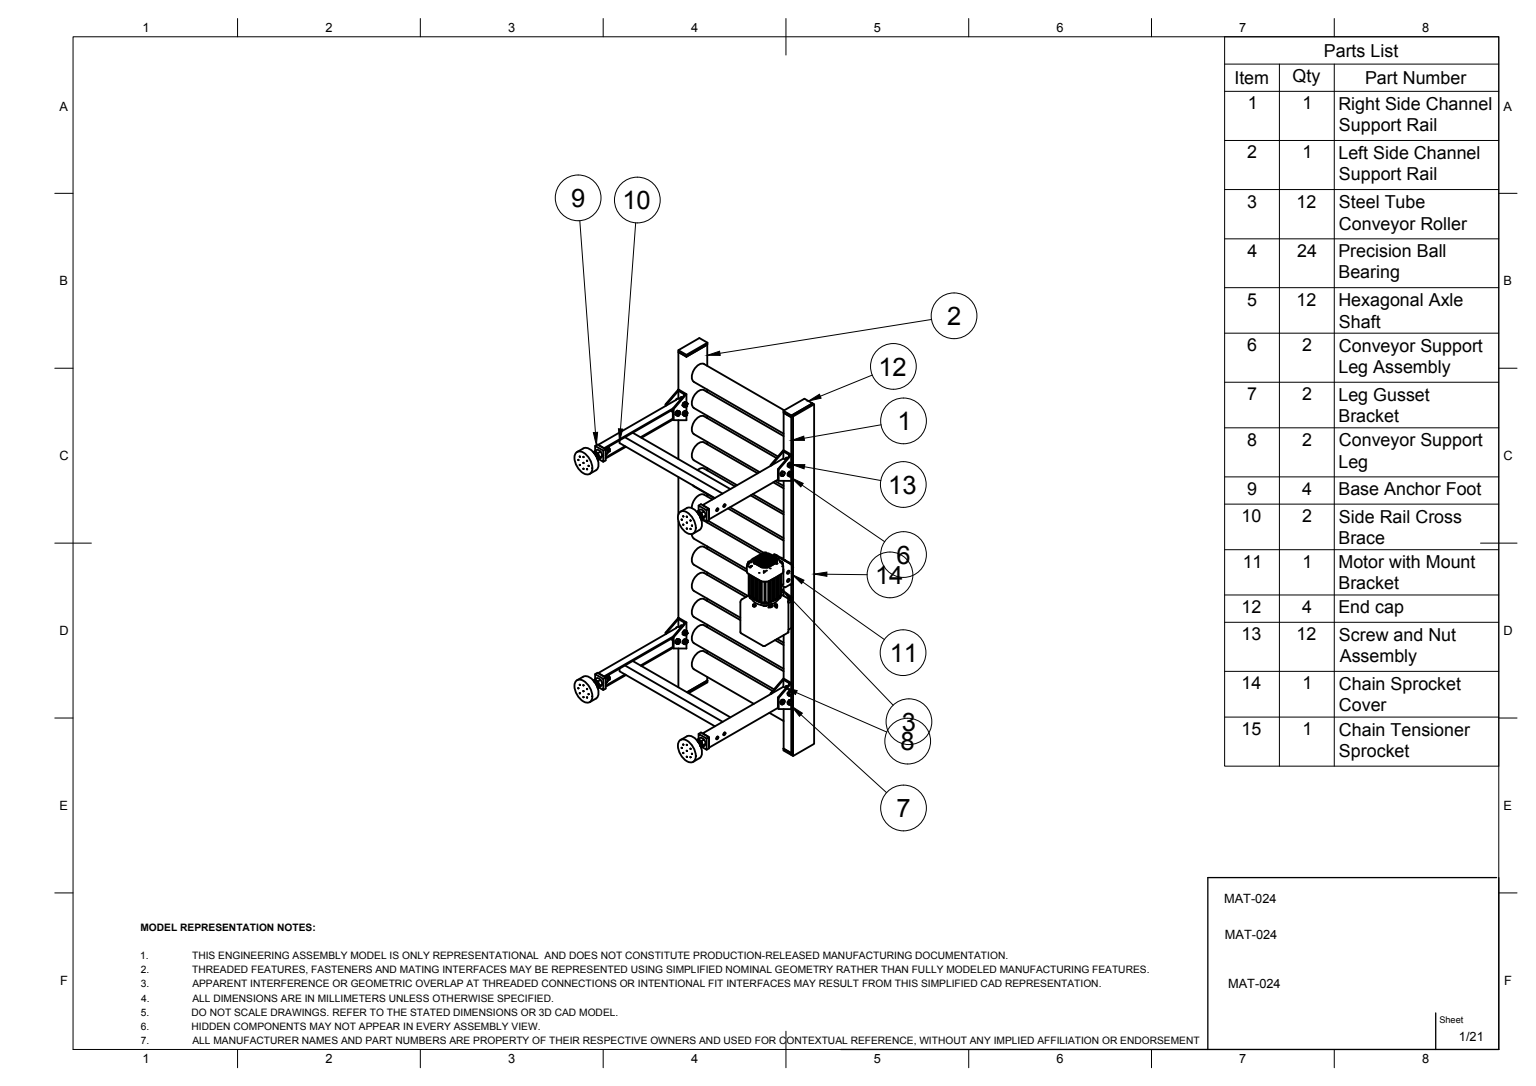
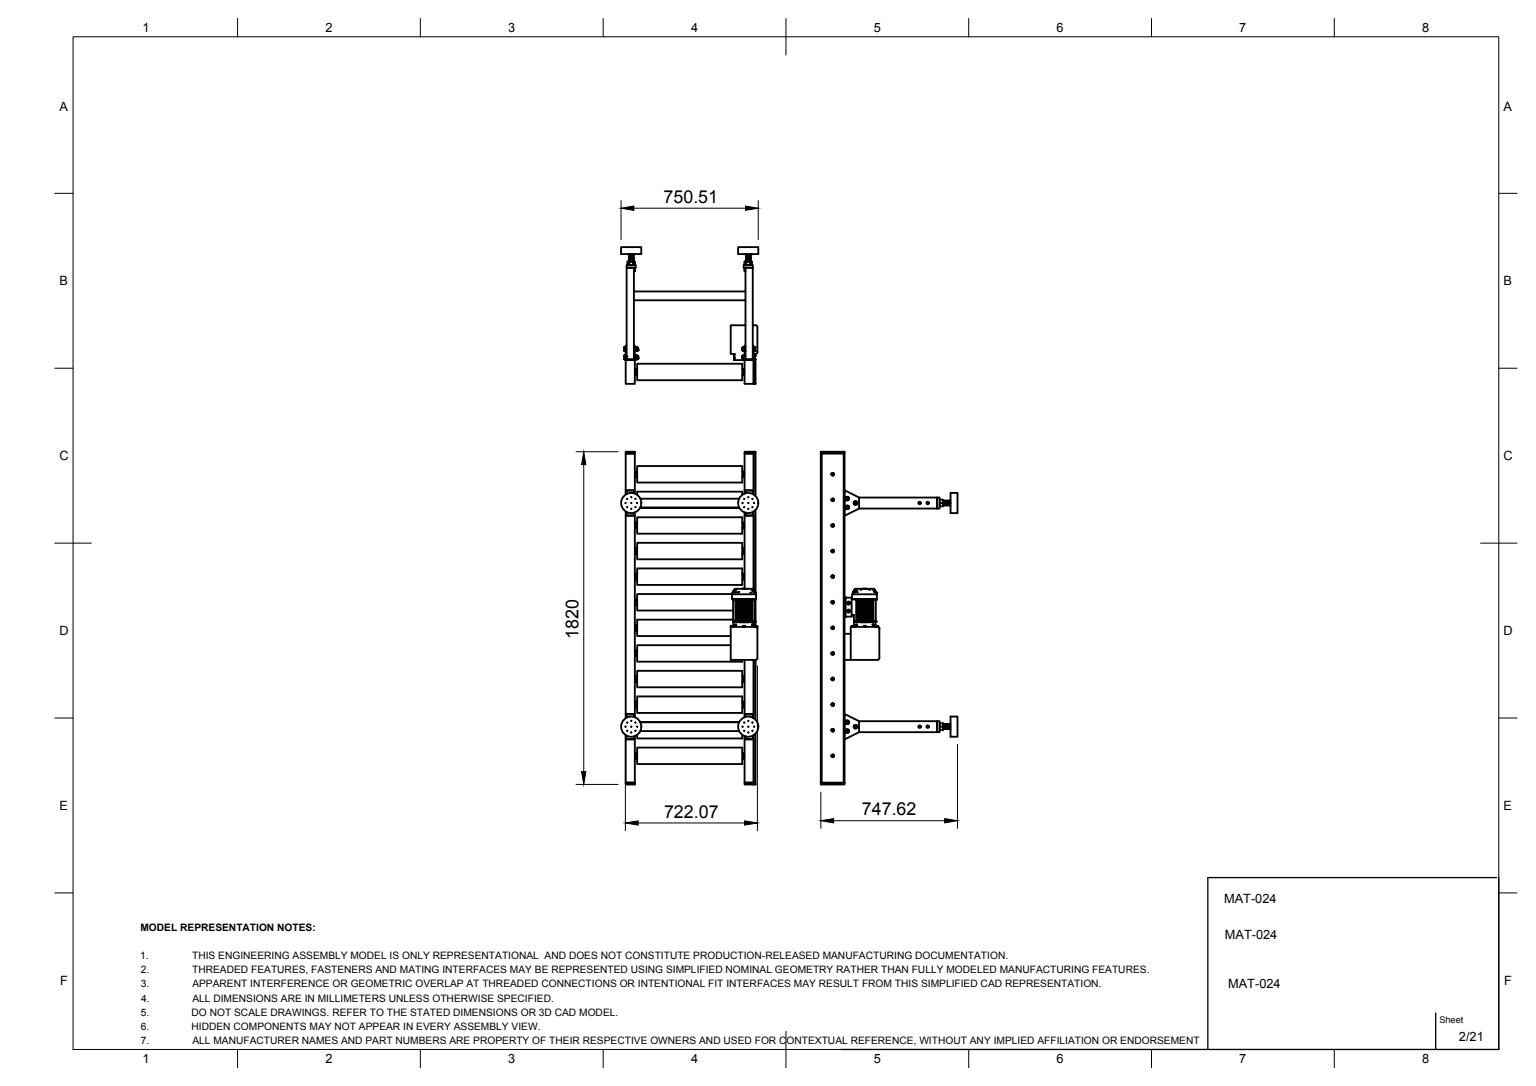
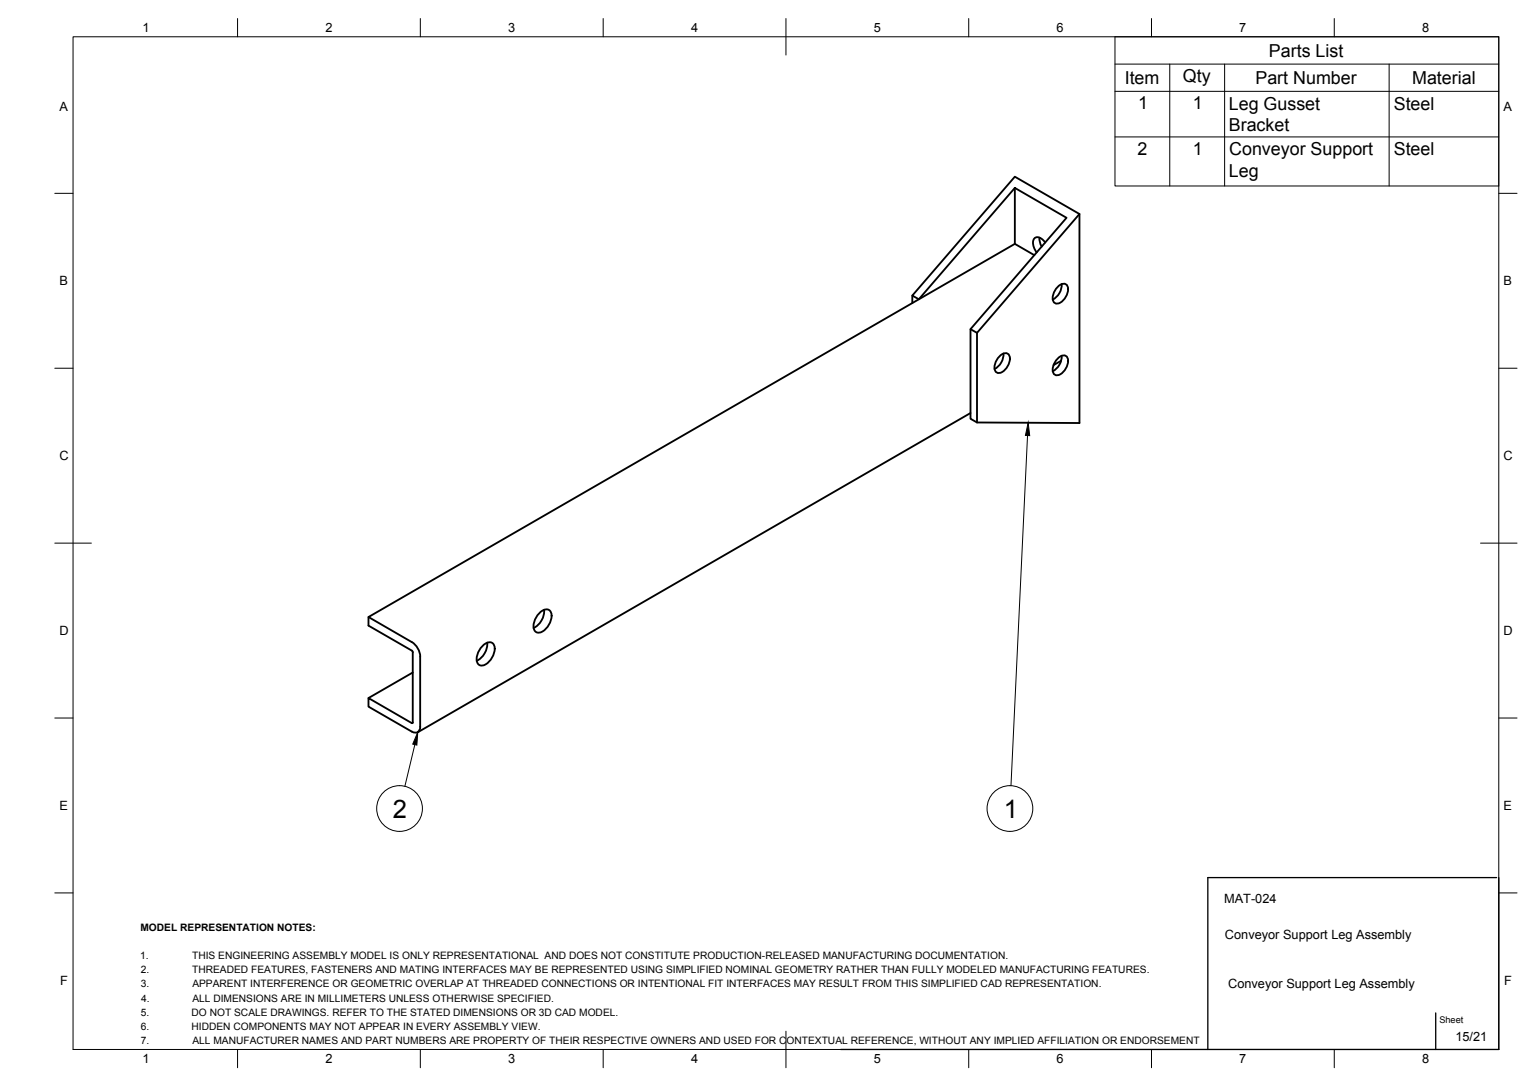
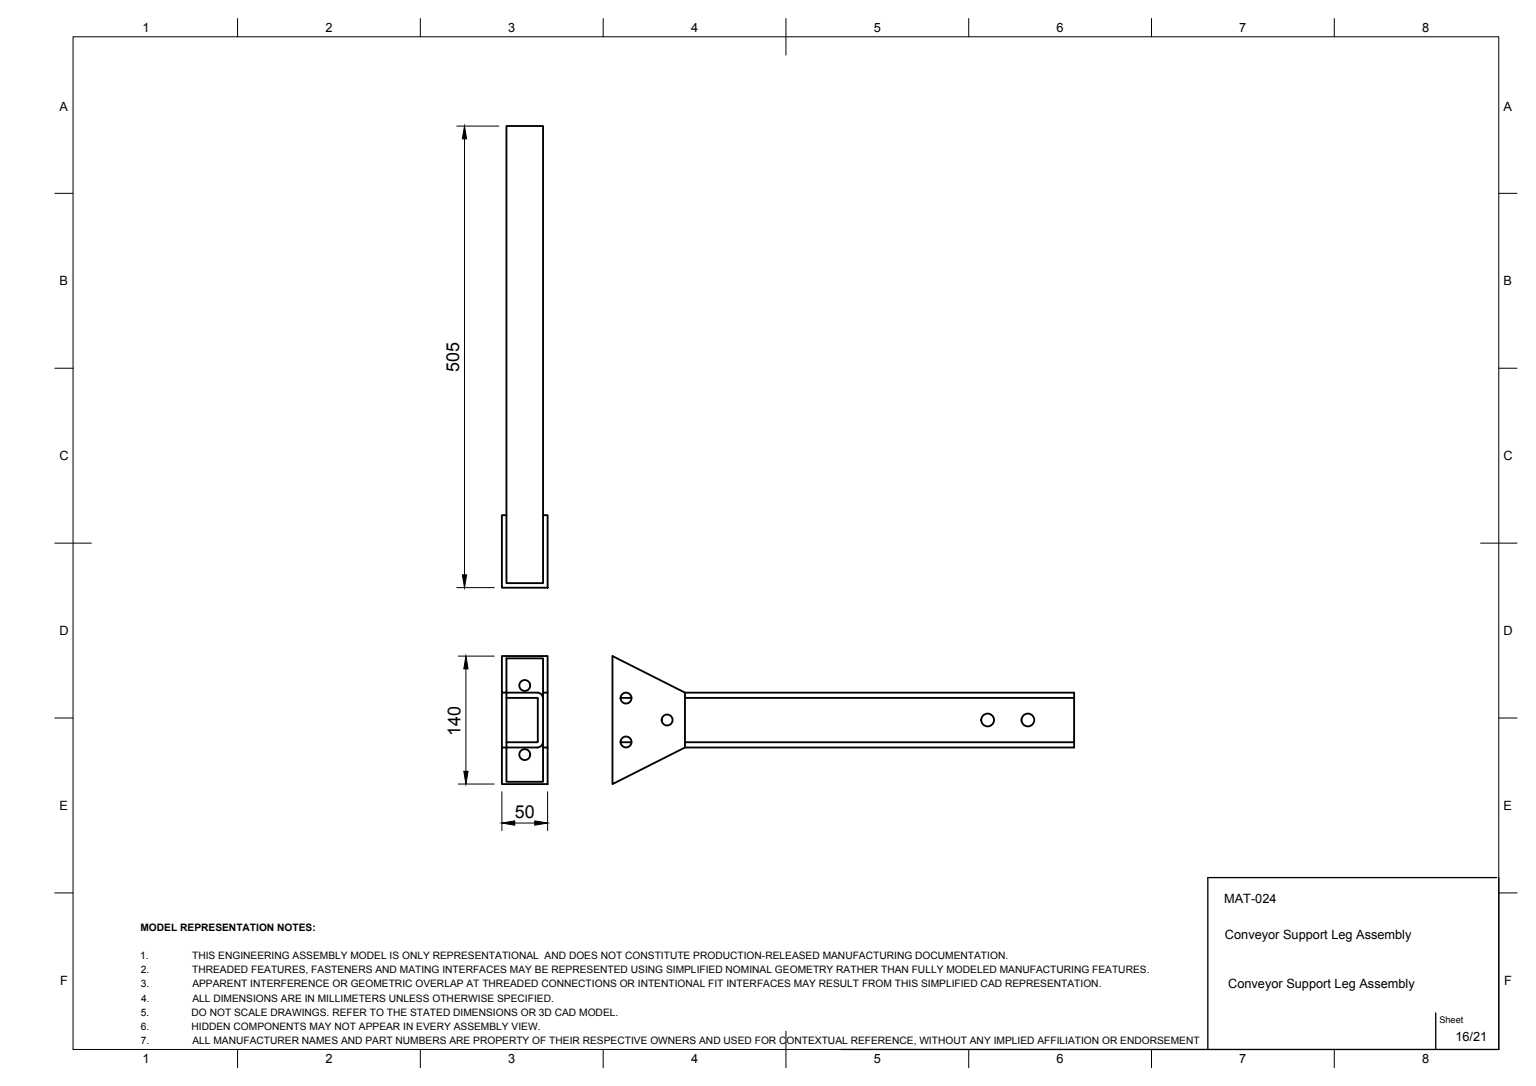
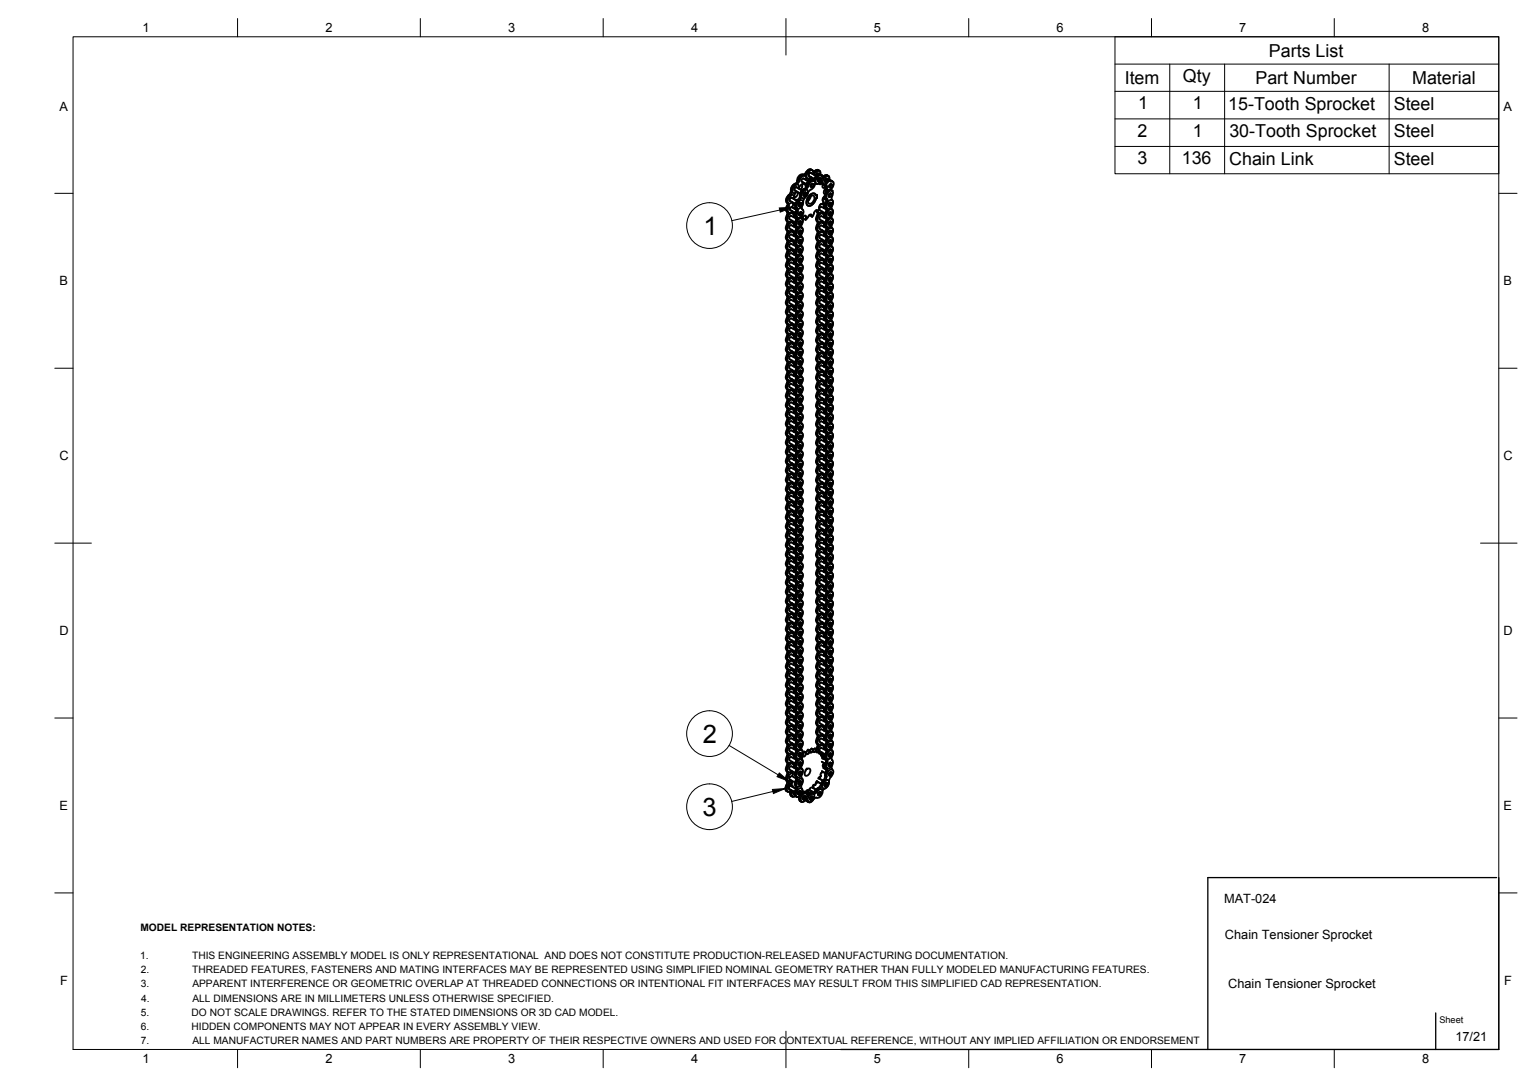
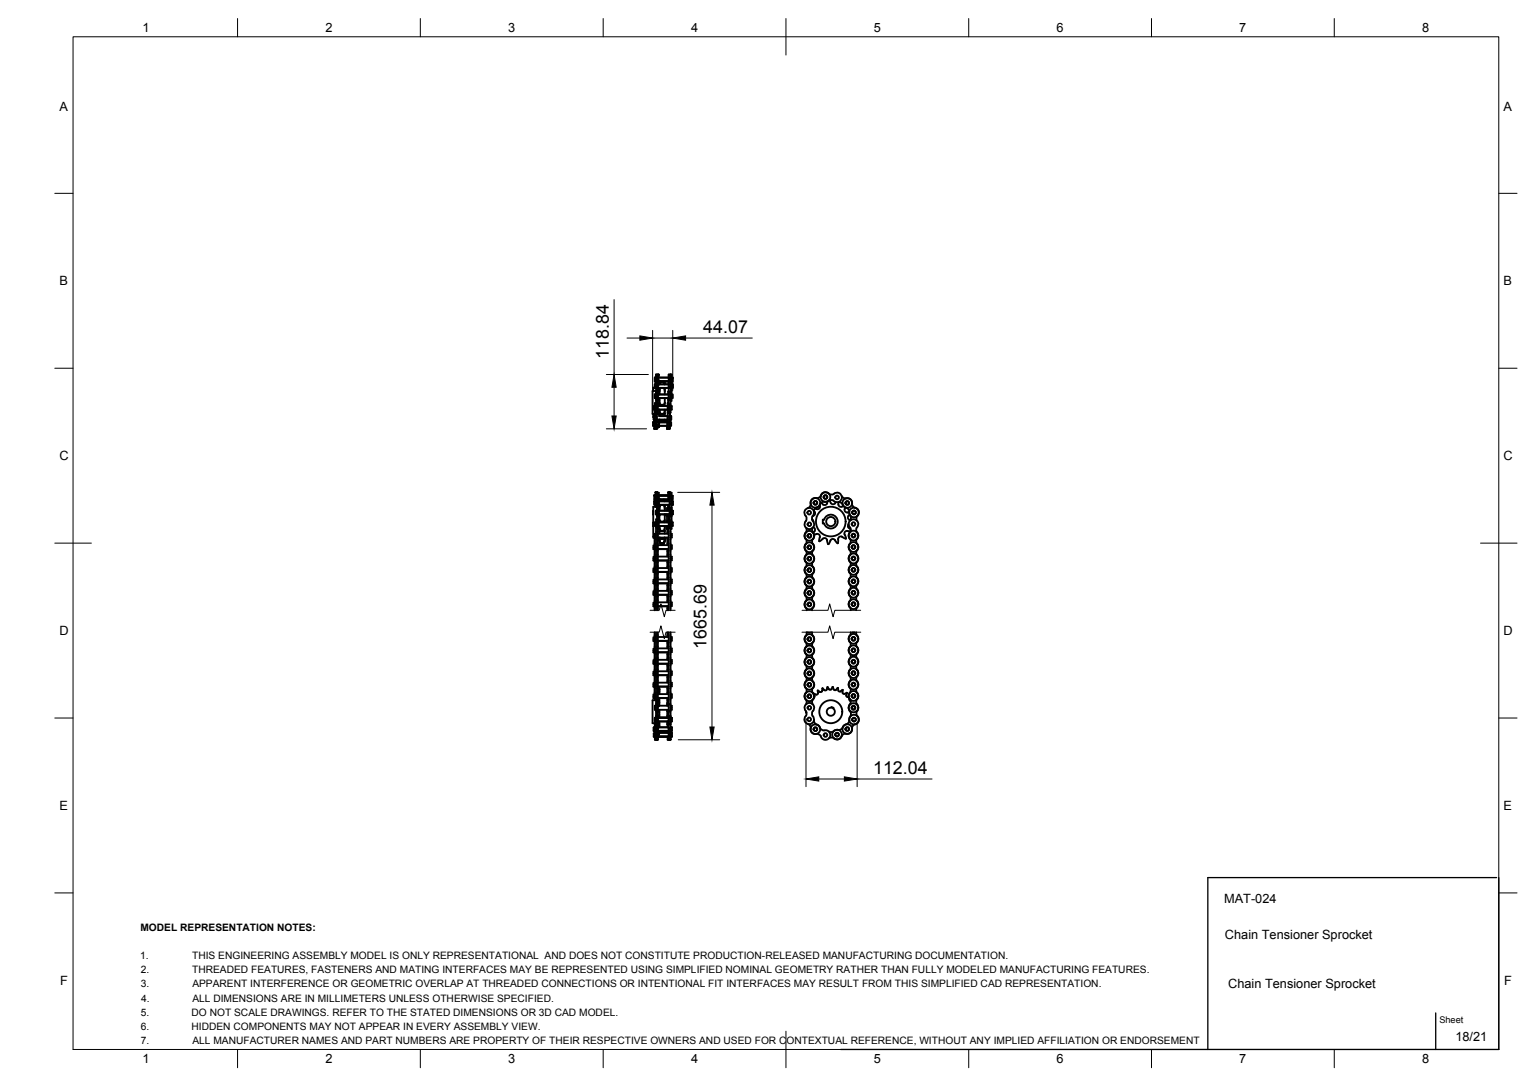
ISO-10303-21;
HEADER;
/* Generated by software containing ST-Developer
 * from STEP Tools, Inc. (www.steptools.com) 
 */

FILE_DESCRIPTION(
/* description */ ('STEP AP214'),
/* implementation_level */ '2;1');

FILE_NAME(
/* name */ 'MAT-024.step',
/* time_stamp */ '2026-11-14T06:34:07-08:00',
/* author */ (''),
/* organization */ (''),
/* preprocessor_version */ 'ST-DEVELOPER v20.2',
/* originating_system */ 'Autodesk Translation Framework v15.17.0.0',
/* authorisation */ '');

FILE_SCHEMA (('AUTOMOTIVE_DESIGN { 1 0 10303 214 3 1 1 }'));
ENDSEC;

DATA;
#10=MECHANICAL_DESIGN_GEOMETRIC_PRESENTATION_REPRESENTATION('',(#7256,#7257,
#7258,#7259,#7260,#7261,#7262,#7263,#7264,#7265,#7266,#7267,#7268,#7269,
#7270,#7271,#7272,#7273,#7274,#7275,#7276,#7277,#7278,#7279,#7280,#7281,
#7282,#7283,#7284,#7285,#7286,#7287,#7288,#7289,#7290,#7291,#7292,#7293,
#7294,#7295,#7296,#7297,#7298,#7299,#7300,#7301,#7302,#7303,#7304,#7305,
#7306,#7307,#7308,#7309,#7310,#7311,#7312,#7313,#7314,#7315,#7316,#7317,
#7318,#7319,#7320,#7321,#7322,#7323),#310623);
#11=ORIENTED_CLOSED_SHELL('',*,#93766,.F.);
#12=BREP_WITH_VOIDS('Body3',#93767,(#11));
#13=ITEM_DEFINED_TRANSFORMATION($,$,#103340,#103974);
#14=ITEM_DEFINED_TRANSFORMATION($,$,#103547,#103975);
#15=ITEM_DEFINED_TRANSFORMATION($,$,#103923,#103976);
#16=ITEM_DEFINED_TRANSFORMATION($,$,#103923,#103977);
#17=ITEM_DEFINED_TRANSFORMATION($,$,#103923,#103978);
#18=ITEM_DEFINED_TRANSFORMATION($,$,#103923,#103979);
#19=ITEM_DEFINED_TRANSFORMATION($,$,#103923,#103980);
#20=ITEM_DEFINED_TRANSFORMATION($,$,#103923,#103981);
#21=ITEM_DEFINED_TRANSFORMATION($,$,#103923,#103982);
#22=ITEM_DEFINED_TRANSFORMATION($,$,#103923,#103983);
#23=ITEM_DEFINED_TRANSFORMATION($,$,#103923,#103984);
#24=ITEM_DEFINED_TRANSFORMATION($,$,#103923,#103985);
#25=ITEM_DEFINED_TRANSFORMATION($,$,#103923,#103986);
#26=ITEM_DEFINED_TRANSFORMATION($,$,#103923,#103987);
#27=ITEM_DEFINED_TRANSFORMATION($,$,#103923,#103988);
#28=ITEM_DEFINED_TRANSFORMATION($,$,#103923,#103989);
#29=ITEM_DEFINED_TRANSFORMATION($,$,#103923,#103990);
#30=ITEM_DEFINED_TRANSFORMATION($,$,#103923,#103991);
#31=ITEM_DEFINED_TRANSFORMATION($,$,#103923,#103992);
#32=ITEM_DEFINED_TRANSFORMATION($,$,#103923,#103993);
#33=ITEM_DEFINED_TRANSFORMATION($,$,#103923,#103994);
#34=ITEM_DEFINED_TRANSFORMATION($,$,#103923,#103995);
#35=ITEM_DEFINED_TRANSFORMATION($,$,#103923,#103996);
#36=ITEM_DEFINED_TRANSFORMATION($,$,#103923,#103997);
#37=ITEM_DEFINED_TRANSFORMATION($,$,#103923,#103998);
#38=ITEM_DEFINED_TRANSFORMATION($,$,#103923,#103999);
#39=ITEM_DEFINED_TRANSFORMATION($,$,#103923,#104000);
#40=ITEM_DEFINED_TRANSFORMATION($,$,#103923,#104001);
#41=ITEM_DEFINED_TRANSFORMATION($,$,#103923,#104002);
#42=ITEM_DEFINED_TRANSFORMATION($,$,#103923,#104003);
#43=ITEM_DEFINED_TRANSFORMATION($,$,#103923,#104004);
#44=ITEM_DEFINED_TRANSFORMATION($,$,#103923,#104005);
#45=ITEM_DEFINED_TRANSFORMATION($,$,#103923,#104006);
#46=ITEM_DEFINED_TRANSFORMATION($,$,#103923,#104007);
#47=ITEM_DEFINED_TRANSFORMATION($,$,#103923,#104008);
#48=ITEM_DEFINED_TRANSFORMATION($,$,#103923,#104009);
#49=ITEM_DEFINED_TRANSFORMATION($,$,#103923,#104010);
#50=ITEM_DEFINED_TRANSFORMATION($,$,#103923,#104011);
#51=ITEM_DEFINED_TRANSFORMATION($,$,#103923,#104012);
#52=ITEM_DEFINED_TRANSFORMATION($,$,#103923,#104013);
#53=ITEM_DEFINED_TRANSFORMATION($,$,#103923,#104014);
#54=ITEM_DEFINED_TRANSFORMATION($,$,#103923,#104015);
#55=ITEM_DEFINED_TRANSFORMATION($,$,#103923,#104016);
#56=ITEM_DEFINED_TRANSFORMATION($,$,#103923,#104017);
#57=ITEM_DEFINED_TRANSFORMATION($,$,#103923,#104018);
#58=ITEM_DEFINED_TRANSFORMATION($,$,#103923,#104019);
#59=ITEM_DEFINED_TRANSFORMATION($,$,#103923,#104020);
#60=ITEM_DEFINED_TRANSFORMATION($,$,#103923,#104021);
#61=ITEM_DEFINED_TRANSFORMATION($,$,#103923,#104022);
#62=ITEM_DEFINED_TRANSFORMATION($,$,#103923,#104023);
#63=ITEM_DEFINED_TRANSFORMATION($,$,#103923,#104024);
#64=ITEM_DEFINED_TRANSFORMATION($,$,#103923,#104025);
#65=ITEM_DEFINED_TRANSFORMATION($,$,#103923,#104026);
#66=ITEM_DEFINED_TRANSFORMATION($,$,#103923,#104027);
#67=ITEM_DEFINED_TRANSFORMATION($,$,#103923,#104028);
#68=ITEM_DEFINED_TRANSFORMATION($,$,#103923,#104029);
#69=ITEM_DEFINED_TRANSFORMATION($,$,#103923,#104030);
#70=ITEM_DEFINED_TRANSFORMATION($,$,#103923,#104031);
#71=ITEM_DEFINED_TRANSFORMATION($,$,#103923,#104032);
#72=ITEM_DEFINED_TRANSFORMATION($,$,#103923,#104033);
#73=ITEM_DEFINED_TRANSFORMATION($,$,#103923,#104034);
#74=ITEM_DEFINED_TRANSFORMATION($,$,#103923,#104035);
#75=ITEM_DEFINED_TRANSFORMATION($,$,#103923,#104036);
#76=ITEM_DEFINED_TRANSFORMATION($,$,#103923,#104037);
#77=ITEM_DEFINED_TRANSFORMATION($,$,#103923,#104038);
#78=ITEM_DEFINED_TRANSFORMATION($,$,#103923,#104039);
#79=ITEM_DEFINED_TRANSFORMATION($,$,#103923,#104040);
#80=ITEM_DEFINED_TRANSFORMATION($,$,#103923,#104041);
#81=ITEM_DEFINED_TRANSFORMATION($,$,#103923,#104042);
#82=ITEM_DEFINED_TRANSFORMATION($,$,#103923,#104043);
#83=ITEM_DEFINED_TRANSFORMATION($,$,#103923,#104044);
#84=ITEM_DEFINED_TRANSFORMATION($,$,#103923,#104045);
#85=ITEM_DEFINED_TRANSFORMATION($,$,#103923,#104046);
#86=ITEM_DEFINED_TRANSFORMATION($,$,#103923,#104047);
#87=ITEM_DEFINED_TRANSFORMATION($,$,#103923,#104048);
#88=ITEM_DEFINED_TRANSFORMATION($,$,#103923,#104049);
#89=ITEM_DEFINED_TRANSFORMATION($,$,#103923,#104050);
#90=ITEM_DEFINED_TRANSFORMATION($,$,#103923,#104051);
#91=ITEM_DEFINED_TRANSFORMATION($,$,#103923,#104052);
#92=ITEM_DEFINED_TRANSFORMATION($,$,#103923,#104053);
#93=ITEM_DEFINED_TRANSFORMATION($,$,#103923,#104054);
#94=ITEM_DEFINED_TRANSFORMATION($,$,#103923,#104055);
#95=ITEM_DEFINED_TRANSFORMATION($,$,#103923,#104056);
#96=ITEM_DEFINED_TRANSFORMATION($,$,#103923,#104057);
#97=ITEM_DEFINED_TRANSFORMATION($,$,#103923,#104058);
#98=ITEM_DEFINED_TRANSFORMATION($,$,#103923,#104059);
#99=ITEM_DEFINED_TRANSFORMATION($,$,#103923,#104060);
#100=ITEM_DEFINED_TRANSFORMATION($,$,#103923,#104061);
#101=ITEM_DEFINED_TRANSFORMATION($,$,#103923,#104062);
#102=ITEM_DEFINED_TRANSFORMATION($,$,#103923,#104063);
#103=ITEM_DEFINED_TRANSFORMATION($,$,#103923,#104064);
#104=ITEM_DEFINED_TRANSFORMATION($,$,#103923,#104065);
#105=ITEM_DEFINED_TRANSFORMATION($,$,#103923,#104066);
#106=ITEM_DEFINED_TRANSFORMATION($,$,#103923,#104067);
#107=ITEM_DEFINED_TRANSFORMATION($,$,#103923,#104068);
#108=ITEM_DEFINED_TRANSFORMATION($,$,#103923,#104069);
#109=ITEM_DEFINED_TRANSFORMATION($,$,#103923,#104070);
#110=ITEM_DEFINED_TRANSFORMATION($,$,#103923,#104071);
#111=ITEM_DEFINED_TRANSFORMATION($,$,#103923,#104072);
#112=ITEM_DEFINED_TRANSFORMATION($,$,#103923,#104073);
#113=ITEM_DEFINED_TRANSFORMATION($,$,#103923,#104074);
#114=ITEM_DEFINED_TRANSFORMATION($,$,#103923,#104075);
#115=ITEM_DEFINED_TRANSFORMATION($,$,#103923,#104076);
#116=ITEM_DEFINED_TRANSFORMATION($,$,#103923,#104077);
#117=ITEM_DEFINED_TRANSFORMATION($,$,#103923,#104078);
#118=ITEM_DEFINED_TRANSFORMATION($,$,#103923,#104079);
#119=ITEM_DEFINED_TRANSFORMATION($,$,#103923,#104080);
#120=ITEM_DEFINED_TRANSFORMATION($,$,#103923,#104081);
#121=ITEM_DEFINED_TRANSFORMATION($,$,#103923,#104082);
#122=ITEM_DEFINED_TRANSFORMATION($,$,#103923,#104083);
#123=ITEM_DEFINED_TRANSFORMATION($,$,#103923,#104084);
#124=ITEM_DEFINED_TRANSFORMATION($,$,#103923,#104085);
#125=ITEM_DEFINED_TRANSFORMATION($,$,#103923,#104086);
#126=ITEM_DEFINED_TRANSFORMATION($,$,#103923,#104087);
#127=ITEM_DEFINED_TRANSFORMATION($,$,#103923,#104088);
#128=ITEM_DEFINED_TRANSFORMATION($,$,#103923,#104089);
#129=ITEM_DEFINED_TRANSFORMATION($,$,#103923,#104090);
#130=ITEM_DEFINED_TRANSFORMATION($,$,#103923,#104091);
#131=ITEM_DEFINED_TRANSFORMATION($,$,#103923,#104092);
#132=ITEM_DEFINED_TRANSFORMATION($,$,#103923,#104093);
#133=ITEM_DEFINED_TRANSFORMATION($,$,#103923,#104094);
#134=ITEM_DEFINED_TRANSFORMATION($,$,#103923,#104095);
#135=ITEM_DEFINED_TRANSFORMATION($,$,#103923,#104096);
#136=ITEM_DEFINED_TRANSFORMATION($,$,#103923,#104097);
#137=ITEM_DEFINED_TRANSFORMATION($,$,#103923,#104098);
#138=ITEM_DEFINED_TRANSFORMATION($,$,#103923,#104099);
#139=ITEM_DEFINED_TRANSFORMATION($,$,#103923,#104100);
#140=ITEM_DEFINED_TRANSFORMATION($,$,#103923,#104101);
#141=ITEM_DEFINED_TRANSFORMATION($,$,#103923,#104102);
#142=ITEM_DEFINED_TRANSFORMATION($,$,#103923,#104103);
#143=ITEM_DEFINED_TRANSFORMATION($,$,#103923,#104104);
#144=ITEM_DEFINED_TRANSFORMATION($,$,#103923,#104105);
#145=ITEM_DEFINED_TRANSFORMATION($,$,#103923,#104106);
#146=ITEM_DEFINED_TRANSFORMATION($,$,#103923,#104107);
#147=ITEM_DEFINED_TRANSFORMATION($,$,#103923,#104108);
#148=ITEM_DEFINED_TRANSFORMATION($,$,#103923,#104109);
#149=ITEM_DEFINED_TRANSFORMATION($,$,#103923,#104110);
#150=ITEM_DEFINED_TRANSFORMATION($,$,#103923,#104111);
#151=ITEM_DEFINED_TRANSFORMATION($,$,#104562,#104634);
#152=ITEM_DEFINED_TRANSFORMATION($,$,#104597,#104635);
#153=ITEM_DEFINED_TRANSFORMATION($,$,#104637,#104781);
#154=ITEM_DEFINED_TRANSFORMATION($,$,#104720,#104782);
#155=ITEM_DEFINED_TRANSFORMATION($,$,#93964,#104783);
#156=ITEM_DEFINED_TRANSFORMATION($,$,#94023,#104784);
#157=ITEM_DEFINED_TRANSFORMATION($,$,#104112,#104785);
#158=ITEM_DEFINED_TRANSFORMATION($,$,#104129,#104786);
#159=ITEM_DEFINED_TRANSFORMATION($,$,#104223,#104787);
#160=ITEM_DEFINED_TRANSFORMATION($,$,#104561,#104788);
#161=ITEM_DEFINED_TRANSFORMATION($,$,#104248,#104789);
#162=ITEM_DEFINED_TRANSFORMATION($,$,#104543,#104790);
#163=ITEM_DEFINED_TRANSFORMATION($,$,#94082,#104791);
#164=ITEM_DEFINED_TRANSFORMATION($,$,#104554,#104792);
#165=ITEM_DEFINED_TRANSFORMATION($,$,#104636,#104793);
#166=ITEM_DEFINED_TRANSFORMATION($,$,#103332,#104794);
#167=ITEM_DEFINED_TRANSFORMATION($,$,#103339,#104795);
#168=ITEM_DEFINED_TRANSFORMATION($,$,#104112,#104796);
#169=ITEM_DEFINED_TRANSFORMATION($,$,#104112,#104797);
#170=ITEM_DEFINED_TRANSFORMATION($,$,#104112,#104798);
#171=ITEM_DEFINED_TRANSFORMATION($,$,#104112,#104799);
#172=ITEM_DEFINED_TRANSFORMATION($,$,#104112,#104800);
#173=ITEM_DEFINED_TRANSFORMATION($,$,#104112,#104801);
#174=ITEM_DEFINED_TRANSFORMATION($,$,#104112,#104802);
#175=ITEM_DEFINED_TRANSFORMATION($,$,#104112,#104803);
#176=ITEM_DEFINED_TRANSFORMATION($,$,#104112,#104804);
#177=ITEM_DEFINED_TRANSFORMATION($,$,#104112,#104805);
#178=ITEM_DEFINED_TRANSFORMATION($,$,#104112,#104806);
#179=ITEM_DEFINED_TRANSFORMATION($,$,#104129,#104807);
#180=ITEM_DEFINED_TRANSFORMATION($,$,#104129,#104808);
#181=ITEM_DEFINED_TRANSFORMATION($,$,#104129,#104809);
#182=ITEM_DEFINED_TRANSFORMATION($,$,#104129,#104810);
#183=ITEM_DEFINED_TRANSFORMATION($,$,#104129,#104811);
#184=ITEM_DEFINED_TRANSFORMATION($,$,#104129,#104812);
#185=ITEM_DEFINED_TRANSFORMATION($,$,#104129,#104813);
#186=ITEM_DEFINED_TRANSFORMATION($,$,#104129,#104814);
#187=ITEM_DEFINED_TRANSFORMATION($,$,#104129,#104815);
#188=ITEM_DEFINED_TRANSFORMATION($,$,#104129,#104816);
#189=ITEM_DEFINED_TRANSFORMATION($,$,#104129,#104817);
#190=ITEM_DEFINED_TRANSFORMATION($,$,#104129,#104818);
#191=ITEM_DEFINED_TRANSFORMATION($,$,#104129,#104819);
#192=ITEM_DEFINED_TRANSFORMATION($,$,#104129,#104820);
#193=ITEM_DEFINED_TRANSFORMATION($,$,#104129,#104821);
#194=ITEM_DEFINED_TRANSFORMATION($,$,#104129,#104822);
#195=ITEM_DEFINED_TRANSFORMATION($,$,#104129,#104823);
#196=ITEM_DEFINED_TRANSFORMATION($,$,#104129,#104824);
#197=ITEM_DEFINED_TRANSFORMATION($,$,#104129,#104825);
#198=ITEM_DEFINED_TRANSFORMATION($,$,#104129,#104826);
#199=ITEM_DEFINED_TRANSFORMATION($,$,#104129,#104827);
#200=ITEM_DEFINED_TRANSFORMATION($,$,#104129,#104828);
#201=ITEM_DEFINED_TRANSFORMATION($,$,#104129,#104829);
#202=ITEM_DEFINED_TRANSFORMATION($,$,#104223,#104830);
#203=ITEM_DEFINED_TRANSFORMATION($,$,#104223,#104831);
#204=ITEM_DEFINED_TRANSFORMATION($,$,#104223,#104832);
#205=ITEM_DEFINED_TRANSFORMATION($,$,#104223,#104833);
#206=ITEM_DEFINED_TRANSFORMATION($,$,#104223,#104834);
#207=ITEM_DEFINED_TRANSFORMATION($,$,#104223,#104835);
#208=ITEM_DEFINED_TRANSFORMATION($,$,#104223,#104836);
#209=ITEM_DEFINED_TRANSFORMATION($,$,#104223,#104837);
#210=ITEM_DEFINED_TRANSFORMATION($,$,#104223,#104838);
#211=ITEM_DEFINED_TRANSFORMATION($,$,#104223,#104839);
#212=ITEM_DEFINED_TRANSFORMATION($,$,#104223,#104840);
#213=ITEM_DEFINED_TRANSFORMATION($,$,#104562,#104841);
#214=ITEM_DEFINED_TRANSFORMATION($,$,#104597,#104842);
#215=ITEM_DEFINED_TRANSFORMATION($,$,#104248,#104843);
#216=ITEM_DEFINED_TRANSFORMATION($,$,#104248,#104844);
#217=ITEM_DEFINED_TRANSFORMATION($,$,#104597,#104845);
#218=ITEM_DEFINED_TRANSFORMATION($,$,#104248,#104846);
#219=ITEM_DEFINED_TRANSFORMATION($,$,#104543,#104847);
#220=ITEM_DEFINED_TRANSFORMATION($,$,#104562,#104848);
#221=ITEM_DEFINED_TRANSFORMATION($,$,#104554,#104849);
#222=ITEM_DEFINED_TRANSFORMATION($,$,#104554,#104850);
#223=ITEM_DEFINED_TRANSFORMATION($,$,#104554,#104851);
#224=ITEM_DEFINED_TRANSFORMATION($,$,#104636,#104852);
#225=ITEM_DEFINED_TRANSFORMATION($,$,#104636,#104853);
#226=ITEM_DEFINED_TRANSFORMATION($,$,#104636,#104854);
#227=ITEM_DEFINED_TRANSFORMATION($,$,#104636,#104855);
#228=ITEM_DEFINED_TRANSFORMATION($,$,#104636,#104856);
#229=ITEM_DEFINED_TRANSFORMATION($,$,#104561,#104857);
#230=ITEM_DEFINED_TRANSFORMATION($,$,#104636,#104858);
#231=ITEM_DEFINED_TRANSFORMATION($,$,#104636,#104859);
#232=ITEM_DEFINED_TRANSFORMATION($,$,#104636,#104860);
#233=ITEM_DEFINED_TRANSFORMATION($,$,#104636,#104861);
#234=ITEM_DEFINED_TRANSFORMATION($,$,#104636,#104862);
#235=ITEM_DEFINED_TRANSFORMATION($,$,#104636,#104863);
#236=(
REPRESENTATION_RELATIONSHIP($,$,#310899,#310898)
REPRESENTATION_RELATIONSHIP_WITH_TRANSFORMATION(#13)
SHAPE_REPRESENTATION_RELATIONSHIP()
);
#237=(
REPRESENTATION_RELATIONSHIP($,$,#310900,#310898)
REPRESENTATION_RELATIONSHIP_WITH_TRANSFORMATION(#14)
SHAPE_REPRESENTATION_RELATIONSHIP()
);
#238=(
REPRESENTATION_RELATIONSHIP($,$,#310901,#310898)
REPRESENTATION_RELATIONSHIP_WITH_TRANSFORMATION(#15)
SHAPE_REPRESENTATION_RELATIONSHIP()
);
#239=(
REPRESENTATION_RELATIONSHIP($,$,#310901,#310898)
REPRESENTATION_RELATIONSHIP_WITH_TRANSFORMATION(#16)
SHAPE_REPRESENTATION_RELATIONSHIP()
);
#240=(
REPRESENTATION_RELATIONSHIP($,$,#310901,#310898)
REPRESENTATION_RELATIONSHIP_WITH_TRANSFORMATION(#17)
SHAPE_REPRESENTATION_RELATIONSHIP()
);
#241=(
REPRESENTATION_RELATIONSHIP($,$,#310901,#310898)
REPRESENTATION_RELATIONSHIP_WITH_TRANSFORMATION(#18)
SHAPE_REPRESENTATION_RELATIONSHIP()
);
#242=(
REPRESENTATION_RELATIONSHIP($,$,#310901,#310898)
REPRESENTATION_RELATIONSHIP_WITH_TRANSFORMATION(#19)
SHAPE_REPRESENTATION_RELATIONSHIP()
);
#243=(
REPRESENTATION_RELATIONSHIP($,$,#310901,#310898)
REPRESENTATION_RELATIONSHIP_WITH_TRANSFORMATION(#20)
SHAPE_REPRESENTATION_RELATIONSHIP()
);
#244=(
REPRESENTATION_RELATIONSHIP($,$,#310901,#310898)
REPRESENTATION_RELATIONSHIP_WITH_TRANSFORMATION(#21)
SHAPE_REPRESENTATION_RELATIONSHIP()
);
#245=(
REPRESENTATION_RELATIONSHIP($,$,#310901,#310898)
REPRESENTATION_RELATIONSHIP_WITH_TRANSFORMATION(#22)
SHAPE_REPRESENTATION_RELATIONSHIP()
);
#246=(
REPRESENTATION_RELATIONSHIP($,$,#310901,#310898)
REPRESENTATION_RELATIONSHIP_WITH_TRANSFORMATION(#23)
SHAPE_REPRESENTATION_RELATIONSHIP()
);
#247=(
REPRESENTATION_RELATIONSHIP($,$,#310901,#310898)
REPRESENTATION_RELATIONSHIP_WITH_TRANSFORMATION(#24)
SHAPE_REPRESENTATION_RELATIONSHIP()
);
#248=(
REPRESENTATION_RELATIONSHIP($,$,#310901,#310898)
REPRESENTATION_RELATIONSHIP_WITH_TRANSFORMATION(#25)
SHAPE_REPRESENTATION_RELATIONSHIP()
);
#249=(
REPRESENTATION_RELATIONSHIP($,$,#310901,#310898)
REPRESENTATION_RELATIONSHIP_WITH_TRANSFORMATION(#26)
SHAPE_REPRESENTATION_RELATIONSHIP()
);
#250=(
REPRESENTATION_RELATIONSHIP($,$,#310901,#310898)
REPRESENTATION_RELATIONSHIP_WITH_TRANSFORMATION(#27)
SHAPE_REPRESENTATION_RELATIONSHIP()
);
#251=(
REPRESENTATION_RELATIONSHIP($,$,#310901,#310898)
REPRESENTATION_RELATIONSHIP_WITH_TRANSFORMATION(#28)
SHAPE_REPRESENTATION_RELATIONSHIP()
);
#252=(
REPRESENTATION_RELATIONSHIP($,$,#310901,#310898)
REPRESENTATION_RELATIONSHIP_WITH_TRANSFORMATION(#29)
SHAPE_REPRESENTATION_RELATIONSHIP()
);
#253=(
REPRESENTATION_RELATIONSHIP($,$,#310901,#310898)
REPRESENTATION_RELATIONSHIP_WITH_TRANSFORMATION(#30)
SHAPE_REPRESENTATION_RELATIONSHIP()
);
#254=(
REPRESENTATION_RELATIONSHIP($,$,#310901,#310898)
REPRESENTATION_RELATIONSHIP_WITH_TRANSFORMATION(#31)
SHAPE_REPRESENTATION_RELATIONSHIP()
);
#255=(
REPRESENTATION_RELATIONSHIP($,$,#310901,#310898)
REPRESENTATION_RELATIONSHIP_WITH_TRANSFORMATION(#32)
SHAPE_REPRESENTATION_RELATIONSHIP()
);
#256=(
REPRESENTATION_RELATIONSHIP($,$,#310901,#310898)
REPRESENTATION_RELATIONSHIP_WITH_TRANSFORMATION(#33)
SHAPE_REPRESENTATION_RELATIONSHIP()
);
#257=(
REPRESENTATION_RELATIONSHIP($,$,#310901,#310898)
REPRESENTATION_RELATIONSHIP_WITH_TRANSFORMATION(#34)
SHAPE_REPRESENTATION_RELATIONSHIP()
);
#258=(
REPRESENTATION_RELATIONSHIP($,$,#310901,#310898)
REPRESENTATION_RELATIONSHIP_WITH_TRANSFORMATION(#35)
SHAPE_REPRESENTATION_RELATIONSHIP()
);
#259=(
REPRESENTATION_RELATIONSHIP($,$,#310901,#310898)
REPRESENTATION_RELATIONSHIP_WITH_TRANSFORMATION(#36)
SHAPE_REPRESENTATION_RELATIONSHIP()
);
#260=(
REPRESENTATION_RELATIONSHIP($,$,#310901,#310898)
REPRESENTATION_RELATIONSHIP_WITH_TRANSFORMATION(#37)
SHAPE_REPRESENTATION_RELATIONSHIP()
);
#261=(
REPRESENTATION_RELATIONSHIP($,$,#310901,#310898)
REPRESENTATION_RELATIONSHIP_WITH_TRANSFORMATION(#38)
SHAPE_REPRESENTATION_RELATIONSHIP()
);
#262=(
REPRESENTATION_RELATIONSHIP($,$,#310901,#310898)
REPRESENTATION_RELATIONSHIP_WITH_TRANSFORMATION(#39)
SHAPE_REPRESENTATION_RELATIONSHIP()
);
#263=(
REPRESENTATION_RELATIONSHIP($,$,#310901,#310898)
REPRESENTATION_RELATIONSHIP_WITH_TRANSFORMATION(#40)
SHAPE_REPRESENTATION_RELATIONSHIP()
);
#264=(
REPRESENTATION_RELATIONSHIP($,$,#310901,#310898)
REPRESENTATION_RELATIONSHIP_WITH_TRANSFORMATION(#41)
SHAPE_REPRESENTATION_RELATIONSHIP()
);
#265=(
REPRESENTATION_RELATIONSHIP($,$,#310901,#310898)
REPRESENTATION_RELATIONSHIP_WITH_TRANSFORMATION(#42)
SHAPE_REPRESENTATION_RELATIONSHIP()
);
#266=(
REPRESENTATION_RELATIONSHIP($,$,#310901,#310898)
REPRESENTATION_RELATIONSHIP_WITH_TRANSFORMATION(#43)
SHAPE_REPRESENTATION_RELATIONSHIP()
);
#267=(
REPRESENTATION_RELATIONSHIP($,$,#310901,#310898)
REPRESENTATION_RELATIONSHIP_WITH_TRANSFORMATION(#44)
SHAPE_REPRESENTATION_RELATIONSHIP()
);
#268=(
REPRESENTATION_RELATIONSHIP($,$,#310901,#310898)
REPRESENTATION_RELATIONSHIP_WITH_TRANSFORMATION(#45)
SHAPE_REPRESENTATION_RELATIONSHIP()
);
#269=(
REPRESENTATION_RELATIONSHIP($,$,#310901,#310898)
REPRESENTATION_RELATIONSHIP_WITH_TRANSFORMATION(#46)
SHAPE_REPRESENTATION_RELATIONSHIP()
);
#270=(
REPRESENTATION_RELATIONSHIP($,$,#310901,#310898)
REPRESENTATION_RELATIONSHIP_WITH_TRANSFORMATION(#47)
SHAPE_REPRESENTATION_RELATIONSHIP()
);
#271=(
REPRESENTATION_RELATIONSHIP($,$,#310901,#310898)
REPRESENTATION_RELATIONSHIP_WITH_TRANSFORMATION(#48)
SHAPE_REPRESENTATION_RELATIONSHIP()
);
#272=(
REPRESENTATION_RELATIONSHIP($,$,#310901,#310898)
REPRESENTATION_RELATIONSHIP_WITH_TRANSFORMATION(#49)
SHAPE_REPRESENTATION_RELATIONSHIP()
);
#273=(
REPRESENTATION_RELATIONSHIP($,$,#310901,#310898)
REPRESENTATION_RELATIONSHIP_WITH_TRANSFORMATION(#50)
SHAPE_REPRESENTATION_RELATIONSHIP()
);
#274=(
REPRESENTATION_RELATIONSHIP($,$,#310901,#310898)
REPRESENTATION_RELATIONSHIP_WITH_TRANSFORMATION(#51)
SHAPE_REPRESENTATION_RELATIONSHIP()
);
#275=(
REPRESENTATION_RELATIONSHIP($,$,#310901,#310898)
REPRESENTATION_RELATIONSHIP_WITH_TRANSFORMATION(#52)
SHAPE_REPRESENTATION_RELATIONSHIP()
);
#276=(
REPRESENTATION_RELATIONSHIP($,$,#310901,#310898)
REPRESENTATION_RELATIONSHIP_WITH_TRANSFORMATION(#53)
SHAPE_REPRESENTATION_RELATIONSHIP()
);
#277=(
REPRESENTATION_RELATIONSHIP($,$,#310901,#310898)
REPRESENTATION_RELATIONSHIP_WITH_TRANSFORMATION(#54)
SHAPE_REPRESENTATION_RELATIONSHIP()
);
#278=(
REPRESENTATION_RELATIONSHIP($,$,#310901,#310898)
REPRESENTATION_RELATIONSHIP_WITH_TRANSFORMATION(#55)
SHAPE_REPRESENTATION_RELATIONSHIP()
);
#279=(
REPRESENTATION_RELATIONSHIP($,$,#310901,#310898)
REPRESENTATION_RELATIONSHIP_WITH_TRANSFORMATION(#56)
SHAPE_REPRESENTATION_RELATIONSHIP()
);
#280=(
REPRESENTATION_RELATIONSHIP($,$,#310901,#310898)
REPRESENTATION_RELATIONSHIP_WITH_TRANSFORMATION(#57)
SHAPE_REPRESENTATION_RELATIONSHIP()
);
#281=(
REPRESENTATION_RELATIONSHIP($,$,#310901,#310898)
REPRESENTATION_RELATIONSHIP_WITH_TRANSFORMATION(#58)
SHAPE_REPRESENTATION_RELATIONSHIP()
);
#282=(
REPRESENTATION_RELATIONSHIP($,$,#310901,#310898)
REPRESENTATION_RELATIONSHIP_WITH_TRANSFORMATION(#59)
SHAPE_REPRESENTATION_RELATIONSHIP()
);
#283=(
REPRESENTATION_RELATIONSHIP($,$,#310901,#310898)
REPRESENTATION_RELATIONSHIP_WITH_TRANSFORMATION(#60)
SHAPE_REPRESENTATION_RELATIONSHIP()
);
#284=(
REPRESENTATION_RELATIONSHIP($,$,#310901,#310898)
REPRESENTATION_RELATIONSHIP_WITH_TRANSFORMATION(#61)
SHAPE_REPRESENTATION_RELATIONSHIP()
);
#285=(
REPRESENTATION_RELATIONSHIP($,$,#310901,#310898)
REPRESENTATION_RELATIONSHIP_WITH_TRANSFORMATION(#62)
SHAPE_REPRESENTATION_RELATIONSHIP()
);
#286=(
REPRESENTATION_RELATIONSHIP($,$,#310901,#310898)
REPRESENTATION_RELATIONSHIP_WITH_TRANSFORMATION(#63)
SHAPE_REPRESENTATION_RELATIONSHIP()
);
#287=(
REPRESENTATION_RELATIONSHIP($,$,#310901,#310898)
REPRESENTATION_RELATIONSHIP_WITH_TRANSFORMATION(#64)
SHAPE_REPRESENTATION_RELATIONSHIP()
);
#288=(
REPRESENTATION_RELATIONSHIP($,$,#310901,#310898)
REPRESENTATION_RELATIONSHIP_WITH_TRANSFORMATION(#65)
SHAPE_REPRESENTATION_RELATIONSHIP()
);
#289=(
REPRESENTATION_RELATIONSHIP($,$,#310901,#310898)
REPRESENTATION_RELATIONSHIP_WITH_TRANSFORMATION(#66)
SHAPE_REPRESENTATION_RELATIONSHIP()
);
#290=(
REPRESENTATION_RELATIONSHIP($,$,#310901,#310898)
REPRESENTATION_RELATIONSHIP_WITH_TRANSFORMATION(#67)
SHAPE_REPRESENTATION_RELATIONSHIP()
);
#291=(
REPRESENTATION_RELATIONSHIP($,$,#310901,#310898)
REPRESENTATION_RELATIONSHIP_WITH_TRANSFORMATION(#68)
SHAPE_REPRESENTATION_RELATIONSHIP()
);
#292=(
REPRESENTATION_RELATIONSHIP($,$,#310901,#310898)
REPRESENTATION_RELATIONSHIP_WITH_TRANSFORMATION(#69)
SHAPE_REPRESENTATION_RELATIONSHIP()
);
#293=(
REPRESENTATION_RELATIONSHIP($,$,#310901,#310898)
REPRESENTATION_RELATIONSHIP_WITH_TRANSFORMATION(#70)
SHAPE_REPRESENTATION_RELATIONSHIP()
);
#294=(
REPRESENTATION_RELATIONSHIP($,$,#310901,#310898)
REPRESENTATION_RELATIONSHIP_WITH_TRANSFORMATION(#71)
SHAPE_REPRESENTATION_RELATIONSHIP()
);
#295=(
REPRESENTATION_RELATIONSHIP($,$,#310901,#310898)
REPRESENTATION_RELATIONSHIP_WITH_TRANSFORMATION(#72)
SHAPE_REPRESENTATION_RELATIONSHIP()
);
#296=(
REPRESENTATION_RELATIONSHIP($,$,#310901,#310898)
REPRESENTATION_RELATIONSHIP_WITH_TRANSFORMATION(#73)
SHAPE_REPRESENTATION_RELATIONSHIP()
);
#297=(
REPRESENTATION_RELATIONSHIP($,$,#310901,#310898)
REPRESENTATION_RELATIONSHIP_WITH_TRANSFORMATION(#74)
SHAPE_REPRESENTATION_RELATIONSHIP()
);
#298=(
REPRESENTATION_RELATIONSHIP($,$,#310901,#310898)
REPRESENTATION_RELATIONSHIP_WITH_TRANSFORMATION(#75)
SHAPE_REPRESENTATION_RELATIONSHIP()
);
#299=(
REPRESENTATION_RELATIONSHIP($,$,#310901,#310898)
REPRESENTATION_RELATIONSHIP_WITH_TRANSFORMATION(#76)
SHAPE_REPRESENTATION_RELATIONSHIP()
);
#300=(
REPRESENTATION_RELATIONSHIP($,$,#310901,#310898)
REPRESENTATION_RELATIONSHIP_WITH_TRANSFORMATION(#77)
SHAPE_REPRESENTATION_RELATIONSHIP()
);
#301=(
REPRESENTATION_RELATIONSHIP($,$,#310901,#310898)
REPRESENTATION_RELATIONSHIP_WITH_TRANSFORMATION(#78)
SHAPE_REPRESENTATION_RELATIONSHIP()
);
#302=(
REPRESENTATION_RELATIONSHIP($,$,#310901,#310898)
REPRESENTATION_RELATIONSHIP_WITH_TRANSFORMATION(#79)
SHAPE_REPRESENTATION_RELATIONSHIP()
);
#303=(
REPRESENTATION_RELATIONSHIP($,$,#310901,#310898)
REPRESENTATION_RELATIONSHIP_WITH_TRANSFORMATION(#80)
SHAPE_REPRESENTATION_RELATIONSHIP()
);
#304=(
REPRESENTATION_RELATIONSHIP($,$,#310901,#310898)
REPRESENTATION_RELATIONSHIP_WITH_TRANSFORMATION(#81)
SHAPE_REPRESENTATION_RELATIONSHIP()
);
#305=(
REPRESENTATION_RELATIONSHIP($,$,#310901,#310898)
REPRESENTATION_RELATIONSHIP_WITH_TRANSFORMATION(#82)
SHAPE_REPRESENTATION_RELATIONSHIP()
);
#306=(
REPRESENTATION_RELATIONSHIP($,$,#310901,#310898)
REPRESENTATION_RELATIONSHIP_WITH_TRANSFORMATION(#83)
SHAPE_REPRESENTATION_RELATIONSHIP()
);
#307=(
REPRESENTATION_RELATIONSHIP($,$,#310901,#310898)
REPRESENTATION_RELATIONSHIP_WITH_TRANSFORMATION(#84)
SHAPE_REPRESENTATION_RELATIONSHIP()
);
#308=(
REPRESENTATION_RELATIONSHIP($,$,#310901,#310898)
REPRESENTATION_RELATIONSHIP_WITH_TRANSFORMATION(#85)
SHAPE_REPRESENTATION_RELATIONSHIP()
);
#309=(
REPRESENTATION_RELATIONSHIP($,$,#310901,#310898)
REPRESENTATION_RELATIONSHIP_WITH_TRANSFORMATION(#86)
SHAPE_REPRESENTATION_RELATIONSHIP()
);
#310=(
REPRESENTATION_RELATIONSHIP($,$,#310901,#310898)
REPRESENTATION_RELATIONSHIP_WITH_TRANSFORMATION(#87)
SHAPE_REPRESENTATION_RELATIONSHIP()
);
#311=(
REPRESENTATION_RELATIONSHIP($,$,#310901,#310898)
REPRESENTATION_RELATIONSHIP_WITH_TRANSFORMATION(#88)
SHAPE_REPRESENTATION_RELATIONSHIP()
);
#312=(
REPRESENTATION_RELATIONSHIP($,$,#310901,#310898)
REPRESENTATION_RELATIONSHIP_WITH_TRANSFORMATION(#89)
SHAPE_REPRESENTATION_RELATIONSHIP()
);
#313=(
REPRESENTATION_RELATIONSHIP($,$,#310901,#310898)
REPRESENTATION_RELATIONSHIP_WITH_TRANSFORMATION(#90)
SHAPE_REPRESENTATION_RELATIONSHIP()
);
#314=(
REPRESENTATION_RELATIONSHIP($,$,#310901,#310898)
REPRESENTATION_RELATIONSHIP_WITH_TRANSFORMATION(#91)
SHAPE_REPRESENTATION_RELATIONSHIP()
);
#315=(
REPRESENTATION_RELATIONSHIP($,$,#310901,#310898)
REPRESENTATION_RELATIONSHIP_WITH_TRANSFORMATION(#92)
SHAPE_REPRESENTATION_RELATIONSHIP()
);
#316=(
REPRESENTATION_RELATIONSHIP($,$,#310901,#310898)
REPRESENTATION_RELATIONSHIP_WITH_TRANSFORMATION(#93)
SHAPE_REPRESENTATION_RELATIONSHIP()
);
#317=(
REPRESENTATION_RELATIONSHIP($,$,#310901,#310898)
REPRESENTATION_RELATIONSHIP_WITH_TRANSFORMATION(#94)
SHAPE_REPRESENTATION_RELATIONSHIP()
);
#318=(
REPRESENTATION_RELATIONSHIP($,$,#310901,#310898)
REPRESENTATION_RELATIONSHIP_WITH_TRANSFORMATION(#95)
SHAPE_REPRESENTATION_RELATIONSHIP()
);
#319=(
REPRESENTATION_RELATIONSHIP($,$,#310901,#310898)
REPRESENTATION_RELATIONSHIP_WITH_TRANSFORMATION(#96)
SHAPE_REPRESENTATION_RELATIONSHIP()
);
#320=(
REPRESENTATION_RELATIONSHIP($,$,#310901,#310898)
REPRESENTATION_RELATIONSHIP_WITH_TRANSFORMATION(#97)
SHAPE_REPRESENTATION_RELATIONSHIP()
);
#321=(
REPRESENTATION_RELATIONSHIP($,$,#310901,#310898)
REPRESENTATION_RELATIONSHIP_WITH_TRANSFORMATION(#98)
SHAPE_REPRESENTATION_RELATIONSHIP()
);
#322=(
REPRESENTATION_RELATIONSHIP($,$,#310901,#310898)
REPRESENTATION_RELATIONSHIP_WITH_TRANSFORMATION(#99)
SHAPE_REPRESENTATION_RELATIONSHIP()
);
#323=(
REPRESENTATION_RELATIONSHIP($,$,#310901,#310898)
REPRESENTATION_RELATIONSHIP_WITH_TRANSFORMATION(#100)
SHAPE_REPRESENTATION_RELATIONSHIP()
);
#324=(
REPRESENTATION_RELATIONSHIP($,$,#310901,#310898)
REPRESENTATION_RELATIONSHIP_WITH_TRANSFORMATION(#101)
SHAPE_REPRESENTATION_RELATIONSHIP()
);
#325=(
REPRESENTATION_RELATIONSHIP($,$,#310901,#310898)
REPRESENTATION_RELATIONSHIP_WITH_TRANSFORMATION(#102)
SHAPE_REPRESENTATION_RELATIONSHIP()
);
#326=(
REPRESENTATION_RELATIONSHIP($,$,#310901,#310898)
REPRESENTATION_RELATIONSHIP_WITH_TRANSFORMATION(#103)
SHAPE_REPRESENTATION_RELATIONSHIP()
);
#327=(
REPRESENTATION_RELATIONSHIP($,$,#310901,#310898)
REPRESENTATION_RELATIONSHIP_WITH_TRANSFORMATION(#104)
SHAPE_REPRESENTATION_RELATIONSHIP()
);
#328=(
REPRESENTATION_RELATIONSHIP($,$,#310901,#310898)
REPRESENTATION_RELATIONSHIP_WITH_TRANSFORMATION(#105)
SHAPE_REPRESENTATION_RELATIONSHIP()
);
#329=(
REPRESENTATION_RELATIONSHIP($,$,#310901,#310898)
REPRESENTATION_RELATIONSHIP_WITH_TRANSFORMATION(#106)
SHAPE_REPRESENTATION_RELATIONSHIP()
);
#330=(
REPRESENTATION_RELATIONSHIP($,$,#310901,#310898)
REPRESENTATION_RELATIONSHIP_WITH_TRANSFORMATION(#107)
SHAPE_REPRESENTATION_RELATIONSHIP()
);
#331=(
REPRESENTATION_RELATIONSHIP($,$,#310901,#310898)
REPRESENTATION_RELATIONSHIP_WITH_TRANSFORMATION(#108)
SHAPE_REPRESENTATION_RELATIONSHIP()
);
#332=(
REPRESENTATION_RELATIONSHIP($,$,#310901,#310898)
REPRESENTATION_RELATIONSHIP_WITH_TRANSFORMATION(#109)
SHAPE_REPRESENTATION_RELATIONSHIP()
);
#333=(
REPRESENTATION_RELATIONSHIP($,$,#310901,#310898)
REPRESENTATION_RELATIONSHIP_WITH_TRANSFORMATION(#110)
SHAPE_REPRESENTATION_RELATIONSHIP()
);
#334=(
REPRESENTATION_RELATIONSHIP($,$,#310901,#310898)
REPRESENTATION_RELATIONSHIP_WITH_TRANSFORMATION(#111)
SHAPE_REPRESENTATION_RELATIONSHIP()
);
#335=(
REPRESENTATION_RELATIONSHIP($,$,#310901,#310898)
REPRESENTATION_RELATIONSHIP_WITH_TRANSFORMATION(#112)
SHAPE_REPRESENTATION_RELATIONSHIP()
);
#336=(
REPRESENTATION_RELATIONSHIP($,$,#310901,#310898)
REPRESENTATION_RELATIONSHIP_WITH_TRANSFORMATION(#113)
SHAPE_REPRESENTATION_RELATIONSHIP()
);
#337=(
REPRESENTATION_RELATIONSHIP($,$,#310901,#310898)
REPRESENTATION_RELATIONSHIP_WITH_TRANSFORMATION(#114)
SHAPE_REPRESENTATION_RELATIONSHIP()
);
#338=(
REPRESENTATION_RELATIONSHIP($,$,#310901,#310898)
REPRESENTATION_RELATIONSHIP_WITH_TRANSFORMATION(#115)
SHAPE_REPRESENTATION_RELATIONSHIP()
);
#339=(
REPRESENTATION_RELATIONSHIP($,$,#310901,#310898)
REPRESENTATION_RELATIONSHIP_WITH_TRANSFORMATION(#116)
SHAPE_REPRESENTATION_RELATIONSHIP()
);
#340=(
REPRESENTATION_RELATIONSHIP($,$,#310901,#310898)
REPRESENTATION_RELATIONSHIP_WITH_TRANSFORMATION(#117)
SHAPE_REPRESENTATION_RELATIONSHIP()
);
#341=(
REPRESENTATION_RELATIONSHIP($,$,#310901,#310898)
REPRESENTATION_RELATIONSHIP_WITH_TRANSFORMATION(#118)
SHAPE_REPRESENTATION_RELATIONSHIP()
);
#342=(
REPRESENTATION_RELATIONSHIP($,$,#310901,#310898)
REPRESENTATION_RELATIONSHIP_WITH_TRANSFORMATION(#119)
SHAPE_REPRESENTATION_RELATIONSHIP()
);
#343=(
REPRESENTATION_RELATIONSHIP($,$,#310901,#310898)
REPRESENTATION_RELATIONSHIP_WITH_TRANSFORMATION(#120)
SHAPE_REPRESENTATION_RELATIONSHIP()
);
#344=(
REPRESENTATION_RELATIONSHIP($,$,#310901,#310898)
REPRESENTATION_RELATIONSHIP_WITH_TRANSFORMATION(#121)
SHAPE_REPRESENTATION_RELATIONSHIP()
);
#345=(
REPRESENTATION_RELATIONSHIP($,$,#310901,#310898)
REPRESENTATION_RELATIONSHIP_WITH_TRANSFORMATION(#122)
SHAPE_REPRESENTATION_RELATIONSHIP()
);
#346=(
REPRESENTATION_RELATIONSHIP($,$,#310901,#310898)
REPRESENTATION_RELATIONSHIP_WITH_TRANSFORMATION(#123)
SHAPE_REPRESENTATION_RELATIONSHIP()
);
#347=(
REPRESENTATION_RELATIONSHIP($,$,#310901,#310898)
REPRESENTATION_RELATIONSHIP_WITH_TRANSFORMATION(#124)
SHAPE_REPRESENTATION_RELATIONSHIP()
);
#348=(
REPRESENTATION_RELATIONSHIP($,$,#310901,#310898)
REPRESENTATION_RELATIONSHIP_WITH_TRANSFORMATION(#125)
SHAPE_REPRESENTATION_RELATIONSHIP()
);
#349=(
REPRESENTATION_RELATIONSHIP($,$,#310901,#310898)
REPRESENTATION_RELATIONSHIP_WITH_TRANSFORMATION(#126)
SHAPE_REPRESENTATION_RELATIONSHIP()
);
#350=(
REPRESENTATION_RELATIONSHIP($,$,#310901,#310898)
REPRESENTATION_RELATIONSHIP_WITH_TRANSFORMATION(#127)
SHAPE_REPRESENTATION_RELATIONSHIP()
);
#351=(
REPRESENTATION_RELATIONSHIP($,$,#310901,#310898)
REPRESENTATION_RELATIONSHIP_WITH_TRANSFORMATION(#128)
SHAPE_REPRESENTATION_RELATIONSHIP()
);
#352=(
REPRESENTATION_RELATIONSHIP($,$,#310901,#310898)
REPRESENTATION_RELATIONSHIP_WITH_TRANSFORMATION(#129)
SHAPE_REPRESENTATION_RELATIONSHIP()
);
#353=(
REPRESENTATION_RELATIONSHIP($,$,#310901,#310898)
REPRESENTATION_RELATIONSHIP_WITH_TRANSFORMATION(#130)
SHAPE_REPRESENTATION_RELATIONSHIP()
);
#354=(
REPRESENTATION_RELATIONSHIP($,$,#310901,#310898)
REPRESENTATION_RELATIONSHIP_WITH_TRANSFORMATION(#131)
SHAPE_REPRESENTATION_RELATIONSHIP()
);
#355=(
REPRESENTATION_RELATIONSHIP($,$,#310901,#310898)
REPRESENTATION_RELATIONSHIP_WITH_TRANSFORMATION(#132)
SHAPE_REPRESENTATION_RELATIONSHIP()
);
#356=(
REPRESENTATION_RELATIONSHIP($,$,#310901,#310898)
REPRESENTATION_RELATIONSHIP_WITH_TRANSFORMATION(#133)
SHAPE_REPRESENTATION_RELATIONSHIP()
);
#357=(
REPRESENTATION_RELATIONSHIP($,$,#310901,#310898)
REPRESENTATION_RELATIONSHIP_WITH_TRANSFORMATION(#134)
SHAPE_REPRESENTATION_RELATIONSHIP()
);
#358=(
REPRESENTATION_RELATIONSHIP($,$,#310901,#310898)
REPRESENTATION_RELATIONSHIP_WITH_TRANSFORMATION(#135)
SHAPE_REPRESENTATION_RELATIONSHIP()
);
#359=(
REPRESENTATION_RELATIONSHIP($,$,#310901,#310898)
REPRESENTATION_RELATIONSHIP_WITH_TRANSFORMATION(#136)
SHAPE_REPRESENTATION_RELATIONSHIP()
);
#360=(
REPRESENTATION_RELATIONSHIP($,$,#310901,#310898)
REPRESENTATION_RELATIONSHIP_WITH_TRANSFORMATION(#137)
SHAPE_REPRESENTATION_RELATIONSHIP()
);
#361=(
REPRESENTATION_RELATIONSHIP($,$,#310901,#310898)
REPRESENTATION_RELATIONSHIP_WITH_TRANSFORMATION(#138)
SHAPE_REPRESENTATION_RELATIONSHIP()
);
#362=(
REPRESENTATION_RELATIONSHIP($,$,#310901,#310898)
REPRESENTATION_RELATIONSHIP_WITH_TRANSFORMATION(#139)
SHAPE_REPRESENTATION_RELATIONSHIP()
);
#363=(
REPRESENTATION_RELATIONSHIP($,$,#310901,#310898)
REPRESENTATION_RELATIONSHIP_WITH_TRANSFORMATION(#140)
SHAPE_REPRESENTATION_RELATIONSHIP()
);
#364=(
REPRESENTATION_RELATIONSHIP($,$,#310901,#310898)
REPRESENTATION_RELATIONSHIP_WITH_TRANSFORMATION(#141)
SHAPE_REPRESENTATION_RELATIONSHIP()
);
#365=(
REPRESENTATION_RELATIONSHIP($,$,#310901,#310898)
REPRESENTATION_RELATIONSHIP_WITH_TRANSFORMATION(#142)
SHAPE_REPRESENTATION_RELATIONSHIP()
);
#366=(
REPRESENTATION_RELATIONSHIP($,$,#310901,#310898)
REPRESENTATION_RELATIONSHIP_WITH_TRANSFORMATION(#143)
SHAPE_REPRESENTATION_RELATIONSHIP()
);
#367=(
REPRESENTATION_RELATIONSHIP($,$,#310901,#310898)
REPRESENTATION_RELATIONSHIP_WITH_TRANSFORMATION(#144)
SHAPE_REPRESENTATION_RELATIONSHIP()
);
#368=(
REPRESENTATION_RELATIONSHIP($,$,#310901,#310898)
REPRESENTATION_RELATIONSHIP_WITH_TRANSFORMATION(#145)
SHAPE_REPRESENTATION_RELATIONSHIP()
);
#369=(
REPRESENTATION_RELATIONSHIP($,$,#310901,#310898)
REPRESENTATION_RELATIONSHIP_WITH_TRANSFORMATION(#146)
SHAPE_REPRESENTATION_RELATIONSHIP()
);
#370=(
REPRESENTATION_RELATIONSHIP($,$,#310901,#310898)
REPRESENTATION_RELATIONSHIP_WITH_TRANSFORMATION(#147)
SHAPE_REPRESENTATION_RELATIONSHIP()
);
#371=(
REPRESENTATION_RELATIONSHIP($,$,#310901,#310898)
REPRESENTATION_RELATIONSHIP_WITH_TRANSFORMATION(#148)
SHAPE_REPRESENTATION_RELATIONSHIP()
);
#372=(
REPRESENTATION_RELATIONSHIP($,$,#310901,#310898)
REPRESENTATION_RELATIONSHIP_WITH_TRANSFORMATION(#149)
SHAPE_REPRESENTATION_RELATIONSHIP()
);
#373=(
REPRESENTATION_RELATIONSHIP($,$,#310901,#310898)
REPRESENTATION_RELATIONSHIP_WITH_TRANSFORMATION(#150)
SHAPE_REPRESENTATION_RELATIONSHIP()
);
#374=(
REPRESENTATION_RELATIONSHIP($,$,#310909,#310908)
REPRESENTATION_RELATIONSHIP_WITH_TRANSFORMATION(#151)
SHAPE_REPRESENTATION_RELATIONSHIP()
);
#375=(
REPRESENTATION_RELATIONSHIP($,$,#310910,#310908)
REPRESENTATION_RELATIONSHIP_WITH_TRANSFORMATION(#152)
SHAPE_REPRESENTATION_RELATIONSHIP()
);
#376=(
REPRESENTATION_RELATIONSHIP($,$,#310912,#310911)
REPRESENTATION_RELATIONSHIP_WITH_TRANSFORMATION(#153)
SHAPE_REPRESENTATION_RELATIONSHIP()
);
#377=(
REPRESENTATION_RELATIONSHIP($,$,#310913,#310911)
REPRESENTATION_RELATIONSHIP_WITH_TRANSFORMATION(#154)
SHAPE_REPRESENTATION_RELATIONSHIP()
);
#378=(
REPRESENTATION_RELATIONSHIP($,$,#310894,#310893)
REPRESENTATION_RELATIONSHIP_WITH_TRANSFORMATION(#155)
SHAPE_REPRESENTATION_RELATIONSHIP()
);
#379=(
REPRESENTATION_RELATIONSHIP($,$,#310895,#310893)
REPRESENTATION_RELATIONSHIP_WITH_TRANSFORMATION(#156)
SHAPE_REPRESENTATION_RELATIONSHIP()
);
#380=(
REPRESENTATION_RELATIONSHIP($,$,#310902,#310893)
REPRESENTATION_RELATIONSHIP_WITH_TRANSFORMATION(#157)
SHAPE_REPRESENTATION_RELATIONSHIP()
);
#381=(
REPRESENTATION_RELATIONSHIP($,$,#310903,#310893)
REPRESENTATION_RELATIONSHIP_WITH_TRANSFORMATION(#158)
SHAPE_REPRESENTATION_RELATIONSHIP()
);
#382=(
REPRESENTATION_RELATIONSHIP($,$,#310904,#310893)
REPRESENTATION_RELATIONSHIP_WITH_TRANSFORMATION(#159)
SHAPE_REPRESENTATION_RELATIONSHIP()
);
#383=(
REPRESENTATION_RELATIONSHIP($,$,#310908,#310893)
REPRESENTATION_RELATIONSHIP_WITH_TRANSFORMATION(#160)
SHAPE_REPRESENTATION_RELATIONSHIP()
);
#384=(
REPRESENTATION_RELATIONSHIP($,$,#310905,#310893)
REPRESENTATION_RELATIONSHIP_WITH_TRANSFORMATION(#161)
SHAPE_REPRESENTATION_RELATIONSHIP()
);
#385=(
REPRESENTATION_RELATIONSHIP($,$,#310906,#310893)
REPRESENTATION_RELATIONSHIP_WITH_TRANSFORMATION(#162)
SHAPE_REPRESENTATION_RELATIONSHIP()
);
#386=(
REPRESENTATION_RELATIONSHIP($,$,#310896,#310893)
REPRESENTATION_RELATIONSHIP_WITH_TRANSFORMATION(#163)
SHAPE_REPRESENTATION_RELATIONSHIP()
);
#387=(
REPRESENTATION_RELATIONSHIP($,$,#310907,#310893)
REPRESENTATION_RELATIONSHIP_WITH_TRANSFORMATION(#164)
SHAPE_REPRESENTATION_RELATIONSHIP()
);
#388=(
REPRESENTATION_RELATIONSHIP($,$,#310911,#310893)
REPRESENTATION_RELATIONSHIP_WITH_TRANSFORMATION(#165)
SHAPE_REPRESENTATION_RELATIONSHIP()
);
#389=(
REPRESENTATION_RELATIONSHIP($,$,#310897,#310893)
REPRESENTATION_RELATIONSHIP_WITH_TRANSFORMATION(#166)
SHAPE_REPRESENTATION_RELATIONSHIP()
);
#390=(
REPRESENTATION_RELATIONSHIP($,$,#310898,#310893)
REPRESENTATION_RELATIONSHIP_WITH_TRANSFORMATION(#167)
SHAPE_REPRESENTATION_RELATIONSHIP()
);
#391=(
REPRESENTATION_RELATIONSHIP($,$,#310902,#310893)
REPRESENTATION_RELATIONSHIP_WITH_TRANSFORMATION(#168)
SHAPE_REPRESENTATION_RELATIONSHIP()
);
#392=(
REPRESENTATION_RELATIONSHIP($,$,#310902,#310893)
REPRESENTATION_RELATIONSHIP_WITH_TRANSFORMATION(#169)
SHAPE_REPRESENTATION_RELATIONSHIP()
);
#393=(
REPRESENTATION_RELATIONSHIP($,$,#310902,#310893)
REPRESENTATION_RELATIONSHIP_WITH_TRANSFORMATION(#170)
SHAPE_REPRESENTATION_RELATIONSHIP()
);
#394=(
REPRESENTATION_RELATIONSHIP($,$,#310902,#310893)
REPRESENTATION_RELATIONSHIP_WITH_TRANSFORMATION(#171)
SHAPE_REPRESENTATION_RELATIONSHIP()
);
#395=(
REPRESENTATION_RELATIONSHIP($,$,#310902,#310893)
REPRESENTATION_RELATIONSHIP_WITH_TRANSFORMATION(#172)
SHAPE_REPRESENTATION_RELATIONSHIP()
);
#396=(
REPRESENTATION_RELATIONSHIP($,$,#310902,#310893)
REPRESENTATION_RELATIONSHIP_WITH_TRANSFORMATION(#173)
SHAPE_REPRESENTATION_RELATIONSHIP()
);
#397=(
REPRESENTATION_RELATIONSHIP($,$,#310902,#310893)
REPRESENTATION_RELATIONSHIP_WITH_TRANSFORMATION(#174)
SHAPE_REPRESENTATION_RELATIONSHIP()
);
#398=(
REPRESENTATION_RELATIONSHIP($,$,#310902,#310893)
REPRESENTATION_RELATIONSHIP_WITH_TRANSFORMATION(#175)
SHAPE_REPRESENTATION_RELATIONSHIP()
);
#399=(
REPRESENTATION_RELATIONSHIP($,$,#310902,#310893)
REPRESENTATION_RELATIONSHIP_WITH_TRANSFORMATION(#176)
SHAPE_REPRESENTATION_RELATIONSHIP()
);
#400=(
REPRESENTATION_RELATIONSHIP($,$,#310902,#310893)
REPRESENTATION_RELATIONSHIP_WITH_TRANSFORMATION(#177)
SHAPE_REPRESENTATION_RELATIONSHIP()
);
#401=(
REPRESENTATION_RELATIONSHIP($,$,#310902,#310893)
REPRESENTATION_RELATIONSHIP_WITH_TRANSFORMATION(#178)
SHAPE_REPRESENTATION_RELATIONSHIP()
);
#402=(
REPRESENTATION_RELATIONSHIP($,$,#310903,#310893)
REPRESENTATION_RELATIONSHIP_WITH_TRANSFORMATION(#179)
SHAPE_REPRESENTATION_RELATIONSHIP()
);
#403=(
REPRESENTATION_RELATIONSHIP($,$,#310903,#310893)
REPRESENTATION_RELATIONSHIP_WITH_TRANSFORMATION(#180)
SHAPE_REPRESENTATION_RELATIONSHIP()
);
#404=(
REPRESENTATION_RELATIONSHIP($,$,#310903,#310893)
REPRESENTATION_RELATIONSHIP_WITH_TRANSFORMATION(#181)
SHAPE_REPRESENTATION_RELATIONSHIP()
);
#405=(
REPRESENTATION_RELATIONSHIP($,$,#310903,#310893)
REPRESENTATION_RELATIONSHIP_WITH_TRANSFORMATION(#182)
SHAPE_REPRESENTATION_RELATIONSHIP()
);
#406=(
REPRESENTATION_RELATIONSHIP($,$,#310903,#310893)
REPRESENTATION_RELATIONSHIP_WITH_TRANSFORMATION(#183)
SHAPE_REPRESENTATION_RELATIONSHIP()
);
#407=(
REPRESENTATION_RELATIONSHIP($,$,#310903,#310893)
REPRESENTATION_RELATIONSHIP_WITH_TRANSFORMATION(#184)
SHAPE_REPRESENTATION_RELATIONSHIP()
);
#408=(
REPRESENTATION_RELATIONSHIP($,$,#310903,#310893)
REPRESENTATION_RELATIONSHIP_WITH_TRANSFORMATION(#185)
SHAPE_REPRESENTATION_RELATIONSHIP()
);
#409=(
REPRESENTATION_RELATIONSHIP($,$,#310903,#310893)
REPRESENTATION_RELATIONSHIP_WITH_TRANSFORMATION(#186)
SHAPE_REPRESENTATION_RELATIONSHIP()
);
#410=(
REPRESENTATION_RELATIONSHIP($,$,#310903,#310893)
REPRESENTATION_RELATIONSHIP_WITH_TRANSFORMATION(#187)
SHAPE_REPRESENTATION_RELATIONSHIP()
);
#411=(
REPRESENTATION_RELATIONSHIP($,$,#310903,#310893)
REPRESENTATION_RELATIONSHIP_WITH_TRANSFORMATION(#188)
SHAPE_REPRESENTATION_RELATIONSHIP()
);
#412=(
REPRESENTATION_RELATIONSHIP($,$,#310903,#310893)
REPRESENTATION_RELATIONSHIP_WITH_TRANSFORMATION(#189)
SHAPE_REPRESENTATION_RELATIONSHIP()
);
#413=(
REPRESENTATION_RELATIONSHIP($,$,#310903,#310893)
REPRESENTATION_RELATIONSHIP_WITH_TRANSFORMATION(#190)
SHAPE_REPRESENTATION_RELATIONSHIP()
);
#414=(
REPRESENTATION_RELATIONSHIP($,$,#310903,#310893)
REPRESENTATION_RELATIONSHIP_WITH_TRANSFORMATION(#191)
SHAPE_REPRESENTATION_RELATIONSHIP()
);
#415=(
REPRESENTATION_RELATIONSHIP($,$,#310903,#310893)
REPRESENTATION_RELATIONSHIP_WITH_TRANSFORMATION(#192)
SHAPE_REPRESENTATION_RELATIONSHIP()
);
#416=(
REPRESENTATION_RELATIONSHIP($,$,#310903,#310893)
REPRESENTATION_RELATIONSHIP_WITH_TRANSFORMATION(#193)
SHAPE_REPRESENTATION_RELATIONSHIP()
);
#417=(
REPRESENTATION_RELATIONSHIP($,$,#310903,#310893)
REPRESENTATION_RELATIONSHIP_WITH_TRANSFORMATION(#194)
SHAPE_REPRESENTATION_RELATIONSHIP()
);
#418=(
REPRESENTATION_RELATIONSHIP($,$,#310903,#310893)
REPRESENTATION_RELATIONSHIP_WITH_TRANSFORMATION(#195)
SHAPE_REPRESENTATION_RELATIONSHIP()
);
#419=(
REPRESENTATION_RELATIONSHIP($,$,#310903,#310893)
REPRESENTATION_RELATIONSHIP_WITH_TRANSFORMATION(#196)
SHAPE_REPRESENTATION_RELATIONSHIP()
);
#420=(
REPRESENTATION_RELATIONSHIP($,$,#310903,#310893)
REPRESENTATION_RELATIONSHIP_WITH_TRANSFORMATION(#197)
SHAPE_REPRESENTATION_RELATIONSHIP()
);
#421=(
REPRESENTATION_RELATIONSHIP($,$,#310903,#310893)
REPRESENTATION_RELATIONSHIP_WITH_TRANSFORMATION(#198)
SHAPE_REPRESENTATION_RELATIONSHIP()
);
#422=(
REPRESENTATION_RELATIONSHIP($,$,#310903,#310893)
REPRESENTATION_RELATIONSHIP_WITH_TRANSFORMATION(#199)
SHAPE_REPRESENTATION_RELATIONSHIP()
);
#423=(
REPRESENTATION_RELATIONSHIP($,$,#310903,#310893)
REPRESENTATION_RELATIONSHIP_WITH_TRANSFORMATION(#200)
SHAPE_REPRESENTATION_RELATIONSHIP()
);
#424=(
REPRESENTATION_RELATIONSHIP($,$,#310903,#310893)
REPRESENTATION_RELATIONSHIP_WITH_TRANSFORMATION(#201)
SHAPE_REPRESENTATION_RELATIONSHIP()
);
#425=(
REPRESENTATION_RELATIONSHIP($,$,#310904,#310893)
REPRESENTATION_RELATIONSHIP_WITH_TRANSFORMATION(#202)
SHAPE_REPRESENTATION_RELATIONSHIP()
);
#426=(
REPRESENTATION_RELATIONSHIP($,$,#310904,#310893)
REPRESENTATION_RELATIONSHIP_WITH_TRANSFORMATION(#203)
SHAPE_REPRESENTATION_RELATIONSHIP()
);
#427=(
REPRESENTATION_RELATIONSHIP($,$,#310904,#310893)
REPRESENTATION_RELATIONSHIP_WITH_TRANSFORMATION(#204)
SHAPE_REPRESENTATION_RELATIONSHIP()
);
#428=(
REPRESENTATION_RELATIONSHIP($,$,#310904,#310893)
REPRESENTATION_RELATIONSHIP_WITH_TRANSFORMATION(#205)
SHAPE_REPRESENTATION_RELATIONSHIP()
);
#429=(
REPRESENTATION_RELATIONSHIP($,$,#310904,#310893)
REPRESENTATION_RELATIONSHIP_WITH_TRANSFORMATION(#206)
SHAPE_REPRESENTATION_RELATIONSHIP()
);
#430=(
REPRESENTATION_RELATIONSHIP($,$,#310904,#310893)
REPRESENTATION_RELATIONSHIP_WITH_TRANSFORMATION(#207)
SHAPE_REPRESENTATION_RELATIONSHIP()
);
#431=(
REPRESENTATION_RELATIONSHIP($,$,#310904,#310893)
REPRESENTATION_RELATIONSHIP_WITH_TRANSFORMATION(#208)
SHAPE_REPRESENTATION_RELATIONSHIP()
);
#432=(
REPRESENTATION_RELATIONSHIP($,$,#310904,#310893)
REPRESENTATION_RELATIONSHIP_WITH_TRANSFORMATION(#209)
SHAPE_REPRESENTATION_RELATIONSHIP()
);
#433=(
REPRESENTATION_RELATIONSHIP($,$,#310904,#310893)
REPRESENTATION_RELATIONSHIP_WITH_TRANSFORMATION(#210)
SHAPE_REPRESENTATION_RELATIONSHIP()
);
#434=(
REPRESENTATION_RELATIONSHIP($,$,#310904,#310893)
REPRESENTATION_RELATIONSHIP_WITH_TRANSFORMATION(#211)
SHAPE_REPRESENTATION_RELATIONSHIP()
);
#435=(
REPRESENTATION_RELATIONSHIP($,$,#310904,#310893)
REPRESENTATION_RELATIONSHIP_WITH_TRANSFORMATION(#212)
SHAPE_REPRESENTATION_RELATIONSHIP()
);
#436=(
REPRESENTATION_RELATIONSHIP($,$,#310909,#310893)
REPRESENTATION_RELATIONSHIP_WITH_TRANSFORMATION(#213)
SHAPE_REPRESENTATION_RELATIONSHIP()
);
#437=(
REPRESENTATION_RELATIONSHIP($,$,#310910,#310893)
REPRESENTATION_RELATIONSHIP_WITH_TRANSFORMATION(#214)
SHAPE_REPRESENTATION_RELATIONSHIP()
);
#438=(
REPRESENTATION_RELATIONSHIP($,$,#310905,#310893)
REPRESENTATION_RELATIONSHIP_WITH_TRANSFORMATION(#215)
SHAPE_REPRESENTATION_RELATIONSHIP()
);
#439=(
REPRESENTATION_RELATIONSHIP($,$,#310905,#310893)
REPRESENTATION_RELATIONSHIP_WITH_TRANSFORMATION(#216)
SHAPE_REPRESENTATION_RELATIONSHIP()
);
#440=(
REPRESENTATION_RELATIONSHIP($,$,#310910,#310893)
REPRESENTATION_RELATIONSHIP_WITH_TRANSFORMATION(#217)
SHAPE_REPRESENTATION_RELATIONSHIP()
);
#441=(
REPRESENTATION_RELATIONSHIP($,$,#310905,#310893)
REPRESENTATION_RELATIONSHIP_WITH_TRANSFORMATION(#218)
SHAPE_REPRESENTATION_RELATIONSHIP()
);
#442=(
REPRESENTATION_RELATIONSHIP($,$,#310906,#310893)
REPRESENTATION_RELATIONSHIP_WITH_TRANSFORMATION(#219)
SHAPE_REPRESENTATION_RELATIONSHIP()
);
#443=(
REPRESENTATION_RELATIONSHIP($,$,#310909,#310893)
REPRESENTATION_RELATIONSHIP_WITH_TRANSFORMATION(#220)
SHAPE_REPRESENTATION_RELATIONSHIP()
);
#444=(
REPRESENTATION_RELATIONSHIP($,$,#310907,#310893)
REPRESENTATION_RELATIONSHIP_WITH_TRANSFORMATION(#221)
SHAPE_REPRESENTATION_RELATIONSHIP()
);
#445=(
REPRESENTATION_RELATIONSHIP($,$,#310907,#310893)
REPRESENTATION_RELATIONSHIP_WITH_TRANSFORMATION(#222)
SHAPE_REPRESENTATION_RELATIONSHIP()
);
#446=(
REPRESENTATION_RELATIONSHIP($,$,#310907,#310893)
REPRESENTATION_RELATIONSHIP_WITH_TRANSFORMATION(#223)
SHAPE_REPRESENTATION_RELATIONSHIP()
);
#447=(
REPRESENTATION_RELATIONSHIP($,$,#310911,#310893)
REPRESENTATION_RELATIONSHIP_WITH_TRANSFORMATION(#224)
SHAPE_REPRESENTATION_RELATIONSHIP()
);
#448=(
REPRESENTATION_RELATIONSHIP($,$,#310911,#310893)
REPRESENTATION_RELATIONSHIP_WITH_TRANSFORMATION(#225)
SHAPE_REPRESENTATION_RELATIONSHIP()
);
#449=(
REPRESENTATION_RELATIONSHIP($,$,#310911,#310893)
REPRESENTATION_RELATIONSHIP_WITH_TRANSFORMATION(#226)
SHAPE_REPRESENTATION_RELATIONSHIP()
);
#450=(
REPRESENTATION_RELATIONSHIP($,$,#310911,#310893)
REPRESENTATION_RELATIONSHIP_WITH_TRANSFORMATION(#227)
SHAPE_REPRESENTATION_RELATIONSHIP()
);
#451=(
REPRESENTATION_RELATIONSHIP($,$,#310911,#310893)
REPRESENTATION_RELATIONSHIP_WITH_TRANSFORMATION(#228)
SHAPE_REPRESENTATION_RELATIONSHIP()
);
#452=(
REPRESENTATION_RELATIONSHIP($,$,#310908,#310893)
REPRESENTATION_RELATIONSHIP_WITH_TRANSFORMATION(#229)
SHAPE_REPRESENTATION_RELATIONSHIP()
);
#453=(
REPRESENTATION_RELATIONSHIP($,$,#310911,#310893)
REPRESENTATION_RELATIONSHIP_WITH_TRANSFORMATION(#230)
SHAPE_REPRESENTATION_RELATIONSHIP()
);
#454=(
REPRESENTATION_RELATIONSHIP($,$,#310911,#310893)
REPRESENTATION_RELATIONSHIP_WITH_TRANSFORMATION(#231)
SHAPE_REPRESENTATION_RELATIONSHIP()
);
#455=(
REPRESENTATION_RELATIONSHIP($,$,#310911,#310893)
REPRESENTATION_RELATIONSHIP_WITH_TRANSFORMATION(#232)
SHAPE_REPRESENTATION_RELATIONSHIP()
);
#456=(
REPRESENTATION_RELATIONSHIP($,$,#310911,#310893)
REPRESENTATION_RELATIONSHIP_WITH_TRANSFORMATION(#233)
SHAPE_REPRESENTATION_RELATIONSHIP()
);
#457=(
REPRESENTATION_RELATIONSHIP($,$,#310911,#310893)
REPRESENTATION_RELATIONSHIP_WITH_TRANSFORMATION(#234)
SHAPE_REPRESENTATION_RELATIONSHIP()
);
#458=(
REPRESENTATION_RELATIONSHIP($,$,#310911,#310893)
REPRESENTATION_RELATIONSHIP_WITH_TRANSFORMATION(#235)
SHAPE_REPRESENTATION_RELATIONSHIP()
);
#459=CONTEXT_DEPENDENT_SHAPE_REPRESENTATION(#236,#310658);
#460=CONTEXT_DEPENDENT_SHAPE_REPRESENTATION(#237,#310659);
#461=CONTEXT_DEPENDENT_SHAPE_REPRESENTATION(#238,#310660);
#462=CONTEXT_DEPENDENT_SHAPE_REPRESENTATION(#239,#310661);
#463=CONTEXT_DEPENDENT_SHAPE_REPRESENTATION(#240,#310662);
#464=CONTEXT_DEPENDENT_SHAPE_REPRESENTATION(#241,#310663);
#465=CONTEXT_DEPENDENT_SHAPE_REPRESENTATION(#242,#310664);
#466=CONTEXT_DEPENDENT_SHAPE_REPRESENTATION(#243,#310665);
#467=CONTEXT_DEPENDENT_SHAPE_REPRESENTATION(#244,#310666);
#468=CONTEXT_DEPENDENT_SHAPE_REPRESENTATION(#245,#310667);
#469=CONTEXT_DEPENDENT_SHAPE_REPRESENTATION(#246,#310668);
#470=CONTEXT_DEPENDENT_SHAPE_REPRESENTATION(#247,#310669);
#471=CONTEXT_DEPENDENT_SHAPE_REPRESENTATION(#248,#310670);
#472=CONTEXT_DEPENDENT_SHAPE_REPRESENTATION(#249,#310671);
#473=CONTEXT_DEPENDENT_SHAPE_REPRESENTATION(#250,#310672);
#474=CONTEXT_DEPENDENT_SHAPE_REPRESENTATION(#251,#310673);
#475=CONTEXT_DEPENDENT_SHAPE_REPRESENTATION(#252,#310674);
#476=CONTEXT_DEPENDENT_SHAPE_REPRESENTATION(#253,#310675);
#477=CONTEXT_DEPENDENT_SHAPE_REPRESENTATION(#254,#310676);
#478=CONTEXT_DEPENDENT_SHAPE_REPRESENTATION(#255,#310677);
#479=CONTEXT_DEPENDENT_SHAPE_REPRESENTATION(#256,#310678);
#480=CONTEXT_DEPENDENT_SHAPE_REPRESENTATION(#257,#310679);
#481=CONTEXT_DEPENDENT_SHAPE_REPRESENTATION(#258,#310680);
#482=CONTEXT_DEPENDENT_SHAPE_REPRESENTATION(#259,#310681);
#483=CONTEXT_DEPENDENT_SHAPE_REPRESENTATION(#260,#310682);
#484=CONTEXT_DEPENDENT_SHAPE_REPRESENTATION(#261,#310683);
#485=CONTEXT_DEPENDENT_SHAPE_REPRESENTATION(#262,#310684);
#486=CONTEXT_DEPENDENT_SHAPE_REPRESENTATION(#263,#310685);
#487=CONTEXT_DEPENDENT_SHAPE_REPRESENTATION(#264,#310686);
#488=CONTEXT_DEPENDENT_SHAPE_REPRESENTATION(#265,#310687);
#489=CONTEXT_DEPENDENT_SHAPE_REPRESENTATION(#266,#310688);
#490=CONTEXT_DEPENDENT_SHAPE_REPRESENTATION(#267,#310689);
#491=CONTEXT_DEPENDENT_SHAPE_REPRESENTATION(#268,#310690);
#492=CONTEXT_DEPENDENT_SHAPE_REPRESENTATION(#269,#310691);
#493=CONTEXT_DEPENDENT_SHAPE_REPRESENTATION(#270,#310692);
#494=CONTEXT_DEPENDENT_SHAPE_REPRESENTATION(#271,#310693);
#495=CONTEXT_DEPENDENT_SHAPE_REPRESENTATION(#272,#310694);
#496=CONTEXT_DEPENDENT_SHAPE_REPRESENTATION(#273,#310695);
#497=CONTEXT_DEPENDENT_SHAPE_REPRESENTATION(#274,#310696);
#498=CONTEXT_DEPENDENT_SHAPE_REPRESENTATION(#275,#310697);
#499=CONTEXT_DEPENDENT_SHAPE_REPRESENTATION(#276,#310698);
#500=CONTEXT_DEPENDENT_SHAPE_REPRESENTATION(#277,#310699);
#501=CONTEXT_DEPENDENT_SHAPE_REPRESENTATION(#278,#310700);
#502=CONTEXT_DEPENDENT_SHAPE_REPRESENTATION(#279,#310701);
#503=CONTEXT_DEPENDENT_SHAPE_REPRESENTATION(#280,#310702);
#504=CONTEXT_DEPENDENT_SHAPE_REPRESENTATION(#281,#310703);
#505=CONTEXT_DEPENDENT_SHAPE_REPRESENTATION(#282,#310704);
#506=CONTEXT_DEPENDENT_SHAPE_REPRESENTATION(#283,#310705);
#507=CONTEXT_DEPENDENT_SHAPE_REPRESENTATION(#284,#310706);
#508=CONTEXT_DEPENDENT_SHAPE_REPRESENTATION(#285,#310707);
#509=CONTEXT_DEPENDENT_SHAPE_REPRESENTATION(#286,#310708);
#510=CONTEXT_DEPENDENT_SHAPE_REPRESENTATION(#287,#310709);
#511=CONTEXT_DEPENDENT_SHAPE_REPRESENTATION(#288,#310710);
#512=CONTEXT_DEPENDENT_SHAPE_REPRESENTATION(#289,#310711);
#513=CONTEXT_DEPENDENT_SHAPE_REPRESENTATION(#290,#310712);
#514=CONTEXT_DEPENDENT_SHAPE_REPRESENTATION(#291,#310713);
#515=CONTEXT_DEPENDENT_SHAPE_REPRESENTATION(#292,#310714);
#516=CONTEXT_DEPENDENT_SHAPE_REPRESENTATION(#293,#310715);
#517=CONTEXT_DEPENDENT_SHAPE_REPRESENTATION(#294,#310716);
#518=CONTEXT_DEPENDENT_SHAPE_REPRESENTATION(#295,#310717);
#519=CONTEXT_DEPENDENT_SHAPE_REPRESENTATION(#296,#310718);
#520=CONTEXT_DEPENDENT_SHAPE_REPRESENTATION(#297,#310719);
#521=CONTEXT_DEPENDENT_SHAPE_REPRESENTATION(#298,#310720);
#522=CONTEXT_DEPENDENT_SHAPE_REPRESENTATION(#299,#310721);
#523=CONTEXT_DEPENDENT_SHAPE_REPRESENTATION(#300,#310722);
#524=CONTEXT_DEPENDENT_SHAPE_REPRESENTATION(#301,#310723);
#525=CONTEXT_DEPENDENT_SHAPE_REPRESENTATION(#302,#310724);
#526=CONTEXT_DEPENDENT_SHAPE_REPRESENTATION(#303,#310725);
#527=CONTEXT_DEPENDENT_SHAPE_REPRESENTATION(#304,#310726);
#528=CONTEXT_DEPENDENT_SHAPE_REPRESENTATION(#305,#310727);
#529=CONTEXT_DEPENDENT_SHAPE_REPRESENTATION(#306,#310728);
#530=CONTEXT_DEPENDENT_SHAPE_REPRESENTATION(#307,#310729);
#531=CONTEXT_DEPENDENT_SHAPE_REPRESENTATION(#308,#310730);
#532=CONTEXT_DEPENDENT_SHAPE_REPRESENTATION(#309,#310731);
#533=CONTEXT_DEPENDENT_SHAPE_REPRESENTATION(#310,#310732);
#534=CONTEXT_DEPENDENT_SHAPE_REPRESENTATION(#311,#310733);
#535=CONTEXT_DEPENDENT_SHAPE_REPRESENTATION(#312,#310734);
#536=CONTEXT_DEPENDENT_SHAPE_REPRESENTATION(#313,#310735);
#537=CONTEXT_DEPENDENT_SHAPE_REPRESENTATION(#314,#310736);
#538=CONTEXT_DEPENDENT_SHAPE_REPRESENTATION(#315,#310737);
#539=CONTEXT_DEPENDENT_SHAPE_REPRESENTATION(#316,#310738);
#540=CONTEXT_DEPENDENT_SHAPE_REPRESENTATION(#317,#310739);
#541=CONTEXT_DEPENDENT_SHAPE_REPRESENTATION(#318,#310740);
#542=CONTEXT_DEPENDENT_SHAPE_REPRESENTATION(#319,#310741);
#543=CONTEXT_DEPENDENT_SHAPE_REPRESENTATION(#320,#310742);
#544=CONTEXT_DEPENDENT_SHAPE_REPRESENTATION(#321,#310743);
#545=CONTEXT_DEPENDENT_SHAPE_REPRESENTATION(#322,#310744);
#546=CONTEXT_DEPENDENT_SHAPE_REPRESENTATION(#323,#310745);
#547=CONTEXT_DEPENDENT_SHAPE_REPRESENTATION(#324,#310746);
#548=CONTEXT_DEPENDENT_SHAPE_REPRESENTATION(#325,#310747);
#549=CONTEXT_DEPENDENT_SHAPE_REPRESENTATION(#326,#310748);
#550=CONTEXT_DEPENDENT_SHAPE_REPRESENTATION(#327,#310749);
#551=CONTEXT_DEPENDENT_SHAPE_REPRESENTATION(#328,#310750);
#552=CONTEXT_DEPENDENT_SHAPE_REPRESENTATION(#329,#310751);
#553=CONTEXT_DEPENDENT_SHAPE_REPRESENTATION(#330,#310752);
#554=CONTEXT_DEPENDENT_SHAPE_REPRESENTATION(#331,#310753);
#555=CONTEXT_DEPENDENT_SHAPE_REPRESENTATION(#332,#310754);
#556=CONTEXT_DEPENDENT_SHAPE_REPRESENTATION(#333,#310755);
#557=CONTEXT_DEPENDENT_SHAPE_REPRESENTATION(#334,#310756);
#558=CONTEXT_DEPENDENT_SHAPE_REPRESENTATION(#335,#310757);
#559=CONTEXT_DEPENDENT_SHAPE_REPRESENTATION(#336,#310758);
#560=CONTEXT_DEPENDENT_SHAPE_REPRESENTATION(#337,#310759);
#561=CONTEXT_DEPENDENT_SHAPE_REPRESENTATION(#338,#310760);
#562=CONTEXT_DEPENDENT_SHAPE_REPRESENTATION(#339,#310761);
#563=CONTEXT_DEPENDENT_SHAPE_REPRESENTATION(#340,#310762);
#564=CONTEXT_DEPENDENT_SHAPE_REPRESENTATION(#341,#310763);
#565=CONTEXT_DEPENDENT_SHAPE_REPRESENTATION(#342,#310764);
#566=CONTEXT_DEPENDENT_SHAPE_REPRESENTATION(#343,#310765);
#567=CONTEXT_DEPENDENT_SHAPE_REPRESENTATION(#344,#310766);
#568=CONTEXT_DEPENDENT_SHAPE_REPRESENTATION(#345,#310767);
#569=CONTEXT_DEPENDENT_SHAPE_REPRESENTATION(#346,#310768);
#570=CONTEXT_DEPENDENT_SHAPE_REPRESENTATION(#347,#310769);
#571=CONTEXT_DEPENDENT_SHAPE_REPRESENTATION(#348,#310770);
#572=CONTEXT_DEPENDENT_SHAPE_REPRESENTATION(#349,#310771);
#573=CONTEXT_DEPENDENT_SHAPE_REPRESENTATION(#350,#310772);
#574=CONTEXT_DEPENDENT_SHAPE_REPRESENTATION(#351,#310773);
#575=CONTEXT_DEPENDENT_SHAPE_REPRESENTATION(#352,#310774);
#576=CONTEXT_DEPENDENT_SHAPE_REPRESENTATION(#353,#310775);
#577=CONTEXT_DEPENDENT_SHAPE_REPRESENTATION(#354,#310776);
#578=CONTEXT_DEPENDENT_SHAPE_REPRESENTATION(#355,#310777);
#579=CONTEXT_DEPENDENT_SHAPE_REPRESENTATION(#356,#310778);
#580=CONTEXT_DEPENDENT_SHAPE_REPRESENTATION(#357,#310779);
#581=CONTEXT_DEPENDENT_SHAPE_REPRESENTATION(#358,#310780);
#582=CONTEXT_DEPENDENT_SHAPE_REPRESENTATION(#359,#310781);
#583=CONTEXT_DEPENDENT_SHAPE_REPRESENTATION(#360,#310782);
#584=CONTEXT_DEPENDENT_SHAPE_REPRESENTATION(#361,#310783);
#585=CONTEXT_DEPENDENT_SHAPE_REPRESENTATION(#362,#310784);
#586=CONTEXT_DEPENDENT_SHAPE_REPRESENTATION(#363,#310785);
#587=CONTEXT_DEPENDENT_SHAPE_REPRESENTATION(#364,#310786);
#588=CONTEXT_DEPENDENT_SHAPE_REPRESENTATION(#365,#310787);
#589=CONTEXT_DEPENDENT_SHAPE_REPRESENTATION(#366,#310788);
#590=CONTEXT_DEPENDENT_SHAPE_REPRESENTATION(#367,#310789);
#591=CONTEXT_DEPENDENT_SHAPE_REPRESENTATION(#368,#310790);
#592=CONTEXT_DEPENDENT_SHAPE_REPRESENTATION(#369,#310791);
#593=CONTEXT_DEPENDENT_SHAPE_REPRESENTATION(#370,#310792);
#594=CONTEXT_DEPENDENT_SHAPE_REPRESENTATION(#371,#310793);
#595=CONTEXT_DEPENDENT_SHAPE_REPRESENTATION(#372,#310794);
#596=CONTEXT_DEPENDENT_SHAPE_REPRESENTATION(#373,#310795);
#597=CONTEXT_DEPENDENT_SHAPE_REPRESENTATION(#374,#310805);
#598=CONTEXT_DEPENDENT_SHAPE_REPRESENTATION(#375,#310806);
#599=CONTEXT_DEPENDENT_SHAPE_REPRESENTATION(#376,#310810);
#600=CONTEXT_DEPENDENT_SHAPE_REPRESENTATION(#377,#310811);
#601=CONTEXT_DEPENDENT_SHAPE_REPRESENTATION(#378,#310812);
#602=CONTEXT_DEPENDENT_SHAPE_REPRESENTATION(#379,#310813);
#603=CONTEXT_DEPENDENT_SHAPE_REPRESENTATION(#380,#310814);
#604=CONTEXT_DEPENDENT_SHAPE_REPRESENTATION(#381,#310815);
#605=CONTEXT_DEPENDENT_SHAPE_REPRESENTATION(#382,#310816);
#606=CONTEXT_DEPENDENT_SHAPE_REPRESENTATION(#383,#310817);
#607=CONTEXT_DEPENDENT_SHAPE_REPRESENTATION(#384,#310818);
#608=CONTEXT_DEPENDENT_SHAPE_REPRESENTATION(#385,#310819);
#609=CONTEXT_DEPENDENT_SHAPE_REPRESENTATION(#386,#310820);
#610=CONTEXT_DEPENDENT_SHAPE_REPRESENTATION(#387,#310821);
#611=CONTEXT_DEPENDENT_SHAPE_REPRESENTATION(#388,#310822);
#612=CONTEXT_DEPENDENT_SHAPE_REPRESENTATION(#389,#310823);
#613=CONTEXT_DEPENDENT_SHAPE_REPRESENTATION(#390,#310824);
#614=CONTEXT_DEPENDENT_SHAPE_REPRESENTATION(#391,#310825);
#615=CONTEXT_DEPENDENT_SHAPE_REPRESENTATION(#392,#310826);
#616=CONTEXT_DEPENDENT_SHAPE_REPRESENTATION(#393,#310827);
#617=CONTEXT_DEPENDENT_SHAPE_REPRESENTATION(#394,#310828);
#618=CONTEXT_DEPENDENT_SHAPE_REPRESENTATION(#395,#310829);
#619=CONTEXT_DEPENDENT_SHAPE_REPRESENTATION(#396,#310830);
#620=CONTEXT_DEPENDENT_SHAPE_REPRESENTATION(#397,#310831);
#621=CONTEXT_DEPENDENT_SHAPE_REPRESENTATION(#398,#310832);
#622=CONTEXT_DEPENDENT_SHAPE_REPRESENTATION(#399,#310833);
#623=CONTEXT_DEPENDENT_SHAPE_REPRESENTATION(#400,#310834);
#624=CONTEXT_DEPENDENT_SHAPE_REPRESENTATION(#401,#310835);
#625=CONTEXT_DEPENDENT_SHAPE_REPRESENTATION(#402,#310836);
#626=CONTEXT_DEPENDENT_SHAPE_REPRESENTATION(#403,#310837);
#627=CONTEXT_DEPENDENT_SHAPE_REPRESENTATION(#404,#310838);
#628=CONTEXT_DEPENDENT_SHAPE_REPRESENTATION(#405,#310839);
#629=CONTEXT_DEPENDENT_SHAPE_REPRESENTATION(#406,#310840);
#630=CONTEXT_DEPENDENT_SHAPE_REPRESENTATION(#407,#310841);
#631=CONTEXT_DEPENDENT_SHAPE_REPRESENTATION(#408,#310842);
#632=CONTEXT_DEPENDENT_SHAPE_REPRESENTATION(#409,#310843);
#633=CONTEXT_DEPENDENT_SHAPE_REPRESENTATION(#410,#310844);
#634=CONTEXT_DEPENDENT_SHAPE_REPRESENTATION(#411,#310845);
#635=CONTEXT_DEPENDENT_SHAPE_REPRESENTATION(#412,#310846);
#636=CONTEXT_DEPENDENT_SHAPE_REPRESENTATION(#413,#310847);
#637=CONTEXT_DEPENDENT_SHAPE_REPRESENTATION(#414,#310848);
#638=CONTEXT_DEPENDENT_SHAPE_REPRESENTATION(#415,#310849);
#639=CONTEXT_DEPENDENT_SHAPE_REPRESENTATION(#416,#310850);
#640=CONTEXT_DEPENDENT_SHAPE_REPRESENTATION(#417,#310851);
#641=CONTEXT_DEPENDENT_SHAPE_REPRESENTATION(#418,#310852);
#642=CONTEXT_DEPENDENT_SHAPE_REPRESENTATION(#419,#310853);
#643=CONTEXT_DEPENDENT_SHAPE_REPRESENTATION(#420,#310854);
#644=CONTEXT_DEPENDENT_SHAPE_REPRESENTATION(#421,#310855);
#645=CONTEXT_DEPENDENT_SHAPE_REPRESENTATION(#422,#310856);
#646=CONTEXT_DEPENDENT_SHAPE_REPRESENTATION(#423,#310857);
#647=CONTEXT_DEPENDENT_SHAPE_REPRESENTATION(#424,#310858);
#648=CONTEXT_DEPENDENT_SHAPE_REPRESENTATION(#425,#310859);
#649=CONTEXT_DEPENDENT_SHAPE_REPRESENTATION(#426,#310860);
#650=CONTEXT_DEPENDENT_SHAPE_REPRESENTATION(#427,#310861);
#651=CONTEXT_DEPENDENT_SHAPE_REPRESENTATION(#428,#310862);
#652=CONTEXT_DEPENDENT_SHAPE_REPRESENTATION(#429,#310863);
#653=CONTEXT_DEPENDENT_SHAPE_REPRESENTATION(#430,#310864);
#654=CONTEXT_DEPENDENT_SHAPE_REPRESENTATION(#431,#310865);
#655=CONTEXT_DEPENDENT_SHAPE_REPRESENTATION(#432,#310866);
#656=CONTEXT_DEPENDENT_SHAPE_REPRESENTATION(#433,#310867);
#657=CONTEXT_DEPENDENT_SHAPE_REPRESENTATION(#434,#310868);
#658=CONTEXT_DEPENDENT_SHAPE_REPRESENTATION(#435,#310869);
#659=CONTEXT_DEPENDENT_SHAPE_REPRESENTATION(#436,#310870);
#660=CONTEXT_DEPENDENT_SHAPE_REPRESENTATION(#437,#310871);
#661=CONTEXT_DEPENDENT_SHAPE_REPRESENTATION(#438,#310872);
#662=CONTEXT_DEPENDENT_SHAPE_REPRESENTATION(#439,#310873);
#663=CONTEXT_DEPENDENT_SHAPE_REPRESENTATION(#440,#310874);
#664=CONTEXT_DEPENDENT_SHAPE_REPRESENTATION(#441,#310875);
#665=CONTEXT_DEPENDENT_SHAPE_REPRESENTATION(#442,#310876);
#666=CONTEXT_DEPENDENT_SHAPE_REPRESENTATION(#443,#310877);
#667=CONTEXT_DEPENDENT_SHAPE_REPRESENTATION(#444,#310878);
#668=CONTEXT_DEPENDENT_SHAPE_REPRESENTATION(#445,#310879);
#669=CONTEXT_DEPENDENT_SHAPE_REPRESENTATION(#446,#310880);
#670=CONTEXT_DEPENDENT_SHAPE_REPRESENTATION(#447,#310881);
#671=CONTEXT_DEPENDENT_SHAPE_REPRESENTATION(#448,#310882);
#672=CONTEXT_DEPENDENT_SHAPE_REPRESENTATION(#449,#310883);
#673=CONTEXT_DEPENDENT_SHAPE_REPRESENTATION(#450,#310884);
#674=CONTEXT_DEPENDENT_SHAPE_REPRESENTATION(#451,#310885);
#675=CONTEXT_DEPENDENT_SHAPE_REPRESENTATION(#452,#310886);
#676=CONTEXT_DEPENDENT_SHAPE_REPRESENTATION(#453,#310887);
#677=CONTEXT_DEPENDENT_SHAPE_REPRESENTATION(#454,#310888);
#678=CONTEXT_DEPENDENT_SHAPE_REPRESENTATION(#455,#310889);
#679=CONTEXT_DEPENDENT_SHAPE_REPRESENTATION(#456,#310890);
#680=CONTEXT_DEPENDENT_SHAPE_REPRESENTATION(#457,#310891);
#681=CONTEXT_DEPENDENT_SHAPE_REPRESENTATION(#458,#310892);
#682=NEXT_ASSEMBLY_USAGE_OCCURRENCE('15-Tooth Sprocket:1',
'15-Tooth Sprocket:1','15-Tooth Sprocket:1',#310920,#310921,
'15-Tooth Sprocket:1');
#683=NEXT_ASSEMBLY_USAGE_OCCURRENCE('30-Tooth Sprocket:1',
'30-Tooth Sprocket:1','30-Tooth Sprocket:1',#310920,#310922,
'30-Tooth Sprocket:1');
#684=NEXT_ASSEMBLY_USAGE_OCCURRENCE('Chain Link:1','Chain Link:1',
'Chain Link:1',#310920,#310923,'Chain Link:1');
#685=NEXT_ASSEMBLY_USAGE_OCCURRENCE('Chain Link:2','Chain Link:2',
'Chain Link:2',#310920,#310923,'Chain Link:2');
#686=NEXT_ASSEMBLY_USAGE_OCCURRENCE('Chain Link:3','Chain Link:3',
'Chain Link:3',#310920,#310923,'Chain Link:3');
#687=NEXT_ASSEMBLY_USAGE_OCCURRENCE('Chain Link:4','Chain Link:4',
'Chain Link:4',#310920,#310923,'Chain Link:4');
#688=NEXT_ASSEMBLY_USAGE_OCCURRENCE('Chain Link:5','Chain Link:5',
'Chain Link:5',#310920,#310923,'Chain Link:5');
#689=NEXT_ASSEMBLY_USAGE_OCCURRENCE('Chain Link:6','Chain Link:6',
'Chain Link:6',#310920,#310923,'Chain Link:6');
#690=NEXT_ASSEMBLY_USAGE_OCCURRENCE('Chain Link:7','Chain Link:7',
'Chain Link:7',#310920,#310923,'Chain Link:7');
#691=NEXT_ASSEMBLY_USAGE_OCCURRENCE('Chain Link:8','Chain Link:8',
'Chain Link:8',#310920,#310923,'Chain Link:8');
#692=NEXT_ASSEMBLY_USAGE_OCCURRENCE('Chain Link:9','Chain Link:9',
'Chain Link:9',#310920,#310923,'Chain Link:9');
#693=NEXT_ASSEMBLY_USAGE_OCCURRENCE('Chain Link:10','Chain Link:10',
'Chain Link:10',#310920,#310923,'Chain Link:10');
#694=NEXT_ASSEMBLY_USAGE_OCCURRENCE('Chain Link:11','Chain Link:11',
'Chain Link:11',#310920,#310923,'Chain Link:11');
#695=NEXT_ASSEMBLY_USAGE_OCCURRENCE('Chain Link:12','Chain Link:12',
'Chain Link:12',#310920,#310923,'Chain Link:12');
#696=NEXT_ASSEMBLY_USAGE_OCCURRENCE('Chain Link:13','Chain Link:13',
'Chain Link:13',#310920,#310923,'Chain Link:13');
#697=NEXT_ASSEMBLY_USAGE_OCCURRENCE('Chain Link:14','Chain Link:14',
'Chain Link:14',#310920,#310923,'Chain Link:14');
#698=NEXT_ASSEMBLY_USAGE_OCCURRENCE('Chain Link:15','Chain Link:15',
'Chain Link:15',#310920,#310923,'Chain Link:15');
#699=NEXT_ASSEMBLY_USAGE_OCCURRENCE('Chain Link:16','Chain Link:16',
'Chain Link:16',#310920,#310923,'Chain Link:16');
#700=NEXT_ASSEMBLY_USAGE_OCCURRENCE('Chain Link:17','Chain Link:17',
'Chain Link:17',#310920,#310923,'Chain Link:17');
#701=NEXT_ASSEMBLY_USAGE_OCCURRENCE('Chain Link:18','Chain Link:18',
'Chain Link:18',#310920,#310923,'Chain Link:18');
#702=NEXT_ASSEMBLY_USAGE_OCCURRENCE('Chain Link:19','Chain Link:19',
'Chain Link:19',#310920,#310923,'Chain Link:19');
#703=NEXT_ASSEMBLY_USAGE_OCCURRENCE('Chain Link:20','Chain Link:20',
'Chain Link:20',#310920,#310923,'Chain Link:20');
#704=NEXT_ASSEMBLY_USAGE_OCCURRENCE('Chain Link:21','Chain Link:21',
'Chain Link:21',#310920,#310923,'Chain Link:21');
#705=NEXT_ASSEMBLY_USAGE_OCCURRENCE('Chain Link:22','Chain Link:22',
'Chain Link:22',#310920,#310923,'Chain Link:22');
#706=NEXT_ASSEMBLY_USAGE_OCCURRENCE('Chain Link:23','Chain Link:23',
'Chain Link:23',#310920,#310923,'Chain Link:23');
#707=NEXT_ASSEMBLY_USAGE_OCCURRENCE('Chain Link:24','Chain Link:24',
'Chain Link:24',#310920,#310923,'Chain Link:24');
#708=NEXT_ASSEMBLY_USAGE_OCCURRENCE('Chain Link:25','Chain Link:25',
'Chain Link:25',#310920,#310923,'Chain Link:25');
#709=NEXT_ASSEMBLY_USAGE_OCCURRENCE('Chain Link:26','Chain Link:26',
'Chain Link:26',#310920,#310923,'Chain Link:26');
#710=NEXT_ASSEMBLY_USAGE_OCCURRENCE('Chain Link:27','Chain Link:27',
'Chain Link:27',#310920,#310923,'Chain Link:27');
#711=NEXT_ASSEMBLY_USAGE_OCCURRENCE('Chain Link:28','Chain Link:28',
'Chain Link:28',#310920,#310923,'Chain Link:28');
#712=NEXT_ASSEMBLY_USAGE_OCCURRENCE('Chain Link:29','Chain Link:29',
'Chain Link:29',#310920,#310923,'Chain Link:29');
#713=NEXT_ASSEMBLY_USAGE_OCCURRENCE('Chain Link:30','Chain Link:30',
'Chain Link:30',#310920,#310923,'Chain Link:30');
#714=NEXT_ASSEMBLY_USAGE_OCCURRENCE('Chain Link:31','Chain Link:31',
'Chain Link:31',#310920,#310923,'Chain Link:31');
#715=NEXT_ASSEMBLY_USAGE_OCCURRENCE('Chain Link:32','Chain Link:32',
'Chain Link:32',#310920,#310923,'Chain Link:32');
#716=NEXT_ASSEMBLY_USAGE_OCCURRENCE('Chain Link:33','Chain Link:33',
'Chain Link:33',#310920,#310923,'Chain Link:33');
#717=NEXT_ASSEMBLY_USAGE_OCCURRENCE('Chain Link:34','Chain Link:34',
'Chain Link:34',#310920,#310923,'Chain Link:34');
#718=NEXT_ASSEMBLY_USAGE_OCCURRENCE('Chain Link:35','Chain Link:35',
'Chain Link:35',#310920,#310923,'Chain Link:35');
#719=NEXT_ASSEMBLY_USAGE_OCCURRENCE('Chain Link:36','Chain Link:36',
'Chain Link:36',#310920,#310923,'Chain Link:36');
#720=NEXT_ASSEMBLY_USAGE_OCCURRENCE('Chain Link:37','Chain Link:37',
'Chain Link:37',#310920,#310923,'Chain Link:37');
#721=NEXT_ASSEMBLY_USAGE_OCCURRENCE('Chain Link:38','Chain Link:38',
'Chain Link:38',#310920,#310923,'Chain Link:38');
#722=NEXT_ASSEMBLY_USAGE_OCCURRENCE('Chain Link:39','Chain Link:39',
'Chain Link:39',#310920,#310923,'Chain Link:39');
#723=NEXT_ASSEMBLY_USAGE_OCCURRENCE('Chain Link:40','Chain Link:40',
'Chain Link:40',#310920,#310923,'Chain Link:40');
#724=NEXT_ASSEMBLY_USAGE_OCCURRENCE('Chain Link:41','Chain Link:41',
'Chain Link:41',#310920,#310923,'Chain Link:41');
#725=NEXT_ASSEMBLY_USAGE_OCCURRENCE('Chain Link:42','Chain Link:42',
'Chain Link:42',#310920,#310923,'Chain Link:42');
#726=NEXT_ASSEMBLY_USAGE_OCCURRENCE('Chain Link:43','Chain Link:43',
'Chain Link:43',#310920,#310923,'Chain Link:43');
#727=NEXT_ASSEMBLY_USAGE_OCCURRENCE('Chain Link:44','Chain Link:44',
'Chain Link:44',#310920,#310923,'Chain Link:44');
#728=NEXT_ASSEMBLY_USAGE_OCCURRENCE('Chain Link:45','Chain Link:45',
'Chain Link:45',#310920,#310923,'Chain Link:45');
#729=NEXT_ASSEMBLY_USAGE_OCCURRENCE('Chain Link:46','Chain Link:46',
'Chain Link:46',#310920,#310923,'Chain Link:46');
#730=NEXT_ASSEMBLY_USAGE_OCCURRENCE('Chain Link:47','Chain Link:47',
'Chain Link:47',#310920,#310923,'Chain Link:47');
#731=NEXT_ASSEMBLY_USAGE_OCCURRENCE('Chain Link:48','Chain Link:48',
'Chain Link:48',#310920,#310923,'Chain Link:48');
#732=NEXT_ASSEMBLY_USAGE_OCCURRENCE('Chain Link:49','Chain Link:49',
'Chain Link:49',#310920,#310923,'Chain Link:49');
#733=NEXT_ASSEMBLY_USAGE_OCCURRENCE('Chain Link:50','Chain Link:50',
'Chain Link:50',#310920,#310923,'Chain Link:50');
#734=NEXT_ASSEMBLY_USAGE_OCCURRENCE('Chain Link:51','Chain Link:51',
'Chain Link:51',#310920,#310923,'Chain Link:51');
#735=NEXT_ASSEMBLY_USAGE_OCCURRENCE('Chain Link:52','Chain Link:52',
'Chain Link:52',#310920,#310923,'Chain Link:52');
#736=NEXT_ASSEMBLY_USAGE_OCCURRENCE('Chain Link:53','Chain Link:53',
'Chain Link:53',#310920,#310923,'Chain Link:53');
#737=NEXT_ASSEMBLY_USAGE_OCCURRENCE('Chain Link:54','Chain Link:54',
'Chain Link:54',#310920,#310923,'Chain Link:54');
#738=NEXT_ASSEMBLY_USAGE_OCCURRENCE('Chain Link:55','Chain Link:55',
'Chain Link:55',#310920,#310923,'Chain Link:55');
#739=NEXT_ASSEMBLY_USAGE_OCCURRENCE('Chain Link:56','Chain Link:56',
'Chain Link:56',#310920,#310923,'Chain Link:56');
#740=NEXT_ASSEMBLY_USAGE_OCCURRENCE('Chain Link:57','Chain Link:57',
'Chain Link:57',#310920,#310923,'Chain Link:57');
#741=NEXT_ASSEMBLY_USAGE_OCCURRENCE('Chain Link:58','Chain Link:58',
'Chain Link:58',#310920,#310923,'Chain Link:58');
#742=NEXT_ASSEMBLY_USAGE_OCCURRENCE('Chain Link:59','Chain Link:59',
'Chain Link:59',#310920,#310923,'Chain Link:59');
#743=NEXT_ASSEMBLY_USAGE_OCCURRENCE('Chain Link:60','Chain Link:60',
'Chain Link:60',#310920,#310923,'Chain Link:60');
#744=NEXT_ASSEMBLY_USAGE_OCCURRENCE('Chain Link:61','Chain Link:61',
'Chain Link:61',#310920,#310923,'Chain Link:61');
#745=NEXT_ASSEMBLY_USAGE_OCCURRENCE('Chain Link:62','Chain Link:62',
'Chain Link:62',#310920,#310923,'Chain Link:62');
#746=NEXT_ASSEMBLY_USAGE_OCCURRENCE('Chain Link:63','Chain Link:63',
'Chain Link:63',#310920,#310923,'Chain Link:63');
#747=NEXT_ASSEMBLY_USAGE_OCCURRENCE('Chain Link:64','Chain Link:64',
'Chain Link:64',#310920,#310923,'Chain Link:64');
#748=NEXT_ASSEMBLY_USAGE_OCCURRENCE('Chain Link:65','Chain Link:65',
'Chain Link:65',#310920,#310923,'Chain Link:65');
#749=NEXT_ASSEMBLY_USAGE_OCCURRENCE('Chain Link:66','Chain Link:66',
'Chain Link:66',#310920,#310923,'Chain Link:66');
#750=NEXT_ASSEMBLY_USAGE_OCCURRENCE('Chain Link:67','Chain Link:67',
'Chain Link:67',#310920,#310923,'Chain Link:67');
#751=NEXT_ASSEMBLY_USAGE_OCCURRENCE('Chain Link:68','Chain Link:68',
'Chain Link:68',#310920,#310923,'Chain Link:68');
#752=NEXT_ASSEMBLY_USAGE_OCCURRENCE('Chain Link:69','Chain Link:69',
'Chain Link:69',#310920,#310923,'Chain Link:69');
#753=NEXT_ASSEMBLY_USAGE_OCCURRENCE('Chain Link:70','Chain Link:70',
'Chain Link:70',#310920,#310923,'Chain Link:70');
#754=NEXT_ASSEMBLY_USAGE_OCCURRENCE('Chain Link:71','Chain Link:71',
'Chain Link:71',#310920,#310923,'Chain Link:71');
#755=NEXT_ASSEMBLY_USAGE_OCCURRENCE('Chain Link:72','Chain Link:72',
'Chain Link:72',#310920,#310923,'Chain Link:72');
#756=NEXT_ASSEMBLY_USAGE_OCCURRENCE('Chain Link:73','Chain Link:73',
'Chain Link:73',#310920,#310923,'Chain Link:73');
#757=NEXT_ASSEMBLY_USAGE_OCCURRENCE('Chain Link:74','Chain Link:74',
'Chain Link:74',#310920,#310923,'Chain Link:74');
#758=NEXT_ASSEMBLY_USAGE_OCCURRENCE('Chain Link:75','Chain Link:75',
'Chain Link:75',#310920,#310923,'Chain Link:75');
#759=NEXT_ASSEMBLY_USAGE_OCCURRENCE('Chain Link:76','Chain Link:76',
'Chain Link:76',#310920,#310923,'Chain Link:76');
#760=NEXT_ASSEMBLY_USAGE_OCCURRENCE('Chain Link:77','Chain Link:77',
'Chain Link:77',#310920,#310923,'Chain Link:77');
#761=NEXT_ASSEMBLY_USAGE_OCCURRENCE('Chain Link:78','Chain Link:78',
'Chain Link:78',#310920,#310923,'Chain Link:78');
#762=NEXT_ASSEMBLY_USAGE_OCCURRENCE('Chain Link:79','Chain Link:79',
'Chain Link:79',#310920,#310923,'Chain Link:79');
#763=NEXT_ASSEMBLY_USAGE_OCCURRENCE('Chain Link:80','Chain Link:80',
'Chain Link:80',#310920,#310923,'Chain Link:80');
#764=NEXT_ASSEMBLY_USAGE_OCCURRENCE('Chain Link:81','Chain Link:81',
'Chain Link:81',#310920,#310923,'Chain Link:81');
#765=NEXT_ASSEMBLY_USAGE_OCCURRENCE('Chain Link:82','Chain Link:82',
'Chain Link:82',#310920,#310923,'Chain Link:82');
#766=NEXT_ASSEMBLY_USAGE_OCCURRENCE('Chain Link:83','Chain Link:83',
'Chain Link:83',#310920,#310923,'Chain Link:83');
#767=NEXT_ASSEMBLY_USAGE_OCCURRENCE('Chain Link:84','Chain Link:84',
'Chain Link:84',#310920,#310923,'Chain Link:84');
#768=NEXT_ASSEMBLY_USAGE_OCCURRENCE('Chain Link:85','Chain Link:85',
'Chain Link:85',#310920,#310923,'Chain Link:85');
#769=NEXT_ASSEMBLY_USAGE_OCCURRENCE('Chain Link:86','Chain Link:86',
'Chain Link:86',#310920,#310923,'Chain Link:86');
#770=NEXT_ASSEMBLY_USAGE_OCCURRENCE('Chain Link:87','Chain Link:87',
'Chain Link:87',#310920,#310923,'Chain Link:87');
#771=NEXT_ASSEMBLY_USAGE_OCCURRENCE('Chain Link:88','Chain Link:88',
'Chain Link:88',#310920,#310923,'Chain Link:88');
#772=NEXT_ASSEMBLY_USAGE_OCCURRENCE('Chain Link:89','Chain Link:89',
'Chain Link:89',#310920,#310923,'Chain Link:89');
#773=NEXT_ASSEMBLY_USAGE_OCCURRENCE('Chain Link:90','Chain Link:90',
'Chain Link:90',#310920,#310923,'Chain Link:90');
#774=NEXT_ASSEMBLY_USAGE_OCCURRENCE('Chain Link:91','Chain Link:91',
'Chain Link:91',#310920,#310923,'Chain Link:91');
#775=NEXT_ASSEMBLY_USAGE_OCCURRENCE('Chain Link:92','Chain Link:92',
'Chain Link:92',#310920,#310923,'Chain Link:92');
#776=NEXT_ASSEMBLY_USAGE_OCCURRENCE('Chain Link:93','Chain Link:93',
'Chain Link:93',#310920,#310923,'Chain Link:93');
#777=NEXT_ASSEMBLY_USAGE_OCCURRENCE('Chain Link:94','Chain Link:94',
'Chain Link:94',#310920,#310923,'Chain Link:94');
#778=NEXT_ASSEMBLY_USAGE_OCCURRENCE('Chain Link:95','Chain Link:95',
'Chain Link:95',#310920,#310923,'Chain Link:95');
#779=NEXT_ASSEMBLY_USAGE_OCCURRENCE('Chain Link:96','Chain Link:96',
'Chain Link:96',#310920,#310923,'Chain Link:96');
#780=NEXT_ASSEMBLY_USAGE_OCCURRENCE('Chain Link:97','Chain Link:97',
'Chain Link:97',#310920,#310923,'Chain Link:97');
#781=NEXT_ASSEMBLY_USAGE_OCCURRENCE('Chain Link:98','Chain Link:98',
'Chain Link:98',#310920,#310923,'Chain Link:98');
#782=NEXT_ASSEMBLY_USAGE_OCCURRENCE('Chain Link:99','Chain Link:99',
'Chain Link:99',#310920,#310923,'Chain Link:99');
#783=NEXT_ASSEMBLY_USAGE_OCCURRENCE('Chain Link:100','Chain Link:100',
'Chain Link:100',#310920,#310923,'Chain Link:100');
#784=NEXT_ASSEMBLY_USAGE_OCCURRENCE('Chain Link:101','Chain Link:101',
'Chain Link:101',#310920,#310923,'Chain Link:101');
#785=NEXT_ASSEMBLY_USAGE_OCCURRENCE('Chain Link:102','Chain Link:102',
'Chain Link:102',#310920,#310923,'Chain Link:102');
#786=NEXT_ASSEMBLY_USAGE_OCCURRENCE('Chain Link:103','Chain Link:103',
'Chain Link:103',#310920,#310923,'Chain Link:103');
#787=NEXT_ASSEMBLY_USAGE_OCCURRENCE('Chain Link:104','Chain Link:104',
'Chain Link:104',#310920,#310923,'Chain Link:104');
#788=NEXT_ASSEMBLY_USAGE_OCCURRENCE('Chain Link:105','Chain Link:105',
'Chain Link:105',#310920,#310923,'Chain Link:105');
#789=NEXT_ASSEMBLY_USAGE_OCCURRENCE('Chain Link:106','Chain Link:106',
'Chain Link:106',#310920,#310923,'Chain Link:106');
#790=NEXT_ASSEMBLY_USAGE_OCCURRENCE('Chain Link:107','Chain Link:107',
'Chain Link:107',#310920,#310923,'Chain Link:107');
#791=NEXT_ASSEMBLY_USAGE_OCCURRENCE('Chain Link:108','Chain Link:108',
'Chain Link:108',#310920,#310923,'Chain Link:108');
#792=NEXT_ASSEMBLY_USAGE_OCCURRENCE('Chain Link:109','Chain Link:109',
'Chain Link:109',#310920,#310923,'Chain Link:109');
#793=NEXT_ASSEMBLY_USAGE_OCCURRENCE('Chain Link:110','Chain Link:110',
'Chain Link:110',#310920,#310923,'Chain Link:110');
#794=NEXT_ASSEMBLY_USAGE_OCCURRENCE('Chain Link:111','Chain Link:111',
'Chain Link:111',#310920,#310923,'Chain Link:111');
#795=NEXT_ASSEMBLY_USAGE_OCCURRENCE('Chain Link:112','Chain Link:112',
'Chain Link:112',#310920,#310923,'Chain Link:112');
#796=NEXT_ASSEMBLY_USAGE_OCCURRENCE('Chain Link:113','Chain Link:113',
'Chain Link:113',#310920,#310923,'Chain Link:113');
#797=NEXT_ASSEMBLY_USAGE_OCCURRENCE('Chain Link:114','Chain Link:114',
'Chain Link:114',#310920,#310923,'Chain Link:114');
#798=NEXT_ASSEMBLY_USAGE_OCCURRENCE('Chain Link:115','Chain Link:115',
'Chain Link:115',#310920,#310923,'Chain Link:115');
#799=NEXT_ASSEMBLY_USAGE_OCCURRENCE('Chain Link:116','Chain Link:116',
'Chain Link:116',#310920,#310923,'Chain Link:116');
#800=NEXT_ASSEMBLY_USAGE_OCCURRENCE('Chain Link:117','Chain Link:117',
'Chain Link:117',#310920,#310923,'Chain Link:117');
#801=NEXT_ASSEMBLY_USAGE_OCCURRENCE('Chain Link:118','Chain Link:118',
'Chain Link:118',#310920,#310923,'Chain Link:118');
#802=NEXT_ASSEMBLY_USAGE_OCCURRENCE('Chain Link:119','Chain Link:119',
'Chain Link:119',#310920,#310923,'Chain Link:119');
#803=NEXT_ASSEMBLY_USAGE_OCCURRENCE('Chain Link:120','Chain Link:120',
'Chain Link:120',#310920,#310923,'Chain Link:120');
#804=NEXT_ASSEMBLY_USAGE_OCCURRENCE('Chain Link:121','Chain Link:121',
'Chain Link:121',#310920,#310923,'Chain Link:121');
#805=NEXT_ASSEMBLY_USAGE_OCCURRENCE('Chain Link:122','Chain Link:122',
'Chain Link:122',#310920,#310923,'Chain Link:122');
#806=NEXT_ASSEMBLY_USAGE_OCCURRENCE('Chain Link:123','Chain Link:123',
'Chain Link:123',#310920,#310923,'Chain Link:123');
#807=NEXT_ASSEMBLY_USAGE_OCCURRENCE('Chain Link:124','Chain Link:124',
'Chain Link:124',#310920,#310923,'Chain Link:124');
#808=NEXT_ASSEMBLY_USAGE_OCCURRENCE('Chain Link:125','Chain Link:125',
'Chain Link:125',#310920,#310923,'Chain Link:125');
#809=NEXT_ASSEMBLY_USAGE_OCCURRENCE('Chain Link:126','Chain Link:126',
'Chain Link:126',#310920,#310923,'Chain Link:126');
#810=NEXT_ASSEMBLY_USAGE_OCCURRENCE('Chain Link:127','Chain Link:127',
'Chain Link:127',#310920,#310923,'Chain Link:127');
#811=NEXT_ASSEMBLY_USAGE_OCCURRENCE('Chain Link:128','Chain Link:128',
'Chain Link:128',#310920,#310923,'Chain Link:128');
#812=NEXT_ASSEMBLY_USAGE_OCCURRENCE('Chain Link:129','Chain Link:129',
'Chain Link:129',#310920,#310923,'Chain Link:129');
#813=NEXT_ASSEMBLY_USAGE_OCCURRENCE('Chain Link:130','Chain Link:130',
'Chain Link:130',#310920,#310923,'Chain Link:130');
#814=NEXT_ASSEMBLY_USAGE_OCCURRENCE('Chain Link:131','Chain Link:131',
'Chain Link:131',#310920,#310923,'Chain Link:131');
#815=NEXT_ASSEMBLY_USAGE_OCCURRENCE('Chain Link:132','Chain Link:132',
'Chain Link:132',#310920,#310923,'Chain Link:132');
#816=NEXT_ASSEMBLY_USAGE_OCCURRENCE('Chain Link:133','Chain Link:133',
'Chain Link:133',#310920,#310923,'Chain Link:133');
#817=NEXT_ASSEMBLY_USAGE_OCCURRENCE('Chain Link:134','Chain Link:134',
'Chain Link:134',#310920,#310923,'Chain Link:134');
#818=NEXT_ASSEMBLY_USAGE_OCCURRENCE('Chain Link:135','Chain Link:135',
'Chain Link:135',#310920,#310923,'Chain Link:135');
#819=NEXT_ASSEMBLY_USAGE_OCCURRENCE('Chain Link:136','Chain Link:136',
'Chain Link:136',#310920,#310923,'Chain Link:136');
#820=NEXT_ASSEMBLY_USAGE_OCCURRENCE('Leg Gusset Bracket:1',
'Leg Gusset Bracket:1','Leg Gusset Bracket:1',#310930,#310931,
'Leg Gusset Bracket:1');
#821=NEXT_ASSEMBLY_USAGE_OCCURRENCE('Conveyor Support Leg:1',
'Conveyor Support Leg:1','Conveyor Support Leg:1',#310930,#310932,
'Conveyor Support Leg:1');
#822=NEXT_ASSEMBLY_USAGE_OCCURRENCE('Class 8.8 Steel Hex Head Screw:1',
'Class 8.8 Steel Hex Head Screw:1','Class 8.8 Steel Hex Head Screw:1',#310933,
#310934,'Class 8.8 Steel Hex Head Screw:1');
#823=NEXT_ASSEMBLY_USAGE_OCCURRENCE('Zinc-Plated Steel Hex Nut:1',
'Zinc-Plated Steel Hex Nut:1','Zinc-Plated Steel Hex Nut:1',#310933,#310935,
'Zinc-Plated Steel Hex Nut:1');
#824=NEXT_ASSEMBLY_USAGE_OCCURRENCE('Right Side Channel Support Rail:1',
'Right Side Channel Support Rail:1','Right Side Channel Support Rail:1',
#310915,#310916,'Right Side Channel Support Rail:1');
#825=NEXT_ASSEMBLY_USAGE_OCCURRENCE('Left Side Channel Support Rail:1',
'Left Side Channel Support Rail:1','Left Side Channel Support Rail:1',#310915,
#310917,'Left Side Channel Support Rail:1');
#826=NEXT_ASSEMBLY_USAGE_OCCURRENCE('Steel Tube Conveyor Roller:1',
'Steel Tube Conveyor Roller:1','Steel Tube Conveyor Roller:1',#310915,#310924,
'Steel Tube Conveyor Roller:1');
#827=NEXT_ASSEMBLY_USAGE_OCCURRENCE('Precision Ball Bearing:1',
'Precision Ball Bearing:1','Precision Ball Bearing:1',#310915,#310925,
'Precision Ball Bearing:1');
#828=NEXT_ASSEMBLY_USAGE_OCCURRENCE('Hexagonal Axle Shaft:1',
'Hexagonal Axle Shaft:1','Hexagonal Axle Shaft:1',#310915,#310926,
'Hexagonal Axle Shaft:1');
#829=NEXT_ASSEMBLY_USAGE_OCCURRENCE('Conveyor Support Leg Assembly:1',
'Conveyor Support Leg Assembly:1','Conveyor Support Leg Assembly:1',#310915,
#310930,'Conveyor Support Leg Assembly:1');
#830=NEXT_ASSEMBLY_USAGE_OCCURRENCE('Base Anchor Foot:1',
'Base Anchor Foot:1','Base Anchor Foot:1',#310915,#310927,
'Base Anchor Foot:1');
#831=NEXT_ASSEMBLY_USAGE_OCCURRENCE('Side Rail Cross Brace:1',
'Side Rail Cross Brace:1','Side Rail Cross Brace:1',#310915,#310928,
'Side Rail Cross Brace:1');
#832=NEXT_ASSEMBLY_USAGE_OCCURRENCE('Motor with Mount Bracket:1',
'Motor with Mount Bracket:1','Motor with Mount Bracket:1',#310915,#310918,
'Motor with Mount Bracket:1');
#833=NEXT_ASSEMBLY_USAGE_OCCURRENCE('End Cap:1','End Cap:1','End Cap:1',
#310915,#310929,'End Cap:1');
#834=NEXT_ASSEMBLY_USAGE_OCCURRENCE('Screw and Nut Assembly:1',
'Screw and Nut Assembly:1','Screw and Nut Assembly:1',#310915,#310933,
'Screw and Nut Assembly:1');
#835=NEXT_ASSEMBLY_USAGE_OCCURRENCE('Chain Sprocket Cover:1',
'Chain Sprocket Cover:1','Chain Sprocket Cover:1',#310915,#310919,
'Chain Sprocket Cover:1');
#836=NEXT_ASSEMBLY_USAGE_OCCURRENCE('Chain Tensioner Sprocket:1',
'Chain Tensioner Sprocket:1','Chain Tensioner Sprocket:1',#310915,#310920,
'Chain Tensioner Sprocket:1');
#837=NEXT_ASSEMBLY_USAGE_OCCURRENCE('Steel Tube Conveyor Roller:2',
'Steel Tube Conveyor Roller:2','Steel Tube Conveyor Roller:2',#310915,#310924,
'Steel Tube Conveyor Roller:2');
#838=NEXT_ASSEMBLY_USAGE_OCCURRENCE('Steel Tube Conveyor Roller:3',
'Steel Tube Conveyor Roller:3','Steel Tube Conveyor Roller:3',#310915,#310924,
'Steel Tube Conveyor Roller:3');
#839=NEXT_ASSEMBLY_USAGE_OCCURRENCE('Steel Tube Conveyor Roller:4',
'Steel Tube Conveyor Roller:4','Steel Tube Conveyor Roller:4',#310915,#310924,
'Steel Tube Conveyor Roller:4');
#840=NEXT_ASSEMBLY_USAGE_OCCURRENCE('Steel Tube Conveyor Roller:5',
'Steel Tube Conveyor Roller:5','Steel Tube Conveyor Roller:5',#310915,#310924,
'Steel Tube Conveyor Roller:5');
#841=NEXT_ASSEMBLY_USAGE_OCCURRENCE('Steel Tube Conveyor Roller:6',
'Steel Tube Conveyor Roller:6','Steel Tube Conveyor Roller:6',#310915,#310924,
'Steel Tube Conveyor Roller:6');
#842=NEXT_ASSEMBLY_USAGE_OCCURRENCE('Steel Tube Conveyor Roller:7',
'Steel Tube Conveyor Roller:7','Steel Tube Conveyor Roller:7',#310915,#310924,
'Steel Tube Conveyor Roller:7');
#843=NEXT_ASSEMBLY_USAGE_OCCURRENCE('Steel Tube Conveyor Roller:8',
'Steel Tube Conveyor Roller:8','Steel Tube Conveyor Roller:8',#310915,#310924,
'Steel Tube Conveyor Roller:8');
#844=NEXT_ASSEMBLY_USAGE_OCCURRENCE('Steel Tube Conveyor Roller:9',
'Steel Tube Conveyor Roller:9','Steel Tube Conveyor Roller:9',#310915,#310924,
'Steel Tube Conveyor Roller:9');
#845=NEXT_ASSEMBLY_USAGE_OCCURRENCE('Steel Tube Conveyor Roller:10',
'Steel Tube Conveyor Roller:10','Steel Tube Conveyor Roller:10',#310915,
#310924,'Steel Tube Conveyor Roller:10');
#846=NEXT_ASSEMBLY_USAGE_OCCURRENCE('Steel Tube Conveyor Roller:11',
'Steel Tube Conveyor Roller:11','Steel Tube Conveyor Roller:11',#310915,
#310924,'Steel Tube Conveyor Roller:11');
#847=NEXT_ASSEMBLY_USAGE_OCCURRENCE('Steel Tube Conveyor Roller:12',
'Steel Tube Conveyor Roller:12','Steel Tube Conveyor Roller:12',#310915,
#310924,'Steel Tube Conveyor Roller:12');
#848=NEXT_ASSEMBLY_USAGE_OCCURRENCE('Precision Ball Bearing:2',
'Precision Ball Bearing:2','Precision Ball Bearing:2',#310915,#310925,
'Precision Ball Bearing:2');
#849=NEXT_ASSEMBLY_USAGE_OCCURRENCE('Precision Ball Bearing:3',
'Precision Ball Bearing:3','Precision Ball Bearing:3',#310915,#310925,
'Precision Ball Bearing:3');
#850=NEXT_ASSEMBLY_USAGE_OCCURRENCE('Precision Ball Bearing:4',
'Precision Ball Bearing:4','Precision Ball Bearing:4',#310915,#310925,
'Precision Ball Bearing:4');
#851=NEXT_ASSEMBLY_USAGE_OCCURRENCE('Precision Ball Bearing:5',
'Precision Ball Bearing:5','Precision Ball Bearing:5',#310915,#310925,
'Precision Ball Bearing:5');
#852=NEXT_ASSEMBLY_USAGE_OCCURRENCE('Precision Ball Bearing:6',
'Precision Ball Bearing:6','Precision Ball Bearing:6',#310915,#310925,
'Precision Ball Bearing:6');
#853=NEXT_ASSEMBLY_USAGE_OCCURRENCE('Precision Ball Bearing:7',
'Precision Ball Bearing:7','Precision Ball Bearing:7',#310915,#310925,
'Precision Ball Bearing:7');
#854=NEXT_ASSEMBLY_USAGE_OCCURRENCE('Precision Ball Bearing:8',
'Precision Ball Bearing:8','Precision Ball Bearing:8',#310915,#310925,
'Precision Ball Bearing:8');
#855=NEXT_ASSEMBLY_USAGE_OCCURRENCE('Precision Ball Bearing:9',
'Precision Ball Bearing:9','Precision Ball Bearing:9',#310915,#310925,
'Precision Ball Bearing:9');
#856=NEXT_ASSEMBLY_USAGE_OCCURRENCE('Precision Ball Bearing:10',
'Precision Ball Bearing:10','Precision Ball Bearing:10',#310915,#310925,
'Precision Ball Bearing:10');
#857=NEXT_ASSEMBLY_USAGE_OCCURRENCE('Precision Ball Bearing:11',
'Precision Ball Bearing:11','Precision Ball Bearing:11',#310915,#310925,
'Precision Ball Bearing:11');
#858=NEXT_ASSEMBLY_USAGE_OCCURRENCE('Precision Ball Bearing:12',
'Precision Ball Bearing:12','Precision Ball Bearing:12',#310915,#310925,
'Precision Ball Bearing:12');
#859=NEXT_ASSEMBLY_USAGE_OCCURRENCE('Precision Ball Bearing:13',
'Precision Ball Bearing:13','Precision Ball Bearing:13',#310915,#310925,
'Precision Ball Bearing:13');
#860=NEXT_ASSEMBLY_USAGE_OCCURRENCE('Precision Ball Bearing:14',
'Precision Ball Bearing:14','Precision Ball Bearing:14',#310915,#310925,
'Precision Ball Bearing:14');
#861=NEXT_ASSEMBLY_USAGE_OCCURRENCE('Precision Ball Bearing:15',
'Precision Ball Bearing:15','Precision Ball Bearing:15',#310915,#310925,
'Precision Ball Bearing:15');
#862=NEXT_ASSEMBLY_USAGE_OCCURRENCE('Precision Ball Bearing:16',
'Precision Ball Bearing:16','Precision Ball Bearing:16',#310915,#310925,
'Precision Ball Bearing:16');
#863=NEXT_ASSEMBLY_USAGE_OCCURRENCE('Precision Ball Bearing:17',
'Precision Ball Bearing:17','Precision Ball Bearing:17',#310915,#310925,
'Precision Ball Bearing:17');
#864=NEXT_ASSEMBLY_USAGE_OCCURRENCE('Precision Ball Bearing:18',
'Precision Ball Bearing:18','Precision Ball Bearing:18',#310915,#310925,
'Precision Ball Bearing:18');
#865=NEXT_ASSEMBLY_USAGE_OCCURRENCE('Precision Ball Bearing:19',
'Precision Ball Bearing:19','Precision Ball Bearing:19',#310915,#310925,
'Precision Ball Bearing:19');
#866=NEXT_ASSEMBLY_USAGE_OCCURRENCE('Precision Ball Bearing:20',
'Precision Ball Bearing:20','Precision Ball Bearing:20',#310915,#310925,
'Precision Ball Bearing:20');
#867=NEXT_ASSEMBLY_USAGE_OCCURRENCE('Precision Ball Bearing:21',
'Precision Ball Bearing:21','Precision Ball Bearing:21',#310915,#310925,
'Precision Ball Bearing:21');
#868=NEXT_ASSEMBLY_USAGE_OCCURRENCE('Precision Ball Bearing:22',
'Precision Ball Bearing:22','Precision Ball Bearing:22',#310915,#310925,
'Precision Ball Bearing:22');
#869=NEXT_ASSEMBLY_USAGE_OCCURRENCE('Precision Ball Bearing:23',
'Precision Ball Bearing:23','Precision Ball Bearing:23',#310915,#310925,
'Precision Ball Bearing:23');
#870=NEXT_ASSEMBLY_USAGE_OCCURRENCE('Precision Ball Bearing:24',
'Precision Ball Bearing:24','Precision Ball Bearing:24',#310915,#310925,
'Precision Ball Bearing:24');
#871=NEXT_ASSEMBLY_USAGE_OCCURRENCE('Hexagonal Axle Shaft:2',
'Hexagonal Axle Shaft:2','Hexagonal Axle Shaft:2',#310915,#310926,
'Hexagonal Axle Shaft:2');
#872=NEXT_ASSEMBLY_USAGE_OCCURRENCE('Hexagonal Axle Shaft:3',
'Hexagonal Axle Shaft:3','Hexagonal Axle Shaft:3',#310915,#310926,
'Hexagonal Axle Shaft:3');
#873=NEXT_ASSEMBLY_USAGE_OCCURRENCE('Hexagonal Axle Shaft:4',
'Hexagonal Axle Shaft:4','Hexagonal Axle Shaft:4',#310915,#310926,
'Hexagonal Axle Shaft:4');
#874=NEXT_ASSEMBLY_USAGE_OCCURRENCE('Hexagonal Axle Shaft:5',
'Hexagonal Axle Shaft:5','Hexagonal Axle Shaft:5',#310915,#310926,
'Hexagonal Axle Shaft:5');
#875=NEXT_ASSEMBLY_USAGE_OCCURRENCE('Hexagonal Axle Shaft:6',
'Hexagonal Axle Shaft:6','Hexagonal Axle Shaft:6',#310915,#310926,
'Hexagonal Axle Shaft:6');
#876=NEXT_ASSEMBLY_USAGE_OCCURRENCE('Hexagonal Axle Shaft:7',
'Hexagonal Axle Shaft:7','Hexagonal Axle Shaft:7',#310915,#310926,
'Hexagonal Axle Shaft:7');
#877=NEXT_ASSEMBLY_USAGE_OCCURRENCE('Hexagonal Axle Shaft:8',
'Hexagonal Axle Shaft:8','Hexagonal Axle Shaft:8',#310915,#310926,
'Hexagonal Axle Shaft:8');
#878=NEXT_ASSEMBLY_USAGE_OCCURRENCE('Hexagonal Axle Shaft:9',
'Hexagonal Axle Shaft:9','Hexagonal Axle Shaft:9',#310915,#310926,
'Hexagonal Axle Shaft:9');
#879=NEXT_ASSEMBLY_USAGE_OCCURRENCE('Hexagonal Axle Shaft:10',
'Hexagonal Axle Shaft:10','Hexagonal Axle Shaft:10',#310915,#310926,
'Hexagonal Axle Shaft:10');
#880=NEXT_ASSEMBLY_USAGE_OCCURRENCE('Hexagonal Axle Shaft:11',
'Hexagonal Axle Shaft:11','Hexagonal Axle Shaft:11',#310915,#310926,
'Hexagonal Axle Shaft:11');
#881=NEXT_ASSEMBLY_USAGE_OCCURRENCE('Hexagonal Axle Shaft:12',
'Hexagonal Axle Shaft:12','Hexagonal Axle Shaft:12',#310915,#310926,
'Hexagonal Axle Shaft:12');
#882=NEXT_ASSEMBLY_USAGE_OCCURRENCE('Leg Gusset Bracket:2',
'Leg Gusset Bracket:2','Leg Gusset Bracket:2',#310915,#310931,
'Leg Gusset Bracket:2');
#883=NEXT_ASSEMBLY_USAGE_OCCURRENCE('Conveyor Support Leg:2',
'Conveyor Support Leg:2','Conveyor Support Leg:2',#310915,#310932,
'Conveyor Support Leg:2');
#884=NEXT_ASSEMBLY_USAGE_OCCURRENCE('Base Anchor Foot:2',
'Base Anchor Foot:2','Base Anchor Foot:2',#310915,#310927,
'Base Anchor Foot:2');
#885=NEXT_ASSEMBLY_USAGE_OCCURRENCE('Base Anchor Foot:3',
'Base Anchor Foot:3','Base Anchor Foot:3',#310915,#310927,
'Base Anchor Foot:3');
#886=NEXT_ASSEMBLY_USAGE_OCCURRENCE('Conveyor Support Leg:3',
'Conveyor Support Leg:3','Conveyor Support Leg:3',#310915,#310932,
'Conveyor Support Leg:3');
#887=NEXT_ASSEMBLY_USAGE_OCCURRENCE('Base Anchor Foot:4',
'Base Anchor Foot:4','Base Anchor Foot:4',#310915,#310927,
'Base Anchor Foot:4');
#888=NEXT_ASSEMBLY_USAGE_OCCURRENCE('Side Rail Cross Brace:2',
'Side Rail Cross Brace:2','Side Rail Cross Brace:2',#310915,#310928,
'Side Rail Cross Brace:2');
#889=NEXT_ASSEMBLY_USAGE_OCCURRENCE('Leg Gusset Bracket:3',
'Leg Gusset Bracket:3','Leg Gusset Bracket:3',#310915,#310931,
'Leg Gusset Bracket:3');
#890=NEXT_ASSEMBLY_USAGE_OCCURRENCE('End Cap:2','End Cap:2','End Cap:2',
#310915,#310929,'End Cap:2');
#891=NEXT_ASSEMBLY_USAGE_OCCURRENCE('End Cap:3','End Cap:3','End Cap:3',
#310915,#310929,'End Cap:3');
#892=NEXT_ASSEMBLY_USAGE_OCCURRENCE('End Cap:4','End Cap:4','End Cap:4',
#310915,#310929,'End Cap:4');
#893=NEXT_ASSEMBLY_USAGE_OCCURRENCE('Screw and Nut Assembly:2',
'Screw and Nut Assembly:2','Screw and Nut Assembly:2',#310915,#310933,
'Screw and Nut Assembly:2');
#894=NEXT_ASSEMBLY_USAGE_OCCURRENCE('Screw and Nut Assembly:3',
'Screw and Nut Assembly:3','Screw and Nut Assembly:3',#310915,#310933,
'Screw and Nut Assembly:3');
#895=NEXT_ASSEMBLY_USAGE_OCCURRENCE('Screw and Nut Assembly:4',
'Screw and Nut Assembly:4','Screw and Nut Assembly:4',#310915,#310933,
'Screw and Nut Assembly:4');
#896=NEXT_ASSEMBLY_USAGE_OCCURRENCE('Screw and Nut Assembly:5',
'Screw and Nut Assembly:5','Screw and Nut Assembly:5',#310915,#310933,
'Screw and Nut Assembly:5');
#897=NEXT_ASSEMBLY_USAGE_OCCURRENCE('Screw and Nut Assembly:6',
'Screw and Nut Assembly:6','Screw and Nut Assembly:6',#310915,#310933,
'Screw and Nut Assembly:6');
#898=NEXT_ASSEMBLY_USAGE_OCCURRENCE('Conveyor Support Leg Assembly:2',
'Conveyor Support Leg Assembly:2','Conveyor Support Leg Assembly:2',#310915,
#310930,'Conveyor Support Leg Assembly:2');
#899=NEXT_ASSEMBLY_USAGE_OCCURRENCE('Screw and Nut Assembly:7',
'Screw and Nut Assembly:7','Screw and Nut Assembly:7',#310915,#310933,
'Screw and Nut Assembly:7');
#900=NEXT_ASSEMBLY_USAGE_OCCURRENCE('Screw and Nut Assembly:8',
'Screw and Nut Assembly:8','Screw and Nut Assembly:8',#310915,#310933,
'Screw and Nut Assembly:8');
#901=NEXT_ASSEMBLY_USAGE_OCCURRENCE('Screw and Nut Assembly:9',
'Screw and Nut Assembly:9','Screw and Nut Assembly:9',#310915,#310933,
'Screw and Nut Assembly:9');
#902=NEXT_ASSEMBLY_USAGE_OCCURRENCE('Screw and Nut Assembly:10',
'Screw and Nut Assembly:10','Screw and Nut Assembly:10',#310915,#310933,
'Screw and Nut Assembly:10');
#903=NEXT_ASSEMBLY_USAGE_OCCURRENCE('Screw and Nut Assembly:11',
'Screw and Nut Assembly:11','Screw and Nut Assembly:11',#310915,#310933,
'Screw and Nut Assembly:11');
#904=NEXT_ASSEMBLY_USAGE_OCCURRENCE('Screw and Nut Assembly:12',
'Screw and Nut Assembly:12','Screw and Nut Assembly:12',#310915,#310933,
'Screw and Nut Assembly:12');
#905=B_SPLINE_SURFACE_WITH_KNOTS('',3,3,((#200297,#200298,#200299,#200300,
#200301,#200302,#200303,#200304,#200305,#200306,#200307,#200308,#200309),
(#200310,#200311,#200312,#200313,#200314,#200315,#200316,#200317,#200318,
#200319,#200320,#200321,#200322),(#200323,#200324,#200325,#200326,#200327,
#200328,#200329,#200330,#200331,#200332,#200333,#200334,#200335),(#200336,
#200337,#200338,#200339,#200340,#200341,#200342,#200343,#200344,#200345,
#200346,#200347,#200348),(#200349,#200350,#200351,#200352,#200353,#200354,
#200355,#200356,#200357,#200358,#200359,#200360,#200361),(#200362,#200363,
#200364,#200365,#200366,#200367,#200368,#200369,#200370,#200371,#200372,
#200373,#200374),(#200375,#200376,#200377,#200378,#200379,#200380,#200381,
#200382,#200383,#200384,#200385,#200386,#200387),(#200388,#200389,#200390,
#200391,#200392,#200393,#200394,#200395,#200396,#200397,#200398,#200399,
#200400),(#200401,#200402,#200403,#200404,#200405,#200406,#200407,#200408,
#200409,#200410,#200411,#200412,#200413),(#200414,#200415,#200416,#200417,
#200418,#200419,#200420,#200421,#200422,#200423,#200424,#200425,#200426),
(#200427,#200428,#200429,#200430,#200431,#200432,#200433,#200434,#200435,
#200436,#200437,#200438,#200439),(#200440,#200441,#200442,#200443,#200444,
#200445,#200446,#200447,#200448,#200449,#200450,#200451,#200452),(#200453,
#200454,#200455,#200456,#200457,#200458,#200459,#200460,#200461,#200462,
#200463,#200464,#200465),(#200466,#200467,#200468,#200469,#200470,#200471,
#200472,#200473,#200474,#200475,#200476,#200477,#200478),(#200479,#200480,
#200481,#200482,#200483,#200484,#200485,#200486,#200487,#200488,#200489,
#200490,#200491),(#200492,#200493,#200494,#200495,#200496,#200497,#200498,
#200499,#200500,#200501,#200502,#200503,#200504),(#200505,#200506,#200507,
#200508,#200509,#200510,#200511,#200512,#200513,#200514,#200515,#200516,
#200517),(#200518,#200519,#200520,#200521,#200522,#200523,#200524,#200525,
#200526,#200527,#200528,#200529,#200530),(#200531,#200532,#200533,#200534,
#200535,#200536,#200537,#200538,#200539,#200540,#200541,#200542,#200543),
(#200544,#200545,#200546,#200547,#200548,#200549,#200550,#200551,#200552,
#200553,#200554,#200555,#200556),(#200557,#200558,#200559,#200560,#200561,
#200562,#200563,#200564,#200565,#200566,#200567,#200568,#200569),(#200570,
#200571,#200572,#200573,#200574,#200575,#200576,#200577,#200578,#200579,
#200580,#200581,#200582),(#200583,#200584,#200585,#200586,#200587,#200588,
#200589,#200590,#200591,#200592,#200593,#200594,#200595),(#200596,#200597,
#200598,#200599,#200600,#200601,#200602,#200603,#200604,#200605,#200606,
#200607,#200608),(#200609,#200610,#200611,#200612,#200613,#200614,#200615,
#200616,#200617,#200618,#200619,#200620,#200621),(#200622,#200623,#200624,
#200625,#200626,#200627,#200628,#200629,#200630,#200631,#200632,#200633,
#200634),(#200635,#200636,#200637,#200638,#200639,#200640,#200641,#200642,
#200643,#200644,#200645,#200646,#200647),(#200648,#200649,#200650,#200651,
#200652,#200653,#200654,#200655,#200656,#200657,#200658,#200659,#200660)),
 .UNSPECIFIED.,.F.,.F.,.F.,(4,3,3,3,3,3,3,3,3,4),(4,3,3,3,4),(-3.98343850650087E-6,
0.125000000000275,0.250000000000551,0.375000000000826,0.500000000001101,
0.625000000001376,0.750000000001651,0.875000000001926,0.937500000002063,
1.0000000000022),(0.0305346534395145,0.148544372614449,0.266554091789383,
0.502573530139252,0.97461240683899),.UNSPECIFIED.);
#906=B_SPLINE_SURFACE_WITH_KNOTS('',3,3,((#200724,#200725,#200726,#200727,
#200728,#200729,#200730,#200731,#200732,#200733,#200734,#200735,#200736),
(#200737,#200738,#200739,#200740,#200741,#200742,#200743,#200744,#200745,
#200746,#200747,#200748,#200749),(#200750,#200751,#200752,#200753,#200754,
#200755,#200756,#200757,#200758,#200759,#200760,#200761,#200762),(#200763,
#200764,#200765,#200766,#200767,#200768,#200769,#200770,#200771,#200772,
#200773,#200774,#200775),(#200776,#200777,#200778,#200779,#200780,#200781,
#200782,#200783,#200784,#200785,#200786,#200787,#200788),(#200789,#200790,
#200791,#200792,#200793,#200794,#200795,#200796,#200797,#200798,#200799,
#200800,#200801),(#200802,#200803,#200804,#200805,#200806,#200807,#200808,
#200809,#200810,#200811,#200812,#200813,#200814),(#200815,#200816,#200817,
#200818,#200819,#200820,#200821,#200822,#200823,#200824,#200825,#200826,
#200827),(#200828,#200829,#200830,#200831,#200832,#200833,#200834,#200835,
#200836,#200837,#200838,#200839,#200840),(#200841,#200842,#200843,#200844,
#200845,#200846,#200847,#200848,#200849,#200850,#200851,#200852,#200853),
(#200854,#200855,#200856,#200857,#200858,#200859,#200860,#200861,#200862,
#200863,#200864,#200865,#200866),(#200867,#200868,#200869,#200870,#200871,
#200872,#200873,#200874,#200875,#200876,#200877,#200878,#200879),(#200880,
#200881,#200882,#200883,#200884,#200885,#200886,#200887,#200888,#200889,
#200890,#200891,#200892),(#200893,#200894,#200895,#200896,#200897,#200898,
#200899,#200900,#200901,#200902,#200903,#200904,#200905),(#200906,#200907,
#200908,#200909,#200910,#200911,#200912,#200913,#200914,#200915,#200916,
#200917,#200918),(#200919,#200920,#200921,#200922,#200923,#200924,#200925,
#200926,#200927,#200928,#200929,#200930,#200931),(#200932,#200933,#200934,
#200935,#200936,#200937,#200938,#200939,#200940,#200941,#200942,#200943,
#200944),(#200945,#200946,#200947,#200948,#200949,#200950,#200951,#200952,
#200953,#200954,#200955,#200956,#200957),(#200958,#200959,#200960,#200961,
#200962,#200963,#200964,#200965,#200966,#200967,#200968,#200969,#200970),
(#200971,#200972,#200973,#200974,#200975,#200976,#200977,#200978,#200979,
#200980,#200981,#200982,#200983),(#200984,#200985,#200986,#200987,#200988,
#200989,#200990,#200991,#200992,#200993,#200994,#200995,#200996),(#200997,
#200998,#200999,#201000,#201001,#201002,#201003,#201004,#201005,#201006,
#201007,#201008,#201009),(#201010,#201011,#201012,#201013,#201014,#201015,
#201016,#201017,#201018,#201019,#201020,#201021,#201022),(#201023,#201024,
#201025,#201026,#201027,#201028,#201029,#201030,#201031,#201032,#201033,
#201034,#201035),(#201036,#201037,#201038,#201039,#201040,#201041,#201042,
#201043,#201044,#201045,#201046,#201047,#201048),(#201049,#201050,#201051,
#201052,#201053,#201054,#201055,#201056,#201057,#201058,#201059,#201060,
#201061),(#201062,#201063,#201064,#201065,#201066,#201067,#201068,#201069,
#201070,#201071,#201072,#201073,#201074),(#201075,#201076,#201077,#201078,
#201079,#201080,#201081,#201082,#201083,#201084,#201085,#201086,#201087),
(#201088,#201089,#201090,#201091,#201092,#201093,#201094,#201095,#201096,
#201097,#201098,#201099,#201100),(#201101,#201102,#201103,#201104,#201105,
#201106,#201107,#201108,#201109,#201110,#201111,#201112,#201113),(#201114,
#201115,#201116,#201117,#201118,#201119,#201120,#201121,#201122,#201123,
#201124,#201125,#201126),(#201127,#201128,#201129,#201130,#201131,#201132,
#201133,#201134,#201135,#201136,#201137,#201138,#201139),(#201140,#201141,
#201142,#201143,#201144,#201145,#201146,#201147,#201148,#201149,#201150,
#201151,#201152),(#201153,#201154,#201155,#201156,#201157,#201158,#201159,
#201160,#201161,#201162,#201163,#201164,#201165),(#201166,#201167,#201168,
#201169,#201170,#201171,#201172,#201173,#201174,#201175,#201176,#201177,
#201178),(#201179,#201180,#201181,#201182,#201183,#201184,#201185,#201186,
#201187,#201188,#201189,#201190,#201191),(#201192,#201193,#201194,#201195,
#201196,#201197,#201198,#201199,#201200,#201201,#201202,#201203,#201204),
(#201205,#201206,#201207,#201208,#201209,#201210,#201211,#201212,#201213,
#201214,#201215,#201216,#201217),(#201218,#201219,#201220,#201221,#201222,
#201223,#201224,#201225,#201226,#201227,#201228,#201229,#201230),(#201231,
#201232,#201233,#201234,#201235,#201236,#201237,#201238,#201239,#201240,
#201241,#201242,#201243),(#201244,#201245,#201246,#201247,#201248,#201249,
#201250,#201251,#201252,#201253,#201254,#201255,#201256),(#201257,#201258,
#201259,#201260,#201261,#201262,#201263,#201264,#201265,#201266,#201267,
#201268,#201269),(#201270,#201271,#201272,#201273,#201274,#201275,#201276,
#201277,#201278,#201279,#201280,#201281,#201282)),.UNSPECIFIED.,.F.,.F.,
 .F.,(4,3,3,3,3,3,3,3,3,3,3,3,3,3,4),(4,3,3,3,4),(0.,0.0628750561902459,
0.125750112380492,0.251500224760983,0.377250337141475,0.503000449521967,
0.628750561902459,0.754500674282951,0.817375730473197,0.880250786663443,
0.943125842853689,0.974563370948812,0.990282134996373,0.998141517020154,
1.00600089904393),(0.0313847250337115,0.149350226349808,0.267315727665905,
0.503246730298099,0.975108735562486),.UNSPECIFIED.);
#907=B_SPLINE_SURFACE_WITH_KNOTS('',3,3,((#201360,#201361,#201362,#201363,
#201364,#201365,#201366,#201367,#201368,#201369,#201370,#201371,#201372),
(#201373,#201374,#201375,#201376,#201377,#201378,#201379,#201380,#201381,
#201382,#201383,#201384,#201385),(#201386,#201387,#201388,#201389,#201390,
#201391,#201392,#201393,#201394,#201395,#201396,#201397,#201398),(#201399,
#201400,#201401,#201402,#201403,#201404,#201405,#201406,#201407,#201408,
#201409,#201410,#201411),(#201412,#201413,#201414,#201415,#201416,#201417,
#201418,#201419,#201420,#201421,#201422,#201423,#201424),(#201425,#201426,
#201427,#201428,#201429,#201430,#201431,#201432,#201433,#201434,#201435,
#201436,#201437),(#201438,#201439,#201440,#201441,#201442,#201443,#201444,
#201445,#201446,#201447,#201448,#201449,#201450),(#201451,#201452,#201453,
#201454,#201455,#201456,#201457,#201458,#201459,#201460,#201461,#201462,
#201463),(#201464,#201465,#201466,#201467,#201468,#201469,#201470,#201471,
#201472,#201473,#201474,#201475,#201476),(#201477,#201478,#201479,#201480,
#201481,#201482,#201483,#201484,#201485,#201486,#201487,#201488,#201489),
(#201490,#201491,#201492,#201493,#201494,#201495,#201496,#201497,#201498,
#201499,#201500,#201501,#201502),(#201503,#201504,#201505,#201506,#201507,
#201508,#201509,#201510,#201511,#201512,#201513,#201514,#201515),(#201516,
#201517,#201518,#201519,#201520,#201521,#201522,#201523,#201524,#201525,
#201526,#201527,#201528),(#201529,#201530,#201531,#201532,#201533,#201534,
#201535,#201536,#201537,#201538,#201539,#201540,#201541),(#201542,#201543,
#201544,#201545,#201546,#201547,#201548,#201549,#201550,#201551,#201552,
#201553,#201554),(#201555,#201556,#201557,#201558,#201559,#201560,#201561,
#201562,#201563,#201564,#201565,#201566,#201567),(#201568,#201569,#201570,
#201571,#201572,#201573,#201574,#201575,#201576,#201577,#201578,#201579,
#201580),(#201581,#201582,#201583,#201584,#201585,#201586,#201587,#201588,
#201589,#201590,#201591,#201592,#201593),(#201594,#201595,#201596,#201597,
#201598,#201599,#201600,#201601,#201602,#201603,#201604,#201605,#201606),
(#201607,#201608,#201609,#201610,#201611,#201612,#201613,#201614,#201615,
#201616,#201617,#201618,#201619),(#201620,#201621,#201622,#201623,#201624,
#201625,#201626,#201627,#201628,#201629,#201630,#201631,#201632),(#201633,
#201634,#201635,#201636,#201637,#201638,#201639,#201640,#201641,#201642,
#201643,#201644,#201645),(#201646,#201647,#201648,#201649,#201650,#201651,
#201652,#201653,#201654,#201655,#201656,#201657,#201658),(#201659,#201660,
#201661,#201662,#201663,#201664,#201665,#201666,#201667,#201668,#201669,
#201670,#201671),(#201672,#201673,#201674,#201675,#201676,#201677,#201678,
#201679,#201680,#201681,#201682,#201683,#201684),(#201685,#201686,#201687,
#201688,#201689,#201690,#201691,#201692,#201693,#201694,#201695,#201696,
#201697),(#201698,#201699,#201700,#201701,#201702,#201703,#201704,#201705,
#201706,#201707,#201708,#201709,#201710),(#201711,#201712,#201713,#201714,
#201715,#201716,#201717,#201718,#201719,#201720,#201721,#201722,#201723)),
 .UNSPECIFIED.,.F.,.F.,.F.,(4,3,3,3,3,3,3,3,3,4),(4,3,3,3,4),(0.,0.125000000000521,
0.250000000001042,0.375000000001564,0.500000000002084,0.625000000002606,
0.750000000003127,0.875000000003648,0.937500000003908,1.00000000000417),
(0.035779394199433,0.153116210014097,0.27045302582876,0.505126657458087,
0.97447392071674),.UNSPECIFIED.);
#908=B_SPLINE_SURFACE_WITH_KNOTS('',3,3,((#201796,#201797,#201798,#201799,
#201800,#201801,#201802,#201803,#201804,#201805),(#201806,#201807,#201808,
#201809,#201810,#201811,#201812,#201813,#201814,#201815),(#201816,#201817,
#201818,#201819,#201820,#201821,#201822,#201823,#201824,#201825),(#201826,
#201827,#201828,#201829,#201830,#201831,#201832,#201833,#201834,#201835),
(#201836,#201837,#201838,#201839,#201840,#201841,#201842,#201843,#201844,
#201845),(#201846,#201847,#201848,#201849,#201850,#201851,#201852,#201853,
#201854,#201855),(#201856,#201857,#201858,#201859,#201860,#201861,#201862,
#201863,#201864,#201865),(#201866,#201867,#201868,#201869,#201870,#201871,
#201872,#201873,#201874,#201875),(#201876,#201877,#201878,#201879,#201880,
#201881,#201882,#201883,#201884,#201885),(#201886,#201887,#201888,#201889,
#201890,#201891,#201892,#201893,#201894,#201895),(#201896,#201897,#201898,
#201899,#201900,#201901,#201902,#201903,#201904,#201905),(#201906,#201907,
#201908,#201909,#201910,#201911,#201912,#201913,#201914,#201915),(#201916,
#201917,#201918,#201919,#201920,#201921,#201922,#201923,#201924,#201925),
(#201926,#201927,#201928,#201929,#201930,#201931,#201932,#201933,#201934,
#201935),(#201936,#201937,#201938,#201939,#201940,#201941,#201942,#201943,
#201944,#201945),(#201946,#201947,#201948,#201949,#201950,#201951,#201952,
#201953,#201954,#201955),(#201956,#201957,#201958,#201959,#201960,#201961,
#201962,#201963,#201964,#201965),(#201966,#201967,#201968,#201969,#201970,
#201971,#201972,#201973,#201974,#201975),(#201976,#201977,#201978,#201979,
#201980,#201981,#201982,#201983,#201984,#201985),(#201986,#201987,#201988,
#201989,#201990,#201991,#201992,#201993,#201994,#201995),(#201996,#201997,
#201998,#201999,#202000,#202001,#202002,#202003,#202004,#202005),(#202006,
#202007,#202008,#202009,#202010,#202011,#202012,#202013,#202014,#202015),
(#202016,#202017,#202018,#202019,#202020,#202021,#202022,#202023,#202024,
#202025),(#202026,#202027,#202028,#202029,#202030,#202031,#202032,#202033,
#202034,#202035),(#202036,#202037,#202038,#202039,#202040,#202041,#202042,
#202043,#202044,#202045),(#202046,#202047,#202048,#202049,#202050,#202051,
#202052,#202053,#202054,#202055),(#202056,#202057,#202058,#202059,#202060,
#202061,#202062,#202063,#202064,#202065),(#202066,#202067,#202068,#202069,
#202070,#202071,#202072,#202073,#202074,#202075),(#202076,#202077,#202078,
#202079,#202080,#202081,#202082,#202083,#202084,#202085),(#202086,#202087,
#202088,#202089,#202090,#202091,#202092,#202093,#202094,#202095),(#202096,
#202097,#202098,#202099,#202100,#202101,#202102,#202103,#202104,#202105),
(#202106,#202107,#202108,#202109,#202110,#202111,#202112,#202113,#202114,
#202115),(#202116,#202117,#202118,#202119,#202120,#202121,#202122,#202123,
#202124,#202125),(#202126,#202127,#202128,#202129,#202130,#202131,#202132,
#202133,#202134,#202135),(#202136,#202137,#202138,#202139,#202140,#202141,
#202142,#202143,#202144,#202145),(#202146,#202147,#202148,#202149,#202150,
#202151,#202152,#202153,#202154,#202155),(#202156,#202157,#202158,#202159,
#202160,#202161,#202162,#202163,#202164,#202165),(#202166,#202167,#202168,
#202169,#202170,#202171,#202172,#202173,#202174,#202175),(#202176,#202177,
#202178,#202179,#202180,#202181,#202182,#202183,#202184,#202185),(#202186,
#202187,#202188,#202189,#202190,#202191,#202192,#202193,#202194,#202195),
(#202196,#202197,#202198,#202199,#202200,#202201,#202202,#202203,#202204,
#202205),(#202206,#202207,#202208,#202209,#202210,#202211,#202212,#202213,
#202214,#202215),(#202216,#202217,#202218,#202219,#202220,#202221,#202222,
#202223,#202224,#202225),(#202226,#202227,#202228,#202229,#202230,#202231,
#202232,#202233,#202234,#202235),(#202236,#202237,#202238,#202239,#202240,
#202241,#202242,#202243,#202244,#202245),(#202246,#202247,#202248,#202249,
#202250,#202251,#202252,#202253,#202254,#202255),(#202256,#202257,#202258,
#202259,#202260,#202261,#202262,#202263,#202264,#202265),(#202266,#202267,
#202268,#202269,#202270,#202271,#202272,#202273,#202274,#202275),(#202276,
#202277,#202278,#202279,#202280,#202281,#202282,#202283,#202284,#202285),
(#202286,#202287,#202288,#202289,#202290,#202291,#202292,#202293,#202294,
#202295),(#202296,#202297,#202298,#202299,#202300,#202301,#202302,#202303,
#202304,#202305),(#202306,#202307,#202308,#202309,#202310,#202311,#202312,
#202313,#202314,#202315)),.UNSPECIFIED.,.F.,.F.,.F.,(4,3,3,3,3,3,3,3,3,
3,3,3,3,3,3,3,3,4),(4,3,3,4),(0.,0.00790626166828645,0.0158125233365729,
0.0316250466731458,0.0632500933462917,0.126500186692583,0.189750280038875,
0.253000373385167,0.37950056007775,0.506000746770334,0.632500933462917,
0.7590011201555,0.885501306848084,0.948751400194375,0.980376446867521,0.996188970204094,
1.00409523187238,1.01200149354067),(0.0341113530318832,0.269267250872974,
0.504423148714065,0.974734944396246),.UNSPECIFIED.);
#909=B_SPLINE_SURFACE_WITH_KNOTS('',3,3,((#202498,#202499,#202500,#202501),
(#202502,#202503,#202504,#202505),(#202506,#202507,#202508,#202509),(#202510,
#202511,#202512,#202513)),.UNSPECIFIED.,.F.,.F.,.F.,(4,4),(4,4),(0.,0.27458600745849),
(0.048728470569204,0.974637180848091),.UNSPECIFIED.);
#910=B_SPLINE_SURFACE_WITH_KNOTS('',3,3,((#202534,#202535,#202536,#202537),
(#202538,#202539,#202540,#202541),(#202542,#202543,#202544,#202545),(#202546,
#202547,#202548,#202549)),.UNSPECIFIED.,.F.,.F.,.F.,(4,4),(4,4),(0.,0.276208371820539),
(0.0491493978854403,0.974752225001403),.UNSPECIFIED.);
#911=B_SPLINE_SURFACE_WITH_KNOTS('',3,3,((#202753,#202754,#202755,#202756),
(#202757,#202758,#202759,#202760),(#202761,#202762,#202763,#202764),(#202765,
#202766,#202767,#202768)),.UNSPECIFIED.,.F.,.F.,.F.,(4,4),(4,4),(0.,0.107439860233905),
(0.0511874640850671,0.974440796609261),.UNSPECIFIED.);
#912=B_SPLINE_SURFACE_WITH_KNOTS('',3,3,((#202889,#202890,#202891,#202892),
(#202893,#202894,#202895,#202896),(#202897,#202898,#202899,#202900),(#202901,
#202902,#202903,#202904)),.UNSPECIFIED.,.F.,.F.,.F.,(4,4),(4,4),(0.,0.0948189441871283),
(0.0504405324641688,0.975107277906268),.UNSPECIFIED.);
#913=B_SPLINE_SURFACE_WITH_KNOTS('',3,3,((#202968,#202969,#202970,#202971,
#202972,#202973,#202974),(#202975,#202976,#202977,#202978,#202979,#202980,
#202981),(#202982,#202983,#202984,#202985,#202986,#202987,#202988),(#202989,
#202990,#202991,#202992,#202993,#202994,#202995),(#202996,#202997,#202998,
#202999,#203000,#203001,#203002),(#203003,#203004,#203005,#203006,#203007,
#203008,#203009),(#203010,#203011,#203012,#203013,#203014,#203015,#203016),
(#203017,#203018,#203019,#203020,#203021,#203022,#203023),(#203024,#203025,
#203026,#203027,#203028,#203029,#203030),(#203031,#203032,#203033,#203034,
#203035,#203036,#203037),(#203038,#203039,#203040,#203041,#203042,#203043,
#203044),(#203045,#203046,#203047,#203048,#203049,#203050,#203051),(#203052,
#203053,#203054,#203055,#203056,#203057,#203058),(#203059,#203060,#203061,
#203062,#203063,#203064,#203065),(#203066,#203067,#203068,#203069,#203070,
#203071,#203072),(#203073,#203074,#203075,#203076,#203077,#203078,#203079),
(#203080,#203081,#203082,#203083,#203084,#203085,#203086),(#203087,#203088,
#203089,#203090,#203091,#203092,#203093),(#203094,#203095,#203096,#203097,
#203098,#203099,#203100),(#203101,#203102,#203103,#203104,#203105,#203106,
#203107),(#203108,#203109,#203110,#203111,#203112,#203113,#203114),(#203115,
#203116,#203117,#203118,#203119,#203120,#203121),(#203122,#203123,#203124,
#203125,#203126,#203127,#203128),(#203129,#203130,#203131,#203132,#203133,
#203134,#203135),(#203136,#203137,#203138,#203139,#203140,#203141,#203142),
(#203143,#203144,#203145,#203146,#203147,#203148,#203149),(#203150,#203151,
#203152,#203153,#203154,#203155,#203156),(#203157,#203158,#203159,#203160,
#203161,#203162,#203163)),.UNSPECIFIED.,.F.,.F.,.F.,(4,3,3,3,3,3,3,3,3,
4),(4,3,4),(0.,0.0078125,0.015625,0.03125,0.0625,0.125,0.25,0.5,0.75,1.),
(0.0332750425089971,0.501824549528,0.970374056547004),.UNSPECIFIED.);
#914=B_SPLINE_SURFACE_WITH_KNOTS('',3,3,((#203245,#203246,#203247,#203248,
#203249,#203250,#203251),(#203252,#203253,#203254,#203255,#203256,#203257,
#203258),(#203259,#203260,#203261,#203262,#203263,#203264,#203265),(#203266,
#203267,#203268,#203269,#203270,#203271,#203272),(#203273,#203274,#203275,
#203276,#203277,#203278,#203279),(#203280,#203281,#203282,#203283,#203284,
#203285,#203286),(#203287,#203288,#203289,#203290,#203291,#203292,#203293),
(#203294,#203295,#203296,#203297,#203298,#203299,#203300),(#203301,#203302,
#203303,#203304,#203305,#203306,#203307),(#203308,#203309,#203310,#203311,
#203312,#203313,#203314),(#203315,#203316,#203317,#203318,#203319,#203320,
#203321),(#203322,#203323,#203324,#203325,#203326,#203327,#203328),(#203329,
#203330,#203331,#203332,#203333,#203334,#203335),(#203336,#203337,#203338,
#203339,#203340,#203341,#203342),(#203343,#203344,#203345,#203346,#203347,
#203348,#203349),(#203350,#203351,#203352,#203353,#203354,#203355,#203356),
(#203357,#203358,#203359,#203360,#203361,#203362,#203363),(#203364,#203365,
#203366,#203367,#203368,#203369,#203370),(#203371,#203372,#203373,#203374,
#203375,#203376,#203377),(#203378,#203379,#203380,#203381,#203382,#203383,
#203384),(#203385,#203386,#203387,#203388,#203389,#203390,#203391),(#203392,
#203393,#203394,#203395,#203396,#203397,#203398),(#203399,#203400,#203401,
#203402,#203403,#203404,#203405),(#203406,#203407,#203408,#203409,#203410,
#203411,#203412),(#203413,#203414,#203415,#203416,#203417,#203418,#203419),
(#203420,#203421,#203422,#203423,#203424,#203425,#203426),(#203427,#203428,
#203429,#203430,#203431,#203432,#203433),(#203434,#203435,#203436,#203437,
#203438,#203439,#203440),(#203441,#203442,#203443,#203444,#203445,#203446,
#203447),(#203448,#203449,#203450,#203451,#203452,#203453,#203454),(#203455,
#203456,#203457,#203458,#203459,#203460,#203461),(#203462,#203463,#203464,
#203465,#203466,#203467,#203468),(#203469,#203470,#203471,#203472,#203473,
#203474,#203475),(#203476,#203477,#203478,#203479,#203480,#203481,#203482),
(#203483,#203484,#203485,#203486,#203487,#203488,#203489),(#203490,#203491,
#203492,#203493,#203494,#203495,#203496),(#203497,#203498,#203499,#203500,
#203501,#203502,#203503),(#203504,#203505,#203506,#203507,#203508,#203509,
#203510),(#203511,#203512,#203513,#203514,#203515,#203516,#203517),(#203518,
#203519,#203520,#203521,#203522,#203523,#203524)),.UNSPECIFIED.,.F.,.F.,
 .F.,(4,3,3,3,3,3,3,3,3,3,3,3,3,4),(4,3,4),(0.,0.0078593752336461,0.0157187504672922,
0.0314375009345845,0.0628750018691691,0.125750003738338,0.251500007476676,
0.503000014953352,0.754500022430028,0.880250026168366,0.943125028037535,
0.974562528972119,0.990281279439412,1.0060000299067),(0.0284242133522742,
0.499005960311874,0.969587707271474),.UNSPECIFIED.);
#915=B_SPLINE_SURFACE_WITH_KNOTS('',3,3,((#203732,#203733,#203734,#203735,
#203736,#203737,#203738),(#203739,#203740,#203741,#203742,#203743,#203744,
#203745),(#203746,#203747,#203748,#203749,#203750,#203751,#203752),(#203753,
#203754,#203755,#203756,#203757,#203758,#203759),(#203760,#203761,#203762,
#203763,#203764,#203765,#203766),(#203767,#203768,#203769,#203770,#203771,
#203772,#203773),(#203774,#203775,#203776,#203777,#203778,#203779,#203780),
(#203781,#203782,#203783,#203784,#203785,#203786,#203787),(#203788,#203789,
#203790,#203791,#203792,#203793,#203794),(#203795,#203796,#203797,#203798,
#203799,#203800,#203801),(#203802,#203803,#203804,#203805,#203806,#203807,
#203808),(#203809,#203810,#203811,#203812,#203813,#203814,#203815),(#203816,
#203817,#203818,#203819,#203820,#203821,#203822),(#203823,#203824,#203825,
#203826,#203827,#203828,#203829),(#203830,#203831,#203832,#203833,#203834,
#203835,#203836),(#203837,#203838,#203839,#203840,#203841,#203842,#203843),
(#203844,#203845,#203846,#203847,#203848,#203849,#203850),(#203851,#203852,
#203853,#203854,#203855,#203856,#203857),(#203858,#203859,#203860,#203861,
#203862,#203863,#203864),(#203865,#203866,#203867,#203868,#203869,#203870,
#203871),(#203872,#203873,#203874,#203875,#203876,#203877,#203878),(#203879,
#203880,#203881,#203882,#203883,#203884,#203885),(#203886,#203887,#203888,
#203889,#203890,#203891,#203892),(#203893,#203894,#203895,#203896,#203897,
#203898,#203899),(#203900,#203901,#203902,#203903,#203904,#203905,#203906),
(#203907,#203908,#203909,#203910,#203911,#203912,#203913),(#203914,#203915,
#203916,#203917,#203918,#203919,#203920),(#203921,#203922,#203923,#203924,
#203925,#203926,#203927),(#203928,#203929,#203930,#203931,#203932,#203933,
#203934),(#203935,#203936,#203937,#203938,#203939,#203940,#203941),(#203942,
#203943,#203944,#203945,#203946,#203947,#203948),(#203949,#203950,#203951,
#203952,#203953,#203954,#203955),(#203956,#203957,#203958,#203959,#203960,
#203961,#203962),(#203963,#203964,#203965,#203966,#203967,#203968,#203969),
(#203970,#203971,#203972,#203973,#203974,#203975,#203976),(#203977,#203978,
#203979,#203980,#203981,#203982,#203983),(#203984,#203985,#203986,#203987,
#203988,#203989,#203990),(#203991,#203992,#203993,#203994,#203995,#203996,
#203997),(#203998,#203999,#204000,#204001,#204002,#204003,#204004),(#204005,
#204006,#204007,#204008,#204009,#204010,#204011),(#204012,#204013,#204014,
#204015,#204016,#204017,#204018),(#204019,#204020,#204021,#204022,#204023,
#204024,#204025),(#204026,#204027,#204028,#204029,#204030,#204031,#204032),
(#204033,#204034,#204035,#204036,#204037,#204038,#204039),(#204040,#204041,
#204042,#204043,#204044,#204045,#204046),(#204047,#204048,#204049,#204050,
#204051,#204052,#204053),(#204054,#204055,#204056,#204057,#204058,#204059,
#204060),(#204061,#204062,#204063,#204064,#204065,#204066,#204067),(#204068,
#204069,#204070,#204071,#204072,#204073,#204074),(#204075,#204076,#204077,
#204078,#204079,#204080,#204081),(#204082,#204083,#204084,#204085,#204086,
#204087,#204088),(#204089,#204090,#204091,#204092,#204093,#204094,#204095),
(#204096,#204097,#204098,#204099,#204100,#204101,#204102),(#204103,#204104,
#204105,#204106,#204107,#204108,#204109),(#204110,#204111,#204112,#204113,
#204114,#204115,#204116),(#204117,#204118,#204119,#204120,#204121,#204122,
#204123),(#204124,#204125,#204126,#204127,#204128,#204129,#204130),(#204131,
#204132,#204133,#204134,#204135,#204136,#204137),(#204138,#204139,#204140,
#204141,#204142,#204143,#204144),(#204145,#204146,#204147,#204148,#204149,
#204150,#204151),(#204152,#204153,#204154,#204155,#204156,#204157,#204158),
(#204159,#204160,#204161,#204162,#204163,#204164,#204165),(#204166,#204167,
#204168,#204169,#204170,#204171,#204172),(#204173,#204174,#204175,#204176,
#204177,#204178,#204179),(#204180,#204181,#204182,#204183,#204184,#204185,
#204186),(#204187,#204188,#204189,#204190,#204191,#204192,#204193),(#204194,
#204195,#204196,#204197,#204198,#204199,#204200),(#204201,#204202,#204203,
#204204,#204205,#204206,#204207),(#204208,#204209,#204210,#204211,#204212,
#204213,#204214),(#204215,#204216,#204217,#204218,#204219,#204220,#204221),
(#204222,#204223,#204224,#204225,#204226,#204227,#204228),(#204229,#204230,
#204231,#204232,#204233,#204234,#204235),(#204236,#204237,#204238,#204239,
#204240,#204241,#204242),(#204243,#204244,#204245,#204246,#204247,#204248,
#204249),(#204250,#204251,#204252,#204253,#204254,#204255,#204256),(#204257,
#204258,#204259,#204260,#204261,#204262,#204263),(#204264,#204265,#204266,
#204267,#204268,#204269,#204270),(#204271,#204272,#204273,#204274,#204275,
#204276,#204277),(#204278,#204279,#204280,#204281,#204282,#204283,#204284),
(#204285,#204286,#204287,#204288,#204289,#204290,#204291),(#204292,#204293,
#204294,#204295,#204296,#204297,#204298),(#204299,#204300,#204301,#204302,
#204303,#204304,#204305),(#204306,#204307,#204308,#204309,#204310,#204311,
#204312),(#204313,#204314,#204315,#204316,#204317,#204318,#204319),(#204320,
#204321,#204322,#204323,#204324,#204325,#204326),(#204327,#204328,#204329,
#204330,#204331,#204332,#204333),(#204334,#204335,#204336,#204337,#204338,
#204339,#204340),(#204341,#204342,#204343,#204344,#204345,#204346,#204347),
(#204348,#204349,#204350,#204351,#204352,#204353,#204354),(#204355,#204356,
#204357,#204358,#204359,#204360,#204361),(#204362,#204363,#204364,#204365,
#204366,#204367,#204368),(#204369,#204370,#204371,#204372,#204373,#204374,
#204375),(#204376,#204377,#204378,#204379,#204380,#204381,#204382),(#204383,
#204384,#204385,#204386,#204387,#204388,#204389),(#204390,#204391,#204392,
#204393,#204394,#204395,#204396),(#204397,#204398,#204399,#204400,#204401,
#204402,#204403),(#204404,#204405,#204406,#204407,#204408,#204409,#204410),
(#204411,#204412,#204413,#204414,#204415,#204416,#204417),(#204418,#204419,
#204420,#204421,#204422,#204423,#204424),(#204425,#204426,#204427,#204428,
#204429,#204430,#204431),(#204432,#204433,#204434,#204435,#204436,#204437,
#204438),(#204439,#204440,#204441,#204442,#204443,#204444,#204445),(#204446,
#204447,#204448,#204449,#204450,#204451,#204452),(#204453,#204454,#204455,
#204456,#204457,#204458,#204459),(#204460,#204461,#204462,#204463,#204464,
#204465,#204466),(#204467,#204468,#204469,#204470,#204471,#204472,#204473),
(#204474,#204475,#204476,#204477,#204478,#204479,#204480),(#204481,#204482,
#204483,#204484,#204485,#204486,#204487),(#204488,#204489,#204490,#204491,
#204492,#204493,#204494),(#204495,#204496,#204497,#204498,#204499,#204500,
#204501),(#204502,#204503,#204504,#204505,#204506,#204507,#204508),(#204509,
#204510,#204511,#204512,#204513,#204514,#204515),(#204516,#204517,#204518,
#204519,#204520,#204521,#204522),(#204523,#204524,#204525,#204526,#204527,
#204528,#204529),(#204530,#204531,#204532,#204533,#204534,#204535,#204536),
(#204537,#204538,#204539,#204540,#204541,#204542,#204543),(#204544,#204545,
#204546,#204547,#204548,#204549,#204550),(#204551,#204552,#204553,#204554,
#204555,#204556,#204557),(#204558,#204559,#204560,#204561,#204562,#204563,
#204564),(#204565,#204566,#204567,#204568,#204569,#204570,#204571),(#204572,
#204573,#204574,#204575,#204576,#204577,#204578),(#204579,#204580,#204581,
#204582,#204583,#204584,#204585),(#204586,#204587,#204588,#204589,#204590,
#204591,#204592),(#204593,#204594,#204595,#204596,#204597,#204598,#204599),
(#204600,#204601,#204602,#204603,#204604,#204605,#204606),(#204607,#204608,
#204609,#204610,#204611,#204612,#204613),(#204614,#204615,#204616,#204617,
#204618,#204619,#204620),(#204621,#204622,#204623,#204624,#204625,#204626,
#204627),(#204628,#204629,#204630,#204631,#204632,#204633,#204634),(#204635,
#204636,#204637,#204638,#204639,#204640,#204641),(#204642,#204643,#204644,
#204645,#204646,#204647,#204648),(#204649,#204650,#204651,#204652,#204653,
#204654,#204655),(#204656,#204657,#204658,#204659,#204660,#204661,#204662),
(#204663,#204664,#204665,#204666,#204667,#204668,#204669),(#204670,#204671,
#204672,#204673,#204674,#204675,#204676),(#204677,#204678,#204679,#204680,
#204681,#204682,#204683),(#204684,#204685,#204686,#204687,#204688,#204689,
#204690),(#204691,#204692,#204693,#204694,#204695,#204696,#204697),(#204698,
#204699,#204700,#204701,#204702,#204703,#204704),(#204705,#204706,#204707,
#204708,#204709,#204710,#204711),(#204712,#204713,#204714,#204715,#204716,
#204717,#204718),(#204719,#204720,#204721,#204722,#204723,#204724,#204725),
(#204726,#204727,#204728,#204729,#204730,#204731,#204732),(#204733,#204734,
#204735,#204736,#204737,#204738,#204739),(#204740,#204741,#204742,#204743,
#204744,#204745,#204746),(#204747,#204748,#204749,#204750,#204751,#204752,
#204753),(#204754,#204755,#204756,#204757,#204758,#204759,#204760),(#204761,
#204762,#204763,#204764,#204765,#204766,#204767),(#204768,#204769,#204770,
#204771,#204772,#204773,#204774),(#204775,#204776,#204777,#204778,#204779,
#204780,#204781),(#204782,#204783,#204784,#204785,#204786,#204787,#204788),
(#204789,#204790,#204791,#204792,#204793,#204794,#204795),(#204796,#204797,
#204798,#204799,#204800,#204801,#204802),(#204803,#204804,#204805,#204806,
#204807,#204808,#204809),(#204810,#204811,#204812,#204813,#204814,#204815,
#204816),(#204817,#204818,#204819,#204820,#204821,#204822,#204823),(#204824,
#204825,#204826,#204827,#204828,#204829,#204830)),.UNSPECIFIED.,.F.,.F.,
 .F.,(4,3,3,3,3,3,3,3,3,3,3,3,3,3,3,3,3,3,3,3,3,3,3,3,3,3,3,3,3,3,3,3,3,
3,3,3,3,3,3,3,3,3,3,3,3,3,3,3,3,3,3,3,4),(4,3,4),(0.,0.125100494684528,
0.156375618355659,0.164194399273443,0.165171746888165,0.166149094502889,
0.168103789732334,0.172013180191225,0.187650742026792,0.250200989369055,
0.281476113040187,0.297113674875754,0.299068370105199,0.301023065334645,
0.304932455793537,0.312751236711319,0.375301484053584,0.406576607724715,
0.422214169560281,0.430032950478064,0.431010298092787,0.431498971900149,
0.43198764570751,0.433942340936955,0.437851731395847,0.500401978738111,
0.562952226080375,0.566861616539267,0.568816311768712,0.569793659383435,
0.570771006998158,0.578589787915941,0.594227349751507,0.625502473422639,
0.688052720764903,0.695871501682686,0.699780892141577,0.7007582397563,0.701246913563662,
0.701735587371023,0.703690282600469,0.719327844436035,0.750602968107167,
0.813153215449431,0.828790777284997,0.832700167743888,0.834654862973334,
0.835632210588057,0.836120884395418,0.83660955820278,0.844428339120562,
0.875703462791694,1.00080395747622),(0.0460660594806178,0.548882757239649,
1.05169945499868),.UNSPECIFIED.);
#916=B_SPLINE_SURFACE_WITH_KNOTS('',3,1,((#204924,#204925),(#204926,#204927),
(#204928,#204929),(#204930,#204931),(#204932,#204933),(#204934,#204935),
(#204936,#204937),(#204938,#204939),(#204940,#204941),(#204942,#204943),
(#204944,#204945),(#204946,#204947),(#204948,#204949),(#204950,#204951),
(#204952,#204953),(#204954,#204955),(#204956,#204957),(#204958,#204959),
(#204960,#204961),(#204962,#204963),(#204964,#204965),(#204966,#204967),
(#204968,#204969),(#204970,#204971),(#204972,#204973),(#204974,#204975),
(#204976,#204977),(#204978,#204979),(#204980,#204981),(#204982,#204983),
(#204984,#204985),(#204986,#204987),(#204988,#204989),(#204990,#204991),
(#204992,#204993),(#204994,#204995),(#204996,#204997),(#204998,#204999),
(#205000,#205001),(#205002,#205003),(#205004,#205005),(#205006,#205007)),
 .UNSPECIFIED.,.F.,.F.,.F.,(4,1,1,1,2,1,1,1,2,1,1,1,2,1,1,1,2,1,1,1,2,1,
1,1,2,1,1,1,2,1,1,1,4),(2,2),(-0.130664626928687,0.0411596607520464,0.0823193215040928,
0.123478982256139,0.164638643008186,0.198458137911997,0.232277632815809,
0.26609712771962,0.299916622623432,0.332619014198497,0.365321405773562,
0.398023797348627,0.430726188923692,0.448044641692768,0.465363094461843,
0.482681547230919,0.499999999999994,0.517318452769073,0.534636905538152,
0.55195535830723,0.569273811076309,0.601976202651373,0.634678594226438,
0.667380985801503,0.700083377376568,0.73390287228038,0.767722367184191,
0.801541862088003,0.835361356991815,0.876521017743861,0.917680678495907,
0.958840339247954,1.12208155081997),(-0.184126650858872,1.18095881489235),
 .UNSPECIFIED.);
#917=B_SPLINE_SURFACE_WITH_KNOTS('',3,3,((#205068,#205069,#205070,#205071,
#205072,#205073,#205074),(#205075,#205076,#205077,#205078,#205079,#205080,
#205081),(#205082,#205083,#205084,#205085,#205086,#205087,#205088),(#205089,
#205090,#205091,#205092,#205093,#205094,#205095),(#205096,#205097,#205098,
#205099,#205100,#205101,#205102),(#205103,#205104,#205105,#205106,#205107,
#205108,#205109),(#205110,#205111,#205112,#205113,#205114,#205115,#205116),
(#205117,#205118,#205119,#205120,#205121,#205122,#205123),(#205124,#205125,
#205126,#205127,#205128,#205129,#205130),(#205131,#205132,#205133,#205134,
#205135,#205136,#205137),(#205138,#205139,#205140,#205141,#205142,#205143,
#205144)),.UNSPECIFIED.,.F.,.F.,.F.,(4,1,1,1,1,1,1,1,4),(4,3,4),(0.,0.124999999999998,
0.249999999999996,0.374999999999993,0.500000000000009,0.625000000000007,
0.75,0.875,1.),(0.,1.,1.01),.UNSPECIFIED.);
#918=B_SPLINE_SURFACE_WITH_KNOTS('',3,3,((#205150,#205151,#205152,#205153,
#205154,#205155,#205156),(#205157,#205158,#205159,#205160,#205161,#205162,
#205163),(#205164,#205165,#205166,#205167,#205168,#205169,#205170),(#205171,
#205172,#205173,#205174,#205175,#205176,#205177),(#205178,#205179,#205180,
#205181,#205182,#205183,#205184),(#205185,#205186,#205187,#205188,#205189,
#205190,#205191),(#205192,#205193,#205194,#205195,#205196,#205197,#205198),
(#205199,#205200,#205201,#205202,#205203,#205204,#205205),(#205206,#205207,
#205208,#205209,#205210,#205211,#205212),(#205213,#205214,#205215,#205216,
#205217,#205218,#205219),(#205220,#205221,#205222,#205223,#205224,#205225,
#205226),(#205227,#205228,#205229,#205230,#205231,#205232,#205233),(#205234,
#205235,#205236,#205237,#205238,#205239,#205240),(#205241,#205242,#205243,
#205244,#205245,#205246,#205247)),.UNSPECIFIED.,.F.,.F.,.F.,(4,3,1,1,1,
1,1,1,1,4),(4,3,4),(-0.01,0.,0.124999999999997,0.249999999999995,0.374999999999992,
0.49999999999999,0.624999999999988,0.749999999999985,0.874999999999983,
1.),(0.,1.,1.01),.UNSPECIFIED.);
#919=B_SPLINE_SURFACE_WITH_KNOTS('',3,3,((#205253,#205254,#205255,#205256,
#205257,#205258,#205259),(#205260,#205261,#205262,#205263,#205264,#205265,
#205266),(#205267,#205268,#205269,#205270,#205271,#205272,#205273),(#205274,
#205275,#205276,#205277,#205278,#205279,#205280),(#205281,#205282,#205283,
#205284,#205285,#205286,#205287),(#205288,#205289,#205290,#205291,#205292,
#205293,#205294),(#205295,#205296,#205297,#205298,#205299,#205300,#205301),
(#205302,#205303,#205304,#205305,#205306,#205307,#205308),(#205309,#205310,
#205311,#205312,#205313,#205314,#205315),(#205316,#205317,#205318,#205319,
#205320,#205321,#205322),(#205323,#205324,#205325,#205326,#205327,#205328,
#205329)),.UNSPECIFIED.,.F.,.F.,.F.,(4,1,1,1,1,1,1,1,4),(4,3,4),(0.,0.124999999999997,
0.249999999999998,0.375,0.5,0.625,0.75,0.875,1.),(0.,1.,1.01),
 .UNSPECIFIED.);
#920=B_SPLINE_SURFACE_WITH_KNOTS('',3,3,((#205335,#205336,#205337,#205338,
#205339,#205340,#205341),(#205342,#205343,#205344,#205345,#205346,#205347,
#205348),(#205349,#205350,#205351,#205352,#205353,#205354,#205355),(#205356,
#205357,#205358,#205359,#205360,#205361,#205362),(#205363,#205364,#205365,
#205366,#205367,#205368,#205369),(#205370,#205371,#205372,#205373,#205374,
#205375,#205376),(#205377,#205378,#205379,#205380,#205381,#205382,#205383),
(#205384,#205385,#205386,#205387,#205388,#205389,#205390),(#205391,#205392,
#205393,#205394,#205395,#205396,#205397),(#205398,#205399,#205400,#205401,
#205402,#205403,#205404),(#205405,#205406,#205407,#205408,#205409,#205410,
#205411),(#205412,#205413,#205414,#205415,#205416,#205417,#205418),(#205419,
#205420,#205421,#205422,#205423,#205424,#205425),(#205426,#205427,#205428,
#205429,#205430,#205431,#205432),(#205433,#205434,#205435,#205436,#205437,
#205438,#205439),(#205440,#205441,#205442,#205443,#205444,#205445,#205446),
(#205447,#205448,#205449,#205450,#205451,#205452,#205453)),
 .UNSPECIFIED.,.F.,.F.,.F.,(4,3,1,1,1,1,1,1,1,3,4),(4,3,4),(-0.01,0.,0.125,
0.25,0.375,0.5,0.625,0.75,0.875,1.,1.01),(0.,1.,1.01),.UNSPECIFIED.);
#921=B_SPLINE_SURFACE_WITH_KNOTS('',3,3,((#205503,#205504,#205505,#205506),
(#205507,#205508,#205509,#205510),(#205511,#205512,#205513,#205514),(#205515,
#205516,#205517,#205518),(#205519,#205520,#205521,#205522),(#205523,#205524,
#205525,#205526),(#205527,#205528,#205529,#205530)),.UNSPECIFIED.,.F.,.F.,
 .F.,(4,1,1,1,4),(4,4),(0.,0.25,0.5,0.75,1.),(0.,1.),.UNSPECIFIED.);
#922=B_SPLINE_SURFACE_WITH_KNOTS('',3,3,((#205531,#205532,#205533,#205534,
#205535,#205536,#205537),(#205538,#205539,#205540,#205541,#205542,#205543,
#205544),(#205545,#205546,#205547,#205548,#205549,#205550,#205551),(#205552,
#205553,#205554,#205555,#205556,#205557,#205558),(#205559,#205560,#205561,
#205562,#205563,#205564,#205565),(#205566,#205567,#205568,#205569,#205570,
#205571,#205572),(#205573,#205574,#205575,#205576,#205577,#205578,#205579)),
 .UNSPECIFIED.,.F.,.F.,.F.,(4,1,1,1,4),(4,3,4),(0.,0.25,0.5,0.75,1.),(0.,
1.,1.01),.UNSPECIFIED.);
#923=B_SPLINE_SURFACE_WITH_KNOTS('',3,3,((#205581,#205582,#205583,#205584,
#205585,#205586,#205587),(#205588,#205589,#205590,#205591,#205592,#205593,
#205594),(#205595,#205596,#205597,#205598,#205599,#205600,#205601),(#205602,
#205603,#205604,#205605,#205606,#205607,#205608),(#205609,#205610,#205611,
#205612,#205613,#205614,#205615),(#205616,#205617,#205618,#205619,#205620,
#205621,#205622),(#205623,#205624,#205625,#205626,#205627,#205628,#205629)),
 .UNSPECIFIED.,.F.,.F.,.F.,(4,1,1,1,4),(4,3,4),(0.,0.25,0.5,0.75,1.),(0.,
1.,1.01),.UNSPECIFIED.);
#924=B_SPLINE_SURFACE_WITH_KNOTS('',3,3,((#205630,#205631,#205632,#205633,
#205634,#205635,#205636),(#205637,#205638,#205639,#205640,#205641,#205642,
#205643),(#205644,#205645,#205646,#205647,#205648,#205649,#205650),(#205651,
#205652,#205653,#205654,#205655,#205656,#205657),(#205658,#205659,#205660,
#205661,#205662,#205663,#205664),(#205665,#205666,#205667,#205668,#205669,
#205670,#205671),(#205672,#205673,#205674,#205675,#205676,#205677,#205678)),
 .UNSPECIFIED.,.F.,.F.,.F.,(4,1,1,1,4),(4,3,4),(0.,0.25,0.5,0.75,1.),(0.,
1.,1.01),.UNSPECIFIED.);
#925=B_SPLINE_SURFACE_WITH_KNOTS('',3,3,((#205680,#205681,#205682,#205683,
#205684,#205685,#205686,#205687,#205688,#205689,#205690,#205691,#205692,
#205693,#205694,#205695),(#205696,#205697,#205698,#205699,#205700,#205701,
#205702,#205703,#205704,#205705,#205706,#205707,#205708,#205709,#205710,
#205711),(#205712,#205713,#205714,#205715,#205716,#205717,#205718,#205719,
#205720,#205721,#205722,#205723,#205724,#205725,#205726,#205727),(#205728,
#205729,#205730,#205731,#205732,#205733,#205734,#205735,#205736,#205737,
#205738,#205739,#205740,#205741,#205742,#205743),(#205744,#205745,#205746,
#205747,#205748,#205749,#205750,#205751,#205752,#205753,#205754,#205755,
#205756,#205757,#205758,#205759),(#205760,#205761,#205762,#205763,#205764,
#205765,#205766,#205767,#205768,#205769,#205770,#205771,#205772,#205773,
#205774,#205775),(#205776,#205777,#205778,#205779,#205780,#205781,#205782,
#205783,#205784,#205785,#205786,#205787,#205788,#205789,#205790,#205791),
(#205792,#205793,#205794,#205795,#205796,#205797,#205798,#205799,#205800,
#205801,#205802,#205803,#205804,#205805,#205806,#205807),(#205808,#205809,
#205810,#205811,#205812,#205813,#205814,#205815,#205816,#205817,#205818,
#205819,#205820,#205821,#205822,#205823),(#205824,#205825,#205826,#205827,
#205828,#205829,#205830,#205831,#205832,#205833,#205834,#205835,#205836,
#205837,#205838,#205839),(#205840,#205841,#205842,#205843,#205844,#205845,
#205846,#205847,#205848,#205849,#205850,#205851,#205852,#205853,#205854,
#205855),(#205856,#205857,#205858,#205859,#205860,#205861,#205862,#205863,
#205864,#205865,#205866,#205867,#205868,#205869,#205870,#205871),(#205872,
#205873,#205874,#205875,#205876,#205877,#205878,#205879,#205880,#205881,
#205882,#205883,#205884,#205885,#205886,#205887),(#205888,#205889,#205890,
#205891,#205892,#205893,#205894,#205895,#205896,#205897,#205898,#205899,
#205900,#205901,#205902,#205903),(#205904,#205905,#205906,#205907,#205908,
#205909,#205910,#205911,#205912,#205913,#205914,#205915,#205916,#205917,
#205918,#205919),(#205920,#205921,#205922,#205923,#205924,#205925,#205926,
#205927,#205928,#205929,#205930,#205931,#205932,#205933,#205934,#205935),
(#205936,#205937,#205938,#205939,#205940,#205941,#205942,#205943,#205944,
#205945,#205946,#205947,#205948,#205949,#205950,#205951),(#205952,#205953,
#205954,#205955,#205956,#205957,#205958,#205959,#205960,#205961,#205962,
#205963,#205964,#205965,#205966,#205967),(#205968,#205969,#205970,#205971,
#205972,#205973,#205974,#205975,#205976,#205977,#205978,#205979,#205980,
#205981,#205982,#205983),(#205984,#205985,#205986,#205987,#205988,#205989,
#205990,#205991,#205992,#205993,#205994,#205995,#205996,#205997,#205998,
#205999),(#206000,#206001,#206002,#206003,#206004,#206005,#206006,#206007,
#206008,#206009,#206010,#206011,#206012,#206013,#206014,#206015),(#206016,
#206017,#206018,#206019,#206020,#206021,#206022,#206023,#206024,#206025,
#206026,#206027,#206028,#206029,#206030,#206031),(#206032,#206033,#206034,
#206035,#206036,#206037,#206038,#206039,#206040,#206041,#206042,#206043,
#206044,#206045,#206046,#206047),(#206048,#206049,#206050,#206051,#206052,
#206053,#206054,#206055,#206056,#206057,#206058,#206059,#206060,#206061,
#206062,#206063),(#206064,#206065,#206066,#206067,#206068,#206069,#206070,
#206071,#206072,#206073,#206074,#206075,#206076,#206077,#206078,#206079),
(#206080,#206081,#206082,#206083,#206084,#206085,#206086,#206087,#206088,
#206089,#206090,#206091,#206092,#206093,#206094,#206095),(#206096,#206097,
#206098,#206099,#206100,#206101,#206102,#206103,#206104,#206105,#206106,
#206107,#206108,#206109,#206110,#206111),(#206112,#206113,#206114,#206115,
#206116,#206117,#206118,#206119,#206120,#206121,#206122,#206123,#206124,
#206125,#206126,#206127),(#206128,#206129,#206130,#206131,#206132,#206133,
#206134,#206135,#206136,#206137,#206138,#206139,#206140,#206141,#206142,
#206143),(#206144,#206145,#206146,#206147,#206148,#206149,#206150,#206151,
#206152,#206153,#206154,#206155,#206156,#206157,#206158,#206159),(#206160,
#206161,#206162,#206163,#206164,#206165,#206166,#206167,#206168,#206169,
#206170,#206171,#206172,#206173,#206174,#206175),(#206176,#206177,#206178,
#206179,#206180,#206181,#206182,#206183,#206184,#206185,#206186,#206187,
#206188,#206189,#206190,#206191),(#206192,#206193,#206194,#206195,#206196,
#206197,#206198,#206199,#206200,#206201,#206202,#206203,#206204,#206205,
#206206,#206207),(#206208,#206209,#206210,#206211,#206212,#206213,#206214,
#206215,#206216,#206217,#206218,#206219,#206220,#206221,#206222,#206223),
(#206224,#206225,#206226,#206227,#206228,#206229,#206230,#206231,#206232,
#206233,#206234,#206235,#206236,#206237,#206238,#206239),(#206240,#206241,
#206242,#206243,#206244,#206245,#206246,#206247,#206248,#206249,#206250,
#206251,#206252,#206253,#206254,#206255),(#206256,#206257,#206258,#206259,
#206260,#206261,#206262,#206263,#206264,#206265,#206266,#206267,#206268,
#206269,#206270,#206271),(#206272,#206273,#206274,#206275,#206276,#206277,
#206278,#206279,#206280,#206281,#206282,#206283,#206284,#206285,#206286,
#206287),(#206288,#206289,#206290,#206291,#206292,#206293,#206294,#206295,
#206296,#206297,#206298,#206299,#206300,#206301,#206302,#206303),(#206304,
#206305,#206306,#206307,#206308,#206309,#206310,#206311,#206312,#206313,
#206314,#206315,#206316,#206317,#206318,#206319),(#206320,#206321,#206322,
#206323,#206324,#206325,#206326,#206327,#206328,#206329,#206330,#206331,
#206332,#206333,#206334,#206335),(#206336,#206337,#206338,#206339,#206340,
#206341,#206342,#206343,#206344,#206345,#206346,#206347,#206348,#206349,
#206350,#206351),(#206352,#206353,#206354,#206355,#206356,#206357,#206358,
#206359,#206360,#206361,#206362,#206363,#206364,#206365,#206366,#206367)),
 .UNSPECIFIED.,.F.,.F.,.F.,(4,3,3,3,3,3,3,1,1,1,3,3,3,3,3,3,4),(4,3,3,3,
3,4),(-364.,-121.,-40.,-13.,-4.,-1.,0.,0.25,0.5,0.75,1.,2.,5.,14.,41.,122.,
365.),(-7.07,-3.03,-1.01,0.,1.,1.01),.UNSPECIFIED.);
#926=B_SPLINE_SURFACE_WITH_KNOTS('',3,3,((#206369,#206370,#206371,#206372,
#206373,#206374,#206375,#206376,#206377,#206378,#206379,#206380,#206381,
#206382,#206383,#206384),(#206385,#206386,#206387,#206388,#206389,#206390,
#206391,#206392,#206393,#206394,#206395,#206396,#206397,#206398,#206399,
#206400),(#206401,#206402,#206403,#206404,#206405,#206406,#206407,#206408,
#206409,#206410,#206411,#206412,#206413,#206414,#206415,#206416),(#206417,
#206418,#206419,#206420,#206421,#206422,#206423,#206424,#206425,#206426,
#206427,#206428,#206429,#206430,#206431,#206432),(#206433,#206434,#206435,
#206436,#206437,#206438,#206439,#206440,#206441,#206442,#206443,#206444,
#206445,#206446,#206447,#206448),(#206449,#206450,#206451,#206452,#206453,
#206454,#206455,#206456,#206457,#206458,#206459,#206460,#206461,#206462,
#206463,#206464),(#206465,#206466,#206467,#206468,#206469,#206470,#206471,
#206472,#206473,#206474,#206475,#206476,#206477,#206478,#206479,#206480),
(#206481,#206482,#206483,#206484,#206485,#206486,#206487,#206488,#206489,
#206490,#206491,#206492,#206493,#206494,#206495,#206496),(#206497,#206498,
#206499,#206500,#206501,#206502,#206503,#206504,#206505,#206506,#206507,
#206508,#206509,#206510,#206511,#206512),(#206513,#206514,#206515,#206516,
#206517,#206518,#206519,#206520,#206521,#206522,#206523,#206524,#206525,
#206526,#206527,#206528),(#206529,#206530,#206531,#206532,#206533,#206534,
#206535,#206536,#206537,#206538,#206539,#206540,#206541,#206542,#206543,
#206544),(#206545,#206546,#206547,#206548,#206549,#206550,#206551,#206552,
#206553,#206554,#206555,#206556,#206557,#206558,#206559,#206560),(#206561,
#206562,#206563,#206564,#206565,#206566,#206567,#206568,#206569,#206570,
#206571,#206572,#206573,#206574,#206575,#206576),(#206577,#206578,#206579,
#206580,#206581,#206582,#206583,#206584,#206585,#206586,#206587,#206588,
#206589,#206590,#206591,#206592),(#206593,#206594,#206595,#206596,#206597,
#206598,#206599,#206600,#206601,#206602,#206603,#206604,#206605,#206606,
#206607,#206608),(#206609,#206610,#206611,#206612,#206613,#206614,#206615,
#206616,#206617,#206618,#206619,#206620,#206621,#206622,#206623,#206624),
(#206625,#206626,#206627,#206628,#206629,#206630,#206631,#206632,#206633,
#206634,#206635,#206636,#206637,#206638,#206639,#206640),(#206641,#206642,
#206643,#206644,#206645,#206646,#206647,#206648,#206649,#206650,#206651,
#206652,#206653,#206654,#206655,#206656),(#206657,#206658,#206659,#206660,
#206661,#206662,#206663,#206664,#206665,#206666,#206667,#206668,#206669,
#206670,#206671,#206672),(#206673,#206674,#206675,#206676,#206677,#206678,
#206679,#206680,#206681,#206682,#206683,#206684,#206685,#206686,#206687,
#206688),(#206689,#206690,#206691,#206692,#206693,#206694,#206695,#206696,
#206697,#206698,#206699,#206700,#206701,#206702,#206703,#206704),(#206705,
#206706,#206707,#206708,#206709,#206710,#206711,#206712,#206713,#206714,
#206715,#206716,#206717,#206718,#206719,#206720),(#206721,#206722,#206723,
#206724,#206725,#206726,#206727,#206728,#206729,#206730,#206731,#206732,
#206733,#206734,#206735,#206736),(#206737,#206738,#206739,#206740,#206741,
#206742,#206743,#206744,#206745,#206746,#206747,#206748,#206749,#206750,
#206751,#206752),(#206753,#206754,#206755,#206756,#206757,#206758,#206759,
#206760,#206761,#206762,#206763,#206764,#206765,#206766,#206767,#206768),
(#206769,#206770,#206771,#206772,#206773,#206774,#206775,#206776,#206777,
#206778,#206779,#206780,#206781,#206782,#206783,#206784),(#206785,#206786,
#206787,#206788,#206789,#206790,#206791,#206792,#206793,#206794,#206795,
#206796,#206797,#206798,#206799,#206800),(#206801,#206802,#206803,#206804,
#206805,#206806,#206807,#206808,#206809,#206810,#206811,#206812,#206813,
#206814,#206815,#206816),(#206817,#206818,#206819,#206820,#206821,#206822,
#206823,#206824,#206825,#206826,#206827,#206828,#206829,#206830,#206831,
#206832),(#206833,#206834,#206835,#206836,#206837,#206838,#206839,#206840,
#206841,#206842,#206843,#206844,#206845,#206846,#206847,#206848),(#206849,
#206850,#206851,#206852,#206853,#206854,#206855,#206856,#206857,#206858,
#206859,#206860,#206861,#206862,#206863,#206864),(#206865,#206866,#206867,
#206868,#206869,#206870,#206871,#206872,#206873,#206874,#206875,#206876,
#206877,#206878,#206879,#206880),(#206881,#206882,#206883,#206884,#206885,
#206886,#206887,#206888,#206889,#206890,#206891,#206892,#206893,#206894,
#206895,#206896),(#206897,#206898,#206899,#206900,#206901,#206902,#206903,
#206904,#206905,#206906,#206907,#206908,#206909,#206910,#206911,#206912),
(#206913,#206914,#206915,#206916,#206917,#206918,#206919,#206920,#206921,
#206922,#206923,#206924,#206925,#206926,#206927,#206928),(#206929,#206930,
#206931,#206932,#206933,#206934,#206935,#206936,#206937,#206938,#206939,
#206940,#206941,#206942,#206943,#206944),(#206945,#206946,#206947,#206948,
#206949,#206950,#206951,#206952,#206953,#206954,#206955,#206956,#206957,
#206958,#206959,#206960)),.UNSPECIFIED.,.F.,.F.,.F.,(4,3,3,3,3,3,1,1,1,
3,3,3,3,3,4),(4,3,3,3,3,4),(-121.,-40.,-13.,-4.,-1.,0.,0.25,0.5,0.75,1.,
2.,5.,14.,41.,122.),(-7.07,-3.03,-1.01,0.,1.,1.01),.UNSPECIFIED.);
#927=B_SPLINE_SURFACE_WITH_KNOTS('',3,3,((#223433,#223434,#223435,#223436,
#223437,#223438,#223439),(#223440,#223441,#223442,#223443,#223444,#223445,
#223446),(#223447,#223448,#223449,#223450,#223451,#223452,#223453),(#223454,
#223455,#223456,#223457,#223458,#223459,#223460),(#223461,#223462,#223463,
#223464,#223465,#223466,#223467),(#223468,#223469,#223470,#223471,#223472,
#223473,#223474),(#223475,#223476,#223477,#223478,#223479,#223480,#223481),
(#223482,#223483,#223484,#223485,#223486,#223487,#223488),(#223489,#223490,
#223491,#223492,#223493,#223494,#223495),(#223496,#223497,#223498,#223499,
#223500,#223501,#223502),(#223503,#223504,#223505,#223506,#223507,#223508,
#223509),(#223510,#223511,#223512,#223513,#223514,#223515,#223516),(#223517,
#223518,#223519,#223520,#223521,#223522,#223523),(#223524,#223525,#223526,
#223527,#223528,#223529,#223530),(#223531,#223532,#223533,#223534,#223535,
#223536,#223537),(#223538,#223539,#223540,#223541,#223542,#223543,#223544),
(#223545,#223546,#223547,#223548,#223549,#223550,#223551),(#223552,#223553,
#223554,#223555,#223556,#223557,#223558),(#223559,#223560,#223561,#223562,
#223563,#223564,#223565),(#223566,#223567,#223568,#223569,#223570,#223571,
#223572),(#223573,#223574,#223575,#223576,#223577,#223578,#223579),(#223580,
#223581,#223582,#223583,#223584,#223585,#223586),(#223587,#223588,#223589,
#223590,#223591,#223592,#223593),(#223594,#223595,#223596,#223597,#223598,
#223599,#223600),(#223601,#223602,#223603,#223604,#223605,#223606,#223607),
(#223608,#223609,#223610,#223611,#223612,#223613,#223614),(#223615,#223616,
#223617,#223618,#223619,#223620,#223621),(#223622,#223623,#223624,#223625,
#223626,#223627,#223628),(#223629,#223630,#223631,#223632,#223633,#223634,
#223635),(#223636,#223637,#223638,#223639,#223640,#223641,#223642),(#223643,
#223644,#223645,#223646,#223647,#223648,#223649),(#223650,#223651,#223652,
#223653,#223654,#223655,#223656),(#223657,#223658,#223659,#223660,#223661,
#223662,#223663),(#223664,#223665,#223666,#223667,#223668,#223669,#223670),
(#223671,#223672,#223673,#223674,#223675,#223676,#223677),(#223678,#223679,
#223680,#223681,#223682,#223683,#223684),(#223685,#223686,#223687,#223688,
#223689,#223690,#223691),(#223692,#223693,#223694,#223695,#223696,#223697,
#223698),(#223699,#223700,#223701,#223702,#223703,#223704,#223705),(#223706,
#223707,#223708,#223709,#223710,#223711,#223712),(#223713,#223714,#223715,
#223716,#223717,#223718,#223719),(#223720,#223721,#223722,#223723,#223724,
#223725,#223726),(#223727,#223728,#223729,#223730,#223731,#223732,#223733),
(#223734,#223735,#223736,#223737,#223738,#223739,#223740),(#223741,#223742,
#223743,#223744,#223745,#223746,#223747),(#223748,#223749,#223750,#223751,
#223752,#223753,#223754),(#223755,#223756,#223757,#223758,#223759,#223760,
#223761),(#223762,#223763,#223764,#223765,#223766,#223767,#223768),(#223769,
#223770,#223771,#223772,#223773,#223774,#223775),(#223776,#223777,#223778,
#223779,#223780,#223781,#223782),(#223783,#223784,#223785,#223786,#223787,
#223788,#223789),(#223790,#223791,#223792,#223793,#223794,#223795,#223796),
(#223797,#223798,#223799,#223800,#223801,#223802,#223803),(#223804,#223805,
#223806,#223807,#223808,#223809,#223810),(#223811,#223812,#223813,#223814,
#223815,#223816,#223817),(#223818,#223819,#223820,#223821,#223822,#223823,
#223824),(#223825,#223826,#223827,#223828,#223829,#223830,#223831),(#223832,
#223833,#223834,#223835,#223836,#223837,#223838),(#223839,#223840,#223841,
#223842,#223843,#223844,#223845),(#223846,#223847,#223848,#223849,#223850,
#223851,#223852),(#223853,#223854,#223855,#223856,#223857,#223858,#223859),
(#223860,#223861,#223862,#223863,#223864,#223865,#223866),(#223867,#223868,
#223869,#223870,#223871,#223872,#223873),(#223874,#223875,#223876,#223877,
#223878,#223879,#223880),(#223881,#223882,#223883,#223884,#223885,#223886,
#223887),(#223888,#223889,#223890,#223891,#223892,#223893,#223894),(#223895,
#223896,#223897,#223898,#223899,#223900,#223901),(#223902,#223903,#223904,
#223905,#223906,#223907,#223908),(#223909,#223910,#223911,#223912,#223913,
#223914,#223915),(#223916,#223917,#223918,#223919,#223920,#223921,#223922),
(#223923,#223924,#223925,#223926,#223927,#223928,#223929),(#223930,#223931,
#223932,#223933,#223934,#223935,#223936),(#223937,#223938,#223939,#223940,
#223941,#223942,#223943),(#223944,#223945,#223946,#223947,#223948,#223949,
#223950),(#223951,#223952,#223953,#223954,#223955,#223956,#223957),(#223958,
#223959,#223960,#223961,#223962,#223963,#223964),(#223965,#223966,#223967,
#223968,#223969,#223970,#223971),(#223972,#223973,#223974,#223975,#223976,
#223977,#223978),(#223979,#223980,#223981,#223982,#223983,#223984,#223985),
(#223986,#223987,#223988,#223989,#223990,#223991,#223992),(#223993,#223994,
#223995,#223996,#223997,#223998,#223999),(#224000,#224001,#224002,#224003,
#224004,#224005,#224006),(#224007,#224008,#224009,#224010,#224011,#224012,
#224013),(#224014,#224015,#224016,#224017,#224018,#224019,#224020),(#224021,
#224022,#224023,#224024,#224025,#224026,#224027),(#224028,#224029,#224030,
#224031,#224032,#224033,#224034),(#224035,#224036,#224037,#224038,#224039,
#224040,#224041),(#224042,#224043,#224044,#224045,#224046,#224047,#224048),
(#224049,#224050,#224051,#224052,#224053,#224054,#224055),(#224056,#224057,
#224058,#224059,#224060,#224061,#224062),(#224063,#224064,#224065,#224066,
#224067,#224068,#224069),(#224070,#224071,#224072,#224073,#224074,#224075,
#224076),(#224077,#224078,#224079,#224080,#224081,#224082,#224083),(#224084,
#224085,#224086,#224087,#224088,#224089,#224090),(#224091,#224092,#224093,
#224094,#224095,#224096,#224097),(#224098,#224099,#224100,#224101,#224102,
#224103,#224104),(#224105,#224106,#224107,#224108,#224109,#224110,#224111),
(#224112,#224113,#224114,#224115,#224116,#224117,#224118),(#224119,#224120,
#224121,#224122,#224123,#224124,#224125),(#224126,#224127,#224128,#224129,
#224130,#224131,#224132),(#224133,#224134,#224135,#224136,#224137,#224138,
#224139),(#224140,#224141,#224142,#224143,#224144,#224145,#224146),(#224147,
#224148,#224149,#224150,#224151,#224152,#224153),(#224154,#224155,#224156,
#224157,#224158,#224159,#224160),(#224161,#224162,#224163,#224164,#224165,
#224166,#224167),(#224168,#224169,#224170,#224171,#224172,#224173,#224174),
(#224175,#224176,#224177,#224178,#224179,#224180,#224181),(#224182,#224183,
#224184,#224185,#224186,#224187,#224188),(#224189,#224190,#224191,#224192,
#224193,#224194,#224195),(#224196,#224197,#224198,#224199,#224200,#224201,
#224202),(#224203,#224204,#224205,#224206,#224207,#224208,#224209),(#224210,
#224211,#224212,#224213,#224214,#224215,#224216),(#224217,#224218,#224219,
#224220,#224221,#224222,#224223),(#224224,#224225,#224226,#224227,#224228,
#224229,#224230),(#224231,#224232,#224233,#224234,#224235,#224236,#224237),
(#224238,#224239,#224240,#224241,#224242,#224243,#224244),(#224245,#224246,
#224247,#224248,#224249,#224250,#224251),(#224252,#224253,#224254,#224255,
#224256,#224257,#224258),(#224259,#224260,#224261,#224262,#224263,#224264,
#224265),(#224266,#224267,#224268,#224269,#224270,#224271,#224272),(#224273,
#224274,#224275,#224276,#224277,#224278,#224279),(#224280,#224281,#224282,
#224283,#224284,#224285,#224286),(#224287,#224288,#224289,#224290,#224291,
#224292,#224293),(#224294,#224295,#224296,#224297,#224298,#224299,#224300),
(#224301,#224302,#224303,#224304,#224305,#224306,#224307),(#224308,#224309,
#224310,#224311,#224312,#224313,#224314),(#224315,#224316,#224317,#224318,
#224319,#224320,#224321),(#224322,#224323,#224324,#224325,#224326,#224327,
#224328),(#224329,#224330,#224331,#224332,#224333,#224334,#224335),(#224336,
#224337,#224338,#224339,#224340,#224341,#224342),(#224343,#224344,#224345,
#224346,#224347,#224348,#224349),(#224350,#224351,#224352,#224353,#224354,
#224355,#224356),(#224357,#224358,#224359,#224360,#224361,#224362,#224363),
(#224364,#224365,#224366,#224367,#224368,#224369,#224370),(#224371,#224372,
#224373,#224374,#224375,#224376,#224377),(#224378,#224379,#224380,#224381,
#224382,#224383,#224384),(#224385,#224386,#224387,#224388,#224389,#224390,
#224391),(#224392,#224393,#224394,#224395,#224396,#224397,#224398),(#224399,
#224400,#224401,#224402,#224403,#224404,#224405),(#224406,#224407,#224408,
#224409,#224410,#224411,#224412),(#224413,#224414,#224415,#224416,#224417,
#224418,#224419),(#224420,#224421,#224422,#224423,#224424,#224425,#224426),
(#224427,#224428,#224429,#224430,#224431,#224432,#224433),(#224434,#224435,
#224436,#224437,#224438,#224439,#224440),(#224441,#224442,#224443,#224444,
#224445,#224446,#224447),(#224448,#224449,#224450,#224451,#224452,#224453,
#224454),(#224455,#224456,#224457,#224458,#224459,#224460,#224461),(#224462,
#224463,#224464,#224465,#224466,#224467,#224468),(#224469,#224470,#224471,
#224472,#224473,#224474,#224475),(#224476,#224477,#224478,#224479,#224480,
#224481,#224482),(#224483,#224484,#224485,#224486,#224487,#224488,#224489),
(#224490,#224491,#224492,#224493,#224494,#224495,#224496),(#224497,#224498,
#224499,#224500,#224501,#224502,#224503),(#224504,#224505,#224506,#224507,
#224508,#224509,#224510),(#224511,#224512,#224513,#224514,#224515,#224516,
#224517),(#224518,#224519,#224520,#224521,#224522,#224523,#224524),(#224525,
#224526,#224527,#224528,#224529,#224530,#224531),(#224532,#224533,#224534,
#224535,#224536,#224537,#224538),(#224539,#224540,#224541,#224542,#224543,
#224544,#224545),(#224546,#224547,#224548,#224549,#224550,#224551,#224552),
(#224553,#224554,#224555,#224556,#224557,#224558,#224559),(#224560,#224561,
#224562,#224563,#224564,#224565,#224566),(#224567,#224568,#224569,#224570,
#224571,#224572,#224573),(#224574,#224575,#224576,#224577,#224578,#224579,
#224580),(#224581,#224582,#224583,#224584,#224585,#224586,#224587),(#224588,
#224589,#224590,#224591,#224592,#224593,#224594),(#224595,#224596,#224597,
#224598,#224599,#224600,#224601),(#224602,#224603,#224604,#224605,#224606,
#224607,#224608),(#224609,#224610,#224611,#224612,#224613,#224614,#224615),
(#224616,#224617,#224618,#224619,#224620,#224621,#224622),(#224623,#224624,
#224625,#224626,#224627,#224628,#224629),(#224630,#224631,#224632,#224633,
#224634,#224635,#224636),(#224637,#224638,#224639,#224640,#224641,#224642,
#224643),(#224644,#224645,#224646,#224647,#224648,#224649,#224650),(#224651,
#224652,#224653,#224654,#224655,#224656,#224657)),.UNSPECIFIED.,.F.,.F.,
 .F.,(4,3,3,3,3,3,3,3,3,3,3,3,3,3,3,3,3,3,3,3,3,3,3,3,3,3,3,3,3,3,3,3,3,
3,3,3,3,3,3,3,3,3,3,3,3,3,3,3,3,3,3,3,3,3,3,3,3,3,4),(4,3,4),(-0.00276391227871182,
0.0600815767561073,0.122927065790926,0.138638438049631,0.1396203988158,
0.140111379198885,0.140602359581969,0.142566281114307,0.146494124178983,
0.154349810308336,0.185772554825745,0.248618043860565,0.264329416119269,
0.272185102248622,0.276112945313298,0.277094906079467,0.278076866845636,
0.280040788377974,0.311463532895383,0.374309021930203,0.405731766447612,
0.421443138706317,0.421934119089401,0.422425099472486,0.423407060238655,
0.425370981770993,0.42929882483567,0.437154510965022,0.468577255482431,
0.499999999999841,0.53142274451725,0.56284548903466,0.570701175164012,0.574629018228689,
0.576592939761027,0.577574900527196,0.57806588091028,0.578556861293365,
0.59426823355207,0.625690978069479,0.688536467104298,0.719959211621708,
0.721923133154046,0.722905093920215,0.723887054686384,0.72781489775106,
0.735670583880413,0.751381956139117,0.814227445173936,0.845650189691346,
0.853505875820698,0.857433718885374,0.859397640417713,0.859888620800797,
0.860379601183882,0.861361561950051,0.877072934208755,0.939918423243574,
1.00276391227839),(-0.034810747309642,0.460156458726841,0.955123664763324),
 .UNSPECIFIED.);
#928=B_SPLINE_SURFACE_WITH_KNOTS('',3,3,((#224988,#224989,#224990,#224991),
(#224992,#224993,#224994,#224995),(#224996,#224997,#224998,#224999),(#225000,
#225001,#225002,#225003),(#225004,#225005,#225006,#225007),(#225008,#225009,
#225010,#225011),(#225012,#225013,#225014,#225015),(#225016,#225017,#225018,
#225019),(#225020,#225021,#225022,#225023),(#225024,#225025,#225026,#225027),
(#225028,#225029,#225030,#225031),(#225032,#225033,#225034,#225035),(#225036,
#225037,#225038,#225039),(#225040,#225041,#225042,#225043),(#225044,#225045,
#225046,#225047),(#225048,#225049,#225050,#225051),(#225052,#225053,#225054,
#225055),(#225056,#225057,#225058,#225059),(#225060,#225061,#225062,#225063),
(#225064,#225065,#225066,#225067),(#225068,#225069,#225070,#225071),(#225072,
#225073,#225074,#225075),(#225076,#225077,#225078,#225079),(#225080,#225081,
#225082,#225083),(#225084,#225085,#225086,#225087),(#225088,#225089,#225090,
#225091),(#225092,#225093,#225094,#225095),(#225096,#225097,#225098,#225099),
(#225100,#225101,#225102,#225103),(#225104,#225105,#225106,#225107),(#225108,
#225109,#225110,#225111),(#225112,#225113,#225114,#225115),(#225116,#225117,
#225118,#225119),(#225120,#225121,#225122,#225123),(#225124,#225125,#225126,
#225127),(#225128,#225129,#225130,#225131),(#225132,#225133,#225134,#225135),
(#225136,#225137,#225138,#225139),(#225140,#225141,#225142,#225143),(#225144,
#225145,#225146,#225147),(#225148,#225149,#225150,#225151),(#225152,#225153,
#225154,#225155),(#225156,#225157,#225158,#225159),(#225160,#225161,#225162,
#225163),(#225164,#225165,#225166,#225167),(#225168,#225169,#225170,#225171),
(#225172,#225173,#225174,#225175),(#225176,#225177,#225178,#225179),(#225180,
#225181,#225182,#225183),(#225184,#225185,#225186,#225187),(#225188,#225189,
#225190,#225191),(#225192,#225193,#225194,#225195),(#225196,#225197,#225198,
#225199),(#225200,#225201,#225202,#225203),(#225204,#225205,#225206,#225207),
(#225208,#225209,#225210,#225211),(#225212,#225213,#225214,#225215),(#225216,
#225217,#225218,#225219),(#225220,#225221,#225222,#225223),(#225224,#225225,
#225226,#225227),(#225228,#225229,#225230,#225231),(#225232,#225233,#225234,
#225235),(#225236,#225237,#225238,#225239),(#225240,#225241,#225242,#225243),
(#225244,#225245,#225246,#225247),(#225248,#225249,#225250,#225251),(#225252,
#225253,#225254,#225255),(#225256,#225257,#225258,#225259),(#225260,#225261,
#225262,#225263),(#225264,#225265,#225266,#225267),(#225268,#225269,#225270,
#225271),(#225272,#225273,#225274,#225275),(#225276,#225277,#225278,#225279),
(#225280,#225281,#225282,#225283),(#225284,#225285,#225286,#225287),(#225288,
#225289,#225290,#225291),(#225292,#225293,#225294,#225295),(#225296,#225297,
#225298,#225299),(#225300,#225301,#225302,#225303),(#225304,#225305,#225306,
#225307),(#225308,#225309,#225310,#225311),(#225312,#225313,#225314,#225315),
(#225316,#225317,#225318,#225319),(#225320,#225321,#225322,#225323),(#225324,
#225325,#225326,#225327),(#225328,#225329,#225330,#225331),(#225332,#225333,
#225334,#225335),(#225336,#225337,#225338,#225339),(#225340,#225341,#225342,
#225343),(#225344,#225345,#225346,#225347),(#225348,#225349,#225350,#225351),
(#225352,#225353,#225354,#225355),(#225356,#225357,#225358,#225359),(#225360,
#225361,#225362,#225363),(#225364,#225365,#225366,#225367),(#225368,#225369,
#225370,#225371),(#225372,#225373,#225374,#225375),(#225376,#225377,#225378,
#225379),(#225380,#225381,#225382,#225383),(#225384,#225385,#225386,#225387),
(#225388,#225389,#225390,#225391),(#225392,#225393,#225394,#225395),(#225396,
#225397,#225398,#225399),(#225400,#225401,#225402,#225403),(#225404,#225405,
#225406,#225407),(#225408,#225409,#225410,#225411),(#225412,#225413,#225414,
#225415),(#225416,#225417,#225418,#225419),(#225420,#225421,#225422,#225423),
(#225424,#225425,#225426,#225427),(#225428,#225429,#225430,#225431),(#225432,
#225433,#225434,#225435),(#225436,#225437,#225438,#225439),(#225440,#225441,
#225442,#225443),(#225444,#225445,#225446,#225447),(#225448,#225449,#225450,
#225451),(#225452,#225453,#225454,#225455),(#225456,#225457,#225458,#225459),
(#225460,#225461,#225462,#225463),(#225464,#225465,#225466,#225467),(#225468,
#225469,#225470,#225471),(#225472,#225473,#225474,#225475),(#225476,#225477,
#225478,#225479),(#225480,#225481,#225482,#225483),(#225484,#225485,#225486,
#225487),(#225488,#225489,#225490,#225491),(#225492,#225493,#225494,#225495),
(#225496,#225497,#225498,#225499),(#225500,#225501,#225502,#225503),(#225504,
#225505,#225506,#225507),(#225508,#225509,#225510,#225511),(#225512,#225513,
#225514,#225515),(#225516,#225517,#225518,#225519),(#225520,#225521,#225522,
#225523),(#225524,#225525,#225526,#225527),(#225528,#225529,#225530,#225531),
(#225532,#225533,#225534,#225535),(#225536,#225537,#225538,#225539),(#225540,
#225541,#225542,#225543),(#225544,#225545,#225546,#225547),(#225548,#225549,
#225550,#225551),(#225552,#225553,#225554,#225555),(#225556,#225557,#225558,
#225559),(#225560,#225561,#225562,#225563),(#225564,#225565,#225566,#225567),
(#225568,#225569,#225570,#225571),(#225572,#225573,#225574,#225575),(#225576,
#225577,#225578,#225579),(#225580,#225581,#225582,#225583),(#225584,#225585,
#225586,#225587),(#225588,#225589,#225590,#225591)),.UNSPECIFIED.,.F.,.F.,
 .F.,(4,3,3,3,3,3,3,3,3,3,3,3,3,3,3,3,3,3,3,3,3,3,3,3,3,3,3,3,3,3,3,3,3,
3,3,3,3,3,3,3,3,3,3,3,3,3,3,3,3,3,4),(4,4),(-0.00109644387045235,0.124177669566463,
0.139836933746078,0.147666565835885,0.151581381880788,0.15353878990324,
0.155496197925692,0.186814726284921,0.249451783003379,0.280770311362608,
0.296429575542222,0.300344391587126,0.302301799609578,0.302791151615191,
0.303280503620803,0.304259207632029,0.312088839721837,0.374725896440295,
0.406044424799524,0.421703688979138,0.42366109700159,0.424639801012816,
0.425618505024042,0.429533321068946,0.437362953158753,0.500000009877211,
0.562637066595668,0.570466698685476,0.574381514730379,0.575360218741605,
0.576338922752831,0.578296330775283,0.593955594954897,0.625274123314126,
0.687911180032584,0.695740812122391,0.696719516133617,0.69720886813923,
0.697698220144843,0.699655628167295,0.703570444212198,0.719229708391813,
0.750548236751042,0.8131852934695,0.844503821828729,0.84646122985118,0.848418637873632,
0.852333453918536,0.860163086008343,0.875822350187958,1.00109646362487),
(0.0477813279241126,1.03891804990681),.UNSPECIFIED.);
#929=B_SPLINE_SURFACE_WITH_KNOTS('',3,3,((#225984,#225985,#225986,#225987,
#225988,#225989,#225990,#225991,#225992,#225993,#225994,#225995,#225996),
(#225997,#225998,#225999,#226000,#226001,#226002,#226003,#226004,#226005,
#226006,#226007,#226008,#226009),(#226010,#226011,#226012,#226013,#226014,
#226015,#226016,#226017,#226018,#226019,#226020,#226021,#226022),(#226023,
#226024,#226025,#226026,#226027,#226028,#226029,#226030,#226031,#226032,
#226033,#226034,#226035),(#226036,#226037,#226038,#226039,#226040,#226041,
#226042,#226043,#226044,#226045,#226046,#226047,#226048),(#226049,#226050,
#226051,#226052,#226053,#226054,#226055,#226056,#226057,#226058,#226059,
#226060,#226061),(#226062,#226063,#226064,#226065,#226066,#226067,#226068,
#226069,#226070,#226071,#226072,#226073,#226074),(#226075,#226076,#226077,
#226078,#226079,#226080,#226081,#226082,#226083,#226084,#226085,#226086,
#226087),(#226088,#226089,#226090,#226091,#226092,#226093,#226094,#226095,
#226096,#226097,#226098,#226099,#226100),(#226101,#226102,#226103,#226104,
#226105,#226106,#226107,#226108,#226109,#226110,#226111,#226112,#226113),
(#226114,#226115,#226116,#226117,#226118,#226119,#226120,#226121,#226122,
#226123,#226124,#226125,#226126),(#226127,#226128,#226129,#226130,#226131,
#226132,#226133,#226134,#226135,#226136,#226137,#226138,#226139),(#226140,
#226141,#226142,#226143,#226144,#226145,#226146,#226147,#226148,#226149,
#226150,#226151,#226152),(#226153,#226154,#226155,#226156,#226157,#226158,
#226159,#226160,#226161,#226162,#226163,#226164,#226165),(#226166,#226167,
#226168,#226169,#226170,#226171,#226172,#226173,#226174,#226175,#226176,
#226177,#226178),(#226179,#226180,#226181,#226182,#226183,#226184,#226185,
#226186,#226187,#226188,#226189,#226190,#226191),(#226192,#226193,#226194,
#226195,#226196,#226197,#226198,#226199,#226200,#226201,#226202,#226203,
#226204),(#226205,#226206,#226207,#226208,#226209,#226210,#226211,#226212,
#226213,#226214,#226215,#226216,#226217),(#226218,#226219,#226220,#226221,
#226222,#226223,#226224,#226225,#226226,#226227,#226228,#226229,#226230),
(#226231,#226232,#226233,#226234,#226235,#226236,#226237,#226238,#226239,
#226240,#226241,#226242,#226243),(#226244,#226245,#226246,#226247,#226248,
#226249,#226250,#226251,#226252,#226253,#226254,#226255,#226256),(#226257,
#226258,#226259,#226260,#226261,#226262,#226263,#226264,#226265,#226266,
#226267,#226268,#226269),(#226270,#226271,#226272,#226273,#226274,#226275,
#226276,#226277,#226278,#226279,#226280,#226281,#226282),(#226283,#226284,
#226285,#226286,#226287,#226288,#226289,#226290,#226291,#226292,#226293,
#226294,#226295),(#226296,#226297,#226298,#226299,#226300,#226301,#226302,
#226303,#226304,#226305,#226306,#226307,#226308),(#226309,#226310,#226311,
#226312,#226313,#226314,#226315,#226316,#226317,#226318,#226319,#226320,
#226321),(#226322,#226323,#226324,#226325,#226326,#226327,#226328,#226329,
#226330,#226331,#226332,#226333,#226334),(#226335,#226336,#226337,#226338,
#226339,#226340,#226341,#226342,#226343,#226344,#226345,#226346,#226347)),
 .UNSPECIFIED.,.F.,.F.,.F.,(4,3,3,3,3,3,3,3,3,4),(4,3,3,3,4),(-2.09329281387815E-12,
0.0624999999980442,0.124999999998182,0.249999999998457,0.374999999998732,
0.499999999999007,0.624999999999282,0.749999999999557,0.874999999999832,
1.00000398343861),(0.0305346534395145,0.148544372614449,0.266554091789383,
0.502573530139252,0.97461240683899),.UNSPECIFIED.);
#930=B_SPLINE_SURFACE_WITH_KNOTS('',3,3,((#226418,#226419,#226420,#226421,
#226422,#226423,#226424,#226425,#226426,#226427,#226428,#226429,#226430),
(#226431,#226432,#226433,#226434,#226435,#226436,#226437,#226438,#226439,
#226440,#226441,#226442,#226443),(#226444,#226445,#226446,#226447,#226448,
#226449,#226450,#226451,#226452,#226453,#226454,#226455,#226456),(#226457,
#226458,#226459,#226460,#226461,#226462,#226463,#226464,#226465,#226466,
#226467,#226468,#226469),(#226470,#226471,#226472,#226473,#226474,#226475,
#226476,#226477,#226478,#226479,#226480,#226481,#226482),(#226483,#226484,
#226485,#226486,#226487,#226488,#226489,#226490,#226491,#226492,#226493,
#226494,#226495),(#226496,#226497,#226498,#226499,#226500,#226501,#226502,
#226503,#226504,#226505,#226506,#226507,#226508),(#226509,#226510,#226511,
#226512,#226513,#226514,#226515,#226516,#226517,#226518,#226519,#226520,
#226521),(#226522,#226523,#226524,#226525,#226526,#226527,#226528,#226529,
#226530,#226531,#226532,#226533,#226534),(#226535,#226536,#226537,#226538,
#226539,#226540,#226541,#226542,#226543,#226544,#226545,#226546,#226547),
(#226548,#226549,#226550,#226551,#226552,#226553,#226554,#226555,#226556,
#226557,#226558,#226559,#226560),(#226561,#226562,#226563,#226564,#226565,
#226566,#226567,#226568,#226569,#226570,#226571,#226572,#226573),(#226574,
#226575,#226576,#226577,#226578,#226579,#226580,#226581,#226582,#226583,
#226584,#226585,#226586),(#226587,#226588,#226589,#226590,#226591,#226592,
#226593,#226594,#226595,#226596,#226597,#226598,#226599),(#226600,#226601,
#226602,#226603,#226604,#226605,#226606,#226607,#226608,#226609,#226610,
#226611,#226612),(#226613,#226614,#226615,#226616,#226617,#226618,#226619,
#226620,#226621,#226622,#226623,#226624,#226625),(#226626,#226627,#226628,
#226629,#226630,#226631,#226632,#226633,#226634,#226635,#226636,#226637,
#226638),(#226639,#226640,#226641,#226642,#226643,#226644,#226645,#226646,
#226647,#226648,#226649,#226650,#226651),(#226652,#226653,#226654,#226655,
#226656,#226657,#226658,#226659,#226660,#226661,#226662,#226663,#226664),
(#226665,#226666,#226667,#226668,#226669,#226670,#226671,#226672,#226673,
#226674,#226675,#226676,#226677),(#226678,#226679,#226680,#226681,#226682,
#226683,#226684,#226685,#226686,#226687,#226688,#226689,#226690),(#226691,
#226692,#226693,#226694,#226695,#226696,#226697,#226698,#226699,#226700,
#226701,#226702,#226703),(#226704,#226705,#226706,#226707,#226708,#226709,
#226710,#226711,#226712,#226713,#226714,#226715,#226716),(#226717,#226718,
#226719,#226720,#226721,#226722,#226723,#226724,#226725,#226726,#226727,
#226728,#226729),(#226730,#226731,#226732,#226733,#226734,#226735,#226736,
#226737,#226738,#226739,#226740,#226741,#226742),(#226743,#226744,#226745,
#226746,#226747,#226748,#226749,#226750,#226751,#226752,#226753,#226754,
#226755),(#226756,#226757,#226758,#226759,#226760,#226761,#226762,#226763,
#226764,#226765,#226766,#226767,#226768),(#226769,#226770,#226771,#226772,
#226773,#226774,#226775,#226776,#226777,#226778,#226779,#226780,#226781),
(#226782,#226783,#226784,#226785,#226786,#226787,#226788,#226789,#226790,
#226791,#226792,#226793,#226794),(#226795,#226796,#226797,#226798,#226799,
#226800,#226801,#226802,#226803,#226804,#226805,#226806,#226807),(#226808,
#226809,#226810,#226811,#226812,#226813,#226814,#226815,#226816,#226817,
#226818,#226819,#226820),(#226821,#226822,#226823,#226824,#226825,#226826,
#226827,#226828,#226829,#226830,#226831,#226832,#226833),(#226834,#226835,
#226836,#226837,#226838,#226839,#226840,#226841,#226842,#226843,#226844,
#226845,#226846),(#226847,#226848,#226849,#226850,#226851,#226852,#226853,
#226854,#226855,#226856,#226857,#226858,#226859),(#226860,#226861,#226862,
#226863,#226864,#226865,#226866,#226867,#226868,#226869,#226870,#226871,
#226872),(#226873,#226874,#226875,#226876,#226877,#226878,#226879,#226880,
#226881,#226882,#226883,#226884,#226885),(#226886,#226887,#226888,#226889,
#226890,#226891,#226892,#226893,#226894,#226895,#226896,#226897,#226898),
(#226899,#226900,#226901,#226902,#226903,#226904,#226905,#226906,#226907,
#226908,#226909,#226910,#226911),(#226912,#226913,#226914,#226915,#226916,
#226917,#226918,#226919,#226920,#226921,#226922,#226923,#226924),(#226925,
#226926,#226927,#226928,#226929,#226930,#226931,#226932,#226933,#226934,
#226935,#226936,#226937),(#226938,#226939,#226940,#226941,#226942,#226943,
#226944,#226945,#226946,#226947,#226948,#226949,#226950),(#226951,#226952,
#226953,#226954,#226955,#226956,#226957,#226958,#226959,#226960,#226961,
#226962,#226963),(#226964,#226965,#226966,#226967,#226968,#226969,#226970,
#226971,#226972,#226973,#226974,#226975,#226976)),.UNSPECIFIED.,.F.,.F.,
 .F.,(4,3,3,3,3,3,3,3,3,3,3,3,3,3,4),(4,3,3,3,4),(-0.00600089904390221,
0.00185848297987854,0.00971786500365927,0.0254366290512207,0.0568741571463437,
0.11974921333659,0.182624269526835,0.245499325717081,0.371249438097573,
0.496999550478065,0.622749662858557,0.748499775239049,0.874249887619541,
0.937124943809787,1.00000000000003),(0.0313847250337115,0.149350226349808,
0.267315727665905,0.503246730298099,0.975108735562486),.UNSPECIFIED.);
#931=B_SPLINE_SURFACE_WITH_KNOTS('',3,3,((#227055,#227056,#227057,#227058,
#227059,#227060,#227061,#227062,#227063,#227064,#227065,#227066,#227067),
(#227068,#227069,#227070,#227071,#227072,#227073,#227074,#227075,#227076,
#227077,#227078,#227079,#227080),(#227081,#227082,#227083,#227084,#227085,
#227086,#227087,#227088,#227089,#227090,#227091,#227092,#227093),(#227094,
#227095,#227096,#227097,#227098,#227099,#227100,#227101,#227102,#227103,
#227104,#227105,#227106),(#227107,#227108,#227109,#227110,#227111,#227112,
#227113,#227114,#227115,#227116,#227117,#227118,#227119),(#227120,#227121,
#227122,#227123,#227124,#227125,#227126,#227127,#227128,#227129,#227130,
#227131,#227132),(#227133,#227134,#227135,#227136,#227137,#227138,#227139,
#227140,#227141,#227142,#227143,#227144,#227145),(#227146,#227147,#227148,
#227149,#227150,#227151,#227152,#227153,#227154,#227155,#227156,#227157,
#227158),(#227159,#227160,#227161,#227162,#227163,#227164,#227165,#227166,
#227167,#227168,#227169,#227170,#227171),(#227172,#227173,#227174,#227175,
#227176,#227177,#227178,#227179,#227180,#227181,#227182,#227183,#227184),
(#227185,#227186,#227187,#227188,#227189,#227190,#227191,#227192,#227193,
#227194,#227195,#227196,#227197),(#227198,#227199,#227200,#227201,#227202,
#227203,#227204,#227205,#227206,#227207,#227208,#227209,#227210),(#227211,
#227212,#227213,#227214,#227215,#227216,#227217,#227218,#227219,#227220,
#227221,#227222,#227223),(#227224,#227225,#227226,#227227,#227228,#227229,
#227230,#227231,#227232,#227233,#227234,#227235,#227236),(#227237,#227238,
#227239,#227240,#227241,#227242,#227243,#227244,#227245,#227246,#227247,
#227248,#227249),(#227250,#227251,#227252,#227253,#227254,#227255,#227256,
#227257,#227258,#227259,#227260,#227261,#227262),(#227263,#227264,#227265,
#227266,#227267,#227268,#227269,#227270,#227271,#227272,#227273,#227274,
#227275),(#227276,#227277,#227278,#227279,#227280,#227281,#227282,#227283,
#227284,#227285,#227286,#227287,#227288),(#227289,#227290,#227291,#227292,
#227293,#227294,#227295,#227296,#227297,#227298,#227299,#227300,#227301),
(#227302,#227303,#227304,#227305,#227306,#227307,#227308,#227309,#227310,
#227311,#227312,#227313,#227314),(#227315,#227316,#227317,#227318,#227319,
#227320,#227321,#227322,#227323,#227324,#227325,#227326,#227327),(#227328,
#227329,#227330,#227331,#227332,#227333,#227334,#227335,#227336,#227337,
#227338,#227339,#227340),(#227341,#227342,#227343,#227344,#227345,#227346,
#227347,#227348,#227349,#227350,#227351,#227352,#227353),(#227354,#227355,
#227356,#227357,#227358,#227359,#227360,#227361,#227362,#227363,#227364,
#227365,#227366),(#227367,#227368,#227369,#227370,#227371,#227372,#227373,
#227374,#227375,#227376,#227377,#227378,#227379),(#227380,#227381,#227382,
#227383,#227384,#227385,#227386,#227387,#227388,#227389,#227390,#227391,
#227392),(#227393,#227394,#227395,#227396,#227397,#227398,#227399,#227400,
#227401,#227402,#227403,#227404,#227405),(#227406,#227407,#227408,#227409,
#227410,#227411,#227412,#227413,#227414,#227415,#227416,#227417,#227418)),
 .UNSPECIFIED.,.F.,.F.,.F.,(4,3,3,3,3,3,3,3,3,4),(4,3,3,3,4),(7.97241441451061E-14,
0.0625000000003403,0.125000000000601,0.250000000001122,0.375000000001643,
0.500000000002164,0.625000000002685,0.750000000003206,0.875000000003727,
1.00000000000425),(0.035779394199433,0.153116210014097,0.27045302582876,
0.505126657458087,0.97447392071674),.UNSPECIFIED.);
#932=B_SPLINE_SURFACE_WITH_KNOTS('',3,3,((#227491,#227492,#227493,#227494,
#227495,#227496,#227497,#227498,#227499,#227500),(#227501,#227502,#227503,
#227504,#227505,#227506,#227507,#227508,#227509,#227510),(#227511,#227512,
#227513,#227514,#227515,#227516,#227517,#227518,#227519,#227520),(#227521,
#227522,#227523,#227524,#227525,#227526,#227527,#227528,#227529,#227530),
(#227531,#227532,#227533,#227534,#227535,#227536,#227537,#227538,#227539,
#227540),(#227541,#227542,#227543,#227544,#227545,#227546,#227547,#227548,
#227549,#227550),(#227551,#227552,#227553,#227554,#227555,#227556,#227557,
#227558,#227559,#227560),(#227561,#227562,#227563,#227564,#227565,#227566,
#227567,#227568,#227569,#227570),(#227571,#227572,#227573,#227574,#227575,
#227576,#227577,#227578,#227579,#227580),(#227581,#227582,#227583,#227584,
#227585,#227586,#227587,#227588,#227589,#227590),(#227591,#227592,#227593,
#227594,#227595,#227596,#227597,#227598,#227599,#227600),(#227601,#227602,
#227603,#227604,#227605,#227606,#227607,#227608,#227609,#227610),(#227611,
#227612,#227613,#227614,#227615,#227616,#227617,#227618,#227619,#227620),
(#227621,#227622,#227623,#227624,#227625,#227626,#227627,#227628,#227629,
#227630),(#227631,#227632,#227633,#227634,#227635,#227636,#227637,#227638,
#227639,#227640),(#227641,#227642,#227643,#227644,#227645,#227646,#227647,
#227648,#227649,#227650),(#227651,#227652,#227653,#227654,#227655,#227656,
#227657,#227658,#227659,#227660),(#227661,#227662,#227663,#227664,#227665,
#227666,#227667,#227668,#227669,#227670),(#227671,#227672,#227673,#227674,
#227675,#227676,#227677,#227678,#227679,#227680),(#227681,#227682,#227683,
#227684,#227685,#227686,#227687,#227688,#227689,#227690),(#227691,#227692,
#227693,#227694,#227695,#227696,#227697,#227698,#227699,#227700),(#227701,
#227702,#227703,#227704,#227705,#227706,#227707,#227708,#227709,#227710),
(#227711,#227712,#227713,#227714,#227715,#227716,#227717,#227718,#227719,
#227720),(#227721,#227722,#227723,#227724,#227725,#227726,#227727,#227728,
#227729,#227730),(#227731,#227732,#227733,#227734,#227735,#227736,#227737,
#227738,#227739,#227740),(#227741,#227742,#227743,#227744,#227745,#227746,
#227747,#227748,#227749,#227750),(#227751,#227752,#227753,#227754,#227755,
#227756,#227757,#227758,#227759,#227760),(#227761,#227762,#227763,#227764,
#227765,#227766,#227767,#227768,#227769,#227770),(#227771,#227772,#227773,
#227774,#227775,#227776,#227777,#227778,#227779,#227780),(#227781,#227782,
#227783,#227784,#227785,#227786,#227787,#227788,#227789,#227790),(#227791,
#227792,#227793,#227794,#227795,#227796,#227797,#227798,#227799,#227800),
(#227801,#227802,#227803,#227804,#227805,#227806,#227807,#227808,#227809,
#227810),(#227811,#227812,#227813,#227814,#227815,#227816,#227817,#227818,
#227819,#227820),(#227821,#227822,#227823,#227824,#227825,#227826,#227827,
#227828,#227829,#227830),(#227831,#227832,#227833,#227834,#227835,#227836,
#227837,#227838,#227839,#227840),(#227841,#227842,#227843,#227844,#227845,
#227846,#227847,#227848,#227849,#227850),(#227851,#227852,#227853,#227854,
#227855,#227856,#227857,#227858,#227859,#227860),(#227861,#227862,#227863,
#227864,#227865,#227866,#227867,#227868,#227869,#227870),(#227871,#227872,
#227873,#227874,#227875,#227876,#227877,#227878,#227879,#227880),(#227881,
#227882,#227883,#227884,#227885,#227886,#227887,#227888,#227889,#227890),
(#227891,#227892,#227893,#227894,#227895,#227896,#227897,#227898,#227899,
#227900),(#227901,#227902,#227903,#227904,#227905,#227906,#227907,#227908,
#227909,#227910),(#227911,#227912,#227913,#227914,#227915,#227916,#227917,
#227918,#227919,#227920),(#227921,#227922,#227923,#227924,#227925,#227926,
#227927,#227928,#227929,#227930),(#227931,#227932,#227933,#227934,#227935,
#227936,#227937,#227938,#227939,#227940),(#227941,#227942,#227943,#227944,
#227945,#227946,#227947,#227948,#227949,#227950),(#227951,#227952,#227953,
#227954,#227955,#227956,#227957,#227958,#227959,#227960),(#227961,#227962,
#227963,#227964,#227965,#227966,#227967,#227968,#227969,#227970),(#227971,
#227972,#227973,#227974,#227975,#227976,#227977,#227978,#227979,#227980),
(#227981,#227982,#227983,#227984,#227985,#227986,#227987,#227988,#227989,
#227990),(#227991,#227992,#227993,#227994,#227995,#227996,#227997,#227998,
#227999,#228000),(#228001,#228002,#228003,#228004,#228005,#228006,#228007,
#228008,#228009,#228010)),.UNSPECIFIED.,.F.,.F.,.F.,(4,3,3,3,3,3,3,3,3,
3,3,3,3,3,3,3,3,4),(4,3,3,4),(-0.00600093757051703,0.00190532409776943,
0.00981158576605589,0.0256241091026288,0.0572491557757747,0.120499249122066,
0.24699943581465,0.373499622507233,0.499999809199817,0.6264999958924,0.753000182584983,
0.816250275931275,0.879500369277567,0.942750462623858,0.974375509297004,
0.990188032633577,0.998094294301864,1.00600055597015),(0.0341113530318832,
0.269267250872974,0.504423148714065,0.974734944396246),.UNSPECIFIED.);
#933=B_SPLINE_SURFACE_WITH_KNOTS('',3,3,((#228207,#228208,#228209,#228210),
(#228211,#228212,#228213,#228214),(#228215,#228216,#228217,#228218),(#228219,
#228220,#228221,#228222)),.UNSPECIFIED.,.F.,.F.,.F.,(4,4),(4,4),(-2.26710392139532E-13,
0.274586007458263),(0.048728470569204,0.974637180848091),.UNSPECIFIED.);
#934=B_SPLINE_SURFACE_WITH_KNOTS('',3,3,((#228243,#228244,#228245,#228246),
(#228247,#228248,#228249,#228250),(#228251,#228252,#228253,#228254),(#228255,
#228256,#228257,#228258)),.UNSPECIFIED.,.F.,.F.,.F.,(4,4),(4,4),(0.723791628179461,
1.),(0.0491493978854403,0.974752225001403),.UNSPECIFIED.);
#935=B_SPLINE_SURFACE_WITH_KNOTS('',3,3,((#228461,#228462,#228463,#228464),
(#228465,#228466,#228467,#228468),(#228469,#228470,#228471,#228472),(#228473,
#228474,#228475,#228476)),.UNSPECIFIED.,.F.,.F.,.F.,(4,4),(4,4),(7.07266882820453E-16,
0.107439860233906),(0.0511874640850671,0.974440796609261),.UNSPECIFIED.);
#936=B_SPLINE_SURFACE_WITH_KNOTS('',3,3,((#228512,#228513,#228514,#228515),
(#228516,#228517,#228518,#228519),(#228520,#228521,#228522,#228523),(#228524,
#228525,#228526,#228527)),.UNSPECIFIED.,.F.,.F.,.F.,(4,4),(4,4),(0.905181055822597,
1.00000000000972),(0.0504405324641688,0.975107277906268),.UNSPECIFIED.);
#937=B_SPLINE_SURFACE_WITH_KNOTS('',3,3,((#228544,#228545,#228546,#228547,
#228548,#228549,#228550),(#228551,#228552,#228553,#228554,#228555,#228556,
#228557),(#228558,#228559,#228560,#228561,#228562,#228563,#228564),(#228565,
#228566,#228567,#228568,#228569,#228570,#228571),(#228572,#228573,#228574,
#228575,#228576,#228577,#228578),(#228579,#228580,#228581,#228582,#228583,
#228584,#228585),(#228586,#228587,#228588,#228589,#228590,#228591,#228592),
(#228593,#228594,#228595,#228596,#228597,#228598,#228599),(#228600,#228601,
#228602,#228603,#228604,#228605,#228606),(#228607,#228608,#228609,#228610,
#228611,#228612,#228613),(#228614,#228615,#228616,#228617,#228618,#228619,
#228620),(#228621,#228622,#228623,#228624,#228625,#228626,#228627),(#228628,
#228629,#228630,#228631,#228632,#228633,#228634),(#228635,#228636,#228637,
#228638,#228639,#228640,#228641),(#228642,#228643,#228644,#228645,#228646,
#228647,#228648),(#228649,#228650,#228651,#228652,#228653,#228654,#228655),
(#228656,#228657,#228658,#228659,#228660,#228661,#228662),(#228663,#228664,
#228665,#228666,#228667,#228668,#228669),(#228670,#228671,#228672,#228673,
#228674,#228675,#228676),(#228677,#228678,#228679,#228680,#228681,#228682,
#228683),(#228684,#228685,#228686,#228687,#228688,#228689,#228690),(#228691,
#228692,#228693,#228694,#228695,#228696,#228697),(#228698,#228699,#228700,
#228701,#228702,#228703,#228704),(#228705,#228706,#228707,#228708,#228709,
#228710,#228711),(#228712,#228713,#228714,#228715,#228716,#228717,#228718),
(#228719,#228720,#228721,#228722,#228723,#228724,#228725),(#228726,#228727,
#228728,#228729,#228730,#228731,#228732),(#228733,#228734,#228735,#228736,
#228737,#228738,#228739)),.UNSPECIFIED.,.F.,.F.,.F.,(4,3,3,3,3,3,3,3,3,
4),(4,3,4),(6.8818812944557E-15,0.250000000000005,0.5,0.75,0.875,0.9375,
0.96875,0.984375,0.9921875,1.),(0.0332750425089971,0.501824549528,0.970374056547004),
 .UNSPECIFIED.);
#938=B_SPLINE_SURFACE_WITH_KNOTS('',3,3,((#228821,#228822,#228823,#228824,
#228825,#228826,#228827),(#228828,#228829,#228830,#228831,#228832,#228833,
#228834),(#228835,#228836,#228837,#228838,#228839,#228840,#228841),(#228842,
#228843,#228844,#228845,#228846,#228847,#228848),(#228849,#228850,#228851,
#228852,#228853,#228854,#228855),(#228856,#228857,#228858,#228859,#228860,
#228861,#228862),(#228863,#228864,#228865,#228866,#228867,#228868,#228869),
(#228870,#228871,#228872,#228873,#228874,#228875,#228876),(#228877,#228878,
#228879,#228880,#228881,#228882,#228883),(#228884,#228885,#228886,#228887,
#228888,#228889,#228890),(#228891,#228892,#228893,#228894,#228895,#228896,
#228897),(#228898,#228899,#228900,#228901,#228902,#228903,#228904),(#228905,
#228906,#228907,#228908,#228909,#228910,#228911),(#228912,#228913,#228914,
#228915,#228916,#228917,#228918),(#228919,#228920,#228921,#228922,#228923,
#228924,#228925),(#228926,#228927,#228928,#228929,#228930,#228931,#228932),
(#228933,#228934,#228935,#228936,#228937,#228938,#228939),(#228940,#228941,
#228942,#228943,#228944,#228945,#228946),(#228947,#228948,#228949,#228950,
#228951,#228952,#228953),(#228954,#228955,#228956,#228957,#228958,#228959,
#228960),(#228961,#228962,#228963,#228964,#228965,#228966,#228967),(#228968,
#228969,#228970,#228971,#228972,#228973,#228974),(#228975,#228976,#228977,
#228978,#228979,#228980,#228981),(#228982,#228983,#228984,#228985,#228986,
#228987,#228988),(#228989,#228990,#228991,#228992,#228993,#228994,#228995),
(#228996,#228997,#228998,#228999,#229000,#229001,#229002),(#229003,#229004,
#229005,#229006,#229007,#229008,#229009),(#229010,#229011,#229012,#229013,
#229014,#229015,#229016),(#229017,#229018,#229019,#229020,#229021,#229022,
#229023),(#229024,#229025,#229026,#229027,#229028,#229029,#229030),(#229031,
#229032,#229033,#229034,#229035,#229036,#229037),(#229038,#229039,#229040,
#229041,#229042,#229043,#229044),(#229045,#229046,#229047,#229048,#229049,
#229050,#229051),(#229052,#229053,#229054,#229055,#229056,#229057,#229058),
(#229059,#229060,#229061,#229062,#229063,#229064,#229065),(#229066,#229067,
#229068,#229069,#229070,#229071,#229072),(#229073,#229074,#229075,#229076,
#229077,#229078,#229079),(#229080,#229081,#229082,#229083,#229084,#229085,
#229086),(#229087,#229088,#229089,#229090,#229091,#229092,#229093),(#229094,
#229095,#229096,#229097,#229098,#229099,#229100)),.UNSPECIFIED.,.F.,.F.,
 .F.,(4,3,3,3,3,3,3,3,3,3,3,3,3,4),(4,3,4),(-0.00600002990670325,0.009718720560589,
0.0254374710278812,0.0568749719624657,0.119749973831635,0.245499977569973,
0.496999985046649,0.748499992523325,0.874249996261663,0.937124998130832,
0.968562499065416,0.984281249532708,0.992140624766354,1.),(0.0284242133522742,
0.499005960311874,0.969587707271474),.UNSPECIFIED.);
#939=B_SPLINE_SURFACE_WITH_KNOTS('',3,3,((#229258,#229259,#229260,#229261,
#229262,#229263,#229264),(#229265,#229266,#229267,#229268,#229269,#229270,
#229271),(#229272,#229273,#229274,#229275,#229276,#229277,#229278),(#229279,
#229280,#229281,#229282,#229283,#229284,#229285),(#229286,#229287,#229288,
#229289,#229290,#229291,#229292),(#229293,#229294,#229295,#229296,#229297,
#229298,#229299),(#229300,#229301,#229302,#229303,#229304,#229305,#229306),
(#229307,#229308,#229309,#229310,#229311,#229312,#229313),(#229314,#229315,
#229316,#229317,#229318,#229319,#229320),(#229321,#229322,#229323,#229324,
#229325,#229326,#229327),(#229328,#229329,#229330,#229331,#229332,#229333,
#229334),(#229335,#229336,#229337,#229338,#229339,#229340,#229341),(#229342,
#229343,#229344,#229345,#229346,#229347,#229348),(#229349,#229350,#229351,
#229352,#229353,#229354,#229355),(#229356,#229357,#229358,#229359,#229360,
#229361,#229362),(#229363,#229364,#229365,#229366,#229367,#229368,#229369),
(#229370,#229371,#229372,#229373,#229374,#229375,#229376),(#229377,#229378,
#229379,#229380,#229381,#229382,#229383),(#229384,#229385,#229386,#229387,
#229388,#229389,#229390),(#229391,#229392,#229393,#229394,#229395,#229396,
#229397),(#229398,#229399,#229400,#229401,#229402,#229403,#229404),(#229405,
#229406,#229407,#229408,#229409,#229410,#229411),(#229412,#229413,#229414,
#229415,#229416,#229417,#229418),(#229419,#229420,#229421,#229422,#229423,
#229424,#229425),(#229426,#229427,#229428,#229429,#229430,#229431,#229432),
(#229433,#229434,#229435,#229436,#229437,#229438,#229439),(#229440,#229441,
#229442,#229443,#229444,#229445,#229446),(#229447,#229448,#229449,#229450,
#229451,#229452,#229453),(#229454,#229455,#229456,#229457,#229458,#229459,
#229460),(#229461,#229462,#229463,#229464,#229465,#229466,#229467),(#229468,
#229469,#229470,#229471,#229472,#229473,#229474),(#229475,#229476,#229477,
#229478,#229479,#229480,#229481),(#229482,#229483,#229484,#229485,#229486,
#229487,#229488),(#229489,#229490,#229491,#229492,#229493,#229494,#229495),
(#229496,#229497,#229498,#229499,#229500,#229501,#229502),(#229503,#229504,
#229505,#229506,#229507,#229508,#229509),(#229510,#229511,#229512,#229513,
#229514,#229515,#229516),(#229517,#229518,#229519,#229520,#229521,#229522,
#229523),(#229524,#229525,#229526,#229527,#229528,#229529,#229530),(#229531,
#229532,#229533,#229534,#229535,#229536,#229537),(#229538,#229539,#229540,
#229541,#229542,#229543,#229544),(#229545,#229546,#229547,#229548,#229549,
#229550,#229551),(#229552,#229553,#229554,#229555,#229556,#229557,#229558),
(#229559,#229560,#229561,#229562,#229563,#229564,#229565),(#229566,#229567,
#229568,#229569,#229570,#229571,#229572),(#229573,#229574,#229575,#229576,
#229577,#229578,#229579),(#229580,#229581,#229582,#229583,#229584,#229585,
#229586),(#229587,#229588,#229589,#229590,#229591,#229592,#229593),(#229594,
#229595,#229596,#229597,#229598,#229599,#229600),(#229601,#229602,#229603,
#229604,#229605,#229606,#229607),(#229608,#229609,#229610,#229611,#229612,
#229613,#229614),(#229615,#229616,#229617,#229618,#229619,#229620,#229621),
(#229622,#229623,#229624,#229625,#229626,#229627,#229628),(#229629,#229630,
#229631,#229632,#229633,#229634,#229635),(#229636,#229637,#229638,#229639,
#229640,#229641,#229642),(#229643,#229644,#229645,#229646,#229647,#229648,
#229649),(#229650,#229651,#229652,#229653,#229654,#229655,#229656),(#229657,
#229658,#229659,#229660,#229661,#229662,#229663),(#229664,#229665,#229666,
#229667,#229668,#229669,#229670),(#229671,#229672,#229673,#229674,#229675,
#229676,#229677),(#229678,#229679,#229680,#229681,#229682,#229683,#229684),
(#229685,#229686,#229687,#229688,#229689,#229690,#229691),(#229692,#229693,
#229694,#229695,#229696,#229697,#229698),(#229699,#229700,#229701,#229702,
#229703,#229704,#229705),(#229706,#229707,#229708,#229709,#229710,#229711,
#229712),(#229713,#229714,#229715,#229716,#229717,#229718,#229719),(#229720,
#229721,#229722,#229723,#229724,#229725,#229726),(#229727,#229728,#229729,
#229730,#229731,#229732,#229733),(#229734,#229735,#229736,#229737,#229738,
#229739,#229740),(#229741,#229742,#229743,#229744,#229745,#229746,#229747),
(#229748,#229749,#229750,#229751,#229752,#229753,#229754),(#229755,#229756,
#229757,#229758,#229759,#229760,#229761),(#229762,#229763,#229764,#229765,
#229766,#229767,#229768),(#229769,#229770,#229771,#229772,#229773,#229774,
#229775),(#229776,#229777,#229778,#229779,#229780,#229781,#229782),(#229783,
#229784,#229785,#229786,#229787,#229788,#229789),(#229790,#229791,#229792,
#229793,#229794,#229795,#229796),(#229797,#229798,#229799,#229800,#229801,
#229802,#229803),(#229804,#229805,#229806,#229807,#229808,#229809,#229810),
(#229811,#229812,#229813,#229814,#229815,#229816,#229817),(#229818,#229819,
#229820,#229821,#229822,#229823,#229824),(#229825,#229826,#229827,#229828,
#229829,#229830,#229831),(#229832,#229833,#229834,#229835,#229836,#229837,
#229838),(#229839,#229840,#229841,#229842,#229843,#229844,#229845),(#229846,
#229847,#229848,#229849,#229850,#229851,#229852),(#229853,#229854,#229855,
#229856,#229857,#229858,#229859),(#229860,#229861,#229862,#229863,#229864,
#229865,#229866),(#229867,#229868,#229869,#229870,#229871,#229872,#229873),
(#229874,#229875,#229876,#229877,#229878,#229879,#229880),(#229881,#229882,
#229883,#229884,#229885,#229886,#229887),(#229888,#229889,#229890,#229891,
#229892,#229893,#229894),(#229895,#229896,#229897,#229898,#229899,#229900,
#229901),(#229902,#229903,#229904,#229905,#229906,#229907,#229908),(#229909,
#229910,#229911,#229912,#229913,#229914,#229915),(#229916,#229917,#229918,
#229919,#229920,#229921,#229922),(#229923,#229924,#229925,#229926,#229927,
#229928,#229929),(#229930,#229931,#229932,#229933,#229934,#229935,#229936),
(#229937,#229938,#229939,#229940,#229941,#229942,#229943),(#229944,#229945,
#229946,#229947,#229948,#229949,#229950),(#229951,#229952,#229953,#229954,
#229955,#229956,#229957),(#229958,#229959,#229960,#229961,#229962,#229963,
#229964),(#229965,#229966,#229967,#229968,#229969,#229970,#229971),(#229972,
#229973,#229974,#229975,#229976,#229977,#229978),(#229979,#229980,#229981,
#229982,#229983,#229984,#229985),(#229986,#229987,#229988,#229989,#229990,
#229991,#229992),(#229993,#229994,#229995,#229996,#229997,#229998,#229999),
(#230000,#230001,#230002,#230003,#230004,#230005,#230006),(#230007,#230008,
#230009,#230010,#230011,#230012,#230013),(#230014,#230015,#230016,#230017,
#230018,#230019,#230020),(#230021,#230022,#230023,#230024,#230025,#230026,
#230027),(#230028,#230029,#230030,#230031,#230032,#230033,#230034),(#230035,
#230036,#230037,#230038,#230039,#230040,#230041),(#230042,#230043,#230044,
#230045,#230046,#230047,#230048),(#230049,#230050,#230051,#230052,#230053,
#230054,#230055),(#230056,#230057,#230058,#230059,#230060,#230061,#230062),
(#230063,#230064,#230065,#230066,#230067,#230068,#230069),(#230070,#230071,
#230072,#230073,#230074,#230075,#230076),(#230077,#230078,#230079,#230080,
#230081,#230082,#230083),(#230084,#230085,#230086,#230087,#230088,#230089,
#230090),(#230091,#230092,#230093,#230094,#230095,#230096,#230097),(#230098,
#230099,#230100,#230101,#230102,#230103,#230104),(#230105,#230106,#230107,
#230108,#230109,#230110,#230111),(#230112,#230113,#230114,#230115,#230116,
#230117,#230118),(#230119,#230120,#230121,#230122,#230123,#230124,#230125),
(#230126,#230127,#230128,#230129,#230130,#230131,#230132),(#230133,#230134,
#230135,#230136,#230137,#230138,#230139),(#230140,#230141,#230142,#230143,
#230144,#230145,#230146),(#230147,#230148,#230149,#230150,#230151,#230152,
#230153),(#230154,#230155,#230156,#230157,#230158,#230159,#230160),(#230161,
#230162,#230163,#230164,#230165,#230166,#230167),(#230168,#230169,#230170,
#230171,#230172,#230173,#230174),(#230175,#230176,#230177,#230178,#230179,
#230180,#230181),(#230182,#230183,#230184,#230185,#230186,#230187,#230188),
(#230189,#230190,#230191,#230192,#230193,#230194,#230195),(#230196,#230197,
#230198,#230199,#230200,#230201,#230202),(#230203,#230204,#230205,#230206,
#230207,#230208,#230209),(#230210,#230211,#230212,#230213,#230214,#230215,
#230216),(#230217,#230218,#230219,#230220,#230221,#230222,#230223),(#230224,
#230225,#230226,#230227,#230228,#230229,#230230),(#230231,#230232,#230233,
#230234,#230235,#230236,#230237),(#230238,#230239,#230240,#230241,#230242,
#230243,#230244),(#230245,#230246,#230247,#230248,#230249,#230250,#230251),
(#230252,#230253,#230254,#230255,#230256,#230257,#230258),(#230259,#230260,
#230261,#230262,#230263,#230264,#230265),(#230266,#230267,#230268,#230269,
#230270,#230271,#230272),(#230273,#230274,#230275,#230276,#230277,#230278,
#230279),(#230280,#230281,#230282,#230283,#230284,#230285,#230286),(#230287,
#230288,#230289,#230290,#230291,#230292,#230293),(#230294,#230295,#230296,
#230297,#230298,#230299,#230300),(#230301,#230302,#230303,#230304,#230305,
#230306,#230307),(#230308,#230309,#230310,#230311,#230312,#230313,#230314),
(#230315,#230316,#230317,#230318,#230319,#230320,#230321),(#230322,#230323,
#230324,#230325,#230326,#230327,#230328),(#230329,#230330,#230331,#230332,
#230333,#230334,#230335),(#230336,#230337,#230338,#230339,#230340,#230341,
#230342),(#230343,#230344,#230345,#230346,#230347,#230348,#230349),(#230350,
#230351,#230352,#230353,#230354,#230355,#230356)),.UNSPECIFIED.,.F.,.F.,
 .F.,(4,3,3,3,3,3,3,3,3,3,3,3,3,3,3,3,3,3,3,3,3,3,3,3,3,3,3,3,3,3,3,3,3,
3,3,3,3,3,3,3,3,3,3,3,3,3,3,3,3,3,3,3,4),(4,3,4),(-7.69660169486442E-5,
0.125023528667579,0.156298652338711,0.164117433256494,0.164606107063856,
0.165094780871217,0.16607212848594,0.168026823715385,0.171936214174277,
0.187573776009843,0.250124023352107,0.281399147023239,0.297036708858805,
0.298991404088251,0.299480077895612,0.299968751702973,0.300946099317697,
0.304855489776588,0.312674270694371,0.375224518036634,0.406499641707767,
0.422137203543333,0.429955984461115,0.430933332075839,0.431910679690562,
0.433865374920007,0.437774765378899,0.500325012721163,0.562875260063426,
0.566784650522318,0.568739345751764,0.569228019559125,0.569716693366486,
0.570694040981209,0.578512821898992,0.594150383734558,0.62542550740569,
0.687975754747954,0.695794535665737,0.699703926124629,0.701658621354074,
0.70361331658352,0.719250878419086,0.750526002090218,0.813076249432482,
0.828713811268048,0.832623201726939,0.834577896956385,0.835555244571108,
0.836532592185831,0.844351373103614,0.875626496774746,1.00072699145927),
(0.0460660594806178,0.548882757239649,1.05169945499868),.UNSPECIFIED.);
#940=B_SPLINE_SURFACE_WITH_KNOTS('',3,1,((#230431,#230432),(#230433,#230434),
(#230435,#230436),(#230437,#230438),(#230439,#230440),(#230441,#230442),
(#230443,#230444),(#230445,#230446),(#230447,#230448),(#230449,#230450),
(#230451,#230452),(#230453,#230454),(#230455,#230456),(#230457,#230458),
(#230459,#230460),(#230461,#230462),(#230463,#230464),(#230465,#230466),
(#230467,#230468),(#230469,#230470),(#230471,#230472),(#230473,#230474),
(#230475,#230476),(#230477,#230478),(#230479,#230480),(#230481,#230482),
(#230483,#230484),(#230485,#230486),(#230487,#230488),(#230489,#230490),
(#230491,#230492),(#230493,#230494),(#230495,#230496),(#230497,#230498),
(#230499,#230500),(#230501,#230502),(#230503,#230504),(#230505,#230506),
(#230507,#230508),(#230509,#230510),(#230511,#230512),(#230513,#230514)),
 .UNSPECIFIED.,.F.,.F.,.F.,(4,1,1,1,2,1,1,1,2,1,1,1,2,1,1,1,2,1,1,1,2,1,
1,1,2,1,1,1,2,1,1,1,4),(2,2),(-0.116364947985043,0.0349237439162043,0.0698474878324086,
0.104771231748613,0.139694975664817,0.174004779710855,0.208314583756892,
0.24262438780293,0.276934191848968,0.313293030205055,0.349651868561143,
0.38601070691723,0.422369545273318,0.441777158954989,0.46118477263666,0.480592386318331,
0.5,0.519407613681673,0.538815227363344,0.558222841045015,0.577630454726686,
0.613989293082773,0.65034813143886,0.686706969794946,0.723065808151033,
0.757375612197071,0.791685416243108,0.825995220289146,0.860305024335184,
0.895228768251388,0.930152512167592,0.965076256083796,1.11636494798509),
(-0.174247524918837,1.18461554289192),.UNSPECIFIED.);
#941=B_SPLINE_SURFACE_WITH_KNOTS('',3,3,((#230515,#230516,#230517,#230518),
(#230519,#230520,#230521,#230522),(#230523,#230524,#230525,#230526),(#230527,
#230528,#230529,#230530),(#230531,#230532,#230533,#230534),(#230535,#230536,
#230537,#230538),(#230539,#230540,#230541,#230542),(#230543,#230544,#230545,
#230546),(#230547,#230548,#230549,#230550),(#230551,#230552,#230553,#230554),
(#230555,#230556,#230557,#230558),(#230559,#230560,#230561,#230562),(#230563,
#230564,#230565,#230566),(#230567,#230568,#230569,#230570),(#230571,#230572,
#230573,#230574),(#230575,#230576,#230577,#230578),(#230579,#230580,#230581,
#230582),(#230583,#230584,#230585,#230586),(#230587,#230588,#230589,#230590),
(#230591,#230592,#230593,#230594),(#230595,#230596,#230597,#230598),(#230599,
#230600,#230601,#230602),(#230603,#230604,#230605,#230606),(#230607,#230608,
#230609,#230610),(#230611,#230612,#230613,#230614),(#230615,#230616,#230617,
#230618),(#230619,#230620,#230621,#230622),(#230623,#230624,#230625,#230626),
(#230627,#230628,#230629,#230630),(#230631,#230632,#230633,#230634),(#230635,
#230636,#230637,#230638),(#230639,#230640,#230641,#230642),(#230643,#230644,
#230645,#230646),(#230647,#230648,#230649,#230650),(#230651,#230652,#230653,
#230654),(#230655,#230656,#230657,#230658),(#230659,#230660,#230661,#230662),
(#230663,#230664,#230665,#230666),(#230667,#230668,#230669,#230670),(#230671,
#230672,#230673,#230674),(#230675,#230676,#230677,#230678),(#230679,#230680,
#230681,#230682)),.UNSPECIFIED.,.F.,.F.,.F.,(4,1,1,1,2,1,1,1,2,1,1,1,2,
1,1,1,2,1,1,1,2,1,1,1,2,1,1,1,2,1,1,1,4),(4,4),(-0.0947053917544244,0.0379780806838576,
0.0759561613677151,0.113934242051573,0.15191232273543,0.189669188200293,
0.227426053665157,0.26518291913002,0.302939784594882,0.333326792628875,
0.363713800662868,0.394100808696861,0.424487816730854,0.44336586254814,
0.462243908365427,0.481121954182713,0.5,0.518878045817286,0.537756091634573,
0.55663413745186,0.575512183269147,0.60589919130314,0.636286199337133,0.666673207371127,
0.697060215405119,0.734817080869983,0.772573946334846,0.810330811799709,
0.848087677264572,0.886065757948429,0.924043838632286,0.962021919316143,
1.09470538922058),(-0.176001360689901,1.1748817259388),.UNSPECIFIED.);
#942=B_SPLINE_SURFACE_WITH_KNOTS('',3,1,((#230683,#230684),(#230685,#230686),
(#230687,#230688),(#230689,#230690),(#230691,#230692),(#230693,#230694),
(#230695,#230696),(#230697,#230698),(#230699,#230700),(#230701,#230702),
(#230703,#230704),(#230705,#230706),(#230707,#230708),(#230709,#230710),
(#230711,#230712),(#230713,#230714),(#230715,#230716),(#230717,#230718),
(#230719,#230720),(#230721,#230722),(#230723,#230724),(#230725,#230726),
(#230727,#230728),(#230729,#230730),(#230731,#230732),(#230733,#230734),
(#230735,#230736),(#230737,#230738),(#230739,#230740),(#230741,#230742),
(#230743,#230744),(#230745,#230746),(#230747,#230748),(#230749,#230750),
(#230751,#230752),(#230753,#230754),(#230755,#230756),(#230757,#230758),
(#230759,#230760),(#230761,#230762),(#230763,#230764),(#230765,#230766)),
 .UNSPECIFIED.,.F.,.F.,.F.,(4,1,1,1,2,1,1,1,2,1,1,1,2,1,1,1,2,1,1,1,2,1,
1,1,2,1,1,1,2,1,1,1,4),(2,2),(-0.130664626928687,0.0411596607520464,0.0823193215040928,
0.123478982256139,0.164638643008186,0.198458137911997,0.232277632815809,
0.26609712771962,0.299916622623432,0.332619014198497,0.365321405773562,
0.398023797348627,0.430726188923692,0.448044641692768,0.465363094461843,
0.482681547230919,0.499999999999994,0.517318452769073,0.534636905538152,
0.55195535830723,0.569273811076309,0.601976202651373,0.634678594226438,
0.667380985801503,0.700083377376568,0.73390287228038,0.767722367184191,
0.801541862088003,0.835361356991815,0.876521017743861,0.917680678495907,
0.958840339247954,1.12208155081997),(-0.184126650858872,1.18095881489235),
 .UNSPECIFIED.);
#943=B_SPLINE_SURFACE_WITH_KNOTS('',3,3,((#230837,#230838,#230839,#230840,
#230841,#230842,#230843),(#230844,#230845,#230846,#230847,#230848,#230849,
#230850),(#230851,#230852,#230853,#230854,#230855,#230856,#230857),(#230858,
#230859,#230860,#230861,#230862,#230863,#230864),(#230865,#230866,#230867,
#230868,#230869,#230870,#230871),(#230872,#230873,#230874,#230875,#230876,
#230877,#230878),(#230879,#230880,#230881,#230882,#230883,#230884,#230885),
(#230886,#230887,#230888,#230889,#230890,#230891,#230892),(#230893,#230894,
#230895,#230896,#230897,#230898,#230899),(#230900,#230901,#230902,#230903,
#230904,#230905,#230906),(#230907,#230908,#230909,#230910,#230911,#230912,
#230913)),.UNSPECIFIED.,.F.,.F.,.F.,(4,1,1,1,1,1,1,1,4),(4,3,4),(0.,0.124999999999998,
0.249999999999996,0.374999999999993,0.500000000000009,0.625000000000007,
0.75,0.875,1.),(0.,1.,1.01),.UNSPECIFIED.);
#944=B_SPLINE_SURFACE_WITH_KNOTS('',3,3,((#230919,#230920,#230921,#230922,
#230923,#230924,#230925),(#230926,#230927,#230928,#230929,#230930,#230931,
#230932),(#230933,#230934,#230935,#230936,#230937,#230938,#230939),(#230940,
#230941,#230942,#230943,#230944,#230945,#230946),(#230947,#230948,#230949,
#230950,#230951,#230952,#230953),(#230954,#230955,#230956,#230957,#230958,
#230959,#230960),(#230961,#230962,#230963,#230964,#230965,#230966,#230967),
(#230968,#230969,#230970,#230971,#230972,#230973,#230974),(#230975,#230976,
#230977,#230978,#230979,#230980,#230981),(#230982,#230983,#230984,#230985,
#230986,#230987,#230988),(#230989,#230990,#230991,#230992,#230993,#230994,
#230995),(#230996,#230997,#230998,#230999,#231000,#231001,#231002),(#231003,
#231004,#231005,#231006,#231007,#231008,#231009),(#231010,#231011,#231012,
#231013,#231014,#231015,#231016)),.UNSPECIFIED.,.F.,.F.,.F.,(4,3,1,1,1,
1,1,1,1,4),(4,3,4),(-0.01,0.,0.124999999999997,0.249999999999995,0.374999999999992,
0.49999999999999,0.624999999999988,0.749999999999985,0.874999999999983,
1.),(0.,1.,1.01),.UNSPECIFIED.);
#945=B_SPLINE_SURFACE_WITH_KNOTS('',3,3,((#231022,#231023,#231024,#231025,
#231026,#231027,#231028),(#231029,#231030,#231031,#231032,#231033,#231034,
#231035),(#231036,#231037,#231038,#231039,#231040,#231041,#231042),(#231043,
#231044,#231045,#231046,#231047,#231048,#231049),(#231050,#231051,#231052,
#231053,#231054,#231055,#231056),(#231057,#231058,#231059,#231060,#231061,
#231062,#231063),(#231064,#231065,#231066,#231067,#231068,#231069,#231070),
(#231071,#231072,#231073,#231074,#231075,#231076,#231077),(#231078,#231079,
#231080,#231081,#231082,#231083,#231084),(#231085,#231086,#231087,#231088,
#231089,#231090,#231091),(#231092,#231093,#231094,#231095,#231096,#231097,
#231098)),.UNSPECIFIED.,.F.,.F.,.F.,(4,1,1,1,1,1,1,1,4),(4,3,4),(0.,0.124999999999997,
0.249999999999998,0.375,0.5,0.625,0.75,0.875,1.),(0.,1.,1.01),
 .UNSPECIFIED.);
#946=B_SPLINE_SURFACE_WITH_KNOTS('',3,3,((#231104,#231105,#231106,#231107,
#231108,#231109,#231110),(#231111,#231112,#231113,#231114,#231115,#231116,
#231117),(#231118,#231119,#231120,#231121,#231122,#231123,#231124),(#231125,
#231126,#231127,#231128,#231129,#231130,#231131),(#231132,#231133,#231134,
#231135,#231136,#231137,#231138),(#231139,#231140,#231141,#231142,#231143,
#231144,#231145),(#231146,#231147,#231148,#231149,#231150,#231151,#231152),
(#231153,#231154,#231155,#231156,#231157,#231158,#231159),(#231160,#231161,
#231162,#231163,#231164,#231165,#231166),(#231167,#231168,#231169,#231170,
#231171,#231172,#231173),(#231174,#231175,#231176,#231177,#231178,#231179,
#231180),(#231181,#231182,#231183,#231184,#231185,#231186,#231187),(#231188,
#231189,#231190,#231191,#231192,#231193,#231194),(#231195,#231196,#231197,
#231198,#231199,#231200,#231201),(#231202,#231203,#231204,#231205,#231206,
#231207,#231208),(#231209,#231210,#231211,#231212,#231213,#231214,#231215),
(#231216,#231217,#231218,#231219,#231220,#231221,#231222)),
 .UNSPECIFIED.,.F.,.F.,.F.,(4,3,1,1,1,1,1,1,1,3,4),(4,3,4),(-0.01,0.,0.125,
0.25,0.375,0.5,0.625,0.75,0.875,1.,1.01),(0.,1.,1.01),.UNSPECIFIED.);
#947=B_SPLINE_SURFACE_WITH_KNOTS('',3,3,((#231279,#231280,#231281,#231282),
(#231283,#231284,#231285,#231286),(#231287,#231288,#231289,#231290),(#231291,
#231292,#231293,#231294),(#231295,#231296,#231297,#231298),(#231299,#231300,
#231301,#231302),(#231303,#231304,#231305,#231306)),.UNSPECIFIED.,.F.,.F.,
 .F.,(4,1,1,1,4),(4,4),(0.,0.25,0.5,0.75,1.),(0.,1.),.UNSPECIFIED.);
#948=B_SPLINE_SURFACE_WITH_KNOTS('',3,3,((#231307,#231308,#231309,#231310,
#231311,#231312,#231313),(#231314,#231315,#231316,#231317,#231318,#231319,
#231320),(#231321,#231322,#231323,#231324,#231325,#231326,#231327),(#231328,
#231329,#231330,#231331,#231332,#231333,#231334),(#231335,#231336,#231337,
#231338,#231339,#231340,#231341),(#231342,#231343,#231344,#231345,#231346,
#231347,#231348),(#231349,#231350,#231351,#231352,#231353,#231354,#231355)),
 .UNSPECIFIED.,.F.,.F.,.F.,(4,1,1,1,4),(4,3,4),(0.,0.25,0.5,0.75,1.),(0.,
1.,1.01),.UNSPECIFIED.);
#949=B_SPLINE_SURFACE_WITH_KNOTS('',3,3,((#231357,#231358,#231359,#231360,
#231361,#231362,#231363),(#231364,#231365,#231366,#231367,#231368,#231369,
#231370),(#231371,#231372,#231373,#231374,#231375,#231376,#231377),(#231378,
#231379,#231380,#231381,#231382,#231383,#231384),(#231385,#231386,#231387,
#231388,#231389,#231390,#231391),(#231392,#231393,#231394,#231395,#231396,
#231397,#231398),(#231399,#231400,#231401,#231402,#231403,#231404,#231405)),
 .UNSPECIFIED.,.F.,.F.,.F.,(4,1,1,1,4),(4,3,4),(0.,0.25,0.5,0.75,1.),(0.,
1.,1.01),.UNSPECIFIED.);
#950=B_SPLINE_SURFACE_WITH_KNOTS('',3,3,((#231408,#231409,#231410,#231411,
#231412,#231413,#231414),(#231415,#231416,#231417,#231418,#231419,#231420,
#231421),(#231422,#231423,#231424,#231425,#231426,#231427,#231428),(#231429,
#231430,#231431,#231432,#231433,#231434,#231435),(#231436,#231437,#231438,
#231439,#231440,#231441,#231442),(#231443,#231444,#231445,#231446,#231447,
#231448,#231449),(#231450,#231451,#231452,#231453,#231454,#231455,#231456)),
 .UNSPECIFIED.,.F.,.F.,.F.,(4,1,1,1,4),(4,3,4),(0.,0.25,0.5,0.75,1.),(0.,
1.,1.01),.UNSPECIFIED.);
#951=B_SPLINE_SURFACE_WITH_KNOTS('',3,3,((#231458,#231459,#231460,#231461,
#231462,#231463,#231464,#231465,#231466,#231467,#231468,#231469,#231470,
#231471,#231472,#231473),(#231474,#231475,#231476,#231477,#231478,#231479,
#231480,#231481,#231482,#231483,#231484,#231485,#231486,#231487,#231488,
#231489),(#231490,#231491,#231492,#231493,#231494,#231495,#231496,#231497,
#231498,#231499,#231500,#231501,#231502,#231503,#231504,#231505),(#231506,
#231507,#231508,#231509,#231510,#231511,#231512,#231513,#231514,#231515,
#231516,#231517,#231518,#231519,#231520,#231521),(#231522,#231523,#231524,
#231525,#231526,#231527,#231528,#231529,#231530,#231531,#231532,#231533,
#231534,#231535,#231536,#231537),(#231538,#231539,#231540,#231541,#231542,
#231543,#231544,#231545,#231546,#231547,#231548,#231549,#231550,#231551,
#231552,#231553),(#231554,#231555,#231556,#231557,#231558,#231559,#231560,
#231561,#231562,#231563,#231564,#231565,#231566,#231567,#231568,#231569),
(#231570,#231571,#231572,#231573,#231574,#231575,#231576,#231577,#231578,
#231579,#231580,#231581,#231582,#231583,#231584,#231585),(#231586,#231587,
#231588,#231589,#231590,#231591,#231592,#231593,#231594,#231595,#231596,
#231597,#231598,#231599,#231600,#231601),(#231602,#231603,#231604,#231605,
#231606,#231607,#231608,#231609,#231610,#231611,#231612,#231613,#231614,
#231615,#231616,#231617),(#231618,#231619,#231620,#231621,#231622,#231623,
#231624,#231625,#231626,#231627,#231628,#231629,#231630,#231631,#231632,
#231633),(#231634,#231635,#231636,#231637,#231638,#231639,#231640,#231641,
#231642,#231643,#231644,#231645,#231646,#231647,#231648,#231649),(#231650,
#231651,#231652,#231653,#231654,#231655,#231656,#231657,#231658,#231659,
#231660,#231661,#231662,#231663,#231664,#231665),(#231666,#231667,#231668,
#231669,#231670,#231671,#231672,#231673,#231674,#231675,#231676,#231677,
#231678,#231679,#231680,#231681),(#231682,#231683,#231684,#231685,#231686,
#231687,#231688,#231689,#231690,#231691,#231692,#231693,#231694,#231695,
#231696,#231697),(#231698,#231699,#231700,#231701,#231702,#231703,#231704,
#231705,#231706,#231707,#231708,#231709,#231710,#231711,#231712,#231713),
(#231714,#231715,#231716,#231717,#231718,#231719,#231720,#231721,#231722,
#231723,#231724,#231725,#231726,#231727,#231728,#231729),(#231730,#231731,
#231732,#231733,#231734,#231735,#231736,#231737,#231738,#231739,#231740,
#231741,#231742,#231743,#231744,#231745),(#231746,#231747,#231748,#231749,
#231750,#231751,#231752,#231753,#231754,#231755,#231756,#231757,#231758,
#231759,#231760,#231761),(#231762,#231763,#231764,#231765,#231766,#231767,
#231768,#231769,#231770,#231771,#231772,#231773,#231774,#231775,#231776,
#231777),(#231778,#231779,#231780,#231781,#231782,#231783,#231784,#231785,
#231786,#231787,#231788,#231789,#231790,#231791,#231792,#231793),(#231794,
#231795,#231796,#231797,#231798,#231799,#231800,#231801,#231802,#231803,
#231804,#231805,#231806,#231807,#231808,#231809),(#231810,#231811,#231812,
#231813,#231814,#231815,#231816,#231817,#231818,#231819,#231820,#231821,
#231822,#231823,#231824,#231825),(#231826,#231827,#231828,#231829,#231830,
#231831,#231832,#231833,#231834,#231835,#231836,#231837,#231838,#231839,
#231840,#231841),(#231842,#231843,#231844,#231845,#231846,#231847,#231848,
#231849,#231850,#231851,#231852,#231853,#231854,#231855,#231856,#231857),
(#231858,#231859,#231860,#231861,#231862,#231863,#231864,#231865,#231866,
#231867,#231868,#231869,#231870,#231871,#231872,#231873),(#231874,#231875,
#231876,#231877,#231878,#231879,#231880,#231881,#231882,#231883,#231884,
#231885,#231886,#231887,#231888,#231889),(#231890,#231891,#231892,#231893,
#231894,#231895,#231896,#231897,#231898,#231899,#231900,#231901,#231902,
#231903,#231904,#231905),(#231906,#231907,#231908,#231909,#231910,#231911,
#231912,#231913,#231914,#231915,#231916,#231917,#231918,#231919,#231920,
#231921),(#231922,#231923,#231924,#231925,#231926,#231927,#231928,#231929,
#231930,#231931,#231932,#231933,#231934,#231935,#231936,#231937),(#231938,
#231939,#231940,#231941,#231942,#231943,#231944,#231945,#231946,#231947,
#231948,#231949,#231950,#231951,#231952,#231953),(#231954,#231955,#231956,
#231957,#231958,#231959,#231960,#231961,#231962,#231963,#231964,#231965,
#231966,#231967,#231968,#231969),(#231970,#231971,#231972,#231973,#231974,
#231975,#231976,#231977,#231978,#231979,#231980,#231981,#231982,#231983,
#231984,#231985),(#231986,#231987,#231988,#231989,#231990,#231991,#231992,
#231993,#231994,#231995,#231996,#231997,#231998,#231999,#232000,#232001),
(#232002,#232003,#232004,#232005,#232006,#232007,#232008,#232009,#232010,
#232011,#232012,#232013,#232014,#232015,#232016,#232017),(#232018,#232019,
#232020,#232021,#232022,#232023,#232024,#232025,#232026,#232027,#232028,
#232029,#232030,#232031,#232032,#232033),(#232034,#232035,#232036,#232037,
#232038,#232039,#232040,#232041,#232042,#232043,#232044,#232045,#232046,
#232047,#232048,#232049),(#232050,#232051,#232052,#232053,#232054,#232055,
#232056,#232057,#232058,#232059,#232060,#232061,#232062,#232063,#232064,
#232065),(#232066,#232067,#232068,#232069,#232070,#232071,#232072,#232073,
#232074,#232075,#232076,#232077,#232078,#232079,#232080,#232081),(#232082,
#232083,#232084,#232085,#232086,#232087,#232088,#232089,#232090,#232091,
#232092,#232093,#232094,#232095,#232096,#232097),(#232098,#232099,#232100,
#232101,#232102,#232103,#232104,#232105,#232106,#232107,#232108,#232109,
#232110,#232111,#232112,#232113),(#232114,#232115,#232116,#232117,#232118,
#232119,#232120,#232121,#232122,#232123,#232124,#232125,#232126,#232127,
#232128,#232129),(#232130,#232131,#232132,#232133,#232134,#232135,#232136,
#232137,#232138,#232139,#232140,#232141,#232142,#232143,#232144,#232145)),
 .UNSPECIFIED.,.F.,.F.,.F.,(4,3,3,3,3,3,3,1,1,1,3,3,3,3,3,3,4),(4,3,3,3,
3,4),(-364.,-121.,-40.,-13.,-4.,-1.,0.,0.25,0.5,0.75,1.,2.,5.,14.,41.,122.,
365.),(-7.07,-3.03,-1.01,0.,1.,1.01),.UNSPECIFIED.);
#952=B_SPLINE_SURFACE_WITH_KNOTS('',3,3,((#232147,#232148,#232149,#232150,
#232151,#232152,#232153,#232154,#232155,#232156,#232157,#232158,#232159,
#232160,#232161,#232162),(#232163,#232164,#232165,#232166,#232167,#232168,
#232169,#232170,#232171,#232172,#232173,#232174,#232175,#232176,#232177,
#232178),(#232179,#232180,#232181,#232182,#232183,#232184,#232185,#232186,
#232187,#232188,#232189,#232190,#232191,#232192,#232193,#232194),(#232195,
#232196,#232197,#232198,#232199,#232200,#232201,#232202,#232203,#232204,
#232205,#232206,#232207,#232208,#232209,#232210),(#232211,#232212,#232213,
#232214,#232215,#232216,#232217,#232218,#232219,#232220,#232221,#232222,
#232223,#232224,#232225,#232226),(#232227,#232228,#232229,#232230,#232231,
#232232,#232233,#232234,#232235,#232236,#232237,#232238,#232239,#232240,
#232241,#232242),(#232243,#232244,#232245,#232246,#232247,#232248,#232249,
#232250,#232251,#232252,#232253,#232254,#232255,#232256,#232257,#232258),
(#232259,#232260,#232261,#232262,#232263,#232264,#232265,#232266,#232267,
#232268,#232269,#232270,#232271,#232272,#232273,#232274),(#232275,#232276,
#232277,#232278,#232279,#232280,#232281,#232282,#232283,#232284,#232285,
#232286,#232287,#232288,#232289,#232290),(#232291,#232292,#232293,#232294,
#232295,#232296,#232297,#232298,#232299,#232300,#232301,#232302,#232303,
#232304,#232305,#232306),(#232307,#232308,#232309,#232310,#232311,#232312,
#232313,#232314,#232315,#232316,#232317,#232318,#232319,#232320,#232321,
#232322),(#232323,#232324,#232325,#232326,#232327,#232328,#232329,#232330,
#232331,#232332,#232333,#232334,#232335,#232336,#232337,#232338),(#232339,
#232340,#232341,#232342,#232343,#232344,#232345,#232346,#232347,#232348,
#232349,#232350,#232351,#232352,#232353,#232354),(#232355,#232356,#232357,
#232358,#232359,#232360,#232361,#232362,#232363,#232364,#232365,#232366,
#232367,#232368,#232369,#232370),(#232371,#232372,#232373,#232374,#232375,
#232376,#232377,#232378,#232379,#232380,#232381,#232382,#232383,#232384,
#232385,#232386),(#232387,#232388,#232389,#232390,#232391,#232392,#232393,
#232394,#232395,#232396,#232397,#232398,#232399,#232400,#232401,#232402),
(#232403,#232404,#232405,#232406,#232407,#232408,#232409,#232410,#232411,
#232412,#232413,#232414,#232415,#232416,#232417,#232418),(#232419,#232420,
#232421,#232422,#232423,#232424,#232425,#232426,#232427,#232428,#232429,
#232430,#232431,#232432,#232433,#232434),(#232435,#232436,#232437,#232438,
#232439,#232440,#232441,#232442,#232443,#232444,#232445,#232446,#232447,
#232448,#232449,#232450),(#232451,#232452,#232453,#232454,#232455,#232456,
#232457,#232458,#232459,#232460,#232461,#232462,#232463,#232464,#232465,
#232466),(#232467,#232468,#232469,#232470,#232471,#232472,#232473,#232474,
#232475,#232476,#232477,#232478,#232479,#232480,#232481,#232482),(#232483,
#232484,#232485,#232486,#232487,#232488,#232489,#232490,#232491,#232492,
#232493,#232494,#232495,#232496,#232497,#232498),(#232499,#232500,#232501,
#232502,#232503,#232504,#232505,#232506,#232507,#232508,#232509,#232510,
#232511,#232512,#232513,#232514),(#232515,#232516,#232517,#232518,#232519,
#232520,#232521,#232522,#232523,#232524,#232525,#232526,#232527,#232528,
#232529,#232530),(#232531,#232532,#232533,#232534,#232535,#232536,#232537,
#232538,#232539,#232540,#232541,#232542,#232543,#232544,#232545,#232546),
(#232547,#232548,#232549,#232550,#232551,#232552,#232553,#232554,#232555,
#232556,#232557,#232558,#232559,#232560,#232561,#232562),(#232563,#232564,
#232565,#232566,#232567,#232568,#232569,#232570,#232571,#232572,#232573,
#232574,#232575,#232576,#232577,#232578),(#232579,#232580,#232581,#232582,
#232583,#232584,#232585,#232586,#232587,#232588,#232589,#232590,#232591,
#232592,#232593,#232594),(#232595,#232596,#232597,#232598,#232599,#232600,
#232601,#232602,#232603,#232604,#232605,#232606,#232607,#232608,#232609,
#232610),(#232611,#232612,#232613,#232614,#232615,#232616,#232617,#232618,
#232619,#232620,#232621,#232622,#232623,#232624,#232625,#232626),(#232627,
#232628,#232629,#232630,#232631,#232632,#232633,#232634,#232635,#232636,
#232637,#232638,#232639,#232640,#232641,#232642),(#232643,#232644,#232645,
#232646,#232647,#232648,#232649,#232650,#232651,#232652,#232653,#232654,
#232655,#232656,#232657,#232658),(#232659,#232660,#232661,#232662,#232663,
#232664,#232665,#232666,#232667,#232668,#232669,#232670,#232671,#232672,
#232673,#232674),(#232675,#232676,#232677,#232678,#232679,#232680,#232681,
#232682,#232683,#232684,#232685,#232686,#232687,#232688,#232689,#232690),
(#232691,#232692,#232693,#232694,#232695,#232696,#232697,#232698,#232699,
#232700,#232701,#232702,#232703,#232704,#232705,#232706),(#232707,#232708,
#232709,#232710,#232711,#232712,#232713,#232714,#232715,#232716,#232717,
#232718,#232719,#232720,#232721,#232722),(#232723,#232724,#232725,#232726,
#232727,#232728,#232729,#232730,#232731,#232732,#232733,#232734,#232735,
#232736,#232737,#232738)),.UNSPECIFIED.,.F.,.F.,.F.,(4,3,3,3,3,3,1,1,1,
3,3,3,3,3,4),(4,3,3,3,3,4),(-121.,-40.,-13.,-4.,-1.,0.,0.25,0.5,0.75,1.,
2.,5.,14.,41.,122.),(-7.07,-3.03,-1.01,0.,1.,1.01),.UNSPECIFIED.);
#953=B_SPLINE_SURFACE_WITH_KNOTS('',1,3,((#244024,#244025,#244026,#244027,
#244028,#244029,#244030,#244031,#244032,#244033,#244034,#244035,#244036,
#244037,#244038,#244039,#244040,#244041,#244042,#244043,#244044,#244045,
#244046,#244047,#244048,#244049,#244050,#244051,#244052,#244053,#244054,
#244055,#244056,#244057,#244058,#244059,#244060,#244061,#244062,#244063,
#244064,#244065,#244066,#244067,#244068,#244069,#244070,#244071,#244072,
#244073,#244074,#244075,#244076,#244077,#244078,#244079,#244080,#244081,
#244082,#244083,#244084,#244085,#244086,#244087,#244088,#244089,#244090,
#244091,#244092,#244093,#244094,#244095,#244096,#244097,#244098,#244099,
#244100,#244101,#244102,#244103,#244104,#244105,#244106,#244107,#244108,
#244109,#244110,#244111,#244112,#244113,#244114,#244115,#244116,#244117,
#244118,#244119,#244120,#244121,#244122,#244123,#244124,#244125,#244126,
#244127,#244128,#244129,#244130,#244131,#244132,#244133,#244134,#244135,
#244136,#244137,#244138,#244139,#244140,#244141,#244142,#244143,#244144,
#244145,#244146,#244147,#244148,#244149,#244150,#244151,#244152,#244153,
#244154,#244155,#244156,#244157,#244158,#244159,#244160,#244161,#244162,
#244163,#244164,#244165,#244166,#244167,#244168,#244169,#244170,#244171,
#244172,#244173,#244174,#244175,#244176,#244177,#244178,#244179,#244180,
#244181,#244182,#244183,#244184,#244185,#244186,#244187,#244188,#244189,
#244190,#244191,#244192,#244193,#244194,#244195,#244196,#244197,#244198),
(#244199,#244200,#244201,#244202,#244203,#244204,#244205,#244206,#244207,
#244208,#244209,#244210,#244211,#244212,#244213,#244214,#244215,#244216,
#244217,#244218,#244219,#244220,#244221,#244222,#244223,#244224,#244225,
#244226,#244227,#244228,#244229,#244230,#244231,#244232,#244233,#244234,
#244235,#244236,#244237,#244238,#244239,#244240,#244241,#244242,#244243,
#244244,#244245,#244246,#244247,#244248,#244249,#244250,#244251,#244252,
#244253,#244254,#244255,#244256,#244257,#244258,#244259,#244260,#244261,
#244262,#244263,#244264,#244265,#244266,#244267,#244268,#244269,#244270,
#244271,#244272,#244273,#244274,#244275,#244276,#244277,#244278,#244279,
#244280,#244281,#244282,#244283,#244284,#244285,#244286,#244287,#244288,
#244289,#244290,#244291,#244292,#244293,#244294,#244295,#244296,#244297,
#244298,#244299,#244300,#244301,#244302,#244303,#244304,#244305,#244306,
#244307,#244308,#244309,#244310,#244311,#244312,#244313,#244314,#244315,
#244316,#244317,#244318,#244319,#244320,#244321,#244322,#244323,#244324,
#244325,#244326,#244327,#244328,#244329,#244330,#244331,#244332,#244333,
#244334,#244335,#244336,#244337,#244338,#244339,#244340,#244341,#244342,
#244343,#244344,#244345,#244346,#244347,#244348,#244349,#244350,#244351,
#244352,#244353,#244354,#244355,#244356,#244357,#244358,#244359,#244360,
#244361,#244362,#244363,#244364,#244365,#244366,#244367,#244368,#244369,
#244370,#244371,#244372,#244373)),.UNSPECIFIED.,.F.,.T.,.F.,(2,2),(4,1,
1,2,1,1,1,1,2,2,1,2,2,2,2,1,1,2,2,2,1,1,1,1,2,2,2,2,2,2,2,2,1,1,1,2,2,2,
2,1,1,1,2,2,2,1,1,1,2,2,2,2,2,2,2,1,2,2,2,2,2,1,1,2,2,2,2,1,2,2,2,1,1,2,
2,2,1,1,1,1,2,2,2,2,2,2,2,1,2,1,1,2,2,2,1,2,2,2,2,2,1,2,2,2,2,4),(0.,4.71475608888856),
(-0.000135430429350568,9.25560474171526E-5,0.000320542524184873,0.000548529000952593,
0.000776515477720314,0.00100450195448803,0.00111849519287189,0.00123248843125575,
0.00134648166963961,0.00146047490802347,0.0016884613847912,0.00191644786155891,
0.00203044109994277,0.00214443433832664,0.00225842757671049,0.00237242081509435,
0.00260040729186208,0.00271440053024594,0.0028283937686298,0.00294238700701366,
0.00305638024539752,0.00317037348378138,0.00328436672216524,0.0033983599605491,
0.00351235319893296,0.00362634643731682,0.00374033967570068,0.0039683261524684,
0.00419631262923612,0.00431030586761998,0.00436730248681191,0.00442429910600384,
0.0045382923443877,0.00465228558277156,0.00488027205953928,0.00499426529792314,
0.005108258536307,0.00522225177469086,0.00533624501307472,0.00556423148984244,
0.0056782247282263,0.00579221796661016,0.00590621120499402,0.00602020444337788,
0.00613419768176174,0.0062481909201456,0.00647617739691333,0.00659017063529719,
0.00670416387368105,0.00681815711206491,0.00693215035044876,0.00716013682721649,
0.00727413006560035,0.00738812330398421,0.00761610978075193,0.00784409625751965,
0.00795808949590351,0.00807208273428737,0.0081290793534793,0.00818607597267123,
0.00830006921105509,0.00852805568782281,0.00864204892620667,0.00875604216459053,
0.00887003540297439,0.00898402864135825,0.00921201511812597,0.00944000159489369,
0.00955399483327755,0.00966798807166141,0.00978198131004527,0.00989597454842913,
0.0101239610251968,0.0102379542635807,0.0103519475019646,0.0104659407403484,
0.0105799339787323,0.0106939272171161,0.0108079204555,0.0109219136938839,
0.0110359069322677,0.0111499001706516,0.0112638934090355,0.0114918798858032,
0.0117198663625709,0.0118338596009548,0.0118908562201467,0.0119478528393386,
0.0120618460777225,0.0121758393161063,0.0124038257928741,0.0125178190312579,
0.0126318122696418,0.0127458055080256,0.0129737919847934,0.0130877852231772,
0.0133157716999449,0.0134297649383288,0.0134867615575207,0.0135437581767127,
0.0137717446534804,0.0139997311302481,0.0142277176070158,0.0142847142262077,
0.0143417108453997,0.0144557040837835),.UNSPECIFIED.);
#954=B_SPLINE_SURFACE_WITH_KNOTS('',1,3,((#245024,#245025,#245026,#245027,
#245028,#245029,#245030,#245031,#245032,#245033,#245034,#245035,#245036,
#245037,#245038,#245039,#245040,#245041,#245042,#245043,#245044,#245045,
#245046,#245047,#245048,#245049,#245050,#245051,#245052,#245053,#245054,
#245055,#245056,#245057,#245058,#245059,#245060,#245061,#245062,#245063,
#245064,#245065,#245066,#245067,#245068,#245069,#245070,#245071,#245072,
#245073,#245074,#245075,#245076,#245077,#245078,#245079,#245080,#245081,
#245082,#245083,#245084,#245085,#245086,#245087,#245088,#245089,#245090,
#245091,#245092,#245093,#245094,#245095,#245096,#245097,#245098,#245099,
#245100,#245101,#245102,#245103,#245104,#245105,#245106,#245107,#245108,
#245109,#245110,#245111,#245112,#245113,#245114,#245115,#245116,#245117,
#245118,#245119,#245120,#245121,#245122,#245123,#245124,#245125,#245126,
#245127,#245128,#245129,#245130,#245131,#245132,#245133,#245134,#245135,
#245136,#245137,#245138,#245139,#245140,#245141,#245142,#245143,#245144,
#245145,#245146,#245147,#245148,#245149,#245150,#245151,#245152,#245153,
#245154,#245155,#245156,#245157,#245158,#245159,#245160,#245161,#245162,
#245163,#245164,#245165,#245166,#245167,#245168,#245169,#245170,#245171,
#245172,#245173,#245174,#245175,#245176,#245177,#245178,#245179,#245180,
#245181,#245182,#245183,#245184,#245185,#245186,#245187,#245188,#245189,
#245190,#245191,#245192,#245193,#245194,#245195,#245196,#245197,#245198),
(#245199,#245200,#245201,#245202,#245203,#245204,#245205,#245206,#245207,
#245208,#245209,#245210,#245211,#245212,#245213,#245214,#245215,#245216,
#245217,#245218,#245219,#245220,#245221,#245222,#245223,#245224,#245225,
#245226,#245227,#245228,#245229,#245230,#245231,#245232,#245233,#245234,
#245235,#245236,#245237,#245238,#245239,#245240,#245241,#245242,#245243,
#245244,#245245,#245246,#245247,#245248,#245249,#245250,#245251,#245252,
#245253,#245254,#245255,#245256,#245257,#245258,#245259,#245260,#245261,
#245262,#245263,#245264,#245265,#245266,#245267,#245268,#245269,#245270,
#245271,#245272,#245273,#245274,#245275,#245276,#245277,#245278,#245279,
#245280,#245281,#245282,#245283,#245284,#245285,#245286,#245287,#245288,
#245289,#245290,#245291,#245292,#245293,#245294,#245295,#245296,#245297,
#245298,#245299,#245300,#245301,#245302,#245303,#245304,#245305,#245306,
#245307,#245308,#245309,#245310,#245311,#245312,#245313,#245314,#245315,
#245316,#245317,#245318,#245319,#245320,#245321,#245322,#245323,#245324,
#245325,#245326,#245327,#245328,#245329,#245330,#245331,#245332,#245333,
#245334,#245335,#245336,#245337,#245338,#245339,#245340,#245341,#245342,
#245343,#245344,#245345,#245346,#245347,#245348,#245349,#245350,#245351,
#245352,#245353,#245354,#245355,#245356,#245357,#245358,#245359,#245360,
#245361,#245362,#245363,#245364,#245365,#245366,#245367,#245368,#245369,
#245370,#245371,#245372,#245373)),.UNSPECIFIED.,.F.,.T.,.F.,(2,2),(4,1,
1,2,1,1,1,1,2,2,1,2,2,2,2,1,1,2,2,2,1,1,1,1,2,2,2,2,2,2,2,2,1,1,1,2,2,2,
2,1,1,1,2,2,2,1,1,1,2,2,2,2,2,2,2,1,2,2,2,2,2,1,1,2,2,2,2,1,2,2,2,1,1,2,
2,2,1,1,1,1,2,2,2,2,2,2,2,1,2,1,1,2,2,2,1,2,2,2,2,2,1,2,2,2,2,4),(0.,5.46382276754873),
(-0.000135430429350568,9.25560474171526E-5,0.000320542524184873,0.000548529000952593,
0.000776515477720314,0.00100450195448803,0.00111849519287189,0.00123248843125575,
0.00134648166963961,0.00146047490802347,0.0016884613847912,0.00191644786155891,
0.00203044109994277,0.00214443433832664,0.00225842757671049,0.00237242081509435,
0.00260040729186208,0.00271440053024594,0.0028283937686298,0.00294238700701366,
0.00305638024539752,0.00317037348378138,0.00328436672216524,0.0033983599605491,
0.00351235319893296,0.00362634643731682,0.00374033967570068,0.0039683261524684,
0.00419631262923612,0.00431030586761998,0.00436730248681191,0.00442429910600384,
0.0045382923443877,0.00465228558277156,0.00488027205953928,0.00499426529792314,
0.005108258536307,0.00522225177469086,0.00533624501307472,0.00556423148984244,
0.0056782247282263,0.00579221796661016,0.00590621120499402,0.00602020444337788,
0.00613419768176174,0.0062481909201456,0.00647617739691333,0.00659017063529719,
0.00670416387368105,0.00681815711206491,0.00693215035044876,0.00716013682721649,
0.00727413006560035,0.00738812330398421,0.00761610978075193,0.00784409625751965,
0.00795808949590351,0.00807208273428737,0.0081290793534793,0.00818607597267123,
0.00830006921105509,0.00852805568782281,0.00864204892620667,0.00875604216459053,
0.00887003540297439,0.00898402864135825,0.00921201511812597,0.00944000159489369,
0.00955399483327755,0.00966798807166141,0.00978198131004527,0.00989597454842913,
0.0101239610251968,0.0102379542635807,0.0103519475019646,0.0104659407403484,
0.0105799339787323,0.0106939272171161,0.0108079204555,0.0109219136938839,
0.0110359069322677,0.0111499001706516,0.0112638934090355,0.0114918798858032,
0.0117198663625709,0.0118338596009548,0.0118908562201467,0.0119478528393386,
0.0120618460777225,0.0121758393161063,0.0124038257928741,0.0125178190312579,
0.0126318122696418,0.0127458055080256,0.0129737919847934,0.0130877852231772,
0.0133157716999449,0.0134297649383288,0.0134867615575207,0.0135437581767127,
0.0137717446534804,0.0139997311302481,0.0142277176070158,0.0142847142262077,
0.0143417108453997,0.0144557040837835),.UNSPECIFIED.);
#955=B_SPLINE_SURFACE_WITH_KNOTS('',1,3,((#249188,#249189,#249190,#249191,
#249192,#249193,#249194,#249195,#249196,#249197,#249198,#249199,#249200,
#249201,#249202,#249203,#249204,#249205,#249206,#249207,#249208,#249209,
#249210,#249211,#249212,#249213,#249214,#249215,#249216,#249217,#249218,
#249219,#249220,#249221,#249222,#249223,#249224,#249225,#249226,#249227,
#249228,#249229,#249230,#249231,#249232,#249233,#249234,#249235,#249236,
#249237,#249238,#249239,#249240,#249241,#249242,#249243,#249244,#249245,
#249246,#249247,#249248,#249249,#249250,#249251,#249252,#249253,#249254,
#249255,#249256,#249257,#249258,#249259,#249260,#249261,#249262,#249263,
#249264,#249265,#249266,#249267,#249268,#249269,#249270,#249271,#249272,
#249273,#249274,#249275,#249276,#249277,#249278,#249279,#249280,#249281,
#249282,#249283,#249284,#249285,#249286,#249287,#249288,#249289,#249290,
#249291,#249292,#249293,#249294,#249295,#249296,#249297,#249298,#249299,
#249300,#249301,#249302,#249303,#249304,#249305,#249306,#249307,#249308,
#249309,#249310,#249311,#249312,#249313,#249314,#249315,#249316,#249317,
#249318,#249319,#249320,#249321,#249322,#249323,#249324,#249325,#249326,
#249327,#249328,#249329,#249330,#249331,#249332,#249333,#249334,#249335,
#249336,#249337,#249338,#249339,#249340,#249341,#249342,#249343,#249344,
#249345,#249346,#249347,#249348,#249349,#249350,#249351,#249352,#249353,
#249354,#249355,#249356,#249357,#249358,#249359,#249360,#249361,#249362,
#249363,#249364,#249365,#249366),(#249367,#249368,#249369,#249370,#249371,
#249372,#249373,#249374,#249375,#249376,#249377,#249378,#249379,#249380,
#249381,#249382,#249383,#249384,#249385,#249386,#249387,#249388,#249389,
#249390,#249391,#249392,#249393,#249394,#249395,#249396,#249397,#249398,
#249399,#249400,#249401,#249402,#249403,#249404,#249405,#249406,#249407,
#249408,#249409,#249410,#249411,#249412,#249413,#249414,#249415,#249416,
#249417,#249418,#249419,#249420,#249421,#249422,#249423,#249424,#249425,
#249426,#249427,#249428,#249429,#249430,#249431,#249432,#249433,#249434,
#249435,#249436,#249437,#249438,#249439,#249440,#249441,#249442,#249443,
#249444,#249445,#249446,#249447,#249448,#249449,#249450,#249451,#249452,
#249453,#249454,#249455,#249456,#249457,#249458,#249459,#249460,#249461,
#249462,#249463,#249464,#249465,#249466,#249467,#249468,#249469,#249470,
#249471,#249472,#249473,#249474,#249475,#249476,#249477,#249478,#249479,
#249480,#249481,#249482,#249483,#249484,#249485,#249486,#249487,#249488,
#249489,#249490,#249491,#249492,#249493,#249494,#249495,#249496,#249497,
#249498,#249499,#249500,#249501,#249502,#249503,#249504,#249505,#249506,
#249507,#249508,#249509,#249510,#249511,#249512,#249513,#249514,#249515,
#249516,#249517,#249518,#249519,#249520,#249521,#249522,#249523,#249524,
#249525,#249526,#249527,#249528,#249529,#249530,#249531,#249532,#249533,
#249534,#249535,#249536,#249537,#249538,#249539,#249540,#249541,#249542,
#249543,#249544,#249545)),.UNSPECIFIED.,.F.,.T.,.F.,(2,2),(4,1,1,2,2,2,
2,1,1,1,2,2,2,1,1,2,2,2,2,2,2,2,2,2,1,1,1,2,2,2,1,2,2,2,1,2,2,2,1,1,1,1,
2,2,2,1,1,1,1,2,2,2,2,2,2,2,1,1,2,2,2,2,1,2,2,2,1,1,2,2,2,2,2,2,2,2,2,2,
1,1,1,2,2,2,1,1,2,2,2,1,2,2,2,2,2,1,2,2,2,2,2,1,1,1,2,2,4),(0.,5.45368304321453),
(-0.000118831294053002,0.000109147352845132,0.000337125999743267,0.000451115323192334,
0.000565104646641402,0.000679093970090469,0.000793083293539536,0.00102106194043767,
0.00113505126388674,0.0012490405873358,0.00136302991078487,0.00142002457250941,
0.00147701923423394,0.00170499788113207,0.00193297652803021,0.00204696585147928,
0.00216095517492835,0.00227494449837741,0.00238893382182648,0.00261691246872462,
0.00284489111562275,0.00290188577734728,0.00295888043907182,0.00307286976252088,
0.00330084840941902,0.00341483773286809,0.00352882705631715,0.00364281637976622,
0.00375680570321528,0.00387079502666435,0.00398478435011342,0.00421276299701156,
0.00444074164390969,0.00466872029080782,0.00489669893770596,0.00512467758460409,
0.00518167224632863,0.00523866690805316,0.00535265623150223,0.0054666455549513,
0.00558063487840036,0.00569462420184943,0.0058086135252985,0.00592260284874756,
0.00603659217219663,0.0061505814956457,0.00626457081909477,0.0064925494659929,
0.00660653878944197,0.00672052811289104,0.0068345174363401,0.00694850675978917,
0.00717648540668731,0.00729047473013637,0.00740446405358544,0.00763244270048357,
0.00786042134738171,0.00797441067083078,0.00808839999427985,0.00820238931772891,
0.00831637864117798,0.00854435728807612,0.00877233593497425,0.00888632525842331,
0.00900031458187238,0.00911430390532145,0.00922829322877052,0.00945627187566865,
0.00957026119911772,0.00968425052256679,0.00974124518429132,0.00979823984601585,
0.00991222916946492,0.0101402078163631,0.0103681864632612,0.0104251811249857,
0.0104821757867103,0.0105961651101593,0.0108241437570575,0.0109381330805065,
0.0110521224039556,0.0111661117274047,0.0112801010508537,0.0113940903743028,
0.0115080796977519,0.01173605834465,0.0118500476680991,0.0119640369915481,
0.0120780263149972,0.0121920156384463,0.0124199942853444,0.0126479729322425,
0.0127049675939671,0.0127619622556916,0.0128759515791407,0.0131039302260388,
0.0133319088729369,0.013445898196386,0.0135028928581105,0.0135598875198351,
0.0136738768432841,0.0137878661667332,0.0140158448136313,0.0141298341370804,
0.0142438234605295,0.0143578127839785,0.0144718021074276),.UNSPECIFIED.);
#956=B_SPLINE_SURFACE_WITH_KNOTS('',1,3,((#250322,#250323,#250324,#250325,
#250326,#250327,#250328,#250329,#250330,#250331,#250332,#250333,#250334,
#250335,#250336,#250337,#250338,#250339,#250340,#250341,#250342,#250343,
#250344,#250345,#250346,#250347,#250348,#250349,#250350,#250351,#250352,
#250353,#250354,#250355,#250356,#250357,#250358,#250359,#250360,#250361,
#250362,#250363,#250364,#250365,#250366,#250367,#250368,#250369,#250370,
#250371,#250372,#250373,#250374,#250375,#250376,#250377,#250378,#250379,
#250380,#250381,#250382,#250383,#250384,#250385,#250386,#250387,#250388,
#250389,#250390,#250391,#250392,#250393,#250394,#250395,#250396,#250397,
#250398,#250399,#250400,#250401,#250402,#250403,#250404,#250405,#250406,
#250407,#250408,#250409,#250410,#250411,#250412,#250413,#250414,#250415,
#250416,#250417,#250418,#250419,#250420,#250421,#250422,#250423,#250424,
#250425,#250426,#250427,#250428,#250429,#250430,#250431,#250432,#250433,
#250434,#250435,#250436,#250437,#250438,#250439,#250440,#250441,#250442,
#250443,#250444,#250445,#250446,#250447,#250448,#250449,#250450,#250451,
#250452,#250453,#250454,#250455,#250456,#250457,#250458,#250459,#250460,
#250461,#250462,#250463,#250464,#250465,#250466,#250467,#250468,#250469,
#250470,#250471,#250472,#250473,#250474,#250475,#250476,#250477,#250478,
#250479,#250480,#250481,#250482,#250483,#250484,#250485,#250486,#250487,
#250488,#250489,#250490,#250491,#250492,#250493,#250494,#250495,#250496,
#250497,#250498,#250499,#250500),(#250501,#250502,#250503,#250504,#250505,
#250506,#250507,#250508,#250509,#250510,#250511,#250512,#250513,#250514,
#250515,#250516,#250517,#250518,#250519,#250520,#250521,#250522,#250523,
#250524,#250525,#250526,#250527,#250528,#250529,#250530,#250531,#250532,
#250533,#250534,#250535,#250536,#250537,#250538,#250539,#250540,#250541,
#250542,#250543,#250544,#250545,#250546,#250547,#250548,#250549,#250550,
#250551,#250552,#250553,#250554,#250555,#250556,#250557,#250558,#250559,
#250560,#250561,#250562,#250563,#250564,#250565,#250566,#250567,#250568,
#250569,#250570,#250571,#250572,#250573,#250574,#250575,#250576,#250577,
#250578,#250579,#250580,#250581,#250582,#250583,#250584,#250585,#250586,
#250587,#250588,#250589,#250590,#250591,#250592,#250593,#250594,#250595,
#250596,#250597,#250598,#250599,#250600,#250601,#250602,#250603,#250604,
#250605,#250606,#250607,#250608,#250609,#250610,#250611,#250612,#250613,
#250614,#250615,#250616,#250617,#250618,#250619,#250620,#250621,#250622,
#250623,#250624,#250625,#250626,#250627,#250628,#250629,#250630,#250631,
#250632,#250633,#250634,#250635,#250636,#250637,#250638,#250639,#250640,
#250641,#250642,#250643,#250644,#250645,#250646,#250647,#250648,#250649,
#250650,#250651,#250652,#250653,#250654,#250655,#250656,#250657,#250658,
#250659,#250660,#250661,#250662,#250663,#250664,#250665,#250666,#250667,
#250668,#250669,#250670,#250671,#250672,#250673,#250674,#250675,#250676,
#250677,#250678,#250679)),.UNSPECIFIED.,.F.,.T.,.F.,(2,2),(4,1,1,2,2,2,
2,1,1,1,2,2,2,1,1,2,2,2,2,2,2,2,2,2,1,1,1,2,2,2,1,2,2,2,1,2,2,2,1,1,1,1,
2,2,2,1,1,1,1,2,2,2,2,2,2,2,1,1,2,2,2,2,1,2,2,2,1,1,2,2,2,2,2,2,2,2,2,2,
1,1,1,2,2,2,1,1,2,2,2,1,2,2,2,2,2,1,2,2,2,2,2,1,1,1,2,2,4),(0.,5.45368304321453),
(-0.000118831294053002,0.000109147352845132,0.000337125999743267,0.000451115323192334,
0.000565104646641402,0.000679093970090469,0.000793083293539536,0.00102106194043767,
0.00113505126388674,0.0012490405873358,0.00136302991078487,0.00142002457250941,
0.00147701923423394,0.00170499788113207,0.00193297652803021,0.00204696585147928,
0.00216095517492835,0.00227494449837741,0.00238893382182648,0.00261691246872462,
0.00284489111562275,0.00290188577734728,0.00295888043907182,0.00307286976252088,
0.00330084840941902,0.00341483773286809,0.00352882705631715,0.00364281637976622,
0.00375680570321528,0.00387079502666435,0.00398478435011342,0.00421276299701156,
0.00444074164390969,0.00466872029080782,0.00489669893770596,0.00512467758460409,
0.00518167224632863,0.00523866690805316,0.00535265623150223,0.0054666455549513,
0.00558063487840036,0.00569462420184943,0.0058086135252985,0.00592260284874756,
0.00603659217219663,0.0061505814956457,0.00626457081909477,0.0064925494659929,
0.00660653878944197,0.00672052811289104,0.0068345174363401,0.00694850675978917,
0.00717648540668731,0.00729047473013637,0.00740446405358544,0.00763244270048357,
0.00786042134738171,0.00797441067083078,0.00808839999427985,0.00820238931772891,
0.00831637864117798,0.00854435728807612,0.00877233593497425,0.00888632525842331,
0.00900031458187238,0.00911430390532145,0.00922829322877052,0.00945627187566865,
0.00957026119911772,0.00968425052256679,0.00974124518429132,0.00979823984601585,
0.00991222916946492,0.0101402078163631,0.0103681864632612,0.0104251811249857,
0.0104821757867103,0.0105961651101593,0.0108241437570575,0.0109381330805065,
0.0110521224039556,0.0111661117274047,0.0112801010508537,0.0113940903743028,
0.0115080796977519,0.01173605834465,0.0118500476680991,0.0119640369915481,
0.0120780263149972,0.0121920156384463,0.0124199942853444,0.0126479729322425,
0.0127049675939671,0.0127619622556916,0.0128759515791407,0.0131039302260388,
0.0133319088729369,0.013445898196386,0.0135028928581105,0.0135598875198351,
0.0136738768432841,0.0137878661667332,0.0140158448136313,0.0141298341370804,
0.0142438234605295,0.0143578127839785,0.0144718021074276),.UNSPECIFIED.);
#957=B_SPLINE_SURFACE_WITH_KNOTS('',1,3,((#250704,#250705,#250706,#250707,
#250708,#250709,#250710,#250711,#250712,#250713,#250714,#250715,#250716,
#250717,#250718,#250719,#250720,#250721,#250722,#250723,#250724,#250725,
#250726,#250727,#250728,#250729,#250730,#250731,#250732,#250733,#250734,
#250735,#250736,#250737,#250738,#250739,#250740,#250741,#250742,#250743,
#250744,#250745,#250746,#250747,#250748,#250749,#250750,#250751,#250752,
#250753,#250754,#250755,#250756,#250757,#250758,#250759,#250760,#250761,
#250762,#250763,#250764,#250765,#250766,#250767,#250768,#250769,#250770,
#250771,#250772,#250773,#250774,#250775,#250776,#250777,#250778,#250779,
#250780,#250781,#250782,#250783,#250784,#250785,#250786,#250787,#250788,
#250789,#250790,#250791,#250792,#250793,#250794,#250795,#250796,#250797,
#250798,#250799,#250800,#250801,#250802,#250803,#250804,#250805,#250806,
#250807,#250808,#250809,#250810,#250811,#250812,#250813,#250814,#250815,
#250816,#250817,#250818,#250819,#250820,#250821,#250822,#250823,#250824,
#250825,#250826,#250827,#250828,#250829,#250830,#250831,#250832,#250833,
#250834,#250835,#250836,#250837,#250838,#250839,#250840,#250841,#250842,
#250843,#250844,#250845,#250846,#250847,#250848,#250849,#250850,#250851,
#250852,#250853,#250854,#250855,#250856,#250857,#250858,#250859,#250860,
#250861,#250862,#250863,#250864,#250865,#250866,#250867,#250868,#250869,
#250870,#250871,#250872,#250873,#250874,#250875,#250876,#250877,#250878,
#250879,#250880,#250881,#250882),(#250883,#250884,#250885,#250886,#250887,
#250888,#250889,#250890,#250891,#250892,#250893,#250894,#250895,#250896,
#250897,#250898,#250899,#250900,#250901,#250902,#250903,#250904,#250905,
#250906,#250907,#250908,#250909,#250910,#250911,#250912,#250913,#250914,
#250915,#250916,#250917,#250918,#250919,#250920,#250921,#250922,#250923,
#250924,#250925,#250926,#250927,#250928,#250929,#250930,#250931,#250932,
#250933,#250934,#250935,#250936,#250937,#250938,#250939,#250940,#250941,
#250942,#250943,#250944,#250945,#250946,#250947,#250948,#250949,#250950,
#250951,#250952,#250953,#250954,#250955,#250956,#250957,#250958,#250959,
#250960,#250961,#250962,#250963,#250964,#250965,#250966,#250967,#250968,
#250969,#250970,#250971,#250972,#250973,#250974,#250975,#250976,#250977,
#250978,#250979,#250980,#250981,#250982,#250983,#250984,#250985,#250986,
#250987,#250988,#250989,#250990,#250991,#250992,#250993,#250994,#250995,
#250996,#250997,#250998,#250999,#251000,#251001,#251002,#251003,#251004,
#251005,#251006,#251007,#251008,#251009,#251010,#251011,#251012,#251013,
#251014,#251015,#251016,#251017,#251018,#251019,#251020,#251021,#251022,
#251023,#251024,#251025,#251026,#251027,#251028,#251029,#251030,#251031,
#251032,#251033,#251034,#251035,#251036,#251037,#251038,#251039,#251040,
#251041,#251042,#251043,#251044,#251045,#251046,#251047,#251048,#251049,
#251050,#251051,#251052,#251053,#251054,#251055,#251056,#251057,#251058,
#251059,#251060,#251061)),.UNSPECIFIED.,.F.,.T.,.F.,(2,2),(4,1,1,2,2,2,
2,1,1,1,2,2,2,1,1,2,2,2,2,2,2,2,2,2,1,1,1,2,2,2,1,2,2,2,1,2,2,2,1,1,1,1,
2,2,2,1,1,1,1,2,2,2,2,2,2,2,1,1,2,2,2,2,1,2,2,2,1,1,2,2,2,2,2,2,2,2,2,2,
1,1,1,2,2,2,1,1,2,2,2,1,2,2,2,2,2,1,2,2,2,2,2,1,1,1,2,2,4),(0.,5.45368304321453),
(-0.000118831294053002,0.000109147352845132,0.000337125999743267,0.000451115323192334,
0.000565104646641402,0.000679093970090469,0.000793083293539536,0.00102106194043767,
0.00113505126388674,0.0012490405873358,0.00136302991078487,0.00142002457250941,
0.00147701923423394,0.00170499788113207,0.00193297652803021,0.00204696585147928,
0.00216095517492835,0.00227494449837741,0.00238893382182648,0.00261691246872462,
0.00284489111562275,0.00290188577734728,0.00295888043907182,0.00307286976252088,
0.00330084840941902,0.00341483773286809,0.00352882705631715,0.00364281637976622,
0.00375680570321528,0.00387079502666435,0.00398478435011342,0.00421276299701156,
0.00444074164390969,0.00466872029080782,0.00489669893770596,0.00512467758460409,
0.00518167224632863,0.00523866690805316,0.00535265623150223,0.0054666455549513,
0.00558063487840036,0.00569462420184943,0.0058086135252985,0.00592260284874756,
0.00603659217219663,0.0061505814956457,0.00626457081909477,0.0064925494659929,
0.00660653878944197,0.00672052811289104,0.0068345174363401,0.00694850675978917,
0.00717648540668731,0.00729047473013637,0.00740446405358544,0.00763244270048357,
0.00786042134738171,0.00797441067083078,0.00808839999427985,0.00820238931772891,
0.00831637864117798,0.00854435728807612,0.00877233593497425,0.00888632525842331,
0.00900031458187238,0.00911430390532145,0.00922829322877052,0.00945627187566865,
0.00957026119911772,0.00968425052256679,0.00974124518429132,0.00979823984601585,
0.00991222916946492,0.0101402078163631,0.0103681864632612,0.0104251811249857,
0.0104821757867103,0.0105961651101593,0.0108241437570575,0.0109381330805065,
0.0110521224039556,0.0111661117274047,0.0112801010508537,0.0113940903743028,
0.0115080796977519,0.01173605834465,0.0118500476680991,0.0119640369915481,
0.0120780263149972,0.0121920156384463,0.0124199942853444,0.0126479729322425,
0.0127049675939671,0.0127619622556916,0.0128759515791407,0.0131039302260388,
0.0133319088729369,0.013445898196386,0.0135028928581105,0.0135598875198351,
0.0136738768432841,0.0137878661667332,0.0140158448136313,0.0141298341370804,
0.0142438234605295,0.0143578127839785,0.0144718021074276),.UNSPECIFIED.);
#958=B_SPLINE_SURFACE_WITH_KNOTS('',1,3,((#251106,#251107,#251108,#251109,
#251110,#251111,#251112,#251113,#251114,#251115,#251116,#251117,#251118,
#251119,#251120,#251121,#251122,#251123,#251124,#251125,#251126,#251127,
#251128,#251129,#251130,#251131,#251132,#251133,#251134,#251135,#251136,
#251137,#251138,#251139,#251140,#251141,#251142,#251143,#251144,#251145,
#251146,#251147,#251148,#251149,#251150,#251151,#251152,#251153,#251154,
#251155,#251156,#251157,#251158,#251159,#251160,#251161,#251162,#251163,
#251164,#251165,#251166,#251167,#251168,#251169,#251170,#251171,#251172,
#251173,#251174,#251175,#251176,#251177,#251178,#251179,#251180,#251181,
#251182,#251183,#251184,#251185,#251186,#251187,#251188,#251189,#251190,
#251191,#251192,#251193,#251194,#251195,#251196,#251197,#251198,#251199,
#251200,#251201,#251202,#251203,#251204,#251205,#251206,#251207,#251208,
#251209,#251210,#251211,#251212,#251213,#251214,#251215,#251216,#251217,
#251218,#251219,#251220,#251221,#251222,#251223,#251224,#251225,#251226,
#251227,#251228,#251229,#251230,#251231,#251232,#251233,#251234,#251235,
#251236,#251237,#251238,#251239,#251240,#251241,#251242,#251243,#251244,
#251245,#251246,#251247,#251248,#251249,#251250,#251251,#251252,#251253,
#251254,#251255,#251256,#251257,#251258,#251259,#251260,#251261,#251262,
#251263,#251264,#251265,#251266,#251267,#251268,#251269,#251270,#251271,
#251272,#251273,#251274,#251275,#251276,#251277,#251278,#251279,#251280,
#251281,#251282,#251283,#251284),(#251285,#251286,#251287,#251288,#251289,
#251290,#251291,#251292,#251293,#251294,#251295,#251296,#251297,#251298,
#251299,#251300,#251301,#251302,#251303,#251304,#251305,#251306,#251307,
#251308,#251309,#251310,#251311,#251312,#251313,#251314,#251315,#251316,
#251317,#251318,#251319,#251320,#251321,#251322,#251323,#251324,#251325,
#251326,#251327,#251328,#251329,#251330,#251331,#251332,#251333,#251334,
#251335,#251336,#251337,#251338,#251339,#251340,#251341,#251342,#251343,
#251344,#251345,#251346,#251347,#251348,#251349,#251350,#251351,#251352,
#251353,#251354,#251355,#251356,#251357,#251358,#251359,#251360,#251361,
#251362,#251363,#251364,#251365,#251366,#251367,#251368,#251369,#251370,
#251371,#251372,#251373,#251374,#251375,#251376,#251377,#251378,#251379,
#251380,#251381,#251382,#251383,#251384,#251385,#251386,#251387,#251388,
#251389,#251390,#251391,#251392,#251393,#251394,#251395,#251396,#251397,
#251398,#251399,#251400,#251401,#251402,#251403,#251404,#251405,#251406,
#251407,#251408,#251409,#251410,#251411,#251412,#251413,#251414,#251415,
#251416,#251417,#251418,#251419,#251420,#251421,#251422,#251423,#251424,
#251425,#251426,#251427,#251428,#251429,#251430,#251431,#251432,#251433,
#251434,#251435,#251436,#251437,#251438,#251439,#251440,#251441,#251442,
#251443,#251444,#251445,#251446,#251447,#251448,#251449,#251450,#251451,
#251452,#251453,#251454,#251455,#251456,#251457,#251458,#251459,#251460,
#251461,#251462,#251463)),.UNSPECIFIED.,.F.,.T.,.F.,(2,2),(4,1,1,2,2,2,
2,1,1,1,2,2,2,1,1,2,2,2,2,2,2,2,2,2,1,1,1,2,2,2,1,2,2,2,1,2,2,2,1,1,1,1,
2,2,2,1,1,1,1,2,2,2,2,2,2,2,1,1,2,2,2,2,1,2,2,2,1,1,2,2,2,2,2,2,2,2,2,2,
1,1,1,2,2,2,1,1,2,2,2,1,2,2,2,2,2,1,2,2,2,2,2,1,1,1,2,2,4),(0.,5.45368304321453),
(-0.000118831294053002,0.000109147352845132,0.000337125999743267,0.000451115323192334,
0.000565104646641402,0.000679093970090469,0.000793083293539536,0.00102106194043767,
0.00113505126388674,0.0012490405873358,0.00136302991078487,0.00142002457250941,
0.00147701923423394,0.00170499788113207,0.00193297652803021,0.00204696585147928,
0.00216095517492835,0.00227494449837741,0.00238893382182648,0.00261691246872462,
0.00284489111562275,0.00290188577734728,0.00295888043907182,0.00307286976252088,
0.00330084840941902,0.00341483773286809,0.00352882705631715,0.00364281637976622,
0.00375680570321528,0.00387079502666435,0.00398478435011342,0.00421276299701156,
0.00444074164390969,0.00466872029080782,0.00489669893770596,0.00512467758460409,
0.00518167224632863,0.00523866690805316,0.00535265623150223,0.0054666455549513,
0.00558063487840036,0.00569462420184943,0.0058086135252985,0.00592260284874756,
0.00603659217219663,0.0061505814956457,0.00626457081909477,0.0064925494659929,
0.00660653878944197,0.00672052811289104,0.0068345174363401,0.00694850675978917,
0.00717648540668731,0.00729047473013637,0.00740446405358544,0.00763244270048357,
0.00786042134738171,0.00797441067083078,0.00808839999427985,0.00820238931772891,
0.00831637864117798,0.00854435728807612,0.00877233593497425,0.00888632525842331,
0.00900031458187238,0.00911430390532145,0.00922829322877052,0.00945627187566865,
0.00957026119911772,0.00968425052256679,0.00974124518429132,0.00979823984601585,
0.00991222916946492,0.0101402078163631,0.0103681864632612,0.0104251811249857,
0.0104821757867103,0.0105961651101593,0.0108241437570575,0.0109381330805065,
0.0110521224039556,0.0111661117274047,0.0112801010508537,0.0113940903743028,
0.0115080796977519,0.01173605834465,0.0118500476680991,0.0119640369915481,
0.0120780263149972,0.0121920156384463,0.0124199942853444,0.0126479729322425,
0.0127049675939671,0.0127619622556916,0.0128759515791407,0.0131039302260388,
0.0133319088729369,0.013445898196386,0.0135028928581105,0.0135598875198351,
0.0136738768432841,0.0137878661667332,0.0140158448136313,0.0141298341370804,
0.0142438234605295,0.0143578127839785,0.0144718021074276),.UNSPECIFIED.);
#959=B_SPLINE_SURFACE_WITH_KNOTS('',1,3,((#251561,#251562,#251563,#251564,
#251565,#251566,#251567,#251568,#251569,#251570,#251571,#251572,#251573,
#251574,#251575,#251576,#251577,#251578,#251579,#251580,#251581,#251582,
#251583,#251584,#251585,#251586,#251587,#251588,#251589,#251590,#251591,
#251592,#251593,#251594,#251595,#251596,#251597,#251598,#251599,#251600,
#251601,#251602,#251603,#251604,#251605,#251606,#251607,#251608,#251609,
#251610,#251611,#251612,#251613,#251614,#251615,#251616,#251617,#251618,
#251619,#251620,#251621,#251622,#251623,#251624,#251625,#251626,#251627,
#251628,#251629,#251630,#251631,#251632,#251633,#251634,#251635,#251636,
#251637,#251638,#251639,#251640,#251641,#251642,#251643,#251644,#251645,
#251646,#251647,#251648,#251649,#251650,#251651,#251652,#251653,#251654,
#251655,#251656,#251657,#251658,#251659,#251660,#251661,#251662,#251663,
#251664,#251665,#251666,#251667,#251668,#251669,#251670,#251671,#251672,
#251673,#251674,#251675,#251676,#251677,#251678,#251679,#251680,#251681,
#251682,#251683,#251684,#251685,#251686,#251687,#251688,#251689,#251690,
#251691,#251692,#251693,#251694,#251695,#251696,#251697,#251698,#251699,
#251700,#251701,#251702,#251703,#251704,#251705,#251706,#251707,#251708,
#251709,#251710,#251711,#251712,#251713,#251714,#251715,#251716,#251717,
#251718,#251719,#251720,#251721,#251722,#251723,#251724,#251725,#251726,
#251727,#251728,#251729,#251730,#251731,#251732,#251733,#251734,#251735,
#251736,#251737,#251738,#251739,#251740,#251741,#251742,#251743,#251744,
#251745,#251746,#251747,#251748,#251749,#251750,#251751,#251752,#251753,
#251754,#251755,#251756,#251757,#251758,#251759,#251760,#251761,#251762,
#251763,#251764,#251765,#251766,#251767,#251768,#251769,#251770,#251771,
#251772,#251773,#251774,#251775,#251776,#251777,#251778,#251779,#251780,
#251781,#251782,#251783,#251784,#251785,#251786),(#251787,#251788,#251789,
#251790,#251791,#251792,#251793,#251794,#251795,#251796,#251797,#251798,
#251799,#251800,#251801,#251802,#251803,#251804,#251805,#251806,#251807,
#251808,#251809,#251810,#251811,#251812,#251813,#251814,#251815,#251816,
#251817,#251818,#251819,#251820,#251821,#251822,#251823,#251824,#251825,
#251826,#251827,#251828,#251829,#251830,#251831,#251832,#251833,#251834,
#251835,#251836,#251837,#251838,#251839,#251840,#251841,#251842,#251843,
#251844,#251845,#251846,#251847,#251848,#251849,#251850,#251851,#251852,
#251853,#251854,#251855,#251856,#251857,#251858,#251859,#251860,#251861,
#251862,#251863,#251864,#251865,#251866,#251867,#251868,#251869,#251870,
#251871,#251872,#251873,#251874,#251875,#251876,#251877,#251878,#251879,
#251880,#251881,#251882,#251883,#251884,#251885,#251886,#251887,#251888,
#251889,#251890,#251891,#251892,#251893,#251894,#251895,#251896,#251897,
#251898,#251899,#251900,#251901,#251902,#251903,#251904,#251905,#251906,
#251907,#251908,#251909,#251910,#251911,#251912,#251913,#251914,#251915,
#251916,#251917,#251918,#251919,#251920,#251921,#251922,#251923,#251924,
#251925,#251926,#251927,#251928,#251929,#251930,#251931,#251932,#251933,
#251934,#251935,#251936,#251937,#251938,#251939,#251940,#251941,#251942,
#251943,#251944,#251945,#251946,#251947,#251948,#251949,#251950,#251951,
#251952,#251953,#251954,#251955,#251956,#251957,#251958,#251959,#251960,
#251961,#251962,#251963,#251964,#251965,#251966,#251967,#251968,#251969,
#251970,#251971,#251972,#251973,#251974,#251975,#251976,#251977,#251978,
#251979,#251980,#251981,#251982,#251983,#251984,#251985,#251986,#251987,
#251988,#251989,#251990,#251991,#251992,#251993,#251994,#251995,#251996,
#251997,#251998,#251999,#252000,#252001,#252002,#252003,#252004,#252005,
#252006,#252007,#252008,#252009,#252010,#252011,#252012)),.UNSPECIFIED.,
 .F.,.T.,.F.,(2,2),(4,2,2,2,2,2,2,2,2,2,2,2,2,2,2,2,2,2,2,2,2,2,2,2,2,2,
2,2,2,2,2,2,2,2,2,2,2,2,2,2,2,2,2,2,2,2,2,2,2,2,2,2,2,2,2,2,2,2,2,2,2,2,
2,2,2,2,2,2,2,2,2,2,2,2,2,2,2,2,2,2,2,2,2,2,2,2,2,2,2,2,2,2,2,2,2,2,2,2,
2,2,2,2,2,2,2,2,2,2,2,2,2,2,4),(-1.02033811129603E-7,1.00000163088848),
(-0.000118831294053002,-4.84197060393493E-6,0.000109147352845132,0.000337125999743267,
0.000451115323192334,0.000565104646641402,0.000679093970090469,0.000793083293539536,
0.00102106194043767,0.00113505126388674,0.0012490405873358,0.00136302991078487,
0.00142002457250941,0.00147701923423394,0.00170499788113207,0.00193297652803021,
0.00204696585147928,0.00216095517492835,0.00227494449837741,0.00238893382182648,
0.00261691246872462,0.00284489111562275,0.00290188577734728,0.00295888043907182,
0.00307286976252088,0.00318685908596995,0.00330084840941902,0.00341483773286809,
0.00352882705631715,0.00364281637976622,0.00375680570321528,0.00387079502666435,
0.00398478435011342,0.00421276299701156,0.00444074164390969,0.00466872029080782,
0.00489669893770596,0.00512467758460409,0.00518167224632863,0.00523866690805316,
0.00535265623150223,0.0054666455549513,0.00558063487840036,0.00569462420184943,
0.0058086135252985,0.00592260284874756,0.00603659217219663,0.0061505814956457,
0.00626457081909477,0.0064925494659929,0.00660653878944197,0.00672052811289104,
0.0068345174363401,0.00694850675978917,0.00706249608323824,0.00717648540668731,
0.00729047473013637,0.00740446405358544,0.00763244270048357,0.00786042134738171,
0.00797441067083078,0.00808839999427985,0.00820238931772891,0.00831637864117798,
0.00854435728807612,0.00865834661152518,0.00877233593497425,0.00888632525842331,
0.00900031458187238,0.00911430390532145,0.00922829322877052,0.00945627187566865,
0.00957026119911772,0.00968425052256679,0.00974124518429132,0.00979823984601585,
0.00991222916946492,0.0101402078163631,0.0103681864632612,0.0104251811249857,
0.0104821757867103,0.0105961651101593,0.0107101544336084,0.0108241437570575,
0.0109381330805065,0.0110521224039556,0.0111661117274047,0.0112801010508537,
0.0113940903743028,0.0115080796977519,0.01173605834465,0.0118500476680991,
0.0119640369915481,0.0120780263149972,0.0121920156384463,0.0124199942853444,
0.0126479729322425,0.0127049675939671,0.0127619622556916,0.0128759515791407,
0.0129899409025897,0.0131039302260388,0.0133319088729369,0.013445898196386,
0.0135028928581105,0.0135598875198351,0.0136738768432841,0.0137878661667332,
0.0140158448136313,0.0141298341370804,0.0142438234605295,0.0143578127839785,
0.0144718021074276),.UNSPECIFIED.);
#960=B_SPLINE_SURFACE_WITH_KNOTS('',1,3,((#254568,#254569,#254570,#254571,
#254572,#254573,#254574,#254575,#254576,#254577,#254578,#254579,#254580,
#254581,#254582,#254583,#254584,#254585,#254586,#254587,#254588,#254589,
#254590,#254591,#254592,#254593,#254594,#254595,#254596,#254597,#254598,
#254599,#254600,#254601,#254602,#254603,#254604,#254605,#254606,#254607,
#254608,#254609,#254610,#254611,#254612,#254613,#254614,#254615,#254616,
#254617,#254618,#254619,#254620,#254621,#254622,#254623,#254624,#254625,
#254626,#254627,#254628,#254629,#254630,#254631,#254632,#254633,#254634,
#254635,#254636,#254637,#254638,#254639,#254640,#254641,#254642,#254643,
#254644,#254645,#254646,#254647,#254648,#254649,#254650,#254651,#254652,
#254653,#254654,#254655,#254656,#254657,#254658,#254659,#254660,#254661,
#254662,#254663,#254664,#254665,#254666,#254667,#254668,#254669,#254670,
#254671,#254672,#254673,#254674,#254675,#254676,#254677,#254678,#254679,
#254680,#254681,#254682,#254683,#254684,#254685,#254686,#254687,#254688,
#254689,#254690,#254691,#254692,#254693,#254694,#254695,#254696,#254697,
#254698,#254699,#254700,#254701,#254702,#254703,#254704,#254705,#254706,
#254707,#254708,#254709,#254710,#254711,#254712,#254713,#254714,#254715,
#254716,#254717,#254718,#254719,#254720,#254721,#254722,#254723,#254724,
#254725,#254726,#254727,#254728,#254729,#254730,#254731,#254732,#254733,
#254734,#254735,#254736,#254737,#254738,#254739,#254740,#254741,#254742,
#254743,#254744,#254745,#254746),(#254747,#254748,#254749,#254750,#254751,
#254752,#254753,#254754,#254755,#254756,#254757,#254758,#254759,#254760,
#254761,#254762,#254763,#254764,#254765,#254766,#254767,#254768,#254769,
#254770,#254771,#254772,#254773,#254774,#254775,#254776,#254777,#254778,
#254779,#254780,#254781,#254782,#254783,#254784,#254785,#254786,#254787,
#254788,#254789,#254790,#254791,#254792,#254793,#254794,#254795,#254796,
#254797,#254798,#254799,#254800,#254801,#254802,#254803,#254804,#254805,
#254806,#254807,#254808,#254809,#254810,#254811,#254812,#254813,#254814,
#254815,#254816,#254817,#254818,#254819,#254820,#254821,#254822,#254823,
#254824,#254825,#254826,#254827,#254828,#254829,#254830,#254831,#254832,
#254833,#254834,#254835,#254836,#254837,#254838,#254839,#254840,#254841,
#254842,#254843,#254844,#254845,#254846,#254847,#254848,#254849,#254850,
#254851,#254852,#254853,#254854,#254855,#254856,#254857,#254858,#254859,
#254860,#254861,#254862,#254863,#254864,#254865,#254866,#254867,#254868,
#254869,#254870,#254871,#254872,#254873,#254874,#254875,#254876,#254877,
#254878,#254879,#254880,#254881,#254882,#254883,#254884,#254885,#254886,
#254887,#254888,#254889,#254890,#254891,#254892,#254893,#254894,#254895,
#254896,#254897,#254898,#254899,#254900,#254901,#254902,#254903,#254904,
#254905,#254906,#254907,#254908,#254909,#254910,#254911,#254912,#254913,
#254914,#254915,#254916,#254917,#254918,#254919,#254920,#254921,#254922,
#254923,#254924,#254925)),.UNSPECIFIED.,.F.,.T.,.F.,(2,2),(4,1,1,2,2,2,
2,1,1,1,2,2,2,1,1,2,2,2,2,2,2,2,2,2,1,1,1,2,2,2,1,2,2,2,1,2,2,2,1,1,1,1,
2,2,2,1,1,1,1,2,2,2,2,2,2,2,1,1,2,2,2,2,1,2,2,2,1,1,2,2,2,2,2,2,2,2,2,2,
1,1,1,2,2,2,1,1,2,2,2,1,2,2,2,2,2,1,2,2,2,2,2,1,1,1,2,2,4),(0.,4.74723717073224),
(-0.000118831294053002,0.000109147352845132,0.000337125999743267,0.000451115323192334,
0.000565104646641402,0.000679093970090469,0.000793083293539536,0.00102106194043767,
0.00113505126388674,0.0012490405873358,0.00136302991078487,0.00142002457250941,
0.00147701923423394,0.00170499788113207,0.00193297652803021,0.00204696585147928,
0.00216095517492835,0.00227494449837741,0.00238893382182648,0.00261691246872462,
0.00284489111562275,0.00290188577734728,0.00295888043907182,0.00307286976252088,
0.00330084840941902,0.00341483773286809,0.00352882705631715,0.00364281637976622,
0.00375680570321528,0.00387079502666435,0.00398478435011342,0.00421276299701156,
0.00444074164390969,0.00466872029080782,0.00489669893770596,0.00512467758460409,
0.00518167224632863,0.00523866690805316,0.00535265623150223,0.0054666455549513,
0.00558063487840036,0.00569462420184943,0.0058086135252985,0.00592260284874756,
0.00603659217219663,0.0061505814956457,0.00626457081909477,0.0064925494659929,
0.00660653878944197,0.00672052811289104,0.0068345174363401,0.00694850675978917,
0.00717648540668731,0.00729047473013637,0.00740446405358544,0.00763244270048357,
0.00786042134738171,0.00797441067083078,0.00808839999427985,0.00820238931772891,
0.00831637864117798,0.00854435728807612,0.00877233593497425,0.00888632525842331,
0.00900031458187238,0.00911430390532145,0.00922829322877052,0.00945627187566865,
0.00957026119911772,0.00968425052256679,0.00974124518429132,0.00979823984601585,
0.00991222916946492,0.0101402078163631,0.0103681864632612,0.0104251811249857,
0.0104821757867103,0.0105961651101593,0.0108241437570575,0.0109381330805065,
0.0110521224039556,0.0111661117274047,0.0112801010508537,0.0113940903743028,
0.0115080796977519,0.01173605834465,0.0118500476680991,0.0119640369915481,
0.0120780263149972,0.0121920156384463,0.0124199942853444,0.0126479729322425,
0.0127049675939671,0.0127619622556916,0.0128759515791407,0.0131039302260388,
0.0133319088729369,0.013445898196386,0.0135028928581105,0.0135598875198351,
0.0136738768432841,0.0137878661667332,0.0140158448136313,0.0141298341370804,
0.0142438234605295,0.0143578127839785,0.0144718021074276),.UNSPECIFIED.);
#961=B_SPLINE_SURFACE_WITH_KNOTS('',1,3,((#254948,#254949,#254950,#254951,
#254952,#254953,#254954,#254955,#254956,#254957,#254958,#254959,#254960,
#254961,#254962,#254963,#254964,#254965,#254966,#254967,#254968,#254969,
#254970,#254971,#254972,#254973,#254974,#254975,#254976,#254977,#254978,
#254979,#254980,#254981,#254982,#254983,#254984,#254985,#254986,#254987,
#254988,#254989,#254990,#254991,#254992,#254993,#254994,#254995,#254996,
#254997,#254998,#254999,#255000,#255001,#255002,#255003,#255004,#255005,
#255006,#255007,#255008,#255009,#255010,#255011,#255012,#255013,#255014,
#255015,#255016,#255017,#255018,#255019,#255020,#255021,#255022,#255023,
#255024,#255025,#255026,#255027,#255028,#255029,#255030,#255031,#255032,
#255033,#255034,#255035,#255036,#255037,#255038,#255039,#255040,#255041,
#255042,#255043,#255044,#255045,#255046,#255047,#255048,#255049,#255050,
#255051,#255052,#255053,#255054,#255055,#255056,#255057,#255058,#255059,
#255060,#255061,#255062,#255063,#255064,#255065,#255066,#255067,#255068,
#255069,#255070,#255071,#255072,#255073,#255074,#255075,#255076,#255077,
#255078,#255079,#255080,#255081,#255082,#255083,#255084,#255085,#255086,
#255087,#255088,#255089,#255090,#255091,#255092,#255093,#255094,#255095,
#255096,#255097,#255098,#255099,#255100,#255101,#255102,#255103,#255104,
#255105,#255106,#255107,#255108,#255109,#255110,#255111,#255112,#255113,
#255114,#255115,#255116,#255117,#255118,#255119,#255120,#255121,#255122,
#255123,#255124,#255125,#255126),(#255127,#255128,#255129,#255130,#255131,
#255132,#255133,#255134,#255135,#255136,#255137,#255138,#255139,#255140,
#255141,#255142,#255143,#255144,#255145,#255146,#255147,#255148,#255149,
#255150,#255151,#255152,#255153,#255154,#255155,#255156,#255157,#255158,
#255159,#255160,#255161,#255162,#255163,#255164,#255165,#255166,#255167,
#255168,#255169,#255170,#255171,#255172,#255173,#255174,#255175,#255176,
#255177,#255178,#255179,#255180,#255181,#255182,#255183,#255184,#255185,
#255186,#255187,#255188,#255189,#255190,#255191,#255192,#255193,#255194,
#255195,#255196,#255197,#255198,#255199,#255200,#255201,#255202,#255203,
#255204,#255205,#255206,#255207,#255208,#255209,#255210,#255211,#255212,
#255213,#255214,#255215,#255216,#255217,#255218,#255219,#255220,#255221,
#255222,#255223,#255224,#255225,#255226,#255227,#255228,#255229,#255230,
#255231,#255232,#255233,#255234,#255235,#255236,#255237,#255238,#255239,
#255240,#255241,#255242,#255243,#255244,#255245,#255246,#255247,#255248,
#255249,#255250,#255251,#255252,#255253,#255254,#255255,#255256,#255257,
#255258,#255259,#255260,#255261,#255262,#255263,#255264,#255265,#255266,
#255267,#255268,#255269,#255270,#255271,#255272,#255273,#255274,#255275,
#255276,#255277,#255278,#255279,#255280,#255281,#255282,#255283,#255284,
#255285,#255286,#255287,#255288,#255289,#255290,#255291,#255292,#255293,
#255294,#255295,#255296,#255297,#255298,#255299,#255300,#255301,#255302,
#255303,#255304,#255305)),.UNSPECIFIED.,.F.,.T.,.F.,(2,2),(4,1,1,2,2,2,
2,1,1,1,2,2,2,1,1,2,2,2,2,2,2,2,2,2,1,1,1,2,2,2,1,2,2,2,1,2,2,2,1,1,1,1,
2,2,2,1,1,1,1,2,2,2,2,2,2,2,1,1,2,2,2,2,1,2,2,2,1,1,2,2,2,2,2,2,2,2,2,2,
1,1,1,2,2,2,1,1,2,2,2,1,2,2,2,2,2,1,2,2,2,2,2,1,1,1,2,2,4),(0.,4.74723717073224),
(-0.000118831294053002,0.000109147352845132,0.000337125999743267,0.000451115323192334,
0.000565104646641402,0.000679093970090469,0.000793083293539536,0.00102106194043767,
0.00113505126388674,0.0012490405873358,0.00136302991078487,0.00142002457250941,
0.00147701923423394,0.00170499788113207,0.00193297652803021,0.00204696585147928,
0.00216095517492835,0.00227494449837741,0.00238893382182648,0.00261691246872462,
0.00284489111562275,0.00290188577734728,0.00295888043907182,0.00307286976252088,
0.00330084840941902,0.00341483773286809,0.00352882705631715,0.00364281637976622,
0.00375680570321528,0.00387079502666435,0.00398478435011342,0.00421276299701156,
0.00444074164390969,0.00466872029080782,0.00489669893770596,0.00512467758460409,
0.00518167224632863,0.00523866690805316,0.00535265623150223,0.0054666455549513,
0.00558063487840036,0.00569462420184943,0.0058086135252985,0.00592260284874756,
0.00603659217219663,0.0061505814956457,0.00626457081909477,0.0064925494659929,
0.00660653878944197,0.00672052811289104,0.0068345174363401,0.00694850675978917,
0.00717648540668731,0.00729047473013637,0.00740446405358544,0.00763244270048357,
0.00786042134738171,0.00797441067083078,0.00808839999427985,0.00820238931772891,
0.00831637864117798,0.00854435728807612,0.00877233593497425,0.00888632525842331,
0.00900031458187238,0.00911430390532145,0.00922829322877052,0.00945627187566865,
0.00957026119911772,0.00968425052256679,0.00974124518429132,0.00979823984601585,
0.00991222916946492,0.0101402078163631,0.0103681864632612,0.0104251811249857,
0.0104821757867103,0.0105961651101593,0.0108241437570575,0.0109381330805065,
0.0110521224039556,0.0111661117274047,0.0112801010508537,0.0113940903743028,
0.0115080796977519,0.01173605834465,0.0118500476680991,0.0119640369915481,
0.0120780263149972,0.0121920156384463,0.0124199942853444,0.0126479729322425,
0.0127049675939671,0.0127619622556916,0.0128759515791407,0.0131039302260388,
0.0133319088729369,0.013445898196386,0.0135028928581105,0.0135598875198351,
0.0136738768432841,0.0137878661667332,0.0140158448136313,0.0141298341370804,
0.0142438234605295,0.0143578127839785,0.0144718021074276),.UNSPECIFIED.);
#962=B_SPLINE_SURFACE_WITH_KNOTS('',1,3,((#255358,#255359,#255360,#255361,
#255362,#255363,#255364,#255365,#255366,#255367,#255368,#255369,#255370,
#255371,#255372,#255373,#255374,#255375,#255376,#255377,#255378,#255379,
#255380,#255381,#255382,#255383,#255384,#255385,#255386,#255387,#255388,
#255389,#255390,#255391,#255392,#255393,#255394,#255395,#255396,#255397,
#255398,#255399,#255400,#255401,#255402,#255403,#255404,#255405,#255406,
#255407,#255408,#255409,#255410,#255411,#255412,#255413,#255414,#255415,
#255416,#255417,#255418,#255419,#255420,#255421,#255422,#255423,#255424,
#255425,#255426,#255427,#255428,#255429,#255430,#255431,#255432,#255433,
#255434,#255435,#255436,#255437,#255438,#255439,#255440,#255441,#255442,
#255443,#255444,#255445,#255446,#255447,#255448,#255449,#255450,#255451,
#255452,#255453,#255454,#255455,#255456,#255457,#255458,#255459,#255460,
#255461,#255462,#255463,#255464,#255465,#255466,#255467,#255468,#255469,
#255470,#255471,#255472,#255473,#255474,#255475,#255476,#255477,#255478,
#255479,#255480,#255481,#255482,#255483,#255484,#255485,#255486,#255487,
#255488,#255489,#255490,#255491,#255492,#255493,#255494,#255495,#255496,
#255497,#255498,#255499,#255500,#255501,#255502,#255503,#255504,#255505,
#255506,#255507,#255508,#255509,#255510,#255511,#255512,#255513,#255514,
#255515,#255516,#255517,#255518,#255519,#255520,#255521,#255522,#255523,
#255524,#255525,#255526,#255527,#255528,#255529,#255530,#255531,#255532,
#255533,#255534,#255535,#255536),(#255537,#255538,#255539,#255540,#255541,
#255542,#255543,#255544,#255545,#255546,#255547,#255548,#255549,#255550,
#255551,#255552,#255553,#255554,#255555,#255556,#255557,#255558,#255559,
#255560,#255561,#255562,#255563,#255564,#255565,#255566,#255567,#255568,
#255569,#255570,#255571,#255572,#255573,#255574,#255575,#255576,#255577,
#255578,#255579,#255580,#255581,#255582,#255583,#255584,#255585,#255586,
#255587,#255588,#255589,#255590,#255591,#255592,#255593,#255594,#255595,
#255596,#255597,#255598,#255599,#255600,#255601,#255602,#255603,#255604,
#255605,#255606,#255607,#255608,#255609,#255610,#255611,#255612,#255613,
#255614,#255615,#255616,#255617,#255618,#255619,#255620,#255621,#255622,
#255623,#255624,#255625,#255626,#255627,#255628,#255629,#255630,#255631,
#255632,#255633,#255634,#255635,#255636,#255637,#255638,#255639,#255640,
#255641,#255642,#255643,#255644,#255645,#255646,#255647,#255648,#255649,
#255650,#255651,#255652,#255653,#255654,#255655,#255656,#255657,#255658,
#255659,#255660,#255661,#255662,#255663,#255664,#255665,#255666,#255667,
#255668,#255669,#255670,#255671,#255672,#255673,#255674,#255675,#255676,
#255677,#255678,#255679,#255680,#255681,#255682,#255683,#255684,#255685,
#255686,#255687,#255688,#255689,#255690,#255691,#255692,#255693,#255694,
#255695,#255696,#255697,#255698,#255699,#255700,#255701,#255702,#255703,
#255704,#255705,#255706,#255707,#255708,#255709,#255710,#255711,#255712,
#255713,#255714,#255715)),.UNSPECIFIED.,.F.,.T.,.F.,(2,2),(4,1,1,2,2,2,
2,1,1,1,2,2,2,1,1,2,2,2,2,2,2,2,2,2,1,1,1,2,2,2,1,2,2,2,1,2,2,2,1,1,1,1,
2,2,2,1,1,1,1,2,2,2,2,2,2,2,1,1,2,2,2,2,1,2,2,2,1,1,2,2,2,2,2,2,2,2,2,2,
1,1,1,2,2,2,1,1,2,2,2,1,2,2,2,2,2,1,2,2,2,2,2,1,1,1,2,2,4),(0.,4.74723717073224),
(-0.000118831294053002,0.000109147352845132,0.000337125999743267,0.000451115323192334,
0.000565104646641402,0.000679093970090469,0.000793083293539536,0.00102106194043767,
0.00113505126388674,0.0012490405873358,0.00136302991078487,0.00142002457250941,
0.00147701923423394,0.00170499788113207,0.00193297652803021,0.00204696585147928,
0.00216095517492835,0.00227494449837741,0.00238893382182648,0.00261691246872462,
0.00284489111562275,0.00290188577734728,0.00295888043907182,0.00307286976252088,
0.00330084840941902,0.00341483773286809,0.00352882705631715,0.00364281637976622,
0.00375680570321528,0.00387079502666435,0.00398478435011342,0.00421276299701156,
0.00444074164390969,0.00466872029080782,0.00489669893770596,0.00512467758460409,
0.00518167224632863,0.00523866690805316,0.00535265623150223,0.0054666455549513,
0.00558063487840036,0.00569462420184943,0.0058086135252985,0.00592260284874756,
0.00603659217219663,0.0061505814956457,0.00626457081909477,0.0064925494659929,
0.00660653878944197,0.00672052811289104,0.0068345174363401,0.00694850675978917,
0.00717648540668731,0.00729047473013637,0.00740446405358544,0.00763244270048357,
0.00786042134738171,0.00797441067083078,0.00808839999427985,0.00820238931772891,
0.00831637864117798,0.00854435728807612,0.00877233593497425,0.00888632525842331,
0.00900031458187238,0.00911430390532145,0.00922829322877052,0.00945627187566865,
0.00957026119911772,0.00968425052256679,0.00974124518429132,0.00979823984601585,
0.00991222916946492,0.0101402078163631,0.0103681864632612,0.0104251811249857,
0.0104821757867103,0.0105961651101593,0.0108241437570575,0.0109381330805065,
0.0110521224039556,0.0111661117274047,0.0112801010508537,0.0113940903743028,
0.0115080796977519,0.01173605834465,0.0118500476680991,0.0119640369915481,
0.0120780263149972,0.0121920156384463,0.0124199942853444,0.0126479729322425,
0.0127049675939671,0.0127619622556916,0.0128759515791407,0.0131039302260388,
0.0133319088729369,0.013445898196386,0.0135028928581105,0.0135598875198351,
0.0136738768432841,0.0137878661667332,0.0140158448136313,0.0141298341370804,
0.0142438234605295,0.0143578127839785,0.0144718021074276),.UNSPECIFIED.);
#963=B_SPLINE_SURFACE_WITH_KNOTS('',1,3,((#255726,#255727,#255728,#255729,
#255730,#255731,#255732,#255733,#255734,#255735,#255736,#255737,#255738,
#255739,#255740,#255741,#255742,#255743,#255744,#255745,#255746,#255747,
#255748,#255749,#255750,#255751,#255752,#255753,#255754,#255755,#255756,
#255757,#255758,#255759,#255760,#255761,#255762,#255763,#255764,#255765,
#255766,#255767,#255768,#255769,#255770,#255771,#255772,#255773,#255774,
#255775,#255776,#255777,#255778,#255779,#255780,#255781,#255782,#255783,
#255784,#255785,#255786,#255787,#255788,#255789,#255790,#255791,#255792,
#255793,#255794,#255795,#255796,#255797,#255798,#255799,#255800,#255801,
#255802,#255803,#255804,#255805,#255806,#255807,#255808,#255809,#255810,
#255811,#255812,#255813,#255814,#255815,#255816,#255817,#255818,#255819,
#255820,#255821,#255822,#255823,#255824,#255825,#255826,#255827,#255828,
#255829,#255830,#255831,#255832,#255833,#255834,#255835,#255836,#255837,
#255838,#255839,#255840,#255841),(#255842,#255843,#255844,#255845,#255846,
#255847,#255848,#255849,#255850,#255851,#255852,#255853,#255854,#255855,
#255856,#255857,#255858,#255859,#255860,#255861,#255862,#255863,#255864,
#255865,#255866,#255867,#255868,#255869,#255870,#255871,#255872,#255873,
#255874,#255875,#255876,#255877,#255878,#255879,#255880,#255881,#255882,
#255883,#255884,#255885,#255886,#255887,#255888,#255889,#255890,#255891,
#255892,#255893,#255894,#255895,#255896,#255897,#255898,#255899,#255900,
#255901,#255902,#255903,#255904,#255905,#255906,#255907,#255908,#255909,
#255910,#255911,#255912,#255913,#255914,#255915,#255916,#255917,#255918,
#255919,#255920,#255921,#255922,#255923,#255924,#255925,#255926,#255927,
#255928,#255929,#255930,#255931,#255932,#255933,#255934,#255935,#255936,
#255937,#255938,#255939,#255940,#255941,#255942,#255943,#255944,#255945,
#255946,#255947,#255948,#255949,#255950,#255951,#255952,#255953,#255954,
#255955,#255956,#255957)),.UNSPECIFIED.,.F.,.F.,.F.,(2,2),(4,2,2,2,2,2,
2,2,2,2,2,2,2,2,2,2,2,2,2,2,2,2,2,2,2,2,2,2,2,2,2,2,2,2,2,2,2,2,2,2,2,2,
2,2,2,2,2,2,2,2,2,2,2,2,2,2,2,4),(0.,1.00000324318157),(0.00717648540668731,
0.00729047473013637,0.00740446405358544,0.00763244270048357,0.00786042134738171,
0.00797441067083078,0.00808839999427985,0.00820238931772891,0.00831637864117798,
0.00854435728807612,0.00865834661152518,0.00877233593497425,0.00888632525842331,
0.00900031458187238,0.00911430390532145,0.00922829322877052,0.00945627187566865,
0.00957026119911772,0.00968425052256679,0.00974124518429132,0.00979823984601585,
0.00991222916946492,0.0101402078163631,0.0103681864632612,0.0104251811249857,
0.0104821757867103,0.0105961651101593,0.0107101544336084,0.0108241437570575,
0.0109381330805065,0.0110521224039556,0.0111661117274047,0.0112801010508537,
0.0113940903743028,0.0115080796977519,0.01173605834465,0.0118500476680991,
0.0119640369915481,0.0120780263149972,0.0121920156384463,0.0124199942853444,
0.0126479729322425,0.0127049675939671,0.0127619622556916,0.0128759515791407,
0.0129899409025897,0.0131039302260388,0.0133319088729369,0.013445898196386,
0.0135028928581105,0.0135598875198351,0.0136738768432841,0.0137878661667332,
0.0140158448136313,0.0141298341370804,0.0142438234605295,0.0143578127839785,
0.0144718021074276),.UNSPECIFIED.);
#964=B_SPLINE_SURFACE_WITH_KNOTS('',1,3,((#258767,#258768,#258769,#258770,
#258771,#258772,#258773,#258774,#258775,#258776,#258777,#258778,#258779,
#258780,#258781,#258782,#258783,#258784,#258785,#258786,#258787,#258788,
#258789,#258790,#258791,#258792,#258793,#258794,#258795,#258796,#258797,
#258798,#258799,#258800,#258801,#258802,#258803,#258804,#258805,#258806,
#258807,#258808,#258809,#258810,#258811,#258812,#258813,#258814,#258815,
#258816,#258817,#258818,#258819,#258820,#258821,#258822,#258823,#258824,
#258825,#258826,#258827,#258828,#258829,#258830,#258831,#258832,#258833,
#258834,#258835,#258836,#258837,#258838,#258839,#258840,#258841,#258842,
#258843,#258844,#258845,#258846,#258847,#258848,#258849,#258850,#258851,
#258852,#258853,#258854,#258855,#258856,#258857,#258858,#258859,#258860,
#258861,#258862,#258863,#258864,#258865,#258866,#258867,#258868,#258869,
#258870,#258871,#258872,#258873,#258874,#258875,#258876,#258877,#258878,
#258879,#258880,#258881,#258882,#258883,#258884,#258885,#258886,#258887,
#258888,#258889,#258890,#258891,#258892,#258893,#258894,#258895,#258896,
#258897,#258898,#258899,#258900,#258901,#258902,#258903,#258904,#258905,
#258906,#258907,#258908,#258909,#258910,#258911,#258912,#258913,#258914,
#258915,#258916,#258917,#258918,#258919,#258920,#258921,#258922,#258923,
#258924,#258925,#258926,#258927,#258928,#258929,#258930,#258931,#258932,
#258933,#258934,#258935,#258936,#258937,#258938,#258939,#258940,#258941),
(#258942,#258943,#258944,#258945,#258946,#258947,#258948,#258949,#258950,
#258951,#258952,#258953,#258954,#258955,#258956,#258957,#258958,#258959,
#258960,#258961,#258962,#258963,#258964,#258965,#258966,#258967,#258968,
#258969,#258970,#258971,#258972,#258973,#258974,#258975,#258976,#258977,
#258978,#258979,#258980,#258981,#258982,#258983,#258984,#258985,#258986,
#258987,#258988,#258989,#258990,#258991,#258992,#258993,#258994,#258995,
#258996,#258997,#258998,#258999,#259000,#259001,#259002,#259003,#259004,
#259005,#259006,#259007,#259008,#259009,#259010,#259011,#259012,#259013,
#259014,#259015,#259016,#259017,#259018,#259019,#259020,#259021,#259022,
#259023,#259024,#259025,#259026,#259027,#259028,#259029,#259030,#259031,
#259032,#259033,#259034,#259035,#259036,#259037,#259038,#259039,#259040,
#259041,#259042,#259043,#259044,#259045,#259046,#259047,#259048,#259049,
#259050,#259051,#259052,#259053,#259054,#259055,#259056,#259057,#259058,
#259059,#259060,#259061,#259062,#259063,#259064,#259065,#259066,#259067,
#259068,#259069,#259070,#259071,#259072,#259073,#259074,#259075,#259076,
#259077,#259078,#259079,#259080,#259081,#259082,#259083,#259084,#259085,
#259086,#259087,#259088,#259089,#259090,#259091,#259092,#259093,#259094,
#259095,#259096,#259097,#259098,#259099,#259100,#259101,#259102,#259103,
#259104,#259105,#259106,#259107,#259108,#259109,#259110,#259111,#259112,
#259113,#259114,#259115,#259116)),.UNSPECIFIED.,.F.,.T.,.F.,(2,2),(4,1,
1,2,1,1,1,1,2,2,1,2,2,2,2,1,1,2,2,2,1,1,1,1,2,2,2,2,2,2,2,2,1,1,1,2,2,2,
2,1,1,1,2,2,2,1,1,1,2,2,2,2,2,2,2,1,2,2,2,2,2,1,1,2,2,2,2,1,2,2,2,1,1,2,
2,2,1,1,1,1,2,2,2,2,2,2,2,1,2,1,1,2,2,2,1,2,2,2,2,2,1,2,2,2,2,4),(0.,4.71475608888856),
(-0.000135430429350568,9.25560474171526E-5,0.000320542524184873,0.000548529000952593,
0.000776515477720314,0.00100450195448803,0.00111849519287189,0.00123248843125575,
0.00134648166963961,0.00146047490802347,0.0016884613847912,0.00191644786155891,
0.00203044109994277,0.00214443433832664,0.00225842757671049,0.00237242081509435,
0.00260040729186208,0.00271440053024594,0.0028283937686298,0.00294238700701366,
0.00305638024539752,0.00317037348378138,0.00328436672216524,0.0033983599605491,
0.00351235319893296,0.00362634643731682,0.00374033967570068,0.0039683261524684,
0.00419631262923612,0.00431030586761998,0.00436730248681191,0.00442429910600384,
0.0045382923443877,0.00465228558277156,0.00488027205953928,0.00499426529792314,
0.005108258536307,0.00522225177469086,0.00533624501307472,0.00556423148984244,
0.0056782247282263,0.00579221796661016,0.00590621120499402,0.00602020444337788,
0.00613419768176174,0.0062481909201456,0.00647617739691333,0.00659017063529719,
0.00670416387368105,0.00681815711206491,0.00693215035044876,0.00716013682721649,
0.00727413006560035,0.00738812330398421,0.00761610978075193,0.00784409625751965,
0.00795808949590351,0.00807208273428737,0.0081290793534793,0.00818607597267123,
0.00830006921105509,0.00852805568782281,0.00864204892620667,0.00875604216459053,
0.00887003540297439,0.00898402864135825,0.00921201511812597,0.00944000159489369,
0.00955399483327755,0.00966798807166141,0.00978198131004527,0.00989597454842913,
0.0101239610251968,0.0102379542635807,0.0103519475019646,0.0104659407403484,
0.0105799339787323,0.0106939272171161,0.0108079204555,0.0109219136938839,
0.0110359069322677,0.0111499001706516,0.0112638934090355,0.0114918798858032,
0.0117198663625709,0.0118338596009548,0.0118908562201467,0.0119478528393386,
0.0120618460777225,0.0121758393161063,0.0124038257928741,0.0125178190312579,
0.0126318122696418,0.0127458055080256,0.0129737919847934,0.0130877852231772,
0.0133157716999449,0.0134297649383288,0.0134867615575207,0.0135437581767127,
0.0137717446534804,0.0139997311302481,0.0142277176070158,0.0142847142262077,
0.0143417108453997,0.0144557040837835),.UNSPECIFIED.);
#965=B_SPLINE_SURFACE_WITH_KNOTS('',1,3,((#259139,#259140,#259141,#259142,
#259143,#259144,#259145,#259146,#259147,#259148,#259149,#259150,#259151,
#259152,#259153,#259154,#259155,#259156,#259157,#259158,#259159,#259160,
#259161,#259162,#259163,#259164,#259165,#259166,#259167,#259168,#259169,
#259170,#259171,#259172,#259173,#259174,#259175,#259176,#259177,#259178,
#259179,#259180,#259181,#259182,#259183,#259184,#259185,#259186,#259187,
#259188,#259189,#259190,#259191,#259192,#259193,#259194,#259195,#259196,
#259197,#259198,#259199,#259200,#259201,#259202,#259203,#259204,#259205,
#259206,#259207,#259208,#259209,#259210,#259211,#259212,#259213,#259214,
#259215,#259216,#259217,#259218,#259219,#259220,#259221,#259222,#259223,
#259224,#259225,#259226,#259227,#259228,#259229,#259230,#259231,#259232,
#259233,#259234,#259235,#259236,#259237,#259238,#259239,#259240,#259241,
#259242,#259243,#259244,#259245,#259246,#259247,#259248,#259249,#259250,
#259251,#259252,#259253,#259254,#259255,#259256,#259257,#259258,#259259,
#259260,#259261,#259262,#259263,#259264,#259265,#259266,#259267,#259268,
#259269,#259270,#259271,#259272,#259273,#259274,#259275,#259276,#259277,
#259278,#259279,#259280,#259281,#259282,#259283,#259284,#259285,#259286,
#259287,#259288,#259289,#259290,#259291,#259292,#259293,#259294,#259295,
#259296,#259297,#259298,#259299,#259300,#259301,#259302,#259303,#259304,
#259305,#259306,#259307,#259308,#259309,#259310,#259311,#259312,#259313),
(#259314,#259315,#259316,#259317,#259318,#259319,#259320,#259321,#259322,
#259323,#259324,#259325,#259326,#259327,#259328,#259329,#259330,#259331,
#259332,#259333,#259334,#259335,#259336,#259337,#259338,#259339,#259340,
#259341,#259342,#259343,#259344,#259345,#259346,#259347,#259348,#259349,
#259350,#259351,#259352,#259353,#259354,#259355,#259356,#259357,#259358,
#259359,#259360,#259361,#259362,#259363,#259364,#259365,#259366,#259367,
#259368,#259369,#259370,#259371,#259372,#259373,#259374,#259375,#259376,
#259377,#259378,#259379,#259380,#259381,#259382,#259383,#259384,#259385,
#259386,#259387,#259388,#259389,#259390,#259391,#259392,#259393,#259394,
#259395,#259396,#259397,#259398,#259399,#259400,#259401,#259402,#259403,
#259404,#259405,#259406,#259407,#259408,#259409,#259410,#259411,#259412,
#259413,#259414,#259415,#259416,#259417,#259418,#259419,#259420,#259421,
#259422,#259423,#259424,#259425,#259426,#259427,#259428,#259429,#259430,
#259431,#259432,#259433,#259434,#259435,#259436,#259437,#259438,#259439,
#259440,#259441,#259442,#259443,#259444,#259445,#259446,#259447,#259448,
#259449,#259450,#259451,#259452,#259453,#259454,#259455,#259456,#259457,
#259458,#259459,#259460,#259461,#259462,#259463,#259464,#259465,#259466,
#259467,#259468,#259469,#259470,#259471,#259472,#259473,#259474,#259475,
#259476,#259477,#259478,#259479,#259480,#259481,#259482,#259483,#259484,
#259485,#259486,#259487,#259488)),.UNSPECIFIED.,.F.,.T.,.F.,(2,2),(4,1,
1,2,1,1,1,1,2,2,1,2,2,2,2,1,1,2,2,2,1,1,1,1,2,2,2,2,2,2,2,2,1,1,1,2,2,2,
2,1,1,1,2,2,2,1,1,1,2,2,2,2,2,2,2,1,2,2,2,2,2,1,1,2,2,2,2,1,2,2,2,1,1,2,
2,2,1,1,1,1,2,2,2,2,2,2,2,1,2,1,1,2,2,2,1,2,2,2,2,2,1,2,2,2,2,4),(0.,4.71475608888856),
(-0.000135430429350568,9.25560474171526E-5,0.000320542524184873,0.000548529000952593,
0.000776515477720314,0.00100450195448803,0.00111849519287189,0.00123248843125575,
0.00134648166963961,0.00146047490802347,0.0016884613847912,0.00191644786155891,
0.00203044109994277,0.00214443433832664,0.00225842757671049,0.00237242081509435,
0.00260040729186208,0.00271440053024594,0.0028283937686298,0.00294238700701366,
0.00305638024539752,0.00317037348378138,0.00328436672216524,0.0033983599605491,
0.00351235319893296,0.00362634643731682,0.00374033967570068,0.0039683261524684,
0.00419631262923612,0.00431030586761998,0.00436730248681191,0.00442429910600384,
0.0045382923443877,0.00465228558277156,0.00488027205953928,0.00499426529792314,
0.005108258536307,0.00522225177469086,0.00533624501307472,0.00556423148984244,
0.0056782247282263,0.00579221796661016,0.00590621120499402,0.00602020444337788,
0.00613419768176174,0.0062481909201456,0.00647617739691333,0.00659017063529719,
0.00670416387368105,0.00681815711206491,0.00693215035044876,0.00716013682721649,
0.00727413006560035,0.00738812330398421,0.00761610978075193,0.00784409625751965,
0.00795808949590351,0.00807208273428737,0.0081290793534793,0.00818607597267123,
0.00830006921105509,0.00852805568782281,0.00864204892620667,0.00875604216459053,
0.00887003540297439,0.00898402864135825,0.00921201511812597,0.00944000159489369,
0.00955399483327755,0.00966798807166141,0.00978198131004527,0.00989597454842913,
0.0101239610251968,0.0102379542635807,0.0103519475019646,0.0104659407403484,
0.0105799339787323,0.0106939272171161,0.0108079204555,0.0109219136938839,
0.0110359069322677,0.0111499001706516,0.0112638934090355,0.0114918798858032,
0.0117198663625709,0.0118338596009548,0.0118908562201467,0.0119478528393386,
0.0120618460777225,0.0121758393161063,0.0124038257928741,0.0125178190312579,
0.0126318122696418,0.0127458055080256,0.0129737919847934,0.0130877852231772,
0.0133157716999449,0.0134297649383288,0.0134867615575207,0.0135437581767127,
0.0137717446534804,0.0139997311302481,0.0142277176070158,0.0142847142262077,
0.0143417108453997,0.0144557040837835),.UNSPECIFIED.);
#966=B_SPLINE_SURFACE_WITH_KNOTS('',1,3,((#259536,#259537,#259538,#259539,
#259540,#259541,#259542,#259543,#259544,#259545,#259546,#259547,#259548,
#259549,#259550,#259551,#259552,#259553,#259554,#259555,#259556,#259557,
#259558,#259559,#259560,#259561,#259562,#259563,#259564,#259565,#259566,
#259567,#259568,#259569,#259570,#259571,#259572,#259573,#259574,#259575,
#259576,#259577,#259578,#259579,#259580,#259581,#259582,#259583,#259584,
#259585,#259586,#259587,#259588,#259589,#259590,#259591,#259592,#259593,
#259594,#259595,#259596,#259597,#259598,#259599,#259600,#259601,#259602,
#259603,#259604,#259605,#259606,#259607,#259608,#259609,#259610,#259611,
#259612,#259613,#259614,#259615,#259616,#259617,#259618,#259619,#259620,
#259621,#259622,#259623,#259624,#259625,#259626,#259627,#259628,#259629,
#259630,#259631,#259632,#259633,#259634,#259635,#259636,#259637,#259638,
#259639,#259640,#259641,#259642,#259643,#259644,#259645,#259646,#259647,
#259648,#259649,#259650,#259651,#259652,#259653,#259654,#259655,#259656,
#259657,#259658,#259659,#259660,#259661,#259662,#259663,#259664,#259665,
#259666,#259667,#259668,#259669,#259670,#259671,#259672,#259673,#259674,
#259675,#259676,#259677,#259678,#259679,#259680,#259681,#259682,#259683,
#259684,#259685,#259686,#259687,#259688,#259689,#259690,#259691,#259692,
#259693,#259694,#259695,#259696,#259697,#259698,#259699,#259700,#259701,
#259702,#259703,#259704,#259705,#259706,#259707,#259708,#259709,#259710),
(#259711,#259712,#259713,#259714,#259715,#259716,#259717,#259718,#259719,
#259720,#259721,#259722,#259723,#259724,#259725,#259726,#259727,#259728,
#259729,#259730,#259731,#259732,#259733,#259734,#259735,#259736,#259737,
#259738,#259739,#259740,#259741,#259742,#259743,#259744,#259745,#259746,
#259747,#259748,#259749,#259750,#259751,#259752,#259753,#259754,#259755,
#259756,#259757,#259758,#259759,#259760,#259761,#259762,#259763,#259764,
#259765,#259766,#259767,#259768,#259769,#259770,#259771,#259772,#259773,
#259774,#259775,#259776,#259777,#259778,#259779,#259780,#259781,#259782,
#259783,#259784,#259785,#259786,#259787,#259788,#259789,#259790,#259791,
#259792,#259793,#259794,#259795,#259796,#259797,#259798,#259799,#259800,
#259801,#259802,#259803,#259804,#259805,#259806,#259807,#259808,#259809,
#259810,#259811,#259812,#259813,#259814,#259815,#259816,#259817,#259818,
#259819,#259820,#259821,#259822,#259823,#259824,#259825,#259826,#259827,
#259828,#259829,#259830,#259831,#259832,#259833,#259834,#259835,#259836,
#259837,#259838,#259839,#259840,#259841,#259842,#259843,#259844,#259845,
#259846,#259847,#259848,#259849,#259850,#259851,#259852,#259853,#259854,
#259855,#259856,#259857,#259858,#259859,#259860,#259861,#259862,#259863,
#259864,#259865,#259866,#259867,#259868,#259869,#259870,#259871,#259872,
#259873,#259874,#259875,#259876,#259877,#259878,#259879,#259880,#259881,
#259882,#259883,#259884,#259885)),.UNSPECIFIED.,.F.,.T.,.F.,(2,2),(4,1,
1,2,1,1,1,1,2,2,1,2,2,2,2,1,1,2,2,2,1,1,1,1,2,2,2,2,2,2,2,2,1,1,1,2,2,2,
2,1,1,1,2,2,2,1,1,1,2,2,2,2,2,2,2,1,2,2,2,2,2,1,1,2,2,2,2,1,2,2,2,1,1,2,
2,2,1,1,1,1,2,2,2,2,2,2,2,1,2,1,1,2,2,2,1,2,2,2,2,2,1,2,2,2,2,4),(0.,4.71475608888856),
(-0.000135430429350568,9.25560474171526E-5,0.000320542524184873,0.000548529000952593,
0.000776515477720314,0.00100450195448803,0.00111849519287189,0.00123248843125575,
0.00134648166963961,0.00146047490802347,0.0016884613847912,0.00191644786155891,
0.00203044109994277,0.00214443433832664,0.00225842757671049,0.00237242081509435,
0.00260040729186208,0.00271440053024594,0.0028283937686298,0.00294238700701366,
0.00305638024539752,0.00317037348378138,0.00328436672216524,0.0033983599605491,
0.00351235319893296,0.00362634643731682,0.00374033967570068,0.0039683261524684,
0.00419631262923612,0.00431030586761998,0.00436730248681191,0.00442429910600384,
0.0045382923443877,0.00465228558277156,0.00488027205953928,0.00499426529792314,
0.005108258536307,0.00522225177469086,0.00533624501307472,0.00556423148984244,
0.0056782247282263,0.00579221796661016,0.00590621120499402,0.00602020444337788,
0.00613419768176174,0.0062481909201456,0.00647617739691333,0.00659017063529719,
0.00670416387368105,0.00681815711206491,0.00693215035044876,0.00716013682721649,
0.00727413006560035,0.00738812330398421,0.00761610978075193,0.00784409625751965,
0.00795808949590351,0.00807208273428737,0.0081290793534793,0.00818607597267123,
0.00830006921105509,0.00852805568782281,0.00864204892620667,0.00875604216459053,
0.00887003540297439,0.00898402864135825,0.00921201511812597,0.00944000159489369,
0.00955399483327755,0.00966798807166141,0.00978198131004527,0.00989597454842913,
0.0101239610251968,0.0102379542635807,0.0103519475019646,0.0104659407403484,
0.0105799339787323,0.0106939272171161,0.0108079204555,0.0109219136938839,
0.0110359069322677,0.0111499001706516,0.0112638934090355,0.0114918798858032,
0.0117198663625709,0.0118338596009548,0.0118908562201467,0.0119478528393386,
0.0120618460777225,0.0121758393161063,0.0124038257928741,0.0125178190312579,
0.0126318122696418,0.0127458055080256,0.0129737919847934,0.0130877852231772,
0.0133157716999449,0.0134297649383288,0.0134867615575207,0.0135437581767127,
0.0137717446534804,0.0139997311302481,0.0142277176070158,0.0142847142262077,
0.0143417108453997,0.0144557040837835),.UNSPECIFIED.);
#967=B_SPLINE_SURFACE_WITH_KNOTS('',1,3,((#259896,#259897,#259898,#259899,
#259900,#259901,#259902,#259903,#259904,#259905,#259906,#259907,#259908,
#259909,#259910,#259911,#259912,#259913,#259914,#259915,#259916,#259917,
#259918,#259919,#259920,#259921,#259922,#259923,#259924,#259925,#259926,
#259927,#259928,#259929,#259930,#259931,#259932,#259933,#259934,#259935,
#259936,#259937,#259938,#259939,#259940,#259941,#259942,#259943,#259944,
#259945,#259946,#259947,#259948,#259949,#259950,#259951,#259952,#259953,
#259954,#259955,#259956,#259957,#259958,#259959,#259960,#259961,#259962,
#259963,#259964,#259965,#259966,#259967,#259968,#259969,#259970,#259971,
#259972,#259973,#259974,#259975,#259976,#259977,#259978,#259979,#259980,
#259981,#259982,#259983,#259984,#259985,#259986,#259987,#259988,#259989,
#259990,#259991,#259992,#259993,#259994,#259995,#259996,#259997,#259998,
#259999,#260000,#260001,#260002,#260003,#260004,#260005,#260006,#260007,
#260008,#260009),(#260010,#260011,#260012,#260013,#260014,#260015,#260016,
#260017,#260018,#260019,#260020,#260021,#260022,#260023,#260024,#260025,
#260026,#260027,#260028,#260029,#260030,#260031,#260032,#260033,#260034,
#260035,#260036,#260037,#260038,#260039,#260040,#260041,#260042,#260043,
#260044,#260045,#260046,#260047,#260048,#260049,#260050,#260051,#260052,
#260053,#260054,#260055,#260056,#260057,#260058,#260059,#260060,#260061,
#260062,#260063,#260064,#260065,#260066,#260067,#260068,#260069,#260070,
#260071,#260072,#260073,#260074,#260075,#260076,#260077,#260078,#260079,
#260080,#260081,#260082,#260083,#260084,#260085,#260086,#260087,#260088,
#260089,#260090,#260091,#260092,#260093,#260094,#260095,#260096,#260097,
#260098,#260099,#260100,#260101,#260102,#260103,#260104,#260105,#260106,
#260107,#260108,#260109,#260110,#260111,#260112,#260113,#260114,#260115,
#260116,#260117,#260118,#260119,#260120,#260121,#260122,#260123)),
 .UNSPECIFIED.,.F.,.F.,.F.,(2,2),(4,2,2,2,2,2,2,2,2,2,2,2,2,2,2,2,2,2,2,
2,2,2,2,2,2,2,2,2,2,2,2,2,2,2,2,2,2,2,2,2,2,2,2,2,2,2,2,2,2,2,2,2,2,2,2,
2,4),(0.,1.00000135803625),(0.00716013682721649,0.00727413006560035,0.00738812330398421,
0.00761610978075193,0.00784409625751965,0.00795808949590351,0.00807208273428737,
0.0081290793534793,0.00818607597267123,0.00830006921105509,0.00852805568782281,
0.00864204892620667,0.00875604216459053,0.00887003540297439,0.00898402864135825,
0.00921201511812597,0.00944000159489369,0.00955399483327755,0.00966798807166141,
0.00978198131004527,0.00989597454842913,0.0101239610251968,0.0102379542635807,
0.0103519475019646,0.0104659407403484,0.0105799339787323,0.0106939272171161,
0.0108079204555,0.0109219136938839,0.0110359069322677,0.0111499001706516,
0.0112638934090355,0.0114918798858032,0.0117198663625709,0.0118338596009548,
0.0118908562201467,0.0119478528393386,0.0120618460777225,0.0121758393161063,
0.0124038257928741,0.0125178190312579,0.0126318122696418,0.0127458055080256,
0.0128597987464095,0.0129737919847934,0.0130877852231772,0.0133157716999449,
0.0134297649383288,0.0134867615575207,0.0135437581767127,0.0136577514150965,
0.0137717446534804,0.0139997311302481,0.0142277176070158,0.0142847142262077,
0.0143417108453997,0.0144557040837835),.UNSPECIFIED.);
#968=B_SPLINE_SURFACE_WITH_KNOTS('',1,3,((#262733,#262734,#262735,#262736,
#262737,#262738,#262739,#262740,#262741,#262742,#262743,#262744,#262745,
#262746,#262747,#262748,#262749,#262750,#262751,#262752,#262753,#262754,
#262755,#262756,#262757,#262758,#262759,#262760,#262761,#262762,#262763,
#262764,#262765,#262766,#262767,#262768,#262769,#262770,#262771,#262772,
#262773,#262774,#262775,#262776,#262777,#262778,#262779,#262780,#262781,
#262782,#262783,#262784,#262785,#262786,#262787,#262788,#262789,#262790,
#262791,#262792,#262793,#262794,#262795,#262796,#262797,#262798,#262799,
#262800,#262801,#262802,#262803,#262804,#262805,#262806,#262807,#262808,
#262809,#262810,#262811,#262812,#262813,#262814,#262815,#262816,#262817,
#262818,#262819,#262820,#262821,#262822,#262823,#262824,#262825,#262826,
#262827,#262828,#262829,#262830,#262831,#262832,#262833,#262834,#262835,
#262836,#262837,#262838,#262839,#262840,#262841,#262842,#262843,#262844,
#262845,#262846,#262847,#262848,#262849,#262850,#262851,#262852,#262853,
#262854,#262855,#262856,#262857,#262858,#262859,#262860,#262861,#262862,
#262863,#262864,#262865,#262866,#262867,#262868,#262869,#262870,#262871,
#262872,#262873,#262874,#262875,#262876,#262877,#262878,#262879,#262880,
#262881,#262882,#262883,#262884,#262885,#262886,#262887,#262888,#262889,
#262890,#262891,#262892,#262893,#262894,#262895,#262896,#262897,#262898,
#262899,#262900,#262901,#262902,#262903,#262904,#262905,#262906,#262907),
(#262908,#262909,#262910,#262911,#262912,#262913,#262914,#262915,#262916,
#262917,#262918,#262919,#262920,#262921,#262922,#262923,#262924,#262925,
#262926,#262927,#262928,#262929,#262930,#262931,#262932,#262933,#262934,
#262935,#262936,#262937,#262938,#262939,#262940,#262941,#262942,#262943,
#262944,#262945,#262946,#262947,#262948,#262949,#262950,#262951,#262952,
#262953,#262954,#262955,#262956,#262957,#262958,#262959,#262960,#262961,
#262962,#262963,#262964,#262965,#262966,#262967,#262968,#262969,#262970,
#262971,#262972,#262973,#262974,#262975,#262976,#262977,#262978,#262979,
#262980,#262981,#262982,#262983,#262984,#262985,#262986,#262987,#262988,
#262989,#262990,#262991,#262992,#262993,#262994,#262995,#262996,#262997,
#262998,#262999,#263000,#263001,#263002,#263003,#263004,#263005,#263006,
#263007,#263008,#263009,#263010,#263011,#263012,#263013,#263014,#263015,
#263016,#263017,#263018,#263019,#263020,#263021,#263022,#263023,#263024,
#263025,#263026,#263027,#263028,#263029,#263030,#263031,#263032,#263033,
#263034,#263035,#263036,#263037,#263038,#263039,#263040,#263041,#263042,
#263043,#263044,#263045,#263046,#263047,#263048,#263049,#263050,#263051,
#263052,#263053,#263054,#263055,#263056,#263057,#263058,#263059,#263060,
#263061,#263062,#263063,#263064,#263065,#263066,#263067,#263068,#263069,
#263070,#263071,#263072,#263073,#263074,#263075,#263076,#263077,#263078,
#263079,#263080,#263081,#263082)),.UNSPECIFIED.,.F.,.T.,.F.,(2,2),(4,1,
1,2,1,1,1,1,2,2,1,2,2,2,2,1,1,2,2,2,1,1,1,1,2,2,2,2,2,2,2,2,1,1,1,2,2,2,
2,1,1,1,2,2,2,1,1,1,2,2,2,2,2,2,2,1,2,2,2,2,2,1,1,2,2,2,2,1,2,2,2,1,1,2,
2,2,1,1,1,1,2,2,2,2,2,2,2,1,2,1,1,2,2,2,1,2,2,2,2,2,1,2,2,2,2,4),(0.,5.46382276754873),
(-0.000135430429350568,9.25560474171526E-5,0.000320542524184873,0.000548529000952593,
0.000776515477720314,0.00100450195448803,0.00111849519287189,0.00123248843125575,
0.00134648166963961,0.00146047490802347,0.0016884613847912,0.00191644786155891,
0.00203044109994277,0.00214443433832664,0.00225842757671049,0.00237242081509435,
0.00260040729186208,0.00271440053024594,0.0028283937686298,0.00294238700701366,
0.00305638024539752,0.00317037348378138,0.00328436672216524,0.0033983599605491,
0.00351235319893296,0.00362634643731682,0.00374033967570068,0.0039683261524684,
0.00419631262923612,0.00431030586761998,0.00436730248681191,0.00442429910600384,
0.0045382923443877,0.00465228558277156,0.00488027205953928,0.00499426529792314,
0.005108258536307,0.00522225177469086,0.00533624501307472,0.00556423148984244,
0.0056782247282263,0.00579221796661016,0.00590621120499402,0.00602020444337788,
0.00613419768176174,0.0062481909201456,0.00647617739691333,0.00659017063529719,
0.00670416387368105,0.00681815711206491,0.00693215035044876,0.00716013682721649,
0.00727413006560035,0.00738812330398421,0.00761610978075193,0.00784409625751965,
0.00795808949590351,0.00807208273428737,0.0081290793534793,0.00818607597267123,
0.00830006921105509,0.00852805568782281,0.00864204892620667,0.00875604216459053,
0.00887003540297439,0.00898402864135825,0.00921201511812597,0.00944000159489369,
0.00955399483327755,0.00966798807166141,0.00978198131004527,0.00989597454842913,
0.0101239610251968,0.0102379542635807,0.0103519475019646,0.0104659407403484,
0.0105799339787323,0.0106939272171161,0.0108079204555,0.0109219136938839,
0.0110359069322677,0.0111499001706516,0.0112638934090355,0.0114918798858032,
0.0117198663625709,0.0118338596009548,0.0118908562201467,0.0119478528393386,
0.0120618460777225,0.0121758393161063,0.0124038257928741,0.0125178190312579,
0.0126318122696418,0.0127458055080256,0.0129737919847934,0.0130877852231772,
0.0133157716999449,0.0134297649383288,0.0134867615575207,0.0135437581767127,
0.0137717446534804,0.0139997311302481,0.0142277176070158,0.0142847142262077,
0.0143417108453997,0.0144557040837835),.UNSPECIFIED.);
#969=B_SPLINE_SURFACE_WITH_KNOTS('',1,3,((#263107,#263108,#263109,#263110,
#263111,#263112,#263113,#263114,#263115,#263116,#263117,#263118,#263119,
#263120,#263121,#263122,#263123,#263124,#263125,#263126,#263127,#263128,
#263129,#263130,#263131,#263132,#263133,#263134,#263135,#263136,#263137,
#263138,#263139,#263140,#263141,#263142,#263143,#263144,#263145,#263146,
#263147,#263148,#263149,#263150,#263151,#263152,#263153,#263154,#263155,
#263156,#263157,#263158,#263159,#263160,#263161,#263162,#263163,#263164,
#263165,#263166,#263167,#263168,#263169,#263170,#263171,#263172,#263173,
#263174,#263175,#263176,#263177,#263178,#263179,#263180,#263181,#263182,
#263183,#263184,#263185,#263186,#263187,#263188,#263189,#263190,#263191,
#263192,#263193,#263194,#263195,#263196,#263197,#263198,#263199,#263200,
#263201,#263202,#263203,#263204,#263205,#263206,#263207,#263208,#263209,
#263210,#263211,#263212,#263213,#263214,#263215,#263216,#263217,#263218,
#263219,#263220,#263221,#263222,#263223,#263224,#263225,#263226,#263227,
#263228,#263229,#263230,#263231,#263232,#263233,#263234,#263235,#263236,
#263237,#263238,#263239,#263240,#263241,#263242,#263243,#263244,#263245,
#263246,#263247,#263248,#263249,#263250,#263251,#263252,#263253,#263254,
#263255,#263256,#263257,#263258,#263259,#263260,#263261,#263262,#263263,
#263264,#263265,#263266,#263267,#263268,#263269,#263270,#263271,#263272,
#263273,#263274,#263275,#263276,#263277,#263278,#263279,#263280,#263281),
(#263282,#263283,#263284,#263285,#263286,#263287,#263288,#263289,#263290,
#263291,#263292,#263293,#263294,#263295,#263296,#263297,#263298,#263299,
#263300,#263301,#263302,#263303,#263304,#263305,#263306,#263307,#263308,
#263309,#263310,#263311,#263312,#263313,#263314,#263315,#263316,#263317,
#263318,#263319,#263320,#263321,#263322,#263323,#263324,#263325,#263326,
#263327,#263328,#263329,#263330,#263331,#263332,#263333,#263334,#263335,
#263336,#263337,#263338,#263339,#263340,#263341,#263342,#263343,#263344,
#263345,#263346,#263347,#263348,#263349,#263350,#263351,#263352,#263353,
#263354,#263355,#263356,#263357,#263358,#263359,#263360,#263361,#263362,
#263363,#263364,#263365,#263366,#263367,#263368,#263369,#263370,#263371,
#263372,#263373,#263374,#263375,#263376,#263377,#263378,#263379,#263380,
#263381,#263382,#263383,#263384,#263385,#263386,#263387,#263388,#263389,
#263390,#263391,#263392,#263393,#263394,#263395,#263396,#263397,#263398,
#263399,#263400,#263401,#263402,#263403,#263404,#263405,#263406,#263407,
#263408,#263409,#263410,#263411,#263412,#263413,#263414,#263415,#263416,
#263417,#263418,#263419,#263420,#263421,#263422,#263423,#263424,#263425,
#263426,#263427,#263428,#263429,#263430,#263431,#263432,#263433,#263434,
#263435,#263436,#263437,#263438,#263439,#263440,#263441,#263442,#263443,
#263444,#263445,#263446,#263447,#263448,#263449,#263450,#263451,#263452,
#263453,#263454,#263455,#263456)),.UNSPECIFIED.,.F.,.T.,.F.,(2,2),(4,1,
1,2,1,1,1,1,2,2,1,2,2,2,2,1,1,2,2,2,1,1,1,1,2,2,2,2,2,2,2,2,1,1,1,2,2,2,
2,1,1,1,2,2,2,1,1,1,2,2,2,2,2,2,2,1,2,2,2,2,2,1,1,2,2,2,2,1,2,2,2,1,1,2,
2,2,1,1,1,1,2,2,2,2,2,2,2,1,2,1,1,2,2,2,1,2,2,2,2,2,1,2,2,2,2,4),(0.,5.46382276754873),
(-0.000135430429350568,9.25560474171526E-5,0.000320542524184873,0.000548529000952593,
0.000776515477720314,0.00100450195448803,0.00111849519287189,0.00123248843125575,
0.00134648166963961,0.00146047490802347,0.0016884613847912,0.00191644786155891,
0.00203044109994277,0.00214443433832664,0.00225842757671049,0.00237242081509435,
0.00260040729186208,0.00271440053024594,0.0028283937686298,0.00294238700701366,
0.00305638024539752,0.00317037348378138,0.00328436672216524,0.0033983599605491,
0.00351235319893296,0.00362634643731682,0.00374033967570068,0.0039683261524684,
0.00419631262923612,0.00431030586761998,0.00436730248681191,0.00442429910600384,
0.0045382923443877,0.00465228558277156,0.00488027205953928,0.00499426529792314,
0.005108258536307,0.00522225177469086,0.00533624501307472,0.00556423148984244,
0.0056782247282263,0.00579221796661016,0.00590621120499402,0.00602020444337788,
0.00613419768176174,0.0062481909201456,0.00647617739691333,0.00659017063529719,
0.00670416387368105,0.00681815711206491,0.00693215035044876,0.00716013682721649,
0.00727413006560035,0.00738812330398421,0.00761610978075193,0.00784409625751965,
0.00795808949590351,0.00807208273428737,0.0081290793534793,0.00818607597267123,
0.00830006921105509,0.00852805568782281,0.00864204892620667,0.00875604216459053,
0.00887003540297439,0.00898402864135825,0.00921201511812597,0.00944000159489369,
0.00955399483327755,0.00966798807166141,0.00978198131004527,0.00989597454842913,
0.0101239610251968,0.0102379542635807,0.0103519475019646,0.0104659407403484,
0.0105799339787323,0.0106939272171161,0.0108079204555,0.0109219136938839,
0.0110359069322677,0.0111499001706516,0.0112638934090355,0.0114918798858032,
0.0117198663625709,0.0118338596009548,0.0118908562201467,0.0119478528393386,
0.0120618460777225,0.0121758393161063,0.0124038257928741,0.0125178190312579,
0.0126318122696418,0.0127458055080256,0.0129737919847934,0.0130877852231772,
0.0133157716999449,0.0134297649383288,0.0134867615575207,0.0135437581767127,
0.0137717446534804,0.0139997311302481,0.0142277176070158,0.0142847142262077,
0.0143417108453997,0.0144557040837835),.UNSPECIFIED.);
#970=B_SPLINE_SURFACE_WITH_KNOTS('',1,3,((#263501,#263502,#263503,#263504,
#263505,#263506,#263507,#263508,#263509,#263510,#263511,#263512,#263513,
#263514,#263515,#263516,#263517,#263518,#263519,#263520,#263521,#263522,
#263523,#263524,#263525,#263526,#263527,#263528,#263529,#263530,#263531,
#263532,#263533,#263534,#263535,#263536,#263537,#263538,#263539,#263540,
#263541,#263542,#263543,#263544,#263545,#263546,#263547,#263548,#263549,
#263550,#263551,#263552,#263553,#263554,#263555,#263556,#263557,#263558,
#263559,#263560,#263561,#263562,#263563,#263564,#263565,#263566,#263567,
#263568,#263569,#263570,#263571,#263572,#263573,#263574,#263575,#263576,
#263577,#263578,#263579,#263580,#263581,#263582,#263583,#263584,#263585,
#263586,#263587,#263588,#263589,#263590,#263591,#263592,#263593,#263594,
#263595,#263596,#263597,#263598,#263599,#263600,#263601,#263602,#263603,
#263604,#263605,#263606,#263607,#263608,#263609,#263610,#263611,#263612,
#263613,#263614,#263615,#263616,#263617,#263618,#263619,#263620,#263621,
#263622,#263623,#263624,#263625,#263626,#263627,#263628,#263629,#263630,
#263631,#263632,#263633,#263634,#263635,#263636,#263637,#263638,#263639,
#263640,#263641,#263642,#263643,#263644,#263645,#263646,#263647,#263648,
#263649,#263650,#263651,#263652,#263653,#263654,#263655,#263656,#263657,
#263658,#263659,#263660,#263661,#263662,#263663,#263664,#263665,#263666,
#263667,#263668,#263669,#263670,#263671,#263672,#263673,#263674,#263675),
(#263676,#263677,#263678,#263679,#263680,#263681,#263682,#263683,#263684,
#263685,#263686,#263687,#263688,#263689,#263690,#263691,#263692,#263693,
#263694,#263695,#263696,#263697,#263698,#263699,#263700,#263701,#263702,
#263703,#263704,#263705,#263706,#263707,#263708,#263709,#263710,#263711,
#263712,#263713,#263714,#263715,#263716,#263717,#263718,#263719,#263720,
#263721,#263722,#263723,#263724,#263725,#263726,#263727,#263728,#263729,
#263730,#263731,#263732,#263733,#263734,#263735,#263736,#263737,#263738,
#263739,#263740,#263741,#263742,#263743,#263744,#263745,#263746,#263747,
#263748,#263749,#263750,#263751,#263752,#263753,#263754,#263755,#263756,
#263757,#263758,#263759,#263760,#263761,#263762,#263763,#263764,#263765,
#263766,#263767,#263768,#263769,#263770,#263771,#263772,#263773,#263774,
#263775,#263776,#263777,#263778,#263779,#263780,#263781,#263782,#263783,
#263784,#263785,#263786,#263787,#263788,#263789,#263790,#263791,#263792,
#263793,#263794,#263795,#263796,#263797,#263798,#263799,#263800,#263801,
#263802,#263803,#263804,#263805,#263806,#263807,#263808,#263809,#263810,
#263811,#263812,#263813,#263814,#263815,#263816,#263817,#263818,#263819,
#263820,#263821,#263822,#263823,#263824,#263825,#263826,#263827,#263828,
#263829,#263830,#263831,#263832,#263833,#263834,#263835,#263836,#263837,
#263838,#263839,#263840,#263841,#263842,#263843,#263844,#263845,#263846,
#263847,#263848,#263849,#263850)),.UNSPECIFIED.,.F.,.T.,.F.,(2,2),(4,1,
1,2,1,1,1,1,2,2,1,2,2,2,2,1,1,2,2,2,1,1,1,1,2,2,2,2,2,2,2,2,1,1,1,2,2,2,
2,1,1,1,2,2,2,1,1,1,2,2,2,2,2,2,2,1,2,2,2,2,2,1,1,2,2,2,2,1,2,2,2,1,1,2,
2,2,1,1,1,1,2,2,2,2,2,2,2,1,2,1,1,2,2,2,1,2,2,2,2,2,1,2,2,2,2,4),(0.,5.46382276754873),
(-0.000135430429350568,9.25560474171526E-5,0.000320542524184873,0.000548529000952593,
0.000776515477720314,0.00100450195448803,0.00111849519287189,0.00123248843125575,
0.00134648166963961,0.00146047490802347,0.0016884613847912,0.00191644786155891,
0.00203044109994277,0.00214443433832664,0.00225842757671049,0.00237242081509435,
0.00260040729186208,0.00271440053024594,0.0028283937686298,0.00294238700701366,
0.00305638024539752,0.00317037348378138,0.00328436672216524,0.0033983599605491,
0.00351235319893296,0.00362634643731682,0.00374033967570068,0.0039683261524684,
0.00419631262923612,0.00431030586761998,0.00436730248681191,0.00442429910600384,
0.0045382923443877,0.00465228558277156,0.00488027205953928,0.00499426529792314,
0.005108258536307,0.00522225177469086,0.00533624501307472,0.00556423148984244,
0.0056782247282263,0.00579221796661016,0.00590621120499402,0.00602020444337788,
0.00613419768176174,0.0062481909201456,0.00647617739691333,0.00659017063529719,
0.00670416387368105,0.00681815711206491,0.00693215035044876,0.00716013682721649,
0.00727413006560035,0.00738812330398421,0.00761610978075193,0.00784409625751965,
0.00795808949590351,0.00807208273428737,0.0081290793534793,0.00818607597267123,
0.00830006921105509,0.00852805568782281,0.00864204892620667,0.00875604216459053,
0.00887003540297439,0.00898402864135825,0.00921201511812597,0.00944000159489369,
0.00955399483327755,0.00966798807166141,0.00978198131004527,0.00989597454842913,
0.0101239610251968,0.0102379542635807,0.0103519475019646,0.0104659407403484,
0.0105799339787323,0.0106939272171161,0.0108079204555,0.0109219136938839,
0.0110359069322677,0.0111499001706516,0.0112638934090355,0.0114918798858032,
0.0117198663625709,0.0118338596009548,0.0118908562201467,0.0119478528393386,
0.0120618460777225,0.0121758393161063,0.0124038257928741,0.0125178190312579,
0.0126318122696418,0.0127458055080256,0.0129737919847934,0.0130877852231772,
0.0133157716999449,0.0134297649383288,0.0134867615575207,0.0135437581767127,
0.0137717446534804,0.0139997311302481,0.0142277176070158,0.0142847142262077,
0.0143417108453997,0.0144557040837835),.UNSPECIFIED.);
#971=B_SPLINE_SURFACE_WITH_KNOTS('',1,3,((#263926,#263927,#263928,#263929,
#263930,#263931,#263932,#263933,#263934,#263935,#263936,#263937,#263938,
#263939,#263940,#263941,#263942,#263943,#263944,#263945,#263946,#263947,
#263948,#263949,#263950,#263951,#263952,#263953,#263954,#263955,#263956,
#263957,#263958,#263959,#263960,#263961,#263962,#263963,#263964,#263965,
#263966,#263967,#263968,#263969,#263970,#263971,#263972,#263973,#263974,
#263975,#263976,#263977,#263978,#263979,#263980,#263981,#263982,#263983,
#263984,#263985,#263986,#263987,#263988,#263989,#263990,#263991,#263992,
#263993,#263994,#263995,#263996,#263997,#263998,#263999,#264000,#264001,
#264002,#264003,#264004,#264005,#264006,#264007,#264008,#264009,#264010,
#264011,#264012,#264013,#264014,#264015,#264016,#264017,#264018,#264019,
#264020,#264021,#264022,#264023,#264024,#264025,#264026,#264027,#264028,
#264029,#264030,#264031,#264032,#264033,#264034,#264035,#264036,#264037,
#264038,#264039,#264040,#264041,#264042,#264043,#264044,#264045,#264046,
#264047,#264048,#264049,#264050,#264051,#264052,#264053,#264054,#264055,
#264056,#264057,#264058,#264059,#264060,#264061,#264062,#264063,#264064,
#264065,#264066,#264067,#264068,#264069,#264070,#264071,#264072,#264073,
#264074,#264075,#264076,#264077,#264078,#264079,#264080,#264081,#264082,
#264083,#264084,#264085,#264086,#264087,#264088,#264089,#264090,#264091,
#264092,#264093,#264094,#264095,#264096,#264097,#264098,#264099,#264100,
#264101,#264102,#264103,#264104,#264105,#264106,#264107,#264108,#264109,
#264110,#264111,#264112,#264113,#264114,#264115,#264116,#264117,#264118,
#264119,#264120,#264121,#264122,#264123,#264124,#264125,#264126,#264127,
#264128,#264129,#264130,#264131,#264132,#264133,#264134,#264135,#264136,
#264137,#264138,#264139,#264140,#264141,#264142,#264143,#264144,#264145,
#264146,#264147,#264148,#264149),(#264150,#264151,#264152,#264153,#264154,
#264155,#264156,#264157,#264158,#264159,#264160,#264161,#264162,#264163,
#264164,#264165,#264166,#264167,#264168,#264169,#264170,#264171,#264172,
#264173,#264174,#264175,#264176,#264177,#264178,#264179,#264180,#264181,
#264182,#264183,#264184,#264185,#264186,#264187,#264188,#264189,#264190,
#264191,#264192,#264193,#264194,#264195,#264196,#264197,#264198,#264199,
#264200,#264201,#264202,#264203,#264204,#264205,#264206,#264207,#264208,
#264209,#264210,#264211,#264212,#264213,#264214,#264215,#264216,#264217,
#264218,#264219,#264220,#264221,#264222,#264223,#264224,#264225,#264226,
#264227,#264228,#264229,#264230,#264231,#264232,#264233,#264234,#264235,
#264236,#264237,#264238,#264239,#264240,#264241,#264242,#264243,#264244,
#264245,#264246,#264247,#264248,#264249,#264250,#264251,#264252,#264253,
#264254,#264255,#264256,#264257,#264258,#264259,#264260,#264261,#264262,
#264263,#264264,#264265,#264266,#264267,#264268,#264269,#264270,#264271,
#264272,#264273,#264274,#264275,#264276,#264277,#264278,#264279,#264280,
#264281,#264282,#264283,#264284,#264285,#264286,#264287,#264288,#264289,
#264290,#264291,#264292,#264293,#264294,#264295,#264296,#264297,#264298,
#264299,#264300,#264301,#264302,#264303,#264304,#264305,#264306,#264307,
#264308,#264309,#264310,#264311,#264312,#264313,#264314,#264315,#264316,
#264317,#264318,#264319,#264320,#264321,#264322,#264323,#264324,#264325,
#264326,#264327,#264328,#264329,#264330,#264331,#264332,#264333,#264334,
#264335,#264336,#264337,#264338,#264339,#264340,#264341,#264342,#264343,
#264344,#264345,#264346,#264347,#264348,#264349,#264350,#264351,#264352,
#264353,#264354,#264355,#264356,#264357,#264358,#264359,#264360,#264361,
#264362,#264363,#264364,#264365,#264366,#264367,#264368,#264369,#264370,
#264371,#264372,#264373)),.UNSPECIFIED.,.F.,.T.,.F.,(2,2),(4,2,2,2,2,2,
2,2,2,2,2,2,2,2,2,2,2,2,2,2,2,2,2,2,2,2,2,2,2,2,2,2,2,2,2,2,2,2,2,2,2,2,
2,2,2,2,2,2,2,2,2,2,2,2,2,2,2,2,2,2,2,2,2,2,2,2,2,2,2,2,2,2,2,2,2,2,2,2,
2,2,2,2,2,2,2,2,2,2,2,2,2,2,2,2,2,2,2,2,2,2,2,2,2,2,2,2,2,2,2,2,2,4),(-1.37747249376985E-7,
1.00000777338949),(-0.000135430429350568,-2.14371909667077E-5,9.25560474171526E-5,
0.000320542524184873,0.000548529000952593,0.000776515477720314,0.00100450195448803,
0.00111849519287189,0.00123248843125575,0.00134648166963961,0.00146047490802347,
0.00157446814640733,0.0016884613847912,0.00191644786155891,0.00203044109994277,
0.00214443433832664,0.00225842757671049,0.00237242081509435,0.00260040729186208,
0.00271440053024594,0.0028283937686298,0.00294238700701366,0.00305638024539752,
0.00317037348378138,0.00328436672216524,0.0033983599605491,0.00351235319893296,
0.00362634643731682,0.00374033967570068,0.0039683261524684,0.00419631262923612,
0.00431030586761998,0.00436730248681191,0.00442429910600384,0.0045382923443877,
0.00465228558277156,0.00488027205953928,0.00499426529792314,0.005108258536307,
0.00522225177469086,0.00533624501307472,0.00545023825145858,0.00556423148984244,
0.0056782247282263,0.00579221796661016,0.00590621120499402,0.00602020444337788,
0.00613419768176174,0.0062481909201456,0.00647617739691333,0.00659017063529719,
0.00670416387368105,0.00681815711206491,0.00693215035044876,0.00704614358883263,
0.00716013682721649,0.00727413006560035,0.00738812330398421,0.00761610978075193,
0.00784409625751965,0.00795808949590351,0.00807208273428737,0.0081290793534793,
0.00818607597267123,0.00830006921105509,0.00852805568782281,0.00864204892620667,
0.00875604216459053,0.00887003540297439,0.00898402864135825,0.00921201511812597,
0.00944000159489369,0.00955399483327755,0.00966798807166141,0.00978198131004527,
0.00989597454842913,0.0101239610251968,0.0102379542635807,0.0103519475019646,
0.0104659407403484,0.0105799339787323,0.0106939272171161,0.0108079204555,
0.0109219136938839,0.0110359069322677,0.0111499001706516,0.0112638934090355,
0.0114918798858032,0.0117198663625709,0.0118338596009548,0.0118908562201467,
0.0119478528393386,0.0120618460777225,0.0121758393161063,0.0124038257928741,
0.0125178190312579,0.0126318122696418,0.0127458055080256,0.0128597987464095,
0.0129737919847934,0.0130877852231772,0.0133157716999449,0.0134297649383288,
0.0134867615575207,0.0135437581767127,0.0136577514150965,0.0137717446534804,
0.0139997311302481,0.0142277176070158,0.0142847142262077,0.0143417108453997,
0.0144557040837835),.UNSPECIFIED.);
#972=B_SPLINE_SURFACE_WITH_KNOTS('',1,3,((#266971,#266972,#266973,#266974,
#266975,#266976,#266977,#266978,#266979,#266980,#266981,#266982,#266983,
#266984,#266985,#266986,#266987,#266988,#266989,#266990,#266991,#266992,
#266993,#266994,#266995,#266996,#266997,#266998,#266999,#267000,#267001,
#267002,#267003,#267004,#267005,#267006,#267007,#267008,#267009,#267010,
#267011,#267012,#267013,#267014,#267015,#267016,#267017,#267018,#267019,
#267020,#267021,#267022,#267023,#267024,#267025,#267026,#267027,#267028,
#267029,#267030,#267031,#267032,#267033,#267034,#267035,#267036,#267037,
#267038,#267039,#267040,#267041,#267042,#267043,#267044,#267045,#267046,
#267047,#267048,#267049,#267050,#267051,#267052,#267053,#267054,#267055,
#267056,#267057,#267058,#267059,#267060,#267061,#267062,#267063,#267064,
#267065,#267066,#267067,#267068,#267069,#267070,#267071,#267072,#267073,
#267074,#267075,#267076,#267077,#267078,#267079,#267080,#267081,#267082,
#267083,#267084,#267085,#267086,#267087,#267088,#267089,#267090,#267091,
#267092,#267093,#267094,#267095,#267096,#267097,#267098,#267099,#267100,
#267101,#267102,#267103,#267104,#267105,#267106,#267107,#267108,#267109,
#267110,#267111,#267112,#267113,#267114,#267115,#267116,#267117,#267118,
#267119,#267120,#267121,#267122,#267123,#267124,#267125,#267126,#267127,
#267128,#267129,#267130,#267131,#267132,#267133,#267134,#267135,#267136,
#267137,#267138,#267139,#267140,#267141,#267142,#267143,#267144,#267145,
#267146,#267147,#267148,#267149,#267150,#267151,#267152,#267153,#267154,
#267155,#267156,#267157,#267158,#267159,#267160,#267161,#267162,#267163,
#267164,#267165,#267166,#267167,#267168,#267169,#267170,#267171,#267172,
#267173,#267174,#267175,#267176,#267177,#267178,#267179,#267180,#267181,
#267182,#267183,#267184,#267185,#267186,#267187,#267188,#267189,#267190,
#267191,#267192,#267193,#267194),(#267195,#267196,#267197,#267198,#267199,
#267200,#267201,#267202,#267203,#267204,#267205,#267206,#267207,#267208,
#267209,#267210,#267211,#267212,#267213,#267214,#267215,#267216,#267217,
#267218,#267219,#267220,#267221,#267222,#267223,#267224,#267225,#267226,
#267227,#267228,#267229,#267230,#267231,#267232,#267233,#267234,#267235,
#267236,#267237,#267238,#267239,#267240,#267241,#267242,#267243,#267244,
#267245,#267246,#267247,#267248,#267249,#267250,#267251,#267252,#267253,
#267254,#267255,#267256,#267257,#267258,#267259,#267260,#267261,#267262,
#267263,#267264,#267265,#267266,#267267,#267268,#267269,#267270,#267271,
#267272,#267273,#267274,#267275,#267276,#267277,#267278,#267279,#267280,
#267281,#267282,#267283,#267284,#267285,#267286,#267287,#267288,#267289,
#267290,#267291,#267292,#267293,#267294,#267295,#267296,#267297,#267298,
#267299,#267300,#267301,#267302,#267303,#267304,#267305,#267306,#267307,
#267308,#267309,#267310,#267311,#267312,#267313,#267314,#267315,#267316,
#267317,#267318,#267319,#267320,#267321,#267322,#267323,#267324,#267325,
#267326,#267327,#267328,#267329,#267330,#267331,#267332,#267333,#267334,
#267335,#267336,#267337,#267338,#267339,#267340,#267341,#267342,#267343,
#267344,#267345,#267346,#267347,#267348,#267349,#267350,#267351,#267352,
#267353,#267354,#267355,#267356,#267357,#267358,#267359,#267360,#267361,
#267362,#267363,#267364,#267365,#267366,#267367,#267368,#267369,#267370,
#267371,#267372,#267373,#267374,#267375,#267376,#267377,#267378,#267379,
#267380,#267381,#267382,#267383,#267384,#267385,#267386,#267387,#267388,
#267389,#267390,#267391,#267392,#267393,#267394,#267395,#267396,#267397,
#267398,#267399,#267400,#267401,#267402,#267403,#267404,#267405,#267406,
#267407,#267408,#267409,#267410,#267411,#267412,#267413,#267414,#267415,
#267416,#267417,#267418)),.UNSPECIFIED.,.F.,.T.,.F.,(2,2),(4,2,2,2,2,2,
2,2,2,2,2,2,2,2,2,2,2,2,2,2,2,2,2,2,2,2,2,2,2,2,2,2,2,2,2,2,2,2,2,2,2,2,
2,2,2,2,2,2,2,2,2,2,2,2,2,2,2,2,2,2,2,2,2,2,2,2,2,2,2,2,2,2,2,2,2,2,2,2,
2,2,2,2,2,2,2,2,2,2,2,2,2,2,2,2,2,2,2,2,2,2,2,2,2,2,2,2,2,2,2,2,2,4),(-3.14488534446183E-8,
1.00000561805477),(-0.000135430429350568,-2.14371909667077E-5,9.25560474171526E-5,
0.000320542524184873,0.000548529000952593,0.000776515477720314,0.00100450195448803,
0.00111849519287189,0.00123248843125575,0.00134648166963961,0.00146047490802347,
0.00157446814640733,0.0016884613847912,0.00191644786155891,0.00203044109994277,
0.00214443433832664,0.00225842757671049,0.00237242081509435,0.00260040729186208,
0.00271440053024594,0.0028283937686298,0.00294238700701366,0.00305638024539752,
0.00317037348378138,0.00328436672216524,0.0033983599605491,0.00351235319893296,
0.00362634643731682,0.00374033967570068,0.0039683261524684,0.00419631262923612,
0.00431030586761998,0.00436730248681191,0.00442429910600384,0.0045382923443877,
0.00465228558277156,0.00488027205953928,0.00499426529792314,0.005108258536307,
0.00522225177469086,0.00533624501307472,0.00545023825145858,0.00556423148984244,
0.0056782247282263,0.00579221796661016,0.00590621120499402,0.00602020444337788,
0.00613419768176174,0.0062481909201456,0.00647617739691333,0.00659017063529719,
0.00670416387368105,0.00681815711206491,0.00693215035044876,0.00704614358883263,
0.00716013682721649,0.00727413006560035,0.00738812330398421,0.00761610978075193,
0.00784409625751965,0.00795808949590351,0.00807208273428737,0.0081290793534793,
0.00818607597267123,0.00830006921105509,0.00852805568782281,0.00864204892620667,
0.00875604216459053,0.00887003540297439,0.00898402864135825,0.00921201511812597,
0.00944000159489369,0.00955399483327755,0.00966798807166141,0.00978198131004527,
0.00989597454842913,0.0101239610251968,0.0102379542635807,0.0103519475019646,
0.0104659407403484,0.0105799339787323,0.0106939272171161,0.0108079204555,
0.0109219136938839,0.0110359069322677,0.0111499001706516,0.0112638934090355,
0.0114918798858032,0.0117198663625709,0.0118338596009548,0.0118908562201467,
0.0119478528393386,0.0120618460777225,0.0121758393161063,0.0124038257928741,
0.0125178190312579,0.0126318122696418,0.0127458055080256,0.0128597987464095,
0.0129737919847934,0.0130877852231772,0.0133157716999449,0.0134297649383288,
0.0134867615575207,0.0135437581767127,0.0136577514150965,0.0137717446534804,
0.0139997311302481,0.0142277176070158,0.0142847142262077,0.0143417108453997,
0.0144557040837835),.UNSPECIFIED.);
#973=B_SPLINE_SURFACE_WITH_KNOTS('',1,3,((#267480,#267481,#267482,#267483,
#267484,#267485,#267486,#267487,#267488,#267489,#267490,#267491,#267492,
#267493,#267494,#267495,#267496,#267497,#267498,#267499,#267500,#267501,
#267502,#267503,#267504,#267505,#267506,#267507,#267508,#267509,#267510,
#267511,#267512,#267513,#267514,#267515,#267516,#267517,#267518,#267519,
#267520,#267521,#267522,#267523,#267524,#267525,#267526,#267527,#267528,
#267529,#267530,#267531,#267532,#267533,#267534,#267535,#267536,#267537,
#267538,#267539,#267540,#267541,#267542,#267543,#267544,#267545,#267546,
#267547,#267548,#267549,#267550,#267551,#267552,#267553,#267554,#267555,
#267556,#267557,#267558,#267559,#267560,#267561,#267562,#267563,#267564,
#267565,#267566,#267567,#267568,#267569,#267570,#267571,#267572,#267573,
#267574,#267575,#267576,#267577,#267578,#267579,#267580,#267581,#267582,
#267583,#267584,#267585,#267586,#267587,#267588,#267589,#267590,#267591,
#267592,#267593,#267594,#267595,#267596,#267597,#267598,#267599,#267600,
#267601,#267602,#267603,#267604,#267605,#267606,#267607,#267608,#267609,
#267610,#267611,#267612,#267613,#267614,#267615,#267616,#267617,#267618,
#267619,#267620,#267621,#267622,#267623,#267624,#267625,#267626,#267627,
#267628,#267629,#267630,#267631,#267632,#267633,#267634,#267635,#267636,
#267637,#267638,#267639,#267640,#267641,#267642,#267643,#267644,#267645,
#267646,#267647,#267648,#267649,#267650,#267651,#267652,#267653,#267654),
(#267655,#267656,#267657,#267658,#267659,#267660,#267661,#267662,#267663,
#267664,#267665,#267666,#267667,#267668,#267669,#267670,#267671,#267672,
#267673,#267674,#267675,#267676,#267677,#267678,#267679,#267680,#267681,
#267682,#267683,#267684,#267685,#267686,#267687,#267688,#267689,#267690,
#267691,#267692,#267693,#267694,#267695,#267696,#267697,#267698,#267699,
#267700,#267701,#267702,#267703,#267704,#267705,#267706,#267707,#267708,
#267709,#267710,#267711,#267712,#267713,#267714,#267715,#267716,#267717,
#267718,#267719,#267720,#267721,#267722,#267723,#267724,#267725,#267726,
#267727,#267728,#267729,#267730,#267731,#267732,#267733,#267734,#267735,
#267736,#267737,#267738,#267739,#267740,#267741,#267742,#267743,#267744,
#267745,#267746,#267747,#267748,#267749,#267750,#267751,#267752,#267753,
#267754,#267755,#267756,#267757,#267758,#267759,#267760,#267761,#267762,
#267763,#267764,#267765,#267766,#267767,#267768,#267769,#267770,#267771,
#267772,#267773,#267774,#267775,#267776,#267777,#267778,#267779,#267780,
#267781,#267782,#267783,#267784,#267785,#267786,#267787,#267788,#267789,
#267790,#267791,#267792,#267793,#267794,#267795,#267796,#267797,#267798,
#267799,#267800,#267801,#267802,#267803,#267804,#267805,#267806,#267807,
#267808,#267809,#267810,#267811,#267812,#267813,#267814,#267815,#267816,
#267817,#267818,#267819,#267820,#267821,#267822,#267823,#267824,#267825,
#267826,#267827,#267828,#267829)),.UNSPECIFIED.,.F.,.T.,.F.,(2,2),(4,1,
1,2,1,1,1,1,2,2,1,2,2,2,2,1,1,2,2,2,1,1,1,1,2,2,2,2,2,2,2,2,1,1,1,2,2,2,
2,1,1,1,2,2,2,1,1,1,2,2,2,2,2,2,2,1,2,2,2,2,2,1,1,2,2,2,2,1,2,2,2,1,1,2,
2,2,1,1,1,1,2,2,2,2,2,2,2,1,2,1,1,2,2,2,1,2,2,2,2,2,1,2,2,2,2,4),(0.,5.46382276754873),
(-0.000135430429350568,9.25560474171526E-5,0.000320542524184873,0.000548529000952593,
0.000776515477720314,0.00100450195448803,0.00111849519287189,0.00123248843125575,
0.00134648166963961,0.00146047490802347,0.0016884613847912,0.00191644786155891,
0.00203044109994277,0.00214443433832664,0.00225842757671049,0.00237242081509435,
0.00260040729186208,0.00271440053024594,0.0028283937686298,0.00294238700701366,
0.00305638024539752,0.00317037348378138,0.00328436672216524,0.0033983599605491,
0.00351235319893296,0.00362634643731682,0.00374033967570068,0.0039683261524684,
0.00419631262923612,0.00431030586761998,0.00436730248681191,0.00442429910600384,
0.0045382923443877,0.00465228558277156,0.00488027205953928,0.00499426529792314,
0.005108258536307,0.00522225177469086,0.00533624501307472,0.00556423148984244,
0.0056782247282263,0.00579221796661016,0.00590621120499402,0.00602020444337788,
0.00613419768176174,0.0062481909201456,0.00647617739691333,0.00659017063529719,
0.00670416387368105,0.00681815711206491,0.00693215035044876,0.00716013682721649,
0.00727413006560035,0.00738812330398421,0.00761610978075193,0.00784409625751965,
0.00795808949590351,0.00807208273428737,0.0081290793534793,0.00818607597267123,
0.00830006921105509,0.00852805568782281,0.00864204892620667,0.00875604216459053,
0.00887003540297439,0.00898402864135825,0.00921201511812597,0.00944000159489369,
0.00955399483327755,0.00966798807166141,0.00978198131004527,0.00989597454842913,
0.0101239610251968,0.0102379542635807,0.0103519475019646,0.0104659407403484,
0.0105799339787323,0.0106939272171161,0.0108079204555,0.0109219136938839,
0.0110359069322677,0.0111499001706516,0.0112638934090355,0.0114918798858032,
0.0117198663625709,0.0118338596009548,0.0118908562201467,0.0119478528393386,
0.0120618460777225,0.0121758393161063,0.0124038257928741,0.0125178190312579,
0.0126318122696418,0.0127458055080256,0.0129737919847934,0.0130877852231772,
0.0133157716999449,0.0134297649383288,0.0134867615575207,0.0135437581767127,
0.0137717446534804,0.0139997311302481,0.0142277176070158,0.0142847142262077,
0.0143417108453997,0.0144557040837835),.UNSPECIFIED.);
#974=B_SPLINE_SURFACE_WITH_KNOTS('',1,3,((#267830,#267831,#267832,#267833,
#267834,#267835,#267836,#267837,#267838,#267839,#267840,#267841,#267842,
#267843,#267844,#267845,#267846,#267847,#267848,#267849,#267850,#267851,
#267852,#267853,#267854,#267855,#267856,#267857,#267858,#267859,#267860,
#267861,#267862,#267863,#267864,#267865,#267866,#267867,#267868,#267869,
#267870,#267871,#267872,#267873,#267874,#267875,#267876,#267877,#267878,
#267879,#267880,#267881,#267882,#267883,#267884,#267885,#267886,#267887,
#267888,#267889,#267890,#267891,#267892,#267893,#267894,#267895,#267896,
#267897,#267898,#267899,#267900,#267901,#267902,#267903,#267904,#267905,
#267906,#267907,#267908,#267909,#267910,#267911,#267912,#267913,#267914,
#267915,#267916,#267917,#267918,#267919,#267920,#267921,#267922,#267923,
#267924,#267925,#267926,#267927,#267928,#267929,#267930,#267931,#267932,
#267933,#267934,#267935,#267936,#267937,#267938,#267939,#267940,#267941,
#267942,#267943,#267944,#267945,#267946,#267947,#267948,#267949,#267950,
#267951,#267952,#267953,#267954,#267955,#267956,#267957,#267958,#267959,
#267960,#267961,#267962,#267963,#267964,#267965,#267966,#267967,#267968,
#267969,#267970,#267971,#267972,#267973,#267974,#267975,#267976,#267977,
#267978,#267979,#267980,#267981,#267982,#267983,#267984,#267985,#267986,
#267987,#267988,#267989,#267990,#267991,#267992,#267993,#267994,#267995,
#267996,#267997,#267998,#267999,#268000,#268001,#268002,#268003,#268004),
(#268005,#268006,#268007,#268008,#268009,#268010,#268011,#268012,#268013,
#268014,#268015,#268016,#268017,#268018,#268019,#268020,#268021,#268022,
#268023,#268024,#268025,#268026,#268027,#268028,#268029,#268030,#268031,
#268032,#268033,#268034,#268035,#268036,#268037,#268038,#268039,#268040,
#268041,#268042,#268043,#268044,#268045,#268046,#268047,#268048,#268049,
#268050,#268051,#268052,#268053,#268054,#268055,#268056,#268057,#268058,
#268059,#268060,#268061,#268062,#268063,#268064,#268065,#268066,#268067,
#268068,#268069,#268070,#268071,#268072,#268073,#268074,#268075,#268076,
#268077,#268078,#268079,#268080,#268081,#268082,#268083,#268084,#268085,
#268086,#268087,#268088,#268089,#268090,#268091,#268092,#268093,#268094,
#268095,#268096,#268097,#268098,#268099,#268100,#268101,#268102,#268103,
#268104,#268105,#268106,#268107,#268108,#268109,#268110,#268111,#268112,
#268113,#268114,#268115,#268116,#268117,#268118,#268119,#268120,#268121,
#268122,#268123,#268124,#268125,#268126,#268127,#268128,#268129,#268130,
#268131,#268132,#268133,#268134,#268135,#268136,#268137,#268138,#268139,
#268140,#268141,#268142,#268143,#268144,#268145,#268146,#268147,#268148,
#268149,#268150,#268151,#268152,#268153,#268154,#268155,#268156,#268157,
#268158,#268159,#268160,#268161,#268162,#268163,#268164,#268165,#268166,
#268167,#268168,#268169,#268170,#268171,#268172,#268173,#268174,#268175,
#268176,#268177,#268178,#268179)),.UNSPECIFIED.,.F.,.T.,.F.,(2,2),(4,1,
1,2,1,1,1,1,2,2,1,2,2,2,2,1,1,2,2,2,1,1,1,1,2,2,2,2,2,2,2,2,1,1,1,2,2,2,
2,1,1,1,2,2,2,1,1,1,2,2,2,2,2,2,2,1,2,2,2,2,2,1,1,2,2,2,2,1,2,2,2,1,1,2,
2,2,1,1,1,1,2,2,2,2,2,2,2,1,2,1,1,2,2,2,1,2,2,2,2,2,1,2,2,2,2,4),(0.,5.46382276754873),
(-0.000135430429350568,9.25560474171526E-5,0.000320542524184873,0.000548529000952593,
0.000776515477720314,0.00100450195448803,0.00111849519287189,0.00123248843125575,
0.00134648166963961,0.00146047490802347,0.0016884613847912,0.00191644786155891,
0.00203044109994277,0.00214443433832664,0.00225842757671049,0.00237242081509435,
0.00260040729186208,0.00271440053024594,0.0028283937686298,0.00294238700701366,
0.00305638024539752,0.00317037348378138,0.00328436672216524,0.0033983599605491,
0.00351235319893296,0.00362634643731682,0.00374033967570068,0.0039683261524684,
0.00419631262923612,0.00431030586761998,0.00436730248681191,0.00442429910600384,
0.0045382923443877,0.00465228558277156,0.00488027205953928,0.00499426529792314,
0.005108258536307,0.00522225177469086,0.00533624501307472,0.00556423148984244,
0.0056782247282263,0.00579221796661016,0.00590621120499402,0.00602020444337788,
0.00613419768176174,0.0062481909201456,0.00647617739691333,0.00659017063529719,
0.00670416387368105,0.00681815711206491,0.00693215035044876,0.00716013682721649,
0.00727413006560035,0.00738812330398421,0.00761610978075193,0.00784409625751965,
0.00795808949590351,0.00807208273428737,0.0081290793534793,0.00818607597267123,
0.00830006921105509,0.00852805568782281,0.00864204892620667,0.00875604216459053,
0.00887003540297439,0.00898402864135825,0.00921201511812597,0.00944000159489369,
0.00955399483327755,0.00966798807166141,0.00978198131004527,0.00989597454842913,
0.0101239610251968,0.0102379542635807,0.0103519475019646,0.0104659407403484,
0.0105799339787323,0.0106939272171161,0.0108079204555,0.0109219136938839,
0.0110359069322677,0.0111499001706516,0.0112638934090355,0.0114918798858032,
0.0117198663625709,0.0118338596009548,0.0118908562201467,0.0119478528393386,
0.0120618460777225,0.0121758393161063,0.0124038257928741,0.0125178190312579,
0.0126318122696418,0.0127458055080256,0.0129737919847934,0.0130877852231772,
0.0133157716999449,0.0134297649383288,0.0134867615575207,0.0135437581767127,
0.0137717446534804,0.0139997311302481,0.0142277176070158,0.0142847142262077,
0.0143417108453997,0.0144557040837835),.UNSPECIFIED.);
#975=B_SPLINE_SURFACE_WITH_KNOTS('',1,3,((#268180,#268181,#268182,#268183,
#268184,#268185,#268186,#268187,#268188,#268189,#268190,#268191,#268192,
#268193,#268194,#268195,#268196,#268197,#268198,#268199,#268200,#268201,
#268202,#268203,#268204,#268205,#268206,#268207,#268208,#268209,#268210,
#268211,#268212,#268213,#268214,#268215,#268216,#268217,#268218,#268219,
#268220,#268221,#268222,#268223,#268224,#268225,#268226,#268227,#268228,
#268229,#268230,#268231,#268232,#268233,#268234,#268235,#268236,#268237,
#268238,#268239,#268240,#268241,#268242,#268243,#268244,#268245,#268246,
#268247,#268248,#268249,#268250,#268251,#268252,#268253,#268254,#268255,
#268256,#268257,#268258,#268259,#268260,#268261,#268262,#268263,#268264,
#268265,#268266,#268267,#268268,#268269,#268270,#268271,#268272,#268273,
#268274,#268275,#268276,#268277,#268278,#268279,#268280,#268281,#268282,
#268283,#268284,#268285,#268286,#268287,#268288,#268289,#268290,#268291),
(#268292,#268293,#268294,#268295,#268296,#268297,#268298,#268299,#268300,
#268301,#268302,#268303,#268304,#268305,#268306,#268307,#268308,#268309,
#268310,#268311,#268312,#268313,#268314,#268315,#268316,#268317,#268318,
#268319,#268320,#268321,#268322,#268323,#268324,#268325,#268326,#268327,
#268328,#268329,#268330,#268331,#268332,#268333,#268334,#268335,#268336,
#268337,#268338,#268339,#268340,#268341,#268342,#268343,#268344,#268345,
#268346,#268347,#268348,#268349,#268350,#268351,#268352,#268353,#268354,
#268355,#268356,#268357,#268358,#268359,#268360,#268361,#268362,#268363,
#268364,#268365,#268366,#268367,#268368,#268369,#268370,#268371,#268372,
#268373,#268374,#268375,#268376,#268377,#268378,#268379,#268380,#268381,
#268382,#268383,#268384,#268385,#268386,#268387,#268388,#268389,#268390,
#268391,#268392,#268393,#268394,#268395,#268396,#268397,#268398,#268399,
#268400,#268401,#268402,#268403)),.UNSPECIFIED.,.F.,.F.,.F.,(2,2),(4,2,
2,2,2,2,2,2,2,2,2,2,2,2,2,2,2,2,2,2,2,2,2,2,2,2,2,2,2,2,2,2,2,2,2,2,2,2,
2,2,2,2,2,2,2,2,2,2,2,2,2,2,2,2,2,4),(0.,1.),(-0.000135430429350568,-2.14371909667077E-5,
9.25560474171526E-5,0.000320542524184873,0.000548529000952593,0.000776515477720314,
0.00100450195448803,0.00111849519287189,0.00123248843125575,0.00134648166963961,
0.00146047490802347,0.00157446814640733,0.0016884613847912,0.00191644786155891,
0.00203044109994277,0.00214443433832664,0.00225842757671049,0.00237242081509435,
0.00260040729186208,0.00271440053024594,0.0028283937686298,0.00294238700701366,
0.00305638024539752,0.00317037348378138,0.00328436672216524,0.0033983599605491,
0.00351235319893296,0.00362634643731682,0.00374033967570068,0.0039683261524684,
0.00419631262923612,0.00431030586761998,0.00436730248681191,0.00442429910600384,
0.0045382923443877,0.00465228558277156,0.00488027205953928,0.00499426529792314,
0.005108258536307,0.00522225177469086,0.00533624501307472,0.00545023825145858,
0.00556423148984244,0.0056782247282263,0.00579221796661016,0.00590621120499402,
0.00602020444337788,0.00613419768176174,0.0062481909201456,0.00647617739691333,
0.00659017063529719,0.00670416387368105,0.00681815711206491,0.00693215035044876,
0.00704614358883263,0.00716013682721649),.UNSPECIFIED.);
#976=B_SPLINE_SURFACE_WITH_KNOTS('',1,3,((#268440,#268441,#268442,#268443,
#268444,#268445,#268446,#268447,#268448,#268449,#268450,#268451,#268452,
#268453,#268454,#268455,#268456,#268457,#268458,#268459,#268460,#268461,
#268462,#268463,#268464,#268465,#268466,#268467,#268468,#268469,#268470,
#268471,#268472,#268473,#268474,#268475,#268476,#268477,#268478,#268479,
#268480,#268481,#268482,#268483,#268484,#268485,#268486,#268487,#268488,
#268489,#268490,#268491,#268492,#268493,#268494,#268495,#268496,#268497,
#268498,#268499,#268500,#268501,#268502,#268503,#268504,#268505,#268506,
#268507,#268508,#268509,#268510,#268511,#268512,#268513,#268514,#268515,
#268516,#268517,#268518,#268519,#268520,#268521,#268522,#268523,#268524,
#268525,#268526,#268527,#268528,#268529,#268530,#268531,#268532,#268533,
#268534,#268535,#268536,#268537,#268538,#268539,#268540,#268541,#268542,
#268543,#268544,#268545,#268546,#268547,#268548,#268549,#268550,#268551,
#268552,#268553,#268554,#268555,#268556,#268557,#268558,#268559,#268560,
#268561,#268562,#268563,#268564,#268565,#268566,#268567,#268568,#268569,
#268570,#268571,#268572,#268573,#268574,#268575,#268576,#268577,#268578,
#268579,#268580,#268581,#268582,#268583,#268584,#268585,#268586,#268587,
#268588,#268589,#268590,#268591,#268592,#268593,#268594,#268595,#268596,
#268597,#268598,#268599,#268600,#268601,#268602,#268603,#268604,#268605,
#268606,#268607,#268608,#268609,#268610,#268611,#268612,#268613,#268614),
(#268615,#268616,#268617,#268618,#268619,#268620,#268621,#268622,#268623,
#268624,#268625,#268626,#268627,#268628,#268629,#268630,#268631,#268632,
#268633,#268634,#268635,#268636,#268637,#268638,#268639,#268640,#268641,
#268642,#268643,#268644,#268645,#268646,#268647,#268648,#268649,#268650,
#268651,#268652,#268653,#268654,#268655,#268656,#268657,#268658,#268659,
#268660,#268661,#268662,#268663,#268664,#268665,#268666,#268667,#268668,
#268669,#268670,#268671,#268672,#268673,#268674,#268675,#268676,#268677,
#268678,#268679,#268680,#268681,#268682,#268683,#268684,#268685,#268686,
#268687,#268688,#268689,#268690,#268691,#268692,#268693,#268694,#268695,
#268696,#268697,#268698,#268699,#268700,#268701,#268702,#268703,#268704,
#268705,#268706,#268707,#268708,#268709,#268710,#268711,#268712,#268713,
#268714,#268715,#268716,#268717,#268718,#268719,#268720,#268721,#268722,
#268723,#268724,#268725,#268726,#268727,#268728,#268729,#268730,#268731,
#268732,#268733,#268734,#268735,#268736,#268737,#268738,#268739,#268740,
#268741,#268742,#268743,#268744,#268745,#268746,#268747,#268748,#268749,
#268750,#268751,#268752,#268753,#268754,#268755,#268756,#268757,#268758,
#268759,#268760,#268761,#268762,#268763,#268764,#268765,#268766,#268767,
#268768,#268769,#268770,#268771,#268772,#268773,#268774,#268775,#268776,
#268777,#268778,#268779,#268780,#268781,#268782,#268783,#268784,#268785,
#268786,#268787,#268788,#268789)),.UNSPECIFIED.,.F.,.T.,.F.,(2,2),(4,1,
1,2,1,1,1,1,2,2,1,2,2,2,2,1,1,2,2,2,1,1,1,1,2,2,2,2,2,2,2,2,1,1,1,2,2,2,
2,1,1,1,2,2,2,1,1,1,2,2,2,2,2,2,2,1,2,2,2,2,2,1,1,2,2,2,2,1,2,2,2,1,1,2,
2,2,1,1,1,1,2,2,2,2,2,2,2,1,2,1,1,2,2,2,1,2,2,2,2,2,1,2,2,2,2,4),(0.,4.71475608888856),
(-0.000135430429350568,9.25560474171526E-5,0.000320542524184873,0.000548529000952593,
0.000776515477720314,0.00100450195448803,0.00111849519287189,0.00123248843125575,
0.00134648166963961,0.00146047490802347,0.0016884613847912,0.00191644786155891,
0.00203044109994277,0.00214443433832664,0.00225842757671049,0.00237242081509435,
0.00260040729186208,0.00271440053024594,0.0028283937686298,0.00294238700701366,
0.00305638024539752,0.00317037348378138,0.00328436672216524,0.0033983599605491,
0.00351235319893296,0.00362634643731682,0.00374033967570068,0.0039683261524684,
0.00419631262923612,0.00431030586761998,0.00436730248681191,0.00442429910600384,
0.0045382923443877,0.00465228558277156,0.00488027205953928,0.00499426529792314,
0.005108258536307,0.00522225177469086,0.00533624501307472,0.00556423148984244,
0.0056782247282263,0.00579221796661016,0.00590621120499402,0.00602020444337788,
0.00613419768176174,0.0062481909201456,0.00647617739691333,0.00659017063529719,
0.00670416387368105,0.00681815711206491,0.00693215035044876,0.00716013682721649,
0.00727413006560035,0.00738812330398421,0.00761610978075193,0.00784409625751965,
0.00795808949590351,0.00807208273428737,0.0081290793534793,0.00818607597267123,
0.00830006921105509,0.00852805568782281,0.00864204892620667,0.00875604216459053,
0.00887003540297439,0.00898402864135825,0.00921201511812597,0.00944000159489369,
0.00955399483327755,0.00966798807166141,0.00978198131004527,0.00989597454842913,
0.0101239610251968,0.0102379542635807,0.0103519475019646,0.0104659407403484,
0.0105799339787323,0.0106939272171161,0.0108079204555,0.0109219136938839,
0.0110359069322677,0.0111499001706516,0.0112638934090355,0.0114918798858032,
0.0117198663625709,0.0118338596009548,0.0118908562201467,0.0119478528393386,
0.0120618460777225,0.0121758393161063,0.0124038257928741,0.0125178190312579,
0.0126318122696418,0.0127458055080256,0.0129737919847934,0.0130877852231772,
0.0133157716999449,0.0134297649383288,0.0134867615575207,0.0135437581767127,
0.0137717446534804,0.0139997311302481,0.0142277176070158,0.0142847142262077,
0.0143417108453997,0.0144557040837835),.UNSPECIFIED.);
#977=B_SPLINE_SURFACE_WITH_KNOTS('',1,3,((#268791,#268792,#268793,#268794,
#268795,#268796,#268797,#268798,#268799,#268800,#268801,#268802,#268803,
#268804,#268805,#268806,#268807,#268808,#268809,#268810,#268811,#268812,
#268813,#268814,#268815,#268816,#268817,#268818,#268819,#268820,#268821,
#268822,#268823,#268824,#268825,#268826,#268827,#268828,#268829,#268830,
#268831,#268832,#268833,#268834,#268835,#268836,#268837,#268838,#268839,
#268840,#268841,#268842,#268843,#268844,#268845,#268846,#268847,#268848,
#268849,#268850,#268851,#268852,#268853,#268854,#268855,#268856,#268857,
#268858,#268859,#268860,#268861,#268862,#268863,#268864,#268865,#268866,
#268867,#268868,#268869,#268870,#268871,#268872,#268873,#268874,#268875,
#268876,#268877,#268878,#268879,#268880,#268881,#268882,#268883,#268884,
#268885,#268886,#268887,#268888,#268889,#268890,#268891,#268892,#268893,
#268894,#268895,#268896,#268897,#268898,#268899,#268900,#268901,#268902,
#268903,#268904,#268905,#268906,#268907,#268908,#268909,#268910,#268911,
#268912,#268913,#268914,#268915,#268916,#268917,#268918,#268919,#268920,
#268921,#268922,#268923,#268924,#268925,#268926,#268927,#268928,#268929,
#268930,#268931,#268932,#268933,#268934,#268935,#268936,#268937,#268938,
#268939,#268940,#268941,#268942,#268943,#268944,#268945,#268946,#268947,
#268948,#268949,#268950,#268951,#268952,#268953,#268954,#268955,#268956,
#268957,#268958,#268959,#268960,#268961,#268962,#268963,#268964,#268965),
(#268966,#268967,#268968,#268969,#268970,#268971,#268972,#268973,#268974,
#268975,#268976,#268977,#268978,#268979,#268980,#268981,#268982,#268983,
#268984,#268985,#268986,#268987,#268988,#268989,#268990,#268991,#268992,
#268993,#268994,#268995,#268996,#268997,#268998,#268999,#269000,#269001,
#269002,#269003,#269004,#269005,#269006,#269007,#269008,#269009,#269010,
#269011,#269012,#269013,#269014,#269015,#269016,#269017,#269018,#269019,
#269020,#269021,#269022,#269023,#269024,#269025,#269026,#269027,#269028,
#269029,#269030,#269031,#269032,#269033,#269034,#269035,#269036,#269037,
#269038,#269039,#269040,#269041,#269042,#269043,#269044,#269045,#269046,
#269047,#269048,#269049,#269050,#269051,#269052,#269053,#269054,#269055,
#269056,#269057,#269058,#269059,#269060,#269061,#269062,#269063,#269064,
#269065,#269066,#269067,#269068,#269069,#269070,#269071,#269072,#269073,
#269074,#269075,#269076,#269077,#269078,#269079,#269080,#269081,#269082,
#269083,#269084,#269085,#269086,#269087,#269088,#269089,#269090,#269091,
#269092,#269093,#269094,#269095,#269096,#269097,#269098,#269099,#269100,
#269101,#269102,#269103,#269104,#269105,#269106,#269107,#269108,#269109,
#269110,#269111,#269112,#269113,#269114,#269115,#269116,#269117,#269118,
#269119,#269120,#269121,#269122,#269123,#269124,#269125,#269126,#269127,
#269128,#269129,#269130,#269131,#269132,#269133,#269134,#269135,#269136,
#269137,#269138,#269139,#269140)),.UNSPECIFIED.,.F.,.T.,.F.,(2,2),(4,1,
1,2,1,1,1,1,2,2,1,2,2,2,2,1,1,2,2,2,1,1,1,1,2,2,2,2,2,2,2,2,1,1,1,2,2,2,
2,1,1,1,2,2,2,1,1,1,2,2,2,2,2,2,2,1,2,2,2,2,2,1,1,2,2,2,2,1,2,2,2,1,1,2,
2,2,1,1,1,1,2,2,2,2,2,2,2,1,2,1,1,2,2,2,1,2,2,2,2,2,1,2,2,2,2,4),(0.,4.71475608888856),
(-0.000135430429350568,9.25560474171526E-5,0.000320542524184873,0.000548529000952593,
0.000776515477720314,0.00100450195448803,0.00111849519287189,0.00123248843125575,
0.00134648166963961,0.00146047490802347,0.0016884613847912,0.00191644786155891,
0.00203044109994277,0.00214443433832664,0.00225842757671049,0.00237242081509435,
0.00260040729186208,0.00271440053024594,0.0028283937686298,0.00294238700701366,
0.00305638024539752,0.00317037348378138,0.00328436672216524,0.0033983599605491,
0.00351235319893296,0.00362634643731682,0.00374033967570068,0.0039683261524684,
0.00419631262923612,0.00431030586761998,0.00436730248681191,0.00442429910600384,
0.0045382923443877,0.00465228558277156,0.00488027205953928,0.00499426529792314,
0.005108258536307,0.00522225177469086,0.00533624501307472,0.00556423148984244,
0.0056782247282263,0.00579221796661016,0.00590621120499402,0.00602020444337788,
0.00613419768176174,0.0062481909201456,0.00647617739691333,0.00659017063529719,
0.00670416387368105,0.00681815711206491,0.00693215035044876,0.00716013682721649,
0.00727413006560035,0.00738812330398421,0.00761610978075193,0.00784409625751965,
0.00795808949590351,0.00807208273428737,0.0081290793534793,0.00818607597267123,
0.00830006921105509,0.00852805568782281,0.00864204892620667,0.00875604216459053,
0.00887003540297439,0.00898402864135825,0.00921201511812597,0.00944000159489369,
0.00955399483327755,0.00966798807166141,0.00978198131004527,0.00989597454842913,
0.0101239610251968,0.0102379542635807,0.0103519475019646,0.0104659407403484,
0.0105799339787323,0.0106939272171161,0.0108079204555,0.0109219136938839,
0.0110359069322677,0.0111499001706516,0.0112638934090355,0.0114918798858032,
0.0117198663625709,0.0118338596009548,0.0118908562201467,0.0119478528393386,
0.0120618460777225,0.0121758393161063,0.0124038257928741,0.0125178190312579,
0.0126318122696418,0.0127458055080256,0.0129737919847934,0.0130877852231772,
0.0133157716999449,0.0134297649383288,0.0134867615575207,0.0135437581767127,
0.0137717446534804,0.0139997311302481,0.0142277176070158,0.0142847142262077,
0.0143417108453997,0.0144557040837835),.UNSPECIFIED.);
#978=B_SPLINE_SURFACE_WITH_KNOTS('',1,3,((#269141,#269142,#269143,#269144,
#269145,#269146,#269147,#269148,#269149,#269150,#269151,#269152,#269153,
#269154,#269155,#269156,#269157,#269158,#269159,#269160,#269161,#269162,
#269163,#269164,#269165,#269166,#269167,#269168,#269169,#269170,#269171,
#269172,#269173,#269174,#269175,#269176,#269177,#269178,#269179,#269180,
#269181,#269182,#269183,#269184,#269185,#269186,#269187,#269188,#269189,
#269190,#269191,#269192,#269193,#269194,#269195,#269196,#269197,#269198,
#269199,#269200,#269201,#269202,#269203,#269204,#269205,#269206,#269207,
#269208,#269209,#269210,#269211,#269212,#269213,#269214,#269215,#269216,
#269217,#269218,#269219,#269220,#269221,#269222,#269223,#269224,#269225,
#269226,#269227,#269228,#269229,#269230,#269231,#269232,#269233,#269234,
#269235,#269236,#269237,#269238,#269239,#269240,#269241,#269242,#269243,
#269244,#269245,#269246,#269247,#269248,#269249,#269250,#269251,#269252),
(#269253,#269254,#269255,#269256,#269257,#269258,#269259,#269260,#269261,
#269262,#269263,#269264,#269265,#269266,#269267,#269268,#269269,#269270,
#269271,#269272,#269273,#269274,#269275,#269276,#269277,#269278,#269279,
#269280,#269281,#269282,#269283,#269284,#269285,#269286,#269287,#269288,
#269289,#269290,#269291,#269292,#269293,#269294,#269295,#269296,#269297,
#269298,#269299,#269300,#269301,#269302,#269303,#269304,#269305,#269306,
#269307,#269308,#269309,#269310,#269311,#269312,#269313,#269314,#269315,
#269316,#269317,#269318,#269319,#269320,#269321,#269322,#269323,#269324,
#269325,#269326,#269327,#269328,#269329,#269330,#269331,#269332,#269333,
#269334,#269335,#269336,#269337,#269338,#269339,#269340,#269341,#269342,
#269343,#269344,#269345,#269346,#269347,#269348,#269349,#269350,#269351,
#269352,#269353,#269354,#269355,#269356,#269357,#269358,#269359,#269360,
#269361,#269362,#269363,#269364)),.UNSPECIFIED.,.F.,.F.,.F.,(2,2),(4,2,
2,2,2,2,2,2,2,2,2,2,2,2,2,2,2,2,2,2,2,2,2,2,2,2,2,2,2,2,2,2,2,2,2,2,2,2,
2,2,2,2,2,2,2,2,2,2,2,2,2,2,2,2,2,4),(0.,1.),(-0.000118831294053002,-4.84197060393493E-6,
0.000109147352845132,0.000337125999743267,0.000451115323192334,0.000565104646641402,
0.000679093970090469,0.000793083293539536,0.00102106194043767,0.00113505126388674,
0.0012490405873358,0.00136302991078487,0.00142002457250941,0.00147701923423394,
0.00170499788113207,0.00193297652803021,0.00204696585147928,0.00216095517492835,
0.00227494449837741,0.00238893382182648,0.00261691246872462,0.00284489111562275,
0.00290188577734728,0.00295888043907182,0.00307286976252088,0.00318685908596995,
0.00330084840941902,0.00341483773286809,0.00352882705631715,0.00364281637976622,
0.00375680570321528,0.00387079502666435,0.00398478435011342,0.00421276299701156,
0.00444074164390969,0.00466872029080782,0.00489669893770596,0.00512467758460409,
0.00518167224632863,0.00523866690805316,0.00535265623150223,0.0054666455549513,
0.00558063487840036,0.00569462420184943,0.0058086135252985,0.00592260284874756,
0.00603659217219663,0.0061505814956457,0.00626457081909477,0.0064925494659929,
0.00660653878944197,0.00672052811289104,0.0068345174363401,0.00694850675978917,
0.00706249608323824,0.00717648540668731),.UNSPECIFIED.);
#979=B_SPLINE_SURFACE_WITH_KNOTS('',1,3,((#269442,#269443,#269444,#269445,
#269446,#269447,#269448,#269449,#269450,#269451,#269452,#269453,#269454,
#269455,#269456,#269457,#269458,#269459,#269460),(#269461,#269462,#269463,
#269464,#269465,#269466,#269467,#269468,#269469,#269470,#269471,#269472,
#269473,#269474,#269475,#269476,#269477,#269478,#269479)),.UNSPECIFIED.,
 .F.,.F.,.F.,(2,2),(4,2,2,2,2,1,1,1,2,2,4),(0.,4.74723717073224),(0.013418536150584,
0.013445898196386,0.0135028928581105,0.0135598875198351,0.0136738768432841,
0.0137878661667332,0.0140158448136313,0.0141298341370804,0.0142438234605295,
0.0143578127839785,0.0144718021074276),.UNSPECIFIED.);
#980=B_SPLINE_SURFACE_WITH_KNOTS('',1,3,((#269481,#269482,#269483,#269484,
#269485,#269486,#269487,#269488,#269489,#269490,#269491,#269492,#269493,
#269494,#269495,#269496,#269497,#269498,#269499,#269500,#269501,#269502,
#269503,#269504,#269505,#269506,#269507,#269508,#269509,#269510,#269511,
#269512,#269513,#269514,#269515,#269516,#269517,#269518,#269519,#269520,
#269521,#269522,#269523,#269524,#269525,#269526,#269527,#269528,#269529,
#269530,#269531,#269532,#269533,#269534,#269535,#269536,#269537,#269538,
#269539,#269540,#269541,#269542,#269543,#269544,#269545,#269546,#269547,
#269548,#269549,#269550,#269551,#269552,#269553,#269554,#269555,#269556,
#269557,#269558,#269559,#269560,#269561,#269562,#269563,#269564,#269565,
#269566,#269567,#269568,#269569,#269570,#269571,#269572,#269573,#269574,
#269575,#269576,#269577,#269578,#269579,#269580,#269581,#269582,#269583,
#269584,#269585,#269586,#269587,#269588,#269589,#269590,#269591,#269592,
#269593,#269594,#269595,#269596,#269597,#269598,#269599,#269600,#269601,
#269602,#269603,#269604,#269605,#269606,#269607,#269608,#269609,#269610,
#269611,#269612,#269613,#269614,#269615,#269616,#269617,#269618,#269619,
#269620,#269621,#269622,#269623,#269624,#269625,#269626,#269627,#269628,
#269629,#269630,#269631,#269632,#269633,#269634,#269635,#269636,#269637,
#269638,#269639,#269640,#269641,#269642,#269643,#269644,#269645,#269646,
#269647,#269648,#269649,#269650,#269651,#269652,#269653,#269654,#269655,
#269656,#269657,#269658,#269659),(#269660,#269661,#269662,#269663,#269664,
#269665,#269666,#269667,#269668,#269669,#269670,#269671,#269672,#269673,
#269674,#269675,#269676,#269677,#269678,#269679,#269680,#269681,#269682,
#269683,#269684,#269685,#269686,#269687,#269688,#269689,#269690,#269691,
#269692,#269693,#269694,#269695,#269696,#269697,#269698,#269699,#269700,
#269701,#269702,#269703,#269704,#269705,#269706,#269707,#269708,#269709,
#269710,#269711,#269712,#269713,#269714,#269715,#269716,#269717,#269718,
#269719,#269720,#269721,#269722,#269723,#269724,#269725,#269726,#269727,
#269728,#269729,#269730,#269731,#269732,#269733,#269734,#269735,#269736,
#269737,#269738,#269739,#269740,#269741,#269742,#269743,#269744,#269745,
#269746,#269747,#269748,#269749,#269750,#269751,#269752,#269753,#269754,
#269755,#269756,#269757,#269758,#269759,#269760,#269761,#269762,#269763,
#269764,#269765,#269766,#269767,#269768,#269769,#269770,#269771,#269772,
#269773,#269774,#269775,#269776,#269777,#269778,#269779,#269780,#269781,
#269782,#269783,#269784,#269785,#269786,#269787,#269788,#269789,#269790,
#269791,#269792,#269793,#269794,#269795,#269796,#269797,#269798,#269799,
#269800,#269801,#269802,#269803,#269804,#269805,#269806,#269807,#269808,
#269809,#269810,#269811,#269812,#269813,#269814,#269815,#269816,#269817,
#269818,#269819,#269820,#269821,#269822,#269823,#269824,#269825,#269826,
#269827,#269828,#269829,#269830,#269831,#269832,#269833,#269834,#269835,
#269836,#269837,#269838)),.UNSPECIFIED.,.F.,.T.,.F.,(2,2),(4,1,1,2,2,2,
2,1,1,1,2,2,2,1,1,2,2,2,2,2,2,2,2,2,1,1,1,2,2,2,1,2,2,2,1,2,2,2,1,1,1,1,
2,2,2,1,1,1,1,2,2,2,2,2,2,2,1,1,2,2,2,2,1,2,2,2,1,1,2,2,2,2,2,2,2,2,2,2,
1,1,1,2,2,2,1,1,2,2,2,1,2,2,2,2,2,1,2,2,2,2,2,1,1,1,2,2,4),(0.,4.74723717073224),
(-0.000118831294053002,0.000109147352845132,0.000337125999743267,0.000451115323192334,
0.000565104646641402,0.000679093970090469,0.000793083293539536,0.00102106194043767,
0.00113505126388674,0.0012490405873358,0.00136302991078487,0.00142002457250941,
0.00147701923423394,0.00170499788113207,0.00193297652803021,0.00204696585147928,
0.00216095517492835,0.00227494449837741,0.00238893382182648,0.00261691246872462,
0.00284489111562275,0.00290188577734728,0.00295888043907182,0.00307286976252088,
0.00330084840941902,0.00341483773286809,0.00352882705631715,0.00364281637976622,
0.00375680570321528,0.00387079502666435,0.00398478435011342,0.00421276299701156,
0.00444074164390969,0.00466872029080782,0.00489669893770596,0.00512467758460409,
0.00518167224632863,0.00523866690805316,0.00535265623150223,0.0054666455549513,
0.00558063487840036,0.00569462420184943,0.0058086135252985,0.00592260284874756,
0.00603659217219663,0.0061505814956457,0.00626457081909477,0.0064925494659929,
0.00660653878944197,0.00672052811289104,0.0068345174363401,0.00694850675978917,
0.00717648540668731,0.00729047473013637,0.00740446405358544,0.00763244270048357,
0.00786042134738171,0.00797441067083078,0.00808839999427985,0.00820238931772891,
0.00831637864117798,0.00854435728807612,0.00877233593497425,0.00888632525842331,
0.00900031458187238,0.00911430390532145,0.00922829322877052,0.00945627187566865,
0.00957026119911772,0.00968425052256679,0.00974124518429132,0.00979823984601585,
0.00991222916946492,0.0101402078163631,0.0103681864632612,0.0104251811249857,
0.0104821757867103,0.0105961651101593,0.0108241437570575,0.0109381330805065,
0.0110521224039556,0.0111661117274047,0.0112801010508537,0.0113940903743028,
0.0115080796977519,0.01173605834465,0.0118500476680991,0.0119640369915481,
0.0120780263149972,0.0121920156384463,0.0124199942853444,0.0126479729322425,
0.0127049675939671,0.0127619622556916,0.0128759515791407,0.0131039302260388,
0.0133319088729369,0.013445898196386,0.0135028928581105,0.0135598875198351,
0.0136738768432841,0.0137878661667332,0.0140158448136313,0.0141298341370804,
0.0142438234605295,0.0143578127839785,0.0144718021074276),.UNSPECIFIED.);
#981=B_SPLINE_SURFACE_WITH_KNOTS('',1,3,((#269839,#269840,#269841,#269842,
#269843,#269844,#269845,#269846,#269847,#269848,#269849,#269850,#269851,
#269852,#269853,#269854,#269855,#269856,#269857,#269858,#269859,#269860,
#269861,#269862,#269863,#269864,#269865,#269866,#269867,#269868,#269869,
#269870,#269871,#269872,#269873,#269874,#269875,#269876,#269877,#269878,
#269879,#269880,#269881,#269882,#269883,#269884,#269885,#269886,#269887,
#269888,#269889,#269890,#269891,#269892,#269893,#269894,#269895,#269896,
#269897,#269898,#269899,#269900,#269901,#269902,#269903,#269904,#269905,
#269906,#269907,#269908,#269909,#269910,#269911,#269912,#269913,#269914,
#269915,#269916,#269917,#269918,#269919,#269920,#269921,#269922,#269923,
#269924,#269925,#269926,#269927,#269928,#269929,#269930,#269931,#269932,
#269933,#269934,#269935,#269936,#269937,#269938,#269939,#269940,#269941,
#269942,#269943,#269944,#269945,#269946,#269947,#269948,#269949,#269950,
#269951,#269952,#269953,#269954,#269955,#269956,#269957,#269958,#269959,
#269960,#269961,#269962,#269963,#269964,#269965,#269966,#269967,#269968,
#269969,#269970,#269971,#269972,#269973,#269974,#269975,#269976,#269977,
#269978,#269979,#269980,#269981,#269982,#269983,#269984,#269985,#269986,
#269987,#269988,#269989,#269990,#269991,#269992,#269993,#269994,#269995,
#269996,#269997,#269998,#269999,#270000,#270001,#270002,#270003,#270004,
#270005,#270006,#270007,#270008,#270009,#270010,#270011,#270012,#270013,
#270014,#270015,#270016,#270017,#270018,#270019,#270020,#270021,#270022,
#270023,#270024,#270025,#270026,#270027,#270028,#270029,#270030,#270031,
#270032,#270033,#270034,#270035,#270036,#270037,#270038,#270039,#270040,
#270041,#270042,#270043,#270044,#270045,#270046,#270047,#270048,#270049,
#270050,#270051,#270052,#270053,#270054,#270055,#270056,#270057,#270058,
#270059,#270060,#270061,#270062,#270063,#270064),(#270065,#270066,#270067,
#270068,#270069,#270070,#270071,#270072,#270073,#270074,#270075,#270076,
#270077,#270078,#270079,#270080,#270081,#270082,#270083,#270084,#270085,
#270086,#270087,#270088,#270089,#270090,#270091,#270092,#270093,#270094,
#270095,#270096,#270097,#270098,#270099,#270100,#270101,#270102,#270103,
#270104,#270105,#270106,#270107,#270108,#270109,#270110,#270111,#270112,
#270113,#270114,#270115,#270116,#270117,#270118,#270119,#270120,#270121,
#270122,#270123,#270124,#270125,#270126,#270127,#270128,#270129,#270130,
#270131,#270132,#270133,#270134,#270135,#270136,#270137,#270138,#270139,
#270140,#270141,#270142,#270143,#270144,#270145,#270146,#270147,#270148,
#270149,#270150,#270151,#270152,#270153,#270154,#270155,#270156,#270157,
#270158,#270159,#270160,#270161,#270162,#270163,#270164,#270165,#270166,
#270167,#270168,#270169,#270170,#270171,#270172,#270173,#270174,#270175,
#270176,#270177,#270178,#270179,#270180,#270181,#270182,#270183,#270184,
#270185,#270186,#270187,#270188,#270189,#270190,#270191,#270192,#270193,
#270194,#270195,#270196,#270197,#270198,#270199,#270200,#270201,#270202,
#270203,#270204,#270205,#270206,#270207,#270208,#270209,#270210,#270211,
#270212,#270213,#270214,#270215,#270216,#270217,#270218,#270219,#270220,
#270221,#270222,#270223,#270224,#270225,#270226,#270227,#270228,#270229,
#270230,#270231,#270232,#270233,#270234,#270235,#270236,#270237,#270238,
#270239,#270240,#270241,#270242,#270243,#270244,#270245,#270246,#270247,
#270248,#270249,#270250,#270251,#270252,#270253,#270254,#270255,#270256,
#270257,#270258,#270259,#270260,#270261,#270262,#270263,#270264,#270265,
#270266,#270267,#270268,#270269,#270270,#270271,#270272,#270273,#270274,
#270275,#270276,#270277,#270278,#270279,#270280,#270281,#270282,#270283,
#270284,#270285,#270286,#270287,#270288,#270289,#270290)),.UNSPECIFIED.,
 .F.,.T.,.F.,(2,2),(4,2,2,2,2,2,2,2,2,2,2,2,2,2,2,2,2,2,2,2,2,2,2,2,2,2,
2,2,2,2,2,2,2,2,2,2,2,2,2,2,2,2,2,2,2,2,2,2,2,2,2,2,2,2,2,2,2,2,2,2,2,2,
2,2,2,2,2,2,2,2,2,2,2,2,2,2,2,2,2,2,2,2,2,2,2,2,2,2,2,2,2,2,2,2,2,2,2,2,
2,2,2,2,2,2,2,2,2,2,2,2,2,2,4),(-1.67052866871372E-8,1.00000923646777),
(-0.000118831294053002,-4.84197060393493E-6,0.000109147352845132,0.000337125999743267,
0.000451115323192334,0.000565104646641402,0.000679093970090469,0.000793083293539536,
0.00102106194043767,0.00113505126388674,0.0012490405873358,0.00136302991078487,
0.00142002457250941,0.00147701923423394,0.00170499788113207,0.00193297652803021,
0.00204696585147928,0.00216095517492835,0.00227494449837741,0.00238893382182648,
0.00261691246872462,0.00284489111562275,0.00290188577734728,0.00295888043907182,
0.00307286976252088,0.00318685908596995,0.00330084840941902,0.00341483773286809,
0.00352882705631715,0.00364281637976622,0.00375680570321528,0.00387079502666435,
0.00398478435011342,0.00421276299701156,0.00444074164390969,0.00466872029080782,
0.00489669893770596,0.00512467758460409,0.00518167224632863,0.00523866690805316,
0.00535265623150223,0.0054666455549513,0.00558063487840036,0.00569462420184943,
0.0058086135252985,0.00592260284874756,0.00603659217219663,0.0061505814956457,
0.00626457081909477,0.0064925494659929,0.00660653878944197,0.00672052811289104,
0.0068345174363401,0.00694850675978917,0.00706249608323824,0.00717648540668731,
0.00729047473013637,0.00740446405358544,0.00763244270048357,0.00786042134738171,
0.00797441067083078,0.00808839999427985,0.00820238931772891,0.00831637864117798,
0.00854435728807612,0.00865834661152518,0.00877233593497425,0.00888632525842331,
0.00900031458187238,0.00911430390532145,0.00922829322877052,0.00945627187566865,
0.00957026119911772,0.00968425052256679,0.00974124518429132,0.00979823984601585,
0.00991222916946492,0.0101402078163631,0.0103681864632612,0.0104251811249857,
0.0104821757867103,0.0105961651101593,0.0107101544336084,0.0108241437570575,
0.0109381330805065,0.0110521224039556,0.0111661117274047,0.0112801010508537,
0.0113940903743028,0.0115080796977519,0.01173605834465,0.0118500476680991,
0.0119640369915481,0.0120780263149972,0.0121920156384463,0.0124199942853444,
0.0126479729322425,0.0127049675939671,0.0127619622556916,0.0128759515791407,
0.0129899409025897,0.0131039302260388,0.0133319088729369,0.013445898196386,
0.0135028928581105,0.0135598875198351,0.0136738768432841,0.0137878661667332,
0.0140158448136313,0.0141298341370804,0.0142438234605295,0.0143578127839785,
0.0144718021074276),.UNSPECIFIED.);
#982=B_SPLINE_SURFACE_WITH_KNOTS('',1,3,((#270358,#270359,#270360,#270361,
#270362,#270363,#270364,#270365,#270366,#270367,#270368,#270369,#270370,
#270371,#270372,#270373,#270374,#270375,#270376,#270377,#270378,#270379,
#270380,#270381,#270382,#270383,#270384,#270385,#270386,#270387,#270388,
#270389,#270390,#270391,#270392,#270393,#270394,#270395,#270396,#270397,
#270398,#270399,#270400,#270401,#270402,#270403,#270404,#270405,#270406,
#270407,#270408,#270409,#270410,#270411,#270412,#270413,#270414,#270415,
#270416,#270417,#270418,#270419,#270420,#270421,#270422,#270423,#270424,
#270425,#270426,#270427,#270428,#270429,#270430,#270431,#270432,#270433,
#270434,#270435,#270436,#270437,#270438,#270439,#270440,#270441,#270442,
#270443,#270444,#270445,#270446,#270447,#270448,#270449,#270450,#270451,
#270452,#270453,#270454,#270455,#270456,#270457,#270458,#270459,#270460,
#270461,#270462,#270463,#270464,#270465,#270466,#270467,#270468,#270469,
#270470,#270471,#270472,#270473,#270474,#270475,#270476,#270477,#270478,
#270479,#270480,#270481,#270482,#270483,#270484,#270485,#270486,#270487,
#270488,#270489,#270490,#270491,#270492,#270493,#270494,#270495,#270496,
#270497,#270498,#270499,#270500,#270501,#270502,#270503,#270504,#270505,
#270506,#270507,#270508,#270509,#270510,#270511,#270512,#270513,#270514,
#270515,#270516,#270517,#270518,#270519,#270520,#270521,#270522,#270523,
#270524,#270525,#270526,#270527,#270528,#270529,#270530,#270531,#270532,
#270533,#270534,#270535,#270536),(#270537,#270538,#270539,#270540,#270541,
#270542,#270543,#270544,#270545,#270546,#270547,#270548,#270549,#270550,
#270551,#270552,#270553,#270554,#270555,#270556,#270557,#270558,#270559,
#270560,#270561,#270562,#270563,#270564,#270565,#270566,#270567,#270568,
#270569,#270570,#270571,#270572,#270573,#270574,#270575,#270576,#270577,
#270578,#270579,#270580,#270581,#270582,#270583,#270584,#270585,#270586,
#270587,#270588,#270589,#270590,#270591,#270592,#270593,#270594,#270595,
#270596,#270597,#270598,#270599,#270600,#270601,#270602,#270603,#270604,
#270605,#270606,#270607,#270608,#270609,#270610,#270611,#270612,#270613,
#270614,#270615,#270616,#270617,#270618,#270619,#270620,#270621,#270622,
#270623,#270624,#270625,#270626,#270627,#270628,#270629,#270630,#270631,
#270632,#270633,#270634,#270635,#270636,#270637,#270638,#270639,#270640,
#270641,#270642,#270643,#270644,#270645,#270646,#270647,#270648,#270649,
#270650,#270651,#270652,#270653,#270654,#270655,#270656,#270657,#270658,
#270659,#270660,#270661,#270662,#270663,#270664,#270665,#270666,#270667,
#270668,#270669,#270670,#270671,#270672,#270673,#270674,#270675,#270676,
#270677,#270678,#270679,#270680,#270681,#270682,#270683,#270684,#270685,
#270686,#270687,#270688,#270689,#270690,#270691,#270692,#270693,#270694,
#270695,#270696,#270697,#270698,#270699,#270700,#270701,#270702,#270703,
#270704,#270705,#270706,#270707,#270708,#270709,#270710,#270711,#270712,
#270713,#270714,#270715)),.UNSPECIFIED.,.F.,.T.,.F.,(2,2),(4,1,1,2,2,2,
2,1,1,1,2,2,2,1,1,2,2,2,2,2,2,2,2,2,1,1,1,2,2,2,1,2,2,2,1,2,2,2,1,1,1,1,
2,2,2,1,1,1,1,2,2,2,2,2,2,2,1,1,2,2,2,2,1,2,2,2,1,1,2,2,2,2,2,2,2,2,2,2,
1,1,1,2,2,2,1,1,2,2,2,1,2,2,2,2,2,1,2,2,2,2,2,1,1,1,2,2,4),(0.,5.45368304321453),
(-0.000118831294053002,0.000109147352845132,0.000337125999743267,0.000451115323192334,
0.000565104646641402,0.000679093970090469,0.000793083293539536,0.00102106194043767,
0.00113505126388674,0.0012490405873358,0.00136302991078487,0.00142002457250941,
0.00147701923423394,0.00170499788113207,0.00193297652803021,0.00204696585147928,
0.00216095517492835,0.00227494449837741,0.00238893382182648,0.00261691246872462,
0.00284489111562275,0.00290188577734728,0.00295888043907182,0.00307286976252088,
0.00330084840941902,0.00341483773286809,0.00352882705631715,0.00364281637976622,
0.00375680570321528,0.00387079502666435,0.00398478435011342,0.00421276299701156,
0.00444074164390969,0.00466872029080782,0.00489669893770596,0.00512467758460409,
0.00518167224632863,0.00523866690805316,0.00535265623150223,0.0054666455549513,
0.00558063487840036,0.00569462420184943,0.0058086135252985,0.00592260284874756,
0.00603659217219663,0.0061505814956457,0.00626457081909477,0.0064925494659929,
0.00660653878944197,0.00672052811289104,0.0068345174363401,0.00694850675978917,
0.00717648540668731,0.00729047473013637,0.00740446405358544,0.00763244270048357,
0.00786042134738171,0.00797441067083078,0.00808839999427985,0.00820238931772891,
0.00831637864117798,0.00854435728807612,0.00877233593497425,0.00888632525842331,
0.00900031458187238,0.00911430390532145,0.00922829322877052,0.00945627187566865,
0.00957026119911772,0.00968425052256679,0.00974124518429132,0.00979823984601585,
0.00991222916946492,0.0101402078163631,0.0103681864632612,0.0104251811249857,
0.0104821757867103,0.0105961651101593,0.0108241437570575,0.0109381330805065,
0.0110521224039556,0.0111661117274047,0.0112801010508537,0.0113940903743028,
0.0115080796977519,0.01173605834465,0.0118500476680991,0.0119640369915481,
0.0120780263149972,0.0121920156384463,0.0124199942853444,0.0126479729322425,
0.0127049675939671,0.0127619622556916,0.0128759515791407,0.0131039302260388,
0.0133319088729369,0.013445898196386,0.0135028928581105,0.0135598875198351,
0.0136738768432841,0.0137878661667332,0.0140158448136313,0.0141298341370804,
0.0142438234605295,0.0143578127839785,0.0144718021074276),.UNSPECIFIED.);
#983=B_SPLINE_SURFACE_WITH_KNOTS('',1,3,((#270716,#270717,#270718,#270719,
#270720,#270721,#270722,#270723,#270724,#270725,#270726,#270727,#270728,
#270729,#270730,#270731,#270732,#270733,#270734,#270735,#270736,#270737,
#270738,#270739,#270740,#270741,#270742,#270743,#270744,#270745,#270746,
#270747,#270748,#270749,#270750,#270751,#270752,#270753,#270754,#270755,
#270756,#270757,#270758,#270759,#270760,#270761,#270762,#270763,#270764,
#270765,#270766,#270767,#270768,#270769,#270770,#270771,#270772,#270773,
#270774,#270775,#270776,#270777,#270778,#270779,#270780,#270781,#270782,
#270783,#270784,#270785,#270786,#270787,#270788,#270789,#270790,#270791,
#270792,#270793,#270794,#270795,#270796,#270797,#270798,#270799,#270800,
#270801,#270802,#270803,#270804,#270805,#270806,#270807,#270808,#270809,
#270810,#270811,#270812,#270813,#270814,#270815,#270816,#270817,#270818,
#270819,#270820,#270821,#270822,#270823,#270824,#270825,#270826,#270827,
#270828,#270829,#270830,#270831,#270832,#270833,#270834,#270835,#270836,
#270837,#270838,#270839,#270840,#270841,#270842,#270843,#270844,#270845,
#270846,#270847,#270848,#270849,#270850,#270851,#270852,#270853,#270854,
#270855,#270856,#270857,#270858,#270859,#270860,#270861,#270862,#270863,
#270864,#270865,#270866,#270867,#270868,#270869,#270870,#270871,#270872,
#270873,#270874,#270875,#270876,#270877,#270878,#270879,#270880,#270881,
#270882,#270883,#270884,#270885,#270886,#270887,#270888,#270889,#270890,
#270891,#270892,#270893,#270894),(#270895,#270896,#270897,#270898,#270899,
#270900,#270901,#270902,#270903,#270904,#270905,#270906,#270907,#270908,
#270909,#270910,#270911,#270912,#270913,#270914,#270915,#270916,#270917,
#270918,#270919,#270920,#270921,#270922,#270923,#270924,#270925,#270926,
#270927,#270928,#270929,#270930,#270931,#270932,#270933,#270934,#270935,
#270936,#270937,#270938,#270939,#270940,#270941,#270942,#270943,#270944,
#270945,#270946,#270947,#270948,#270949,#270950,#270951,#270952,#270953,
#270954,#270955,#270956,#270957,#270958,#270959,#270960,#270961,#270962,
#270963,#270964,#270965,#270966,#270967,#270968,#270969,#270970,#270971,
#270972,#270973,#270974,#270975,#270976,#270977,#270978,#270979,#270980,
#270981,#270982,#270983,#270984,#270985,#270986,#270987,#270988,#270989,
#270990,#270991,#270992,#270993,#270994,#270995,#270996,#270997,#270998,
#270999,#271000,#271001,#271002,#271003,#271004,#271005,#271006,#271007,
#271008,#271009,#271010,#271011,#271012,#271013,#271014,#271015,#271016,
#271017,#271018,#271019,#271020,#271021,#271022,#271023,#271024,#271025,
#271026,#271027,#271028,#271029,#271030,#271031,#271032,#271033,#271034,
#271035,#271036,#271037,#271038,#271039,#271040,#271041,#271042,#271043,
#271044,#271045,#271046,#271047,#271048,#271049,#271050,#271051,#271052,
#271053,#271054,#271055,#271056,#271057,#271058,#271059,#271060,#271061,
#271062,#271063,#271064,#271065,#271066,#271067,#271068,#271069,#271070,
#271071,#271072,#271073)),.UNSPECIFIED.,.F.,.T.,.F.,(2,2),(4,1,1,2,2,2,
2,1,1,1,2,2,2,1,1,2,2,2,2,2,2,2,2,2,1,1,1,2,2,2,1,2,2,2,1,2,2,2,1,1,1,1,
2,2,2,1,1,1,1,2,2,2,2,2,2,2,1,1,2,2,2,2,1,2,2,2,1,1,2,2,2,2,2,2,2,2,2,2,
1,1,1,2,2,2,1,1,2,2,2,1,2,2,2,2,2,1,2,2,2,2,2,1,1,1,2,2,4),(0.,5.45368304321453),
(-0.000118831294053002,0.000109147352845132,0.000337125999743267,0.000451115323192334,
0.000565104646641402,0.000679093970090469,0.000793083293539536,0.00102106194043767,
0.00113505126388674,0.0012490405873358,0.00136302991078487,0.00142002457250941,
0.00147701923423394,0.00170499788113207,0.00193297652803021,0.00204696585147928,
0.00216095517492835,0.00227494449837741,0.00238893382182648,0.00261691246872462,
0.00284489111562275,0.00290188577734728,0.00295888043907182,0.00307286976252088,
0.00330084840941902,0.00341483773286809,0.00352882705631715,0.00364281637976622,
0.00375680570321528,0.00387079502666435,0.00398478435011342,0.00421276299701156,
0.00444074164390969,0.00466872029080782,0.00489669893770596,0.00512467758460409,
0.00518167224632863,0.00523866690805316,0.00535265623150223,0.0054666455549513,
0.00558063487840036,0.00569462420184943,0.0058086135252985,0.00592260284874756,
0.00603659217219663,0.0061505814956457,0.00626457081909477,0.0064925494659929,
0.00660653878944197,0.00672052811289104,0.0068345174363401,0.00694850675978917,
0.00717648540668731,0.00729047473013637,0.00740446405358544,0.00763244270048357,
0.00786042134738171,0.00797441067083078,0.00808839999427985,0.00820238931772891,
0.00831637864117798,0.00854435728807612,0.00877233593497425,0.00888632525842331,
0.00900031458187238,0.00911430390532145,0.00922829322877052,0.00945627187566865,
0.00957026119911772,0.00968425052256679,0.00974124518429132,0.00979823984601585,
0.00991222916946492,0.0101402078163631,0.0103681864632612,0.0104251811249857,
0.0104821757867103,0.0105961651101593,0.0108241437570575,0.0109381330805065,
0.0110521224039556,0.0111661117274047,0.0112801010508537,0.0113940903743028,
0.0115080796977519,0.01173605834465,0.0118500476680991,0.0119640369915481,
0.0120780263149972,0.0121920156384463,0.0124199942853444,0.0126479729322425,
0.0127049675939671,0.0127619622556916,0.0128759515791407,0.0131039302260388,
0.0133319088729369,0.013445898196386,0.0135028928581105,0.0135598875198351,
0.0136738768432841,0.0137878661667332,0.0140158448136313,0.0141298341370804,
0.0142438234605295,0.0143578127839785,0.0144718021074276),.UNSPECIFIED.);
#984=B_SPLINE_SURFACE_WITH_KNOTS('',3,1,((#306944,#306945),(#306946,#306947),
(#306948,#306949),(#306950,#306951),(#306952,#306953),(#306954,#306955),
(#306956,#306957),(#306958,#306959),(#306960,#306961),(#306962,#306963),
(#306964,#306965),(#306966,#306967),(#306968,#306969),(#306970,#306971),
(#306972,#306973),(#306974,#306975),(#306976,#306977),(#306978,#306979),
(#306980,#306981)),.UNSPECIFIED.,.F.,.F.,.F.,(4,1,1,1,1,1,1,1,1,1,1,1,1,
1,1,1,4),(2,2),(0.,0.0580692684342556,0.114001303445375,0.169772099070702,
0.224674954494909,0.280054150165824,0.336957215314267,0.395112576113712,
0.456649482459617,0.519182398591372,0.582165728137028,0.645753825355143,
0.710908012329458,0.778341319290106,0.848949505917864,0.922850140892551,
1.),(0.,0.024),.UNSPECIFIED.);
#985=B_SPLINE_SURFACE_WITH_KNOTS('',3,1,((#307005,#307006),(#307007,#307008),
(#307009,#307010),(#307011,#307012),(#307013,#307014),(#307015,#307016),
(#307017,#307018),(#307019,#307020),(#307021,#307022),(#307023,#307024),
(#307025,#307026),(#307027,#307028),(#307029,#307030),(#307031,#307032),
(#307033,#307034),(#307035,#307036),(#307037,#307038),(#307039,#307040),
(#307041,#307042)),.UNSPECIFIED.,.F.,.F.,.F.,(4,1,1,1,1,1,1,1,1,1,1,1,1,
1,1,1,4),(2,2),(0.,0.0766164418639844,0.150101977842741,0.220268821680907,
0.287483908975341,0.35290178839726,0.417338409308383,0.480866360224848,
0.543808187325834,0.605854592868513,0.665047756996982,0.722013651121557,
0.777789178028364,0.832724479504672,0.887128050755955,0.942855781853261,
1.),(0.,0.024),.UNSPECIFIED.);
#986=B_SPLINE_SURFACE_WITH_KNOTS('',3,1,((#307064,#307065),(#307066,#307067),
(#307068,#307069),(#307070,#307071),(#307072,#307073),(#307074,#307075),
(#307076,#307077),(#307078,#307079),(#307080,#307081),(#307082,#307083),
(#307084,#307085),(#307086,#307087),(#307088,#307089),(#307090,#307091),
(#307092,#307093),(#307094,#307095),(#307096,#307097),(#307098,#307099),
(#307100,#307101)),.UNSPECIFIED.,.F.,.F.,.F.,(4,1,1,1,1,1,1,1,1,1,1,1,1,
1,1,1,4),(2,2),(0.,0.0577170366867072,0.113994474768008,0.16893758423175,
0.224179487123504,0.279968804571931,0.337633163696686,0.397092193126611,
0.459041827583877,0.522525900750905,0.586121573329079,0.650102352916103,
0.71540731027663,0.782762550840158,0.852275272320573,0.924507298607219,
1.),(0.,0.024),.UNSPECIFIED.);
#987=B_SPLINE_SURFACE_WITH_KNOTS('',3,1,((#307123,#307124),(#307125,#307126),
(#307127,#307128),(#307129,#307130),(#307131,#307132),(#307133,#307134),
(#307135,#307136),(#307137,#307138),(#307139,#307140),(#307141,#307142),
(#307143,#307144),(#307145,#307146),(#307147,#307148),(#307149,#307150),
(#307151,#307152),(#307153,#307154),(#307155,#307156),(#307157,#307158),
(#307159,#307160)),.UNSPECIFIED.,.F.,.F.,.F.,(4,1,1,1,1,1,1,1,1,1,1,1,1,
1,1,1,4),(2,2),(0.,0.0768723536038944,0.150603343572851,0.220876273582275,
0.288315870518755,0.35395225660761,0.418604106617997,0.481972048717606,
0.545247561534372,0.606993813632933,0.665860906234417,0.723420981486814,
0.778433488719744,0.833552283298071,0.88813757158342,0.943362448943921,
1.),(0.,0.024),.UNSPECIFIED.);
#988=B_SPLINE_SURFACE_WITH_KNOTS('',3,1,((#307180,#307181),(#307182,#307183),
(#307184,#307185),(#307186,#307187),(#307188,#307189),(#307190,#307191),
(#307192,#307193),(#307194,#307195),(#307196,#307197),(#307198,#307199),
(#307200,#307201)),.UNSPECIFIED.,.F.,.F.,.F.,(4,1,1,1,1,1,1,1,4),(2,2),
(0.,0.113008663357688,0.223447121007772,0.335763095333029,0.457240997711765,
0.584219963833153,0.714811315114105,0.851997802140335,1.),(0.,0.024),
 .UNSPECIFIED.);
#989=B_SPLINE_SURFACE_WITH_KNOTS('',3,1,((#307217,#307218),(#307219,#307220),
(#307221,#307222),(#307223,#307224),(#307225,#307226),(#307227,#307228),
(#307229,#307230),(#307231,#307232),(#307233,#307234),(#307235,#307236),
(#307237,#307238)),.UNSPECIFIED.,.F.,.F.,.F.,(4,1,1,1,1,1,1,1,4),(2,2),
(0.,0.149379665294656,0.288273014687601,0.418942648167458,0.547753389590675,
0.670496533301504,0.782663672045753,0.890203158268387,1.),(0.,0.024),
 .UNSPECIFIED.);
#990=B_SPLINE_SURFACE_WITH_KNOTS('',3,1,((#307252,#307253),(#307254,#307255),
(#307256,#307257),(#307258,#307259),(#307260,#307261),(#307262,#307263),
(#307264,#307265),(#307266,#307267),(#307268,#307269),(#307270,#307271),
(#307272,#307273)),.UNSPECIFIED.,.F.,.F.,.F.,(4,1,1,1,1,1,1,1,4),(2,2),
(0.,0.113035127206385,0.22352787461649,0.337812984577189,0.462304974001557,
0.590889524052717,0.720496476039469,0.855414628911259,1.),(0.,0.024),
 .UNSPECIFIED.);
#991=B_SPLINE_SURFACE_WITH_KNOTS('',3,1,((#307287,#307288),(#307289,#307290),
(#307291,#307292),(#307293,#307294),(#307295,#307296),(#307297,#307298),
(#307299,#307300),(#307301,#307302),(#307303,#307304),(#307305,#307306),
(#307307,#307308)),.UNSPECIFIED.,.F.,.F.,.F.,(4,1,1,1,1,1,1,1,4),(2,2),
(0.,0.153975786043391,0.294620990206987,0.425952943236339,0.551063084753368,
0.669883873511439,0.780296648018842,0.888858324162197,1.),(0.,0.024),
 .UNSPECIFIED.);
#992=B_SPLINE_SURFACE_WITH_KNOTS('',3,1,((#307320,#307321),(#307322,#307323),
(#307324,#307325),(#307326,#307327),(#307328,#307329),(#307330,#307331),
(#307332,#307333),(#307334,#307335),(#307336,#307337),(#307338,#307339),
(#307340,#307341),(#307342,#307343),(#307344,#307345),(#307346,#307347),
(#307348,#307349),(#307350,#307351),(#307352,#307353),(#307354,#307355),
(#307356,#307357)),.UNSPECIFIED.,.F.,.F.,.F.,(4,1,1,1,1,1,1,1,1,1,1,1,1,
1,1,1,4),(2,2),(0.,0.0580692684342556,0.114001303445375,0.169772099070702,
0.224674954494909,0.280054150165824,0.336957215314267,0.395112576113712,
0.456649482459617,0.519182398591372,0.582165728137028,0.645753825355143,
0.710908012329458,0.778341319290106,0.848949505917864,0.922850140892551,
1.),(0.,0.024),.UNSPECIFIED.);
#993=B_SPLINE_SURFACE_WITH_KNOTS('',3,1,((#307381,#307382),(#307383,#307384),
(#307385,#307386),(#307387,#307388),(#307389,#307390),(#307391,#307392),
(#307393,#307394),(#307395,#307396),(#307397,#307398),(#307399,#307400),
(#307401,#307402),(#307403,#307404),(#307405,#307406),(#307407,#307408),
(#307409,#307410),(#307411,#307412),(#307413,#307414),(#307415,#307416),
(#307417,#307418)),.UNSPECIFIED.,.F.,.F.,.F.,(4,1,1,1,1,1,1,1,1,1,1,1,1,
1,1,1,4),(2,2),(0.,0.0766164418639844,0.150101977842741,0.220268821680907,
0.287483908975341,0.35290178839726,0.417338409308383,0.480866360224848,
0.543808187325834,0.605854592868513,0.665047756996982,0.722013651121557,
0.777789178028364,0.832724479504672,0.887128050755955,0.942855781853261,
1.),(0.,0.024),.UNSPECIFIED.);
#994=B_SPLINE_SURFACE_WITH_KNOTS('',3,1,((#307440,#307441),(#307442,#307443),
(#307444,#307445),(#307446,#307447),(#307448,#307449),(#307450,#307451),
(#307452,#307453),(#307454,#307455),(#307456,#307457),(#307458,#307459),
(#307460,#307461),(#307462,#307463),(#307464,#307465),(#307466,#307467),
(#307468,#307469),(#307470,#307471),(#307472,#307473),(#307474,#307475),
(#307476,#307477)),.UNSPECIFIED.,.F.,.F.,.F.,(4,1,1,1,1,1,1,1,1,1,1,1,1,
1,1,1,4),(2,2),(0.,0.0577170366867072,0.113994474768008,0.16893758423175,
0.224179487123505,0.279968804571931,0.337633163696686,0.397092193126611,
0.459041827583877,0.522525900750905,0.586121573329079,0.650102352916103,
0.71540731027663,0.782762550840158,0.852275272320572,0.924507298607219,
1.),(0.,0.024),.UNSPECIFIED.);
#995=B_SPLINE_SURFACE_WITH_KNOTS('',3,1,((#307499,#307500),(#307501,#307502),
(#307503,#307504),(#307505,#307506),(#307507,#307508),(#307509,#307510),
(#307511,#307512),(#307513,#307514),(#307515,#307516),(#307517,#307518),
(#307519,#307520),(#307521,#307522),(#307523,#307524),(#307525,#307526),
(#307527,#307528),(#307529,#307530),(#307531,#307532),(#307533,#307534),
(#307535,#307536)),.UNSPECIFIED.,.F.,.F.,.F.,(4,1,1,1,1,1,1,1,1,1,1,1,1,
1,1,1,4),(2,2),(0.,0.0768723536038944,0.150603343572851,0.220876273582275,
0.288315870518755,0.35395225660761,0.418604106617997,0.481972048717605,
0.545247561534372,0.606993813632933,0.665860906234417,0.723420981486814,
0.778433488719744,0.833552283298071,0.88813757158342,0.943362448943921,
1.),(0.,0.024),.UNSPECIFIED.);
#996=B_SPLINE_SURFACE_WITH_KNOTS('',3,1,((#307556,#307557),(#307558,#307559),
(#307560,#307561),(#307562,#307563),(#307564,#307565),(#307566,#307567),
(#307568,#307569),(#307570,#307571),(#307572,#307573),(#307574,#307575),
(#307576,#307577)),.UNSPECIFIED.,.F.,.F.,.F.,(4,1,1,1,1,1,1,1,4),(2,2),
(0.,0.113008663357688,0.223447121007772,0.335763095333029,0.457240997711765,
0.584219963833153,0.714811315114105,0.851997802140335,1.),(0.,0.024),
 .UNSPECIFIED.);
#997=B_SPLINE_SURFACE_WITH_KNOTS('',3,1,((#307593,#307594),(#307595,#307596),
(#307597,#307598),(#307599,#307600),(#307601,#307602),(#307603,#307604),
(#307605,#307606),(#307607,#307608),(#307609,#307610),(#307611,#307612),
(#307613,#307614)),.UNSPECIFIED.,.F.,.F.,.F.,(4,1,1,1,1,1,1,1,4),(2,2),
(0.,0.149379665294656,0.288273014687601,0.418942648167458,0.547753389590675,
0.670496533301504,0.782663672045753,0.890203158268387,1.),(0.,0.024),
 .UNSPECIFIED.);
#998=B_SPLINE_SURFACE_WITH_KNOTS('',3,1,((#307628,#307629),(#307630,#307631),
(#307632,#307633),(#307634,#307635),(#307636,#307637),(#307638,#307639),
(#307640,#307641),(#307642,#307643),(#307644,#307645),(#307646,#307647),
(#307648,#307649)),.UNSPECIFIED.,.F.,.F.,.F.,(4,1,1,1,1,1,1,1,4),(2,2),
(0.,0.113035127206385,0.22352787461649,0.337812984577189,0.462304974001557,
0.590889524052717,0.720496476039469,0.855414628911259,1.),(0.,0.024),
 .UNSPECIFIED.);
#999=B_SPLINE_SURFACE_WITH_KNOTS('',3,1,((#307663,#307664),(#307665,#307666),
(#307667,#307668),(#307669,#307670),(#307671,#307672),(#307673,#307674),
(#307675,#307676),(#307677,#307678),(#307679,#307680),(#307681,#307682),
(#307683,#307684)),.UNSPECIFIED.,.F.,.F.,.F.,(4,1,1,1,1,1,1,1,4),(2,2),
(0.,0.153975786043391,0.294620990206987,0.42595294323634,0.551063084753368,
0.669883873511439,0.780296648018842,0.888858324162197,1.),(0.,0.024),
 .UNSPECIFIED.);
#1000=B_SPLINE_SURFACE_WITH_KNOTS('',3,1,((#307995,#307996),(#307997,#307998),
(#307999,#308000),(#308001,#308002),(#308003,#308004),(#308005,#308006),
(#308007,#308008),(#308009,#308010),(#308011,#308012),(#308013,#308014),
(#308015,#308016),(#308017,#308018),(#308019,#308020),(#308021,#308022),
(#308023,#308024),(#308025,#308026),(#308027,#308028),(#308029,#308030),
(#308031,#308032)),.UNSPECIFIED.,.F.,.F.,.F.,(4,1,1,1,1,1,1,1,1,1,1,1,1,
1,1,1,4),(2,2),(0.,0.0624074292203441,0.123580758253191,0.183030548059535,
0.241487894622227,0.299476288588136,0.357776621678218,0.416397215359044,
0.475293297309649,0.535174551555035,0.596373380100883,0.65843295832835,
0.722087328991003,0.787866252937039,0.856053064935337,0.926280127267363,
1.),(0.,0.024),.UNSPECIFIED.);
#1001=B_SPLINE_SURFACE_WITH_KNOTS('',3,1,((#308056,#308057),(#308058,#308059),
(#308060,#308061),(#308062,#308063),(#308064,#308065),(#308066,#308067),
(#308068,#308069),(#308070,#308071),(#308072,#308073),(#308074,#308075),
(#308076,#308077)),.UNSPECIFIED.,.F.,.F.,.F.,(4,1,1,1,1,1,1,1,4),(2,2),
(0.,0.140786050719229,0.271192292477146,0.394820533419766,0.51366840541228,
0.630249521887138,0.748635241534156,0.870539222318192,1.),(0.,0.024),
 .UNSPECIFIED.);
#1002=B_SPLINE_SURFACE_WITH_KNOTS('',3,1,((#308091,#308092),(#308093,#308094),
(#308095,#308096),(#308097,#308098),(#308099,#308100),(#308101,#308102),
(#308103,#308104),(#308105,#308106),(#308107,#308108),(#308109,#308110),
(#308111,#308112),(#308113,#308114),(#308115,#308116),(#308117,#308118),
(#308119,#308120),(#308121,#308122),(#308123,#308124),(#308125,#308126),
(#308127,#308128)),.UNSPECIFIED.,.F.,.F.,.F.,(4,1,1,1,1,1,1,1,1,1,1,1,1,
1,1,1,4),(2,2),(0.,0.061579283211466,0.121651367349155,0.179800294989198,
0.237201673292092,0.294780234992934,0.353324880649131,0.412515530286399,
0.474433538402357,0.537108068033057,0.599269077379891,0.66175044463838,
0.725142484567205,0.790290611404277,0.857751363050287,0.927508428952717,
1.),(0.,0.024),.UNSPECIFIED.);
#1003=B_SPLINE_SURFACE_WITH_KNOTS('',3,1,((#308150,#308151),(#308152,#308153),
(#308154,#308155),(#308156,#308157),(#308158,#308159),(#308160,#308161),
(#308162,#308163),(#308164,#308165),(#308166,#308167),(#308168,#308169),
(#308170,#308171),(#308172,#308173),(#308174,#308175),(#308176,#308177),
(#308178,#308179),(#308180,#308181),(#308182,#308183),(#308184,#308185),
(#308186,#308187)),.UNSPECIFIED.,.F.,.F.,.F.,(4,1,1,1,1,1,1,1,1,1,1,1,1,
1,1,1,4),(2,2),(0.,0.0728455592253727,0.142402257701936,0.209648156853246,
0.274427985226561,0.337611609749171,0.399896985087157,0.462371952688158,
0.524655094094133,0.586203391626632,0.645775819776357,0.704006503444922,
0.762043319649332,0.81964939871453,0.877994662833982,0.938199028971844,
1.),(0.,0.024),.UNSPECIFIED.);
#1004=B_SPLINE_SURFACE_WITH_KNOTS('',3,1,((#308209,#308210),(#308211,#308212),
(#308213,#308214),(#308215,#308216),(#308217,#308218),(#308219,#308220),
(#308221,#308222),(#308223,#308224),(#308225,#308226),(#308227,#308228),
(#308229,#308230)),.UNSPECIFIED.,.F.,.F.,.F.,(4,1,1,1,1,1,1,1,4),(2,2),
(0.,0.126037809173243,0.24590192439148,0.362706754432767,0.479405225937116,
0.59860340945283,0.723279815939465,0.85618139156474,1.),(0.,0.024),
 .UNSPECIFIED.);
#1005=B_SPLINE_SURFACE_WITH_KNOTS('',3,1,((#308244,#308245),(#308246,#308247),
(#308248,#308249),(#308250,#308251),(#308252,#308253),(#308254,#308255),
(#308256,#308257),(#308258,#308259),(#308260,#308261),(#308262,#308263),
(#308264,#308265),(#308266,#308267),(#308268,#308269),(#308270,#308271),
(#308272,#308273),(#308274,#308275),(#308276,#308277),(#308278,#308279),
(#308280,#308281)),.UNSPECIFIED.,.F.,.F.,.F.,(4,1,1,1,1,1,1,1,1,1,1,1,1,
1,1,1,4),(2,2),(0.,0.0756779287595513,0.148475385165302,0.218686839383758,
0.285894163869826,0.350394511043543,0.41333034849776,0.475131662182092,
0.535395707628871,0.595069793647295,0.653190706601446,0.71022527848224,
0.767064167323289,0.824126149789293,0.882061797546221,0.940276800846585,
1.),(0.,0.024),.UNSPECIFIED.);
#1006=B_SPLINE_SURFACE_WITH_KNOTS('',3,1,((#308303,#308304),(#308305,#308306),
(#308307,#308308),(#308309,#308310),(#308311,#308312),(#308313,#308314),
(#308315,#308316),(#308317,#308318),(#308319,#308320),(#308321,#308322),
(#308323,#308324),(#308325,#308326),(#308327,#308328),(#308329,#308330),
(#308331,#308332),(#308333,#308334),(#308335,#308336),(#308337,#308338),
(#308339,#308340)),.UNSPECIFIED.,.F.,.F.,.F.,(4,1,1,1,1,1,1,1,1,1,1,1,1,
1,1,1,4),(2,2),(0.,0.061560808552986,0.120975543465591,0.179004419802313,
0.236102291207156,0.293686508428115,0.351514938997191,0.410728891353352,
0.472160594099565,0.534227146274051,0.596384774286223,0.658759168877887,
0.722544817104037,0.787964999387698,0.855593119477614,0.926440609783223,
1.),(0.,0.024),.UNSPECIFIED.);
#1007=B_SPLINE_SURFACE_WITH_KNOTS('',3,1,((#308362,#308363),(#308364,#308365),
(#308366,#308367),(#308368,#308369),(#308370,#308371),(#308372,#308373),
(#308374,#308375),(#308376,#308377),(#308378,#308379),(#308380,#308381),
(#308382,#308383),(#308384,#308385),(#308386,#308387),(#308388,#308389),
(#308390,#308391),(#308392,#308393),(#308394,#308395),(#308396,#308397),
(#308398,#308399)),.UNSPECIFIED.,.F.,.F.,.F.,(4,1,1,1,1,1,1,1,1,1,1,1,1,
1,1,1,4),(2,2),(0.,0.0724843729385586,0.142190024778259,0.209247943639616,
0.274447923967761,0.33802582267117,0.400406532440542,0.463046285981066,
0.525723189050567,0.587758999700955,0.647207274703619,0.705604379270503,
0.76335494041328,0.821014301633402,0.879178712895835,0.938732443992665,
1.),(0.,0.024),.UNSPECIFIED.);
#1008=B_SPLINE_SURFACE_WITH_KNOTS('',3,1,((#308419,#308420),(#308421,#308422),
(#308423,#308424),(#308425,#308426),(#308427,#308428),(#308429,#308430),
(#308431,#308432),(#308433,#308434),(#308435,#308436),(#308437,#308438),
(#308439,#308440),(#308441,#308442),(#308443,#308444),(#308445,#308446),
(#308447,#308448),(#308449,#308450),(#308451,#308452),(#308453,#308454),
(#308455,#308456)),.UNSPECIFIED.,.F.,.F.,.F.,(4,1,1,1,1,1,1,1,1,1,1,1,1,
1,1,1,4),(2,2),(0.,0.0624074292203441,0.123580758253191,0.183030548059535,
0.241487894622227,0.299476288588135,0.357776621678218,0.416397215359044,
0.475293297309649,0.535174551555035,0.596373380100883,0.65843295832835,
0.722087328991003,0.787866252937039,0.856053064935338,0.926280127267363,
1.),(0.,0.024),.UNSPECIFIED.);
#1009=B_SPLINE_SURFACE_WITH_KNOTS('',3,1,((#308480,#308481),(#308482,#308483),
(#308484,#308485),(#308486,#308487),(#308488,#308489),(#308490,#308491),
(#308492,#308493),(#308494,#308495),(#308496,#308497),(#308498,#308499),
(#308500,#308501)),.UNSPECIFIED.,.F.,.F.,.F.,(4,1,1,1,1,1,1,1,4),(2,2),
(0.,0.140786050719229,0.271192292477146,0.394820533419766,0.51366840541228,
0.630249521887138,0.748635241534156,0.870539222318192,1.),(0.,0.024),
 .UNSPECIFIED.);
#1010=B_SPLINE_SURFACE_WITH_KNOTS('',3,1,((#308515,#308516),(#308517,#308518),
(#308519,#308520),(#308521,#308522),(#308523,#308524),(#308525,#308526),
(#308527,#308528),(#308529,#308530),(#308531,#308532),(#308533,#308534),
(#308535,#308536),(#308537,#308538),(#308539,#308540),(#308541,#308542),
(#308543,#308544),(#308545,#308546),(#308547,#308548),(#308549,#308550),
(#308551,#308552)),.UNSPECIFIED.,.F.,.F.,.F.,(4,1,1,1,1,1,1,1,1,1,1,1,1,
1,1,1,4),(2,2),(0.,0.061579283211466,0.121651367349155,0.179800294989198,
0.237201673292092,0.294780234992934,0.353324880649131,0.412515530286399,
0.474433538402357,0.537108068033057,0.599269077379891,0.66175044463838,
0.725142484567205,0.790290611404277,0.857751363050287,0.927508428952717,
1.),(0.,0.024),.UNSPECIFIED.);
#1011=B_SPLINE_SURFACE_WITH_KNOTS('',3,1,((#308574,#308575),(#308576,#308577),
(#308578,#308579),(#308580,#308581),(#308582,#308583),(#308584,#308585),
(#308586,#308587),(#308588,#308589),(#308590,#308591),(#308592,#308593),
(#308594,#308595),(#308596,#308597),(#308598,#308599),(#308600,#308601),
(#308602,#308603),(#308604,#308605),(#308606,#308607),(#308608,#308609),
(#308610,#308611)),.UNSPECIFIED.,.F.,.F.,.F.,(4,1,1,1,1,1,1,1,1,1,1,1,1,
1,1,1,4),(2,2),(0.,0.0728455592253727,0.142402257701936,0.209648156853246,
0.274427985226561,0.337611609749171,0.399896985087157,0.462371952688158,
0.524655094094133,0.586203391626633,0.645775819776357,0.704006503444922,
0.762043319649332,0.81964939871453,0.877994662833982,0.938199028971844,
1.),(0.,0.024),.UNSPECIFIED.);
#1012=B_SPLINE_SURFACE_WITH_KNOTS('',3,1,((#308633,#308634),(#308635,#308636),
(#308637,#308638),(#308639,#308640),(#308641,#308642),(#308643,#308644),
(#308645,#308646),(#308647,#308648),(#308649,#308650),(#308651,#308652),
(#308653,#308654)),.UNSPECIFIED.,.F.,.F.,.F.,(4,1,1,1,1,1,1,1,4),(2,2),
(0.,0.126037809173244,0.24590192439148,0.362706754432767,0.479405225937116,
0.59860340945283,0.723279815939465,0.85618139156474,1.),(0.,0.024),
 .UNSPECIFIED.);
#1013=B_SPLINE_SURFACE_WITH_KNOTS('',3,1,((#308668,#308669),(#308670,#308671),
(#308672,#308673),(#308674,#308675),(#308676,#308677),(#308678,#308679),
(#308680,#308681),(#308682,#308683),(#308684,#308685),(#308686,#308687),
(#308688,#308689),(#308690,#308691),(#308692,#308693),(#308694,#308695),
(#308696,#308697),(#308698,#308699),(#308700,#308701),(#308702,#308703),
(#308704,#308705)),.UNSPECIFIED.,.F.,.F.,.F.,(4,1,1,1,1,1,1,1,1,1,1,1,1,
1,1,1,4),(2,2),(0.,0.0756779287595513,0.148475385165302,0.218686839383758,
0.285894163869826,0.350394511043543,0.41333034849776,0.475131662182092,
0.535395707628871,0.595069793647295,0.653190706601445,0.71022527848224,
0.767064167323289,0.824126149789293,0.882061797546221,0.940276800846584,
1.),(0.,0.024),.UNSPECIFIED.);
#1014=B_SPLINE_SURFACE_WITH_KNOTS('',3,1,((#308727,#308728),(#308729,#308730),
(#308731,#308732),(#308733,#308734),(#308735,#308736),(#308737,#308738),
(#308739,#308740),(#308741,#308742),(#308743,#308744),(#308745,#308746),
(#308747,#308748),(#308749,#308750),(#308751,#308752),(#308753,#308754),
(#308755,#308756),(#308757,#308758),(#308759,#308760),(#308761,#308762),
(#308763,#308764)),.UNSPECIFIED.,.F.,.F.,.F.,(4,1,1,1,1,1,1,1,1,1,1,1,1,
1,1,1,4),(2,2),(0.,0.061560808552986,0.120975543465591,0.179004419802313,
0.236102291207156,0.293686508428115,0.351514938997191,0.410728891353352,
0.472160594099565,0.534227146274051,0.596384774286223,0.658759168877887,
0.722544817104037,0.787964999387698,0.855593119477614,0.926440609783223,
1.),(0.,0.024),.UNSPECIFIED.);
#1015=B_SPLINE_SURFACE_WITH_KNOTS('',3,1,((#308786,#308787),(#308788,#308789),
(#308790,#308791),(#308792,#308793),(#308794,#308795),(#308796,#308797),
(#308798,#308799),(#308800,#308801),(#308802,#308803),(#308804,#308805),
(#308806,#308807),(#308808,#308809),(#308810,#308811),(#308812,#308813),
(#308814,#308815),(#308816,#308817),(#308818,#308819),(#308820,#308821),
(#308822,#308823)),.UNSPECIFIED.,.F.,.F.,.F.,(4,1,1,1,1,1,1,1,1,1,1,1,1,
1,1,1,4),(2,2),(0.,0.0724843729385586,0.142190024778259,0.209247943639616,
0.274447923967761,0.33802582267117,0.400406532440542,0.463046285981066,
0.525723189050567,0.587758999700955,0.647207274703619,0.705604379270503,
0.76335494041328,0.821014301633402,0.879178712895835,0.938732443992665,
1.),(0.,0.024),.UNSPECIFIED.);
#1016=SPHERICAL_SURFACE('',#95826,0.5);
#1017=SPHERICAL_SURFACE('',#96300,0.5);
#1018=SPHERICAL_SURFACE('',#97991,0.5);
#1019=SPHERICAL_SURFACE('',#98013,0.5);
#1020=SPHERICAL_SURFACE('',#98021,0.5);
#1021=SPHERICAL_SURFACE('',#98031,0.5);
#1022=SPHERICAL_SURFACE('',#99893,0.5);
#1023=SPHERICAL_SURFACE('',#99915,0.5);
#1024=SPHERICAL_SURFACE('',#99923,0.5);
#1025=SPHERICAL_SURFACE('',#99933,0.5);
#1026=SPHERICAL_SURFACE('',#101999,20.36);
#1027=SPHERICAL_SURFACE('',#102137,20.36);
#1028=SPHERICAL_SURFACE('',#102743,0.75);
#1029=SPHERICAL_SURFACE('',#102749,0.75);
#1030=SPHERICAL_SURFACE('',#102756,0.75);
#1031=SPHERICAL_SURFACE('',#102764,0.75);
#1032=SPHERICAL_SURFACE('',#102790,0.75);
#1033=SPHERICAL_SURFACE('',#102796,0.75);
#1034=SPHERICAL_SURFACE('',#102803,0.75);
#1035=SPHERICAL_SURFACE('',#102811,0.75);
#1036=SPHERICAL_SURFACE('',#103151,1.);
#1037=SPHERICAL_SURFACE('',#103161,1.);
#1038=SPHERICAL_SURFACE('',#103323,10.);
#1039=SPHERICAL_SURFACE('',#103325,10.);
#1040=SPHERICAL_SURFACE('',#104160,32.6421664440783);
#1041=SPHERICAL_SURFACE('',#104175,5.238);
#1042=SPHERICAL_SURFACE('',#104177,5.238);
#1043=SPHERICAL_SURFACE('',#104179,5.238);
#1044=SPHERICAL_SURFACE('',#104181,5.238);
#1045=SPHERICAL_SURFACE('',#104183,5.238);
#1046=SPHERICAL_SURFACE('',#104185,5.238);
#1047=SPHERICAL_SURFACE('',#104187,5.238);
#1048=SPHERICAL_SURFACE('',#104189,5.238);
#1049=SPHERICAL_SURFACE('',#104191,5.238);
#1050=SPHERICAL_SURFACE('',#104193,5.238);
#1051=SPHERICAL_SURFACE('',#104195,5.238);
#1052=SPHERICAL_SURFACE('',#104197,5.238);
#1053=SPHERICAL_SURFACE('',#104199,5.238);
#1054=SPHERICAL_SURFACE('',#104201,5.238);
#1055=SPHERICAL_SURFACE('',#104203,5.238);
#1056=SPHERICAL_SURFACE('',#104205,5.238);
#1057=SPHERICAL_SURFACE('',#104207,5.238);
#1058=SPHERICAL_SURFACE('',#104209,5.238);
#1059=SPHERICAL_SURFACE('',#104211,5.238);
#1060=SPHERICAL_SURFACE('',#104213,5.238);
#1061=SPHERICAL_SURFACE('',#104215,5.238);
#1062=SPHERICAL_SURFACE('',#104217,5.238);
#1063=SPHERICAL_SURFACE('',#104219,5.238);
#1064=SPHERICAL_SURFACE('',#104221,5.238);
#1065=SPHERICAL_SURFACE('',#104324,64.4688722290585);
#1066=SPHERICAL_SURFACE('',#104326,25.0876428025235);
#1067=SPHERICAL_SURFACE('',#104511,25.2860803025235);
#1068=(
BOUNDED_CURVE()
B_SPLINE_CURVE(3,(#134716,#134717,#134718,#134719,#134720,#134721),
 .UNSPECIFIED.,.F.,.F.)
B_SPLINE_CURVE_WITH_KNOTS((4,2,4),(0.,0.5,1.),.UNSPECIFIED.)
CURVE()
GEOMETRIC_REPRESENTATION_ITEM()
RATIONAL_B_SPLINE_CURVE((0.999999968420324,0.999999972427659,0.999999976025392,
0.999999982652427,0.99999998567993,0.999999988486397))
REPRESENTATION_ITEM('')
);
#1069=(
BOUNDED_CURVE()
B_SPLINE_CURVE(3,(#135210,#135211,#135212,#135213,#135214,#135215,#135216,
#135217,#135218,#135219,#135220,#135221,#135222,#135223),.UNSPECIFIED.,
 .F.,.F.)
B_SPLINE_CURVE_WITH_KNOTS((4,2,2,2,2,2,4),(0.,0.0419812889255314,0.201651074104609,
0.361320859283688,0.520990644462766,0.680660429641844,1.),.UNSPECIFIED.)
CURVE()
GEOMETRIC_REPRESENTATION_ITEM()
RATIONAL_B_SPLINE_CURVE((0.999998374495664,0.999998374493274,0.999998374583376,
0.999998375464702,0.999998377524268,0.999998384150543,0.999998388666334,
0.999998400123408,0.999998406847051,0.999998422090857,0.99999843067397,
0.999998457730094,0.999998478258162,0.999998498329814))
REPRESENTATION_ITEM('')
);
#1070=(
BOUNDED_CURVE()
B_SPLINE_CURVE(3,(#135565,#135566,#135567,#135568,#135569,#135570,#135571,
#135572,#135573,#135574),.UNSPECIFIED.,.F.,.F.)
B_SPLINE_CURVE_WITH_KNOTS((4,2,2,2,4),(4.71238898038469,5.10508806208341,
5.49778714378214,5.89048622548086,6.28318530717959),.UNSPECIFIED.)
CURVE()
GEOMETRIC_REPRESENTATION_ITEM()
RATIONAL_B_SPLINE_CURVE((1.,1.,1.,1.,1.,1.,1.,1.,1.,1.))
REPRESENTATION_ITEM('')
);
#1071=(
BOUNDED_CURVE()
B_SPLINE_CURVE(3,(#136470,#136471,#136472,#136473,#136474,#136475,#136476,
#136477,#136478,#136479),.UNSPECIFIED.,.F.,.F.)
B_SPLINE_CURVE_WITH_KNOTS((4,2,2,2,4),(0.,0.245429606613382,0.496953071075587,
0.748476535537792,1.),.UNSPECIFIED.)
CURVE()
GEOMETRIC_REPRESENTATION_ITEM()
RATIONAL_B_SPLINE_CURVE((0.999999984853823,0.999999984852031,0.99999998484993,
0.999999984845045,0.999999984842238,0.999999984836252,0.999999984832989,
0.999999984826274,0.999999984822825,0.99999998481928))
REPRESENTATION_ITEM('')
);
#1072=(
BOUNDED_CURVE()
B_SPLINE_CURVE(3,(#136618,#136619,#136620,#136621),.UNSPECIFIED.,.F.,.F.)
B_SPLINE_CURVE_WITH_KNOTS((4,4),(0.,0.038317388945353),.UNSPECIFIED.)
CURVE()
GEOMETRIC_REPRESENTATION_ITEM()
RATIONAL_B_SPLINE_CURVE((1.,1.,1.,1.))
REPRESENTATION_ITEM('')
);
#1073=(
BOUNDED_CURVE()
B_SPLINE_CURVE(3,(#136629,#136630,#136631,#136632),.UNSPECIFIED.,.F.,.F.)
B_SPLINE_CURVE_WITH_KNOTS((4,4),(0.,0.0385835973699829),.UNSPECIFIED.)
CURVE()
GEOMETRIC_REPRESENTATION_ITEM()
RATIONAL_B_SPLINE_CURVE((1.,1.,1.,1.))
REPRESENTATION_ITEM('')
);
#1074=(
BOUNDED_CURVE()
B_SPLINE_CURVE(3,(#136756,#136757,#136758,#136759),.UNSPECIFIED.,.F.,.F.)
B_SPLINE_CURVE_WITH_KNOTS((4,4),(0.,0.0372541843113205),.UNSPECIFIED.)
CURVE()
GEOMETRIC_REPRESENTATION_ITEM()
RATIONAL_B_SPLINE_CURVE((1.,1.,1.,1.))
REPRESENTATION_ITEM('')
);
#1075=(
BOUNDED_CURVE()
B_SPLINE_CURVE(3,(#136790,#136791,#136792,#136793),.UNSPECIFIED.,.F.,.F.)
B_SPLINE_CURVE_WITH_KNOTS((4,4),(0.,0.0369876550821707),.UNSPECIFIED.)
CURVE()
GEOMETRIC_REPRESENTATION_ITEM()
RATIONAL_B_SPLINE_CURVE((1.,1.,1.,1.))
REPRESENTATION_ITEM('')
);
#1076=(
BOUNDED_CURVE()
B_SPLINE_CURVE(3,(#136837,#136838,#136839,#136840,#136841,#136842,#136843,
#136844,#136845,#136846,#136847,#136848,#136849,#136850),.UNSPECIFIED.,
 .F.,.F.)
B_SPLINE_CURVE_WITH_KNOTS((4,2,2,2,2,2,4),(0.,0.245468499204218,0.371223749336846,
0.496978999469476,0.622734249602107,0.748489499734738,1.),.UNSPECIFIED.)
CURVE()
GEOMETRIC_REPRESENTATION_ITEM()
RATIONAL_B_SPLINE_CURVE((0.99999993495641,0.999999935048577,0.999999935181178,
0.999999935424418,0.999999935514307,0.999999935708972,0.999999935814682,
0.999999936034834,0.999999936149644,0.999999936388505,0.999999936513549,
0.999999936895779,0.999999937156295,0.999999937422256))
REPRESENTATION_ITEM('')
);
#1077=(
BOUNDED_CURVE()
B_SPLINE_CURVE(3,(#137033,#137034,#137035,#137036),.UNSPECIFIED.,.F.,.F.)
B_SPLINE_CURVE_WITH_KNOTS((4,4),(0.,0.0358270578054484),.UNSPECIFIED.)
CURVE()
GEOMETRIC_REPRESENTATION_ITEM()
RATIONAL_B_SPLINE_CURVE((1.,1.,1.,1.))
REPRESENTATION_ITEM('')
);
#1078=(
BOUNDED_CURVE()
B_SPLINE_CURVE(3,(#137068,#137069,#137070,#137071),.UNSPECIFIED.,.F.,.F.)
B_SPLINE_CURVE_WITH_KNOTS((4,4),(0.,0.0360938777358061),.UNSPECIFIED.)
CURVE()
GEOMETRIC_REPRESENTATION_ITEM()
RATIONAL_B_SPLINE_CURVE((1.,1.,1.,1.))
REPRESENTATION_ITEM('')
);
#1079=(
BOUNDED_CURVE()
B_SPLINE_CURVE(3,(#137082,#137083,#137084,#137085),.UNSPECIFIED.,.F.,.F.)
B_SPLINE_CURVE_WITH_KNOTS((4,4),(0.,1.),.UNSPECIFIED.)
CURVE()
GEOMETRIC_REPRESENTATION_ITEM()
RATIONAL_B_SPLINE_CURVE((0.999999995222607,0.999999995303701,0.999999995402298,
0.999999995544337))
REPRESENTATION_ITEM('')
);
#1080=(
BOUNDED_CURVE()
B_SPLINE_CURVE(3,(#137248,#137249,#137250,#137251),.UNSPECIFIED.,.F.,.F.)
B_SPLINE_CURVE_WITH_KNOTS((4,4),(0.,1.),.UNSPECIFIED.)
CURVE()
GEOMETRIC_REPRESENTATION_ITEM()
RATIONAL_B_SPLINE_CURVE((0.999999920677172,0.999999923035118,0.999999925829014,
0.999999929482952))
REPRESENTATION_ITEM('')
);
#1081=(
BOUNDED_CURVE()
B_SPLINE_CURVE(3,(#137464,#137465,#137466,#137467),.UNSPECIFIED.,.F.,.F.)
B_SPLINE_CURVE_WITH_KNOTS((4,4),(0.,1.),.UNSPECIFIED.)
CURVE()
GEOMETRIC_REPRESENTATION_ITEM()
RATIONAL_B_SPLINE_CURVE((0.999999954619029,0.999999952528045,0.999999951009961,
0.999999949748637))
REPRESENTATION_ITEM('')
);
#1082=(
BOUNDED_CURVE()
B_SPLINE_CURVE(3,(#137900,#137901,#137902,#137903),.UNSPECIFIED.,.F.,.F.)
B_SPLINE_CURVE_WITH_KNOTS((4,4),(-1.38777878078145E-17,0.0332202089949022),
 .UNSPECIFIED.)
CURVE()
GEOMETRIC_REPRESENTATION_ITEM()
RATIONAL_B_SPLINE_CURVE((1.,1.,1.,1.))
REPRESENTATION_ITEM('')
);
#1083=(
BOUNDED_CURVE()
B_SPLINE_CURVE(3,(#137941,#137942,#137943,#137944,#137945,#137946,#137947,
#137948,#137949,#137950,#137951,#137952),.UNSPECIFIED.,.F.,.F.)
B_SPLINE_CURVE_WITH_KNOTS((4,2,2,2,2,4),(0.,0.244321743484906,0.496214495656607,
0.622160871742453,0.748107247828304,1.),.UNSPECIFIED.)
CURVE()
GEOMETRIC_REPRESENTATION_ITEM()
RATIONAL_B_SPLINE_CURVE((0.999999971111316,0.999999971052111,0.999999970982043,
0.999999970817943,0.99999997072254,0.999999970569587,0.999999970516657,
0.999999970406767,0.999999970349674,0.999999970177141,0.999999970058889,
0.999999969937273))
REPRESENTATION_ITEM('')
);
#1084=(
BOUNDED_CURVE()
B_SPLINE_CURVE(3,(#138175,#138176,#138177,#138178,#138179,#138180),
 .UNSPECIFIED.,.F.,.F.)
B_SPLINE_CURVE_WITH_KNOTS((4,2,4),(0.,0.5,1.),.UNSPECIFIED.)
CURVE()
GEOMETRIC_REPRESENTATION_ITEM()
RATIONAL_B_SPLINE_CURVE((0.999999994912409,0.999999994848392,0.999999994777208,
0.999999994613678,0.999999994521381,0.999999994413334))
REPRESENTATION_ITEM('')
);
#1085=(
BOUNDED_CURVE()
B_SPLINE_CURVE(3,(#138365,#138366,#138367,#138368),.UNSPECIFIED.,.F.,.F.)
B_SPLINE_CURVE_WITH_KNOTS((4,4),(0.,1.),.UNSPECIFIED.)
CURVE()
GEOMETRIC_REPRESENTATION_ITEM()
RATIONAL_B_SPLINE_CURVE((0.999999987573952,0.999999987041702,0.999999986704629,
0.99999998643111))
REPRESENTATION_ITEM('')
);
#1086=(
BOUNDED_CURVE()
B_SPLINE_CURVE(3,(#138745,#138746,#138747,#138748),.UNSPECIFIED.,.F.,.F.)
B_SPLINE_CURVE_WITH_KNOTS((4,4),(0.,0.0430361525536219),.UNSPECIFIED.)
CURVE()
GEOMETRIC_REPRESENTATION_ITEM()
RATIONAL_B_SPLINE_CURVE((1.,1.,1.,1.))
REPRESENTATION_ITEM('')
);
#1087=(
BOUNDED_CURVE()
B_SPLINE_CURVE(3,(#138780,#138781,#138782,#138783),.UNSPECIFIED.,.F.,.F.)
B_SPLINE_CURVE_WITH_KNOTS((4,4),(-2.77555756156289E-17,0.0433026927553429),
 .UNSPECIFIED.)
CURVE()
GEOMETRIC_REPRESENTATION_ITEM()
RATIONAL_B_SPLINE_CURVE((1.,1.,1.,1.))
REPRESENTATION_ITEM('')
);
#1088=(
BOUNDED_CURVE()
B_SPLINE_CURVE(3,(#138796,#138797,#138798,#138799),.UNSPECIFIED.,.F.,.F.)
B_SPLINE_CURVE_WITH_KNOTS((4,4),(0.,1.),.UNSPECIFIED.)
CURVE()
GEOMETRIC_REPRESENTATION_ITEM()
RATIONAL_B_SPLINE_CURVE((0.999999999134233,0.999999999123191,0.999999999109547,
0.999999999086375))
REPRESENTATION_ITEM('')
);
#1089=(
BOUNDED_CURVE()
B_SPLINE_CURVE(3,(#138882,#138883,#138884,#138885),.UNSPECIFIED.,.F.,.F.)
B_SPLINE_CURVE_WITH_KNOTS((4,4),(0.,0.044753309356401),.UNSPECIFIED.)
CURVE()
GEOMETRIC_REPRESENTATION_ITEM()
RATIONAL_B_SPLINE_CURVE((1.,1.,1.,1.))
REPRESENTATION_ITEM('')
);
#1090=(
BOUNDED_CURVE()
B_SPLINE_CURVE(3,(#138892,#138893,#138894,#138895),.UNSPECIFIED.,.F.,.F.)
B_SPLINE_CURVE_WITH_KNOTS((4,4),(0.,0.0444870989094409),.UNSPECIFIED.)
CURVE()
GEOMETRIC_REPRESENTATION_ITEM()
RATIONAL_B_SPLINE_CURVE((1.,1.,1.,1.))
REPRESENTATION_ITEM('')
);
#1091=(
BOUNDED_CURVE()
B_SPLINE_CURVE(3,(#138927,#138928,#138929,#138930,#138931,#138932,#138933,
#138934,#138935,#138936),.UNSPECIFIED.,.F.,.F.)
B_SPLINE_CURVE_WITH_KNOTS((4,2,2,2,4),(0.,0.245398115008223,0.49693207667215,
0.748466038336073,1.),.UNSPECIFIED.)
CURVE()
GEOMETRIC_REPRESENTATION_ITEM()
RATIONAL_B_SPLINE_CURVE((0.999999977858779,0.999999977854974,0.999999977850512,
0.999999977840136,0.999999977834171,0.999999977821454,0.999999977814521,
0.999999977800252,0.999999977792922,0.999999977785388))
REPRESENTATION_ITEM('')
);
#1092=(
BOUNDED_CURVE()
B_SPLINE_CURVE(3,(#138951,#138952,#138953,#138954,#138955,#138956,#138957,
#138958,#138959,#138960),.UNSPECIFIED.,.F.,.F.)
B_SPLINE_CURVE_WITH_KNOTS((4,2,2,2,4),(0.,0.251502574391383,0.503005148782772,
0.754507723174155,1.),.UNSPECIFIED.)
CURVE()
GEOMETRIC_REPRESENTATION_ITEM()
RATIONAL_B_SPLINE_CURVE((0.999999995351172,0.999999995351771,0.999999995352353,
0.999999995353486,0.999999995354037,0.999999995355048,0.999999995355522,
0.999999995356347,0.999999995356702,0.999999995357005))
REPRESENTATION_ITEM('')
);
#1093=(
BOUNDED_CURVE()
B_SPLINE_CURVE(3,(#139039,#139040,#139041,#139042),.UNSPECIFIED.,.F.,.F.)
B_SPLINE_CURVE_WITH_KNOTS((4,4),(0.,0.0445045070401677),.UNSPECIFIED.)
CURVE()
GEOMETRIC_REPRESENTATION_ITEM()
RATIONAL_B_SPLINE_CURVE((1.,1.,1.,1.))
REPRESENTATION_ITEM('')
);
#1094=(
BOUNDED_CURVE()
B_SPLINE_CURVE(3,(#139088,#139089,#139090,#139091,#139092,#139093,#139094,
#139095),.UNSPECIFIED.,.F.,.F.)
B_SPLINE_CURVE_WITH_KNOTS((4,2,2,4),(0.,0.233211998637451,0.490844615148963,
1.),.UNSPECIFIED.)
CURVE()
GEOMETRIC_REPRESENTATION_ITEM()
RATIONAL_B_SPLINE_CURVE((0.999999996506968,0.999999996496103,0.99999999647882,
0.999999996429016,0.999999996394958,0.999999996273789,0.999999996166972,
0.999999996039415))
REPRESENTATION_ITEM('')
);
#1095=(
BOUNDED_CURVE()
B_SPLINE_CURVE(3,(#139100,#139101,#139102,#139103),.UNSPECIFIED.,.F.,.F.)
B_SPLINE_CURVE_WITH_KNOTS((4,4),(0.,1.),.UNSPECIFIED.)
CURVE()
GEOMETRIC_REPRESENTATION_ITEM()
RATIONAL_B_SPLINE_CURVE((0.999999998576403,0.999999998611592,0.999999998632289,
0.999999998649038))
REPRESENTATION_ITEM('')
);
#1096=(
BOUNDED_CURVE()
B_SPLINE_CURVE(3,(#139203,#139204,#139205,#139206),.UNSPECIFIED.,.F.,.F.)
B_SPLINE_CURVE_WITH_KNOTS((4,4),(0.,0.0433970829567688),.UNSPECIFIED.)
CURVE()
GEOMETRIC_REPRESENTATION_ITEM()
RATIONAL_B_SPLINE_CURVE((1.,1.,1.,1.))
REPRESENTATION_ITEM('')
);
#1097=(
BOUNDED_CURVE()
B_SPLINE_CURVE(3,(#139237,#139238,#139239,#139240),.UNSPECIFIED.,.F.,.F.)
B_SPLINE_CURVE_WITH_KNOTS((4,4),(-1.38777878078145E-17,0.0431305646498159),
 .UNSPECIFIED.)
CURVE()
GEOMETRIC_REPRESENTATION_ITEM()
RATIONAL_B_SPLINE_CURVE((1.,1.,1.,1.))
REPRESENTATION_ITEM('')
);
#1098=(
BOUNDED_CURVE()
B_SPLINE_CURVE(3,(#139284,#139285,#139286,#139287,#139288,#139289,#139290,
#139291,#139292,#139293,#139294,#139295,#139296,#139297),.UNSPECIFIED.,
 .F.,.F.)
B_SPLINE_CURVE_WITH_KNOTS((4,2,2,2,2,2,4),(0.,0.245486421447413,0.371238684539511,
0.496990947631609,0.622743210723706,0.748495473815804,1.),.UNSPECIFIED.)
CURVE()
GEOMETRIC_REPRESENTATION_ITEM()
RATIONAL_B_SPLINE_CURVE((0.999999936096482,0.999999936209566,0.999999936365119,
0.999999936644208,0.999999936746728,0.999999936967832,0.999999937086967,
0.999999937333646,0.999999937462032,0.999999937728739,0.999999937868259,
0.999999938292486,0.99999993858141,0.99999993887622))
REPRESENTATION_ITEM('')
);
#1099=(
BOUNDED_CURVE()
B_SPLINE_CURVE(3,(#139524,#139525,#139526,#139527),.UNSPECIFIED.,.F.,.F.)
B_SPLINE_CURVE_WITH_KNOTS((4,4),(0.,1.),.UNSPECIFIED.)
CURVE()
GEOMETRIC_REPRESENTATION_ITEM()
RATIONAL_B_SPLINE_CURVE((0.999999988352499,0.999999988581759,0.999999988864347,
0.999999989311818))
REPRESENTATION_ITEM('')
);
#1100=(
BOUNDED_CURVE()
B_SPLINE_CURVE(3,(#139703,#139704,#139705,#139706,#139707,#139708),
 .UNSPECIFIED.,.F.,.F.)
B_SPLINE_CURVE_WITH_KNOTS((4,2,4),(0.,0.500000000000001,1.),
 .UNSPECIFIED.)
CURVE()
GEOMETRIC_REPRESENTATION_ITEM()
RATIONAL_B_SPLINE_CURVE((0.999999994872226,0.999999994962405,0.999999995062978,
0.999999995295095,0.999999995426566,0.999999995581248))
REPRESENTATION_ITEM('')
);
#1101=(
BOUNDED_CURVE()
B_SPLINE_CURVE(3,(#139709,#139710,#139711,#139712,#139713,#139714),
 .UNSPECIFIED.,.F.,.F.)
B_SPLINE_CURVE_WITH_KNOTS((4,2,4),(0.,0.5,1.),.UNSPECIFIED.)
CURVE()
GEOMETRIC_REPRESENTATION_ITEM()
RATIONAL_B_SPLINE_CURVE((0.999999988435972,0.999999988660851,0.999999988852627,
0.999999989192075,0.999999989339638,0.999999989472243))
REPRESENTATION_ITEM('')
);
#1102=(
BOUNDED_CURVE()
B_SPLINE_CURVE(3,(#139852,#139853,#139854,#139855,#139856,#139857,#139858,
#139859,#139860,#139861),.UNSPECIFIED.,.F.,.F.)
B_SPLINE_CURVE_WITH_KNOTS((4,2,2,2,4),(1.18015353016497E-15,0.392699081698726,
0.785398163397449,1.17809724509617,1.5707963267949),.UNSPECIFIED.)
CURVE()
GEOMETRIC_REPRESENTATION_ITEM()
RATIONAL_B_SPLINE_CURVE((1.,1.,1.,1.,1.,1.,1.,1.,1.,1.))
REPRESENTATION_ITEM('')
);
#1103=(
BOUNDED_CURVE()
B_SPLINE_CURVE(3,(#139894,#139895,#139896,#139897,#139898,#139899,#139900,
#139901,#139902,#139903),.UNSPECIFIED.,.F.,.F.)
B_SPLINE_CURVE_WITH_KNOTS((4,2,2,2,4),(4.71238898038469,5.10508806208341,
5.49778714378214,5.89048622548086,6.28318530717959),.UNSPECIFIED.)
CURVE()
GEOMETRIC_REPRESENTATION_ITEM()
RATIONAL_B_SPLINE_CURVE((1.,1.,1.,1.,1.,1.,1.,1.,1.,1.))
REPRESENTATION_ITEM('')
);
#1104=(
BOUNDED_CURVE()
B_SPLINE_CURVE(3,(#139907,#139908,#139909,#139910,#139911,#139912,#139913,
#139914,#139915,#139916),.UNSPECIFIED.,.F.,.F.)
B_SPLINE_CURVE_WITH_KNOTS((4,2,2,2,4),(1.5707963267949,1.96349540849362,
2.35619449019234,2.74889357189107,3.1415926535898),.UNSPECIFIED.)
CURVE()
GEOMETRIC_REPRESENTATION_ITEM()
RATIONAL_B_SPLINE_CURVE((1.,1.,1.,1.,1.,1.,1.,1.,1.,1.))
REPRESENTATION_ITEM('')
);
#1105=(
BOUNDED_CURVE()
B_SPLINE_CURVE(3,(#140064,#140065,#140066,#140067,#140068,#140069,#140070,
#140071,#140072,#140073),.UNSPECIFIED.,.F.,.F.)
B_SPLINE_CURVE_WITH_KNOTS((4,2,2,2,4),(3.1415926535898,3.53429173528852,
3.92699081698724,4.31968989868597,4.71238898038469),.UNSPECIFIED.)
CURVE()
GEOMETRIC_REPRESENTATION_ITEM()
RATIONAL_B_SPLINE_CURVE((1.,1.,1.,1.,1.,1.,1.,1.,1.,1.))
REPRESENTATION_ITEM('')
);
#1106=(
BOUNDED_CURVE()
B_SPLINE_CURVE(3,(#140084,#140085,#140086,#140087,#140088,#140089,#140090,
#140091,#140092,#140093),.UNSPECIFIED.,.F.,.F.)
B_SPLINE_CURVE_WITH_KNOTS((4,2,2,2,4),(4.71238898038469,5.10508806208342,
5.49778714378214,5.89048622548086,6.28318530717959),.UNSPECIFIED.)
CURVE()
GEOMETRIC_REPRESENTATION_ITEM()
RATIONAL_B_SPLINE_CURVE((1.,1.,1.,1.,1.,1.,1.,1.,1.,1.))
REPRESENTATION_ITEM('')
);
#1107=(
BOUNDED_CURVE()
B_SPLINE_CURVE(3,(#140350,#140351,#140352,#140353,#140354,#140355,#140356,
#140357,#140358,#140359),.UNSPECIFIED.,.F.,.F.)
B_SPLINE_CURVE_WITH_KNOTS((4,2,2,2,4),(0.,0.392699081698724,0.785398163397448,
1.17809724509617,1.5707963267949),.UNSPECIFIED.)
CURVE()
GEOMETRIC_REPRESENTATION_ITEM()
RATIONAL_B_SPLINE_CURVE((1.,1.,1.,1.,1.,1.,1.,1.,1.,1.))
REPRESENTATION_ITEM('')
);
#1108=(
BOUNDED_CURVE()
B_SPLINE_CURVE(3,(#140374,#140375,#140376,#140377,#140378,#140379,#140380,
#140381,#140382,#140383),.UNSPECIFIED.,.F.,.F.)
B_SPLINE_CURVE_WITH_KNOTS((4,2,2,2,4),(1.5707963267949,1.96349540849362,
2.35619449019234,2.74889357189107,3.1415926535898),.UNSPECIFIED.)
CURVE()
GEOMETRIC_REPRESENTATION_ITEM()
RATIONAL_B_SPLINE_CURVE((1.,1.,1.,1.,1.,1.,1.,1.,1.,1.))
REPRESENTATION_ITEM('')
);
#1109=(
BOUNDED_CURVE()
B_SPLINE_CURVE(3,(#140585,#140586,#140587,#140588,#140589,#140590,#140591,
#140592,#140593,#140594),.UNSPECIFIED.,.F.,.F.)
B_SPLINE_CURVE_WITH_KNOTS((4,2,2,2,4),(3.1415926535898,3.53429173528852,
3.92699081698724,4.31968989868597,4.71238898038469),.UNSPECIFIED.)
CURVE()
GEOMETRIC_REPRESENTATION_ITEM()
RATIONAL_B_SPLINE_CURVE((1.,1.,1.,1.,1.,1.,1.,1.,1.,1.))
REPRESENTATION_ITEM('')
);
#1110=(
BOUNDED_CURVE()
B_SPLINE_CURVE(3,(#140633,#140634,#140635,#140636,#140637,#140638,#140639,
#140640,#140641,#140642),.UNSPECIFIED.,.F.,.F.)
B_SPLINE_CURVE_WITH_KNOTS((4,2,2,2,4),(3.1415926535898,3.53429173528852,
3.92699081698724,4.31968989868597,4.71238898038469),.UNSPECIFIED.)
CURVE()
GEOMETRIC_REPRESENTATION_ITEM()
RATIONAL_B_SPLINE_CURVE((1.,1.,1.,1.,1.,1.,1.,1.,1.,1.))
REPRESENTATION_ITEM('')
);
#1111=(
BOUNDED_CURVE()
B_SPLINE_CURVE(3,(#140676,#140677,#140678,#140679,#140680,#140681,#140682,
#140683,#140684,#140685),.UNSPECIFIED.,.F.,.F.)
B_SPLINE_CURVE_WITH_KNOTS((4,2,2,2,4),(1.5707963267949,1.96349540849362,
2.35619449019234,2.74889357189106,3.14159265358979),.UNSPECIFIED.)
CURVE()
GEOMETRIC_REPRESENTATION_ITEM()
RATIONAL_B_SPLINE_CURVE((1.,1.,1.,1.,1.,1.,1.,1.,1.,1.))
REPRESENTATION_ITEM('')
);
#1112=(
BOUNDED_CURVE()
B_SPLINE_CURVE(3,(#140968,#140969,#140970,#140971),.UNSPECIFIED.,.F.,.F.)
B_SPLINE_CURVE_WITH_KNOTS((4,4),(0.,0.00407947372412412),.UNSPECIFIED.)
CURVE()
GEOMETRIC_REPRESENTATION_ITEM()
RATIONAL_B_SPLINE_CURVE((1.,1.,1.,1.))
REPRESENTATION_ITEM('')
);
#1113=(
BOUNDED_CURVE()
B_SPLINE_CURVE(3,(#141029,#141030,#141031,#141032,#141033,#141034,#141035,
#141036,#141037,#141038),.UNSPECIFIED.,.F.,.F.)
B_SPLINE_CURVE_WITH_KNOTS((4,2,2,2,4),(-1.77635683940025E-15,0.392699081698723,
0.785398163397447,1.17809724509617,1.5707963267949),.UNSPECIFIED.)
CURVE()
GEOMETRIC_REPRESENTATION_ITEM()
RATIONAL_B_SPLINE_CURVE((1.,1.,1.,1.,1.,1.,1.,1.,1.,1.))
REPRESENTATION_ITEM('')
);
#1114=(
BOUNDED_CURVE()
B_SPLINE_CURVE(3,(#141072,#141073,#141074,#141075,#141076,#141077,#141078,
#141079,#141080,#141081),.UNSPECIFIED.,.F.,.F.)
B_SPLINE_CURVE_WITH_KNOTS((4,2,2,2,4),(4.71238898038469,5.10508806208342,
5.49778714378214,5.89048622548086,6.28318530717959),.UNSPECIFIED.)
CURVE()
GEOMETRIC_REPRESENTATION_ITEM()
RATIONAL_B_SPLINE_CURVE((1.,1.,1.,1.,1.,1.,1.,1.,1.,1.))
REPRESENTATION_ITEM('')
);
#1115=(
BOUNDED_CURVE()
B_SPLINE_CURVE(3,(#141085,#141086,#141087,#141088,#141089,#141090,#141091,
#141092,#141093,#141094),.UNSPECIFIED.,.F.,.F.)
B_SPLINE_CURVE_WITH_KNOTS((4,2,2,2,4),(1.5707963267949,1.96349540849362,
2.35619449019234,2.74889357189107,3.14159265358979),.UNSPECIFIED.)
CURVE()
GEOMETRIC_REPRESENTATION_ITEM()
RATIONAL_B_SPLINE_CURVE((1.,1.,1.,1.,1.,1.,1.,1.,1.,1.))
REPRESENTATION_ITEM('')
);
#1116=(
BOUNDED_CURVE()
B_SPLINE_CURVE(3,(#141118,#141119,#141120,#141121),.UNSPECIFIED.,.F.,.F.)
B_SPLINE_CURVE_WITH_KNOTS((4,4),(-1.00613961606655E-16,0.00454919832189776),
 .UNSPECIFIED.)
CURVE()
GEOMETRIC_REPRESENTATION_ITEM()
RATIONAL_B_SPLINE_CURVE((1.,1.,1.,1.))
REPRESENTATION_ITEM('')
);
#1117=(
BOUNDED_CURVE()
B_SPLINE_CURVE(3,(#141162,#141163,#141164,#141165),.UNSPECIFIED.,.F.,.F.)
B_SPLINE_CURVE_WITH_KNOTS((4,4),(1.7347234759768E-18,0.00426411906192034),
 .UNSPECIFIED.)
CURVE()
GEOMETRIC_REPRESENTATION_ITEM()
RATIONAL_B_SPLINE_CURVE((1.,1.,1.,1.))
REPRESENTATION_ITEM('')
);
#1118=(
BOUNDED_CURVE()
B_SPLINE_CURVE(3,(#141236,#141237,#141238,#141239,#141240,#141241,#141242,
#141243,#141244,#141245),.UNSPECIFIED.,.F.,.F.)
B_SPLINE_CURVE_WITH_KNOTS((4,2,2,2,4),(4.71238898038469,5.10508806208342,
5.49778714378214,5.89048622548086,6.28318530717959),.UNSPECIFIED.)
CURVE()
GEOMETRIC_REPRESENTATION_ITEM()
RATIONAL_B_SPLINE_CURVE((1.,1.,1.,1.,1.,1.,1.,1.,1.,1.))
REPRESENTATION_ITEM('')
);
#1119=(
BOUNDED_CURVE()
B_SPLINE_CURVE(3,(#141275,#141276,#141277,#141278,#141279,#141280,#141281,
#141282,#141283,#141284),.UNSPECIFIED.,.F.,.F.)
B_SPLINE_CURVE_WITH_KNOTS((4,2,2,2,4),(3.1415926535898,3.53429173528852,
3.92699081698724,4.31968989868597,4.71238898038469),.UNSPECIFIED.)
CURVE()
GEOMETRIC_REPRESENTATION_ITEM()
RATIONAL_B_SPLINE_CURVE((1.,1.,1.,1.,1.,1.,1.,1.,1.,1.))
REPRESENTATION_ITEM('')
);
#1120=(
BOUNDED_CURVE()
B_SPLINE_CURVE(3,(#141500,#141501,#141502,#141503,#141504,#141505,#141506,
#141507,#141508,#141509),.UNSPECIFIED.,.F.,.F.)
B_SPLINE_CURVE_WITH_KNOTS((4,2,2,2,4),(-1.77635683940025E-15,0.392699081698723,
0.785398163397447,1.17809724509617,1.5707963267949),.UNSPECIFIED.)
CURVE()
GEOMETRIC_REPRESENTATION_ITEM()
RATIONAL_B_SPLINE_CURVE((1.,1.,1.,1.,1.,1.,1.,1.,1.,1.))
REPRESENTATION_ITEM('')
);
#1121=(
BOUNDED_CURVE()
B_SPLINE_CURVE(3,(#141524,#141525,#141526,#141527,#141528,#141529,#141530,
#141531,#141532,#141533),.UNSPECIFIED.,.F.,.F.)
B_SPLINE_CURVE_WITH_KNOTS((4,2,2,2,4),(1.5707963267949,1.96349540849362,
2.35619449019234,2.74889357189107,3.14159265358979),.UNSPECIFIED.)
CURVE()
GEOMETRIC_REPRESENTATION_ITEM()
RATIONAL_B_SPLINE_CURVE((1.,1.,1.,1.,1.,1.,1.,1.,1.,1.))
REPRESENTATION_ITEM('')
);
#1122=(
BOUNDED_CURVE()
B_SPLINE_CURVE(3,(#141732,#141733,#141734,#141735,#141736,#141737,#141738,
#141739,#141740,#141741),.UNSPECIFIED.,.F.,.F.)
B_SPLINE_CURVE_WITH_KNOTS((4,2,2,2,4),(3.1415926535898,3.53429173528852,
3.92699081698724,4.31968989868597,4.71238898038469),.UNSPECIFIED.)
CURVE()
GEOMETRIC_REPRESENTATION_ITEM()
RATIONAL_B_SPLINE_CURVE((1.,1.,1.,1.,1.,1.,1.,1.,1.,1.))
REPRESENTATION_ITEM('')
);
#1123=(
BOUNDED_CURVE()
B_SPLINE_CURVE(3,(#141935,#141936,#141937,#141938,#141939,#141940,#141941,
#141942,#141943,#141944),.UNSPECIFIED.,.F.,.F.)
B_SPLINE_CURVE_WITH_KNOTS((4,2,2,2,4),(3.1415926535898,3.53429173528852,
3.92699081698724,4.31968989868597,4.71238898038469),.UNSPECIFIED.)
CURVE()
GEOMETRIC_REPRESENTATION_ITEM()
RATIONAL_B_SPLINE_CURVE((1.,1.,1.,1.,1.,1.,1.,1.,1.,1.))
REPRESENTATION_ITEM('')
);
#1124=(
BOUNDED_CURVE()
B_SPLINE_CURVE(3,(#141948,#141949,#141950,#141951,#141952,#141953,#141954,
#141955,#141956,#141957),.UNSPECIFIED.,.F.,.F.)
B_SPLINE_CURVE_WITH_KNOTS((4,2,2,2,4),(4.71238898038469,5.10508806208341,
5.49778714378214,5.89048622548086,6.28318530717959),.UNSPECIFIED.)
CURVE()
GEOMETRIC_REPRESENTATION_ITEM()
RATIONAL_B_SPLINE_CURVE((1.,1.,1.,1.,1.,1.,1.,1.,1.,1.))
REPRESENTATION_ITEM('')
);
#1125=(
BOUNDED_CURVE()
B_SPLINE_CURVE(3,(#142061,#142062,#142063,#142064,#142065,#142066,#142067,
#142068,#142069,#142070),.UNSPECIFIED.,.F.,.F.)
B_SPLINE_CURVE_WITH_KNOTS((4,2,2,2,4),(1.5707963267949,1.96349540849362,
2.35619449019234,2.74889357189107,3.14159265358979),.UNSPECIFIED.)
CURVE()
GEOMETRIC_REPRESENTATION_ITEM()
RATIONAL_B_SPLINE_CURVE((1.,1.,1.,1.,1.,1.,1.,1.,1.,1.))
REPRESENTATION_ITEM('')
);
#1126=(
BOUNDED_CURVE()
B_SPLINE_CURVE(3,(#142094,#142095,#142096,#142097),.UNSPECIFIED.,.F.,.F.)
B_SPLINE_CURVE_WITH_KNOTS((4,4),(-5.03069808033274E-17,0.00385726433182564),
 .UNSPECIFIED.)
CURVE()
GEOMETRIC_REPRESENTATION_ITEM()
RATIONAL_B_SPLINE_CURVE((1.,1.,1.,1.))
REPRESENTATION_ITEM('')
);
#1127=(
BOUNDED_CURVE()
B_SPLINE_CURVE(3,(#142138,#142139,#142140,#142141),.UNSPECIFIED.,.F.,.F.)
B_SPLINE_CURVE_WITH_KNOTS((4,4),(0.,0.00414272899747597),.UNSPECIFIED.)
CURVE()
GEOMETRIC_REPRESENTATION_ITEM()
RATIONAL_B_SPLINE_CURVE((1.,1.,1.,1.))
REPRESENTATION_ITEM('')
);
#1128=(
BOUNDED_CURVE()
B_SPLINE_CURVE(3,(#142159,#142160,#142161,#142162,#142163,#142164,#142165,
#142166,#142167,#142168),.UNSPECIFIED.,.F.,.F.)
B_SPLINE_CURVE_WITH_KNOTS((4,2,2,2,4),(-8.88178419700125E-16,0.392699081698724,
0.785398163397448,1.17809724509617,1.5707963267949),.UNSPECIFIED.)
CURVE()
GEOMETRIC_REPRESENTATION_ITEM()
RATIONAL_B_SPLINE_CURVE((1.,1.,1.,1.,1.,1.,1.,1.,1.,1.))
REPRESENTATION_ITEM('')
);
#1129=(
BOUNDED_CURVE()
B_SPLINE_CURVE(3,(#142266,#142267,#142268,#142269,#142270,#142271,#142272,
#142273,#142274,#142275),.UNSPECIFIED.,.F.,.F.)
B_SPLINE_CURVE_WITH_KNOTS((4,2,2,2,4),(4.71238898038469,5.10508806208341,
5.49778714378214,5.89048622548086,6.28318530717959),.UNSPECIFIED.)
CURVE()
GEOMETRIC_REPRESENTATION_ITEM()
RATIONAL_B_SPLINE_CURVE((1.,1.,1.,1.,1.,1.,1.,1.,1.,1.))
REPRESENTATION_ITEM('')
);
#1130=(
BOUNDED_CURVE()
B_SPLINE_CURVE(3,(#142412,#142413,#142414,#142415,#142416,#142417,#142418,
#142419,#142420,#142421),.UNSPECIFIED.,.F.,.F.)
B_SPLINE_CURVE_WITH_KNOTS((4,2,2,2,4),(1.5707963267949,1.96349540849362,
2.35619449019234,2.74889357189107,3.14159265358979),.UNSPECIFIED.)
CURVE()
GEOMETRIC_REPRESENTATION_ITEM()
RATIONAL_B_SPLINE_CURVE((1.,1.,1.,1.,1.,1.,1.,1.,1.,1.))
REPRESENTATION_ITEM('')
);
#1131=(
BOUNDED_CURVE()
B_SPLINE_CURVE(3,(#142528,#142529,#142530,#142531,#142532,#142533,#142534,
#142535,#142536,#142537),.UNSPECIFIED.,.F.,.F.)
B_SPLINE_CURVE_WITH_KNOTS((4,2,2,2,4),(-8.88178419700125E-16,0.392699081698724,
0.785398163397448,1.17809724509617,1.5707963267949),.UNSPECIFIED.)
CURVE()
GEOMETRIC_REPRESENTATION_ITEM()
RATIONAL_B_SPLINE_CURVE((1.,1.,1.,1.,1.,1.,1.,1.,1.,1.))
REPRESENTATION_ITEM('')
);
#1132=(
BOUNDED_CURVE()
B_SPLINE_CURVE(3,(#144003,#144004,#144005,#144006),.UNSPECIFIED.,.F.,.F.)
B_SPLINE_CURVE_WITH_KNOTS((4,4),(0.,1.),.UNSPECIFIED.)
CURVE()
GEOMETRIC_REPRESENTATION_ITEM()
RATIONAL_B_SPLINE_CURVE((0.999999927380708,0.999999923584106,0.999999920688567,
0.999999918247059))
REPRESENTATION_ITEM('')
);
#1133=(
BOUNDED_CURVE()
B_SPLINE_CURVE(3,(#144057,#144058,#144059,#144060),.UNSPECIFIED.,.F.,.F.)
B_SPLINE_CURVE_WITH_KNOTS((4,4),(0.,1.),.UNSPECIFIED.)
CURVE()
GEOMETRIC_REPRESENTATION_ITEM()
RATIONAL_B_SPLINE_CURVE((0.999999995487232,0.999999995342312,0.999999995242007,
0.999999995159558))
REPRESENTATION_ITEM('')
);
#1134=(
BOUNDED_CURVE()
B_SPLINE_CURVE(3,(#144253,#144254,#144255,#144256),.UNSPECIFIED.,.F.,.F.)
B_SPLINE_CURVE_WITH_KNOTS((4,4),(0.,1.),.UNSPECIFIED.)
CURVE()
GEOMETRIC_REPRESENTATION_ITEM()
RATIONAL_B_SPLINE_CURVE((0.999999999408156,0.999999999401785,0.999999999393965,
0.999999999382027))
REPRESENTATION_ITEM('')
);
#1135=(
BOUNDED_CURVE()
B_SPLINE_CURVE(3,(#144311,#144312,#144313,#144314),.UNSPECIFIED.,.F.,.F.)
B_SPLINE_CURVE_WITH_KNOTS((4,4),(0.,1.),.UNSPECIFIED.)
CURVE()
GEOMETRIC_REPRESENTATION_ITEM()
RATIONAL_B_SPLINE_CURVE((0.99999987960117,0.999999865674974,0.999999841276082,
0.999999808047049))
REPRESENTATION_ITEM('')
);
#1136=(
BOUNDED_CURVE()
B_SPLINE_CURVE(3,(#144668,#144669,#144670,#144671,#144672,#144673),
 .UNSPECIFIED.,.F.,.F.)
B_SPLINE_CURVE_WITH_KNOTS((4,2,4),(0.,0.5,1.),.UNSPECIFIED.)
CURVE()
GEOMETRIC_REPRESENTATION_ITEM()
RATIONAL_B_SPLINE_CURVE((0.999999999903741,0.999999999897905,0.999999999891833,
0.999999999879122,0.999999999872429,0.999999999865662))
REPRESENTATION_ITEM('')
);
#1137=(
BOUNDED_CURVE()
B_SPLINE_CURVE(3,(#144928,#144929,#144930,#144931,#144932,#144933),
 .UNSPECIFIED.,.F.,.F.)
B_SPLINE_CURVE_WITH_KNOTS((4,2,4),(0.,0.499999999999999,0.999999989281006),
 .UNSPECIFIED.)
CURVE()
GEOMETRIC_REPRESENTATION_ITEM()
RATIONAL_B_SPLINE_CURVE((0.999999999934743,0.999999999928937,0.999999999922868,
0.999999999909996,0.99999999990313,0.999999999896125))
REPRESENTATION_ITEM('')
);
#1138=(
BOUNDED_CURVE()
B_SPLINE_CURVE(3,(#145054,#145055,#145056,#145057),.UNSPECIFIED.,.F.,.F.)
B_SPLINE_CURVE_WITH_KNOTS((4,4),(0.,1.),.UNSPECIFIED.)
CURVE()
GEOMETRIC_REPRESENTATION_ITEM()
RATIONAL_B_SPLINE_CURVE((0.999999907463791,0.99999990228317,0.999999898054214,
0.999999894391216))
REPRESENTATION_ITEM('')
);
#1139=(
BOUNDED_CURVE()
B_SPLINE_CURVE(3,(#145708,#145709,#145710,#145711,#145712,#145713),
 .UNSPECIFIED.,.F.,.F.)
B_SPLINE_CURVE_WITH_KNOTS((4,2,4),(0.,0.5,1.),.UNSPECIFIED.)
CURVE()
GEOMETRIC_REPRESENTATION_ITEM()
RATIONAL_B_SPLINE_CURVE((0.999999998284567,0.999999998319219,0.99999999834714,
0.999999998395064,0.999999998415023,0.999999998432575))
REPRESENTATION_ITEM('')
);
#1140=(
BOUNDED_CURVE()
B_SPLINE_CURVE(3,(#145734,#145735,#145736,#145737,#145738,#145739),
 .UNSPECIFIED.,.F.,.F.)
B_SPLINE_CURVE_WITH_KNOTS((4,2,4),(0.,0.499999999999999,1.),
 .UNSPECIFIED.)
CURVE()
GEOMETRIC_REPRESENTATION_ITEM()
RATIONAL_B_SPLINE_CURVE((0.99999999988276,0.999999999875186,0.999999999867293,
0.999999999850728,0.999999999841986,0.999999999833128))
REPRESENTATION_ITEM('')
);
#1141=(
BOUNDED_CURVE()
B_SPLINE_CURVE(3,(#145935,#145936,#145937,#145938),.UNSPECIFIED.,.F.,.F.)
B_SPLINE_CURVE_WITH_KNOTS((4,4),(0.,1.),.UNSPECIFIED.)
CURVE()
GEOMETRIC_REPRESENTATION_ITEM()
RATIONAL_B_SPLINE_CURVE((0.999999985881004,0.999999986166315,0.999999986518015,
0.99999998707511))
REPRESENTATION_ITEM('')
);
#1142=(
BOUNDED_CURVE()
B_SPLINE_CURVE(3,(#146091,#146092,#146093,#146094,#146095,#146096,#146097,
#146098,#146099,#146100,#146101,#146102,#146103,#146104),.UNSPECIFIED.,
 .F.,.F.)
B_SPLINE_CURVE_WITH_KNOTS((4,2,2,2,2,2,4),(0.,0.245502202551198,0.371251835459332,
0.497001468367467,0.622751101275599,0.748500734183734,1.),.UNSPECIFIED.)
CURVE()
GEOMETRIC_REPRESENTATION_ITEM()
RATIONAL_B_SPLINE_CURVE((0.999999945516601,0.999999945630438,0.999999945782265,
0.999999946051757,0.999999946150377,0.999999946362488,0.999999946475958,
0.99999994671043,0.999999946832282,0.999999947085115,0.999999947217219,
0.999999947617593,0.999999947890007,0.999999948167728))
REPRESENTATION_ITEM('')
);
#1143=(
BOUNDED_CURVE()
B_SPLINE_CURVE(3,(#146180,#146181,#146182,#146183),.UNSPECIFIED.,.F.,.F.)
B_SPLINE_CURVE_WITH_KNOTS((4,4),(0.,1.),.UNSPECIFIED.)
CURVE()
GEOMETRIC_REPRESENTATION_ITEM()
RATIONAL_B_SPLINE_CURVE((0.999999999051513,0.999999999075715,0.999999999089916,
0.999999999101407))
REPRESENTATION_ITEM('')
);
#1144=(
BOUNDED_CURVE()
B_SPLINE_CURVE(3,(#146412,#146413,#146414,#146415,#146416,#146417,#146418,
#146419,#146420,#146421),.UNSPECIFIED.,.F.,.F.)
B_SPLINE_CURVE_WITH_KNOTS((4,2,2,2,4),(0.,0.251507516180303,0.50301503236061,
0.754522548540912,1.),.UNSPECIFIED.)
CURVE()
GEOMETRIC_REPRESENTATION_ITEM()
RATIONAL_B_SPLINE_CURVE((0.999999987939898,0.999999987944251,0.999999987948487,
0.999999987956739,0.999999987960767,0.999999987968182,0.999999987971664,
0.999999987977827,0.999999987980498,0.999999987982808))
REPRESENTATION_ITEM('')
);
#1145=(
BOUNDED_CURVE()
B_SPLINE_CURVE(3,(#146520,#146521,#146522,#146523,#146524,#146525,#146526,
#146527,#146528,#146529),.UNSPECIFIED.,.F.,.F.)
B_SPLINE_CURVE_WITH_KNOTS((4,2,2,2,4),(0.,0.24546127409179,0.496974182727859,
0.748487091363931,1.),.UNSPECIFIED.)
CURVE()
GEOMETRIC_REPRESENTATION_ITEM()
RATIONAL_B_SPLINE_CURVE((0.999999992164428,0.999999992163856,0.999999992163196,
0.999999992161673,0.999999992160813,0.999999992158981,0.999999992157986,
0.999999992155948,0.999999992154902,0.999999992153827))
REPRESENTATION_ITEM('')
);
#1146=(
BOUNDED_CURVE()
B_SPLINE_CURVE(3,(#146762,#146763,#146764,#146765),.UNSPECIFIED.,.F.,.F.)
B_SPLINE_CURVE_WITH_KNOTS((4,4),(0.,1.),.UNSPECIFIED.)
CURVE()
GEOMETRIC_REPRESENTATION_ITEM()
RATIONAL_B_SPLINE_CURVE((0.999999998598817,0.999999998581398,0.999999998559873,
0.999999998523147))
REPRESENTATION_ITEM('')
);
#1147=(
BOUNDED_CURVE()
B_SPLINE_CURVE(3,(#147003,#147004,#147005,#147006),.UNSPECIFIED.,.F.,.F.)
B_SPLINE_CURVE_WITH_KNOTS((4,4),(0.,1.),.UNSPECIFIED.)
CURVE()
GEOMETRIC_REPRESENTATION_ITEM()
RATIONAL_B_SPLINE_CURVE((0.99999998938962,0.999999988942626,0.999999988661227,
0.999999988432992))
REPRESENTATION_ITEM('')
);
#1148=(
BOUNDED_CURVE()
B_SPLINE_CURVE(3,(#147124,#147125,#147126,#147127,#147128,#147129),
 .UNSPECIFIED.,.F.,.F.)
B_SPLINE_CURVE_WITH_KNOTS((4,2,4),(0.,0.5,1.),.UNSPECIFIED.)
CURVE()
GEOMETRIC_REPRESENTATION_ITEM()
RATIONAL_B_SPLINE_CURVE((0.999999999894234,0.999999999887496,0.999999999880475,
0.999999999865743,0.999999999857971,0.999999999850097))
REPRESENTATION_ITEM('')
);
#1149=(
BOUNDED_CURVE()
B_SPLINE_CURVE(3,(#148141,#148142,#148143,#148144),.UNSPECIFIED.,.F.,.F.)
B_SPLINE_CURVE_WITH_KNOTS((4,4),(0.,1.),.UNSPECIFIED.)
CURVE()
GEOMETRIC_REPRESENTATION_ITEM()
RATIONAL_B_SPLINE_CURVE((0.999999927469661,0.999999923649506,0.999999920386278,
0.999999917494068))
REPRESENTATION_ITEM('')
);
#1150=(
BOUNDED_CURVE()
B_SPLINE_CURVE(3,(#148246,#148247,#148248,#148249),.UNSPECIFIED.,.F.,.F.)
B_SPLINE_CURVE_WITH_KNOTS((4,4),(0.,1.),.UNSPECIFIED.)
CURVE()
GEOMETRIC_REPRESENTATION_ITEM()
RATIONAL_B_SPLINE_CURVE((0.999999892411738,0.999999896151516,0.999999900365766,
0.999999905288505))
REPRESENTATION_ITEM('')
);
#1151=(
BOUNDED_CURVE()
B_SPLINE_CURVE(3,(#148262,#148263,#148264,#148265),.UNSPECIFIED.,.F.,.F.)
B_SPLINE_CURVE_WITH_KNOTS((4,4),(0.,1.),.UNSPECIFIED.)
CURVE()
GEOMETRIC_REPRESENTATION_ITEM()
RATIONAL_B_SPLINE_CURVE((0.999999978616913,0.999999978977049,0.999999979295994,
0.999999979585313))
REPRESENTATION_ITEM('')
);
#1152=(
BOUNDED_CURVE()
B_SPLINE_CURVE(3,(#148432,#148433,#148434,#148435),.UNSPECIFIED.,.F.,.F.)
B_SPLINE_CURVE_WITH_KNOTS((4,4),(0.,1.),.UNSPECIFIED.)
CURVE()
GEOMETRIC_REPRESENTATION_ITEM()
RATIONAL_B_SPLINE_CURVE((0.999999998794032,0.999999998776629,0.99999999875741,
0.999999998735649))
REPRESENTATION_ITEM('')
);
#1153=(
BOUNDED_CURVE()
B_SPLINE_CURVE(3,(#149798,#149799,#149800,#149801,#149802,#149803),
 .UNSPECIFIED.,.F.,.F.)
B_SPLINE_CURVE_WITH_KNOTS((4,2,4),(0.,0.5,1.),.UNSPECIFIED.)
CURVE()
GEOMETRIC_REPRESENTATION_ITEM()
RATIONAL_B_SPLINE_CURVE((0.999999996854374,0.999999996923258,0.999999996997747,
0.999999997161208,0.999999997250172,0.999999997348475))
REPRESENTATION_ITEM('')
);
#1154=(
BOUNDED_CURVE()
B_SPLINE_CURVE(3,(#150640,#150641,#150642,#150643,#150644,#150645),
 .UNSPECIFIED.,.F.,.F.)
B_SPLINE_CURVE_WITH_KNOTS((4,2,4),(0.,0.5,1.),.UNSPECIFIED.)
CURVE()
GEOMETRIC_REPRESENTATION_ITEM()
RATIONAL_B_SPLINE_CURVE((0.999999996756183,0.999999996827757,0.999999996905132,
0.999999997074846,0.999999997167179,0.999999997269145))
REPRESENTATION_ITEM('')
);
#1155=(
BOUNDED_CURVE()
B_SPLINE_CURVE(3,(#151836,#151837,#151838,#151839,#151840,#151841),
 .UNSPECIFIED.,.F.,.F.)
B_SPLINE_CURVE_WITH_KNOTS((4,2,4),(0.,0.5,1.),.UNSPECIFIED.)
CURVE()
GEOMETRIC_REPRESENTATION_ITEM()
RATIONAL_B_SPLINE_CURVE((0.999999999990438,0.999999999987754,0.999999999984833,
0.999999999978368,0.999999999974827,0.999999999970832))
REPRESENTATION_ITEM('')
);
#1156=(
BOUNDED_CURVE()
B_SPLINE_CURVE(3,(#151873,#151874,#151875,#151876),.UNSPECIFIED.,.F.,.F.)
B_SPLINE_CURVE_WITH_KNOTS((4,4),(0.,1.),.UNSPECIFIED.)
CURVE()
GEOMETRIC_REPRESENTATION_ITEM()
RATIONAL_B_SPLINE_CURVE((0.999999764205276,0.999999729074058,0.999999662874959,
0.999999569832623))
REPRESENTATION_ITEM('')
);
#1157=(
BOUNDED_CURVE()
B_SPLINE_CURVE(3,(#152419,#152420,#152421,#152422,#152423,#152424),
 .UNSPECIFIED.,.F.,.F.)
B_SPLINE_CURVE_WITH_KNOTS((4,2,4),(0.,0.5,1.),.UNSPECIFIED.)
CURVE()
GEOMETRIC_REPRESENTATION_ITEM()
RATIONAL_B_SPLINE_CURVE((0.999999938557239,0.999999946973332,0.999999954433094,
0.999999968051422,0.999999974205021,0.999999979856827))
REPRESENTATION_ITEM('')
);
#1158=(
BOUNDED_CURVE()
B_SPLINE_CURVE(3,(#152846,#152847,#152848,#152849,#152850,#152851,#152852,
#152853),.UNSPECIFIED.,.F.,.F.)
B_SPLINE_CURVE_WITH_KNOTS((4,2,2,4),(0.,0.230529842217703,0.489063635927588,
1.),.UNSPECIFIED.)
CURVE()
GEOMETRIC_REPRESENTATION_ITEM()
RATIONAL_B_SPLINE_CURVE((0.999999995461409,0.999999995444687,0.999999995419802,
0.999999995349838,0.999999995302614,0.999999995136626,0.999999994992415,
0.999999994821643))
REPRESENTATION_ITEM('')
);
#1159=(
BOUNDED_CURVE()
B_SPLINE_CURVE(3,(#165191,#165192,#165193,#165194,#165195,#165196,#165197,
#165198,#165199,#165200),.UNSPECIFIED.,.F.,.F.)
B_SPLINE_CURVE_WITH_KNOTS((4,2,2,2,4),(-8.88178419700125E-16,0.392699081698724,
0.785398163397448,1.17809724509617,1.5707963267949),.UNSPECIFIED.)
CURVE()
GEOMETRIC_REPRESENTATION_ITEM()
RATIONAL_B_SPLINE_CURVE((1.,1.,1.,1.,1.,1.,1.,1.,1.,1.))
REPRESENTATION_ITEM('')
);
#1160=(
BOUNDED_CURVE()
B_SPLINE_CURVE(3,(#165277,#165278,#165279,#165280,#165281,#165282,#165283,
#165284,#165285,#165286),.UNSPECIFIED.,.F.,.F.)
B_SPLINE_CURVE_WITH_KNOTS((4,2,2,2,4),(4.71238898038469,5.10508806208341,
5.49778714378214,5.89048622548086,6.28318530717959),.UNSPECIFIED.)
CURVE()
GEOMETRIC_REPRESENTATION_ITEM()
RATIONAL_B_SPLINE_CURVE((1.,1.,1.,1.,1.,1.,1.,1.,1.,1.))
REPRESENTATION_ITEM('')
);
#1161=(
BOUNDED_CURVE()
B_SPLINE_CURVE(3,(#165729,#165730,#165731,#165732),.UNSPECIFIED.,.F.,.F.)
B_SPLINE_CURVE_WITH_KNOTS((4,4),(-5.03069808033274E-17,0.00385726433182564),
 .UNSPECIFIED.)
CURVE()
GEOMETRIC_REPRESENTATION_ITEM()
RATIONAL_B_SPLINE_CURVE((1.,1.,1.,1.))
REPRESENTATION_ITEM('')
);
#1162=(
BOUNDED_CURVE()
B_SPLINE_CURVE(3,(#165857,#165858,#165859,#165860),.UNSPECIFIED.,.F.,.F.)
B_SPLINE_CURVE_WITH_KNOTS((4,4),(0.,0.00414272899747597),.UNSPECIFIED.)
CURVE()
GEOMETRIC_REPRESENTATION_ITEM()
RATIONAL_B_SPLINE_CURVE((1.,1.,1.,1.))
REPRESENTATION_ITEM('')
);
#1163=(
BOUNDED_CURVE()
B_SPLINE_CURVE(3,(#165944,#165945,#165946,#165947,#165948,#165949,#165950,
#165951,#165952,#165953),.UNSPECIFIED.,.F.,.F.)
B_SPLINE_CURVE_WITH_KNOTS((4,2,2,2,4),(-8.88178419700125E-16,0.392699081698724,
0.785398163397448,1.17809724509617,1.5707963267949),.UNSPECIFIED.)
CURVE()
GEOMETRIC_REPRESENTATION_ITEM()
RATIONAL_B_SPLINE_CURVE((1.,1.,1.,1.,1.,1.,1.,1.,1.,1.))
REPRESENTATION_ITEM('')
);
#1164=(
BOUNDED_CURVE()
B_SPLINE_CURVE(3,(#166125,#166126,#166127,#166128,#166129,#166130,#166131,
#166132,#166133,#166134),.UNSPECIFIED.,.F.,.F.)
B_SPLINE_CURVE_WITH_KNOTS((4,2,2,2,4),(4.71238898038469,5.10508806208341,
5.49778714378214,5.89048622548086,6.28318530717959),.UNSPECIFIED.)
CURVE()
GEOMETRIC_REPRESENTATION_ITEM()
RATIONAL_B_SPLINE_CURVE((1.,1.,1.,1.,1.,1.,1.,1.,1.,1.))
REPRESENTATION_ITEM('')
);
#1165=(
BOUNDED_CURVE()
B_SPLINE_CURVE(3,(#166770,#166771,#166772,#166773,#166774,#166775,#166776,
#166777,#166778,#166779),.UNSPECIFIED.,.F.,.F.)
B_SPLINE_CURVE_WITH_KNOTS((4,2,2,2,4),(3.1415926535898,3.53429173528852,
3.92699081698724,4.31968989868597,4.71238898038469),.UNSPECIFIED.)
CURVE()
GEOMETRIC_REPRESENTATION_ITEM()
RATIONAL_B_SPLINE_CURVE((1.,1.,1.,1.,1.,1.,1.,1.,1.,1.))
REPRESENTATION_ITEM('')
);
#1166=(
BOUNDED_CURVE()
B_SPLINE_CURVE(3,(#166847,#166848,#166849,#166850,#166851,#166852,#166853,
#166854,#166855,#166856),.UNSPECIFIED.,.F.,.F.)
B_SPLINE_CURVE_WITH_KNOTS((4,2,2,2,4),(1.5707963267949,1.96349540849362,
2.35619449019234,2.74889357189107,3.14159265358979),.UNSPECIFIED.)
CURVE()
GEOMETRIC_REPRESENTATION_ITEM()
RATIONAL_B_SPLINE_CURVE((1.,1.,1.,1.,1.,1.,1.,1.,1.,1.))
REPRESENTATION_ITEM('')
);
#1167=(
BOUNDED_CURVE()
B_SPLINE_CURVE(3,(#167521,#167522,#167523,#167524,#167525,#167526,#167527,
#167528,#167529,#167530),.UNSPECIFIED.,.F.,.F.)
B_SPLINE_CURVE_WITH_KNOTS((4,2,2,2,4),(3.1415926535898,3.53429173528852,
3.92699081698724,4.31968989868597,4.71238898038469),.UNSPECIFIED.)
CURVE()
GEOMETRIC_REPRESENTATION_ITEM()
RATIONAL_B_SPLINE_CURVE((1.,1.,1.,1.,1.,1.,1.,1.,1.,1.))
REPRESENTATION_ITEM('')
);
#1168=(
BOUNDED_CURVE()
B_SPLINE_CURVE(3,(#167735,#167736,#167737,#167738),.UNSPECIFIED.,.F.,.F.)
B_SPLINE_CURVE_WITH_KNOTS((4,4),(-1.00613961606655E-16,0.00454919832189776),
 .UNSPECIFIED.)
CURVE()
GEOMETRIC_REPRESENTATION_ITEM()
RATIONAL_B_SPLINE_CURVE((1.,1.,1.,1.))
REPRESENTATION_ITEM('')
);
#1169=(
BOUNDED_CURVE()
B_SPLINE_CURVE(3,(#167862,#167863,#167864,#167865),.UNSPECIFIED.,.F.,.F.)
B_SPLINE_CURVE_WITH_KNOTS((4,4),(1.7347234759768E-18,0.00426411906192034),
 .UNSPECIFIED.)
CURVE()
GEOMETRIC_REPRESENTATION_ITEM()
RATIONAL_B_SPLINE_CURVE((1.,1.,1.,1.))
REPRESENTATION_ITEM('')
);
#1170=(
BOUNDED_CURVE()
B_SPLINE_CURVE(3,(#168044,#168045,#168046,#168047,#168048,#168049,#168050,
#168051,#168052,#168053),.UNSPECIFIED.,.F.,.F.)
B_SPLINE_CURVE_WITH_KNOTS((4,2,2,2,4),(1.5707963267949,1.96349540849362,
2.35619449019234,2.74889357189107,3.14159265358979),.UNSPECIFIED.)
CURVE()
GEOMETRIC_REPRESENTATION_ITEM()
RATIONAL_B_SPLINE_CURVE((1.,1.,1.,1.,1.,1.,1.,1.,1.,1.))
REPRESENTATION_ITEM('')
);
#1171=(
BOUNDED_CURVE()
B_SPLINE_CURVE(3,(#168202,#168203,#168204,#168205),.UNSPECIFIED.,.F.,.F.)
B_SPLINE_CURVE_WITH_KNOTS((4,4),(0.,0.00407947372412412),.UNSPECIFIED.)
CURVE()
GEOMETRIC_REPRESENTATION_ITEM()
RATIONAL_B_SPLINE_CURVE((1.,1.,1.,1.))
REPRESENTATION_ITEM('')
);
#1172=(
BOUNDED_CURVE()
B_SPLINE_CURVE(3,(#169018,#169019,#169020,#169021,#169022,#169023,#169024,
#169025,#169026,#169027),.UNSPECIFIED.,.F.,.F.)
B_SPLINE_CURVE_WITH_KNOTS((4,2,2,2,4),(3.1415926535898,3.53429173528852,
3.92699081698724,4.31968989868597,4.71238898038469),.UNSPECIFIED.)
CURVE()
GEOMETRIC_REPRESENTATION_ITEM()
RATIONAL_B_SPLINE_CURVE((1.,1.,1.,1.,1.,1.,1.,1.,1.,1.))
REPRESENTATION_ITEM('')
);
#1173=(
BOUNDED_CURVE()
B_SPLINE_CURVE(3,(#169095,#169096,#169097,#169098,#169099,#169100,#169101,
#169102,#169103,#169104),.UNSPECIFIED.,.F.,.F.)
B_SPLINE_CURVE_WITH_KNOTS((4,2,2,2,4),(1.5707963267949,1.96349540849362,
2.35619449019234,2.74889357189107,3.1415926535898),.UNSPECIFIED.)
CURVE()
GEOMETRIC_REPRESENTATION_ITEM()
RATIONAL_B_SPLINE_CURVE((1.,1.,1.,1.,1.,1.,1.,1.,1.,1.))
REPRESENTATION_ITEM('')
);
#1174=(
BOUNDED_CURVE()
B_SPLINE_CURVE(3,(#169731,#169732,#169733,#169734,#169735,#169736,#169737,
#169738,#169739,#169740),.UNSPECIFIED.,.F.,.F.)
B_SPLINE_CURVE_WITH_KNOTS((4,2,2,2,4),(3.1415926535898,3.53429173528852,
3.92699081698724,4.31968989868597,4.71238898038469),.UNSPECIFIED.)
CURVE()
GEOMETRIC_REPRESENTATION_ITEM()
RATIONAL_B_SPLINE_CURVE((1.,1.,1.,1.,1.,1.,1.,1.,1.,1.))
REPRESENTATION_ITEM('')
);
#1175=(
BOUNDED_CURVE()
B_SPLINE_CURVE(3,(#170157,#170158,#170159,#170160,#170161,#170162,#170163,
#170164,#170165,#170166),.UNSPECIFIED.,.F.,.F.)
B_SPLINE_CURVE_WITH_KNOTS((4,2,2,2,4),(1.5707963267949,1.96349540849362,
2.35619449019234,2.74889357189107,3.1415926535898),.UNSPECIFIED.)
CURVE()
GEOMETRIC_REPRESENTATION_ITEM()
RATIONAL_B_SPLINE_CURVE((1.,1.,1.,1.,1.,1.,1.,1.,1.,1.))
REPRESENTATION_ITEM('')
);
#1176=(
BOUNDED_CURVE()
B_SPLINE_CURVE(3,(#171513,#171514,#171515,#171516),.UNSPECIFIED.,.F.,.F.)
B_SPLINE_CURVE_WITH_KNOTS((4,4),(0.,0.0433970829567688),.UNSPECIFIED.)
CURVE()
GEOMETRIC_REPRESENTATION_ITEM()
RATIONAL_B_SPLINE_CURVE((1.,1.,1.,1.))
REPRESENTATION_ITEM('')
);
#1177=(
BOUNDED_CURVE()
B_SPLINE_CURVE(3,(#171666,#171667,#171668,#171669),.UNSPECIFIED.,.F.,.F.)
B_SPLINE_CURVE_WITH_KNOTS((4,4),(-1.38777878078145E-17,0.0431305646498159),
 .UNSPECIFIED.)
CURVE()
GEOMETRIC_REPRESENTATION_ITEM()
RATIONAL_B_SPLINE_CURVE((1.,1.,1.,1.))
REPRESENTATION_ITEM('')
);
#1178=(
BOUNDED_CURVE()
B_SPLINE_CURVE(3,(#171908,#171909,#171910,#171911),.UNSPECIFIED.,.F.,.F.)
B_SPLINE_CURVE_WITH_KNOTS((4,4),(0.,0.0445045070401677),.UNSPECIFIED.)
CURVE()
GEOMETRIC_REPRESENTATION_ITEM()
RATIONAL_B_SPLINE_CURVE((1.,1.,1.,1.))
REPRESENTATION_ITEM('')
);
#1179=(
BOUNDED_CURVE()
B_SPLINE_CURVE(3,(#172016,#172017,#172018,#172019),.UNSPECIFIED.,.F.,.F.)
B_SPLINE_CURVE_WITH_KNOTS((4,4),(0.,0.044753309356401),.UNSPECIFIED.)
CURVE()
GEOMETRIC_REPRESENTATION_ITEM()
RATIONAL_B_SPLINE_CURVE((1.,1.,1.,1.))
REPRESENTATION_ITEM('')
);
#1180=(
BOUNDED_CURVE()
B_SPLINE_CURVE(3,(#172070,#172071,#172072,#172073),.UNSPECIFIED.,.F.,.F.)
B_SPLINE_CURVE_WITH_KNOTS((4,4),(0.,0.0444870989094409),.UNSPECIFIED.)
CURVE()
GEOMETRIC_REPRESENTATION_ITEM()
RATIONAL_B_SPLINE_CURVE((1.,1.,1.,1.))
REPRESENTATION_ITEM('')
);
#1181=(
BOUNDED_CURVE()
B_SPLINE_CURVE(3,(#172295,#172296,#172297,#172298),.UNSPECIFIED.,.F.,.F.)
B_SPLINE_CURVE_WITH_KNOTS((4,4),(-2.77555756156289E-17,0.0433026927553429),
 .UNSPECIFIED.)
CURVE()
GEOMETRIC_REPRESENTATION_ITEM()
RATIONAL_B_SPLINE_CURVE((1.,1.,1.,1.))
REPRESENTATION_ITEM('')
);
#1182=(
BOUNDED_CURVE()
B_SPLINE_CURVE(3,(#172425,#172426,#172427,#172428),.UNSPECIFIED.,.F.,.F.)
B_SPLINE_CURVE_WITH_KNOTS((4,4),(0.,0.0430361525536219),.UNSPECIFIED.)
CURVE()
GEOMETRIC_REPRESENTATION_ITEM()
RATIONAL_B_SPLINE_CURVE((1.,1.,1.,1.))
REPRESENTATION_ITEM('')
);
#1183=(
BOUNDED_CURVE()
B_SPLINE_CURVE(3,(#173780,#173781,#173782,#173783),.UNSPECIFIED.,.F.,.F.)
B_SPLINE_CURVE_WITH_KNOTS((4,4),(-1.38777878078145E-17,0.0332202089949022),
 .UNSPECIFIED.)
CURVE()
GEOMETRIC_REPRESENTATION_ITEM()
RATIONAL_B_SPLINE_CURVE((1.,1.,1.,1.))
REPRESENTATION_ITEM('')
);
#1184=(
BOUNDED_CURVE()
B_SPLINE_CURVE(3,(#175236,#175237,#175238,#175239),.UNSPECIFIED.,.F.,.F.)
B_SPLINE_CURVE_WITH_KNOTS((4,4),(0.,0.0360938777358061),.UNSPECIFIED.)
CURVE()
GEOMETRIC_REPRESENTATION_ITEM()
RATIONAL_B_SPLINE_CURVE((1.,1.,1.,1.))
REPRESENTATION_ITEM('')
);
#1185=(
BOUNDED_CURVE()
B_SPLINE_CURVE(3,(#175270,#175271,#175272,#175273),.UNSPECIFIED.,.F.,.F.)
B_SPLINE_CURVE_WITH_KNOTS((4,4),(0.,0.0358270578054484),.UNSPECIFIED.)
CURVE()
GEOMETRIC_REPRESENTATION_ITEM()
RATIONAL_B_SPLINE_CURVE((1.,1.,1.,1.))
REPRESENTATION_ITEM('')
);
#1186=(
BOUNDED_CURVE()
B_SPLINE_CURVE(3,(#175317,#175318,#175319,#175320),.UNSPECIFIED.,.F.,.F.)
B_SPLINE_CURVE_WITH_KNOTS((4,4),(0.,0.0372541843113205),.UNSPECIFIED.)
CURVE()
GEOMETRIC_REPRESENTATION_ITEM()
RATIONAL_B_SPLINE_CURVE((1.,1.,1.,1.))
REPRESENTATION_ITEM('')
);
#1187=(
BOUNDED_CURVE()
B_SPLINE_CURVE(3,(#175490,#175491,#175492,#175493),.UNSPECIFIED.,.F.,.F.)
B_SPLINE_CURVE_WITH_KNOTS((4,4),(0.,0.0369876550821707),.UNSPECIFIED.)
CURVE()
GEOMETRIC_REPRESENTATION_ITEM()
RATIONAL_B_SPLINE_CURVE((1.,1.,1.,1.))
REPRESENTATION_ITEM('')
);
#1188=(
BOUNDED_CURVE()
B_SPLINE_CURVE(3,(#175650,#175651,#175652,#175653),.UNSPECIFIED.,.F.,.F.)
B_SPLINE_CURVE_WITH_KNOTS((4,4),(0.,0.0385835973699829),.UNSPECIFIED.)
CURVE()
GEOMETRIC_REPRESENTATION_ITEM()
RATIONAL_B_SPLINE_CURVE((1.,1.,1.,1.))
REPRESENTATION_ITEM('')
);
#1189=(
BOUNDED_CURVE()
B_SPLINE_CURVE(3,(#175681,#175682,#175683,#175684),.UNSPECIFIED.,.F.,.F.)
B_SPLINE_CURVE_WITH_KNOTS((4,4),(0.,0.038317388945353),.UNSPECIFIED.)
CURVE()
GEOMETRIC_REPRESENTATION_ITEM()
RATIONAL_B_SPLINE_CURVE((1.,1.,1.,1.))
REPRESENTATION_ITEM('')
);
#1190=(
BOUNDED_CURVE()
B_SPLINE_CURVE(3,(#176882,#176883,#176884,#176885,#176886,#176887,#176888,
#176889,#176890,#176891),.UNSPECIFIED.,.F.,.F.)
B_SPLINE_CURVE_WITH_KNOTS((4,2,2,2,4),(4.71238898038469,5.10508806208341,
5.49778714378214,5.89048622548086,6.28318530717959),.UNSPECIFIED.)
CURVE()
GEOMETRIC_REPRESENTATION_ITEM()
RATIONAL_B_SPLINE_CURVE((1.,1.,1.,1.,1.,1.,1.,1.,1.,1.))
REPRESENTATION_ITEM('')
);
#1191=(
BOUNDED_CURVE()
B_SPLINE_CURVE(3,(#177941,#177942,#177943,#177944,#177945,#177946,#177947,
#177948,#177949,#177950),.UNSPECIFIED.,.F.,.F.)
B_SPLINE_CURVE_WITH_KNOTS((4,2,2,2,4),(1.5707963267949,1.96349540849362,
2.35619449019234,2.74889357189107,3.14159265358979),.UNSPECIFIED.)
CURVE()
GEOMETRIC_REPRESENTATION_ITEM()
RATIONAL_B_SPLINE_CURVE((1.,1.,1.,1.,1.,1.,1.,1.,1.,1.))
REPRESENTATION_ITEM('')
);
#1192=(
BOUNDED_CURVE()
B_SPLINE_CURVE(3,(#178325,#178326,#178327,#178328,#178329,#178330,#178331,
#178332,#178333,#178334),.UNSPECIFIED.,.F.,.F.)
B_SPLINE_CURVE_WITH_KNOTS((4,2,2,2,4),(1.5707963267949,1.96349540849362,
2.35619449019234,2.74889357189107,3.14159265358979),.UNSPECIFIED.)
CURVE()
GEOMETRIC_REPRESENTATION_ITEM()
RATIONAL_B_SPLINE_CURVE((1.,1.,1.,1.,1.,1.,1.,1.,1.,1.))
REPRESENTATION_ITEM('')
);
#1193=(
BOUNDED_CURVE()
B_SPLINE_CURVE(3,(#178526,#178527,#178528,#178529,#178530,#178531,#178532,
#178533,#178534,#178535),.UNSPECIFIED.,.F.,.F.)
B_SPLINE_CURVE_WITH_KNOTS((4,2,2,2,4),(3.1415926535898,3.53429173528852,
3.92699081698724,4.31968989868597,4.71238898038469),.UNSPECIFIED.)
CURVE()
GEOMETRIC_REPRESENTATION_ITEM()
RATIONAL_B_SPLINE_CURVE((1.,1.,1.,1.,1.,1.,1.,1.,1.,1.))
REPRESENTATION_ITEM('')
);
#1194=(
BOUNDED_CURVE()
B_SPLINE_CURVE(3,(#178822,#178823,#178824,#178825,#178826,#178827,#178828,
#178829,#178830,#178831),.UNSPECIFIED.,.F.,.F.)
B_SPLINE_CURVE_WITH_KNOTS((4,2,2,2,4),(4.71238898038469,5.10508806208342,
5.49778714378214,5.89048622548086,6.28318530717959),.UNSPECIFIED.)
CURVE()
GEOMETRIC_REPRESENTATION_ITEM()
RATIONAL_B_SPLINE_CURVE((1.,1.,1.,1.,1.,1.,1.,1.,1.,1.))
REPRESENTATION_ITEM('')
);
#1195=(
BOUNDED_CURVE()
B_SPLINE_CURVE(3,(#178949,#178950,#178951,#178952,#178953,#178954,#178955,
#178956,#178957,#178958),.UNSPECIFIED.,.F.,.F.)
B_SPLINE_CURVE_WITH_KNOTS((4,2,2,2,4),(-1.77635683940025E-15,0.392699081698723,
0.785398163397447,1.17809724509617,1.5707963267949),.UNSPECIFIED.)
CURVE()
GEOMETRIC_REPRESENTATION_ITEM()
RATIONAL_B_SPLINE_CURVE((1.,1.,1.,1.,1.,1.,1.,1.,1.,1.))
REPRESENTATION_ITEM('')
);
#1196=(
BOUNDED_CURVE()
B_SPLINE_CURVE(3,(#179176,#179177,#179178,#179179,#179180,#179181,#179182,
#179183,#179184,#179185),.UNSPECIFIED.,.F.,.F.)
B_SPLINE_CURVE_WITH_KNOTS((4,2,2,2,4),(4.71238898038469,5.10508806208342,
5.49778714378214,5.89048622548086,6.28318530717959),.UNSPECIFIED.)
CURVE()
GEOMETRIC_REPRESENTATION_ITEM()
RATIONAL_B_SPLINE_CURVE((1.,1.,1.,1.,1.,1.,1.,1.,1.,1.))
REPRESENTATION_ITEM('')
);
#1197=(
BOUNDED_CURVE()
B_SPLINE_CURVE(3,(#179405,#179406,#179407,#179408,#179409,#179410,#179411,
#179412,#179413,#179414),.UNSPECIFIED.,.F.,.F.)
B_SPLINE_CURVE_WITH_KNOTS((4,2,2,2,4),(-1.77635683940025E-15,0.392699081698723,
0.785398163397447,1.17809724509617,1.5707963267949),.UNSPECIFIED.)
CURVE()
GEOMETRIC_REPRESENTATION_ITEM()
RATIONAL_B_SPLINE_CURVE((1.,1.,1.,1.,1.,1.,1.,1.,1.,1.))
REPRESENTATION_ITEM('')
);
#1198=(
BOUNDED_CURVE()
B_SPLINE_CURVE(3,(#179630,#179631,#179632,#179633,#179634,#179635,#179636,
#179637,#179638,#179639),.UNSPECIFIED.,.F.,.F.)
B_SPLINE_CURVE_WITH_KNOTS((4,2,2,2,4),(1.5707963267949,1.96349540849362,
2.35619449019234,2.74889357189106,3.14159265358979),.UNSPECIFIED.)
CURVE()
GEOMETRIC_REPRESENTATION_ITEM()
RATIONAL_B_SPLINE_CURVE((1.,1.,1.,1.,1.,1.,1.,1.,1.,1.))
REPRESENTATION_ITEM('')
);
#1199=(
BOUNDED_CURVE()
B_SPLINE_CURVE(3,(#180140,#180141,#180142,#180143,#180144,#180145,#180146,
#180147,#180148,#180149),.UNSPECIFIED.,.F.,.F.)
B_SPLINE_CURVE_WITH_KNOTS((4,2,2,2,4),(3.1415926535898,3.53429173528852,
3.92699081698724,4.31968989868597,4.71238898038469),.UNSPECIFIED.)
CURVE()
GEOMETRIC_REPRESENTATION_ITEM()
RATIONAL_B_SPLINE_CURVE((1.,1.,1.,1.,1.,1.,1.,1.,1.,1.))
REPRESENTATION_ITEM('')
);
#1200=(
BOUNDED_CURVE()
B_SPLINE_CURVE(3,(#180362,#180363,#180364,#180365,#180366,#180367,#180368,
#180369,#180370,#180371),.UNSPECIFIED.,.F.,.F.)
B_SPLINE_CURVE_WITH_KNOTS((4,2,2,2,4),(4.71238898038469,5.10508806208341,
5.49778714378214,5.89048622548086,6.28318530717959),.UNSPECIFIED.)
CURVE()
GEOMETRIC_REPRESENTATION_ITEM()
RATIONAL_B_SPLINE_CURVE((1.,1.,1.,1.,1.,1.,1.,1.,1.,1.))
REPRESENTATION_ITEM('')
);
#1201=(
BOUNDED_CURVE()
B_SPLINE_CURVE(3,(#180489,#180490,#180491,#180492,#180493,#180494,#180495,
#180496,#180497,#180498),.UNSPECIFIED.,.F.,.F.)
B_SPLINE_CURVE_WITH_KNOTS((4,2,2,2,4),(0.,0.392699081698724,0.785398163397448,
1.17809724509617,1.5707963267949),.UNSPECIFIED.)
CURVE()
GEOMETRIC_REPRESENTATION_ITEM()
RATIONAL_B_SPLINE_CURVE((1.,1.,1.,1.,1.,1.,1.,1.,1.,1.))
REPRESENTATION_ITEM('')
);
#1202=(
BOUNDED_CURVE()
B_SPLINE_CURVE(3,(#180738,#180739,#180740,#180741,#180742,#180743,#180744,
#180745,#180746,#180747),.UNSPECIFIED.,.F.,.F.)
B_SPLINE_CURVE_WITH_KNOTS((4,2,2,2,4),(4.71238898038469,5.10508806208342,
5.49778714378214,5.89048622548086,6.28318530717959),.UNSPECIFIED.)
CURVE()
GEOMETRIC_REPRESENTATION_ITEM()
RATIONAL_B_SPLINE_CURVE((1.,1.,1.,1.,1.,1.,1.,1.,1.,1.))
REPRESENTATION_ITEM('')
);
#1203=(
BOUNDED_CURVE()
B_SPLINE_CURVE(3,(#180936,#180937,#180938,#180939,#180940,#180941,#180942,
#180943,#180944,#180945),.UNSPECIFIED.,.F.,.F.)
B_SPLINE_CURVE_WITH_KNOTS((4,2,2,2,4),(1.18015353016497E-15,0.392699081698726,
0.785398163397449,1.17809724509617,1.5707963267949),.UNSPECIFIED.)
CURVE()
GEOMETRIC_REPRESENTATION_ITEM()
RATIONAL_B_SPLINE_CURVE((1.,1.,1.,1.,1.,1.,1.,1.,1.,1.))
REPRESENTATION_ITEM('')
);
#1204=(
BOUNDED_CURVE()
B_SPLINE_CURVE(2,(#189315,#189316,#189317),.UNSPECIFIED.,.F.,.F.)
B_SPLINE_CURVE_WITH_KNOTS((3,3),(0.130611113351463,0.388312804292302),
 .UNSPECIFIED.)
CURVE()
GEOMETRIC_REPRESENTATION_ITEM()
RATIONAL_B_SPLINE_CURVE((1.30940107675848,1.51196612828735,1.30940107675849))
REPRESENTATION_ITEM('')
);
#1205=(
BOUNDED_CURVE()
B_SPLINE_CURVE(2,(#189320,#189321,#189322),.UNSPECIFIED.,.F.,.F.)
B_SPLINE_CURVE_WITH_KNOTS((3,3),(-1.16209721084497,-0.594066455576381),
 .UNSPECIFIED.)
CURVE()
GEOMETRIC_REPRESENTATION_ITEM()
RATIONAL_B_SPLINE_CURVE((2.95854811567268,3.41623710198805,2.95854811567267))
REPRESENTATION_ITEM('')
);
#1206=(
BOUNDED_CURVE()
B_SPLINE_CURVE(2,(#189327,#189328,#189329),.UNSPECIFIED.,.F.,.F.)
B_SPLINE_CURVE_WITH_KNOTS((3,3),(0.130611113351462,0.388312804292336),
 .UNSPECIFIED.)
CURVE()
GEOMETRIC_REPRESENTATION_ITEM()
RATIONAL_B_SPLINE_CURVE((1.30940107675853,1.51196612828747,1.30940107675849))
REPRESENTATION_ITEM('')
);
#1207=(
BOUNDED_CURVE()
B_SPLINE_CURVE(2,(#189330,#189331,#189332),.UNSPECIFIED.,.F.,.F.)
B_SPLINE_CURVE_WITH_KNOTS((3,3),(-1.16209721084502,-0.594066455576397),
 .UNSPECIFIED.)
CURVE()
GEOMETRIC_REPRESENTATION_ITEM()
RATIONAL_B_SPLINE_CURVE((2.95854811567274,3.41623710198818,2.95854811567276))
REPRESENTATION_ITEM('')
);
#1208=(
BOUNDED_CURVE()
B_SPLINE_CURVE(2,(#189337,#189338,#189339),.UNSPECIFIED.,.F.,.F.)
B_SPLINE_CURVE_WITH_KNOTS((3,3),(0.130611113351459,0.388312804292314),
 .UNSPECIFIED.)
CURVE()
GEOMETRIC_REPRESENTATION_ITEM()
RATIONAL_B_SPLINE_CURVE((1.30940107675849,1.51196612828739,1.3094010767585))
REPRESENTATION_ITEM('')
);
#1209=(
BOUNDED_CURVE()
B_SPLINE_CURVE(2,(#189340,#189341,#189342),.UNSPECIFIED.,.F.,.F.)
B_SPLINE_CURVE_WITH_KNOTS((3,3),(-1.16209721084514,-0.594066455576369),
 .UNSPECIFIED.)
CURVE()
GEOMETRIC_REPRESENTATION_ITEM()
RATIONAL_B_SPLINE_CURVE((2.95854811567259,3.4162371019884,2.95854811567281))
REPRESENTATION_ITEM('')
);
#1210=(
BOUNDED_CURVE()
B_SPLINE_CURVE(2,(#189347,#189348,#189349),.UNSPECIFIED.,.F.,.F.)
B_SPLINE_CURVE_WITH_KNOTS((3,3),(0.130611113351462,0.388312804292323),
 .UNSPECIFIED.)
CURVE()
GEOMETRIC_REPRESENTATION_ITEM()
RATIONAL_B_SPLINE_CURVE((1.30940107675851,1.51196612828743,1.30940107675851))
REPRESENTATION_ITEM('')
);
#1211=(
BOUNDED_CURVE()
B_SPLINE_CURVE(2,(#189350,#189351,#189352),.UNSPECIFIED.,.F.,.F.)
B_SPLINE_CURVE_WITH_KNOTS((3,3),(-1.16209721084512,-0.594066455576527),
 .UNSPECIFIED.)
CURVE()
GEOMETRIC_REPRESENTATION_ITEM()
RATIONAL_B_SPLINE_CURVE((2.95854811567258,3.41623710198823,2.95854811567305))
REPRESENTATION_ITEM('')
);
#1212=(
BOUNDED_CURVE()
B_SPLINE_CURVE(2,(#189357,#189358,#189359),.UNSPECIFIED.,.F.,.F.)
B_SPLINE_CURVE_WITH_KNOTS((3,3),(0.130611113351459,0.388312804292301),
 .UNSPECIFIED.)
CURVE()
GEOMETRIC_REPRESENTATION_ITEM()
RATIONAL_B_SPLINE_CURVE((1.30940107675849,1.51196612828738,1.30940107675852))
REPRESENTATION_ITEM('')
);
#1213=(
BOUNDED_CURVE()
B_SPLINE_CURVE(2,(#189360,#189361,#189362),.UNSPECIFIED.,.F.,.F.)
B_SPLINE_CURVE_WITH_KNOTS((3,3),(-1.16209721084525,-0.594066455576358),
 .UNSPECIFIED.)
CURVE()
GEOMETRIC_REPRESENTATION_ITEM()
RATIONAL_B_SPLINE_CURVE((2.95854811567222,3.41623710198829,2.95854811567264))
REPRESENTATION_ITEM('')
);
#1214=(
BOUNDED_CURVE()
B_SPLINE_CURVE(2,(#189364,#189365,#189366),.UNSPECIFIED.,.F.,.F.)
B_SPLINE_CURVE_WITH_KNOTS((3,3),(0.130611113351455,0.388312804292296),
 .UNSPECIFIED.)
CURVE()
GEOMETRIC_REPRESENTATION_ITEM()
RATIONAL_B_SPLINE_CURVE((1.30940107675851,1.51196612828741,1.30940107675853))
REPRESENTATION_ITEM('')
);
#1215=(
BOUNDED_CURVE()
B_SPLINE_CURVE(2,(#189367,#189368,#189369),.UNSPECIFIED.,.F.,.F.)
B_SPLINE_CURVE_WITH_KNOTS((3,3),(-1.16209721084501,-0.594066455576361),
 .UNSPECIFIED.)
CURVE()
GEOMETRIC_REPRESENTATION_ITEM()
RATIONAL_B_SPLINE_CURVE((2.95854811567265,3.41623710198812,2.95854811567266))
REPRESENTATION_ITEM('')
);
#1216=(
BOUNDED_CURVE()
B_SPLINE_CURVE(3,(#189448,#189449,#189450,#189451,#189452,#189453),
 .UNSPECIFIED.,.F.,.F.)
B_SPLINE_CURVE_WITH_KNOTS((4,2,4),(0.,0.5,1.),.UNSPECIFIED.)
CURVE()
GEOMETRIC_REPRESENTATION_ITEM()
RATIONAL_B_SPLINE_CURVE((0.999999993165193,0.99999999218853,0.99999999162755,
0.999999991625647,0.999999992188242,0.999999993165193))
REPRESENTATION_ITEM('')
);
#1217=(
BOUNDED_CURVE()
B_SPLINE_CURVE(3,(#195905,#195906,#195907,#195908),.UNSPECIFIED.,.F.,.F.)
B_SPLINE_CURVE_WITH_KNOTS((4,4),(0.,1.),.UNSPECIFIED.)
CURVE()
GEOMETRIC_REPRESENTATION_ITEM()
RATIONAL_B_SPLINE_CURVE((0.999999992674717,0.999999992656022,0.999999992624103,
0.999999992588127))
REPRESENTATION_ITEM('')
);
#1218=(
BOUNDED_CURVE()
B_SPLINE_CURVE(3,(#198545,#198546,#198547,#198548),.UNSPECIFIED.,.F.,.F.)
B_SPLINE_CURVE_WITH_KNOTS((4,4),(0.,1.),.UNSPECIFIED.)
CURVE()
GEOMETRIC_REPRESENTATION_ITEM()
RATIONAL_B_SPLINE_CURVE((0.999999999851496,0.999999999851229,0.999999999850917,
0.999999999850552))
REPRESENTATION_ITEM('')
);
#1219=(
BOUNDED_CURVE()
B_SPLINE_CURVE(3,(#198765,#198766,#198767,#198768,#198769,#198770,#198771,
#198772,#198773,#198774,#198775,#198776,#198777,#198778,#198779,#198780,
#198781,#198782,#198783,#198784),.UNSPECIFIED.,.F.,.F.)
B_SPLINE_CURVE_WITH_KNOTS((4,2,2,2,2,2,2,2,2,4),(0.,0.12500000000001,0.25,
0.37499999999999,0.437500000000004,0.5,0.62499999999999,0.75,0.87499999999999,
1.),.UNSPECIFIED.)
CURVE()
GEOMETRIC_REPRESENTATION_ITEM()
RATIONAL_B_SPLINE_CURVE((0.999999999812713,0.999999999813312,0.999999999814157,
0.999999999815449,0.999999999817637,0.999999999820964,0.999999999822179,
0.999999999824503,0.999999999825349,0.999999999827408,0.999999999828626,
0.999999999831746,0.999999999833571,0.999999999837455,0.999999999839621,
0.999999999844372,0.999999999846902,0.999999999851427,0.999999999853478,
0.999999999855875))
REPRESENTATION_ITEM('')
);
#1220=(
BOUNDED_CURVE()
B_SPLINE_CURVE(3,(#198941,#198942,#198943,#198944),.UNSPECIFIED.,.F.,.F.)
B_SPLINE_CURVE_WITH_KNOTS((4,4),(0.,1.),.UNSPECIFIED.)
CURVE()
GEOMETRIC_REPRESENTATION_ITEM()
RATIONAL_B_SPLINE_CURVE((0.999999998386268,0.999999998378396,0.999999998366988,
0.999999998354755))
REPRESENTATION_ITEM('')
);
#1221=(
BOUNDED_CURVE()
B_SPLINE_CURVE(3,(#199096,#199097,#199098,#199099,#199100,#199101),
 .UNSPECIFIED.,.F.,.F.)
B_SPLINE_CURVE_WITH_KNOTS((4,2,4),(0.,0.494420432466491,1.),
 .UNSPECIFIED.)
CURVE()
GEOMETRIC_REPRESENTATION_ITEM()
RATIONAL_B_SPLINE_CURVE((0.999999966703371,0.999999968198516,0.999999968156611,
0.999999966169366,0.999999964170887,0.999999961536821))
REPRESENTATION_ITEM('')
);
#1222=(
BOUNDED_CURVE()
B_SPLINE_CURVE(2,(#200177,#200178,#200179),.UNSPECIFIED.,.F.,.F.)
B_SPLINE_CURVE_WITH_KNOTS((3,3),(-0.866812823403001,-0.259568682604973),
 .UNSPECIFIED.)
CURVE()
GEOMETRIC_REPRESENTATION_ITEM()
RATIONAL_B_SPLINE_CURVE((1.00000103881537,1.00000117281535,1.00000060925137))
REPRESENTATION_ITEM('')
);
#1223=(
BOUNDED_CURVE()
B_SPLINE_CURVE(2,(#200193,#200194,#200195),.UNSPECIFIED.,.F.,.F.)
B_SPLINE_CURVE_WITH_KNOTS((3,3),(-1.23967788329125,-0.633513201114164),
 .UNSPECIFIED.)
CURVE()
GEOMETRIC_REPRESENTATION_ITEM()
RATIONAL_B_SPLINE_CURVE((1.00000061114393,1.00000117236832,1.00000103863036))
REPRESENTATION_ITEM('')
);
#1224=(
BOUNDED_CURVE()
B_SPLINE_CURVE(2,(#200212,#200213,#200214),.UNSPECIFIED.,.F.,.F.)
B_SPLINE_CURVE_WITH_KNOTS((3,3),(-1.24811202076719,-0.633513201181538),
 .UNSPECIFIED.)
CURVE()
GEOMETRIC_REPRESENTATION_ITEM()
RATIONAL_B_SPLINE_CURVE((1.00000059564287,1.00000117472449,1.00000103906851))
REPRESENTATION_ITEM('')
);
#1225=(
BOUNDED_CURVE()
B_SPLINE_CURVE(2,(#200228,#200229,#200230),.UNSPECIFIED.,.F.,.F.)
B_SPLINE_CURVE_WITH_KNOTS((3,3),(-0.866812823519123,-0.251975230958864),
 .UNSPECIFIED.)
CURVE()
GEOMETRIC_REPRESENTATION_ITEM()
RATIONAL_B_SPLINE_CURVE((1.00000103877905,1.00000117444993,1.00000059502701))
REPRESENTATION_ITEM('')
);
#1226=(
BOUNDED_CURVE()
B_SPLINE_CURVE(2,(#223366,#223367,#223368),.UNSPECIFIED.,.F.,.F.)
B_SPLINE_CURVE_WITH_KNOTS((3,3),(0.633513201322797,1.24075734212083),
 .UNSPECIFIED.)
CURVE()
GEOMETRIC_REPRESENTATION_ITEM()
RATIONAL_B_SPLINE_CURVE((1.00000103881537,1.00000117281535,1.00000060925137))
REPRESENTATION_ITEM('')
);
#1227=(
BOUNDED_CURVE()
B_SPLINE_CURVE(2,(#223382,#223383,#223384),.UNSPECIFIED.,.F.,.F.)
B_SPLINE_CURVE_WITH_KNOTS((3,3),(0.260648141434546,0.866812823611635),
 .UNSPECIFIED.)
CURVE()
GEOMETRIC_REPRESENTATION_ITEM()
RATIONAL_B_SPLINE_CURVE((1.00000061114393,1.00000117236832,1.00000103863036))
REPRESENTATION_ITEM('')
);
#1228=(
BOUNDED_CURVE()
B_SPLINE_CURVE(2,(#223401,#223402,#223403),.UNSPECIFIED.,.F.,.F.)
B_SPLINE_CURVE_WITH_KNOTS((3,3),(0.252214003958614,0.866812823544261),
 .UNSPECIFIED.)
CURVE()
GEOMETRIC_REPRESENTATION_ITEM()
RATIONAL_B_SPLINE_CURVE((1.00000059564287,1.00000117472449,1.00000103906851))
REPRESENTATION_ITEM('')
);
#1229=(
BOUNDED_CURVE()
B_SPLINE_CURVE(2,(#223417,#223418,#223419),.UNSPECIFIED.,.F.,.F.)
B_SPLINE_CURVE_WITH_KNOTS((3,3),(0.633513201206708,1.24835079376697),
 .UNSPECIFIED.)
CURVE()
GEOMETRIC_REPRESENTATION_ITEM()
RATIONAL_B_SPLINE_CURVE((1.00000103877905,1.00000117444993,1.00000059502701))
REPRESENTATION_ITEM('')
);
#1230=(
BOUNDED_CURVE()
B_SPLINE_CURVE(2,(#232817,#232818,#232819),.UNSPECIFIED.,.F.,.F.)
B_SPLINE_CURVE_WITH_KNOTS((3,3),(0.594066455576382,1.16209721084497),
 .UNSPECIFIED.)
CURVE()
GEOMETRIC_REPRESENTATION_ITEM()
RATIONAL_B_SPLINE_CURVE((2.95854811567267,3.41623710198805,2.95854811567268))
REPRESENTATION_ITEM('')
);
#1231=(
BOUNDED_CURVE()
B_SPLINE_CURVE(2,(#232822,#232823,#232824),.UNSPECIFIED.,.F.,.F.)
B_SPLINE_CURVE_WITH_KNOTS((3,3),(-0.388312804292316,-0.130611113351459),
 .UNSPECIFIED.)
CURVE()
GEOMETRIC_REPRESENTATION_ITEM()
RATIONAL_B_SPLINE_CURVE((1.30940107675847,1.51196612828737,1.30940107675848))
REPRESENTATION_ITEM('')
);
#1232=(
BOUNDED_CURVE()
B_SPLINE_CURVE(2,(#232829,#232830,#232831),.UNSPECIFIED.,.F.,.F.)
B_SPLINE_CURVE_WITH_KNOTS((3,3),(0.594066455576367,1.16209721084493),
 .UNSPECIFIED.)
CURVE()
GEOMETRIC_REPRESENTATION_ITEM()
RATIONAL_B_SPLINE_CURVE((2.95854811567267,3.41623710198805,2.95854811567278))
REPRESENTATION_ITEM('')
);
#1233=(
BOUNDED_CURVE()
B_SPLINE_CURVE(2,(#232832,#232833,#232834),.UNSPECIFIED.,.F.,.F.)
B_SPLINE_CURVE_WITH_KNOTS((3,3),(-0.388312804292315,-0.130611113351461),
 .UNSPECIFIED.)
CURVE()
GEOMETRIC_REPRESENTATION_ITEM()
RATIONAL_B_SPLINE_CURVE((1.30940107675852,1.51196612828742,1.30940107675851))
REPRESENTATION_ITEM('')
);
#1234=(
BOUNDED_CURVE()
B_SPLINE_CURVE(2,(#232839,#232840,#232841),.UNSPECIFIED.,.F.,.F.)
B_SPLINE_CURVE_WITH_KNOTS((3,3),(0.594066455576351,1.16209721084505),
 .UNSPECIFIED.)
CURVE()
GEOMETRIC_REPRESENTATION_ITEM()
RATIONAL_B_SPLINE_CURVE((2.95854811567277,3.41623710198832,2.95854811567269))
REPRESENTATION_ITEM('')
);
#1235=(
BOUNDED_CURVE()
B_SPLINE_CURVE(2,(#232842,#232843,#232844),.UNSPECIFIED.,.F.,.F.)
B_SPLINE_CURVE_WITH_KNOTS((3,3),(-0.388312804292322,-0.130611113351455),
 .UNSPECIFIED.)
CURVE()
GEOMETRIC_REPRESENTATION_ITEM()
RATIONAL_B_SPLINE_CURVE((1.30940107675848,1.5119661282874,1.30940107675849))
REPRESENTATION_ITEM('')
);
#1236=(
BOUNDED_CURVE()
B_SPLINE_CURVE(2,(#232849,#232850,#232851),.UNSPECIFIED.,.F.,.F.)
B_SPLINE_CURVE_WITH_KNOTS((3,3),(0.594066455576352,1.16209721084485),
 .UNSPECIFIED.)
CURVE()
GEOMETRIC_REPRESENTATION_ITEM()
RATIONAL_B_SPLINE_CURVE((2.95854811567277,3.41623710198815,2.95854811567302))
REPRESENTATION_ITEM('')
);
#1237=(
BOUNDED_CURVE()
B_SPLINE_CURVE(2,(#232852,#232853,#232854),.UNSPECIFIED.,.F.,.F.)
B_SPLINE_CURVE_WITH_KNOTS((3,3),(-0.388312804292316,-0.130611113351461),
 .UNSPECIFIED.)
CURVE()
GEOMETRIC_REPRESENTATION_ITEM()
RATIONAL_B_SPLINE_CURVE((1.30940107675852,1.51196612828743,1.30940107675851))
REPRESENTATION_ITEM('')
);
#1238=(
BOUNDED_CURVE()
B_SPLINE_CURVE(2,(#232859,#232860,#232861),.UNSPECIFIED.,.F.,.F.)
B_SPLINE_CURVE_WITH_KNOTS((3,3),(0.594066455576162,1.16209721084505),
 .UNSPECIFIED.)
CURVE()
GEOMETRIC_REPRESENTATION_ITEM()
RATIONAL_B_SPLINE_CURVE((2.95854811567234,3.41623710198832,2.95854811567258))
REPRESENTATION_ITEM('')
);
#1239=(
BOUNDED_CURVE()
B_SPLINE_CURVE(2,(#232862,#232863,#232864),.UNSPECIFIED.,.F.,.F.)
B_SPLINE_CURVE_WITH_KNOTS((3,3),(-0.388312804292327,-0.130611113351463),
 .UNSPECIFIED.)
CURVE()
GEOMETRIC_REPRESENTATION_ITEM()
RATIONAL_B_SPLINE_CURVE((1.30940107675851,1.51196612828743,1.30940107675852))
REPRESENTATION_ITEM('')
);
#1240=(
BOUNDED_CURVE()
B_SPLINE_CURVE(2,(#232866,#232867,#232868),.UNSPECIFIED.,.F.,.F.)
B_SPLINE_CURVE_WITH_KNOTS((3,3),(0.594066455576369,1.16209721084496),
 .UNSPECIFIED.)
CURVE()
GEOMETRIC_REPRESENTATION_ITEM()
RATIONAL_B_SPLINE_CURVE((2.95854811567278,3.4162371019882,2.95854811567281))
REPRESENTATION_ITEM('')
);
#1241=(
BOUNDED_CURVE()
B_SPLINE_CURVE(2,(#232869,#232870,#232871),.UNSPECIFIED.,.F.,.F.)
B_SPLINE_CURVE_WITH_KNOTS((3,3),(-0.388312804292311,-0.130611113351464),
 .UNSPECIFIED.)
CURVE()
GEOMETRIC_REPRESENTATION_ITEM()
RATIONAL_B_SPLINE_CURVE((1.30940107675851,1.51196612828742,1.30940107675852))
REPRESENTATION_ITEM('')
);
#1242=(
BOUNDED_CURVE()
B_SPLINE_CURVE(2,(#232916,#232917,#232918),.UNSPECIFIED.,.F.,.F.)
B_SPLINE_CURVE_WITH_KNOTS((3,3),(-1.46410161513778,-1.00000000000002),
 .UNSPECIFIED.)
CURVE()
GEOMETRIC_REPRESENTATION_ITEM()
RATIONAL_B_SPLINE_CURVE((1.39230484541328,1.50000000000003,1.50000000000003))
REPRESENTATION_ITEM('')
);
#1243=(
BOUNDED_CURVE()
B_SPLINE_CURVE(2,(#232919,#232920,#232921),.UNSPECIFIED.,.F.,.F.)
B_SPLINE_CURVE_WITH_KNOTS((3,3),(-1.00000000000002,-0.535898384862265),
 .UNSPECIFIED.)
CURVE()
GEOMETRIC_REPRESENTATION_ITEM()
RATIONAL_B_SPLINE_CURVE((1.50000000000001,1.50000000000001,1.39230484541328))
REPRESENTATION_ITEM('')
);
#1244=(
BOUNDED_CURVE()
B_SPLINE_CURVE(2,(#232924,#232925,#232926),.UNSPECIFIED.,.F.,.F.)
B_SPLINE_CURVE_WITH_KNOTS((3,3),(-1.00000000000002,-0.535898384862256),
 .UNSPECIFIED.)
CURVE()
GEOMETRIC_REPRESENTATION_ITEM()
RATIONAL_B_SPLINE_CURVE((1.50000000000003,1.50000000000003,1.39230484541329))
REPRESENTATION_ITEM('')
);
#1245=(
BOUNDED_CURVE()
B_SPLINE_CURVE(2,(#232927,#232928,#232929),.UNSPECIFIED.,.F.,.F.)
B_SPLINE_CURVE_WITH_KNOTS((3,3),(-1.46410161513777,-1.00000000000001),
 .UNSPECIFIED.)
CURVE()
GEOMETRIC_REPRESENTATION_ITEM()
RATIONAL_B_SPLINE_CURVE((1.39230484541327,1.50000000000001,1.50000000000001))
REPRESENTATION_ITEM('')
);
#1246=(
BOUNDED_CURVE()
B_SPLINE_CURVE(2,(#232932,#232933,#232934),.UNSPECIFIED.,.F.,.F.)
B_SPLINE_CURVE_WITH_KNOTS((3,3),(-1.00000000000001,-0.535898384862254),
 .UNSPECIFIED.)
CURVE()
GEOMETRIC_REPRESENTATION_ITEM()
RATIONAL_B_SPLINE_CURVE((1.50000000000001,1.50000000000001,1.39230484541328))
REPRESENTATION_ITEM('')
);
#1247=(
BOUNDED_CURVE()
B_SPLINE_CURVE(2,(#232935,#232936,#232937),.UNSPECIFIED.,.F.,.F.)
B_SPLINE_CURVE_WITH_KNOTS((3,3),(-1.46410161513775,-1.),.UNSPECIFIED.)
CURVE()
GEOMETRIC_REPRESENTATION_ITEM()
RATIONAL_B_SPLINE_CURVE((1.39230484541327,1.5,1.5))
REPRESENTATION_ITEM('')
);
#1248=(
BOUNDED_CURVE()
B_SPLINE_CURVE(2,(#232940,#232941,#232942),.UNSPECIFIED.,.F.,.F.)
B_SPLINE_CURVE_WITH_KNOTS((3,3),(-1.,-0.535898384862256),.UNSPECIFIED.)
CURVE()
GEOMETRIC_REPRESENTATION_ITEM()
RATIONAL_B_SPLINE_CURVE((1.5,1.5,1.39230484541327))
REPRESENTATION_ITEM('')
);
#1249=(
BOUNDED_CURVE()
B_SPLINE_CURVE(2,(#232943,#232944,#232945),.UNSPECIFIED.,.F.,.F.)
B_SPLINE_CURVE_WITH_KNOTS((3,3),(-1.46410161513776,-1.00000000000001),
 .UNSPECIFIED.)
CURVE()
GEOMETRIC_REPRESENTATION_ITEM()
RATIONAL_B_SPLINE_CURVE((1.39230484541327,1.5,1.5))
REPRESENTATION_ITEM('')
);
#1250=(
BOUNDED_CURVE()
B_SPLINE_CURVE(2,(#232948,#232949,#232950),.UNSPECIFIED.,.F.,.F.)
B_SPLINE_CURVE_WITH_KNOTS((3,3),(-1.00000000000001,-0.535898384862251),
 .UNSPECIFIED.)
CURVE()
GEOMETRIC_REPRESENTATION_ITEM()
RATIONAL_B_SPLINE_CURVE((1.5,1.50000000000001,1.39230484541327))
REPRESENTATION_ITEM('')
);
#1251=(
BOUNDED_CURVE()
B_SPLINE_CURVE(2,(#232951,#232952,#232953),.UNSPECIFIED.,.F.,.F.)
B_SPLINE_CURVE_WITH_KNOTS((3,3),(-1.46410161513775,-1.00000000000001),
 .UNSPECIFIED.)
CURVE()
GEOMETRIC_REPRESENTATION_ITEM()
RATIONAL_B_SPLINE_CURVE((1.39230484541326,1.49999999999999,1.49999999999999))
REPRESENTATION_ITEM('')
);
#1252=(
BOUNDED_CURVE()
B_SPLINE_CURVE(2,(#232956,#232957,#232958),.UNSPECIFIED.,.F.,.F.)
B_SPLINE_CURVE_WITH_KNOTS((3,3),(-1.00000000000001,-0.535898384862264),
 .UNSPECIFIED.)
CURVE()
GEOMETRIC_REPRESENTATION_ITEM()
RATIONAL_B_SPLINE_CURVE((1.49999999999999,1.49999999999999,1.39230484541326))
REPRESENTATION_ITEM('')
);
#1253=(
BOUNDED_CURVE()
B_SPLINE_CURVE(2,(#232959,#232960,#232961),.UNSPECIFIED.,.F.,.F.)
B_SPLINE_CURVE_WITH_KNOTS((3,3),(-1.46410161513776,-1.00000000000002),
 .UNSPECIFIED.)
CURVE()
GEOMETRIC_REPRESENTATION_ITEM()
RATIONAL_B_SPLINE_CURVE((1.39230484541327,1.5,1.50000000000001))
REPRESENTATION_ITEM('')
);
#1254=(
BOUNDED_CURVE()
B_SPLINE_CURVE(2,(#232977,#232978,#232979),.UNSPECIFIED.,.F.,.F.)
B_SPLINE_CURVE_WITH_KNOTS((3,3),(0.82874043787133,1.36602540378442),
 .UNSPECIFIED.)
CURVE()
GEOMETRIC_REPRESENTATION_ITEM()
RATIONAL_B_SPLINE_CURVE((1.73205080756822,1.86602540378445,1.86602540378445))
REPRESENTATION_ITEM('')
);
#1255=(
BOUNDED_CURVE()
B_SPLINE_CURVE(2,(#232980,#232981,#232982),.UNSPECIFIED.,.F.,.F.)
B_SPLINE_CURVE_WITH_KNOTS((3,3),(1.36602540378443,1.90331036969748),
 .UNSPECIFIED.)
CURVE()
GEOMETRIC_REPRESENTATION_ITEM()
RATIONAL_B_SPLINE_CURVE((1.86602540378443,1.86602540378443,1.73205080756823))
REPRESENTATION_ITEM('')
);
#1256=(
BOUNDED_CURVE()
B_SPLINE_CURVE(2,(#232985,#232986,#232987),.UNSPECIFIED.,.F.,.F.)
B_SPLINE_CURVE_WITH_KNOTS((3,3),(0.82874043787135,1.36602540378443),
 .UNSPECIFIED.)
CURVE()
GEOMETRIC_REPRESENTATION_ITEM()
RATIONAL_B_SPLINE_CURVE((1.73205080756821,1.86602540378443,1.86602540378443))
REPRESENTATION_ITEM('')
);
#1257=(
BOUNDED_CURVE()
B_SPLINE_CURVE(2,(#232988,#232989,#232990),.UNSPECIFIED.,.F.,.F.)
B_SPLINE_CURVE_WITH_KNOTS((3,3),(1.36602540378445,1.90331036969754),
 .UNSPECIFIED.)
CURVE()
GEOMETRIC_REPRESENTATION_ITEM()
RATIONAL_B_SPLINE_CURVE((1.86602540378445,1.86602540378445,1.73205080756823))
REPRESENTATION_ITEM('')
);
#1258=(
BOUNDED_CURVE()
B_SPLINE_CURVE(2,(#232993,#232994,#232995),.UNSPECIFIED.,.F.,.F.)
B_SPLINE_CURVE_WITH_KNOTS((3,3),(0.828740437871358,1.36602540378445),
 .UNSPECIFIED.)
CURVE()
GEOMETRIC_REPRESENTATION_ITEM()
RATIONAL_B_SPLINE_CURVE((1.73205080756824,1.86602540378446,1.86602540378445))
REPRESENTATION_ITEM('')
);
#1259=(
BOUNDED_CURVE()
B_SPLINE_CURVE(2,(#232996,#232997,#232998),.UNSPECIFIED.,.F.,.F.)
B_SPLINE_CURVE_WITH_KNOTS((3,3),(1.36602540378445,1.90331036969753),
 .UNSPECIFIED.)
CURVE()
GEOMETRIC_REPRESENTATION_ITEM()
RATIONAL_B_SPLINE_CURVE((1.86602540378444,1.86602540378444,1.73205080756822))
REPRESENTATION_ITEM('')
);
#1260=(
BOUNDED_CURVE()
B_SPLINE_CURVE(2,(#233001,#233002,#233003),.UNSPECIFIED.,.F.,.F.)
B_SPLINE_CURVE_WITH_KNOTS((3,3),(0.828740437871363,1.36602540378445),
 .UNSPECIFIED.)
CURVE()
GEOMETRIC_REPRESENTATION_ITEM()
RATIONAL_B_SPLINE_CURVE((1.73205080756823,1.86602540378444,1.86602540378444))
REPRESENTATION_ITEM('')
);
#1261=(
BOUNDED_CURVE()
B_SPLINE_CURVE(2,(#233004,#233005,#233006),.UNSPECIFIED.,.F.,.F.)
B_SPLINE_CURVE_WITH_KNOTS((3,3),(1.36602540378447,1.90331036969755),
 .UNSPECIFIED.)
CURVE()
GEOMETRIC_REPRESENTATION_ITEM()
RATIONAL_B_SPLINE_CURVE((1.86602540378447,1.86602540378447,1.73205080756825))
REPRESENTATION_ITEM('')
);
#1262=(
BOUNDED_CURVE()
B_SPLINE_CURVE(2,(#233009,#233010,#233011),.UNSPECIFIED.,.F.,.F.)
B_SPLINE_CURVE_WITH_KNOTS((3,3),(0.828740437871365,1.36602540378447),
 .UNSPECIFIED.)
CURVE()
GEOMETRIC_REPRESENTATION_ITEM()
RATIONAL_B_SPLINE_CURVE((1.73205080756825,1.86602540378447,1.86602540378447))
REPRESENTATION_ITEM('')
);
#1263=(
BOUNDED_CURVE()
B_SPLINE_CURVE(2,(#233012,#233013,#233014),.UNSPECIFIED.,.F.,.F.)
B_SPLINE_CURVE_WITH_KNOTS((3,3),(1.36602540378446,1.90331036969757),
 .UNSPECIFIED.)
CURVE()
GEOMETRIC_REPRESENTATION_ITEM()
RATIONAL_B_SPLINE_CURVE((1.8660254037845,1.8660254037845,1.73205080756827))
REPRESENTATION_ITEM('')
);
#1264=(
BOUNDED_CURVE()
B_SPLINE_CURVE(2,(#233017,#233018,#233019),.UNSPECIFIED.,.F.,.F.)
B_SPLINE_CURVE_WITH_KNOTS((3,3),(1.36602540378442,1.90331036969753),
 .UNSPECIFIED.)
CURVE()
GEOMETRIC_REPRESENTATION_ITEM()
RATIONAL_B_SPLINE_CURVE((1.86602540378445,1.86602540378446,1.73205080756824))
REPRESENTATION_ITEM('')
);
#1265=(
BOUNDED_CURVE()
B_SPLINE_CURVE(2,(#233020,#233021,#233022),.UNSPECIFIED.,.F.,.F.)
B_SPLINE_CURVE_WITH_KNOTS((3,3),(0.82874043787136,1.36602540378446),
 .UNSPECIFIED.)
CURVE()
GEOMETRIC_REPRESENTATION_ITEM()
RATIONAL_B_SPLINE_CURVE((1.73205080756826,1.86602540378449,1.8660254037845))
REPRESENTATION_ITEM('')
);
#1266=(
BOUNDED_CURVE()
B_SPLINE_CURVE(2,(#233050,#233051,#233052),.UNSPECIFIED.,.F.,.F.)
B_SPLINE_CURVE_WITH_KNOTS((3,3),(-1.46410161513776,-1.00000000000001),
 .UNSPECIFIED.)
CURVE()
GEOMETRIC_REPRESENTATION_ITEM()
RATIONAL_B_SPLINE_CURVE((1.39230484541327,1.50000000000001,1.50000000000001))
REPRESENTATION_ITEM('')
);
#1267=(
BOUNDED_CURVE()
B_SPLINE_CURVE(2,(#233053,#233054,#233055),.UNSPECIFIED.,.F.,.F.)
B_SPLINE_CURVE_WITH_KNOTS((3,3),(-1.,-0.535898384862256),.UNSPECIFIED.)
CURVE()
GEOMETRIC_REPRESENTATION_ITEM()
RATIONAL_B_SPLINE_CURVE((1.5,1.5,1.39230484541327))
REPRESENTATION_ITEM('')
);
#1268=(
BOUNDED_CURVE()
B_SPLINE_CURVE(2,(#233058,#233059,#233060),.UNSPECIFIED.,.F.,.F.)
B_SPLINE_CURVE_WITH_KNOTS((3,3),(-1.00000000000001,-0.535898384862251),
 .UNSPECIFIED.)
CURVE()
GEOMETRIC_REPRESENTATION_ITEM()
RATIONAL_B_SPLINE_CURVE((1.50000000000001,1.50000000000001,1.39230484541327))
REPRESENTATION_ITEM('')
);
#1269=(
BOUNDED_CURVE()
B_SPLINE_CURVE(2,(#233061,#233062,#233063),.UNSPECIFIED.,.F.,.F.)
B_SPLINE_CURVE_WITH_KNOTS((3,3),(-1.46410161513775,-1.),.UNSPECIFIED.)
CURVE()
GEOMETRIC_REPRESENTATION_ITEM()
RATIONAL_B_SPLINE_CURVE((1.39230484541326,1.5,1.5))
REPRESENTATION_ITEM('')
);
#1270=(
BOUNDED_CURVE()
B_SPLINE_CURVE(2,(#233066,#233067,#233068),.UNSPECIFIED.,.F.,.F.)
B_SPLINE_CURVE_WITH_KNOTS((3,3),(-1.,-0.535898384862256),.UNSPECIFIED.)
CURVE()
GEOMETRIC_REPRESENTATION_ITEM()
RATIONAL_B_SPLINE_CURVE((1.5,1.5,1.39230484541327))
REPRESENTATION_ITEM('')
);
#1271=(
BOUNDED_CURVE()
B_SPLINE_CURVE(2,(#233069,#233070,#233071),.UNSPECIFIED.,.F.,.F.)
B_SPLINE_CURVE_WITH_KNOTS((3,3),(-1.46410161513777,-1.),.UNSPECIFIED.)
CURVE()
GEOMETRIC_REPRESENTATION_ITEM()
RATIONAL_B_SPLINE_CURVE((1.39230484541326,1.5,1.5))
REPRESENTATION_ITEM('')
);
#1272=(
BOUNDED_CURVE()
B_SPLINE_CURVE(2,(#233074,#233075,#233076),.UNSPECIFIED.,.F.,.F.)
B_SPLINE_CURVE_WITH_KNOTS((3,3),(-1.,-0.535898384862258),.UNSPECIFIED.)
CURVE()
GEOMETRIC_REPRESENTATION_ITEM()
RATIONAL_B_SPLINE_CURVE((1.5,1.5,1.39230484541327))
REPRESENTATION_ITEM('')
);
#1273=(
BOUNDED_CURVE()
B_SPLINE_CURVE(2,(#233077,#233078,#233079),.UNSPECIFIED.,.F.,.F.)
B_SPLINE_CURVE_WITH_KNOTS((3,3),(-1.46410161513776,-1.),.UNSPECIFIED.)
CURVE()
GEOMETRIC_REPRESENTATION_ITEM()
RATIONAL_B_SPLINE_CURVE((1.39230484541327,1.50000000000001,1.50000000000001))
REPRESENTATION_ITEM('')
);
#1274=(
BOUNDED_CURVE()
B_SPLINE_CURVE(2,(#233082,#233083,#233084),.UNSPECIFIED.,.F.,.F.)
B_SPLINE_CURVE_WITH_KNOTS((3,3),(-1.,-0.535898384862256),.UNSPECIFIED.)
CURVE()
GEOMETRIC_REPRESENTATION_ITEM()
RATIONAL_B_SPLINE_CURVE((1.50000000000001,1.5,1.39230484541327))
REPRESENTATION_ITEM('')
);
#1275=(
BOUNDED_CURVE()
B_SPLINE_CURVE(2,(#233085,#233086,#233087),.UNSPECIFIED.,.F.,.F.)
B_SPLINE_CURVE_WITH_KNOTS((3,3),(-1.46410161513776,-1.00000000000001),
 .UNSPECIFIED.)
CURVE()
GEOMETRIC_REPRESENTATION_ITEM()
RATIONAL_B_SPLINE_CURVE((1.39230484541328,1.50000000000002,1.50000000000002))
REPRESENTATION_ITEM('')
);
#1276=(
BOUNDED_CURVE()
B_SPLINE_CURVE(2,(#233090,#233091,#233092),.UNSPECIFIED.,.F.,.F.)
B_SPLINE_CURVE_WITH_KNOTS((3,3),(-1.00000000000001,-0.535898384862248),
 .UNSPECIFIED.)
CURVE()
GEOMETRIC_REPRESENTATION_ITEM()
RATIONAL_B_SPLINE_CURVE((1.50000000000002,1.50000000000002,1.39230484541328))
REPRESENTATION_ITEM('')
);
#1277=(
BOUNDED_CURVE()
B_SPLINE_CURVE(2,(#233093,#233094,#233095),.UNSPECIFIED.,.F.,.F.)
B_SPLINE_CURVE_WITH_KNOTS((3,3),(-1.46410161513775,-1.),.UNSPECIFIED.)
CURVE()
GEOMETRIC_REPRESENTATION_ITEM()
RATIONAL_B_SPLINE_CURVE((1.39230484541327,1.5,1.5))
REPRESENTATION_ITEM('')
);
#1278=(
BOUNDED_CURVE()
B_SPLINE_CURVE(2,(#233111,#233112,#233113),.UNSPECIFIED.,.F.,.F.)
B_SPLINE_CURVE_WITH_KNOTS((3,3),(0.828740437871337,1.36602540378444),
 .UNSPECIFIED.)
CURVE()
GEOMETRIC_REPRESENTATION_ITEM()
RATIONAL_B_SPLINE_CURVE((1.73205080756821,1.86602540378444,1.86602540378444))
REPRESENTATION_ITEM('')
);
#1279=(
BOUNDED_CURVE()
B_SPLINE_CURVE(2,(#233114,#233115,#233116),.UNSPECIFIED.,.F.,.F.)
B_SPLINE_CURVE_WITH_KNOTS((3,3),(1.36602540378446,1.90331036969753),
 .UNSPECIFIED.)
CURVE()
GEOMETRIC_REPRESENTATION_ITEM()
RATIONAL_B_SPLINE_CURVE((1.86602540378447,1.86602540378447,1.73205080756826))
REPRESENTATION_ITEM('')
);
#1280=(
BOUNDED_CURVE()
B_SPLINE_CURVE(2,(#233119,#233120,#233121),.UNSPECIFIED.,.F.,.F.)
B_SPLINE_CURVE_WITH_KNOTS((3,3),(0.828740437871367,1.36602540378446),
 .UNSPECIFIED.)
CURVE()
GEOMETRIC_REPRESENTATION_ITEM()
RATIONAL_B_SPLINE_CURVE((1.73205080756825,1.86602540378447,1.86602540378447))
REPRESENTATION_ITEM('')
);
#1281=(
BOUNDED_CURVE()
B_SPLINE_CURVE(2,(#233122,#233123,#233124),.UNSPECIFIED.,.F.,.F.)
B_SPLINE_CURVE_WITH_KNOTS((3,3),(1.36602540378445,1.90331036969753),
 .UNSPECIFIED.)
CURVE()
GEOMETRIC_REPRESENTATION_ITEM()
RATIONAL_B_SPLINE_CURVE((1.86602540378445,1.86602540378445,1.73205080756823))
REPRESENTATION_ITEM('')
);
#1282=(
BOUNDED_CURVE()
B_SPLINE_CURVE(2,(#233127,#233128,#233129),.UNSPECIFIED.,.F.,.F.)
B_SPLINE_CURVE_WITH_KNOTS((3,3),(0.828740437871355,1.36602540378445),
 .UNSPECIFIED.)
CURVE()
GEOMETRIC_REPRESENTATION_ITEM()
RATIONAL_B_SPLINE_CURVE((1.73205080756823,1.86602540378445,1.86602540378445))
REPRESENTATION_ITEM('')
);
#1283=(
BOUNDED_CURVE()
B_SPLINE_CURVE(2,(#233130,#233131,#233132),.UNSPECIFIED.,.F.,.F.)
B_SPLINE_CURVE_WITH_KNOTS((3,3),(1.36602540378444,1.90331036969752),
 .UNSPECIFIED.)
CURVE()
GEOMETRIC_REPRESENTATION_ITEM()
RATIONAL_B_SPLINE_CURVE((1.86602540378444,1.86602540378444,1.73205080756823))
REPRESENTATION_ITEM('')
);
#1284=(
BOUNDED_CURVE()
B_SPLINE_CURVE(2,(#233135,#233136,#233137),.UNSPECIFIED.,.F.,.F.)
B_SPLINE_CURVE_WITH_KNOTS((3,3),(0.828740437871347,1.36602540378444),
 .UNSPECIFIED.)
CURVE()
GEOMETRIC_REPRESENTATION_ITEM()
RATIONAL_B_SPLINE_CURVE((1.73205080756822,1.86602540378444,1.86602540378444))
REPRESENTATION_ITEM('')
);
#1285=(
BOUNDED_CURVE()
B_SPLINE_CURVE(2,(#233138,#233139,#233140),.UNSPECIFIED.,.F.,.F.)
B_SPLINE_CURVE_WITH_KNOTS((3,3),(1.36602540378443,1.90331036969751),
 .UNSPECIFIED.)
CURVE()
GEOMETRIC_REPRESENTATION_ITEM()
RATIONAL_B_SPLINE_CURVE((1.86602540378443,1.86602540378444,1.73205080756823))
REPRESENTATION_ITEM('')
);
#1286=(
BOUNDED_CURVE()
B_SPLINE_CURVE(2,(#233143,#233144,#233145),.UNSPECIFIED.,.F.,.F.)
B_SPLINE_CURVE_WITH_KNOTS((3,3),(0.828740437871352,1.36602540378443),
 .UNSPECIFIED.)
CURVE()
GEOMETRIC_REPRESENTATION_ITEM()
RATIONAL_B_SPLINE_CURVE((1.73205080756822,1.86602540378443,1.86602540378443))
REPRESENTATION_ITEM('')
);
#1287=(
BOUNDED_CURVE()
B_SPLINE_CURVE(2,(#233146,#233147,#233148),.UNSPECIFIED.,.F.,.F.)
B_SPLINE_CURVE_WITH_KNOTS((3,3),(1.36602540378444,1.90331036969754),
 .UNSPECIFIED.)
CURVE()
GEOMETRIC_REPRESENTATION_ITEM()
RATIONAL_B_SPLINE_CURVE((1.86602540378445,1.86602540378445,1.73205080756823))
REPRESENTATION_ITEM('')
);
#1288=(
BOUNDED_CURVE()
B_SPLINE_CURVE(2,(#233151,#233152,#233153),.UNSPECIFIED.,.F.,.F.)
B_SPLINE_CURVE_WITH_KNOTS((3,3),(1.36602540378444,1.90331036969753),
 .UNSPECIFIED.)
CURVE()
GEOMETRIC_REPRESENTATION_ITEM()
RATIONAL_B_SPLINE_CURVE((1.86602540378444,1.86602540378444,1.73205080756822))
REPRESENTATION_ITEM('')
);
#1289=(
BOUNDED_CURVE()
B_SPLINE_CURVE(2,(#233154,#233155,#233156),.UNSPECIFIED.,.F.,.F.)
B_SPLINE_CURVE_WITH_KNOTS((3,3),(0.828740437871356,1.36602540378444),
 .UNSPECIFIED.)
CURVE()
GEOMETRIC_REPRESENTATION_ITEM()
RATIONAL_B_SPLINE_CURVE((1.73205080756823,1.86602540378445,1.86602540378445))
REPRESENTATION_ITEM('')
);
#1290=(
BOUNDED_CURVE()
B_SPLINE_CURVE(2,(#233174,#233175,#233176),.UNSPECIFIED.,.F.,.F.)
B_SPLINE_CURVE_WITH_KNOTS((3,3),(0.130611113351464,0.388312804292288),
 .UNSPECIFIED.)
CURVE()
GEOMETRIC_REPRESENTATION_ITEM()
RATIONAL_B_SPLINE_CURVE((1.30940107675847,1.51196612828731,1.30940107675848))
REPRESENTATION_ITEM('')
);
#1291=(
BOUNDED_CURVE()
B_SPLINE_CURVE(2,(#233179,#233180,#233181),.UNSPECIFIED.,.F.,.F.)
B_SPLINE_CURVE_WITH_KNOTS((3,3),(-1.16209721084502,-0.594066455576398),
 .UNSPECIFIED.)
CURVE()
GEOMETRIC_REPRESENTATION_ITEM()
RATIONAL_B_SPLINE_CURVE((2.95854811567252,3.41623710198795,2.95854811567259))
REPRESENTATION_ITEM('')
);
#1292=(
BOUNDED_CURVE()
B_SPLINE_CURVE(2,(#233186,#233187,#233188),.UNSPECIFIED.,.F.,.F.)
B_SPLINE_CURVE_WITH_KNOTS((3,3),(0.130611113351459,0.388312804292326),
 .UNSPECIFIED.)
CURVE()
GEOMETRIC_REPRESENTATION_ITEM()
RATIONAL_B_SPLINE_CURVE((1.30940107675853,1.51196612828746,1.30940107675851))
REPRESENTATION_ITEM('')
);
#1293=(
BOUNDED_CURVE()
B_SPLINE_CURVE(2,(#233189,#233190,#233191),.UNSPECIFIED.,.F.,.F.)
B_SPLINE_CURVE_WITH_KNOTS((3,3),(-1.16209721084504,-0.594066455576386),
 .UNSPECIFIED.)
CURVE()
GEOMETRIC_REPRESENTATION_ITEM()
RATIONAL_B_SPLINE_CURVE((2.95854811567252,3.416237101988,2.95854811567259))
REPRESENTATION_ITEM('')
);
#1294=(
BOUNDED_CURVE()
B_SPLINE_CURVE(2,(#233196,#233197,#233198),.UNSPECIFIED.,.F.,.F.)
B_SPLINE_CURVE_WITH_KNOTS((3,3),(0.130611113351456,0.388312804292303),
 .UNSPECIFIED.)
CURVE()
GEOMETRIC_REPRESENTATION_ITEM()
RATIONAL_B_SPLINE_CURVE((1.30940107675853,1.51196612828745,1.30940107675855))
REPRESENTATION_ITEM('')
);
#1295=(
BOUNDED_CURVE()
B_SPLINE_CURVE(2,(#233199,#233200,#233201),.UNSPECIFIED.,.F.,.F.)
B_SPLINE_CURVE_WITH_KNOTS((3,3),(-1.16209721084501,-0.594066455576338),
 .UNSPECIFIED.)
CURVE()
GEOMETRIC_REPRESENTATION_ITEM()
RATIONAL_B_SPLINE_CURVE((2.95854811567261,3.41623710198812,2.9585481156726))
REPRESENTATION_ITEM('')
);
#1296=(
BOUNDED_CURVE()
B_SPLINE_CURVE(2,(#233206,#233207,#233208),.UNSPECIFIED.,.F.,.F.)
B_SPLINE_CURVE_WITH_KNOTS((3,3),(0.130611113351459,0.388312804292329),
 .UNSPECIFIED.)
CURVE()
GEOMETRIC_REPRESENTATION_ITEM()
RATIONAL_B_SPLINE_CURVE((1.30940107675851,1.51196612828744,1.3094010767585))
REPRESENTATION_ITEM('')
);
#1297=(
BOUNDED_CURVE()
B_SPLINE_CURVE(2,(#233209,#233210,#233211),.UNSPECIFIED.,.F.,.F.)
B_SPLINE_CURVE_WITH_KNOTS((3,3),(-1.16209721084508,-0.594066455576527),
 .UNSPECIFIED.)
CURVE()
GEOMETRIC_REPRESENTATION_ITEM()
RATIONAL_B_SPLINE_CURVE((2.95854811567269,3.41623710198822,2.95854811567307))
REPRESENTATION_ITEM('')
);
#1298=(
BOUNDED_CURVE()
B_SPLINE_CURVE(2,(#233216,#233217,#233218),.UNSPECIFIED.,.F.,.F.)
B_SPLINE_CURVE_WITH_KNOTS((3,3),(0.130611113351453,0.388312804292305),
 .UNSPECIFIED.)
CURVE()
GEOMETRIC_REPRESENTATION_ITEM()
RATIONAL_B_SPLINE_CURVE((1.30940107675848,1.51196612828739,1.30940107675851))
REPRESENTATION_ITEM('')
);
#1299=(
BOUNDED_CURVE()
B_SPLINE_CURVE(2,(#233219,#233220,#233221),.UNSPECIFIED.,.F.,.F.)
B_SPLINE_CURVE_WITH_KNOTS((3,3),(-1.16209721084514,-0.594066455576349),
 .UNSPECIFIED.)
CURVE()
GEOMETRIC_REPRESENTATION_ITEM()
RATIONAL_B_SPLINE_CURVE((2.9585481156724,3.41623710198821,2.95854811567262))
REPRESENTATION_ITEM('')
);
#1300=(
BOUNDED_CURVE()
B_SPLINE_CURVE(2,(#233223,#233224,#233225),.UNSPECIFIED.,.F.,.F.)
B_SPLINE_CURVE_WITH_KNOTS((3,3),(0.130611113351457,0.388312804292304),
 .UNSPECIFIED.)
CURVE()
GEOMETRIC_REPRESENTATION_ITEM()
RATIONAL_B_SPLINE_CURVE((1.30940107675851,1.51196612828742,1.30940107675852))
REPRESENTATION_ITEM('')
);
#1301=(
BOUNDED_CURVE()
B_SPLINE_CURVE(2,(#233226,#233227,#233228),.UNSPECIFIED.,.F.,.F.)
B_SPLINE_CURVE_WITH_KNOTS((3,3),(-1.16209721084494,-0.594066455576379),
 .UNSPECIFIED.)
CURVE()
GEOMETRIC_REPRESENTATION_ITEM()
RATIONAL_B_SPLINE_CURVE((2.95854811567261,3.41623710198787,2.95854811567254))
REPRESENTATION_ITEM('')
);
#1302=(
BOUNDED_CURVE()
B_SPLINE_CURVE(2,(#234764,#234765,#234766),.UNSPECIFIED.,.F.,.F.)
B_SPLINE_CURVE_WITH_KNOTS((3,3),(-1.46410161513777,-1.00000000000001),
 .UNSPECIFIED.)
CURVE()
GEOMETRIC_REPRESENTATION_ITEM()
RATIONAL_B_SPLINE_CURVE((1.39230484541328,1.50000000000002,1.50000000000002))
REPRESENTATION_ITEM('')
);
#1303=(
BOUNDED_CURVE()
B_SPLINE_CURVE(2,(#234767,#234768,#234769),.UNSPECIFIED.,.F.,.F.)
B_SPLINE_CURVE_WITH_KNOTS((3,3),(-1.00000000000001,-0.535898384862261),
 .UNSPECIFIED.)
CURVE()
GEOMETRIC_REPRESENTATION_ITEM()
RATIONAL_B_SPLINE_CURVE((1.5,1.5,1.39230484541327))
REPRESENTATION_ITEM('')
);
#1304=(
BOUNDED_CURVE()
B_SPLINE_CURVE(2,(#234772,#234773,#234774),.UNSPECIFIED.,.F.,.F.)
B_SPLINE_CURVE_WITH_KNOTS((3,3),(-1.00000000000001,-0.535898384862254),
 .UNSPECIFIED.)
CURVE()
GEOMETRIC_REPRESENTATION_ITEM()
RATIONAL_B_SPLINE_CURVE((1.50000000000002,1.50000000000002,1.39230484541328))
REPRESENTATION_ITEM('')
);
#1305=(
BOUNDED_CURVE()
B_SPLINE_CURVE(2,(#234775,#234776,#234777),.UNSPECIFIED.,.F.,.F.)
B_SPLINE_CURVE_WITH_KNOTS((3,3),(-1.46410161513777,-1.),.UNSPECIFIED.)
CURVE()
GEOMETRIC_REPRESENTATION_ITEM()
RATIONAL_B_SPLINE_CURVE((1.39230484541327,1.50000000000001,1.50000000000001))
REPRESENTATION_ITEM('')
);
#1306=(
BOUNDED_CURVE()
B_SPLINE_CURVE(2,(#234780,#234781,#234782),.UNSPECIFIED.,.F.,.F.)
B_SPLINE_CURVE_WITH_KNOTS((3,3),(-1.,-0.535898384862249),.UNSPECIFIED.)
CURVE()
GEOMETRIC_REPRESENTATION_ITEM()
RATIONAL_B_SPLINE_CURVE((1.50000000000001,1.50000000000001,1.39230484541327))
REPRESENTATION_ITEM('')
);
#1307=(
BOUNDED_CURVE()
B_SPLINE_CURVE(2,(#234783,#234784,#234785),.UNSPECIFIED.,.F.,.F.)
B_SPLINE_CURVE_WITH_KNOTS((3,3),(-1.46410161513774,-0.99999999999999),
 .UNSPECIFIED.)
CURVE()
GEOMETRIC_REPRESENTATION_ITEM()
RATIONAL_B_SPLINE_CURVE((1.39230484541328,1.50000000000001,1.50000000000001))
REPRESENTATION_ITEM('')
);
#1308=(
BOUNDED_CURVE()
B_SPLINE_CURVE(2,(#234788,#234789,#234790),.UNSPECIFIED.,.F.,.F.)
B_SPLINE_CURVE_WITH_KNOTS((3,3),(-0.99999999999999,-0.535898384862251),
 .UNSPECIFIED.)
CURVE()
GEOMETRIC_REPRESENTATION_ITEM()
RATIONAL_B_SPLINE_CURVE((1.50000000000001,1.5,1.39230484541327))
REPRESENTATION_ITEM('')
);
#1309=(
BOUNDED_CURVE()
B_SPLINE_CURVE(2,(#234791,#234792,#234793),.UNSPECIFIED.,.F.,.F.)
B_SPLINE_CURVE_WITH_KNOTS((3,3),(-1.46410161513775,-1.),.UNSPECIFIED.)
CURVE()
GEOMETRIC_REPRESENTATION_ITEM()
RATIONAL_B_SPLINE_CURVE((1.39230484541327,1.5,1.5))
REPRESENTATION_ITEM('')
);
#1310=(
BOUNDED_CURVE()
B_SPLINE_CURVE(2,(#234796,#234797,#234798),.UNSPECIFIED.,.F.,.F.)
B_SPLINE_CURVE_WITH_KNOTS((3,3),(-1.,-0.53589838486225),.UNSPECIFIED.)
CURVE()
GEOMETRIC_REPRESENTATION_ITEM()
RATIONAL_B_SPLINE_CURVE((1.5,1.5,1.39230484541326))
REPRESENTATION_ITEM('')
);
#1311=(
BOUNDED_CURVE()
B_SPLINE_CURVE(2,(#234799,#234800,#234801),.UNSPECIFIED.,.F.,.F.)
B_SPLINE_CURVE_WITH_KNOTS((3,3),(-1.46410161513774,-1.),.UNSPECIFIED.)
CURVE()
GEOMETRIC_REPRESENTATION_ITEM()
RATIONAL_B_SPLINE_CURVE((1.39230484541326,1.49999999999999,1.49999999999999))
REPRESENTATION_ITEM('')
);
#1312=(
BOUNDED_CURVE()
B_SPLINE_CURVE(2,(#234804,#234805,#234806),.UNSPECIFIED.,.F.,.F.)
B_SPLINE_CURVE_WITH_KNOTS((3,3),(-1.,-0.535898384862254),.UNSPECIFIED.)
CURVE()
GEOMETRIC_REPRESENTATION_ITEM()
RATIONAL_B_SPLINE_CURVE((1.49999999999999,1.49999999999999,1.39230484541326))
REPRESENTATION_ITEM('')
);
#1313=(
BOUNDED_CURVE()
B_SPLINE_CURVE(2,(#234807,#234808,#234809),.UNSPECIFIED.,.F.,.F.)
B_SPLINE_CURVE_WITH_KNOTS((3,3),(-1.46410161513775,-1.00000000000001),
 .UNSPECIFIED.)
CURVE()
GEOMETRIC_REPRESENTATION_ITEM()
RATIONAL_B_SPLINE_CURVE((1.39230484541327,1.5,1.5))
REPRESENTATION_ITEM('')
);
#1314=(
BOUNDED_CURVE()
B_SPLINE_CURVE(2,(#234825,#234826,#234827),.UNSPECIFIED.,.F.,.F.)
B_SPLINE_CURVE_WITH_KNOTS((3,3),(0.828740437871318,1.36602540378443),
 .UNSPECIFIED.)
CURVE()
GEOMETRIC_REPRESENTATION_ITEM()
RATIONAL_B_SPLINE_CURVE((1.73205080756821,1.86602540378444,1.86602540378444))
REPRESENTATION_ITEM('')
);
#1315=(
BOUNDED_CURVE()
B_SPLINE_CURVE(2,(#234828,#234829,#234830),.UNSPECIFIED.,.F.,.F.)
B_SPLINE_CURVE_WITH_KNOTS((3,3),(1.36602540378443,1.90331036969749),
 .UNSPECIFIED.)
CURVE()
GEOMETRIC_REPRESENTATION_ITEM()
RATIONAL_B_SPLINE_CURVE((1.86602540378444,1.86602540378444,1.73205080756824))
REPRESENTATION_ITEM('')
);
#1316=(
BOUNDED_CURVE()
B_SPLINE_CURVE(2,(#234833,#234834,#234835),.UNSPECIFIED.,.F.,.F.)
B_SPLINE_CURVE_WITH_KNOTS((3,3),(0.828740437871351,1.36602540378443),
 .UNSPECIFIED.)
CURVE()
GEOMETRIC_REPRESENTATION_ITEM()
RATIONAL_B_SPLINE_CURVE((1.73205080756822,1.86602540378444,1.86602540378444))
REPRESENTATION_ITEM('')
);
#1317=(
BOUNDED_CURVE()
B_SPLINE_CURVE(2,(#234836,#234837,#234838),.UNSPECIFIED.,.F.,.F.)
B_SPLINE_CURVE_WITH_KNOTS((3,3),(1.36602540378444,1.90331036969753),
 .UNSPECIFIED.)
CURVE()
GEOMETRIC_REPRESENTATION_ITEM()
RATIONAL_B_SPLINE_CURVE((1.86602540378444,1.86602540378444,1.73205080756822))
REPRESENTATION_ITEM('')
);
#1318=(
BOUNDED_CURVE()
B_SPLINE_CURVE(2,(#234841,#234842,#234843),.UNSPECIFIED.,.F.,.F.)
B_SPLINE_CURVE_WITH_KNOTS((3,3),(0.82874043787136,1.36602540378444),
 .UNSPECIFIED.)
CURVE()
GEOMETRIC_REPRESENTATION_ITEM()
RATIONAL_B_SPLINE_CURVE((1.73205080756822,1.86602540378444,1.86602540378444))
REPRESENTATION_ITEM('')
);
#1319=(
BOUNDED_CURVE()
B_SPLINE_CURVE(2,(#234844,#234845,#234846),.UNSPECIFIED.,.F.,.F.)
B_SPLINE_CURVE_WITH_KNOTS((3,3),(1.36602540378446,1.90331036969753),
 .UNSPECIFIED.)
CURVE()
GEOMETRIC_REPRESENTATION_ITEM()
RATIONAL_B_SPLINE_CURVE((1.86602540378445,1.86602540378444,1.73205080756823))
REPRESENTATION_ITEM('')
);
#1320=(
BOUNDED_CURVE()
B_SPLINE_CURVE(2,(#234849,#234850,#234851),.UNSPECIFIED.,.F.,.F.)
B_SPLINE_CURVE_WITH_KNOTS((3,3),(0.82874043787137,1.36602540378446),
 .UNSPECIFIED.)
CURVE()
GEOMETRIC_REPRESENTATION_ITEM()
RATIONAL_B_SPLINE_CURVE((1.73205080756824,1.86602540378445,1.86602540378445))
REPRESENTATION_ITEM('')
);
#1321=(
BOUNDED_CURVE()
B_SPLINE_CURVE(2,(#234852,#234853,#234854),.UNSPECIFIED.,.F.,.F.)
B_SPLINE_CURVE_WITH_KNOTS((3,3),(1.36602540378446,1.90331036969755),
 .UNSPECIFIED.)
CURVE()
GEOMETRIC_REPRESENTATION_ITEM()
RATIONAL_B_SPLINE_CURVE((1.86602540378447,1.86602540378446,1.73205080756824))
REPRESENTATION_ITEM('')
);
#1322=(
BOUNDED_CURVE()
B_SPLINE_CURVE(2,(#234857,#234858,#234859),.UNSPECIFIED.,.F.,.F.)
B_SPLINE_CURVE_WITH_KNOTS((3,3),(0.828740437871358,1.36602540378446),
 .UNSPECIFIED.)
CURVE()
GEOMETRIC_REPRESENTATION_ITEM()
RATIONAL_B_SPLINE_CURVE((1.73205080756824,1.86602540378447,1.86602540378447))
REPRESENTATION_ITEM('')
);
#1323=(
BOUNDED_CURVE()
B_SPLINE_CURVE(2,(#234860,#234861,#234862),.UNSPECIFIED.,.F.,.F.)
B_SPLINE_CURVE_WITH_KNOTS((3,3),(1.36602540378446,1.90331036969755),
 .UNSPECIFIED.)
CURVE()
GEOMETRIC_REPRESENTATION_ITEM()
RATIONAL_B_SPLINE_CURVE((1.86602540378446,1.86602540378446,1.73205080756824))
REPRESENTATION_ITEM('')
);
#1324=(
BOUNDED_CURVE()
B_SPLINE_CURVE(2,(#234865,#234866,#234867),.UNSPECIFIED.,.F.,.F.)
B_SPLINE_CURVE_WITH_KNOTS((3,3),(1.36602540378443,1.90331036969752),
 .UNSPECIFIED.)
CURVE()
GEOMETRIC_REPRESENTATION_ITEM()
RATIONAL_B_SPLINE_CURVE((1.86602540378444,1.86602540378445,1.73205080756823))
REPRESENTATION_ITEM('')
);
#1325=(
BOUNDED_CURVE()
B_SPLINE_CURVE(2,(#234868,#234869,#234870),.UNSPECIFIED.,.F.,.F.)
B_SPLINE_CURVE_WITH_KNOTS((3,3),(0.828740437871363,1.36602540378446),
 .UNSPECIFIED.)
CURVE()
GEOMETRIC_REPRESENTATION_ITEM()
RATIONAL_B_SPLINE_CURVE((1.73205080756824,1.86602540378447,1.86602540378446))
REPRESENTATION_ITEM('')
);
#1326=(
BOUNDED_CURVE()
B_SPLINE_CURVE(2,(#234898,#234899,#234900),.UNSPECIFIED.,.F.,.F.)
B_SPLINE_CURVE_WITH_KNOTS((3,3),(-1.46410161513776,-1.00000000000001),
 .UNSPECIFIED.)
CURVE()
GEOMETRIC_REPRESENTATION_ITEM()
RATIONAL_B_SPLINE_CURVE((1.39230484541327,1.5,1.5))
REPRESENTATION_ITEM('')
);
#1327=(
BOUNDED_CURVE()
B_SPLINE_CURVE(2,(#234901,#234902,#234903),.UNSPECIFIED.,.F.,.F.)
B_SPLINE_CURVE_WITH_KNOTS((3,3),(-1.,-0.535898384862256),.UNSPECIFIED.)
CURVE()
GEOMETRIC_REPRESENTATION_ITEM()
RATIONAL_B_SPLINE_CURVE((1.5,1.5,1.39230484541327))
REPRESENTATION_ITEM('')
);
#1328=(
BOUNDED_CURVE()
B_SPLINE_CURVE(2,(#234906,#234907,#234908),.UNSPECIFIED.,.F.,.F.)
B_SPLINE_CURVE_WITH_KNOTS((3,3),(-1.00000000000001,-0.535898384862261),
 .UNSPECIFIED.)
CURVE()
GEOMETRIC_REPRESENTATION_ITEM()
RATIONAL_B_SPLINE_CURVE((1.5,1.5,1.39230484541327))
REPRESENTATION_ITEM('')
);
#1329=(
BOUNDED_CURVE()
B_SPLINE_CURVE(2,(#234909,#234910,#234911),.UNSPECIFIED.,.F.,.F.)
B_SPLINE_CURVE_WITH_KNOTS((3,3),(-1.46410161513776,-1.),.UNSPECIFIED.)
CURVE()
GEOMETRIC_REPRESENTATION_ITEM()
RATIONAL_B_SPLINE_CURVE((1.39230484541328,1.50000000000002,1.50000000000002))
REPRESENTATION_ITEM('')
);
#1330=(
BOUNDED_CURVE()
B_SPLINE_CURVE(2,(#234914,#234915,#234916),.UNSPECIFIED.,.F.,.F.)
B_SPLINE_CURVE_WITH_KNOTS((3,3),(-1.,-0.53589838486225),.UNSPECIFIED.)
CURVE()
GEOMETRIC_REPRESENTATION_ITEM()
RATIONAL_B_SPLINE_CURVE((1.50000000000002,1.50000000000002,1.39230484541328))
REPRESENTATION_ITEM('')
);
#1331=(
BOUNDED_CURVE()
B_SPLINE_CURVE(2,(#234917,#234918,#234919),.UNSPECIFIED.,.F.,.F.)
B_SPLINE_CURVE_WITH_KNOTS((3,3),(-1.46410161513775,-1.00000000000001),
 .UNSPECIFIED.)
CURVE()
GEOMETRIC_REPRESENTATION_ITEM()
RATIONAL_B_SPLINE_CURVE((1.39230484541327,1.5,1.50000000000001))
REPRESENTATION_ITEM('')
);
#1332=(
BOUNDED_CURVE()
B_SPLINE_CURVE(2,(#234922,#234923,#234924),.UNSPECIFIED.,.F.,.F.)
B_SPLINE_CURVE_WITH_KNOTS((3,3),(-1.00000000000001,-0.535898384862254),
 .UNSPECIFIED.)
CURVE()
GEOMETRIC_REPRESENTATION_ITEM()
RATIONAL_B_SPLINE_CURVE((1.50000000000001,1.50000000000001,1.39230484541327))
REPRESENTATION_ITEM('')
);
#1333=(
BOUNDED_CURVE()
B_SPLINE_CURVE(2,(#234925,#234926,#234927),.UNSPECIFIED.,.F.,.F.)
B_SPLINE_CURVE_WITH_KNOTS((3,3),(-1.46410161513775,-1.00000000000001),
 .UNSPECIFIED.)
CURVE()
GEOMETRIC_REPRESENTATION_ITEM()
RATIONAL_B_SPLINE_CURVE((1.39230484541328,1.50000000000001,1.50000000000001))
REPRESENTATION_ITEM('')
);
#1334=(
BOUNDED_CURVE()
B_SPLINE_CURVE(2,(#234930,#234931,#234932),.UNSPECIFIED.,.F.,.F.)
B_SPLINE_CURVE_WITH_KNOTS((3,3),(-1.00000000000001,-0.535898384862257),
 .UNSPECIFIED.)
CURVE()
GEOMETRIC_REPRESENTATION_ITEM()
RATIONAL_B_SPLINE_CURVE((1.5,1.5,1.39230484541327))
REPRESENTATION_ITEM('')
);
#1335=(
BOUNDED_CURVE()
B_SPLINE_CURVE(2,(#234933,#234934,#234935),.UNSPECIFIED.,.F.,.F.)
B_SPLINE_CURVE_WITH_KNOTS((3,3),(-1.46410161513775,-1.00000000000001),
 .UNSPECIFIED.)
CURVE()
GEOMETRIC_REPRESENTATION_ITEM()
RATIONAL_B_SPLINE_CURVE((1.39230484541328,1.50000000000001,1.50000000000001))
REPRESENTATION_ITEM('')
);
#1336=(
BOUNDED_CURVE()
B_SPLINE_CURVE(2,(#234938,#234939,#234940),.UNSPECIFIED.,.F.,.F.)
B_SPLINE_CURVE_WITH_KNOTS((3,3),(-1.00000000000001,-0.535898384862249),
 .UNSPECIFIED.)
CURVE()
GEOMETRIC_REPRESENTATION_ITEM()
RATIONAL_B_SPLINE_CURVE((1.50000000000002,1.50000000000002,1.39230484541328))
REPRESENTATION_ITEM('')
);
#1337=(
BOUNDED_CURVE()
B_SPLINE_CURVE(2,(#234941,#234942,#234943),.UNSPECIFIED.,.F.,.F.)
B_SPLINE_CURVE_WITH_KNOTS((3,3),(-1.46410161513775,-1.),.UNSPECIFIED.)
CURVE()
GEOMETRIC_REPRESENTATION_ITEM()
RATIONAL_B_SPLINE_CURVE((1.39230484541327,1.5,1.5))
REPRESENTATION_ITEM('')
);
#1338=(
BOUNDED_CURVE()
B_SPLINE_CURVE(2,(#234959,#234960,#234961),.UNSPECIFIED.,.F.,.F.)
B_SPLINE_CURVE_WITH_KNOTS((3,3),(0.828740437871322,1.36602540378445),
 .UNSPECIFIED.)
CURVE()
GEOMETRIC_REPRESENTATION_ITEM()
RATIONAL_B_SPLINE_CURVE((1.7320508075682,1.86602540378444,1.86602540378444))
REPRESENTATION_ITEM('')
);
#1339=(
BOUNDED_CURVE()
B_SPLINE_CURVE(2,(#234962,#234963,#234964),.UNSPECIFIED.,.F.,.F.)
B_SPLINE_CURVE_WITH_KNOTS((3,3),(1.36602540378446,1.90331036969753),
 .UNSPECIFIED.)
CURVE()
GEOMETRIC_REPRESENTATION_ITEM()
RATIONAL_B_SPLINE_CURVE((1.86602540378447,1.86602540378447,1.73205080756826))
REPRESENTATION_ITEM('')
);
#1340=(
BOUNDED_CURVE()
B_SPLINE_CURVE(2,(#234967,#234968,#234969),.UNSPECIFIED.,.F.,.F.)
B_SPLINE_CURVE_WITH_KNOTS((3,3),(0.828740437871366,1.36602540378446),
 .UNSPECIFIED.)
CURVE()
GEOMETRIC_REPRESENTATION_ITEM()
RATIONAL_B_SPLINE_CURVE((1.73205080756825,1.86602540378447,1.86602540378447))
REPRESENTATION_ITEM('')
);
#1341=(
BOUNDED_CURVE()
B_SPLINE_CURVE(2,(#234970,#234971,#234972),.UNSPECIFIED.,.F.,.F.)
B_SPLINE_CURVE_WITH_KNOTS((3,3),(1.36602540378446,1.90331036969754),
 .UNSPECIFIED.)
CURVE()
GEOMETRIC_REPRESENTATION_ITEM()
RATIONAL_B_SPLINE_CURVE((1.86602540378445,1.86602540378445,1.73205080756824))
REPRESENTATION_ITEM('')
);
#1342=(
BOUNDED_CURVE()
B_SPLINE_CURVE(2,(#234975,#234976,#234977),.UNSPECIFIED.,.F.,.F.)
B_SPLINE_CURVE_WITH_KNOTS((3,3),(0.828740437871359,1.36602540378446),
 .UNSPECIFIED.)
CURVE()
GEOMETRIC_REPRESENTATION_ITEM()
RATIONAL_B_SPLINE_CURVE((1.73205080756823,1.86602540378446,1.86602540378445))
REPRESENTATION_ITEM('')
);
#1343=(
BOUNDED_CURVE()
B_SPLINE_CURVE(2,(#234978,#234979,#234980),.UNSPECIFIED.,.F.,.F.)
B_SPLINE_CURVE_WITH_KNOTS((3,3),(1.36602540378444,1.90331036969751),
 .UNSPECIFIED.)
CURVE()
GEOMETRIC_REPRESENTATION_ITEM()
RATIONAL_B_SPLINE_CURVE((1.86602540378444,1.86602540378444,1.73205080756823))
REPRESENTATION_ITEM('')
);
#1344=(
BOUNDED_CURVE()
B_SPLINE_CURVE(2,(#234983,#234984,#234985),.UNSPECIFIED.,.F.,.F.)
B_SPLINE_CURVE_WITH_KNOTS((3,3),(0.828740437871355,1.36602540378444),
 .UNSPECIFIED.)
CURVE()
GEOMETRIC_REPRESENTATION_ITEM()
RATIONAL_B_SPLINE_CURVE((1.73205080756823,1.86602540378444,1.86602540378444))
REPRESENTATION_ITEM('')
);
#1345=(
BOUNDED_CURVE()
B_SPLINE_CURVE(2,(#234986,#234987,#234988),.UNSPECIFIED.,.F.,.F.)
B_SPLINE_CURVE_WITH_KNOTS((3,3),(1.36602540378447,1.90331036969758),
 .UNSPECIFIED.)
CURVE()
GEOMETRIC_REPRESENTATION_ITEM()
RATIONAL_B_SPLINE_CURVE((1.8660254037845,1.86602540378449,1.73205080756826))
REPRESENTATION_ITEM('')
);
#1346=(
BOUNDED_CURVE()
B_SPLINE_CURVE(2,(#234991,#234992,#234993),.UNSPECIFIED.,.F.,.F.)
B_SPLINE_CURVE_WITH_KNOTS((3,3),(0.828740437871367,1.36602540378446),
 .UNSPECIFIED.)
CURVE()
GEOMETRIC_REPRESENTATION_ITEM()
RATIONAL_B_SPLINE_CURVE((1.73205080756826,1.86602540378449,1.86602540378449))
REPRESENTATION_ITEM('')
);
#1347=(
BOUNDED_CURVE()
B_SPLINE_CURVE(2,(#234994,#234995,#234996),.UNSPECIFIED.,.F.,.F.)
B_SPLINE_CURVE_WITH_KNOTS((3,3),(1.36602540378445,1.90331036969752),
 .UNSPECIFIED.)
CURVE()
GEOMETRIC_REPRESENTATION_ITEM()
RATIONAL_B_SPLINE_CURVE((1.86602540378444,1.86602540378444,1.73205080756823))
REPRESENTATION_ITEM('')
);
#1348=(
BOUNDED_CURVE()
B_SPLINE_CURVE(2,(#234999,#235000,#235001),.UNSPECIFIED.,.F.,.F.)
B_SPLINE_CURVE_WITH_KNOTS((3,3),(1.36602540378445,1.90331036969753),
 .UNSPECIFIED.)
CURVE()
GEOMETRIC_REPRESENTATION_ITEM()
RATIONAL_B_SPLINE_CURVE((1.86602540378444,1.86602540378444,1.73205080756822))
REPRESENTATION_ITEM('')
);
#1349=(
BOUNDED_CURVE()
B_SPLINE_CURVE(2,(#235002,#235003,#235004),.UNSPECIFIED.,.F.,.F.)
B_SPLINE_CURVE_WITH_KNOTS((3,3),(0.828740437871357,1.36602540378444),
 .UNSPECIFIED.)
CURVE()
GEOMETRIC_REPRESENTATION_ITEM()
RATIONAL_B_SPLINE_CURVE((1.73205080756823,1.86602540378444,1.86602540378444))
REPRESENTATION_ITEM('')
);
#1350=(
BOUNDED_CURVE()
B_SPLINE_CURVE(2,(#235022,#235023,#235024),.UNSPECIFIED.,.F.,.F.)
B_SPLINE_CURVE_WITH_KNOTS((3,3),(0.594066455576395,1.16209721084489),
 .UNSPECIFIED.)
CURVE()
GEOMETRIC_REPRESENTATION_ITEM()
RATIONAL_B_SPLINE_CURVE((2.95854811567256,3.4162371019878,2.95854811567265))
REPRESENTATION_ITEM('')
);
#1351=(
BOUNDED_CURVE()
B_SPLINE_CURVE(2,(#235027,#235028,#235029),.UNSPECIFIED.,.F.,.F.)
B_SPLINE_CURVE_WITH_KNOTS((3,3),(-0.388312804292301,-0.130611113351461),
 .UNSPECIFIED.)
CURVE()
GEOMETRIC_REPRESENTATION_ITEM()
RATIONAL_B_SPLINE_CURVE((1.30940107675846,1.51196612828732,1.30940107675846))
REPRESENTATION_ITEM('')
);
#1352=(
BOUNDED_CURVE()
B_SPLINE_CURVE(2,(#235034,#235035,#235036),.UNSPECIFIED.,.F.,.F.)
B_SPLINE_CURVE_WITH_KNOTS((3,3),(0.594066455576358,1.16209721084491),
 .UNSPECIFIED.)
CURVE()
GEOMETRIC_REPRESENTATION_ITEM()
RATIONAL_B_SPLINE_CURVE((2.95854811567265,3.41623710198804,2.95854811567281))
REPRESENTATION_ITEM('')
);
#1353=(
BOUNDED_CURVE()
B_SPLINE_CURVE(2,(#235037,#235038,#235039),.UNSPECIFIED.,.F.,.F.)
B_SPLINE_CURVE_WITH_KNOTS((3,3),(-0.388312804292316,-0.130611113351459),
 .UNSPECIFIED.)
CURVE()
GEOMETRIC_REPRESENTATION_ITEM()
RATIONAL_B_SPLINE_CURVE((1.30940107675852,1.51196612828743,1.30940107675851))
REPRESENTATION_ITEM('')
);
#1354=(
BOUNDED_CURVE()
B_SPLINE_CURVE(2,(#235044,#235045,#235046),.UNSPECIFIED.,.F.,.F.)
B_SPLINE_CURVE_WITH_KNOTS((3,3),(0.59406645557637,1.16209721084499),
 .UNSPECIFIED.)
CURVE()
GEOMETRIC_REPRESENTATION_ITEM()
RATIONAL_B_SPLINE_CURVE((2.95854811567266,3.41623710198807,2.95854811567265))
REPRESENTATION_ITEM('')
);
#1355=(
BOUNDED_CURVE()
B_SPLINE_CURVE(2,(#235047,#235048,#235049),.UNSPECIFIED.,.F.,.F.)
B_SPLINE_CURVE_WITH_KNOTS((3,3),(-0.38831280429231,-0.130611113351455),
 .UNSPECIFIED.)
CURVE()
GEOMETRIC_REPRESENTATION_ITEM()
RATIONAL_B_SPLINE_CURVE((1.30940107675854,1.51196612828746,1.30940107675852))
REPRESENTATION_ITEM('')
);
#1356=(
BOUNDED_CURVE()
B_SPLINE_CURVE(2,(#235054,#235055,#235056),.UNSPECIFIED.,.F.,.F.)
B_SPLINE_CURVE_WITH_KNOTS((3,3),(0.594066455576365,1.16209721084486),
 .UNSPECIFIED.)
CURVE()
GEOMETRIC_REPRESENTATION_ITEM()
RATIONAL_B_SPLINE_CURVE((2.95854811567265,3.41623710198797,2.95854811567285))
REPRESENTATION_ITEM('')
);
#1357=(
BOUNDED_CURVE()
B_SPLINE_CURVE(2,(#235057,#235058,#235059),.UNSPECIFIED.,.F.,.F.)
B_SPLINE_CURVE_WITH_KNOTS((3,3),(-0.388312804292318,-0.13061111335146),
 .UNSPECIFIED.)
CURVE()
GEOMETRIC_REPRESENTATION_ITEM()
RATIONAL_B_SPLINE_CURVE((1.30940107675852,1.51196612828743,1.30940107675851))
REPRESENTATION_ITEM('')
);
#1358=(
BOUNDED_CURVE()
B_SPLINE_CURVE(2,(#235064,#235065,#235066),.UNSPECIFIED.,.F.,.F.)
B_SPLINE_CURVE_WITH_KNOTS((3,3),(0.594066455576169,1.16209721084492),
 .UNSPECIFIED.)
CURVE()
GEOMETRIC_REPRESENTATION_ITEM()
RATIONAL_B_SPLINE_CURVE((2.95854811567235,3.41623710198821,2.95854811567279))
REPRESENTATION_ITEM('')
);
#1359=(
BOUNDED_CURVE()
B_SPLINE_CURVE(2,(#235067,#235068,#235069),.UNSPECIFIED.,.F.,.F.)
B_SPLINE_CURVE_WITH_KNOTS((3,3),(-0.388312804292328,-0.130611113351469),
 .UNSPECIFIED.)
CURVE()
GEOMETRIC_REPRESENTATION_ITEM()
RATIONAL_B_SPLINE_CURVE((1.3094010767585,1.51196612828743,1.30940107675853))
REPRESENTATION_ITEM('')
);
#1360=(
BOUNDED_CURVE()
B_SPLINE_CURVE(2,(#235071,#235072,#235073),.UNSPECIFIED.,.F.,.F.)
B_SPLINE_CURVE_WITH_KNOTS((3,3),(0.594066455576378,1.16209721084502),
 .UNSPECIFIED.)
CURVE()
GEOMETRIC_REPRESENTATION_ITEM()
RATIONAL_B_SPLINE_CURVE((2.95854811567253,3.41623710198792,2.95854811567244))
REPRESENTATION_ITEM('')
);
#1361=(
BOUNDED_CURVE()
B_SPLINE_CURVE(2,(#235074,#235075,#235076),.UNSPECIFIED.,.F.,.F.)
B_SPLINE_CURVE_WITH_KNOTS((3,3),(-0.388312804292317,-0.13061111335146),
 .UNSPECIFIED.)
CURVE()
GEOMETRIC_REPRESENTATION_ITEM()
RATIONAL_B_SPLINE_CURVE((1.3094010767585,1.51196612828743,1.30940107675851))
REPRESENTATION_ITEM('')
);
#1362=(
BOUNDED_CURVE()
B_SPLINE_CURVE(3,(#235504,#235505,#235506,#235507,#235508,#235509,#235510,
#235511,#235512,#235513),.UNSPECIFIED.,.F.,.F.)
B_SPLINE_CURVE_WITH_KNOTS((4,2,2,2,4),(4.71238898038469,5.10508806208341,
5.49778714378214,5.89048622548086,6.28318530717959),.UNSPECIFIED.)
CURVE()
GEOMETRIC_REPRESENTATION_ITEM()
RATIONAL_B_SPLINE_CURVE((1.,1.,1.,1.,1.,1.,1.,1.,1.,1.))
REPRESENTATION_ITEM('')
);
#1363=(
BOUNDED_CURVE()
B_SPLINE_CURVE(3,(#235591,#235592,#235593,#235594,#235595,#235596,#235597,
#235598,#235599,#235600),.UNSPECIFIED.,.F.,.F.)
B_SPLINE_CURVE_WITH_KNOTS((4,2,2,2,4),(4.71238898038469,5.10508806208341,
5.49778714378214,5.89048622548086,6.28318530717959),.UNSPECIFIED.)
CURVE()
GEOMETRIC_REPRESENTATION_ITEM()
RATIONAL_B_SPLINE_CURVE((1.,1.,1.,1.,1.,1.,1.,1.,1.,1.))
REPRESENTATION_ITEM('')
);
#1364=(
BOUNDED_CURVE()
B_SPLINE_CURVE(2,(#238415,#238416,#238417),.UNSPECIFIED.,.F.,.F.)
B_SPLINE_CURVE_WITH_KNOTS((3,3),(0.809350832147077,0.812919471044032),
 .UNSPECIFIED.)
CURVE()
GEOMETRIC_REPRESENTATION_ITEM()
RATIONAL_B_SPLINE_CURVE((1.,0.934429088195473,0.933042650109519))
REPRESENTATION_ITEM('')
);
#1365=(
BOUNDED_CURVE()
B_SPLINE_CURVE(2,(#238425,#238426,#238427),.UNSPECIFIED.,.F.,.F.)
B_SPLINE_CURVE_WITH_KNOTS((3,3),(0.804347826086956,0.80995470719394),
 .UNSPECIFIED.)
CURVE()
GEOMETRIC_REPRESENTATION_ITEM()
RATIONAL_B_SPLINE_CURVE((1.,0.89633721073752,0.953092503428239))
REPRESENTATION_ITEM('')
);
#1366=(
BOUNDED_CURVE()
B_SPLINE_CURVE(2,(#238433,#238434,#238435,#238436,#238437,#238438,#238439),
 .UNSPECIFIED.,.F.,.F.)
B_SPLINE_CURVE_WITH_KNOTS((3,2,2,3),(0.76560213851751,0.772893587455772,
0.780185036394034,0.78020664750063),.UNSPECIFIED.)
CURVE()
GEOMETRIC_REPRESENTATION_ITEM()
RATIONAL_B_SPLINE_CURVE((1.,0.866025403784439,1.,0.866025403784439,1.,0.99960291304177,
0.999208179933552))
REPRESENTATION_ITEM('')
);
#1367=(
BOUNDED_CURVE()
B_SPLINE_CURVE(2,(#238453,#238454,#238455,#238456,#238457,#238458,#238459),
 .UNSPECIFIED.,.F.,.F.)
B_SPLINE_CURVE_WITH_KNOTS((3,2,2,3),(0.787646415600072,0.794767934270535,
0.802059383208806,0.809350832147077),.UNSPECIFIED.)
CURVE()
GEOMETRIC_REPRESENTATION_ITEM()
RATIONAL_B_SPLINE_CURVE((0.993900866577314,0.86914773779612,1.,0.866025403784439,
1.,0.866025403784439,1.))
REPRESENTATION_ITEM('')
);
#1368=(
BOUNDED_CURVE()
B_SPLINE_CURVE(2,(#238460,#238461,#238462,#238463,#238464,#238465,#238466,
#238467,#238468,#238469,#238470,#238471,#238472),.UNSPECIFIED.,.F.,.F.)
B_SPLINE_CURVE_WITH_KNOTS((3,2,2,2,2,2,3),(0.760869565217391,0.768115942028986,
0.77536231884058,0.782608695652174,0.789855072463768,0.797101449275362,
0.804347826086956),.UNSPECIFIED.)
CURVE()
GEOMETRIC_REPRESENTATION_ITEM()
RATIONAL_B_SPLINE_CURVE((1.,0.866025403784439,1.,0.866025403784439,1.,0.866025403784439,
1.,0.866025403784439,1.,0.866025403784439,1.,0.866025403784439,1.))
REPRESENTATION_ITEM('')
);
#1369=(
BOUNDED_CURVE()
B_SPLINE_CURVE(2,(#238477,#238478,#238479,#238480,#238481,#238482,#238483,
#238484,#238485,#238486,#238487,#238488,#238489),.UNSPECIFIED.,.F.,.F.)
B_SPLINE_CURVE_WITH_KNOTS((3,2,2,2,2,2,3),(0.721853444887938,0.7291448938262,
0.736436342764462,0.743727791702724,0.751019240640986,0.758310689579248,
0.76560213851751),.UNSPECIFIED.)
CURVE()
GEOMETRIC_REPRESENTATION_ITEM()
RATIONAL_B_SPLINE_CURVE((1.,0.866025403784439,1.,0.866025403784439,1.,0.866025403784439,
1.,0.866025403784439,1.,0.866025403784439,1.,0.866025403784439,1.))
REPRESENTATION_ITEM('')
);
#1370=(
BOUNDED_CURVE()
B_SPLINE_CURVE(2,(#238490,#238491,#238492,#238493,#238494,#238495,#238496,
#238497,#238498,#238499,#238500,#238501,#238502),.UNSPECIFIED.,.F.,.F.)
B_SPLINE_CURVE_WITH_KNOTS((3,2,2,2,2,2,3),(0.717391304347826,0.72463768115942,
0.731884057971015,0.739130434782609,0.746376811594203,0.753623188405797,
0.760869565217391),.UNSPECIFIED.)
CURVE()
GEOMETRIC_REPRESENTATION_ITEM()
RATIONAL_B_SPLINE_CURVE((1.,0.866025403784439,1.,0.866025403784439,1.,0.866025403784439,
1.,0.866025403784439,1.,0.866025403784439,1.,0.866025403784439,1.))
REPRESENTATION_ITEM('')
);
#1371=(
BOUNDED_CURVE()
B_SPLINE_CURVE(2,(#238507,#238508,#238509,#238510,#238511,#238512,#238513,
#238514,#238515,#238516,#238517,#238518,#238519),.UNSPECIFIED.,.F.,.F.)
B_SPLINE_CURVE_WITH_KNOTS((3,2,2,2,2,2,3),(0.678104751258366,0.685396200196628,
0.69268764913489,0.699979098073152,0.707270547011414,0.714561995949676,
0.721853444887938),.UNSPECIFIED.)
CURVE()
GEOMETRIC_REPRESENTATION_ITEM()
RATIONAL_B_SPLINE_CURVE((1.,0.866025403784439,1.,0.866025403784439,1.,0.866025403784439,
1.,0.866025403784439,1.,0.866025403784439,1.,0.866025403784439,1.))
REPRESENTATION_ITEM('')
);
#1372=(
BOUNDED_CURVE()
B_SPLINE_CURVE(2,(#238520,#238521,#238522,#238523,#238524,#238525,#238526,
#238527,#238528,#238529,#238530,#238531,#238532),.UNSPECIFIED.,.F.,.F.)
B_SPLINE_CURVE_WITH_KNOTS((3,2,2,2,2,2,3),(0.673913043478261,0.681159420289855,
0.688405797101449,0.695652173913044,0.702898550724638,0.710144927536232,
0.717391304347826),.UNSPECIFIED.)
CURVE()
GEOMETRIC_REPRESENTATION_ITEM()
RATIONAL_B_SPLINE_CURVE((1.,0.866025403784439,1.,0.866025403784439,1.,0.866025403784439,
1.,0.866025403784439,1.,0.866025403784439,1.,0.866025403784439,1.))
REPRESENTATION_ITEM('')
);
#1373=(
BOUNDED_CURVE()
B_SPLINE_CURVE(2,(#238537,#238538,#238539,#238540,#238541,#238542,#238543,
#238544,#238545,#238546,#238547,#238548,#238549),.UNSPECIFIED.,.F.,.F.)
B_SPLINE_CURVE_WITH_KNOTS((3,2,2,2,2,2,3),(0.634356057628794,0.641647506567056,
0.648938955505318,0.65623040444358,0.663521853381842,0.670813302320104,
0.678104751258366),.UNSPECIFIED.)
CURVE()
GEOMETRIC_REPRESENTATION_ITEM()
RATIONAL_B_SPLINE_CURVE((1.,0.866025403784439,1.,0.866025403784439,1.,0.866025403784439,
1.,0.866025403784439,1.,0.866025403784439,1.,0.866025403784439,1.))
REPRESENTATION_ITEM('')
);
#1374=(
BOUNDED_CURVE()
B_SPLINE_CURVE(2,(#238550,#238551,#238552,#238553,#238554,#238555,#238556,
#238557,#238558,#238559,#238560,#238561,#238562),.UNSPECIFIED.,.F.,.F.)
B_SPLINE_CURVE_WITH_KNOTS((3,2,2,2,2,2,3),(0.630434782608696,0.63768115942029,
0.644927536231884,0.652173913043478,0.659420289855073,0.666666666666667,
0.673913043478261),.UNSPECIFIED.)
CURVE()
GEOMETRIC_REPRESENTATION_ITEM()
RATIONAL_B_SPLINE_CURVE((1.,0.866025403784439,1.,0.866025403784439,1.,0.866025403784439,
1.,0.866025403784439,1.,0.866025403784439,1.,0.866025403784439,1.))
REPRESENTATION_ITEM('')
);
#1375=(
BOUNDED_CURVE()
B_SPLINE_CURVE(2,(#238567,#238568,#238569,#238570,#238571,#238572,#238573,
#238574,#238575,#238576,#238577,#238578,#238579),.UNSPECIFIED.,.F.,.F.)
B_SPLINE_CURVE_WITH_KNOTS((3,2,2,2,2,2,3),(0.590607363999222,0.597898812937484,
0.605190261875746,0.612481710814008,0.61977315975227,0.627064608690532,
0.634356057628794),.UNSPECIFIED.)
CURVE()
GEOMETRIC_REPRESENTATION_ITEM()
RATIONAL_B_SPLINE_CURVE((1.,0.866025403784439,1.,0.866025403784439,1.,0.866025403784439,
1.,0.866025403784439,1.,0.866025403784439,1.,0.866025403784439,1.))
REPRESENTATION_ITEM('')
);
#1376=(
BOUNDED_CURVE()
B_SPLINE_CURVE(2,(#238580,#238581,#238582,#238583,#238584,#238585,#238586,
#238587,#238588,#238589,#238590,#238591,#238592),.UNSPECIFIED.,.F.,.F.)
B_SPLINE_CURVE_WITH_KNOTS((3,2,2,2,2,2,3),(0.586956521739131,0.594202898550725,
0.601449275362319,0.608695652173913,0.615942028985507,0.623188405797102,
0.630434782608696),.UNSPECIFIED.)
CURVE()
GEOMETRIC_REPRESENTATION_ITEM()
RATIONAL_B_SPLINE_CURVE((1.,0.866025403784439,1.,0.866025403784439,1.,0.866025403784439,
1.,0.866025403784439,1.,0.866025403784439,1.,0.866025403784439,1.))
REPRESENTATION_ITEM('')
);
#1377=(
BOUNDED_CURVE()
B_SPLINE_CURVE(2,(#238597,#238598,#238599,#238600,#238601,#238602,#238603,
#238604,#238605,#238606,#238607,#238608,#238609),.UNSPECIFIED.,.F.,.F.)
B_SPLINE_CURVE_WITH_KNOTS((3,2,2,2,2,2,3),(0.54685867036965,0.554150119307912,
0.561441568246174,0.568733017184436,0.576024466122698,0.58331591506096,
0.590607363999222),.UNSPECIFIED.)
CURVE()
GEOMETRIC_REPRESENTATION_ITEM()
RATIONAL_B_SPLINE_CURVE((1.,0.866025403784439,1.,0.866025403784439,1.,0.866025403784439,
1.,0.866025403784439,1.,0.866025403784439,1.,0.866025403784439,1.))
REPRESENTATION_ITEM('')
);
#1378=(
BOUNDED_CURVE()
B_SPLINE_CURVE(2,(#238610,#238611,#238612,#238613,#238614,#238615,#238616,
#238617,#238618,#238619,#238620,#238621,#238622),.UNSPECIFIED.,.F.,.F.)
B_SPLINE_CURVE_WITH_KNOTS((3,2,2,2,2,2,3),(0.543478260869565,0.550724637681159,
0.557971014492754,0.565217391304348,0.572463768115942,0.579710144927536,
0.586956521739131),.UNSPECIFIED.)
CURVE()
GEOMETRIC_REPRESENTATION_ITEM()
RATIONAL_B_SPLINE_CURVE((1.,0.866025403784439,1.,0.866025403784439,1.,0.866025403784439,
1.,0.866025403784439,1.,0.866025403784439,1.,0.866025403784439,1.))
REPRESENTATION_ITEM('')
);
#1379=(
BOUNDED_CURVE()
B_SPLINE_CURVE(2,(#238627,#238628,#238629,#238630,#238631,#238632,#238633,
#238634,#238635,#238636,#238637,#238638,#238639),.UNSPECIFIED.,.F.,.F.)
B_SPLINE_CURVE_WITH_KNOTS((3,2,2,2,2,2,3),(0.503109976740078,0.51040142567834,
0.517692874616602,0.524984323554864,0.532275772493126,0.539567221431388,
0.54685867036965),.UNSPECIFIED.)
CURVE()
GEOMETRIC_REPRESENTATION_ITEM()
RATIONAL_B_SPLINE_CURVE((1.,0.866025403784439,1.,0.866025403784439,1.,0.866025403784439,
1.,0.866025403784439,1.,0.866025403784439,1.,0.866025403784439,1.))
REPRESENTATION_ITEM('')
);
#1380=(
BOUNDED_CURVE()
B_SPLINE_CURVE(2,(#238640,#238641,#238642,#238643,#238644,#238645,#238646,
#238647,#238648,#238649,#238650,#238651,#238652),.UNSPECIFIED.,.F.,.F.)
B_SPLINE_CURVE_WITH_KNOTS((3,2,2,2,2,2,3),(0.5,0.507246376811594,0.514492753623189,
0.521739130434783,0.528985507246377,0.536231884057971,0.543478260869565),
 .UNSPECIFIED.)
CURVE()
GEOMETRIC_REPRESENTATION_ITEM()
RATIONAL_B_SPLINE_CURVE((1.,0.866025403784439,1.,0.866025403784439,1.,0.866025403784439,
1.,0.866025403784439,1.,0.866025403784439,1.,0.866025403784439,1.))
REPRESENTATION_ITEM('')
);
#1381=(
BOUNDED_CURVE()
B_SPLINE_CURVE(2,(#238657,#238658,#238659,#238660,#238661,#238662,#238663,
#238664,#238665,#238666,#238667,#238668,#238669),.UNSPECIFIED.,.F.,.F.)
B_SPLINE_CURVE_WITH_KNOTS((3,2,2,2,2,2,3),(0.459361283110506,0.466652732048768,
0.47394418098703,0.481235629925292,0.488527078863554,0.495818527801816,
0.503109976740078),.UNSPECIFIED.)
CURVE()
GEOMETRIC_REPRESENTATION_ITEM()
RATIONAL_B_SPLINE_CURVE((1.,0.866025403784439,1.,0.866025403784439,1.,0.866025403784439,
1.,0.866025403784439,1.,0.866025403784439,1.,0.866025403784439,1.))
REPRESENTATION_ITEM('')
);
#1382=(
BOUNDED_CURVE()
B_SPLINE_CURVE(2,(#238670,#238671,#238672,#238673,#238674,#238675,#238676,
#238677,#238678,#238679,#238680,#238681,#238682),.UNSPECIFIED.,.F.,.F.)
B_SPLINE_CURVE_WITH_KNOTS((3,2,2,2,2,2,3),(0.456521739130435,0.463768115942029,
0.471014492753623,0.478260869565218,0.485507246376812,0.492753623188406,
0.5),.UNSPECIFIED.)
CURVE()
GEOMETRIC_REPRESENTATION_ITEM()
RATIONAL_B_SPLINE_CURVE((1.,0.866025403784439,1.,0.866025403784439,1.,0.866025403784439,
1.,0.866025403784439,1.,0.866025403784439,1.,0.866025403784439,1.))
REPRESENTATION_ITEM('')
);
#1383=(
BOUNDED_CURVE()
B_SPLINE_CURVE(2,(#238687,#238688,#238689,#238690,#238691,#238692,#238693,
#238694,#238695,#238696,#238697,#238698,#238699),.UNSPECIFIED.,.F.,.F.)
B_SPLINE_CURVE_WITH_KNOTS((3,2,2,2,2,2,3),(0.415612589480934,0.422904038419196,
0.430195487357458,0.43748693629572,0.444778385233982,0.452069834172244,
0.459361283110506),.UNSPECIFIED.)
CURVE()
GEOMETRIC_REPRESENTATION_ITEM()
RATIONAL_B_SPLINE_CURVE((1.,0.866025403784439,1.,0.866025403784439,1.,0.866025403784439,
1.,0.866025403784439,1.,0.866025403784439,1.,0.866025403784439,1.))
REPRESENTATION_ITEM('')
);
#1384=(
BOUNDED_CURVE()
B_SPLINE_CURVE(2,(#238700,#238701,#238702,#238703,#238704,#238705,#238706,
#238707,#238708,#238709,#238710,#238711,#238712),.UNSPECIFIED.,.F.,.F.)
B_SPLINE_CURVE_WITH_KNOTS((3,2,2,2,2,2,3),(0.41304347826087,0.420289855072464,
0.427536231884058,0.434782608695652,0.442028985507247,0.449275362318841,
0.456521739130435),.UNSPECIFIED.)
CURVE()
GEOMETRIC_REPRESENTATION_ITEM()
RATIONAL_B_SPLINE_CURVE((1.,0.866025403784439,1.,0.866025403784439,1.,0.866025403784439,
1.,0.866025403784439,1.,0.866025403784439,1.,0.866025403784439,1.))
REPRESENTATION_ITEM('')
);
#1385=(
BOUNDED_CURVE()
B_SPLINE_CURVE(2,(#238717,#238718,#238719,#238720,#238721,#238722,#238723,
#238724,#238725,#238726,#238727,#238728,#238729),.UNSPECIFIED.,.F.,.F.)
B_SPLINE_CURVE_WITH_KNOTS((3,2,2,2,2,2,3),(0.371863895851362,0.379155344789624,
0.386446793727886,0.393738242666148,0.40102969160441,0.408321140542672,
0.415612589480934),.UNSPECIFIED.)
CURVE()
GEOMETRIC_REPRESENTATION_ITEM()
RATIONAL_B_SPLINE_CURVE((1.,0.866025403784439,1.,0.866025403784439,1.,0.866025403784439,
1.,0.866025403784439,1.,0.866025403784439,1.,0.866025403784439,1.))
REPRESENTATION_ITEM('')
);
#1386=(
BOUNDED_CURVE()
B_SPLINE_CURVE(2,(#238730,#238731,#238732,#238733,#238734,#238735,#238736,
#238737,#238738,#238739,#238740,#238741,#238742),.UNSPECIFIED.,.F.,.F.)
B_SPLINE_CURVE_WITH_KNOTS((3,2,2,2,2,2,3),(0.369565217391304,0.376811594202899,
0.384057971014493,0.391304347826087,0.398550724637681,0.405797101449275,
0.41304347826087),.UNSPECIFIED.)
CURVE()
GEOMETRIC_REPRESENTATION_ITEM()
RATIONAL_B_SPLINE_CURVE((1.,0.866025403784439,1.,0.866025403784439,1.,0.866025403784439,
1.,0.866025403784439,1.,0.866025403784439,1.,0.866025403784439,1.))
REPRESENTATION_ITEM('')
);
#1387=(
BOUNDED_CURVE()
B_SPLINE_CURVE(2,(#238747,#238748,#238749,#238750,#238751,#238752,#238753,
#238754,#238755,#238756,#238757,#238758,#238759),.UNSPECIFIED.,.F.,.F.)
B_SPLINE_CURVE_WITH_KNOTS((3,2,2,2,2,2,3),(0.32811520222179,0.335406651160052,
0.342698100098314,0.349989549036576,0.357280997974838,0.3645724469131,0.371863895851362),
 .UNSPECIFIED.)
CURVE()
GEOMETRIC_REPRESENTATION_ITEM()
RATIONAL_B_SPLINE_CURVE((1.,0.866025403784439,1.,0.866025403784439,1.,0.866025403784439,
1.,0.866025403784439,1.,0.866025403784439,1.,0.866025403784439,1.))
REPRESENTATION_ITEM('')
);
#1388=(
BOUNDED_CURVE()
B_SPLINE_CURVE(2,(#238760,#238761,#238762,#238763,#238764,#238765,#238766,
#238767,#238768,#238769,#238770,#238771,#238772),.UNSPECIFIED.,.F.,.F.)
B_SPLINE_CURVE_WITH_KNOTS((3,2,2,2,2,2,3),(0.326086956521739,0.333333333333334,
0.340579710144927,0.347826086956522,0.355072463768116,0.36231884057971,
0.369565217391304),.UNSPECIFIED.)
CURVE()
GEOMETRIC_REPRESENTATION_ITEM()
RATIONAL_B_SPLINE_CURVE((1.,0.866025403784439,1.,0.866025403784439,1.,0.866025403784439,
1.,0.866025403784439,1.,0.866025403784439,1.,0.866025403784439,1.))
REPRESENTATION_ITEM('')
);
#1389=(
BOUNDED_CURVE()
B_SPLINE_CURVE(2,(#238777,#238778,#238779,#238780,#238781,#238782,#238783,
#238784,#238785,#238786,#238787,#238788,#238789),.UNSPECIFIED.,.F.,.F.)
B_SPLINE_CURVE_WITH_KNOTS((3,2,2,2,2,2,3),(0.284366508592218,0.29165795753048,
0.298949406468742,0.306240855407004,0.313532304345266,0.320823753283528,
0.32811520222179),.UNSPECIFIED.)
CURVE()
GEOMETRIC_REPRESENTATION_ITEM()
RATIONAL_B_SPLINE_CURVE((1.,0.866025403784439,1.,0.866025403784439,1.,0.866025403784439,
1.,0.866025403784439,1.,0.866025403784439,1.,0.866025403784439,1.))
REPRESENTATION_ITEM('')
);
#1390=(
BOUNDED_CURVE()
B_SPLINE_CURVE(2,(#238790,#238791,#238792,#238793,#238794,#238795,#238796,
#238797,#238798,#238799,#238800,#238801,#238802),.UNSPECIFIED.,.F.,.F.)
B_SPLINE_CURVE_WITH_KNOTS((3,2,2,2,2,2,3),(0.282608695652174,0.289855072463769,
0.297101449275363,0.304347826086956,0.311594202898551,0.318840579710145,
0.326086956521739),.UNSPECIFIED.)
CURVE()
GEOMETRIC_REPRESENTATION_ITEM()
RATIONAL_B_SPLINE_CURVE((1.,0.866025403784439,1.,0.866025403784439,1.,0.866025403784439,
1.,0.866025403784439,1.,0.866025403784439,1.,0.866025403784439,1.))
REPRESENTATION_ITEM('')
);
#1391=(
BOUNDED_CURVE()
B_SPLINE_CURVE(2,(#238807,#238808,#238809,#238810,#238811,#238812,#238813,
#238814,#238815,#238816,#238817,#238818,#238819),.UNSPECIFIED.,.F.,.F.)
B_SPLINE_CURVE_WITH_KNOTS((3,2,2,2,2,2,3),(0.240617814962646,0.247909263900908,
0.25520071283917,0.262492161777432,0.269783610715694,0.277075059653956,
0.284366508592218),.UNSPECIFIED.)
CURVE()
GEOMETRIC_REPRESENTATION_ITEM()
RATIONAL_B_SPLINE_CURVE((1.,0.866025403784439,1.,0.866025403784439,1.,0.866025403784439,
1.,0.866025403784439,1.,0.866025403784439,1.,0.866025403784439,1.))
REPRESENTATION_ITEM('')
);
#1392=(
BOUNDED_CURVE()
B_SPLINE_CURVE(2,(#238820,#238821,#238822,#238823,#238824,#238825,#238826,
#238827,#238828,#238829,#238830,#238831,#238832),.UNSPECIFIED.,.F.,.F.)
B_SPLINE_CURVE_WITH_KNOTS((3,2,2,2,2,2,3),(0.239130434782609,0.246376811594203,
0.253623188405797,0.260869565217392,0.268115942028985,0.27536231884058,
0.282608695652174),.UNSPECIFIED.)
CURVE()
GEOMETRIC_REPRESENTATION_ITEM()
RATIONAL_B_SPLINE_CURVE((1.,0.866025403784439,1.,0.866025403784439,1.,0.866025403784439,
1.,0.866025403784439,1.,0.866025403784439,1.,0.866025403784439,1.))
REPRESENTATION_ITEM('')
);
#1393=(
BOUNDED_CURVE()
B_SPLINE_CURVE(2,(#238837,#238838,#238839,#238840,#238841,#238842,#238843,
#238844,#238845,#238846,#238847,#238848,#238849),.UNSPECIFIED.,.F.,.F.)
B_SPLINE_CURVE_WITH_KNOTS((3,2,2,2,2,2,3),(0.196869121333074,0.204160570271336,
0.211452019209598,0.21874346814786,0.226034917086122,0.233326366024384,
0.240617814962646),.UNSPECIFIED.)
CURVE()
GEOMETRIC_REPRESENTATION_ITEM()
RATIONAL_B_SPLINE_CURVE((1.,0.866025403784439,1.,0.866025403784439,1.,0.866025403784439,
1.,0.866025403784439,1.,0.866025403784439,1.,0.866025403784439,1.))
REPRESENTATION_ITEM('')
);
#1394=(
BOUNDED_CURVE()
B_SPLINE_CURVE(2,(#238850,#238851,#238852,#238853,#238854,#238855,#238856,
#238857,#238858,#238859,#238860,#238861,#238862),.UNSPECIFIED.,.F.,.F.)
B_SPLINE_CURVE_WITH_KNOTS((3,2,2,2,2,2,3),(0.195652173913044,0.202898550724638,
0.210144927536232,0.217391304347826,0.224637681159421,0.231884057971014,
0.239130434782609),.UNSPECIFIED.)
CURVE()
GEOMETRIC_REPRESENTATION_ITEM()
RATIONAL_B_SPLINE_CURVE((1.,0.866025403784439,1.,0.866025403784439,1.,0.866025403784439,
1.,0.866025403784439,1.,0.866025403784439,1.,0.866025403784439,1.))
REPRESENTATION_ITEM('')
);
#1395=(
BOUNDED_CURVE()
B_SPLINE_CURVE(2,(#238867,#238868,#238869,#238870,#238871,#238872,#238873,
#238874,#238875,#238876,#238877,#238878,#238879),.UNSPECIFIED.,.F.,.F.)
B_SPLINE_CURVE_WITH_KNOTS((3,2,2,2,2,2,3),(0.153120427703502,0.160411876641764,
0.167703325580026,0.174994774518288,0.18228622345655,0.189577672394812,
0.196869121333074),.UNSPECIFIED.)
CURVE()
GEOMETRIC_REPRESENTATION_ITEM()
RATIONAL_B_SPLINE_CURVE((1.,0.866025403784439,1.,0.866025403784439,1.,0.866025403784439,
1.,0.866025403784439,1.,0.866025403784439,1.,0.866025403784439,1.))
REPRESENTATION_ITEM('')
);
#1396=(
BOUNDED_CURVE()
B_SPLINE_CURVE(2,(#238880,#238881,#238882,#238883,#238884,#238885,#238886,
#238887,#238888,#238889,#238890,#238891,#238892),.UNSPECIFIED.,.F.,.F.)
B_SPLINE_CURVE_WITH_KNOTS((3,2,2,2,2,2,3),(0.152173913043478,0.159420289855073,
0.166666666666667,0.173913043478261,0.181159420289855,0.18840579710145,
0.195652173913044),.UNSPECIFIED.)
CURVE()
GEOMETRIC_REPRESENTATION_ITEM()
RATIONAL_B_SPLINE_CURVE((1.,0.866025403784439,1.,0.866025403784439,1.,0.866025403784439,
1.,0.866025403784439,1.,0.866025403784439,1.,0.866025403784439,1.))
REPRESENTATION_ITEM('')
);
#1397=(
BOUNDED_CURVE()
B_SPLINE_CURVE(2,(#238897,#238898,#238899,#238900,#238901,#238902,#238903,
#238904,#238905,#238906,#238907,#238908,#238909),.UNSPECIFIED.,.F.,.F.)
B_SPLINE_CURVE_WITH_KNOTS((3,2,2,2,2,2,3),(0.10937173407393,0.116663183012192,
0.123954631950454,0.131246080888716,0.138537529826978,0.14582897876524,
0.153120427703502),.UNSPECIFIED.)
CURVE()
GEOMETRIC_REPRESENTATION_ITEM()
RATIONAL_B_SPLINE_CURVE((1.,0.866025403784439,1.,0.866025403784439,1.,0.866025403784439,
1.,0.866025403784439,1.,0.866025403784439,1.,0.866025403784439,1.))
REPRESENTATION_ITEM('')
);
#1398=(
BOUNDED_CURVE()
B_SPLINE_CURVE(2,(#238910,#238911,#238912,#238913,#238914,#238915,#238916,
#238917,#238918,#238919,#238920,#238921,#238922),.UNSPECIFIED.,.F.,.F.)
B_SPLINE_CURVE_WITH_KNOTS((3,2,2,2,2,2,3),(0.108695652173913,0.115942028985507,
0.123188405797102,0.130434782608696,0.13768115942029,0.144927536231884,
0.152173913043478),.UNSPECIFIED.)
CURVE()
GEOMETRIC_REPRESENTATION_ITEM()
RATIONAL_B_SPLINE_CURVE((1.,0.866025403784439,1.,0.866025403784439,1.,0.866025403784439,
1.,0.866025403784439,1.,0.866025403784439,1.,0.866025403784439,1.))
REPRESENTATION_ITEM('')
);
#1399=(
BOUNDED_CURVE()
B_SPLINE_CURVE(2,(#238927,#238928,#238929,#238930,#238931,#238932,#238933,
#238934,#238935,#238936,#238937,#238938,#238939),.UNSPECIFIED.,.F.,.F.)
B_SPLINE_CURVE_WITH_KNOTS((3,2,2,2,2,2,3),(0.065623040444358,0.07291448938262,
0.080205938320882,0.087497387259144,0.094788836197406,0.102080285135668,
0.10937173407393),.UNSPECIFIED.)
CURVE()
GEOMETRIC_REPRESENTATION_ITEM()
RATIONAL_B_SPLINE_CURVE((1.,0.866025403784439,1.,0.866025403784439,1.,0.866025403784439,
1.,0.866025403784439,1.,0.866025403784439,1.,0.866025403784439,1.))
REPRESENTATION_ITEM('')
);
#1400=(
BOUNDED_CURVE()
B_SPLINE_CURVE(2,(#238940,#238941,#238942,#238943,#238944,#238945,#238946,
#238947,#238948,#238949,#238950,#238951,#238952),.UNSPECIFIED.,.F.,.F.)
B_SPLINE_CURVE_WITH_KNOTS((3,2,2,2,2,2,3),(0.065217391304348,0.0724637681159422,
0.0797101449275364,0.0869565217391306,0.0942028985507248,0.101449275362319,
0.108695652173913),.UNSPECIFIED.)
CURVE()
GEOMETRIC_REPRESENTATION_ITEM()
RATIONAL_B_SPLINE_CURVE((1.,0.866025403784439,1.,0.866025403784439,1.,0.866025403784439,
1.,0.866025403784439,1.,0.866025403784439,1.,0.866025403784439,1.))
REPRESENTATION_ITEM('')
);
#1401=(
BOUNDED_CURVE()
B_SPLINE_CURVE(2,(#238959,#238960,#238961,#238962,#238963),
 .UNSPECIFIED.,.F.,.F.)
B_SPLINE_CURVE_WITH_KNOTS((3,2,3),(0.0118893770663295,0.014582897876524,
0.021874346814786),.UNSPECIFIED.)
CURVE()
GEOMETRIC_REPRESENTATION_ITEM()
RATIONAL_B_SPLINE_CURVE((0.937582367981151,0.950508689562319,1.,0.866025403784439,
1.))
REPRESENTATION_ITEM('')
);
#1402=(
BOUNDED_CURVE()
B_SPLINE_CURVE(2,(#240349,#240350,#240351),.UNSPECIFIED.,.F.,.F.)
B_SPLINE_CURVE_WITH_KNOTS((3,3),(0.809350832147077,0.812919456587346),
 .UNSPECIFIED.)
CURVE()
GEOMETRIC_REPRESENTATION_ITEM()
RATIONAL_B_SPLINE_CURVE((1.,0.934429353825615,0.933042661343594))
REPRESENTATION_ITEM('')
);
#1403=(
BOUNDED_CURVE()
B_SPLINE_CURVE(2,(#240369,#240370,#240371),.UNSPECIFIED.,.F.,.F.)
B_SPLINE_CURVE_WITH_KNOTS((3,3),(0.804347826086956,0.809954707839571),
 .UNSPECIFIED.)
CURVE()
GEOMETRIC_REPRESENTATION_ITEM()
RATIONAL_B_SPLINE_CURVE((1.,0.896337198800779,0.953092516498953))
REPRESENTATION_ITEM('')
);
#1404=(
BOUNDED_CURVE()
B_SPLINE_CURVE(2,(#240377,#240378,#240379,#240380,#240381,#240382,#240383),
 .UNSPECIFIED.,.F.,.F.)
B_SPLINE_CURVE_WITH_KNOTS((3,2,2,3),(0.76560213851751,0.772893587455772,
0.780185036394034,0.780206648355897),.UNSPECIFIED.)
CURVE()
GEOMETRIC_REPRESENTATION_ITEM()
RATIONAL_B_SPLINE_CURVE((1.,0.866025403784439,1.,0.866025403784439,1.,0.99960289732691,
0.999208148690144))
REPRESENTATION_ITEM('')
);
#1405=(
BOUNDED_CURVE()
B_SPLINE_CURVE(2,(#240397,#240398,#240399,#240400,#240401,#240402,#240403),
 .UNSPECIFIED.,.F.,.F.)
B_SPLINE_CURVE_WITH_KNOTS((3,2,2,3),(0.787646397966073,0.794767934270535,
0.802059383208806,0.809350832147077),.UNSPECIFIED.)
CURVE()
GEOMETRIC_REPRESENTATION_ITEM()
RATIONAL_B_SPLINE_CURVE((0.99390148439558,0.869147413785358,1.,0.866025403784439,
1.,0.866025403784439,1.))
REPRESENTATION_ITEM('')
);
#1406=(
BOUNDED_CURVE()
B_SPLINE_CURVE(2,(#240404,#240405,#240406,#240407,#240408,#240409,#240410,
#240411,#240412,#240413,#240414,#240415,#240416),.UNSPECIFIED.,.F.,.F.)
B_SPLINE_CURVE_WITH_KNOTS((3,2,2,2,2,2,3),(0.760869565217391,0.768115942028986,
0.77536231884058,0.782608695652174,0.789855072463768,0.797101449275362,
0.804347826086956),.UNSPECIFIED.)
CURVE()
GEOMETRIC_REPRESENTATION_ITEM()
RATIONAL_B_SPLINE_CURVE((1.,0.866025403784439,1.,0.866025403784439,1.,0.866025403784439,
1.,0.866025403784439,1.,0.866025403784439,1.,0.866025403784439,1.))
REPRESENTATION_ITEM('')
);
#1407=(
BOUNDED_CURVE()
B_SPLINE_CURVE(2,(#240421,#240422,#240423,#240424,#240425,#240426,#240427,
#240428,#240429,#240430,#240431,#240432,#240433),.UNSPECIFIED.,.F.,.F.)
B_SPLINE_CURVE_WITH_KNOTS((3,2,2,2,2,2,3),(0.721853444887938,0.7291448938262,
0.736436342764462,0.743727791702724,0.751019240640986,0.758310689579248,
0.76560213851751),.UNSPECIFIED.)
CURVE()
GEOMETRIC_REPRESENTATION_ITEM()
RATIONAL_B_SPLINE_CURVE((1.,0.866025403784439,1.,0.866025403784439,1.,0.866025403784439,
1.,0.866025403784439,1.,0.866025403784439,1.,0.866025403784439,1.))
REPRESENTATION_ITEM('')
);
#1408=(
BOUNDED_CURVE()
B_SPLINE_CURVE(2,(#240434,#240435,#240436,#240437,#240438,#240439,#240440,
#240441,#240442,#240443,#240444,#240445,#240446),.UNSPECIFIED.,.F.,.F.)
B_SPLINE_CURVE_WITH_KNOTS((3,2,2,2,2,2,3),(0.717391304347826,0.724637681159421,
0.731884057971015,0.739130434782609,0.746376811594203,0.753623188405797,
0.760869565217391),.UNSPECIFIED.)
CURVE()
GEOMETRIC_REPRESENTATION_ITEM()
RATIONAL_B_SPLINE_CURVE((1.,0.866025403784439,1.,0.866025403784439,1.,0.866025403784439,
1.,0.866025403784439,1.,0.866025403784439,1.,0.866025403784439,1.))
REPRESENTATION_ITEM('')
);
#1409=(
BOUNDED_CURVE()
B_SPLINE_CURVE(2,(#240451,#240452,#240453,#240454,#240455,#240456,#240457,
#240458,#240459,#240460,#240461,#240462,#240463),.UNSPECIFIED.,.F.,.F.)
B_SPLINE_CURVE_WITH_KNOTS((3,2,2,2,2,2,3),(0.678104751258366,0.685396200196628,
0.69268764913489,0.699979098073152,0.707270547011414,0.714561995949676,
0.721853444887938),.UNSPECIFIED.)
CURVE()
GEOMETRIC_REPRESENTATION_ITEM()
RATIONAL_B_SPLINE_CURVE((1.,0.866025403784439,1.,0.866025403784439,1.,0.866025403784439,
1.,0.866025403784439,1.,0.866025403784439,1.,0.866025403784439,1.))
REPRESENTATION_ITEM('')
);
#1410=(
BOUNDED_CURVE()
B_SPLINE_CURVE(2,(#240464,#240465,#240466,#240467,#240468,#240469,#240470,
#240471,#240472,#240473,#240474,#240475,#240476),.UNSPECIFIED.,.F.,.F.)
B_SPLINE_CURVE_WITH_KNOTS((3,2,2,2,2,2,3),(0.673913043478261,0.681159420289855,
0.688405797101449,0.695652173913044,0.702898550724638,0.710144927536232,
0.717391304347826),.UNSPECIFIED.)
CURVE()
GEOMETRIC_REPRESENTATION_ITEM()
RATIONAL_B_SPLINE_CURVE((1.,0.866025403784439,1.,0.866025403784439,1.,0.866025403784439,
1.,0.866025403784439,1.,0.866025403784439,1.,0.866025403784439,1.))
REPRESENTATION_ITEM('')
);
#1411=(
BOUNDED_CURVE()
B_SPLINE_CURVE(2,(#240481,#240482,#240483,#240484,#240485,#240486,#240487,
#240488,#240489,#240490,#240491,#240492,#240493),.UNSPECIFIED.,.F.,.F.)
B_SPLINE_CURVE_WITH_KNOTS((3,2,2,2,2,2,3),(0.634356057628794,0.641647506567056,
0.648938955505318,0.65623040444358,0.663521853381842,0.670813302320104,
0.678104751258366),.UNSPECIFIED.)
CURVE()
GEOMETRIC_REPRESENTATION_ITEM()
RATIONAL_B_SPLINE_CURVE((1.,0.866025403784439,1.,0.866025403784439,1.,0.866025403784439,
1.,0.866025403784439,1.,0.866025403784439,1.,0.866025403784439,1.))
REPRESENTATION_ITEM('')
);
#1412=(
BOUNDED_CURVE()
B_SPLINE_CURVE(2,(#240494,#240495,#240496,#240497,#240498,#240499,#240500,
#240501,#240502,#240503,#240504,#240505,#240506),.UNSPECIFIED.,.F.,.F.)
B_SPLINE_CURVE_WITH_KNOTS((3,2,2,2,2,2,3),(0.630434782608696,0.63768115942029,
0.644927536231884,0.652173913043478,0.659420289855073,0.666666666666667,
0.673913043478261),.UNSPECIFIED.)
CURVE()
GEOMETRIC_REPRESENTATION_ITEM()
RATIONAL_B_SPLINE_CURVE((1.,0.866025403784439,1.,0.866025403784439,1.,0.866025403784439,
1.,0.866025403784439,1.,0.866025403784439,1.,0.866025403784439,1.))
REPRESENTATION_ITEM('')
);
#1413=(
BOUNDED_CURVE()
B_SPLINE_CURVE(2,(#240511,#240512,#240513,#240514,#240515,#240516,#240517,
#240518,#240519,#240520,#240521,#240522,#240523),.UNSPECIFIED.,.F.,.F.)
B_SPLINE_CURVE_WITH_KNOTS((3,2,2,2,2,2,3),(0.590607363999222,0.597898812937484,
0.605190261875746,0.612481710814008,0.61977315975227,0.627064608690532,
0.634356057628794),.UNSPECIFIED.)
CURVE()
GEOMETRIC_REPRESENTATION_ITEM()
RATIONAL_B_SPLINE_CURVE((1.,0.866025403784439,1.,0.866025403784439,1.,0.866025403784439,
1.,0.866025403784439,1.,0.866025403784439,1.,0.866025403784439,1.))
REPRESENTATION_ITEM('')
);
#1414=(
BOUNDED_CURVE()
B_SPLINE_CURVE(2,(#240524,#240525,#240526,#240527,#240528,#240529,#240530,
#240531,#240532,#240533,#240534,#240535,#240536),.UNSPECIFIED.,.F.,.F.)
B_SPLINE_CURVE_WITH_KNOTS((3,2,2,2,2,2,3),(0.586956521739131,0.594202898550725,
0.601449275362319,0.608695652173913,0.615942028985507,0.623188405797101,
0.630434782608696),.UNSPECIFIED.)
CURVE()
GEOMETRIC_REPRESENTATION_ITEM()
RATIONAL_B_SPLINE_CURVE((1.,0.866025403784439,1.,0.866025403784439,1.,0.866025403784439,
1.,0.866025403784439,1.,0.866025403784439,1.,0.866025403784439,1.))
REPRESENTATION_ITEM('')
);
#1415=(
BOUNDED_CURVE()
B_SPLINE_CURVE(2,(#240541,#240542,#240543,#240544,#240545,#240546,#240547,
#240548,#240549,#240550,#240551,#240552,#240553),.UNSPECIFIED.,.F.,.F.)
B_SPLINE_CURVE_WITH_KNOTS((3,2,2,2,2,2,3),(0.54685867036965,0.554150119307912,
0.561441568246174,0.568733017184436,0.576024466122698,0.58331591506096,
0.590607363999222),.UNSPECIFIED.)
CURVE()
GEOMETRIC_REPRESENTATION_ITEM()
RATIONAL_B_SPLINE_CURVE((1.,0.866025403784439,1.,0.866025403784439,1.,0.866025403784439,
1.,0.866025403784439,1.,0.866025403784439,1.,0.866025403784439,1.))
REPRESENTATION_ITEM('')
);
#1416=(
BOUNDED_CURVE()
B_SPLINE_CURVE(2,(#240554,#240555,#240556,#240557,#240558,#240559,#240560,
#240561,#240562,#240563,#240564,#240565,#240566),.UNSPECIFIED.,.F.,.F.)
B_SPLINE_CURVE_WITH_KNOTS((3,2,2,2,2,2,3),(0.543478260869565,0.55072463768116,
0.557971014492754,0.565217391304348,0.572463768115942,0.579710144927536,
0.586956521739131),.UNSPECIFIED.)
CURVE()
GEOMETRIC_REPRESENTATION_ITEM()
RATIONAL_B_SPLINE_CURVE((1.,0.866025403784439,1.,0.866025403784439,1.,0.866025403784439,
1.,0.866025403784439,1.,0.866025403784439,1.,0.866025403784439,1.))
REPRESENTATION_ITEM('')
);
#1417=(
BOUNDED_CURVE()
B_SPLINE_CURVE(2,(#240571,#240572,#240573,#240574,#240575,#240576,#240577,
#240578,#240579,#240580,#240581,#240582,#240583),.UNSPECIFIED.,.F.,.F.)
B_SPLINE_CURVE_WITH_KNOTS((3,2,2,2,2,2,3),(0.503109976740078,0.51040142567834,
0.517692874616602,0.524984323554864,0.532275772493126,0.539567221431388,
0.54685867036965),.UNSPECIFIED.)
CURVE()
GEOMETRIC_REPRESENTATION_ITEM()
RATIONAL_B_SPLINE_CURVE((1.,0.866025403784439,1.,0.866025403784439,1.,0.866025403784439,
1.,0.866025403784439,1.,0.866025403784439,1.,0.866025403784439,1.))
REPRESENTATION_ITEM('')
);
#1418=(
BOUNDED_CURVE()
B_SPLINE_CURVE(2,(#240584,#240585,#240586,#240587,#240588,#240589,#240590,
#240591,#240592,#240593,#240594,#240595,#240596),.UNSPECIFIED.,.F.,.F.)
B_SPLINE_CURVE_WITH_KNOTS((3,2,2,2,2,2,3),(0.5,0.507246376811594,0.514492753623189,
0.521739130434783,0.528985507246377,0.536231884057971,0.543478260869565),
 .UNSPECIFIED.)
CURVE()
GEOMETRIC_REPRESENTATION_ITEM()
RATIONAL_B_SPLINE_CURVE((1.,0.866025403784439,1.,0.866025403784439,1.,0.866025403784439,
1.,0.866025403784439,1.,0.866025403784439,1.,0.866025403784439,1.))
REPRESENTATION_ITEM('')
);
#1419=(
BOUNDED_CURVE()
B_SPLINE_CURVE(2,(#240601,#240602,#240603,#240604,#240605,#240606,#240607,
#240608,#240609,#240610,#240611,#240612,#240613),.UNSPECIFIED.,.F.,.F.)
B_SPLINE_CURVE_WITH_KNOTS((3,2,2,2,2,2,3),(0.459361283110506,0.466652732048768,
0.47394418098703,0.481235629925292,0.488527078863554,0.495818527801816,
0.503109976740078),.UNSPECIFIED.)
CURVE()
GEOMETRIC_REPRESENTATION_ITEM()
RATIONAL_B_SPLINE_CURVE((1.,0.866025403784439,1.,0.866025403784439,1.,0.866025403784439,
1.,0.866025403784439,1.,0.866025403784439,1.,0.866025403784439,1.))
REPRESENTATION_ITEM('')
);
#1420=(
BOUNDED_CURVE()
B_SPLINE_CURVE(2,(#240614,#240615,#240616,#240617,#240618,#240619,#240620,
#240621,#240622,#240623,#240624,#240625,#240626),.UNSPECIFIED.,.F.,.F.)
B_SPLINE_CURVE_WITH_KNOTS((3,2,2,2,2,2,3),(0.456521739130435,0.463768115942029,
0.471014492753623,0.478260869565218,0.485507246376812,0.492753623188406,
0.5),.UNSPECIFIED.)
CURVE()
GEOMETRIC_REPRESENTATION_ITEM()
RATIONAL_B_SPLINE_CURVE((1.,0.866025403784439,1.,0.866025403784439,1.,0.866025403784439,
1.,0.866025403784439,1.,0.866025403784439,1.,0.866025403784439,1.))
REPRESENTATION_ITEM('')
);
#1421=(
BOUNDED_CURVE()
B_SPLINE_CURVE(2,(#240631,#240632,#240633,#240634,#240635,#240636,#240637,
#240638,#240639,#240640,#240641,#240642,#240643),.UNSPECIFIED.,.F.,.F.)
B_SPLINE_CURVE_WITH_KNOTS((3,2,2,2,2,2,3),(0.415612589480934,0.422904038419196,
0.430195487357458,0.43748693629572,0.444778385233982,0.452069834172244,
0.459361283110506),.UNSPECIFIED.)
CURVE()
GEOMETRIC_REPRESENTATION_ITEM()
RATIONAL_B_SPLINE_CURVE((1.,0.866025403784439,1.,0.866025403784439,1.,0.866025403784439,
1.,0.866025403784439,1.,0.866025403784439,1.,0.866025403784439,1.))
REPRESENTATION_ITEM('')
);
#1422=(
BOUNDED_CURVE()
B_SPLINE_CURVE(2,(#240644,#240645,#240646,#240647,#240648,#240649,#240650,
#240651,#240652,#240653,#240654,#240655,#240656),.UNSPECIFIED.,.F.,.F.)
B_SPLINE_CURVE_WITH_KNOTS((3,2,2,2,2,2,3),(0.413043478260869,0.420289855072464,
0.427536231884058,0.434782608695652,0.442028985507246,0.449275362318841,
0.456521739130435),.UNSPECIFIED.)
CURVE()
GEOMETRIC_REPRESENTATION_ITEM()
RATIONAL_B_SPLINE_CURVE((1.,0.866025403784439,1.,0.866025403784439,1.,0.866025403784439,
1.,0.866025403784439,1.,0.866025403784439,1.,0.866025403784439,1.))
REPRESENTATION_ITEM('')
);
#1423=(
BOUNDED_CURVE()
B_SPLINE_CURVE(2,(#240661,#240662,#240663,#240664,#240665,#240666,#240667,
#240668,#240669,#240670,#240671,#240672,#240673),.UNSPECIFIED.,.F.,.F.)
B_SPLINE_CURVE_WITH_KNOTS((3,2,2,2,2,2,3),(0.371863895851362,0.379155344789624,
0.386446793727886,0.393738242666148,0.40102969160441,0.408321140542672,
0.415612589480934),.UNSPECIFIED.)
CURVE()
GEOMETRIC_REPRESENTATION_ITEM()
RATIONAL_B_SPLINE_CURVE((1.,0.866025403784439,1.,0.866025403784439,1.,0.866025403784439,
1.,0.866025403784439,1.,0.866025403784439,1.,0.866025403784439,1.))
REPRESENTATION_ITEM('')
);
#1424=(
BOUNDED_CURVE()
B_SPLINE_CURVE(2,(#240674,#240675,#240676,#240677,#240678,#240679,#240680,
#240681,#240682,#240683,#240684,#240685,#240686),.UNSPECIFIED.,.F.,.F.)
B_SPLINE_CURVE_WITH_KNOTS((3,2,2,2,2,2,3),(0.369565217391304,0.376811594202899,
0.384057971014493,0.391304347826087,0.398550724637682,0.405797101449275,
0.413043478260869),.UNSPECIFIED.)
CURVE()
GEOMETRIC_REPRESENTATION_ITEM()
RATIONAL_B_SPLINE_CURVE((1.,0.866025403784439,1.,0.866025403784439,1.,0.866025403784439,
1.,0.866025403784439,1.,0.866025403784439,1.,0.866025403784439,1.))
REPRESENTATION_ITEM('')
);
#1425=(
BOUNDED_CURVE()
B_SPLINE_CURVE(2,(#240691,#240692,#240693,#240694,#240695,#240696,#240697,
#240698,#240699,#240700,#240701,#240702,#240703),.UNSPECIFIED.,.F.,.F.)
B_SPLINE_CURVE_WITH_KNOTS((3,2,2,2,2,2,3),(0.32811520222179,0.335406651160052,
0.342698100098314,0.349989549036576,0.357280997974838,0.3645724469131,0.371863895851362),
 .UNSPECIFIED.)
CURVE()
GEOMETRIC_REPRESENTATION_ITEM()
RATIONAL_B_SPLINE_CURVE((1.,0.866025403784439,1.,0.866025403784439,1.,0.866025403784439,
1.,0.866025403784439,1.,0.866025403784439,1.,0.866025403784439,1.))
REPRESENTATION_ITEM('')
);
#1426=(
BOUNDED_CURVE()
B_SPLINE_CURVE(2,(#240704,#240705,#240706,#240707,#240708,#240709,#240710,
#240711,#240712,#240713,#240714,#240715,#240716),.UNSPECIFIED.,.F.,.F.)
B_SPLINE_CURVE_WITH_KNOTS((3,2,2,2,2,2,3),(0.326086956521739,0.333333333333334,
0.340579710144927,0.347826086956522,0.355072463768116,0.36231884057971,
0.369565217391304),.UNSPECIFIED.)
CURVE()
GEOMETRIC_REPRESENTATION_ITEM()
RATIONAL_B_SPLINE_CURVE((1.,0.866025403784439,1.,0.866025403784439,1.,0.866025403784439,
1.,0.866025403784439,1.,0.866025403784439,1.,0.866025403784439,1.))
REPRESENTATION_ITEM('')
);
#1427=(
BOUNDED_CURVE()
B_SPLINE_CURVE(2,(#240721,#240722,#240723,#240724,#240725,#240726,#240727,
#240728,#240729,#240730,#240731,#240732,#240733),.UNSPECIFIED.,.F.,.F.)
B_SPLINE_CURVE_WITH_KNOTS((3,2,2,2,2,2,3),(0.284366508592218,0.29165795753048,
0.298949406468742,0.306240855407004,0.313532304345266,0.320823753283528,
0.32811520222179),.UNSPECIFIED.)
CURVE()
GEOMETRIC_REPRESENTATION_ITEM()
RATIONAL_B_SPLINE_CURVE((1.,0.866025403784439,1.,0.866025403784439,1.,0.866025403784439,
1.,0.866025403784439,1.,0.866025403784439,1.,0.866025403784439,1.))
REPRESENTATION_ITEM('')
);
#1428=(
BOUNDED_CURVE()
B_SPLINE_CURVE(2,(#240734,#240735,#240736,#240737,#240738,#240739,#240740,
#240741,#240742,#240743,#240744,#240745,#240746),.UNSPECIFIED.,.F.,.F.)
B_SPLINE_CURVE_WITH_KNOTS((3,2,2,2,2,2,3),(0.282608695652174,0.289855072463769,
0.297101449275363,0.304347826086956,0.311594202898551,0.318840579710145,
0.326086956521739),.UNSPECIFIED.)
CURVE()
GEOMETRIC_REPRESENTATION_ITEM()
RATIONAL_B_SPLINE_CURVE((1.,0.866025403784439,1.,0.866025403784439,1.,0.866025403784439,
1.,0.866025403784439,1.,0.866025403784439,1.,0.866025403784439,1.))
REPRESENTATION_ITEM('')
);
#1429=(
BOUNDED_CURVE()
B_SPLINE_CURVE(2,(#240751,#240752,#240753,#240754,#240755,#240756,#240757,
#240758,#240759,#240760,#240761,#240762,#240763),.UNSPECIFIED.,.F.,.F.)
B_SPLINE_CURVE_WITH_KNOTS((3,2,2,2,2,2,3),(0.240617814962646,0.247909263900908,
0.25520071283917,0.262492161777432,0.269783610715694,0.277075059653956,
0.284366508592218),.UNSPECIFIED.)
CURVE()
GEOMETRIC_REPRESENTATION_ITEM()
RATIONAL_B_SPLINE_CURVE((1.,0.866025403784439,1.,0.866025403784439,1.,0.866025403784439,
1.,0.866025403784439,1.,0.866025403784439,1.,0.866025403784439,1.))
REPRESENTATION_ITEM('')
);
#1430=(
BOUNDED_CURVE()
B_SPLINE_CURVE(2,(#240764,#240765,#240766,#240767,#240768,#240769,#240770,
#240771,#240772,#240773,#240774,#240775,#240776),.UNSPECIFIED.,.F.,.F.)
B_SPLINE_CURVE_WITH_KNOTS((3,2,2,2,2,2,3),(0.239130434782609,0.246376811594203,
0.253623188405797,0.260869565217392,0.268115942028985,0.27536231884058,
0.282608695652174),.UNSPECIFIED.)
CURVE()
GEOMETRIC_REPRESENTATION_ITEM()
RATIONAL_B_SPLINE_CURVE((1.,0.866025403784439,1.,0.866025403784439,1.,0.866025403784439,
1.,0.866025403784439,1.,0.866025403784439,1.,0.866025403784439,1.))
REPRESENTATION_ITEM('')
);
#1431=(
BOUNDED_CURVE()
B_SPLINE_CURVE(2,(#240781,#240782,#240783,#240784,#240785,#240786,#240787,
#240788,#240789,#240790,#240791,#240792,#240793),.UNSPECIFIED.,.F.,.F.)
B_SPLINE_CURVE_WITH_KNOTS((3,2,2,2,2,2,3),(0.196869121333074,0.204160570271336,
0.211452019209598,0.21874346814786,0.226034917086122,0.233326366024384,
0.240617814962646),.UNSPECIFIED.)
CURVE()
GEOMETRIC_REPRESENTATION_ITEM()
RATIONAL_B_SPLINE_CURVE((1.,0.866025403784439,1.,0.866025403784439,1.,0.866025403784439,
1.,0.866025403784439,1.,0.866025403784439,1.,0.866025403784439,1.))
REPRESENTATION_ITEM('')
);
#1432=(
BOUNDED_CURVE()
B_SPLINE_CURVE(2,(#240794,#240795,#240796,#240797,#240798,#240799,#240800,
#240801,#240802,#240803,#240804,#240805,#240806),.UNSPECIFIED.,.F.,.F.)
B_SPLINE_CURVE_WITH_KNOTS((3,2,2,2,2,2,3),(0.195652173913044,0.202898550724638,
0.210144927536232,0.217391304347826,0.224637681159421,0.231884057971015,
0.239130434782609),.UNSPECIFIED.)
CURVE()
GEOMETRIC_REPRESENTATION_ITEM()
RATIONAL_B_SPLINE_CURVE((1.,0.866025403784439,1.,0.866025403784439,1.,0.866025403784439,
1.,0.866025403784439,1.,0.866025403784439,1.,0.866025403784439,1.))
REPRESENTATION_ITEM('')
);
#1433=(
BOUNDED_CURVE()
B_SPLINE_CURVE(2,(#240811,#240812,#240813,#240814,#240815,#240816,#240817,
#240818,#240819,#240820,#240821,#240822,#240823),.UNSPECIFIED.,.F.,.F.)
B_SPLINE_CURVE_WITH_KNOTS((3,2,2,2,2,2,3),(0.153120427703502,0.160411876641764,
0.167703325580026,0.174994774518288,0.18228622345655,0.189577672394812,
0.196869121333074),.UNSPECIFIED.)
CURVE()
GEOMETRIC_REPRESENTATION_ITEM()
RATIONAL_B_SPLINE_CURVE((1.,0.866025403784439,1.,0.866025403784439,1.,0.866025403784439,
1.,0.866025403784439,1.,0.866025403784439,1.,0.866025403784439,1.))
REPRESENTATION_ITEM('')
);
#1434=(
BOUNDED_CURVE()
B_SPLINE_CURVE(2,(#240824,#240825,#240826,#240827,#240828,#240829,#240830,
#240831,#240832,#240833,#240834,#240835,#240836),.UNSPECIFIED.,.F.,.F.)
B_SPLINE_CURVE_WITH_KNOTS((3,2,2,2,2,2,3),(0.152173913043478,0.159420289855073,
0.166666666666667,0.173913043478261,0.181159420289855,0.18840579710145,
0.195652173913044),.UNSPECIFIED.)
CURVE()
GEOMETRIC_REPRESENTATION_ITEM()
RATIONAL_B_SPLINE_CURVE((1.,0.866025403784439,1.,0.866025403784439,1.,0.866025403784439,
1.,0.866025403784439,1.,0.866025403784439,1.,0.866025403784439,1.))
REPRESENTATION_ITEM('')
);
#1435=(
BOUNDED_CURVE()
B_SPLINE_CURVE(2,(#240841,#240842,#240843,#240844,#240845,#240846,#240847,
#240848,#240849,#240850,#240851,#240852,#240853),.UNSPECIFIED.,.F.,.F.)
B_SPLINE_CURVE_WITH_KNOTS((3,2,2,2,2,2,3),(0.10937173407393,0.116663183012192,
0.123954631950454,0.131246080888716,0.138537529826978,0.14582897876524,
0.153120427703502),.UNSPECIFIED.)
CURVE()
GEOMETRIC_REPRESENTATION_ITEM()
RATIONAL_B_SPLINE_CURVE((1.,0.866025403784439,1.,0.866025403784439,1.,0.866025403784439,
1.,0.866025403784439,1.,0.866025403784439,1.,0.866025403784439,1.))
REPRESENTATION_ITEM('')
);
#1436=(
BOUNDED_CURVE()
B_SPLINE_CURVE(2,(#240854,#240855,#240856,#240857,#240858,#240859,#240860,
#240861,#240862,#240863,#240864,#240865,#240866),.UNSPECIFIED.,.F.,.F.)
B_SPLINE_CURVE_WITH_KNOTS((3,2,2,2,2,2,3),(0.108695652173913,0.115942028985507,
0.123188405797102,0.130434782608696,0.13768115942029,0.144927536231884,
0.152173913043478),.UNSPECIFIED.)
CURVE()
GEOMETRIC_REPRESENTATION_ITEM()
RATIONAL_B_SPLINE_CURVE((1.,0.866025403784439,1.,0.866025403784439,1.,0.866025403784439,
1.,0.866025403784439,1.,0.866025403784439,1.,0.866025403784439,1.))
REPRESENTATION_ITEM('')
);
#1437=(
BOUNDED_CURVE()
B_SPLINE_CURVE(2,(#240871,#240872,#240873,#240874,#240875,#240876,#240877,
#240878,#240879,#240880,#240881,#240882,#240883),.UNSPECIFIED.,.F.,.F.)
B_SPLINE_CURVE_WITH_KNOTS((3,2,2,2,2,2,3),(0.065623040444358,0.07291448938262,
0.080205938320882,0.087497387259144,0.094788836197406,0.102080285135668,
0.10937173407393),.UNSPECIFIED.)
CURVE()
GEOMETRIC_REPRESENTATION_ITEM()
RATIONAL_B_SPLINE_CURVE((1.,0.866025403784439,1.,0.866025403784439,1.,0.866025403784439,
1.,0.866025403784439,1.,0.866025403784439,1.,0.866025403784439,1.))
REPRESENTATION_ITEM('')
);
#1438=(
BOUNDED_CURVE()
B_SPLINE_CURVE(2,(#240884,#240885,#240886,#240887,#240888,#240889,#240890,
#240891,#240892,#240893,#240894,#240895,#240896),.UNSPECIFIED.,.F.,.F.)
B_SPLINE_CURVE_WITH_KNOTS((3,2,2,2,2,2,3),(0.065217391304348,0.0724637681159421,
0.0797101449275364,0.0869565217391305,0.0942028985507248,0.101449275362319,
0.108695652173913),.UNSPECIFIED.)
CURVE()
GEOMETRIC_REPRESENTATION_ITEM()
RATIONAL_B_SPLINE_CURVE((1.,0.866025403784439,1.,0.866025403784439,1.,0.866025403784439,
1.,0.866025403784439,1.,0.866025403784439,1.,0.866025403784439,1.))
REPRESENTATION_ITEM('')
);
#1439=(
BOUNDED_CURVE()
B_SPLINE_CURVE(2,(#240903,#240904,#240905,#240906,#240907),
 .UNSPECIFIED.,.F.,.F.)
B_SPLINE_CURVE_WITH_KNOTS((3,2,3),(0.0118893770663288,0.014582897876524,
0.021874346814786),.UNSPECIFIED.)
CURVE()
GEOMETRIC_REPRESENTATION_ITEM()
RATIONAL_B_SPLINE_CURVE((0.937582367981144,0.950508689562306,1.,0.866025403784439,
1.))
REPRESENTATION_ITEM('')
);
#1440=(
BOUNDED_CURVE()
B_SPLINE_CURVE(2,(#242295,#242296,#242297),.UNSPECIFIED.,.F.,.F.)
B_SPLINE_CURVE_WITH_KNOTS((3,3),(0.809350832147077,0.81291946675533),
 .UNSPECIFIED.)
CURVE()
GEOMETRIC_REPRESENTATION_ITEM()
RATIONAL_B_SPLINE_CURVE((1.,0.934429166996968,0.933042653441986))
REPRESENTATION_ITEM('')
);
#1441=(
BOUNDED_CURVE()
B_SPLINE_CURVE(2,(#242305,#242306,#242307),.UNSPECIFIED.,.F.,.F.)
B_SPLINE_CURVE_WITH_KNOTS((3,3),(0.804347826086956,0.809954704477924),
 .UNSPECIFIED.)
CURVE()
GEOMETRIC_REPRESENTATION_ITEM()
RATIONAL_B_SPLINE_CURVE((1.,0.896337260952566,0.953092448442884))
REPRESENTATION_ITEM('')
);
#1442=(
BOUNDED_CURVE()
B_SPLINE_CURVE(2,(#242313,#242314,#242315,#242316,#242317,#242318,#242319),
 .UNSPECIFIED.,.F.,.F.)
B_SPLINE_CURVE_WITH_KNOTS((3,2,2,3),(0.76560213851751,0.772893587455772,
0.780185036394034,0.780206651397652),.UNSPECIFIED.)
CURVE()
GEOMETRIC_REPRESENTATION_ITEM()
RATIONAL_B_SPLINE_CURVE((1.,0.866025403784439,1.,0.866025403784439,1.,0.999602841437075,
0.999208037573154))
REPRESENTATION_ITEM('')
);
#1443=(
BOUNDED_CURVE()
B_SPLINE_CURVE(2,(#242333,#242334,#242335,#242336,#242337,#242338,#242339),
 .UNSPECIFIED.,.F.,.F.)
B_SPLINE_CURVE_WITH_KNOTS((3,2,2,3),(0.787646407455994,0.794767934270535,
0.802059383208806,0.809350832147077),.UNSPECIFIED.)
CURVE()
GEOMETRIC_REPRESENTATION_ITEM()
RATIONAL_B_SPLINE_CURVE((0.993901151909826,0.86914758815514,1.,0.866025403784439,
1.,0.866025403784439,1.))
REPRESENTATION_ITEM('')
);
#1444=(
BOUNDED_CURVE()
B_SPLINE_CURVE(2,(#242340,#242341,#242342,#242343,#242344,#242345,#242346,
#242347,#242348,#242349,#242350,#242351,#242352),.UNSPECIFIED.,.F.,.F.)
B_SPLINE_CURVE_WITH_KNOTS((3,2,2,2,2,2,3),(0.760869565217391,0.768115942028986,
0.77536231884058,0.782608695652174,0.789855072463768,0.797101449275362,
0.804347826086956),.UNSPECIFIED.)
CURVE()
GEOMETRIC_REPRESENTATION_ITEM()
RATIONAL_B_SPLINE_CURVE((1.,0.866025403784439,1.,0.866025403784439,1.,0.866025403784439,
1.,0.866025403784439,1.,0.866025403784439,1.,0.866025403784439,1.))
REPRESENTATION_ITEM('')
);
#1445=(
BOUNDED_CURVE()
B_SPLINE_CURVE(2,(#242357,#242358,#242359,#242360,#242361,#242362,#242363,
#242364,#242365,#242366,#242367,#242368,#242369),.UNSPECIFIED.,.F.,.F.)
B_SPLINE_CURVE_WITH_KNOTS((3,2,2,2,2,2,3),(0.721853444887938,0.7291448938262,
0.736436342764462,0.743727791702724,0.751019240640986,0.758310689579248,
0.76560213851751),.UNSPECIFIED.)
CURVE()
GEOMETRIC_REPRESENTATION_ITEM()
RATIONAL_B_SPLINE_CURVE((1.,0.866025403784439,1.,0.866025403784439,1.,0.866025403784439,
1.,0.866025403784439,1.,0.866025403784439,1.,0.866025403784439,1.))
REPRESENTATION_ITEM('')
);
#1446=(
BOUNDED_CURVE()
B_SPLINE_CURVE(2,(#242370,#242371,#242372,#242373,#242374,#242375,#242376,
#242377,#242378,#242379,#242380,#242381,#242382),.UNSPECIFIED.,.F.,.F.)
B_SPLINE_CURVE_WITH_KNOTS((3,2,2,2,2,2,3),(0.717391304347826,0.72463768115942,
0.731884057971015,0.739130434782609,0.746376811594203,0.753623188405797,
0.760869565217391),.UNSPECIFIED.)
CURVE()
GEOMETRIC_REPRESENTATION_ITEM()
RATIONAL_B_SPLINE_CURVE((1.,0.866025403784439,1.,0.866025403784439,1.,0.866025403784439,
1.,0.866025403784439,1.,0.866025403784439,1.,0.866025403784439,1.))
REPRESENTATION_ITEM('')
);
#1447=(
BOUNDED_CURVE()
B_SPLINE_CURVE(2,(#242387,#242388,#242389,#242390,#242391,#242392,#242393,
#242394,#242395,#242396,#242397,#242398,#242399),.UNSPECIFIED.,.F.,.F.)
B_SPLINE_CURVE_WITH_KNOTS((3,2,2,2,2,2,3),(0.678104751258366,0.685396200196628,
0.69268764913489,0.699979098073152,0.707270547011414,0.714561995949676,
0.721853444887938),.UNSPECIFIED.)
CURVE()
GEOMETRIC_REPRESENTATION_ITEM()
RATIONAL_B_SPLINE_CURVE((1.,0.866025403784439,1.,0.866025403784439,1.,0.866025403784439,
1.,0.866025403784439,1.,0.866025403784439,1.,0.866025403784439,1.))
REPRESENTATION_ITEM('')
);
#1448=(
BOUNDED_CURVE()
B_SPLINE_CURVE(2,(#242400,#242401,#242402,#242403,#242404,#242405,#242406,
#242407,#242408,#242409,#242410,#242411,#242412),.UNSPECIFIED.,.F.,.F.)
B_SPLINE_CURVE_WITH_KNOTS((3,2,2,2,2,2,3),(0.673913043478261,0.681159420289855,
0.688405797101449,0.695652173913044,0.702898550724638,0.710144927536232,
0.717391304347826),.UNSPECIFIED.)
CURVE()
GEOMETRIC_REPRESENTATION_ITEM()
RATIONAL_B_SPLINE_CURVE((1.,0.866025403784439,1.,0.866025403784439,1.,0.866025403784439,
1.,0.866025403784439,1.,0.866025403784439,1.,0.866025403784439,1.))
REPRESENTATION_ITEM('')
);
#1449=(
BOUNDED_CURVE()
B_SPLINE_CURVE(2,(#242417,#242418,#242419,#242420,#242421,#242422,#242423,
#242424,#242425,#242426,#242427,#242428,#242429),.UNSPECIFIED.,.F.,.F.)
B_SPLINE_CURVE_WITH_KNOTS((3,2,2,2,2,2,3),(0.634356057628794,0.641647506567056,
0.648938955505318,0.65623040444358,0.663521853381842,0.670813302320104,
0.678104751258366),.UNSPECIFIED.)
CURVE()
GEOMETRIC_REPRESENTATION_ITEM()
RATIONAL_B_SPLINE_CURVE((1.,0.866025403784439,1.,0.866025403784439,1.,0.866025403784439,
1.,0.866025403784439,1.,0.866025403784439,1.,0.866025403784439,1.))
REPRESENTATION_ITEM('')
);
#1450=(
BOUNDED_CURVE()
B_SPLINE_CURVE(2,(#242430,#242431,#242432,#242433,#242434,#242435,#242436,
#242437,#242438,#242439,#242440,#242441,#242442),.UNSPECIFIED.,.F.,.F.)
B_SPLINE_CURVE_WITH_KNOTS((3,2,2,2,2,2,3),(0.630434782608696,0.63768115942029,
0.644927536231884,0.652173913043478,0.659420289855073,0.666666666666667,
0.673913043478261),.UNSPECIFIED.)
CURVE()
GEOMETRIC_REPRESENTATION_ITEM()
RATIONAL_B_SPLINE_CURVE((1.,0.866025403784439,1.,0.866025403784439,1.,0.866025403784439,
1.,0.866025403784439,1.,0.866025403784439,1.,0.866025403784439,1.))
REPRESENTATION_ITEM('')
);
#1451=(
BOUNDED_CURVE()
B_SPLINE_CURVE(2,(#242447,#242448,#242449,#242450,#242451,#242452,#242453,
#242454,#242455,#242456,#242457,#242458,#242459),.UNSPECIFIED.,.F.,.F.)
B_SPLINE_CURVE_WITH_KNOTS((3,2,2,2,2,2,3),(0.590607363999222,0.597898812937484,
0.605190261875746,0.612481710814008,0.61977315975227,0.627064608690532,
0.634356057628794),.UNSPECIFIED.)
CURVE()
GEOMETRIC_REPRESENTATION_ITEM()
RATIONAL_B_SPLINE_CURVE((1.,0.866025403784439,1.,0.866025403784439,1.,0.866025403784439,
1.,0.866025403784439,1.,0.866025403784439,1.,0.866025403784439,1.))
REPRESENTATION_ITEM('')
);
#1452=(
BOUNDED_CURVE()
B_SPLINE_CURVE(2,(#242460,#242461,#242462,#242463,#242464,#242465,#242466,
#242467,#242468,#242469,#242470,#242471,#242472),.UNSPECIFIED.,.F.,.F.)
B_SPLINE_CURVE_WITH_KNOTS((3,2,2,2,2,2,3),(0.586956521739131,0.594202898550725,
0.601449275362319,0.608695652173913,0.615942028985507,0.623188405797101,
0.630434782608696),.UNSPECIFIED.)
CURVE()
GEOMETRIC_REPRESENTATION_ITEM()
RATIONAL_B_SPLINE_CURVE((1.,0.866025403784439,1.,0.866025403784439,1.,0.866025403784439,
1.,0.866025403784439,1.,0.866025403784439,1.,0.866025403784439,1.))
REPRESENTATION_ITEM('')
);
#1453=(
BOUNDED_CURVE()
B_SPLINE_CURVE(2,(#242477,#242478,#242479,#242480,#242481,#242482,#242483,
#242484,#242485,#242486,#242487,#242488,#242489),.UNSPECIFIED.,.F.,.F.)
B_SPLINE_CURVE_WITH_KNOTS((3,2,2,2,2,2,3),(0.54685867036965,0.554150119307912,
0.561441568246174,0.568733017184436,0.576024466122698,0.58331591506096,
0.590607363999222),.UNSPECIFIED.)
CURVE()
GEOMETRIC_REPRESENTATION_ITEM()
RATIONAL_B_SPLINE_CURVE((1.,0.866025403784439,1.,0.866025403784439,1.,0.866025403784439,
1.,0.866025403784439,1.,0.866025403784439,1.,0.866025403784439,1.))
REPRESENTATION_ITEM('')
);
#1454=(
BOUNDED_CURVE()
B_SPLINE_CURVE(2,(#242490,#242491,#242492,#242493,#242494,#242495,#242496,
#242497,#242498,#242499,#242500,#242501,#242502),.UNSPECIFIED.,.F.,.F.)
B_SPLINE_CURVE_WITH_KNOTS((3,2,2,2,2,2,3),(0.543478260869565,0.55072463768116,
0.557971014492754,0.565217391304348,0.572463768115942,0.579710144927536,
0.586956521739131),.UNSPECIFIED.)
CURVE()
GEOMETRIC_REPRESENTATION_ITEM()
RATIONAL_B_SPLINE_CURVE((1.,0.866025403784439,1.,0.866025403784439,1.,0.866025403784439,
1.,0.866025403784439,1.,0.866025403784439,1.,0.866025403784439,1.))
REPRESENTATION_ITEM('')
);
#1455=(
BOUNDED_CURVE()
B_SPLINE_CURVE(2,(#242507,#242508,#242509,#242510,#242511,#242512,#242513,
#242514,#242515,#242516,#242517,#242518,#242519),.UNSPECIFIED.,.F.,.F.)
B_SPLINE_CURVE_WITH_KNOTS((3,2,2,2,2,2,3),(0.503109976740078,0.51040142567834,
0.517692874616602,0.524984323554864,0.532275772493126,0.539567221431388,
0.54685867036965),.UNSPECIFIED.)
CURVE()
GEOMETRIC_REPRESENTATION_ITEM()
RATIONAL_B_SPLINE_CURVE((1.,0.866025403784439,1.,0.866025403784439,1.,0.866025403784439,
1.,0.866025403784439,1.,0.866025403784439,1.,0.866025403784439,1.))
REPRESENTATION_ITEM('')
);
#1456=(
BOUNDED_CURVE()
B_SPLINE_CURVE(2,(#242520,#242521,#242522,#242523,#242524,#242525,#242526,
#242527,#242528,#242529,#242530,#242531,#242532),.UNSPECIFIED.,.F.,.F.)
B_SPLINE_CURVE_WITH_KNOTS((3,2,2,2,2,2,3),(0.5,0.507246376811594,0.514492753623188,
0.521739130434783,0.528985507246377,0.536231884057971,0.543478260869565),
 .UNSPECIFIED.)
CURVE()
GEOMETRIC_REPRESENTATION_ITEM()
RATIONAL_B_SPLINE_CURVE((1.,0.866025403784439,1.,0.866025403784439,1.,0.866025403784439,
1.,0.866025403784439,1.,0.866025403784439,1.,0.866025403784439,1.))
REPRESENTATION_ITEM('')
);
#1457=(
BOUNDED_CURVE()
B_SPLINE_CURVE(2,(#242537,#242538,#242539,#242540,#242541,#242542,#242543,
#242544,#242545,#242546,#242547,#242548,#242549),.UNSPECIFIED.,.F.,.F.)
B_SPLINE_CURVE_WITH_KNOTS((3,2,2,2,2,2,3),(0.459361283110506,0.466652732048768,
0.47394418098703,0.481235629925292,0.488527078863554,0.495818527801816,
0.503109976740078),.UNSPECIFIED.)
CURVE()
GEOMETRIC_REPRESENTATION_ITEM()
RATIONAL_B_SPLINE_CURVE((1.,0.866025403784439,1.,0.866025403784439,1.,0.866025403784439,
1.,0.866025403784439,1.,0.866025403784439,1.,0.866025403784439,1.))
REPRESENTATION_ITEM('')
);
#1458=(
BOUNDED_CURVE()
B_SPLINE_CURVE(2,(#242550,#242551,#242552,#242553,#242554,#242555,#242556,
#242557,#242558,#242559,#242560,#242561,#242562),.UNSPECIFIED.,.F.,.F.)
B_SPLINE_CURVE_WITH_KNOTS((3,2,2,2,2,2,3),(0.456521739130435,0.463768115942029,
0.471014492753623,0.478260869565218,0.485507246376812,0.492753623188406,
0.5),.UNSPECIFIED.)
CURVE()
GEOMETRIC_REPRESENTATION_ITEM()
RATIONAL_B_SPLINE_CURVE((1.,0.866025403784439,1.,0.866025403784439,1.,0.866025403784439,
1.,0.866025403784439,1.,0.866025403784439,1.,0.866025403784439,1.))
REPRESENTATION_ITEM('')
);
#1459=(
BOUNDED_CURVE()
B_SPLINE_CURVE(2,(#242567,#242568,#242569,#242570,#242571,#242572,#242573,
#242574,#242575,#242576,#242577,#242578,#242579),.UNSPECIFIED.,.F.,.F.)
B_SPLINE_CURVE_WITH_KNOTS((3,2,2,2,2,2,3),(0.415612589480934,0.422904038419196,
0.430195487357458,0.43748693629572,0.444778385233982,0.452069834172244,
0.459361283110506),.UNSPECIFIED.)
CURVE()
GEOMETRIC_REPRESENTATION_ITEM()
RATIONAL_B_SPLINE_CURVE((1.,0.866025403784439,1.,0.866025403784439,1.,0.866025403784439,
1.,0.866025403784439,1.,0.866025403784439,1.,0.866025403784439,1.))
REPRESENTATION_ITEM('')
);
#1460=(
BOUNDED_CURVE()
B_SPLINE_CURVE(2,(#242580,#242581,#242582,#242583,#242584,#242585,#242586,
#242587,#242588,#242589,#242590,#242591,#242592),.UNSPECIFIED.,.F.,.F.)
B_SPLINE_CURVE_WITH_KNOTS((3,2,2,2,2,2,3),(0.41304347826087,0.420289855072464,
0.427536231884058,0.434782608695652,0.442028985507247,0.449275362318841,
0.456521739130435),.UNSPECIFIED.)
CURVE()
GEOMETRIC_REPRESENTATION_ITEM()
RATIONAL_B_SPLINE_CURVE((1.,0.866025403784439,1.,0.866025403784439,1.,0.866025403784439,
1.,0.866025403784439,1.,0.866025403784439,1.,0.866025403784439,1.))
REPRESENTATION_ITEM('')
);
#1461=(
BOUNDED_CURVE()
B_SPLINE_CURVE(2,(#242597,#242598,#242599,#242600,#242601,#242602,#242603,
#242604,#242605,#242606,#242607,#242608,#242609),.UNSPECIFIED.,.F.,.F.)
B_SPLINE_CURVE_WITH_KNOTS((3,2,2,2,2,2,3),(0.371863895851362,0.379155344789624,
0.386446793727886,0.393738242666148,0.40102969160441,0.408321140542672,
0.415612589480934),.UNSPECIFIED.)
CURVE()
GEOMETRIC_REPRESENTATION_ITEM()
RATIONAL_B_SPLINE_CURVE((1.,0.866025403784439,1.,0.866025403784439,1.,0.866025403784439,
1.,0.866025403784439,1.,0.866025403784439,1.,0.866025403784439,1.))
REPRESENTATION_ITEM('')
);
#1462=(
BOUNDED_CURVE()
B_SPLINE_CURVE(2,(#242610,#242611,#242612,#242613,#242614,#242615,#242616,
#242617,#242618,#242619,#242620,#242621,#242622),.UNSPECIFIED.,.F.,.F.)
B_SPLINE_CURVE_WITH_KNOTS((3,2,2,2,2,2,3),(0.369565217391304,0.376811594202899,
0.384057971014493,0.391304347826087,0.398550724637681,0.405797101449275,
0.41304347826087),.UNSPECIFIED.)
CURVE()
GEOMETRIC_REPRESENTATION_ITEM()
RATIONAL_B_SPLINE_CURVE((1.,0.866025403784439,1.,0.866025403784439,1.,0.866025403784439,
1.,0.866025403784439,1.,0.866025403784439,1.,0.866025403784439,1.))
REPRESENTATION_ITEM('')
);
#1463=(
BOUNDED_CURVE()
B_SPLINE_CURVE(2,(#242627,#242628,#242629,#242630,#242631,#242632,#242633,
#242634,#242635,#242636,#242637,#242638,#242639),.UNSPECIFIED.,.F.,.F.)
B_SPLINE_CURVE_WITH_KNOTS((3,2,2,2,2,2,3),(0.32811520222179,0.335406651160052,
0.342698100098314,0.349989549036576,0.357280997974838,0.3645724469131,0.371863895851362),
 .UNSPECIFIED.)
CURVE()
GEOMETRIC_REPRESENTATION_ITEM()
RATIONAL_B_SPLINE_CURVE((1.,0.866025403784439,1.,0.866025403784439,1.,0.866025403784439,
1.,0.866025403784439,1.,0.866025403784439,1.,0.866025403784439,1.))
REPRESENTATION_ITEM('')
);
#1464=(
BOUNDED_CURVE()
B_SPLINE_CURVE(2,(#242640,#242641,#242642,#242643,#242644,#242645,#242646,
#242647,#242648,#242649,#242650,#242651,#242652),.UNSPECIFIED.,.F.,.F.)
B_SPLINE_CURVE_WITH_KNOTS((3,2,2,2,2,2,3),(0.326086956521739,0.333333333333334,
0.340579710144927,0.347826086956522,0.355072463768116,0.36231884057971,
0.369565217391304),.UNSPECIFIED.)
CURVE()
GEOMETRIC_REPRESENTATION_ITEM()
RATIONAL_B_SPLINE_CURVE((1.,0.866025403784439,1.,0.866025403784439,1.,0.866025403784439,
1.,0.866025403784439,1.,0.866025403784439,1.,0.866025403784439,1.))
REPRESENTATION_ITEM('')
);
#1465=(
BOUNDED_CURVE()
B_SPLINE_CURVE(2,(#242657,#242658,#242659,#242660,#242661,#242662,#242663,
#242664,#242665,#242666,#242667,#242668,#242669),.UNSPECIFIED.,.F.,.F.)
B_SPLINE_CURVE_WITH_KNOTS((3,2,2,2,2,2,3),(0.284366508592218,0.29165795753048,
0.298949406468742,0.306240855407004,0.313532304345266,0.320823753283528,
0.32811520222179),.UNSPECIFIED.)
CURVE()
GEOMETRIC_REPRESENTATION_ITEM()
RATIONAL_B_SPLINE_CURVE((1.,0.866025403784439,1.,0.866025403784439,1.,0.866025403784439,
1.,0.866025403784439,1.,0.866025403784439,1.,0.866025403784439,1.))
REPRESENTATION_ITEM('')
);
#1466=(
BOUNDED_CURVE()
B_SPLINE_CURVE(2,(#242670,#242671,#242672,#242673,#242674,#242675,#242676,
#242677,#242678,#242679,#242680,#242681,#242682),.UNSPECIFIED.,.F.,.F.)
B_SPLINE_CURVE_WITH_KNOTS((3,2,2,2,2,2,3),(0.282608695652174,0.289855072463769,
0.297101449275363,0.304347826086956,0.311594202898551,0.318840579710145,
0.326086956521739),.UNSPECIFIED.)
CURVE()
GEOMETRIC_REPRESENTATION_ITEM()
RATIONAL_B_SPLINE_CURVE((1.,0.866025403784439,1.,0.866025403784439,1.,0.866025403784439,
1.,0.866025403784439,1.,0.866025403784439,1.,0.866025403784439,1.))
REPRESENTATION_ITEM('')
);
#1467=(
BOUNDED_CURVE()
B_SPLINE_CURVE(2,(#242687,#242688,#242689,#242690,#242691,#242692,#242693,
#242694,#242695,#242696,#242697,#242698,#242699),.UNSPECIFIED.,.F.,.F.)
B_SPLINE_CURVE_WITH_KNOTS((3,2,2,2,2,2,3),(0.240617814962646,0.247909263900908,
0.25520071283917,0.262492161777432,0.269783610715694,0.277075059653956,
0.284366508592218),.UNSPECIFIED.)
CURVE()
GEOMETRIC_REPRESENTATION_ITEM()
RATIONAL_B_SPLINE_CURVE((1.,0.866025403784439,1.,0.866025403784439,1.,0.866025403784439,
1.,0.866025403784439,1.,0.866025403784439,1.,0.866025403784439,1.))
REPRESENTATION_ITEM('')
);
#1468=(
BOUNDED_CURVE()
B_SPLINE_CURVE(2,(#242700,#242701,#242702,#242703,#242704,#242705,#242706,
#242707,#242708,#242709,#242710,#242711,#242712),.UNSPECIFIED.,.F.,.F.)
B_SPLINE_CURVE_WITH_KNOTS((3,2,2,2,2,2,3),(0.239130434782609,0.246376811594203,
0.253623188405797,0.260869565217392,0.268115942028985,0.27536231884058,
0.282608695652174),.UNSPECIFIED.)
CURVE()
GEOMETRIC_REPRESENTATION_ITEM()
RATIONAL_B_SPLINE_CURVE((1.,0.866025403784439,1.,0.866025403784439,1.,0.866025403784439,
1.,0.866025403784439,1.,0.866025403784439,1.,0.866025403784439,1.))
REPRESENTATION_ITEM('')
);
#1469=(
BOUNDED_CURVE()
B_SPLINE_CURVE(2,(#242717,#242718,#242719,#242720,#242721,#242722,#242723,
#242724,#242725,#242726,#242727,#242728,#242729),.UNSPECIFIED.,.F.,.F.)
B_SPLINE_CURVE_WITH_KNOTS((3,2,2,2,2,2,3),(0.196869121333074,0.204160570271336,
0.211452019209598,0.21874346814786,0.226034917086122,0.233326366024384,
0.240617814962646),.UNSPECIFIED.)
CURVE()
GEOMETRIC_REPRESENTATION_ITEM()
RATIONAL_B_SPLINE_CURVE((1.,0.866025403784439,1.,0.866025403784439,1.,0.866025403784439,
1.,0.866025403784439,1.,0.866025403784439,1.,0.866025403784439,1.))
REPRESENTATION_ITEM('')
);
#1470=(
BOUNDED_CURVE()
B_SPLINE_CURVE(2,(#242730,#242731,#242732,#242733,#242734,#242735,#242736,
#242737,#242738,#242739,#242740,#242741,#242742),.UNSPECIFIED.,.F.,.F.)
B_SPLINE_CURVE_WITH_KNOTS((3,2,2,2,2,2,3),(0.195652173913044,0.202898550724638,
0.210144927536232,0.217391304347826,0.224637681159421,0.231884057971014,
0.239130434782609),.UNSPECIFIED.)
CURVE()
GEOMETRIC_REPRESENTATION_ITEM()
RATIONAL_B_SPLINE_CURVE((1.,0.866025403784439,1.,0.866025403784439,1.,0.866025403784439,
1.,0.866025403784439,1.,0.866025403784439,1.,0.866025403784439,1.))
REPRESENTATION_ITEM('')
);
#1471=(
BOUNDED_CURVE()
B_SPLINE_CURVE(2,(#242747,#242748,#242749,#242750,#242751,#242752,#242753,
#242754,#242755,#242756,#242757,#242758,#242759),.UNSPECIFIED.,.F.,.F.)
B_SPLINE_CURVE_WITH_KNOTS((3,2,2,2,2,2,3),(0.153120427703502,0.160411876641764,
0.167703325580026,0.174994774518288,0.18228622345655,0.189577672394812,
0.196869121333074),.UNSPECIFIED.)
CURVE()
GEOMETRIC_REPRESENTATION_ITEM()
RATIONAL_B_SPLINE_CURVE((1.,0.866025403784439,1.,0.866025403784439,1.,0.866025403784439,
1.,0.866025403784439,1.,0.866025403784439,1.,0.866025403784439,1.))
REPRESENTATION_ITEM('')
);
#1472=(
BOUNDED_CURVE()
B_SPLINE_CURVE(2,(#242760,#242761,#242762,#242763,#242764,#242765,#242766,
#242767,#242768,#242769,#242770,#242771,#242772),.UNSPECIFIED.,.F.,.F.)
B_SPLINE_CURVE_WITH_KNOTS((3,2,2,2,2,2,3),(0.152173913043478,0.159420289855073,
0.166666666666667,0.173913043478261,0.181159420289855,0.18840579710145,
0.195652173913044),.UNSPECIFIED.)
CURVE()
GEOMETRIC_REPRESENTATION_ITEM()
RATIONAL_B_SPLINE_CURVE((1.,0.866025403784439,1.,0.866025403784439,1.,0.866025403784439,
1.,0.866025403784439,1.,0.866025403784439,1.,0.866025403784439,1.))
REPRESENTATION_ITEM('')
);
#1473=(
BOUNDED_CURVE()
B_SPLINE_CURVE(2,(#242777,#242778,#242779,#242780,#242781,#242782,#242783,
#242784,#242785,#242786,#242787,#242788,#242789),.UNSPECIFIED.,.F.,.F.)
B_SPLINE_CURVE_WITH_KNOTS((3,2,2,2,2,2,3),(0.10937173407393,0.116663183012192,
0.123954631950454,0.131246080888716,0.138537529826978,0.14582897876524,
0.153120427703502),.UNSPECIFIED.)
CURVE()
GEOMETRIC_REPRESENTATION_ITEM()
RATIONAL_B_SPLINE_CURVE((1.,0.866025403784439,1.,0.866025403784439,1.,0.866025403784439,
1.,0.866025403784439,1.,0.866025403784439,1.,0.866025403784439,1.))
REPRESENTATION_ITEM('')
);
#1474=(
BOUNDED_CURVE()
B_SPLINE_CURVE(2,(#242790,#242791,#242792,#242793,#242794,#242795,#242796,
#242797,#242798,#242799,#242800,#242801,#242802),.UNSPECIFIED.,.F.,.F.)
B_SPLINE_CURVE_WITH_KNOTS((3,2,2,2,2,2,3),(0.108695652173913,0.115942028985507,
0.123188405797102,0.130434782608696,0.13768115942029,0.144927536231884,
0.152173913043478),.UNSPECIFIED.)
CURVE()
GEOMETRIC_REPRESENTATION_ITEM()
RATIONAL_B_SPLINE_CURVE((1.,0.866025403784439,1.,0.866025403784439,1.,0.866025403784439,
1.,0.866025403784439,1.,0.866025403784439,1.,0.866025403784439,1.))
REPRESENTATION_ITEM('')
);
#1475=(
BOUNDED_CURVE()
B_SPLINE_CURVE(2,(#242807,#242808,#242809,#242810,#242811,#242812,#242813,
#242814,#242815,#242816,#242817,#242818,#242819),.UNSPECIFIED.,.F.,.F.)
B_SPLINE_CURVE_WITH_KNOTS((3,2,2,2,2,2,3),(0.065623040444358,0.07291448938262,
0.080205938320882,0.087497387259144,0.094788836197406,0.102080285135668,
0.10937173407393),.UNSPECIFIED.)
CURVE()
GEOMETRIC_REPRESENTATION_ITEM()
RATIONAL_B_SPLINE_CURVE((1.,0.866025403784439,1.,0.866025403784439,1.,0.866025403784439,
1.,0.866025403784439,1.,0.866025403784439,1.,0.866025403784439,1.))
REPRESENTATION_ITEM('')
);
#1476=(
BOUNDED_CURVE()
B_SPLINE_CURVE(2,(#242820,#242821,#242822,#242823,#242824,#242825,#242826,
#242827,#242828,#242829,#242830,#242831,#242832),.UNSPECIFIED.,.F.,.F.)
B_SPLINE_CURVE_WITH_KNOTS((3,2,2,2,2,2,3),(0.065217391304348,0.0724637681159422,
0.0797101449275364,0.0869565217391306,0.0942028985507248,0.101449275362319,
0.108695652173913),.UNSPECIFIED.)
CURVE()
GEOMETRIC_REPRESENTATION_ITEM()
RATIONAL_B_SPLINE_CURVE((1.,0.866025403784439,1.,0.866025403784439,1.,0.866025403784439,
1.,0.866025403784439,1.,0.866025403784439,1.,0.866025403784439,1.))
REPRESENTATION_ITEM('')
);
#1477=(
BOUNDED_CURVE()
B_SPLINE_CURVE(2,(#242839,#242840,#242841,#242842,#242843),
 .UNSPECIFIED.,.F.,.F.)
B_SPLINE_CURVE_WITH_KNOTS((3,2,3),(0.0118893770663289,0.014582897876524,
0.021874346814786),.UNSPECIFIED.)
CURVE()
GEOMETRIC_REPRESENTATION_ITEM()
RATIONAL_B_SPLINE_CURVE((0.937582367981145,0.950508689562308,1.,0.866025403784439,
1.))
REPRESENTATION_ITEM('')
);
#1478=(
BOUNDED_CURVE()
B_SPLINE_CURVE(2,(#242849,#242850,#242851),.UNSPECIFIED.,.F.,.F.)
B_SPLINE_CURVE_WITH_KNOTS((3,3),(0.809350832147077,0.812919467682267),
 .UNSPECIFIED.)
CURVE()
GEOMETRIC_REPRESENTATION_ITEM()
RATIONAL_B_SPLINE_CURVE((1.,0.934429149965244,0.933042652721709))
REPRESENTATION_ITEM('')
);
#1479=(
BOUNDED_CURVE()
B_SPLINE_CURVE(2,(#242859,#242860,#242861),.UNSPECIFIED.,.F.,.F.)
B_SPLINE_CURVE_WITH_KNOTS((3,3),(0.804347826086957,0.809954707320484),
 .UNSPECIFIED.)
CURVE()
GEOMETRIC_REPRESENTATION_ITEM()
RATIONAL_B_SPLINE_CURVE((1.,0.896337208397912,0.953092505990106))
REPRESENTATION_ITEM('')
);
#1480=(
BOUNDED_CURVE()
B_SPLINE_CURVE(2,(#242867,#242868,#242869,#242870,#242871,#242872,#242873),
 .UNSPECIFIED.,.F.,.F.)
B_SPLINE_CURVE_WITH_KNOTS((3,2,2,3),(0.76560213851751,0.772893587455772,
0.780185036394034,0.780206571546235),.UNSPECIFIED.)
CURVE()
GEOMETRIC_REPRESENTATION_ITEM()
RATIONAL_B_SPLINE_CURVE((1.,0.866025403784439,1.,0.866025403784439,1.,0.99960430864359,
0.999210954620584))
REPRESENTATION_ITEM('')
);
#1481=(
BOUNDED_CURVE()
B_SPLINE_CURVE(2,(#242887,#242888,#242889,#242890,#242891,#242892,#242893),
 .UNSPECIFIED.,.F.,.F.)
B_SPLINE_CURVE_WITH_KNOTS((3,2,2,3),(0.787646418746451,0.794767934270535,
0.802059383208806,0.809350832147077),.UNSPECIFIED.)
CURVE()
GEOMETRIC_REPRESENTATION_ITEM()
RATIONAL_B_SPLINE_CURVE((0.993900756342288,0.869147795608333,1.,0.866025403784439,
1.,0.866025403784439,1.))
REPRESENTATION_ITEM('')
);
#1482=(
BOUNDED_CURVE()
B_SPLINE_CURVE(2,(#242894,#242895,#242896,#242897,#242898,#242899,#242900,
#242901,#242902,#242903,#242904,#242905,#242906),.UNSPECIFIED.,.F.,.F.)
B_SPLINE_CURVE_WITH_KNOTS((3,2,2,2,2,2,3),(0.760869565217391,0.768115942028986,
0.77536231884058,0.782608695652174,0.789855072463768,0.797101449275362,
0.804347826086957),.UNSPECIFIED.)
CURVE()
GEOMETRIC_REPRESENTATION_ITEM()
RATIONAL_B_SPLINE_CURVE((1.,0.866025403784439,1.,0.866025403784439,1.,0.866025403784439,
1.,0.866025403784439,1.,0.866025403784439,1.,0.866025403784439,1.))
REPRESENTATION_ITEM('')
);
#1483=(
BOUNDED_CURVE()
B_SPLINE_CURVE(2,(#242911,#242912,#242913,#242914,#242915,#242916,#242917,
#242918,#242919,#242920,#242921,#242922,#242923),.UNSPECIFIED.,.F.,.F.)
B_SPLINE_CURVE_WITH_KNOTS((3,2,2,2,2,2,3),(0.721853444887938,0.7291448938262,
0.736436342764462,0.743727791702724,0.751019240640986,0.758310689579248,
0.76560213851751),.UNSPECIFIED.)
CURVE()
GEOMETRIC_REPRESENTATION_ITEM()
RATIONAL_B_SPLINE_CURVE((1.,0.866025403784439,1.,0.866025403784439,1.,0.866025403784439,
1.,0.866025403784439,1.,0.866025403784439,1.,0.866025403784439,1.))
REPRESENTATION_ITEM('')
);
#1484=(
BOUNDED_CURVE()
B_SPLINE_CURVE(2,(#242924,#242925,#242926,#242927,#242928,#242929,#242930,
#242931,#242932,#242933,#242934,#242935,#242936),.UNSPECIFIED.,.F.,.F.)
B_SPLINE_CURVE_WITH_KNOTS((3,2,2,2,2,2,3),(0.717391304347826,0.72463768115942,
0.731884057971015,0.739130434782609,0.746376811594203,0.753623188405797,
0.760869565217391),.UNSPECIFIED.)
CURVE()
GEOMETRIC_REPRESENTATION_ITEM()
RATIONAL_B_SPLINE_CURVE((1.,0.866025403784439,1.,0.866025403784439,1.,0.866025403784439,
1.,0.866025403784439,1.,0.866025403784439,1.,0.866025403784439,1.))
REPRESENTATION_ITEM('')
);
#1485=(
BOUNDED_CURVE()
B_SPLINE_CURVE(2,(#242941,#242942,#242943,#242944,#242945,#242946,#242947,
#242948,#242949,#242950,#242951,#242952,#242953),.UNSPECIFIED.,.F.,.F.)
B_SPLINE_CURVE_WITH_KNOTS((3,2,2,2,2,2,3),(0.678104751258366,0.685396200196628,
0.69268764913489,0.699979098073152,0.707270547011414,0.714561995949676,
0.721853444887938),.UNSPECIFIED.)
CURVE()
GEOMETRIC_REPRESENTATION_ITEM()
RATIONAL_B_SPLINE_CURVE((1.,0.866025403784439,1.,0.866025403784439,1.,0.866025403784439,
1.,0.866025403784439,1.,0.866025403784439,1.,0.866025403784439,1.))
REPRESENTATION_ITEM('')
);
#1486=(
BOUNDED_CURVE()
B_SPLINE_CURVE(2,(#242954,#242955,#242956,#242957,#242958,#242959,#242960,
#242961,#242962,#242963,#242964,#242965,#242966),.UNSPECIFIED.,.F.,.F.)
B_SPLINE_CURVE_WITH_KNOTS((3,2,2,2,2,2,3),(0.673913043478261,0.681159420289855,
0.688405797101449,0.695652173913044,0.702898550724638,0.710144927536232,
0.717391304347826),.UNSPECIFIED.)
CURVE()
GEOMETRIC_REPRESENTATION_ITEM()
RATIONAL_B_SPLINE_CURVE((1.,0.866025403784439,1.,0.866025403784439,1.,0.866025403784439,
1.,0.866025403784439,1.,0.866025403784439,1.,0.866025403784439,1.))
REPRESENTATION_ITEM('')
);
#1487=(
BOUNDED_CURVE()
B_SPLINE_CURVE(2,(#242971,#242972,#242973,#242974,#242975,#242976,#242977,
#242978,#242979,#242980,#242981,#242982,#242983),.UNSPECIFIED.,.F.,.F.)
B_SPLINE_CURVE_WITH_KNOTS((3,2,2,2,2,2,3),(0.634356057628794,0.641647506567056,
0.648938955505318,0.65623040444358,0.663521853381842,0.670813302320104,
0.678104751258366),.UNSPECIFIED.)
CURVE()
GEOMETRIC_REPRESENTATION_ITEM()
RATIONAL_B_SPLINE_CURVE((1.,0.866025403784439,1.,0.866025403784439,1.,0.866025403784439,
1.,0.866025403784439,1.,0.866025403784439,1.,0.866025403784439,1.))
REPRESENTATION_ITEM('')
);
#1488=(
BOUNDED_CURVE()
B_SPLINE_CURVE(2,(#242984,#242985,#242986,#242987,#242988,#242989,#242990,
#242991,#242992,#242993,#242994,#242995,#242996),.UNSPECIFIED.,.F.,.F.)
B_SPLINE_CURVE_WITH_KNOTS((3,2,2,2,2,2,3),(0.630434782608696,0.63768115942029,
0.644927536231884,0.652173913043478,0.659420289855073,0.666666666666667,
0.673913043478261),.UNSPECIFIED.)
CURVE()
GEOMETRIC_REPRESENTATION_ITEM()
RATIONAL_B_SPLINE_CURVE((1.,0.866025403784439,1.,0.866025403784439,1.,0.866025403784439,
1.,0.866025403784439,1.,0.866025403784439,1.,0.866025403784439,1.))
REPRESENTATION_ITEM('')
);
#1489=(
BOUNDED_CURVE()
B_SPLINE_CURVE(2,(#243001,#243002,#243003,#243004,#243005,#243006,#243007,
#243008,#243009,#243010,#243011,#243012,#243013),.UNSPECIFIED.,.F.,.F.)
B_SPLINE_CURVE_WITH_KNOTS((3,2,2,2,2,2,3),(0.590607363999222,0.597898812937484,
0.605190261875746,0.612481710814008,0.61977315975227,0.627064608690532,
0.634356057628794),.UNSPECIFIED.)
CURVE()
GEOMETRIC_REPRESENTATION_ITEM()
RATIONAL_B_SPLINE_CURVE((1.,0.866025403784439,1.,0.866025403784439,1.,0.866025403784439,
1.,0.866025403784439,1.,0.866025403784439,1.,0.866025403784439,1.))
REPRESENTATION_ITEM('')
);
#1490=(
BOUNDED_CURVE()
B_SPLINE_CURVE(2,(#243014,#243015,#243016,#243017,#243018,#243019,#243020,
#243021,#243022,#243023,#243024,#243025,#243026),.UNSPECIFIED.,.F.,.F.)
B_SPLINE_CURVE_WITH_KNOTS((3,2,2,2,2,2,3),(0.586956521739131,0.594202898550725,
0.601449275362319,0.608695652173913,0.615942028985507,0.623188405797101,
0.630434782608696),.UNSPECIFIED.)
CURVE()
GEOMETRIC_REPRESENTATION_ITEM()
RATIONAL_B_SPLINE_CURVE((1.,0.866025403784439,1.,0.866025403784439,1.,0.866025403784439,
1.,0.866025403784439,1.,0.866025403784439,1.,0.866025403784439,1.))
REPRESENTATION_ITEM('')
);
#1491=(
BOUNDED_CURVE()
B_SPLINE_CURVE(2,(#243031,#243032,#243033,#243034,#243035,#243036,#243037,
#243038,#243039,#243040,#243041,#243042,#243043),.UNSPECIFIED.,.F.,.F.)
B_SPLINE_CURVE_WITH_KNOTS((3,2,2,2,2,2,3),(0.54685867036965,0.554150119307912,
0.561441568246174,0.568733017184436,0.576024466122698,0.58331591506096,
0.590607363999222),.UNSPECIFIED.)
CURVE()
GEOMETRIC_REPRESENTATION_ITEM()
RATIONAL_B_SPLINE_CURVE((1.,0.866025403784439,1.,0.866025403784439,1.,0.866025403784439,
1.,0.866025403784439,1.,0.866025403784439,1.,0.866025403784439,1.))
REPRESENTATION_ITEM('')
);
#1492=(
BOUNDED_CURVE()
B_SPLINE_CURVE(2,(#243044,#243045,#243046,#243047,#243048,#243049,#243050,
#243051,#243052,#243053,#243054,#243055,#243056),.UNSPECIFIED.,.F.,.F.)
B_SPLINE_CURVE_WITH_KNOTS((3,2,2,2,2,2,3),(0.543478260869565,0.55072463768116,
0.557971014492754,0.565217391304348,0.572463768115942,0.579710144927536,
0.586956521739131),.UNSPECIFIED.)
CURVE()
GEOMETRIC_REPRESENTATION_ITEM()
RATIONAL_B_SPLINE_CURVE((1.,0.866025403784439,1.,0.866025403784439,1.,0.866025403784439,
1.,0.866025403784439,1.,0.866025403784439,1.,0.866025403784439,1.))
REPRESENTATION_ITEM('')
);
#1493=(
BOUNDED_CURVE()
B_SPLINE_CURVE(2,(#243061,#243062,#243063,#243064,#243065,#243066,#243067,
#243068,#243069,#243070,#243071,#243072,#243073),.UNSPECIFIED.,.F.,.F.)
B_SPLINE_CURVE_WITH_KNOTS((3,2,2,2,2,2,3),(0.503109976740078,0.51040142567834,
0.517692874616602,0.524984323554864,0.532275772493126,0.539567221431388,
0.54685867036965),.UNSPECIFIED.)
CURVE()
GEOMETRIC_REPRESENTATION_ITEM()
RATIONAL_B_SPLINE_CURVE((1.,0.866025403784439,1.,0.866025403784439,1.,0.866025403784439,
1.,0.866025403784439,1.,0.866025403784439,1.,0.866025403784439,1.))
REPRESENTATION_ITEM('')
);
#1494=(
BOUNDED_CURVE()
B_SPLINE_CURVE(2,(#243074,#243075,#243076,#243077,#243078,#243079,#243080,
#243081,#243082,#243083,#243084,#243085,#243086),.UNSPECIFIED.,.F.,.F.)
B_SPLINE_CURVE_WITH_KNOTS((3,2,2,2,2,2,3),(0.5,0.507246376811594,0.514492753623189,
0.521739130434783,0.528985507246377,0.536231884057971,0.543478260869565),
 .UNSPECIFIED.)
CURVE()
GEOMETRIC_REPRESENTATION_ITEM()
RATIONAL_B_SPLINE_CURVE((1.,0.866025403784439,1.,0.866025403784439,1.,0.866025403784439,
1.,0.866025403784439,1.,0.866025403784439,1.,0.866025403784439,1.))
REPRESENTATION_ITEM('')
);
#1495=(
BOUNDED_CURVE()
B_SPLINE_CURVE(2,(#243091,#243092,#243093,#243094,#243095,#243096,#243097,
#243098,#243099,#243100,#243101,#243102,#243103),.UNSPECIFIED.,.F.,.F.)
B_SPLINE_CURVE_WITH_KNOTS((3,2,2,2,2,2,3),(0.459361283110506,0.466652732048768,
0.47394418098703,0.481235629925292,0.488527078863554,0.495818527801816,
0.503109976740078),.UNSPECIFIED.)
CURVE()
GEOMETRIC_REPRESENTATION_ITEM()
RATIONAL_B_SPLINE_CURVE((1.,0.866025403784439,1.,0.866025403784439,1.,0.866025403784439,
1.,0.866025403784439,1.,0.866025403784439,1.,0.866025403784439,1.))
REPRESENTATION_ITEM('')
);
#1496=(
BOUNDED_CURVE()
B_SPLINE_CURVE(2,(#243104,#243105,#243106,#243107,#243108,#243109,#243110,
#243111,#243112,#243113,#243114,#243115,#243116),.UNSPECIFIED.,.F.,.F.)
B_SPLINE_CURVE_WITH_KNOTS((3,2,2,2,2,2,3),(0.456521739130435,0.463768115942029,
0.471014492753623,0.478260869565218,0.485507246376812,0.492753623188406,
0.5),.UNSPECIFIED.)
CURVE()
GEOMETRIC_REPRESENTATION_ITEM()
RATIONAL_B_SPLINE_CURVE((1.,0.866025403784439,1.,0.866025403784439,1.,0.866025403784439,
1.,0.866025403784439,1.,0.866025403784439,1.,0.866025403784439,1.))
REPRESENTATION_ITEM('')
);
#1497=(
BOUNDED_CURVE()
B_SPLINE_CURVE(2,(#243121,#243122,#243123,#243124,#243125,#243126,#243127,
#243128,#243129,#243130,#243131,#243132,#243133),.UNSPECIFIED.,.F.,.F.)
B_SPLINE_CURVE_WITH_KNOTS((3,2,2,2,2,2,3),(0.415612589480934,0.422904038419196,
0.430195487357458,0.43748693629572,0.444778385233982,0.452069834172244,
0.459361283110506),.UNSPECIFIED.)
CURVE()
GEOMETRIC_REPRESENTATION_ITEM()
RATIONAL_B_SPLINE_CURVE((1.,0.866025403784439,1.,0.866025403784439,1.,0.866025403784439,
1.,0.866025403784439,1.,0.866025403784439,1.,0.866025403784439,1.))
REPRESENTATION_ITEM('')
);
#1498=(
BOUNDED_CURVE()
B_SPLINE_CURVE(2,(#243134,#243135,#243136,#243137,#243138,#243139,#243140,
#243141,#243142,#243143,#243144,#243145,#243146),.UNSPECIFIED.,.F.,.F.)
B_SPLINE_CURVE_WITH_KNOTS((3,2,2,2,2,2,3),(0.41304347826087,0.420289855072464,
0.427536231884058,0.434782608695652,0.442028985507247,0.449275362318841,
0.456521739130435),.UNSPECIFIED.)
CURVE()
GEOMETRIC_REPRESENTATION_ITEM()
RATIONAL_B_SPLINE_CURVE((1.,0.866025403784439,1.,0.866025403784439,1.,0.866025403784439,
1.,0.866025403784439,1.,0.866025403784439,1.,0.866025403784439,1.))
REPRESENTATION_ITEM('')
);
#1499=(
BOUNDED_CURVE()
B_SPLINE_CURVE(2,(#243151,#243152,#243153,#243154,#243155,#243156,#243157,
#243158,#243159,#243160,#243161,#243162,#243163),.UNSPECIFIED.,.F.,.F.)
B_SPLINE_CURVE_WITH_KNOTS((3,2,2,2,2,2,3),(0.371863895851362,0.379155344789624,
0.386446793727886,0.393738242666148,0.40102969160441,0.408321140542672,
0.415612589480934),.UNSPECIFIED.)
CURVE()
GEOMETRIC_REPRESENTATION_ITEM()
RATIONAL_B_SPLINE_CURVE((1.,0.866025403784439,1.,0.866025403784439,1.,0.866025403784439,
1.,0.866025403784439,1.,0.866025403784439,1.,0.866025403784439,1.))
REPRESENTATION_ITEM('')
);
#1500=(
BOUNDED_CURVE()
B_SPLINE_CURVE(2,(#243164,#243165,#243166,#243167,#243168,#243169,#243170,
#243171,#243172,#243173,#243174,#243175,#243176),.UNSPECIFIED.,.F.,.F.)
B_SPLINE_CURVE_WITH_KNOTS((3,2,2,2,2,2,3),(0.369565217391304,0.376811594202899,
0.384057971014493,0.391304347826087,0.398550724637682,0.405797101449275,
0.41304347826087),.UNSPECIFIED.)
CURVE()
GEOMETRIC_REPRESENTATION_ITEM()
RATIONAL_B_SPLINE_CURVE((1.,0.866025403784439,1.,0.866025403784439,1.,0.866025403784439,
1.,0.866025403784439,1.,0.866025403784439,1.,0.866025403784439,1.))
REPRESENTATION_ITEM('')
);
#1501=(
BOUNDED_CURVE()
B_SPLINE_CURVE(2,(#243181,#243182,#243183,#243184,#243185,#243186,#243187,
#243188,#243189,#243190,#243191,#243192,#243193),.UNSPECIFIED.,.F.,.F.)
B_SPLINE_CURVE_WITH_KNOTS((3,2,2,2,2,2,3),(0.32811520222179,0.335406651160052,
0.342698100098314,0.349989549036576,0.357280997974838,0.3645724469131,0.371863895851362),
 .UNSPECIFIED.)
CURVE()
GEOMETRIC_REPRESENTATION_ITEM()
RATIONAL_B_SPLINE_CURVE((1.,0.866025403784439,1.,0.866025403784439,1.,0.866025403784439,
1.,0.866025403784439,1.,0.866025403784439,1.,0.866025403784439,1.))
REPRESENTATION_ITEM('')
);
#1502=(
BOUNDED_CURVE()
B_SPLINE_CURVE(2,(#243194,#243195,#243196,#243197,#243198,#243199,#243200,
#243201,#243202,#243203,#243204,#243205,#243206),.UNSPECIFIED.,.F.,.F.)
B_SPLINE_CURVE_WITH_KNOTS((3,2,2,2,2,2,3),(0.326086956521739,0.333333333333334,
0.340579710144927,0.347826086956522,0.355072463768116,0.36231884057971,
0.369565217391304),.UNSPECIFIED.)
CURVE()
GEOMETRIC_REPRESENTATION_ITEM()
RATIONAL_B_SPLINE_CURVE((1.,0.866025403784439,1.,0.866025403784439,1.,0.866025403784439,
1.,0.866025403784439,1.,0.866025403784439,1.,0.866025403784439,1.))
REPRESENTATION_ITEM('')
);
#1503=(
BOUNDED_CURVE()
B_SPLINE_CURVE(2,(#243211,#243212,#243213,#243214,#243215,#243216,#243217,
#243218,#243219,#243220,#243221,#243222,#243223),.UNSPECIFIED.,.F.,.F.)
B_SPLINE_CURVE_WITH_KNOTS((3,2,2,2,2,2,3),(0.284366508592218,0.29165795753048,
0.298949406468742,0.306240855407004,0.313532304345266,0.320823753283528,
0.32811520222179),.UNSPECIFIED.)
CURVE()
GEOMETRIC_REPRESENTATION_ITEM()
RATIONAL_B_SPLINE_CURVE((1.,0.866025403784439,1.,0.866025403784439,1.,0.866025403784439,
1.,0.866025403784439,1.,0.866025403784439,1.,0.866025403784439,1.))
REPRESENTATION_ITEM('')
);
#1504=(
BOUNDED_CURVE()
B_SPLINE_CURVE(2,(#243224,#243225,#243226,#243227,#243228,#243229,#243230,
#243231,#243232,#243233,#243234,#243235,#243236),.UNSPECIFIED.,.F.,.F.)
B_SPLINE_CURVE_WITH_KNOTS((3,2,2,2,2,2,3),(0.282608695652174,0.289855072463769,
0.297101449275363,0.304347826086956,0.311594202898551,0.318840579710145,
0.326086956521739),.UNSPECIFIED.)
CURVE()
GEOMETRIC_REPRESENTATION_ITEM()
RATIONAL_B_SPLINE_CURVE((1.,0.866025403784439,1.,0.866025403784439,1.,0.866025403784439,
1.,0.866025403784439,1.,0.866025403784439,1.,0.866025403784439,1.))
REPRESENTATION_ITEM('')
);
#1505=(
BOUNDED_CURVE()
B_SPLINE_CURVE(2,(#243241,#243242,#243243,#243244,#243245,#243246,#243247,
#243248,#243249,#243250,#243251,#243252,#243253),.UNSPECIFIED.,.F.,.F.)
B_SPLINE_CURVE_WITH_KNOTS((3,2,2,2,2,2,3),(0.240617814962646,0.247909263900908,
0.25520071283917,0.262492161777432,0.269783610715694,0.277075059653956,
0.284366508592218),.UNSPECIFIED.)
CURVE()
GEOMETRIC_REPRESENTATION_ITEM()
RATIONAL_B_SPLINE_CURVE((1.,0.866025403784439,1.,0.866025403784439,1.,0.866025403784439,
1.,0.866025403784439,1.,0.866025403784439,1.,0.866025403784439,1.))
REPRESENTATION_ITEM('')
);
#1506=(
BOUNDED_CURVE()
B_SPLINE_CURVE(2,(#243254,#243255,#243256,#243257,#243258,#243259,#243260,
#243261,#243262,#243263,#243264,#243265,#243266),.UNSPECIFIED.,.F.,.F.)
B_SPLINE_CURVE_WITH_KNOTS((3,2,2,2,2,2,3),(0.239130434782609,0.246376811594203,
0.253623188405797,0.260869565217392,0.268115942028985,0.27536231884058,
0.282608695652174),.UNSPECIFIED.)
CURVE()
GEOMETRIC_REPRESENTATION_ITEM()
RATIONAL_B_SPLINE_CURVE((1.,0.866025403784439,1.,0.866025403784439,1.,0.866025403784439,
1.,0.866025403784439,1.,0.866025403784439,1.,0.866025403784439,1.))
REPRESENTATION_ITEM('')
);
#1507=(
BOUNDED_CURVE()
B_SPLINE_CURVE(2,(#243271,#243272,#243273,#243274,#243275,#243276,#243277,
#243278,#243279,#243280,#243281,#243282,#243283),.UNSPECIFIED.,.F.,.F.)
B_SPLINE_CURVE_WITH_KNOTS((3,2,2,2,2,2,3),(0.196869121333074,0.204160570271336,
0.211452019209598,0.21874346814786,0.226034917086122,0.233326366024384,
0.240617814962646),.UNSPECIFIED.)
CURVE()
GEOMETRIC_REPRESENTATION_ITEM()
RATIONAL_B_SPLINE_CURVE((1.,0.866025403784439,1.,0.866025403784439,1.,0.866025403784439,
1.,0.866025403784439,1.,0.866025403784439,1.,0.866025403784439,1.))
REPRESENTATION_ITEM('')
);
#1508=(
BOUNDED_CURVE()
B_SPLINE_CURVE(2,(#243284,#243285,#243286,#243287,#243288,#243289,#243290,
#243291,#243292,#243293,#243294,#243295,#243296),.UNSPECIFIED.,.F.,.F.)
B_SPLINE_CURVE_WITH_KNOTS((3,2,2,2,2,2,3),(0.195652173913044,0.202898550724638,
0.210144927536232,0.217391304347826,0.224637681159421,0.231884057971015,
0.239130434782609),.UNSPECIFIED.)
CURVE()
GEOMETRIC_REPRESENTATION_ITEM()
RATIONAL_B_SPLINE_CURVE((1.,0.866025403784439,1.,0.866025403784439,1.,0.866025403784439,
1.,0.866025403784439,1.,0.866025403784439,1.,0.866025403784439,1.))
REPRESENTATION_ITEM('')
);
#1509=(
BOUNDED_CURVE()
B_SPLINE_CURVE(2,(#243301,#243302,#243303,#243304,#243305,#243306,#243307,
#243308,#243309,#243310,#243311,#243312,#243313),.UNSPECIFIED.,.F.,.F.)
B_SPLINE_CURVE_WITH_KNOTS((3,2,2,2,2,2,3),(0.153120427703502,0.160411876641764,
0.167703325580026,0.174994774518288,0.18228622345655,0.189577672394812,
0.196869121333074),.UNSPECIFIED.)
CURVE()
GEOMETRIC_REPRESENTATION_ITEM()
RATIONAL_B_SPLINE_CURVE((1.,0.866025403784439,1.,0.866025403784439,1.,0.866025403784439,
1.,0.866025403784439,1.,0.866025403784439,1.,0.866025403784439,1.))
REPRESENTATION_ITEM('')
);
#1510=(
BOUNDED_CURVE()
B_SPLINE_CURVE(2,(#243314,#243315,#243316,#243317,#243318,#243319,#243320,
#243321,#243322,#243323,#243324,#243325,#243326),.UNSPECIFIED.,.F.,.F.)
B_SPLINE_CURVE_WITH_KNOTS((3,2,2,2,2,2,3),(0.152173913043478,0.159420289855073,
0.166666666666667,0.173913043478261,0.181159420289855,0.18840579710145,
0.195652173913044),.UNSPECIFIED.)
CURVE()
GEOMETRIC_REPRESENTATION_ITEM()
RATIONAL_B_SPLINE_CURVE((1.,0.866025403784439,1.,0.866025403784439,1.,0.866025403784439,
1.,0.866025403784439,1.,0.866025403784439,1.,0.866025403784439,1.))
REPRESENTATION_ITEM('')
);
#1511=(
BOUNDED_CURVE()
B_SPLINE_CURVE(2,(#243331,#243332,#243333,#243334,#243335,#243336,#243337,
#243338,#243339,#243340,#243341,#243342,#243343),.UNSPECIFIED.,.F.,.F.)
B_SPLINE_CURVE_WITH_KNOTS((3,2,2,2,2,2,3),(0.10937173407393,0.116663183012192,
0.123954631950454,0.131246080888716,0.138537529826978,0.14582897876524,
0.153120427703502),.UNSPECIFIED.)
CURVE()
GEOMETRIC_REPRESENTATION_ITEM()
RATIONAL_B_SPLINE_CURVE((1.,0.866025403784439,1.,0.866025403784439,1.,0.866025403784439,
1.,0.866025403784439,1.,0.866025403784439,1.,0.866025403784439,1.))
REPRESENTATION_ITEM('')
);
#1512=(
BOUNDED_CURVE()
B_SPLINE_CURVE(2,(#243344,#243345,#243346,#243347,#243348,#243349,#243350,
#243351,#243352,#243353,#243354,#243355,#243356),.UNSPECIFIED.,.F.,.F.)
B_SPLINE_CURVE_WITH_KNOTS((3,2,2,2,2,2,3),(0.108695652173913,0.115942028985507,
0.123188405797102,0.130434782608696,0.13768115942029,0.144927536231884,
0.152173913043478),.UNSPECIFIED.)
CURVE()
GEOMETRIC_REPRESENTATION_ITEM()
RATIONAL_B_SPLINE_CURVE((1.,0.866025403784439,1.,0.866025403784439,1.,0.866025403784439,
1.,0.866025403784439,1.,0.866025403784439,1.,0.866025403784439,1.))
REPRESENTATION_ITEM('')
);
#1513=(
BOUNDED_CURVE()
B_SPLINE_CURVE(2,(#243361,#243362,#243363,#243364,#243365,#243366,#243367,
#243368,#243369,#243370,#243371,#243372,#243373),.UNSPECIFIED.,.F.,.F.)
B_SPLINE_CURVE_WITH_KNOTS((3,2,2,2,2,2,3),(0.065623040444358,0.07291448938262,
0.080205938320882,0.087497387259144,0.094788836197406,0.102080285135668,
0.10937173407393),.UNSPECIFIED.)
CURVE()
GEOMETRIC_REPRESENTATION_ITEM()
RATIONAL_B_SPLINE_CURVE((1.,0.866025403784439,1.,0.866025403784439,1.,0.866025403784439,
1.,0.866025403784439,1.,0.866025403784439,1.,0.866025403784439,1.))
REPRESENTATION_ITEM('')
);
#1514=(
BOUNDED_CURVE()
B_SPLINE_CURVE(2,(#243374,#243375,#243376,#243377,#243378,#243379,#243380,
#243381,#243382,#243383,#243384,#243385,#243386),.UNSPECIFIED.,.F.,.F.)
B_SPLINE_CURVE_WITH_KNOTS((3,2,2,2,2,2,3),(0.065217391304348,0.0724637681159422,
0.0797101449275364,0.0869565217391306,0.0942028985507248,0.101449275362319,
0.108695652173913),.UNSPECIFIED.)
CURVE()
GEOMETRIC_REPRESENTATION_ITEM()
RATIONAL_B_SPLINE_CURVE((1.,0.866025403784439,1.,0.866025403784439,1.,0.866025403784439,
1.,0.866025403784439,1.,0.866025403784439,1.,0.866025403784439,1.))
REPRESENTATION_ITEM('')
);
#1515=(
BOUNDED_CURVE()
B_SPLINE_CURVE(2,(#243393,#243394,#243395,#243396,#243397),
 .UNSPECIFIED.,.F.,.F.)
B_SPLINE_CURVE_WITH_KNOTS((3,2,3),(0.0118893770663285,0.014582897876524,
0.021874346814786),.UNSPECIFIED.)
CURVE()
GEOMETRIC_REPRESENTATION_ITEM()
RATIONAL_B_SPLINE_CURVE((0.937582367981142,0.950508689562301,1.,0.866025403784439,
1.))
REPRESENTATION_ITEM('')
);
#1516=(
BOUNDED_CURVE()
B_SPLINE_CURVE(2,(#243949,#243950,#243951),.UNSPECIFIED.,.F.,.F.)
B_SPLINE_CURVE_WITH_KNOTS((3,3),(0.305379135947461,0.795630657118022),
 .UNSPECIFIED.)
CURVE()
GEOMETRIC_REPRESENTATION_ITEM()
RATIONAL_B_SPLINE_CURVE((1.45513171305057,1.68024137247218,1.45513171305058))
REPRESENTATION_ITEM('')
);
#1517=(
BOUNDED_CURVE()
B_SPLINE_CURVE(2,(#243954,#243955,#243956),.UNSPECIFIED.,.F.,.F.)
B_SPLINE_CURVE_WITH_KNOTS((3,3),(-1.92744743716646,-0.984663180908388),
 .UNSPECIFIED.)
CURVE()
GEOMETRIC_REPRESENTATION_ITEM()
RATIONAL_B_SPLINE_CURVE((2.94675698395174,3.40262187584188,2.94675698395181))
REPRESENTATION_ITEM('')
);
#1518=(
BOUNDED_CURVE()
B_SPLINE_CURVE(2,(#243961,#243962,#243963),.UNSPECIFIED.,.F.,.F.)
B_SPLINE_CURVE_WITH_KNOTS((3,3),(0.313853530401117,0.810060947929668),
 .UNSPECIFIED.)
CURVE()
GEOMETRIC_REPRESENTATION_ITEM()
RATIONAL_B_SPLINE_CURVE((1.46945873729773,1.69678479508373,1.46945873729773))
REPRESENTATION_ITEM('')
);
#1519=(
BOUNDED_CURVE()
B_SPLINE_CURVE(2,(#243964,#243965,#243966),.UNSPECIFIED.,.F.,.F.)
B_SPLINE_CURVE_WITH_KNOTS((3,3),(-1.9274474371665,-0.98466318090834),
 .UNSPECIFIED.)
CURVE()
GEOMETRIC_REPRESENTATION_ITEM()
RATIONAL_B_SPLINE_CURVE((2.94675698395173,3.40262187584197,2.94675698395179))
REPRESENTATION_ITEM('')
);
#1520=(
BOUNDED_CURVE()
B_SPLINE_CURVE(2,(#243971,#243972,#243973),.UNSPECIFIED.,.F.,.F.)
B_SPLINE_CURVE_WITH_KNOTS((3,3),(0.337455036462552,0.850307797466422),
 .UNSPECIFIED.)
CURVE()
GEOMETRIC_REPRESENTATION_ITEM()
RATIONAL_B_SPLINE_CURVE((1.5095308677303,1.74305610566815,1.5095308677303))
REPRESENTATION_ITEM('')
);
#1521=(
BOUNDED_CURVE()
B_SPLINE_CURVE(2,(#243974,#243975,#243976),.UNSPECIFIED.,.F.,.F.)
B_SPLINE_CURVE_WITH_KNOTS((3,3),(-1.75023669514897,-0.881692746819963),
 .UNSPECIFIED.)
CURVE()
GEOMETRIC_REPRESENTATION_ITEM()
RATIONAL_B_SPLINE_CURVE((2.72423919983985,3.14568047072895,2.72423919983986))
REPRESENTATION_ITEM('')
);
#1522=(
BOUNDED_CURVE()
B_SPLINE_CURVE(2,(#243981,#243982,#243983),.UNSPECIFIED.,.F.,.F.)
B_SPLINE_CURVE_WITH_KNOTS((3,3),(0.296747814710797,0.78094561467123),
 .UNSPECIFIED.)
CURVE()
GEOMETRIC_REPRESENTATION_ITEM()
RATIONAL_B_SPLINE_CURVE((1.44057579043547,1.66343364079194,1.44057579043547))
REPRESENTATION_ITEM('')
);
#1523=(
BOUNDED_CURVE()
B_SPLINE_CURVE(2,(#243984,#243985,#243986),.UNSPECIFIED.,.F.,.F.)
B_SPLINE_CURVE_WITH_KNOTS((3,3),(-1.65890795248092,-0.828567311293231),
 .UNSPECIFIED.)
CURVE()
GEOMETRIC_REPRESENTATION_ITEM()
RATIONAL_B_SPLINE_CURVE((2.60974794608846,3.01347735838248,2.60974794608845))
REPRESENTATION_ITEM('')
);
#1524=(
BOUNDED_CURVE()
B_SPLINE_CURVE(2,(#243991,#243992,#243993),.UNSPECIFIED.,.F.,.F.)
B_SPLINE_CURVE_WITH_KNOTS((3,3),(0.327461385305039,0.833256095326246),
 .UNSPECIFIED.)
CURVE()
GEOMETRIC_REPRESENTATION_ITEM()
RATIONAL_B_SPLINE_CURVE((1.49253377429497,1.72342955272753,1.49253377429496))
REPRESENTATION_ITEM('')
);
#1525=(
BOUNDED_CURVE()
B_SPLINE_CURVE(2,(#243994,#243995,#243996),.UNSPECIFIED.,.F.,.F.)
B_SPLINE_CURVE_WITH_KNOTS((3,3),(-1.63785199431076,-0.816312569741005),
 .UNSPECIFIED.)
CURVE()
GEOMETRIC_REPRESENTATION_ITEM()
RATIONAL_B_SPLINE_CURVE((2.58337319633923,2.9830224206474,2.58337319633922))
REPRESENTATION_ITEM('')
);
#1526=(
BOUNDED_CURVE()
B_SPLINE_CURVE(2,(#243998,#243999,#244000),.UNSPECIFIED.,.F.,.F.)
B_SPLINE_CURVE_WITH_KNOTS((3,3),(0.336410883504879,0.848525565411443),
 .UNSPECIFIED.)
CURVE()
GEOMETRIC_REPRESENTATION_ITEM()
RATIONAL_B_SPLINE_CURVE((1.50775306979144,1.74100328143105,1.50775306979145))
REPRESENTATION_ITEM('')
);
#1527=(
BOUNDED_CURVE()
B_SPLINE_CURVE(2,(#244001,#244002,#244003),.UNSPECIFIED.,.F.,.F.)
B_SPLINE_CURVE_WITH_KNOTS((3,3),(-1.93645569281037,-0.989894173396402),
 .UNSPECIFIED.)
CURVE()
GEOMETRIC_REPRESENTATION_ITEM()
RATIONAL_B_SPLINE_CURVE((2.9580792886783,3.41569574720537,2.9580792886783))
REPRESENTATION_ITEM('')
);
#1528=(
BOUNDED_CURVE()
B_SPLINE_CURVE(2,(#247964,#247965,#247966),.UNSPECIFIED.,.F.,.F.)
B_SPLINE_CURVE_WITH_KNOTS((3,3),(-1.19817642475198,-1.13405670867392),
 .UNSPECIFIED.)
CURVE()
GEOMETRIC_REPRESENTATION_ITEM()
RATIONAL_B_SPLINE_CURVE((1.00675929761165,1.00683091269735,1.00687550567357))
REPRESENTATION_ITEM('')
);
#1529=(
BOUNDED_CURVE()
B_SPLINE_CURVE(3,(#248095,#248096,#248097,#248098,#248099,#248100),
 .UNSPECIFIED.,.F.,.F.)
B_SPLINE_CURVE_WITH_KNOTS((4,2,4),(0.,0.5,1.),.UNSPECIFIED.)
CURVE()
GEOMETRIC_REPRESENTATION_ITEM()
RATIONAL_B_SPLINE_CURVE((0.99999997576651,0.999999976303432,0.999999976712256,
0.999999977274856,0.999999977413013,0.999999977414642))
REPRESENTATION_ITEM('')
);
#1530=(
BOUNDED_CURVE()
B_SPLINE_CURVE(3,(#248243,#248244,#248245,#248246,#248247,#248248),
 .UNSPECIFIED.,.F.,.F.)
B_SPLINE_CURVE_WITH_KNOTS((4,2,4),(0.,0.5,1.),.UNSPECIFIED.)
CURVE()
GEOMETRIC_REPRESENTATION_ITEM()
RATIONAL_B_SPLINE_CURVE((0.999999975766518,0.999999976303441,0.999999976712265,
0.999999977274864,0.999999977413021,0.99999997741465))
REPRESENTATION_ITEM('')
);
#1531=(
BOUNDED_CURVE()
B_SPLINE_CURVE(2,(#252039,#252040,#252041,#252042,#252043,#252044,#252045,
#252046,#252047,#252048,#252049,#252050,#252051),.UNSPECIFIED.,.F.,.F.)
B_SPLINE_CURVE_WITH_KNOTS((3,2,2,2,2,2,3),(0.021874346814786,0.029165795753048,
0.03645724469131,0.043748693629572,0.051040142567834,0.058331591506096,
0.065623040444358),.UNSPECIFIED.)
CURVE()
GEOMETRIC_REPRESENTATION_ITEM()
RATIONAL_B_SPLINE_CURVE((1.,0.866025403784439,1.,0.866025403784439,1.,0.866025403784439,
1.,0.866025403784439,1.,0.866025403784439,1.,0.866025403784439,1.))
REPRESENTATION_ITEM('')
);
#1532=(
BOUNDED_CURVE()
B_SPLINE_CURVE(2,(#252052,#252053,#252054,#252055,#252056,#252057,#252058,
#252059,#252060,#252061,#252062,#252063,#252064),.UNSPECIFIED.,.F.,.F.)
B_SPLINE_CURVE_WITH_KNOTS((3,2,2,2,2,2,3),(0.0217391304347828,0.028985507246377,
0.0362318840579712,0.0434782608695654,0.0507246376811596,0.0579710144927538,
0.065217391304348),.UNSPECIFIED.)
CURVE()
GEOMETRIC_REPRESENTATION_ITEM()
RATIONAL_B_SPLINE_CURVE((1.,0.866025403784442,1.,0.866025403784439,1.,0.866025403784439,
1.,0.866025403784439,1.,0.866025403784439,1.,0.866025403784439,1.))
REPRESENTATION_ITEM('')
);
#1533=(
BOUNDED_CURVE()
B_SPLINE_CURVE(2,(#256140,#256141,#256142,#256143,#256144,#256145,#256146,
#256147,#256148,#256149,#256150,#256151,#256152),.UNSPECIFIED.,.F.,.F.)
B_SPLINE_CURVE_WITH_KNOTS((3,2,2,2,2,2,3),(0.021874346814786,0.029165795753048,
0.03645724469131,0.043748693629572,0.051040142567834,0.058331591506096,
0.065623040444358),.UNSPECIFIED.)
CURVE()
GEOMETRIC_REPRESENTATION_ITEM()
RATIONAL_B_SPLINE_CURVE((1.,0.866025403784439,1.,0.866025403784439,1.,0.866025403784439,
1.,0.866025403784439,1.,0.866025403784439,1.,0.866025403784439,1.))
REPRESENTATION_ITEM('')
);
#1534=(
BOUNDED_CURVE()
B_SPLINE_CURVE(2,(#256153,#256154,#256155,#256156,#256157,#256158,#256159,
#256160,#256161,#256162,#256163,#256164,#256165),.UNSPECIFIED.,.F.,.F.)
B_SPLINE_CURVE_WITH_KNOTS((3,2,2,2,2,2,3),(0.0217391304347828,0.028985507246377,
0.0362318840579712,0.0434782608695654,0.0507246376811596,0.0579710144927538,
0.065217391304348),.UNSPECIFIED.)
CURVE()
GEOMETRIC_REPRESENTATION_ITEM()
RATIONAL_B_SPLINE_CURVE((1.,0.866025403784442,1.,0.866025403784439,1.,0.866025403784439,
1.,0.866025403784439,1.,0.866025403784439,1.,0.866025403784439,1.))
REPRESENTATION_ITEM('')
);
#1535=(
BOUNDED_CURVE()
B_SPLINE_CURVE(2,(#260278,#260279,#260280,#260281,#260282,#260283,#260284,
#260285,#260286,#260287,#260288,#260289,#260290),.UNSPECIFIED.,.F.,.F.)
B_SPLINE_CURVE_WITH_KNOTS((3,2,2,2,2,2,3),(0.021874346814786,0.029165795753048,
0.03645724469131,0.043748693629572,0.051040142567834,0.058331591506096,
0.065623040444358),.UNSPECIFIED.)
CURVE()
GEOMETRIC_REPRESENTATION_ITEM()
RATIONAL_B_SPLINE_CURVE((1.,0.866025403784439,1.,0.866025403784439,1.,0.866025403784439,
1.,0.866025403784439,1.,0.866025403784439,1.,0.866025403784439,1.))
REPRESENTATION_ITEM('')
);
#1536=(
BOUNDED_CURVE()
B_SPLINE_CURVE(2,(#260291,#260292,#260293,#260294,#260295,#260296,#260297,
#260298,#260299,#260300,#260301,#260302,#260303),.UNSPECIFIED.,.F.,.F.)
B_SPLINE_CURVE_WITH_KNOTS((3,2,2,2,2,2,3),(0.0217391304347828,0.028985507246377,
0.0362318840579711,0.0434782608695653,0.0507246376811596,0.0579710144927538,
0.065217391304348),.UNSPECIFIED.)
CURVE()
GEOMETRIC_REPRESENTATION_ITEM()
RATIONAL_B_SPLINE_CURVE((1.,0.866025403784441,1.,0.866025403784439,1.,0.866025403784439,
1.,0.866025403784439,1.,0.866025403784439,1.,0.866025403784439,1.))
REPRESENTATION_ITEM('')
);
#1537=(
BOUNDED_CURVE()
B_SPLINE_CURVE(2,(#264429,#264430,#264431,#264432,#264433,#264434,#264435,
#264436,#264437,#264438,#264439,#264440,#264441),.UNSPECIFIED.,.F.,.F.)
B_SPLINE_CURVE_WITH_KNOTS((3,2,2,2,2,2,3),(0.021874346814786,0.029165795753048,
0.03645724469131,0.043748693629572,0.051040142567834,0.058331591506096,
0.065623040444358),.UNSPECIFIED.)
CURVE()
GEOMETRIC_REPRESENTATION_ITEM()
RATIONAL_B_SPLINE_CURVE((1.,0.866025403784439,1.,0.866025403784439,1.,0.866025403784439,
1.,0.866025403784439,1.,0.866025403784439,1.,0.866025403784439,1.))
REPRESENTATION_ITEM('')
);
#1538=(
BOUNDED_CURVE()
B_SPLINE_CURVE(2,(#264442,#264443,#264444,#264445,#264446,#264447,#264448,
#264449,#264450,#264451,#264452,#264453,#264454),.UNSPECIFIED.,.F.,.F.)
B_SPLINE_CURVE_WITH_KNOTS((3,2,2,2,2,2,3),(0.0217391304347828,0.028985507246377,
0.0362318840579712,0.0434782608695654,0.0507246376811596,0.0579710144927538,
0.065217391304348),.UNSPECIFIED.)
CURVE()
GEOMETRIC_REPRESENTATION_ITEM()
RATIONAL_B_SPLINE_CURVE((1.,0.866025403784442,1.,0.866025403784439,1.,0.866025403784439,
1.,0.866025403784439,1.,0.866025403784439,1.,0.866025403784439,1.))
REPRESENTATION_ITEM('')
);
#1539=(
BOUNDED_CURVE()
B_SPLINE_CURVE(2,(#275566,#275567,#275568),.UNSPECIFIED.,.F.,.F.)
B_SPLINE_CURVE_WITH_KNOTS((3,3),(0.701923076923077,0.701927534605613),
 .UNSPECIFIED.)
CURVE()
GEOMETRIC_REPRESENTATION_ITEM()
RATIONAL_B_SPLINE_CURVE((1.,0.99988654925346,0.999773624463427))
REPRESENTATION_ITEM('')
);
#1540=(
BOUNDED_CURVE()
B_SPLINE_CURVE(2,(#275574,#275575,#275576,#275577,#275578,#275579,#275580,
#275581,#275582,#275583,#275584,#275585,#275586,#275587,#275588,#275589,
#275590,#275591,#275592),.UNSPECIFIED.,.F.,.F.)
B_SPLINE_CURVE_WITH_KNOTS((3,2,2,2,2,2,2,2,2,3),(0.682692307692308,0.684615384615385,
0.686538461538462,0.688461538461538,0.690384615384615,0.692307692307692,
0.694230769230769,0.696153846153846,0.698076923076923,0.699514511997895),
 .UNSPECIFIED.)
CURVE()
GEOMETRIC_REPRESENTATION_ITEM()
RATIONAL_B_SPLINE_CURVE((1.,0.951056516295154,1.,0.951056516295154,1.,0.951056516295154,
1.,0.951056516295154,1.,0.951056516295154,1.,0.951056516295154,1.,0.951056516295154,
1.,0.951056516295154,1.,0.963412482837523,0.981526687366426))
REPRESENTATION_ITEM('')
);
#1541=(
BOUNDED_CURVE()
B_SPLINE_CURVE(2,(#275594,#275595,#275596,#275597,#275598,#275599,#275600,
#275601,#275602,#275603,#275604,#275605,#275606,#275607,#275608,#275609,
#275610,#275611,#275612,#275613,#275614),.UNSPECIFIED.,.F.,.F.)
B_SPLINE_CURVE_WITH_KNOTS((3,2,2,2,2,2,2,2,2,2,3),(0.682692307692308,0.684615384615385,
0.686538461538462,0.688461538461538,0.690384615384615,0.692307692307692,
0.694230769230769,0.696153846153846,0.698076923076923,0.7,0.701923076923077),
 .UNSPECIFIED.)
CURVE()
GEOMETRIC_REPRESENTATION_ITEM()
RATIONAL_B_SPLINE_CURVE((1.,0.951056516295154,1.,0.951056516295154,1.,0.951056516295154,
1.,0.951056516295154,1.,0.951056516295154,1.,0.951056516295154,1.,0.951056516295154,
1.,0.951056516295154,1.,0.951056516295154,1.,0.951056516295154,1.))
REPRESENTATION_ITEM('')
);
#1542=(
BOUNDED_CURVE()
B_SPLINE_CURVE(2,(#275619,#275620,#275621,#275622,#275623,#275624,#275625,
#275626,#275627,#275628,#275629,#275630,#275631,#275632,#275633,#275634,
#275635,#275636,#275637,#275638,#275639),.UNSPECIFIED.,.F.,.F.)
B_SPLINE_CURVE_WITH_KNOTS((3,2,2,2,2,2,2,2,2,2,3),(0.663461538461538,0.665384615384615,
0.667307692307692,0.669230769230769,0.671153846153846,0.673076923076923,
0.675,0.676923076923077,0.678846153846154,0.680769230769231,0.682692307692308),
 .UNSPECIFIED.)
CURVE()
GEOMETRIC_REPRESENTATION_ITEM()
RATIONAL_B_SPLINE_CURVE((1.,0.951056516295154,1.,0.951056516295154,1.,0.951056516295154,
1.,0.951056516295154,1.,0.951056516295154,1.,0.951056516295154,1.,0.951056516295154,
1.,0.951056516295154,1.,0.951056516295154,1.,0.951056516295154,1.))
REPRESENTATION_ITEM('')
);
#1543=(
BOUNDED_CURVE()
B_SPLINE_CURVE(2,(#275640,#275641,#275642,#275643,#275644,#275645,#275646,
#275647,#275648,#275649,#275650,#275651,#275652,#275653,#275654,#275655,
#275656,#275657,#275658,#275659,#275660),.UNSPECIFIED.,.F.,.F.)
B_SPLINE_CURVE_WITH_KNOTS((3,2,2,2,2,2,2,2,2,2,3),(0.663461538461538,0.665384615384615,
0.667307692307692,0.669230769230769,0.671153846153846,0.673076923076923,
0.675,0.676923076923077,0.678846153846154,0.680769230769231,0.682692307692308),
 .UNSPECIFIED.)
CURVE()
GEOMETRIC_REPRESENTATION_ITEM()
RATIONAL_B_SPLINE_CURVE((1.,0.951056516295154,1.,0.951056516295154,1.,0.951056516295154,
1.,0.951056516295154,1.,0.951056516295154,1.,0.951056516295154,1.,0.951056516295154,
1.,0.951056516295154,1.,0.951056516295154,1.,0.951056516295154,1.))
REPRESENTATION_ITEM('')
);
#1544=(
BOUNDED_CURVE()
B_SPLINE_CURVE(2,(#275665,#275666,#275667,#275668,#275669,#275670,#275671,
#275672,#275673,#275674,#275675,#275676,#275677,#275678,#275679,#275680,
#275681,#275682,#275683,#275684,#275685),.UNSPECIFIED.,.F.,.F.)
B_SPLINE_CURVE_WITH_KNOTS((3,2,2,2,2,2,2,2,2,2,3),(0.644230769230769,0.646153846153846,
0.648076923076923,0.65,0.651923076923077,0.653846153846154,0.655769230769231,
0.657692307692308,0.659615384615385,0.661538461538462,0.663461538461538),
 .UNSPECIFIED.)
CURVE()
GEOMETRIC_REPRESENTATION_ITEM()
RATIONAL_B_SPLINE_CURVE((1.,0.951056516295154,1.,0.951056516295154,1.,0.951056516295154,
1.,0.951056516295154,1.,0.951056516295154,1.,0.951056516295154,1.,0.951056516295154,
1.,0.951056516295154,1.,0.951056516295154,1.,0.951056516295154,1.))
REPRESENTATION_ITEM('')
);
#1545=(
BOUNDED_CURVE()
B_SPLINE_CURVE(2,(#275686,#275687,#275688,#275689,#275690,#275691,#275692,
#275693,#275694,#275695,#275696,#275697,#275698,#275699,#275700,#275701,
#275702,#275703,#275704,#275705,#275706),.UNSPECIFIED.,.F.,.F.)
B_SPLINE_CURVE_WITH_KNOTS((3,2,2,2,2,2,2,2,2,2,3),(0.644230769230769,0.646153846153846,
0.648076923076923,0.65,0.651923076923077,0.653846153846154,0.655769230769231,
0.657692307692308,0.659615384615385,0.661538461538462,0.663461538461538),
 .UNSPECIFIED.)
CURVE()
GEOMETRIC_REPRESENTATION_ITEM()
RATIONAL_B_SPLINE_CURVE((1.,0.951056516295154,1.,0.951056516295154,1.,0.951056516295154,
1.,0.951056516295154,1.,0.951056516295154,1.,0.951056516295154,1.,0.951056516295154,
1.,0.951056516295154,1.,0.951056516295154,1.,0.951056516295154,1.))
REPRESENTATION_ITEM('')
);
#1546=(
BOUNDED_CURVE()
B_SPLINE_CURVE(2,(#275712,#275713,#275714,#275715,#275716,#275717,#275718,
#275719,#275720),.UNSPECIFIED.,.F.,.F.)
B_SPLINE_CURVE_WITH_KNOTS((3,2,2,2,3),(0.618568719050757,0.619230769230769,
0.621153846153846,0.623076923076923,0.625),.UNSPECIFIED.)
CURVE()
GEOMETRIC_REPRESENTATION_ITEM()
RATIONAL_B_SPLINE_CURVE((0.977902315623412,0.983150418057436,1.,0.951056516295154,
1.,0.951056516295154,1.,0.951056516295154,1.))
REPRESENTATION_ITEM('')
);
#1547=(
BOUNDED_CURVE()
B_SPLINE_CURVE(2,(#275723,#275724,#275725,#275726,#275727,#275728,#275729,
#275730,#275731,#275732,#275733),.UNSPECIFIED.,.F.,.F.)
B_SPLINE_CURVE_WITH_KNOTS((3,2,2,2,2,3),(0.616175777003085,0.617307692307692,
0.619230769230769,0.621153846153846,0.623076923076923,0.625),
 .UNSPECIFIED.)
CURVE()
GEOMETRIC_REPRESENTATION_ITEM()
RATIONAL_B_SPLINE_CURVE((0.976296596823935,0.971192063301508,1.,0.951056516295154,
1.,0.951056516295154,1.,0.951056516295154,1.,0.951056516295154,1.))
REPRESENTATION_ITEM('')
);
#1548=(
BOUNDED_CURVE()
B_SPLINE_CURVE(2,(#276333,#276334,#276335),.UNSPECIFIED.,.F.,.F.)
B_SPLINE_CURVE_WITH_KNOTS((3,3),(-7.37746868484566,-5.33580039117808),
 .UNSPECIFIED.)
CURVE()
GEOMETRIC_REPRESENTATION_ITEM()
RATIONAL_B_SPLINE_CURVE((1.82136720504436,1.96225044864938,1.96225044864938))
REPRESENTATION_ITEM('')
);
#1549=(
BOUNDED_CURVE()
B_SPLINE_CURVE(2,(#276339,#276340,#276341),.UNSPECIFIED.,.F.,.F.)
B_SPLINE_CURVE_WITH_KNOTS((3,3),(3.29413209751051,5.33580039117807),
 .UNSPECIFIED.)
CURVE()
GEOMETRIC_REPRESENTATION_ITEM()
RATIONAL_B_SPLINE_CURVE((1.82136720504436,1.96225044864938,1.96225044864938))
REPRESENTATION_ITEM('')
);
#1550=(
BOUNDED_CURVE()
B_SPLINE_CURVE(2,(#276343,#276344,#276345),.UNSPECIFIED.,.F.,.F.)
B_SPLINE_CURVE_WITH_KNOTS((3,3),(5.33580039117807,7.37746868484567),
 .UNSPECIFIED.)
CURVE()
GEOMETRIC_REPRESENTATION_ITEM()
RATIONAL_B_SPLINE_CURVE((1.96225044864938,1.96225044864939,1.82136720504436))
REPRESENTATION_ITEM('')
);
#1551=(
BOUNDED_CURVE()
B_SPLINE_CURVE(2,(#276348,#276349,#276350),.UNSPECIFIED.,.F.,.F.)
B_SPLINE_CURVE_WITH_KNOTS((3,3),(-5.33580039117808,-3.2941320975105),
 .UNSPECIFIED.)
CURVE()
GEOMETRIC_REPRESENTATION_ITEM()
RATIONAL_B_SPLINE_CURVE((1.96225044864938,1.96225044864938,1.82136720504436))
REPRESENTATION_ITEM('')
);
#1552=(
BOUNDED_CURVE()
B_SPLINE_CURVE(2,(#276352,#276353,#276354),.UNSPECIFIED.,.F.,.F.)
B_SPLINE_CURVE_WITH_KNOTS((3,3),(-7.37746868484565,-5.33580039117808),
 .UNSPECIFIED.)
CURVE()
GEOMETRIC_REPRESENTATION_ITEM()
RATIONAL_B_SPLINE_CURVE((1.82136720504435,1.96225044864937,1.96225044864937))
REPRESENTATION_ITEM('')
);
#1553=(
BOUNDED_CURVE()
B_SPLINE_CURVE(2,(#276356,#276357,#276358),.UNSPECIFIED.,.F.,.F.)
B_SPLINE_CURVE_WITH_KNOTS((3,3),(3.29413209751051,5.33580039117807),
 .UNSPECIFIED.)
CURVE()
GEOMETRIC_REPRESENTATION_ITEM()
RATIONAL_B_SPLINE_CURVE((1.82136720504436,1.96225044864937,1.96225044864937))
REPRESENTATION_ITEM('')
);
#1554=(
BOUNDED_CURVE()
B_SPLINE_CURVE(2,(#276360,#276361,#276362),.UNSPECIFIED.,.F.,.F.)
B_SPLINE_CURVE_WITH_KNOTS((3,3),(5.33580039117807,7.37746868484565),
 .UNSPECIFIED.)
CURVE()
GEOMETRIC_REPRESENTATION_ITEM()
RATIONAL_B_SPLINE_CURVE((1.96225044864937,1.96225044864937,1.82136720504436))
REPRESENTATION_ITEM('')
);
#1555=(
BOUNDED_CURVE()
B_SPLINE_CURVE(2,(#276365,#276366,#276367),.UNSPECIFIED.,.F.,.F.)
B_SPLINE_CURVE_WITH_KNOTS((3,3),(-5.33580039117808,-3.29413209751051),
 .UNSPECIFIED.)
CURVE()
GEOMETRIC_REPRESENTATION_ITEM()
RATIONAL_B_SPLINE_CURVE((1.96225044864937,1.96225044864937,1.82136720504436))
REPRESENTATION_ITEM('')
);
#1556=(
BOUNDED_CURVE()
B_SPLINE_CURVE(2,(#276369,#276370,#276371),.UNSPECIFIED.,.F.,.F.)
B_SPLINE_CURVE_WITH_KNOTS((3,3),(-7.37746868484568,-5.33580039117808),
 .UNSPECIFIED.)
CURVE()
GEOMETRIC_REPRESENTATION_ITEM()
RATIONAL_B_SPLINE_CURVE((1.82136720504436,1.96225044864938,1.96225044864938))
REPRESENTATION_ITEM('')
);
#1557=(
BOUNDED_CURVE()
B_SPLINE_CURVE(2,(#276373,#276374,#276375),.UNSPECIFIED.,.F.,.F.)
B_SPLINE_CURVE_WITH_KNOTS((3,3),(3.29413209751049,5.3358003911781),
 .UNSPECIFIED.)
CURVE()
GEOMETRIC_REPRESENTATION_ITEM()
RATIONAL_B_SPLINE_CURVE((1.82136720504436,1.96225044864939,1.96225044864938))
REPRESENTATION_ITEM('')
);
#1558=(
BOUNDED_CURVE()
B_SPLINE_CURVE(2,(#276377,#276378,#276379),.UNSPECIFIED.,.F.,.F.)
B_SPLINE_CURVE_WITH_KNOTS((3,3),(5.3358003911781,7.37746868484565),
 .UNSPECIFIED.)
CURVE()
GEOMETRIC_REPRESENTATION_ITEM()
RATIONAL_B_SPLINE_CURVE((1.96225044864938,1.96225044864938,1.82136720504436))
REPRESENTATION_ITEM('')
);
#1559=(
BOUNDED_CURVE()
B_SPLINE_CURVE(2,(#276382,#276383,#276384),.UNSPECIFIED.,.F.,.F.)
B_SPLINE_CURVE_WITH_KNOTS((3,3),(-5.33580039117808,-3.29413209751051),
 .UNSPECIFIED.)
CURVE()
GEOMETRIC_REPRESENTATION_ITEM()
RATIONAL_B_SPLINE_CURVE((1.96225044864938,1.96225044864938,1.82136720504436))
REPRESENTATION_ITEM('')
);
#1560=(
BOUNDED_CURVE()
B_SPLINE_CURVE(2,(#276386,#276387,#276388),.UNSPECIFIED.,.F.,.F.)
B_SPLINE_CURVE_WITH_KNOTS((3,3),(-7.37746868484567,-5.33580039117808),
 .UNSPECIFIED.)
CURVE()
GEOMETRIC_REPRESENTATION_ITEM()
RATIONAL_B_SPLINE_CURVE((1.82136720504436,1.96225044864938,1.96225044864938))
REPRESENTATION_ITEM('')
);
#1561=(
BOUNDED_CURVE()
B_SPLINE_CURVE(2,(#276390,#276391,#276392),.UNSPECIFIED.,.F.,.F.)
B_SPLINE_CURVE_WITH_KNOTS((3,3),(3.29413209751051,5.33580039117811),
 .UNSPECIFIED.)
CURVE()
GEOMETRIC_REPRESENTATION_ITEM()
RATIONAL_B_SPLINE_CURVE((1.82136720504437,1.96225044864939,1.96225044864939))
REPRESENTATION_ITEM('')
);
#1562=(
BOUNDED_CURVE()
B_SPLINE_CURVE(2,(#276394,#276395,#276396),.UNSPECIFIED.,.F.,.F.)
B_SPLINE_CURVE_WITH_KNOTS((3,3),(5.33580039117811,7.37746868484567),
 .UNSPECIFIED.)
CURVE()
GEOMETRIC_REPRESENTATION_ITEM()
RATIONAL_B_SPLINE_CURVE((1.96225044864939,1.96225044864939,1.82136720504437))
REPRESENTATION_ITEM('')
);
#1563=(
BOUNDED_CURVE()
B_SPLINE_CURVE(2,(#276399,#276400,#276401),.UNSPECIFIED.,.F.,.F.)
B_SPLINE_CURVE_WITH_KNOTS((3,3),(-5.3358003911781,-3.29413209751052),
 .UNSPECIFIED.)
CURVE()
GEOMETRIC_REPRESENTATION_ITEM()
RATIONAL_B_SPLINE_CURVE((1.96225044864939,1.96225044864939,1.82136720504437))
REPRESENTATION_ITEM('')
);
#1564=(
BOUNDED_CURVE()
B_SPLINE_CURVE(2,(#276403,#276404,#276405),.UNSPECIFIED.,.F.,.F.)
B_SPLINE_CURVE_WITH_KNOTS((3,3),(-7.37746868484567,-5.33580039117809),
 .UNSPECIFIED.)
CURVE()
GEOMETRIC_REPRESENTATION_ITEM()
RATIONAL_B_SPLINE_CURVE((1.82136720504437,1.96225044864939,1.96225044864939))
REPRESENTATION_ITEM('')
);
#1565=(
BOUNDED_CURVE()
B_SPLINE_CURVE(2,(#276407,#276408,#276409),.UNSPECIFIED.,.F.,.F.)
B_SPLINE_CURVE_WITH_KNOTS((3,3),(3.29413209751051,5.33580039117809),
 .UNSPECIFIED.)
CURVE()
GEOMETRIC_REPRESENTATION_ITEM()
RATIONAL_B_SPLINE_CURVE((1.82136720504437,1.96225044864939,1.96225044864939))
REPRESENTATION_ITEM('')
);
#1566=(
BOUNDED_CURVE()
B_SPLINE_CURVE(2,(#276411,#276412,#276413),.UNSPECIFIED.,.F.,.F.)
B_SPLINE_CURVE_WITH_KNOTS((3,3),(5.33580039117809,7.37746868484569),
 .UNSPECIFIED.)
CURVE()
GEOMETRIC_REPRESENTATION_ITEM()
RATIONAL_B_SPLINE_CURVE((1.96225044864939,1.96225044864939,1.82136720504436))
REPRESENTATION_ITEM('')
);
#1567=(
BOUNDED_CURVE()
B_SPLINE_CURVE(2,(#276416,#276417,#276418),.UNSPECIFIED.,.F.,.F.)
B_SPLINE_CURVE_WITH_KNOTS((3,3),(-5.33580039117809,-3.29413209751051),
 .UNSPECIFIED.)
CURVE()
GEOMETRIC_REPRESENTATION_ITEM()
RATIONAL_B_SPLINE_CURVE((1.96225044864939,1.96225044864939,1.82136720504436))
REPRESENTATION_ITEM('')
);
#1568=(
BOUNDED_CURVE()
B_SPLINE_CURVE(2,(#276420,#276421,#276422),.UNSPECIFIED.,.F.,.F.)
B_SPLINE_CURVE_WITH_KNOTS((3,3),(-7.37746868484564,-5.33580039117808),
 .UNSPECIFIED.)
CURVE()
GEOMETRIC_REPRESENTATION_ITEM()
RATIONAL_B_SPLINE_CURVE((1.82136720504437,1.96225044864938,1.96225044864938))
REPRESENTATION_ITEM('')
);
#1569=(
BOUNDED_CURVE()
B_SPLINE_CURVE(2,(#276424,#276425,#276426),.UNSPECIFIED.,.F.,.F.)
B_SPLINE_CURVE_WITH_KNOTS((3,3),(3.29413209751051,5.3358003911781),
 .UNSPECIFIED.)
CURVE()
GEOMETRIC_REPRESENTATION_ITEM()
RATIONAL_B_SPLINE_CURVE((1.82136720504436,1.96225044864939,1.96225044864938))
REPRESENTATION_ITEM('')
);
#1570=(
BOUNDED_CURVE()
B_SPLINE_CURVE(2,(#276427,#276428,#276429),.UNSPECIFIED.,.F.,.F.)
B_SPLINE_CURVE_WITH_KNOTS((3,3),(5.3358003911781,7.37746868484565),
 .UNSPECIFIED.)
CURVE()
GEOMETRIC_REPRESENTATION_ITEM()
RATIONAL_B_SPLINE_CURVE((1.96225044864938,1.96225044864938,1.82136720504436))
REPRESENTATION_ITEM('')
);
#1571=(
BOUNDED_CURVE()
B_SPLINE_CURVE(2,(#276430,#276431,#276432),.UNSPECIFIED.,.F.,.F.)
B_SPLINE_CURVE_WITH_KNOTS((3,3),(-5.33580039117809,-3.2941320975105),
 .UNSPECIFIED.)
CURVE()
GEOMETRIC_REPRESENTATION_ITEM()
RATIONAL_B_SPLINE_CURVE((1.96225044864938,1.96225044864938,1.82136720504436))
REPRESENTATION_ITEM('')
);
#1572=(
BOUNDED_CURVE()
B_SPLINE_CURVE(2,(#278526,#278527,#278528,#278529,#278530,#278531,#278532,
#278533,#278534,#278535,#278536,#278537,#278538,#278539,#278540,#278541,
#278542,#278543,#278544,#278545,#278546),.UNSPECIFIED.,.F.,.F.)
B_SPLINE_CURVE_WITH_KNOTS((3,2,2,2,2,2,2,2,2,2,3),(0.625,0.626923076923077,
0.628846153846154,0.630769230769231,0.632692307692308,0.634615384615385,
0.636538461538461,0.638461538461538,0.640384615384615,0.642307692307692,
0.644230769230769),.UNSPECIFIED.)
CURVE()
GEOMETRIC_REPRESENTATION_ITEM()
RATIONAL_B_SPLINE_CURVE((1.,0.951056516295154,1.,0.951056516295154,1.,0.951056516295154,
1.,0.951056516295154,1.,0.951056516295154,1.,0.951056516295154,1.,0.951056516295154,
1.,0.951056516295154,1.,0.951056516295154,1.,0.951056516295154,1.))
REPRESENTATION_ITEM('')
);
#1573=(
BOUNDED_CURVE()
B_SPLINE_CURVE(2,(#280621,#280622,#280623,#280624,#280625,#280626,#280627,
#280628,#280629,#280630,#280631,#280632,#280633,#280634,#280635,#280636,
#280637,#280638,#280639,#280640,#280641),.UNSPECIFIED.,.F.,.F.)
B_SPLINE_CURVE_WITH_KNOTS((3,2,2,2,2,2,2,2,2,2,3),(0.625,0.626923076923077,
0.628846153846154,0.630769230769231,0.632692307692308,0.634615384615385,
0.636538461538461,0.638461538461538,0.640384615384615,0.642307692307692,
0.644230769230769),.UNSPECIFIED.)
CURVE()
GEOMETRIC_REPRESENTATION_ITEM()
RATIONAL_B_SPLINE_CURVE((1.,0.951056516295154,1.,0.951056516295154,1.,0.951056516295154,
1.,0.951056516295154,1.,0.951056516295154,1.,0.951056516295154,1.,0.951056516295154,
1.,0.951056516295154,1.,0.951056516295154,1.,0.951056516295154,1.))
REPRESENTATION_ITEM('')
);
#1574=(
BOUNDED_CURVE()
B_SPLINE_CURVE(2,(#280648,#280649,#280650,#280651,#280652,#280653,#280654,
#280655,#280656),.UNSPECIFIED.,.F.,.F.)
B_SPLINE_CURVE_WITH_KNOTS((3,2,2,2,3),(0.125,0.126923076923077,0.128846153846154,
0.130769230769231,0.132372212319224),.UNSPECIFIED.)
CURVE()
GEOMETRIC_REPRESENTATION_ITEM()
RATIONAL_B_SPLINE_CURVE((1.,0.951056516295154,1.,0.951056516295154,1.,0.951056516295154,
1.,0.959203139286952,0.986418758195375))
REPRESENTATION_ITEM('')
);
#1575=(
BOUNDED_CURVE()
B_SPLINE_CURVE(2,(#280659,#280660,#280661,#280662,#280663,#280664,#280665,
#280666,#280667,#280668,#280669,#280670,#280671),.UNSPECIFIED.,.F.,.F.)
B_SPLINE_CURVE_WITH_KNOTS((3,2,2,2,2,2,3),(0.125,0.126923076923077,0.128846153846154,
0.130769230769231,0.132692307692308,0.134615384615385,0.134791334496805),
 .UNSPECIFIED.)
CURVE()
GEOMETRIC_REPRESENTATION_ITEM()
RATIONAL_B_SPLINE_CURVE((1.,0.951056516295154,1.,0.951056516295154,1.,0.951056516295154,
1.,0.951056516295154,1.,0.951056516295154,1.,0.99552196791982,0.991863361421687))
REPRESENTATION_ITEM('')
);
#1576=(
BOUNDED_CURVE()
B_SPLINE_CURVE(2,(#280676,#280677,#280678,#280679,#280680,#280681,#280682,
#280683,#280684,#280685,#280686,#280687,#280688,#280689,#280690,#280691,
#280692,#280693,#280694,#280695,#280696),.UNSPECIFIED.,.F.,.F.)
B_SPLINE_CURVE_WITH_KNOTS((3,2,2,2,2,2,2,2,2,2,3),(0.105769230769231,0.107692307692308,
0.109615384615385,0.111538461538462,0.113461538461538,0.115384615384615,
0.117307692307692,0.119230769230769,0.121153846153846,0.123076923076923,
0.125),.UNSPECIFIED.)
CURVE()
GEOMETRIC_REPRESENTATION_ITEM()
RATIONAL_B_SPLINE_CURVE((1.,0.951056516295154,1.,0.951056516295154,1.,0.951056516295154,
1.,0.951056516295154,1.,0.951056516295154,1.,0.951056516295154,1.,0.951056516295154,
1.,0.951056516295154,1.,0.951056516295154,1.,0.951056516295154,1.))
REPRESENTATION_ITEM('')
);
#1577=(
BOUNDED_CURVE()
B_SPLINE_CURVE(2,(#280697,#280698,#280699,#280700,#280701,#280702,#280703,
#280704,#280705,#280706,#280707,#280708,#280709,#280710,#280711,#280712,
#280713,#280714,#280715,#280716,#280717),.UNSPECIFIED.,.F.,.F.)
B_SPLINE_CURVE_WITH_KNOTS((3,2,2,2,2,2,2,2,2,2,3),(0.105769230769231,0.107692307692308,
0.109615384615385,0.111538461538462,0.113461538461538,0.115384615384615,
0.117307692307692,0.119230769230769,0.121153846153846,0.123076923076923,
0.125),.UNSPECIFIED.)
CURVE()
GEOMETRIC_REPRESENTATION_ITEM()
RATIONAL_B_SPLINE_CURVE((1.,0.951056516295154,1.,0.951056516295154,1.,0.951056516295154,
1.,0.951056516295154,1.,0.951056516295154,1.,0.951056516295154,1.,0.951056516295154,
1.,0.951056516295154,1.,0.951056516295154,1.,0.951056516295154,1.))
REPRESENTATION_ITEM('')
);
#1578=(
BOUNDED_CURVE()
B_SPLINE_CURVE(2,(#280722,#280723,#280724,#280725,#280726,#280727,#280728,
#280729,#280730,#280731,#280732,#280733,#280734,#280735,#280736,#280737,
#280738,#280739,#280740,#280741,#280742),.UNSPECIFIED.,.F.,.F.)
B_SPLINE_CURVE_WITH_KNOTS((3,2,2,2,2,2,2,2,2,2,3),(0.0865384615384615,0.0884615384615385,
0.0903846153846154,0.0923076923076923,0.0942307692307692,0.0961538461538462,
0.0980769230769231,0.1,0.101923076923077,0.103846153846154,0.105769230769231),
 .UNSPECIFIED.)
CURVE()
GEOMETRIC_REPRESENTATION_ITEM()
RATIONAL_B_SPLINE_CURVE((1.,0.951056516295154,1.,0.951056516295154,1.,0.951056516295154,
1.,0.951056516295154,1.,0.951056516295154,1.,0.951056516295154,1.,0.951056516295154,
1.,0.951056516295154,1.,0.951056516295154,1.,0.951056516295154,1.))
REPRESENTATION_ITEM('')
);
#1579=(
BOUNDED_CURVE()
B_SPLINE_CURVE(2,(#280743,#280744,#280745,#280746,#280747,#280748,#280749,
#280750,#280751,#280752,#280753,#280754,#280755,#280756,#280757,#280758,
#280759,#280760,#280761,#280762,#280763),.UNSPECIFIED.,.F.,.F.)
B_SPLINE_CURVE_WITH_KNOTS((3,2,2,2,2,2,2,2,2,2,3),(0.0865384615384615,0.0884615384615385,
0.0903846153846154,0.0923076923076923,0.0942307692307692,0.0961538461538462,
0.0980769230769231,0.1,0.101923076923077,0.103846153846154,0.105769230769231),
 .UNSPECIFIED.)
CURVE()
GEOMETRIC_REPRESENTATION_ITEM()
RATIONAL_B_SPLINE_CURVE((1.,0.951056516295154,1.,0.951056516295154,1.,0.951056516295154,
1.,0.951056516295154,1.,0.951056516295154,1.,0.951056516295154,1.,0.951056516295154,
1.,0.951056516295154,1.,0.951056516295154,1.,0.951056516295154,1.))
REPRESENTATION_ITEM('')
);
#1580=(
BOUNDED_CURVE()
B_SPLINE_CURVE(2,(#280768,#280769,#280770,#280771,#280772,#280773,#280774,
#280775,#280776,#280777,#280778,#280779,#280780,#280781,#280782,#280783,
#280784,#280785,#280786,#280787,#280788),.UNSPECIFIED.,.F.,.F.)
B_SPLINE_CURVE_WITH_KNOTS((3,2,2,2,2,2,2,2,2,2,3),(0.0673076923076923,0.0692307692307692,
0.0711538461538461,0.0730769230769231,0.075,0.0769230769230769,0.0788461538461538,
0.0807692307692308,0.0826923076923077,0.0846153846153846,0.0865384615384615),
 .UNSPECIFIED.)
CURVE()
GEOMETRIC_REPRESENTATION_ITEM()
RATIONAL_B_SPLINE_CURVE((1.,0.951056516295154,1.,0.951056516295154,1.,0.951056516295154,
1.,0.951056516295154,1.,0.951056516295154,1.,0.951056516295154,1.,0.951056516295154,
1.,0.951056516295154,1.,0.951056516295154,1.,0.951056516295154,1.))
REPRESENTATION_ITEM('')
);
#1581=(
BOUNDED_CURVE()
B_SPLINE_CURVE(2,(#280789,#280790,#280791,#280792,#280793,#280794,#280795,
#280796,#280797,#280798,#280799,#280800,#280801,#280802,#280803,#280804,
#280805,#280806,#280807,#280808,#280809),.UNSPECIFIED.,.F.,.F.)
B_SPLINE_CURVE_WITH_KNOTS((3,2,2,2,2,2,2,2,2,2,3),(0.0673076923076923,0.0692307692307692,
0.0711538461538462,0.0730769230769231,0.075,0.0769230769230769,0.0788461538461538,
0.0807692307692308,0.0826923076923077,0.0846153846153846,0.0865384615384615),
 .UNSPECIFIED.)
CURVE()
GEOMETRIC_REPRESENTATION_ITEM()
RATIONAL_B_SPLINE_CURVE((1.,0.951056516295154,1.,0.951056516295154,1.,0.951056516295154,
1.,0.951056516295154,1.,0.951056516295154,1.,0.951056516295154,1.,0.951056516295154,
1.,0.951056516295154,1.,0.951056516295154,1.,0.951056516295154,1.))
REPRESENTATION_ITEM('')
);
#1582=(
BOUNDED_CURVE()
B_SPLINE_CURVE(2,(#280814,#280815,#280816,#280817,#280818,#280819,#280820,
#280821,#280822,#280823,#280824,#280825,#280826,#280827,#280828,#280829,
#280830,#280831,#280832,#280833,#280834),.UNSPECIFIED.,.F.,.F.)
B_SPLINE_CURVE_WITH_KNOTS((3,2,2,2,2,2,2,2,2,2,3),(0.0480769230769231,0.05,
0.0519230769230769,0.0538461538461538,0.0557692307692308,0.0576923076923077,
0.0596153846153846,0.0615384615384615,0.0634615384615385,0.0653846153846154,
0.0673076923076923),.UNSPECIFIED.)
CURVE()
GEOMETRIC_REPRESENTATION_ITEM()
RATIONAL_B_SPLINE_CURVE((1.,0.951056516295154,1.,0.951056516295154,1.,0.951056516295154,
1.,0.951056516295154,1.,0.951056516295154,1.,0.951056516295154,1.,0.951056516295154,
1.,0.951056516295154,1.,0.951056516295154,1.,0.951056516295154,1.))
REPRESENTATION_ITEM('')
);
#1583=(
BOUNDED_CURVE()
B_SPLINE_CURVE(2,(#280835,#280836,#280837,#280838,#280839,#280840,#280841,
#280842,#280843,#280844,#280845,#280846,#280847,#280848,#280849,#280850,
#280851,#280852,#280853,#280854,#280855),.UNSPECIFIED.,.F.,.F.)
B_SPLINE_CURVE_WITH_KNOTS((3,2,2,2,2,2,2,2,2,2,3),(0.0480769230769231,0.05,
0.0519230769230769,0.0538461538461538,0.0557692307692308,0.0576923076923077,
0.0596153846153846,0.0615384615384615,0.0634615384615385,0.0653846153846154,
0.0673076923076923),.UNSPECIFIED.)
CURVE()
GEOMETRIC_REPRESENTATION_ITEM()
RATIONAL_B_SPLINE_CURVE((1.,0.951056516295154,1.,0.951056516295154,1.,0.951056516295154,
1.,0.951056516295154,1.,0.951056516295154,1.,0.951056516295154,1.,0.951056516295154,
1.,0.951056516295154,1.,0.951056516295154,1.,0.951056516295154,1.))
REPRESENTATION_ITEM('')
);
#1584=(
BOUNDED_CURVE()
B_SPLINE_CURVE(2,(#280862,#280863,#280864,#280865,#280866),
 .UNSPECIFIED.,.F.,.F.)
B_SPLINE_CURVE_WITH_KNOTS((3,2,3),(0.0264333754686713,0.0269230769230769,
0.0288461538461538),.UNSPECIFIED.)
CURVE()
GEOMETRIC_REPRESENTATION_ITEM()
RATIONAL_B_SPLINE_CURVE((0.981420974846885,0.987536798519951,1.,0.951056516295154,
1.))
REPRESENTATION_ITEM('')
);
#1585=(
BOUNDED_CURVE()
B_SPLINE_CURVE(2,(#281378,#281379,#281380),.UNSPECIFIED.,.F.,.F.)
B_SPLINE_CURVE_WITH_KNOTS((3,3),(-3.18750279702086,-0.878323675844115),
 .UNSPECIFIED.)
CURVE()
GEOMETRIC_REPRESENTATION_ITEM()
RATIONAL_B_SPLINE_CURVE((1.1939543172175,1.37865969289105,1.1939543172175))
REPRESENTATION_ITEM('')
);
#1586=(
BOUNDED_CURVE()
B_SPLINE_CURVE(2,(#281382,#281383,#281384),.UNSPECIFIED.,.F.,.F.)
B_SPLINE_CURVE_WITH_KNOTS((3,3),(0.878323675844114,3.18750279702085),
 .UNSPECIFIED.)
CURVE()
GEOMETRIC_REPRESENTATION_ITEM()
RATIONAL_B_SPLINE_CURVE((1.1939543172175,1.37865969289105,1.1939543172175))
REPRESENTATION_ITEM('')
);
#1587=(
BOUNDED_CURVE()
B_SPLINE_CURVE(2,(#281386,#281387,#281388),.UNSPECIFIED.,.F.,.F.)
B_SPLINE_CURVE_WITH_KNOTS((3,3),(0.878323675844118,3.18750279702086),
 .UNSPECIFIED.)
CURVE()
GEOMETRIC_REPRESENTATION_ITEM()
RATIONAL_B_SPLINE_CURVE((1.1939543172175,1.37865969289105,1.1939543172175))
REPRESENTATION_ITEM('')
);
#1588=(
BOUNDED_CURVE()
B_SPLINE_CURVE(2,(#281390,#281391,#281392),.UNSPECIFIED.,.F.,.F.)
B_SPLINE_CURVE_WITH_KNOTS((3,3),(0.878323675844117,2.03291323643249),
 .UNSPECIFIED.)
CURVE()
GEOMETRIC_REPRESENTATION_ITEM()
RATIONAL_B_SPLINE_CURVE((1.1939543172175,1.28630700505428,1.28630700505428))
REPRESENTATION_ITEM('')
);
#1589=(
BOUNDED_CURVE()
B_SPLINE_CURVE(2,(#281397,#281398,#281399),.UNSPECIFIED.,.F.,.F.)
B_SPLINE_CURVE_WITH_KNOTS((3,3),(2.03291323643249,3.18750279702086),
 .UNSPECIFIED.)
CURVE()
GEOMETRIC_REPRESENTATION_ITEM()
RATIONAL_B_SPLINE_CURVE((1.28630700505428,1.28630700505428,1.1939543172175))
REPRESENTATION_ITEM('')
);
#1590=(
BOUNDED_CURVE()
B_SPLINE_CURVE(2,(#281401,#281402,#281403),.UNSPECIFIED.,.F.,.F.)
B_SPLINE_CURVE_WITH_KNOTS((3,3),(-3.18750279702086,-0.878323675844113),
 .UNSPECIFIED.)
CURVE()
GEOMETRIC_REPRESENTATION_ITEM()
RATIONAL_B_SPLINE_CURVE((1.1939543172175,1.37865969289105,1.1939543172175))
REPRESENTATION_ITEM('')
);
#1591=(
BOUNDED_CURVE()
B_SPLINE_CURVE(2,(#281404,#281405,#281406),.UNSPECIFIED.,.F.,.F.)
B_SPLINE_CURVE_WITH_KNOTS((3,3),(-3.18750279702087,-0.878323675844119),
 .UNSPECIFIED.)
CURVE()
GEOMETRIC_REPRESENTATION_ITEM()
RATIONAL_B_SPLINE_CURVE((1.1939543172175,1.37865969289105,1.1939543172175))
REPRESENTATION_ITEM('')
);
#1592=(
BOUNDED_CURVE()
B_SPLINE_CURVE(2,(#283589,#283590,#283591,#283592,#283593,#283594,#283595,
#283596,#283597,#283598,#283599,#283600,#283601,#283602,#283603,#283604,
#283605,#283606,#283607,#283608,#283609),.UNSPECIFIED.,.F.,.F.)
B_SPLINE_CURVE_WITH_KNOTS((3,2,2,2,2,2,2,2,2,2,3),(0.0288461538461538,0.0307692307692308,
0.0326923076923077,0.0346153846153846,0.0365384615384615,0.0384615384615385,
0.0403846153846154,0.0423076923076923,0.0442307692307692,0.0461538461538462,
0.0480769230769231),.UNSPECIFIED.)
CURVE()
GEOMETRIC_REPRESENTATION_ITEM()
RATIONAL_B_SPLINE_CURVE((1.,0.951056516295154,1.,0.951056516295154,1.,0.951056516295154,
1.,0.951056516295154,1.,0.951056516295154,1.,0.951056516295154,1.,0.951056516295154,
1.,0.951056516295154,1.,0.951056516295154,1.,0.951056516295154,1.))
REPRESENTATION_ITEM('')
);
#1593=(
BOUNDED_CURVE()
B_SPLINE_CURVE(2,(#285684,#285685,#285686,#285687,#285688,#285689,#285690,
#285691,#285692,#285693,#285694,#285695,#285696,#285697,#285698,#285699,
#285700,#285701,#285702,#285703,#285704),.UNSPECIFIED.,.F.,.F.)
B_SPLINE_CURVE_WITH_KNOTS((3,2,2,2,2,2,2,2,2,2,3),(0.0288461538461538,0.0307692307692308,
0.0326923076923077,0.0346153846153846,0.0365384615384615,0.0384615384615385,
0.0403846153846154,0.0423076923076923,0.0442307692307692,0.0461538461538462,
0.0480769230769231),.UNSPECIFIED.)
CURVE()
GEOMETRIC_REPRESENTATION_ITEM()
RATIONAL_B_SPLINE_CURVE((1.,0.951056516295154,1.,0.951056516295154,1.,0.951056516295154,
1.,0.951056516295154,1.,0.951056516295154,1.,0.951056516295154,1.,0.951056516295154,
1.,0.951056516295154,1.,0.951056516295154,1.,0.951056516295154,1.))
REPRESENTATION_ITEM('')
);
#1594=(
BOUNDED_CURVE()
B_SPLINE_CURVE(2,(#285711,#285712,#285713,#285714,#285715,#285716,#285717,
#285718,#285719,#285720,#285721,#285722,#285723),.UNSPECIFIED.,.F.,.F.)
B_SPLINE_CURVE_WITH_KNOTS((3,2,2,2,2,2,3),(0.480090915688519,0.480769230769231,
0.482692307692308,0.484615384615385,0.486538461538462,0.488461538461538,
0.490384615384615),.UNSPECIFIED.)
CURVE()
GEOMETRIC_REPRESENTATION_ITEM()
RATIONAL_B_SPLINE_CURVE((0.977651452579507,0.982736466388236,1.,0.951056516295154,
1.,0.951056516295154,1.,0.951056516295154,1.,0.951056516295154,1.,0.951056516295154,
1.))
REPRESENTATION_ITEM('')
);
#1595=(
BOUNDED_CURVE()
B_SPLINE_CURVE(2,(#285726,#285727,#285728,#285729,#285730,#285731,#285732,
#285733,#285734,#285735,#285736),.UNSPECIFIED.,.F.,.F.)
B_SPLINE_CURVE_WITH_KNOTS((3,2,2,2,2,3),(0.482494269360453,0.482692307692308,
0.484615384615385,0.486538461538462,0.488461538461538,0.490384615384615),
 .UNSPECIFIED.)
CURVE()
GEOMETRIC_REPRESENTATION_ITEM()
RATIONAL_B_SPLINE_CURVE((0.990957684919766,0.994959803348612,1.,0.951056516295154,
1.,0.951056516295154,1.,0.951056516295154,1.,0.951056516295154,1.))
REPRESENTATION_ITEM('')
);
#1596=(
BOUNDED_CURVE()
B_SPLINE_CURVE(2,(#285805,#285806,#285807,#285808,#285809,#285810,#285811,
#285812,#285813),.UNSPECIFIED.,.F.,.F.)
B_SPLINE_CURVE_WITH_KNOTS((3,2,2,2,3),(0.48722585646854,0.488461538461539,
0.490384615384615,0.492307692307692,0.493941807988044),.UNSPECIFIED.)
CURVE()
GEOMETRIC_REPRESENTATION_ITEM()
RATIONAL_B_SPLINE_CURVE((0.97751749990519,0.968551137625873,1.,0.951056516295154,
1.,0.951056516295154,1.,0.958410756629963,0.987501613373882))
REPRESENTATION_ITEM('')
);
#1597=(
BOUNDED_CURVE()
B_SPLINE_CURVE(2,(#287903,#287904,#287905,#287906,#287907,#287908,#287909,
#287910,#287911,#287912,#287913),.UNSPECIFIED.,.F.,.F.)
B_SPLINE_CURVE_WITH_KNOTS((3,2,2,2,2,3),(0.490384615384615,0.492307692307692,
0.494230769230769,0.496153846153846,0.498076923076923,0.499312605069927),
 .UNSPECIFIED.)
CURVE()
GEOMETRIC_REPRESENTATION_ITEM()
RATIONAL_B_SPLINE_CURVE((1.,0.951056516295154,1.,0.951056516295154,1.,0.951056516295154,
1.,0.951056516295154,1.,0.968551137625747,0.977517499905262))
REPRESENTATION_ITEM('')
);
#1598=(
BOUNDED_CURVE()
B_SPLINE_CURVE(2,(#290023,#290024,#290025,#290026,#290027,#290028,#290029,
#290030,#290031,#290032,#290033,#290034,#290035),.UNSPECIFIED.,.F.,.F.)
B_SPLINE_CURVE_WITH_KNOTS((3,2,2,2,2,2,3),(0.490384615384615,0.492307692307692,
0.494230769230769,0.496153846153846,0.498076923076923,0.5,0.501715584159741),
 .UNSPECIFIED.)
CURVE()
GEOMETRIC_REPRESENTATION_ITEM()
RATIONAL_B_SPLINE_CURVE((1.,0.951056516295154,1.,0.951056516295154,1.,0.951056516295154,
1.,0.951056516295154,1.,0.951056516295154,1.,0.956337334009382,0.99057792529015))
REPRESENTATION_ITEM('')
);
#1599=(
BOUNDED_CURVE()
B_SPLINE_CURVE(2,(#290044,#290045,#290046,#290047,#290048),
 .UNSPECIFIED.,.F.,.F.)
B_SPLINE_CURVE_WITH_KNOTS((3,2,3),(0.0264333754686713,0.0269230769230769,
0.0288461538461538),.UNSPECIFIED.)
CURVE()
GEOMETRIC_REPRESENTATION_ITEM()
RATIONAL_B_SPLINE_CURVE((0.981420974846885,0.987536798519951,1.,0.951056516295154,
1.))
REPRESENTATION_ITEM('')
);
#1600=(
BOUNDED_CURVE()
B_SPLINE_CURVE(2,(#290054,#290055,#290056,#290057,#290058,#290059,#290060,
#290061,#290062,#290063,#290064,#290065,#290066,#290067,#290068,#290069,
#290070,#290071,#290072,#290073,#290074),.UNSPECIFIED.,.F.,.F.)
B_SPLINE_CURVE_WITH_KNOTS((3,2,2,2,2,2,2,2,2,2,3),(0.0288461538461538,0.0307692307692308,
0.0326923076923077,0.0346153846153846,0.0365384615384615,0.0384615384615385,
0.0403846153846154,0.0423076923076923,0.0442307692307692,0.0461538461538462,
0.0480769230769231),.UNSPECIFIED.)
CURVE()
GEOMETRIC_REPRESENTATION_ITEM()
RATIONAL_B_SPLINE_CURVE((1.,0.951056516295154,1.,0.951056516295154,1.,0.951056516295154,
1.,0.951056516295154,1.,0.951056516295154,1.,0.951056516295154,1.,0.951056516295154,
1.,0.951056516295154,1.,0.951056516295154,1.,0.951056516295154,1.))
REPRESENTATION_ITEM('')
);
#1601=(
BOUNDED_CURVE()
B_SPLINE_CURVE(2,(#290075,#290076,#290077,#290078,#290079,#290080,#290081,
#290082,#290083,#290084,#290085,#290086,#290087,#290088,#290089,#290090,
#290091,#290092,#290093,#290094,#290095),.UNSPECIFIED.,.F.,.F.)
B_SPLINE_CURVE_WITH_KNOTS((3,2,2,2,2,2,2,2,2,2,3),(0.0288461538461538,0.0307692307692308,
0.0326923076923077,0.0346153846153846,0.0365384615384615,0.0384615384615385,
0.0403846153846154,0.0423076923076923,0.0442307692307692,0.0461538461538462,
0.0480769230769231),.UNSPECIFIED.)
CURVE()
GEOMETRIC_REPRESENTATION_ITEM()
RATIONAL_B_SPLINE_CURVE((1.,0.951056516295154,1.,0.951056516295154,1.,0.951056516295154,
1.,0.951056516295154,1.,0.951056516295154,1.,0.951056516295154,1.,0.951056516295154,
1.,0.951056516295154,1.,0.951056516295154,1.,0.951056516295154,1.))
REPRESENTATION_ITEM('')
);
#1602=(
BOUNDED_CURVE()
B_SPLINE_CURVE(2,(#290100,#290101,#290102,#290103,#290104,#290105,#290106,
#290107,#290108,#290109,#290110,#290111,#290112,#290113,#290114,#290115,
#290116,#290117,#290118,#290119,#290120),.UNSPECIFIED.,.F.,.F.)
B_SPLINE_CURVE_WITH_KNOTS((3,2,2,2,2,2,2,2,2,2,3),(0.0480769230769231,0.05,
0.0519230769230769,0.0538461538461538,0.0557692307692308,0.0576923076923077,
0.0596153846153846,0.0615384615384615,0.0634615384615385,0.0653846153846154,
0.0673076923076923),.UNSPECIFIED.)
CURVE()
GEOMETRIC_REPRESENTATION_ITEM()
RATIONAL_B_SPLINE_CURVE((1.,0.951056516295154,1.,0.951056516295154,1.,0.951056516295154,
1.,0.951056516295154,1.,0.951056516295154,1.,0.951056516295154,1.,0.951056516295154,
1.,0.951056516295154,1.,0.951056516295154,1.,0.951056516295154,1.))
REPRESENTATION_ITEM('')
);
#1603=(
BOUNDED_CURVE()
B_SPLINE_CURVE(2,(#290121,#290122,#290123,#290124,#290125,#290126,#290127,
#290128,#290129,#290130,#290131,#290132,#290133,#290134,#290135,#290136,
#290137,#290138,#290139,#290140,#290141),.UNSPECIFIED.,.F.,.F.)
B_SPLINE_CURVE_WITH_KNOTS((3,2,2,2,2,2,2,2,2,2,3),(0.0480769230769231,0.05,
0.0519230769230769,0.0538461538461538,0.0557692307692308,0.0576923076923077,
0.0596153846153846,0.0615384615384615,0.0634615384615385,0.0653846153846154,
0.0673076923076923),.UNSPECIFIED.)
CURVE()
GEOMETRIC_REPRESENTATION_ITEM()
RATIONAL_B_SPLINE_CURVE((1.,0.951056516295154,1.,0.951056516295154,1.,0.951056516295154,
1.,0.951056516295154,1.,0.951056516295154,1.,0.951056516295154,1.,0.951056516295154,
1.,0.951056516295154,1.,0.951056516295154,1.,0.951056516295154,1.))
REPRESENTATION_ITEM('')
);
#1604=(
BOUNDED_CURVE()
B_SPLINE_CURVE(2,(#290146,#290147,#290148,#290149,#290150,#290151,#290152,
#290153,#290154,#290155,#290156,#290157,#290158,#290159,#290160,#290161,
#290162,#290163,#290164,#290165,#290166),.UNSPECIFIED.,.F.,.F.)
B_SPLINE_CURVE_WITH_KNOTS((3,2,2,2,2,2,2,2,2,2,3),(0.0673076923076923,0.0692307692307692,
0.0711538461538462,0.0730769230769231,0.075,0.0769230769230769,0.0788461538461538,
0.0807692307692308,0.0826923076923077,0.0846153846153846,0.0865384615384615),
 .UNSPECIFIED.)
CURVE()
GEOMETRIC_REPRESENTATION_ITEM()
RATIONAL_B_SPLINE_CURVE((1.,0.951056516295154,1.,0.951056516295154,1.,0.951056516295154,
1.,0.951056516295154,1.,0.951056516295154,1.,0.951056516295154,1.,0.951056516295154,
1.,0.951056516295154,1.,0.951056516295154,1.,0.951056516295154,1.))
REPRESENTATION_ITEM('')
);
#1605=(
BOUNDED_CURVE()
B_SPLINE_CURVE(2,(#290167,#290168,#290169,#290170,#290171,#290172,#290173,
#290174,#290175,#290176,#290177,#290178,#290179,#290180,#290181,#290182,
#290183,#290184,#290185,#290186,#290187),.UNSPECIFIED.,.F.,.F.)
B_SPLINE_CURVE_WITH_KNOTS((3,2,2,2,2,2,2,2,2,2,3),(0.0673076923076923,0.0692307692307692,
0.0711538461538462,0.0730769230769231,0.075,0.0769230769230769,0.0788461538461538,
0.0807692307692308,0.0826923076923077,0.0846153846153846,0.0865384615384615),
 .UNSPECIFIED.)
CURVE()
GEOMETRIC_REPRESENTATION_ITEM()
RATIONAL_B_SPLINE_CURVE((1.,0.951056516295154,1.,0.951056516295154,1.,0.951056516295154,
1.,0.951056516295154,1.,0.951056516295154,1.,0.951056516295154,1.,0.951056516295154,
1.,0.951056516295154,1.,0.951056516295154,1.,0.951056516295154,1.))
REPRESENTATION_ITEM('')
);
#1606=(
BOUNDED_CURVE()
B_SPLINE_CURVE(2,(#290192,#290193,#290194,#290195,#290196,#290197,#290198,
#290199,#290200,#290201,#290202,#290203,#290204,#290205,#290206,#290207,
#290208,#290209,#290210,#290211,#290212),.UNSPECIFIED.,.F.,.F.)
B_SPLINE_CURVE_WITH_KNOTS((3,2,2,2,2,2,2,2,2,2,3),(0.0865384615384615,0.0884615384615385,
0.0903846153846154,0.0923076923076923,0.0942307692307692,0.0961538461538462,
0.0980769230769231,0.1,0.101923076923077,0.103846153846154,0.105769230769231),
 .UNSPECIFIED.)
CURVE()
GEOMETRIC_REPRESENTATION_ITEM()
RATIONAL_B_SPLINE_CURVE((1.,0.951056516295154,1.,0.951056516295154,1.,0.951056516295154,
1.,0.951056516295154,1.,0.951056516295154,1.,0.951056516295154,1.,0.951056516295154,
1.,0.951056516295154,1.,0.951056516295154,1.,0.951056516295154,1.))
REPRESENTATION_ITEM('')
);
#1607=(
BOUNDED_CURVE()
B_SPLINE_CURVE(2,(#290213,#290214,#290215,#290216,#290217,#290218,#290219,
#290220,#290221,#290222,#290223,#290224,#290225,#290226,#290227,#290228,
#290229,#290230,#290231,#290232,#290233),.UNSPECIFIED.,.F.,.F.)
B_SPLINE_CURVE_WITH_KNOTS((3,2,2,2,2,2,2,2,2,2,3),(0.0865384615384615,0.0884615384615385,
0.0903846153846154,0.0923076923076923,0.0942307692307692,0.0961538461538462,
0.0980769230769231,0.1,0.101923076923077,0.103846153846154,0.105769230769231),
 .UNSPECIFIED.)
CURVE()
GEOMETRIC_REPRESENTATION_ITEM()
RATIONAL_B_SPLINE_CURVE((1.,0.951056516295154,1.,0.951056516295154,1.,0.951056516295154,
1.,0.951056516295154,1.,0.951056516295154,1.,0.951056516295154,1.,0.951056516295154,
1.,0.951056516295154,1.,0.951056516295154,1.,0.951056516295154,1.))
REPRESENTATION_ITEM('')
);
#1608=(
BOUNDED_CURVE()
B_SPLINE_CURVE(2,(#290238,#290239,#290240,#290241,#290242,#290243,#290244,
#290245,#290246,#290247,#290248,#290249,#290250,#290251,#290252,#290253,
#290254,#290255,#290256,#290257,#290258),.UNSPECIFIED.,.F.,.F.)
B_SPLINE_CURVE_WITH_KNOTS((3,2,2,2,2,2,2,2,2,2,3),(0.105769230769231,0.107692307692308,
0.109615384615385,0.111538461538462,0.113461538461538,0.115384615384615,
0.117307692307692,0.119230769230769,0.121153846153846,0.123076923076923,
0.125),.UNSPECIFIED.)
CURVE()
GEOMETRIC_REPRESENTATION_ITEM()
RATIONAL_B_SPLINE_CURVE((1.,0.951056516295154,1.,0.951056516295154,1.,0.951056516295154,
1.,0.951056516295154,1.,0.951056516295154,1.,0.951056516295154,1.,0.951056516295154,
1.,0.951056516295154,1.,0.951056516295154,1.,0.951056516295154,1.))
REPRESENTATION_ITEM('')
);
#1609=(
BOUNDED_CURVE()
B_SPLINE_CURVE(2,(#290259,#290260,#290261,#290262,#290263,#290264,#290265,
#290266,#290267,#290268,#290269,#290270,#290271,#290272,#290273,#290274,
#290275,#290276,#290277,#290278,#290279),.UNSPECIFIED.,.F.,.F.)
B_SPLINE_CURVE_WITH_KNOTS((3,2,2,2,2,2,2,2,2,2,3),(0.105769230769231,0.107692307692308,
0.109615384615385,0.111538461538462,0.113461538461538,0.115384615384615,
0.117307692307692,0.119230769230769,0.121153846153846,0.123076923076923,
0.125),.UNSPECIFIED.)
CURVE()
GEOMETRIC_REPRESENTATION_ITEM()
RATIONAL_B_SPLINE_CURVE((1.,0.951056516295154,1.,0.951056516295154,1.,0.951056516295154,
1.,0.951056516295154,1.,0.951056516295154,1.,0.951056516295154,1.,0.951056516295154,
1.,0.951056516295154,1.,0.951056516295154,1.,0.951056516295154,1.))
REPRESENTATION_ITEM('')
);
#1610=(
BOUNDED_CURVE()
B_SPLINE_CURVE(2,(#290284,#290285,#290286,#290287,#290288,#290289,#290290,
#290291,#290292,#290293,#290294,#290295,#290296,#290297,#290298,#290299,
#290300,#290301,#290302,#290303,#290304),.UNSPECIFIED.,.F.,.F.)
B_SPLINE_CURVE_WITH_KNOTS((3,2,2,2,2,2,2,2,2,2,3),(0.125,0.126923076923077,
0.128846153846154,0.130769230769231,0.132692307692308,0.134615384615385,
0.136538461538462,0.138461538461538,0.140384615384615,0.142307692307692,
0.144230769230769),.UNSPECIFIED.)
CURVE()
GEOMETRIC_REPRESENTATION_ITEM()
RATIONAL_B_SPLINE_CURVE((1.,0.951056516295154,1.,0.951056516295154,1.,0.951056516295154,
1.,0.951056516295154,1.,0.951056516295154,1.,0.951056516295154,1.,0.951056516295154,
1.,0.951056516295154,1.,0.951056516295154,1.,0.951056516295154,1.))
REPRESENTATION_ITEM('')
);
#1611=(
BOUNDED_CURVE()
B_SPLINE_CURVE(2,(#290305,#290306,#290307,#290308,#290309,#290310,#290311,
#290312,#290313,#290314,#290315,#290316,#290317,#290318,#290319,#290320,
#290321,#290322,#290323,#290324,#290325),.UNSPECIFIED.,.F.,.F.)
B_SPLINE_CURVE_WITH_KNOTS((3,2,2,2,2,2,2,2,2,2,3),(0.125,0.126923076923077,
0.128846153846154,0.130769230769231,0.132692307692308,0.134615384615385,
0.136538461538462,0.138461538461538,0.140384615384615,0.142307692307692,
0.144230769230769),.UNSPECIFIED.)
CURVE()
GEOMETRIC_REPRESENTATION_ITEM()
RATIONAL_B_SPLINE_CURVE((1.,0.951056516295154,1.,0.951056516295154,1.,0.951056516295154,
1.,0.951056516295154,1.,0.951056516295154,1.,0.951056516295154,1.,0.951056516295154,
1.,0.951056516295154,1.,0.951056516295154,1.,0.951056516295154,1.))
REPRESENTATION_ITEM('')
);
#1612=(
BOUNDED_CURVE()
B_SPLINE_CURVE(2,(#290330,#290331,#290332,#290333,#290334,#290335,#290336,
#290337,#290338,#290339,#290340,#290341,#290342,#290343,#290344,#290345,
#290346,#290347,#290348,#290349,#290350),.UNSPECIFIED.,.F.,.F.)
B_SPLINE_CURVE_WITH_KNOTS((3,2,2,2,2,2,2,2,2,2,3),(0.144230769230769,0.146153846153846,
0.148076923076923,0.15,0.151923076923077,0.153846153846154,0.155769230769231,
0.157692307692308,0.159615384615385,0.161538461538462,0.163461538461538),
 .UNSPECIFIED.)
CURVE()
GEOMETRIC_REPRESENTATION_ITEM()
RATIONAL_B_SPLINE_CURVE((1.,0.951056516295154,1.,0.951056516295154,1.,0.951056516295154,
1.,0.951056516295154,1.,0.951056516295154,1.,0.951056516295154,1.,0.951056516295154,
1.,0.951056516295154,1.,0.951056516295154,1.,0.951056516295154,1.))
REPRESENTATION_ITEM('')
);
#1613=(
BOUNDED_CURVE()
B_SPLINE_CURVE(2,(#290351,#290352,#290353,#290354,#290355,#290356,#290357,
#290358,#290359,#290360,#290361,#290362,#290363,#290364,#290365,#290366,
#290367,#290368,#290369,#290370,#290371),.UNSPECIFIED.,.F.,.F.)
B_SPLINE_CURVE_WITH_KNOTS((3,2,2,2,2,2,2,2,2,2,3),(0.144230769230769,0.146153846153846,
0.148076923076923,0.15,0.151923076923077,0.153846153846154,0.155769230769231,
0.157692307692308,0.159615384615385,0.161538461538462,0.163461538461538),
 .UNSPECIFIED.)
CURVE()
GEOMETRIC_REPRESENTATION_ITEM()
RATIONAL_B_SPLINE_CURVE((1.,0.951056516295154,1.,0.951056516295154,1.,0.951056516295154,
1.,0.951056516295154,1.,0.951056516295154,1.,0.951056516295154,1.,0.951056516295154,
1.,0.951056516295154,1.,0.951056516295154,1.,0.951056516295154,1.))
REPRESENTATION_ITEM('')
);
#1614=(
BOUNDED_CURVE()
B_SPLINE_CURVE(2,(#290376,#290377,#290378,#290379,#290380,#290381,#290382,
#290383,#290384,#290385,#290386,#290387,#290388,#290389,#290390,#290391,
#290392,#290393,#290394,#290395,#290396),.UNSPECIFIED.,.F.,.F.)
B_SPLINE_CURVE_WITH_KNOTS((3,2,2,2,2,2,2,2,2,2,3),(0.163461538461538,0.165384615384615,
0.167307692307692,0.169230769230769,0.171153846153846,0.173076923076923,
0.175,0.176923076923077,0.178846153846154,0.180769230769231,0.182692307692308),
 .UNSPECIFIED.)
CURVE()
GEOMETRIC_REPRESENTATION_ITEM()
RATIONAL_B_SPLINE_CURVE((1.,0.951056516295154,1.,0.951056516295154,1.,0.951056516295154,
1.,0.951056516295154,1.,0.951056516295154,1.,0.951056516295154,1.,0.951056516295154,
1.,0.951056516295154,1.,0.951056516295154,1.,0.951056516295154,1.))
REPRESENTATION_ITEM('')
);
#1615=(
BOUNDED_CURVE()
B_SPLINE_CURVE(2,(#290397,#290398,#290399,#290400,#290401,#290402,#290403,
#290404,#290405,#290406,#290407,#290408,#290409,#290410,#290411,#290412,
#290413,#290414,#290415,#290416,#290417),.UNSPECIFIED.,.F.,.F.)
B_SPLINE_CURVE_WITH_KNOTS((3,2,2,2,2,2,2,2,2,2,3),(0.163461538461538,0.165384615384615,
0.167307692307692,0.169230769230769,0.171153846153846,0.173076923076923,
0.175,0.176923076923077,0.178846153846154,0.180769230769231,0.182692307692308),
 .UNSPECIFIED.)
CURVE()
GEOMETRIC_REPRESENTATION_ITEM()
RATIONAL_B_SPLINE_CURVE((1.,0.951056516295154,1.,0.951056516295154,1.,0.951056516295154,
1.,0.951056516295154,1.,0.951056516295154,1.,0.951056516295154,1.,0.951056516295154,
1.,0.951056516295154,1.,0.951056516295154,1.,0.951056516295154,1.))
REPRESENTATION_ITEM('')
);
#1616=(
BOUNDED_CURVE()
B_SPLINE_CURVE(2,(#290422,#290423,#290424,#290425,#290426,#290427,#290428,
#290429,#290430,#290431,#290432,#290433,#290434,#290435,#290436,#290437,
#290438,#290439,#290440,#290441,#290442),.UNSPECIFIED.,.F.,.F.)
B_SPLINE_CURVE_WITH_KNOTS((3,2,2,2,2,2,2,2,2,2,3),(0.182692307692308,0.184615384615385,
0.186538461538462,0.188461538461538,0.190384615384615,0.192307692307692,
0.194230769230769,0.196153846153846,0.198076923076923,0.2,0.201923076923077),
 .UNSPECIFIED.)
CURVE()
GEOMETRIC_REPRESENTATION_ITEM()
RATIONAL_B_SPLINE_CURVE((1.,0.951056516295154,1.,0.951056516295154,1.,0.951056516295154,
1.,0.951056516295154,1.,0.951056516295154,1.,0.951056516295154,1.,0.951056516295154,
1.,0.951056516295154,1.,0.951056516295154,1.,0.951056516295154,1.))
REPRESENTATION_ITEM('')
);
#1617=(
BOUNDED_CURVE()
B_SPLINE_CURVE(2,(#290443,#290444,#290445,#290446,#290447,#290448,#290449,
#290450,#290451,#290452,#290453,#290454,#290455,#290456,#290457,#290458,
#290459,#290460,#290461,#290462,#290463),.UNSPECIFIED.,.F.,.F.)
B_SPLINE_CURVE_WITH_KNOTS((3,2,2,2,2,2,2,2,2,2,3),(0.182692307692308,0.184615384615385,
0.186538461538462,0.188461538461538,0.190384615384615,0.192307692307692,
0.194230769230769,0.196153846153846,0.198076923076923,0.2,0.201923076923077),
 .UNSPECIFIED.)
CURVE()
GEOMETRIC_REPRESENTATION_ITEM()
RATIONAL_B_SPLINE_CURVE((1.,0.951056516295154,1.,0.951056516295154,1.,0.951056516295154,
1.,0.951056516295154,1.,0.951056516295154,1.,0.951056516295154,1.,0.951056516295154,
1.,0.951056516295154,1.,0.951056516295154,1.,0.951056516295154,1.))
REPRESENTATION_ITEM('')
);
#1618=(
BOUNDED_CURVE()
B_SPLINE_CURVE(2,(#290468,#290469,#290470,#290471,#290472,#290473,#290474,
#290475,#290476,#290477,#290478,#290479,#290480,#290481,#290482,#290483,
#290484,#290485,#290486,#290487,#290488),.UNSPECIFIED.,.F.,.F.)
B_SPLINE_CURVE_WITH_KNOTS((3,2,2,2,2,2,2,2,2,2,3),(0.201923076923077,0.203846153846154,
0.205769230769231,0.207692307692308,0.209615384615385,0.211538461538462,
0.213461538461538,0.215384615384615,0.217307692307692,0.219230769230769,
0.221153846153846),.UNSPECIFIED.)
CURVE()
GEOMETRIC_REPRESENTATION_ITEM()
RATIONAL_B_SPLINE_CURVE((1.,0.951056516295154,1.,0.951056516295154,1.,0.951056516295154,
1.,0.951056516295154,1.,0.951056516295154,1.,0.951056516295154,1.,0.951056516295154,
1.,0.951056516295154,1.,0.951056516295154,1.,0.951056516295154,1.))
REPRESENTATION_ITEM('')
);
#1619=(
BOUNDED_CURVE()
B_SPLINE_CURVE(2,(#290489,#290490,#290491,#290492,#290493,#290494,#290495,
#290496,#290497,#290498,#290499,#290500,#290501,#290502,#290503,#290504,
#290505,#290506,#290507,#290508,#290509),.UNSPECIFIED.,.F.,.F.)
B_SPLINE_CURVE_WITH_KNOTS((3,2,2,2,2,2,2,2,2,2,3),(0.201923076923077,0.203846153846154,
0.205769230769231,0.207692307692308,0.209615384615385,0.211538461538462,
0.213461538461538,0.215384615384615,0.217307692307692,0.219230769230769,
0.221153846153846),.UNSPECIFIED.)
CURVE()
GEOMETRIC_REPRESENTATION_ITEM()
RATIONAL_B_SPLINE_CURVE((1.,0.951056516295154,1.,0.951056516295154,1.,0.951056516295154,
1.,0.951056516295154,1.,0.951056516295154,1.,0.951056516295154,1.,0.951056516295154,
1.,0.951056516295154,1.,0.951056516295154,1.,0.951056516295154,1.))
REPRESENTATION_ITEM('')
);
#1620=(
BOUNDED_CURVE()
B_SPLINE_CURVE(2,(#290514,#290515,#290516,#290517,#290518,#290519,#290520,
#290521,#290522,#290523,#290524,#290525,#290526,#290527,#290528,#290529,
#290530,#290531,#290532,#290533,#290534),.UNSPECIFIED.,.F.,.F.)
B_SPLINE_CURVE_WITH_KNOTS((3,2,2,2,2,2,2,2,2,2,3),(0.221153846153846,0.223076923076923,
0.225,0.226923076923077,0.228846153846154,0.230769230769231,0.232692307692308,
0.234615384615385,0.236538461538462,0.238461538461538,0.240384615384615),
 .UNSPECIFIED.)
CURVE()
GEOMETRIC_REPRESENTATION_ITEM()
RATIONAL_B_SPLINE_CURVE((1.,0.951056516295154,1.,0.951056516295154,1.,0.951056516295154,
1.,0.951056516295154,1.,0.951056516295154,1.,0.951056516295154,1.,0.951056516295154,
1.,0.951056516295154,1.,0.951056516295154,1.,0.951056516295154,1.))
REPRESENTATION_ITEM('')
);
#1621=(
BOUNDED_CURVE()
B_SPLINE_CURVE(2,(#290535,#290536,#290537,#290538,#290539,#290540,#290541,
#290542,#290543,#290544,#290545,#290546,#290547,#290548,#290549,#290550,
#290551,#290552,#290553,#290554,#290555),.UNSPECIFIED.,.F.,.F.)
B_SPLINE_CURVE_WITH_KNOTS((3,2,2,2,2,2,2,2,2,2,3),(0.221153846153846,0.223076923076923,
0.225,0.226923076923077,0.228846153846154,0.230769230769231,0.232692307692308,
0.234615384615385,0.236538461538462,0.238461538461538,0.240384615384615),
 .UNSPECIFIED.)
CURVE()
GEOMETRIC_REPRESENTATION_ITEM()
RATIONAL_B_SPLINE_CURVE((1.,0.951056516295154,1.,0.951056516295154,1.,0.951056516295154,
1.,0.951056516295154,1.,0.951056516295154,1.,0.951056516295154,1.,0.951056516295154,
1.,0.951056516295154,1.,0.951056516295154,1.,0.951056516295154,1.))
REPRESENTATION_ITEM('')
);
#1622=(
BOUNDED_CURVE()
B_SPLINE_CURVE(2,(#290560,#290561,#290562,#290563,#290564,#290565,#290566,
#290567,#290568,#290569,#290570,#290571,#290572,#290573,#290574,#290575,
#290576,#290577,#290578,#290579,#290580),.UNSPECIFIED.,.F.,.F.)
B_SPLINE_CURVE_WITH_KNOTS((3,2,2,2,2,2,2,2,2,2,3),(0.240384615384615,0.242307692307692,
0.244230769230769,0.246153846153846,0.248076923076923,0.25,0.251923076923077,
0.253846153846154,0.255769230769231,0.257692307692308,0.259615384615385),
 .UNSPECIFIED.)
CURVE()
GEOMETRIC_REPRESENTATION_ITEM()
RATIONAL_B_SPLINE_CURVE((1.,0.951056516295154,1.,0.951056516295154,1.,0.951056516295154,
1.,0.951056516295154,1.,0.951056516295154,1.,0.951056516295154,1.,0.951056516295154,
1.,0.951056516295154,1.,0.951056516295154,1.,0.951056516295154,1.))
REPRESENTATION_ITEM('')
);
#1623=(
BOUNDED_CURVE()
B_SPLINE_CURVE(2,(#290581,#290582,#290583,#290584,#290585,#290586,#290587,
#290588,#290589,#290590,#290591,#290592,#290593,#290594,#290595,#290596,
#290597,#290598,#290599,#290600,#290601),.UNSPECIFIED.,.F.,.F.)
B_SPLINE_CURVE_WITH_KNOTS((3,2,2,2,2,2,2,2,2,2,3),(0.240384615384615,0.242307692307692,
0.244230769230769,0.246153846153846,0.248076923076923,0.25,0.251923076923077,
0.253846153846154,0.255769230769231,0.257692307692308,0.259615384615385),
 .UNSPECIFIED.)
CURVE()
GEOMETRIC_REPRESENTATION_ITEM()
RATIONAL_B_SPLINE_CURVE((1.,0.951056516295154,1.,0.951056516295154,1.,0.951056516295154,
1.,0.951056516295154,1.,0.951056516295154,1.,0.951056516295154,1.,0.951056516295154,
1.,0.951056516295154,1.,0.951056516295154,1.,0.951056516295154,1.))
REPRESENTATION_ITEM('')
);
#1624=(
BOUNDED_CURVE()
B_SPLINE_CURVE(2,(#290606,#290607,#290608,#290609,#290610,#290611,#290612,
#290613,#290614,#290615,#290616,#290617,#290618,#290619,#290620,#290621,
#290622,#290623,#290624,#290625,#290626),.UNSPECIFIED.,.F.,.F.)
B_SPLINE_CURVE_WITH_KNOTS((3,2,2,2,2,2,2,2,2,2,3),(0.259615384615385,0.261538461538462,
0.263461538461538,0.265384615384615,0.267307692307692,0.269230769230769,
0.271153846153846,0.273076923076923,0.275,0.276923076923077,0.278846153846154),
 .UNSPECIFIED.)
CURVE()
GEOMETRIC_REPRESENTATION_ITEM()
RATIONAL_B_SPLINE_CURVE((1.,0.951056516295154,1.,0.951056516295154,1.,0.951056516295154,
1.,0.951056516295154,1.,0.951056516295154,1.,0.951056516295154,1.,0.951056516295154,
1.,0.951056516295154,1.,0.951056516295154,1.,0.951056516295154,1.))
REPRESENTATION_ITEM('')
);
#1625=(
BOUNDED_CURVE()
B_SPLINE_CURVE(2,(#290627,#290628,#290629,#290630,#290631,#290632,#290633,
#290634,#290635,#290636,#290637,#290638,#290639,#290640,#290641,#290642,
#290643,#290644,#290645,#290646,#290647),.UNSPECIFIED.,.F.,.F.)
B_SPLINE_CURVE_WITH_KNOTS((3,2,2,2,2,2,2,2,2,2,3),(0.259615384615385,0.261538461538462,
0.263461538461538,0.265384615384615,0.267307692307692,0.269230769230769,
0.271153846153846,0.273076923076923,0.275,0.276923076923077,0.278846153846154),
 .UNSPECIFIED.)
CURVE()
GEOMETRIC_REPRESENTATION_ITEM()
RATIONAL_B_SPLINE_CURVE((1.,0.951056516295154,1.,0.951056516295154,1.,0.951056516295154,
1.,0.951056516295154,1.,0.951056516295154,1.,0.951056516295154,1.,0.951056516295154,
1.,0.951056516295154,1.,0.951056516295154,1.,0.951056516295154,1.))
REPRESENTATION_ITEM('')
);
#1626=(
BOUNDED_CURVE()
B_SPLINE_CURVE(2,(#290652,#290653,#290654,#290655,#290656,#290657,#290658,
#290659,#290660,#290661,#290662,#290663,#290664,#290665,#290666,#290667,
#290668,#290669,#290670,#290671,#290672),.UNSPECIFIED.,.F.,.F.)
B_SPLINE_CURVE_WITH_KNOTS((3,2,2,2,2,2,2,2,2,2,3),(0.278846153846154,0.280769230769231,
0.282692307692308,0.284615384615385,0.286538461538462,0.288461538461538,
0.290384615384615,0.292307692307692,0.294230769230769,0.296153846153846,
0.298076923076923),.UNSPECIFIED.)
CURVE()
GEOMETRIC_REPRESENTATION_ITEM()
RATIONAL_B_SPLINE_CURVE((1.,0.951056516295154,1.,0.951056516295154,1.,0.951056516295154,
1.,0.951056516295154,1.,0.951056516295154,1.,0.951056516295154,1.,0.951056516295154,
1.,0.951056516295154,1.,0.951056516295154,1.,0.951056516295154,1.))
REPRESENTATION_ITEM('')
);
#1627=(
BOUNDED_CURVE()
B_SPLINE_CURVE(2,(#290673,#290674,#290675,#290676,#290677,#290678,#290679,
#290680,#290681,#290682,#290683,#290684,#290685,#290686,#290687,#290688,
#290689,#290690,#290691,#290692,#290693),.UNSPECIFIED.,.F.,.F.)
B_SPLINE_CURVE_WITH_KNOTS((3,2,2,2,2,2,2,2,2,2,3),(0.278846153846154,0.280769230769231,
0.282692307692308,0.284615384615385,0.286538461538462,0.288461538461538,
0.290384615384615,0.292307692307692,0.294230769230769,0.296153846153846,
0.298076923076923),.UNSPECIFIED.)
CURVE()
GEOMETRIC_REPRESENTATION_ITEM()
RATIONAL_B_SPLINE_CURVE((1.,0.951056516295154,1.,0.951056516295154,1.,0.951056516295154,
1.,0.951056516295154,1.,0.951056516295154,1.,0.951056516295154,1.,0.951056516295154,
1.,0.951056516295154,1.,0.951056516295154,1.,0.951056516295154,1.))
REPRESENTATION_ITEM('')
);
#1628=(
BOUNDED_CURVE()
B_SPLINE_CURVE(2,(#290698,#290699,#290700,#290701,#290702,#290703,#290704,
#290705,#290706,#290707,#290708,#290709,#290710,#290711,#290712,#290713,
#290714,#290715,#290716,#290717,#290718),.UNSPECIFIED.,.F.,.F.)
B_SPLINE_CURVE_WITH_KNOTS((3,2,2,2,2,2,2,2,2,2,3),(0.298076923076923,0.3,
0.301923076923077,0.303846153846154,0.305769230769231,0.307692307692308,
0.309615384615385,0.311538461538462,0.313461538461538,0.315384615384615,
0.317307692307692),.UNSPECIFIED.)
CURVE()
GEOMETRIC_REPRESENTATION_ITEM()
RATIONAL_B_SPLINE_CURVE((1.,0.951056516295154,1.,0.951056516295154,1.,0.951056516295154,
1.,0.951056516295154,1.,0.951056516295154,1.,0.951056516295154,1.,0.951056516295154,
1.,0.951056516295154,1.,0.951056516295154,1.,0.951056516295154,1.))
REPRESENTATION_ITEM('')
);
#1629=(
BOUNDED_CURVE()
B_SPLINE_CURVE(2,(#290719,#290720,#290721,#290722,#290723,#290724,#290725,
#290726,#290727,#290728,#290729,#290730,#290731,#290732,#290733,#290734,
#290735,#290736,#290737,#290738,#290739),.UNSPECIFIED.,.F.,.F.)
B_SPLINE_CURVE_WITH_KNOTS((3,2,2,2,2,2,2,2,2,2,3),(0.298076923076923,0.3,
0.301923076923077,0.303846153846154,0.305769230769231,0.307692307692308,
0.309615384615385,0.311538461538462,0.313461538461538,0.315384615384615,
0.317307692307692),.UNSPECIFIED.)
CURVE()
GEOMETRIC_REPRESENTATION_ITEM()
RATIONAL_B_SPLINE_CURVE((1.,0.951056516295154,1.,0.951056516295154,1.,0.951056516295154,
1.,0.951056516295154,1.,0.951056516295154,1.,0.951056516295154,1.,0.951056516295154,
1.,0.951056516295154,1.,0.951056516295154,1.,0.951056516295154,1.))
REPRESENTATION_ITEM('')
);
#1630=(
BOUNDED_CURVE()
B_SPLINE_CURVE(2,(#290744,#290745,#290746,#290747,#290748,#290749,#290750,
#290751,#290752,#290753,#290754,#290755,#290756,#290757,#290758,#290759,
#290760,#290761,#290762,#290763,#290764),.UNSPECIFIED.,.F.,.F.)
B_SPLINE_CURVE_WITH_KNOTS((3,2,2,2,2,2,2,2,2,2,3),(0.317307692307692,0.319230769230769,
0.321153846153846,0.323076923076923,0.325,0.326923076923077,0.328846153846154,
0.330769230769231,0.332692307692308,0.334615384615385,0.336538461538462),
 .UNSPECIFIED.)
CURVE()
GEOMETRIC_REPRESENTATION_ITEM()
RATIONAL_B_SPLINE_CURVE((1.,0.951056516295154,1.,0.951056516295154,1.,0.951056516295154,
1.,0.951056516295154,1.,0.951056516295154,1.,0.951056516295154,1.,0.951056516295154,
1.,0.951056516295154,1.,0.951056516295154,1.,0.951056516295154,1.))
REPRESENTATION_ITEM('')
);
#1631=(
BOUNDED_CURVE()
B_SPLINE_CURVE(2,(#290765,#290766,#290767,#290768,#290769,#290770,#290771,
#290772,#290773,#290774,#290775,#290776,#290777,#290778,#290779,#290780,
#290781,#290782,#290783,#290784,#290785),.UNSPECIFIED.,.F.,.F.)
B_SPLINE_CURVE_WITH_KNOTS((3,2,2,2,2,2,2,2,2,2,3),(0.317307692307692,0.319230769230769,
0.321153846153846,0.323076923076923,0.325,0.326923076923077,0.328846153846154,
0.330769230769231,0.332692307692308,0.334615384615385,0.336538461538462),
 .UNSPECIFIED.)
CURVE()
GEOMETRIC_REPRESENTATION_ITEM()
RATIONAL_B_SPLINE_CURVE((1.,0.951056516295154,1.,0.951056516295154,1.,0.951056516295154,
1.,0.951056516295154,1.,0.951056516295154,1.,0.951056516295154,1.,0.951056516295154,
1.,0.951056516295154,1.,0.951056516295154,1.,0.951056516295154,1.))
REPRESENTATION_ITEM('')
);
#1632=(
BOUNDED_CURVE()
B_SPLINE_CURVE(2,(#290790,#290791,#290792,#290793,#290794,#290795,#290796,
#290797,#290798,#290799,#290800,#290801,#290802,#290803,#290804,#290805,
#290806,#290807,#290808,#290809,#290810),.UNSPECIFIED.,.F.,.F.)
B_SPLINE_CURVE_WITH_KNOTS((3,2,2,2,2,2,2,2,2,2,3),(0.336538461538462,0.338461538461538,
0.340384615384615,0.342307692307692,0.344230769230769,0.346153846153846,
0.348076923076923,0.35,0.351923076923077,0.353846153846154,0.355769230769231),
 .UNSPECIFIED.)
CURVE()
GEOMETRIC_REPRESENTATION_ITEM()
RATIONAL_B_SPLINE_CURVE((1.,0.951056516295154,1.,0.951056516295154,1.,0.951056516295154,
1.,0.951056516295154,1.,0.951056516295154,1.,0.951056516295154,1.,0.951056516295154,
1.,0.951056516295154,1.,0.951056516295154,1.,0.951056516295154,1.))
REPRESENTATION_ITEM('')
);
#1633=(
BOUNDED_CURVE()
B_SPLINE_CURVE(2,(#290811,#290812,#290813,#290814,#290815,#290816,#290817,
#290818,#290819,#290820,#290821,#290822,#290823,#290824,#290825,#290826,
#290827,#290828,#290829,#290830,#290831),.UNSPECIFIED.,.F.,.F.)
B_SPLINE_CURVE_WITH_KNOTS((3,2,2,2,2,2,2,2,2,2,3),(0.336538461538462,0.338461538461538,
0.340384615384615,0.342307692307692,0.344230769230769,0.346153846153846,
0.348076923076923,0.35,0.351923076923077,0.353846153846154,0.355769230769231),
 .UNSPECIFIED.)
CURVE()
GEOMETRIC_REPRESENTATION_ITEM()
RATIONAL_B_SPLINE_CURVE((1.,0.951056516295154,1.,0.951056516295154,1.,0.951056516295154,
1.,0.951056516295154,1.,0.951056516295154,1.,0.951056516295154,1.,0.951056516295154,
1.,0.951056516295154,1.,0.951056516295154,1.,0.951056516295154,1.))
REPRESENTATION_ITEM('')
);
#1634=(
BOUNDED_CURVE()
B_SPLINE_CURVE(2,(#290836,#290837,#290838,#290839,#290840,#290841,#290842,
#290843,#290844,#290845,#290846,#290847,#290848,#290849,#290850,#290851,
#290852,#290853,#290854,#290855,#290856),.UNSPECIFIED.,.F.,.F.)
B_SPLINE_CURVE_WITH_KNOTS((3,2,2,2,2,2,2,2,2,2,3),(0.355769230769231,0.357692307692308,
0.359615384615385,0.361538461538462,0.363461538461538,0.365384615384615,
0.367307692307692,0.369230769230769,0.371153846153846,0.373076923076923,
0.375),.UNSPECIFIED.)
CURVE()
GEOMETRIC_REPRESENTATION_ITEM()
RATIONAL_B_SPLINE_CURVE((1.,0.951056516295154,1.,0.951056516295154,1.,0.951056516295154,
1.,0.951056516295154,1.,0.951056516295154,1.,0.951056516295154,1.,0.951056516295154,
1.,0.951056516295154,1.,0.951056516295154,1.,0.951056516295154,1.))
REPRESENTATION_ITEM('')
);
#1635=(
BOUNDED_CURVE()
B_SPLINE_CURVE(2,(#290857,#290858,#290859,#290860,#290861,#290862,#290863,
#290864,#290865,#290866,#290867,#290868,#290869,#290870,#290871,#290872,
#290873,#290874,#290875,#290876,#290877),.UNSPECIFIED.,.F.,.F.)
B_SPLINE_CURVE_WITH_KNOTS((3,2,2,2,2,2,2,2,2,2,3),(0.355769230769231,0.357692307692308,
0.359615384615385,0.361538461538462,0.363461538461538,0.365384615384615,
0.367307692307692,0.369230769230769,0.371153846153846,0.373076923076923,
0.375),.UNSPECIFIED.)
CURVE()
GEOMETRIC_REPRESENTATION_ITEM()
RATIONAL_B_SPLINE_CURVE((1.,0.951056516295154,1.,0.951056516295154,1.,0.951056516295154,
1.,0.951056516295154,1.,0.951056516295154,1.,0.951056516295154,1.,0.951056516295154,
1.,0.951056516295154,1.,0.951056516295154,1.,0.951056516295154,1.))
REPRESENTATION_ITEM('')
);
#1636=(
BOUNDED_CURVE()
B_SPLINE_CURVE(2,(#290882,#290883,#290884,#290885,#290886,#290887,#290888,
#290889,#290890,#290891,#290892,#290893,#290894,#290895,#290896,#290897,
#290898,#290899,#290900,#290901,#290902),.UNSPECIFIED.,.F.,.F.)
B_SPLINE_CURVE_WITH_KNOTS((3,2,2,2,2,2,2,2,2,2,3),(0.375,0.376923076923077,
0.378846153846154,0.380769230769231,0.382692307692308,0.384615384615385,
0.386538461538462,0.388461538461538,0.390384615384615,0.392307692307692,
0.394230769230769),.UNSPECIFIED.)
CURVE()
GEOMETRIC_REPRESENTATION_ITEM()
RATIONAL_B_SPLINE_CURVE((1.,0.951056516295154,1.,0.951056516295154,1.,0.951056516295154,
1.,0.951056516295154,1.,0.951056516295154,1.,0.951056516295154,1.,0.951056516295154,
1.,0.951056516295154,1.,0.951056516295154,1.,0.951056516295154,1.))
REPRESENTATION_ITEM('')
);
#1637=(
BOUNDED_CURVE()
B_SPLINE_CURVE(2,(#290903,#290904,#290905,#290906,#290907,#290908,#290909,
#290910,#290911,#290912,#290913,#290914,#290915,#290916,#290917,#290918,
#290919,#290920,#290921,#290922,#290923),.UNSPECIFIED.,.F.,.F.)
B_SPLINE_CURVE_WITH_KNOTS((3,2,2,2,2,2,2,2,2,2,3),(0.375,0.376923076923077,
0.378846153846154,0.380769230769231,0.382692307692308,0.384615384615385,
0.386538461538462,0.388461538461538,0.390384615384615,0.392307692307692,
0.394230769230769),.UNSPECIFIED.)
CURVE()
GEOMETRIC_REPRESENTATION_ITEM()
RATIONAL_B_SPLINE_CURVE((1.,0.951056516295154,1.,0.951056516295154,1.,0.951056516295154,
1.,0.951056516295154,1.,0.951056516295154,1.,0.951056516295154,1.,0.951056516295154,
1.,0.951056516295154,1.,0.951056516295154,1.,0.951056516295154,1.))
REPRESENTATION_ITEM('')
);
#1638=(
BOUNDED_CURVE()
B_SPLINE_CURVE(2,(#290929,#290930,#290931,#290932,#290933,#290934,#290935,
#290936,#290937,#290938,#290939,#290940,#290941),.UNSPECIFIED.,.F.,.F.)
B_SPLINE_CURVE_WITH_KNOTS((3,2,2,2,2,2,3),(0.595378520967158,0.596153846153846,
0.598076923076923,0.6,0.601923076923077,0.603846153846154,0.605769230769231),
 .UNSPECIFIED.)
CURVE()
GEOMETRIC_REPRESENTATION_ITEM()
RATIONAL_B_SPLINE_CURVE((0.976446068257266,0.980267499866866,1.,0.951056516295154,
1.,0.951056516295154,1.,0.951056516295154,1.,0.951056516295154,1.,0.951056516295154,
1.))
REPRESENTATION_ITEM('')
);
#1639=(
BOUNDED_CURVE()
B_SPLINE_CURVE(2,(#290944,#290945,#290946,#290947,#290948,#290949,#290950,
#290951,#290952,#290953,#290954),.UNSPECIFIED.,.F.,.F.)
B_SPLINE_CURVE_WITH_KNOTS((3,2,2,2,2,3),(0.597778235786775,0.598076923076923,
0.6,0.601923076923077,0.603846153846154,0.605769230769231),
 .UNSPECIFIED.)
CURVE()
GEOMETRIC_REPRESENTATION_ITEM()
RATIONAL_B_SPLINE_CURVE((0.987157827087347,0.992398225810528,1.,0.951056516295154,
1.,0.951056516295154,1.,0.951056516295154,1.,0.951056516295154,1.))
REPRESENTATION_ITEM('')
);
#1640=(
BOUNDED_CURVE()
B_SPLINE_CURVE(2,(#290959,#290960,#290961,#290962,#290963,#290964,#290965,
#290966,#290967,#290968,#290969,#290970,#290971,#290972,#290973,#290974,
#290975,#290976,#290977,#290978,#290979),.UNSPECIFIED.,.F.,.F.)
B_SPLINE_CURVE_WITH_KNOTS((3,2,2,2,2,2,2,2,2,2,3),(0.605769230769231,0.607692307692308,
0.609615384615385,0.611538461538462,0.613461538461539,0.615384615384615,
0.617307692307692,0.619230769230769,0.621153846153846,0.623076923076923,
0.625),.UNSPECIFIED.)
CURVE()
GEOMETRIC_REPRESENTATION_ITEM()
RATIONAL_B_SPLINE_CURVE((1.,0.951056516295154,1.,0.951056516295154,1.,0.951056516295154,
1.,0.951056516295154,1.,0.951056516295154,1.,0.951056516295154,1.,0.951056516295154,
1.,0.951056516295154,1.,0.951056516295154,1.,0.951056516295154,1.))
REPRESENTATION_ITEM('')
);
#1641=(
BOUNDED_CURVE()
B_SPLINE_CURVE(2,(#290980,#290981,#290982,#290983,#290984,#290985,#290986,
#290987,#290988,#290989,#290990,#290991,#290992,#290993,#290994,#290995,
#290996,#290997,#290998,#290999,#291000),.UNSPECIFIED.,.F.,.F.)
B_SPLINE_CURVE_WITH_KNOTS((3,2,2,2,2,2,2,2,2,2,3),(0.605769230769231,0.607692307692308,
0.609615384615385,0.611538461538462,0.613461538461539,0.615384615384615,
0.617307692307692,0.619230769230769,0.621153846153846,0.623076923076923,
0.625),.UNSPECIFIED.)
CURVE()
GEOMETRIC_REPRESENTATION_ITEM()
RATIONAL_B_SPLINE_CURVE((1.,0.951056516295154,1.,0.951056516295154,1.,0.951056516295154,
1.,0.951056516295154,1.,0.951056516295154,1.,0.951056516295154,1.,0.951056516295154,
1.,0.951056516295154,1.,0.951056516295154,1.,0.951056516295154,1.))
REPRESENTATION_ITEM('')
);
#1642=(
BOUNDED_CURVE()
B_SPLINE_CURVE(2,(#291005,#291006,#291007,#291008,#291009,#291010,#291011,
#291012,#291013,#291014,#291015,#291016,#291017,#291018,#291019,#291020,
#291021,#291022,#291023,#291024,#291025),.UNSPECIFIED.,.F.,.F.)
B_SPLINE_CURVE_WITH_KNOTS((3,2,2,2,2,2,2,2,2,2,3),(0.625,0.626923076923077,
0.628846153846154,0.630769230769231,0.632692307692308,0.634615384615385,
0.636538461538461,0.638461538461538,0.640384615384615,0.642307692307692,
0.644230769230769),.UNSPECIFIED.)
CURVE()
GEOMETRIC_REPRESENTATION_ITEM()
RATIONAL_B_SPLINE_CURVE((1.,0.951056516295154,1.,0.951056516295154,1.,0.951056516295154,
1.,0.951056516295154,1.,0.951056516295154,1.,0.951056516295154,1.,0.951056516295154,
1.,0.951056516295154,1.,0.951056516295154,1.,0.951056516295154,1.))
REPRESENTATION_ITEM('')
);
#1643=(
BOUNDED_CURVE()
B_SPLINE_CURVE(2,(#291026,#291027,#291028,#291029,#291030,#291031,#291032,
#291033,#291034,#291035,#291036,#291037,#291038,#291039,#291040,#291041,
#291042,#291043,#291044,#291045,#291046),.UNSPECIFIED.,.F.,.F.)
B_SPLINE_CURVE_WITH_KNOTS((3,2,2,2,2,2,2,2,2,2,3),(0.625,0.626923076923077,
0.628846153846154,0.630769230769231,0.632692307692308,0.634615384615385,
0.636538461538461,0.638461538461538,0.640384615384615,0.642307692307692,
0.644230769230769),.UNSPECIFIED.)
CURVE()
GEOMETRIC_REPRESENTATION_ITEM()
RATIONAL_B_SPLINE_CURVE((1.,0.951056516295154,1.,0.951056516295154,1.,0.951056516295154,
1.,0.951056516295154,1.,0.951056516295154,1.,0.951056516295154,1.,0.951056516295154,
1.,0.951056516295154,1.,0.951056516295154,1.,0.951056516295154,1.))
REPRESENTATION_ITEM('')
);
#1644=(
BOUNDED_CURVE()
B_SPLINE_CURVE(2,(#291051,#291052,#291053,#291054,#291055,#291056,#291057,
#291058,#291059,#291060,#291061,#291062,#291063,#291064,#291065,#291066,
#291067,#291068,#291069,#291070,#291071),.UNSPECIFIED.,.F.,.F.)
B_SPLINE_CURVE_WITH_KNOTS((3,2,2,2,2,2,2,2,2,2,3),(0.644230769230769,0.646153846153846,
0.648076923076923,0.65,0.651923076923077,0.653846153846154,0.655769230769231,
0.657692307692308,0.659615384615385,0.661538461538462,0.663461538461538),
 .UNSPECIFIED.)
CURVE()
GEOMETRIC_REPRESENTATION_ITEM()
RATIONAL_B_SPLINE_CURVE((1.,0.951056516295154,1.,0.951056516295154,1.,0.951056516295154,
1.,0.951056516295154,1.,0.951056516295154,1.,0.951056516295154,1.,0.951056516295154,
1.,0.951056516295154,1.,0.951056516295154,1.,0.951056516295154,1.))
REPRESENTATION_ITEM('')
);
#1645=(
BOUNDED_CURVE()
B_SPLINE_CURVE(2,(#291072,#291073,#291074,#291075,#291076,#291077,#291078,
#291079,#291080,#291081,#291082,#291083,#291084,#291085,#291086,#291087,
#291088,#291089,#291090,#291091,#291092),.UNSPECIFIED.,.F.,.F.)
B_SPLINE_CURVE_WITH_KNOTS((3,2,2,2,2,2,2,2,2,2,3),(0.644230769230769,0.646153846153846,
0.648076923076923,0.65,0.651923076923077,0.653846153846154,0.655769230769231,
0.657692307692308,0.659615384615385,0.661538461538462,0.663461538461538),
 .UNSPECIFIED.)
CURVE()
GEOMETRIC_REPRESENTATION_ITEM()
RATIONAL_B_SPLINE_CURVE((1.,0.951056516295154,1.,0.951056516295154,1.,0.951056516295154,
1.,0.951056516295154,1.,0.951056516295154,1.,0.951056516295154,1.,0.951056516295154,
1.,0.951056516295154,1.,0.951056516295154,1.,0.951056516295154,1.))
REPRESENTATION_ITEM('')
);
#1646=(
BOUNDED_CURVE()
B_SPLINE_CURVE(2,(#291097,#291098,#291099,#291100,#291101,#291102,#291103,
#291104,#291105,#291106,#291107,#291108,#291109,#291110,#291111,#291112,
#291113,#291114,#291115,#291116,#291117),.UNSPECIFIED.,.F.,.F.)
B_SPLINE_CURVE_WITH_KNOTS((3,2,2,2,2,2,2,2,2,2,3),(0.663461538461538,0.665384615384615,
0.667307692307692,0.669230769230769,0.671153846153846,0.673076923076923,
0.675,0.676923076923077,0.678846153846154,0.680769230769231,0.682692307692308),
 .UNSPECIFIED.)
CURVE()
GEOMETRIC_REPRESENTATION_ITEM()
RATIONAL_B_SPLINE_CURVE((1.,0.951056516295154,1.,0.951056516295154,1.,0.951056516295154,
1.,0.951056516295154,1.,0.951056516295154,1.,0.951056516295154,1.,0.951056516295154,
1.,0.951056516295154,1.,0.951056516295154,1.,0.951056516295154,1.))
REPRESENTATION_ITEM('')
);
#1647=(
BOUNDED_CURVE()
B_SPLINE_CURVE(2,(#291118,#291119,#291120,#291121,#291122,#291123,#291124,
#291125,#291126,#291127,#291128,#291129,#291130,#291131,#291132,#291133,
#291134,#291135,#291136,#291137,#291138),.UNSPECIFIED.,.F.,.F.)
B_SPLINE_CURVE_WITH_KNOTS((3,2,2,2,2,2,2,2,2,2,3),(0.663461538461538,0.665384615384615,
0.667307692307692,0.669230769230769,0.671153846153846,0.673076923076923,
0.675,0.676923076923077,0.678846153846154,0.680769230769231,0.682692307692308),
 .UNSPECIFIED.)
CURVE()
GEOMETRIC_REPRESENTATION_ITEM()
RATIONAL_B_SPLINE_CURVE((1.,0.951056516295154,1.,0.951056516295154,1.,0.951056516295154,
1.,0.951056516295154,1.,0.951056516295154,1.,0.951056516295154,1.,0.951056516295154,
1.,0.951056516295154,1.,0.951056516295154,1.,0.951056516295154,1.))
REPRESENTATION_ITEM('')
);
#1648=(
BOUNDED_CURVE()
B_SPLINE_CURVE(2,(#291143,#291144,#291145,#291146,#291147,#291148,#291149,
#291150,#291151,#291152,#291153,#291154,#291155,#291156,#291157,#291158,
#291159,#291160,#291161,#291162,#291163),.UNSPECIFIED.,.F.,.F.)
B_SPLINE_CURVE_WITH_KNOTS((3,2,2,2,2,2,2,2,2,2,3),(0.682692307692308,0.684615384615385,
0.686538461538462,0.688461538461538,0.690384615384615,0.692307692307692,
0.694230769230769,0.696153846153846,0.698076923076923,0.7,0.701923076923077),
 .UNSPECIFIED.)
CURVE()
GEOMETRIC_REPRESENTATION_ITEM()
RATIONAL_B_SPLINE_CURVE((1.,0.951056516295154,1.,0.951056516295154,1.,0.951056516295154,
1.,0.951056516295154,1.,0.951056516295154,1.,0.951056516295154,1.,0.951056516295154,
1.,0.951056516295154,1.,0.951056516295154,1.,0.951056516295154,1.))
REPRESENTATION_ITEM('')
);
#1649=(
BOUNDED_CURVE()
B_SPLINE_CURVE(2,(#291164,#291165,#291166,#291167,#291168,#291169,#291170,
#291171,#291172,#291173,#291174,#291175,#291176,#291177,#291178,#291179,
#291180,#291181,#291182,#291183,#291184),.UNSPECIFIED.,.F.,.F.)
B_SPLINE_CURVE_WITH_KNOTS((3,2,2,2,2,2,2,2,2,2,3),(0.682692307692308,0.684615384615385,
0.686538461538462,0.688461538461538,0.690384615384615,0.692307692307692,
0.694230769230769,0.696153846153846,0.698076923076923,0.7,0.701923076923077),
 .UNSPECIFIED.)
CURVE()
GEOMETRIC_REPRESENTATION_ITEM()
RATIONAL_B_SPLINE_CURVE((1.,0.951056516295154,1.,0.951056516295154,1.,0.951056516295154,
1.,0.951056516295154,1.,0.951056516295154,1.,0.951056516295154,1.,0.951056516295154,
1.,0.951056516295154,1.,0.951056516295154,1.,0.951056516295154,1.))
REPRESENTATION_ITEM('')
);
#1650=(
BOUNDED_CURVE()
B_SPLINE_CURVE(2,(#291189,#291190,#291191,#291192,#291193,#291194,#291195,
#291196,#291197,#291198,#291199,#291200,#291201,#291202,#291203,#291204,
#291205,#291206,#291207,#291208,#291209),.UNSPECIFIED.,.F.,.F.)
B_SPLINE_CURVE_WITH_KNOTS((3,2,2,2,2,2,2,2,2,2,3),(0.701923076923077,0.703846153846154,
0.705769230769231,0.707692307692308,0.709615384615385,0.711538461538462,
0.713461538461538,0.715384615384615,0.717307692307692,0.719230769230769,
0.721153846153846),.UNSPECIFIED.)
CURVE()
GEOMETRIC_REPRESENTATION_ITEM()
RATIONAL_B_SPLINE_CURVE((1.,0.951056516295154,1.,0.951056516295154,1.,0.951056516295154,
1.,0.951056516295154,1.,0.951056516295154,1.,0.951056516295154,1.,0.951056516295154,
1.,0.951056516295154,1.,0.951056516295154,1.,0.951056516295154,1.))
REPRESENTATION_ITEM('')
);
#1651=(
BOUNDED_CURVE()
B_SPLINE_CURVE(2,(#291210,#291211,#291212,#291213,#291214,#291215,#291216,
#291217,#291218,#291219,#291220,#291221,#291222,#291223,#291224,#291225,
#291226,#291227,#291228,#291229,#291230),.UNSPECIFIED.,.F.,.F.)
B_SPLINE_CURVE_WITH_KNOTS((3,2,2,2,2,2,2,2,2,2,3),(0.701923076923077,0.703846153846154,
0.705769230769231,0.707692307692308,0.709615384615385,0.711538461538462,
0.713461538461538,0.715384615384615,0.717307692307692,0.719230769230769,
0.721153846153846),.UNSPECIFIED.)
CURVE()
GEOMETRIC_REPRESENTATION_ITEM()
RATIONAL_B_SPLINE_CURVE((1.,0.951056516295154,1.,0.951056516295154,1.,0.951056516295154,
1.,0.951056516295154,1.,0.951056516295154,1.,0.951056516295154,1.,0.951056516295154,
1.,0.951056516295154,1.,0.951056516295154,1.,0.951056516295154,1.))
REPRESENTATION_ITEM('')
);
#1652=(
BOUNDED_CURVE()
B_SPLINE_CURVE(2,(#291235,#291236,#291237,#291238,#291239,#291240,#291241,
#291242,#291243,#291244,#291245,#291246,#291247,#291248,#291249,#291250,
#291251,#291252,#291253,#291254,#291255),.UNSPECIFIED.,.F.,.F.)
B_SPLINE_CURVE_WITH_KNOTS((3,2,2,2,2,2,2,2,2,2,3),(0.721153846153846,0.723076923076923,
0.725,0.726923076923077,0.728846153846154,0.730769230769231,0.732692307692308,
0.734615384615385,0.736538461538462,0.738461538461539,0.740384615384615),
 .UNSPECIFIED.)
CURVE()
GEOMETRIC_REPRESENTATION_ITEM()
RATIONAL_B_SPLINE_CURVE((1.,0.951056516295154,1.,0.951056516295154,1.,0.951056516295154,
1.,0.951056516295154,1.,0.951056516295154,1.,0.951056516295154,1.,0.951056516295154,
1.,0.951056516295154,1.,0.951056516295154,1.,0.951056516295154,1.))
REPRESENTATION_ITEM('')
);
#1653=(
BOUNDED_CURVE()
B_SPLINE_CURVE(2,(#291256,#291257,#291258,#291259,#291260,#291261,#291262,
#291263,#291264,#291265,#291266,#291267,#291268,#291269,#291270,#291271,
#291272,#291273,#291274,#291275,#291276),.UNSPECIFIED.,.F.,.F.)
B_SPLINE_CURVE_WITH_KNOTS((3,2,2,2,2,2,2,2,2,2,3),(0.721153846153846,0.723076923076923,
0.725,0.726923076923077,0.728846153846154,0.730769230769231,0.732692307692308,
0.734615384615385,0.736538461538462,0.738461538461539,0.740384615384615),
 .UNSPECIFIED.)
CURVE()
GEOMETRIC_REPRESENTATION_ITEM()
RATIONAL_B_SPLINE_CURVE((1.,0.951056516295154,1.,0.951056516295154,1.,0.951056516295154,
1.,0.951056516295154,1.,0.951056516295154,1.,0.951056516295154,1.,0.951056516295154,
1.,0.951056516295154,1.,0.951056516295154,1.,0.951056516295154,1.))
REPRESENTATION_ITEM('')
);
#1654=(
BOUNDED_CURVE()
B_SPLINE_CURVE(2,(#291281,#291282,#291283,#291284,#291285,#291286,#291287,
#291288,#291289,#291290,#291291,#291292,#291293,#291294,#291295,#291296,
#291297,#291298,#291299,#291300,#291301),.UNSPECIFIED.,.F.,.F.)
B_SPLINE_CURVE_WITH_KNOTS((3,2,2,2,2,2,2,2,2,2,3),(0.740384615384615,0.742307692307692,
0.744230769230769,0.746153846153846,0.748076923076923,0.75,0.751923076923077,
0.753846153846154,0.755769230769231,0.757692307692308,0.759615384615385),
 .UNSPECIFIED.)
CURVE()
GEOMETRIC_REPRESENTATION_ITEM()
RATIONAL_B_SPLINE_CURVE((1.,0.951056516295154,1.,0.951056516295154,1.,0.951056516295154,
1.,0.951056516295154,1.,0.951056516295154,1.,0.951056516295154,1.,0.951056516295154,
1.,0.951056516295154,1.,0.951056516295154,1.,0.951056516295154,1.))
REPRESENTATION_ITEM('')
);
#1655=(
BOUNDED_CURVE()
B_SPLINE_CURVE(2,(#291302,#291303,#291304,#291305,#291306,#291307,#291308,
#291309,#291310,#291311,#291312,#291313,#291314,#291315,#291316,#291317,
#291318,#291319,#291320,#291321,#291322),.UNSPECIFIED.,.F.,.F.)
B_SPLINE_CURVE_WITH_KNOTS((3,2,2,2,2,2,2,2,2,2,3),(0.740384615384615,0.742307692307692,
0.744230769230769,0.746153846153846,0.748076923076923,0.75,0.751923076923077,
0.753846153846154,0.755769230769231,0.757692307692308,0.759615384615385),
 .UNSPECIFIED.)
CURVE()
GEOMETRIC_REPRESENTATION_ITEM()
RATIONAL_B_SPLINE_CURVE((1.,0.951056516295154,1.,0.951056516295154,1.,0.951056516295154,
1.,0.951056516295154,1.,0.951056516295154,1.,0.951056516295154,1.,0.951056516295154,
1.,0.951056516295154,1.,0.951056516295154,1.,0.951056516295154,1.))
REPRESENTATION_ITEM('')
);
#1656=(
BOUNDED_CURVE()
B_SPLINE_CURVE(2,(#291327,#291328,#291329,#291330,#291331,#291332,#291333,
#291334,#291335,#291336,#291337,#291338,#291339,#291340,#291341,#291342,
#291343,#291344,#291345,#291346,#291347),.UNSPECIFIED.,.F.,.F.)
B_SPLINE_CURVE_WITH_KNOTS((3,2,2,2,2,2,2,2,2,2,3),(0.759615384615385,0.761538461538461,
0.763461538461538,0.765384615384615,0.767307692307692,0.769230769230769,
0.771153846153846,0.773076923076923,0.775,0.776923076923077,0.778846153846154),
 .UNSPECIFIED.)
CURVE()
GEOMETRIC_REPRESENTATION_ITEM()
RATIONAL_B_SPLINE_CURVE((1.,0.951056516295154,1.,0.951056516295154,1.,0.951056516295154,
1.,0.951056516295154,1.,0.951056516295154,1.,0.951056516295154,1.,0.951056516295154,
1.,0.951056516295154,1.,0.951056516295154,1.,0.951056516295154,1.))
REPRESENTATION_ITEM('')
);
#1657=(
BOUNDED_CURVE()
B_SPLINE_CURVE(2,(#291348,#291349,#291350,#291351,#291352,#291353,#291354,
#291355,#291356,#291357,#291358,#291359,#291360,#291361,#291362,#291363,
#291364,#291365,#291366,#291367,#291368),.UNSPECIFIED.,.F.,.F.)
B_SPLINE_CURVE_WITH_KNOTS((3,2,2,2,2,2,2,2,2,2,3),(0.759615384615385,0.761538461538461,
0.763461538461538,0.765384615384615,0.767307692307692,0.769230769230769,
0.771153846153846,0.773076923076923,0.775,0.776923076923077,0.778846153846154),
 .UNSPECIFIED.)
CURVE()
GEOMETRIC_REPRESENTATION_ITEM()
RATIONAL_B_SPLINE_CURVE((1.,0.951056516295154,1.,0.951056516295154,1.,0.951056516295154,
1.,0.951056516295154,1.,0.951056516295154,1.,0.951056516295154,1.,0.951056516295154,
1.,0.951056516295154,1.,0.951056516295154,1.,0.951056516295154,1.))
REPRESENTATION_ITEM('')
);
#1658=(
BOUNDED_CURVE()
B_SPLINE_CURVE(2,(#291373,#291374,#291375,#291376,#291377,#291378,#291379,
#291380,#291381,#291382,#291383,#291384,#291385,#291386,#291387,#291388,
#291389,#291390,#291391,#291392,#291393),.UNSPECIFIED.,.F.,.F.)
B_SPLINE_CURVE_WITH_KNOTS((3,2,2,2,2,2,2,2,2,2,3),(0.778846153846154,0.780769230769231,
0.782692307692308,0.784615384615385,0.786538461538462,0.788461538461538,
0.790384615384615,0.792307692307692,0.794230769230769,0.796153846153846,
0.798076923076923),.UNSPECIFIED.)
CURVE()
GEOMETRIC_REPRESENTATION_ITEM()
RATIONAL_B_SPLINE_CURVE((1.,0.951056516295154,1.,0.951056516295154,1.,0.951056516295154,
1.,0.951056516295154,1.,0.951056516295154,1.,0.951056516295154,1.,0.951056516295154,
1.,0.951056516295154,1.,0.951056516295154,1.,0.951056516295154,1.))
REPRESENTATION_ITEM('')
);
#1659=(
BOUNDED_CURVE()
B_SPLINE_CURVE(2,(#291394,#291395,#291396,#291397,#291398,#291399,#291400,
#291401,#291402,#291403,#291404,#291405,#291406,#291407,#291408,#291409,
#291410,#291411,#291412,#291413,#291414),.UNSPECIFIED.,.F.,.F.)
B_SPLINE_CURVE_WITH_KNOTS((3,2,2,2,2,2,2,2,2,2,3),(0.778846153846154,0.780769230769231,
0.782692307692308,0.784615384615385,0.786538461538462,0.788461538461538,
0.790384615384615,0.792307692307692,0.794230769230769,0.796153846153846,
0.798076923076923),.UNSPECIFIED.)
CURVE()
GEOMETRIC_REPRESENTATION_ITEM()
RATIONAL_B_SPLINE_CURVE((1.,0.951056516295154,1.,0.951056516295154,1.,0.951056516295154,
1.,0.951056516295154,1.,0.951056516295154,1.,0.951056516295154,1.,0.951056516295154,
1.,0.951056516295154,1.,0.951056516295154,1.,0.951056516295154,1.))
REPRESENTATION_ITEM('')
);
#1660=(
BOUNDED_CURVE()
B_SPLINE_CURVE(2,(#291419,#291420,#291421,#291422,#291423,#291424,#291425,
#291426,#291427,#291428,#291429,#291430,#291431,#291432,#291433,#291434,
#291435,#291436,#291437,#291438,#291439),.UNSPECIFIED.,.F.,.F.)
B_SPLINE_CURVE_WITH_KNOTS((3,2,2,2,2,2,2,2,2,2,3),(0.798076923076923,0.8,
0.801923076923077,0.803846153846154,0.805769230769231,0.807692307692308,
0.809615384615385,0.811538461538462,0.813461538461538,0.815384615384615,
0.817307692307692),.UNSPECIFIED.)
CURVE()
GEOMETRIC_REPRESENTATION_ITEM()
RATIONAL_B_SPLINE_CURVE((1.,0.951056516295154,1.,0.951056516295154,1.,0.951056516295154,
1.,0.951056516295154,1.,0.951056516295154,1.,0.951056516295154,1.,0.951056516295154,
1.,0.951056516295154,1.,0.951056516295154,1.,0.951056516295154,1.))
REPRESENTATION_ITEM('')
);
#1661=(
BOUNDED_CURVE()
B_SPLINE_CURVE(2,(#291440,#291441,#291442,#291443,#291444,#291445,#291446,
#291447,#291448,#291449,#291450,#291451,#291452,#291453,#291454,#291455,
#291456,#291457,#291458,#291459,#291460),.UNSPECIFIED.,.F.,.F.)
B_SPLINE_CURVE_WITH_KNOTS((3,2,2,2,2,2,2,2,2,2,3),(0.798076923076923,0.8,
0.801923076923077,0.803846153846154,0.805769230769231,0.807692307692308,
0.809615384615385,0.811538461538462,0.813461538461538,0.815384615384615,
0.817307692307692),.UNSPECIFIED.)
CURVE()
GEOMETRIC_REPRESENTATION_ITEM()
RATIONAL_B_SPLINE_CURVE((1.,0.951056516295154,1.,0.951056516295154,1.,0.951056516295154,
1.,0.951056516295154,1.,0.951056516295154,1.,0.951056516295154,1.,0.951056516295154,
1.,0.951056516295154,1.,0.951056516295154,1.,0.951056516295154,1.))
REPRESENTATION_ITEM('')
);
#1662=(
BOUNDED_CURVE()
B_SPLINE_CURVE(2,(#291465,#291466,#291467,#291468,#291469,#291470,#291471,
#291472,#291473,#291474,#291475,#291476,#291477,#291478,#291479,#291480,
#291481,#291482,#291483,#291484,#291485),.UNSPECIFIED.,.F.,.F.)
B_SPLINE_CURVE_WITH_KNOTS((3,2,2,2,2,2,2,2,2,2,3),(0.817307692307692,0.819230769230769,
0.821153846153846,0.823076923076923,0.825,0.826923076923077,0.828846153846154,
0.830769230769231,0.832692307692308,0.834615384615385,0.836538461538462),
 .UNSPECIFIED.)
CURVE()
GEOMETRIC_REPRESENTATION_ITEM()
RATIONAL_B_SPLINE_CURVE((1.,0.951056516295154,1.,0.951056516295154,1.,0.951056516295154,
1.,0.951056516295154,1.,0.951056516295154,1.,0.951056516295154,1.,0.951056516295154,
1.,0.951056516295154,1.,0.951056516295154,1.,0.951056516295154,1.))
REPRESENTATION_ITEM('')
);
#1663=(
BOUNDED_CURVE()
B_SPLINE_CURVE(2,(#291486,#291487,#291488,#291489,#291490,#291491,#291492,
#291493,#291494,#291495,#291496,#291497,#291498,#291499,#291500,#291501,
#291502,#291503,#291504,#291505,#291506),.UNSPECIFIED.,.F.,.F.)
B_SPLINE_CURVE_WITH_KNOTS((3,2,2,2,2,2,2,2,2,2,3),(0.817307692307692,0.819230769230769,
0.821153846153846,0.823076923076923,0.825,0.826923076923077,0.828846153846154,
0.830769230769231,0.832692307692308,0.834615384615385,0.836538461538462),
 .UNSPECIFIED.)
CURVE()
GEOMETRIC_REPRESENTATION_ITEM()
RATIONAL_B_SPLINE_CURVE((1.,0.951056516295154,1.,0.951056516295154,1.,0.951056516295154,
1.,0.951056516295154,1.,0.951056516295154,1.,0.951056516295154,1.,0.951056516295154,
1.,0.951056516295154,1.,0.951056516295154,1.,0.951056516295154,1.))
REPRESENTATION_ITEM('')
);
#1664=(
BOUNDED_CURVE()
B_SPLINE_CURVE(2,(#296144,#296145,#296146,#296147,#296148,#296149,#296150,
#296151,#296152,#296153,#296154,#296155,#296156,#296157,#296158),
 .UNSPECIFIED.,.F.,.F.)
B_SPLINE_CURVE_WITH_KNOTS((3,2,2,2,2,2,2,3),(0.836538461538462,0.838461538461538,
0.840384615384615,0.842307692307692,0.844230769230769,0.846153846153846,
0.848076923076923,0.849421797849676),.UNSPECIFIED.)
CURVE()
GEOMETRIC_REPRESENTATION_ITEM()
RATIONAL_B_SPLINE_CURVE((1.,0.951056516295154,1.,0.951056516295154,1.,0.951056516295154,
1.,0.951056516295154,1.,0.951056516295154,1.,0.951056516295154,1.,0.965772114606848,
0.979417737587222))
REPRESENTATION_ITEM('')
);
#1665=(
BOUNDED_CURVE()
B_SPLINE_CURVE(2,(#298251,#298252,#298253,#298254,#298255,#298256,#298257,
#298258,#298259,#298260,#298261,#298262,#298263,#298264,#298265,#298266,
#298267),.UNSPECIFIED.,.F.,.F.)
B_SPLINE_CURVE_WITH_KNOTS((3,2,2,2,2,2,2,2,3),(0.836538461538462,0.838461538461538,
0.840384615384615,0.842307692307692,0.844230769230769,0.846153846153846,
0.848076923076923,0.85,0.851829757961637),.UNSPECIFIED.)
CURVE()
GEOMETRIC_REPRESENTATION_ITEM()
RATIONAL_B_SPLINE_CURVE((1.,0.951056516295154,1.,0.951056516295154,1.,0.951056516295154,
1.,0.951056516295154,1.,0.951056516295154,1.,0.951056516295154,1.,0.951056516295154,
1.,0.953431540930822,0.995480450954353))
REPRESENTATION_ITEM('')
);
#1666=(
BOUNDED_CURVE()
B_SPLINE_CURVE(2,(#298312,#298313,#298314),.UNSPECIFIED.,.F.,.F.)
B_SPLINE_CURVE_WITH_KNOTS((3,3),(3.2941320975105,5.33580039117811),
 .UNSPECIFIED.)
CURVE()
GEOMETRIC_REPRESENTATION_ITEM()
RATIONAL_B_SPLINE_CURVE((1.82136720504436,1.96225044864938,1.96225044864938))
REPRESENTATION_ITEM('')
);
#1667=(
BOUNDED_CURVE()
B_SPLINE_CURVE(2,(#298316,#298317,#298318),.UNSPECIFIED.,.F.,.F.)
B_SPLINE_CURVE_WITH_KNOTS((3,3),(5.33580039117811,7.37746868484565),
 .UNSPECIFIED.)
CURVE()
GEOMETRIC_REPRESENTATION_ITEM()
RATIONAL_B_SPLINE_CURVE((1.96225044864938,1.96225044864938,1.82136720504436))
REPRESENTATION_ITEM('')
);
#1668=(
BOUNDED_CURVE()
B_SPLINE_CURVE(2,(#298322,#298323,#298324),.UNSPECIFIED.,.F.,.F.)
B_SPLINE_CURVE_WITH_KNOTS((3,3),(-5.33580039117806,-3.29413209751052),
 .UNSPECIFIED.)
CURVE()
GEOMETRIC_REPRESENTATION_ITEM()
RATIONAL_B_SPLINE_CURVE((1.96225044864938,1.96225044864937,1.82136720504436))
REPRESENTATION_ITEM('')
);
#1669=(
BOUNDED_CURVE()
B_SPLINE_CURVE(2,(#298325,#298326,#298327),.UNSPECIFIED.,.F.,.F.)
B_SPLINE_CURVE_WITH_KNOTS((3,3),(-7.37746868484564,-5.33580039117806),
 .UNSPECIFIED.)
CURVE()
GEOMETRIC_REPRESENTATION_ITEM()
RATIONAL_B_SPLINE_CURVE((1.82136720504435,1.96225044864937,1.96225044864937))
REPRESENTATION_ITEM('')
);
#1670=(
BOUNDED_CURVE()
B_SPLINE_CURVE(2,(#298329,#298330,#298331),.UNSPECIFIED.,.F.,.F.)
B_SPLINE_CURVE_WITH_KNOTS((3,3),(3.29413209751049,5.33580039117809),
 .UNSPECIFIED.)
CURVE()
GEOMETRIC_REPRESENTATION_ITEM()
RATIONAL_B_SPLINE_CURVE((1.82136720504436,1.96225044864938,1.96225044864938))
REPRESENTATION_ITEM('')
);
#1671=(
BOUNDED_CURVE()
B_SPLINE_CURVE(2,(#298333,#298334,#298335),.UNSPECIFIED.,.F.,.F.)
B_SPLINE_CURVE_WITH_KNOTS((3,3),(5.33580039117807,7.37746868484566),
 .UNSPECIFIED.)
CURVE()
GEOMETRIC_REPRESENTATION_ITEM()
RATIONAL_B_SPLINE_CURVE((1.96225044864938,1.96225044864938,1.82136720504436))
REPRESENTATION_ITEM('')
);
#1672=(
BOUNDED_CURVE()
B_SPLINE_CURVE(2,(#298339,#298340,#298341),.UNSPECIFIED.,.F.,.F.)
B_SPLINE_CURVE_WITH_KNOTS((3,3),(-5.33580039117809,-3.29413209751052),
 .UNSPECIFIED.)
CURVE()
GEOMETRIC_REPRESENTATION_ITEM()
RATIONAL_B_SPLINE_CURVE((1.96225044864938,1.96225044864938,1.82136720504436))
REPRESENTATION_ITEM('')
);
#1673=(
BOUNDED_CURVE()
B_SPLINE_CURVE(2,(#298342,#298343,#298344),.UNSPECIFIED.,.F.,.F.)
B_SPLINE_CURVE_WITH_KNOTS((3,3),(-7.37746868484567,-5.33580039117808),
 .UNSPECIFIED.)
CURVE()
GEOMETRIC_REPRESENTATION_ITEM()
RATIONAL_B_SPLINE_CURVE((1.82136720504436,1.96225044864939,1.96225044864939))
REPRESENTATION_ITEM('')
);
#1674=(
BOUNDED_CURVE()
B_SPLINE_CURVE(2,(#298346,#298347,#298348),.UNSPECIFIED.,.F.,.F.)
B_SPLINE_CURVE_WITH_KNOTS((3,3),(3.2941320975105,5.33580039117809),
 .UNSPECIFIED.)
CURVE()
GEOMETRIC_REPRESENTATION_ITEM()
RATIONAL_B_SPLINE_CURVE((1.82136720504437,1.9622504486494,1.9622504486494))
REPRESENTATION_ITEM('')
);
#1675=(
BOUNDED_CURVE()
B_SPLINE_CURVE(2,(#298350,#298351,#298352),.UNSPECIFIED.,.F.,.F.)
B_SPLINE_CURVE_WITH_KNOTS((3,3),(5.33580039117805,7.37746868484568),
 .UNSPECIFIED.)
CURVE()
GEOMETRIC_REPRESENTATION_ITEM()
RATIONAL_B_SPLINE_CURVE((1.96225044864939,1.9622504486494,1.82136720504437))
REPRESENTATION_ITEM('')
);
#1676=(
BOUNDED_CURVE()
B_SPLINE_CURVE(2,(#298356,#298357,#298358),.UNSPECIFIED.,.F.,.F.)
B_SPLINE_CURVE_WITH_KNOTS((3,3),(-5.33580039117813,-3.29413209751052),
 .UNSPECIFIED.)
CURVE()
GEOMETRIC_REPRESENTATION_ITEM()
RATIONAL_B_SPLINE_CURVE((1.96225044864939,1.96225044864939,1.82136720504437))
REPRESENTATION_ITEM('')
);
#1677=(
BOUNDED_CURVE()
B_SPLINE_CURVE(2,(#298359,#298360,#298361),.UNSPECIFIED.,.F.,.F.)
B_SPLINE_CURVE_WITH_KNOTS((3,3),(-7.37746868484571,-5.33580039117813),
 .UNSPECIFIED.)
CURVE()
GEOMETRIC_REPRESENTATION_ITEM()
RATIONAL_B_SPLINE_CURVE((1.82136720504437,1.96225044864939,1.96225044864939))
REPRESENTATION_ITEM('')
);
#1678=(
BOUNDED_CURVE()
B_SPLINE_CURVE(2,(#298363,#298364,#298365),.UNSPECIFIED.,.F.,.F.)
B_SPLINE_CURVE_WITH_KNOTS((3,3),(3.29413209751053,5.33580039117809),
 .UNSPECIFIED.)
CURVE()
GEOMETRIC_REPRESENTATION_ITEM()
RATIONAL_B_SPLINE_CURVE((1.82136720504437,1.96225044864939,1.96225044864939))
REPRESENTATION_ITEM('')
);
#1679=(
BOUNDED_CURVE()
B_SPLINE_CURVE(2,(#298367,#298368,#298369),.UNSPECIFIED.,.F.,.F.)
B_SPLINE_CURVE_WITH_KNOTS((3,3),(5.33580039117809,7.37746868484569),
 .UNSPECIFIED.)
CURVE()
GEOMETRIC_REPRESENTATION_ITEM()
RATIONAL_B_SPLINE_CURVE((1.96225044864938,1.96225044864938,1.82136720504436))
REPRESENTATION_ITEM('')
);
#1680=(
BOUNDED_CURVE()
B_SPLINE_CURVE(2,(#298373,#298374,#298375),.UNSPECIFIED.,.F.,.F.)
B_SPLINE_CURVE_WITH_KNOTS((3,3),(-5.33580039117811,-3.2941320975105),
 .UNSPECIFIED.)
CURVE()
GEOMETRIC_REPRESENTATION_ITEM()
RATIONAL_B_SPLINE_CURVE((1.96225044864939,1.96225044864939,1.82136720504437))
REPRESENTATION_ITEM('')
);
#1681=(
BOUNDED_CURVE()
B_SPLINE_CURVE(2,(#298376,#298377,#298378),.UNSPECIFIED.,.F.,.F.)
B_SPLINE_CURVE_WITH_KNOTS((3,3),(-7.37746868484567,-5.33580039117811),
 .UNSPECIFIED.)
CURVE()
GEOMETRIC_REPRESENTATION_ITEM()
RATIONAL_B_SPLINE_CURVE((1.82136720504437,1.96225044864939,1.96225044864939))
REPRESENTATION_ITEM('')
);
#1682=(
BOUNDED_CURVE()
B_SPLINE_CURVE(2,(#298380,#298381,#298382),.UNSPECIFIED.,.F.,.F.)
B_SPLINE_CURVE_WITH_KNOTS((3,3),(3.29413209751053,5.33580039117807),
 .UNSPECIFIED.)
CURVE()
GEOMETRIC_REPRESENTATION_ITEM()
RATIONAL_B_SPLINE_CURVE((1.82136720504437,1.96225044864938,1.96225044864938))
REPRESENTATION_ITEM('')
);
#1683=(
BOUNDED_CURVE()
B_SPLINE_CURVE(2,(#298384,#298385,#298386),.UNSPECIFIED.,.F.,.F.)
B_SPLINE_CURVE_WITH_KNOTS((3,3),(5.33580039117811,7.37746868484569),
 .UNSPECIFIED.)
CURVE()
GEOMETRIC_REPRESENTATION_ITEM()
RATIONAL_B_SPLINE_CURVE((1.96225044864938,1.96225044864938,1.82136720504436))
REPRESENTATION_ITEM('')
);
#1684=(
BOUNDED_CURVE()
B_SPLINE_CURVE(2,(#298390,#298391,#298392),.UNSPECIFIED.,.F.,.F.)
B_SPLINE_CURVE_WITH_KNOTS((3,3),(-5.33580039117809,-3.2941320975105),
 .UNSPECIFIED.)
CURVE()
GEOMETRIC_REPRESENTATION_ITEM()
RATIONAL_B_SPLINE_CURVE((1.96225044864938,1.96225044864938,1.82136720504436))
REPRESENTATION_ITEM('')
);
#1685=(
BOUNDED_CURVE()
B_SPLINE_CURVE(2,(#298393,#298394,#298395),.UNSPECIFIED.,.F.,.F.)
B_SPLINE_CURVE_WITH_KNOTS((3,3),(-7.37746868484566,-5.3358003911781),
 .UNSPECIFIED.)
CURVE()
GEOMETRIC_REPRESENTATION_ITEM()
RATIONAL_B_SPLINE_CURVE((1.82136720504436,1.96225044864938,1.96225044864938))
REPRESENTATION_ITEM('')
);
#1686=(
BOUNDED_CURVE()
B_SPLINE_CURVE(2,(#298397,#298398,#298399),.UNSPECIFIED.,.F.,.F.)
B_SPLINE_CURVE_WITH_KNOTS((3,3),(3.29413209751053,5.33580039117807),
 .UNSPECIFIED.)
CURVE()
GEOMETRIC_REPRESENTATION_ITEM()
RATIONAL_B_SPLINE_CURVE((1.82136720504436,1.96225044864937,1.96225044864937))
REPRESENTATION_ITEM('')
);
#1687=(
BOUNDED_CURVE()
B_SPLINE_CURVE(2,(#298400,#298401,#298402),.UNSPECIFIED.,.F.,.F.)
B_SPLINE_CURVE_WITH_KNOTS((3,3),(5.33580039117807,7.37746868484566),
 .UNSPECIFIED.)
CURVE()
GEOMETRIC_REPRESENTATION_ITEM()
RATIONAL_B_SPLINE_CURVE((1.96225044864937,1.96225044864937,1.82136720504435))
REPRESENTATION_ITEM('')
);
#1688=(
BOUNDED_CURVE()
B_SPLINE_CURVE(2,(#298404,#298405,#298406),.UNSPECIFIED.,.F.,.F.)
B_SPLINE_CURVE_WITH_KNOTS((3,3),(-5.33580039117805,-3.29413209751049),
 .UNSPECIFIED.)
CURVE()
GEOMETRIC_REPRESENTATION_ITEM()
RATIONAL_B_SPLINE_CURVE((1.96225044864937,1.96225044864937,1.82136720504435))
REPRESENTATION_ITEM('')
);
#1689=(
BOUNDED_CURVE()
B_SPLINE_CURVE(2,(#298407,#298408,#298409),.UNSPECIFIED.,.F.,.F.)
B_SPLINE_CURVE_WITH_KNOTS((3,3),(-7.37746868484564,-5.33580039117806),
 .UNSPECIFIED.)
CURVE()
GEOMETRIC_REPRESENTATION_ITEM()
RATIONAL_B_SPLINE_CURVE((1.82136720504436,1.96225044864938,1.96225044864938))
REPRESENTATION_ITEM('')
);
#1690=(
BOUNDED_CURVE()
B_SPLINE_CURVE(2,(#300536,#300537,#300538,#300539,#300540),
 .UNSPECIFIED.,.F.,.F.)
B_SPLINE_CURVE_WITH_KNOTS((3,2,3),(0.394230769230769,0.396153846153846,
0.396753325815344),.UNSPECIFIED.)
CURVE()
GEOMETRIC_REPRESENTATION_ITEM()
RATIONAL_B_SPLINE_CURVE((1.,0.951056516295154,1.,0.984742876017165,0.978997940975819))
REPRESENTATION_ITEM('')
);
#1691=(
BOUNDED_CURVE()
B_SPLINE_CURVE(2,(#302615,#302616,#302617,#302618,#302619,#302620,#302621),
 .UNSPECIFIED.,.F.,.F.)
B_SPLINE_CURVE_WITH_KNOTS((3,2,2,3),(0.394230769230769,0.396153846153846,
0.398076923076923,0.399146724305703),.UNSPECIFIED.)
CURVE()
GEOMETRIC_REPRESENTATION_ITEM()
RATIONAL_B_SPLINE_CURVE((1.,0.951056516295154,1.,0.951056516295154,1.,0.972772904515738,
0.975838492444844))
REPRESENTATION_ITEM('')
);
#1692=(
BOUNDED_CURVE()
B_SPLINE_CURVE(2,(#304329,#304330,#304331),.UNSPECIFIED.,.F.,.F.)
B_SPLINE_CURVE_WITH_KNOTS((3,3),(0.868421052631579,0.871442538302458),
 .UNSPECIFIED.)
CURVE()
GEOMETRIC_REPRESENTATION_ITEM()
RATIONAL_B_SPLINE_CURVE((1.,0.971902413407548,0.976065479819744))
REPRESENTATION_ITEM('')
);
#1693=(
BOUNDED_CURVE()
B_SPLINE_CURVE(2,(#304336,#304337,#304338,#304339,#304340,#304341,#304342,
#304343,#304344,#304345,#304346,#304347,#304348,#304349,#304350,#304351,
#304352,#304353,#304354,#304355,#304356),.UNSPECIFIED.,.F.,.F.)
B_SPLINE_CURVE_WITH_KNOTS((3,2,2,2,2,2,2,2,2,2,3),(0.815789473684211,0.821052631578947,
0.826315789473684,0.831578947368421,0.836842105263158,0.842105263157895,
0.847368421052632,0.852631578947368,0.857894736842105,0.863157894736842,
0.868421052631579),.UNSPECIFIED.)
CURVE()
GEOMETRIC_REPRESENTATION_ITEM()
RATIONAL_B_SPLINE_CURVE((1.,0.951056516295154,1.,0.951056516295154,1.,0.951056516295154,
1.,0.951056516295154,1.,0.951056516295154,1.,0.951056516295154,1.,0.951056516295154,
1.,0.951056516295154,1.,0.951056516295154,1.,0.951056516295154,1.))
REPRESENTATION_ITEM('')
);
#1694=(
BOUNDED_CURVE()
B_SPLINE_CURVE(2,(#304357,#304358,#304359,#304360,#304361,#304362,#304363,
#304364,#304365,#304366,#304367,#304368,#304369,#304370,#304371,#304372,
#304373,#304374,#304375,#304376,#304377),.UNSPECIFIED.,.F.,.F.)
B_SPLINE_CURVE_WITH_KNOTS((3,2,2,2,2,2,2,2,2,2,3),(0.815789473684211,0.821052631578947,
0.826315789473684,0.831578947368421,0.836842105263158,0.842105263157895,
0.847368421052632,0.852631578947368,0.857894736842105,0.863157894736842,
0.864892973551299),.UNSPECIFIED.)
CURVE()
GEOMETRIC_REPRESENTATION_ITEM()
RATIONAL_B_SPLINE_CURVE((1.,0.951056516295154,1.,0.951056516295154,1.,0.951056516295154,
1.,0.951056516295154,1.,0.951056516295154,1.,0.951056516295154,1.,0.951056516295154,
1.,0.951056516295154,1.,0.951056516295154,1.,0.983865047680423,0.978368352658793))
REPRESENTATION_ITEM('')
);
#1695=(
BOUNDED_CURVE()
B_SPLINE_CURVE(2,(#304382,#304383,#304384,#304385,#304386,#304387,#304388,
#304389,#304390,#304391,#304392,#304393,#304394,#304395,#304396,#304397,
#304398,#304399,#304400,#304401,#304402),.UNSPECIFIED.,.F.,.F.)
B_SPLINE_CURVE_WITH_KNOTS((3,2,2,2,2,2,2,2,2,2,3),(0.763157894736842,0.768421052631579,
0.773684210526316,0.778947368421053,0.78421052631579,0.789473684210526,
0.794736842105263,0.8,0.805263157894737,0.810526315789474,0.815789473684211),
 .UNSPECIFIED.)
CURVE()
GEOMETRIC_REPRESENTATION_ITEM()
RATIONAL_B_SPLINE_CURVE((1.,0.951056516295154,1.,0.951056516295154,1.,0.951056516295154,
1.,0.951056516295154,1.,0.951056516295154,1.,0.951056516295154,1.,0.951056516295154,
1.,0.951056516295154,1.,0.951056516295154,1.,0.951056516295154,1.))
REPRESENTATION_ITEM('')
);
#1696=(
BOUNDED_CURVE()
B_SPLINE_CURVE(2,(#304403,#304404,#304405,#304406,#304407,#304408,#304409,
#304410,#304411,#304412,#304413,#304414,#304415,#304416,#304417,#304418,
#304419,#304420,#304421,#304422,#304423),.UNSPECIFIED.,.F.,.F.)
B_SPLINE_CURVE_WITH_KNOTS((3,2,2,2,2,2,2,2,2,2,3),(0.763157894736842,0.768421052631579,
0.773684210526316,0.778947368421053,0.78421052631579,0.789473684210526,
0.794736842105263,0.8,0.805263157894737,0.810526315789474,0.815789473684211),
 .UNSPECIFIED.)
CURVE()
GEOMETRIC_REPRESENTATION_ITEM()
RATIONAL_B_SPLINE_CURVE((1.,0.951056516295154,1.,0.951056516295154,1.,0.951056516295154,
1.,0.951056516295154,1.,0.951056516295154,1.,0.951056516295154,1.,0.951056516295154,
1.,0.951056516295154,1.,0.951056516295154,1.,0.951056516295154,1.))
REPRESENTATION_ITEM('')
);
#1697=(
BOUNDED_CURVE()
B_SPLINE_CURVE(2,(#304428,#304429,#304430,#304431,#304432,#304433,#304434,
#304435,#304436,#304437,#304438,#304439,#304440,#304441,#304442,#304443,
#304444,#304445,#304446,#304447,#304448),.UNSPECIFIED.,.F.,.F.)
B_SPLINE_CURVE_WITH_KNOTS((3,2,2,2,2,2,2,2,2,2,3),(0.710526315789474,0.715789473684211,
0.721052631578947,0.726315789473684,0.731578947368421,0.736842105263158,
0.742105263157895,0.747368421052632,0.752631578947368,0.757894736842105,
0.763157894736842),.UNSPECIFIED.)
CURVE()
GEOMETRIC_REPRESENTATION_ITEM()
RATIONAL_B_SPLINE_CURVE((1.,0.951056516295154,1.,0.951056516295154,1.,0.951056516295154,
1.,0.951056516295154,1.,0.951056516295154,1.,0.951056516295154,1.,0.951056516295154,
1.,0.951056516295154,1.,0.951056516295154,1.,0.951056516295154,1.))
REPRESENTATION_ITEM('')
);
#1698=(
BOUNDED_CURVE()
B_SPLINE_CURVE(2,(#304449,#304450,#304451,#304452,#304453,#304454,#304455,
#304456,#304457,#304458,#304459,#304460,#304461,#304462,#304463,#304464,
#304465,#304466,#304467,#304468,#304469),.UNSPECIFIED.,.F.,.F.)
B_SPLINE_CURVE_WITH_KNOTS((3,2,2,2,2,2,2,2,2,2,3),(0.710526315789474,0.715789473684211,
0.721052631578947,0.726315789473684,0.731578947368421,0.736842105263158,
0.742105263157895,0.747368421052632,0.752631578947368,0.757894736842105,
0.763157894736842),.UNSPECIFIED.)
CURVE()
GEOMETRIC_REPRESENTATION_ITEM()
RATIONAL_B_SPLINE_CURVE((1.,0.951056516295154,1.,0.951056516295154,1.,0.951056516295154,
1.,0.951056516295154,1.,0.951056516295154,1.,0.951056516295154,1.,0.951056516295154,
1.,0.951056516295154,1.,0.951056516295154,1.,0.951056516295154,1.))
REPRESENTATION_ITEM('')
);
#1699=(
BOUNDED_CURVE()
B_SPLINE_CURVE(2,(#304474,#304475,#304476,#304477,#304478,#304479,#304480,
#304481,#304482,#304483,#304484,#304485,#304486,#304487,#304488,#304489,
#304490,#304491,#304492,#304493,#304494),.UNSPECIFIED.,.F.,.F.)
B_SPLINE_CURVE_WITH_KNOTS((3,2,2,2,2,2,2,2,2,2,3),(0.657894736842105,0.663157894736842,
0.668421052631579,0.673684210526316,0.678947368421053,0.68421052631579,
0.689473684210526,0.694736842105263,0.7,0.705263157894737,0.710526315789474),
 .UNSPECIFIED.)
CURVE()
GEOMETRIC_REPRESENTATION_ITEM()
RATIONAL_B_SPLINE_CURVE((1.,0.951056516295154,1.,0.951056516295154,1.,0.951056516295154,
1.,0.951056516295154,1.,0.951056516295154,1.,0.951056516295154,1.,0.951056516295154,
1.,0.951056516295154,1.,0.951056516295154,1.,0.951056516295154,1.))
REPRESENTATION_ITEM('')
);
#1700=(
BOUNDED_CURVE()
B_SPLINE_CURVE(2,(#304495,#304496,#304497,#304498,#304499,#304500,#304501,
#304502,#304503,#304504,#304505,#304506,#304507,#304508,#304509,#304510,
#304511,#304512,#304513,#304514,#304515),.UNSPECIFIED.,.F.,.F.)
B_SPLINE_CURVE_WITH_KNOTS((3,2,2,2,2,2,2,2,2,2,3),(0.657894736842105,0.663157894736842,
0.668421052631579,0.673684210526316,0.678947368421053,0.68421052631579,
0.689473684210526,0.694736842105263,0.7,0.705263157894737,0.710526315789474),
 .UNSPECIFIED.)
CURVE()
GEOMETRIC_REPRESENTATION_ITEM()
RATIONAL_B_SPLINE_CURVE((1.,0.951056516295154,1.,0.951056516295154,1.,0.951056516295154,
1.,0.951056516295154,1.,0.951056516295154,1.,0.951056516295154,1.,0.951056516295154,
1.,0.951056516295154,1.,0.951056516295154,1.,0.951056516295154,1.))
REPRESENTATION_ITEM('')
);
#1701=(
BOUNDED_CURVE()
B_SPLINE_CURVE(2,(#304520,#304521,#304522,#304523,#304524,#304525,#304526,
#304527,#304528,#304529,#304530,#304531,#304532,#304533,#304534,#304535,
#304536,#304537,#304538,#304539,#304540),.UNSPECIFIED.,.F.,.F.)
B_SPLINE_CURVE_WITH_KNOTS((3,2,2,2,2,2,2,2,2,2,3),(0.605263157894737,0.610526315789474,
0.615789473684211,0.621052631578947,0.626315789473684,0.631578947368421,
0.636842105263158,0.642105263157895,0.647368421052632,0.652631578947369,
0.657894736842105),.UNSPECIFIED.)
CURVE()
GEOMETRIC_REPRESENTATION_ITEM()
RATIONAL_B_SPLINE_CURVE((1.,0.951056516295154,1.,0.951056516295154,1.,0.951056516295154,
1.,0.951056516295154,1.,0.951056516295154,1.,0.951056516295154,1.,0.951056516295154,
1.,0.951056516295154,1.,0.951056516295154,1.,0.951056516295154,1.))
REPRESENTATION_ITEM('')
);
#1702=(
BOUNDED_CURVE()
B_SPLINE_CURVE(2,(#304541,#304542,#304543,#304544,#304545,#304546,#304547,
#304548,#304549,#304550,#304551,#304552,#304553,#304554,#304555,#304556,
#304557,#304558,#304559,#304560,#304561),.UNSPECIFIED.,.F.,.F.)
B_SPLINE_CURVE_WITH_KNOTS((3,2,2,2,2,2,2,2,2,2,3),(0.605263157894737,0.610526315789474,
0.615789473684211,0.621052631578947,0.626315789473684,0.631578947368421,
0.636842105263158,0.642105263157895,0.647368421052632,0.652631578947369,
0.657894736842105),.UNSPECIFIED.)
CURVE()
GEOMETRIC_REPRESENTATION_ITEM()
RATIONAL_B_SPLINE_CURVE((1.,0.951056516295154,1.,0.951056516295154,1.,0.951056516295154,
1.,0.951056516295154,1.,0.951056516295154,1.,0.951056516295154,1.,0.951056516295154,
1.,0.951056516295154,1.,0.951056516295154,1.,0.951056516295154,1.))
REPRESENTATION_ITEM('')
);
#1703=(
BOUNDED_CURVE()
B_SPLINE_CURVE(2,(#304566,#304567,#304568,#304569,#304570,#304571,#304572,
#304573,#304574,#304575,#304576,#304577,#304578,#304579,#304580,#304581,
#304582,#304583,#304584,#304585,#304586),.UNSPECIFIED.,.F.,.F.)
B_SPLINE_CURVE_WITH_KNOTS((3,2,2,2,2,2,2,2,2,2,3),(0.552631578947369,0.557894736842105,
0.563157894736842,0.568421052631579,0.573684210526316,0.578947368421053,
0.58421052631579,0.589473684210526,0.594736842105263,0.6,0.605263157894737),
 .UNSPECIFIED.)
CURVE()
GEOMETRIC_REPRESENTATION_ITEM()
RATIONAL_B_SPLINE_CURVE((1.,0.951056516295154,1.,0.951056516295154,1.,0.951056516295154,
1.,0.951056516295154,1.,0.951056516295154,1.,0.951056516295154,1.,0.951056516295154,
1.,0.951056516295154,1.,0.951056516295154,1.,0.951056516295154,1.))
REPRESENTATION_ITEM('')
);
#1704=(
BOUNDED_CURVE()
B_SPLINE_CURVE(2,(#304587,#304588,#304589,#304590,#304591,#304592,#304593,
#304594,#304595,#304596,#304597,#304598,#304599,#304600,#304601,#304602,
#304603,#304604,#304605,#304606,#304607),.UNSPECIFIED.,.F.,.F.)
B_SPLINE_CURVE_WITH_KNOTS((3,2,2,2,2,2,2,2,2,2,3),(0.552631578947369,0.557894736842105,
0.563157894736842,0.568421052631579,0.573684210526316,0.578947368421053,
0.58421052631579,0.589473684210526,0.594736842105263,0.6,0.605263157894737),
 .UNSPECIFIED.)
CURVE()
GEOMETRIC_REPRESENTATION_ITEM()
RATIONAL_B_SPLINE_CURVE((1.,0.951056516295154,1.,0.951056516295154,1.,0.951056516295154,
1.,0.951056516295154,1.,0.951056516295154,1.,0.951056516295154,1.,0.951056516295154,
1.,0.951056516295154,1.,0.951056516295154,1.,0.951056516295154,1.))
REPRESENTATION_ITEM('')
);
#1705=(
BOUNDED_CURVE()
B_SPLINE_CURVE(2,(#304612,#304613,#304614,#304615,#304616,#304617,#304618,
#304619,#304620,#304621,#304622,#304623,#304624,#304625,#304626,#304627,
#304628,#304629,#304630,#304631,#304632),.UNSPECIFIED.,.F.,.F.)
B_SPLINE_CURVE_WITH_KNOTS((3,2,2,2,2,2,2,2,2,2,3),(0.5,0.505263157894737,
0.510526315789474,0.515789473684211,0.521052631578947,0.526315789473684,
0.531578947368421,0.536842105263158,0.542105263157895,0.547368421052632,
0.552631578947369),.UNSPECIFIED.)
CURVE()
GEOMETRIC_REPRESENTATION_ITEM()
RATIONAL_B_SPLINE_CURVE((1.,0.951056516295154,1.,0.951056516295154,1.,0.951056516295154,
1.,0.951056516295154,1.,0.951056516295154,1.,0.951056516295154,1.,0.951056516295154,
1.,0.951056516295154,1.,0.951056516295154,1.,0.951056516295154,1.))
REPRESENTATION_ITEM('')
);
#1706=(
BOUNDED_CURVE()
B_SPLINE_CURVE(2,(#304633,#304634,#304635,#304636,#304637,#304638,#304639,
#304640,#304641,#304642,#304643,#304644,#304645,#304646,#304647,#304648,
#304649,#304650,#304651,#304652,#304653),.UNSPECIFIED.,.F.,.F.)
B_SPLINE_CURVE_WITH_KNOTS((3,2,2,2,2,2,2,2,2,2,3),(0.5,0.505263157894737,
0.510526315789474,0.515789473684211,0.521052631578947,0.526315789473684,
0.531578947368421,0.536842105263158,0.542105263157895,0.547368421052632,
0.552631578947369),.UNSPECIFIED.)
CURVE()
GEOMETRIC_REPRESENTATION_ITEM()
RATIONAL_B_SPLINE_CURVE((1.,0.951056516295154,1.,0.951056516295154,1.,0.951056516295154,
1.,0.951056516295154,1.,0.951056516295154,1.,0.951056516295154,1.,0.951056516295154,
1.,0.951056516295154,1.,0.951056516295154,1.,0.951056516295154,1.))
REPRESENTATION_ITEM('')
);
#1707=(
BOUNDED_CURVE()
B_SPLINE_CURVE(2,(#304658,#304659,#304660,#304661,#304662,#304663,#304664,
#304665,#304666,#304667,#304668,#304669,#304670,#304671,#304672,#304673,
#304674,#304675,#304676,#304677,#304678),.UNSPECIFIED.,.F.,.F.)
B_SPLINE_CURVE_WITH_KNOTS((3,2,2,2,2,2,2,2,2,2,3),(0.447368421052632,0.452631578947368,
0.457894736842105,0.463157894736842,0.468421052631579,0.473684210526316,
0.478947368421053,0.48421052631579,0.489473684210526,0.494736842105263,
0.5),.UNSPECIFIED.)
CURVE()
GEOMETRIC_REPRESENTATION_ITEM()
RATIONAL_B_SPLINE_CURVE((1.,0.951056516295154,1.,0.951056516295154,1.,0.951056516295154,
1.,0.951056516295154,1.,0.951056516295154,1.,0.951056516295154,1.,0.951056516295154,
1.,0.951056516295154,1.,0.951056516295154,1.,0.951056516295154,1.))
REPRESENTATION_ITEM('')
);
#1708=(
BOUNDED_CURVE()
B_SPLINE_CURVE(2,(#304679,#304680,#304681,#304682,#304683,#304684,#304685,
#304686,#304687,#304688,#304689,#304690,#304691,#304692,#304693,#304694,
#304695,#304696,#304697,#304698,#304699),.UNSPECIFIED.,.F.,.F.)
B_SPLINE_CURVE_WITH_KNOTS((3,2,2,2,2,2,2,2,2,2,3),(0.447368421052631,0.452631578947369,
0.457894736842105,0.463157894736842,0.468421052631579,0.473684210526316,
0.478947368421053,0.48421052631579,0.489473684210526,0.494736842105263,
0.5),.UNSPECIFIED.)
CURVE()
GEOMETRIC_REPRESENTATION_ITEM()
RATIONAL_B_SPLINE_CURVE((1.,0.951056516295154,1.,0.951056516295154,1.,0.951056516295154,
1.,0.951056516295154,1.,0.951056516295154,1.,0.951056516295154,1.,0.951056516295154,
1.,0.951056516295154,1.,0.951056516295154,1.,0.951056516295154,1.))
REPRESENTATION_ITEM('')
);
#1709=(
BOUNDED_CURVE()
B_SPLINE_CURVE(2,(#304704,#304705,#304706,#304707,#304708,#304709,#304710,
#304711,#304712,#304713,#304714,#304715,#304716,#304717,#304718,#304719,
#304720,#304721,#304722,#304723,#304724),.UNSPECIFIED.,.F.,.F.)
B_SPLINE_CURVE_WITH_KNOTS((3,2,2,2,2,2,2,2,2,2,3),(0.394736842105263,0.4,
0.405263157894737,0.410526315789473,0.415789473684211,0.421052631578948,
0.426315789473684,0.431578947368421,0.436842105263158,0.442105263157895,
0.447368421052632),.UNSPECIFIED.)
CURVE()
GEOMETRIC_REPRESENTATION_ITEM()
RATIONAL_B_SPLINE_CURVE((1.,0.951056516295154,1.,0.951056516295154,1.,0.951056516295154,
1.,0.951056516295154,1.,0.951056516295154,1.,0.951056516295154,1.,0.951056516295154,
1.,0.951056516295154,1.,0.951056516295154,1.,0.951056516295154,1.))
REPRESENTATION_ITEM('')
);
#1710=(
BOUNDED_CURVE()
B_SPLINE_CURVE(2,(#304725,#304726,#304727,#304728,#304729,#304730,#304731,
#304732,#304733,#304734,#304735,#304736,#304737,#304738,#304739,#304740,
#304741,#304742,#304743,#304744,#304745),.UNSPECIFIED.,.F.,.F.)
B_SPLINE_CURVE_WITH_KNOTS((3,2,2,2,2,2,2,2,2,2,3),(0.394736842105263,0.4,
0.405263157894737,0.410526315789473,0.415789473684211,0.421052631578948,
0.426315789473684,0.431578947368421,0.436842105263158,0.442105263157894,
0.447368421052631),.UNSPECIFIED.)
CURVE()
GEOMETRIC_REPRESENTATION_ITEM()
RATIONAL_B_SPLINE_CURVE((1.,0.951056516295154,1.,0.951056516295154,1.,0.951056516295154,
1.,0.951056516295154,1.,0.951056516295154,1.,0.951056516295154,1.,0.951056516295154,
1.,0.951056516295154,1.,0.951056516295154,1.,0.951056516295154,1.))
REPRESENTATION_ITEM('')
);
#1711=(
BOUNDED_CURVE()
B_SPLINE_CURVE(2,(#304750,#304751,#304752,#304753,#304754,#304755,#304756,
#304757,#304758,#304759,#304760,#304761,#304762,#304763,#304764,#304765,
#304766,#304767,#304768,#304769,#304770),.UNSPECIFIED.,.F.,.F.)
B_SPLINE_CURVE_WITH_KNOTS((3,2,2,2,2,2,2,2,2,2,3),(0.342105263157895,0.347368421052631,
0.352631578947369,0.357894736842105,0.363157894736842,0.368421052631579,
0.373684210526316,0.378947368421053,0.38421052631579,0.389473684210526,
0.394736842105263),.UNSPECIFIED.)
CURVE()
GEOMETRIC_REPRESENTATION_ITEM()
RATIONAL_B_SPLINE_CURVE((1.,0.951056516295154,1.,0.951056516295154,1.,0.951056516295154,
1.,0.951056516295154,1.,0.951056516295154,1.,0.951056516295154,1.,0.951056516295154,
1.,0.951056516295154,1.,0.951056516295154,1.,0.951056516295154,1.))
REPRESENTATION_ITEM('')
);
#1712=(
BOUNDED_CURVE()
B_SPLINE_CURVE(2,(#304771,#304772,#304773,#304774,#304775,#304776,#304777,
#304778,#304779,#304780,#304781,#304782,#304783,#304784,#304785,#304786,
#304787,#304788,#304789,#304790,#304791),.UNSPECIFIED.,.F.,.F.)
B_SPLINE_CURVE_WITH_KNOTS((3,2,2,2,2,2,2,2,2,2,3),(0.342105263157895,0.347368421052632,
0.352631578947369,0.357894736842105,0.363157894736842,0.368421052631579,
0.373684210526316,0.378947368421053,0.38421052631579,0.389473684210527,
0.394736842105263),.UNSPECIFIED.)
CURVE()
GEOMETRIC_REPRESENTATION_ITEM()
RATIONAL_B_SPLINE_CURVE((1.,0.951056516295154,1.,0.951056516295154,1.,0.951056516295154,
1.,0.951056516295154,1.,0.951056516295154,1.,0.951056516295154,1.,0.951056516295154,
1.,0.951056516295154,1.,0.951056516295154,1.,0.951056516295154,1.))
REPRESENTATION_ITEM('')
);
#1713=(
BOUNDED_CURVE()
B_SPLINE_CURVE(2,(#304796,#304797,#304798,#304799,#304800,#304801,#304802,
#304803,#304804,#304805,#304806,#304807,#304808,#304809,#304810,#304811,
#304812,#304813,#304814,#304815,#304816),.UNSPECIFIED.,.F.,.F.)
B_SPLINE_CURVE_WITH_KNOTS((3,2,2,2,2,2,2,2,2,2,3),(0.289473684210526,0.294736842105263,
0.3,0.305263157894737,0.310526315789473,0.315789473684211,0.321052631578947,
0.326315789473685,0.331578947368421,0.336842105263158,0.342105263157895),
 .UNSPECIFIED.)
CURVE()
GEOMETRIC_REPRESENTATION_ITEM()
RATIONAL_B_SPLINE_CURVE((1.,0.951056516295154,1.,0.951056516295154,1.,0.951056516295154,
1.,0.951056516295154,1.,0.951056516295154,1.,0.951056516295154,1.,0.951056516295154,
1.,0.951056516295154,1.,0.951056516295154,1.,0.951056516295154,1.))
REPRESENTATION_ITEM('')
);
#1714=(
BOUNDED_CURVE()
B_SPLINE_CURVE(2,(#304817,#304818,#304819,#304820,#304821,#304822,#304823,
#304824,#304825,#304826,#304827,#304828,#304829,#304830,#304831,#304832,
#304833,#304834,#304835,#304836,#304837),.UNSPECIFIED.,.F.,.F.)
B_SPLINE_CURVE_WITH_KNOTS((3,2,2,2,2,2,2,2,2,2,3),(0.289473684210526,0.294736842105263,
0.3,0.305263157894737,0.310526315789473,0.315789473684211,0.321052631578947,
0.326315789473685,0.331578947368421,0.336842105263158,0.342105263157895),
 .UNSPECIFIED.)
CURVE()
GEOMETRIC_REPRESENTATION_ITEM()
RATIONAL_B_SPLINE_CURVE((1.,0.951056516295154,1.,0.951056516295154,1.,0.951056516295154,
1.,0.951056516295154,1.,0.951056516295154,1.,0.951056516295154,1.,0.951056516295154,
1.,0.951056516295154,1.,0.951056516295154,1.,0.951056516295154,1.))
REPRESENTATION_ITEM('')
);
#1715=(
BOUNDED_CURVE()
B_SPLINE_CURVE(2,(#304842,#304843,#304844,#304845,#304846,#304847,#304848,
#304849,#304850,#304851,#304852,#304853,#304854,#304855,#304856,#304857,
#304858,#304859,#304860,#304861,#304862),.UNSPECIFIED.,.F.,.F.)
B_SPLINE_CURVE_WITH_KNOTS((3,2,2,2,2,2,2,2,2,2,3),(0.236842105263158,0.242105263157895,
0.247368421052632,0.252631578947369,0.257894736842106,0.263157894736842,
0.268421052631579,0.273684210526316,0.278947368421052,0.28421052631579,
0.289473684210526),.UNSPECIFIED.)
CURVE()
GEOMETRIC_REPRESENTATION_ITEM()
RATIONAL_B_SPLINE_CURVE((1.,0.951056516295154,1.,0.951056516295154,1.,0.951056516295154,
1.,0.951056516295154,1.,0.951056516295154,1.,0.951056516295154,1.,0.951056516295154,
1.,0.951056516295154,1.,0.951056516295154,1.,0.951056516295154,1.))
REPRESENTATION_ITEM('')
);
#1716=(
BOUNDED_CURVE()
B_SPLINE_CURVE(2,(#304863,#304864,#304865,#304866,#304867,#304868,#304869,
#304870,#304871,#304872,#304873,#304874,#304875,#304876,#304877,#304878,
#304879,#304880,#304881,#304882,#304883),.UNSPECIFIED.,.F.,.F.)
B_SPLINE_CURVE_WITH_KNOTS((3,2,2,2,2,2,2,2,2,2,3),(0.236842105263158,0.242105263157895,
0.247368421052632,0.252631578947369,0.257894736842106,0.263157894736842,
0.268421052631579,0.273684210526316,0.278947368421052,0.28421052631579,
0.289473684210526),.UNSPECIFIED.)
CURVE()
GEOMETRIC_REPRESENTATION_ITEM()
RATIONAL_B_SPLINE_CURVE((1.,0.951056516295154,1.,0.951056516295154,1.,0.951056516295154,
1.,0.951056516295154,1.,0.951056516295154,1.,0.951056516295154,1.,0.951056516295154,
1.,0.951056516295154,1.,0.951056516295154,1.,0.951056516295154,1.))
REPRESENTATION_ITEM('')
);
#1717=(
BOUNDED_CURVE()
B_SPLINE_CURVE(2,(#304888,#304889,#304890,#304891,#304892,#304893,#304894,
#304895,#304896,#304897,#304898,#304899,#304900,#304901,#304902,#304903,
#304904,#304905,#304906,#304907,#304908),.UNSPECIFIED.,.F.,.F.)
B_SPLINE_CURVE_WITH_KNOTS((3,2,2,2,2,2,2,2,2,2,3),(0.18421052631579,0.189473684210526,
0.194736842105263,0.2,0.205263157894737,0.210526315789474,0.215789473684211,
0.221052631578948,0.226315789473684,0.231578947368421,0.236842105263158),
 .UNSPECIFIED.)
CURVE()
GEOMETRIC_REPRESENTATION_ITEM()
RATIONAL_B_SPLINE_CURVE((1.,0.951056516295154,1.,0.951056516295154,1.,0.951056516295154,
1.,0.951056516295154,1.,0.951056516295154,1.,0.951056516295154,1.,0.951056516295154,
1.,0.951056516295154,1.,0.951056516295154,1.,0.951056516295154,1.))
REPRESENTATION_ITEM('')
);
#1718=(
BOUNDED_CURVE()
B_SPLINE_CURVE(2,(#304909,#304910,#304911,#304912,#304913,#304914,#304915,
#304916,#304917,#304918,#304919,#304920,#304921,#304922,#304923,#304924,
#304925,#304926,#304927,#304928,#304929),.UNSPECIFIED.,.F.,.F.)
B_SPLINE_CURVE_WITH_KNOTS((3,2,2,2,2,2,2,2,2,2,3),(0.18421052631579,0.189473684210526,
0.194736842105263,0.2,0.205263157894737,0.210526315789474,0.215789473684211,
0.221052631578948,0.226315789473685,0.231578947368421,0.236842105263158),
 .UNSPECIFIED.)
CURVE()
GEOMETRIC_REPRESENTATION_ITEM()
RATIONAL_B_SPLINE_CURVE((1.,0.951056516295154,1.,0.951056516295154,1.,0.951056516295154,
1.,0.951056516295154,1.,0.951056516295154,1.,0.951056516295154,1.,0.951056516295154,
1.,0.951056516295154,1.,0.951056516295154,1.,0.951056516295154,1.))
REPRESENTATION_ITEM('')
);
#1719=(
BOUNDED_CURVE()
B_SPLINE_CURVE(2,(#304934,#304935,#304936,#304937,#304938,#304939,#304940,
#304941,#304942,#304943,#304944,#304945,#304946,#304947,#304948,#304949,
#304950,#304951,#304952,#304953,#304954),.UNSPECIFIED.,.F.,.F.)
B_SPLINE_CURVE_WITH_KNOTS((3,2,2,2,2,2,2,2,2,2,3),(0.131578947368421,0.136842105263158,
0.142105263157895,0.147368421052632,0.152631578947369,0.157894736842105,
0.163157894736842,0.168421052631579,0.173684210526316,0.178947368421052,
0.18421052631579),.UNSPECIFIED.)
CURVE()
GEOMETRIC_REPRESENTATION_ITEM()
RATIONAL_B_SPLINE_CURVE((1.,0.951056516295154,1.,0.951056516295154,1.,0.951056516295154,
1.,0.951056516295154,1.,0.951056516295154,1.,0.951056516295154,1.,0.951056516295154,
1.,0.951056516295154,1.,0.951056516295154,1.,0.951056516295154,1.))
REPRESENTATION_ITEM('')
);
#1720=(
BOUNDED_CURVE()
B_SPLINE_CURVE(2,(#304955,#304956,#304957,#304958,#304959,#304960,#304961,
#304962,#304963,#304964,#304965,#304966,#304967,#304968,#304969,#304970,
#304971,#304972,#304973,#304974,#304975),.UNSPECIFIED.,.F.,.F.)
B_SPLINE_CURVE_WITH_KNOTS((3,2,2,2,2,2,2,2,2,2,3),(0.131578947368421,0.136842105263158,
0.142105263157895,0.147368421052632,0.152631578947369,0.157894736842105,
0.163157894736842,0.168421052631579,0.173684210526316,0.178947368421053,
0.18421052631579),.UNSPECIFIED.)
CURVE()
GEOMETRIC_REPRESENTATION_ITEM()
RATIONAL_B_SPLINE_CURVE((1.,0.951056516295154,1.,0.951056516295154,1.,0.951056516295154,
1.,0.951056516295154,1.,0.951056516295154,1.,0.951056516295154,1.,0.951056516295154,
1.,0.951056516295154,1.,0.951056516295154,1.,0.951056516295154,1.))
REPRESENTATION_ITEM('')
);
#1721=(
BOUNDED_CURVE()
B_SPLINE_CURVE(2,(#304980,#304981,#304982,#304983,#304984,#304985,#304986,
#304987,#304988,#304989,#304990,#304991,#304992,#304993,#304994,#304995,
#304996,#304997,#304998,#304999,#305000),.UNSPECIFIED.,.F.,.F.)
B_SPLINE_CURVE_WITH_KNOTS((3,2,2,2,2,2,2,2,2,2,3),(0.0789473684210526,0.0842105263157895,
0.0894736842105263,0.0947368421052632,0.1,0.105263157894737,0.110526315789474,
0.11578947368421,0.121052631578947,0.126315789473684,0.131578947368421),
 .UNSPECIFIED.)
CURVE()
GEOMETRIC_REPRESENTATION_ITEM()
RATIONAL_B_SPLINE_CURVE((1.,0.951056516295154,1.,0.951056516295154,1.,0.951056516295154,
1.,0.951056516295154,1.,0.951056516295154,1.,0.951056516295154,1.,0.951056516295154,
1.,0.951056516295154,1.,0.951056516295154,1.,0.951056516295154,1.))
REPRESENTATION_ITEM('')
);
#1722=(
BOUNDED_CURVE()
B_SPLINE_CURVE(2,(#305001,#305002,#305003,#305004,#305005,#305006,#305007,
#305008,#305009,#305010,#305011,#305012,#305013,#305014,#305015,#305016,
#305017,#305018,#305019,#305020,#305021),.UNSPECIFIED.,.F.,.F.)
B_SPLINE_CURVE_WITH_KNOTS((3,2,2,2,2,2,2,2,2,2,3),(0.0789473684210526,0.0842105263157895,
0.0894736842105263,0.0947368421052632,0.1,0.105263157894737,0.110526315789474,
0.11578947368421,0.121052631578947,0.126315789473684,0.131578947368421),
 .UNSPECIFIED.)
CURVE()
GEOMETRIC_REPRESENTATION_ITEM()
RATIONAL_B_SPLINE_CURVE((1.,0.951056516295154,1.,0.951056516295154,1.,0.951056516295154,
1.,0.951056516295154,1.,0.951056516295154,1.,0.951056516295154,1.,0.951056516295154,
1.,0.951056516295154,1.,0.951056516295154,1.,0.951056516295154,1.))
REPRESENTATION_ITEM('')
);
#1723=(
BOUNDED_CURVE()
B_SPLINE_CURVE(2,(#305028,#305029,#305030,#305031,#305032,#305033,#305034,
#305035,#305036,#305037,#305038,#305039,#305040,#305041,#305042,#305043,
#305044,#305045,#305046),.UNSPECIFIED.,.F.,.F.)
B_SPLINE_CURVE_WITH_KNOTS((3,2,2,2,2,2,2,2,2,3),(0.0316055430258635,0.0368421052631579,
0.0421052631578947,0.0473684210526316,0.0526315789473684,0.0578947368421053,
0.0631578947368421,0.068421052631579,0.0736842105263158,0.0789473684210526),
 .UNSPECIFIED.)
CURVE()
GEOMETRIC_REPRESENTATION_ITEM()
RATIONAL_B_SPLINE_CURVE((0.999507859534149,0.951303836279218,1.,0.951056516295154,
1.,0.951056516295154,1.,0.951056516295154,1.,0.951056516295154,1.,0.951056516295154,
1.,0.951056516295154,1.,0.951056516295154,1.,0.951056516295154,1.))
REPRESENTATION_ITEM('')
);
#1724=(
BOUNDED_CURVE()
B_SPLINE_CURVE(2,(#305047,#305048,#305049,#305050,#305051,#305052,#305053,
#305054,#305055,#305056,#305057,#305058,#305059,#305060,#305061,#305062,
#305063,#305064,#305065,#305066,#305067),.UNSPECIFIED.,.F.,.F.)
B_SPLINE_CURVE_WITH_KNOTS((3,2,2,2,2,2,2,2,2,2,3),(0.0263157894736842,0.031578947368421,
0.0368421052631579,0.0421052631578947,0.0473684210526316,0.0526315789473684,
0.0578947368421053,0.0631578947368421,0.068421052631579,0.0736842105263158,
0.0789473684210526),.UNSPECIFIED.)
CURVE()
GEOMETRIC_REPRESENTATION_ITEM()
RATIONAL_B_SPLINE_CURVE((1.,0.951056516295154,1.,0.951056516295154,1.,0.951056516295154,
1.,0.951056516295154,1.,0.951056516295154,1.,0.951056516295154,1.,0.951056516295154,
1.,0.951056516295154,1.,0.951056516295154,1.,0.951056516295154,1.))
REPRESENTATION_ITEM('')
);
#1725=(
BOUNDED_CURVE()
B_SPLINE_CURVE(2,(#305900,#305901,#305902),.UNSPECIFIED.,.F.,.F.)
B_SPLINE_CURVE_WITH_KNOTS((3,3),(0.0250007074989804,0.0263157894736842),
 .UNSPECIFIED.)
CURVE()
GEOMETRIC_REPRESENTATION_ITEM()
RATIONAL_B_SPLINE_CURVE((0.981652774597819,0.987770708292104,1.))
REPRESENTATION_ITEM('')
);
#1726=(
BOUNDED_CURVE()
B_SPLINE_CURVE(2,(#308874,#308875,#308876),.UNSPECIFIED.,.F.,.F.)
B_SPLINE_CURVE_WITH_KNOTS((3,3),(-2.38479811603073,-1.41769287070735),
 .UNSPECIFIED.)
CURVE()
GEOMETRIC_REPRESENTATION_ITEM()
RATIONAL_B_SPLINE_CURVE((1.77486483496503,1.77486483496502,1.6474352731167))
REPRESENTATION_ITEM('')
);
#1727=(
BOUNDED_CURVE()
B_SPLINE_CURVE(2,(#308877,#308878,#308879),.UNSPECIFIED.,.F.,.F.)
B_SPLINE_CURVE_WITH_KNOTS((3,3),(-3.35190336135413,-2.38479811603074),
 .UNSPECIFIED.)
CURVE()
GEOMETRIC_REPRESENTATION_ITEM()
RATIONAL_B_SPLINE_CURVE((1.6474352731167,1.77486483496503,1.77486483496503))
REPRESENTATION_ITEM('')
);
#1728=(
BOUNDED_CURVE()
B_SPLINE_CURVE(2,(#308882,#308883,#308884),.UNSPECIFIED.,.F.,.F.)
B_SPLINE_CURVE_WITH_KNOTS((3,3),(-2.38479811603074,-1.41769287070735),
 .UNSPECIFIED.)
CURVE()
GEOMETRIC_REPRESENTATION_ITEM()
RATIONAL_B_SPLINE_CURVE((1.77486483496503,1.77486483496503,1.6474352731167))
REPRESENTATION_ITEM('')
);
#1729=(
BOUNDED_CURVE()
B_SPLINE_CURVE(2,(#308885,#308886,#308887),.UNSPECIFIED.,.F.,.F.)
B_SPLINE_CURVE_WITH_KNOTS((3,3),(-3.35190336135412,-2.38479811603073),
 .UNSPECIFIED.)
CURVE()
GEOMETRIC_REPRESENTATION_ITEM()
RATIONAL_B_SPLINE_CURVE((1.6474352731167,1.77486483496503,1.77486483496503))
REPRESENTATION_ITEM('')
);
#1730=(
BOUNDED_CURVE()
B_SPLINE_CURVE(2,(#308890,#308891,#308892),.UNSPECIFIED.,.F.,.F.)
B_SPLINE_CURVE_WITH_KNOTS((3,3),(-2.38479811603073,-1.41769287070735),
 .UNSPECIFIED.)
CURVE()
GEOMETRIC_REPRESENTATION_ITEM()
RATIONAL_B_SPLINE_CURVE((1.77486483496503,1.77486483496503,1.6474352731167))
REPRESENTATION_ITEM('')
);
#1731=(
BOUNDED_CURVE()
B_SPLINE_CURVE(2,(#308893,#308894,#308895),.UNSPECIFIED.,.F.,.F.)
B_SPLINE_CURVE_WITH_KNOTS((3,3),(-3.35190336135412,-2.38479811603073),
 .UNSPECIFIED.)
CURVE()
GEOMETRIC_REPRESENTATION_ITEM()
RATIONAL_B_SPLINE_CURVE((1.6474352731167,1.77486483496503,1.77486483496503))
REPRESENTATION_ITEM('')
);
#1732=(
BOUNDED_CURVE()
B_SPLINE_CURVE(2,(#308898,#308899,#308900),.UNSPECIFIED.,.F.,.F.)
B_SPLINE_CURVE_WITH_KNOTS((3,3),(-2.38479811603073,-1.41769287070735),
 .UNSPECIFIED.)
CURVE()
GEOMETRIC_REPRESENTATION_ITEM()
RATIONAL_B_SPLINE_CURVE((1.77486483496503,1.77486483496503,1.6474352731167))
REPRESENTATION_ITEM('')
);
#1733=(
BOUNDED_CURVE()
B_SPLINE_CURVE(2,(#308901,#308902,#308903),.UNSPECIFIED.,.F.,.F.)
B_SPLINE_CURVE_WITH_KNOTS((3,3),(-3.35190336135412,-2.38479811603073),
 .UNSPECIFIED.)
CURVE()
GEOMETRIC_REPRESENTATION_ITEM()
RATIONAL_B_SPLINE_CURVE((1.6474352731167,1.77486483496502,1.77486483496502))
REPRESENTATION_ITEM('')
);
#1734=(
BOUNDED_CURVE()
B_SPLINE_CURVE(2,(#308906,#308907,#308908),.UNSPECIFIED.,.F.,.F.)
B_SPLINE_CURVE_WITH_KNOTS((3,3),(-2.38479811603073,-1.41769287070735),
 .UNSPECIFIED.)
CURVE()
GEOMETRIC_REPRESENTATION_ITEM()
RATIONAL_B_SPLINE_CURVE((1.77486483496503,1.77486483496503,1.6474352731167))
REPRESENTATION_ITEM('')
);
#1735=(
BOUNDED_CURVE()
B_SPLINE_CURVE(2,(#308909,#308910,#308911),.UNSPECIFIED.,.F.,.F.)
B_SPLINE_CURVE_WITH_KNOTS((3,3),(-3.35190336135413,-2.38479811603073),
 .UNSPECIFIED.)
CURVE()
GEOMETRIC_REPRESENTATION_ITEM()
RATIONAL_B_SPLINE_CURVE((1.6474352731167,1.77486483496503,1.77486483496503))
REPRESENTATION_ITEM('')
);
#1736=(
BOUNDED_CURVE()
B_SPLINE_CURVE(2,(#308914,#308915,#308916),.UNSPECIFIED.,.F.,.F.)
B_SPLINE_CURVE_WITH_KNOTS((3,3),(-3.35190336135412,-2.38479811603073),
 .UNSPECIFIED.)
CURVE()
GEOMETRIC_REPRESENTATION_ITEM()
RATIONAL_B_SPLINE_CURVE((1.6474352731167,1.77486483496503,1.77486483496503))
REPRESENTATION_ITEM('')
);
#1737=(
BOUNDED_CURVE()
B_SPLINE_CURVE(2,(#308917,#308918,#308919),.UNSPECIFIED.,.F.,.F.)
B_SPLINE_CURVE_WITH_KNOTS((3,3),(-2.38479811603073,-1.41769287070735),
 .UNSPECIFIED.)
CURVE()
GEOMETRIC_REPRESENTATION_ITEM()
RATIONAL_B_SPLINE_CURVE((1.77486483496502,1.77486483496502,1.6474352731167))
REPRESENTATION_ITEM('')
);
#1738=(
BOUNDED_CURVE()
B_SPLINE_CURVE(2,(#309301,#309302,#309303,#309304,#309305,#309306,#309307,
#309308,#309309,#309310,#309311,#309312,#309313),.UNSPECIFIED.,.F.,.F.)
B_SPLINE_CURVE_WITH_KNOTS((3,2,2,2,2,2,3),(0.670198248522263,0.685091542933869,
0.699984837345475,0.714878131757081,0.729771426168687,0.744664720580293,
0.750623093706636),.UNSPECIFIED.)
CURVE()
GEOMETRIC_REPRESENTATION_ITEM()
RATIONAL_B_SPLINE_CURVE((1.,0.951056516295154,1.,0.951056516295154,1.,0.951056516295154,
1.,0.951056516295154,1.,0.951056516295154,1.,0.980419138307685,0.976505741029048))
REPRESENTATION_ITEM('')
);
#1739=(
BOUNDED_CURVE()
B_SPLINE_CURVE(2,(#309314,#309315,#309316,#309317,#309318,#309319,#309320,
#309321,#309322,#309323,#309324,#309325,#309326,#309327,#309328),
 .UNSPECIFIED.,.F.,.F.)
B_SPLINE_CURVE_WITH_KNOTS((3,2,2,2,2,2,2,3),(0.642857142857143,0.657142857142857,
0.671428571428571,0.685714285714286,0.7,0.714285714285714,0.728571428571428,
0.737776488038992),.UNSPECIFIED.)
CURVE()
GEOMETRIC_REPRESENTATION_ITEM()
RATIONAL_B_SPLINE_CURVE((1.,0.951056516295154,1.,0.951056516295154,1.,0.951056516295154,
1.,0.951056516295154,1.,0.951056516295154,1.,0.951056516295154,1.,0.968463062536303,
0.977568038941547))
REPRESENTATION_ITEM('')
);
#1740=(
BOUNDED_CURVE()
B_SPLINE_CURVE(2,(#309333,#309334,#309335,#309336,#309337,#309338,#309339,
#309340,#309341,#309342,#309343,#309344,#309345,#309346,#309347,#309348,
#309349,#309350,#309351,#309352,#309353),.UNSPECIFIED.,.F.,.F.)
B_SPLINE_CURVE_WITH_KNOTS((3,2,2,2,2,2,2,2,2,2,3),(0.521265304406204,0.53615859881781,
0.551051893229416,0.565945187641022,0.580838482052628,0.595731776464233,
0.610625070875839,0.625518365287445,0.640411659699051,0.655304954110657,
0.670198248522263),.UNSPECIFIED.)
CURVE()
GEOMETRIC_REPRESENTATION_ITEM()
RATIONAL_B_SPLINE_CURVE((1.,0.951056516295154,1.,0.951056516295154,1.,0.951056516295154,
1.,0.951056516295154,1.,0.951056516295154,1.,0.951056516295154,1.,0.951056516295154,
1.,0.951056516295154,1.,0.951056516295154,1.,0.951056516295154,1.))
REPRESENTATION_ITEM('')
);
#1741=(
BOUNDED_CURVE()
B_SPLINE_CURVE(2,(#309354,#309355,#309356,#309357,#309358,#309359,#309360,
#309361,#309362,#309363,#309364,#309365,#309366,#309367,#309368,#309369,
#309370,#309371,#309372,#309373,#309374),.UNSPECIFIED.,.F.,.F.)
B_SPLINE_CURVE_WITH_KNOTS((3,2,2,2,2,2,2,2,2,2,3),(0.5,0.514285714285714,
0.528571428571429,0.542857142857143,0.557142857142857,0.571428571428571,
0.585714285714286,0.6,0.614285714285714,0.628571428571429,0.642857142857143),
 .UNSPECIFIED.)
CURVE()
GEOMETRIC_REPRESENTATION_ITEM()
RATIONAL_B_SPLINE_CURVE((1.,0.951056516295154,1.,0.951056516295154,1.,0.951056516295154,
1.,0.951056516295154,1.,0.951056516295154,1.,0.951056516295154,1.,0.951056516295154,
1.,0.951056516295154,1.,0.951056516295154,1.,0.951056516295154,1.))
REPRESENTATION_ITEM('')
);
#1742=(
BOUNDED_CURVE()
B_SPLINE_CURVE(2,(#309379,#309380,#309381,#309382,#309383,#309384,#309385,
#309386,#309387,#309388,#309389,#309390,#309391,#309392,#309393,#309394,
#309395,#309396,#309397,#309398,#309399),.UNSPECIFIED.,.F.,.F.)
B_SPLINE_CURVE_WITH_KNOTS((3,2,2,2,2,2,2,2,2,2,3),(0.372332360290144,0.38722565470175,
0.402118949113356,0.417012243524962,0.431905537936568,0.446798832348174,
0.46169212675978,0.476585421171386,0.491478715582992,0.506372009994598,
0.521265304406204),.UNSPECIFIED.)
CURVE()
GEOMETRIC_REPRESENTATION_ITEM()
RATIONAL_B_SPLINE_CURVE((1.,0.951056516295154,1.,0.951056516295154,1.,0.951056516295154,
1.,0.951056516295154,1.,0.951056516295154,1.,0.951056516295154,1.,0.951056516295154,
1.,0.951056516295154,1.,0.951056516295154,1.,0.951056516295154,1.))
REPRESENTATION_ITEM('')
);
#1743=(
BOUNDED_CURVE()
B_SPLINE_CURVE(2,(#309400,#309401,#309402,#309403,#309404,#309405,#309406,
#309407,#309408,#309409,#309410,#309411,#309412,#309413,#309414,#309415,
#309416,#309417,#309418,#309419,#309420),.UNSPECIFIED.,.F.,.F.)
B_SPLINE_CURVE_WITH_KNOTS((3,2,2,2,2,2,2,2,2,2,3),(0.357142857142857,0.371428571428571,
0.385714285714286,0.4,0.414285714285715,0.428571428571428,0.442857142857143,
0.457142857142857,0.471428571428571,0.485714285714286,0.5),
 .UNSPECIFIED.)
CURVE()
GEOMETRIC_REPRESENTATION_ITEM()
RATIONAL_B_SPLINE_CURVE((1.,0.951056516295154,1.,0.951056516295154,1.,0.951056516295154,
1.,0.951056516295154,1.,0.951056516295154,1.,0.951056516295154,1.,0.951056516295154,
1.,0.951056516295154,1.,0.951056516295154,1.,0.951056516295154,1.))
REPRESENTATION_ITEM('')
);
#1744=(
BOUNDED_CURVE()
B_SPLINE_CURVE(2,(#309427,#309428,#309429),.UNSPECIFIED.,.F.,.F.)
B_SPLINE_CURVE_WITH_KNOTS((3,3),(0.212227443337166,0.223399416174085),
 .UNSPECIFIED.)
CURVE()
GEOMETRIC_REPRESENTATION_ITEM()
RATIONAL_B_SPLINE_CURVE((0.981652774597814,0.963285808003053,1.))
REPRESENTATION_ITEM('')
);
#1745=(
BOUNDED_CURVE()
B_SPLINE_CURVE(2,(#309746,#309747,#309748,#309749,#309750,#309751,#309752,
#309753,#309754,#309755,#309756,#309757,#309758,#309759,#309760,#309761,
#309762,#309763,#309764,#309765,#309766),.UNSPECIFIED.,.F.,.F.)
B_SPLINE_CURVE_WITH_KNOTS((3,2,2,2,2,2,2,2,2,2,3),(0.223399416174085,0.23829271058569,
0.253186004997297,0.268079299408903,0.282972593820508,0.297865888232115,
0.312759182643721,0.327652477055327,0.342545771466932,0.357439065878539,
0.372332360290144),.UNSPECIFIED.)
CURVE()
GEOMETRIC_REPRESENTATION_ITEM()
RATIONAL_B_SPLINE_CURVE((1.,0.951056516295154,1.,0.951056516295154,1.,0.951056516295154,
1.,0.951056516295154,1.,0.951056516295154,1.,0.951056516295154,1.,0.951056516295154,
1.,0.951056516295154,1.,0.951056516295154,1.,0.951056516295154,1.))
REPRESENTATION_ITEM('')
);
#1746=(
BOUNDED_CURVE()
B_SPLINE_CURVE(2,(#309820,#309821,#309822,#309823,#309824,#309825,#309826,
#309827,#309828,#309829,#309830,#309831,#309832,#309833,#309834,#309835,
#309836,#309837,#309838,#309839,#309840),.UNSPECIFIED.,.F.,.F.)
B_SPLINE_CURVE_WITH_KNOTS((3,2,2,2,2,2,2,2,2,2,3),(0.221361545916683,0.228571428571428,
0.242857142857143,0.257142857142857,0.271428571428572,0.285714285714286,
0.3,0.314285714285715,0.328571428571429,0.342857142857143,0.357142857142857),
 .UNSPECIFIED.)
CURVE()
GEOMETRIC_REPRESENTATION_ITEM()
RATIONAL_B_SPLINE_CURVE((0.975530412919128,0.97529862580415,1.,0.951056516295154,
1.,0.951056516295154,1.,0.951056516295154,1.,0.951056516295154,1.,0.951056516295154,
1.,0.951056516295154,1.,0.951056516295154,1.,0.951056516295154,1.,0.951056516295154,
1.))
REPRESENTATION_ITEM('')
);
#1747=(
BOUNDED_CURVE()
B_SPLINE_CURVE(2,(#310374,#310375,#310376),.UNSPECIFIED.,.F.,.F.)
B_SPLINE_CURVE_WITH_KNOTS((3,3),(1.8359668034886,2.908605540086),
 .UNSPECIFIED.)
CURVE()
GEOMETRIC_REPRESENTATION_ITEM()
RATIONAL_B_SPLINE_CURVE((1.8663905512715,2.00276625701356,2.00276625701356))
REPRESENTATION_ITEM('')
);
#1748=(
BOUNDED_CURVE()
B_SPLINE_CURVE(2,(#310378,#310379,#310380),.UNSPECIFIED.,.F.,.F.)
B_SPLINE_CURVE_WITH_KNOTS((3,3),(2.908605540086,3.98124427668513),
 .UNSPECIFIED.)
CURVE()
GEOMETRIC_REPRESENTATION_ITEM()
RATIONAL_B_SPLINE_CURVE((2.00276625701356,2.00276625701356,1.86639055127106))
REPRESENTATION_ITEM('')
);
#1749=(
BOUNDED_CURVE()
B_SPLINE_CURVE(2,(#310383,#310384,#310385),.UNSPECIFIED.,.F.,.F.)
B_SPLINE_CURVE_WITH_KNOTS((3,3),(1.83596680348874,2.908605540086),
 .UNSPECIFIED.)
CURVE()
GEOMETRIC_REPRESENTATION_ITEM()
RATIONAL_B_SPLINE_CURVE((1.86639055127154,2.00276625701356,2.00276625701356))
REPRESENTATION_ITEM('')
);
#1750=(
BOUNDED_CURVE()
B_SPLINE_CURVE(2,(#310387,#310388,#310389),.UNSPECIFIED.,.F.,.F.)
B_SPLINE_CURVE_WITH_KNOTS((3,3),(2.908605540086,3.98124427668513),
 .UNSPECIFIED.)
CURVE()
GEOMETRIC_REPRESENTATION_ITEM()
RATIONAL_B_SPLINE_CURVE((2.00276625701356,2.00276625701356,1.86639055127106))
REPRESENTATION_ITEM('')
);
#1751=(
BOUNDED_CURVE()
B_SPLINE_CURVE(2,(#310392,#310393,#310394),.UNSPECIFIED.,.F.,.F.)
B_SPLINE_CURVE_WITH_KNOTS((3,3),(1.83596680348874,2.908605540086),
 .UNSPECIFIED.)
CURVE()
GEOMETRIC_REPRESENTATION_ITEM()
RATIONAL_B_SPLINE_CURVE((1.86639055127154,2.00276625701356,2.00276625701356))
REPRESENTATION_ITEM('')
);
#1752=(
BOUNDED_CURVE()
B_SPLINE_CURVE(2,(#310396,#310397,#310398),.UNSPECIFIED.,.F.,.F.)
B_SPLINE_CURVE_WITH_KNOTS((3,3),(2.908605540086,3.9812442766844),
 .UNSPECIFIED.)
CURVE()
GEOMETRIC_REPRESENTATION_ITEM()
RATIONAL_B_SPLINE_CURVE((2.00276625701356,2.00276625701356,1.86639055127125))
REPRESENTATION_ITEM('')
);
#1753=(
BOUNDED_CURVE()
B_SPLINE_CURVE(2,(#310401,#310402,#310403),.UNSPECIFIED.,.F.,.F.)
B_SPLINE_CURVE_WITH_KNOTS((3,3),(1.8359668034886,2.908605540086),
 .UNSPECIFIED.)
CURVE()
GEOMETRIC_REPRESENTATION_ITEM()
RATIONAL_B_SPLINE_CURVE((1.8663905512715,2.00276625701356,2.00276625701356))
REPRESENTATION_ITEM('')
);
#1754=(
BOUNDED_CURVE()
B_SPLINE_CURVE(2,(#310405,#310406,#310407),.UNSPECIFIED.,.F.,.F.)
B_SPLINE_CURVE_WITH_KNOTS((3,3),(2.908605540086,3.98124427668513),
 .UNSPECIFIED.)
CURVE()
GEOMETRIC_REPRESENTATION_ITEM()
RATIONAL_B_SPLINE_CURVE((2.00276625701356,2.00276625701356,1.86639055127106))
REPRESENTATION_ITEM('')
);
#1755=(
BOUNDED_CURVE()
B_SPLINE_CURVE(2,(#310410,#310411,#310412),.UNSPECIFIED.,.F.,.F.)
B_SPLINE_CURVE_WITH_KNOTS((3,3),(1.83596680348875,2.908605540086),
 .UNSPECIFIED.)
CURVE()
GEOMETRIC_REPRESENTATION_ITEM()
RATIONAL_B_SPLINE_CURVE((1.86639055127154,2.00276625701356,2.00276625701356))
REPRESENTATION_ITEM('')
);
#1756=(
BOUNDED_CURVE()
B_SPLINE_CURVE(2,(#310414,#310415,#310416),.UNSPECIFIED.,.F.,.F.)
B_SPLINE_CURVE_WITH_KNOTS((3,3),(2.908605540086,3.98124427668513),
 .UNSPECIFIED.)
CURVE()
GEOMETRIC_REPRESENTATION_ITEM()
RATIONAL_B_SPLINE_CURVE((2.00276625701356,2.00276625701356,1.86639055127106))
REPRESENTATION_ITEM('')
);
#1757=(
BOUNDED_CURVE()
B_SPLINE_CURVE(2,(#310419,#310420,#310421),.UNSPECIFIED.,.F.,.F.)
B_SPLINE_CURVE_WITH_KNOTS((3,3),(1.83596680348874,2.908605540086),
 .UNSPECIFIED.)
CURVE()
GEOMETRIC_REPRESENTATION_ITEM()
RATIONAL_B_SPLINE_CURVE((1.86639055127154,2.00276625701356,2.00276625701356))
REPRESENTATION_ITEM('')
);
#1758=(
BOUNDED_CURVE()
B_SPLINE_CURVE(2,(#310422,#310423,#310424),.UNSPECIFIED.,.F.,.F.)
B_SPLINE_CURVE_WITH_KNOTS((3,3),(2.908605540086,3.9812442766844),
 .UNSPECIFIED.)
CURVE()
GEOMETRIC_REPRESENTATION_ITEM()
RATIONAL_B_SPLINE_CURVE((2.00276625701356,2.00276625701356,1.86639055127125))
REPRESENTATION_ITEM('')
);
#1759=(
BOUNDED_CURVE()
B_SPLINE_CURVE(2,(#310428,#310429,#310430),.UNSPECIFIED.,.F.,.F.)
B_SPLINE_CURVE_WITH_KNOTS((3,3),(-2.908605540086,-1.83596680348895),
 .UNSPECIFIED.)
CURVE()
GEOMETRIC_REPRESENTATION_ITEM()
RATIONAL_B_SPLINE_CURVE((2.00276625701356,2.00276625701356,1.86639055127159))
REPRESENTATION_ITEM('')
);
#1760=(
BOUNDED_CURVE()
B_SPLINE_CURVE(2,(#310432,#310433,#310434),.UNSPECIFIED.,.F.,.F.)
B_SPLINE_CURVE_WITH_KNOTS((3,3),(-3.98124427668322,-2.90860554008599),
 .UNSPECIFIED.)
CURVE()
GEOMETRIC_REPRESENTATION_ITEM()
RATIONAL_B_SPLINE_CURVE((1.86639055127155,2.00276625701356,2.00276625701356))
REPRESENTATION_ITEM('')
);
#1761=(
BOUNDED_CURVE()
B_SPLINE_CURVE(2,(#310437,#310438,#310439),.UNSPECIFIED.,.F.,.F.)
B_SPLINE_CURVE_WITH_KNOTS((3,3),(-2.90860554008599,-1.83596680348895),
 .UNSPECIFIED.)
CURVE()
GEOMETRIC_REPRESENTATION_ITEM()
RATIONAL_B_SPLINE_CURVE((2.00276625701356,2.00276625701356,1.86639055127159))
REPRESENTATION_ITEM('')
);
#1762=(
BOUNDED_CURVE()
B_SPLINE_CURVE(2,(#310441,#310442,#310443),.UNSPECIFIED.,.F.,.F.)
B_SPLINE_CURVE_WITH_KNOTS((3,3),(-3.98124427668324,-2.908605540086),
 .UNSPECIFIED.)
CURVE()
GEOMETRIC_REPRESENTATION_ITEM()
RATIONAL_B_SPLINE_CURVE((1.86639055127154,2.00276625701356,2.00276625701356))
REPRESENTATION_ITEM('')
);
#1763=(
BOUNDED_CURVE()
B_SPLINE_CURVE(2,(#310446,#310447,#310448),.UNSPECIFIED.,.F.,.F.)
B_SPLINE_CURVE_WITH_KNOTS((3,3),(-2.908605540086,-1.83596680348886),
 .UNSPECIFIED.)
CURVE()
GEOMETRIC_REPRESENTATION_ITEM()
RATIONAL_B_SPLINE_CURVE((2.00276625701356,2.00276625701356,1.86639055127157))
REPRESENTATION_ITEM('')
);
#1764=(
BOUNDED_CURVE()
B_SPLINE_CURVE(2,(#310450,#310451,#310452),.UNSPECIFIED.,.F.,.F.)
B_SPLINE_CURVE_WITH_KNOTS((3,3),(-3.98124427668322,-2.908605540086),
 .UNSPECIFIED.)
CURVE()
GEOMETRIC_REPRESENTATION_ITEM()
RATIONAL_B_SPLINE_CURVE((1.86639055127154,2.00276625701356,2.00276625701356))
REPRESENTATION_ITEM('')
);
#1765=(
BOUNDED_CURVE()
B_SPLINE_CURVE(2,(#310455,#310456,#310457),.UNSPECIFIED.,.F.,.F.)
B_SPLINE_CURVE_WITH_KNOTS((3,3),(-2.908605540086,-1.83596680348895),
 .UNSPECIFIED.)
CURVE()
GEOMETRIC_REPRESENTATION_ITEM()
RATIONAL_B_SPLINE_CURVE((2.00276625701356,2.00276625701356,1.86639055127159))
REPRESENTATION_ITEM('')
);
#1766=(
BOUNDED_CURVE()
B_SPLINE_CURVE(2,(#310459,#310460,#310461),.UNSPECIFIED.,.F.,.F.)
B_SPLINE_CURVE_WITH_KNOTS((3,3),(-3.98124427668322,-2.908605540086),
 .UNSPECIFIED.)
CURVE()
GEOMETRIC_REPRESENTATION_ITEM()
RATIONAL_B_SPLINE_CURVE((1.86639055127154,2.00276625701356,2.00276625701356))
REPRESENTATION_ITEM('')
);
#1767=(
BOUNDED_CURVE()
B_SPLINE_CURVE(2,(#310464,#310465,#310466),.UNSPECIFIED.,.F.,.F.)
B_SPLINE_CURVE_WITH_KNOTS((3,3),(-2.908605540086,-1.83596680348895),
 .UNSPECIFIED.)
CURVE()
GEOMETRIC_REPRESENTATION_ITEM()
RATIONAL_B_SPLINE_CURVE((2.00276625701356,2.00276625701356,1.86639055127159))
REPRESENTATION_ITEM('')
);
#1768=(
BOUNDED_CURVE()
B_SPLINE_CURVE(2,(#310468,#310469,#310470),.UNSPECIFIED.,.F.,.F.)
B_SPLINE_CURVE_WITH_KNOTS((3,3),(-3.98124427668324,-2.908605540086),
 .UNSPECIFIED.)
CURVE()
GEOMETRIC_REPRESENTATION_ITEM()
RATIONAL_B_SPLINE_CURVE((1.86639055127154,2.00276625701356,2.00276625701356))
REPRESENTATION_ITEM('')
);
#1769=(
BOUNDED_CURVE()
B_SPLINE_CURVE(2,(#310473,#310474,#310475),.UNSPECIFIED.,.F.,.F.)
B_SPLINE_CURVE_WITH_KNOTS((3,3),(-2.908605540086,-1.83596680348886),
 .UNSPECIFIED.)
CURVE()
GEOMETRIC_REPRESENTATION_ITEM()
RATIONAL_B_SPLINE_CURVE((2.00276625701356,2.00276625701356,1.86639055127157))
REPRESENTATION_ITEM('')
);
#1770=(
BOUNDED_CURVE()
B_SPLINE_CURVE(2,(#310476,#310477,#310478),.UNSPECIFIED.,.F.,.F.)
B_SPLINE_CURVE_WITH_KNOTS((3,3),(-3.98124427668322,-2.908605540086),
 .UNSPECIFIED.)
CURVE()
GEOMETRIC_REPRESENTATION_ITEM()
RATIONAL_B_SPLINE_CURVE((1.86639055127154,2.00276625701356,2.00276625701356))
REPRESENTATION_ITEM('')
);
#1771=ELLIPSE('',#94133,0.937885965405836,0.86675406492929);
#1772=ELLIPSE('',#94142,1.46972525436131,1.19984572304843);
#1773=ELLIPSE('',#94157,1.04665693996376,1.00906146746166);
#1774=ELLIPSE('',#94159,1.37504974877692,1.13183911208508);
#1775=ELLIPSE('',#94174,1.14567646024684,1.02014379851209);
#1776=ELLIPSE('',#94176,1.25196838933939,1.02863480032067);
#1777=ELLIPSE('',#94203,1.29935811091585,1.07153805568279);
#1778=ELLIPSE('',#94205,1.09610411986708,1.01541339803192);
#1779=ELLIPSE('',#94218,1.42337813156552,1.16710237101683);
#1780=ELLIPSE('',#94264,0.908597175301873,0.820141976513812);
#1781=ELLIPSE('',#94283,1.06703722879645,0.943876034909289);
#1782=ELLIPSE('',#94284,1.14336482056826,1.01842172929862);
#1783=ELLIPSE('',#94297,1.3737241452667,1.13065652311915);
#1784=ELLIPSE('',#94298,1.04669178748828,1.00873018684506);
#1785=ELLIPSE('',#94310,1.46903943622045,1.1992965413372);
#1786=ELLIPSE('',#94324,1.47061008469222,1.20045580538409);
#1787=ELLIPSE('',#94336,1.04558723045975,1.0088761098663);
#1788=ELLIPSE('',#94337,1.37669607957637,1.13307292819281);
#1789=ELLIPSE('',#94350,1.14413769841436,1.02008736650461);
#1790=ELLIPSE('',#94351,1.25359260924378,1.03019400968285);
#1791=ELLIPSE('',#94415,0.455015549306865,0.414682781673397);
#1792=ELLIPSE('',#94434,0.470322150347728,0.437408695773927);
#1793=ELLIPSE('',#94470,2.23591051322783,1.82312386243465);
#1794=ELLIPSE('',#94471,1.49234872661747,1.21529881462133);
#1795=ELLIPSE('',#94499,0.796819240888165,0.626540578311605);
#1796=ELLIPSE('',#94501,0.817675517046813,0.657962952441664);
#1797=ELLIPSE('',#94642,1.14142675533965,1.0183769149773);
#1798=ELLIPSE('',#94644,1.25155489583491,1.02861695892357);
#1799=ELLIPSE('',#94658,1.04546867609948,1.00852772291651);
#1800=ELLIPSE('',#94660,1.37581189656266,1.13221924904961);
#1801=ELLIPSE('',#94675,1.47003669918833,1.19998639117251);
#1802=ELLIPSE('',#94690,2.24478172556828,1.82751302619863);
#1803=ELLIPSE('',#94692,6.74379813677969,5.49640701624088);
#1804=ELLIPSE('',#94693,6.74471830677379,5.49677536022385);
#1805=ELLIPSE('',#94694,2.24478717905741,1.82751618959032);
#1806=ELLIPSE('',#94697,2.19060648404767,1.80054773483043);
#1807=ELLIPSE('',#94699,2.19081358780445,1.80064181344396);
#1808=ELLIPSE('',#94703,1.43187143532244,1.37961189378668);
#1809=ELLIPSE('',#94705,2.14457779788183,1.77729531483311);
#1810=ELLIPSE('',#94708,1.45260602254477,1.42951177173056);
#1811=ELLIPSE('',#94712,1.45276135118972,1.42923490730472);
#1812=ELLIPSE('',#94719,1.48146874195372,1.44883544422854);
#1813=ELLIPSE('',#94723,1.48049428484162,1.44867655321776);
#1814=ELLIPSE('',#94726,1.59183749500213,1.48024250564481);
#1815=ELLIPSE('',#94730,1.59230054944377,1.48054973563609);
#1816=ELLIPSE('',#94736,1.34503947636183,1.23514518656413);
#1817=ELLIPSE('',#94748,1.52235692825161,1.4619644584823);
#1818=ELLIPSE('',#94753,1.44688208751335,1.42026986218873);
#1819=ELLIPSE('',#94761,1.43683810397249,1.39553674726878);
#1820=ELLIPSE('',#94764,2.21081023708958,1.81065351492543);
#1821=ELLIPSE('',#94783,1.4677889282425,1.40956355520622);
#1822=ELLIPSE('',#94784,1.59354891790328,1.48067275522773);
#1823=ELLIPSE('',#94787,1.48261995869119,1.44952139994979);
#1824=ELLIPSE('',#94792,1.48262920837846,1.44930064696724);
#1825=ELLIPSE('',#94799,1.45380901900664,1.43054003732522);
#1826=ELLIPSE('',#94801,1.45322066357761,1.43028995785239);
#1827=ELLIPSE('',#94806,2.14181401024915,1.77588874339951);
#1828=ELLIPSE('',#94808,1.43208157244053,1.38029189146704);
#1829=ELLIPSE('',#94812,2.18879207398525,1.79962727559316);
#1830=ELLIPSE('',#94814,2.18901509550273,1.79974914074665);
#1831=ELLIPSE('',#94817,2.2444282619244,1.82733890923556);
#1832=ELLIPSE('',#94819,2.24443876108746,1.82734353773875);
#1833=ELLIPSE('',#94820,6.74573450851259,5.50047048351084);
#1834=ELLIPSE('',#94821,6.74598671172703,5.50057144500526);
#1835=ELLIPSE('',#94826,2.24510297414266,1.8276717674473);
#1836=ELLIPSE('',#94828,6.74390240939121,5.49585078304806);
#1837=ELLIPSE('',#94829,6.74404990886307,5.4959097928901);
#1838=ELLIPSE('',#94830,2.24510748390125,1.82767438434328);
#1839=ELLIPSE('',#94833,2.19238797298482,1.80144123645576);
#1840=ELLIPSE('',#94835,2.19259034569564,1.80153305864657);
#1841=ELLIPSE('',#94839,1.4316254101432,1.37881184106309);
#1842=ELLIPSE('',#94841,2.14692927256853,1.77849116248874);
#1843=ELLIPSE('',#94843,1.45181104759523,1.42845526063355);
#1844=ELLIPSE('',#94848,1.45196348821223,1.42817952802932);
#1845=ELLIPSE('',#94855,1.47984354908539,1.44816756164213);
#1846=ELLIPSE('',#94857,1.47888863188348,1.44801453428131);
#1847=ELLIPSE('',#94861,1.58904382174786,1.4795419860971);
#1848=ELLIPSE('',#94864,1.58949098795625,1.47983751651523);
#1849=ELLIPSE('',#94887,0.749685754907703,0.60185647341446);
#1850=ELLIPSE('',#94890,1.41328440310968,1.18460827309285);
#1851=ELLIPSE('',#94952,2.88179127866164,2.12564226548654);
#1852=ELLIPSE('',#94953,1.43722552537773,1.32204636451836);
#1853=ELLIPSE('',#94954,0.987429753876356,0.693960884248331);
#1854=ELLIPSE('',#94958,1.87599164352097,1.3631837367251);
#1855=ELLIPSE('',#94976,0.977632591669663,0.93380624359465);
#1856=ELLIPSE('',#94979,0.523318313869799,0.469519600058616);
#1857=ELLIPSE('',#95067,17.5713723065032,4.52112060210991);
#1858=ELLIPSE('',#95068,4.50277672631039,3.19320827117429);
#1859=ELLIPSE('',#95108,9.1303217691259,3.27937044288807);
#1860=ELLIPSE('',#95112,5.58690768783904,2.31976556616765);
#1861=ELLIPSE('',#95177,7.49339813124813,6.10504954200232);
#1862=ELLIPSE('',#95180,7.49235439337033,6.10463249190312);
#1863=ELLIPSE('',#95265,1.25100010657953,1.02769269305806);
#1864=ELLIPSE('',#95282,1.14675177068285,1.02017737933149);
#1865=ELLIPSE('',#95308,1.37382679960868,1.13091857689604);
#1866=ELLIPSE('',#95320,1.04756140277279,1.00921649017983);
#1867=ELLIPSE('',#95333,1.46893565132849,1.19930046752296);
#1868=ELLIPSE('',#95338,7.49433291871596,6.10831258037442);
#1869=ELLIPSE('',#95344,7.4940138380099,6.10818593644246);
#1870=ELLIPSE('',#95364,7.49253505210954,6.10416626992353);
#1871=ELLIPSE('',#95367,7.49234362041712,6.10409043317082);
#1872=ELLIPSE('',#95375,1.47091283278985,1.20059247389518);
#1873=ELLIPSE('',#95388,1.04442811078714,1.00835504871987);
#1874=ELLIPSE('',#95400,1.3774591382642,1.13345236867699);
#1875=ELLIPSE('',#95426,1.13994052039406,1.01834002153806);
#1876=ELLIPSE('',#95434,1.25321023290178,1.03018791386508);
#1877=ELLIPSE('',#95475,11.6751690359376,3.71302998352787);
#1878=ELLIPSE('',#95715,0.678690131415711,0.494805844211885);
#1879=ELLIPSE('',#95726,34.5904711318704,5.84597391203818);
#1880=ELLIPSE('',#96078,11.7565014068008,3.72593447424617);
#1881=ELLIPSE('',#96110,7.46086400325983,6.09136338114254);
#1882=ELLIPSE('',#96116,7.53518791407952,6.1247960459708);
#1883=ELLIPSE('',#96150,7.45763201025,6.09058811436398);
#1884=ELLIPSE('',#96203,9.1303217691259,3.27937044288807);
#1885=ELLIPSE('',#96205,6.16525689027633,2.36185455359168);
#1886=ELLIPSE('',#96212,1.33669592490101,1.1019523707532);
#1887=ELLIPSE('',#96213,1.25109689071003,1.02773417463857);
#1888=ELLIPSE('',#96221,5.58690768783904,2.31976556616765);
#1889=ELLIPSE('',#96224,1.44645360831276,1.18341499862822);
#1890=ELLIPSE('',#96225,1.37376569032744,1.13089346959656);
#1891=ELLIPSE('',#96233,1.49685474119579,1.21828695523177);
#1892=ELLIPSE('',#96234,1.46882736484448,1.19925664387663);
#1893=ELLIPSE('',#96242,1.47121822864674,1.20071603818299);
#1894=ELLIPSE('',#96243,1.49679583489779,1.21835526315613);
#1895=ELLIPSE('',#96251,1.37792699674947,1.13364466418821);
#1896=ELLIPSE('',#96252,1.44801280663984,1.18476784522542);
#1897=ELLIPSE('',#96262,1.25404132664573,1.03054296143257);
#1898=ELLIPSE('',#96263,1.3394502339077,1.10450276996805);
#1899=ELLIPSE('',#96432,0.979743096898815,0.937213104467219);
#1900=ELLIPSE('',#96433,0.523318313830269,0.469519600018551);
#1901=ELLIPSE('',#96496,1.43722552532624,1.32204636444341);
#1902=ELLIPSE('',#96498,0.987429753852244,0.693960884240177);
#1903=ELLIPSE('',#96500,1.01009247479397,0.982994833669031);
#1904=ELLIPSE('',#96682,0.749685755431834,0.601856473637416);
#1905=ELLIPSE('',#96752,1.58949098802822,1.479837516555);
#1906=ELLIPSE('',#96760,1.47888863176487,1.4480145341903);
#1907=ELLIPSE('',#96787,1.45196348827863,1.42817952812272);
#1908=ELLIPSE('',#96802,2.14692927256853,1.77849116248874);
#1909=ELLIPSE('',#96814,2.19259034569564,1.80153305864657);
#1910=ELLIPSE('',#96822,7.53325800757047,6.12058869275862);
#1911=ELLIPSE('',#96825,6.74390240934933,5.49585078303102);
#1912=ELLIPSE('',#96829,6.74404990885783,5.49590979288799);
#1913=ELLIPSE('',#96832,2.24510748390125,1.82767438434328);
#1914=ELLIPSE('',#96845,2.24443876108746,1.82734353773875);
#1915=ELLIPSE('',#96848,6.7457345089557,5.50047048368992);
#1916=ELLIPSE('',#96852,6.7459867118041,5.50057144503682);
#1917=ELLIPSE('',#96854,7.46237077505305,6.09538628449527);
#1918=ELLIPSE('',#96863,2.18901509550273,1.79974914074665);
#1919=ELLIPSE('',#96875,1.43208157237843,1.38029189134632);
#1920=ELLIPSE('',#96889,1.45322066372077,1.43028995804929);
#1921=ELLIPSE('',#96916,1.48262920850352,1.44930064705618);
#1922=ELLIPSE('',#96937,1.59354891806686,1.48067275531);
#1923=ELLIPSE('',#96964,4.50277672631039,3.19320827117429);
#1924=ELLIPSE('',#97067,7.540726371712,6.12413561514585);
#1925=ELLIPSE('',#97070,6.743798136932,5.49640701630224);
#1926=ELLIPSE('',#97074,6.74471830680559,5.49677536023675);
#1927=ELLIPSE('',#97084,1.49663539150943,1.21824685106957);
#1928=ELLIPSE('',#97085,2.24478717905741,1.82751618959032);
#1929=ELLIPSE('',#97089,2.19081358780445,1.80064181344396);
#1930=ELLIPSE('',#97090,1.47034339388813,1.20011049466526);
#1931=ELLIPSE('',#97093,1.4468541246316,1.18395401892993);
#1932=ELLIPSE('',#97094,2.14457779788183,1.77729531483311);
#1933=ELLIPSE('',#97098,1.45276135105947,1.42923490713001);
#1934=ELLIPSE('',#97099,1.37628311373034,1.13241299577346);
#1935=ELLIPSE('',#97105,1.33772997969343,1.1031395948871);
#1936=ELLIPSE('',#97106,1.48049428500572,1.4486765533338);
#1937=ELLIPSE('',#97110,1.59230054967801,1.48054973575714);
#1938=ELLIPSE('',#97111,1.25239319344149,1.02897532635693);
#1939=ELLIPSE('',#97183,17.5713723091178,4.52112060324491);
#1940=ELLIPSE('',#97197,0.872532027987849,0.761015579916806);
#1941=ELLIPSE('',#97198,0.872242253742692,0.756153787356879);
#1942=ELLIPSE('',#97289,2.88179127901306,2.12564226561543);
#1943=ELLIPSE('',#97336,1.58904382162818,1.47954198603725);
#1944=ELLIPSE('',#97338,1.25368354036916,1.03023294677774);
#1945=ELLIPSE('',#97342,1.47984354894719,1.44816756153839);
#1946=ELLIPSE('',#97343,1.33964027941621,1.10428915808927);
#1947=ELLIPSE('',#97350,1.45181104761723,1.42845526066408);
#1948=ELLIPSE('',#97352,1.37663299645276,1.13304702413717);
#1949=ELLIPSE('',#97356,1.4316254101432,1.37881184106309);
#1950=ELLIPSE('',#97357,1.44858750676641,1.18492005208182);
#1951=ELLIPSE('',#97361,2.19238797298482,1.80144123645576);
#1952=ELLIPSE('',#97363,1.47050130285363,1.20041179042018);
#1953=ELLIPSE('',#97367,2.24510297414266,1.8276717674473);
#1954=ELLIPSE('',#97368,1.49718443147311,1.21851081499056);
#1955=ELLIPSE('',#97372,2.2444282619244,1.82733890923556);
#1956=ELLIPSE('',#97374,1.496455657919,1.21812538939567);
#1957=ELLIPSE('',#97378,2.18879207398525,1.79962727559316);
#1958=ELLIPSE('',#97379,1.46934753477481,1.19942122868132);
#1959=ELLIPSE('',#97383,2.14181401024915,1.77588874339951);
#1960=ELLIPSE('',#97385,1.44549176500332,1.18299703423917);
#1961=ELLIPSE('',#97389,1.45380901901781,1.43054003733421);
#1962=ELLIPSE('',#97390,1.37419951292197,1.13085206801441);
#1963=ELLIPSE('',#97397,1.48261995859359,1.44952139988389);
#1964=ELLIPSE('',#97399,1.33548546759184,1.10135868188479);
#1965=ELLIPSE('',#97403,1.46778892822304,1.40956355519549);
#1966=ELLIPSE('',#97409,0.470344661252933,0.437456112172233);
#1967=ELLIPSE('',#97411,0.455017224729773,0.414686073541653);
#1968=ELLIPSE('',#97416,2.23591051322783,1.82312386243465);
#1969=ELLIPSE('',#97419,2.21081023703135,1.81065351490182);
#1970=ELLIPSE('',#97421,1.47966360607638,1.20670524509602);
#1971=ELLIPSE('',#97426,1.43683810399907,1.39553674731997);
#1972=ELLIPSE('',#97427,1.42375962264705,1.16725779022872);
#1973=ELLIPSE('',#97431,1.44688208750104,1.42026986217179);
#1974=ELLIPSE('',#97433,1.39004657997782,1.14302890167313);
#1975=ELLIPSE('',#97437,1.52235692801125,1.4619644583464);
#1976=ELLIPSE('',#97438,1.30002012621557,1.07181606140101);
#1977=ELLIPSE('',#97445,1.34503947637202,1.23514518658134);
#1978=ELLIPSE('',#97451,1.59183749527776,1.48024250578175);
#1979=ELLIPSE('',#97453,1.25206291218026,1.02867529869755);
#1980=ELLIPSE('',#97457,1.48146874171335,1.4488354440584);
#1981=ELLIPSE('',#97458,1.33790496197122,1.1029159114908);
#1982=ELLIPSE('',#97465,1.45260602245606,1.42951177160569);
#1983=ELLIPSE('',#97468,1.37498779933069,1.13181366553965);
#1984=ELLIPSE('',#97472,1.4318714352199,1.37961189358987);
#1985=ELLIPSE('',#97473,1.44743072160946,1.18410503354282);
#1986=ELLIPSE('',#97477,2.19060648404767,1.80054773483043);
#1987=ELLIPSE('',#97480,1.46961676159926,1.19980182022532);
#1988=ELLIPSE('',#97484,2.24478172556828,1.82751302619863);
#1989=ELLIPSE('',#97485,1.49702492666268,1.21840253533698);
#1990=ELLIPSE('',#97642,0.872188006859956,0.755196727163197);
#1991=ELLIPSE('',#97644,1.49262340192896,1.21540966767209);
#1992=ELLIPSE('',#97677,0.937885965402937,0.866754064923446);
#1993=ELLIPSE('',#97692,0.908597175301873,0.820141976513812);
#1994=ELLIPSE('',#98012,3.52383305788943,2.05269137889129);
#1995=ELLIPSE('',#98075,61.9730832448324,42.9788571518931);
#1996=ELLIPSE('',#99192,13.1271153497978,2.2815651398259);
#1997=ELLIPSE('',#99195,1.19618791882944,0.501602687323024);
#1998=ELLIPSE('',#99196,1.29981244177848,1.04628846257511);
#1999=ELLIPSE('',#99204,12.6883691454053,2.13068730228645);
#2000=ELLIPSE('',#99207,1.1878650987102,0.0615784629608745);
#2001=ELLIPSE('',#99209,9.77817556377705,5.31069546080688);
#2002=ELLIPSE('',#99212,88.5846814729442,33.7972522652792);
#2003=ELLIPSE('',#99914,3.52785922818763,2.05416344169751);
#2004=ELLIPSE('',#99983,61.9730832448324,42.9788571518931);
#2005=ELLIPSE('',#101082,2.92401254191216,2.73356722767542);
#2006=ELLIPSE('',#101109,5.10101304780922,2.0080086469997);
#2007=ELLIPSE('',#101114,5.6075381031809,3.56592930826501);
#2008=ELLIPSE('',#101127,13.1302942292056,2.28259278464871);
#2009=ELLIPSE('',#101129,4.57456085127438,4.1484359323234);
#2010=ELLIPSE('',#101131,1.29981239432824,1.04628842702785);
#2011=ELLIPSE('',#101132,1.19618830369613,0.501602775052797);
#2012=ELLIPSE('',#101140,12.6871422926546,2.13028400375921);
#2013=ELLIPSE('',#101142,9.77817556377705,5.31069546080688);
#2014=ELLIPSE('',#101144,1.18790481732873,0.0615825826882351);
#2015=ELLIPSE('',#101147,88.5846058090516,33.7973158081396);
#2016=ELLIPSE('',#102738,0.922279678089193,0.749999999999809);
#2017=ELLIPSE('',#102739,1.28870175757961,0.749999999999421);
#2018=ELLIPSE('',#102741,1.2887017575839,0.750000000003065);
#2019=ELLIPSE('',#102777,0.859134505046975,0.499999999989815);
#2020=ELLIPSE('',#102778,0.614853118726872,0.500000000000419);
#2021=ELLIPSE('',#102780,0.859134505053703,0.499999999999708);
#2022=ELLIPSE('',#102785,1.28870175757994,0.749999999999587);
#2023=ELLIPSE('',#102786,0.922279678089253,0.749999999999816);
#2024=ELLIPSE('',#102789,1.28870175760062,0.750000000020496);
#2025=ELLIPSE('',#102824,0.859134505046725,0.499999999989502);
#2026=ELLIPSE('',#102825,0.614853118726913,0.500000000000432);
#2027=ELLIPSE('',#102827,0.859134505054217,0.500000000000012);
#2028=ELLIPSE('',#103055,20.4666308011442,7.0000000000003);
#2029=ELLIPSE('',#103124,2.41725606676382,0.463770738124485);
#2030=ELLIPSE('',#103128,18.7300337971543,16.644499908438);
#2031=ELLIPSE('',#103129,18.4563717977211,16.4307217995611);
#2032=ELLIPSE('',#103137,1.99975887730092,1.99623716560152);
#2033=ELLIPSE('',#103142,2.00289288489225,1.97864499243066);
#2034=ELLIPSE('',#103145,1.70825186416551,1.63934150110833);
#2035=ELLIPSE('',#103294,2.05999726017368,1.96170207629362);
#2036=ELLIPSE('',#103328,14.1421356237285,9.99999999999842);
#2037=ELLIPSE('',#103330,14.14213562373,9.99999999999928);
#2038=(
BOUNDED_SURFACE()
B_SPLINE_SURFACE(3,2,((#131389,#131390,#131391),(#131392,#131393,#131394),
(#131395,#131396,#131397),(#131398,#131399,#131400)),.UNSPECIFIED.,.F.,
 .F.,.F.)
B_SPLINE_SURFACE_WITH_KNOTS((4,4),(3,3),(0.,0.00040046484477139),(0.,1.),
 .UNSPECIFIED.)
GEOMETRIC_REPRESENTATION_ITEM()
RATIONAL_B_SPLINE_SURFACE(((1.,0.707106781186548,1.),(1.,0.718332690797356,
1.),(1.,0.721890377876178,1.),(1.,0.71893387489533,1.)))
REPRESENTATION_ITEM('')
SURFACE()
);
#2039=(
BOUNDED_SURFACE()
B_SPLINE_SURFACE(3,2,((#131632,#131633,#131634),(#131635,#131636,#131637),
(#131638,#131639,#131640),(#131641,#131642,#131643),(#131644,#131645,#131646),
(#131647,#131648,#131649),(#131650,#131651,#131652),(#131653,#131654,#131655)),
 .UNSPECIFIED.,.F.,.F.,.F.)
B_SPLINE_SURFACE_WITH_KNOTS((4,2,2,4),(3,3),(-6.93889390390723E-18,0.000883592517330617,
0.00132538877599593,0.00176718503466124),(0.,1.),.UNSPECIFIED.)
GEOMETRIC_REPRESENTATION_ITEM()
RATIONAL_B_SPLINE_SURFACE(((1.,0.714572220188102,1.),(1.,0.766482020905858,
1.),(1.,0.804713539964754,1.),(1.,0.843200382681728,1.),(1.,0.852495764772597,
1.),(1.,0.865090875406593,1.),(1.,0.86808633519291,1.),(1.,0.868041451421723,
1.)))
REPRESENTATION_ITEM('')
SURFACE()
);
#2040=(
BOUNDED_SURFACE()
B_SPLINE_SURFACE(3,2,((#131704,#131705,#131706),(#131707,#131708,#131709),
(#131710,#131711,#131712),(#131713,#131714,#131715),(#131716,#131717,#131718),
(#131719,#131720,#131721),(#131722,#131723,#131724),(#131725,#131726,#131727),
(#131728,#131729,#131730),(#131731,#131732,#131733)),.UNSPECIFIED.,.F.,
 .F.,.F.)
B_SPLINE_SURFACE_WITH_KNOTS((4,2,2,2,4),(3,3),(-4.62791697325438E-16,0.00043428534736775,
0.000868570694735964,0.00130285604210418,0.00173714138947239),(0.,1.),
 .UNSPECIFIED.)
GEOMETRIC_REPRESENTATION_ITEM()
RATIONAL_B_SPLINE_SURFACE(((1.,0.823084066989561,1.),(1.,0.819254444805576,
1.),(1.,0.813299508531675,1.),(1.,0.797300511206505,1.),(1.,0.787129420739965,
1.),(1.,0.761999300344554,1.),(1.,0.746886433981532,1.),(1.,0.710597168436061,
1.),(1.,0.68930848675479,1.),(1.,0.664389729441784,1.)))
REPRESENTATION_ITEM('')
SURFACE()
);
#2041=(
BOUNDED_SURFACE()
B_SPLINE_SURFACE(3,2,((#131793,#131794,#131795),(#131796,#131797,#131798),
(#131799,#131800,#131801),(#131802,#131803,#131804)),.UNSPECIFIED.,.F.,
 .F.,.F.)
B_SPLINE_SURFACE_WITH_KNOTS((4,4),(3,3),(0.,0.000503800937603746),(0.,1.),
 .UNSPECIFIED.)
GEOMETRIC_REPRESENTATION_ITEM()
RATIONAL_B_SPLINE_SURFACE(((1.,0.816955285488328,1.),(1.,0.819071576866324,
1.),(1.,0.821113754793722,1.),(1.,0.823084066989369,1.)))
REPRESENTATION_ITEM('')
SURFACE()
);
#2042=(
BOUNDED_SURFACE()
B_SPLINE_SURFACE(3,2,((#131810,#131811,#131812),(#131813,#131814,#131815),
(#131816,#131817,#131818),(#131819,#131820,#131821),(#131822,#131823,#131824),
(#131825,#131826,#131827),(#131828,#131829,#131830),(#131831,#131832,#131833),
(#131834,#131835,#131836),(#131837,#131838,#131839)),.UNSPECIFIED.,.F.,
 .F.,.F.)
B_SPLINE_SURFACE_WITH_KNOTS((4,2,2,2,4),(3,3),(-7.15573433840433E-18,0.000392138229924569,
0.000784276459849145,0.00117641468977372,0.00156855291969829),(0.,1.),
 .UNSPECIFIED.)
GEOMETRIC_REPRESENTATION_ITEM()
RATIONAL_B_SPLINE_SURFACE(((1.,0.761454662564716,1.),(1.,0.777350220421001,
1.),(1.,0.789525254479917,1.),(1.,0.80808932428192,1.),(1.,0.814267286660623,
1.),(1.,0.822043050215882,1.),(1.,0.8235601071816,1.),(1.,0.82291335354639,
1.),(1.,0.820747192732019,1.),(1.,0.816955285488498,1.)))
REPRESENTATION_ITEM('')
SURFACE()
);
#2043=(
BOUNDED_SURFACE()
B_SPLINE_SURFACE(3,2,((#131914,#131915,#131916),(#131917,#131918,#131919),
(#131920,#131921,#131922),(#131923,#131924,#131925),(#131926,#131927,#131928),
(#131929,#131930,#131931)),.UNSPECIFIED.,.F.,.F.,.F.)
B_SPLINE_SURFACE_WITH_KNOTS((4,2,4),(3,3),(-9.86081875875566E-17,0.000795696580732677,
0.00159139316146545),(0.,1.),.UNSPECIFIED.)
GEOMETRIC_REPRESENTATION_ITEM()
RATIONAL_B_SPLINE_SURFACE(((1.,0.707106781186548,1.),(1.,0.682426263182222,
1.),(1.,0.657497772192221,1.),(1.,0.621173394621865,1.),(1.,0.609936188780092,
1.),(1.,0.610093408676581,1.)))
REPRESENTATION_ITEM('')
SURFACE()
);
#2044=(
BOUNDED_SURFACE()
B_SPLINE_SURFACE(3,2,((#131953,#131954,#131955),(#131956,#131957,#131958),
(#131959,#131960,#131961),(#131962,#131963,#131964),(#131965,#131966,#131967),
(#131968,#131969,#131970),(#131971,#131972,#131973),(#131974,#131975,#131976),
(#131977,#131978,#131979),(#131980,#131981,#131982)),.UNSPECIFIED.,.F.,
 .F.,.F.)
B_SPLINE_SURFACE_WITH_KNOTS((4,2,2,2,4),(3,3),(0.,0.000399257182160439,
0.000798514364320879,0.00119777154648132,0.00159702872864176),(0.,1.),
 .UNSPECIFIED.)
GEOMETRIC_REPRESENTATION_ITEM()
RATIONAL_B_SPLINE_SURFACE(((1.,0.805613398857371,1.),(1.,0.805643268651268,
1.),(1.,0.802937363700045,1.),(1.,0.792810049002322,1.),(1.,0.785336419192136,
1.),(1.,0.767086380955436,1.),(1.,0.756158224894836,1.),(1.,0.732687821688199,
1.),(1.,0.719866291289219,1.),(1.,0.707106781186559,1.)))
REPRESENTATION_ITEM('')
SURFACE()
);
#2045=(
BOUNDED_SURFACE()
B_SPLINE_SURFACE(3,2,((#132088,#132089,#132090),(#132091,#132092,#132093),
(#132094,#132095,#132096),(#132097,#132098,#132099),(#132100,#132101,#132102),
(#132103,#132104,#132105),(#132106,#132107,#132108),(#132109,#132110,#132111),
(#132112,#132113,#132114),(#132115,#132116,#132117)),.UNSPECIFIED.,.F.,
 .F.,.F.)
B_SPLINE_SURFACE_WITH_KNOTS((4,2,2,2,4),(3,3),(0.,0.000408971318093432,
0.000817942636186865,0.0012269139542803,0.00163588527237373),(0.,1.),
 .UNSPECIFIED.)
GEOMETRIC_REPRESENTATION_ITEM()
RATIONAL_B_SPLINE_SURFACE(((1.,0.707106781186548,1.),(1.,0.688859876352089,
1.),(1.,0.670469148037181,1.),(1.,0.634232875326911,1.),(1.,0.617116919953528,
1.),(1.,0.586509610415134,1.),(1.,0.573603373050602,1.),(1.,0.555466576286827,
1.),(1.,0.550482231415542,1.),(1.,0.55046727607882,1.)))
REPRESENTATION_ITEM('')
SURFACE()
);
#2046=(
BOUNDED_SURFACE()
B_SPLINE_SURFACE(3,2,((#132223,#132224,#132225),(#132226,#132227,#132228),
(#132229,#132230,#132231),(#132232,#132233,#132234),(#132235,#132236,#132237),
(#132238,#132239,#132240)),.UNSPECIFIED.,.F.,.F.,.F.)
B_SPLINE_SURFACE_WITH_KNOTS((4,2,4),(3,3),(0.,0.0008117357936932,0.0016234715873864),
(0.,1.),.UNSPECIFIED.)
GEOMETRIC_REPRESENTATION_ITEM()
RATIONAL_B_SPLINE_SURFACE(((1.,0.707106781186543,1.),(1.,0.739826804639566,
1.),(1.,0.771134330273905,1.),(1.,0.817260896513624,1.),(1.,0.831377708695547,
1.),(1.,0.831289505264087,1.)))
REPRESENTATION_ITEM('')
SURFACE()
);
#2047=(
BOUNDED_SURFACE()
B_SPLINE_SURFACE(3,2,((#132262,#132263,#132264),(#132265,#132266,#132267),
(#132268,#132269,#132270),(#132271,#132272,#132273),(#132274,#132275,#132276),
(#132277,#132278,#132279),(#132280,#132281,#132282),(#132283,#132284,#132285),
(#132286,#132287,#132288),(#132289,#132290,#132291)),.UNSPECIFIED.,.F.,
 .F.,.F.)
B_SPLINE_SURFACE_WITH_KNOTS((4,2,2,2,4),(3,3),(0.,0.000403813407730069,
0.00080762681546014,0.00121144022319021,0.00161525363092028),(0.,1.),
 .UNSPECIFIED.)
GEOMETRIC_REPRESENTATION_ITEM()
RATIONAL_B_SPLINE_SURFACE(((1.,0.574616980402532,1.),(1.,0.574559944255782,
1.),(1.,0.578580805360036,1.),(1.,0.593205211704828,1.),(1.,0.603887596362185,
1.),(1.,0.629170763939607,1.),(1.,0.643946507952345,1.),(1.,0.674809145535283,
1.),(1.,0.691194307570675,1.),(1.,0.707106781186543,1.)))
REPRESENTATION_ITEM('')
SURFACE()
);
#2048=(
BOUNDED_SURFACE()
B_SPLINE_SURFACE(3,2,((#132373,#132374,#132375),(#132376,#132377,#132378),
(#132379,#132380,#132381),(#132382,#132383,#132384),(#132385,#132386,#132387),
(#132388,#132389,#132390),(#132391,#132392,#132393),(#132394,#132395,#132396),
(#132397,#132398,#132399),(#132400,#132401,#132402)),.UNSPECIFIED.,.F.,
 .F.,.F.)
B_SPLINE_SURFACE_WITH_KNOTS((4,2,2,2,4),(3,3),(-3.25260651745651E-18,0.000393055033931551,
0.000786110067863104,0.00117916510179466,0.00157222013572621),(0.,1.),
 .UNSPECIFIED.)
GEOMETRIC_REPRESENTATION_ITEM()
RATIONAL_B_SPLINE_SURFACE(((1.,0.759233451646328,1.),(1.,0.765853834182409,
1.),(1.,0.77182063876785,1.),(1.,0.782085007421256,1.),(1.,0.786377884755709,
1.),(1.,0.792439775573655,1.),(1.,0.794229619467717,1.),(1.,0.793882695203775,
1.),(1.,0.791736824593394,1.),(1.,0.786683372191859,1.)))
REPRESENTATION_ITEM('')
SURFACE()
);
#2049=(
BOUNDED_SURFACE()
B_SPLINE_SURFACE(3,2,((#132459,#132460,#132461),(#132462,#132463,#132464),
(#132465,#132466,#132467),(#132468,#132469,#132470)),.UNSPECIFIED.,.F.,
 .F.,.F.)
B_SPLINE_SURFACE_WITH_KNOTS((4,4),(3,3),(2.16840434497101E-19,0.000504355062152837),
(0.,1.),.UNSPECIFIED.)
GEOMETRIC_REPRESENTATION_ITEM()
RATIONAL_B_SPLINE_SURFACE(((1.,0.759233451646319,1.),(1.,0.762871393877082,
1.),(1.,0.766403968732707,1.),(1.,0.769836971136898,1.)))
REPRESENTATION_ITEM('')
SURFACE()
);
#2050=(
BOUNDED_SURFACE()
B_SPLINE_SURFACE(3,2,((#132476,#132477,#132478),(#132479,#132480,#132481),
(#132482,#132483,#132484),(#132485,#132486,#132487),(#132488,#132489,#132490),
(#132491,#132492,#132493)),.UNSPECIFIED.,.F.,.F.,.F.)
B_SPLINE_SURFACE_WITH_KNOTS((4,2,4),(3,3),(-7.10152422978005E-18,0.000826467086096255,
0.00165293417219252),(0.,1.),.UNSPECIFIED.)
GEOMETRIC_REPRESENTATION_ITEM()
RATIONAL_B_SPLINE_SURFACE(((1.,0.634315526883885,1.),(1.,0.669226935131166,
1.),(1.,0.696507858185965,1.),(1.,0.739984504397939,1.),(1.,0.756420113602562,
1.),(1.,0.769836971137166,1.)))
REPRESENTATION_ITEM('')
SURFACE()
);
#2051=(
BOUNDED_SURFACE()
B_SPLINE_SURFACE(3,2,((#132531,#132532,#132533),(#132534,#132535,#132536),
(#132537,#132538,#132539),(#132540,#132541,#132542),(#132543,#132544,#132545),
(#132546,#132547,#132548),(#132549,#132550,#132551),(#132552,#132553,#132554),
(#132555,#132556,#132557),(#132558,#132559,#132560)),.UNSPECIFIED.,.F.,
 .F.,.F.)
B_SPLINE_SURFACE_WITH_KNOTS((4,2,2,2,4),(3,3),(-9.01822866961737E-5,0.000428050429885702,
0.000856100859773762,0.00128415128966182,0.0018023840062437),(-0.000709751295981599,
1.),.UNSPECIFIED.)
GEOMETRIC_REPRESENTATION_ITEM()
RATIONAL_B_SPLINE_SURFACE(((1.00018329866537,0.870871200656103,1.),(1.00017803427841,
0.874579814490897,1.),(1.00017912606777,0.873810679327735,1.),(1.00019317825117,
0.863911307902413,1.),(1.000204118,0.856204559855697,1.),(1.00023569027009,
0.833962775819186,1.),(1.00025618433367,0.819525279404997,1.),(1.00031175778272,
0.780375333947188,1.),(1.00034836088001,0.754589472410892,1.),(1.00039261225142,
0.723415614990589,1.)))
REPRESENTATION_ITEM('')
SURFACE()
);
#2052=(
BOUNDED_SURFACE()
B_SPLINE_SURFACE(3,2,((#132586,#132587,#132588),(#132589,#132590,#132591),
(#132592,#132593,#132594),(#132595,#132596,#132597)),.UNSPECIFIED.,.F.,
 .F.,.F.)
B_SPLINE_SURFACE_WITH_KNOTS((4,4),(3,3),(0.,0.000504208024932662),(0.,1.),
 .UNSPECIFIED.)
GEOMETRIC_REPRESENTATION_ITEM()
RATIONAL_B_SPLINE_SURFACE(((1.,0.872490094680101,1.),(1.,0.873532316568381,
1.),(1.,0.874514063294085,1.),(1.,0.875436198637085,1.)))
REPRESENTATION_ITEM('')
SURFACE()
);
#2053=(
BOUNDED_SURFACE()
B_SPLINE_SURFACE(3,2,((#132603,#132604,#132605),(#132606,#132607,#132608),
(#132609,#132610,#132611),(#132612,#132613,#132614),(#132615,#132616,#132617),
(#132618,#132619,#132620),(#132621,#132622,#132623),(#132624,#132625,#132626),
(#132627,#132628,#132629),(#132630,#132631,#132632),(#132633,#132634,#132635),
(#132636,#132637,#132638)),.UNSPECIFIED.,.F.,.F.,.F.)
B_SPLINE_SURFACE_WITH_KNOTS((4,2,2,2,2,4),(3,3),(0.,0.000471787629256711,
0.000943575258513421,0.00117946907314178,0.00141536288777013,0.00188715051702685),
(0.,1.),.UNSPECIFIED.)
GEOMETRIC_REPRESENTATION_ITEM()
RATIONAL_B_SPLINE_SURFACE(((1.,0.688859710774758,1.),(1.,0.717278497414175,
1.),(1.,0.742415568607548,1.),(1.,0.786827943379553,1.),(1.,0.806155596178757,
1.),(1.,0.829868996905786,1.),(1.,0.837032764561711,1.),(1.,0.849395444084014,
1.),(1.,0.854694123459555,1.),(1.,0.86824784980175,1.),(1.,0.873676740317145,
1.),(1.,0.875436198637081,1.)))
REPRESENTATION_ITEM('')
SURFACE()
);
#2054=(
BOUNDED_SURFACE()
B_SPLINE_SURFACE(3,2,((#132703,#132704,#132705),(#132706,#132707,#132708),
(#132709,#132710,#132711),(#132712,#132713,#132714)),.UNSPECIFIED.,.F.,
 .F.,.F.)
B_SPLINE_SURFACE_WITH_KNOTS((4,4),(3,3),(0.000909429960036056,0.00157021148057203),
(0.,1.),.UNSPECIFIED.)
GEOMETRIC_REPRESENTATION_ITEM()
RATIONAL_B_SPLINE_SURFACE(((1.,0.72569894652024,1.),(1.,0.728856973451895,
1.),(1.,0.724481780670466,1.),(1.,0.707106781186543,1.)))
REPRESENTATION_ITEM('')
SURFACE()
);
#2055=(
BOUNDED_SURFACE()
B_SPLINE_SURFACE(3,2,((#132727,#132728,#132729),(#132730,#132731,#132732),
(#132733,#132734,#132735),(#132736,#132737,#132738)),.UNSPECIFIED.,.F.,
 .F.,.F.)
B_SPLINE_SURFACE_WITH_KNOTS((4,4),(3,3),(-1.50704101975485E-17,0.000358861832009556),
(0.,1.),.UNSPECIFIED.)
GEOMETRIC_REPRESENTATION_ITEM()
RATIONAL_B_SPLINE_SURFACE(((1.,0.707106781186544,1.),(1.,0.693584131808955,
1.),(1.,0.67719600445086,1.),(1.,0.65799444631037,1.)))
REPRESENTATION_ITEM('')
SURFACE()
);
#2056=(
BOUNDED_SURFACE()
B_SPLINE_SURFACE(3,2,((#133123,#133124,#133125),(#133126,#133127,#133128),
(#133129,#133130,#133131),(#133132,#133133,#133134)),.UNSPECIFIED.,.F.,
 .F.,.F.)
B_SPLINE_SURFACE_WITH_KNOTS((4,4),(3,3),(5.42101086242752E-20,0.000113625826113285),
(0.,1.),.UNSPECIFIED.)
GEOMETRIC_REPRESENTATION_ITEM()
RATIONAL_B_SPLINE_SURFACE(((1.,0.691935594449019,1.),(1.,0.697297182114951,
1.),(1.,0.702351867303478,1.),(1.,0.70710678118654,1.)))
REPRESENTATION_ITEM('')
SURFACE()
);
#2057=(
BOUNDED_SURFACE()
B_SPLINE_SURFACE(3,2,((#133147,#133148,#133149),(#133150,#133151,#133152),
(#133153,#133154,#133155),(#133156,#133157,#133158),(#133159,#133160,#133161),
(#133162,#133163,#133164)),.UNSPECIFIED.,.F.,.F.,.F.)
B_SPLINE_SURFACE_WITH_KNOTS((4,2,4),(3,3),(0.,0.000500133683539797,0.00100026736707959),
(0.,1.),.UNSPECIFIED.)
GEOMETRIC_REPRESENTATION_ITEM()
RATIONAL_B_SPLINE_SURFACE(((1.,0.707106781186538,1.),(1.,0.722794581177,
1.),(1.,0.731463278267736,1.),(1.,0.737752025312339,1.),(1.,0.735567484186947,
1.),(1.,0.732423362569068,1.)))
REPRESENTATION_ITEM('')
SURFACE()
);
#2058=(
BOUNDED_SURFACE()
B_SPLINE_SURFACE(3,2,((#133347,#133348,#133349),(#133350,#133351,#133352),
(#133353,#133354,#133355),(#133356,#133357,#133358),(#133359,#133360,#133361),
(#133362,#133363,#133364)),.UNSPECIFIED.,.F.,.F.,.F.)
B_SPLINE_SURFACE_WITH_KNOTS((4,2,4),(3,3),(0.,0.000635851334990063,0.00127170266998013),
(0.,1.),.UNSPECIFIED.)
GEOMETRIC_REPRESENTATION_ITEM()
RATIONAL_B_SPLINE_SURFACE(((1.,0.549598954535088,1.),(1.,0.549481216714779,
1.),(1.,0.561870616792487,1.),(1.,0.602538835999935,1.),(1.,0.629604434612806,
1.),(1.,0.65799444631184,1.)))
REPRESENTATION_ITEM('')
SURFACE()
);
#2059=(
BOUNDED_SURFACE()
B_SPLINE_SURFACE(3,2,((#133389,#133390,#133391),(#133392,#133393,#133394),
(#133395,#133396,#133397),(#133398,#133399,#133400),(#133401,#133402,#133403),
(#133404,#133405,#133406),(#133407,#133408,#133409),(#133410,#133411,#133412)),
 .UNSPECIFIED.,.F.,.F.,.F.)
B_SPLINE_SURFACE_WITH_KNOTS((4,2,2,4),(3,3),(0.,0.000399389907139719,0.000798779814279438,
0.00159755962855888),(0.,1.),.UNSPECIFIED.)
GEOMETRIC_REPRESENTATION_ITEM()
RATIONAL_B_SPLINE_SURFACE(((1.,0.707106781186543,1.),(1.,0.719972059607527,
1.),(1.,0.732679659198347,1.),(1.,0.756479572209125,1.),(1.,0.767365377234031,
1.),(1.,0.79501980381119,1.),(1.,0.806340389868128,1.),(1.,0.806206028026398,
1.)))
REPRESENTATION_ITEM('')
SURFACE()
);
#2060=(
BOUNDED_SURFACE()
B_SPLINE_SURFACE(3,2,((#133427,#133428,#133429),(#133430,#133431,#133432),
(#133433,#133434,#133435),(#133436,#133437,#133438),(#133439,#133440,#133441),
(#133442,#133443,#133444),(#133445,#133446,#133447),(#133448,#133449,#133450),
(#133451,#133452,#133453),(#133454,#133455,#133456)),.UNSPECIFIED.,.F.,
 .F.,.F.)
B_SPLINE_SURFACE_WITH_KNOTS((4,2,2,2,4),(3,3),(0.,0.000397955182835291,
0.000795910365670582,0.00119386554850587,0.00159182073134117),(0.,1.),
 .UNSPECIFIED.)
GEOMETRIC_REPRESENTATION_ITEM()
RATIONAL_B_SPLINE_SURFACE(((1.,0.60931006565052,1.),(1.,0.60928110676943,
1.),(1.,0.611992414032709,1.),(1.,0.622151576786515,1.),(1.,0.629646305612374,
1.),(1.,0.647895096091951,1.),(1.,0.658798646820943,1.),(1.,0.682038372243284,
1.),(1.,0.694657643733687,1.),(1.,0.707106781186553,1.)))
REPRESENTATION_ITEM('')
SURFACE()
);
#2061=(
BOUNDED_SURFACE()
B_SPLINE_SURFACE(3,2,((#133485,#133486,#133487),(#133488,#133489,#133490),
(#133491,#133492,#133493),(#133494,#133495,#133496),(#133497,#133498,#133499),
(#133500,#133501,#133502),(#133503,#133504,#133505),(#133506,#133507,#133508),
(#133509,#133510,#133511),(#133512,#133513,#133514)),.UNSPECIFIED.,.F.,
 .F.,.F.)
B_SPLINE_SURFACE_WITH_KNOTS((4,2,2,2,4),(3,3),(0.,0.00039329942356206,0.000786598847124121,
0.00117989827068618,0.00157319769424824),(0.,1.),.UNSPECIFIED.)
GEOMETRIC_REPRESENTATION_ITEM()
RATIONAL_B_SPLINE_SURFACE(((1.,0.825370895892916,1.),(1.,0.829081051796027,
1.),(1.,0.831084991111337,1.),(1.,0.831059675364535,1.),(1.,0.829021889329635,
1.),(1.,0.819977402296451,1.),(1.,0.812885056457023,1.),(1.,0.792515337687537,
1.),(1.,0.779105591645567,1.),(1.,0.762081632340355,1.)))
REPRESENTATION_ITEM('')
SURFACE()
);
#2062=(
BOUNDED_SURFACE()
B_SPLINE_SURFACE(3,2,((#133527,#133528,#133529),(#133530,#133531,#133532),
(#133533,#133534,#133535),(#133536,#133537,#133538)),.UNSPECIFIED.,.F.,
 .F.,.F.)
B_SPLINE_SURFACE_WITH_KNOTS((4,4),(3,3),(-2.62810606610486E-16,0.000504136652582459),
(0.,1.),.UNSPECIFIED.)
GEOMETRIC_REPRESENTATION_ITEM()
RATIONAL_B_SPLINE_SURFACE(((1.,0.831517473467334,1.),(1.,0.829540548856785,
1.),(1.,0.827492428459287,1.),(1.,0.825370895892945,1.)))
REPRESENTATION_ITEM('')
SURFACE()
);
#2063=(
BOUNDED_SURFACE()
B_SPLINE_SURFACE(3,2,((#133542,#133543,#133544),(#133545,#133546,#133547),
(#133548,#133549,#133550),(#133551,#133552,#133553),(#133554,#133555,#133556),
(#133557,#133558,#133559),(#133560,#133561,#133562),(#133563,#133564,#133565),
(#133566,#133567,#133568),(#133569,#133570,#133571),(#133572,#133573,#133574),
(#133575,#133576,#133577)),.UNSPECIFIED.,.F.,.F.,.F.)
B_SPLINE_SURFACE_WITH_KNOTS((4,2,2,2,2,4),(3,3),(-0.000176150978763801,
0.000440377446917856,0.000880754893835713,0.00110094361729464,0.00132113234075357,
0.00193766076643857),(0.,1.00051287559994),.UNSPECIFIED.)
GEOMETRIC_REPRESENTATION_ITEM()
RATIONAL_B_SPLINE_SURFACE(((1.,0.629431973271816,1.00038011059806),(1.,
0.671936522340933,1.00033651150585),(1.,0.704322705400091,1.00030329133971),
(1.,0.750691692792477,1.00025572829526),(1.,0.766670204641027,1.00023933831756),
(1.,0.786800026967206,1.00021869012815),(1.,0.792954061695274,1.00021237761965),
(1.,0.80379124513689,1.00020126136573),(1.,0.808563806838397,1.00019636590484),
(1.,0.824745084867243,1.00017976793948),(1.,0.832099980342898,1.00017222364662),
(1.,0.835028609003294,1.00016921960226)))
REPRESENTATION_ITEM('')
SURFACE()
);
#2064=(
BOUNDED_SURFACE()
B_SPLINE_SURFACE(3,2,((#133645,#133646,#133647),(#133648,#133649,#133650),
(#133651,#133652,#133653),(#133654,#133655,#133656),(#133657,#133658,#133659),
(#133660,#133661,#133662),(#133663,#133664,#133665),(#133666,#133667,#133668),
(#133669,#133670,#133671),(#133672,#133673,#133674)),.UNSPECIFIED.,.F.,
 .F.,.F.)
B_SPLINE_SURFACE_WITH_KNOTS((4,2,2,2,4),(3,3),(-0.000135704889425893,0.000453061765036137,
0.000906123530072295,0.00135918529510845,0.00194795194957144),(-0.000781731935573401,
1.00013570488943),.UNSPECIFIED.)
GEOMETRIC_REPRESENTATION_ITEM()
RATIONAL_B_SPLINE_SURFACE(((1.00019390081514,0.8759631402042,1.00003363851682),
(1.00018914318116,0.879006562062377,1.00003281314767),(1.00019402369835,
0.875884532760928,1.00003365983498),(1.00021859753591,0.860164837917186,
1.00003792298079),(1.00023473046334,0.84984472834809,1.00004072177124),
(1.00027794935235,0.822197937521576,1.0000482195186),(1.00030475494617,
0.805050605368179,1.00005286983644),(1.00037753551171,0.758493437481938,
1.00006549603544),(1.00042634862193,0.727268066383258,1.0000739642857),
(1.00048406431786,0.690347779692363,1.00008397698424)))
REPRESENTATION_ITEM('')
SURFACE()
);
#2065=(
BOUNDED_SURFACE()
B_SPLINE_SURFACE(3,2,((#133726,#133727,#133728),(#133729,#133730,#133731),
(#133732,#133733,#133734),(#133735,#133736,#133737)),.UNSPECIFIED.,.F.,
 .F.,.F.)
B_SPLINE_SURFACE_WITH_KNOTS((4,4),(3,3),(0.,0.000503779257761556),(0.,1.),
 .UNSPECIFIED.)
GEOMETRIC_REPRESENTATION_ITEM()
RATIONAL_B_SPLINE_SURFACE(((1.,0.877279917170998,1.),(1.,0.877311423474687,
1.),(1.,0.877285649811871,1.),(1.,0.877202574460126,1.)))
REPRESENTATION_ITEM('')
SURFACE()
);
#2066=(
BOUNDED_SURFACE()
B_SPLINE_SURFACE(3,2,((#133741,#133742,#133743),(#133744,#133745,#133746),
(#133747,#133748,#133749),(#133750,#133751,#133752),(#133753,#133754,#133755),
(#133756,#133757,#133758),(#133759,#133760,#133761),(#133762,#133763,#133764),
(#133765,#133766,#133767),(#133768,#133769,#133770)),.UNSPECIFIED.,.F.,
 .F.,.F.)
B_SPLINE_SURFACE_WITH_KNOTS((4,2,2,2,4),(3,3),(-0.000155617325212005,0.000907880296577857,
0.00113485037072232,0.00136182044486679,0.00197137791837065),(0.,1.00015561732522),
 .UNSPECIFIED.)
GEOMETRIC_REPRESENTATION_ITEM()
RATIONAL_B_SPLINE_SURFACE(((1.,0.68550557359324,1.00009788156287),(1.,0.752540961090915,
1.00007701782747),(1.,0.80291249495684,1.00006134046074),(1.,0.8425596182679,
1.00004900090217),(1.,0.848571644906788,1.00004712975116),(1.,0.858970162163407,
1.00004389337228),(1.,0.8633849038709,1.00004251935169),(1.,0.876162786879574,
1.00003854243174),(1.,0.879321122197454,1.00003755944835),(1.,0.875948401811248,
1.0000386091558)))
REPRESENTATION_ITEM('')
SURFACE()
);
#2067=(
BOUNDED_SURFACE()
B_SPLINE_SURFACE(3,2,((#133838,#133839,#133840),(#133841,#133842,#133843),
(#133844,#133845,#133846),(#133847,#133848,#133849),(#133850,#133851,#133852),
(#133853,#133854,#133855),(#133856,#133857,#133858),(#133859,#133860,#133861),
(#133862,#133863,#133864),(#133865,#133866,#133867)),.UNSPECIFIED.,.F.,
 .F.,.F.)
B_SPLINE_SURFACE_WITH_KNOTS((4,2,2,2,4),(3,3),(-8.34022521184474E-16,0.000443043867974425,
0.000886087735949684,0.00132913160392494,0.00177217547190021),(0.,1.),
 .UNSPECIFIED.)
GEOMETRIC_REPRESENTATION_ITEM()
RATIONAL_B_SPLINE_SURFACE(((1.,0.834143101464621,1.),(1.,0.83044410875076,
1.),(1.,0.824302497883951,1.),(1.,0.80744078994961,1.),(1.,0.79657978834944,
1.),(1.,0.769588124839812,1.),(1.,0.753384767045469,1.),(1.,0.714346006222175,
1.),(1.,0.691706791956038,1.),(1.,0.665108204576645,1.)))
REPRESENTATION_ITEM('')
SURFACE()
);
#2068=(
BOUNDED_SURFACE()
B_SPLINE_SURFACE(3,2,((#133880,#133881,#133882),(#133883,#133884,#133885),
(#133886,#133887,#133888),(#133889,#133890,#133891)),.UNSPECIFIED.,.F.,
 .F.,.F.)
B_SPLINE_SURFACE_WITH_KNOTS((4,4),(3,3),(0.,0.000504125640440226),(0.,1.),
 .UNSPECIFIED.)
GEOMETRIC_REPRESENTATION_ITEM()
RATIONAL_B_SPLINE_SURFACE(((1.,0.828190603154496,1.),(1.,0.830246482056442,
1.),(1.,0.832229943187683,1.),(1.,0.834143101464675,1.)))
REPRESENTATION_ITEM('')
SURFACE()
);
#2069=(
BOUNDED_SURFACE()
B_SPLINE_SURFACE(3,2,((#133895,#133896,#133897),(#133898,#133899,#133900),
(#133901,#133902,#133903),(#133904,#133905,#133906),(#133907,#133908,#133909),
(#133910,#133911,#133912),(#133913,#133914,#133915),(#133916,#133917,#133918)),
 .UNSPECIFIED.,.F.,.F.,.F.)
B_SPLINE_SURFACE_WITH_KNOTS((4,2,2,4),(3,3),(0.,0.000394166264145648,0.000788332528291295,
0.00157666505658259),(0.,1.),.UNSPECIFIED.)
GEOMETRIC_REPRESENTATION_ITEM()
RATIONAL_B_SPLINE_SURFACE(((1.,0.760827176127386,1.),(1.,0.778398802886113,
1.),(1.,0.792083552136379,1.),(1.,0.813520155171949,1.),(1.,0.820889309284053,
1.),(1.,0.835705990917082,1.),(1.,0.835268319089816,1.),(1.,0.828190603154679,
1.)))
REPRESENTATION_ITEM('')
SURFACE()
);
#2070=(
BOUNDED_SURFACE()
B_SPLINE_SURFACE(3,2,((#133945,#133946,#133947),(#133948,#133949,#133950),
(#133951,#133952,#133953),(#133954,#133955,#133956),(#133957,#133958,#133959),
(#133960,#133961,#133962)),.UNSPECIFIED.,.F.,.F.,.F.)
B_SPLINE_SURFACE_WITH_KNOTS((4,2,4),(3,3),(0.,0.000795474163050539,0.00159094832610108),
(0.,1.),.UNSPECIFIED.)
GEOMETRIC_REPRESENTATION_ITEM()
RATIONAL_B_SPLINE_SURFACE(((1.,0.707106781186543,1.),(1.,0.682590952101739,
1.),(1.,0.657853637690047,1.),(1.,0.62184399984072,1.),(1.,0.610720170210845,
1.),(1.,0.610875747200839,1.)))
REPRESENTATION_ITEM('')
SURFACE()
);
#2071=(
BOUNDED_SURFACE()
B_SPLINE_SURFACE(3,2,((#133975,#133976,#133977),(#133978,#133979,#133980),
(#133981,#133982,#133983),(#133984,#133985,#133986),(#133987,#133988,#133989),
(#133990,#133991,#133992),(#133993,#133994,#133995),(#133996,#133997,#133998),
(#133999,#134000,#134001),(#134002,#134003,#134004)),.UNSPECIFIED.,.F.,
 .F.,.F.)
B_SPLINE_SURFACE_WITH_KNOTS((4,2,2,2,4),(3,3),(0.,0.000399133477242608,
0.000798266954485216,0.00119740043172782,0.00159653390897044),(0.,1.),
 .UNSPECIFIED.)
GEOMETRIC_REPRESENTATION_ITEM()
RATIONAL_B_SPLINE_SURFACE(((1.,0.805020333414601,1.),(1.,0.805049923545582,
1.),(1.,0.802360394037482,1.),(1.,0.792292516045722,1.),(1.,0.784862653088995,
1.),(1.,0.766719225973379,1.),(1.,0.755854623801483,1.),(1.,0.732526059701691,
1.),(1.,0.719783513455905,1.),(1.,0.707106781186554,1.)))
REPRESENTATION_ITEM('')
SURFACE()
);
#2072=(
BOUNDED_SURFACE()
B_SPLINE_SURFACE(3,2,((#134060,#134061,#134062),(#134063,#134064,#134065),
(#134066,#134067,#134068),(#134069,#134070,#134071),(#134072,#134073,#134074),
(#134075,#134076,#134077),(#134078,#134079,#134080),(#134081,#134082,#134083)),
 .UNSPECIFIED.,.F.,.F.,.F.)
B_SPLINE_SURFACE_WITH_KNOTS((4,2,2,4),(3,3),(-3.14418630020796E-18,0.000761037462531171,
0.00114155619379676,0.00152207492506235),(0.,1.),.UNSPECIFIED.)
GEOMETRIC_REPRESENTATION_ITEM()
RATIONAL_B_SPLINE_SURFACE(((1.,0.691935594449023,1.),(1.,0.657938057153071,
1.),(1.,0.623321566128117,1.),(1.,0.582569634693765,1.),(1.,0.571407182182735,
1.),(1.,0.5555307216223,1.),(1.,0.551373498869702,1.),(1.,0.551334230064852,
1.)))
REPRESENTATION_ITEM('')
SURFACE()
);
#2073=(
BOUNDED_SURFACE()
B_SPLINE_SURFACE(3,2,((#134122,#134123,#134124),(#134125,#134126,#134127),
(#134128,#134129,#134130),(#134131,#134132,#134133),(#134134,#134135,#134136),
(#134137,#134138,#134139)),.UNSPECIFIED.,.F.,.F.,.F.)
B_SPLINE_SURFACE_WITH_KNOTS((4,2,4),(3,3),(4.71238898038469,5.49778714378214,
6.28318530717959),(0.,1.),.UNSPECIFIED.)
GEOMETRIC_REPRESENTATION_ITEM()
RATIONAL_B_SPLINE_SURFACE(((1.,0.707106781186548,1.),(1.,0.699025295935929,
1.),(1.,0.690860049127223,1.),(1.,0.679082711198032,1.),(1.,0.675526278180878,
1.),(1.,0.675590207615665,1.)))
REPRESENTATION_ITEM('')
SURFACE()
);
#2074=(
BOUNDED_SURFACE()
B_SPLINE_SURFACE(3,2,((#134152,#134153,#134154),(#134155,#134156,#134157),
(#134158,#134159,#134160),(#134161,#134162,#134163),(#134164,#134165,#134166),
(#134167,#134168,#134169)),.UNSPECIFIED.,.F.,.F.,.F.)
B_SPLINE_SURFACE_WITH_KNOTS((4,2,4),(3,3),(1.41124413247309E-15,0.78539816339745,
1.5707963267949),(0.,1.),.UNSPECIFIED.)
GEOMETRIC_REPRESENTATION_ITEM()
RATIONAL_B_SPLINE_SURFACE(((1.,0.73727733681012,1.),(1.,0.737326538316275,
1.),(1.,0.734106258287724,1.),(1.,0.723033691556635,1.),(1.,0.715202981902879,
1.),(1.,0.707106781186548,1.)))
REPRESENTATION_ITEM('')
SURFACE()
);
#2075=(
BOUNDED_SURFACE()
B_SPLINE_SURFACE(3,2,((#134195,#134196,#134197),(#134198,#134199,#134200),
(#134201,#134202,#134203),(#134204,#134205,#134206),(#134207,#134208,#134209),
(#134210,#134211,#134212)),.UNSPECIFIED.,.F.,.F.,.F.)
B_SPLINE_SURFACE_WITH_KNOTS((4,2,4),(3,3),(3.1415926535898,3.72828696246945,
4.31498127134909),(0.,1.),.UNSPECIFIED.)
GEOMETRIC_REPRESENTATION_ITEM()
RATIONAL_B_SPLINE_SURFACE(((1.,0.737277336810115,1.),(1.,0.73729299178243,
1.),(1.,0.735539930277599,1.),(1.,0.729097328045697,1.),(1.,0.724411344440144,
1.),(1.,0.71893387489533,1.)))
REPRESENTATION_ITEM('')
SURFACE()
);
#2076=(
BOUNDED_SURFACE()
B_SPLINE_SURFACE(3,2,((#134225,#134226,#134227),(#134228,#134229,#134230),
(#134231,#134232,#134233),(#134234,#134235,#134236),(#134237,#134238,#134239),
(#134240,#134241,#134242)),.UNSPECIFIED.,.F.,.F.,.F.)
B_SPLINE_SURFACE_WITH_KNOTS((4,2,4),(3,3),(0.,0.00169934430350512,0.00339868860701024),
(0.,1.),.UNSPECIFIED.)
GEOMETRIC_REPRESENTATION_ITEM()
RATIONAL_B_SPLINE_SURFACE(((1.,0.707106781186547,1.),(1.,0.74482559038907,
1.),(1.,0.778551967557851,1.),(1.,0.840511428018892,1.),(1.,0.868726285027217,
1.),(1.,0.894799245647903,1.)))
REPRESENTATION_ITEM('')
SURFACE()
);
#2077=(
BOUNDED_SURFACE()
B_SPLINE_SURFACE(3,2,((#134277,#134278,#134279),(#134280,#134281,#134282),
(#134283,#134284,#134285),(#134286,#134287,#134288),(#134289,#134290,#134291),
(#134292,#134293,#134294)),.UNSPECIFIED.,.F.,.F.,.F.)
B_SPLINE_SURFACE_WITH_KNOTS((4,2,4),(3,3),(4.71238898038469,5.49778714378214,
6.28318530717959),(0.,1.),.UNSPECIFIED.)
GEOMETRIC_REPRESENTATION_ITEM()
RATIONAL_B_SPLINE_SURFACE(((1.,0.707106781186548,1.),(1.,0.699025295935929,
1.),(1.,0.690860049127223,1.),(1.,0.679082711198032,1.),(1.,0.675526278180878,
1.),(1.,0.675590207615665,1.)))
REPRESENTATION_ITEM('')
SURFACE()
);
#2078=(
BOUNDED_SURFACE()
B_SPLINE_SURFACE(3,2,((#134307,#134308,#134309),(#134310,#134311,#134312),
(#134313,#134314,#134315),(#134316,#134317,#134318),(#134319,#134320,#134321),
(#134322,#134323,#134324)),.UNSPECIFIED.,.F.,.F.,.F.)
B_SPLINE_SURFACE_WITH_KNOTS((4,2,4),(3,3),(3.1415926535898,3.92699081698724,
4.71238898038469),(0.,1.),.UNSPECIFIED.)
GEOMETRIC_REPRESENTATION_ITEM()
RATIONAL_B_SPLINE_SURFACE(((1.,0.73727733681012,1.),(1.,0.737326538316634,
1.),(1.,0.734106258287243,1.),(1.,0.723033691557116,1.),(1.,0.715202981902516,
1.),(1.,0.707106781186548,1.)))
REPRESENTATION_ITEM('')
SURFACE()
);
#2079=(
BOUNDED_SURFACE()
B_SPLINE_SURFACE(3,2,((#134339,#134340,#134341),(#134342,#134343,#134344),
(#134345,#134346,#134347),(#134348,#134349,#134350),(#134351,#134352,#134353),
(#134354,#134355,#134356)),.UNSPECIFIED.,.F.,.F.,.F.)
B_SPLINE_SURFACE_WITH_KNOTS((4,2,4),(3,3),(-3.25260651745651E-18,0.00101351621082632,
0.00202703242165263),(0.,1.),.UNSPECIFIED.)
GEOMETRIC_REPRESENTATION_ITEM()
RATIONAL_B_SPLINE_SURFACE(((1.,0.893214344719542,1.),(1.,0.912305000874927,
1.),(1.,0.927255525935639,1.),(1.,0.94789383214718,1.),(1.,0.953590869545161,
1.),(1.,0.953555223991885,1.)))
REPRESENTATION_ITEM('')
SURFACE()
);
#2080=(
BOUNDED_SURFACE()
B_SPLINE_SURFACE(3,2,((#134395,#134396,#134397),(#134398,#134399,#134400),
(#134401,#134402,#134403),(#134404,#134405,#134406),(#134407,#134408,#134409),
(#134410,#134411,#134412)),.UNSPECIFIED.,.F.,.F.,.F.)
B_SPLINE_SURFACE_WITH_KNOTS((4,2,4),(3,3),(4.71238898038469,5.49778714378214,
6.28318530717959),(0.,1.),.UNSPECIFIED.)
GEOMETRIC_REPRESENTATION_ITEM()
RATIONAL_B_SPLINE_SURFACE(((1.,0.707106781186543,1.),(1.,0.715202981902221,
1.),(1.,0.723033691557525,1.),(1.,0.734106258286841,1.),(1.,0.737326538316939,
1.),(1.,0.737277336810125,1.)))
REPRESENTATION_ITEM('')
SURFACE()
);
#2081=(
BOUNDED_SURFACE()
B_SPLINE_SURFACE(3,2,((#134425,#134426,#134427),(#134428,#134429,#134430),
(#134431,#134432,#134433),(#134434,#134435,#134436),(#134437,#134438,#134439),
(#134440,#134441,#134442)),.UNSPECIFIED.,.F.,.F.,.F.)
B_SPLINE_SURFACE_WITH_KNOTS((4,2,4),(3,3),(3.1415926535898,3.92699081698724,
4.71238898038469),(0.,1.),.UNSPECIFIED.)
GEOMETRIC_REPRESENTATION_ITEM()
RATIONAL_B_SPLINE_SURFACE(((1.,0.675590207615659,1.),(1.,0.675526278181242,
1.),(1.,0.679082711197541,1.),(1.,0.690860049127717,1.),(1.,0.699025295935567,
1.),(1.,0.707106781186543,1.)))
REPRESENTATION_ITEM('')
SURFACE()
);
#2082=(
BOUNDED_SURFACE()
B_SPLINE_SURFACE(3,2,((#134455,#134456,#134457),(#134458,#134459,#134460),
(#134461,#134462,#134463),(#134464,#134465,#134466),(#134467,#134468,#134469),
(#134470,#134471,#134472)),.UNSPECIFIED.,.F.,.F.,.F.)
B_SPLINE_SURFACE_WITH_KNOTS((4,2,4),(3,3),(0.,0.00162565899344706,0.00325131798689413),
(0.,1.),.UNSPECIFIED.)
GEOMETRIC_REPRESENTATION_ITEM()
RATIONAL_B_SPLINE_SURFACE(((1.,0.893214344719539,1.),(1.,0.868075018581634,
1.),(1.,0.841018189595232,1.),(1.,0.782003386508022,1.),(1.,0.750058517040659,
1.),(1.,0.714668958264373,1.)))
REPRESENTATION_ITEM('')
SURFACE()
);
#2083=(
BOUNDED_SURFACE()
B_SPLINE_SURFACE(3,2,((#134511,#134512,#134513),(#134514,#134515,#134516),
(#134517,#134518,#134519),(#134520,#134521,#134522),(#134523,#134524,#134525),
(#134526,#134527,#134528)),.UNSPECIFIED.,.F.,.F.,.F.)
B_SPLINE_SURFACE_WITH_KNOTS((4,2,4),(3,3),(1.5707963267949,2.35619449019234,
3.1415926535898),(0.,1.),.UNSPECIFIED.)
GEOMETRIC_REPRESENTATION_ITEM()
RATIONAL_B_SPLINE_SURFACE(((1.,0.707106781186543,1.),(1.,0.71520298190223,
1.),(1.,0.723033691557516,1.),(1.,0.734106258286857,1.),(1.,0.737326538316932,
1.),(1.,0.737277336810125,1.)))
REPRESENTATION_ITEM('')
SURFACE()
);
#2084=(
BOUNDED_SURFACE()
B_SPLINE_SURFACE(3,2,((#134541,#134542,#134543),(#134544,#134545,#134546),
(#134547,#134548,#134549),(#134550,#134551,#134552),(#134553,#134554,#134555),
(#134556,#134557,#134558)),.UNSPECIFIED.,.F.,.F.,.F.)
B_SPLINE_SURFACE_WITH_KNOTS((4,2,4),(3,3),(3.1415926535898,3.92699081698724,
4.71238898038469),(0.,1.),.UNSPECIFIED.)
GEOMETRIC_REPRESENTATION_ITEM()
RATIONAL_B_SPLINE_SURFACE(((1.,0.675590207615659,1.),(1.,0.675526278181249,
1.),(1.,0.679082711197525,1.),(1.,0.69086004912773,1.),(1.,0.699025295935556,
1.),(1.,0.707106781186543,1.)))
REPRESENTATION_ITEM('')
SURFACE()
);
#2085=(
BOUNDED_SURFACE()
B_SPLINE_SURFACE(3,2,((#134603,#134604,#134605),(#134606,#134607,#134608),
(#134609,#134610,#134611),(#134612,#134613,#134614),(#134615,#134616,#134617),
(#134618,#134619,#134620)),.UNSPECIFIED.,.F.,.F.,.F.)
B_SPLINE_SURFACE_WITH_KNOTS((4,2,4),(3,3),(4.71238898038469,5.49778714378214,
6.28318530717959),(0.,1.),.UNSPECIFIED.)
GEOMETRIC_REPRESENTATION_ITEM()
RATIONAL_B_SPLINE_SURFACE(((1.,0.707106781186543,1.),(1.,0.699025295935225,
1.),(1.,0.690860049128176,1.),(1.,0.679082711197064,1.),(1.,0.6755262781816,
1.),(1.,0.675590207615662,1.)))
REPRESENTATION_ITEM('')
SURFACE()
);
#2086=(
BOUNDED_SURFACE()
B_SPLINE_SURFACE(3,2,((#134633,#134634,#134635),(#134636,#134637,#134638),
(#134639,#134640,#134641),(#134642,#134643,#134644),(#134645,#134646,#134647),
(#134648,#134649,#134650)),.UNSPECIFIED.,.F.,.F.,.F.)
B_SPLINE_SURFACE_WITH_KNOTS((4,2,4),(3,3),(0.,0.785398163397448,1.5707963267949),
(0.,1.),.UNSPECIFIED.)
GEOMETRIC_REPRESENTATION_ITEM()
RATIONAL_B_SPLINE_SURFACE(((1.,0.737277336810127,1.),(1.,0.737326538316762,
1.),(1.,0.734106258287074,1.),(1.,0.723033691557295,1.),(1.,0.715202981902387,
1.),(1.,0.707106781186548,1.)))
REPRESENTATION_ITEM('')
SURFACE()
);
#2087=(
BOUNDED_SURFACE()
B_SPLINE_SURFACE(3,2,((#134676,#134677,#134678),(#134679,#134680,#134681),
(#134682,#134683,#134684),(#134685,#134686,#134687)),.UNSPECIFIED.,.F.,
 .F.,.F.)
B_SPLINE_SURFACE_WITH_KNOTS((4,4),(3,3),(3.1415926535898,3.72189740710945),
(0.,1.),.UNSPECIFIED.)
GEOMETRIC_REPRESENTATION_ITEM()
RATIONAL_B_SPLINE_SURFACE(((1.,0.737277336810124,1.),(1.,0.737285953283754,
1.),(1.,0.735586930398308,1.),(1.,0.732423362569238,1.)))
REPRESENTATION_ITEM('')
SURFACE()
);
#2088=(
BOUNDED_SURFACE()
B_SPLINE_SURFACE(3,2,((#134695,#134696,#134697),(#134698,#134699,#134700),
(#134701,#134702,#134703),(#134704,#134705,#134706),(#134707,#134708,#134709),
(#134710,#134711,#134712)),.UNSPECIFIED.,.F.,.F.,.F.)
B_SPLINE_SURFACE_WITH_KNOTS((4,2,4),(3,3),(0.,0.00168309713341273,0.00336619426682545),
(0.,1.),.UNSPECIFIED.)
GEOMETRIC_REPRESENTATION_ITEM()
RATIONAL_B_SPLINE_SURFACE(((1.,0.707106781186545,1.),(1.,0.744273762477552,
1.),(1.,0.7776417896067,1.),(1.,0.83910580954319,1.),(1.,0.867185102973278,
1.),(1.,0.89321434471954,1.)))
REPRESENTATION_ITEM('')
SURFACE()
);
#2089=(
BOUNDED_SURFACE()
B_SPLINE_SURFACE(3,2,((#134756,#134757,#134758),(#134759,#134760,#134761),
(#134762,#134763,#134764),(#134765,#134766,#134767),(#134768,#134769,#134770),
(#134771,#134772,#134773)),.UNSPECIFIED.,.F.,.F.,.F.)
B_SPLINE_SURFACE_WITH_KNOTS((4,2,4),(3,3),(4.71238898038469,5.49778714378214,
6.28318530717959),(0.,1.),.UNSPECIFIED.)
GEOMETRIC_REPRESENTATION_ITEM()
RATIONAL_B_SPLINE_SURFACE(((1.,0.707106781186543,1.),(1.,0.699025295935037,
1.),(1.,0.690860049128415,1.),(1.,0.679082711196836,1.),(1.,0.675526278181767,
1.),(1.,0.675590207615662,1.)))
REPRESENTATION_ITEM('')
SURFACE()
);
#2090=(
BOUNDED_SURFACE()
B_SPLINE_SURFACE(3,2,((#134786,#134787,#134788),(#134789,#134790,#134791),
(#134792,#134793,#134794),(#134795,#134796,#134797),(#134798,#134799,#134800),
(#134801,#134802,#134803)),.UNSPECIFIED.,.F.,.F.,.F.)
B_SPLINE_SURFACE_WITH_KNOTS((4,2,4),(3,3),(3.1415926535898,3.92699081698724,
4.71238898038469),(0.,1.),.UNSPECIFIED.)
GEOMETRIC_REPRESENTATION_ITEM()
RATIONAL_B_SPLINE_SURFACE(((1.,0.737277336810123,1.),(1.,0.737326538316937,
1.),(1.,0.73410625828684,1.),(1.,0.723033691557529,1.),(1.,0.715202981902217,
1.),(1.,0.707106781186543,1.)))
REPRESENTATION_ITEM('')
SURFACE()
);
#2091=(
BOUNDED_SURFACE()
B_SPLINE_SURFACE(3,2,((#134816,#134817,#134818),(#134819,#134820,#134821),
(#134822,#134823,#134824),(#134825,#134826,#134827),(#134828,#134829,#134830),
(#134831,#134832,#134833)),.UNSPECIFIED.,.F.,.F.,.F.)
B_SPLINE_SURFACE_WITH_KNOTS((4,2,4),(3,3),(9.63948754967748E-5,0.00173129457116097,
0.00336619426682516),(0.,1.),.UNSPECIFIED.)
GEOMETRIC_REPRESENTATION_ITEM()
RATIONAL_B_SPLINE_SURFACE(((1.,0.88872394157032,1.),(1.,0.863203710383462,
1.),(1.,0.835728844788038,1.),(1.,0.775725241916869,1.),(1.,0.743211702946043,
1.),(1.,0.707106781186548,1.)))
REPRESENTATION_ITEM('')
SURFACE()
);
#2092=(
BOUNDED_SURFACE()
B_SPLINE_SURFACE(3,2,((#134855,#134856,#134857),(#134858,#134859,#134860),
(#134861,#134862,#134863),(#134864,#134865,#134866)),.UNSPECIFIED.,.F.,
 .F.,.F.)
B_SPLINE_SURFACE_WITH_KNOTS((4,4),(3,3),(2.22847122787664,3.14161440295379),
(-2.1749363990258E-5,1.),.UNSPECIFIED.)
GEOMETRIC_REPRESENTATION_ITEM()
RATIONAL_B_SPLINE_SURFACE(((1.00001193202905,0.725692460307629,1.),(1.00001161526324,
0.732974645844473,1.),(1.00001142611057,0.737323110435419,1.),(1.00001142835037,
0.737271619087495,0.999999999999999)))
REPRESENTATION_ITEM('')
SURFACE()
);
#2093=(
BOUNDED_SURFACE()
B_SPLINE_SURFACE(3,2,((#134887,#134888,#134889),(#134890,#134891,#134892),
(#134893,#134894,#134895),(#134896,#134897,#134898),(#134899,#134900,#134901),
(#134902,#134903,#134904)),.UNSPECIFIED.,.F.,.F.,.F.)
B_SPLINE_SURFACE_WITH_KNOTS((4,2,4),(3,3),(4.71238898038469,5.49778714378214,
6.28318530717959),(0.,1.),.UNSPECIFIED.)
GEOMETRIC_REPRESENTATION_ITEM()
RATIONAL_B_SPLINE_SURFACE(((1.,0.707106781186538,1.),(1.,0.715202981902668,
1.),(1.,0.723033691556936,1.),(1.,0.734106258287417,1.),(1.,0.737326538316498,
1.),(1.,0.737277336810125,1.)))
REPRESENTATION_ITEM('')
SURFACE()
);
#2094=(
BOUNDED_SURFACE()
B_SPLINE_SURFACE(3,2,((#134917,#134918,#134919),(#134920,#134921,#134922),
(#134923,#134924,#134925),(#134926,#134927,#134928),(#134929,#134930,#134931),
(#134932,#134933,#134934)),.UNSPECIFIED.,.F.,.F.,.F.)
B_SPLINE_SURFACE_WITH_KNOTS((4,2,4),(3,3),(0.,0.785398163397448,1.5707963267949),
(0.,1.),.UNSPECIFIED.)
GEOMETRIC_REPRESENTATION_ITEM()
RATIONAL_B_SPLINE_SURFACE(((1.,0.675590207615664,1.),(1.,0.675526278181461,
1.),(1.,0.679082711197251,1.),(1.,0.690860049128011,1.),(1.,0.699025295935341,
1.),(1.,0.707106781186543,1.)))
REPRESENTATION_ITEM('')
SURFACE()
);
#2095=(
BOUNDED_SURFACE()
B_SPLINE_SURFACE(3,2,((#134977,#134978,#134979),(#134980,#134981,#134982),
(#134983,#134984,#134985),(#134986,#134987,#134988),(#134989,#134990,#134991),
(#134992,#134993,#134994)),.UNSPECIFIED.,.F.,.F.,.F.)
B_SPLINE_SURFACE_WITH_KNOTS((4,2,4),(3,3),(1.5707963267949,2.35619449019234,
3.1415926535898),(0.,1.),.UNSPECIFIED.)
GEOMETRIC_REPRESENTATION_ITEM()
RATIONAL_B_SPLINE_SURFACE(((1.,0.707106781186543,1.),(1.,0.715202981902222,
1.),(1.,0.723033691557528,1.),(1.,0.73410625828684,1.),(1.,0.737326538316928,
1.),(1.,0.737277336810125,1.)))
REPRESENTATION_ITEM('')
SURFACE()
);
#2096=(
BOUNDED_SURFACE()
B_SPLINE_SURFACE(3,2,((#135007,#135008,#135009),(#135010,#135011,#135012),
(#135013,#135014,#135015),(#135016,#135017,#135018),(#135019,#135020,#135021),
(#135022,#135023,#135024)),.UNSPECIFIED.,.F.,.F.,.F.)
B_SPLINE_SURFACE_WITH_KNOTS((4,2,4),(3,3),(0.,0.785398163397448,1.5707963267949),
(0.,1.),.UNSPECIFIED.)
GEOMETRIC_REPRESENTATION_ITEM()
RATIONAL_B_SPLINE_SURFACE(((1.,0.675590207615664,1.),(1.,0.675526278181762,
1.),(1.,0.679082711196844,1.),(1.,0.690860049128418,1.),(1.,0.699025295935035,
1.),(1.,0.707106781186543,1.)))
REPRESENTATION_ITEM('')
SURFACE()
);
#2097=(
BOUNDED_SURFACE()
B_SPLINE_SURFACE(3,2,((#135086,#135087,#135088),(#135089,#135090,#135091),
(#135092,#135093,#135094),(#135095,#135096,#135097)),.UNSPECIFIED.,.F.,
 .F.,.F.)
B_SPLINE_SURFACE_WITH_KNOTS((4,4),(3,3),(0.,0.000650162698700256),(0.,1.),
 .UNSPECIFIED.)
GEOMETRIC_REPRESENTATION_ITEM()
RATIONAL_B_SPLINE_SURFACE(((1.,0.690549802660026,1.),(1.,0.689437188232559,
1.),(1.,0.688863085247593,1.),(1.,0.688859710772113,1.)))
REPRESENTATION_ITEM('')
SURFACE()
);
#2098=(
BOUNDED_SURFACE()
B_SPLINE_SURFACE(3,2,((#135103,#135104,#135105),(#135106,#135107,#135108),
(#135109,#135110,#135111),(#135112,#135113,#135114)),.UNSPECIFIED.,.F.,
 .F.,.F.)
B_SPLINE_SURFACE_WITH_KNOTS((4,4),(3,3),(-6.93889390390723E-18,0.0331958858056162),
(0.,1.),.UNSPECIFIED.)
GEOMETRIC_REPRESENTATION_ITEM()
RATIONAL_B_SPLINE_SURFACE(((1.,0.685275128444715,1.),(1.,0.687584548418076,
1.),(1.,0.689209215689052,1.),(1.,0.690549802660031,1.)))
REPRESENTATION_ITEM('')
SURFACE()
);
#2099=(
BOUNDED_SURFACE()
B_SPLINE_SURFACE(3,2,((#135126,#135127,#135128),(#135129,#135130,#135131),
(#135132,#135133,#135134),(#135135,#135136,#135137),(#135138,#135139,#135140),
(#135141,#135142,#135143),(#135144,#135145,#135146),(#135147,#135148,#135149),
(#135150,#135151,#135152),(#135153,#135154,#135155),(#135156,#135157,#135158),
(#135159,#135160,#135161),(#135162,#135163,#135164),(#135165,#135166,#135167)),
 .UNSPECIFIED.,.F.,.F.,.F.)
B_SPLINE_SURFACE_WITH_KNOTS((4,2,2,2,2,2,4),(3,3),(-9.99593665452618E-5,
0.000249898416362892,0.000374847624544338,0.000499796832725785,0.000624746040907231,
0.000749695249088677,0.00109955303199673),(-0.00121399112232759,1.00003012118409),
 .UNSPECIFIED.)
GEOMETRIC_REPRESENTATION_ITEM()
RATIONAL_B_SPLINE_SURFACE(((1.00075881319157,0.687462263241503,1.0000188051834),
(1.0007674207464,0.683917008974209,1.00001901849894),(1.00077151552536,
0.682230463507457,1.00001911997723),(1.00077025819397,0.682748329448053,
1.00001908881759),(1.00076928167011,0.683150537212566,1.00001906461702),
(1.00076613988363,0.684444566951248,1.00001898675613),(1.00076399876361,
0.685326445139633,1.00001893369412),(1.00075856649934,0.687563870106642,
1.00001879906978),(1.000755378547,0.688876914504211,1.00001872006479),(1.0007481508392,
0.69185384145156,1.00001854094512),(1.00074408123656,0.693530017369103,
1.00001844009075),(1.00072783192001,0.700222737891797,1.0000180373943),
(1.00071354413798,0.706107547365276,1.00001768330931),(1.00070077601211,
0.711366445349713,1.00001736688499)))
REPRESENTATION_ITEM('')
SURFACE()
);
#2100=(
BOUNDED_SURFACE()
B_SPLINE_SURFACE(3,2,((#135420,#135421,#135422),(#135423,#135424,#135425),
(#135426,#135427,#135428),(#135429,#135430,#135431),(#135432,#135433,#135434),
(#135435,#135436,#135437)),.UNSPECIFIED.,.F.,.F.,.F.)
B_SPLINE_SURFACE_WITH_KNOTS((4,2,4),(3,3),(0.0202634924775631,0.0220347355863407,
0.0238059786951184),(0.,1.),.UNSPECIFIED.)
GEOMETRIC_REPRESENTATION_ITEM()
RATIONAL_B_SPLINE_SURFACE(((1.,0.707106781186538,1.),(1.,0.681614664404396,
1.),(1.,0.655059254259685,1.),(1.,0.598852069172831,1.),(1.,0.569209502658738,
1.),(1.,0.537299608347133,1.)))
REPRESENTATION_ITEM('')
SURFACE()
);
#2101=(
BOUNDED_SURFACE()
B_SPLINE_SURFACE(3,2,((#135836,#135837,#135838),(#135839,#135840,#135841),
(#135842,#135843,#135844),(#135845,#135846,#135847),(#135848,#135849,#135850),
(#135851,#135852,#135853),(#135854,#135855,#135856),(#135857,#135858,#135859),
(#135860,#135861,#135862),(#135863,#135864,#135865)),.UNSPECIFIED.,.F.,
 .F.,.F.)
B_SPLINE_SURFACE_WITH_KNOTS((4,2,2,2,4),(3,3),(-4.08272591082004E-15,0.000408890006701704,
0.000817780013407491,0.00122667002011328,0.00163556002681907),(0.,1.),
 .UNSPECIFIED.)
GEOMETRIC_REPRESENTATION_ITEM()
RATIONAL_B_SPLINE_SURFACE(((1.,0.707106781186878,1.),(1.,0.688891921544893,
1.),(1.,0.670532818962991,1.),(1.,0.634368444020432,1.),(1.,0.617287210907485,
1.),(1.,0.586753298958185,1.),(1.,0.573879231151052,1.),(1.,0.555793216592158,
1.),(1.,0.550823008344725,1.),(1.,0.550808342809435,1.)))
REPRESENTATION_ITEM('')
SURFACE()
);
#2102=(
BOUNDED_SURFACE()
B_SPLINE_SURFACE(3,2,((#135947,#135948,#135949),(#135950,#135951,#135952),
(#135953,#135954,#135955),(#135956,#135957,#135958),(#135959,#135960,#135961),
(#135962,#135963,#135964),(#135965,#135966,#135967),(#135968,#135969,#135970),
(#135971,#135972,#135973),(#135974,#135975,#135976)),.UNSPECIFIED.,.F.,
 .F.,.F.)
B_SPLINE_SURFACE_WITH_KNOTS((4,2,2,2,4),(3,3),(-5.38853734303535E-5,0.000399221470224828,
0.000798442940449655,0.00119766441067448,0.00165077125432966),(-5.38853734303535E-5,
1.),.UNSPECIFIED.)
GEOMETRIC_REPRESENTATION_ITEM()
RATIONAL_B_SPLINE_SURFACE(((1.00002098681007,0.805264316328848,1.),(1.00002089216129,
0.806142558161274,1.),(1.00002118366649,0.803437694284019,1.),(1.00002234668521,
0.79264609497424,1.),(1.00002315070481,0.785185632613891,1.),(1.00002511413113,
0.766967086537006,1.),(1.0000262898705,0.756057452790845,1.),(1.00002898535259,
0.731046193594127,1.),(1.00003056885291,0.716352964024592,1.),(1.00003212218393,
0.701939674122364,1.)))
REPRESENTATION_ITEM('')
SURFACE()
);
#2103=(
BOUNDED_SURFACE()
B_SPLINE_SURFACE(3,2,((#136069,#136070,#136071),(#136072,#136073,#136074),
(#136075,#136076,#136077),(#136078,#136079,#136080),(#136081,#136082,#136083),
(#136084,#136085,#136086)),.UNSPECIFIED.,.F.,.F.,.F.)
B_SPLINE_SURFACE_WITH_KNOTS((4,2,4),(3,3),(-1.94017978766281E-16,0.000795637462001992,
0.00159127492400417),(0.,1.),.UNSPECIFIED.)
GEOMETRIC_REPRESENTATION_ITEM()
RATIONAL_B_SPLINE_SURFACE(((1.,0.707106781186555,1.),(1.,0.682471170316176,
1.),(1.,0.657591859959034,1.),(1.,0.621346223380964,1.),(1.,0.610136165392898,
1.),(1.,0.610293066582478,1.)))
REPRESENTATION_ITEM('')
SURFACE()
);
#2104=(
BOUNDED_SURFACE()
B_SPLINE_SURFACE(3,2,((#136124,#136125,#136126),(#136127,#136128,#136129),
(#136130,#136131,#136132),(#136133,#136134,#136135),(#136136,#136137,#136138),
(#136139,#136140,#136141),(#136142,#136143,#136144),(#136145,#136146,#136147)),
 .UNSPECIFIED.,.F.,.F.,.F.)
B_SPLINE_SURFACE_WITH_KNOTS((4,2,2,4),(3,3),(0.,0.000393730579424048,0.000787461158848096,
0.00157492231769619),(0.,1.),.UNSPECIFIED.)
GEOMETRIC_REPRESENTATION_ITEM()
RATIONAL_B_SPLINE_SURFACE(((1.,0.761354724782829,1.),(1.,0.778699482201342,
1.),(1.,0.792177303062869,1.),(1.,0.813203501689393,1.),(1.,0.820397856397578,
1.),(1.,0.834724000629532,1.),(1.,0.834081767050111,1.),(1.,0.826892724830075,
1.)))
REPRESENTATION_ITEM('')
SURFACE()
);
#2105=(
BOUNDED_SURFACE()
B_SPLINE_SURFACE(3,2,((#136167,#136168,#136169),(#136170,#136171,#136172),
(#136173,#136174,#136175),(#136176,#136177,#136178)),.UNSPECIFIED.,.F.,
 .F.,.F.)
B_SPLINE_SURFACE_WITH_KNOTS((4,4),(3,3),(-2.30501381870419E-16,0.000504122926429285),
(0.,1.),.UNSPECIFIED.)
GEOMETRIC_REPRESENTATION_ITEM()
RATIONAL_B_SPLINE_SURFACE(((1.,0.832929291663028,1.),(1.,0.830988393206304,
1.),(1.,0.828976922242354,1.),(1.,0.82689272482991,1.)))
REPRESENTATION_ITEM('')
SURFACE()
);
#2106=(
BOUNDED_SURFACE()
B_SPLINE_SURFACE(3,2,((#136184,#136185,#136186),(#136187,#136188,#136189),
(#136190,#136191,#136192),(#136193,#136194,#136195),(#136196,#136197,#136198),
(#136199,#136200,#136201),(#136202,#136203,#136204),(#136205,#136206,#136207),
(#136208,#136209,#136210),(#136211,#136212,#136213)),.UNSPECIFIED.,.F.,
 .F.,.F.)
B_SPLINE_SURFACE_WITH_KNOTS((4,2,2,2,4),(3,3),(-1.86157513015761E-16,0.000442340065143073,
0.000884680130286332,0.00132702019542959,0.00176936026057285),(0.,1.),
 .UNSPECIFIED.)
GEOMETRIC_REPRESENTATION_ITEM()
RATIONAL_B_SPLINE_SURFACE(((1.,0.83292929166297,1.),(1.,0.829173169481911,
1.),(1.,0.823008202027213,1.),(1.,0.806154887727085,1.),(1.,0.795326013033949,
1.),(1.,0.768452086196073,1.),(1.,0.752322946736307,1.),(1.,0.713492386952618,
1.),(1.,0.69094524448308,1.),(1.,0.664473794614023,1.)))
REPRESENTATION_ITEM('')
SURFACE()
);
#2107=(
BOUNDED_SURFACE()
B_SPLINE_SURFACE(3,2,((#136301,#136302,#136303),(#136304,#136305,#136306),
(#136307,#136308,#136309),(#136310,#136311,#136312),(#136313,#136314,#136315),
(#136316,#136317,#136318),(#136319,#136320,#136321),(#136322,#136323,#136324),
(#136325,#136326,#136327),(#136328,#136329,#136330)),.UNSPECIFIED.,.F.,
 .F.,.F.)
B_SPLINE_SURFACE_WITH_KNOTS((4,2,2,2,4),(3,3),(-0.000154485852495398,0.000906588491342359,
0.00113323561417795,0.00135988273701354,0.00196766283517968),(-0.000154485852495398,
1.),.UNSPECIFIED.)
GEOMETRIC_REPRESENTATION_ITEM()
RATIONAL_B_SPLINE_SURFACE(((1.00009689723556,0.686387996056344,1.),(1.00007625016334,
0.753213119168533,1.),(1.00006074765387,0.803387647186572,1.),(1.00004855990641,
0.842833807662968,1.),(1.00004671134296,0.848816761518043,1.),(1.00004351687879,
0.859155779998294,1.),(1.0000421620718,0.863540670176529,1.),(1.00003825071871,
0.876199929974803,1.),(1.00003729591827,0.879290182030031,1.),(1.00003834620117,
0.875890896968986,1.)))
REPRESENTATION_ITEM('')
SURFACE()
);
#2108=(
BOUNDED_SURFACE()
B_SPLINE_SURFACE(3,2,((#136411,#136412,#136413),(#136414,#136415,#136416),
(#136417,#136418,#136419),(#136420,#136421,#136422)),.UNSPECIFIED.,.F.,
 .F.,.F.)
B_SPLINE_SURFACE_WITH_KNOTS((4,4),(3,3),(-2.91650384398601E-17,0.000810744804887501),
(0.,1.),.UNSPECIFIED.)
GEOMETRIC_REPRESENTATION_ITEM()
RATIONAL_B_SPLINE_SURFACE(((1.,0.804104907750019,1.),(1.,0.778265384411316,
1.),(1.,0.743775615594857,1.),(1.,0.707106781186549,1.)))
REPRESENTATION_ITEM('')
SURFACE()
);
#2109=(
BOUNDED_SURFACE()
B_SPLINE_SURFACE(3,2,((#136439,#136440,#136441),(#136442,#136443,#136444),
(#136445,#136446,#136447),(#136448,#136449,#136450),(#136451,#136452,#136453),
(#136454,#136455,#136456),(#136457,#136458,#136459),(#136460,#136461,#136462),
(#136463,#136464,#136465),(#136466,#136467,#136468)),.UNSPECIFIED.,.F.,
 .F.,.F.)
B_SPLINE_SURFACE_WITH_KNOTS((4,2,2,2,4),(3,3),(0.00807567872552143,0.00870243807057167,
0.0093291974156219,0.00995595676067213,0.0105827161057224),(0.,1.),
 .UNSPECIFIED.)
GEOMETRIC_REPRESENTATION_ITEM()
RATIONAL_B_SPLINE_SURFACE(((1.,0.707106781186547,1.),(1.,0.707175173315664,
1.),(1.,0.707241719347897,1.),(1.,0.707371272007346,1.),(1.,0.70743422794471,
1.),(1.,0.707549712034256,1.),(1.,0.707603875852248,1.),(1.,0.707699291327501,
1.),(1.,0.707740674853624,1.),(1.,0.707775806502368,1.)))
REPRESENTATION_ITEM('')
SURFACE()
);
#2110=(
BOUNDED_SURFACE()
B_SPLINE_SURFACE(3,2,((#136516,#136517,#136518),(#136519,#136520,#136521),
(#136522,#136523,#136524),(#136525,#136526,#136527),(#136528,#136529,#136530),
(#136531,#136532,#136533),(#136534,#136535,#136536),(#136537,#136538,#136539),
(#136540,#136541,#136542),(#136543,#136544,#136545),(#136546,#136547,#136548),
(#136549,#136550,#136551)),.UNSPECIFIED.,.F.,.F.,.F.)
B_SPLINE_SURFACE_WITH_KNOTS((4,2,2,2,2,4),(3,3),(0.00807567643991074,0.0087258483708248,
0.00905093433628183,0.00937602030173886,0.0100261922326529,0.010676364163567),
(0.,1.),.UNSPECIFIED.)
GEOMETRIC_REPRESENTATION_ITEM()
RATIONAL_B_SPLINE_SURFACE(((1.,0.707106781186547,1.),(1.,0.707170635637275,
1.),(1.,0.707232744268554,1.),(1.,0.70732338528182,1.),(1.,0.707353375007997,
1.),(1.,0.707410998957093,1.),(1.,0.707438747129451,1.),(1.,0.707518900645085,
1.),(1.,0.707568814651682,1.),(1.,0.707655521042551,1.),(1.,0.707692858707996,
1.),(1.,0.707723858215708,1.)))
REPRESENTATION_ITEM('')
SURFACE()
);
#2111=(
BOUNDED_SURFACE()
B_SPLINE_SURFACE(3,2,((#136601,#136602,#136603),(#136604,#136605,#136606),
(#136607,#136608,#136609),(#136610,#136611,#136612)),.UNSPECIFIED.,.F.,
 .F.,.F.)
B_SPLINE_SURFACE_WITH_KNOTS((4,4),(3,3),(0.,0.000650122897330092),(0.,1.),
 .UNSPECIFIED.)
GEOMETRIC_REPRESENTATION_ITEM()
RATIONAL_B_SPLINE_SURFACE(((1.,0.713892198341303,1.),(1.,0.714340614318511,
1.),(1.,0.714570777789516,1.),(1.,0.714572220188112,1.)))
REPRESENTATION_ITEM('')
SURFACE()
);
#2112=(
BOUNDED_SURFACE()
B_SPLINE_SURFACE(3,2,((#136660,#136661,#136662),(#136663,#136664,#136665),
(#136666,#136667,#136668),(#136669,#136670,#136671)),.UNSPECIFIED.,.F.,
 .F.,.F.)
B_SPLINE_SURFACE_WITH_KNOTS((4,4),(3,3),(0.,0.000650368158908551),(0.,1.),
 .UNSPECIFIED.)
GEOMETRIC_REPRESENTATION_ITEM()
RATIONAL_B_SPLINE_SURFACE(((1.,0.66438972944168,1.),(1.,0.664393217905862,
1.),(1.,0.665747114157887,1.),(1.,0.66841287307604,1.)))
REPRESENTATION_ITEM('')
SURFACE()
);
#2113=(
BOUNDED_SURFACE()
B_SPLINE_SURFACE(3,2,((#136794,#136795,#136796),(#136797,#136798,#136799),
(#136800,#136801,#136802),(#136803,#136804,#136805),(#136806,#136807,#136808),
(#136809,#136810,#136811),(#136812,#136813,#136814),(#136815,#136816,#136817),
(#136818,#136819,#136820),(#136821,#136822,#136823),(#136824,#136825,#136826),
(#136827,#136828,#136829),(#136830,#136831,#136832),(#136833,#136834,#136835)),
 .UNSPECIFIED.,.F.,.F.,.F.)
B_SPLINE_SURFACE_WITH_KNOTS((4,2,2,2,2,2,4),(3,3),(0.00807831625971351,
0.00883535021604665,0.00921386719421322,0.00959238417237979,0.00997090115054636,
0.0103494181287129,0.0111064520850461),(0.,1.),.UNSPECIFIED.)
GEOMETRIC_REPRESENTATION_ITEM()
RATIONAL_B_SPLINE_SURFACE(((1.,0.707106781186548,1.),(1.,0.705861961062141,
1.),(1.,0.704642623504988,1.),(1.,0.702853606538468,1.),(1.,0.702268342990035,
1.),(1.,0.701150362247141,1.),(1.,0.700612993986993,1.),(1.,0.699582583564998,
1.),(1.,0.699087807793684,1.),(1.,0.698176683118393,1.),(1.,0.697755963868462,
1.),(1.,0.696598958196255,1.),(1.,0.695966377684547,1.),(1.,0.695533955710884,
1.)))
REPRESENTATION_ITEM('')
SURFACE()
);
#2114=(
BOUNDED_SURFACE()
B_SPLINE_SURFACE(3,2,((#136852,#136853,#136854),(#136855,#136856,#136857),
(#136858,#136859,#136860),(#136861,#136862,#136863)),.UNSPECIFIED.,.F.,
 .F.,.F.)
B_SPLINE_SURFACE_WITH_KNOTS((4,4),(3,3),(0.0316780996002149,0.0322721596780966),
(0.0854777406552673,1.),.UNSPECIFIED.)
GEOMETRIC_REPRESENTATION_ITEM()
RATIONAL_B_SPLINE_SURFACE(((0.96702384016161,0.807106741558701,1.),(0.966583587972177,
0.804531496904019,1.),(0.966125339262662,0.801850982035457,1.),(0.96564868941755,
0.799062830164232,1.)))
REPRESENTATION_ITEM('')
SURFACE()
);
#2115=(
BOUNDED_SURFACE()
B_SPLINE_SURFACE(3,2,((#136881,#136882,#136883),(#136884,#136885,#136886),
(#136887,#136888,#136889),(#136890,#136891,#136892),(#136893,#136894,#136895),
(#136896,#136897,#136898),(#136899,#136900,#136901),(#136902,#136903,#136904),
(#136905,#136906,#136907),(#136908,#136909,#136910),(#136911,#136912,#136913),
(#136914,#136915,#136916)),.UNSPECIFIED.,.F.,.F.,.F.)
B_SPLINE_SURFACE_WITH_KNOTS((4,2,2,2,2,4),(3,3),(0.00807807165860127,0.00885401549830484,
0.00962995933800841,0.0100179312578602,0.010405903177712,0.0111818470174155),
(0.,1.),.UNSPECIFIED.)
GEOMETRIC_REPRESENTATION_ITEM()
RATIONAL_B_SPLINE_SURFACE(((1.,0.707106781186548,1.),(1.,0.708323960348238,
1.),(1.,0.709510365636766,1.),(1.,0.711820403892163,1.),(1.,0.712901935204825,
1.),(1.,0.714375984986412,1.),(1.,0.714843782196838,1.),(1.,0.715700614088123,
1.),(1.,0.716094239791898,1.),(1.,0.71717000694229,1.),(1.,0.717742537382462,
1.),(1.,0.718120418666571,1.)))
REPRESENTATION_ITEM('')
SURFACE()
);
#2116=(
BOUNDED_SURFACE()
B_SPLINE_SURFACE(3,2,((#136965,#136966,#136967),(#136968,#136969,#136970),
(#136971,#136972,#136973),(#136974,#136975,#136976)),.UNSPECIFIED.,.F.,
 .F.,.F.)
B_SPLINE_SURFACE_WITH_KNOTS((4,4),(3,3),(-6.50599722386063E-5,0.000715659694624667),
(0.,1.00019764385803),.UNSPECIFIED.)
GEOMETRIC_REPRESENTATION_ITEM()
RATIONAL_B_SPLINE_SURFACE(((1.,0.755595413549798,1.00009661013077),(1.,
0.759778183122694,1.00009495673334),(1.,0.761738166948689,1.00009418197581),
(1.,0.761362101277913,1.00009433062995)))
REPRESENTATION_ITEM('')
SURFACE()
);
#2117=(
BOUNDED_SURFACE()
B_SPLINE_SURFACE(3,2,((#137090,#137091,#137092),(#137093,#137094,#137095),
(#137096,#137097,#137098),(#137099,#137100,#137101)),.UNSPECIFIED.,.F.,
 .F.,.F.)
B_SPLINE_SURFACE_WITH_KNOTS((4,4),(3,3),(-6.51392861930307E-5,0.000716532148123338),
(0.,1.00012789259532),.UNSPECIFIED.)
GEOMETRIC_REPRESENTATION_ITEM()
RATIONAL_B_SPLINE_SURFACE(((1.,0.610140967503591,1.00009972016695),(1.,
0.609358872291236,1.00009992021532),(1.,0.613297600455477,1.00009891274699),
(1.,0.621522254435954,1.0000968090023)))
REPRESENTATION_ITEM('')
SURFACE()
);
#2118=(
BOUNDED_SURFACE()
B_SPLINE_SURFACE(3,2,((#137171,#137172,#137173),(#137174,#137175,#137176),
(#137177,#137178,#137179),(#137180,#137181,#137182)),.UNSPECIFIED.,.F.,
 .F.,.F.)
B_SPLINE_SURFACE_WITH_KNOTS((4,4),(3,3),(-6.51938878740145E-5,0.000717132766614092),
(0.,1.00014042207762),.UNSPECIFIED.)
GEOMETRIC_REPRESENTATION_ITEM()
RATIONAL_B_SPLINE_SURFACE(((1.,0.795313299193259,1.00005748506358),(1.,
0.802685972468766,1.00005541449138),(1.,0.806177096184803,1.00005443402969),
(1.,0.805504544806421,1.00005462291181)))
REPRESENTATION_ITEM('')
SURFACE()
);
#2119=(
BOUNDED_SURFACE()
B_SPLINE_SURFACE(3,2,((#137256,#137257,#137258),(#137259,#137260,#137261),
(#137262,#137263,#137264),(#137265,#137266,#137267)),.UNSPECIFIED.,.F.,
 .F.,.F.)
B_SPLINE_SURFACE_WITH_KNOTS((4,4),(3,3),(-3.51472717058904E-5,0.00068864672702981),
(0.,1.00003514727171),.UNSPECIFIED.)
GEOMETRIC_REPRESENTATION_ITEM()
RATIONAL_B_SPLINE_SURFACE(((1.,0.550503741378763,1.00003159713427),(1.,
0.549804011257131,1.00003164632147),(1.,0.556145239310861,1.00003120056774),
(1.,0.568324276981185,1.00003034444785)))
REPRESENTATION_ITEM('')
SURFACE()
);
#2120=(
BOUNDED_SURFACE()
B_SPLINE_SURFACE(3,2,((#137355,#137356,#137357),(#137358,#137359,#137360),
(#137361,#137362,#137363),(#137364,#137365,#137366)),.UNSPECIFIED.,.F.,
 .F.,.F.)
B_SPLINE_SURFACE_WITH_KNOTS((4,4),(3,3),(0.,0.000921798889909707),(0.,1.),
 .UNSPECIFIED.)
GEOMETRIC_REPRESENTATION_ITEM()
RATIONAL_B_SPLINE_SURFACE(((1.,0.831289505264087,1.),(1.,0.831333394817592,
1.),(1.,0.824011622363235,1.),(1.,0.810617639934149,1.)))
REPRESENTATION_ITEM('')
SURFACE()
);
#2121=(
BOUNDED_SURFACE()
B_SPLINE_SURFACE(3,2,((#137438,#137439,#137440),(#137441,#137442,#137443),
(#137444,#137445,#137446),(#137447,#137448,#137449)),.UNSPECIFIED.,.F.,
 .F.,.F.)
B_SPLINE_SURFACE_WITH_KNOTS((4,4),(3,3),(-6.52563961816919E-5,0.000717820357998483),
(0.,1.00007660676733),.UNSPECIFIED.)
GEOMETRIC_REPRESENTATION_ITEM()
RATIONAL_B_SPLINE_SURFACE(((1.,0.590666869146129,1.00006271537583),(1.,
0.579347829852759,1.00006444960585),(1.,0.573596789585218,1.00006533074306),
(0.999999999999999,0.574723554882887,1.00006515810736)))
REPRESENTATION_ITEM('')
SURFACE()
);
#2122=(
BOUNDED_SURFACE()
B_SPLINE_SURFACE(3,2,((#137468,#137469,#137470),(#137471,#137472,#137473),
(#137474,#137475,#137476),(#137477,#137478,#137479)),.UNSPECIFIED.,.F.,
 .F.,.F.)
B_SPLINE_SURFACE_WITH_KNOTS((4,4),(3,3),(-6.51209638471727E-5,0.000716330602318899),
(0.,1.00017301493665),.UNSPECIFIED.)
GEOMETRIC_REPRESENTATION_ITEM()
RATIONAL_B_SPLINE_SURFACE(((1.,0.786579319308494,1.0000738499311),(1.,0.787125222591245,
1.00007366103225),(1.,0.784342967102359,1.00007462377577),(1.,0.778244201129582,
1.00007673413099)))
REPRESENTATION_ITEM('')
SURFACE()
);
#2123=(
BOUNDED_SURFACE()
B_SPLINE_SURFACE(3,2,((#137596,#137597,#137598),(#137599,#137600,#137601),
(#137602,#137603,#137604),(#137605,#137606,#137607),(#137608,#137609,#137610),
(#137611,#137612,#137613),(#137614,#137615,#137616),(#137617,#137618,#137619),
(#137620,#137621,#137622),(#137623,#137624,#137625),(#137626,#137627,#137628),
(#137629,#137630,#137631),(#137632,#137633,#137634),(#137635,#137636,#137637)),
 .UNSPECIFIED.,.F.,.F.,.F.)
B_SPLINE_SURFACE_WITH_KNOTS((4,2,2,2,2,2,4),(3,3),(0.00807568025026493,
0.00898700204274496,0.00944266293898498,0.009898323835225,0.010353984731465,
0.010809645627705,0.0117209674201851),(0.,1.),.UNSPECIFIED.)
GEOMETRIC_REPRESENTATION_ITEM()
RATIONAL_B_SPLINE_SURFACE(((1.,0.707106781186546,1.),(1.,0.707214557916128,
1.),(1.,0.707322930753557,1.),(1.,0.707478596210236,1.),(1.,0.707528365558662,
1.),(1.,0.70762361150633,1.),(1.,0.70766951928712,1.),(1.,0.70775397022188,
1.),(1.,0.707792549798564,1.),(1.,0.707862266510969,1.),(1.,0.707893578069266,
1.),(1.,0.707972242595767,1.),(1.,0.70800597758526,1.),(1.,0.708018339291814,
1.)))
REPRESENTATION_ITEM('')
SURFACE()
);
#2124=(
BOUNDED_SURFACE()
B_SPLINE_SURFACE(3,2,((#137654,#137655,#137656),(#137657,#137658,#137659),
(#137660,#137661,#137662),(#137663,#137664,#137665)),.UNSPECIFIED.,.F.,
 .F.,.F.)
B_SPLINE_SURFACE_WITH_KNOTS((4,4),(3,3),(0.0370067204754696,0.0375452288399126),
(0.,0.906596046514924),.UNSPECIFIED.)
GEOMETRIC_REPRESENTATION_ITEM()
RATIONAL_B_SPLINE_SURFACE(((1.,0.74984328911729,0.953268748425464),(1.,
0.745960134338133,0.952543344408728),(1.,0.741971405566699,0.951798218335465),
(1.,0.737872605222811,0.951032530022135)))
REPRESENTATION_ITEM('')
SURFACE()
);
#2125=(
BOUNDED_SURFACE()
B_SPLINE_SURFACE(3,2,((#137680,#137681,#137682),(#137683,#137684,#137685),
(#137686,#137687,#137688),(#137689,#137690,#137691),(#137692,#137693,#137694),
(#137695,#137696,#137697),(#137698,#137699,#137700),(#137701,#137702,#137703),
(#137704,#137705,#137706),(#137707,#137708,#137709),(#137710,#137711,#137712),
(#137713,#137714,#137715)),.UNSPECIFIED.,.F.,.F.,.F.)
B_SPLINE_SURFACE_WITH_KNOTS((4,2,2,2,2,4),(3,3),(0.00807589507756136,0.00894079878156724,
0.00980570248557312,0.010238154337576,0.010670606189579,0.0115355098935849),
(0.,1.),.UNSPECIFIED.)
GEOMETRIC_REPRESENTATION_ITEM()
RATIONAL_B_SPLINE_SURFACE(((1.,0.707106781186548,1.),(1.,0.706684802682679,
1.),(1.,0.706265611788784,1.),(1.,0.705449765784865,1.),(1.,0.705070572349072,
1.),(1.,0.704559600788765,1.),(1.,0.704402907652403,1.),(1.,0.7041166887103,
1.),(1.,0.703986299022118,1.),(1.,0.703645597188673,1.),(1.,0.703488957328521,
1.),(1.,0.703406029216022,1.)))
REPRESENTATION_ITEM('')
SURFACE()
);
#2126=(
BOUNDED_SURFACE()
B_SPLINE_SURFACE(3,2,((#137779,#137780,#137781),(#137782,#137783,#137784),
(#137785,#137786,#137787),(#137788,#137789,#137790)),.UNSPECIFIED.,.F.,
 .F.,.F.)
B_SPLINE_SURFACE_WITH_KNOTS((4,4),(3,3),(-6.50851503337948E-5,0.000715936653671955),
(0.,1.00015557324313),.UNSPECIFIED.)
GEOMETRIC_REPRESENTATION_ITEM()
RATIONAL_B_SPLINE_SURFACE(((0.999999999999999,0.64270572393334,1.00011117085856),
(1.,0.636685742162938,1.00011304395473),(1.,0.633761479841935,1.00011395382868),
(1.,0.634327701648552,1.00011377765075)))
REPRESENTATION_ITEM('')
SURFACE()
);
#2127=(
BOUNDED_SURFACE()
B_SPLINE_SURFACE(3,2,((#137844,#137845,#137846),(#137847,#137848,#137849),
(#137850,#137851,#137852),(#137853,#137854,#137855)),.UNSPECIFIED.,.F.,
 .F.,.F.)
B_SPLINE_SURFACE_WITH_KNOTS((4,4),(3,3),(0.,0.000650274811908555),(0.,1.),
 .UNSPECIFIED.)
GEOMETRIC_REPRESENTATION_ITEM()
RATIONAL_B_SPLINE_SURFACE(((1.,0.73939111071482,1.),(1.,0.73938749716724,
1.),(1.,0.738423154307972,1.),(1.,0.736495153922513,1.)))
REPRESENTATION_ITEM('')
SURFACE()
);
#2128=(
BOUNDED_SURFACE()
B_SPLINE_SURFACE(3,2,((#137904,#137905,#137906),(#137907,#137908,#137909),
(#137910,#137911,#137912),(#137913,#137914,#137915),(#137916,#137917,#137918),
(#137919,#137920,#137921),(#137922,#137923,#137924),(#137925,#137926,#137927),
(#137928,#137929,#137930),(#137931,#137932,#137933),(#137934,#137935,#137936),
(#137937,#137938,#137939)),.UNSPECIFIED.,.F.,.F.,.F.)
B_SPLINE_SURFACE_WITH_KNOTS((4,2,2,2,2,4),(3,3),(0.00807907499033046,0.00872002967587247,
0.00904050701864348,0.00936098436141448,0.0100019390469565,0.0106428937324985),
(0.,1.),.UNSPECIFIED.)
GEOMETRIC_REPRESENTATION_ITEM()
RATIONAL_B_SPLINE_SURFACE(((1.,0.707106781186548,1.),(1.,0.708291653108703,
1.),(1.,0.709443749235048,1.),(1.,0.71112469687116,1.),(1.,0.711680940824733,
1.),(1.,0.712751570007901,1.),(1.,0.713267249229028,1.),(1.,0.714757432797168,
1.),(1.,0.715686917775259,1.),(1.,0.717310091250008,1.),(1.,0.718010566750711,
1.),(1.,0.718598488256614,1.)))
REPRESENTATION_ITEM('')
SURFACE()
);
#2129=(
BOUNDED_SURFACE()
B_SPLINE_SURFACE(3,2,((#137954,#137955,#137956),(#137957,#137958,#137959),
(#137960,#137961,#137962),(#137963,#137964,#137965)),.UNSPECIFIED.,.F.,
 .F.,.F.)
B_SPLINE_SURFACE_WITH_KNOTS((4,4),(3,3),(0.0283524505452003,0.0289409470909155),
(0.,0.920633110097118),.UNSPECIFIED.)
GEOMETRIC_REPRESENTATION_ITEM()
RATIONAL_B_SPLINE_SURFACE(((1.,0.864312975626627,0.978461885750618),(1.,
0.86308788835206,0.978267423016934),(1.,0.861770510916135,0.978058310717099),
(1.,0.860360064997711,0.977834425305256)))
REPRESENTATION_ITEM('')
SURFACE()
);
#2130=(
BOUNDED_SURFACE()
B_SPLINE_SURFACE(3,2,((#137981,#137982,#137983),(#137984,#137985,#137986),
(#137987,#137988,#137989),(#137990,#137991,#137992),(#137993,#137994,#137995),
(#137996,#137997,#137998),(#137999,#138000,#138001),(#138002,#138003,#138004),
(#138005,#138006,#138007),(#138008,#138009,#138010)),.UNSPECIFIED.,.F.,
 .F.,.F.)
B_SPLINE_SURFACE_WITH_KNOTS((4,2,2,2,4),(3,3),(0.00807856278467327,0.00871080510931882,
0.00934304743396438,0.00997528975860994,0.0106075320832555),(0.,1.),
 .UNSPECIFIED.)
GEOMETRIC_REPRESENTATION_ITEM()
RATIONAL_B_SPLINE_SURFACE(((1.,0.707106781186548,1.),(1.,0.706030220592194,
1.),(1.,0.704978540375902,1.),(1.,0.702923837367757,1.),(1.,0.701922380471311,
1.),(1.,0.700080728636545,1.),(1.,0.699214393311896,1.),(1.,0.697689255248067,
1.),(1.,0.697026914527849,1.),(1.,0.696465765714756,1.)))
REPRESENTATION_ITEM('')
SURFACE()
);
#2131=(
BOUNDED_SURFACE()
B_SPLINE_SURFACE(3,2,((#138152,#138153,#138154),(#138155,#138156,#138157),
(#138158,#138159,#138160),(#138161,#138162,#138163)),.UNSPECIFIED.,.F.,
 .F.,.F.)
B_SPLINE_SURFACE_WITH_KNOTS((4,4),(3,3),(0.00489732211254449,0.00554953903232782),
(0.,1.),.UNSPECIFIED.)
GEOMETRIC_REPRESENTATION_ITEM()
RATIONAL_B_SPLINE_SURFACE(((1.,0.565840417962196,1.),(1.,0.555341099754398,
1.),(1.,0.549566935115175,1.),(1.,0.549598954535096,1.)))
REPRESENTATION_ITEM('')
SURFACE()
);
#2132=(
BOUNDED_SURFACE()
B_SPLINE_SURFACE(3,2,((#138187,#138188,#138189),(#138190,#138191,#138192),
(#138193,#138194,#138195),(#138196,#138197,#138198)),.UNSPECIFIED.,.F.,
 .F.,.F.)
B_SPLINE_SURFACE_WITH_KNOTS((4,4),(3,3),(-6.51926395977061E-5,0.000717119035574751),
(0.,1.00013881592609),.UNSPECIFIED.)
GEOMETRIC_REPRESENTATION_ITEM()
RATIONAL_B_SPLINE_SURFACE(((1.,0.806095432842625,1.00005383408413),(1.,
0.806773570717767,1.00005364581145),(1.,0.803329499666744,1.00005460199528),
(0.999999999999999,0.795829536739348,1.00005668422387)))
REPRESENTATION_ITEM('')
SURFACE()
);
#2133=(
BOUNDED_SURFACE()
B_SPLINE_SURFACE(3,2,((#138272,#138273,#138274),(#138275,#138276,#138277),
(#138278,#138279,#138280),(#138281,#138282,#138283)),.UNSPECIFIED.,.F.,
 .F.,.F.)
B_SPLINE_SURFACE_WITH_KNOTS((4,4),(3,3),(-6.51439314691727E-5,0.000716583246160882),
(0.,1.00012692018127),.UNSPECIFIED.)
GEOMETRIC_REPRESENTATION_ITEM()
RATIONAL_B_SPLINE_SURFACE(((1.,0.620818202688319,1.0000962516449),(1.,0.612618963298309,
1.0000983329428),(1.,0.608569430840875,1.00009936087759),(1.,0.609356995261979,
1.00009916096195)))
REPRESENTATION_ITEM('')
SURFACE()
);
#2134=(
BOUNDED_SURFACE()
B_SPLINE_SURFACE(3,2,((#138369,#138370,#138371),(#138372,#138373,#138374),
(#138375,#138376,#138377),(#138378,#138379,#138380)),.UNSPECIFIED.,.F.,
 .F.,.F.)
B_SPLINE_SURFACE_WITH_KNOTS((4,4),(3,3),(0.,0.00065060314950297),(0.,1.),
 .UNSPECIFIED.)
GEOMETRIC_REPRESENTATION_ITEM()
RATIONAL_B_SPLINE_SURFACE(((1.,0.762081632339421,1.),(1.,0.762075781187422,
1.),(1.,0.760455646763466,1.),(1.,0.757216058458816,1.)))
REPRESENTATION_ITEM('')
SURFACE()
);
#2135=(
BOUNDED_SURFACE()
B_SPLINE_SURFACE(3,2,((#138521,#138522,#138523),(#138524,#138525,#138526),
(#138527,#138528,#138529),(#138530,#138531,#138532),(#138533,#138534,#138535),
(#138536,#138537,#138538),(#138539,#138540,#138541),(#138542,#138543,#138544),
(#138545,#138546,#138547),(#138548,#138549,#138550),(#138551,#138552,#138553),
(#138554,#138555,#138556),(#138557,#138558,#138559),(#138560,#138561,#138562)),
 .UNSPECIFIED.,.F.,.F.,.F.)
B_SPLINE_SURFACE_WITH_KNOTS((4,2,2,2,2,2,4),(3,3),(0.00807895877935271,
0.00883634587130868,0.00921503941728666,0.00959373296326465,0.00997242650924264,
0.0103511200552206,0.0111085071471766),(0.,1.),.UNSPECIFIED.)
GEOMETRIC_REPRESENTATION_ITEM()
RATIONAL_B_SPLINE_SURFACE(((1.,0.707106781186548,1.),(1.,0.708496200821205,
1.),(1.,0.70985049824013,1.),(1.,0.711828637936002,1.),(1.,0.712474210732742,
1.),(1.,0.71370482119381,1.),(1.,0.714294998379545,1.),(1.,0.715424510819791,
1.),(1.,0.715965704866287,1.),(1.,0.716960611510995,1.),(1.,0.71741913219781,
1.),(1.,0.71867831515119,1.),(1.,0.719364099598229,1.),(1.,0.719832136235989,
1.)))
REPRESENTATION_ITEM('')
SURFACE()
);
#2136=(
BOUNDED_SURFACE()
B_SPLINE_SURFACE(3,2,((#138579,#138580,#138581),(#138582,#138583,#138584),
(#138585,#138586,#138587),(#138588,#138589,#138590)),.UNSPECIFIED.,.F.,
 .F.,.F.)
B_SPLINE_SURFACE_WITH_KNOTS((4,4),(3,3),(0.0154746506919765,0.0160816000283851),
(0.0845570889131019,1.),.UNSPECIFIED.)
GEOMETRIC_REPRESENTATION_ITEM()
RATIONAL_B_SPLINE_SURFACE(((0.967520924037566,0.807945871955148,1.),(0.96800421232544,
0.810803635237245,1.),(0.968468725982054,0.813550381031034,1.),(0.968914883389343,
0.81618858329783,1.)))
REPRESENTATION_ITEM('')
SURFACE()
);
#2137=(
BOUNDED_SURFACE()
B_SPLINE_SURFACE(3,2,((#138610,#138611,#138612),(#138613,#138614,#138615),
(#138616,#138617,#138618),(#138619,#138620,#138621),(#138622,#138623,#138624),
(#138625,#138626,#138627),(#138628,#138629,#138630),(#138631,#138632,#138633),
(#138634,#138635,#138636),(#138637,#138638,#138639),(#138640,#138641,#138642),
(#138643,#138644,#138645),(#138646,#138647,#138648),(#138649,#138650,#138651)),
 .UNSPECIFIED.,.F.,.F.,.F.)
B_SPLINE_SURFACE_WITH_KNOTS((4,2,2,2,2,2,4),(3,3),(0.00807922902311453,
0.00881773053780572,0.00918698129515131,0.0095562320524969,0.0099254828098425,
0.0102947335671881,0.0110332350818793),(0.,1.),.UNSPECIFIED.)
GEOMETRIC_REPRESENTATION_ITEM()
RATIONAL_B_SPLINE_SURFACE(((1.,0.707106781186548,1.),(1.,0.705699386801107,
1.),(1.,0.704319784944778,1.),(1.,0.702293838625036,1.),(1.,0.701628229397446,
1.),(1.,0.700355977320158,1.),(1.,0.699743668156969,1.),(1.,0.698567591087498,
1.),(1.,0.698000119405105,1.),(1.,0.696949115865192,1.),(1.,0.696462203809247,
1.),(1.,0.695116916536575,1.),(1.,0.694367821279467,1.),(1.,0.693837065201558,
1.)))
REPRESENTATION_ITEM('')
SURFACE()
);
#2138=(
BOUNDED_SURFACE()
B_SPLINE_SURFACE(3,2,((#138691,#138692,#138693),(#138694,#138695,#138696),
(#138697,#138698,#138699),(#138700,#138701,#138702)),.UNSPECIFIED.,.F.,
 .F.,.F.)
B_SPLINE_SURFACE_WITH_KNOTS((4,4),(3,3),(0.,0.0006503810773206),(0.,1.),
 .UNSPECIFIED.)
GEOMETRIC_REPRESENTATION_ITEM()
RATIONAL_B_SPLINE_SURFACE(((1.,0.667763418073535,1.),(1.,0.665075430476096,
1.),(1.,0.663677894706716,1.),(1.,0.663670476501713,1.)))
REPRESENTATION_ITEM('')
SURFACE()
);
#2139=(
BOUNDED_SURFACE()
B_SPLINE_SURFACE(3,2,((#138804,#138805,#138806),(#138807,#138808,#138809),
(#138810,#138811,#138812),(#138813,#138814,#138815)),.UNSPECIFIED.,.F.,
 .F.,.F.)
B_SPLINE_SURFACE_WITH_KNOTS((4,4),(3,3),(0.,0.000650124307745721),(0.,1.),
 .UNSPECIFIED.)
GEOMETRIC_REPRESENTATION_ITEM()
RATIONAL_B_SPLINE_SURFACE(((1.,0.715240287646145,1.),(1.,0.715239393380683,
1.),(1.,0.714992351911572,1.),(1.,0.71449972514277,1.)))
REPRESENTATION_ITEM('')
SURFACE()
);
#2140=(
BOUNDED_SURFACE()
B_SPLINE_SURFACE(3,2,((#138896,#138897,#138898),(#138899,#138900,#138901),
(#138902,#138903,#138904),(#138905,#138906,#138907),(#138908,#138909,#138910),
(#138911,#138912,#138913),(#138914,#138915,#138916),(#138917,#138918,#138919),
(#138920,#138921,#138922),(#138923,#138924,#138925)),.UNSPECIFIED.,.F.,
 .F.,.F.)
B_SPLINE_SURFACE_WITH_KNOTS((4,2,2,2,4),(3,3),(0.00807569195610403,0.00870260410927289,
0.00932951626244174,0.0099564284156106,0.0105833405687795),(0.,1.),
 .UNSPECIFIED.)
GEOMETRIC_REPRESENTATION_ITEM()
RATIONAL_B_SPLINE_SURFACE(((1.,0.707106781186548,1.),(1.,0.707206112905989,
1.),(1.,0.707302756119535,1.),(1.,0.707490889447615,1.),(1.,0.707582303244654,
1.),(1.,0.707749976398179,1.),(1.,0.707828611057685,1.),(1.,0.70796711497316,
1.),(1.,0.708027180199908,1.),(1.,0.708078164615097,1.)))
REPRESENTATION_ITEM('')
SURFACE()
);
#2141=(
BOUNDED_SURFACE()
B_SPLINE_SURFACE(3,2,((#138938,#138939,#138940),(#138941,#138942,#138943),
(#138944,#138945,#138946),(#138947,#138948,#138949)),.UNSPECIFIED.,.F.,
 .F.,.F.)
B_SPLINE_SURFACE_WITH_KNOTS((4,4),(3,3),(0.0237206528291238,0.0242322821884044),
(0.0789621674491627,1.),.UNSPECIFIED.)
GEOMETRIC_REPRESENTATION_ITEM()
RATIONAL_B_SPLINE_SURFACE(((0.978911250155251,0.866462949751686,1.),(0.978926955451664,
0.866562397986968,1.),(0.9789317875721,0.866592995680722,1.),(0.978925751378407,
0.866554773618892,1.)))
REPRESENTATION_ITEM('')
SURFACE()
);
#2142=(
BOUNDED_SURFACE()
B_SPLINE_SURFACE(3,2,((#138962,#138963,#138964),(#138965,#138966,#138967),
(#138968,#138969,#138970),(#138971,#138972,#138973),(#138974,#138975,#138976),
(#138977,#138978,#138979),(#138980,#138981,#138982),(#138983,#138984,#138985),
(#138986,#138987,#138988),(#138989,#138990,#138991)),.UNSPECIFIED.,.F.,
 .F.,.F.)
B_SPLINE_SURFACE_WITH_KNOTS((4,2,2,2,4),(3,3),(0.00807567041695258,0.00870229794915108,
0.00932892548134959,0.00995555301354809,0.0105821805457466),(0.,1.),
 .UNSPECIFIED.)
GEOMETRIC_REPRESENTATION_ITEM()
RATIONAL_B_SPLINE_SURFACE(((1.,0.707106781186548,1.),(1.,0.707144476742774,
1.),(1.,0.707181156772813,1.),(1.,0.707252569458078,1.),(1.,0.707287275051322,
1.),(1.,0.707350941456054,1.),(1.,0.707380803865577,1.),(1.,0.707433415861318,
1.),(1.,0.707456236659423,1.),(1.,0.707475611987371,1.)))
REPRESENTATION_ITEM('')
SURFACE()
);
#2143=(
BOUNDED_SURFACE()
B_SPLINE_SURFACE(3,2,((#139022,#139023,#139024),(#139025,#139026,#139027),
(#139028,#139029,#139030),(#139031,#139032,#139033)),.UNSPECIFIED.,.F.,
 .F.,.F.)
B_SPLINE_SURFACE_WITH_KNOTS((4,4),(3,3),(0.,0.000650121463573334),(0.,1.),
 .UNSPECIFIED.)
GEOMETRIC_REPRESENTATION_ITEM()
RATIONAL_B_SPLINE_SURFACE(((1.,0.713284154090124,1.),(1.,0.713692564168438,
1.),(1.,0.713902215282654,1.),(1.,0.713903527556066,1.)))
REPRESENTATION_ITEM('')
SURFACE()
);
#2144=(
BOUNDED_SURFACE()
B_SPLINE_SURFACE(3,2,((#139104,#139105,#139106),(#139107,#139108,#139109),
(#139110,#139111,#139112),(#139113,#139114,#139115)),.UNSPECIFIED.,.F.,
 .F.,.F.)
B_SPLINE_SURFACE_WITH_KNOTS((4,4),(3,3),(0.,0.000650359837711272),(0.,1.),
 .UNSPECIFIED.)
GEOMETRIC_REPRESENTATION_ITEM()
RATIONAL_B_SPLINE_SURFACE(((1.,0.665108204576639,1.),(1.,0.66511166059484,
1.),(1.,0.666441892349684,1.),(1.,0.669061697655964,1.)))
REPRESENTATION_ITEM('')
SURFACE()
);
#2145=(
BOUNDED_SURFACE()
B_SPLINE_SURFACE(3,2,((#139241,#139242,#139243),(#139244,#139245,#139246),
(#139247,#139248,#139249),(#139250,#139251,#139252),(#139253,#139254,#139255),
(#139256,#139257,#139258),(#139259,#139260,#139261),(#139262,#139263,#139264),
(#139265,#139266,#139267),(#139268,#139269,#139270),(#139271,#139272,#139273),
(#139274,#139275,#139276),(#139277,#139278,#139279),(#139280,#139281,#139282)),
 .UNSPECIFIED.,.F.,.F.,.F.)
B_SPLINE_SURFACE_WITH_KNOTS((4,2,2,2,2,2,4),(3,3),(0.00807931853788568,
0.00881187542632408,0.00917815387054328,0.00954443231476248,0.00991071075898168,
0.0102769892032009,0.0110095460916393),(0.,1.),.UNSPECIFIED.)
GEOMETRIC_REPRESENTATION_ITEM()
RATIONAL_B_SPLINE_SURFACE(((1.,0.707106781186552,1.),(1.,0.705694108475444,
1.),(1.,0.704309639709031,1.),(1.,0.702276829363826,1.),(1.,0.701608277715413,
1.),(1.,0.700330266875156,1.),(1.,0.699715065357364,1.),(1.,0.698533028725346,
1.),(1.,0.697962156582885,1.),(1.,0.696902668323859,1.),(1.,0.696411414935025,
1.),(1.,0.695052392645847,1.),(1.,0.69429223033984,1.),(1.,0.69374733452232,
1.)))
REPRESENTATION_ITEM('')
SURFACE()
);
#2146=(
BOUNDED_SURFACE()
B_SPLINE_SURFACE(3,2,((#139299,#139300,#139301),(#139302,#139303,#139304),
(#139305,#139306,#139307),(#139308,#139309,#139310)),.UNSPECIFIED.,.F.,
 .F.,.F.)
B_SPLINE_SURFACE_WITH_KNOTS((4,4),(3,3),(0.0318721040045715,0.0324798405467945),
(0.0842204782052437,1.),.UNSPECIFIED.)
GEOMETRIC_REPRESENTATION_ITEM()
RATIONAL_B_SPLINE_SURFACE(((0.96952117077485,0.819053335514945,1.),(0.96908988447244,
0.816492875686171,1.),(0.968640411425079,0.813824444819121,1.),(0.968172353055208,
0.811045676639188,1.)))
REPRESENTATION_ITEM('')
SURFACE()
);
#2147=(
BOUNDED_SURFACE()
B_SPLINE_SURFACE(3,2,((#139330,#139331,#139332),(#139333,#139334,#139335),
(#139336,#139337,#139338),(#139339,#139340,#139341),(#139342,#139343,#139344),
(#139345,#139346,#139347),(#139348,#139349,#139350),(#139351,#139352,#139353),
(#139354,#139355,#139356),(#139357,#139358,#139359),(#139360,#139361,#139362),
(#139363,#139364,#139365),(#139366,#139367,#139368),(#139369,#139370,#139371)),
 .UNSPECIFIED.,.F.,.F.,.F.)
B_SPLINE_SURFACE_WITH_KNOTS((4,2,2,2,2,2,4),(3,3),(0.00807909221698663,
0.00882982802565525,0.00920519592998956,0.00958056383432386,0.00995593173865817,
0.0103312996429925,0.0110820354516611),(0.,1.),.UNSPECIFIED.)
GEOMETRIC_REPRESENTATION_ITEM()
RATIONAL_B_SPLINE_SURFACE(((1.,0.707106781186556,1.),(1.,0.708510771074171,
1.),(1.,0.709878889431803,1.),(1.,0.711876867675041,1.),(1.,0.712529775389558,
1.),(1.,0.713774284861137,1.),(1.,0.714371256763372,1.),(1.,0.715514222535529,
1.),(1.,0.716062813357328,1.),(1.,0.717072969030255,1.),(1.,0.717538977439758,
1.),(1.,0.718820706504871,1.),(1.,0.719523481892828,1.),(1.,0.720009098745653,
1.)))
REPRESENTATION_ITEM('')
SURFACE()
);
#2148=(
BOUNDED_SURFACE()
B_SPLINE_SURFACE(3,2,((#139411,#139412,#139413),(#139414,#139415,#139416),
(#139417,#139418,#139419),(#139420,#139421,#139422)),.UNSPECIFIED.,.F.,
 .F.,.F.)
B_SPLINE_SURFACE_WITH_KNOTS((4,4),(3,3),(-6.50587846610038E-5,0.000715646631271042),
(0.,1.00019802018696),.UNSPECIFIED.)
GEOMETRIC_REPRESENTATION_ITEM()
RATIONAL_B_SPLINE_SURFACE(((1.,0.755032712249889,1.00009701693624),(1.,
0.75916874975514,1.0000953788984),(1.,0.761106752395798,1.00009461137111),
(1.,0.760734912009425,1.00009475863492)))
REPRESENTATION_ITEM('')
SURFACE()
);
#2149=(
BOUNDED_SURFACE()
B_SPLINE_SURFACE(3,2,((#139534,#139535,#139536),(#139537,#139538,#139539),
(#139540,#139541,#139542),(#139543,#139544,#139545)),.UNSPECIFIED.,.F.,
 .F.,.F.)
B_SPLINE_SURFACE_WITH_KNOTS((4,4),(3,3),(-6.5137241604418E-5,0.000716509657648589),
(0.,1.00012888352926),.UNSPECIFIED.)
GEOMETRIC_REPRESENTATION_ITEM()
RATIONAL_B_SPLINE_SURFACE(((1.,0.610922104164594,1.00010029146475),(1.,
0.610147227047923,1.00010049120254),(1.,0.614050298485334,1.0000994851193),
(1.,0.622205101827845,1.00009738307963)))
REPRESENTATION_ITEM('')
SURFACE()
);
#2150=(
BOUNDED_SURFACE()
B_SPLINE_SURFACE(3,2,((#139622,#139623,#139624),(#139625,#139626,#139627),
(#139628,#139629,#139630),(#139631,#139632,#139633)),.UNSPECIFIED.,.F.,
 .F.,.F.)
B_SPLINE_SURFACE_WITH_KNOTS((4,4),(3,3),(-6.51913040321435E-5,0.00071710434435357),
(0.,1.00014170095501),.UNSPECIFIED.)
GEOMETRIC_REPRESENTATION_ITEM()
RATIONAL_B_SPLINE_SURFACE(((1.,0.794778369766658,1.00005816020198),(1.,
0.80210956676765,1.00005608252675),(1.,0.805580179391815,1.0000550989485),
(1.,0.804911641151859,1.00005528841352)))
REPRESENTATION_ITEM('')
SURFACE()
);
#2151=(
BOUNDED_SURFACE()
B_SPLINE_SURFACE(3,2,((#139715,#139716,#139717),(#139718,#139719,#139720),
(#139721,#139722,#139723),(#139724,#139725,#139726)),.UNSPECIFIED.,.F.,
 .F.,.F.)
B_SPLINE_SURFACE_WITH_KNOTS((4,4),(3,3),(-3.67368196064713E-5,0.0006901971826107),
(0.,1.00003673681961),.UNSPECIFIED.)
GEOMETRIC_REPRESENTATION_ITEM()
RATIONAL_B_SPLINE_SURFACE(((1.,0.551374288254534,1.00003296216369),(1.,
0.550645752158029,1.00003301569188),(1.,0.556973926885096,1.00003255073786),
(0.999999999999999,0.569158328192581,1.00003165550555)))
REPRESENTATION_ITEM('')
SURFACE()
);
#2152=(
BOUNDED_SURFACE()
B_SPLINE_SURFACE(3,2,((#139820,#139821,#139822),(#139823,#139824,#139825),
(#139826,#139827,#139828),(#139829,#139830,#139831),(#139832,#139833,#139834),
(#139835,#139836,#139837),(#139838,#139839,#139840),(#139841,#139842,#139843),
(#139844,#139845,#139846),(#139847,#139848,#139849)),.UNSPECIFIED.,.F.,
 .F.,.F.)
B_SPLINE_SURFACE_WITH_KNOTS((4,2,2,2,4),(3,3),(1.18015353016497E-15,0.392699081698726,
0.785398163397449,1.17809724509617,1.5707963267949),(0.,1.),
 .UNSPECIFIED.)
GEOMETRIC_REPRESENTATION_ITEM()
RATIONAL_B_SPLINE_SURFACE(((1.,0.67559020761567,1.),(1.,0.675585785528194,
1.),(1.,0.676431027860885,1.),(1.,0.679650528045421,1.),(1.,0.682027045382314,
1.),(1.,0.687915714942951,1.),(1.,0.691424416305301,1.),(1.,0.699004971484679,
1.),(1.,0.703073130220216,1.),(1.,0.707106781186548,1.)))
REPRESENTATION_ITEM('')
SURFACE()
);
#2153=(
BOUNDED_SURFACE()
B_SPLINE_SURFACE(3,2,((#139862,#139863,#139864),(#139865,#139866,#139867),
(#139868,#139869,#139870),(#139871,#139872,#139873),(#139874,#139875,#139876),
(#139877,#139878,#139879),(#139880,#139881,#139882),(#139883,#139884,#139885),
(#139886,#139887,#139888),(#139889,#139890,#139891)),.UNSPECIFIED.,.F.,
 .F.,.F.)
B_SPLINE_SURFACE_WITH_KNOTS((4,2,2,2,4),(3,3),(4.71238898038469,5.10508806208341,
5.49778714378214,5.89048622548086,6.28318530717959),(0.,1.),
 .UNSPECIFIED.)
GEOMETRIC_REPRESENTATION_ITEM()
RATIONAL_B_SPLINE_SURFACE(((1.,0.707106781186548,1.),(1.,0.71114164850559,
1.),(1.,0.71513624913423,1.),(1.,0.722468048845566,1.),(1.,0.725801833007554,
1.),(1.,0.731338116836806,1.),(1.,0.733539335051299,1.),(1.,0.736509240245015,
1.),(1.,0.737280525008035,1.),(1.,0.73727733681012,1.)))
REPRESENTATION_ITEM('')
SURFACE()
);
#2154=(
BOUNDED_SURFACE()
B_SPLINE_SURFACE(3,2,((#140139,#140140,#140141),(#140142,#140143,#140144),
(#140145,#140146,#140147),(#140148,#140149,#140150),(#140151,#140152,#140153),
(#140154,#140155,#140156),(#140157,#140158,#140159),(#140160,#140161,#140162),
(#140163,#140164,#140165),(#140166,#140167,#140168)),.UNSPECIFIED.,.F.,
 .F.,.F.)
B_SPLINE_SURFACE_WITH_KNOTS((4,2,2,2,4),(3,3),(4.71238898038469,5.10508806208342,
5.49778714378214,5.89048622548086,6.28318530717959),(0.,1.),
 .UNSPECIFIED.)
GEOMETRIC_REPRESENTATION_ITEM()
RATIONAL_B_SPLINE_SURFACE(((1.,0.707106781186548,1.),(1.,0.711141648505921,
1.),(1.,0.715136249133786,1.),(1.,0.722468048846019,1.),(1.,0.725801833007554,
1.),(1.,0.731338116836806,1.),(1.,0.733539335051135,1.),(1.,0.736509240245178,
1.),(1.,0.737280525007913,1.),(1.,0.73727733681012,1.)))
REPRESENTATION_ITEM('')
SURFACE()
);
#2155=(
BOUNDED_SURFACE()
B_SPLINE_SURFACE(3,2,((#140170,#140171,#140172),(#140173,#140174,#140175),
(#140176,#140177,#140178),(#140179,#140180,#140181),(#140182,#140183,#140184),
(#140185,#140186,#140187)),.UNSPECIFIED.,.F.,.F.,.F.)
B_SPLINE_SURFACE_WITH_KNOTS((4,2,4),(3,3),(0.,0.00070803381389838,0.00141606762779676),
(0.,1.),.UNSPECIFIED.)
GEOMETRIC_REPRESENTATION_ITEM()
RATIONAL_B_SPLINE_SURFACE(((1.,0.800108937437262,1.),(1.,0.794442999342884,
1.),(1.,0.785169683107043,1.),(1.,0.763289065038484,1.),(1.,0.750458153314313,
1.),(1.,0.737277336810115,1.)))
REPRESENTATION_ITEM('')
SURFACE()
);
#2156=(
BOUNDED_SURFACE()
B_SPLINE_SURFACE(3,2,((#140318,#140319,#140320),(#140321,#140322,#140323),
(#140324,#140325,#140326),(#140327,#140328,#140329),(#140330,#140331,#140332),
(#140333,#140334,#140335),(#140336,#140337,#140338),(#140339,#140340,#140341),
(#140342,#140343,#140344),(#140345,#140346,#140347)),.UNSPECIFIED.,.F.,
 .F.,.F.)
B_SPLINE_SURFACE_WITH_KNOTS((4,2,2,2,4),(3,3),(0.,0.392699081698724,0.785398163397448,
1.17809724509617,1.5707963267949),(0.,1.),.UNSPECIFIED.)
GEOMETRIC_REPRESENTATION_ITEM()
RATIONAL_B_SPLINE_SURFACE(((1.,0.67559020761567,1.),(1.,0.675585785528568,
1.),(1.,0.676431027860386,1.),(1.,0.679650528045925,1.),(1.,0.682027045382314,
1.),(1.,0.687915714942951,1.),(1.,0.69142441630529,1.),(1.,0.69900497148469,
1.),(1.,0.703073130220208,1.),(1.,0.707106781186548,1.)))
REPRESENTATION_ITEM('')
SURFACE()
);
#2157=(
BOUNDED_SURFACE()
B_SPLINE_SURFACE(3,2,((#140602,#140603,#140604),(#140605,#140606,#140607),
(#140608,#140609,#140610),(#140611,#140612,#140613),(#140614,#140615,#140616),
(#140617,#140618,#140619),(#140620,#140621,#140622),(#140623,#140624,#140625),
(#140626,#140627,#140628),(#140629,#140630,#140631)),.UNSPECIFIED.,.F.,
 .F.,.F.)
B_SPLINE_SURFACE_WITH_KNOTS((4,2,2,2,4),(3,3),(3.1415926535898,3.53429173528852,
3.92699081698724,4.31968989868597,4.71238898038469),(0.,1.),
 .UNSPECIFIED.)
GEOMETRIC_REPRESENTATION_ITEM()
RATIONAL_B_SPLINE_SURFACE(((1.,0.737277336810125,1.),(1.,0.737280525008216,
1.),(1.,0.736509240244793,1.),(1.,0.733539335051535,1.),(1.,0.731338116837053,
1.),(1.,0.725801833007317,1.),(1.,0.722468048845379,1.),(1.,0.715136249134436,
1.),(1.,0.711141648505436,1.),(1.,0.707106781186548,1.)))
REPRESENTATION_ITEM('')
SURFACE()
);
#2158=(
BOUNDED_SURFACE()
B_SPLINE_SURFACE(3,2,((#140644,#140645,#140646),(#140647,#140648,#140649),
(#140650,#140651,#140652),(#140653,#140654,#140655),(#140656,#140657,#140658),
(#140659,#140660,#140661),(#140662,#140663,#140664),(#140665,#140666,#140667),
(#140668,#140669,#140670),(#140671,#140672,#140673)),.UNSPECIFIED.,.F.,
 .F.,.F.)
B_SPLINE_SURFACE_WITH_KNOTS((4,2,2,2,4),(3,3),(1.5707963267949,1.96349540849362,
2.35619449019234,2.74889357189106,3.14159265358979),(0.,1.),
 .UNSPECIFIED.)
GEOMETRIC_REPRESENTATION_ITEM()
RATIONAL_B_SPLINE_SURFACE(((1.,0.707106781186548,1.),(1.,0.703073130219847,
1.),(1.,0.699004971485165,1.),(1.,0.691424416304824,1.),(1.,0.687915714942826,
1.),(1.,0.682027045382428,1.),(1.,0.679650528045614,1.),(1.,0.676431027860685,
1.),(1.,0.675585785528338,1.),(1.,0.675590207615664,1.)))
REPRESENTATION_ITEM('')
SURFACE()
);
#2159=(
BOUNDED_SURFACE()
B_SPLINE_SURFACE(3,2,((#140835,#140836,#140837),(#140838,#140839,#140840),
(#140841,#140842,#140843),(#140844,#140845,#140846),(#140847,#140848,#140849),
(#140850,#140851,#140852),(#140853,#140854,#140855),(#140856,#140857,#140858),
(#140859,#140860,#140861),(#140862,#140863,#140864),(#140865,#140866,#140867),
(#140868,#140869,#140870)),.UNSPECIFIED.,.F.,.F.,.F.)
B_SPLINE_SURFACE_WITH_KNOTS((4,2,2,2,2,4),(3,3),(0.00373720614906648,0.00431441150266452,
0.00489161685626256,0.00518021953306157,0.00546882220986059,0.00604602756345863),
(0.,1.),.UNSPECIFIED.)
GEOMETRIC_REPRESENTATION_ITEM()
RATIONAL_B_SPLINE_SURFACE(((1.,0.702399276808564,1.),(1.,0.697901374758016,
1.),(1.,0.693446103155503,1.),(1.,0.685742881148842,1.),(1.,0.682394877642487,
1.),(1.,0.6786862147386,1.),(1.,0.677675780152448,1.),(1.,0.676083839724519,
1.),(1.,0.675500346164623,1.),(1.,0.674441428307327,1.),(1.,0.674627601820987,
1.),(1.,0.675590207615657,1.)))
REPRESENTATION_ITEM('')
SURFACE()
);
#2160=(
BOUNDED_SURFACE()
B_SPLINE_SURFACE(3,2,((#140872,#140873,#140874),(#140875,#140876,#140877),
(#140878,#140879,#140880),(#140881,#140882,#140883),(#140884,#140885,#140886),
(#140887,#140888,#140889),(#140890,#140891,#140892),(#140893,#140894,#140895),
(#140896,#140897,#140898),(#140899,#140900,#140901)),.UNSPECIFIED.,.F.,
 .F.,.F.)
B_SPLINE_SURFACE_WITH_KNOTS((4,2,2,2,4),(3,3),(1.5707963267949,1.96349540849362,
2.35619449019234,2.74889357189107,3.1415926535898),(0.,1.),
 .UNSPECIFIED.)
GEOMETRIC_REPRESENTATION_ITEM()
RATIONAL_B_SPLINE_SURFACE(((1.,0.707106781186548,1.),(1.,0.711141648505595,
1.),(1.,0.715136249134216,1.),(1.,0.722468048845599,1.),(1.,0.725801833007891,
1.),(1.,0.731338116836469,1.),(1.,0.733539335051304,1.),(1.,0.73650924024502,
1.),(1.,0.737280525008041,1.),(1.,0.737277336810125,1.)))
REPRESENTATION_ITEM('')
SURFACE()
);
#2161=(
BOUNDED_SURFACE()
B_SPLINE_SURFACE(3,2,((#140998,#140999,#141000),(#141001,#141002,#141003),
(#141004,#141005,#141006),(#141007,#141008,#141009),(#141010,#141011,#141012),
(#141013,#141014,#141015),(#141016,#141017,#141018),(#141019,#141020,#141021),
(#141022,#141023,#141024),(#141025,#141026,#141027)),.UNSPECIFIED.,.F.,
 .F.,.F.)
B_SPLINE_SURFACE_WITH_KNOTS((4,2,2,2,4),(3,3),(-1.77635683940025E-15,0.392699081698723,
0.785398163397447,1.17809724509617,1.5707963267949),(0.,1.),
 .UNSPECIFIED.)
GEOMETRIC_REPRESENTATION_ITEM()
RATIONAL_B_SPLINE_SURFACE(((1.,0.675590207615668,1.),(1.,0.675585785528724,
1.),(1.,0.676431027860173,1.),(1.,0.679650528046127,1.),(1.,0.682027045382925,
1.),(1.,0.687915714942339,1.),(1.,0.69142441630503,1.),(1.,0.699004971484955,
1.),(1.,0.703073130220009,1.),(1.,0.70710678118655,1.)))
REPRESENTATION_ITEM('')
SURFACE()
);
#2162=(
BOUNDED_SURFACE()
B_SPLINE_SURFACE(3,2,((#141040,#141041,#141042),(#141043,#141044,#141045),
(#141046,#141047,#141048),(#141049,#141050,#141051),(#141052,#141053,#141054),
(#141055,#141056,#141057),(#141058,#141059,#141060),(#141061,#141062,#141063),
(#141064,#141065,#141066),(#141067,#141068,#141069)),.UNSPECIFIED.,.F.,
 .F.,.F.)
B_SPLINE_SURFACE_WITH_KNOTS((4,2,2,2,4),(3,3),(4.71238898038469,5.10508806208342,
5.49778714378214,5.89048622548086,6.28318530717959),(0.,1.),
 .UNSPECIFIED.)
GEOMETRIC_REPRESENTATION_ITEM()
RATIONAL_B_SPLINE_SURFACE(((1.,0.707106781186545,1.),(1.,0.711141648505882,
1.),(1.,0.715136249133832,1.),(1.,0.722468048845978,1.),(1.,0.725801833007229,
1.),(1.,0.731338116837136,1.),(1.,0.733539335051522,1.),(1.,0.736509240244802,
1.),(1.,0.737280525008203,1.),(1.,0.737277336810123,1.)))
REPRESENTATION_ITEM('')
SURFACE()
);
#2163=(
BOUNDED_SURFACE()
B_SPLINE_SURFACE(3,2,((#141204,#141205,#141206),(#141207,#141208,#141209),
(#141210,#141211,#141212),(#141213,#141214,#141215),(#141216,#141217,#141218),
(#141219,#141220,#141221),(#141222,#141223,#141224),(#141225,#141226,#141227),
(#141228,#141229,#141230),(#141231,#141232,#141233)),.UNSPECIFIED.,.F.,
 .F.,.F.)
B_SPLINE_SURFACE_WITH_KNOTS((4,2,2,2,4),(3,3),(4.71238898038469,5.10508806208342,
5.49778714378214,5.89048622548086,6.28318530717959),(0.,1.),
 .UNSPECIFIED.)
GEOMETRIC_REPRESENTATION_ITEM()
RATIONAL_B_SPLINE_SURFACE(((1.,0.707106781186545,1.),(1.,0.711141648505767,
1.),(1.,0.715136249133983,1.),(1.,0.722468048845823,1.),(1.,0.725801833007033,
1.),(1.,0.731338116837333,1.),(1.,0.73353933505153,1.),(1.,0.736509240244789,
1.),(1.,0.737280525008216,1.),(1.,0.737277336810123,1.)))
REPRESENTATION_ITEM('')
SURFACE()
);
#2164=(
BOUNDED_SURFACE()
B_SPLINE_SURFACE(3,2,((#141417,#141418,#141419),(#141420,#141421,#141422),
(#141423,#141424,#141425),(#141426,#141427,#141428)),.UNSPECIFIED.,.F.,
 .F.,.F.)
B_SPLINE_SURFACE_WITH_KNOTS((4,4),(3,3),(-5.74627151417317E-18,0.000655078443521525),
(0.,1.),.UNSPECIFIED.)
GEOMETRIC_REPRESENTATION_ITEM()
RATIONAL_B_SPLINE_SURFACE(((1.,0.773398994756356,1.),(1.,0.76231666392952,
1.),(1.,0.750153503473797,1.),(1.,0.737277336810164,1.)))
REPRESENTATION_ITEM('')
SURFACE()
);
#2165=(
BOUNDED_SURFACE()
B_SPLINE_SURFACE(3,2,((#141430,#141431,#141432),(#141433,#141434,#141435),
(#141436,#141437,#141438),(#141439,#141440,#141441)),.UNSPECIFIED.,.F.,
 .F.,.F.)
B_SPLINE_SURFACE_WITH_KNOTS((4,4),(3,3),(-8.23993651088983E-18,0.000144871551798125),
(0.,0.546238879221174),.UNSPECIFIED.)
GEOMETRIC_REPRESENTATION_ITEM()
RATIONAL_B_SPLINE_SURFACE(((1.,0.941669523342704,0.947063795072844),(1.,
0.94316141436526,0.948417719357794),(1.,0.944606420735039,0.949729094777561),
(1.,0.946004055482066,0.950997479396062)))
REPRESENTATION_ITEM('')
SURFACE()
);
#2166=(
BOUNDED_SURFACE()
B_SPLINE_SURFACE(3,2,((#141468,#141469,#141470),(#141471,#141472,#141473),
(#141474,#141475,#141476),(#141477,#141478,#141479),(#141480,#141481,#141482),
(#141483,#141484,#141485),(#141486,#141487,#141488),(#141489,#141490,#141491),
(#141492,#141493,#141494),(#141495,#141496,#141497)),.UNSPECIFIED.,.F.,
 .F.,.F.)
B_SPLINE_SURFACE_WITH_KNOTS((4,2,2,2,4),(3,3),(-1.77635683940025E-15,0.392699081698723,
0.785398163397447,1.17809724509617,1.5707963267949),(0.,1.),
 .UNSPECIFIED.)
GEOMETRIC_REPRESENTATION_ITEM()
RATIONAL_B_SPLINE_SURFACE(((1.,0.675590207615662,1.),(1.,0.675585785528387,
1.),(1.,0.676431027860615,1.),(1.,0.679650528045674,1.),(1.,0.682027045382935,
1.),(1.,0.687915714942327,1.),(1.,0.691424416304369,1.),(1.,0.699004971485606,
1.),(1.,0.703073130219524,1.),(1.,0.707106781186548,1.)))
REPRESENTATION_ITEM('')
SURFACE()
);
#2167=(
BOUNDED_SURFACE()
B_SPLINE_SURFACE(3,2,((#141760,#141761,#141762),(#141763,#141764,#141765),
(#141766,#141767,#141768),(#141769,#141770,#141771),(#141772,#141773,#141774),
(#141775,#141776,#141777)),.UNSPECIFIED.,.F.,.F.,.F.)
B_SPLINE_SURFACE_WITH_KNOTS((4,2,4),(3,3),(0.00432986646256736,0.00505584518302534,
0.00578182390348332),(0.,1.),.UNSPECIFIED.)
GEOMETRIC_REPRESENTATION_ITEM()
RATIONAL_B_SPLINE_SURFACE(((1.,0.737277336810087,1.),(1.,0.750110373322841,
1.),(1.,0.762782449795825,1.),(1.,0.783852338027907,1.),(1.,0.792419881107176,
1.),(1.,0.79736306112227,1.)))
REPRESENTATION_ITEM('')
SURFACE()
);
#2168=(
BOUNDED_SURFACE()
B_SPLINE_SURFACE(3,2,((#141903,#141904,#141905),(#141906,#141907,#141908),
(#141909,#141910,#141911),(#141912,#141913,#141914),(#141915,#141916,#141917),
(#141918,#141919,#141920),(#141921,#141922,#141923),(#141924,#141925,#141926),
(#141927,#141928,#141929),(#141930,#141931,#141932)),.UNSPECIFIED.,.F.,
 .F.,.F.)
B_SPLINE_SURFACE_WITH_KNOTS((4,2,2,2,4),(3,3),(3.1415926535898,3.53429173528852,
3.92699081698724,4.31968989868597,4.71238898038469),(0.,1.),
 .UNSPECIFIED.)
GEOMETRIC_REPRESENTATION_ITEM()
RATIONAL_B_SPLINE_SURFACE(((1.,0.73727733681012,1.),(1.,0.737280525007918,
1.),(1.,0.736509240245177,1.),(1.,0.733539335051133,1.),(1.,0.731338116836513,
1.),(1.,0.725801833007847,1.),(1.,0.722468048844965,1.),(1.,0.715136249134831,
1.),(1.,0.711141648505139,1.),(1.,0.707106781186548,1.)))
REPRESENTATION_ITEM('')
SURFACE()
);
#2169=(
BOUNDED_SURFACE()
B_SPLINE_SURFACE(3,2,((#142170,#142171,#142172),(#142173,#142174,#142175),
(#142176,#142177,#142178),(#142179,#142180,#142181),(#142182,#142183,#142184),
(#142185,#142186,#142187),(#142188,#142189,#142190),(#142191,#142192,#142193),
(#142194,#142195,#142196),(#142197,#142198,#142199)),.UNSPECIFIED.,.F.,
 .F.,.F.)
B_SPLINE_SURFACE_WITH_KNOTS((4,2,2,2,4),(3,3),(1.5707963267949,1.96349540849362,
2.35619449019234,2.74889357189107,3.14159265358979),(0.,1.),
 .UNSPECIFIED.)
GEOMETRIC_REPRESENTATION_ITEM()
RATIONAL_B_SPLINE_SURFACE(((1.,0.707106781186548,1.),(1.,0.703073130219484,
1.),(1.,0.699004971485652,1.),(1.,0.691424416304328,1.),(1.,0.687915714942076,
1.),(1.,0.682027045383186,1.),(1.,0.679650528045925,1.),(1.,0.676431027860385,
1.),(1.,0.675585785528569,1.),(1.,0.67559020761567,1.)))
REPRESENTATION_ITEM('')
SURFACE()
);
#2170=(
BOUNDED_SURFACE()
B_SPLINE_SURFACE(3,2,((#142207,#142208,#142209),(#142210,#142211,#142212),
(#142213,#142214,#142215),(#142216,#142217,#142218),(#142219,#142220,#142221),
(#142222,#142223,#142224),(#142225,#142226,#142227),(#142228,#142229,#142230),
(#142231,#142232,#142233),(#142234,#142235,#142236)),.UNSPECIFIED.,.F.,
 .F.,.F.)
B_SPLINE_SURFACE_WITH_KNOTS((4,2,2,2,4),(3,3),(3.1415926535898,3.53429173528852,
3.92699081698724,4.31968989868597,4.71238898038469),(0.,1.),
 .UNSPECIFIED.)
GEOMETRIC_REPRESENTATION_ITEM()
RATIONAL_B_SPLINE_SURFACE(((1.,0.73727733681012,1.),(1.,0.737280525007918,
1.),(1.,0.736509240245186,1.),(1.,0.733539335051142,1.),(1.,0.731338116837293,
1.),(1.,0.725801833007076,1.),(1.,0.722468048845319,1.),(1.,0.715136249134486,
1.),(1.,0.711141648505406,1.),(1.,0.707106781186552,1.)))
REPRESENTATION_ITEM('')
SURFACE()
);
#2171=(
BOUNDED_SURFACE()
B_SPLINE_SURFACE(3,2,((#142380,#142381,#142382),(#142383,#142384,#142385),
(#142386,#142387,#142388),(#142389,#142390,#142391),(#142392,#142393,#142394),
(#142395,#142396,#142397),(#142398,#142399,#142400),(#142401,#142402,#142403),
(#142404,#142405,#142406),(#142407,#142408,#142409)),.UNSPECIFIED.,.F.,
 .F.,.F.)
B_SPLINE_SURFACE_WITH_KNOTS((4,2,2,2,4),(3,3),(1.5707963267949,1.96349540849362,
2.35619449019234,2.74889357189107,3.14159265358979),(0.,1.),
 .UNSPECIFIED.)
GEOMETRIC_REPRESENTATION_ITEM()
RATIONAL_B_SPLINE_SURFACE(((1.,0.707106781186543,1.),(1.,0.703073130219691,
1.),(1.,0.699004971485369,1.),(1.,0.691424416304591,1.),(1.,0.687915714942475,
1.),(1.,0.682027045382777,1.),(1.,0.679650528045923,1.),(1.,0.676431027860383,
1.),(1.,0.675585785528567,1.),(1.,0.675590207615659,1.)))
REPRESENTATION_ITEM('')
SURFACE()
);
#2172=(
BOUNDED_SURFACE()
B_SPLINE_SURFACE(2,2,((#142574,#142575,#142576),(#142577,#142578,#142579),
(#142580,#142581,#142582)),.UNSPECIFIED.,.F.,.F.,.F.)
B_SPLINE_SURFACE_WITH_KNOTS((3,3),(3,3),(-1.5707963267949,-1.75915766232281E-16),
(2.36370134837197,3.14159265358979),.UNSPECIFIED.)
GEOMETRIC_REPRESENTATION_ITEM()
RATIONAL_B_SPLINE_SURFACE(((1.,0.925309396359852,1.),(0.707106781186554,
0.654292548861688,0.707106781186554),(1.,0.925309396359852,1.)))
REPRESENTATION_ITEM('')
SURFACE()
);
#2173=(
BOUNDED_SURFACE()
B_SPLINE_SURFACE(2,2,((#142590,#142591,#142592),(#142593,#142594,#142595),
(#142596,#142597,#142598)),.UNSPECIFIED.,.F.,.F.,.F.)
B_SPLINE_SURFACE_WITH_KNOTS((3,3),(3,3),(-1.5707963267949,0.),(1.5707963267949,
2.40432329481773),.UNSPECIFIED.)
GEOMETRIC_REPRESENTATION_ITEM()
RATIONAL_B_SPLINE_SURFACE(((1.,0.914403878918655,1.),(0.707106781186554,
0.64658118352667,0.707106781186554),(1.,0.914403878918655,1.)))
REPRESENTATION_ITEM('')
SURFACE()
);
#2174=(
BOUNDED_SURFACE()
B_SPLINE_SURFACE(3,2,((#142680,#142681,#142682),(#142683,#142684,#142685),
(#142686,#142687,#142688),(#142689,#142690,#142691),(#142692,#142693,#142694),
(#142695,#142696,#142697),(#142698,#142699,#142700),(#142701,#142702,#142703),
(#142704,#142705,#142706),(#142707,#142708,#142709)),.UNSPECIFIED.,.F.,
 .F.,.F.)
B_SPLINE_SURFACE_WITH_KNOTS((4,2,2,2,4),(3,3),(0.00328497804042337,0.00367780251889487,
0.00407062699736637,0.00446345147583787,0.00485627595430937),(0.,1.),
 .UNSPECIFIED.)
GEOMETRIC_REPRESENTATION_ITEM()
RATIONAL_B_SPLINE_SURFACE(((1.,0.801783725737274,1.),(1.,0.801875346909261,
1.),(1.,0.796940392589261,1.),(1.,0.780100098278086,1.),(1.,0.768150144755555,
1.),(1.,0.743627445145758,1.),(1.,0.730956034974261,1.),(1.,0.712691010436091,
1.),(1.,0.706946596929733,1.),(1.,0.707106781186548,1.)))
REPRESENTATION_ITEM('')
SURFACE()
);
#2175=(
BOUNDED_SURFACE()
B_SPLINE_SURFACE(3,2,((#142721,#142722,#142723),(#142724,#142725,#142726),
(#142727,#142728,#142729),(#142730,#142731,#142732),(#142733,#142734,#142735),
(#142736,#142737,#142738)),.UNSPECIFIED.,.F.,.F.,.F.)
B_SPLINE_SURFACE_WITH_KNOTS((4,2,4),(3,3),(-1.97866896478604E-18,0.00038804539867497,
0.000776090797349943),(0.,1.),.UNSPECIFIED.)
GEOMETRIC_REPRESENTATION_ITEM()
RATIONAL_B_SPLINE_SURFACE(((1.,0.889512696472455,1.),(1.,0.863343118435834,
1.),(1.,0.832896241151233,1.),(1.,0.770252595987774,1.),(1.,0.738321744191135,
1.),(1.,0.707106781186616,1.)))
REPRESENTATION_ITEM('')
SURFACE()
);
#2176=(
BOUNDED_SURFACE()
B_SPLINE_SURFACE(3,2,((#142752,#142753,#142754),(#142755,#142756,#142757),
(#142758,#142759,#142760),(#142761,#142762,#142763)),.UNSPECIFIED.,.F.,
 .F.,.F.)
B_SPLINE_SURFACE_WITH_KNOTS((4,4),(3,3),(-3.41523684332934E-18,0.000418670815451504),
(0.,1.),.UNSPECIFIED.)
GEOMETRIC_REPRESENTATION_ITEM()
RATIONAL_B_SPLINE_SURFACE(((1.,0.80178372573727,1.),(1.,0.801581038760284,
1.),(1.,0.797360979426379,1.),(1.,0.782160982635977,1.)))
REPRESENTATION_ITEM('')
SURFACE()
);
#2177=(
BOUNDED_SURFACE()
B_SPLINE_SURFACE(3,2,((#142770,#142771,#142772),(#142773,#142774,#142775),
(#142776,#142777,#142778),(#142779,#142780,#142781),(#142782,#142783,#142784),
(#142785,#142786,#142787)),.UNSPECIFIED.,.F.,.F.,.F.)
B_SPLINE_SURFACE_WITH_KNOTS((4,2,4),(3,3),(0.,0.00138008432392828,0.00276016864785656),
(0.,1.),.UNSPECIFIED.)
GEOMETRIC_REPRESENTATION_ITEM()
RATIONAL_B_SPLINE_SURFACE(((1.,0.889512696472458,1.),(1.,0.875621469665309,
1.),(1.,0.859481975708513,1.),(1.,0.823331923932046,1.),(1.,0.803217377248123,
1.),(1.,0.782160982635976,1.)))
REPRESENTATION_ITEM('')
SURFACE()
);
#2178=(
BOUNDED_SURFACE()
B_SPLINE_SURFACE(3,2,((#142799,#142800,#142801),(#142802,#142803,#142804),
(#142805,#142806,#142807),(#142808,#142809,#142810),(#142811,#142812,#142813),
(#142814,#142815,#142816),(#142817,#142818,#142819),(#142820,#142821,#142822),
(#142823,#142824,#142825),(#142826,#142827,#142828),(#142829,#142830,#142831),
(#142832,#142833,#142834)),.UNSPECIFIED.,.F.,.F.,.F.)
B_SPLINE_SURFACE_WITH_KNOTS((4,2,2,2,2,4),(3,3),(0.,0.000250417359226946,
0.000375626038840418,0.000500834718453891,0.000751252077680836,0.00100166943690778),
(-0.00140468204160171,1.),.UNSPECIFIED.)
GEOMETRIC_REPRESENTATION_ITEM()
RATIONAL_B_SPLINE_SURFACE(((1.0008239995229,0.706695359341974,1.),(1.00080388922191,
0.713853670046833,1.),(1.00078381509905,0.720999103057124,1.),(1.00075782359272,
0.7302508431544,1.),(1.00074967829203,0.73315018280726,1.),(1.00073524706918,
0.738287011792902,1.),(1.00072896513201,0.740523082654128,1.),(1.00071294399062,
0.746225847024512,1.),(1.00070666903946,0.748459431199004,1.),(1.00070405563711,
0.749389678142165,1.),(1.00070770913775,0.748089205673413,1.),(1.00071606406546,
0.745115248770045,1.)))
REPRESENTATION_ITEM('')
SURFACE()
);
#2179=(
BOUNDED_SURFACE()
B_SPLINE_SURFACE(3,2,((#142836,#142837,#142838),(#142839,#142840,#142841),
(#142842,#142843,#142844),(#142845,#142846,#142847),(#142848,#142849,#142850),
(#142851,#142852,#142853),(#142854,#142855,#142856),(#142857,#142858,#142859),
(#142860,#142861,#142862),(#142863,#142864,#142865),(#142866,#142867,#142868),
(#142869,#142870,#142871)),.UNSPECIFIED.,.F.,.F.,.F.)
B_SPLINE_SURFACE_WITH_KNOTS((4,2,2,2,2,4),(3,3),(-2.00577401909819E-18,
0.000253295312002929,0.000379942968004394,0.00050659062400586,0.000759885936008791,
0.00101318124801172),(0.,1.),.UNSPECIFIED.)
GEOMETRIC_REPRESENTATION_ITEM()
RATIONAL_B_SPLINE_SURFACE(((1.,0.619253049823351,1.),(1.,0.611711019709536,
1.),(1.,0.608322651255403,1.),(1.,0.610256821027379,1.),(1.,0.612081873728276,
1.),(1.,0.61778814027945,1.),(1.,0.621690668847742,1.),(1.,0.636005795097188,
1.),(1.,0.648854597242623,1.),(1.,0.676998182563378,1.),(1.,0.692438011698887,
1.),(1.,0.707106781186548,1.)))
REPRESENTATION_ITEM('')
SURFACE()
);
#2180=(
BOUNDED_SURFACE()
B_SPLINE_SURFACE(3,2,((#142878,#142879,#142880),(#142881,#142882,#142883),
(#142884,#142885,#142886),(#142887,#142888,#142889)),.UNSPECIFIED.,.F.,
 .F.,.F.)
B_SPLINE_SURFACE_WITH_KNOTS((4,4),(3,3),(0.00165976994196512,0.00175987143987977),
(0.,1.),.UNSPECIFIED.)
GEOMETRIC_REPRESENTATION_ITEM()
RATIONAL_B_SPLINE_SURFACE(((1.,0.707106781186549,1.),(1.,0.714158119082749,
1.),(1.,0.721010468727715,1.),(1.,0.727682857483054,1.)))
REPRESENTATION_ITEM('')
SURFACE()
);
#2181=(
BOUNDED_SURFACE()
B_SPLINE_SURFACE(3,2,((#142891,#142892,#142893),(#142894,#142895,#142896),
(#142897,#142898,#142899),(#142900,#142901,#142902),(#142903,#142904,#142905),
(#142906,#142907,#142908),(#142909,#142910,#142911),(#142912,#142913,#142914),
(#142915,#142916,#142917),(#142918,#142919,#142920)),.UNSPECIFIED.,.F.,
 .F.,.F.)
B_SPLINE_SURFACE_WITH_KNOTS((4,2,2,2,4),(3,3),(0.00166905748884283,0.00189688228523533,
0.00212470708162783,0.00235253187802032,0.00258035667441282),(0.,1.),
 .UNSPECIFIED.)
GEOMETRIC_REPRESENTATION_ITEM()
RATIONAL_B_SPLINE_SURFACE(((1.,0.727682857482998,1.),(1.,0.742747587336582,
1.),(1.,0.756565090576503,1.),(1.,0.779563382898484,1.),(1.,0.788904601358709,
1.),(1.,0.801793098601248,1.),(1.,0.805447378128131,1.),(1.,0.806422615061365,
1.),(1.,0.803776299349016,1.),(1.,0.798143461625347,1.)))
REPRESENTATION_ITEM('')
SURFACE()
);
#2182=(
BOUNDED_SURFACE()
B_SPLINE_SURFACE(3,2,((#142922,#142923,#142924),(#142925,#142926,#142927),
(#142928,#142929,#142930),(#142931,#142932,#142933),(#142934,#142935,#142936),
(#142937,#142938,#142939)),.UNSPECIFIED.,.F.,.F.,.F.)
B_SPLINE_SURFACE_WITH_KNOTS((4,2,4),(3,3),(0.19058679356565,0.194723599184011,
0.198860404802373),(0.,1.),.UNSPECIFIED.)
GEOMETRIC_REPRESENTATION_ITEM()
RATIONAL_B_SPLINE_SURFACE(((1.,0.954062806827576,1.),(1.,0.95589180838713,
1.),(1.,0.957713181483215,1.),(1.,0.961295526062221,1.),(1.,0.963047831711069,
1.),(1.,0.964700553047209,1.)))
REPRESENTATION_ITEM('')
SURFACE()
);
#2183=(
BOUNDED_SURFACE()
B_SPLINE_SURFACE(2,2,((#142973,#142974,#142975),(#142976,#142977,#142978),
(#142979,#142980,#142981)),.UNSPECIFIED.,.F.,.F.,.F.)
B_SPLINE_SURFACE_WITH_KNOTS((3,3),(3,3),(-3.74064361396611E-16,1.57079632679501),
(0.,1.5707963267949),.UNSPECIFIED.)
GEOMETRIC_REPRESENTATION_ITEM()
RATIONAL_B_SPLINE_SURFACE(((1.,0.707106781186548,1.),(0.707106781186506,
0.49999999999997,0.707106781186506),(1.,0.707106781186548,1.)))
REPRESENTATION_ITEM('')
SURFACE()
);
#2184=(
BOUNDED_SURFACE()
B_SPLINE_SURFACE(2,2,((#142993,#142994,#142995),(#142996,#142997,#142998),
(#142999,#143000,#143001)),.UNSPECIFIED.,.F.,.F.,.F.)
B_SPLINE_SURFACE_WITH_KNOTS((3,3),(3,3),(0.,1.57079632679501),(1.5707963267949,
3.14159265358979),.UNSPECIFIED.)
GEOMETRIC_REPRESENTATION_ITEM()
RATIONAL_B_SPLINE_SURFACE(((1.,0.707106781186548,1.),(0.707106781186506,
0.49999999999997,0.707106781186506),(1.,0.707106781186548,1.)))
REPRESENTATION_ITEM('')
SURFACE()
);
#2185=(
BOUNDED_SURFACE()
B_SPLINE_SURFACE(2,2,((#143024,#143025,#143026),(#143027,#143028,#143029),
(#143030,#143031,#143032)),.UNSPECIFIED.,.F.,.F.,.F.)
B_SPLINE_SURFACE_WITH_KNOTS((3,3),(3,3),(-3.74064361396611E-16,1.57079632679492),
(0.,1.5707963267949),.UNSPECIFIED.)
GEOMETRIC_REPRESENTATION_ITEM()
RATIONAL_B_SPLINE_SURFACE(((1.,0.707106781186548,1.),(0.707106781186552,
0.500000000000003,0.707106781186552),(1.,0.707106781186548,1.)))
REPRESENTATION_ITEM('')
SURFACE()
);
#2186=(
BOUNDED_SURFACE()
B_SPLINE_SURFACE(2,2,((#143044,#143045,#143046),(#143047,#143048,#143049),
(#143050,#143051,#143052)),.UNSPECIFIED.,.F.,.F.,.F.)
B_SPLINE_SURFACE_WITH_KNOTS((3,3),(3,3),(0.,1.57079632679492),(1.5707963267949,
3.14159265358979),.UNSPECIFIED.)
GEOMETRIC_REPRESENTATION_ITEM()
RATIONAL_B_SPLINE_SURFACE(((1.,0.707106781186548,1.),(0.707106781186552,
0.500000000000003,0.707106781186552),(1.,0.707106781186548,1.)))
REPRESENTATION_ITEM('')
SURFACE()
);
#2187=(
BOUNDED_SURFACE()
B_SPLINE_SURFACE(2,2,((#143072,#143073,#143074),(#143075,#143076,#143077),
(#143078,#143079,#143080)),.UNSPECIFIED.,.F.,.F.,.F.)
B_SPLINE_SURFACE_WITH_KNOTS((3,3),(3,3),(-3.74064361396611E-16,1.57079632679492),
(0.,1.5707963267949),.UNSPECIFIED.)
GEOMETRIC_REPRESENTATION_ITEM()
RATIONAL_B_SPLINE_SURFACE(((1.,0.707106781186548,1.),(0.707106781186552,
0.500000000000003,0.707106781186552),(1.,0.707106781186548,1.)))
REPRESENTATION_ITEM('')
SURFACE()
);
#2188=(
BOUNDED_SURFACE()
B_SPLINE_SURFACE(3,2,((#143089,#143090,#143091),(#143092,#143093,#143094),
(#143095,#143096,#143097),(#143098,#143099,#143100),(#143101,#143102,#143103),
(#143104,#143105,#143106),(#143107,#143108,#143109),(#143110,#143111,#143112),
(#143113,#143114,#143115),(#143116,#143117,#143118)),.UNSPECIFIED.,.F.,
 .F.,.F.)
B_SPLINE_SURFACE_WITH_KNOTS((4,2,2,2,4),(3,3),(0.00116892975483561,0.00173273620432837,
0.00229654265382113,0.00286034910331391,0.00342415555280667),(-8.73672651670295E-5,
1.),.UNSPECIFIED.)
GEOMETRIC_REPRESENTATION_ITEM()
RATIONAL_B_SPLINE_SURFACE(((1.00005118303036,0.707081191907034,1.),(1.00004250803408,
0.75672791175003,1.),(1.00003576403205,0.795323614743255,1.),(1.0000266067815,
0.847730260009664,1.),(1.00002422236724,0.86137618483401,1.),(1.00002421067414,
0.861443104051655,1.),(1.0000265855687,0.847851660205381,1.),(1.00003574715403,
0.795420207077597,1.),(1.00004250128307,0.756766547571557,1.),(1.00005118303036,
0.707081191907034,1.)))
REPRESENTATION_ITEM('')
SURFACE()
);
#2189=(
BOUNDED_SURFACE()
B_SPLINE_SURFACE(3,2,((#143124,#143125,#143126),(#143127,#143128,#143129),
(#143130,#143131,#143132),(#143133,#143134,#143135),(#143136,#143137,#143138),
(#143139,#143140,#143141),(#143142,#143143,#143144),(#143145,#143146,#143147),
(#143148,#143149,#143150),(#143151,#143152,#143153)),.UNSPECIFIED.,.F.,
 .F.,.F.)
B_SPLINE_SURFACE_WITH_KNOTS((4,2,2,2,4),(3,3),(4.71238898038469,5.10508806208341,
5.49778714378214,5.89048622548086,6.28318530717959),(0.,1.),
 .UNSPECIFIED.)
GEOMETRIC_REPRESENTATION_ITEM()
RATIONAL_B_SPLINE_SURFACE(((1.,0.707106781186548,1.),(1.,0.71355026185156,
1.),(1.,0.719894264862189,1.),(1.,0.73149075639733,1.),(1.,0.73673812929671,
1.),(1.,0.745429366938189,1.),(1.,0.748871927696634,1.),(1.,0.753512297096161,
1.),(1.,0.754714219730837,1.),(1.,0.754709580222772,1.)))
REPRESENTATION_ITEM('')
SURFACE()
);
#2190=(
BOUNDED_SURFACE()
B_SPLINE_SURFACE(3,2,((#143170,#143171,#143172),(#143173,#143174,#143175),
(#143176,#143177,#143178),(#143179,#143180,#143181),(#143182,#143183,#143184),
(#143185,#143186,#143187),(#143188,#143189,#143190),(#143191,#143192,#143193),
(#143194,#143195,#143196),(#143197,#143198,#143199)),.UNSPECIFIED.,.F.,
 .F.,.F.)
B_SPLINE_SURFACE_WITH_KNOTS((4,2,2,2,4),(3,3),(8.78519494496445E-16,0.392699081698725,
0.785398163397449,1.17809724509617,1.5707963267949),(0.,1.),
 .UNSPECIFIED.)
GEOMETRIC_REPRESENTATION_ITEM()
RATIONAL_B_SPLINE_SURFACE(((1.,0.754709580222768,1.),(1.,0.754714219644573,
1.),(1.,0.753512297211018,1.),(1.,0.748871927581762,1.),(1.,0.745429367161016,
1.),(1.,0.736738129073881,1.),(1.,0.73149075671205,1.),(1.,0.719894264547496,
1.),(1.,0.713550262087909,1.),(1.,0.707106781186548,1.)))
REPRESENTATION_ITEM('')
SURFACE()
);
#2191=(
BOUNDED_SURFACE()
B_SPLINE_SURFACE(3,2,((#143854,#143855,#143856),(#143857,#143858,#143859),
(#143860,#143861,#143862),(#143863,#143864,#143865),(#143866,#143867,#143868),
(#143869,#143870,#143871),(#143872,#143873,#143874),(#143875,#143876,#143877),
(#143878,#143879,#143880),(#143881,#143882,#143883)),.UNSPECIFIED.,.F.,
 .F.,.F.)
B_SPLINE_SURFACE_WITH_KNOTS((4,2,2,2,4),(3,3),(0.00116892975483565,0.00173273620432837,
0.00229654265382108,0.0028603491033138,0.00342415555280651),(-8.73672651410431E-5,
1.),.UNSPECIFIED.)
GEOMETRIC_REPRESENTATION_ITEM()
RATIONAL_B_SPLINE_SURFACE(((1.00005118303034,0.707081191907037,1.),(1.00004250803407,
0.756727911750281,1.),(1.00003576403204,0.795323614742893,1.),(1.00002660678149,
0.847730260009987,1.),(1.00002422236723,0.861376184832614,1.),(1.00002421067413,
0.861443104052995,1.),(1.00002658556869,0.847851660205354,1.),(1.00003574715402,
0.795420207077597,1.),(1.00004250128306,0.756766547571537,1.),(1.00005118303034,
0.707081191907037,1.)))
REPRESENTATION_ITEM('')
SURFACE()
);
#2192=(
BOUNDED_SURFACE()
B_SPLINE_SURFACE(3,2,((#143900,#143901,#143902),(#143903,#143904,#143905),
(#143906,#143907,#143908),(#143909,#143910,#143911),(#143912,#143913,#143914),
(#143915,#143916,#143917),(#143918,#143919,#143920),(#143921,#143922,#143923),
(#143924,#143925,#143926),(#143927,#143928,#143929)),.UNSPECIFIED.,.F.,
 .F.,.F.)
B_SPLINE_SURFACE_WITH_KNOTS((4,2,2,2,4),(3,3),(0.00108313181642967,0.00175636478508591,
0.00242959775374216,0.0031028307223984,0.00377606369105465),(-0.000209460012303618,
1.),.UNSPECIFIED.)
GEOMETRIC_REPRESENTATION_ITEM()
RATIONAL_B_SPLINE_SURFACE(((1.00012272453493,0.707045431769336,1.),(1.00009434426229,
0.774791710231057,1.),(1.00007166829574,0.828921293970649,1.),(1.0000403086156,
0.903779687679754,1.),(1.00003179560244,0.924101020320101,1.),(1.00003154660919,
0.92469538973271,1.),(1.00003985538718,0.90486158494707,1.),(1.00007114262335,
0.830176121522528,1.),(1.00009383870822,0.775998513536341,1.),(1.00012272453493,
0.707045431769336,1.)))
REPRESENTATION_ITEM('')
SURFACE()
);
#2193=(
BOUNDED_SURFACE()
B_SPLINE_SURFACE(3,2,((#143938,#143939,#143940),(#143941,#143942,#143943),
(#143944,#143945,#143946),(#143947,#143948,#143949),(#143950,#143951,#143952),
(#143953,#143954,#143955),(#143956,#143957,#143958),(#143959,#143960,#143961),
(#143962,#143963,#143964),(#143965,#143966,#143967)),.UNSPECIFIED.,.F.,
 .F.,.F.)
B_SPLINE_SURFACE_WITH_KNOTS((4,2,2,2,4),(3,3),(0.00131180726843869,0.00173116479138241,
0.00215052231432612,0.00256987983726984,0.00298923736021356),(-7.19536616060548E-6,
1.),.UNSPECIFIED.)
GEOMETRIC_REPRESENTATION_ITEM()
RATIONAL_B_SPLINE_SURFACE(((1.00000421497824,0.707104673712593,1.),(1.00000380693473,
0.735459277067922,1.),(1.00000349584298,0.757076784024011,1.),(1.00000307861086,
0.78606989643,1.),(1.00000297270686,0.793429076618424,1.),(1.00000297242631,
0.793448571747567,1.),(1.00000307812254,0.786103829136133,1.),(1.0000034951559,
0.757124528684544,1.),(1.00000380600669,0.735523766261729,1.),(1.00000421497824,
0.707104673712593,1.)))
REPRESENTATION_ITEM('')
SURFACE()
);
#2194=(
BOUNDED_SURFACE()
B_SPLINE_SURFACE(3,2,((#143988,#143989,#143990),(#143991,#143992,#143993),
(#143994,#143995,#143996),(#143997,#143998,#143999)),.UNSPECIFIED.,.F.,
 .F.,.F.)
B_SPLINE_SURFACE_WITH_KNOTS((4,4),(3,3),(-3.51851606259766E-5,0.000688755160509476),
(0.,1.00003518516063),.UNSPECIFIED.)
GEOMETRIC_REPRESENTATION_ITEM()
RATIONAL_B_SPLINE_SURFACE(((1.,0.568606220888424,1.00003035731882),(1.,
0.556584756681385,1.00003120327312),(1.,0.550157943671747,1.00003165553002),
(1.,0.550842070368378,1.0000316073878)))
REPRESENTATION_ITEM('')
SURFACE()
);
#2195=(
BOUNDED_SURFACE()
B_SPLINE_SURFACE(3,2,((#144019,#144020,#144021),(#144022,#144023,#144024),
(#144025,#144026,#144027),(#144028,#144029,#144030)),.UNSPECIFIED.,.F.,
 .F.,.F.)
B_SPLINE_SURFACE_WITH_KNOTS((4,4),(3,3),(-6.51893458122614E-5,0.000717082803934822),
(0.,1.00014047630858),.UNSPECIFIED.)
GEOMETRIC_REPRESENTATION_ITEM()
RATIONAL_B_SPLINE_SURFACE(((1.,0.80532666321776,1.00005469398346),(1.,0.805999592802023,
1.00005450492213),(1.,0.80258142750598,1.00005546526462),(1.,0.795135566176566,
1.00005755719884)))
REPRESENTATION_ITEM('')
SURFACE()
);
#2196=(
BOUNDED_SURFACE()
B_SPLINE_SURFACE(3,2,((#144042,#144043,#144044),(#144045,#144046,#144047),
(#144048,#144049,#144050),(#144051,#144052,#144053)),.UNSPECIFIED.,.F.,
 .F.,.F.)
B_SPLINE_SURFACE_WITH_KNOTS((4,4),(3,3),(-6.51412822692208E-5,0.000716554104961429),
(0.,1.00012817146333),.UNSPECIFIED.)
GEOMETRIC_REPRESENTATION_ITEM()
RATIONAL_B_SPLINE_SURFACE(((1.,0.62167678976432,1.00009698047894),(1.,0.613563994562104,
1.0000990601366),(1.,0.609559936451189,1.00010008654858),(1.,0.610338513229397,
1.00009988696593)))
REPRESENTATION_ITEM('')
SURFACE()
);
#2197=(
BOUNDED_SURFACE()
B_SPLINE_SURFACE(3,2,((#144072,#144073,#144074),(#144075,#144076,#144077),
(#144078,#144079,#144080),(#144081,#144082,#144083)),.UNSPECIFIED.,.F.,
 .F.,.F.)
B_SPLINE_SURFACE_WITH_KNOTS((4,4),(3,3),(0.,0.000650589467290063),(0.,1.),
 .UNSPECIFIED.)
GEOMETRIC_REPRESENTATION_ITEM()
RATIONAL_B_SPLINE_SURFACE(((1.,0.761354724782838,1.),(1.,0.761348936155314,
1.),(1.,0.759749503531854,1.),(1.,0.756551244268667,1.)))
REPRESENTATION_ITEM('')
SURFACE()
);
#2198=(
BOUNDED_SURFACE()
B_SPLINE_SURFACE(3,2,((#144085,#144086,#144087),(#144088,#144089,#144090),
(#144091,#144092,#144093),(#144094,#144095,#144096),(#144097,#144098,#144099),
(#144100,#144101,#144102),(#144103,#144104,#144105),(#144106,#144107,#144108),
(#144109,#144110,#144111),(#144112,#144113,#144114),(#144115,#144116,#144117),
(#144118,#144119,#144120),(#144121,#144122,#144123),(#144124,#144125,#144126)),
 .UNSPECIFIED.,.F.,.F.,.F.)
B_SPLINE_SURFACE_WITH_KNOTS((4,2,2,2,2,2,4),(3,3),(0.00807902625150492,
0.00883280378349999,0.00920969254949752,0.00958658131549505,0.00996347008149258,
0.0103403588474901,0.0110941363794852),(0.,1.),.UNSPECIFIED.)
GEOMETRIC_REPRESENTATION_ITEM()
RATIONAL_B_SPLINE_SURFACE(((1.,0.707106781186548,1.),(1.,0.708503208405905,
1.),(1.,0.709864127404626,1.),(1.,0.711851747119499,1.),(1.,0.712500882329163,
1.),(1.,0.713738228851022,1.),(1.,0.714331705876986,1.),(1.,0.715467776552351,
1.),(1.,0.716012641761659,1.),(1.,0.71701515809269,1.),(1.,0.717477434704573,
1.),(1.,0.718748007011303,1.),(1.,0.719442582755427,1.),(1.,0.719919801430648,
1.)))
REPRESENTATION_ITEM('')
SURFACE()
);
#2199=(
BOUNDED_SURFACE()
B_SPLINE_SURFACE(3,2,((#144143,#144144,#144145),(#144146,#144147,#144148),
(#144149,#144150,#144151),(#144152,#144153,#144154)),.UNSPECIFIED.,.F.,
 .F.,.F.)
B_SPLINE_SURFACE_WITH_KNOTS((4,4),(3,3),(0.0156098999423859,0.0162171358932854),
(0.0843742085712764,1.),.UNSPECIFIED.)
GEOMETRIC_REPRESENTATION_ITEM()
RATIONAL_B_SPLINE_SURFACE(((0.967873953213285,0.809621640719886,1.),(0.968348523789084,
0.812433937177747,1.),(0.968804462122364,0.815135819310926,1.),(0.969242174215226,
0.817729693080374,1.)))
REPRESENTATION_ITEM('')
SURFACE()
);
#2200=(
BOUNDED_SURFACE()
B_SPLINE_SURFACE(3,2,((#144174,#144175,#144176),(#144177,#144178,#144179),
(#144180,#144181,#144182),(#144183,#144184,#144185),(#144186,#144187,#144188),
(#144189,#144190,#144191),(#144192,#144193,#144194),(#144195,#144196,#144197),
(#144198,#144199,#144200),(#144201,#144202,#144203),(#144204,#144205,#144206),
(#144207,#144208,#144209),(#144210,#144211,#144212),(#144213,#144214,#144215)),
 .UNSPECIFIED.,.F.,.F.,.F.)
B_SPLINE_SURFACE_WITH_KNOTS((4,2,2,2,2,2,4),(3,3),(0.00807927244133089,
0.00881458117408921,0.00918223554046837,0.00954988990684753,0.0099175442732267,
0.0102851986396059,0.0110205073723642),(0.,1.),.UNSPECIFIED.)
GEOMETRIC_REPRESENTATION_ITEM()
RATIONAL_B_SPLINE_SURFACE(((1.,0.707106781186548,1.),(1.,0.705697402766896,
1.),(1.,0.704316028414221,1.),(1.,0.702287640598182,1.),(1.,0.70162085852966,
1.),(1.,0.700346303389684,1.),(1.,0.699732822392533,1.),(1.,0.69855427952325,
1.),(1.,0.697985323371657,1.),(1.,0.696930428409623,1.),(1.,0.69644149384419,
1.),(1.,0.695089684342733,1.),(1.,0.694335092820993,1.),(1.,0.693797102764879,
1.)))
REPRESENTATION_ITEM('')
SURFACE()
);
#2201=(
BOUNDED_SURFACE()
B_SPLINE_SURFACE(3,2,((#144217,#144218,#144219),(#144220,#144221,#144222),
(#144223,#144224,#144225),(#144226,#144227,#144228)),.UNSPECIFIED.,.F.,
 .F.,.F.)
B_SPLINE_SURFACE_WITH_KNOTS((4,4),(3,3),(-1.0842021724855E-19,0.000650371461981817),
(0.,1.),.UNSPECIFIED.)
GEOMETRIC_REPRESENTATION_ITEM()
RATIONAL_B_SPLINE_SURFACE(((1.,0.668488966322264,1.),(1.,0.665851831765851,
1.),(1.,0.664481097979681,1.),(1.,0.664473794614064,1.)))
REPRESENTATION_ITEM('')
SURFACE()
);
#2202=(
BOUNDED_SURFACE()
B_SPLINE_SURFACE(3,2,((#144257,#144258,#144259),(#144260,#144261,#144262),
(#144263,#144264,#144265),(#144266,#144267,#144268)),.UNSPECIFIED.,.F.,
 .F.,.F.)
B_SPLINE_SURFACE_WITH_KNOTS((4,4),(3,3),(0.,0.000650122732446382),(0.,1.),
 .UNSPECIFIED.)
GEOMETRIC_REPRESENTATION_ITEM()
RATIONAL_B_SPLINE_SURFACE(((1.,0.714558059459819,1.),(1.,0.714557241617472,
1.),(1.,0.714330794970796,1.),(1.,0.71387929067142,1.)))
REPRESENTATION_ITEM('')
SURFACE()
);
#2203=(
BOUNDED_SURFACE()
B_SPLINE_SURFACE(3,2,((#144273,#144274,#144275),(#144276,#144277,#144278),
(#144279,#144280,#144281),(#144282,#144283,#144284),(#144285,#144286,#144287),
(#144288,#144289,#144290)),.UNSPECIFIED.,.F.,.F.,.F.)
B_SPLINE_SURFACE_WITH_KNOTS((4,2,4),(3,3),(0.,0.000414679582686121,0.000829359165372242),
(0.,1.),.UNSPECIFIED.)
GEOMETRIC_REPRESENTATION_ITEM()
RATIONAL_B_SPLINE_SURFACE(((1.,0.807089511457031,1.),(1.,0.806982451123016,
1.),(1.,0.808254776113455,1.),(1.,0.809251473726326,1.),(1.,0.80886183729917,
1.),(1.,0.804104907750028,1.)))
REPRESENTATION_ITEM('')
SURFACE()
);
#2204=(
BOUNDED_SURFACE()
B_SPLINE_SURFACE(3,2,((#144297,#144298,#144299),(#144300,#144301,#144302),
(#144303,#144304,#144305),(#144306,#144307,#144308)),.UNSPECIFIED.,.F.,
 .F.,.F.)
B_SPLINE_SURFACE_WITH_KNOTS((4,4),(3,3),(2.16840434497101E-19,0.000794016598505311),
(0.,1.),.UNSPECIFIED.)
GEOMETRIC_REPRESENTATION_ITEM()
RATIONAL_B_SPLINE_SURFACE(((1.,0.917068097704896,1.),(1.,0.931812274712855,
1.),(1.,0.942532558511199,1.),(1.,0.948460216910911,1.)))
REPRESENTATION_ITEM('')
SURFACE()
);
#2205=(
BOUNDED_SURFACE()
B_SPLINE_SURFACE(3,2,((#144328,#144329,#144330),(#144331,#144332,#144333),
(#144334,#144335,#144336),(#144337,#144338,#144339)),.UNSPECIFIED.,.F.,
 .F.,.F.)
B_SPLINE_SURFACE_WITH_KNOTS((4,4),(3,3),(0.,0.038317388945353),(0.,1.),
 .UNSPECIFIED.)
GEOMETRIC_REPRESENTATION_ITEM()
RATIONAL_B_SPLINE_SURFACE(((1.,0.716457303923414,1.),(1.,0.715285870443621,
1.),(1.,0.714517981140503,1.),(1.,0.713892198341303,1.)))
REPRESENTATION_ITEM('')
SURFACE()
);
#2206=(
BOUNDED_SURFACE()
B_SPLINE_SURFACE(3,2,((#144341,#144342,#144343),(#144344,#144345,#144346),
(#144347,#144348,#144349),(#144350,#144351,#144352)),.UNSPECIFIED.,.F.,
 .F.,.F.)
B_SPLINE_SURFACE_WITH_KNOTS((4,4),(3,3),(0.,0.0385835973699829),(0.,1.),
 .UNSPECIFIED.)
GEOMETRIC_REPRESENTATION_ITEM()
RATIONAL_B_SPLINE_SURFACE(((1.,0.713879290671428,1.),(1.,0.71450712730611,
1.),(1.,0.715277846561214,1.),(1.,0.716457303923418,1.)))
REPRESENTATION_ITEM('')
SURFACE()
);
#2207=(
BOUNDED_SURFACE()
B_SPLINE_SURFACE(3,2,((#144354,#144355,#144356),(#144357,#144358,#144359),
(#144360,#144361,#144362),(#144363,#144364,#144365)),.UNSPECIFIED.,.F.,
 .F.,.F.)
B_SPLINE_SURFACE_WITH_KNOTS((4,4),(3,3),(0.,0.00195778753723149),(0.,1.),
 .UNSPECIFIED.)
GEOMETRIC_REPRESENTATION_ITEM()
RATIONAL_B_SPLINE_SURFACE(((1.,0.707106781186543,1.),(1.,0.710074099671655,
1.),(1.,0.713236629341983,1.),(1.,0.716457303923398,1.)))
REPRESENTATION_ITEM('')
SURFACE()
);
#2208=(
BOUNDED_SURFACE()
B_SPLINE_SURFACE(3,2,((#144373,#144374,#144375),(#144376,#144377,#144378),
(#144379,#144380,#144381),(#144382,#144383,#144384)),.UNSPECIFIED.,.F.,
 .F.,.F.)
B_SPLINE_SURFACE_WITH_KNOTS((4,4),(3,3),(-4.11996825544492E-18,0.00195778789380024),
(0.,1.),.UNSPECIFIED.)
GEOMETRIC_REPRESENTATION_ITEM()
RATIONAL_B_SPLINE_SURFACE(((1.,0.716457303923414,1.),(1.,0.713268765085681,
1.),(1.,0.710104564531573,1.),(1.,0.707106781186529,1.)))
REPRESENTATION_ITEM('')
SURFACE()
);
#2209=(
BOUNDED_SURFACE()
B_SPLINE_SURFACE(3,2,((#144386,#144387,#144388),(#144389,#144390,#144391),
(#144392,#144393,#144394),(#144395,#144396,#144397),(#144398,#144399,#144400),
(#144401,#144402,#144403)),.UNSPECIFIED.,.F.,.F.,.F.)
B_SPLINE_SURFACE_WITH_KNOTS((4,2,4),(3,3),(0.024832888249526,0.028058706716499,
0.0312845251834718),(0.,1.),.UNSPECIFIED.)
GEOMETRIC_REPRESENTATION_ITEM()
RATIONAL_B_SPLINE_SURFACE(((1.,0.973275621725783,1.),(1.,0.974072863725218,
1.),(1.,0.974738796346974,1.),(1.,0.975743605366306,1.),(1.,0.976080910223402,
1.),(1.,0.976217656750926,1.)))
REPRESENTATION_ITEM('')
SURFACE()
);
#2210=(
BOUNDED_SURFACE()
B_SPLINE_SURFACE(3,2,((#144437,#144438,#144439),(#144440,#144441,#144442),
(#144443,#144444,#144445),(#144446,#144447,#144448)),.UNSPECIFIED.,.F.,
 .F.,.F.)
B_SPLINE_SURFACE_WITH_KNOTS((4,4),(3,3),(0.,0.0369876550821707),(0.,1.),
 .UNSPECIFIED.)
GEOMETRIC_REPRESENTATION_ITEM()
RATIONAL_B_SPLINE_SURFACE(((1.,0.668412873076039,1.),(1.,0.66485630627401,
1.),(1.,0.660493096380151,1.),(1.,0.653853118868808,1.)))
REPRESENTATION_ITEM('')
SURFACE()
);
#2211=(
BOUNDED_SURFACE()
B_SPLINE_SURFACE(3,2,((#144450,#144451,#144452),(#144453,#144454,#144455),
(#144456,#144457,#144458),(#144459,#144460,#144461),(#144462,#144463,#144464),
(#144465,#144466,#144467)),.UNSPECIFIED.,.F.,.F.,.F.)
B_SPLINE_SURFACE_WITH_KNOTS((4,2,4),(3,3),(0.,0.00108572934543333,0.00217145869086666),
(0.,1.),.UNSPECIFIED.)
GEOMETRIC_REPRESENTATION_ITEM()
RATIONAL_B_SPLINE_SURFACE(((1.,0.707106781186548,1.),(1.,0.698862672165929,
1.),(1.,0.690309395332211,1.),(1.,0.672521089753096,1.),(1.,0.663221545283971,
1.),(1.,0.653853118868808,1.)))
REPRESENTATION_ITEM('')
SURFACE()
);
#2212=(
BOUNDED_SURFACE()
B_SPLINE_SURFACE(3,2,((#144473,#144474,#144475),(#144476,#144477,#144478),
(#144479,#144480,#144481),(#144482,#144483,#144484),(#144485,#144486,#144487),
(#144488,#144489,#144490)),.UNSPECIFIED.,.F.,.F.,.F.)
B_SPLINE_SURFACE_WITH_KNOTS((4,2,4),(3,3),(-3.59995409638982E-5,0.00108574887884081,
0.00220749732422829),(0.,1.00003599956655),.UNSPECIFIED.)
GEOMETRIC_REPRESENTATION_ITEM()
RATIONAL_B_SPLINE_SURFACE(((1.,0.652908618523184,1.00002499027857),(1.,
0.662597041194131,1.00002429272054),(1.,0.672048287583566,1.00002361223899),
(1.,0.690435350993111,1.00002228838636),(1.,0.699430385989609,1.00002164075164),
(1.,0.70791464495416,1.00002102989235)))
REPRESENTATION_ITEM('')
SURFACE()
);
#2213=(
BOUNDED_SURFACE()
B_SPLINE_SURFACE(3,2,((#144517,#144518,#144519),(#144520,#144521,#144522),
(#144523,#144524,#144525),(#144526,#144527,#144528)),.UNSPECIFIED.,.F.,
 .F.,.F.)
B_SPLINE_SURFACE_WITH_KNOTS((4,4),(3,3),(0.,0.0372541843113205),(0.,1.),
 .UNSPECIFIED.)
GEOMETRIC_REPRESENTATION_ITEM()
RATIONAL_B_SPLINE_SURFACE(((1.,0.653853118868809,1.),(1.,0.660540277946251,
1.),(1.,0.664920252154014,1.),(1.,0.668488966322263,1.)))
REPRESENTATION_ITEM('')
SURFACE()
);
#2214=(
BOUNDED_SURFACE()
B_SPLINE_SURFACE(3,2,((#144534,#144535,#144536),(#144537,#144538,#144539),
(#144540,#144541,#144542),(#144543,#144544,#144545)),.UNSPECIFIED.,.F.,
 .F.,.F.)
B_SPLINE_SURFACE_WITH_KNOTS((4,4),(3,3),(0.,0.0358270578054484),(0.,1.),
 .UNSPECIFIED.)
GEOMETRIC_REPRESENTATION_ITEM()
RATIONAL_B_SPLINE_SURFACE(((1.,0.773031559588625,1.),(1.,0.765796148320668,
1.),(1.,0.760773695826815,1.),(1.,0.756642830410354,1.)))
REPRESENTATION_ITEM('')
SURFACE()
);
#2215=(
BOUNDED_SURFACE()
B_SPLINE_SURFACE(3,2,((#144547,#144548,#144549),(#144550,#144551,#144552),
(#144553,#144554,#144555),(#144556,#144557,#144558)),.UNSPECIFIED.,.F.,
 .F.,.F.)
B_SPLINE_SURFACE_WITH_KNOTS((4,4),(3,3),(0.,0.0360938777358061),(0.,1.),
 .UNSPECIFIED.)
GEOMETRIC_REPRESENTATION_ITEM()
RATIONAL_B_SPLINE_SURFACE(((1.,0.756551244268665,1.),(1.,0.760698019999951,
1.),(1.,0.765742819248909,1.),(1.,0.77303155958863,1.)))
REPRESENTATION_ITEM('')
SURFACE()
);
#2216=(
BOUNDED_SURFACE()
B_SPLINE_SURFACE(3,2,((#144560,#144561,#144562),(#144563,#144564,#144565),
(#144566,#144567,#144568),(#144569,#144570,#144571),(#144572,#144573,#144574),
(#144575,#144576,#144577)),.UNSPECIFIED.,.F.,.F.,.F.)
B_SPLINE_SURFACE_WITH_KNOTS((4,2,4),(3,3),(-2.53870287234617E-5,0.00117590500970525,
0.00237716614312564),(0.,1.00002538702872),.UNSPECIFIED.)
GEOMETRIC_REPRESENTATION_ITEM()
RATIONAL_B_SPLINE_SURFACE(((1.,0.706372183938724,1.0000149086756),(1.,0.717843868865426,
1.00001432621161),(1.,0.729214574731599,1.00001374887474),(1.,0.751742343795836,
1.0000126050485),(1.,0.762975777222459,1.0000120346815),(1.,0.773705940022985,
1.0000114898676)))
REPRESENTATION_ITEM('')
SURFACE()
);
#2217=(
BOUNDED_SURFACE()
B_SPLINE_SURFACE(3,2,((#144609,#144610,#144611),(#144612,#144613,#144614),
(#144615,#144616,#144617),(#144618,#144619,#144620),(#144621,#144622,#144623),
(#144624,#144625,#144626)),.UNSPECIFIED.,.F.,.F.,.F.)
B_SPLINE_SURFACE_WITH_KNOTS((4,2,4),(3,3),(0.,0.00117596609447381,0.00235193218894761),
(0.,1.),.UNSPECIFIED.)
GEOMETRIC_REPRESENTATION_ITEM()
RATIONAL_B_SPLINE_SURFACE(((1.,0.773031559588625,1.),(1.,0.762507689934388,
1.),(1.,0.751714784265694,1.),(1.,0.729663967046365,1.),(1.,0.718328240933523,
1.),(1.,0.707106781186548,1.)))
REPRESENTATION_ITEM('')
SURFACE()
);
#2218=(
BOUNDED_SURFACE()
B_SPLINE_SURFACE(3,2,((#144633,#144634,#144635),(#144636,#144637,#144638),
(#144639,#144640,#144641),(#144642,#144643,#144644),(#144645,#144646,#144647),
(#144648,#144649,#144650)),.UNSPECIFIED.,.F.,.F.,.F.)
B_SPLINE_SURFACE_WITH_KNOTS((4,2,4),(3,3),(0.0131958327712131,0.0172517018793722,
0.0213075709875312),(0.,1.),.UNSPECIFIED.)
GEOMETRIC_REPRESENTATION_ITEM()
RATIONAL_B_SPLINE_SURFACE(((1.,0.962986864031359,1.),(1.,0.964634124968522,
1.),(1.,0.966223563289428,1.),(1.,0.969200421482677,1.),(1.,0.970562510847277,
1.),(1.,0.97174760310377,1.)))
REPRESENTATION_ITEM('')
SURFACE()
);
#2219=(
BOUNDED_SURFACE()
B_SPLINE_SURFACE(3,2,((#144674,#144675,#144676),(#144677,#144678,#144679),
(#144680,#144681,#144682),(#144683,#144684,#144685)),.UNSPECIFIED.,.F.,
 .F.,.F.)
B_SPLINE_SURFACE_WITH_KNOTS((4,4),(3,3),(0.,0.0319950621716305),(0.,1.),
 .UNSPECIFIED.)
GEOMETRIC_REPRESENTATION_ITEM()
RATIONAL_B_SPLINE_SURFACE(((1.,0.619604282534389,1.),(1.,0.612421729644488,
1.),(1.,0.603704627405285,1.),(1.,0.591243989422539,1.)))
REPRESENTATION_ITEM('')
SURFACE()
);
#2220=(
BOUNDED_SURFACE()
B_SPLINE_SURFACE(3,2,((#144687,#144688,#144689),(#144690,#144691,#144692),
(#144693,#144694,#144695),(#144696,#144697,#144698),(#144699,#144700,#144701),
(#144702,#144703,#144704)),.UNSPECIFIED.,.F.,.F.,.F.)
B_SPLINE_SURFACE_WITH_KNOTS((4,2,4),(3,3),(0.,0.00145467289932797,0.00290934579865593),
(0.,1.),.UNSPECIFIED.)
GEOMETRIC_REPRESENTATION_ITEM()
RATIONAL_B_SPLINE_SURFACE(((1.,0.707106781186548,1.),(1.,0.689351003959322,
1.),(1.,0.670875374619751,1.),(1.,0.63219865253591,1.),(1.,0.61183462187758,
1.),(1.,0.591243989422533,1.)))
REPRESENTATION_ITEM('')
SURFACE()
);
#2221=(
BOUNDED_SURFACE()
B_SPLINE_SURFACE(3,2,((#144710,#144711,#144712),(#144713,#144714,#144715),
(#144716,#144717,#144718),(#144719,#144720,#144721),(#144722,#144723,#144724),
(#144725,#144726,#144727)),.UNSPECIFIED.,.F.,.F.,.F.)
B_SPLINE_SURFACE_WITH_KNOTS((4,2,4),(3,3),(-0.000112903673830276,0.00145505538520654,
0.00302301461672063),(0.,1.00011290384629),.UNSPECIFIED.)
GEOMETRIC_REPRESENTATION_ITEM()
RATIONAL_B_SPLINE_SURFACE(((0.999999999999999,0.586393787062724,1.00009339546458),
(1.,0.608684432923124,1.00008836206527),(1.,0.630255928913141,1.00008349105554),
(1.,0.671993040490121,1.00007406649468),(1.,0.692297992883085,1.00006948148023),
(1.,0.711173028308929,1.00006521935203)))
REPRESENTATION_ITEM('')
SURFACE()
);
#2222=(
BOUNDED_SURFACE()
B_SPLINE_SURFACE(3,2,((#144757,#144758,#144759),(#144760,#144761,#144762),
(#144763,#144764,#144765),(#144766,#144767,#144768)),.UNSPECIFIED.,.F.,
 .F.,.F.)
B_SPLINE_SURFACE_WITH_KNOTS((4,4),(3,3),(0.,0.0322629186945109),(0.,1.),
 .UNSPECIFIED.)
GEOMETRIC_REPRESENTATION_ITEM()
RATIONAL_B_SPLINE_SURFACE(((1.,0.591243989422541,1.),(1.,0.603807915079894,
1.),(1.,0.612569262394175,1.),(1.,0.619783312569531,1.)))
REPRESENTATION_ITEM('')
SURFACE()
);
#2223=(
BOUNDED_SURFACE()
B_SPLINE_SURFACE(3,2,((#144785,#144786,#144787),(#144788,#144789,#144790),
(#144791,#144792,#144793),(#144794,#144795,#144796)),.UNSPECIFIED.,.F.,
 .F.,.F.)
B_SPLINE_SURFACE_WITH_KNOTS((4,4),(3,3),(0.,0.0298008594779328),(0.,1.),
 .UNSPECIFIED.)
GEOMETRIC_REPRESENTATION_ITEM()
RATIONAL_B_SPLINE_SURFACE(((1.,0.819627815321769,1.),(1.,0.81028158060527,
1.),(1.,0.803135207628788,1.),(1.,0.797103929716951,1.)))
REPRESENTATION_ITEM('')
SURFACE()
);
#2224=(
BOUNDED_SURFACE()
B_SPLINE_SURFACE(3,2,((#144798,#144799,#144800),(#144801,#144802,#144803),
(#144804,#144805,#144806),(#144807,#144808,#144809)),.UNSPECIFIED.,.F.,
 .F.,.F.)
B_SPLINE_SURFACE_WITH_KNOTS((4,4),(3,3),(0.,0.0300693678107436),(0.,1.),
 .UNSPECIFIED.)
GEOMETRIC_REPRESENTATION_ITEM()
RATIONAL_B_SPLINE_SURFACE(((1.,0.79694160937888,1.),(1.,0.803005840650144,
1.),(1.,0.810197796192684,1.),(1.,0.819627815321757,1.)))
REPRESENTATION_ITEM('')
SURFACE()
);
#2225=(
BOUNDED_SURFACE()
B_SPLINE_SURFACE(3,2,((#144811,#144812,#144813),(#144814,#144815,#144816),
(#144817,#144818,#144819),(#144820,#144821,#144822),(#144823,#144824,#144825),
(#144826,#144827,#144828)),.UNSPECIFIED.,.F.,.F.,.F.)
B_SPLINE_SURFACE_WITH_KNOTS((4,2,4),(3,3),(-8.43401684374147E-5,0.00160216910094088,
0.00328860201455053),(0.,1.00008434016844),.UNSPECIFIED.)
GEOMETRIC_REPRESENTATION_ITEM()
RATIONAL_B_SPLINE_SURFACE(((1.,0.703841529342767,1.0000499561106),(1.,0.725491849855086,
1.00004630412724),(1.,0.746131243723142,1.00004282266733),(1.,0.785697186856154,
1.00003614867071),(1.,0.804770925859817,1.00003293130599),(1.,0.822243584210538,
1.0000299840121)))
REPRESENTATION_ITEM('')
SURFACE()
);
#2226=(
BOUNDED_SURFACE()
B_SPLINE_SURFACE(3,2,((#144863,#144864,#144865),(#144866,#144867,#144868),
(#144869,#144870,#144871),(#144872,#144873,#144874),(#144875,#144876,#144877),
(#144878,#144879,#144880)),.UNSPECIFIED.,.F.,.F.,.F.)
B_SPLINE_SURFACE_WITH_KNOTS((4,2,4),(3,3),(0.,0.00160286774303482,0.00320573548606963),
(0.,1.),.UNSPECIFIED.)
GEOMETRIC_REPRESENTATION_ITEM()
RATIONAL_B_SPLINE_SURFACE(((1.,0.819627815321769,1.),(1.,0.802865620897526,
1.),(1.,0.785107826354221,1.),(1.,0.747495184421159,1.),(1.,0.727508688529169,
1.),(1.,0.707106781186548,1.)))
REPRESENTATION_ITEM('')
SURFACE()
);
#2227=(
BOUNDED_SURFACE()
B_SPLINE_SURFACE(3,2,((#144893,#144894,#144895),(#144896,#144897,#144898),
(#144899,#144900,#144901),(#144902,#144903,#144904),(#144905,#144906,#144907),
(#144908,#144909,#144910)),.UNSPECIFIED.,.F.,.F.,.F.)
B_SPLINE_SURFACE_WITH_KNOTS((4,2,4),(3,3),(0.28787290846928,0.292960043496213,
0.298047178523145),(0.,1.),.UNSPECIFIED.)
GEOMETRIC_REPRESENTATION_ITEM()
RATIONAL_B_SPLINE_SURFACE(((1.,0.948000837587232,1.),(1.,0.950253148926149,
1.),(1.,0.952526342948766,1.),(1.,0.957029990073055,1.),(1.,0.959243464400477,
1.),(1.,0.961372004230729,1.)))
REPRESENTATION_ITEM('')
SURFACE()
);
#2228=(
BOUNDED_SURFACE()
B_SPLINE_SURFACE(3,2,((#144934,#144935,#144936),(#144937,#144938,#144939),
(#144940,#144941,#144942),(#144943,#144944,#144945)),.UNSPECIFIED.,.F.,
 .F.,.F.)
B_SPLINE_SURFACE_WITH_KNOTS((4,4),(3,3),(1.38777878078145E-17,0.0238258198664154),
(0.,1.),.UNSPECIFIED.)
GEOMETRIC_REPRESENTATION_ITEM()
RATIONAL_B_SPLINE_SURFACE(((1.,0.566606711022863,1.),(1.,0.557709627588123,
1.),(1.,0.547241836069268,1.),(1.,0.533775524284033,1.)))
REPRESENTATION_ITEM('')
SURFACE()
);
#2229=(
BOUNDED_SURFACE()
B_SPLINE_SURFACE(3,2,((#144947,#144948,#144949),(#144950,#144951,#144952),
(#144953,#144954,#144955),(#144956,#144957,#144958),(#144959,#144960,#144961),
(#144962,#144963,#144964)),.UNSPECIFIED.,.F.,.F.,.F.)
B_SPLINE_SURFACE_WITH_KNOTS((4,2,4),(3,3),(0.,0.00196532227871992,0.00393064455743984),
(0.,1.),.UNSPECIFIED.)
GEOMETRIC_REPRESENTATION_ITEM()
RATIONAL_B_SPLINE_SURFACE(((1.,0.70710678118655,1.),(1.,0.681045297773967,
1.),(1.,0.653805231917789,1.),(1.,0.596033371554667,1.),(1.,0.565216504169612,
1.),(1.,0.533775524284038,1.)))
REPRESENTATION_ITEM('')
SURFACE()
);
#2230=(
BOUNDED_SURFACE()
B_SPLINE_SURFACE(3,2,((#144970,#144971,#144972),(#144973,#144974,#144975),
(#144976,#144977,#144978),(#144979,#144980,#144981),(#144982,#144983,#144984),
(#144985,#144986,#144987)),.UNSPECIFIED.,.F.,.F.,.F.)
B_SPLINE_SURFACE_WITH_KNOTS((4,2,4),(3,3),(-0.000393284609852448,0.00196642364705715,
0.00432613202352569),(0.,1.00045991623863),.UNSPECIFIED.)
GEOMETRIC_REPRESENTATION_ITEM()
RATIONAL_B_SPLINE_SURFACE(((1.,0.514485821122662,1.0004465917099),(1.,0.552975432690279,
1.00041118771514),(1.,0.589408021414007,1.0003776758368),(1.,0.658978456167228,
1.00031368269146),(1.,0.692168964479326,1.00028315298398),(1.,0.722275405990915,
1.0002554601013)))
REPRESENTATION_ITEM('')
SURFACE()
);
#2231=(
BOUNDED_SURFACE()
B_SPLINE_SURFACE(3,2,((#145020,#145021,#145022),(#145023,#145024,#145025),
(#145026,#145027,#145028),(#145029,#145030,#145031)),.UNSPECIFIED.,.F.,
 .F.,.F.)
B_SPLINE_SURFACE_WITH_KNOTS((4,4),(3,3),(0.,0.0240963563036403),(0.,1.),
 .UNSPECIFIED.)
GEOMETRIC_REPRESENTATION_ITEM()
RATIONAL_B_SPLINE_SURFACE(((1.,0.533775524284036,1.),(1.,0.547394060950047,
1.),(1.,0.557948204678947,1.),(1.,0.566908467907053,1.)))
REPRESENTATION_ITEM('')
SURFACE()
);
#2232=(
BOUNDED_SURFACE()
B_SPLINE_SURFACE(3,2,((#145058,#145059,#145060),(#145061,#145062,#145063),
(#145064,#145065,#145066),(#145067,#145068,#145069)),.UNSPECIFIED.,.F.,
 .F.,.F.)
B_SPLINE_SURFACE_WITH_KNOTS((4,4),(3,3),(0.,8.95703543583319E-5),(0.,1.),
 .UNSPECIFIED.)
GEOMETRIC_REPRESENTATION_ITEM()
RATIONAL_B_SPLINE_SURFACE(((1.,0.821022196159299,1.),(1.,0.818079073177133,
1.),(1.,0.814610488520586,1.),(1.,0.810617639934139,1.)))
REPRESENTATION_ITEM('')
SURFACE()
);
#2233=(
BOUNDED_SURFACE()
B_SPLINE_SURFACE(3,2,((#145071,#145072,#145073),(#145074,#145075,#145076),
(#145077,#145078,#145079),(#145080,#145081,#145082),(#145083,#145084,#145085),
(#145086,#145087,#145088),(#145089,#145090,#145091),(#145092,#145093,#145094)),
 .UNSPECIFIED.,.F.,.F.,.F.)
B_SPLINE_SURFACE_WITH_KNOTS((4,2,2,4),(3,3),(0.,0.000301902853038141,0.000452854279557211,
0.000603805706076282),(0.,1.),.UNSPECIFIED.)
GEOMETRIC_REPRESENTATION_ITEM()
RATIONAL_B_SPLINE_SURFACE(((1.,0.702399276808562,1.),(1.,0.672208297052869,
1.),(1.,0.639172707788597,1.),(1.,0.593013313775285,1.),(1.,0.577958663413849,
1.),(1.,0.550545486207946,1.),(1.,0.538469268822416,1.),(1.,0.528679393385783,
1.)))
REPRESENTATION_ITEM('')
SURFACE()
);
#2234=(
BOUNDED_SURFACE()
B_SPLINE_SURFACE(3,2,((#145096,#145097,#145098),(#145099,#145100,#145101),
(#145102,#145103,#145104),(#145105,#145106,#145107)),.UNSPECIFIED.,.F.,
 .F.,.F.)
B_SPLINE_SURFACE_WITH_KNOTS((4,4),(3,3),(0.,0.024690830875569),(0.,1.),
 .UNSPECIFIED.)
GEOMETRIC_REPRESENTATION_ITEM()
RATIONAL_B_SPLINE_SURFACE(((1.,0.821022196159299,1.),(1.,0.827229968384993,
1.),(1.,0.834396885388283,1.),(1.,0.84317661051583,1.)))
REPRESENTATION_ITEM('')
SURFACE()
);
#2235=(
BOUNDED_SURFACE()
B_SPLINE_SURFACE(3,2,((#145109,#145110,#145111),(#145112,#145113,#145114),
(#145115,#145116,#145117),(#145118,#145119,#145120),(#145121,#145122,#145123),
(#145124,#145125,#145126)),.UNSPECIFIED.,.F.,.F.,.F.)
B_SPLINE_SURFACE_WITH_KNOTS((4,2,4),(3,3),(-0.000125633631190664,0.00192660600180124,
0.00397876574878657),(0.,1.00012563363119),.UNSPECIFIED.)
GEOMETRIC_REPRESENTATION_ITEM()
RATIONAL_B_SPLINE_SURFACE(((1.,0.702058786892261,1.00007486287297),(1.,
0.729454174087526,1.00006797930903),(1.,0.755057429332917,1.00006154604917),
(1.,0.803448625603955,1.00004938692576),(1.,0.826420664059153,1.00004361480455),
(1.,0.846952528006408,1.0000384558193)))
REPRESENTATION_ITEM('')
SURFACE()
);
#2236=(
BOUNDED_SURFACE()
B_SPLINE_SURFACE(3,2,((#145167,#145168,#145169),(#145170,#145171,#145172),
(#145173,#145174,#145175),(#145176,#145177,#145178),(#145179,#145180,#145181),
(#145182,#145183,#145184)),.UNSPECIFIED.,.F.,.F.,.F.)
B_SPLINE_SURFACE_WITH_KNOTS((4,2,4),(3,3),(-0.000277756685671561,0.00176358033920161,
0.00380491746723071),(0.,1.00027775678883),.UNSPECIFIED.)
GEOMETRIC_REPRESENTATION_ITEM()
RATIONAL_B_SPLINE_SURFACE(((1.,0.541612572103269,1.00025464044002),(1.,
0.573730160641759,1.00023679868351),(1.,0.60443290548972,1.00021974289187),
(1.,0.66339296977674,1.00018698977562),(1.,0.691792553884413,1.00017121342105),
(1.,0.717755310902421,1.00015679075701)))
REPRESENTATION_ITEM('')
SURFACE()
);
#2237=(
BOUNDED_SURFACE()
B_SPLINE_SURFACE(3,2,((#145186,#145187,#145188),(#145189,#145190,#145191),
(#145192,#145193,#145194),(#145195,#145196,#145197)),.UNSPECIFIED.,.F.,
 .F.,.F.)
B_SPLINE_SURFACE_WITH_KNOTS((4,4),(3,3),(0.,0.0278605201857756),(0.,1.),
 .UNSPECIFIED.)
GEOMETRIC_REPRESENTATION_ITEM()
RATIONAL_B_SPLINE_SURFACE(((1.,0.55476848021506,1.),(1.,0.56887897086178,
1.),(1.,0.579290070452688,1.),(1.,0.587985430396658,1.)))
REPRESENTATION_ITEM('')
SURFACE()
);
#2238=(
BOUNDED_SURFACE()
B_SPLINE_SURFACE(3,2,((#145198,#145199,#145200),(#145201,#145202,#145203),
(#145204,#145205,#145206),(#145207,#145208,#145209)),.UNSPECIFIED.,.F.,
 .F.,.F.)
B_SPLINE_SURFACE_WITH_KNOTS((4,4),(3,3),(-1.38777878078145E-17,0.0333345287175385),
(0.,1.),.UNSPECIFIED.)
GEOMETRIC_REPRESENTATION_ITEM()
RATIONAL_B_SPLINE_SURFACE(((1.,0.779737900546642,1.),(1.,0.785266544814036,
1.),(1.,0.791920621206337,1.),(1.,0.801085834760578,1.)))
REPRESENTATION_ITEM('')
SURFACE()
);
#2239=(
BOUNDED_SURFACE()
B_SPLINE_SURFACE(3,2,((#145211,#145212,#145213),(#145214,#145215,#145216),
(#145217,#145218,#145219),(#145220,#145221,#145222)),.UNSPECIFIED.,.F.,
 .F.,.F.)
B_SPLINE_SURFACE_WITH_KNOTS((4,4),(3,3),(0.,9.64176041888312E-5),(0.,1.),
 .UNSPECIFIED.)
GEOMETRIC_REPRESENTATION_ITEM()
RATIONAL_B_SPLINE_SURFACE(((1.,0.801085834760579,1.),(1.,0.800109483270879,
1.),(1.,0.799128688610329,1.),(1.,0.798143461627153,1.)))
REPRESENTATION_ITEM('')
SURFACE()
);
#2240=(
BOUNDED_SURFACE()
B_SPLINE_SURFACE(3,2,((#145223,#145224,#145225),(#145226,#145227,#145228),
(#145229,#145230,#145231),(#145232,#145233,#145234)),.UNSPECIFIED.,.F.,
 .F.,.F.)
B_SPLINE_SURFACE_WITH_KNOTS((4,4),(3,3),(0.,0.0333425790106738),(0.,1.),
 .UNSPECIFIED.)
GEOMETRIC_REPRESENTATION_ITEM()
RATIONAL_B_SPLINE_SURFACE(((1.,0.619253049823353,1.),(1.,0.62903050118076,
1.),(1.,0.635777469330956,1.),(1.,0.641321251913794,1.)))
REPRESENTATION_ITEM('')
SURFACE()
);
#2241=(
BOUNDED_SURFACE()
B_SPLINE_SURFACE(3,2,((#145235,#145236,#145237),(#145238,#145239,#145240),
(#145241,#145242,#145243),(#145244,#145245,#145246)),.UNSPECIFIED.,.F.,
 .F.,.F.)
B_SPLINE_SURFACE_WITH_KNOTS((4,4),(3,3),(-1.38777878078145E-17,0.0332202089949022),
(0.,1.),.UNSPECIFIED.)
GEOMETRIC_REPRESENTATION_ITEM()
RATIONAL_B_SPLINE_SURFACE(((1.,0.736495153922513,1.),(1.,0.738798609451216,
1.),(1.,0.741580133014481,1.),(1.,0.745472778587061,1.)))
REPRESENTATION_ITEM('')
SURFACE()
);
#2242=(
BOUNDED_SURFACE()
B_SPLINE_SURFACE(3,2,((#145285,#145286,#145287),(#145288,#145289,#145290),
(#145291,#145292,#145293),(#145294,#145295,#145296)),.UNSPECIFIED.,.F.,
 .F.,.F.)
B_SPLINE_SURFACE_WITH_KNOTS((4,4),(3,3),(-3.41800396632663E-5,0.000687703280430334),
(0.,1.00003418003966),.UNSPECIFIED.)
GEOMETRIC_REPRESENTATION_ITEM()
RATIONAL_B_SPLINE_SURFACE(((1.,0.549976566282829,1.00003076363763),(1.,
0.549294416403988,1.00003081026945),(1.,0.555643671106273,1.00003037623389),
(1.,0.567819410633178,1.00002954389937)))
REPRESENTATION_ITEM('')
SURFACE()
);
#2243=(
BOUNDED_SURFACE()
B_SPLINE_SURFACE(3,2,((#145300,#145301,#145302),(#145303,#145304,#145305),
(#145306,#145307,#145308),(#145309,#145310,#145311),(#145312,#145313,#145314),
(#145315,#145316,#145317)),.UNSPECIFIED.,.F.,.F.,.F.)
B_SPLINE_SURFACE_WITH_KNOTS((4,2,4),(3,3),(1.38777878078145E-17,0.0146992078328598,
0.0293984156657196),(0.,1.),.UNSPECIFIED.)
GEOMETRIC_REPRESENTATION_ITEM()
RATIONAL_B_SPLINE_SURFACE(((1.,0.566144048133053,1.),(1.,0.560653267979146,
1.),(1.,0.554543800692172,1.),(1.,0.540492753126539,1.),(1.,0.532555598048173,
1.),(1.,0.523250899838466,1.)))
REPRESENTATION_ITEM('')
SURFACE()
);
#2244=(
BOUNDED_SURFACE()
B_SPLINE_SURFACE(3,2,((#145326,#145327,#145328),(#145329,#145330,#145331),
(#145332,#145333,#145334),(#145335,#145336,#145337),(#145338,#145339,#145340),
(#145341,#145342,#145343)),.UNSPECIFIED.,.F.,.F.,.F.)
B_SPLINE_SURFACE_WITH_KNOTS((4,2,4),(3,3),(0.,0.00207126900955203,0.00414253801910405),
(0.,1.),.UNSPECIFIED.)
GEOMETRIC_REPRESENTATION_ITEM()
RATIONAL_B_SPLINE_SURFACE(((1.,0.707106781186548,1.),(1.,0.679626330234824,
1.),(1.,0.650848145227602,1.),(1.,0.589569252159033,1.),(1.,0.556778618705704,
1.),(1.,0.523250899838466,1.)))
REPRESENTATION_ITEM('')
SURFACE()
);
#2245=(
BOUNDED_SURFACE()
B_SPLINE_SURFACE(3,2,((#145356,#145357,#145358),(#145359,#145360,#145361),
(#145362,#145363,#145364),(#145365,#145366,#145367),(#145368,#145369,#145370),
(#145371,#145372,#145373)),.UNSPECIFIED.,.F.,.F.,.F.)
B_SPLINE_SURFACE_WITH_KNOTS((4,2,4),(3,3),(-0.000414433024293954,0.00207216577676188,
0.00455876470887616),(0.,1.00057450279771),.UNSPECIFIED.)
GEOMETRIC_REPRESENTATION_ITEM()
RATIONAL_B_SPLINE_SURFACE(((1.,0.502594029997045,1.00057152224273),(1.,
0.543754583372273,1.00052422853659),(1.,0.582517660127345,1.0004796895445),
(1.,0.656326486548337,1.00039488278995),(1.,0.691338987574868,1.00035465323036),
(1.,0.723071803322265,1.00031819204751)))
REPRESENTATION_ITEM('')
SURFACE()
);
#2246=(
BOUNDED_SURFACE()
B_SPLINE_SURFACE(3,2,((#145406,#145407,#145408),(#145409,#145410,#145411),
(#145412,#145413,#145414),(#145415,#145416,#145417),(#145418,#145419,#145420),
(#145421,#145422,#145423)),.UNSPECIFIED.,.F.,.F.,.F.)
B_SPLINE_SURFACE_WITH_KNOTS((4,2,4),(3,3),(0.,0.0145632072393804,0.0291264144787609),
(0.,1.),.UNSPECIFIED.)
GEOMETRIC_REPRESENTATION_ITEM()
RATIONAL_B_SPLINE_SURFACE(((1.,0.523250899838464,1.),(1.,0.532471350763147,
1.),(1.,0.540347653844846,1.),(1.,0.554302832144208,1.),(1.,0.560377433574518,
1.),(1.,0.565840417962188,1.)))
REPRESENTATION_ITEM('')
SURFACE()
);
#2247=(
BOUNDED_SURFACE()
B_SPLINE_SURFACE(3,2,((#145430,#145431,#145432),(#145433,#145434,#145435),
(#145436,#145437,#145438),(#145439,#145440,#145441),(#145442,#145443,#145444),
(#145445,#145446,#145447)),.UNSPECIFIED.,.F.,.F.,.F.)
B_SPLINE_SURFACE_WITH_KNOTS((4,2,4),(3,3),(0.320579494062015,0.325851056440119,
0.331122618818223),(0.,1.),.UNSPECIFIED.)
GEOMETRIC_REPRESENTATION_ITEM()
RATIONAL_B_SPLINE_SURFACE(((1.,0.944716550693843,1.),(1.,0.947183014496352,
1.),(1.,0.949681733718157,1.),(1.,0.954674150124444,1.),(1.,0.957142659869515,
1.),(1.,0.959530911310534,1.)))
REPRESENTATION_ITEM('')
SURFACE()
);
#2248=(
BOUNDED_SURFACE()
B_SPLINE_SURFACE(3,2,((#145499,#145500,#145501),(#145502,#145503,#145504),
(#145505,#145506,#145507),(#145508,#145509,#145510),(#145511,#145512,#145513),
(#145514,#145515,#145516)),.UNSPECIFIED.,.F.,.F.,.F.)
B_SPLINE_SURFACE_WITH_KNOTS((4,2,4),(3,3),(0.,0.0176980703187956,0.0353961406375911),
(0.,1.),.UNSPECIFIED.)
GEOMETRIC_REPRESENTATION_ITEM()
RATIONAL_B_SPLINE_SURFACE(((1.,0.797648081014877,1.),(1.,0.801243745289675,
1.),(1.,0.805251011590647,1.),(1.,0.814487862093865,1.),(1.,0.819714636457853,
1.),(1.,0.825853968826193,1.)))
REPRESENTATION_ITEM('')
SURFACE()
);
#2249=(
BOUNDED_SURFACE()
B_SPLINE_SURFACE(3,2,((#145518,#145519,#145520),(#145521,#145522,#145523),
(#145524,#145525,#145526),(#145527,#145528,#145529),(#145530,#145531,#145532),
(#145533,#145534,#145535)),.UNSPECIFIED.,.F.,.F.,.F.)
B_SPLINE_SURFACE_WITH_KNOTS((4,2,4),(3,3),(-9.9063038639367E-5,0.00167878022781669,
0.00345653198876773),(0.,1.00009906303864),.UNSPECIFIED.)
GEOMETRIC_REPRESENTATION_ITEM()
RATIONAL_B_SPLINE_SURFACE(((0.999999999999999,0.70321690031505,1.00005880047134),
(1.,0.726378747565388,1.0000542115054),(1.,0.748363388483742,1.00004985577474),
(1.,0.790366013422709,1.00004153395942),(1.,0.810543585884598,1.00003753625614),
(1.,0.828922930782749,1.00003389482864)))
REPRESENTATION_ITEM('')
SURFACE()
);
#2250=(
BOUNDED_SURFACE()
B_SPLINE_SURFACE(3,2,((#145541,#145542,#145543),(#145544,#145545,#145546),
(#145547,#145548,#145549),(#145550,#145551,#145552),(#145553,#145554,#145555),
(#145556,#145557,#145558)),.UNSPECIFIED.,.F.,.F.,.F.)
B_SPLINE_SURFACE_WITH_KNOTS((4,2,4),(3,3),(-3.90312782094781E-18,0.00167965794371986,
0.00335931588743972),(0.,1.),.UNSPECIFIED.)
GEOMETRIC_REPRESENTATION_ITEM()
RATIONAL_B_SPLINE_SURFACE(((1.,0.825853968826192,1.),(1.,0.808295365083271,
1.),(1.,0.789625920673805,1.),(1.,0.749928217285841,1.),(1.,0.728769006116152,
1.),(1.,0.707106781186548,1.)))
REPRESENTATION_ITEM('')
SURFACE()
);
#2251=(
BOUNDED_SURFACE()
B_SPLINE_SURFACE(3,2,((#145567,#145568,#145569),(#145570,#145571,#145572),
(#145573,#145574,#145575),(#145576,#145577,#145578),(#145579,#145580,#145581),
(#145582,#145583,#145584)),.UNSPECIFIED.,.F.,.F.,.F.)
B_SPLINE_SURFACE_WITH_KNOTS((4,2,4),(3,3),(0.,0.0178323395635859,0.0356646791271718),
(0.,1.),.UNSPECIFIED.)
GEOMETRIC_REPRESENTATION_ITEM()
RATIONAL_B_SPLINE_SURFACE(((1.,0.825853968826192,1.),(1.,0.819668171116131,
1.),(1.,0.814408476706928,1.),(1.,0.80512037347301,1.),(1.,0.801094867709694,
1.),(1.,0.79748483152198,1.)))
REPRESENTATION_ITEM('')
SURFACE()
);
#2252=(
BOUNDED_SURFACE()
B_SPLINE_SURFACE(3,2,((#145593,#145594,#145595),(#145596,#145597,#145598),
(#145599,#145600,#145601),(#145602,#145603,#145604)),.UNSPECIFIED.,.F.,
 .F.,.F.)
B_SPLINE_SURFACE_WITH_KNOTS((4,4),(3,3),(-6.51957114117417E-5,0.000717152825529202),
(0.,1.0001395156952),.UNSPECIFIED.)
GEOMETRIC_REPRESENTATION_ITEM()
RATIONAL_B_SPLINE_SURFACE(((1.,0.795687417707187,1.00005700962391),(1.,
0.80308940810469,1.00005494423624),(1.,0.806595093358397,1.00005396604001),
(1.,0.80591968995395,1.00005415449876)))
REPRESENTATION_ITEM('')
SURFACE()
);
#2253=(
BOUNDED_SURFACE()
B_SPLINE_SURFACE(3,2,((#145638,#145639,#145640),(#145641,#145642,#145643),
(#145644,#145645,#145646),(#145647,#145648,#145649),(#145650,#145651,#145652),
(#145653,#145654,#145655)),.UNSPECIFIED.,.F.,.F.,.F.)
B_SPLINE_SURFACE_WITH_KNOTS((4,2,4),(3,3),(0.,0.0188568492058762,0.0377136984117525),
(0.,1.),.UNSPECIFIED.)
GEOMETRIC_REPRESENTATION_ITEM()
RATIONAL_B_SPLINE_SURFACE(((1.,0.583115115460263,1.),(1.,0.591477165975886,
1.),(1.,0.59822556054293,1.),(1.,0.609817503669346,1.),(1.,0.614651018359553,
1.),(1.,0.618903611686376,1.)))
REPRESENTATION_ITEM('')
SURFACE()
);
#2254=(
BOUNDED_SURFACE()
B_SPLINE_SURFACE(3,2,((#145673,#145674,#145675),(#145676,#145677,#145678),
(#145679,#145680,#145681),(#145682,#145683,#145684)),.UNSPECIFIED.,.F.,
 .F.,.F.)
B_SPLINE_SURFACE_WITH_KNOTS((4,4),(3,3),(-6.51408174375087E-5,0.000716548991812596),
(0.,1.00012715075799),.UNSPECIFIED.)
GEOMETRIC_REPRESENTATION_ITEM()
RATIONAL_B_SPLINE_SURFACE(((1.,0.609559938200355,1.00009928949961),(1.,
0.608772413245087,1.0000994897684),(1.,0.612737943163139,1.00009848132813),
(1.,0.621014916147782,1.00009637648136)))
REPRESENTATION_ITEM('')
SURFACE()
);
#2255=(
BOUNDED_SURFACE()
B_SPLINE_SURFACE(3,2,((#145688,#145689,#145690),(#145691,#145692,#145693),
(#145694,#145695,#145696),(#145697,#145698,#145699),(#145700,#145701,#145702),
(#145703,#145704,#145705)),.UNSPECIFIED.,.F.,.F.,.F.)
B_SPLINE_SURFACE_WITH_KNOTS((4,2,4),(3,3),(0.,0.018990790064314,0.0379815801286281),
(0.,1.),.UNSPECIFIED.)
GEOMETRIC_REPRESENTATION_ITEM()
RATIONAL_B_SPLINE_SURFACE(((1.,0.619084183929308,1.),(1.,0.61481875400451,
1.),(1.,0.609968099232784,1.),(1.,0.598321687913226,1.),(1.,0.591536257853193,
1.),(1.,0.583115115460264,1.)))
REPRESENTATION_ITEM('')
SURFACE()
);
#2256=(
BOUNDED_SURFACE()
B_SPLINE_SURFACE(3,2,((#145714,#145715,#145716),(#145717,#145718,#145719),
(#145720,#145721,#145722),(#145723,#145724,#145725),(#145726,#145727,#145728),
(#145729,#145730,#145731)),.UNSPECIFIED.,.F.,.F.,.F.)
B_SPLINE_SURFACE_WITH_KNOTS((4,2,4),(3,3),(0.,0.00151694200897944,0.00303388401795888),
(0.,1.),.UNSPECIFIED.)
GEOMETRIC_REPRESENTATION_ITEM()
RATIONAL_B_SPLINE_SURFACE(((1.,0.70710678118655,1.),(1.,0.688185240537986,
1.),(1.,0.6684652198449,1.),(1.,0.627083641349078,1.),(1.,0.605243055947471,
1.),(1.,0.583115115460264,1.)))
REPRESENTATION_ITEM('')
SURFACE()
);
#2257=(
BOUNDED_SURFACE()
B_SPLINE_SURFACE(3,2,((#145744,#145745,#145746),(#145747,#145748,#145749),
(#145750,#145751,#145752),(#145753,#145754,#145755),(#145756,#145757,#145758),
(#145759,#145760,#145761)),.UNSPECIFIED.,.F.,.F.,.F.)
B_SPLINE_SURFACE_WITH_KNOTS((4,2,4),(3,3),(-0.000134068678628998,0.00151741931723474,
0.00316890735964793),(0.,1.00013406872517),.UNSPECIFIED.)
GEOMETRIC_REPRESENTATION_ITEM()
RATIONAL_B_SPLINE_SURFACE(((1.,0.577176787432037,1.00011337473816),(1.,
0.601399673404762,1.00010687967528),(1.,0.624769559778014,1.00010061333353),
(1.,0.669881131114838,1.00008851723181),(1.,0.691769778729462,1.00008264806565),
(1.,0.712034386796128,1.00007721436531)))
REPRESENTATION_ITEM('')
SURFACE()
);
#2258=(
BOUNDED_SURFACE()
B_SPLINE_SURFACE(3,2,((#145790,#145791,#145792),(#145793,#145794,#145795),
(#145796,#145797,#145798),(#145799,#145800,#145801),(#145802,#145803,#145804),
(#145805,#145806,#145807),(#145808,#145809,#145810),(#145811,#145812,#145813)),
 .UNSPECIFIED.,.F.,.F.,.F.)
B_SPLINE_SURFACE_WITH_KNOTS((4,2,2,4),(3,3),(0.017818580704263,0.0199004486313254,
0.0219823165583878,0.0261460524125126),(0.,1.),.UNSPECIFIED.)
GEOMETRIC_REPRESENTATION_ITEM()
RATIONAL_B_SPLINE_SURFACE(((1.,0.961171308030857,1.),(1.,0.962092810628593,
1.),(1.,0.963001088261132,1.),(1.,0.964780402726978,1.),(1.,0.965653853257041,
1.),(1.,0.968176214233281,1.),(1.,0.969729042204957,1.),(1.,0.971089731516655,
1.)))
REPRESENTATION_ITEM('')
SURFACE()
);
#2259=(
BOUNDED_SURFACE()
B_SPLINE_SURFACE(3,2,((#145859,#145860,#145861),(#145862,#145863,#145864),
(#145865,#145866,#145867),(#145868,#145869,#145870)),.UNSPECIFIED.,.F.,
 .F.,.F.)
B_SPLINE_SURFACE_WITH_KNOTS((4,4),(3,3),(-8.32667268468867E-17,0.0417901757617077),
(0.,1.),.UNSPECIFIED.)
GEOMETRIC_REPRESENTATION_ITEM()
RATIONAL_B_SPLINE_SURFACE(((1.,0.757216058458815,1.),(1.,0.76211005468913,
1.),(1.,0.768141195659961,1.),(1.,0.777664586555055,1.)))
REPRESENTATION_ITEM('')
SURFACE()
);
#2260=(
BOUNDED_SURFACE()
B_SPLINE_SURFACE(3,2,((#145872,#145873,#145874),(#145875,#145876,#145877),
(#145878,#145879,#145880),(#145881,#145882,#145883),(#145884,#145885,#145886),
(#145887,#145888,#145889)),.UNSPECIFIED.,.F.,.F.,.F.)
B_SPLINE_SURFACE_WITH_KNOTS((4,2,4),(3,3),(-2.92956119863222E-5,0.00120613678608598,
0.00244151698435041),(0.,1.00002929561199),.UNSPECIFIED.)
GEOMETRIC_REPRESENTATION_ITEM()
RATIONAL_B_SPLINE_SURFACE(((1.,0.706220266280328,1.00001721291418),(1.,
0.718564407685336,1.00001648965582),(1.,0.730784372547602,1.00001577367312),
(1.,0.754961474849659,1.00001435710711),(1.,0.767001288465581,1.00001365167969),
(1.,0.778473732954666,1.00001297949513)))
REPRESENTATION_ITEM('')
SURFACE()
);
#2261=(
BOUNDED_SURFACE()
B_SPLINE_SURFACE(3,2,((#145895,#145896,#145897),(#145898,#145899,#145900),
(#145901,#145902,#145903),(#145904,#145905,#145906),(#145907,#145908,#145909),
(#145910,#145911,#145912)),.UNSPECIFIED.,.F.,.F.,.F.)
B_SPLINE_SURFACE_WITH_KNOTS((4,2,4),(3,3),(0.,0.00120620763625507,0.00241241527251014),
(0.,1.),.UNSPECIFIED.)
GEOMETRIC_REPRESENTATION_ITEM()
RATIONAL_B_SPLINE_SURFACE(((1.,0.777664586555049,1.),(1.,0.766436783957212,
1.),(1.,0.754901973237173,1.),(1.,0.73129895059372,1.),(1.,0.719146552484787,
1.),(1.,0.707106781186548,1.)))
REPRESENTATION_ITEM('')
SURFACE()
);
#2262=(
BOUNDED_SURFACE()
B_SPLINE_SURFACE(3,2,((#145921,#145922,#145923),(#145924,#145925,#145926),
(#145927,#145928,#145929),(#145930,#145931,#145932)),.UNSPECIFIED.,.F.,
 .F.,.F.)
B_SPLINE_SURFACE_WITH_KNOTS((4,4),(3,3),(0.,0.0420570108120997),(0.,1.),
 .UNSPECIFIED.)
GEOMETRIC_REPRESENTATION_ITEM()
RATIONAL_B_SPLINE_SURFACE(((1.,0.777664586555049,1.),(1.,0.768081385918698,
1.),(1.,0.762031405880593,1.),(1.,0.757123446310248,1.)))
REPRESENTATION_ITEM('')
SURFACE()
);
#2263=(
BOUNDED_SURFACE()
B_SPLINE_SURFACE(3,2,((#145939,#145940,#145941),(#145942,#145943,#145944),
(#145945,#145946,#145947),(#145948,#145949,#145950)),.UNSPECIFIED.,.F.,
 .F.,.F.)
B_SPLINE_SURFACE_WITH_KNOTS((4,4),(3,3),(-6.50609804213592E-5,0.000715670784634903),
(0.,1.00019732104438),.UNSPECIFIED.)
GEOMETRIC_REPRESENTATION_ITEM()
RATIONAL_B_SPLINE_SURFACE(((1.,0.756066809424476,1.00009626630384),(1.,
0.760288887453374,1.00009460009415),(1.,0.762267398805321,1.0000938192903),
(1.,0.761887769744426,1.00009396910791)))
REPRESENTATION_ITEM('')
SURFACE()
);
#2264=(
BOUNDED_SURFACE()
B_SPLINE_SURFACE(3,2,((#145955,#145956,#145957),(#145958,#145959,#145960),
(#145961,#145962,#145963),(#145964,#145965,#145966),(#145967,#145968,#145969),
(#145970,#145971,#145972),(#145973,#145974,#145975),(#145976,#145977,#145978),
(#145979,#145980,#145981),(#145982,#145983,#145984),(#145985,#145986,#145987),
(#145988,#145989,#145990),(#145991,#145992,#145993),(#145994,#145995,#145996)),
 .UNSPECIFIED.,.F.,.F.,.F.)
B_SPLINE_SURFACE_WITH_KNOTS((4,2,2,2,2,2,4),(3,3),(0.00808011141552929,
0.00881517523662049,0.00918270714716608,0.00955023905771168,0.00991777096825728,
0.0102853028788029,0.0110203666998941),(0.,1.),.UNSPECIFIED.)
GEOMETRIC_REPRESENTATION_ITEM()
RATIONAL_B_SPLINE_SURFACE(((1.,0.707106781186548,1.),(1.,0.708672362536739,
1.),(1.,0.710198222857537,1.),(1.,0.712427305746575,1.),(1.,0.71315813872198,
1.),(1.,0.714551782754775,1.),(1.,0.715220876802376,1.),(1.,0.71650348303418,
1.),(1.,0.717121230234592,1.),(1.,0.718264550261012,1.),(1.,0.718793336138408,
1.),(1.,0.720253112545596,1.),(1.,0.721064801594907,1.),(1.,0.721643051700349,
1.)))
REPRESENTATION_ITEM('')
SURFACE()
);
#2265=(
BOUNDED_SURFACE()
B_SPLINE_SURFACE(3,2,((#146035,#146036,#146037),(#146038,#146039,#146040),
(#146041,#146042,#146043),(#146044,#146045,#146046)),.UNSPECIFIED.,.F.,
 .F.,.F.)
B_SPLINE_SURFACE_WITH_KNOTS((4,4),(3,3),(0.,0.0430361525536219),(0.,1.),
 .UNSPECIFIED.)
GEOMETRIC_REPRESENTATION_ITEM()
RATIONAL_B_SPLINE_SURFACE(((1.,0.649397749909071,1.),(1.,0.658290092659334,
1.),(1.,0.663526138769308,1.),(1.,0.667763418073535,1.)))
REPRESENTATION_ITEM('')
SURFACE()
);
#2266=(
BOUNDED_SURFACE()
B_SPLINE_SURFACE(3,2,((#146048,#146049,#146050),(#146051,#146052,#146053),
(#146054,#146055,#146056),(#146057,#146058,#146059),(#146060,#146061,#146062),
(#146063,#146064,#146065),(#146066,#146067,#146068),(#146069,#146070,#146071),
(#146072,#146073,#146074),(#146075,#146076,#146077),(#146078,#146079,#146080),
(#146081,#146082,#146083),(#146084,#146085,#146086),(#146087,#146088,#146089)),
 .UNSPECIFIED.,.F.,.F.,.F.)
B_SPLINE_SURFACE_WITH_KNOTS((4,2,2,2,2,2,4),(3,3),(0.0080803797182093,0.00879690254712659,
0.00915516396158524,0.00951342537604388,0.00987168679050253,0.0102299482049612,
0.0109464710338785),(0.,1.),.UNSPECIFIED.)
GEOMETRIC_REPRESENTATION_ITEM()
RATIONAL_B_SPLINE_SURFACE(((1.,0.707106781186548,1.),(1.,0.705537440672151,
1.),(1.,0.703998083945123,1.),(1.,0.701735656940981,1.),(1.,0.700989163179782,
1.),(1.,0.699560461823081,1.),(1.,0.698871897343629,1.),(1.,0.697546947950716,
1.),(1.,0.696905752213842,1.),(1.,0.695707159507179,1.),(1.,0.695149875554341,
1.),(1.,0.693602432259692,1.),(1.,0.692727265033204,1.),(1.,0.692079067931822,
1.)))
REPRESENTATION_ITEM('')
SURFACE()
);
#2267=(
BOUNDED_SURFACE()
B_SPLINE_SURFACE(3,2,((#146151,#146152,#146153),(#146154,#146155,#146156),
(#146157,#146158,#146159),(#146160,#146161,#146162)),.UNSPECIFIED.,.F.,
 .F.,.F.)
B_SPLINE_SURFACE_WITH_KNOTS((4,4),(3,3),(0.,0.000650375609766158),(0.,1.),
 .UNSPECIFIED.)
GEOMETRIC_REPRESENTATION_ITEM()
RATIONAL_B_SPLINE_SURFACE(((1.,0.663756004792833,1.),(1.,0.663759519746911,
1.),(1.,0.665134391960157,1.),(1.,0.66784082710355,1.)))
REPRESENTATION_ITEM('')
SURFACE()
);
#2268=(
BOUNDED_SURFACE()
B_SPLINE_SURFACE(3,2,((#146166,#146167,#146168),(#146169,#146170,#146171),
(#146172,#146173,#146174),(#146175,#146176,#146177)),.UNSPECIFIED.,.F.,
 .F.,.F.)
B_SPLINE_SURFACE_WITH_KNOTS((4,4),(3,3),(-2.77555756156289E-17,0.0433026927553429),
(0.,1.),.UNSPECIFIED.)
GEOMETRIC_REPRESENTATION_ITEM()
RATIONAL_B_SPLINE_SURFACE(((1.,0.667840827103545,1.),(1.,0.66359300941018,
1.),(1.,0.658343952018749,1.),(1.,0.649397749909072,1.)))
REPRESENTATION_ITEM('')
SURFACE()
);
#2269=(
BOUNDED_SURFACE()
B_SPLINE_SURFACE(3,2,((#146184,#146185,#146186),(#146187,#146188,#146189),
(#146190,#146191,#146192),(#146193,#146194,#146195),(#146196,#146197,#146198),
(#146199,#146200,#146201)),.UNSPECIFIED.,.F.,.F.,.F.)
B_SPLINE_SURFACE_WITH_KNOTS((4,2,4),(3,3),(0.,0.00110388220976991,0.00220776441953981),
(0.,1.),.UNSPECIFIED.)
GEOMETRIC_REPRESENTATION_ITEM()
RATIONAL_B_SPLINE_SURFACE(((1.,0.707106781186548,1.),(1.,0.69822152219183,
1.),(1.,0.68897986867167,1.),(1.,0.66970545013756,1.),(1.,0.659601845960695,
1.),(1.,0.649397749909072,1.)))
REPRESENTATION_ITEM('')
SURFACE()
);
#2270=(
BOUNDED_SURFACE()
B_SPLINE_SURFACE(3,2,((#146215,#146216,#146217),(#146218,#146219,#146220),
(#146221,#146222,#146223),(#146224,#146225,#146226),(#146227,#146228,#146229),
(#146230,#146231,#146232)),.UNSPECIFIED.,.F.,.F.,.F.)
B_SPLINE_SURFACE_WITH_KNOTS((4,2,4),(3,3),(-4.18082381682501E-5,0.00110390261829224,
0.00224961359036052),(0.,1.00004180835378),.UNSPECIFIED.)
GEOMETRIC_REPRESENTATION_ITEM()
RATIONAL_B_SPLINE_SURFACE(((1.,0.648223184306046,1.00002941441912),(1.,
0.658829102191687,1.00002852758719),(1.,0.669145628051642,1.00002766495326),
(1.,0.68916060951258,1.00002599136641),(1.,0.698923845802076,1.00002517499674),
(1.,0.708101577151724,1.00002440758506)))
REPRESENTATION_ITEM('')
SURFACE()
);
#2271=(
BOUNDED_SURFACE()
B_SPLINE_SURFACE(3,2,((#146258,#146259,#146260),(#146261,#146262,#146263),
(#146264,#146265,#146266),(#146267,#146268,#146269),(#146270,#146271,#146272),
(#146273,#146274,#146275)),.UNSPECIFIED.,.F.,.F.,.F.)
B_SPLINE_SURFACE_WITH_KNOTS((4,2,4),(3,3),(0.012499301108314,0.0157975372010094,
0.0190957732937049),(0.,1.),.UNSPECIFIED.)
GEOMETRIC_REPRESENTATION_ITEM()
RATIONAL_B_SPLINE_SURFACE(((1.,0.976191060180328,1.),(1.,0.976018964367352,
1.),(1.,0.975629721882182,1.),(1.,0.974451430140223,1.),(1.,0.97367913510036,
1.),(1.,0.972768244198254,1.)))
REPRESENTATION_ITEM('')
SURFACE()
);
#2272=(
BOUNDED_SURFACE()
B_SPLINE_SURFACE(3,2,((#146300,#146301,#146302),(#146303,#146304,#146305),
(#146306,#146307,#146308),(#146309,#146310,#146311)),.UNSPECIFIED.,.F.,
 .F.,.F.)
B_SPLINE_SURFACE_WITH_KNOTS((4,4),(3,3),(0.,0.0444870989094409),(0.,1.),
 .UNSPECIFIED.)
GEOMETRIC_REPRESENTATION_ITEM()
RATIONAL_B_SPLINE_SURFACE(((1.,0.71449972514277,1.),(1.,0.715296138993144,
1.),(1.,0.71628014758797,1.),(1.,0.717952606100523,1.)))
REPRESENTATION_ITEM('')
SURFACE()
);
#2273=(
BOUNDED_SURFACE()
B_SPLINE_SURFACE(3,2,((#146313,#146314,#146315),(#146316,#146317,#146318),
(#146319,#146320,#146321),(#146322,#146323,#146324)),.UNSPECIFIED.,.F.,
 .F.,.F.)
B_SPLINE_SURFACE_WITH_KNOTS((4,4),(3,3),(0.,0.00196035438616165),(0.,1.),
 .UNSPECIFIED.)
GEOMETRIC_REPRESENTATION_ITEM()
RATIONAL_B_SPLINE_SURFACE(((1.,0.707106781186548,1.),(1.,0.710533388681839,
1.),(1.,0.714200483631581,1.),(1.,0.717952606100467,1.)))
REPRESENTATION_ITEM('')
SURFACE()
);
#2274=(
BOUNDED_SURFACE()
B_SPLINE_SURFACE(3,2,((#146330,#146331,#146332),(#146333,#146334,#146335),
(#146336,#146337,#146338),(#146339,#146340,#146341)),.UNSPECIFIED.,.F.,
 .F.,.F.)
B_SPLINE_SURFACE_WITH_KNOTS((4,4),(3,3),(-3.90312782094781E-18,0.0019603544817943),
(0.,1.),.UNSPECIFIED.)
GEOMETRIC_REPRESENTATION_ITEM()
RATIONAL_B_SPLINE_SURFACE(((1.,0.717952606100523,1.),(1.,0.714237876912109,
1.),(1.,0.710568615888393,1.),(1.,0.707106781186514,1.)))
REPRESENTATION_ITEM('')
SURFACE()
);
#2275=(
BOUNDED_SURFACE()
B_SPLINE_SURFACE(3,2,((#146345,#146346,#146347),(#146348,#146349,#146350),
(#146351,#146352,#146353),(#146354,#146355,#146356)),.UNSPECIFIED.,.F.,
 .F.,.F.)
B_SPLINE_SURFACE_WITH_KNOTS((4,4),(3,3),(0.,0.044753309356401),(0.,1.),
 .UNSPECIFIED.)
GEOMETRIC_REPRESENTATION_ITEM()
RATIONAL_B_SPLINE_SURFACE(((1.,0.717952606100523,1.),(1.,0.716270361073643,
1.),(1.,0.715283994577086,1.),(1.,0.714485667734334,1.)))
REPRESENTATION_ITEM('')
SURFACE()
);
#2276=(
BOUNDED_SURFACE()
B_SPLINE_SURFACE(3,2,((#146363,#146364,#146365),(#146366,#146367,#146368),
(#146369,#146370,#146371),(#146372,#146373,#146374)),.UNSPECIFIED.,.F.,
 .F.,.F.)
B_SPLINE_SURFACE_WITH_KNOTS((4,4),(3,3),(0.,0.000650124428678587),(0.,1.),
 .UNSPECIFIED.)
GEOMETRIC_REPRESENTATION_ITEM()
RATIONAL_B_SPLINE_SURFACE(((1.,0.714485667734326,1.),(1.,0.714973119513317,
1.),(1.,0.715223297464931,1.),(1.,0.715224866856049,1.)))
REPRESENTATION_ITEM('')
SURFACE()
);
#2277=(
BOUNDED_SURFACE()
B_SPLINE_SURFACE(3,2,((#146379,#146380,#146381),(#146382,#146383,#146384),
(#146385,#146386,#146387),(#146388,#146389,#146390),(#146391,#146392,#146393),
(#146394,#146395,#146396),(#146397,#146398,#146399),(#146400,#146401,#146402),
(#146403,#146404,#146405),(#146406,#146407,#146408)),.UNSPECIFIED.,.F.,
 .F.,.F.)
B_SPLINE_SURFACE_WITH_KNOTS((4,2,2,2,4),(3,3),(0.00807569768389314,0.00867847980331418,
0.00928126192273523,0.00988404404215627,0.0104868261615773),(0.,1.),
 .UNSPECIFIED.)
GEOMETRIC_REPRESENTATION_ITEM()
RATIONAL_B_SPLINE_SURFACE(((1.,0.707106781186548,1.),(1.,0.707212493429049,
1.),(1.,0.707315385014487,1.),(1.,0.707515784384109,1.),(1.,0.707613608127955,
1.),(1.,0.707793680404111,1.),(1.,0.707878261047732,1.),(1.,0.708029744860286,
1.),(1.,0.7080959680978,1.),(1.,0.708153025875396,1.)))
REPRESENTATION_ITEM('')
SURFACE()
);
#2278=(
BOUNDED_SURFACE()
B_SPLINE_SURFACE(3,2,((#146476,#146477,#146478),(#146479,#146480,#146481),
(#146482,#146483,#146484),(#146485,#146486,#146487)),.UNSPECIFIED.,.F.,
 .F.,.F.)
B_SPLINE_SURFACE_WITH_KNOTS((4,4),(3,3),(0.,0.0445045070401677),(0.,1.),
 .UNSPECIFIED.)
GEOMETRIC_REPRESENTATION_ITEM()
RATIONAL_B_SPLINE_SURFACE(((1.,0.71617462512364,1.),(1.,0.714773807595299,
1.),(1.,0.713950503107743,1.),(1.,0.713284154090124,1.)))
REPRESENTATION_ITEM('')
SURFACE()
);
#2279=(
BOUNDED_SURFACE()
B_SPLINE_SURFACE(3,2,((#146489,#146490,#146491),(#146492,#146493,#146494),
(#146495,#146496,#146497),(#146498,#146499,#146500),(#146501,#146502,#146503),
(#146504,#146505,#146506),(#146507,#146508,#146509),(#146510,#146511,#146512),
(#146513,#146514,#146515),(#146516,#146517,#146518)),.UNSPECIFIED.,.F.,
 .F.,.F.)
B_SPLINE_SURFACE_WITH_KNOTS((4,2,2,2,4),(3,3),(0.0080756712423913,0.00867825313759154,
0.00928083503279179,0.00988341692799203,0.0104859988231923),(0.,1.),
 .UNSPECIFIED.)
GEOMETRIC_REPRESENTATION_ITEM()
RATIONAL_B_SPLINE_SURFACE(((1.,0.707106781186548,1.),(1.,0.707146901961909,
1.),(1.,0.707185957443845,1.),(1.,0.707262034097608,1.),(1.,0.707299176477847,
1.),(1.,0.7073675568103,1.),(1.,0.707399679105567,1.),(1.,0.707457223307409,
1.),(1.,0.707482383732919,1.),(1.,0.707504065565917,1.)))
REPRESENTATION_ITEM('')
SURFACE()
);
#2280=(
BOUNDED_SURFACE()
B_SPLINE_SURFACE(3,2,((#146545,#146546,#146547),(#146548,#146549,#146550),
(#146551,#146552,#146553),(#146554,#146555,#146556)),.UNSPECIFIED.,.F.,
 .F.,.F.)
B_SPLINE_SURFACE_WITH_KNOTS((4,4),(3,3),(0.,0.000650121327073412),(0.,1.),
 .UNSPECIFIED.)
GEOMETRIC_REPRESENTATION_ITEM()
RATIONAL_B_SPLINE_SURFACE(((1.,0.713890629234418,1.),(1.,0.713889885788569,
1.),(1.,0.71368362023966,1.),(1.,0.713272398106985,1.)))
REPRESENTATION_ITEM('')
SURFACE()
);
#2281=(
BOUNDED_SURFACE()
B_SPLINE_SURFACE(3,2,((#146560,#146561,#146562),(#146563,#146564,#146565),
(#146566,#146567,#146568),(#146569,#146570,#146571)),.UNSPECIFIED.,.F.,
 .F.,.F.)
B_SPLINE_SURFACE_WITH_KNOTS((4,4),(3,3),(0.,0.0447707136167657),(0.,1.),
 .UNSPECIFIED.)
GEOMETRIC_REPRESENTATION_ITEM()
RATIONAL_B_SPLINE_SURFACE(((1.,0.713272398106993,1.),(1.,0.713940344609358,
1.),(1.,0.714765614654658,1.),(1.,0.71617462512364,1.)))
REPRESENTATION_ITEM('')
SURFACE()
);
#2282=(
BOUNDED_SURFACE()
B_SPLINE_SURFACE(3,2,((#146578,#146579,#146580),(#146581,#146582,#146583),
(#146584,#146585,#146586),(#146587,#146588,#146589)),.UNSPECIFIED.,.F.,
 .F.,.F.)
B_SPLINE_SURFACE_WITH_KNOTS((4,4),(3,3),(0.,0.00195732360009946),(0.,1.),
 .UNSPECIFIED.)
GEOMETRIC_REPRESENTATION_ITEM()
RATIONAL_B_SPLINE_SURFACE(((1.,0.707106781186548,1.),(1.,0.709967301734631,
1.),(1.,0.713032729764421,1.),(1.,0.716174625123614,1.)))
REPRESENTATION_ITEM('')
SURFACE()
);
#2283=(
BOUNDED_SURFACE()
B_SPLINE_SURFACE(3,2,((#146597,#146598,#146599),(#146600,#146601,#146602),
(#146603,#146604,#146605),(#146606,#146607,#146608)),.UNSPECIFIED.,.F.,
 .F.,.F.)
B_SPLINE_SURFACE_WITH_KNOTS((4,4),(3,3),(0.,0.00195732365556561),(0.,1.),
 .UNSPECIFIED.)
GEOMETRIC_REPRESENTATION_ITEM()
RATIONAL_B_SPLINE_SURFACE(((1.,0.71617462512364,1.),(1.,0.713064019807532,
1.),(1.,0.709996713322441,1.),(1.,0.707106781186534,1.)))
REPRESENTATION_ITEM('')
SURFACE()
);
#2284=(
BOUNDED_SURFACE()
B_SPLINE_SURFACE(3,2,((#146610,#146611,#146612),(#146613,#146614,#146615),
(#146616,#146617,#146618),(#146619,#146620,#146621),(#146622,#146623,#146624),
(#146625,#146626,#146627),(#146628,#146629,#146630),(#146631,#146632,#146633)),
 .UNSPECIFIED.,.F.,.F.,.F.)
B_SPLINE_SURFACE_WITH_KNOTS((4,2,2,4),(3,3),(0.023727979672696,0.0269788291349169,
0.0286042538660274,0.0302296785971378),(0.,1.),.UNSPECIFIED.)
GEOMETRIC_REPRESENTATION_ITEM()
RATIONAL_B_SPLINE_SURFACE(((1.,0.972985060853882,1.),(1.,0.973867966894579,
1.),(1.,0.974606628833735,1.),(1.,0.975438732489742,1.),(1.,0.975670772749385,
1.),(1.,0.976026965697327,1.),(1.,0.976152018462137,1.),(1.,0.976223679017856,
1.)))
REPRESENTATION_ITEM('')
SURFACE()
);
#2285=(
BOUNDED_SURFACE()
B_SPLINE_SURFACE(3,2,((#146667,#146668,#146669),(#146670,#146671,#146672),
(#146673,#146674,#146675),(#146676,#146677,#146678)),.UNSPECIFIED.,.F.,
 .F.,.F.)
B_SPLINE_SURFACE_WITH_KNOTS((4,4),(3,3),(-1.38777878078145E-17,0.0431305646498159),
(0.,1.),.UNSPECIFIED.)
GEOMETRIC_REPRESENTATION_ITEM()
RATIONAL_B_SPLINE_SURFACE(((1.,0.669061697655964,1.),(1.,0.66495869705799,
1.),(1.,0.659888610517475,1.),(1.,0.65126854630498,1.)))
REPRESENTATION_ITEM('')
SURFACE()
);
#2286=(
BOUNDED_SURFACE()
B_SPLINE_SURFACE(3,2,((#146680,#146681,#146682),(#146683,#146684,#146685),
(#146686,#146687,#146688),(#146689,#146690,#146691),(#146692,#146693,#146694),
(#146695,#146696,#146697)),.UNSPECIFIED.,.F.,.F.,.F.)
B_SPLINE_SURFACE_WITH_KNOTS((4,2,4),(3,3),(0.,0.00109598668217933,0.00219197336435865),
(0.,1.),.UNSPECIFIED.)
GEOMETRIC_REPRESENTATION_ITEM()
RATIONAL_B_SPLINE_SURFACE(((1.,0.707106781186548,1.),(1.,0.698507203291837,
1.),(1.,0.689563761715544,1.),(1.,0.670914228806854,1.),(1.,0.661139818833385,
1.),(1.,0.65126854630498,1.)))
REPRESENTATION_ITEM('')
SURFACE()
);
#2287=(
BOUNDED_SURFACE()
B_SPLINE_SURFACE(3,2,((#146703,#146704,#146705),(#146706,#146707,#146708),
(#146709,#146710,#146711),(#146712,#146713,#146714),(#146715,#146716,#146717),
(#146718,#146719,#146720)),.UNSPECIFIED.,.F.,.F.,.F.)
B_SPLINE_SURFACE_WITH_KNOTS((4,2,4),(3,3),(-4.05963276307181E-5,0.00109600456666539,
0.0022326050184341),(0.,1.00004059633081),.UNSPECIFIED.)
GEOMETRIC_REPRESENTATION_ITEM()
RATIONAL_B_SPLINE_SURFACE(((1.,0.650157040100188,1.00002840468107),(1.,
0.660408047293388,1.00002757237451),(1.,0.670380682621654,1.0000267626697),
(1.,0.689731025456819,1.00002519156386),(1.,0.699171182287062,1.0000244250924),
(1.,0.708048211870778,1.00002370434275)))
REPRESENTATION_ITEM('')
SURFACE()
);
#2288=(
BOUNDED_SURFACE()
B_SPLINE_SURFACE(3,2,((#146748,#146749,#146750),(#146751,#146752,#146753),
(#146754,#146755,#146756),(#146757,#146758,#146759)),.UNSPECIFIED.,.F.,
 .F.,.F.)
B_SPLINE_SURFACE_WITH_KNOTS((4,4),(3,3),(0.,0.0433970829567688),(0.,1.),
 .UNSPECIFIED.)
GEOMETRIC_REPRESENTATION_ITEM()
RATIONAL_B_SPLINE_SURFACE(((1.,0.651268546304981,1.),(1.,0.659940697395559,
1.),(1.,0.665023311775857,1.),(1.,0.669136477740405,1.)))
REPRESENTATION_ITEM('')
SURFACE()
);
#2289=(
BOUNDED_SURFACE()
B_SPLINE_SURFACE(3,2,((#146766,#146767,#146768),(#146769,#146770,#146771),
(#146772,#146773,#146774),(#146775,#146776,#146777)),.UNSPECIFIED.,.F.,
 .F.,.F.)
B_SPLINE_SURFACE_WITH_KNOTS((4,4),(3,3),(0.,0.000650363027228679),(0.,1.),
 .UNSPECIFIED.)
GEOMETRIC_REPRESENTATION_ITEM()
RATIONAL_B_SPLINE_SURFACE(((1.,0.66913647774042,1.),(1.,0.666544790513632,
1.),(1.,0.665198010610878,1.),(1.,0.665190809887722,1.)))
REPRESENTATION_ITEM('')
SURFACE()
);
#2290=(
BOUNDED_SURFACE()
B_SPLINE_SURFACE(3,2,((#146782,#146783,#146784),(#146785,#146786,#146787),
(#146788,#146789,#146790),(#146791,#146792,#146793),(#146794,#146795,#146796),
(#146797,#146798,#146799),(#146800,#146801,#146802),(#146803,#146804,#146805),
(#146806,#146807,#146808),(#146809,#146810,#146811),(#146812,#146813,#146814),
(#146815,#146816,#146817),(#146818,#146819,#146820),(#146821,#146822,#146823)),
 .UNSPECIFIED.,.F.,.F.,.F.)
B_SPLINE_SURFACE_WITH_KNOTS((4,2,2,2,2,2,4),(3,3),(0.00808046157075938,
0.00879095475051749,0.00914620134039654,0.0095014479302756,0.00985669452015465,
0.0102119411100337,0.0109224342897918),(0.,1.),.UNSPECIFIED.)
GEOMETRIC_REPRESENTATION_ITEM()
RATIONAL_B_SPLINE_SURFACE(((1.,0.707106781186552,1.),(1.,0.705538120216095,
1.),(1.,0.703999772329756,1.),(1.,0.701739154413458,1.),(1.,0.700992634705956,
1.),(1.,0.699563445722461,1.),(1.,0.698874516085242,1.),(1.,0.697548436732303,
1.),(1.,0.696906638208049,1.),(1.,0.695703451829647,1.),(1.,0.695143596113536,
1.),(1.,0.693587190992306,1.),(1.,0.692704331853457,1.),(1.,0.69204248906153,
1.)))
REPRESENTATION_ITEM('')
SURFACE()
);
#2291=(
BOUNDED_SURFACE()
B_SPLINE_SURFACE(3,2,((#146895,#146896,#146897),(#146898,#146899,#146900),
(#146901,#146902,#146903),(#146904,#146905,#146906)),.UNSPECIFIED.,.F.,
 .F.,.F.)
B_SPLINE_SURFACE_WITH_KNOTS((4,4),(3,3),(0.,0.0419168978153696),(0.,1.),
 .UNSPECIFIED.)
GEOMETRIC_REPRESENTATION_ITEM()
RATIONAL_B_SPLINE_SURFACE(((1.,0.776159951988518,1.),(1.,0.766788671732685,
1.),(1.,0.760870494736068,1.),(1.,0.756069167758398,1.)))
REPRESENTATION_ITEM('')
SURFACE()
);
#2292=(
BOUNDED_SURFACE()
B_SPLINE_SURFACE(3,2,((#146908,#146909,#146910),(#146911,#146912,#146913),
(#146914,#146915,#146916),(#146917,#146918,#146919),(#146920,#146921,#146922),
(#146923,#146924,#146925),(#146926,#146927,#146928),(#146929,#146930,#146931),
(#146932,#146933,#146934),(#146935,#146936,#146937),(#146938,#146939,#146940),
(#146941,#146942,#146943),(#146944,#146945,#146946),(#146947,#146948,#146949)),
 .UNSPECIFIED.,.F.,.F.,.F.)
B_SPLINE_SURFACE_WITH_KNOTS((4,2,2,2,2,2,4),(3,3),(0.00808024661615471,
0.00880850598034447,0.00917263566243935,0.00953676534453423,0.00990089502662911,
0.010265024708724,0.0109932840729137),(0.,1.),.UNSPECIFIED.)
GEOMETRIC_REPRESENTATION_ITEM()
RATIONAL_B_SPLINE_SURFACE(((1.,0.707106781186552,1.),(1.,0.7086803042033,
1.),(1.,0.710213526000588,1.),(1.,0.712453026336305,1.),(1.,0.713188114139461,
1.),(1.,0.714590095265908,1.),(1.,0.715263343050717,1.),(1.,0.716554408796435,
1.),(1.,0.71717678241798,1.),(1.,0.718331565221162,1.),(1.,0.718866152975084,
1.),(1.,0.720344053893136,1.),(1.,0.721169771392395,1.),(1.,0.721765931188049,
1.)))
REPRESENTATION_ITEM('')
SURFACE()
);
#2293=(
BOUNDED_SURFACE()
B_SPLINE_SURFACE(3,2,((#146974,#146975,#146976),(#146977,#146978,#146979),
(#146980,#146981,#146982),(#146983,#146984,#146985)),.UNSPECIFIED.,.F.,
 .F.,.F.)
B_SPLINE_SURFACE_WITH_KNOTS((4,4),(3,3),(0.,0.000650577858517379),(0.,1.),
 .UNSPECIFIED.)
GEOMETRIC_REPRESENTATION_ITEM()
RATIONAL_B_SPLINE_SURFACE(((1.,0.760728353039955,1.),(1.,0.760722617942438,
1.),(1.,0.759141109939139,1.),(1.,0.755978609126096,1.)))
REPRESENTATION_ITEM('')
SURFACE()
);
#2294=(
BOUNDED_SURFACE()
B_SPLINE_SURFACE(3,2,((#146989,#146990,#146991),(#146992,#146993,#146994),
(#146995,#146996,#146997),(#146998,#146999,#147000)),.UNSPECIFIED.,.F.,
 .F.,.F.)
B_SPLINE_SURFACE_WITH_KNOTS((4,4),(3,3),(0.,0.0421837023697854),(0.,1.),
 .UNSPECIFIED.)
GEOMETRIC_REPRESENTATION_ITEM()
RATIONAL_B_SPLINE_SURFACE(((1.,0.755978609126094,1.),(1.,0.760793534959097,
1.),(1.,0.766730014383061,1.),(1.,0.776159951988524,1.)))
REPRESENTATION_ITEM('')
SURFACE()
);
#2295=(
BOUNDED_SURFACE()
B_SPLINE_SURFACE(3,2,((#147007,#147008,#147009),(#147010,#147011,#147012),
(#147013,#147014,#147015),(#147016,#147017,#147018),(#147019,#147020,#147021),
(#147022,#147023,#147024)),.UNSPECIFIED.,.F.,.F.,.F.)
B_SPLINE_SURFACE_WITH_KNOTS((4,2,4),(3,3),(-2.81603468776107E-5,0.00119589979970271,
0.00241995509742885),(0.,1.00002816034688),.UNSPECIFIED.)
GEOMETRIC_REPRESENTATION_ITEM()
RATIONAL_B_SPLINE_SURFACE(((1.,0.706267412093565,1.00001654322313),(1.,
0.718312133068377,1.00001586485609),(1.,0.730249727038935,1.00001519252251),
(1.,0.753894775002322,1.00001386081701),(1.,0.765682964669419,1.00001319689799),
(1.,0.776930652130126,1.00001256342043)))
REPRESENTATION_ITEM('')
SURFACE()
);
#2296=(
BOUNDED_SURFACE()
B_SPLINE_SURFACE(3,2,((#147056,#147057,#147058),(#147059,#147060,#147061),
(#147062,#147063,#147064),(#147065,#147066,#147067),(#147068,#147069,#147070),
(#147071,#147072,#147073)),.UNSPECIFIED.,.F.,.F.,.F.)
B_SPLINE_SURFACE_WITH_KNOTS((4,2,4),(3,3),(0.,0.00119596402151854,0.00239192804303707),
(0.,1.),.UNSPECIFIED.)
GEOMETRIC_REPRESENTATION_ITEM()
RATIONAL_B_SPLINE_SURFACE(((1.,0.776159951988518,1.),(1.,0.765146332033717,
1.),(1.,0.753844155392208,1.),(1.,0.730744284614809,1.),(1.,0.718864587348138,
1.),(1.,0.707106781186548,1.)))
REPRESENTATION_ITEM('')
SURFACE()
);
#2297=(
BOUNDED_SURFACE()
B_SPLINE_SURFACE(3,2,((#147080,#147081,#147082),(#147083,#147084,#147085),
(#147086,#147087,#147088),(#147089,#147090,#147091),(#147092,#147093,#147094),
(#147095,#147096,#147097),(#147098,#147099,#147100),(#147101,#147102,#147103)),
 .UNSPECIFIED.,.F.,.F.,.F.)
B_SPLINE_SURFACE_WITH_KNOTS((4,2,2,4),(3,3),(0.0758061741912965,0.0799264930317429,
0.081986652451966,0.0840468118721892),(0.,1.),.UNSPECIFIED.)
GEOMETRIC_REPRESENTATION_ITEM()
RATIONAL_B_SPLINE_SURFACE(((1.,0.961573839605902,1.),(1.,0.963379794804551,
1.),(1.,0.965135301445735,1.),(1.,0.967619049505042,1.),(1.,0.968423938543271,
1.),(1.,0.96994350882013,1.),(1.,0.970660771468208,1.),(1.,0.971327129982678,
1.)))
REPRESENTATION_ITEM('')
SURFACE()
);
#2298=(
BOUNDED_SURFACE()
B_SPLINE_SURFACE(3,2,((#147130,#147131,#147132),(#147133,#147134,#147135),
(#147136,#147137,#147138),(#147139,#147140,#147141),(#147142,#147143,#147144),
(#147145,#147146,#147147)),.UNSPECIFIED.,.F.,.F.,.F.)
B_SPLINE_SURFACE_WITH_KNOTS((4,2,4),(3,3),(-1.38777878078145E-17,0.0189537577590876,
0.0379075155181751),(0.,1.),.UNSPECIFIED.)
GEOMETRIC_REPRESENTATION_ITEM()
RATIONAL_B_SPLINE_SURFACE(((1.,0.620304161933054,1.),(1.,0.616101722702546,
1.),(1.,0.61132314280393,1.),(1.,0.599852065362239,1.),(1.,0.593169697629851,
1.),(1.,0.584878694958868,1.)))
REPRESENTATION_ITEM('')
SURFACE()
);
#2299=(
BOUNDED_SURFACE()
B_SPLINE_SURFACE(3,2,((#147149,#147150,#147151),(#147152,#147153,#147154),
(#147155,#147156,#147157),(#147158,#147159,#147160),(#147161,#147162,#147163),
(#147164,#147165,#147166)),.UNSPECIFIED.,.F.,.F.,.F.)
B_SPLINE_SURFACE_WITH_KNOTS((4,2,4),(3,3),(-1.06251812903579E-17,0.00150294083257491,
0.00300588166514984),(0.,1.),.UNSPECIFIED.)
GEOMETRIC_REPRESENTATION_ITEM()
RATIONAL_B_SPLINE_SURFACE(((1.,0.707106781186548,1.),(1.,0.688447591630839,
1.),(1.,0.669002122235948,1.),(1.,0.628207099426844,1.),(1.,0.606682052630604,
1.),(1.,0.584878694958868,1.)))
REPRESENTATION_ITEM('')
SURFACE()
);
#2300=(
BOUNDED_SURFACE()
B_SPLINE_SURFACE(3,2,((#147172,#147173,#147174),(#147175,#147176,#147177),
(#147178,#147179,#147180),(#147181,#147182,#147183),(#147184,#147185,#147186),
(#147187,#147188,#147189)),.UNSPECIFIED.,.F.,.F.,.F.)
B_SPLINE_SURFACE_WITH_KNOTS((4,2,4),(3,3),(-0.000128927283350436,0.00150339017752321,
0.00313570783234569),(0.,1.00012892747725),.UNSPECIFIED.)
GEOMETRIC_REPRESENTATION_ITEM()
RATIONAL_B_SPLINE_SURFACE(((1.,0.579199953812914,1.00010850537676),(1.,
0.603005180155982,1.0001023670812),(1.,0.625981897604081,1.00009644242077),
(1.,0.670345420760658,1.00008500306653),(1.,0.691877771030212,1.00007945084333),
(1.,0.711824716728862,1.00007430742455)))
REPRESENTATION_ITEM('')
SURFACE()
);
#2301=(
BOUNDED_SURFACE()
B_SPLINE_SURFACE(3,2,((#147220,#147221,#147222),(#147223,#147224,#147225),
(#147226,#147227,#147228),(#147229,#147230,#147231),(#147232,#147233,#147234),
(#147235,#147236,#147237)),.UNSPECIFIED.,.F.,.F.,.F.)
B_SPLINE_SURFACE_WITH_KNOTS((4,2,4),(3,3),(0.,0.0190876722191456,0.0381753444382913),
(0.,1.),.UNSPECIFIED.)
GEOMETRIC_REPRESENTATION_ITEM()
RATIONAL_B_SPLINE_SURFACE(((1.,0.584878694958869,1.),(1.,0.593227971935905,
1.),(1.,0.599946751815832,1.),(1.,0.611471310523657,1.),(1.,0.616266665820404,
1.),(1.,0.620481653466,1.)))
REPRESENTATION_ITEM('')
SURFACE()
);
#2302=(
BOUNDED_SURFACE()
B_SPLINE_SURFACE(3,2,((#147246,#147247,#147248),(#147249,#147250,#147251),
(#147252,#147253,#147254),(#147255,#147256,#147257)),.UNSPECIFIED.,.F.,
 .F.,.F.)
B_SPLINE_SURFACE_WITH_KNOTS((4,4),(3,3),(-6.51391992791641E-5,0.000716531192070805),
(0.,1.00012915786925),.UNSPECIFIED.)
GEOMETRIC_REPRESENTATION_ITEM()
RATIONAL_B_SPLINE_SURFACE(((1.,0.622358323103107,1.00009755078866),(1.,
0.614314362823104,1.0000996286702),(1.,0.610346508423654,1.00010065362944),
(1.,0.611117930705946,1.00010045435892)))
REPRESENTATION_ITEM('')
SURFACE()
);
#2303=(
BOUNDED_SURFACE()
B_SPLINE_SURFACE(3,2,((#147285,#147286,#147287),(#147288,#147289,#147290),
(#147291,#147292,#147293),(#147294,#147295,#147296),(#147297,#147298,#147299),
(#147300,#147301,#147302)),.UNSPECIFIED.,.F.,.F.,.F.)
B_SPLINE_SURFACE_WITH_KNOTS((4,2,4),(3,3),(0.,0.0178083890192188,0.0356167780384377),
(0.,1.),.UNSPECIFIED.)
GEOMETRIC_REPRESENTATION_ITEM()
RATIONAL_B_SPLINE_SURFACE(((1.,0.824689321081978,1.),(1.,0.818552442915159,
1.),(1.,0.813336414682689,1.),(1.,0.80412734431217,1.),(1.,0.800137214821899,
1.),(1.,0.796559406694623,1.)))
REPRESENTATION_ITEM('')
SURFACE()
);
#2304=(
BOUNDED_SURFACE()
B_SPLINE_SURFACE(3,2,((#147355,#147356,#147357),(#147358,#147359,#147360),
(#147361,#147362,#147363),(#147364,#147365,#147366)),.UNSPECIFIED.,.F.,
 .F.,.F.)
B_SPLINE_SURFACE_WITH_KNOTS((4,4),(3,3),(-6.5186839171593E-5,0.000717055230887516),
(0.,1.00014173624585),.UNSPECIFIED.)
GEOMETRIC_REPRESENTATION_ITEM()
RATIONAL_B_SPLINE_SURFACE(((1.,0.804734778555417,1.00005535231887),(1.,
0.805403669437747,1.0000551627067),(1.,0.802005595787365,1.00005612596711),
(1.,0.794601667527971,1.0000582247771)))
REPRESENTATION_ITEM('')
SURFACE()
);
#2305=(
BOUNDED_SURFACE()
B_SPLINE_SURFACE(3,2,((#147370,#147371,#147372),(#147373,#147374,#147375),
(#147376,#147377,#147378),(#147379,#147380,#147381),(#147382,#147383,#147384),
(#147385,#147386,#147387)),.UNSPECIFIED.,.F.,.F.,.F.)
B_SPLINE_SURFACE_WITH_KNOTS((4,2,4),(3,3),(0.,0.0179426259581151,0.0358852519162302),
(0.,1.),.UNSPECIFIED.)
GEOMETRIC_REPRESENTATION_ITEM()
RATIONAL_B_SPLINE_SURFACE(((1.,0.796398016704685,1.),(1.,0.799989941027341,
1.),(1.,0.80399801610487,1.),(1.,0.81325769888663,1.),(1.,0.81850629826423,
1.),(1.,0.824689321081979,1.)))
REPRESENTATION_ITEM('')
SURFACE()
);
#2306=(
BOUNDED_SURFACE()
B_SPLINE_SURFACE(3,2,((#147396,#147397,#147398),(#147399,#147400,#147401),
(#147402,#147403,#147404),(#147405,#147406,#147407),(#147408,#147409,#147410),
(#147411,#147412,#147413)),.UNSPECIFIED.,.F.,.F.,.F.)
B_SPLINE_SURFACE_WITH_KNOTS((4,2,4),(3,3),(-9.67458881849461E-5,0.0016638050806964,
0.00342426416910809),(0.,1.00009674588818),.UNSPECIFIED.)
GEOMETRIC_REPRESENTATION_ITEM()
RATIONAL_B_SPLINE_SURFACE(((1.,0.703317663028854,1.0000574055924),(1.,0.726192599003532,
1.0000529794804),(1.,0.747928069556768,1.00004877384559),(1.,0.789487375132482,
1.00004073246173),(1.,0.809468493425914,1.00003686627966),(1.,0.827689223724241,
1.00003334071819)))
REPRESENTATION_ITEM('')
SURFACE()
);
#2307=(
BOUNDED_SURFACE()
B_SPLINE_SURFACE(3,2,((#147448,#147449,#147450),(#147451,#147452,#147453),
(#147454,#147455,#147456),(#147457,#147458,#147459),(#147460,#147461,#147462),
(#147463,#147464,#147465)),.UNSPECIFIED.,.F.,.F.,.F.)
B_SPLINE_SURFACE_WITH_KNOTS((4,2,4),(3,3),(0.,0.00166463949867057,0.00332927899734113),
(0.,1.),.UNSPECIFIED.)
GEOMETRIC_REPRESENTATION_ITEM()
RATIONAL_B_SPLINE_SURFACE(((1.,0.824689321081979,1.),(1.,0.807273117786527,
1.),(1.,0.78876985537206,1.),(1.,0.749461319834452,1.),(1.,0.728524445804063,
1.),(1.,0.707106781186548,1.)))
REPRESENTATION_ITEM('')
SURFACE()
);
#2308=(
BOUNDED_SURFACE()
B_SPLINE_SURFACE(3,2,((#147473,#147474,#147475),(#147476,#147477,#147478),
(#147479,#147480,#147481),(#147482,#147483,#147484),(#147485,#147486,#147487),
(#147488,#147489,#147490)),.UNSPECIFIED.,.F.,.F.,.F.)
B_SPLINE_SURFACE_WITH_KNOTS((4,2,4),(3,3),(0.312244141975826,0.317485429411984,
0.322726716848141),(0.,1.),.UNSPECIFIED.)
GEOMETRIC_REPRESENTATION_ITEM()
RATIONAL_B_SPLINE_SURFACE(((1.,0.945205509755643,1.),(1.,0.94765942841632,
1.),(1.,0.950143082313928,1.),(1.,0.955101624050304,1.),(1.,0.957550590969702,
1.),(1.,0.959916006973269,1.)))
REPRESENTATION_ITEM('')
SURFACE()
);
#2309=(
BOUNDED_SURFACE()
B_SPLINE_SURFACE(3,2,((#147517,#147518,#147519),(#147520,#147521,#147522),
(#147523,#147524,#147525),(#147526,#147527,#147528),(#147529,#147530,#147531),
(#147532,#147533,#147534)),.UNSPECIFIED.,.F.,.F.,.F.)
B_SPLINE_SURFACE_WITH_KNOTS((4,2,4),(3,3),(0.,0.0147014688781887,0.0294029377563774),
(0.,1.),.UNSPECIFIED.)
GEOMETRIC_REPRESENTATION_ITEM()
RATIONAL_B_SPLINE_SURFACE(((1.,0.567371969128416,1.),(1.,0.561922702387361,
1.),(1.,0.555858739311734,1.),(1.,0.541909480588213,1.),(1.,0.534028604774054,
1.),(1.,0.524787419125872,1.)))
REPRESENTATION_ITEM('')
SURFACE()
);
#2310=(
BOUNDED_SURFACE()
B_SPLINE_SURFACE(3,2,((#147536,#147537,#147538),(#147539,#147540,#147541),
(#147542,#147543,#147544),(#147545,#147546,#147547)),.UNSPECIFIED.,.F.,
 .F.,.F.)
B_SPLINE_SURFACE_WITH_KNOTS((4,4),(3,3),(-3.67928601655754E-5,0.000690322634236133),
(0.,1.00003679286017),.UNSPECIFIED.)
GEOMETRIC_REPRESENTATION_ITEM()
RATIONAL_B_SPLINE_SURFACE(((1.,0.569438382608578,1.00003168318676),(1.,
0.557411392496524,1.00003256820149),(1.,0.550996682930264,1.00003304023252),
(1.,0.551710399363625,1.00003298771318)))
REPRESENTATION_ITEM('')
SURFACE()
);
#2311=(
BOUNDED_SURFACE()
B_SPLINE_SURFACE(3,2,((#147575,#147576,#147577),(#147578,#147579,#147580),
(#147581,#147582,#147583),(#147584,#147585,#147586),(#147587,#147588,#147589),
(#147590,#147591,#147592)),.UNSPECIFIED.,.F.,.F.,.F.)
B_SPLINE_SURFACE_WITH_KNOTS((4,2,4),(3,3),(0.,0.002055311285568,0.00411062257113599),
(0.,1.),.UNSPECIFIED.)
GEOMETRIC_REPRESENTATION_ITEM()
RATIONAL_B_SPLINE_SURFACE(((1.,0.707106781186549,1.),(1.,0.67983601545864,
1.),(1.,0.651283059470391,1.),(1.,0.590515772030266,1.),(1.,0.55801180255865,
1.),(1.,0.524787419125864,1.)))
REPRESENTATION_ITEM('')
SURFACE()
);
#2312=(
BOUNDED_SURFACE()
B_SPLINE_SURFACE(3,2,((#147598,#147599,#147600),(#147601,#147602,#147603),
(#147604,#147605,#147606),(#147607,#147608,#147609),(#147610,#147611,#147612),
(#147613,#147614,#147615)),.UNSPECIFIED.,.F.,.F.,.F.)
B_SPLINE_SURFACE_WITH_KNOTS((4,2,4),(3,3),(-0.000411246537817809,0.00205623335330194,
0.00452371337726426),(0.,1.00055466892243),.UNSPECIFIED.)
GEOMETRIC_REPRESENTATION_ITEM()
RATIONAL_B_SPLINE_SURFACE(((1.,0.50433079517456,1.00054986460745),(1.,0.545103499610019,
1.00050463390338),(1.,0.583527669535412,1.00046200851752),(1.,0.656716898757763,
1.00038081693571),(1.,0.691464019865608,1.00034227063927),(1.,0.722954371107003,
1.00030733720088)))
REPRESENTATION_ITEM('')
SURFACE()
);
#2313=(
BOUNDED_SURFACE()
B_SPLINE_SURFACE(3,2,((#147649,#147650,#147651),(#147652,#147653,#147654),
(#147655,#147656,#147657),(#147658,#147659,#147660),(#147661,#147662,#147663),
(#147664,#147665,#147666)),.UNSPECIFIED.,.F.,.F.,.F.)
B_SPLINE_SURFACE_WITH_KNOTS((4,2,4),(3,3),(-6.93889390390723E-18,0.0148367096635454,
0.0296734193270908),(0.,1.),.UNSPECIFIED.)
GEOMETRIC_REPRESENTATION_ITEM()
RATIONAL_B_SPLINE_SURFACE(((1.,0.524787419125867,1.),(1.,0.534113414550019,
1.),(1.,0.542054608658765,1.),(1.,0.556098130983184,1.),(1.,0.562195863398439,
1.),(1.,0.56767185832395,1.)))
REPRESENTATION_ITEM('')
SURFACE()
);
#2314=(
BOUNDED_SURFACE()
B_SPLINE_SURFACE(3,2,((#147673,#147674,#147675),(#147676,#147677,#147678),
(#147679,#147680,#147681),(#147682,#147683,#147684)),.UNSPECIFIED.,.F.,
 .F.,.F.)
B_SPLINE_SURFACE_WITH_KNOTS((4,4),(3,3),(0.,0.000433489251034108),(0.,1.),
 .UNSPECIFIED.)
GEOMETRIC_REPRESENTATION_ITEM()
RATIONAL_B_SPLINE_SURFACE(((1.,0.843391445812886,1.),(1.,0.83955525384858,
1.),(1.,0.835558949072738,1.),(1.,0.831408647420015,1.)))
REPRESENTATION_ITEM('')
SURFACE()
);
#2315=(
BOUNDED_SURFACE()
B_SPLINE_SURFACE(3,2,((#147715,#147716,#147717),(#147718,#147719,#147720),
(#147721,#147722,#147723),(#147724,#147725,#147726),(#147727,#147728,#147729),
(#147730,#147731,#147732),(#147733,#147734,#147735),(#147736,#147737,#147738),
(#147739,#147740,#147741),(#147742,#147743,#147744)),.UNSPECIFIED.,.F.,
 .F.,.F.)
B_SPLINE_SURFACE_WITH_KNOTS((4,2,2,2,4),(3,3),(1.5707963267949,1.96349540849362,
2.35619449019234,2.74889357189107,3.1415926535898),(0.,1.),
 .UNSPECIFIED.)
GEOMETRIC_REPRESENTATION_ITEM()
RATIONAL_B_SPLINE_SURFACE(((1.,0.707106781186548,1.),(1.,0.700666378834291,
1.),(1.,0.694134907060803,1.),(1.,0.681903435451243,1.),(1.,0.676209154064001,
1.),(1.,0.666616044204474,1.),(1.,0.662724068472647,1.),(1.,0.657443209221265,
1.),(1.,0.656051196071914,1.),(1.,0.656059028990508,1.)))
REPRESENTATION_ITEM('')
SURFACE()
);
#2316=(
BOUNDED_SURFACE()
B_SPLINE_SURFACE(3,2,((#147783,#147784,#147785),(#147786,#147787,#147788),
(#147789,#147790,#147791),(#147792,#147793,#147794),(#147795,#147796,#147797),
(#147798,#147799,#147800),(#147801,#147802,#147803),(#147804,#147805,#147806),
(#147807,#147808,#147809),(#147810,#147811,#147812)),.UNSPECIFIED.,.F.,
 .F.,.F.)
B_SPLINE_SURFACE_WITH_KNOTS((4,2,2,2,4),(3,3),(0.,0.000174105410412539,
0.000348210820825077,0.000522316231237617,0.000696421641650155),(0.,1.),
 .UNSPECIFIED.)
GEOMETRIC_REPRESENTATION_ITEM()
RATIONAL_B_SPLINE_SURFACE(((1.,0.4747595709467,1.),(1.,0.487194273605061,
1.),(1.,0.503322485825965,1.),(1.,0.54047069549172,1.),(1.,0.560568699342516,
1.),(1.,0.602438533850501,1.),(1.,0.623450047599376,1.),(1.,0.665484286819028,
1.),(1.,0.686628698725959,1.),(1.,0.707106781186548,1.)))
REPRESENTATION_ITEM('')
SURFACE()
);
#2317=(
BOUNDED_SURFACE()
B_SPLINE_SURFACE(3,2,((#147814,#147815,#147816),(#147817,#147818,#147819),
(#147820,#147821,#147822),(#147823,#147824,#147825),(#147826,#147827,#147828),
(#147829,#147830,#147831),(#147832,#147833,#147834),(#147835,#147836,#147837)),
 .UNSPECIFIED.,.F.,.F.,.F.)
B_SPLINE_SURFACE_WITH_KNOTS((4,2,2,4),(3,3),(0.,0.00267885639561352,0.00401828459342028,
0.00535771279122705),(0.,1.),.UNSPECIFIED.)
GEOMETRIC_REPRESENTATION_ITEM()
RATIONAL_B_SPLINE_SURFACE(((1.,0.707106781186871,1.),(1.,0.673473842386368,
1.),(1.,0.638019211186003,1.),(1.,0.580269195298477,1.),(1.,0.560144321783745,
1.),(1.,0.518526712842715,1.),(1.,0.497044145980004,1.),(1.,0.474759570947005,
1.)))
REPRESENTATION_ITEM('')
SURFACE()
);
#2318=(
BOUNDED_SURFACE()
B_SPLINE_SURFACE(3,2,((#147854,#147855,#147856),(#147857,#147858,#147859),
(#147860,#147861,#147862),(#147863,#147864,#147865),(#147866,#147867,#147868),
(#147869,#147870,#147871),(#147872,#147873,#147874),(#147875,#147876,#147877),
(#147878,#147879,#147880),(#147881,#147882,#147883)),.UNSPECIFIED.,.F.,
 .F.,.F.)
B_SPLINE_SURFACE_WITH_KNOTS((4,2,2,2,4),(3,3),(-0.000563963881013773,0.00140990970253443,
0.00281981940506887,0.0042297291076033,0.0062036026911515),(0.,1.00067621131492),
 .UNSPECIFIED.)
GEOMETRIC_REPRESENTATION_ITEM()
RATIONAL_B_SPLINE_SURFACE(((1.,0.431302648803683,1.00076911916729),(1.,
0.465713233921,1.00072258151327),(1.,0.498089262024449,1.0006787954402),
(1.,0.550868342653017,1.00060741581717),(1.,0.572053437981938,1.00057876461484),
(1.,0.613155696744348,1.00052317698995),(1.,0.632943112728916,1.00049641604078),
(1.,0.678527474844668,1.00043476671789),(1.,0.703702763966988,1.00040071908717),
(1.,0.727897090333189,1.00036799813268)))
REPRESENTATION_ITEM('')
SURFACE()
);
#2319=(
BOUNDED_SURFACE()
B_SPLINE_SURFACE(3,2,((#147929,#147930,#147931),(#147932,#147933,#147934),
(#147935,#147936,#147937),(#147938,#147939,#147940),(#147941,#147942,#147943),
(#147944,#147945,#147946)),.UNSPECIFIED.,.F.,.F.,.F.)
B_SPLINE_SURFACE_WITH_KNOTS((4,2,4),(3,3),(0.00191966951912585,0.00217079434687949,
0.00242191917463315),(0.,1.),.UNSPECIFIED.)
GEOMETRIC_REPRESENTATION_ITEM()
RATIONAL_B_SPLINE_SURFACE(((1.,0.460674285272032,1.),(1.,0.480581991146479,
1.),(1.,0.508992468088204,1.),(1.,0.568988175192947,1.),(1.,0.601196374063936,
1.),(1.,0.631879234223659,1.)))
REPRESENTATION_ITEM('')
SURFACE()
);
#2320=(
BOUNDED_SURFACE()
B_SPLINE_SURFACE(3,2,((#147955,#147956,#147957),(#147958,#147959,#147960),
(#147961,#147962,#147963),(#147964,#147965,#147966)),.UNSPECIFIED.,.F.,
 .F.,.F.)
B_SPLINE_SURFACE_WITH_KNOTS((4,4),(3,3),(-6.9931040125315E-18,0.000203650363220118),
(0.,1.),.UNSPECIFIED.)
GEOMETRIC_REPRESENTATION_ITEM()
RATIONAL_B_SPLINE_SURFACE(((1.,0.707106781186548,1.),(1.,0.683088481213104,
1.),(1.,0.658130799535722,1.),(1.,0.631879234223615,1.)))
REPRESENTATION_ITEM('')
SURFACE()
);
#2321=(
BOUNDED_SURFACE()
B_SPLINE_SURFACE(3,2,((#147988,#147989,#147990),(#147991,#147992,#147993),
(#147994,#147995,#147996),(#147997,#147998,#147999),(#148000,#148001,#148002),
(#148003,#148004,#148005),(#148006,#148007,#148008),(#148009,#148010,#148011),
(#148012,#148013,#148014),(#148015,#148016,#148017)),.UNSPECIFIED.,.F.,
 .F.,.F.)
B_SPLINE_SURFACE_WITH_KNOTS((4,2,2,2,4),(3,3),(0.00116892975483546,0.00173273620432841,
0.00229654265382136,0.0028603491033143,0.00342415555280725),(0.,1.00008736726511),
 .UNSPECIFIED.)
GEOMETRIC_REPRESENTATION_ITEM()
RATIONAL_B_SPLINE_SURFACE(((1.,0.707081191907056,1.00005118303032),(1.,
0.756727911750155,1.00004250803406),(1.,0.795323614743188,1.00003576403202),
(1.,0.847730260009882,1.00002660678148),(1.,0.86137618483429,1.00002422236722),
(1.,0.861443104051581,1.00002421067412),(1.,0.847851660205464,1.00002658556868),
(1.,0.795420207077645,1.00003574715401),(1.,0.756766547571617,1.00004250128304),
(1.,0.707081191907056,1.00005118303032)))
REPRESENTATION_ITEM('')
SURFACE()
);
#2322=(
BOUNDED_SURFACE()
B_SPLINE_SURFACE(3,2,((#148038,#148039,#148040),(#148041,#148042,#148043),
(#148044,#148045,#148046),(#148047,#148048,#148049),(#148050,#148051,#148052),
(#148053,#148054,#148055),(#148056,#148057,#148058),(#148059,#148060,#148061),
(#148062,#148063,#148064),(#148065,#148066,#148067)),.UNSPECIFIED.,.F.,
 .F.,.F.)
B_SPLINE_SURFACE_WITH_KNOTS((4,2,2,2,4),(3,3),(3.1415926535898,3.53429173528852,
3.92699081698724,4.31968989868597,4.71238898038469),(0.,1.),
 .UNSPECIFIED.)
GEOMETRIC_REPRESENTATION_ITEM()
RATIONAL_B_SPLINE_SURFACE(((1.,0.754709580222767,1.),(1.,0.754714219730801,
1.),(1.,0.753512297096199,1.),(1.,0.748871927696587,1.),(1.,0.745429366938708,
1.),(1.,0.736738129296182,1.),(1.,0.731490756397336,1.),(1.,0.719894264862173,
1.),(1.,0.71355026185156,1.),(1.,0.707106781186543,1.)))
REPRESENTATION_ITEM('')
SURFACE()
);
#2323=(
BOUNDED_SURFACE()
B_SPLINE_SURFACE(3,2,((#148080,#148081,#148082),(#148083,#148084,#148085),
(#148086,#148087,#148088),(#148089,#148090,#148091)),.UNSPECIFIED.,.F.,
 .F.,.F.)
B_SPLINE_SURFACE_WITH_KNOTS((4,4),(3,3),(-2.71050543121376E-20,0.00022779825406313),
(0.,1.),.UNSPECIFIED.)
GEOMETRIC_REPRESENTATION_ITEM()
RATIONAL_B_SPLINE_SURFACE(((1.,0.800108937437274,1.),(1.,0.815261773270244,
1.),(1.,0.827452668690902,1.),(1.,0.835963592436001,1.)))
REPRESENTATION_ITEM('')
SURFACE()
);
#2324=(
BOUNDED_SURFACE()
B_SPLINE_SURFACE(3,2,((#148093,#148094,#148095),(#148096,#148097,#148098),
(#148099,#148100,#148101),(#148102,#148103,#148104),(#148105,#148106,#148107),
(#148108,#148109,#148110)),.UNSPECIFIED.,.F.,.F.,.F.)
B_SPLINE_SURFACE_WITH_KNOTS((4,2,4),(3,3),(0.,0.000488238270881924,0.000976476541763847),
(0.,1.),.UNSPECIFIED.)
GEOMETRIC_REPRESENTATION_ITEM()
RATIONAL_B_SPLINE_SURFACE(((1.,0.807089511457258,1.),(1.,0.816558112905035,
1.),(1.,0.821286794224823,1.),(1.,0.825205555407875,1.),(1.,0.824318362071196,
1.),(1.,0.822092089912778,1.)))
REPRESENTATION_ITEM('')
SURFACE()
);
#2325=(
BOUNDED_SURFACE()
B_SPLINE_SURFACE(3,2,((#148112,#148113,#148114),(#148115,#148116,#148117),
(#148118,#148119,#148120),(#148121,#148122,#148123)),.UNSPECIFIED.,.F.,
 .F.,.F.)
B_SPLINE_SURFACE_WITH_KNOTS((4,4),(3,3),(0.,0.000103369667661675),(0.,1.),
 .UNSPECIFIED.)
GEOMETRIC_REPRESENTATION_ITEM()
RATIONAL_B_SPLINE_SURFACE(((1.,0.835735574810027,1.),(1.,0.831946521393585,
1.),(1.,0.827395718030991,1.),(1.,0.822092089912784,1.)))
REPRESENTATION_ITEM('')
SURFACE()
);
#2326=(
BOUNDED_SURFACE()
B_SPLINE_SURFACE(3,2,((#148127,#148128,#148129),(#148130,#148131,#148132),
(#148133,#148134,#148135),(#148136,#148137,#148138)),.UNSPECIFIED.,.F.,
 .F.,.F.)
B_SPLINE_SURFACE_WITH_KNOTS((4,4),(3,3),(0.,0.0206148669995797),(0.,1.),
 .UNSPECIFIED.)
GEOMETRIC_REPRESENTATION_ITEM()
RATIONAL_B_SPLINE_SURFACE(((1.,0.835735574810025,1.),(1.,0.841493793210698,
1.),(1.,0.847990686938055,1.),(1.,0.855596390789697,1.)))
REPRESENTATION_ITEM('')
SURFACE()
);
#2327=(
BOUNDED_SURFACE()
B_SPLINE_SURFACE(3,2,((#148145,#148146,#148147),(#148148,#148149,#148150),
(#148151,#148152,#148153),(#148154,#148155,#148156),(#148157,#148158,#148159),
(#148160,#148161,#148162)),.UNSPECIFIED.,.F.,.F.,.F.)
B_SPLINE_SURFACE_WITH_KNOTS((4,2,4),(3,3),(-0.000138519827310576,0.00213206083322637,
0.00440235036966729),(0.,1.00013851982731),.UNSPECIFIED.)
GEOMETRIC_REPRESENTATION_ITEM()
RATIONAL_B_SPLINE_SURFACE(((1.,0.701536032441349,1.00008268635449),(1.,
0.731888497336716,1.0000742775181),(1.,0.759999697565549,1.0000664896009),
(1.,0.812818114669199,1.00005185680486),(1.,0.837690840276735,1.00004496607355),
(1.,0.859613164458893,1.00003889272043)))
REPRESENTATION_ITEM('')
SURFACE()
);
#2328=(
BOUNDED_SURFACE()
B_SPLINE_SURFACE(3,2,((#148200,#148201,#148202),(#148203,#148204,#148205),
(#148206,#148207,#148208),(#148209,#148210,#148211),(#148212,#148213,#148214),
(#148215,#148216,#148217),(#148218,#148219,#148220),(#148221,#148222,#148223)),
 .UNSPECIFIED.,.F.,.F.,.F.)
B_SPLINE_SURFACE_WITH_KNOTS((4,2,2,4),(3,3),(0.,0.00213290337237644,0.00319935505856466,
0.00426580674475288),(0.,1.),.UNSPECIFIED.)
GEOMETRIC_REPRESENTATION_ITEM()
RATIONAL_B_SPLINE_SURFACE(((1.,0.855596390789701,1.),(1.,0.834565892891844,
1.),(1.,0.811730594666637,1.),(1.,0.77446817058652,1.),(1.,0.761499431653623,
1.),(1.,0.734903385695778,1.),(1.,0.721225679237929,1.),(1.,0.707106781186545,
1.)))
REPRESENTATION_ITEM('')
SURFACE()
);
#2329=(
BOUNDED_SURFACE()
B_SPLINE_SURFACE(3,2,((#148234,#148235,#148236),(#148237,#148238,#148239),
(#148240,#148241,#148242),(#148243,#148244,#148245)),.UNSPECIFIED.,.F.,
 .F.,.F.)
B_SPLINE_SURFACE_WITH_KNOTS((4,4),(3,3),(-2.08166817117217E-17,0.0203430832871546),
(0.,1.),.UNSPECIFIED.)
GEOMETRIC_REPRESENTATION_ITEM()
RATIONAL_B_SPLINE_SURFACE(((1.,0.855596390789699,1.),(1.,0.848090845809161,
1.),(1.,0.841665513049531,1.),(1.,0.835963592435998,1.)))
REPRESENTATION_ITEM('')
SURFACE()
);
#2330=(
BOUNDED_SURFACE()
B_SPLINE_SURFACE(3,2,((#148266,#148267,#148268),(#148269,#148270,#148271),
(#148272,#148273,#148274),(#148275,#148276,#148277),(#148278,#148279,#148280),
(#148281,#148282,#148283),(#148284,#148285,#148286),(#148287,#148288,#148289)),
 .UNSPECIFIED.,.F.,.F.,.F.)
B_SPLINE_SURFACE_WITH_KNOTS((4,2,2,4),(3,3),(-1.5368565794982E-17,0.000158339556725866,
0.000316679113451747,0.000633358226903509),(0.,1.),.UNSPECIFIED.)
GEOMETRIC_REPRESENTATION_ITEM()
RATIONAL_B_SPLINE_SURFACE(((1.,0.507397370006824,1.),(1.,0.519070630879541,
1.),(1.,0.533426892711081,1.),(1.,0.565658432465259,1.),(1.,0.583100719918817,
1.),(1.,0.636529920575075,1.),(1.,0.673198940992506,1.),(1.,0.707106781186548,
1.)))
REPRESENTATION_ITEM('')
SURFACE()
);
#2331=(
BOUNDED_SURFACE()
B_SPLINE_SURFACE(3,2,((#148293,#148294,#148295),(#148296,#148297,#148298),
(#148299,#148300,#148301),(#148302,#148303,#148304)),.UNSPECIFIED.,.F.,
 .F.,.F.)
B_SPLINE_SURFACE_WITH_KNOTS((4,4),(3,3),(0.,0.0125680158145827),(0.,1.),
 .UNSPECIFIED.)
GEOMETRIC_REPRESENTATION_ITEM()
RATIONAL_B_SPLINE_SURFACE(((1.,0.507397370006812,1.),(1.,0.500416139715127,
1.),(1.,0.49272006913241,1.),(1.,0.484030052331115,1.)))
REPRESENTATION_ITEM('')
SURFACE()
);
#2332=(
BOUNDED_SURFACE()
B_SPLINE_SURFACE(3,2,((#148306,#148307,#148308),(#148309,#148310,#148311),
(#148312,#148313,#148314),(#148315,#148316,#148317),(#148318,#148319,#148320),
(#148321,#148322,#148323),(#148324,#148325,#148326),(#148327,#148328,#148329)),
 .UNSPECIFIED.,.F.,.F.,.F.)
B_SPLINE_SURFACE_WITH_KNOTS((4,2,2,4),(3,3),(-5.42101086242752E-20,0.00250485829616721,
0.00375728744425081,0.00500971659233441),(0.,1.),.UNSPECIFIED.)
GEOMETRIC_REPRESENTATION_ITEM()
RATIONAL_B_SPLINE_SURFACE(((1.,0.70710678118722,1.),(1.,0.674452105060394,
1.),(1.,0.640073400404409,1.),(1.,0.584341050151977,1.),(1.,0.564951135845581,
1.),(1.,0.525261922605914,1.),(1.,0.504912110655119,1.),(1.,0.484030052331115,
1.)))
REPRESENTATION_ITEM('')
SURFACE()
);
#2333=(
BOUNDED_SURFACE()
B_SPLINE_SURFACE(3,2,((#148346,#148347,#148348),(#148349,#148350,#148351),
(#148352,#148353,#148354),(#148355,#148356,#148357),(#148358,#148359,#148360),
(#148361,#148362,#148363),(#148364,#148365,#148366),(#148367,#148368,#148369),
(#148370,#148371,#148372),(#148373,#148374,#148375)),.UNSPECIFIED.,.F.,
 .F.,.F.)
B_SPLINE_SURFACE_WITH_KNOTS((4,2,2,2,4),(3,3),(-0.000453575048684217,0.00125260629929845,
0.00250521259859689,0.00375781889789535,0.00546400047376828),(0.,1.00045357527164),
 .UNSPECIFIED.)
GEOMETRIC_REPRESENTATION_ITEM()
RATIONAL_B_SPLINE_SURFACE(((1.,0.460833248862991,1.00048910541122),(1.,
0.4899429330804,1.00046269854536),(1.,0.517846279275575,1.0004373860097),
(1.,0.564400235579759,1.00039515456295),(1.,0.583541342515348,1.00037779069739),
(1.,0.620882778440762,1.00034391639351),(1.,0.63899642320703,1.00032748459082),
(1.,0.680146964965137,1.0002901548545),(1.,0.702746029066762,1.00026965410123),
(1.,0.724519821938228,1.00024990199319)))
REPRESENTATION_ITEM('')
SURFACE()
);
#2334=(
BOUNDED_SURFACE()
B_SPLINE_SURFACE(3,2,((#148418,#148419,#148420),(#148421,#148422,#148423),
(#148424,#148425,#148426),(#148427,#148428,#148429)),.UNSPECIFIED.,.F.,
 .F.,.F.)
B_SPLINE_SURFACE_WITH_KNOTS((4,4),(3,3),(0.,0.01284355850178),(0.,1.),
 .UNSPECIFIED.)
GEOMETRIC_REPRESENTATION_ITEM()
RATIONAL_B_SPLINE_SURFACE(((1.,0.484030052331127,1.),(1.,0.492910462848522,
1.),(1.,0.500753390328389,1.),(1.,0.507855360856573,1.)))
REPRESENTATION_ITEM('')
SURFACE()
);
#2335=(
BOUNDED_SURFACE()
B_SPLINE_SURFACE(3,2,((#148436,#148437,#148438),(#148439,#148440,#148441),
(#148442,#148443,#148444),(#148445,#148446,#148447),(#148448,#148449,#148450),
(#148451,#148452,#148453),(#148454,#148455,#148456),(#148457,#148458,#148459),
(#148460,#148461,#148462),(#148463,#148464,#148465)),.UNSPECIFIED.,.F.,
 .F.,.F.)
B_SPLINE_SURFACE_WITH_KNOTS((4,2,2,2,4),(3,3),(0.,0.000158019212117338,
0.000316038424234677,0.000474057636352015,0.000632076848469353),(0.,1.),
 .UNSPECIFIED.)
GEOMETRIC_REPRESENTATION_ITEM()
RATIONAL_B_SPLINE_SURFACE(((1.,0.707106781186548,1.),(1.,0.690072170678528,
1.),(1.,0.67275310971826,1.),(1.,0.637401910188738,1.),(1.,0.619074074320766,
1.),(1.,0.5836606862513,1.),(1.,0.566468213012793,1.),(1.,0.53406367243224,
1.),(1.,0.519473083497879,1.),(1.,0.507855360856575,1.)))
REPRESENTATION_ITEM('')
SURFACE()
);
#2336=(
BOUNDED_SURFACE()
B_SPLINE_SURFACE(3,2,((#148482,#148483,#148484),(#148485,#148486,#148487),
(#148488,#148489,#148490),(#148491,#148492,#148493),(#148494,#148495,#148496),
(#148497,#148498,#148499),(#148500,#148501,#148502),(#148503,#148504,#148505),
(#148506,#148507,#148508),(#148509,#148510,#148511)),.UNSPECIFIED.,.F.,
 .F.,.F.)
B_SPLINE_SURFACE_WITH_KNOTS((4,2,2,2,4),(3,3),(1.5707963267949,1.96349540849362,
2.35619449019234,2.74889357189107,3.1415926535898),(0.,1.),
 .UNSPECIFIED.)
GEOMETRIC_REPRESENTATION_ITEM()
RATIONAL_B_SPLINE_SURFACE(((1.,0.707106781186548,1.),(1.,0.700666378834307,
1.),(1.,0.694134907060781,1.),(1.,0.681903435451265,1.),(1.,0.676209154064001,
1.),(1.,0.666616044204474,1.),(1.,0.662724068472647,1.),(1.,0.657443209221265,
1.),(1.,0.656051196071904,1.),(1.,0.656059028990508,1.)))
REPRESENTATION_ITEM('')
SURFACE()
);
#2337=(
BOUNDED_SURFACE()
B_SPLINE_SURFACE(3,2,((#148566,#148567,#148568),(#148569,#148570,#148571),
(#148572,#148573,#148574),(#148575,#148576,#148577),(#148578,#148579,#148580),
(#148581,#148582,#148583),(#148584,#148585,#148586),(#148587,#148588,#148589),
(#148590,#148591,#148592),(#148593,#148594,#148595)),.UNSPECIFIED.,.F.,
 .F.,.F.)
B_SPLINE_SURFACE_WITH_KNOTS((4,2,2,2,4),(3,3),(3.1415926535898,3.53429173528852,
3.92699081698724,4.31968989868597,4.71238898038469),(0.,1.),
 .UNSPECIFIED.)
GEOMETRIC_REPRESENTATION_ITEM()
RATIONAL_B_SPLINE_SURFACE(((1.,0.754709580222772,1.),(1.,0.754714219730806,
1.),(1.,0.753512297096203,1.),(1.,0.748871927696591,1.),(1.,0.745429366938691,
1.),(1.,0.736738129296209,1.),(1.,0.73149075639733,1.),(1.,0.719894264862189,
1.),(1.,0.713550261851557,1.),(1.,0.707106781186548,1.)))
REPRESENTATION_ITEM('')
SURFACE()
);
#2338=(
BOUNDED_SURFACE()
B_SPLINE_SURFACE(3,2,((#148612,#148613,#148614),(#148615,#148616,#148617),
(#148618,#148619,#148620),(#148621,#148622,#148623),(#148624,#148625,#148626),
(#148627,#148628,#148629)),.UNSPECIFIED.,.F.,.F.,.F.)
B_SPLINE_SURFACE_WITH_KNOTS((4,2,4),(3,3),(-3.07642366442762E-17,0.000324428028333684,
0.000648856056667399),(0.,1.),.UNSPECIFIED.)
GEOMETRIC_REPRESENTATION_ITEM()
RATIONAL_B_SPLINE_SURFACE(((1.,0.872575378690131,1.),(1.,0.857798601408145,
1.),(1.,0.834121076196936,1.),(1.,0.776835192876573,1.),(1.,0.743446077163894,
1.),(1.,0.707106781186548,1.)))
REPRESENTATION_ITEM('')
SURFACE()
);
#2339=(
BOUNDED_SURFACE()
B_SPLINE_SURFACE(3,2,((#148638,#148639,#148640),(#148641,#148642,#148643),
(#148644,#148645,#148646),(#148647,#148648,#148649)),.UNSPECIFIED.,.F.,
 .F.,.F.)
B_SPLINE_SURFACE_WITH_KNOTS((4,4),(3,3),(-3.46944695195361E-18,0.00904291806877092),
(0.,1.),.UNSPECIFIED.)
GEOMETRIC_REPRESENTATION_ITEM()
RATIONAL_B_SPLINE_SURFACE(((1.,0.872575378690133,1.),(1.,0.875691129720726,
1.),(1.,0.878972255663315,1.),(1.,0.882443751548002,1.)))
REPRESENTATION_ITEM('')
SURFACE()
);
#2340=(
BOUNDED_SURFACE()
B_SPLINE_SURFACE(3,2,((#148656,#148657,#148658),(#148659,#148660,#148661),
(#148662,#148663,#148664),(#148665,#148666,#148667),(#148668,#148669,#148670),
(#148671,#148672,#148673),(#148674,#148675,#148676),(#148677,#148678,#148679)),
 .UNSPECIFIED.,.F.,.F.,.F.)
B_SPLINE_SURFACE_WITH_KNOTS((4,2,2,4),(3,3),(-0.000144062567305207,0.0026640399986995,
0.00399605999804924,0.00547189964699229),(0.,1.00014406256731),
 .UNSPECIFIED.)
GEOMETRIC_REPRESENTATION_ITEM()
RATIONAL_B_SPLINE_SURFACE(((1.,0.701472497284949,1.0000860132769),(1.,0.73797281472355,
1.00007549661803),(1.,0.771217551452112,1.00006591797378),(1.,0.816811286567555,
1.00005278127272),(1.,0.831011743157808,1.00004868976425),(1.,0.859267298198093,
1.00004054862865),(1.,0.873224671977378,1.00003652715845),(1.,0.886265321053273,
1.00003276981968)))
REPRESENTATION_ITEM('')
SURFACE()
);
#2341=(
BOUNDED_SURFACE()
B_SPLINE_SURFACE(3,2,((#148726,#148727,#148728),(#148729,#148730,#148731),
(#148732,#148733,#148734),(#148735,#148736,#148737),(#148738,#148739,#148740),
(#148741,#148742,#148743),(#148744,#148745,#148746),(#148747,#148748,#148749)),
 .UNSPECIFIED.,.F.,.F.,.F.)
B_SPLINE_SURFACE_WITH_KNOTS((4,2,2,4),(3,3),(0.,0.00133214690895888,0.00266429381791776,
0.00532858763583552),(0.,1.),.UNSPECIFIED.)
GEOMETRIC_REPRESENTATION_ITEM()
RATIONAL_B_SPLINE_SURFACE(((1.,0.882443751548025,1.),(1.,0.870504695835311,
1.),(1.,0.857867656996629,1.),(1.,0.831237498116469,1.),(1.,0.81724531074011,
1.),(1.,0.773060112442974,1.),(1.,0.741342239036411,1.),(1.,0.707106781185704,
1.)))
REPRESENTATION_ITEM('')
SURFACE()
);
#2342=(
BOUNDED_SURFACE()
B_SPLINE_SURFACE(3,2,((#148760,#148761,#148762),(#148763,#148764,#148765),
(#148766,#148767,#148768),(#148769,#148770,#148771)),.UNSPECIFIED.,.F.,
 .F.,.F.)
B_SPLINE_SURFACE_WITH_KNOTS((4,4),(3,3),(0.,0.00876509433037234),(0.,1.),
 .UNSPECIFIED.)
GEOMETRIC_REPRESENTATION_ITEM()
RATIONAL_B_SPLINE_SURFACE(((1.,0.882443751548025,1.),(1.,0.879078911067312,
1.),(1.,0.875892933141997,1.),(1.,0.872863017557589,1.)))
REPRESENTATION_ITEM('')
SURFACE()
);
#2343=(
BOUNDED_SURFACE()
B_SPLINE_SURFACE(3,2,((#148777,#148778,#148779),(#148780,#148781,#148782),
(#148783,#148784,#148785),(#148786,#148787,#148788),(#148789,#148790,#148791),
(#148792,#148793,#148794)),.UNSPECIFIED.,.F.,.F.,.F.)
B_SPLINE_SURFACE_WITH_KNOTS((4,2,4),(3,3),(0.,0.000324772070278169,0.000649544140556338),
(0.,1.),.UNSPECIFIED.)
GEOMETRIC_REPRESENTATION_ITEM()
RATIONAL_B_SPLINE_SURFACE(((1.,0.707106781186543,1.),(1.,0.743104095569232,
1.),(1.,0.776957430466177,1.),(1.,0.834022397797079,1.),(1.,0.857828418485942,
1.),(1.,0.872863017557589,1.)))
REPRESENTATION_ITEM('')
SURFACE()
);
#2344=(
BOUNDED_SURFACE()
B_SPLINE_SURFACE(3,2,((#148823,#148824,#148825),(#148826,#148827,#148828),
(#148829,#148830,#148831),(#148832,#148833,#148834),(#148835,#148836,#148837),
(#148838,#148839,#148840)),.UNSPECIFIED.,.F.,.F.,.F.)
B_SPLINE_SURFACE_WITH_KNOTS((4,2,4),(3,3),(0.,0.000315675390911493,0.000631350781822986),
(0.,1.),.UNSPECIFIED.)
GEOMETRIC_REPRESENTATION_ITEM()
RATIONAL_B_SPLINE_SURFACE(((1.,0.860139545375527,1.),(1.,0.846673137247607,
1.),(1.,0.824923291377528,1.),(1.,0.771907958235216,1.),(1.,0.740773829846737,
1.),(1.,0.70710678118655,1.)))
REPRESENTATION_ITEM('')
SURFACE()
);
#2345=(
BOUNDED_SURFACE()
B_SPLINE_SURFACE(3,2,((#148842,#148843,#148844),(#148845,#148846,#148847),
(#148848,#148849,#148850),(#148851,#148852,#148853)),.UNSPECIFIED.,.F.,
 .F.,.F.)
B_SPLINE_SURFACE_WITH_KNOTS((4,4),(3,3),(0.,0.0135233968444947),(0.,1.),
 .UNSPECIFIED.)
GEOMETRIC_REPRESENTATION_ITEM()
RATIONAL_B_SPLINE_SURFACE(((1.,0.860139545375529,1.),(1.,0.864525021855929,
1.),(1.,0.869269442591942,1.),(1.,0.874466916621369,1.)))
REPRESENTATION_ITEM('')
SURFACE()
);
#2346=(
BOUNDED_SURFACE()
B_SPLINE_SURFACE(3,2,((#148860,#148861,#148862),(#148863,#148864,#148865),
(#148866,#148867,#148868),(#148869,#148870,#148871),(#148872,#148873,#148874),
(#148875,#148876,#148877),(#148878,#148879,#148880),(#148881,#148882,#148883)),
 .UNSPECIFIED.,.F.,.F.,.F.)
B_SPLINE_SURFACE_WITH_KNOTS((4,2,2,4),(3,3),(-0.000144843990829094,0.00249252731595781,
0.00373879097393672,0.00512986098279815),(0.,1.00014484399083),
 .UNSPECIFIED.)
GEOMETRIC_REPRESENTATION_ITEM()
RATIONAL_B_SPLINE_SURFACE(((1.,0.70137438171017,1.00008650825263),(1.,0.736070522946198,
1.00007645719751),(1.,0.767818414112902,1.00006726021499),(1.,0.811420652293743,
1.00005462917062),(1.,0.824998507459968,1.00005069582916),(1.,0.852223941818717,
1.00004280894803),(1.,0.865751049224885,1.00003889030759),(1.,0.878438086880466,
1.00003521502526)))
REPRESENTATION_ITEM('')
SURFACE()
);
#2347=(
BOUNDED_SURFACE()
B_SPLINE_SURFACE(3,2,((#148933,#148934,#148935),(#148936,#148937,#148938),
(#148939,#148940,#148941),(#148942,#148943,#148944),(#148945,#148946,#148947),
(#148948,#148949,#148950),(#148951,#148952,#148953),(#148954,#148955,#148956),
(#148957,#148958,#148959),(#148960,#148961,#148962)),.UNSPECIFIED.,.F.,
 .F.,.F.)
B_SPLINE_SURFACE_WITH_KNOTS((4,2,2,2,4),(3,3),(-0.000328574018954638,0.00116432048255243,
0.00232864096510486,0.0034929614476573,0.00498585604475646),(0.,1.00032857411453),
 .UNSPECIFIED.)
GEOMETRIC_REPRESENTATION_ITEM()
RATIONAL_B_SPLINE_SURFACE(((1.,0.483022826201985,1.00033973063422),(1.,
0.508075627896709,1.00032326722996),(1.,0.53225061289853,1.00030738068138),
(1.,0.573877072079261,1.00028002592744),(1.,0.591639012002754,1.00026835370008),
(1.,0.626354777911338,1.00024554029599),(1.,0.643300055532478,1.00023440473681),
(1.,0.680527266030163,1.00020994094136),(1.,0.700545105936671,1.00019678625332),
(1.,0.719876715686407,1.0001840825202)))
REPRESENTATION_ITEM('')
SURFACE()
);
#2348=(
BOUNDED_SURFACE()
B_SPLINE_SURFACE(3,2,((#149004,#149005,#149006),(#149007,#149008,#149009),
(#149010,#149011,#149012),(#149013,#149014,#149015)),.UNSPECIFIED.,.F.,
 .F.,.F.)
B_SPLINE_SURFACE_WITH_KNOTS((4,4),(3,3),(-1.7347234759768E-18,0.0170848224870981),
(0.,1.),.UNSPECIFIED.)
GEOMETRIC_REPRESENTATION_ITEM()
RATIONAL_B_SPLINE_SURFACE(((1.,0.499602392377301,1.),(1.,0.510855798801923,
1.),(1.,0.520331406035946,1.),(1.,0.528679393385783,1.)))
REPRESENTATION_ITEM('')
SURFACE()
);
#2349=(
BOUNDED_SURFACE()
B_SPLINE_SURFACE(3,2,((#149027,#149028,#149029),(#149030,#149031,#149032),
(#149033,#149034,#149035),(#149036,#149037,#149038),(#149039,#149040,#149041),
(#149042,#149043,#149044),(#149045,#149046,#149047),(#149048,#149049,#149050)),
 .UNSPECIFIED.,.F.,.F.,.F.)
B_SPLINE_SURFACE_WITH_KNOTS((4,2,2,4),(3,3),(0.,0.001434338214324,0.002868676428648,
0.005737352857296),(0.,1.),.UNSPECIFIED.)
GEOMETRIC_REPRESENTATION_ITEM()
RATIONAL_B_SPLINE_SURFACE(((1.,0.45339384727684,1.),(1.,0.47771228976057,
1.),(1.,0.501151853233145,1.),(1.,0.546461020466456,1.),(1.,0.568350660511087,
1.),(1.,0.632070189677047,1.),(1.,0.670684004768455,1.),(1.,0.707106781186548,
1.)))
REPRESENTATION_ITEM('')
SURFACE()
);
#2350=(
BOUNDED_SURFACE()
B_SPLINE_SURFACE(3,2,((#149061,#149062,#149063),(#149064,#149065,#149066),
(#149067,#149068,#149069),(#149070,#149071,#149072)),.UNSPECIFIED.,.F.,
 .F.,.F.)
B_SPLINE_SURFACE_WITH_KNOTS((4,4),(3,3),(0.,0.00407947372412412),(0.,1.),
 .UNSPECIFIED.)
GEOMETRIC_REPRESENTATION_ITEM()
RATIONAL_B_SPLINE_SURFACE(((1.,0.453393847276564,1.),(1.,0.456475766016567,
1.),(1.,0.459447353892611,1.),(1.,0.462319489161104,1.)))
REPRESENTATION_ITEM('')
SURFACE()
);
#2351=(
BOUNDED_SURFACE()
B_SPLINE_SURFACE(3,2,((#149078,#149079,#149080),(#149081,#149082,#149083),
(#149084,#149085,#149086),(#149087,#149088,#149089),(#149090,#149091,#149092),
(#149093,#149094,#149095),(#149096,#149097,#149098),(#149099,#149100,#149101)),
 .UNSPECIFIED.,.F.,.F.,.F.)
B_SPLINE_SURFACE_WITH_KNOTS((4,2,2,4),(3,3),(0.,0.000337961269725901,0.000506941904588851,
0.000675922539451801),(0.,1.),.UNSPECIFIED.)
GEOMETRIC_REPRESENTATION_ITEM()
RATIONAL_B_SPLINE_SURFACE(((1.,0.707106781186548,1.),(1.,0.66833529952704,
1.),(1.,0.625126311995779,1.),(1.,0.560329805282816,1.),(1.,0.53845874286336,
1.),(1.,0.497198802480914,1.),(1.,0.478168468596388,1.),(1.,0.462319489161107,
1.)))
REPRESENTATION_ITEM('')
SURFACE()
);
#2352=(
BOUNDED_SURFACE()
B_SPLINE_SURFACE(3,2,((#149126,#149127,#149128),(#149129,#149130,#149131),
(#149132,#149133,#149134),(#149135,#149136,#149137),(#149138,#149139,#149140),
(#149141,#149142,#149143),(#149144,#149145,#149146),(#149147,#149148,#149149),
(#149150,#149151,#149152),(#149153,#149154,#149155)),.UNSPECIFIED.,.F.,
 .F.,.F.)
B_SPLINE_SURFACE_WITH_KNOTS((4,2,2,2,4),(3,3),(1.5707963267949,1.96349540849362,
2.35619449019234,2.74889357189107,3.14159265358979),(0.,1.),
 .UNSPECIFIED.)
GEOMETRIC_REPRESENTATION_ITEM()
RATIONAL_B_SPLINE_SURFACE(((1.,0.70710678118655,1.),(1.,0.7006663788345,
1.),(1.,0.694134907060529,1.),(1.,0.681903435451519,1.),(1.,0.676209154063276,
1.),(1.,0.666616044205195,1.),(1.,0.662724068472661,1.),(1.,0.657443209221257,
1.),(1.,0.656051196071916,1.),(1.,0.656059028990507,1.)))
REPRESENTATION_ITEM('')
SURFACE()
);
#2353=(
BOUNDED_SURFACE()
B_SPLINE_SURFACE(3,2,((#149194,#149195,#149196),(#149197,#149198,#149199),
(#149200,#149201,#149202),(#149203,#149204,#149205),(#149206,#149207,#149208),
(#149209,#149210,#149211),(#149212,#149213,#149214),(#149215,#149216,#149217),
(#149218,#149219,#149220),(#149221,#149222,#149223)),.UNSPECIFIED.,.F.,
 .F.,.F.)
B_SPLINE_SURFACE_WITH_KNOTS((4,2,2,2,4),(3,3),(0.,0.000175112702239915,
0.000350225404479831,0.000525338106719747,0.000700450808959663),(0.,1.),
 .UNSPECIFIED.)
GEOMETRIC_REPRESENTATION_ITEM()
RATIONAL_B_SPLINE_SURFACE(((1.,0.441891116431771,1.),(1.,0.459945578495206,
1.),(1.,0.481391225572596,1.),(1.,0.52725624746098,1.),(1.,0.550835433567685,
1.),(1.,0.597437830540943,1.),(1.,0.62070290968502,1.),(1.,0.665021344579013,
1.),(1.,0.68636937449165,1.),(1.,0.707106781186548,1.)))
REPRESENTATION_ITEM('')
SURFACE()
);
#2354=(
BOUNDED_SURFACE()
B_SPLINE_SURFACE(3,2,((#149225,#149226,#149227),(#149228,#149229,#149230),
(#149231,#149232,#149233),(#149234,#149235,#149236)),.UNSPECIFIED.,.F.,
 .F.,.F.)
B_SPLINE_SURFACE_WITH_KNOTS((4,4),(3,3),(1.7347234759768E-18,0.00426411906192034),
(0.,1.),.UNSPECIFIED.)
GEOMETRIC_REPRESENTATION_ITEM()
RATIONAL_B_SPLINE_SURFACE(((1.,0.441891116431774,1.),(1.,0.438589787881315,
1.),(1.,0.435168043398159,1.),(1.,0.431612184895232,1.)))
REPRESENTATION_ITEM('')
SURFACE()
);
#2355=(
BOUNDED_SURFACE()
B_SPLINE_SURFACE(3,2,((#149243,#149244,#149245),(#149246,#149247,#149248),
(#149249,#149250,#149251),(#149252,#149253,#149254),(#149255,#149256,#149257),
(#149258,#149259,#149260),(#149261,#149262,#149263),(#149264,#149265,#149266),
(#149267,#149268,#149269),(#149270,#149271,#149272)),.UNSPECIFIED.,.F.,
 .F.,.F.)
B_SPLINE_SURFACE_WITH_KNOTS((4,2,2,2,4),(3,3),(-0.000627077628646835,0.00156769407161709,
0.00313538814323418,0.00470308221485126,0.00689785374126868),(0.,1.00120059479706),
 .UNSPECIFIED.)
GEOMETRIC_REPRESENTATION_ITEM()
RATIONAL_B_SPLINE_SURFACE(((1.,0.729847250011682,1.00064868797209),(1.,
0.70323368126333,1.00071259219644),(1.,0.675527972127855,1.00077911885691),
(1.,0.62520314302849,1.00089995831287),(1.,0.603398245983805,1.00095231600475),
(1.,0.55753734457264,1.001062436724),(1.,0.533442814445538,1.00112029225901),
(1.,0.47370313538274,1.00126373855474),(1.,0.436994504158806,1.00135188293805),
(1.,0.398153145892338,1.00144514840334)))
REPRESENTATION_ITEM('')
SURFACE()
);
#2356=(
BOUNDED_SURFACE()
B_SPLINE_SURFACE(3,2,((#149328,#149329,#149330),(#149331,#149332,#149333),
(#149334,#149335,#149336),(#149337,#149338,#149339),(#149340,#149341,#149342),
(#149343,#149344,#149345),(#149346,#149347,#149348),(#149349,#149350,#149351),
(#149352,#149353,#149354),(#149355,#149356,#149357),(#149358,#149359,#149360),
(#149361,#149362,#149363)),.UNSPECIFIED.,.F.,.F.,.F.)
B_SPLINE_SURFACE_WITH_KNOTS((4,2,2,2,2,4),(3,3),(-0.000627228261712472,
0.0015680710888481,0.00235210663327216,0.0031361421776962,0.00470421326654431,
0.00689951279093165),(0.,1.00121732095691),.UNSPECIFIED.)
GEOMETRIC_REPRESENTATION_ITEM()
RATIONAL_B_SPLINE_SURFACE(((1.,0.398113494737596,1.00146537811308),(1.,
0.437012270486998,1.00137067352324),(1.,0.473696248960092,1.00128136117168),
(1.,0.520905142750056,1.00116642442016),(1.,0.533089323815758,1.00113676030225),
(1.,0.557031366991619,1.00107847000043),(1.,0.568823900888959,1.00104975940313),
(1.,0.603302051221277,1.00096581745322),(1.,0.625142666027295,1.00091264337699),
(1.,0.675522559468756,1.00078998637681),(1.,0.703234839482815,1.00072251689836),
(1.,0.729837417574121,1.00065774914672)))
REPRESENTATION_ITEM('')
SURFACE()
);
#2357=(
BOUNDED_SURFACE()
B_SPLINE_SURFACE(3,2,((#149415,#149416,#149417),(#149418,#149419,#149420),
(#149421,#149422,#149423),(#149424,#149425,#149426)),.UNSPECIFIED.,.F.,
 .F.,.F.)
B_SPLINE_SURFACE_WITH_KNOTS((4,4),(3,3),(-1.00613961606655E-16,0.00454919832189776),
(0.,1.),.UNSPECIFIED.)
GEOMETRIC_REPRESENTATION_ITEM()
RATIONAL_B_SPLINE_SURFACE(((1.,0.43161218489519,1.),(1.,0.4354057728044,
1.),(1.,0.439046733702441,1.),(1.,0.442551630563568,1.)))
REPRESENTATION_ITEM('')
SURFACE()
);
#2358=(
BOUNDED_SURFACE()
B_SPLINE_SURFACE(3,2,((#149433,#149434,#149435),(#149436,#149437,#149438),
(#149439,#149440,#149441),(#149442,#149443,#149444),(#149445,#149446,#149447),
(#149448,#149449,#149450),(#149451,#149452,#149453),(#149454,#149455,#149456)),
 .UNSPECIFIED.,.F.,.F.,.F.)
B_SPLINE_SURFACE_WITH_KNOTS((4,2,2,4),(3,3),(0.,0.000350059279280428,0.000525088918920643,
0.000700118558560857),(0.,1.),.UNSPECIFIED.)
GEOMETRIC_REPRESENTATION_ITEM()
RATIONAL_B_SPLINE_SURFACE(((1.,0.707106781186548,1.),(1.,0.666269021153261,
1.),(1.,0.620643690025591,1.),(1.,0.551020195303415,1.),(1.,0.527243635346707,
1.),(1.,0.48184496425994,1.),(1.,0.460546552679624,1.),(1.,0.442551630563558,
1.)))
REPRESENTATION_ITEM('')
SURFACE()
);
#2359=(
BOUNDED_SURFACE()
B_SPLINE_SURFACE(3,2,((#149477,#149478,#149479),(#149480,#149481,#149482),
(#149483,#149484,#149485),(#149486,#149487,#149488),(#149489,#149490,#149491),
(#149492,#149493,#149494),(#149495,#149496,#149497),(#149498,#149499,#149500),
(#149501,#149502,#149503),(#149504,#149505,#149506)),.UNSPECIFIED.,.F.,
 .F.,.F.)
B_SPLINE_SURFACE_WITH_KNOTS((4,2,2,2,4),(3,3),(0.00131180726843867,0.00173116479138242,
0.00215052231432617,0.00256987983726992,0.00298923736021366),(0.,1.00000719536586),
 .UNSPECIFIED.)
GEOMETRIC_REPRESENTATION_ITEM()
RATIONAL_B_SPLINE_SURFACE(((1.,0.70710467371268,1.00000421497806),(1.,0.735459277069437,
1.00000380693457),(1.,0.75707678402216,1.00000349584283),(1.,0.786069896432003,
1.00000307861073),(1.,0.793429076618853,1.00000297270674),(1.,0.793448571747271,
1.00000297242619),(1.,0.786103829137559,1.00000307812241),(1.,0.757124528683257,
1.00000349515575),(1.,0.735523766262829,1.00000380600653),(1.,0.70710467371268,
1.00000421497806)))
REPRESENTATION_ITEM('')
SURFACE()
);
#2360=(
BOUNDED_SURFACE()
B_SPLINE_SURFACE(3,2,((#149527,#149528,#149529),(#149530,#149531,#149532),
(#149533,#149534,#149535),(#149536,#149537,#149538),(#149539,#149540,#149541),
(#149542,#149543,#149544),(#149545,#149546,#149547),(#149548,#149549,#149550),
(#149551,#149552,#149553),(#149554,#149555,#149556)),.UNSPECIFIED.,.F.,
 .F.,.F.)
B_SPLINE_SURFACE_WITH_KNOTS((4,2,2,2,4),(3,3),(3.1415926535898,3.53429173528852,
3.92699081698724,4.31968989868597,4.71238898038469),(0.,1.),
 .UNSPECIFIED.)
GEOMETRIC_REPRESENTATION_ITEM()
RATIONAL_B_SPLINE_SURFACE(((1.,0.754709580222776,1.),(1.,0.75471421973084,
1.),(1.,0.753512297096162,1.),(1.,0.748871927696637,1.),(1.,0.745429366938649,
1.),(1.,0.736738129296255,1.),(1.,0.73149075639724,1.),(1.,0.719894264862275,
1.),(1.,0.713550261851491,1.),(1.,0.707106781186548,1.)))
REPRESENTATION_ITEM('')
SURFACE()
);
#2361=(
BOUNDED_SURFACE()
B_SPLINE_SURFACE(3,2,((#149596,#149597,#149598),(#149599,#149600,#149601),
(#149602,#149603,#149604),(#149605,#149606,#149607),(#149608,#149609,#149610),
(#149611,#149612,#149613)),.UNSPECIFIED.,.F.,.F.,.F.)
B_SPLINE_SURFACE_WITH_KNOTS((4,2,4),(3,3),(-3.80119597236557E-5,0.000488761174293955,
0.00101555203427385),(-3.80296856860089E-5,1.),.UNSPECIFIED.)
GEOMETRIC_REPRESENTATION_ITEM()
RATIONAL_B_SPLINE_SURFACE(((1.00001434166179,0.81144122631948,1.),(1.00001374938095,
0.819228311950262,1.),(1.00001345333693,0.823120587367281,1.),(1.00001327853937,
0.825418760007561,1.),(1.00001340351003,0.823775692776788,1.),(1.00001365395156,
0.820482981788876,1.)))
REPRESENTATION_ITEM('')
SURFACE()
);
#2362=(
BOUNDED_SURFACE()
B_SPLINE_SURFACE(3,2,((#149641,#149642,#149643),(#149644,#149645,#149646),
(#149647,#149648,#149649),(#149650,#149651,#149652)),.UNSPECIFIED.,.F.,
 .F.,.F.)
B_SPLINE_SURFACE_WITH_KNOTS((4,4),(3,3),(0.,0.000106239733749475),(0.,1.),
 .UNSPECIFIED.)
GEOMETRIC_REPRESENTATION_ITEM()
RATIONAL_B_SPLINE_SURFACE(((1.,0.835215680136664,1.),(1.,0.831333836917881,
1.),(1.,0.826651097750167,1.),(1.,0.821176675475199,1.)))
REPRESENTATION_ITEM('')
SURFACE()
);
#2363=(
BOUNDED_SURFACE()
B_SPLINE_SURFACE(3,2,((#149656,#149657,#149658),(#149659,#149660,#149661),
(#149662,#149663,#149664),(#149665,#149666,#149667),(#149668,#149669,#149670),
(#149671,#149672,#149673)),.UNSPECIFIED.,.F.,.F.,.F.)
B_SPLINE_SURFACE_WITH_KNOTS((4,2,4),(3,3),(0.,0.0130414224518927,0.0260828449037854),
(0.,1.),.UNSPECIFIED.)
GEOMETRIC_REPRESENTATION_ITEM()
RATIONAL_B_SPLINE_SURFACE(((1.,0.835215680136663,1.),(1.,0.838844513950773,
1.),(1.,0.842771271110783,1.),(1.,0.851396246528345,1.),(1.,0.856094111052002,
1.),(1.,0.861290731803024,1.)))
REPRESENTATION_ITEM('')
SURFACE()
);
#2364=(
BOUNDED_SURFACE()
B_SPLINE_SURFACE(3,2,((#149682,#149683,#149684),(#149685,#149686,#149687),
(#149688,#149689,#149690),(#149691,#149692,#149693),(#149694,#149695,#149696),
(#149697,#149698,#149699)),.UNSPECIFIED.,.F.,.F.,.F.)
B_SPLINE_SURFACE_WITH_KNOTS((4,2,4),(3,3),(-0.00015233523741089,0.0022325368353913,
0.00461734601372613),(0.,1.00015233523741),.UNSPECIFIED.)
GEOMETRIC_REPRESENTATION_ITEM()
RATIONAL_B_SPLINE_SURFACE(((1.,0.700994279879693,1.00009109821472),(1.,
0.732815663384495,1.0000814031787),(1.,0.762177009942305,1.0000724576433),
(1.,0.817213761356616,1.00005568957012),(1.,0.843031394120544,1.00004782369969),
(1.,0.865639026170535,1.00004093582169)))
REPRESENTATION_ITEM('')
SURFACE()
);
#2365=(
BOUNDED_SURFACE()
B_SPLINE_SURFACE(3,2,((#149743,#149744,#149745),(#149746,#149747,#149748),
(#149749,#149750,#149751),(#149752,#149753,#149754),(#149755,#149756,#149757),
(#149758,#149759,#149760),(#149761,#149762,#149763),(#149764,#149765,#149766)),
 .UNSPECIFIED.,.F.,.F.,.F.)
B_SPLINE_SURFACE_WITH_KNOTS((4,2,2,4),(3,3),(0.,0.00223318354977648,0.00334977532466471,
0.00446636709955295),(0.,1.),.UNSPECIFIED.)
GEOMETRIC_REPRESENTATION_ITEM()
RATIONAL_B_SPLINE_SURFACE(((1.,0.861290731803006,1.),(1.,0.839613661895165,
1.),(1.,0.815980432119487,1.),(1.,0.777267373295742,1.),(1.,0.763786842194511,
1.),(1.,0.736109943319361,1.),(1.,0.721853181403518,1.),(1.,0.707106781186545,
1.)))
REPRESENTATION_ITEM('')
SURFACE()
);
#2366=(
BOUNDED_SURFACE()
B_SPLINE_SURFACE(3,2,((#149779,#149780,#149781),(#149782,#149783,#149784),
(#149785,#149786,#149787),(#149788,#149789,#149790),(#149791,#149792,#149793),
(#149794,#149795,#149796)),.UNSPECIFIED.,.F.,.F.,.F.)
B_SPLINE_SURFACE_WITH_KNOTS((4,2,4),(3,3),(0.,0.0129055642122842,0.0258111284245685),
(0.,1.),.UNSPECIFIED.)
GEOMETRIC_REPRESENTATION_ITEM()
RATIONAL_B_SPLINE_SURFACE(((1.,0.861290731803006,1.),(1.,0.856148221578915,
1.),(1.,0.851494227257712,1.),(1.,0.842943112520738,1.),(1.,0.839046328378941,
1.),(1.,0.835442841040481,1.)))
REPRESENTATION_ITEM('')
SURFACE()
);
#2367=(
BOUNDED_SURFACE()
B_SPLINE_SURFACE(3,2,((#149804,#149805,#149806),(#149807,#149808,#149809),
(#149810,#149811,#149812),(#149813,#149814,#149815)),.UNSPECIFIED.,.F.,
 .F.,.F.)
B_SPLINE_SURFACE_WITH_KNOTS((4,4),(3,3),(0.,0.000212668013534773),(0.,1.),
 .UNSPECIFIED.)
GEOMETRIC_REPRESENTATION_ITEM()
RATIONAL_B_SPLINE_SURFACE(((1.,0.802684671197877,1.),(1.,0.816456497832501,
1.),(1.,0.82752079624252,1.),(1.,0.835442841040483,1.)))
REPRESENTATION_ITEM('')
SURFACE()
);
#2368=(
BOUNDED_SURFACE()
B_SPLINE_SURFACE(3,2,((#149817,#149818,#149819),(#149820,#149821,#149822),
(#149823,#149824,#149825),(#149826,#149827,#149828)),.UNSPECIFIED.,.F.,
 .F.,.F.)
B_SPLINE_SURFACE_WITH_KNOTS((4,4),(3,3),(-1.1328828500301E-15,0.000723745383907254),
(0.,1.),.UNSPECIFIED.)
GEOMETRIC_REPRESENTATION_ITEM()
RATIONAL_B_SPLINE_SURFACE(((1.,0.802684671198269,1.),(1.,0.797620722711664,
1.),(1.,0.787749610789602,1.),(1.,0.773398994756355,1.)))
REPRESENTATION_ITEM('')
SURFACE()
);
#2369=(
BOUNDED_SURFACE()
B_SPLINE_SURFACE(3,2,((#149848,#149849,#149850),(#149851,#149852,#149853),
(#149854,#149855,#149856),(#149857,#149858,#149859),(#149860,#149861,#149862),
(#149863,#149864,#149865),(#149866,#149867,#149868),(#149869,#149870,#149871)),
 .UNSPECIFIED.,.F.,.F.,.F.)
B_SPLINE_SURFACE_WITH_KNOTS((4,2,2,4),(3,3),(-6.50521303491303E-18,0.000158176853950714,
0.000316353707901435,0.000632707415802875),(0.,1.),.UNSPECIFIED.)
GEOMETRIC_REPRESENTATION_ITEM()
RATIONAL_B_SPLINE_SURFACE(((1.,0.50825434412561,1.),(1.,0.519857702736613,
1.),(1.,0.534132547044037,1.),(1.,0.566198696596924,1.),(1.,0.583560620774966,
1.),(1.,0.636763258069658,1.),(1.,0.673308410857549,1.),(1.,0.707106781186552,
1.)))
REPRESENTATION_ITEM('')
SURFACE()
);
#2370=(
BOUNDED_SURFACE()
B_SPLINE_SURFACE(3,2,((#149875,#149876,#149877),(#149878,#149879,#149880),
(#149881,#149882,#149883),(#149884,#149885,#149886)),.UNSPECIFIED.,.F.,
 .F.,.F.)
B_SPLINE_SURFACE_WITH_KNOTS((4,4),(3,3),(-6.93889390390723E-18,0.0177935197894076),
(0.,1.),.UNSPECIFIED.)
GEOMETRIC_REPRESENTATION_ITEM()
RATIONAL_B_SPLINE_SURFACE(((1.,0.508254344125608,1.),(1.,0.498412666571477,
1.),(1.,0.487173250319529,1.),(1.,0.473671517629131,1.)))
REPRESENTATION_ITEM('')
SURFACE()
);
#2371=(
BOUNDED_SURFACE()
B_SPLINE_SURFACE(3,2,((#149888,#149889,#149890),(#149891,#149892,#149893),
(#149894,#149895,#149896),(#149897,#149898,#149899),(#149900,#149901,#149902),
(#149903,#149904,#149905),(#149906,#149907,#149908),(#149909,#149910,#149911)),
 .UNSPECIFIED.,.F.,.F.,.F.)
B_SPLINE_SURFACE_WITH_KNOTS((4,2,2,4),(3,3),(0.,0.00262348010799063,0.00393522016198593,
0.00524696021598125),(0.,1.),.UNSPECIFIED.)
GEOMETRIC_REPRESENTATION_ITEM()
RATIONAL_B_SPLINE_SURFACE(((1.,0.70710678118732,1.),(1.,0.673159051373371,
1.),(1.,0.637356734328886,1.),(1.,0.579048422068377,1.),(1.,0.558729842945168,
1.),(1.,0.517089292555981,1.),(1.,0.495689661102028,1.),(1.,0.473671517629131,
1.)))
REPRESENTATION_ITEM('')
SURFACE()
);
#2372=(
BOUNDED_SURFACE()
B_SPLINE_SURFACE(3,2,((#149928,#149929,#149930),(#149931,#149932,#149933),
(#149934,#149935,#149936),(#149937,#149938,#149939),(#149940,#149941,#149942),
(#149943,#149944,#149945),(#149946,#149947,#149948),(#149949,#149950,#149951),
(#149952,#149953,#149954),(#149955,#149956,#149957)),.UNSPECIFIED.,.F.,
 .F.,.F.)
B_SPLINE_SURFACE_WITH_KNOTS((4,2,2,2,4),(3,3),(-4.33680868994201E-18,0.00131184996336558,
0.00262369992673117,0.00393554989009676,0.00524739985346235),(0.,1.),
 .UNSPECIFIED.)
GEOMETRIC_REPRESENTATION_ITEM()
RATIONAL_B_SPLINE_SURFACE(((1.,0.473671517629133,1.),(1.,0.495707594803631,
1.),(1.,0.517034522428114,1.),(1.,0.558412152901823,1.),(1.,0.578466470542957,
1.),(1.,0.617536962037478,1.),(1.,0.636393525150058,1.),(1.,0.672664546785766,
1.),(1.,0.690145348310819,1.),(1.,0.707106781186548,1.)))
REPRESENTATION_ITEM('')
SURFACE()
);
#2373=(
BOUNDED_SURFACE()
B_SPLINE_SURFACE(3,2,((#149970,#149971,#149972),(#149973,#149974,#149975),
(#149976,#149977,#149978),(#149979,#149980,#149981)),.UNSPECIFIED.,.F.,
 .F.,.F.)
B_SPLINE_SURFACE_WITH_KNOTS((4,4),(3,3),(0.,0.0180689587739334),(0.,1.),
 .UNSPECIFIED.)
GEOMETRIC_REPRESENTATION_ITEM()
RATIONAL_B_SPLINE_SURFACE(((1.,0.473671517629134,1.),(1.,0.487381853083234,
1.),(1.,0.49876090260372,1.),(1.,0.508709923441297,1.)))
REPRESENTATION_ITEM('')
SURFACE()
);
#2374=(
BOUNDED_SURFACE()
B_SPLINE_SURFACE(3,2,((#149988,#149989,#149990),(#149991,#149992,#149993),
(#149994,#149995,#149996),(#149997,#149998,#149999),(#150000,#150001,#150002),
(#150003,#150004,#150005),(#150006,#150007,#150008),(#150009,#150010,#150011),
(#150012,#150013,#150014),(#150015,#150016,#150017)),.UNSPECIFIED.,.F.,
 .F.,.F.)
B_SPLINE_SURFACE_WITH_KNOTS((4,2,2,2,4),(3,3),(0.,0.000157845161260656,
0.000315690322521312,0.000473535483781968,0.000631380645042625),(0.,1.),
 .UNSPECIFIED.)
GEOMETRIC_REPRESENTATION_ITEM()
RATIONAL_B_SPLINE_SURFACE(((1.,0.707106781186548,1.),(1.,0.690126575842363,
1.),(1.,0.672866331348439,1.),(1.,0.637644189799934,1.),(1.,0.619386686649187,
1.),(1.,0.584119465416144,1.),(1.,0.567005655158962,1.),(1.,0.534765171917349,
1.),(1.,0.520258799319389,1.),(1.,0.508709923441296,1.)))
REPRESENTATION_ITEM('')
SURFACE()
);
#2375=(
BOUNDED_SURFACE()
B_SPLINE_SURFACE(3,2,((#150034,#150035,#150036),(#150037,#150038,#150039),
(#150040,#150041,#150042),(#150043,#150044,#150045),(#150046,#150047,#150048),
(#150049,#150050,#150051),(#150052,#150053,#150054),(#150055,#150056,#150057),
(#150058,#150059,#150060),(#150061,#150062,#150063)),.UNSPECIFIED.,.F.,
 .F.,.F.)
B_SPLINE_SURFACE_WITH_KNOTS((4,2,2,2,4),(3,3),(1.5707963267949,1.96349540849362,
2.35619449019234,2.74889357189107,3.14159265358979),(0.,1.),
 .UNSPECIFIED.)
GEOMETRIC_REPRESENTATION_ITEM()
RATIONAL_B_SPLINE_SURFACE(((1.,0.707106781186548,1.),(1.,0.700666378834645,
1.),(1.,0.694134907060333,1.),(1.,0.681903435451719,1.),(1.,0.676209154063922,
1.),(1.,0.666616044204548,1.),(1.,0.662724068472644,1.),(1.,0.657443209221262,
1.),(1.,0.656051196071901,1.),(1.,0.656059028990513,1.)))
REPRESENTATION_ITEM('')
SURFACE()
);
#2376=(
BOUNDED_SURFACE()
B_SPLINE_SURFACE(3,2,((#150118,#150119,#150120),(#150121,#150122,#150123),
(#150124,#150125,#150126),(#150127,#150128,#150129),(#150130,#150131,#150132),
(#150133,#150134,#150135),(#150136,#150137,#150138),(#150139,#150140,#150141),
(#150142,#150143,#150144),(#150145,#150146,#150147)),.UNSPECIFIED.,.F.,
 .F.,.F.)
B_SPLINE_SURFACE_WITH_KNOTS((4,2,2,2,4),(3,3),(3.1415926535898,3.53429173528852,
3.92699081698724,4.31968989868597,4.71238898038469),(0.,1.),
 .UNSPECIFIED.)
GEOMETRIC_REPRESENTATION_ITEM()
RATIONAL_B_SPLINE_SURFACE(((1.,0.754709580222772,1.),(1.,0.754714219730848,
1.),(1.,0.753512297096158,1.),(1.,0.748871927696634,1.),(1.,0.745429366938649,
1.),(1.,0.736738129296255,1.),(1.,0.731490756397077,1.),(1.,0.719894264862441,
1.),(1.,0.713550261851367,1.),(1.,0.707106781186548,1.)))
REPRESENTATION_ITEM('')
SURFACE()
);
#2377=(
BOUNDED_SURFACE()
B_SPLINE_SURFACE(3,2,((#150164,#150165,#150166),(#150167,#150168,#150169),
(#150170,#150171,#150172),(#150173,#150174,#150175),(#150176,#150177,#150178),
(#150179,#150180,#150181)),.UNSPECIFIED.,.F.,.F.,.F.)
B_SPLINE_SURFACE_WITH_KNOTS((4,2,4),(3,3),(0.,0.000324038763230374,0.000648077526460748),
(0.,1.),.UNSPECIFIED.)
GEOMETRIC_REPRESENTATION_ITEM()
RATIONAL_B_SPLINE_SURFACE(((1.,0.87207744658335,1.),(1.,0.857354948275163,
1.),(1.,0.833755771861677,1.),(1.,0.776640613237984,1.),(1.,0.743340108181467,
1.),(1.,0.707106781186543,1.)))
REPRESENTATION_ITEM('')
SURFACE()
);
#2378=(
BOUNDED_SURFACE()
B_SPLINE_SURFACE(3,2,((#150190,#150191,#150192),(#150193,#150194,#150195),
(#150196,#150197,#150198),(#150199,#150200,#150201)),.UNSPECIFIED.,.F.,
 .F.,.F.)
B_SPLINE_SURFACE_WITH_KNOTS((4,4),(3,3),(0.,0.0141656229616797),(0.,1.),
 .UNSPECIFIED.)
GEOMETRIC_REPRESENTATION_ITEM()
RATIONAL_B_SPLINE_SURFACE(((1.,0.872077446583348,1.),(1.,0.876947206822174,
1.),(1.,0.882221222508023,1.),(1.,0.887998771276578,1.)))
REPRESENTATION_ITEM('')
SURFACE()
);
#2379=(
BOUNDED_SURFACE()
B_SPLINE_SURFACE(3,2,((#150208,#150209,#150210),(#150211,#150212,#150213),
(#150214,#150215,#150216),(#150217,#150218,#150219),(#150220,#150221,#150222),
(#150223,#150224,#150225),(#150226,#150227,#150228),(#150229,#150230,#150231)),
 .UNSPECIFIED.,.F.,.F.,.F.)
B_SPLINE_SURFACE_WITH_KNOTS((4,2,2,4),(3,3),(-0.000151407848110819,0.00278824321172774,
0.00418236481759161,0.0057276222743267),(0.,1.00015140784811),
 .UNSPECIFIED.)
GEOMETRIC_REPRESENTATION_ITEM()
RATIONAL_B_SPLINE_SURFACE(((1.,0.701236390783137,1.00009047031033),(1.,
0.739120426865072,1.00007899842957),(1.,0.773512306563008,1.00006858402857),
(1.,0.820586923934616,1.00005432909554),(1.,0.835217331499987,1.00004989877849),
(1.,0.864264001665827,1.00004110299084),(1.,0.878586452051055,1.00003676592805),
(1.,0.891923360613614,1.0000327273028)))
REPRESENTATION_ITEM('')
SURFACE()
);
#2380=(
BOUNDED_SURFACE()
B_SPLINE_SURFACE(3,2,((#150278,#150279,#150280),(#150281,#150282,#150283),
(#150284,#150285,#150286),(#150287,#150288,#150289),(#150290,#150291,#150292),
(#150293,#150294,#150295),(#150296,#150297,#150298),(#150299,#150300,#150301)),
 .UNSPECIFIED.,.F.,.F.,.F.)
B_SPLINE_SURFACE_WITH_KNOTS((4,2,2,4),(3,3),(-8.78076470147105E-5,0.00139422219513554,
0.00278844439027108,0.0056649682329014),(0.,1.00008807945236),
 .UNSPECIFIED.)
GEOMETRIC_REPRESENTATION_ITEM()
RATIONAL_B_SPLINE_SURFACE(((1.,0.890287745294558,1.00001932679062),(1.,
0.87740523386917,1.00002159615973),(1.,0.863663500716923,1.00002401688839),
(1.,0.835397058527914,1.00002899627389),(1.,0.820967815861932,1.00003153811347),
(1.,0.774347259046824,1.0000397507397),(1.,0.740581186868133,1.00004569893399),
(0.999999999999999,0.703701983503653,1.00005219553406)))
REPRESENTATION_ITEM('')
SURFACE()
);
#2381=(
BOUNDED_SURFACE()
B_SPLINE_SURFACE(3,2,((#150350,#150351,#150352),(#150353,#150354,#150355),
(#150356,#150357,#150358),(#150359,#150360,#150361)),.UNSPECIFIED.,.F.,
 .F.,.F.)
B_SPLINE_SURFACE_WITH_KNOTS((4,4),(3,3),(0.,0.0138879247081574),(0.,1.),
 .UNSPECIFIED.)
GEOMETRIC_REPRESENTATION_ITEM()
RATIONAL_B_SPLINE_SURFACE(((1.,0.887998771276556,1.),(1.,0.882334484690674,
1.),(1.,0.877154223922122,1.),(1.,0.872364293278347,1.)))
REPRESENTATION_ITEM('')
SURFACE()
);
#2382=(
BOUNDED_SURFACE()
B_SPLINE_SURFACE(3,2,((#150367,#150368,#150369),(#150370,#150371,#150372),
(#150373,#150374,#150375),(#150376,#150377,#150378),(#150379,#150380,#150381),
(#150382,#150383,#150384)),.UNSPECIFIED.,.F.,.F.,.F.)
B_SPLINE_SURFACE_WITH_KNOTS((4,2,4),(3,3),(0.,0.000324353517959648,0.000648707035919297),
(0.,1.),.UNSPECIFIED.)
GEOMETRIC_REPRESENTATION_ITEM()
RATIONAL_B_SPLINE_SURFACE(((1.,0.707106781186548,1.),(1.,0.742998991655634,
1.),(1.,0.776756965569408,1.),(1.,0.833658724502819,1.),(1.,0.857385369677227,
1.),(1.,0.872364293278349,1.)))
REPRESENTATION_ITEM('')
SURFACE()
);
#2383=(
BOUNDED_SURFACE()
B_SPLINE_SURFACE(3,2,((#150411,#150412,#150413),(#150414,#150415,#150416),
(#150417,#150418,#150419),(#150420,#150421,#150422)),.UNSPECIFIED.,.F.,
 .F.,.F.)
B_SPLINE_SURFACE_WITH_KNOTS((4,4),(3,3),(0.00167806205423436,0.0019221164224989),
(0.,1.),.UNSPECIFIED.)
GEOMETRIC_REPRESENTATION_ITEM()
RATIONAL_B_SPLINE_SURFACE(((1.,0.83648401963888,1.),(1.,0.827500667105214,
1.),(1.,0.81402442184051,1.),(1.,0.797363061122239,1.)))
REPRESENTATION_ITEM('')
SURFACE()
);
#2384=(
BOUNDED_SURFACE()
B_SPLINE_SURFACE(3,2,((#150424,#150425,#150426),(#150427,#150428,#150429),
(#150430,#150431,#150432),(#150433,#150434,#150435),(#150436,#150437,#150438),
(#150439,#150440,#150441),(#150442,#150443,#150444),(#150445,#150446,#150447),
(#150448,#150449,#150450),(#150451,#150452,#150453)),.UNSPECIFIED.,.F.,
 .F.,.F.)
B_SPLINE_SURFACE_WITH_KNOTS((4,2,2,2,4),(3,3),(0.,0.000158289020679031,
0.000316578041358062,0.000474867062037094,0.000633156082716125),(0.,1.),
 .UNSPECIFIED.)
GEOMETRIC_REPRESENTATION_ITEM()
RATIONAL_B_SPLINE_SURFACE(((1.,0.707106781186548,1.),(1.,0.689988873362392,
1.),(1.,0.672579653000586,1.),(1.,0.63703033863955,1.),(1.,0.61859446393025,
1.),(1.,0.582956103977724,1.),(1.,0.565642356156971,1.),(1.,0.532984405418804,
1.),(1.,0.518263379167526,1.),(1.,0.506538946041792,1.)))
REPRESENTATION_ITEM('')
SURFACE()
);
#2385=(
BOUNDED_SURFACE()
B_SPLINE_SURFACE(3,2,((#150456,#150457,#150458),(#150459,#150460,#150461),
(#150462,#150463,#150464),(#150465,#150466,#150467),(#150468,#150469,#150470),
(#150471,#150472,#150473)),.UNSPECIFIED.,.F.,.F.,.F.)
B_SPLINE_SURFACE_WITH_KNOTS((4,2,4),(3,3),(0.,0.000518347860385374,0.00103669572077075),
(0.,1.),.UNSPECIFIED.)
GEOMETRIC_REPRESENTATION_ITEM()
RATIONAL_B_SPLINE_SURFACE(((1.,0.819851970694872,1.),(1.,0.821199393891468,
1.),(1.,0.820620061026224,1.),(1.,0.813565992888811,1.),(1.,0.807280082867884,
1.),(1.,0.797551754323293,1.)))
REPRESENTATION_ITEM('')
SURFACE()
);
#2386=(
BOUNDED_SURFACE()
B_SPLINE_SURFACE(3,2,((#150504,#150505,#150506),(#150507,#150508,#150509),
(#150510,#150511,#150512),(#150513,#150514,#150515),(#150516,#150517,#150518),
(#150519,#150520,#150521)),.UNSPECIFIED.,.F.,.F.,.F.)
B_SPLINE_SURFACE_WITH_KNOTS((4,2,4),(3,3),(0.,0.0127570403976527,0.0255140807953054),
(0.,1.),.UNSPECIFIED.)
GEOMETRIC_REPRESENTATION_ITEM()
RATIONAL_B_SPLINE_SURFACE(((1.,0.83648401963888,1.),(1.,0.840071262854844,
1.),(1.,0.843946769546665,1.),(1.,0.852439323016447,1.),(1.,0.857056062862677,
1.),(1.,0.862148985649771,1.)))
REPRESENTATION_ITEM('')
SURFACE()
);
#2387=(
BOUNDED_SURFACE()
B_SPLINE_SURFACE(3,2,((#150523,#150524,#150525),(#150526,#150527,#150528),
(#150529,#150530,#150531),(#150532,#150533,#150534),(#150535,#150536,#150537),
(#150538,#150539,#150540)),.UNSPECIFIED.,.F.,.F.,.F.)
B_SPLINE_SURFACE_WITH_KNOTS((4,2,4),(3,3),(-0.000152927716596379,0.00224843555189379,
0.00464973688355988),(0.,1.0001529277166),.UNSPECIFIED.)
GEOMETRIC_REPRESENTATION_ITEM()
RATIONAL_B_SPLINE_SURFACE(((1.,0.700973962712928,1.00009145873817),(1.,
0.732997839700047,1.0000816640614),(1.,0.76252859926943,1.00007263191814),
(1.,0.817862932084816,1.00005570761181),(1.,0.843804501741489,1.00004777324178),
(1.,0.866501623387319,1.00004083120381)))
REPRESENTATION_ITEM('')
SURFACE()
);
#2388=(
BOUNDED_SURFACE()
B_SPLINE_SURFACE(3,2,((#150584,#150585,#150586),(#150587,#150588,#150589),
(#150590,#150591,#150592),(#150593,#150594,#150595),(#150596,#150597,#150598),
(#150599,#150600,#150601),(#150602,#150603,#150604),(#150605,#150606,#150607)),
 .UNSPECIFIED.,.F.,.F.,.F.)
B_SPLINE_SURFACE_WITH_KNOTS((4,2,2,4),(3,3),(2.16840434497101E-19,0.00224905873968498,
0.00337358810952747,0.00449811747936996),(0.,1.),.UNSPECIFIED.)
GEOMETRIC_REPRESENTATION_ITEM()
RATIONAL_B_SPLINE_SURFACE(((1.,0.862148985649768,1.),(1.,0.840377424690098,
1.),(1.,0.816625499326475,1.),(1.,0.777693385283957,1.),(1.,0.764135973582955,
1.),(1.,0.736295007876384,1.),(1.,0.721949804627483,1.),(1.,0.707106781186548,
1.)))
REPRESENTATION_ITEM('')
SURFACE()
);
#2389=(
BOUNDED_SURFACE()
B_SPLINE_SURFACE(3,2,((#150620,#150621,#150622),(#150623,#150624,#150625),
(#150626,#150627,#150628),(#150629,#150630,#150631),(#150632,#150633,#150634),
(#150635,#150636,#150637)),.UNSPECIFIED.,.F.,.F.,.F.)
B_SPLINE_SURFACE_WITH_KNOTS((4,2,4),(3,3),(0.,0.0128929585057523,0.0257859170115046),
(0.,1.),.UNSPECIFIED.)
GEOMETRIC_REPRESENTATION_ITEM()
RATIONAL_B_SPLINE_SURFACE(((1.,0.862148985649771,1.),(1.,0.857001824466315,
1.),(1.,0.852340953158334,1.),(1.,0.843773924789864,1.),(1.,0.839868090827823,
1.),(1.,0.83625514626814,1.)))
REPRESENTATION_ITEM('')
SURFACE()
);
#2390=(
BOUNDED_SURFACE()
B_SPLINE_SURFACE(3,2,((#150646,#150647,#150648),(#150649,#150650,#150651),
(#150652,#150653,#150654),(#150655,#150656,#150657)),.UNSPECIFIED.,.F.,
 .F.,.F.)
B_SPLINE_SURFACE_WITH_KNOTS((4,4),(3,3),(-1.68213967061126E-16,0.000120540380538488),
(0.,1.),.UNSPECIFIED.)
GEOMETRIC_REPRESENTATION_ITEM()
RATIONAL_B_SPLINE_SURFACE(((1.,0.819851970694933,1.),(1.,0.826338730586804,
1.),(1.,0.831810971765196,1.),(1.,0.836255146268139,1.)))
REPRESENTATION_ITEM('')
SURFACE()
);
#2391=(
BOUNDED_SURFACE()
B_SPLINE_SURFACE(3,2,((#150659,#150660,#150661),(#150662,#150663,#150664),
(#150665,#150666,#150667),(#150668,#150669,#150670),(#150671,#150672,#150673),
(#150674,#150675,#150676),(#150677,#150678,#150679),(#150680,#150681,#150682),
(#150683,#150684,#150685),(#150686,#150687,#150688)),.UNSPECIFIED.,.F.,
 .F.,.F.)
B_SPLINE_SURFACE_WITH_KNOTS((4,2,2,2,4),(3,3),(4.71238898038469,5.10508806208341,
5.49778714378214,5.89048622548086,6.28318530717959),(0.,1.),
 .UNSPECIFIED.)
GEOMETRIC_REPRESENTATION_ITEM()
RATIONAL_B_SPLINE_SURFACE(((1.,0.707106781186552,1.),(1.,0.713550261851678,
1.),(1.,0.71989426486204,1.),(1.,0.731490756397489,1.),(1.,0.736738129296849,
1.),(1.,0.745429366938066,1.),(1.,0.748871927696599,1.),(1.,0.753512297096214,
1.),(1.,0.754714219730812,1.),(1.,0.754709580222777,1.)))
REPRESENTATION_ITEM('')
SURFACE()
);
#2392=(
BOUNDED_SURFACE()
B_SPLINE_SURFACE(3,2,((#150724,#150725,#150726),(#150727,#150728,#150729),
(#150730,#150731,#150732),(#150733,#150734,#150735),(#150736,#150737,#150738),
(#150739,#150740,#150741),(#150742,#150743,#150744),(#150745,#150746,#150747),
(#150748,#150749,#150750),(#150751,#150752,#150753)),.UNSPECIFIED.,.F.,
 .F.,.F.)
B_SPLINE_SURFACE_WITH_KNOTS((4,2,2,2,4),(3,3),(0.00108313181642978,0.00175636478508586,
0.00242959775374195,0.00310283072239804,0.00377606369105412),(0.,1.00020946001193),
 .UNSPECIFIED.)
GEOMETRIC_REPRESENTATION_ITEM()
RATIONAL_B_SPLINE_SURFACE(((1.,0.707045431769442,1.00012272453471),(1.,
0.774791710231453,1.00009434426212),(1.,0.828921293970199,1.00007166829561),
(1.,0.90377968768014,1.00004030861553),(1.,0.924101020320238,1.00003179560238),
(1.,0.924695389732398,1.00003154660913),(1.,0.904861584946617,1.0000398553871),
(1.,0.830176121522932,1.00007114262322),(1.,0.775998513536094,1.00009383870805),
(1.,0.707045431769442,1.00012272453471)))
REPRESENTATION_ITEM('')
SURFACE()
);
#2393=(
BOUNDED_SURFACE()
B_SPLINE_SURFACE(3,2,((#150784,#150785,#150786),(#150787,#150788,#150789),
(#150790,#150791,#150792),(#150793,#150794,#150795),(#150796,#150797,#150798),
(#150799,#150800,#150801),(#150802,#150803,#150804),(#150805,#150806,#150807),
(#150808,#150809,#150810),(#150811,#150812,#150813)),.UNSPECIFIED.,.F.,
 .F.,.F.)
B_SPLINE_SURFACE_WITH_KNOTS((4,2,2,2,4),(3,3),(-8.88178419700125E-16,0.392699081698724,
0.785398163397448,1.17809724509617,1.5707963267949),(0.,1.),
 .UNSPECIFIED.)
GEOMETRIC_REPRESENTATION_ITEM()
RATIONAL_B_SPLINE_SURFACE(((1.,0.656059028990513,1.),(1.,0.656051196071901,
1.),(1.,0.657443209221259,1.),(1.,0.662724068472642,1.),(1.,0.666616044204551,
1.),(1.,0.676209154063925,1.),(1.,0.681903435451265,1.),(1.,0.694134907060781,
1.),(1.,0.70066637883431,1.),(1.,0.707106781186548,1.)))
REPRESENTATION_ITEM('')
SURFACE()
);
#2394=(
BOUNDED_SURFACE()
B_SPLINE_SURFACE(3,2,((#150830,#150831,#150832),(#150833,#150834,#150835),
(#150836,#150837,#150838),(#150839,#150840,#150841),(#150842,#150843,#150844),
(#150845,#150846,#150847),(#150848,#150849,#150850),(#150851,#150852,#150853),
(#150854,#150855,#150856),(#150857,#150858,#150859)),.UNSPECIFIED.,.F.,
 .F.,.F.)
B_SPLINE_SURFACE_WITH_KNOTS((4,2,2,2,4),(3,3),(-6.16097884514888E-17,0.000175529658750937,
0.000351059317501936,0.000526588976252934,0.000702118635003933),(0.,1.),
 .UNSPECIFIED.)
GEOMETRIC_REPRESENTATION_ITEM()
RATIONAL_B_SPLINE_SURFACE(((1.,0.440584280700845,1.),(1.,0.458788905458512,
1.),(1.,0.480391768923104,1.),(1.,0.526541516020855,1.),(1.,0.550240391579637,
1.),(1.,0.597052366816548,1.),(1.,0.620407250394368,1.),(1.,0.664886737818671,
1.),(1.,0.686305427599538,1.),(1.,0.707106781186548,1.)))
REPRESENTATION_ITEM('')
SURFACE()
);
#2395=(
BOUNDED_SURFACE()
B_SPLINE_SURFACE(3,2,((#150872,#150873,#150874),(#150875,#150876,#150877),
(#150878,#150879,#150880),(#150881,#150882,#150883)),.UNSPECIFIED.,.F.,
 .F.,.F.)
B_SPLINE_SURFACE_WITH_KNOTS((4,4),(3,3),(0.,0.00414272899747597),(0.,1.),
 .UNSPECIFIED.)
GEOMETRIC_REPRESENTATION_ITEM()
RATIONAL_B_SPLINE_SURFACE(((1.,0.440584280700845,1.),(1.,0.437364321804866,
1.),(1.,0.434030421143282,1.),(1.,0.43057004911423,1.)))
REPRESENTATION_ITEM('')
SURFACE()
);
#2396=(
BOUNDED_SURFACE()
B_SPLINE_SURFACE(3,2,((#150890,#150891,#150892),(#150893,#150894,#150895),
(#150896,#150897,#150898),(#150899,#150900,#150901),(#150902,#150903,#150904),
(#150905,#150906,#150907),(#150908,#150909,#150910),(#150911,#150912,#150913),
(#150914,#150915,#150916),(#150917,#150918,#150919)),.UNSPECIFIED.,.F.,
 .F.,.F.)
B_SPLINE_SURFACE_WITH_KNOTS((4,2,2,2,4),(3,3),(-0.000629686196911106,0.00157421549227777,
0.00314843098455553,0.0047226464768333,0.00692654799509362),(0.,1.00122484286925),
 .UNSPECIFIED.)
GEOMETRIC_REPRESENTATION_ITEM()
RATIONAL_B_SPLINE_SURFACE(((1.,0.729910044545915,1.00066163551199),(1.,
0.703216914697168,1.00072702529149),(1.,0.675425262315014,1.00079510610598),
(1.,0.62493198685998,1.00091879876276),(1.,0.603050731781505,1.00097240096126),
(1.,0.557017477276785,1.00108516796832),(1.,0.532829811862376,1.00114442014733),
(1.,0.472843951657849,1.00129136665359),(1.,0.435970647158995,1.00138169466175),
(1.,0.396939037364919,1.00147730983961)))
REPRESENTATION_ITEM('')
SURFACE()
);
#2397=(
BOUNDED_SURFACE()
B_SPLINE_SURFACE(3,2,((#150975,#150976,#150977),(#150978,#150979,#150980),
(#150981,#150982,#150983),(#150984,#150985,#150986),(#150987,#150988,#150989),
(#150990,#150991,#150992),(#150993,#150994,#150995),(#150996,#150997,#150998),
(#150999,#151000,#151001),(#151002,#151003,#151004),(#151005,#151006,#151007),
(#151008,#151009,#151010)),.UNSPECIFIED.,.F.,.F.,.F.)
B_SPLINE_SURFACE_WITH_KNOTS((4,2,2,2,2,4),(3,3),(-0.000629845251684256,
0.00157461356268982,0.00236192034403473,0.00314922712537965,0.00472384068806947,
0.00692829967583523),(0.,1.00123997501886),.UNSPECIFIED.)
GEOMETRIC_REPRESENTATION_ITEM()
RATIONAL_B_SPLINE_SURFACE(((1.,0.396902198869997,1.00149565241467),(1.,
0.435987544303699,1.00139872271078),(1.,0.47283780294273,1.00130733591048),
(1.,0.520247360808013,1.00118976257566),(1.,0.532482074736246,1.0011594210964),
(1.,0.556521348730162,1.00109980489795),(1.,0.568360302311468,1.00107044488457),
(1.,0.602961724073934,1.00098463508736),(1.,0.624876074265694,1.00093028859378),
(1.,0.67542036326162,1.00080494128238),(1.,0.703218088558977,1.00073600431248),
(1.,0.72990104380667,1.0006698319166)))
REPRESENTATION_ITEM('')
SURFACE()
);
#2398=(
BOUNDED_SURFACE()
B_SPLINE_SURFACE(3,2,((#151062,#151063,#151064),(#151065,#151066,#151067),
(#151068,#151069,#151070),(#151071,#151072,#151073)),.UNSPECIFIED.,.F.,
 .F.,.F.)
B_SPLINE_SURFACE_WITH_KNOTS((4,4),(3,3),(-5.03069808033274E-17,0.00385726433182564),
(0.,1.),.UNSPECIFIED.)
GEOMETRIC_REPRESENTATION_ITEM()
RATIONAL_B_SPLINE_SURFACE(((1.,0.430570049114201,1.),(1.,0.433791974258431,
1.),(1.,0.436904245661489,1.),(1.,0.439917019807019,1.)))
REPRESENTATION_ITEM('')
SURFACE()
);
#2399=(
BOUNDED_SURFACE()
B_SPLINE_SURFACE(3,2,((#151080,#151081,#151082),(#151083,#151084,#151085),
(#151086,#151087,#151088),(#151089,#151090,#151091),(#151092,#151093,#151094),
(#151095,#151096,#151097),(#151098,#151099,#151100),(#151101,#151102,#151103)),
 .UNSPECIFIED.,.F.,.F.,.F.)
B_SPLINE_SURFACE_WITH_KNOTS((4,2,2,4),(3,3),(0.,0.000351812098911224,0.000527718148366836,
0.000703624197822447),(0.,1.),.UNSPECIFIED.)
GEOMETRIC_REPRESENTATION_ITEM()
RATIONAL_B_SPLINE_SURFACE(((1.,0.707106781186548,1.),(1.,0.666004685610564,
1.),(1.,0.620075381085077,1.),(1.,0.549819108711631,1.),(1.,0.525790037137517,
1.),(1.,0.479829608303299,1.),(1.,0.458216765529125,1.),(1.,0.439917019807004,
1.)))
REPRESENTATION_ITEM('')
SURFACE()
);
#2400=(
BOUNDED_SURFACE()
B_SPLINE_SURFACE(3,2,((#151131,#151132,#151133),(#151134,#151135,#151136),
(#151137,#151138,#151139),(#151140,#151141,#151142),(#151143,#151144,#151145),
(#151146,#151147,#151148)),.UNSPECIFIED.,.F.,.F.,.F.)
B_SPLINE_SURFACE_WITH_KNOTS((4,2,4),(3,3),(-6.47810798060089E-18,0.000325048915579083,
0.000650097831158172),(0.,1.),.UNSPECIFIED.)
GEOMETRIC_REPRESENTATION_ITEM()
RATIONAL_B_SPLINE_SURFACE(((1.,0.873361457045401,1.),(1.,0.85849847792363,
1.),(1.,0.834696857457215,1.),(1.,0.77714142509596,1.),(1.,0.743612803250452,
1.),(1.,0.707106781186552,1.)))
REPRESENTATION_ITEM('')
SURFACE()
);
#2401=(
BOUNDED_SURFACE()
B_SPLINE_SURFACE(3,2,((#151150,#151151,#151152),(#151153,#151154,#151155),
(#151156,#151157,#151158),(#151159,#151160,#151161)),.UNSPECIFIED.,.F.,
 .F.,.F.)
B_SPLINE_SURFACE_WITH_KNOTS((4,4),(3,3),(-6.93889390390723E-18,0.0135258923233721),
(0.,1.),.UNSPECIFIED.)
GEOMETRIC_REPRESENTATION_ITEM()
RATIONAL_B_SPLINE_SURFACE(((1.,0.873361457045398,1.),(1.,0.878048383336236,
1.),(1.,0.883106305929072,1.),(1.,0.888620714475961,1.)))
REPRESENTATION_ITEM('')
SURFACE()
);
#2402=(
BOUNDED_SURFACE()
B_SPLINE_SURFACE(3,2,((#151168,#151169,#151170),(#151171,#151172,#151173),
(#151174,#151175,#151176),(#151177,#151178,#151179),(#151180,#151181,#151182),
(#151183,#151184,#151185),(#151186,#151187,#151188),(#151189,#151190,#151191)),
 .UNSPECIFIED.,.F.,.F.,.F.)
B_SPLINE_SURFACE_WITH_KNOTS((4,2,2,4),(3,3),(-0.000151078666148884,0.00280275939636971,
0.00420413909455456,0.00575632475223853),(0.,1.00015107866615),
 .UNSPECIFIED.)
GEOMETRIC_REPRESENTATION_ITEM()
RATIONAL_B_SPLINE_SURFACE(((1.,0.701255881851812,1.00009026772578),(1.,
0.739278029586967,1.00007877905505),(1.,0.773783756716406,1.00006835289659),
(1.,0.82101132809148,1.00005408273962),(1.,0.835689666549691,1.00004964757202),
(1.,0.864812919803629,1.00004084776751),(1.,0.879165644906446,1.00003651098639),
(1.,0.892526157585967,1.00003247400952)))
REPRESENTATION_ITEM('')
SURFACE()
);
#2403=(
BOUNDED_SURFACE()
B_SPLINE_SURFACE(3,2,((#151241,#151242,#151243),(#151244,#151245,#151246),
(#151247,#151248,#151249),(#151250,#151251,#151252),(#151253,#151254,#151255),
(#151256,#151257,#151258),(#151259,#151260,#151261),(#151262,#151263,#151264)),
 .UNSPECIFIED.,.F.,.F.,.F.)
B_SPLINE_SURFACE_WITH_KNOTS((4,2,2,4),(3,3),(-9.4832710962814E-5,0.00140148291572316,
0.00280296583144632,0.00570103232705891),(0.,1.00009510066417),
 .UNSPECIFIED.)
GEOMETRIC_REPRESENTATION_ITEM()
RATIONAL_B_SPLINE_SURFACE(((1.,0.891085304843231,1.0000207157197),(1.,0.878122527114681,
1.00002318125724),(1.,0.864284413164116,1.00002581328489),(1.,0.835864397104656,
1.0000312188097),(1.,0.821386039943232,1.00003397261246),(1.,0.774524182759367,
1.00004288579995),(1.,0.740570301233833,1.00004934387332),(1.,0.703433195559746,
1.00005640740015)))
REPRESENTATION_ITEM('')
SURFACE()
);
#2404=(
BOUNDED_SURFACE()
B_SPLINE_SURFACE(3,2,((#151313,#151314,#151315),(#151316,#151317,#151318),
(#151319,#151320,#151321),(#151322,#151323,#151324)),.UNSPECIFIED.,.F.,
 .F.,.F.)
B_SPLINE_SURFACE_WITH_KNOTS((4,4),(3,3),(-6.93889390390723E-18,0.0138038180377133),
(0.,1.),.UNSPECIFIED.)
GEOMETRIC_REPRESENTATION_ITEM()
RATIONAL_B_SPLINE_SURFACE(((1.,0.888620714475959,1.),(1.,0.882992994712188,
1.),(1.,0.877840677983261,1.),(1.,0.873073026815702,1.)))
REPRESENTATION_ITEM('')
SURFACE()
);
#2405=(
BOUNDED_SURFACE()
B_SPLINE_SURFACE(3,2,((#151331,#151332,#151333),(#151334,#151335,#151336),
(#151337,#151338,#151339),(#151340,#151341,#151342),(#151343,#151344,#151345),
(#151346,#151347,#151348)),.UNSPECIFIED.,.F.,.F.,.F.)
B_SPLINE_SURFACE_WITH_KNOTS((4,2,4),(3,3),(0.,0.000324950456877623,0.000649900913755246),
(0.,1.),.UNSPECIFIED.)
GEOMETRIC_REPRESENTATION_ITEM()
RATIONAL_B_SPLINE_SURFACE(((1.,0.707106781186552,1.),(1.,0.743148709395921,
1.),(1.,0.777042261126144,1.),(1.,0.834175818048995,1.),(1.,0.858015095896893,
1.),(1.,0.873073026815704,1.)))
REPRESENTATION_ITEM('')
SURFACE()
);
#2406=(
BOUNDED_SURFACE()
B_SPLINE_SURFACE(3,2,((#151361,#151362,#151363),(#151364,#151365,#151366),
(#151367,#151368,#151369),(#151370,#151371,#151372),(#151373,#151374,#151375),
(#151376,#151377,#151378),(#151379,#151380,#151381),(#151382,#151383,#151384),
(#151385,#151386,#151387),(#151388,#151389,#151390)),.UNSPECIFIED.,.F.,
 .F.,.F.)
B_SPLINE_SURFACE_WITH_KNOTS((4,2,2,2,4),(3,3),(4.71238898038469,5.10508806208341,
5.49778714378214,5.89048622548086,6.28318530717959),(0.,1.),
 .UNSPECIFIED.)
GEOMETRIC_REPRESENTATION_ITEM()
RATIONAL_B_SPLINE_SURFACE(((1.,0.707106781186552,1.),(1.,0.713550261851565,
1.),(1.,0.719894264862192,1.),(1.,0.731490756397333,1.),(1.,0.736738129296254,
1.),(1.,0.745429366938654,1.),(1.,0.748871927696603,1.),(1.,0.753512297096217,
1.),(1.,0.754714219730812,1.),(1.,0.754709580222777,1.)))
REPRESENTATION_ITEM('')
SURFACE()
);
#2407=(
BOUNDED_SURFACE()
B_SPLINE_SURFACE(3,2,((#151448,#151449,#151450),(#151451,#151452,#151453),
(#151454,#151455,#151456),(#151457,#151458,#151459),(#151460,#151461,#151462),
(#151463,#151464,#151465),(#151466,#151467,#151468),(#151469,#151470,#151471),
(#151472,#151473,#151474),(#151475,#151476,#151477)),.UNSPECIFIED.,.F.,
 .F.,.F.)
B_SPLINE_SURFACE_WITH_KNOTS((4,2,2,2,4),(3,3),(-8.88178419700125E-16,0.392699081698724,
0.785398163397448,1.17809724509617,1.5707963267949),(0.,1.),
 .UNSPECIFIED.)
GEOMETRIC_REPRESENTATION_ITEM()
RATIONAL_B_SPLINE_SURFACE(((1.,0.656059028990507,1.),(1.,0.65605119607191,
1.),(1.,0.657443209221259,1.),(1.,0.662724068472642,1.),(1.,0.666616044204551,
1.),(1.,0.676209154063925,1.),(1.,0.681903435451068,1.),(1.,0.694134907060979,
1.),(1.,0.70066637883416,1.),(1.,0.707106781186548,1.)))
REPRESENTATION_ITEM('')
SURFACE()
);
#2408=(
BOUNDED_SURFACE()
B_SPLINE_SURFACE(3,2,((#151494,#151495,#151496),(#151497,#151498,#151499),
(#151500,#151501,#151502),(#151503,#151504,#151505),(#151506,#151507,#151508),
(#151509,#151510,#151511),(#151512,#151513,#151514),(#151515,#151516,#151517)),
 .UNSPECIFIED.,.F.,.F.,.F.)
B_SPLINE_SURFACE_WITH_KNOTS((4,2,2,4),(3,3),(-2.83789918648081E-17,0.000158415844625727,
0.000316831689251482,0.000633663378502992),(0.,1.),.UNSPECIFIED.)
GEOMETRIC_REPRESENTATION_ITEM()
RATIONAL_B_SPLINE_SURFACE(((1.,0.506999357883079,1.),(1.,0.518705031372287,
1.),(1.,0.533099046918872,1.),(1.,0.565407295868411,1.),(1.,0.582886848388227,
1.),(1.,0.636421215472814,1.),(1.,0.67314781771756,1.),(1.,0.707106781186543,
1.)))
REPRESENTATION_ITEM('')
SURFACE()
);
#2409=(
BOUNDED_SURFACE()
B_SPLINE_SURFACE(3,2,((#151528,#151529,#151530),(#151531,#151532,#151533),
(#151534,#151535,#151536),(#151537,#151538,#151539)),.UNSPECIFIED.,.F.,
 .F.,.F.)
B_SPLINE_SURFACE_WITH_KNOTS((4,4),(3,3),(6.93889390390723E-18,0.0177264565684137),
(0.,1.),.UNSPECIFIED.)
GEOMETRIC_REPRESENTATION_ITEM()
RATIONAL_B_SPLINE_SURFACE(((1.,0.506999357883079,1.),(1.,0.497142617029225,
1.),(1.,0.485892200859361,1.),(1.,0.472392340793768,1.)))
REPRESENTATION_ITEM('')
SURFACE()
);
#2410=(
BOUNDED_SURFACE()
B_SPLINE_SURFACE(3,2,((#151546,#151547,#151548),(#151549,#151550,#151551),
(#151552,#151553,#151554),(#151555,#151556,#151557),(#151558,#151559,#151560),
(#151561,#151562,#151563),(#151564,#151565,#151566),(#151567,#151568,#151569)),
 .UNSPECIFIED.,.F.,.F.,.F.)
B_SPLINE_SURFACE_WITH_KNOTS((4,2,2,4),(3,3),(0.,0.00263855694108943,0.00395783541163415,
0.00527711388217887),(0.,1.),.UNSPECIFIED.)
GEOMETRIC_REPRESENTATION_ITEM()
RATIONAL_B_SPLINE_SURFACE(((1.,0.707106781186999,1.),(1.,0.673000035720727,
1.),(1.,0.63702309328796,1.),(1.,0.578397249219397,1.),(1.,0.557964247865131,
1.),(1.,0.516081850109694,1.),(1.,0.494551837223282,1.),(1.,0.472392340793768,
1.)))
REPRESENTATION_ITEM('')
SURFACE()
);
#2411=(
BOUNDED_SURFACE()
B_SPLINE_SURFACE(3,2,((#151586,#151587,#151588),(#151589,#151590,#151591),
(#151592,#151593,#151594),(#151595,#151596,#151597),(#151598,#151599,#151600),
(#151601,#151602,#151603),(#151604,#151605,#151606),(#151607,#151608,#151609)),
 .UNSPECIFIED.,.F.,.F.,.F.)
B_SPLINE_SURFACE_WITH_KNOTS((4,2,2,4),(3,3),(-0.00052775387520704,0.0013193848583342,
0.00263876971666841,0.00580529337667048),(0.,1.00056372827132),
 .UNSPECIFIED.)
GEOMETRIC_REPRESENTATION_ITEM()
RATIONAL_B_SPLINE_SURFACE(((1.,0.445116797210528,1.00062560669739),(1.,
0.477005124809063,1.0005896539938),(1.,0.507425993631993,1.00055535578622),
(1.,0.557401754212246,1.00049901028798),(1.,0.577581621789236,1.00047625836425),
(1.,0.644406491906409,1.00040091622722),(1.,0.687357348800982,1.0003524910026),
(1.,0.727074127757439,1.00030771206032)))
REPRESENTATION_ITEM('')
SURFACE()
);
#2412=(
BOUNDED_SURFACE()
B_SPLINE_SURFACE(3,2,((#151654,#151655,#151656),(#151657,#151658,#151659),
(#151660,#151661,#151662),(#151663,#151664,#151665)),.UNSPECIFIED.,.F.,
 .F.,.F.)
B_SPLINE_SURFACE_WITH_KNOTS((4,4),(3,3),(0.,0.0174508326761739),(0.,1.),
 .UNSPECIFIED.)
GEOMETRIC_REPRESENTATION_ITEM()
RATIONAL_B_SPLINE_SURFACE(((1.,0.472392340793765,1.),(1.,0.485682667654673,
1.),(1.,0.49679147679375,1.),(1.,0.506538946041787,1.)))
REPRESENTATION_ITEM('')
SURFACE()
);
#2413=(
BOUNDED_SURFACE()
B_SPLINE_SURFACE(3,2,((#151677,#151678,#151679),(#151680,#151681,#151682),
(#151683,#151684,#151685),(#151686,#151687,#151688),(#151689,#151690,#151691),
(#151692,#151693,#151694)),.UNSPECIFIED.,.F.,.F.,.F.)
B_SPLINE_SURFACE_WITH_KNOTS((4,2,4),(3,3),(0.269041526988586,0.27511900362718,
0.281196480265774),(0.,1.),.UNSPECIFIED.)
GEOMETRIC_REPRESENTATION_ITEM()
RATIONAL_B_SPLINE_SURFACE(((1.,0.936757701036177,1.),(1.,0.939378149853558,
1.),(1.,0.942051042550488,1.),(1.,0.947449038066665,1.),(1.,0.950158897999453,
1.),(1.,0.952840299126697,1.)))
REPRESENTATION_ITEM('')
SURFACE()
);
#2414=(
BOUNDED_SURFACE()
B_SPLINE_SURFACE(3,2,((#151695,#151696,#151697),(#151698,#151699,#151700),
(#151701,#151702,#151703),(#151704,#151705,#151706),(#151707,#151708,#151709),
(#151710,#151711,#151712)),.UNSPECIFIED.,.F.,.F.,.F.)
B_SPLINE_SURFACE_WITH_KNOTS((4,2,4),(3,3),(0.0740543944727613,0.0811932403219739,
0.0883320861711864),(0.,1.),.UNSPECIFIED.)
GEOMETRIC_REPRESENTATION_ITEM()
RATIONAL_B_SPLINE_SURFACE(((1.,0.918849788108586,1.),(1.,0.921623427170992,
1.),(1.,0.924482745526459,1.),(1.,0.930368049939493,1.),(1.,0.933390296558584,
1.),(1.,0.936467000373499,1.)))
REPRESENTATION_ITEM('')
SURFACE()
);
#2415=(
BOUNDED_SURFACE()
B_SPLINE_SURFACE(3,2,((#151730,#151731,#151732),(#151733,#151734,#151735),
(#151736,#151737,#151738),(#151739,#151740,#151741),(#151742,#151743,#151744),
(#151745,#151746,#151747)),.UNSPECIFIED.,.F.,.F.,.F.)
B_SPLINE_SURFACE_WITH_KNOTS((4,2,4),(3,3),(4.71238898038469,5.49778714378214,
6.28318530717959),(0.,1.),.UNSPECIFIED.)
GEOMETRIC_REPRESENTATION_ITEM()
RATIONAL_B_SPLINE_SURFACE(((1.,0.707106781186552,1.),(1.,0.720039765645528,
1.),(1.,0.732392511163776,1.),(1.,0.749774985071127,1.),(1.,0.754782222113857,
1.),(1.,0.754709580222772,1.)))
REPRESENTATION_ITEM('')
SURFACE()
);
#2416=(
BOUNDED_SURFACE()
B_SPLINE_SURFACE(3,2,((#151752,#151753,#151754),(#151755,#151756,#151757),
(#151758,#151759,#151760),(#151761,#151762,#151763),(#151764,#151765,#151766),
(#151767,#151768,#151769)),.UNSPECIFIED.,.F.,.F.,.F.)
B_SPLINE_SURFACE_WITH_KNOTS((4,2,4),(3,3),(0.,0.785398163397448,1.5707963267949),
(0.,1.),.UNSPECIFIED.)
GEOMETRIC_REPRESENTATION_ITEM()
RATIONAL_B_SPLINE_SURFACE(((1.,0.656059028990507,1.),(1.,0.655948674699742,
1.),(1.,0.661819490286637,1.),(1.,0.681005707981833,1.),(1.,0.694211427469263,
1.),(1.,0.707106781186548,1.)))
REPRESENTATION_ITEM('')
SURFACE()
);
#2417=(
BOUNDED_SURFACE()
B_SPLINE_SURFACE(3,2,((#151772,#151773,#151774),(#151775,#151776,#151777),
(#151778,#151779,#151780),(#151781,#151782,#151783),(#151784,#151785,#151786),
(#151787,#151788,#151789)),.UNSPECIFIED.,.F.,.F.,.F.)
B_SPLINE_SURFACE_WITH_KNOTS((4,2,4),(3,3),(1.5707963267949,2.35619449019234,
3.1415926535898),(0.,1.),.UNSPECIFIED.)
GEOMETRIC_REPRESENTATION_ITEM()
RATIONAL_B_SPLINE_SURFACE(((1.,0.707106781186548,1.),(1.,0.72003976564552,
1.),(1.,0.732392511163791,1.),(1.,0.749774985071113,1.),(1.,0.75478222211386,
1.),(1.,0.754709580222772,1.)))
REPRESENTATION_ITEM('')
SURFACE()
);
#2418=(
BOUNDED_SURFACE()
B_SPLINE_SURFACE(3,2,((#151794,#151795,#151796),(#151797,#151798,#151799),
(#151800,#151801,#151802),(#151803,#151804,#151805),(#151806,#151807,#151808),
(#151809,#151810,#151811)),.UNSPECIFIED.,.F.,.F.,.F.)
B_SPLINE_SURFACE_WITH_KNOTS((4,2,4),(3,3),(0.,0.785398163397448,1.5707963267949),
(0.,1.),.UNSPECIFIED.)
GEOMETRIC_REPRESENTATION_ITEM()
RATIONAL_B_SPLINE_SURFACE(((1.,0.656059028990507,1.),(1.,0.655948674699894,
1.),(1.,0.661819490286433,1.),(1.,0.681005707982038,1.),(1.,0.694211427469109,
1.),(1.,0.707106781186548,1.)))
REPRESENTATION_ITEM('')
SURFACE()
);
#2419=(
BOUNDED_SURFACE()
B_SPLINE_SURFACE(3,2,((#151816,#151817,#151818),(#151819,#151820,#151821),
(#151822,#151823,#151824),(#151825,#151826,#151827),(#151828,#151829,#151830),
(#151831,#151832,#151833)),.UNSPECIFIED.,.F.,.F.,.F.)
B_SPLINE_SURFACE_WITH_KNOTS((4,2,4),(3,3),(-4.77048955893622E-18,0.00191432655883667,
0.00382865311767335),(0.,1.),.UNSPECIFIED.)
GEOMETRIC_REPRESENTATION_ITEM()
RATIONAL_B_SPLINE_SURFACE(((1.,0.903978945212085,1.),(1.,0.877037193452108,
1.),(1.,0.847703426978615,1.),(1.,0.782785838918396,1.),(1.,0.74722569047758,
1.),(1.,0.707106781186548,1.)))
REPRESENTATION_ITEM('')
SURFACE()
);
#2420=(
BOUNDED_SURFACE()
B_SPLINE_SURFACE(3,2,((#151842,#151843,#151844),(#151845,#151846,#151847),
(#151848,#151849,#151850),(#151851,#151852,#151853),(#151854,#151855,#151856),
(#151857,#151858,#151859)),.UNSPECIFIED.,.F.,.F.,.F.)
B_SPLINE_SURFACE_WITH_KNOTS((4,2,4),(3,3),(0.,0.000512893057734432,0.00102578611546886),
(0.,1.),.UNSPECIFIED.)
GEOMETRIC_REPRESENTATION_ITEM()
RATIONAL_B_SPLINE_SURFACE(((1.,0.813073674901549,1.),(1.,0.812982901655522,
1.),(1.,0.811992001632673,1.),(1.,0.803971289951385,1.),(1.,0.796694115012665,
1.),(1.,0.78334887142417,1.)))
REPRESENTATION_ITEM('')
SURFACE()
);
#2421=(
BOUNDED_SURFACE()
B_SPLINE_SURFACE(3,2,((#151861,#151862,#151863),(#151864,#151865,#151866),
(#151867,#151868,#151869),(#151870,#151871,#151872)),.UNSPECIFIED.,.F.,
 .F.,.F.)
B_SPLINE_SURFACE_WITH_KNOTS((4,4),(3,3),(0.,0.00123332093723591),(0.,1.),
 .UNSPECIFIED.)
GEOMETRIC_REPRESENTATION_ITEM()
RATIONAL_B_SPLINE_SURFACE(((1.,0.903978945212084,1.),(1.,0.925250261712233,
1.),(1.,0.940236171156205,1.),(1.,0.947923524237147,1.)))
REPRESENTATION_ITEM('')
SURFACE()
);
#2422=(
BOUNDED_SURFACE()
B_SPLINE_SURFACE(3,2,((#151877,#151878,#151879),(#151880,#151881,#151882),
(#151883,#151884,#151885),(#151886,#151887,#151888)),.UNSPECIFIED.,.F.,
 .F.,.F.)
B_SPLINE_SURFACE_WITH_KNOTS((4,4),(3,3),(-2.22874639202747E-5,0.000633198052120762),
(-2.22874639202404E-5,1.),.UNSPECIFIED.)
GEOMETRIC_REPRESENTATION_ITEM()
RATIONAL_B_SPLINE_SURFACE(((1.00000954900466,0.785776329440857,1.),(1.00001060519385,
0.762081637234299,1.),(1.0000118597036,0.733937794771298,1.),(1.00001319156803,
0.70405856681235,1.)))
REPRESENTATION_ITEM('')
SURFACE()
);
#2423=(
BOUNDED_SURFACE()
B_SPLINE_SURFACE(3,2,((#151893,#151894,#151895),(#151896,#151897,#151898),
(#151899,#151900,#151901),(#151902,#151903,#151904),(#151905,#151906,#151907),
(#151908,#151909,#151910),(#151911,#151912,#151913),(#151914,#151915,#151916),
(#151917,#151918,#151919),(#151920,#151921,#151922)),.UNSPECIFIED.,.F.,
 .F.,.F.)
B_SPLINE_SURFACE_WITH_KNOTS((4,2,2,2,4),(3,3),(0.,0.000408689684844658,
0.000817379369689317,0.00122606905453398,0.00163475873937863),(0.,1.),
 .UNSPECIFIED.)
GEOMETRIC_REPRESENTATION_ITEM()
RATIONAL_B_SPLINE_SURFACE(((1.,0.707106781186864,1.),(1.,0.688970136944317,
1.),(1.,0.670689426918774,1.),(1.,0.634705388858963,1.),(1.,0.617712576312848,
1.),(1.,0.58736619029857,1.),(1.,0.574575334017929,1.),(1.,0.556620432342278,
1.),(1.,0.551687087704826,1.),(1.,0.55167311003777,1.)))
REPRESENTATION_ITEM('')
SURFACE()
);
#2424=(
BOUNDED_SURFACE()
B_SPLINE_SURFACE(3,2,((#151925,#151926,#151927),(#151928,#151929,#151930),
(#151931,#151932,#151933),(#151934,#151935,#151936),(#151937,#151938,#151939),
(#151940,#151941,#151942),(#151943,#151944,#151945),(#151946,#151947,#151948),
(#151949,#151950,#151951),(#151952,#151953,#151954)),.UNSPECIFIED.,.F.,
 .F.,.F.)
B_SPLINE_SURFACE_WITH_KNOTS((4,2,2,2,4),(3,3),(-5.33083174934941E-5,0.000399098307138592,
0.000798196614277184,0.00119729492141578,0.00164970154604786),(-5.33083174934941E-5,
1.),.UNSPECIFIED.)
GEOMETRIC_REPRESENTATION_ITEM()
RATIONAL_B_SPLINE_SURFACE(((1.00002082472519,0.804676585507141,1.),(1.00002073272724,
0.805539470966454,1.),(1.00002101939354,0.802850713304667,1.),(1.00002216245292,
0.792129502840601,1.),(1.0000229532041,0.784712731694325,1.),(1.00002488425564,
0.766600628144248,1.),(1.00002604063762,0.755754459706965,1.),(1.00002868939129,
0.730910741180952,1.),(1.00003024414844,0.716328052911061,1.),(1.00003176891541,
0.702026654549035,1.)))
REPRESENTATION_ITEM('')
SURFACE()
);
#2425=(
BOUNDED_SURFACE()
B_SPLINE_SURFACE(3,2,((#151960,#151961,#151962),(#151963,#151964,#151965),
(#151966,#151967,#151968),(#151969,#151970,#151971)),.UNSPECIFIED.,.F.,
 .F.,.F.)
B_SPLINE_SURFACE_WITH_KNOTS((4,4),(3,3),(0.00330239163309442,0.00410592895993832),
(0.,1.),.UNSPECIFIED.)
GEOMETRIC_REPRESENTATION_ITEM()
RATIONAL_B_SPLINE_SURFACE(((1.,0.707106781186551,1.),(1.,0.682330721002586,
1.),(1.,0.657517255942454,1.),(1.,0.639433225268795,1.)))
REPRESENTATION_ITEM('')
SURFACE()
);
#2426=(
BOUNDED_SURFACE()
B_SPLINE_SURFACE(3,2,((#151977,#151978,#151979),(#151980,#151981,#151982),
(#151983,#151984,#151985),(#151986,#151987,#151988)),.UNSPECIFIED.,.F.,
 .F.,.F.)
B_SPLINE_SURFACE_WITH_KNOTS((4,4),(3,3),(-3.25260651745652E-19,0.0007884708222344),
(0.,1.),.UNSPECIFIED.)
GEOMETRIC_REPRESENTATION_ITEM()
RATIONAL_B_SPLINE_SURFACE(((1.,0.639433225268789,1.),(1.,0.625985289878347,
1.),(1.,0.614551947533885,1.),(1.,0.61107365918432,1.)))
REPRESENTATION_ITEM('')
SURFACE()
);
#2427=(
BOUNDED_SURFACE()
B_SPLINE_SURFACE(3,2,((#151991,#151992,#151993),(#151994,#151995,#151996),
(#151997,#151998,#151999),(#152000,#152001,#152002),(#152003,#152004,#152005),
(#152006,#152007,#152008)),.UNSPECIFIED.,.F.,.F.,.F.)
B_SPLINE_SURFACE_WITH_KNOTS((4,2,4),(3,3),(0.,0.000792989481313416,0.00158597896262684),
(0.,1.),.UNSPECIFIED.)
GEOMETRIC_REPRESENTATION_ITEM()
RATIONAL_B_SPLINE_SURFACE(((1.,0.760728353039959,1.),(1.,0.798498231399495,
1.),(1.,0.82089578223655,1.),(1.,0.844341385725833,1.),(1.,0.844813563409958,
1.),(1.,0.837989542743388,1.)))
REPRESENTATION_ITEM('')
SURFACE()
);
#2428=(
BOUNDED_SURFACE()
B_SPLINE_SURFACE(3,2,((#152010,#152011,#152012),(#152013,#152014,#152015),
(#152016,#152017,#152018),(#152019,#152020,#152021)),.UNSPECIFIED.,.F.,
 .F.,.F.)
B_SPLINE_SURFACE_WITH_KNOTS((4,4),(3,3),(0.,0.000504443591143906),(0.,1.),
 .UNSPECIFIED.)
GEOMETRIC_REPRESENTATION_ITEM()
RATIONAL_B_SPLINE_SURFACE(((1.,0.843854525156016,1.),(1.,0.841969285469978,
1.),(1.,0.840014967913779,1.),(1.,0.837989542743208,1.)))
REPRESENTATION_ITEM('')
SURFACE()
);
#2429=(
BOUNDED_SURFACE()
B_SPLINE_SURFACE(3,2,((#152024,#152025,#152026),(#152027,#152028,#152029),
(#152030,#152031,#152032),(#152033,#152034,#152035),(#152036,#152037,#152038),
(#152039,#152040,#152041),(#152042,#152043,#152044),(#152045,#152046,#152047),
(#152048,#152049,#152050),(#152051,#152052,#152053)),.UNSPECIFIED.,.F.,
 .F.,.F.)
B_SPLINE_SURFACE_WITH_KNOTS((4,2,2,2,4),(3,3),(-0.000180960259681038,0.00045240064920256,
0.00090480129840513,0.0013572019476077,0.0019905628564913),(-0.000555000723925246,
1.),.UNSPECIFIED.)
GEOMETRIC_REPRESENTATION_ITEM()
RATIONAL_B_SPLINE_SURFACE(((1.00017007065858,0.846783390316832,1.),(1.00017222379657,
0.844843628895718,1.),(1.00018057705553,0.837318180189595,1.),(1.00020429784683,
0.815948125808373,1.),(1.00021713987135,0.804378749442043,1.),(1.00024916216878,
0.775529870463418,1.),(1.00026828613008,0.758301098979412,1.),(1.00032368050176,
0.708396324719543,1.),(1.00036234037351,0.673567656857712,1.),(1.00041151994587,
0.629261793605653,1.)))
REPRESENTATION_ITEM('')
SURFACE()
);
#2430=(
BOUNDED_SURFACE()
B_SPLINE_SURFACE(3,2,((#152056,#152057,#152058),(#152059,#152060,#152061),
(#152062,#152063,#152064),(#152065,#152066,#152067),(#152068,#152069,#152070),
(#152071,#152072,#152073),(#152074,#152075,#152076),(#152077,#152078,#152079),
(#152080,#152081,#152082),(#152083,#152084,#152085),(#152086,#152087,#152088),
(#152089,#152090,#152091)),.UNSPECIFIED.,.F.,.F.,.F.)
B_SPLINE_SURFACE_WITH_KNOTS((4,2,2,2,2,4),(3,3),(0.,0.000464847896993965,
0.00092969579398793,0.00116211974248491,0.00139454369098189,0.00185939158797586),
(0.,1.),.UNSPECIFIED.)
GEOMETRIC_REPRESENTATION_ITEM()
RATIONAL_B_SPLINE_SURFACE(((1.,0.713890629234418,1.),(1.,0.74043984709427,
1.),(1.,0.764405928904485,1.),(1.,0.806784773788238,1.),(1.,0.825414433535011,
1.),(1.,0.847876574774264,1.),(1.,0.854606009430438,1.),(1.,0.866028143804753,
1.),(1.,0.87079122929337,1.),(1.,0.882487982894785,1.),(1.,0.886433234017275,
1.),(1.,0.886392435203049,1.)))
REPRESENTATION_ITEM('')
SURFACE()
);
#2431=(
BOUNDED_SURFACE()
B_SPLINE_SURFACE(3,2,((#152093,#152094,#152095),(#152096,#152097,#152098),
(#152099,#152100,#152101),(#152102,#152103,#152104)),.UNSPECIFIED.,.F.,
 .F.,.F.)
B_SPLINE_SURFACE_WITH_KNOTS((4,4),(3,3),(0.,0.000504070263719173),(0.,1.),
 .UNSPECIFIED.)
GEOMETRIC_REPRESENTATION_ITEM()
RATIONAL_B_SPLINE_SURFACE(((1.,0.886316114436169,1.),(1.,0.886398092028818,
1.),(1.,0.886423525277845,1.),(1.,0.886392435202391,1.)))
REPRESENTATION_ITEM('')
SURFACE()
);
#2432=(
BOUNDED_SURFACE()
B_SPLINE_SURFACE(3,2,((#152107,#152108,#152109),(#152110,#152111,#152112),
(#152113,#152114,#152115),(#152116,#152117,#152118),(#152119,#152120,#152121),
(#152122,#152123,#152124),(#152125,#152126,#152127),(#152128,#152129,#152130)),
 .UNSPECIFIED.,.F.,.F.,.F.)
B_SPLINE_SURFACE_WITH_KNOTS((4,2,2,4),(3,3),(-0.00017279642425018,0.000466811173310166,
0.000933622346620337,0.00204004111749139),(-0.000172796424253642,1.),
 .UNSPECIFIED.)
GEOMETRIC_REPRESENTATION_ITEM()
RATIONAL_B_SPLINE_SURFACE(((1.00003993733279,0.884438196676905,1.),(1.00003842620951,
0.888810750363417,1.),(1.00003959918162,0.885416663590792,1.),(1.00004581699226,
0.867424941052306,1.),(1.00004978263944,0.855950030055177,1.),(1.00006709382113,
0.805858768736276,1.),(1.0000858454205,0.751599545903121,1.),(1.0001089190889,
0.684834077514369,1.)))
REPRESENTATION_ITEM('')
SURFACE()
);
#2433=(
BOUNDED_SURFACE()
B_SPLINE_SURFACE(3,2,((#152133,#152134,#152135),(#152136,#152137,#152138),
(#152139,#152140,#152141),(#152142,#152143,#152144),(#152145,#152146,#152147),
(#152148,#152149,#152150),(#152151,#152152,#152153),(#152154,#152155,#152156)),
 .UNSPECIFIED.,.F.,.F.,.F.)
B_SPLINE_SURFACE_WITH_KNOTS((4,2,2,4),(3,3),(-0.00017992504535195,0.000899625226760169,
0.00134943784014025,0.00197917549887237),(-0.000964860374386562,1.),
 .UNSPECIFIED.)
GEOMETRIC_REPRESENTATION_ITEM()
RATIONAL_B_SPLINE_SURFACE(((1.00071732884499,0.628273238267874,1.),(1.00057400293934,
0.702546112070203,1.),(1.00047742991241,0.75259119087058,1.),(1.00038270957014,
0.801676190515576,1.),(1.00036092726382,0.812963992823138,1.),(1.00031924704205,
0.83456308781941,1.),(1.00030545716438,0.841709136113667,1.),(1.00029954974065,
0.844770420362849,1.)))
REPRESENTATION_ITEM('')
SURFACE()
);
#2434=(
BOUNDED_SURFACE()
B_SPLINE_SURFACE(3,2,((#152158,#152159,#152160),(#152161,#152162,#152163),
(#152164,#152165,#152166),(#152167,#152168,#152169)),.UNSPECIFIED.,.F.,
 .F.,.F.)
B_SPLINE_SURFACE_WITH_KNOTS((4,4),(3,3),(-2.16840434497101E-19,0.000504456607560921),
(0.,1.),.UNSPECIFIED.)
GEOMETRIC_REPRESENTATION_ITEM()
RATIONAL_B_SPLINE_SURFACE(((1.,0.835211735760659,1.),(1.,0.83730162444359,
1.),(1.,0.839319452171524,1.),(1.,0.841267344812682,1.)))
REPRESENTATION_ITEM('')
SURFACE()
);
#2435=(
BOUNDED_SURFACE()
B_SPLINE_SURFACE(3,2,((#152172,#152173,#152174),(#152175,#152176,#152177),
(#152178,#152179,#152180),(#152181,#152182,#152183),(#152184,#152185,#152186),
(#152187,#152188,#152189),(#152190,#152191,#152192),(#152193,#152194,#152195),
(#152196,#152197,#152198),(#152199,#152200,#152201)),.UNSPECIFIED.,.F.,
 .F.,.F.)
B_SPLINE_SURFACE_WITH_KNOTS((4,2,2,2,4),(3,3),(0.,0.00039540981677153,0.00079081963354306,
0.00118622945031459,0.00158163926708612),(0.,1.),.UNSPECIFIED.)
GEOMETRIC_REPRESENTATION_ITEM()
RATIONAL_B_SPLINE_SURFACE(((1.,0.835211735760644,1.),(1.,0.838806334780784,
1.),(1.,0.840513202341181,1.),(1.,0.839504260685003,1.),(1.,0.836771095032971,
1.),(1.,0.825966649242057,1.),(1.,0.817815337411177,1.),(1.,0.795024845130666,
1.),(1.,0.780342956064905,1.),(1.,0.761980581628842,1.)))
REPRESENTATION_ITEM('')
SURFACE()
);
#2436=(
BOUNDED_SURFACE()
B_SPLINE_SURFACE(3,2,((#152204,#152205,#152206),(#152207,#152208,#152209),
(#152210,#152211,#152212),(#152213,#152214,#152215)),.UNSPECIFIED.,.F.,
 .F.,.F.)
B_SPLINE_SURFACE_WITH_KNOTS((4,4),(3,3),(0.,0.000372129922795447),(0.,1.),
 .UNSPECIFIED.)
GEOMETRIC_REPRESENTATION_ITEM()
RATIONAL_B_SPLINE_SURFACE(((1.,0.609511474287707,1.),(1.,0.609908567799612,
1.),(1.,0.612427474748796,1.),(1.,0.616304832905386,1.)))
REPRESENTATION_ITEM('')
SURFACE()
);
#2437=(
BOUNDED_SURFACE()
B_SPLINE_SURFACE(3,2,((#152217,#152218,#152219),(#152220,#152221,#152222),
(#152223,#152224,#152225),(#152226,#152227,#152228),(#152229,#152230,#152231),
(#152232,#152233,#152234)),.UNSPECIFIED.,.F.,.F.,.F.)
B_SPLINE_SURFACE_WITH_KNOTS((4,2,4),(3,3),(0.0033044647217104,0.00391466500066162,
0.00452486527961284),(0.,1.),.UNSPECIFIED.)
GEOMETRIC_REPRESENTATION_ITEM()
RATIONAL_B_SPLINE_SURFACE(((1.,0.707106781186548,1.),(1.,0.688071275370979,
1.),(1.,0.668909963668733,1.),(1.,0.636714772442526,1.),(1.,0.623520947306417,
1.),(1.,0.61630483290538,1.)))
REPRESENTATION_ITEM('')
SURFACE()
);
#2438=(
BOUNDED_SURFACE()
B_SPLINE_SURFACE(3,2,((#152246,#152247,#152248),(#152249,#152250,#152251),
(#152252,#152253,#152254),(#152255,#152256,#152257),(#152258,#152259,#152260),
(#152261,#152262,#152263),(#152264,#152265,#152266),(#152267,#152268,#152269)),
 .UNSPECIFIED.,.F.,.F.,.F.)
B_SPLINE_SURFACE_WITH_KNOTS((4,2,2,4),(3,3),(-1.29128478743024E-16,0.000399353616616221,
0.00079870723323257,0.00159741446646527),(0.,1.),.UNSPECIFIED.)
GEOMETRIC_REPRESENTATION_ITEM()
RATIONAL_B_SPLINE_SURFACE(((1.,0.70710678118656,1.),(1.,0.719948338626786,
1.),(1.,0.732633692835949,1.),(1.,0.756391361283625,1.),(1.,0.767258343653063,
1.),(1.,0.794863148134095,1.),(1.,0.806163077037293,1.),(1.,0.806028661642745,
1.)))
REPRESENTATION_ITEM('')
SURFACE()
);
#2439=(
BOUNDED_SURFACE()
B_SPLINE_SURFACE(3,2,((#152272,#152273,#152274),(#152275,#152276,#152277),
(#152278,#152279,#152280),(#152281,#152282,#152283),(#152284,#152285,#152286),
(#152287,#152288,#152289),(#152290,#152291,#152292),(#152293,#152294,#152295),
(#152296,#152297,#152298),(#152299,#152300,#152301)),.UNSPECIFIED.,.F.,
 .F.,.F.)
B_SPLINE_SURFACE_WITH_KNOTS((4,2,2,2,4),(3,3),(0.,0.000409091700616903,
0.000818183401233805,0.00122727510185071,0.00163636680246761),(0.,1.),
 .UNSPECIFIED.)
GEOMETRIC_REPRESENTATION_ITEM()
RATIONAL_B_SPLINE_SURFACE(((1.,0.549942215762897,1.),(1.,0.54985788278214,
1.),(1.,0.554957454495403,1.),(1.,0.573078296428378,1.),(1.,0.58619337630722,
1.),(1.,0.61662144853447,1.),(1.,0.634085743304818,1.),(1.,0.670152902628418,
1.),(1.,0.688944445542904,1.),(1.,0.707106781186548,1.)))
REPRESENTATION_ITEM('')
SURFACE()
);
#2440=(
BOUNDED_SURFACE()
B_SPLINE_SURFACE(3,2,((#152306,#152307,#152308),(#152309,#152310,#152311),
(#152312,#152313,#152314),(#152315,#152316,#152317)),.UNSPECIFIED.,.F.,
 .F.,.F.)
B_SPLINE_SURFACE_WITH_KNOTS((4,4),(3,3),(0.,0.000344272120907045),(0.,1.),
 .UNSPECIFIED.)
GEOMETRIC_REPRESENTATION_ITEM()
RATIONAL_B_SPLINE_SURFACE(((1.,0.707106781186548,1.),(1.,0.722743638846974,
1.),(1.,0.737730816488031,1.),(1.,0.752153393551655,1.)))
REPRESENTATION_ITEM('')
SURFACE()
);
#2441=(
BOUNDED_SURFACE()
B_SPLINE_SURFACE(3,2,((#152319,#152320,#152321),(#152322,#152323,#152324),
(#152325,#152326,#152327),(#152328,#152329,#152330),(#152331,#152332,#152333),
(#152334,#152335,#152336)),.UNSPECIFIED.,.F.,.F.,.F.)
B_SPLINE_SURFACE_WITH_KNOTS((4,2,4),(3,3),(-1.54498809579185E-17,0.000643111039450966,
0.00128622207890195),(0.,1.),.UNSPECIFIED.)
GEOMETRIC_REPRESENTATION_ITEM()
RATIONAL_B_SPLINE_SURFACE(((1.,0.752153393551656,1.),(1.,0.774602351077688,
1.),(1.,0.786049290204429,1.),(1.,0.797170335299084,1.),(1.,0.797315472489739,
1.),(1.,0.797551754323297,1.)))
REPRESENTATION_ITEM('')
SURFACE()
);
#2442=(
BOUNDED_SURFACE()
B_SPLINE_SURFACE(3,2,((#152337,#152338,#152339),(#152340,#152341,#152342),
(#152343,#152344,#152345),(#152346,#152347,#152348)),.UNSPECIFIED.,.F.,
 .F.,.F.)
B_SPLINE_SURFACE_WITH_KNOTS((4,4),(3,3),(0.,0.00096907076046529),(0.,1.),
 .UNSPECIFIED.)
GEOMETRIC_REPRESENTATION_ITEM()
RATIONAL_B_SPLINE_SURFACE(((1.,0.903978945212084,1.),(1.,0.920702565586523,
1.),(1.,0.933513016958348,1.),(1.,0.941989694367876,1.)))
REPRESENTATION_ITEM('')
SURFACE()
);
#2443=(
BOUNDED_SURFACE()
B_SPLINE_SURFACE(3,2,((#152357,#152358,#152359),(#152360,#152361,#152362),
(#152363,#152364,#152365),(#152366,#152367,#152368),(#152369,#152370,#152371),
(#152372,#152373,#152374)),.UNSPECIFIED.,.F.,.F.,.F.)
B_SPLINE_SURFACE_WITH_KNOTS((4,2,4),(3,3),(4.71238898038469,5.49778714378214,
6.28318530717959),(0.,1.),.UNSPECIFIED.)
GEOMETRIC_REPRESENTATION_ITEM()
RATIONAL_B_SPLINE_SURFACE(((1.,0.707106781186552,1.),(1.,0.694211427469738,
1.),(1.,0.681005707981193,1.),(1.,0.661819490287278,1.),(1.,0.65594867469926,
1.),(1.,0.656059028990507,1.)))
REPRESENTATION_ITEM('')
SURFACE()
);
#2444=(
BOUNDED_SURFACE()
B_SPLINE_SURFACE(3,2,((#152379,#152380,#152381),(#152382,#152383,#152384),
(#152385,#152386,#152387),(#152388,#152389,#152390),(#152391,#152392,#152393),
(#152394,#152395,#152396)),.UNSPECIFIED.,.F.,.F.,.F.)
B_SPLINE_SURFACE_WITH_KNOTS((4,2,4),(3,3),(0.,0.785398163397448,1.5707963267949),
(0.,1.),.UNSPECIFIED.)
GEOMETRIC_REPRESENTATION_ITEM()
RATIONAL_B_SPLINE_SURFACE(((1.,0.754709580222772,1.),(1.,0.754782222114301,
1.),(1.,0.749774985070531,1.),(1.,0.732392511164381,1.),(1.,0.720039765645079,
1.),(1.,0.707106781186548,1.)))
REPRESENTATION_ITEM('')
SURFACE()
);
#2445=(
BOUNDED_SURFACE()
B_SPLINE_SURFACE(3,2,((#152399,#152400,#152401),(#152402,#152403,#152404),
(#152405,#152406,#152407),(#152408,#152409,#152410),(#152411,#152412,#152413),
(#152414,#152415,#152416)),.UNSPECIFIED.,.F.,.F.,.F.)
B_SPLINE_SURFACE_WITH_KNOTS((4,2,4),(3,3),(0.,0.00191432655883665,0.0038286531176733),
(0.,1.),.UNSPECIFIED.)
GEOMETRIC_REPRESENTATION_ITEM()
RATIONAL_B_SPLINE_SURFACE(((1.,0.707106781186548,1.),(1.,0.747225690478532,
1.),(1.,0.78278583891712,1.),(1.,0.847703426979888,1.),(1.,0.877037193451153,
1.),(1.,0.903978945212084,1.)))
REPRESENTATION_ITEM('')
SURFACE()
);
#2446=(
BOUNDED_SURFACE()
B_SPLINE_SURFACE(3,2,((#152427,#152428,#152429),(#152430,#152431,#152432),
(#152433,#152434,#152435),(#152436,#152437,#152438),(#152439,#152440,#152441),
(#152442,#152443,#152444)),.UNSPECIFIED.,.F.,.F.,.F.)
B_SPLINE_SURFACE_WITH_KNOTS((4,2,4),(3,3),(4.71238898038469,5.49778714378214,
6.28318530717959),(0.,1.),.UNSPECIFIED.)
GEOMETRIC_REPRESENTATION_ITEM()
RATIONAL_B_SPLINE_SURFACE(((1.,0.707106781186548,1.),(1.,0.694211427468419,
1.),(1.,0.68100570798296,1.),(1.,0.661819490285511,1.),(1.,0.655948674700594,
1.),(1.,0.656059028990501,1.)))
REPRESENTATION_ITEM('')
SURFACE()
);
#2447=(
BOUNDED_SURFACE()
B_SPLINE_SURFACE(3,2,((#152449,#152450,#152451),(#152452,#152453,#152454),
(#152455,#152456,#152457),(#152458,#152459,#152460),(#152461,#152462,#152463),
(#152464,#152465,#152466)),.UNSPECIFIED.,.F.,.F.,.F.)
B_SPLINE_SURFACE_WITH_KNOTS((4,2,4),(3,3),(3.1415926535898,3.92699081698724,
4.71238898038469),(0.,1.),.UNSPECIFIED.)
GEOMETRIC_REPRESENTATION_ITEM()
RATIONAL_B_SPLINE_SURFACE(((1.,0.754709580222777,1.),(1.,0.754782222115066,
1.),(1.,0.749774985069503,1.),(1.,0.732392511165393,1.),(1.,0.720039765644325,
1.),(1.,0.707106781186548,1.)))
REPRESENTATION_ITEM('')
SURFACE()
);
#2448=(
BOUNDED_SURFACE()
B_SPLINE_SURFACE(3,2,((#152474,#152475,#152476),(#152477,#152478,#152479),
(#152480,#152481,#152482),(#152483,#152484,#152485),(#152486,#152487,#152488),
(#152489,#152490,#152491)),.UNSPECIFIED.,.F.,.F.,.F.)
B_SPLINE_SURFACE_WITH_KNOTS((4,2,4),(3,3),(4.71238898038469,5.49778714378214,
6.28318530717959),(0.,1.),.UNSPECIFIED.)
GEOMETRIC_REPRESENTATION_ITEM()
RATIONAL_B_SPLINE_SURFACE(((1.,0.707106781186548,1.),(1.,0.720039765645103,
1.),(1.,0.732392511164345,1.),(1.,0.749774985070558,1.),(1.,0.754782222114279,
1.),(1.,0.754709580222763,1.)))
REPRESENTATION_ITEM('')
SURFACE()
);
#2449=(
BOUNDED_SURFACE()
B_SPLINE_SURFACE(3,2,((#152496,#152497,#152498),(#152499,#152500,#152501),
(#152502,#152503,#152504),(#152505,#152506,#152507),(#152508,#152509,#152510),
(#152511,#152512,#152513)),.UNSPECIFIED.,.F.,.F.,.F.)
B_SPLINE_SURFACE_WITH_KNOTS((4,2,4),(3,3),(8.78519494496442E-16,0.785398163397449,
1.5707963267949),(0.,1.),.UNSPECIFIED.)
GEOMETRIC_REPRESENTATION_ITEM()
RATIONAL_B_SPLINE_SURFACE(((1.,0.656059028990513,1.),(1.,0.655948674700453,
1.),(1.,0.661819490285707,1.),(1.,0.681005707982772,1.),(1.,0.694211427468564,
1.),(1.,0.707106781186548,1.)))
REPRESENTATION_ITEM('')
SURFACE()
);
#2450=(
BOUNDED_SURFACE()
B_SPLINE_SURFACE(3,2,((#152516,#152517,#152518),(#152519,#152520,#152521),
(#152522,#152523,#152524),(#152525,#152526,#152527),(#152528,#152529,#152530),
(#152531,#152532,#152533)),.UNSPECIFIED.,.F.,.F.,.F.)
B_SPLINE_SURFACE_WITH_KNOTS((4,2,4),(3,3),(1.5707963267949,2.35619449019234,
3.1415926535898),(0.,1.),.UNSPECIFIED.)
GEOMETRIC_REPRESENTATION_ITEM()
RATIONAL_B_SPLINE_SURFACE(((1.,0.707106781186548,1.),(1.,0.720039765645106,
1.),(1.,0.732392511164342,1.),(1.,0.749774985070554,1.),(1.,0.754782222114274,
1.),(1.,0.754709580222767,1.)))
REPRESENTATION_ITEM('')
SURFACE()
);
#2451=(
BOUNDED_SURFACE()
B_SPLINE_SURFACE(3,2,((#152538,#152539,#152540),(#152541,#152542,#152543),
(#152544,#152545,#152546),(#152547,#152548,#152549),(#152550,#152551,#152552),
(#152553,#152554,#152555)),.UNSPECIFIED.,.F.,.F.,.F.)
B_SPLINE_SURFACE_WITH_KNOTS((4,2,4),(3,3),(8.78519494496442E-16,0.785398163397449,
1.5707963267949),(0.,1.),.UNSPECIFIED.)
GEOMETRIC_REPRESENTATION_ITEM()
RATIONAL_B_SPLINE_SURFACE(((1.,0.656059028990513,1.),(1.,0.65594867470042,
1.),(1.,0.661819490285751,1.),(1.,0.681005707982728,1.),(1.,0.694211427468597,
1.),(1.,0.707106781186548,1.)))
REPRESENTATION_ITEM('')
SURFACE()
);
#2452=(
BOUNDED_SURFACE()
B_SPLINE_SURFACE(3,2,((#152560,#152561,#152562),(#152563,#152564,#152565),
(#152566,#152567,#152568),(#152569,#152570,#152571),(#152572,#152573,#152574),
(#152575,#152576,#152577),(#152578,#152579,#152580),(#152581,#152582,#152583)),
 .UNSPECIFIED.,.F.,.F.,.F.)
B_SPLINE_SURFACE_WITH_KNOTS((4,2,2,4),(3,3),(0.,0.00103600378053286,0.00207200756106572,
0.00414401512213144),(0.,1.),.UNSPECIFIED.)
GEOMETRIC_REPRESENTATION_ITEM()
RATIONAL_B_SPLINE_SURFACE(((1.,0.917068097704898,1.),(1.,0.902969174287913,
1.),(1.,0.888154932928049,1.),(1.,0.856959094818643,1.),(1.,0.840579087750432,
1.),(1.,0.788725570722382,1.),(1.,0.750598222445163,1.),(1.,0.707106781186548,
1.)))
REPRESENTATION_ITEM('')
SURFACE()
);
#2453=(
BOUNDED_SURFACE()
B_SPLINE_SURFACE(2,2,((#152592,#152593,#152594),(#152595,#152596,#152597),
(#152598,#152599,#152600)),.UNSPECIFIED.,.F.,.F.,.F.)
B_SPLINE_SURFACE_WITH_KNOTS((3,3),(3,3),(0.,1.5707963267949),(0.,1.5707963267949),
 .UNSPECIFIED.)
GEOMETRIC_REPRESENTATION_ITEM()
RATIONAL_B_SPLINE_SURFACE(((1.,0.707106781186547,1.),(0.707106781186621,
0.500000000000052,0.707106781186621),(1.,0.707106781186547,1.)))
REPRESENTATION_ITEM('')
SURFACE()
);
#2454=(
BOUNDED_SURFACE()
B_SPLINE_SURFACE(3,2,((#152601,#152602,#152603),(#152604,#152605,#152606),
(#152607,#152608,#152609),(#152610,#152611,#152612),(#152613,#152614,#152615),
(#152616,#152617,#152618)),.UNSPECIFIED.,.F.,.F.,.F.)
B_SPLINE_SURFACE_WITH_KNOTS((4,2,4),(3,3),(0.283188163394013,0.288276169473932,
0.293364175553851),(0.,1.),.UNSPECIFIED.)
GEOMETRIC_REPRESENTATION_ITEM()
RATIONAL_B_SPLINE_SURFACE(((1.,0.948000855586274,1.),(1.,0.950253931198463,
1.),(1.,0.952523267214703,1.),(1.,0.957028867337525,1.),(1.,0.959243070764605,
1.),(1.,0.961372018922465,1.)))
REPRESENTATION_ITEM('')
SURFACE()
);
#2455=(
BOUNDED_SURFACE()
B_SPLINE_SURFACE(3,2,((#152640,#152641,#152642),(#152643,#152644,#152645),
(#152646,#152647,#152648),(#152649,#152650,#152651),(#152652,#152653,#152654),
(#152655,#152656,#152657)),.UNSPECIFIED.,.F.,.F.,.F.)
B_SPLINE_SURFACE_WITH_KNOTS((4,2,4),(3,3),(0.0131888298509929,0.0172446796820237,
0.0213005295130545),(0.,1.),.UNSPECIFIED.)
GEOMETRIC_REPRESENTATION_ITEM()
RATIONAL_B_SPLINE_SURFACE(((1.,0.962986864789684,1.),(1.,0.964634105108703,
1.),(1.,0.96622351418111,1.),(1.,0.969200309542686,1.),(1.,0.970562566403692,
1.),(1.,0.971747603318281,1.)))
REPRESENTATION_ITEM('')
SURFACE()
);
#2456=(
BOUNDED_SURFACE()
B_SPLINE_SURFACE(3,2,((#152674,#152675,#152676),(#152677,#152678,#152679),
(#152680,#152681,#152682),(#152683,#152684,#152685),(#152686,#152687,#152688),
(#152689,#152690,#152691),(#152692,#152693,#152694),(#152695,#152696,#152697)),
 .UNSPECIFIED.,.F.,.F.,.F.)
B_SPLINE_SURFACE_WITH_KNOTS((4,2,2,4),(3,3),(0.0122567706991037,0.0155118977534076,
0.0171394612805594,0.0187670248077113),(0.,1.),.UNSPECIFIED.)
GEOMETRIC_REPRESENTATION_ITEM()
RATIONAL_B_SPLINE_SURFACE(((1.,0.976217638119343,1.),(1.,0.976078404720299,
1.),(1.,0.975752989031438,1.),(1.,0.975002468017128,1.),(1.,0.974707022042782,
1.),(1.,0.97404359369431,1.),(1.,0.973675473821347,1.),(1.,0.973275528580344,
1.)))
REPRESENTATION_ITEM('')
SURFACE()
);
#2457=(
BOUNDED_SURFACE()
B_SPLINE_SURFACE(3,2,((#152745,#152746,#152747),(#152748,#152749,#152750),
(#152751,#152752,#152753),(#152754,#152755,#152756),(#152757,#152758,#152759),
(#152760,#152761,#152762)),.UNSPECIFIED.,.F.,.F.,.F.)
B_SPLINE_SURFACE_WITH_KNOTS((4,2,4),(3,3),(0.320593732793275,0.325865292398914,
0.331136852004555),(0.,1.),.UNSPECIFIED.)
GEOMETRIC_REPRESENTATION_ITEM()
RATIONAL_B_SPLINE_SURFACE(((1.,0.944716550630948,1.),(1.,0.947183012056064,
1.),(1.,0.949681743560583,1.),(1.,0.954674153969892,1.),(1.,0.957142661330136,
1.),(1.,0.959530911256235,1.)))
REPRESENTATION_ITEM('')
SURFACE()
);
#2458=(
BOUNDED_SURFACE()
B_SPLINE_SURFACE(3,2,((#152798,#152799,#152800),(#152801,#152802,#152803),
(#152804,#152805,#152806),(#152807,#152808,#152809),(#152810,#152811,#152812),
(#152813,#152814,#152815)),.UNSPECIFIED.,.F.,.F.,.F.)
B_SPLINE_SURFACE_WITH_KNOTS((4,2,4),(3,3),(0.0161036610523817,0.0202680863362144,
0.0244325116200472),(0.,1.),.UNSPECIFIED.)
GEOMETRIC_REPRESENTATION_ITEM()
RATIONAL_B_SPLINE_SURFACE(((1.,0.961171400688072,1.),(1.,0.963011198169074,
1.),(1.,0.964799382389448,1.),(1.,0.968173271553358,1.),(1.,0.969728922082773,
1.),(1.,0.971089741366958,1.)))
REPRESENTATION_ITEM('')
SURFACE()
);
#2459=(
BOUNDED_SURFACE()
B_SPLINE_SURFACE(3,2,((#152833,#152834,#152835),(#152836,#152837,#152838),
(#152839,#152840,#152841),(#152842,#152843,#152844)),.UNSPECIFIED.,.F.,
 .F.,.F.)
B_SPLINE_SURFACE_WITH_KNOTS((4,4),(3,3),(0.0324061838408421,0.0330259723062236),
(0.0834883624373275,1.),.UNSPECIFIED.)
GEOMETRIC_REPRESENTATION_ITEM()
RATIONAL_B_SPLINE_SURFACE(((0.97106385378676,0.826705510992856,1.),(0.97062009002177,
0.824047872538613,1.),(0.970157734863912,0.821278892860728,1.),(0.969676371182953,
0.8183960738252,1.)))
REPRESENTATION_ITEM('')
SURFACE()
);
#2460=(
BOUNDED_SURFACE()
B_SPLINE_SURFACE(3,2,((#152854,#152855,#152856),(#152857,#152858,#152859),
(#152860,#152861,#152862),(#152863,#152864,#152865),(#152866,#152867,#152868),
(#152869,#152870,#152871),(#152872,#152873,#152874),(#152875,#152876,#152877)),
 .UNSPECIFIED.,.F.,.F.,.F.)
B_SPLINE_SURFACE_WITH_KNOTS((4,2,2,4),(3,3),(0.0238269657788709,0.0270983492768517,
0.0287340410258421,0.0303697327748325),(0.,1.),.UNSPECIFIED.)
GEOMETRIC_REPRESENTATION_ITEM()
RATIONAL_B_SPLINE_SURFACE(((1.,0.972768240458926,1.),(1.,0.973679370262107,
1.),(1.,0.974448100441956,1.),(1.,0.975326902749563,1.),(1.,0.975574944117527,
1.),(1.,0.975963474394985,1.),(1.,0.976104268047958,1.),(1.,0.976191081059459,
1.)))
REPRESENTATION_ITEM('')
SURFACE()
);
#2461=(
BOUNDED_SURFACE()
B_SPLINE_SURFACE(3,2,((#152904,#152905,#152906),(#152907,#152908,#152909),
(#152910,#152911,#152912),(#152913,#152914,#152915)),.UNSPECIFIED.,.F.,
 .F.,.F.)
B_SPLINE_SURFACE_WITH_KNOTS((4,4),(3,3),(0.0242632023351278,0.0247749981337221),
(0.078087948024069,1.),.UNSPECIFIED.)
GEOMETRIC_REPRESENTATION_ITEM()
RATIONAL_B_SPLINE_SURFACE(((0.980707816377885,0.876471439509661,1.),(0.980713728265565,
0.876509293543672,1.),(0.98070899383337,0.876478978800394,1.),(0.980693615408901,
0.876380510183544,1.)))
REPRESENTATION_ITEM('')
SURFACE()
);
#2462=(
BOUNDED_SURFACE()
B_SPLINE_SURFACE(3,2,((#152923,#152924,#152925),(#152926,#152927,#152928),
(#152929,#152930,#152931),(#152932,#152933,#152934),(#152935,#152936,#152937),
(#152938,#152939,#152940)),.UNSPECIFIED.,.F.,.F.,.F.)
B_SPLINE_SURFACE_WITH_KNOTS((4,2,4),(3,3),(0.0123698333451925,0.0156488944469233,
0.018927955548654),(0.,1.),.UNSPECIFIED.)
GEOMETRIC_REPRESENTATION_ITEM()
RATIONAL_B_SPLINE_SURFACE(((1.,0.976223664541016,1.),(1.,0.976080968954893,
1.),(1.,0.975725566325668,1.),(1.,0.974611093487067,1.),(1.,0.973867270455976,
1.),(1.,0.972985060473524,1.)))
REPRESENTATION_ITEM('')
SURFACE()
);
#2463=(
BOUNDED_SURFACE()
B_SPLINE_SURFACE(3,2,((#152961,#152962,#152963),(#152964,#152965,#152966),
(#152967,#152968,#152969),(#152970,#152971,#152972)),.UNSPECIFIED.,.F.,
 .F.,.F.)
B_SPLINE_SURFACE_WITH_KNOTS((4,4),(3,3),(0.0160154644119955,0.0166352988433916),
(0.0831643362494566,1.),.UNSPECIFIED.)
GEOMETRIC_REPRESENTATION_ITEM()
RATIONAL_B_SPLINE_SURFACE(((0.970304695662226,0.821466113499056,1.),(0.970770685596721,
0.824267734695772,1.),(0.971217880665933,0.826956357544095,1.),(0.971646673892332,
0.829534344970778,1.)))
REPRESENTATION_ITEM('')
SURFACE()
);
#2464=(
BOUNDED_SURFACE()
B_SPLINE_SURFACE(3,2,((#152982,#152983,#152984),(#152985,#152986,#152987),
(#152988,#152989,#152990),(#152991,#152992,#152993),(#152994,#152995,#152996),
(#152997,#152998,#152999),(#153000,#153001,#153002),(#153003,#153004,#153005)),
 .UNSPECIFIED.,.F.,.F.,.F.)
B_SPLINE_SURFACE_WITH_KNOTS((4,2,2,4),(3,3),(0.0125275809691397,0.0146002660392865,
0.0166729511094333,0.0208183212497269),(0.,1.),.UNSPECIFIED.)
GEOMETRIC_REPRESENTATION_ITEM()
RATIONAL_B_SPLINE_SURFACE(((1.,0.971326932216839,1.),(1.,0.970663335907126,
1.),(1.,0.969949535519179,1.),(1.,0.968438208203061,1.),(1.,0.967638304877362,
1.),(1.,0.965155032314022,1.),(1.,0.963392662012641,1.),(1.,0.961573369372794,
1.)))
REPRESENTATION_ITEM('')
SURFACE()
);
#2465=(
BOUNDED_SURFACE()
B_SPLINE_SURFACE(3,2,((#153041,#153042,#153043),(#153044,#153045,#153046),
(#153047,#153048,#153049),(#153050,#153051,#153052),(#153053,#153054,#153055),
(#153056,#153057,#153058)),.UNSPECIFIED.,.F.,.F.,.F.)
B_SPLINE_SURFACE_WITH_KNOTS((4,2,4),(3,3),(0.312823500866356,0.318064669632816,
0.323305838399276),(0.,1.),.UNSPECIFIED.)
GEOMETRIC_REPRESENTATION_ITEM()
RATIONAL_B_SPLINE_SURFACE(((1.,0.945205507217168,1.),(1.,0.947659322083022,
1.),(1.,0.950143491189858,1.),(1.,0.955101782056076,1.),(1.,0.957550650194803,
1.),(1.,0.959916004770377,1.)))
REPRESENTATION_ITEM('')
SURFACE()
);
#2466=(
BOUNDED_SURFACE()
B_SPLINE_SURFACE(3,2,((#153082,#153083,#153084),(#153085,#153086,#153087),
(#153088,#153089,#153090),(#153091,#153092,#153093)),.UNSPECIFIED.,.F.,
 .F.,.F.)
B_SPLINE_SURFACE_WITH_KNOTS((4,4),(3,3),(0.419404298305653,0.433181348372439),
(0.,1.),.UNSPECIFIED.)
GEOMETRIC_REPRESENTATION_ITEM()
RATIONAL_B_SPLINE_SURFACE(((1.,0.914650799019394,1.),(1.,0.919810342661608,
1.),(1.,0.925303402418372,1.),(1.,0.931052782541994,1.)))
REPRESENTATION_ITEM('')
SURFACE()
);
#2467=(
BOUNDED_SURFACE()
B_SPLINE_SURFACE(3,2,((#153113,#153114,#153115),(#153116,#153117,#153118),
(#153119,#153120,#153121),(#153122,#153123,#153124)),.UNSPECIFIED.,.F.,
 .F.,.F.)
B_SPLINE_SURFACE_WITH_KNOTS((4,4),(3,3),(0.419208811459411,0.43319545022518),
(0.,1.),.UNSPECIFIED.)
GEOMETRIC_REPRESENTATION_ITEM()
RATIONAL_B_SPLINE_SURFACE(((1.,0.914416798650558,1.),(1.,0.91964499776707,
1.),(1.,0.925217323809603,1.),(1.,0.931054338234342,1.)))
REPRESENTATION_ITEM('')
SURFACE()
);
#2468=(
BOUNDED_SURFACE()
B_SPLINE_SURFACE(3,2,((#153131,#153132,#153133),(#153134,#153135,#153136),
(#153137,#153138,#153139),(#153140,#153141,#153142)),.UNSPECIFIED.,.F.,
 .F.,.F.)
B_SPLINE_SURFACE_WITH_KNOTS((4,4),(3,3),(0.,0.000244695081784474),(0.27005445281224,
1.),.UNSPECIFIED.)
GEOMETRIC_REPRESENTATION_ITEM()
RATIONAL_B_SPLINE_SURFACE(((0.938257063314061,0.885684283219602,1.),(0.937405524229094,
0.884107676953533,1.),(0.936533776434415,0.882493654696909,1.),(0.935642351405452,
0.88084320046503,1.)))
REPRESENTATION_ITEM('')
SURFACE()
);
#2469=(
BOUNDED_SURFACE()
B_SPLINE_SURFACE(2,2,((#153148,#153149,#153150),(#153151,#153152,#153153),
(#153154,#153155,#153156)),.UNSPECIFIED.,.F.,.F.,.F.)
B_SPLINE_SURFACE_WITH_KNOTS((3,3),(3,3),(-1.5707963267949,2.46935726117696E-16),
(0.,1.5707963267949),.UNSPECIFIED.)
GEOMETRIC_REPRESENTATION_ITEM()
RATIONAL_B_SPLINE_SURFACE(((1.,0.707106781186548,1.),(0.707106781186554,
0.500000000000005,0.707106781186554),(1.,0.707106781186548,1.)))
REPRESENTATION_ITEM('')
SURFACE()
);
#2470=(
BOUNDED_SURFACE()
B_SPLINE_SURFACE(3,2,((#153162,#153163,#153164),(#153165,#153166,#153167),
(#153168,#153169,#153170),(#153171,#153172,#153173)),.UNSPECIFIED.,.F.,
 .F.,.F.)
B_SPLINE_SURFACE_WITH_KNOTS((4,4),(3,3),(0.38512996553569,0.397461118597566),
(0.,1.),.UNSPECIFIED.)
GEOMETRIC_REPRESENTATION_ITEM()
RATIONAL_B_SPLINE_SURFACE(((1.,0.93107684669709,1.),(1.,0.936225605355842,
1.),(1.,0.941660652469138,1.),(1.,0.947109873173451,1.)))
REPRESENTATION_ITEM('')
SURFACE()
);
#2471=(
BOUNDED_SURFACE()
B_SPLINE_SURFACE(3,2,((#153183,#153184,#153185),(#153186,#153187,#153188),
(#153189,#153190,#153191),(#153192,#153193,#153194)),.UNSPECIFIED.,.F.,
 .F.,.F.)
B_SPLINE_SURFACE_WITH_KNOTS((4,4),(3,3),(0.385104144430477,0.397435259869197),
(0.,1.),.UNSPECIFIED.)
GEOMETRIC_REPRESENTATION_ITEM()
RATIONAL_B_SPLINE_SURFACE(((1.,0.931076847239609,1.),(1.,0.936225547402437,
1.),(1.,0.941660619426866,1.),(1.,0.947109873449768,1.)))
REPRESENTATION_ITEM('')
SURFACE()
);
#2472=(
BOUNDED_SURFACE()
B_SPLINE_SURFACE(3,2,((#153213,#153214,#153215),(#153216,#153217,#153218),
(#153219,#153220,#153221),(#153222,#153223,#153224)),.UNSPECIFIED.,.F.,
 .F.,.F.)
B_SPLINE_SURFACE_WITH_KNOTS((4,4),(3,3),(0.404488952792596,0.419203847024178),
(0.,1.),.UNSPECIFIED.)
GEOMETRIC_REPRESENTATION_ITEM()
RATIONAL_B_SPLINE_SURFACE(((1.,0.909299925506085,1.),(1.,0.914893743921987,
1.),(1.,0.920902622704526,1.),(1.,0.927264329586823,1.)))
REPRESENTATION_ITEM('')
SURFACE()
);
#2473=(
BOUNDED_SURFACE()
B_SPLINE_SURFACE(3,2,((#153234,#153235,#153236),(#153237,#153238,#153239),
(#153240,#153241,#153242),(#153243,#153244,#153245)),.UNSPECIFIED.,.F.,
 .F.,.F.)
B_SPLINE_SURFACE_WITH_KNOTS((4,4),(3,3),(0.404502936988592,0.419217840791179),
(0.,1.),.UNSPECIFIED.)
GEOMETRIC_REPRESENTATION_ITEM()
RATIONAL_B_SPLINE_SURFACE(((1.,0.909299925389086,1.),(1.,0.914893755639716,
1.),(1.,0.920902631303307,1.),(1.,0.927264329485076,1.)))
REPRESENTATION_ITEM('')
SURFACE()
);
#2474=(
BOUNDED_SURFACE()
B_SPLINE_SURFACE(3,2,((#153266,#153267,#153268),(#153269,#153270,#153271),
(#153272,#153273,#153274),(#153275,#153276,#153277),(#153278,#153279,#153280),
(#153281,#153282,#153283)),.UNSPECIFIED.,.F.,.F.,.F.)
B_SPLINE_SURFACE_WITH_KNOTS((4,2,4),(3,3),(0.369267573830044,0.375649620241937,
0.382031666653828),(0.,1.),.UNSPECIFIED.)
GEOMETRIC_REPRESENTATION_ITEM()
RATIONAL_B_SPLINE_SURFACE(((1.,0.927093956641406,1.),(1.,0.929854789980195,
1.),(1.,0.932694024545401,1.),(1.,0.938495042437814,1.),(1.,0.941445780893249,
1.),(1.,0.944420998665188,1.)))
REPRESENTATION_ITEM('')
SURFACE()
);
#2475=(
BOUNDED_SURFACE()
B_SPLINE_SURFACE(3,2,((#153311,#153312,#153313),(#153314,#153315,#153316),
(#153317,#153318,#153319),(#153320,#153321,#153322),(#153323,#153324,#153325),
(#153326,#153327,#153328)),.UNSPECIFIED.,.F.,.F.,.F.)
B_SPLINE_SURFACE_WITH_KNOTS((4,2,4),(3,3),(0.369297600957186,0.375679664308256,
0.382061727659326),(0.,1.),.UNSPECIFIED.)
GEOMETRIC_REPRESENTATION_ITEM()
RATIONAL_B_SPLINE_SURFACE(((1.,0.927093956100417,1.),(1.,0.929854781017749,
1.),(1.,0.932694090912752,1.),(1.,0.938495064212398,1.),(1.,0.941445786720263,
1.),(1.,0.944420998446809,1.)))
REPRESENTATION_ITEM('')
SURFACE()
);
#2476=(
BOUNDED_SURFACE()
B_SPLINE_SURFACE(3,2,((#153335,#153336,#153337),(#153338,#153339,#153340),
(#153341,#153342,#153343),(#153344,#153345,#153346),(#153347,#153348,#153349),
(#153350,#153351,#153352)),.UNSPECIFIED.,.F.,.F.,.F.)
B_SPLINE_SURFACE_WITH_KNOTS((4,2,4),(3,3),(0.370125164623157,0.376536577097884,
0.382947989572612),(0.,1.),.UNSPECIFIED.)
GEOMETRIC_REPRESENTATION_ITEM()
RATIONAL_B_SPLINE_SURFACE(((1.,0.926591820711723,1.),(1.,0.929356779319319,
1.),(1.,0.932200966596534,1.),(1.,0.938014929520768,1.),(1.,0.94097390228205,
1.),(1.,0.943959859033813,1.)))
REPRESENTATION_ITEM('')
SURFACE()
);
#2477=(
BOUNDED_SURFACE()
B_SPLINE_SURFACE(3,2,((#153380,#153381,#153382),(#153383,#153384,#153385),
(#153386,#153387,#153388),(#153389,#153390,#153391),(#153392,#153393,#153394),
(#153395,#153396,#153397)),.UNSPECIFIED.,.F.,.F.,.F.)
B_SPLINE_SURFACE_WITH_KNOTS((4,2,4),(3,3),(0.370163239489449,0.376574672522443,
0.382986105555437),(0.,1.),.UNSPECIFIED.)
GEOMETRIC_REPRESENTATION_ITEM()
RATIONAL_B_SPLINE_SURFACE(((1.,0.926591820049981,1.),(1.,0.929356768176447,
1.),(1.,0.932201048041363,1.),(1.,0.938014956099503,1.),(1.,0.940973909290998,
1.),(1.,0.943959858771035,1.)))
REPRESENTATION_ITEM('')
SURFACE()
);
#2478=(
BOUNDED_SURFACE()
B_SPLINE_SURFACE(3,2,((#153423,#153424,#153425),(#153426,#153427,#153428),
(#153429,#153430,#153431),(#153432,#153433,#153434)),.UNSPECIFIED.,.F.,
 .F.,.F.)
B_SPLINE_SURFACE_WITH_KNOTS((4,4),(3,3),(0.405561464018681,0.420324995017399),
(0.,1.),.UNSPECIFIED.)
GEOMETRIC_REPRESENTATION_ITEM()
RATIONAL_B_SPLINE_SURFACE(((1.,0.908824629255916,1.),(1.,0.914415103092982,
1.),(1.,0.920421753472993,1.),(1.,0.926785562004255,1.)))
REPRESENTATION_ITEM('')
SURFACE()
);
#2479=(
BOUNDED_SURFACE()
B_SPLINE_SURFACE(3,2,((#153444,#153445,#153446),(#153447,#153448,#153449),
(#153450,#153451,#153452),(#153453,#153454,#153455)),.UNSPECIFIED.,.F.,
 .F.,.F.)
B_SPLINE_SURFACE_WITH_KNOTS((4,4),(3,3),(0.410308427502393,0.42507565892922),
(0.,1.),.UNSPECIFIED.)
GEOMETRIC_REPRESENTATION_ITEM()
RATIONAL_B_SPLINE_SURFACE(((1.,0.908824587192128,1.),(1.,0.914419456338754,
1.),(1.,0.920423871098494,1.),(1.,0.926785532009406,1.)))
REPRESENTATION_ITEM('')
SURFACE()
);
#2480=(
BOUNDED_SURFACE()
B_SPLINE_SURFACE(3,2,((#153537,#153538,#153539),(#153540,#153541,#153542),
(#153543,#153544,#153545),(#153546,#153547,#153548)),.UNSPECIFIED.,.F.,
 .F.,.F.)
B_SPLINE_SURFACE_WITH_KNOTS((4,4),(3,3),(0.410308427502393,0.42507565892922),
(0.,1.),.UNSPECIFIED.)
GEOMETRIC_REPRESENTATION_ITEM()
RATIONAL_B_SPLINE_SURFACE(((1.,0.908824587192128,1.),(1.,0.914419456338754,
1.),(1.,0.920423871098494,1.),(1.,0.926785532009406,1.)))
REPRESENTATION_ITEM('')
SURFACE()
);
#2481=(
BOUNDED_SURFACE()
B_SPLINE_SURFACE(3,2,((#153800,#153801,#153802),(#153803,#153804,#153805),
(#153806,#153807,#153808),(#153809,#153810,#153811)),.UNSPECIFIED.,.F.,
 .F.,.F.)
B_SPLINE_SURFACE_WITH_KNOTS((4,4),(3,3),(0.405561464018681,0.420324995017399),
(0.,1.),.UNSPECIFIED.)
GEOMETRIC_REPRESENTATION_ITEM()
RATIONAL_B_SPLINE_SURFACE(((1.,0.908824629255916,1.),(1.,0.914415103092982,
1.),(1.,0.920421753472993,1.),(1.,0.926785562004255,1.)))
REPRESENTATION_ITEM('')
SURFACE()
);
#2482=(
BOUNDED_SURFACE()
B_SPLINE_SURFACE(3,2,((#154434,#154435,#154436),(#154437,#154438,#154439),
(#154440,#154441,#154442),(#154443,#154444,#154445),(#154446,#154447,#154448),
(#154449,#154450,#154451)),.UNSPECIFIED.,.F.,.F.,.F.)
B_SPLINE_SURFACE_WITH_KNOTS((4,2,4),(3,3),(0.370163239489449,0.376574672522443,
0.382986105555437),(0.,1.),.UNSPECIFIED.)
GEOMETRIC_REPRESENTATION_ITEM()
RATIONAL_B_SPLINE_SURFACE(((1.,0.926591820049981,1.),(1.,0.929356768176447,
1.),(1.,0.932201048041363,1.),(1.,0.938014956099503,1.),(1.,0.940973909290998,
1.),(1.,0.943959858771035,1.)))
REPRESENTATION_ITEM('')
SURFACE()
);
#2483=(
BOUNDED_SURFACE()
B_SPLINE_SURFACE(3,2,((#154619,#154620,#154621),(#154622,#154623,#154624),
(#154625,#154626,#154627),(#154628,#154629,#154630),(#154631,#154632,#154633),
(#154634,#154635,#154636)),.UNSPECIFIED.,.F.,.F.,.F.)
B_SPLINE_SURFACE_WITH_KNOTS((4,2,4),(3,3),(0.370125164623157,0.376536577097884,
0.382947989572612),(0.,1.),.UNSPECIFIED.)
GEOMETRIC_REPRESENTATION_ITEM()
RATIONAL_B_SPLINE_SURFACE(((1.,0.926591820711723,1.),(1.,0.929356779319319,
1.),(1.,0.932200966596534,1.),(1.,0.938014929520768,1.),(1.,0.94097390228205,
1.),(1.,0.943959859033813,1.)))
REPRESENTATION_ITEM('')
SURFACE()
);
#2484=(
BOUNDED_SURFACE()
B_SPLINE_SURFACE(3,2,((#154835,#154836,#154837),(#154838,#154839,#154840),
(#154841,#154842,#154843),(#154844,#154845,#154846),(#154847,#154848,#154849),
(#154850,#154851,#154852)),.UNSPECIFIED.,.F.,.F.,.F.)
B_SPLINE_SURFACE_WITH_KNOTS((4,2,4),(3,3),(0.369297600957186,0.375679664308256,
0.382061727659326),(0.,1.),.UNSPECIFIED.)
GEOMETRIC_REPRESENTATION_ITEM()
RATIONAL_B_SPLINE_SURFACE(((1.,0.927093956100417,1.),(1.,0.929854781017749,
1.),(1.,0.932694090912752,1.),(1.,0.938495064212398,1.),(1.,0.941445786720263,
1.),(1.,0.944420998446809,1.)))
REPRESENTATION_ITEM('')
SURFACE()
);
#2485=(
BOUNDED_SURFACE()
B_SPLINE_SURFACE(3,2,((#154999,#155000,#155001),(#155002,#155003,#155004),
(#155005,#155006,#155007),(#155008,#155009,#155010),(#155011,#155012,#155013),
(#155014,#155015,#155016)),.UNSPECIFIED.,.F.,.F.,.F.)
B_SPLINE_SURFACE_WITH_KNOTS((4,2,4),(3,3),(0.369267573830044,0.375649620241937,
0.382031666653828),(0.,1.),.UNSPECIFIED.)
GEOMETRIC_REPRESENTATION_ITEM()
RATIONAL_B_SPLINE_SURFACE(((1.,0.927093956641406,1.),(1.,0.929854789980195,
1.),(1.,0.932694024545401,1.),(1.,0.938495042437814,1.),(1.,0.941445780893249,
1.),(1.,0.944420998665188,1.)))
REPRESENTATION_ITEM('')
SURFACE()
);
#2486=(
BOUNDED_SURFACE()
B_SPLINE_SURFACE(3,2,((#155557,#155558,#155559),(#155560,#155561,#155562),
(#155563,#155564,#155565),(#155566,#155567,#155568)),.UNSPECIFIED.,.F.,
 .F.,.F.)
B_SPLINE_SURFACE_WITH_KNOTS((4,4),(3,3),(0.404502936988592,0.419217840791179),
(0.,1.),.UNSPECIFIED.)
GEOMETRIC_REPRESENTATION_ITEM()
RATIONAL_B_SPLINE_SURFACE(((1.,0.909299925389086,1.),(1.,0.914893755639716,
1.),(1.,0.920902631303307,1.),(1.,0.927264329485076,1.)))
REPRESENTATION_ITEM('')
SURFACE()
);
#2487=(
BOUNDED_SURFACE()
B_SPLINE_SURFACE(3,2,((#155817,#155818,#155819),(#155820,#155821,#155822),
(#155823,#155824,#155825),(#155826,#155827,#155828)),.UNSPECIFIED.,.F.,
 .F.,.F.)
B_SPLINE_SURFACE_WITH_KNOTS((4,4),(3,3),(0.404488952792596,0.419203847024178),
(0.,1.00010378411472),.UNSPECIFIED.)
GEOMETRIC_REPRESENTATION_ITEM()
RATIONAL_B_SPLINE_SURFACE(((1.,0.909290512279149,1.00001882840776),(1.,
0.914884911244543,1.00001766718827),(1.,0.920894413653247,1.0000164198065),
(1.,0.927256780779661,1.00001509918122)))
REPRESENTATION_ITEM('')
SURFACE()
);
#2488=(
BOUNDED_SURFACE()
B_SPLINE_SURFACE(3,2,((#156265,#156266,#156267),(#156268,#156269,#156270),
(#156271,#156272,#156273),(#156274,#156275,#156276)),.UNSPECIFIED.,.F.,
 .F.,.F.)
B_SPLINE_SURFACE_WITH_KNOTS((4,4),(3,3),(0.385104144430477,0.397435259869197),
(0.,1.),.UNSPECIFIED.)
GEOMETRIC_REPRESENTATION_ITEM()
RATIONAL_B_SPLINE_SURFACE(((1.,0.931076847239609,1.),(1.,0.936225547402437,
1.),(1.,0.941660619426866,1.),(1.,0.947109873449768,1.)))
REPRESENTATION_ITEM('')
SURFACE()
);
#2489=(
BOUNDED_SURFACE()
B_SPLINE_SURFACE(3,2,((#156429,#156430,#156431),(#156432,#156433,#156434),
(#156435,#156436,#156437),(#156438,#156439,#156440)),.UNSPECIFIED.,.F.,
 .F.,.F.)
B_SPLINE_SURFACE_WITH_KNOTS((4,4),(3,3),(0.38512996553569,0.397461118597566),
(0.,1.),.UNSPECIFIED.)
GEOMETRIC_REPRESENTATION_ITEM()
RATIONAL_B_SPLINE_SURFACE(((1.,0.93107684669709,1.),(1.,0.936225605355842,
1.),(1.,0.941660652469138,1.),(1.,0.947109873173451,1.)))
REPRESENTATION_ITEM('')
SURFACE()
);
#2490=(
BOUNDED_SURFACE()
B_SPLINE_SURFACE(2,2,((#156689,#156690,#156691),(#156692,#156693,#156694),
(#156695,#156696,#156697)),.UNSPECIFIED.,.F.,.F.,.F.)
B_SPLINE_SURFACE_WITH_KNOTS((3,3),(3,3),(-1.5707963267949,2.46935726117696E-16),
(-1.5707963267949,0.),.UNSPECIFIED.)
GEOMETRIC_REPRESENTATION_ITEM()
RATIONAL_B_SPLINE_SURFACE(((1.,0.707106781186548,1.),(0.707106781186554,
0.500000000000005,0.707106781186554),(1.,0.707106781186548,1.)))
REPRESENTATION_ITEM('')
SURFACE()
);
#2491=(
BOUNDED_SURFACE()
B_SPLINE_SURFACE(3,2,((#156786,#156787,#156788),(#156789,#156790,#156791),
(#156792,#156793,#156794),(#156795,#156796,#156797)),.UNSPECIFIED.,.F.,
 .F.,.F.)
B_SPLINE_SURFACE_WITH_KNOTS((4,4),(3,3),(0.,0.000244695081784474),(0.,0.729945547187775),
 .UNSPECIFIED.)
GEOMETRIC_REPRESENTATION_ITEM()
RATIONAL_B_SPLINE_SURFACE(((1.,0.8856842832196,0.938257063314063),(1.,0.884107676953531,
0.937405524229096),(1.,0.882493654696906,0.936533776434417),(1.,0.880843200465028,
0.935642351405454)))
REPRESENTATION_ITEM('')
SURFACE()
);
#2492=(
BOUNDED_SURFACE()
B_SPLINE_SURFACE(3,2,((#156852,#156853,#156854),(#156855,#156856,#156857),
(#156858,#156859,#156860),(#156861,#156862,#156863)),.UNSPECIFIED.,.F.,
 .F.,.F.)
B_SPLINE_SURFACE_WITH_KNOTS((4,4),(3,3),(0.419208811459411,0.43319545022518),
(0.,1.),.UNSPECIFIED.)
GEOMETRIC_REPRESENTATION_ITEM()
RATIONAL_B_SPLINE_SURFACE(((1.,0.914416798650558,1.),(1.,0.91964499776707,
1.),(1.,0.925217323809603,1.),(1.,0.931054338234342,1.)))
REPRESENTATION_ITEM('')
SURFACE()
);
#2493=(
BOUNDED_SURFACE()
B_SPLINE_SURFACE(3,2,((#157146,#157147,#157148),(#157149,#157150,#157151),
(#157152,#157153,#157154),(#157155,#157156,#157157)),.UNSPECIFIED.,.F.,
 .F.,.F.)
B_SPLINE_SURFACE_WITH_KNOTS((4,4),(3,3),(0.419404298305653,0.433181348372439),
(0.,1.),.UNSPECIFIED.)
GEOMETRIC_REPRESENTATION_ITEM()
RATIONAL_B_SPLINE_SURFACE(((1.,0.914650799019394,1.),(1.,0.919810342661608,
1.),(1.,0.925303402418372,1.),(1.,0.931052782541994,1.)))
REPRESENTATION_ITEM('')
SURFACE()
);
#2494=(
BOUNDED_SURFACE()
B_SPLINE_SURFACE(3,2,((#157401,#157402,#157403),(#157404,#157405,#157406),
(#157407,#157408,#157409),(#157410,#157411,#157412),(#157413,#157414,#157415),
(#157416,#157417,#157418)),.UNSPECIFIED.,.F.,.F.,.F.)
B_SPLINE_SURFACE_WITH_KNOTS((4,2,4),(3,3),(0.312823500866356,0.318064669632816,
0.323305838399276),(-5.72660618870878E-8,1.),.UNSPECIFIED.)
GEOMETRIC_REPRESENTATION_ITEM()
RATIONAL_B_SPLINE_SURFACE(((1.00000000627573,0.945205504079303,1.),(1.00000000599469,
0.947659319085678,1.),(1.00000000571017,0.950143488334772,1.),(1.00000000514229,
0.955101779484932,1.),(1.00000000486181,0.957550647763896,1.),(1.00000000459091,
0.959916002474924,1.)))
REPRESENTATION_ITEM('')
SURFACE()
);
#2495=(
BOUNDED_SURFACE()
B_SPLINE_SURFACE(3,2,((#157744,#157745,#157746),(#157747,#157748,#157749),
(#157750,#157751,#157752),(#157753,#157754,#157755),(#157756,#157757,#157758),
(#157759,#157760,#157761),(#157762,#157763,#157764),(#157765,#157766,#157767)),
 .UNSPECIFIED.,.F.,.F.,.F.)
B_SPLINE_SURFACE_WITH_KNOTS((4,2,2,4),(3,3),(0.0125275809691397,0.0146002660392865,
0.0166729511094333,0.0208183212497269),(0.,1.),.UNSPECIFIED.)
GEOMETRIC_REPRESENTATION_ITEM()
RATIONAL_B_SPLINE_SURFACE(((1.,0.971326932216839,1.),(1.,0.970663335907126,
1.),(1.,0.969949535519179,1.),(1.,0.968438208203061,1.),(1.,0.967638304877362,
1.),(1.,0.965155032314022,1.),(1.,0.963392662012641,1.),(1.,0.961573369372794,
1.)))
REPRESENTATION_ITEM('')
SURFACE()
);
#2496=(
BOUNDED_SURFACE()
B_SPLINE_SURFACE(3,2,((#157998,#157999,#158000),(#158001,#158002,#158003),
(#158004,#158005,#158006),(#158007,#158008,#158009)),.UNSPECIFIED.,.F.,
 .F.,.F.)
B_SPLINE_SURFACE_WITH_KNOTS((4,4),(3,3),(0.0160154644119955,0.0166352988433916),
(0.,0.916835663750545),.UNSPECIFIED.)
GEOMETRIC_REPRESENTATION_ITEM()
RATIONAL_B_SPLINE_SURFACE(((1.,0.821466113499055,0.970304695662227),(1.,
0.824267734695769,0.970770685596721),(1.,0.826956357544096,0.971217880665933),
(1.,0.829534344970778,0.971646673892332)))
REPRESENTATION_ITEM('')
SURFACE()
);
#2497=(
BOUNDED_SURFACE()
B_SPLINE_SURFACE(3,2,((#158282,#158283,#158284),(#158285,#158286,#158287),
(#158288,#158289,#158290),(#158291,#158292,#158293),(#158294,#158295,#158296),
(#158297,#158298,#158299)),.UNSPECIFIED.,.F.,.F.,.F.)
B_SPLINE_SURFACE_WITH_KNOTS((4,2,4),(3,3),(0.0123698333451925,0.0156488944469233,
0.018927955548654),(0.,1.00002228978397),.UNSPECIFIED.)
GEOMETRIC_REPRESENTATION_ITEM()
RATIONAL_B_SPLINE_SURFACE(((1.,0.976223134571635,1.00000105996239),(1.,
0.976080435804858,1.00000106632384),(1.,0.975725025253786,1.00000108216789),
(1.,0.974610527573826,1.00000113185171),(1.,0.97386668796308,1.00000116501176),
(1.,0.972984458316358,1.00000120434118)))
REPRESENTATION_ITEM('')
SURFACE()
);
#2498=(
BOUNDED_SURFACE()
B_SPLINE_SURFACE(3,2,((#158421,#158422,#158423),(#158424,#158425,#158426),
(#158427,#158428,#158429),(#158430,#158431,#158432)),.UNSPECIFIED.,.F.,
 .F.,.F.)
B_SPLINE_SURFACE_WITH_KNOTS((4,4),(3,3),(0.0242632023351278,0.0247749981337221),
(0.,0.921912051975923),.UNSPECIFIED.)
GEOMETRIC_REPRESENTATION_ITEM()
RATIONAL_B_SPLINE_SURFACE(((1.,0.876471439509662,0.980707816377883),(1.,
0.876509293543674,0.980713728265564),(1.,0.876478978800395,0.980708993833368),
(1.,0.876380510183545,0.980693615408899)))
REPRESENTATION_ITEM('')
SURFACE()
);
#2499=(
BOUNDED_SURFACE()
B_SPLINE_SURFACE(3,2,((#158594,#158595,#158596),(#158597,#158598,#158599),
(#158600,#158601,#158602),(#158603,#158604,#158605),(#158606,#158607,#158608),
(#158609,#158610,#158611),(#158612,#158613,#158614),(#158615,#158616,#158617)),
 .UNSPECIFIED.,.F.,.F.,.F.)
B_SPLINE_SURFACE_WITH_KNOTS((4,2,2,4),(3,3),(0.0238269657788709,0.0270983492768517,
0.0287340410258421,0.0303697327748325),(0.,1.),.UNSPECIFIED.)
GEOMETRIC_REPRESENTATION_ITEM()
RATIONAL_B_SPLINE_SURFACE(((1.,0.972768240458926,1.),(1.,0.973679370262107,
1.),(1.,0.974448100441956,1.),(1.,0.975326902749563,1.),(1.,0.975574944117527,
1.),(1.,0.975963474394985,1.),(1.,0.976104268047958,1.),(1.,0.976191081059459,
1.)))
REPRESENTATION_ITEM('')
SURFACE()
);
#2500=(
BOUNDED_SURFACE()
B_SPLINE_SURFACE(3,2,((#158773,#158774,#158775),(#158776,#158777,#158778),
(#158779,#158780,#158781),(#158782,#158783,#158784)),.UNSPECIFIED.,.F.,
 .F.,.F.)
B_SPLINE_SURFACE_WITH_KNOTS((4,4),(3,3),(0.0324061838408421,0.0330259723062236),
(0.,0.916511637562676),.UNSPECIFIED.)
GEOMETRIC_REPRESENTATION_ITEM()
RATIONAL_B_SPLINE_SURFACE(((1.,0.826705510992856,0.971063853786761),(1.,
0.824047872538611,0.970620090021771),(1.,0.821278892860727,0.970157734863913),
(1.,0.818396073825199,0.969676371182954)))
REPRESENTATION_ITEM('')
SURFACE()
);
#2501=(
BOUNDED_SURFACE()
B_SPLINE_SURFACE(3,2,((#158996,#158997,#158998),(#158999,#159000,#159001),
(#159002,#159003,#159004),(#159005,#159006,#159007),(#159008,#159009,#159010),
(#159011,#159012,#159013)),.UNSPECIFIED.,.F.,.F.,.F.)
B_SPLINE_SURFACE_WITH_KNOTS((4,2,4),(3,3),(0.0161036610523817,0.0202680863362144,
0.0244325116200472),(0.,1.),.UNSPECIFIED.)
GEOMETRIC_REPRESENTATION_ITEM()
RATIONAL_B_SPLINE_SURFACE(((1.,0.961171400688072,1.),(1.,0.963011198169074,
1.),(1.,0.964799382389448,1.),(1.,0.968173271553358,1.),(1.,0.969728922082773,
1.),(1.,0.971089741366958,1.)))
REPRESENTATION_ITEM('')
SURFACE()
);
#2502=(
BOUNDED_SURFACE()
B_SPLINE_SURFACE(3,2,((#159339,#159340,#159341),(#159342,#159343,#159344),
(#159345,#159346,#159347),(#159348,#159349,#159350),(#159351,#159352,#159353),
(#159354,#159355,#159356)),.UNSPECIFIED.,.F.,.F.,.F.)
B_SPLINE_SURFACE_WITH_KNOTS((4,2,4),(3,3),(0.320593732793275,0.325865292398914,
0.331136852004555),(0.,1.),.UNSPECIFIED.)
GEOMETRIC_REPRESENTATION_ITEM()
RATIONAL_B_SPLINE_SURFACE(((1.,0.944716550630948,1.),(1.,0.947183012056064,
1.),(1.,0.949681743560583,1.),(1.,0.954674153969892,1.),(1.,0.957142661330136,
1.),(1.,0.959530911256235,1.)))
REPRESENTATION_ITEM('')
SURFACE()
);
#2503=(
BOUNDED_SURFACE()
B_SPLINE_SURFACE(3,2,((#159807,#159808,#159809),(#159810,#159811,#159812),
(#159813,#159814,#159815),(#159816,#159817,#159818),(#159819,#159820,#159821),
(#159822,#159823,#159824),(#159825,#159826,#159827),(#159828,#159829,#159830)),
 .UNSPECIFIED.,.F.,.F.,.F.)
B_SPLINE_SURFACE_WITH_KNOTS((4,2,2,4),(3,3),(0.0122567706991037,0.0155118977534076,
0.0171394612805594,0.0187670248077113),(0.,1.00001496733849),
 .UNSPECIFIED.)
GEOMETRIC_REPRESENTATION_ITEM()
RATIONAL_B_SPLINE_SURFACE(((1.,0.976217282160683,1.00000071192798),(1.,
0.976078046677685,1.00000071609595),(1.,0.975752626118217,1.0000007258373),
(1.,0.975002093870605,1.00000074830424),(1.,0.97470664347422,1.00000075714846),
(1.,0.974043205195991,1.00000077700827),(1.,0.973675079813253,1.00000078802798),
(1.,0.973275128586134,1.00000080000039)))
REPRESENTATION_ITEM('')
SURFACE()
);
#2504=(
BOUNDED_SURFACE()
B_SPLINE_SURFACE(3,2,((#159910,#159911,#159912),(#159913,#159914,#159915),
(#159916,#159917,#159918),(#159919,#159920,#159921),(#159922,#159923,#159924),
(#159925,#159926,#159927)),.UNSPECIFIED.,.F.,.F.,.F.)
B_SPLINE_SURFACE_WITH_KNOTS((4,2,4),(3,3),(0.0131888298509929,0.0172446796820237,
0.0213005295130545),(0.,1.),.UNSPECIFIED.)
GEOMETRIC_REPRESENTATION_ITEM()
RATIONAL_B_SPLINE_SURFACE(((1.,0.962986864789684,1.),(1.,0.964634105108703,
1.),(1.,0.96622351418111,1.),(1.,0.969200309542686,1.),(1.,0.970562566403692,
1.),(1.,0.971747603318281,1.)))
REPRESENTATION_ITEM('')
SURFACE()
);
#2505=(
BOUNDED_SURFACE()
B_SPLINE_SURFACE(3,2,((#160107,#160108,#160109),(#160110,#160111,#160112),
(#160113,#160114,#160115),(#160116,#160117,#160118),(#160119,#160120,#160121),
(#160122,#160123,#160124)),.UNSPECIFIED.,.F.,.F.,.F.)
B_SPLINE_SURFACE_WITH_KNOTS((4,2,4),(3,3),(0.283188163394013,0.288276169473932,
0.293364175553851),(0.,1.),.UNSPECIFIED.)
GEOMETRIC_REPRESENTATION_ITEM()
RATIONAL_B_SPLINE_SURFACE(((1.,0.948000855586274,1.),(1.,0.950253931198463,
1.),(1.,0.952523267214703,1.),(1.,0.957028867337525,1.),(1.,0.959243070764605,
1.),(1.,0.961372018922465,1.)))
REPRESENTATION_ITEM('')
SURFACE()
);
#2506=(
BOUNDED_SURFACE()
B_SPLINE_SURFACE(2,2,((#160355,#160356,#160357),(#160358,#160359,#160360),
(#160361,#160362,#160363)),.UNSPECIFIED.,.F.,.F.,.F.)
B_SPLINE_SURFACE_WITH_KNOTS((3,3),(3,3),(0.,1.5707963267949),(-1.5707963267949,
0.),.UNSPECIFIED.)
GEOMETRIC_REPRESENTATION_ITEM()
RATIONAL_B_SPLINE_SURFACE(((1.,0.707106781186547,1.),(0.707106781186621,
0.500000000000052,0.707106781186621),(1.,0.707106781186547,1.)))
REPRESENTATION_ITEM('')
SURFACE()
);
#2507=(
BOUNDED_SURFACE()
B_SPLINE_SURFACE(3,2,((#160372,#160373,#160374),(#160375,#160376,#160377),
(#160378,#160379,#160380),(#160381,#160382,#160383),(#160384,#160385,#160386),
(#160387,#160388,#160389),(#160390,#160391,#160392),(#160393,#160394,#160395)),
 .UNSPECIFIED.,.F.,.F.,.F.)
B_SPLINE_SURFACE_WITH_KNOTS((4,2,2,4),(3,3),(0.,0.00103600378053286,0.00207200756106572,
0.00414401512213144),(0.,1.),.UNSPECIFIED.)
GEOMETRIC_REPRESENTATION_ITEM()
RATIONAL_B_SPLINE_SURFACE(((1.,0.917068097704898,1.),(1.,0.902969174287913,
1.),(1.,0.888154932928049,1.),(1.,0.856959094818643,1.),(1.,0.840579087750432,
1.),(1.,0.788725570722382,1.),(1.,0.750598222445163,1.),(1.,0.707106781186548,
1.)))
REPRESENTATION_ITEM('')
SURFACE()
);
#2508=(
BOUNDED_SURFACE()
B_SPLINE_SURFACE(3,2,((#160489,#160490,#160491),(#160492,#160493,#160494),
(#160495,#160496,#160497),(#160498,#160499,#160500),(#160501,#160502,#160503),
(#160504,#160505,#160506)),.UNSPECIFIED.,.F.,.F.,.F.)
B_SPLINE_SURFACE_WITH_KNOTS((4,2,4),(3,3),(8.78519494496442E-16,0.785398163397449,
1.5707963267949),(0.,1.),.UNSPECIFIED.)
GEOMETRIC_REPRESENTATION_ITEM()
RATIONAL_B_SPLINE_SURFACE(((1.,0.656059028990513,1.),(1.,0.65594867470042,
1.),(1.,0.661819490285751,1.),(1.,0.681005707982728,1.),(1.,0.694211427468597,
1.),(1.,0.707106781186548,1.)))
REPRESENTATION_ITEM('')
SURFACE()
);
#2509=(
BOUNDED_SURFACE()
B_SPLINE_SURFACE(3,2,((#160578,#160579,#160580),(#160581,#160582,#160583),
(#160584,#160585,#160586),(#160587,#160588,#160589),(#160590,#160591,#160592),
(#160593,#160594,#160595)),.UNSPECIFIED.,.F.,.F.,.F.)
B_SPLINE_SURFACE_WITH_KNOTS((4,2,4),(3,3),(1.5707963267949,2.35619449019234,
3.1415926535898),(0.,1.),.UNSPECIFIED.)
GEOMETRIC_REPRESENTATION_ITEM()
RATIONAL_B_SPLINE_SURFACE(((1.,0.707106781186548,1.),(1.,0.720039765645106,
1.),(1.,0.732392511164342,1.),(1.,0.749774985070554,1.),(1.,0.754782222114274,
1.),(1.,0.754709580222767,1.)))
REPRESENTATION_ITEM('')
SURFACE()
);
#2510=(
BOUNDED_SURFACE()
B_SPLINE_SURFACE(3,2,((#160799,#160800,#160801),(#160802,#160803,#160804),
(#160805,#160806,#160807),(#160808,#160809,#160810),(#160811,#160812,#160813),
(#160814,#160815,#160816)),.UNSPECIFIED.,.F.,.F.,.F.)
B_SPLINE_SURFACE_WITH_KNOTS((4,2,4),(3,3),(8.78519494496442E-16,0.785398163397449,
1.5707963267949),(0.,1.),.UNSPECIFIED.)
GEOMETRIC_REPRESENTATION_ITEM()
RATIONAL_B_SPLINE_SURFACE(((1.,0.656059028990513,1.),(1.,0.655948674700453,
1.),(1.,0.661819490285707,1.),(1.,0.681005707982772,1.),(1.,0.694211427468564,
1.),(1.,0.707106781186548,1.)))
REPRESENTATION_ITEM('')
SURFACE()
);
#2511=(
BOUNDED_SURFACE()
B_SPLINE_SURFACE(3,2,((#160888,#160889,#160890),(#160891,#160892,#160893),
(#160894,#160895,#160896),(#160897,#160898,#160899),(#160900,#160901,#160902),
(#160903,#160904,#160905)),.UNSPECIFIED.,.F.,.F.,.F.)
B_SPLINE_SURFACE_WITH_KNOTS((4,2,4),(3,3),(4.71238898038469,5.49778714378214,
6.28318530717959),(0.,1.),.UNSPECIFIED.)
GEOMETRIC_REPRESENTATION_ITEM()
RATIONAL_B_SPLINE_SURFACE(((1.,0.707106781186548,1.),(1.,0.720039765645103,
1.),(1.,0.732392511164345,1.),(1.,0.749774985070558,1.),(1.,0.754782222114279,
1.),(1.,0.754709580222763,1.)))
REPRESENTATION_ITEM('')
SURFACE()
);
#2512=(
BOUNDED_SURFACE()
B_SPLINE_SURFACE(3,2,((#161058,#161059,#161060),(#161061,#161062,#161063),
(#161064,#161065,#161066),(#161067,#161068,#161069),(#161070,#161071,#161072),
(#161073,#161074,#161075)),.UNSPECIFIED.,.F.,.F.,.F.)
B_SPLINE_SURFACE_WITH_KNOTS((4,2,4),(3,3),(3.1415926535898,3.92699081698724,
4.71238898038469),(0.,1.),.UNSPECIFIED.)
GEOMETRIC_REPRESENTATION_ITEM()
RATIONAL_B_SPLINE_SURFACE(((1.,0.754709580222777,1.),(1.,0.754782222115066,
1.),(1.,0.749774985069503,1.),(1.,0.732392511165393,1.),(1.,0.720039765644325,
1.),(1.,0.707106781186548,1.)))
REPRESENTATION_ITEM('')
SURFACE()
);
#2513=(
BOUNDED_SURFACE()
B_SPLINE_SURFACE(3,2,((#161141,#161142,#161143),(#161144,#161145,#161146),
(#161147,#161148,#161149),(#161150,#161151,#161152),(#161153,#161154,#161155),
(#161156,#161157,#161158)),.UNSPECIFIED.,.F.,.F.,.F.)
B_SPLINE_SURFACE_WITH_KNOTS((4,2,4),(3,3),(4.71232237546293,5.49778714378214,
6.28325191210135),(-6.66049217571579E-5,1.),.UNSPECIFIED.)
GEOMETRIC_REPRESENTATION_ITEM()
RATIONAL_B_SPLINE_SURFACE(((1.00003901842147,0.707090554001954,1.),(1.0000407364626,
0.694193300415841,1.),(1.0000424959016,0.680985274981482,1.),(1.00004505208164,
0.661796152210739,1.),(1.00004583420842,0.655924763411915,1.),(1.00004581937076,
0.656036149035425,1.)))
REPRESENTATION_ITEM('')
SURFACE()
);
#2514=(
BOUNDED_SURFACE()
B_SPLINE_SURFACE(3,2,((#161302,#161303,#161304),(#161305,#161306,#161307),
(#161308,#161309,#161310),(#161311,#161312,#161313),(#161314,#161315,#161316),
(#161317,#161318,#161319)),.UNSPECIFIED.,.F.,.F.,.F.)
B_SPLINE_SURFACE_WITH_KNOTS((4,2,4),(3,3),(0.,0.00191432655883665,0.0038286531176733),
(0.,1.),.UNSPECIFIED.)
GEOMETRIC_REPRESENTATION_ITEM()
RATIONAL_B_SPLINE_SURFACE(((1.,0.707106781186548,1.),(1.,0.747225690478532,
1.),(1.,0.78278583891712,1.),(1.,0.847703426979888,1.),(1.,0.877037193451153,
1.),(1.,0.903978945212084,1.)))
REPRESENTATION_ITEM('')
SURFACE()
);
#2515=(
BOUNDED_SURFACE()
B_SPLINE_SURFACE(3,2,((#161410,#161411,#161412),(#161413,#161414,#161415),
(#161416,#161417,#161418),(#161419,#161420,#161421),(#161422,#161423,#161424),
(#161425,#161426,#161427)),.UNSPECIFIED.,.F.,.F.,.F.)
B_SPLINE_SURFACE_WITH_KNOTS((4,2,4),(3,3),(0.,0.785398163397448,1.5707963267949),
(0.,1.),.UNSPECIFIED.)
GEOMETRIC_REPRESENTATION_ITEM()
RATIONAL_B_SPLINE_SURFACE(((1.,0.754709580222772,1.),(1.,0.754782222114301,
1.),(1.,0.749774985070531,1.),(1.,0.732392511164381,1.),(1.,0.720039765645079,
1.),(1.,0.707106781186548,1.)))
REPRESENTATION_ITEM('')
SURFACE()
);
#2516=(
BOUNDED_SURFACE()
B_SPLINE_SURFACE(3,2,((#161493,#161494,#161495),(#161496,#161497,#161498),
(#161499,#161500,#161501),(#161502,#161503,#161504),(#161505,#161506,#161507),
(#161508,#161509,#161510)),.UNSPECIFIED.,.F.,.F.,.F.)
B_SPLINE_SURFACE_WITH_KNOTS((4,2,4),(3,3),(4.71232237546302,5.49778714378214,
6.28325191210126),(-6.6604921673139E-5,1.),.UNSPECIFIED.)
GEOMETRIC_REPRESENTATION_ITEM()
RATIONAL_B_SPLINE_SURFACE(((1.00003901842142,0.707090554001977,0.999999999999999),
(1.00004073646254,0.694193300417183,1.),(1.00004249590154,0.68098527497974,
1.),(1.00004505208158,0.661796152212536,1.),(1.00004583420837,0.65592476341061,
1.),(1.0000458193707,0.65603614903546,1.)))
REPRESENTATION_ITEM('')
SURFACE()
);
#2517=(
BOUNDED_SURFACE()
B_SPLINE_SURFACE(3,2,((#161723,#161724,#161725),(#161726,#161727,#161728),
(#161729,#161730,#161731),(#161732,#161733,#161734)),.UNSPECIFIED.,.F.,
 .F.,.F.)
B_SPLINE_SURFACE_WITH_KNOTS((4,4),(3,3),(0.,0.00096907076046529),(0.,1.),
 .UNSPECIFIED.)
GEOMETRIC_REPRESENTATION_ITEM()
RATIONAL_B_SPLINE_SURFACE(((1.,0.903978945212084,1.),(1.,0.920702565586523,
1.),(1.,0.933513016958348,1.),(1.,0.941989694367876,1.)))
REPRESENTATION_ITEM('')
SURFACE()
);
#2518=(
BOUNDED_SURFACE()
B_SPLINE_SURFACE(3,2,((#161807,#161808,#161809),(#161810,#161811,#161812),
(#161813,#161814,#161815),(#161816,#161817,#161818),(#161819,#161820,#161821),
(#161822,#161823,#161824)),.UNSPECIFIED.,.F.,.F.,.F.)
B_SPLINE_SURFACE_WITH_KNOTS((4,2,4),(3,3),(-0.000128622207890212,0.000643111039450966,
0.00141484428679216),(-0.00251732068448168,1.),.UNSPECIFIED.)
GEOMETRIC_REPRESENTATION_ITEM()
RATIONAL_B_SPLINE_SURFACE(((1.00132581435537,0.736661609395596,1.),(1.00116195192182,
0.769208601633366,1.),(1.0010854898064,0.784395803624051,1.),(1.00101813210278,
0.797774652021856,1.),(1.00102381299662,0.796646290850486,1.),(1.00102082699956,
0.797239381168936,1.)))
REPRESENTATION_ITEM('')
SURFACE()
);
#2519=(
BOUNDED_SURFACE()
B_SPLINE_SURFACE(3,2,((#161873,#161874,#161875),(#161876,#161877,#161878),
(#161879,#161880,#161881),(#161882,#161883,#161884)),.UNSPECIFIED.,.F.,
 .F.,.F.)
B_SPLINE_SURFACE_WITH_KNOTS((4,4),(3,3),(0.,0.000344272120907045),(0.,1.),
 .UNSPECIFIED.)
GEOMETRIC_REPRESENTATION_ITEM()
RATIONAL_B_SPLINE_SURFACE(((1.,0.707106781186548,1.),(1.,0.722743638846974,
1.),(1.,0.737730816488031,1.),(1.,0.752153393551655,1.)))
REPRESENTATION_ITEM('')
SURFACE()
);
#2520=(
BOUNDED_SURFACE()
B_SPLINE_SURFACE(3,2,((#161893,#161894,#161895),(#161896,#161897,#161898),
(#161899,#161900,#161901),(#161902,#161903,#161904),(#161905,#161906,#161907),
(#161908,#161909,#161910),(#161911,#161912,#161913),(#161914,#161915,#161916),
(#161917,#161918,#161919),(#161920,#161921,#161922)),.UNSPECIFIED.,.F.,
 .F.,.F.)
B_SPLINE_SURFACE_WITH_KNOTS((4,2,2,2,4),(3,3),(0.,0.000409091700616903,
0.000818183401233805,0.00122727510185071,0.00163636680246761),(0.,1.),
 .UNSPECIFIED.)
GEOMETRIC_REPRESENTATION_ITEM()
RATIONAL_B_SPLINE_SURFACE(((1.,0.549942215762897,1.),(1.,0.54985788278214,
1.),(1.,0.554957454495403,1.),(1.,0.573078296428378,1.),(1.,0.58619337630722,
1.),(1.,0.61662144853447,1.),(1.,0.634085743304818,1.),(1.,0.670152902628418,
1.),(1.,0.688944445542904,1.),(1.,0.707106781186548,1.)))
REPRESENTATION_ITEM('')
SURFACE()
);
#2521=(
BOUNDED_SURFACE()
B_SPLINE_SURFACE(3,2,((#162039,#162040,#162041),(#162042,#162043,#162044),
(#162045,#162046,#162047),(#162048,#162049,#162050),(#162051,#162052,#162053),
(#162054,#162055,#162056),(#162057,#162058,#162059),(#162060,#162061,#162062)),
 .UNSPECIFIED.,.F.,.F.,.F.)
B_SPLINE_SURFACE_WITH_KNOTS((4,2,2,4),(3,3),(-0.000109471601813517,0.000399353616616221,
0.00079870723323257,0.00170688606827854),(-0.000609991948385842,1.),
 .UNSPECIFIED.)
GEOMETRIC_REPRESENTATION_ITEM()
RATIONAL_B_SPLINE_SURFACE(((1.00037046105782,0.696339387097673,1.),(1.00035043066668,
0.712757957212574,1.),(1.00033035655321,0.729212365766033,1.),(1.00029737990511,
0.756242761975451,1.),(1.00028411427462,0.767116373116637,1.),(1.00024733719763,
0.797261916093909,1.),(1.00023300379127,0.809010764906677,1.),(1.00023765398644,
0.805199079207076,1.)))
REPRESENTATION_ITEM('')
SURFACE()
);
#2522=(
BOUNDED_SURFACE()
B_SPLINE_SURFACE(3,2,((#162155,#162156,#162157),(#162158,#162159,#162160),
(#162161,#162162,#162163),(#162164,#162165,#162166),(#162167,#162168,#162169),
(#162170,#162171,#162172)),.UNSPECIFIED.,.F.,.F.,.F.)
B_SPLINE_SURFACE_WITH_KNOTS((4,2,4),(3,3),(0.0033044647217104,0.00391466500066162,
0.00452486527961284),(0.,1.),.UNSPECIFIED.)
GEOMETRIC_REPRESENTATION_ITEM()
RATIONAL_B_SPLINE_SURFACE(((1.,0.707106781186548,1.),(1.,0.688071275370979,
1.),(1.,0.668909963668733,1.),(1.,0.636714772442526,1.),(1.,0.623520947306417,
1.),(1.,0.61630483290538,1.)))
REPRESENTATION_ITEM('')
SURFACE()
);
#2523=(
BOUNDED_SURFACE()
B_SPLINE_SURFACE(3,2,((#162206,#162207,#162208),(#162209,#162210,#162211),
(#162212,#162213,#162214),(#162215,#162216,#162217)),.UNSPECIFIED.,.F.,
 .F.,.F.)
B_SPLINE_SURFACE_WITH_KNOTS((4,4),(3,3),(-3.72129922795447E-5,0.000409342915074972),
(0.,1.00007018282617),.UNSPECIFIED.)
GEOMETRIC_REPRESENTATION_ITEM()
RATIONAL_B_SPLINE_SURFACE(((1.,0.609429354571442,1.00005482270343),(1.,
0.60938746827453,1.00005482858282),(1.,0.612511139640593,1.00005439012666),
(1.,0.617481186158951,1.00005369250283)))
REPRESENTATION_ITEM('')
SURFACE()
);
#2524=(
BOUNDED_SURFACE()
B_SPLINE_SURFACE(3,2,((#162238,#162239,#162240),(#162241,#162242,#162243),
(#162244,#162245,#162246),(#162247,#162248,#162249),(#162250,#162251,#162252),
(#162253,#162254,#162255),(#162256,#162257,#162258),(#162259,#162260,#162261),
(#162262,#162263,#162264),(#162265,#162266,#162267)),.UNSPECIFIED.,.F.,
 .F.,.F.)
B_SPLINE_SURFACE_WITH_KNOTS((4,2,2,2,4),(3,3),(0.,0.00039540981677153,0.00079081963354306,
0.00118622945031459,0.00158163926708612),(0.,1.),.UNSPECIFIED.)
GEOMETRIC_REPRESENTATION_ITEM()
RATIONAL_B_SPLINE_SURFACE(((1.,0.835211735760644,1.),(1.,0.838806334780784,
1.),(1.,0.840513202341181,1.),(1.,0.839504260685003,1.),(1.,0.836771095032971,
1.),(1.,0.825966649242057,1.),(1.,0.817815337411177,1.),(1.,0.795024845130666,
1.),(1.,0.780342956064905,1.),(1.,0.761980581628842,1.)))
REPRESENTATION_ITEM('')
SURFACE()
);
#2525=(
BOUNDED_SURFACE()
B_SPLINE_SURFACE(3,2,((#162380,#162381,#162382),(#162383,#162384,#162385),
(#162386,#162387,#162388),(#162389,#162390,#162391)),.UNSPECIFIED.,.F.,
 .F.,.F.)
B_SPLINE_SURFACE_WITH_KNOTS((4,4),(3,3),(-2.16840434497101E-19,0.000504456607560921),
(0.,1.),.UNSPECIFIED.)
GEOMETRIC_REPRESENTATION_ITEM()
RATIONAL_B_SPLINE_SURFACE(((1.,0.835211735760659,1.),(1.,0.83730162444359,
1.),(1.,0.839319452171524,1.),(1.,0.841267344812682,1.)))
REPRESENTATION_ITEM('')
SURFACE()
);
#2526=(
BOUNDED_SURFACE()
B_SPLINE_SURFACE(3,2,((#162395,#162396,#162397),(#162398,#162399,#162400),
(#162401,#162402,#162403),(#162404,#162405,#162406),(#162407,#162408,#162409),
(#162410,#162411,#162412),(#162413,#162414,#162415),(#162416,#162417,#162418)),
 .UNSPECIFIED.,.F.,.F.,.F.)
B_SPLINE_SURFACE_WITH_KNOTS((4,2,2,4),(3,3),(-0.000179925045351958,0.000899625226760169,
0.00134943784014025,0.00197917549887236),(0.,1.00242125618315),
 .UNSPECIFIED.)
GEOMETRIC_REPRESENTATION_ITEM()
RATIONAL_B_SPLINE_SURFACE(((1.,0.627732378823926,1.00180271055912),(1.,
0.702113319059347,1.00144251993621),(1.,0.752231213046251,1.00119982341481),
(1.,0.801387630970335,1.00096178285313),(1.,0.812691856939329,1.00090704199908),
(1.,0.834322378444833,1.0008022959312),(1.,0.841478824181795,1.00076764075422),
(1.,0.8445445625749,1.00075279487814)))
REPRESENTATION_ITEM('')
SURFACE()
);
#2527=(
BOUNDED_SURFACE()
B_SPLINE_SURFACE(3,2,((#162525,#162526,#162527),(#162528,#162529,#162530),
(#162531,#162532,#162533),(#162534,#162535,#162536),(#162537,#162538,#162539),
(#162540,#162541,#162542),(#162543,#162544,#162545),(#162546,#162547,#162548)),
 .UNSPECIFIED.,.F.,.F.,.F.)
B_SPLINE_SURFACE_WITH_KNOTS((4,2,2,4),(3,3),(-5.14996031930615E-18,0.000466811173310166,
0.000933622346620337,0.00186724469324068),(-0.00180391133637782,1.),
 .UNSPECIFIED.)
GEOMETRIC_REPRESENTATION_ITEM()
RATIONAL_B_SPLINE_SURFACE(((1.00041089117644,0.886111038786231,1.),(1.00041028049095,
0.886280305833524,1.),(1.0004242246253,0.882415333629096,1.),(1.0004790873429,
0.867208733256615,1.),(1.00052055430255,0.855715108594697,1.),(1.00068168753861,
0.811052925699315,1.),(1.00083807861781,0.767705152435299,1.),(1.00102927155329,
0.714711157767394,1.)))
REPRESENTATION_ITEM('')
SURFACE()
);
#2528=(
BOUNDED_SURFACE()
B_SPLINE_SURFACE(3,2,((#162647,#162648,#162649),(#162650,#162651,#162652),
(#162653,#162654,#162655),(#162656,#162657,#162658)),.UNSPECIFIED.,.F.,
 .F.,.F.)
B_SPLINE_SURFACE_WITH_KNOTS((4,4),(3,3),(0.,0.000504070263719173),(0.,1.),
 .UNSPECIFIED.)
GEOMETRIC_REPRESENTATION_ITEM()
RATIONAL_B_SPLINE_SURFACE(((1.,0.886316114436169,1.),(1.,0.886398092028818,
1.),(1.,0.886423525277845,1.),(1.,0.886392435202391,1.)))
REPRESENTATION_ITEM('')
SURFACE()
);
#2529=(
BOUNDED_SURFACE()
B_SPLINE_SURFACE(3,2,((#162662,#162663,#162664),(#162665,#162666,#162667),
(#162668,#162669,#162670),(#162671,#162672,#162673),(#162674,#162675,#162676),
(#162677,#162678,#162679),(#162680,#162681,#162682),(#162683,#162684,#162685),
(#162686,#162687,#162688),(#162689,#162690,#162691),(#162692,#162693,#162694),
(#162695,#162696,#162697)),.UNSPECIFIED.,.F.,.F.,.F.)
B_SPLINE_SURFACE_WITH_KNOTS((4,2,2,2,2,4),(3,3),(0.,0.000464847896993965,
0.00092969579398793,0.00116211974248491,0.00139454369098189,0.00185939158797586),
(0.,1.),.UNSPECIFIED.)
GEOMETRIC_REPRESENTATION_ITEM()
RATIONAL_B_SPLINE_SURFACE(((1.,0.713890629234418,1.),(1.,0.74043984709427,
1.),(1.,0.764405928904485,1.),(1.,0.806784773788238,1.),(1.,0.825414433535011,
1.),(1.,0.847876574774264,1.),(1.,0.854606009430438,1.),(1.,0.866028143804753,
1.),(1.,0.87079122929337,1.),(1.,0.882487982894785,1.),(1.,0.886433234017274,
1.),(1.,0.886392435203049,1.)))
REPRESENTATION_ITEM('')
SURFACE()
);
#2530=(
BOUNDED_SURFACE()
B_SPLINE_SURFACE(3,2,((#162835,#162836,#162837),(#162838,#162839,#162840),
(#162841,#162842,#162843),(#162844,#162845,#162846),(#162847,#162848,#162849),
(#162850,#162851,#162852),(#162853,#162854,#162855),(#162856,#162857,#162858),
(#162859,#162860,#162861),(#162862,#162863,#162864)),.UNSPECIFIED.,.F.,
 .F.,.F.)
B_SPLINE_SURFACE_WITH_KNOTS((4,2,2,2,4),(3,3),(-1.01915004213637E-17,0.00045240064920256,
0.00090480129840513,0.0013572019476077,0.00180960259681027),(0.,1.),
 .UNSPECIFIED.)
GEOMETRIC_REPRESENTATION_ITEM()
RATIONAL_B_SPLINE_SURFACE(((1.,0.843854525155974,1.),(1.,0.840228746359808,
1.),(1.,0.833848718540882,1.),(1.,0.81605021807051,1.),(1.,0.804487259154749,
1.),(1.,0.775654382443571,1.),(1.,0.758435167636249,1.),(1.,0.716870923938366,
1.),(1.,0.693173303079418,1.),(1.,0.665190809887608,1.)))
REPRESENTATION_ITEM('')
SURFACE()
);
#2531=(
BOUNDED_SURFACE()
B_SPLINE_SURFACE(3,2,((#162989,#162990,#162991),(#162992,#162993,#162994),
(#162995,#162996,#162997),(#162998,#162999,#163000)),.UNSPECIFIED.,.F.,
 .F.,.F.)
B_SPLINE_SURFACE_WITH_KNOTS((4,4),(3,3),(0.,0.000504443591143906),(0.,1.),
 .UNSPECIFIED.)
GEOMETRIC_REPRESENTATION_ITEM()
RATIONAL_B_SPLINE_SURFACE(((1.,0.843854525156016,1.),(1.,0.841969285469978,
1.),(1.,0.840014967913779,1.),(1.,0.837989542743208,1.)))
REPRESENTATION_ITEM('')
SURFACE()
);
#2532=(
BOUNDED_SURFACE()
B_SPLINE_SURFACE(3,2,((#163004,#163005,#163006),(#163007,#163008,#163009),
(#163010,#163011,#163012),(#163013,#163014,#163015),(#163016,#163017,#163018),
(#163019,#163020,#163021)),.UNSPECIFIED.,.F.,.F.,.F.)
B_SPLINE_SURFACE_WITH_KNOTS((4,2,4),(3,3),(-0.000158597896262736,0.000792989481313416,
0.00174457685888895),(-0.00240453499929849,1.),.UNSPECIFIED.)
GEOMETRIC_REPRESENTATION_ITEM()
RATIONAL_B_SPLINE_SURFACE(((1.00127175946673,0.735549811688094,1.),(1.00101661270767,
0.788605134055686,1.),(1.00087469807204,0.81811492195007,1.),(1.00073907087598,
0.846317297066205,1.),(1.00074935587393,0.844178630349327,1.),(1.00080479888491,
0.832649787767144,1.)))
REPRESENTATION_ITEM('')
SURFACE()
);
#2533=(
BOUNDED_SURFACE()
B_SPLINE_SURFACE(3,2,((#163108,#163109,#163110),(#163111,#163112,#163113),
(#163114,#163115,#163116),(#163117,#163118,#163119)),.UNSPECIFIED.,.F.,
 .F.,.F.)
B_SPLINE_SURFACE_WITH_KNOTS((4,4),(3,3),(-3.25260651745652E-19,0.0007884708222344),
(0.,1.),.UNSPECIFIED.)
GEOMETRIC_REPRESENTATION_ITEM()
RATIONAL_B_SPLINE_SURFACE(((1.,0.639433225268789,1.),(1.,0.625985289878347,
1.),(1.,0.614551947533885,1.),(1.,0.61107365918432,1.)))
REPRESENTATION_ITEM('')
SURFACE()
);
#2534=(
BOUNDED_SURFACE()
B_SPLINE_SURFACE(3,2,((#163168,#163169,#163170),(#163171,#163172,#163173),
(#163174,#163175,#163176),(#163177,#163178,#163179)),.UNSPECIFIED.,.F.,
 .F.,.F.)
B_SPLINE_SURFACE_WITH_KNOTS((4,4),(3,3),(0.00330239163309442,0.00410592895993832),
(0.,1.),.UNSPECIFIED.)
GEOMETRIC_REPRESENTATION_ITEM()
RATIONAL_B_SPLINE_SURFACE(((1.,0.707106781186551,1.),(1.,0.682330721002586,
1.),(1.,0.657517255942454,1.),(1.,0.639433225268795,1.)))
REPRESENTATION_ITEM('')
SURFACE()
);
#2535=(
BOUNDED_SURFACE()
B_SPLINE_SURFACE(3,2,((#163214,#163215,#163216),(#163217,#163218,#163219),
(#163220,#163221,#163222),(#163223,#163224,#163225),(#163226,#163227,#163228),
(#163229,#163230,#163231),(#163232,#163233,#163234),(#163235,#163236,#163237),
(#163238,#163239,#163240),(#163241,#163242,#163243)),.UNSPECIFIED.,.F.,
 .F.,.F.)
B_SPLINE_SURFACE_WITH_KNOTS((4,2,2,2,4),(3,3),(-0.000159639322855436,0.000399098307138592,
0.000798196614277184,0.00119729492141578,0.0017560325514098),(0.,1.00227173482475),
 .UNSPECIFIED.)
GEOMETRIC_REPRESENTATION_ITEM()
RATIONAL_B_SPLINE_SURFACE(((1.,0.803036549228823,1.00089489746064),(1.,
0.806208297931994,1.00088048671667),(1.,0.80375514797508,1.00089163252905),
(1.,0.791668382001202,1.00094654838341),(1.,0.784235158170282,1.00098032101028),
(1.,0.766082876391421,1.00106279535161),(1.,0.755212647809181,1.00111218390526),
(1.,0.727204596596005,1.00123943763589),(1.,0.708752138742072,1.00132327581811),
(1.,0.691327715635498,1.00140244315565)))
REPRESENTATION_ITEM('')
SURFACE()
);
#2536=(
BOUNDED_SURFACE()
B_SPLINE_SURFACE(3,2,((#163315,#163316,#163317),(#163318,#163319,#163320),
(#163321,#163322,#163323),(#163324,#163325,#163326),(#163327,#163328,#163329),
(#163330,#163331,#163332),(#163333,#163334,#163335),(#163336,#163337,#163338),
(#163339,#163340,#163341),(#163342,#163343,#163344)),.UNSPECIFIED.,.F.,
 .F.,.F.)
B_SPLINE_SURFACE_WITH_KNOTS((4,2,2,2,4),(3,3),(0.,0.000408689684844658,
0.000817379369689317,0.00122606905453398,0.00163475873937863),(0.,1.),
 .UNSPECIFIED.)
GEOMETRIC_REPRESENTATION_ITEM()
RATIONAL_B_SPLINE_SURFACE(((1.,0.707106781186864,1.),(1.,0.688970136944317,
1.),(1.,0.670689426918774,1.),(1.,0.634705388858963,1.),(1.,0.617712576312848,
1.),(1.,0.58736619029857,1.),(1.,0.574575334017929,1.),(1.,0.556620432342278,
1.),(1.,0.551687087704826,1.),(1.,0.55167311003777,1.)))
REPRESENTATION_ITEM('')
SURFACE()
);
#2537=(
BOUNDED_SURFACE()
B_SPLINE_SURFACE(3,2,((#163467,#163468,#163469),(#163470,#163471,#163472),
(#163473,#163474,#163475),(#163476,#163477,#163478)),.UNSPECIFIED.,.F.,
 .F.,.F.)
B_SPLINE_SURFACE_WITH_KNOTS((4,4),(3,3),(-6.10910588200899E-5,0.000672001647020572),
(-0.000116090865111071,1.),.UNSPECIFIED.)
GEOMETRIC_REPRESENTATION_ITEM()
RATIONAL_B_SPLINE_SURFACE(((1.00004877735551,0.789917339908843,1.),(1.00005479149462,
0.764014616617302,1.),(1.00006214451632,0.73234536470319,1.),(1.00006995490833,
0.698706232130948,1.)))
REPRESENTATION_ITEM('')
SURFACE()
);
#2538=(
BOUNDED_SURFACE()
B_SPLINE_SURFACE(3,2,((#163526,#163527,#163528),(#163529,#163530,#163531),
(#163532,#163533,#163534),(#163535,#163536,#163537)),.UNSPECIFIED.,.F.,
 .F.,.F.)
B_SPLINE_SURFACE_WITH_KNOTS((4,4),(3,3),(0.,0.00123332093723591),(0.,1.),
 .UNSPECIFIED.)
GEOMETRIC_REPRESENTATION_ITEM()
RATIONAL_B_SPLINE_SURFACE(((1.,0.903978945212084,1.),(1.,0.925250261712233,
1.),(1.,0.940236171156205,1.),(1.,0.947923524237147,1.)))
REPRESENTATION_ITEM('')
SURFACE()
);
#2539=(
BOUNDED_SURFACE()
B_SPLINE_SURFACE(3,2,((#163612,#163613,#163614),(#163615,#163616,#163617),
(#163618,#163619,#163620),(#163621,#163622,#163623),(#163624,#163625,#163626),
(#163627,#163628,#163629)),.UNSPECIFIED.,.F.,.F.,.F.)
B_SPLINE_SURFACE_WITH_KNOTS((4,2,4),(3,3),(-2.91766628346879E-5,0.000512893057734432,
0.00105496277830351),(-0.00146324405675922,1.00002917666283),
 .UNSPECIFIED.)
GEOMETRIC_REPRESENTATION_ITEM()
RATIONAL_B_SPLINE_SURFACE(((1.00054781718412,0.812801839713216,1.00001090767416),
(1.0005478023828,0.812806897568977,1.00001090737945),(1.00055033964304,
0.811939873927939,1.00001095789923),(1.00057518372836,0.80345024052436,
1.00001145257373),(1.00059830034578,0.795550911371957,1.00001191285233),
(1.00064180365305,0.780685114305911,1.00001277905353)))
REPRESENTATION_ITEM('')
SURFACE()
);
#2540=(
BOUNDED_SURFACE()
B_SPLINE_SURFACE(3,2,((#163651,#163652,#163653),(#163654,#163655,#163656),
(#163657,#163658,#163659),(#163660,#163661,#163662),(#163663,#163664,#163665),
(#163666,#163667,#163668)),.UNSPECIFIED.,.F.,.F.,.F.)
B_SPLINE_SURFACE_WITH_KNOTS((4,2,4),(3,3),(-4.77048955893622E-18,0.00191432655883667,
0.00382865311767335),(0.,1.),.UNSPECIFIED.)
GEOMETRIC_REPRESENTATION_ITEM()
RATIONAL_B_SPLINE_SURFACE(((1.,0.903978945212085,1.),(1.,0.877037193452108,
1.),(1.,0.847703426978615,1.),(1.,0.782785838918396,1.),(1.,0.74722569047758,
1.),(1.,0.707106781186548,1.)))
REPRESENTATION_ITEM('')
SURFACE()
);
#2541=(
BOUNDED_SURFACE()
B_SPLINE_SURFACE(3,2,((#163760,#163761,#163762),(#163763,#163764,#163765),
(#163766,#163767,#163768),(#163769,#163770,#163771),(#163772,#163773,#163774),
(#163775,#163776,#163777)),.UNSPECIFIED.,.F.,.F.,.F.)
B_SPLINE_SURFACE_WITH_KNOTS((4,2,4),(3,3),(0.,0.785398163397448,1.5707963267949),
(0.,1.),.UNSPECIFIED.)
GEOMETRIC_REPRESENTATION_ITEM()
RATIONAL_B_SPLINE_SURFACE(((1.,0.656059028990507,1.),(1.,0.655948674699894,
1.),(1.,0.661819490286433,1.),(1.,0.681005707982038,1.),(1.,0.694211427469109,
1.),(1.,0.707106781186548,1.)))
REPRESENTATION_ITEM('')
SURFACE()
);
#2542=(
BOUNDED_SURFACE()
B_SPLINE_SURFACE(3,2,((#163849,#163850,#163851),(#163852,#163853,#163854),
(#163855,#163856,#163857),(#163858,#163859,#163860),(#163861,#163862,#163863),
(#163864,#163865,#163866)),.UNSPECIFIED.,.F.,.F.,.F.)
B_SPLINE_SURFACE_WITH_KNOTS((4,2,4),(3,3),(1.5707963267949,2.35619449019234,
3.1415926535898),(0.,1.),.UNSPECIFIED.)
GEOMETRIC_REPRESENTATION_ITEM()
RATIONAL_B_SPLINE_SURFACE(((1.,0.707106781186548,1.),(1.,0.72003976564552,
1.),(1.,0.732392511163791,1.),(1.,0.749774985071113,1.),(1.,0.75478222211386,
1.),(1.,0.754709580222772,1.)))
REPRESENTATION_ITEM('')
SURFACE()
);
#2543=(
BOUNDED_SURFACE()
B_SPLINE_SURFACE(3,2,((#164070,#164071,#164072),(#164073,#164074,#164075),
(#164076,#164077,#164078),(#164079,#164080,#164081),(#164082,#164083,#164084),
(#164085,#164086,#164087)),.UNSPECIFIED.,.F.,.F.,.F.)
B_SPLINE_SURFACE_WITH_KNOTS((4,2,4),(3,3),(0.,0.785398163397448,1.5707963267949),
(0.,1.),.UNSPECIFIED.)
GEOMETRIC_REPRESENTATION_ITEM()
RATIONAL_B_SPLINE_SURFACE(((1.,0.656059028990507,1.),(1.,0.655948674699742,
1.),(1.,0.661819490286637,1.),(1.,0.681005707981833,1.),(1.,0.694211427469263,
1.),(1.,0.707106781186548,1.)))
REPRESENTATION_ITEM('')
SURFACE()
);
#2544=(
BOUNDED_SURFACE()
B_SPLINE_SURFACE(3,2,((#164159,#164160,#164161),(#164162,#164163,#164164),
(#164165,#164166,#164167),(#164168,#164169,#164170),(#164171,#164172,#164173),
(#164174,#164175,#164176)),.UNSPECIFIED.,.F.,.F.,.F.)
B_SPLINE_SURFACE_WITH_KNOTS((4,2,4),(3,3),(4.71238898038469,5.49778714378214,
6.28318530717959),(0.,1.),.UNSPECIFIED.)
GEOMETRIC_REPRESENTATION_ITEM()
RATIONAL_B_SPLINE_SURFACE(((1.,0.707106781186552,1.),(1.,0.720039765645528,
1.),(1.,0.732392511163776,1.),(1.,0.749774985071127,1.),(1.,0.754782222113857,
1.),(1.,0.754709580222772,1.)))
REPRESENTATION_ITEM('')
SURFACE()
);
#2545=(
BOUNDED_SURFACE()
B_SPLINE_SURFACE(3,2,((#164411,#164412,#164413),(#164414,#164415,#164416),
(#164417,#164418,#164419),(#164420,#164421,#164422),(#164423,#164424,#164425),
(#164426,#164427,#164428)),.UNSPECIFIED.,.F.,.F.,.F.)
B_SPLINE_SURFACE_WITH_KNOTS((4,2,4),(3,3),(0.0740543944727613,0.0811932403219739,
0.0883320861711864),(0.,1.),.UNSPECIFIED.)
GEOMETRIC_REPRESENTATION_ITEM()
RATIONAL_B_SPLINE_SURFACE(((1.,0.918849788108586,1.),(1.,0.921623427170992,
1.),(1.,0.924482745526459,1.),(1.,0.930368049939493,1.),(1.,0.933390296558584,
1.),(1.,0.936467000373499,1.)))
REPRESENTATION_ITEM('')
SURFACE()
);
#2546=(
BOUNDED_SURFACE()
B_SPLINE_SURFACE(3,2,((#164641,#164642,#164643),(#164644,#164645,#164646),
(#164647,#164648,#164649),(#164650,#164651,#164652),(#164653,#164654,#164655),
(#164656,#164657,#164658)),.UNSPECIFIED.,.F.,.F.,.F.)
B_SPLINE_SURFACE_WITH_KNOTS((4,2,4),(3,3),(0.269041526988586,0.27511900362718,
0.281196480265774),(0.,1.),.UNSPECIFIED.)
GEOMETRIC_REPRESENTATION_ITEM()
RATIONAL_B_SPLINE_SURFACE(((1.,0.936757701036177,1.),(1.,0.939378149853558,
1.),(1.,0.942051042550488,1.),(1.,0.947449038066665,1.),(1.,0.950158897999453,
1.),(1.,0.952840299126697,1.)))
REPRESENTATION_ITEM('')
SURFACE()
);
#2547=(
BOUNDED_SURFACE()
B_SPLINE_SURFACE(3,2,((#164959,#164960,#164961),(#164962,#164963,#164964),
(#164965,#164966,#164967),(#164968,#164969,#164970)),.UNSPECIFIED.,.F.,
 .F.,.F.)
B_SPLINE_SURFACE_WITH_KNOTS((4,4),(3,3),(0.,0.0174508326761739),(0.,1.),
 .UNSPECIFIED.)
GEOMETRIC_REPRESENTATION_ITEM()
RATIONAL_B_SPLINE_SURFACE(((1.,0.472392340793765,1.),(1.,0.485682667654673,
1.),(1.,0.49679147679375,1.),(1.,0.506538946041787,1.)))
REPRESENTATION_ITEM('')
SURFACE()
);
#2548=(
BOUNDED_SURFACE()
B_SPLINE_SURFACE(3,2,((#164996,#164997,#164998),(#164999,#165000,#165001),
(#165002,#165003,#165004),(#165005,#165006,#165007),(#165008,#165009,#165010),
(#165011,#165012,#165013),(#165014,#165015,#165016),(#165017,#165018,#165019)),
 .UNSPECIFIED.,.F.,.F.,.F.)
B_SPLINE_SURFACE_WITH_KNOTS((4,2,2,4),(3,3),(0.,0.0013193848583342,0.00263876971666841,
0.00527753943333681),(0.,1.),.UNSPECIFIED.)
GEOMETRIC_REPRESENTATION_ITEM()
RATIONAL_B_SPLINE_SURFACE(((1.,0.472392340793765,1.),(1.,0.494569863951139,
1.),(1.,0.516028114800238,1.),(1.,0.557651118782376,1.),(1.,0.577819616806839,
1.),(1.,0.636749517047671,1.),(1.,0.673107462854922,1.),(1.,0.707106781186548,
1.)))
REPRESENTATION_ITEM('')
SURFACE()
);
#2549=(
BOUNDED_SURFACE()
B_SPLINE_SURFACE(3,2,((#165054,#165055,#165056),(#165057,#165058,#165059),
(#165060,#165061,#165062),(#165063,#165064,#165065),(#165066,#165067,#165068),
(#165069,#165070,#165071),(#165072,#165073,#165074),(#165075,#165076,#165077)),
 .UNSPECIFIED.,.F.,.F.,.F.)
B_SPLINE_SURFACE_WITH_KNOTS((4,2,2,4),(3,3),(-0.000342067638939368,0.00263855694108943,
0.00395783541163415,0.00561918145328965),(-0.00153661657981784,1.),
 .UNSPECIFIED.)
GEOMETRIC_REPRESENTATION_ITEM()
RATIONAL_B_SPLINE_SURFACE(((1.00086096519304,0.71985035032541,1.),(1.00097794016698,
0.681787838351873,1.),(1.00110163105103,0.641540034937012,1.),(1.00129767452272,
0.577749407442451,1.),(1.00136056639245,0.557285008399528,1.),(1.00150619096957,
0.509900195875283,1.),(1.00159023347395,0.482553587266646,1.),(1.00167739996307,
0.454190464588956,1.)))
REPRESENTATION_ITEM('')
SURFACE()
);
#2550=(
BOUNDED_SURFACE()
B_SPLINE_SURFACE(3,2,((#165096,#165097,#165098),(#165099,#165100,#165101),
(#165102,#165103,#165104),(#165105,#165106,#165107)),.UNSPECIFIED.,.F.,
 .F.,.F.)
B_SPLINE_SURFACE_WITH_KNOTS((4,4),(3,3),(6.93889390390723E-18,0.0177264565684137),
(0.,1.),.UNSPECIFIED.)
GEOMETRIC_REPRESENTATION_ITEM()
RATIONAL_B_SPLINE_SURFACE(((1.,0.506999357883079,1.),(1.,0.497142617029225,
1.),(1.,0.485892200859361,1.),(1.,0.472392340793768,1.)))
REPRESENTATION_ITEM('')
SURFACE()
);
#2551=(
BOUNDED_SURFACE()
B_SPLINE_SURFACE(3,2,((#165114,#165115,#165116),(#165117,#165118,#165119),
(#165120,#165121,#165122),(#165123,#165124,#165125),(#165126,#165127,#165128),
(#165129,#165130,#165131),(#165132,#165133,#165134),(#165135,#165136,#165137)),
 .UNSPECIFIED.,.F.,.F.,.F.)
B_SPLINE_SURFACE_WITH_KNOTS((4,2,2,4),(3,3),(-2.83789918648081E-17,0.000158415844625727,
0.000316831689251482,0.000633663378502992),(0.,1.),.UNSPECIFIED.)
GEOMETRIC_REPRESENTATION_ITEM()
RATIONAL_B_SPLINE_SURFACE(((1.,0.506999357883079,1.),(1.,0.518705031372287,
1.),(1.,0.533099046918872,1.),(1.,0.565407295868411,1.),(1.,0.582886848388227,
1.),(1.,0.636421215472814,1.),(1.,0.67314781771756,1.),(1.,0.707106781186543,
1.)))
REPRESENTATION_ITEM('')
SURFACE()
);
#2552=(
BOUNDED_SURFACE()
B_SPLINE_SURFACE(3,2,((#165157,#165158,#165159),(#165160,#165161,#165162),
(#165163,#165164,#165165),(#165166,#165167,#165168),(#165169,#165170,#165171),
(#165172,#165173,#165174),(#165175,#165176,#165177),(#165178,#165179,#165180),
(#165181,#165182,#165183),(#165184,#165185,#165186)),.UNSPECIFIED.,.F.,
 .F.,.F.)
B_SPLINE_SURFACE_WITH_KNOTS((4,2,2,2,4),(3,3),(-8.88178419700125E-16,0.392699081698724,
0.785398163397448,1.17809724509617,1.5707963267949),(0.,1.),
 .UNSPECIFIED.)
GEOMETRIC_REPRESENTATION_ITEM()
RATIONAL_B_SPLINE_SURFACE(((1.,0.656059028990507,1.),(1.,0.65605119607191,
1.),(1.,0.657443209221259,1.),(1.,0.662724068472642,1.),(1.,0.666616044204551,
1.),(1.,0.676209154063925,1.),(1.,0.681903435451068,1.),(1.,0.694134907060979,
1.),(1.,0.70066637883416,1.),(1.,0.707106781186548,1.)))
REPRESENTATION_ITEM('')
SURFACE()
);
#2553=(
BOUNDED_SURFACE()
B_SPLINE_SURFACE(3,2,((#165246,#165247,#165248),(#165249,#165250,#165251),
(#165252,#165253,#165254),(#165255,#165256,#165257),(#165258,#165259,#165260),
(#165261,#165262,#165263),(#165264,#165265,#165266),(#165267,#165268,#165269),
(#165270,#165271,#165272),(#165273,#165274,#165275)),.UNSPECIFIED.,.F.,
 .F.,.F.)
B_SPLINE_SURFACE_WITH_KNOTS((4,2,2,2,4),(3,3),(4.71238898038469,5.10508806208341,
5.49778714378214,5.89048622548086,6.28318530717959),(0.,1.),
 .UNSPECIFIED.)
GEOMETRIC_REPRESENTATION_ITEM()
RATIONAL_B_SPLINE_SURFACE(((1.,0.707106781186552,1.),(1.,0.713550261851565,
1.),(1.,0.719894264862192,1.),(1.,0.731490756397333,1.),(1.,0.736738129296254,
1.),(1.,0.745429366938654,1.),(1.,0.748871927696603,1.),(1.,0.753512297096217,
1.),(1.,0.754714219730812,1.),(1.,0.754709580222777,1.)))
REPRESENTATION_ITEM('')
SURFACE()
);
#2554=(
BOUNDED_SURFACE()
B_SPLINE_SURFACE(3,2,((#165292,#165293,#165294),(#165295,#165296,#165297),
(#165298,#165299,#165300),(#165301,#165302,#165303),(#165304,#165305,#165306),
(#165307,#165308,#165309)),.UNSPECIFIED.,.F.,.F.,.F.)
B_SPLINE_SURFACE_WITH_KNOTS((4,2,4),(3,3),(-6.49900913755202E-5,0.000324950456877623,
0.000714891005130771),(-0.0004124377275279,1.),.UNSPECIFIED.)
GEOMETRIC_REPRESENTATION_ITEM()
RATIONAL_B_SPLINE_SURFACE(((1.0002597372525,0.685119431172141,1.),(1.00022332133393,
0.7292666031402,1.),(1.00018870296933,0.771234592847265,1.),(1.00013212596193,
0.839823137995945,1.),(1.00010945519713,0.867307001975368,1.),(1.00009818284526,
0.880972521781153,1.)))
REPRESENTATION_ITEM('')
SURFACE()
);
#2555=(
BOUNDED_SURFACE()
B_SPLINE_SURFACE(3,2,((#165334,#165335,#165336),(#165337,#165338,#165339),
(#165340,#165341,#165342),(#165343,#165344,#165345)),.UNSPECIFIED.,.F.,
 .F.,.F.)
B_SPLINE_SURFACE_WITH_KNOTS((4,4),(3,3),(-6.93889390390723E-18,0.0138038180377133),
(0.,1.),.UNSPECIFIED.)
GEOMETRIC_REPRESENTATION_ITEM()
RATIONAL_B_SPLINE_SURFACE(((1.,0.888620714475959,1.),(1.,0.882992994712188,
1.),(1.,0.877840677983261,1.),(1.,0.873073026815702,1.)))
REPRESENTATION_ITEM('')
SURFACE()
);
#2556=(
BOUNDED_SURFACE()
B_SPLINE_SURFACE(3,2,((#165352,#165353,#165354),(#165355,#165356,#165357),
(#165358,#165359,#165360),(#165361,#165362,#165363),(#165364,#165365,#165366),
(#165367,#165368,#165369),(#165370,#165371,#165372),(#165373,#165374,#165375)),
 .UNSPECIFIED.,.F.,.F.,.F.)
B_SPLINE_SURFACE_WITH_KNOTS((4,2,2,4),(3,3),(0.,0.00140148291572316,0.00280296583144632,
0.00560593166289265),(0.,1.),.UNSPECIFIED.)
GEOMETRIC_REPRESENTATION_ITEM()
RATIONAL_B_SPLINE_SURFACE(((1.,0.888620714475959,1.),(1.,0.876376872535401,
1.),(1.,0.863367339892611,1.),(1.,0.835880005025182,1.),(1.,0.821403024634208,
1.),(1.,0.775582050820272,1.),(1.,0.742820617730576,1.),(1.,0.707106781185993,
1.)))
REPRESENTATION_ITEM('')
SURFACE()
);
#2557=(
BOUNDED_SURFACE()
B_SPLINE_SURFACE(3,2,((#165401,#165402,#165403),(#165404,#165405,#165406),
(#165407,#165408,#165409),(#165410,#165411,#165412),(#165413,#165414,#165415),
(#165416,#165417,#165418),(#165419,#165420,#165421),(#165422,#165423,#165424)),
 .UNSPECIFIED.,.F.,.F.,.F.)
B_SPLINE_SURFACE_WITH_KNOTS((4,2,2,4),(3,3),(0.,0.00280275939636971,0.00420413909455456,
0.00560551879273941),(0.,1.),.UNSPECIFIED.)
GEOMETRIC_REPRESENTATION_ITEM()
RATIONAL_B_SPLINE_SURFACE(((1.,0.707106781186548,1.),(1.,0.742840106247676,
1.),(1.,0.77545596336237,1.),(1.,0.821038365376531,1.),(1.,0.835714486585925,
1.),(1.,0.863346562356171,1.),(1.,0.876386389875133,1.),(1.,0.888620714475965,
1.)))
REPRESENTATION_ITEM('')
SURFACE()
);
#2558=(
BOUNDED_SURFACE()
B_SPLINE_SURFACE(3,2,((#165443,#165444,#165445),(#165446,#165447,#165448),
(#165449,#165450,#165451),(#165452,#165453,#165454)),.UNSPECIFIED.,.F.,
 .F.,.F.)
B_SPLINE_SURFACE_WITH_KNOTS((4,4),(3,3),(-6.93889390390723E-18,0.0135258923233721),
(0.,1.),.UNSPECIFIED.)
GEOMETRIC_REPRESENTATION_ITEM()
RATIONAL_B_SPLINE_SURFACE(((1.,0.873361457045398,1.),(1.,0.878048383336236,
1.),(1.,0.883106305929072,1.),(1.,0.888620714475961,1.)))
REPRESENTATION_ITEM('')
SURFACE()
);
#2559=(
BOUNDED_SURFACE()
B_SPLINE_SURFACE(3,2,((#165461,#165462,#165463),(#165464,#165465,#165466),
(#165467,#165468,#165469),(#165470,#165471,#165472),(#165473,#165474,#165475),
(#165476,#165477,#165478)),.UNSPECIFIED.,.F.,.F.,.F.)
B_SPLINE_SURFACE_WITH_KNOTS((4,2,4),(3,3),(-6.47810798060089E-18,0.000325048915579083,
0.000650097831158172),(0.,1.),.UNSPECIFIED.)
GEOMETRIC_REPRESENTATION_ITEM()
RATIONAL_B_SPLINE_SURFACE(((1.,0.873361457045401,1.),(1.,0.85849847792363,
1.),(1.,0.834696857457215,1.),(1.,0.77714142509596,1.),(1.,0.743612803250452,
1.),(1.,0.707106781186552,1.)))
REPRESENTATION_ITEM('')
SURFACE()
);
#2560=(
BOUNDED_SURFACE()
B_SPLINE_SURFACE(3,2,((#165671,#165672,#165673),(#165674,#165675,#165676),
(#165677,#165678,#165679),(#165680,#165681,#165682),(#165683,#165684,#165685),
(#165686,#165687,#165688),(#165689,#165690,#165691),(#165692,#165693,#165694)),
 .UNSPECIFIED.,.F.,.F.,.F.)
B_SPLINE_SURFACE_WITH_KNOTS((4,2,2,4),(3,3),(0.,0.000351812098911224,0.000527718148366836,
0.000703624197822447),(0.,1.),.UNSPECIFIED.)
GEOMETRIC_REPRESENTATION_ITEM()
RATIONAL_B_SPLINE_SURFACE(((1.,0.707106781186548,1.),(1.,0.666004685610564,
1.),(1.,0.620075381085077,1.),(1.,0.549819108711631,1.),(1.,0.525790037137517,
1.),(1.,0.479829608303299,1.),(1.,0.458216765529125,1.),(1.,0.439917019807004,
1.)))
REPRESENTATION_ITEM('')
SURFACE()
);
#2561=(
BOUNDED_SURFACE()
B_SPLINE_SURFACE(3,2,((#165716,#165717,#165718),(#165719,#165720,#165721),
(#165722,#165723,#165724),(#165725,#165726,#165727)),.UNSPECIFIED.,.F.,
 .F.,.F.)
B_SPLINE_SURFACE_WITH_KNOTS((4,4),(3,3),(-5.03069808033274E-17,0.00385726433182564),
(0.,1.),.UNSPECIFIED.)
GEOMETRIC_REPRESENTATION_ITEM()
RATIONAL_B_SPLINE_SURFACE(((1.,0.430570049114201,1.),(1.,0.433791974258431,
1.),(1.,0.436904245661489,1.),(1.,0.439917019807019,1.)))
REPRESENTATION_ITEM('')
SURFACE()
);
#2562=(
BOUNDED_SURFACE()
B_SPLINE_SURFACE(3,2,((#165734,#165735,#165736),(#165737,#165738,#165739),
(#165740,#165741,#165742),(#165743,#165744,#165745),(#165746,#165747,#165748),
(#165749,#165750,#165751),(#165752,#165753,#165754),(#165755,#165756,#165757),
(#165758,#165759,#165760),(#165761,#165762,#165763),(#165764,#165765,#165766),
(#165767,#165768,#165769)),.UNSPECIFIED.,.F.,.F.,.F.)
B_SPLINE_SURFACE_WITH_KNOTS((4,2,2,2,2,4),(3,3),(0.,0.00157461356268982,
0.00236192034403473,0.00314922712537965,0.00472384068806947,0.0062984542507593),
(0.,1.),.UNSPECIFIED.)
GEOMETRIC_REPRESENTATION_ITEM()
RATIONAL_B_SPLINE_SURFACE(((1.,0.430570049114667,1.),(1.,0.457560960025303,
1.),(1.,0.483459257940472,1.),(1.,0.520841505371429,1.),(1.,0.533061067348069,
1.),(1.,0.557070570158285,1.),(1.,0.5688948619132,1.),(1.,0.603453431912179,
1.),(1.,0.625340642509566,1.),(1.,0.667408719974356,1.),(1.,0.687583394050722,
1.),(1.,0.707106781186543,1.)))
REPRESENTATION_ITEM('')
SURFACE()
);
#2563=(
BOUNDED_SURFACE()
B_SPLINE_SURFACE(3,2,((#165795,#165796,#165797),(#165798,#165799,#165800),
(#165801,#165802,#165803),(#165804,#165805,#165806),(#165807,#165808,#165809),
(#165810,#165811,#165812),(#165813,#165814,#165815),(#165816,#165817,#165818),
(#165819,#165820,#165821),(#165822,#165823,#165824)),.UNSPECIFIED.,.F.,
 .F.,.F.)
B_SPLINE_SURFACE_WITH_KNOTS((4,2,2,2,4),(3,3),(0.,0.00157421549227777,0.00314843098455553,
0.0047226464768333,0.00629686196911106),(0.,1.),.UNSPECIFIED.)
GEOMETRIC_REPRESENTATION_ITEM()
RATIONAL_B_SPLINE_SURFACE(((1.,0.707106781187362,1.),(1.,0.68758289696825,
1.),(1.,0.667417078226011,1.),(1.,0.625390824237668,1.),(1.,0.60353633747147,
1.),(1.,0.557559397493831,1.),(1.,0.533401321926016,1.),(1.,0.483474255638482,
1.),(1.,0.457551920277023,1.),(1.,0.430570049114227,1.)))
REPRESENTATION_ITEM('')
SURFACE()
);
#2564=(
BOUNDED_SURFACE()
B_SPLINE_SURFACE(3,2,((#165843,#165844,#165845),(#165846,#165847,#165848),
(#165849,#165850,#165851),(#165852,#165853,#165854)),.UNSPECIFIED.,.F.,
 .F.,.F.)
B_SPLINE_SURFACE_WITH_KNOTS((4,4),(3,3),(0.,0.00414272899747597),(0.,1.),
 .UNSPECIFIED.)
GEOMETRIC_REPRESENTATION_ITEM()
RATIONAL_B_SPLINE_SURFACE(((1.,0.440584280700845,1.),(1.,0.437364321804866,
1.),(1.,0.434030421143282,1.),(1.,0.43057004911423,1.)))
REPRESENTATION_ITEM('')
SURFACE()
);
#2565=(
BOUNDED_SURFACE()
B_SPLINE_SURFACE(3,2,((#165861,#165862,#165863),(#165864,#165865,#165866),
(#165867,#165868,#165869),(#165870,#165871,#165872),(#165873,#165874,#165875),
(#165876,#165877,#165878),(#165879,#165880,#165881),(#165882,#165883,#165884),
(#165885,#165886,#165887),(#165888,#165889,#165890)),.UNSPECIFIED.,.F.,
 .F.,.F.)
B_SPLINE_SURFACE_WITH_KNOTS((4,2,2,2,4),(3,3),(-6.16097884514888E-17,0.000175529658750937,
0.000351059317501936,0.000526588976252934,0.000702118635003933),(0.,1.),
 .UNSPECIFIED.)
GEOMETRIC_REPRESENTATION_ITEM()
RATIONAL_B_SPLINE_SURFACE(((1.,0.440584280700845,1.),(1.,0.458788905458512,
1.),(1.,0.480391768923104,1.),(1.,0.526541516020855,1.),(1.,0.550240391579637,
1.),(1.,0.597052366816548,1.),(1.,0.620407250394368,1.),(1.,0.664886737818671,
1.),(1.,0.686305427599538,1.),(1.,0.707106781186548,1.)))
REPRESENTATION_ITEM('')
SURFACE()
);
#2566=(
BOUNDED_SURFACE()
B_SPLINE_SURFACE(3,2,((#165910,#165911,#165912),(#165913,#165914,#165915),
(#165916,#165917,#165918),(#165919,#165920,#165921),(#165922,#165923,#165924),
(#165925,#165926,#165927),(#165928,#165929,#165930),(#165931,#165932,#165933),
(#165934,#165935,#165936),(#165937,#165938,#165939)),.UNSPECIFIED.,.F.,
 .F.,.F.)
B_SPLINE_SURFACE_WITH_KNOTS((4,2,2,2,4),(3,3),(-8.88178419700125E-16,0.392699081698724,
0.785398163397448,1.17809724509617,1.5707963267949),(0.,1.),
 .UNSPECIFIED.)
GEOMETRIC_REPRESENTATION_ITEM()
RATIONAL_B_SPLINE_SURFACE(((1.,0.656059028990513,1.),(1.,0.656051196071901,
1.),(1.,0.657443209221259,1.),(1.,0.662724068472642,1.),(1.,0.666616044204551,
1.),(1.,0.676209154063925,1.),(1.,0.681903435451265,1.),(1.,0.694134907060781,
1.),(1.,0.70066637883431,1.),(1.,0.707106781186548,1.)))
REPRESENTATION_ITEM('')
SURFACE()
);
#2567=(
BOUNDED_SURFACE()
B_SPLINE_SURFACE(3,2,((#165987,#165988,#165989),(#165990,#165991,#165992),
(#165993,#165994,#165995),(#165996,#165997,#165998),(#165999,#166000,#166001),
(#166002,#166003,#166004),(#166005,#166006,#166007),(#166008,#166009,#166010),
(#166011,#166012,#166013),(#166014,#166015,#166016)),.UNSPECIFIED.,.F.,
 .F.,.F.)
B_SPLINE_SURFACE_WITH_KNOTS((4,2,2,2,4),(3,3),(0.00108313181642978,0.00175636478508586,
0.00242959775374195,0.00310283072239804,0.00377606369105412),(-0.000209460012389645,
1.),.UNSPECIFIED.)
GEOMETRIC_REPRESENTATION_ITEM()
RATIONAL_B_SPLINE_SURFACE(((1.00012272453498,0.707045431769307,1.),(1.00009434426233,
0.774791710231349,1.),(1.00007166829577,0.82892129397012,1.),(1.00004030861562,
0.903779687680096,1.),(1.00003179560245,0.924101020320203,1.),(1.0000315466092,
0.924695389732363,1.),(1.00003985538719,0.904861584947119,1.),(1.00007114262338,
0.830176121522307,1.),(1.00009383870826,0.775998513536397,1.),(1.00012272453498,
0.707045431769307,1.)))
REPRESENTATION_ITEM('')
SURFACE()
);
#2568=(
BOUNDED_SURFACE()
B_SPLINE_SURFACE(3,2,((#166095,#166096,#166097),(#166098,#166099,#166100),
(#166101,#166102,#166103),(#166104,#166105,#166106),(#166107,#166108,#166109),
(#166110,#166111,#166112),(#166113,#166114,#166115),(#166116,#166117,#166118),
(#166119,#166120,#166121),(#166122,#166123,#166124)),.UNSPECIFIED.,.F.,
 .F.,.F.)
B_SPLINE_SURFACE_WITH_KNOTS((4,2,2,2,4),(3,3),(4.71238898038469,5.10508806208341,
5.49778714378214,5.89048622548086,6.28318530717959),(0.,1.),
 .UNSPECIFIED.)
GEOMETRIC_REPRESENTATION_ITEM()
RATIONAL_B_SPLINE_SURFACE(((1.,0.707106781186552,1.),(1.,0.713550261851678,
1.),(1.,0.71989426486204,1.),(1.,0.731490756397489,1.),(1.,0.736738129296849,
1.),(1.,0.745429366938066,1.),(1.,0.748871927696599,1.),(1.,0.753512297096214,
1.),(1.,0.754714219730812,1.),(1.,0.754709580222777,1.)))
REPRESENTATION_ITEM('')
SURFACE()
);
#2569=(
BOUNDED_SURFACE()
B_SPLINE_SURFACE(3,2,((#166135,#166136,#166137),(#166138,#166139,#166140),
(#166141,#166142,#166143),(#166144,#166145,#166146)),.UNSPECIFIED.,.F.,
 .F.,.F.)
B_SPLINE_SURFACE_WITH_KNOTS((4,4),(3,3),(-1.68213967061126E-16,0.000120540380538488),
(0.,1.),.UNSPECIFIED.)
GEOMETRIC_REPRESENTATION_ITEM()
RATIONAL_B_SPLINE_SURFACE(((1.,0.819851970694933,1.),(1.,0.826338730586804,
1.),(1.,0.831810971765196,1.),(1.,0.836255146268139,1.)))
REPRESENTATION_ITEM('')
SURFACE()
);
#2570=(
BOUNDED_SURFACE()
B_SPLINE_SURFACE(3,2,((#166155,#166156,#166157),(#166158,#166159,#166160),
(#166161,#166162,#166163),(#166164,#166165,#166166),(#166167,#166168,#166169),
(#166170,#166171,#166172)),.UNSPECIFIED.,.F.,.F.,.F.)
B_SPLINE_SURFACE_WITH_KNOTS((4,2,4),(3,3),(0.,0.0128929585057523,0.0257859170115046),
(0.,1.),.UNSPECIFIED.)
GEOMETRIC_REPRESENTATION_ITEM()
RATIONAL_B_SPLINE_SURFACE(((1.,0.862148985649771,1.),(1.,0.857001824466315,
1.),(1.,0.852340953158334,1.),(1.,0.843773924789864,1.),(1.,0.839868090827823,
1.),(1.,0.83625514626814,1.)))
REPRESENTATION_ITEM('')
SURFACE()
);
#2571=(
BOUNDED_SURFACE()
B_SPLINE_SURFACE(3,2,((#166182,#166183,#166184),(#166185,#166186,#166187),
(#166188,#166189,#166190),(#166191,#166192,#166193),(#166194,#166195,#166196),
(#166197,#166198,#166199),(#166200,#166201,#166202),(#166203,#166204,#166205)),
 .UNSPECIFIED.,.F.,.F.,.F.)
B_SPLINE_SURFACE_WITH_KNOTS((4,2,2,4),(3,3),(-0.000114297678441313,0.00224905873968498,
0.00337358810952747,0.00461247683191633),(-0.000114359352546393,1.),
 .UNSPECIFIED.)
GEOMETRIC_REPRESENTATION_ITEM()
RATIONAL_B_SPLINE_SURFACE(((1.0000307769399,0.865437591192138,1.),(1.00003596191931,
0.842767913115381,1.),(1.0000416442543,0.817923705527529,1.),(1.00005085149573,
0.777667962443431,1.),(1.00005395268399,0.764109000325605,1.),(1.00006064498396,
0.734849041160352,1.),(1.00006427096229,0.718995600871095,1.),(1.00006803721689,
0.702528847114332,1.)))
REPRESENTATION_ITEM('')
SURFACE()
);
#2572=(
BOUNDED_SURFACE()
B_SPLINE_SURFACE(3,2,((#166228,#166229,#166230),(#166231,#166232,#166233),
(#166234,#166235,#166236),(#166237,#166238,#166239),(#166240,#166241,#166242),
(#166243,#166244,#166245)),.UNSPECIFIED.,.F.,.F.,.F.)
B_SPLINE_SURFACE_WITH_KNOTS((4,2,4),(3,3),(0.,0.00224843555189379,0.00449687110378757),
(0.,1.),.UNSPECIFIED.)
GEOMETRIC_REPRESENTATION_ITEM()
RATIONAL_B_SPLINE_SURFACE(((1.,0.707106781186548,1.),(1.,0.736791791485942,
1.),(1.,0.764326610725229,1.),(1.,0.81612979408374,1.),(1.,0.840519041516535,
1.),(1.,0.862148985649773,1.)))
REPRESENTATION_ITEM('')
SURFACE()
);
#2573=(
BOUNDED_SURFACE()
B_SPLINE_SURFACE(3,2,((#166273,#166274,#166275),(#166276,#166277,#166278),
(#166279,#166280,#166281),(#166282,#166283,#166284),(#166285,#166286,#166287),
(#166288,#166289,#166290)),.UNSPECIFIED.,.F.,.F.,.F.)
B_SPLINE_SURFACE_WITH_KNOTS((4,2,4),(3,3),(0.,0.0127570403976527,0.0255140807953054),
(0.,1.),.UNSPECIFIED.)
GEOMETRIC_REPRESENTATION_ITEM()
RATIONAL_B_SPLINE_SURFACE(((1.,0.83648401963888,1.),(1.,0.840071262854844,
1.),(1.,0.843946769546665,1.),(1.,0.852439323016447,1.),(1.,0.857056062862677,
1.),(1.,0.862148985649771,1.)))
REPRESENTATION_ITEM('')
SURFACE()
);
#2574=(
BOUNDED_SURFACE()
B_SPLINE_SURFACE(3,2,((#166346,#166347,#166348),(#166349,#166350,#166351),
(#166352,#166353,#166354),(#166355,#166356,#166357),(#166358,#166359,#166360),
(#166361,#166362,#166363)),.UNSPECIFIED.,.F.,.F.,.F.)
B_SPLINE_SURFACE_WITH_KNOTS((4,2,4),(3,3),(0.,0.000518347860385374,0.00103669572077075),
(0.,1.),.UNSPECIFIED.)
GEOMETRIC_REPRESENTATION_ITEM()
RATIONAL_B_SPLINE_SURFACE(((1.,0.819851970694872,1.),(1.,0.821199393891468,
1.),(1.,0.820620061026224,1.),(1.,0.813565992888811,1.),(1.,0.807280082867884,
1.),(1.,0.797551754323293,1.)))
REPRESENTATION_ITEM('')
SURFACE()
);
#2575=(
BOUNDED_SURFACE()
B_SPLINE_SURFACE(3,2,((#166377,#166378,#166379),(#166380,#166381,#166382),
(#166383,#166384,#166385),(#166386,#166387,#166388),(#166389,#166390,#166391),
(#166392,#166393,#166394),(#166395,#166396,#166397),(#166398,#166399,#166400),
(#166401,#166402,#166403),(#166404,#166405,#166406)),.UNSPECIFIED.,.F.,
 .F.,.F.)
B_SPLINE_SURFACE_WITH_KNOTS((4,2,2,2,4),(3,3),(0.,0.000158289020679031,
0.000316578041358062,0.000474867062037094,0.000633156082716125),(-0.000663546784200084,
1.),.UNSPECIFIED.)
GEOMETRIC_REPRESENTATION_ITEM()
RATIONAL_B_SPLINE_SURFACE(((1.00038895462537,0.70691243283309,1.),(1.00041168676458,
0.689783166476245,1.),(1.00043480575931,0.672362394282253,1.),(1.00048201433009,
0.636789491287992,1.),(1.00050649669526,0.618341383513315,1.),(1.00055382351628,
0.582679375841648,1.),(1.00057681572595,0.565354139539206,1.),(1.00062018464055,
0.532674518722848,1.),(1.00063973378298,0.517943724381941,1.),(1.00065530352718,
0.50621151154631,1.)))
REPRESENTATION_ITEM('')
SURFACE()
);
#2576=(
BOUNDED_SURFACE()
B_SPLINE_SURFACE(3,2,((#166442,#166443,#166444),(#166445,#166446,#166447),
(#166448,#166449,#166450),(#166451,#166452,#166453)),.UNSPECIFIED.,.F.,
 .F.,.F.)
B_SPLINE_SURFACE_WITH_KNOTS((4,4),(3,3),(0.00167806205423436,0.0019221164224989),
(0.,1.),.UNSPECIFIED.)
GEOMETRIC_REPRESENTATION_ITEM()
RATIONAL_B_SPLINE_SURFACE(((1.,0.83648401963888,1.),(1.,0.827500667105214,
1.),(1.,0.81402442184051,1.),(1.,0.797363061122239,1.)))
REPRESENTATION_ITEM('')
SURFACE()
);
#2577=(
BOUNDED_SURFACE()
B_SPLINE_SURFACE(3,2,((#166471,#166472,#166473),(#166474,#166475,#166476),
(#166477,#166478,#166479),(#166480,#166481,#166482),(#166483,#166484,#166485),
(#166486,#166487,#166488)),.UNSPECIFIED.,.F.,.F.,.F.)
B_SPLINE_SURFACE_WITH_KNOTS((4,2,4),(3,3),(-6.48707035919281E-5,0.000324353517959648,
0.000713577739511227),(-0.000405636278254878,1.),.UNSPECIFIED.)
GEOMETRIC_REPRESENTATION_ITEM()
RATIONAL_B_SPLINE_SURFACE(((1.00025537797947,0.685213092166142,1.),(1.00021971394,
0.729173705886148,1.),(1.00018580256851,0.770973926060662,1.),(1.0001303846956,
0.839283734482019,1.),(1.0001081970018,0.866632981809814,1.),(1.00009717328087,
0.88022116601206,1.)))
REPRESENTATION_ITEM('')
SURFACE()
);
#2578=(
BOUNDED_SURFACE()
B_SPLINE_SURFACE(3,2,((#166571,#166572,#166573),(#166574,#166575,#166576),
(#166577,#166578,#166579),(#166580,#166581,#166582)),.UNSPECIFIED.,.F.,
 .F.,.F.)
B_SPLINE_SURFACE_WITH_KNOTS((4,4),(3,3),(0.,0.0138879247081574),(0.,1.),
 .UNSPECIFIED.)
GEOMETRIC_REPRESENTATION_ITEM()
RATIONAL_B_SPLINE_SURFACE(((1.,0.887998771276556,1.),(1.,0.882334484690674,
1.),(1.,0.877154223922122,1.),(1.,0.872364293278347,1.)))
REPRESENTATION_ITEM('')
SURFACE()
);
#2579=(
BOUNDED_SURFACE()
B_SPLINE_SURFACE(3,2,((#166589,#166590,#166591),(#166592,#166593,#166594),
(#166595,#166596,#166597),(#166598,#166599,#166600),(#166601,#166602,#166603),
(#166604,#166605,#166606),(#166607,#166608,#166609),(#166610,#166611,#166612)),
 .UNSPECIFIED.,.F.,.F.,.F.)
B_SPLINE_SURFACE_WITH_KNOTS((4,2,2,4),(3,3),(0.,0.00139422219513554,0.00278844439027108,
0.00557688878054216),(-0.000307172053122608,1.),.UNSPECIFIED.)
GEOMETRIC_REPRESENTATION_ITEM()
RATIONAL_B_SPLINE_SURFACE(((1.00006882843044,0.887964367629177,1.),(1.00007633423115,
0.875746783638711,1.),(1.00008430612713,0.862770512034486,1.),(1.00010114500028,
0.835360998417529,1.),(1.00011001146245,0.820928594689669,1.),(1.00013806798131,
0.775259533038872,1.),(1.00015813805149,0.742590431185938,1.),(1.00017999249442,
0.707016812574673,1.)))
REPRESENTATION_ITEM('')
SURFACE()
);
#2580=(
BOUNDED_SURFACE()
B_SPLINE_SURFACE(3,2,((#166638,#166639,#166640),(#166641,#166642,#166643),
(#166644,#166645,#166646),(#166647,#166648,#166649),(#166650,#166651,#166652),
(#166653,#166654,#166655),(#166656,#166657,#166658),(#166659,#166660,#166661)),
 .UNSPECIFIED.,.F.,.F.,.F.)
B_SPLINE_SURFACE_WITH_KNOTS((4,2,2,4),(3,3),(0.,0.00278824321172774,0.00418236481759161,
0.00557648642345548),(0.,1.),.UNSPECIFIED.)
GEOMETRIC_REPRESENTATION_ITEM()
RATIONAL_B_SPLINE_SURFACE(((1.,0.707106781186548,1.),(1.,0.742695591047798,
1.),(1.,0.775190977638611,1.),(1.,0.820614084370083,1.),(1.,0.835242277112269,
1.),(1.,0.862791265741296,1.),(1.,0.875794541967241,1.),(1.,0.887998771276056,
1.)))
REPRESENTATION_ITEM('')
SURFACE()
);
#2581=(
BOUNDED_SURFACE()
B_SPLINE_SURFACE(3,2,((#166680,#166681,#166682),(#166683,#166684,#166685),
(#166686,#166687,#166688),(#166689,#166690,#166691)),.UNSPECIFIED.,.F.,
 .F.,.F.)
B_SPLINE_SURFACE_WITH_KNOTS((4,4),(3,3),(0.,0.0141656229616797),(0.,1.),
 .UNSPECIFIED.)
GEOMETRIC_REPRESENTATION_ITEM()
RATIONAL_B_SPLINE_SURFACE(((1.,0.872077446583348,1.),(1.,0.876947206822174,
1.),(1.,0.882221222508023,1.),(1.,0.887998771276578,1.)))
REPRESENTATION_ITEM('')
SURFACE()
);
#2582=(
BOUNDED_SURFACE()
B_SPLINE_SURFACE(3,2,((#166698,#166699,#166700),(#166701,#166702,#166703),
(#166704,#166705,#166706),(#166707,#166708,#166709),(#166710,#166711,#166712),
(#166713,#166714,#166715)),.UNSPECIFIED.,.F.,.F.,.F.)
B_SPLINE_SURFACE_WITH_KNOTS((4,2,4),(3,3),(-6.48077526460634E-5,0.000324038763230374,
0.000712885279106823),(-0.000106163867131493,1.),.UNSPECIFIED.)
GEOMETRIC_REPRESENTATION_ITEM()
RATIONAL_B_SPLINE_SURFACE(((1.00002552144573,0.879801638625688,1.),(1.00002832831616,
0.866582120070106,1.),(1.00003408916573,0.839450244950509,1.),(1.00004864326935,
0.770904778322745,1.),(1.00005737063385,0.729801506857169,1.),(1.00006688410924,
0.684995888682771,1.)))
REPRESENTATION_ITEM('')
SURFACE()
);
#2583=(
BOUNDED_SURFACE()
B_SPLINE_SURFACE(3,2,((#166738,#166739,#166740),(#166741,#166742,#166743),
(#166744,#166745,#166746),(#166747,#166748,#166749),(#166750,#166751,#166752),
(#166753,#166754,#166755),(#166756,#166757,#166758),(#166759,#166760,#166761),
(#166762,#166763,#166764),(#166765,#166766,#166767)),.UNSPECIFIED.,.F.,
 .F.,.F.)
B_SPLINE_SURFACE_WITH_KNOTS((4,2,2,2,4),(3,3),(3.1415926535898,3.53429173528852,
3.92699081698724,4.31968989868597,4.71238898038469),(0.,1.),
 .UNSPECIFIED.)
GEOMETRIC_REPRESENTATION_ITEM()
RATIONAL_B_SPLINE_SURFACE(((1.,0.754709580222772,1.),(1.,0.754714219730848,
1.),(1.,0.753512297096158,1.),(1.,0.748871927696634,1.),(1.,0.745429366938649,
1.),(1.,0.736738129296255,1.),(1.,0.731490756397077,1.),(1.,0.719894264862441,
1.),(1.,0.713550261851367,1.),(1.,0.707106781186548,1.)))
REPRESENTATION_ITEM('')
SURFACE()
);
#2584=(
BOUNDED_SURFACE()
B_SPLINE_SURFACE(3,2,((#166816,#166817,#166818),(#166819,#166820,#166821),
(#166822,#166823,#166824),(#166825,#166826,#166827),(#166828,#166829,#166830),
(#166831,#166832,#166833),(#166834,#166835,#166836),(#166837,#166838,#166839),
(#166840,#166841,#166842),(#166843,#166844,#166845)),.UNSPECIFIED.,.F.,
 .F.,.F.)
B_SPLINE_SURFACE_WITH_KNOTS((4,2,2,2,4),(3,3),(1.5706633618744,1.96349540849362,
2.35619449019234,2.74889357189107,3.14172561851029),(0.,1.0001329649205),
 .UNSPECIFIED.)
GEOMETRIC_REPRESENTATION_ITEM()
RATIONAL_B_SPLINE_SURFACE(((1.,0.707074379515176,1.00007789766368),(1.,
0.700631001612551,1.00007961115014),(1.,0.694096308749504,1.00008134891997),
(1.,0.681861139767303,1.00008460261652),(1.,0.676166101239835,1.00008611709721),
(1.,0.666571715833371,1.00008866853059),(1.,0.662679222605223,1.0000897036607),
(1.,0.657396767036559,1.00009110842327),(1.,0.656004520314218,1.00009147866321),
(0.999999999999999,0.65601330534573,1.00009147632701)))
REPRESENTATION_ITEM('')
SURFACE()
);
#2585=(
BOUNDED_SURFACE()
B_SPLINE_SURFACE(3,2,((#166862,#166863,#166864),(#166865,#166866,#166867),
(#166868,#166869,#166870),(#166871,#166872,#166873),(#166874,#166875,#166876),
(#166877,#166878,#166879),(#166880,#166881,#166882),(#166883,#166884,#166885),
(#166886,#166887,#166888),(#166889,#166890,#166891)),.UNSPECIFIED.,.F.,
 .F.,.F.)
B_SPLINE_SURFACE_WITH_KNOTS((4,2,2,2,4),(3,3),(0.,0.000157845161260656,
0.000315690322521312,0.000473535483781968,0.000631380645042625),(-0.000656128803624682,
1.),.UNSPECIFIED.)
GEOMETRIC_REPRESENTATION_ITEM()
RATIONAL_B_SPLINE_SURFACE(((1.00038460353849,0.706914605509298,1.),(1.00040690056226,
0.689923258963295,1.),(1.00042956531064,0.672651689525801,1.),(1.00047581616045,
0.637406437715701,1.),(1.00049979042774,0.619136955291255,1.),(1.00054610047252,
0.583846594218537,1.),(1.00056857293538,0.566721555097505,1.),(1.00061090851415,
0.534459917946195,1.),(1.00062995710208,0.519944027299337,1.),(1.00064512214601,
0.508387573871131,1.)))
REPRESENTATION_ITEM('')
SURFACE()
);
#2586=(
BOUNDED_SURFACE()
B_SPLINE_SURFACE(3,2,((#166913,#166914,#166915),(#166916,#166917,#166918),
(#166919,#166920,#166921),(#166922,#166923,#166924)),.UNSPECIFIED.,.F.,
 .F.,.F.)
B_SPLINE_SURFACE_WITH_KNOTS((4,4),(3,3),(0.,0.0180689587739334),(0.,1.),
 .UNSPECIFIED.)
GEOMETRIC_REPRESENTATION_ITEM()
RATIONAL_B_SPLINE_SURFACE(((1.,0.473671517629134,1.),(1.,0.487381853083234,
1.),(1.,0.49876090260372,1.),(1.,0.508709923441297,1.)))
REPRESENTATION_ITEM('')
SURFACE()
);
#2587=(
BOUNDED_SURFACE()
B_SPLINE_SURFACE(3,2,((#166931,#166932,#166933),(#166934,#166935,#166936),
(#166937,#166938,#166939),(#166940,#166941,#166942),(#166943,#166944,#166945),
(#166946,#166947,#166948),(#166949,#166950,#166951),(#166952,#166953,#166954),
(#166955,#166956,#166957),(#166958,#166959,#166960)),.UNSPECIFIED.,.F.,
 .F.,.F.)
B_SPLINE_SURFACE_WITH_KNOTS((4,2,2,2,4),(3,3),(-4.33680868994201E-18,0.00131184996336558,
0.00262369992673117,0.00393554989009676,0.00524739985346235),(0.,1.),
 .UNSPECIFIED.)
GEOMETRIC_REPRESENTATION_ITEM()
RATIONAL_B_SPLINE_SURFACE(((1.,0.473671517629133,1.),(1.,0.495707594803631,
1.),(1.,0.517034522428114,1.),(1.,0.558412152901823,1.),(1.,0.578466470542957,
1.),(1.,0.617536962037478,1.),(1.,0.636393525150058,1.),(1.,0.672664546785766,
1.),(1.,0.690145348310819,1.),(1.,0.707106781186548,1.)))
REPRESENTATION_ITEM('')
SURFACE()
);
#2588=(
BOUNDED_SURFACE()
B_SPLINE_SURFACE(3,2,((#166983,#166984,#166985),(#166986,#166987,#166988),
(#166989,#166990,#166991),(#166992,#166993,#166994),(#166995,#166996,#166997),
(#166998,#166999,#167000),(#167001,#167002,#167003),(#167004,#167005,#167006)),
 .UNSPECIFIED.,.F.,.F.,.F.)
B_SPLINE_SURFACE_WITH_KNOTS((4,2,2,4),(3,3),(0.,0.00262348010799063,0.00393522016198593,
0.00524696021598125),(0.,1.),.UNSPECIFIED.)
GEOMETRIC_REPRESENTATION_ITEM()
RATIONAL_B_SPLINE_SURFACE(((1.,0.70710678118732,1.),(1.,0.673159051373371,
1.),(1.,0.637356734328886,1.),(1.,0.579048422068377,1.),(1.,0.558729842945168,
1.),(1.,0.517089292555981,1.),(1.,0.495689661102028,1.),(1.,0.473671517629131,
1.)))
REPRESENTATION_ITEM('')
SURFACE()
);
#2589=(
BOUNDED_SURFACE()
B_SPLINE_SURFACE(3,2,((#167025,#167026,#167027),(#167028,#167029,#167030),
(#167031,#167032,#167033),(#167034,#167035,#167036)),.UNSPECIFIED.,.F.,
 .F.,.F.)
B_SPLINE_SURFACE_WITH_KNOTS((4,4),(3,3),(-6.93889390390723E-18,0.0177935197894076),
(0.,1.),.UNSPECIFIED.)
GEOMETRIC_REPRESENTATION_ITEM()
RATIONAL_B_SPLINE_SURFACE(((1.,0.508254344125608,1.),(1.,0.498412666571477,
1.),(1.,0.487173250319529,1.),(1.,0.473671517629131,1.)))
REPRESENTATION_ITEM('')
SURFACE()
);
#2590=(
BOUNDED_SURFACE()
B_SPLINE_SURFACE(3,2,((#167072,#167073,#167074),(#167075,#167076,#167077),
(#167078,#167079,#167080),(#167081,#167082,#167083),(#167084,#167085,#167086),
(#167087,#167088,#167089),(#167090,#167091,#167092),(#167093,#167094,#167095)),
 .UNSPECIFIED.,.F.,.F.,.F.)
B_SPLINE_SURFACE_WITH_KNOTS((4,2,2,4),(3,3),(-6.50521303491303E-18,0.000158176853950714,
0.000316353707901435,0.000632707415802875),(0.,1.),.UNSPECIFIED.)
GEOMETRIC_REPRESENTATION_ITEM()
RATIONAL_B_SPLINE_SURFACE(((1.,0.50825434412561,1.),(1.,0.519857702736613,
1.),(1.,0.534132547044037,1.),(1.,0.566198696596924,1.),(1.,0.583560620774966,
1.),(1.,0.636763258069658,1.),(1.,0.673308410857549,1.),(1.,0.707106781186552,
1.)))
REPRESENTATION_ITEM('')
SURFACE()
);
#2591=(
BOUNDED_SURFACE()
B_SPLINE_SURFACE(3,2,((#167226,#167227,#167228),(#167229,#167230,#167231),
(#167232,#167233,#167234),(#167235,#167236,#167237)),.UNSPECIFIED.,.F.,
 .F.,.F.)
B_SPLINE_SURFACE_WITH_KNOTS((4,4),(3,3),(-1.1328828500301E-15,0.000723745383907254),
(0.,1.),.UNSPECIFIED.)
GEOMETRIC_REPRESENTATION_ITEM()
RATIONAL_B_SPLINE_SURFACE(((1.,0.802684671198269,1.),(1.,0.797620722711664,
1.),(1.,0.787749610789602,1.),(1.,0.773398994756355,1.)))
REPRESENTATION_ITEM('')
SURFACE()
);
#2592=(
BOUNDED_SURFACE()
B_SPLINE_SURFACE(3,2,((#167258,#167259,#167260),(#167261,#167262,#167263),
(#167264,#167265,#167266),(#167267,#167268,#167269)),.UNSPECIFIED.,.F.,
 .F.,.F.)
B_SPLINE_SURFACE_WITH_KNOTS((4,4),(3,3),(-2.12668013510612E-5,0.00023393481488825),
(-2.58890273307494E-5,1.),.UNSPECIFIED.)
GEOMETRIC_REPRESENTATION_ITEM()
RATIONAL_B_SPLINE_SURFACE(((1.00001043498075,0.798467114731324,1.),(1.00000954588804,
0.815638341296739,1.),(1.00000885543353,0.828973228358054,1.),(1.00000840251418,
0.837720550997796,0.999999999999999)))
REPRESENTATION_ITEM('')
SURFACE()
);
#2593=(
BOUNDED_SURFACE()
B_SPLINE_SURFACE(3,2,((#167274,#167275,#167276),(#167277,#167278,#167279),
(#167280,#167281,#167282),(#167283,#167284,#167285),(#167286,#167287,#167288),
(#167289,#167290,#167291)),.UNSPECIFIED.,.F.,.F.,.F.)
B_SPLINE_SURFACE_WITH_KNOTS((4,2,4),(3,3),(0.,0.0129055642122842,0.0258111284245685),
(0.,1.),.UNSPECIFIED.)
GEOMETRIC_REPRESENTATION_ITEM()
RATIONAL_B_SPLINE_SURFACE(((1.,0.861290731803006,1.),(1.,0.856148221578915,
1.),(1.,0.851494227257712,1.),(1.,0.842943112520738,1.),(1.,0.839046328378941,
1.),(1.,0.835442841040481,1.)))
REPRESENTATION_ITEM('')
SURFACE()
);
#2594=(
BOUNDED_SURFACE()
B_SPLINE_SURFACE(3,2,((#167301,#167302,#167303),(#167304,#167305,#167306),
(#167307,#167308,#167309),(#167310,#167311,#167312),(#167313,#167314,#167315),
(#167316,#167317,#167318),(#167319,#167320,#167321),(#167322,#167323,#167324)),
 .UNSPECIFIED.,.F.,.F.,.F.)
B_SPLINE_SURFACE_WITH_KNOTS((4,2,2,4),(3,3),(-0.000118679703551729,0.00223318354977648,
0.00334977532466471,0.00458504680310467),(-0.000118679703551729,1.),
 .UNSPECIFIED.)
GEOMETRIC_REPRESENTATION_ITEM()
RATIONAL_B_SPLINE_SURFACE(((1.00003211137202,0.864714137900249,1.),(1.00003747888505,
0.842100696538067,1.),(1.00004335836542,0.817330326405749,1.),(1.00005287395854,
0.777240939453633,1.),(1.00005607406915,0.763758808486968,1.),(1.00006299338349,
0.734607596724851,1.),(1.00006674915501,0.718784455078024,1.),(1.00007064938466,
0.702352708408401,0.999999999999999)))
REPRESENTATION_ITEM('')
SURFACE()
);
#2595=(
BOUNDED_SURFACE()
B_SPLINE_SURFACE(3,2,((#167347,#167348,#167349),(#167350,#167351,#167352),
(#167353,#167354,#167355),(#167356,#167357,#167358),(#167359,#167360,#167361),
(#167362,#167363,#167364)),.UNSPECIFIED.,.F.,.F.,.F.)
B_SPLINE_SURFACE_WITH_KNOTS((4,2,4),(3,3),(4.33680868994202E-19,0.0022325368353913,
0.00446507367078261),(0.,1.),.UNSPECIFIED.)
GEOMETRIC_REPRESENTATION_ITEM()
RATIONAL_B_SPLINE_SURFACE(((1.,0.707106781186548,1.),(1.,0.736599220372578,
1.),(1.,0.763970742639471,1.),(1.,0.815484818127782,1.),(1.,0.839751912193024,
1.),(1.,0.861290731802537,1.)))
REPRESENTATION_ITEM('')
SURFACE()
);
#2596=(
BOUNDED_SURFACE()
B_SPLINE_SURFACE(3,2,((#167392,#167393,#167394),(#167395,#167396,#167397),
(#167398,#167399,#167400),(#167401,#167402,#167403),(#167404,#167405,#167406),
(#167407,#167408,#167409)),.UNSPECIFIED.,.F.,.F.,.F.)
B_SPLINE_SURFACE_WITH_KNOTS((4,2,4),(3,3),(0.,0.0130414224518927,0.0260828449037854),
(0.,1.),.UNSPECIFIED.)
GEOMETRIC_REPRESENTATION_ITEM()
RATIONAL_B_SPLINE_SURFACE(((1.,0.835215680136663,1.),(1.,0.838844513950773,
1.),(1.,0.842771271110783,1.),(1.,0.851396246528345,1.),(1.,0.856094111052002,
1.),(1.,0.861290731803024,1.)))
REPRESENTATION_ITEM('')
SURFACE()
);
#2597=(
BOUNDED_SURFACE()
B_SPLINE_SURFACE(3,2,((#167419,#167420,#167421),(#167422,#167423,#167424),
(#167425,#167426,#167427),(#167428,#167429,#167430)),.UNSPECIFIED.,.F.,
 .F.,.F.)
B_SPLINE_SURFACE_WITH_KNOTS((4,4),(3,3),(0.,0.000106239733749475),(0.,1.),
 .UNSPECIFIED.)
GEOMETRIC_REPRESENTATION_ITEM()
RATIONAL_B_SPLINE_SURFACE(((1.,0.835215680136664,1.),(1.,0.831333836917881,
1.),(1.,0.826651097750167,1.),(1.,0.821176675475199,1.)))
REPRESENTATION_ITEM('')
SURFACE()
);
#2598=(
BOUNDED_SURFACE()
B_SPLINE_SURFACE(3,2,((#167437,#167438,#167439),(#167440,#167441,#167442),
(#167443,#167444,#167445),(#167446,#167447,#167448),(#167449,#167450,#167451),
(#167452,#167453,#167454)),.UNSPECIFIED.,.F.,.F.,.F.)
B_SPLINE_SURFACE_WITH_KNOTS((4,2,4),(3,3),(0.,0.000488761174293955,0.00097752234858791),
(0.,1.),.UNSPECIFIED.)
GEOMETRIC_REPRESENTATION_ITEM()
RATIONAL_B_SPLINE_SURFACE(((1.,0.813073674901529,1.),(1.,0.819782614828204,
1.),(1.,0.82321022732318,1.),(1.,0.825342446816795,1.),(1.,0.824005064313242,
1.),(1.,0.821176675475194,1.)))
REPRESENTATION_ITEM('')
SURFACE()
);
#2599=(
BOUNDED_SURFACE()
B_SPLINE_SURFACE(3,2,((#167489,#167490,#167491),(#167492,#167493,#167494),
(#167495,#167496,#167497),(#167498,#167499,#167500),(#167501,#167502,#167503),
(#167504,#167505,#167506),(#167507,#167508,#167509),(#167510,#167511,#167512),
(#167513,#167514,#167515),(#167516,#167517,#167518)),.UNSPECIFIED.,.F.,
 .F.,.F.)
B_SPLINE_SURFACE_WITH_KNOTS((4,2,2,2,4),(3,3),(3.1415926535898,3.53429173528852,
3.92699081698724,4.31968989868597,4.71238898038469),(0.,1.),
 .UNSPECIFIED.)
GEOMETRIC_REPRESENTATION_ITEM()
RATIONAL_B_SPLINE_SURFACE(((1.,0.754709580222776,1.),(1.,0.75471421973084,
1.),(1.,0.753512297096162,1.),(1.,0.748871927696637,1.),(1.,0.745429366938649,
1.),(1.,0.736738129296255,1.),(1.,0.73149075639724,1.),(1.,0.719894264862275,
1.),(1.,0.713550261851491,1.),(1.,0.707106781186548,1.)))
REPRESENTATION_ITEM('')
SURFACE()
);
#2600=(
BOUNDED_SURFACE()
B_SPLINE_SURFACE(3,2,((#167546,#167547,#167548),(#167549,#167550,#167551),
(#167552,#167553,#167554),(#167555,#167556,#167557),(#167558,#167559,#167560),
(#167561,#167562,#167563),(#167564,#167565,#167566),(#167567,#167568,#167569),
(#167570,#167571,#167572),(#167573,#167574,#167575)),.UNSPECIFIED.,.F.,
 .F.,.F.)
B_SPLINE_SURFACE_WITH_KNOTS((4,2,2,2,4),(3,3),(0.00131180726843867,0.00173116479138242,
0.00215052231432617,0.00256987983726992,0.00298923736021366),(-7.19536585550859E-6,
1.),.UNSPECIFIED.)
GEOMETRIC_REPRESENTATION_ITEM()
RATIONAL_B_SPLINE_SURFACE(((1.00000421497806,0.707104673712682,1.),(1.00000380693457,
0.735459277069438,1.),(1.00000349584283,0.757076784022164,1.),(1.00000307861073,
0.786069896432006,1.),(1.00000297270674,0.793429076618855,1.),(1.00000297242619,
0.793448571747273,1.),(1.00000307812241,0.786103829137561,1.),(1.00000349515575,
0.757124528683259,1.),(1.00000380600652,0.735523766262835,1.),(1.00000421497806,
0.707104673712682,1.)))
REPRESENTATION_ITEM('')
SURFACE()
);
#2601=(
BOUNDED_SURFACE()
B_SPLINE_SURFACE(3,2,((#167676,#167677,#167678),(#167679,#167680,#167681),
(#167682,#167683,#167684),(#167685,#167686,#167687),(#167688,#167689,#167690),
(#167691,#167692,#167693),(#167694,#167695,#167696),(#167697,#167698,#167699)),
 .UNSPECIFIED.,.F.,.F.,.F.)
B_SPLINE_SURFACE_WITH_KNOTS((4,2,2,4),(3,3),(0.,0.000350059279280428,0.000525088918920643,
0.000700118558560857),(0.,1.),.UNSPECIFIED.)
GEOMETRIC_REPRESENTATION_ITEM()
RATIONAL_B_SPLINE_SURFACE(((1.,0.707106781186548,1.),(1.,0.666269021153261,
1.),(1.,0.620643690025591,1.),(1.,0.551020195303415,1.),(1.,0.527243635346707,
1.),(1.,0.48184496425994,1.),(1.,0.460546552679624,1.),(1.,0.442551630563558,
1.)))
REPRESENTATION_ITEM('')
SURFACE()
);
#2602=(
BOUNDED_SURFACE()
B_SPLINE_SURFACE(3,2,((#167721,#167722,#167723),(#167724,#167725,#167726),
(#167727,#167728,#167729),(#167730,#167731,#167732)),.UNSPECIFIED.,.F.,
 .F.,.F.)
B_SPLINE_SURFACE_WITH_KNOTS((4,4),(3,3),(-1.00613961606655E-16,0.00454919832189776),
(0.,1.),.UNSPECIFIED.)
GEOMETRIC_REPRESENTATION_ITEM()
RATIONAL_B_SPLINE_SURFACE(((1.,0.43161218489519,1.),(1.,0.4354057728044,
1.),(1.,0.439046733702441,1.),(1.,0.442551630563568,1.)))
REPRESENTATION_ITEM('')
SURFACE()
);
#2603=(
BOUNDED_SURFACE()
B_SPLINE_SURFACE(3,2,((#167739,#167740,#167741),(#167742,#167743,#167744),
(#167745,#167746,#167747),(#167748,#167749,#167750),(#167751,#167752,#167753),
(#167754,#167755,#167756),(#167757,#167758,#167759),(#167760,#167761,#167762),
(#167763,#167764,#167765),(#167766,#167767,#167768),(#167769,#167770,#167771),
(#167772,#167773,#167774)),.UNSPECIFIED.,.F.,.F.,.F.)
B_SPLINE_SURFACE_WITH_KNOTS((4,2,2,2,2,4),(3,3),(0.,0.0015680710888481,
0.00235210663327216,0.0031361421776962,0.00470421326654431,0.00627228435539241),
(0.,1.),.UNSPECIFIED.)
GEOMETRIC_REPRESENTATION_ITEM()
RATIONAL_B_SPLINE_SURFACE(((1.,0.431612184896198,1.),(1.,0.458478767119797,
1.),(1.,0.484262778995081,1.),(1.,0.521487645866883,1.),(1.,0.533657012907055,
1.),(1.,0.557569946367873,1.),(1.,0.569348142420323,1.),(1.,0.603784372807714,
1.),(1.,0.625598432901225,1.),(1.,0.667530632490446,1.),(1.,0.687642674416921,
1.),(1.,0.707106781186545,1.)))
REPRESENTATION_ITEM('')
SURFACE()
);
#2604=(
BOUNDED_SURFACE()
B_SPLINE_SURFACE(3,2,((#167800,#167801,#167802),(#167803,#167804,#167805),
(#167806,#167807,#167808),(#167809,#167810,#167811),(#167812,#167813,#167814),
(#167815,#167816,#167817),(#167818,#167819,#167820),(#167821,#167822,#167823),
(#167824,#167825,#167826),(#167827,#167828,#167829)),.UNSPECIFIED.,.F.,
 .F.,.F.)
B_SPLINE_SURFACE_WITH_KNOTS((4,2,2,2,4),(3,3),(0.,0.00156769407161709,0.00313538814323418,
0.00470308221485126,0.00627077628646835),(0.,1.),.UNSPECIFIED.)
GEOMETRIC_REPRESENTATION_ITEM()
RATIONAL_B_SPLINE_SURFACE(((1.,0.707106781185944,1.),(1.,0.687642132810167,
1.),(1.,0.6675396507768,1.),(1.,0.625652582590125,1.),(1.,0.603873832998886,
1.),(1.,0.558067925921433,1.),(1.,0.534002288872959,1.),(1.,0.484278918307038,
1.),(1.,0.458469143464434,1.),(1.,0.431612184895232,1.)))
REPRESENTATION_ITEM('')
SURFACE()
);
#2605=(
BOUNDED_SURFACE()
B_SPLINE_SURFACE(3,2,((#167848,#167849,#167850),(#167851,#167852,#167853),
(#167854,#167855,#167856),(#167857,#167858,#167859)),.UNSPECIFIED.,.F.,
 .F.,.F.)
B_SPLINE_SURFACE_WITH_KNOTS((4,4),(3,3),(1.7347234759768E-18,0.00426411906192034),
(0.,1.),.UNSPECIFIED.)
GEOMETRIC_REPRESENTATION_ITEM()
RATIONAL_B_SPLINE_SURFACE(((1.,0.441891116431774,1.),(1.,0.438589787881315,
1.),(1.,0.435168043398159,1.),(1.,0.431612184895232,1.)))
REPRESENTATION_ITEM('')
SURFACE()
);
#2606=(
BOUNDED_SURFACE()
B_SPLINE_SURFACE(3,2,((#167866,#167867,#167868),(#167869,#167870,#167871),
(#167872,#167873,#167874),(#167875,#167876,#167877),(#167878,#167879,#167880),
(#167881,#167882,#167883),(#167884,#167885,#167886),(#167887,#167888,#167889),
(#167890,#167891,#167892),(#167893,#167894,#167895)),.UNSPECIFIED.,.F.,
 .F.,.F.)
B_SPLINE_SURFACE_WITH_KNOTS((4,2,2,2,4),(3,3),(0.,0.000175112702239915,
0.000350225404479831,0.000525338106719747,0.000700450808959663),(0.,1.),
 .UNSPECIFIED.)
GEOMETRIC_REPRESENTATION_ITEM()
RATIONAL_B_SPLINE_SURFACE(((1.,0.441891116431771,1.),(1.,0.459945578495206,
1.),(1.,0.481391225572596,1.),(1.,0.52725624746098,1.),(1.,0.550835433567685,
1.),(1.,0.597437830540943,1.),(1.,0.62070290968502,1.),(1.,0.665021344579013,
1.),(1.,0.68636937449165,1.),(1.,0.707106781186548,1.)))
REPRESENTATION_ITEM('')
SURFACE()
);
#2607=(
BOUNDED_SURFACE()
B_SPLINE_SURFACE(3,2,((#168014,#168015,#168016),(#168017,#168018,#168019),
(#168020,#168021,#168022),(#168023,#168024,#168025),(#168026,#168027,#168028),
(#168029,#168030,#168031),(#168032,#168033,#168034),(#168035,#168036,#168037),
(#168038,#168039,#168040),(#168041,#168042,#168043)),.UNSPECIFIED.,.F.,
 .F.,.F.)
B_SPLINE_SURFACE_WITH_KNOTS((4,2,2,2,4),(3,3),(1.57066336187496,1.96349540849362,
2.35619449019234,2.74889357189107,3.14172561850969),(0.,1.00013296491993),
 .UNSPECIFIED.)
GEOMETRIC_REPRESENTATION_ITEM()
RATIONAL_B_SPLINE_SURFACE(((1.,0.707074379515315,1.00007789766335),(1.,
0.700631001612556,1.0000796111498),(1.,0.694096308749865,1.00008134891963),
(1.,0.681861139767284,1.00008460261615),(1.,0.676166101239372,1.00008611709684),
(1.,0.666571715834207,1.00008866853021),(1.,0.662679222605431,1.00008970366031),
(1.,0.657396767036752,1.00009110842288),(1.,0.656004520314433,1.00009147866283),
(1.,0.656013305345919,1.00009147632662)))
REPRESENTATION_ITEM('')
SURFACE()
);
#2608=(
BOUNDED_SURFACE()
B_SPLINE_SURFACE(3,2,((#168068,#168069,#168070),(#168071,#168072,#168073),
(#168074,#168075,#168076),(#168077,#168078,#168079),(#168080,#168081,#168082),
(#168083,#168084,#168085),(#168086,#168087,#168088),(#168089,#168090,#168091)),
 .UNSPECIFIED.,.F.,.F.,.F.)
B_SPLINE_SURFACE_WITH_KNOTS((4,2,2,4),(3,3),(0.,0.000337961269725901,0.000506941904588851,
0.000675922539451801),(0.,1.),.UNSPECIFIED.)
GEOMETRIC_REPRESENTATION_ITEM()
RATIONAL_B_SPLINE_SURFACE(((1.,0.707106781186548,1.),(1.,0.66833529952704,
1.),(1.,0.625126311995779,1.),(1.,0.560329805282816,1.),(1.,0.53845874286336,
1.),(1.,0.497198802480914,1.),(1.,0.478168468596388,1.),(1.,0.462319489161107,
1.)))
REPRESENTATION_ITEM('')
SURFACE()
);
#2609=(
BOUNDED_SURFACE()
B_SPLINE_SURFACE(3,2,((#168189,#168190,#168191),(#168192,#168193,#168194),
(#168195,#168196,#168197),(#168198,#168199,#168200)),.UNSPECIFIED.,.F.,
 .F.,.F.)
B_SPLINE_SURFACE_WITH_KNOTS((4,4),(3,3),(0.,0.00407947372412412),(0.,1.),
 .UNSPECIFIED.)
GEOMETRIC_REPRESENTATION_ITEM()
RATIONAL_B_SPLINE_SURFACE(((1.,0.453393847276564,1.),(1.,0.456475766016567,
1.),(1.,0.459447353892611,1.),(1.,0.462319489161104,1.)))
REPRESENTATION_ITEM('')
SURFACE()
);
#2610=(
BOUNDED_SURFACE()
B_SPLINE_SURFACE(3,2,((#168207,#168208,#168209),(#168210,#168211,#168212),
(#168213,#168214,#168215),(#168216,#168217,#168218),(#168219,#168220,#168221),
(#168222,#168223,#168224),(#168225,#168226,#168227),(#168228,#168229,#168230)),
 .UNSPECIFIED.,.F.,.F.,.F.)
B_SPLINE_SURFACE_WITH_KNOTS((4,2,2,4),(3,3),(0.,0.001434338214324,0.002868676428648,
0.005737352857296),(0.,1.),.UNSPECIFIED.)
GEOMETRIC_REPRESENTATION_ITEM()
RATIONAL_B_SPLINE_SURFACE(((1.,0.45339384727684,1.),(1.,0.47771228976057,
1.),(1.,0.501151853233145,1.),(1.,0.546461020466456,1.),(1.,0.568350660511087,
1.),(1.,0.632070189677047,1.),(1.,0.670684004768455,1.),(1.,0.707106781186548,
1.)))
REPRESENTATION_ITEM('')
SURFACE()
);
#2611=(
BOUNDED_SURFACE()
B_SPLINE_SURFACE(3,2,((#168399,#168400,#168401),(#168402,#168403,#168404),
(#168405,#168406,#168407),(#168408,#168409,#168410)),.UNSPECIFIED.,.F.,
 .F.,.F.)
B_SPLINE_SURFACE_WITH_KNOTS((4,4),(3,3),(-1.7347234759768E-18,0.0170848224870981),
(0.,1.),.UNSPECIFIED.)
GEOMETRIC_REPRESENTATION_ITEM()
RATIONAL_B_SPLINE_SURFACE(((1.,0.499602392377301,1.),(1.,0.510855798801923,
1.),(1.,0.520331406035946,1.),(1.,0.528679393385783,1.)))
REPRESENTATION_ITEM('')
SURFACE()
);
#2612=(
BOUNDED_SURFACE()
B_SPLINE_SURFACE(3,2,((#168436,#168437,#168438),(#168439,#168440,#168441),
(#168442,#168443,#168444),(#168445,#168446,#168447),(#168448,#168449,#168450),
(#168451,#168452,#168453),(#168454,#168455,#168456),(#168457,#168458,#168459),
(#168460,#168461,#168462),(#168463,#168464,#168465)),.UNSPECIFIED.,.F.,
 .F.,.F.)
B_SPLINE_SURFACE_WITH_KNOTS((4,2,2,2,4),(3,3),(-1.8702487475375E-18,0.00116432048255243,
0.00232864096510486,0.0034929614476573,0.00465728193020974),(0.,1.),
 .UNSPECIFIED.)
GEOMETRIC_REPRESENTATION_ITEM()
RATIONAL_B_SPLINE_SURFACE(((1.,0.499602392377304,1.),(1.,0.518836986211321,
1.),(1.,0.537549820773013,1.),(1.,0.574017039053458,1.),(1.,0.591773144780234,
1.),(1.,0.62647750773349,1.),(1.,0.643417219403868,1.),(1.,0.676030436791849,
1.),(1.,0.691791372953169,1.),(1.,0.707106781186548,1.)))
REPRESENTATION_ITEM('')
SURFACE()
);
#2613=(
BOUNDED_SURFACE()
B_SPLINE_SURFACE(3,2,((#168516,#168517,#168518),(#168519,#168520,#168521),
(#168522,#168523,#168524),(#168525,#168526,#168527),(#168528,#168529,#168530),
(#168531,#168532,#168533),(#168534,#168535,#168536),(#168537,#168538,#168539)),
 .UNSPECIFIED.,.F.,.F.,.F.)
B_SPLINE_SURFACE_WITH_KNOTS((4,2,2,4),(3,3),(-4.33680868994202E-19,0.00249252731595781,
0.00373879097393672,0.00498505463191562),(0.,1.),.UNSPECIFIED.)
GEOMETRIC_REPRESENTATION_ITEM()
RATIONAL_B_SPLINE_SURFACE(((1.,0.70710678118655,1.),(1.,0.739588972045703,
1.),(1.,0.769477992255324,1.),(1.,0.811447962923272,1.),(1.,0.825023851703587,
1.),(1.,0.850750710603259,1.),(1.,0.862945608551043,1.),(1.,0.874466916621005,
1.)))
REPRESENTATION_ITEM('')
SURFACE()
);
#2614=(
BOUNDED_SURFACE()
B_SPLINE_SURFACE(3,2,((#168555,#168556,#168557),(#168558,#168559,#168560),
(#168561,#168562,#168563),(#168564,#168565,#168566)),.UNSPECIFIED.,.F.,
 .F.,.F.)
B_SPLINE_SURFACE_WITH_KNOTS((4,4),(3,3),(0.,0.0135233968444947),(0.,1.),
 .UNSPECIFIED.)
GEOMETRIC_REPRESENTATION_ITEM()
RATIONAL_B_SPLINE_SURFACE(((1.,0.860139545375529,1.),(1.,0.864525021855929,
1.),(1.,0.869269442591942,1.),(1.,0.874466916621369,1.)))
REPRESENTATION_ITEM('')
SURFACE()
);
#2615=(
BOUNDED_SURFACE()
B_SPLINE_SURFACE(3,2,((#168573,#168574,#168575),(#168576,#168577,#168578),
(#168579,#168580,#168581),(#168582,#168583,#168584),(#168585,#168586,#168587),
(#168588,#168589,#168590)),.UNSPECIFIED.,.F.,.F.,.F.)
B_SPLINE_SURFACE_WITH_KNOTS((4,2,4),(3,3),(0.,0.000315675390911493,0.000631350781822986),
(0.,1.),.UNSPECIFIED.)
GEOMETRIC_REPRESENTATION_ITEM()
RATIONAL_B_SPLINE_SURFACE(((1.,0.860139545375527,1.),(1.,0.846673137247607,
1.),(1.,0.824923291377528,1.),(1.,0.771907958235216,1.),(1.,0.740773829846737,
1.),(1.,0.70710678118655,1.)))
REPRESENTATION_ITEM('')
SURFACE()
);
#2616=(
BOUNDED_SURFACE()
B_SPLINE_SURFACE(3,2,((#168713,#168714,#168715),(#168716,#168717,#168718),
(#168719,#168720,#168721),(#168722,#168723,#168724),(#168725,#168726,#168727),
(#168728,#168729,#168730)),.UNSPECIFIED.,.F.,.F.,.F.)
B_SPLINE_SURFACE_WITH_KNOTS((4,2,4),(3,3),(-6.4954414055628E-5,0.000324772070278169,
0.000714498554611972),(-0.000410438713922671,1.),.UNSPECIFIED.)
GEOMETRIC_REPRESENTATION_ITEM()
RATIONAL_B_SPLINE_SURFACE(((1.00025845542913,0.685147355296338,1.),(1.0002222617227,
0.729238842293541,1.),(1.00018785201525,0.771157046260518,1.),(1.00013161693134,
0.839663113063761,1.),(1.00010908866185,0.867107246289421,1.),(1.00009788969732,
0.880749921969343,1.)))
REPRESENTATION_ITEM('')
SURFACE()
);
#2617=(
BOUNDED_SURFACE()
B_SPLINE_SURFACE(3,2,((#168813,#168814,#168815),(#168816,#168817,#168818),
(#168819,#168820,#168821),(#168822,#168823,#168824)),.UNSPECIFIED.,.F.,
 .F.,.F.)
B_SPLINE_SURFACE_WITH_KNOTS((4,4),(3,3),(0.,0.00876509433037234),(0.,1.),
 .UNSPECIFIED.)
GEOMETRIC_REPRESENTATION_ITEM()
RATIONAL_B_SPLINE_SURFACE(((1.,0.882443751548025,1.),(1.,0.879078911067312,
1.),(1.,0.875892933141997,1.),(1.,0.872863017557589,1.)))
REPRESENTATION_ITEM('')
SURFACE()
);
#2618=(
BOUNDED_SURFACE()
B_SPLINE_SURFACE(3,2,((#168831,#168832,#168833),(#168834,#168835,#168836),
(#168837,#168838,#168839),(#168840,#168841,#168842),(#168843,#168844,#168845),
(#168846,#168847,#168848),(#168849,#168850,#168851),(#168852,#168853,#168854)),
 .UNSPECIFIED.,.F.,.F.,.F.)
B_SPLINE_SURFACE_WITH_KNOTS((4,2,2,4),(3,3),(-4.21496351932344E-5,0.00133214690895888,
0.00266429381791776,0.00537073727101886),(-0.000298701407012629,1.),
 .UNSPECIFIED.)
GEOMETRIC_REPRESENTATION_ITEM()
RATIONAL_B_SPLINE_SURFACE(((1.00006957344384,0.883540147100468,1.),(1.0000769064979,
0.871265256709866,1.),(1.00008468386698,0.858246621887947,1.),(1.00010084930836,
0.831187088519705,1.),(1.00010921077731,0.81719072165729,1.),(1.00013589350388,
0.772526173817441,1.),(1.00015516908062,0.740260546179961,1.),(1.00017599959926,
0.705392081983662,0.999999999999999)))
REPRESENTATION_ITEM('')
SURFACE()
);
#2619=(
BOUNDED_SURFACE()
B_SPLINE_SURFACE(3,2,((#168886,#168887,#168888),(#168889,#168890,#168891),
(#168892,#168893,#168894),(#168895,#168896,#168897),(#168898,#168899,#168900),
(#168901,#168902,#168903),(#168904,#168905,#168906),(#168907,#168908,#168909)),
 .UNSPECIFIED.,.F.,.F.,.F.)
B_SPLINE_SURFACE_WITH_KNOTS((4,2,2,4),(3,3),(0.,0.0026640399986995,0.00399605999804924,
0.00532807999739899),(0.,1.),.UNSPECIFIED.)
GEOMETRIC_REPRESENTATION_ITEM()
RATIONAL_B_SPLINE_SURFACE(((1.,0.707106781186548,1.),(1.,0.741415034329509,
1.),(1.,0.772836788298617,1.),(1.,0.816837673402558,1.),(1.,0.831036084533252,
1.),(1.,0.857840517676878,1.),(1.,0.87051456122688,1.),(1.,0.882443751548482,
1.)))
REPRESENTATION_ITEM('')
SURFACE()
);
#2620=(
BOUNDED_SURFACE()
B_SPLINE_SURFACE(3,2,((#168928,#168929,#168930),(#168931,#168932,#168933),
(#168934,#168935,#168936),(#168937,#168938,#168939)),.UNSPECIFIED.,.F.,
 .F.,.F.)
B_SPLINE_SURFACE_WITH_KNOTS((4,4),(3,3),(-3.46944695195361E-18,0.00904291806877092),
(0.,1.),.UNSPECIFIED.)
GEOMETRIC_REPRESENTATION_ITEM()
RATIONAL_B_SPLINE_SURFACE(((1.,0.872575378690133,1.),(1.,0.875691129720726,
1.),(1.,0.878972255663315,1.),(1.,0.882443751548002,1.)))
REPRESENTATION_ITEM('')
SURFACE()
);
#2621=(
BOUNDED_SURFACE()
B_SPLINE_SURFACE(3,2,((#168946,#168947,#168948),(#168949,#168950,#168951),
(#168952,#168953,#168954),(#168955,#168956,#168957),(#168958,#168959,#168960),
(#168961,#168962,#168963)),.UNSPECIFIED.,.F.,.F.,.F.)
B_SPLINE_SURFACE_WITH_KNOTS((4,2,4),(3,3),(-6.48856056667737E-5,0.000324428028333684,
0.000713741662334142),(-0.000106621799618699,1.),.UNSPECIFIED.)
GEOMETRIC_REPRESENTATION_ITEM()
RATIONAL_B_SPLINE_SURFACE(((1.00002551905035,0.880329114491097,1.),(1.00002834928183,
0.867056821704917,1.),(1.0000341546752,0.839832589011995,1.),(1.0000488152557,
0.771082199518792,1.),(1.00005760311273,0.729871785430903,1.),(1.00006718666931,
0.68492996016543,1.)))
REPRESENTATION_ITEM('')
SURFACE()
);
#2622=(
BOUNDED_SURFACE()
B_SPLINE_SURFACE(3,2,((#168986,#168987,#168988),(#168989,#168990,#168991),
(#168992,#168993,#168994),(#168995,#168996,#168997),(#168998,#168999,#169000),
(#169001,#169002,#169003),(#169004,#169005,#169006),(#169007,#169008,#169009),
(#169010,#169011,#169012),(#169013,#169014,#169015)),.UNSPECIFIED.,.F.,
 .F.,.F.)
B_SPLINE_SURFACE_WITH_KNOTS((4,2,2,2,4),(3,3),(3.1415926535898,3.53429173528852,
3.92699081698724,4.31968989868597,4.71238898038469),(0.,1.),
 .UNSPECIFIED.)
GEOMETRIC_REPRESENTATION_ITEM()
RATIONAL_B_SPLINE_SURFACE(((1.,0.754709580222772,1.),(1.,0.754714219730806,
1.),(1.,0.753512297096203,1.),(1.,0.748871927696591,1.),(1.,0.745429366938691,
1.),(1.,0.736738129296209,1.),(1.,0.73149075639733,1.),(1.,0.719894264862189,
1.),(1.,0.713550261851557,1.),(1.,0.707106781186548,1.)))
REPRESENTATION_ITEM('')
SURFACE()
);
#2623=(
BOUNDED_SURFACE()
B_SPLINE_SURFACE(3,2,((#169064,#169065,#169066),(#169067,#169068,#169069),
(#169070,#169071,#169072),(#169073,#169074,#169075),(#169076,#169077,#169078),
(#169079,#169080,#169081),(#169082,#169083,#169084),(#169085,#169086,#169087),
(#169088,#169089,#169090),(#169091,#169092,#169093)),.UNSPECIFIED.,.F.,
 .F.,.F.)
B_SPLINE_SURFACE_WITH_KNOTS((4,2,2,2,4),(3,3),(1.57066336187449,1.96349540849362,
2.35619449019234,2.74889357189107,3.1417256185102),(0.,1.00013296492041),
 .UNSPECIFIED.)
GEOMETRIC_REPRESENTATION_ITEM()
RATIONAL_B_SPLINE_SURFACE(((1.,0.707074379515197,1.00007789766363),(1.,
0.700631001612236,1.00007961115009),(1.,0.694096308749978,1.00008134891992),
(1.,0.681861139766877,1.00008460261646),(1.,0.676166101239942,1.00008611709715),
(1.,0.666571715833326,1.00008866853053),(1.,0.662679222605256,1.00008970366064),
(1.,0.657396767036593,1.00009110842321),(1.,0.656004520314252,1.00009147866316),
(1.,0.656013305345755,1.00009147632695)))
REPRESENTATION_ITEM('')
SURFACE()
);
#2624=(
BOUNDED_SURFACE()
B_SPLINE_SURFACE(3,2,((#169110,#169111,#169112),(#169113,#169114,#169115),
(#169116,#169117,#169118),(#169119,#169120,#169121),(#169122,#169123,#169124),
(#169125,#169126,#169127),(#169128,#169129,#169130),(#169131,#169132,#169133),
(#169134,#169135,#169136),(#169137,#169138,#169139)),.UNSPECIFIED.,.F.,
 .F.,.F.)
B_SPLINE_SURFACE_WITH_KNOTS((4,2,2,2,4),(3,3),(0.,0.000158019212117338,
0.000316038424234677,0.000474057636352015,0.000632076848469353),(-0.000659009817274179,
1.),.UNSPECIFIED.)
GEOMETRIC_REPRESENTATION_ITEM()
RATIONAL_B_SPLINE_SURFACE(((1.00038629341672,0.706913761679937,1.),(1.00040876016389,
0.689867925196359,1.),(1.00043160206942,0.672537450804892,1.),(1.00047822635013,
0.637162954487827,1.),(1.000502398717,0.618823040396089,1.),(1.00054910501744,
0.583386314556222,1.),(1.0005717799679,0.566182511309068,1.),(1.00061451793483,
0.533756615818148,1.),(1.00063376129073,0.519156411542439,1.),(1.0006490837683,
0.507531032707861,1.)))
REPRESENTATION_ITEM('')
SURFACE()
);
#2625=(
BOUNDED_SURFACE()
B_SPLINE_SURFACE(3,2,((#169161,#169162,#169163),(#169164,#169165,#169166),
(#169167,#169168,#169169),(#169170,#169171,#169172)),.UNSPECIFIED.,.F.,
 .F.,.F.)
B_SPLINE_SURFACE_WITH_KNOTS((4,4),(3,3),(0.,0.01284355850178),(0.,1.),
 .UNSPECIFIED.)
GEOMETRIC_REPRESENTATION_ITEM()
RATIONAL_B_SPLINE_SURFACE(((1.,0.484030052331127,1.),(1.,0.492910462848522,
1.),(1.,0.500753390328389,1.),(1.,0.507855360856573,1.)))
REPRESENTATION_ITEM('')
SURFACE()
);
#2626=(
BOUNDED_SURFACE()
B_SPLINE_SURFACE(3,2,((#169179,#169180,#169181),(#169182,#169183,#169184),
(#169185,#169186,#169187),(#169188,#169189,#169190),(#169191,#169192,#169193),
(#169194,#169195,#169196),(#169197,#169198,#169199),(#169200,#169201,#169202),
(#169203,#169204,#169205),(#169206,#169207,#169208)),.UNSPECIFIED.,.F.,
 .F.,.F.)
B_SPLINE_SURFACE_WITH_KNOTS((4,2,2,2,4),(3,3),(-4.33680868994201E-18,0.00125260629929845,
0.00250521259859689,0.00375781889789535,0.0050104251971938),(0.,1.),
 .UNSPECIFIED.)
GEOMETRIC_REPRESENTATION_ITEM()
RATIONAL_B_SPLINE_SURFACE(((1.,0.484030052331112,1.),(1.,0.504928485114276,
1.),(1.,0.525198247435633,1.),(1.,0.564597723285694,1.),(1.,0.583730152224629,
1.),(1.,0.62105465867689,1.),(1.,0.639160091266653,1.),(1.,0.67398655458045,
1.),(1.,0.690790819130117,1.),(1.,0.707106781186548,1.)))
REPRESENTATION_ITEM('')
SURFACE()
);
#2627=(
BOUNDED_SURFACE()
B_SPLINE_SURFACE(3,2,((#169231,#169232,#169233),(#169234,#169235,#169236),
(#169237,#169238,#169239),(#169240,#169241,#169242),(#169243,#169244,#169245),
(#169246,#169247,#169248),(#169249,#169250,#169251),(#169252,#169253,#169254)),
 .UNSPECIFIED.,.F.,.F.,.F.)
B_SPLINE_SURFACE_WITH_KNOTS((4,2,2,4),(3,3),(-5.42101086242752E-20,0.00250485829616721,
0.00375728744425081,0.00500971659233441),(0.,1.),.UNSPECIFIED.)
GEOMETRIC_REPRESENTATION_ITEM()
RATIONAL_B_SPLINE_SURFACE(((1.,0.70710678118722,1.),(1.,0.674452105060394,
1.),(1.,0.640073400404409,1.),(1.,0.584341050151977,1.),(1.,0.564951135845581,
1.),(1.,0.525261922605914,1.),(1.,0.504912110655119,1.),(1.,0.484030052331115,
1.)))
REPRESENTATION_ITEM('')
SURFACE()
);
#2628=(
BOUNDED_SURFACE()
B_SPLINE_SURFACE(3,2,((#169270,#169271,#169272),(#169273,#169274,#169275),
(#169276,#169277,#169278),(#169279,#169280,#169281)),.UNSPECIFIED.,.F.,
 .F.,.F.)
B_SPLINE_SURFACE_WITH_KNOTS((4,4),(3,3),(0.,0.0125680158145827),(0.,1.),
 .UNSPECIFIED.)
GEOMETRIC_REPRESENTATION_ITEM()
RATIONAL_B_SPLINE_SURFACE(((1.,0.507397370006812,1.),(1.,0.500416139715127,
1.),(1.,0.49272006913241,1.),(1.,0.484030052331115,1.)))
REPRESENTATION_ITEM('')
SURFACE()
);
#2629=(
BOUNDED_SURFACE()
B_SPLINE_SURFACE(3,2,((#169311,#169312,#169313),(#169314,#169315,#169316),
(#169317,#169318,#169319),(#169320,#169321,#169322),(#169323,#169324,#169325),
(#169326,#169327,#169328),(#169329,#169330,#169331),(#169332,#169333,#169334)),
 .UNSPECIFIED.,.F.,.F.,.F.)
B_SPLINE_SURFACE_WITH_KNOTS((4,2,2,4),(3,3),(-1.5368565794982E-17,0.000158339556725866,
0.000316679113451747,0.000633358226903509),(0.,1.),.UNSPECIFIED.)
GEOMETRIC_REPRESENTATION_ITEM()
RATIONAL_B_SPLINE_SURFACE(((1.,0.507397370006824,1.),(1.,0.519070630879541,
1.),(1.,0.533426892711081,1.),(1.,0.565658432465259,1.),(1.,0.583100719918817,
1.),(1.,0.636529920575075,1.),(1.,0.673198940992506,1.),(1.,0.707106781186548,
1.)))
REPRESENTATION_ITEM('')
SURFACE()
);
#2630=(
BOUNDED_SURFACE()
B_SPLINE_SURFACE(3,2,((#169453,#169454,#169455),(#169456,#169457,#169458),
(#169459,#169460,#169461),(#169462,#169463,#169464)),.UNSPECIFIED.,.F.,
 .F.,.F.)
B_SPLINE_SURFACE_WITH_KNOTS((4,4),(3,3),(-2.08166817117217E-17,0.0203430832871546),
(0.,1.),.UNSPECIFIED.)
GEOMETRIC_REPRESENTATION_ITEM()
RATIONAL_B_SPLINE_SURFACE(((1.,0.855596390789699,1.),(1.,0.848090845809161,
1.),(1.,0.841665513049531,1.),(1.,0.835963592435998,1.)))
REPRESENTATION_ITEM('')
SURFACE()
);
#2631=(
BOUNDED_SURFACE()
B_SPLINE_SURFACE(3,2,((#169473,#169474,#169475),(#169476,#169477,#169478),
(#169479,#169480,#169481),(#169482,#169483,#169484),(#169485,#169486,#169487),
(#169488,#169489,#169490),(#169491,#169492,#169493),(#169494,#169495,#169496)),
 .UNSPECIFIED.,.F.,.F.,.F.)
B_SPLINE_SURFACE_WITH_KNOTS((4,2,2,4),(3,3),(-0.000280270643381287,0.00213290337237644,
0.00319935505856466,0.00454607738813407),(-0.00139944814386632,1.),
 .UNSPECIFIED.)
GEOMETRIC_REPRESENTATION_ITEM()
RATIONAL_B_SPLINE_SURFACE(((1.0003817605577,0.863603178378214,1.),(1.00044695755931,
0.840309352917159,1.),(1.00051853483077,0.814735961086389,1.),(1.00063212358804,
0.774152550486465,1.),(1.00066847254068,0.76116566247594,1.),(1.00075281158742,
0.731032696452739,1.),(1.00080157579018,0.713610042037807,1.),(1.00085238418929,
0.695457029605283,1.)))
REPRESENTATION_ITEM('')
SURFACE()
);
#2632=(
BOUNDED_SURFACE()
B_SPLINE_SURFACE(3,2,((#169516,#169517,#169518),(#169519,#169520,#169521),
(#169522,#169523,#169524),(#169525,#169526,#169527),(#169528,#169529,#169530),
(#169531,#169532,#169533)),.UNSPECIFIED.,.F.,.F.,.F.)
B_SPLINE_SURFACE_WITH_KNOTS((4,2,4),(3,3),(0.,0.00213206083322637,0.00426412166645274),
(0.,1.),.UNSPECIFIED.)
GEOMETRIC_REPRESENTATION_ITEM()
RATIONAL_B_SPLINE_SURFACE(((1.,0.707106781186545,1.),(1.,0.735348751818402,
1.),(1.,0.761643947187706,1.),(1.,0.811236415877723,1.),(1.,0.834679252508647,
1.),(1.,0.855596390789698,1.)))
REPRESENTATION_ITEM('')
SURFACE()
);
#2633=(
BOUNDED_SURFACE()
B_SPLINE_SURFACE(3,2,((#169558,#169559,#169560),(#169561,#169562,#169563),
(#169564,#169565,#169566),(#169567,#169568,#169569)),.UNSPECIFIED.,.F.,
 .F.,.F.)
B_SPLINE_SURFACE_WITH_KNOTS((4,4),(3,3),(0.,0.0206148669995797),(0.,1.),
 .UNSPECIFIED.)
GEOMETRIC_REPRESENTATION_ITEM()
RATIONAL_B_SPLINE_SURFACE(((1.,0.835735574810025,1.),(1.,0.841493793210698,
1.),(1.,0.847990686938055,1.),(1.,0.855596390789697,1.)))
REPRESENTATION_ITEM('')
SURFACE()
);
#2634=(
BOUNDED_SURFACE()
B_SPLINE_SURFACE(3,2,((#169576,#169577,#169578),(#169579,#169580,#169581),
(#169582,#169583,#169584),(#169585,#169586,#169587)),.UNSPECIFIED.,.F.,
 .F.,.F.)
B_SPLINE_SURFACE_WITH_KNOTS((4,4),(3,3),(0.,0.000103369667661675),(0.,1.),
 .UNSPECIFIED.)
GEOMETRIC_REPRESENTATION_ITEM()
RATIONAL_B_SPLINE_SURFACE(((1.,0.835735574810027,1.),(1.,0.831946521393585,
1.),(1.,0.827395718030991,1.),(1.,0.822092089912784,1.)))
REPRESENTATION_ITEM('')
SURFACE()
);
#2635=(
BOUNDED_SURFACE()
B_SPLINE_SURFACE(3,2,((#169594,#169595,#169596),(#169597,#169598,#169599),
(#169600,#169601,#169602),(#169603,#169604,#169605),(#169606,#169607,#169608),
(#169609,#169610,#169611)),.UNSPECIFIED.,.F.,.F.,.F.)
B_SPLINE_SURFACE_WITH_KNOTS((4,2,4),(3,3),(0.,0.000488238270881924,0.000976476541763847),
(0.,1.),.UNSPECIFIED.)
GEOMETRIC_REPRESENTATION_ITEM()
RATIONAL_B_SPLINE_SURFACE(((1.,0.807089511457258,1.),(1.,0.816558112905035,
1.),(1.,0.821286794224823,1.),(1.,0.825205555407875,1.),(1.,0.824318362071196,
1.),(1.,0.822092089912778,1.)))
REPRESENTATION_ITEM('')
SURFACE()
);
#2636=(
BOUNDED_SURFACE()
B_SPLINE_SURFACE(3,2,((#169662,#169663,#169664),(#169665,#169666,#169667),
(#169668,#169669,#169670),(#169671,#169672,#169673)),.UNSPECIFIED.,.F.,
 .F.,.F.)
B_SPLINE_SURFACE_WITH_KNOTS((4,4),(3,3),(-2.2779825405953E-5,0.000250578079469443),
(-9.62977912475538E-5,1.),.UNSPECIFIED.)
GEOMETRIC_REPRESENTATION_ITEM()
RATIONAL_B_SPLINE_SURFACE(((1.00003939441504,0.795455251195445,1.),(1.00003575677157,
0.814342722165374,1.),(1.00003292074913,0.829067994671566,1.),(1.00003112533526,
0.838390191208877,1.)))
REPRESENTATION_ITEM('')
SURFACE()
);
#2637=(
BOUNDED_SURFACE()
B_SPLINE_SURFACE(3,2,((#169699,#169700,#169701),(#169702,#169703,#169704),
(#169705,#169706,#169707),(#169708,#169709,#169710),(#169711,#169712,#169713),
(#169714,#169715,#169716),(#169717,#169718,#169719),(#169720,#169721,#169722),
(#169723,#169724,#169725),(#169726,#169727,#169728)),.UNSPECIFIED.,.F.,
 .F.,.F.)
B_SPLINE_SURFACE_WITH_KNOTS((4,2,2,2,4),(3,3),(3.1415926535898,3.53429173528852,
3.92699081698724,4.31968989868597,4.71238898038469),(0.,1.),
 .UNSPECIFIED.)
GEOMETRIC_REPRESENTATION_ITEM()
RATIONAL_B_SPLINE_SURFACE(((1.,0.754709580222767,1.),(1.,0.754714219730801,
1.),(1.,0.753512297096199,1.),(1.,0.748871927696587,1.),(1.,0.745429366938708,
1.),(1.,0.736738129296182,1.),(1.,0.731490756397336,1.),(1.,0.719894264862173,
1.),(1.,0.71355026185156,1.),(1.,0.707106781186543,1.)))
REPRESENTATION_ITEM('')
SURFACE()
);
#2638=(
BOUNDED_SURFACE()
B_SPLINE_SURFACE(3,2,((#169756,#169757,#169758),(#169759,#169760,#169761),
(#169762,#169763,#169764),(#169765,#169766,#169767),(#169768,#169769,#169770),
(#169771,#169772,#169773),(#169774,#169775,#169776),(#169777,#169778,#169779),
(#169780,#169781,#169782),(#169783,#169784,#169785)),.UNSPECIFIED.,.F.,
 .F.,.F.)
B_SPLINE_SURFACE_WITH_KNOTS((4,2,2,2,4),(3,3),(0.00116892975483546,0.00173273620432841,
0.00229654265382136,0.0028603491033143,0.00342415555280725),(-8.73672651017134E-5,
1.),.UNSPECIFIED.)
GEOMETRIC_REPRESENTATION_ITEM()
RATIONAL_B_SPLINE_SURFACE(((1.00005118303032,0.707081191907057,1.),(1.00004250803405,
0.756727911750157,1.),(1.00003576403202,0.795323614743189,1.),(1.00002660678148,
0.847730260009883,1.),(1.00002422236722,0.86137618483429,1.),(1.00002421067412,
0.861443104051582,1.),(1.00002658556867,0.847851660205465,1.),(1.00003574715401,
0.795420207077646,1.),(1.00004250128304,0.756766547571618,1.),(1.00005118303032,
0.707081191907057,1.)))
REPRESENTATION_ITEM('')
SURFACE()
);
#2639=(
BOUNDED_SURFACE()
B_SPLINE_SURFACE(3,2,((#169873,#169874,#169875),(#169876,#169877,#169878),
(#169879,#169880,#169881),(#169882,#169883,#169884)),.UNSPECIFIED.,.F.,
 .F.,.F.)
B_SPLINE_SURFACE_WITH_KNOTS((4,4),(3,3),(-6.9931040125315E-18,0.000203650363220118),
(0.,1.),.UNSPECIFIED.)
GEOMETRIC_REPRESENTATION_ITEM()
RATIONAL_B_SPLINE_SURFACE(((1.,0.707106781186548,1.),(1.,0.683088481213104,
1.),(1.,0.658130799535722,1.),(1.,0.631879234223615,1.)))
REPRESENTATION_ITEM('')
SURFACE()
);
#2640=(
BOUNDED_SURFACE()
B_SPLINE_SURFACE(3,2,((#169891,#169892,#169893),(#169894,#169895,#169896),
(#169897,#169898,#169899),(#169900,#169901,#169902),(#169903,#169904,#169905),
(#169906,#169907,#169908)),.UNSPECIFIED.,.F.,.F.,.F.)
B_SPLINE_SURFACE_WITH_KNOTS((4,2,4),(3,3),(0.00191966951912585,0.00217079434687949,
0.00242191917463315),(0.,1.),.UNSPECIFIED.)
GEOMETRIC_REPRESENTATION_ITEM()
RATIONAL_B_SPLINE_SURFACE(((1.,0.460674285272032,1.),(1.,0.480581991146479,
1.),(1.,0.508992468088204,1.),(1.,0.568988175192947,1.),(1.,0.601196374063936,
1.),(1.,0.631879234223659,1.)))
REPRESENTATION_ITEM('')
SURFACE()
);
#2641=(
BOUNDED_SURFACE()
B_SPLINE_SURFACE(3,2,((#169936,#169937,#169938),(#169939,#169940,#169941),
(#169942,#169943,#169944),(#169945,#169946,#169947),(#169948,#169949,#169950),
(#169951,#169952,#169953),(#169954,#169955,#169956),(#169957,#169958,#169959),
(#169960,#169961,#169962),(#169963,#169964,#169965)),.UNSPECIFIED.,.F.,
 .F.,.F.)
B_SPLINE_SURFACE_WITH_KNOTS((4,2,2,2,4),(3,3),(0.,0.00140990970253443,0.00281981940506887,
0.0042297291076033,0.00563963881013773),(0.,1.),.UNSPECIFIED.)
GEOMETRIC_REPRESENTATION_ITEM()
RATIONAL_B_SPLINE_SURFACE(((1.,0.460674285271834,1.),(1.,0.484432802265468,
1.),(1.,0.507218999550826,1.),(1.,0.55117184532966,1.),(1.,0.572342624738,
1.),(1.,0.613417108469756,1.),(1.,0.633191153021656,1.),(1.,0.671152451591827,
1.),(1.,0.689411349760462,1.),(1.,0.707106781186548,1.)))
REPRESENTATION_ITEM('')
SURFACE()
);
#2642=(
BOUNDED_SURFACE()
B_SPLINE_SURFACE(3,2,((#169988,#169989,#169990),(#169991,#169992,#169993),
(#169994,#169995,#169996),(#169997,#169998,#169999),(#170000,#170001,#170002),
(#170003,#170004,#170005),(#170006,#170007,#170008),(#170009,#170010,#170011)),
 .UNSPECIFIED.,.F.,.F.,.F.)
B_SPLINE_SURFACE_WITH_KNOTS((4,2,2,4),(3,3),(0.,0.00267885639561352,0.00401828459342028,
0.00535771279122705),(0.,1.),.UNSPECIFIED.)
GEOMETRIC_REPRESENTATION_ITEM()
RATIONAL_B_SPLINE_SURFACE(((1.,0.707106781186871,1.),(1.,0.673473842386368,
1.),(1.,0.638019211186003,1.),(1.,0.580269195298477,1.),(1.,0.560144321783745,
1.),(1.,0.518526712842715,1.),(1.,0.497044145980004,1.),(1.,0.474759570947005,
1.)))
REPRESENTATION_ITEM('')
SURFACE()
);
#2643=(
BOUNDED_SURFACE()
B_SPLINE_SURFACE(3,2,((#170027,#170028,#170029),(#170030,#170031,#170032),
(#170033,#170034,#170035),(#170036,#170037,#170038),(#170039,#170040,#170041),
(#170042,#170043,#170044),(#170045,#170046,#170047),(#170048,#170049,#170050),
(#170051,#170052,#170053),(#170054,#170055,#170056)),.UNSPECIFIED.,.F.,
 .F.,.F.)
B_SPLINE_SURFACE_WITH_KNOTS((4,2,2,2,4),(3,3),(0.,0.000174105410412539,
0.000348210820825077,0.000522316231237617,0.000696421641650155),(-0.000483059379797502,
1.),.UNSPECIFIED.)
GEOMETRIC_REPRESENTATION_ITEM()
RATIONAL_B_SPLINE_SURFACE(((1.0005076897577,0.474505848630797,1.),(1.000495670555,
0.486946557988912,1.),(1.0004800812597,0.503082561094009,1.),(1.00044417434065,
0.540248715550885,1.),(1.00042474790251,0.560356427930957,1.),(1.00038427712958,
0.602246488055232,1.),(1.00036396770606,0.623268151612906,1.),(1.00032333802193,
0.665322695866086,1.),(1.00030290014099,0.686477321779519,1.),(1.00028310632439,
0.706965296369921,1.)))
REPRESENTATION_ITEM('')
SURFACE()
);
#2644=(
BOUNDED_SURFACE()
B_SPLINE_SURFACE(3,2,((#170127,#170128,#170129),(#170130,#170131,#170132),
(#170133,#170134,#170135),(#170136,#170137,#170138),(#170139,#170140,#170141),
(#170142,#170143,#170144),(#170145,#170146,#170147),(#170148,#170149,#170150),
(#170151,#170152,#170153),(#170154,#170155,#170156)),.UNSPECIFIED.,.F.,
 .F.,.F.)
B_SPLINE_SURFACE_WITH_KNOTS((4,2,2,2,4),(3,3),(1.57066336187483,1.96349540849362,
2.35619449019234,2.74889357189107,3.14172561850986),(0.,1.00013296492006),
 .UNSPECIFIED.)
GEOMETRIC_REPRESENTATION_ITEM()
RATIONAL_B_SPLINE_SURFACE(((1.,0.707074379515281,1.00007789766343),(1.,
0.700631001612311,1.00007961114988),(1.,0.6940963087501,1.00008134891971),
(1.,0.681861139766965,1.00008460261624),(1.,0.676166101240053,1.00008611709693),
(1.,0.666571715833441,1.0000886685303),(1.,0.662679222605372,1.00008970366041),
(1.,0.657396767036713,1.00009110842297),(1.,0.656004520314383,1.00009147866292),
(1.,0.656013305345874,1.00009147632672)))
REPRESENTATION_ITEM('')
SURFACE()
);
#2645=(
BOUNDED_SURFACE()
B_SPLINE_SURFACE(3,2,((#170183,#170184,#170185),(#170186,#170187,#170188),
(#170189,#170190,#170191),(#170192,#170193,#170194)),.UNSPECIFIED.,.F.,
 .F.,.F.)
B_SPLINE_SURFACE_WITH_KNOTS((4,4),(3,3),(0.,0.000433489251034108),(0.,1.),
 .UNSPECIFIED.)
GEOMETRIC_REPRESENTATION_ITEM()
RATIONAL_B_SPLINE_SURFACE(((1.,0.843391445812886,1.),(1.,0.83955525384858,
1.),(1.,0.835558949072738,1.),(1.,0.831408647420015,1.)))
REPRESENTATION_ITEM('')
SURFACE()
);
#2646=(
BOUNDED_SURFACE()
B_SPLINE_SURFACE(3,2,((#170199,#170200,#170201),(#170202,#170203,#170204),
(#170205,#170206,#170207),(#170208,#170209,#170210),(#170211,#170212,#170213),
(#170214,#170215,#170216)),.UNSPECIFIED.,.F.,.F.,.F.)
B_SPLINE_SURFACE_WITH_KNOTS((4,2,4),(3,3),(-6.93889390390723E-18,0.0148367096635454,
0.0296734193270908),(0.,1.),.UNSPECIFIED.)
GEOMETRIC_REPRESENTATION_ITEM()
RATIONAL_B_SPLINE_SURFACE(((1.,0.524787419125867,1.),(1.,0.534113414550019,
1.),(1.,0.542054608658765,1.),(1.,0.556098130983184,1.),(1.,0.562195863398439,
1.),(1.,0.56767185832395,1.)))
REPRESENTATION_ITEM('')
SURFACE()
);
#2647=(
BOUNDED_SURFACE()
B_SPLINE_SURFACE(3,2,((#170228,#170229,#170230),(#170231,#170232,#170233),
(#170234,#170235,#170236),(#170237,#170238,#170239),(#170240,#170241,#170242),
(#170243,#170244,#170245)),.UNSPECIFIED.,.F.,.F.,.F.)
B_SPLINE_SURFACE_WITH_KNOTS((4,2,4),(3,3),(-0.000210164559996447,0.00205623335330194,
0.00432263126660034),(-0.000445187292128403,1.),.UNSPECIFIED.)
GEOMETRIC_REPRESENTATION_ITEM()
RATIONAL_B_SPLINE_SURFACE(((1.0004324500486,0.514305488672343,1.),(1.00039941933963,
0.551403031161431,1.),(1.00036812081892,0.58655511350849,1.),(1.00030827208983,
0.653772585966662,1.),(1.00027973535443,0.68582284425181,1.),(1.00025355847735,
0.71522269184906,1.)))
REPRESENTATION_ITEM('')
SURFACE()
);
#2648=(
BOUNDED_SURFACE()
B_SPLINE_SURFACE(3,2,((#170277,#170278,#170279),(#170280,#170281,#170282),
(#170283,#170284,#170285),(#170286,#170287,#170288),(#170289,#170290,#170291),
(#170292,#170293,#170294)),.UNSPECIFIED.,.F.,.F.,.F.)
B_SPLINE_SURFACE_WITH_KNOTS((4,2,4),(3,3),(0.,0.002055311285568,0.00411062257113599),
(0.,1.),.UNSPECIFIED.)
GEOMETRIC_REPRESENTATION_ITEM()
RATIONAL_B_SPLINE_SURFACE(((1.,0.707106781186549,1.),(1.,0.67983601545864,
1.),(1.,0.651283059470391,1.),(1.,0.590515772030266,1.),(1.,0.55801180255865,
1.),(1.,0.524787419125864,1.)))
REPRESENTATION_ITEM('')
SURFACE()
);
#2649=(
BOUNDED_SURFACE()
B_SPLINE_SURFACE(3,2,((#170376,#170377,#170378),(#170379,#170380,#170381),
(#170382,#170383,#170384),(#170385,#170386,#170387)),.UNSPECIFIED.,.F.,
 .F.,.F.)
B_SPLINE_SURFACE_WITH_KNOTS((4,4),(3,3),(-3.67928601881599E-5,0.000690322634258718),
(-3.67928601881599E-5,1.),.UNSPECIFIED.)
GEOMETRIC_REPRESENTATION_ITEM()
RATIONAL_B_SPLINE_SURFACE(((1.00003168318678,0.569438382609689,1.),(1.00003256820151,
0.557411392496539,1.),(1.00003304023254,0.550996682929833,1.),(1.0000329877132,
0.551710399363681,1.)))
REPRESENTATION_ITEM('')
SURFACE()
);
#2650=(
BOUNDED_SURFACE()
B_SPLINE_SURFACE(3,2,((#170389,#170390,#170391),(#170392,#170393,#170394),
(#170395,#170396,#170397),(#170398,#170399,#170400),(#170401,#170402,#170403),
(#170404,#170405,#170406)),.UNSPECIFIED.,.F.,.F.,.F.)
B_SPLINE_SURFACE_WITH_KNOTS((4,2,4),(3,3),(-3.37037386498138E-5,0.0147014688781887,
0.0294366414950272),(0.,1.00003370373865),.UNSPECIFIED.)
GEOMETRIC_REPRESENTATION_ITEM()
RATIONAL_B_SPLINE_SURFACE(((1.,0.567394857543477,1.00002916082132),(1.,
0.561935737478507,1.00002952880683),(1.,0.555859760262213,1.00002993837313),
(1.,0.541878051053617,1.00003088084487),(1.,0.533976759333239,1.00003141345102),
(1.,0.524707821662759,1.00003203824672)))
REPRESENTATION_ITEM('')
SURFACE()
);
#2651=(
BOUNDED_SURFACE()
B_SPLINE_SURFACE(3,2,((#170433,#170434,#170435),(#170436,#170437,#170438),
(#170439,#170440,#170441),(#170442,#170443,#170444),(#170445,#170446,#170447),
(#170448,#170449,#170450)),.UNSPECIFIED.,.F.,.F.,.F.)
B_SPLINE_SURFACE_WITH_KNOTS((4,2,4),(3,3),(0.312244141975826,0.317485429411984,
0.322726716848141),(0.,1.),.UNSPECIFIED.)
GEOMETRIC_REPRESENTATION_ITEM()
RATIONAL_B_SPLINE_SURFACE(((1.,0.945205509755643,1.),(1.,0.94765942841632,
1.),(1.,0.950143082313928,1.),(1.,0.955101624050304,1.),(1.,0.957550590969702,
1.),(1.,0.959916006973269,1.)))
REPRESENTATION_ITEM('')
SURFACE()
);
#2652=(
BOUNDED_SURFACE()
B_SPLINE_SURFACE(3,2,((#170550,#170551,#170552),(#170553,#170554,#170555),
(#170556,#170557,#170558),(#170559,#170560,#170561),(#170562,#170563,#170564),
(#170565,#170566,#170567)),.UNSPECIFIED.,.F.,.F.,.F.)
B_SPLINE_SURFACE_WITH_KNOTS((4,2,4),(3,3),(0.,0.00166463949867057,0.00332927899734113),
(0.,1.),.UNSPECIFIED.)
GEOMETRIC_REPRESENTATION_ITEM()
RATIONAL_B_SPLINE_SURFACE(((1.,0.824689321081979,1.),(1.,0.807273117786527,
1.),(1.,0.78876985537206,1.),(1.,0.749461319834452,1.),(1.,0.728524445804063,
1.),(1.,0.707106781186548,1.)))
REPRESENTATION_ITEM('')
SURFACE()
);
#2653=(
BOUNDED_SURFACE()
B_SPLINE_SURFACE(3,2,((#170584,#170585,#170586),(#170587,#170588,#170589),
(#170590,#170591,#170592),(#170593,#170594,#170595),(#170596,#170597,#170598),
(#170599,#170600,#170601)),.UNSPECIFIED.,.F.,.F.,.F.)
B_SPLINE_SURFACE_WITH_KNOTS((4,2,4),(3,3),(0.,0.0016638050806964,0.0033276101613928),
(0.,1.),.UNSPECIFIED.)
GEOMETRIC_REPRESENTATION_ITEM()
RATIONAL_B_SPLINE_SURFACE(((1.,0.707106781186548,1.),(1.,0.728604788113201,
1.),(1.,0.749094258011124,1.),(1.,0.788367019884298,1.),(1.,0.807290696029469,
1.),(1.,0.824689321081979,1.)))
REPRESENTATION_ITEM('')
SURFACE()
);
#2654=(
BOUNDED_SURFACE()
B_SPLINE_SURFACE(3,2,((#170620,#170621,#170622),(#170623,#170624,#170625),
(#170626,#170627,#170628),(#170629,#170630,#170631),(#170632,#170633,#170634),
(#170635,#170636,#170637)),.UNSPECIFIED.,.F.,.F.,.F.)
B_SPLINE_SURFACE_WITH_KNOTS((4,2,4),(3,3),(0.,0.0179426259581151,0.0358852519162302),
(0.,1.),.UNSPECIFIED.)
GEOMETRIC_REPRESENTATION_ITEM()
RATIONAL_B_SPLINE_SURFACE(((1.,0.796398016704685,1.),(1.,0.799989941027341,
1.),(1.,0.80399801610487,1.),(1.,0.81325769888663,1.),(1.,0.81850629826423,
1.),(1.,0.824689321081979,1.)))
REPRESENTATION_ITEM('')
SURFACE()
);
#2655=(
BOUNDED_SURFACE()
B_SPLINE_SURFACE(3,2,((#170647,#170648,#170649),(#170650,#170651,#170652),
(#170653,#170654,#170655),(#170656,#170657,#170658)),.UNSPECIFIED.,.F.,
 .F.,.F.)
B_SPLINE_SURFACE_WITH_KNOTS((4,4),(3,3),(-6.51868391715497E-5,0.000717055230887523),
(-0.00014173624593116,1.),.UNSPECIFIED.)
GEOMETRIC_REPRESENTATION_ITEM()
RATIONAL_B_SPLINE_SURFACE(((1.0000553523189,0.804734778555401,1.),(1.00005516270673,
0.805403669437731,1.),(1.00005612596714,0.802005595787349,1.),(1.00005822477713,
0.794601667527954,1.)))
REPRESENTATION_ITEM('')
SURFACE()
);
#2656=(
BOUNDED_SURFACE()
B_SPLINE_SURFACE(3,2,((#170677,#170678,#170679),(#170680,#170681,#170682),
(#170683,#170684,#170685),(#170686,#170687,#170688),(#170689,#170690,#170691),
(#170692,#170693,#170694)),.UNSPECIFIED.,.F.,.F.,.F.)
B_SPLINE_SURFACE_WITH_KNOTS((4,2,4),(3,3),(0.,0.0178083890192188,0.0356167780384377),
(0.,1.),.UNSPECIFIED.)
GEOMETRIC_REPRESENTATION_ITEM()
RATIONAL_B_SPLINE_SURFACE(((1.,0.824689321081978,1.),(1.,0.818552442915159,
1.),(1.,0.813336414682689,1.),(1.,0.80412734431217,1.),(1.,0.800137214821899,
1.),(1.,0.796559406694623,1.)))
REPRESENTATION_ITEM('')
SURFACE()
);
#2657=(
BOUNDED_SURFACE()
B_SPLINE_SURFACE(3,2,((#170763,#170764,#170765),(#170766,#170767,#170768),
(#170769,#170770,#170771),(#170772,#170773,#170774)),.UNSPECIFIED.,.F.,
 .F.,.F.)
B_SPLINE_SURFACE_WITH_KNOTS((4,4),(3,3),(-6.51391992791641E-5,0.00071653119207077),
(-0.000129157869248124,1.),.UNSPECIFIED.)
GEOMETRIC_REPRESENTATION_ITEM()
RATIONAL_B_SPLINE_SURFACE(((1.00009755078865,0.622358323103109,1.),(1.00009962867019,
0.614314362823106,1.),(1.00010065362943,0.610346508423656,1.),(1.00010045435892,
0.611117930705948,1.)))
REPRESENTATION_ITEM('')
SURFACE()
);
#2658=(
BOUNDED_SURFACE()
B_SPLINE_SURFACE(3,2,((#170778,#170779,#170780),(#170781,#170782,#170783),
(#170784,#170785,#170786),(#170787,#170788,#170789),(#170790,#170791,#170792),
(#170793,#170794,#170795)),.UNSPECIFIED.,.F.,.F.,.F.)
B_SPLINE_SURFACE_WITH_KNOTS((4,2,4),(3,3),(0.,0.0190876722191456,0.0381753444382913),
(0.,1.),.UNSPECIFIED.)
GEOMETRIC_REPRESENTATION_ITEM()
RATIONAL_B_SPLINE_SURFACE(((1.,0.584878694958869,1.),(1.,0.593227971935905,
1.),(1.,0.599946751815832,1.),(1.,0.611471310523657,1.),(1.,0.616266665820404,
1.),(1.,0.620481653466,1.)))
REPRESENTATION_ITEM('')
SURFACE()
);
#2659=(
BOUNDED_SURFACE()
B_SPLINE_SURFACE(3,2,((#170805,#170806,#170807),(#170808,#170809,#170810),
(#170811,#170812,#170813),(#170814,#170815,#170816),(#170817,#170818,#170819),
(#170820,#170821,#170822)),.UNSPECIFIED.,.F.,.F.,.F.)
B_SPLINE_SURFACE_WITH_KNOTS((4,2,4),(3,3),(-3.90312782094781E-18,0.00150339017752321,
0.00300678035504644),(0.,1.),.UNSPECIFIED.)
GEOMETRIC_REPRESENTATION_ITEM()
RATIONAL_B_SPLINE_SURFACE(((1.,0.58487869495887,1.),(1.,0.60668052563981,
1.),(1.,0.627781895260115,1.),(1.,0.668636131517873,1.),(1.,0.688512443471572,
1.),(1.,0.707106781186547,1.)))
REPRESENTATION_ITEM('')
SURFACE()
);
#2660=(
BOUNDED_SURFACE()
B_SPLINE_SURFACE(3,2,((#170845,#170846,#170847),(#170848,#170849,#170850),
(#170851,#170852,#170853),(#170854,#170855,#170856),(#170857,#170858,#170859),
(#170860,#170861,#170862)),.UNSPECIFIED.,.F.,.F.,.F.)
B_SPLINE_SURFACE_WITH_KNOTS((4,2,4),(3,3),(-1.06251812903579E-17,0.00150294083257491,
0.00300588166514984),(0.,1.),.UNSPECIFIED.)
GEOMETRIC_REPRESENTATION_ITEM()
RATIONAL_B_SPLINE_SURFACE(((1.,0.707106781186548,1.),(1.,0.688447591630839,
1.),(1.,0.669002122235948,1.),(1.,0.628207099426844,1.),(1.,0.606682052630604,
1.),(1.,0.584878694958868,1.)))
REPRESENTATION_ITEM('')
SURFACE()
);
#2661=(
BOUNDED_SURFACE()
B_SPLINE_SURFACE(3,2,((#170982,#170983,#170984),(#170985,#170986,#170987),
(#170988,#170989,#170990),(#170991,#170992,#170993),(#170994,#170995,#170996),
(#170997,#170998,#170999)),.UNSPECIFIED.,.F.,.F.,.F.)
B_SPLINE_SURFACE_WITH_KNOTS((4,2,4),(3,3),(-1.83478794364492E-5,0.0189537577590876,
0.0379258633976115),(0.,1.00001834787944),.UNSPECIFIED.)
GEOMETRIC_REPRESENTATION_ITEM()
RATIONAL_B_SPLINE_SURFACE(((0.999999999999999,0.620309398234657,1.00001393303477),
(1.,0.616103929910579,1.00001408735762),(1.,0.611321563705418,1.00001426285018),
(1.,0.599839171198574,1.00001468420528),(1.,0.593149294515289,1.00001492969539),
(0.999999999999999,0.584846995484289,1.00001523435455)))
REPRESENTATION_ITEM('')
SURFACE()
);
#2662=(
BOUNDED_SURFACE()
B_SPLINE_SURFACE(3,2,((#171026,#171027,#171028),(#171029,#171030,#171031),
(#171032,#171033,#171034),(#171035,#171036,#171037),(#171038,#171039,#171040),
(#171041,#171042,#171043),(#171044,#171045,#171046),(#171047,#171048,#171049)),
 .UNSPECIFIED.,.F.,.F.,.F.)
B_SPLINE_SURFACE_WITH_KNOTS((4,2,2,4),(3,3),(0.0758061741912965,0.0799264930317429,
0.081986652451966,0.0840468118721892),(0.,1.00000233834524),
 .UNSPECIFIED.)
GEOMETRIC_REPRESENTATION_ITEM()
RATIONAL_B_SPLINE_SURFACE(((1.,0.961573749752273,1.00000017970768),(1.,
0.963379709173868,1.00000017126177),(1.,0.965135219920033,1.00000016305179),
(1.,0.9676189737872,1.00000015143604),(1.,0.968423864707538,1.00000014767181),
(1.,0.969943438537677,1.00000014056524),(1.,0.970660702862963,1.00000013721081),
(1.,0.971327062935609,1.00000013409445)))
REPRESENTATION_ITEM('')
SURFACE()
);
#2663=(
BOUNDED_SURFACE()
B_SPLINE_SURFACE(3,2,((#171155,#171156,#171157),(#171158,#171159,#171160),
(#171161,#171162,#171163),(#171164,#171165,#171166),(#171167,#171168,#171169),
(#171170,#171171,#171172)),.UNSPECIFIED.,.F.,.F.,.F.)
B_SPLINE_SURFACE_WITH_KNOTS((4,2,4),(3,3),(-0.00011033835690659,0.00119596402151854,
0.00250226639994571),(-0.000284389303992256,1.),.UNSPECIFIED.)
GEOMETRIC_REPRESENTATION_ITEM()
RATIONAL_B_SPLINE_SURFACE(((1.00012562153941,0.779138072972314,1.),(1.00013243243221,
0.767163479163878,1.),(1.00013944174136,0.754840038985303,1.),(1.00015379669844,
0.729601823486879,1.),(1.00016119800703,0.716589188185346,1.),(1.00016848829712,
0.703771740441114,1.)))
REPRESENTATION_ITEM('')
SURFACE()
);
#2664=(
BOUNDED_SURFACE()
B_SPLINE_SURFACE(3,2,((#171194,#171195,#171196),(#171197,#171198,#171199),
(#171200,#171201,#171202),(#171203,#171204,#171205),(#171206,#171207,#171208),
(#171209,#171210,#171211)),.UNSPECIFIED.,.F.,.F.,.F.)
B_SPLINE_SURFACE_WITH_KNOTS((4,2,4),(3,3),(0.,0.00119589979970271,0.00239179959940542),
(0.,1.),.UNSPECIFIED.)
GEOMETRIC_REPRESENTATION_ITEM()
RATIONAL_B_SPLINE_SURFACE(((1.,0.707106781186548,1.),(1.,0.718869254063191,
1.),(1.,0.730529301274249,1.),(1.,0.753629773858896,1.),(1.,0.765147260447909,
1.),(1.,0.776159951988232,1.)))
REPRESENTATION_ITEM('')
SURFACE()
);
#2665=(
BOUNDED_SURFACE()
B_SPLINE_SURFACE(3,2,((#171227,#171228,#171229),(#171230,#171231,#171232),
(#171233,#171234,#171235),(#171236,#171237,#171238)),.UNSPECIFIED.,.F.,
 .F.,.F.)
B_SPLINE_SURFACE_WITH_KNOTS((4,4),(3,3),(0.,0.0421837023697854),(0.,1.),
 .UNSPECIFIED.)
GEOMETRIC_REPRESENTATION_ITEM()
RATIONAL_B_SPLINE_SURFACE(((1.,0.755978609126094,1.),(1.,0.760793534959097,
1.),(1.,0.766730014383061,1.),(1.,0.776159951988524,1.)))
REPRESENTATION_ITEM('')
SURFACE()
);
#2666=(
BOUNDED_SURFACE()
B_SPLINE_SURFACE(3,2,((#171245,#171246,#171247),(#171248,#171249,#171250),
(#171251,#171252,#171253),(#171254,#171255,#171256)),.UNSPECIFIED.,.F.,
 .F.,.F.)
B_SPLINE_SURFACE_WITH_KNOTS((4,4),(3,3),(0.,0.000650577858517379),(0.,1.),
 .UNSPECIFIED.)
GEOMETRIC_REPRESENTATION_ITEM()
RATIONAL_B_SPLINE_SURFACE(((1.,0.760728353039955,1.),(1.,0.760722617942438,
1.),(1.,0.759141109939139,1.),(1.,0.755978609126096,1.)))
REPRESENTATION_ITEM('')
SURFACE()
);
#2667=(
BOUNDED_SURFACE()
B_SPLINE_SURFACE(3,2,((#171263,#171264,#171265),(#171266,#171267,#171268),
(#171269,#171270,#171271),(#171272,#171273,#171274),(#171275,#171276,#171277),
(#171278,#171279,#171280),(#171281,#171282,#171283),(#171284,#171285,#171286),
(#171287,#171288,#171289),(#171290,#171291,#171292),(#171293,#171294,#171295),
(#171296,#171297,#171298),(#171299,#171300,#171301),(#171302,#171303,#171304)),
 .UNSPECIFIED.,.F.,.F.,.F.)
B_SPLINE_SURFACE_WITH_KNOTS((4,2,2,2,2,2,4),(3,3),(0.00808024661615471,
0.00880850598034447,0.00917263566243935,0.00953676534453423,0.00990089502662911,
0.010265024708724,0.0109932840729137),(0.,1.),.UNSPECIFIED.)
GEOMETRIC_REPRESENTATION_ITEM()
RATIONAL_B_SPLINE_SURFACE(((1.,0.707106781186552,1.),(1.,0.7086803042033,
1.),(1.,0.710213526000588,1.),(1.,0.712453026336305,1.),(1.,0.713188114139461,
1.),(1.,0.714590095265908,1.),(1.,0.715263343050717,1.),(1.,0.716554408796435,
1.),(1.,0.71717678241798,1.),(1.,0.718331565221162,1.),(1.,0.718866152975084,
1.),(1.,0.720344053893136,1.),(1.,0.721169771392395,1.),(1.,0.721765931188049,
1.)))
REPRESENTATION_ITEM('')
SURFACE()
);
#2668=(
BOUNDED_SURFACE()
B_SPLINE_SURFACE(3,2,((#171347,#171348,#171349),(#171350,#171351,#171352),
(#171353,#171354,#171355),(#171356,#171357,#171358)),.UNSPECIFIED.,.F.,
 .F.,.F.)
B_SPLINE_SURFACE_WITH_KNOTS((4,4),(3,3),(0.,0.0419168978153696),(0.,1.),
 .UNSPECIFIED.)
GEOMETRIC_REPRESENTATION_ITEM()
RATIONAL_B_SPLINE_SURFACE(((1.,0.776159951988518,1.),(1.,0.766788671732685,
1.),(1.,0.760870494736068,1.),(1.,0.756069167758398,1.)))
REPRESENTATION_ITEM('')
SURFACE()
);
#2669=(
BOUNDED_SURFACE()
B_SPLINE_SURFACE(3,2,((#171401,#171402,#171403),(#171404,#171405,#171406),
(#171407,#171408,#171409),(#171410,#171411,#171412),(#171413,#171414,#171415),
(#171416,#171417,#171418),(#171419,#171420,#171421),(#171422,#171423,#171424),
(#171425,#171426,#171427),(#171428,#171429,#171430),(#171431,#171432,#171433),
(#171434,#171435,#171436),(#171437,#171438,#171439),(#171440,#171441,#171442)),
 .UNSPECIFIED.,.F.,.F.,.F.)
B_SPLINE_SURFACE_WITH_KNOTS((4,2,2,2,2,2,4),(3,3),(0.00808046157075938,
0.00879095475051749,0.00914620134039654,0.0095014479302756,0.00985669452015465,
0.0102119411100337,0.0109224342897918),(0.,1.),.UNSPECIFIED.)
GEOMETRIC_REPRESENTATION_ITEM()
RATIONAL_B_SPLINE_SURFACE(((1.,0.707106781186552,1.),(1.,0.705538120216095,
1.),(1.,0.703999772329756,1.),(1.,0.701739154413458,1.),(1.,0.700992634705956,
1.),(1.,0.699563445722461,1.),(1.,0.698874516085242,1.),(1.,0.697548436732303,
1.),(1.,0.696906638208049,1.),(1.,0.695703451829647,1.),(1.,0.695143596113536,
1.),(1.,0.693587190992306,1.),(1.,0.692704331853457,1.),(1.,0.69204248906153,
1.)))
REPRESENTATION_ITEM('')
SURFACE()
);
#2670=(
BOUNDED_SURFACE()
B_SPLINE_SURFACE(3,2,((#171485,#171486,#171487),(#171488,#171489,#171490),
(#171491,#171492,#171493),(#171494,#171495,#171496)),.UNSPECIFIED.,.F.,
 .F.,.F.)
B_SPLINE_SURFACE_WITH_KNOTS((4,4),(3,3),(0.,0.000650363027228679),(0.,1.),
 .UNSPECIFIED.)
GEOMETRIC_REPRESENTATION_ITEM()
RATIONAL_B_SPLINE_SURFACE(((1.,0.66913647774042,1.),(1.,0.666544790513632,
1.),(1.,0.665198010610878,1.),(1.,0.665190809887722,1.)))
REPRESENTATION_ITEM('')
SURFACE()
);
#2671=(
BOUNDED_SURFACE()
B_SPLINE_SURFACE(3,2,((#171500,#171501,#171502),(#171503,#171504,#171505),
(#171506,#171507,#171508),(#171509,#171510,#171511)),.UNSPECIFIED.,.F.,
 .F.,.F.)
B_SPLINE_SURFACE_WITH_KNOTS((4,4),(3,3),(0.,0.0433970829567688),(0.,1.),
 .UNSPECIFIED.)
GEOMETRIC_REPRESENTATION_ITEM()
RATIONAL_B_SPLINE_SURFACE(((1.,0.651268546304981,1.),(1.,0.659940697395559,
1.),(1.,0.665023311775857,1.),(1.,0.669136477740405,1.)))
REPRESENTATION_ITEM('')
SURFACE()
);
#2672=(
BOUNDED_SURFACE()
B_SPLINE_SURFACE(3,2,((#171518,#171519,#171520),(#171521,#171522,#171523),
(#171524,#171525,#171526),(#171527,#171528,#171529),(#171530,#171531,#171532),
(#171533,#171534,#171535)),.UNSPECIFIED.,.F.,.F.,.F.)
B_SPLINE_SURFACE_WITH_KNOTS((4,2,4),(3,3),(-0.00017231904915643,0.00109600456666539,
0.00236432773995983),(-0.000172319052339097,1.),.UNSPECIFIED.)
GEOMETRIC_REPRESENTATION_ITEM()
RATIONAL_B_SPLINE_SURFACE(((1.00012181741146,0.646535279167556,1.),(1.00011784985333,
0.658047523674751,1.),(1.0001140008242,0.669215845107308,1.),(1.00010655811155,
0.690811578565519,1.),(1.00010293762449,0.701316763613497,1.),(1.00009957515527,
0.711073285509502,1.)))
REPRESENTATION_ITEM('')
SURFACE()
);
#2673=(
BOUNDED_SURFACE()
B_SPLINE_SURFACE(3,2,((#171555,#171556,#171557),(#171558,#171559,#171560),
(#171561,#171562,#171563),(#171564,#171565,#171566),(#171567,#171568,#171569),
(#171570,#171571,#171572)),.UNSPECIFIED.,.F.,.F.,.F.)
B_SPLINE_SURFACE_WITH_KNOTS((4,2,4),(3,3),(0.,0.00109598668217933,0.00219197336435865),
(0.,1.),.UNSPECIFIED.)
GEOMETRIC_REPRESENTATION_ITEM()
RATIONAL_B_SPLINE_SURFACE(((1.,0.707106781186548,1.),(1.,0.698507203291837,
1.),(1.,0.689563761715544,1.),(1.,0.670914228806854,1.),(1.,0.661139818833385,
1.),(1.,0.65126854630498,1.)))
REPRESENTATION_ITEM('')
SURFACE()
);
#2674=(
BOUNDED_SURFACE()
B_SPLINE_SURFACE(3,2,((#171653,#171654,#171655),(#171656,#171657,#171658),
(#171659,#171660,#171661),(#171662,#171663,#171664)),.UNSPECIFIED.,.F.,
 .F.,.F.)
B_SPLINE_SURFACE_WITH_KNOTS((4,4),(3,3),(-1.38777878078145E-17,0.0431305646498159),
(0.,1.),.UNSPECIFIED.)
GEOMETRIC_REPRESENTATION_ITEM()
RATIONAL_B_SPLINE_SURFACE(((1.,0.669061697655964,1.),(1.,0.66495869705799,
1.),(1.,0.659888610517475,1.),(1.,0.65126854630498,1.)))
REPRESENTATION_ITEM('')
SURFACE()
);
#2675=(
BOUNDED_SURFACE()
B_SPLINE_SURFACE(3,2,((#171688,#171689,#171690),(#171691,#171692,#171693),
(#171694,#171695,#171696),(#171697,#171698,#171699),(#171700,#171701,#171702),
(#171703,#171704,#171705),(#171706,#171707,#171708),(#171709,#171710,#171711)),
 .UNSPECIFIED.,.F.,.F.,.F.)
B_SPLINE_SURFACE_WITH_KNOTS((4,2,2,4),(3,3),(0.023727979672696,0.0269788291349169,
0.0286042538660274,0.0302296785971378),(0.,1.),.UNSPECIFIED.)
GEOMETRIC_REPRESENTATION_ITEM()
RATIONAL_B_SPLINE_SURFACE(((1.,0.972985060853882,1.),(1.,0.973867966894579,
1.),(1.,0.974606628833735,1.),(1.,0.975438732489742,1.),(1.,0.975670772749385,
1.),(1.,0.976026965697327,1.),(1.,0.976152018462137,1.),(1.,0.976223679017856,
1.)))
REPRESENTATION_ITEM('')
SURFACE()
);
#2676=(
BOUNDED_SURFACE()
B_SPLINE_SURFACE(3,2,((#171754,#171755,#171756),(#171757,#171758,#171759),
(#171760,#171761,#171762),(#171763,#171764,#171765)),.UNSPECIFIED.,.F.,
 .F.,.F.)
B_SPLINE_SURFACE_WITH_KNOTS((4,4),(3,3),(0.,0.00195732365556561),(0.,1.),
 .UNSPECIFIED.)
GEOMETRIC_REPRESENTATION_ITEM()
RATIONAL_B_SPLINE_SURFACE(((1.,0.71617462512364,1.),(1.,0.713064019807532,
1.),(1.,0.709996713322441,1.),(1.,0.707106781186534,1.)))
REPRESENTATION_ITEM('')
SURFACE()
);
#2677=(
BOUNDED_SURFACE()
B_SPLINE_SURFACE(3,2,((#171775,#171776,#171777),(#171778,#171779,#171780),
(#171781,#171782,#171783),(#171784,#171785,#171786)),.UNSPECIFIED.,.F.,
 .F.,.F.)
B_SPLINE_SURFACE_WITH_KNOTS((4,4),(3,3),(0.,0.00195732360009946),(0.,1.),
 .UNSPECIFIED.)
GEOMETRIC_REPRESENTATION_ITEM()
RATIONAL_B_SPLINE_SURFACE(((1.,0.707106781186548,1.),(1.,0.709967301734631,
1.),(1.,0.713032729764421,1.),(1.,0.716174625123614,1.)))
REPRESENTATION_ITEM('')
SURFACE()
);
#2678=(
BOUNDED_SURFACE()
B_SPLINE_SURFACE(3,2,((#171790,#171791,#171792),(#171793,#171794,#171795),
(#171796,#171797,#171798),(#171799,#171800,#171801)),.UNSPECIFIED.,.F.,
 .F.,.F.)
B_SPLINE_SURFACE_WITH_KNOTS((4,4),(3,3),(0.,0.0447707136167657),(0.,1.),
 .UNSPECIFIED.)
GEOMETRIC_REPRESENTATION_ITEM()
RATIONAL_B_SPLINE_SURFACE(((1.,0.713272398106993,1.),(1.,0.713940344609358,
1.),(1.,0.714765614654658,1.),(1.,0.71617462512364,1.)))
REPRESENTATION_ITEM('')
SURFACE()
);
#2679=(
BOUNDED_SURFACE()
B_SPLINE_SURFACE(3,2,((#171808,#171809,#171810),(#171811,#171812,#171813),
(#171814,#171815,#171816),(#171817,#171818,#171819)),.UNSPECIFIED.,.F.,
 .F.,.F.)
B_SPLINE_SURFACE_WITH_KNOTS((4,4),(3,3),(0.,0.000650121327073412),(0.,1.),
 .UNSPECIFIED.)
GEOMETRIC_REPRESENTATION_ITEM()
RATIONAL_B_SPLINE_SURFACE(((1.,0.713890629234418,1.),(1.,0.713889885788569,
1.),(1.,0.71368362023966,1.),(1.,0.713272398106985,1.)))
REPRESENTATION_ITEM('')
SURFACE()
);
#2680=(
BOUNDED_SURFACE()
B_SPLINE_SURFACE(3,2,((#171826,#171827,#171828),(#171829,#171830,#171831),
(#171832,#171833,#171834),(#171835,#171836,#171837),(#171838,#171839,#171840),
(#171841,#171842,#171843),(#171844,#171845,#171846),(#171847,#171848,#171849),
(#171850,#171851,#171852),(#171853,#171854,#171855)),.UNSPECIFIED.,.F.,
 .F.,.F.)
B_SPLINE_SURFACE_WITH_KNOTS((4,2,2,2,4),(3,3),(0.0080756712423913,0.00867825313759154,
0.00928083503279179,0.00988341692799203,0.0104859988231923),(0.,1.),
 .UNSPECIFIED.)
GEOMETRIC_REPRESENTATION_ITEM()
RATIONAL_B_SPLINE_SURFACE(((1.,0.707106781186548,1.),(1.,0.707146901961909,
1.),(1.,0.707185957443845,1.),(1.,0.707262034097608,1.),(1.,0.707299176477847,
1.),(1.,0.7073675568103,1.),(1.,0.707399679105567,1.),(1.,0.707457223307409,
1.),(1.,0.707482383732919,1.),(1.,0.707504065565917,1.)))
REPRESENTATION_ITEM('')
SURFACE()
);
#2681=(
BOUNDED_SURFACE()
B_SPLINE_SURFACE(3,2,((#171883,#171884,#171885),(#171886,#171887,#171888),
(#171889,#171890,#171891),(#171892,#171893,#171894)),.UNSPECIFIED.,.F.,
 .F.,.F.)
B_SPLINE_SURFACE_WITH_KNOTS((4,4),(3,3),(0.,0.0445045070401677),(0.,1.),
 .UNSPECIFIED.)
GEOMETRIC_REPRESENTATION_ITEM()
RATIONAL_B_SPLINE_SURFACE(((1.,0.71617462512364,1.),(1.,0.714773807595299,
1.),(1.,0.713950503107743,1.),(1.,0.713284154090124,1.)))
REPRESENTATION_ITEM('')
SURFACE()
);
#2682=(
BOUNDED_SURFACE()
B_SPLINE_SURFACE(3,2,((#171928,#171929,#171930),(#171931,#171932,#171933),
(#171934,#171935,#171936),(#171937,#171938,#171939),(#171940,#171941,#171942),
(#171943,#171944,#171945),(#171946,#171947,#171948),(#171949,#171950,#171951),
(#171952,#171953,#171954),(#171955,#171956,#171957)),.UNSPECIFIED.,.F.,
 .F.,.F.)
B_SPLINE_SURFACE_WITH_KNOTS((4,2,2,2,4),(3,3),(0.00807569768389314,0.00867847980331418,
0.00928126192273523,0.00988404404215627,0.0104868261615773),(0.,1.),
 .UNSPECIFIED.)
GEOMETRIC_REPRESENTATION_ITEM()
RATIONAL_B_SPLINE_SURFACE(((1.,0.707106781186548,1.),(1.,0.707212493429049,
1.),(1.,0.707315385014487,1.),(1.,0.707515784384109,1.),(1.,0.707613608127955,
1.),(1.,0.707793680404111,1.),(1.,0.707878261047732,1.),(1.,0.708029744860286,
1.),(1.,0.7080959680978,1.),(1.,0.708153025875396,1.)))
REPRESENTATION_ITEM('')
SURFACE()
);
#2683=(
BOUNDED_SURFACE()
B_SPLINE_SURFACE(3,2,((#171988,#171989,#171990),(#171991,#171992,#171993),
(#171994,#171995,#171996),(#171997,#171998,#171999)),.UNSPECIFIED.,.F.,
 .F.,.F.)
B_SPLINE_SURFACE_WITH_KNOTS((4,4),(3,3),(0.,0.000650124428678587),(0.,1.),
 .UNSPECIFIED.)
GEOMETRIC_REPRESENTATION_ITEM()
RATIONAL_B_SPLINE_SURFACE(((1.,0.714485667734326,1.),(1.,0.714973119513317,
1.),(1.,0.715223297464931,1.),(1.,0.715224866856049,1.)))
REPRESENTATION_ITEM('')
SURFACE()
);
#2684=(
BOUNDED_SURFACE()
B_SPLINE_SURFACE(3,2,((#172003,#172004,#172005),(#172006,#172007,#172008),
(#172009,#172010,#172011),(#172012,#172013,#172014)),.UNSPECIFIED.,.F.,
 .F.,.F.)
B_SPLINE_SURFACE_WITH_KNOTS((4,4),(3,3),(0.,0.044753309356401),(0.,1.),
 .UNSPECIFIED.)
GEOMETRIC_REPRESENTATION_ITEM()
RATIONAL_B_SPLINE_SURFACE(((1.,0.717952606100523,1.),(1.,0.716270361073643,
1.),(1.,0.715283994577086,1.),(1.,0.714485667734334,1.)))
REPRESENTATION_ITEM('')
SURFACE()
);
#2685=(
BOUNDED_SURFACE()
B_SPLINE_SURFACE(3,2,((#172021,#172022,#172023),(#172024,#172025,#172026),
(#172027,#172028,#172029),(#172030,#172031,#172032)),.UNSPECIFIED.,.F.,
 .F.,.F.)
B_SPLINE_SURFACE_WITH_KNOTS((4,4),(3,3),(-3.90312782094781E-18,0.0019603544817943),
(0.,1.),.UNSPECIFIED.)
GEOMETRIC_REPRESENTATION_ITEM()
RATIONAL_B_SPLINE_SURFACE(((1.,0.717952606100523,1.),(1.,0.714237876912109,
1.),(1.,0.710568615888393,1.),(1.,0.707106781186514,1.)))
REPRESENTATION_ITEM('')
SURFACE()
);
#2686=(
BOUNDED_SURFACE()
B_SPLINE_SURFACE(3,2,((#172040,#172041,#172042),(#172043,#172044,#172045),
(#172046,#172047,#172048),(#172049,#172050,#172051)),.UNSPECIFIED.,.F.,
 .F.,.F.)
B_SPLINE_SURFACE_WITH_KNOTS((4,4),(3,3),(0.,0.00196035438616165),(0.,1.),
 .UNSPECIFIED.)
GEOMETRIC_REPRESENTATION_ITEM()
RATIONAL_B_SPLINE_SURFACE(((1.,0.707106781186548,1.),(1.,0.710533388681839,
1.),(1.,0.714200483631581,1.),(1.,0.717952606100467,1.)))
REPRESENTATION_ITEM('')
SURFACE()
);
#2687=(
BOUNDED_SURFACE()
B_SPLINE_SURFACE(3,2,((#172057,#172058,#172059),(#172060,#172061,#172062),
(#172063,#172064,#172065),(#172066,#172067,#172068)),.UNSPECIFIED.,.F.,
 .F.,.F.)
B_SPLINE_SURFACE_WITH_KNOTS((4,4),(3,3),(0.,0.0444870989094409),(0.,1.),
 .UNSPECIFIED.)
GEOMETRIC_REPRESENTATION_ITEM()
RATIONAL_B_SPLINE_SURFACE(((1.,0.71449972514277,1.),(1.,0.715296138993144,
1.),(1.,0.71628014758797,1.),(1.,0.717952606100523,1.)))
REPRESENTATION_ITEM('')
SURFACE()
);
#2688=(
BOUNDED_SURFACE()
B_SPLINE_SURFACE(3,2,((#172101,#172102,#172103),(#172104,#172105,#172106),
(#172107,#172108,#172109),(#172110,#172111,#172112),(#172113,#172114,#172115),
(#172116,#172117,#172118)),.UNSPECIFIED.,.F.,.F.,.F.)
B_SPLINE_SURFACE_WITH_KNOTS((4,2,4),(3,3),(0.012499301108314,0.0157975372010094,
0.0190957732937049),(0.,1.),.UNSPECIFIED.)
GEOMETRIC_REPRESENTATION_ITEM()
RATIONAL_B_SPLINE_SURFACE(((1.,0.976191060180328,1.),(1.,0.976018964367352,
1.),(1.,0.975629721882182,1.),(1.,0.974451430140223,1.),(1.,0.97367913510036,
1.),(1.,0.972768244198254,1.)))
REPRESENTATION_ITEM('')
SURFACE()
);
#2689=(
BOUNDED_SURFACE()
B_SPLINE_SURFACE(3,2,((#172209,#172210,#172211),(#172212,#172213,#172214),
(#172215,#172216,#172217),(#172218,#172219,#172220),(#172221,#172222,#172223),
(#172224,#172225,#172226)),.UNSPECIFIED.,.F.,.F.,.F.)
B_SPLINE_SURFACE_WITH_KNOTS((4,2,4),(3,3),(-0.00018317133585458,0.00110390261829224,
0.00239097668804685),(-0.000183171451462374,1.),.UNSPECIFIED.)
GEOMETRIC_REPRESENTATION_ITEM()
RATIONAL_B_SPLINE_SURFACE(((1.00013033238588,0.644233899891368,1.),(1.00012593769652,
0.656230008786567,1.),(1.00012167569773,0.667863914494213,1.),(1.00011343748823,
0.690351615044338,1.),(1.00010943132374,0.701287174225601,1.),(1.00010571535824,
0.711430582116219,1.)))
REPRESENTATION_ITEM('')
SURFACE()
);
#2690=(
BOUNDED_SURFACE()
B_SPLINE_SURFACE(3,2,((#172248,#172249,#172250),(#172251,#172252,#172253),
(#172254,#172255,#172256),(#172257,#172258,#172259),(#172260,#172261,#172262),
(#172263,#172264,#172265)),.UNSPECIFIED.,.F.,.F.,.F.)
B_SPLINE_SURFACE_WITH_KNOTS((4,2,4),(3,3),(0.,0.00110388220976991,0.00220776441953981),
(0.,1.),.UNSPECIFIED.)
GEOMETRIC_REPRESENTATION_ITEM()
RATIONAL_B_SPLINE_SURFACE(((1.,0.707106781186548,1.),(1.,0.69822152219183,
1.),(1.,0.68897986867167,1.),(1.,0.66970545013756,1.),(1.,0.659601845960695,
1.),(1.,0.649397749909072,1.)))
REPRESENTATION_ITEM('')
SURFACE()
);
#2691=(
BOUNDED_SURFACE()
B_SPLINE_SURFACE(3,2,((#172281,#172282,#172283),(#172284,#172285,#172286),
(#172287,#172288,#172289),(#172290,#172291,#172292)),.UNSPECIFIED.,.F.,
 .F.,.F.)
B_SPLINE_SURFACE_WITH_KNOTS((4,4),(3,3),(-2.77555756156289E-17,0.0433026927553429),
(0.,1.),.UNSPECIFIED.)
GEOMETRIC_REPRESENTATION_ITEM()
RATIONAL_B_SPLINE_SURFACE(((1.,0.667840827103545,1.),(1.,0.66359300941018,
1.),(1.,0.658343952018749,1.),(1.,0.649397749909072,1.)))
REPRESENTATION_ITEM('')
SURFACE()
);
#2692=(
BOUNDED_SURFACE()
B_SPLINE_SURFACE(3,2,((#172299,#172300,#172301),(#172302,#172303,#172304),
(#172305,#172306,#172307),(#172308,#172309,#172310)),.UNSPECIFIED.,.F.,
 .F.,.F.)
B_SPLINE_SURFACE_WITH_KNOTS((4,4),(3,3),(0.,0.000650375609766158),(0.,1.),
 .UNSPECIFIED.)
GEOMETRIC_REPRESENTATION_ITEM()
RATIONAL_B_SPLINE_SURFACE(((1.,0.663756004792833,1.),(1.,0.663759519746911,
1.),(1.,0.665134391960157,1.),(1.,0.66784082710355,1.)))
REPRESENTATION_ITEM('')
SURFACE()
);
#2693=(
BOUNDED_SURFACE()
B_SPLINE_SURFACE(3,2,((#172317,#172318,#172319),(#172320,#172321,#172322),
(#172323,#172324,#172325),(#172326,#172327,#172328),(#172329,#172330,#172331),
(#172332,#172333,#172334),(#172335,#172336,#172337),(#172338,#172339,#172340),
(#172341,#172342,#172343),(#172344,#172345,#172346),(#172347,#172348,#172349),
(#172350,#172351,#172352),(#172353,#172354,#172355),(#172356,#172357,#172358)),
 .UNSPECIFIED.,.F.,.F.,.F.)
B_SPLINE_SURFACE_WITH_KNOTS((4,2,2,2,2,2,4),(3,3),(0.0080803797182093,0.00879690254712659,
0.00915516396158524,0.00951342537604388,0.00987168679050253,0.0102299482049612,
0.0109464710338785),(0.,1.),.UNSPECIFIED.)
GEOMETRIC_REPRESENTATION_ITEM()
RATIONAL_B_SPLINE_SURFACE(((1.,0.707106781186548,1.),(1.,0.705537440672151,
1.),(1.,0.703998083945123,1.),(1.,0.701735656940981,1.),(1.,0.700989163179782,
1.),(1.,0.699560461823081,1.),(1.,0.698871897343629,1.),(1.,0.697546947950716,
1.),(1.,0.696905752213842,1.),(1.,0.695707159507179,1.),(1.,0.695149875554341,
1.),(1.,0.693602432259692,1.),(1.,0.692727265033204,1.),(1.,0.692079067931822,
1.)))
REPRESENTATION_ITEM('')
SURFACE()
);
#2694=(
BOUNDED_SURFACE()
B_SPLINE_SURFACE(3,2,((#172395,#172396,#172397),(#172398,#172399,#172400),
(#172401,#172402,#172403),(#172404,#172405,#172406)),.UNSPECIFIED.,.F.,
 .F.,.F.)
B_SPLINE_SURFACE_WITH_KNOTS((4,4),(3,3),(0.,0.0430361525536219),(0.,1.),
 .UNSPECIFIED.)
GEOMETRIC_REPRESENTATION_ITEM()
RATIONAL_B_SPLINE_SURFACE(((1.,0.649397749909071,1.),(1.,0.658290092659334,
1.),(1.,0.663526138769308,1.),(1.,0.667763418073535,1.)))
REPRESENTATION_ITEM('')
SURFACE()
);
#2695=(
BOUNDED_SURFACE()
B_SPLINE_SURFACE(3,2,((#172448,#172449,#172450),(#172451,#172452,#172453),
(#172454,#172455,#172456),(#172457,#172458,#172459),(#172460,#172461,#172462),
(#172463,#172464,#172465),(#172466,#172467,#172468),(#172469,#172470,#172471),
(#172472,#172473,#172474),(#172475,#172476,#172477),(#172478,#172479,#172480),
(#172481,#172482,#172483),(#172484,#172485,#172486),(#172487,#172488,#172489)),
 .UNSPECIFIED.,.F.,.F.,.F.)
B_SPLINE_SURFACE_WITH_KNOTS((4,2,2,2,2,2,4),(3,3),(0.00808011141552929,
0.00881517523662049,0.00918270714716608,0.00955023905771168,0.00991777096825728,
0.0102853028788029,0.0110203666998941),(0.,1.),.UNSPECIFIED.)
GEOMETRIC_REPRESENTATION_ITEM()
RATIONAL_B_SPLINE_SURFACE(((1.,0.707106781186548,1.),(1.,0.708672362536739,
1.),(1.,0.710198222857537,1.),(1.,0.712427305746575,1.),(1.,0.71315813872198,
1.),(1.,0.714551782754775,1.),(1.,0.715220876802376,1.),(1.,0.71650348303418,
1.),(1.,0.717121230234592,1.),(1.,0.718264550261012,1.),(1.,0.718793336138408,
1.),(1.,0.720253112545596,1.),(1.,0.721064801594907,1.),(1.,0.721643051700349,
1.)))
REPRESENTATION_ITEM('')
SURFACE()
);
#2696=(
BOUNDED_SURFACE()
B_SPLINE_SURFACE(3,2,((#172532,#172533,#172534),(#172535,#172536,#172537),
(#172538,#172539,#172540),(#172541,#172542,#172543)),.UNSPECIFIED.,.F.,
 .F.,.F.)
B_SPLINE_SURFACE_WITH_KNOTS((4,4),(3,3),(-6.5060980421357E-5,0.000715670784634951),
(-0.000197321044369628,1.),.UNSPECIFIED.)
GEOMETRIC_REPRESENTATION_ITEM()
RATIONAL_B_SPLINE_SURFACE(((1.00009626630384,0.756066809424477,1.),(1.00009460009415,
0.760288887453376,1.),(1.0000938192903,0.762267398805323,1.),(1.0000939691079,
0.761887769744427,1.)))
REPRESENTATION_ITEM('')
SURFACE()
);
#2697=(
BOUNDED_SURFACE()
B_SPLINE_SURFACE(3,2,((#172547,#172548,#172549),(#172550,#172551,#172552),
(#172553,#172554,#172555),(#172556,#172557,#172558)),.UNSPECIFIED.,.F.,
 .F.,.F.)
B_SPLINE_SURFACE_WITH_KNOTS((4,4),(3,3),(0.,0.0420570108120997),(0.,1.),
 .UNSPECIFIED.)
GEOMETRIC_REPRESENTATION_ITEM()
RATIONAL_B_SPLINE_SURFACE(((1.,0.777664586555049,1.),(1.,0.768081385918698,
1.),(1.,0.762031405880593,1.),(1.,0.757123446310248,1.)))
REPRESENTATION_ITEM('')
SURFACE()
);
#2698=(
BOUNDED_SURFACE()
B_SPLINE_SURFACE(3,2,((#172565,#172566,#172567),(#172568,#172569,#172570),
(#172571,#172572,#172573),(#172574,#172575,#172576),(#172577,#172578,#172579),
(#172580,#172581,#172582)),.UNSPECIFIED.,.F.,.F.,.F.)
B_SPLINE_SURFACE_WITH_KNOTS((4,2,4),(3,3),(0.,0.00120620763625507,0.00241241527251014),
(0.,1.),.UNSPECIFIED.)
GEOMETRIC_REPRESENTATION_ITEM()
RATIONAL_B_SPLINE_SURFACE(((1.,0.777664586555049,1.),(1.,0.766436783957212,
1.),(1.,0.754901973237173,1.),(1.,0.73129895059372,1.),(1.,0.719146552484787,
1.),(1.,0.707106781186548,1.)))
REPRESENTATION_ITEM('')
SURFACE()
);
#2699=(
BOUNDED_SURFACE()
B_SPLINE_SURFACE(3,2,((#172602,#172603,#172604),(#172605,#172606,#172607),
(#172608,#172609,#172610),(#172611,#172612,#172613),(#172614,#172615,#172616),
(#172617,#172618,#172619)),.UNSPECIFIED.,.F.,.F.,.F.)
B_SPLINE_SURFACE_WITH_KNOTS((4,2,4),(3,3),(0.,0.00120613678608598,0.00241227357217196),
(0.,1.),.UNSPECIFIED.)
GEOMETRIC_REPRESENTATION_ITEM()
RATIONAL_B_SPLINE_SURFACE(((1.,0.707106781186548,1.),(1.,0.719152101713129,
1.),(1.,0.731078910702522,1.),(1.,0.754682512407923,1.),(1.,0.766438100601174,
1.),(1.,0.777664586554854,1.)))
REPRESENTATION_ITEM('')
SURFACE()
);
#2700=(
BOUNDED_SURFACE()
B_SPLINE_SURFACE(3,2,((#172700,#172701,#172702),(#172703,#172704,#172705),
(#172706,#172707,#172708),(#172709,#172710,#172711)),.UNSPECIFIED.,.F.,
 .F.,.F.)
B_SPLINE_SURFACE_WITH_KNOTS((4,4),(3,3),(-8.32667268468867E-17,0.0417901757617077),
(0.,1.),.UNSPECIFIED.)
GEOMETRIC_REPRESENTATION_ITEM()
RATIONAL_B_SPLINE_SURFACE(((1.,0.757216058458815,1.),(1.,0.76211005468913,
1.),(1.,0.768141195659961,1.),(1.,0.777664586555055,1.)))
REPRESENTATION_ITEM('')
SURFACE()
);
#2701=(
BOUNDED_SURFACE()
B_SPLINE_SURFACE(3,2,((#172735,#172736,#172737),(#172738,#172739,#172740),
(#172741,#172742,#172743),(#172744,#172745,#172746),(#172747,#172748,#172749),
(#172750,#172751,#172752),(#172753,#172754,#172755),(#172756,#172757,#172758)),
 .UNSPECIFIED.,.F.,.F.,.F.)
B_SPLINE_SURFACE_WITH_KNOTS((4,2,2,4),(3,3),(0.017818580704263,0.0199004486313254,
0.0219823165583878,0.0261460524125126),(0.,1.),.UNSPECIFIED.)
GEOMETRIC_REPRESENTATION_ITEM()
RATIONAL_B_SPLINE_SURFACE(((1.,0.961171308030857,1.),(1.,0.962092810628593,
1.),(1.,0.963001088261132,1.),(1.,0.964780402726978,1.),(1.,0.965653853257041,
1.),(1.,0.968176214233281,1.),(1.,0.969729042204957,1.),(1.,0.971089731516655,
1.)))
REPRESENTATION_ITEM('')
SURFACE()
);
#2702=(
BOUNDED_SURFACE()
B_SPLINE_SURFACE(3,2,((#172864,#172865,#172866),(#172867,#172868,#172869),
(#172870,#172871,#172872),(#172873,#172874,#172875),(#172876,#172877,#172878),
(#172879,#172880,#172881)),.UNSPECIFIED.,.F.,.F.,.F.)
B_SPLINE_SURFACE_WITH_KNOTS((4,2,4),(3,3),(-1.5178830414797E-17,0.00151741931723474,
0.0030348386344695),(0.,1.),.UNSPECIFIED.)
GEOMETRIC_REPRESENTATION_ITEM()
RATIONAL_B_SPLINE_SURFACE(((1.,0.583115115460263,1.),(1.,0.605241592753533,
1.),(1.,0.62665070495839,1.),(1.,0.668094537904905,1.),(1.,0.688253312209368,
1.),(1.,0.70710678118655,1.)))
REPRESENTATION_ITEM('')
SURFACE()
);
#2703=(
BOUNDED_SURFACE()
B_SPLINE_SURFACE(3,2,((#172906,#172907,#172908),(#172909,#172910,#172911),
(#172912,#172913,#172914),(#172915,#172916,#172917),(#172918,#172919,#172920),
(#172921,#172922,#172923)),.UNSPECIFIED.,.F.,.F.,.F.)
B_SPLINE_SURFACE_WITH_KNOTS((4,2,4),(3,3),(0.,0.00151694200897944,0.00303388401795888),
(0.,1.),.UNSPECIFIED.)
GEOMETRIC_REPRESENTATION_ITEM()
RATIONAL_B_SPLINE_SURFACE(((1.,0.70710678118655,1.),(1.,0.688185240537986,
1.),(1.,0.6684652198449,1.),(1.,0.627083641349078,1.),(1.,0.605243055947471,
1.),(1.,0.583115115460264,1.)))
REPRESENTATION_ITEM('')
SURFACE()
);
#2704=(
BOUNDED_SURFACE()
B_SPLINE_SURFACE(3,2,((#172939,#172940,#172941),(#172942,#172943,#172944),
(#172945,#172946,#172947),(#172948,#172949,#172950),(#172951,#172952,#172953),
(#172954,#172955,#172956)),.UNSPECIFIED.,.F.,.F.,.F.)
B_SPLINE_SURFACE_WITH_KNOTS((4,2,4),(3,3),(-1.94201995013153E-5,0.018990790064314,
0.0380010003281294),(0.,1.0000194201995),.UNSPECIFIED.)
GEOMETRIC_REPRESENTATION_ITEM()
RATIONAL_B_SPLINE_SURFACE(((1.,0.619089870519235,1.00001479470141),(1.,
0.61482119355377,1.00001496049853),(1.,0.60996647972793,1.00001514905755),
(1.,0.5983079322478,1.00001560188019),(1.,0.59151444641303,1.00001586574189),
(0.999999999999999,0.58308117916846,1.00001619329335)))
REPRESENTATION_ITEM('')
SURFACE()
);
#2705=(
BOUNDED_SURFACE()
B_SPLINE_SURFACE(3,2,((#172966,#172967,#172968),(#172969,#172970,#172971),
(#172972,#172973,#172974),(#172975,#172976,#172977)),.UNSPECIFIED.,.F.,
 .F.,.F.)
B_SPLINE_SURFACE_WITH_KNOTS((4,4),(3,3),(-6.51408174375083E-5,0.000716548991812596),
(-0.000127150757950157,1.),.UNSPECIFIED.)
GEOMETRIC_REPRESENTATION_ITEM()
RATIONAL_B_SPLINE_SURFACE(((1.00009928949958,0.60955993820037,1.),(1.00009948976837,
0.608772413245102,1.),(1.0000984813281,0.612737943163154,1.),(1.00009637648133,
0.621014916147796,1.)))
REPRESENTATION_ITEM('')
SURFACE()
);
#2706=(
BOUNDED_SURFACE()
B_SPLINE_SURFACE(3,2,((#172992,#172993,#172994),(#172995,#172996,#172997),
(#172998,#172999,#173000),(#173001,#173002,#173003),(#173004,#173005,#173006),
(#173007,#173008,#173009)),.UNSPECIFIED.,.F.,.F.,.F.)
B_SPLINE_SURFACE_WITH_KNOTS((4,2,4),(3,3),(0.,0.0188568492058762,0.0377136984117525),
(0.,1.),.UNSPECIFIED.)
GEOMETRIC_REPRESENTATION_ITEM()
RATIONAL_B_SPLINE_SURFACE(((1.,0.583115115460263,1.),(1.,0.591477165975886,
1.),(1.,0.59822556054293,1.),(1.,0.609817503669346,1.),(1.,0.614651018359553,
1.),(1.,0.618903611686376,1.)))
REPRESENTATION_ITEM('')
SURFACE()
);
#2707=(
BOUNDED_SURFACE()
B_SPLINE_SURFACE(3,2,((#173094,#173095,#173096),(#173097,#173098,#173099),
(#173100,#173101,#173102),(#173103,#173104,#173105)),.UNSPECIFIED.,.F.,
 .F.,.F.)
B_SPLINE_SURFACE_WITH_KNOTS((4,4),(3,3),(-6.51957114117336E-5,0.000717152825529202),
(-0.000139515695195982,1.),.UNSPECIFIED.)
GEOMETRIC_REPRESENTATION_ITEM()
RATIONAL_B_SPLINE_SURFACE(((1.00005700962391,0.795687417707188,1.),(1.00005494423624,
0.80308940810469,1.),(1.00005396604001,0.806595093358397,1.),(1.00005415449876,
0.805919689953951,1.)))
REPRESENTATION_ITEM('')
SURFACE()
);
#2708=(
BOUNDED_SURFACE()
B_SPLINE_SURFACE(3,2,((#173109,#173110,#173111),(#173112,#173113,#173114),
(#173115,#173116,#173117),(#173118,#173119,#173120),(#173121,#173122,#173123),
(#173124,#173125,#173126)),.UNSPECIFIED.,.F.,.F.,.F.)
B_SPLINE_SURFACE_WITH_KNOTS((4,2,4),(3,3),(0.,0.0178323395635859,0.0356646791271718),
(0.,1.),.UNSPECIFIED.)
GEOMETRIC_REPRESENTATION_ITEM()
RATIONAL_B_SPLINE_SURFACE(((1.,0.825853968826192,1.),(1.,0.819668171116131,
1.),(1.,0.814408476706928,1.),(1.,0.80512037347301,1.),(1.,0.801094867709694,
1.),(1.,0.79748483152198,1.)))
REPRESENTATION_ITEM('')
SURFACE()
);
#2709=(
BOUNDED_SURFACE()
B_SPLINE_SURFACE(3,2,((#173136,#173137,#173138),(#173139,#173140,#173141),
(#173142,#173143,#173144),(#173145,#173146,#173147),(#173148,#173149,#173150),
(#173151,#173152,#173153)),.UNSPECIFIED.,.F.,.F.,.F.)
B_SPLINE_SURFACE_WITH_KNOTS((4,2,4),(3,3),(-3.90312782094781E-18,0.00167965794371986,
0.00335931588743972),(0.,1.),.UNSPECIFIED.)
GEOMETRIC_REPRESENTATION_ITEM()
RATIONAL_B_SPLINE_SURFACE(((1.,0.825853968826192,1.),(1.,0.808295365083271,
1.),(1.,0.789625920673805,1.),(1.,0.749928217285841,1.),(1.,0.728769006116152,
1.),(1.,0.707106781186548,1.)))
REPRESENTATION_ITEM('')
SURFACE()
);
#2710=(
BOUNDED_SURFACE()
B_SPLINE_SURFACE(3,2,((#173168,#173169,#173170),(#173171,#173172,#173173),
(#173174,#173175,#173176),(#173177,#173178,#173179),(#173180,#173181,#173182),
(#173183,#173184,#173185)),.UNSPECIFIED.,.F.,.F.,.F.)
B_SPLINE_SURFACE_WITH_KNOTS((4,2,4),(3,3),(0.,0.00167878022781669,0.00335756045563338),
(0.,1.),.UNSPECIFIED.)
GEOMETRIC_REPRESENTATION_ITEM()
RATIONAL_B_SPLINE_SURFACE(((1.,0.707106781186548,1.),(1.,0.728852565122502,
1.),(1.,0.749558440272865,1.),(1.,0.789217732831704,1.),(1.,0.808313359696353,
1.),(1.,0.825853968826191,1.)))
REPRESENTATION_ITEM('')
SURFACE()
);
#2711=(
BOUNDED_SURFACE()
B_SPLINE_SURFACE(3,2,((#173302,#173303,#173304),(#173305,#173306,#173307),
(#173308,#173309,#173310),(#173311,#173312,#173313),(#173314,#173315,#173316),
(#173317,#173318,#173319)),.UNSPECIFIED.,.F.,.F.,.F.)
B_SPLINE_SURFACE_WITH_KNOTS((4,2,4),(3,3),(0.,0.0176980703187956,0.0353961406375911),
(0.,1.),.UNSPECIFIED.)
GEOMETRIC_REPRESENTATION_ITEM()
RATIONAL_B_SPLINE_SURFACE(((1.,0.797648081014877,1.),(1.,0.801243745289675,
1.),(1.,0.805251011590647,1.),(1.,0.814487862093865,1.),(1.,0.819714636457853,
1.),(1.,0.825853968826193,1.)))
REPRESENTATION_ITEM('')
SURFACE()
);
#2712=(
BOUNDED_SURFACE()
B_SPLINE_SURFACE(3,2,((#173361,#173362,#173363),(#173364,#173365,#173366),
(#173367,#173368,#173369),(#173370,#173371,#173372),(#173373,#173374,#173375),
(#173376,#173377,#173378)),.UNSPECIFIED.,.F.,.F.,.F.)
B_SPLINE_SURFACE_WITH_KNOTS((4,2,4),(3,3),(0.320579494062015,0.325851056440119,
0.331122618818223),(0.,1.),.UNSPECIFIED.)
GEOMETRIC_REPRESENTATION_ITEM()
RATIONAL_B_SPLINE_SURFACE(((1.,0.944716550693843,1.),(1.,0.947183014496352,
1.),(1.,0.949681733718157,1.),(1.,0.954674150124444,1.),(1.,0.957142659869515,
1.),(1.,0.959530911310534,1.)))
REPRESENTATION_ITEM('')
SURFACE()
);
#2713=(
BOUNDED_SURFACE()
B_SPLINE_SURFACE(3,2,((#173512,#173513,#173514),(#173515,#173516,#173517),
(#173518,#173519,#173520),(#173521,#173522,#173523),(#173524,#173525,#173526),
(#173527,#173528,#173529)),.UNSPECIFIED.,.F.,.F.,.F.)
B_SPLINE_SURFACE_WITH_KNOTS((4,2,4),(3,3),(0.,0.0145632072393804,0.0291264144787609),
(0.,1.),.UNSPECIFIED.)
GEOMETRIC_REPRESENTATION_ITEM()
RATIONAL_B_SPLINE_SURFACE(((1.,0.523250899838464,1.),(1.,0.532471350763147,
1.),(1.,0.540347653844846,1.),(1.,0.554302832144208,1.),(1.,0.560377433574518,
1.),(1.,0.565840417962188,1.)))
REPRESENTATION_ITEM('')
SURFACE()
);
#2714=(
BOUNDED_SURFACE()
B_SPLINE_SURFACE(3,2,((#173582,#173583,#173584),(#173585,#173586,#173587),
(#173588,#173589,#173590),(#173591,#173592,#173593),(#173594,#173595,#173596),
(#173597,#173598,#173599)),.UNSPECIFIED.,.F.,.F.,.F.)
B_SPLINE_SURFACE_WITH_KNOTS((4,2,4),(3,3),(-0.000106024816734168,0.00207216577676188,
0.00425035650131637),(-0.000106024947792593,1.),.UNSPECIFIED.)
GEOMETRIC_REPRESENTATION_ITEM()
RATIONAL_B_SPLINE_SURFACE(((1.00010220266629,0.518025387314371,1.),(1.00009466956028,
0.553550545186674,1.),(1.00008751550017,0.587288171340496,1.),(1.00007381194872,
0.651912355251542,1.),(1.00006726786479,0.682773412363203,1.),(1.00006122918042,
0.711251070175717,1.)))
REPRESENTATION_ITEM('')
SURFACE()
);
#2715=(
BOUNDED_SURFACE()
B_SPLINE_SURFACE(3,2,((#173631,#173632,#173633),(#173634,#173635,#173636),
(#173637,#173638,#173639),(#173640,#173641,#173642),(#173643,#173644,#173645),
(#173646,#173647,#173648)),.UNSPECIFIED.,.F.,.F.,.F.)
B_SPLINE_SURFACE_WITH_KNOTS((4,2,4),(3,3),(0.,0.00207126900955203,0.00414253801910405),
(0.,1.),.UNSPECIFIED.)
GEOMETRIC_REPRESENTATION_ITEM()
RATIONAL_B_SPLINE_SURFACE(((1.,0.707106781186548,1.),(1.,0.679626330234824,
1.),(1.,0.650848145227602,1.),(1.,0.589569252159033,1.),(1.,0.556778618705704,
1.),(1.,0.523250899838466,1.)))
REPRESENTATION_ITEM('')
SURFACE()
);
#2716=(
BOUNDED_SURFACE()
B_SPLINE_SURFACE(3,2,((#173673,#173674,#173675),(#173676,#173677,#173678),
(#173679,#173680,#173681),(#173682,#173683,#173684),(#173685,#173686,#173687),
(#173688,#173689,#173690)),.UNSPECIFIED.,.F.,.F.,.F.)
B_SPLINE_SURFACE_WITH_KNOTS((4,2,4),(3,3),(-3.45632130015141E-5,0.0146992078328598,
0.029432978878721),(0.,1.000034563213),.UNSPECIFIED.)
GEOMETRIC_REPRESENTATION_ITEM()
RATIONAL_B_SPLINE_SURFACE(((1.,0.566167776253824,1.00002998927111),(1.,
0.560666809856082,1.00003036953326),(1.,0.554544924441235,1.00003079271732),
(1.,0.540460350933127,1.00003176633355),(1.,0.532502109028823,1.00003231645837),
(1.,0.523168760654905,1.00003296163938)))
REPRESENTATION_ITEM('')
SURFACE()
);
#2717=(
BOUNDED_SURFACE()
B_SPLINE_SURFACE(3,2,((#173700,#173701,#173702),(#173703,#173704,#173705),
(#173706,#173707,#173708),(#173709,#173710,#173711)),.UNSPECIFIED.,.F.,
 .F.,.F.)
B_SPLINE_SURFACE_WITH_KNOTS((4,4),(3,3),(-3.41800396463488E-5,0.000687703280413445),
(-3.41800396463774E-5,1.),.UNSPECIFIED.)
GEOMETRIC_REPRESENTATION_ITEM()
RATIONAL_B_SPLINE_SURFACE(((1.00003076363761,0.549976566282789,1.),(1.00003081026943,
0.549294416404309,1.),(1.00003037623388,0.555643671106268,1.),(1.00002954389936,
0.56781941063233,1.)))
REPRESENTATION_ITEM('')
SURFACE()
);
#2718=(
BOUNDED_SURFACE()
B_SPLINE_SURFACE(3,2,((#173748,#173749,#173750),(#173751,#173752,#173753),
(#173754,#173755,#173756),(#173757,#173758,#173759)),.UNSPECIFIED.,.F.,
 .F.,.F.)
B_SPLINE_SURFACE_WITH_KNOTS((4,4),(3,3),(-1.38777878078145E-17,0.0332202089949022),
(0.,1.),.UNSPECIFIED.)
GEOMETRIC_REPRESENTATION_ITEM()
RATIONAL_B_SPLINE_SURFACE(((1.,0.736495153922513,1.),(1.,0.738798609451216,
1.),(1.,0.741580133014481,1.),(1.,0.745472778587061,1.)))
REPRESENTATION_ITEM('')
SURFACE()
);
#2719=(
BOUNDED_SURFACE()
B_SPLINE_SURFACE(3,2,((#173784,#173785,#173786),(#173787,#173788,#173789),
(#173790,#173791,#173792),(#173793,#173794,#173795)),.UNSPECIFIED.,.F.,
 .F.,.F.)
B_SPLINE_SURFACE_WITH_KNOTS((4,4),(3,3),(0.,0.0333425790106738),(0.,1.),
 .UNSPECIFIED.)
GEOMETRIC_REPRESENTATION_ITEM()
RATIONAL_B_SPLINE_SURFACE(((1.,0.619253049823353,1.),(1.,0.62903050118076,
1.),(1.,0.635777469330956,1.),(1.,0.641321251913794,1.)))
REPRESENTATION_ITEM('')
SURFACE()
);
#2720=(
BOUNDED_SURFACE()
B_SPLINE_SURFACE(3,2,((#173820,#173821,#173822),(#173823,#173824,#173825),
(#173826,#173827,#173828),(#173829,#173830,#173831)),.UNSPECIFIED.,.F.,
 .F.,.F.)
B_SPLINE_SURFACE_WITH_KNOTS((4,4),(3,3),(0.,9.64176041888312E-5),(0.,1.),
 .UNSPECIFIED.)
GEOMETRIC_REPRESENTATION_ITEM()
RATIONAL_B_SPLINE_SURFACE(((1.,0.801085834760579,1.),(1.,0.800109483270879,
1.),(1.,0.799128688610329,1.),(1.,0.798143461627153,1.)))
REPRESENTATION_ITEM('')
SURFACE()
);
#2721=(
BOUNDED_SURFACE()
B_SPLINE_SURFACE(3,2,((#173843,#173844,#173845),(#173846,#173847,#173848),
(#173849,#173850,#173851),(#173852,#173853,#173854)),.UNSPECIFIED.,.F.,
 .F.,.F.)
B_SPLINE_SURFACE_WITH_KNOTS((4,4),(3,3),(-1.38777878078145E-17,0.0333345287175385),
(0.,1.),.UNSPECIFIED.)
GEOMETRIC_REPRESENTATION_ITEM()
RATIONAL_B_SPLINE_SURFACE(((1.,0.779737900546642,1.),(1.,0.785266544814036,
1.),(1.,0.791920621206337,1.),(1.,0.801085834760578,1.)))
REPRESENTATION_ITEM('')
SURFACE()
);
#2722=(
BOUNDED_SURFACE()
B_SPLINE_SURFACE(3,2,((#173881,#173882,#173883),(#173884,#173885,#173886),
(#173887,#173888,#173889),(#173890,#173891,#173892)),.UNSPECIFIED.,.F.,
 .F.,.F.)
B_SPLINE_SURFACE_WITH_KNOTS((4,4),(3,3),(0.,0.0278605201857756),(0.,1.),
 .UNSPECIFIED.)
GEOMETRIC_REPRESENTATION_ITEM()
RATIONAL_B_SPLINE_SURFACE(((1.,0.55476848021506,1.),(1.,0.56887897086178,
1.),(1.,0.579290070452688,1.),(1.,0.587985430396658,1.)))
REPRESENTATION_ITEM('')
SURFACE()
);
#2723=(
BOUNDED_SURFACE()
B_SPLINE_SURFACE(3,2,((#173922,#173923,#173924),(#173925,#173926,#173927),
(#173928,#173929,#173930),(#173931,#173932,#173933),(#173934,#173935,#173936),
(#173937,#173938,#173939)),.UNSPECIFIED.,.F.,.F.,.F.)
B_SPLINE_SURFACE_WITH_KNOTS((4,2,4),(3,3),(-1.95156391047391E-18,0.00176358033920161,
0.00352716067840323),(0.,1.),.UNSPECIFIED.)
GEOMETRIC_REPRESENTATION_ITEM()
RATIONAL_B_SPLINE_SURFACE(((1.,0.554768480215054,1.),(1.,0.582178779071266,
1.),(1.,0.608552864303934,1.),(1.,0.659476319336264,1.),(1.,0.684131843499319,
1.),(1.,0.707106781186548,1.)))
REPRESENTATION_ITEM('')
SURFACE()
);
#2724=(
BOUNDED_SURFACE()
B_SPLINE_SURFACE(3,2,((#174089,#174090,#174091),(#174092,#174093,#174094),
(#174095,#174096,#174097),(#174098,#174099,#174100),(#174101,#174102,#174103),
(#174104,#174105,#174106)),.UNSPECIFIED.,.F.,.F.,.F.)
B_SPLINE_SURFACE_WITH_KNOTS((4,2,4),(3,3),(0.,0.00192660600180124,0.00385321200360248),
(0.,1.),.UNSPECIFIED.)
GEOMETRIC_REPRESENTATION_ITEM()
RATIONAL_B_SPLINE_SURFACE(((1.,0.707106781186548,1.),(1.,0.732617243564259,
1.),(1.,0.7565692429617,1.),(1.,0.801993213239136,1.),(1.,0.823627327095932,
1.),(1.,0.843176610515832,1.)))
REPRESENTATION_ITEM('')
SURFACE()
);
#2725=(
BOUNDED_SURFACE()
B_SPLINE_SURFACE(3,2,((#174125,#174126,#174127),(#174128,#174129,#174130),
(#174131,#174132,#174133),(#174134,#174135,#174136)),.UNSPECIFIED.,.F.,
 .F.,.F.)
B_SPLINE_SURFACE_WITH_KNOTS((4,4),(3,3),(0.,0.024690830875569),(0.,1.),
 .UNSPECIFIED.)
GEOMETRIC_REPRESENTATION_ITEM()
RATIONAL_B_SPLINE_SURFACE(((1.,0.821022196159299,1.),(1.,0.827229968384993,
1.),(1.,0.834396885388283,1.),(1.,0.84317661051583,1.)))
REPRESENTATION_ITEM('')
SURFACE()
);
#2726=(
BOUNDED_SURFACE()
B_SPLINE_SURFACE(3,2,((#174163,#174164,#174165),(#174166,#174167,#174168),
(#174169,#174170,#174171),(#174172,#174173,#174174),(#174175,#174176,#174177),
(#174178,#174179,#174180),(#174181,#174182,#174183),(#174184,#174185,#174186)),
 .UNSPECIFIED.,.F.,.F.,.F.)
B_SPLINE_SURFACE_WITH_KNOTS((4,2,2,4),(3,3),(0.,0.000301902853038141,0.000452854279557211,
0.000603805706076282),(0.,1.),.UNSPECIFIED.)
GEOMETRIC_REPRESENTATION_ITEM()
RATIONAL_B_SPLINE_SURFACE(((1.,0.702399276808562,1.),(1.,0.672208297052869,
1.),(1.,0.639172707788597,1.),(1.,0.593013313775285,1.),(1.,0.577958663413849,
1.),(1.,0.550545486207946,1.),(1.,0.538469268822416,1.),(1.,0.528679393385783,
1.)))
REPRESENTATION_ITEM('')
SURFACE()
);
#2727=(
BOUNDED_SURFACE()
B_SPLINE_SURFACE(3,2,((#174264,#174265,#174266),(#174267,#174268,#174269),
(#174270,#174271,#174272),(#174273,#174274,#174275)),.UNSPECIFIED.,.F.,
 .F.,.F.)
B_SPLINE_SURFACE_WITH_KNOTS((4,4),(3,3),(0.,8.95703543583319E-5),(0.,1.),
 .UNSPECIFIED.)
GEOMETRIC_REPRESENTATION_ITEM()
RATIONAL_B_SPLINE_SURFACE(((1.,0.821022196159299,1.),(1.,0.818079073177133,
1.),(1.,0.814610488520586,1.),(1.,0.810617639934139,1.)))
REPRESENTATION_ITEM('')
SURFACE()
);
#2728=(
BOUNDED_SURFACE()
B_SPLINE_SURFACE(3,2,((#174299,#174300,#174301),(#174302,#174303,#174304),
(#174305,#174306,#174307),(#174308,#174309,#174310)),.UNSPECIFIED.,.F.,
 .F.,.F.)
B_SPLINE_SURFACE_WITH_KNOTS((4,4),(3,3),(0.,0.0240963563036403),(0.,1.),
 .UNSPECIFIED.)
GEOMETRIC_REPRESENTATION_ITEM()
RATIONAL_B_SPLINE_SURFACE(((1.,0.533775524284036,1.),(1.,0.547394060950047,
1.),(1.,0.557948204678947,1.),(1.,0.566908467907053,1.)))
REPRESENTATION_ITEM('')
SURFACE()
);
#2729=(
BOUNDED_SURFACE()
B_SPLINE_SURFACE(3,2,((#174339,#174340,#174341),(#174342,#174343,#174344),
(#174345,#174346,#174347),(#174348,#174349,#174350),(#174351,#174352,#174353),
(#174354,#174355,#174356)),.UNSPECIFIED.,.F.,.F.,.F.)
B_SPLINE_SURFACE_WITH_KNOTS((4,2,4),(3,3),(0.,0.00196642364705715,0.0039328472941143),
(0.,1.),.UNSPECIFIED.)
GEOMETRIC_REPRESENTATION_ITEM()
RATIONAL_B_SPLINE_SURFACE(((1.,0.533775524284043,1.),(1.,0.565273803175765,
1.),(1.,0.595391641981992,1.),(1.,0.653340354191305,1.),(1.,0.681207781927973,
1.),(1.,0.707106781186552,1.)))
REPRESENTATION_ITEM('')
SURFACE()
);
#2730=(
BOUNDED_SURFACE()
B_SPLINE_SURFACE(3,2,((#174388,#174389,#174390),(#174391,#174392,#174393),
(#174394,#174395,#174396),(#174397,#174398,#174399),(#174400,#174401,#174402),
(#174403,#174404,#174405)),.UNSPECIFIED.,.F.,.F.,.F.)
B_SPLINE_SURFACE_WITH_KNOTS((4,2,4),(3,3),(0.,0.00196532227871992,0.00393064455743984),
(0.,1.),.UNSPECIFIED.)
GEOMETRIC_REPRESENTATION_ITEM()
RATIONAL_B_SPLINE_SURFACE(((1.,0.70710678118655,1.),(1.,0.681045297773967,
1.),(1.,0.653805231917789,1.),(1.,0.596033371554667,1.),(1.,0.565216504169612,
1.),(1.,0.533775524284038,1.)))
REPRESENTATION_ITEM('')
SURFACE()
);
#2731=(
BOUNDED_SURFACE()
B_SPLINE_SURFACE(3,2,((#174467,#174468,#174469),(#174470,#174471,#174472),
(#174473,#174474,#174475),(#174476,#174477,#174478)),.UNSPECIFIED.,.F.,
 .F.,.F.)
B_SPLINE_SURFACE_WITH_KNOTS((4,4),(3,3),(1.38777878078145E-17,0.0238258198664154),
(0.,1.),.UNSPECIFIED.)
GEOMETRIC_REPRESENTATION_ITEM()
RATIONAL_B_SPLINE_SURFACE(((1.,0.566606711022863,1.),(1.,0.557709627588123,
1.),(1.,0.547241836069268,1.),(1.,0.533775524284033,1.)))
REPRESENTATION_ITEM('')
SURFACE()
);
#2732=(
BOUNDED_SURFACE()
B_SPLINE_SURFACE(3,2,((#174505,#174506,#174507),(#174508,#174509,#174510),
(#174511,#174512,#174513),(#174514,#174515,#174516),(#174517,#174518,#174519),
(#174520,#174521,#174522)),.UNSPECIFIED.,.F.,.F.,.F.)
B_SPLINE_SURFACE_WITH_KNOTS((4,2,4),(3,3),(0.28787290846928,0.292960043496213,
0.298047178523145),(0.,1.),.UNSPECIFIED.)
GEOMETRIC_REPRESENTATION_ITEM()
RATIONAL_B_SPLINE_SURFACE(((1.,0.948000837587232,1.),(1.,0.950253148926149,
1.),(1.,0.952526342948766,1.),(1.,0.957029990073055,1.),(1.,0.959243464400477,
1.),(1.,0.961372004230729,1.)))
REPRESENTATION_ITEM('')
SURFACE()
);
#2733=(
BOUNDED_SURFACE()
B_SPLINE_SURFACE(3,2,((#174589,#174590,#174591),(#174592,#174593,#174594),
(#174595,#174596,#174597),(#174598,#174599,#174600),(#174601,#174602,#174603),
(#174604,#174605,#174606)),.UNSPECIFIED.,.F.,.F.,.F.)
B_SPLINE_SURFACE_WITH_KNOTS((4,2,4),(3,3),(0.,0.00160286774303482,0.00320573548606963),
(0.,1.),.UNSPECIFIED.)
GEOMETRIC_REPRESENTATION_ITEM()
RATIONAL_B_SPLINE_SURFACE(((1.,0.819627815321769,1.),(1.,0.802865620897526,
1.),(1.,0.785107826354221,1.),(1.,0.747495184421159,1.),(1.,0.727508688529169,
1.),(1.,0.707106781186548,1.)))
REPRESENTATION_ITEM('')
SURFACE()
);
#2734=(
BOUNDED_SURFACE()
B_SPLINE_SURFACE(3,2,((#174631,#174632,#174633),(#174634,#174635,#174636),
(#174637,#174638,#174639),(#174640,#174641,#174642),(#174643,#174644,#174645),
(#174646,#174647,#174648)),.UNSPECIFIED.,.F.,.F.,.F.)
B_SPLINE_SURFACE_WITH_KNOTS((4,2,4),(3,3),(0.,0.00160216910094088,0.00320433820188177),
(0.,1.),.UNSPECIFIED.)
GEOMETRIC_REPRESENTATION_ITEM()
RATIONAL_B_SPLINE_SURFACE(((1.,0.707106781186548,1.),(1.,0.727576984679287,
1.),(1.,0.747141913282259,1.),(1.,0.784726895243881,1.),(1.,0.80287971578069,
1.),(1.,0.819627815322113,1.)))
REPRESENTATION_ITEM('')
SURFACE()
);
#2735=(
BOUNDED_SURFACE()
B_SPLINE_SURFACE(3,2,((#174664,#174665,#174666),(#174667,#174668,#174669),
(#174670,#174671,#174672),(#174673,#174674,#174675)),.UNSPECIFIED.,.F.,
 .F.,.F.)
B_SPLINE_SURFACE_WITH_KNOTS((4,4),(3,3),(0.,0.0300693678107436),(0.,1.),
 .UNSPECIFIED.)
GEOMETRIC_REPRESENTATION_ITEM()
RATIONAL_B_SPLINE_SURFACE(((1.,0.79694160937888,1.),(1.,0.803005840650144,
1.),(1.,0.810197796192684,1.),(1.,0.819627815321757,1.)))
REPRESENTATION_ITEM('')
SURFACE()
);
#2736=(
BOUNDED_SURFACE()
B_SPLINE_SURFACE(3,2,((#174702,#174703,#174704),(#174705,#174706,#174707),
(#174708,#174709,#174710),(#174711,#174712,#174713)),.UNSPECIFIED.,.F.,
 .F.,.F.)
B_SPLINE_SURFACE_WITH_KNOTS((4,4),(3,3),(0.,0.0298008594779328),(0.,1.),
 .UNSPECIFIED.)
GEOMETRIC_REPRESENTATION_ITEM()
RATIONAL_B_SPLINE_SURFACE(((1.,0.819627815321769,1.),(1.,0.81028158060527,
1.),(1.,0.803135207628788,1.),(1.,0.797103929716951,1.)))
REPRESENTATION_ITEM('')
SURFACE()
);
#2737=(
BOUNDED_SURFACE()
B_SPLINE_SURFACE(3,2,((#174764,#174765,#174766),(#174767,#174768,#174769),
(#174770,#174771,#174772),(#174773,#174774,#174775)),.UNSPECIFIED.,.F.,
 .F.,.F.)
B_SPLINE_SURFACE_WITH_KNOTS((4,4),(3,3),(0.,0.0322629186945109),(0.,1.),
 .UNSPECIFIED.)
GEOMETRIC_REPRESENTATION_ITEM()
RATIONAL_B_SPLINE_SURFACE(((1.,0.591243989422541,1.),(1.,0.603807915079894,
1.),(1.,0.612569262394175,1.),(1.,0.619783312569531,1.)))
REPRESENTATION_ITEM('')
SURFACE()
);
#2738=(
BOUNDED_SURFACE()
B_SPLINE_SURFACE(3,2,((#174804,#174805,#174806),(#174807,#174808,#174809),
(#174810,#174811,#174812),(#174813,#174814,#174815),(#174816,#174817,#174818),
(#174819,#174820,#174821)),.UNSPECIFIED.,.F.,.F.,.F.)
B_SPLINE_SURFACE_WITH_KNOTS((4,2,4),(3,3),(-4.11996825544492E-18,0.00145505538520654,
0.00291011077041309),(0.,1.),.UNSPECIFIED.)
GEOMETRIC_REPRESENTATION_ITEM()
RATIONAL_B_SPLINE_SURFACE(((1.,0.591243989422539,1.),(1.,0.611831201619161,
1.),(1.,0.631800177390031,1.),(1.,0.67052755959961,1.),(1.,0.68940594547505,
1.),(1.,0.707106781186548,1.)))
REPRESENTATION_ITEM('')
SURFACE()
);
#2739=(
BOUNDED_SURFACE()
B_SPLINE_SURFACE(3,2,((#174844,#174845,#174846),(#174847,#174848,#174849),
(#174850,#174851,#174852),(#174853,#174854,#174855),(#174856,#174857,#174858),
(#174859,#174860,#174861)),.UNSPECIFIED.,.F.,.F.,.F.)
B_SPLINE_SURFACE_WITH_KNOTS((4,2,4),(3,3),(0.,0.00145467289932797,0.00290934579865593),
(0.,1.),.UNSPECIFIED.)
GEOMETRIC_REPRESENTATION_ITEM()
RATIONAL_B_SPLINE_SURFACE(((1.,0.707106781186548,1.),(1.,0.689351003959322,
1.),(1.,0.670875374619751,1.),(1.,0.63219865253591,1.),(1.,0.61183462187758,
1.),(1.,0.591243989422533,1.)))
REPRESENTATION_ITEM('')
SURFACE()
);
#2740=(
BOUNDED_SURFACE()
B_SPLINE_SURFACE(3,2,((#174975,#174976,#174977),(#174978,#174979,#174980),
(#174981,#174982,#174983),(#174984,#174985,#174986)),.UNSPECIFIED.,.F.,
 .F.,.F.)
B_SPLINE_SURFACE_WITH_KNOTS((4,4),(3,3),(0.,0.0319950621716305),(0.,1.),
 .UNSPECIFIED.)
GEOMETRIC_REPRESENTATION_ITEM()
RATIONAL_B_SPLINE_SURFACE(((1.,0.619604282534389,1.),(1.,0.612421729644488,
1.),(1.,0.603704627405285,1.),(1.,0.591243989422539,1.)))
REPRESENTATION_ITEM('')
SURFACE()
);
#2741=(
BOUNDED_SURFACE()
B_SPLINE_SURFACE(3,2,((#175013,#175014,#175015),(#175016,#175017,#175018),
(#175019,#175020,#175021),(#175022,#175023,#175024),(#175025,#175026,#175027),
(#175028,#175029,#175030)),.UNSPECIFIED.,.F.,.F.,.F.)
B_SPLINE_SURFACE_WITH_KNOTS((4,2,4),(3,3),(0.0131958327712131,0.0172517018793722,
0.0213075709875312),(0.,1.),.UNSPECIFIED.)
GEOMETRIC_REPRESENTATION_ITEM()
RATIONAL_B_SPLINE_SURFACE(((1.,0.962986864031359,1.),(1.,0.964634124968522,
1.),(1.,0.966223563289428,1.),(1.,0.969200421482677,1.),(1.,0.970562510847277,
1.),(1.,0.97174760310377,1.)))
REPRESENTATION_ITEM('')
SURFACE()
);
#2742=(
BOUNDED_SURFACE()
B_SPLINE_SURFACE(3,2,((#175133,#175134,#175135),(#175136,#175137,#175138),
(#175139,#175140,#175141),(#175142,#175143,#175144),(#175145,#175146,#175147),
(#175148,#175149,#175150)),.UNSPECIFIED.,.F.,.F.,.F.)
B_SPLINE_SURFACE_WITH_KNOTS((4,2,4),(3,3),(0.,0.00117596609447381,0.00235193218894761),
(0.,1.),.UNSPECIFIED.)
GEOMETRIC_REPRESENTATION_ITEM()
RATIONAL_B_SPLINE_SURFACE(((1.,0.773031559588625,1.),(1.,0.762507689934388,
1.),(1.,0.751714784265694,1.),(1.,0.729663967046365,1.),(1.,0.718328240933523,
1.),(1.,0.707106781186548,1.)))
REPRESENTATION_ITEM('')
SURFACE()
);
#2743=(
BOUNDED_SURFACE()
B_SPLINE_SURFACE(3,2,((#175172,#175173,#175174),(#175175,#175176,#175177),
(#175178,#175179,#175180),(#175181,#175182,#175183),(#175184,#175185,#175186),
(#175187,#175188,#175189)),.UNSPECIFIED.,.F.,.F.,.F.)
B_SPLINE_SURFACE_WITH_KNOTS((4,2,4),(3,3),(0.,0.00117590500970525,0.00235181001941051),
(0.,1.),.UNSPECIFIED.)
GEOMETRIC_REPRESENTATION_ITEM()
RATIONAL_B_SPLINE_SURFACE(((1.,0.707106781186548,1.),(1.,0.718331568550412,
1.),(1.,0.729459486848599,1.),(1.,0.751510898082342,1.),(1.,0.762507564122321,
1.),(1.,0.773031559588357,1.)))
REPRESENTATION_ITEM('')
SURFACE()
);
#2744=(
BOUNDED_SURFACE()
B_SPLINE_SURFACE(3,2,((#175205,#175206,#175207),(#175208,#175209,#175210),
(#175211,#175212,#175213),(#175214,#175215,#175216)),.UNSPECIFIED.,.F.,
 .F.,.F.)
B_SPLINE_SURFACE_WITH_KNOTS((4,4),(3,3),(0.,0.0360938777358061),(0.,1.),
 .UNSPECIFIED.)
GEOMETRIC_REPRESENTATION_ITEM()
RATIONAL_B_SPLINE_SURFACE(((1.,0.756551244268665,1.),(1.,0.760698019999951,
1.),(1.,0.765742819248909,1.),(1.,0.77303155958863,1.)))
REPRESENTATION_ITEM('')
SURFACE()
);
#2745=(
BOUNDED_SURFACE()
B_SPLINE_SURFACE(3,2,((#175240,#175241,#175242),(#175243,#175244,#175245),
(#175246,#175247,#175248),(#175249,#175250,#175251)),.UNSPECIFIED.,.F.,
 .F.,.F.)
B_SPLINE_SURFACE_WITH_KNOTS((4,4),(3,3),(0.,0.0358270578054484),(0.,1.),
 .UNSPECIFIED.)
GEOMETRIC_REPRESENTATION_ITEM()
RATIONAL_B_SPLINE_SURFACE(((1.,0.773031559588625,1.),(1.,0.765796148320668,
1.),(1.,0.760773695826815,1.),(1.,0.756642830410354,1.)))
REPRESENTATION_ITEM('')
SURFACE()
);
#2746=(
BOUNDED_SURFACE()
B_SPLINE_SURFACE(3,2,((#175301,#175302,#175303),(#175304,#175305,#175306),
(#175307,#175308,#175309),(#175310,#175311,#175312)),.UNSPECIFIED.,.F.,
 .F.,.F.)
B_SPLINE_SURFACE_WITH_KNOTS((4,4),(3,3),(0.,0.0372541843113205),(0.,1.),
 .UNSPECIFIED.)
GEOMETRIC_REPRESENTATION_ITEM()
RATIONAL_B_SPLINE_SURFACE(((1.,0.653853118868809,1.),(1.,0.660540277946251,
1.),(1.,0.664920252154014,1.),(1.,0.668488966322263,1.)))
REPRESENTATION_ITEM('')
SURFACE()
);
#2747=(
BOUNDED_SURFACE()
B_SPLINE_SURFACE(3,2,((#175336,#175337,#175338),(#175339,#175340,#175341),
(#175342,#175343,#175344),(#175345,#175346,#175347),(#175348,#175349,#175350),
(#175351,#175352,#175353)),.UNSPECIFIED.,.F.,.F.,.F.)
B_SPLINE_SURFACE_WITH_KNOTS((4,2,4),(3,3),(-0.000172720172426045,0.00108574887884081,
0.00234421795569043),(-0.000172720198008812,1.),.UNSPECIFIED.)
GEOMETRIC_REPRESENTATION_ITEM()
RATIONAL_B_SPLINE_SURFACE(((1.00012114331385,0.649307622257087,1.),(1.00011736582696,
0.660242900607159,1.),(1.00011369038462,0.670882774756897,1.),(1.0001065636278,
0.691513705317947,1.),(1.00010308656314,0.70157930476702,1.),(1.00009984815327,
0.710954033119057,1.)))
REPRESENTATION_ITEM('')
SURFACE()
);
#2748=(
BOUNDED_SURFACE()
B_SPLINE_SURFACE(3,2,((#175373,#175374,#175375),(#175376,#175377,#175378),
(#175379,#175380,#175381),(#175382,#175383,#175384),(#175385,#175386,#175387),
(#175388,#175389,#175390)),.UNSPECIFIED.,.F.,.F.,.F.)
B_SPLINE_SURFACE_WITH_KNOTS((4,2,4),(3,3),(0.,0.00108572934543333,0.00217145869086666),
(0.,1.),.UNSPECIFIED.)
GEOMETRIC_REPRESENTATION_ITEM()
RATIONAL_B_SPLINE_SURFACE(((1.,0.707106781186548,1.),(1.,0.698862672165929,
1.),(1.,0.690309395332211,1.),(1.,0.672521089753096,1.),(1.,0.663221545283971,
1.),(1.,0.653853118868808,1.)))
REPRESENTATION_ITEM('')
SURFACE()
);
#2749=(
BOUNDED_SURFACE()
B_SPLINE_SURFACE(3,2,((#175477,#175478,#175479),(#175480,#175481,#175482),
(#175483,#175484,#175485),(#175486,#175487,#175488)),.UNSPECIFIED.,.F.,
 .F.,.F.)
B_SPLINE_SURFACE_WITH_KNOTS((4,4),(3,3),(0.,0.0369876550821707),(0.,1.),
 .UNSPECIFIED.)
GEOMETRIC_REPRESENTATION_ITEM()
RATIONAL_B_SPLINE_SURFACE(((1.,0.668412873076039,1.),(1.,0.66485630627401,
1.),(1.,0.660493096380151,1.),(1.,0.653853118868808,1.)))
REPRESENTATION_ITEM('')
SURFACE()
);
#2750=(
BOUNDED_SURFACE()
B_SPLINE_SURFACE(3,2,((#175554,#175555,#175556),(#175557,#175558,#175559),
(#175560,#175561,#175562),(#175563,#175564,#175565),(#175566,#175567,#175568),
(#175569,#175570,#175571)),.UNSPECIFIED.,.F.,.F.,.F.)
B_SPLINE_SURFACE_WITH_KNOTS((4,2,4),(3,3),(0.024832888249526,0.028058706716499,
0.0312845251834718),(0.,1.),.UNSPECIFIED.)
GEOMETRIC_REPRESENTATION_ITEM()
RATIONAL_B_SPLINE_SURFACE(((1.,0.973275621725783,1.),(1.,0.974072863725218,
1.),(1.,0.974738796346974,1.),(1.,0.975743605366306,1.),(1.,0.976080910223402,
1.),(1.,0.976217656750926,1.)))
REPRESENTATION_ITEM('')
SURFACE()
);
#2751=(
BOUNDED_SURFACE()
B_SPLINE_SURFACE(3,2,((#175587,#175588,#175589),(#175590,#175591,#175592),
(#175593,#175594,#175595),(#175596,#175597,#175598)),.UNSPECIFIED.,.F.,
 .F.,.F.)
B_SPLINE_SURFACE_WITH_KNOTS((4,4),(3,3),(-4.11996825544492E-18,0.00195778789380024),
(0.,1.),.UNSPECIFIED.)
GEOMETRIC_REPRESENTATION_ITEM()
RATIONAL_B_SPLINE_SURFACE(((1.,0.716457303923414,1.),(1.,0.713268765085681,
1.),(1.,0.710104564531573,1.),(1.,0.707106781186529,1.)))
REPRESENTATION_ITEM('')
SURFACE()
);
#2752=(
BOUNDED_SURFACE()
B_SPLINE_SURFACE(3,2,((#175608,#175609,#175610),(#175611,#175612,#175613),
(#175614,#175615,#175616),(#175617,#175618,#175619)),.UNSPECIFIED.,.F.,
 .F.,.F.)
B_SPLINE_SURFACE_WITH_KNOTS((4,4),(3,3),(0.,0.00195778753723149),(0.,1.),
 .UNSPECIFIED.)
GEOMETRIC_REPRESENTATION_ITEM()
RATIONAL_B_SPLINE_SURFACE(((1.,0.707106781186543,1.),(1.,0.710074099671655,
1.),(1.,0.713236629341983,1.),(1.,0.716457303923398,1.)))
REPRESENTATION_ITEM('')
SURFACE()
);
#2753=(
BOUNDED_SURFACE()
B_SPLINE_SURFACE(3,2,((#175623,#175624,#175625),(#175626,#175627,#175628),
(#175629,#175630,#175631),(#175632,#175633,#175634)),.UNSPECIFIED.,.F.,
 .F.,.F.)
B_SPLINE_SURFACE_WITH_KNOTS((4,4),(3,3),(0.,0.0385835973699829),(0.,1.),
 .UNSPECIFIED.)
GEOMETRIC_REPRESENTATION_ITEM()
RATIONAL_B_SPLINE_SURFACE(((1.,0.713879290671428,1.),(1.,0.71450712730611,
1.),(1.,0.715277846561214,1.),(1.,0.716457303923418,1.)))
REPRESENTATION_ITEM('')
SURFACE()
);
#2754=(
BOUNDED_SURFACE()
B_SPLINE_SURFACE(3,2,((#175654,#175655,#175656),(#175657,#175658,#175659),
(#175660,#175661,#175662),(#175663,#175664,#175665)),.UNSPECIFIED.,.F.,
 .F.,.F.)
B_SPLINE_SURFACE_WITH_KNOTS((4,4),(3,3),(0.,0.038317388945353),(0.,1.),
 .UNSPECIFIED.)
GEOMETRIC_REPRESENTATION_ITEM()
RATIONAL_B_SPLINE_SURFACE(((1.,0.716457303923414,1.),(1.,0.715285870443621,
1.),(1.,0.714517981140503,1.),(1.,0.713892198341303,1.)))
REPRESENTATION_ITEM('')
SURFACE()
);
#2755=(
BOUNDED_SURFACE()
B_SPLINE_SURFACE(3,2,((#175747,#175748,#175749),(#175750,#175751,#175752),
(#175753,#175754,#175755),(#175756,#175757,#175758)),.UNSPECIFIED.,.F.,
 .F.,.F.)
B_SPLINE_SURFACE_WITH_KNOTS((4,4),(3,3),(-1.62187915626604E-5,0.000794016598505311),
(0.,1.00001621879156),.UNSPECIFIED.)
GEOMETRIC_REPRESENTATION_ITEM()
RATIONAL_B_SPLINE_SURFACE(((1.,0.916158202477454,1.00000271962528),(1.,
0.931371211352859,1.00000222615204),(1.,0.942410544587803,1.00000186806275),
(1.,0.948459380997912,1.00000167185311)))
REPRESENTATION_ITEM('')
SURFACE()
);
#2756=(
BOUNDED_SURFACE()
B_SPLINE_SURFACE(3,2,((#175770,#175771,#175772),(#175773,#175774,#175775),
(#175776,#175777,#175778),(#175779,#175780,#175781),(#175782,#175783,#175784),
(#175785,#175786,#175787)),.UNSPECIFIED.,.F.,.F.,.F.)
B_SPLINE_SURFACE_WITH_KNOTS((4,2,4),(3,3),(-2.35539541778838E-5,0.000414679582686121,
0.000852913119550131),(-0.00068744155822166,1.00002355395418),
 .UNSPECIFIED.)
GEOMETRIC_REPRESENTATION_ITEM()
RATIONAL_B_SPLINE_SURFACE(((1.00026536769246,0.806984358134055,1.00000908631671),
(1.00026576129372,0.806698071587169,1.00000909979381),(1.00026384744406,
0.80809011338651,1.00000903426268),(1.00026239826983,0.809144172726734,
1.00000898464226),(1.00026303812725,0.808678771345985,1.00000900655128),
(1.00027069226676,0.803111519968988,1.00000926863268)))
REPRESENTATION_ITEM('')
SURFACE()
);
#2757=(
BOUNDED_SURFACE()
B_SPLINE_SURFACE(3,2,((#175807,#175808,#175809),(#175810,#175811,#175812),
(#175813,#175814,#175815),(#175816,#175817,#175818)),.UNSPECIFIED.,.F.,
 .F.,.F.)
B_SPLINE_SURFACE_WITH_KNOTS((4,4),(3,3),(0.,0.000650122732446382),(0.,1.),
 .UNSPECIFIED.)
GEOMETRIC_REPRESENTATION_ITEM()
RATIONAL_B_SPLINE_SURFACE(((1.,0.714558059459819,1.),(1.,0.714557241617472,
1.),(1.,0.714330794970796,1.),(1.,0.71387929067142,1.)))
REPRESENTATION_ITEM('')
SURFACE()
);
#2758=(
BOUNDED_SURFACE()
B_SPLINE_SURFACE(3,2,((#175826,#175827,#175828),(#175829,#175830,#175831),
(#175832,#175833,#175834),(#175835,#175836,#175837)),.UNSPECIFIED.,.F.,
 .F.,.F.)
B_SPLINE_SURFACE_WITH_KNOTS((4,4),(3,3),(-1.0842021724855E-19,0.000650371461981817),
(0.,1.),.UNSPECIFIED.)
GEOMETRIC_REPRESENTATION_ITEM()
RATIONAL_B_SPLINE_SURFACE(((1.,0.668488966322264,1.),(1.,0.665851831765851,
1.),(1.,0.664481097979681,1.),(1.,0.664473794614064,1.)))
REPRESENTATION_ITEM('')
SURFACE()
);
#2759=(
BOUNDED_SURFACE()
B_SPLINE_SURFACE(3,2,((#175843,#175844,#175845),(#175846,#175847,#175848),
(#175849,#175850,#175851),(#175852,#175853,#175854),(#175855,#175856,#175857),
(#175858,#175859,#175860),(#175861,#175862,#175863),(#175864,#175865,#175866),
(#175867,#175868,#175869),(#175870,#175871,#175872),(#175873,#175874,#175875),
(#175876,#175877,#175878),(#175879,#175880,#175881),(#175882,#175883,#175884)),
 .UNSPECIFIED.,.F.,.F.,.F.)
B_SPLINE_SURFACE_WITH_KNOTS((4,2,2,2,2,2,4),(3,3),(0.00807927244133089,
0.00881458117408921,0.00918223554046837,0.00954988990684753,0.0099175442732267,
0.0102851986396059,0.0110205073723642),(0.,1.),.UNSPECIFIED.)
GEOMETRIC_REPRESENTATION_ITEM()
RATIONAL_B_SPLINE_SURFACE(((1.,0.707106781186548,1.),(1.,0.705697402766896,
1.),(1.,0.704316028414221,1.),(1.,0.702287640598182,1.),(1.,0.70162085852966,
1.),(1.,0.700346303389684,1.),(1.,0.699732822392533,1.),(1.,0.69855427952325,
1.),(1.,0.697985323371657,1.),(1.,0.696930428409623,1.),(1.,0.69644149384419,
1.),(1.,0.695089684342733,1.),(1.,0.694335092820993,1.),(1.,0.693797102764879,
1.)))
REPRESENTATION_ITEM('')
SURFACE()
);
#2760=(
BOUNDED_SURFACE()
B_SPLINE_SURFACE(3,2,((#176024,#176025,#176026),(#176027,#176028,#176029),
(#176030,#176031,#176032),(#176033,#176034,#176035)),.UNSPECIFIED.,.F.,
 .F.,.F.)
B_SPLINE_SURFACE_WITH_KNOTS((4,4),(3,3),(0.0156098999423859,0.0162171358932854),
(0.,0.915625791428726),.UNSPECIFIED.)
GEOMETRIC_REPRESENTATION_ITEM()
RATIONAL_B_SPLINE_SURFACE(((1.,0.809621640719886,0.967873953213285),(1.,
0.812433937177746,0.968348523789085),(1.,0.815135819310926,0.968804462122364),
(1.,0.817729693080373,0.969242174215226)))
REPRESENTATION_ITEM('')
SURFACE()
);
#2761=(
BOUNDED_SURFACE()
B_SPLINE_SURFACE(3,2,((#176070,#176071,#176072),(#176073,#176074,#176075),
(#176076,#176077,#176078),(#176079,#176080,#176081),(#176082,#176083,#176084),
(#176085,#176086,#176087),(#176088,#176089,#176090),(#176091,#176092,#176093),
(#176094,#176095,#176096),(#176097,#176098,#176099),(#176100,#176101,#176102),
(#176103,#176104,#176105),(#176106,#176107,#176108),(#176109,#176110,#176111)),
 .UNSPECIFIED.,.F.,.F.,.F.)
B_SPLINE_SURFACE_WITH_KNOTS((4,2,2,2,2,2,4),(3,3),(0.00807902625150492,
0.00883280378349999,0.00920969254949752,0.00958658131549505,0.00996347008149258,
0.0103403588474901,0.0110941363794852),(0.,1.),.UNSPECIFIED.)
GEOMETRIC_REPRESENTATION_ITEM()
RATIONAL_B_SPLINE_SURFACE(((1.,0.707106781186548,1.),(1.,0.708503208405905,
1.),(1.,0.709864127404626,1.),(1.,0.711851747119499,1.),(1.,0.712500882329163,
1.),(1.,0.713738228851022,1.),(1.,0.714331705876986,1.),(1.,0.715467776552351,
1.),(1.,0.716012641761659,1.),(1.,0.71701515809269,1.),(1.,0.717477434704573,
1.),(1.,0.718748007011303,1.),(1.,0.719442582755427,1.),(1.,0.719919801430648,
1.)))
REPRESENTATION_ITEM('')
SURFACE()
);
#2762=(
BOUNDED_SURFACE()
B_SPLINE_SURFACE(3,2,((#176211,#176212,#176213),(#176214,#176215,#176216),
(#176217,#176218,#176219),(#176220,#176221,#176222)),.UNSPECIFIED.,.F.,
 .F.,.F.)
B_SPLINE_SURFACE_WITH_KNOTS((4,4),(3,3),(0.,0.000650589467290063),(0.,1.),
 .UNSPECIFIED.)
GEOMETRIC_REPRESENTATION_ITEM()
RATIONAL_B_SPLINE_SURFACE(((1.,0.761354724782838,1.),(1.,0.761348936155314,
1.),(1.,0.759749503531854,1.),(1.,0.756551244268667,1.)))
REPRESENTATION_ITEM('')
SURFACE()
);
#2763=(
BOUNDED_SURFACE()
B_SPLINE_SURFACE(3,2,((#176230,#176231,#176232),(#176233,#176234,#176235),
(#176236,#176237,#176238),(#176239,#176240,#176241)),.UNSPECIFIED.,.F.,
 .F.,.F.)
B_SPLINE_SURFACE_WITH_KNOTS((4,4),(3,3),(-6.51412822692206E-5,0.000716554104961429),
(-0.000128171463349183,1.),.UNSPECIFIED.)
GEOMETRIC_REPRESENTATION_ITEM()
RATIONAL_B_SPLINE_SURFACE(((1.00009698047895,0.621676789764313,1.),(1.00009906013662,
0.613563994562098,1.),(1.00010008654859,0.609559936451183,1.),(1.00009988696594,
0.610338513229391,1.)))
REPRESENTATION_ITEM('')
SURFACE()
);
#2764=(
BOUNDED_SURFACE()
B_SPLINE_SURFACE(3,2,((#176291,#176292,#176293),(#176294,#176295,#176296),
(#176297,#176298,#176299),(#176300,#176301,#176302)),.UNSPECIFIED.,.F.,
 .F.,.F.)
B_SPLINE_SURFACE_WITH_KNOTS((4,4),(3,3),(-6.51893458122614E-5,0.000717082803934875),
(-0.000140476308568739,1.),.UNSPECIFIED.)
GEOMETRIC_REPRESENTATION_ITEM()
RATIONAL_B_SPLINE_SURFACE(((1.00005469398346,0.805326663217762,1.),(1.00005450492213,
0.805999592802024,1.),(1.00005546526461,0.802581427505982,1.),(1.00005755719884,
0.795135566176566,1.)))
REPRESENTATION_ITEM('')
SURFACE()
);
#2765=(
BOUNDED_SURFACE()
B_SPLINE_SURFACE(3,2,((#176310,#176311,#176312),(#176313,#176314,#176315),
(#176316,#176317,#176318),(#176319,#176320,#176321)),.UNSPECIFIED.,.F.,
 .F.,.F.)
B_SPLINE_SURFACE_WITH_KNOTS((4,4),(3,3),(-3.51851606592903E-5,0.00068875516054279),
(-3.51851606592598E-5,1.),.UNSPECIFIED.)
GEOMETRIC_REPRESENTATION_ITEM()
RATIONAL_B_SPLINE_SURFACE(((1.00003035731885,0.568606220890069,1.),(1.00003120327315,
0.556584756681408,1.),(1.00003165553005,0.550157943671109,1.),(1.00003160738783,
0.550842070368458,1.)))
REPRESENTATION_ITEM('')
SURFACE()
);
#2766=(
BOUNDED_SURFACE()
B_SPLINE_SURFACE(3,2,((#176408,#176409,#176410),(#176411,#176412,#176413),
(#176414,#176415,#176416),(#176417,#176418,#176419),(#176420,#176421,#176422),
(#176423,#176424,#176425),(#176426,#176427,#176428),(#176429,#176430,#176431),
(#176432,#176433,#176434),(#176435,#176436,#176437)),.UNSPECIFIED.,.F.,
 .F.,.F.)
B_SPLINE_SURFACE_WITH_KNOTS((4,2,2,2,4),(3,3),(0.00131180726843869,0.00173116479138241,
0.00215052231432612,0.00256987983726984,0.00298923736021356),(0.,1.00000719536613),
 .UNSPECIFIED.)
GEOMETRIC_REPRESENTATION_ITEM()
RATIONAL_B_SPLINE_SURFACE(((1.,0.707104673712603,1.00000421497822),(1.,
0.735459277067931,1.00000380693471),(1.,0.757076784024019,1.00000349584296),
(1.,0.786069896430007,1.00000307861084),(1.,0.793429076618431,1.00000297270685),
(1.,0.793448571747574,1.0000029724263),(1.,0.78610382913614,1.00000307812252),
(1.,0.757124528684552,1.00000349515588),(1.,0.735523766261738,1.00000380600667),
(1.,0.707104673712603,1.00000421497822)))
REPRESENTATION_ITEM('')
SURFACE()
);
#2767=(
BOUNDED_SURFACE()
B_SPLINE_SURFACE(3,2,((#176476,#176477,#176478),(#176479,#176480,#176481),
(#176482,#176483,#176484),(#176485,#176486,#176487),(#176488,#176489,#176490),
(#176491,#176492,#176493),(#176494,#176495,#176496),(#176497,#176498,#176499),
(#176500,#176501,#176502),(#176503,#176504,#176505)),.UNSPECIFIED.,.F.,
 .F.,.F.)
B_SPLINE_SURFACE_WITH_KNOTS((4,2,2,2,4),(3,3),(0.00108313181642967,0.00175636478508591,
0.00242959775374216,0.0031028307223984,0.00377606369105465),(0.,1.00020946001139),
 .UNSPECIFIED.)
GEOMETRIC_REPRESENTATION_ITEM()
RATIONAL_B_SPLINE_SURFACE(((1.,0.707045431769604,1.00012272453439),(1.,
0.774791710231264,1.00009434426188),(1.,0.828921293970805,1.00007166829543),
(1.,0.903779687679842,1.00004030861543),(1.,0.92410102032017,1.0000317956023),
(1.,0.924695389732779,1.00003154660905),(1.,0.904861584947158,1.000039855387),
(1.,0.830176121522683,1.00007114262304),(1.,0.775998513536546,1.00009383870781),
(1.,0.707045431769604,1.00012272453439)))
REPRESENTATION_ITEM('')
SURFACE()
);
#2768=(
BOUNDED_SURFACE()
B_SPLINE_SURFACE(3,2,((#176567,#176568,#176569),(#176570,#176571,#176572),
(#176573,#176574,#176575),(#176576,#176577,#176578),(#176579,#176580,#176581),
(#176582,#176583,#176584),(#176585,#176586,#176587),(#176588,#176589,#176590),
(#176591,#176592,#176593),(#176594,#176595,#176596)),.UNSPECIFIED.,.F.,
 .F.,.F.)
B_SPLINE_SURFACE_WITH_KNOTS((4,2,2,2,4),(3,3),(0.00116892975483565,0.00173273620432837,
0.00229654265382108,0.0028603491033138,0.00342415555280651),(0.,1.00008736726516),
 .UNSPECIFIED.)
GEOMETRIC_REPRESENTATION_ITEM()
RATIONAL_B_SPLINE_SURFACE(((1.,0.707081191907032,1.00005118303035),(1.,
0.756727911750276,1.00004250803408),(1.,0.79532361474289,1.00003576403205),
(1.,0.847730260009984,1.0000266067815),(1.,0.861376184832611,1.00002422236723),
(1.,0.861443104052992,1.00002421067414),(1.,0.847851660205351,1.00002658556869),
(1.,0.795420207077594,1.00003574715403),(1.,0.756766547571532,1.00004250128307),
(1.,0.707081191907032,1.00005118303035)))
REPRESENTATION_ITEM('')
SURFACE()
);
#2769=(
BOUNDED_SURFACE()
B_SPLINE_SURFACE(3,2,((#176718,#176719,#176720),(#176721,#176722,#176723),
(#176724,#176725,#176726),(#176727,#176728,#176729),(#176730,#176731,#176732),
(#176733,#176734,#176735),(#176736,#176737,#176738),(#176739,#176740,#176741),
(#176742,#176743,#176744),(#176745,#176746,#176747)),.UNSPECIFIED.,.F.,
 .F.,.F.)
B_SPLINE_SURFACE_WITH_KNOTS((4,2,2,2,4),(3,3),(8.78519494496445E-16,0.392699081698725,
0.785398163397449,1.17809724509617,1.5707963267949),(0.,1.),
 .UNSPECIFIED.)
GEOMETRIC_REPRESENTATION_ITEM()
RATIONAL_B_SPLINE_SURFACE(((1.,0.754709580222768,1.),(1.,0.754714219644573,
1.),(1.,0.753512297211018,1.),(1.,0.748871927581762,1.),(1.,0.745429367161016,
1.),(1.,0.736738129073881,1.),(1.,0.73149075671205,1.),(1.,0.719894264547496,
1.),(1.,0.713550262087909,1.),(1.,0.707106781186548,1.)))
REPRESENTATION_ITEM('')
SURFACE()
);
#2770=(
BOUNDED_SURFACE()
B_SPLINE_SURFACE(3,2,((#176850,#176851,#176852),(#176853,#176854,#176855),
(#176856,#176857,#176858),(#176859,#176860,#176861),(#176862,#176863,#176864),
(#176865,#176866,#176867),(#176868,#176869,#176870),(#176871,#176872,#176873),
(#176874,#176875,#176876),(#176877,#176878,#176879)),.UNSPECIFIED.,.F.,
 .F.,.F.)
B_SPLINE_SURFACE_WITH_KNOTS((4,2,2,2,4),(3,3),(4.71238898038469,5.10508806208341,
5.49778714378214,5.89048622548086,6.28318530717959),(0.,1.),
 .UNSPECIFIED.)
GEOMETRIC_REPRESENTATION_ITEM()
RATIONAL_B_SPLINE_SURFACE(((1.,0.707106781186548,1.),(1.,0.71355026185156,
1.),(1.,0.719894264862189,1.),(1.,0.73149075639733,1.),(1.,0.73673812929671,
1.),(1.,0.745429366938189,1.),(1.,0.748871927696634,1.),(1.,0.753512297096161,
1.),(1.,0.754714219730837,1.),(1.,0.754709580222772,1.)))
REPRESENTATION_ITEM('')
SURFACE()
);
#2771=(
BOUNDED_SURFACE()
B_SPLINE_SURFACE(3,2,((#176896,#176897,#176898),(#176899,#176900,#176901),
(#176902,#176903,#176904),(#176905,#176906,#176907),(#176908,#176909,#176910),
(#176911,#176912,#176913),(#176914,#176915,#176916),(#176917,#176918,#176919),
(#176920,#176921,#176922),(#176923,#176924,#176925)),.UNSPECIFIED.,.F.,
 .F.,.F.)
B_SPLINE_SURFACE_WITH_KNOTS((4,2,2,2,4),(3,3),(0.00116892975483561,0.00173273620432837,
0.00229654265382113,0.00286034910331391,0.00342415555280667),(0.,1.00008736726517),
 .UNSPECIFIED.)
GEOMETRIC_REPRESENTATION_ITEM()
RATIONAL_B_SPLINE_SURFACE(((1.,0.707081191907034,1.00005118303036),(1.,
0.75672791175003,1.00004250803408),(1.,0.795323614743255,1.00003576403205),
(1.,0.847730260009664,1.0000266067815),(1.,0.861376184834009,1.00002422236724),
(1.,0.861443104051655,1.00002421067414),(1.,0.847851660205381,1.0000265855687),
(1.,0.795420207077597,1.00003574715403),(1.,0.756766547571556,1.00004250128307),
(1.,0.707081191907034,1.00005118303036)))
REPRESENTATION_ITEM('')
SURFACE()
);
#2772=(
BOUNDED_SURFACE()
B_SPLINE_SURFACE(2,2,((#176985,#176986,#176987),(#176988,#176989,#176990),
(#176991,#176992,#176993)),.UNSPECIFIED.,.F.,.F.,.F.)
B_SPLINE_SURFACE_WITH_KNOTS((3,3),(3,3),(-3.74064361396611E-16,1.57079632679492),
(-1.5707963267949,0.),.UNSPECIFIED.)
GEOMETRIC_REPRESENTATION_ITEM()
RATIONAL_B_SPLINE_SURFACE(((1.,0.707106781186548,1.),(0.707106781186552,
0.500000000000003,0.707106781186552),(1.,0.707106781186548,1.)))
REPRESENTATION_ITEM('')
SURFACE()
);
#2773=(
BOUNDED_SURFACE()
B_SPLINE_SURFACE(2,2,((#177001,#177002,#177003),(#177004,#177005,#177006),
(#177007,#177008,#177009)),.UNSPECIFIED.,.F.,.F.,.F.)
B_SPLINE_SURFACE_WITH_KNOTS((3,3),(3,3),(0.,1.57079632679492),(-3.14159265358979,
-1.5707963267949),.UNSPECIFIED.)
GEOMETRIC_REPRESENTATION_ITEM()
RATIONAL_B_SPLINE_SURFACE(((1.,0.707106781186548,1.),(0.707106781186552,
0.500000000000003,0.707106781186552),(1.,0.707106781186548,1.)))
REPRESENTATION_ITEM('')
SURFACE()
);
#2774=(
BOUNDED_SURFACE()
B_SPLINE_SURFACE(2,2,((#177029,#177030,#177031),(#177032,#177033,#177034),
(#177035,#177036,#177037)),.UNSPECIFIED.,.F.,.F.,.F.)
B_SPLINE_SURFACE_WITH_KNOTS((3,3),(3,3),(-3.74064361396611E-16,1.57079632679492),
(-1.5707963267949,0.),.UNSPECIFIED.)
GEOMETRIC_REPRESENTATION_ITEM()
RATIONAL_B_SPLINE_SURFACE(((1.,0.707106781186548,1.),(0.707106781186552,
0.500000000000003,0.707106781186552),(1.,0.707106781186548,1.)))
REPRESENTATION_ITEM('')
SURFACE()
);
#2775=(
BOUNDED_SURFACE()
B_SPLINE_SURFACE(2,2,((#177045,#177046,#177047),(#177048,#177049,#177050),
(#177051,#177052,#177053)),.UNSPECIFIED.,.F.,.F.,.F.)
B_SPLINE_SURFACE_WITH_KNOTS((3,3),(3,3),(0.,1.57079632679501),(-3.14159265358979,
-1.5707963267949),.UNSPECIFIED.)
GEOMETRIC_REPRESENTATION_ITEM()
RATIONAL_B_SPLINE_SURFACE(((1.,0.707106781186548,1.),(0.707106781186506,
0.49999999999997,0.707106781186506),(1.,0.707106781186548,1.)))
REPRESENTATION_ITEM('')
SURFACE()
);
#2776=(
BOUNDED_SURFACE()
B_SPLINE_SURFACE(2,2,((#177073,#177074,#177075),(#177076,#177077,#177078),
(#177079,#177080,#177081)),.UNSPECIFIED.,.F.,.F.,.F.)
B_SPLINE_SURFACE_WITH_KNOTS((3,3),(3,3),(-3.74064361396611E-16,1.57079632679501),
(-1.5707963267949,0.),.UNSPECIFIED.)
GEOMETRIC_REPRESENTATION_ITEM()
RATIONAL_B_SPLINE_SURFACE(((1.,0.707106781186548,1.),(0.707106781186506,
0.49999999999997,0.707106781186506),(1.,0.707106781186548,1.)))
REPRESENTATION_ITEM('')
SURFACE()
);
#2777=(
BOUNDED_SURFACE()
B_SPLINE_SURFACE(3,2,((#177091,#177092,#177093),(#177094,#177095,#177096),
(#177097,#177098,#177099),(#177100,#177101,#177102),(#177103,#177104,#177105),
(#177106,#177107,#177108)),.UNSPECIFIED.,.F.,.F.,.F.)
B_SPLINE_SURFACE_WITH_KNOTS((4,2,4),(3,3),(0.19058679356565,0.194723599184011,
0.198860404802373),(0.,1.),.UNSPECIFIED.)
GEOMETRIC_REPRESENTATION_ITEM()
RATIONAL_B_SPLINE_SURFACE(((1.,0.954062806827576,1.),(1.,0.95589180838713,
1.),(1.,0.957713181483215,1.),(1.,0.961295526062221,1.),(1.,0.963047831711069,
1.),(1.,0.964700553047209,1.)))
REPRESENTATION_ITEM('')
SURFACE()
);
#2778=(
BOUNDED_SURFACE()
B_SPLINE_SURFACE(3,2,((#177180,#177181,#177182),(#177183,#177184,#177185),
(#177186,#177187,#177188),(#177189,#177190,#177191),(#177192,#177193,#177194),
(#177195,#177196,#177197),(#177198,#177199,#177200),(#177201,#177202,#177203),
(#177204,#177205,#177206),(#177207,#177208,#177209)),.UNSPECIFIED.,.F.,
 .F.,.F.)
B_SPLINE_SURFACE_WITH_KNOTS((4,2,2,2,4),(3,3),(0.00166905748884283,0.00189688228523533,
0.00212470708162783,0.00235253187802032,0.00258035667441282),(0.,1.),
 .UNSPECIFIED.)
GEOMETRIC_REPRESENTATION_ITEM()
RATIONAL_B_SPLINE_SURFACE(((1.,0.727682857482998,1.),(1.,0.742747587336582,
1.),(1.,0.756565090576503,1.),(1.,0.779563382898484,1.),(1.,0.788904601358709,
1.),(1.,0.801793098601248,1.),(1.,0.805447378128131,1.),(1.,0.806422615061365,
1.),(1.,0.803776299349016,1.),(1.,0.798143461625347,1.)))
REPRESENTATION_ITEM('')
SURFACE()
);
#2779=(
BOUNDED_SURFACE()
B_SPLINE_SURFACE(3,2,((#177347,#177348,#177349),(#177350,#177351,#177352),
(#177353,#177354,#177355),(#177356,#177357,#177358)),.UNSPECIFIED.,.F.,
 .F.,.F.)
B_SPLINE_SURFACE_WITH_KNOTS((4,4),(3,3),(0.00165976994196512,0.00175987143987977),
(0.,1.),.UNSPECIFIED.)
GEOMETRIC_REPRESENTATION_ITEM()
RATIONAL_B_SPLINE_SURFACE(((1.,0.707106781186549,1.),(1.,0.714158119082749,
1.),(1.,0.721010468727715,1.),(1.,0.727682857483054,1.)))
REPRESENTATION_ITEM('')
SURFACE()
);
#2780=(
BOUNDED_SURFACE()
B_SPLINE_SURFACE(3,2,((#177385,#177386,#177387),(#177388,#177389,#177390),
(#177391,#177392,#177393),(#177394,#177395,#177396),(#177397,#177398,#177399),
(#177400,#177401,#177402),(#177403,#177404,#177405),(#177406,#177407,#177408),
(#177409,#177410,#177411),(#177412,#177413,#177414),(#177415,#177416,#177417),
(#177418,#177419,#177420)),.UNSPECIFIED.,.F.,.F.,.F.)
B_SPLINE_SURFACE_WITH_KNOTS((4,2,2,2,2,4),(3,3),(-2.00577401909819E-18,
0.000253295312002929,0.000379942968004394,0.00050659062400586,0.000759885936008791,
0.00107305843962858),(-0.000819314453937797,1.),.UNSPECIFIED.)
GEOMETRIC_REPRESENTATION_ITEM()
RATIONAL_B_SPLINE_SURFACE(((1.00062441413186,0.618941098343779,1.),(1.000636782846,
0.611392888935679,1.),(1.00064233967356,0.608001744342297,1.),(1.00063916769033,
0.609937498807523,1.),(1.00063617465599,0.611764046800477,1.),(1.0006268165417,
0.617474988578315,1.),(1.00062041650623,0.621380714544669,1.),(1.00059694010773,
0.635707569383962,1.),(1.00057586843891,0.64856689873871,1.),(1.00052425844524,
0.680062738598407,1.),(1.00049229616275,0.699568242459855,1.),(1.00046353459627,
0.717120457208093,1.)))
REPRESENTATION_ITEM('')
SURFACE()
);
#2781=(
BOUNDED_SURFACE()
B_SPLINE_SURFACE(3,2,((#177478,#177479,#177480),(#177481,#177482,#177483),
(#177484,#177485,#177486),(#177487,#177488,#177489),(#177490,#177491,#177492),
(#177493,#177494,#177495),(#177496,#177497,#177498),(#177499,#177500,#177501),
(#177502,#177503,#177504),(#177505,#177506,#177507),(#177508,#177509,#177510),
(#177511,#177512,#177513)),.UNSPECIFIED.,.F.,.F.,.F.)
B_SPLINE_SURFACE_WITH_KNOTS((4,2,2,2,2,4),(3,3),(0.,0.000250417359226946,
0.000375626038840418,0.000500834718453891,0.000751252077680836,0.00100166943690778),
(0.,1.00140468204324),.UNSPECIFIED.)
GEOMETRIC_REPRESENTATION_ITEM()
RATIONAL_B_SPLINE_SURFACE(((1.,0.706695359341495,1.00082399952386),(1.,
0.713853670046366,1.00080388922285),(1.,0.720999103056668,1.00078381509997),
(1.,0.73025084315396,1.0007578235936),(1.,0.733150182806824,1.00074967829291),
(1.,0.738287011792474,1.00073524707003),(1.,0.740523082653704,1.00072896513286),
(1.,0.746225847024098,1.00071294399145),(1.,0.748459431198593,1.00070666904028),
(1.,0.749389678141756,1.00070405563793),(1.,0.748089205673001,1.00070770913858),
(1.,0.745115248769628,1.0007160640663)))
REPRESENTATION_ITEM('')
SURFACE()
);
#2782=(
BOUNDED_SURFACE()
B_SPLINE_SURFACE(3,2,((#177610,#177611,#177612),(#177613,#177614,#177615),
(#177616,#177617,#177618),(#177619,#177620,#177621),(#177622,#177623,#177624),
(#177625,#177626,#177627)),.UNSPECIFIED.,.F.,.F.,.F.)
B_SPLINE_SURFACE_WITH_KNOTS((4,2,4),(3,3),(0.,0.00138008432392828,0.00276016864785656),
(0.,1.),.UNSPECIFIED.)
GEOMETRIC_REPRESENTATION_ITEM()
RATIONAL_B_SPLINE_SURFACE(((1.,0.889512696472458,1.),(1.,0.875621469665309,
1.),(1.,0.859481975708513,1.),(1.,0.823331923932046,1.),(1.,0.803217377248123,
1.),(1.,0.782160982635976,1.)))
REPRESENTATION_ITEM('')
SURFACE()
);
#2783=(
BOUNDED_SURFACE()
B_SPLINE_SURFACE(3,2,((#177678,#177679,#177680),(#177681,#177682,#177683),
(#177684,#177685,#177686),(#177687,#177688,#177689)),.UNSPECIFIED.,.F.,
 .F.,.F.)
B_SPLINE_SURFACE_WITH_KNOTS((4,4),(3,3),(-3.41523684332934E-18,0.000418670815451504),
(0.,1.),.UNSPECIFIED.)
GEOMETRIC_REPRESENTATION_ITEM()
RATIONAL_B_SPLINE_SURFACE(((1.,0.80178372573727,1.),(1.,0.801581038760284,
1.),(1.,0.797360979426379,1.),(1.,0.782160982635977,1.)))
REPRESENTATION_ITEM('')
SURFACE()
);
#2784=(
BOUNDED_SURFACE()
B_SPLINE_SURFACE(3,2,((#177736,#177737,#177738),(#177739,#177740,#177741),
(#177742,#177743,#177744),(#177745,#177746,#177747),(#177748,#177749,#177750),
(#177751,#177752,#177753)),.UNSPECIFIED.,.F.,.F.,.F.)
B_SPLINE_SURFACE_WITH_KNOTS((4,2,4),(3,3),(-1.97866896478604E-18,0.00038804539867497,
0.000776090797349943),(0.,1.),.UNSPECIFIED.)
GEOMETRIC_REPRESENTATION_ITEM()
RATIONAL_B_SPLINE_SURFACE(((1.,0.889512696472455,1.),(1.,0.863343118435834,
1.),(1.,0.832896241151233,1.),(1.,0.770252595987774,1.),(1.,0.738321744191135,
1.),(1.,0.707106781186616,1.)))
REPRESENTATION_ITEM('')
SURFACE()
);
#2785=(
BOUNDED_SURFACE()
B_SPLINE_SURFACE(3,2,((#177788,#177789,#177790),(#177791,#177792,#177793),
(#177794,#177795,#177796),(#177797,#177798,#177799),(#177800,#177801,#177802),
(#177803,#177804,#177805),(#177806,#177807,#177808),(#177809,#177810,#177811),
(#177812,#177813,#177814),(#177815,#177816,#177817)),.UNSPECIFIED.,.F.,
 .F.,.F.)
B_SPLINE_SURFACE_WITH_KNOTS((4,2,2,2,4),(3,3),(0.00312784824903477,0.00367780251889487,
0.00407062699736637,0.00446345147583787,0.00501340574569797),(0.,1.00073967576989),
 .UNSPECIFIED.)
GEOMETRIC_REPRESENTATION_ITEM()
RATIONAL_B_SPLINE_SURFACE(((1.,0.799013820880279,1.00029732921356),(1.,
0.805121639253135,1.00028829360304),(1.,0.800160744451582,1.00029563251041),
(1.,0.77993744364898,1.00032554988159),(1.,0.767978651035377,1.00034324113985),
(1.,0.743437812578867,1.00037954566701),(1.,0.730757029672295,1.00039830500273),
(1.,0.708822787991186,1.00043075345694),(1.,0.70267339919749,1.00043985056472),
(1.,0.710079976844615,1.00042889363267)))
REPRESENTATION_ITEM('')
SURFACE()
);
#2786=(
BOUNDED_SURFACE()
B_SPLINE_SURFACE(2,2,((#177886,#177887,#177888),(#177889,#177890,#177891),
(#177892,#177893,#177894)),.UNSPECIFIED.,.F.,.F.,.F.)
B_SPLINE_SURFACE_WITH_KNOTS((3,3),(3,3),(-1.5707963267949,0.),(-2.40432329481773,
-1.5707963267949),.UNSPECIFIED.)
GEOMETRIC_REPRESENTATION_ITEM()
RATIONAL_B_SPLINE_SURFACE(((1.,0.914403878918655,1.),(0.707106781186554,
0.64658118352667,0.707106781186554),(1.,0.914403878918655,1.)))
REPRESENTATION_ITEM('')
SURFACE()
);
#2787=(
BOUNDED_SURFACE()
B_SPLINE_SURFACE(2,2,((#177902,#177903,#177904),(#177905,#177906,#177907),
(#177908,#177909,#177910)),.UNSPECIFIED.,.F.,.F.,.F.)
B_SPLINE_SURFACE_WITH_KNOTS((3,3),(3,3),(-1.5707963267949,-1.75915766232281E-16),
(-3.14159265358979,-2.36370134837197),.UNSPECIFIED.)
GEOMETRIC_REPRESENTATION_ITEM()
RATIONAL_B_SPLINE_SURFACE(((1.,0.925309396359852,1.),(0.707106781186554,
0.654292548861688,0.707106781186554),(1.,0.925309396359852,1.)))
REPRESENTATION_ITEM('')
SURFACE()
);
#2788=(
BOUNDED_SURFACE()
B_SPLINE_SURFACE(3,2,((#177954,#177955,#177956),(#177957,#177958,#177959),
(#177960,#177961,#177962),(#177963,#177964,#177965),(#177966,#177967,#177968),
(#177969,#177970,#177971),(#177972,#177973,#177974),(#177975,#177976,#177977),
(#177978,#177979,#177980),(#177981,#177982,#177983)),.UNSPECIFIED.,.F.,
 .F.,.F.)
B_SPLINE_SURFACE_WITH_KNOTS((4,2,2,2,4),(3,3),(1.57071221042854,1.96349540849362,
2.35619449019234,2.74889357189107,3.14167676995614),(0.,1.00008411636635),
 .UNSPECIFIED.)
GEOMETRIC_REPRESENTATION_ITEM()
RATIONAL_B_SPLINE_SURFACE(((1.,0.707084736317511,1.00004927793526),(1.,
0.703049896773505,1.00004995672734),(1.,0.698980464825185,1.000050641339),
(1.,0.691398460047746,1.00005191688038),(1.,0.68788946354642,1.00005250720845),
(1.,0.682000298653236,1.00005349795876),(1.,0.679623581412379,1.00005389780039),
(1.,0.676403465575794,1.00005443952928),(1.,0.675558134885499,1.00005458174157),
(1.,0.675562922401557,1.00005458093616)))
REPRESENTATION_ITEM('')
SURFACE()
);
#2789=(
BOUNDED_SURFACE()
B_SPLINE_SURFACE(3,2,((#178188,#178189,#178190),(#178191,#178192,#178193),
(#178194,#178195,#178196),(#178197,#178198,#178199),(#178200,#178201,#178202),
(#178203,#178204,#178205),(#178206,#178207,#178208),(#178209,#178210,#178211),
(#178212,#178213,#178214),(#178215,#178216,#178217)),.UNSPECIFIED.,.F.,
 .F.,.F.)
B_SPLINE_SURFACE_WITH_KNOTS((4,2,2,2,4),(3,3),(3.1415926535898,3.53429173528852,
3.92699081698724,4.31968989868597,4.71238898038469),(0.,1.),
 .UNSPECIFIED.)
GEOMETRIC_REPRESENTATION_ITEM()
RATIONAL_B_SPLINE_SURFACE(((1.,0.73727733681012,1.),(1.,0.737280525007918,
1.),(1.,0.736509240245186,1.),(1.,0.733539335051142,1.),(1.,0.731338116837293,
1.),(1.,0.725801833007076,1.),(1.,0.722468048845319,1.),(1.,0.715136249134486,
1.),(1.,0.711141648505406,1.),(1.,0.707106781186552,1.)))
REPRESENTATION_ITEM('')
SURFACE()
);
#2790=(
BOUNDED_SURFACE()
B_SPLINE_SURFACE(3,2,((#178292,#178293,#178294),(#178295,#178296,#178297),
(#178298,#178299,#178300),(#178301,#178302,#178303),(#178304,#178305,#178306),
(#178307,#178308,#178309),(#178310,#178311,#178312),(#178313,#178314,#178315),
(#178316,#178317,#178318),(#178319,#178320,#178321)),.UNSPECIFIED.,.F.,
 .F.,.F.)
B_SPLINE_SURFACE_WITH_KNOTS((4,2,2,2,4),(3,3),(1.57071221043463,1.96349540849362,
2.35619449019234,2.74889357189107,3.14167676995005),(0.,1.00008411636026),
 .UNSPECIFIED.)
GEOMETRIC_REPRESENTATION_ITEM()
RATIONAL_B_SPLINE_SURFACE(((0.999999999999999,0.707084736319112,1.00004927793169),
(1.,0.70304989677498,1.00004995672372),(1.,0.698980464827243,1.00005064133533),
(1.,0.691398460049362,1.00005191687662),(1.,0.687889463547922,1.00005250720465),
(1.,0.682000298655582,1.00005349795488),(1.,0.679623581414333,1.00005389779649),
(1.,0.676403465577792,1.00005443952534),(1.,0.675558134887503,1.00005458173762),
(1.,0.675562922403545,1.0000545809322)))
REPRESENTATION_ITEM('')
SURFACE()
);
#2791=(
BOUNDED_SURFACE()
B_SPLINE_SURFACE(3,2,((#178536,#178537,#178538),(#178539,#178540,#178541),
(#178542,#178543,#178544),(#178545,#178546,#178547),(#178548,#178549,#178550),
(#178551,#178552,#178553),(#178554,#178555,#178556),(#178557,#178558,#178559),
(#178560,#178561,#178562),(#178563,#178564,#178565)),.UNSPECIFIED.,.F.,
 .F.,.F.)
B_SPLINE_SURFACE_WITH_KNOTS((4,2,2,2,4),(3,3),(3.1415926535898,3.53429173528852,
3.92699081698724,4.31968989868597,4.71238898038469),(0.,1.),
 .UNSPECIFIED.)
GEOMETRIC_REPRESENTATION_ITEM()
RATIONAL_B_SPLINE_SURFACE(((1.,0.73727733681012,1.),(1.,0.737280525007918,
1.),(1.,0.736509240245177,1.),(1.,0.733539335051133,1.),(1.,0.731338116836513,
1.),(1.,0.725801833007847,1.),(1.,0.722468048844965,1.),(1.,0.715136249134831,
1.),(1.,0.711141648505139,1.),(1.,0.707106781186548,1.)))
REPRESENTATION_ITEM('')
SURFACE()
);
#2792=(
BOUNDED_SURFACE()
B_SPLINE_SURFACE(3,2,((#178674,#178675,#178676),(#178677,#178678,#178679),
(#178680,#178681,#178682),(#178683,#178684,#178685),(#178686,#178687,#178688),
(#178689,#178690,#178691)),.UNSPECIFIED.,.F.,.F.,.F.)
B_SPLINE_SURFACE_WITH_KNOTS((4,2,4),(3,3),(0.00432986646256736,0.00505584518302534,
0.00578182390348332),(0.,1.),.UNSPECIFIED.)
GEOMETRIC_REPRESENTATION_ITEM()
RATIONAL_B_SPLINE_SURFACE(((1.,0.737277336810087,1.),(1.,0.750110373322841,
1.),(1.,0.762782449795825,1.),(1.,0.783852338027907,1.),(1.,0.792419881107176,
1.),(1.,0.79736306112227,1.)))
REPRESENTATION_ITEM('')
SURFACE()
);
#2793=(
BOUNDED_SURFACE()
B_SPLINE_SURFACE(3,2,((#178959,#178960,#178961),(#178962,#178963,#178964),
(#178965,#178966,#178967),(#178968,#178969,#178970),(#178971,#178972,#178973),
(#178974,#178975,#178976),(#178977,#178978,#178979),(#178980,#178981,#178982),
(#178983,#178984,#178985),(#178986,#178987,#178988)),.UNSPECIFIED.,.F.,
 .F.,.F.)
B_SPLINE_SURFACE_WITH_KNOTS((4,2,2,2,4),(3,3),(-1.77635683940025E-15,0.392699081698723,
0.785398163397447,1.17809724509617,1.5707963267949),(0.,1.),
 .UNSPECIFIED.)
GEOMETRIC_REPRESENTATION_ITEM()
RATIONAL_B_SPLINE_SURFACE(((1.,0.675590207615662,1.),(1.,0.675585785528387,
1.),(1.,0.676431027860615,1.),(1.,0.679650528045674,1.),(1.,0.682027045382935,
1.),(1.,0.687915714942327,1.),(1.,0.691424416304369,1.),(1.,0.699004971485606,
1.),(1.,0.703073130219524,1.),(1.,0.707106781186548,1.)))
REPRESENTATION_ITEM('')
SURFACE()
);
#2794=(
BOUNDED_SURFACE()
B_SPLINE_SURFACE(3,2,((#179098,#179099,#179100),(#179101,#179102,#179103),
(#179104,#179105,#179106),(#179107,#179108,#179109)),.UNSPECIFIED.,.F.,
 .F.,.F.)
B_SPLINE_SURFACE_WITH_KNOTS((4,4),(3,3),(-8.23993651088983E-18,0.000144871551798125),
(0.453761120778822,1.),.UNSPECIFIED.)
GEOMETRIC_REPRESENTATION_ITEM()
RATIONAL_B_SPLINE_SURFACE(((0.947063795072845,0.941669523342704,1.),(0.948417719357794,
0.943161414365259,1.),(0.949729094777561,0.944606420735039,1.),(0.950997479396062,
0.946004055482066,1.)))
REPRESENTATION_ITEM('')
SURFACE()
);
#2795=(
BOUNDED_SURFACE()
B_SPLINE_SURFACE(3,2,((#179111,#179112,#179113),(#179114,#179115,#179116),
(#179117,#179118,#179119),(#179120,#179121,#179122)),.UNSPECIFIED.,.F.,
 .F.,.F.)
B_SPLINE_SURFACE_WITH_KNOTS((4,4),(3,3),(-5.74627151417317E-18,0.000655078443521525),
(0.,1.),.UNSPECIFIED.)
GEOMETRIC_REPRESENTATION_ITEM()
RATIONAL_B_SPLINE_SURFACE(((1.,0.773398994756356,1.),(1.,0.76231666392952,
1.),(1.,0.750153503473797,1.),(1.,0.737277336810164,1.)))
REPRESENTATION_ITEM('')
SURFACE()
);
#2796=(
BOUNDED_SURFACE()
B_SPLINE_SURFACE(3,2,((#179189,#179190,#179191),(#179192,#179193,#179194),
(#179195,#179196,#179197),(#179198,#179199,#179200),(#179201,#179202,#179203),
(#179204,#179205,#179206),(#179207,#179208,#179209),(#179210,#179211,#179212),
(#179213,#179214,#179215),(#179216,#179217,#179218)),.UNSPECIFIED.,.F.,
 .F.,.F.)
B_SPLINE_SURFACE_WITH_KNOTS((4,2,2,2,4),(3,3),(4.71238898038469,5.10508806208342,
5.49778714378214,5.89048622548086,6.28318530717959),(0.,1.),
 .UNSPECIFIED.)
GEOMETRIC_REPRESENTATION_ITEM()
RATIONAL_B_SPLINE_SURFACE(((1.,0.707106781186545,1.),(1.,0.711141648505767,
1.),(1.,0.715136249133983,1.),(1.,0.722468048845823,1.),(1.,0.725801833007033,
1.),(1.,0.731338116837333,1.),(1.,0.73353933505153,1.),(1.,0.736509240244789,
1.),(1.,0.737280525008216,1.),(1.,0.737277336810123,1.)))
REPRESENTATION_ITEM('')
SURFACE()
);
#2797=(
BOUNDED_SURFACE()
B_SPLINE_SURFACE(3,2,((#179415,#179416,#179417),(#179418,#179419,#179420),
(#179421,#179422,#179423),(#179424,#179425,#179426),(#179427,#179428,#179429),
(#179430,#179431,#179432),(#179433,#179434,#179435),(#179436,#179437,#179438),
(#179439,#179440,#179441),(#179442,#179443,#179444)),.UNSPECIFIED.,.F.,
 .F.,.F.)
B_SPLINE_SURFACE_WITH_KNOTS((4,2,2,2,4),(3,3),(4.71238898038469,5.10508806208342,
5.49778714378214,5.89048622548086,6.28318530717959),(0.,1.),
 .UNSPECIFIED.)
GEOMETRIC_REPRESENTATION_ITEM()
RATIONAL_B_SPLINE_SURFACE(((1.,0.707106781186545,1.),(1.,0.711141648505882,
1.),(1.,0.715136249133832,1.),(1.,0.722468048845978,1.),(1.,0.725801833007229,
1.),(1.,0.731338116837136,1.),(1.,0.733539335051522,1.),(1.,0.736509240244802,
1.),(1.,0.737280525008203,1.),(1.,0.737277336810123,1.)))
REPRESENTATION_ITEM('')
SURFACE()
);
#2798=(
BOUNDED_SURFACE()
B_SPLINE_SURFACE(3,2,((#179517,#179518,#179519),(#179520,#179521,#179522),
(#179523,#179524,#179525),(#179526,#179527,#179528),(#179529,#179530,#179531),
(#179532,#179533,#179534),(#179535,#179536,#179537),(#179538,#179539,#179540),
(#179541,#179542,#179543),(#179544,#179545,#179546)),.UNSPECIFIED.,.F.,
 .F.,.F.)
B_SPLINE_SURFACE_WITH_KNOTS((4,2,2,2,4),(3,3),(-1.77635683940025E-15,0.392699081698723,
0.785398163397447,1.17809724509617,1.5707963267949),(0.,1.),
 .UNSPECIFIED.)
GEOMETRIC_REPRESENTATION_ITEM()
RATIONAL_B_SPLINE_SURFACE(((1.,0.675590207615668,1.),(1.,0.675585785528724,
1.),(1.,0.676431027860173,1.),(1.,0.679650528046127,1.),(1.,0.682027045382925,
1.),(1.,0.687915714942339,1.),(1.,0.69142441630503,1.),(1.,0.699004971484955,
1.),(1.,0.703073130220009,1.),(1.,0.70710678118655,1.)))
REPRESENTATION_ITEM('')
SURFACE()
);
#2799=(
BOUNDED_SURFACE()
B_SPLINE_SURFACE(3,2,((#179770,#179771,#179772),(#179773,#179774,#179775),
(#179776,#179777,#179778),(#179779,#179780,#179781),(#179782,#179783,#179784),
(#179785,#179786,#179787),(#179788,#179789,#179790),(#179791,#179792,#179793),
(#179794,#179795,#179796),(#179797,#179798,#179799)),.UNSPECIFIED.,.F.,
 .F.,.F.)
B_SPLINE_SURFACE_WITH_KNOTS((4,2,2,2,4),(3,3),(1.5707963267949,1.96349540849362,
2.35619449019234,2.74889357189107,3.1415926535898),(0.,1.),
 .UNSPECIFIED.)
GEOMETRIC_REPRESENTATION_ITEM()
RATIONAL_B_SPLINE_SURFACE(((1.,0.707106781186548,1.),(1.,0.711141648505595,
1.),(1.,0.715136249134216,1.),(1.,0.722468048845599,1.),(1.,0.725801833007891,
1.),(1.,0.731338116836469,1.),(1.,0.733539335051304,1.),(1.,0.73650924024502,
1.),(1.,0.737280525008041,1.),(1.,0.737277336810125,1.)))
REPRESENTATION_ITEM('')
SURFACE()
);
#2800=(
BOUNDED_SURFACE()
B_SPLINE_SURFACE(3,2,((#179872,#179873,#179874),(#179875,#179876,#179877),
(#179878,#179879,#179880),(#179881,#179882,#179883),(#179884,#179885,#179886),
(#179887,#179888,#179889),(#179890,#179891,#179892),(#179893,#179894,#179895),
(#179896,#179897,#179898),(#179899,#179900,#179901),(#179902,#179903,#179904),
(#179905,#179906,#179907)),.UNSPECIFIED.,.F.,.F.,.F.)
B_SPLINE_SURFACE_WITH_KNOTS((4,2,2,2,2,4),(3,3),(0.00373720614906648,0.00431441150266452,
0.00489161685626256,0.00518021953306157,0.00546882220986059,0.00604602756345863),
(0.,1.),.UNSPECIFIED.)
GEOMETRIC_REPRESENTATION_ITEM()
RATIONAL_B_SPLINE_SURFACE(((1.,0.702399276808564,1.),(1.,0.697901374758016,
1.),(1.,0.693446103155503,1.),(1.,0.685742881148842,1.),(1.,0.682394877642487,
1.),(1.,0.6786862147386,1.),(1.,0.677675780152448,1.),(1.,0.676083839724519,
1.),(1.,0.675500346164623,1.),(1.,0.674441428307327,1.),(1.,0.674627601820987,
1.),(1.,0.675590207615657,1.)))
REPRESENTATION_ITEM('')
SURFACE()
);
#2801=(
BOUNDED_SURFACE()
B_SPLINE_SURFACE(3,2,((#180151,#180152,#180153),(#180154,#180155,#180156),
(#180157,#180158,#180159),(#180160,#180161,#180162),(#180163,#180164,#180165),
(#180166,#180167,#180168),(#180169,#180170,#180171),(#180172,#180173,#180174),
(#180175,#180176,#180177),(#180178,#180179,#180180)),.UNSPECIFIED.,.F.,
 .F.,.F.)
B_SPLINE_SURFACE_WITH_KNOTS((4,2,2,2,4),(3,3),(1.5707122104307,1.96349540849362,
2.35619449019234,2.74889357189106,3.14167676995398),(0.,1.0000841163642),
 .UNSPECIFIED.)
GEOMETRIC_REPRESENTATION_ITEM()
RATIONAL_B_SPLINE_SURFACE(((1.,0.70708473631808,1.000049277934),(1.,0.703049896774256,
1.00004995672606),(1.,0.698980464825608,1.0000506413377),(1.,0.691398460048643,
1.00005191687905),(1.,0.687889463547443,1.00005250720711),(1.,0.682000298653572,
1.00005349795739),(1.,0.67962358141276,1.00005389779901),(1.,0.676403465576801,
1.00005443952789),(1.,0.675558134885977,1.00005458174018),(1.,0.675562922402261,
1.00005458093476)))
REPRESENTATION_ITEM('')
SURFACE()
);
#2802=(
BOUNDED_SURFACE()
B_SPLINE_SURFACE(3,2,((#180256,#180257,#180258),(#180259,#180260,#180261),
(#180262,#180263,#180264),(#180265,#180266,#180267),(#180268,#180269,#180270),
(#180271,#180272,#180273),(#180274,#180275,#180276),(#180277,#180278,#180279),
(#180280,#180281,#180282),(#180283,#180284,#180285)),.UNSPECIFIED.,.F.,
 .F.,.F.)
B_SPLINE_SURFACE_WITH_KNOTS((4,2,2,2,4),(3,3),(3.1415926535898,3.53429173528852,
3.92699081698724,4.31968989868597,4.71238898038469),(0.,1.),
 .UNSPECIFIED.)
GEOMETRIC_REPRESENTATION_ITEM()
RATIONAL_B_SPLINE_SURFACE(((1.,0.737277336810125,1.),(1.,0.737280525008216,
1.),(1.,0.736509240244793,1.),(1.,0.733539335051535,1.),(1.,0.731338116837053,
1.),(1.,0.725801833007317,1.),(1.,0.722468048845379,1.),(1.,0.715136249134436,
1.),(1.,0.711141648505436,1.),(1.,0.707106781186548,1.)))
REPRESENTATION_ITEM('')
SURFACE()
);
#2803=(
BOUNDED_SURFACE()
B_SPLINE_SURFACE(3,2,((#180499,#180500,#180501),(#180502,#180503,#180504),
(#180505,#180506,#180507),(#180508,#180509,#180510),(#180511,#180512,#180513),
(#180514,#180515,#180516),(#180517,#180518,#180519),(#180520,#180521,#180522),
(#180523,#180524,#180525),(#180526,#180527,#180528)),.UNSPECIFIED.,.F.,
 .F.,.F.)
B_SPLINE_SURFACE_WITH_KNOTS((4,2,2,2,4),(3,3),(0.,0.392699081698724,0.785398163397448,
1.17809724509617,1.5707963267949),(0.,1.),.UNSPECIFIED.)
GEOMETRIC_REPRESENTATION_ITEM()
RATIONAL_B_SPLINE_SURFACE(((1.,0.67559020761567,1.),(1.,0.675585785528568,
1.),(1.,0.676431027860386,1.),(1.,0.679650528045925,1.),(1.,0.682027045382314,
1.),(1.,0.687915714942951,1.),(1.,0.69142441630529,1.),(1.,0.69900497148469,
1.),(1.,0.703073130220208,1.),(1.,0.707106781186548,1.)))
REPRESENTATION_ITEM('')
SURFACE()
);
#2804=(
BOUNDED_SURFACE()
B_SPLINE_SURFACE(3,2,((#180669,#180670,#180671),(#180672,#180673,#180674),
(#180675,#180676,#180677),(#180678,#180679,#180680),(#180681,#180682,#180683),
(#180684,#180685,#180686)),.UNSPECIFIED.,.F.,.F.,.F.)
B_SPLINE_SURFACE_WITH_KNOTS((4,2,4),(3,3),(-0.000141606762778327,0.00070803381389838,
0.00155767439057644),(0.,1.00109719399777),.UNSPECIFIED.)
GEOMETRIC_REPRESENTATION_ITEM()
RATIONAL_B_SPLINE_SURFACE(((1.,0.802844010548984,1.0004326367365),(1.,0.797864106908113,
1.00044356457727),(1.,0.787124435107925,1.00046713158414),(1.,0.7608388846863,
1.00052481228045),(1.,0.744970654526623,1.00055963333422),(1.,0.729042216494434,
1.00059458650742)))
REPRESENTATION_ITEM('')
SURFACE()
);
#2805=(
BOUNDED_SURFACE()
B_SPLINE_SURFACE(3,2,((#180705,#180706,#180707),(#180708,#180709,#180710),
(#180711,#180712,#180713),(#180714,#180715,#180716),(#180717,#180718,#180719),
(#180720,#180721,#180722),(#180723,#180724,#180725),(#180726,#180727,#180728),
(#180729,#180730,#180731),(#180732,#180733,#180734)),.UNSPECIFIED.,.F.,
 .F.,.F.)
B_SPLINE_SURFACE_WITH_KNOTS((4,2,2,2,4),(3,3),(4.71238898038469,5.10508806208342,
5.49778714378214,5.89048622548086,6.28318530717959),(0.,1.),
 .UNSPECIFIED.)
GEOMETRIC_REPRESENTATION_ITEM()
RATIONAL_B_SPLINE_SURFACE(((1.,0.707106781186548,1.),(1.,0.711141648505921,
1.),(1.,0.715136249133786,1.),(1.,0.722468048846019,1.),(1.,0.725801833007554,
1.),(1.,0.731338116836806,1.),(1.,0.733539335051135,1.),(1.,0.736509240245178,
1.),(1.,0.737280525007913,1.),(1.,0.73727733681012,1.)))
REPRESENTATION_ITEM('')
SURFACE()
);
#2806=(
BOUNDED_SURFACE()
B_SPLINE_SURFACE(3,2,((#180946,#180947,#180948),(#180949,#180950,#180951),
(#180952,#180953,#180954),(#180955,#180956,#180957),(#180958,#180959,#180960),
(#180961,#180962,#180963),(#180964,#180965,#180966),(#180967,#180968,#180969),
(#180970,#180971,#180972),(#180973,#180974,#180975)),.UNSPECIFIED.,.F.,
 .F.,.F.)
B_SPLINE_SURFACE_WITH_KNOTS((4,2,2,2,4),(3,3),(4.71238898038469,5.10508806208341,
5.49778714378214,5.89048622548086,6.28318530717959),(0.,1.),
 .UNSPECIFIED.)
GEOMETRIC_REPRESENTATION_ITEM()
RATIONAL_B_SPLINE_SURFACE(((1.,0.707106781186548,1.),(1.,0.71114164850559,
1.),(1.,0.71513624913423,1.),(1.,0.722468048845566,1.),(1.,0.725801833007554,
1.),(1.,0.731338116836806,1.),(1.,0.733539335051299,1.),(1.,0.736509240245015,
1.),(1.,0.737280525008035,1.),(1.,0.73727733681012,1.)))
REPRESENTATION_ITEM('')
SURFACE()
);
#2807=(
BOUNDED_SURFACE()
B_SPLINE_SURFACE(3,2,((#181048,#181049,#181050),(#181051,#181052,#181053),
(#181054,#181055,#181056),(#181057,#181058,#181059),(#181060,#181061,#181062),
(#181063,#181064,#181065),(#181066,#181067,#181068),(#181069,#181070,#181071),
(#181072,#181073,#181074),(#181075,#181076,#181077)),.UNSPECIFIED.,.F.,
 .F.,.F.)
B_SPLINE_SURFACE_WITH_KNOTS((4,2,2,2,4),(3,3),(1.18015353016497E-15,0.392699081698726,
0.785398163397449,1.17809724509617,1.5707963267949),(0.,1.),
 .UNSPECIFIED.)
GEOMETRIC_REPRESENTATION_ITEM()
RATIONAL_B_SPLINE_SURFACE(((1.,0.67559020761567,1.),(1.,0.675585785528194,
1.),(1.,0.676431027860885,1.),(1.,0.679650528045421,1.),(1.,0.682027045382314,
1.),(1.,0.687915714942951,1.),(1.,0.691424416305301,1.),(1.,0.699004971484679,
1.),(1.,0.703073130220216,1.),(1.,0.707106781186548,1.)))
REPRESENTATION_ITEM('')
SURFACE()
);
#2808=(
BOUNDED_SURFACE()
B_SPLINE_SURFACE(3,2,((#181164,#181165,#181166),(#181167,#181168,#181169),
(#181170,#181171,#181172),(#181173,#181174,#181175)),.UNSPECIFIED.,.F.,
 .F.,.F.)
B_SPLINE_SURFACE_WITH_KNOTS((4,4),(3,3),(-3.67368196280255E-5,0.000690197182632251),
(-3.67368196280259E-5,1.),.UNSPECIFIED.)
GEOMETRIC_REPRESENTATION_ITEM()
RATIONAL_B_SPLINE_SURFACE(((1.00003296216371,0.551374288254589,1.),(1.0000330156919,
0.550645752157623,1.),(1.00003255073788,0.5569739268851,1.),(1.00003165550557,
0.569158328193655,1.)))
REPRESENTATION_ITEM('')
SURFACE()
);
#2809=(
BOUNDED_SURFACE()
B_SPLINE_SURFACE(3,2,((#181187,#181188,#181189),(#181190,#181191,#181192),
(#181193,#181194,#181195),(#181196,#181197,#181198)),.UNSPECIFIED.,.F.,
 .F.,.F.)
B_SPLINE_SURFACE_WITH_KNOTS((4,4),(3,3),(-6.51913040321377E-5,0.000717104344353579),
(-0.000141700954976534,1.),.UNSPECIFIED.)
GEOMETRIC_REPRESENTATION_ITEM()
RATIONAL_B_SPLINE_SURFACE(((1.00005816020197,0.794778369766663,1.),(1.00005608252674,
0.802109566767656,1.),(1.00005509894849,0.805580179391821,1.),(1.00005528841351,
0.804911641151865,1.)))
REPRESENTATION_ITEM('')
SURFACE()
);
#2810=(
BOUNDED_SURFACE()
B_SPLINE_SURFACE(3,2,((#181286,#181287,#181288),(#181289,#181290,#181291),
(#181292,#181293,#181294),(#181295,#181296,#181297)),.UNSPECIFIED.,.F.,
 .F.,.F.)
B_SPLINE_SURFACE_WITH_KNOTS((4,4),(3,3),(-6.5137241604418E-5,0.000716509657648598),
(-0.000128883529287276,1.),.UNSPECIFIED.)
GEOMETRIC_REPRESENTATION_ITEM()
RATIONAL_B_SPLINE_SURFACE(((1.00010029146477,0.610922104164585,1.),(1.00010049120256,
0.610147227047914,1.),(1.00009948511932,0.614050298485325,1.),(1.00009738307965,
0.622205101827837,1.)))
REPRESENTATION_ITEM('')
SURFACE()
);
#2811=(
BOUNDED_SURFACE()
B_SPLINE_SURFACE(3,2,((#181345,#181346,#181347),(#181348,#181349,#181350),
(#181351,#181352,#181353),(#181354,#181355,#181356)),.UNSPECIFIED.,.F.,
 .F.,.F.)
B_SPLINE_SURFACE_WITH_KNOTS((4,4),(3,3),(-6.50587846610001E-5,0.000715646631271033),
(-0.000198020186981615,1.),.UNSPECIFIED.)
GEOMETRIC_REPRESENTATION_ITEM()
RATIONAL_B_SPLINE_SURFACE(((1.00009701693625,0.755032712249884,1.),(1.00009537889841,
0.759168749755136,1.),(1.00009461137112,0.761106752395794,1.),(1.00009475863492,
0.760734912009421,1.)))
REPRESENTATION_ITEM('')
SURFACE()
);
#2812=(
BOUNDED_SURFACE()
B_SPLINE_SURFACE(3,2,((#181360,#181361,#181362),(#181363,#181364,#181365),
(#181366,#181367,#181368),(#181369,#181370,#181371),(#181372,#181373,#181374),
(#181375,#181376,#181377),(#181378,#181379,#181380),(#181381,#181382,#181383),
(#181384,#181385,#181386),(#181387,#181388,#181389),(#181390,#181391,#181392),
(#181393,#181394,#181395),(#181396,#181397,#181398),(#181399,#181400,#181401)),
 .UNSPECIFIED.,.F.,.F.,.F.)
B_SPLINE_SURFACE_WITH_KNOTS((4,2,2,2,2,2,4),(3,3),(0.00807909221698663,
0.00882982802565525,0.00920519592998956,0.00958056383432386,0.00995593173865817,
0.0103312996429925,0.0110820354516611),(0.,1.),.UNSPECIFIED.)
GEOMETRIC_REPRESENTATION_ITEM()
RATIONAL_B_SPLINE_SURFACE(((1.,0.707106781186556,1.),(1.,0.708510771074171,
1.),(1.,0.709878889431803,1.),(1.,0.711876867675041,1.),(1.,0.712529775389558,
1.),(1.,0.713774284861137,1.),(1.,0.714371256763372,1.),(1.,0.715514222535529,
1.),(1.,0.716062813357328,1.),(1.,0.717072969030255,1.),(1.,0.717538977439758,
1.),(1.,0.718820706504871,1.),(1.,0.719523481892828,1.),(1.,0.720009098745653,
1.)))
REPRESENTATION_ITEM('')
SURFACE()
);
#2813=(
BOUNDED_SURFACE()
B_SPLINE_SURFACE(3,2,((#181447,#181448,#181449),(#181450,#181451,#181452),
(#181453,#181454,#181455),(#181456,#181457,#181458)),.UNSPECIFIED.,.F.,
 .F.,.F.)
B_SPLINE_SURFACE_WITH_KNOTS((4,4),(3,3),(0.0318721040045715,0.0324798405467945),
(0.,0.915779521794752),.UNSPECIFIED.)
GEOMETRIC_REPRESENTATION_ITEM()
RATIONAL_B_SPLINE_SURFACE(((1.,0.819053335514945,0.969521170774848),(1.,
0.81649287568617,0.969089884472439),(1.,0.813824444819125,0.968640411425078),
(1.,0.811045676639188,0.968172353055207)))
REPRESENTATION_ITEM('')
SURFACE()
);
#2814=(
BOUNDED_SURFACE()
B_SPLINE_SURFACE(3,2,((#181591,#181592,#181593),(#181594,#181595,#181596),
(#181597,#181598,#181599),(#181600,#181601,#181602),(#181603,#181604,#181605),
(#181606,#181607,#181608),(#181609,#181610,#181611),(#181612,#181613,#181614),
(#181615,#181616,#181617),(#181618,#181619,#181620),(#181621,#181622,#181623),
(#181624,#181625,#181626),(#181627,#181628,#181629),(#181630,#181631,#181632)),
 .UNSPECIFIED.,.F.,.F.,.F.)
B_SPLINE_SURFACE_WITH_KNOTS((4,2,2,2,2,2,4),(3,3),(0.00807931853788568,
0.00881187542632408,0.00917815387054328,0.00954443231476248,0.00991071075898168,
0.0102769892032009,0.0110095460916393),(0.,1.),.UNSPECIFIED.)
GEOMETRIC_REPRESENTATION_ITEM()
RATIONAL_B_SPLINE_SURFACE(((1.,0.707106781186552,1.),(1.,0.705694108475444,
1.),(1.,0.704309639709031,1.),(1.,0.702276829363826,1.),(1.,0.701608277715413,
1.),(1.,0.700330266875156,1.),(1.,0.699715065357364,1.),(1.,0.698533028725346,
1.),(1.,0.697962156582885,1.),(1.,0.696902668323859,1.),(1.,0.696411414935025,
1.),(1.,0.695052392645847,1.),(1.,0.69429223033984,1.),(1.,0.69374733452232,
1.)))
REPRESENTATION_ITEM('')
SURFACE()
);
#2815=(
BOUNDED_SURFACE()
B_SPLINE_SURFACE(3,2,((#181733,#181734,#181735),(#181736,#181737,#181738),
(#181739,#181740,#181741),(#181742,#181743,#181744)),.UNSPECIFIED.,.F.,
 .F.,.F.)
B_SPLINE_SURFACE_WITH_KNOTS((4,4),(3,3),(0.,0.000650359837711272),(0.,1.),
 .UNSPECIFIED.)
GEOMETRIC_REPRESENTATION_ITEM()
RATIONAL_B_SPLINE_SURFACE(((1.,0.665108204576639,1.),(1.,0.66511166059484,
1.),(1.,0.666441892349684,1.),(1.,0.669061697655964,1.)))
REPRESENTATION_ITEM('')
SURFACE()
);
#2816=(
BOUNDED_SURFACE()
B_SPLINE_SURFACE(3,2,((#181783,#181784,#181785),(#181786,#181787,#181788),
(#181789,#181790,#181791),(#181792,#181793,#181794)),.UNSPECIFIED.,.F.,
 .F.,.F.)
B_SPLINE_SURFACE_WITH_KNOTS((4,4),(3,3),(0.,0.000650121463573334),(0.,1.),
 .UNSPECIFIED.)
GEOMETRIC_REPRESENTATION_ITEM()
RATIONAL_B_SPLINE_SURFACE(((1.,0.713284154090124,1.),(1.,0.713692564168438,
1.),(1.,0.713902215282654,1.),(1.,0.713903527556066,1.)))
REPRESENTATION_ITEM('')
SURFACE()
);
#2817=(
BOUNDED_SURFACE()
B_SPLINE_SURFACE(3,2,((#181798,#181799,#181800),(#181801,#181802,#181803),
(#181804,#181805,#181806),(#181807,#181808,#181809),(#181810,#181811,#181812),
(#181813,#181814,#181815),(#181816,#181817,#181818),(#181819,#181820,#181821),
(#181822,#181823,#181824),(#181825,#181826,#181827)),.UNSPECIFIED.,.F.,
 .F.,.F.)
B_SPLINE_SURFACE_WITH_KNOTS((4,2,2,2,4),(3,3),(0.00807567041695258,0.00870229794915108,
0.00932892548134959,0.00995555301354809,0.0105821805457466),(0.,1.),
 .UNSPECIFIED.)
GEOMETRIC_REPRESENTATION_ITEM()
RATIONAL_B_SPLINE_SURFACE(((1.,0.707106781186548,1.),(1.,0.707144476742774,
1.),(1.,0.707181156772813,1.),(1.,0.707252569458078,1.),(1.,0.707287275051322,
1.),(1.,0.707350941456054,1.),(1.,0.707380803865577,1.),(1.,0.707433415861318,
1.),(1.,0.707456236659423,1.),(1.,0.707475611987371,1.)))
REPRESENTATION_ITEM('')
SURFACE()
);
#2818=(
BOUNDED_SURFACE()
B_SPLINE_SURFACE(3,2,((#181942,#181943,#181944),(#181945,#181946,#181947),
(#181948,#181949,#181950),(#181951,#181952,#181953)),.UNSPECIFIED.,.F.,
 .F.,.F.)
B_SPLINE_SURFACE_WITH_KNOTS((4,4),(3,3),(0.0237206528291238,0.0242322821884044),
(0.,0.921037832550836),.UNSPECIFIED.)
GEOMETRIC_REPRESENTATION_ITEM()
RATIONAL_B_SPLINE_SURFACE(((1.,0.866462949751686,0.97891125015525),(1.,
0.866562397986968,0.978926955451664),(1.,0.866592995680722,0.9789317875721),
(1.,0.866554773618892,0.978925751378407)))
REPRESENTATION_ITEM('')
SURFACE()
);
#2819=(
BOUNDED_SURFACE()
B_SPLINE_SURFACE(3,2,((#182017,#182018,#182019),(#182020,#182021,#182022),
(#182023,#182024,#182025),(#182026,#182027,#182028),(#182029,#182030,#182031),
(#182032,#182033,#182034),(#182035,#182036,#182037),(#182038,#182039,#182040),
(#182041,#182042,#182043),(#182044,#182045,#182046)),.UNSPECIFIED.,.F.,
 .F.,.F.)
B_SPLINE_SURFACE_WITH_KNOTS((4,2,2,2,4),(3,3),(0.00807569195610403,0.00870260410927289,
0.00932951626244174,0.0099564284156106,0.0105833405687795),(0.,1.),
 .UNSPECIFIED.)
GEOMETRIC_REPRESENTATION_ITEM()
RATIONAL_B_SPLINE_SURFACE(((1.,0.707106781186548,1.),(1.,0.707206112905989,
1.),(1.,0.707302756119535,1.),(1.,0.707490889447615,1.),(1.,0.707582303244654,
1.),(1.,0.707749976398179,1.),(1.,0.707828611057685,1.),(1.,0.70796711497316,
1.),(1.,0.708027180199908,1.),(1.,0.708078164615097,1.)))
REPRESENTATION_ITEM('')
SURFACE()
);
#2820=(
BOUNDED_SURFACE()
B_SPLINE_SURFACE(3,2,((#182150,#182151,#182152),(#182153,#182154,#182155),
(#182156,#182157,#182158),(#182159,#182160,#182161)),.UNSPECIFIED.,.F.,
 .F.,.F.)
B_SPLINE_SURFACE_WITH_KNOTS((4,4),(3,3),(0.,0.000650124307745721),(0.,1.),
 .UNSPECIFIED.)
GEOMETRIC_REPRESENTATION_ITEM()
RATIONAL_B_SPLINE_SURFACE(((1.,0.715240287646145,1.),(1.,0.715239393380683,
1.),(1.,0.714992351911572,1.),(1.,0.71449972514277,1.)))
REPRESENTATION_ITEM('')
SURFACE()
);
#2821=(
BOUNDED_SURFACE()
B_SPLINE_SURFACE(3,2,((#182209,#182210,#182211),(#182212,#182213,#182214),
(#182215,#182216,#182217),(#182218,#182219,#182220)),.UNSPECIFIED.,.F.,
 .F.,.F.)
B_SPLINE_SURFACE_WITH_KNOTS((4,4),(3,3),(0.,0.0006503810773206),(0.,1.),
 .UNSPECIFIED.)
GEOMETRIC_REPRESENTATION_ITEM()
RATIONAL_B_SPLINE_SURFACE(((1.,0.667763418073535,1.),(1.,0.665075430476096,
1.),(1.,0.663677894706716,1.),(1.,0.663670476501713,1.)))
REPRESENTATION_ITEM('')
SURFACE()
);
#2822=(
BOUNDED_SURFACE()
B_SPLINE_SURFACE(3,2,((#182224,#182225,#182226),(#182227,#182228,#182229),
(#182230,#182231,#182232),(#182233,#182234,#182235),(#182236,#182237,#182238),
(#182239,#182240,#182241),(#182242,#182243,#182244),(#182245,#182246,#182247),
(#182248,#182249,#182250),(#182251,#182252,#182253),(#182254,#182255,#182256),
(#182257,#182258,#182259),(#182260,#182261,#182262),(#182263,#182264,#182265)),
 .UNSPECIFIED.,.F.,.F.,.F.)
B_SPLINE_SURFACE_WITH_KNOTS((4,2,2,2,2,2,4),(3,3),(0.00807922902311453,
0.00881773053780572,0.00918698129515131,0.0095562320524969,0.0099254828098425,
0.0102947335671881,0.0110332350818793),(0.,1.),.UNSPECIFIED.)
GEOMETRIC_REPRESENTATION_ITEM()
RATIONAL_B_SPLINE_SURFACE(((1.,0.707106781186548,1.),(1.,0.705699386801107,
1.),(1.,0.704319784944778,1.),(1.,0.702293838625036,1.),(1.,0.701628229397446,
1.),(1.,0.700355977320158,1.),(1.,0.699743668156969,1.),(1.,0.698567591087498,
1.),(1.,0.698000119405105,1.),(1.,0.696949115865192,1.),(1.,0.696462203809247,
1.),(1.,0.695116916536575,1.),(1.,0.694367821279467,1.),(1.,0.693837065201558,
1.)))
REPRESENTATION_ITEM('')
SURFACE()
);
#2823=(
BOUNDED_SURFACE()
B_SPLINE_SURFACE(3,2,((#182373,#182374,#182375),(#182376,#182377,#182378),
(#182379,#182380,#182381),(#182382,#182383,#182384)),.UNSPECIFIED.,.F.,
 .F.,.F.)
B_SPLINE_SURFACE_WITH_KNOTS((4,4),(3,3),(0.0154746506919765,0.0160816000283851),
(0.,0.915442911086902),.UNSPECIFIED.)
GEOMETRIC_REPRESENTATION_ITEM()
RATIONAL_B_SPLINE_SURFACE(((1.,0.807945871955147,0.967520924037568),(1.,
0.810803635237244,0.968004212325442),(1.,0.813550381031034,0.968468725982056),
(1.,0.816188583297829,0.968914883389344)))
REPRESENTATION_ITEM('')
SURFACE()
);
#2824=(
BOUNDED_SURFACE()
B_SPLINE_SURFACE(3,2,((#182419,#182420,#182421),(#182422,#182423,#182424),
(#182425,#182426,#182427),(#182428,#182429,#182430),(#182431,#182432,#182433),
(#182434,#182435,#182436),(#182437,#182438,#182439),(#182440,#182441,#182442),
(#182443,#182444,#182445),(#182446,#182447,#182448),(#182449,#182450,#182451),
(#182452,#182453,#182454),(#182455,#182456,#182457),(#182458,#182459,#182460)),
 .UNSPECIFIED.,.F.,.F.,.F.)
B_SPLINE_SURFACE_WITH_KNOTS((4,2,2,2,2,2,4),(3,3),(0.00807895877935271,
0.00883634587130868,0.00921503941728666,0.00959373296326465,0.00997242650924264,
0.0103511200552206,0.0111085071471766),(0.,1.),.UNSPECIFIED.)
GEOMETRIC_REPRESENTATION_ITEM()
RATIONAL_B_SPLINE_SURFACE(((1.,0.707106781186548,1.),(1.,0.708496200821205,
1.),(1.,0.70985049824013,1.),(1.,0.711828637936002,1.),(1.,0.712474210732742,
1.),(1.,0.71370482119381,1.),(1.,0.714294998379545,1.),(1.,0.715424510819791,
1.),(1.,0.715965704866287,1.),(1.,0.716960611510995,1.),(1.,0.71741913219781,
1.),(1.,0.71867831515119,1.),(1.,0.719364099598229,1.),(1.,0.719832136235989,
1.)))
REPRESENTATION_ITEM('')
SURFACE()
);
#2825=(
BOUNDED_SURFACE()
B_SPLINE_SURFACE(3,2,((#182582,#182583,#182584),(#182585,#182586,#182587),
(#182588,#182589,#182590),(#182591,#182592,#182593)),.UNSPECIFIED.,.F.,
 .F.,.F.)
B_SPLINE_SURFACE_WITH_KNOTS((4,4),(3,3),(0.,0.00065060314950297),(0.,1.),
 .UNSPECIFIED.)
GEOMETRIC_REPRESENTATION_ITEM()
RATIONAL_B_SPLINE_SURFACE(((1.,0.762081632339421,1.),(1.,0.762075781187422,
1.),(1.,0.760455646763466,1.),(1.,0.757216058458816,1.)))
REPRESENTATION_ITEM('')
SURFACE()
);
#2826=(
BOUNDED_SURFACE()
B_SPLINE_SURFACE(3,2,((#182605,#182606,#182607),(#182608,#182609,#182610),
(#182611,#182612,#182613),(#182614,#182615,#182616)),.UNSPECIFIED.,.F.,
 .F.,.F.)
B_SPLINE_SURFACE_WITH_KNOTS((4,4),(3,3),(-6.51439314691719E-5,0.0007165832461609),
(-0.00012692018125823,1.),.UNSPECIFIED.)
GEOMETRIC_REPRESENTATION_ITEM()
RATIONAL_B_SPLINE_SURFACE(((1.00009625164489,0.620818202688323,1.),(1.00009833294279,
0.612618963298313,1.),(1.00009936087757,0.608569430840879,1.),(1.00009916096194,
0.609356995261984,1.)))
REPRESENTATION_ITEM('')
SURFACE()
);
#2827=(
BOUNDED_SURFACE()
B_SPLINE_SURFACE(3,2,((#182759,#182760,#182761),(#182762,#182763,#182764),
(#182765,#182766,#182767),(#182768,#182769,#182770)),.UNSPECIFIED.,.F.,
 .F.,.F.)
B_SPLINE_SURFACE_WITH_KNOTS((4,4),(3,3),(-6.51926395977004E-5,0.000717119035574768),
(-0.000138815926047248,1.),.UNSPECIFIED.)
GEOMETRIC_REPRESENTATION_ITEM()
RATIONAL_B_SPLINE_SURFACE(((1.00005383408411,0.806095432842632,1.),(1.00005364581143,
0.806773570717775,1.),(1.00005460199526,0.803329499666753,1.),(1.00005668422386,
0.795829536739356,1.)))
REPRESENTATION_ITEM('')
SURFACE()
);
#2828=(
BOUNDED_SURFACE()
B_SPLINE_SURFACE(3,2,((#182776,#182777,#182778),(#182779,#182780,#182781),
(#182782,#182783,#182784),(#182785,#182786,#182787)),.UNSPECIFIED.,.F.,
 .F.,.F.)
B_SPLINE_SURFACE_WITH_KNOTS((4,4),(3,3),(0.00485453262895891,0.0055923285159134),
(0.,1.00004278948359),.UNSPECIFIED.)
GEOMETRIC_REPRESENTATION_ITEM()
RATIONAL_B_SPLINE_SURFACE(((1.,0.567949101515402,1.00003697446966),(1.,
0.55537551727941,1.00003805050401),(1.,0.548757935635794,1.00003861682981),
(1.,0.549661265383694,1.00003853952379)))
REPRESENTATION_ITEM('')
SURFACE()
);
#2829=(
BOUNDED_SURFACE()
B_SPLINE_SURFACE(3,2,((#183025,#183026,#183027),(#183028,#183029,#183030),
(#183031,#183032,#183033),(#183034,#183035,#183036),(#183037,#183038,#183039),
(#183040,#183041,#183042),(#183043,#183044,#183045),(#183046,#183047,#183048),
(#183049,#183050,#183051),(#183052,#183053,#183054)),.UNSPECIFIED.,.F.,
 .F.,.F.)
B_SPLINE_SURFACE_WITH_KNOTS((4,2,2,2,4),(3,3),(0.00807856278467327,0.00871080510931882,
0.00934304743396438,0.00997528975860994,0.0106075320832555),(0.,1.),
 .UNSPECIFIED.)
GEOMETRIC_REPRESENTATION_ITEM()
RATIONAL_B_SPLINE_SURFACE(((1.,0.707106781186548,1.),(1.,0.706030220592194,
1.),(1.,0.704978540375902,1.),(1.,0.702923837367757,1.),(1.,0.701922380471311,
1.),(1.,0.700080728636545,1.),(1.,0.699214393311896,1.),(1.,0.697689255248067,
1.),(1.,0.697026914527849,1.),(1.,0.696465765714756,1.)))
REPRESENTATION_ITEM('')
SURFACE()
);
#2830=(
BOUNDED_SURFACE()
B_SPLINE_SURFACE(3,2,((#183211,#183212,#183213),(#183214,#183215,#183216),
(#183217,#183218,#183219),(#183220,#183221,#183222)),.UNSPECIFIED.,.F.,
 .F.,.F.)
B_SPLINE_SURFACE_WITH_KNOTS((4,4),(3,3),(0.0283524505452003,0.0289409470909155),
(0.0793668899028847,1.),.UNSPECIFIED.)
GEOMETRIC_REPRESENTATION_ITEM()
RATIONAL_B_SPLINE_SURFACE(((0.978461885750617,0.864312975626627,1.),(0.978267423016933,
0.863087888352061,1.),(0.978058310717098,0.861770510916135,1.),(0.977834425305255,
0.860360064997711,1.)))
REPRESENTATION_ITEM('')
SURFACE()
);
#2831=(
BOUNDED_SURFACE()
B_SPLINE_SURFACE(3,2,((#183319,#183320,#183321),(#183322,#183323,#183324),
(#183325,#183326,#183327),(#183328,#183329,#183330),(#183331,#183332,#183333),
(#183334,#183335,#183336),(#183337,#183338,#183339),(#183340,#183341,#183342),
(#183343,#183344,#183345),(#183346,#183347,#183348),(#183349,#183350,#183351),
(#183352,#183353,#183354)),.UNSPECIFIED.,.F.,.F.,.F.)
B_SPLINE_SURFACE_WITH_KNOTS((4,2,2,2,2,4),(3,3),(0.00807907499033046,0.00872002967587247,
0.00904050701864348,0.00936098436141448,0.0100019390469565,0.0106428937324985),
(0.,1.),.UNSPECIFIED.)
GEOMETRIC_REPRESENTATION_ITEM()
RATIONAL_B_SPLINE_SURFACE(((1.,0.707106781186548,1.),(1.,0.708291653108703,
1.),(1.,0.709443749235048,1.),(1.,0.71112469687116,1.),(1.,0.711680940824733,
1.),(1.,0.712751570007901,1.),(1.,0.713267249229028,1.),(1.,0.714757432797168,
1.),(1.,0.715686917775259,1.),(1.,0.717310091250008,1.),(1.,0.718010566750711,
1.),(1.,0.718598488256614,1.)))
REPRESENTATION_ITEM('')
SURFACE()
);
#2832=(
BOUNDED_SURFACE()
B_SPLINE_SURFACE(3,2,((#183462,#183463,#183464),(#183465,#183466,#183467),
(#183468,#183469,#183470),(#183471,#183472,#183473)),.UNSPECIFIED.,.F.,
 .F.,.F.)
B_SPLINE_SURFACE_WITH_KNOTS((4,4),(3,3),(0.,0.000650274811908555),(0.,1.),
 .UNSPECIFIED.)
GEOMETRIC_REPRESENTATION_ITEM()
RATIONAL_B_SPLINE_SURFACE(((1.,0.73939111071482,1.),(1.,0.73938749716724,
1.),(1.,0.738423154307972,1.),(1.,0.736495153922513,1.)))
REPRESENTATION_ITEM('')
SURFACE()
);
#2833=(
BOUNDED_SURFACE()
B_SPLINE_SURFACE(3,2,((#183547,#183548,#183549),(#183550,#183551,#183552),
(#183553,#183554,#183555),(#183556,#183557,#183558)),.UNSPECIFIED.,.F.,
 .F.,.F.)
B_SPLINE_SURFACE_WITH_KNOTS((4,4),(3,3),(-6.5085150333794E-5,0.000715936653671951),
(-0.00015557324309298,1.),.UNSPECIFIED.)
GEOMETRIC_REPRESENTATION_ITEM()
RATIONAL_B_SPLINE_SURFACE(((1.00011117085853,0.642705723933352,1.),(1.00011304395471,
0.636685742162949,1.),(1.00011395382865,0.633761479841946,1.),(1.00011377765073,
0.634327701648564,1.)))
REPRESENTATION_ITEM('')
SURFACE()
);
#2834=(
BOUNDED_SURFACE()
B_SPLINE_SURFACE(3,2,((#183562,#183563,#183564),(#183565,#183566,#183567),
(#183568,#183569,#183570),(#183571,#183572,#183573),(#183574,#183575,#183576),
(#183577,#183578,#183579),(#183580,#183581,#183582),(#183583,#183584,#183585),
(#183586,#183587,#183588),(#183589,#183590,#183591),(#183592,#183593,#183594),
(#183595,#183596,#183597)),.UNSPECIFIED.,.F.,.F.,.F.)
B_SPLINE_SURFACE_WITH_KNOTS((4,2,2,2,2,4),(3,3),(0.00807589507756136,0.00894079878156724,
0.00980570248557312,0.010238154337576,0.010670606189579,0.0115355098935849),
(0.,1.),.UNSPECIFIED.)
GEOMETRIC_REPRESENTATION_ITEM()
RATIONAL_B_SPLINE_SURFACE(((1.,0.707106781186548,1.),(1.,0.706684802682679,
1.),(1.,0.706265611788784,1.),(1.,0.705449765784865,1.),(1.,0.705070572349072,
1.),(1.,0.704559600788765,1.),(1.,0.704402907652403,1.),(1.,0.7041166887103,
1.),(1.,0.703986299022118,1.),(1.,0.703645597188673,1.),(1.,0.703488957328521,
1.),(1.,0.703406029216022,1.)))
REPRESENTATION_ITEM('')
SURFACE()
);
#2835=(
BOUNDED_SURFACE()
B_SPLINE_SURFACE(3,2,((#183769,#183770,#183771),(#183772,#183773,#183774),
(#183775,#183776,#183777),(#183778,#183779,#183780)),.UNSPECIFIED.,.F.,
 .F.,.F.)
B_SPLINE_SURFACE_WITH_KNOTS((4,4),(3,3),(0.0370067204754696,0.0375452288399126),
(0.093403953485077,1.),.UNSPECIFIED.)
GEOMETRIC_REPRESENTATION_ITEM()
RATIONAL_B_SPLINE_SURFACE(((0.953268748425463,0.74984328911729,1.),(0.952543344408727,
0.745960134338133,1.),(0.951798218335464,0.741971405566697,1.),(0.951032530022134,
0.737872605222811,1.)))
REPRESENTATION_ITEM('')
SURFACE()
);
#2836=(
BOUNDED_SURFACE()
B_SPLINE_SURFACE(3,2,((#183865,#183866,#183867),(#183868,#183869,#183870),
(#183871,#183872,#183873),(#183874,#183875,#183876),(#183877,#183878,#183879),
(#183880,#183881,#183882),(#183883,#183884,#183885),(#183886,#183887,#183888),
(#183889,#183890,#183891),(#183892,#183893,#183894),(#183895,#183896,#183897),
(#183898,#183899,#183900),(#183901,#183902,#183903),(#183904,#183905,#183906)),
 .UNSPECIFIED.,.F.,.F.,.F.)
B_SPLINE_SURFACE_WITH_KNOTS((4,2,2,2,2,2,4),(3,3),(0.00807568025026493,
0.00898700204274496,0.00944266293898498,0.009898323835225,0.010353984731465,
0.010809645627705,0.0117209674201851),(0.,1.),.UNSPECIFIED.)
GEOMETRIC_REPRESENTATION_ITEM()
RATIONAL_B_SPLINE_SURFACE(((1.,0.707106781186546,1.),(1.,0.707214557916128,
1.),(1.,0.707322930753557,1.),(1.,0.707478596210236,1.),(1.,0.707528365558662,
1.),(1.,0.70762361150633,1.),(1.,0.70766951928712,1.),(1.,0.70775397022188,
1.),(1.,0.707792549798564,1.),(1.,0.707862266510969,1.),(1.,0.707893578069266,
1.),(1.,0.707972242595767,1.),(1.,0.70800597758526,1.),(1.,0.708018339291814,
1.)))
REPRESENTATION_ITEM('')
SURFACE()
);
#2837=(
BOUNDED_SURFACE()
B_SPLINE_SURFACE(3,2,((#184041,#184042,#184043),(#184044,#184045,#184046),
(#184047,#184048,#184049),(#184050,#184051,#184052)),.UNSPECIFIED.,.F.,
 .F.,.F.)
B_SPLINE_SURFACE_WITH_KNOTS((4,4),(3,3),(-6.51209638471711E-5,0.0007163306023189),
(-0.000173014936682415,1.),.UNSPECIFIED.)
GEOMETRIC_REPRESENTATION_ITEM()
RATIONAL_B_SPLINE_SURFACE(((1.00007384993111,0.786579319308486,1.),(1.00007366103227,
0.787125222591237,1.),(1.00007462377578,0.784342967102351,1.),(1.000076734131,
0.778244201129574,1.)))
REPRESENTATION_ITEM('')
SURFACE()
);
#2838=(
BOUNDED_SURFACE()
B_SPLINE_SURFACE(3,2,((#184058,#184059,#184060),(#184061,#184062,#184063),
(#184064,#184065,#184066),(#184067,#184068,#184069)),.UNSPECIFIED.,.F.,
 .F.,.F.)
B_SPLINE_SURFACE_WITH_KNOTS((4,4),(3,3),(-6.52563961816873E-5,0.000717820357998492),
(-7.66067673815307E-5,1.),.UNSPECIFIED.)
GEOMETRIC_REPRESENTATION_ITEM()
RATIONAL_B_SPLINE_SURFACE(((1.00006271537587,0.590666869146107,1.),(1.00006444960589,
0.579347829852736,1.),(1.0000653307431,0.573596789585195,1.),(1.00006515810741,
0.574723554882865,1.)))
REPRESENTATION_ITEM('')
SURFACE()
);
#2839=(
BOUNDED_SURFACE()
B_SPLINE_SURFACE(3,2,((#184193,#184194,#184195),(#184196,#184197,#184198),
(#184199,#184200,#184201),(#184202,#184203,#184204)),.UNSPECIFIED.,.F.,
 .F.,.F.)
B_SPLINE_SURFACE_WITH_KNOTS((4,4),(3,3),(0.,0.000921798889909707),(0.,1.),
 .UNSPECIFIED.)
GEOMETRIC_REPRESENTATION_ITEM()
RATIONAL_B_SPLINE_SURFACE(((1.,0.831289505264087,1.),(1.,0.831333394817592,
1.),(1.,0.824011622363235,1.),(1.,0.810617639934149,1.)))
REPRESENTATION_ITEM('')
SURFACE()
);
#2840=(
BOUNDED_SURFACE()
B_SPLINE_SURFACE(3,2,((#184372,#184373,#184374),(#184375,#184376,#184377),
(#184378,#184379,#184380),(#184381,#184382,#184383)),.UNSPECIFIED.,.F.,
 .F.,.F.)
B_SPLINE_SURFACE_WITH_KNOTS((4,4),(3,3),(-3.51472716647773E-5,0.000688646726988702),
(-3.51472716647773E-5,1.),.UNSPECIFIED.)
GEOMETRIC_REPRESENTATION_ITEM()
RATIONAL_B_SPLINE_SURFACE(((1.00003159713423,0.550503741378662,1.),(1.00003164632144,
0.54980401125791,1.),(1.00003120056771,0.556145239310851,1.),(1.00003034444782,
0.568324276979128,1.)))
REPRESENTATION_ITEM('')
SURFACE()
);
#2841=(
BOUNDED_SURFACE()
B_SPLINE_SURFACE(3,2,((#184396,#184397,#184398),(#184399,#184400,#184401),
(#184402,#184403,#184404),(#184405,#184406,#184407)),.UNSPECIFIED.,.F.,
 .F.,.F.)
B_SPLINE_SURFACE_WITH_KNOTS((4,4),(3,3),(-6.51938878740144E-5,0.000717132766614092),
(-0.000140422077604399,1.),.UNSPECIFIED.)
GEOMETRIC_REPRESENTATION_ITEM()
RATIONAL_B_SPLINE_SURFACE(((1.00005748506357,0.795313299193262,1.),(1.00005541449137,
0.802685972468769,1.),(1.00005443402968,0.806177096184806,1.),(1.00005462291181,
0.805504544806424,1.)))
REPRESENTATION_ITEM('')
SURFACE()
);
#2842=(
BOUNDED_SURFACE()
B_SPLINE_SURFACE(3,2,((#184496,#184497,#184498),(#184499,#184500,#184501),
(#184502,#184503,#184504),(#184505,#184506,#184507)),.UNSPECIFIED.,.F.,
 .F.,.F.)
B_SPLINE_SURFACE_WITH_KNOTS((4,4),(3,3),(-6.51392861930307E-5,0.000716532148123338),
(-0.000127892595311363,1.),.UNSPECIFIED.)
GEOMETRIC_REPRESENTATION_ITEM()
RATIONAL_B_SPLINE_SURFACE(((1.00009972016694,0.610140967503593,1.),(1.00009992021532,
0.609358872291238,1.),(1.00009891274698,0.613297600455479,1.),(1.0000968090023,
0.621522254435956,1.)))
REPRESENTATION_ITEM('')
SURFACE()
);
#2843=(
BOUNDED_SURFACE()
B_SPLINE_SURFACE(3,2,((#184567,#184568,#184569),(#184570,#184571,#184572),
(#184573,#184574,#184575),(#184576,#184577,#184578)),.UNSPECIFIED.,.F.,
 .F.,.F.)
B_SPLINE_SURFACE_WITH_KNOTS((4,4),(3,3),(-6.5059972238603E-5,0.000715659694624669),
(-0.000197643858000933,1.),.UNSPECIFIED.)
GEOMETRIC_REPRESENTATION_ITEM()
RATIONAL_B_SPLINE_SURFACE(((1.00009661013076,0.755595413549805,1.),(1.00009495673333,
0.759778183122702,1.),(1.0000941819758,0.761738166948696,1.),(1.00009433062994,
0.761362101277921,1.)))
REPRESENTATION_ITEM('')
SURFACE()
);
#2844=(
BOUNDED_SURFACE()
B_SPLINE_SURFACE(3,2,((#184582,#184583,#184584),(#184585,#184586,#184587),
(#184588,#184589,#184590),(#184591,#184592,#184593),(#184594,#184595,#184596),
(#184597,#184598,#184599),(#184600,#184601,#184602),(#184603,#184604,#184605),
(#184606,#184607,#184608),(#184609,#184610,#184611),(#184612,#184613,#184614),
(#184615,#184616,#184617)),.UNSPECIFIED.,.F.,.F.,.F.)
B_SPLINE_SURFACE_WITH_KNOTS((4,2,2,2,2,4),(3,3),(0.00807807165860127,0.00885401549830484,
0.00962995933800841,0.0100179312578602,0.010405903177712,0.0111818470174155),
(0.,1.),.UNSPECIFIED.)
GEOMETRIC_REPRESENTATION_ITEM()
RATIONAL_B_SPLINE_SURFACE(((1.,0.707106781186548,1.),(1.,0.708323960348238,
1.),(1.,0.709510365636766,1.),(1.,0.711820403892163,1.),(1.,0.712901935204825,
1.),(1.,0.714375984986412,1.),(1.,0.714843782196838,1.),(1.,0.715700614088123,
1.),(1.,0.716094239791898,1.),(1.,0.71717000694229,1.),(1.,0.717742537382462,
1.),(1.,0.718120418666571,1.)))
REPRESENTATION_ITEM('')
SURFACE()
);
#2845=(
BOUNDED_SURFACE()
B_SPLINE_SURFACE(3,2,((#184765,#184766,#184767),(#184768,#184769,#184770),
(#184771,#184772,#184773),(#184774,#184775,#184776)),.UNSPECIFIED.,.F.,
 .F.,.F.)
B_SPLINE_SURFACE_WITH_KNOTS((4,4),(3,3),(0.0316780996002149,0.032272159678108),
(0.,0.914522259344732),.UNSPECIFIED.)
GEOMETRIC_REPRESENTATION_ITEM()
RATIONAL_B_SPLINE_SURFACE(((1.,0.807106741558702,0.96702384016161),(1.,
0.804531496903973,0.966583587972169),(1.,0.801850982035351,0.966125339262643),
(1.,0.799062830164071,0.965648689417522)))
REPRESENTATION_ITEM('')
SURFACE()
);
#2846=(
BOUNDED_SURFACE()
B_SPLINE_SURFACE(3,2,((#184867,#184868,#184869),(#184870,#184871,#184872),
(#184873,#184874,#184875),(#184876,#184877,#184878),(#184879,#184880,#184881),
(#184882,#184883,#184884),(#184885,#184886,#184887),(#184888,#184889,#184890),
(#184891,#184892,#184893),(#184894,#184895,#184896),(#184897,#184898,#184899),
(#184900,#184901,#184902),(#184903,#184904,#184905),(#184906,#184907,#184908)),
 .UNSPECIFIED.,.F.,.F.,.F.)
B_SPLINE_SURFACE_WITH_KNOTS((4,2,2,2,2,2,4),(3,3),(0.00807831625971351,
0.00883535021604665,0.00921386719421322,0.00959238417237979,0.00997090115054636,
0.0103494181287129,0.0111064520850461),(0.,1.),.UNSPECIFIED.)
GEOMETRIC_REPRESENTATION_ITEM()
RATIONAL_B_SPLINE_SURFACE(((1.,0.707106781186548,1.),(1.,0.705861961062141,
1.),(1.,0.704642623504988,1.),(1.,0.702853606538468,1.),(1.,0.702268342990035,
1.),(1.,0.701150362247141,1.),(1.,0.700612993986993,1.),(1.,0.699582583564998,
1.),(1.,0.699087807793684,1.),(1.,0.698176683118393,1.),(1.,0.697755963868462,
1.),(1.,0.696598958196255,1.),(1.,0.695966377684547,1.),(1.,0.695533955710884,
1.)))
REPRESENTATION_ITEM('')
SURFACE()
);
#2847=(
BOUNDED_SURFACE()
B_SPLINE_SURFACE(3,2,((#185016,#185017,#185018),(#185019,#185020,#185021),
(#185022,#185023,#185024),(#185025,#185026,#185027)),.UNSPECIFIED.,.F.,
 .F.,.F.)
B_SPLINE_SURFACE_WITH_KNOTS((4,4),(3,3),(0.,0.000650368158908551),(0.,1.),
 .UNSPECIFIED.)
GEOMETRIC_REPRESENTATION_ITEM()
RATIONAL_B_SPLINE_SURFACE(((1.,0.66438972944168,1.),(1.,0.664393217905862,
1.),(1.,0.665747114157887,1.),(1.,0.66841287307604,1.)))
REPRESENTATION_ITEM('')
SURFACE()
);
#2848=(
BOUNDED_SURFACE()
B_SPLINE_SURFACE(3,2,((#185110,#185111,#185112),(#185113,#185114,#185115),
(#185116,#185117,#185118),(#185119,#185120,#185121)),.UNSPECIFIED.,.F.,
 .F.,.F.)
B_SPLINE_SURFACE_WITH_KNOTS((4,4),(3,3),(0.,0.000650122897330092),(0.,1.),
 .UNSPECIFIED.)
GEOMETRIC_REPRESENTATION_ITEM()
RATIONAL_B_SPLINE_SURFACE(((1.,0.713892198341303,1.),(1.,0.714340614318511,
1.),(1.,0.714570777789516,1.),(1.,0.714572220188112,1.)))
REPRESENTATION_ITEM('')
SURFACE()
);
#2849=(
BOUNDED_SURFACE()
B_SPLINE_SURFACE(3,2,((#185125,#185126,#185127),(#185128,#185129,#185130),
(#185131,#185132,#185133),(#185134,#185135,#185136),(#185137,#185138,#185139),
(#185140,#185141,#185142),(#185143,#185144,#185145),(#185146,#185147,#185148),
(#185149,#185150,#185151),(#185152,#185153,#185154),(#185155,#185156,#185157),
(#185158,#185159,#185160)),.UNSPECIFIED.,.F.,.F.,.F.)
B_SPLINE_SURFACE_WITH_KNOTS((4,2,2,2,2,4),(3,3),(0.00807567643991074,0.0087258483708248,
0.00905093433628183,0.00937602030173886,0.0100261922326529,0.010676364163567),
(0.,1.),.UNSPECIFIED.)
GEOMETRIC_REPRESENTATION_ITEM()
RATIONAL_B_SPLINE_SURFACE(((1.,0.707106781186547,1.),(1.,0.707170635637275,
1.),(1.,0.707232744268554,1.),(1.,0.70732338528182,1.),(1.,0.707353375007997,
1.),(1.,0.707410998957093,1.),(1.,0.707438747129451,1.),(1.,0.707518900645085,
1.),(1.,0.707568814651682,1.),(1.,0.707655521042551,1.),(1.,0.707692858707996,
1.),(1.,0.707723858215708,1.)))
REPRESENTATION_ITEM('')
SURFACE()
);
#2850=(
BOUNDED_SURFACE()
B_SPLINE_SURFACE(3,2,((#185275,#185276,#185277),(#185278,#185279,#185280),
(#185281,#185282,#185283),(#185284,#185285,#185286),(#185287,#185288,#185289),
(#185290,#185291,#185292),(#185293,#185294,#185295),(#185296,#185297,#185298),
(#185299,#185300,#185301),(#185302,#185303,#185304)),.UNSPECIFIED.,.F.,
 .F.,.F.)
B_SPLINE_SURFACE_WITH_KNOTS((4,2,2,2,4),(3,3),(0.00807567872552143,0.00870243807057167,
0.0093291974156219,0.00995595676067213,0.0105827161057224),(0.,1.),
 .UNSPECIFIED.)
GEOMETRIC_REPRESENTATION_ITEM()
RATIONAL_B_SPLINE_SURFACE(((1.,0.707106781186547,1.),(1.,0.707175173315664,
1.),(1.,0.707241719347897,1.),(1.,0.707371272007346,1.),(1.,0.70743422794471,
1.),(1.,0.707549712034256,1.),(1.,0.707603875852248,1.),(1.,0.707699291327501,
1.),(1.,0.707740674853624,1.),(1.,0.707775806502368,1.)))
REPRESENTATION_ITEM('')
SURFACE()
);
#2851=(
BOUNDED_SURFACE()
B_SPLINE_SURFACE(3,2,((#185425,#185426,#185427),(#185428,#185429,#185430),
(#185431,#185432,#185433),(#185434,#185435,#185436)),.UNSPECIFIED.,.F.,
 .F.,.F.)
B_SPLINE_SURFACE_WITH_KNOTS((4,4),(3,3),(-2.91650384398601E-17,0.000810744804887501),
(0.,1.),.UNSPECIFIED.)
GEOMETRIC_REPRESENTATION_ITEM()
RATIONAL_B_SPLINE_SURFACE(((1.,0.804104907750019,1.),(1.,0.778265384411316,
1.),(1.,0.743775615594857,1.),(1.,0.707106781186549,1.)))
REPRESENTATION_ITEM('')
SURFACE()
);
#2852=(
BOUNDED_SURFACE()
B_SPLINE_SURFACE(3,2,((#185472,#185473,#185474),(#185475,#185476,#185477),
(#185478,#185479,#185480),(#185481,#185482,#185483),(#185484,#185485,#185486),
(#185487,#185488,#185489),(#185490,#185491,#185492),(#185493,#185494,#185495),
(#185496,#185497,#185498),(#185499,#185500,#185501)),.UNSPECIFIED.,.F.,
 .F.,.F.)
B_SPLINE_SURFACE_WITH_KNOTS((4,2,2,2,4),(3,3),(-0.00010658318899339,0.000906588491342359,
0.00113323561417795,0.00135988273701354,0.00191976017167813),(-0.00126250237001865,
1.),.UNSPECIFIED.)
GEOMETRIC_REPRESENTATION_ITEM()
RATIONAL_B_SPLINE_SURFACE(((1.0007701286604,0.694999122897755,1.),(1.0006124677188,
0.757438982554043,1.),(1.0004932878644,0.804638836285473,1.),(1.00039728502394,
0.842659691824301,1.),(1.00038216130089,0.848649273867104,1.),(1.00035602630873,
0.858999746381121,1.),(1.00034494217433,0.863389494339642,1.),(1.00031477912816,
0.875335232776448,1.),(1.00030645813634,0.878630668891778,1.),(1.00031199678186,
0.876437150031478,1.)))
REPRESENTATION_ITEM('')
SURFACE()
);
#2853=(
BOUNDED_SURFACE()
B_SPLINE_SURFACE(3,2,((#185532,#185533,#185534),(#185535,#185536,#185537),
(#185538,#185539,#185540),(#185541,#185542,#185543),(#185544,#185545,#185546),
(#185547,#185548,#185549),(#185550,#185551,#185552),(#185553,#185554,#185555),
(#185556,#185557,#185558),(#185559,#185560,#185561)),.UNSPECIFIED.,.F.,
 .F.,.F.)
B_SPLINE_SURFACE_WITH_KNOTS((4,2,2,2,4),(3,3),(-1.86157513015761E-16,0.000442340065143073,
0.000884680130286332,0.00132702019542959,0.00176936026057285),(0.,1.),
 .UNSPECIFIED.)
GEOMETRIC_REPRESENTATION_ITEM()
RATIONAL_B_SPLINE_SURFACE(((1.,0.83292929166297,1.),(1.,0.829173169481905,
1.),(1.,0.823008202027213,1.),(1.,0.806154887727085,1.),(1.,0.795326013033949,
1.),(1.,0.768452086196073,1.),(1.,0.752322946736307,1.),(1.,0.713492386952618,
1.),(1.,0.690945244483084,1.),(1.,0.664473794614023,1.)))
REPRESENTATION_ITEM('')
SURFACE()
);
#2854=(
BOUNDED_SURFACE()
B_SPLINE_SURFACE(3,2,((#185616,#185617,#185618),(#185619,#185620,#185621),
(#185622,#185623,#185624),(#185625,#185626,#185627)),.UNSPECIFIED.,.F.,
 .F.,.F.)
B_SPLINE_SURFACE_WITH_KNOTS((4,4),(3,3),(-2.30501381870419E-16,0.000504122926429285),
(0.,1.),.UNSPECIFIED.)
GEOMETRIC_REPRESENTATION_ITEM()
RATIONAL_B_SPLINE_SURFACE(((1.,0.832929291663028,1.),(1.,0.830988393206304,
1.),(1.,0.828976922242354,1.),(1.,0.82689272482991,1.)))
REPRESENTATION_ITEM('')
SURFACE()
);
#2855=(
BOUNDED_SURFACE()
B_SPLINE_SURFACE(3,2,((#185631,#185632,#185633),(#185634,#185635,#185636),
(#185637,#185638,#185639),(#185640,#185641,#185642),(#185643,#185644,#185645),
(#185646,#185647,#185648),(#185649,#185650,#185651),(#185652,#185653,#185654)),
 .UNSPECIFIED.,.F.,.F.,.F.)
B_SPLINE_SURFACE_WITH_KNOTS((4,2,2,4),(3,3),(-0.000157492231769603,0.000393730579424047,
0.000787461158848095,0.00173241454946589),(-0.00194680660466252,1.),
 .UNSPECIFIED.)
GEOMETRIC_REPRESENTATION_ITEM()
RATIONAL_B_SPLINE_SURFACE(((1.00101966603795,0.738118302171479,1.),(1.00090725032211,
0.766990126307879,1.),(1.00082716197042,0.787559285950097,1.),(1.00072872925164,
0.812839845032754,1.),(1.0007006626831,0.820048205758201,1.),(1.00063732175048,
0.836316111484255,1.),(1.00064987188718,0.833092849177034,1.),(1.00069510349992,
0.82147597551466,1.)))
REPRESENTATION_ITEM('')
SURFACE()
);
#2856=(
BOUNDED_SURFACE()
B_SPLINE_SURFACE(3,2,((#185690,#185691,#185692),(#185693,#185694,#185695),
(#185696,#185697,#185698),(#185699,#185700,#185701),(#185702,#185703,#185704),
(#185705,#185706,#185707)),.UNSPECIFIED.,.F.,.F.,.F.)
B_SPLINE_SURFACE_WITH_KNOTS((4,2,4),(3,3),(-0.000159127492400632,0.000795637462001992,
0.00175040241640461),(-0.00149890992630704,1.),.UNSPECIFIED.)
GEOMETRIC_REPRESENTATION_ITEM()
RATIONAL_B_SPLINE_SURFACE(((1.00083523485068,0.721385909846626,1.),(1.00092263143497,
0.692232528860078,1.),(1.00101713444213,0.66070861755133,1.),(1.00114771935088,
0.617148658924304,1.),(1.00118312565315,0.605337975155434,1.),(1.0011655374311,
0.611204979483453,1.)))
REPRESENTATION_ITEM('')
SURFACE()
);
#2857=(
BOUNDED_SURFACE()
B_SPLINE_SURFACE(3,2,((#185736,#185737,#185738),(#185739,#185740,#185741),
(#185742,#185743,#185744),(#185745,#185746,#185747),(#185748,#185749,#185750),
(#185751,#185752,#185753),(#185754,#185755,#185756),(#185757,#185758,#185759),
(#185760,#185761,#185762),(#185763,#185764,#185765)),.UNSPECIFIED.,.F.,
 .F.,.F.)
B_SPLINE_SURFACE_WITH_KNOTS((4,2,2,2,4),(3,3),(-0.000159688588089931,0.000399221470224828,
0.000798442940449655,0.00119766441067448,0.00175657446898924),(0.,1.0022804026225),
 .UNSPECIFIED.)
GEOMETRIC_REPRESENTATION_ITEM()
RATIONAL_B_SPLINE_SURFACE(((1.,0.803619719160217,1.00089565221487),(1.,
0.806811279572102,1.0008810961294),(1.,0.804342659083832,1.00089235502667),
(1.,0.792184442804338,1.00094780628325),(1.,0.784707370490891,1.00098190775387),
(1.,0.766448262692597,1.00106518398849),(1.,0.75551433976755,1.00111505148151),
(1.,0.727335726940382,1.00124356864669),(1.,0.708767918151572,1.00132825280641),
(1.,0.691224111502863,1.00140826669179)))
REPRESENTATION_ITEM('')
SURFACE()
);
#2858=(
BOUNDED_SURFACE()
B_SPLINE_SURFACE(3,2,((#185822,#185823,#185824),(#185825,#185826,#185827),
(#185828,#185829,#185830),(#185831,#185832,#185833),(#185834,#185835,#185836),
(#185837,#185838,#185839),(#185840,#185841,#185842),(#185843,#185844,#185845),
(#185846,#185847,#185848),(#185849,#185850,#185851)),.UNSPECIFIED.,.F.,
 .F.,.F.)
B_SPLINE_SURFACE_WITH_KNOTS((4,2,2,2,4),(3,3),(-4.08272591082004E-15,0.000408890006701704,
0.000817780013407491,0.00122667002011328,0.00163556002681907),(0.,1.),
 .UNSPECIFIED.)
GEOMETRIC_REPRESENTATION_ITEM()
RATIONAL_B_SPLINE_SURFACE(((1.,0.707106781186878,1.),(1.,0.688891921544893,
1.),(1.,0.670532818962991,1.),(1.,0.634368444020432,1.),(1.,0.617287210907485,
1.),(1.,0.586753298958185,1.),(1.,0.573879231151052,1.),(1.,0.555793216592158,
1.),(1.,0.550823008344725,1.),(1.,0.550808342809435,1.)))
REPRESENTATION_ITEM('')
SURFACE()
);
#2859=(
BOUNDED_SURFACE()
B_SPLINE_SURFACE(3,2,((#186037,#186038,#186039),(#186040,#186041,#186042),
(#186043,#186044,#186045),(#186046,#186047,#186048),(#186049,#186050,#186051),
(#186052,#186053,#186054)),.UNSPECIFIED.,.F.,.F.,.F.)
B_SPLINE_SURFACE_WITH_KNOTS((4,2,4),(3,3),(0.0202634924775631,0.0220347355863407,
0.0238059786951184),(0.,1.),.UNSPECIFIED.)
GEOMETRIC_REPRESENTATION_ITEM()
RATIONAL_B_SPLINE_SURFACE(((1.,0.707106781186538,1.),(1.,0.681614664404396,
1.),(1.,0.655059254259685,1.),(1.,0.598852069172831,1.),(1.,0.569209502658738,
1.),(1.,0.537299608347133,1.)))
REPRESENTATION_ITEM('')
SURFACE()
);
#2860=(
BOUNDED_SURFACE()
B_SPLINE_SURFACE(3,2,((#186115,#186116,#186117),(#186118,#186119,#186120),
(#186121,#186122,#186123),(#186124,#186125,#186126),(#186127,#186128,#186129),
(#186130,#186131,#186132),(#186133,#186134,#186135),(#186136,#186137,#186138),
(#186139,#186140,#186141),(#186142,#186143,#186144),(#186145,#186146,#186147),
(#186148,#186149,#186150),(#186151,#186152,#186153),(#186154,#186155,#186156)),
 .UNSPECIFIED.,.F.,.F.,.F.)
B_SPLINE_SURFACE_WITH_KNOTS((4,2,2,2,2,2,4),(3,3),(-9.99593665452691E-5,
0.000249898416362892,0.000374847624544338,0.000499796832725785,0.000624746040907231,
0.000749695249088677,0.00109955303199673),(0.,1.00121399112233),
 .UNSPECIFIED.)
GEOMETRIC_REPRESENTATION_ITEM()
RATIONAL_B_SPLINE_SURFACE(((1.,0.68747168837863,1.00075881319157),(1.,0.683926541024849,
1.0007674207464),(1.,0.682240046418907,1.00077151552536),(1.,0.682757896742324,
1.00077025819397),(1.,0.68316009237754,1.00076928167011),(1.,0.684454083092429,
1.00076613988363),(1.,0.685335934686193,1.00076399876362),(1.,0.687573292179631,
1.00075856649935),(1.,0.688886296979987,1.000755378547),(1.,0.691863134152753,
1.0007481508392),(1.,0.693539259522199,1.00074408123657),(1.,0.700231778213878,
1.00072783192001),(1.,0.706116410220352,1.00071354413798),(1.,0.711375149613269,
1.00070077601211)))
REPRESENTATION_ITEM('')
SURFACE()
);
#2861=(
BOUNDED_SURFACE()
B_SPLINE_SURFACE(3,2,((#186234,#186235,#186236),(#186237,#186238,#186239),
(#186240,#186241,#186242),(#186243,#186244,#186245)),.UNSPECIFIED.,.F.,
 .F.,.F.)
B_SPLINE_SURFACE_WITH_KNOTS((4,4),(3,3),(-6.93889390390723E-18,0.0331958858056162),
(0.,1.),.UNSPECIFIED.)
GEOMETRIC_REPRESENTATION_ITEM()
RATIONAL_B_SPLINE_SURFACE(((1.,0.685275128444715,1.),(1.,0.687584548418076,
1.),(1.,0.689209215689052,1.),(1.,0.690549802660031,1.)))
REPRESENTATION_ITEM('')
SURFACE()
);
#2862=(
BOUNDED_SURFACE()
B_SPLINE_SURFACE(3,2,((#186258,#186259,#186260),(#186261,#186262,#186263),
(#186264,#186265,#186266),(#186267,#186268,#186269)),.UNSPECIFIED.,.F.,
 .F.,.F.)
B_SPLINE_SURFACE_WITH_KNOTS((4,4),(3,3),(0.,0.000650162698700256),(0.,1.),
 .UNSPECIFIED.)
GEOMETRIC_REPRESENTATION_ITEM()
RATIONAL_B_SPLINE_SURFACE(((1.,0.690549802660026,1.),(1.,0.689437188232559,
1.),(1.,0.688863085247593,1.),(1.,0.688859710772113,1.)))
REPRESENTATION_ITEM('')
SURFACE()
);
#2863=(
BOUNDED_SURFACE()
B_SPLINE_SURFACE(3,2,((#186361,#186362,#186363),(#186364,#186365,#186366),
(#186367,#186368,#186369),(#186370,#186371,#186372),(#186373,#186374,#186375),
(#186376,#186377,#186378)),.UNSPECIFIED.,.F.,.F.,.F.)
B_SPLINE_SURFACE_WITH_KNOTS((4,2,4),(3,3),(0.,0.785398163397448,1.5707963267949),
(0.,1.),.UNSPECIFIED.)
GEOMETRIC_REPRESENTATION_ITEM()
RATIONAL_B_SPLINE_SURFACE(((1.,0.675590207615664,1.),(1.,0.675526278181762,
1.),(1.,0.679082711196844,1.),(1.,0.690860049128418,1.),(1.,0.699025295935035,
1.),(1.,0.707106781186543,1.)))
REPRESENTATION_ITEM('')
SURFACE()
);
#2864=(
BOUNDED_SURFACE()
B_SPLINE_SURFACE(3,2,((#186392,#186393,#186394),(#186395,#186396,#186397),
(#186398,#186399,#186400),(#186401,#186402,#186403),(#186404,#186405,#186406),
(#186407,#186408,#186409)),.UNSPECIFIED.,.F.,.F.,.F.)
B_SPLINE_SURFACE_WITH_KNOTS((4,2,4),(3,3),(1.5707963267949,2.35619449019234,
3.1415926535898),(0.,1.),.UNSPECIFIED.)
GEOMETRIC_REPRESENTATION_ITEM()
RATIONAL_B_SPLINE_SURFACE(((1.,0.707106781186543,1.),(1.,0.715202981902222,
1.),(1.,0.723033691557528,1.),(1.,0.73410625828684,1.),(1.,0.737326538316928,
1.),(1.,0.737277336810125,1.)))
REPRESENTATION_ITEM('')
SURFACE()
);
#2865=(
BOUNDED_SURFACE()
B_SPLINE_SURFACE(3,2,((#186427,#186428,#186429),(#186430,#186431,#186432),
(#186433,#186434,#186435),(#186436,#186437,#186438),(#186439,#186440,#186441),
(#186442,#186443,#186444)),.UNSPECIFIED.,.F.,.F.,.F.)
B_SPLINE_SURFACE_WITH_KNOTS((4,2,4),(3,3),(0.,0.785398163397448,1.5707963267949),
(0.,1.),.UNSPECIFIED.)
GEOMETRIC_REPRESENTATION_ITEM()
RATIONAL_B_SPLINE_SURFACE(((1.,0.675590207615664,1.),(1.,0.675526278181461,
1.),(1.,0.679082711197251,1.),(1.,0.690860049128011,1.),(1.,0.699025295935341,
1.),(1.,0.707106781186543,1.)))
REPRESENTATION_ITEM('')
SURFACE()
);
#2866=(
BOUNDED_SURFACE()
B_SPLINE_SURFACE(3,2,((#186458,#186459,#186460),(#186461,#186462,#186463),
(#186464,#186465,#186466),(#186467,#186468,#186469),(#186470,#186471,#186472),
(#186473,#186474,#186475)),.UNSPECIFIED.,.F.,.F.,.F.)
B_SPLINE_SURFACE_WITH_KNOTS((4,2,4),(3,3),(4.71238898038469,5.49778714378214,
6.28318530717959),(0.,1.),.UNSPECIFIED.)
GEOMETRIC_REPRESENTATION_ITEM()
RATIONAL_B_SPLINE_SURFACE(((1.,0.707106781186538,1.),(1.,0.715202981902668,
1.),(1.,0.723033691556936,1.),(1.,0.734106258287417,1.),(1.,0.737326538316498,
1.),(1.,0.737277336810125,1.)))
REPRESENTATION_ITEM('')
SURFACE()
);
#2867=(
BOUNDED_SURFACE()
B_SPLINE_SURFACE(3,2,((#186491,#186492,#186493),(#186494,#186495,#186496),
(#186497,#186498,#186499),(#186500,#186501,#186502)),.UNSPECIFIED.,.F.,
 .F.,.F.)
B_SPLINE_SURFACE_WITH_KNOTS((4,4),(3,3),(2.22847122787663,3.14161440295379),
(0.,1.000021749364),.UNSPECIFIED.)
GEOMETRIC_REPRESENTATION_ITEM()
RATIONAL_B_SPLINE_SURFACE(((1.,0.725692460307628,1.00001193202905),(1.,
0.732974645844472,1.00001161526325),(1.,0.737323110435418,1.00001142611057),
(1.,0.737271619087494,1.00001142835038)))
REPRESENTATION_ITEM('')
SURFACE()
);
#2868=(
BOUNDED_SURFACE()
B_SPLINE_SURFACE(3,2,((#186510,#186511,#186512),(#186513,#186514,#186515),
(#186516,#186517,#186518),(#186519,#186520,#186521),(#186522,#186523,#186524),
(#186525,#186526,#186527)),.UNSPECIFIED.,.F.,.F.,.F.)
B_SPLINE_SURFACE_WITH_KNOTS((4,2,4),(3,3),(9.63948754967748E-5,0.00173129457116097,
0.00336619426682516),(0.,1.),.UNSPECIFIED.)
GEOMETRIC_REPRESENTATION_ITEM()
RATIONAL_B_SPLINE_SURFACE(((1.,0.88872394157032,1.),(1.,0.863203710383462,
1.),(1.,0.835728844788038,1.),(1.,0.775725241916869,1.),(1.,0.743211702946043,
1.),(1.,0.707106781186548,1.)))
REPRESENTATION_ITEM('')
SURFACE()
);
#2869=(
BOUNDED_SURFACE()
B_SPLINE_SURFACE(3,2,((#186551,#186552,#186553),(#186554,#186555,#186556),
(#186557,#186558,#186559),(#186560,#186561,#186562),(#186563,#186564,#186565),
(#186566,#186567,#186568)),.UNSPECIFIED.,.F.,.F.,.F.)
B_SPLINE_SURFACE_WITH_KNOTS((4,2,4),(3,3),(3.1415926535898,3.92699081698724,
4.71238898038469),(0.,1.),.UNSPECIFIED.)
GEOMETRIC_REPRESENTATION_ITEM()
RATIONAL_B_SPLINE_SURFACE(((1.,0.737277336810123,1.),(1.,0.737326538316937,
1.),(1.,0.73410625828684,1.),(1.,0.723033691557529,1.),(1.,0.715202981902217,
1.),(1.,0.707106781186543,1.)))
REPRESENTATION_ITEM('')
SURFACE()
);
#2870=(
BOUNDED_SURFACE()
B_SPLINE_SURFACE(3,2,((#186582,#186583,#186584),(#186585,#186586,#186587),
(#186588,#186589,#186590),(#186591,#186592,#186593),(#186594,#186595,#186596),
(#186597,#186598,#186599)),.UNSPECIFIED.,.F.,.F.,.F.)
B_SPLINE_SURFACE_WITH_KNOTS((4,2,4),(3,3),(4.71234651107924,5.49778714378214,
6.28322777648504),(-4.24693054514115E-5,1.),.UNSPECIFIED.)
GEOMETRIC_REPRESENTATION_ITEM()
RATIONAL_B_SPLINE_SURFACE(((1.00002487888834,0.707095653254892,1.),(1.00002556538397,
0.699013396841122,1.),(1.00002625900611,0.690847238604463,1.),(1.00002725945341,
0.679068763627425,1.),(1.00002756155034,0.675512113380383,1.),(1.00002755608648,
0.675576440559981,1.)))
REPRESENTATION_ITEM('')
SURFACE()
);
#2871=(
BOUNDED_SURFACE()
B_SPLINE_SURFACE(3,2,((#186615,#186616,#186617),(#186618,#186619,#186620),
(#186621,#186622,#186623),(#186624,#186625,#186626),(#186627,#186628,#186629),
(#186630,#186631,#186632)),.UNSPECIFIED.,.F.,.F.,.F.)
B_SPLINE_SURFACE_WITH_KNOTS((4,2,4),(3,3),(0.,0.00168309713341273,0.00336619426682545),
(0.,1.),.UNSPECIFIED.)
GEOMETRIC_REPRESENTATION_ITEM()
RATIONAL_B_SPLINE_SURFACE(((1.,0.707106781186545,1.),(1.,0.744273762477552,
1.),(1.,0.7776417896067,1.),(1.,0.83910580954319,1.),(1.,0.867185102973278,
1.),(1.,0.89321434471954,1.)))
REPRESENTATION_ITEM('')
SURFACE()
);
#2872=(
BOUNDED_SURFACE()
B_SPLINE_SURFACE(3,2,((#186656,#186657,#186658),(#186659,#186660,#186661),
(#186662,#186663,#186664),(#186665,#186666,#186667)),.UNSPECIFIED.,.F.,
 .F.,.F.)
B_SPLINE_SURFACE_WITH_KNOTS((4,4),(3,3),(3.1415926535898,3.72189740710945),
(0.,1.),.UNSPECIFIED.)
GEOMETRIC_REPRESENTATION_ITEM()
RATIONAL_B_SPLINE_SURFACE(((1.,0.737277336810124,1.),(1.,0.737285953283754,
1.),(1.,0.735586930398308,1.),(1.,0.732423362569238,1.)))
REPRESENTATION_ITEM('')
SURFACE()
);
#2873=(
BOUNDED_SURFACE()
B_SPLINE_SURFACE(3,2,((#186679,#186680,#186681),(#186682,#186683,#186684),
(#186685,#186686,#186687),(#186688,#186689,#186690),(#186691,#186692,#186693),
(#186694,#186695,#186696)),.UNSPECIFIED.,.F.,.F.,.F.)
B_SPLINE_SURFACE_WITH_KNOTS((4,2,4),(3,3),(0.,0.785398163397448,1.5707963267949),
(0.,1.),.UNSPECIFIED.)
GEOMETRIC_REPRESENTATION_ITEM()
RATIONAL_B_SPLINE_SURFACE(((1.,0.737277336810127,1.),(1.,0.737326538316762,
1.),(1.,0.734106258287074,1.),(1.,0.723033691557295,1.),(1.,0.715202981902387,
1.),(1.,0.707106781186548,1.)))
REPRESENTATION_ITEM('')
SURFACE()
);
#2874=(
BOUNDED_SURFACE()
B_SPLINE_SURFACE(3,2,((#186710,#186711,#186712),(#186713,#186714,#186715),
(#186716,#186717,#186718),(#186719,#186720,#186721),(#186722,#186723,#186724),
(#186725,#186726,#186727)),.UNSPECIFIED.,.F.,.F.,.F.)
B_SPLINE_SURFACE_WITH_KNOTS((4,2,4),(3,3),(4.7123465110751,5.49778714378214,
6.28322777648918),(-4.24693095901446E-5,1.),.UNSPECIFIED.)
GEOMETRIC_REPRESENTATION_ITEM()
RATIONAL_B_SPLINE_SURFACE(((1.00002487889076,0.707095653253807,0.999999999999999),
(1.00002556538646,0.69901339684015,1.),(1.00002625900867,0.690847238602975,
1.),(1.00002725945607,0.679068763626294,1.),(1.00002756155303,0.675512113378835,
1.),(1.00002755608917,0.675576440558639,0.999999999999999)))
REPRESENTATION_ITEM('')
SURFACE()
);
#2875=(
BOUNDED_SURFACE()
B_SPLINE_SURFACE(3,2,((#186751,#186752,#186753),(#186754,#186755,#186756),
(#186757,#186758,#186759),(#186760,#186761,#186762),(#186763,#186764,#186765),
(#186766,#186767,#186768)),.UNSPECIFIED.,.F.,.F.,.F.)
B_SPLINE_SURFACE_WITH_KNOTS((4,2,4),(3,3),(3.1415926535898,3.92699081698724,
4.71238898038469),(0.,1.),.UNSPECIFIED.)
GEOMETRIC_REPRESENTATION_ITEM()
RATIONAL_B_SPLINE_SURFACE(((1.,0.675590207615659,1.),(1.,0.675526278181249,
1.),(1.,0.679082711197525,1.),(1.,0.69086004912773,1.),(1.,0.699025295935556,
1.),(1.,0.707106781186543,1.)))
REPRESENTATION_ITEM('')
SURFACE()
);
#2876=(
BOUNDED_SURFACE()
B_SPLINE_SURFACE(3,2,((#186782,#186783,#186784),(#186785,#186786,#186787),
(#186788,#186789,#186790),(#186791,#186792,#186793),(#186794,#186795,#186796),
(#186797,#186798,#186799)),.UNSPECIFIED.,.F.,.F.,.F.)
B_SPLINE_SURFACE_WITH_KNOTS((4,2,4),(3,3),(1.5707963267949,2.35619449019234,
3.1415926535898),(0.,1.),.UNSPECIFIED.)
GEOMETRIC_REPRESENTATION_ITEM()
RATIONAL_B_SPLINE_SURFACE(((1.,0.707106781186543,1.),(1.,0.71520298190223,
1.),(1.,0.723033691557516,1.),(1.,0.734106258286857,1.),(1.,0.737326538316932,
1.),(1.,0.737277336810125,1.)))
REPRESENTATION_ITEM('')
SURFACE()
);
#2877=(
BOUNDED_SURFACE()
B_SPLINE_SURFACE(3,2,((#186815,#186816,#186817),(#186818,#186819,#186820),
(#186821,#186822,#186823),(#186824,#186825,#186826),(#186827,#186828,#186829),
(#186830,#186831,#186832)),.UNSPECIFIED.,.F.,.F.,.F.)
B_SPLINE_SURFACE_WITH_KNOTS((4,2,4),(3,3),(0.,0.00162565899344706,0.00325131798689413),
(0.,1.),.UNSPECIFIED.)
GEOMETRIC_REPRESENTATION_ITEM()
RATIONAL_B_SPLINE_SURFACE(((1.,0.893214344719539,1.),(1.,0.868075018581634,
1.),(1.,0.841018189595232,1.),(1.,0.782003386508022,1.),(1.,0.750058517040659,
1.),(1.,0.714668958264373,1.)))
REPRESENTATION_ITEM('')
SURFACE()
);
#2878=(
BOUNDED_SURFACE()
B_SPLINE_SURFACE(3,2,((#186855,#186856,#186857),(#186858,#186859,#186860),
(#186861,#186862,#186863),(#186864,#186865,#186866),(#186867,#186868,#186869),
(#186870,#186871,#186872)),.UNSPECIFIED.,.F.,.F.,.F.)
B_SPLINE_SURFACE_WITH_KNOTS((4,2,4),(3,3),(3.1415926535898,3.92699081698724,
4.71238898038469),(0.,1.),.UNSPECIFIED.)
GEOMETRIC_REPRESENTATION_ITEM()
RATIONAL_B_SPLINE_SURFACE(((1.,0.675590207615659,1.),(1.,0.675526278181242,
1.),(1.,0.679082711197541,1.),(1.,0.690860049127717,1.),(1.,0.699025295935567,
1.),(1.,0.707106781186543,1.)))
REPRESENTATION_ITEM('')
SURFACE()
);
#2879=(
BOUNDED_SURFACE()
B_SPLINE_SURFACE(3,2,((#186886,#186887,#186888),(#186889,#186890,#186891),
(#186892,#186893,#186894),(#186895,#186896,#186897),(#186898,#186899,#186900),
(#186901,#186902,#186903)),.UNSPECIFIED.,.F.,.F.,.F.)
B_SPLINE_SURFACE_WITH_KNOTS((4,2,4),(3,3),(4.71238898038469,5.49778714378214,
6.28318530717959),(0.,1.),.UNSPECIFIED.)
GEOMETRIC_REPRESENTATION_ITEM()
RATIONAL_B_SPLINE_SURFACE(((1.,0.707106781186543,1.),(1.,0.715202981902221,
1.),(1.,0.723033691557525,1.),(1.,0.734106258286841,1.),(1.,0.737326538316939,
1.),(1.,0.737277336810125,1.)))
REPRESENTATION_ITEM('')
SURFACE()
);
#2880=(
BOUNDED_SURFACE()
B_SPLINE_SURFACE(3,2,((#186917,#186918,#186919),(#186920,#186921,#186922),
(#186923,#186924,#186925),(#186926,#186927,#186928),(#186929,#186930,#186931),
(#186932,#186933,#186934)),.UNSPECIFIED.,.F.,.F.,.F.)
B_SPLINE_SURFACE_WITH_KNOTS((4,2,4),(3,3),(-3.25260651745651E-18,0.00101351621082632,
0.00202703242165263),(0.,1.),.UNSPECIFIED.)
GEOMETRIC_REPRESENTATION_ITEM()
RATIONAL_B_SPLINE_SURFACE(((1.,0.893214344719542,1.),(1.,0.912305000874927,
1.),(1.,0.927255525935639,1.),(1.,0.94789383214718,1.),(1.,0.953590869545161,
1.),(1.,0.953555223991885,1.)))
REPRESENTATION_ITEM('')
SURFACE()
);
#2881=(
BOUNDED_SURFACE()
B_SPLINE_SURFACE(3,2,((#187005,#187006,#187007),(#187008,#187009,#187010),
(#187011,#187012,#187013),(#187014,#187015,#187016),(#187017,#187018,#187019),
(#187020,#187021,#187022)),.UNSPECIFIED.,.F.,.F.,.F.)
B_SPLINE_SURFACE_WITH_KNOTS((4,2,4),(3,3),(3.1415926535898,3.92699081698724,
4.71238898038469),(0.,1.),.UNSPECIFIED.)
GEOMETRIC_REPRESENTATION_ITEM()
RATIONAL_B_SPLINE_SURFACE(((1.,0.73727733681012,1.),(1.,0.737326538316634,
1.),(1.,0.734106258287243,1.),(1.,0.723033691557116,1.),(1.,0.715202981902516,
1.),(1.,0.707106781186548,1.)))
REPRESENTATION_ITEM('')
SURFACE()
);
#2882=(
BOUNDED_SURFACE()
B_SPLINE_SURFACE(3,2,((#187036,#187037,#187038),(#187039,#187040,#187041),
(#187042,#187043,#187044),(#187045,#187046,#187047),(#187048,#187049,#187050),
(#187051,#187052,#187053)),.UNSPECIFIED.,.F.,.F.,.F.)
B_SPLINE_SURFACE_WITH_KNOTS((4,2,4),(3,3),(4.71234651106924,5.49778714378214,
6.28322777649504),(-4.24693154496904E-5,1.),.UNSPECIFIED.)
GEOMETRIC_REPRESENTATION_ITEM()
RATIONAL_B_SPLINE_SURFACE(((1.0000248788942,0.707095653252277,1.),(1.00002556538999,
0.699013396839213,1.),(1.00002625901229,0.690847238600254,1.),(1.00002725945983,
0.679068763625337,1.),(1.00002756155683,0.675512113376159,1.),(1.00002755609297,
0.675576440556743,1.)))
REPRESENTATION_ITEM('')
SURFACE()
);
#2883=(
BOUNDED_SURFACE()
B_SPLINE_SURFACE(3,2,((#187069,#187070,#187071),(#187072,#187073,#187074),
(#187075,#187076,#187077),(#187078,#187079,#187080),(#187081,#187082,#187083),
(#187084,#187085,#187086)),.UNSPECIFIED.,.F.,.F.,.F.)
B_SPLINE_SURFACE_WITH_KNOTS((4,2,4),(3,3),(0.,0.00169934430350512,0.00339868860701024),
(0.,1.),.UNSPECIFIED.)
GEOMETRIC_REPRESENTATION_ITEM()
RATIONAL_B_SPLINE_SURFACE(((1.,0.707106781186547,1.),(1.,0.74482559038907,
1.),(1.,0.778551967557851,1.),(1.,0.840511428018892,1.),(1.,0.868726285027217,
1.),(1.,0.894799245647903,1.)))
REPRESENTATION_ITEM('')
SURFACE()
);
#2884=(
BOUNDED_SURFACE()
B_SPLINE_SURFACE(3,2,((#187110,#187111,#187112),(#187113,#187114,#187115),
(#187116,#187117,#187118),(#187119,#187120,#187121),(#187122,#187123,#187124),
(#187125,#187126,#187127)),.UNSPECIFIED.,.F.,.F.,.F.)
B_SPLINE_SURFACE_WITH_KNOTS((4,2,4),(3,3),(3.1415926535898,3.72828696246945,
4.31498127134909),(0.,1.),.UNSPECIFIED.)
GEOMETRIC_REPRESENTATION_ITEM()
RATIONAL_B_SPLINE_SURFACE(((1.,0.737277336810115,1.),(1.,0.73729299178243,
1.),(1.,0.735539930277599,1.),(1.,0.729097328045697,1.),(1.,0.724411344440144,
1.),(1.,0.71893387489533,1.)))
REPRESENTATION_ITEM('')
SURFACE()
);
#2885=(
BOUNDED_SURFACE()
B_SPLINE_SURFACE(3,2,((#187175,#187176,#187177),(#187178,#187179,#187180),
(#187181,#187182,#187183),(#187184,#187185,#187186),(#187187,#187188,#187189),
(#187190,#187191,#187192)),.UNSPECIFIED.,.F.,.F.,.F.)
B_SPLINE_SURFACE_WITH_KNOTS((4,2,4),(3,3),(1.41124413247309E-15,0.78539816339745,
1.5707963267949),(0.,1.),.UNSPECIFIED.)
GEOMETRIC_REPRESENTATION_ITEM()
RATIONAL_B_SPLINE_SURFACE(((1.,0.73727733681012,1.),(1.,0.737326538316275,
1.),(1.,0.734106258287724,1.),(1.,0.723033691556635,1.),(1.,0.715202981902879,
1.),(1.,0.707106781186548,1.)))
REPRESENTATION_ITEM('')
SURFACE()
);
#2886=(
BOUNDED_SURFACE()
B_SPLINE_SURFACE(3,2,((#187206,#187207,#187208),(#187209,#187210,#187211),
(#187212,#187213,#187214),(#187215,#187216,#187217),(#187218,#187219,#187220),
(#187221,#187222,#187223)),.UNSPECIFIED.,.F.,.F.,.F.)
B_SPLINE_SURFACE_WITH_KNOTS((4,2,4),(3,3),(4.71234651107879,5.49778714378214,
6.28322777648549),(-4.24693058989126E-5,1.),.UNSPECIFIED.)
GEOMETRIC_REPRESENTATION_ITEM()
RATIONAL_B_SPLINE_SURFACE(((1.0000248788886,0.70709565325478,1.),(1.00002556538424,
0.699013396841888,1.),(1.00002625900639,0.690847238603135,1.),(1.0000272594537,
0.679068763628474,1.),(1.00002756155063,0.675512113379344,1.),(1.00002755608677,
0.675576440559839,1.)))
REPRESENTATION_ITEM('')
SURFACE()
);
#2887=(
BOUNDED_SURFACE()
B_SPLINE_SURFACE(3,2,((#187237,#187238,#187239),(#187240,#187241,#187242),
(#187243,#187244,#187245),(#187246,#187247,#187248),(#187249,#187250,#187251),
(#187252,#187253,#187254),(#187255,#187256,#187257),(#187258,#187259,#187260)),
 .UNSPECIFIED.,.F.,.F.,.F.)
B_SPLINE_SURFACE_WITH_KNOTS((4,2,2,4),(3,3),(-3.14418630020796E-18,0.000761037462531171,
0.00114155619379676,0.00152207492506235),(0.,1.),.UNSPECIFIED.)
GEOMETRIC_REPRESENTATION_ITEM()
RATIONAL_B_SPLINE_SURFACE(((1.,0.691935594449023,1.),(1.,0.657938057153071,
1.),(1.,0.623321566128117,1.),(1.,0.582569634693765,1.),(1.,0.571407182182735,
1.),(1.,0.5555307216223,1.),(1.,0.551373498869702,1.),(1.,0.551334230064852,
1.)))
REPRESENTATION_ITEM('')
SURFACE()
);
#2888=(
BOUNDED_SURFACE()
B_SPLINE_SURFACE(3,2,((#187340,#187341,#187342),(#187343,#187344,#187345),
(#187346,#187347,#187348),(#187349,#187350,#187351),(#187352,#187353,#187354),
(#187355,#187356,#187357),(#187358,#187359,#187360),(#187361,#187362,#187363),
(#187364,#187365,#187366),(#187367,#187368,#187369)),.UNSPECIFIED.,.F.,
 .F.,.F.)
B_SPLINE_SURFACE_WITH_KNOTS((4,2,2,2,4),(3,3),(-0.000159653390897044,0.000399133477242608,
0.000798266954485216,0.00119740043172782,0.00175618729986758),(-0.00202899497456342,
1.),.UNSPECIFIED.)
GEOMETRIC_REPRESENTATION_ITEM()
RATIONAL_B_SPLINE_SURFACE(((1.00079837996119,0.803257284714785,1.),(1.00078548688006,
0.806434493454874,1.),(1.00079545917955,0.803977045403331,1.),(1.00084458507115,
0.791871078604599,1.),(1.00087479655517,0.784426140493272,1.),(1.00094857178652,
0.766245900455217,1.),(1.00099274968817,0.755359254060113,1.),(1.00110658067738,
0.727308176893173,1.),(1.00118157563583,0.70882736264828,1.),(1.0012523988413,
0.691374582737139,1.)))
REPRESENTATION_ITEM('')
SURFACE()
);
#2889=(
BOUNDED_SURFACE()
B_SPLINE_SURFACE(3,2,((#187419,#187420,#187421),(#187422,#187423,#187424),
(#187425,#187426,#187427),(#187428,#187429,#187430),(#187431,#187432,#187433),
(#187434,#187435,#187436)),.UNSPECIFIED.,.F.,.F.,.F.)
B_SPLINE_SURFACE_WITH_KNOTS((4,2,4),(3,3),(-0.000140547083940185,0.000795474163050539,
0.00173149541004126),(-0.000140547083940185,1.00127446610899),
 .UNSPECIFIED.)
GEOMETRIC_REPRESENTATION_ITEM()
RATIONAL_B_SPLINE_SURFACE(((1.00007870553575,0.719646060326318,1.00071450264019),
(1.00008671779993,0.691105884499127,1.00078723937792),(1.00009529453502,
0.660555028733005,1.00086510048138),(1.00010720671514,0.618123113407254,
1.0009732413392),(1.0001104843585,0.606447946977011,1.00100299635976),(1.00010906895813,
0.611489689798581,1.00099014710727)))
REPRESENTATION_ITEM('')
SURFACE()
);
#2890=(
BOUNDED_SURFACE()
B_SPLINE_SURFACE(3,2,((#187466,#187467,#187468),(#187469,#187470,#187471),
(#187472,#187473,#187474),(#187475,#187476,#187477),(#187478,#187479,#187480),
(#187481,#187482,#187483),(#187484,#187485,#187486),(#187487,#187488,#187489)),
 .UNSPECIFIED.,.F.,.F.,.F.)
B_SPLINE_SURFACE_WITH_KNOTS((4,2,2,4),(3,3),(-0.000157666505658259,0.000394166264145648,
0.000788332528291295,0.00173433156224098),(-0.00241203109543842,1.00210445955167),
 .UNSPECIFIED.)
GEOMETRIC_REPRESENTATION_ITEM()
RATIONAL_B_SPLINE_SURFACE(((1.00126783966346,0.736629804805208,1.00110583094575),
(1.00112683188768,0.765921557145529,1.00098284160685),(1.00102615333431,
0.786835660891743,1.0008950280898),(1.00090176020874,0.812676027545364,
1.00078653032651),(1.00086612520509,0.820078539185068,1.00075544888071),
(1.00078492300801,0.836946790835935,1.00068462296716),(1.00079943453383,
0.833932290266678,1.00069728016253),(1.00085506469522,0.822376155144815,
1.00074580171913)))
REPRESENTATION_ITEM('')
SURFACE()
);
#2891=(
BOUNDED_SURFACE()
B_SPLINE_SURFACE(3,2,((#187520,#187521,#187522),(#187523,#187524,#187525),
(#187526,#187527,#187528),(#187529,#187530,#187531)),.UNSPECIFIED.,.F.,
 .F.,.F.)
B_SPLINE_SURFACE_WITH_KNOTS((4,4),(3,3),(0.,0.000504125640440226),(0.,1.),
 .UNSPECIFIED.)
GEOMETRIC_REPRESENTATION_ITEM()
RATIONAL_B_SPLINE_SURFACE(((1.,0.828190603154496,1.),(1.,0.830246482056442,
1.),(1.,0.832229943187683,1.),(1.,0.834143101464675,1.)))
REPRESENTATION_ITEM('')
SURFACE()
);
#2892=(
BOUNDED_SURFACE()
B_SPLINE_SURFACE(3,2,((#187535,#187536,#187537),(#187538,#187539,#187540),
(#187541,#187542,#187543),(#187544,#187545,#187546),(#187547,#187548,#187549),
(#187550,#187551,#187552),(#187553,#187554,#187555),(#187556,#187557,#187558),
(#187559,#187560,#187561),(#187562,#187563,#187564)),.UNSPECIFIED.,.F.,
 .F.,.F.)
B_SPLINE_SURFACE_WITH_KNOTS((4,2,2,2,4),(3,3),(-8.34022521184474E-16,0.000443043867974425,
0.000886087735949684,0.00132913160392494,0.00177217547190021),(0.,1.),
 .UNSPECIFIED.)
GEOMETRIC_REPRESENTATION_ITEM()
RATIONAL_B_SPLINE_SURFACE(((1.,0.834143101464621,1.),(1.,0.830444108750761,
1.),(1.,0.824302497883951,1.),(1.,0.80744078994961,1.),(1.,0.79657978834944,
1.),(1.,0.769588124839812,1.),(1.,0.753384767045469,1.),(1.,0.714346006222175,
1.),(1.,0.691706791956038,1.),(1.,0.665108204576645,1.)))
REPRESENTATION_ITEM('')
SURFACE()
);
#2893=(
BOUNDED_SURFACE()
B_SPLINE_SURFACE(3,2,((#187627,#187628,#187629),(#187630,#187631,#187632),
(#187633,#187634,#187635),(#187636,#187637,#187638),(#187639,#187640,#187641),
(#187642,#187643,#187644),(#187645,#187646,#187647),(#187648,#187649,#187650),
(#187651,#187652,#187653),(#187654,#187655,#187656)),.UNSPECIFIED.,.F.,
 .F.,.F.)
B_SPLINE_SURFACE_WITH_KNOTS((4,2,2,2,4),(3,3),(-0.000173686186586184,0.000907880296577857,
0.00113485037072232,0.00136182044486679,0.00198944677974189),(0.,1.00144242662926),
 .UNSPECIFIED.)
GEOMETRIC_REPRESENTATION_ITEM()
RATIONAL_B_SPLINE_SURFACE(((1.,0.681665301346584,1.00091834889271),(1.,
0.750503632449571,1.00071976040892),(1.,0.8021030753377,1.00057090358796),
(1.,0.842357054042358,1.00045477676633),(1.,0.848376815809341,1.00043741063698),
(1.,0.858788711892737,1.00040737384464),(1.,0.863209133647019,1.00039462157653),
(1.,0.876279812131844,1.00035691458712),(1.,0.879347925892028,1.00034806352914),
(1.,0.875471233314833,1.00035924721835)))
REPRESENTATION_ITEM('')
SURFACE()
);
#2894=(
BOUNDED_SURFACE()
B_SPLINE_SURFACE(3,2,((#187676,#187677,#187678),(#187679,#187680,#187681),
(#187682,#187683,#187684),(#187685,#187686,#187687)),.UNSPECIFIED.,.F.,
 .F.,.F.)
B_SPLINE_SURFACE_WITH_KNOTS((4,4),(3,3),(0.,0.000503779257761556),(0.,1.),
 .UNSPECIFIED.)
GEOMETRIC_REPRESENTATION_ITEM()
RATIONAL_B_SPLINE_SURFACE(((1.,0.877279917170998,1.),(1.,0.877311423474942,
1.),(1.,0.87728564981134,1.),(1.,0.877202574460556,1.)))
REPRESENTATION_ITEM('')
SURFACE()
);
#2895=(
BOUNDED_SURFACE()
B_SPLINE_SURFACE(3,2,((#187691,#187692,#187693),(#187694,#187695,#187696),
(#187697,#187698,#187699),(#187700,#187701,#187702),(#187703,#187704,#187705),
(#187706,#187707,#187708),(#187709,#187710,#187711),(#187712,#187713,#187714),
(#187715,#187716,#187717),(#187718,#187719,#187720)),.UNSPECIFIED.,.F.,
 .F.,.F.)
B_SPLINE_SURFACE_WITH_KNOTS((4,2,2,2,4),(3,3),(-0.000115990203183372,0.000453061765036137,
0.000906123530072295,0.00135918529510845,0.00192823726332794),(0.,1.00079444254916),
 .UNSPECIFIED.)
GEOMETRIC_REPRESENTATION_ITEM()
RATIONAL_B_SPLINE_SURFACE(((1.,0.876263374194623,1.00019660328086),(1.,
0.878805941473907,1.0001925634336),(1.,0.875602380876755,1.00019765352329),
(1.,0.86018205071516,1.0002221546561),(1.,0.849863211484357,1.00023855010598),
(1.,0.822219823797783,1.00028247227274),(1.,0.805074602369326,1.00030971405958),
(1.,0.759404065674411,1.00038227929477),(1.,0.729387016381409,1.00042997293708),
(1.,0.694075111441602,1.00048607949663)))
REPRESENTATION_ITEM('')
SURFACE()
);
#2896=(
BOUNDED_SURFACE()
B_SPLINE_SURFACE(3,2,((#187753,#187754,#187755),(#187756,#187757,#187758),
(#187759,#187760,#187761),(#187762,#187763,#187764),(#187765,#187766,#187767),
(#187768,#187769,#187770),(#187771,#187772,#187773),(#187774,#187775,#187776),
(#187777,#187778,#187779),(#187780,#187781,#187782),(#187783,#187784,#187785),
(#187786,#187787,#187788)),.UNSPECIFIED.,.F.,.F.,.F.)
B_SPLINE_SURFACE_WITH_KNOTS((4,2,2,2,2,4),(3,3),(0.,0.000440377446917856,
0.000880754893835713,0.00110094361729464,0.00132113234075357,0.00176150978767142),
(0.,1.),.UNSPECIFIED.)
GEOMETRIC_REPRESENTATION_ITEM()
RATIONAL_B_SPLINE_SURFACE(((1.,0.663670476503535,1.),(1.,0.690166095882704,
1.),(1.,0.712198476344476,1.),(1.,0.750819491395322,1.),(1.,0.766789812455876,
1.),(1.,0.786909315979615,1.),(1.,0.793060196071366,1.),(1.,0.803891824235189,
1.),(1.,0.808661939460988,1.),(1.,0.821430084171777,1.),(1.,0.827612685850937,
1.),(1.,0.831517473467322,1.)))
REPRESENTATION_ITEM('')
SURFACE()
);
#2897=(
BOUNDED_SURFACE()
B_SPLINE_SURFACE(3,2,((#187834,#187835,#187836),(#187837,#187838,#187839),
(#187840,#187841,#187842),(#187843,#187844,#187845)),.UNSPECIFIED.,.F.,
 .F.,.F.)
B_SPLINE_SURFACE_WITH_KNOTS((4,4),(3,3),(-2.62810606610486E-16,0.000504136652582459),
(0.,1.),.UNSPECIFIED.)
GEOMETRIC_REPRESENTATION_ITEM()
RATIONAL_B_SPLINE_SURFACE(((1.,0.831517473467334,1.),(1.,0.829540548856785,
1.),(1.,0.827492428459287,1.),(1.,0.825370895892945,1.)))
REPRESENTATION_ITEM('')
SURFACE()
);
#2898=(
BOUNDED_SURFACE()
B_SPLINE_SURFACE(3,2,((#187849,#187850,#187851),(#187852,#187853,#187854),
(#187855,#187856,#187857),(#187858,#187859,#187860),(#187861,#187862,#187863),
(#187864,#187865,#187866),(#187867,#187868,#187869),(#187870,#187871,#187872),
(#187873,#187874,#187875),(#187876,#187877,#187878)),.UNSPECIFIED.,.F.,
 .F.,.F.)
B_SPLINE_SURFACE_WITH_KNOTS((4,2,2,2,4),(3,3),(0.,0.00039329942356206,0.000786598847124121,
0.00117989827068618,0.00157319769424824),(0.,1.),.UNSPECIFIED.)
GEOMETRIC_REPRESENTATION_ITEM()
RATIONAL_B_SPLINE_SURFACE(((1.,0.825370895892916,1.),(1.,0.829081051796028,
1.),(1.,0.831084991111337,1.),(1.,0.831059675364535,1.),(1.,0.829021889329635,
1.),(1.,0.819977402296451,1.),(1.,0.812885056457023,1.),(1.,0.792515337687537,
1.),(1.,0.779105591645567,1.),(1.,0.762081632340355,1.)))
REPRESENTATION_ITEM('')
SURFACE()
);
#2899=(
BOUNDED_SURFACE()
B_SPLINE_SURFACE(3,2,((#187935,#187936,#187937),(#187938,#187939,#187940),
(#187941,#187942,#187943),(#187944,#187945,#187946),(#187947,#187948,#187949),
(#187950,#187951,#187952),(#187953,#187954,#187955),(#187956,#187957,#187958),
(#187959,#187960,#187961),(#187962,#187963,#187964)),.UNSPECIFIED.,.F.,
 .F.,.F.)
B_SPLINE_SURFACE_WITH_KNOTS((4,2,2,2,4),(3,3),(0.,0.000397955182835291,
0.000795910365670582,0.00119386554850587,0.00159182073134117),(0.,1.),
 .UNSPECIFIED.)
GEOMETRIC_REPRESENTATION_ITEM()
RATIONAL_B_SPLINE_SURFACE(((1.,0.60931006565052,1.),(1.,0.60928110676943,
1.),(1.,0.611992414032709,1.),(1.,0.622151576786515,1.),(1.,0.629646305612374,
1.),(1.,0.647895096091951,1.),(1.,0.658798646820943,1.),(1.,0.682038372243284,
1.),(1.,0.694657643733687,1.),(1.,0.707106781186553,1.)))
REPRESENTATION_ITEM('')
SURFACE()
);
#2900=(
BOUNDED_SURFACE()
B_SPLINE_SURFACE(3,2,((#188014,#188015,#188016),(#188017,#188018,#188019),
(#188020,#188021,#188022),(#188023,#188024,#188025),(#188026,#188027,#188028),
(#188029,#188030,#188031),(#188032,#188033,#188034),(#188035,#188036,#188037)),
 .UNSPECIFIED.,.F.,.F.,.F.)
B_SPLINE_SURFACE_WITH_KNOTS((4,2,2,4),(3,3),(0.,0.000399389907139719,0.000798779814279438,
0.00159755962855888),(0.,1.),.UNSPECIFIED.)
GEOMETRIC_REPRESENTATION_ITEM()
RATIONAL_B_SPLINE_SURFACE(((1.,0.707106781186543,1.),(1.,0.719972059607527,
1.),(1.,0.732679659198347,1.),(1.,0.756479572209125,1.),(1.,0.767365377234031,
1.),(1.,0.79501980381119,1.),(1.,0.806340389868128,1.),(1.,0.806206028026398,
1.)))
REPRESENTATION_ITEM('')
SURFACE()
);
#2901=(
BOUNDED_SURFACE()
B_SPLINE_SURFACE(3,2,((#188109,#188110,#188111),(#188112,#188113,#188114),
(#188115,#188116,#188117),(#188118,#188119,#188120),(#188121,#188122,#188123),
(#188124,#188125,#188126)),.UNSPECIFIED.,.F.,.F.,.F.)
B_SPLINE_SURFACE_WITH_KNOTS((4,2,4),(3,3),(0.,0.000635851334990063,0.00127170266998013),
(0.,1.),.UNSPECIFIED.)
GEOMETRIC_REPRESENTATION_ITEM()
RATIONAL_B_SPLINE_SURFACE(((1.,0.549598954535088,1.),(1.,0.549481216714779,
1.),(1.,0.561870616792487,1.),(1.,0.602538835999935,1.),(1.,0.629604434612806,
1.),(1.,0.65799444631184,1.)))
REPRESENTATION_ITEM('')
SURFACE()
);
#2902=(
BOUNDED_SURFACE()
B_SPLINE_SURFACE(3,2,((#188207,#188208,#188209),(#188210,#188211,#188212),
(#188213,#188214,#188215),(#188216,#188217,#188218),(#188219,#188220,#188221),
(#188222,#188223,#188224)),.UNSPECIFIED.,.F.,.F.,.F.)
B_SPLINE_SURFACE_WITH_KNOTS((4,2,4),(3,3),(0.,0.000500133683539797,0.00100026736707959),
(-0.00102329236961724,1.),.UNSPECIFIED.)
GEOMETRIC_REPRESENTATION_ITEM()
RATIONAL_B_SPLINE_SURFACE(((1.0006000441848,0.706807065790613,1.),(1.00056790491851,
0.722510918987102,1.),(1.00055014554087,0.731188486689425,1.),(1.0005372619169,
0.737483668960894,1.),(1.00054173734042,0.735296892411237,1.),(1.00054817863633,
0.732149553437697,1.)))
REPRESENTATION_ITEM('')
SURFACE()
);
#2903=(
BOUNDED_SURFACE()
B_SPLINE_SURFACE(3,2,((#188242,#188243,#188244),(#188245,#188246,#188247),
(#188248,#188249,#188250),(#188251,#188252,#188253)),.UNSPECIFIED.,.F.,
 .F.,.F.)
B_SPLINE_SURFACE_WITH_KNOTS((4,4),(3,3),(5.42101086242752E-20,0.000113625826113285),
(0.,1.),.UNSPECIFIED.)
GEOMETRIC_REPRESENTATION_ITEM()
RATIONAL_B_SPLINE_SURFACE(((1.,0.691935594449019,1.),(1.,0.697297182114951,
1.),(1.,0.702351867303478,1.),(1.,0.70710678118654,1.)))
REPRESENTATION_ITEM('')
SURFACE()
);
#2904=(
BOUNDED_SURFACE()
B_SPLINE_SURFACE(3,2,((#188263,#188264,#188265),(#188266,#188267,#188268),
(#188269,#188270,#188271),(#188272,#188273,#188274)),.UNSPECIFIED.,.F.,
 .F.,.F.)
B_SPLINE_SURFACE_WITH_KNOTS((4,4),(3,3),(-1.50704101975485E-17,0.000358861832009556),
(0.,1.),.UNSPECIFIED.)
GEOMETRIC_REPRESENTATION_ITEM()
RATIONAL_B_SPLINE_SURFACE(((1.,0.707106781186544,1.),(1.,0.693584131808955,
1.),(1.,0.67719600445086,1.),(1.,0.65799444631037,1.)))
REPRESENTATION_ITEM('')
SURFACE()
);
#2905=(
BOUNDED_SURFACE()
B_SPLINE_SURFACE(3,2,((#188288,#188289,#188290),(#188291,#188292,#188293),
(#188294,#188295,#188296),(#188297,#188298,#188299)),.UNSPECIFIED.,.F.,
 .F.,.F.)
B_SPLINE_SURFACE_WITH_KNOTS((4,4),(3,3),(0.000909429960036056,0.00157021148057203),
(0.,1.),.UNSPECIFIED.)
GEOMETRIC_REPRESENTATION_ITEM()
RATIONAL_B_SPLINE_SURFACE(((1.,0.72569894652024,1.),(1.,0.728856973451895,
1.),(1.,0.724481780670466,1.),(1.,0.707106781186543,1.)))
REPRESENTATION_ITEM('')
SURFACE()
);
#2906=(
BOUNDED_SURFACE()
B_SPLINE_SURFACE(3,2,((#188335,#188336,#188337),(#188338,#188339,#188340),
(#188341,#188342,#188343),(#188344,#188345,#188346),(#188347,#188348,#188349),
(#188350,#188351,#188352),(#188353,#188354,#188355),(#188356,#188357,#188358),
(#188359,#188360,#188361),(#188362,#188363,#188364),(#188365,#188366,#188367),
(#188368,#188369,#188370)),.UNSPECIFIED.,.F.,.F.,.F.)
B_SPLINE_SURFACE_WITH_KNOTS((4,2,2,2,2,4),(3,3),(0.,0.000471787629256711,
0.000943575258513421,0.00117946907314178,0.00141536288777013,0.00188715051702685),
(0.,1.),.UNSPECIFIED.)
GEOMETRIC_REPRESENTATION_ITEM()
RATIONAL_B_SPLINE_SURFACE(((1.,0.688859710774758,1.),(1.,0.717278497414175,
1.),(1.,0.742415568607548,1.),(1.,0.786827943379553,1.),(1.,0.806155596178757,
1.),(1.,0.829868996905786,1.),(1.,0.837032764561711,1.),(1.,0.849395444084014,
1.),(1.,0.854694123459555,1.),(1.,0.86824784980175,1.),(1.,0.873676740317143,
1.),(1.,0.875436198637081,1.)))
REPRESENTATION_ITEM('')
SURFACE()
);
#2907=(
BOUNDED_SURFACE()
B_SPLINE_SURFACE(3,2,((#188416,#188417,#188418),(#188419,#188420,#188421),
(#188422,#188423,#188424),(#188425,#188426,#188427)),.UNSPECIFIED.,.F.,
 .F.,.F.)
B_SPLINE_SURFACE_WITH_KNOTS((4,4),(3,3),(0.,0.000504208024932662),(0.,1.),
 .UNSPECIFIED.)
GEOMETRIC_REPRESENTATION_ITEM()
RATIONAL_B_SPLINE_SURFACE(((1.,0.872490094680101,1.),(1.,0.873532316568381,
1.),(1.,0.874514063294085,1.),(1.,0.875436198637085,1.)))
REPRESENTATION_ITEM('')
SURFACE()
);
#2908=(
BOUNDED_SURFACE()
B_SPLINE_SURFACE(3,2,((#188431,#188432,#188433),(#188434,#188435,#188436),
(#188437,#188438,#188439),(#188440,#188441,#188442),(#188443,#188444,#188445),
(#188446,#188447,#188448),(#188449,#188450,#188451),(#188452,#188453,#188454),
(#188455,#188456,#188457),(#188458,#188459,#188460)),.UNSPECIFIED.,.F.,
 .F.,.F.)
B_SPLINE_SURFACE_WITH_KNOTS((4,2,2,2,4),(3,3),(-9.01822866958479E-5,0.000428050429885702,
0.000856100859773762,0.00128415128966182,0.00180238400624337),(0.,1.00070975129598),
 .UNSPECIFIED.)
GEOMETRIC_REPRESENTATION_ITEM()
RATIONAL_B_SPLINE_SURFACE(((1.,0.87087120065611,1.00018329866537),(1.,0.874579814490895,
1.00017803427842),(1.,0.873810679327731,1.00017912606777),(1.,0.863911307902413,
1.00019317825117),(1.,0.856204559855697,1.000204118),(1.,0.833962775819185,
1.00023569027009),(1.,0.819525279404997,1.00025618433367),(1.,0.780375333947201,
1.00031175778272),(1.,0.754589472410923,1.00034836088001),(1.,0.723415614990647,
1.00039261225142)))
REPRESENTATION_ITEM('')
SURFACE()
);
#2909=(
BOUNDED_SURFACE()
B_SPLINE_SURFACE(3,2,((#188483,#188484,#188485),(#188486,#188487,#188488),
(#188489,#188490,#188491),(#188492,#188493,#188494),(#188495,#188496,#188497),
(#188498,#188499,#188500)),.UNSPECIFIED.,.F.,.F.,.F.)
B_SPLINE_SURFACE_WITH_KNOTS((4,2,4),(3,3),(-0.000165293417219257,0.000826467086096255,
0.0018182275894121),(-0.00110131312783401,1.00167262876028),
 .UNSPECIFIED.)
GEOMETRIC_REPRESENTATION_ITEM()
RATIONAL_B_SPLINE_SURFACE(((1.00085459808061,0.61135981365314,1.00129866887682),
(1.00075392303127,0.657143171733025,1.00114568052331),(1.00067880279221,
0.691305129694834,1.00103152590643),(1.00056376087147,0.743622019388052,
1.00085670529147),(1.00052307748563,0.762123346519561,1.00079488178847),
(1.00049052902468,0.77692520509168,1.00074542032329)))
REPRESENTATION_ITEM('')
SURFACE()
);
#2910=(
BOUNDED_SURFACE()
B_SPLINE_SURFACE(3,2,((#188515,#188516,#188517),(#188518,#188519,#188520),
(#188521,#188522,#188523),(#188524,#188525,#188526)),.UNSPECIFIED.,.F.,
 .F.,.F.)
B_SPLINE_SURFACE_WITH_KNOTS((4,4),(3,3),(2.16840434497101E-19,0.000504355062152837),
(0.,1.),.UNSPECIFIED.)
GEOMETRIC_REPRESENTATION_ITEM()
RATIONAL_B_SPLINE_SURFACE(((1.,0.759233451646319,1.),(1.,0.762871393877082,
1.),(1.,0.766403968732707,1.),(1.,0.769836971136898,1.)))
REPRESENTATION_ITEM('')
SURFACE()
);
#2911=(
BOUNDED_SURFACE()
B_SPLINE_SURFACE(3,2,((#188530,#188531,#188532),(#188533,#188534,#188535),
(#188536,#188537,#188538),(#188539,#188540,#188541),(#188542,#188543,#188544),
(#188545,#188546,#188547),(#188548,#188549,#188550),(#188551,#188552,#188553),
(#188554,#188555,#188556),(#188557,#188558,#188559)),.UNSPECIFIED.,.F.,
 .F.,.F.)
B_SPLINE_SURFACE_WITH_KNOTS((4,2,2,2,4),(3,3),(-3.25260651745651E-18,0.000393055033931551,
0.000786110067863104,0.00117916510179466,0.00157222013572621),(0.,1.),
 .UNSPECIFIED.)
GEOMETRIC_REPRESENTATION_ITEM()
RATIONAL_B_SPLINE_SURFACE(((1.,0.759233451646328,1.),(1.,0.765853834182409,
1.),(1.,0.77182063876785,1.),(1.,0.782085007421256,1.),(1.,0.786377884755709,
1.),(1.,0.792439775573655,1.),(1.,0.794229619467717,1.),(1.,0.793882695203775,
1.),(1.,0.791736824593394,1.),(1.,0.786683372191859,1.)))
REPRESENTATION_ITEM('')
SURFACE()
);
#2912=(
BOUNDED_SURFACE()
B_SPLINE_SURFACE(3,2,((#188613,#188614,#188615),(#188616,#188617,#188618),
(#188619,#188620,#188621),(#188622,#188623,#188624),(#188625,#188626,#188627),
(#188628,#188629,#188630),(#188631,#188632,#188633),(#188634,#188635,#188636),
(#188637,#188638,#188639),(#188640,#188641,#188642)),.UNSPECIFIED.,.F.,
 .F.,.F.)
B_SPLINE_SURFACE_WITH_KNOTS((4,2,2,2,4),(3,3),(0.,0.000403813407730069,
0.00080762681546014,0.00121144022319021,0.00161525363092028),(0.,1.),
 .UNSPECIFIED.)
GEOMETRIC_REPRESENTATION_ITEM()
RATIONAL_B_SPLINE_SURFACE(((1.,0.574616980402532,1.),(1.,0.574559944255782,
1.),(1.,0.578580805360036,1.),(1.,0.593205211704828,1.),(1.,0.603887596362185,
1.),(1.,0.629170763939607,1.),(1.,0.643946507952345,1.),(1.,0.674809145535283,
1.),(1.,0.691194307570675,1.),(1.,0.707106781186543,1.)))
REPRESENTATION_ITEM('')
SURFACE()
);
#2913=(
BOUNDED_SURFACE()
B_SPLINE_SURFACE(3,2,((#188695,#188696,#188697),(#188698,#188699,#188700),
(#188701,#188702,#188703),(#188704,#188705,#188706),(#188707,#188708,#188709),
(#188710,#188711,#188712)),.UNSPECIFIED.,.F.,.F.,.F.)
B_SPLINE_SURFACE_WITH_KNOTS((4,2,4),(3,3),(-0.00016234715873864,0.0008117357936932,
0.00178581874612504),(-0.00233857113343664,1.00211339902085),
 .UNSPECIFIED.)
GEOMETRIC_REPRESENTATION_ITEM()
RATIONAL_B_SPLINE_SURFACE(((1.00146568173025,0.685964966691454,1.00132425925821),
(1.00127996764077,0.725755822420716,1.00115646457449),(1.00109456509479,
0.765479927253636,1.00098895137367),(1.00083507105024,0.821078778791707,
1.00075449570444),(1.00076572018014,0.83593780469964,1.000691836445),(1.00079936494528,
0.828729121720177,1.00072223485333)))
REPRESENTATION_ITEM('')
SURFACE()
);
#2914=(
BOUNDED_SURFACE()
B_SPLINE_SURFACE(3,2,((#188743,#188744,#188745),(#188746,#188747,#188748),
(#188749,#188750,#188751),(#188752,#188753,#188754),(#188755,#188756,#188757),
(#188758,#188759,#188760),(#188761,#188762,#188763),(#188764,#188765,#188766),
(#188767,#188768,#188769),(#188770,#188771,#188772)),.UNSPECIFIED.,.F.,
 .F.,.F.)
B_SPLINE_SURFACE_WITH_KNOTS((4,2,2,2,4),(3,3),(0.,0.000408971318093432,
0.000817942636186865,0.0012269139542803,0.00163588527237373),(0.,1.),
 .UNSPECIFIED.)
GEOMETRIC_REPRESENTATION_ITEM()
RATIONAL_B_SPLINE_SURFACE(((1.,0.707106781186548,1.),(1.,0.688859876352089,
1.),(1.,0.670469148037181,1.),(1.,0.634232875326911,1.),(1.,0.617116919953528,
1.),(1.,0.586509610415134,1.),(1.,0.573603373050602,1.),(1.,0.555466576286827,
1.),(1.,0.550482231415542,1.),(1.,0.55046727607882,1.)))
REPRESENTATION_ITEM('')
SURFACE()
);
#2915=(
BOUNDED_SURFACE()
B_SPLINE_SURFACE(3,2,((#188826,#188827,#188828),(#188829,#188830,#188831),
(#188832,#188833,#188834),(#188835,#188836,#188837),(#188838,#188839,#188840),
(#188841,#188842,#188843),(#188844,#188845,#188846),(#188847,#188848,#188849),
(#188850,#188851,#188852),(#188853,#188854,#188855)),.UNSPECIFIED.,.F.,
 .F.,.F.)
B_SPLINE_SURFACE_WITH_KNOTS((4,2,2,2,4),(3,3),(-0.000159702872864176,0.000399257182160439,
0.000798514364320879,0.00119777154648132,0.00175673160150589),(-0.00203488447750748,
1.),.UNSPECIFIED.)
GEOMETRIC_REPRESENTATION_ITEM()
RATIONAL_B_SPLINE_SURFACE(((1.00079831838497,0.803841841197695,1.),(1.00078530711036,
0.807038896055489,1.),(1.00079537143545,0.804565948522982,1.),(1.00084493107595,
0.792388441387141,1.),(1.00087540891547,0.784899603603664,1.),(1.00094983349238,
0.766612428647442,1.),(1.00099439906428,0.755662035051707,1.),(1.00110925525072,
0.727440239732745,1.),(1.00118493769597,0.708843988672124,1.),(1.00125645292226,
0.691271682458585,1.)))
REPRESENTATION_ITEM('')
SURFACE()
);
#2916=(
BOUNDED_SURFACE()
B_SPLINE_SURFACE(3,2,((#188905,#188906,#188907),(#188908,#188909,#188910),
(#188911,#188912,#188913),(#188914,#188915,#188916),(#188917,#188918,#188919),
(#188920,#188921,#188922)),.UNSPECIFIED.,.F.,.F.,.F.)
B_SPLINE_SURFACE_WITH_KNOTS((4,2,4),(3,3),(-9.2024572792766E-5,0.000795696580732677,
0.00168341773425804),(0.,1.00126533647542),.UNSPECIFIED.)
GEOMETRIC_REPRESENTATION_ITEM()
RATIONAL_B_SPLINE_SURFACE(((1.,0.715289297039673,1.0007205096748),(1.,0.687888441120641,
1.0007898522797),(1.,0.659167558273284,1.00086253544105),(1.,0.618590884857398,
1.0009652217309),(1.,0.606932851144685,1.00099472440148),(1.,0.610119385799617,
1.00098666032442)))
REPRESENTATION_ITEM('')
SURFACE()
);
#2917=(
BOUNDED_SURFACE()
B_SPLINE_SURFACE(3,2,((#188952,#188953,#188954),(#188955,#188956,#188957),
(#188958,#188959,#188960),(#188961,#188962,#188963),(#188964,#188965,#188966),
(#188967,#188968,#188969),(#188970,#188971,#188972),(#188973,#188974,#188975),
(#188976,#188977,#188978),(#188979,#188980,#188981)),.UNSPECIFIED.,.F.,
 .F.,.F.)
B_SPLINE_SURFACE_WITH_KNOTS((4,2,2,2,4),(3,3),(-7.15573433840433E-18,0.000392138229924569,
0.000784276459849145,0.00117641468977372,0.00156855291969829),(0.,1.),
 .UNSPECIFIED.)
GEOMETRIC_REPRESENTATION_ITEM()
RATIONAL_B_SPLINE_SURFACE(((1.,0.761454662564716,1.),(1.,0.777350220421001,
1.),(1.,0.789525254479917,1.),(1.,0.80808932428192,1.),(1.,0.814267286660623,
1.),(1.,0.822043050215882,1.),(1.,0.823560107182087,1.),(1.,0.822913353545903,
1.),(1.,0.820747192732385,1.),(1.,0.816955285488498,1.)))
REPRESENTATION_ITEM('')
SURFACE()
);
#2918=(
BOUNDED_SURFACE()
B_SPLINE_SURFACE(3,2,((#189021,#189022,#189023),(#189024,#189025,#189026),
(#189027,#189028,#189029),(#189030,#189031,#189032)),.UNSPECIFIED.,.F.,
 .F.,.F.)
B_SPLINE_SURFACE_WITH_KNOTS((4,4),(3,3),(0.,0.000503800937603746),(0.,1.),
 .UNSPECIFIED.)
GEOMETRIC_REPRESENTATION_ITEM()
RATIONAL_B_SPLINE_SURFACE(((1.,0.816955285488328,1.),(1.,0.819071576866324,
1.),(1.,0.821113754793722,1.),(1.,0.823084066989369,1.)))
REPRESENTATION_ITEM('')
SURFACE()
);
#2919=(
BOUNDED_SURFACE()
B_SPLINE_SURFACE(3,2,((#189036,#189037,#189038),(#189039,#189040,#189041),
(#189042,#189043,#189044),(#189045,#189046,#189047),(#189048,#189049,#189050),
(#189051,#189052,#189053),(#189054,#189055,#189056),(#189057,#189058,#189059),
(#189060,#189061,#189062),(#189063,#189064,#189065)),.UNSPECIFIED.,.F.,
 .F.,.F.)
B_SPLINE_SURFACE_WITH_KNOTS((4,2,2,2,4),(3,3),(-4.62791697325438E-16,0.00043428534736775,
0.000868570694735964,0.00130285604210418,0.00173714138947239),(0.,1.),
 .UNSPECIFIED.)
GEOMETRIC_REPRESENTATION_ITEM()
RATIONAL_B_SPLINE_SURFACE(((1.,0.823084066989561,1.),(1.,0.819254444805576,
1.),(1.,0.813299508531675,1.),(1.,0.797300511206505,1.),(1.,0.787129420739965,
1.),(1.,0.761999300344554,1.),(1.,0.746886433981532,1.),(1.,0.710597168436061,
1.),(1.,0.68930848675479,1.),(1.,0.664389729441784,1.)))
REPRESENTATION_ITEM('')
SURFACE()
);
#2920=(
BOUNDED_SURFACE()
B_SPLINE_SURFACE(3,2,((#189124,#189125,#189126),(#189127,#189128,#189129),
(#189130,#189131,#189132),(#189133,#189134,#189135),(#189136,#189137,#189138),
(#189139,#189140,#189141),(#189142,#189143,#189144),(#189145,#189146,#189147)),
 .UNSPECIFIED.,.F.,.F.,.F.)
B_SPLINE_SURFACE_WITH_KNOTS((4,2,2,4),(3,3),(-2.3396834471962E-5,0.000883592517330617,
0.00132538877599593,0.00179058186913343),(0.,1.00056892075226),
 .UNSPECIFIED.)
GEOMETRIC_REPRESENTATION_ITEM()
RATIONAL_B_SPLINE_SURFACE(((1.,0.710255087975394,1.00032968378662),(1.,
0.764314513729547,1.00026817272829),(1.,0.803922650049074,1.00022310494687),
(1.,0.84311117612549,1.0001785146154),(1.,0.852411846552129,1.00016793192657),
(1.,0.865347821163161,1.00015321283775),(1.,0.86831947063463,1.00014983157165),
(1.,0.867933686036368,1.00015027053338)))
REPRESENTATION_ITEM('')
SURFACE()
);
#2921=(
BOUNDED_SURFACE()
B_SPLINE_SURFACE(3,2,((#189196,#189197,#189198),(#189199,#189200,#189201),
(#189202,#189203,#189204),(#189205,#189206,#189207)),.UNSPECIFIED.,.F.,
 .F.,.F.)
B_SPLINE_SURFACE_WITH_KNOTS((4,4),(3,3),(0.,0.00040046484477139),(0.,1.),
 .UNSPECIFIED.)
GEOMETRIC_REPRESENTATION_ITEM()
RATIONAL_B_SPLINE_SURFACE(((1.,0.707106781186548,1.),(1.,0.718332690797356,
1.),(1.,0.721890377876178,1.),(1.,0.71893387489533,1.)))
REPRESENTATION_ITEM('')
SURFACE()
);
#2922=(
BOUNDED_SURFACE()
B_SPLINE_SURFACE(3,2,((#189227,#189228,#189229),(#189230,#189231,#189232),
(#189233,#189234,#189235),(#189236,#189237,#189238)),.UNSPECIFIED.,.F.,
 .F.,.F.)
B_SPLINE_SURFACE_WITH_KNOTS((4,4),(3,3),(0.,0.000502699148463484),(0.,1.),
 .UNSPECIFIED.)
GEOMETRIC_REPRESENTATION_ITEM()
RATIONAL_B_SPLINE_SURFACE(((1.,0.868041451421792,1.),(1.,0.868099423952364,
1.),(1.,0.868099396145349,1.),(1.,0.868041451421496,1.)))
REPRESENTATION_ITEM('')
SURFACE()
);
#2923=(
BOUNDED_SURFACE()
B_SPLINE_SURFACE(3,2,((#189240,#189241,#189242),(#189243,#189244,#189245),
(#189246,#189247,#189248),(#189249,#189250,#189251)),.UNSPECIFIED.,.F.,
 .F.,.F.)
B_SPLINE_SURFACE_WITH_KNOTS((4,4),(3,3),(0.0235251249547107,0.0240364247854912),
(0.,0.920133931130292),.UNSPECIFIED.)
GEOMETRIC_REPRESENTATION_ITEM()
RATIONAL_B_SPLINE_SURFACE(((1.,0.856496456488226,0.977077872221683),(1.,
0.856565845946365,0.977088955948168),(1.,0.856565846106366,0.977088955973725),
(1.,0.85649645648538,0.977077872221228)))
REPRESENTATION_ITEM('')
SURFACE()
);
#2924=(
BOUNDED_SURFACE()
B_SPLINE_SURFACE(3,2,((#189255,#189256,#189257),(#189258,#189259,#189260),
(#189261,#189262,#189263),(#189264,#189265,#189266)),.UNSPECIFIED.,.F.,
 .F.,.F.)
B_SPLINE_SURFACE_WITH_KNOTS((4,4),(3,3),(0.0238558353156833,0.0243674807756399),
(0.,0.921037717824849),.UNSPECIFIED.)
GEOMETRIC_REPRESENTATION_ITEM()
RATIONAL_B_SPLINE_SURFACE(((1.,0.866519190723957,0.978920101345955),(1.,
0.866587888331177,0.978930950385647),(1.,0.866587880203078,0.978930949102021),
(1.,0.866519190868502,0.978920101368782)))
REPRESENTATION_ITEM('')
SURFACE()
);
#2925=(
BOUNDED_SURFACE()
B_SPLINE_SURFACE(3,2,((#189268,#189269,#189270),(#189271,#189272,#189273),
(#189274,#189275,#189276),(#189277,#189278,#189279)),.UNSPECIFIED.,.F.,
 .F.,.F.)
B_SPLINE_SURFACE_WITH_KNOTS((4,4),(3,3),(-8.67361737988404E-19,0.00050299424914367),
(0.,1.),.UNSPECIFIED.)
GEOMETRIC_REPRESENTATION_ITEM()
RATIONAL_B_SPLINE_SURFACE(((1.,0.877250029438358,1.),(1.,0.877307222991301,
1.),(1.,0.877307195652826,1.),(1.,0.877250029437921,1.)))
REPRESENTATION_ITEM('')
SURFACE()
);
#2926=(
BOUNDED_SURFACE()
B_SPLINE_SURFACE(3,2,((#189418,#189419,#189420),(#189421,#189422,#189423),
(#189424,#189425,#189426),(#189427,#189428,#189429),(#189430,#189431,#189432),
(#189433,#189434,#189435)),.UNSPECIFIED.,.F.,.F.,.F.)
B_SPLINE_SURFACE_WITH_KNOTS((4,2,4),(3,3),(0.,0.000611885440421095,0.00122377088084219),
(0.,1.),.UNSPECIFIED.)
GEOMETRIC_REPRESENTATION_ITEM()
RATIONAL_B_SPLINE_SURFACE(((1.,0.713250449154079,1.),(1.,0.672263173507019,
1.),(1.,0.648659882421647,1.),(1.,0.648739723662275,1.),(1.,0.672275262307808,
1.),(1.,0.713250449154082,1.)))
REPRESENTATION_ITEM('')
SURFACE()
);
#2927=(
BOUNDED_SURFACE()
B_SPLINE_SURFACE(3,2,((#189462,#189463,#189464),(#189465,#189466,#189467),
(#189468,#189469,#189470),(#189471,#189472,#189473),(#189474,#189475,#189476),
(#189477,#189478,#189479),(#189480,#189481,#189482),(#189483,#189484,#189485),
(#189486,#189487,#189488),(#189489,#189490,#189491)),.UNSPECIFIED.,.F.,
 .F.,.F.)
B_SPLINE_SURFACE_WITH_KNOTS((4,2,2,2,4),(3,3),(-1.10588621593521E-17,0.00061030576480229,
0.00122061152960459,0.00183091729440689,0.0024412230592092),(0.,1.),
 .UNSPECIFIED.)
GEOMETRIC_REPRESENTATION_ITEM()
RATIONAL_B_SPLINE_SURFACE(((1.,0.727552664059041,1.),(1.,0.745088511631937,
1.),(1.,0.761651043043578,1.),(1.,0.793171709476032,1.),(1.,0.808261553244041,
1.),(1.,0.836218122215552,1.),(1.,0.8491155211034,1.),(1.,0.872797166619207,
1.),(1.,0.883451618896772,1.),(1.,0.892325300547709,1.)))
REPRESENTATION_ITEM('')
SURFACE()
);
#2928=(
BOUNDED_SURFACE()
B_SPLINE_SURFACE(3,2,((#189539,#189540,#189541),(#189542,#189543,#189544),
(#189545,#189546,#189547),(#189548,#189549,#189550)),.UNSPECIFIED.,.F.,
 .F.,.F.)
B_SPLINE_SURFACE_WITH_KNOTS((4,4),(3,3),(0.,0.010514647628205),(0.,1.),
 .UNSPECIFIED.)
GEOMETRIC_REPRESENTATION_ITEM()
RATIONAL_B_SPLINE_SURFACE(((1.,0.727552664059029,1.),(1.,0.728396913847474,
1.),(1.,0.728235528042243,1.),(1.,0.727880838895167,1.)))
REPRESENTATION_ITEM('')
SURFACE()
);
#2929=(
BOUNDED_SURFACE()
B_SPLINE_SURFACE(3,2,((#189581,#189582,#189583),(#189584,#189585,#189586),
(#189587,#189588,#189589),(#189590,#189591,#189592),(#189593,#189594,#189595),
(#189596,#189597,#189598),(#189599,#189600,#189601),(#189602,#189603,#189604),
(#189605,#189606,#189607),(#189608,#189609,#189610)),.UNSPECIFIED.,.F.,
 .F.,.F.)
B_SPLINE_SURFACE_WITH_KNOTS((4,2,2,2,4),(3,3),(-0.000237785429372242,0.000594463573430658,
0.00118892714686131,0.00178339072029198,0.00261563972309489),(0.,1.00128235392051),
 .UNSPECIFIED.)
GEOMETRIC_REPRESENTATION_ITEM()
RATIONAL_B_SPLINE_SURFACE(((1.,0.922004222179873,1.00020003638294),(1.,
0.933851150468113,1.00016965247307),(1.,0.92880531270258,1.00018259357275),
(1.,0.902012680283328,1.0002513088472),(1.,0.885879697912423,1.00029268523358),
(1.,0.848390934561697,1.0003888329589),(1.,0.826950983044361,1.00044382017067),
(1.,0.770649871834025,1.00058821607204),(1.,0.734476704092988,1.00068098967898),
(1.,0.693640011354707,1.00078572386505)))
REPRESENTATION_ITEM('')
SURFACE()
);
#2930=(
BOUNDED_SURFACE()
B_SPLINE_SURFACE(3,2,((#189682,#189683,#189684),(#189685,#189686,#189687),
(#189688,#189689,#189690),(#189691,#189692,#189693),(#189694,#189695,#189696),
(#189697,#189698,#189699)),.UNSPECIFIED.,.F.,.F.,.F.)
B_SPLINE_SURFACE_WITH_KNOTS((4,2,4),(3,3),(-1.38777878078145E-17,0.0041604828508626,
0.00832096570172521),(0.,1.),.UNSPECIFIED.)
GEOMETRIC_REPRESENTATION_ITEM()
RATIONAL_B_SPLINE_SURFACE(((1.,0.928260885086434,1.),(1.,0.928493402693592,
1.),(1.,0.928615016565842,1.),(1.,0.928561249118847,1.),(1.,0.928391240061757,
1.),(1.,0.928132015153712,1.)))
REPRESENTATION_ITEM('')
SURFACE()
);
#2931=(
BOUNDED_SURFACE()
B_SPLINE_SURFACE(3,2,((#189722,#189723,#189724),(#189725,#189726,#189727),
(#189728,#189729,#189730),(#189731,#189732,#189733),(#189734,#189735,#189736),
(#189737,#189738,#189739),(#189740,#189741,#189742),(#189743,#189744,#189745),
(#189746,#189747,#189748),(#189749,#189750,#189751)),.UNSPECIFIED.,.F.,
 .F.,.F.)
B_SPLINE_SURFACE_WITH_KNOTS((4,2,2,2,4),(3,3),(-0.00023493367097703,0.000587334177442414,
0.00117466835488487,0.00176200253232733,0.00258427038074678),(0.,1.00065879078994),
 .UNSPECIFIED.)
GEOMETRIC_REPRESENTATION_ITEM()
RATIONAL_B_SPLINE_SURFACE(((1.,0.701334864614367,1.00039351568094),(1.,
0.741616670565157,1.00034044111541),(1.,0.777121913763768,1.00029366006098),
(1.,0.832030184715688,1.00022131393459),(1.,0.853267713621314,1.00019333175771),
(1.,0.889718813400979,1.00014530446007),(1.,0.905272975779917,1.00012481058223),
(1.,0.930301816583754,1.00009183304262),(1.,0.933805909408884,1.00008721611446),
(1.,0.920947462794136,1.00010415816686)))
REPRESENTATION_ITEM('')
SURFACE()
);
#2932=(
BOUNDED_SURFACE()
B_SPLINE_SURFACE(3,2,((#189820,#189821,#189822),(#189823,#189824,#189825),
(#189826,#189827,#189828),(#189829,#189830,#189831)),.UNSPECIFIED.,.F.,
 .F.,.F.)
B_SPLINE_SURFACE_WITH_KNOTS((4,4),(3,3),(0.,0.0107001581246114),(0.,1.),
 .UNSPECIFIED.)
GEOMETRIC_REPRESENTATION_ITEM()
RATIONAL_B_SPLINE_SURFACE(((1.,0.73489735095993,1.),(1.,0.734875794442845,
1.),(1.,0.734252034560147,1.),(1.,0.73129868040477,1.)))
REPRESENTATION_ITEM('')
SURFACE()
);
#2933=(
BOUNDED_SURFACE()
B_SPLINE_SURFACE(3,2,((#189843,#189844,#189845),(#189846,#189847,#189848),
(#189849,#189850,#189851),(#189852,#189853,#189854)),.UNSPECIFIED.,.F.,
 .F.,.F.)
B_SPLINE_SURFACE_WITH_KNOTS((4,4),(3,3),(0.,0.000517122404042923),(0.,1.),
 .UNSPECIFIED.)
GEOMETRIC_REPRESENTATION_ITEM()
RATIONAL_B_SPLINE_SURFACE(((1.,0.707106781186546,1.),(1.,0.731070766440982,
1.),(1.,0.753745435486364,1.),(1.,0.77196935846749,1.)))
REPRESENTATION_ITEM('')
SURFACE()
);
#2934=(
BOUNDED_SURFACE()
B_SPLINE_SURFACE(3,2,((#189866,#189867,#189868),(#189869,#189870,#189871),
(#189872,#189873,#189874),(#189875,#189876,#189877),(#189878,#189879,#189880),
(#189881,#189882,#189883)),.UNSPECIFIED.,.F.,.F.,.F.)
B_SPLINE_SURFACE_WITH_KNOTS((4,2,4),(3,3),(-2.92626166353837E-16,0.00117037761632422,
0.00247736720267303),(0.,1.00013661197002),.UNSPECIFIED.)
GEOMETRIC_REPRESENTATION_ITEM()
RATIONAL_B_SPLINE_SURFACE(((1.,0.888632222864986,1.00003042834286),(1.,
0.871230572502141,1.00003518289034),(1.,0.84777527697816,1.0000415914386),
(1.,0.791539704054847,1.0000569563434),(1.,0.757531651118529,1.00006624815762),
(1.,0.719456177971868,1.00007665128841)))
REPRESENTATION_ITEM('')
SURFACE()
);
#2935=(
BOUNDED_SURFACE()
B_SPLINE_SURFACE(3,2,((#189921,#189922,#189923),(#189924,#189925,#189926),
(#189927,#189928,#189929),(#189930,#189931,#189932),(#189933,#189934,#189935),
(#189936,#189937,#189938),(#189939,#189940,#189941),(#189942,#189943,#189944),
(#189945,#189946,#189947),(#189948,#189949,#189950),(#189951,#189952,#189953),
(#189954,#189955,#189956)),.UNSPECIFIED.,.F.,.F.,.F.)
B_SPLINE_SURFACE_WITH_KNOTS((4,2,2,2,2,4),(3,3),(-0.000229639107487331,
0.000574097768718188,0.00114819553743641,0.00143524442179553,0.00172229330615464,
0.00252603018236012),(0.,1.0004970139285),.UNSPECIFIED.)
GEOMETRIC_REPRESENTATION_ITEM()
RATIONAL_B_SPLINE_SURFACE(((1.,0.700923021341121,1.00029729084818),(1.,
0.7401895073962,1.00025825886719),(1.,0.774929246625952,1.00022372659865),
(1.,0.828726764317455,1.00017025036743),(1.,0.848866331641938,1.00015023107648),
(1.,0.875086581874444,1.00012416741733),(1.,0.883052096108772,1.00011624947429),
(1.,0.896973719729107,1.00010241099259),(1.,0.903053458090336,1.0000963675633),
(1.,0.921003114707731,1.0000785251046),(1.,0.923996083572407,1.00007555001017),
(1.,0.912082123762018,1.00008739281811)))
REPRESENTATION_ITEM('')
SURFACE()
);
#2936=(
BOUNDED_SURFACE()
B_SPLINE_SURFACE(3,2,((#190030,#190031,#190032),(#190033,#190034,#190035),
(#190036,#190037,#190038),(#190039,#190040,#190041)),.UNSPECIFIED.,.F.,
 .F.,.F.)
B_SPLINE_SURFACE_WITH_KNOTS((4,4),(3,3),(-0.00012025625334337,0.00992992973959445),
(0.,1.00012025625329),.UNSPECIFIED.)
GEOMETRIC_REPRESENTATION_ITEM()
RATIONAL_B_SPLINE_SURFACE(((1.,0.733625250090197,1.00006406645879),(1.,
0.732900523743408,1.00006424076454),(1.,0.731718785769699,1.0000645249873),
(1.,0.729605009136797,1.00006503337702)))
REPRESENTATION_ITEM('')
SURFACE()
);
#2937=(
BOUNDED_SURFACE()
B_SPLINE_SURFACE(3,2,((#190062,#190063,#190064),(#190065,#190066,#190067),
(#190068,#190069,#190070),(#190071,#190072,#190073),(#190074,#190075,#190076),
(#190077,#190078,#190079)),.UNSPECIFIED.,.F.,.F.,.F.)
B_SPLINE_SURFACE_WITH_KNOTS((4,2,4),(3,3),(-1.04083408558608E-17,0.00416021787251448,
0.00832043574502897),(0.,1.),.UNSPECIFIED.)
GEOMETRIC_REPRESENTATION_ITEM()
RATIONAL_B_SPLINE_SURFACE(((1.,0.91815876419713,1.),(1.,0.918478576988139,
1.),(1.,0.918702883828552,1.),(1.,0.918900670636956,1.),(1.,0.918880394705029,
1.),(1.,0.918792784744087,1.)))
REPRESENTATION_ITEM('')
SURFACE()
);
#2938=(
BOUNDED_SURFACE()
B_SPLINE_SURFACE(3,2,((#190115,#190116,#190117),(#190118,#190119,#190120),
(#190121,#190122,#190123),(#190124,#190125,#190126),(#190127,#190128,#190129),
(#190130,#190131,#190132)),.UNSPECIFIED.,.F.,.F.,.F.)
B_SPLINE_SURFACE_WITH_KNOTS((4,2,4),(3,3),(0.,0.00128099832444667,0.00256199664889334),
(0.,1.),.UNSPECIFIED.)
GEOMETRIC_REPRESENTATION_ITEM()
RATIONAL_B_SPLINE_SURFACE(((1.,0.901968956514557,1.),(1.,0.883369478136272,
1.),(1.,0.857628018061933,1.),(1.,0.799434735382796,1.),(1.,0.766284883168506,
1.),(1.,0.729712990977659,1.)))
REPRESENTATION_ITEM('')
SURFACE()
);
#2939=(
BOUNDED_SURFACE()
B_SPLINE_SURFACE(3,2,((#190148,#190149,#190150),(#190151,#190152,#190153),
(#190154,#190155,#190156),(#190157,#190158,#190159),(#190160,#190161,#190162),
(#190163,#190164,#190165),(#190166,#190167,#190168),(#190169,#190170,#190171),
(#190172,#190173,#190174),(#190175,#190176,#190177)),.UNSPECIFIED.,.F.,
 .F.,.F.)
B_SPLINE_SURFACE_WITH_KNOTS((4,2,2,2,4),(3,3),(-0.000230073755017583,0.000575184387543924,
0.00115036877508786,0.00172555316263179,0.0025308113051933),(0.,1.00091870395598),
 .UNSPECIFIED.)
GEOMETRIC_REPRESENTATION_ITEM()
RATIONAL_B_SPLINE_SURFACE(((1.,0.912190934045583,1.00016134107253),(1.,
0.923169507875512,1.00014116895411),(1.,0.919328473509897,1.00014822650104),
(1.,0.895550804689188,1.00019191577786),(1.,0.880755800234217,1.00021910023611),
(1.,0.845438547487969,1.00028399243573),(1.,0.825154962787659,1.00032126165474),
(1.,0.771085355509094,1.00042060957895),(1.,0.736236157458662,1.00048464177118),
(1.,0.696833914618885,1.00055703976392)))
REPRESENTATION_ITEM('')
SURFACE()
);
#2940=(
BOUNDED_SURFACE()
B_SPLINE_SURFACE(3,2,((#190247,#190248,#190249),(#190250,#190251,#190252),
(#190253,#190254,#190255),(#190256,#190257,#190258)),.UNSPECIFIED.,.F.,
 .F.,.F.)
B_SPLINE_SURFACE_WITH_KNOTS((4,4),(3,3),(-8.33055367281454E-5,0.00981269153950731),
(0.,1.00008330553673),.UNSPECIFIED.)
GEOMETRIC_REPRESENTATION_ITEM()
RATIONAL_B_SPLINE_SURFACE(((1.,0.729482986426254,1.00004507113002),(1.,
0.730583093938839,1.00004488783993),(1.,0.730289958374372,1.00004493667956),
(1.,0.729733000633497,1.00004502947488)))
REPRESENTATION_ITEM('')
SURFACE()
);
#2941=(
BOUNDED_SURFACE()
B_SPLINE_SURFACE(3,2,((#190285,#190286,#190287),(#190288,#190289,#190290),
(#190291,#190292,#190293),(#190294,#190295,#190296)),.UNSPECIFIED.,.F.,
 .F.,.F.)
B_SPLINE_SURFACE_WITH_KNOTS((4,4),(3,3),(-6.39679281766448E-18,3.42512019832298E-5),
(0.,1.),.UNSPECIFIED.)
GEOMETRIC_REPRESENTATION_ITEM()
RATIONAL_B_SPLINE_SURFACE(((1.,0.707106781186548,1.),(1.,0.70842711846827,
1.),(1.,0.709730890158149,1.),(1.,0.711017327239758,1.)))
REPRESENTATION_ITEM('')
SURFACE()
);
#2942=(
BOUNDED_SURFACE()
B_SPLINE_SURFACE(3,2,((#190308,#190309,#190310),(#190311,#190312,#190313),
(#190314,#190315,#190316),(#190317,#190318,#190319),(#190320,#190321,#190322),
(#190323,#190324,#190325),(#190326,#190327,#190328),(#190329,#190330,#190331)),
 .UNSPECIFIED.,.F.,.F.,.F.)
B_SPLINE_SURFACE_WITH_KNOTS((4,2,2,4),(3,3),(-4.40186082029115E-17,0.00128517876997136,
0.00192776815495707,0.00257035753994277),(0.,1.),.UNSPECIFIED.)
GEOMETRIC_REPRESENTATION_ITEM()
RATIONAL_B_SPLINE_SURFACE(((1.,0.729533004763577,1.),(1.,0.766429181343272,
1.),(1.,0.799163813689396,1.),(1.,0.843673470277402,1.),(1.,0.857403797497954,
1.),(1.,0.882315838156852,1.),(1.,0.8936522353954,1.),(1.,0.903015666115932,
1.)))
REPRESENTATION_ITEM('')
SURFACE()
);
#2943=(
BOUNDED_SURFACE()
B_SPLINE_SURFACE(3,2,((#190367,#190368,#190369),(#190370,#190371,#190372),
(#190373,#190374,#190375),(#190376,#190377,#190378)),.UNSPECIFIED.,.F.,
 .F.,.F.)
B_SPLINE_SURFACE_WITH_KNOTS((4,4),(3,3),(-6.61363325216158E-18,2.21589532008063E-5),
(0.,1.),.UNSPECIFIED.)
GEOMETRIC_REPRESENTATION_ITEM()
RATIONAL_B_SPLINE_SURFACE(((1.,0.707106781186552,1.),(1.,0.707961610595566,
1.),(1.,0.708809519028292,1.),(1.,0.709650295730098,1.)))
REPRESENTATION_ITEM('')
SURFACE()
);
#2944=(
BOUNDED_SURFACE()
B_SPLINE_SURFACE(3,2,((#190438,#190439,#190440),(#190441,#190442,#190443),
(#190444,#190445,#190446),(#190447,#190448,#190449)),.UNSPECIFIED.,.F.,
 .F.,.F.)
B_SPLINE_SURFACE_WITH_KNOTS((4,4),(3,3),(0.00880203782093236,0.00917783640854858),
(0.,1.),.UNSPECIFIED.)
GEOMETRIC_REPRESENTATION_ITEM()
RATIONAL_B_SPLINE_SURFACE(((1.,0.928452770819608,1.),(1.,0.928460035446427,
1.),(1.,0.928468213633899,1.),(1.,0.928477160954731,1.)))
REPRESENTATION_ITEM('')
SURFACE()
);
#2945=(
BOUNDED_SURFACE()
B_SPLINE_SURFACE(3,2,((#190455,#190456,#190457),(#190458,#190459,#190460),
(#190461,#190462,#190463),(#190464,#190465,#190466)),.UNSPECIFIED.,.F.,
 .F.,.F.)
B_SPLINE_SURFACE_WITH_KNOTS((4,4),(3,3),(0.,0.000210836370419711),(0.,1.),
 .UNSPECIFIED.)
GEOMETRIC_REPRESENTATION_ITEM()
RATIONAL_B_SPLINE_SURFACE(((1.,0.928492930368189,1.),(1.,0.928487440815482,
1.),(1.,0.928482179049582,1.),(1.,0.928477160954739,1.)))
REPRESENTATION_ITEM('')
SURFACE()
);
#2946=(
BOUNDED_SURFACE()
B_SPLINE_SURFACE(3,2,((#190475,#190476,#190477),(#190478,#190479,#190480),
(#190481,#190482,#190483),(#190484,#190485,#190486),(#190487,#190488,#190489),
(#190490,#190491,#190492),(#190493,#190494,#190495),(#190496,#190497,#190498),
(#190499,#190500,#190501),(#190502,#190503,#190504),(#190505,#190506,#190507),
(#190508,#190509,#190510)),.UNSPECIFIED.,.F.,.F.,.F.)
B_SPLINE_SURFACE_WITH_KNOTS((4,2,2,2,2,4),(3,3),(0.,0.000515857252641128,
0.00103171450528226,0.00154757175792339,0.00180550038424395,0.00206342901056451),
(0.,1.),.UNSPECIFIED.)
GEOMETRIC_REPRESENTATION_ITEM()
RATIONAL_B_SPLINE_SURFACE(((1.,0.833636261310757,1.),(1.,0.852503152936051,
1.),(1.,0.870009925957043,1.),(1.,0.902231799969848,1.),(1.,0.917257297026174,
1.),(1.,0.941890812780404,1.),(1.,0.951540383616161,1.),(1.,0.957012273115604,
1.),(1.,0.957266013039511,1.),(1.,0.954585364787499,1.),(1.,0.951691174223743,
1.),(1.,0.94762543845782,1.)))
REPRESENTATION_ITEM('')
SURFACE()
);
#2947=(
BOUNDED_SURFACE()
B_SPLINE_SURFACE(3,2,((#190538,#190539,#190540),(#190541,#190542,#190543),
(#190544,#190545,#190546),(#190547,#190548,#190549),(#190550,#190551,#190552),
(#190553,#190554,#190555),(#190556,#190557,#190558),(#190559,#190560,#190561),
(#190562,#190563,#190564),(#190565,#190566,#190567),(#190568,#190569,#190570),
(#190571,#190572,#190573)),.UNSPECIFIED.,.F.,.F.,.F.)
B_SPLINE_SURFACE_WITH_KNOTS((4,2,2,2,2,4),(3,3),(-0.000236631349860531,
0.000591578374651329,0.000887367561976994,0.00118315674930266,0.00177473512395399,
0.00260294484846585),(-0.000316350823376031,1.),.UNSPECIFIED.)
GEOMETRIC_REPRESENTATION_ITEM()
RATIONAL_B_SPLINE_SURFACE(((1.00005654889587,0.910623125196701,1.),(1.00004251824259,
0.932798906393937,1.),(1.00003076168259,0.951380429072687,1.),(1.00002821571298,
0.95540439459059,1.),(1.00002884406971,0.954411261834663,1.),(1.0000324794467,
0.94866546204241,1.),(1.00003543438326,0.943995114528206,1.),(1.00004647347567,
0.926547566441873,1.),(1.00005663693604,0.910483975614549,1.),(1.00008366922795,
0.867758795350838,1.),(1.00010211678816,0.838601987700274,1.),(1.00012218890575,
0.806877528490201,1.)))
REPRESENTATION_ITEM('')
SURFACE()
);
#2948=(
BOUNDED_SURFACE()
B_SPLINE_SURFACE(3,2,((#190623,#190624,#190625),(#190626,#190627,#190628),
(#190629,#190630,#190631),(#190632,#190633,#190634)),.UNSPECIFIED.,.F.,
 .F.,.F.)
B_SPLINE_SURFACE_WITH_KNOTS((4,4),(3,3),(-5.20417042793042E-18,0.000729297262992661),
(0.,1.),.UNSPECIFIED.)
GEOMETRIC_REPRESENTATION_ITEM()
RATIONAL_B_SPLINE_SURFACE(((1.,0.833636261310766,1.),(1.,0.833189131672253,
1.),(1.,0.83273693675361,1.),(1.,0.832279622729512,1.)))
REPRESENTATION_ITEM('')
SURFACE()
);
#2949=(
BOUNDED_SURFACE()
B_SPLINE_SURFACE(3,2,((#190640,#190641,#190642),(#190643,#190644,#190645),
(#190646,#190647,#190648),(#190649,#190650,#190651)),.UNSPECIFIED.,.F.,
 .F.,.F.)
B_SPLINE_SURFACE_WITH_KNOTS((4,4),(3,3),(-1.04083408558608E-17,0.000723082784825488),
(0.,1.),.UNSPECIFIED.)
GEOMETRIC_REPRESENTATION_ITEM()
RATIONAL_B_SPLINE_SURFACE(((1.,0.832455503270619,1.),(1.,0.832789231498785,
1.),(1.,0.833122604759493,1.),(1.,0.833454935865631,1.)))
REPRESENTATION_ITEM('')
SURFACE()
);
#2950=(
BOUNDED_SURFACE()
B_SPLINE_SURFACE(3,2,((#190657,#190658,#190659),(#190660,#190661,#190662),
(#190663,#190664,#190665),(#190666,#190667,#190668)),.UNSPECIFIED.,.F.,
 .F.,.F.)
B_SPLINE_SURFACE_WITH_KNOTS((4,4),(3,3),(-5.74122752815573E-5,0.0016458175534959),
(0.,1.0000582174393),.UNSPECIFIED.)
GEOMETRIC_REPRESENTATION_ITEM()
RATIONAL_B_SPLINE_SURFACE(((1.,0.831178243785979,1.00001965674069),(1.,
0.842029459925232,1.00001839328066),(1.,0.851208165407911,1.0000173245592),
(1.,0.858742600214373,1.0000164472882)))
REPRESENTATION_ITEM('')
SURFACE()
);
#2951=(
BOUNDED_SURFACE()
B_SPLINE_SURFACE(3,2,((#190695,#190696,#190697),(#190698,#190699,#190700),
(#190701,#190702,#190703),(#190704,#190705,#190706)),.UNSPECIFIED.,.F.,
 .F.,.F.)
B_SPLINE_SURFACE_WITH_KNOTS((4,4),(3,3),(-5.23390230695915E-5,0.00157016878280004),
(0.,1.00005233902307),.UNSPECIFIED.)
GEOMETRIC_REPRESENTATION_ITEM()
RATIONAL_B_SPLINE_SURFACE(((1.,0.857807746985037,1.00001488440722),(1.,
0.850509611749564,1.00001564836176),(1.,0.841739216144316,1.00001656642963),
(1.,0.831471023017743,1.00001764128403)))
REPRESENTATION_ITEM('')
SURFACE()
);
#2952=(
BOUNDED_SURFACE()
B_SPLINE_SURFACE(3,2,((#190733,#190734,#190735),(#190736,#190737,#190738),
(#190739,#190740,#190741),(#190742,#190743,#190744),(#190745,#190746,#190747),
(#190748,#190749,#190750),(#190751,#190752,#190753),(#190754,#190755,#190756)),
 .UNSPECIFIED.,.F.,.F.,.F.)
B_SPLINE_SURFACE_WITH_KNOTS((4,2,2,4),(3,3),(-2.40757934422131E-15,0.000787383129295151,
0.00157476625859271,0.00314953251718783),(0.,1.),.UNSPECIFIED.)
GEOMETRIC_REPRESENTATION_ITEM()
RATIONAL_B_SPLINE_SURFACE(((1.,0.989234343678173,1.),(1.,0.988443605143724,
1.),(1.,0.984599769902277,1.),(1.,0.971863446961927,1.),(1.,0.962926004132788,
1.),(1.,0.929467293227288,1.),(1.,0.898004938874792,1.),(1.,0.857972509692102,
1.)))
REPRESENTATION_ITEM('')
SURFACE()
);
#2953=(
BOUNDED_SURFACE()
B_SPLINE_SURFACE(3,2,((#190776,#190777,#190778),(#190779,#190780,#190781),
(#190782,#190783,#190784),(#190785,#190786,#190787),(#190788,#190789,#190790),
(#190791,#190792,#190793),(#190794,#190795,#190796),(#190797,#190798,#190799)),
 .UNSPECIFIED.,.F.,.F.,.F.)
B_SPLINE_SURFACE_WITH_KNOTS((4,2,2,4),(3,3),(2.16840434497101E-19,0.00157702467408662,
0.00236553701112993,0.00315404934817324),(0.,1.),.UNSPECIFIED.)
GEOMETRIC_REPRESENTATION_ITEM()
RATIONAL_B_SPLINE_SURFACE(((1.,0.857104357126295,1.),(1.,0.897186993221649,
1.),(1.,0.928714693488658,1.),(1.,0.962508133039243,1.),(1.,0.971517540750285,
1.),(1.,0.984393580256014,1.),(1.,0.988371316630897,1.),(1.,0.989172917436462,
1.)))
REPRESENTATION_ITEM('')
SURFACE()
);
#2954=(
BOUNDED_SURFACE()
B_SPLINE_SURFACE(3,2,((#190819,#190820,#190821),(#190822,#190823,#190824),
(#190825,#190826,#190827),(#190828,#190829,#190830),(#190831,#190832,#190833),
(#190834,#190835,#190836),(#190837,#190838,#190839),(#190840,#190841,#190842),
(#190843,#190844,#190845),(#190846,#190847,#190848),(#190849,#190850,#190851),
(#190852,#190853,#190854),(#190855,#190856,#190857),(#190858,#190859,#190860),
(#190861,#190862,#190863),(#190864,#190865,#190866),(#190867,#190868,#190869),
(#190870,#190871,#190872)),.UNSPECIFIED.,.F.,.F.,.F.)
B_SPLINE_SURFACE_WITH_KNOTS((4,2,2,2,2,2,2,2,4),(3,3),(-0.000508741685376785,
0.00254370842688261,0.00381556264032431,0.00445148974704516,0.00476945330040559,
0.0049284350770858,0.00500792596542591,0.00504767140959596,0.0055961585391427),
(0.,1.00567142871774),.UNSPECIFIED.)
GEOMETRIC_REPRESENTATION_ITEM()
RATIONAL_B_SPLINE_SURFACE(((1.,0.988073899798154,1.00013527605435),(1.,
0.990274117753828,1.00011031929575),(1.,0.992465877278408,1.00008545847993),
(1.,0.995553721434854,1.00005043350388),(1.,0.996459905831034,1.00004015478347),
(1.,0.997814118238599,1.00002479414519),(1.,0.998264976714179,1.00001968012178),
(1.,0.99893609089222,1.00001206776933),(1.,0.999159203039956,1.00000953704005),
(1.,0.999488994833662,1.00000579625875),(1.,0.999598301582193,1.00000455640789),
(1.,0.999757142399174,1.00000275469914),(1.,0.999809501617783,1.00000216079599),
(1.,0.999882023724343,1.00000133818808),(1.,0.999905504951442,1.00000107184386),
(1.,1.00019880923877,0.999997744935148),(1.,0.999814228249837,1.00000210718248),
(1.,0.965387876575238,1.00039260038155)))
REPRESENTATION_ITEM('')
SURFACE()
);
#2955=(
BOUNDED_SURFACE()
B_SPLINE_SURFACE(3,2,((#190912,#190913,#190914),(#190915,#190916,#190917),
(#190918,#190919,#190920),(#190921,#190922,#190923),(#190924,#190925,#190926),
(#190927,#190928,#190929),(#190930,#190931,#190932),(#190933,#190934,#190935),
(#190936,#190937,#190938),(#190939,#190940,#190941),(#190942,#190943,#190944),
(#190945,#190946,#190947),(#190948,#190949,#190950),(#190951,#190952,#190953),
(#190954,#190955,#190956),(#190957,#190958,#190959),(#190960,#190961,#190962),
(#190963,#190964,#190965)),.UNSPECIFIED.,.F.,.F.,.F.)
B_SPLINE_SURFACE_WITH_KNOTS((4,2,2,2,2,2,2,2,4),(3,3),(-7.45388993583784E-20,
4.05793239028379E-5,8.11586478056759E-5,0.000162317295611352,0.000324634591222704,
0.000649269182445408,0.00129853836489082,0.00259707672978163,0.00519415345956326),
(0.,1.),.UNSPECIFIED.)
GEOMETRIC_REPRESENTATION_ITEM()
RATIONAL_B_SPLINE_SURFACE(((1.,0.999961923064171,1.),(1.,0.999961833753432,
1.),(1.,0.999944633098586,1.),(1.,0.999904212270329,1.),(1.,0.99988023258917,
1.),(1.,0.999806855851567,1.),(1.,0.999754783512162,1.),(1.,0.999595776401296,
1.),(1.,0.999485889992571,1.),(1.,0.999156267866573,1.),(1.,0.998933623645324,
1.),(1.,0.998262897761582,1.),(1.,0.997812273447783,1.),(1.,0.996459235447427,
1.),(1.,0.995553264664008,1.),(1.,0.992828768547989,1.),(1.,0.991003554465269,
1.),(1.,0.989172917436461,1.)))
REPRESENTATION_ITEM('')
SURFACE()
);
#2956=(
BOUNDED_SURFACE()
B_SPLINE_SURFACE(3,2,((#191015,#191016,#191017),(#191018,#191019,#191020),
(#191021,#191022,#191023),(#191024,#191025,#191026),(#191027,#191028,#191029),
(#191030,#191031,#191032),(#191033,#191034,#191035),(#191036,#191037,#191038),
(#191039,#191040,#191041),(#191042,#191043,#191044),(#191045,#191046,#191047),
(#191048,#191049,#191050),(#191051,#191052,#191053),(#191054,#191055,#191056),
(#191057,#191058,#191059),(#191060,#191061,#191062),(#191063,#191064,#191065),
(#191066,#191067,#191068)),.UNSPECIFIED.,.F.,.F.,.F.)
B_SPLINE_SURFACE_WITH_KNOTS((4,2,2,2,2,2,2,2,4),(3,3),(-0.000525941938450675,
0.00262970969225337,0.00394456453838006,0.00460199196144341,0.00493070567297508,
0.00509506252874091,0.00517724095662383,0.00521833017056529,0.00578536132295742),
(0.,1.00671701195453),.UNSPECIFIED.)
GEOMETRIC_REPRESENTATION_ITEM()
RATIONAL_B_SPLINE_SURFACE(((1.,0.987652440486347,1.00016587740972),(1.,
0.989930475499347,1.00013527423289),(1.,0.992199484515042,1.00010479231153),
(1.,0.995396092253403,1.00006184900674),(1.,0.996334181463897,1.00004924669386),
(1.,0.997736167759121,1.00003041237645),(1.,0.998202686027925,1.00002414515887),
(1.,0.998897407157577,1.00001481225861),(1.,0.999128412532823,1.00001170892687),
(1.,0.999469951933241,1.0000071206784),(1.,0.999583268571811,1.00000559837997),
(1.,0.999747958495426,1.0000033859316),(1.,0.999802181877435,1.00000265749339),
(1.,0.999877976982937,1.00000163926013),(1.,0.999902135273186,1.00000131471708),
(1.,1.000210891347,0.999997166880602),(1.,0.999880980100307,1.00000159891618),
(1.,0.96165859498486,1.00051507935168)))
REPRESENTATION_ITEM('')
SURFACE()
);
#2957=(
BOUNDED_SURFACE()
B_SPLINE_SURFACE(3,2,((#191117,#191118,#191119),(#191120,#191121,#191122),
(#191123,#191124,#191125),(#191126,#191127,#191128),(#191129,#191130,#191131),
(#191132,#191133,#191134),(#191135,#191136,#191137),(#191138,#191139,#191140)),
 .UNSPECIFIED.,.F.,.F.,.F.)
B_SPLINE_SURFACE_WITH_KNOTS((4,2,2,4),(3,3),(0.,0.000786373253240854,0.0015727465064817,
0.00314549301296342),(0.,1.),.UNSPECIFIED.)
GEOMETRIC_REPRESENTATION_ITEM()
RATIONAL_B_SPLINE_SURFACE(((1.,0.988865480076014,1.),(1.,0.988061700311495,
1.),(1.,0.984209057857027,1.),(1.,0.971450599512814,1.),(1.,0.962500813802613,
1.),(1.,0.929017994266129,1.),(1.,0.897560549282588,1.),(1.,0.857509777230937,
1.)))
REPRESENTATION_ITEM('')
SURFACE()
);
#2958=(
BOUNDED_SURFACE()
B_SPLINE_SURFACE(3,2,((#191160,#191161,#191162),(#191163,#191164,#191165),
(#191166,#191167,#191168),(#191169,#191170,#191171),(#191172,#191173,#191174),
(#191175,#191176,#191177),(#191178,#191179,#191180),(#191181,#191182,#191183),
(#191184,#191185,#191186),(#191187,#191188,#191189),(#191190,#191191,#191192),
(#191193,#191194,#191195),(#191196,#191197,#191198),(#191199,#191200,#191201),
(#191202,#191203,#191204),(#191205,#191206,#191207),(#191208,#191209,#191210),
(#191211,#191212,#191213)),.UNSPECIFIED.,.F.,.F.,.F.)
B_SPLINE_SURFACE_WITH_KNOTS((4,2,2,2,2,2,2,2,4),(3,3),(-1.32137139771671E-19,
4.17669388829254E-5,8.35338777658508E-5,0.000167067755531702,0.000334135511063404,
0.000668271022126808,0.00133654204425361,0.00267308408850723,0.00534616817701446),
(0.,1.),.UNSPECIFIED.)
GEOMETRIC_REPRESENTATION_ITEM()
RATIONAL_B_SPLINE_SURFACE(((1.,0.999961923064171,1.),(1.,0.999961782802257,
1.),(1.,0.999943671528414,1.),(1.,0.999901604878771,1.),(1.,0.999876750335241,
1.),(1.,0.999800908054986,1.),(1.,0.99974715657318,1.),(1.,0.999583072363253,
1.),(1.,0.999469900307565,1.),(1.,0.999130340955253,1.),(1.,0.998901033022514,
1.),(1.,0.998210264756137,1.),(1.,0.997746391825068,1.),(1.,0.996353373847482,
1.),(1.,0.9954206326127,1.),(1.,0.992615540215937,1.),(1.,0.990736373728666,
1.),(1.,0.988851372352096,1.)))
REPRESENTATION_ITEM('')
SURFACE()
);
#2959=(
BOUNDED_SURFACE()
B_SPLINE_SURFACE(3,2,((#191260,#191261,#191262),(#191263,#191264,#191265),
(#191266,#191267,#191268),(#191269,#191270,#191271)),.UNSPECIFIED.,.F.,
 .F.,.F.)
B_SPLINE_SURFACE_WITH_KNOTS((4,4),(3,3),(-1.85521401386541E-5,0.00125436719122141),
(0.,1.00001918161636),.UNSPECIFIED.)
GEOMETRIC_REPRESENTATION_ITEM()
RATIONAL_B_SPLINE_SURFACE(((1.,0.837815237008462,1.0000062219318),(1.,0.84540513832919,
1.00000593075865),(1.,0.852052930826092,1.00000567572784),(1.,0.857765949207726,
1.00000545655799)))
REPRESENTATION_ITEM('')
SURFACE()
);
#2960=(
BOUNDED_SURFACE()
B_SPLINE_SURFACE(3,2,((#191295,#191296,#191297),(#191298,#191299,#191300),
(#191301,#191302,#191303),(#191304,#191305,#191306),(#191307,#191308,#191309),
(#191310,#191311,#191312),(#191313,#191314,#191315),(#191316,#191317,#191318)),
 .UNSPECIFIED.,.F.,.F.,.F.)
B_SPLINE_SURFACE_WITH_KNOTS((4,2,2,4),(3,3),(8.13151629364128E-20,0.00157235613934946,
0.00235853420902418,0.00314471227869891),(0.,1.),.UNSPECIFIED.)
GEOMETRIC_REPRESENTATION_ITEM()
RATIONAL_B_SPLINE_SURFACE(((1.,0.857407773863101,1.),(1.,0.897293426532578,
1.),(1.,0.928679392158714,1.),(1.,0.962320286971746,1.),(1.,0.971291611639875,
1.),(1.,0.984107082217988,1.),(1.,0.988059746314391,1.),(1.,0.988851372352099,
1.)))
REPRESENTATION_ITEM('')
SURFACE()
);
#2961=(
BOUNDED_SURFACE()
B_SPLINE_SURFACE(3,2,((#191348,#191349,#191350),(#191351,#191352,#191353),
(#191354,#191355,#191356),(#191357,#191358,#191359)),.UNSPECIFIED.,.F.,
 .F.,.F.)
B_SPLINE_SURFACE_WITH_KNOTS((4,4),(3,3),(0.,0.000753104234298227),(0.,1.),
 .UNSPECIFIED.)
GEOMETRIC_REPRESENTATION_ITEM()
RATIONAL_B_SPLINE_SURFACE(((1.,0.839275484760762,1.),(1.,0.838901603374917,
1.),(1.,0.838526082980222,1.),(1.,0.83814959787298,1.)))
REPRESENTATION_ITEM('')
SURFACE()
);
#2962=(
BOUNDED_SURFACE()
B_SPLINE_SURFACE(3,2,((#191365,#191366,#191367),(#191368,#191369,#191370),
(#191371,#191372,#191373),(#191374,#191375,#191376)),.UNSPECIFIED.,.F.,
 .F.,.F.)
B_SPLINE_SURFACE_WITH_KNOTS((4,4),(3,3),(0.,0.00121469382512386),(0.,1.),
 .UNSPECIFIED.)
GEOMETRIC_REPRESENTATION_ITEM()
RATIONAL_B_SPLINE_SURFACE(((1.,0.857407773863101,1.),(1.,0.851918824817362,
1.),(1.,0.845578741226857,1.),(1.,0.83838293312654,1.)))
REPRESENTATION_ITEM('')
SURFACE()
);
#2963=(
BOUNDED_SURFACE()
B_SPLINE_SURFACE(3,2,((#191397,#191398,#191399),(#191400,#191401,#191402),
(#191403,#191404,#191405),(#191406,#191407,#191408),(#191409,#191410,#191411),
(#191412,#191413,#191414),(#191415,#191416,#191417),(#191418,#191419,#191420),
(#191421,#191422,#191423),(#191424,#191425,#191426),(#191427,#191428,#191429),
(#191430,#191431,#191432),(#191433,#191434,#191435),(#191436,#191437,#191438)),
 .UNSPECIFIED.,.F.,.F.,.F.)
B_SPLINE_SURFACE_WITH_KNOTS((4,2,2,2,2,2,4),(3,3),(-0.000226840284413293,
0.000567100711032879,0.000850651066549369,0.00113420142206586,0.00141775177758235,
0.00170130213309884,0.00249524312854497),(-0.000282176477353801,1.00009539139101),
 .UNSPECIFIED.)
GEOMETRIC_REPRESENTATION_ITEM()
RATIONAL_B_SPLINE_SURFACE(((1.00010528003724,0.813432211160089,1.0000355838799),
(1.00008775714205,0.844484705969625,1.00002966126993),(1.00007212354181,
0.872189162633845,1.00002437722779),(1.00005392748604,0.90443457190974,
1.00001822709449),(1.0000494556467,0.912359162369374,1.00001671564561),
(1.00004150285258,0.926452386996823,1.00001402765957),(1.00003795528609,
0.932739064433654,1.00001282860813),(1.00003236888526,0.942638780270556,
1.00001094044565),(1.00003027209024,0.946354531320264,1.00001023174432),
(1.00002812425189,0.950160736773148,1.00000950579073),(1.00002807138552,
0.950254421792609,1.00000948792228),(1.00003175744819,0.943722313910005,
1.00001073378441),(1.00004241856759,0.924829639419119,1.00001433716452),
(1.00005485908397,0.902783678063587,1.00001854196775)))
REPRESENTATION_ITEM('')
SURFACE()
);
#2964=(
BOUNDED_SURFACE()
B_SPLINE_SURFACE(3,2,((#191537,#191538,#191539),(#191540,#191541,#191542),
(#191543,#191544,#191545),(#191546,#191547,#191548)),.UNSPECIFIED.,.F.,
 .F.,.F.)
B_SPLINE_SURFACE_WITH_KNOTS((4,4),(3,3),(0.,0.000758627814399393),(0.,1.),
 .UNSPECIFIED.)
GEOMETRIC_REPRESENTATION_ITEM()
RATIONAL_B_SPLINE_SURFACE(((1.,0.838382933127103,1.),(1.,0.838759998356351,
1.),(1.,0.839135655634363,1.),(1.,0.839509576764081,1.)))
REPRESENTATION_ITEM('')
SURFACE()
);
#2965=(
BOUNDED_SURFACE()
B_SPLINE_SURFACE(3,2,((#191554,#191555,#191556),(#191557,#191558,#191559),
(#191560,#191561,#191562),(#191563,#191564,#191565),(#191566,#191567,#191568),
(#191569,#191570,#191571),(#191572,#191573,#191574),(#191575,#191576,#191577),
(#191578,#191579,#191580),(#191581,#191582,#191583),(#191584,#191585,#191586),
(#191587,#191588,#191589)),.UNSPECIFIED.,.F.,.F.,.F.)
B_SPLINE_SURFACE_WITH_KNOTS((4,2,2,2,2,4),(3,3),(-0.000216256680534375,
0.000582607613633213,0.000867916290121638,0.00115322496661006,0.00172384231958692,
0.00252270661375451),(-0.000244207734780689,1.),.UNSPECIFIED.)
GEOMETRIC_REPRESENTATION_ITEM()
RATIONAL_B_SPLINE_SURFACE(((1.00004816059777,0.901394200701356,1.),(1.00003731388615,
0.923602161531115,1.),(1.00002813164864,0.942402216152368,1.),(1.00002468431679,
0.94946041162475,1.),(1.00002465107978,0.949528462309686,1.),(1.00002636666531,
0.946015908672132,1.),(1.00002810233345,0.942462237161793,1.),(1.00003527537775,
0.927775879444964,1.),(1.0000424644099,0.913056787614755,1.),(1.0000622011378,
0.872647076777095,1.),(1.00007580610643,0.844791757926684,1.),(1.00009107581698,
0.813527984557883,1.)))
REPRESENTATION_ITEM('')
SURFACE()
);
#2966=(
BOUNDED_SURFACE()
B_SPLINE_SURFACE(2,2,((#191642,#191643,#191644),(#191645,#191646,#191647),
(#191648,#191649,#191650)),.UNSPECIFIED.,.F.,.F.,.F.)
B_SPLINE_SURFACE_WITH_KNOTS((3,3),(3,3),(1.74317346290508E-16,1.57079632679495),
(-0.736541846753928,0.787072384273275),.UNSPECIFIED.)
GEOMETRIC_REPRESENTATION_ITEM()
RATIONAL_B_SPLINE_SURFACE(((1.,0.723589867251388,1.),(0.707106781186616,
0.51165530193138,0.707106781186616),(1.,0.723589867251388,1.)))
REPRESENTATION_ITEM('')
SURFACE()
);
#2967=(
BOUNDED_SURFACE()
B_SPLINE_SURFACE(2,2,((#191663,#191664,#191665),(#191666,#191667,#191668),
(#191669,#191670,#191671)),.UNSPECIFIED.,.F.,.F.,.F.)
B_SPLINE_SURFACE_WITH_KNOTS((3,3),(3,3),(-1.74317346290519E-16,1.57079632679496),
(-2.35452026931659,-0.830906038289448),.UNSPECIFIED.)
GEOMETRIC_REPRESENTATION_ITEM()
RATIONAL_B_SPLINE_SURFACE(((1.,0.72358986725141,1.),(0.707106781186587,
0.511655301931375,0.707106781186587),(1.,0.72358986725141,1.)))
REPRESENTATION_ITEM('')
SURFACE()
);
#2968=(
BOUNDED_SURFACE()
B_SPLINE_SURFACE(2,2,((#191686,#191687,#191688),(#191689,#191690,#191691),
(#191692,#191693,#191694)),.UNSPECIFIED.,.F.,.F.,.F.)
B_SPLINE_SURFACE_WITH_KNOTS((3,3),(3,3),(1.81714697791953E-16,1.57079632679495),
(-0.74383310368946,0.26549733202973),.UNSPECIFIED.)
GEOMETRIC_REPRESENTATION_ITEM()
RATIONAL_B_SPLINE_SURFACE(((1.,0.875336395469216,1.),(0.707106781186606,
0.618956301055724,0.707106781186606),(1.,0.875336395469216,1.)))
REPRESENTATION_ITEM('')
SURFACE()
);
#2969=(
BOUNDED_SURFACE()
B_SPLINE_SURFACE(2,2,((#191706,#191707,#191708),(#191709,#191710,#191711),
(#191712,#191713,#191714)),.UNSPECIFIED.,.F.,.F.,.F.)
B_SPLINE_SURFACE_WITH_KNOTS((3,3),(3,3),(-6.30291942997115E-17,1.57079632679495),
(-1.82889777036346,-0.819567334644225),.UNSPECIFIED.)
GEOMETRIC_REPRESENTATION_ITEM()
RATIONAL_B_SPLINE_SURFACE(((1.,0.875336395469206,1.),(0.707106781186601,
0.618956301055712,0.707106781186601),(1.,0.875336395469206,1.)))
REPRESENTATION_ITEM('')
SURFACE()
);
#2970=(
BOUNDED_SURFACE()
B_SPLINE_SURFACE(2,2,((#191729,#191730,#191731),(#191732,#191733,#191734),
(#191735,#191736,#191737)),.UNSPECIFIED.,.F.,.F.,.F.)
B_SPLINE_SURFACE_WITH_KNOTS((3,3),(3,3),(-1.57079632679491,1.68131336473773E-16),
(-1.83117576062825,-0.821845324909055),.UNSPECIFIED.)
GEOMETRIC_REPRESENTATION_ITEM()
RATIONAL_B_SPLINE_SURFACE(((1.,0.875336395469216,1.),(0.70710678118653,
0.618956301055656,0.70710678118653),(1.,0.875336395469216,1.)))
REPRESENTATION_ITEM('')
SURFACE()
);
#2971=(
BOUNDED_SURFACE()
B_SPLINE_SURFACE(2,2,((#191749,#191750,#191751),(#191752,#191753,#191754),
(#191755,#191756,#191757)),.UNSPECIFIED.,.F.,.F.,.F.)
B_SPLINE_SURFACE_WITH_KNOTS((3,3),(3,3),(-1.5707963267949,2.47147205475768E-16),
(-0.746111093954295,0.263219341764958),.UNSPECIFIED.)
GEOMETRIC_REPRESENTATION_ITEM()
RATIONAL_B_SPLINE_SURFACE(((1.,0.875336395469201,1.),(0.707106781186519,
0.618956301055637,0.707106781186519),(1.,0.875336395469201,1.)))
REPRESENTATION_ITEM('')
SURFACE()
);
#2972=(
BOUNDED_SURFACE()
B_SPLINE_SURFACE(2,2,((#191772,#191773,#191774),(#191775,#191776,#191777),
(#191778,#191779,#191780)),.UNSPECIFIED.,.F.,.F.,.F.)
B_SPLINE_SURFACE_WITH_KNOTS((3,3),(3,3),(-1.57079632679491,1.67905497988288E-16),
(-2.34670754812599,-0.823093317098874),.UNSPECIFIED.)
GEOMETRIC_REPRESENTATION_ITEM()
RATIONAL_B_SPLINE_SURFACE(((1.,0.723589867251417,1.),(0.70710678118653,
0.511655301931338,0.70710678118653),(1.,0.723589867251417,1.)))
REPRESENTATION_ITEM('')
SURFACE()
);
#2973=(
BOUNDED_SURFACE()
B_SPLINE_SURFACE(2,2,((#191792,#191793,#191794),(#191795,#191796,#191797),
(#191798,#191799,#191800)),.UNSPECIFIED.,.F.,.F.,.F.)
B_SPLINE_SURFACE_WITH_KNOTS((3,3),(3,3),(-1.57079632679491,2.478375474118E-16),
(-0.728729125563299,0.794885105463935),.UNSPECIFIED.)
GEOMETRIC_REPRESENTATION_ITEM()
RATIONAL_B_SPLINE_SURFACE(((1.,0.723589867251377,1.),(0.70710678118653,
0.511655301931309,0.70710678118653),(1.,0.723589867251377,1.)))
REPRESENTATION_ITEM('')
SURFACE()
);
#2974=(
BOUNDED_SURFACE()
B_SPLINE_SURFACE(3,2,((#193720,#193721,#193722),(#193723,#193724,#193725),
(#193726,#193727,#193728),(#193729,#193730,#193731),(#193732,#193733,#193734),
(#193735,#193736,#193737),(#193738,#193739,#193740),(#193741,#193742,#193743),
(#193744,#193745,#193746),(#193747,#193748,#193749),(#193750,#193751,#193752),
(#193753,#193754,#193755),(#193756,#193757,#193758),(#193759,#193760,#193761),
(#193762,#193763,#193764),(#193765,#193766,#193767),(#193768,#193769,#193770),
(#193771,#193772,#193773),(#193774,#193775,#193776),(#193777,#193778,#193779),
(#193780,#193781,#193782),(#193783,#193784,#193785),(#193786,#193787,#193788),
(#193789,#193790,#193791),(#193792,#193793,#193794),(#193795,#193796,#193797),
(#193798,#193799,#193800),(#193801,#193802,#193803),(#193804,#193805,#193806),
(#193807,#193808,#193809),(#193810,#193811,#193812),(#193813,#193814,#193815),
(#193816,#193817,#193818),(#193819,#193820,#193821),(#193822,#193823,#193824),
(#193825,#193826,#193827),(#193828,#193829,#193830),(#193831,#193832,#193833),
(#193834,#193835,#193836),(#193837,#193838,#193839),(#193840,#193841,#193842),
(#193843,#193844,#193845),(#193846,#193847,#193848),(#193849,#193850,#193851),
(#193852,#193853,#193854),(#193855,#193856,#193857),(#193858,#193859,#193860),
(#193861,#193862,#193863)),.UNSPECIFIED.,.F.,.F.,.F.)
B_SPLINE_SURFACE_WITH_KNOTS((4,2,2,2,2,2,2,2,2,2,2,2,2,2,2,2,2,2,2,2,2,
2,2,4),(3,3),(0.,0.0059149619404375,0.00739370242554688,0.00743991306570655,
0.00748612370586621,0.00757854498618555,0.00776338754682422,0.00813307266810157,
0.00887244291065625,0.011829923880875,0.0133086643659844,0.0140480346085391,
0.0140942452486987,0.0141404558888584,0.0142328771691777,0.0144177197298164,
0.0147874048510938,0.0177448858213125,0.0192236263064219,0.0199629965489765,
0.0201478391096152,0.0203326816702539,0.0207023667915313,0.02365984776175),
(-0.000128696703876237,1.),.UNSPECIFIED.)
GEOMETRIC_REPRESENTATION_ITEM()
RATIONAL_B_SPLINE_SURFACE(((1.00003576453942,0.861051066802645,1.),(1.00003300380643,
0.871776799904612,1.),(1.00003114473836,0.878999471558354,1.),(1.00002957069443,
0.885114794930814,1.),(1.0000292946172,0.886187383506178,1.),(1.00002904679648,
0.887150192641286,1.),(1.00002905930675,0.887101588964017,1.),(1.00002907039925,
0.88705849344574,1.),(1.00002907595876,0.887036894169038,1.),(1.0000290926768,
0.886971942860521,1.),(1.00002910387483,0.886928437357747,1.),(1.00002913762479,
0.886797315265569,1.),(1.00002916033256,0.886709093220405,1.),(1.00002922906338,
0.886442066884952,1.),(1.00002927569335,0.886260904621482,1.),(1.00002941790449,
0.885708399652157,1.),(1.00002951579679,0.885328077943985,1.),(1.00003001983054,
0.883369854726223,1.),(1.0000304754155,0.881599860064861,1.),(1.00003124833757,
0.878596977882908,1.),(1.00003152026012,0.877540530673196,1.),(1.00003195407994,
0.875855095812049,1.),(1.00003210266429,0.875277830252333,1.),(1.00003226456337,
0.874648835593434,1.),(1.00003223907406,0.874747864199818,1.),(1.00003222073887,
0.87481909833159,1.),(1.00003221161445,0.874854547615397,1.),(1.00003218436966,
0.874960396475737,1.),(1.00003216637769,0.875030297104221,1.),(1.00003211290697,
0.875238036387284,1.),(1.0000320779332,0.87537391310078,1.),(1.00003197496994,
0.875773936029893,1.),(1.00003190893599,0.876030484733642,1.),(1.00003133689918,
0.878252906904018,1.),(1.00003098535817,0.879618680051682,1.),(1.00003066804144,
0.880851488372246,1.),(1.00003059686398,0.881128020145932,1.),(1.00003054204845,
0.88134098415604,1.),(1.00003053232869,0.881378746411579,1.),(1.00003053090852,
0.881384263936795,1.),(1.00003053116352,0.881383273219239,1.),(1.00003053276312,
0.881377058605224,1.),(1.00003053808665,0.881356376158469,1.),(1.00003051977626,
0.881427513909725,1.),(1.00003050821747,0.881472421022649,1.),(1.00003041011411,
0.88185356269165,1.),(1.0000303659271,0.882025233799165,1.),(1.00003036612293,
0.882024472999063,1.)))
REPRESENTATION_ITEM('')
SURFACE()
);
#2975=(
BOUNDED_SURFACE()
B_SPLINE_SURFACE(3,2,((#194043,#194044,#194045),(#194046,#194047,#194048),
(#194049,#194050,#194051),(#194052,#194053,#194054)),.UNSPECIFIED.,.F.,
 .F.,.F.)
B_SPLINE_SURFACE_WITH_KNOTS((4,4),(3,3),(1.0842021724855E-19,0.000322395538615675),
(0.,1.),.UNSPECIFIED.)
GEOMETRIC_REPRESENTATION_ITEM()
RATIONAL_B_SPLINE_SURFACE(((1.,0.861068946771251,1.),(1.,0.868023491094222,
1.),(1.,0.874094710294855,1.),(1.,0.879223463974629,1.)))
REPRESENTATION_ITEM('')
SURFACE()
);
#2976=(
BOUNDED_SURFACE()
B_SPLINE_SURFACE(3,2,((#194066,#194067,#194068),(#194069,#194070,#194071),
(#194072,#194073,#194074),(#194075,#194076,#194077)),.UNSPECIFIED.,.F.,
 .F.,.F.)
B_SPLINE_SURFACE_WITH_KNOTS((4,4),(3,3),(-1.56125112837912E-17,0.00371972595076131),
(0.,1.),.UNSPECIFIED.)
GEOMETRIC_REPRESENTATION_ITEM()
RATIONAL_B_SPLINE_SURFACE(((1.,0.879223463974645,1.),(1.,0.879197541860131,
1.),(1.,0.879166735457461,1.),(1.,0.879131676488835,1.)))
REPRESENTATION_ITEM('')
SURFACE()
);
#2977=(
BOUNDED_SURFACE()
B_SPLINE_SURFACE(3,2,((#194083,#194084,#194085),(#194086,#194087,#194088),
(#194089,#194090,#194091),(#194092,#194093,#194094),(#194095,#194096,#194097),
(#194098,#194099,#194100),(#194101,#194102,#194103),(#194104,#194105,#194106),
(#194107,#194108,#194109),(#194110,#194111,#194112),(#194113,#194114,#194115),
(#194116,#194117,#194118),(#194119,#194120,#194121),(#194122,#194123,#194124),
(#194125,#194126,#194127),(#194128,#194129,#194130),(#194131,#194132,#194133),
(#194134,#194135,#194136),(#194137,#194138,#194139),(#194140,#194141,#194142),
(#194143,#194144,#194145),(#194146,#194147,#194148),(#194149,#194150,#194151),
(#194152,#194153,#194154),(#194155,#194156,#194157),(#194158,#194159,#194160)),
 .UNSPECIFIED.,.F.,.F.,.F.)
B_SPLINE_SURFACE_WITH_KNOTS((4,2,2,2,2,2,2,2,2,2,2,2,4),(3,3),(0.,0.000191440896835587,
0.00028716134525338,0.000382881793671173,0.00057432269050676,0.000670043138924553,
0.000765763587342347,0.000957204484177933,0.00114864538101352,0.00124436582943131,
0.00129222605364021,0.00134008627784911,0.00153152717468469),(0.,1.),
 .UNSPECIFIED.)
GEOMETRIC_REPRESENTATION_ITEM()
RATIONAL_B_SPLINE_SURFACE(((1.,0.879131676489345,1.),(1.,0.880626887596785,
1.),(1.,0.882841814432506,1.),(1.,0.886761296901068,1.),(1.,0.888121788557817,
1.),(1.,0.890288150019219,1.),(1.,0.891026608347966,1.),(1.,0.892657535905197,
1.),(1.,0.894092695678742,1.),(1.,0.897075330661339,1.),(1.,0.898026040345514,
1.),(1.,0.899562222232299,1.),(1.,0.900146620417538,1.),(1.,0.901818107518504,
1.),(1.,0.902658365336305,1.),(1.,0.905247057738554,1.),(1.,0.906646088930788,
1.),(1.,0.907839183414567,1.),(1.,0.908162443627513,1.),(1.,0.90858816846029,
1.),(1.,0.908692441152182,1.),(1.,0.909187146997205,1.),(1.,0.909555346803908,
1.),(1.,0.911583034137221,1.),(1.,0.912990115533129,1.),(1.,0.913476533865317,
1.)))
REPRESENTATION_ITEM('')
SURFACE()
);
#2978=(
BOUNDED_SURFACE()
B_SPLINE_SURFACE(3,2,((#194227,#194228,#194229),(#194230,#194231,#194232),
(#194233,#194234,#194235),(#194236,#194237,#194238),(#194239,#194240,#194241),
(#194242,#194243,#194244),(#194245,#194246,#194247),(#194248,#194249,#194250),
(#194251,#194252,#194253),(#194254,#194255,#194256),(#194257,#194258,#194259),
(#194260,#194261,#194262)),.UNSPECIFIED.,.F.,.F.,.F.)
B_SPLINE_SURFACE_WITH_KNOTS((4,2,2,2,2,4),(3,3),(-0.000409539429897566,
0.00646885457540742,0.0129377091508148,0.0161721364385186,0.0194065637262222,
0.0262849577315271),(0.,1.0004095394299),.UNSPECIFIED.)
GEOMETRIC_REPRESENTATION_ITEM()
RATIONAL_B_SPLINE_SURFACE(((1.,0.913179721902361,1.00007111265439),(1.,
0.914649363023394,1.00006990890242),(1.,0.916017546687799,1.0000687882521),
(1.,0.918006651041594,1.00006715901878),(1.,0.918577734918004,1.00006669125605),
(1.,0.918977605127172,1.00006636373081),(1.,0.919016659308045,1.00006633174236),
(1.,0.918937808682391,1.00006639632724),(1.,0.918820432299286,1.00006649246775),
(1.,0.918221056281877,1.00006698340398),(1.,0.917500522000491,1.00006757357837),
(0.999999999999999,0.916883429763216,1.00006807902558)))
REPRESENTATION_ITEM('')
SURFACE()
);
#2979=(
BOUNDED_SURFACE()
B_SPLINE_SURFACE(3,2,((#194367,#194368,#194369),(#194370,#194371,#194372),
(#194373,#194374,#194375),(#194376,#194377,#194378),(#194379,#194380,#194381),
(#194382,#194383,#194384),(#194385,#194386,#194387),(#194388,#194389,#194390),
(#194391,#194392,#194393),(#194394,#194395,#194396),(#194397,#194398,#194399),
(#194400,#194401,#194402),(#194403,#194404,#194405),(#194406,#194407,#194408),
(#194409,#194410,#194411),(#194412,#194413,#194414),(#194415,#194416,#194417),
(#194418,#194419,#194420),(#194421,#194422,#194423),(#194424,#194425,#194426),
(#194427,#194428,#194429),(#194430,#194431,#194432),(#194433,#194434,#194435),
(#194436,#194437,#194438),(#194439,#194440,#194441),(#194442,#194443,#194444),
(#194445,#194446,#194447),(#194448,#194449,#194450),(#194451,#194452,#194453),
(#194454,#194455,#194456),(#194457,#194458,#194459),(#194460,#194461,#194462),
(#194463,#194464,#194465),(#194466,#194467,#194468)),.UNSPECIFIED.,.F.,
 .F.,.F.)
B_SPLINE_SURFACE_WITH_KNOTS((4,2,2,2,2,2,2,2,2,2,2,2,2,2,2,2,4),(3,3),(0.,
0.000127304511784401,0.000254609023568802,0.000318261279461002,0.000381913535353202,
0.000509218047137603,0.000636522558922004,0.000763827070706405,0.000891131582490806,
0.00101843609427521,0.00114574060605961,0.00127304511784401,0.00140034962962841,
0.00152765414141281,0.00165495865319721,0.00178226316498161,0.00203687218855042),
(0.,1.),.UNSPECIFIED.)
GEOMETRIC_REPRESENTATION_ITEM()
RATIONAL_B_SPLINE_SURFACE(((1.,0.91702864701937,1.),(1.,0.916747691343526,
1.),(1.,0.916396650974015,1.),(1.,0.915391285047532,1.),(1.,0.91466902297872,
1.),(1.,0.913617961828943,1.),(1.,0.913301894872966,1.),(1.,0.91288722963512,
1.),(1.,0.912808085796895,1.),(1.,0.912445288290209,1.),(1.,0.912155502184342,
1.),(1.,0.911390085208123,1.),(1.,0.910897099188983,1.),(1.,0.909571313750726,
1.),(1.,0.908903094531974,1.),(1.,0.907795271007775,1.),(1.,0.907436030525757,
1.),(1.,0.9066073942613,1.),(1.,0.906098571567135,1.),(1.,0.904785338999927,
1.),(1.,0.903901015235201,1.),(1.,0.9022896096654,1.),(1.,0.90153583977931,
1.),(1.,0.900209640235172,1.),(1.,0.899552878447653,1.),(1.,0.897909996734079,
1.),(1.,0.896964437998137,1.),(1.,0.894976204823856,1.),(1.,0.894010134201253,
1.),(1.,0.892205555807536,1.),(1.,0.89146980148389,1.),(1.,0.88870491520376,
1.),(1.,0.885769567646591,1.),(1.,0.884000563436218,1.)))
REPRESENTATION_ITEM('')
SURFACE()
);
#2980=(
BOUNDED_SURFACE()
B_SPLINE_SURFACE(3,2,((#194555,#194556,#194557),(#194558,#194559,#194560),
(#194561,#194562,#194563),(#194564,#194565,#194566)),.UNSPECIFIED.,.F.,
 .F.,.F.)
B_SPLINE_SURFACE_WITH_KNOTS((4,4),(3,3),(0.,0.00767500517967513),(0.,1.),
 .UNSPECIFIED.)
GEOMETRIC_REPRESENTATION_ITEM()
RATIONAL_B_SPLINE_SURFACE(((1.,0.884000563436129,1.),(1.,0.883607612825216,
1.),(1.,0.883267077927119,1.),(1.,0.882986276630499,1.)))
REPRESENTATION_ITEM('')
SURFACE()
);
#2981=(
BOUNDED_SURFACE()
B_SPLINE_SURFACE(3,2,((#194572,#194573,#194574),(#194575,#194576,#194577),
(#194578,#194579,#194580),(#194581,#194582,#194583)),.UNSPECIFIED.,.F.,
 .F.,.F.)
B_SPLINE_SURFACE_WITH_KNOTS((4,4),(3,3),(-1.19804340059648E-17,0.000463834979289297),
(0.,1.),.UNSPECIFIED.)
GEOMETRIC_REPRESENTATION_ITEM()
RATIONAL_B_SPLINE_SURFACE(((1.,0.882986276630509,1.),(1.,0.873185362893501,
1.),(1.,0.861832566029531,1.),(1.,0.849056746210421,1.)))
REPRESENTATION_ITEM('')
SURFACE()
);
#2982=(
BOUNDED_SURFACE()
B_SPLINE_SURFACE(3,2,((#194595,#194596,#194597),(#194598,#194599,#194600),
(#194601,#194602,#194603),(#194604,#194605,#194606),(#194607,#194608,#194609),
(#194610,#194611,#194612),(#194613,#194614,#194615),(#194616,#194617,#194618),
(#194619,#194620,#194621),(#194622,#194623,#194624),(#194625,#194626,#194627),
(#194628,#194629,#194630),(#194631,#194632,#194633),(#194634,#194635,#194636),
(#194637,#194638,#194639),(#194640,#194641,#194642),(#194643,#194644,#194645),
(#194646,#194647,#194648),(#194649,#194650,#194651),(#194652,#194653,#194654),
(#194655,#194656,#194657),(#194658,#194659,#194660),(#194661,#194662,#194663),
(#194664,#194665,#194666),(#194667,#194668,#194669),(#194670,#194671,#194672),
(#194673,#194674,#194675),(#194676,#194677,#194678),(#194679,#194680,#194681),
(#194682,#194683,#194684),(#194685,#194686,#194687),(#194688,#194689,#194690),
(#194691,#194692,#194693),(#194694,#194695,#194696),(#194697,#194698,#194699),
(#194700,#194701,#194702),(#194703,#194704,#194705),(#194706,#194707,#194708),
(#194709,#194710,#194711),(#194712,#194713,#194714),(#194715,#194716,#194717),
(#194718,#194719,#194720),(#194721,#194722,#194723),(#194724,#194725,#194726),
(#194727,#194728,#194729),(#194730,#194731,#194732),(#194733,#194734,#194735),
(#194736,#194737,#194738),(#194739,#194740,#194741),(#194742,#194743,#194744),
(#194745,#194746,#194747),(#194748,#194749,#194750),(#194751,#194752,#194753),
(#194754,#194755,#194756),(#194757,#194758,#194759),(#194760,#194761,#194762),
(#194763,#194764,#194765),(#194766,#194767,#194768),(#194769,#194770,#194771),
(#194772,#194773,#194774),(#194775,#194776,#194777),(#194778,#194779,#194780),
(#194781,#194782,#194783),(#194784,#194785,#194786),(#194787,#194788,#194789),
(#194790,#194791,#194792),(#194793,#194794,#194795),(#194796,#194797,#194798),
(#194799,#194800,#194801),(#194802,#194803,#194804),(#194805,#194806,#194807),
(#194808,#194809,#194810),(#194811,#194812,#194813),(#194814,#194815,#194816),
(#194817,#194818,#194819),(#194820,#194821,#194822),(#194823,#194824,#194825),
(#194826,#194827,#194828),(#194829,#194830,#194831),(#194832,#194833,#194834),
(#194835,#194836,#194837),(#194838,#194839,#194840),(#194841,#194842,#194843),
(#194844,#194845,#194846),(#194847,#194848,#194849),(#194850,#194851,#194852),
(#194853,#194854,#194855),(#194856,#194857,#194858),(#194859,#194860,#194861),
(#194862,#194863,#194864),(#194865,#194866,#194867),(#194868,#194869,#194870),
(#194871,#194872,#194873),(#194874,#194875,#194876),(#194877,#194878,#194879),
(#194880,#194881,#194882),(#194883,#194884,#194885),(#194886,#194887,#194888),
(#194889,#194890,#194891),(#194892,#194893,#194894),(#194895,#194896,#194897),
(#194898,#194899,#194900),(#194901,#194902,#194903),(#194904,#194905,#194906)),
 .UNSPECIFIED.,.F.,.F.,.F.)
B_SPLINE_SURFACE_WITH_KNOTS((4,2,2,2,2,2,2,2,2,2,2,2,2,2,2,2,2,2,2,2,2,
2,2,2,2,2,2,2,2,2,2,2,2,2,2,2,2,2,2,2,2,2,2,2,2,2,2,2,2,2,2,4),(3,3),(-1.90819582357449E-17,
0.00250327328955147,0.00500654657910296,0.0062581832238787,0.00688400154626657,
0.00696222883656506,0.00704045612686354,0.00719691070746051,0.00750981986865445,
0.0100130931582059,0.0112647298029817,0.0115776389641756,0.0117340935447726,
0.0117732071899218,0.0118123208350711,0.0118905481253695,0.0125163664477574,
0.0137680030925332,0.0150196397373089,0.0175229130268604,0.0175620266720097,
0.0176011403171589,0.0176793676074573,0.0178358221880543,0.0181487313492483,
0.0187745496716362,0.0200261863164119,0.0225294596059634,0.0226076868962618,
0.0226468005414111,0.0226859141865603,0.0228423687671573,0.0231552779283512,
0.0237810962507391,0.0250327328955148,0.0275360061850663,0.0281618245074543,
0.0283182790880512,0.0283965063783497,0.0284356200234989,0.0284747336686481,
0.0287876428298421,0.0300392794746179,0.0325425527641693,0.0331683710865572,
0.0332465983768557,0.0333248256671542,0.0334812802477511,0.0337941894089451,
0.0350458260537208,0.0375490993432723,0.0401656877060997),(0.,1.00015179601854),
 .UNSPECIFIED.)
GEOMETRIC_REPRESENTATION_ITEM()
RATIONAL_B_SPLINE_SURFACE(((1.,0.849033833625475,1.00004583212598),(1.,
0.857897119742638,1.00004314130289),(1.,0.865043679059864,1.00004097166439),
(1.,0.876686517055576,1.00003743699149),(1.,0.881205024794411,1.00003606520852),
(1.,0.886414625564822,1.00003448361521),(1.,0.887881243937061,1.00003403836155),
(1.,0.889692656429651,1.00003348843114),(1.,0.890232954947349,1.00003332440081),
(1.,0.890771831880103,1.00003316080207),(1.,0.890856320713948,1.00003313515193),
(1.,0.890681329796628,1.00003318827778),(1.,0.890593656796271,1.0000332148946),
(1.,0.890330116618983,1.0000332949033),(1.,0.890153728390971,1.00003334845336),
(1.,0.889622566425299,1.00003350970991),(1.,0.889265797639508,1.00003361802207),
(1.,0.886032789860672,1.00003459953749),(1.,0.883009418597165,1.00003551740893),
(1.,0.878217284280675,1.00003697226275),(1.,0.876593412053755,1.00003746525742),
(1.,0.874525462184782,1.00003809307054),(1.,0.874110131143723,1.00003821916173),
(1.,0.873484749154558,1.00003840902273),(1.,0.873275890241246,1.00003847243063),
(1.,0.873014337068072,1.00003855183609),(1.,0.872962002442414,1.00003856772447),
(1.,0.872857285608954,1.00003859951566),(1.,0.872731930863508,1.00003863757236),
(1.,0.872890560350215,1.00003858941372),(1.,0.872995125812693,1.00003855766847),
(1.,0.873925639885731,1.00003827517181),(1.,0.874677728758358,1.00003804684362),
(1.,0.876724634752812,1.00003742541926),(1.,0.877812640553407,1.00003709510936),
(1.,0.879464189151955,1.00003659371236),(1.,0.880031794826061,1.00003642139179),
(1.,0.880962615838148,1.00003613880195),(1.,0.880576605528814,1.0000362559916),
(1.,0.879126719140342,1.00003669616556),(1.,0.879157178625721,1.00003668691831),
(1.,0.879182665775382,1.00003667918061),(1.,0.879195407511513,1.00003667531232),
(1.,0.879233627689003,1.00003666370898),(1.,0.879259101093747,1.00003665597546),
(1.,0.879335505234512,1.00003663277977),(1.,0.879386419815118,1.00003661732251),
(1.,0.879539134556379,1.00003657095953),(1.,0.879640904470776,1.00003654006299),
(1.,0.879946424969611,1.0000364473094),(1.,0.88014929469008,1.00003638571977),
(1.,0.880757599478193,1.00003620104328),(1.,0.881161368633861,1.00003607846218),
(1.,0.882351219988641,1.00003571723278),(1.,0.883116027430274,1.00003548504333),
(1.,0.883884077234136,1.00003525186953),(1.,0.883907336025334,1.00003524480835),
(1.,0.883942203551939,1.00003523422284),(1.,0.883958490107036,1.00003522927837),
(1.,0.883961132532197,1.00003522847615),(1.,0.883962211382421,1.00003522814862),
(1.,0.883966395700204,1.0000352268783),(1.,0.883965871907594,1.00003522703732),
(1.,0.883952745623932,1.00003523102235),(1.,0.883928595048457,1.00003523835428),
(1.,0.883810165971008,1.0000352743084),(1.,0.883670016928064,1.00003531685653),
(1.,0.88306386319684,1.00003550087998),(1.,0.882412138697386,1.00003569873835),
(1.,0.879709919903232,1.00003651911046),(1.,0.876914343405723,1.00003736782522),
(1.,0.871931382756172,1.00003888061239),(1.,0.870860364968084,1.00003920576487),
(1.,0.869420643269702,1.00003964285291),(1.,0.869127634755716,1.00003973180796),
(1.,0.868680339242782,1.00003986760332),(1.,0.86852994348834,1.00003991326227),
(1.,0.868302379480849,1.00003998234889),(1.,0.868226196408592,1.00004000547747),
(1.,0.868073169270762,1.00004005193529),(1.,0.86818422111107,1.00004001822083),
(1.,0.868924411953888,1.00003979350479),(1.,0.869577997769037,1.00003959508134),
(1.,0.872822984740276,1.00003860992913),(1.,0.87533860305511,1.00003784620744),
(1.,0.882672172604018,1.00003561979413),(1.,0.88727751836787,1.00003422164782),
(1.,0.892665553038707,1.0000325858834),(1.,0.893724673510805,1.00003226434286),
(1.,0.894892968317747,1.00003190965786),(1.,0.89502245580098,1.00003187034649),
(1.,0.895280775266388,1.00003179192276),(1.,0.89516331129965,1.00003182758388),
(1.,0.894880513654593,1.000031913439),(1.,0.894687925962448,1.00003197190709),
(1.,0.894097865318725,1.0000321510448),(1.,0.893688100021225,1.00003227544628),
(1.,0.891555270434203,1.00003292295636),(1.,0.889581836674106,1.00003352207513),
(1.,0.882741932058345,1.00003559861571),(1.,0.877005189271263,1.00003734024514),
(1.,0.862041840928008,1.00004188299854),(1.,0.852645436799408,1.00004473567201),
(0.999999999999999,0.840867469721541,1.00004831136903)))
REPRESENTATION_ITEM('')
SURFACE()
);
#2983=(
BOUNDED_SURFACE()
B_SPLINE_SURFACE(3,2,((#195298,#195299,#195300),(#195301,#195302,#195303),
(#195304,#195305,#195306),(#195307,#195308,#195309)),.UNSPECIFIED.,.F.,
 .F.,.F.)
B_SPLINE_SURFACE_WITH_KNOTS((4,4),(3,3),(-8.29532866279615E-6,0.00052578299168427),
(-8.29532866279615E-6,1.),.UNSPECIFIED.)
GEOMETRIC_REPRESENTATION_ITEM()
RATIONAL_B_SPLINE_SURFACE(((1.00000262679448,0.841670258828196,1.),(1.00000236409525,
0.857504425499066,1.),(1.00000212772213,0.871751788438872,1.),(1.00000191989843,
0.884278338845134,1.)))
REPRESENTATION_ITEM('')
SURFACE()
);
#2984=(
BOUNDED_SURFACE()
B_SPLINE_SURFACE(3,2,((#195321,#195322,#195323),(#195324,#195325,#195326),
(#195327,#195328,#195329),(#195330,#195331,#195332)),.UNSPECIFIED.,.F.,
 .F.,.F.)
B_SPLINE_SURFACE_WITH_KNOTS((4,4),(3,3),(1.7347234759768E-18,0.00761738954978064),
(0.,1.),.UNSPECIFIED.)
GEOMETRIC_REPRESENTATION_ITEM()
RATIONAL_B_SPLINE_SURFACE(((1.,0.883694369886725,1.),(1.,0.884057799195121,
1.),(1.,0.884477978068247,1.),(1.,0.884949126929568,1.)))
REPRESENTATION_ITEM('')
SURFACE()
);
#2985=(
BOUNDED_SURFACE()
B_SPLINE_SURFACE(3,2,((#195338,#195339,#195340),(#195341,#195342,#195343),
(#195344,#195345,#195346),(#195347,#195348,#195349),(#195350,#195351,#195352),
(#195353,#195354,#195355),(#195356,#195357,#195358),(#195359,#195360,#195361),
(#195362,#195363,#195364),(#195365,#195366,#195367),(#195368,#195369,#195370),
(#195371,#195372,#195373),(#195374,#195375,#195376),(#195377,#195378,#195379),
(#195380,#195381,#195382),(#195383,#195384,#195385),(#195386,#195387,#195388),
(#195389,#195390,#195391),(#195392,#195393,#195394),(#195395,#195396,#195397),
(#195398,#195399,#195400),(#195401,#195402,#195403),(#195404,#195405,#195406),
(#195407,#195408,#195409),(#195410,#195411,#195412),(#195413,#195414,#195415),
(#195416,#195417,#195418),(#195419,#195420,#195421),(#195422,#195423,#195424),
(#195425,#195426,#195427),(#195428,#195429,#195430),(#195431,#195432,#195433)),
 .UNSPECIFIED.,.F.,.F.,.F.)
B_SPLINE_SURFACE_WITH_KNOTS((4,2,2,2,2,2,2,2,2,2,2,2,2,2,2,4),(3,3),(0.,
0.0002498236013634,0.0003747354020451,0.0004996472027268,0.0006245590034085,
0.0007494708040902,0.0008743826047719,0.0009992944054536,0.001249118006817,
0.0013740298074987,0.0014989416081804,0.0016238534088621,0.00168630930920295,
0.0017487652095438,0.0018736770102255,0.0019985888109072),(0.,1.),
 .UNSPECIFIED.)
GEOMETRIC_REPRESENTATION_ITEM()
RATIONAL_B_SPLINE_SURFACE(((1.,0.884949126929531,1.),(1.,0.887143782528108,
1.),(1.,0.890918336240603,1.),(1.,0.894210449378273,1.),(1.,0.895128089226685,
1.),(1.,0.897367518060138,1.),(1.,0.898575478737319,1.),(1.,0.901068236159139,
1.),(1.,0.902188804939834,1.),(1.,0.904118344604245,1.),(1.,0.904836730307214,
1.),(1.,0.906457435203586,1.),(1.,0.907401903391372,1.),(1.,0.909436312125094,
1.),(1.,0.910504885825633,1.),(1.,0.912732113906766,1.),(1.,0.913182649173379,
1.),(1.,0.915295706676324,1.),(1.,0.916179642793504,1.),(1.,0.917783643221206,
1.),(1.,0.918289173478595,1.),(1.,0.919115574923275,1.),(1.,0.919419128152901,
1.),(1.,0.919791548547683,1.),(1.,0.91988587489381,1.),(1.,0.920431178830713,
1.),(1.,0.920846680282669,1.),(1.,0.922176939320294,1.),(1.,0.923013849094452,
1.),(1.,0.924153386273243,1.),(1.,0.924540045823644,1.),(1.,0.924853416885498,
1.)))
REPRESENTATION_ITEM('')
SURFACE()
);
#2986=(
BOUNDED_SURFACE()
B_SPLINE_SURFACE(3,2,((#195515,#195516,#195517),(#195518,#195519,#195520),
(#195521,#195522,#195523),(#195524,#195525,#195526),(#195527,#195528,#195529),
(#195530,#195531,#195532),(#195533,#195534,#195535),(#195536,#195537,#195538),
(#195539,#195540,#195541),(#195542,#195543,#195544),(#195545,#195546,#195547),
(#195548,#195549,#195550)),.UNSPECIFIED.,.F.,.F.,.F.)
B_SPLINE_SURFACE_WITH_KNOTS((4,2,2,2,2,4),(3,3),(-0.000625729109945204,
0.00715193125010649,0.014303862500213,0.0178798281252662,0.0214557937503195,
0.0292334541103712),(0.,1.00062572910995),.UNSPECIFIED.)
GEOMETRIC_REPRESENTATION_ITEM()
RATIONAL_B_SPLINE_SURFACE(((1.,0.924499160265099,1.00009448614649),(1.,
0.925778544860493,1.00009288505013),(1.,0.926988832520574,1.00009137042569),
(1.,0.928403005961066,1.00008960064671),(1.,0.928672278179807,1.00008926366378),
(1.,0.928396618697272,1.0000896086401),(1.,0.928197998538414,1.00008985720493),
(1.,0.927602144330102,1.00009060289158),(1.,0.927204819604613,1.00009110012687),
(1.,0.925564164183759,1.00009315333859),(1.,0.923967382217261,1.0000951516445),
(1.,0.922538732838579,1.00009693953951)))
REPRESENTATION_ITEM('')
SURFACE()
);
#2987=(
BOUNDED_SURFACE()
B_SPLINE_SURFACE(3,2,((#195664,#195665,#195666),(#195667,#195668,#195669),
(#195670,#195671,#195672),(#195673,#195674,#195675),(#195676,#195677,#195678),
(#195679,#195680,#195681),(#195682,#195683,#195684),(#195685,#195686,#195687),
(#195688,#195689,#195690),(#195691,#195692,#195693),(#195694,#195695,#195696),
(#195697,#195698,#195699),(#195700,#195701,#195702),(#195703,#195704,#195705),
(#195706,#195707,#195708),(#195709,#195710,#195711),(#195712,#195713,#195714),
(#195715,#195716,#195717),(#195718,#195719,#195720),(#195721,#195722,#195723),
(#195724,#195725,#195726),(#195727,#195728,#195729),(#195730,#195731,#195732),
(#195733,#195734,#195735),(#195736,#195737,#195738),(#195739,#195740,#195741),
(#195742,#195743,#195744),(#195745,#195746,#195747),(#195748,#195749,#195750),
(#195751,#195752,#195753),(#195754,#195755,#195756),(#195757,#195758,#195759),
(#195760,#195761,#195762),(#195763,#195764,#195765)),.UNSPECIFIED.,.F.,
 .F.,.F.)
B_SPLINE_SURFACE_WITH_KNOTS((4,2,2,2,2,2,2,2,2,2,2,2,2,2,2,2,4),(3,3),(0.,
0.000209917658866865,0.000262397073583582,0.000314876488300298,0.000419835317733731,
0.000524794147167163,0.000629752976600596,0.000839670635467461,0.000892150050184177,
0.000944629464900893,0.00104958829433433,0.00115454712376776,0.00125950595320119,
0.00136446478263462,0.00146942361206806,0.00157438244150149,0.00167934127093492),
(0.,1.),.UNSPECIFIED.)
GEOMETRIC_REPRESENTATION_ITEM()
RATIONAL_B_SPLINE_SURFACE(((1.,0.922934699314368,1.),(1.,0.922418139396395,
1.),(1.,0.921306581502972,1.),(1.,0.918237743219156,1.),(1.,0.917652150959428,
1.),(1.,0.91703035541482,1.),(1.,0.917005626549279,1.),(1.,0.916857059572335,
1.),(1.,0.916688851599089,1.),(1.,0.916103666089295,1.),(1.,0.915719829580818,
1.),(1.,0.914172806704204,1.),(1.,0.912988290535927,1.),(1.,0.910591006023012,
1.),(1.,0.910578234409646,1.),(1.,0.908859123022388,1.),(1.,0.908450616432512,
1.),(1.,0.90741169941527,1.),(1.,0.906720027731936,1.),(1.,0.904857077146999,
1.),(1.,0.903782469918774,1.),(1.,0.902111434863952,1.),(1.,0.901503491191089,
1.),(1.,0.899540977424082,1.),(1.,0.898323167261007,1.),(1.,0.895415117868645,
1.),(1.,0.894063264652639,1.),(1.,0.891702659041491,1.),(1.,0.890819635354087,
1.),(1.,0.888591057203743,1.),(1.,0.88687758303178,1.),(1.,0.883673322831122,
1.),(1.,0.882221756932481,1.),(1.,0.881068987522013,1.)))
REPRESENTATION_ITEM('')
SURFACE()
);
#2988=(
BOUNDED_SURFACE()
B_SPLINE_SURFACE(3,2,((#195852,#195853,#195854),(#195855,#195856,#195857),
(#195858,#195859,#195860),(#195861,#195862,#195863)),.UNSPECIFIED.,.F.,
 .F.,.F.)
B_SPLINE_SURFACE_WITH_KNOTS((4,4),(3,3),(-6.93889390390723E-18,0.00418923766731893),
(0.,1.),.UNSPECIFIED.)
GEOMETRIC_REPRESENTATION_ITEM()
RATIONAL_B_SPLINE_SURFACE(((1.,0.881068987521719,1.),(1.,0.880840248614593,
1.),(1.,0.880630793895676,1.),(1.,0.880439575617234,1.)))
REPRESENTATION_ITEM('')
SURFACE()
);
#2989=(
BOUNDED_SURFACE()
B_SPLINE_SURFACE(3,2,((#195869,#195870,#195871),(#195872,#195873,#195874),
(#195875,#195876,#195877),(#195878,#195879,#195880)),.UNSPECIFIED.,.F.,
 .F.,.F.)
B_SPLINE_SURFACE_WITH_KNOTS((4,4),(3,3),(-7.25197858200355E-6,0.00049505136265659),
(-7.25197858200355E-6,1.),.UNSPECIFIED.)
GEOMETRIC_REPRESENTATION_ITEM()
RATIONAL_B_SPLINE_SURFACE(((1.00000172705636,0.880925161180393,1.),(1.00000188960186,
0.86971818519116,1.),(1.00000207656143,0.856827939964767,1.),(1.00000228609307,
0.842381424617121,0.999999999999999)))
REPRESENTATION_ITEM('')
SURFACE()
);
#2990=(
BOUNDED_SURFACE()
B_SPLINE_SURFACE(3,2,((#195892,#195893,#195894),(#195895,#195896,#195897),
(#195898,#195899,#195900),(#195901,#195902,#195903)),.UNSPECIFIED.,.F.,
 .F.,.F.)
B_SPLINE_SURFACE_WITH_KNOTS((4,4),(3,3),(0.0429271655601134,0.046749382327419),
(0.,1.),.UNSPECIFIED.)
GEOMETRIC_REPRESENTATION_ITEM()
RATIONAL_B_SPLINE_SURFACE(((1.,0.922487559402275,1.),(1.,0.922290239059189,
1.),(1.,0.921950699598134,1.),(1.,0.921567721510049,1.)))
REPRESENTATION_ITEM('')
SURFACE()
);
#2991=(
BOUNDED_SURFACE()
B_SPLINE_SURFACE(3,2,((#195912,#195913,#195914),(#195915,#195916,#195917),
(#195918,#195919,#195920),(#195921,#195922,#195923)),.UNSPECIFIED.,.F.,
 .F.,.F.)
B_SPLINE_SURFACE_WITH_KNOTS((4,4),(3,3),(0.0243367909416761,0.0248833749525317),
(0.,1.),.UNSPECIFIED.)
GEOMETRIC_REPRESENTATION_ITEM()
RATIONAL_B_SPLINE_SURFACE(((1.,0.920889968635124,1.),(1.,0.921315643311136,
1.),(1.,0.921538438398832,1.),(1.,0.921567721510049,1.)))
REPRESENTATION_ITEM('')
SURFACE()
);
#2992=(
BOUNDED_SURFACE()
B_SPLINE_SURFACE(3,2,((#195929,#195930,#195931),(#195932,#195933,#195934),
(#195935,#195936,#195937),(#195938,#195939,#195940),(#195941,#195942,#195943),
(#195944,#195945,#195946),(#195947,#195948,#195949),(#195950,#195951,#195952),
(#195953,#195954,#195955),(#195956,#195957,#195958),(#195959,#195960,#195961),
(#195962,#195963,#195964),(#195965,#195966,#195967),(#195968,#195969,#195970),
(#195971,#195972,#195973),(#195974,#195975,#195976),(#195977,#195978,#195979),
(#195980,#195981,#195982),(#195983,#195984,#195985),(#195986,#195987,#195988),
(#195989,#195990,#195991),(#195992,#195993,#195994),(#195995,#195996,#195997),
(#195998,#195999,#196000),(#196001,#196002,#196003),(#196004,#196005,#196006)),
 .UNSPECIFIED.,.F.,.F.,.F.)
B_SPLINE_SURFACE_WITH_KNOTS((4,2,2,2,2,2,2,2,2,2,2,2,4),(3,3),(0.0236362382318929,
0.0238608230039569,0.023973115389989,0.0240854077760209,0.0243099925480849,
0.0245345773201489,0.0249837468642769,0.0252083316363409,0.0254329164084048,
0.0258820859525328,0.0263312554966607,0.0267804250407887,0.0272295945849166),
(0.,1.),.UNSPECIFIED.)
GEOMETRIC_REPRESENTATION_ITEM()
RATIONAL_B_SPLINE_SURFACE(((1.,0.920889968635126,1.),(1.,0.921094720125926,
1.),(1.,0.92133483228952,1.),(1.,0.921629553215121,1.),(1.,0.921717663867405,
1.),(1.,0.921866856601366,1.),(1.,0.92191190374927,1.),(1.,0.922251469700973,
1.),(1.,0.922692650412903,1.),(1.,0.923603719687576,1.),(1.,0.924055408647065,
1.),(1.,0.925181588378585,1.),(1.,0.925771557037175,1.),(1.,0.927073550275403,
1.),(1.,0.927638435549014,1.),(1.,0.92876341969282,1.),(1.,0.929280825357496,
1.),(1.,0.930786786259919,1.),(1.,0.931716896300058,1.),(1.,0.933882873767671,
1.),(1.,0.935142096438581,1.),(1.,0.937701084319509,1.),(1.,0.938925602458109,
1.),(1.,0.941308524649693,1.),(1.,0.942521337023694,1.),(1.,0.944221776843192,
1.)))
REPRESENTATION_ITEM('')
SURFACE()
);
#2993=(
BOUNDED_SURFACE()
B_SPLINE_SURFACE(3,2,((#196062,#196063,#196064),(#196065,#196066,#196067),
(#196068,#196069,#196070),(#196071,#196072,#196073),(#196074,#196075,#196076),
(#196077,#196078,#196079),(#196080,#196081,#196082),(#196083,#196084,#196085)),
 .UNSPECIFIED.,.F.,.F.,.F.)
B_SPLINE_SURFACE_WITH_KNOTS((4,2,2,4),(3,3),(0.,0.00023361260625816,0.00046722521251632,
0.000934450425032639),(0.,1.),.UNSPECIFIED.)
GEOMETRIC_REPRESENTATION_ITEM()
RATIONAL_B_SPLINE_SURFACE(((1.,0.957684062981954,1.),(1.,0.956682131117891,
1.),(1.,0.955470098743404,1.),(1.,0.953098741844667,1.),(1.,0.951960835596806,
1.),(1.,0.948724989903624,1.),(1.,0.946647027979619,1.),(1.,0.944221776843184,
1.)))
REPRESENTATION_ITEM('')
SURFACE()
);
#2994=(
BOUNDED_SURFACE()
B_SPLINE_SURFACE(3,2,((#196135,#196136,#196137),(#196138,#196139,#196140),
(#196141,#196142,#196143),(#196144,#196145,#196146)),.UNSPECIFIED.,.F.,
 .F.,.F.)
B_SPLINE_SURFACE_WITH_KNOTS((4,4),(3,3),(0.0114568846502287,0.0192019541084939),
(0.,1.),.UNSPECIFIED.)
GEOMETRIC_REPRESENTATION_ITEM()
RATIONAL_B_SPLINE_SURFACE(((1.,0.957684062981984,1.),(1.,0.957879658663776,
1.),(1.,0.958058054935734,1.),(1.,0.958218732174581,1.)))
REPRESENTATION_ITEM('')
SURFACE()
);
#2995=(
BOUNDED_SURFACE()
B_SPLINE_SURFACE(3,2,((#196162,#196163,#196164),(#196165,#196166,#196167),
(#196168,#196169,#196170),(#196171,#196172,#196173)),.UNSPECIFIED.,.F.,
 .F.,.F.)
B_SPLINE_SURFACE_WITH_KNOTS((4,4),(3,3),(0.00545299542660057,0.00564442024814154),
(0.,1.),.UNSPECIFIED.)
GEOMETRIC_REPRESENTATION_ITEM()
RATIONAL_B_SPLINE_SURFACE(((1.,0.992160193962408,1.),(1.,0.99307558921891,
1.),(1.,0.993813024865429,1.),(1.,0.994220746859028,1.)))
REPRESENTATION_ITEM('')
SURFACE()
);
#2996=(
BOUNDED_SURFACE()
B_SPLINE_SURFACE(3,2,((#196188,#196189,#196190),(#196191,#196192,#196193),
(#196194,#196195,#196196),(#196197,#196198,#196199),(#196200,#196201,#196202),
(#196203,#196204,#196205)),.UNSPECIFIED.,.F.,.F.,.F.)
B_SPLINE_SURFACE_WITH_KNOTS((4,2,4),(3,3),(-1.09829680072782E-16,0.000498949606022071,
0.000997899212044251),(0.,1.),.UNSPECIFIED.)
GEOMETRIC_REPRESENTATION_ITEM()
RATIONAL_B_SPLINE_SURFACE(((1.,0.994220746859027,1.),(1.,0.996098915568006,
1.),(1.,0.997550054459957,1.),(1.,0.99950507842482,1.),(1.,1.00000638742927,
1.),(1.,1.,1.)))
REPRESENTATION_ITEM('')
SURFACE()
);
#2997=(
BOUNDED_SURFACE()
B_SPLINE_SURFACE(3,2,((#196264,#196265,#196266),(#196267,#196268,#196269),
(#196270,#196271,#196272),(#196273,#196274,#196275),(#196276,#196277,#196278),
(#196279,#196280,#196281),(#196282,#196283,#196284),(#196285,#196286,#196287),
(#196288,#196289,#196290),(#196291,#196292,#196293),(#196294,#196295,#196296),
(#196297,#196298,#196299),(#196300,#196301,#196302),(#196303,#196304,#196305),
(#196306,#196307,#196308),(#196309,#196310,#196311),(#196312,#196313,#196314),
(#196315,#196316,#196317),(#196318,#196319,#196320),(#196321,#196322,#196323),
(#196324,#196325,#196326),(#196327,#196328,#196329),(#196330,#196331,#196332),
(#196333,#196334,#196335),(#196336,#196337,#196338),(#196339,#196340,#196341),
(#196342,#196343,#196344),(#196345,#196346,#196347),(#196348,#196349,#196350),
(#196351,#196352,#196353),(#196354,#196355,#196356),(#196357,#196358,#196359),
(#196360,#196361,#196362),(#196363,#196364,#196365),(#196366,#196367,#196368),
(#196369,#196370,#196371),(#196372,#196373,#196374),(#196375,#196376,#196377),
(#196378,#196379,#196380),(#196381,#196382,#196383),(#196384,#196385,#196386),
(#196387,#196388,#196389),(#196390,#196391,#196392),(#196393,#196394,#196395),
(#196396,#196397,#196398),(#196399,#196400,#196401),(#196402,#196403,#196404),
(#196405,#196406,#196407),(#196408,#196409,#196410),(#196411,#196412,#196413),
(#196414,#196415,#196416),(#196417,#196418,#196419),(#196420,#196421,#196422),
(#196423,#196424,#196425),(#196426,#196427,#196428),(#196429,#196430,#196431),
(#196432,#196433,#196434),(#196435,#196436,#196437),(#196438,#196439,#196440),
(#196441,#196442,#196443),(#196444,#196445,#196446),(#196447,#196448,#196449),
(#196450,#196451,#196452),(#196453,#196454,#196455),(#196456,#196457,#196458),
(#196459,#196460,#196461),(#196462,#196463,#196464),(#196465,#196466,#196467),
(#196468,#196469,#196470),(#196471,#196472,#196473),(#196474,#196475,#196476),
(#196477,#196478,#196479),(#196480,#196481,#196482),(#196483,#196484,#196485),
(#196486,#196487,#196488),(#196489,#196490,#196491),(#196492,#196493,#196494),
(#196495,#196496,#196497),(#196498,#196499,#196500),(#196501,#196502,#196503),
(#196504,#196505,#196506),(#196507,#196508,#196509),(#196510,#196511,#196512),
(#196513,#196514,#196515),(#196516,#196517,#196518),(#196519,#196520,#196521),
(#196522,#196523,#196524),(#196525,#196526,#196527),(#196528,#196529,#196530),
(#196531,#196532,#196533),(#196534,#196535,#196536),(#196537,#196538,#196539),
(#196540,#196541,#196542),(#196543,#196544,#196545),(#196546,#196547,#196548),
(#196549,#196550,#196551),(#196552,#196553,#196554),(#196555,#196556,#196557),
(#196558,#196559,#196560),(#196561,#196562,#196563),(#196564,#196565,#196566),
(#196567,#196568,#196569),(#196570,#196571,#196572),(#196573,#196574,#196575),
(#196576,#196577,#196578),(#196579,#196580,#196581),(#196582,#196583,#196584),
(#196585,#196586,#196587),(#196588,#196589,#196590),(#196591,#196592,#196593),
(#196594,#196595,#196596),(#196597,#196598,#196599),(#196600,#196601,#196602),
(#196603,#196604,#196605),(#196606,#196607,#196608),(#196609,#196610,#196611),
(#196612,#196613,#196614),(#196615,#196616,#196617),(#196618,#196619,#196620),
(#196621,#196622,#196623),(#196624,#196625,#196626),(#196627,#196628,#196629),
(#196630,#196631,#196632),(#196633,#196634,#196635),(#196636,#196637,#196638),
(#196639,#196640,#196641),(#196642,#196643,#196644),(#196645,#196646,#196647),
(#196648,#196649,#196650),(#196651,#196652,#196653),(#196654,#196655,#196656),
(#196657,#196658,#196659),(#196660,#196661,#196662),(#196663,#196664,#196665)),
 .UNSPECIFIED.,.F.,.F.,.F.)
B_SPLINE_SURFACE_WITH_KNOTS((4,2,2,2,2,2,2,2,2,2,2,2,2,2,2,2,2,2,2,2,2,
2,2,2,2,2,2,2,2,2,2,2,2,2,2,2,2,2,2,2,2,2,2,2,2,2,2,2,2,2,2,2,2,2,2,2,2,
2,2,2,2,2,2,2,2,2,4),(3,3),(0.0401209448553485,0.0422079288610133,0.0442949128666782,
0.046381896872343,0.0484688808780079,0.0526428488893376,0.0527732853896916,
0.0528385036398687,0.0529037218900457,0.0531645948907538,0.05368634089217,
0.0547298328950024,0.0568168169006673,0.0578603089034997,0.0589038009063321,
0.0599472929091645,0.0602081659098726,0.0603386024102267,0.0603712115353152,
0.0604038206604037,0.0604690389105808,0.060990784911997,0.0651647529233267,
0.0693387209346564,0.0698604669360726,0.0701213399367807,0.0701865581869577,
0.0702191673120462,0.0702517764371347,0.0703822129374888,0.0714257049403212,
0.0724691969431537,0.0735126889459861,0.0755996729516509,0.0766431649544833,
0.0771649109558996,0.0774257839566077,0.0775562204569617,0.0776214387071387,
0.0776540478322272,0.0776866569573158,0.0818606249686455,0.0860345929799752,
0.0870780849828076,0.0873389579835157,0.0874041762336927,0.0874367853587812,
0.0874530899213255,0.0874693944838697,0.0875998309842238,0.08812157698564,
0.0902085609913048,0.0943825290026346,0.0946434020033427,0.0947086202535197,
0.0947412293786082,0.0947738385036967,0.0949042750040508,0.095426021005467,
0.0964695130082994,0.0985564970139642,0.100643481019629,0.101686973022461,
0.102730465025294,0.104817449030959,0.105860941033791,0.106904433036624),
(-0.000150331225571141,1.),.UNSPECIFIED.)
GEOMETRIC_REPRESENTATION_ITEM()
RATIONAL_B_SPLINE_SURFACE(((1.00000971526928,0.967687121417261,1.),(1.00000979368702,
0.967426304860057,1.),(1.00000993438659,0.966958339653348,1.),(1.00001029017888,
0.965774978398451,1.),(1.00001050549399,0.965058842720181,1.),(1.00001098728375,
0.963456415296758,1.),(1.00001125422659,0.962568566336671,1.),(1.0000118294071,
0.960655522326197,1.),(1.00001213342102,0.959644375358026,1.),(1.00001308594142,
0.956476303020351,1.),(1.00001377412596,0.954187408806267,1.),(1.00001454155145,
0.951634960071011,1.),(1.00001456486356,0.951557424250059,1.),(1.00001459991773,
0.951440834491396,1.),(1.00001457230817,0.951532663561032,1.),(1.00001453962294,
0.951641374304724,1.),(1.00001452333201,0.951695557756684,1.),(1.00001444213708,
0.951965611176811,1.),(1.00001437801212,0.952178890092796,1.),(1.00001418818244,
0.952810261506986,1.),(1.00001406502106,0.953219894923565,1.),(1.0000137061962,
0.954413342436734,1.),(1.00001348115785,0.955161817519688,1.),(1.00001285359615,
0.957249080809413,1.),(1.00001250436141,0.958410631712903,1.),(1.00001210988278,
0.95972266329395,1.),(1.00001200110933,0.960084442603283,1.),(1.00001183261586,
0.960644850011032,1.),(1.00001177287885,0.960843534658787,1.),(1.00001170804724,
0.96105916386307,1.),(1.00001170266968,0.961077049592171,1.),(1.00001173086546,
0.960983270719707,1.),(1.00001173825265,0.960958701013246,1.),(1.00001175198371,
0.960913031660308,1.),(1.00001175700248,0.960896339292811,1.),(1.00001176383135,
0.960873626543695,1.),(1.00001176522489,0.960868991626948,1.),(1.00001176806761,
0.960859536780326,1.),(1.00001177105464,0.960849601956462,1.),(1.00001176869476,
0.960857450901041,1.),(1.00001176715196,0.96086258223084,1.),(1.00001175353863,
0.960907860010547,1.),(1.00001174336965,0.96094168192141,1.),(1.0000116681701,
0.961191794790978,1.),(1.00001171285899,0.961043160058672,1.),(1.00001196988856,
0.96018828251794,1.),(1.00001218283227,0.959480034084875,1.),(1.00001253635177,
0.958304232125271,1.),(1.00001257727477,0.958168122675296,1.),(1.00001264122898,
0.957955411672161,1.),(1.00001266294138,0.957883196469429,1.),(1.00001269058339,
0.957791259469782,1.),(1.00001269613687,0.957772788660441,1.),(1.00001270450487,
0.957744956766385,1.),(1.0000127126013,0.957718028118306,1.),(1.00001270395433,
0.957746787852822,1.),(1.00001269965221,0.9577610966519,1.),(1.00001267824887,
0.957832283944761,1.),(1.00001266146939,0.957888092294895,1.),(1.00001251358919,
0.958379940224678,1.),(1.00001240455658,0.958742581485571,1.),(1.00001223534349,
0.959305382336318,1.),(1.00001217514497,0.959505601958515,1.),(1.00001210726764,
0.959731361219486,1.),(1.00001209931732,0.959757803879631,1.),(1.00001215129706,
0.959584919863517,1.),(1.0000122874652,0.959132026118958,1.),(1.00001262675854,
0.95800354019393,1.),(1.00001276231487,0.957552681348205,1.),(1.00001299609705,
0.956775124398884,1.),(1.00001307914247,0.95649891625436,1.),(1.00001321097066,
0.956060457128587,1.),(1.0000132561197,0.955910291938057,1.),(1.00001332558918,
0.955679237196541,1.),(1.00001334903664,0.955601251202993,1.),(1.00001338463613,
0.955482847702871,1.),(1.000013396574,0.955443142455131,1.),(1.00001341458686,
0.955383231893246,1.),(1.00001342060882,0.955363202924128,1.),(1.00001343268791,
0.955323027998288,1.),(1.00001342097891,0.955361972010516,1.),(1.0000128917049,
0.957122331530358,1.),(1.00001245359404,0.958579483414712,1.),(1.00001173531401,
0.960968474900111,1.),(1.00001145207891,0.96191051170025,1.),(1.00001123165748,
0.962643630951223,1.),(1.00001119459058,0.962766915069294,1.),(1.00001115856949,
0.962886720799798,1.),(1.00001115188289,0.962908960376103,1.),(1.00001114420108,
0.962934509975404,1.),(1.00001114269855,0.962939507370241,1.),(1.00001114049609,
0.962946832741217,1.),(1.00001113977049,0.962949246077756,1.),(1.000011138695,
0.962952823156129,1.),(1.00001113833865,0.962954008361232,1.),(1.00001113763027,
0.962956364421279,1.),(1.00001113829343,0.962954158761119,1.),(1.00001114110855,
0.962944795699858,1.),(1.00001114414817,0.962934685949314,1.),(1.00001116199795,
0.962875317780209,1.),(1.00001118475773,0.962799619030819,1.),(1.00001133896015,
0.96228674347642,1.),(1.00001159320074,0.961441142056957,1.),(1.00001265659516,
0.957904303941762,1.),(1.00001376678907,0.954211811223626,1.),(1.00001513580773,
0.949658470243662,1.),(1.0000152171122,0.949388052460497,1.),(1.00001531968671,
0.949046890784209,1.),(1.00001534024882,0.948978501441861,1.),(1.00001537116238,
0.948875683285007,1.),(1.00001538147863,0.948841371541406,1.),(1.00001540213453,
0.948772670228394,1.),(1.00001538091888,0.948843233269349,1.),(1.00001534454108,
0.948964225425651,1.),(1.00001531549173,0.94906084323558,1.),(1.00001517050652,
0.949543062447052,1.),(1.0000150553548,0.949926055790804,1.),(1.00001471230728,
0.951067028082035,1.),(1.00001448692643,0.951816642300841,1.),(1.00001381880759,
0.954038798202261,1.),(1.00001338374559,0.955485809633019,1.),(1.00001253497379,
0.958308815288275,1.),(1.00001212137949,0.959684425368754,1.),(1.00001152065592,
0.961682425350425,1.),(1.00001132312401,0.962339414286871,1.),(1.00001094046962,
0.963612118576129,1.),(1.00001075510022,0.964228655148104,1.),(1.00001021993682,
0.966008602726101,1.),(1.00000989010539,0.967105618448797,1.),(1.0000094600318,
0.968536038448202,1.),(1.00000932763788,0.968976379179426,1.),(1.00000909187148,
0.969760535622473,1.),(1.00000898814038,0.970105544128433,1.),(1.0000089057079,
0.97037971365699,1.)))
REPRESENTATION_ITEM('')
SURFACE()
);
#2998=(
BOUNDED_SURFACE()
B_SPLINE_SURFACE(3,2,((#197269,#197270,#197271),(#197272,#197273,#197274),
(#197275,#197276,#197277),(#197278,#197279,#197280),(#197281,#197282,#197283),
(#197284,#197285,#197286)),.UNSPECIFIED.,.F.,.F.,.F.)
B_SPLINE_SURFACE_WITH_KNOTS((4,2,4),(3,3),(-2.65828754408143E-15,0.000518614521426172,
0.001037229042855),(0.,1.),.UNSPECIFIED.)
GEOMETRIC_REPRESENTATION_ITEM()
RATIONAL_B_SPLINE_SURFACE(((1.,0.994246489501235,1.),(1.,0.99609478928193,
1.),(1.,0.997541267372286,1.),(1.,0.999499888835022,1.),(1.,1.00000732330262,
1.),(1.,1.,1.)))
REPRESENTATION_ITEM('')
SURFACE()
);
#2999=(
BOUNDED_SURFACE()
B_SPLINE_SURFACE(3,2,((#197303,#197304,#197305),(#197306,#197307,#197308),
(#197309,#197310,#197311),(#197312,#197313,#197314)),.UNSPECIFIED.,.F.,
 .F.,.F.)
B_SPLINE_SURFACE_WITH_KNOTS((4,4),(3,3),(0.0119444722538381,0.0121107952282446),
(0.,1.00002036952005),.UNSPECIFIED.)
GEOMETRIC_REPRESENTATION_ITEM()
RATIONAL_B_SPLINE_SURFACE(((1.,0.99280936423786,1.0000002929396),(1.,0.993510643385736,
1.00000026437016),(1.,0.994041174404923,1.00000024275684),(1.,0.99432165622759,
1.00000023133027)))
REPRESENTATION_ITEM('')
SURFACE()
);
#3000=(
BOUNDED_SURFACE()
B_SPLINE_SURFACE(3,2,((#197329,#197330,#197331),(#197332,#197333,#197334),
(#197335,#197336,#197337),(#197338,#197339,#197340)),.UNSPECIFIED.,.F.,
 .F.,.F.)
B_SPLINE_SURFACE_WITH_KNOTS((4,4),(3,3),(0.0657640091385094,0.0735516090029935),
(0.,1.),.UNSPECIFIED.)
GEOMETRIC_REPRESENTATION_ITEM()
RATIONAL_B_SPLINE_SURFACE(((1.,0.958250447061442,1.),(1.,0.958411329127679,
1.),(1.,0.958554518262528,1.),(1.,0.958680046125676,1.)))
REPRESENTATION_ITEM('')
SURFACE()
);
#3001=(
BOUNDED_SURFACE()
B_SPLINE_SURFACE(3,2,((#197346,#197347,#197348),(#197349,#197350,#197351),
(#197352,#197353,#197354),(#197355,#197356,#197357),(#197358,#197359,#197360),
(#197361,#197362,#197363)),.UNSPECIFIED.,.F.,.F.,.F.)
B_SPLINE_SURFACE_WITH_KNOTS((4,2,4),(3,3),(-3.33934269125535E-17,0.000375063365810863,
0.00075012673162176),(0.,1.),.UNSPECIFIED.)
GEOMETRIC_REPRESENTATION_ITEM()
RATIONAL_B_SPLINE_SURFACE(((1.,0.949971414633671,1.),(1.,0.951436745841567,
1.),(1.,0.952767928482916,1.),(1.,0.955568668815872,1.),(1.,0.957047312721609,
1.),(1.,0.958250447045288,1.)))
REPRESENTATION_ITEM('')
SURFACE()
);
#3002=(
BOUNDED_SURFACE()
B_SPLINE_SURFACE(3,2,((#197380,#197381,#197382),(#197383,#197384,#197385),
(#197386,#197387,#197388),(#197389,#197390,#197391),(#197392,#197393,#197394),
(#197395,#197396,#197397),(#197398,#197399,#197400),(#197401,#197402,#197403),
(#197404,#197405,#197406),(#197407,#197408,#197409),(#197410,#197411,#197412),
(#197413,#197414,#197415),(#197416,#197417,#197418),(#197419,#197420,#197421),
(#197422,#197423,#197424),(#197425,#197426,#197427),(#197428,#197429,#197430),
(#197431,#197432,#197433),(#197434,#197435,#197436),(#197437,#197438,#197439),
(#197440,#197441,#197442),(#197443,#197444,#197445),(#197446,#197447,#197448),
(#197449,#197450,#197451),(#197452,#197453,#197454),(#197455,#197456,#197457)),
 .UNSPECIFIED.,.F.,.F.,.F.)
B_SPLINE_SURFACE_WITH_KNOTS((4,2,2,2,2,2,2,2,2,2,2,2,4),(3,3),(0.0241420258550515,
0.0246199912180732,0.0250868407533039,0.0255536902885345,0.0260205398237651,
0.0262539645913804,0.0264873893589957,0.0269542388942264,0.0271876636618417,
0.0274210884294571,0.0275378008132647,0.0276545131970724,0.0278990537924757),
(0.,1.00001111582779),.UNSPECIFIED.)
GEOMETRIC_REPRESENTATION_ITEM()
RATIONAL_B_SPLINE_SURFACE(((1.,0.950055426454912,1.00000111035056),(1.,
0.948849226790929,1.00000113716637),(1.,0.947384468413781,1.00000116973038),
(1.,0.945196499226927,1.00000121837255),(1.,0.944259740621461,1.00000123919825),
(1.,0.942078306513855,1.00000128769514),(1.,0.940957878707281,1.00000131260411),
(1.,0.938972382400276,1.00000135674498),(1.,0.938140754494424,1.00000137523344),
(1.,0.936869151046711,1.00000140350329),(1.,0.936440925028753,1.00000141302346),
(1.,0.93553683485142,1.00000143312289),(1.,0.935022314137583,1.00000144456153),
(1.,0.933816624278113,1.00000147136601),(1.,0.933295910820293,1.00000148294234),
(1.,0.932361200720811,1.00000150372249),(1.,0.932002008792242,1.00000151170792),
(1.,0.931284282765525,1.00000152766416),(1.,0.930932917594263,1.00000153547559),
(1.,0.930603729964699,1.00000154279397),(1.,0.930541982836373,1.00000154416671),
(1.,0.930392431492657,1.00000154749149),(1.,0.93030830454879,1.00000154936177),
(1.,0.930032458299446,1.00000155549429),(1.,0.929822127885655,1.00000156017028),
(1.,0.929675939651775,1.00000156342029)))
REPRESENTATION_ITEM('')
SURFACE()
);
#3003=(
BOUNDED_SURFACE()
B_SPLINE_SURFACE(3,2,((#197620,#197621,#197622),(#197623,#197624,#197625),
(#197626,#197627,#197628),(#197629,#197630,#197631)),.UNSPECIFIED.,.F.,
 .F.,.F.)
B_SPLINE_SURFACE_WITH_KNOTS((4,4),(3,3),(0.0249863231317726,0.0253614725245169),
(0.,1.),.UNSPECIFIED.)
GEOMETRIC_REPRESENTATION_ITEM()
RATIONAL_B_SPLINE_SURFACE(((1.,0.930070526504304,1.),(1.,0.930041043693298,
1.),(1.,0.929915461335265,1.),(1.,0.929697045866142,1.)))
REPRESENTATION_ITEM('')
SURFACE()
);
#3004=(
BOUNDED_SURFACE()
B_SPLINE_SURFACE(3,2,((#197637,#197638,#197639),(#197640,#197641,#197642),
(#197643,#197644,#197645),(#197646,#197647,#197648)),.UNSPECIFIED.,.F.,
 .F.,.F.)
B_SPLINE_SURFACE_WITH_KNOTS((4,4),(3,3),(0.0387340315057144,0.0427072915207099),
(0.,1.),.UNSPECIFIED.)
GEOMETRIC_REPRESENTATION_ITEM()
RATIONAL_B_SPLINE_SURFACE(((1.,0.930070526504304,1.),(1.,0.930612186341166,
1.),(1.,0.931191283587817,1.),(1.,0.931676951123116,1.)))
REPRESENTATION_ITEM('')
SURFACE()
);
#3005=(
BOUNDED_SURFACE()
B_SPLINE_SURFACE(3,2,((#197654,#197655,#197656),(#197657,#197658,#197659),
(#197660,#197661,#197662),(#197663,#197664,#197665)),.UNSPECIFIED.,.F.,
 .F.,.F.)
B_SPLINE_SURFACE_WITH_KNOTS((4,4),(3,3),(-0.000102945165535128,0.00102945165511774),
(0.,1.00671370076984),.UNSPECIFIED.)
GEOMETRIC_REPRESENTATION_ITEM()
RATIONAL_B_SPLINE_SURFACE(((0.999999999999999,0.997903207556182,1.00002815447409),
(1.,0.999219022833365,1.00001048649401),(1.,1.00001169204399,0.99999984300623),
(1.,1.,1.)))
REPRESENTATION_ITEM('')
SURFACE()
);
#3006=(
BOUNDED_SURFACE()
B_SPLINE_SURFACE(3,2,((#197735,#197736,#197737),(#197738,#197739,#197740),
(#197741,#197742,#197743),(#197744,#197745,#197746)),.UNSPECIFIED.,.F.,
 .F.,.F.)
B_SPLINE_SURFACE_WITH_KNOTS((4,4),(3,3),(0.0105620870905992,0.0106719618085628),
(0.,1.),.UNSPECIFIED.)
GEOMETRIC_REPRESENTATION_ITEM()
RATIONAL_B_SPLINE_SURFACE(((1.,0.997703261465162,1.),(1.,0.997980295466877,
1.),(1.,0.998184609657421,1.),(1.,0.998260562486345,1.)))
REPRESENTATION_ITEM('')
SURFACE()
);
#3007=(
BOUNDED_SURFACE()
B_SPLINE_SURFACE(3,2,((#197752,#197753,#197754),(#197755,#197756,#197757),
(#197758,#197759,#197760),(#197761,#197762,#197763)),.UNSPECIFIED.,.F.,
 .F.,.F.)
B_SPLINE_SURFACE_WITH_KNOTS((4,4),(3,3),(0.0270627267990643,0.0348275700538469),
(0.,1.),.UNSPECIFIED.)
GEOMETRIC_REPRESENTATION_ITEM()
RATIONAL_B_SPLINE_SURFACE(((1.,0.959662285900567,1.),(1.,0.959827071897822,
1.),(1.,0.959976275192286,1.),(1.,0.960109658705298,1.)))
REPRESENTATION_ITEM('')
SURFACE()
);
#3008=(
BOUNDED_SURFACE()
B_SPLINE_SURFACE(3,2,((#197769,#197770,#197771),(#197772,#197773,#197774),
(#197775,#197776,#197777),(#197778,#197779,#197780),(#197781,#197782,#197783),
(#197784,#197785,#197786),(#197787,#197788,#197789),(#197790,#197791,#197792),
(#197793,#197794,#197795),(#197796,#197797,#197798)),.UNSPECIFIED.,.F.,
 .F.,.F.)
B_SPLINE_SURFACE_WITH_KNOTS((4,2,2,2,4),(3,3),(-8.76035355368288E-17,0.000261575538067988,
0.000523151076136064,0.00078472661420414,0.00104630215227222),(0.,1.),
 .UNSPECIFIED.)
GEOMETRIC_REPRESENTATION_ITEM()
RATIONAL_B_SPLINE_SURFACE(((1.,0.941539462223513,1.),(1.,0.942944078103832,
1.),(1.,0.944666632267536,1.),(1.,0.947704870094427,1.),(1.,0.949116332566031,
1.),(1.,0.951938364158755,1.),(1.,0.953364849053626,1.),(1.,0.956562808919945,
1.),(1.,0.958303880696362,1.),(1.,0.959662285866081,1.)))
REPRESENTATION_ITEM('')
SURFACE()
);
#3009=(
BOUNDED_SURFACE()
B_SPLINE_SURFACE(3,2,((#197825,#197826,#197827),(#197828,#197829,#197830),
(#197831,#197832,#197833),(#197834,#197835,#197836),(#197837,#197838,#197839),
(#197840,#197841,#197842),(#197843,#197844,#197845),(#197846,#197847,#197848),
(#197849,#197850,#197851),(#197852,#197853,#197854),(#197855,#197856,#197857),
(#197858,#197859,#197860),(#197861,#197862,#197863),(#197864,#197865,#197866),
(#197867,#197868,#197869),(#197870,#197871,#197872),(#197873,#197874,#197875),
(#197876,#197877,#197878),(#197879,#197880,#197881),(#197882,#197883,#197884),
(#197885,#197886,#197887),(#197888,#197889,#197890),(#197891,#197892,#197893),
(#197894,#197895,#197896),(#197897,#197898,#197899),(#197900,#197901,#197902)),
 .UNSPECIFIED.,.F.,.F.,.F.)
B_SPLINE_SURFACE_WITH_KNOTS((4,2,2,2,2,2,2,2,2,2,2,2,4),(3,3),(0.0234563246751814,
0.0238865203213557,0.0243167159675301,0.0247469116137044,0.0251771072598787,
0.0253922050829658,0.0256073029060529,0.0260374985522272,0.0262525963753144,
0.0264676941984016,0.0265752431099451,0.0266827920214887,0.0268978898445759),
(0.,1.),.UNSPECIFIED.)
GEOMETRIC_REPRESENTATION_ITEM()
RATIONAL_B_SPLINE_SURFACE(((1.,0.941539462223482,1.),(1.,0.94001314415555,
1.),(1.,0.938778552928411,1.),(1.,0.936146669124993,1.),(1.,0.934687355972348,
1.),(1.,0.931881901141109,1.),(1.,0.930584405145522,1.),(1.,0.928334675540862,
1.),(1.,0.927304800261896,1.),(1.,0.925560477902519,1.),(1.,0.924898629931803,
1.),(1.,0.923648361190968,1.),(1.,0.923163635402122,1.),(1.,0.921866592945891,
1.),(1.,0.921255551609143,1.),(1.,0.919961545322548,1.),(1.,0.91942646515046,
1.),(1.,0.918406367469313,1.),(1.,0.917958926413567,1.),(1.,0.917720801012666,
1.),(1.,0.917685854938757,1.),(1.,0.917559269654572,1.),(1.,0.917489604007006,
1.),(1.,0.917284127651096,1.),(1.,0.917152514069398,1.),(1.,0.917108339181246,
1.)))
REPRESENTATION_ITEM('')
SURFACE()
);
#3010=(
BOUNDED_SURFACE()
B_SPLINE_SURFACE(3,2,((#197958,#197959,#197960),(#197961,#197962,#197963),
(#197964,#197965,#197966),(#197967,#197968,#197969)),.UNSPECIFIED.,.F.,
 .F.,.F.)
B_SPLINE_SURFACE_WITH_KNOTS((4,4),(3,3),(0.0245397910410617,0.0252336582652646),
(0.,1.),.UNSPECIFIED.)
GEOMETRIC_REPRESENTATION_ITEM()
RATIONAL_B_SPLINE_SURFACE(((1.,0.91828031569264,1.),(1.,0.918191277007662,
1.),(1.,0.917795655860169,1.),(1.,0.917108339181228,1.)))
REPRESENTATION_ITEM('')
SURFACE()
);
#3011=(
BOUNDED_SURFACE()
B_SPLINE_SURFACE(3,2,((#197984,#197985,#197986),(#197987,#197988,#197989),
(#197990,#197991,#197992),(#197993,#197994,#197995)),.UNSPECIFIED.,.F.,
 .F.,.F.)
B_SPLINE_SURFACE_WITH_KNOTS((4,4),(3,3),(0.0408577781618264,0.0446742483522374),
(0.,1.),.UNSPECIFIED.)
GEOMETRIC_REPRESENTATION_ITEM()
RATIONAL_B_SPLINE_SURFACE(((1.,0.918280315692642,1.),(1.,0.919146142525415,
1.),(1.,0.920060572994544,1.),(1.,0.920885718130539,1.)))
REPRESENTATION_ITEM('')
SURFACE()
);
#3012=(
BOUNDED_SURFACE()
B_SPLINE_SURFACE(3,2,((#198010,#198011,#198012),(#198013,#198014,#198015),
(#198016,#198017,#198018),(#198019,#198020,#198021),(#198022,#198023,#198024),
(#198025,#198026,#198027),(#198028,#198029,#198030),(#198031,#198032,#198033),
(#198034,#198035,#198036),(#198037,#198038,#198039),(#198040,#198041,#198042),
(#198043,#198044,#198045),(#198046,#198047,#198048),(#198049,#198050,#198051),
(#198052,#198053,#198054),(#198055,#198056,#198057),(#198058,#198059,#198060),
(#198061,#198062,#198063),(#198064,#198065,#198066),(#198067,#198068,#198069),
(#198070,#198071,#198072),(#198073,#198074,#198075),(#198076,#198077,#198078),
(#198079,#198080,#198081),(#198082,#198083,#198084),(#198085,#198086,#198087),
(#198088,#198089,#198090),(#198091,#198092,#198093),(#198094,#198095,#198096),
(#198097,#198098,#198099),(#198100,#198101,#198102),(#198103,#198104,#198105),
(#198106,#198107,#198108),(#198109,#198110,#198111),(#198112,#198113,#198114),
(#198115,#198116,#198117),(#198118,#198119,#198120),(#198121,#198122,#198123),
(#198124,#198125,#198126),(#198127,#198128,#198129),(#198130,#198131,#198132),
(#198133,#198134,#198135),(#198136,#198137,#198138),(#198139,#198140,#198141),
(#198142,#198143,#198144),(#198145,#198146,#198147),(#198148,#198149,#198150),
(#198151,#198152,#198153),(#198154,#198155,#198156),(#198157,#198158,#198159),
(#198160,#198161,#198162),(#198163,#198164,#198165),(#198166,#198167,#198168),
(#198169,#198170,#198171),(#198172,#198173,#198174),(#198175,#198176,#198177),
(#198178,#198179,#198180),(#198181,#198182,#198183),(#198184,#198185,#198186),
(#198187,#198188,#198189),(#198190,#198191,#198192),(#198193,#198194,#198195)),
 .UNSPECIFIED.,.F.,.F.,.F.)
B_SPLINE_SURFACE_WITH_KNOTS((4,2,2,2,2,2,2,2,2,2,2,2,2,2,2,2,2,2,2,2,2,
2,2,2,2,2,2,2,2,2,4),(3,3),(8.67361737988404E-19,0.00422017278643856,0.00435205318601475,
0.00438502328590881,0.00441799338580286,0.00448393358559096,0.00474769438474337,
0.00527521598304819,0.00633025917965783,0.00844034557287711,0.0126605183593157,
0.0137155615559253,0.0137815017557134,0.0138474419555015,0.0139793223550777,
0.0142430831542301,0.0147706047525349,0.0168806911457542,0.0211008639321928,
0.0221559071288024,0.0224196679279548,0.0224856081277429,0.0225185782276369,
0.022551548327531,0.0226834287271072,0.0232109503254121,0.0253210367186313,
0.0274311231118506,0.0284861663084603,0.0295412095050698,0.0337613822915084),
(-3.60075492201877E-5,1.),.UNSPECIFIED.)
GEOMETRIC_REPRESENTATION_ITEM()
RATIONAL_B_SPLINE_SURFACE(((1.00000292637104,0.959364479127511,1.),(1.00000292757611,
0.959347745547871,1.),(1.0000029869754,0.958522928388227,1.),(1.00000309965914,
0.956958204480126,1.),(1.00000310312445,0.956910085312184,1.),(1.00000310752022,
0.956849045791879,1.),(1.0000031057735,0.956873300638878,1.),(1.0000031039675,
0.956898378742207,1.),(1.00000310306648,0.956910890223367,1.),(1.0000031003694,
0.956948341850289,1.),(1.0000030985793,0.956973199179412,1.),(1.00000308966864,
0.957096932329961,1.),(1.00000308266768,0.957194147589323,1.),(1.00000306205115,
0.957480428238286,1.),(1.00000304882204,0.957664127258792,1.),(1.00000301070718,
0.958193389415057,1.),(1.00000298738066,0.958517300910559,1.),(1.00000292394881,
0.95939811406461,1.),(1.00000289040681,0.959863877542923,1.),(1.0000028158029,
0.960899825671287,1.),(1.00000280023093,0.961116057785621,1.),(1.00000283026338,
0.960699027834766,1.),(1.0000028387997,0.960580492677261,1.),(1.0000028506814,
0.96041550366659,1.),(1.00000285139065,0.960405655023073,1.),(1.00000285282986,
0.960385670240394,1.),(1.00000285177099,0.96040037370118,1.),(1.00000285025679,
0.960421399773948,1.),(1.000002849315,0.960434477515303,1.),(1.00000284669049,
0.960470921313707,1.),(1.00000284520862,0.960491498623802,1.),(1.00000284155124,
0.960542284905421,1.),(1.00000284016333,0.960561557334819,1.),(1.00000283831761,
0.960587186968871,1.),(1.00000285326178,0.960379672542332,1.),(1.00000294182501,
0.959149885586877,1.),(1.00000306027874,0.957505039829061,1.),(1.00000326284385,
0.954692225357289,1.),(1.00000330607674,0.954091894504147,1.),(1.00000336322261,
0.953298368221104,1.),(1.00000337481016,0.953137463832346,1.),(1.00000338949359,
0.952933570057739,1.),(1.00000339244022,0.952892653107387,1.),(1.00000339687514,
0.952831070026665,1.),(1.00000339835593,0.952810507723471,1.),(1.00000340132251,
0.952769313832698,1.),(1.00000340517493,0.952715819204016,1.),(1.00000339803007,
0.9528150326048,1.),(1.0000033923405,0.952894037921842,1.),(1.0000033640243,
0.953287236017829,1.),(1.0000033417926,0.953595944837787,1.),(1.00000323275155,
0.95511008637556,1.),(1.00000315226282,0.956227751003349,1.),(1.00000300554034,
0.95826513604973,1.),(1.00000293927507,0.959185294029097,1.),(1.0000028519299,
0.960398167032383,1.),(1.00000282483424,0.960774416805573,1.),(1.00000277506302,
0.961465538790771,1.),(1.00000275232028,0.961781343928606,1.),(1.00000265174015,
0.96317799730065,1.),(1.00000261355939,0.963708174443108,1.),(1.00000263292298,
0.963439292028068,1.)))
REPRESENTATION_ITEM('')
SURFACE()
);
#3013=(
BOUNDED_SURFACE()
B_SPLINE_SURFACE(3,2,((#198480,#198481,#198482),(#198483,#198484,#198485),
(#198486,#198487,#198488),(#198489,#198490,#198491),(#198492,#198493,#198494),
(#198495,#198496,#198497)),.UNSPECIFIED.,.F.,.F.,.F.)
B_SPLINE_SURFACE_WITH_KNOTS((4,2,4),(3,3),(-0.000109518730889342,0.000547593654446629,
0.00109518730889329),(-0.00197443491225529,1.),.UNSPECIFIED.)
GEOMETRIC_REPRESENTATION_ITEM()
RATIONAL_B_SPLINE_SURFACE(((1.00002435441833,0.993832559842802,1.),(1.00001601188437,
0.995945198226732,1.),(1.0000094741473,0.997600795233666,1.),(1.00000179564523,
0.999545276164647,1.),(0.999999971260214,1.00000727797757,1.),(1.,1.,1.)))
REPRESENTATION_ITEM('')
SURFACE()
);
#3014=(
BOUNDED_SURFACE()
B_SPLINE_SURFACE(3,2,((#198531,#198532,#198533),(#198534,#198535,#198536),
(#198537,#198538,#198539),(#198540,#198541,#198542)),.UNSPECIFIED.,.F.,
 .F.,.F.)
B_SPLINE_SURFACE_WITH_KNOTS((4,4),(3,3),(0.0169795328233838,0.0259332885708231),
(0.,1.),.UNSPECIFIED.)
GEOMETRIC_REPRESENTATION_ITEM()
RATIONAL_B_SPLINE_SURFACE(((1.,0.957225253293536,1.),(1.,0.957330219064779,
1.),(1.,0.957420194105006,1.),(1.,0.95749691742527,1.)))
REPRESENTATION_ITEM('')
SURFACE()
);
#3015=(
BOUNDED_SURFACE()
B_SPLINE_SURFACE(3,2,((#198553,#198554,#198555),(#198556,#198557,#198558),
(#198559,#198560,#198561),(#198562,#198563,#198564)),.UNSPECIFIED.,.F.,
 .F.,.F.)
B_SPLINE_SURFACE_WITH_KNOTS((4,4),(3,3),(0.00708837036243835,0.00717746991701786),
(0.,1.),.UNSPECIFIED.)
GEOMETRIC_REPRESENTATION_ITEM()
RATIONAL_B_SPLINE_SURFACE(((1.,0.994244619571122,1.),(1.,0.994515217115564,
1.),(1.,0.994723691418642,1.),(1.,0.99486030168986,1.)))
REPRESENTATION_ITEM('')
SURFACE()
);
#3016=(
BOUNDED_SURFACE()
B_SPLINE_SURFACE(3,2,((#198574,#198575,#198576),(#198577,#198578,#198579),
(#198580,#198581,#198582),(#198583,#198584,#198585),(#198586,#198587,#198588),
(#198589,#198590,#198591),(#198592,#198593,#198594),(#198595,#198596,#198597),
(#198598,#198599,#198600),(#198601,#198602,#198603)),.UNSPECIFIED.,.F.,
 .F.,.F.)
B_SPLINE_SURFACE_WITH_KNOTS((4,2,2,2,4),(3,3),(2.16840434497101E-19,0.000213802025234883,
0.000427604050469766,0.000641406075704648,0.00085520810093953),(0.,1.),
 .UNSPECIFIED.)
GEOMETRIC_REPRESENTATION_ITEM()
RATIONAL_B_SPLINE_SURFACE(((1.,0.946111573410138,1.),(1.,0.947006419495448,
1.),(1.,0.94806750540417,1.),(1.,0.949985245580726,1.),(1.,0.950885821685186,
1.),(1.,0.952671230936143,1.),(1.,0.95357069077605,1.),(1.,0.955449705779053,
1.),(1.,0.956409634187462,1.),(1.,0.957225253284162,1.)))
REPRESENTATION_ITEM('')
SURFACE()
);
#3017=(
BOUNDED_SURFACE()
B_SPLINE_SURFACE(3,2,((#198702,#198703,#198704),(#198705,#198706,#198707),
(#198708,#198709,#198710),(#198711,#198712,#198713),(#198714,#198715,#198716),
(#198717,#198718,#198719),(#198720,#198721,#198722),(#198723,#198724,#198725),
(#198726,#198727,#198728),(#198729,#198730,#198731),(#198732,#198733,#198734),
(#198735,#198736,#198737),(#198738,#198739,#198740),(#198741,#198742,#198743),
(#198744,#198745,#198746),(#198747,#198748,#198749),(#198750,#198751,#198752),
(#198753,#198754,#198755),(#198756,#198757,#198758),(#198759,#198760,#198761)),
 .UNSPECIFIED.,.F.,.F.,.F.)
B_SPLINE_SURFACE_WITH_KNOTS((4,2,2,2,2,2,2,2,2,4),(3,3),(0.0241892472826494,
0.0245055239061063,0.0248218005295631,0.0251380771530199,0.0252962154647483,
0.0254543537764767,0.0257706303999336,0.0260869070233904,0.0264031836468472,
0.0267194602703041),(0.,1.),.UNSPECIFIED.)
GEOMETRIC_REPRESENTATION_ITEM()
RATIONAL_B_SPLINE_SURFACE(((1.,0.929973550212778,1.),(1.,0.930197351202751,
1.),(1.,0.930513290387209,1.),(1.,0.930996534931652,1.),(1.,0.931814475301649,
1.),(1.,0.93305861889435,1.),(1.,0.933512667464957,1.),(1.,0.934381592790984,
1.),(1.,0.934697923125669,1.),(1.,0.935467938930732,1.),(1.,0.935923141258381,
1.),(1.,0.937089763990058,1.),(1.,0.937772194692309,1.),(1.,0.939224429356622,
1.),(1.,0.94003447069213,1.),(1.,0.941810586362858,1.),(1.,0.942756891232808,
1.),(1.,0.944448481966905,1.),(1.,0.945215424202475,1.),(1.,0.946111573410157,
1.)))
REPRESENTATION_ITEM('')
SURFACE()
);
#3018=(
BOUNDED_SURFACE()
B_SPLINE_SURFACE(3,2,((#198912,#198913,#198914),(#198915,#198916,#198917),
(#198918,#198919,#198920),(#198921,#198922,#198923)),.UNSPECIFIED.,.F.,
 .F.,.F.)
B_SPLINE_SURFACE_WITH_KNOTS((4,4),(3,3),(0.0252170418335343,0.0258229913570786),
(0.,1.),.UNSPECIFIED.)
GEOMETRIC_REPRESENTATION_ITEM()
RATIONAL_B_SPLINE_SURFACE(((1.,0.930836001346604,1.),(1.,0.9307923293152,
1.),(1.,0.930500666506043,1.),(1.,0.929973550212784,1.)))
REPRESENTATION_ITEM('')
SURFACE()
);
#3019=(
BOUNDED_SURFACE()
B_SPLINE_SURFACE(3,2,((#198929,#198930,#198931),(#198932,#198933,#198934),
(#198935,#198936,#198937),(#198938,#198939,#198940)),.UNSPECIFIED.,.F.,
 .F.,.F.)
B_SPLINE_SURFACE_WITH_KNOTS((4,4),(3,3),(0.0413352581734093,0.045313001148136),
(0.,1.),.UNSPECIFIED.)
GEOMETRIC_REPRESENTATION_ITEM()
RATIONAL_B_SPLINE_SURFACE(((1.,0.932166688794147,1.),(1.,0.93183558573748,
1.),(1.,0.931353352247314,1.),(1.,0.930836001346602,1.)))
REPRESENTATION_ITEM('')
SURFACE()
);
#3020=(
BOUNDED_SURFACE()
B_SPLINE_SURFACE(3,2,((#198949,#198950,#198951),(#198952,#198953,#198954),
(#198955,#198956,#198957),(#198958,#198959,#198960),(#198961,#198962,#198963),
(#198964,#198965,#198966)),.UNSPECIFIED.,.F.,.F.,.F.)
B_SPLINE_SURFACE_WITH_KNOTS((4,2,4),(3,3),(0.0163865690223841,0.0292596031542503,
0.0419823306135875),(0.,1.00027232565654),.UNSPECIFIED.)
GEOMETRIC_REPRESENTATION_ITEM()
RATIONAL_B_SPLINE_SURFACE(((1.,0.997741854080557,1.00000122990214),(1.,
0.997128059065537,1.0000015642064),(1.,0.996318687779106,1.00000200503153),
(1.,0.994008737908883,1.00000326314876),(1.,0.992515369868671,1.00000407651363),
(1.,0.990483423032272,1.00000518321614)))
REPRESENTATION_ITEM('')
SURFACE()
);
#3021=(
BOUNDED_SURFACE()
B_SPLINE_SURFACE(3,2,((#198996,#198997,#198998),(#198999,#199000,#199001),
(#199002,#199003,#199004),(#199005,#199006,#199007)),.UNSPECIFIED.,.F.,
 .F.,.F.)
B_SPLINE_SURFACE_WITH_KNOTS((4,4),(3,3),(0.0181935747412957,0.0490322053436587),
(0.,1.00237065770204),.UNSPECIFIED.)
GEOMETRIC_REPRESENTATION_ITEM()
RATIONAL_B_SPLINE_SURFACE(((1.,0.989924970143594,1.00004776889425),(1.,
0.991156791509079,1.00004192844064),(1.,0.991768207325747,1.00003902952541),
(1.,0.992256661054546,1.00003671361222)))
REPRESENTATION_ITEM('')
SURFACE()
);
#3022=(
BOUNDED_SURFACE()
B_SPLINE_SURFACE(3,2,((#199037,#199038,#199039),(#199040,#199041,#199042),
(#199043,#199044,#199045),(#199046,#199047,#199048)),.UNSPECIFIED.,.F.,
 .F.,.F.)
B_SPLINE_SURFACE_WITH_KNOTS((4,4),(3,3),(0.0486839608469686,0.0783506339606883),
(0.,1.00251465406579),.UNSPECIFIED.)
GEOMETRIC_REPRESENTATION_ITEM()
RATIONAL_B_SPLINE_SURFACE(((1.,0.993081781376145,1.00003479385318),(1.,
0.992621487987293,1.00003710881046),(1.,0.992054572782517,1.00003996000171),
(1.,0.990843694193378,1.00004604988325)))
REPRESENTATION_ITEM('')
SURFACE()
);
#3023=(
BOUNDED_SURFACE()
B_SPLINE_SURFACE(3,2,((#199078,#199079,#199080),(#199081,#199082,#199083),
(#199084,#199085,#199086),(#199087,#199088,#199089),(#199090,#199091,#199092),
(#199093,#199094,#199095)),.UNSPECIFIED.,.F.,.F.,.F.)
B_SPLINE_SURFACE_WITH_KNOTS((4,2,4),(3,3),(0.0166253761100808,0.0283648343214889,
0.0401042925328971),(0.,1.),.UNSPECIFIED.)
GEOMETRIC_REPRESENTATION_ITEM()
RATIONAL_B_SPLINE_SURFACE(((1.,0.99500220761949,1.),(1.,0.995241643636696,
1.),(1.,0.995238480184742,1.),(1.,0.994937803535913,1.),(1.,0.99463876407346,
1.),(1.,0.994244619571122,1.)))
REPRESENTATION_ITEM('')
SURFACE()
);
#3024=(
BOUNDED_SURFACE()
B_SPLINE_SURFACE(3,2,((#207098,#207099,#207100),(#207101,#207102,#207103),
(#207104,#207105,#207106),(#207107,#207108,#207109),(#207110,#207111,#207112),
(#207113,#207114,#207115)),.UNSPECIFIED.,.F.,.F.,.F.)
B_SPLINE_SURFACE_WITH_KNOTS((4,2,4),(3,3),(0.,0.000611885440421095,0.00122377088084219),
(0.,1.),.UNSPECIFIED.)
GEOMETRIC_REPRESENTATION_ITEM()
RATIONAL_B_SPLINE_SURFACE(((1.,0.713250449154079,1.),(1.,0.672263173507019,
1.),(1.,0.648659882421647,1.),(1.,0.648739723662275,1.),(1.,0.672275262307808,
1.),(1.,0.713250449154082,1.)))
REPRESENTATION_ITEM('')
SURFACE()
);
#3025=(
BOUNDED_SURFACE()
B_SPLINE_SURFACE(3,2,((#207212,#207213,#207214),(#207215,#207216,#207217),
(#207218,#207219,#207220),(#207221,#207222,#207223),(#207224,#207225,#207226),
(#207227,#207228,#207229),(#207230,#207231,#207232),(#207233,#207234,#207235),
(#207236,#207237,#207238),(#207239,#207240,#207241)),.UNSPECIFIED.,.F.,
 .F.,.F.)
B_SPLINE_SURFACE_WITH_KNOTS((4,2,2,2,4),(3,3),(-1.10588621593521E-17,0.00061030576480229,
0.00122061152960459,0.00183091729440689,0.0024412230592092),(0.,1.),
 .UNSPECIFIED.)
GEOMETRIC_REPRESENTATION_ITEM()
RATIONAL_B_SPLINE_SURFACE(((1.,0.727552664059041,1.),(1.,0.745088511631937,
1.),(1.,0.761651043043578,1.),(1.,0.793171709476032,1.),(1.,0.808261553243384,
1.),(1.,0.836218122216209,1.),(1.,0.849115521102991,1.),(1.,0.872797166619617,
1.),(1.,0.883451618896464,1.),(1.,0.892325300547709,1.)))
REPRESENTATION_ITEM('')
SURFACE()
);
#3026=(
BOUNDED_SURFACE()
B_SPLINE_SURFACE(3,2,((#207358,#207359,#207360),(#207361,#207362,#207363),
(#207364,#207365,#207366),(#207367,#207368,#207369)),.UNSPECIFIED.,.F.,
 .F.,.F.)
B_SPLINE_SURFACE_WITH_KNOTS((4,4),(3,3),(0.,0.010514647628205),(0.,1.),
 .UNSPECIFIED.)
GEOMETRIC_REPRESENTATION_ITEM()
RATIONAL_B_SPLINE_SURFACE(((1.,0.727552664059029,1.),(1.,0.728396913847474,
1.),(1.,0.728235528042243,1.),(1.,0.727880838895167,1.)))
REPRESENTATION_ITEM('')
SURFACE()
);
#3027=(
BOUNDED_SURFACE()
B_SPLINE_SURFACE(3,2,((#207427,#207428,#207429),(#207430,#207431,#207432),
(#207433,#207434,#207435),(#207436,#207437,#207438),(#207439,#207440,#207441),
(#207442,#207443,#207444),(#207445,#207446,#207447),(#207448,#207449,#207450),
(#207451,#207452,#207453),(#207454,#207455,#207456)),.UNSPECIFIED.,.F.,
 .F.,.F.)
B_SPLINE_SURFACE_WITH_KNOTS((4,2,2,2,4),(3,3),(-8.17201003445707E-5,0.000594463573430658,
0.00118892714686131,0.00178339072029198,0.00245957439406716),(0.,1.00071180428484),
 .UNSPECIFIED.)
GEOMETRIC_REPRESENTATION_ITEM()
RATIONAL_B_SPLINE_SURFACE(((1.,0.926970074644159,1.00010396602758),(1.,
0.931625564084532,1.00009733843292),(1.,0.925916756569445,1.00010546554022),
(1.,0.902068515312624,1.00013941610084),(1.,0.885944725818379,1.00016237006574),
(1.,0.848477324278585,1.00021570897966),(1.,0.827049589649371,1.0002462136863),
(1.,0.776935720203443,1.00031755622031),(1.,0.74806977061884,1.00035865003351),
(1.,0.716291963603933,1.0004038891919)))
REPRESENTATION_ITEM('')
SURFACE()
);
#3028=(
BOUNDED_SURFACE()
B_SPLINE_SURFACE(3,2,((#207529,#207530,#207531),(#207532,#207533,#207534),
(#207535,#207536,#207537),(#207538,#207539,#207540),(#207541,#207542,#207543),
(#207544,#207545,#207546)),.UNSPECIFIED.,.F.,.F.,.F.)
B_SPLINE_SURFACE_WITH_KNOTS((4,2,4),(3,3),(-1.38777878078145E-17,0.0041604828508626,
0.00832096570172521),(0.,1.),.UNSPECIFIED.)
GEOMETRIC_REPRESENTATION_ITEM()
RATIONAL_B_SPLINE_SURFACE(((1.,0.928260885086434,1.),(1.,0.928493402693592,
1.),(1.,0.928615016565842,1.),(1.,0.928561249118847,1.),(1.,0.928391240061757,
1.),(1.,0.928132015153712,1.)))
REPRESENTATION_ITEM('')
SURFACE()
);
#3029=(
BOUNDED_SURFACE()
B_SPLINE_SURFACE(3,2,((#207588,#207589,#207590),(#207591,#207592,#207593),
(#207594,#207595,#207596),(#207597,#207598,#207599),(#207600,#207601,#207602),
(#207603,#207604,#207605),(#207606,#207607,#207608),(#207609,#207610,#207611),
(#207612,#207613,#207614),(#207615,#207616,#207617)),.UNSPECIFIED.,.F.,
 .F.,.F.)
B_SPLINE_SURFACE_WITH_KNOTS((4,2,2,2,4),(3,3),(-0.00023493367097703,0.000587334177442414,
0.00117466835488487,0.00176200253232733,0.00258427038074678),(-0.000330771740685424,
1.),.UNSPECIFIED.)
GEOMETRIC_REPRESENTATION_ITEM()
RATIONAL_B_SPLINE_SURFACE(((1.0001975152061,0.701432767973641,1.),(1.00017087577531,
0.741701369416836,1.),(1.00014739521264,0.777194973892298,1.),(1.00011108291111,
0.832085245739731,1.),(1.00009703796778,0.853315812919012,1.),(1.00007293188498,
0.889754963915332,1.),(1.00006264550326,0.905304027592269,1.),(1.00004609326443,
0.930324663863228,1.),(1.00004377591455,0.933827608038183,1.),(1.00005227954766,
0.920973376459142,1.)))
REPRESENTATION_ITEM('')
SURFACE()
);
#3030=(
BOUNDED_SURFACE()
B_SPLINE_SURFACE(3,2,((#207749,#207750,#207751),(#207752,#207753,#207754),
(#207755,#207756,#207757),(#207758,#207759,#207760)),.UNSPECIFIED.,.F.,
 .F.,.F.)
B_SPLINE_SURFACE_WITH_KNOTS((4,4),(3,3),(0.,0.0107001581246114),(0.,1.),
 .UNSPECIFIED.)
GEOMETRIC_REPRESENTATION_ITEM()
RATIONAL_B_SPLINE_SURFACE(((1.,0.73489735095993,1.),(1.,0.734875794442845,
1.),(1.,0.734252034560147,1.),(1.,0.73129868040477,1.)))
REPRESENTATION_ITEM('')
SURFACE()
);
#3031=(
BOUNDED_SURFACE()
B_SPLINE_SURFACE(3,2,((#207783,#207784,#207785),(#207786,#207787,#207788),
(#207789,#207790,#207791),(#207792,#207793,#207794)),.UNSPECIFIED.,.F.,
 .F.,.F.)
B_SPLINE_SURFACE_WITH_KNOTS((4,4),(3,3),(0.,0.000517122404042923),(0.,1.),
 .UNSPECIFIED.)
GEOMETRIC_REPRESENTATION_ITEM()
RATIONAL_B_SPLINE_SURFACE(((1.,0.707106781186546,1.),(1.,0.731070766440982,
1.),(1.,0.753745435486364,1.),(1.,0.77196935846749,1.)))
REPRESENTATION_ITEM('')
SURFACE()
);
#3032=(
BOUNDED_SURFACE()
B_SPLINE_SURFACE(3,2,((#207836,#207837,#207838),(#207839,#207840,#207841),
(#207842,#207843,#207844),(#207845,#207846,#207847),(#207848,#207849,#207850),
(#207851,#207852,#207853)),.UNSPECIFIED.,.F.,.F.,.F.)
B_SPLINE_SURFACE_WITH_KNOTS((4,2,4),(3,3),(-2.92626166353837E-16,0.00117037761632422,
0.00234075523264872),(0.,1.),.UNSPECIFIED.)
GEOMETRIC_REPRESENTATION_ITEM()
RATIONAL_B_SPLINE_SURFACE(((1.,0.888647434958264,1.),(1.,0.871248161544161,
1.),(1.,0.84779606985727,1.),(1.,0.794668809935237,1.),(1.,0.764625718490638,
1.),(1.,0.731298680404815,1.)))
REPRESENTATION_ITEM('')
SURFACE()
);
#3033=(
BOUNDED_SURFACE()
B_SPLINE_SURFACE(3,2,((#207964,#207965,#207966),(#207967,#207968,#207969),
(#207970,#207971,#207972),(#207973,#207974,#207975),(#207976,#207977,#207978),
(#207979,#207980,#207981),(#207982,#207983,#207984),(#207985,#207986,#207987),
(#207988,#207989,#207990),(#207991,#207992,#207993),(#207994,#207995,#207996),
(#207997,#207998,#207999)),.UNSPECIFIED.,.F.,.F.,.F.)
B_SPLINE_SURFACE_WITH_KNOTS((4,2,2,2,2,4),(3,3),(-0.000229639107487331,
0.000574097768718188,0.00114819553743641,0.00143524442179553,0.00172229330615464,
0.00252603018236012),(-0.000695063111154208,1.00310110558421),
 .UNSPECIFIED.)
GEOMETRIC_REPRESENTATION_ITEM()
RATIONAL_B_SPLINE_SURFACE(((1.00041583704952,0.699935521594427,1.00185976660778),
(1.00036124087235,0.739331658718599,1.00161559368639),(1.00031293869035,
0.774186102461259,1.00139956968065),(1.00023813854648,0.82816125013087,
1.00106503765666),(1.0002101364639,0.848367314777069,1.00093980269216),
(1.00017367979131,0.874674139669543,1.00077675588718),(1.00016260452917,
0.882665954637282,1.0007272234977),(1.00014324788421,0.896633545018679,
1.00064065390999),(1.00013479460749,0.902733357609951,1.00060284794298),
(1.00010983737982,0.920742280843341,1.0004912306191),(1.00010567595172,
0.92374513197171,1.00047261927834),(1.00012224113811,0.911791834348499,
1.00054670450126)))
REPRESENTATION_ITEM('')
SURFACE()
);
#3034=(
BOUNDED_SURFACE()
B_SPLINE_SURFACE(3,2,((#208067,#208068,#208069),(#208070,#208071,#208072),
(#208073,#208074,#208075),(#208076,#208077,#208078)),.UNSPECIFIED.,.F.,
 .F.,.F.)
B_SPLINE_SURFACE_WITH_KNOTS((4,4),(3,3),(0.,0.00980967348625105),(0.,1.),
 .UNSPECIFIED.)
GEOMETRIC_REPRESENTATION_ITEM()
RATIONAL_B_SPLINE_SURFACE(((1.,0.733631070205817,1.),(1.,0.732913032274794,
1.),(1.,0.731754232439324,1.),(1.,0.729712990977684,1.)))
REPRESENTATION_ITEM('')
SURFACE()
);
#3035=(
BOUNDED_SURFACE()
B_SPLINE_SURFACE(3,2,((#208090,#208091,#208092),(#208093,#208094,#208095),
(#208096,#208097,#208098),(#208099,#208100,#208101),(#208102,#208103,#208104),
(#208105,#208106,#208107)),.UNSPECIFIED.,.F.,.F.,.F.)
B_SPLINE_SURFACE_WITH_KNOTS((4,2,4),(3,3),(-1.04083408558608E-17,0.00416021787251448,
0.00832043574502897),(0.,1.),.UNSPECIFIED.)
GEOMETRIC_REPRESENTATION_ITEM()
RATIONAL_B_SPLINE_SURFACE(((1.,0.91815876419713,1.),(1.,0.918478576988139,
1.),(1.,0.918702883828552,1.),(1.,0.918900670636956,1.),(1.,0.918880394705029,
1.),(1.,0.918792784744087,1.)))
REPRESENTATION_ITEM('')
SURFACE()
);
#3036=(
BOUNDED_SURFACE()
B_SPLINE_SURFACE(3,2,((#208140,#208141,#208142),(#208143,#208144,#208145),
(#208146,#208147,#208148),(#208149,#208150,#208151),(#208152,#208153,#208154),
(#208155,#208156,#208157)),.UNSPECIFIED.,.F.,.F.,.F.)
B_SPLINE_SURFACE_WITH_KNOTS((4,2,4),(3,3),(0.,0.00128099832444667,0.00256199664889334),
(0.,1.),.UNSPECIFIED.)
GEOMETRIC_REPRESENTATION_ITEM()
RATIONAL_B_SPLINE_SURFACE(((1.,0.901968956514557,1.),(1.,0.883369478142107,
1.),(1.,0.857628018054164,1.),(1.,0.799434735390564,1.),(1.,0.766284883162671,
1.),(1.,0.729712990977659,1.)))
REPRESENTATION_ITEM('')
SURFACE()
);
#3037=(
BOUNDED_SURFACE()
B_SPLINE_SURFACE(3,2,((#208301,#208302,#208303),(#208304,#208305,#208306),
(#208307,#208308,#208309),(#208310,#208311,#208312),(#208313,#208314,#208315),
(#208316,#208317,#208318),(#208319,#208320,#208321),(#208322,#208323,#208324),
(#208325,#208326,#208327),(#208328,#208329,#208330)),.UNSPECIFIED.,.F.,
 .F.,.F.)
B_SPLINE_SURFACE_WITH_KNOTS((4,2,2,2,4),(3,3),(-9.48676900924816E-18,0.000575184387543924,
0.00115036877508786,0.00172555316263179,0.00230073755017573),(0.,1.00079242647114),
 .UNSPECIFIED.)
GEOMETRIC_REPRESENTATION_ITEM()
RATIONAL_B_SPLINE_SURFACE(((1.,0.918093911035446,1.00012980910609),(1.,
0.92016598823334,1.00012652516844),(1.,0.91537620632456,1.00013411626839),
(1.,0.895563982165149,1.00016551573015),(1.,0.880770844269308,1.00018896067827),
(1.,0.8454580472065,1.00024492626859),(1.,0.825177021514163,1.00027706871183),
(1.,0.780124700037101,1.00034847001608),(1.,0.75591069420419,1.00038684565447),
(1.,0.729555383368477,1.00042861494639)))
REPRESENTATION_ITEM('')
SURFACE()
);
#3038=(
BOUNDED_SURFACE()
B_SPLINE_SURFACE(3,2,((#208401,#208402,#208403),(#208404,#208405,#208406),
(#208407,#208408,#208409),(#208410,#208411,#208412)),.UNSPECIFIED.,.F.,
 .F.,.F.)
B_SPLINE_SURFACE_WITH_KNOTS((4,4),(3,3),(0.,0.00972938600277916),(0.,1.),
 .UNSPECIFIED.)
GEOMETRIC_REPRESENTATION_ITEM()
RATIONAL_B_SPLINE_SURFACE(((1.,0.729533004763605,1.),(1.,0.730591519138966,
1.),(1.,0.730312610923774,1.),(1.,0.729769521153222,1.)))
REPRESENTATION_ITEM('')
SURFACE()
);
#3039=(
BOUNDED_SURFACE()
B_SPLINE_SURFACE(3,2,((#208435,#208436,#208437),(#208438,#208439,#208440),
(#208441,#208442,#208443),(#208444,#208445,#208446)),.UNSPECIFIED.,.F.,
 .F.,.F.)
B_SPLINE_SURFACE_WITH_KNOTS((4,4),(3,3),(-6.39679281766448E-18,3.42512019832298E-5),
(0.,1.),.UNSPECIFIED.)
GEOMETRIC_REPRESENTATION_ITEM()
RATIONAL_B_SPLINE_SURFACE(((1.,0.707106781186548,1.),(1.,0.70842711846827,
1.),(1.,0.709730890158149,1.),(1.,0.711017327239758,1.)))
REPRESENTATION_ITEM('')
SURFACE()
);
#3040=(
BOUNDED_SURFACE()
B_SPLINE_SURFACE(3,2,((#208458,#208459,#208460),(#208461,#208462,#208463),
(#208464,#208465,#208466),(#208467,#208468,#208469),(#208470,#208471,#208472),
(#208473,#208474,#208475),(#208476,#208477,#208478),(#208479,#208480,#208481)),
 .UNSPECIFIED.,.F.,.F.,.F.)
B_SPLINE_SURFACE_WITH_KNOTS((4,2,2,4),(3,3),(-4.40186082029115E-17,0.00128517876997136,
0.00192776815495707,0.00257035753994277),(0.,1.),.UNSPECIFIED.)
GEOMETRIC_REPRESENTATION_ITEM()
RATIONAL_B_SPLINE_SURFACE(((1.,0.729533004763577,1.),(1.,0.766429181343272,
1.),(1.,0.799163813689396,1.),(1.,0.843673470277402,1.),(1.,0.857403797499188,
1.),(1.,0.882315838155618,1.),(1.,0.893652235396326,1.),(1.,0.903015666115932,
1.)))
REPRESENTATION_ITEM('')
SURFACE()
);
#3041=(
BOUNDED_SURFACE()
B_SPLINE_SURFACE(3,2,((#208605,#208606,#208607),(#208608,#208609,#208610),
(#208611,#208612,#208613),(#208614,#208615,#208616)),.UNSPECIFIED.,.F.,
 .F.,.F.)
B_SPLINE_SURFACE_WITH_KNOTS((4,4),(3,3),(-6.61363325216158E-18,2.21589532008063E-5),
(0.,1.),.UNSPECIFIED.)
GEOMETRIC_REPRESENTATION_ITEM()
RATIONAL_B_SPLINE_SURFACE(((1.,0.707106781186552,1.),(1.,0.707961610595566,
1.),(1.,0.708809519028292,1.),(1.,0.709650295730098,1.)))
REPRESENTATION_ITEM('')
SURFACE()
);
#3042=(
BOUNDED_SURFACE()
B_SPLINE_SURFACE(3,2,((#208682,#208683,#208684),(#208685,#208686,#208687),
(#208688,#208689,#208690),(#208691,#208692,#208693)),.UNSPECIFIED.,.F.,
 .F.,.F.)
B_SPLINE_SURFACE_WITH_KNOTS((4,4),(3,3),(0.00880203782093267,0.00917783640854858),
(0.,1.),.UNSPECIFIED.)
GEOMETRIC_REPRESENTATION_ITEM()
RATIONAL_B_SPLINE_SURFACE(((1.,0.928452770819611,1.),(1.,0.928460035446405,
1.),(1.,0.928468213633922,1.),(1.,0.928477160954726,1.)))
REPRESENTATION_ITEM('')
SURFACE()
);
#3043=(
BOUNDED_SURFACE()
B_SPLINE_SURFACE(3,2,((#208699,#208700,#208701),(#208702,#208703,#208704),
(#208705,#208706,#208707),(#208708,#208709,#208710)),.UNSPECIFIED.,.F.,
 .F.,.F.)
B_SPLINE_SURFACE_WITH_KNOTS((4,4),(3,3),(0.,0.000210836370419711),(0.,1.),
 .UNSPECIFIED.)
GEOMETRIC_REPRESENTATION_ITEM()
RATIONAL_B_SPLINE_SURFACE(((1.,0.928492930368189,1.),(1.,0.928487440815482,
1.),(1.,0.928482179049582,1.),(1.,0.928477160954739,1.)))
REPRESENTATION_ITEM('')
SURFACE()
);
#3044=(
BOUNDED_SURFACE()
B_SPLINE_SURFACE(3,2,((#208719,#208720,#208721),(#208722,#208723,#208724),
(#208725,#208726,#208727),(#208728,#208729,#208730),(#208731,#208732,#208733),
(#208734,#208735,#208736),(#208737,#208738,#208739),(#208740,#208741,#208742),
(#208743,#208744,#208745),(#208746,#208747,#208748),(#208749,#208750,#208751),
(#208752,#208753,#208754)),.UNSPECIFIED.,.F.,.F.,.F.)
B_SPLINE_SURFACE_WITH_KNOTS((4,2,2,2,2,4),(3,3),(-0.000206342901056451,
0.000515857252641128,0.00103171450528226,0.00154757175792339,0.00180550038424395,
0.00226977191162085),(-0.00146001009681673,1.00056090637502),
 .UNSPECIFIED.)
GEOMETRIC_REPRESENTATION_ITEM()
RATIONAL_B_SPLINE_SURFACE(((1.00055460374899,0.809961833654899,1.00021287626228),
(1.00047293149373,0.837947301944298,1.00018152760215),(1.00039897300112,
0.863289605070118,1.00015313975317),(1.00028590192954,0.90203405847295,
1.00010973913222),(1.00024196311713,0.917089945412939,1.00009287388352),
(1.00016992773463,0.941773283793271,1.00006522419127),(1.00014170965431,
0.951442371408365,1.00005439310786),(1.00012570829839,0.956925328102896,
1.00004825122936),(1.00012496629093,0.957179581229155,1.00004796642102),
(1.00013594085639,0.953419083216919,1.00005217884201),(1.00015771831893,
0.945956910345841,1.00006053779169),(1.00018769789889,0.935684234741691,
1.0000720450001)))
REPRESENTATION_ITEM('')
SURFACE()
);
#3045=(
BOUNDED_SURFACE()
B_SPLINE_SURFACE(3,2,((#208813,#208814,#208815),(#208816,#208817,#208818),
(#208819,#208820,#208821),(#208822,#208823,#208824),(#208825,#208826,#208827),
(#208828,#208829,#208830),(#208831,#208832,#208833),(#208834,#208835,#208836),
(#208837,#208838,#208839),(#208840,#208841,#208842),(#208843,#208844,#208845),
(#208846,#208847,#208848)),.UNSPECIFIED.,.F.,.F.,.F.)
B_SPLINE_SURFACE_WITH_KNOTS((4,2,2,2,2,4),(3,3),(-0.000236631349860531,
0.000591578374651329,0.000887367561976994,0.00118315674930266,0.00177473512395399,
0.00260294484846584),(-0.00119575409929547,1.),.UNSPECIFIED.)
GEOMETRIC_REPRESENTATION_ITEM()
RATIONAL_B_SPLINE_SURFACE(((1.00021393343793,0.910544551738771,1.),(1.00016085325225,
0.932739828219605,1.),(1.00011637632197,0.951337686385449,1.),(1.00010674451532,
0.955365189471307,1.),(1.00010912168845,0.954371183627145,1.),(1.00012287489593,
0.948620332558914,1.),(1.0001340538894,0.943945879224083,1.),(1.00017581652603,
0.926482992559179,1.),(1.00021426650785,0.910405279824543,1.),(1.00031653395365,
0.86764253878067,1.),(1.00038632399849,0.838460098645234,1.),(1.0004622600014,
0.80670774966673,1.)))
REPRESENTATION_ITEM('')
SURFACE()
);
#3046=(
BOUNDED_SURFACE()
B_SPLINE_SURFACE(3,2,((#208999,#209000,#209001),(#209002,#209003,#209004),
(#209005,#209006,#209007),(#209008,#209009,#209010)),.UNSPECIFIED.,.F.,
 .F.,.F.)
B_SPLINE_SURFACE_WITH_KNOTS((4,4),(3,3),(-5.20417042793042E-18,0.000729297262992661),
(0.,1.),.UNSPECIFIED.)
GEOMETRIC_REPRESENTATION_ITEM()
RATIONAL_B_SPLINE_SURFACE(((1.,0.833636261310766,1.),(1.,0.833189131672253,
1.),(1.,0.83273693675361,1.),(1.,0.832279622729512,1.)))
REPRESENTATION_ITEM('')
SURFACE()
);
#3047=(
BOUNDED_SURFACE()
B_SPLINE_SURFACE(3,2,((#209016,#209017,#209018),(#209019,#209020,#209021),
(#209022,#209023,#209024),(#209025,#209026,#209027)),.UNSPECIFIED.,.F.,
 .F.,.F.)
B_SPLINE_SURFACE_WITH_KNOTS((4,4),(3,3),(-1.04083408558608E-17,0.000723082784825488),
(0.,1.),.UNSPECIFIED.)
GEOMETRIC_REPRESENTATION_ITEM()
RATIONAL_B_SPLINE_SURFACE(((1.,0.832455503270619,1.),(1.,0.832789231498785,
1.),(1.,0.833122604759493,1.),(1.,0.833454935865631,1.)))
REPRESENTATION_ITEM('')
SURFACE()
);
#3048=(
BOUNDED_SURFACE()
B_SPLINE_SURFACE(3,2,((#209033,#209034,#209035),(#209036,#209037,#209038),
(#209039,#209040,#209041),(#209042,#209043,#209044)),.UNSPECIFIED.,.F.,
 .F.,.F.)
B_SPLINE_SURFACE_WITH_KNOTS((4,4),(3,3),(0.,0.00158760011419447),(0.,1.),
 .UNSPECIFIED.)
GEOMETRIC_REPRESENTATION_ITEM()
RATIONAL_B_SPLINE_SURFACE(((1.,0.832279622729481,1.),(1.,0.842288514399813,
1.),(1.,0.850845187132399,1.),(1.,0.857972509692097,1.)))
REPRESENTATION_ITEM('')
SURFACE()
);
#3049=(
BOUNDED_SURFACE()
B_SPLINE_SURFACE(3,2,((#209107,#209108,#209109),(#209110,#209111,#209112),
(#209113,#209114,#209115),(#209116,#209117,#209118)),.UNSPECIFIED.,.F.,
 .F.,.F.)
B_SPLINE_SURFACE_WITH_KNOTS((4,4),(3,3),(-3.10081821330854E-17,0.00151853748946949),
(0.,1.),.UNSPECIFIED.)
GEOMETRIC_REPRESENTATION_ITEM()
RATIONAL_B_SPLINE_SURFACE(((1.,0.857104357126303,1.),(1.,0.850185325699861,
1.),(1.,0.84197601930101,1.),(1.,0.83245550327062,1.)))
REPRESENTATION_ITEM('')
SURFACE()
);
#3050=(
BOUNDED_SURFACE()
B_SPLINE_SURFACE(3,2,((#209184,#209185,#209186),(#209187,#209188,#209189),
(#209190,#209191,#209192),(#209193,#209194,#209195),(#209196,#209197,#209198),
(#209199,#209200,#209201),(#209202,#209203,#209204),(#209205,#209206,#209207)),
 .UNSPECIFIED.,.F.,.F.,.F.)
B_SPLINE_SURFACE_WITH_KNOTS((4,2,2,4),(3,3),(-0.000314953251722383,0.000787383129295151,
0.00157476625859271,0.00346448576890691),(0.,1.00393321929414),
 .UNSPECIFIED.)
GEOMETRIC_REPRESENTATION_ITEM()
RATIONAL_B_SPLINE_SURFACE(((1.,0.988639393495295,1.00008936751339),(1.,
0.99107983362604,1.00007016994098),(1.,0.987096480958425,1.00010150474011),
(1.,0.971752779728647,1.00022220502355),(1.,0.962780183976932,1.00029278739701),
(1.,0.924711164443769,1.00059225500129),(1.,0.884601626384202,1.00090777421924),
(1.,0.832272209417737,1.00131942036416)))
REPRESENTATION_ITEM('')
SURFACE()
);
#3051=(
BOUNDED_SURFACE()
B_SPLINE_SURFACE(3,2,((#209353,#209354,#209355),(#209356,#209357,#209358),
(#209359,#209360,#209361),(#209362,#209363,#209364),(#209365,#209366,#209367),
(#209368,#209369,#209370),(#209371,#209372,#209373),(#209374,#209375,#209376)),
 .UNSPECIFIED.,.F.,.F.,.F.)
B_SPLINE_SURFACE_WITH_KNOTS((4,2,2,4),(3,3),(-0.000315404934817324,0.00157702467408662,
0.00236553701112993,0.00346945428299001),(0.,1.00901231170094),
 .UNSPECIFIED.)
GEOMETRIC_REPRESENTATION_ITEM()
RATIONAL_B_SPLINE_SURFACE(((1.,0.830517951234993,1.00305485010237),(1.,
0.88317248166518,1.00210577202096),(1.,0.923525848545179,1.00137841777995),
(1.,0.962170244647943,1.00068186709361),(1.,0.971260847949517,1.0005180123926),
(1.,0.986851346814187,1.00023699952192),(1.,0.99108019029668,1.00016077621072),
(1.,0.988461418308015,1.00020797858959)))
REPRESENTATION_ITEM('')
SURFACE()
);
#3052=(
BOUNDED_SURFACE()
B_SPLINE_SURFACE(3,2,((#209509,#209510,#209511),(#209512,#209513,#209514),
(#209515,#209516,#209517),(#209518,#209519,#209520),(#209521,#209522,#209523),
(#209524,#209525,#209526),(#209527,#209528,#209529),(#209530,#209531,#209532),
(#209533,#209534,#209535),(#209536,#209537,#209538),(#209539,#209540,#209541),
(#209542,#209543,#209544),(#209545,#209546,#209547),(#209548,#209549,#209550),
(#209551,#209552,#209553),(#209554,#209555,#209556),(#209557,#209558,#209559),
(#209560,#209561,#209562)),.UNSPECIFIED.,.F.,.F.,.F.)
B_SPLINE_SURFACE_WITH_KNOTS((4,2,2,2,2,2,2,2,4),(3,3),(-0.000508741685376785,
0.00254370842688261,0.00381556264032431,0.00445148974704516,0.00476945330040559,
0.0049284350770858,0.00500792596542591,0.00504767140959596,0.0055961585391427),
(-0.00567142872297958,1.),.UNSPECIFIED.)
GEOMETRIC_REPRESENTATION_ITEM()
RATIONAL_B_SPLINE_SURFACE(((1.00013527605448,0.988073899798091,1.),(1.00011031929585,
0.990274117753778,1.),(1.00008545848001,0.992465877278369,1.),(1.00005043350393,
0.995553721434831,1.),(1.0000401547835,0.996459905831016,1.),(1.00002479414521,
0.997814118238588,1.),(1.0000196801218,0.99826497671417,1.),(1.00001206776935,
0.998936090892214,1.),(1.00000953704006,0.999159203039952,1.),(1.00000579625876,
0.999488994833659,1.),(1.00000455640789,0.999598301582191,1.),(1.00000275469915,
0.999757142399172,1.),(1.00000216079599,0.999809501617783,1.),(1.00000133818808,
0.999882023724343,1.),(1.00000107184386,0.999905504951442,1.),(0.999997744935146,
1.00019880923877,1.),(1.00000210718248,0.999814228249836,1.),(1.00039260038191,
0.965387876575058,1.)))
REPRESENTATION_ITEM('')
SURFACE()
);
#3053=(
BOUNDED_SURFACE()
B_SPLINE_SURFACE(3,2,((#209681,#209682,#209683),(#209684,#209685,#209686),
(#209687,#209688,#209689),(#209690,#209691,#209692),(#209693,#209694,#209695),
(#209696,#209697,#209698),(#209699,#209700,#209701),(#209702,#209703,#209704),
(#209705,#209706,#209707),(#209708,#209709,#209710),(#209711,#209712,#209713),
(#209714,#209715,#209716),(#209717,#209718,#209719),(#209720,#209721,#209722),
(#209723,#209724,#209725),(#209726,#209727,#209728),(#209729,#209730,#209731),
(#209732,#209733,#209734)),.UNSPECIFIED.,.F.,.F.,.F.)
B_SPLINE_SURFACE_WITH_KNOTS((4,2,2,2,2,2,2,2,4),(3,3),(-7.45388993583784E-20,
4.05793239028379E-5,8.11586478056759E-5,0.000162317295611352,0.000324634591222704,
0.000649269182445408,0.00129853836489082,0.00259707672978163,0.00519415345956326),
(0.,1.),.UNSPECIFIED.)
GEOMETRIC_REPRESENTATION_ITEM()
RATIONAL_B_SPLINE_SURFACE(((1.,0.999961923064171,1.),(1.,0.999961833753432,
1.),(1.,0.999944633098586,1.),(1.,0.999904212270329,1.),(1.,0.99988023258917,
1.),(1.,0.999806855851567,1.),(1.,0.999754783512162,1.),(1.,0.999595776401296,
1.),(1.,0.999485889992571,1.),(1.,0.999156267866573,1.),(1.,0.998933623645324,
1.),(1.,0.998262897761582,1.),(1.,0.997812273447783,1.),(1.,0.996459235447427,
1.),(1.,0.995553264664008,1.),(1.,0.992828768547989,1.),(1.,0.991003554465269,
1.),(1.,0.989172917436461,1.)))
REPRESENTATION_ITEM('')
SURFACE()
);
#3054=(
BOUNDED_SURFACE()
B_SPLINE_SURFACE(3,2,((#209860,#209861,#209862),(#209863,#209864,#209865),
(#209866,#209867,#209868),(#209869,#209870,#209871),(#209872,#209873,#209874),
(#209875,#209876,#209877),(#209878,#209879,#209880),(#209881,#209882,#209883),
(#209884,#209885,#209886),(#209887,#209888,#209889),(#209890,#209891,#209892),
(#209893,#209894,#209895),(#209896,#209897,#209898),(#209899,#209900,#209901),
(#209902,#209903,#209904),(#209905,#209906,#209907),(#209908,#209909,#209910),
(#209911,#209912,#209913)),.UNSPECIFIED.,.F.,.F.,.F.)
B_SPLINE_SURFACE_WITH_KNOTS((4,2,2,2,2,2,2,2,4),(3,3),(-0.000525941938450675,
0.00262970969225337,0.00394456453838006,0.00460199196144341,0.00493070567297508,
0.00509506252874091,0.00517724095662383,0.00521833017056529,0.00578536132295742),
(-0.00671701195452941,1.),.UNSPECIFIED.)
GEOMETRIC_REPRESENTATION_ITEM()
RATIONAL_B_SPLINE_SURFACE(((1.00016587740973,0.987652440486347,1.),(1.00013527423289,
0.989930475499347,1.),(1.00010479231153,0.992199484515042,1.),(1.00006184900674,
0.995396092253403,1.),(1.00004924669386,0.996334181463897,1.),(1.00003041237645,
0.997736167759121,1.),(1.00002414515887,0.998202686027925,1.),(1.00001481225861,
0.998897407157577,1.),(1.00001170892687,0.999128412532823,1.),(1.0000071206784,
0.999469951933241,1.),(1.00000559837997,0.999583268571811,1.),(1.0000033859316,
0.999747958495426,1.),(1.00000265749339,0.999802181877435,1.),(1.00000163926013,
0.999877976982937,1.),(1.00000131471708,0.999902135273186,1.),(0.999997166880602,
1.000210891347,1.),(1.00000159891618,0.999880980100307,1.),(1.00051507935168,
0.96165859498486,1.)))
REPRESENTATION_ITEM('')
SURFACE()
);
#3055=(
BOUNDED_SURFACE()
B_SPLINE_SURFACE(3,2,((#210041,#210042,#210043),(#210044,#210045,#210046),
(#210047,#210048,#210049),(#210050,#210051,#210052),(#210053,#210054,#210055),
(#210056,#210057,#210058),(#210059,#210060,#210061),(#210062,#210063,#210064)),
 .UNSPECIFIED.,.F.,.F.,.F.)
B_SPLINE_SURFACE_WITH_KNOTS((4,2,2,4),(3,3),(-0.000314549301296344,0.000786373253240854,
0.0015727465064817,0.00346004231425976),(0.,1.00377255784672),
 .UNSPECIFIED.)
GEOMETRIC_REPRESENTATION_ITEM()
RATIONAL_B_SPLINE_SURFACE(((1.,0.988289122120854,1.00008835992847),(1.,
0.990704624856171,1.00007013468087),(1.,0.986710803687609,1.00010026852365),
(1.,0.971342895247987,1.00021622117079),(1.,0.962359345953478,1.00028400308956),
(1.,0.924268992488747,1.00057139921325),(1.,0.884176841333546,1.00087389913212),
(1.,0.831820369843143,1.00126893476681)))
REPRESENTATION_ITEM('')
SURFACE()
);
#3056=(
BOUNDED_SURFACE()
B_SPLINE_SURFACE(3,2,((#210203,#210204,#210205),(#210206,#210207,#210208),
(#210209,#210210,#210211),(#210212,#210213,#210214),(#210215,#210216,#210217),
(#210218,#210219,#210220),(#210221,#210222,#210223),(#210224,#210225,#210226),
(#210227,#210228,#210229),(#210230,#210231,#210232),(#210233,#210234,#210235),
(#210236,#210237,#210238),(#210239,#210240,#210241),(#210242,#210243,#210244),
(#210245,#210246,#210247),(#210248,#210249,#210250),(#210251,#210252,#210253),
(#210254,#210255,#210256)),.UNSPECIFIED.,.F.,.F.,.F.)
B_SPLINE_SURFACE_WITH_KNOTS((4,2,2,2,2,2,2,2,4),(3,3),(-1.32137139771671E-19,
4.17669388829254E-5,8.35338777658508E-5,0.000167067755531702,0.000334135511063404,
0.000668271022126808,0.00133654204425361,0.00267308408850723,0.00534616817701446),
(0.,1.),.UNSPECIFIED.)
GEOMETRIC_REPRESENTATION_ITEM()
RATIONAL_B_SPLINE_SURFACE(((1.,0.999961923064171,1.),(1.,0.999961782802257,
1.),(1.,0.999943671528414,1.),(1.,0.999901604878771,1.),(1.,0.999876750335241,
1.),(1.,0.999800908054986,1.),(1.,0.99974715657318,1.),(1.,0.999583072363253,
1.),(1.,0.999469900307565,1.),(1.,0.999130340955253,1.),(1.,0.998901033022514,
1.),(1.,0.998210264756137,1.),(1.,0.997746391825068,1.),(1.,0.996353373847482,
1.),(1.,0.9954206326127,1.),(1.,0.992615540215937,1.),(1.,0.990736373728666,
1.),(1.,0.988851372352096,1.)))
REPRESENTATION_ITEM('')
SURFACE()
);
#3057=(
BOUNDED_SURFACE()
B_SPLINE_SURFACE(3,2,((#210379,#210380,#210381),(#210382,#210383,#210384),
(#210385,#210386,#210387),(#210388,#210389,#210390)),.UNSPECIFIED.,.F.,
 .F.,.F.)
B_SPLINE_SURFACE_WITH_KNOTS((4,4),(3,3),(-1.02728155843001E-17,0.0012351855748658),
(0.,1.),.UNSPECIFIED.)
GEOMETRIC_REPRESENTATION_ITEM()
RATIONAL_B_SPLINE_SURFACE(((1.,0.838149597872977,1.),(1.,0.845487721431554,
1.),(1.,0.851938880735554,1.),(1.,0.857509777230923,1.)))
REPRESENTATION_ITEM('')
SURFACE()
);
#3058=(
BOUNDED_SURFACE()
B_SPLINE_SURFACE(3,2,((#210447,#210448,#210449),(#210450,#210451,#210452),
(#210453,#210454,#210455),(#210456,#210457,#210458),(#210459,#210460,#210461),
(#210462,#210463,#210464),(#210465,#210466,#210467),(#210468,#210469,#210470)),
 .UNSPECIFIED.,.F.,.F.,.F.)
B_SPLINE_SURFACE_WITH_KNOTS((4,2,2,4),(3,3),(-0.000314471227869891,0.00157235613934946,
0.00235853420902418,0.00345918350656882),(-0.0010818761735745,1.00850572874588),
 .UNSPECIFIED.)
GEOMETRIC_REPRESENTATION_ITEM()
RATIONAL_B_SPLINE_SURFACE(((1.00036290706551,0.830850702039335,1.00287434018484),
(1.0002504422033,0.883270052049706,1.00198358245771),(1.00016420299662,
0.923465745801804,1.00130054032154),(1.0000816177724,0.961958335301367,
1.00064643889664),(1.00006218504651,0.971015838596884,1.00049252548399),
(1.00002887364119,0.986542129924704,1.00022868848542),(1.00001986509788,
0.990740970126149,1.00015733793731),(1.00002547576192,0.988125865671606,
1.00020177619341)))
REPRESENTATION_ITEM('')
SURFACE()
);
#3059=(
BOUNDED_SURFACE()
B_SPLINE_SURFACE(3,2,((#210542,#210543,#210544),(#210545,#210546,#210547),
(#210548,#210549,#210550),(#210551,#210552,#210553)),.UNSPECIFIED.,.F.,
 .F.,.F.)
B_SPLINE_SURFACE_WITH_KNOTS((4,4),(3,3),(0.,0.000753104234298227),(0.,1.),
 .UNSPECIFIED.)
GEOMETRIC_REPRESENTATION_ITEM()
RATIONAL_B_SPLINE_SURFACE(((1.,0.839275484760762,1.),(1.,0.838901603374917,
1.),(1.,0.838526082980222,1.),(1.,0.83814959787298,1.)))
REPRESENTATION_ITEM('')
SURFACE()
);
#3060=(
BOUNDED_SURFACE()
B_SPLINE_SURFACE(3,2,((#210559,#210560,#210561),(#210562,#210563,#210564),
(#210565,#210566,#210567),(#210568,#210569,#210570)),.UNSPECIFIED.,.F.,
 .F.,.F.)
B_SPLINE_SURFACE_WITH_KNOTS((4,4),(3,3),(0.,0.00121469382512386),(0.,1.),
 .UNSPECIFIED.)
GEOMETRIC_REPRESENTATION_ITEM()
RATIONAL_B_SPLINE_SURFACE(((1.,0.857407773863101,1.),(1.,0.851918824817362,
1.),(1.,0.845578741226857,1.),(1.,0.83838293312654,1.)))
REPRESENTATION_ITEM('')
SURFACE()
);
#3061=(
BOUNDED_SURFACE()
B_SPLINE_SURFACE(3,2,((#210627,#210628,#210629),(#210630,#210631,#210632),
(#210633,#210634,#210635),(#210636,#210637,#210638),(#210639,#210640,#210641),
(#210642,#210643,#210644),(#210645,#210646,#210647),(#210648,#210649,#210650),
(#210651,#210652,#210653),(#210654,#210655,#210656),(#210657,#210658,#210659),
(#210660,#210661,#210662),(#210663,#210664,#210665),(#210666,#210667,#210668)),
 .UNSPECIFIED.,.F.,.F.,.F.)
B_SPLINE_SURFACE_WITH_KNOTS((4,2,2,2,2,2,4),(3,3),(-0.000226840284413363,
0.000567100711032879,0.000850651066549369,0.00113420142206586,0.00141775177758235,
0.00170130213309884,0.00249524312854497),(-0.00170901498463875,1.00351063153609),
 .UNSPECIFIED.)
GEOMETRIC_REPRESENTATION_ITEM()
RATIONAL_B_SPLINE_SURFACE(((1.00063854299496,0.812526948435515,1.00131404403671),
(1.00053226337854,0.843730115906702,1.00109533347645),(1.00043744268712,
0.871568999916444,1.00090020399402),(1.0003270802267,0.903970870106644,
1.00067309143599),(1.00029995768986,0.911933912200606,1.00061727654478),
(1.00025172251529,0.926095519859969,1.00051801440582),(1.00023020586516,
0.932412701462029,1.00047373574954),(1.00019632330569,0.942360452621125,
1.00040400955167),(1.00018360585421,0.946094233207541,1.00037783857897),
(1.00017057881538,0.949918907100824,1.00035103051306),(1.000170258171,0.950013046697734,
1.00035037066582),(1.00019261482622,0.943449243773019,1.00039637795071),
(1.00025727649706,0.924464898400181,1.00052944382668),(1.0003327305413,
0.902311965806151,1.00068471909813)))
REPRESENTATION_ITEM('')
SURFACE()
);
#3062=(
BOUNDED_SURFACE()
B_SPLINE_SURFACE(3,2,((#210720,#210721,#210722),(#210723,#210724,#210725),
(#210726,#210727,#210728),(#210729,#210730,#210731)),.UNSPECIFIED.,.F.,
 .F.,.F.)
B_SPLINE_SURFACE_WITH_KNOTS((4,4),(3,3),(0.,0.000758627814399393),(0.,1.),
 .UNSPECIFIED.)
GEOMETRIC_REPRESENTATION_ITEM()
RATIONAL_B_SPLINE_SURFACE(((1.,0.838382933127103,1.),(1.,0.838759998356351,
1.),(1.,0.839135655634363,1.),(1.,0.839509576764081,1.)))
REPRESENTATION_ITEM('')
SURFACE()
);
#3063=(
BOUNDED_SURFACE()
B_SPLINE_SURFACE(3,2,((#210737,#210738,#210739),(#210740,#210741,#210742),
(#210743,#210744,#210745),(#210746,#210747,#210748),(#210749,#210750,#210751),
(#210752,#210753,#210754),(#210755,#210756,#210757),(#210758,#210759,#210760),
(#210761,#210762,#210763),(#210764,#210765,#210766),(#210767,#210768,#210769),
(#210770,#210771,#210772)),.UNSPECIFIED.,.F.,.F.,.F.)
B_SPLINE_SURFACE_WITH_KNOTS((4,2,2,2,2,4),(3,3),(-0.000216256680534387,
0.000582607613633213,0.000867916290121638,0.00115322496661006,0.00172384231958692,
0.00252270661375453),(-0.00157135189843493,1.00088857311935),
 .UNSPECIFIED.)
GEOMETRIC_REPRESENTATION_ITEM()
RATIONAL_B_SPLINE_SURFACE(((1.00031029998659,0.901175496173816,1.00017534981439),
(1.00024041434093,0.923432713562446,1.00013585759549),(1.00018125294539,
0.942274466099237,1.00010242562586),(1.00015904169639,0.949348316427786,
1.00008987409973),(1.00015882754949,0.949416518046249,1.00008975308581),
(1.0001698811118,0.945896173676258,1.00009599942865),(1.00018106406685,
0.942334620236191,1.00010231889103),(1.00022728017823,0.927615688644421,
1.00012843551011),(1.00027359929972,0.912863950337352,1.00015461033998),
(1.00040076355192,0.872364612049113,1.00022647056873),(1.00048842071942,
0.844447510986039,1.00027600543408),(1.00058680386245,0.813114395566315,
1.00033160152371)))
REPRESENTATION_ITEM('')
SURFACE()
);
#3064=(
BOUNDED_SURFACE()
B_SPLINE_SURFACE(2,2,((#210835,#210836,#210837),(#210838,#210839,#210840),
(#210841,#210842,#210843)),.UNSPECIFIED.,.F.,.F.,.F.)
B_SPLINE_SURFACE_WITH_KNOTS((3,3),(3,3),(1.74317346290508E-16,1.57079632679495),
(-0.787072384273275,0.736541846753928),.UNSPECIFIED.)
GEOMETRIC_REPRESENTATION_ITEM()
RATIONAL_B_SPLINE_SURFACE(((1.,0.723589867251388,1.),(0.707106781186616,
0.51165530193138,0.707106781186616),(1.,0.723589867251388,1.)))
REPRESENTATION_ITEM('')
SURFACE()
);
#3065=(
BOUNDED_SURFACE()
B_SPLINE_SURFACE(2,2,((#210856,#210857,#210858),(#210859,#210860,#210861),
(#210862,#210863,#210864)),.UNSPECIFIED.,.F.,.F.,.F.)
B_SPLINE_SURFACE_WITH_KNOTS((3,3),(3,3),(-1.74317346290519E-16,1.57079632679496),
(0.830906038289448,2.35452026931659),.UNSPECIFIED.)
GEOMETRIC_REPRESENTATION_ITEM()
RATIONAL_B_SPLINE_SURFACE(((1.,0.72358986725141,1.),(0.707106781186587,
0.511655301931375,0.707106781186587),(1.,0.72358986725141,1.)))
REPRESENTATION_ITEM('')
SURFACE()
);
#3066=(
BOUNDED_SURFACE()
B_SPLINE_SURFACE(2,2,((#210879,#210880,#210881),(#210882,#210883,#210884),
(#210885,#210886,#210887)),.UNSPECIFIED.,.F.,.F.,.F.)
B_SPLINE_SURFACE_WITH_KNOTS((3,3),(3,3),(1.81714697791953E-16,1.57079632679495),
(-0.26549733202973,0.74383310368946),.UNSPECIFIED.)
GEOMETRIC_REPRESENTATION_ITEM()
RATIONAL_B_SPLINE_SURFACE(((1.,0.875336395469216,1.),(0.707106781186606,
0.618956301055724,0.707106781186606),(1.,0.875336395469216,1.)))
REPRESENTATION_ITEM('')
SURFACE()
);
#3067=(
BOUNDED_SURFACE()
B_SPLINE_SURFACE(2,2,((#210899,#210900,#210901),(#210902,#210903,#210904),
(#210905,#210906,#210907)),.UNSPECIFIED.,.F.,.F.,.F.)
B_SPLINE_SURFACE_WITH_KNOTS((3,3),(3,3),(-6.30291942997115E-17,1.57079632679495),
(0.819567334644225,1.82889777036346),.UNSPECIFIED.)
GEOMETRIC_REPRESENTATION_ITEM()
RATIONAL_B_SPLINE_SURFACE(((1.,0.875336395469206,1.),(0.707106781186601,
0.618956301055712,0.707106781186601),(1.,0.875336395469206,1.)))
REPRESENTATION_ITEM('')
SURFACE()
);
#3068=(
BOUNDED_SURFACE()
B_SPLINE_SURFACE(2,2,((#210922,#210923,#210924),(#210925,#210926,#210927),
(#210928,#210929,#210930)),.UNSPECIFIED.,.F.,.F.,.F.)
B_SPLINE_SURFACE_WITH_KNOTS((3,3),(3,3),(-1.57079632679491,1.68131336473773E-16),
(0.821845324909055,1.83117576062825),.UNSPECIFIED.)
GEOMETRIC_REPRESENTATION_ITEM()
RATIONAL_B_SPLINE_SURFACE(((1.,0.875336395469216,1.),(0.70710678118653,
0.618956301055656,0.70710678118653),(1.,0.875336395469216,1.)))
REPRESENTATION_ITEM('')
SURFACE()
);
#3069=(
BOUNDED_SURFACE()
B_SPLINE_SURFACE(2,2,((#210942,#210943,#210944),(#210945,#210946,#210947),
(#210948,#210949,#210950)),.UNSPECIFIED.,.F.,.F.,.F.)
B_SPLINE_SURFACE_WITH_KNOTS((3,3),(3,3),(-1.5707963267949,2.47147205475768E-16),
(-0.263219341764958,0.746111093954295),.UNSPECIFIED.)
GEOMETRIC_REPRESENTATION_ITEM()
RATIONAL_B_SPLINE_SURFACE(((1.,0.875336395469201,1.),(0.707106781186519,
0.618956301055637,0.707106781186519),(1.,0.875336395469201,1.)))
REPRESENTATION_ITEM('')
SURFACE()
);
#3070=(
BOUNDED_SURFACE()
B_SPLINE_SURFACE(2,2,((#210965,#210966,#210967),(#210968,#210969,#210970),
(#210971,#210972,#210973)),.UNSPECIFIED.,.F.,.F.,.F.)
B_SPLINE_SURFACE_WITH_KNOTS((3,3),(3,3),(-1.57079632679491,1.67905497988288E-16),
(0.823093317098874,2.34670754812599),.UNSPECIFIED.)
GEOMETRIC_REPRESENTATION_ITEM()
RATIONAL_B_SPLINE_SURFACE(((1.,0.723589867251417,1.),(0.70710678118653,
0.511655301931338,0.70710678118653),(1.,0.723589867251417,1.)))
REPRESENTATION_ITEM('')
SURFACE()
);
#3071=(
BOUNDED_SURFACE()
B_SPLINE_SURFACE(2,2,((#210985,#210986,#210987),(#210988,#210989,#210990),
(#210991,#210992,#210993)),.UNSPECIFIED.,.F.,.F.,.F.)
B_SPLINE_SURFACE_WITH_KNOTS((3,3),(3,3),(-1.57079632679491,2.478375474118E-16),
(-0.794885105463935,0.728729125563299),.UNSPECIFIED.)
GEOMETRIC_REPRESENTATION_ITEM()
RATIONAL_B_SPLINE_SURFACE(((1.,0.723589867251377,1.),(0.70710678118653,
0.511655301931309,0.70710678118653),(1.,0.723589867251377,1.)))
REPRESENTATION_ITEM('')
SURFACE()
);
#3072=(
BOUNDED_SURFACE()
B_SPLINE_SURFACE(3,2,((#212943,#212944,#212945),(#212946,#212947,#212948),
(#212949,#212950,#212951),(#212952,#212953,#212954),(#212955,#212956,#212957),
(#212958,#212959,#212960),(#212961,#212962,#212963),(#212964,#212965,#212966),
(#212967,#212968,#212969),(#212970,#212971,#212972),(#212973,#212974,#212975),
(#212976,#212977,#212978),(#212979,#212980,#212981),(#212982,#212983,#212984),
(#212985,#212986,#212987),(#212988,#212989,#212990),(#212991,#212992,#212993),
(#212994,#212995,#212996),(#212997,#212998,#212999),(#213000,#213001,#213002),
(#213003,#213004,#213005),(#213006,#213007,#213008),(#213009,#213010,#213011),
(#213012,#213013,#213014),(#213015,#213016,#213017),(#213018,#213019,#213020),
(#213021,#213022,#213023),(#213024,#213025,#213026),(#213027,#213028,#213029),
(#213030,#213031,#213032),(#213033,#213034,#213035),(#213036,#213037,#213038),
(#213039,#213040,#213041),(#213042,#213043,#213044),(#213045,#213046,#213047),
(#213048,#213049,#213050),(#213051,#213052,#213053),(#213054,#213055,#213056),
(#213057,#213058,#213059),(#213060,#213061,#213062),(#213063,#213064,#213065),
(#213066,#213067,#213068),(#213069,#213070,#213071),(#213072,#213073,#213074),
(#213075,#213076,#213077),(#213078,#213079,#213080),(#213081,#213082,#213083),
(#213084,#213085,#213086)),.UNSPECIFIED.,.F.,.F.,.F.)
B_SPLINE_SURFACE_WITH_KNOTS((4,2,2,2,2,2,2,2,2,2,2,2,2,2,2,2,2,2,2,2,2,
2,2,4),(3,3),(0.,0.0059149619408077,0.00739370242600962,0.00743991306617218,
0.00748612370633474,0.00757854498665986,0.0077633875473101,0.00813307266861059,
0.00887244291121155,0.0118299238816154,0.0133086643668173,0.0140480346094183,
0.0140942452495808,0.0141404558897434,0.0142328771700685,0.0144177197307188,
0.0147874048520192,0.0177448858224231,0.019223626307625,0.019962996550226,
0.0201478391108762,0.0203326816715265,0.0207023667928269,0.0236598477632308),
(0.,1.),.UNSPECIFIED.)
GEOMETRIC_REPRESENTATION_ITEM()
RATIONAL_B_SPLINE_SURFACE(((1.,0.861068946771262,1.),(1.,0.871793299675347,
1.),(1.,0.879015041937488,1.),(1.,0.885129578373153,1.),(1.,0.886202028929654,
1.),(1.,0.887164714171582,1.),(1.,0.887116116747139,1.),(1.,0.887073026774255,
1.),(1.,0.887051430276885,1.),(1.,0.886986487326662,1.),(1.,0.886942987422201,
1.),(1.,0.886811882202044,1.),(1.,0.886723671509742,1.),(1.,0.886456679535479,
1.),(1.,0.886275540586052,1.),(1.,0.88572310670639,1.),(1.,0.885342833942064,
1.),(1.,0.883384862710688,1.),(1.,0.881615095800445,1.),(1.,0.878612600044596,
1.),(1.,0.877556288775192,1.),(1.,0.875871070793252,1.),(1.,0.875293879519929,
1.),(1.,0.874664965796897,1.),(1.,0.874763981664806,1.),(1.,0.874835206629783,
1.),(1.,0.874870651351952,1.),(1.,0.87497648659221,1.),(1.,0.875046378225363,
1.),(1.,0.875254090776843,1.),(1.,0.875389950005275,1.),(1.,0.875789921459867,
1.),(1.,0.876046437149636,1.),(1.,0.878268573346079,1.),(1.,0.879634170738163,
1.),(1.,0.880866820420691,1.),(1.,0.881143316614213,1.),(1.,0.881356253213235,
1.),(1.,0.881394010610288,1.),(1.,0.88139952742701,1.),(1.,0.881398536837081,
1.),(1.,0.881392323021745,1.),(1.,0.881371643237072,1.),(1.,0.881442771835474,
1.),(1.,0.881487673169753,1.),(1.,0.881868765786043,1.),(1.,0.882040414813943,
1.),(1.,0.88203965410677,1.)))
REPRESENTATION_ITEM('')
SURFACE()
);
#3073=(
BOUNDED_SURFACE()
B_SPLINE_SURFACE(3,2,((#213396,#213397,#213398),(#213399,#213400,#213401),
(#213402,#213403,#213404),(#213405,#213406,#213407)),.UNSPECIFIED.,.F.,
 .F.,.F.)
B_SPLINE_SURFACE_WITH_KNOTS((4,4),(3,3),(-8.16115679863473E-6,0.000330556732041574),
(-8.16118966828803E-6,1.),.UNSPECIFIED.)
GEOMETRIC_REPRESENTATION_ITEM()
RATIONAL_B_SPLINE_SURFACE(((1.0000022763522,0.860537967104879,1.),(1.00000215632319,
0.867891613986121,1.),(1.00000205218217,0.874271873585881,1.),(1.00000196504864,
0.8796101599594,1.)))
REPRESENTATION_ITEM('')
SURFACE()
);
#3074=(
BOUNDED_SURFACE()
B_SPLINE_SURFACE(3,2,((#213416,#213417,#213418),(#213419,#213420,#213421),
(#213422,#213423,#213424),(#213425,#213426,#213427)),.UNSPECIFIED.,.F.,
 .F.,.F.)
B_SPLINE_SURFACE_WITH_KNOTS((4,4),(3,3),(-1.56125112837912E-17,0.00371972595076131),
(0.,1.),.UNSPECIFIED.)
GEOMETRIC_REPRESENTATION_ITEM()
RATIONAL_B_SPLINE_SURFACE(((1.,0.879223463974645,1.),(1.,0.879197541860131,
1.),(1.,0.879166735457461,1.),(1.,0.879131676488835,1.)))
REPRESENTATION_ITEM('')
SURFACE()
);
#3075=(
BOUNDED_SURFACE()
B_SPLINE_SURFACE(3,2,((#213433,#213434,#213435),(#213436,#213437,#213438),
(#213439,#213440,#213441),(#213442,#213443,#213444),(#213445,#213446,#213447),
(#213448,#213449,#213450),(#213451,#213452,#213453),(#213454,#213455,#213456),
(#213457,#213458,#213459),(#213460,#213461,#213462),(#213463,#213464,#213465),
(#213466,#213467,#213468),(#213469,#213470,#213471),(#213472,#213473,#213474),
(#213475,#213476,#213477),(#213478,#213479,#213480),(#213481,#213482,#213483),
(#213484,#213485,#213486),(#213487,#213488,#213489),(#213490,#213491,#213492),
(#213493,#213494,#213495),(#213496,#213497,#213498),(#213499,#213500,#213501),
(#213502,#213503,#213504),(#213505,#213506,#213507),(#213508,#213509,#213510)),
 .UNSPECIFIED.,.F.,.F.,.F.)
B_SPLINE_SURFACE_WITH_KNOTS((4,2,2,2,2,2,2,2,2,2,2,2,4),(3,3),(-2.020502013395E-5,
0.000191440896835587,0.00028716134525338,0.000382881793671173,0.00057432269050676,
0.000670043138924553,0.000765763587342347,0.000957204484177933,0.00114864538101352,
0.00124436582943131,0.00129222605364021,0.00134008627784911,0.00155173219481786),
(-0.000614322987741022,1.),.UNSPECIFIED.)
GEOMETRIC_REPRESENTATION_ITEM()
RATIONAL_B_SPLINE_SURFACE(((1.00014914760104,0.878608155632912,1.),(1.00014732673166,
0.880090168686671,1.),(1.00014437340606,0.882493892513453,1.),(1.00013921574776,
0.886691731762652,1.),(1.00013754315828,0.888053059200701,1.),(1.00013487983185,
0.890220751507748,1.),(1.00013397197062,0.890959663488422,1.),(1.00013196690704,
0.892591592961943,1.),(1.00013020252052,0.894027634387128,1.),(1.00012653566681,
0.897012101670959,1.),(1.0001253668636,0.897963395397947,1.),(1.00012347828042,
0.899500520996579,1.),(1.00012275982084,0.900085278191057,1.),(1.00012070489333,
0.901757792124973,1.),(1.00011967187973,0.902598566132467,1.),(1.00011648933932,
0.905188848827967,1.),(1.00011476936931,0.906588739477223,1.),(1.00011330257804,
0.90778256690637,1.),(1.00011290516169,0.908106025705496,1.),(1.00011238177525,
0.908532012070824,1.),(1.00011225358233,0.908636348819827,1.),(1.00011164539059,
0.909131358574023,1.),(1.00011119272546,0.909499784574332,1.),(1.00010848940599,
0.911700027382186,1.),(1.0001066078168,0.913231460541444,1.),(1.00010622151568,
0.913545872609453,1.)))
REPRESENTATION_ITEM('')
SURFACE()
);
#3076=(
BOUNDED_SURFACE()
B_SPLINE_SURFACE(3,2,((#213626,#213627,#213628),(#213629,#213630,#213631),
(#213632,#213633,#213634),(#213635,#213636,#213637),(#213638,#213639,#213640),
(#213641,#213642,#213643),(#213644,#213645,#213646),(#213647,#213648,#213649),
(#213650,#213651,#213652),(#213653,#213654,#213655),(#213656,#213657,#213658),
(#213659,#213660,#213661)),.UNSPECIFIED.,.F.,.F.,.F.)
B_SPLINE_SURFACE_WITH_KNOTS((4,2,2,2,2,4),(3,3),(0.,0.00646885457540742,
0.0129377091508148,0.0161721364385186,0.0194065637262222,0.0258754183016297),
(0.,1.),.UNSPECIFIED.)
GEOMETRIC_REPRESENTATION_ITEM()
RATIONAL_B_SPLINE_SURFACE(((1.,0.913476533865333,1.),(1.,0.914845943871889,
1.),(1.,0.916112934302359,1.),(1.,0.918040216804478,1.),(1.,0.918611066895268,
1.),(1.,0.919010773408858,1.),(1.,0.919049811602052,1.),(1.,0.918970993255618,
1.),(1.,0.918853664923092,1.),(1.,0.918278797297209,1.),(1.,0.917618952389758,
1.),(1.,0.917028647019402,1.)))
REPRESENTATION_ITEM('')
SURFACE()
);
#3077=(
BOUNDED_SURFACE()
B_SPLINE_SURFACE(3,2,((#213793,#213794,#213795),(#213796,#213797,#213798),
(#213799,#213800,#213801),(#213802,#213803,#213804),(#213805,#213806,#213807),
(#213808,#213809,#213810),(#213811,#213812,#213813),(#213814,#213815,#213816),
(#213817,#213818,#213819),(#213820,#213821,#213822),(#213823,#213824,#213825),
(#213826,#213827,#213828),(#213829,#213830,#213831),(#213832,#213833,#213834),
(#213835,#213836,#213837),(#213838,#213839,#213840),(#213841,#213842,#213843),
(#213844,#213845,#213846),(#213847,#213848,#213849),(#213850,#213851,#213852),
(#213853,#213854,#213855),(#213856,#213857,#213858),(#213859,#213860,#213861),
(#213862,#213863,#213864),(#213865,#213866,#213867),(#213868,#213869,#213870),
(#213871,#213872,#213873),(#213874,#213875,#213876),(#213877,#213878,#213879),
(#213880,#213881,#213882),(#213883,#213884,#213885),(#213886,#213887,#213888),
(#213889,#213890,#213891),(#213892,#213893,#213894)),.UNSPECIFIED.,.F.,
 .F.,.F.)
B_SPLINE_SURFACE_WITH_KNOTS((4,2,2,2,2,2,2,2,2,2,2,2,2,2,2,2,4),(3,3),(0.,
0.000127304511784401,0.000254609023568802,0.000318261279461002,0.000381913535353202,
0.000509218047137603,0.000636522558922004,0.000763827070706405,0.000891131582490806,
0.00101843609427521,0.00114574060605961,0.00127304511784401,0.00140034962962841,
0.00152765414141281,0.00165495865319721,0.00178226316498161,0.00203687218855042),
(-0.000961805720933131,1.),.UNSPECIFIED.)
GEOMETRIC_REPRESENTATION_ITEM()
RATIONAL_B_SPLINE_SURFACE(((1.0001597581526,0.916948844697399,1.),(1.00016029912196,
0.916667618796779,1.),(1.00016097503671,0.916316240794633,1.),(1.00016291083017,
0.91530990790145,1.),(1.00016430151804,0.914586951156848,1.),(1.0001663252959,
0.913534879090444,1.),(1.00016693387069,0.913218508139461,1.),(1.00016773229267,
0.912803444074217,1.),(1.00016788468109,0.912724224114995,1.),(1.00016858323375,
0.912361077667592,1.),(1.00016914120577,0.91207101284379,1.),(1.00017061498675,
0.911304859685145,1.),(1.00017156421239,0.910811399509231,1.),(1.00017411696132,
0.909484338922955,1.),(1.00017540359175,0.908815477007135,1.),(1.00017753666339,
0.907706587971933,1.),(1.00017822836713,0.907347001970364,1.),(1.00017982387443,
0.906517568718808,1.),(1.00018080359298,0.906008256636064,1.),(1.00018333217183,
0.90469376099426,1.),(1.00018503490327,0.903808586681878,1.),(1.00018813760279,
0.902195631252981,1.),(1.00018958895774,0.901441136386703,1.),(1.00019214250402,
0.900113661296256,1.),(1.00019340707361,0.899456267831493,1.),(1.00019657037923,
0.897811805984888,1.),(1.00019839101625,0.896865337805144,1.),(1.00020221928284,
0.894875192336821,1.),(1.00020407941471,0.893908192541967,1.),(1.00020755406108,
0.892101878494427,1.),(1.00020897072777,0.891365416518063,1.),(1.00021429441008,
0.888597870954491,1.),(1.00021994630903,0.885659700163249,1.),(1.00022335245868,
0.883888994514506,1.)))
REPRESENTATION_ITEM('')
SURFACE()
);
#3078=(
BOUNDED_SURFACE()
B_SPLINE_SURFACE(3,2,((#214040,#214041,#214042),(#214043,#214044,#214045),
(#214046,#214047,#214048),(#214049,#214050,#214051)),.UNSPECIFIED.,.F.,
 .F.,.F.)
B_SPLINE_SURFACE_WITH_KNOTS((4,4),(3,3),(0.,0.00767500517967513),(0.,1.),
 .UNSPECIFIED.)
GEOMETRIC_REPRESENTATION_ITEM()
RATIONAL_B_SPLINE_SURFACE(((1.,0.884000563436129,1.),(1.,0.883607612825216,
1.),(1.,0.883267077927119,1.),(1.,0.882986276630499,1.)))
REPRESENTATION_ITEM('')
SURFACE()
);
#3079=(
BOUNDED_SURFACE()
B_SPLINE_SURFACE(3,2,((#214057,#214058,#214059),(#214060,#214061,#214062),
(#214063,#214064,#214065),(#214066,#214067,#214068)),.UNSPECIFIED.,.F.,
 .F.,.F.)
B_SPLINE_SURFACE_WITH_KNOTS((4,4),(3,3),(-4.63829152513897E-5,0.000510218477218229),
(-8.53868048819074E-5,1.),.UNSPECIFIED.)
GEOMETRIC_REPRESENTATION_ITEM()
RATIONAL_B_SPLINE_SURFACE(((1.00001949037752,0.885870085279226,1.),(1.0000214351582,
0.874482021962947,1.),(1.00002376476953,0.860840503630916,1.),(1.00002644118215,
0.845168218973911,1.)))
REPRESENTATION_ITEM('')
SURFACE()
);
#3080=(
BOUNDED_SURFACE()
B_SPLINE_SURFACE(3,2,((#214089,#214090,#214091),(#214092,#214093,#214094),
(#214095,#214096,#214097),(#214098,#214099,#214100),(#214101,#214102,#214103),
(#214104,#214105,#214106),(#214107,#214108,#214109),(#214110,#214111,#214112),
(#214113,#214114,#214115),(#214116,#214117,#214118),(#214119,#214120,#214121),
(#214122,#214123,#214124),(#214125,#214126,#214127),(#214128,#214129,#214130),
(#214131,#214132,#214133),(#214134,#214135,#214136),(#214137,#214138,#214139),
(#214140,#214141,#214142),(#214143,#214144,#214145),(#214146,#214147,#214148),
(#214149,#214150,#214151),(#214152,#214153,#214154),(#214155,#214156,#214157),
(#214158,#214159,#214160),(#214161,#214162,#214163),(#214164,#214165,#214166),
(#214167,#214168,#214169),(#214170,#214171,#214172),(#214173,#214174,#214175),
(#214176,#214177,#214178),(#214179,#214180,#214181),(#214182,#214183,#214184),
(#214185,#214186,#214187),(#214188,#214189,#214190),(#214191,#214192,#214193),
(#214194,#214195,#214196),(#214197,#214198,#214199),(#214200,#214201,#214202),
(#214203,#214204,#214205),(#214206,#214207,#214208),(#214209,#214210,#214211),
(#214212,#214213,#214214),(#214215,#214216,#214217),(#214218,#214219,#214220),
(#214221,#214222,#214223),(#214224,#214225,#214226),(#214227,#214228,#214229),
(#214230,#214231,#214232),(#214233,#214234,#214235),(#214236,#214237,#214238),
(#214239,#214240,#214241),(#214242,#214243,#214244),(#214245,#214246,#214247),
(#214248,#214249,#214250),(#214251,#214252,#214253),(#214254,#214255,#214256),
(#214257,#214258,#214259),(#214260,#214261,#214262),(#214263,#214264,#214265),
(#214266,#214267,#214268),(#214269,#214270,#214271),(#214272,#214273,#214274),
(#214275,#214276,#214277),(#214278,#214279,#214280),(#214281,#214282,#214283),
(#214284,#214285,#214286),(#214287,#214288,#214289),(#214290,#214291,#214292),
(#214293,#214294,#214295),(#214296,#214297,#214298),(#214299,#214300,#214301),
(#214302,#214303,#214304),(#214305,#214306,#214307),(#214308,#214309,#214310),
(#214311,#214312,#214313),(#214314,#214315,#214316),(#214317,#214318,#214319),
(#214320,#214321,#214322),(#214323,#214324,#214325),(#214326,#214327,#214328),
(#214329,#214330,#214331),(#214332,#214333,#214334),(#214335,#214336,#214337),
(#214338,#214339,#214340),(#214341,#214342,#214343),(#214344,#214345,#214346),
(#214347,#214348,#214349),(#214350,#214351,#214352),(#214353,#214354,#214355),
(#214356,#214357,#214358),(#214359,#214360,#214361),(#214362,#214363,#214364),
(#214365,#214366,#214367),(#214368,#214369,#214370),(#214371,#214372,#214373),
(#214374,#214375,#214376),(#214377,#214378,#214379),(#214380,#214381,#214382),
(#214383,#214384,#214385),(#214386,#214387,#214388),(#214389,#214390,#214391),
(#214392,#214393,#214394),(#214395,#214396,#214397),(#214398,#214399,#214400)),
 .UNSPECIFIED.,.F.,.F.,.F.)
B_SPLINE_SURFACE_WITH_KNOTS((4,2,2,2,2,2,2,2,2,2,2,2,2,2,2,2,2,2,2,2,2,
2,2,2,2,2,2,2,2,2,2,2,2,2,2,2,2,2,2,2,2,2,2,2,2,2,2,2,2,2,2,4),(3,3),(-1.90819582357449E-17,
0.00250327328955147,0.00500654657910296,0.0062581832238787,0.00688400154626657,
0.00696222883656506,0.00704045612686354,0.00719691070746051,0.00750981986865445,
0.0100130931582059,0.0112647298029817,0.0115776389641756,0.0117340935447726,
0.0117732071899218,0.0118123208350711,0.0118905481253695,0.0125163664477574,
0.0137680030925332,0.0150196397373089,0.0175229130268604,0.0175620266720097,
0.0176011403171589,0.0176793676074573,0.0178358221880543,0.0181487313492483,
0.0187745496716362,0.0200261863164119,0.0225294596059634,0.0226076868962618,
0.0226468005414111,0.0226859141865603,0.0228423687671573,0.0231552779283512,
0.0237810962507391,0.0250327328955148,0.0275360061850663,0.0281618245074543,
0.0283182790880512,0.0283965063783497,0.0284356200234989,0.0284747336686481,
0.0287876428298421,0.0300392794746179,0.0325425527641693,0.0331683710865572,
0.0332465983768557,0.0333248256671542,0.0334812802477511,0.0337941894089451,
0.0350458260537208,0.0375490993432723,0.0400523726328238),(-0.0381612915992707,
1.),.UNSPECIFIED.)
GEOMETRIC_REPRESENTATION_ITEM()
RATIONAL_B_SPLINE_SURFACE(((1.01196001158971,0.843296556687619,1.),(1.01125783435868,
0.85249668070863,1.),(1.01069166159088,0.859914835913468,1.),(1.00976927957171,
0.872000145143153,1.),(1.00941130926471,0.876690373015487,1.),(1.00899858840752,
0.882097958030137,1.),(1.00888239831572,0.883620313366265,1.),(1.00873889255595,
0.885500566284285,1.),(1.00869608841852,0.886061398159222,1.),(1.00865339690349,
0.886620754423689,1.),(1.00864670343397,0.88670845414809,1.),(1.00866056676143,
0.886526812923762,1.),(1.00866751249057,0.886435808022655,1.),(1.00868839096718,
0.886162252336477,1.),(1.00870236499396,0.885979160698443,1.),(1.00874444530519,
0.885427812598559,1.),(1.00877270964358,0.885057485269314,1.),(1.00902883862555,
0.881701611146218,1.),(1.00926835954748,0.878563340507299,1.),(1.00964800740727,
0.873589087227618,1.),(1.00977665564098,0.871903501804282,1.),(1.00994048509359,
0.869756962133522,1.),(1.00997338891691,0.869325846965062,1.),(1.01002293363291,
0.868676698129656,1.),(1.01003948008887,0.86845990179927,1.),(1.01006020114881,
0.868188408630767,1.),(1.01006434726144,0.868134085094295,1.),(1.01007264325631,
0.868025388630908,1.),(1.01008257425108,0.867895269937968,1.),(1.0100700071273,
0.868059927936344,1.),(1.01006172312451,0.868168467276088,1.),(1.00998800489105,
0.86913434435171,1.),(1.00992842205968,0.869915015404356,1.),(1.00976625976859,
0.87203971145494,1.),(1.00968006454818,0.873169065530701,1.),(1.0095492237058,
0.87488337913093,1.),(1.00950425621008,0.875472555935985,1.),(1.00943051365994,
0.876438751615483,1.),(1.00946109460324,0.876038071475825,1.),(1.00957595913498,
0.874533084001203,1.),(1.00957354603934,0.874564701060542,1.),(1.00957152686768,
0.874591156816875,1.),(1.00957051742751,0.874604382786464,1.),(1.00956748950558,
0.874644055473136,1.),(1.00956547142283,0.874670496962195,1.),(1.00955941844798,
0.874749804745048,1.),(1.00955538483576,0.874802654269464,1.),(1.0095432862966,
0.874961172740026,1.),(1.00953522376587,0.875066810290442,1.),(1.00951101947695,
0.875383941706837,1.),(1.00949494750357,0.875594521232732,1.),(1.00944675569682,
0.876225943869802,1.),(1.00941476784221,0.876645057758139,1.),(1.00932050409865,
0.877880127898698,1.),(1.00925991366249,0.878674000873372,1.),(1.00919906635626,
0.879471239432123,1.),(1.00919722372212,0.879495382144067,1.),(1.00919446140767,
0.879531574766626,1.),(1.00919317113587,0.879548480271513,1.),(1.00919296179469,
0.879551223118678,1.),(1.0091928763248,0.879552342969231,1.),(1.00919254483007,
0.879556686306683,1.),(1.00919258632655,0.879556142608002,1.),(1.00919362623178,
0.879542517476642,1.),(1.00919553951585,0.879517449089296,1.),(1.00920492183756,
0.879394519265546,1.),(1.00921602488281,0.879249044036668,1.),(1.00926404627612,
0.878619854204664,1.),(1.00931567792812,0.877943361745405,1.),(1.00952975614758,
0.875138448566535,1.),(1.00975123045612,0.872236629743661,1.),(1.01014599617449,
0.867064298019097,1.),(1.01023084555145,0.865952577563629,1.),(1.01034490480467,
0.864458141075202,1.),(1.01036811785504,0.86415399714571,1.),(1.01040355400373,
0.863689702736319,1.),(1.0104154688255,0.863533591382718,1.),(1.01043349715749,
0.863297379094865,1.),(1.01043953261861,0.863218300781946,1.),(1.0104516559068,
0.863059458042581,1.),(1.01044285803288,0.863174730266686,1.),(1.01038421780063,
0.863943051120049,1.),(1.01033243868938,0.864621475631935,1.),(1.01007536067835,
0.867989784201389,1.),(1.00987606553213,0.870601005387309,1.),(1.00929507722922,
0.878213277909576,1.),(1.00893022734244,0.882993643975501,1.),(1.00850337039391,
0.888586444043777,1.),(1.00841946355952,0.889685815040908,1.),(1.00832690759306,
0.890898509404476,1.),(1.00831664918989,0.891032917894642,1.),(1.00829618431438,
0.891301054462431,1.),(1.008305490177,0.891179126427196,1.),(1.00832789429041,
0.890885581417706,1.),(1.00834315168937,0.89068567467553,1.),(1.00838989813797,
0.890073189528329,1.),(1.00842236102569,0.889647851622424,1.),(1.00859133045236,
0.887433966562537,1.),(1.00874767204339,0.88538553496503,1.),(1.0092895506672,
0.878285688483144,1.),(1.00974403336268,0.872330928090653,1.),(1.01090323982987,
0.857142678183397,1.),(1.01160967330184,0.847886787693706,1.),(1.01248680792497,
0.836394322601919,1.)))
REPRESENTATION_ITEM('')
SURFACE()
);
#3081=(
BOUNDED_SURFACE()
B_SPLINE_SURFACE(3,2,((#214913,#214914,#214915),(#214916,#214917,#214918),
(#214919,#214920,#214921),(#214922,#214923,#214924)),.UNSPECIFIED.,.F.,
 .F.,.F.)
B_SPLINE_SURFACE_WITH_KNOTS((4,4),(3,3),(-5.17487663021493E-5,0.000569235683520745),
(-0.000120686675199996,1.00000829533119),.UNSPECIFIED.)
GEOMETRIC_REPRESENTATION_ITEM()
RATIONAL_B_SPLINE_SURFACE(((1.0000391614481,0.837754362995105,1.00000269143776),
(1.00003464486359,0.856466544625889,1.00000238102774),(1.00003064258142,
0.873047974894796,1.00000210596402),(1.00002720545249,0.887287978772295,
1.00000186974144)))
REPRESENTATION_ITEM('')
SURFACE()
);
#3082=(
BOUNDED_SURFACE()
B_SPLINE_SURFACE(3,2,((#214948,#214949,#214950),(#214951,#214952,#214953),
(#214954,#214955,#214956),(#214957,#214958,#214959)),.UNSPECIFIED.,.F.,
 .F.,.F.)
B_SPLINE_SURFACE_WITH_KNOTS((4,4),(3,3),(1.7347234759768E-18,0.00761738954978064),
(0.,1.),.UNSPECIFIED.)
GEOMETRIC_REPRESENTATION_ITEM()
RATIONAL_B_SPLINE_SURFACE(((1.,0.883694369886725,1.),(1.,0.884057799195121,
1.),(1.,0.884477978068247,1.),(1.,0.884949126929568,1.)))
REPRESENTATION_ITEM('')
SURFACE()
);
#3083=(
BOUNDED_SURFACE()
B_SPLINE_SURFACE(3,2,((#214965,#214966,#214967),(#214968,#214969,#214970),
(#214971,#214972,#214973),(#214974,#214975,#214976),(#214977,#214978,#214979),
(#214980,#214981,#214982),(#214983,#214984,#214985),(#214986,#214987,#214988),
(#214989,#214990,#214991),(#214992,#214993,#214994),(#214995,#214996,#214997),
(#214998,#214999,#215000),(#215001,#215002,#215003),(#215004,#215005,#215006),
(#215007,#215008,#215009),(#215010,#215011,#215012),(#215013,#215014,#215015),
(#215016,#215017,#215018),(#215019,#215020,#215021),(#215022,#215023,#215024),
(#215025,#215026,#215027),(#215028,#215029,#215030),(#215031,#215032,#215033),
(#215034,#215035,#215036),(#215037,#215038,#215039),(#215040,#215041,#215042),
(#215043,#215044,#215045),(#215046,#215047,#215048),(#215049,#215050,#215051),
(#215052,#215053,#215054),(#215055,#215056,#215057),(#215058,#215059,#215060)),
 .UNSPECIFIED.,.F.,.F.,.F.)
B_SPLINE_SURFACE_WITH_KNOTS((4,2,2,2,2,2,2,2,2,2,2,2,2,2,2,4),(3,3),(-4.4986094344704E-5,
0.0002498236013634,0.0003747354020451,0.0004996472027268,0.0006245590034085,
0.0007494708040902,0.0008743826047719,0.0009992944054536,0.001249118006817,
0.0013740298074987,0.0014989416081804,0.0016238534088621,0.00168630930920295,
0.0017487652095438,0.0018736770102255,0.00204357490525167),(-0.000928863206409833,
1.),.UNSPECIFIED.)
GEOMETRIC_REPRESENTATION_ITEM()
RATIONAL_B_SPLINE_SURFACE(((1.00021581603045,0.883827872090034,1.),(1.00021247367029,
0.885627039143543,1.),(1.00020356699106,0.890421436842798,1.),(1.00019671059006,
0.894112185357078,1.),(1.00019500428282,0.895030677567382,1.),(1.00019084017243,
0.897272186523882,1.),(1.00018859402754,0.89848126923129,1.),(1.0001839588648,
0.900976342083762,1.),(1.00018187522096,0.902097951719568,1.),(1.0001782873346,
0.904029283662378,1.),(1.00017695153087,0.904748336647395,1.),(1.00017393790794,
0.906370546956913,1.),(1.00017218171469,0.907315892426449,1.),(1.00016839882933,
0.90935219084759,1.),(1.00016641186784,0.910421757106923,1.),(1.00016227044416,
0.912651053978273,1.),(1.00016143269546,0.913102007730518,1.),(1.00015750356649,
0.915217027974831,1.),(1.00015585992972,0.916101785147747,1.),(1.00015287736794,
0.917707275472429,1.),(1.0001519373587,0.918213275298274,1.),(1.00015040070489,
0.91904044435685,1.),(1.00014983626223,0.919344279545902,1.),(1.00014914376439,
0.919717045868286,1.),(1.00014896836908,0.919811459830685,1.),(1.00014795440259,
0.920357270280351,1.),(1.00014718179759,0.920773157676318,1.),(1.00014470824478,
0.922104652342618,1.),(1.00014315205124,0.922942339491473,1.),(1.00014065158056,
0.924288323840175,1.),(1.00013984045591,0.924724946070919,1.),(1.00013914538674,
0.925099096520833,1.)))
REPRESENTATION_ITEM('')
SURFACE()
);
#3084=(
BOUNDED_SURFACE()
B_SPLINE_SURFACE(3,2,((#215354,#215355,#215356),(#215357,#215358,#215359),
(#215360,#215361,#215362),(#215363,#215364,#215365),(#215366,#215367,#215368),
(#215369,#215370,#215371),(#215372,#215373,#215374),(#215375,#215376,#215377),
(#215378,#215379,#215380),(#215381,#215382,#215383),(#215384,#215385,#215386),
(#215387,#215388,#215389)),.UNSPECIFIED.,.F.,.F.,.F.)
B_SPLINE_SURFACE_WITH_KNOTS((4,2,2,2,2,4),(3,3),(0.,0.00715193125010649,
0.014303862500213,0.0178798281252662,0.0214557937503195,0.028607725000426),
(0.,1.),.UNSPECIFIED.)
GEOMETRIC_REPRESENTATION_ITEM()
RATIONAL_B_SPLINE_SURFACE(((1.,0.924853416885499,1.),(1.,0.926016513677579,
1.),(1.,0.927093722943951,1.),(1.,0.928447778269084,1.),(1.,0.928716882101724,
1.),(1.,0.928441394999488,1.),(1.,0.928242899045327,1.),(1.,0.927647417447185,
1.),(1.,0.927250341183873,1.),(1.,0.92570107615163,1.),(1.,0.924268637781389,
1.),(1.,0.922934699314373,1.)))
REPRESENTATION_ITEM('')
SURFACE()
);
#3085=(
BOUNDED_SURFACE()
B_SPLINE_SURFACE(3,2,((#215533,#215534,#215535),(#215536,#215537,#215538),
(#215539,#215540,#215541),(#215542,#215543,#215544),(#215545,#215546,#215547),
(#215548,#215549,#215550),(#215551,#215552,#215553),(#215554,#215555,#215556),
(#215557,#215558,#215559),(#215560,#215561,#215562),(#215563,#215564,#215565),
(#215566,#215567,#215568),(#215569,#215570,#215571),(#215572,#215573,#215574),
(#215575,#215576,#215577),(#215578,#215579,#215580),(#215581,#215582,#215583),
(#215584,#215585,#215586),(#215587,#215588,#215589),(#215590,#215591,#215592),
(#215593,#215594,#215595),(#215596,#215597,#215598),(#215599,#215600,#215601),
(#215602,#215603,#215604),(#215605,#215606,#215607),(#215608,#215609,#215610),
(#215611,#215612,#215613),(#215614,#215615,#215616),(#215617,#215618,#215619),
(#215620,#215621,#215622),(#215623,#215624,#215625),(#215626,#215627,#215628),
(#215629,#215630,#215631),(#215632,#215633,#215634)),.UNSPECIFIED.,.F.,
 .F.,.F.)
B_SPLINE_SURFACE_WITH_KNOTS((4,2,2,2,2,2,2,2,2,2,2,2,2,2,2,2,4),(3,3),(-0.00016793412709353,
0.000209917658866865,0.000262397073583582,0.000314876488300298,0.000419835317733731,
0.000524794147167163,0.000629752976600596,0.000839670635467461,0.000892150050184177,
0.000944629464900893,0.00104958829433433,0.00115454712376776,0.00125950595320119,
0.00136446478263462,0.00146942361206806,0.00157438244150149,0.00184727539802677),
(-0.00143652655570475,1.),.UNSPECIFIED.)
GEOMETRIC_REPRESENTATION_ITEM()
RATIONAL_B_SPLINE_SURFACE(((1.00022034803097,0.923305270586211,1.),(1.00022057389735,
0.923226655130542,1.),(1.00022076421095,0.923160414238506,1.),(1.00023524475682,
0.918120289566036,1.),(1.00023692961135,0.917533856087476,1.),(1.00023871862926,
0.916911167317056,1.),(1.00023878977867,0.916886402927843,1.),(1.00023921723265,
0.916737622530491,1.),(1.00023970119732,0.916569172922025,1.),(1.00024138488156,
0.915983146777706,1.),(1.00024248924841,0.915598758877892,1.),(1.0002469403122,
0.914049513661833,1.),(1.00025034837882,0.912863295904625,1.),(1.00025724579866,
0.910462567628845,1.),(1.0002572825449,0.910449777668718,1.),(1.00026222873836,
0.9087281967323,1.),(1.00026340408549,0.908319103311859,1.),(1.00026639323709,
0.907278693862733,1.),(1.00026838330125,0.906586028574658,1.),(1.00027374334603,
0.904720401811733,1.),(1.00027683518481,0.903644250881688,1.),(1.00028164305399,
0.901970815340634,1.),(1.00028339221757,0.901361998340541,1.),(1.00028903872358,
0.899396665370392,1.),(1.00029254258302,0.898177105790678,1.),(1.00030090956553,
0.895264878908138,1.),(1.00030479909101,0.893911083719088,1.),(1.00031159097903,
0.891547087035292,1.),(1.00031413159742,0.890662794860912,1.),(1.00032054361863,
0.888431015298873,1.),(1.00032547359281,0.88671507967576,1.),(1.00034206821476,
0.880939125905835,1.),(1.00035112478508,0.877786879858916,1.),(1.00034975691482,
0.87826298322615,1.)))
REPRESENTATION_ITEM('')
SURFACE()
);
#3086=(
BOUNDED_SURFACE()
B_SPLINE_SURFACE(3,2,((#215761,#215762,#215763),(#215764,#215765,#215766),
(#215767,#215768,#215769),(#215770,#215771,#215772)),.UNSPECIFIED.,.F.,
 .F.,.F.)
B_SPLINE_SURFACE_WITH_KNOTS((4,4),(3,3),(-6.93889390390723E-18,0.00418923766731893),
(0.,1.),.UNSPECIFIED.)
GEOMETRIC_REPRESENTATION_ITEM()
RATIONAL_B_SPLINE_SURFACE(((1.,0.881068987521719,1.),(1.,0.880840248614593,
1.),(1.,0.880630793895676,1.),(1.,0.880439575617234,1.)))
REPRESENTATION_ITEM('')
SURFACE()
);
#3087=(
BOUNDED_SURFACE()
B_SPLINE_SURFACE(3,2,((#215778,#215779,#215780),(#215781,#215782,#215783),
(#215784,#215785,#215786),(#215787,#215788,#215789)),.UNSPECIFIED.,.F.,
 .F.,.F.)
B_SPLINE_SURFACE_WITH_KNOTS((4,4),(3,3),(-4.87796775942825E-5,0.000536579322482048),
(-9.19097232831942E-5,1.00000725198376),.UNSPECIFIED.)
GEOMETRIC_REPRESENTATION_ITEM()
RATIONAL_B_SPLINE_SURFACE(((1.00002138549554,0.883659476497807,1.0000016872441),
(1.00002372657649,0.870923620884117,1.00000187194756),(1.00002649051571,
0.85588734854124,1.00000209001312),(1.00002964036462,0.838751665603248,
1.00000233852567)))
REPRESENTATION_ITEM('')
SURFACE()
);
#3088=(
BOUNDED_SURFACE()
B_SPLINE_SURFACE(3,2,((#215810,#215811,#215812),(#215813,#215814,#215815),
(#215816,#215817,#215818),(#215819,#215820,#215821),(#215822,#215823,#215824),
(#215825,#215826,#215827),(#215828,#215829,#215830),(#215831,#215832,#215833),
(#215834,#215835,#215836),(#215837,#215838,#215839),(#215840,#215841,#215842),
(#215843,#215844,#215845),(#215846,#215847,#215848),(#215849,#215850,#215851),
(#215852,#215853,#215854),(#215855,#215856,#215857),(#215858,#215859,#215860),
(#215861,#215862,#215863),(#215864,#215865,#215866),(#215867,#215868,#215869),
(#215870,#215871,#215872),(#215873,#215874,#215875),(#215876,#215877,#215878),
(#215879,#215880,#215881),(#215882,#215883,#215884),(#215885,#215886,#215887),
(#215888,#215889,#215890),(#215891,#215892,#215893),(#215894,#215895,#215896),
(#215897,#215898,#215899),(#215900,#215901,#215902),(#215903,#215904,#215905),
(#215906,#215907,#215908),(#215909,#215910,#215911),(#215912,#215913,#215914),
(#215915,#215916,#215917),(#215918,#215919,#215920),(#215921,#215922,#215923),
(#215924,#215925,#215926),(#215927,#215928,#215929),(#215930,#215931,#215932),
(#215933,#215934,#215935),(#215936,#215937,#215938),(#215939,#215940,#215941),
(#215942,#215943,#215944),(#215945,#215946,#215947),(#215948,#215949,#215950),
(#215951,#215952,#215953),(#215954,#215955,#215956),(#215957,#215958,#215959),
(#215960,#215961,#215962),(#215963,#215964,#215965),(#215966,#215967,#215968),
(#215969,#215970,#215971),(#215972,#215973,#215974),(#215975,#215976,#215977),
(#215978,#215979,#215980),(#215981,#215982,#215983),(#215984,#215985,#215986),
(#215987,#215988,#215989),(#215990,#215991,#215992),(#215993,#215994,#215995),
(#215996,#215997,#215998),(#215999,#216000,#216001),(#216002,#216003,#216004),
(#216005,#216006,#216007),(#216008,#216009,#216010),(#216011,#216012,#216013),
(#216014,#216015,#216016),(#216017,#216018,#216019),(#216020,#216021,#216022),
(#216023,#216024,#216025),(#216026,#216027,#216028),(#216029,#216030,#216031),
(#216032,#216033,#216034),(#216035,#216036,#216037),(#216038,#216039,#216040),
(#216041,#216042,#216043),(#216044,#216045,#216046),(#216047,#216048,#216049),
(#216050,#216051,#216052),(#216053,#216054,#216055),(#216056,#216057,#216058),
(#216059,#216060,#216061),(#216062,#216063,#216064),(#216065,#216066,#216067),
(#216068,#216069,#216070),(#216071,#216072,#216073),(#216074,#216075,#216076),
(#216077,#216078,#216079),(#216080,#216081,#216082),(#216083,#216084,#216085),
(#216086,#216087,#216088),(#216089,#216090,#216091),(#216092,#216093,#216094),
(#216095,#216096,#216097),(#216098,#216099,#216100),(#216101,#216102,#216103),
(#216104,#216105,#216106),(#216107,#216108,#216109),(#216110,#216111,#216112),
(#216113,#216114,#216115),(#216116,#216117,#216118),(#216119,#216120,#216121)),
 .UNSPECIFIED.,.F.,.F.,.F.)
B_SPLINE_SURFACE_WITH_KNOTS((4,2,2,2,2,2,2,2,2,2,2,2,2,2,2,2,2,2,2,2,2,
2,2,2,2,2,2,2,2,2,2,2,2,2,2,2,2,2,2,2,2,2,2,2,2,2,2,2,2,2,2,4),(3,3),(-3.46944695195361E-18,
0.00252618215747139,0.00505236431494278,0.00631545539367848,0.00639439858609946,
0.00647334177852044,0.0066312281633624,0.00694700093304633,0.00757854647241417,
0.0101047286298856,0.0107362741692534,0.0110520469389373,0.0111309901313583,
0.0111704617275688,0.0112099333237793,0.0113678197086213,0.012630910787357,
0.0151570929448283,0.016420184023564,0.0170517295629319,0.0173675023326158,
0.0174464455250368,0.0174859171212473,0.0175253887174578,0.0176832751022998,
0.0189463661810354,0.0202094572597711,0.0227356394172426,0.0228145826096635,
0.022854054205874,0.0228935258020845,0.0230514121869265,0.0233671849566104,
0.0239987304959783,0.025261821574714,0.0277880037321854,0.029051094810921,
0.029208981195763,0.029287924388184,0.029366867580605,0.0296826403502888,
0.0303141858896567,0.0328403680471281,0.0341034591258638,0.0341824023182848,
0.0342218739144953,0.0342613455107057,0.0344192318955477,0.0347350046652317,
0.0353665502045995,0.0378927323620709,0.0404189145195423),(-0.00400343516766361,
1.),.UNSPECIFIED.)
GEOMETRIC_REPRESENTATION_ITEM()
RATIONAL_B_SPLINE_SURFACE(((1.00126205257496,0.842378791948742,1.),(1.00116206025281,
0.854867107353403,1.),(1.00108355000387,0.864672467707073,1.),(1.00095888244726,
0.880242540830635,1.),(1.00091226223324,0.886065067244628,1.),(1.00086179031195,
0.892368643945316,1.),(1.00084832168461,0.894050777759472,1.),(1.00083725616009,
0.89543278147101,1.),(1.00083939692912,0.89516541495365,1.),(1.0008423307566,
0.894799001192412,1.),(1.00084380125902,0.894615346111281,1.),(1.00084822302296,
0.894063099883762,1.),(1.00085118454391,0.893693227408759,1.),(1.00086010596924,
0.892579006126042,1.),(1.00086610276788,0.891830049494227,1.),(1.00088420600063,
0.889569087096759,1.),(1.00089642239576,0.888043347997252,1.),(1.00095780436928,
0.880377184946395,1.),(1.00100879881346,0.874008348928721,1.),(1.00107119105981,
0.866216010132179,1.),(1.00108365614793,0.864659211083758,1.),(1.00110223373256,
0.862339005579313,1.),(1.00110840636504,0.86156808857656,1.),(1.0011160880171,
0.860608705979043,1.),(1.00111762264437,0.860417042169444,1.),(1.0011199218686,
0.860129885748125,1.),(1.00112136395188,0.859949780012029,1.),(1.00111940556711,
0.860194368058238,1.),(1.0011184314474,0.860316028541052,1.),(1.00111358603219,
0.86092118573824,1.),(1.00110979027839,0.861395247842052,1.),(1.00107633361689,
0.86557374207204,1.),(1.00105157373995,0.868666071022459,1.),(1.00098953843601,
0.876413830301835,1.),(1.00096444592774,0.879547702492012,1.),(1.00094661068597,
0.8817751947611,1.),(1.00094402396992,0.882098256823662,1.),(1.00094525304224,
0.881944754610406,1.),(1.00094651635627,0.881786975855158,1.),(1.00094973604407,
0.881384860213925,1.),(1.00095103043371,0.881223200342202,1.),(1.00095293246182,
0.880985650833325,1.),(1.00095332707769,0.880936366175553,1.),(1.00095394048422,
0.88085975615034,1.),(1.00095414853362,0.880833772290365,1.),(1.00095457182273,
0.880780906552175,1.),(1.00095468954101,0.880766204393413,1.),(1.00095544962206,
0.880671275785742,1.),(1.0009560445374,0.880596975178003,1.),(1.00096127208582,
0.879944092315028,1.),(1.0009650012442,0.879478347496011,1.),(1.00096997719539,
0.878856887301876,1.),(1.00097130929268,0.878690518017464,1.),(1.00097096264402,
0.878733811919358,1.),(1.00096516997834,0.879457273826079,1.),(1.0009556328047,
0.880648397604047,1.),(1.00095534056217,0.880684896575533,1.),(1.0009548975107,
0.880740230488282,1.),(1.00095474904569,0.880758772690539,1.),(1.00095445058259,
0.880796048566581,1.),(1.00095424553061,0.880821658070792,1.),(1.00095323023239,
0.880948461449914,1.),(1.00095247254334,0.881043091314579,1.),(1.00095036084046,
0.881306827679129,1.),(1.00094916809947,0.881455792373385,1.),(1.00094622018284,
0.881823965768153,1.),(1.00094509490487,0.881964504820641,1.),(1.00094416392081,
0.882080777973223,1.),(1.00094679343264,0.881752371027292,1.),(1.00096430182822,
0.879565699475922,1.),(1.00098858666124,0.876532700064088,1.),(1.00104815881752,
0.869092570052193,1.),(1.00107185053063,0.866133647012636,1.),(1.00110348918137,
0.862182209133539,1.),(1.00110707459538,0.861734416942979,1.),(1.00111256022933,
0.861049301070322,1.),(1.00111440669401,0.860818691031526,1.),(1.00111813589513,
0.860352940874234,1.),(1.00112173560586,0.859903363126305,1.),(1.00111433813456,
0.860827253609506,1.),(1.00110838255543,0.861571062223461,1.),(1.00109042205054,
0.863814198947867,1.),(1.00107832275572,0.865325313066906,1.),(1.00101749555892,
0.872922188531655,1.),(1.00096720718229,0.879202841836596,1.),(1.00089304098,
0.888465662287133,1.),(1.00086839099238,0.891544266859536,1.),(1.00084316866518,
0.894694352491815,1.),(1.00084168868037,0.894879191853632,1.),(1.00083947448171,
0.895155729198434,1.),(1.00083873737851,0.895247788038785,1.),(1.00083726514029,
0.895431659908763,1.),(1.0008378809652,0.895354747846773,1.),(1.00083952894906,
0.89514892662193,1.),(1.00084089654681,0.894978123586918,1.),(1.00084514785539,
0.894447165996617,1.),(1.0008481799721,0.894068476623283,1.),(1.00085788119072,
0.892856864818009,1.),(1.000865153556,0.891948599169143,1.),(1.0009057894337,
0.886873472934737,1.),(1.00095157280583,0.881155461999917,1.),(1.00107806329298,
0.865357718081277,1.),(1.00116014641827,0.855106131398954,1.),(1.00126205257496,
0.842378791948798,1.)))
REPRESENTATION_ITEM('')
SURFACE()
);
#3089=(
BOUNDED_SURFACE()
B_SPLINE_SURFACE(3,2,((#216727,#216728,#216729),(#216730,#216731,#216732),
(#216733,#216734,#216735),(#216736,#216737,#216738)),.UNSPECIFIED.,.F.,
 .F.,.F.)
B_SPLINE_SURFACE_WITH_KNOTS((4,4),(3,3),(0.0429271655601134,0.046749382327419),
(0.,1.),.UNSPECIFIED.)
GEOMETRIC_REPRESENTATION_ITEM()
RATIONAL_B_SPLINE_SURFACE(((1.,0.922487559402275,1.),(1.,0.922290239059189,
1.),(1.,0.921950699598134,1.),(1.,0.921567721510049,1.)))
REPRESENTATION_ITEM('')
SURFACE()
);
#3090=(
BOUNDED_SURFACE()
B_SPLINE_SURFACE(3,2,((#216765,#216766,#216767),(#216768,#216769,#216770),
(#216771,#216772,#216773),(#216774,#216775,#216776)),.UNSPECIFIED.,.F.,
 .F.,.F.)
B_SPLINE_SURFACE_WITH_KNOTS((4,4),(3,3),(0.0243367909416761,0.0248833749525317),
(0.,1.),.UNSPECIFIED.)
GEOMETRIC_REPRESENTATION_ITEM()
RATIONAL_B_SPLINE_SURFACE(((1.,0.920889968635124,1.),(1.,0.921315643311137,
1.),(1.,0.921538438398832,1.),(1.,0.921567721510049,1.)))
REPRESENTATION_ITEM('')
SURFACE()
);
#3091=(
BOUNDED_SURFACE()
B_SPLINE_SURFACE(3,2,((#216782,#216783,#216784),(#216785,#216786,#216787),
(#216788,#216789,#216790),(#216791,#216792,#216793),(#216794,#216795,#216796),
(#216797,#216798,#216799),(#216800,#216801,#216802),(#216803,#216804,#216805),
(#216806,#216807,#216808),(#216809,#216810,#216811),(#216812,#216813,#216814),
(#216815,#216816,#216817),(#216818,#216819,#216820),(#216821,#216822,#216823),
(#216824,#216825,#216826),(#216827,#216828,#216829),(#216830,#216831,#216832),
(#216833,#216834,#216835),(#216836,#216837,#216838),(#216839,#216840,#216841),
(#216842,#216843,#216844),(#216845,#216846,#216847),(#216848,#216849,#216850),
(#216851,#216852,#216853),(#216854,#216855,#216856),(#216857,#216858,#216859)),
 .UNSPECIFIED.,.F.,.F.,.F.)
B_SPLINE_SURFACE_WITH_KNOTS((4,2,2,2,2,2,2,2,2,2,2,2,4),(3,3),(0.0235924208938234,
0.0238608230039568,0.0239731153899888,0.0240854077760208,0.0243099925480848,
0.0245345773201488,0.0249837468642768,0.0252083316363408,0.0254329164084048,
0.0258820859525327,0.0263312554966607,0.0267804250407887,0.0272734119229856),
(-0.000493556320524505,1.),.UNSPECIFIED.)
GEOMETRIC_REPRESENTATION_ITEM()
RATIONAL_B_SPLINE_SURFACE(((1.00007824284398,0.920735647859346,1.),(1.00007802101355,
0.920960374425325,1.),(1.00007772756555,0.921257653567913,1.),(1.00007739864045,
0.921590872985578,1.),(1.00007731162238,0.92167902712557,1.),(1.00007716427966,
0.921828293494607,1.),(1.00007711979111,0.92187336287521,1.),(1.00007678443583,
0.922213096423567,1.),(1.00007634872583,0.922654494882402,1.),(1.00007544895396,
0.92356601382016,1.),(1.00007500286602,0.924017925712546,1.),(1.0000738906511,
0.925144661281554,1.),(1.00007330799815,0.92573492111959,1.),(1.00007202214984,
0.927037556965429,1.),(1.00007146426924,0.927602721040608,1.),(1.00007035323508,
0.928728260429265,1.),(1.00006984224533,0.929245921461416,1.),(1.00006835495859,
0.930752625641717,1.),(1.00006743638207,0.931683194740616,1.),(1.00006529726307,
0.933850241244143,1.),(1.00006405365497,0.935110085410391,1.),(1.00006152639895,
0.937670336295846,1.),(1.00006031706504,0.938895458806362,1.),(1.00005784890346,
0.941395843745346,1.),(1.0000565320274,0.942729912423448,1.),(1.00005458091539,
0.944706497397475,1.)))
REPRESENTATION_ITEM('')
SURFACE()
);
#3092=(
BOUNDED_SURFACE()
B_SPLINE_SURFACE(3,2,((#217189,#217190,#217191),(#217192,#217193,#217194),
(#217195,#217196,#217197),(#217198,#217199,#217200),(#217201,#217202,#217203),
(#217204,#217205,#217206),(#217207,#217208,#217209),(#217210,#217211,#217212)),
 .UNSPECIFIED.,.F.,.F.,.F.)
B_SPLINE_SURFACE_WITH_KNOTS((4,2,2,4),(3,3),(-6.62670003357417E-5,0.000233612606258176,
0.000467225212516351,0.00100071742536861),(0.,1.00006626700034),
 .UNSPECIFIED.)
GEOMETRIC_REPRESENTATION_ITEM()
RATIONAL_B_SPLINE_SURFACE(((1.,0.958477827751749,1.0000055030996),(1.,0.957369041680115,
1.00000565005146),(1.,0.955803501995477,1.0000058575387),(1.,0.953095633837129,
1.0000062164233),(1.,0.951957652185137,1.00000636724456),(1.,0.9484156097212,
1.00000683668562),(1.,0.946055609381867,1.0000071494659),(1.,0.943163908413987,
1.0000075327146)))
REPRESENTATION_ITEM('')
SURFACE()
);
#3093=(
BOUNDED_SURFACE()
B_SPLINE_SURFACE(3,2,((#217248,#217249,#217250),(#217251,#217252,#217253),
(#217254,#217255,#217256),(#217257,#217258,#217259)),.UNSPECIFIED.,.F.,
 .F.,.F.)
B_SPLINE_SURFACE_WITH_KNOTS((4,4),(3,3),(0.0114568846502287,0.0192019541084939),
(0.,1.),.UNSPECIFIED.)
GEOMETRIC_REPRESENTATION_ITEM()
RATIONAL_B_SPLINE_SURFACE(((1.,0.957684062981984,1.),(1.,0.957879658663776,
1.),(1.,0.958058054935734,1.),(1.,0.958218732174581,1.)))
REPRESENTATION_ITEM('')
SURFACE()
);
#3094=(
BOUNDED_SURFACE()
B_SPLINE_SURFACE(3,2,((#217281,#217282,#217283),(#217284,#217285,#217286),
(#217287,#217288,#217289),(#217290,#217291,#217292)),.UNSPECIFIED.,.F.,
 .F.,.F.)
B_SPLINE_SURFACE_WITH_KNOTS((4,4),(3,3),(0.00543385294581827,0.00566356273029558),
(0.,1.0000263042412),.UNSPECIFIED.)
GEOMETRIC_REPRESENTATION_ITEM()
RATIONAL_B_SPLINE_SURFACE(((1.,0.991880174791391,1.00000042717168),(1.,
0.993019568317563,1.00000036722992),(1.,0.993924546422819,1.00000031962039),
(0.999999999999999,0.994332871227875,1.00000029813904)))
REPRESENTATION_ITEM('')
SURFACE()
);
#3095=(
BOUNDED_SURFACE()
B_SPLINE_SURFACE(3,2,((#217307,#217308,#217309),(#217310,#217311,#217312),
(#217313,#217314,#217315),(#217316,#217317,#217318),(#217319,#217320,#217321),
(#217322,#217323,#217324)),.UNSPECIFIED.,.F.,.F.,.F.)
B_SPLINE_SURFACE_WITH_KNOTS((4,2,4),(3,3),(-1.09829680072782E-16,0.000498949606022071,
0.000997899212044251),(0.,1.),.UNSPECIFIED.)
GEOMETRIC_REPRESENTATION_ITEM()
RATIONAL_B_SPLINE_SURFACE(((1.,0.994220746859027,1.),(1.,0.996098915568006,
1.),(1.,0.997550054459957,1.),(1.,0.99950507842482,1.),(1.,1.00000638742927,
1.),(1.,1.,1.)))
REPRESENTATION_ITEM('')
SURFACE()
);
#3096=(
BOUNDED_SURFACE()
B_SPLINE_SURFACE(3,2,((#217350,#217351,#217352),(#217353,#217354,#217355),
(#217356,#217357,#217358),(#217359,#217360,#217361),(#217362,#217363,#217364),
(#217365,#217366,#217367),(#217368,#217369,#217370),(#217371,#217372,#217373),
(#217374,#217375,#217376),(#217377,#217378,#217379),(#217380,#217381,#217382),
(#217383,#217384,#217385),(#217386,#217387,#217388),(#217389,#217390,#217391),
(#217392,#217393,#217394),(#217395,#217396,#217397),(#217398,#217399,#217400),
(#217401,#217402,#217403),(#217404,#217405,#217406),(#217407,#217408,#217409),
(#217410,#217411,#217412),(#217413,#217414,#217415),(#217416,#217417,#217418),
(#217419,#217420,#217421),(#217422,#217423,#217424),(#217425,#217426,#217427),
(#217428,#217429,#217430),(#217431,#217432,#217433),(#217434,#217435,#217436),
(#217437,#217438,#217439),(#217440,#217441,#217442),(#217443,#217444,#217445),
(#217446,#217447,#217448),(#217449,#217450,#217451),(#217452,#217453,#217454),
(#217455,#217456,#217457),(#217458,#217459,#217460),(#217461,#217462,#217463),
(#217464,#217465,#217466),(#217467,#217468,#217469),(#217470,#217471,#217472),
(#217473,#217474,#217475),(#217476,#217477,#217478),(#217479,#217480,#217481),
(#217482,#217483,#217484),(#217485,#217486,#217487),(#217488,#217489,#217490),
(#217491,#217492,#217493),(#217494,#217495,#217496),(#217497,#217498,#217499),
(#217500,#217501,#217502),(#217503,#217504,#217505),(#217506,#217507,#217508),
(#217509,#217510,#217511),(#217512,#217513,#217514),(#217515,#217516,#217517),
(#217518,#217519,#217520),(#217521,#217522,#217523),(#217524,#217525,#217526),
(#217527,#217528,#217529),(#217530,#217531,#217532),(#217533,#217534,#217535),
(#217536,#217537,#217538),(#217539,#217540,#217541),(#217542,#217543,#217544),
(#217545,#217546,#217547),(#217548,#217549,#217550),(#217551,#217552,#217553),
(#217554,#217555,#217556),(#217557,#217558,#217559),(#217560,#217561,#217562),
(#217563,#217564,#217565),(#217566,#217567,#217568),(#217569,#217570,#217571),
(#217572,#217573,#217574),(#217575,#217576,#217577),(#217578,#217579,#217580),
(#217581,#217582,#217583),(#217584,#217585,#217586),(#217587,#217588,#217589),
(#217590,#217591,#217592),(#217593,#217594,#217595),(#217596,#217597,#217598),
(#217599,#217600,#217601),(#217602,#217603,#217604),(#217605,#217606,#217607),
(#217608,#217609,#217610),(#217611,#217612,#217613),(#217614,#217615,#217616),
(#217617,#217618,#217619),(#217620,#217621,#217622),(#217623,#217624,#217625),
(#217626,#217627,#217628),(#217629,#217630,#217631),(#217632,#217633,#217634),
(#217635,#217636,#217637),(#217638,#217639,#217640),(#217641,#217642,#217643),
(#217644,#217645,#217646),(#217647,#217648,#217649),(#217650,#217651,#217652),
(#217653,#217654,#217655),(#217656,#217657,#217658),(#217659,#217660,#217661),
(#217662,#217663,#217664),(#217665,#217666,#217667),(#217668,#217669,#217670),
(#217671,#217672,#217673),(#217674,#217675,#217676),(#217677,#217678,#217679),
(#217680,#217681,#217682),(#217683,#217684,#217685),(#217686,#217687,#217688),
(#217689,#217690,#217691),(#217692,#217693,#217694),(#217695,#217696,#217697),
(#217698,#217699,#217700),(#217701,#217702,#217703),(#217704,#217705,#217706),
(#217707,#217708,#217709),(#217710,#217711,#217712),(#217713,#217714,#217715),
(#217716,#217717,#217718),(#217719,#217720,#217721),(#217722,#217723,#217724),
(#217725,#217726,#217727),(#217728,#217729,#217730),(#217731,#217732,#217733),
(#217734,#217735,#217736),(#217737,#217738,#217739),(#217740,#217741,#217742),
(#217743,#217744,#217745),(#217746,#217747,#217748),(#217749,#217750,#217751)),
 .UNSPECIFIED.,.F.,.F.,.F.)
B_SPLINE_SURFACE_WITH_KNOTS((4,2,2,2,2,2,2,2,2,2,2,2,2,2,2,2,2,2,2,2,2,
2,2,2,2,2,2,2,2,2,2,2,2,2,2,2,2,2,2,2,2,2,2,2,2,2,2,2,2,2,2,2,2,2,2,2,2,
2,2,2,2,2,2,2,2,2,4),(3,3),(0.0401209448553485,0.0422079288610133,0.0442949128666782,
0.046381896872343,0.0484688808780079,0.0526428488893376,0.0527732853896916,
0.0528385036398687,0.0529037218900457,0.0531645948907538,0.05368634089217,
0.0547298328950024,0.0568168169006673,0.0578603089034997,0.0589038009063321,
0.0599472929091645,0.0602081659098726,0.0603386024102267,0.0603712115353152,
0.0604038206604037,0.0604690389105808,0.060990784911997,0.0651647529233267,
0.0693387209346564,0.0698604669360726,0.0701213399367807,0.0701865581869577,
0.0702191673120462,0.0702517764371347,0.0703822129374888,0.0714257049403212,
0.0724691969431537,0.0735126889459861,0.0755996729516509,0.0766431649544833,
0.0771649109558996,0.0774257839566077,0.0775562204569617,0.0776214387071387,
0.0776540478322272,0.0776866569573158,0.0818606249686455,0.0860345929799752,
0.0870780849828076,0.0873389579835157,0.0874041762336927,0.0874367853587812,
0.0874530899213255,0.0874693944838697,0.0875998309842238,0.08812157698564,
0.0902085609913048,0.0943825290026346,0.0946434020033427,0.0947086202535197,
0.0947412293786082,0.0947738385036967,0.0949042750040508,0.095426021005467,
0.0964695130082994,0.0985564970139642,0.100643481019629,0.101686973022461,
0.102730465025294,0.104817449030959,0.105860941033791,0.106904433036624),
(0.,1.00211619801959),.UNSPECIFIED.)
GEOMETRIC_REPRESENTATION_ITEM()
RATIONAL_B_SPLINE_SURFACE(((1.,0.967623608150263,1.00013702971263),(1.,
0.967362278939665,1.00013813576134),(1.,0.966893393913631,1.00014012026847),
(1.,0.965707706678196,1.00014513856643),(1.,0.964990163383989,1.00014817549383),
(1.,0.9633845862752,1.00015497093202),(1.,0.962494992184358,1.00015873604653),
(1.,0.960578187950096,1.00016684872118),(1.,0.959565053500142,1.00017113670741),
(1.,0.956390754090381,1.00018457159966),(1.,0.954097360891505,1.00019427814795),
(1.,0.951539895136251,1.00020510235588),(1.,0.951462206912974,1.00020543116321),
(1.,0.951345387989037,1.00020592558716),(1.,0.951437397555211,1.00020553616624),
(1.,0.951546321977574,1.00020507515495),(1.,0.951600611930997,1.00020484537836),
(1.,0.951871196160378,1.00020370015874),(1.,0.95208489429128,1.00020279570362),
(1.,0.952717506711006,1.00020011823732),(1.,0.9531279452915,1.0001983810987),
(1.,0.954323738610181,1.00019332002779),(1.,0.955073684874735,1.00019014595819),
(1.,0.957165050829292,1.00018129446921),(1.,0.95832888484391,1.00017636866273),
(1.,0.959643495316587,1.00017080471058),(1.,0.96000598572915,1.00016927050759),
(1.,0.960567494657221,1.00016689397943),(1.,0.960766569834018,1.00016605141444),
(1.,0.960982622872878,1.00016513699241),(1.,0.961000543757655,1.00016506114413),
(1.,0.96090658055613,1.00016545883361),(1.,0.960881962556224,1.00016556302674),
(1.,0.960836203436817,1.00016575669745),(1.,0.960819478259316,1.00016582748503),
(1.,0.960796720866671,1.00016592380333),(1.,0.960792076839665,1.00016594345869),
(1.,0.960782603408868,1.000165983554),(1.,0.960772649057408,1.00016602568476),
(1.,0.960780513429616,1.00016599239962),(1.,0.960785654845429,1.00016597063911),
(1.,0.960831021621874,1.00016577862895),(1.,0.960864910012085,1.00016563519986),
(1.,0.961115514496332,1.00016457454243),(1.,0.960966587611861,1.00016520485999),
(1.,0.960110029748364,1.0001688301521),(1.,0.959400389202501,1.00017183363193),
(1.,0.958222276120302,1.00017681987307),(1.,0.958085899137497,1.00017739707448),
(1.,0.957872770035717,1.00017829912124),(1.,0.957800412888855,1.00017860536534),
(1.,0.95770829518048,1.00017899524397),(1.,0.957689788065446,1.00017907357341),
(1.,0.957661901465818,1.00017919160054),(1.,0.95763491988757,1.00017930579727),
(1.,0.957663736151373,1.00017918383543),(1.,0.957678073075429,1.00017912315589),
(1.,0.95774940029199,1.00017882127086),(1.,0.957805318337416,1.00017858460354),
(1.,0.958298133029376,1.00017649881659),(1.,0.958661487087527,1.00017496095832),
(1.,0.959225394163478,1.00017257428024),(1.,0.95942600733162,1.00017172520586),
(1.,0.959652210338516,1.00017076782515),(1.,0.959678704973595,1.00017065568936),
(1.,0.959505481141619,1.00017138884122),(1.,0.959051697202111,1.00017330943457),
(1.,0.957920993157528,1.00017809502189),(1.,0.957469248115843,1.00018000698582),
(1.,0.956690162824021,1.00018330438332),(1.,0.956413411772314,1.00018447570338),
(1.,0.955974090823865,1.00018633508362),(1.,0.955823630472945,1.00018697189141),
(1.,0.955592121576858,1.00018795172875),(1.,0.955513982296279,1.00018828244513),
(1.,0.955395346065634,1.00018878456064),(1.,0.955355562774398,1.00018895293929),
(1.,0.955295534454033,1.00018920700291),(1.,0.955275466116547,1.00018929194006),
(1.,0.955235212224026,1.00018946231048),(1.,0.955274232783486,1.00018929716002),
(1.,0.957038052415492,1.00018183197679),(1.,0.95849806843578,1.00017565261077),
(1.,0.960891755654296,1.00016552157847),(1.,0.961835644094202,1.00016152666877),
(1.,0.962570204344262,1.00015841771888),(1.,0.962693730785603,1.00015789490606),
(1.,0.962813772003151,1.00015738684409),(1.,0.962836055292866,1.00015729253238),
(1.,0.96286165511172,1.00015718418381),(1.,0.962866662329318,1.00015716299128),
(1.,0.962874002098797,1.00015713192647),(1.,0.962876420178934,1.00015712169219),
(1.,0.962880004288309,1.00015710652282),(1.,0.962881191823016,1.00015710149671),
(1.,0.962883552514071,1.00015709150533),(1.,0.962881342518526,1.0001571008589),
(1.,0.9628719610535,1.00015714056498),(1.,0.9628618314315,1.00015718343755),
(1.,0.96280234657013,1.00015743520104),(1.,0.962726499029366,1.00015775621787),
(1.,0.962212615381494,1.00015993117699),(1.,0.961365351871455,1.00016351713171),
(1.,0.957821561850805,1.00017851585456),(1.,0.954121811281669,1.00019417466422),
(1.,0.949559520376701,1.00021348408617),(1.,0.949288571068739,1.00021463085095),
(1.,0.948946738814693,1.00021607762043),(1.,0.948878215048348,1.00021636764015),
(1.,0.94877519479492,1.00021680366266),(1.,0.948740815609189,1.00021694916899),
(1.,0.948671979258847,1.00021724051168),(1.,0.94874268099657,1.00021694127393),
(1.,0.948863910971176,1.00021642818066),(1.,0.948960718690678,1.00021601845206),
(1.,0.949443885738123,1.00021397349776),(1.,0.949827631882834,1.0002123493321),
(1.,0.950970846836433,1.00020751079365),(1.,0.951721934475459,1.00020433189331),
(1.,0.95394845818276,1.00019490836319),(1.,0.955398313814889,1.00018877199995),
(1.,0.958226868294617,1.00017680043717),(1.,0.95960518223231,1.00017096686672),
(1.,0.961607109424986,1.000162493918),(1.,0.962265389719952,1.00015970781509),
(1.,0.963540595600696,1.00015431063877),(1.,0.96415834401959,1.00015169608281),
(1.,0.965941790209826,1.00014414783222),(1.,0.967040962196452,1.00013949570105),
(1.,0.96847419378806,1.00013342969734),(1.,0.968915400040616,1.00013156233775),
(1.,0.969701097798822,1.00012823695367),(1.,0.970046784443818,1.00012677387088),
(1.,0.970321492872041,1.00012561119602)))
REPRESENTATION_ITEM('')
SURFACE()
);
#3097=(
BOUNDED_SURFACE()
B_SPLINE_SURFACE(3,2,((#218553,#218554,#218555),(#218556,#218557,#218558),
(#218559,#218560,#218561),(#218562,#218563,#218564),(#218565,#218566,#218567),
(#218568,#218569,#218570)),.UNSPECIFIED.,.F.,.F.,.F.)
B_SPLINE_SURFACE_WITH_KNOTS((4,2,4),(3,3),(-2.65828754408143E-15,0.000518614521426172,
0.001037229042855),(0.,1.),.UNSPECIFIED.)
GEOMETRIC_REPRESENTATION_ITEM()
RATIONAL_B_SPLINE_SURFACE(((1.,0.994246489501235,1.),(1.,0.99609478928193,
1.),(1.,0.997541267372286,1.),(1.,0.999499888835022,1.),(1.,1.00000732330262,
1.),(1.,1.,1.)))
REPRESENTATION_ITEM('')
SURFACE()
);
#3098=(
BOUNDED_SURFACE()
B_SPLINE_SURFACE(3,2,((#218579,#218580,#218581),(#218582,#218583,#218584),
(#218585,#218586,#218587),(#218588,#218589,#218590)),.UNSPECIFIED.,.F.,
 .F.,.F.)
B_SPLINE_SURFACE_WITH_KNOTS((4,4),(3,3),(0.0119444722538381,0.0121107952282447),
(-2.03695309557864E-5,1.),.UNSPECIFIED.)
GEOMETRIC_REPRESENTATION_ITEM()
RATIONAL_B_SPLINE_SURFACE(((1.00000029293976,0.992809364237771,1.),(1.0000002643703,
0.993510643385671,1.),(1.00000024275696,0.994041174404857,1.),(1.0000002313304,
0.994321656227528,1.)))
REPRESENTATION_ITEM('')
SURFACE()
);
#3099=(
BOUNDED_SURFACE()
B_SPLINE_SURFACE(3,2,((#218605,#218606,#218607),(#218608,#218609,#218610),
(#218611,#218612,#218613),(#218614,#218615,#218616)),.UNSPECIFIED.,.F.,
 .F.,.F.)
B_SPLINE_SURFACE_WITH_KNOTS((4,4),(3,3),(0.0657640091385094,0.0735516090029935),
(0.,1.),.UNSPECIFIED.)
GEOMETRIC_REPRESENTATION_ITEM()
RATIONAL_B_SPLINE_SURFACE(((1.,0.958250447061442,1.),(1.,0.958411329127679,
1.),(1.,0.958554518262528,1.),(1.,0.958680046125676,1.)))
REPRESENTATION_ITEM('')
SURFACE()
);
#3100=(
BOUNDED_SURFACE()
B_SPLINE_SURFACE(3,2,((#218622,#218623,#218624),(#218625,#218626,#218627),
(#218628,#218629,#218630),(#218631,#218632,#218633),(#218634,#218635,#218636),
(#218637,#218638,#218639)),.UNSPECIFIED.,.F.,.F.,.F.)
B_SPLINE_SURFACE_WITH_KNOTS((4,2,4),(3,3),(-7.50126731622146E-5,0.000375063365810873,
0.000825139404783385),(0.,1.00007657360774),.UNSPECIFIED.)
GEOMETRIC_REPRESENTATION_ITEM()
RATIONAL_B_SPLINE_SURFACE(((1.,0.949070591842026,1.00000779969705),(1.,
0.950903281061525,1.00000751902579),(1.,0.952484216272804,1.00000727690997),
(1.,0.955845362028548,1.00000676215986),(1.,0.957638657720463,1.00000648752161),
(1.,0.95893329183817,1.000006289252)))
REPRESENTATION_ITEM('')
SURFACE()
);
#3101=(
BOUNDED_SURFACE()
B_SPLINE_SURFACE(3,2,((#218663,#218664,#218665),(#218666,#218667,#218668),
(#218669,#218670,#218671),(#218672,#218673,#218674),(#218675,#218676,#218677),
(#218678,#218679,#218680),(#218681,#218682,#218683),(#218684,#218685,#218686),
(#218687,#218688,#218689),(#218690,#218691,#218692),(#218693,#218694,#218695),
(#218696,#218697,#218698),(#218699,#218700,#218701),(#218702,#218703,#218704),
(#218705,#218706,#218707),(#218708,#218709,#218710),(#218711,#218712,#218713),
(#218714,#218715,#218716),(#218717,#218718,#218719),(#218720,#218721,#218722),
(#218723,#218724,#218725),(#218726,#218727,#218728),(#218729,#218730,#218731),
(#218732,#218733,#218734),(#218735,#218736,#218737),(#218738,#218739,#218740)),
 .UNSPECIFIED.,.F.,.F.,.F.)
B_SPLINE_SURFACE_WITH_KNOTS((4,2,2,2,2,2,2,2,2,2,2,2,4),(3,3),(0.0241531416828426,
0.0246199912180733,0.0250868407533039,0.0255536902885345,0.0260205398237651,
0.0262539645913804,0.0264873893589958,0.0269542388942264,0.0271876636618417,
0.0274210884294571,0.0275378008132647,0.0276545131970724,0.0278879379646877),
(-0.000276129488825748,1.),.UNSPECIFIED.)
GEOMETRIC_REPRESENTATION_ITEM()
RATIONAL_B_SPLINE_SURFACE(((1.00002763636452,0.949957600265961,1.),(1.00002829348857,
0.948767716395043,1.),(1.00002907932003,0.947344776267276,1.),(1.00003027374605,
0.945181975713108,1.),(1.0000307912165,0.944244968855354,1.),(1.00003199625233,
0.942062956644543,1.),(1.00003261518263,0.940942231912179,1.),(1.00003371198137,
0.938956209428044,1.),(1.00003417137706,0.938124361131481,1.),(1.00003487381759,
0.936852420695295,1.),(1.00003511037192,0.936424081193685,1.),(1.00003560979616,
0.935519751421037,1.),(1.00003589402015,0.935005094353774,1.),(1.00003656004965,
0.933799084975963,1.),(1.00003684769454,0.933278233520713,1.),(1.00003736403339,
0.93234327571486,1.),(1.00003756245292,0.931983988594581,1.),(1.00003795892861,
0.931266072365573,1.),(1.0000381530246,0.930914614077073,1.),(1.0000383348696,
0.930585339209706,1.),(1.00003836897905,0.930523575717338,1.),(1.000038451592,
0.930373984741388,1.),(1.00003849806418,0.930289835502992,1.),(1.00003864575439,
0.930022406245385,1.),(1.00003875609486,0.929822607823737,1.),(1.00003883615842,
0.929677633147427,1.)))
REPRESENTATION_ITEM('')
SURFACE()
);
#3102=(
BOUNDED_SURFACE()
B_SPLINE_SURFACE(3,2,((#219004,#219005,#219006),(#219007,#219008,#219009),
(#219010,#219011,#219012),(#219013,#219014,#219015)),.UNSPECIFIED.,.F.,
 .F.,.F.)
B_SPLINE_SURFACE_WITH_KNOTS((4,4),(3,3),(0.0249863231317726,0.0253614725245169),
(0.,1.),.UNSPECIFIED.)
GEOMETRIC_REPRESENTATION_ITEM()
RATIONAL_B_SPLINE_SURFACE(((1.,0.930070526504304,1.),(1.,0.930041043693297,
1.),(1.,0.929915461335265,1.),(1.,0.929697045866144,1.)))
REPRESENTATION_ITEM('')
SURFACE()
);
#3103=(
BOUNDED_SURFACE()
B_SPLINE_SURFACE(3,2,((#219021,#219022,#219023),(#219024,#219025,#219026),
(#219027,#219028,#219029),(#219030,#219031,#219032)),.UNSPECIFIED.,.F.,
 .F.,.F.)
B_SPLINE_SURFACE_WITH_KNOTS((4,4),(3,3),(0.0387340315057144,0.0427072915207103),
(0.,1.),.UNSPECIFIED.)
GEOMETRIC_REPRESENTATION_ITEM()
RATIONAL_B_SPLINE_SURFACE(((1.,0.930070526504304,1.),(1.,0.930612186341169,
1.),(1.,0.931191283587816,1.),(1.,0.931676951123116,1.)))
REPRESENTATION_ITEM('')
SURFACE()
);
#3104=(
BOUNDED_SURFACE()
B_SPLINE_SURFACE(3,2,((#219068,#219069,#219070),(#219071,#219072,#219073),
(#219074,#219075,#219076),(#219077,#219078,#219079),(#219080,#219081,#219082),
(#219083,#219084,#219085),(#219086,#219087,#219088),(#219089,#219090,#219091),
(#219092,#219093,#219094),(#219095,#219096,#219097),(#219098,#219099,#219100),
(#219101,#219102,#219103),(#219104,#219105,#219106),(#219107,#219108,#219109),
(#219110,#219111,#219112),(#219113,#219114,#219115),(#219116,#219117,#219118),
(#219119,#219120,#219121),(#219122,#219123,#219124),(#219125,#219126,#219127),
(#219128,#219129,#219130),(#219131,#219132,#219133),(#219134,#219135,#219136),
(#219137,#219138,#219139),(#219140,#219141,#219142),(#219143,#219144,#219145),
(#219146,#219147,#219148),(#219149,#219150,#219151),(#219152,#219153,#219154),
(#219155,#219156,#219157),(#219158,#219159,#219160),(#219161,#219162,#219163),
(#219164,#219165,#219166),(#219167,#219168,#219169),(#219170,#219171,#219172),
(#219173,#219174,#219175),(#219176,#219177,#219178),(#219179,#219180,#219181),
(#219182,#219183,#219184),(#219185,#219186,#219187),(#219188,#219189,#219190),
(#219191,#219192,#219193),(#219194,#219195,#219196),(#219197,#219198,#219199),
(#219200,#219201,#219202),(#219203,#219204,#219205),(#219206,#219207,#219208),
(#219209,#219210,#219211),(#219212,#219213,#219214),(#219215,#219216,#219217),
(#219218,#219219,#219220),(#219221,#219222,#219223),(#219224,#219225,#219226),
(#219227,#219228,#219229),(#219230,#219231,#219232),(#219233,#219234,#219235),
(#219236,#219237,#219238),(#219239,#219240,#219241),(#219242,#219243,#219244),
(#219245,#219246,#219247),(#219248,#219249,#219250),(#219251,#219252,#219253),
(#219254,#219255,#219256),(#219257,#219258,#219259),(#219260,#219261,#219262),
(#219263,#219264,#219265),(#219266,#219267,#219268),(#219269,#219270,#219271),
(#219272,#219273,#219274),(#219275,#219276,#219277),(#219278,#219279,#219280),
(#219281,#219282,#219283),(#219284,#219285,#219286),(#219287,#219288,#219289),
(#219290,#219291,#219292),(#219293,#219294,#219295),(#219296,#219297,#219298),
(#219299,#219300,#219301),(#219302,#219303,#219304),(#219305,#219306,#219307),
(#219308,#219309,#219310),(#219311,#219312,#219313),(#219314,#219315,#219316),
(#219317,#219318,#219319),(#219320,#219321,#219322),(#219323,#219324,#219325),
(#219326,#219327,#219328),(#219329,#219330,#219331),(#219332,#219333,#219334),
(#219335,#219336,#219337),(#219338,#219339,#219340),(#219341,#219342,#219343),
(#219344,#219345,#219346),(#219347,#219348,#219349),(#219350,#219351,#219352),
(#219353,#219354,#219355),(#219356,#219357,#219358),(#219359,#219360,#219361),
(#219362,#219363,#219364),(#219365,#219366,#219367),(#219368,#219369,#219370),
(#219371,#219372,#219373),(#219374,#219375,#219376),(#219377,#219378,#219379),
(#219380,#219381,#219382),(#219383,#219384,#219385),(#219386,#219387,#219388),
(#219389,#219390,#219391),(#219392,#219393,#219394),(#219395,#219396,#219397),
(#219398,#219399,#219400),(#219401,#219402,#219403),(#219404,#219405,#219406),
(#219407,#219408,#219409),(#219410,#219411,#219412),(#219413,#219414,#219415),
(#219416,#219417,#219418),(#219419,#219420,#219421),(#219422,#219423,#219424),
(#219425,#219426,#219427),(#219428,#219429,#219430),(#219431,#219432,#219433),
(#219434,#219435,#219436),(#219437,#219438,#219439),(#219440,#219441,#219442),
(#219443,#219444,#219445)),.UNSPECIFIED.,.F.,.F.,.F.)
B_SPLINE_SURFACE_WITH_KNOTS((4,2,2,2,2,2,2,2,2,2,2,2,2,2,2,2,2,2,2,2,2,
2,2,2,2,2,2,2,2,2,2,2,2,2,2,2,2,2,2,2,2,2,2,2,2,2,2,2,2,2,2,2,2,2,2,2,2,
2,2,2,2,2,4),(3,3),(-0.0208001925820885,-0.0186971148351636,-0.0165940370882388,
-0.0123878815943892,-0.0113363427209268,-0.0108105732841956,-0.0107448521046042,
-0.0106791309250128,-0.01054768856583,-0.0102848038474644,-0.00818172610053958,
-0.00397557060668997,-0.00292403173322756,-0.00279258937404477,-0.00272686819445337,
-0.00266114701486196,-0.00239826229649636,-0.00187249285976516,0.000230584887159648,
0.00443674038100926,0.00653981812793407,0.00759135700139648,0.00811712643812768,
0.00824856879731048,0.00831428997690188,0.00834715056669758,0.00838001115649328,
0.00864289587485888,0.0107459736217837,0.0117975124952461,0.0128490513687085,
0.0139005902421709,0.0149521291156333,0.0170552068625581,0.0181067457360205,
0.0181724669156119,0.0182053275054076,0.0182381880952033,0.0183696304543861,
0.0186325151727517,0.0191582846094829,0.0212613623564077,0.0254675178502573,
0.0275705955971822,0.0286221344706445,0.0291479039073758,0.0291807644971715,
0.0292136250869671,0.0292464856767628,0.0292793462665586,0.0294107886257414,
0.029673673344107,0.0338798288379566,0.0359829065848814,0.0365086760216126,
0.0367715607399782,0.036903003099161,0.0369687242787524,0.0370344454583438,
0.0380859843318062,0.0422921398256558,0.0443952175725807,0.0464982953195054),
(-0.000276885655367279,1.),.UNSPECIFIED.)
GEOMETRIC_REPRESENTATION_ITEM()
RATIONAL_B_SPLINE_SURFACE(((1.0000178221674,0.967816737606249,1.),(1.00001842741335,
0.966723784718768,1.),(1.00001902799113,0.965639261620645,1.),(1.00002019116422,
0.963538804148879,1.),(1.00002075669582,0.962517567422574,1.),(1.00002238403677,
0.959578915815827,1.),(1.00002337031455,0.957797895819759,1.),(1.00002455994145,
0.955649668060796,1.),(1.00002479580039,0.955223754076267,1.),(1.00002514701149,
0.954589537228534,1.),(1.00002526365088,0.954378909864324,1.),(1.00002539442655,
0.954142755210289,1.),(1.00002535993735,0.954205035799784,1.),(1.00002530498449,
0.954304269644752,1.),(1.00002527759341,0.95435373244978,1.),(1.00002519567715,
0.954501656806086,1.),(1.00002514140894,0.954599654306862,1.),(1.00002497963994,
0.954891776693891,1.),(1.00002487317471,0.955084031573329,1.),(1.00002392760603,
0.956791539099975,1.),(1.00002317337716,0.958153525278607,1.),(1.00002124289493,
0.961639589270802,1.),(1.00002040044771,0.963160880111278,1.),(1.00002005485079,
0.963784958886781,1.),(1.00002002036804,0.96384722781288,1.),(1.00002002020255,
0.96384752666274,1.),(1.00002002072063,0.963846591104061,1.),(1.00002002230128,
0.963843736761046,1.),(1.00002003224056,0.963825788430608,1.),(1.00002004614413,
0.963800681366758,1.),(1.0000200530961,0.963788127505428,1.),(1.00002008785585,
0.963725358348255,1.),(1.00002011566327,0.963675143731717,1.),(1.00002019904931,
0.963524565254967,1.),(1.00002025459039,0.963424269201259,1.),(1.00002053167059,
0.962923917881688,1.),(1.00002075111335,0.962527648246921,1.),(1.00002139578426,
0.961363501776867,1.),(1.00002180611404,0.960622528444111,1.),(1.00002240703783,
0.959537380513288,1.),(1.00002260586054,0.959178346540822,1.),(1.00002290466648,
0.958638762910466,1.),(1.00002300423325,0.958458965270393,1.),(1.00002315445808,
0.958187689342807,1.),(1.00002320468023,0.958096998204385,1.),(1.00002326775072,
0.957983105536474,1.),(1.00002328037942,0.957960300638801,1.),(1.00002329935517,
0.957926034231589,1.),(1.00002330568552,0.957914602889172,1.),(1.00002331518898,
0.957897441554315,1.),(1.00002331835812,0.957891718722412,1.),(1.00002332469909,
0.957880268198829,1.),(1.0000233342893,0.957862950189563,1.),(1.00002326570032,
0.957986808148111,1.),(1.00002320624477,0.958094172961626,1.),(1.00002268469492,
0.959035987448788,1.),(1.00002231597137,0.959701828289977,1.),(1.00002192048742,
0.960415993042883,1.),(1.00002181534814,0.960605853508497,1.),(1.00002165963563,
0.960887039090721,1.),(1.00002161074628,0.960975323464167,1.),(1.00002156885829,
0.961050964778899,1.),(1.00002157262121,0.961044169689148,1.),(1.00002163274295,
0.960935601880239,1.),(1.00002169236395,0.960827938305037,1.),(1.00002195462671,
0.960354344324168,1.),(1.00002223986213,0.959839266325176,1.),(1.00002282165689,
0.95878866158457,1.),(1.00002304014723,0.958394111825039,1.),(1.00002329817088,
0.957928172825059,1.),(1.00002331344442,0.957900591864297,1.),(1.00002333649845,
0.957858960912326,1.),(1.00002332375725,0.957881968962704,1.),(1.00002331736747,
0.957893507631862,1.),(1.00002331417392,0.957899274538583,1.),(1.00002329821279,
0.957928097152465,1.),(1.000023285465,0.957951117104651,1.),(1.0000232472804,
0.9580200708351,1.),(1.00002322190232,0.958065898550066,1.),(1.00002314596772,
0.958203021226092,1.),(1.00002309561029,0.958293956657091,1.),(1.00002284471333,
0.958747026277197,1.),(1.00002264663059,0.959104724004719,1.),(1.00002204771429,
0.960186246811101,1.),(1.00002164152455,0.960919744067784,1.),(1.00002099795675,
0.962081898526066,1.),(1.00002077788797,0.962479298636387,1.),(1.00002044118626,
0.963087314445631,1.),(1.00002032779168,0.963292082332173,1.),(1.00002015724606,
0.963600053539546,1.),(1.0000201003211,0.963702848610252,1.),(1.00002003985951,
0.963812030128801,1.),(1.00002003630303,0.963818452413985,1.),(1.0000200291903,
0.963831296571643,1.),(1.00002002404297,0.963840591621128,1.),(1.00002002011293,
0.963847688499234,1.),(1.00002002151763,0.963845151877356,1.),(1.0000200210696,
0.963845960940693,1.),(1.00002002088064,0.963846302169928,1.),(1.00002002011118,
0.963847691658443,1.),(1.00002002005674,0.963847789958493,1.),(1.0000200215801,
0.963845039083613,1.),(1.00002002484447,0.96383914428714,1.),(1.00002011873487,
0.963669597025071,1.),(1.00002080897953,0.962423153516154,1.),(1.00002261635824,
0.95915938980657,1.),(1.00002334790121,0.957838369809624,1.),(1.00002438902999,
0.955958299899251,1.),(1.00002460376163,0.955570537600982,1.),(1.00002493505981,
0.954972279475213,1.),(1.00002504702576,0.954770091421123,1.),(1.00002521723854,
0.954462721246432,1.),(1.00002527435347,0.954359583139847,1.),(1.00002536058752,
0.954203861714998,1.),(1.0000253934109,0.954144589270825,1.),(1.00002536300565,
0.954199495063233,1.),(1.00002534779637,0.954226959973017,1.),(1.0000250891242,
0.954694070074855,1.),(1.00002484395155,0.955136802747112,1.),(1.00002360770641,
0.95736921369098,1.),(1.00002258796812,0.959210656666961,1.),(1.00002090417295,
0.962251253288119,1.),(1.000020317103,0.963311383954806,1.),(1.00001908992458,
0.965527422225216,1.),(1.0000184437515,0.966694281295037,1.),(1.00001779951518,
0.967857642975733,1.)))
REPRESENTATION_ITEM('')
SURFACE()
);
#3105=(
BOUNDED_SURFACE()
B_SPLINE_SURFACE(3,2,((#220102,#220103,#220104),(#220105,#220106,#220107),
(#220108,#220109,#220110),(#220111,#220112,#220113)),.UNSPECIFIED.,.F.,
 .F.,.F.)
B_SPLINE_SURFACE_WITH_KNOTS((4,4),(3,3),(-0.000102945165535282,0.00102945165511775),
(0.,1.00456220410723),.UNSPECIFIED.)
GEOMETRIC_REPRESENTATION_ITEM()
RATIONAL_B_SPLINE_SURFACE(((1.,0.99790768871298,1.00001909110229),(1.,0.999220691897535,
1.00000711072525),(1.,1.00001166705636,0.999999893545015),(1.,1.,1.)))
REPRESENTATION_ITEM('')
SURFACE()
);
#3106=(
BOUNDED_SURFACE()
B_SPLINE_SURFACE(3,2,((#220117,#220118,#220119),(#220120,#220121,#220122),
(#220123,#220124,#220125),(#220126,#220127,#220128)),.UNSPECIFIED.,.F.,
 .F.,.F.)
B_SPLINE_SURFACE_WITH_KNOTS((4,4),(3,3),(0.0105620870905992,0.0106719618085628),
(0.,1.),.UNSPECIFIED.)
GEOMETRIC_REPRESENTATION_ITEM()
RATIONAL_B_SPLINE_SURFACE(((1.,0.997703261465161,1.),(1.,0.997980295466883,
1.),(1.,0.998184609657418,1.),(1.,0.998260562486346,1.)))
REPRESENTATION_ITEM('')
SURFACE()
);
#3107=(
BOUNDED_SURFACE()
B_SPLINE_SURFACE(3,2,((#220134,#220135,#220136),(#220137,#220138,#220139),
(#220140,#220141,#220142),(#220143,#220144,#220145)),.UNSPECIFIED.,.F.,
 .F.,.F.)
B_SPLINE_SURFACE_WITH_KNOTS((4,4),(3,3),(0.0270627267990834,0.0348275700538468),
(0.,1.),.UNSPECIFIED.)
GEOMETRIC_REPRESENTATION_ITEM()
RATIONAL_B_SPLINE_SURFACE(((1.,0.959662285900572,1.),(1.,0.959827071897818,
1.),(1.,0.959976275192295,1.),(1.,0.960109658705296,1.)))
REPRESENTATION_ITEM('')
SURFACE()
);
#3108=(
BOUNDED_SURFACE()
B_SPLINE_SURFACE(3,2,((#220151,#220152,#220153),(#220154,#220155,#220156),
(#220157,#220158,#220159),(#220160,#220161,#220162),(#220163,#220164,#220165),
(#220166,#220167,#220168),(#220169,#220170,#220171),(#220172,#220173,#220174),
(#220175,#220176,#220177),(#220178,#220179,#220180)),.UNSPECIFIED.,.F.,
 .F.,.F.)
B_SPLINE_SURFACE_WITH_KNOTS((4,2,2,2,4),(3,3),(-8.76035355368288E-17,0.000261575538067988,
0.000523151076136064,0.00078472661420414,0.00104630215227222),(0.,1.),
 .UNSPECIFIED.)
GEOMETRIC_REPRESENTATION_ITEM()
RATIONAL_B_SPLINE_SURFACE(((1.,0.941539462223513,1.),(1.,0.942944078103613,
1.),(1.,0.944666632267826,1.),(1.,0.947704870094144,1.),(1.,0.949116332566215,
1.),(1.,0.951938364158571,1.),(1.,0.953364849054759,1.),(1.,0.956562808918851,
1.),(1.,0.958303880697236,1.),(1.,0.959662285866025,1.)))
REPRESENTATION_ITEM('')
SURFACE()
);
#3109=(
BOUNDED_SURFACE()
B_SPLINE_SURFACE(3,2,((#220318,#220319,#220320),(#220321,#220322,#220323),
(#220324,#220325,#220326),(#220327,#220328,#220329),(#220330,#220331,#220332),
(#220333,#220334,#220335),(#220336,#220337,#220338),(#220339,#220340,#220341),
(#220342,#220343,#220344),(#220345,#220346,#220347),(#220348,#220349,#220350),
(#220351,#220352,#220353),(#220354,#220355,#220356),(#220357,#220358,#220359),
(#220360,#220361,#220362),(#220363,#220364,#220365),(#220366,#220367,#220368),
(#220369,#220370,#220371),(#220372,#220373,#220374),(#220375,#220376,#220377),
(#220378,#220379,#220380),(#220381,#220382,#220383),(#220384,#220385,#220386),
(#220387,#220388,#220389),(#220390,#220391,#220392),(#220393,#220394,#220395)),
 .UNSPECIFIED.,.F.,.F.,.F.)
B_SPLINE_SURFACE_WITH_KNOTS((4,2,2,2,2,2,2,2,2,2,2,2,4),(3,3),(0.0232773420264243,
0.0238865203213561,0.0243167159675304,0.0247469116137046,0.0251771072598788,
0.025392205082966,0.0256073029060531,0.0260374985522273,0.0262525963753145,
0.0264676941984016,0.0265752431099451,0.0266827920214887,0.0270768724933326),
(-0.000622430556160899,1.),.UNSPECIFIED.)
GEOMETRIC_REPRESENTATION_ITEM()
RATIONAL_B_SPLINE_SURFACE(((1.00007022535184,0.94358780176874,1.),(1.00007345968059,
0.940989657513307,1.),(1.00007557765372,0.939288284476128,1.),(1.00007953800459,
0.936106924857717,1.),(1.00008135577751,0.93464670339122,1.),(1.00008485035292,
0.931839502350726,1.),(1.00008646656058,0.930541198756514,1.),(1.00008926890465,
0.928290068854851,1.),(1.00009055175433,0.927259552546139,1.),(1.00009272454497,
0.925514144470467,1.),(1.00009354896659,0.924851884544549,1.),(1.00009510634629,
0.923600837597642,1.),(1.00009571013816,0.923115810099967,1.),(1.00009732578087,
0.92181796032787,1.),(1.00009808691593,0.921206538657284,1.),(1.00009969877668,
0.919911726943257,1.),(1.00010036529178,0.919376313722562,1.),(1.00010163596213,
0.918355581096937,1.),(1.00010219331079,0.917907861542757,1.),(1.00010248992835,
0.917669587924958,1.),(1.00010253345844,0.917634620099449,1.),(1.00010269113762,
0.917507956025272,1.),(1.00010277791566,0.917438247014893,1.),(1.00010317584749,
0.917118587394104,1.),(1.00010346600792,0.916885500804008,1.),(1.00010310505887,
0.917175452062668,1.)))
REPRESENTATION_ITEM('')
SURFACE()
);
#3110=(
BOUNDED_SURFACE()
B_SPLINE_SURFACE(3,2,((#220594,#220595,#220596),(#220597,#220598,#220599),
(#220600,#220601,#220602),(#220603,#220604,#220605)),.UNSPECIFIED.,.F.,
 .F.,.F.)
B_SPLINE_SURFACE_WITH_KNOTS((4,4),(3,3),(0.0245397910410617,0.0252336582652646),
(0.,1.),.UNSPECIFIED.)
GEOMETRIC_REPRESENTATION_ITEM()
RATIONAL_B_SPLINE_SURFACE(((1.,0.91828031569264,1.),(1.,0.918191277007669,
1.),(1.,0.917795655860158,1.),(1.,0.917108339181228,1.)))
REPRESENTATION_ITEM('')
SURFACE()
);
#3111=(
BOUNDED_SURFACE()
B_SPLINE_SURFACE(3,2,((#220620,#220621,#220622),(#220623,#220624,#220625),
(#220626,#220627,#220628),(#220629,#220630,#220631)),.UNSPECIFIED.,.F.,
 .F.,.F.)
B_SPLINE_SURFACE_WITH_KNOTS((4,4),(3,3),(0.0408577781618264,0.0446742483522374),
(0.,1.),.UNSPECIFIED.)
GEOMETRIC_REPRESENTATION_ITEM()
RATIONAL_B_SPLINE_SURFACE(((1.,0.918280315692642,1.),(1.,0.919146142525415,
1.),(1.,0.920060572994544,1.),(1.,0.920885718130539,1.)))
REPRESENTATION_ITEM('')
SURFACE()
);
#3112=(
BOUNDED_SURFACE()
B_SPLINE_SURFACE(3,2,((#220649,#220650,#220651),(#220652,#220653,#220654),
(#220655,#220656,#220657),(#220658,#220659,#220660),(#220661,#220662,#220663),
(#220664,#220665,#220666),(#220667,#220668,#220669),(#220670,#220671,#220672),
(#220673,#220674,#220675),(#220676,#220677,#220678),(#220679,#220680,#220681),
(#220682,#220683,#220684),(#220685,#220686,#220687),(#220688,#220689,#220690),
(#220691,#220692,#220693),(#220694,#220695,#220696),(#220697,#220698,#220699),
(#220700,#220701,#220702),(#220703,#220704,#220705),(#220706,#220707,#220708),
(#220709,#220710,#220711),(#220712,#220713,#220714),(#220715,#220716,#220717),
(#220718,#220719,#220720),(#220721,#220722,#220723),(#220724,#220725,#220726),
(#220727,#220728,#220729),(#220730,#220731,#220732),(#220733,#220734,#220735),
(#220736,#220737,#220738),(#220739,#220740,#220741),(#220742,#220743,#220744),
(#220745,#220746,#220747),(#220748,#220749,#220750),(#220751,#220752,#220753),
(#220754,#220755,#220756),(#220757,#220758,#220759),(#220760,#220761,#220762),
(#220763,#220764,#220765),(#220766,#220767,#220768),(#220769,#220770,#220771),
(#220772,#220773,#220774),(#220775,#220776,#220777),(#220778,#220779,#220780),
(#220781,#220782,#220783),(#220784,#220785,#220786),(#220787,#220788,#220789),
(#220790,#220791,#220792),(#220793,#220794,#220795),(#220796,#220797,#220798),
(#220799,#220800,#220801),(#220802,#220803,#220804),(#220805,#220806,#220807),
(#220808,#220809,#220810),(#220811,#220812,#220813),(#220814,#220815,#220816),
(#220817,#220818,#220819),(#220820,#220821,#220822),(#220823,#220824,#220825),
(#220826,#220827,#220828),(#220829,#220830,#220831),(#220832,#220833,#220834)),
 .UNSPECIFIED.,.F.,.F.,.F.)
B_SPLINE_SURFACE_WITH_KNOTS((4,2,2,2,2,2,2,2,2,2,2,2,2,2,2,2,2,2,2,2,2,
2,2,2,2,2,2,2,2,2,4),(3,3),(8.67361737988404E-19,0.00422017278643856,0.00435205318601475,
0.00438502328590881,0.00441799338580286,0.00448393358559096,0.00474769438474337,
0.00527521598304819,0.00633025917965783,0.00844034557287711,0.0126605183593157,
0.0137155615559253,0.0137815017557134,0.0138474419555015,0.0139793223550777,
0.0142430831542301,0.0147706047525349,0.0168806911457542,0.0211008639321928,
0.0221559071288024,0.0224196679279548,0.0224856081277429,0.0225185782276369,
0.022551548327531,0.0226834287271072,0.0232109503254121,0.0253210367186313,
0.0274311231118506,0.0284861663084603,0.0295412095050698,0.0337613822915084),
(0.,1.00028876552603),.UNSPECIFIED.)
GEOMETRIC_REPRESENTATION_ITEM()
RATIONAL_B_SPLINE_SURFACE(((1.,0.959354208545287,1.0000234742067),(1.,0.959337470736254,
1.0000234838733),(1.,0.958512445104999,1.00002396035123),(1.,0.95694732571469,
1.00002486425627),(1.,0.956899194384682,1.00002489205361),(1.,0.956838139436707,
1.00002492731474),(1.,0.956862400414095,1.00002491330327),(1.,0.956887484855878,
1.00002489881623),(1.,0.956899999499305,1.00002489158863),(1.,0.956937460592084,
1.00002486995369),(1.,0.956962324203891,1.00002485559418),(1.,0.957086088627733,
1.00002478411638),(1.,0.957183328458195,1.00002472795736),(1.,0.957469681464417,
1.00002456257961),(1.,0.957653426914545,1.0000244564609),(1.,0.958182822841225,
1.00002415071832),(1.,0.958506816204993,1.00002396360209),(1.,0.959387851983579,
1.00002345477657),(1.,0.959853733183088,1.00002318571571),(1.,0.960889943146176,
1.00002258727228),(1.,0.961106229913013,1.00002246235996),(1.,0.960689094558209,
1.00002270326858),(1.,0.960570529441095,1.00002277174361),(1.,0.960405498729637,
1.00002286705397),(1.,0.960395647596876,1.00002287274331),(1.,0.960375657763087,
1.00002288428806),(1.,0.960390364940156,1.00002287579421),(1.,0.960411396327207,
1.00002286364793),(1.,0.960424477373958,1.00002285609322),(1.,0.960460930383527,
1.00002283504047),(1.,0.960481512894489,1.00002282315343),(1.,0.960532312012284,
1.00002279381537),(1.,0.960551589312845,1.00002278268213),(1.,0.960577225424367,
1.00002276787648),(1.,0.960369658550149,1.00002288775279),(1.,0.959139560764285,
1.00002359817246),(1.,0.957494299277627,1.00002454836206),(1.,0.954680773867681,
1.00002617326035),(1.,0.954080291282266,1.00002652005769),(1.,0.953286564436122,
1.00002697845959),(1.,0.95312561937944,1.00002707141035),(1.,0.952921674070366,
1.0000271891951),(1.,0.952880746778416,1.00002721283189),(1.,0.952819148132629,
1.00002724840702),(1.,0.952798580632323,1.00002726028539),(1.,0.952757376329878,
1.00002728408215),(1.,0.952703868180498,1.00002731498477),(1.,0.952803106657217,
1.00002725767147),(1.,0.952882131942925,1.00002721203191),(1.,0.953275429419064,
1.0000269848904),(1.,0.953584216264606,1.00002680655641),(1.,0.955098740501949,
1.00002593187164),(1.,0.956216687617054,1.00002528622246),(1.,0.958254587609343,
1.00002410927194),(1.,0.959174978159034,1.00002357771781),(1.,0.960388157713114,
1.00002287706895),(1.,0.960764502584019,1.0000226597181),(1.,0.961455799248518,
1.00002226047281),(1.,0.961771684206244,1.00002207803944),(1.,0.963168690580858,
1.00002127122488),(1.,0.963699001724993,1.00002096495372),(1.,0.963430051350225,
1.00002112028092)))
REPRESENTATION_ITEM('')
SURFACE()
);
#3113=(
BOUNDED_SURFACE()
B_SPLINE_SURFACE(3,2,((#221269,#221270,#221271),(#221272,#221273,#221274),
(#221275,#221276,#221277),(#221278,#221279,#221280),(#221281,#221282,#221283),
(#221284,#221285,#221286)),.UNSPECIFIED.,.F.,.F.,.F.)
B_SPLINE_SURFACE_WITH_KNOTS((4,2,4),(3,3),(-3.10081821330854E-17,0.000547593654446629,
0.00109518730889329),(0.,1.),.UNSPECIFIED.)
GEOMETRIC_REPRESENTATION_ITEM()
RATIONAL_B_SPLINE_SURFACE(((1.,0.994860301689857,1.),(1.,0.996487472179808,
1.),(1.,0.997781945631374,1.),(1.,0.999546172218064,1.),(1.,1.00000726363599,
1.),(1.,1.,1.)))
REPRESENTATION_ITEM('')
SURFACE()
);
#3114=(
BOUNDED_SURFACE()
B_SPLINE_SURFACE(3,2,((#221317,#221318,#221319),(#221320,#221321,#221322),
(#221323,#221324,#221325),(#221326,#221327,#221328)),.UNSPECIFIED.,.F.,
 .F.,.F.)
B_SPLINE_SURFACE_WITH_KNOTS((4,4),(3,3),(0.0169795328233838,0.0259332885708231),
(0.,1.),.UNSPECIFIED.)
GEOMETRIC_REPRESENTATION_ITEM()
RATIONAL_B_SPLINE_SURFACE(((1.,0.957225253293536,1.),(1.,0.957330219064779,
1.),(1.,0.957420194105006,1.),(1.,0.95749691742527,1.)))
REPRESENTATION_ITEM('')
SURFACE()
);
#3115=(
BOUNDED_SURFACE()
B_SPLINE_SURFACE(3,2,((#221345,#221346,#221347),(#221348,#221349,#221350),
(#221351,#221352,#221353),(#221354,#221355,#221356)),.UNSPECIFIED.,.F.,
 .F.,.F.)
B_SPLINE_SURFACE_WITH_KNOTS((4,4),(3,3),(0.00708837036243835,0.00717746991701786),
(0.,1.),.UNSPECIFIED.)
GEOMETRIC_REPRESENTATION_ITEM()
RATIONAL_B_SPLINE_SURFACE(((1.,0.994244619571122,1.),(1.,0.99451521711556,
1.),(1.,0.994723691418652,1.),(1.,0.994860301689858,1.)))
REPRESENTATION_ITEM('')
SURFACE()
);
#3116=(
BOUNDED_SURFACE()
B_SPLINE_SURFACE(3,2,((#221366,#221367,#221368),(#221369,#221370,#221371),
(#221372,#221373,#221374),(#221375,#221376,#221377),(#221378,#221379,#221380),
(#221381,#221382,#221383),(#221384,#221385,#221386),(#221387,#221388,#221389),
(#221390,#221391,#221392),(#221393,#221394,#221395)),.UNSPECIFIED.,.F.,
 .F.,.F.)
B_SPLINE_SURFACE_WITH_KNOTS((4,2,2,2,4),(3,3),(-3.64042682515704E-5,0.000213802025234883,
0.000427604050469766,0.000641406075704648,0.000891612369191551),(-3.64042682525183E-5,
1.),.UNSPECIFIED.)
GEOMETRIC_REPRESENTATION_ITEM()
RATIONAL_B_SPLINE_SURFACE(((1.00000395581295,0.945668280974287,1.),(1.00000388505117,
0.946640169426575,1.),(1.00000379315429,0.947902341199865,1.),(1.00000364163364,
0.949983424830958,1.),(1.00000357606162,0.950884033719279,1.),(1.00000344606386,
0.95266950796714,1.),(1.00000338057312,0.953569000549728,1.),(1.00000323211214,
0.955608060593106,1.),(1.0000031500215,0.956735547071876,1.),(1.00000308511796,
0.957626974709355,1.)))
REPRESENTATION_ITEM('')
SURFACE()
);
#3117=(
BOUNDED_SURFACE()
B_SPLINE_SURFACE(3,2,((#221439,#221440,#221441),(#221442,#221443,#221444),
(#221445,#221446,#221447),(#221448,#221449,#221450),(#221451,#221452,#221453),
(#221454,#221455,#221456),(#221457,#221458,#221459),(#221460,#221461,#221462),
(#221463,#221464,#221465),(#221466,#221467,#221468),(#221469,#221470,#221471),
(#221472,#221473,#221474),(#221475,#221476,#221477),(#221478,#221479,#221480),
(#221481,#221482,#221483),(#221484,#221485,#221486),(#221487,#221488,#221489),
(#221490,#221491,#221492),(#221493,#221494,#221495),(#221496,#221497,#221498)),
 .UNSPECIFIED.,.F.,.F.,.F.)
B_SPLINE_SURFACE_WITH_KNOTS((4,2,2,2,2,2,2,2,2,4),(3,3),(0.0241832201811484,
0.0245055239061063,0.0248218005295632,0.02513807715302,0.0252962154647484,
0.0254543537764769,0.0257706303999337,0.0260869070233905,0.0264031836468474,
0.0267254873718053),(-6.02710150104311E-6,1.),.UNSPECIFIED.)
GEOMETRIC_REPRESENTATION_ITEM()
RATIONAL_B_SPLINE_SURFACE(((1.00000084427113,0.929960435071147,1.),(1.00000084156585,
0.930184862090941,1.),(1.00000083766746,0.930508267100976,1.),(1.00000083178679,
0.930996119039314,1.),(1.00000082192711,0.931814064338866,1.),(1.00000080692986,
0.933058215433481,1.),(1.00000080145663,0.933512266741312,1.),(1.00000079098237,
0.934381197300965,1.),(1.00000078716924,0.934697529544281,1.),(1.00000077788725,
0.935467549988599,1.),(1.00000077240012,0.935922755061344,1.),(1.00000075833733,
0.937089384822285,1.),(1.00000075011112,0.937771819638465,1.),(1.00000073260548,
0.939224063056665,1.),(1.00000072284102,0.940034109274095,1.),(1.00000070143123,
0.941810235649062,1.),(1.00000069002421,0.942756546224953,1.),(1.00000066943902,
0.944464265082494,1.),(1.00000066003637,0.945244295905894,1.),(1.00000064896667,
0.946162623330347,1.)))
REPRESENTATION_ITEM('')
SURFACE()
);
#3118=(
BOUNDED_SURFACE()
B_SPLINE_SURFACE(3,2,((#221813,#221814,#221815),(#221816,#221817,#221818),
(#221819,#221820,#221821),(#221822,#221823,#221824)),.UNSPECIFIED.,.F.,
 .F.,.F.)
B_SPLINE_SURFACE_WITH_KNOTS((4,4),(3,3),(0.0252170418335343,0.0258229913570787),
(0.,1.),.UNSPECIFIED.)
GEOMETRIC_REPRESENTATION_ITEM()
RATIONAL_B_SPLINE_SURFACE(((1.,0.930836001346604,1.),(1.,0.930792329315189,
1.),(1.,0.93050066650605,1.),(1.,0.929973550212784,1.)))
REPRESENTATION_ITEM('')
SURFACE()
);
#3119=(
BOUNDED_SURFACE()
B_SPLINE_SURFACE(3,2,((#221842,#221843,#221844),(#221845,#221846,#221847),
(#221848,#221849,#221850),(#221851,#221852,#221853)),.UNSPECIFIED.,.F.,
 .F.,.F.)
B_SPLINE_SURFACE_WITH_KNOTS((4,4),(3,3),(0.0413352581734094,0.0453130011481359),
(0.,1.),.UNSPECIFIED.)
GEOMETRIC_REPRESENTATION_ITEM()
RATIONAL_B_SPLINE_SURFACE(((1.,0.932166688794147,1.),(1.,0.931835585737477,
1.),(1.,0.931353352247319,1.),(1.,0.930836001346601,1.)))
REPRESENTATION_ITEM('')
SURFACE()
);
#3120=(
BOUNDED_SURFACE()
B_SPLINE_SURFACE(3,2,((#221886,#221887,#221888),(#221889,#221890,#221891),
(#221892,#221893,#221894),(#221895,#221896,#221897),(#221898,#221899,#221900),
(#221901,#221902,#221903)),.UNSPECIFIED.,.F.,.F.,.F.)
B_SPLINE_SURFACE_WITH_KNOTS((4,2,4),(3,3),(0.0166588946789198,0.0292596031542503,
0.0418603116295807),(0.,1.),.UNSPECIFIED.)
GEOMETRIC_REPRESENTATION_ITEM()
RATIONAL_B_SPLINE_SURFACE(((1.,0.997703261465172,1.),(1.,0.997094448547928,
1.),(1.,0.996295120040444,1.),(1.,0.994021377933446,1.),(1.,0.992546012713842,
1.),(1.,0.990544312570191,1.)))
REPRESENTATION_ITEM('')
SURFACE()
);
#3121=(
BOUNDED_SURFACE()
B_SPLINE_SURFACE(3,2,((#221942,#221943,#221944),(#221945,#221946,#221947),
(#221948,#221949,#221950),(#221951,#221952,#221953)),.UNSPECIFIED.,.F.,
 .F.,.F.)
B_SPLINE_SURFACE_WITH_KNOTS((4,4),(3,3),(0.0204076478587134,0.0466615476412126),
(0.,1.),.UNSPECIFIED.)
GEOMETRIC_REPRESENTATION_ITEM()
RATIONAL_B_SPLINE_SURFACE(((1.,0.990204100637796,1.),(1.,0.991176825451801,
1.),(1.,0.991726788386978,1.),(1.,0.99216019396246,1.)))
REPRESENTATION_ITEM('')
SURFACE()
);
#3122=(
BOUNDED_SURFACE()
B_SPLINE_SURFACE(3,2,((#222037,#222038,#222039),(#222040,#222041,#222042),
(#222043,#222044,#222045),(#222046,#222047,#222048)),.UNSPECIFIED.,.F.,
 .F.,.F.)
B_SPLINE_SURFACE_WITH_KNOTS((4,4),(3,3),(0.0511685324324545,0.0760142482873155),
(0.,1.),.UNSPECIFIED.)
GEOMETRIC_REPRESENTATION_ITEM()
RATIONAL_B_SPLINE_SURFACE(((1.,0.992981223849425,1.),(1.,0.992578629089082,
1.),(1.,0.992069952154663,1.),(1.,0.99114034013539,1.)))
REPRESENTATION_ITEM('')
SURFACE()
);
#3123=(
BOUNDED_SURFACE()
B_SPLINE_SURFACE(3,2,((#222119,#222120,#222121),(#222122,#222123,#222124),
(#222125,#222126,#222127),(#222128,#222129,#222130),(#222131,#222132,#222133),
(#222134,#222135,#222136)),.UNSPECIFIED.,.F.,.F.,.F.)
B_SPLINE_SURFACE_WITH_KNOTS((4,2,4),(3,3),(0.0166253761100813,0.0283648343214891,
0.0402199721685829),(-0.000115679635685861,1.),.UNSPECIFIED.)
GEOMETRIC_REPRESENTATION_ITEM()
RATIONAL_B_SPLINE_SURFACE(((1.00000115641936,0.995001629476687,1.),(1.00000110101721,
0.995241093190461,1.),(1.00000110174919,0.995237929375604,1.),(1.00000117166435,
0.994935736348517,1.),(1.00000124188212,0.994632235347241,1.),(1.00000133441707,
0.994232273186486,1.)))
REPRESENTATION_ITEM('')
SURFACE()
);
#3124=(
BOUNDED_SURFACE()
B_SPLINE_SURFACE(3,2,((#235472,#235473,#235474),(#235475,#235476,#235477),
(#235478,#235479,#235480),(#235481,#235482,#235483),(#235484,#235485,#235486),
(#235487,#235488,#235489),(#235490,#235491,#235492),(#235493,#235494,#235495),
(#235496,#235497,#235498),(#235499,#235500,#235501)),.UNSPECIFIED.,.F.,
 .F.,.F.)
B_SPLINE_SURFACE_WITH_KNOTS((4,2,2,2,4),(3,3),(4.71238898038469,5.10508806208341,
5.49778714378214,5.89048622548086,6.28318530717959),(0.,1.),
 .UNSPECIFIED.)
GEOMETRIC_REPRESENTATION_ITEM()
RATIONAL_B_SPLINE_SURFACE(((1.,0.707106781186554,1.),(1.,0.7340577581143,
1.),(1.,0.759389607022087,1.),(1.,0.804397146462884,1.),(1.,0.824065680681991,
1.),(1.,0.856126418973412,1.),(1.,0.868523258375879,1.),(1.,0.885147394261533,
1.),(1.,0.889385678509254,1.),(1.,0.889376480585547,1.)))
REPRESENTATION_ITEM('')
SURFACE()
);
#3125=(
BOUNDED_SURFACE()
B_SPLINE_SURFACE(3,2,((#235559,#235560,#235561),(#235562,#235563,#235564),
(#235565,#235566,#235567),(#235568,#235569,#235570),(#235571,#235572,#235573),
(#235574,#235575,#235576),(#235577,#235578,#235579),(#235580,#235581,#235582),
(#235583,#235584,#235585),(#235586,#235587,#235588)),.UNSPECIFIED.,.F.,
 .F.,.F.)
B_SPLINE_SURFACE_WITH_KNOTS((4,2,2,2,4),(3,3),(4.71238898038469,5.10508806208341,
5.49778714378214,5.89048622548086,6.28318530717959),(0.,1.),
 .UNSPECIFIED.)
GEOMETRIC_REPRESENTATION_ITEM()
RATIONAL_B_SPLINE_SURFACE(((1.,0.707106781186555,1.),(1.,0.7340577581143,
1.),(1.,0.759389607022087,1.),(1.,0.804397146462884,1.),(1.,0.82406568068196,
1.),(1.,0.856126418973443,1.),(1.,0.868523258375851,1.),(1.,0.885147394261561,
1.),(1.,0.889385678509233,1.),(1.,0.889376480585547,1.)))
REPRESENTATION_ITEM('')
SURFACE()
);
#3126=(
BOUNDED_SURFACE()
B_SPLINE_SURFACE(1,2,((#244439,#244440,#244441,#244442,#244443,#244444,
#244445,#244446,#244447,#244448,#244449,#244450,#244451,#244452,#244453,
#244454,#244455,#244456,#244457,#244458,#244459,#244460,#244461,#244462,
#244463,#244464,#244465,#244466,#244467,#244468,#244469,#244470,#244471,
#244472,#244473,#244474,#244475,#244476,#244477,#244478,#244479,#244480,
#244481,#244482,#244483,#244484,#244485,#244486,#244487,#244488,#244489,
#244490,#244491,#244492,#244493,#244494,#244495,#244496,#244497,#244498,
#244499,#244500,#244501,#244502,#244503,#244504,#244505,#244506,#244507,
#244508,#244509,#244510,#244511,#244512,#244513,#244514,#244515,#244516,
#244517,#244518,#244519,#244520,#244521,#244522,#244523,#244524,#244525,
#244526,#244527,#244528,#244529,#244530,#244531,#244532,#244533,#244534,
#244535,#244536,#244537,#244538,#244539,#244540,#244541,#244542,#244543,
#244544,#244545,#244546,#244547,#244548,#244549,#244550,#244551,#244552,
#244553,#244554,#244555,#244556,#244557,#244558,#244559,#244560,#244561,
#244562,#244563,#244564,#244565,#244566,#244567,#244568,#244569,#244570,
#244571,#244572,#244573,#244574,#244575,#244576,#244577,#244578,#244579,
#244580,#244581,#244582,#244583,#244584,#244585,#244586,#244587,#244588,
#244589,#244590,#244591,#244592,#244593,#244594,#244595,#244596,#244597,
#244598,#244599,#244600,#244601,#244602,#244603,#244604,#244605,#244606,
#244607,#244608,#244609,#244610,#244611,#244612,#244613,#244614,#244615,
#244616,#244617,#244618,#244619,#244620,#244621,#244622,#244623,#244624,
#244625,#244626,#244627,#244628,#244629,#244630,#244631,#244632,#244633,
#244634,#244635,#244636,#244637,#244638,#244639,#244640,#244641,#244642,
#244643,#244644,#244645,#244646,#244647,#244648,#244649,#244650,#244651,
#244652,#244653,#244654,#244655,#244656,#244657,#244658,#244659,#244660,
#244661,#244662,#244663,#244664,#244665,#244666,#244667,#244668,#244669,
#244670,#244671,#244672,#244673,#244674,#244675,#244676,#244677,#244678,
#244679,#244680,#244681,#244682,#244683,#244684,#244685,#244686,#244687,
#244688,#244689,#244690,#244691,#244692,#244693,#244694,#244695,#244696,
#244697,#244698,#244699,#244700,#244701,#244702,#244703,#244704,#244705,
#244706,#244707,#244708,#244709,#244710,#244711,#244712,#244713,#244714,
#244715),(#244716,#244717,#244718,#244719,#244720,#244721,#244722,#244723,
#244724,#244725,#244726,#244727,#244728,#244729,#244730,#244731,#244732,
#244733,#244734,#244735,#244736,#244737,#244738,#244739,#244740,#244741,
#244742,#244743,#244744,#244745,#244746,#244747,#244748,#244749,#244750,
#244751,#244752,#244753,#244754,#244755,#244756,#244757,#244758,#244759,
#244760,#244761,#244762,#244763,#244764,#244765,#244766,#244767,#244768,
#244769,#244770,#244771,#244772,#244773,#244774,#244775,#244776,#244777,
#244778,#244779,#244780,#244781,#244782,#244783,#244784,#244785,#244786,
#244787,#244788,#244789,#244790,#244791,#244792,#244793,#244794,#244795,
#244796,#244797,#244798,#244799,#244800,#244801,#244802,#244803,#244804,
#244805,#244806,#244807,#244808,#244809,#244810,#244811,#244812,#244813,
#244814,#244815,#244816,#244817,#244818,#244819,#244820,#244821,#244822,
#244823,#244824,#244825,#244826,#244827,#244828,#244829,#244830,#244831,
#244832,#244833,#244834,#244835,#244836,#244837,#244838,#244839,#244840,
#244841,#244842,#244843,#244844,#244845,#244846,#244847,#244848,#244849,
#244850,#244851,#244852,#244853,#244854,#244855,#244856,#244857,#244858,
#244859,#244860,#244861,#244862,#244863,#244864,#244865,#244866,#244867,
#244868,#244869,#244870,#244871,#244872,#244873,#244874,#244875,#244876,
#244877,#244878,#244879,#244880,#244881,#244882,#244883,#244884,#244885,
#244886,#244887,#244888,#244889,#244890,#244891,#244892,#244893,#244894,
#244895,#244896,#244897,#244898,#244899,#244900,#244901,#244902,#244903,
#244904,#244905,#244906,#244907,#244908,#244909,#244910,#244911,#244912,
#244913,#244914,#244915,#244916,#244917,#244918,#244919,#244920,#244921,
#244922,#244923,#244924,#244925,#244926,#244927,#244928,#244929,#244930,
#244931,#244932,#244933,#244934,#244935,#244936,#244937,#244938,#244939,
#244940,#244941,#244942,#244943,#244944,#244945,#244946,#244947,#244948,
#244949,#244950,#244951,#244952,#244953,#244954,#244955,#244956,#244957,
#244958,#244959,#244960,#244961,#244962,#244963,#244964,#244965,#244966,
#244967,#244968,#244969,#244970,#244971,#244972,#244973,#244974,#244975,
#244976,#244977,#244978,#244979,#244980,#244981,#244982,#244983,#244984,
#244985,#244986,#244987,#244988,#244989,#244990,#244991,#244992)),
 .UNSPECIFIED.,.F.,.F.,.F.)
B_SPLINE_SURFACE_WITH_KNOTS((2,2),(3,2,2,2,2,2,2,2,2,2,2,2,2,2,2,2,2,2,
2,2,2,2,2,2,2,2,2,2,2,2,2,2,2,2,2,2,2,2,2,2,2,2,2,2,2,2,2,2,2,2,2,2,2,2,
2,2,2,2,2,2,2,2,2,2,2,2,2,2,2,2,2,2,2,2,2,2,2,2,2,2,2,2,2,2,2,2,2,2,2,2,
2,2,2,2,2,2,2,2,2,2,2,2,2,2,2,2,2,2,2,2,2,2,2,2,2,2,2,2,2,2,2,2,2,2,2,2,
2,2,2,2,2,2,2,2,2,2,2,2,3),(0.,1.),(0.,0.0072463768115942,0.0144927536231884,
0.0217391304347826,0.0289855072463768,0.036231884057971,0.0434782608695652,
0.0507246376811594,0.0579710144927536,0.0652173913043478,0.072463768115942,
0.0797101449275362,0.0869565217391304,0.0942028985507246,0.101449275362319,
0.108695652173913,0.115942028985507,0.123188405797101,0.130434782608696,
0.13768115942029,0.144927536231884,0.152173913043478,0.159420289855073,
0.166666666666667,0.173913043478261,0.181159420289855,0.18840579710145,
0.195652173913044,0.202898550724637,0.210144927536232,0.217391304347826,
0.224637681159421,0.231884057971014,0.239130434782609,0.246376811594203,
0.253623188405797,0.260869565217392,0.268115942028985,0.275362318840579,
0.282608695652174,0.289855072463768,0.297101449275363,0.304347826086956,
0.31159420289855,0.318840579710145,0.326086956521739,0.333333333333334,
0.340579710144927,0.347826086956521,0.355072463768116,0.36231884057971,
0.369565217391304,0.376811594202899,0.384057971014493,0.391304347826087,
0.398550724637681,0.405797101449275,0.41304347826087,0.420289855072463,
0.427536231884058,0.434782608695652,0.442028985507247,0.449275362318841,
0.456521739130435,0.463768115942029,0.471014492753623,0.478260869565218,
0.485507246376812,0.492753623188406,0.5,0.507246376811594,0.514492753623188,
0.521739130434783,0.528985507246377,0.536231884057971,0.543478260869565,
0.550724637681159,0.557971014492754,0.565217391304348,0.572463768115942,
0.579710144927536,0.586956521739131,0.594202898550725,0.601449275362319,
0.608695652173913,0.615942028985507,0.623188405797101,0.630434782608696,
0.63768115942029,0.644927536231884,0.652173913043478,0.659420289855073,
0.666666666666667,0.673913043478261,0.681159420289855,0.688405797101449,
0.695652173913044,0.702898550724638,0.710144927536232,0.717391304347826,
0.72463768115942,0.731884057971015,0.739130434782609,0.746376811594203,
0.753623188405797,0.760869565217391,0.768115942028986,0.77536231884058,
0.782608695652174,0.789855072463768,0.797101449275362,0.804347826086956,
0.811594202898551,0.818840579710145,0.826086956521739,0.833333333333333,
0.840579710144928,0.847826086956522,0.855072463768116,0.86231884057971,
0.869565217391304,0.876811594202899,0.884057971014493,0.891304347826087,
0.898550724637681,0.905797101449275,0.91304347826087,0.920289855072464,
0.927536231884058,0.934782608695652,0.942028985507246,0.94927536231884,
0.956521739130435,0.963768115942029,0.971014492753623,0.978260869565217,
0.985507246376812,0.992753623188406,0.993818585798284),.UNSPECIFIED.)
GEOMETRIC_REPRESENTATION_ITEM()
RATIONAL_B_SPLINE_SURFACE(((1.,0.866025403784439,1.,0.866025403784439,1.,
0.866025403784439,1.,0.866025403784439,1.,0.866025403784439,1.,0.866025403784439,
1.,0.866025403784439,1.,0.866025403784439,1.,0.866025403784439,1.,0.866025403784439,
1.,0.866025403784439,1.,0.866025403784439,1.,0.866025403784439,1.,0.866025403784439,
1.,0.866025403784439,1.,0.866025403784439,1.,0.866025403784439,1.,0.866025403784439,
1.,0.866025403784439,1.,0.866025403784439,1.,0.866025403784439,1.,0.866025403784439,
1.,0.866025403784439,1.,0.866025403784439,1.,0.866025403784439,1.,0.866025403784439,
1.,0.866025403784439,1.,0.866025403784439,1.,0.866025403784439,1.,0.866025403784439,
1.,0.866025403784439,1.,0.866025403784439,1.,0.866025403784439,1.,0.866025403784439,
1.,0.866025403784439,1.,0.866025403784439,1.,0.866025403784439,1.,0.866025403784439,
1.,0.866025403784439,1.,0.866025403784439,1.,0.866025403784439,1.,0.866025403784439,
1.,0.866025403784439,1.,0.866025403784439,1.,0.866025403784439,1.,0.866025403784439,
1.,0.866025403784439,1.,0.866025403784439,1.,0.866025403784439,1.,0.866025403784439,
1.,0.866025403784439,1.,0.866025403784439,1.,0.866025403784439,1.,0.866025403784439,
1.,0.866025403784439,1.,0.866025403784439,1.,0.866025403784439,1.,0.866025403784439,
1.,0.866025403784439,1.,0.866025403784439,1.,0.866025403784439,1.,0.866025403784439,
1.,0.866025403784439,1.,0.866025403784439,1.,0.866025403784439,1.,0.866025403784439,
1.,0.866025403784439,1.,0.866025403784439,1.,0.866025403784439,1.,0.866025403784439,
1.,0.866025403784439,1.,0.866025403784439,1.,0.866025403784439,1.,0.866025403784439,
1.,0.866025403784439,1.,0.866025403784439,1.,0.866025403784439,1.,0.866025403784439,
1.,0.866025403784439,1.,0.866025403784439,1.,0.866025403784439,1.,0.866025403784439,
1.,0.866025403784439,1.,0.866025403784439,1.,0.866025403784439,1.,0.866025403784439,
1.,0.866025403784439,1.,0.866025403784439,1.,0.866025403784439,1.,0.866025403784439,
1.,0.866025403784439,1.,0.866025403784439,1.,0.866025403784439,1.,0.866025403784439,
1.,0.866025403784439,1.,0.866025403784439,1.,0.866025403784439,1.,0.866025403784439,
1.,0.866025403784439,1.,0.866025403784439,1.,0.866025403784439,1.,0.866025403784439,
1.,0.866025403784439,1.,0.866025403784439,1.,0.866025403784439,1.,0.866025403784439,
1.,0.866025403784439,1.,0.866025403784439,1.,0.866025403784439,1.,0.866025403784439,
1.,0.866025403784439,1.,0.866025403784439,1.,0.866025403784439,1.,0.866025403784439,
1.,0.866025403784439,1.,0.866025403784439,1.,0.866025403784439,1.,0.866025403784439,
1.,0.866025403784439,1.,0.866025403784439,1.,0.866025403784439,1.,0.866025403784439,
1.,0.866025403784439,1.,0.866025403784439,1.,0.866025403784439,1.,0.866025403784439,
1.,0.866025403784439,1.,0.866025403784439,1.,0.866025403784439,1.,0.866025403784439,
1.,0.866025403784439,1.,0.866025403784439,1.,0.866025403784439,1.,0.866025403784439,
1.,0.866025403784439,1.,0.866025403784439,1.,0.866025403784439,1.,0.98031044488126,
0.966408234404338),(1.,0.866025403784439,1.,0.866025403784439,1.,0.866025403784439,
1.,0.866025403784439,1.,0.866025403784439,1.,0.866025403784439,1.,0.866025403784439,
1.,0.866025403784439,1.,0.866025403784439,1.,0.866025403784439,1.,0.866025403784439,
1.,0.866025403784439,1.,0.866025403784439,1.,0.866025403784439,1.,0.866025403784439,
1.,0.866025403784439,1.,0.866025403784439,1.,0.866025403784439,1.,0.866025403784439,
1.,0.866025403784439,1.,0.866025403784439,1.,0.866025403784439,1.,0.866025403784439,
1.,0.866025403784439,1.,0.866025403784439,1.,0.866025403784439,1.,0.866025403784439,
1.,0.866025403784439,1.,0.866025403784439,1.,0.866025403784439,1.,0.866025403784439,
1.,0.866025403784439,1.,0.866025403784439,1.,0.866025403784439,1.,0.866025403784439,
1.,0.866025403784439,1.,0.866025403784439,1.,0.866025403784439,1.,0.866025403784439,
1.,0.866025403784439,1.,0.866025403784439,1.,0.866025403784439,1.,0.866025403784439,
1.,0.866025403784439,1.,0.866025403784439,1.,0.866025403784439,1.,0.866025403784439,
1.,0.866025403784439,1.,0.866025403784439,1.,0.866025403784439,1.,0.866025403784439,
1.,0.866025403784439,1.,0.866025403784439,1.,0.866025403784439,1.,0.866025403784439,
1.,0.866025403784439,1.,0.866025403784439,1.,0.866025403784439,1.,0.866025403784439,
1.,0.866025403784439,1.,0.866025403784439,1.,0.866025403784439,1.,0.866025403784439,
1.,0.866025403784439,1.,0.866025403784439,1.,0.866025403784439,1.,0.866025403784439,
1.,0.866025403784439,1.,0.866025403784439,1.,0.866025403784439,1.,0.866025403784439,
1.,0.866025403784439,1.,0.866025403784439,1.,0.866025403784439,1.,0.866025403784439,
1.,0.866025403784439,1.,0.866025403784439,1.,0.866025403784439,1.,0.866025403784439,
1.,0.866025403784439,1.,0.866025403784439,1.,0.866025403784439,1.,0.866025403784439,
1.,0.866025403784439,1.,0.866025403784439,1.,0.866025403784439,1.,0.866025403784439,
1.,0.866025403784439,1.,0.866025403784439,1.,0.866025403784439,1.,0.866025403784439,
1.,0.866025403784439,1.,0.866025403784439,1.,0.866025403784439,1.,0.866025403784439,
1.,0.866025403784439,1.,0.866025403784439,1.,0.866025403784439,1.,0.866025403784439,
1.,0.866025403784439,1.,0.866025403784439,1.,0.866025403784439,1.,0.866025403784439,
1.,0.866025403784439,1.,0.866025403784439,1.,0.866025403784439,1.,0.866025403784439,
1.,0.866025403784439,1.,0.866025403784439,1.,0.866025403784439,1.,0.866025403784439,
1.,0.866025403784439,1.,0.866025403784439,1.,0.866025403784439,1.,0.866025403784439,
1.,0.866025403784439,1.,0.866025403784439,1.,0.866025403784439,1.,0.866025403784439,
1.,0.866025403784439,1.,0.866025403784439,1.,0.866025403784439,1.,0.866025403784439,
1.,0.866025403784439,1.,0.866025403784439,1.,0.866025403784439,1.,0.866025403784439,
1.,0.866025403784439,1.,0.866025403784439,1.,0.866025403784439,1.,0.866025403784439,
1.,0.866025403784439,1.,0.866025403784439,1.,0.866025403784439,1.,0.866025403784439,
1.,0.866025403784439,1.,0.866025403784439,1.,0.98031044488126,0.966408234404338)))
REPRESENTATION_ITEM('')
SURFACE()
);
#3127=(
BOUNDED_SURFACE()
B_SPLINE_SURFACE(1,2,((#245436,#245437,#245438,#245439,#245440,#245441,
#245442,#245443,#245444,#245445,#245446,#245447,#245448,#245449,#245450,
#245451,#245452,#245453,#245454,#245455,#245456,#245457,#245458,#245459,
#245460,#245461,#245462,#245463,#245464,#245465,#245466,#245467,#245468,
#245469,#245470,#245471,#245472,#245473,#245474,#245475,#245476,#245477,
#245478,#245479,#245480,#245481,#245482,#245483,#245484,#245485,#245486,
#245487,#245488,#245489,#245490,#245491,#245492,#245493,#245494,#245495,
#245496,#245497,#245498,#245499,#245500,#245501,#245502,#245503,#245504,
#245505,#245506,#245507,#245508,#245509,#245510,#245511,#245512,#245513,
#245514,#245515,#245516,#245517,#245518,#245519,#245520,#245521,#245522,
#245523,#245524,#245525,#245526,#245527,#245528,#245529,#245530,#245531,
#245532,#245533,#245534,#245535,#245536,#245537,#245538,#245539,#245540,
#245541,#245542,#245543,#245544,#245545,#245546,#245547,#245548,#245549,
#245550,#245551,#245552,#245553,#245554,#245555,#245556,#245557,#245558,
#245559,#245560,#245561,#245562,#245563,#245564,#245565,#245566,#245567,
#245568,#245569,#245570,#245571,#245572,#245573,#245574,#245575,#245576,
#245577,#245578,#245579,#245580,#245581,#245582,#245583,#245584,#245585,
#245586,#245587,#245588,#245589,#245590,#245591,#245592,#245593,#245594,
#245595,#245596,#245597,#245598,#245599,#245600,#245601,#245602,#245603,
#245604,#245605,#245606,#245607,#245608,#245609,#245610,#245611,#245612,
#245613,#245614,#245615,#245616,#245617,#245618,#245619,#245620,#245621,
#245622,#245623,#245624,#245625,#245626,#245627,#245628,#245629,#245630,
#245631,#245632,#245633,#245634,#245635,#245636,#245637,#245638,#245639,
#245640,#245641,#245642,#245643,#245644,#245645,#245646,#245647,#245648,
#245649,#245650,#245651,#245652,#245653,#245654,#245655,#245656,#245657,
#245658,#245659,#245660,#245661,#245662,#245663,#245664,#245665,#245666,
#245667,#245668,#245669,#245670,#245671,#245672,#245673,#245674,#245675,
#245676,#245677,#245678,#245679,#245680,#245681,#245682,#245683,#245684,
#245685,#245686,#245687,#245688,#245689,#245690,#245691,#245692,#245693,
#245694,#245695,#245696,#245697,#245698,#245699,#245700,#245701,#245702,
#245703,#245704,#245705,#245706,#245707,#245708,#245709,#245710,#245711,
#245712),(#245713,#245714,#245715,#245716,#245717,#245718,#245719,#245720,
#245721,#245722,#245723,#245724,#245725,#245726,#245727,#245728,#245729,
#245730,#245731,#245732,#245733,#245734,#245735,#245736,#245737,#245738,
#245739,#245740,#245741,#245742,#245743,#245744,#245745,#245746,#245747,
#245748,#245749,#245750,#245751,#245752,#245753,#245754,#245755,#245756,
#245757,#245758,#245759,#245760,#245761,#245762,#245763,#245764,#245765,
#245766,#245767,#245768,#245769,#245770,#245771,#245772,#245773,#245774,
#245775,#245776,#245777,#245778,#245779,#245780,#245781,#245782,#245783,
#245784,#245785,#245786,#245787,#245788,#245789,#245790,#245791,#245792,
#245793,#245794,#245795,#245796,#245797,#245798,#245799,#245800,#245801,
#245802,#245803,#245804,#245805,#245806,#245807,#245808,#245809,#245810,
#245811,#245812,#245813,#245814,#245815,#245816,#245817,#245818,#245819,
#245820,#245821,#245822,#245823,#245824,#245825,#245826,#245827,#245828,
#245829,#245830,#245831,#245832,#245833,#245834,#245835,#245836,#245837,
#245838,#245839,#245840,#245841,#245842,#245843,#245844,#245845,#245846,
#245847,#245848,#245849,#245850,#245851,#245852,#245853,#245854,#245855,
#245856,#245857,#245858,#245859,#245860,#245861,#245862,#245863,#245864,
#245865,#245866,#245867,#245868,#245869,#245870,#245871,#245872,#245873,
#245874,#245875,#245876,#245877,#245878,#245879,#245880,#245881,#245882,
#245883,#245884,#245885,#245886,#245887,#245888,#245889,#245890,#245891,
#245892,#245893,#245894,#245895,#245896,#245897,#245898,#245899,#245900,
#245901,#245902,#245903,#245904,#245905,#245906,#245907,#245908,#245909,
#245910,#245911,#245912,#245913,#245914,#245915,#245916,#245917,#245918,
#245919,#245920,#245921,#245922,#245923,#245924,#245925,#245926,#245927,
#245928,#245929,#245930,#245931,#245932,#245933,#245934,#245935,#245936,
#245937,#245938,#245939,#245940,#245941,#245942,#245943,#245944,#245945,
#245946,#245947,#245948,#245949,#245950,#245951,#245952,#245953,#245954,
#245955,#245956,#245957,#245958,#245959,#245960,#245961,#245962,#245963,
#245964,#245965,#245966,#245967,#245968,#245969,#245970,#245971,#245972,
#245973,#245974,#245975,#245976,#245977,#245978,#245979,#245980,#245981,
#245982,#245983,#245984,#245985,#245986,#245987,#245988,#245989)),
 .UNSPECIFIED.,.F.,.F.,.F.)
B_SPLINE_SURFACE_WITH_KNOTS((2,2),(3,2,2,2,2,2,2,2,2,2,2,2,2,2,2,2,2,2,
2,2,2,2,2,2,2,2,2,2,2,2,2,2,2,2,2,2,2,2,2,2,2,2,2,2,2,2,2,2,2,2,2,2,2,2,
2,2,2,2,2,2,2,2,2,2,2,2,2,2,2,2,2,2,2,2,2,2,2,2,2,2,2,2,2,2,2,2,2,2,2,2,
2,2,2,2,2,2,2,2,2,2,2,2,2,2,2,2,2,2,2,2,2,2,2,2,2,2,2,2,2,2,2,2,2,2,2,2,
2,2,2,2,2,2,2,2,2,2,2,2,3),(0.,1.),(0.,0.0072463768115942,0.0144927536231884,
0.0217391304347826,0.0289855072463768,0.036231884057971,0.0434782608695652,
0.0507246376811594,0.0579710144927536,0.0652173913043478,0.072463768115942,
0.0797101449275362,0.0869565217391304,0.0942028985507246,0.101449275362319,
0.108695652173913,0.115942028985507,0.123188405797101,0.130434782608696,
0.13768115942029,0.144927536231884,0.152173913043478,0.159420289855073,
0.166666666666667,0.173913043478261,0.181159420289855,0.18840579710145,
0.195652173913044,0.202898550724637,0.210144927536232,0.217391304347826,
0.224637681159421,0.231884057971014,0.239130434782609,0.246376811594203,
0.253623188405797,0.260869565217392,0.268115942028985,0.275362318840579,
0.282608695652174,0.289855072463768,0.297101449275363,0.304347826086956,
0.31159420289855,0.318840579710145,0.326086956521739,0.333333333333334,
0.340579710144927,0.347826086956521,0.355072463768116,0.36231884057971,
0.369565217391304,0.376811594202899,0.384057971014493,0.391304347826087,
0.398550724637681,0.405797101449275,0.41304347826087,0.420289855072463,
0.427536231884058,0.434782608695652,0.442028985507247,0.449275362318841,
0.456521739130435,0.463768115942029,0.471014492753623,0.478260869565218,
0.485507246376812,0.492753623188406,0.5,0.507246376811594,0.514492753623188,
0.521739130434783,0.528985507246377,0.536231884057971,0.543478260869565,
0.550724637681159,0.557971014492754,0.565217391304348,0.572463768115942,
0.579710144927536,0.586956521739131,0.594202898550725,0.601449275362319,
0.608695652173913,0.615942028985507,0.623188405797101,0.630434782608696,
0.63768115942029,0.644927536231884,0.652173913043478,0.659420289855073,
0.666666666666667,0.673913043478261,0.681159420289855,0.688405797101449,
0.695652173913044,0.702898550724638,0.710144927536232,0.717391304347826,
0.72463768115942,0.731884057971015,0.739130434782609,0.746376811594203,
0.753623188405797,0.760869565217391,0.768115942028986,0.77536231884058,
0.782608695652174,0.789855072463768,0.797101449275362,0.804347826086956,
0.811594202898551,0.818840579710145,0.826086956521739,0.833333333333333,
0.840579710144928,0.847826086956522,0.855072463768116,0.86231884057971,
0.869565217391304,0.876811594202899,0.884057971014493,0.891304347826087,
0.898550724637681,0.905797101449275,0.91304347826087,0.920289855072464,
0.927536231884058,0.934782608695652,0.942028985507246,0.94927536231884,
0.956521739130435,0.963768115942029,0.971014492753623,0.978260869565217,
0.985507246376812,0.992753623188406,0.993818585798284),.UNSPECIFIED.)
GEOMETRIC_REPRESENTATION_ITEM()
RATIONAL_B_SPLINE_SURFACE(((1.,0.866025403784439,1.,0.866025403784439,1.,
0.866025403784439,1.,0.866025403784439,1.,0.866025403784439,1.,0.866025403784439,
1.,0.866025403784439,1.,0.866025403784439,1.,0.866025403784439,1.,0.866025403784439,
1.,0.866025403784439,1.,0.866025403784439,1.,0.866025403784439,1.,0.866025403784439,
1.,0.866025403784439,1.,0.866025403784439,1.,0.866025403784439,1.,0.866025403784439,
1.,0.866025403784439,1.,0.866025403784439,1.,0.866025403784439,1.,0.866025403784439,
1.,0.866025403784439,1.,0.866025403784439,1.,0.866025403784439,1.,0.866025403784439,
1.,0.866025403784439,1.,0.866025403784439,1.,0.866025403784439,1.,0.866025403784439,
1.,0.866025403784439,1.,0.866025403784439,1.,0.866025403784439,1.,0.866025403784439,
1.,0.866025403784439,1.,0.866025403784439,1.,0.866025403784439,1.,0.866025403784439,
1.,0.866025403784439,1.,0.866025403784439,1.,0.866025403784439,1.,0.866025403784439,
1.,0.866025403784439,1.,0.866025403784439,1.,0.866025403784439,1.,0.866025403784439,
1.,0.866025403784439,1.,0.866025403784439,1.,0.866025403784439,1.,0.866025403784439,
1.,0.866025403784439,1.,0.866025403784439,1.,0.866025403784439,1.,0.866025403784439,
1.,0.866025403784439,1.,0.866025403784439,1.,0.866025403784439,1.,0.866025403784439,
1.,0.866025403784439,1.,0.866025403784439,1.,0.866025403784439,1.,0.866025403784439,
1.,0.866025403784439,1.,0.866025403784439,1.,0.866025403784439,1.,0.866025403784439,
1.,0.866025403784439,1.,0.866025403784439,1.,0.866025403784439,1.,0.866025403784439,
1.,0.866025403784439,1.,0.866025403784439,1.,0.866025403784439,1.,0.866025403784439,
1.,0.866025403784439,1.,0.866025403784439,1.,0.866025403784439,1.,0.866025403784439,
1.,0.866025403784439,1.,0.866025403784439,1.,0.866025403784439,1.,0.866025403784439,
1.,0.866025403784439,1.,0.866025403784439,1.,0.866025403784439,1.,0.866025403784439,
1.,0.866025403784439,1.,0.866025403784439,1.,0.866025403784439,1.,0.866025403784439,
1.,0.866025403784439,1.,0.866025403784439,1.,0.866025403784439,1.,0.866025403784439,
1.,0.866025403784439,1.,0.866025403784439,1.,0.866025403784439,1.,0.866025403784439,
1.,0.866025403784439,1.,0.866025403784439,1.,0.866025403784439,1.,0.866025403784439,
1.,0.866025403784439,1.,0.866025403784439,1.,0.866025403784439,1.,0.866025403784439,
1.,0.866025403784439,1.,0.866025403784439,1.,0.866025403784439,1.,0.866025403784439,
1.,0.866025403784439,1.,0.866025403784439,1.,0.866025403784439,1.,0.866025403784439,
1.,0.866025403784439,1.,0.866025403784439,1.,0.866025403784439,1.,0.866025403784439,
1.,0.866025403784439,1.,0.866025403784439,1.,0.866025403784439,1.,0.866025403784439,
1.,0.866025403784439,1.,0.866025403784439,1.,0.866025403784439,1.,0.866025403784439,
1.,0.866025403784439,1.,0.866025403784439,1.,0.866025403784439,1.,0.866025403784439,
1.,0.866025403784439,1.,0.866025403784439,1.,0.866025403784439,1.,0.866025403784439,
1.,0.866025403784439,1.,0.866025403784439,1.,0.866025403784439,1.,0.98031044488126,
0.966408234404338),(1.,0.866025403784439,1.,0.866025403784439,1.,0.866025403784439,
1.,0.866025403784439,1.,0.866025403784439,1.,0.866025403784439,1.,0.866025403784439,
1.,0.866025403784439,1.,0.866025403784439,1.,0.866025403784439,1.,0.866025403784439,
1.,0.866025403784439,1.,0.866025403784439,1.,0.866025403784439,1.,0.866025403784439,
1.,0.866025403784439,1.,0.866025403784439,1.,0.866025403784439,1.,0.866025403784439,
1.,0.866025403784439,1.,0.866025403784439,1.,0.866025403784439,1.,0.866025403784439,
1.,0.866025403784439,1.,0.866025403784439,1.,0.866025403784439,1.,0.866025403784439,
1.,0.866025403784439,1.,0.866025403784439,1.,0.866025403784439,1.,0.866025403784439,
1.,0.866025403784439,1.,0.866025403784439,1.,0.866025403784439,1.,0.866025403784439,
1.,0.866025403784439,1.,0.866025403784439,1.,0.866025403784439,1.,0.866025403784439,
1.,0.866025403784439,1.,0.866025403784439,1.,0.866025403784439,1.,0.866025403784439,
1.,0.866025403784439,1.,0.866025403784439,1.,0.866025403784439,1.,0.866025403784439,
1.,0.866025403784439,1.,0.866025403784439,1.,0.866025403784439,1.,0.866025403784439,
1.,0.866025403784439,1.,0.866025403784439,1.,0.866025403784439,1.,0.866025403784439,
1.,0.866025403784439,1.,0.866025403784439,1.,0.866025403784439,1.,0.866025403784439,
1.,0.866025403784439,1.,0.866025403784439,1.,0.866025403784439,1.,0.866025403784439,
1.,0.866025403784439,1.,0.866025403784439,1.,0.866025403784439,1.,0.866025403784439,
1.,0.866025403784439,1.,0.866025403784439,1.,0.866025403784439,1.,0.866025403784439,
1.,0.866025403784439,1.,0.866025403784439,1.,0.866025403784439,1.,0.866025403784439,
1.,0.866025403784439,1.,0.866025403784439,1.,0.866025403784439,1.,0.866025403784439,
1.,0.866025403784439,1.,0.866025403784439,1.,0.866025403784439,1.,0.866025403784439,
1.,0.866025403784439,1.,0.866025403784439,1.,0.866025403784439,1.,0.866025403784439,
1.,0.866025403784439,1.,0.866025403784439,1.,0.866025403784439,1.,0.866025403784439,
1.,0.866025403784439,1.,0.866025403784439,1.,0.866025403784439,1.,0.866025403784439,
1.,0.866025403784439,1.,0.866025403784439,1.,0.866025403784439,1.,0.866025403784439,
1.,0.866025403784439,1.,0.866025403784439,1.,0.866025403784439,1.,0.866025403784439,
1.,0.866025403784439,1.,0.866025403784439,1.,0.866025403784439,1.,0.866025403784439,
1.,0.866025403784439,1.,0.866025403784439,1.,0.866025403784439,1.,0.866025403784439,
1.,0.866025403784439,1.,0.866025403784439,1.,0.866025403784439,1.,0.866025403784439,
1.,0.866025403784439,1.,0.866025403784439,1.,0.866025403784439,1.,0.866025403784439,
1.,0.866025403784439,1.,0.866025403784439,1.,0.866025403784439,1.,0.866025403784439,
1.,0.866025403784439,1.,0.866025403784439,1.,0.866025403784439,1.,0.866025403784439,
1.,0.866025403784439,1.,0.866025403784439,1.,0.866025403784439,1.,0.866025403784439,
1.,0.866025403784439,1.,0.866025403784439,1.,0.866025403784439,1.,0.866025403784439,
1.,0.866025403784439,1.,0.866025403784439,1.,0.98031044488126,0.966408234404338)))
REPRESENTATION_ITEM('')
SURFACE()
);
#3128=(
BOUNDED_SURFACE()
B_SPLINE_SURFACE(3,2,((#246021,#246022,#246023),(#246024,#246025,#246026),
(#246027,#246028,#246029),(#246030,#246031,#246032)),.UNSPECIFIED.,.F.,
 .F.,.F.)
B_SPLINE_SURFACE_WITH_KNOTS((4,4),(3,3),(0.,0.000928457009668218),(0.,0.749952265697638),
 .UNSPECIFIED.)
GEOMETRIC_REPRESENTATION_ITEM()
RATIONAL_B_SPLINE_SURFACE(((1.,0.97561107945597,0.98780321135177),(1.,0.97592437041105,
0.98795988673876),(1.,0.97623752029395,0.988116491576193),(1.,0.97655053044864,
0.988273026536181)))
REPRESENTATION_ITEM('')
SURFACE()
);
#3129=(
BOUNDED_SURFACE()
B_SPLINE_SURFACE(3,2,((#246039,#246040,#246041),(#246042,#246043,#246044),
(#246045,#246046,#246047),(#246048,#246049,#246050),(#246051,#246052,#246053),
(#246054,#246055,#246056),(#246057,#246058,#246059),(#246060,#246061,#246062),
(#246063,#246064,#246065),(#246066,#246067,#246068),(#246069,#246070,#246071),
(#246072,#246073,#246074),(#246075,#246076,#246077),(#246078,#246079,#246080)),
 .UNSPECIFIED.,.F.,.F.,.F.)
B_SPLINE_SURFACE_WITH_KNOTS((4,2,2,2,2,2,4),(3,3),(0.012210545256649,0.012913253531591,
0.0134151880136936,0.0136661552547448,0.0139171224957961,0.0141680897368473,
0.0144191053734446),(-0.00118607011455501,1.00106010974999),
 .UNSPECIFIED.)
GEOMETRIC_REPRESENTATION_ITEM()
RATIONAL_B_SPLINE_SURFACE(((1.00042223753196,0.821812523909012,1.00037734852569),
(1.00036561497319,0.845707677874531,1.00032674563643),(1.00031052998004,
0.868953967361828,1.00027751685078),(1.00022051976633,0.906938967721429,
1.00019707582205),(1.00018420004347,0.922266169259384,1.00016461732929),
(1.0001333136267,0.943740627317328,1.00011914076008),(1.00011734829418,
0.950478120060816,1.00010487273738),(1.00008857958998,0.962618733823534,
1.00007916249778),(1.00007587856666,0.967978663051886,1.00006781174835),
(1.00005828162361,0.975404707950268,1.00005208557525),(1.00005406471308,
0.977184276526349,1.00004831697381),(1.00005807698422,0.975491067339927,
1.00005190269153),(1.00006613372506,0.972091060928923,1.00005910290242),
(1.00007724141785,0.96740352939868,1.00006902971182)))
REPRESENTATION_ITEM('')
SURFACE()
);
#3130=(
BOUNDED_SURFACE()
B_SPLINE_SURFACE(3,2,((#246236,#246237,#246238),(#246239,#246240,#246241),
(#246242,#246243,#246244),(#246245,#246246,#246247)),.UNSPECIFIED.,.F.,
 .F.,.F.)
B_SPLINE_SURFACE_WITH_KNOTS((4,4),(3,3),(2.58410722075169,2.75084833243122),
(0.,1.),.UNSPECIFIED.)
GEOMETRIC_REPRESENTATION_ITEM()
RATIONAL_B_SPLINE_SURFACE(((1.,0.832178067339829,1.),(1.,0.836186490185363,
1.),(1.,0.83962897728861,1.),(1.,0.84247914424116,1.)))
REPRESENTATION_ITEM('')
SURFACE()
);
#3131=(
BOUNDED_SURFACE()
B_SPLINE_SURFACE(3,2,((#246253,#246254,#246255),(#246256,#246257,#246258),
(#246259,#246260,#246261),(#246262,#246263,#246264)),.UNSPECIFIED.,.F.,
 .F.,.F.)
B_SPLINE_SURFACE_WITH_KNOTS((4,4),(3,3),(0.,0.00132498435822727),(0.,1.),
 .UNSPECIFIED.)
GEOMETRIC_REPRESENTATION_ITEM()
RATIONAL_B_SPLINE_SURFACE(((1.,0.832178067339829,1.),(1.,0.82686356673151,
1.),(1.,0.821151298721319,1.),(1.,0.815289268529491,1.)))
REPRESENTATION_ITEM('')
SURFACE()
);
#3132=(
BOUNDED_SURFACE()
B_SPLINE_SURFACE(3,2,((#246297,#246298,#246299),(#246300,#246301,#246302),
(#246303,#246304,#246305),(#246306,#246307,#246308),(#246309,#246310,#246311),
(#246312,#246313,#246314),(#246315,#246316,#246317),(#246318,#246319,#246320),
(#246321,#246322,#246323),(#246324,#246325,#246326)),.UNSPECIFIED.,.F.,
 .F.,.F.)
B_SPLINE_SURFACE_WITH_KNOTS((4,2,2,2,4),(3,3),(-3.38271077815477E-17,0.0053077668156845,
0.00663470851960563,0.00796165022352677,0.010615533631369),(0.,1.),
 .UNSPECIFIED.)
GEOMETRIC_REPRESENTATION_ITEM()
RATIONAL_B_SPLINE_SURFACE(((1.,0.815289268529492,1.),(1.,0.819667585266128,
1.),(1.,0.820338423873395,1.),(1.,0.816466016787285,1.),(1.,0.815452764187778,
1.),(1.,0.812995487572161,1.),(1.,0.81154866816968,1.),(1.,0.806583085327115,
1.),(1.,0.802440012727956,1.),(1.,0.797521159322293,1.)))
REPRESENTATION_ITEM('')
SURFACE()
);
#3133=(
BOUNDED_SURFACE()
B_SPLINE_SURFACE(3,2,((#246443,#246444,#246445),(#246446,#246447,#246448),
(#246449,#246450,#246451),(#246452,#246453,#246454),(#246455,#246456,#246457),
(#246458,#246459,#246460)),.UNSPECIFIED.,.F.,.F.,.F.)
B_SPLINE_SURFACE_WITH_KNOTS((4,2,4),(3,3),(0.00808931143172237,0.0087165405671442,
0.00934376970256604),(0.,1.),.UNSPECIFIED.)
GEOMETRIC_REPRESENTATION_ITEM()
RATIONAL_B_SPLINE_SURFACE(((1.,0.797521159322292,1.),(1.,0.820509064499797,
1.),(1.,0.842744492243191,1.),(1.,0.885608693575932,1.),(1.,0.906523136189702,
1.),(1.,0.925255145240244,1.)))
REPRESENTATION_ITEM('')
SURFACE()
);
#3134=(
BOUNDED_SURFACE()
B_SPLINE_SURFACE(3,2,((#246523,#246524,#246525),(#246526,#246527,#246528),
(#246529,#246530,#246531),(#246532,#246533,#246534),(#246535,#246536,#246537),
(#246538,#246539,#246540),(#246541,#246542,#246543),(#246544,#246545,#246546),
(#246547,#246548,#246549),(#246550,#246551,#246552),(#246553,#246554,#246555),
(#246556,#246557,#246558),(#246559,#246560,#246561),(#246562,#246563,#246564),
(#246565,#246566,#246567),(#246568,#246569,#246570),(#246571,#246572,#246573),
(#246574,#246575,#246576),(#246577,#246578,#246579),(#246580,#246581,#246582)),
 .UNSPECIFIED.,.F.,.F.,.F.)
B_SPLINE_SURFACE_WITH_KNOTS((4,2,2,2,2,2,2,2,2,4),(3,3),(0.00111929193439265,
0.00178147539823544,0.00211256713015685,0.00227811299611754,0.00236088592909789,
0.00240227239558807,0.00242296562883316,0.00243331224545569,0.00243848555376697,
0.00244365886207824),(0.,1.),.UNSPECIFIED.)
GEOMETRIC_REPRESENTATION_ITEM()
RATIONAL_B_SPLINE_SURFACE(((1.,0.849234981733232,1.),(1.,0.870241987650574,
1.),(1.,0.895121832531114,1.),(1.,0.933989529870412,1.),(1.,0.947468186626281,
1.),(1.,0.967283733305218,1.),(1.,0.973827959689554,1.),(1.,0.983885895426172,
1.),(1.,0.987109304535727,1.),(1.,0.991867531035233,1.),(1.,0.993380275833142,
1.),(1.,0.996085964157165,1.),(1.,0.99695187264233,1.),(1.,0.99815729362421,
1.),(1.,0.998544146160859,1.),(1.,0.999082128717776,1.),(1.,0.999255712640949,
1.),(1.,0.999568658539456,1.),(1.,0.999758809035204,1.),(1.,0.99967095488344,
1.)))
REPRESENTATION_ITEM('')
SURFACE()
);
#3135=(
BOUNDED_SURFACE()
B_SPLINE_SURFACE(3,2,((#246601,#246602,#246603),(#246604,#246605,#246606),
(#246607,#246608,#246609),(#246610,#246611,#246612),(#246613,#246614,#246615),
(#246616,#246617,#246618)),.UNSPECIFIED.,.F.,.F.,.F.)
B_SPLINE_SURFACE_WITH_KNOTS((4,2,4),(3,3),(-1.368745591061E-5,0.000558644410170963,
0.00113103749536398),(0.,1.0001876508054),.UNSPECIFIED.)
GEOMETRIC_REPRESENTATION_ITEM()
RATIONAL_B_SPLINE_SURFACE(((1.,0.776510200206641,1.00008387608186),(1.,
0.780671305424827,1.00008231441237),(1.,0.789444453094105,1.00007902183592),
(1.,0.815105956743532,1.00006939103226),(1.,0.831679493744461,1.00006317095713),
(1.,0.850563496104669,1.00005608376062)))
REPRESENTATION_ITEM('')
SURFACE()
);
#3136=(
BOUNDED_SURFACE()
B_SPLINE_SURFACE(3,2,((#246676,#246677,#246678),(#246679,#246680,#246681),
(#246682,#246683,#246684),(#246685,#246686,#246687)),.UNSPECIFIED.,.F.,
 .F.,.F.)
B_SPLINE_SURFACE_WITH_KNOTS((4,4),(3,3),(0.00612686414750675,0.00733563944177598),
(0.,1.),.UNSPECIFIED.)
GEOMETRIC_REPRESENTATION_ITEM()
RATIONAL_B_SPLINE_SURFACE(((1.,0.776858520243962,1.),(1.,0.757903633195438,
1.),(1.,0.733510495431111,1.),(1.,0.707106781186548,1.)))
REPRESENTATION_ITEM('')
SURFACE()
);
#3137=(
BOUNDED_SURFACE()
B_SPLINE_SURFACE(3,2,((#246689,#246690,#246691),(#246692,#246693,#246694),
(#246695,#246696,#246697),(#246698,#246699,#246700)),.UNSPECIFIED.,.F.,
 .F.,.F.)
B_SPLINE_SURFACE_WITH_KNOTS((4,4),(3,3),(0.00603197572710737,0.00723932307207816),
(0.,1.),.UNSPECIFIED.)
GEOMETRIC_REPRESENTATION_ITEM()
RATIONAL_B_SPLINE_SURFACE(((1.,0.707106781186549,1.),(1.,0.733656875693368,
1.),(1.,0.758260023147512,1.),(1.,0.776858520243961,1.)))
REPRESENTATION_ITEM('')
SURFACE()
);
#3138=(
BOUNDED_SURFACE()
B_SPLINE_SURFACE(3,2,((#246704,#246705,#246706),(#246707,#246708,#246709),
(#246710,#246711,#246712),(#246713,#246714,#246715),(#246716,#246717,#246718),
(#246719,#246720,#246721)),.UNSPECIFIED.,.F.,.F.,.F.)
B_SPLINE_SURFACE_WITH_KNOTS((4,2,4),(3,3),(-0.000111927549594358,0.000559637745952908,
0.00123115031984094),(0.,1.00031845895621),.UNSPECIFIED.)
GEOMETRIC_REPRESENTATION_ITEM()
RATIONAL_B_SPLINE_SURFACE(((1.,0.860513397693372,1.00008884151555),(1.,
0.837277590186421,1.00010364081756),(1.,0.817467037853214,1.0001162585132),
(1.,0.787333305184159,1.0001354512273),(1.,0.777597790956806,1.0001416519507),
(1.,0.774832571355172,1.0001434131686)))
REPRESENTATION_ITEM('')
SURFACE()
);
#3139=(
BOUNDED_SURFACE()
B_SPLINE_SURFACE(3,2,((#246776,#246777,#246778),(#246779,#246780,#246781),
(#246782,#246783,#246784),(#246785,#246786,#246787),(#246788,#246789,#246790),
(#246791,#246792,#246793),(#246794,#246795,#246796),(#246797,#246798,#246799),
(#246800,#246801,#246802),(#246803,#246804,#246805),(#246806,#246807,#246808),
(#246809,#246810,#246811),(#246812,#246813,#246814),(#246815,#246816,#246817),
(#246818,#246819,#246820),(#246821,#246822,#246823),(#246824,#246825,#246826),
(#246827,#246828,#246829),(#246830,#246831,#246832),(#246833,#246834,#246835)),
 .UNSPECIFIED.,.F.,.F.,.F.)
B_SPLINE_SURFACE_WITH_KNOTS((4,2,2,2,2,2,2,2,2,4),(3,3),(0.00111929193439371,
0.00178158198025093,0.00211272700317955,0.00227829951464385,0.00236108577037601,
0.00240247889824208,0.00242317546217512,0.00243352374414164,0.0024386978851249,
0.00244387202610816),(0.,1.),.UNSPECIFIED.)
GEOMETRIC_REPRESENTATION_ITEM()
RATIONAL_B_SPLINE_SURFACE(((1.,0.849234981733213,1.),(1.,0.870241987653356,
1.),(1.,0.89512183252925,1.),(1.,0.933989529872486,1.),(1.,0.947468186625073,
1.),(1.,0.967283733305516,1.),(1.,0.973827959687474,1.),(1.,0.983885895428084,
1.),(1.,0.98710930453863,1.),(1.,0.99186753103398,1.),(1.,0.993380275830688,
1.),(1.,0.996085964157665,1.),(1.,0.99695187264221,1.),(1.,0.998157293624355,
1.),(1.,0.998544146162347,1.),(1.,0.999082128717726,1.),(1.,0.999255712642408,
1.),(1.,0.999568658539312,1.),(1.,0.999758809037123,1.),(1.,0.999670954879881,
1.)))
REPRESENTATION_ITEM('')
SURFACE()
);
#3140=(
BOUNDED_SURFACE()
B_SPLINE_SURFACE(3,2,((#246852,#246853,#246854),(#246855,#246856,#246857),
(#246858,#246859,#246860),(#246861,#246862,#246863)),.UNSPECIFIED.,.F.,
 .F.,.F.)
B_SPLINE_SURFACE_WITH_KNOTS((4,4),(3,3),(0.0408455795445267,0.042773718086462),
(0.,1.),.UNSPECIFIED.)
GEOMETRIC_REPRESENTATION_ITEM()
RATIONAL_B_SPLINE_SURFACE(((1.,0.967701496827011,1.),(1.,0.968545704393032,
1.),(1.,0.969390043334334,1.),(1.,0.970233777086396,1.)))
REPRESENTATION_ITEM('')
SURFACE()
);
#3141=(
BOUNDED_SURFACE()
B_SPLINE_SURFACE(3,2,((#246884,#246885,#246886),(#246887,#246888,#246889),
(#246890,#246891,#246892),(#246893,#246894,#246895),(#246896,#246897,#246898),
(#246899,#246900,#246901),(#246902,#246903,#246904),(#246905,#246906,#246907),
(#246908,#246909,#246910),(#246911,#246912,#246913),(#246914,#246915,#246916),
(#246917,#246918,#246919),(#246920,#246921,#246922),(#246923,#246924,#246925)),
 .UNSPECIFIED.,.F.,.F.,.F.)
B_SPLINE_SURFACE_WITH_KNOTS((4,2,2,2,2,2,4),(3,3),(0.00641476504360471,
0.00720885616391255,0.00758281066823651,0.00795676517256048,0.00833071967688444,
0.0087046741812084,0.00945258318985632),(0.,1.00004618211165),
 .UNSPECIFIED.)
GEOMETRIC_REPRESENTATION_ITEM()
RATIONAL_B_SPLINE_SURFACE(((1.,0.706895776308564,1.00002707234397),(1.,
0.708010377644408,1.00002696939468),(1.,0.709414341304934,1.00002683971867),
(1.,0.712474126198451,1.00002655710402),(1.,0.713589100039244,1.00002645412032),
(1.,0.716224859765459,1.00002621067042),(1.,0.717766798011333,1.00002606825049),
(1.,0.721310542436779,1.00002574093529),(1.,0.723318075519062,1.00002555551106),
(1.,0.727854283400673,1.00002513652774),(1.,0.730408561181452,1.00002490060386),
(1.,0.738132660070436,1.00002418717346),(1.,0.743606172212938,1.00002368161677),
(1.,0.745071384918521,1.00002354628353)))
REPRESENTATION_ITEM('')
SURFACE()
);
#3142=(
BOUNDED_SURFACE()
B_SPLINE_SURFACE(3,2,((#247118,#247119,#247120),(#247121,#247122,#247123),
(#247124,#247125,#247126),(#247127,#247128,#247129),(#247130,#247131,#247132),
(#247133,#247134,#247135),(#247136,#247137,#247138),(#247139,#247140,#247141),
(#247142,#247143,#247144),(#247145,#247146,#247147)),.UNSPECIFIED.,.F.,
 .F.,.F.)
B_SPLINE_SURFACE_WITH_KNOTS((4,2,2,2,4),(3,3),(0.,0.392699081698725,0.785398163397449,
1.17809724509617,1.5707963267949),(0.,1.),.UNSPECIFIED.)
GEOMETRIC_REPRESENTATION_ITEM()
RATIONAL_B_SPLINE_SURFACE(((1.,0.819152044288993,1.),(1.,0.819160091424011,
1.),(1.,0.816447805244711,1.),(1.,0.805887184900773,1.),(1.,0.798030050106979,
1.),(1.,0.777942514786192,1.),(1.,0.765710795400617,1.),(1.,0.738207714616384,
1.),(1.,0.722944887324406,1.),(1.,0.707106781186549,1.)))
REPRESENTATION_ITEM('')
SURFACE()
);
#3143=(
BOUNDED_SURFACE()
B_SPLINE_SURFACE(3,2,((#247249,#247250,#247251),(#247252,#247253,#247254),
(#247255,#247256,#247257),(#247258,#247259,#247260),(#247261,#247262,#247263),
(#247264,#247265,#247266),(#247267,#247268,#247269),(#247270,#247271,#247272),
(#247273,#247274,#247275),(#247276,#247277,#247278),(#247279,#247280,#247281),
(#247282,#247283,#247284),(#247285,#247286,#247287),(#247288,#247289,#247290)),
 .UNSPECIFIED.,.F.,.F.,.F.)
B_SPLINE_SURFACE_WITH_KNOTS((4,2,2,2,2,2,4),(3,3),(0.00646808747938269,
0.00724932038878676,0.00763316097925953,0.0080170015697323,0.00840084216020507,
0.00878468275067784,0.00955236393162338),(-1.35517284585259E-5,1.),
 .UNSPECIFIED.)
GEOMETRIC_REPRESENTATION_ITEM()
RATIONAL_B_SPLINE_SURFACE(((1.00000793151294,0.707361574991507,1.),(1.00000806626139,
0.7023899417983,1.),(1.00000820227477,0.697371638210326,1.),(1.00000839312539,
0.690330078134294,1.),(1.00000845317796,0.688114398442112,1.),(1.00000856755574,
0.683894354745816,1.),(1.00000862230378,0.681874389455888,1.),(1.00000872143439,
0.678216899825171,1.),(1.00000876629923,0.676561581859308,1.),(1.00000884629199,
0.673610195926044,1.),(1.00000888117563,0.672323140891743,1.),(1.00000896617579,
0.669187003750694,1.),(1.00000899882615,0.667982347216541,1.),(1.0000090031805,
0.667821690638002,1.)))
REPRESENTATION_ITEM('')
SURFACE()
);
#3144=(
BOUNDED_SURFACE()
B_SPLINE_SURFACE(3,2,((#247491,#247492,#247493),(#247494,#247495,#247496),
(#247497,#247498,#247499),(#247500,#247501,#247502),(#247503,#247504,#247505),
(#247506,#247507,#247508),(#247509,#247510,#247511),(#247512,#247513,#247514),
(#247515,#247516,#247517),(#247518,#247519,#247520)),.UNSPECIFIED.,.F.,
 .F.,.F.)
B_SPLINE_SURFACE_WITH_KNOTS((4,2,2,2,4),(3,3),(1.5707963267949,1.96585160298382,
2.36090687917273,2.75596215536165,3.15101743155057),(0.,1.),
 .UNSPECIFIED.)
GEOMETRIC_REPRESENTATION_ITEM()
RATIONAL_B_SPLINE_SURFACE(((1.,0.707106781186549,1.),(1.,0.723040087310248,
1.),(1.,0.738390656304015,1.),(1.,0.766022585770263,1.),(1.,0.778295218542395,
1.),(1.,0.7983986260281,1.),(1.,0.806230755417563,1.),(1.,0.816669539143349,
1.),(1.,0.819285194795031,1.),(1.,0.819147408352828,1.)))
REPRESENTATION_ITEM('')
SURFACE()
);
#3145=(
BOUNDED_SURFACE()
B_SPLINE_SURFACE(3,2,((#247631,#247632,#247633),(#247634,#247635,#247636),
(#247637,#247638,#247639),(#247640,#247641,#247642)),.UNSPECIFIED.,.F.,
 .F.,.F.)
B_SPLINE_SURFACE_WITH_KNOTS((4,4),(3,3),(0.,0.000561888377921629),(0.,1.),
 .UNSPECIFIED.)
GEOMETRIC_REPRESENTATION_ITEM()
RATIONAL_B_SPLINE_SURFACE(((1.,0.721830660407024,1.),(1.,0.726161642227015,
1.),(1.,0.730217605430419,1.),(1.,0.734028581001202,1.)))
REPRESENTATION_ITEM('')
SURFACE()
);
#3146=(
BOUNDED_SURFACE()
B_SPLINE_SURFACE(3,2,((#247648,#247649,#247650),(#247651,#247652,#247653),
(#247654,#247655,#247656),(#247657,#247658,#247659)),.UNSPECIFIED.,.F.,
 .F.,.F.)
B_SPLINE_SURFACE_WITH_KNOTS((4,4),(3,3),(-8.67361737988403E-18,0.0027255914917872),
(0.,1.),.UNSPECIFIED.)
GEOMETRIC_REPRESENTATION_ITEM()
RATIONAL_B_SPLINE_SURFACE(((1.,0.721830660407024,1.),(1.,0.722050915678773,
1.),(1.,0.722280885253549,1.),(1.,0.722521956262064,1.)))
REPRESENTATION_ITEM('')
SURFACE()
);
#3147=(
BOUNDED_SURFACE()
B_SPLINE_SURFACE(3,2,((#247675,#247676,#247677),(#247678,#247679,#247680),
(#247681,#247682,#247683),(#247684,#247685,#247686),(#247687,#247688,#247689),
(#247690,#247691,#247692),(#247693,#247694,#247695),(#247696,#247697,#247698),
(#247699,#247700,#247701),(#247702,#247703,#247704),(#247705,#247706,#247707),
(#247708,#247709,#247710)),.UNSPECIFIED.,.F.,.F.,.F.)
B_SPLINE_SURFACE_WITH_KNOTS((4,2,2,2,2,4),(3,3),(-2.71050543121376E-20,
0.000196917635222578,0.000295376452833867,0.000393835270445156,0.000590752905667733,
0.000787670540890311),(0.,1.),.UNSPECIFIED.)
GEOMETRIC_REPRESENTATION_ITEM()
RATIONAL_B_SPLINE_SURFACE(((1.,0.768827303401079,1.),(1.,0.768839794086584,
1.),(1.,0.767245932333086,1.),(1.,0.76267317155594,1.),(1.,0.760806266526503,
1.),(1.,0.756383065794974,1.),(1.,0.753812076955945,1.),(1.,0.745366037508728,
1.),(1.,0.738532036970522,1.),(1.,0.723650553821477,1.),(1.,0.715418707911078,
1.),(1.,0.707106781186548,1.)))
REPRESENTATION_ITEM('')
SURFACE()
);
#3148=(
BOUNDED_SURFACE()
B_SPLINE_SURFACE(3,2,((#247840,#247841,#247842),(#247843,#247844,#247845),
(#247846,#247847,#247848),(#247849,#247850,#247851)),.UNSPECIFIED.,.F.,
 .F.,.F.)
B_SPLINE_SURFACE_WITH_KNOTS((4,4),(3,3),(0.,0.00308554567306433),(0.,1.),
 .UNSPECIFIED.)
GEOMETRIC_REPRESENTATION_ITEM()
RATIONAL_B_SPLINE_SURFACE(((1.,0.722521956262063,1.),(1.,0.722249049952648,
1.),(1.,0.721990362413173,1.),(1.,0.721743903804635,1.)))
REPRESENTATION_ITEM('')
SURFACE()
);
#3149=(
BOUNDED_SURFACE()
B_SPLINE_SURFACE(3,2,((#247867,#247868,#247869),(#247870,#247871,#247872),
(#247873,#247874,#247875),(#247876,#247877,#247878),(#247879,#247880,#247881),
(#247882,#247883,#247884),(#247885,#247886,#247887),(#247888,#247889,#247890),
(#247891,#247892,#247893),(#247894,#247895,#247896),(#247897,#247898,#247899),
(#247900,#247901,#247902)),.UNSPECIFIED.,.F.,.F.,.F.)
B_SPLINE_SURFACE_WITH_KNOTS((4,2,2,2,2,4),(3,3),(0.,0.000196919474660801,
0.000295379211991202,0.000393838949321602,0.000590758423982404,0.000787677898643205),
(0.,1.),.UNSPECIFIED.)
GEOMETRIC_REPRESENTATION_ITEM()
RATIONAL_B_SPLINE_SURFACE(((1.,0.707106781186546,1.),(1.,0.715396063584809,
1.),(1.,0.723543617208936,1.),(1.,0.734788510950855,1.),(1.,0.738325118179662,
1.),(1.,0.744992206539526,1.),(1.,0.748144662339383,1.),(1.,0.756608512730963,
1.),(1.,0.761139004306969,1.),(1.,0.767215293085605,1.),(1.,0.768836106148694,
1.),(1.,0.768827303401081,1.)))
REPRESENTATION_ITEM('')
SURFACE()
);
#3150=(
BOUNDED_SURFACE()
B_SPLINE_SURFACE(3,2,((#248044,#248045,#248046),(#248047,#248048,#248049),
(#248050,#248051,#248052),(#248053,#248054,#248055)),.UNSPECIFIED.,.F.,
 .F.,.F.)
B_SPLINE_SURFACE_WITH_KNOTS((4,4),(3,3),(0.,0.00168726762248989),(0.,1.),
 .UNSPECIFIED.)
GEOMETRIC_REPRESENTATION_ITEM()
RATIONAL_B_SPLINE_SURFACE(((1.,0.788010753606719,1.),(1.,0.787995580138724,
1.),(1.,0.785892129585524,1.),(1.,0.781757935428468,1.)))
REPRESENTATION_ITEM('')
SURFACE()
);
#3151=(
BOUNDED_SURFACE()
B_SPLINE_SURFACE(3,2,((#248107,#248108,#248109),(#248110,#248111,#248112),
(#248113,#248114,#248115),(#248116,#248117,#248118),(#248119,#248120,#248121),
(#248122,#248123,#248124)),.UNSPECIFIED.,.F.,.F.,.F.)
B_SPLINE_SURFACE_WITH_KNOTS((4,2,4),(3,3),(0.,0.000492064922826377,0.000984129845652755),
(0.,1.),.UNSPECIFIED.)
GEOMETRIC_REPRESENTATION_ITEM()
RATIONAL_B_SPLINE_SURFACE(((1.,0.788010753606719,1.),(1.,0.787995463701203,
1.),(1.,0.786698704019208,1.),(1.,0.781418067371145,1.),(1.,0.777580790644453,
1.),(1.,0.772541161150265,1.)))
REPRESENTATION_ITEM('')
SURFACE()
);
#3152=(
BOUNDED_SURFACE()
B_SPLINE_SURFACE(3,2,((#248148,#248149,#248150),(#248151,#248152,#248153),
(#248154,#248155,#248156),(#248157,#248158,#248159),(#248160,#248161,#248162),
(#248163,#248164,#248165)),.UNSPECIFIED.,.F.,.F.,.F.)
B_SPLINE_SURFACE_WITH_KNOTS((4,2,4),(3,3),(1.0842021724855E-19,0.000492127602558551,
0.000984255205117102),(0.,1.),.UNSPECIFIED.)
GEOMETRIC_REPRESENTATION_ITEM()
RATIONAL_B_SPLINE_SURFACE(((1.,0.772541161150265,1.),(1.,0.7775811913717,
1.),(1.,0.781415995839735,1.),(1.,0.786696090924191,1.),(1.,0.787997416142609,
1.),(1.,0.788010753606718,1.)))
REPRESENTATION_ITEM('')
SURFACE()
);
#3153=(
BOUNDED_SURFACE()
B_SPLINE_SURFACE(3,2,((#248192,#248193,#248194),(#248195,#248196,#248197),
(#248198,#248199,#248200),(#248201,#248202,#248203)),.UNSPECIFIED.,.F.,
 .F.,.F.)
B_SPLINE_SURFACE_WITH_KNOTS((4,4),(3,3),(-3.46944695195361E-18,0.00168726762248988),
(0.,1.),.UNSPECIFIED.)
GEOMETRIC_REPRESENTATION_ITEM()
RATIONAL_B_SPLINE_SURFACE(((1.,0.781757935428468,1.),(1.,0.785892129585526,
1.),(1.,0.787995580138721,1.),(1.,0.78801075360672,1.)))
REPRESENTATION_ITEM('')
SURFACE()
);
#3154=(
BOUNDED_SURFACE()
B_SPLINE_SURFACE(3,2,((#248257,#248258,#248259),(#248260,#248261,#248262),
(#248263,#248264,#248265),(#248266,#248267,#248268),(#248269,#248270,#248271),
(#248272,#248273,#248274)),.UNSPECIFIED.,.F.,.F.,.F.)
B_SPLINE_SURFACE_WITH_KNOTS((4,2,4),(3,3),(0.,0.000492064922826383,0.000984129845652766),
(0.,1.),.UNSPECIFIED.)
GEOMETRIC_REPRESENTATION_ITEM()
RATIONAL_B_SPLINE_SURFACE(((1.,0.78801075360672,1.),(1.,0.787995463701083,
1.),(1.,0.786698704019365,1.),(1.,0.781418067370988,1.),(1.,0.777580790644572,
1.),(1.,0.772541161150265,1.)))
REPRESENTATION_ITEM('')
SURFACE()
);
#3155=(
BOUNDED_SURFACE()
B_SPLINE_SURFACE(3,2,((#248298,#248299,#248300),(#248301,#248302,#248303),
(#248304,#248305,#248306),(#248307,#248308,#248309),(#248310,#248311,#248312),
(#248313,#248314,#248315)),.UNSPECIFIED.,.F.,.F.,.F.)
B_SPLINE_SURFACE_WITH_KNOTS((4,2,4),(3,3),(0.,0.000492127602558548,0.000984255205117095),
(0.,1.),.UNSPECIFIED.)
GEOMETRIC_REPRESENTATION_ITEM()
RATIONAL_B_SPLINE_SURFACE(((1.,0.772541161150265,1.),(1.,0.777581191371582,
1.),(1.,0.781415995839892,1.),(1.,0.786696090924034,1.),(1.,0.787997416142728,
1.),(1.,0.78801075360672,1.)))
REPRESENTATION_ITEM('')
SURFACE()
);
#3156=(
BOUNDED_SURFACE()
B_SPLINE_SURFACE(3,2,((#248342,#248343,#248344),(#248345,#248346,#248347),
(#248348,#248349,#248350),(#248351,#248352,#248353)),.UNSPECIFIED.,.F.,
 .F.,.F.)
B_SPLINE_SURFACE_WITH_KNOTS((4,4),(3,3),(0.,0.00168726762248988),(0.,1.),
 .UNSPECIFIED.)
GEOMETRIC_REPRESENTATION_ITEM()
RATIONAL_B_SPLINE_SURFACE(((1.,0.78175793542847,1.),(1.,0.785892129585525,
1.),(1.,0.787995580138723,1.),(1.,0.788010753606719,1.)))
REPRESENTATION_ITEM('')
SURFACE()
);
#3157=(
BOUNDED_SURFACE()
B_SPLINE_SURFACE(3,2,((#248371,#248372,#248373),(#248374,#248375,#248376),
(#248377,#248378,#248379),(#248380,#248381,#248382)),.UNSPECIFIED.,.F.,
 .F.,.F.)
B_SPLINE_SURFACE_WITH_KNOTS((4,4),(3,3),(-0.000914415610118037,0.0178445500057952),
(0.,1.00091441561012),.UNSPECIFIED.)
GEOMETRIC_REPRESENTATION_ITEM()
RATIONAL_B_SPLINE_SURFACE(((1.,0.771817621836307,1.00041730705709),(1.,
0.77533655889149,1.00041087151514),(1.,0.779001978127809,1.00040416808201),
(1.,0.782001690466344,1.00039868211443)))
REPRESENTATION_ITEM('')
SURFACE()
);
#3158=(
BOUNDED_SURFACE()
B_SPLINE_SURFACE(3,2,((#248413,#248414,#248415),(#248416,#248417,#248418),
(#248419,#248420,#248421),(#248422,#248423,#248424)),.UNSPECIFIED.,.F.,
 .F.,.F.)
B_SPLINE_SURFACE_WITH_KNOTS((4,4),(3,3),(-0.000914415609804201,0.0178445500054813),
(0.,1.0009144156098),.UNSPECIFIED.)
GEOMETRIC_REPRESENTATION_ITEM()
RATIONAL_B_SPLINE_SURFACE(((1.,0.771817621836556,1.00041730705695),(1.,
0.77533655889162,1.000410871515),(1.,0.779001978127809,1.00040416808187),
(0.999999999999999,0.782001690466259,1.0003986821143)))
REPRESENTATION_ITEM('')
SURFACE()
);
#3159=(
BOUNDED_SURFACE()
B_SPLINE_SURFACE(3,2,((#248455,#248456,#248457),(#248458,#248459,#248460),
(#248461,#248462,#248463),(#248464,#248465,#248466)),.UNSPECIFIED.,.F.,
 .F.,.F.)
B_SPLINE_SURFACE_WITH_KNOTS((4,4),(3,3),(-0.000914415609905059,0.0178445500055823),
(0.,1.00091441560991),.UNSPECIFIED.)
GEOMETRIC_REPRESENTATION_ITEM()
RATIONAL_B_SPLINE_SURFACE(((0.999999999999999,0.782001690466286,1.00039868211434),
(1.,0.779001978127807,1.00040416808192),(1.,0.775336558891579,1.00041087151505),
(1.,0.771817621836475,1.000417307057)))
REPRESENTATION_ITEM('')
SURFACE()
);
#3160=(
BOUNDED_SURFACE()
B_SPLINE_SURFACE(3,2,((#248606,#248607,#248608),(#248609,#248610,#248611),
(#248612,#248613,#248614),(#248615,#248616,#248617)),.UNSPECIFIED.,.F.,
 .F.,.F.)
B_SPLINE_SURFACE_WITH_KNOTS((4,4),(3,3),(0.,0.00168726762248989),(0.,1.),
 .UNSPECIFIED.)
GEOMETRIC_REPRESENTATION_ITEM()
RATIONAL_B_SPLINE_SURFACE(((1.,0.788010753606719,1.),(1.,0.787995580138724,
1.),(1.,0.785892129585524,1.),(1.,0.781757935428468,1.)))
REPRESENTATION_ITEM('')
SURFACE()
);
#3161=(
BOUNDED_SURFACE()
B_SPLINE_SURFACE(3,2,((#248701,#248702,#248703),(#248704,#248705,#248706),
(#248707,#248708,#248709),(#248710,#248711,#248712),(#248713,#248714,#248715),
(#248716,#248717,#248718)),.UNSPECIFIED.,.F.,.F.,.F.)
B_SPLINE_SURFACE_WITH_KNOTS((4,2,4),(3,3),(0.,0.000492064922826377,0.000984129845652755),
(0.,1.),.UNSPECIFIED.)
GEOMETRIC_REPRESENTATION_ITEM()
RATIONAL_B_SPLINE_SURFACE(((1.,0.788010753606719,1.),(1.,0.787995463701203,
1.),(1.,0.786698704019208,1.),(1.,0.781418067371145,1.),(1.,0.777580790644453,
1.),(1.,0.772541161150265,1.)))
REPRESENTATION_ITEM('')
SURFACE()
);
#3162=(
BOUNDED_SURFACE()
B_SPLINE_SURFACE(3,2,((#248742,#248743,#248744),(#248745,#248746,#248747),
(#248748,#248749,#248750),(#248751,#248752,#248753),(#248754,#248755,#248756),
(#248757,#248758,#248759)),.UNSPECIFIED.,.F.,.F.,.F.)
B_SPLINE_SURFACE_WITH_KNOTS((4,2,4),(3,3),(1.0842021724855E-19,0.000492127602558551,
0.000984255205117102),(0.,1.),.UNSPECIFIED.)
GEOMETRIC_REPRESENTATION_ITEM()
RATIONAL_B_SPLINE_SURFACE(((1.,0.772541161150265,1.),(1.,0.7775811913717,
1.),(1.,0.781415995839735,1.),(1.,0.786696090924191,1.),(1.,0.787997416142609,
1.),(1.,0.788010753606718,1.)))
REPRESENTATION_ITEM('')
SURFACE()
);
#3163=(
BOUNDED_SURFACE()
B_SPLINE_SURFACE(3,2,((#248786,#248787,#248788),(#248789,#248790,#248791),
(#248792,#248793,#248794),(#248795,#248796,#248797)),.UNSPECIFIED.,.F.,
 .F.,.F.)
B_SPLINE_SURFACE_WITH_KNOTS((4,4),(3,3),(-3.46944695195361E-18,0.00168726762248988),
(0.,1.),.UNSPECIFIED.)
GEOMETRIC_REPRESENTATION_ITEM()
RATIONAL_B_SPLINE_SURFACE(((1.,0.781757935428468,1.),(1.,0.785892129585526,
1.),(1.,0.787995580138721,1.),(1.,0.78801075360672,1.)))
REPRESENTATION_ITEM('')
SURFACE()
);
#3164=(
BOUNDED_SURFACE()
B_SPLINE_SURFACE(3,2,((#248818,#248819,#248820),(#248821,#248822,#248823),
(#248824,#248825,#248826),(#248827,#248828,#248829)),.UNSPECIFIED.,.F.,
 .F.,.F.)
B_SPLINE_SURFACE_WITH_KNOTS((4,4),(3,3),(0.,0.00168726762248987),(0.,1.),
 .UNSPECIFIED.)
GEOMETRIC_REPRESENTATION_ITEM()
RATIONAL_B_SPLINE_SURFACE(((1.,0.78801075360672,1.),(1.,0.787995580138721,
1.),(1.,0.785892129585525,1.),(1.,0.78175793542847,1.)))
REPRESENTATION_ITEM('')
SURFACE()
);
#3165=(
BOUNDED_SURFACE()
B_SPLINE_SURFACE(3,2,((#248913,#248914,#248915),(#248916,#248917,#248918),
(#248919,#248920,#248921),(#248922,#248923,#248924),(#248925,#248926,#248927),
(#248928,#248929,#248930)),.UNSPECIFIED.,.F.,.F.,.F.)
B_SPLINE_SURFACE_WITH_KNOTS((4,2,4),(3,3),(0.,0.000492064922826383,0.000984129845652766),
(0.,1.),.UNSPECIFIED.)
GEOMETRIC_REPRESENTATION_ITEM()
RATIONAL_B_SPLINE_SURFACE(((1.,0.78801075360672,1.),(1.,0.787995463701083,
1.),(1.,0.786698704019365,1.),(1.,0.781418067370988,1.),(1.,0.777580790644572,
1.),(1.,0.772541161150265,1.)))
REPRESENTATION_ITEM('')
SURFACE()
);
#3166=(
BOUNDED_SURFACE()
B_SPLINE_SURFACE(3,2,((#248954,#248955,#248956),(#248957,#248958,#248959),
(#248960,#248961,#248962),(#248963,#248964,#248965),(#248966,#248967,#248968),
(#248969,#248970,#248971)),.UNSPECIFIED.,.F.,.F.,.F.)
B_SPLINE_SURFACE_WITH_KNOTS((4,2,4),(3,3),(0.,0.000492127602558548,0.000984255205117095),
(0.,1.),.UNSPECIFIED.)
GEOMETRIC_REPRESENTATION_ITEM()
RATIONAL_B_SPLINE_SURFACE(((1.,0.772541161150265,1.),(1.,0.777581191371582,
1.),(1.,0.781415995839892,1.),(1.,0.786696090924034,1.),(1.,0.787997416142728,
1.),(1.,0.78801075360672,1.)))
REPRESENTATION_ITEM('')
SURFACE()
);
#3167=(
BOUNDED_SURFACE()
B_SPLINE_SURFACE(3,2,((#248998,#248999,#249000),(#249001,#249002,#249003),
(#249004,#249005,#249006),(#249007,#249008,#249009)),.UNSPECIFIED.,.F.,
 .F.,.F.)
B_SPLINE_SURFACE_WITH_KNOTS((4,4),(3,3),(0.,0.00168726762248988),(0.,1.),
 .UNSPECIFIED.)
GEOMETRIC_REPRESENTATION_ITEM()
RATIONAL_B_SPLINE_SURFACE(((1.,0.78175793542847,1.),(1.,0.785892129585525,
1.),(1.,0.787995580138723,1.),(1.,0.788010753606719,1.)))
REPRESENTATION_ITEM('')
SURFACE()
);
#3168=(
BOUNDED_SURFACE()
B_SPLINE_SURFACE(3,2,((#249041,#249042,#249043),(#249044,#249045,#249046),
(#249047,#249048,#249049),(#249050,#249051,#249052)),.UNSPECIFIED.,.F.,
 .F.,.F.)
B_SPLINE_SURFACE_WITH_KNOTS((4,4),(3,3),(-1.38777878078145E-17,0.0169301343956772),
(0.,1.),.UNSPECIFIED.)
GEOMETRIC_REPRESENTATION_ITEM()
RATIONAL_B_SPLINE_SURFACE(((1.,0.772541161150265,1.),(1.,0.775725268487667,
1.),(1.,0.778996361886149,1.),(1.,0.78175793542847,1.)))
REPRESENTATION_ITEM('')
SURFACE()
);
#3169=(
BOUNDED_SURFACE()
B_SPLINE_SURFACE(3,2,((#249071,#249072,#249073),(#249074,#249075,#249076),
(#249077,#249078,#249079),(#249080,#249081,#249082)),.UNSPECIFIED.,.F.,
 .F.,.F.)
B_SPLINE_SURFACE_WITH_KNOTS((4,4),(3,3),(-6.93889390390723E-18,0.0169301343956773),
(0.,1.),.UNSPECIFIED.)
GEOMETRIC_REPRESENTATION_ITEM()
RATIONAL_B_SPLINE_SURFACE(((1.,0.781757935428468,1.),(1.,0.778996361886152,
1.),(1.,0.775725268487663,1.),(1.,0.772541161150265,1.)))
REPRESENTATION_ITEM('')
SURFACE()
);
#3170=(
BOUNDED_SURFACE()
B_SPLINE_SURFACE(3,2,((#249102,#249103,#249104),(#249105,#249106,#249107),
(#249108,#249109,#249110),(#249111,#249112,#249113)),.UNSPECIFIED.,.F.,
 .F.,.F.)
B_SPLINE_SURFACE_WITH_KNOTS((4,4),(3,3),(-6.93889390390723E-18,0.0169301343956771),
(0.,1.),.UNSPECIFIED.)
GEOMETRIC_REPRESENTATION_ITEM()
RATIONAL_B_SPLINE_SURFACE(((1.,0.772541161150265,1.),(1.,0.775725268487663,
1.),(1.,0.778996361886151,1.),(1.,0.781757935428468,1.)))
REPRESENTATION_ITEM('')
SURFACE()
);
#3171=(
BOUNDED_SURFACE()
B_SPLINE_SURFACE(3,2,((#249132,#249133,#249134),(#249135,#249136,#249137),
(#249138,#249139,#249140),(#249141,#249142,#249143)),.UNSPECIFIED.,.F.,
 .F.,.F.)
B_SPLINE_SURFACE_WITH_KNOTS((4,4),(3,3),(0.,0.0169301343956772),(0.,1.),
 .UNSPECIFIED.)
GEOMETRIC_REPRESENTATION_ITEM()
RATIONAL_B_SPLINE_SURFACE(((1.,0.781757935428468,1.),(1.,0.778996361886149,
1.),(1.,0.775725268487665,1.),(1.,0.772541161150265,1.)))
REPRESENTATION_ITEM('')
SURFACE()
);
#3172=(
BOUNDED_SURFACE()
B_SPLINE_SURFACE(3,2,((#249172,#249173,#249174),(#249175,#249176,#249177),
(#249178,#249179,#249180),(#249181,#249182,#249183)),.UNSPECIFIED.,.F.,
 .F.,.F.)
B_SPLINE_SURFACE_WITH_KNOTS((4,4),(3,3),(0.00337631140392896,0.0169301343956773),
(0.,1.),.UNSPECIFIED.)
GEOMETRIC_REPRESENTATION_ITEM()
RATIONAL_B_SPLINE_SURFACE(((1.,0.780050659744625,1.),(1.,0.777690973944284,
1.),(1.,0.775093372307372,1.),(1.,0.772541161150265,1.)))
REPRESENTATION_ITEM('')
SURFACE()
);
#3173=(
BOUNDED_SURFACE()
B_SPLINE_SURFACE(1,2,((#249602,#249603,#249604,#249605,#249606,#249607,
#249608,#249609,#249610,#249611,#249612,#249613,#249614,#249615,#249616,
#249617,#249618,#249619,#249620,#249621,#249622,#249623,#249624,#249625,
#249626,#249627,#249628,#249629,#249630,#249631,#249632,#249633,#249634,
#249635,#249636,#249637,#249638,#249639,#249640,#249641,#249642,#249643,
#249644,#249645,#249646,#249647,#249648,#249649,#249650,#249651,#249652,
#249653,#249654,#249655,#249656,#249657,#249658,#249659,#249660,#249661,
#249662,#249663,#249664,#249665,#249666,#249667,#249668,#249669,#249670,
#249671,#249672,#249673,#249674,#249675,#249676,#249677,#249678,#249679,
#249680,#249681,#249682,#249683,#249684,#249685,#249686,#249687,#249688,
#249689,#249690,#249691,#249692,#249693,#249694,#249695,#249696,#249697,
#249698,#249699,#249700,#249701,#249702,#249703,#249704,#249705,#249706,
#249707,#249708,#249709,#249710,#249711,#249712,#249713,#249714,#249715,
#249716,#249717,#249718,#249719,#249720,#249721,#249722,#249723,#249724,
#249725,#249726,#249727,#249728,#249729,#249730,#249731,#249732,#249733,
#249734,#249735,#249736,#249737,#249738,#249739,#249740,#249741,#249742,
#249743,#249744,#249745,#249746,#249747,#249748,#249749,#249750,#249751,
#249752,#249753,#249754,#249755,#249756,#249757,#249758,#249759,#249760,
#249761,#249762,#249763,#249764,#249765,#249766,#249767,#249768,#249769,
#249770,#249771,#249772,#249773,#249774,#249775,#249776,#249777,#249778,
#249779,#249780,#249781,#249782,#249783,#249784,#249785,#249786,#249787,
#249788,#249789,#249790,#249791,#249792,#249793,#249794,#249795,#249796,
#249797,#249798,#249799,#249800,#249801,#249802,#249803,#249804,#249805,
#249806,#249807,#249808,#249809,#249810,#249811,#249812,#249813,#249814,
#249815,#249816,#249817,#249818,#249819,#249820,#249821,#249822,#249823,
#249824,#249825,#249826,#249827,#249828,#249829,#249830,#249831,#249832,
#249833,#249834,#249835,#249836,#249837,#249838,#249839,#249840,#249841,
#249842,#249843,#249844,#249845,#249846,#249847,#249848,#249849,#249850,
#249851,#249852,#249853,#249854,#249855,#249856,#249857,#249858,#249859,
#249860,#249861,#249862,#249863,#249864,#249865,#249866,#249867,#249868,
#249869,#249870,#249871,#249872,#249873,#249874,#249875,#249876,#249877,
#249878),(#249879,#249880,#249881,#249882,#249883,#249884,#249885,#249886,
#249887,#249888,#249889,#249890,#249891,#249892,#249893,#249894,#249895,
#249896,#249897,#249898,#249899,#249900,#249901,#249902,#249903,#249904,
#249905,#249906,#249907,#249908,#249909,#249910,#249911,#249912,#249913,
#249914,#249915,#249916,#249917,#249918,#249919,#249920,#249921,#249922,
#249923,#249924,#249925,#249926,#249927,#249928,#249929,#249930,#249931,
#249932,#249933,#249934,#249935,#249936,#249937,#249938,#249939,#249940,
#249941,#249942,#249943,#249944,#249945,#249946,#249947,#249948,#249949,
#249950,#249951,#249952,#249953,#249954,#249955,#249956,#249957,#249958,
#249959,#249960,#249961,#249962,#249963,#249964,#249965,#249966,#249967,
#249968,#249969,#249970,#249971,#249972,#249973,#249974,#249975,#249976,
#249977,#249978,#249979,#249980,#249981,#249982,#249983,#249984,#249985,
#249986,#249987,#249988,#249989,#249990,#249991,#249992,#249993,#249994,
#249995,#249996,#249997,#249998,#249999,#250000,#250001,#250002,#250003,
#250004,#250005,#250006,#250007,#250008,#250009,#250010,#250011,#250012,
#250013,#250014,#250015,#250016,#250017,#250018,#250019,#250020,#250021,
#250022,#250023,#250024,#250025,#250026,#250027,#250028,#250029,#250030,
#250031,#250032,#250033,#250034,#250035,#250036,#250037,#250038,#250039,
#250040,#250041,#250042,#250043,#250044,#250045,#250046,#250047,#250048,
#250049,#250050,#250051,#250052,#250053,#250054,#250055,#250056,#250057,
#250058,#250059,#250060,#250061,#250062,#250063,#250064,#250065,#250066,
#250067,#250068,#250069,#250070,#250071,#250072,#250073,#250074,#250075,
#250076,#250077,#250078,#250079,#250080,#250081,#250082,#250083,#250084,
#250085,#250086,#250087,#250088,#250089,#250090,#250091,#250092,#250093,
#250094,#250095,#250096,#250097,#250098,#250099,#250100,#250101,#250102,
#250103,#250104,#250105,#250106,#250107,#250108,#250109,#250110,#250111,
#250112,#250113,#250114,#250115,#250116,#250117,#250118,#250119,#250120,
#250121,#250122,#250123,#250124,#250125,#250126,#250127,#250128,#250129,
#250130,#250131,#250132,#250133,#250134,#250135,#250136,#250137,#250138,
#250139,#250140,#250141,#250142,#250143,#250144,#250145,#250146,#250147,
#250148,#250149,#250150,#250151,#250152,#250153,#250154,#250155)),
 .UNSPECIFIED.,.F.,.F.,.F.)
B_SPLINE_SURFACE_WITH_KNOTS((2,2),(3,2,2,2,2,2,2,2,2,2,2,2,2,2,2,2,2,2,
2,2,2,2,2,2,2,2,2,2,2,2,2,2,2,2,2,2,2,2,2,2,2,2,2,2,2,2,2,2,2,2,2,2,2,2,
2,2,2,2,2,2,2,2,2,2,2,2,2,2,2,2,2,2,2,2,2,2,2,2,2,2,2,2,2,2,2,2,2,2,2,2,
2,2,2,2,2,2,2,2,2,2,2,2,2,2,2,2,2,2,2,2,2,2,2,2,2,2,2,2,2,2,2,2,2,2,2,2,
2,2,2,2,2,2,2,2,2,2,2,2,3),(0.,1.),(0.,0.0072463768115942,0.0144927536231884,
0.0217391304347826,0.0289855072463768,0.036231884057971,0.0434782608695652,
0.0507246376811594,0.0579710144927536,0.0652173913043478,0.072463768115942,
0.0797101449275362,0.0869565217391304,0.0942028985507246,0.101449275362319,
0.108695652173913,0.115942028985507,0.123188405797101,0.130434782608696,
0.13768115942029,0.144927536231884,0.152173913043478,0.159420289855073,
0.166666666666667,0.173913043478261,0.181159420289855,0.18840579710145,
0.195652173913044,0.202898550724637,0.210144927536232,0.217391304347826,
0.224637681159421,0.231884057971014,0.239130434782609,0.246376811594203,
0.253623188405797,0.260869565217392,0.268115942028985,0.275362318840579,
0.282608695652174,0.289855072463768,0.297101449275363,0.304347826086956,
0.31159420289855,0.318840579710145,0.326086956521739,0.333333333333334,
0.340579710144927,0.347826086956521,0.355072463768116,0.36231884057971,
0.369565217391304,0.376811594202899,0.384057971014493,0.391304347826087,
0.398550724637681,0.405797101449275,0.41304347826087,0.420289855072463,
0.427536231884058,0.434782608695652,0.442028985507247,0.449275362318841,
0.456521739130435,0.463768115942029,0.471014492753623,0.478260869565218,
0.485507246376812,0.492753623188406,0.5,0.507246376811594,0.514492753623188,
0.521739130434783,0.528985507246377,0.536231884057971,0.543478260869565,
0.550724637681159,0.557971014492754,0.565217391304348,0.572463768115942,
0.579710144927536,0.586956521739131,0.594202898550725,0.601449275362319,
0.608695652173913,0.615942028985507,0.623188405797101,0.630434782608696,
0.63768115942029,0.644927536231884,0.652173913043478,0.659420289855073,
0.666666666666667,0.673913043478261,0.681159420289855,0.688405797101449,
0.695652173913044,0.702898550724638,0.710144927536232,0.717391304347826,
0.72463768115942,0.731884057971015,0.739130434782609,0.746376811594203,
0.753623188405797,0.760869565217391,0.768115942028986,0.77536231884058,
0.782608695652174,0.789855072463768,0.797101449275362,0.804347826086956,
0.811594202898551,0.818840579710145,0.826086956521739,0.833333333333333,
0.840579710144928,0.847826086956522,0.855072463768116,0.86231884057971,
0.869565217391304,0.876811594202899,0.884057971014493,0.891304347826087,
0.898550724637681,0.905797101449275,0.91304347826087,0.920289855072464,
0.927536231884058,0.934782608695652,0.942028985507246,0.94927536231884,
0.956521739130435,0.963768115942029,0.971014492753623,0.978260869565217,
0.985507246376812,0.992753623188406,0.993818585798284),.UNSPECIFIED.)
GEOMETRIC_REPRESENTATION_ITEM()
RATIONAL_B_SPLINE_SURFACE(((1.,0.866025403784439,1.,0.866025403784439,1.,
0.866025403784439,1.,0.866025403784439,1.,0.866025403784439,1.,0.866025403784439,
1.,0.866025403784439,1.,0.866025403784439,1.,0.866025403784439,1.,0.866025403784439,
1.,0.866025403784439,1.,0.866025403784439,1.,0.866025403784439,1.,0.866025403784439,
1.,0.866025403784439,1.,0.866025403784439,1.,0.866025403784439,1.,0.866025403784439,
1.,0.866025403784439,1.,0.866025403784439,1.,0.866025403784439,1.,0.866025403784439,
1.,0.866025403784439,1.,0.866025403784439,1.,0.866025403784439,1.,0.866025403784439,
1.,0.866025403784439,1.,0.866025403784439,1.,0.866025403784439,1.,0.866025403784439,
1.,0.866025403784439,1.,0.866025403784439,1.,0.866025403784439,1.,0.866025403784439,
1.,0.866025403784439,1.,0.866025403784439,1.,0.866025403784439,1.,0.866025403784439,
1.,0.866025403784439,1.,0.866025403784439,1.,0.866025403784439,1.,0.866025403784439,
1.,0.866025403784439,1.,0.866025403784439,1.,0.866025403784439,1.,0.866025403784439,
1.,0.866025403784439,1.,0.866025403784439,1.,0.866025403784439,1.,0.866025403784439,
1.,0.866025403784439,1.,0.866025403784439,1.,0.866025403784439,1.,0.866025403784439,
1.,0.866025403784439,1.,0.866025403784439,1.,0.866025403784439,1.,0.866025403784439,
1.,0.866025403784439,1.,0.866025403784439,1.,0.866025403784439,1.,0.866025403784439,
1.,0.866025403784439,1.,0.866025403784439,1.,0.866025403784439,1.,0.866025403784439,
1.,0.866025403784439,1.,0.866025403784439,1.,0.866025403784439,1.,0.866025403784439,
1.,0.866025403784439,1.,0.866025403784439,1.,0.866025403784439,1.,0.866025403784439,
1.,0.866025403784439,1.,0.866025403784439,1.,0.866025403784439,1.,0.866025403784439,
1.,0.866025403784439,1.,0.866025403784439,1.,0.866025403784439,1.,0.866025403784439,
1.,0.866025403784439,1.,0.866025403784439,1.,0.866025403784439,1.,0.866025403784439,
1.,0.866025403784439,1.,0.866025403784439,1.,0.866025403784439,1.,0.866025403784439,
1.,0.866025403784439,1.,0.866025403784439,1.,0.866025403784439,1.,0.866025403784439,
1.,0.866025403784439,1.,0.866025403784439,1.,0.866025403784439,1.,0.866025403784439,
1.,0.866025403784439,1.,0.866025403784439,1.,0.866025403784439,1.,0.866025403784439,
1.,0.866025403784439,1.,0.866025403784439,1.,0.866025403784439,1.,0.866025403784439,
1.,0.866025403784439,1.,0.866025403784439,1.,0.866025403784439,1.,0.866025403784439,
1.,0.866025403784439,1.,0.866025403784439,1.,0.866025403784439,1.,0.866025403784439,
1.,0.866025403784439,1.,0.866025403784439,1.,0.866025403784439,1.,0.866025403784439,
1.,0.866025403784439,1.,0.866025403784439,1.,0.866025403784439,1.,0.866025403784439,
1.,0.866025403784439,1.,0.866025403784439,1.,0.866025403784439,1.,0.866025403784439,
1.,0.866025403784439,1.,0.866025403784439,1.,0.866025403784439,1.,0.866025403784439,
1.,0.866025403784439,1.,0.866025403784439,1.,0.866025403784439,1.,0.866025403784439,
1.,0.866025403784439,1.,0.866025403784439,1.,0.866025403784439,1.,0.98031044488126,
0.966408234404338),(1.,0.866025403784439,1.,0.866025403784439,1.,0.866025403784439,
1.,0.866025403784439,1.,0.866025403784439,1.,0.866025403784439,1.,0.866025403784439,
1.,0.866025403784439,1.,0.866025403784439,1.,0.866025403784439,1.,0.866025403784439,
1.,0.866025403784439,1.,0.866025403784439,1.,0.866025403784439,1.,0.866025403784439,
1.,0.866025403784439,1.,0.866025403784439,1.,0.866025403784439,1.,0.866025403784439,
1.,0.866025403784439,1.,0.866025403784439,1.,0.866025403784439,1.,0.866025403784439,
1.,0.866025403784439,1.,0.866025403784439,1.,0.866025403784439,1.,0.866025403784439,
1.,0.866025403784439,1.,0.866025403784439,1.,0.866025403784439,1.,0.866025403784439,
1.,0.866025403784439,1.,0.866025403784439,1.,0.866025403784439,1.,0.866025403784439,
1.,0.866025403784439,1.,0.866025403784439,1.,0.866025403784439,1.,0.866025403784439,
1.,0.866025403784439,1.,0.866025403784439,1.,0.866025403784439,1.,0.866025403784439,
1.,0.866025403784439,1.,0.866025403784439,1.,0.866025403784439,1.,0.866025403784439,
1.,0.866025403784439,1.,0.866025403784439,1.,0.866025403784439,1.,0.866025403784439,
1.,0.866025403784439,1.,0.866025403784439,1.,0.866025403784439,1.,0.866025403784439,
1.,0.866025403784439,1.,0.866025403784439,1.,0.866025403784439,1.,0.866025403784439,
1.,0.866025403784439,1.,0.866025403784439,1.,0.866025403784439,1.,0.866025403784439,
1.,0.866025403784439,1.,0.866025403784439,1.,0.866025403784439,1.,0.866025403784439,
1.,0.866025403784439,1.,0.866025403784439,1.,0.866025403784439,1.,0.866025403784439,
1.,0.866025403784439,1.,0.866025403784439,1.,0.866025403784439,1.,0.866025403784439,
1.,0.866025403784439,1.,0.866025403784439,1.,0.866025403784439,1.,0.866025403784439,
1.,0.866025403784439,1.,0.866025403784439,1.,0.866025403784439,1.,0.866025403784439,
1.,0.866025403784439,1.,0.866025403784439,1.,0.866025403784439,1.,0.866025403784439,
1.,0.866025403784439,1.,0.866025403784439,1.,0.866025403784439,1.,0.866025403784439,
1.,0.866025403784439,1.,0.866025403784439,1.,0.866025403784439,1.,0.866025403784439,
1.,0.866025403784439,1.,0.866025403784439,1.,0.866025403784439,1.,0.866025403784439,
1.,0.866025403784439,1.,0.866025403784439,1.,0.866025403784439,1.,0.866025403784439,
1.,0.866025403784439,1.,0.866025403784439,1.,0.866025403784439,1.,0.866025403784439,
1.,0.866025403784439,1.,0.866025403784439,1.,0.866025403784439,1.,0.866025403784439,
1.,0.866025403784439,1.,0.866025403784439,1.,0.866025403784439,1.,0.866025403784439,
1.,0.866025403784439,1.,0.866025403784439,1.,0.866025403784439,1.,0.866025403784439,
1.,0.866025403784439,1.,0.866025403784439,1.,0.866025403784439,1.,0.866025403784439,
1.,0.866025403784439,1.,0.866025403784439,1.,0.866025403784439,1.,0.866025403784439,
1.,0.866025403784439,1.,0.866025403784439,1.,0.866025403784439,1.,0.866025403784439,
1.,0.866025403784439,1.,0.866025403784439,1.,0.866025403784439,1.,0.866025403784439,
1.,0.866025403784439,1.,0.866025403784439,1.,0.98031044488126,0.966408234404338)))
REPRESENTATION_ITEM('')
SURFACE()
);
#3174=(
BOUNDED_SURFACE()
B_SPLINE_SURFACE(1,2,((#252065,#252066,#252067,#252068,#252069,#252070,
#252071,#252072,#252073,#252074,#252075,#252076,#252077,#252078,#252079,
#252080,#252081,#252082,#252083,#252084,#252085,#252086,#252087,#252088,
#252089,#252090,#252091,#252092,#252093,#252094,#252095,#252096,#252097,
#252098,#252099,#252100,#252101,#252102,#252103,#252104,#252105,#252106,
#252107,#252108,#252109,#252110,#252111,#252112,#252113,#252114,#252115,
#252116,#252117,#252118,#252119,#252120,#252121,#252122,#252123,#252124,
#252125,#252126,#252127,#252128,#252129,#252130,#252131,#252132,#252133,
#252134,#252135,#252136,#252137,#252138,#252139,#252140,#252141,#252142,
#252143,#252144,#252145,#252146,#252147,#252148,#252149,#252150,#252151,
#252152,#252153,#252154,#252155,#252156,#252157,#252158,#252159,#252160,
#252161,#252162,#252163,#252164,#252165,#252166,#252167,#252168,#252169,
#252170,#252171,#252172,#252173,#252174,#252175,#252176,#252177,#252178,
#252179,#252180,#252181,#252182,#252183,#252184,#252185,#252186,#252187,
#252188,#252189,#252190,#252191,#252192,#252193,#252194,#252195,#252196,
#252197,#252198,#252199,#252200,#252201,#252202,#252203,#252204,#252205,
#252206,#252207,#252208,#252209,#252210,#252211,#252212,#252213,#252214,
#252215,#252216,#252217,#252218,#252219,#252220,#252221,#252222,#252223,
#252224,#252225,#252226,#252227,#252228,#252229,#252230,#252231,#252232,
#252233,#252234,#252235,#252236,#252237,#252238,#252239,#252240,#252241,
#252242,#252243,#252244,#252245,#252246,#252247,#252248,#252249,#252250,
#252251,#252252,#252253,#252254,#252255,#252256,#252257,#252258,#252259,
#252260,#252261,#252262,#252263,#252264,#252265,#252266,#252267,#252268,
#252269,#252270,#252271,#252272,#252273,#252274,#252275,#252276,#252277,
#252278,#252279,#252280,#252281,#252282,#252283,#252284,#252285,#252286,
#252287,#252288,#252289,#252290,#252291,#252292,#252293,#252294,#252295,
#252296,#252297,#252298,#252299,#252300,#252301,#252302,#252303,#252304,
#252305,#252306,#252307,#252308,#252309,#252310,#252311,#252312,#252313,
#252314,#252315,#252316,#252317,#252318,#252319,#252320,#252321,#252322,
#252323,#252324,#252325,#252326,#252327,#252328,#252329,#252330,#252331,
#252332,#252333,#252334,#252335,#252336,#252337,#252338,#252339,#252340,
#252341),(#252342,#252343,#252344,#252345,#252346,#252347,#252348,#252349,
#252350,#252351,#252352,#252353,#252354,#252355,#252356,#252357,#252358,
#252359,#252360,#252361,#252362,#252363,#252364,#252365,#252366,#252367,
#252368,#252369,#252370,#252371,#252372,#252373,#252374,#252375,#252376,
#252377,#252378,#252379,#252380,#252381,#252382,#252383,#252384,#252385,
#252386,#252387,#252388,#252389,#252390,#252391,#252392,#252393,#252394,
#252395,#252396,#252397,#252398,#252399,#252400,#252401,#252402,#252403,
#252404,#252405,#252406,#252407,#252408,#252409,#252410,#252411,#252412,
#252413,#252414,#252415,#252416,#252417,#252418,#252419,#252420,#252421,
#252422,#252423,#252424,#252425,#252426,#252427,#252428,#252429,#252430,
#252431,#252432,#252433,#252434,#252435,#252436,#252437,#252438,#252439,
#252440,#252441,#252442,#252443,#252444,#252445,#252446,#252447,#252448,
#252449,#252450,#252451,#252452,#252453,#252454,#252455,#252456,#252457,
#252458,#252459,#252460,#252461,#252462,#252463,#252464,#252465,#252466,
#252467,#252468,#252469,#252470,#252471,#252472,#252473,#252474,#252475,
#252476,#252477,#252478,#252479,#252480,#252481,#252482,#252483,#252484,
#252485,#252486,#252487,#252488,#252489,#252490,#252491,#252492,#252493,
#252494,#252495,#252496,#252497,#252498,#252499,#252500,#252501,#252502,
#252503,#252504,#252505,#252506,#252507,#252508,#252509,#252510,#252511,
#252512,#252513,#252514,#252515,#252516,#252517,#252518,#252519,#252520,
#252521,#252522,#252523,#252524,#252525,#252526,#252527,#252528,#252529,
#252530,#252531,#252532,#252533,#252534,#252535,#252536,#252537,#252538,
#252539,#252540,#252541,#252542,#252543,#252544,#252545,#252546,#252547,
#252548,#252549,#252550,#252551,#252552,#252553,#252554,#252555,#252556,
#252557,#252558,#252559,#252560,#252561,#252562,#252563,#252564,#252565,
#252566,#252567,#252568,#252569,#252570,#252571,#252572,#252573,#252574,
#252575,#252576,#252577,#252578,#252579,#252580,#252581,#252582,#252583,
#252584,#252585,#252586,#252587,#252588,#252589,#252590,#252591,#252592,
#252593,#252594,#252595,#252596,#252597,#252598,#252599,#252600,#252601,
#252602,#252603,#252604,#252605,#252606,#252607,#252608,#252609,#252610,
#252611,#252612,#252613,#252614,#252615,#252616,#252617,#252618)),
 .UNSPECIFIED.,.F.,.F.,.F.)
B_SPLINE_SURFACE_WITH_KNOTS((2,2),(3,2,2,2,2,2,2,2,2,2,2,2,2,2,2,2,2,2,
2,2,2,2,2,2,2,2,2,2,2,2,2,2,2,2,2,2,2,2,2,2,2,2,2,2,2,2,2,2,2,2,2,2,2,2,
2,2,2,2,2,2,2,2,2,2,2,2,2,2,2,2,2,2,2,2,2,2,2,2,2,2,2,2,2,2,2,2,2,2,2,2,
2,2,2,2,2,2,2,2,2,2,2,2,2,2,2,2,2,2,2,2,2,2,2,2,2,2,2,2,2,2,2,2,2,2,2,2,
2,2,2,2,2,2,2,2,2,2,2,2,3),(0.,1.),(0.,0.0072463768115942,0.0144927536231884,
0.0217391304347826,0.0289855072463768,0.036231884057971,0.0434782608695652,
0.0507246376811594,0.0579710144927536,0.0652173913043478,0.072463768115942,
0.0797101449275362,0.0869565217391304,0.0942028985507246,0.101449275362319,
0.108695652173913,0.115942028985507,0.123188405797101,0.130434782608696,
0.13768115942029,0.144927536231884,0.152173913043478,0.159420289855073,
0.166666666666667,0.173913043478261,0.181159420289855,0.18840579710145,
0.195652173913044,0.202898550724637,0.210144927536232,0.217391304347826,
0.224637681159421,0.231884057971014,0.239130434782609,0.246376811594203,
0.253623188405797,0.260869565217392,0.268115942028985,0.275362318840579,
0.282608695652174,0.289855072463768,0.297101449275363,0.304347826086956,
0.31159420289855,0.318840579710145,0.326086956521739,0.333333333333334,
0.340579710144927,0.347826086956521,0.355072463768116,0.36231884057971,
0.369565217391304,0.376811594202899,0.384057971014493,0.391304347826087,
0.398550724637681,0.405797101449275,0.41304347826087,0.420289855072463,
0.427536231884058,0.434782608695652,0.442028985507247,0.449275362318841,
0.456521739130435,0.463768115942029,0.471014492753623,0.478260869565218,
0.485507246376812,0.492753623188406,0.5,0.507246376811594,0.514492753623188,
0.521739130434783,0.528985507246377,0.536231884057971,0.543478260869565,
0.550724637681159,0.557971014492754,0.565217391304348,0.572463768115942,
0.579710144927536,0.586956521739131,0.594202898550725,0.601449275362319,
0.608695652173913,0.615942028985507,0.623188405797101,0.630434782608696,
0.63768115942029,0.644927536231884,0.652173913043478,0.659420289855073,
0.666666666666667,0.673913043478261,0.681159420289855,0.688405797101449,
0.695652173913044,0.702898550724638,0.710144927536232,0.717391304347826,
0.72463768115942,0.731884057971015,0.739130434782609,0.746376811594203,
0.753623188405797,0.760869565217391,0.768115942028986,0.77536231884058,
0.782608695652174,0.789855072463768,0.797101449275362,0.804347826086956,
0.811594202898551,0.818840579710145,0.826086956521739,0.833333333333333,
0.840579710144928,0.847826086956522,0.855072463768116,0.86231884057971,
0.869565217391304,0.876811594202899,0.884057971014493,0.891304347826087,
0.898550724637681,0.905797101449275,0.91304347826087,0.920289855072464,
0.927536231884058,0.934782608695652,0.942028985507246,0.94927536231884,
0.956521739130435,0.963768115942029,0.971014492753623,0.978260869565217,
0.985507246376812,0.992753623188406,0.993818495192186),.UNSPECIFIED.)
GEOMETRIC_REPRESENTATION_ITEM()
RATIONAL_B_SPLINE_SURFACE(((1.,0.866025403784439,1.,0.866025403784439,1.,
0.866025403784439,1.,0.866025403784439,1.,0.866025403784439,1.,0.866025403784439,
1.,0.866025403784439,1.,0.866025403784439,1.,0.866025403784439,1.,0.866025403784439,
1.,0.866025403784439,1.,0.866025403784439,1.,0.866025403784439,1.,0.866025403784439,
1.,0.866025403784439,1.,0.866025403784439,1.,0.866025403784439,1.,0.866025403784439,
1.,0.866025403784439,1.,0.866025403784439,1.,0.866025403784439,1.,0.866025403784439,
1.,0.866025403784439,1.,0.866025403784439,1.,0.866025403784439,1.,0.866025403784439,
1.,0.866025403784439,1.,0.866025403784439,1.,0.866025403784439,1.,0.866025403784439,
1.,0.866025403784439,1.,0.866025403784439,1.,0.866025403784439,1.,0.866025403784439,
1.,0.866025403784439,1.,0.866025403784439,1.,0.866025403784439,1.,0.866025403784439,
1.,0.866025403784439,1.,0.866025403784439,1.,0.866025403784439,1.,0.866025403784439,
1.,0.866025403784439,1.,0.866025403784439,1.,0.866025403784439,1.,0.866025403784439,
1.,0.866025403784439,1.,0.866025403784439,1.,0.866025403784439,1.,0.866025403784439,
1.,0.866025403784439,1.,0.866025403784439,1.,0.866025403784439,1.,0.866025403784439,
1.,0.866025403784439,1.,0.866025403784439,1.,0.866025403784439,1.,0.866025403784439,
1.,0.866025403784439,1.,0.866025403784439,1.,0.866025403784439,1.,0.866025403784439,
1.,0.866025403784439,1.,0.866025403784439,1.,0.866025403784439,1.,0.866025403784439,
1.,0.866025403784439,1.,0.866025403784439,1.,0.866025403784439,1.,0.866025403784439,
1.,0.866025403784439,1.,0.866025403784439,1.,0.866025403784439,1.,0.866025403784439,
1.,0.866025403784439,1.,0.866025403784439,1.,0.866025403784439,1.,0.866025403784439,
1.,0.866025403784439,1.,0.866025403784439,1.,0.866025403784439,1.,0.866025403784439,
1.,0.866025403784439,1.,0.866025403784439,1.,0.866025403784439,1.,0.866025403784439,
1.,0.866025403784439,1.,0.866025403784439,1.,0.866025403784439,1.,0.866025403784439,
1.,0.866025403784439,1.,0.866025403784439,1.,0.866025403784439,1.,0.866025403784439,
1.,0.866025403784439,1.,0.866025403784439,1.,0.866025403784439,1.,0.866025403784439,
1.,0.866025403784439,1.,0.866025403784439,1.,0.866025403784439,1.,0.866025403784439,
1.,0.866025403784439,1.,0.866025403784439,1.,0.866025403784439,1.,0.866025403784439,
1.,0.866025403784439,1.,0.866025403784439,1.,0.866025403784439,1.,0.866025403784439,
1.,0.866025403784439,1.,0.866025403784439,1.,0.866025403784439,1.,0.866025403784439,
1.,0.866025403784439,1.,0.866025403784439,1.,0.866025403784439,1.,0.866025403784439,
1.,0.866025403784439,1.,0.866025403784439,1.,0.866025403784439,1.,0.866025403784439,
1.,0.866025403784439,1.,0.866025403784439,1.,0.866025403784439,1.,0.866025403784439,
1.,0.866025403784439,1.,0.866025403784439,1.,0.866025403784439,1.,0.866025403784439,
1.,0.866025403784439,1.,0.866025403784439,1.,0.866025403784439,1.,0.866025403784439,
1.,0.866025403784439,1.,0.866025403784439,1.,0.866025403784439,1.,0.980312120051573,
0.966410600022306),(1.,0.866025403784439,1.,0.866025403784439,1.,0.866025403784439,
1.,0.866025403784439,1.,0.866025403784439,1.,0.866025403784439,1.,0.866025403784439,
1.,0.866025403784439,1.,0.866025403784439,1.,0.866025403784439,1.,0.866025403784439,
1.,0.866025403784439,1.,0.866025403784439,1.,0.866025403784439,1.,0.866025403784439,
1.,0.866025403784439,1.,0.866025403784439,1.,0.866025403784439,1.,0.866025403784439,
1.,0.866025403784439,1.,0.866025403784439,1.,0.866025403784439,1.,0.866025403784439,
1.,0.866025403784439,1.,0.866025403784439,1.,0.866025403784439,1.,0.866025403784439,
1.,0.866025403784439,1.,0.866025403784439,1.,0.866025403784439,1.,0.866025403784439,
1.,0.866025403784439,1.,0.866025403784439,1.,0.866025403784439,1.,0.866025403784439,
1.,0.866025403784439,1.,0.866025403784439,1.,0.866025403784439,1.,0.866025403784439,
1.,0.866025403784439,1.,0.866025403784439,1.,0.866025403784439,1.,0.866025403784439,
1.,0.866025403784439,1.,0.866025403784439,1.,0.866025403784439,1.,0.866025403784439,
1.,0.866025403784439,1.,0.866025403784439,1.,0.866025403784439,1.,0.866025403784439,
1.,0.866025403784439,1.,0.866025403784439,1.,0.866025403784439,1.,0.866025403784439,
1.,0.866025403784439,1.,0.866025403784439,1.,0.866025403784439,1.,0.866025403784439,
1.,0.866025403784439,1.,0.866025403784439,1.,0.866025403784439,1.,0.866025403784439,
1.,0.866025403784439,1.,0.866025403784439,1.,0.866025403784439,1.,0.866025403784439,
1.,0.866025403784439,1.,0.866025403784439,1.,0.866025403784439,1.,0.866025403784439,
1.,0.866025403784439,1.,0.866025403784439,1.,0.866025403784439,1.,0.866025403784439,
1.,0.866025403784439,1.,0.866025403784439,1.,0.866025403784439,1.,0.866025403784439,
1.,0.866025403784439,1.,0.866025403784439,1.,0.866025403784439,1.,0.866025403784439,
1.,0.866025403784439,1.,0.866025403784439,1.,0.866025403784439,1.,0.866025403784439,
1.,0.866025403784439,1.,0.866025403784439,1.,0.866025403784439,1.,0.866025403784439,
1.,0.866025403784439,1.,0.866025403784439,1.,0.866025403784439,1.,0.866025403784439,
1.,0.866025403784439,1.,0.866025403784439,1.,0.866025403784439,1.,0.866025403784439,
1.,0.866025403784439,1.,0.866025403784439,1.,0.866025403784439,1.,0.866025403784439,
1.,0.866025403784439,1.,0.866025403784439,1.,0.866025403784439,1.,0.866025403784439,
1.,0.866025403784439,1.,0.866025403784439,1.,0.866025403784439,1.,0.866025403784439,
1.,0.866025403784439,1.,0.866025403784439,1.,0.866025403784439,1.,0.866025403784439,
1.,0.866025403784439,1.,0.866025403784439,1.,0.866025403784439,1.,0.866025403784439,
1.,0.866025403784439,1.,0.866025403784439,1.,0.866025403784439,1.,0.866025403784439,
1.,0.866025403784439,1.,0.866025403784439,1.,0.866025403784439,1.,0.866025403784439,
1.,0.866025403784439,1.,0.866025403784439,1.,0.866025403784439,1.,0.866025403784439,
1.,0.866025403784439,1.,0.866025403784439,1.,0.866025403784439,1.,0.866025403784439,
1.,0.866025403784439,1.,0.866025403784439,1.,0.980312120051573,0.966410600022306)))
REPRESENTATION_ITEM('')
SURFACE()
);
#3175=(
BOUNDED_SURFACE()
B_SPLINE_SURFACE(1,2,((#252619,#252620,#252621,#252622,#252623,#252624,
#252625,#252626,#252627,#252628,#252629,#252630,#252631,#252632,#252633,
#252634,#252635,#252636,#252637,#252638,#252639,#252640,#252641,#252642,
#252643,#252644,#252645,#252646,#252647,#252648,#252649,#252650,#252651,
#252652,#252653,#252654,#252655,#252656,#252657,#252658,#252659,#252660,
#252661,#252662,#252663,#252664,#252665,#252666,#252667,#252668,#252669,
#252670,#252671,#252672,#252673,#252674,#252675,#252676,#252677,#252678,
#252679,#252680,#252681,#252682,#252683,#252684,#252685,#252686,#252687,
#252688,#252689,#252690,#252691,#252692,#252693,#252694,#252695,#252696,
#252697,#252698,#252699,#252700,#252701,#252702,#252703,#252704,#252705,
#252706,#252707,#252708,#252709,#252710,#252711,#252712,#252713,#252714,
#252715,#252716,#252717,#252718,#252719,#252720,#252721,#252722,#252723,
#252724,#252725,#252726,#252727,#252728,#252729,#252730,#252731,#252732,
#252733,#252734,#252735,#252736,#252737,#252738,#252739,#252740,#252741,
#252742,#252743,#252744,#252745,#252746,#252747,#252748,#252749,#252750,
#252751,#252752,#252753,#252754,#252755,#252756,#252757,#252758,#252759,
#252760,#252761,#252762,#252763,#252764,#252765,#252766,#252767,#252768,
#252769,#252770,#252771,#252772,#252773,#252774,#252775,#252776,#252777,
#252778,#252779,#252780,#252781,#252782,#252783,#252784,#252785,#252786,
#252787,#252788,#252789,#252790,#252791,#252792,#252793,#252794,#252795,
#252796,#252797,#252798,#252799,#252800,#252801,#252802,#252803,#252804,
#252805,#252806,#252807,#252808,#252809,#252810,#252811,#252812,#252813,
#252814,#252815,#252816,#252817,#252818,#252819,#252820,#252821,#252822,
#252823,#252824,#252825,#252826,#252827,#252828,#252829,#252830,#252831,
#252832,#252833,#252834,#252835,#252836,#252837,#252838,#252839,#252840,
#252841,#252842,#252843,#252844,#252845,#252846,#252847,#252848,#252849,
#252850,#252851,#252852,#252853,#252854,#252855,#252856,#252857,#252858,
#252859,#252860,#252861,#252862,#252863,#252864,#252865,#252866,#252867,
#252868,#252869,#252870,#252871,#252872,#252873,#252874,#252875,#252876,
#252877,#252878,#252879,#252880,#252881,#252882,#252883,#252884,#252885,
#252886,#252887,#252888,#252889,#252890,#252891,#252892,#252893,#252894,
#252895),(#252896,#252897,#252898,#252899,#252900,#252901,#252902,#252903,
#252904,#252905,#252906,#252907,#252908,#252909,#252910,#252911,#252912,
#252913,#252914,#252915,#252916,#252917,#252918,#252919,#252920,#252921,
#252922,#252923,#252924,#252925,#252926,#252927,#252928,#252929,#252930,
#252931,#252932,#252933,#252934,#252935,#252936,#252937,#252938,#252939,
#252940,#252941,#252942,#252943,#252944,#252945,#252946,#252947,#252948,
#252949,#252950,#252951,#252952,#252953,#252954,#252955,#252956,#252957,
#252958,#252959,#252960,#252961,#252962,#252963,#252964,#252965,#252966,
#252967,#252968,#252969,#252970,#252971,#252972,#252973,#252974,#252975,
#252976,#252977,#252978,#252979,#252980,#252981,#252982,#252983,#252984,
#252985,#252986,#252987,#252988,#252989,#252990,#252991,#252992,#252993,
#252994,#252995,#252996,#252997,#252998,#252999,#253000,#253001,#253002,
#253003,#253004,#253005,#253006,#253007,#253008,#253009,#253010,#253011,
#253012,#253013,#253014,#253015,#253016,#253017,#253018,#253019,#253020,
#253021,#253022,#253023,#253024,#253025,#253026,#253027,#253028,#253029,
#253030,#253031,#253032,#253033,#253034,#253035,#253036,#253037,#253038,
#253039,#253040,#253041,#253042,#253043,#253044,#253045,#253046,#253047,
#253048,#253049,#253050,#253051,#253052,#253053,#253054,#253055,#253056,
#253057,#253058,#253059,#253060,#253061,#253062,#253063,#253064,#253065,
#253066,#253067,#253068,#253069,#253070,#253071,#253072,#253073,#253074,
#253075,#253076,#253077,#253078,#253079,#253080,#253081,#253082,#253083,
#253084,#253085,#253086,#253087,#253088,#253089,#253090,#253091,#253092,
#253093,#253094,#253095,#253096,#253097,#253098,#253099,#253100,#253101,
#253102,#253103,#253104,#253105,#253106,#253107,#253108,#253109,#253110,
#253111,#253112,#253113,#253114,#253115,#253116,#253117,#253118,#253119,
#253120,#253121,#253122,#253123,#253124,#253125,#253126,#253127,#253128,
#253129,#253130,#253131,#253132,#253133,#253134,#253135,#253136,#253137,
#253138,#253139,#253140,#253141,#253142,#253143,#253144,#253145,#253146,
#253147,#253148,#253149,#253150,#253151,#253152,#253153,#253154,#253155,
#253156,#253157,#253158,#253159,#253160,#253161,#253162,#253163,#253164,
#253165,#253166,#253167,#253168,#253169,#253170,#253171,#253172)),
 .UNSPECIFIED.,.F.,.F.,.F.)
B_SPLINE_SURFACE_WITH_KNOTS((2,2),(3,2,2,2,2,2,2,2,2,2,2,2,2,2,2,2,2,2,
2,2,2,2,2,2,2,2,2,2,2,2,2,2,2,2,2,2,2,2,2,2,2,2,2,2,2,2,2,2,2,2,2,2,2,2,
2,2,2,2,2,2,2,2,2,2,2,2,2,2,2,2,2,2,2,2,2,2,2,2,2,2,2,2,2,2,2,2,2,2,2,2,
2,2,2,2,2,2,2,2,2,2,2,2,2,2,2,2,2,2,2,2,2,2,2,2,2,2,2,2,2,2,2,2,2,2,2,2,
2,2,2,2,2,2,2,2,2,2,2,2,3),(0.,1.00000048160228),(0.,0.0072463768115942,
0.0144927536231884,0.0217391304347826,0.0289855072463768,0.036231884057971,
0.0434782608695652,0.0507246376811594,0.0579710144927536,0.0652173913043478,
0.072463768115942,0.0797101449275362,0.0869565217391304,0.0942028985507246,
0.101449275362319,0.108695652173913,0.115942028985507,0.123188405797101,
0.130434782608696,0.13768115942029,0.144927536231884,0.152173913043478,
0.159420289855073,0.166666666666667,0.173913043478261,0.181159420289855,
0.18840579710145,0.195652173913044,0.202898550724637,0.210144927536232,
0.217391304347826,0.224637681159421,0.231884057971014,0.239130434782609,
0.246376811594203,0.253623188405797,0.260869565217392,0.268115942028985,
0.275362318840579,0.282608695652174,0.289855072463768,0.297101449275363,
0.304347826086956,0.31159420289855,0.318840579710145,0.326086956521739,
0.333333333333334,0.340579710144927,0.347826086956521,0.355072463768116,
0.36231884057971,0.369565217391304,0.376811594202899,0.384057971014493,
0.391304347826087,0.398550724637681,0.405797101449275,0.41304347826087,
0.420289855072463,0.427536231884058,0.434782608695652,0.442028985507247,
0.449275362318841,0.456521739130435,0.463768115942029,0.471014492753623,
0.478260869565218,0.485507246376812,0.492753623188406,0.5,0.507246376811594,
0.514492753623188,0.521739130434783,0.528985507246377,0.536231884057971,
0.543478260869565,0.550724637681159,0.557971014492754,0.565217391304348,
0.572463768115942,0.579710144927536,0.586956521739131,0.594202898550725,
0.601449275362319,0.608695652173913,0.615942028985507,0.623188405797101,
0.630434782608696,0.63768115942029,0.644927536231884,0.652173913043478,
0.659420289855073,0.666666666666667,0.673913043478261,0.681159420289855,
0.688405797101449,0.695652173913044,0.702898550724638,0.710144927536232,
0.717391304347826,0.72463768115942,0.731884057971015,0.739130434782609,
0.746376811594203,0.753623188405797,0.760869565217391,0.768115942028986,
0.77536231884058,0.782608695652174,0.789855072463768,0.797101449275362,
0.804347826086956,0.811594202898551,0.818840579710145,0.826086956521739,
0.833333333333333,0.840579710144928,0.847826086956522,0.855072463768116,
0.86231884057971,0.869565217391304,0.876811594202899,0.884057971014493,
0.891304347826087,0.898550724637681,0.905797101449275,0.91304347826087,
0.920289855072464,0.927536231884058,0.934782608695652,0.942028985507246,
0.94927536231884,0.956521739130435,0.963768115942029,0.971014492753623,
0.978260869565217,0.985507246376812,0.992753623188406,0.993818495192186),
 .UNSPECIFIED.)
GEOMETRIC_REPRESENTATION_ITEM()
RATIONAL_B_SPLINE_SURFACE(((1.,0.866025403784439,1.,0.866025403784439,1.,
0.866025403784439,1.,0.866025403784439,1.,0.866025403784439,1.,0.866025403784439,
1.,0.866025403784439,1.,0.866025403784439,1.,0.866025403784439,1.,0.866025403784439,
1.,0.866025403784439,1.,0.866025403784439,1.,0.866025403784439,1.,0.866025403784439,
1.,0.866025403784439,1.,0.866025403784439,1.,0.866025403784439,1.,0.866025403784439,
1.,0.866025403784439,1.,0.866025403784439,1.,0.866025403784439,1.,0.866025403784439,
1.,0.866025403784439,1.,0.866025403784439,1.,0.866025403784439,1.,0.866025403784439,
1.,0.866025403784439,1.,0.866025403784439,1.,0.866025403784439,1.,0.866025403784439,
1.,0.866025403784439,1.,0.866025403784439,1.,0.866025403784439,1.,0.866025403784439,
1.,0.866025403784439,1.,0.866025403784439,1.,0.866025403784439,1.,0.866025403784439,
1.,0.866025403784439,1.,0.866025403784439,1.,0.866025403784439,1.,0.866025403784439,
1.,0.866025403784439,1.,0.866025403784439,1.,0.866025403784439,1.,0.866025403784439,
1.,0.866025403784439,1.,0.866025403784439,1.,0.866025403784439,1.,0.866025403784439,
1.,0.866025403784439,1.,0.866025403784439,1.,0.866025403784439,1.,0.866025403784439,
1.,0.866025403784439,1.,0.866025403784439,1.,0.866025403784439,1.,0.866025403784439,
1.,0.866025403784439,1.,0.866025403784439,1.,0.866025403784439,1.,0.866025403784439,
1.,0.866025403784439,1.,0.866025403784439,1.,0.866025403784439,1.,0.866025403784439,
1.,0.866025403784439,1.,0.866025403784439,1.,0.866025403784439,1.,0.866025403784439,
1.,0.866025403784439,1.,0.866025403784439,1.,0.866025403784439,1.,0.866025403784439,
1.,0.866025403784439,1.,0.866025403784439,1.,0.866025403784439,1.,0.866025403784439,
1.,0.866025403784439,1.,0.866025403784439,1.,0.866025403784439,1.,0.866025403784439,
1.,0.866025403784439,1.,0.866025403784439,1.,0.866025403784439,1.,0.866025403784439,
1.,0.866025403784439,1.,0.866025403784439,1.,0.866025403784439,1.,0.866025403784439,
1.,0.866025403784439,1.,0.866025403784439,1.,0.866025403784439,1.,0.866025403784439,
1.,0.866025403784439,1.,0.866025403784439,1.,0.866025403784439,1.,0.866025403784439,
1.,0.866025403784439,1.,0.866025403784439,1.,0.866025403784439,1.,0.866025403784439,
1.,0.866025403784439,1.,0.866025403784439,1.,0.866025403784439,1.,0.866025403784439,
1.,0.866025403784439,1.,0.866025403784439,1.,0.866025403784439,1.,0.866025403784439,
1.,0.866025403784439,1.,0.866025403784439,1.,0.866025403784439,1.,0.866025403784439,
1.,0.866025403784439,1.,0.866025403784439,1.,0.866025403784439,1.,0.866025403784439,
1.,0.866025403784439,1.,0.866025403784439,1.,0.866025403784439,1.,0.866025403784439,
1.,0.866025403784439,1.,0.866025403784439,1.,0.866025403784439,1.,0.866025403784439,
1.,0.866025403784439,1.,0.866025403784439,1.,0.866025403784439,1.,0.866025403784439,
1.,0.866025403784439,1.,0.866025403784439,1.,0.866025403784439,1.,0.866025403784439,
1.,0.866025403784439,1.,0.866025403784439,1.,0.866025403784439,1.,0.980312120051573,
0.966410600022306),(1.,0.866025403784439,1.,0.866025403784439,1.,0.866025403784439,
1.,0.866025403784439,1.,0.866025403784439,1.,0.866025403784439,1.,0.866025403784439,
1.,0.866025403784439,1.,0.866025403784439,1.,0.866025403784439,1.,0.866025403784439,
1.,0.866025403784439,1.,0.866025403784439,1.,0.866025403784439,1.,0.866025403784439,
1.,0.866025403784439,1.,0.866025403784439,1.,0.866025403784439,1.,0.866025403784439,
1.,0.866025403784439,1.,0.866025403784439,1.,0.866025403784439,1.,0.866025403784439,
1.,0.866025403784439,1.,0.866025403784439,1.,0.866025403784439,1.,0.866025403784439,
1.,0.866025403784439,1.,0.866025403784439,1.,0.866025403784439,1.,0.866025403784439,
1.,0.866025403784439,1.,0.866025403784439,1.,0.866025403784439,1.,0.866025403784439,
1.,0.866025403784439,1.,0.866025403784439,1.,0.866025403784439,1.,0.866025403784439,
1.,0.866025403784439,1.,0.866025403784439,1.,0.866025403784439,1.,0.866025403784439,
1.,0.866025403784439,1.,0.866025403784439,1.,0.866025403784439,1.,0.866025403784439,
1.,0.866025403784439,1.,0.866025403784439,1.,0.866025403784439,1.,0.866025403784439,
1.,0.866025403784439,1.,0.866025403784439,1.,0.866025403784439,1.,0.866025403784439,
1.,0.866025403784439,1.,0.866025403784439,1.,0.866025403784439,1.,0.866025403784439,
1.,0.866025403784439,1.,0.866025403784439,1.,0.866025403784439,1.,0.866025403784439,
1.,0.866025403784439,1.,0.866025403784439,1.,0.866025403784439,1.,0.866025403784439,
1.,0.866025403784439,1.,0.866025403784439,1.,0.866025403784439,1.,0.866025403784439,
1.,0.866025403784439,1.,0.866025403784439,1.,0.866025403784439,1.,0.866025403784439,
1.,0.866025403784439,1.,0.866025403784439,1.,0.866025403784439,1.,0.866025403784439,
1.,0.866025403784439,1.,0.866025403784439,1.,0.866025403784439,1.,0.866025403784439,
1.,0.866025403784439,1.,0.866025403784439,1.,0.866025403784439,1.,0.866025403784439,
1.,0.866025403784439,1.,0.866025403784439,1.,0.866025403784439,1.,0.866025403784439,
1.,0.866025403784439,1.,0.866025403784439,1.,0.866025403784439,1.,0.866025403784439,
1.,0.866025403784439,1.,0.866025403784439,1.,0.866025403784439,1.,0.866025403784439,
1.,0.866025403784439,1.,0.866025403784439,1.,0.866025403784439,1.,0.866025403784439,
1.,0.866025403784439,1.,0.866025403784439,1.,0.866025403784439,1.,0.866025403784439,
1.,0.866025403784439,1.,0.866025403784439,1.,0.866025403784439,1.,0.866025403784439,
1.,0.866025403784439,1.,0.866025403784439,1.,0.866025403784439,1.,0.866025403784439,
1.,0.866025403784439,1.,0.866025403784439,1.,0.866025403784439,1.,0.866025403784439,
1.,0.866025403784439,1.,0.866025403784439,1.,0.866025403784439,1.,0.866025403784439,
1.,0.866025403784439,1.,0.866025403784439,1.,0.866025403784439,1.,0.866025403784439,
1.,0.866025403784439,1.,0.866025403784439,1.,0.866025403784439,1.,0.866025403784439,
1.,0.866025403784439,1.,0.866025403784439,1.,0.866025403784439,1.,0.866025403784439,
1.,0.866025403784439,1.,0.866025403784439,1.,0.980312120051573,0.966410600022306)))
REPRESENTATION_ITEM('')
SURFACE()
);
#3176=(
BOUNDED_SURFACE()
B_SPLINE_SURFACE(1,2,((#253229,#253230,#253231,#253232,#253233,#253234,
#253235,#253236,#253237,#253238,#253239,#253240,#253241,#253242,#253243,
#253244,#253245,#253246,#253247,#253248,#253249,#253250,#253251,#253252,
#253253,#253254,#253255,#253256,#253257,#253258,#253259,#253260,#253261,
#253262,#253263,#253264,#253265,#253266,#253267,#253268,#253269,#253270,
#253271,#253272,#253273,#253274,#253275,#253276,#253277,#253278,#253279,
#253280,#253281,#253282,#253283,#253284,#253285,#253286,#253287,#253288,
#253289,#253290,#253291,#253292,#253293,#253294,#253295,#253296,#253297,
#253298,#253299,#253300,#253301,#253302,#253303,#253304,#253305,#253306,
#253307,#253308,#253309,#253310,#253311,#253312,#253313,#253314,#253315,
#253316,#253317,#253318,#253319,#253320,#253321,#253322,#253323,#253324,
#253325,#253326,#253327,#253328,#253329,#253330,#253331,#253332,#253333,
#253334,#253335,#253336,#253337,#253338,#253339,#253340,#253341,#253342,
#253343,#253344,#253345,#253346,#253347,#253348,#253349,#253350,#253351,
#253352,#253353,#253354,#253355,#253356,#253357,#253358,#253359,#253360,
#253361,#253362,#253363,#253364,#253365,#253366,#253367,#253368,#253369,
#253370,#253371,#253372,#253373,#253374,#253375,#253376,#253377,#253378,
#253379,#253380,#253381,#253382,#253383,#253384,#253385,#253386,#253387,
#253388,#253389,#253390,#253391,#253392,#253393,#253394,#253395,#253396,
#253397,#253398,#253399,#253400,#253401,#253402,#253403,#253404,#253405,
#253406,#253407,#253408,#253409,#253410,#253411,#253412,#253413,#253414,
#253415,#253416,#253417,#253418,#253419,#253420,#253421,#253422,#253423,
#253424,#253425,#253426,#253427,#253428,#253429,#253430,#253431,#253432,
#253433,#253434,#253435,#253436,#253437,#253438,#253439,#253440,#253441,
#253442,#253443,#253444,#253445,#253446,#253447,#253448,#253449,#253450,
#253451,#253452,#253453,#253454,#253455,#253456,#253457,#253458,#253459,
#253460,#253461,#253462,#253463,#253464,#253465,#253466,#253467,#253468,
#253469,#253470,#253471,#253472,#253473,#253474,#253475,#253476,#253477,
#253478,#253479,#253480,#253481,#253482,#253483,#253484,#253485,#253486,
#253487,#253488,#253489,#253490,#253491,#253492,#253493,#253494,#253495,
#253496,#253497,#253498,#253499,#253500,#253501,#253502,#253503,#253504,
#253505),(#253506,#253507,#253508,#253509,#253510,#253511,#253512,#253513,
#253514,#253515,#253516,#253517,#253518,#253519,#253520,#253521,#253522,
#253523,#253524,#253525,#253526,#253527,#253528,#253529,#253530,#253531,
#253532,#253533,#253534,#253535,#253536,#253537,#253538,#253539,#253540,
#253541,#253542,#253543,#253544,#253545,#253546,#253547,#253548,#253549,
#253550,#253551,#253552,#253553,#253554,#253555,#253556,#253557,#253558,
#253559,#253560,#253561,#253562,#253563,#253564,#253565,#253566,#253567,
#253568,#253569,#253570,#253571,#253572,#253573,#253574,#253575,#253576,
#253577,#253578,#253579,#253580,#253581,#253582,#253583,#253584,#253585,
#253586,#253587,#253588,#253589,#253590,#253591,#253592,#253593,#253594,
#253595,#253596,#253597,#253598,#253599,#253600,#253601,#253602,#253603,
#253604,#253605,#253606,#253607,#253608,#253609,#253610,#253611,#253612,
#253613,#253614,#253615,#253616,#253617,#253618,#253619,#253620,#253621,
#253622,#253623,#253624,#253625,#253626,#253627,#253628,#253629,#253630,
#253631,#253632,#253633,#253634,#253635,#253636,#253637,#253638,#253639,
#253640,#253641,#253642,#253643,#253644,#253645,#253646,#253647,#253648,
#253649,#253650,#253651,#253652,#253653,#253654,#253655,#253656,#253657,
#253658,#253659,#253660,#253661,#253662,#253663,#253664,#253665,#253666,
#253667,#253668,#253669,#253670,#253671,#253672,#253673,#253674,#253675,
#253676,#253677,#253678,#253679,#253680,#253681,#253682,#253683,#253684,
#253685,#253686,#253687,#253688,#253689,#253690,#253691,#253692,#253693,
#253694,#253695,#253696,#253697,#253698,#253699,#253700,#253701,#253702,
#253703,#253704,#253705,#253706,#253707,#253708,#253709,#253710,#253711,
#253712,#253713,#253714,#253715,#253716,#253717,#253718,#253719,#253720,
#253721,#253722,#253723,#253724,#253725,#253726,#253727,#253728,#253729,
#253730,#253731,#253732,#253733,#253734,#253735,#253736,#253737,#253738,
#253739,#253740,#253741,#253742,#253743,#253744,#253745,#253746,#253747,
#253748,#253749,#253750,#253751,#253752,#253753,#253754,#253755,#253756,
#253757,#253758,#253759,#253760,#253761,#253762,#253763,#253764,#253765,
#253766,#253767,#253768,#253769,#253770,#253771,#253772,#253773,#253774,
#253775,#253776,#253777,#253778,#253779,#253780,#253781,#253782)),
 .UNSPECIFIED.,.F.,.F.,.F.)
B_SPLINE_SURFACE_WITH_KNOTS((2,2),(3,2,2,2,2,2,2,2,2,2,2,2,2,2,2,2,2,2,
2,2,2,2,2,2,2,2,2,2,2,2,2,2,2,2,2,2,2,2,2,2,2,2,2,2,2,2,2,2,2,2,2,2,2,2,
2,2,2,2,2,2,2,2,2,2,2,2,2,2,2,2,2,2,2,2,2,2,2,2,2,2,2,2,2,2,2,2,2,2,2,2,
2,2,2,2,2,2,2,2,2,2,2,2,2,2,2,2,2,2,2,2,2,2,2,2,2,2,2,2,2,2,2,2,2,2,2,2,
2,2,2,2,2,2,2,2,2,2,2,2,3),(0.,1.),(0.,0.0072463768115942,0.0144927536231884,
0.0217391304347826,0.0289855072463768,0.036231884057971,0.0434782608695652,
0.0507246376811594,0.0579710144927536,0.0652173913043478,0.072463768115942,
0.0797101449275362,0.0869565217391304,0.0942028985507246,0.101449275362319,
0.108695652173913,0.115942028985507,0.123188405797101,0.130434782608696,
0.13768115942029,0.144927536231884,0.152173913043478,0.159420289855073,
0.166666666666667,0.173913043478261,0.181159420289855,0.18840579710145,
0.195652173913044,0.202898550724637,0.210144927536232,0.217391304347826,
0.224637681159421,0.231884057971014,0.239130434782609,0.246376811594203,
0.253623188405797,0.260869565217392,0.268115942028985,0.275362318840579,
0.282608695652174,0.289855072463768,0.297101449275363,0.304347826086956,
0.31159420289855,0.318840579710145,0.326086956521739,0.333333333333334,
0.340579710144927,0.347826086956521,0.355072463768116,0.36231884057971,
0.369565217391304,0.376811594202899,0.384057971014493,0.391304347826087,
0.398550724637681,0.405797101449275,0.41304347826087,0.420289855072463,
0.427536231884058,0.434782608695652,0.442028985507247,0.449275362318841,
0.456521739130435,0.463768115942029,0.471014492753623,0.478260869565218,
0.485507246376812,0.492753623188406,0.5,0.507246376811594,0.514492753623188,
0.521739130434783,0.528985507246377,0.536231884057971,0.543478260869565,
0.550724637681159,0.557971014492754,0.565217391304348,0.572463768115942,
0.579710144927536,0.586956521739131,0.594202898550725,0.601449275362319,
0.608695652173913,0.615942028985507,0.623188405797101,0.630434782608696,
0.63768115942029,0.644927536231884,0.652173913043478,0.659420289855073,
0.666666666666667,0.673913043478261,0.681159420289855,0.688405797101449,
0.695652173913044,0.702898550724638,0.710144927536232,0.717391304347826,
0.72463768115942,0.731884057971015,0.739130434782609,0.746376811594203,
0.753623188405797,0.760869565217391,0.768115942028986,0.77536231884058,
0.782608695652174,0.789855072463768,0.797101449275362,0.804347826086956,
0.811594202898551,0.818840579710145,0.826086956521739,0.833333333333333,
0.840579710144928,0.847826086956522,0.855072463768116,0.86231884057971,
0.869565217391304,0.876811594202899,0.884057971014493,0.891304347826087,
0.898550724637681,0.905797101449275,0.91304347826087,0.920289855072464,
0.927536231884058,0.934782608695652,0.942028985507246,0.94927536231884,
0.956521739130435,0.963768115942029,0.971014492753623,0.978260869565217,
0.985507246376812,0.992753623188406,0.993818585798284),.UNSPECIFIED.)
GEOMETRIC_REPRESENTATION_ITEM()
RATIONAL_B_SPLINE_SURFACE(((1.,0.866025403784439,1.,0.866025403784439,1.,
0.866025403784439,1.,0.866025403784439,1.,0.866025403784439,1.,0.866025403784439,
1.,0.866025403784439,1.,0.866025403784439,1.,0.866025403784439,1.,0.866025403784439,
1.,0.866025403784439,1.,0.866025403784439,1.,0.866025403784439,1.,0.866025403784439,
1.,0.866025403784439,1.,0.866025403784439,1.,0.866025403784439,1.,0.866025403784439,
1.,0.866025403784439,1.,0.866025403784439,1.,0.866025403784439,1.,0.866025403784439,
1.,0.866025403784439,1.,0.866025403784439,1.,0.866025403784439,1.,0.866025403784439,
1.,0.866025403784439,1.,0.866025403784439,1.,0.866025403784439,1.,0.866025403784439,
1.,0.866025403784439,1.,0.866025403784439,1.,0.866025403784439,1.,0.866025403784439,
1.,0.866025403784439,1.,0.866025403784439,1.,0.866025403784439,1.,0.866025403784439,
1.,0.866025403784439,1.,0.866025403784439,1.,0.866025403784439,1.,0.866025403784439,
1.,0.866025403784439,1.,0.866025403784439,1.,0.866025403784439,1.,0.866025403784439,
1.,0.866025403784439,1.,0.866025403784439,1.,0.866025403784439,1.,0.866025403784439,
1.,0.866025403784439,1.,0.866025403784439,1.,0.866025403784439,1.,0.866025403784439,
1.,0.866025403784439,1.,0.866025403784439,1.,0.866025403784439,1.,0.866025403784439,
1.,0.866025403784439,1.,0.866025403784439,1.,0.866025403784439,1.,0.866025403784439,
1.,0.866025403784439,1.,0.866025403784439,1.,0.866025403784439,1.,0.866025403784439,
1.,0.866025403784439,1.,0.866025403784439,1.,0.866025403784439,1.,0.866025403784439,
1.,0.866025403784439,1.,0.866025403784439,1.,0.866025403784439,1.,0.866025403784439,
1.,0.866025403784439,1.,0.866025403784439,1.,0.866025403784439,1.,0.866025403784439,
1.,0.866025403784439,1.,0.866025403784439,1.,0.866025403784439,1.,0.866025403784439,
1.,0.866025403784439,1.,0.866025403784439,1.,0.866025403784439,1.,0.866025403784439,
1.,0.866025403784439,1.,0.866025403784439,1.,0.866025403784439,1.,0.866025403784439,
1.,0.866025403784439,1.,0.866025403784439,1.,0.866025403784439,1.,0.866025403784439,
1.,0.866025403784439,1.,0.866025403784439,1.,0.866025403784439,1.,0.866025403784439,
1.,0.866025403784439,1.,0.866025403784439,1.,0.866025403784439,1.,0.866025403784439,
1.,0.866025403784439,1.,0.866025403784439,1.,0.866025403784439,1.,0.866025403784439,
1.,0.866025403784439,1.,0.866025403784439,1.,0.866025403784439,1.,0.866025403784439,
1.,0.866025403784439,1.,0.866025403784439,1.,0.866025403784439,1.,0.866025403784439,
1.,0.866025403784439,1.,0.866025403784439,1.,0.866025403784439,1.,0.866025403784439,
1.,0.866025403784439,1.,0.866025403784439,1.,0.866025403784439,1.,0.866025403784439,
1.,0.866025403784439,1.,0.866025403784439,1.,0.866025403784439,1.,0.866025403784439,
1.,0.866025403784439,1.,0.866025403784439,1.,0.866025403784439,1.,0.866025403784439,
1.,0.866025403784439,1.,0.866025403784439,1.,0.866025403784439,1.,0.866025403784439,
1.,0.866025403784439,1.,0.866025403784439,1.,0.866025403784439,1.,0.98031044488126,
0.966408234404338),(1.,0.866025403784439,1.,0.866025403784439,1.,0.866025403784439,
1.,0.866025403784439,1.,0.866025403784439,1.,0.866025403784439,1.,0.866025403784439,
1.,0.866025403784439,1.,0.866025403784439,1.,0.866025403784439,1.,0.866025403784439,
1.,0.866025403784439,1.,0.866025403784439,1.,0.866025403784439,1.,0.866025403784439,
1.,0.866025403784439,1.,0.866025403784439,1.,0.866025403784439,1.,0.866025403784439,
1.,0.866025403784439,1.,0.866025403784439,1.,0.866025403784439,1.,0.866025403784439,
1.,0.866025403784439,1.,0.866025403784439,1.,0.866025403784439,1.,0.866025403784439,
1.,0.866025403784439,1.,0.866025403784439,1.,0.866025403784439,1.,0.866025403784439,
1.,0.866025403784439,1.,0.866025403784439,1.,0.866025403784439,1.,0.866025403784439,
1.,0.866025403784439,1.,0.866025403784439,1.,0.866025403784439,1.,0.866025403784439,
1.,0.866025403784439,1.,0.866025403784439,1.,0.866025403784439,1.,0.866025403784439,
1.,0.866025403784439,1.,0.866025403784439,1.,0.866025403784439,1.,0.866025403784439,
1.,0.866025403784439,1.,0.866025403784439,1.,0.866025403784439,1.,0.866025403784439,
1.,0.866025403784439,1.,0.866025403784439,1.,0.866025403784439,1.,0.866025403784439,
1.,0.866025403784439,1.,0.866025403784439,1.,0.866025403784439,1.,0.866025403784439,
1.,0.866025403784439,1.,0.866025403784439,1.,0.866025403784439,1.,0.866025403784439,
1.,0.866025403784439,1.,0.866025403784439,1.,0.866025403784439,1.,0.866025403784439,
1.,0.866025403784439,1.,0.866025403784439,1.,0.866025403784439,1.,0.866025403784439,
1.,0.866025403784439,1.,0.866025403784439,1.,0.866025403784439,1.,0.866025403784439,
1.,0.866025403784439,1.,0.866025403784439,1.,0.866025403784439,1.,0.866025403784439,
1.,0.866025403784439,1.,0.866025403784439,1.,0.866025403784439,1.,0.866025403784439,
1.,0.866025403784439,1.,0.866025403784439,1.,0.866025403784439,1.,0.866025403784439,
1.,0.866025403784439,1.,0.866025403784439,1.,0.866025403784439,1.,0.866025403784439,
1.,0.866025403784439,1.,0.866025403784439,1.,0.866025403784439,1.,0.866025403784439,
1.,0.866025403784439,1.,0.866025403784439,1.,0.866025403784439,1.,0.866025403784439,
1.,0.866025403784439,1.,0.866025403784439,1.,0.866025403784439,1.,0.866025403784439,
1.,0.866025403784439,1.,0.866025403784439,1.,0.866025403784439,1.,0.866025403784439,
1.,0.866025403784439,1.,0.866025403784439,1.,0.866025403784439,1.,0.866025403784439,
1.,0.866025403784439,1.,0.866025403784439,1.,0.866025403784439,1.,0.866025403784439,
1.,0.866025403784439,1.,0.866025403784439,1.,0.866025403784439,1.,0.866025403784439,
1.,0.866025403784439,1.,0.866025403784439,1.,0.866025403784439,1.,0.866025403784439,
1.,0.866025403784439,1.,0.866025403784439,1.,0.866025403784439,1.,0.866025403784439,
1.,0.866025403784439,1.,0.866025403784439,1.,0.866025403784439,1.,0.866025403784439,
1.,0.866025403784439,1.,0.866025403784439,1.,0.866025403784439,1.,0.866025403784439,
1.,0.866025403784439,1.,0.866025403784439,1.,0.98031044488126,0.966408234404338)))
REPRESENTATION_ITEM('')
SURFACE()
);
#3177=(
BOUNDED_SURFACE()
B_SPLINE_SURFACE(1,2,((#253816,#253817,#253818,#253819,#253820,#253821,
#253822,#253823,#253824,#253825,#253826,#253827,#253828,#253829,#253830,
#253831,#253832,#253833,#253834,#253835,#253836,#253837,#253838,#253839,
#253840,#253841,#253842,#253843,#253844,#253845,#253846,#253847,#253848,
#253849,#253850,#253851,#253852,#253853,#253854,#253855,#253856,#253857,
#253858,#253859,#253860,#253861,#253862,#253863,#253864,#253865,#253866,
#253867,#253868,#253869,#253870,#253871,#253872,#253873,#253874,#253875,
#253876,#253877,#253878,#253879,#253880,#253881,#253882,#253883,#253884,
#253885,#253886,#253887,#253888,#253889,#253890,#253891,#253892,#253893,
#253894,#253895,#253896,#253897,#253898,#253899,#253900,#253901,#253902,
#253903,#253904,#253905,#253906,#253907,#253908,#253909,#253910,#253911,
#253912,#253913,#253914,#253915,#253916,#253917,#253918,#253919,#253920,
#253921,#253922,#253923,#253924,#253925,#253926,#253927,#253928,#253929,
#253930,#253931,#253932,#253933,#253934,#253935,#253936,#253937,#253938,
#253939,#253940,#253941,#253942,#253943,#253944,#253945,#253946,#253947,
#253948,#253949,#253950,#253951,#253952,#253953,#253954,#253955,#253956,
#253957,#253958,#253959,#253960,#253961,#253962,#253963,#253964,#253965,
#253966,#253967,#253968,#253969,#253970,#253971,#253972,#253973,#253974,
#253975,#253976,#253977,#253978,#253979,#253980,#253981,#253982,#253983,
#253984,#253985,#253986,#253987,#253988,#253989,#253990,#253991,#253992,
#253993,#253994,#253995,#253996,#253997,#253998,#253999,#254000,#254001,
#254002,#254003,#254004,#254005,#254006,#254007,#254008,#254009,#254010,
#254011,#254012,#254013,#254014,#254015,#254016,#254017,#254018,#254019,
#254020,#254021,#254022,#254023,#254024,#254025,#254026,#254027,#254028,
#254029,#254030,#254031,#254032,#254033,#254034,#254035,#254036,#254037,
#254038,#254039,#254040,#254041,#254042,#254043,#254044,#254045,#254046,
#254047,#254048,#254049,#254050,#254051,#254052,#254053,#254054,#254055,
#254056,#254057,#254058,#254059,#254060,#254061,#254062,#254063,#254064,
#254065,#254066,#254067,#254068,#254069,#254070,#254071,#254072,#254073,
#254074,#254075,#254076,#254077,#254078,#254079,#254080,#254081,#254082,
#254083,#254084,#254085,#254086,#254087,#254088,#254089,#254090,#254091,
#254092),(#254093,#254094,#254095,#254096,#254097,#254098,#254099,#254100,
#254101,#254102,#254103,#254104,#254105,#254106,#254107,#254108,#254109,
#254110,#254111,#254112,#254113,#254114,#254115,#254116,#254117,#254118,
#254119,#254120,#254121,#254122,#254123,#254124,#254125,#254126,#254127,
#254128,#254129,#254130,#254131,#254132,#254133,#254134,#254135,#254136,
#254137,#254138,#254139,#254140,#254141,#254142,#254143,#254144,#254145,
#254146,#254147,#254148,#254149,#254150,#254151,#254152,#254153,#254154,
#254155,#254156,#254157,#254158,#254159,#254160,#254161,#254162,#254163,
#254164,#254165,#254166,#254167,#254168,#254169,#254170,#254171,#254172,
#254173,#254174,#254175,#254176,#254177,#254178,#254179,#254180,#254181,
#254182,#254183,#254184,#254185,#254186,#254187,#254188,#254189,#254190,
#254191,#254192,#254193,#254194,#254195,#254196,#254197,#254198,#254199,
#254200,#254201,#254202,#254203,#254204,#254205,#254206,#254207,#254208,
#254209,#254210,#254211,#254212,#254213,#254214,#254215,#254216,#254217,
#254218,#254219,#254220,#254221,#254222,#254223,#254224,#254225,#254226,
#254227,#254228,#254229,#254230,#254231,#254232,#254233,#254234,#254235,
#254236,#254237,#254238,#254239,#254240,#254241,#254242,#254243,#254244,
#254245,#254246,#254247,#254248,#254249,#254250,#254251,#254252,#254253,
#254254,#254255,#254256,#254257,#254258,#254259,#254260,#254261,#254262,
#254263,#254264,#254265,#254266,#254267,#254268,#254269,#254270,#254271,
#254272,#254273,#254274,#254275,#254276,#254277,#254278,#254279,#254280,
#254281,#254282,#254283,#254284,#254285,#254286,#254287,#254288,#254289,
#254290,#254291,#254292,#254293,#254294,#254295,#254296,#254297,#254298,
#254299,#254300,#254301,#254302,#254303,#254304,#254305,#254306,#254307,
#254308,#254309,#254310,#254311,#254312,#254313,#254314,#254315,#254316,
#254317,#254318,#254319,#254320,#254321,#254322,#254323,#254324,#254325,
#254326,#254327,#254328,#254329,#254330,#254331,#254332,#254333,#254334,
#254335,#254336,#254337,#254338,#254339,#254340,#254341,#254342,#254343,
#254344,#254345,#254346,#254347,#254348,#254349,#254350,#254351,#254352,
#254353,#254354,#254355,#254356,#254357,#254358,#254359,#254360,#254361,
#254362,#254363,#254364,#254365,#254366,#254367,#254368,#254369)),
 .UNSPECIFIED.,.F.,.F.,.F.)
B_SPLINE_SURFACE_WITH_KNOTS((2,2),(3,2,2,2,2,2,2,2,2,2,2,2,2,2,2,2,2,2,
2,2,2,2,2,2,2,2,2,2,2,2,2,2,2,2,2,2,2,2,2,2,2,2,2,2,2,2,2,2,2,2,2,2,2,2,
2,2,2,2,2,2,2,2,2,2,2,2,2,2,2,2,2,2,2,2,2,2,2,2,2,2,2,2,2,2,2,2,2,2,2,2,
2,2,2,2,2,2,2,2,2,2,2,2,2,2,2,2,2,2,2,2,2,2,2,2,2,2,2,2,2,2,2,2,2,2,2,2,
2,2,2,2,2,2,2,2,2,2,2,2,3),(0.,1.),(0.,0.0072463768115942,0.0144927536231884,
0.0217391304347826,0.0289855072463768,0.036231884057971,0.0434782608695652,
0.0507246376811594,0.0579710144927536,0.0652173913043478,0.072463768115942,
0.0797101449275362,0.0869565217391304,0.0942028985507246,0.101449275362319,
0.108695652173913,0.115942028985507,0.123188405797101,0.130434782608696,
0.13768115942029,0.144927536231884,0.152173913043478,0.159420289855073,
0.166666666666667,0.173913043478261,0.181159420289855,0.18840579710145,
0.195652173913044,0.202898550724637,0.210144927536232,0.217391304347826,
0.224637681159421,0.231884057971014,0.239130434782609,0.246376811594203,
0.253623188405797,0.260869565217392,0.268115942028985,0.275362318840579,
0.282608695652174,0.289855072463768,0.297101449275363,0.304347826086956,
0.31159420289855,0.318840579710145,0.326086956521739,0.333333333333334,
0.340579710144927,0.347826086956521,0.355072463768116,0.36231884057971,
0.369565217391304,0.376811594202899,0.384057971014493,0.391304347826087,
0.398550724637681,0.405797101449275,0.41304347826087,0.420289855072463,
0.427536231884058,0.434782608695652,0.442028985507247,0.449275362318841,
0.456521739130435,0.463768115942029,0.471014492753623,0.478260869565218,
0.485507246376812,0.492753623188406,0.5,0.507246376811594,0.514492753623188,
0.521739130434783,0.528985507246377,0.536231884057971,0.543478260869565,
0.550724637681159,0.557971014492754,0.565217391304348,0.572463768115942,
0.579710144927536,0.586956521739131,0.594202898550725,0.601449275362319,
0.608695652173913,0.615942028985507,0.623188405797101,0.630434782608696,
0.63768115942029,0.644927536231884,0.652173913043478,0.659420289855073,
0.666666666666667,0.673913043478261,0.681159420289855,0.688405797101449,
0.695652173913044,0.702898550724638,0.710144927536232,0.717391304347826,
0.72463768115942,0.731884057971015,0.739130434782609,0.746376811594203,
0.753623188405797,0.760869565217391,0.768115942028986,0.77536231884058,
0.782608695652174,0.789855072463768,0.797101449275362,0.804347826086956,
0.811594202898551,0.818840579710145,0.826086956521739,0.833333333333333,
0.840579710144928,0.847826086956522,0.855072463768116,0.86231884057971,
0.869565217391304,0.876811594202899,0.884057971014493,0.891304347826087,
0.898550724637681,0.905797101449275,0.91304347826087,0.920289855072464,
0.927536231884058,0.934782608695652,0.942028985507246,0.94927536231884,
0.956521739130435,0.963768115942029,0.971014492753623,0.978260869565217,
0.985507246376812,0.992753623188406,0.993818585798284),.UNSPECIFIED.)
GEOMETRIC_REPRESENTATION_ITEM()
RATIONAL_B_SPLINE_SURFACE(((1.,0.866025403784439,1.,0.866025403784439,1.,
0.866025403784439,1.,0.866025403784439,1.,0.866025403784439,1.,0.866025403784439,
1.,0.866025403784439,1.,0.866025403784439,1.,0.866025403784439,1.,0.866025403784439,
1.,0.866025403784439,1.,0.866025403784439,1.,0.866025403784439,1.,0.866025403784439,
1.,0.866025403784439,1.,0.866025403784439,1.,0.866025403784439,1.,0.866025403784439,
1.,0.866025403784439,1.,0.866025403784439,1.,0.866025403784439,1.,0.866025403784439,
1.,0.866025403784439,1.,0.866025403784439,1.,0.866025403784439,1.,0.866025403784439,
1.,0.866025403784439,1.,0.866025403784439,1.,0.866025403784439,1.,0.866025403784439,
1.,0.866025403784439,1.,0.866025403784439,1.,0.866025403784439,1.,0.866025403784439,
1.,0.866025403784439,1.,0.866025403784439,1.,0.866025403784439,1.,0.866025403784439,
1.,0.866025403784439,1.,0.866025403784439,1.,0.866025403784439,1.,0.866025403784439,
1.,0.866025403784439,1.,0.866025403784439,1.,0.866025403784439,1.,0.866025403784439,
1.,0.866025403784439,1.,0.866025403784439,1.,0.866025403784439,1.,0.866025403784439,
1.,0.866025403784439,1.,0.866025403784439,1.,0.866025403784439,1.,0.866025403784439,
1.,0.866025403784439,1.,0.866025403784439,1.,0.866025403784439,1.,0.866025403784439,
1.,0.866025403784439,1.,0.866025403784439,1.,0.866025403784439,1.,0.866025403784439,
1.,0.866025403784439,1.,0.866025403784439,1.,0.866025403784439,1.,0.866025403784439,
1.,0.866025403784439,1.,0.866025403784439,1.,0.866025403784439,1.,0.866025403784439,
1.,0.866025403784439,1.,0.866025403784439,1.,0.866025403784439,1.,0.866025403784439,
1.,0.866025403784439,1.,0.866025403784439,1.,0.866025403784439,1.,0.866025403784439,
1.,0.866025403784439,1.,0.866025403784439,1.,0.866025403784439,1.,0.866025403784439,
1.,0.866025403784439,1.,0.866025403784439,1.,0.866025403784439,1.,0.866025403784439,
1.,0.866025403784439,1.,0.866025403784439,1.,0.866025403784439,1.,0.866025403784439,
1.,0.866025403784439,1.,0.866025403784439,1.,0.866025403784439,1.,0.866025403784439,
1.,0.866025403784439,1.,0.866025403784439,1.,0.866025403784439,1.,0.866025403784439,
1.,0.866025403784439,1.,0.866025403784439,1.,0.866025403784439,1.,0.866025403784439,
1.,0.866025403784439,1.,0.866025403784439,1.,0.866025403784439,1.,0.866025403784439,
1.,0.866025403784439,1.,0.866025403784439,1.,0.866025403784439,1.,0.866025403784439,
1.,0.866025403784439,1.,0.866025403784439,1.,0.866025403784439,1.,0.866025403784439,
1.,0.866025403784439,1.,0.866025403784439,1.,0.866025403784439,1.,0.866025403784439,
1.,0.866025403784439,1.,0.866025403784439,1.,0.866025403784439,1.,0.866025403784439,
1.,0.866025403784439,1.,0.866025403784439,1.,0.866025403784439,1.,0.866025403784439,
1.,0.866025403784439,1.,0.866025403784439,1.,0.866025403784439,1.,0.866025403784439,
1.,0.866025403784439,1.,0.866025403784439,1.,0.866025403784439,1.,0.866025403784439,
1.,0.866025403784439,1.,0.866025403784439,1.,0.866025403784439,1.,0.98031044488126,
0.966408234404338),(1.,0.866025403784439,1.,0.866025403784439,1.,0.866025403784439,
1.,0.866025403784439,1.,0.866025403784439,1.,0.866025403784439,1.,0.866025403784439,
1.,0.866025403784439,1.,0.866025403784439,1.,0.866025403784439,1.,0.866025403784439,
1.,0.866025403784439,1.,0.866025403784439,1.,0.866025403784439,1.,0.866025403784439,
1.,0.866025403784439,1.,0.866025403784439,1.,0.866025403784439,1.,0.866025403784439,
1.,0.866025403784439,1.,0.866025403784439,1.,0.866025403784439,1.,0.866025403784439,
1.,0.866025403784439,1.,0.866025403784439,1.,0.866025403784439,1.,0.866025403784439,
1.,0.866025403784439,1.,0.866025403784439,1.,0.866025403784439,1.,0.866025403784439,
1.,0.866025403784439,1.,0.866025403784439,1.,0.866025403784439,1.,0.866025403784439,
1.,0.866025403784439,1.,0.866025403784439,1.,0.866025403784439,1.,0.866025403784439,
1.,0.866025403784439,1.,0.866025403784439,1.,0.866025403784439,1.,0.866025403784439,
1.,0.866025403784439,1.,0.866025403784439,1.,0.866025403784439,1.,0.866025403784439,
1.,0.866025403784439,1.,0.866025403784439,1.,0.866025403784439,1.,0.866025403784439,
1.,0.866025403784439,1.,0.866025403784439,1.,0.866025403784439,1.,0.866025403784439,
1.,0.866025403784439,1.,0.866025403784439,1.,0.866025403784439,1.,0.866025403784439,
1.,0.866025403784439,1.,0.866025403784439,1.,0.866025403784439,1.,0.866025403784439,
1.,0.866025403784439,1.,0.866025403784439,1.,0.866025403784439,1.,0.866025403784439,
1.,0.866025403784439,1.,0.866025403784439,1.,0.866025403784439,1.,0.866025403784439,
1.,0.866025403784439,1.,0.866025403784439,1.,0.866025403784439,1.,0.866025403784439,
1.,0.866025403784439,1.,0.866025403784439,1.,0.866025403784439,1.,0.866025403784439,
1.,0.866025403784439,1.,0.866025403784439,1.,0.866025403784439,1.,0.866025403784439,
1.,0.866025403784439,1.,0.866025403784439,1.,0.866025403784439,1.,0.866025403784439,
1.,0.866025403784439,1.,0.866025403784439,1.,0.866025403784439,1.,0.866025403784439,
1.,0.866025403784439,1.,0.866025403784439,1.,0.866025403784439,1.,0.866025403784439,
1.,0.866025403784439,1.,0.866025403784439,1.,0.866025403784439,1.,0.866025403784439,
1.,0.866025403784439,1.,0.866025403784439,1.,0.866025403784439,1.,0.866025403784439,
1.,0.866025403784439,1.,0.866025403784439,1.,0.866025403784439,1.,0.866025403784439,
1.,0.866025403784439,1.,0.866025403784439,1.,0.866025403784439,1.,0.866025403784439,
1.,0.866025403784439,1.,0.866025403784439,1.,0.866025403784439,1.,0.866025403784439,
1.,0.866025403784439,1.,0.866025403784439,1.,0.866025403784439,1.,0.866025403784439,
1.,0.866025403784439,1.,0.866025403784439,1.,0.866025403784439,1.,0.866025403784439,
1.,0.866025403784439,1.,0.866025403784439,1.,0.866025403784439,1.,0.866025403784439,
1.,0.866025403784439,1.,0.866025403784439,1.,0.866025403784439,1.,0.866025403784439,
1.,0.866025403784439,1.,0.866025403784439,1.,0.866025403784439,1.,0.866025403784439,
1.,0.866025403784439,1.,0.866025403784439,1.,0.98031044488126,0.966408234404338)))
REPRESENTATION_ITEM('')
SURFACE()
);
#3178=(
BOUNDED_SURFACE()
B_SPLINE_SURFACE(1,2,((#256166,#256167,#256168,#256169,#256170,#256171,
#256172,#256173,#256174,#256175,#256176,#256177,#256178,#256179,#256180,
#256181,#256182,#256183,#256184,#256185,#256186,#256187,#256188,#256189,
#256190,#256191,#256192,#256193,#256194,#256195,#256196,#256197,#256198,
#256199,#256200,#256201,#256202,#256203,#256204,#256205,#256206,#256207,
#256208,#256209,#256210,#256211,#256212,#256213,#256214,#256215,#256216,
#256217,#256218,#256219,#256220,#256221,#256222,#256223,#256224,#256225,
#256226,#256227,#256228,#256229,#256230,#256231,#256232,#256233,#256234,
#256235,#256236,#256237,#256238,#256239,#256240,#256241,#256242,#256243,
#256244,#256245,#256246,#256247,#256248,#256249,#256250,#256251,#256252,
#256253,#256254,#256255,#256256,#256257,#256258,#256259,#256260,#256261,
#256262,#256263,#256264,#256265,#256266,#256267,#256268,#256269,#256270,
#256271,#256272,#256273,#256274,#256275,#256276,#256277,#256278,#256279,
#256280,#256281,#256282,#256283,#256284,#256285,#256286,#256287,#256288,
#256289,#256290,#256291,#256292,#256293,#256294,#256295,#256296,#256297,
#256298,#256299,#256300,#256301,#256302,#256303,#256304,#256305,#256306,
#256307,#256308,#256309,#256310,#256311,#256312,#256313,#256314,#256315,
#256316,#256317,#256318,#256319,#256320,#256321,#256322,#256323,#256324,
#256325,#256326,#256327,#256328,#256329,#256330,#256331,#256332,#256333,
#256334,#256335,#256336,#256337,#256338,#256339,#256340,#256341,#256342,
#256343,#256344,#256345,#256346,#256347,#256348,#256349,#256350,#256351,
#256352,#256353,#256354,#256355,#256356,#256357,#256358,#256359,#256360,
#256361,#256362,#256363,#256364,#256365,#256366,#256367,#256368,#256369,
#256370,#256371,#256372,#256373,#256374,#256375,#256376,#256377,#256378,
#256379,#256380,#256381,#256382,#256383,#256384,#256385,#256386,#256387,
#256388,#256389,#256390,#256391,#256392,#256393,#256394,#256395,#256396,
#256397,#256398,#256399,#256400,#256401,#256402,#256403,#256404,#256405,
#256406,#256407,#256408,#256409,#256410,#256411,#256412,#256413,#256414,
#256415,#256416,#256417,#256418,#256419,#256420,#256421,#256422,#256423,
#256424,#256425,#256426,#256427,#256428,#256429,#256430,#256431,#256432,
#256433,#256434,#256435,#256436,#256437,#256438,#256439,#256440,#256441,
#256442),(#256443,#256444,#256445,#256446,#256447,#256448,#256449,#256450,
#256451,#256452,#256453,#256454,#256455,#256456,#256457,#256458,#256459,
#256460,#256461,#256462,#256463,#256464,#256465,#256466,#256467,#256468,
#256469,#256470,#256471,#256472,#256473,#256474,#256475,#256476,#256477,
#256478,#256479,#256480,#256481,#256482,#256483,#256484,#256485,#256486,
#256487,#256488,#256489,#256490,#256491,#256492,#256493,#256494,#256495,
#256496,#256497,#256498,#256499,#256500,#256501,#256502,#256503,#256504,
#256505,#256506,#256507,#256508,#256509,#256510,#256511,#256512,#256513,
#256514,#256515,#256516,#256517,#256518,#256519,#256520,#256521,#256522,
#256523,#256524,#256525,#256526,#256527,#256528,#256529,#256530,#256531,
#256532,#256533,#256534,#256535,#256536,#256537,#256538,#256539,#256540,
#256541,#256542,#256543,#256544,#256545,#256546,#256547,#256548,#256549,
#256550,#256551,#256552,#256553,#256554,#256555,#256556,#256557,#256558,
#256559,#256560,#256561,#256562,#256563,#256564,#256565,#256566,#256567,
#256568,#256569,#256570,#256571,#256572,#256573,#256574,#256575,#256576,
#256577,#256578,#256579,#256580,#256581,#256582,#256583,#256584,#256585,
#256586,#256587,#256588,#256589,#256590,#256591,#256592,#256593,#256594,
#256595,#256596,#256597,#256598,#256599,#256600,#256601,#256602,#256603,
#256604,#256605,#256606,#256607,#256608,#256609,#256610,#256611,#256612,
#256613,#256614,#256615,#256616,#256617,#256618,#256619,#256620,#256621,
#256622,#256623,#256624,#256625,#256626,#256627,#256628,#256629,#256630,
#256631,#256632,#256633,#256634,#256635,#256636,#256637,#256638,#256639,
#256640,#256641,#256642,#256643,#256644,#256645,#256646,#256647,#256648,
#256649,#256650,#256651,#256652,#256653,#256654,#256655,#256656,#256657,
#256658,#256659,#256660,#256661,#256662,#256663,#256664,#256665,#256666,
#256667,#256668,#256669,#256670,#256671,#256672,#256673,#256674,#256675,
#256676,#256677,#256678,#256679,#256680,#256681,#256682,#256683,#256684,
#256685,#256686,#256687,#256688,#256689,#256690,#256691,#256692,#256693,
#256694,#256695,#256696,#256697,#256698,#256699,#256700,#256701,#256702,
#256703,#256704,#256705,#256706,#256707,#256708,#256709,#256710,#256711,
#256712,#256713,#256714,#256715,#256716,#256717,#256718,#256719)),
 .UNSPECIFIED.,.F.,.F.,.F.)
B_SPLINE_SURFACE_WITH_KNOTS((2,2),(3,2,2,2,2,2,2,2,2,2,2,2,2,2,2,2,2,2,
2,2,2,2,2,2,2,2,2,2,2,2,2,2,2,2,2,2,2,2,2,2,2,2,2,2,2,2,2,2,2,2,2,2,2,2,
2,2,2,2,2,2,2,2,2,2,2,2,2,2,2,2,2,2,2,2,2,2,2,2,2,2,2,2,2,2,2,2,2,2,2,2,
2,2,2,2,2,2,2,2,2,2,2,2,2,2,2,2,2,2,2,2,2,2,2,2,2,2,2,2,2,2,2,2,2,2,2,2,
2,2,2,2,2,2,2,2,2,2,2,2,3),(0.,1.),(0.,0.0072463768115942,0.0144927536231884,
0.0217391304347826,0.0289855072463768,0.036231884057971,0.0434782608695652,
0.0507246376811594,0.0579710144927536,0.0652173913043478,0.072463768115942,
0.0797101449275362,0.0869565217391304,0.0942028985507246,0.101449275362319,
0.108695652173913,0.115942028985507,0.123188405797101,0.130434782608696,
0.13768115942029,0.144927536231884,0.152173913043478,0.159420289855073,
0.166666666666667,0.173913043478261,0.181159420289855,0.18840579710145,
0.195652173913044,0.202898550724637,0.210144927536232,0.217391304347826,
0.224637681159421,0.231884057971014,0.239130434782609,0.246376811594203,
0.253623188405797,0.260869565217392,0.268115942028985,0.275362318840579,
0.282608695652174,0.289855072463768,0.297101449275363,0.304347826086956,
0.31159420289855,0.318840579710145,0.326086956521739,0.333333333333334,
0.340579710144927,0.347826086956521,0.355072463768116,0.36231884057971,
0.369565217391304,0.376811594202899,0.384057971014493,0.391304347826087,
0.398550724637681,0.405797101449275,0.41304347826087,0.420289855072463,
0.427536231884058,0.434782608695652,0.442028985507247,0.449275362318841,
0.456521739130435,0.463768115942029,0.471014492753623,0.478260869565218,
0.485507246376812,0.492753623188406,0.5,0.507246376811594,0.514492753623188,
0.521739130434783,0.528985507246377,0.536231884057971,0.543478260869565,
0.550724637681159,0.557971014492754,0.565217391304348,0.572463768115942,
0.579710144927536,0.586956521739131,0.594202898550725,0.601449275362319,
0.608695652173913,0.615942028985507,0.623188405797101,0.630434782608696,
0.63768115942029,0.644927536231884,0.652173913043478,0.659420289855073,
0.666666666666667,0.673913043478261,0.681159420289855,0.688405797101449,
0.695652173913044,0.702898550724638,0.710144927536232,0.717391304347826,
0.72463768115942,0.731884057971015,0.739130434782609,0.746376811594203,
0.753623188405797,0.760869565217391,0.768115942028986,0.77536231884058,
0.782608695652174,0.789855072463768,0.797101449275362,0.804347826086956,
0.811594202898551,0.818840579710145,0.826086956521739,0.833333333333333,
0.840579710144928,0.847826086956522,0.855072463768116,0.86231884057971,
0.869565217391304,0.876811594202899,0.884057971014493,0.891304347826087,
0.898550724637681,0.905797101449275,0.91304347826087,0.920289855072464,
0.927536231884058,0.934782608695652,0.942028985507246,0.94927536231884,
0.956521739130435,0.963768115942029,0.971014492753623,0.978260869565217,
0.985507246376812,0.992753623188406,0.993818495192186),.UNSPECIFIED.)
GEOMETRIC_REPRESENTATION_ITEM()
RATIONAL_B_SPLINE_SURFACE(((1.,0.866025403784439,1.,0.866025403784439,1.,
0.866025403784439,1.,0.866025403784439,1.,0.866025403784439,1.,0.866025403784439,
1.,0.866025403784439,1.,0.866025403784439,1.,0.866025403784439,1.,0.866025403784439,
1.,0.866025403784439,1.,0.866025403784439,1.,0.866025403784439,1.,0.866025403784439,
1.,0.866025403784439,1.,0.866025403784439,1.,0.866025403784439,1.,0.866025403784439,
1.,0.866025403784439,1.,0.866025403784439,1.,0.866025403784439,1.,0.866025403784439,
1.,0.866025403784439,1.,0.866025403784439,1.,0.866025403784439,1.,0.866025403784439,
1.,0.866025403784439,1.,0.866025403784439,1.,0.866025403784439,1.,0.866025403784439,
1.,0.866025403784439,1.,0.866025403784439,1.,0.866025403784439,1.,0.866025403784439,
1.,0.866025403784439,1.,0.866025403784439,1.,0.866025403784439,1.,0.866025403784439,
1.,0.866025403784439,1.,0.866025403784439,1.,0.866025403784439,1.,0.866025403784439,
1.,0.866025403784439,1.,0.866025403784439,1.,0.866025403784439,1.,0.866025403784439,
1.,0.866025403784439,1.,0.866025403784439,1.,0.866025403784439,1.,0.866025403784439,
1.,0.866025403784439,1.,0.866025403784439,1.,0.866025403784439,1.,0.866025403784439,
1.,0.866025403784439,1.,0.866025403784439,1.,0.866025403784439,1.,0.866025403784439,
1.,0.866025403784439,1.,0.866025403784439,1.,0.866025403784439,1.,0.866025403784439,
1.,0.866025403784439,1.,0.866025403784439,1.,0.866025403784439,1.,0.866025403784439,
1.,0.866025403784439,1.,0.866025403784439,1.,0.866025403784439,1.,0.866025403784439,
1.,0.866025403784439,1.,0.866025403784439,1.,0.866025403784439,1.,0.866025403784439,
1.,0.866025403784439,1.,0.866025403784439,1.,0.866025403784439,1.,0.866025403784439,
1.,0.866025403784439,1.,0.866025403784439,1.,0.866025403784439,1.,0.866025403784439,
1.,0.866025403784439,1.,0.866025403784439,1.,0.866025403784439,1.,0.866025403784439,
1.,0.866025403784439,1.,0.866025403784439,1.,0.866025403784439,1.,0.866025403784439,
1.,0.866025403784439,1.,0.866025403784439,1.,0.866025403784439,1.,0.866025403784439,
1.,0.866025403784439,1.,0.866025403784439,1.,0.866025403784439,1.,0.866025403784439,
1.,0.866025403784439,1.,0.866025403784439,1.,0.866025403784439,1.,0.866025403784439,
1.,0.866025403784439,1.,0.866025403784439,1.,0.866025403784439,1.,0.866025403784439,
1.,0.866025403784439,1.,0.866025403784439,1.,0.866025403784439,1.,0.866025403784439,
1.,0.866025403784439,1.,0.866025403784439,1.,0.866025403784439,1.,0.866025403784439,
1.,0.866025403784439,1.,0.866025403784439,1.,0.866025403784439,1.,0.866025403784439,
1.,0.866025403784439,1.,0.866025403784439,1.,0.866025403784439,1.,0.866025403784439,
1.,0.866025403784439,1.,0.866025403784439,1.,0.866025403784439,1.,0.866025403784439,
1.,0.866025403784439,1.,0.866025403784439,1.,0.866025403784439,1.,0.866025403784439,
1.,0.866025403784439,1.,0.866025403784439,1.,0.866025403784439,1.,0.866025403784439,
1.,0.866025403784439,1.,0.866025403784439,1.,0.866025403784439,1.,0.980312120051573,
0.966410600022306),(1.,0.866025403784439,1.,0.866025403784439,1.,0.866025403784439,
1.,0.866025403784439,1.,0.866025403784439,1.,0.866025403784439,1.,0.866025403784439,
1.,0.866025403784439,1.,0.866025403784439,1.,0.866025403784439,1.,0.866025403784439,
1.,0.866025403784439,1.,0.866025403784439,1.,0.866025403784439,1.,0.866025403784439,
1.,0.866025403784439,1.,0.866025403784439,1.,0.866025403784439,1.,0.866025403784439,
1.,0.866025403784439,1.,0.866025403784439,1.,0.866025403784439,1.,0.866025403784439,
1.,0.866025403784439,1.,0.866025403784439,1.,0.866025403784439,1.,0.866025403784439,
1.,0.866025403784439,1.,0.866025403784439,1.,0.866025403784439,1.,0.866025403784439,
1.,0.866025403784439,1.,0.866025403784439,1.,0.866025403784439,1.,0.866025403784439,
1.,0.866025403784439,1.,0.866025403784439,1.,0.866025403784439,1.,0.866025403784439,
1.,0.866025403784439,1.,0.866025403784439,1.,0.866025403784439,1.,0.866025403784439,
1.,0.866025403784439,1.,0.866025403784439,1.,0.866025403784439,1.,0.866025403784439,
1.,0.866025403784439,1.,0.866025403784439,1.,0.866025403784439,1.,0.866025403784439,
1.,0.866025403784439,1.,0.866025403784439,1.,0.866025403784439,1.,0.866025403784439,
1.,0.866025403784439,1.,0.866025403784439,1.,0.866025403784439,1.,0.866025403784439,
1.,0.866025403784439,1.,0.866025403784439,1.,0.866025403784439,1.,0.866025403784439,
1.,0.866025403784439,1.,0.866025403784439,1.,0.866025403784439,1.,0.866025403784439,
1.,0.866025403784439,1.,0.866025403784439,1.,0.866025403784439,1.,0.866025403784439,
1.,0.866025403784439,1.,0.866025403784439,1.,0.866025403784439,1.,0.866025403784439,
1.,0.866025403784439,1.,0.866025403784439,1.,0.866025403784439,1.,0.866025403784439,
1.,0.866025403784439,1.,0.866025403784439,1.,0.866025403784439,1.,0.866025403784439,
1.,0.866025403784439,1.,0.866025403784439,1.,0.866025403784439,1.,0.866025403784439,
1.,0.866025403784439,1.,0.866025403784439,1.,0.866025403784439,1.,0.866025403784439,
1.,0.866025403784439,1.,0.866025403784439,1.,0.866025403784439,1.,0.866025403784439,
1.,0.866025403784439,1.,0.866025403784439,1.,0.866025403784439,1.,0.866025403784439,
1.,0.866025403784439,1.,0.866025403784439,1.,0.866025403784439,1.,0.866025403784439,
1.,0.866025403784439,1.,0.866025403784439,1.,0.866025403784439,1.,0.866025403784439,
1.,0.866025403784439,1.,0.866025403784439,1.,0.866025403784439,1.,0.866025403784439,
1.,0.866025403784439,1.,0.866025403784439,1.,0.866025403784439,1.,0.866025403784439,
1.,0.866025403784439,1.,0.866025403784439,1.,0.866025403784439,1.,0.866025403784439,
1.,0.866025403784439,1.,0.866025403784439,1.,0.866025403784439,1.,0.866025403784439,
1.,0.866025403784439,1.,0.866025403784439,1.,0.866025403784439,1.,0.866025403784439,
1.,0.866025403784439,1.,0.866025403784439,1.,0.866025403784439,1.,0.866025403784439,
1.,0.866025403784439,1.,0.866025403784439,1.,0.866025403784439,1.,0.866025403784439,
1.,0.866025403784439,1.,0.866025403784439,1.,0.980312120051573,0.966410600022306)))
REPRESENTATION_ITEM('')
SURFACE()
);
#3179=(
BOUNDED_SURFACE()
B_SPLINE_SURFACE(1,2,((#256742,#256743,#256744,#256745,#256746,#256747,
#256748,#256749,#256750,#256751,#256752,#256753,#256754,#256755,#256756,
#256757,#256758,#256759,#256760,#256761,#256762,#256763,#256764,#256765,
#256766,#256767,#256768,#256769,#256770,#256771,#256772,#256773,#256774,
#256775,#256776,#256777,#256778,#256779,#256780,#256781,#256782,#256783,
#256784,#256785,#256786,#256787,#256788,#256789,#256790,#256791,#256792,
#256793,#256794,#256795,#256796,#256797,#256798,#256799,#256800,#256801,
#256802,#256803,#256804,#256805,#256806,#256807,#256808,#256809,#256810,
#256811,#256812,#256813,#256814,#256815,#256816,#256817,#256818,#256819,
#256820,#256821,#256822,#256823,#256824,#256825,#256826,#256827,#256828,
#256829,#256830,#256831,#256832,#256833,#256834,#256835,#256836,#256837,
#256838,#256839,#256840,#256841,#256842,#256843,#256844,#256845,#256846,
#256847,#256848,#256849,#256850,#256851,#256852,#256853,#256854,#256855,
#256856,#256857,#256858,#256859,#256860,#256861,#256862,#256863,#256864,
#256865,#256866,#256867,#256868,#256869,#256870,#256871,#256872,#256873,
#256874,#256875,#256876,#256877,#256878,#256879,#256880,#256881,#256882,
#256883,#256884,#256885,#256886,#256887,#256888,#256889,#256890,#256891,
#256892,#256893,#256894,#256895,#256896,#256897,#256898,#256899,#256900,
#256901,#256902,#256903,#256904,#256905,#256906,#256907,#256908,#256909,
#256910,#256911,#256912,#256913,#256914,#256915,#256916,#256917,#256918,
#256919,#256920,#256921,#256922,#256923,#256924,#256925,#256926,#256927,
#256928,#256929,#256930,#256931,#256932,#256933,#256934,#256935,#256936,
#256937,#256938,#256939,#256940,#256941,#256942,#256943,#256944,#256945,
#256946,#256947,#256948,#256949,#256950,#256951,#256952,#256953,#256954,
#256955,#256956,#256957,#256958,#256959,#256960,#256961,#256962,#256963,
#256964,#256965,#256966,#256967,#256968,#256969,#256970,#256971,#256972,
#256973,#256974,#256975,#256976,#256977,#256978,#256979,#256980,#256981,
#256982,#256983,#256984,#256985,#256986,#256987,#256988,#256989,#256990,
#256991,#256992,#256993,#256994,#256995,#256996,#256997,#256998,#256999,
#257000,#257001,#257002,#257003,#257004,#257005,#257006,#257007,#257008,
#257009,#257010,#257011,#257012,#257013,#257014,#257015,#257016,#257017,
#257018),(#257019,#257020,#257021,#257022,#257023,#257024,#257025,#257026,
#257027,#257028,#257029,#257030,#257031,#257032,#257033,#257034,#257035,
#257036,#257037,#257038,#257039,#257040,#257041,#257042,#257043,#257044,
#257045,#257046,#257047,#257048,#257049,#257050,#257051,#257052,#257053,
#257054,#257055,#257056,#257057,#257058,#257059,#257060,#257061,#257062,
#257063,#257064,#257065,#257066,#257067,#257068,#257069,#257070,#257071,
#257072,#257073,#257074,#257075,#257076,#257077,#257078,#257079,#257080,
#257081,#257082,#257083,#257084,#257085,#257086,#257087,#257088,#257089,
#257090,#257091,#257092,#257093,#257094,#257095,#257096,#257097,#257098,
#257099,#257100,#257101,#257102,#257103,#257104,#257105,#257106,#257107,
#257108,#257109,#257110,#257111,#257112,#257113,#257114,#257115,#257116,
#257117,#257118,#257119,#257120,#257121,#257122,#257123,#257124,#257125,
#257126,#257127,#257128,#257129,#257130,#257131,#257132,#257133,#257134,
#257135,#257136,#257137,#257138,#257139,#257140,#257141,#257142,#257143,
#257144,#257145,#257146,#257147,#257148,#257149,#257150,#257151,#257152,
#257153,#257154,#257155,#257156,#257157,#257158,#257159,#257160,#257161,
#257162,#257163,#257164,#257165,#257166,#257167,#257168,#257169,#257170,
#257171,#257172,#257173,#257174,#257175,#257176,#257177,#257178,#257179,
#257180,#257181,#257182,#257183,#257184,#257185,#257186,#257187,#257188,
#257189,#257190,#257191,#257192,#257193,#257194,#257195,#257196,#257197,
#257198,#257199,#257200,#257201,#257202,#257203,#257204,#257205,#257206,
#257207,#257208,#257209,#257210,#257211,#257212,#257213,#257214,#257215,
#257216,#257217,#257218,#257219,#257220,#257221,#257222,#257223,#257224,
#257225,#257226,#257227,#257228,#257229,#257230,#257231,#257232,#257233,
#257234,#257235,#257236,#257237,#257238,#257239,#257240,#257241,#257242,
#257243,#257244,#257245,#257246,#257247,#257248,#257249,#257250,#257251,
#257252,#257253,#257254,#257255,#257256,#257257,#257258,#257259,#257260,
#257261,#257262,#257263,#257264,#257265,#257266,#257267,#257268,#257269,
#257270,#257271,#257272,#257273,#257274,#257275,#257276,#257277,#257278,
#257279,#257280,#257281,#257282,#257283,#257284,#257285,#257286,#257287,
#257288,#257289,#257290,#257291,#257292,#257293,#257294,#257295)),
 .UNSPECIFIED.,.F.,.F.,.F.)
B_SPLINE_SURFACE_WITH_KNOTS((2,2),(3,2,2,2,2,2,2,2,2,2,2,2,2,2,2,2,2,2,
2,2,2,2,2,2,2,2,2,2,2,2,2,2,2,2,2,2,2,2,2,2,2,2,2,2,2,2,2,2,2,2,2,2,2,2,
2,2,2,2,2,2,2,2,2,2,2,2,2,2,2,2,2,2,2,2,2,2,2,2,2,2,2,2,2,2,2,2,2,2,2,2,
2,2,2,2,2,2,2,2,2,2,2,2,2,2,2,2,2,2,2,2,2,2,2,2,2,2,2,2,2,2,2,2,2,2,2,2,
2,2,2,2,2,2,2,2,2,2,2,2,3),(0.,1.00000038849803),(0.,0.0072463768115942,
0.0144927536231884,0.0217391304347826,0.0289855072463768,0.036231884057971,
0.0434782608695652,0.0507246376811594,0.0579710144927536,0.0652173913043478,
0.072463768115942,0.0797101449275362,0.0869565217391304,0.0942028985507246,
0.101449275362319,0.108695652173913,0.115942028985507,0.123188405797101,
0.130434782608696,0.13768115942029,0.144927536231884,0.152173913043478,
0.159420289855073,0.166666666666667,0.173913043478261,0.181159420289855,
0.18840579710145,0.195652173913044,0.202898550724637,0.210144927536232,
0.217391304347826,0.224637681159421,0.231884057971014,0.239130434782609,
0.246376811594203,0.253623188405797,0.260869565217392,0.268115942028985,
0.275362318840579,0.282608695652174,0.289855072463768,0.297101449275363,
0.304347826086956,0.31159420289855,0.318840579710145,0.326086956521739,
0.333333333333334,0.340579710144927,0.347826086956521,0.355072463768116,
0.36231884057971,0.369565217391304,0.376811594202899,0.384057971014493,
0.391304347826087,0.398550724637681,0.405797101449275,0.41304347826087,
0.420289855072463,0.427536231884058,0.434782608695652,0.442028985507247,
0.449275362318841,0.456521739130435,0.463768115942029,0.471014492753623,
0.478260869565218,0.485507246376812,0.492753623188406,0.5,0.507246376811594,
0.514492753623188,0.521739130434783,0.528985507246377,0.536231884057971,
0.543478260869565,0.550724637681159,0.557971014492754,0.565217391304348,
0.572463768115942,0.579710144927536,0.586956521739131,0.594202898550725,
0.601449275362319,0.608695652173913,0.615942028985507,0.623188405797101,
0.630434782608696,0.63768115942029,0.644927536231884,0.652173913043478,
0.659420289855073,0.666666666666667,0.673913043478261,0.681159420289855,
0.688405797101449,0.695652173913044,0.702898550724638,0.710144927536232,
0.717391304347826,0.72463768115942,0.731884057971015,0.739130434782609,
0.746376811594203,0.753623188405797,0.760869565217391,0.768115942028986,
0.77536231884058,0.782608695652174,0.789855072463768,0.797101449275362,
0.804347826086956,0.811594202898551,0.818840579710145,0.826086956521739,
0.833333333333333,0.840579710144928,0.847826086956522,0.855072463768116,
0.86231884057971,0.869565217391304,0.876811594202899,0.884057971014493,
0.891304347826087,0.898550724637681,0.905797101449275,0.91304347826087,
0.920289855072464,0.927536231884058,0.934782608695652,0.942028985507246,
0.94927536231884,0.956521739130435,0.963768115942029,0.971014492753623,
0.978260869565217,0.985507246376812,0.992753623188406,0.993818495192186),
 .UNSPECIFIED.)
GEOMETRIC_REPRESENTATION_ITEM()
RATIONAL_B_SPLINE_SURFACE(((1.,0.866025403784439,1.,0.866025403784439,1.,
0.866025403784439,1.,0.866025403784439,1.,0.866025403784439,1.,0.866025403784439,
1.,0.866025403784439,1.,0.866025403784439,1.,0.866025403784439,1.,0.866025403784439,
1.,0.866025403784439,1.,0.866025403784439,1.,0.866025403784439,1.,0.866025403784439,
1.,0.866025403784439,1.,0.866025403784439,1.,0.866025403784439,1.,0.866025403784439,
1.,0.866025403784439,1.,0.866025403784439,1.,0.866025403784439,1.,0.866025403784439,
1.,0.866025403784439,1.,0.866025403784439,1.,0.866025403784439,1.,0.866025403784439,
1.,0.866025403784439,1.,0.866025403784439,1.,0.866025403784439,1.,0.866025403784439,
1.,0.866025403784439,1.,0.866025403784439,1.,0.866025403784439,1.,0.866025403784439,
1.,0.866025403784439,1.,0.866025403784439,1.,0.866025403784439,1.,0.866025403784439,
1.,0.866025403784439,1.,0.866025403784439,1.,0.866025403784439,1.,0.866025403784439,
1.,0.866025403784439,1.,0.866025403784439,1.,0.866025403784439,1.,0.866025403784439,
1.,0.866025403784439,1.,0.866025403784439,1.,0.866025403784439,1.,0.866025403784439,
1.,0.866025403784439,1.,0.866025403784439,1.,0.866025403784439,1.,0.866025403784439,
1.,0.866025403784439,1.,0.866025403784439,1.,0.866025403784439,1.,0.866025403784439,
1.,0.866025403784439,1.,0.866025403784439,1.,0.866025403784439,1.,0.866025403784439,
1.,0.866025403784439,1.,0.866025403784439,1.,0.866025403784439,1.,0.866025403784439,
1.,0.866025403784439,1.,0.866025403784439,1.,0.866025403784439,1.,0.866025403784439,
1.,0.866025403784439,1.,0.866025403784439,1.,0.866025403784439,1.,0.866025403784439,
1.,0.866025403784439,1.,0.866025403784439,1.,0.866025403784439,1.,0.866025403784439,
1.,0.866025403784439,1.,0.866025403784439,1.,0.866025403784439,1.,0.866025403784439,
1.,0.866025403784439,1.,0.866025403784439,1.,0.866025403784439,1.,0.866025403784439,
1.,0.866025403784439,1.,0.866025403784439,1.,0.866025403784439,1.,0.866025403784439,
1.,0.866025403784439,1.,0.866025403784439,1.,0.866025403784439,1.,0.866025403784439,
1.,0.866025403784439,1.,0.866025403784439,1.,0.866025403784439,1.,0.866025403784439,
1.,0.866025403784439,1.,0.866025403784439,1.,0.866025403784439,1.,0.866025403784439,
1.,0.866025403784439,1.,0.866025403784439,1.,0.866025403784439,1.,0.866025403784439,
1.,0.866025403784439,1.,0.866025403784439,1.,0.866025403784439,1.,0.866025403784439,
1.,0.866025403784439,1.,0.866025403784439,1.,0.866025403784439,1.,0.866025403784439,
1.,0.866025403784439,1.,0.866025403784439,1.,0.866025403784439,1.,0.866025403784439,
1.,0.866025403784439,1.,0.866025403784439,1.,0.866025403784439,1.,0.866025403784439,
1.,0.866025403784439,1.,0.866025403784439,1.,0.866025403784439,1.,0.866025403784439,
1.,0.866025403784439,1.,0.866025403784439,1.,0.866025403784439,1.,0.866025403784439,
1.,0.866025403784439,1.,0.866025403784439,1.,0.866025403784439,1.,0.866025403784439,
1.,0.866025403784439,1.,0.866025403784439,1.,0.866025403784439,1.,0.980312120051573,
0.966410600022306),(1.,0.866025403784439,1.,0.866025403784439,1.,0.866025403784439,
1.,0.866025403784439,1.,0.866025403784439,1.,0.866025403784439,1.,0.866025403784439,
1.,0.866025403784439,1.,0.866025403784439,1.,0.866025403784439,1.,0.866025403784439,
1.,0.866025403784439,1.,0.866025403784439,1.,0.866025403784439,1.,0.866025403784439,
1.,0.866025403784439,1.,0.866025403784439,1.,0.866025403784439,1.,0.866025403784439,
1.,0.866025403784439,1.,0.866025403784439,1.,0.866025403784439,1.,0.866025403784439,
1.,0.866025403784439,1.,0.866025403784439,1.,0.866025403784439,1.,0.866025403784439,
1.,0.866025403784439,1.,0.866025403784439,1.,0.866025403784439,1.,0.866025403784439,
1.,0.866025403784439,1.,0.866025403784439,1.,0.866025403784439,1.,0.866025403784439,
1.,0.866025403784439,1.,0.866025403784439,1.,0.866025403784439,1.,0.866025403784439,
1.,0.866025403784439,1.,0.866025403784439,1.,0.866025403784439,1.,0.866025403784439,
1.,0.866025403784439,1.,0.866025403784439,1.,0.866025403784439,1.,0.866025403784439,
1.,0.866025403784439,1.,0.866025403784439,1.,0.866025403784439,1.,0.866025403784439,
1.,0.866025403784439,1.,0.866025403784439,1.,0.866025403784439,1.,0.866025403784439,
1.,0.866025403784439,1.,0.866025403784439,1.,0.866025403784439,1.,0.866025403784439,
1.,0.866025403784439,1.,0.866025403784439,1.,0.866025403784439,1.,0.866025403784439,
1.,0.866025403784439,1.,0.866025403784439,1.,0.866025403784439,1.,0.866025403784439,
1.,0.866025403784439,1.,0.866025403784439,1.,0.866025403784439,1.,0.866025403784439,
1.,0.866025403784439,1.,0.866025403784439,1.,0.866025403784439,1.,0.866025403784439,
1.,0.866025403784439,1.,0.866025403784439,1.,0.866025403784439,1.,0.866025403784439,
1.,0.866025403784439,1.,0.866025403784439,1.,0.866025403784439,1.,0.866025403784439,
1.,0.866025403784439,1.,0.866025403784439,1.,0.866025403784439,1.,0.866025403784439,
1.,0.866025403784439,1.,0.866025403784439,1.,0.866025403784439,1.,0.866025403784439,
1.,0.866025403784439,1.,0.866025403784439,1.,0.866025403784439,1.,0.866025403784439,
1.,0.866025403784439,1.,0.866025403784439,1.,0.866025403784439,1.,0.866025403784439,
1.,0.866025403784439,1.,0.866025403784439,1.,0.866025403784439,1.,0.866025403784439,
1.,0.866025403784439,1.,0.866025403784439,1.,0.866025403784439,1.,0.866025403784439,
1.,0.866025403784439,1.,0.866025403784439,1.,0.866025403784439,1.,0.866025403784439,
1.,0.866025403784439,1.,0.866025403784439,1.,0.866025403784439,1.,0.866025403784439,
1.,0.866025403784439,1.,0.866025403784439,1.,0.866025403784439,1.,0.866025403784439,
1.,0.866025403784439,1.,0.866025403784439,1.,0.866025403784439,1.,0.866025403784439,
1.,0.866025403784439,1.,0.866025403784439,1.,0.866025403784439,1.,0.866025403784439,
1.,0.866025403784439,1.,0.866025403784439,1.,0.866025403784439,1.,0.866025403784439,
1.,0.866025403784439,1.,0.866025403784439,1.,0.866025403784439,1.,0.866025403784439,
1.,0.866025403784439,1.,0.866025403784439,1.,0.980312120051573,0.966410600022306)))
REPRESENTATION_ITEM('')
SURFACE()
);
#3180=(
BOUNDED_SURFACE()
B_SPLINE_SURFACE(1,2,((#257346,#257347,#257348,#257349,#257350,#257351,
#257352,#257353,#257354,#257355,#257356,#257357,#257358,#257359,#257360,
#257361,#257362,#257363,#257364,#257365,#257366,#257367,#257368,#257369,
#257370,#257371,#257372,#257373,#257374,#257375,#257376,#257377,#257378,
#257379,#257380,#257381,#257382,#257383,#257384,#257385,#257386,#257387,
#257388,#257389,#257390,#257391,#257392,#257393,#257394,#257395,#257396,
#257397,#257398,#257399,#257400,#257401,#257402,#257403,#257404,#257405,
#257406,#257407,#257408,#257409,#257410,#257411,#257412,#257413,#257414,
#257415,#257416,#257417,#257418,#257419,#257420,#257421,#257422,#257423,
#257424,#257425,#257426,#257427,#257428,#257429,#257430,#257431,#257432,
#257433,#257434,#257435,#257436,#257437,#257438,#257439,#257440,#257441,
#257442,#257443,#257444,#257445,#257446,#257447,#257448,#257449,#257450,
#257451,#257452,#257453,#257454,#257455,#257456,#257457,#257458,#257459,
#257460,#257461,#257462,#257463,#257464,#257465,#257466,#257467,#257468,
#257469,#257470,#257471,#257472,#257473,#257474,#257475,#257476,#257477,
#257478,#257479,#257480,#257481,#257482,#257483,#257484,#257485,#257486,
#257487,#257488,#257489,#257490,#257491,#257492,#257493,#257494,#257495,
#257496,#257497,#257498,#257499,#257500,#257501,#257502,#257503,#257504,
#257505,#257506,#257507,#257508,#257509,#257510,#257511,#257512,#257513,
#257514,#257515,#257516,#257517,#257518,#257519,#257520,#257521,#257522,
#257523,#257524,#257525,#257526,#257527,#257528,#257529,#257530,#257531,
#257532,#257533,#257534,#257535,#257536,#257537,#257538,#257539,#257540,
#257541,#257542,#257543,#257544,#257545,#257546,#257547,#257548,#257549,
#257550,#257551,#257552,#257553,#257554,#257555,#257556,#257557,#257558,
#257559,#257560,#257561,#257562,#257563,#257564,#257565,#257566,#257567,
#257568,#257569,#257570,#257571,#257572,#257573,#257574,#257575,#257576,
#257577,#257578,#257579,#257580,#257581,#257582,#257583,#257584,#257585,
#257586,#257587,#257588,#257589,#257590,#257591,#257592,#257593,#257594,
#257595,#257596,#257597,#257598,#257599,#257600,#257601,#257602,#257603,
#257604,#257605,#257606,#257607,#257608,#257609,#257610,#257611,#257612,
#257613,#257614,#257615,#257616,#257617,#257618,#257619,#257620,#257621,
#257622),(#257623,#257624,#257625,#257626,#257627,#257628,#257629,#257630,
#257631,#257632,#257633,#257634,#257635,#257636,#257637,#257638,#257639,
#257640,#257641,#257642,#257643,#257644,#257645,#257646,#257647,#257648,
#257649,#257650,#257651,#257652,#257653,#257654,#257655,#257656,#257657,
#257658,#257659,#257660,#257661,#257662,#257663,#257664,#257665,#257666,
#257667,#257668,#257669,#257670,#257671,#257672,#257673,#257674,#257675,
#257676,#257677,#257678,#257679,#257680,#257681,#257682,#257683,#257684,
#257685,#257686,#257687,#257688,#257689,#257690,#257691,#257692,#257693,
#257694,#257695,#257696,#257697,#257698,#257699,#257700,#257701,#257702,
#257703,#257704,#257705,#257706,#257707,#257708,#257709,#257710,#257711,
#257712,#257713,#257714,#257715,#257716,#257717,#257718,#257719,#257720,
#257721,#257722,#257723,#257724,#257725,#257726,#257727,#257728,#257729,
#257730,#257731,#257732,#257733,#257734,#257735,#257736,#257737,#257738,
#257739,#257740,#257741,#257742,#257743,#257744,#257745,#257746,#257747,
#257748,#257749,#257750,#257751,#257752,#257753,#257754,#257755,#257756,
#257757,#257758,#257759,#257760,#257761,#257762,#257763,#257764,#257765,
#257766,#257767,#257768,#257769,#257770,#257771,#257772,#257773,#257774,
#257775,#257776,#257777,#257778,#257779,#257780,#257781,#257782,#257783,
#257784,#257785,#257786,#257787,#257788,#257789,#257790,#257791,#257792,
#257793,#257794,#257795,#257796,#257797,#257798,#257799,#257800,#257801,
#257802,#257803,#257804,#257805,#257806,#257807,#257808,#257809,#257810,
#257811,#257812,#257813,#257814,#257815,#257816,#257817,#257818,#257819,
#257820,#257821,#257822,#257823,#257824,#257825,#257826,#257827,#257828,
#257829,#257830,#257831,#257832,#257833,#257834,#257835,#257836,#257837,
#257838,#257839,#257840,#257841,#257842,#257843,#257844,#257845,#257846,
#257847,#257848,#257849,#257850,#257851,#257852,#257853,#257854,#257855,
#257856,#257857,#257858,#257859,#257860,#257861,#257862,#257863,#257864,
#257865,#257866,#257867,#257868,#257869,#257870,#257871,#257872,#257873,
#257874,#257875,#257876,#257877,#257878,#257879,#257880,#257881,#257882,
#257883,#257884,#257885,#257886,#257887,#257888,#257889,#257890,#257891,
#257892,#257893,#257894,#257895,#257896,#257897,#257898,#257899)),
 .UNSPECIFIED.,.F.,.F.,.F.)
B_SPLINE_SURFACE_WITH_KNOTS((2,2),(3,2,2,2,2,2,2,2,2,2,2,2,2,2,2,2,2,2,
2,2,2,2,2,2,2,2,2,2,2,2,2,2,2,2,2,2,2,2,2,2,2,2,2,2,2,2,2,2,2,2,2,2,2,2,
2,2,2,2,2,2,2,2,2,2,2,2,2,2,2,2,2,2,2,2,2,2,2,2,2,2,2,2,2,2,2,2,2,2,2,2,
2,2,2,2,2,2,2,2,2,2,2,2,2,2,2,2,2,2,2,2,2,2,2,2,2,2,2,2,2,2,2,2,2,2,2,2,
2,2,2,2,2,2,2,2,2,2,2,2,3),(0.,1.),(0.,0.0072463768115942,0.0144927536231884,
0.0217391304347826,0.0289855072463768,0.036231884057971,0.0434782608695652,
0.0507246376811594,0.0579710144927536,0.0652173913043478,0.072463768115942,
0.0797101449275362,0.0869565217391304,0.0942028985507246,0.101449275362319,
0.108695652173913,0.115942028985507,0.123188405797101,0.130434782608696,
0.13768115942029,0.144927536231884,0.152173913043478,0.159420289855073,
0.166666666666667,0.173913043478261,0.181159420289855,0.18840579710145,
0.195652173913044,0.202898550724637,0.210144927536232,0.217391304347826,
0.224637681159421,0.231884057971014,0.239130434782609,0.246376811594203,
0.253623188405797,0.260869565217392,0.268115942028985,0.275362318840579,
0.282608695652174,0.289855072463768,0.297101449275363,0.304347826086956,
0.31159420289855,0.318840579710145,0.326086956521739,0.333333333333334,
0.340579710144927,0.347826086956521,0.355072463768116,0.36231884057971,
0.369565217391304,0.376811594202899,0.384057971014493,0.391304347826087,
0.398550724637681,0.405797101449275,0.41304347826087,0.420289855072463,
0.427536231884058,0.434782608695652,0.442028985507247,0.449275362318841,
0.456521739130435,0.463768115942029,0.471014492753623,0.478260869565218,
0.485507246376812,0.492753623188406,0.5,0.507246376811594,0.514492753623188,
0.521739130434783,0.528985507246377,0.536231884057971,0.543478260869565,
0.550724637681159,0.557971014492754,0.565217391304348,0.572463768115942,
0.579710144927536,0.586956521739131,0.594202898550725,0.601449275362319,
0.608695652173913,0.615942028985507,0.623188405797101,0.630434782608696,
0.63768115942029,0.644927536231884,0.652173913043478,0.659420289855073,
0.666666666666667,0.673913043478261,0.681159420289855,0.688405797101449,
0.695652173913044,0.702898550724638,0.710144927536232,0.717391304347826,
0.72463768115942,0.731884057971015,0.739130434782609,0.746376811594203,
0.753623188405797,0.760869565217391,0.768115942028986,0.77536231884058,
0.782608695652174,0.789855072463768,0.797101449275362,0.804347826086956,
0.811594202898551,0.818840579710145,0.826086956521739,0.833333333333333,
0.840579710144928,0.847826086956522,0.855072463768116,0.86231884057971,
0.869565217391304,0.876811594202899,0.884057971014493,0.891304347826087,
0.898550724637681,0.905797101449275,0.91304347826087,0.920289855072464,
0.927536231884058,0.934782608695652,0.942028985507246,0.94927536231884,
0.956521739130435,0.963768115942029,0.971014492753623,0.978260869565217,
0.985507246376812,0.992753623188406,0.993818585798284),.UNSPECIFIED.)
GEOMETRIC_REPRESENTATION_ITEM()
RATIONAL_B_SPLINE_SURFACE(((1.,0.866025403784439,1.,0.866025403784439,1.,
0.866025403784439,1.,0.866025403784439,1.,0.866025403784439,1.,0.866025403784439,
1.,0.866025403784439,1.,0.866025403784439,1.,0.866025403784439,1.,0.866025403784439,
1.,0.866025403784439,1.,0.866025403784439,1.,0.866025403784439,1.,0.866025403784439,
1.,0.866025403784439,1.,0.866025403784439,1.,0.866025403784439,1.,0.866025403784439,
1.,0.866025403784439,1.,0.866025403784439,1.,0.866025403784439,1.,0.866025403784439,
1.,0.866025403784439,1.,0.866025403784439,1.,0.866025403784439,1.,0.866025403784439,
1.,0.866025403784439,1.,0.866025403784439,1.,0.866025403784439,1.,0.866025403784439,
1.,0.866025403784439,1.,0.866025403784439,1.,0.866025403784439,1.,0.866025403784439,
1.,0.866025403784439,1.,0.866025403784439,1.,0.866025403784439,1.,0.866025403784439,
1.,0.866025403784439,1.,0.866025403784439,1.,0.866025403784439,1.,0.866025403784439,
1.,0.866025403784439,1.,0.866025403784439,1.,0.866025403784439,1.,0.866025403784439,
1.,0.866025403784439,1.,0.866025403784439,1.,0.866025403784439,1.,0.866025403784439,
1.,0.866025403784439,1.,0.866025403784439,1.,0.866025403784439,1.,0.866025403784439,
1.,0.866025403784439,1.,0.866025403784439,1.,0.866025403784439,1.,0.866025403784439,
1.,0.866025403784439,1.,0.866025403784439,1.,0.866025403784439,1.,0.866025403784439,
1.,0.866025403784439,1.,0.866025403784439,1.,0.866025403784439,1.,0.866025403784439,
1.,0.866025403784439,1.,0.866025403784439,1.,0.866025403784439,1.,0.866025403784439,
1.,0.866025403784439,1.,0.866025403784439,1.,0.866025403784439,1.,0.866025403784439,
1.,0.866025403784439,1.,0.866025403784439,1.,0.866025403784439,1.,0.866025403784439,
1.,0.866025403784439,1.,0.866025403784439,1.,0.866025403784439,1.,0.866025403784439,
1.,0.866025403784439,1.,0.866025403784439,1.,0.866025403784439,1.,0.866025403784439,
1.,0.866025403784439,1.,0.866025403784439,1.,0.866025403784439,1.,0.866025403784439,
1.,0.866025403784439,1.,0.866025403784439,1.,0.866025403784439,1.,0.866025403784439,
1.,0.866025403784439,1.,0.866025403784439,1.,0.866025403784439,1.,0.866025403784439,
1.,0.866025403784439,1.,0.866025403784439,1.,0.866025403784439,1.,0.866025403784439,
1.,0.866025403784439,1.,0.866025403784439,1.,0.866025403784439,1.,0.866025403784439,
1.,0.866025403784439,1.,0.866025403784439,1.,0.866025403784439,1.,0.866025403784439,
1.,0.866025403784439,1.,0.866025403784439,1.,0.866025403784439,1.,0.866025403784439,
1.,0.866025403784439,1.,0.866025403784439,1.,0.866025403784439,1.,0.866025403784439,
1.,0.866025403784439,1.,0.866025403784439,1.,0.866025403784439,1.,0.866025403784439,
1.,0.866025403784439,1.,0.866025403784439,1.,0.866025403784439,1.,0.866025403784439,
1.,0.866025403784439,1.,0.866025403784439,1.,0.866025403784439,1.,0.866025403784439,
1.,0.866025403784439,1.,0.866025403784439,1.,0.866025403784439,1.,0.866025403784439,
1.,0.866025403784439,1.,0.866025403784439,1.,0.866025403784439,1.,0.98031044488126,
0.966408234404338),(1.,0.866025403784439,1.,0.866025403784439,1.,0.866025403784439,
1.,0.866025403784439,1.,0.866025403784439,1.,0.866025403784439,1.,0.866025403784439,
1.,0.866025403784439,1.,0.866025403784439,1.,0.866025403784439,1.,0.866025403784439,
1.,0.866025403784439,1.,0.866025403784439,1.,0.866025403784439,1.,0.866025403784439,
1.,0.866025403784439,1.,0.866025403784439,1.,0.866025403784439,1.,0.866025403784439,
1.,0.866025403784439,1.,0.866025403784439,1.,0.866025403784439,1.,0.866025403784439,
1.,0.866025403784439,1.,0.866025403784439,1.,0.866025403784439,1.,0.866025403784439,
1.,0.866025403784439,1.,0.866025403784439,1.,0.866025403784439,1.,0.866025403784439,
1.,0.866025403784439,1.,0.866025403784439,1.,0.866025403784439,1.,0.866025403784439,
1.,0.866025403784439,1.,0.866025403784439,1.,0.866025403784439,1.,0.866025403784439,
1.,0.866025403784439,1.,0.866025403784439,1.,0.866025403784439,1.,0.866025403784439,
1.,0.866025403784439,1.,0.866025403784439,1.,0.866025403784439,1.,0.866025403784439,
1.,0.866025403784439,1.,0.866025403784439,1.,0.866025403784439,1.,0.866025403784439,
1.,0.866025403784439,1.,0.866025403784439,1.,0.866025403784439,1.,0.866025403784439,
1.,0.866025403784439,1.,0.866025403784439,1.,0.866025403784439,1.,0.866025403784439,
1.,0.866025403784439,1.,0.866025403784439,1.,0.866025403784439,1.,0.866025403784439,
1.,0.866025403784439,1.,0.866025403784439,1.,0.866025403784439,1.,0.866025403784439,
1.,0.866025403784439,1.,0.866025403784439,1.,0.866025403784439,1.,0.866025403784439,
1.,0.866025403784439,1.,0.866025403784439,1.,0.866025403784439,1.,0.866025403784439,
1.,0.866025403784439,1.,0.866025403784439,1.,0.866025403784439,1.,0.866025403784439,
1.,0.866025403784439,1.,0.866025403784439,1.,0.866025403784439,1.,0.866025403784439,
1.,0.866025403784439,1.,0.866025403784439,1.,0.866025403784439,1.,0.866025403784439,
1.,0.866025403784439,1.,0.866025403784439,1.,0.866025403784439,1.,0.866025403784439,
1.,0.866025403784439,1.,0.866025403784439,1.,0.866025403784439,1.,0.866025403784439,
1.,0.866025403784439,1.,0.866025403784439,1.,0.866025403784439,1.,0.866025403784439,
1.,0.866025403784439,1.,0.866025403784439,1.,0.866025403784439,1.,0.866025403784439,
1.,0.866025403784439,1.,0.866025403784439,1.,0.866025403784439,1.,0.866025403784439,
1.,0.866025403784439,1.,0.866025403784439,1.,0.866025403784439,1.,0.866025403784439,
1.,0.866025403784439,1.,0.866025403784439,1.,0.866025403784439,1.,0.866025403784439,
1.,0.866025403784439,1.,0.866025403784439,1.,0.866025403784439,1.,0.866025403784439,
1.,0.866025403784439,1.,0.866025403784439,1.,0.866025403784439,1.,0.866025403784439,
1.,0.866025403784439,1.,0.866025403784439,1.,0.866025403784439,1.,0.866025403784439,
1.,0.866025403784439,1.,0.866025403784439,1.,0.866025403784439,1.,0.866025403784439,
1.,0.866025403784439,1.,0.866025403784439,1.,0.866025403784439,1.,0.866025403784439,
1.,0.866025403784439,1.,0.866025403784439,1.,0.98031044488126,0.966408234404338)))
REPRESENTATION_ITEM('')
SURFACE()
);
#3181=(
BOUNDED_SURFACE()
B_SPLINE_SURFACE(1,2,((#257947,#257948,#257949,#257950,#257951,#257952,
#257953,#257954,#257955,#257956,#257957,#257958,#257959,#257960,#257961,
#257962,#257963,#257964,#257965,#257966,#257967,#257968,#257969,#257970,
#257971,#257972,#257973,#257974,#257975,#257976,#257977,#257978,#257979,
#257980,#257981,#257982,#257983,#257984,#257985,#257986,#257987,#257988,
#257989,#257990,#257991,#257992,#257993,#257994,#257995,#257996,#257997,
#257998,#257999,#258000,#258001,#258002,#258003,#258004,#258005,#258006,
#258007,#258008,#258009,#258010,#258011,#258012,#258013,#258014,#258015,
#258016,#258017,#258018,#258019,#258020,#258021,#258022,#258023,#258024,
#258025,#258026,#258027,#258028,#258029,#258030,#258031,#258032,#258033,
#258034,#258035,#258036,#258037,#258038,#258039,#258040,#258041,#258042,
#258043,#258044,#258045,#258046,#258047,#258048,#258049,#258050,#258051,
#258052,#258053,#258054,#258055,#258056,#258057,#258058,#258059,#258060,
#258061,#258062,#258063,#258064,#258065,#258066,#258067,#258068,#258069,
#258070,#258071,#258072,#258073,#258074,#258075,#258076,#258077,#258078,
#258079,#258080,#258081,#258082,#258083,#258084,#258085,#258086,#258087,
#258088,#258089,#258090,#258091,#258092,#258093,#258094,#258095,#258096,
#258097,#258098,#258099,#258100,#258101,#258102,#258103,#258104,#258105,
#258106,#258107,#258108,#258109,#258110,#258111,#258112,#258113,#258114,
#258115,#258116,#258117,#258118,#258119,#258120,#258121,#258122,#258123,
#258124,#258125,#258126,#258127,#258128,#258129,#258130,#258131,#258132,
#258133,#258134,#258135,#258136,#258137,#258138,#258139,#258140,#258141,
#258142,#258143,#258144,#258145,#258146,#258147,#258148,#258149,#258150,
#258151,#258152,#258153,#258154,#258155,#258156,#258157,#258158,#258159,
#258160,#258161,#258162,#258163,#258164,#258165,#258166,#258167,#258168,
#258169,#258170,#258171,#258172,#258173,#258174,#258175,#258176,#258177,
#258178,#258179,#258180,#258181,#258182,#258183,#258184,#258185,#258186,
#258187,#258188,#258189,#258190,#258191,#258192,#258193,#258194,#258195,
#258196,#258197,#258198,#258199,#258200,#258201,#258202,#258203,#258204,
#258205,#258206,#258207,#258208,#258209,#258210,#258211,#258212,#258213,
#258214,#258215,#258216,#258217,#258218,#258219,#258220,#258221,#258222,
#258223),(#258224,#258225,#258226,#258227,#258228,#258229,#258230,#258231,
#258232,#258233,#258234,#258235,#258236,#258237,#258238,#258239,#258240,
#258241,#258242,#258243,#258244,#258245,#258246,#258247,#258248,#258249,
#258250,#258251,#258252,#258253,#258254,#258255,#258256,#258257,#258258,
#258259,#258260,#258261,#258262,#258263,#258264,#258265,#258266,#258267,
#258268,#258269,#258270,#258271,#258272,#258273,#258274,#258275,#258276,
#258277,#258278,#258279,#258280,#258281,#258282,#258283,#258284,#258285,
#258286,#258287,#258288,#258289,#258290,#258291,#258292,#258293,#258294,
#258295,#258296,#258297,#258298,#258299,#258300,#258301,#258302,#258303,
#258304,#258305,#258306,#258307,#258308,#258309,#258310,#258311,#258312,
#258313,#258314,#258315,#258316,#258317,#258318,#258319,#258320,#258321,
#258322,#258323,#258324,#258325,#258326,#258327,#258328,#258329,#258330,
#258331,#258332,#258333,#258334,#258335,#258336,#258337,#258338,#258339,
#258340,#258341,#258342,#258343,#258344,#258345,#258346,#258347,#258348,
#258349,#258350,#258351,#258352,#258353,#258354,#258355,#258356,#258357,
#258358,#258359,#258360,#258361,#258362,#258363,#258364,#258365,#258366,
#258367,#258368,#258369,#258370,#258371,#258372,#258373,#258374,#258375,
#258376,#258377,#258378,#258379,#258380,#258381,#258382,#258383,#258384,
#258385,#258386,#258387,#258388,#258389,#258390,#258391,#258392,#258393,
#258394,#258395,#258396,#258397,#258398,#258399,#258400,#258401,#258402,
#258403,#258404,#258405,#258406,#258407,#258408,#258409,#258410,#258411,
#258412,#258413,#258414,#258415,#258416,#258417,#258418,#258419,#258420,
#258421,#258422,#258423,#258424,#258425,#258426,#258427,#258428,#258429,
#258430,#258431,#258432,#258433,#258434,#258435,#258436,#258437,#258438,
#258439,#258440,#258441,#258442,#258443,#258444,#258445,#258446,#258447,
#258448,#258449,#258450,#258451,#258452,#258453,#258454,#258455,#258456,
#258457,#258458,#258459,#258460,#258461,#258462,#258463,#258464,#258465,
#258466,#258467,#258468,#258469,#258470,#258471,#258472,#258473,#258474,
#258475,#258476,#258477,#258478,#258479,#258480,#258481,#258482,#258483,
#258484,#258485,#258486,#258487,#258488,#258489,#258490,#258491,#258492,
#258493,#258494,#258495,#258496,#258497,#258498,#258499,#258500)),
 .UNSPECIFIED.,.F.,.F.,.F.)
B_SPLINE_SURFACE_WITH_KNOTS((2,2),(3,2,2,2,2,2,2,2,2,2,2,2,2,2,2,2,2,2,
2,2,2,2,2,2,2,2,2,2,2,2,2,2,2,2,2,2,2,2,2,2,2,2,2,2,2,2,2,2,2,2,2,2,2,2,
2,2,2,2,2,2,2,2,2,2,2,2,2,2,2,2,2,2,2,2,2,2,2,2,2,2,2,2,2,2,2,2,2,2,2,2,
2,2,2,2,2,2,2,2,2,2,2,2,2,2,2,2,2,2,2,2,2,2,2,2,2,2,2,2,2,2,2,2,2,2,2,2,
2,2,2,2,2,2,2,2,2,2,2,2,3),(0.,1.),(0.,0.0072463768115942,0.0144927536231884,
0.0217391304347826,0.0289855072463768,0.036231884057971,0.0434782608695652,
0.0507246376811594,0.0579710144927536,0.0652173913043478,0.072463768115942,
0.0797101449275362,0.0869565217391304,0.0942028985507246,0.101449275362319,
0.108695652173913,0.115942028985507,0.123188405797101,0.130434782608696,
0.13768115942029,0.144927536231884,0.152173913043478,0.159420289855073,
0.166666666666667,0.173913043478261,0.181159420289855,0.18840579710145,
0.195652173913044,0.202898550724637,0.210144927536232,0.217391304347826,
0.224637681159421,0.231884057971014,0.239130434782609,0.246376811594203,
0.253623188405797,0.260869565217392,0.268115942028985,0.275362318840579,
0.282608695652174,0.289855072463768,0.297101449275363,0.304347826086956,
0.31159420289855,0.318840579710145,0.326086956521739,0.333333333333334,
0.340579710144927,0.347826086956521,0.355072463768116,0.36231884057971,
0.369565217391304,0.376811594202899,0.384057971014493,0.391304347826087,
0.398550724637681,0.405797101449275,0.41304347826087,0.420289855072463,
0.427536231884058,0.434782608695652,0.442028985507247,0.449275362318841,
0.456521739130435,0.463768115942029,0.471014492753623,0.478260869565218,
0.485507246376812,0.492753623188406,0.5,0.507246376811594,0.514492753623188,
0.521739130434783,0.528985507246377,0.536231884057971,0.543478260869565,
0.550724637681159,0.557971014492754,0.565217391304348,0.572463768115942,
0.579710144927536,0.586956521739131,0.594202898550725,0.601449275362319,
0.608695652173913,0.615942028985507,0.623188405797101,0.630434782608696,
0.63768115942029,0.644927536231884,0.652173913043478,0.659420289855073,
0.666666666666667,0.673913043478261,0.681159420289855,0.688405797101449,
0.695652173913044,0.702898550724638,0.710144927536232,0.717391304347826,
0.72463768115942,0.731884057971015,0.739130434782609,0.746376811594203,
0.753623188405797,0.760869565217391,0.768115942028986,0.77536231884058,
0.782608695652174,0.789855072463768,0.797101449275362,0.804347826086956,
0.811594202898551,0.818840579710145,0.826086956521739,0.833333333333333,
0.840579710144928,0.847826086956522,0.855072463768116,0.86231884057971,
0.869565217391304,0.876811594202899,0.884057971014493,0.891304347826087,
0.898550724637681,0.905797101449275,0.91304347826087,0.920289855072464,
0.927536231884058,0.934782608695652,0.942028985507246,0.94927536231884,
0.956521739130435,0.963768115942029,0.971014492753623,0.978260869565217,
0.985507246376812,0.992753623188406,0.993818585798284),.UNSPECIFIED.)
GEOMETRIC_REPRESENTATION_ITEM()
RATIONAL_B_SPLINE_SURFACE(((1.,0.866025403784439,1.,0.866025403784439,1.,
0.866025403784439,1.,0.866025403784439,1.,0.866025403784439,1.,0.866025403784439,
1.,0.866025403784439,1.,0.866025403784439,1.,0.866025403784439,1.,0.866025403784439,
1.,0.866025403784439,1.,0.866025403784439,1.,0.866025403784439,1.,0.866025403784439,
1.,0.866025403784439,1.,0.866025403784439,1.,0.866025403784439,1.,0.866025403784439,
1.,0.866025403784439,1.,0.866025403784439,1.,0.866025403784439,1.,0.866025403784439,
1.,0.866025403784439,1.,0.866025403784439,1.,0.866025403784439,1.,0.866025403784439,
1.,0.866025403784439,1.,0.866025403784439,1.,0.866025403784439,1.,0.866025403784439,
1.,0.866025403784439,1.,0.866025403784439,1.,0.866025403784439,1.,0.866025403784439,
1.,0.866025403784439,1.,0.866025403784439,1.,0.866025403784439,1.,0.866025403784439,
1.,0.866025403784439,1.,0.866025403784439,1.,0.866025403784439,1.,0.866025403784439,
1.,0.866025403784439,1.,0.866025403784439,1.,0.866025403784439,1.,0.866025403784439,
1.,0.866025403784439,1.,0.866025403784439,1.,0.866025403784439,1.,0.866025403784439,
1.,0.866025403784439,1.,0.866025403784439,1.,0.866025403784439,1.,0.866025403784439,
1.,0.866025403784439,1.,0.866025403784439,1.,0.866025403784439,1.,0.866025403784439,
1.,0.866025403784439,1.,0.866025403784439,1.,0.866025403784439,1.,0.866025403784439,
1.,0.866025403784439,1.,0.866025403784439,1.,0.866025403784439,1.,0.866025403784439,
1.,0.866025403784439,1.,0.866025403784439,1.,0.866025403784439,1.,0.866025403784439,
1.,0.866025403784439,1.,0.866025403784439,1.,0.866025403784439,1.,0.866025403784439,
1.,0.866025403784439,1.,0.866025403784439,1.,0.866025403784439,1.,0.866025403784439,
1.,0.866025403784439,1.,0.866025403784439,1.,0.866025403784439,1.,0.866025403784439,
1.,0.866025403784439,1.,0.866025403784439,1.,0.866025403784439,1.,0.866025403784439,
1.,0.866025403784439,1.,0.866025403784439,1.,0.866025403784439,1.,0.866025403784439,
1.,0.866025403784439,1.,0.866025403784439,1.,0.866025403784439,1.,0.866025403784439,
1.,0.866025403784439,1.,0.866025403784439,1.,0.866025403784439,1.,0.866025403784439,
1.,0.866025403784439,1.,0.866025403784439,1.,0.866025403784439,1.,0.866025403784439,
1.,0.866025403784439,1.,0.866025403784439,1.,0.866025403784439,1.,0.866025403784439,
1.,0.866025403784439,1.,0.866025403784439,1.,0.866025403784439,1.,0.866025403784439,
1.,0.866025403784439,1.,0.866025403784439,1.,0.866025403784439,1.,0.866025403784439,
1.,0.866025403784439,1.,0.866025403784439,1.,0.866025403784439,1.,0.866025403784439,
1.,0.866025403784439,1.,0.866025403784439,1.,0.866025403784439,1.,0.866025403784439,
1.,0.866025403784439,1.,0.866025403784439,1.,0.866025403784439,1.,0.866025403784439,
1.,0.866025403784439,1.,0.866025403784439,1.,0.866025403784439,1.,0.866025403784439,
1.,0.866025403784439,1.,0.866025403784439,1.,0.866025403784439,1.,0.866025403784439,
1.,0.866025403784439,1.,0.866025403784439,1.,0.866025403784439,1.,0.98031044488126,
0.966408234404338),(1.,0.866025403784439,1.,0.866025403784439,1.,0.866025403784439,
1.,0.866025403784439,1.,0.866025403784439,1.,0.866025403784439,1.,0.866025403784439,
1.,0.866025403784439,1.,0.866025403784439,1.,0.866025403784439,1.,0.866025403784439,
1.,0.866025403784439,1.,0.866025403784439,1.,0.866025403784439,1.,0.866025403784439,
1.,0.866025403784439,1.,0.866025403784439,1.,0.866025403784439,1.,0.866025403784439,
1.,0.866025403784439,1.,0.866025403784439,1.,0.866025403784439,1.,0.866025403784439,
1.,0.866025403784439,1.,0.866025403784439,1.,0.866025403784439,1.,0.866025403784439,
1.,0.866025403784439,1.,0.866025403784439,1.,0.866025403784439,1.,0.866025403784439,
1.,0.866025403784439,1.,0.866025403784439,1.,0.866025403784439,1.,0.866025403784439,
1.,0.866025403784439,1.,0.866025403784439,1.,0.866025403784439,1.,0.866025403784439,
1.,0.866025403784439,1.,0.866025403784439,1.,0.866025403784439,1.,0.866025403784439,
1.,0.866025403784439,1.,0.866025403784439,1.,0.866025403784439,1.,0.866025403784439,
1.,0.866025403784439,1.,0.866025403784439,1.,0.866025403784439,1.,0.866025403784439,
1.,0.866025403784439,1.,0.866025403784439,1.,0.866025403784439,1.,0.866025403784439,
1.,0.866025403784439,1.,0.866025403784439,1.,0.866025403784439,1.,0.866025403784439,
1.,0.866025403784439,1.,0.866025403784439,1.,0.866025403784439,1.,0.866025403784439,
1.,0.866025403784439,1.,0.866025403784439,1.,0.866025403784439,1.,0.866025403784439,
1.,0.866025403784439,1.,0.866025403784439,1.,0.866025403784439,1.,0.866025403784439,
1.,0.866025403784439,1.,0.866025403784439,1.,0.866025403784439,1.,0.866025403784439,
1.,0.866025403784439,1.,0.866025403784439,1.,0.866025403784439,1.,0.866025403784439,
1.,0.866025403784439,1.,0.866025403784439,1.,0.866025403784439,1.,0.866025403784439,
1.,0.866025403784439,1.,0.866025403784439,1.,0.866025403784439,1.,0.866025403784439,
1.,0.866025403784439,1.,0.866025403784439,1.,0.866025403784439,1.,0.866025403784439,
1.,0.866025403784439,1.,0.866025403784439,1.,0.866025403784439,1.,0.866025403784439,
1.,0.866025403784439,1.,0.866025403784439,1.,0.866025403784439,1.,0.866025403784439,
1.,0.866025403784439,1.,0.866025403784439,1.,0.866025403784439,1.,0.866025403784439,
1.,0.866025403784439,1.,0.866025403784439,1.,0.866025403784439,1.,0.866025403784439,
1.,0.866025403784439,1.,0.866025403784439,1.,0.866025403784439,1.,0.866025403784439,
1.,0.866025403784439,1.,0.866025403784439,1.,0.866025403784439,1.,0.866025403784439,
1.,0.866025403784439,1.,0.866025403784439,1.,0.866025403784439,1.,0.866025403784439,
1.,0.866025403784439,1.,0.866025403784439,1.,0.866025403784439,1.,0.866025403784439,
1.,0.866025403784439,1.,0.866025403784439,1.,0.866025403784439,1.,0.866025403784439,
1.,0.866025403784439,1.,0.866025403784439,1.,0.866025403784439,1.,0.866025403784439,
1.,0.866025403784439,1.,0.866025403784439,1.,0.866025403784439,1.,0.866025403784439,
1.,0.866025403784439,1.,0.866025403784439,1.,0.98031044488126,0.966408234404338)))
REPRESENTATION_ITEM('')
SURFACE()
);
#3182=(
BOUNDED_SURFACE()
B_SPLINE_SURFACE(1,2,((#260304,#260305,#260306,#260307,#260308,#260309,
#260310,#260311,#260312,#260313,#260314,#260315,#260316,#260317,#260318,
#260319,#260320,#260321,#260322,#260323,#260324,#260325,#260326,#260327,
#260328,#260329,#260330,#260331,#260332,#260333,#260334,#260335,#260336,
#260337,#260338,#260339,#260340,#260341,#260342,#260343,#260344,#260345,
#260346,#260347,#260348,#260349,#260350,#260351,#260352,#260353,#260354,
#260355,#260356,#260357,#260358,#260359,#260360,#260361,#260362,#260363,
#260364,#260365,#260366,#260367,#260368,#260369,#260370,#260371,#260372,
#260373,#260374,#260375,#260376,#260377,#260378,#260379,#260380,#260381,
#260382,#260383,#260384,#260385,#260386,#260387,#260388,#260389,#260390,
#260391,#260392,#260393,#260394,#260395,#260396,#260397,#260398,#260399,
#260400,#260401,#260402,#260403,#260404,#260405,#260406,#260407,#260408,
#260409,#260410,#260411,#260412,#260413,#260414,#260415,#260416,#260417,
#260418,#260419,#260420,#260421,#260422,#260423,#260424,#260425,#260426,
#260427,#260428,#260429,#260430,#260431,#260432,#260433,#260434,#260435,
#260436,#260437,#260438,#260439,#260440,#260441,#260442,#260443,#260444,
#260445,#260446,#260447,#260448,#260449,#260450,#260451,#260452,#260453,
#260454,#260455,#260456,#260457,#260458,#260459,#260460,#260461,#260462,
#260463,#260464,#260465,#260466,#260467,#260468,#260469,#260470,#260471,
#260472,#260473,#260474,#260475,#260476,#260477,#260478,#260479,#260480,
#260481,#260482,#260483,#260484,#260485,#260486,#260487,#260488,#260489,
#260490,#260491,#260492,#260493,#260494,#260495,#260496,#260497,#260498,
#260499,#260500,#260501,#260502,#260503,#260504,#260505,#260506,#260507,
#260508,#260509,#260510,#260511,#260512,#260513,#260514,#260515,#260516,
#260517,#260518,#260519,#260520,#260521,#260522,#260523,#260524,#260525,
#260526,#260527,#260528,#260529,#260530,#260531,#260532,#260533,#260534,
#260535,#260536,#260537,#260538,#260539,#260540,#260541,#260542,#260543,
#260544,#260545,#260546,#260547,#260548,#260549,#260550,#260551,#260552,
#260553,#260554,#260555,#260556,#260557,#260558,#260559,#260560,#260561,
#260562,#260563,#260564,#260565,#260566,#260567,#260568,#260569,#260570,
#260571,#260572,#260573,#260574,#260575,#260576,#260577,#260578,#260579,
#260580),(#260581,#260582,#260583,#260584,#260585,#260586,#260587,#260588,
#260589,#260590,#260591,#260592,#260593,#260594,#260595,#260596,#260597,
#260598,#260599,#260600,#260601,#260602,#260603,#260604,#260605,#260606,
#260607,#260608,#260609,#260610,#260611,#260612,#260613,#260614,#260615,
#260616,#260617,#260618,#260619,#260620,#260621,#260622,#260623,#260624,
#260625,#260626,#260627,#260628,#260629,#260630,#260631,#260632,#260633,
#260634,#260635,#260636,#260637,#260638,#260639,#260640,#260641,#260642,
#260643,#260644,#260645,#260646,#260647,#260648,#260649,#260650,#260651,
#260652,#260653,#260654,#260655,#260656,#260657,#260658,#260659,#260660,
#260661,#260662,#260663,#260664,#260665,#260666,#260667,#260668,#260669,
#260670,#260671,#260672,#260673,#260674,#260675,#260676,#260677,#260678,
#260679,#260680,#260681,#260682,#260683,#260684,#260685,#260686,#260687,
#260688,#260689,#260690,#260691,#260692,#260693,#260694,#260695,#260696,
#260697,#260698,#260699,#260700,#260701,#260702,#260703,#260704,#260705,
#260706,#260707,#260708,#260709,#260710,#260711,#260712,#260713,#260714,
#260715,#260716,#260717,#260718,#260719,#260720,#260721,#260722,#260723,
#260724,#260725,#260726,#260727,#260728,#260729,#260730,#260731,#260732,
#260733,#260734,#260735,#260736,#260737,#260738,#260739,#260740,#260741,
#260742,#260743,#260744,#260745,#260746,#260747,#260748,#260749,#260750,
#260751,#260752,#260753,#260754,#260755,#260756,#260757,#260758,#260759,
#260760,#260761,#260762,#260763,#260764,#260765,#260766,#260767,#260768,
#260769,#260770,#260771,#260772,#260773,#260774,#260775,#260776,#260777,
#260778,#260779,#260780,#260781,#260782,#260783,#260784,#260785,#260786,
#260787,#260788,#260789,#260790,#260791,#260792,#260793,#260794,#260795,
#260796,#260797,#260798,#260799,#260800,#260801,#260802,#260803,#260804,
#260805,#260806,#260807,#260808,#260809,#260810,#260811,#260812,#260813,
#260814,#260815,#260816,#260817,#260818,#260819,#260820,#260821,#260822,
#260823,#260824,#260825,#260826,#260827,#260828,#260829,#260830,#260831,
#260832,#260833,#260834,#260835,#260836,#260837,#260838,#260839,#260840,
#260841,#260842,#260843,#260844,#260845,#260846,#260847,#260848,#260849,
#260850,#260851,#260852,#260853,#260854,#260855,#260856,#260857)),
 .UNSPECIFIED.,.F.,.F.,.F.)
B_SPLINE_SURFACE_WITH_KNOTS((2,2),(3,2,2,2,2,2,2,2,2,2,2,2,2,2,2,2,2,2,
2,2,2,2,2,2,2,2,2,2,2,2,2,2,2,2,2,2,2,2,2,2,2,2,2,2,2,2,2,2,2,2,2,2,2,2,
2,2,2,2,2,2,2,2,2,2,2,2,2,2,2,2,2,2,2,2,2,2,2,2,2,2,2,2,2,2,2,2,2,2,2,2,
2,2,2,2,2,2,2,2,2,2,2,2,2,2,2,2,2,2,2,2,2,2,2,2,2,2,2,2,2,2,2,2,2,2,2,2,
2,2,2,2,2,2,2,2,2,2,2,2,3),(0.,1.),(0.,0.0072463768115942,0.0144927536231884,
0.0217391304347826,0.0289855072463768,0.036231884057971,0.0434782608695652,
0.0507246376811594,0.0579710144927536,0.0652173913043478,0.072463768115942,
0.0797101449275362,0.0869565217391304,0.0942028985507246,0.101449275362319,
0.108695652173913,0.115942028985507,0.123188405797101,0.130434782608696,
0.13768115942029,0.144927536231884,0.152173913043478,0.159420289855073,
0.166666666666667,0.173913043478261,0.181159420289855,0.18840579710145,
0.195652173913044,0.202898550724637,0.210144927536232,0.217391304347826,
0.224637681159421,0.231884057971014,0.239130434782609,0.246376811594203,
0.253623188405797,0.260869565217392,0.268115942028985,0.275362318840579,
0.282608695652174,0.289855072463768,0.297101449275363,0.304347826086956,
0.31159420289855,0.318840579710145,0.326086956521739,0.333333333333334,
0.340579710144927,0.347826086956521,0.355072463768116,0.36231884057971,
0.369565217391304,0.376811594202899,0.384057971014493,0.391304347826087,
0.398550724637681,0.405797101449275,0.41304347826087,0.420289855072463,
0.427536231884058,0.434782608695652,0.442028985507247,0.449275362318841,
0.456521739130435,0.463768115942029,0.471014492753623,0.478260869565218,
0.485507246376812,0.492753623188406,0.5,0.507246376811594,0.514492753623188,
0.521739130434783,0.528985507246377,0.536231884057971,0.543478260869565,
0.550724637681159,0.557971014492754,0.565217391304348,0.572463768115942,
0.579710144927536,0.586956521739131,0.594202898550725,0.601449275362319,
0.608695652173913,0.615942028985507,0.623188405797101,0.630434782608696,
0.63768115942029,0.644927536231884,0.652173913043478,0.659420289855073,
0.666666666666667,0.673913043478261,0.681159420289855,0.688405797101449,
0.695652173913044,0.702898550724638,0.710144927536232,0.717391304347826,
0.72463768115942,0.731884057971015,0.739130434782609,0.746376811594203,
0.753623188405797,0.760869565217391,0.768115942028986,0.77536231884058,
0.782608695652174,0.789855072463768,0.797101449275362,0.804347826086956,
0.811594202898551,0.818840579710145,0.826086956521739,0.833333333333333,
0.840579710144928,0.847826086956522,0.855072463768116,0.86231884057971,
0.869565217391304,0.876811594202899,0.884057971014493,0.891304347826087,
0.898550724637681,0.905797101449275,0.91304347826087,0.920289855072464,
0.927536231884058,0.934782608695652,0.942028985507246,0.94927536231884,
0.956521739130435,0.963768115942029,0.971014492753623,0.978260869565217,
0.985507246376812,0.992753623188406,0.993818495192186),.UNSPECIFIED.)
GEOMETRIC_REPRESENTATION_ITEM()
RATIONAL_B_SPLINE_SURFACE(((1.,0.866025403784439,1.,0.866025403784439,1.,
0.866025403784439,1.,0.866025403784439,1.,0.866025403784439,1.,0.866025403784439,
1.,0.866025403784439,1.,0.866025403784439,1.,0.866025403784439,1.,0.866025403784439,
1.,0.866025403784439,1.,0.866025403784439,1.,0.866025403784439,1.,0.866025403784439,
1.,0.866025403784439,1.,0.866025403784439,1.,0.866025403784439,1.,0.866025403784439,
1.,0.866025403784439,1.,0.866025403784439,1.,0.866025403784439,1.,0.866025403784439,
1.,0.866025403784439,1.,0.866025403784439,1.,0.866025403784439,1.,0.866025403784439,
1.,0.866025403784439,1.,0.866025403784439,1.,0.866025403784439,1.,0.866025403784439,
1.,0.866025403784439,1.,0.866025403784439,1.,0.866025403784439,1.,0.866025403784439,
1.,0.866025403784439,1.,0.866025403784439,1.,0.866025403784439,1.,0.866025403784439,
1.,0.866025403784439,1.,0.866025403784439,1.,0.866025403784439,1.,0.866025403784439,
1.,0.866025403784439,1.,0.866025403784439,1.,0.866025403784439,1.,0.866025403784439,
1.,0.866025403784439,1.,0.866025403784439,1.,0.866025403784439,1.,0.866025403784439,
1.,0.866025403784439,1.,0.866025403784439,1.,0.866025403784439,1.,0.866025403784439,
1.,0.866025403784439,1.,0.866025403784439,1.,0.866025403784439,1.,0.866025403784439,
1.,0.866025403784439,1.,0.866025403784439,1.,0.866025403784439,1.,0.866025403784439,
1.,0.866025403784439,1.,0.866025403784439,1.,0.866025403784439,1.,0.866025403784439,
1.,0.866025403784439,1.,0.866025403784439,1.,0.866025403784439,1.,0.866025403784439,
1.,0.866025403784439,1.,0.866025403784439,1.,0.866025403784439,1.,0.866025403784439,
1.,0.866025403784439,1.,0.866025403784439,1.,0.866025403784439,1.,0.866025403784439,
1.,0.866025403784439,1.,0.866025403784439,1.,0.866025403784439,1.,0.866025403784439,
1.,0.866025403784439,1.,0.866025403784439,1.,0.866025403784439,1.,0.866025403784439,
1.,0.866025403784439,1.,0.866025403784439,1.,0.866025403784439,1.,0.866025403784439,
1.,0.866025403784439,1.,0.866025403784439,1.,0.866025403784439,1.,0.866025403784439,
1.,0.866025403784439,1.,0.866025403784439,1.,0.866025403784439,1.,0.866025403784439,
1.,0.866025403784439,1.,0.866025403784439,1.,0.866025403784439,1.,0.866025403784439,
1.,0.866025403784439,1.,0.866025403784439,1.,0.866025403784439,1.,0.866025403784439,
1.,0.866025403784439,1.,0.866025403784439,1.,0.866025403784439,1.,0.866025403784439,
1.,0.866025403784439,1.,0.866025403784439,1.,0.866025403784439,1.,0.866025403784439,
1.,0.866025403784439,1.,0.866025403784439,1.,0.866025403784439,1.,0.866025403784439,
1.,0.866025403784439,1.,0.866025403784439,1.,0.866025403784439,1.,0.866025403784439,
1.,0.866025403784439,1.,0.866025403784439,1.,0.866025403784439,1.,0.866025403784439,
1.,0.866025403784439,1.,0.866025403784439,1.,0.866025403784439,1.,0.866025403784439,
1.,0.866025403784439,1.,0.866025403784439,1.,0.866025403784439,1.,0.866025403784439,
1.,0.866025403784439,1.,0.866025403784439,1.,0.866025403784439,1.,0.980312120051573,
0.966410600022306),(1.,0.866025403784439,1.,0.866025403784439,1.,0.866025403784439,
1.,0.866025403784439,1.,0.866025403784439,1.,0.866025403784439,1.,0.866025403784439,
1.,0.866025403784439,1.,0.866025403784439,1.,0.866025403784439,1.,0.866025403784439,
1.,0.866025403784439,1.,0.866025403784439,1.,0.866025403784439,1.,0.866025403784439,
1.,0.866025403784439,1.,0.866025403784439,1.,0.866025403784439,1.,0.866025403784439,
1.,0.866025403784439,1.,0.866025403784439,1.,0.866025403784439,1.,0.866025403784439,
1.,0.866025403784439,1.,0.866025403784439,1.,0.866025403784439,1.,0.866025403784439,
1.,0.866025403784439,1.,0.866025403784439,1.,0.866025403784439,1.,0.866025403784439,
1.,0.866025403784439,1.,0.866025403784439,1.,0.866025403784439,1.,0.866025403784439,
1.,0.866025403784439,1.,0.866025403784439,1.,0.866025403784439,1.,0.866025403784439,
1.,0.866025403784439,1.,0.866025403784439,1.,0.866025403784439,1.,0.866025403784439,
1.,0.866025403784439,1.,0.866025403784439,1.,0.866025403784439,1.,0.866025403784439,
1.,0.866025403784439,1.,0.866025403784439,1.,0.866025403784439,1.,0.866025403784439,
1.,0.866025403784439,1.,0.866025403784439,1.,0.866025403784439,1.,0.866025403784439,
1.,0.866025403784439,1.,0.866025403784439,1.,0.866025403784439,1.,0.866025403784439,
1.,0.866025403784439,1.,0.866025403784439,1.,0.866025403784439,1.,0.866025403784439,
1.,0.866025403784439,1.,0.866025403784439,1.,0.866025403784439,1.,0.866025403784439,
1.,0.866025403784439,1.,0.866025403784439,1.,0.866025403784439,1.,0.866025403784439,
1.,0.866025403784439,1.,0.866025403784439,1.,0.866025403784439,1.,0.866025403784439,
1.,0.866025403784439,1.,0.866025403784439,1.,0.866025403784439,1.,0.866025403784439,
1.,0.866025403784439,1.,0.866025403784439,1.,0.866025403784439,1.,0.866025403784439,
1.,0.866025403784439,1.,0.866025403784439,1.,0.866025403784439,1.,0.866025403784439,
1.,0.866025403784439,1.,0.866025403784439,1.,0.866025403784439,1.,0.866025403784439,
1.,0.866025403784439,1.,0.866025403784439,1.,0.866025403784439,1.,0.866025403784439,
1.,0.866025403784439,1.,0.866025403784439,1.,0.866025403784439,1.,0.866025403784439,
1.,0.866025403784439,1.,0.866025403784439,1.,0.866025403784439,1.,0.866025403784439,
1.,0.866025403784439,1.,0.866025403784439,1.,0.866025403784439,1.,0.866025403784439,
1.,0.866025403784439,1.,0.866025403784439,1.,0.866025403784439,1.,0.866025403784439,
1.,0.866025403784439,1.,0.866025403784439,1.,0.866025403784439,1.,0.866025403784439,
1.,0.866025403784439,1.,0.866025403784439,1.,0.866025403784439,1.,0.866025403784439,
1.,0.866025403784439,1.,0.866025403784439,1.,0.866025403784439,1.,0.866025403784439,
1.,0.866025403784439,1.,0.866025403784439,1.,0.866025403784439,1.,0.866025403784439,
1.,0.866025403784439,1.,0.866025403784439,1.,0.866025403784439,1.,0.866025403784439,
1.,0.866025403784439,1.,0.866025403784439,1.,0.866025403784439,1.,0.866025403784439,
1.,0.866025403784439,1.,0.866025403784439,1.,0.980312120051573,0.966410600022306)))
REPRESENTATION_ITEM('')
SURFACE()
);
#3183=(
BOUNDED_SURFACE()
B_SPLINE_SURFACE(1,2,((#260880,#260881,#260882,#260883,#260884,#260885,
#260886,#260887,#260888,#260889,#260890,#260891,#260892,#260893,#260894,
#260895,#260896,#260897,#260898,#260899,#260900,#260901,#260902,#260903,
#260904,#260905,#260906,#260907,#260908,#260909,#260910,#260911,#260912,
#260913,#260914,#260915,#260916,#260917,#260918,#260919,#260920,#260921,
#260922,#260923,#260924,#260925,#260926,#260927,#260928,#260929,#260930,
#260931,#260932,#260933,#260934,#260935,#260936,#260937,#260938,#260939,
#260940,#260941,#260942,#260943,#260944,#260945,#260946,#260947,#260948,
#260949,#260950,#260951,#260952,#260953,#260954,#260955,#260956,#260957,
#260958,#260959,#260960,#260961,#260962,#260963,#260964,#260965,#260966,
#260967,#260968,#260969,#260970,#260971,#260972,#260973,#260974,#260975,
#260976,#260977,#260978,#260979,#260980,#260981,#260982,#260983,#260984,
#260985,#260986,#260987,#260988,#260989,#260990,#260991,#260992,#260993,
#260994,#260995,#260996,#260997,#260998,#260999,#261000,#261001,#261002,
#261003,#261004,#261005,#261006,#261007,#261008,#261009,#261010,#261011,
#261012,#261013,#261014,#261015,#261016,#261017,#261018,#261019,#261020,
#261021,#261022,#261023,#261024,#261025,#261026,#261027,#261028,#261029,
#261030,#261031,#261032,#261033,#261034,#261035,#261036,#261037,#261038,
#261039,#261040,#261041,#261042,#261043,#261044,#261045,#261046,#261047,
#261048,#261049,#261050,#261051,#261052,#261053,#261054,#261055,#261056,
#261057,#261058,#261059,#261060,#261061,#261062,#261063,#261064,#261065,
#261066,#261067,#261068,#261069,#261070,#261071,#261072,#261073,#261074,
#261075,#261076,#261077,#261078,#261079,#261080,#261081,#261082,#261083,
#261084,#261085,#261086,#261087,#261088,#261089,#261090,#261091,#261092,
#261093,#261094,#261095,#261096,#261097,#261098,#261099,#261100,#261101,
#261102,#261103,#261104,#261105,#261106,#261107,#261108,#261109,#261110,
#261111,#261112,#261113,#261114,#261115,#261116,#261117,#261118,#261119,
#261120,#261121,#261122,#261123,#261124,#261125,#261126,#261127,#261128,
#261129,#261130,#261131,#261132,#261133,#261134,#261135,#261136,#261137,
#261138,#261139,#261140,#261141,#261142,#261143,#261144,#261145,#261146,
#261147,#261148,#261149,#261150,#261151,#261152,#261153,#261154,#261155,
#261156),(#261157,#261158,#261159,#261160,#261161,#261162,#261163,#261164,
#261165,#261166,#261167,#261168,#261169,#261170,#261171,#261172,#261173,
#261174,#261175,#261176,#261177,#261178,#261179,#261180,#261181,#261182,
#261183,#261184,#261185,#261186,#261187,#261188,#261189,#261190,#261191,
#261192,#261193,#261194,#261195,#261196,#261197,#261198,#261199,#261200,
#261201,#261202,#261203,#261204,#261205,#261206,#261207,#261208,#261209,
#261210,#261211,#261212,#261213,#261214,#261215,#261216,#261217,#261218,
#261219,#261220,#261221,#261222,#261223,#261224,#261225,#261226,#261227,
#261228,#261229,#261230,#261231,#261232,#261233,#261234,#261235,#261236,
#261237,#261238,#261239,#261240,#261241,#261242,#261243,#261244,#261245,
#261246,#261247,#261248,#261249,#261250,#261251,#261252,#261253,#261254,
#261255,#261256,#261257,#261258,#261259,#261260,#261261,#261262,#261263,
#261264,#261265,#261266,#261267,#261268,#261269,#261270,#261271,#261272,
#261273,#261274,#261275,#261276,#261277,#261278,#261279,#261280,#261281,
#261282,#261283,#261284,#261285,#261286,#261287,#261288,#261289,#261290,
#261291,#261292,#261293,#261294,#261295,#261296,#261297,#261298,#261299,
#261300,#261301,#261302,#261303,#261304,#261305,#261306,#261307,#261308,
#261309,#261310,#261311,#261312,#261313,#261314,#261315,#261316,#261317,
#261318,#261319,#261320,#261321,#261322,#261323,#261324,#261325,#261326,
#261327,#261328,#261329,#261330,#261331,#261332,#261333,#261334,#261335,
#261336,#261337,#261338,#261339,#261340,#261341,#261342,#261343,#261344,
#261345,#261346,#261347,#261348,#261349,#261350,#261351,#261352,#261353,
#261354,#261355,#261356,#261357,#261358,#261359,#261360,#261361,#261362,
#261363,#261364,#261365,#261366,#261367,#261368,#261369,#261370,#261371,
#261372,#261373,#261374,#261375,#261376,#261377,#261378,#261379,#261380,
#261381,#261382,#261383,#261384,#261385,#261386,#261387,#261388,#261389,
#261390,#261391,#261392,#261393,#261394,#261395,#261396,#261397,#261398,
#261399,#261400,#261401,#261402,#261403,#261404,#261405,#261406,#261407,
#261408,#261409,#261410,#261411,#261412,#261413,#261414,#261415,#261416,
#261417,#261418,#261419,#261420,#261421,#261422,#261423,#261424,#261425,
#261426,#261427,#261428,#261429,#261430,#261431,#261432,#261433)),
 .UNSPECIFIED.,.F.,.F.,.F.)
B_SPLINE_SURFACE_WITH_KNOTS((2,2),(3,2,2,2,2,2,2,2,2,2,2,2,2,2,2,2,2,2,
2,2,2,2,2,2,2,2,2,2,2,2,2,2,2,2,2,2,2,2,2,2,2,2,2,2,2,2,2,2,2,2,2,2,2,2,
2,2,2,2,2,2,2,2,2,2,2,2,2,2,2,2,2,2,2,2,2,2,2,2,2,2,2,2,2,2,2,2,2,2,2,2,
2,2,2,2,2,2,2,2,2,2,2,2,2,2,2,2,2,2,2,2,2,2,2,2,2,2,2,2,2,2,2,2,2,2,2,2,
2,2,2,2,2,2,2,2,2,2,2,2,3),(0.,1.00000038195933),(0.,0.0072463768115942,
0.0144927536231884,0.0217391304347826,0.0289855072463768,0.036231884057971,
0.0434782608695652,0.0507246376811594,0.0579710144927536,0.0652173913043478,
0.072463768115942,0.0797101449275362,0.0869565217391304,0.0942028985507246,
0.101449275362319,0.108695652173913,0.115942028985507,0.123188405797101,
0.130434782608696,0.13768115942029,0.144927536231884,0.152173913043478,
0.159420289855073,0.166666666666667,0.173913043478261,0.181159420289855,
0.18840579710145,0.195652173913044,0.202898550724637,0.210144927536232,
0.217391304347826,0.224637681159421,0.231884057971014,0.239130434782609,
0.246376811594203,0.253623188405797,0.260869565217392,0.268115942028985,
0.275362318840579,0.282608695652174,0.289855072463768,0.297101449275363,
0.304347826086956,0.31159420289855,0.318840579710145,0.326086956521739,
0.333333333333334,0.340579710144927,0.347826086956521,0.355072463768116,
0.36231884057971,0.369565217391304,0.376811594202899,0.384057971014493,
0.391304347826087,0.398550724637681,0.405797101449275,0.41304347826087,
0.420289855072463,0.427536231884058,0.434782608695652,0.442028985507247,
0.449275362318841,0.456521739130435,0.463768115942029,0.471014492753623,
0.478260869565218,0.485507246376812,0.492753623188406,0.5,0.507246376811594,
0.514492753623188,0.521739130434783,0.528985507246377,0.536231884057971,
0.543478260869565,0.550724637681159,0.557971014492754,0.565217391304348,
0.572463768115942,0.579710144927536,0.586956521739131,0.594202898550725,
0.601449275362319,0.608695652173913,0.615942028985507,0.623188405797101,
0.630434782608696,0.63768115942029,0.644927536231884,0.652173913043478,
0.659420289855073,0.666666666666667,0.673913043478261,0.681159420289855,
0.688405797101449,0.695652173913044,0.702898550724638,0.710144927536232,
0.717391304347826,0.72463768115942,0.731884057971015,0.739130434782609,
0.746376811594203,0.753623188405797,0.760869565217391,0.768115942028986,
0.77536231884058,0.782608695652174,0.789855072463768,0.797101449275362,
0.804347826086956,0.811594202898551,0.818840579710145,0.826086956521739,
0.833333333333333,0.840579710144928,0.847826086956522,0.855072463768116,
0.86231884057971,0.869565217391304,0.876811594202899,0.884057971014493,
0.891304347826087,0.898550724637681,0.905797101449275,0.91304347826087,
0.920289855072464,0.927536231884058,0.934782608695652,0.942028985507246,
0.94927536231884,0.956521739130435,0.963768115942029,0.971014492753623,
0.978260869565217,0.985507246376812,0.992753623188406,0.993818495192186),
 .UNSPECIFIED.)
GEOMETRIC_REPRESENTATION_ITEM()
RATIONAL_B_SPLINE_SURFACE(((1.,0.866025403784439,1.,0.866025403784439,1.,
0.866025403784439,1.,0.866025403784439,1.,0.866025403784439,1.,0.866025403784439,
1.,0.866025403784439,1.,0.866025403784439,1.,0.866025403784439,1.,0.866025403784439,
1.,0.866025403784439,1.,0.866025403784439,1.,0.866025403784439,1.,0.866025403784439,
1.,0.866025403784439,1.,0.866025403784439,1.,0.866025403784439,1.,0.866025403784439,
1.,0.866025403784439,1.,0.866025403784439,1.,0.866025403784439,1.,0.866025403784439,
1.,0.866025403784439,1.,0.866025403784439,1.,0.866025403784439,1.,0.866025403784439,
1.,0.866025403784439,1.,0.866025403784439,1.,0.866025403784439,1.,0.866025403784439,
1.,0.866025403784439,1.,0.866025403784439,1.,0.866025403784439,1.,0.866025403784439,
1.,0.866025403784439,1.,0.866025403784439,1.,0.866025403784439,1.,0.866025403784439,
1.,0.866025403784439,1.,0.866025403784439,1.,0.866025403784439,1.,0.866025403784439,
1.,0.866025403784439,1.,0.866025403784439,1.,0.866025403784439,1.,0.866025403784439,
1.,0.866025403784439,1.,0.866025403784439,1.,0.866025403784439,1.,0.866025403784439,
1.,0.866025403784439,1.,0.866025403784439,1.,0.866025403784439,1.,0.866025403784439,
1.,0.866025403784439,1.,0.866025403784439,1.,0.866025403784439,1.,0.866025403784439,
1.,0.866025403784439,1.,0.866025403784439,1.,0.866025403784439,1.,0.866025403784439,
1.,0.866025403784439,1.,0.866025403784439,1.,0.866025403784439,1.,0.866025403784439,
1.,0.866025403784439,1.,0.866025403784439,1.,0.866025403784439,1.,0.866025403784439,
1.,0.866025403784439,1.,0.866025403784439,1.,0.866025403784439,1.,0.866025403784439,
1.,0.866025403784439,1.,0.866025403784439,1.,0.866025403784439,1.,0.866025403784439,
1.,0.866025403784439,1.,0.866025403784439,1.,0.866025403784439,1.,0.866025403784439,
1.,0.866025403784439,1.,0.866025403784439,1.,0.866025403784439,1.,0.866025403784439,
1.,0.866025403784439,1.,0.866025403784439,1.,0.866025403784439,1.,0.866025403784439,
1.,0.866025403784439,1.,0.866025403784439,1.,0.866025403784439,1.,0.866025403784439,
1.,0.866025403784439,1.,0.866025403784439,1.,0.866025403784439,1.,0.866025403784439,
1.,0.866025403784439,1.,0.866025403784439,1.,0.866025403784439,1.,0.866025403784439,
1.,0.866025403784439,1.,0.866025403784439,1.,0.866025403784439,1.,0.866025403784439,
1.,0.866025403784439,1.,0.866025403784439,1.,0.866025403784439,1.,0.866025403784439,
1.,0.866025403784439,1.,0.866025403784439,1.,0.866025403784439,1.,0.866025403784439,
1.,0.866025403784439,1.,0.866025403784439,1.,0.866025403784439,1.,0.866025403784439,
1.,0.866025403784439,1.,0.866025403784439,1.,0.866025403784439,1.,0.866025403784439,
1.,0.866025403784439,1.,0.866025403784439,1.,0.866025403784439,1.,0.866025403784439,
1.,0.866025403784439,1.,0.866025403784439,1.,0.866025403784439,1.,0.866025403784439,
1.,0.866025403784439,1.,0.866025403784439,1.,0.866025403784439,1.,0.866025403784439,
1.,0.866025403784439,1.,0.866025403784439,1.,0.866025403784439,1.,0.980312120051573,
0.966410600022306),(1.,0.866025403784439,1.,0.866025403784439,1.,0.866025403784439,
1.,0.866025403784439,1.,0.866025403784439,1.,0.866025403784439,1.,0.866025403784439,
1.,0.866025403784439,1.,0.866025403784439,1.,0.866025403784439,1.,0.866025403784439,
1.,0.866025403784439,1.,0.866025403784439,1.,0.866025403784439,1.,0.866025403784439,
1.,0.866025403784439,1.,0.866025403784439,1.,0.866025403784439,1.,0.866025403784439,
1.,0.866025403784439,1.,0.866025403784439,1.,0.866025403784439,1.,0.866025403784439,
1.,0.866025403784439,1.,0.866025403784439,1.,0.866025403784439,1.,0.866025403784439,
1.,0.866025403784439,1.,0.866025403784439,1.,0.866025403784439,1.,0.866025403784439,
1.,0.866025403784439,1.,0.866025403784439,1.,0.866025403784439,1.,0.866025403784439,
1.,0.866025403784439,1.,0.866025403784439,1.,0.866025403784439,1.,0.866025403784439,
1.,0.866025403784439,1.,0.866025403784439,1.,0.866025403784439,1.,0.866025403784439,
1.,0.866025403784439,1.,0.866025403784439,1.,0.866025403784439,1.,0.866025403784439,
1.,0.866025403784439,1.,0.866025403784439,1.,0.866025403784439,1.,0.866025403784439,
1.,0.866025403784439,1.,0.866025403784439,1.,0.866025403784439,1.,0.866025403784439,
1.,0.866025403784439,1.,0.866025403784439,1.,0.866025403784439,1.,0.866025403784439,
1.,0.866025403784439,1.,0.866025403784439,1.,0.866025403784439,1.,0.866025403784439,
1.,0.866025403784439,1.,0.866025403784439,1.,0.866025403784439,1.,0.866025403784439,
1.,0.866025403784439,1.,0.866025403784439,1.,0.866025403784439,1.,0.866025403784439,
1.,0.866025403784439,1.,0.866025403784439,1.,0.866025403784439,1.,0.866025403784439,
1.,0.866025403784439,1.,0.866025403784439,1.,0.866025403784439,1.,0.866025403784439,
1.,0.866025403784439,1.,0.866025403784439,1.,0.866025403784439,1.,0.866025403784439,
1.,0.866025403784439,1.,0.866025403784439,1.,0.866025403784439,1.,0.866025403784439,
1.,0.866025403784439,1.,0.866025403784439,1.,0.866025403784439,1.,0.866025403784439,
1.,0.866025403784439,1.,0.866025403784439,1.,0.866025403784439,1.,0.866025403784439,
1.,0.866025403784439,1.,0.866025403784439,1.,0.866025403784439,1.,0.866025403784439,
1.,0.866025403784439,1.,0.866025403784439,1.,0.866025403784439,1.,0.866025403784439,
1.,0.866025403784439,1.,0.866025403784439,1.,0.866025403784439,1.,0.866025403784439,
1.,0.866025403784439,1.,0.866025403784439,1.,0.866025403784439,1.,0.866025403784439,
1.,0.866025403784439,1.,0.866025403784439,1.,0.866025403784439,1.,0.866025403784439,
1.,0.866025403784439,1.,0.866025403784439,1.,0.866025403784439,1.,0.866025403784439,
1.,0.866025403784439,1.,0.866025403784439,1.,0.866025403784439,1.,0.866025403784439,
1.,0.866025403784439,1.,0.866025403784439,1.,0.866025403784439,1.,0.866025403784439,
1.,0.866025403784439,1.,0.866025403784439,1.,0.866025403784439,1.,0.866025403784439,
1.,0.866025403784439,1.,0.866025403784439,1.,0.866025403784439,1.,0.866025403784439,
1.,0.866025403784439,1.,0.866025403784439,1.,0.980312120051573,0.966410600022306)))
REPRESENTATION_ITEM('')
SURFACE()
);
#3184=(
BOUNDED_SURFACE()
B_SPLINE_SURFACE(1,2,((#261448,#261449,#261450,#261451,#261452,#261453,
#261454,#261455,#261456,#261457,#261458,#261459,#261460,#261461,#261462,
#261463,#261464,#261465,#261466,#261467,#261468,#261469,#261470,#261471,
#261472,#261473,#261474,#261475,#261476,#261477,#261478,#261479,#261480,
#261481,#261482,#261483,#261484,#261485,#261486,#261487,#261488,#261489,
#261490,#261491,#261492,#261493,#261494,#261495,#261496,#261497,#261498,
#261499,#261500,#261501,#261502,#261503,#261504,#261505,#261506,#261507,
#261508,#261509,#261510,#261511,#261512,#261513,#261514,#261515,#261516,
#261517,#261518,#261519,#261520,#261521,#261522,#261523,#261524,#261525,
#261526,#261527,#261528,#261529,#261530,#261531,#261532,#261533,#261534,
#261535,#261536,#261537,#261538,#261539,#261540,#261541,#261542,#261543,
#261544,#261545,#261546,#261547,#261548,#261549,#261550,#261551,#261552,
#261553,#261554,#261555,#261556,#261557,#261558,#261559,#261560,#261561,
#261562,#261563,#261564,#261565,#261566,#261567,#261568,#261569,#261570,
#261571,#261572,#261573,#261574,#261575,#261576,#261577,#261578,#261579,
#261580,#261581,#261582,#261583,#261584,#261585,#261586,#261587,#261588,
#261589,#261590,#261591,#261592,#261593,#261594,#261595,#261596,#261597,
#261598,#261599,#261600,#261601,#261602,#261603,#261604,#261605,#261606,
#261607,#261608,#261609,#261610,#261611,#261612,#261613,#261614,#261615,
#261616,#261617,#261618,#261619,#261620,#261621,#261622,#261623,#261624,
#261625,#261626,#261627,#261628,#261629,#261630,#261631,#261632,#261633,
#261634,#261635,#261636,#261637,#261638,#261639,#261640,#261641,#261642,
#261643,#261644,#261645,#261646,#261647,#261648,#261649,#261650,#261651,
#261652,#261653,#261654,#261655,#261656,#261657,#261658,#261659,#261660,
#261661,#261662,#261663,#261664,#261665,#261666,#261667,#261668,#261669,
#261670,#261671,#261672,#261673,#261674,#261675,#261676,#261677,#261678,
#261679,#261680,#261681,#261682,#261683,#261684,#261685,#261686,#261687,
#261688,#261689,#261690,#261691,#261692,#261693,#261694,#261695,#261696,
#261697,#261698,#261699,#261700,#261701,#261702,#261703,#261704,#261705,
#261706,#261707,#261708,#261709,#261710,#261711,#261712,#261713,#261714,
#261715,#261716,#261717,#261718,#261719,#261720,#261721,#261722,#261723,
#261724),(#261725,#261726,#261727,#261728,#261729,#261730,#261731,#261732,
#261733,#261734,#261735,#261736,#261737,#261738,#261739,#261740,#261741,
#261742,#261743,#261744,#261745,#261746,#261747,#261748,#261749,#261750,
#261751,#261752,#261753,#261754,#261755,#261756,#261757,#261758,#261759,
#261760,#261761,#261762,#261763,#261764,#261765,#261766,#261767,#261768,
#261769,#261770,#261771,#261772,#261773,#261774,#261775,#261776,#261777,
#261778,#261779,#261780,#261781,#261782,#261783,#261784,#261785,#261786,
#261787,#261788,#261789,#261790,#261791,#261792,#261793,#261794,#261795,
#261796,#261797,#261798,#261799,#261800,#261801,#261802,#261803,#261804,
#261805,#261806,#261807,#261808,#261809,#261810,#261811,#261812,#261813,
#261814,#261815,#261816,#261817,#261818,#261819,#261820,#261821,#261822,
#261823,#261824,#261825,#261826,#261827,#261828,#261829,#261830,#261831,
#261832,#261833,#261834,#261835,#261836,#261837,#261838,#261839,#261840,
#261841,#261842,#261843,#261844,#261845,#261846,#261847,#261848,#261849,
#261850,#261851,#261852,#261853,#261854,#261855,#261856,#261857,#261858,
#261859,#261860,#261861,#261862,#261863,#261864,#261865,#261866,#261867,
#261868,#261869,#261870,#261871,#261872,#261873,#261874,#261875,#261876,
#261877,#261878,#261879,#261880,#261881,#261882,#261883,#261884,#261885,
#261886,#261887,#261888,#261889,#261890,#261891,#261892,#261893,#261894,
#261895,#261896,#261897,#261898,#261899,#261900,#261901,#261902,#261903,
#261904,#261905,#261906,#261907,#261908,#261909,#261910,#261911,#261912,
#261913,#261914,#261915,#261916,#261917,#261918,#261919,#261920,#261921,
#261922,#261923,#261924,#261925,#261926,#261927,#261928,#261929,#261930,
#261931,#261932,#261933,#261934,#261935,#261936,#261937,#261938,#261939,
#261940,#261941,#261942,#261943,#261944,#261945,#261946,#261947,#261948,
#261949,#261950,#261951,#261952,#261953,#261954,#261955,#261956,#261957,
#261958,#261959,#261960,#261961,#261962,#261963,#261964,#261965,#261966,
#261967,#261968,#261969,#261970,#261971,#261972,#261973,#261974,#261975,
#261976,#261977,#261978,#261979,#261980,#261981,#261982,#261983,#261984,
#261985,#261986,#261987,#261988,#261989,#261990,#261991,#261992,#261993,
#261994,#261995,#261996,#261997,#261998,#261999,#262000,#262001)),
 .UNSPECIFIED.,.F.,.F.,.F.)
B_SPLINE_SURFACE_WITH_KNOTS((2,2),(3,2,2,2,2,2,2,2,2,2,2,2,2,2,2,2,2,2,
2,2,2,2,2,2,2,2,2,2,2,2,2,2,2,2,2,2,2,2,2,2,2,2,2,2,2,2,2,2,2,2,2,2,2,2,
2,2,2,2,2,2,2,2,2,2,2,2,2,2,2,2,2,2,2,2,2,2,2,2,2,2,2,2,2,2,2,2,2,2,2,2,
2,2,2,2,2,2,2,2,2,2,2,2,2,2,2,2,2,2,2,2,2,2,2,2,2,2,2,2,2,2,2,2,2,2,2,2,
2,2,2,2,2,2,2,2,2,2,2,2,3),(0.,1.),(0.,0.0072463768115942,0.0144927536231884,
0.0217391304347826,0.0289855072463768,0.036231884057971,0.0434782608695652,
0.0507246376811594,0.0579710144927536,0.0652173913043478,0.072463768115942,
0.0797101449275362,0.0869565217391304,0.0942028985507246,0.101449275362319,
0.108695652173913,0.115942028985507,0.123188405797101,0.130434782608696,
0.13768115942029,0.144927536231884,0.152173913043478,0.159420289855073,
0.166666666666667,0.173913043478261,0.181159420289855,0.18840579710145,
0.195652173913044,0.202898550724637,0.210144927536232,0.217391304347826,
0.224637681159421,0.231884057971014,0.239130434782609,0.246376811594203,
0.253623188405797,0.260869565217392,0.268115942028985,0.275362318840579,
0.282608695652174,0.289855072463768,0.297101449275363,0.304347826086956,
0.31159420289855,0.318840579710145,0.326086956521739,0.333333333333334,
0.340579710144927,0.347826086956521,0.355072463768116,0.36231884057971,
0.369565217391304,0.376811594202899,0.384057971014493,0.391304347826087,
0.398550724637681,0.405797101449275,0.41304347826087,0.420289855072463,
0.427536231884058,0.434782608695652,0.442028985507247,0.449275362318841,
0.456521739130435,0.463768115942029,0.471014492753623,0.478260869565218,
0.485507246376812,0.492753623188406,0.5,0.507246376811594,0.514492753623188,
0.521739130434783,0.528985507246377,0.536231884057971,0.543478260869565,
0.550724637681159,0.557971014492754,0.565217391304348,0.572463768115942,
0.579710144927536,0.586956521739131,0.594202898550725,0.601449275362319,
0.608695652173913,0.615942028985507,0.623188405797101,0.630434782608696,
0.63768115942029,0.644927536231884,0.652173913043478,0.659420289855073,
0.666666666666667,0.673913043478261,0.681159420289855,0.688405797101449,
0.695652173913044,0.702898550724638,0.710144927536232,0.717391304347826,
0.72463768115942,0.731884057971015,0.739130434782609,0.746376811594203,
0.753623188405797,0.760869565217391,0.768115942028986,0.77536231884058,
0.782608695652174,0.789855072463768,0.797101449275362,0.804347826086956,
0.811594202898551,0.818840579710145,0.826086956521739,0.833333333333333,
0.840579710144928,0.847826086956522,0.855072463768116,0.86231884057971,
0.869565217391304,0.876811594202899,0.884057971014493,0.891304347826087,
0.898550724637681,0.905797101449275,0.91304347826087,0.920289855072464,
0.927536231884058,0.934782608695652,0.942028985507246,0.94927536231884,
0.956521739130435,0.963768115942029,0.971014492753623,0.978260869565217,
0.985507246376812,0.992753623188406,0.993818585798284),.UNSPECIFIED.)
GEOMETRIC_REPRESENTATION_ITEM()
RATIONAL_B_SPLINE_SURFACE(((1.,0.866025403784439,1.,0.866025403784439,1.,
0.866025403784439,1.,0.866025403784439,1.,0.866025403784439,1.,0.866025403784439,
1.,0.866025403784439,1.,0.866025403784439,1.,0.866025403784439,1.,0.866025403784439,
1.,0.866025403784439,1.,0.866025403784439,1.,0.866025403784439,1.,0.866025403784439,
1.,0.866025403784439,1.,0.866025403784439,1.,0.866025403784439,1.,0.866025403784439,
1.,0.866025403784439,1.,0.866025403784439,1.,0.866025403784439,1.,0.866025403784439,
1.,0.866025403784439,1.,0.866025403784439,1.,0.866025403784439,1.,0.866025403784439,
1.,0.866025403784439,1.,0.866025403784439,1.,0.866025403784439,1.,0.866025403784439,
1.,0.866025403784439,1.,0.866025403784439,1.,0.866025403784439,1.,0.866025403784439,
1.,0.866025403784439,1.,0.866025403784439,1.,0.866025403784439,1.,0.866025403784439,
1.,0.866025403784439,1.,0.866025403784439,1.,0.866025403784439,1.,0.866025403784439,
1.,0.866025403784439,1.,0.866025403784439,1.,0.866025403784439,1.,0.866025403784439,
1.,0.866025403784439,1.,0.866025403784439,1.,0.866025403784439,1.,0.866025403784439,
1.,0.866025403784439,1.,0.866025403784439,1.,0.866025403784439,1.,0.866025403784439,
1.,0.866025403784439,1.,0.866025403784439,1.,0.866025403784439,1.,0.866025403784439,
1.,0.866025403784439,1.,0.866025403784439,1.,0.866025403784439,1.,0.866025403784439,
1.,0.866025403784439,1.,0.866025403784439,1.,0.866025403784439,1.,0.866025403784439,
1.,0.866025403784439,1.,0.866025403784439,1.,0.866025403784439,1.,0.866025403784439,
1.,0.866025403784439,1.,0.866025403784439,1.,0.866025403784439,1.,0.866025403784439,
1.,0.866025403784439,1.,0.866025403784439,1.,0.866025403784439,1.,0.866025403784439,
1.,0.866025403784439,1.,0.866025403784439,1.,0.866025403784439,1.,0.866025403784439,
1.,0.866025403784439,1.,0.866025403784439,1.,0.866025403784439,1.,0.866025403784439,
1.,0.866025403784439,1.,0.866025403784439,1.,0.866025403784439,1.,0.866025403784439,
1.,0.866025403784439,1.,0.866025403784439,1.,0.866025403784439,1.,0.866025403784439,
1.,0.866025403784439,1.,0.866025403784439,1.,0.866025403784439,1.,0.866025403784439,
1.,0.866025403784439,1.,0.866025403784439,1.,0.866025403784439,1.,0.866025403784439,
1.,0.866025403784439,1.,0.866025403784439,1.,0.866025403784439,1.,0.866025403784439,
1.,0.866025403784439,1.,0.866025403784439,1.,0.866025403784439,1.,0.866025403784439,
1.,0.866025403784439,1.,0.866025403784439,1.,0.866025403784439,1.,0.866025403784439,
1.,0.866025403784439,1.,0.866025403784439,1.,0.866025403784439,1.,0.866025403784439,
1.,0.866025403784439,1.,0.866025403784439,1.,0.866025403784439,1.,0.866025403784439,
1.,0.866025403784439,1.,0.866025403784439,1.,0.866025403784439,1.,0.866025403784439,
1.,0.866025403784439,1.,0.866025403784439,1.,0.866025403784439,1.,0.866025403784439,
1.,0.866025403784439,1.,0.866025403784439,1.,0.866025403784439,1.,0.866025403784439,
1.,0.866025403784439,1.,0.866025403784439,1.,0.866025403784439,1.,0.98031044488126,
0.966408234404338),(1.,0.866025403784439,1.,0.866025403784439,1.,0.866025403784439,
1.,0.866025403784439,1.,0.866025403784439,1.,0.866025403784439,1.,0.866025403784439,
1.,0.866025403784439,1.,0.866025403784439,1.,0.866025403784439,1.,0.866025403784439,
1.,0.866025403784439,1.,0.866025403784439,1.,0.866025403784439,1.,0.866025403784439,
1.,0.866025403784439,1.,0.866025403784439,1.,0.866025403784439,1.,0.866025403784439,
1.,0.866025403784439,1.,0.866025403784439,1.,0.866025403784439,1.,0.866025403784439,
1.,0.866025403784439,1.,0.866025403784439,1.,0.866025403784439,1.,0.866025403784439,
1.,0.866025403784439,1.,0.866025403784439,1.,0.866025403784439,1.,0.866025403784439,
1.,0.866025403784439,1.,0.866025403784439,1.,0.866025403784439,1.,0.866025403784439,
1.,0.866025403784439,1.,0.866025403784439,1.,0.866025403784439,1.,0.866025403784439,
1.,0.866025403784439,1.,0.866025403784439,1.,0.866025403784439,1.,0.866025403784439,
1.,0.866025403784439,1.,0.866025403784439,1.,0.866025403784439,1.,0.866025403784439,
1.,0.866025403784439,1.,0.866025403784439,1.,0.866025403784439,1.,0.866025403784439,
1.,0.866025403784439,1.,0.866025403784439,1.,0.866025403784439,1.,0.866025403784439,
1.,0.866025403784439,1.,0.866025403784439,1.,0.866025403784439,1.,0.866025403784439,
1.,0.866025403784439,1.,0.866025403784439,1.,0.866025403784439,1.,0.866025403784439,
1.,0.866025403784439,1.,0.866025403784439,1.,0.866025403784439,1.,0.866025403784439,
1.,0.866025403784439,1.,0.866025403784439,1.,0.866025403784439,1.,0.866025403784439,
1.,0.866025403784439,1.,0.866025403784439,1.,0.866025403784439,1.,0.866025403784439,
1.,0.866025403784439,1.,0.866025403784439,1.,0.866025403784439,1.,0.866025403784439,
1.,0.866025403784439,1.,0.866025403784439,1.,0.866025403784439,1.,0.866025403784439,
1.,0.866025403784439,1.,0.866025403784439,1.,0.866025403784439,1.,0.866025403784439,
1.,0.866025403784439,1.,0.866025403784439,1.,0.866025403784439,1.,0.866025403784439,
1.,0.866025403784439,1.,0.866025403784439,1.,0.866025403784439,1.,0.866025403784439,
1.,0.866025403784439,1.,0.866025403784439,1.,0.866025403784439,1.,0.866025403784439,
1.,0.866025403784439,1.,0.866025403784439,1.,0.866025403784439,1.,0.866025403784439,
1.,0.866025403784439,1.,0.866025403784439,1.,0.866025403784439,1.,0.866025403784439,
1.,0.866025403784439,1.,0.866025403784439,1.,0.866025403784439,1.,0.866025403784439,
1.,0.866025403784439,1.,0.866025403784439,1.,0.866025403784439,1.,0.866025403784439,
1.,0.866025403784439,1.,0.866025403784439,1.,0.866025403784439,1.,0.866025403784439,
1.,0.866025403784439,1.,0.866025403784439,1.,0.866025403784439,1.,0.866025403784439,
1.,0.866025403784439,1.,0.866025403784439,1.,0.866025403784439,1.,0.866025403784439,
1.,0.866025403784439,1.,0.866025403784439,1.,0.866025403784439,1.,0.866025403784439,
1.,0.866025403784439,1.,0.866025403784439,1.,0.866025403784439,1.,0.866025403784439,
1.,0.866025403784439,1.,0.866025403784439,1.,0.98031044488126,0.966408234404338)))
REPRESENTATION_ITEM('')
SURFACE()
);
#3185=(
BOUNDED_SURFACE()
B_SPLINE_SURFACE(1,2,((#262037,#262038,#262039,#262040,#262041,#262042,
#262043,#262044,#262045,#262046,#262047,#262048,#262049,#262050,#262051,
#262052,#262053,#262054,#262055,#262056,#262057,#262058,#262059,#262060,
#262061,#262062,#262063,#262064,#262065,#262066,#262067,#262068,#262069,
#262070,#262071,#262072,#262073,#262074,#262075,#262076,#262077,#262078,
#262079,#262080,#262081,#262082,#262083,#262084,#262085,#262086,#262087,
#262088,#262089,#262090,#262091,#262092,#262093,#262094,#262095,#262096,
#262097,#262098,#262099,#262100,#262101,#262102,#262103,#262104,#262105,
#262106,#262107,#262108,#262109,#262110,#262111,#262112,#262113,#262114,
#262115,#262116,#262117,#262118,#262119,#262120,#262121,#262122,#262123,
#262124,#262125,#262126,#262127,#262128,#262129,#262130,#262131,#262132,
#262133,#262134,#262135,#262136,#262137,#262138,#262139,#262140,#262141,
#262142,#262143,#262144,#262145,#262146,#262147,#262148,#262149,#262150,
#262151,#262152,#262153,#262154,#262155,#262156,#262157,#262158,#262159,
#262160,#262161,#262162,#262163,#262164,#262165,#262166,#262167,#262168,
#262169,#262170,#262171,#262172,#262173,#262174,#262175,#262176,#262177,
#262178,#262179,#262180,#262181,#262182,#262183,#262184,#262185,#262186,
#262187,#262188,#262189,#262190,#262191,#262192,#262193,#262194,#262195,
#262196,#262197,#262198,#262199,#262200,#262201,#262202,#262203,#262204,
#262205,#262206,#262207,#262208,#262209,#262210,#262211,#262212,#262213,
#262214,#262215,#262216,#262217,#262218,#262219,#262220,#262221,#262222,
#262223,#262224,#262225,#262226,#262227,#262228,#262229,#262230,#262231,
#262232,#262233,#262234,#262235,#262236,#262237,#262238,#262239,#262240,
#262241,#262242,#262243,#262244,#262245,#262246,#262247,#262248,#262249,
#262250,#262251,#262252,#262253,#262254,#262255,#262256,#262257,#262258,
#262259,#262260,#262261,#262262,#262263,#262264,#262265,#262266,#262267,
#262268,#262269,#262270,#262271,#262272,#262273,#262274,#262275,#262276,
#262277,#262278,#262279,#262280,#262281,#262282,#262283,#262284,#262285,
#262286,#262287,#262288,#262289,#262290,#262291,#262292,#262293,#262294,
#262295,#262296,#262297,#262298,#262299,#262300,#262301,#262302,#262303,
#262304,#262305,#262306,#262307,#262308,#262309,#262310,#262311,#262312,
#262313),(#262314,#262315,#262316,#262317,#262318,#262319,#262320,#262321,
#262322,#262323,#262324,#262325,#262326,#262327,#262328,#262329,#262330,
#262331,#262332,#262333,#262334,#262335,#262336,#262337,#262338,#262339,
#262340,#262341,#262342,#262343,#262344,#262345,#262346,#262347,#262348,
#262349,#262350,#262351,#262352,#262353,#262354,#262355,#262356,#262357,
#262358,#262359,#262360,#262361,#262362,#262363,#262364,#262365,#262366,
#262367,#262368,#262369,#262370,#262371,#262372,#262373,#262374,#262375,
#262376,#262377,#262378,#262379,#262380,#262381,#262382,#262383,#262384,
#262385,#262386,#262387,#262388,#262389,#262390,#262391,#262392,#262393,
#262394,#262395,#262396,#262397,#262398,#262399,#262400,#262401,#262402,
#262403,#262404,#262405,#262406,#262407,#262408,#262409,#262410,#262411,
#262412,#262413,#262414,#262415,#262416,#262417,#262418,#262419,#262420,
#262421,#262422,#262423,#262424,#262425,#262426,#262427,#262428,#262429,
#262430,#262431,#262432,#262433,#262434,#262435,#262436,#262437,#262438,
#262439,#262440,#262441,#262442,#262443,#262444,#262445,#262446,#262447,
#262448,#262449,#262450,#262451,#262452,#262453,#262454,#262455,#262456,
#262457,#262458,#262459,#262460,#262461,#262462,#262463,#262464,#262465,
#262466,#262467,#262468,#262469,#262470,#262471,#262472,#262473,#262474,
#262475,#262476,#262477,#262478,#262479,#262480,#262481,#262482,#262483,
#262484,#262485,#262486,#262487,#262488,#262489,#262490,#262491,#262492,
#262493,#262494,#262495,#262496,#262497,#262498,#262499,#262500,#262501,
#262502,#262503,#262504,#262505,#262506,#262507,#262508,#262509,#262510,
#262511,#262512,#262513,#262514,#262515,#262516,#262517,#262518,#262519,
#262520,#262521,#262522,#262523,#262524,#262525,#262526,#262527,#262528,
#262529,#262530,#262531,#262532,#262533,#262534,#262535,#262536,#262537,
#262538,#262539,#262540,#262541,#262542,#262543,#262544,#262545,#262546,
#262547,#262548,#262549,#262550,#262551,#262552,#262553,#262554,#262555,
#262556,#262557,#262558,#262559,#262560,#262561,#262562,#262563,#262564,
#262565,#262566,#262567,#262568,#262569,#262570,#262571,#262572,#262573,
#262574,#262575,#262576,#262577,#262578,#262579,#262580,#262581,#262582,
#262583,#262584,#262585,#262586,#262587,#262588,#262589,#262590)),
 .UNSPECIFIED.,.F.,.F.,.F.)
B_SPLINE_SURFACE_WITH_KNOTS((2,2),(3,2,2,2,2,2,2,2,2,2,2,2,2,2,2,2,2,2,
2,2,2,2,2,2,2,2,2,2,2,2,2,2,2,2,2,2,2,2,2,2,2,2,2,2,2,2,2,2,2,2,2,2,2,2,
2,2,2,2,2,2,2,2,2,2,2,2,2,2,2,2,2,2,2,2,2,2,2,2,2,2,2,2,2,2,2,2,2,2,2,2,
2,2,2,2,2,2,2,2,2,2,2,2,2,2,2,2,2,2,2,2,2,2,2,2,2,2,2,2,2,2,2,2,2,2,2,2,
2,2,2,2,2,2,2,2,2,2,2,2,3),(0.,1.),(0.,0.0072463768115942,0.0144927536231884,
0.0217391304347826,0.0289855072463768,0.036231884057971,0.0434782608695652,
0.0507246376811594,0.0579710144927536,0.0652173913043478,0.072463768115942,
0.0797101449275362,0.0869565217391304,0.0942028985507246,0.101449275362319,
0.108695652173913,0.115942028985507,0.123188405797101,0.130434782608696,
0.13768115942029,0.144927536231884,0.152173913043478,0.159420289855073,
0.166666666666667,0.173913043478261,0.181159420289855,0.18840579710145,
0.195652173913044,0.202898550724637,0.210144927536232,0.217391304347826,
0.224637681159421,0.231884057971014,0.239130434782609,0.246376811594203,
0.253623188405797,0.260869565217392,0.268115942028985,0.275362318840579,
0.282608695652174,0.289855072463768,0.297101449275363,0.304347826086956,
0.31159420289855,0.318840579710145,0.326086956521739,0.333333333333334,
0.340579710144927,0.347826086956521,0.355072463768116,0.36231884057971,
0.369565217391304,0.376811594202899,0.384057971014493,0.391304347826087,
0.398550724637681,0.405797101449275,0.41304347826087,0.420289855072463,
0.427536231884058,0.434782608695652,0.442028985507247,0.449275362318841,
0.456521739130435,0.463768115942029,0.471014492753623,0.478260869565218,
0.485507246376812,0.492753623188406,0.5,0.507246376811594,0.514492753623188,
0.521739130434783,0.528985507246377,0.536231884057971,0.543478260869565,
0.550724637681159,0.557971014492754,0.565217391304348,0.572463768115942,
0.579710144927536,0.586956521739131,0.594202898550725,0.601449275362319,
0.608695652173913,0.615942028985507,0.623188405797101,0.630434782608696,
0.63768115942029,0.644927536231884,0.652173913043478,0.659420289855073,
0.666666666666667,0.673913043478261,0.681159420289855,0.688405797101449,
0.695652173913044,0.702898550724638,0.710144927536232,0.717391304347826,
0.72463768115942,0.731884057971015,0.739130434782609,0.746376811594203,
0.753623188405797,0.760869565217391,0.768115942028986,0.77536231884058,
0.782608695652174,0.789855072463768,0.797101449275362,0.804347826086956,
0.811594202898551,0.818840579710145,0.826086956521739,0.833333333333333,
0.840579710144928,0.847826086956522,0.855072463768116,0.86231884057971,
0.869565217391304,0.876811594202899,0.884057971014493,0.891304347826087,
0.898550724637681,0.905797101449275,0.91304347826087,0.920289855072464,
0.927536231884058,0.934782608695652,0.942028985507246,0.94927536231884,
0.956521739130435,0.963768115942029,0.971014492753623,0.978260869565217,
0.985507246376812,0.992753623188406,0.993818585798284),.UNSPECIFIED.)
GEOMETRIC_REPRESENTATION_ITEM()
RATIONAL_B_SPLINE_SURFACE(((1.,0.866025403784439,1.,0.866025403784439,1.,
0.866025403784439,1.,0.866025403784439,1.,0.866025403784439,1.,0.866025403784439,
1.,0.866025403784439,1.,0.866025403784439,1.,0.866025403784439,1.,0.866025403784439,
1.,0.866025403784439,1.,0.866025403784439,1.,0.866025403784439,1.,0.866025403784439,
1.,0.866025403784439,1.,0.866025403784439,1.,0.866025403784439,1.,0.866025403784439,
1.,0.866025403784439,1.,0.866025403784439,1.,0.866025403784439,1.,0.866025403784439,
1.,0.866025403784439,1.,0.866025403784439,1.,0.866025403784439,1.,0.866025403784439,
1.,0.866025403784439,1.,0.866025403784439,1.,0.866025403784439,1.,0.866025403784439,
1.,0.866025403784439,1.,0.866025403784439,1.,0.866025403784439,1.,0.866025403784439,
1.,0.866025403784439,1.,0.866025403784439,1.,0.866025403784439,1.,0.866025403784439,
1.,0.866025403784439,1.,0.866025403784439,1.,0.866025403784439,1.,0.866025403784439,
1.,0.866025403784439,1.,0.866025403784439,1.,0.866025403784439,1.,0.866025403784439,
1.,0.866025403784439,1.,0.866025403784439,1.,0.866025403784439,1.,0.866025403784439,
1.,0.866025403784439,1.,0.866025403784439,1.,0.866025403784439,1.,0.866025403784439,
1.,0.866025403784439,1.,0.866025403784439,1.,0.866025403784439,1.,0.866025403784439,
1.,0.866025403784439,1.,0.866025403784439,1.,0.866025403784439,1.,0.866025403784439,
1.,0.866025403784439,1.,0.866025403784439,1.,0.866025403784439,1.,0.866025403784439,
1.,0.866025403784439,1.,0.866025403784439,1.,0.866025403784439,1.,0.866025403784439,
1.,0.866025403784439,1.,0.866025403784439,1.,0.866025403784439,1.,0.866025403784439,
1.,0.866025403784439,1.,0.866025403784439,1.,0.866025403784439,1.,0.866025403784439,
1.,0.866025403784439,1.,0.866025403784439,1.,0.866025403784439,1.,0.866025403784439,
1.,0.866025403784439,1.,0.866025403784439,1.,0.866025403784439,1.,0.866025403784439,
1.,0.866025403784439,1.,0.866025403784439,1.,0.866025403784439,1.,0.866025403784439,
1.,0.866025403784439,1.,0.866025403784439,1.,0.866025403784439,1.,0.866025403784439,
1.,0.866025403784439,1.,0.866025403784439,1.,0.866025403784439,1.,0.866025403784439,
1.,0.866025403784439,1.,0.866025403784439,1.,0.866025403784439,1.,0.866025403784439,
1.,0.866025403784439,1.,0.866025403784439,1.,0.866025403784439,1.,0.866025403784439,
1.,0.866025403784439,1.,0.866025403784439,1.,0.866025403784439,1.,0.866025403784439,
1.,0.866025403784439,1.,0.866025403784439,1.,0.866025403784439,1.,0.866025403784439,
1.,0.866025403784439,1.,0.866025403784439,1.,0.866025403784439,1.,0.866025403784439,
1.,0.866025403784439,1.,0.866025403784439,1.,0.866025403784439,1.,0.866025403784439,
1.,0.866025403784439,1.,0.866025403784439,1.,0.866025403784439,1.,0.866025403784439,
1.,0.866025403784439,1.,0.866025403784439,1.,0.866025403784439,1.,0.866025403784439,
1.,0.866025403784439,1.,0.866025403784439,1.,0.866025403784439,1.,0.866025403784439,
1.,0.866025403784439,1.,0.866025403784439,1.,0.866025403784439,1.,0.98031044488126,
0.966408234404338),(1.,0.866025403784439,1.,0.866025403784439,1.,0.866025403784439,
1.,0.866025403784439,1.,0.866025403784439,1.,0.866025403784439,1.,0.866025403784439,
1.,0.866025403784439,1.,0.866025403784439,1.,0.866025403784439,1.,0.866025403784439,
1.,0.866025403784439,1.,0.866025403784439,1.,0.866025403784439,1.,0.866025403784439,
1.,0.866025403784439,1.,0.866025403784439,1.,0.866025403784439,1.,0.866025403784439,
1.,0.866025403784439,1.,0.866025403784439,1.,0.866025403784439,1.,0.866025403784439,
1.,0.866025403784439,1.,0.866025403784439,1.,0.866025403784439,1.,0.866025403784439,
1.,0.866025403784439,1.,0.866025403784439,1.,0.866025403784439,1.,0.866025403784439,
1.,0.866025403784439,1.,0.866025403784439,1.,0.866025403784439,1.,0.866025403784439,
1.,0.866025403784439,1.,0.866025403784439,1.,0.866025403784439,1.,0.866025403784439,
1.,0.866025403784439,1.,0.866025403784439,1.,0.866025403784439,1.,0.866025403784439,
1.,0.866025403784439,1.,0.866025403784439,1.,0.866025403784439,1.,0.866025403784439,
1.,0.866025403784439,1.,0.866025403784439,1.,0.866025403784439,1.,0.866025403784439,
1.,0.866025403784439,1.,0.866025403784439,1.,0.866025403784439,1.,0.866025403784439,
1.,0.866025403784439,1.,0.866025403784439,1.,0.866025403784439,1.,0.866025403784439,
1.,0.866025403784439,1.,0.866025403784439,1.,0.866025403784439,1.,0.866025403784439,
1.,0.866025403784439,1.,0.866025403784439,1.,0.866025403784439,1.,0.866025403784439,
1.,0.866025403784439,1.,0.866025403784439,1.,0.866025403784439,1.,0.866025403784439,
1.,0.866025403784439,1.,0.866025403784439,1.,0.866025403784439,1.,0.866025403784439,
1.,0.866025403784439,1.,0.866025403784439,1.,0.866025403784439,1.,0.866025403784439,
1.,0.866025403784439,1.,0.866025403784439,1.,0.866025403784439,1.,0.866025403784439,
1.,0.866025403784439,1.,0.866025403784439,1.,0.866025403784439,1.,0.866025403784439,
1.,0.866025403784439,1.,0.866025403784439,1.,0.866025403784439,1.,0.866025403784439,
1.,0.866025403784439,1.,0.866025403784439,1.,0.866025403784439,1.,0.866025403784439,
1.,0.866025403784439,1.,0.866025403784439,1.,0.866025403784439,1.,0.866025403784439,
1.,0.866025403784439,1.,0.866025403784439,1.,0.866025403784439,1.,0.866025403784439,
1.,0.866025403784439,1.,0.866025403784439,1.,0.866025403784439,1.,0.866025403784439,
1.,0.866025403784439,1.,0.866025403784439,1.,0.866025403784439,1.,0.866025403784439,
1.,0.866025403784439,1.,0.866025403784439,1.,0.866025403784439,1.,0.866025403784439,
1.,0.866025403784439,1.,0.866025403784439,1.,0.866025403784439,1.,0.866025403784439,
1.,0.866025403784439,1.,0.866025403784439,1.,0.866025403784439,1.,0.866025403784439,
1.,0.866025403784439,1.,0.866025403784439,1.,0.866025403784439,1.,0.866025403784439,
1.,0.866025403784439,1.,0.866025403784439,1.,0.866025403784439,1.,0.866025403784439,
1.,0.866025403784439,1.,0.866025403784439,1.,0.866025403784439,1.,0.866025403784439,
1.,0.866025403784439,1.,0.866025403784439,1.,0.98031044488126,0.966408234404338)))
REPRESENTATION_ITEM('')
SURFACE()
);
#3186=(
BOUNDED_SURFACE()
B_SPLINE_SURFACE(1,2,((#264455,#264456,#264457,#264458,#264459,#264460,
#264461,#264462,#264463,#264464,#264465,#264466,#264467,#264468,#264469,
#264470,#264471,#264472,#264473,#264474,#264475,#264476,#264477,#264478,
#264479,#264480,#264481,#264482,#264483,#264484,#264485,#264486,#264487,
#264488,#264489,#264490,#264491,#264492,#264493,#264494,#264495,#264496,
#264497,#264498,#264499,#264500,#264501,#264502,#264503,#264504,#264505,
#264506,#264507,#264508,#264509,#264510,#264511,#264512,#264513,#264514,
#264515,#264516,#264517,#264518,#264519,#264520,#264521,#264522,#264523,
#264524,#264525,#264526,#264527,#264528,#264529,#264530,#264531,#264532,
#264533,#264534,#264535,#264536,#264537,#264538,#264539,#264540,#264541,
#264542,#264543,#264544,#264545,#264546,#264547,#264548,#264549,#264550,
#264551,#264552,#264553,#264554,#264555,#264556,#264557,#264558,#264559,
#264560,#264561,#264562,#264563,#264564,#264565,#264566,#264567,#264568,
#264569,#264570,#264571,#264572,#264573,#264574,#264575,#264576,#264577,
#264578,#264579,#264580,#264581,#264582,#264583,#264584,#264585,#264586,
#264587,#264588,#264589,#264590,#264591,#264592,#264593,#264594,#264595,
#264596,#264597,#264598,#264599,#264600,#264601,#264602,#264603,#264604,
#264605,#264606,#264607,#264608,#264609,#264610,#264611,#264612,#264613,
#264614,#264615,#264616,#264617,#264618,#264619,#264620,#264621,#264622,
#264623,#264624,#264625,#264626,#264627,#264628,#264629,#264630,#264631,
#264632,#264633,#264634,#264635,#264636,#264637,#264638,#264639,#264640,
#264641,#264642,#264643,#264644,#264645,#264646,#264647,#264648,#264649,
#264650,#264651,#264652,#264653,#264654,#264655,#264656,#264657,#264658,
#264659,#264660,#264661,#264662,#264663,#264664,#264665,#264666,#264667,
#264668,#264669,#264670,#264671,#264672,#264673,#264674,#264675,#264676,
#264677,#264678,#264679,#264680,#264681,#264682,#264683,#264684,#264685,
#264686,#264687,#264688,#264689,#264690,#264691,#264692,#264693,#264694,
#264695,#264696,#264697,#264698,#264699,#264700,#264701,#264702,#264703,
#264704,#264705,#264706,#264707,#264708,#264709,#264710,#264711,#264712,
#264713,#264714,#264715,#264716,#264717,#264718,#264719,#264720,#264721,
#264722,#264723,#264724,#264725,#264726,#264727,#264728,#264729,#264730,
#264731),(#264732,#264733,#264734,#264735,#264736,#264737,#264738,#264739,
#264740,#264741,#264742,#264743,#264744,#264745,#264746,#264747,#264748,
#264749,#264750,#264751,#264752,#264753,#264754,#264755,#264756,#264757,
#264758,#264759,#264760,#264761,#264762,#264763,#264764,#264765,#264766,
#264767,#264768,#264769,#264770,#264771,#264772,#264773,#264774,#264775,
#264776,#264777,#264778,#264779,#264780,#264781,#264782,#264783,#264784,
#264785,#264786,#264787,#264788,#264789,#264790,#264791,#264792,#264793,
#264794,#264795,#264796,#264797,#264798,#264799,#264800,#264801,#264802,
#264803,#264804,#264805,#264806,#264807,#264808,#264809,#264810,#264811,
#264812,#264813,#264814,#264815,#264816,#264817,#264818,#264819,#264820,
#264821,#264822,#264823,#264824,#264825,#264826,#264827,#264828,#264829,
#264830,#264831,#264832,#264833,#264834,#264835,#264836,#264837,#264838,
#264839,#264840,#264841,#264842,#264843,#264844,#264845,#264846,#264847,
#264848,#264849,#264850,#264851,#264852,#264853,#264854,#264855,#264856,
#264857,#264858,#264859,#264860,#264861,#264862,#264863,#264864,#264865,
#264866,#264867,#264868,#264869,#264870,#264871,#264872,#264873,#264874,
#264875,#264876,#264877,#264878,#264879,#264880,#264881,#264882,#264883,
#264884,#264885,#264886,#264887,#264888,#264889,#264890,#264891,#264892,
#264893,#264894,#264895,#264896,#264897,#264898,#264899,#264900,#264901,
#264902,#264903,#264904,#264905,#264906,#264907,#264908,#264909,#264910,
#264911,#264912,#264913,#264914,#264915,#264916,#264917,#264918,#264919,
#264920,#264921,#264922,#264923,#264924,#264925,#264926,#264927,#264928,
#264929,#264930,#264931,#264932,#264933,#264934,#264935,#264936,#264937,
#264938,#264939,#264940,#264941,#264942,#264943,#264944,#264945,#264946,
#264947,#264948,#264949,#264950,#264951,#264952,#264953,#264954,#264955,
#264956,#264957,#264958,#264959,#264960,#264961,#264962,#264963,#264964,
#264965,#264966,#264967,#264968,#264969,#264970,#264971,#264972,#264973,
#264974,#264975,#264976,#264977,#264978,#264979,#264980,#264981,#264982,
#264983,#264984,#264985,#264986,#264987,#264988,#264989,#264990,#264991,
#264992,#264993,#264994,#264995,#264996,#264997,#264998,#264999,#265000,
#265001,#265002,#265003,#265004,#265005,#265006,#265007,#265008)),
 .UNSPECIFIED.,.F.,.F.,.F.)
B_SPLINE_SURFACE_WITH_KNOTS((2,2),(3,2,2,2,2,2,2,2,2,2,2,2,2,2,2,2,2,2,
2,2,2,2,2,2,2,2,2,2,2,2,2,2,2,2,2,2,2,2,2,2,2,2,2,2,2,2,2,2,2,2,2,2,2,2,
2,2,2,2,2,2,2,2,2,2,2,2,2,2,2,2,2,2,2,2,2,2,2,2,2,2,2,2,2,2,2,2,2,2,2,2,
2,2,2,2,2,2,2,2,2,2,2,2,2,2,2,2,2,2,2,2,2,2,2,2,2,2,2,2,2,2,2,2,2,2,2,2,
2,2,2,2,2,2,2,2,2,2,2,2,3),(0.,1.),(0.,0.0072463768115942,0.0144927536231884,
0.0217391304347826,0.0289855072463768,0.036231884057971,0.0434782608695652,
0.0507246376811594,0.0579710144927536,0.0652173913043478,0.072463768115942,
0.0797101449275362,0.0869565217391304,0.0942028985507246,0.101449275362319,
0.108695652173913,0.115942028985507,0.123188405797101,0.130434782608696,
0.13768115942029,0.144927536231884,0.152173913043478,0.159420289855073,
0.166666666666667,0.173913043478261,0.181159420289855,0.18840579710145,
0.195652173913044,0.202898550724637,0.210144927536232,0.217391304347826,
0.224637681159421,0.231884057971014,0.239130434782609,0.246376811594203,
0.253623188405797,0.260869565217392,0.268115942028985,0.275362318840579,
0.282608695652174,0.289855072463768,0.297101449275363,0.304347826086956,
0.31159420289855,0.318840579710145,0.326086956521739,0.333333333333334,
0.340579710144927,0.347826086956521,0.355072463768116,0.36231884057971,
0.369565217391304,0.376811594202899,0.384057971014493,0.391304347826087,
0.398550724637681,0.405797101449275,0.41304347826087,0.420289855072463,
0.427536231884058,0.434782608695652,0.442028985507247,0.449275362318841,
0.456521739130435,0.463768115942029,0.471014492753623,0.478260869565218,
0.485507246376812,0.492753623188406,0.5,0.507246376811594,0.514492753623188,
0.521739130434783,0.528985507246377,0.536231884057971,0.543478260869565,
0.550724637681159,0.557971014492754,0.565217391304348,0.572463768115942,
0.579710144927536,0.586956521739131,0.594202898550725,0.601449275362319,
0.608695652173913,0.615942028985507,0.623188405797101,0.630434782608696,
0.63768115942029,0.644927536231884,0.652173913043478,0.659420289855073,
0.666666666666667,0.673913043478261,0.681159420289855,0.688405797101449,
0.695652173913044,0.702898550724638,0.710144927536232,0.717391304347826,
0.72463768115942,0.731884057971015,0.739130434782609,0.746376811594203,
0.753623188405797,0.760869565217391,0.768115942028986,0.77536231884058,
0.782608695652174,0.789855072463768,0.797101449275362,0.804347826086956,
0.811594202898551,0.818840579710145,0.826086956521739,0.833333333333333,
0.840579710144928,0.847826086956522,0.855072463768116,0.86231884057971,
0.869565217391304,0.876811594202899,0.884057971014493,0.891304347826087,
0.898550724637681,0.905797101449275,0.91304347826087,0.920289855072464,
0.927536231884058,0.934782608695652,0.942028985507246,0.94927536231884,
0.956521739130435,0.963768115942029,0.971014492753623,0.978260869565217,
0.985507246376812,0.992753623188406,0.993818495192186),.UNSPECIFIED.)
GEOMETRIC_REPRESENTATION_ITEM()
RATIONAL_B_SPLINE_SURFACE(((1.,0.866025403784439,1.,0.866025403784439,1.,
0.866025403784439,1.,0.866025403784439,1.,0.866025403784439,1.,0.866025403784439,
1.,0.866025403784439,1.,0.866025403784439,1.,0.866025403784439,1.,0.866025403784439,
1.,0.866025403784439,1.,0.866025403784439,1.,0.866025403784439,1.,0.866025403784439,
1.,0.866025403784439,1.,0.866025403784439,1.,0.866025403784439,1.,0.866025403784439,
1.,0.866025403784439,1.,0.866025403784439,1.,0.866025403784439,1.,0.866025403784439,
1.,0.866025403784439,1.,0.866025403784439,1.,0.866025403784439,1.,0.866025403784439,
1.,0.866025403784439,1.,0.866025403784439,1.,0.866025403784439,1.,0.866025403784439,
1.,0.866025403784439,1.,0.866025403784439,1.,0.866025403784439,1.,0.866025403784439,
1.,0.866025403784439,1.,0.866025403784439,1.,0.866025403784439,1.,0.866025403784439,
1.,0.866025403784439,1.,0.866025403784439,1.,0.866025403784439,1.,0.866025403784439,
1.,0.866025403784439,1.,0.866025403784439,1.,0.866025403784439,1.,0.866025403784439,
1.,0.866025403784439,1.,0.866025403784439,1.,0.866025403784439,1.,0.866025403784439,
1.,0.866025403784439,1.,0.866025403784439,1.,0.866025403784439,1.,0.866025403784439,
1.,0.866025403784439,1.,0.866025403784439,1.,0.866025403784439,1.,0.866025403784439,
1.,0.866025403784439,1.,0.866025403784439,1.,0.866025403784439,1.,0.866025403784439,
1.,0.866025403784439,1.,0.866025403784439,1.,0.866025403784439,1.,0.866025403784439,
1.,0.866025403784439,1.,0.866025403784439,1.,0.866025403784439,1.,0.866025403784439,
1.,0.866025403784439,1.,0.866025403784439,1.,0.866025403784439,1.,0.866025403784439,
1.,0.866025403784439,1.,0.866025403784439,1.,0.866025403784439,1.,0.866025403784439,
1.,0.866025403784439,1.,0.866025403784439,1.,0.866025403784439,1.,0.866025403784439,
1.,0.866025403784439,1.,0.866025403784439,1.,0.866025403784439,1.,0.866025403784439,
1.,0.866025403784439,1.,0.866025403784439,1.,0.866025403784439,1.,0.866025403784439,
1.,0.866025403784439,1.,0.866025403784439,1.,0.866025403784439,1.,0.866025403784439,
1.,0.866025403784439,1.,0.866025403784439,1.,0.866025403784439,1.,0.866025403784439,
1.,0.866025403784439,1.,0.866025403784439,1.,0.866025403784439,1.,0.866025403784439,
1.,0.866025403784439,1.,0.866025403784439,1.,0.866025403784439,1.,0.866025403784439,
1.,0.866025403784439,1.,0.866025403784439,1.,0.866025403784439,1.,0.866025403784439,
1.,0.866025403784439,1.,0.866025403784439,1.,0.866025403784439,1.,0.866025403784439,
1.,0.866025403784439,1.,0.866025403784439,1.,0.866025403784439,1.,0.866025403784439,
1.,0.866025403784439,1.,0.866025403784439,1.,0.866025403784439,1.,0.866025403784439,
1.,0.866025403784439,1.,0.866025403784439,1.,0.866025403784439,1.,0.866025403784439,
1.,0.866025403784439,1.,0.866025403784439,1.,0.866025403784439,1.,0.866025403784439,
1.,0.866025403784439,1.,0.866025403784439,1.,0.866025403784439,1.,0.866025403784439,
1.,0.866025403784439,1.,0.866025403784439,1.,0.866025403784439,1.,0.980312120051573,
0.966410600022306),(1.,0.866025403784439,1.,0.866025403784439,1.,0.866025403784439,
1.,0.866025403784439,1.,0.866025403784439,1.,0.866025403784439,1.,0.866025403784439,
1.,0.866025403784439,1.,0.866025403784439,1.,0.866025403784439,1.,0.866025403784439,
1.,0.866025403784439,1.,0.866025403784439,1.,0.866025403784439,1.,0.866025403784439,
1.,0.866025403784439,1.,0.866025403784439,1.,0.866025403784439,1.,0.866025403784439,
1.,0.866025403784439,1.,0.866025403784439,1.,0.866025403784439,1.,0.866025403784439,
1.,0.866025403784439,1.,0.866025403784439,1.,0.866025403784439,1.,0.866025403784439,
1.,0.866025403784439,1.,0.866025403784439,1.,0.866025403784439,1.,0.866025403784439,
1.,0.866025403784439,1.,0.866025403784439,1.,0.866025403784439,1.,0.866025403784439,
1.,0.866025403784439,1.,0.866025403784439,1.,0.866025403784439,1.,0.866025403784439,
1.,0.866025403784439,1.,0.866025403784439,1.,0.866025403784439,1.,0.866025403784439,
1.,0.866025403784439,1.,0.866025403784439,1.,0.866025403784439,1.,0.866025403784439,
1.,0.866025403784439,1.,0.866025403784439,1.,0.866025403784439,1.,0.866025403784439,
1.,0.866025403784439,1.,0.866025403784439,1.,0.866025403784439,1.,0.866025403784439,
1.,0.866025403784439,1.,0.866025403784439,1.,0.866025403784439,1.,0.866025403784439,
1.,0.866025403784439,1.,0.866025403784439,1.,0.866025403784439,1.,0.866025403784439,
1.,0.866025403784439,1.,0.866025403784439,1.,0.866025403784439,1.,0.866025403784439,
1.,0.866025403784439,1.,0.866025403784439,1.,0.866025403784439,1.,0.866025403784439,
1.,0.866025403784439,1.,0.866025403784439,1.,0.866025403784439,1.,0.866025403784439,
1.,0.866025403784439,1.,0.866025403784439,1.,0.866025403784439,1.,0.866025403784439,
1.,0.866025403784439,1.,0.866025403784439,1.,0.866025403784439,1.,0.866025403784439,
1.,0.866025403784439,1.,0.866025403784439,1.,0.866025403784439,1.,0.866025403784439,
1.,0.866025403784439,1.,0.866025403784439,1.,0.866025403784439,1.,0.866025403784439,
1.,0.866025403784439,1.,0.866025403784439,1.,0.866025403784439,1.,0.866025403784439,
1.,0.866025403784439,1.,0.866025403784439,1.,0.866025403784439,1.,0.866025403784439,
1.,0.866025403784439,1.,0.866025403784439,1.,0.866025403784439,1.,0.866025403784439,
1.,0.866025403784439,1.,0.866025403784439,1.,0.866025403784439,1.,0.866025403784439,
1.,0.866025403784439,1.,0.866025403784439,1.,0.866025403784439,1.,0.866025403784439,
1.,0.866025403784439,1.,0.866025403784439,1.,0.866025403784439,1.,0.866025403784439,
1.,0.866025403784439,1.,0.866025403784439,1.,0.866025403784439,1.,0.866025403784439,
1.,0.866025403784439,1.,0.866025403784439,1.,0.866025403784439,1.,0.866025403784439,
1.,0.866025403784439,1.,0.866025403784439,1.,0.866025403784439,1.,0.866025403784439,
1.,0.866025403784439,1.,0.866025403784439,1.,0.866025403784439,1.,0.866025403784439,
1.,0.866025403784439,1.,0.866025403784439,1.,0.866025403784439,1.,0.866025403784439,
1.,0.866025403784439,1.,0.866025403784439,1.,0.980312120051573,0.966410600022306)))
REPRESENTATION_ITEM('')
SURFACE()
);
#3187=(
BOUNDED_SURFACE()
B_SPLINE_SURFACE(1,2,((#265009,#265010,#265011,#265012,#265013,#265014,
#265015,#265016,#265017,#265018,#265019,#265020,#265021,#265022,#265023,
#265024,#265025,#265026,#265027,#265028,#265029,#265030,#265031,#265032,
#265033,#265034,#265035,#265036,#265037,#265038,#265039,#265040,#265041,
#265042,#265043,#265044,#265045,#265046,#265047,#265048,#265049,#265050,
#265051,#265052,#265053,#265054,#265055,#265056,#265057,#265058,#265059,
#265060,#265061,#265062,#265063,#265064,#265065,#265066,#265067,#265068,
#265069,#265070,#265071,#265072,#265073,#265074,#265075,#265076,#265077,
#265078,#265079,#265080,#265081,#265082,#265083,#265084,#265085,#265086,
#265087,#265088,#265089,#265090,#265091,#265092,#265093,#265094,#265095,
#265096,#265097,#265098,#265099,#265100,#265101,#265102,#265103,#265104,
#265105,#265106,#265107,#265108,#265109,#265110,#265111,#265112,#265113,
#265114,#265115,#265116,#265117,#265118,#265119,#265120,#265121,#265122,
#265123,#265124,#265125,#265126,#265127,#265128,#265129,#265130,#265131,
#265132,#265133,#265134,#265135,#265136,#265137,#265138,#265139,#265140,
#265141,#265142,#265143,#265144,#265145,#265146,#265147,#265148,#265149,
#265150,#265151,#265152,#265153,#265154,#265155,#265156,#265157,#265158,
#265159,#265160,#265161,#265162,#265163,#265164,#265165,#265166,#265167,
#265168,#265169,#265170,#265171,#265172,#265173,#265174,#265175,#265176,
#265177,#265178,#265179,#265180,#265181,#265182,#265183,#265184,#265185,
#265186,#265187,#265188,#265189,#265190,#265191,#265192,#265193,#265194,
#265195,#265196,#265197,#265198,#265199,#265200,#265201,#265202,#265203,
#265204,#265205,#265206,#265207,#265208,#265209,#265210,#265211,#265212,
#265213,#265214,#265215,#265216,#265217,#265218,#265219,#265220,#265221,
#265222,#265223,#265224,#265225,#265226,#265227,#265228,#265229,#265230,
#265231,#265232,#265233,#265234,#265235,#265236,#265237,#265238,#265239,
#265240,#265241,#265242,#265243,#265244,#265245,#265246,#265247,#265248,
#265249,#265250,#265251,#265252,#265253,#265254,#265255,#265256,#265257,
#265258,#265259,#265260,#265261,#265262,#265263,#265264,#265265,#265266,
#265267,#265268,#265269,#265270,#265271,#265272,#265273,#265274,#265275,
#265276,#265277,#265278,#265279,#265280,#265281,#265282,#265283,#265284,
#265285),(#265286,#265287,#265288,#265289,#265290,#265291,#265292,#265293,
#265294,#265295,#265296,#265297,#265298,#265299,#265300,#265301,#265302,
#265303,#265304,#265305,#265306,#265307,#265308,#265309,#265310,#265311,
#265312,#265313,#265314,#265315,#265316,#265317,#265318,#265319,#265320,
#265321,#265322,#265323,#265324,#265325,#265326,#265327,#265328,#265329,
#265330,#265331,#265332,#265333,#265334,#265335,#265336,#265337,#265338,
#265339,#265340,#265341,#265342,#265343,#265344,#265345,#265346,#265347,
#265348,#265349,#265350,#265351,#265352,#265353,#265354,#265355,#265356,
#265357,#265358,#265359,#265360,#265361,#265362,#265363,#265364,#265365,
#265366,#265367,#265368,#265369,#265370,#265371,#265372,#265373,#265374,
#265375,#265376,#265377,#265378,#265379,#265380,#265381,#265382,#265383,
#265384,#265385,#265386,#265387,#265388,#265389,#265390,#265391,#265392,
#265393,#265394,#265395,#265396,#265397,#265398,#265399,#265400,#265401,
#265402,#265403,#265404,#265405,#265406,#265407,#265408,#265409,#265410,
#265411,#265412,#265413,#265414,#265415,#265416,#265417,#265418,#265419,
#265420,#265421,#265422,#265423,#265424,#265425,#265426,#265427,#265428,
#265429,#265430,#265431,#265432,#265433,#265434,#265435,#265436,#265437,
#265438,#265439,#265440,#265441,#265442,#265443,#265444,#265445,#265446,
#265447,#265448,#265449,#265450,#265451,#265452,#265453,#265454,#265455,
#265456,#265457,#265458,#265459,#265460,#265461,#265462,#265463,#265464,
#265465,#265466,#265467,#265468,#265469,#265470,#265471,#265472,#265473,
#265474,#265475,#265476,#265477,#265478,#265479,#265480,#265481,#265482,
#265483,#265484,#265485,#265486,#265487,#265488,#265489,#265490,#265491,
#265492,#265493,#265494,#265495,#265496,#265497,#265498,#265499,#265500,
#265501,#265502,#265503,#265504,#265505,#265506,#265507,#265508,#265509,
#265510,#265511,#265512,#265513,#265514,#265515,#265516,#265517,#265518,
#265519,#265520,#265521,#265522,#265523,#265524,#265525,#265526,#265527,
#265528,#265529,#265530,#265531,#265532,#265533,#265534,#265535,#265536,
#265537,#265538,#265539,#265540,#265541,#265542,#265543,#265544,#265545,
#265546,#265547,#265548,#265549,#265550,#265551,#265552,#265553,#265554,
#265555,#265556,#265557,#265558,#265559,#265560,#265561,#265562)),
 .UNSPECIFIED.,.F.,.F.,.F.)
B_SPLINE_SURFACE_WITH_KNOTS((2,2),(3,2,2,2,2,2,2,2,2,2,2,2,2,2,2,2,2,2,
2,2,2,2,2,2,2,2,2,2,2,2,2,2,2,2,2,2,2,2,2,2,2,2,2,2,2,2,2,2,2,2,2,2,2,2,
2,2,2,2,2,2,2,2,2,2,2,2,2,2,2,2,2,2,2,2,2,2,2,2,2,2,2,2,2,2,2,2,2,2,2,2,
2,2,2,2,2,2,2,2,2,2,2,2,2,2,2,2,2,2,2,2,2,2,2,2,2,2,2,2,2,2,2,2,2,2,2,2,
2,2,2,2,2,2,2,2,2,2,2,2,3),(0.,1.00000035866471),(0.,0.0072463768115942,
0.0144927536231884,0.0217391304347826,0.0289855072463768,0.036231884057971,
0.0434782608695652,0.0507246376811594,0.0579710144927536,0.0652173913043478,
0.072463768115942,0.0797101449275362,0.0869565217391304,0.0942028985507246,
0.101449275362319,0.108695652173913,0.115942028985507,0.123188405797101,
0.130434782608696,0.13768115942029,0.144927536231884,0.152173913043478,
0.159420289855073,0.166666666666667,0.173913043478261,0.181159420289855,
0.18840579710145,0.195652173913044,0.202898550724637,0.210144927536232,
0.217391304347826,0.224637681159421,0.231884057971014,0.239130434782609,
0.246376811594203,0.253623188405797,0.260869565217392,0.268115942028985,
0.275362318840579,0.282608695652174,0.289855072463768,0.297101449275363,
0.304347826086956,0.31159420289855,0.318840579710145,0.326086956521739,
0.333333333333334,0.340579710144927,0.347826086956521,0.355072463768116,
0.36231884057971,0.369565217391304,0.376811594202899,0.384057971014493,
0.391304347826087,0.398550724637681,0.405797101449275,0.41304347826087,
0.420289855072463,0.427536231884058,0.434782608695652,0.442028985507247,
0.449275362318841,0.456521739130435,0.463768115942029,0.471014492753623,
0.478260869565218,0.485507246376812,0.492753623188406,0.5,0.507246376811594,
0.514492753623188,0.521739130434783,0.528985507246377,0.536231884057971,
0.543478260869565,0.550724637681159,0.557971014492754,0.565217391304348,
0.572463768115942,0.579710144927536,0.586956521739131,0.594202898550725,
0.601449275362319,0.608695652173913,0.615942028985507,0.623188405797101,
0.630434782608696,0.63768115942029,0.644927536231884,0.652173913043478,
0.659420289855073,0.666666666666667,0.673913043478261,0.681159420289855,
0.688405797101449,0.695652173913044,0.702898550724638,0.710144927536232,
0.717391304347826,0.72463768115942,0.731884057971015,0.739130434782609,
0.746376811594203,0.753623188405797,0.760869565217391,0.768115942028986,
0.77536231884058,0.782608695652174,0.789855072463768,0.797101449275362,
0.804347826086956,0.811594202898551,0.818840579710145,0.826086956521739,
0.833333333333333,0.840579710144928,0.847826086956522,0.855072463768116,
0.86231884057971,0.869565217391304,0.876811594202899,0.884057971014493,
0.891304347826087,0.898550724637681,0.905797101449275,0.91304347826087,
0.920289855072464,0.927536231884058,0.934782608695652,0.942028985507246,
0.94927536231884,0.956521739130435,0.963768115942029,0.971014492753623,
0.978260869565217,0.985507246376812,0.992753623188406,0.993818495192186),
 .UNSPECIFIED.)
GEOMETRIC_REPRESENTATION_ITEM()
RATIONAL_B_SPLINE_SURFACE(((1.,0.866025403784439,1.,0.866025403784439,1.,
0.866025403784439,1.,0.866025403784439,1.,0.866025403784439,1.,0.866025403784439,
1.,0.866025403784439,1.,0.866025403784439,1.,0.866025403784439,1.,0.866025403784439,
1.,0.866025403784439,1.,0.866025403784439,1.,0.866025403784439,1.,0.866025403784439,
1.,0.866025403784439,1.,0.866025403784439,1.,0.866025403784439,1.,0.866025403784439,
1.,0.866025403784439,1.,0.866025403784439,1.,0.866025403784439,1.,0.866025403784439,
1.,0.866025403784439,1.,0.866025403784439,1.,0.866025403784439,1.,0.866025403784439,
1.,0.866025403784439,1.,0.866025403784439,1.,0.866025403784439,1.,0.866025403784439,
1.,0.866025403784439,1.,0.866025403784439,1.,0.866025403784439,1.,0.866025403784439,
1.,0.866025403784439,1.,0.866025403784439,1.,0.866025403784439,1.,0.866025403784439,
1.,0.866025403784439,1.,0.866025403784439,1.,0.866025403784439,1.,0.866025403784439,
1.,0.866025403784439,1.,0.866025403784439,1.,0.866025403784439,1.,0.866025403784439,
1.,0.866025403784439,1.,0.866025403784439,1.,0.866025403784439,1.,0.866025403784439,
1.,0.866025403784439,1.,0.866025403784439,1.,0.866025403784439,1.,0.866025403784439,
1.,0.866025403784439,1.,0.866025403784439,1.,0.866025403784439,1.,0.866025403784439,
1.,0.866025403784439,1.,0.866025403784439,1.,0.866025403784439,1.,0.866025403784439,
1.,0.866025403784439,1.,0.866025403784439,1.,0.866025403784439,1.,0.866025403784439,
1.,0.866025403784439,1.,0.866025403784439,1.,0.866025403784439,1.,0.866025403784439,
1.,0.866025403784439,1.,0.866025403784439,1.,0.866025403784439,1.,0.866025403784439,
1.,0.866025403784439,1.,0.866025403784439,1.,0.866025403784439,1.,0.866025403784439,
1.,0.866025403784439,1.,0.866025403784439,1.,0.866025403784439,1.,0.866025403784439,
1.,0.866025403784439,1.,0.866025403784439,1.,0.866025403784439,1.,0.866025403784439,
1.,0.866025403784439,1.,0.866025403784439,1.,0.866025403784439,1.,0.866025403784439,
1.,0.866025403784439,1.,0.866025403784439,1.,0.866025403784439,1.,0.866025403784439,
1.,0.866025403784439,1.,0.866025403784439,1.,0.866025403784439,1.,0.866025403784439,
1.,0.866025403784439,1.,0.866025403784439,1.,0.866025403784439,1.,0.866025403784439,
1.,0.866025403784439,1.,0.866025403784439,1.,0.866025403784439,1.,0.866025403784439,
1.,0.866025403784439,1.,0.866025403784439,1.,0.866025403784439,1.,0.866025403784439,
1.,0.866025403784439,1.,0.866025403784439,1.,0.866025403784439,1.,0.866025403784439,
1.,0.866025403784439,1.,0.866025403784439,1.,0.866025403784439,1.,0.866025403784439,
1.,0.866025403784439,1.,0.866025403784439,1.,0.866025403784439,1.,0.866025403784439,
1.,0.866025403784439,1.,0.866025403784439,1.,0.866025403784439,1.,0.866025403784439,
1.,0.866025403784439,1.,0.866025403784439,1.,0.866025403784439,1.,0.866025403784439,
1.,0.866025403784439,1.,0.866025403784439,1.,0.866025403784439,1.,0.866025403784439,
1.,0.866025403784439,1.,0.866025403784439,1.,0.866025403784439,1.,0.980312120051573,
0.966410600022306),(1.,0.866025403784439,1.,0.866025403784439,1.,0.866025403784439,
1.,0.866025403784439,1.,0.866025403784439,1.,0.866025403784439,1.,0.866025403784439,
1.,0.866025403784439,1.,0.866025403784439,1.,0.866025403784439,1.,0.866025403784439,
1.,0.866025403784439,1.,0.866025403784439,1.,0.866025403784439,1.,0.866025403784439,
1.,0.866025403784439,1.,0.866025403784439,1.,0.866025403784439,1.,0.866025403784439,
1.,0.866025403784439,1.,0.866025403784439,1.,0.866025403784439,1.,0.866025403784439,
1.,0.866025403784439,1.,0.866025403784439,1.,0.866025403784439,1.,0.866025403784439,
1.,0.866025403784439,1.,0.866025403784439,1.,0.866025403784439,1.,0.866025403784439,
1.,0.866025403784439,1.,0.866025403784439,1.,0.866025403784439,1.,0.866025403784439,
1.,0.866025403784439,1.,0.866025403784439,1.,0.866025403784439,1.,0.866025403784439,
1.,0.866025403784439,1.,0.866025403784439,1.,0.866025403784439,1.,0.866025403784439,
1.,0.866025403784439,1.,0.866025403784439,1.,0.866025403784439,1.,0.866025403784439,
1.,0.866025403784439,1.,0.866025403784439,1.,0.866025403784439,1.,0.866025403784439,
1.,0.866025403784439,1.,0.866025403784439,1.,0.866025403784439,1.,0.866025403784439,
1.,0.866025403784439,1.,0.866025403784439,1.,0.866025403784439,1.,0.866025403784439,
1.,0.866025403784439,1.,0.866025403784439,1.,0.866025403784439,1.,0.866025403784439,
1.,0.866025403784439,1.,0.866025403784439,1.,0.866025403784439,1.,0.866025403784439,
1.,0.866025403784439,1.,0.866025403784439,1.,0.866025403784439,1.,0.866025403784439,
1.,0.866025403784439,1.,0.866025403784439,1.,0.866025403784439,1.,0.866025403784439,
1.,0.866025403784439,1.,0.866025403784439,1.,0.866025403784439,1.,0.866025403784439,
1.,0.866025403784439,1.,0.866025403784439,1.,0.866025403784439,1.,0.866025403784439,
1.,0.866025403784439,1.,0.866025403784439,1.,0.866025403784439,1.,0.866025403784439,
1.,0.866025403784439,1.,0.866025403784439,1.,0.866025403784439,1.,0.866025403784439,
1.,0.866025403784439,1.,0.866025403784439,1.,0.866025403784439,1.,0.866025403784439,
1.,0.866025403784439,1.,0.866025403784439,1.,0.866025403784439,1.,0.866025403784439,
1.,0.866025403784439,1.,0.866025403784439,1.,0.866025403784439,1.,0.866025403784439,
1.,0.866025403784439,1.,0.866025403784439,1.,0.866025403784439,1.,0.866025403784439,
1.,0.866025403784439,1.,0.866025403784439,1.,0.866025403784439,1.,0.866025403784439,
1.,0.866025403784439,1.,0.866025403784439,1.,0.866025403784439,1.,0.866025403784439,
1.,0.866025403784439,1.,0.866025403784439,1.,0.866025403784439,1.,0.866025403784439,
1.,0.866025403784439,1.,0.866025403784439,1.,0.866025403784439,1.,0.866025403784439,
1.,0.866025403784439,1.,0.866025403784439,1.,0.866025403784439,1.,0.866025403784439,
1.,0.866025403784439,1.,0.866025403784439,1.,0.866025403784439,1.,0.866025403784439,
1.,0.866025403784439,1.,0.866025403784439,1.,0.866025403784439,1.,0.866025403784439,
1.,0.866025403784439,1.,0.866025403784439,1.,0.980312120051573,0.966410600022306)))
REPRESENTATION_ITEM('')
SURFACE()
);
#3188=(
BOUNDED_SURFACE()
B_SPLINE_SURFACE(1,2,((#265569,#265570,#265571,#265572,#265573,#265574,
#265575,#265576,#265577,#265578,#265579,#265580,#265581,#265582,#265583,
#265584,#265585,#265586,#265587,#265588,#265589,#265590,#265591,#265592,
#265593,#265594,#265595,#265596,#265597,#265598,#265599,#265600,#265601,
#265602,#265603,#265604,#265605,#265606,#265607,#265608,#265609,#265610,
#265611,#265612,#265613,#265614,#265615,#265616,#265617,#265618,#265619,
#265620,#265621,#265622,#265623,#265624,#265625,#265626,#265627,#265628,
#265629,#265630,#265631,#265632,#265633,#265634,#265635,#265636,#265637,
#265638,#265639,#265640,#265641,#265642,#265643,#265644,#265645,#265646,
#265647,#265648,#265649,#265650,#265651,#265652,#265653,#265654,#265655,
#265656,#265657,#265658,#265659,#265660,#265661,#265662,#265663,#265664,
#265665,#265666,#265667,#265668,#265669,#265670,#265671,#265672,#265673,
#265674,#265675,#265676,#265677,#265678,#265679,#265680,#265681,#265682,
#265683,#265684,#265685,#265686,#265687,#265688,#265689,#265690,#265691,
#265692,#265693,#265694,#265695,#265696,#265697,#265698,#265699,#265700,
#265701,#265702,#265703,#265704,#265705,#265706,#265707,#265708,#265709,
#265710,#265711,#265712,#265713,#265714,#265715,#265716,#265717,#265718,
#265719,#265720,#265721,#265722,#265723,#265724,#265725,#265726,#265727,
#265728,#265729,#265730,#265731,#265732,#265733,#265734,#265735,#265736,
#265737,#265738,#265739,#265740,#265741,#265742,#265743,#265744,#265745,
#265746,#265747,#265748,#265749,#265750,#265751,#265752,#265753,#265754,
#265755,#265756,#265757,#265758,#265759,#265760,#265761,#265762,#265763,
#265764,#265765,#265766,#265767,#265768,#265769,#265770,#265771,#265772,
#265773,#265774,#265775,#265776,#265777,#265778,#265779,#265780,#265781,
#265782,#265783,#265784,#265785,#265786,#265787,#265788,#265789,#265790,
#265791,#265792,#265793,#265794,#265795,#265796,#265797,#265798,#265799,
#265800,#265801,#265802,#265803,#265804,#265805,#265806,#265807,#265808,
#265809,#265810,#265811,#265812,#265813,#265814,#265815,#265816,#265817,
#265818,#265819,#265820,#265821,#265822,#265823,#265824,#265825,#265826,
#265827,#265828,#265829,#265830,#265831,#265832,#265833,#265834,#265835,
#265836,#265837,#265838,#265839,#265840,#265841,#265842,#265843,#265844,
#265845),(#265846,#265847,#265848,#265849,#265850,#265851,#265852,#265853,
#265854,#265855,#265856,#265857,#265858,#265859,#265860,#265861,#265862,
#265863,#265864,#265865,#265866,#265867,#265868,#265869,#265870,#265871,
#265872,#265873,#265874,#265875,#265876,#265877,#265878,#265879,#265880,
#265881,#265882,#265883,#265884,#265885,#265886,#265887,#265888,#265889,
#265890,#265891,#265892,#265893,#265894,#265895,#265896,#265897,#265898,
#265899,#265900,#265901,#265902,#265903,#265904,#265905,#265906,#265907,
#265908,#265909,#265910,#265911,#265912,#265913,#265914,#265915,#265916,
#265917,#265918,#265919,#265920,#265921,#265922,#265923,#265924,#265925,
#265926,#265927,#265928,#265929,#265930,#265931,#265932,#265933,#265934,
#265935,#265936,#265937,#265938,#265939,#265940,#265941,#265942,#265943,
#265944,#265945,#265946,#265947,#265948,#265949,#265950,#265951,#265952,
#265953,#265954,#265955,#265956,#265957,#265958,#265959,#265960,#265961,
#265962,#265963,#265964,#265965,#265966,#265967,#265968,#265969,#265970,
#265971,#265972,#265973,#265974,#265975,#265976,#265977,#265978,#265979,
#265980,#265981,#265982,#265983,#265984,#265985,#265986,#265987,#265988,
#265989,#265990,#265991,#265992,#265993,#265994,#265995,#265996,#265997,
#265998,#265999,#266000,#266001,#266002,#266003,#266004,#266005,#266006,
#266007,#266008,#266009,#266010,#266011,#266012,#266013,#266014,#266015,
#266016,#266017,#266018,#266019,#266020,#266021,#266022,#266023,#266024,
#266025,#266026,#266027,#266028,#266029,#266030,#266031,#266032,#266033,
#266034,#266035,#266036,#266037,#266038,#266039,#266040,#266041,#266042,
#266043,#266044,#266045,#266046,#266047,#266048,#266049,#266050,#266051,
#266052,#266053,#266054,#266055,#266056,#266057,#266058,#266059,#266060,
#266061,#266062,#266063,#266064,#266065,#266066,#266067,#266068,#266069,
#266070,#266071,#266072,#266073,#266074,#266075,#266076,#266077,#266078,
#266079,#266080,#266081,#266082,#266083,#266084,#266085,#266086,#266087,
#266088,#266089,#266090,#266091,#266092,#266093,#266094,#266095,#266096,
#266097,#266098,#266099,#266100,#266101,#266102,#266103,#266104,#266105,
#266106,#266107,#266108,#266109,#266110,#266111,#266112,#266113,#266114,
#266115,#266116,#266117,#266118,#266119,#266120,#266121,#266122)),
 .UNSPECIFIED.,.F.,.F.,.F.)
B_SPLINE_SURFACE_WITH_KNOTS((2,2),(3,2,2,2,2,2,2,2,2,2,2,2,2,2,2,2,2,2,
2,2,2,2,2,2,2,2,2,2,2,2,2,2,2,2,2,2,2,2,2,2,2,2,2,2,2,2,2,2,2,2,2,2,2,2,
2,2,2,2,2,2,2,2,2,2,2,2,2,2,2,2,2,2,2,2,2,2,2,2,2,2,2,2,2,2,2,2,2,2,2,2,
2,2,2,2,2,2,2,2,2,2,2,2,2,2,2,2,2,2,2,2,2,2,2,2,2,2,2,2,2,2,2,2,2,2,2,2,
2,2,2,2,2,2,2,2,2,2,2,2,3),(0.,1.),(0.,0.0072463768115942,0.0144927536231884,
0.0217391304347826,0.0289855072463768,0.036231884057971,0.0434782608695652,
0.0507246376811594,0.0579710144927536,0.0652173913043478,0.072463768115942,
0.0797101449275362,0.0869565217391304,0.0942028985507246,0.101449275362319,
0.108695652173913,0.115942028985507,0.123188405797101,0.130434782608696,
0.13768115942029,0.144927536231884,0.152173913043478,0.159420289855073,
0.166666666666667,0.173913043478261,0.181159420289855,0.18840579710145,
0.195652173913044,0.202898550724637,0.210144927536232,0.217391304347826,
0.224637681159421,0.231884057971014,0.239130434782609,0.246376811594203,
0.253623188405797,0.260869565217392,0.268115942028985,0.275362318840579,
0.282608695652174,0.289855072463768,0.297101449275363,0.304347826086956,
0.31159420289855,0.318840579710145,0.326086956521739,0.333333333333334,
0.340579710144927,0.347826086956521,0.355072463768116,0.36231884057971,
0.369565217391304,0.376811594202899,0.384057971014493,0.391304347826087,
0.398550724637681,0.405797101449275,0.41304347826087,0.420289855072463,
0.427536231884058,0.434782608695652,0.442028985507247,0.449275362318841,
0.456521739130435,0.463768115942029,0.471014492753623,0.478260869565218,
0.485507246376812,0.492753623188406,0.5,0.507246376811594,0.514492753623188,
0.521739130434783,0.528985507246377,0.536231884057971,0.543478260869565,
0.550724637681159,0.557971014492754,0.565217391304348,0.572463768115942,
0.579710144927536,0.586956521739131,0.594202898550725,0.601449275362319,
0.608695652173913,0.615942028985507,0.623188405797101,0.630434782608696,
0.63768115942029,0.644927536231884,0.652173913043478,0.659420289855073,
0.666666666666667,0.673913043478261,0.681159420289855,0.688405797101449,
0.695652173913044,0.702898550724638,0.710144927536232,0.717391304347826,
0.72463768115942,0.731884057971015,0.739130434782609,0.746376811594203,
0.753623188405797,0.760869565217391,0.768115942028986,0.77536231884058,
0.782608695652174,0.789855072463768,0.797101449275362,0.804347826086956,
0.811594202898551,0.818840579710145,0.826086956521739,0.833333333333333,
0.840579710144928,0.847826086956522,0.855072463768116,0.86231884057971,
0.869565217391304,0.876811594202899,0.884057971014493,0.891304347826087,
0.898550724637681,0.905797101449275,0.91304347826087,0.920289855072464,
0.927536231884058,0.934782608695652,0.942028985507246,0.94927536231884,
0.956521739130435,0.963768115942029,0.971014492753623,0.978260869565217,
0.985507246376812,0.992753623188406,0.993818585798284),.UNSPECIFIED.)
GEOMETRIC_REPRESENTATION_ITEM()
RATIONAL_B_SPLINE_SURFACE(((1.,0.866025403784439,1.,0.866025403784439,1.,
0.866025403784439,1.,0.866025403784439,1.,0.866025403784439,1.,0.866025403784439,
1.,0.866025403784439,1.,0.866025403784439,1.,0.866025403784439,1.,0.866025403784439,
1.,0.866025403784439,1.,0.866025403784439,1.,0.866025403784439,1.,0.866025403784439,
1.,0.866025403784439,1.,0.866025403784439,1.,0.866025403784439,1.,0.866025403784439,
1.,0.866025403784439,1.,0.866025403784439,1.,0.866025403784439,1.,0.866025403784439,
1.,0.866025403784439,1.,0.866025403784439,1.,0.866025403784439,1.,0.866025403784439,
1.,0.866025403784439,1.,0.866025403784439,1.,0.866025403784439,1.,0.866025403784439,
1.,0.866025403784439,1.,0.866025403784439,1.,0.866025403784439,1.,0.866025403784439,
1.,0.866025403784439,1.,0.866025403784439,1.,0.866025403784439,1.,0.866025403784439,
1.,0.866025403784439,1.,0.866025403784439,1.,0.866025403784439,1.,0.866025403784439,
1.,0.866025403784439,1.,0.866025403784439,1.,0.866025403784439,1.,0.866025403784439,
1.,0.866025403784439,1.,0.866025403784439,1.,0.866025403784439,1.,0.866025403784439,
1.,0.866025403784439,1.,0.866025403784439,1.,0.866025403784439,1.,0.866025403784439,
1.,0.866025403784439,1.,0.866025403784439,1.,0.866025403784439,1.,0.866025403784439,
1.,0.866025403784439,1.,0.866025403784439,1.,0.866025403784439,1.,0.866025403784439,
1.,0.866025403784439,1.,0.866025403784439,1.,0.866025403784439,1.,0.866025403784439,
1.,0.866025403784439,1.,0.866025403784439,1.,0.866025403784439,1.,0.866025403784439,
1.,0.866025403784439,1.,0.866025403784439,1.,0.866025403784439,1.,0.866025403784439,
1.,0.866025403784439,1.,0.866025403784439,1.,0.866025403784439,1.,0.866025403784439,
1.,0.866025403784439,1.,0.866025403784439,1.,0.866025403784439,1.,0.866025403784439,
1.,0.866025403784439,1.,0.866025403784439,1.,0.866025403784439,1.,0.866025403784439,
1.,0.866025403784439,1.,0.866025403784439,1.,0.866025403784439,1.,0.866025403784439,
1.,0.866025403784439,1.,0.866025403784439,1.,0.866025403784439,1.,0.866025403784439,
1.,0.866025403784439,1.,0.866025403784439,1.,0.866025403784439,1.,0.866025403784439,
1.,0.866025403784439,1.,0.866025403784439,1.,0.866025403784439,1.,0.866025403784439,
1.,0.866025403784439,1.,0.866025403784439,1.,0.866025403784439,1.,0.866025403784439,
1.,0.866025403784439,1.,0.866025403784439,1.,0.866025403784439,1.,0.866025403784439,
1.,0.866025403784439,1.,0.866025403784439,1.,0.866025403784439,1.,0.866025403784439,
1.,0.866025403784439,1.,0.866025403784439,1.,0.866025403784439,1.,0.866025403784439,
1.,0.866025403784439,1.,0.866025403784439,1.,0.866025403784439,1.,0.866025403784439,
1.,0.866025403784439,1.,0.866025403784439,1.,0.866025403784439,1.,0.866025403784439,
1.,0.866025403784439,1.,0.866025403784439,1.,0.866025403784439,1.,0.866025403784439,
1.,0.866025403784439,1.,0.866025403784439,1.,0.866025403784439,1.,0.866025403784439,
1.,0.866025403784439,1.,0.866025403784439,1.,0.866025403784439,1.,0.98031044488126,
0.966408234404338),(1.,0.866025403784439,1.,0.866025403784439,1.,0.866025403784439,
1.,0.866025403784439,1.,0.866025403784439,1.,0.866025403784439,1.,0.866025403784439,
1.,0.866025403784439,1.,0.866025403784439,1.,0.866025403784439,1.,0.866025403784439,
1.,0.866025403784439,1.,0.866025403784439,1.,0.866025403784439,1.,0.866025403784439,
1.,0.866025403784439,1.,0.866025403784439,1.,0.866025403784439,1.,0.866025403784439,
1.,0.866025403784439,1.,0.866025403784439,1.,0.866025403784439,1.,0.866025403784439,
1.,0.866025403784439,1.,0.866025403784439,1.,0.866025403784439,1.,0.866025403784439,
1.,0.866025403784439,1.,0.866025403784439,1.,0.866025403784439,1.,0.866025403784439,
1.,0.866025403784439,1.,0.866025403784439,1.,0.866025403784439,1.,0.866025403784439,
1.,0.866025403784439,1.,0.866025403784439,1.,0.866025403784439,1.,0.866025403784439,
1.,0.866025403784439,1.,0.866025403784439,1.,0.866025403784439,1.,0.866025403784439,
1.,0.866025403784439,1.,0.866025403784439,1.,0.866025403784439,1.,0.866025403784439,
1.,0.866025403784439,1.,0.866025403784439,1.,0.866025403784439,1.,0.866025403784439,
1.,0.866025403784439,1.,0.866025403784439,1.,0.866025403784439,1.,0.866025403784439,
1.,0.866025403784439,1.,0.866025403784439,1.,0.866025403784439,1.,0.866025403784439,
1.,0.866025403784439,1.,0.866025403784439,1.,0.866025403784439,1.,0.866025403784439,
1.,0.866025403784439,1.,0.866025403784439,1.,0.866025403784439,1.,0.866025403784439,
1.,0.866025403784439,1.,0.866025403784439,1.,0.866025403784439,1.,0.866025403784439,
1.,0.866025403784439,1.,0.866025403784439,1.,0.866025403784439,1.,0.866025403784439,
1.,0.866025403784439,1.,0.866025403784439,1.,0.866025403784439,1.,0.866025403784439,
1.,0.866025403784439,1.,0.866025403784439,1.,0.866025403784439,1.,0.866025403784439,
1.,0.866025403784439,1.,0.866025403784439,1.,0.866025403784439,1.,0.866025403784439,
1.,0.866025403784439,1.,0.866025403784439,1.,0.866025403784439,1.,0.866025403784439,
1.,0.866025403784439,1.,0.866025403784439,1.,0.866025403784439,1.,0.866025403784439,
1.,0.866025403784439,1.,0.866025403784439,1.,0.866025403784439,1.,0.866025403784439,
1.,0.866025403784439,1.,0.866025403784439,1.,0.866025403784439,1.,0.866025403784439,
1.,0.866025403784439,1.,0.866025403784439,1.,0.866025403784439,1.,0.866025403784439,
1.,0.866025403784439,1.,0.866025403784439,1.,0.866025403784439,1.,0.866025403784439,
1.,0.866025403784439,1.,0.866025403784439,1.,0.866025403784439,1.,0.866025403784439,
1.,0.866025403784439,1.,0.866025403784439,1.,0.866025403784439,1.,0.866025403784439,
1.,0.866025403784439,1.,0.866025403784439,1.,0.866025403784439,1.,0.866025403784439,
1.,0.866025403784439,1.,0.866025403784439,1.,0.866025403784439,1.,0.866025403784439,
1.,0.866025403784439,1.,0.866025403784439,1.,0.866025403784439,1.,0.866025403784439,
1.,0.866025403784439,1.,0.866025403784439,1.,0.866025403784439,1.,0.866025403784439,
1.,0.866025403784439,1.,0.866025403784439,1.,0.98031044488126,0.966408234404338)))
REPRESENTATION_ITEM('')
SURFACE()
);
#3189=(
BOUNDED_SURFACE()
B_SPLINE_SURFACE(1,2,((#266133,#266134,#266135,#266136,#266137,#266138,
#266139,#266140,#266141,#266142,#266143,#266144,#266145,#266146,#266147,
#266148,#266149,#266150,#266151,#266152,#266153,#266154,#266155,#266156,
#266157,#266158,#266159,#266160,#266161,#266162,#266163,#266164,#266165,
#266166,#266167,#266168,#266169,#266170,#266171,#266172,#266173,#266174,
#266175,#266176,#266177,#266178,#266179,#266180,#266181,#266182,#266183,
#266184,#266185,#266186,#266187,#266188,#266189,#266190,#266191,#266192,
#266193,#266194,#266195,#266196,#266197,#266198,#266199,#266200,#266201,
#266202,#266203,#266204,#266205,#266206,#266207,#266208,#266209,#266210,
#266211,#266212,#266213,#266214,#266215,#266216,#266217,#266218,#266219,
#266220,#266221,#266222,#266223,#266224,#266225,#266226,#266227,#266228,
#266229,#266230,#266231,#266232,#266233,#266234,#266235,#266236,#266237,
#266238,#266239,#266240,#266241,#266242,#266243,#266244,#266245,#266246,
#266247,#266248,#266249,#266250,#266251,#266252,#266253,#266254,#266255,
#266256,#266257,#266258,#266259,#266260,#266261,#266262,#266263,#266264,
#266265,#266266,#266267,#266268,#266269,#266270,#266271,#266272,#266273,
#266274,#266275,#266276,#266277,#266278,#266279,#266280,#266281,#266282,
#266283,#266284,#266285,#266286,#266287,#266288,#266289,#266290,#266291,
#266292,#266293,#266294,#266295,#266296,#266297,#266298,#266299,#266300,
#266301,#266302,#266303,#266304,#266305,#266306,#266307,#266308,#266309,
#266310,#266311,#266312,#266313,#266314,#266315,#266316,#266317,#266318,
#266319,#266320,#266321,#266322,#266323,#266324,#266325,#266326,#266327,
#266328,#266329,#266330,#266331,#266332,#266333,#266334,#266335,#266336,
#266337,#266338,#266339,#266340,#266341,#266342,#266343,#266344,#266345,
#266346,#266347,#266348,#266349,#266350,#266351,#266352,#266353,#266354,
#266355,#266356,#266357,#266358,#266359,#266360,#266361,#266362,#266363,
#266364,#266365,#266366,#266367,#266368,#266369,#266370,#266371,#266372,
#266373,#266374,#266375,#266376,#266377,#266378,#266379,#266380,#266381,
#266382,#266383,#266384,#266385,#266386,#266387,#266388,#266389,#266390,
#266391,#266392,#266393,#266394,#266395,#266396,#266397,#266398,#266399,
#266400,#266401,#266402,#266403,#266404,#266405,#266406,#266407,#266408,
#266409),(#266410,#266411,#266412,#266413,#266414,#266415,#266416,#266417,
#266418,#266419,#266420,#266421,#266422,#266423,#266424,#266425,#266426,
#266427,#266428,#266429,#266430,#266431,#266432,#266433,#266434,#266435,
#266436,#266437,#266438,#266439,#266440,#266441,#266442,#266443,#266444,
#266445,#266446,#266447,#266448,#266449,#266450,#266451,#266452,#266453,
#266454,#266455,#266456,#266457,#266458,#266459,#266460,#266461,#266462,
#266463,#266464,#266465,#266466,#266467,#266468,#266469,#266470,#266471,
#266472,#266473,#266474,#266475,#266476,#266477,#266478,#266479,#266480,
#266481,#266482,#266483,#266484,#266485,#266486,#266487,#266488,#266489,
#266490,#266491,#266492,#266493,#266494,#266495,#266496,#266497,#266498,
#266499,#266500,#266501,#266502,#266503,#266504,#266505,#266506,#266507,
#266508,#266509,#266510,#266511,#266512,#266513,#266514,#266515,#266516,
#266517,#266518,#266519,#266520,#266521,#266522,#266523,#266524,#266525,
#266526,#266527,#266528,#266529,#266530,#266531,#266532,#266533,#266534,
#266535,#266536,#266537,#266538,#266539,#266540,#266541,#266542,#266543,
#266544,#266545,#266546,#266547,#266548,#266549,#266550,#266551,#266552,
#266553,#266554,#266555,#266556,#266557,#266558,#266559,#266560,#266561,
#266562,#266563,#266564,#266565,#266566,#266567,#266568,#266569,#266570,
#266571,#266572,#266573,#266574,#266575,#266576,#266577,#266578,#266579,
#266580,#266581,#266582,#266583,#266584,#266585,#266586,#266587,#266588,
#266589,#266590,#266591,#266592,#266593,#266594,#266595,#266596,#266597,
#266598,#266599,#266600,#266601,#266602,#266603,#266604,#266605,#266606,
#266607,#266608,#266609,#266610,#266611,#266612,#266613,#266614,#266615,
#266616,#266617,#266618,#266619,#266620,#266621,#266622,#266623,#266624,
#266625,#266626,#266627,#266628,#266629,#266630,#266631,#266632,#266633,
#266634,#266635,#266636,#266637,#266638,#266639,#266640,#266641,#266642,
#266643,#266644,#266645,#266646,#266647,#266648,#266649,#266650,#266651,
#266652,#266653,#266654,#266655,#266656,#266657,#266658,#266659,#266660,
#266661,#266662,#266663,#266664,#266665,#266666,#266667,#266668,#266669,
#266670,#266671,#266672,#266673,#266674,#266675,#266676,#266677,#266678,
#266679,#266680,#266681,#266682,#266683,#266684,#266685,#266686)),
 .UNSPECIFIED.,.F.,.F.,.F.)
B_SPLINE_SURFACE_WITH_KNOTS((2,2),(3,2,2,2,2,2,2,2,2,2,2,2,2,2,2,2,2,2,
2,2,2,2,2,2,2,2,2,2,2,2,2,2,2,2,2,2,2,2,2,2,2,2,2,2,2,2,2,2,2,2,2,2,2,2,
2,2,2,2,2,2,2,2,2,2,2,2,2,2,2,2,2,2,2,2,2,2,2,2,2,2,2,2,2,2,2,2,2,2,2,2,
2,2,2,2,2,2,2,2,2,2,2,2,2,2,2,2,2,2,2,2,2,2,2,2,2,2,2,2,2,2,2,2,2,2,2,2,
2,2,2,2,2,2,2,2,2,2,2,2,3),(0.,1.),(0.,0.0072463768115942,0.0144927536231884,
0.0217391304347826,0.0289855072463768,0.036231884057971,0.0434782608695652,
0.0507246376811594,0.0579710144927536,0.0652173913043478,0.072463768115942,
0.0797101449275362,0.0869565217391304,0.0942028985507246,0.101449275362319,
0.108695652173913,0.115942028985507,0.123188405797101,0.130434782608696,
0.13768115942029,0.144927536231884,0.152173913043478,0.159420289855073,
0.166666666666667,0.173913043478261,0.181159420289855,0.18840579710145,
0.195652173913044,0.202898550724637,0.210144927536232,0.217391304347826,
0.224637681159421,0.231884057971014,0.239130434782609,0.246376811594203,
0.253623188405797,0.260869565217392,0.268115942028985,0.275362318840579,
0.282608695652174,0.289855072463768,0.297101449275363,0.304347826086956,
0.31159420289855,0.318840579710145,0.326086956521739,0.333333333333334,
0.340579710144927,0.347826086956521,0.355072463768116,0.36231884057971,
0.369565217391304,0.376811594202899,0.384057971014493,0.391304347826087,
0.398550724637681,0.405797101449275,0.41304347826087,0.420289855072463,
0.427536231884058,0.434782608695652,0.442028985507247,0.449275362318841,
0.456521739130435,0.463768115942029,0.471014492753623,0.478260869565218,
0.485507246376812,0.492753623188406,0.5,0.507246376811594,0.514492753623188,
0.521739130434783,0.528985507246377,0.536231884057971,0.543478260869565,
0.550724637681159,0.557971014492754,0.565217391304348,0.572463768115942,
0.579710144927536,0.586956521739131,0.594202898550725,0.601449275362319,
0.608695652173913,0.615942028985507,0.623188405797101,0.630434782608696,
0.63768115942029,0.644927536231884,0.652173913043478,0.659420289855073,
0.666666666666667,0.673913043478261,0.681159420289855,0.688405797101449,
0.695652173913044,0.702898550724638,0.710144927536232,0.717391304347826,
0.72463768115942,0.731884057971015,0.739130434782609,0.746376811594203,
0.753623188405797,0.760869565217391,0.768115942028986,0.77536231884058,
0.782608695652174,0.789855072463768,0.797101449275362,0.804347826086956,
0.811594202898551,0.818840579710145,0.826086956521739,0.833333333333333,
0.840579710144928,0.847826086956522,0.855072463768116,0.86231884057971,
0.869565217391304,0.876811594202899,0.884057971014493,0.891304347826087,
0.898550724637681,0.905797101449275,0.91304347826087,0.920289855072464,
0.927536231884058,0.934782608695652,0.942028985507246,0.94927536231884,
0.956521739130435,0.963768115942029,0.971014492753623,0.978260869565217,
0.985507246376812,0.992753623188406,0.993818585798284),.UNSPECIFIED.)
GEOMETRIC_REPRESENTATION_ITEM()
RATIONAL_B_SPLINE_SURFACE(((1.,0.866025403784439,1.,0.866025403784439,1.,
0.866025403784439,1.,0.866025403784439,1.,0.866025403784439,1.,0.866025403784439,
1.,0.866025403784439,1.,0.866025403784439,1.,0.866025403784439,1.,0.866025403784439,
1.,0.866025403784439,1.,0.866025403784439,1.,0.866025403784439,1.,0.866025403784439,
1.,0.866025403784439,1.,0.866025403784439,1.,0.866025403784439,1.,0.866025403784439,
1.,0.866025403784439,1.,0.866025403784439,1.,0.866025403784439,1.,0.866025403784439,
1.,0.866025403784439,1.,0.866025403784439,1.,0.866025403784439,1.,0.866025403784439,
1.,0.866025403784439,1.,0.866025403784439,1.,0.866025403784439,1.,0.866025403784439,
1.,0.866025403784439,1.,0.866025403784439,1.,0.866025403784439,1.,0.866025403784439,
1.,0.866025403784439,1.,0.866025403784439,1.,0.866025403784439,1.,0.866025403784439,
1.,0.866025403784439,1.,0.866025403784439,1.,0.866025403784439,1.,0.866025403784439,
1.,0.866025403784439,1.,0.866025403784439,1.,0.866025403784439,1.,0.866025403784439,
1.,0.866025403784439,1.,0.866025403784439,1.,0.866025403784439,1.,0.866025403784439,
1.,0.866025403784439,1.,0.866025403784439,1.,0.866025403784439,1.,0.866025403784439,
1.,0.866025403784439,1.,0.866025403784439,1.,0.866025403784439,1.,0.866025403784439,
1.,0.866025403784439,1.,0.866025403784439,1.,0.866025403784439,1.,0.866025403784439,
1.,0.866025403784439,1.,0.866025403784439,1.,0.866025403784439,1.,0.866025403784439,
1.,0.866025403784439,1.,0.866025403784439,1.,0.866025403784439,1.,0.866025403784439,
1.,0.866025403784439,1.,0.866025403784439,1.,0.866025403784439,1.,0.866025403784439,
1.,0.866025403784439,1.,0.866025403784439,1.,0.866025403784439,1.,0.866025403784439,
1.,0.866025403784439,1.,0.866025403784439,1.,0.866025403784439,1.,0.866025403784439,
1.,0.866025403784439,1.,0.866025403784439,1.,0.866025403784439,1.,0.866025403784439,
1.,0.866025403784439,1.,0.866025403784439,1.,0.866025403784439,1.,0.866025403784439,
1.,0.866025403784439,1.,0.866025403784439,1.,0.866025403784439,1.,0.866025403784439,
1.,0.866025403784439,1.,0.866025403784439,1.,0.866025403784439,1.,0.866025403784439,
1.,0.866025403784439,1.,0.866025403784439,1.,0.866025403784439,1.,0.866025403784439,
1.,0.866025403784439,1.,0.866025403784439,1.,0.866025403784439,1.,0.866025403784439,
1.,0.866025403784439,1.,0.866025403784439,1.,0.866025403784439,1.,0.866025403784439,
1.,0.866025403784439,1.,0.866025403784439,1.,0.866025403784439,1.,0.866025403784439,
1.,0.866025403784439,1.,0.866025403784439,1.,0.866025403784439,1.,0.866025403784439,
1.,0.866025403784439,1.,0.866025403784439,1.,0.866025403784439,1.,0.866025403784439,
1.,0.866025403784439,1.,0.866025403784439,1.,0.866025403784439,1.,0.866025403784439,
1.,0.866025403784439,1.,0.866025403784439,1.,0.866025403784439,1.,0.866025403784439,
1.,0.866025403784439,1.,0.866025403784439,1.,0.866025403784439,1.,0.866025403784439,
1.,0.866025403784439,1.,0.866025403784439,1.,0.866025403784439,1.,0.98031044488126,
0.966408234404338),(1.,0.866025403784439,1.,0.866025403784439,1.,0.866025403784439,
1.,0.866025403784439,1.,0.866025403784439,1.,0.866025403784439,1.,0.866025403784439,
1.,0.866025403784439,1.,0.866025403784439,1.,0.866025403784439,1.,0.866025403784439,
1.,0.866025403784439,1.,0.866025403784439,1.,0.866025403784439,1.,0.866025403784439,
1.,0.866025403784439,1.,0.866025403784439,1.,0.866025403784439,1.,0.866025403784439,
1.,0.866025403784439,1.,0.866025403784439,1.,0.866025403784439,1.,0.866025403784439,
1.,0.866025403784439,1.,0.866025403784439,1.,0.866025403784439,1.,0.866025403784439,
1.,0.866025403784439,1.,0.866025403784439,1.,0.866025403784439,1.,0.866025403784439,
1.,0.866025403784439,1.,0.866025403784439,1.,0.866025403784439,1.,0.866025403784439,
1.,0.866025403784439,1.,0.866025403784439,1.,0.866025403784439,1.,0.866025403784439,
1.,0.866025403784439,1.,0.866025403784439,1.,0.866025403784439,1.,0.866025403784439,
1.,0.866025403784439,1.,0.866025403784439,1.,0.866025403784439,1.,0.866025403784439,
1.,0.866025403784439,1.,0.866025403784439,1.,0.866025403784439,1.,0.866025403784439,
1.,0.866025403784439,1.,0.866025403784439,1.,0.866025403784439,1.,0.866025403784439,
1.,0.866025403784439,1.,0.866025403784439,1.,0.866025403784439,1.,0.866025403784439,
1.,0.866025403784439,1.,0.866025403784439,1.,0.866025403784439,1.,0.866025403784439,
1.,0.866025403784439,1.,0.866025403784439,1.,0.866025403784439,1.,0.866025403784439,
1.,0.866025403784439,1.,0.866025403784439,1.,0.866025403784439,1.,0.866025403784439,
1.,0.866025403784439,1.,0.866025403784439,1.,0.866025403784439,1.,0.866025403784439,
1.,0.866025403784439,1.,0.866025403784439,1.,0.866025403784439,1.,0.866025403784439,
1.,0.866025403784439,1.,0.866025403784439,1.,0.866025403784439,1.,0.866025403784439,
1.,0.866025403784439,1.,0.866025403784439,1.,0.866025403784439,1.,0.866025403784439,
1.,0.866025403784439,1.,0.866025403784439,1.,0.866025403784439,1.,0.866025403784439,
1.,0.866025403784439,1.,0.866025403784439,1.,0.866025403784439,1.,0.866025403784439,
1.,0.866025403784439,1.,0.866025403784439,1.,0.866025403784439,1.,0.866025403784439,
1.,0.866025403784439,1.,0.866025403784439,1.,0.866025403784439,1.,0.866025403784439,
1.,0.866025403784439,1.,0.866025403784439,1.,0.866025403784439,1.,0.866025403784439,
1.,0.866025403784439,1.,0.866025403784439,1.,0.866025403784439,1.,0.866025403784439,
1.,0.866025403784439,1.,0.866025403784439,1.,0.866025403784439,1.,0.866025403784439,
1.,0.866025403784439,1.,0.866025403784439,1.,0.866025403784439,1.,0.866025403784439,
1.,0.866025403784439,1.,0.866025403784439,1.,0.866025403784439,1.,0.866025403784439,
1.,0.866025403784439,1.,0.866025403784439,1.,0.866025403784439,1.,0.866025403784439,
1.,0.866025403784439,1.,0.866025403784439,1.,0.866025403784439,1.,0.866025403784439,
1.,0.866025403784439,1.,0.866025403784439,1.,0.866025403784439,1.,0.866025403784439,
1.,0.866025403784439,1.,0.866025403784439,1.,0.98031044488126,0.966408234404338)))
REPRESENTATION_ITEM('')
SURFACE()
);
#3190=(
BOUNDED_SURFACE()
B_SPLINE_SURFACE(3,2,((#271081,#271082,#271083),(#271084,#271085,#271086),
(#271087,#271088,#271089),(#271090,#271091,#271092),(#271093,#271094,#271095),
(#271096,#271097,#271098),(#271099,#271100,#271101),(#271102,#271103,#271104),
(#271105,#271106,#271107),(#271108,#271109,#271110),(#271111,#271112,#271113),
(#271114,#271115,#271116),(#271117,#271118,#271119),(#271120,#271121,#271122),
(#271123,#271124,#271125),(#271126,#271127,#271128)),.UNSPECIFIED.,.F.,
 .F.,.F.)
B_SPLINE_SURFACE_WITH_KNOTS((4,2,2,2,2,2,2,4),(3,3),(0.021246894993388,
0.0219851502508119,0.0226493629442376,0.0233135756376633,0.023977788331089,
0.0246420010245147,0.0253062137179403,0.02670868166879),(-7.40425639982891E-5,
1.),.UNSPECIFIED.)
GEOMETRIC_REPRESENTATION_ITEM()
RATIONAL_B_SPLINE_SURFACE(((1.00002710501715,0.816963272991268,1.),(1.00002702241829,
0.817521052555119,1.),(1.00002733502832,0.815410036827724,1.),(1.00002846649364,
0.807769395738777,1.),(1.00002922674044,0.802635545928914,1.),(1.00003092826825,
0.791145345435121,1.),(1.00003186568695,0.784815076400909,1.),(1.00003372138338,
0.772283794894346,1.),(1.00003464066055,0.76607603331725,1.),(1.00003637793641,
0.754344430769809,1.),(1.00003719750955,0.748809957783788,1.),(1.00003871890084,
0.738536196261916,1.),(1.00003942162688,0.733790776873006,1.),(1.00004143922335,
0.720166205006836,1.),(1.00004256778357,0.712545181611092,1.),(1.00004353016739,
0.706046326330694,1.)))
REPRESENTATION_ITEM('')
SURFACE()
);
#3191=(
BOUNDED_SURFACE()
B_SPLINE_SURFACE(3,2,((#271130,#271131,#271132),(#271133,#271134,#271135),
(#271136,#271137,#271138),(#271139,#271140,#271141),(#271142,#271143,#271144),
(#271145,#271146,#271147),(#271148,#271149,#271150),(#271151,#271152,#271153),
(#271154,#271155,#271156),(#271157,#271158,#271159),(#271160,#271161,#271162),
(#271163,#271164,#271165),(#271166,#271167,#271168),(#271169,#271170,#271171),
(#271172,#271173,#271174),(#271175,#271176,#271177)),.UNSPECIFIED.,.F.,
 .F.,.F.)
B_SPLINE_SURFACE_WITH_KNOTS((4,2,2,2,2,2,2,4),(3,3),(0.0159102555591329,
0.0173176440494504,0.0179848596341063,0.0186520752187623,0.0193192908034183,
0.0199865063880743,0.0206537219727303,0.0213938948783918),(-7.2957321005512E-5,
1.),.UNSPECIFIED.)
GEOMETRIC_REPRESENTATION_ITEM()
RATIONAL_B_SPLINE_SURFACE(((1.00004288879452,0.706069288657398,1.),(1.00004194432714,
0.71254202756886,1.),(1.00004082887242,0.720186597774606,1.),(1.00003884013724,
0.733816039950407,1.),(1.00003814748,0.7385630429368,1.),(1.00003664903336,
0.748832379971001,1.),(1.00003584236797,0.754360717483753,1.),(1.00003413328098,
0.766073640691051,1.),(1.00003322932712,0.772268727405263,1.),(1.0000314042151,
0.78477680737215,1.),(1.00003048201287,0.791096956071881,1.),(1.00002880594349,
0.802583598909048,1.),(1.00002805569383,0.807725301287472,1.),(1.00002693784998,
0.815386244970287,1.),(1.00002662695858,0.817516883782438,1.),(1.00002670733337,
0.816966049480649,1.)))
REPRESENTATION_ITEM('')
SURFACE()
);
#3192=(
BOUNDED_SURFACE()
B_SPLINE_SURFACE(1,2,((#276452,#276453,#276454,#276455,#276456,#276457,
#276458,#276459,#276460,#276461,#276462,#276463,#276464,#276465,#276466,
#276467,#276468,#276469,#276470,#276471,#276472,#276473,#276474,#276475,
#276476,#276477,#276478,#276479,#276480,#276481,#276482,#276483,#276484,
#276485,#276486,#276487,#276488,#276489,#276490,#276491,#276492,#276493,
#276494,#276495,#276496,#276497,#276498,#276499,#276500,#276501,#276502,
#276503,#276504,#276505,#276506,#276507,#276508,#276509,#276510,#276511,
#276512,#276513,#276514,#276515,#276516,#276517,#276518,#276519,#276520,
#276521,#276522,#276523,#276524,#276525,#276526,#276527,#276528,#276529,
#276530,#276531,#276532,#276533,#276534,#276535,#276536,#276537,#276538,
#276539,#276540,#276541,#276542,#276543,#276544,#276545,#276546,#276547,
#276548,#276549,#276550,#276551,#276552,#276553,#276554,#276555,#276556,
#276557,#276558,#276559,#276560,#276561,#276562,#276563,#276564,#276565,
#276566,#276567,#276568,#276569,#276570,#276571,#276572,#276573,#276574,
#276575,#276576,#276577,#276578,#276579,#276580,#276581,#276582,#276583,
#276584,#276585,#276586,#276587,#276588,#276589,#276590,#276591,#276592,
#276593,#276594,#276595,#276596,#276597,#276598,#276599,#276600,#276601,
#276602,#276603,#276604,#276605,#276606,#276607,#276608,#276609,#276610,
#276611,#276612,#276613,#276614,#276615,#276616,#276617,#276618,#276619,
#276620,#276621,#276622,#276623,#276624,#276625,#276626,#276627,#276628,
#276629,#276630,#276631,#276632,#276633,#276634,#276635,#276636,#276637,
#276638,#276639,#276640,#276641,#276642,#276643,#276644,#276645,#276646,
#276647,#276648,#276649,#276650,#276651,#276652,#276653,#276654,#276655,
#276656,#276657,#276658,#276659,#276660,#276661,#276662,#276663,#276664,
#276665,#276666,#276667,#276668,#276669,#276670,#276671,#276672,#276673,
#276674,#276675,#276676,#276677,#276678,#276679,#276680,#276681,#276682,
#276683,#276684,#276685,#276686,#276687,#276688,#276689,#276690,#276691,
#276692,#276693,#276694,#276695,#276696,#276697,#276698,#276699,#276700,
#276701,#276702,#276703,#276704,#276705,#276706,#276707,#276708,#276709,
#276710,#276711,#276712,#276713,#276714,#276715,#276716,#276717,#276718,
#276719,#276720,#276721,#276722,#276723,#276724,#276725,#276726,#276727,
#276728,#276729,#276730,#276731,#276732,#276733,#276734,#276735,#276736,
#276737,#276738,#276739,#276740,#276741,#276742,#276743,#276744,#276745,
#276746,#276747,#276748,#276749,#276750,#276751,#276752,#276753,#276754,
#276755,#276756,#276757,#276758,#276759,#276760,#276761,#276762,#276763,
#276764,#276765,#276766,#276767,#276768,#276769,#276770,#276771,#276772,
#276773,#276774,#276775,#276776,#276777,#276778,#276779,#276780,#276781,
#276782,#276783,#276784,#276785,#276786,#276787,#276788,#276789,#276790,
#276791,#276792,#276793,#276794,#276795,#276796,#276797,#276798,#276799,
#276800,#276801,#276802,#276803,#276804,#276805,#276806,#276807,#276808,
#276809,#276810,#276811,#276812,#276813,#276814,#276815,#276816,#276817,
#276818,#276819,#276820,#276821,#276822,#276823,#276824,#276825,#276826,
#276827,#276828,#276829,#276830,#276831,#276832,#276833,#276834,#276835,
#276836,#276837,#276838,#276839,#276840,#276841,#276842,#276843,#276844,
#276845,#276846,#276847,#276848,#276849,#276850,#276851,#276852,#276853,
#276854,#276855,#276856,#276857,#276858,#276859,#276860,#276861,#276862,
#276863,#276864,#276865,#276866,#276867,#276868,#276869,#276870,#276871,
#276872,#276873,#276874,#276875,#276876,#276877,#276878,#276879,#276880,
#276881,#276882,#276883,#276884,#276885,#276886,#276887,#276888,#276889,
#276890,#276891,#276892,#276893,#276894,#276895,#276896,#276897,#276898,
#276899,#276900,#276901,#276902,#276903,#276904,#276905,#276906,#276907,
#276908,#276909,#276910,#276911,#276912,#276913,#276914,#276915,#276916,
#276917,#276918,#276919,#276920,#276921,#276922,#276923,#276924,#276925,
#276926,#276927,#276928,#276929,#276930,#276931,#276932,#276933,#276934,
#276935,#276936,#276937,#276938,#276939,#276940,#276941,#276942,#276943,
#276944,#276945,#276946,#276947,#276948,#276949,#276950,#276951,#276952,
#276953,#276954,#276955,#276956,#276957,#276958,#276959,#276960,#276961,
#276962,#276963,#276964,#276965,#276966,#276967,#276968,#276969,#276970,
#276971,#276972,#276973,#276974,#276975,#276976,#276977,#276978,#276979,
#276980,#276981,#276982,#276983,#276984,#276985,#276986,#276987,#276988,
#276989,#276990,#276991,#276992,#276993,#276994,#276995,#276996,#276997,
#276998,#276999,#277000,#277001,#277002,#277003,#277004,#277005,#277006,
#277007,#277008,#277009,#277010,#277011,#277012,#277013,#277014,#277015,
#277016,#277017,#277018,#277019,#277020,#277021,#277022,#277023,#277024,
#277025,#277026,#277027,#277028,#277029,#277030,#277031,#277032,#277033,
#277034,#277035,#277036,#277037,#277038,#277039,#277040,#277041,#277042,
#277043,#277044,#277045,#277046,#277047,#277048,#277049,#277050,#277051,
#277052,#277053,#277054,#277055,#277056,#277057,#277058,#277059,#277060,
#277061,#277062,#277063,#277064,#277065,#277066,#277067,#277068,#277069,
#277070,#277071,#277072,#277073,#277074,#277075,#277076,#277077,#277078,
#277079,#277080,#277081,#277082,#277083,#277084,#277085,#277086,#277087,
#277088,#277089,#277090,#277091,#277092,#277093,#277094,#277095,#277096,
#277097,#277098,#277099,#277100,#277101,#277102,#277103,#277104,#277105,
#277106,#277107,#277108,#277109,#277110,#277111,#277112,#277113,#277114,
#277115,#277116,#277117,#277118,#277119,#277120,#277121,#277122,#277123,
#277124,#277125,#277126,#277127,#277128,#277129,#277130,#277131,#277132,
#277133,#277134,#277135,#277136,#277137,#277138,#277139,#277140,#277141,
#277142,#277143,#277144,#277145,#277146,#277147,#277148,#277149,#277150,
#277151,#277152,#277153,#277154,#277155,#277156,#277157,#277158,#277159,
#277160,#277161,#277162,#277163,#277164,#277165,#277166,#277167,#277168,
#277169,#277170,#277171,#277172,#277173,#277174,#277175,#277176,#277177,
#277178,#277179,#277180,#277181,#277182,#277183,#277184,#277185,#277186,
#277187,#277188,#277189,#277190,#277191,#277192,#277193,#277194,#277195,
#277196,#277197,#277198,#277199,#277200,#277201,#277202,#277203,#277204,
#277205,#277206,#277207,#277208,#277209,#277210,#277211,#277212,#277213,
#277214,#277215,#277216,#277217,#277218,#277219,#277220,#277221,#277222,
#277223,#277224,#277225,#277226,#277227,#277228,#277229,#277230,#277231,
#277232,#277233,#277234,#277235,#277236,#277237,#277238,#277239,#277240,
#277241,#277242,#277243,#277244,#277245,#277246,#277247,#277248,#277249,
#277250,#277251,#277252,#277253,#277254,#277255,#277256,#277257,#277258,
#277259,#277260,#277261,#277262,#277263,#277264,#277265,#277266,#277267,
#277268,#277269,#277270,#277271,#277272,#277273,#277274,#277275,#277276,
#277277,#277278,#277279,#277280,#277281,#277282,#277283,#277284,#277285,
#277286,#277287,#277288,#277289,#277290,#277291,#277292,#277293,#277294,
#277295,#277296,#277297,#277298,#277299,#277300,#277301,#277302,#277303,
#277304,#277305,#277306,#277307,#277308,#277309,#277310,#277311,#277312,
#277313,#277314,#277315,#277316,#277317,#277318,#277319,#277320,#277321,
#277322,#277323,#277324,#277325,#277326,#277327,#277328,#277329,#277330,
#277331,#277332,#277333,#277334,#277335,#277336,#277337,#277338,#277339,
#277340,#277341,#277342,#277343,#277344,#277345,#277346,#277347,#277348,
#277349,#277350,#277351,#277352,#277353,#277354,#277355,#277356,#277357,
#277358,#277359,#277360,#277361,#277362,#277363,#277364,#277365,#277366,
#277367,#277368,#277369,#277370,#277371,#277372,#277373,#277374,#277375,
#277376,#277377,#277378,#277379,#277380,#277381,#277382,#277383,#277384,
#277385,#277386,#277387,#277388,#277389,#277390,#277391,#277392,#277393,
#277394,#277395,#277396,#277397,#277398,#277399,#277400,#277401,#277402,
#277403,#277404,#277405,#277406,#277407,#277408,#277409,#277410,#277411,
#277412,#277413,#277414,#277415,#277416,#277417,#277418,#277419,#277420,
#277421,#277422,#277423,#277424,#277425,#277426,#277427,#277428,#277429,
#277430,#277431,#277432,#277433,#277434,#277435,#277436,#277437,#277438,
#277439,#277440,#277441,#277442,#277443,#277444,#277445,#277446,#277447,
#277448,#277449,#277450,#277451,#277452,#277453,#277454,#277455,#277456,
#277457,#277458,#277459,#277460,#277461,#277462,#277463,#277464,#277465,
#277466,#277467,#277468,#277469,#277470,#277471,#277472,#277473,#277474,
#277475,#277476,#277477,#277478,#277479,#277480,#277481,#277482,#277483,
#277484,#277485,#277486,#277487,#277488),(#277489,#277490,#277491,#277492,
#277493,#277494,#277495,#277496,#277497,#277498,#277499,#277500,#277501,
#277502,#277503,#277504,#277505,#277506,#277507,#277508,#277509,#277510,
#277511,#277512,#277513,#277514,#277515,#277516,#277517,#277518,#277519,
#277520,#277521,#277522,#277523,#277524,#277525,#277526,#277527,#277528,
#277529,#277530,#277531,#277532,#277533,#277534,#277535,#277536,#277537,
#277538,#277539,#277540,#277541,#277542,#277543,#277544,#277545,#277546,
#277547,#277548,#277549,#277550,#277551,#277552,#277553,#277554,#277555,
#277556,#277557,#277558,#277559,#277560,#277561,#277562,#277563,#277564,
#277565,#277566,#277567,#277568,#277569,#277570,#277571,#277572,#277573,
#277574,#277575,#277576,#277577,#277578,#277579,#277580,#277581,#277582,
#277583,#277584,#277585,#277586,#277587,#277588,#277589,#277590,#277591,
#277592,#277593,#277594,#277595,#277596,#277597,#277598,#277599,#277600,
#277601,#277602,#277603,#277604,#277605,#277606,#277607,#277608,#277609,
#277610,#277611,#277612,#277613,#277614,#277615,#277616,#277617,#277618,
#277619,#277620,#277621,#277622,#277623,#277624,#277625,#277626,#277627,
#277628,#277629,#277630,#277631,#277632,#277633,#277634,#277635,#277636,
#277637,#277638,#277639,#277640,#277641,#277642,#277643,#277644,#277645,
#277646,#277647,#277648,#277649,#277650,#277651,#277652,#277653,#277654,
#277655,#277656,#277657,#277658,#277659,#277660,#277661,#277662,#277663,
#277664,#277665,#277666,#277667,#277668,#277669,#277670,#277671,#277672,
#277673,#277674,#277675,#277676,#277677,#277678,#277679,#277680,#277681,
#277682,#277683,#277684,#277685,#277686,#277687,#277688,#277689,#277690,
#277691,#277692,#277693,#277694,#277695,#277696,#277697,#277698,#277699,
#277700,#277701,#277702,#277703,#277704,#277705,#277706,#277707,#277708,
#277709,#277710,#277711,#277712,#277713,#277714,#277715,#277716,#277717,
#277718,#277719,#277720,#277721,#277722,#277723,#277724,#277725,#277726,
#277727,#277728,#277729,#277730,#277731,#277732,#277733,#277734,#277735,
#277736,#277737,#277738,#277739,#277740,#277741,#277742,#277743,#277744,
#277745,#277746,#277747,#277748,#277749,#277750,#277751,#277752,#277753,
#277754,#277755,#277756,#277757,#277758,#277759,#277760,#277761,#277762,
#277763,#277764,#277765,#277766,#277767,#277768,#277769,#277770,#277771,
#277772,#277773,#277774,#277775,#277776,#277777,#277778,#277779,#277780,
#277781,#277782,#277783,#277784,#277785,#277786,#277787,#277788,#277789,
#277790,#277791,#277792,#277793,#277794,#277795,#277796,#277797,#277798,
#277799,#277800,#277801,#277802,#277803,#277804,#277805,#277806,#277807,
#277808,#277809,#277810,#277811,#277812,#277813,#277814,#277815,#277816,
#277817,#277818,#277819,#277820,#277821,#277822,#277823,#277824,#277825,
#277826,#277827,#277828,#277829,#277830,#277831,#277832,#277833,#277834,
#277835,#277836,#277837,#277838,#277839,#277840,#277841,#277842,#277843,
#277844,#277845,#277846,#277847,#277848,#277849,#277850,#277851,#277852,
#277853,#277854,#277855,#277856,#277857,#277858,#277859,#277860,#277861,
#277862,#277863,#277864,#277865,#277866,#277867,#277868,#277869,#277870,
#277871,#277872,#277873,#277874,#277875,#277876,#277877,#277878,#277879,
#277880,#277881,#277882,#277883,#277884,#277885,#277886,#277887,#277888,
#277889,#277890,#277891,#277892,#277893,#277894,#277895,#277896,#277897,
#277898,#277899,#277900,#277901,#277902,#277903,#277904,#277905,#277906,
#277907,#277908,#277909,#277910,#277911,#277912,#277913,#277914,#277915,
#277916,#277917,#277918,#277919,#277920,#277921,#277922,#277923,#277924,
#277925,#277926,#277927,#277928,#277929,#277930,#277931,#277932,#277933,
#277934,#277935,#277936,#277937,#277938,#277939,#277940,#277941,#277942,
#277943,#277944,#277945,#277946,#277947,#277948,#277949,#277950,#277951,
#277952,#277953,#277954,#277955,#277956,#277957,#277958,#277959,#277960,
#277961,#277962,#277963,#277964,#277965,#277966,#277967,#277968,#277969,
#277970,#277971,#277972,#277973,#277974,#277975,#277976,#277977,#277978,
#277979,#277980,#277981,#277982,#277983,#277984,#277985,#277986,#277987,
#277988,#277989,#277990,#277991,#277992,#277993,#277994,#277995,#277996,
#277997,#277998,#277999,#278000,#278001,#278002,#278003,#278004,#278005,
#278006,#278007,#278008,#278009,#278010,#278011,#278012,#278013,#278014,
#278015,#278016,#278017,#278018,#278019,#278020,#278021,#278022,#278023,
#278024,#278025,#278026,#278027,#278028,#278029,#278030,#278031,#278032,
#278033,#278034,#278035,#278036,#278037,#278038,#278039,#278040,#278041,
#278042,#278043,#278044,#278045,#278046,#278047,#278048,#278049,#278050,
#278051,#278052,#278053,#278054,#278055,#278056,#278057,#278058,#278059,
#278060,#278061,#278062,#278063,#278064,#278065,#278066,#278067,#278068,
#278069,#278070,#278071,#278072,#278073,#278074,#278075,#278076,#278077,
#278078,#278079,#278080,#278081,#278082,#278083,#278084,#278085,#278086,
#278087,#278088,#278089,#278090,#278091,#278092,#278093,#278094,#278095,
#278096,#278097,#278098,#278099,#278100,#278101,#278102,#278103,#278104,
#278105,#278106,#278107,#278108,#278109,#278110,#278111,#278112,#278113,
#278114,#278115,#278116,#278117,#278118,#278119,#278120,#278121,#278122,
#278123,#278124,#278125,#278126,#278127,#278128,#278129,#278130,#278131,
#278132,#278133,#278134,#278135,#278136,#278137,#278138,#278139,#278140,
#278141,#278142,#278143,#278144,#278145,#278146,#278147,#278148,#278149,
#278150,#278151,#278152,#278153,#278154,#278155,#278156,#278157,#278158,
#278159,#278160,#278161,#278162,#278163,#278164,#278165,#278166,#278167,
#278168,#278169,#278170,#278171,#278172,#278173,#278174,#278175,#278176,
#278177,#278178,#278179,#278180,#278181,#278182,#278183,#278184,#278185,
#278186,#278187,#278188,#278189,#278190,#278191,#278192,#278193,#278194,
#278195,#278196,#278197,#278198,#278199,#278200,#278201,#278202,#278203,
#278204,#278205,#278206,#278207,#278208,#278209,#278210,#278211,#278212,
#278213,#278214,#278215,#278216,#278217,#278218,#278219,#278220,#278221,
#278222,#278223,#278224,#278225,#278226,#278227,#278228,#278229,#278230,
#278231,#278232,#278233,#278234,#278235,#278236,#278237,#278238,#278239,
#278240,#278241,#278242,#278243,#278244,#278245,#278246,#278247,#278248,
#278249,#278250,#278251,#278252,#278253,#278254,#278255,#278256,#278257,
#278258,#278259,#278260,#278261,#278262,#278263,#278264,#278265,#278266,
#278267,#278268,#278269,#278270,#278271,#278272,#278273,#278274,#278275,
#278276,#278277,#278278,#278279,#278280,#278281,#278282,#278283,#278284,
#278285,#278286,#278287,#278288,#278289,#278290,#278291,#278292,#278293,
#278294,#278295,#278296,#278297,#278298,#278299,#278300,#278301,#278302,
#278303,#278304,#278305,#278306,#278307,#278308,#278309,#278310,#278311,
#278312,#278313,#278314,#278315,#278316,#278317,#278318,#278319,#278320,
#278321,#278322,#278323,#278324,#278325,#278326,#278327,#278328,#278329,
#278330,#278331,#278332,#278333,#278334,#278335,#278336,#278337,#278338,
#278339,#278340,#278341,#278342,#278343,#278344,#278345,#278346,#278347,
#278348,#278349,#278350,#278351,#278352,#278353,#278354,#278355,#278356,
#278357,#278358,#278359,#278360,#278361,#278362,#278363,#278364,#278365,
#278366,#278367,#278368,#278369,#278370,#278371,#278372,#278373,#278374,
#278375,#278376,#278377,#278378,#278379,#278380,#278381,#278382,#278383,
#278384,#278385,#278386,#278387,#278388,#278389,#278390,#278391,#278392,
#278393,#278394,#278395,#278396,#278397,#278398,#278399,#278400,#278401,
#278402,#278403,#278404,#278405,#278406,#278407,#278408,#278409,#278410,
#278411,#278412,#278413,#278414,#278415,#278416,#278417,#278418,#278419,
#278420,#278421,#278422,#278423,#278424,#278425,#278426,#278427,#278428,
#278429,#278430,#278431,#278432,#278433,#278434,#278435,#278436,#278437,
#278438,#278439,#278440,#278441,#278442,#278443,#278444,#278445,#278446,
#278447,#278448,#278449,#278450,#278451,#278452,#278453,#278454,#278455,
#278456,#278457,#278458,#278459,#278460,#278461,#278462,#278463,#278464,
#278465,#278466,#278467,#278468,#278469,#278470,#278471,#278472,#278473,
#278474,#278475,#278476,#278477,#278478,#278479,#278480,#278481,#278482,
#278483,#278484,#278485,#278486,#278487,#278488,#278489,#278490,#278491,
#278492,#278493,#278494,#278495,#278496,#278497,#278498,#278499,#278500,
#278501,#278502,#278503,#278504,#278505,#278506,#278507,#278508,#278509,
#278510,#278511,#278512,#278513,#278514,#278515,#278516,#278517,#278518,
#278519,#278520,#278521,#278522,#278523,#278524,#278525)),.UNSPECIFIED.,
 .F.,.F.,.F.)
B_SPLINE_SURFACE_WITH_KNOTS((2,2),(3,2,2,2,2,2,2,2,2,2,2,2,2,2,2,2,2,2,
2,2,2,2,2,2,2,2,2,2,2,2,2,2,2,2,2,2,2,2,2,2,2,2,2,2,2,2,2,2,2,2,2,2,2,2,
2,2,2,2,2,2,2,2,2,2,2,2,2,2,2,2,2,2,2,2,2,2,2,2,2,2,2,2,2,2,2,2,2,2,2,2,
2,2,2,2,2,2,2,2,2,2,2,2,2,2,2,2,2,2,2,2,2,2,2,2,2,2,2,2,2,2,2,2,2,2,2,2,
2,2,2,2,2,2,2,2,2,2,2,2,2,2,2,2,2,2,2,2,2,2,2,2,2,2,2,2,2,2,2,2,2,2,2,2,
2,2,2,2,2,2,2,2,2,2,2,2,2,2,2,2,2,2,2,2,2,2,2,2,2,2,2,2,2,2,2,2,2,2,2,2,
2,2,2,2,2,2,2,2,2,2,2,2,2,2,2,2,2,2,2,2,2,2,2,2,2,2,2,2,2,2,2,2,2,2,2,2,
2,2,2,2,2,2,2,2,2,2,2,2,2,2,2,2,2,2,2,2,2,2,2,2,2,2,2,2,2,2,2,2,2,2,2,2,
2,2,2,2,2,2,2,2,2,2,2,2,2,2,2,2,2,2,2,2,2,2,2,2,2,2,2,2,2,2,2,2,2,2,2,2,
2,2,2,2,2,2,2,2,2,2,2,2,2,2,2,2,2,2,2,2,2,2,2,2,2,2,2,2,2,2,2,2,2,2,2,2,
2,2,2,2,2,2,2,2,2,2,2,2,2,2,2,2,2,2,2,2,2,2,2,2,2,2,2,2,2,2,2,2,2,2,2,2,
2,2,2,2,2,2,2,2,2,2,2,2,2,2,2,2,2,2,2,2,2,2,2,2,2,2,2,2,2,2,2,2,2,2,2,2,
2,2,2,2,2,2,2,2,2,2,2,2,2,2,2,2,2,2,2,2,2,2,2,2,2,2,2,2,2,2,2,2,2,2,2,2,
2,2,2,2,2,2,2,2,2,2,2,2,2,2,2,2,2,2,2,2,2,2,2,2,2,2,2,2,2,2,2,2,2,2,2,2,
2,2,2,2,2,2,2,2,2,2,2,2,2,2,2,2,2,2,2,2,2,2,2,2,2,2,2,2,2,2,2,2,3),(-2.04414063882605E-6,
1.),(0.,0.00192307692307692,0.00384615384615385,0.00576923076923077,0.00769230769230769,
0.00961538461538462,0.0115384615384615,0.0134615384615385,0.0153846153846154,
0.0173076923076923,0.0192307692307692,0.0211538461538462,0.0230769230769231,
0.025,0.0269230769230769,0.0288461538461538,0.0307692307692308,0.0326923076923077,
0.0346153846153846,0.0365384615384615,0.0384615384615385,0.0403846153846154,
0.0423076923076923,0.0442307692307692,0.0461538461538462,0.0480769230769231,
0.05,0.0519230769230769,0.0538461538461538,0.0557692307692308,0.0576923076923077,
0.0596153846153846,0.0615384615384615,0.0634615384615385,0.0653846153846154,
0.0673076923076923,0.0692307692307692,0.0711538461538462,0.0730769230769231,
0.075,0.0769230769230769,0.0788461538461538,0.0807692307692308,0.0826923076923077,
0.0846153846153846,0.0865384615384615,0.0884615384615385,0.0903846153846154,
0.0923076923076923,0.0942307692307692,0.0961538461538462,0.0980769230769231,
0.1,0.101923076923077,0.103846153846154,0.105769230769231,0.107692307692308,
0.109615384615385,0.111538461538462,0.113461538461538,0.115384615384615,
0.117307692307692,0.119230769230769,0.121153846153846,0.123076923076923,
0.125,0.126923076923077,0.128846153846154,0.130769230769231,0.132692307692308,
0.134615384615385,0.136538461538462,0.138461538461538,0.140384615384615,
0.142307692307692,0.144230769230769,0.146153846153846,0.148076923076923,
0.15,0.151923076923077,0.153846153846154,0.155769230769231,0.157692307692308,
0.159615384615385,0.161538461538462,0.163461538461538,0.165384615384615,
0.167307692307692,0.169230769230769,0.171153846153846,0.173076923076923,
0.175,0.176923076923077,0.178846153846154,0.180769230769231,0.182692307692308,
0.184615384615385,0.186538461538462,0.188461538461538,0.190384615384615,
0.192307692307692,0.194230769230769,0.196153846153846,0.198076923076923,
0.2,0.201923076923077,0.203846153846154,0.205769230769231,0.207692307692308,
0.209615384615385,0.211538461538462,0.213461538461538,0.215384615384615,
0.217307692307692,0.219230769230769,0.221153846153846,0.223076923076923,
0.225,0.226923076923077,0.228846153846154,0.230769230769231,0.232692307692308,
0.234615384615385,0.236538461538462,0.238461538461538,0.240384615384615,
0.242307692307692,0.244230769230769,0.246153846153846,0.248076923076923,
0.25,0.251923076923077,0.253846153846154,0.255769230769231,0.257692307692308,
0.259615384615385,0.261538461538462,0.263461538461538,0.265384615384615,
0.267307692307692,0.269230769230769,0.271153846153846,0.273076923076923,
0.275,0.276923076923077,0.278846153846154,0.280769230769231,0.282692307692308,
0.284615384615385,0.286538461538462,0.288461538461538,0.290384615384615,
0.292307692307692,0.294230769230769,0.296153846153846,0.298076923076923,
0.3,0.301923076923077,0.303846153846154,0.305769230769231,0.307692307692308,
0.309615384615385,0.311538461538462,0.313461538461538,0.315384615384615,
0.317307692307692,0.319230769230769,0.321153846153846,0.323076923076923,
0.325,0.326923076923077,0.328846153846154,0.330769230769231,0.332692307692308,
0.334615384615385,0.336538461538462,0.338461538461538,0.340384615384615,
0.342307692307692,0.344230769230769,0.346153846153846,0.348076923076923,
0.35,0.351923076923077,0.353846153846154,0.355769230769231,0.357692307692308,
0.359615384615385,0.361538461538462,0.363461538461538,0.365384615384615,
0.367307692307692,0.369230769230769,0.371153846153846,0.373076923076923,
0.375,0.376923076923077,0.378846153846154,0.380769230769231,0.382692307692308,
0.384615384615385,0.386538461538462,0.388461538461538,0.390384615384615,
0.392307692307692,0.394230769230769,0.396153846153846,0.398076923076923,
0.4,0.401923076923077,0.403846153846154,0.405769230769231,0.407692307692308,
0.409615384615385,0.411538461538462,0.413461538461538,0.415384615384615,
0.417307692307692,0.419230769230769,0.421153846153846,0.423076923076923,
0.425,0.426923076923077,0.428846153846154,0.430769230769231,0.432692307692308,
0.434615384615385,0.436538461538462,0.438461538461538,0.440384615384615,
0.442307692307692,0.444230769230769,0.446153846153846,0.448076923076923,
0.45,0.451923076923077,0.453846153846154,0.455769230769231,0.457692307692308,
0.459615384615385,0.461538461538462,0.463461538461538,0.465384615384615,
0.467307692307692,0.469230769230769,0.471153846153846,0.473076923076923,
0.475,0.476923076923077,0.478846153846154,0.480769230769231,0.482692307692308,
0.484615384615385,0.486538461538462,0.488461538461538,0.490384615384615,
0.492307692307692,0.494230769230769,0.496153846153846,0.498076923076923,
0.5,0.501923076923077,0.503846153846154,0.505769230769231,0.507692307692308,
0.509615384615385,0.511538461538461,0.513461538461538,0.515384615384615,
0.517307692307692,0.519230769230769,0.521153846153846,0.523076923076923,
0.525,0.526923076923077,0.528846153846154,0.530769230769231,0.532692307692308,
0.534615384615385,0.536538461538462,0.538461538461538,0.540384615384615,
0.542307692307692,0.544230769230769,0.546153846153846,0.548076923076923,
0.55,0.551923076923077,0.553846153846154,0.555769230769231,0.557692307692308,
0.559615384615385,0.561538461538462,0.563461538461538,0.565384615384615,
0.567307692307692,0.569230769230769,0.571153846153846,0.573076923076923,
0.575,0.576923076923077,0.578846153846154,0.580769230769231,0.582692307692308,
0.584615384615385,0.586538461538462,0.588461538461538,0.590384615384615,
0.592307692307692,0.594230769230769,0.596153846153846,0.598076923076923,
0.6,0.601923076923077,0.603846153846154,0.605769230769231,0.607692307692308,
0.609615384615385,0.611538461538462,0.613461538461539,0.615384615384615,
0.617307692307692,0.619230769230769,0.621153846153846,0.623076923076923,
0.625,0.626923076923077,0.628846153846154,0.630769230769231,0.632692307692308,
0.634615384615385,0.636538461538461,0.638461538461538,0.640384615384615,
0.642307692307692,0.644230769230769,0.646153846153846,0.648076923076923,
0.65,0.651923076923077,0.653846153846154,0.655769230769231,0.657692307692308,
0.659615384615385,0.661538461538462,0.663461538461538,0.665384615384615,
0.667307692307692,0.669230769230769,0.671153846153846,0.673076923076923,
0.675,0.676923076923077,0.678846153846154,0.680769230769231,0.682692307692308,
0.684615384615385,0.686538461538462,0.688461538461538,0.690384615384615,
0.692307692307692,0.694230769230769,0.696153846153846,0.698076923076923,
0.7,0.701923076923077,0.703846153846154,0.705769230769231,0.707692307692308,
0.709615384615385,0.711538461538462,0.713461538461538,0.715384615384615,
0.717307692307692,0.719230769230769,0.721153846153846,0.723076923076923,
0.725,0.726923076923077,0.728846153846154,0.730769230769231,0.732692307692308,
0.734615384615385,0.736538461538462,0.738461538461539,0.740384615384615,
0.742307692307692,0.744230769230769,0.746153846153846,0.748076923076923,
0.75,0.751923076923077,0.753846153846154,0.755769230769231,0.757692307692308,
0.759615384615385,0.761538461538461,0.763461538461538,0.765384615384615,
0.767307692307692,0.769230769230769,0.771153846153846,0.773076923076923,
0.775,0.776923076923077,0.778846153846154,0.780769230769231,0.782692307692308,
0.784615384615385,0.786538461538462,0.788461538461538,0.790384615384615,
0.792307692307692,0.794230769230769,0.796153846153846,0.798076923076923,
0.8,0.801923076923077,0.803846153846154,0.805769230769231,0.807692307692308,
0.809615384615385,0.811538461538462,0.813461538461538,0.815384615384615,
0.817307692307692,0.819230769230769,0.821153846153846,0.823076923076923,
0.825,0.826923076923077,0.828846153846154,0.830769230769231,0.832692307692308,
0.834615384615385,0.836538461538462,0.838461538461538,0.840384615384615,
0.842307692307692,0.844230769230769,0.846153846153846,0.848076923076923,
0.85,0.851923076923077,0.853846153846154,0.855769230769231,0.857692307692308,
0.859615384615385,0.861538461538462,0.863461538461539,0.865384615384615,
0.867307692307692,0.869230769230769,0.871153846153846,0.873076923076923,
0.875,0.876923076923077,0.878846153846154,0.880769230769231,0.882692307692308,
0.884615384615385,0.886538461538461,0.888461538461538,0.890384615384615,
0.892307692307692,0.894230769230769,0.896153846153846,0.898076923076923,
0.9,0.901923076923077,0.903846153846154,0.905769230769231,0.907692307692308,
0.909615384615385,0.911538461538462,0.913461538461538,0.915384615384615,
0.917307692307692,0.919230769230769,0.921153846153846,0.923076923076923,
0.925,0.926923076923077,0.928846153846154,0.930769230769231,0.932692307692308,
0.934615384615385,0.936538461538462,0.938461538461538,0.940384615384615,
0.942307692307692,0.944230769230769,0.946153846153846,0.948076923076923,
0.95,0.951923076923077,0.953846153846154,0.955769230769231,0.957692307692308,
0.959615384615385,0.961538461538462,0.963461538461538,0.965384615384615,
0.967307692307692,0.969230769230769,0.971153846153846,0.973076923076923,
0.975,0.976923076923077,0.978846153846154,0.980769230769231,0.982692307692308,
0.984615384615385,0.986538461538462,0.988461538461539,0.990384615384615,
0.992307692307692,0.994230769230769,0.996153846153846),.UNSPECIFIED.)
GEOMETRIC_REPRESENTATION_ITEM()
RATIONAL_B_SPLINE_SURFACE(((1.,0.951056516295153,1.,0.951056516295153,1.,
0.951056516295153,1.,0.951056516295153,1.,0.951056516295153,1.,0.951056516295153,
1.,0.951056516295153,1.,0.951056516295153,1.,0.951056516295153,1.,0.951056516295153,
1.,0.951056516295153,1.,0.951056516295153,1.,0.951056516295153,1.,0.951056516295153,
1.,0.951056516295153,1.,0.951056516295153,1.,0.951056516295153,1.,0.951056516295153,
1.,0.951056516295153,1.,0.951056516295153,1.,0.951056516295153,1.,0.951056516295153,
1.,0.951056516295153,1.,0.951056516295153,1.,0.951056516295153,1.,0.951056516295153,
1.,0.951056516295153,1.,0.951056516295153,1.,0.951056516295153,1.,0.951056516295153,
1.,0.951056516295153,1.,0.951056516295153,1.,0.951056516295153,1.,0.951056516295153,
1.,0.951056516295153,1.,0.951056516295153,1.,0.951056516295153,1.,0.951056516295153,
1.,0.951056516295153,1.,0.951056516295153,1.,0.951056516295153,1.,0.951056516295153,
1.,0.951056516295153,1.,0.951056516295153,1.,0.951056516295153,1.,0.951056516295153,
1.,0.951056516295153,1.,0.951056516295153,1.,0.951056516295153,1.,0.951056516295153,
1.,0.951056516295153,1.,0.951056516295153,1.,0.951056516295153,1.,0.951056516295153,
1.,0.951056516295153,1.,0.951056516295153,1.,0.951056516295153,1.,0.951056516295153,
1.,0.951056516295153,1.,0.951056516295153,1.,0.951056516295153,1.,0.951056516295153,
1.,0.951056516295153,1.,0.951056516295153,1.,0.951056516295153,1.,0.951056516295153,
1.,0.951056516295153,1.,0.951056516295153,1.,0.951056516295153,1.,0.951056516295153,
1.,0.951056516295153,1.,0.951056516295153,1.,0.951056516295153,1.,0.951056516295153,
1.,0.951056516295153,1.,0.951056516295153,1.,0.951056516295153,1.,0.951056516295153,
1.,0.951056516295153,1.,0.951056516295153,1.,0.951056516295153,1.,0.951056516295153,
1.,0.951056516295153,1.,0.951056516295153,1.,0.951056516295153,1.,0.951056516295153,
1.,0.951056516295153,1.,0.951056516295153,1.,0.951056516295153,1.,0.951056516295153,
1.,0.951056516295153,1.,0.951056516295153,1.,0.951056516295153,1.,0.951056516295153,
1.,0.951056516295153,1.,0.951056516295153,1.,0.951056516295153,1.,0.951056516295153,
1.,0.951056516295153,1.,0.951056516295153,1.,0.951056516295153,1.,0.951056516295153,
1.,0.951056516295153,1.,0.951056516295153,1.,0.951056516295153,1.,0.951056516295153,
1.,0.951056516295153,1.,0.951056516295153,1.,0.951056516295153,1.,0.951056516295153,
1.,0.951056516295153,1.,0.951056516295153,1.,0.951056516295153,1.,0.951056516295153,
1.,0.951056516295153,1.,0.951056516295153,1.,0.951056516295153,1.,0.951056516295153,
1.,0.951056516295153,1.,0.951056516295153,1.,0.951056516295153,1.,0.951056516295153,
1.,0.951056516295153,1.,0.951056516295153,1.,0.951056516295153,1.,0.951056516295153,
1.,0.951056516295153,1.,0.951056516295153,1.,0.951056516295153,1.,0.951056516295153,
1.,0.951056516295153,1.,0.951056516295153,1.,0.951056516295153,1.,0.951056516295153,
1.,0.951056516295153,1.,0.951056516295153,1.,0.951056516295153,1.,0.951056516295153,
1.,0.951056516295153,1.,0.951056516295153,1.,0.951056516295153,1.,0.951056516295153,
1.,0.951056516295153,1.,0.951056516295153,1.,0.951056516295153,1.,0.951056516295153,
1.,0.951056516295153,1.,0.951056516295153,1.,0.951056516295153,1.,0.951056516295153,
1.,0.951056516295153,1.,0.951056516295153,1.,0.951056516295153,1.,0.951056516295153,
1.,0.951056516295153,1.,0.951056516295153,1.,0.951056516295153,1.,0.951056516295153,
1.,0.951056516295153,1.,0.951056516295153,1.,0.951056516295153,1.,0.951056516295153,
1.,0.951056516295153,1.,0.951056516295153,1.,0.951056516295153,1.,0.951056516295153,
1.,0.951056516295153,1.,0.951056516295153,1.,0.951056516295153,1.,0.951056516295153,
1.,0.951056516295153,1.,0.951056516295153,1.,0.951056516295153,1.,0.951056516295153,
1.,0.951056516295153,1.,0.951056516295153,1.,0.951056516295153,1.,0.951056516295153,
1.,0.951056516295153,1.,0.951056516295153,1.,0.951056516295153,1.,0.951056516295153,
1.,0.951056516295153,1.,0.951056516295153,1.,0.951056516295153,1.,0.951056516295153,
1.,0.951056516295153,1.,0.951056516295153,1.,0.951056516295153,1.,0.951056516295153,
1.,0.951056516295153,1.,0.951056516295153,1.,0.951056516295153,1.,0.951056516295153,
1.,0.951056516295153,1.,0.951056516295153,1.,0.951056516295153,1.,0.951056516295153,
1.,0.951056516295153,1.,0.951056516295153,1.,0.951056516295153,1.,0.951056516295153,
1.,0.951056516295153,1.,0.951056516295153,1.,0.951056516295153,1.,0.951056516295153,
1.,0.951056516295153,1.,0.951056516295153,1.,0.951056516295153,1.,0.951056516295153,
1.,0.951056516295153,1.,0.951056516295153,1.,0.951056516295153,1.,0.951056516295153,
1.,0.951056516295153,1.,0.951056516295153,1.,0.951056516295153,1.,0.951056516295153,
1.,0.951056516295153,1.,0.951056516295153,1.,0.951056516295153,1.,0.951056516295153,
1.,0.951056516295153,1.,0.951056516295153,1.,0.951056516295153,1.,0.951056516295153,
1.,0.951056516295153,1.,0.951056516295153,1.,0.951056516295153,1.,0.951056516295153,
1.,0.951056516295153,1.,0.951056516295153,1.,0.951056516295153,1.,0.951056516295153,
1.,0.951056516295153,1.,0.951056516295153,1.,0.951056516295153,1.,0.951056516295153,
1.,0.951056516295153,1.,0.951056516295153,1.,0.951056516295153,1.,0.951056516295153,
1.,0.951056516295153,1.,0.951056516295153,1.,0.951056516295153,1.,0.951056516295153,
1.,0.951056516295153,1.,0.951056516295153,1.,0.951056516295153,1.,0.951056516295153,
1.,0.951056516295153,1.,0.951056516295153,1.,0.951056516295153,1.,0.951056516295153,
1.,0.951056516295153,1.,0.951056516295153,1.,0.951056516295153,1.,0.951056516295153,
1.,0.951056516295153,1.,0.951056516295153,1.,0.951056516295153,1.,0.951056516295153,
1.,0.951056516295153,1.,0.951056516295153,1.,0.951056516295153,1.,0.951056516295153,
1.,0.951056516295153,1.,0.951056516295153,1.,0.951056516295153,1.,0.951056516295153,
1.,0.951056516295153,1.,0.951056516295153,1.,0.951056516295153,1.,0.951056516295153,
1.,0.951056516295153,1.,0.951056516295153,1.,0.951056516295153,1.,0.951056516295153,
1.,0.951056516295153,1.,0.951056516295153,1.,0.951056516295153,1.,0.951056516295153,
1.,0.951056516295153,1.,0.951056516295153,1.,0.951056516295153,1.,0.951056516295153,
1.,0.951056516295153,1.,0.951056516295153,1.,0.951056516295153,1.,0.951056516295153,
1.,0.951056516295153,1.,0.951056516295153,1.,0.951056516295153,1.,0.951056516295153,
1.,0.951056516295153,1.,0.951056516295153,1.,0.951056516295153,1.,0.951056516295153,
1.,0.951056516295153,1.,0.951056516295153,1.,0.951056516295153,1.,0.951056516295153,
1.,0.951056516295153,1.,0.951056516295153,1.,0.951056516295153,1.,0.951056516295153,
1.,0.951056516295153,1.,0.951056516295153,1.,0.951056516295153,1.,0.951056516295153,
1.,0.951056516295153,1.,0.951056516295153,1.,0.951056516295153,1.,0.951056516295153,
1.,0.951056516295153,1.,0.951056516295153,1.,0.951056516295153,1.,0.951056516295153,
1.,0.951056516295153,1.,0.951056516295153,1.,0.951056516295153,1.,0.951056516295153,
1.,0.951056516295153,1.,0.951056516295153,1.,0.951056516295153,1.,0.951056516295153,
1.,0.951056516295153,1.,0.951056516295153,1.,0.951056516295153,1.,0.951056516295153,
1.,0.951056516295153,1.,0.951056516295153,1.,0.951056516295153,1.,0.951056516295153,
1.,0.951056516295153,1.,0.951056516295153,1.,0.951056516295153,1.,0.951056516295153,
1.,0.951056516295153,1.,0.951056516295153,1.,0.951056516295153,1.,0.951056516295153,
1.,0.951056516295153,1.,0.951056516295153,1.,0.951056516295153,1.,0.951056516295153,
1.,0.951056516295153,1.,0.951056516295153,1.,0.951056516295153,1.,0.951056516295153,
1.,0.951056516295153,1.,0.951056516295153,1.,0.951056516295153,1.,0.951056516295153,
1.,0.951056516295153,1.,0.951056516295153,1.,0.951056516295153,1.,0.951056516295153,
1.,0.951056516295153,1.,0.951056516295153,1.,0.951056516295153,1.,0.951056516295153,
1.,0.951056516295153,1.,0.951056516295153,1.,0.951056516295153,1.,0.951056516295153,
1.,0.951056516295153,1.,0.951056516295153,1.,0.951056516295153,1.,0.951056516295153,
1.,0.951056516295153,1.,0.951056516295153,1.,0.951056516295153,1.,0.951056516295153,
1.,0.951056516295153,1.,0.951056516295153,1.,0.951056516295153,1.,0.951056516295153,
1.,0.951056516295153,1.,0.951056516295153,1.,0.951056516295153,1.,0.951056516295153,
1.,0.951056516295153,1.,0.951056516295153,1.,0.951056516295153,1.,0.951056516295153,
1.,0.951056516295153,1.,0.951056516295153,1.,0.951056516295153,1.,0.951056516295153,
1.,0.951056516295153,1.,0.951056516295153,1.,0.951056516295153,1.,0.951056516295153,
1.,0.951056516295153,1.,0.951056516295153,1.,0.951056516295153,1.,0.951056516295153,
1.,0.951056516295153,1.,0.951056516295153,1.,0.951056516295153,1.,0.951056516295153,
1.,0.951056516295153,1.,0.951056516295153,1.,0.951056516295153,1.,0.951056516295153,
1.,0.951056516295153,1.,0.951056516295153,1.,0.951056516295153,1.,0.951056516295153,
1.,0.951056516295153,1.,0.951056516295153,1.,0.951056516295153,1.,0.951056516295153,
1.,0.951056516295153,1.,0.951056516295153,1.,0.951056516295153,1.,0.951056516295153,
1.,0.951056516295153,1.,0.951056516295153,1.,0.951056516295153,1.,0.951056516295153,
1.,0.951056516295153,1.,0.951056516295153,1.,0.951056516295153,1.,0.951056516295153,
1.,0.951056516295153,1.,0.951056516295153,1.,0.951056516295153,1.,0.951056516295153,
1.,0.951056516295153,1.,0.951056516295153,1.,0.951056516295153,1.,0.951056516295153,
1.,0.951056516295153,1.,0.951056516295153,1.,0.951056516295153,1.,0.951056516295153,
1.,0.951056516295153,1.,0.951056516295153,1.,0.951056516295153,1.,0.951056516295153,
1.,0.951056516295153,1.,0.951056516295153,1.,0.951056516295153,1.,0.951056516295153,
1.,0.951056516295153,1.,0.951056516295153,1.,0.951056516295153,1.,0.951056516295153,
1.,0.951056516295153,1.,0.951056516295153,1.,0.951056516295153,1.,0.951056516295153,
1.,0.951056516295153,1.,0.951056516295153,1.,0.951056516295153,1.,0.951056516295153,
1.,0.951056516295153,1.,0.951056516295153,1.,0.951056516295153,1.,0.951056516295153,
1.,0.951056516295153,1.,0.951056516295153,1.,0.951056516295153,1.,0.951056516295153,
1.,0.951056516295153,1.,0.951056516295153,1.,0.951056516295153,1.,0.951056516295153,
1.,0.951056516295153,1.,0.951056516295153,1.,0.951056516295153,1.,0.951056516295153,
1.,0.951056516295153,1.,0.951056516295153,1.,0.951056516295153,1.,0.951056516295153,
1.,0.951056516295153,1.,0.951056516295153,1.,0.951056516295153,1.,0.951056516295153,
1.,0.951056516295153,1.,0.951056516295153,1.,0.951056516295153,1.,0.951056516295153,
1.,0.951056516295153,1.,0.951056516295153,1.,0.951056516295153,1.,0.951056516295153,
1.,0.951056516295153,1.,0.951056516295153,1.,0.951056516295153,1.,0.951056516295153,
1.,0.951056516295153,1.,0.951056516295153,1.,0.951056516295153,1.,0.951056516295153,
1.,0.951056516295153,1.,0.951056516295153,1.,0.951056516295153,1.,0.951056516295153,
1.,0.951056516295153,1.,0.951056516295153,1.,0.951056516295153,1.,0.951056516295153,
1.,0.951056516295153,1.,0.951056516295153,1.,0.951056516295153,1.,0.951056516295153,
1.,0.951056516295153,1.,0.951056516295153,1.,0.951056516295153,1.,0.951056516295153,
1.,0.951056516295153,1.,0.951056516295153,1.,0.951056516295153,1.,0.951056516295153,
1.),(1.,0.951056516295154,1.,0.951056516295154,1.,0.951056516295154,1.,
0.951056516295154,1.,0.951056516295154,1.,0.951056516295154,1.,0.951056516295154,
1.,0.951056516295154,1.,0.951056516295154,1.,0.951056516295154,1.,0.951056516295154,
1.,0.951056516295154,1.,0.951056516295154,1.,0.951056516295154,1.,0.951056516295154,
1.,0.951056516295154,1.,0.951056516295154,1.,0.951056516295154,1.,0.951056516295154,
1.,0.951056516295154,1.,0.951056516295154,1.,0.951056516295154,1.,0.951056516295154,
1.,0.951056516295154,1.,0.951056516295154,1.,0.951056516295154,1.,0.951056516295154,
1.,0.951056516295154,1.,0.951056516295154,1.,0.951056516295154,1.,0.951056516295154,
1.,0.951056516295154,1.,0.951056516295154,1.,0.951056516295154,1.,0.951056516295154,
1.,0.951056516295154,1.,0.951056516295154,1.,0.951056516295154,1.,0.951056516295154,
1.,0.951056516295154,1.,0.951056516295154,1.,0.951056516295154,1.,0.951056516295154,
1.,0.951056516295154,1.,0.951056516295154,1.,0.951056516295154,1.,0.951056516295154,
1.,0.951056516295154,1.,0.951056516295154,1.,0.951056516295154,1.,0.951056516295154,
1.,0.951056516295154,1.,0.951056516295154,1.,0.951056516295154,1.,0.951056516295154,
1.,0.951056516295154,1.,0.951056516295154,1.,0.951056516295154,1.,0.951056516295154,
1.,0.951056516295154,1.,0.951056516295154,1.,0.951056516295154,1.,0.951056516295154,
1.,0.951056516295154,1.,0.951056516295154,1.,0.951056516295154,1.,0.951056516295154,
1.,0.951056516295154,1.,0.951056516295154,1.,0.951056516295154,1.,0.951056516295154,
1.,0.951056516295154,1.,0.951056516295154,1.,0.951056516295154,1.,0.951056516295154,
1.,0.951056516295154,1.,0.951056516295154,1.,0.951056516295154,1.,0.951056516295154,
1.,0.951056516295154,1.,0.951056516295154,1.,0.951056516295154,1.,0.951056516295154,
1.,0.951056516295154,1.,0.951056516295154,1.,0.951056516295154,1.,0.951056516295154,
1.,0.951056516295154,1.,0.951056516295154,1.,0.951056516295154,1.,0.951056516295154,
1.,0.951056516295154,1.,0.951056516295154,1.,0.951056516295154,1.,0.951056516295154,
1.,0.951056516295154,1.,0.951056516295154,1.,0.951056516295154,1.,0.951056516295154,
1.,0.951056516295154,1.,0.951056516295154,1.,0.951056516295154,1.,0.951056516295154,
1.,0.951056516295154,1.,0.951056516295154,1.,0.951056516295154,1.,0.951056516295154,
1.,0.951056516295154,1.,0.951056516295154,1.,0.951056516295154,1.,0.951056516295154,
1.,0.951056516295154,1.,0.951056516295154,1.,0.951056516295154,1.,0.951056516295154,
1.,0.951056516295154,1.,0.951056516295154,1.,0.951056516295154,1.,0.951056516295154,
1.,0.951056516295154,1.,0.951056516295154,1.,0.951056516295154,1.,0.951056516295154,
1.,0.951056516295154,1.,0.951056516295154,1.,0.951056516295154,1.,0.951056516295154,
1.,0.951056516295154,1.,0.951056516295154,1.,0.951056516295154,1.,0.951056516295154,
1.,0.951056516295154,1.,0.951056516295154,1.,0.951056516295154,1.,0.951056516295154,
1.,0.951056516295154,1.,0.951056516295154,1.,0.951056516295154,1.,0.951056516295154,
1.,0.951056516295154,1.,0.951056516295154,1.,0.951056516295154,1.,0.951056516295154,
1.,0.951056516295154,1.,0.951056516295154,1.,0.951056516295154,1.,0.951056516295154,
1.,0.951056516295154,1.,0.951056516295154,1.,0.951056516295154,1.,0.951056516295154,
1.,0.951056516295154,1.,0.951056516295154,1.,0.951056516295154,1.,0.951056516295154,
1.,0.951056516295154,1.,0.951056516295154,1.,0.951056516295154,1.,0.951056516295154,
1.,0.951056516295154,1.,0.951056516295154,1.,0.951056516295154,1.,0.951056516295154,
1.,0.951056516295154,1.,0.951056516295154,1.,0.951056516295154,1.,0.951056516295154,
1.,0.951056516295154,1.,0.951056516295154,1.,0.951056516295154,1.,0.951056516295154,
1.,0.951056516295154,1.,0.951056516295154,1.,0.951056516295154,1.,0.951056516295154,
1.,0.951056516295154,1.,0.951056516295154,1.,0.951056516295154,1.,0.951056516295154,
1.,0.951056516295154,1.,0.951056516295154,1.,0.951056516295154,1.,0.951056516295154,
1.,0.951056516295154,1.,0.951056516295154,1.,0.951056516295154,1.,0.951056516295154,
1.,0.951056516295154,1.,0.951056516295154,1.,0.951056516295154,1.,0.951056516295154,
1.,0.951056516295154,1.,0.951056516295154,1.,0.951056516295154,1.,0.951056516295154,
1.,0.951056516295154,1.,0.951056516295154,1.,0.951056516295154,1.,0.951056516295154,
1.,0.951056516295154,1.,0.951056516295154,1.,0.951056516295154,1.,0.951056516295154,
1.,0.951056516295154,1.,0.951056516295154,1.,0.951056516295154,1.,0.951056516295154,
1.,0.951056516295154,1.,0.951056516295154,1.,0.951056516295154,1.,0.951056516295154,
1.,0.951056516295154,1.,0.951056516295154,1.,0.951056516295154,1.,0.951056516295154,
1.,0.951056516295154,1.,0.951056516295154,1.,0.951056516295154,1.,0.951056516295154,
1.,0.951056516295154,1.,0.951056516295154,1.,0.951056516295154,1.,0.951056516295154,
1.,0.951056516295154,1.,0.951056516295154,1.,0.951056516295154,1.,0.951056516295154,
1.,0.951056516295154,1.,0.951056516295154,1.,0.951056516295154,1.,0.951056516295154,
1.,0.951056516295154,1.,0.951056516295154,1.,0.951056516295154,1.,0.951056516295154,
1.,0.951056516295154,1.,0.951056516295154,1.,0.951056516295154,1.,0.951056516295154,
1.,0.951056516295154,1.,0.951056516295154,1.,0.951056516295154,1.,0.951056516295154,
1.,0.951056516295154,1.,0.951056516295154,1.,0.951056516295154,1.,0.951056516295154,
1.,0.951056516295154,1.,0.951056516295154,1.,0.951056516295154,1.,0.951056516295154,
1.,0.951056516295154,1.,0.951056516295154,1.,0.951056516295154,1.,0.951056516295154,
1.,0.951056516295154,1.,0.951056516295154,1.,0.951056516295154,1.,0.951056516295154,
1.,0.951056516295154,1.,0.951056516295154,1.,0.951056516295154,1.,0.951056516295154,
1.,0.951056516295154,1.,0.951056516295154,1.,0.951056516295154,1.,0.951056516295154,
1.,0.951056516295154,1.,0.951056516295154,1.,0.951056516295154,1.,0.951056516295154,
1.,0.951056516295154,1.,0.951056516295154,1.,0.951056516295154,1.,0.951056516295154,
1.,0.951056516295154,1.,0.951056516295154,1.,0.951056516295154,1.,0.951056516295154,
1.,0.951056516295154,1.,0.951056516295154,1.,0.951056516295154,1.,0.951056516295154,
1.,0.951056516295154,1.,0.951056516295154,1.,0.951056516295154,1.,0.951056516295154,
1.,0.951056516295154,1.,0.951056516295154,1.,0.951056516295154,1.,0.951056516295154,
1.,0.951056516295154,1.,0.951056516295154,1.,0.951056516295154,1.,0.951056516295154,
1.,0.951056516295154,1.,0.951056516295154,1.,0.951056516295154,1.,0.951056516295154,
1.,0.951056516295154,1.,0.951056516295154,1.,0.951056516295154,1.,0.951056516295154,
1.,0.951056516295154,1.,0.951056516295154,1.,0.951056516295154,1.,0.951056516295154,
1.,0.951056516295154,1.,0.951056516295154,1.,0.951056516295154,1.,0.951056516295154,
1.,0.951056516295154,1.,0.951056516295154,1.,0.951056516295154,1.,0.951056516295154,
1.,0.951056516295154,1.,0.951056516295154,1.,0.951056516295154,1.,0.951056516295154,
1.,0.951056516295154,1.,0.951056516295154,1.,0.951056516295154,1.,0.951056516295154,
1.,0.951056516295154,1.,0.951056516295154,1.,0.951056516295154,1.,0.951056516295154,
1.,0.951056516295154,1.,0.951056516295154,1.,0.951056516295154,1.,0.951056516295154,
1.,0.951056516295154,1.,0.951056516295154,1.,0.951056516295154,1.,0.951056516295154,
1.,0.951056516295154,1.,0.951056516295154,1.,0.951056516295154,1.,0.951056516295154,
1.,0.951056516295154,1.,0.951056516295154,1.,0.951056516295154,1.,0.951056516295154,
1.,0.951056516295154,1.,0.951056516295154,1.,0.951056516295154,1.,0.951056516295154,
1.,0.951056516295154,1.,0.951056516295154,1.,0.951056516295154,1.,0.951056516295154,
1.,0.951056516295154,1.,0.951056516295154,1.,0.951056516295154,1.,0.951056516295154,
1.,0.951056516295154,1.,0.951056516295154,1.,0.951056516295154,1.,0.951056516295154,
1.,0.951056516295154,1.,0.951056516295154,1.,0.951056516295154,1.,0.951056516295154,
1.,0.951056516295154,1.,0.951056516295154,1.,0.951056516295154,1.,0.951056516295154,
1.,0.951056516295154,1.,0.951056516295154,1.,0.951056516295154,1.,0.951056516295154,
1.,0.951056516295154,1.,0.951056516295154,1.,0.951056516295154,1.,0.951056516295154,
1.,0.951056516295154,1.,0.951056516295154,1.,0.951056516295154,1.,0.951056516295154,
1.,0.951056516295154,1.,0.951056516295154,1.,0.951056516295154,1.,0.951056516295154,
1.,0.951056516295154,1.,0.951056516295154,1.,0.951056516295154,1.,0.951056516295154,
1.,0.951056516295154,1.,0.951056516295154,1.,0.951056516295154,1.,0.951056516295154,
1.,0.951056516295154,1.,0.951056516295154,1.,0.951056516295154,1.,0.951056516295154,
1.,0.951056516295154,1.,0.951056516295154,1.,0.951056516295154,1.,0.951056516295154,
1.,0.951056516295154,1.,0.951056516295154,1.,0.951056516295154,1.,0.951056516295154,
1.,0.951056516295154,1.,0.951056516295154,1.,0.951056516295154,1.,0.951056516295154,
1.,0.951056516295154,1.,0.951056516295154,1.,0.951056516295154,1.,0.951056516295154,
1.,0.951056516295154,1.,0.951056516295154,1.,0.951056516295154,1.,0.951056516295154,
1.,0.951056516295154,1.,0.951056516295154,1.,0.951056516295154,1.,0.951056516295154,
1.,0.951056516295154,1.,0.951056516295154,1.,0.951056516295154,1.,0.951056516295154,
1.,0.951056516295154,1.,0.951056516295154,1.,0.951056516295154,1.,0.951056516295154,
1.,0.951056516295154,1.,0.951056516295154,1.,0.951056516295154,1.,0.951056516295154,
1.,0.951056516295154,1.,0.951056516295154,1.,0.951056516295154,1.,0.951056516295154,
1.,0.951056516295154,1.,0.951056516295154,1.,0.951056516295154,1.,0.951056516295154,
1.,0.951056516295154,1.,0.951056516295154,1.,0.951056516295154,1.,0.951056516295154,
1.,0.951056516295154,1.,0.951056516295154,1.,0.951056516295154,1.,0.951056516295154,
1.,0.951056516295154,1.,0.951056516295154,1.,0.951056516295154,1.,0.951056516295154,
1.,0.951056516295154,1.,0.951056516295154,1.,0.951056516295154,1.,0.951056516295154,
1.,0.951056516295154,1.,0.951056516295154,1.,0.951056516295154,1.,0.951056516295154,
1.,0.951056516295154,1.,0.951056516295154,1.,0.951056516295154,1.,0.951056516295154,
1.,0.951056516295154,1.,0.951056516295154,1.,0.951056516295154,1.,0.951056516295154,
1.,0.951056516295154,1.,0.951056516295154,1.,0.951056516295154,1.,0.951056516295154,
1.,0.951056516295154,1.,0.951056516295154,1.,0.951056516295154,1.,0.951056516295154,
1.,0.951056516295154,1.,0.951056516295154,1.,0.951056516295154,1.,0.951056516295154,
1.,0.951056516295154,1.,0.951056516295154,1.,0.951056516295154,1.,0.951056516295154,
1.,0.951056516295154,1.,0.951056516295154,1.,0.951056516295154,1.,0.951056516295154,
1.,0.951056516295154,1.,0.951056516295154,1.,0.951056516295154,1.,0.951056516295154,
1.,0.951056516295154,1.,0.951056516295154,1.,0.951056516295154,1.,0.951056516295154,
1.,0.951056516295154,1.,0.951056516295154,1.,0.951056516295154,1.,0.951056516295154,
1.,0.951056516295154,1.,0.951056516295154,1.,0.951056516295154,1.,0.951056516295154,
1.,0.951056516295154,1.,0.951056516295154,1.,0.951056516295154,1.,0.951056516295154,
1.,0.951056516295154,1.,0.951056516295154,1.,0.951056516295154,1.,0.951056516295154,
1.,0.951056516295154,1.,0.951056516295154,1.,0.951056516295154,1.,0.951056516295154,
1.,0.951056516295154,1.,0.951056516295154,1.,0.951056516295154,1.)))
REPRESENTATION_ITEM('')
SURFACE()
);
#3193=(
BOUNDED_SURFACE()
B_SPLINE_SURFACE(1,2,((#278547,#278548,#278549,#278550,#278551,#278552,
#278553,#278554,#278555,#278556,#278557,#278558,#278559,#278560,#278561,
#278562,#278563,#278564,#278565,#278566,#278567,#278568,#278569,#278570,
#278571,#278572,#278573,#278574,#278575,#278576,#278577,#278578,#278579,
#278580,#278581,#278582,#278583,#278584,#278585,#278586,#278587,#278588,
#278589,#278590,#278591,#278592,#278593,#278594,#278595,#278596,#278597,
#278598,#278599,#278600,#278601,#278602,#278603,#278604,#278605,#278606,
#278607,#278608,#278609,#278610,#278611,#278612,#278613,#278614,#278615,
#278616,#278617,#278618,#278619,#278620,#278621,#278622,#278623,#278624,
#278625,#278626,#278627,#278628,#278629,#278630,#278631,#278632,#278633,
#278634,#278635,#278636,#278637,#278638,#278639,#278640,#278641,#278642,
#278643,#278644,#278645,#278646,#278647,#278648,#278649,#278650,#278651,
#278652,#278653,#278654,#278655,#278656,#278657,#278658,#278659,#278660,
#278661,#278662,#278663,#278664,#278665,#278666,#278667,#278668,#278669,
#278670,#278671,#278672,#278673,#278674,#278675,#278676,#278677,#278678,
#278679,#278680,#278681,#278682,#278683,#278684,#278685,#278686,#278687,
#278688,#278689,#278690,#278691,#278692,#278693,#278694,#278695,#278696,
#278697,#278698,#278699,#278700,#278701,#278702,#278703,#278704,#278705,
#278706,#278707,#278708,#278709,#278710,#278711,#278712,#278713,#278714,
#278715,#278716,#278717,#278718,#278719,#278720,#278721,#278722,#278723,
#278724,#278725,#278726,#278727,#278728,#278729,#278730,#278731,#278732,
#278733,#278734,#278735,#278736,#278737,#278738,#278739,#278740,#278741,
#278742,#278743,#278744,#278745,#278746,#278747,#278748,#278749,#278750,
#278751,#278752,#278753,#278754,#278755,#278756,#278757,#278758,#278759,
#278760,#278761,#278762,#278763,#278764,#278765,#278766,#278767,#278768,
#278769,#278770,#278771,#278772,#278773,#278774,#278775,#278776,#278777,
#278778,#278779,#278780,#278781,#278782,#278783,#278784,#278785,#278786,
#278787,#278788,#278789,#278790,#278791,#278792,#278793,#278794,#278795,
#278796,#278797,#278798,#278799,#278800,#278801,#278802,#278803,#278804,
#278805,#278806,#278807,#278808,#278809,#278810,#278811,#278812,#278813,
#278814,#278815,#278816,#278817,#278818,#278819,#278820,#278821,#278822,
#278823,#278824,#278825,#278826,#278827,#278828,#278829,#278830,#278831,
#278832,#278833,#278834,#278835,#278836,#278837,#278838,#278839,#278840,
#278841,#278842,#278843,#278844,#278845,#278846,#278847,#278848,#278849,
#278850,#278851,#278852,#278853,#278854,#278855,#278856,#278857,#278858,
#278859,#278860,#278861,#278862,#278863,#278864,#278865,#278866,#278867,
#278868,#278869,#278870,#278871,#278872,#278873,#278874,#278875,#278876,
#278877,#278878,#278879,#278880,#278881,#278882,#278883,#278884,#278885,
#278886,#278887,#278888,#278889,#278890,#278891,#278892,#278893,#278894,
#278895,#278896,#278897,#278898,#278899,#278900,#278901,#278902,#278903,
#278904,#278905,#278906,#278907,#278908,#278909,#278910,#278911,#278912,
#278913,#278914,#278915,#278916,#278917,#278918,#278919,#278920,#278921,
#278922,#278923,#278924,#278925,#278926,#278927,#278928,#278929,#278930,
#278931,#278932,#278933,#278934,#278935,#278936,#278937,#278938,#278939,
#278940,#278941,#278942,#278943,#278944,#278945,#278946,#278947,#278948,
#278949,#278950,#278951,#278952,#278953,#278954,#278955,#278956,#278957,
#278958,#278959,#278960,#278961,#278962,#278963,#278964,#278965,#278966,
#278967,#278968,#278969,#278970,#278971,#278972,#278973,#278974,#278975,
#278976,#278977,#278978,#278979,#278980,#278981,#278982,#278983,#278984,
#278985,#278986,#278987,#278988,#278989,#278990,#278991,#278992,#278993,
#278994,#278995,#278996,#278997,#278998,#278999,#279000,#279001,#279002,
#279003,#279004,#279005,#279006,#279007,#279008,#279009,#279010,#279011,
#279012,#279013,#279014,#279015,#279016,#279017,#279018,#279019,#279020,
#279021,#279022,#279023,#279024,#279025,#279026,#279027,#279028,#279029,
#279030,#279031,#279032,#279033,#279034,#279035,#279036,#279037,#279038,
#279039,#279040,#279041,#279042,#279043,#279044,#279045,#279046,#279047,
#279048,#279049,#279050,#279051,#279052,#279053,#279054,#279055,#279056,
#279057,#279058,#279059,#279060,#279061,#279062,#279063,#279064,#279065,
#279066,#279067,#279068,#279069,#279070,#279071,#279072,#279073,#279074,
#279075,#279076,#279077,#279078,#279079,#279080,#279081,#279082,#279083,
#279084,#279085,#279086,#279087,#279088,#279089,#279090,#279091,#279092,
#279093,#279094,#279095,#279096,#279097,#279098,#279099,#279100,#279101,
#279102,#279103,#279104,#279105,#279106,#279107,#279108,#279109,#279110,
#279111,#279112,#279113,#279114,#279115,#279116,#279117,#279118,#279119,
#279120,#279121,#279122,#279123,#279124,#279125,#279126,#279127,#279128,
#279129,#279130,#279131,#279132,#279133,#279134,#279135,#279136,#279137,
#279138,#279139,#279140,#279141,#279142,#279143,#279144,#279145,#279146,
#279147,#279148,#279149,#279150,#279151,#279152,#279153,#279154,#279155,
#279156,#279157,#279158,#279159,#279160,#279161,#279162,#279163,#279164,
#279165,#279166,#279167,#279168,#279169,#279170,#279171,#279172,#279173,
#279174,#279175,#279176,#279177,#279178,#279179,#279180,#279181,#279182,
#279183,#279184,#279185,#279186,#279187,#279188,#279189,#279190,#279191,
#279192,#279193,#279194,#279195,#279196,#279197,#279198,#279199,#279200,
#279201,#279202,#279203,#279204,#279205,#279206,#279207,#279208,#279209,
#279210,#279211,#279212,#279213,#279214,#279215,#279216,#279217,#279218,
#279219,#279220,#279221,#279222,#279223,#279224,#279225,#279226,#279227,
#279228,#279229,#279230,#279231,#279232,#279233,#279234,#279235,#279236,
#279237,#279238,#279239,#279240,#279241,#279242,#279243,#279244,#279245,
#279246,#279247,#279248,#279249,#279250,#279251,#279252,#279253,#279254,
#279255,#279256,#279257,#279258,#279259,#279260,#279261,#279262,#279263,
#279264,#279265,#279266,#279267,#279268,#279269,#279270,#279271,#279272,
#279273,#279274,#279275,#279276,#279277,#279278,#279279,#279280,#279281,
#279282,#279283,#279284,#279285,#279286,#279287,#279288,#279289,#279290,
#279291,#279292,#279293,#279294,#279295,#279296,#279297,#279298,#279299,
#279300,#279301,#279302,#279303,#279304,#279305,#279306,#279307,#279308,
#279309,#279310,#279311,#279312,#279313,#279314,#279315,#279316,#279317,
#279318,#279319,#279320,#279321,#279322,#279323,#279324,#279325,#279326,
#279327,#279328,#279329,#279330,#279331,#279332,#279333,#279334,#279335,
#279336,#279337,#279338,#279339,#279340,#279341,#279342,#279343,#279344,
#279345,#279346,#279347,#279348,#279349,#279350,#279351,#279352,#279353,
#279354,#279355,#279356,#279357,#279358,#279359,#279360,#279361,#279362,
#279363,#279364,#279365,#279366,#279367,#279368,#279369,#279370,#279371,
#279372,#279373,#279374,#279375,#279376,#279377,#279378,#279379,#279380,
#279381,#279382,#279383,#279384,#279385,#279386,#279387,#279388,#279389,
#279390,#279391,#279392,#279393,#279394,#279395,#279396,#279397,#279398,
#279399,#279400,#279401,#279402,#279403,#279404,#279405,#279406,#279407,
#279408,#279409,#279410,#279411,#279412,#279413,#279414,#279415,#279416,
#279417,#279418,#279419,#279420,#279421,#279422,#279423,#279424,#279425,
#279426,#279427,#279428,#279429,#279430,#279431,#279432,#279433,#279434,
#279435,#279436,#279437,#279438,#279439,#279440,#279441,#279442,#279443,
#279444,#279445,#279446,#279447,#279448,#279449,#279450,#279451,#279452,
#279453,#279454,#279455,#279456,#279457,#279458,#279459,#279460,#279461,
#279462,#279463,#279464,#279465,#279466,#279467,#279468,#279469,#279470,
#279471,#279472,#279473,#279474,#279475,#279476,#279477,#279478,#279479,
#279480,#279481,#279482,#279483,#279484,#279485,#279486,#279487,#279488,
#279489,#279490,#279491,#279492,#279493,#279494,#279495,#279496,#279497,
#279498,#279499,#279500,#279501,#279502,#279503,#279504,#279505,#279506,
#279507,#279508,#279509,#279510,#279511,#279512,#279513,#279514,#279515,
#279516,#279517,#279518,#279519,#279520,#279521,#279522,#279523,#279524,
#279525,#279526,#279527,#279528,#279529,#279530,#279531,#279532,#279533,
#279534,#279535,#279536,#279537,#279538,#279539,#279540,#279541,#279542,
#279543,#279544,#279545,#279546,#279547,#279548,#279549,#279550,#279551,
#279552,#279553,#279554,#279555,#279556,#279557,#279558,#279559,#279560,
#279561,#279562,#279563,#279564,#279565,#279566,#279567,#279568,#279569,
#279570,#279571,#279572,#279573,#279574,#279575,#279576,#279577,#279578,
#279579,#279580,#279581,#279582,#279583),(#279584,#279585,#279586,#279587,
#279588,#279589,#279590,#279591,#279592,#279593,#279594,#279595,#279596,
#279597,#279598,#279599,#279600,#279601,#279602,#279603,#279604,#279605,
#279606,#279607,#279608,#279609,#279610,#279611,#279612,#279613,#279614,
#279615,#279616,#279617,#279618,#279619,#279620,#279621,#279622,#279623,
#279624,#279625,#279626,#279627,#279628,#279629,#279630,#279631,#279632,
#279633,#279634,#279635,#279636,#279637,#279638,#279639,#279640,#279641,
#279642,#279643,#279644,#279645,#279646,#279647,#279648,#279649,#279650,
#279651,#279652,#279653,#279654,#279655,#279656,#279657,#279658,#279659,
#279660,#279661,#279662,#279663,#279664,#279665,#279666,#279667,#279668,
#279669,#279670,#279671,#279672,#279673,#279674,#279675,#279676,#279677,
#279678,#279679,#279680,#279681,#279682,#279683,#279684,#279685,#279686,
#279687,#279688,#279689,#279690,#279691,#279692,#279693,#279694,#279695,
#279696,#279697,#279698,#279699,#279700,#279701,#279702,#279703,#279704,
#279705,#279706,#279707,#279708,#279709,#279710,#279711,#279712,#279713,
#279714,#279715,#279716,#279717,#279718,#279719,#279720,#279721,#279722,
#279723,#279724,#279725,#279726,#279727,#279728,#279729,#279730,#279731,
#279732,#279733,#279734,#279735,#279736,#279737,#279738,#279739,#279740,
#279741,#279742,#279743,#279744,#279745,#279746,#279747,#279748,#279749,
#279750,#279751,#279752,#279753,#279754,#279755,#279756,#279757,#279758,
#279759,#279760,#279761,#279762,#279763,#279764,#279765,#279766,#279767,
#279768,#279769,#279770,#279771,#279772,#279773,#279774,#279775,#279776,
#279777,#279778,#279779,#279780,#279781,#279782,#279783,#279784,#279785,
#279786,#279787,#279788,#279789,#279790,#279791,#279792,#279793,#279794,
#279795,#279796,#279797,#279798,#279799,#279800,#279801,#279802,#279803,
#279804,#279805,#279806,#279807,#279808,#279809,#279810,#279811,#279812,
#279813,#279814,#279815,#279816,#279817,#279818,#279819,#279820,#279821,
#279822,#279823,#279824,#279825,#279826,#279827,#279828,#279829,#279830,
#279831,#279832,#279833,#279834,#279835,#279836,#279837,#279838,#279839,
#279840,#279841,#279842,#279843,#279844,#279845,#279846,#279847,#279848,
#279849,#279850,#279851,#279852,#279853,#279854,#279855,#279856,#279857,
#279858,#279859,#279860,#279861,#279862,#279863,#279864,#279865,#279866,
#279867,#279868,#279869,#279870,#279871,#279872,#279873,#279874,#279875,
#279876,#279877,#279878,#279879,#279880,#279881,#279882,#279883,#279884,
#279885,#279886,#279887,#279888,#279889,#279890,#279891,#279892,#279893,
#279894,#279895,#279896,#279897,#279898,#279899,#279900,#279901,#279902,
#279903,#279904,#279905,#279906,#279907,#279908,#279909,#279910,#279911,
#279912,#279913,#279914,#279915,#279916,#279917,#279918,#279919,#279920,
#279921,#279922,#279923,#279924,#279925,#279926,#279927,#279928,#279929,
#279930,#279931,#279932,#279933,#279934,#279935,#279936,#279937,#279938,
#279939,#279940,#279941,#279942,#279943,#279944,#279945,#279946,#279947,
#279948,#279949,#279950,#279951,#279952,#279953,#279954,#279955,#279956,
#279957,#279958,#279959,#279960,#279961,#279962,#279963,#279964,#279965,
#279966,#279967,#279968,#279969,#279970,#279971,#279972,#279973,#279974,
#279975,#279976,#279977,#279978,#279979,#279980,#279981,#279982,#279983,
#279984,#279985,#279986,#279987,#279988,#279989,#279990,#279991,#279992,
#279993,#279994,#279995,#279996,#279997,#279998,#279999,#280000,#280001,
#280002,#280003,#280004,#280005,#280006,#280007,#280008,#280009,#280010,
#280011,#280012,#280013,#280014,#280015,#280016,#280017,#280018,#280019,
#280020,#280021,#280022,#280023,#280024,#280025,#280026,#280027,#280028,
#280029,#280030,#280031,#280032,#280033,#280034,#280035,#280036,#280037,
#280038,#280039,#280040,#280041,#280042,#280043,#280044,#280045,#280046,
#280047,#280048,#280049,#280050,#280051,#280052,#280053,#280054,#280055,
#280056,#280057,#280058,#280059,#280060,#280061,#280062,#280063,#280064,
#280065,#280066,#280067,#280068,#280069,#280070,#280071,#280072,#280073,
#280074,#280075,#280076,#280077,#280078,#280079,#280080,#280081,#280082,
#280083,#280084,#280085,#280086,#280087,#280088,#280089,#280090,#280091,
#280092,#280093,#280094,#280095,#280096,#280097,#280098,#280099,#280100,
#280101,#280102,#280103,#280104,#280105,#280106,#280107,#280108,#280109,
#280110,#280111,#280112,#280113,#280114,#280115,#280116,#280117,#280118,
#280119,#280120,#280121,#280122,#280123,#280124,#280125,#280126,#280127,
#280128,#280129,#280130,#280131,#280132,#280133,#280134,#280135,#280136,
#280137,#280138,#280139,#280140,#280141,#280142,#280143,#280144,#280145,
#280146,#280147,#280148,#280149,#280150,#280151,#280152,#280153,#280154,
#280155,#280156,#280157,#280158,#280159,#280160,#280161,#280162,#280163,
#280164,#280165,#280166,#280167,#280168,#280169,#280170,#280171,#280172,
#280173,#280174,#280175,#280176,#280177,#280178,#280179,#280180,#280181,
#280182,#280183,#280184,#280185,#280186,#280187,#280188,#280189,#280190,
#280191,#280192,#280193,#280194,#280195,#280196,#280197,#280198,#280199,
#280200,#280201,#280202,#280203,#280204,#280205,#280206,#280207,#280208,
#280209,#280210,#280211,#280212,#280213,#280214,#280215,#280216,#280217,
#280218,#280219,#280220,#280221,#280222,#280223,#280224,#280225,#280226,
#280227,#280228,#280229,#280230,#280231,#280232,#280233,#280234,#280235,
#280236,#280237,#280238,#280239,#280240,#280241,#280242,#280243,#280244,
#280245,#280246,#280247,#280248,#280249,#280250,#280251,#280252,#280253,
#280254,#280255,#280256,#280257,#280258,#280259,#280260,#280261,#280262,
#280263,#280264,#280265,#280266,#280267,#280268,#280269,#280270,#280271,
#280272,#280273,#280274,#280275,#280276,#280277,#280278,#280279,#280280,
#280281,#280282,#280283,#280284,#280285,#280286,#280287,#280288,#280289,
#280290,#280291,#280292,#280293,#280294,#280295,#280296,#280297,#280298,
#280299,#280300,#280301,#280302,#280303,#280304,#280305,#280306,#280307,
#280308,#280309,#280310,#280311,#280312,#280313,#280314,#280315,#280316,
#280317,#280318,#280319,#280320,#280321,#280322,#280323,#280324,#280325,
#280326,#280327,#280328,#280329,#280330,#280331,#280332,#280333,#280334,
#280335,#280336,#280337,#280338,#280339,#280340,#280341,#280342,#280343,
#280344,#280345,#280346,#280347,#280348,#280349,#280350,#280351,#280352,
#280353,#280354,#280355,#280356,#280357,#280358,#280359,#280360,#280361,
#280362,#280363,#280364,#280365,#280366,#280367,#280368,#280369,#280370,
#280371,#280372,#280373,#280374,#280375,#280376,#280377,#280378,#280379,
#280380,#280381,#280382,#280383,#280384,#280385,#280386,#280387,#280388,
#280389,#280390,#280391,#280392,#280393,#280394,#280395,#280396,#280397,
#280398,#280399,#280400,#280401,#280402,#280403,#280404,#280405,#280406,
#280407,#280408,#280409,#280410,#280411,#280412,#280413,#280414,#280415,
#280416,#280417,#280418,#280419,#280420,#280421,#280422,#280423,#280424,
#280425,#280426,#280427,#280428,#280429,#280430,#280431,#280432,#280433,
#280434,#280435,#280436,#280437,#280438,#280439,#280440,#280441,#280442,
#280443,#280444,#280445,#280446,#280447,#280448,#280449,#280450,#280451,
#280452,#280453,#280454,#280455,#280456,#280457,#280458,#280459,#280460,
#280461,#280462,#280463,#280464,#280465,#280466,#280467,#280468,#280469,
#280470,#280471,#280472,#280473,#280474,#280475,#280476,#280477,#280478,
#280479,#280480,#280481,#280482,#280483,#280484,#280485,#280486,#280487,
#280488,#280489,#280490,#280491,#280492,#280493,#280494,#280495,#280496,
#280497,#280498,#280499,#280500,#280501,#280502,#280503,#280504,#280505,
#280506,#280507,#280508,#280509,#280510,#280511,#280512,#280513,#280514,
#280515,#280516,#280517,#280518,#280519,#280520,#280521,#280522,#280523,
#280524,#280525,#280526,#280527,#280528,#280529,#280530,#280531,#280532,
#280533,#280534,#280535,#280536,#280537,#280538,#280539,#280540,#280541,
#280542,#280543,#280544,#280545,#280546,#280547,#280548,#280549,#280550,
#280551,#280552,#280553,#280554,#280555,#280556,#280557,#280558,#280559,
#280560,#280561,#280562,#280563,#280564,#280565,#280566,#280567,#280568,
#280569,#280570,#280571,#280572,#280573,#280574,#280575,#280576,#280577,
#280578,#280579,#280580,#280581,#280582,#280583,#280584,#280585,#280586,
#280587,#280588,#280589,#280590,#280591,#280592,#280593,#280594,#280595,
#280596,#280597,#280598,#280599,#280600,#280601,#280602,#280603,#280604,
#280605,#280606,#280607,#280608,#280609,#280610,#280611,#280612,#280613,
#280614,#280615,#280616,#280617,#280618,#280619,#280620)),.UNSPECIFIED.,
 .F.,.F.,.F.)
B_SPLINE_SURFACE_WITH_KNOTS((2,2),(3,2,2,2,2,2,2,2,2,2,2,2,2,2,2,2,2,2,
2,2,2,2,2,2,2,2,2,2,2,2,2,2,2,2,2,2,2,2,2,2,2,2,2,2,2,2,2,2,2,2,2,2,2,2,
2,2,2,2,2,2,2,2,2,2,2,2,2,2,2,2,2,2,2,2,2,2,2,2,2,2,2,2,2,2,2,2,2,2,2,2,
2,2,2,2,2,2,2,2,2,2,2,2,2,2,2,2,2,2,2,2,2,2,2,2,2,2,2,2,2,2,2,2,2,2,2,2,
2,2,2,2,2,2,2,2,2,2,2,2,2,2,2,2,2,2,2,2,2,2,2,2,2,2,2,2,2,2,2,2,2,2,2,2,
2,2,2,2,2,2,2,2,2,2,2,2,2,2,2,2,2,2,2,2,2,2,2,2,2,2,2,2,2,2,2,2,2,2,2,2,
2,2,2,2,2,2,2,2,2,2,2,2,2,2,2,2,2,2,2,2,2,2,2,2,2,2,2,2,2,2,2,2,2,2,2,2,
2,2,2,2,2,2,2,2,2,2,2,2,2,2,2,2,2,2,2,2,2,2,2,2,2,2,2,2,2,2,2,2,2,2,2,2,
2,2,2,2,2,2,2,2,2,2,2,2,2,2,2,2,2,2,2,2,2,2,2,2,2,2,2,2,2,2,2,2,2,2,2,2,
2,2,2,2,2,2,2,2,2,2,2,2,2,2,2,2,2,2,2,2,2,2,2,2,2,2,2,2,2,2,2,2,2,2,2,2,
2,2,2,2,2,2,2,2,2,2,2,2,2,2,2,2,2,2,2,2,2,2,2,2,2,2,2,2,2,2,2,2,2,2,2,2,
2,2,2,2,2,2,2,2,2,2,2,2,2,2,2,2,2,2,2,2,2,2,2,2,2,2,2,2,2,2,2,2,2,2,2,2,
2,2,2,2,2,2,2,2,2,2,2,2,2,2,2,2,2,2,2,2,2,2,2,2,2,2,2,2,2,2,2,2,2,2,2,2,
2,2,2,2,2,2,2,2,2,2,2,2,2,2,2,2,2,2,2,2,2,2,2,2,2,2,2,2,2,2,2,2,2,2,2,2,
2,2,2,2,2,2,2,2,2,2,2,2,2,2,2,2,2,2,2,2,2,2,2,2,2,2,2,2,2,2,2,2,3),(0.,
1.00000707949272),(0.,0.00192307692307692,0.00384615384615385,0.00576923076923077,
0.00769230769230769,0.00961538461538462,0.0115384615384615,0.0134615384615385,
0.0153846153846154,0.0173076923076923,0.0192307692307692,0.0211538461538462,
0.0230769230769231,0.025,0.0269230769230769,0.0288461538461538,0.0307692307692308,
0.0326923076923077,0.0346153846153846,0.0365384615384615,0.0384615384615385,
0.0403846153846154,0.0423076923076923,0.0442307692307692,0.0461538461538462,
0.0480769230769231,0.05,0.0519230769230769,0.0538461538461538,0.0557692307692308,
0.0576923076923077,0.0596153846153846,0.0615384615384615,0.0634615384615385,
0.0653846153846154,0.0673076923076923,0.0692307692307692,0.0711538461538462,
0.0730769230769231,0.075,0.0769230769230769,0.0788461538461538,0.0807692307692308,
0.0826923076923077,0.0846153846153846,0.0865384615384615,0.0884615384615385,
0.0903846153846154,0.0923076923076923,0.0942307692307692,0.0961538461538462,
0.0980769230769231,0.1,0.101923076923077,0.103846153846154,0.105769230769231,
0.107692307692308,0.109615384615385,0.111538461538462,0.113461538461538,
0.115384615384615,0.117307692307692,0.119230769230769,0.121153846153846,
0.123076923076923,0.125,0.126923076923077,0.128846153846154,0.130769230769231,
0.132692307692308,0.134615384615385,0.136538461538462,0.138461538461538,
0.140384615384615,0.142307692307692,0.144230769230769,0.146153846153846,
0.148076923076923,0.15,0.151923076923077,0.153846153846154,0.155769230769231,
0.157692307692308,0.159615384615385,0.161538461538462,0.163461538461538,
0.165384615384615,0.167307692307692,0.169230769230769,0.171153846153846,
0.173076923076923,0.175,0.176923076923077,0.178846153846154,0.180769230769231,
0.182692307692308,0.184615384615385,0.186538461538462,0.188461538461538,
0.190384615384615,0.192307692307692,0.194230769230769,0.196153846153846,
0.198076923076923,0.2,0.201923076923077,0.203846153846154,0.205769230769231,
0.207692307692308,0.209615384615385,0.211538461538462,0.213461538461538,
0.215384615384615,0.217307692307692,0.219230769230769,0.221153846153846,
0.223076923076923,0.225,0.226923076923077,0.228846153846154,0.230769230769231,
0.232692307692308,0.234615384615385,0.236538461538462,0.238461538461538,
0.240384615384615,0.242307692307692,0.244230769230769,0.246153846153846,
0.248076923076923,0.25,0.251923076923077,0.253846153846154,0.255769230769231,
0.257692307692308,0.259615384615385,0.261538461538462,0.263461538461538,
0.265384615384615,0.267307692307692,0.269230769230769,0.271153846153846,
0.273076923076923,0.275,0.276923076923077,0.278846153846154,0.280769230769231,
0.282692307692308,0.284615384615385,0.286538461538462,0.288461538461538,
0.290384615384615,0.292307692307692,0.294230769230769,0.296153846153846,
0.298076923076923,0.3,0.301923076923077,0.303846153846154,0.305769230769231,
0.307692307692308,0.309615384615385,0.311538461538462,0.313461538461538,
0.315384615384615,0.317307692307692,0.319230769230769,0.321153846153846,
0.323076923076923,0.325,0.326923076923077,0.328846153846154,0.330769230769231,
0.332692307692308,0.334615384615385,0.336538461538462,0.338461538461538,
0.340384615384615,0.342307692307692,0.344230769230769,0.346153846153846,
0.348076923076923,0.35,0.351923076923077,0.353846153846154,0.355769230769231,
0.357692307692308,0.359615384615385,0.361538461538462,0.363461538461538,
0.365384615384615,0.367307692307692,0.369230769230769,0.371153846153846,
0.373076923076923,0.375,0.376923076923077,0.378846153846154,0.380769230769231,
0.382692307692308,0.384615384615385,0.386538461538462,0.388461538461538,
0.390384615384615,0.392307692307692,0.394230769230769,0.396153846153846,
0.398076923076923,0.4,0.401923076923077,0.403846153846154,0.405769230769231,
0.407692307692308,0.409615384615385,0.411538461538462,0.413461538461538,
0.415384615384615,0.417307692307692,0.419230769230769,0.421153846153846,
0.423076923076923,0.425,0.426923076923077,0.428846153846154,0.430769230769231,
0.432692307692308,0.434615384615385,0.436538461538462,0.438461538461538,
0.440384615384615,0.442307692307692,0.444230769230769,0.446153846153846,
0.448076923076923,0.45,0.451923076923077,0.453846153846154,0.455769230769231,
0.457692307692308,0.459615384615385,0.461538461538462,0.463461538461538,
0.465384615384615,0.467307692307692,0.469230769230769,0.471153846153846,
0.473076923076923,0.475,0.476923076923077,0.478846153846154,0.480769230769231,
0.482692307692308,0.484615384615385,0.486538461538462,0.488461538461538,
0.490384615384615,0.492307692307692,0.494230769230769,0.496153846153846,
0.498076923076923,0.5,0.501923076923077,0.503846153846154,0.505769230769231,
0.507692307692308,0.509615384615385,0.511538461538461,0.513461538461538,
0.515384615384615,0.517307692307692,0.519230769230769,0.521153846153846,
0.523076923076923,0.525,0.526923076923077,0.528846153846154,0.530769230769231,
0.532692307692308,0.534615384615385,0.536538461538462,0.538461538461538,
0.540384615384615,0.542307692307692,0.544230769230769,0.546153846153846,
0.548076923076923,0.55,0.551923076923077,0.553846153846154,0.555769230769231,
0.557692307692308,0.559615384615385,0.561538461538462,0.563461538461538,
0.565384615384615,0.567307692307692,0.569230769230769,0.571153846153846,
0.573076923076923,0.575,0.576923076923077,0.578846153846154,0.580769230769231,
0.582692307692308,0.584615384615385,0.586538461538462,0.588461538461538,
0.590384615384615,0.592307692307692,0.594230769230769,0.596153846153846,
0.598076923076923,0.6,0.601923076923077,0.603846153846154,0.605769230769231,
0.607692307692308,0.609615384615385,0.611538461538462,0.613461538461539,
0.615384615384615,0.617307692307692,0.619230769230769,0.621153846153846,
0.623076923076923,0.625,0.626923076923077,0.628846153846154,0.630769230769231,
0.632692307692308,0.634615384615385,0.636538461538461,0.638461538461538,
0.640384615384615,0.642307692307692,0.644230769230769,0.646153846153846,
0.648076923076923,0.65,0.651923076923077,0.653846153846154,0.655769230769231,
0.657692307692308,0.659615384615385,0.661538461538462,0.663461538461538,
0.665384615384615,0.667307692307692,0.669230769230769,0.671153846153846,
0.673076923076923,0.675,0.676923076923077,0.678846153846154,0.680769230769231,
0.682692307692308,0.684615384615385,0.686538461538462,0.688461538461538,
0.690384615384615,0.692307692307692,0.694230769230769,0.696153846153846,
0.698076923076923,0.7,0.701923076923077,0.703846153846154,0.705769230769231,
0.707692307692308,0.709615384615385,0.711538461538462,0.713461538461538,
0.715384615384615,0.717307692307692,0.719230769230769,0.721153846153846,
0.723076923076923,0.725,0.726923076923077,0.728846153846154,0.730769230769231,
0.732692307692308,0.734615384615385,0.736538461538462,0.738461538461539,
0.740384615384615,0.742307692307692,0.744230769230769,0.746153846153846,
0.748076923076923,0.75,0.751923076923077,0.753846153846154,0.755769230769231,
0.757692307692308,0.759615384615385,0.761538461538461,0.763461538461538,
0.765384615384615,0.767307692307692,0.769230769230769,0.771153846153846,
0.773076923076923,0.775,0.776923076923077,0.778846153846154,0.780769230769231,
0.782692307692308,0.784615384615385,0.786538461538462,0.788461538461538,
0.790384615384615,0.792307692307692,0.794230769230769,0.796153846153846,
0.798076923076923,0.8,0.801923076923077,0.803846153846154,0.805769230769231,
0.807692307692308,0.809615384615385,0.811538461538462,0.813461538461538,
0.815384615384615,0.817307692307692,0.819230769230769,0.821153846153846,
0.823076923076923,0.825,0.826923076923077,0.828846153846154,0.830769230769231,
0.832692307692308,0.834615384615385,0.836538461538462,0.838461538461538,
0.840384615384615,0.842307692307692,0.844230769230769,0.846153846153846,
0.848076923076923,0.85,0.851923076923077,0.853846153846154,0.855769230769231,
0.857692307692308,0.859615384615385,0.861538461538462,0.863461538461539,
0.865384615384615,0.867307692307692,0.869230769230769,0.871153846153846,
0.873076923076923,0.875,0.876923076923077,0.878846153846154,0.880769230769231,
0.882692307692308,0.884615384615385,0.886538461538461,0.888461538461538,
0.890384615384615,0.892307692307692,0.894230769230769,0.896153846153846,
0.898076923076923,0.9,0.901923076923077,0.903846153846154,0.905769230769231,
0.907692307692308,0.909615384615385,0.911538461538462,0.913461538461538,
0.915384615384615,0.917307692307692,0.919230769230769,0.921153846153846,
0.923076923076923,0.925,0.926923076923077,0.928846153846154,0.930769230769231,
0.932692307692308,0.934615384615385,0.936538461538462,0.938461538461538,
0.940384615384615,0.942307692307692,0.944230769230769,0.946153846153846,
0.948076923076923,0.95,0.951923076923077,0.953846153846154,0.955769230769231,
0.957692307692308,0.959615384615385,0.961538461538462,0.963461538461538,
0.965384615384615,0.967307692307692,0.969230769230769,0.971153846153846,
0.973076923076923,0.975,0.976923076923077,0.978846153846154,0.980769230769231,
0.982692307692308,0.984615384615385,0.986538461538462,0.988461538461539,
0.990384615384615,0.992307692307692,0.994230769230769,0.996153846153846),
 .UNSPECIFIED.)
GEOMETRIC_REPRESENTATION_ITEM()
RATIONAL_B_SPLINE_SURFACE(((1.,0.951056516295154,1.,0.951056516295154,1.,
0.951056516295154,1.,0.951056516295154,1.,0.951056516295154,1.,0.951056516295154,
1.,0.951056516295154,1.,0.951056516295154,1.,0.951056516295154,1.,0.951056516295154,
1.,0.951056516295154,1.,0.951056516295154,1.,0.951056516295154,1.,0.951056516295154,
1.,0.951056516295154,1.,0.951056516295154,1.,0.951056516295154,1.,0.951056516295154,
1.,0.951056516295154,1.,0.951056516295154,1.,0.951056516295154,1.,0.951056516295154,
1.,0.951056516295154,1.,0.951056516295154,1.,0.951056516295154,1.,0.951056516295154,
1.,0.951056516295154,1.,0.951056516295154,1.,0.951056516295154,1.,0.951056516295154,
1.,0.951056516295154,1.,0.951056516295154,1.,0.951056516295154,1.,0.951056516295154,
1.,0.951056516295154,1.,0.951056516295154,1.,0.951056516295154,1.,0.951056516295154,
1.,0.951056516295154,1.,0.951056516295154,1.,0.951056516295154,1.,0.951056516295154,
1.,0.951056516295154,1.,0.951056516295154,1.,0.951056516295154,1.,0.951056516295154,
1.,0.951056516295154,1.,0.951056516295154,1.,0.951056516295154,1.,0.951056516295154,
1.,0.951056516295154,1.,0.951056516295154,1.,0.951056516295154,1.,0.951056516295154,
1.,0.951056516295154,1.,0.951056516295154,1.,0.951056516295154,1.,0.951056516295154,
1.,0.951056516295154,1.,0.951056516295154,1.,0.951056516295154,1.,0.951056516295154,
1.,0.951056516295154,1.,0.951056516295154,1.,0.951056516295154,1.,0.951056516295154,
1.,0.951056516295154,1.,0.951056516295154,1.,0.951056516295154,1.,0.951056516295154,
1.,0.951056516295154,1.,0.951056516295154,1.,0.951056516295154,1.,0.951056516295154,
1.,0.951056516295154,1.,0.951056516295154,1.,0.951056516295154,1.,0.951056516295154,
1.,0.951056516295154,1.,0.951056516295154,1.,0.951056516295154,1.,0.951056516295154,
1.,0.951056516295154,1.,0.951056516295154,1.,0.951056516295154,1.,0.951056516295154,
1.,0.951056516295154,1.,0.951056516295154,1.,0.951056516295154,1.,0.951056516295154,
1.,0.951056516295154,1.,0.951056516295154,1.,0.951056516295154,1.,0.951056516295154,
1.,0.951056516295154,1.,0.951056516295154,1.,0.951056516295154,1.,0.951056516295154,
1.,0.951056516295154,1.,0.951056516295154,1.,0.951056516295154,1.,0.951056516295154,
1.,0.951056516295154,1.,0.951056516295154,1.,0.951056516295154,1.,0.951056516295154,
1.,0.951056516295154,1.,0.951056516295154,1.,0.951056516295154,1.,0.951056516295154,
1.,0.951056516295154,1.,0.951056516295154,1.,0.951056516295154,1.,0.951056516295154,
1.,0.951056516295154,1.,0.951056516295154,1.,0.951056516295154,1.,0.951056516295154,
1.,0.951056516295154,1.,0.951056516295154,1.,0.951056516295154,1.,0.951056516295154,
1.,0.951056516295154,1.,0.951056516295154,1.,0.951056516295154,1.,0.951056516295154,
1.,0.951056516295154,1.,0.951056516295154,1.,0.951056516295154,1.,0.951056516295154,
1.,0.951056516295154,1.,0.951056516295154,1.,0.951056516295154,1.,0.951056516295154,
1.,0.951056516295154,1.,0.951056516295154,1.,0.951056516295154,1.,0.951056516295154,
1.,0.951056516295154,1.,0.951056516295154,1.,0.951056516295154,1.,0.951056516295154,
1.,0.951056516295154,1.,0.951056516295154,1.,0.951056516295154,1.,0.951056516295154,
1.,0.951056516295154,1.,0.951056516295154,1.,0.951056516295154,1.,0.951056516295154,
1.,0.951056516295154,1.,0.951056516295154,1.,0.951056516295154,1.,0.951056516295154,
1.,0.951056516295154,1.,0.951056516295154,1.,0.951056516295154,1.,0.951056516295154,
1.,0.951056516295154,1.,0.951056516295154,1.,0.951056516295154,1.,0.951056516295154,
1.,0.951056516295154,1.,0.951056516295154,1.,0.951056516295154,1.,0.951056516295154,
1.,0.951056516295154,1.,0.951056516295154,1.,0.951056516295154,1.,0.951056516295154,
1.,0.951056516295154,1.,0.951056516295154,1.,0.951056516295154,1.,0.951056516295154,
1.,0.951056516295154,1.,0.951056516295154,1.,0.951056516295154,1.,0.951056516295154,
1.,0.951056516295154,1.,0.951056516295154,1.,0.951056516295154,1.,0.951056516295154,
1.,0.951056516295154,1.,0.951056516295154,1.,0.951056516295154,1.,0.951056516295154,
1.,0.951056516295154,1.,0.951056516295154,1.,0.951056516295154,1.,0.951056516295154,
1.,0.951056516295154,1.,0.951056516295154,1.,0.951056516295154,1.,0.951056516295154,
1.,0.951056516295154,1.,0.951056516295154,1.,0.951056516295154,1.,0.951056516295154,
1.,0.951056516295154,1.,0.951056516295154,1.,0.951056516295154,1.,0.951056516295154,
1.,0.951056516295154,1.,0.951056516295154,1.,0.951056516295154,1.,0.951056516295154,
1.,0.951056516295154,1.,0.951056516295154,1.,0.951056516295154,1.,0.951056516295154,
1.,0.951056516295154,1.,0.951056516295154,1.,0.951056516295154,1.,0.951056516295154,
1.,0.951056516295154,1.,0.951056516295154,1.,0.951056516295154,1.,0.951056516295154,
1.,0.951056516295154,1.,0.951056516295154,1.,0.951056516295154,1.,0.951056516295154,
1.,0.951056516295154,1.,0.951056516295154,1.,0.951056516295154,1.,0.951056516295154,
1.,0.951056516295154,1.,0.951056516295154,1.,0.951056516295154,1.,0.951056516295154,
1.,0.951056516295154,1.,0.951056516295154,1.,0.951056516295154,1.,0.951056516295154,
1.,0.951056516295154,1.,0.951056516295154,1.,0.951056516295154,1.,0.951056516295154,
1.,0.951056516295154,1.,0.951056516295154,1.,0.951056516295154,1.,0.951056516295154,
1.,0.951056516295154,1.,0.951056516295154,1.,0.951056516295154,1.,0.951056516295154,
1.,0.951056516295154,1.,0.951056516295154,1.,0.951056516295154,1.,0.951056516295154,
1.,0.951056516295154,1.,0.951056516295154,1.,0.951056516295154,1.,0.951056516295154,
1.,0.951056516295154,1.,0.951056516295154,1.,0.951056516295154,1.,0.951056516295154,
1.,0.951056516295154,1.,0.951056516295154,1.,0.951056516295154,1.,0.951056516295154,
1.,0.951056516295154,1.,0.951056516295154,1.,0.951056516295154,1.,0.951056516295154,
1.,0.951056516295154,1.,0.951056516295154,1.,0.951056516295154,1.,0.951056516295154,
1.,0.951056516295154,1.,0.951056516295154,1.,0.951056516295154,1.,0.951056516295154,
1.,0.951056516295154,1.,0.951056516295154,1.,0.951056516295154,1.,0.951056516295154,
1.,0.951056516295154,1.,0.951056516295154,1.,0.951056516295154,1.,0.951056516295154,
1.,0.951056516295154,1.,0.951056516295154,1.,0.951056516295154,1.,0.951056516295154,
1.,0.951056516295154,1.,0.951056516295154,1.,0.951056516295154,1.,0.951056516295154,
1.,0.951056516295154,1.,0.951056516295154,1.,0.951056516295154,1.,0.951056516295154,
1.,0.951056516295154,1.,0.951056516295154,1.,0.951056516295154,1.,0.951056516295154,
1.,0.951056516295154,1.,0.951056516295154,1.,0.951056516295154,1.,0.951056516295154,
1.,0.951056516295154,1.,0.951056516295154,1.,0.951056516295154,1.,0.951056516295154,
1.,0.951056516295154,1.,0.951056516295154,1.,0.951056516295154,1.,0.951056516295154,
1.,0.951056516295154,1.,0.951056516295154,1.,0.951056516295154,1.,0.951056516295154,
1.,0.951056516295154,1.,0.951056516295154,1.,0.951056516295154,1.,0.951056516295154,
1.,0.951056516295154,1.,0.951056516295154,1.,0.951056516295154,1.,0.951056516295154,
1.,0.951056516295154,1.,0.951056516295154,1.,0.951056516295154,1.,0.951056516295154,
1.,0.951056516295154,1.,0.951056516295154,1.,0.951056516295154,1.,0.951056516295154,
1.,0.951056516295154,1.,0.951056516295154,1.,0.951056516295154,1.,0.951056516295154,
1.,0.951056516295154,1.,0.951056516295154,1.,0.951056516295154,1.,0.951056516295154,
1.,0.951056516295154,1.,0.951056516295154,1.,0.951056516295154,1.,0.951056516295154,
1.,0.951056516295154,1.,0.951056516295154,1.,0.951056516295154,1.,0.951056516295154,
1.,0.951056516295154,1.,0.951056516295154,1.,0.951056516295154,1.,0.951056516295154,
1.,0.951056516295154,1.,0.951056516295154,1.,0.951056516295154,1.,0.951056516295154,
1.,0.951056516295154,1.,0.951056516295154,1.,0.951056516295154,1.,0.951056516295154,
1.,0.951056516295154,1.,0.951056516295154,1.,0.951056516295154,1.,0.951056516295154,
1.,0.951056516295154,1.,0.951056516295154,1.,0.951056516295154,1.,0.951056516295154,
1.,0.951056516295154,1.,0.951056516295154,1.,0.951056516295154,1.,0.951056516295154,
1.,0.951056516295154,1.,0.951056516295154,1.,0.951056516295154,1.,0.951056516295154,
1.,0.951056516295154,1.,0.951056516295154,1.,0.951056516295154,1.,0.951056516295154,
1.,0.951056516295154,1.,0.951056516295154,1.,0.951056516295154,1.,0.951056516295154,
1.,0.951056516295154,1.,0.951056516295154,1.,0.951056516295154,1.,0.951056516295154,
1.,0.951056516295154,1.,0.951056516295154,1.,0.951056516295154,1.,0.951056516295154,
1.,0.951056516295154,1.,0.951056516295154,1.,0.951056516295154,1.,0.951056516295154,
1.,0.951056516295154,1.,0.951056516295154,1.,0.951056516295154,1.,0.951056516295154,
1.,0.951056516295154,1.,0.951056516295154,1.,0.951056516295154,1.,0.951056516295154,
1.,0.951056516295154,1.,0.951056516295154,1.,0.951056516295154,1.,0.951056516295154,
1.,0.951056516295154,1.,0.951056516295154,1.,0.951056516295154,1.,0.951056516295154,
1.,0.951056516295154,1.,0.951056516295154,1.,0.951056516295154,1.,0.951056516295154,
1.,0.951056516295154,1.,0.951056516295154,1.,0.951056516295154,1.,0.951056516295154,
1.,0.951056516295154,1.,0.951056516295154,1.,0.951056516295154,1.,0.951056516295154,
1.,0.951056516295154,1.,0.951056516295154,1.,0.951056516295154,1.,0.951056516295154,
1.,0.951056516295154,1.,0.951056516295154,1.,0.951056516295154,1.,0.951056516295154,
1.,0.951056516295154,1.,0.951056516295154,1.,0.951056516295154,1.,0.951056516295154,
1.,0.951056516295154,1.,0.951056516295154,1.,0.951056516295154,1.,0.951056516295154,
1.,0.951056516295154,1.,0.951056516295154,1.,0.951056516295154,1.,0.951056516295154,
1.,0.951056516295154,1.,0.951056516295154,1.,0.951056516295154,1.,0.951056516295154,
1.,0.951056516295154,1.,0.951056516295154,1.,0.951056516295154,1.,0.951056516295154,
1.,0.951056516295154,1.,0.951056516295154,1.,0.951056516295154,1.,0.951056516295154,
1.,0.951056516295154,1.,0.951056516295154,1.,0.951056516295154,1.,0.951056516295154,
1.,0.951056516295154,1.,0.951056516295154,1.,0.951056516295154,1.,0.951056516295154,
1.,0.951056516295154,1.,0.951056516295154,1.,0.951056516295154,1.,0.951056516295154,
1.,0.951056516295154,1.,0.951056516295154,1.,0.951056516295154,1.,0.951056516295154,
1.,0.951056516295154,1.,0.951056516295154,1.,0.951056516295154,1.,0.951056516295154,
1.,0.951056516295154,1.,0.951056516295154,1.,0.951056516295154,1.,0.951056516295154,
1.,0.951056516295154,1.,0.951056516295154,1.,0.951056516295154,1.,0.951056516295154,
1.,0.951056516295154,1.,0.951056516295154,1.,0.951056516295154,1.,0.951056516295154,
1.,0.951056516295154,1.,0.951056516295154,1.,0.951056516295154,1.,0.951056516295154,
1.,0.951056516295154,1.,0.951056516295154,1.,0.951056516295154,1.,0.951056516295154,
1.,0.951056516295154,1.,0.951056516295154,1.,0.951056516295154,1.,0.951056516295154,
1.,0.951056516295154,1.,0.951056516295154,1.,0.951056516295154,1.,0.951056516295154,
1.,0.951056516295154,1.,0.951056516295154,1.,0.951056516295154,1.,0.951056516295154,
1.,0.951056516295154,1.,0.951056516295154,1.,0.951056516295154,1.,0.951056516295154,
1.,0.951056516295154,1.,0.951056516295154,1.,0.951056516295154,1.,0.951056516295154,
1.,0.951056516295154,1.,0.951056516295154,1.,0.951056516295154,1.,0.951056516295154,
1.),(1.,0.951056516295154,1.,0.951056516295154,1.,0.951056516295154,1.,
0.951056516295154,1.,0.951056516295154,1.,0.951056516295154,1.,0.951056516295154,
1.,0.951056516295154,1.,0.951056516295154,1.,0.951056516295154,1.,0.951056516295154,
1.,0.951056516295154,1.,0.951056516295154,1.,0.951056516295154,1.,0.951056516295154,
1.,0.951056516295154,1.,0.951056516295154,1.,0.951056516295154,1.,0.951056516295154,
1.,0.951056516295154,1.,0.951056516295154,1.,0.951056516295154,1.,0.951056516295154,
1.,0.951056516295154,1.,0.951056516295154,1.,0.951056516295154,1.,0.951056516295154,
1.,0.951056516295154,1.,0.951056516295154,1.,0.951056516295154,1.,0.951056516295154,
1.,0.951056516295154,1.,0.951056516295154,1.,0.951056516295154,1.,0.951056516295154,
1.,0.951056516295154,1.,0.951056516295154,1.,0.951056516295154,1.,0.951056516295154,
1.,0.951056516295154,1.,0.951056516295154,1.,0.951056516295154,1.,0.951056516295154,
1.,0.951056516295154,1.,0.951056516295154,1.,0.951056516295154,1.,0.951056516295154,
1.,0.951056516295154,1.,0.951056516295154,1.,0.951056516295154,1.,0.951056516295154,
1.,0.951056516295154,1.,0.951056516295154,1.,0.951056516295154,1.,0.951056516295154,
1.,0.951056516295154,1.,0.951056516295154,1.,0.951056516295154,1.,0.951056516295154,
1.,0.951056516295154,1.,0.951056516295154,1.,0.951056516295154,1.,0.951056516295154,
1.,0.951056516295154,1.,0.951056516295154,1.,0.951056516295154,1.,0.951056516295154,
1.,0.951056516295154,1.,0.951056516295154,1.,0.951056516295154,1.,0.951056516295154,
1.,0.951056516295154,1.,0.951056516295154,1.,0.951056516295154,1.,0.951056516295154,
1.,0.951056516295154,1.,0.951056516295154,1.,0.951056516295154,1.,0.951056516295154,
1.,0.951056516295154,1.,0.951056516295154,1.,0.951056516295154,1.,0.951056516295154,
1.,0.951056516295154,1.,0.951056516295154,1.,0.951056516295154,1.,0.951056516295154,
1.,0.951056516295154,1.,0.951056516295154,1.,0.951056516295154,1.,0.951056516295154,
1.,0.951056516295154,1.,0.951056516295154,1.,0.951056516295154,1.,0.951056516295154,
1.,0.951056516295154,1.,0.951056516295154,1.,0.951056516295154,1.,0.951056516295154,
1.,0.951056516295154,1.,0.951056516295154,1.,0.951056516295154,1.,0.951056516295154,
1.,0.951056516295154,1.,0.951056516295154,1.,0.951056516295154,1.,0.951056516295154,
1.,0.951056516295154,1.,0.951056516295154,1.,0.951056516295154,1.,0.951056516295154,
1.,0.951056516295154,1.,0.951056516295154,1.,0.951056516295154,1.,0.951056516295154,
1.,0.951056516295154,1.,0.951056516295154,1.,0.951056516295154,1.,0.951056516295154,
1.,0.951056516295154,1.,0.951056516295154,1.,0.951056516295154,1.,0.951056516295154,
1.,0.951056516295154,1.,0.951056516295154,1.,0.951056516295154,1.,0.951056516295154,
1.,0.951056516295154,1.,0.951056516295154,1.,0.951056516295154,1.,0.951056516295154,
1.,0.951056516295154,1.,0.951056516295154,1.,0.951056516295154,1.,0.951056516295154,
1.,0.951056516295154,1.,0.951056516295154,1.,0.951056516295154,1.,0.951056516295154,
1.,0.951056516295154,1.,0.951056516295154,1.,0.951056516295154,1.,0.951056516295154,
1.,0.951056516295154,1.,0.951056516295154,1.,0.951056516295154,1.,0.951056516295154,
1.,0.951056516295154,1.,0.951056516295154,1.,0.951056516295154,1.,0.951056516295154,
1.,0.951056516295154,1.,0.951056516295154,1.,0.951056516295154,1.,0.951056516295154,
1.,0.951056516295154,1.,0.951056516295154,1.,0.951056516295154,1.,0.951056516295154,
1.,0.951056516295154,1.,0.951056516295154,1.,0.951056516295154,1.,0.951056516295154,
1.,0.951056516295154,1.,0.951056516295154,1.,0.951056516295154,1.,0.951056516295154,
1.,0.951056516295154,1.,0.951056516295154,1.,0.951056516295154,1.,0.951056516295154,
1.,0.951056516295154,1.,0.951056516295154,1.,0.951056516295154,1.,0.951056516295154,
1.,0.951056516295154,1.,0.951056516295154,1.,0.951056516295154,1.,0.951056516295154,
1.,0.951056516295154,1.,0.951056516295154,1.,0.951056516295154,1.,0.951056516295154,
1.,0.951056516295154,1.,0.951056516295154,1.,0.951056516295154,1.,0.951056516295154,
1.,0.951056516295154,1.,0.951056516295154,1.,0.951056516295154,1.,0.951056516295154,
1.,0.951056516295154,1.,0.951056516295154,1.,0.951056516295154,1.,0.951056516295154,
1.,0.951056516295154,1.,0.951056516295154,1.,0.951056516295154,1.,0.951056516295154,
1.,0.951056516295154,1.,0.951056516295154,1.,0.951056516295154,1.,0.951056516295154,
1.,0.951056516295154,1.,0.951056516295154,1.,0.951056516295154,1.,0.951056516295154,
1.,0.951056516295154,1.,0.951056516295154,1.,0.951056516295154,1.,0.951056516295154,
1.,0.951056516295154,1.,0.951056516295154,1.,0.951056516295154,1.,0.951056516295154,
1.,0.951056516295154,1.,0.951056516295154,1.,0.951056516295154,1.,0.951056516295154,
1.,0.951056516295154,1.,0.951056516295154,1.,0.951056516295154,1.,0.951056516295154,
1.,0.951056516295154,1.,0.951056516295154,1.,0.951056516295154,1.,0.951056516295154,
1.,0.951056516295154,1.,0.951056516295154,1.,0.951056516295154,1.,0.951056516295154,
1.,0.951056516295154,1.,0.951056516295154,1.,0.951056516295154,1.,0.951056516295154,
1.,0.951056516295154,1.,0.951056516295154,1.,0.951056516295154,1.,0.951056516295154,
1.,0.951056516295154,1.,0.951056516295154,1.,0.951056516295154,1.,0.951056516295154,
1.,0.951056516295154,1.,0.951056516295154,1.,0.951056516295154,1.,0.951056516295154,
1.,0.951056516295154,1.,0.951056516295154,1.,0.951056516295154,1.,0.951056516295154,
1.,0.951056516295154,1.,0.951056516295154,1.,0.951056516295154,1.,0.951056516295154,
1.,0.951056516295154,1.,0.951056516295154,1.,0.951056516295154,1.,0.951056516295154,
1.,0.951056516295154,1.,0.951056516295154,1.,0.951056516295154,1.,0.951056516295154,
1.,0.951056516295154,1.,0.951056516295154,1.,0.951056516295154,1.,0.951056516295154,
1.,0.951056516295154,1.,0.951056516295154,1.,0.951056516295154,1.,0.951056516295154,
1.,0.951056516295154,1.,0.951056516295154,1.,0.951056516295154,1.,0.951056516295154,
1.,0.951056516295154,1.,0.951056516295154,1.,0.951056516295154,1.,0.951056516295154,
1.,0.951056516295154,1.,0.951056516295154,1.,0.951056516295154,1.,0.951056516295154,
1.,0.951056516295154,1.,0.951056516295154,1.,0.951056516295154,1.,0.951056516295154,
1.,0.951056516295154,1.,0.951056516295154,1.,0.951056516295154,1.,0.951056516295154,
1.,0.951056516295154,1.,0.951056516295154,1.,0.951056516295154,1.,0.951056516295154,
1.,0.951056516295154,1.,0.951056516295154,1.,0.951056516295154,1.,0.951056516295154,
1.,0.951056516295154,1.,0.951056516295154,1.,0.951056516295154,1.,0.951056516295154,
1.,0.951056516295154,1.,0.951056516295154,1.,0.951056516295154,1.,0.951056516295154,
1.,0.951056516295154,1.,0.951056516295154,1.,0.951056516295154,1.,0.951056516295154,
1.,0.951056516295154,1.,0.951056516295154,1.,0.951056516295154,1.,0.951056516295154,
1.,0.951056516295154,1.,0.951056516295154,1.,0.951056516295154,1.,0.951056516295154,
1.,0.951056516295154,1.,0.951056516295154,1.,0.951056516295154,1.,0.951056516295154,
1.,0.951056516295154,1.,0.951056516295154,1.,0.951056516295154,1.,0.951056516295154,
1.,0.951056516295154,1.,0.951056516295154,1.,0.951056516295154,1.,0.951056516295154,
1.,0.951056516295154,1.,0.951056516295154,1.,0.951056516295154,1.,0.951056516295154,
1.,0.951056516295154,1.,0.951056516295154,1.,0.951056516295154,1.,0.951056516295154,
1.,0.951056516295154,1.,0.951056516295154,1.,0.951056516295154,1.,0.951056516295154,
1.,0.951056516295154,1.,0.951056516295154,1.,0.951056516295154,1.,0.951056516295154,
1.,0.951056516295154,1.,0.951056516295154,1.,0.951056516295154,1.,0.951056516295154,
1.,0.951056516295154,1.,0.951056516295154,1.,0.951056516295154,1.,0.951056516295154,
1.,0.951056516295154,1.,0.951056516295154,1.,0.951056516295154,1.,0.951056516295154,
1.,0.951056516295154,1.,0.951056516295154,1.,0.951056516295154,1.,0.951056516295154,
1.,0.951056516295154,1.,0.951056516295154,1.,0.951056516295154,1.,0.951056516295154,
1.,0.951056516295154,1.,0.951056516295154,1.,0.951056516295154,1.,0.951056516295154,
1.,0.951056516295154,1.,0.951056516295154,1.,0.951056516295154,1.,0.951056516295154,
1.,0.951056516295154,1.,0.951056516295154,1.,0.951056516295154,1.,0.951056516295154,
1.,0.951056516295154,1.,0.951056516295154,1.,0.951056516295154,1.,0.951056516295154,
1.,0.951056516295154,1.,0.951056516295154,1.,0.951056516295154,1.,0.951056516295154,
1.,0.951056516295154,1.,0.951056516295154,1.,0.951056516295154,1.,0.951056516295154,
1.,0.951056516295154,1.,0.951056516295154,1.,0.951056516295154,1.,0.951056516295154,
1.,0.951056516295154,1.,0.951056516295154,1.,0.951056516295154,1.,0.951056516295154,
1.,0.951056516295154,1.,0.951056516295154,1.,0.951056516295154,1.,0.951056516295154,
1.,0.951056516295154,1.,0.951056516295154,1.,0.951056516295154,1.,0.951056516295154,
1.,0.951056516295154,1.,0.951056516295154,1.,0.951056516295154,1.,0.951056516295154,
1.,0.951056516295154,1.,0.951056516295154,1.,0.951056516295154,1.,0.951056516295154,
1.,0.951056516295154,1.,0.951056516295154,1.,0.951056516295154,1.,0.951056516295154,
1.,0.951056516295154,1.,0.951056516295154,1.,0.951056516295154,1.,0.951056516295154,
1.,0.951056516295154,1.,0.951056516295154,1.,0.951056516295154,1.,0.951056516295154,
1.,0.951056516295154,1.,0.951056516295154,1.,0.951056516295154,1.,0.951056516295154,
1.,0.951056516295154,1.,0.951056516295154,1.,0.951056516295154,1.,0.951056516295154,
1.,0.951056516295154,1.,0.951056516295154,1.,0.951056516295154,1.,0.951056516295154,
1.,0.951056516295154,1.,0.951056516295154,1.,0.951056516295154,1.,0.951056516295154,
1.,0.951056516295154,1.,0.951056516295154,1.,0.951056516295154,1.,0.951056516295154,
1.,0.951056516295154,1.,0.951056516295154,1.,0.951056516295154,1.,0.951056516295154,
1.,0.951056516295154,1.,0.951056516295154,1.,0.951056516295154,1.,0.951056516295154,
1.,0.951056516295154,1.,0.951056516295154,1.,0.951056516295154,1.,0.951056516295154,
1.,0.951056516295154,1.,0.951056516295154,1.,0.951056516295154,1.,0.951056516295154,
1.,0.951056516295154,1.,0.951056516295154,1.,0.951056516295154,1.,0.951056516295154,
1.,0.951056516295154,1.,0.951056516295154,1.,0.951056516295154,1.,0.951056516295154,
1.,0.951056516295154,1.,0.951056516295154,1.,0.951056516295154,1.,0.951056516295154,
1.,0.951056516295154,1.,0.951056516295154,1.,0.951056516295154,1.,0.951056516295154,
1.,0.951056516295154,1.,0.951056516295154,1.,0.951056516295154,1.,0.951056516295154,
1.,0.951056516295154,1.,0.951056516295154,1.,0.951056516295154,1.,0.951056516295154,
1.,0.951056516295154,1.,0.951056516295154,1.,0.951056516295154,1.,0.951056516295154,
1.,0.951056516295154,1.,0.951056516295154,1.,0.951056516295154,1.,0.951056516295154,
1.,0.951056516295154,1.,0.951056516295154,1.,0.951056516295154,1.,0.951056516295154,
1.,0.951056516295154,1.,0.951056516295154,1.,0.951056516295154,1.,0.951056516295154,
1.,0.951056516295154,1.,0.951056516295154,1.,0.951056516295154,1.,0.951056516295154,
1.,0.951056516295154,1.,0.951056516295154,1.,0.951056516295154,1.,0.951056516295154,
1.,0.951056516295154,1.,0.951056516295154,1.,0.951056516295154,1.,0.951056516295154,
1.,0.951056516295154,1.,0.951056516295154,1.,0.951056516295154,1.)))
REPRESENTATION_ITEM('')
SURFACE()
);
#3194=(
BOUNDED_SURFACE()
B_SPLINE_SURFACE(1,2,((#281515,#281516,#281517,#281518,#281519,#281520,
#281521,#281522,#281523,#281524,#281525,#281526,#281527,#281528,#281529,
#281530,#281531,#281532,#281533,#281534,#281535,#281536,#281537,#281538,
#281539,#281540,#281541,#281542,#281543,#281544,#281545,#281546,#281547,
#281548,#281549,#281550,#281551,#281552,#281553,#281554,#281555,#281556,
#281557,#281558,#281559,#281560,#281561,#281562,#281563,#281564,#281565,
#281566,#281567,#281568,#281569,#281570,#281571,#281572,#281573,#281574,
#281575,#281576,#281577,#281578,#281579,#281580,#281581,#281582,#281583,
#281584,#281585,#281586,#281587,#281588,#281589,#281590,#281591,#281592,
#281593,#281594,#281595,#281596,#281597,#281598,#281599,#281600,#281601,
#281602,#281603,#281604,#281605,#281606,#281607,#281608,#281609,#281610,
#281611,#281612,#281613,#281614,#281615,#281616,#281617,#281618,#281619,
#281620,#281621,#281622,#281623,#281624,#281625,#281626,#281627,#281628,
#281629,#281630,#281631,#281632,#281633,#281634,#281635,#281636,#281637,
#281638,#281639,#281640,#281641,#281642,#281643,#281644,#281645,#281646,
#281647,#281648,#281649,#281650,#281651,#281652,#281653,#281654,#281655,
#281656,#281657,#281658,#281659,#281660,#281661,#281662,#281663,#281664,
#281665,#281666,#281667,#281668,#281669,#281670,#281671,#281672,#281673,
#281674,#281675,#281676,#281677,#281678,#281679,#281680,#281681,#281682,
#281683,#281684,#281685,#281686,#281687,#281688,#281689,#281690,#281691,
#281692,#281693,#281694,#281695,#281696,#281697,#281698,#281699,#281700,
#281701,#281702,#281703,#281704,#281705,#281706,#281707,#281708,#281709,
#281710,#281711,#281712,#281713,#281714,#281715,#281716,#281717,#281718,
#281719,#281720,#281721,#281722,#281723,#281724,#281725,#281726,#281727,
#281728,#281729,#281730,#281731,#281732,#281733,#281734,#281735,#281736,
#281737,#281738,#281739,#281740,#281741,#281742,#281743,#281744,#281745,
#281746,#281747,#281748,#281749,#281750,#281751,#281752,#281753,#281754,
#281755,#281756,#281757,#281758,#281759,#281760,#281761,#281762,#281763,
#281764,#281765,#281766,#281767,#281768,#281769,#281770,#281771,#281772,
#281773,#281774,#281775,#281776,#281777,#281778,#281779,#281780,#281781,
#281782,#281783,#281784,#281785,#281786,#281787,#281788,#281789,#281790,
#281791,#281792,#281793,#281794,#281795,#281796,#281797,#281798,#281799,
#281800,#281801,#281802,#281803,#281804,#281805,#281806,#281807,#281808,
#281809,#281810,#281811,#281812,#281813,#281814,#281815,#281816,#281817,
#281818,#281819,#281820,#281821,#281822,#281823,#281824,#281825,#281826,
#281827,#281828,#281829,#281830,#281831,#281832,#281833,#281834,#281835,
#281836,#281837,#281838,#281839,#281840,#281841,#281842,#281843,#281844,
#281845,#281846,#281847,#281848,#281849,#281850,#281851,#281852,#281853,
#281854,#281855,#281856,#281857,#281858,#281859,#281860,#281861,#281862,
#281863,#281864,#281865,#281866,#281867,#281868,#281869,#281870,#281871,
#281872,#281873,#281874,#281875,#281876,#281877,#281878,#281879,#281880,
#281881,#281882,#281883,#281884,#281885,#281886,#281887,#281888,#281889,
#281890,#281891,#281892,#281893,#281894,#281895,#281896,#281897,#281898,
#281899,#281900,#281901,#281902,#281903,#281904,#281905,#281906,#281907,
#281908,#281909,#281910,#281911,#281912,#281913,#281914,#281915,#281916,
#281917,#281918,#281919,#281920,#281921,#281922,#281923,#281924,#281925,
#281926,#281927,#281928,#281929,#281930,#281931,#281932,#281933,#281934,
#281935,#281936,#281937,#281938,#281939,#281940,#281941,#281942,#281943,
#281944,#281945,#281946,#281947,#281948,#281949,#281950,#281951,#281952,
#281953,#281954,#281955,#281956,#281957,#281958,#281959,#281960,#281961,
#281962,#281963,#281964,#281965,#281966,#281967,#281968,#281969,#281970,
#281971,#281972,#281973,#281974,#281975,#281976,#281977,#281978,#281979,
#281980,#281981,#281982,#281983,#281984,#281985,#281986,#281987,#281988,
#281989,#281990,#281991,#281992,#281993,#281994,#281995,#281996,#281997,
#281998,#281999,#282000,#282001,#282002,#282003,#282004,#282005,#282006,
#282007,#282008,#282009,#282010,#282011,#282012,#282013,#282014,#282015,
#282016,#282017,#282018,#282019,#282020,#282021,#282022,#282023,#282024,
#282025,#282026,#282027,#282028,#282029,#282030,#282031,#282032,#282033,
#282034,#282035,#282036,#282037,#282038,#282039,#282040,#282041,#282042,
#282043,#282044,#282045,#282046,#282047,#282048,#282049,#282050,#282051,
#282052,#282053,#282054,#282055,#282056,#282057,#282058,#282059,#282060,
#282061,#282062,#282063,#282064,#282065,#282066,#282067,#282068,#282069,
#282070,#282071,#282072,#282073,#282074,#282075,#282076,#282077,#282078,
#282079,#282080,#282081,#282082,#282083,#282084,#282085,#282086,#282087,
#282088,#282089,#282090,#282091,#282092,#282093,#282094,#282095,#282096,
#282097,#282098,#282099,#282100,#282101,#282102,#282103,#282104,#282105,
#282106,#282107,#282108,#282109,#282110,#282111,#282112,#282113,#282114,
#282115,#282116,#282117,#282118,#282119,#282120,#282121,#282122,#282123,
#282124,#282125,#282126,#282127,#282128,#282129,#282130,#282131,#282132,
#282133,#282134,#282135,#282136,#282137,#282138,#282139,#282140,#282141,
#282142,#282143,#282144,#282145,#282146,#282147,#282148,#282149,#282150,
#282151,#282152,#282153,#282154,#282155,#282156,#282157,#282158,#282159,
#282160,#282161,#282162,#282163,#282164,#282165,#282166,#282167,#282168,
#282169,#282170,#282171,#282172,#282173,#282174,#282175,#282176,#282177,
#282178,#282179,#282180,#282181,#282182,#282183,#282184,#282185,#282186,
#282187,#282188,#282189,#282190,#282191,#282192,#282193,#282194,#282195,
#282196,#282197,#282198,#282199,#282200,#282201,#282202,#282203,#282204,
#282205,#282206,#282207,#282208,#282209,#282210,#282211,#282212,#282213,
#282214,#282215,#282216,#282217,#282218,#282219,#282220,#282221,#282222,
#282223,#282224,#282225,#282226,#282227,#282228,#282229,#282230,#282231,
#282232,#282233,#282234,#282235,#282236,#282237,#282238,#282239,#282240,
#282241,#282242,#282243,#282244,#282245,#282246,#282247,#282248,#282249,
#282250,#282251,#282252,#282253,#282254,#282255,#282256,#282257,#282258,
#282259,#282260,#282261,#282262,#282263,#282264,#282265,#282266,#282267,
#282268,#282269,#282270,#282271,#282272,#282273,#282274,#282275,#282276,
#282277,#282278,#282279,#282280,#282281,#282282,#282283,#282284,#282285,
#282286,#282287,#282288,#282289,#282290,#282291,#282292,#282293,#282294,
#282295,#282296,#282297,#282298,#282299,#282300,#282301,#282302,#282303,
#282304,#282305,#282306,#282307,#282308,#282309,#282310,#282311,#282312,
#282313,#282314,#282315,#282316,#282317,#282318,#282319,#282320,#282321,
#282322,#282323,#282324,#282325,#282326,#282327,#282328,#282329,#282330,
#282331,#282332,#282333,#282334,#282335,#282336,#282337,#282338,#282339,
#282340,#282341,#282342,#282343,#282344,#282345,#282346,#282347,#282348,
#282349,#282350,#282351,#282352,#282353,#282354,#282355,#282356,#282357,
#282358,#282359,#282360,#282361,#282362,#282363,#282364,#282365,#282366,
#282367,#282368,#282369,#282370,#282371,#282372,#282373,#282374,#282375,
#282376,#282377,#282378,#282379,#282380,#282381,#282382,#282383,#282384,
#282385,#282386,#282387,#282388,#282389,#282390,#282391,#282392,#282393,
#282394,#282395,#282396,#282397,#282398,#282399,#282400,#282401,#282402,
#282403,#282404,#282405,#282406,#282407,#282408,#282409,#282410,#282411,
#282412,#282413,#282414,#282415,#282416,#282417,#282418,#282419,#282420,
#282421,#282422,#282423,#282424,#282425,#282426,#282427,#282428,#282429,
#282430,#282431,#282432,#282433,#282434,#282435,#282436,#282437,#282438,
#282439,#282440,#282441,#282442,#282443,#282444,#282445,#282446,#282447,
#282448,#282449,#282450,#282451,#282452,#282453,#282454,#282455,#282456,
#282457,#282458,#282459,#282460,#282461,#282462,#282463,#282464,#282465,
#282466,#282467,#282468,#282469,#282470,#282471,#282472,#282473,#282474,
#282475,#282476,#282477,#282478,#282479,#282480,#282481,#282482,#282483,
#282484,#282485,#282486,#282487,#282488,#282489,#282490,#282491,#282492,
#282493,#282494,#282495,#282496,#282497,#282498,#282499,#282500,#282501,
#282502,#282503,#282504,#282505,#282506,#282507,#282508,#282509,#282510,
#282511,#282512,#282513,#282514,#282515,#282516,#282517,#282518,#282519,
#282520,#282521,#282522,#282523,#282524,#282525,#282526,#282527,#282528,
#282529,#282530,#282531,#282532,#282533,#282534,#282535,#282536,#282537,
#282538,#282539,#282540,#282541,#282542,#282543,#282544,#282545,#282546,
#282547,#282548,#282549,#282550,#282551),(#282552,#282553,#282554,#282555,
#282556,#282557,#282558,#282559,#282560,#282561,#282562,#282563,#282564,
#282565,#282566,#282567,#282568,#282569,#282570,#282571,#282572,#282573,
#282574,#282575,#282576,#282577,#282578,#282579,#282580,#282581,#282582,
#282583,#282584,#282585,#282586,#282587,#282588,#282589,#282590,#282591,
#282592,#282593,#282594,#282595,#282596,#282597,#282598,#282599,#282600,
#282601,#282602,#282603,#282604,#282605,#282606,#282607,#282608,#282609,
#282610,#282611,#282612,#282613,#282614,#282615,#282616,#282617,#282618,
#282619,#282620,#282621,#282622,#282623,#282624,#282625,#282626,#282627,
#282628,#282629,#282630,#282631,#282632,#282633,#282634,#282635,#282636,
#282637,#282638,#282639,#282640,#282641,#282642,#282643,#282644,#282645,
#282646,#282647,#282648,#282649,#282650,#282651,#282652,#282653,#282654,
#282655,#282656,#282657,#282658,#282659,#282660,#282661,#282662,#282663,
#282664,#282665,#282666,#282667,#282668,#282669,#282670,#282671,#282672,
#282673,#282674,#282675,#282676,#282677,#282678,#282679,#282680,#282681,
#282682,#282683,#282684,#282685,#282686,#282687,#282688,#282689,#282690,
#282691,#282692,#282693,#282694,#282695,#282696,#282697,#282698,#282699,
#282700,#282701,#282702,#282703,#282704,#282705,#282706,#282707,#282708,
#282709,#282710,#282711,#282712,#282713,#282714,#282715,#282716,#282717,
#282718,#282719,#282720,#282721,#282722,#282723,#282724,#282725,#282726,
#282727,#282728,#282729,#282730,#282731,#282732,#282733,#282734,#282735,
#282736,#282737,#282738,#282739,#282740,#282741,#282742,#282743,#282744,
#282745,#282746,#282747,#282748,#282749,#282750,#282751,#282752,#282753,
#282754,#282755,#282756,#282757,#282758,#282759,#282760,#282761,#282762,
#282763,#282764,#282765,#282766,#282767,#282768,#282769,#282770,#282771,
#282772,#282773,#282774,#282775,#282776,#282777,#282778,#282779,#282780,
#282781,#282782,#282783,#282784,#282785,#282786,#282787,#282788,#282789,
#282790,#282791,#282792,#282793,#282794,#282795,#282796,#282797,#282798,
#282799,#282800,#282801,#282802,#282803,#282804,#282805,#282806,#282807,
#282808,#282809,#282810,#282811,#282812,#282813,#282814,#282815,#282816,
#282817,#282818,#282819,#282820,#282821,#282822,#282823,#282824,#282825,
#282826,#282827,#282828,#282829,#282830,#282831,#282832,#282833,#282834,
#282835,#282836,#282837,#282838,#282839,#282840,#282841,#282842,#282843,
#282844,#282845,#282846,#282847,#282848,#282849,#282850,#282851,#282852,
#282853,#282854,#282855,#282856,#282857,#282858,#282859,#282860,#282861,
#282862,#282863,#282864,#282865,#282866,#282867,#282868,#282869,#282870,
#282871,#282872,#282873,#282874,#282875,#282876,#282877,#282878,#282879,
#282880,#282881,#282882,#282883,#282884,#282885,#282886,#282887,#282888,
#282889,#282890,#282891,#282892,#282893,#282894,#282895,#282896,#282897,
#282898,#282899,#282900,#282901,#282902,#282903,#282904,#282905,#282906,
#282907,#282908,#282909,#282910,#282911,#282912,#282913,#282914,#282915,
#282916,#282917,#282918,#282919,#282920,#282921,#282922,#282923,#282924,
#282925,#282926,#282927,#282928,#282929,#282930,#282931,#282932,#282933,
#282934,#282935,#282936,#282937,#282938,#282939,#282940,#282941,#282942,
#282943,#282944,#282945,#282946,#282947,#282948,#282949,#282950,#282951,
#282952,#282953,#282954,#282955,#282956,#282957,#282958,#282959,#282960,
#282961,#282962,#282963,#282964,#282965,#282966,#282967,#282968,#282969,
#282970,#282971,#282972,#282973,#282974,#282975,#282976,#282977,#282978,
#282979,#282980,#282981,#282982,#282983,#282984,#282985,#282986,#282987,
#282988,#282989,#282990,#282991,#282992,#282993,#282994,#282995,#282996,
#282997,#282998,#282999,#283000,#283001,#283002,#283003,#283004,#283005,
#283006,#283007,#283008,#283009,#283010,#283011,#283012,#283013,#283014,
#283015,#283016,#283017,#283018,#283019,#283020,#283021,#283022,#283023,
#283024,#283025,#283026,#283027,#283028,#283029,#283030,#283031,#283032,
#283033,#283034,#283035,#283036,#283037,#283038,#283039,#283040,#283041,
#283042,#283043,#283044,#283045,#283046,#283047,#283048,#283049,#283050,
#283051,#283052,#283053,#283054,#283055,#283056,#283057,#283058,#283059,
#283060,#283061,#283062,#283063,#283064,#283065,#283066,#283067,#283068,
#283069,#283070,#283071,#283072,#283073,#283074,#283075,#283076,#283077,
#283078,#283079,#283080,#283081,#283082,#283083,#283084,#283085,#283086,
#283087,#283088,#283089,#283090,#283091,#283092,#283093,#283094,#283095,
#283096,#283097,#283098,#283099,#283100,#283101,#283102,#283103,#283104,
#283105,#283106,#283107,#283108,#283109,#283110,#283111,#283112,#283113,
#283114,#283115,#283116,#283117,#283118,#283119,#283120,#283121,#283122,
#283123,#283124,#283125,#283126,#283127,#283128,#283129,#283130,#283131,
#283132,#283133,#283134,#283135,#283136,#283137,#283138,#283139,#283140,
#283141,#283142,#283143,#283144,#283145,#283146,#283147,#283148,#283149,
#283150,#283151,#283152,#283153,#283154,#283155,#283156,#283157,#283158,
#283159,#283160,#283161,#283162,#283163,#283164,#283165,#283166,#283167,
#283168,#283169,#283170,#283171,#283172,#283173,#283174,#283175,#283176,
#283177,#283178,#283179,#283180,#283181,#283182,#283183,#283184,#283185,
#283186,#283187,#283188,#283189,#283190,#283191,#283192,#283193,#283194,
#283195,#283196,#283197,#283198,#283199,#283200,#283201,#283202,#283203,
#283204,#283205,#283206,#283207,#283208,#283209,#283210,#283211,#283212,
#283213,#283214,#283215,#283216,#283217,#283218,#283219,#283220,#283221,
#283222,#283223,#283224,#283225,#283226,#283227,#283228,#283229,#283230,
#283231,#283232,#283233,#283234,#283235,#283236,#283237,#283238,#283239,
#283240,#283241,#283242,#283243,#283244,#283245,#283246,#283247,#283248,
#283249,#283250,#283251,#283252,#283253,#283254,#283255,#283256,#283257,
#283258,#283259,#283260,#283261,#283262,#283263,#283264,#283265,#283266,
#283267,#283268,#283269,#283270,#283271,#283272,#283273,#283274,#283275,
#283276,#283277,#283278,#283279,#283280,#283281,#283282,#283283,#283284,
#283285,#283286,#283287,#283288,#283289,#283290,#283291,#283292,#283293,
#283294,#283295,#283296,#283297,#283298,#283299,#283300,#283301,#283302,
#283303,#283304,#283305,#283306,#283307,#283308,#283309,#283310,#283311,
#283312,#283313,#283314,#283315,#283316,#283317,#283318,#283319,#283320,
#283321,#283322,#283323,#283324,#283325,#283326,#283327,#283328,#283329,
#283330,#283331,#283332,#283333,#283334,#283335,#283336,#283337,#283338,
#283339,#283340,#283341,#283342,#283343,#283344,#283345,#283346,#283347,
#283348,#283349,#283350,#283351,#283352,#283353,#283354,#283355,#283356,
#283357,#283358,#283359,#283360,#283361,#283362,#283363,#283364,#283365,
#283366,#283367,#283368,#283369,#283370,#283371,#283372,#283373,#283374,
#283375,#283376,#283377,#283378,#283379,#283380,#283381,#283382,#283383,
#283384,#283385,#283386,#283387,#283388,#283389,#283390,#283391,#283392,
#283393,#283394,#283395,#283396,#283397,#283398,#283399,#283400,#283401,
#283402,#283403,#283404,#283405,#283406,#283407,#283408,#283409,#283410,
#283411,#283412,#283413,#283414,#283415,#283416,#283417,#283418,#283419,
#283420,#283421,#283422,#283423,#283424,#283425,#283426,#283427,#283428,
#283429,#283430,#283431,#283432,#283433,#283434,#283435,#283436,#283437,
#283438,#283439,#283440,#283441,#283442,#283443,#283444,#283445,#283446,
#283447,#283448,#283449,#283450,#283451,#283452,#283453,#283454,#283455,
#283456,#283457,#283458,#283459,#283460,#283461,#283462,#283463,#283464,
#283465,#283466,#283467,#283468,#283469,#283470,#283471,#283472,#283473,
#283474,#283475,#283476,#283477,#283478,#283479,#283480,#283481,#283482,
#283483,#283484,#283485,#283486,#283487,#283488,#283489,#283490,#283491,
#283492,#283493,#283494,#283495,#283496,#283497,#283498,#283499,#283500,
#283501,#283502,#283503,#283504,#283505,#283506,#283507,#283508,#283509,
#283510,#283511,#283512,#283513,#283514,#283515,#283516,#283517,#283518,
#283519,#283520,#283521,#283522,#283523,#283524,#283525,#283526,#283527,
#283528,#283529,#283530,#283531,#283532,#283533,#283534,#283535,#283536,
#283537,#283538,#283539,#283540,#283541,#283542,#283543,#283544,#283545,
#283546,#283547,#283548,#283549,#283550,#283551,#283552,#283553,#283554,
#283555,#283556,#283557,#283558,#283559,#283560,#283561,#283562,#283563,
#283564,#283565,#283566,#283567,#283568,#283569,#283570,#283571,#283572,
#283573,#283574,#283575,#283576,#283577,#283578,#283579,#283580,#283581,
#283582,#283583,#283584,#283585,#283586,#283587,#283588)),.UNSPECIFIED.,
 .F.,.F.,.F.)
B_SPLINE_SURFACE_WITH_KNOTS((2,2),(3,2,2,2,2,2,2,2,2,2,2,2,2,2,2,2,2,2,
2,2,2,2,2,2,2,2,2,2,2,2,2,2,2,2,2,2,2,2,2,2,2,2,2,2,2,2,2,2,2,2,2,2,2,2,
2,2,2,2,2,2,2,2,2,2,2,2,2,2,2,2,2,2,2,2,2,2,2,2,2,2,2,2,2,2,2,2,2,2,2,2,
2,2,2,2,2,2,2,2,2,2,2,2,2,2,2,2,2,2,2,2,2,2,2,2,2,2,2,2,2,2,2,2,2,2,2,2,
2,2,2,2,2,2,2,2,2,2,2,2,2,2,2,2,2,2,2,2,2,2,2,2,2,2,2,2,2,2,2,2,2,2,2,2,
2,2,2,2,2,2,2,2,2,2,2,2,2,2,2,2,2,2,2,2,2,2,2,2,2,2,2,2,2,2,2,2,2,2,2,2,
2,2,2,2,2,2,2,2,2,2,2,2,2,2,2,2,2,2,2,2,2,2,2,2,2,2,2,2,2,2,2,2,2,2,2,2,
2,2,2,2,2,2,2,2,2,2,2,2,2,2,2,2,2,2,2,2,2,2,2,2,2,2,2,2,2,2,2,2,2,2,2,2,
2,2,2,2,2,2,2,2,2,2,2,2,2,2,2,2,2,2,2,2,2,2,2,2,2,2,2,2,2,2,2,2,2,2,2,2,
2,2,2,2,2,2,2,2,2,2,2,2,2,2,2,2,2,2,2,2,2,2,2,2,2,2,2,2,2,2,2,2,2,2,2,2,
2,2,2,2,2,2,2,2,2,2,2,2,2,2,2,2,2,2,2,2,2,2,2,2,2,2,2,2,2,2,2,2,2,2,2,2,
2,2,2,2,2,2,2,2,2,2,2,2,2,2,2,2,2,2,2,2,2,2,2,2,2,2,2,2,2,2,2,2,2,2,2,2,
2,2,2,2,2,2,2,2,2,2,2,2,2,2,2,2,2,2,2,2,2,2,2,2,2,2,2,2,2,2,2,2,2,2,2,2,
2,2,2,2,2,2,2,2,2,2,2,2,2,2,2,2,2,2,2,2,2,2,2,2,2,2,2,2,2,2,2,2,2,2,2,2,
2,2,2,2,2,2,2,2,2,2,2,2,2,2,2,2,2,2,2,2,2,2,2,2,2,2,2,2,2,2,2,2,3),(-2.99434144680572E-6,
1.),(0.,0.00192307692307692,0.00384615384615385,0.00576923076923077,0.00769230769230769,
0.00961538461538462,0.0115384615384615,0.0134615384615385,0.0153846153846154,
0.0173076923076923,0.0192307692307692,0.0211538461538462,0.0230769230769231,
0.025,0.0269230769230769,0.0288461538461538,0.0307692307692308,0.0326923076923077,
0.0346153846153846,0.0365384615384615,0.0384615384615385,0.0403846153846154,
0.0423076923076923,0.0442307692307692,0.0461538461538462,0.0480769230769231,
0.05,0.0519230769230769,0.0538461538461538,0.0557692307692308,0.0576923076923077,
0.0596153846153846,0.0615384615384615,0.0634615384615385,0.0653846153846154,
0.0673076923076923,0.0692307692307692,0.0711538461538462,0.0730769230769231,
0.075,0.0769230769230769,0.0788461538461538,0.0807692307692308,0.0826923076923077,
0.0846153846153846,0.0865384615384615,0.0884615384615385,0.0903846153846154,
0.0923076923076923,0.0942307692307692,0.0961538461538462,0.0980769230769231,
0.1,0.101923076923077,0.103846153846154,0.105769230769231,0.107692307692308,
0.109615384615385,0.111538461538462,0.113461538461538,0.115384615384615,
0.117307692307692,0.119230769230769,0.121153846153846,0.123076923076923,
0.125,0.126923076923077,0.128846153846154,0.130769230769231,0.132692307692308,
0.134615384615385,0.136538461538462,0.138461538461538,0.140384615384615,
0.142307692307692,0.144230769230769,0.146153846153846,0.148076923076923,
0.15,0.151923076923077,0.153846153846154,0.155769230769231,0.157692307692308,
0.159615384615385,0.161538461538462,0.163461538461538,0.165384615384615,
0.167307692307692,0.169230769230769,0.171153846153846,0.173076923076923,
0.175,0.176923076923077,0.178846153846154,0.180769230769231,0.182692307692308,
0.184615384615385,0.186538461538462,0.188461538461538,0.190384615384615,
0.192307692307692,0.194230769230769,0.196153846153846,0.198076923076923,
0.2,0.201923076923077,0.203846153846154,0.205769230769231,0.207692307692308,
0.209615384615385,0.211538461538462,0.213461538461538,0.215384615384615,
0.217307692307692,0.219230769230769,0.221153846153846,0.223076923076923,
0.225,0.226923076923077,0.228846153846154,0.230769230769231,0.232692307692308,
0.234615384615385,0.236538461538462,0.238461538461538,0.240384615384615,
0.242307692307692,0.244230769230769,0.246153846153846,0.248076923076923,
0.25,0.251923076923077,0.253846153846154,0.255769230769231,0.257692307692308,
0.259615384615385,0.261538461538462,0.263461538461538,0.265384615384615,
0.267307692307692,0.269230769230769,0.271153846153846,0.273076923076923,
0.275,0.276923076923077,0.278846153846154,0.280769230769231,0.282692307692308,
0.284615384615385,0.286538461538462,0.288461538461538,0.290384615384615,
0.292307692307692,0.294230769230769,0.296153846153846,0.298076923076923,
0.3,0.301923076923077,0.303846153846154,0.305769230769231,0.307692307692308,
0.309615384615385,0.311538461538462,0.313461538461538,0.315384615384615,
0.317307692307692,0.319230769230769,0.321153846153846,0.323076923076923,
0.325,0.326923076923077,0.328846153846154,0.330769230769231,0.332692307692308,
0.334615384615385,0.336538461538462,0.338461538461538,0.340384615384615,
0.342307692307692,0.344230769230769,0.346153846153846,0.348076923076923,
0.35,0.351923076923077,0.353846153846154,0.355769230769231,0.357692307692308,
0.359615384615385,0.361538461538462,0.363461538461538,0.365384615384615,
0.367307692307692,0.369230769230769,0.371153846153846,0.373076923076923,
0.375,0.376923076923077,0.378846153846154,0.380769230769231,0.382692307692308,
0.384615384615385,0.386538461538462,0.388461538461538,0.390384615384615,
0.392307692307692,0.394230769230769,0.396153846153846,0.398076923076923,
0.4,0.401923076923077,0.403846153846154,0.405769230769231,0.407692307692308,
0.409615384615385,0.411538461538462,0.413461538461538,0.415384615384615,
0.417307692307692,0.419230769230769,0.421153846153846,0.423076923076923,
0.425,0.426923076923077,0.428846153846154,0.430769230769231,0.432692307692308,
0.434615384615385,0.436538461538462,0.438461538461538,0.440384615384615,
0.442307692307692,0.444230769230769,0.446153846153846,0.448076923076923,
0.45,0.451923076923077,0.453846153846154,0.455769230769231,0.457692307692308,
0.459615384615385,0.461538461538462,0.463461538461538,0.465384615384615,
0.467307692307692,0.469230769230769,0.471153846153846,0.473076923076923,
0.475,0.476923076923077,0.478846153846154,0.480769230769231,0.482692307692308,
0.484615384615385,0.486538461538462,0.488461538461538,0.490384615384615,
0.492307692307692,0.494230769230769,0.496153846153846,0.498076923076923,
0.5,0.501923076923077,0.503846153846154,0.505769230769231,0.507692307692308,
0.509615384615385,0.511538461538461,0.513461538461538,0.515384615384615,
0.517307692307692,0.519230769230769,0.521153846153846,0.523076923076923,
0.525,0.526923076923077,0.528846153846154,0.530769230769231,0.532692307692308,
0.534615384615385,0.536538461538462,0.538461538461538,0.540384615384615,
0.542307692307692,0.544230769230769,0.546153846153846,0.548076923076923,
0.55,0.551923076923077,0.553846153846154,0.555769230769231,0.557692307692308,
0.559615384615385,0.561538461538462,0.563461538461538,0.565384615384615,
0.567307692307692,0.569230769230769,0.571153846153846,0.573076923076923,
0.575,0.576923076923077,0.578846153846154,0.580769230769231,0.582692307692308,
0.584615384615385,0.586538461538462,0.588461538461538,0.590384615384615,
0.592307692307692,0.594230769230769,0.596153846153846,0.598076923076923,
0.6,0.601923076923077,0.603846153846154,0.605769230769231,0.607692307692308,
0.609615384615385,0.611538461538462,0.613461538461539,0.615384615384615,
0.617307692307692,0.619230769230769,0.621153846153846,0.623076923076923,
0.625,0.626923076923077,0.628846153846154,0.630769230769231,0.632692307692308,
0.634615384615385,0.636538461538461,0.638461538461538,0.640384615384615,
0.642307692307692,0.644230769230769,0.646153846153846,0.648076923076923,
0.65,0.651923076923077,0.653846153846154,0.655769230769231,0.657692307692308,
0.659615384615385,0.661538461538462,0.663461538461538,0.665384615384615,
0.667307692307692,0.669230769230769,0.671153846153846,0.673076923076923,
0.675,0.676923076923077,0.678846153846154,0.680769230769231,0.682692307692308,
0.684615384615385,0.686538461538462,0.688461538461538,0.690384615384615,
0.692307692307692,0.694230769230769,0.696153846153846,0.698076923076923,
0.7,0.701923076923077,0.703846153846154,0.705769230769231,0.707692307692308,
0.709615384615385,0.711538461538462,0.713461538461538,0.715384615384615,
0.717307692307692,0.719230769230769,0.721153846153846,0.723076923076923,
0.725,0.726923076923077,0.728846153846154,0.730769230769231,0.732692307692308,
0.734615384615385,0.736538461538462,0.738461538461539,0.740384615384615,
0.742307692307692,0.744230769230769,0.746153846153846,0.748076923076923,
0.75,0.751923076923077,0.753846153846154,0.755769230769231,0.757692307692308,
0.759615384615385,0.761538461538461,0.763461538461538,0.765384615384615,
0.767307692307692,0.769230769230769,0.771153846153846,0.773076923076923,
0.775,0.776923076923077,0.778846153846154,0.780769230769231,0.782692307692308,
0.784615384615385,0.786538461538462,0.788461538461538,0.790384615384615,
0.792307692307692,0.794230769230769,0.796153846153846,0.798076923076923,
0.8,0.801923076923077,0.803846153846154,0.805769230769231,0.807692307692308,
0.809615384615385,0.811538461538462,0.813461538461538,0.815384615384615,
0.817307692307692,0.819230769230769,0.821153846153846,0.823076923076923,
0.825,0.826923076923077,0.828846153846154,0.830769230769231,0.832692307692308,
0.834615384615385,0.836538461538462,0.838461538461538,0.840384615384615,
0.842307692307692,0.844230769230769,0.846153846153846,0.848076923076923,
0.85,0.851923076923077,0.853846153846154,0.855769230769231,0.857692307692308,
0.859615384615385,0.861538461538462,0.863461538461539,0.865384615384615,
0.867307692307692,0.869230769230769,0.871153846153846,0.873076923076923,
0.875,0.876923076923077,0.878846153846154,0.880769230769231,0.882692307692308,
0.884615384615385,0.886538461538461,0.888461538461538,0.890384615384615,
0.892307692307692,0.894230769230769,0.896153846153846,0.898076923076923,
0.9,0.901923076923077,0.903846153846154,0.905769230769231,0.907692307692308,
0.909615384615385,0.911538461538462,0.913461538461538,0.915384615384615,
0.917307692307692,0.919230769230769,0.921153846153846,0.923076923076923,
0.925,0.926923076923077,0.928846153846154,0.930769230769231,0.932692307692308,
0.934615384615385,0.936538461538462,0.938461538461538,0.940384615384615,
0.942307692307692,0.944230769230769,0.946153846153846,0.948076923076923,
0.95,0.951923076923077,0.953846153846154,0.955769230769231,0.957692307692308,
0.959615384615385,0.961538461538462,0.963461538461538,0.965384615384615,
0.967307692307692,0.969230769230769,0.971153846153846,0.973076923076923,
0.975,0.976923076923077,0.978846153846154,0.980769230769231,0.982692307692308,
0.984615384615385,0.986538461538462,0.988461538461539,0.990384615384615,
0.992307692307692,0.994230769230769,0.996153846153846),.UNSPECIFIED.)
GEOMETRIC_REPRESENTATION_ITEM()
RATIONAL_B_SPLINE_SURFACE(((1.,0.951056516295154,1.,0.951056516295154,1.,
0.951056516295154,1.,0.951056516295154,1.,0.951056516295154,1.,0.951056516295154,
1.,0.951056516295154,1.,0.951056516295154,1.,0.951056516295154,1.,0.951056516295154,
1.,0.951056516295154,1.,0.951056516295154,1.,0.951056516295154,1.,0.951056516295154,
1.,0.951056516295154,1.,0.951056516295154,1.,0.951056516295154,1.,0.951056516295154,
1.,0.951056516295154,1.,0.951056516295154,1.,0.951056516295154,1.,0.951056516295154,
1.,0.951056516295154,1.,0.951056516295154,1.,0.951056516295154,1.,0.951056516295154,
1.,0.951056516295154,1.,0.951056516295154,1.,0.951056516295154,1.,0.951056516295154,
1.,0.951056516295154,1.,0.951056516295154,1.,0.951056516295154,1.,0.951056516295154,
1.,0.951056516295154,1.,0.951056516295154,1.,0.951056516295154,1.,0.951056516295154,
1.,0.951056516295154,1.,0.951056516295154,1.,0.951056516295154,1.,0.951056516295154,
1.,0.951056516295154,1.,0.951056516295154,1.,0.951056516295154,1.,0.951056516295154,
1.,0.951056516295154,1.,0.951056516295154,1.,0.951056516295154,1.,0.951056516295154,
1.,0.951056516295154,1.,0.951056516295154,1.,0.951056516295154,1.,0.951056516295154,
1.,0.951056516295154,1.,0.951056516295154,1.,0.951056516295154,1.,0.951056516295154,
1.,0.951056516295154,1.,0.951056516295154,1.,0.951056516295154,1.,0.951056516295154,
1.,0.951056516295154,1.,0.951056516295154,1.,0.951056516295154,1.,0.951056516295154,
1.,0.951056516295154,1.,0.951056516295154,1.,0.951056516295154,1.,0.951056516295154,
1.,0.951056516295154,1.,0.951056516295154,1.,0.951056516295154,1.,0.951056516295154,
1.,0.951056516295154,1.,0.951056516295154,1.,0.951056516295154,1.,0.951056516295154,
1.,0.951056516295154,1.,0.951056516295154,1.,0.951056516295154,1.,0.951056516295154,
1.,0.951056516295154,1.,0.951056516295154,1.,0.951056516295154,1.,0.951056516295154,
1.,0.951056516295154,1.,0.951056516295154,1.,0.951056516295154,1.,0.951056516295154,
1.,0.951056516295154,1.,0.951056516295154,1.,0.951056516295154,1.,0.951056516295154,
1.,0.951056516295154,1.,0.951056516295154,1.,0.951056516295154,1.,0.951056516295154,
1.,0.951056516295154,1.,0.951056516295154,1.,0.951056516295154,1.,0.951056516295154,
1.,0.951056516295154,1.,0.951056516295154,1.,0.951056516295154,1.,0.951056516295154,
1.,0.951056516295154,1.,0.951056516295154,1.,0.951056516295154,1.,0.951056516295154,
1.,0.951056516295154,1.,0.951056516295154,1.,0.951056516295154,1.,0.951056516295154,
1.,0.951056516295154,1.,0.951056516295154,1.,0.951056516295154,1.,0.951056516295154,
1.,0.951056516295154,1.,0.951056516295154,1.,0.951056516295154,1.,0.951056516295154,
1.,0.951056516295154,1.,0.951056516295154,1.,0.951056516295154,1.,0.951056516295154,
1.,0.951056516295154,1.,0.951056516295154,1.,0.951056516295154,1.,0.951056516295154,
1.,0.951056516295154,1.,0.951056516295154,1.,0.951056516295154,1.,0.951056516295154,
1.,0.951056516295154,1.,0.951056516295154,1.,0.951056516295154,1.,0.951056516295154,
1.,0.951056516295154,1.,0.951056516295154,1.,0.951056516295154,1.,0.951056516295154,
1.,0.951056516295154,1.,0.951056516295154,1.,0.951056516295154,1.,0.951056516295154,
1.,0.951056516295154,1.,0.951056516295154,1.,0.951056516295154,1.,0.951056516295154,
1.,0.951056516295154,1.,0.951056516295154,1.,0.951056516295154,1.,0.951056516295154,
1.,0.951056516295154,1.,0.951056516295154,1.,0.951056516295154,1.,0.951056516295154,
1.,0.951056516295154,1.,0.951056516295154,1.,0.951056516295154,1.,0.951056516295154,
1.,0.951056516295154,1.,0.951056516295154,1.,0.951056516295154,1.,0.951056516295154,
1.,0.951056516295154,1.,0.951056516295154,1.,0.951056516295154,1.,0.951056516295154,
1.,0.951056516295154,1.,0.951056516295154,1.,0.951056516295154,1.,0.951056516295154,
1.,0.951056516295154,1.,0.951056516295154,1.,0.951056516295154,1.,0.951056516295154,
1.,0.951056516295154,1.,0.951056516295154,1.,0.951056516295154,1.,0.951056516295154,
1.,0.951056516295154,1.,0.951056516295154,1.,0.951056516295154,1.,0.951056516295154,
1.,0.951056516295154,1.,0.951056516295154,1.,0.951056516295154,1.,0.951056516295154,
1.,0.951056516295154,1.,0.951056516295154,1.,0.951056516295154,1.,0.951056516295154,
1.,0.951056516295154,1.,0.951056516295154,1.,0.951056516295154,1.,0.951056516295154,
1.,0.951056516295154,1.,0.951056516295154,1.,0.951056516295154,1.,0.951056516295154,
1.,0.951056516295154,1.,0.951056516295154,1.,0.951056516295154,1.,0.951056516295154,
1.,0.951056516295154,1.,0.951056516295154,1.,0.951056516295154,1.,0.951056516295154,
1.,0.951056516295154,1.,0.951056516295154,1.,0.951056516295154,1.,0.951056516295154,
1.,0.951056516295154,1.,0.951056516295154,1.,0.951056516295154,1.,0.951056516295154,
1.,0.951056516295154,1.,0.951056516295154,1.,0.951056516295154,1.,0.951056516295154,
1.,0.951056516295154,1.,0.951056516295154,1.,0.951056516295154,1.,0.951056516295154,
1.,0.951056516295154,1.,0.951056516295154,1.,0.951056516295154,1.,0.951056516295154,
1.,0.951056516295154,1.,0.951056516295154,1.,0.951056516295154,1.,0.951056516295154,
1.,0.951056516295154,1.,0.951056516295154,1.,0.951056516295154,1.,0.951056516295154,
1.,0.951056516295154,1.,0.951056516295154,1.,0.951056516295154,1.,0.951056516295154,
1.,0.951056516295154,1.,0.951056516295154,1.,0.951056516295154,1.,0.951056516295154,
1.,0.951056516295154,1.,0.951056516295154,1.,0.951056516295154,1.,0.951056516295154,
1.,0.951056516295154,1.,0.951056516295154,1.,0.951056516295154,1.,0.951056516295154,
1.,0.951056516295154,1.,0.951056516295154,1.,0.951056516295154,1.,0.951056516295154,
1.,0.951056516295154,1.,0.951056516295154,1.,0.951056516295154,1.,0.951056516295154,
1.,0.951056516295154,1.,0.951056516295154,1.,0.951056516295154,1.,0.951056516295154,
1.,0.951056516295154,1.,0.951056516295154,1.,0.951056516295154,1.,0.951056516295154,
1.,0.951056516295154,1.,0.951056516295154,1.,0.951056516295154,1.,0.951056516295154,
1.,0.951056516295154,1.,0.951056516295154,1.,0.951056516295154,1.,0.951056516295154,
1.,0.951056516295154,1.,0.951056516295154,1.,0.951056516295154,1.,0.951056516295154,
1.,0.951056516295154,1.,0.951056516295154,1.,0.951056516295154,1.,0.951056516295154,
1.,0.951056516295154,1.,0.951056516295154,1.,0.951056516295154,1.,0.951056516295154,
1.,0.951056516295154,1.,0.951056516295154,1.,0.951056516295154,1.,0.951056516295154,
1.,0.951056516295154,1.,0.951056516295154,1.,0.951056516295154,1.,0.951056516295154,
1.,0.951056516295154,1.,0.951056516295154,1.,0.951056516295154,1.,0.951056516295154,
1.,0.951056516295154,1.,0.951056516295154,1.,0.951056516295154,1.,0.951056516295154,
1.,0.951056516295154,1.,0.951056516295154,1.,0.951056516295154,1.,0.951056516295154,
1.,0.951056516295154,1.,0.951056516295154,1.,0.951056516295154,1.,0.951056516295154,
1.,0.951056516295154,1.,0.951056516295154,1.,0.951056516295154,1.,0.951056516295154,
1.,0.951056516295154,1.,0.951056516295154,1.,0.951056516295154,1.,0.951056516295154,
1.,0.951056516295154,1.,0.951056516295154,1.,0.951056516295154,1.,0.951056516295154,
1.,0.951056516295154,1.,0.951056516295154,1.,0.951056516295154,1.,0.951056516295154,
1.,0.951056516295154,1.,0.951056516295154,1.,0.951056516295154,1.,0.951056516295154,
1.,0.951056516295154,1.,0.951056516295154,1.,0.951056516295154,1.,0.951056516295154,
1.,0.951056516295154,1.,0.951056516295154,1.,0.951056516295154,1.,0.951056516295154,
1.,0.951056516295154,1.,0.951056516295154,1.,0.951056516295154,1.,0.951056516295154,
1.,0.951056516295154,1.,0.951056516295154,1.,0.951056516295154,1.,0.951056516295154,
1.,0.951056516295154,1.,0.951056516295154,1.,0.951056516295154,1.,0.951056516295154,
1.,0.951056516295154,1.,0.951056516295154,1.,0.951056516295154,1.,0.951056516295154,
1.,0.951056516295154,1.,0.951056516295154,1.,0.951056516295154,1.,0.951056516295154,
1.,0.951056516295154,1.,0.951056516295154,1.,0.951056516295154,1.,0.951056516295154,
1.,0.951056516295154,1.,0.951056516295154,1.,0.951056516295154,1.,0.951056516295154,
1.,0.951056516295154,1.,0.951056516295154,1.,0.951056516295154,1.,0.951056516295154,
1.,0.951056516295154,1.,0.951056516295154,1.,0.951056516295154,1.,0.951056516295154,
1.,0.951056516295154,1.,0.951056516295154,1.,0.951056516295154,1.,0.951056516295154,
1.,0.951056516295154,1.,0.951056516295154,1.,0.951056516295154,1.,0.951056516295154,
1.,0.951056516295154,1.,0.951056516295154,1.,0.951056516295154,1.,0.951056516295154,
1.,0.951056516295154,1.,0.951056516295154,1.,0.951056516295154,1.,0.951056516295154,
1.,0.951056516295154,1.,0.951056516295154,1.,0.951056516295154,1.,0.951056516295154,
1.,0.951056516295154,1.,0.951056516295154,1.,0.951056516295154,1.,0.951056516295154,
1.,0.951056516295154,1.,0.951056516295154,1.,0.951056516295154,1.,0.951056516295154,
1.,0.951056516295154,1.,0.951056516295154,1.,0.951056516295154,1.,0.951056516295154,
1.,0.951056516295154,1.,0.951056516295154,1.,0.951056516295154,1.,0.951056516295154,
1.,0.951056516295154,1.,0.951056516295154,1.,0.951056516295154,1.,0.951056516295154,
1.,0.951056516295154,1.,0.951056516295154,1.,0.951056516295154,1.,0.951056516295154,
1.,0.951056516295154,1.,0.951056516295154,1.,0.951056516295154,1.,0.951056516295154,
1.,0.951056516295154,1.,0.951056516295154,1.,0.951056516295154,1.,0.951056516295154,
1.,0.951056516295154,1.,0.951056516295154,1.,0.951056516295154,1.,0.951056516295154,
1.,0.951056516295154,1.,0.951056516295154,1.,0.951056516295154,1.,0.951056516295154,
1.,0.951056516295154,1.,0.951056516295154,1.,0.951056516295154,1.,0.951056516295154,
1.,0.951056516295154,1.,0.951056516295154,1.,0.951056516295154,1.,0.951056516295154,
1.,0.951056516295154,1.,0.951056516295154,1.,0.951056516295154,1.,0.951056516295154,
1.,0.951056516295154,1.,0.951056516295154,1.,0.951056516295154,1.,0.951056516295154,
1.,0.951056516295154,1.,0.951056516295154,1.,0.951056516295154,1.,0.951056516295154,
1.,0.951056516295154,1.,0.951056516295154,1.,0.951056516295154,1.,0.951056516295154,
1.,0.951056516295154,1.,0.951056516295154,1.,0.951056516295154,1.,0.951056516295154,
1.,0.951056516295154,1.,0.951056516295154,1.,0.951056516295154,1.,0.951056516295154,
1.,0.951056516295154,1.,0.951056516295154,1.,0.951056516295154,1.,0.951056516295154,
1.,0.951056516295154,1.,0.951056516295154,1.,0.951056516295154,1.,0.951056516295154,
1.,0.951056516295154,1.,0.951056516295154,1.,0.951056516295154,1.,0.951056516295154,
1.,0.951056516295154,1.,0.951056516295154,1.,0.951056516295154,1.,0.951056516295154,
1.,0.951056516295154,1.,0.951056516295154,1.,0.951056516295154,1.,0.951056516295154,
1.,0.951056516295154,1.,0.951056516295154,1.,0.951056516295154,1.,0.951056516295154,
1.,0.951056516295154,1.,0.951056516295154,1.,0.951056516295154,1.,0.951056516295154,
1.,0.951056516295154,1.,0.951056516295154,1.,0.951056516295154,1.,0.951056516295154,
1.,0.951056516295154,1.,0.951056516295154,1.,0.951056516295154,1.,0.951056516295154,
1.,0.951056516295154,1.,0.951056516295154,1.,0.951056516295154,1.,0.951056516295154,
1.,0.951056516295154,1.,0.951056516295154,1.,0.951056516295154,1.,0.951056516295154,
1.,0.951056516295154,1.,0.951056516295154,1.,0.951056516295154,1.,0.951056516295154,
1.),(1.,0.951056516295154,1.,0.951056516295154,1.,0.951056516295154,1.,
0.951056516295154,1.,0.951056516295154,1.,0.951056516295154,1.,0.951056516295154,
1.,0.951056516295154,1.,0.951056516295154,1.,0.951056516295154,1.,0.951056516295154,
1.,0.951056516295154,1.,0.951056516295154,1.,0.951056516295154,1.,0.951056516295154,
1.,0.951056516295154,1.,0.951056516295154,1.,0.951056516295154,1.,0.951056516295154,
1.,0.951056516295154,1.,0.951056516295154,1.,0.951056516295154,1.,0.951056516295154,
1.,0.951056516295154,1.,0.951056516295154,1.,0.951056516295154,1.,0.951056516295154,
1.,0.951056516295154,1.,0.951056516295154,1.,0.951056516295154,1.,0.951056516295154,
1.,0.951056516295154,1.,0.951056516295154,1.,0.951056516295154,1.,0.951056516295154,
1.,0.951056516295154,1.,0.951056516295154,1.,0.951056516295154,1.,0.951056516295154,
1.,0.951056516295154,1.,0.951056516295154,1.,0.951056516295154,1.,0.951056516295154,
1.,0.951056516295154,1.,0.951056516295154,1.,0.951056516295154,1.,0.951056516295154,
1.,0.951056516295154,1.,0.951056516295154,1.,0.951056516295154,1.,0.951056516295154,
1.,0.951056516295154,1.,0.951056516295154,1.,0.951056516295154,1.,0.951056516295154,
1.,0.951056516295154,1.,0.951056516295154,1.,0.951056516295154,1.,0.951056516295154,
1.,0.951056516295154,1.,0.951056516295154,1.,0.951056516295154,1.,0.951056516295154,
1.,0.951056516295154,1.,0.951056516295154,1.,0.951056516295154,1.,0.951056516295154,
1.,0.951056516295154,1.,0.951056516295154,1.,0.951056516295154,1.,0.951056516295154,
1.,0.951056516295154,1.,0.951056516295154,1.,0.951056516295154,1.,0.951056516295154,
1.,0.951056516295154,1.,0.951056516295154,1.,0.951056516295154,1.,0.951056516295154,
1.,0.951056516295154,1.,0.951056516295154,1.,0.951056516295154,1.,0.951056516295154,
1.,0.951056516295154,1.,0.951056516295154,1.,0.951056516295154,1.,0.951056516295154,
1.,0.951056516295154,1.,0.951056516295154,1.,0.951056516295154,1.,0.951056516295154,
1.,0.951056516295154,1.,0.951056516295154,1.,0.951056516295154,1.,0.951056516295154,
1.,0.951056516295154,1.,0.951056516295154,1.,0.951056516295154,1.,0.951056516295154,
1.,0.951056516295154,1.,0.951056516295154,1.,0.951056516295154,1.,0.951056516295154,
1.,0.951056516295154,1.,0.951056516295154,1.,0.951056516295154,1.,0.951056516295154,
1.,0.951056516295154,1.,0.951056516295154,1.,0.951056516295154,1.,0.951056516295154,
1.,0.951056516295154,1.,0.951056516295154,1.,0.951056516295154,1.,0.951056516295154,
1.,0.951056516295154,1.,0.951056516295154,1.,0.951056516295154,1.,0.951056516295154,
1.,0.951056516295154,1.,0.951056516295154,1.,0.951056516295154,1.,0.951056516295154,
1.,0.951056516295154,1.,0.951056516295154,1.,0.951056516295154,1.,0.951056516295154,
1.,0.951056516295154,1.,0.951056516295154,1.,0.951056516295154,1.,0.951056516295154,
1.,0.951056516295154,1.,0.951056516295154,1.,0.951056516295154,1.,0.951056516295154,
1.,0.951056516295154,1.,0.951056516295154,1.,0.951056516295154,1.,0.951056516295154,
1.,0.951056516295154,1.,0.951056516295154,1.,0.951056516295154,1.,0.951056516295154,
1.,0.951056516295154,1.,0.951056516295154,1.,0.951056516295154,1.,0.951056516295154,
1.,0.951056516295154,1.,0.951056516295154,1.,0.951056516295154,1.,0.951056516295154,
1.,0.951056516295154,1.,0.951056516295154,1.,0.951056516295154,1.,0.951056516295154,
1.,0.951056516295154,1.,0.951056516295154,1.,0.951056516295154,1.,0.951056516295154,
1.,0.951056516295154,1.,0.951056516295154,1.,0.951056516295154,1.,0.951056516295154,
1.,0.951056516295154,1.,0.951056516295154,1.,0.951056516295154,1.,0.951056516295154,
1.,0.951056516295154,1.,0.951056516295154,1.,0.951056516295154,1.,0.951056516295154,
1.,0.951056516295154,1.,0.951056516295154,1.,0.951056516295154,1.,0.951056516295154,
1.,0.951056516295154,1.,0.951056516295154,1.,0.951056516295154,1.,0.951056516295154,
1.,0.951056516295154,1.,0.951056516295154,1.,0.951056516295154,1.,0.951056516295154,
1.,0.951056516295154,1.,0.951056516295154,1.,0.951056516295154,1.,0.951056516295154,
1.,0.951056516295154,1.,0.951056516295154,1.,0.951056516295154,1.,0.951056516295154,
1.,0.951056516295154,1.,0.951056516295154,1.,0.951056516295154,1.,0.951056516295154,
1.,0.951056516295154,1.,0.951056516295154,1.,0.951056516295154,1.,0.951056516295154,
1.,0.951056516295154,1.,0.951056516295154,1.,0.951056516295154,1.,0.951056516295154,
1.,0.951056516295154,1.,0.951056516295154,1.,0.951056516295154,1.,0.951056516295154,
1.,0.951056516295154,1.,0.951056516295154,1.,0.951056516295154,1.,0.951056516295154,
1.,0.951056516295154,1.,0.951056516295154,1.,0.951056516295154,1.,0.951056516295154,
1.,0.951056516295154,1.,0.951056516295154,1.,0.951056516295154,1.,0.951056516295154,
1.,0.951056516295154,1.,0.951056516295154,1.,0.951056516295154,1.,0.951056516295154,
1.,0.951056516295154,1.,0.951056516295154,1.,0.951056516295154,1.,0.951056516295154,
1.,0.951056516295154,1.,0.951056516295154,1.,0.951056516295154,1.,0.951056516295154,
1.,0.951056516295154,1.,0.951056516295154,1.,0.951056516295154,1.,0.951056516295154,
1.,0.951056516295154,1.,0.951056516295154,1.,0.951056516295154,1.,0.951056516295154,
1.,0.951056516295154,1.,0.951056516295154,1.,0.951056516295154,1.,0.951056516295154,
1.,0.951056516295154,1.,0.951056516295154,1.,0.951056516295154,1.,0.951056516295154,
1.,0.951056516295154,1.,0.951056516295154,1.,0.951056516295154,1.,0.951056516295154,
1.,0.951056516295154,1.,0.951056516295154,1.,0.951056516295154,1.,0.951056516295154,
1.,0.951056516295154,1.,0.951056516295154,1.,0.951056516295154,1.,0.951056516295154,
1.,0.951056516295154,1.,0.951056516295154,1.,0.951056516295154,1.,0.951056516295154,
1.,0.951056516295154,1.,0.951056516295154,1.,0.951056516295154,1.,0.951056516295154,
1.,0.951056516295154,1.,0.951056516295154,1.,0.951056516295154,1.,0.951056516295154,
1.,0.951056516295154,1.,0.951056516295154,1.,0.951056516295154,1.,0.951056516295154,
1.,0.951056516295154,1.,0.951056516295154,1.,0.951056516295154,1.,0.951056516295154,
1.,0.951056516295154,1.,0.951056516295154,1.,0.951056516295154,1.,0.951056516295154,
1.,0.951056516295154,1.,0.951056516295154,1.,0.951056516295154,1.,0.951056516295154,
1.,0.951056516295154,1.,0.951056516295154,1.,0.951056516295154,1.,0.951056516295154,
1.,0.951056516295154,1.,0.951056516295154,1.,0.951056516295154,1.,0.951056516295154,
1.,0.951056516295154,1.,0.951056516295154,1.,0.951056516295154,1.,0.951056516295154,
1.,0.951056516295154,1.,0.951056516295154,1.,0.951056516295154,1.,0.951056516295154,
1.,0.951056516295154,1.,0.951056516295154,1.,0.951056516295154,1.,0.951056516295154,
1.,0.951056516295154,1.,0.951056516295154,1.,0.951056516295154,1.,0.951056516295154,
1.,0.951056516295154,1.,0.951056516295154,1.,0.951056516295154,1.,0.951056516295154,
1.,0.951056516295154,1.,0.951056516295154,1.,0.951056516295154,1.,0.951056516295154,
1.,0.951056516295154,1.,0.951056516295154,1.,0.951056516295154,1.,0.951056516295154,
1.,0.951056516295154,1.,0.951056516295154,1.,0.951056516295154,1.,0.951056516295154,
1.,0.951056516295154,1.,0.951056516295154,1.,0.951056516295154,1.,0.951056516295154,
1.,0.951056516295154,1.,0.951056516295154,1.,0.951056516295154,1.,0.951056516295154,
1.,0.951056516295154,1.,0.951056516295154,1.,0.951056516295154,1.,0.951056516295154,
1.,0.951056516295154,1.,0.951056516295154,1.,0.951056516295154,1.,0.951056516295154,
1.,0.951056516295154,1.,0.951056516295154,1.,0.951056516295154,1.,0.951056516295154,
1.,0.951056516295154,1.,0.951056516295154,1.,0.951056516295154,1.,0.951056516295154,
1.,0.951056516295154,1.,0.951056516295154,1.,0.951056516295154,1.,0.951056516295154,
1.,0.951056516295154,1.,0.951056516295154,1.,0.951056516295154,1.,0.951056516295154,
1.,0.951056516295154,1.,0.951056516295154,1.,0.951056516295154,1.,0.951056516295154,
1.,0.951056516295154,1.,0.951056516295154,1.,0.951056516295154,1.,0.951056516295154,
1.,0.951056516295154,1.,0.951056516295154,1.,0.951056516295154,1.,0.951056516295154,
1.,0.951056516295154,1.,0.951056516295154,1.,0.951056516295154,1.,0.951056516295154,
1.,0.951056516295154,1.,0.951056516295154,1.,0.951056516295154,1.,0.951056516295154,
1.,0.951056516295154,1.,0.951056516295154,1.,0.951056516295154,1.,0.951056516295154,
1.,0.951056516295154,1.,0.951056516295154,1.,0.951056516295154,1.,0.951056516295154,
1.,0.951056516295154,1.,0.951056516295154,1.,0.951056516295154,1.,0.951056516295154,
1.,0.951056516295154,1.,0.951056516295154,1.,0.951056516295154,1.,0.951056516295154,
1.,0.951056516295154,1.,0.951056516295154,1.,0.951056516295154,1.,0.951056516295154,
1.,0.951056516295154,1.,0.951056516295154,1.,0.951056516295154,1.,0.951056516295154,
1.,0.951056516295154,1.,0.951056516295154,1.,0.951056516295154,1.,0.951056516295154,
1.,0.951056516295154,1.,0.951056516295154,1.,0.951056516295154,1.,0.951056516295154,
1.,0.951056516295154,1.,0.951056516295154,1.,0.951056516295154,1.,0.951056516295154,
1.,0.951056516295154,1.,0.951056516295154,1.,0.951056516295154,1.,0.951056516295154,
1.,0.951056516295154,1.,0.951056516295154,1.,0.951056516295154,1.,0.951056516295154,
1.,0.951056516295154,1.,0.951056516295154,1.,0.951056516295154,1.,0.951056516295154,
1.,0.951056516295154,1.,0.951056516295154,1.,0.951056516295154,1.,0.951056516295154,
1.,0.951056516295154,1.,0.951056516295154,1.,0.951056516295154,1.,0.951056516295154,
1.,0.951056516295154,1.,0.951056516295154,1.,0.951056516295154,1.,0.951056516295154,
1.,0.951056516295154,1.,0.951056516295154,1.,0.951056516295154,1.,0.951056516295154,
1.,0.951056516295154,1.,0.951056516295154,1.,0.951056516295154,1.,0.951056516295154,
1.,0.951056516295154,1.,0.951056516295154,1.,0.951056516295154,1.,0.951056516295154,
1.,0.951056516295154,1.,0.951056516295154,1.,0.951056516295154,1.,0.951056516295154,
1.,0.951056516295154,1.,0.951056516295154,1.,0.951056516295154,1.,0.951056516295154,
1.,0.951056516295154,1.,0.951056516295154,1.,0.951056516295154,1.,0.951056516295154,
1.,0.951056516295154,1.,0.951056516295154,1.,0.951056516295154,1.,0.951056516295154,
1.,0.951056516295154,1.,0.951056516295154,1.,0.951056516295154,1.,0.951056516295154,
1.,0.951056516295154,1.,0.951056516295154,1.,0.951056516295154,1.,0.951056516295154,
1.,0.951056516295154,1.,0.951056516295154,1.,0.951056516295154,1.,0.951056516295154,
1.,0.951056516295154,1.,0.951056516295154,1.,0.951056516295154,1.,0.951056516295154,
1.,0.951056516295154,1.,0.951056516295154,1.,0.951056516295154,1.,0.951056516295154,
1.,0.951056516295154,1.,0.951056516295154,1.,0.951056516295154,1.,0.951056516295154,
1.,0.951056516295154,1.,0.951056516295154,1.,0.951056516295154,1.,0.951056516295154,
1.,0.951056516295154,1.,0.951056516295154,1.,0.951056516295154,1.,0.951056516295154,
1.,0.951056516295154,1.,0.951056516295154,1.,0.951056516295154,1.,0.951056516295154,
1.,0.951056516295154,1.,0.951056516295154,1.,0.951056516295154,1.,0.951056516295154,
1.,0.951056516295154,1.,0.951056516295154,1.,0.951056516295154,1.,0.951056516295154,
1.,0.951056516295154,1.,0.951056516295154,1.,0.951056516295154,1.,0.951056516295154,
1.,0.951056516295154,1.,0.951056516295154,1.,0.951056516295154,1.)))
REPRESENTATION_ITEM('')
SURFACE()
);
#3195=(
BOUNDED_SURFACE()
B_SPLINE_SURFACE(1,2,((#283610,#283611,#283612,#283613,#283614,#283615,
#283616,#283617,#283618,#283619,#283620,#283621,#283622,#283623,#283624,
#283625,#283626,#283627,#283628,#283629,#283630,#283631,#283632,#283633,
#283634,#283635,#283636,#283637,#283638,#283639,#283640,#283641,#283642,
#283643,#283644,#283645,#283646,#283647,#283648,#283649,#283650,#283651,
#283652,#283653,#283654,#283655,#283656,#283657,#283658,#283659,#283660,
#283661,#283662,#283663,#283664,#283665,#283666,#283667,#283668,#283669,
#283670,#283671,#283672,#283673,#283674,#283675,#283676,#283677,#283678,
#283679,#283680,#283681,#283682,#283683,#283684,#283685,#283686,#283687,
#283688,#283689,#283690,#283691,#283692,#283693,#283694,#283695,#283696,
#283697,#283698,#283699,#283700,#283701,#283702,#283703,#283704,#283705,
#283706,#283707,#283708,#283709,#283710,#283711,#283712,#283713,#283714,
#283715,#283716,#283717,#283718,#283719,#283720,#283721,#283722,#283723,
#283724,#283725,#283726,#283727,#283728,#283729,#283730,#283731,#283732,
#283733,#283734,#283735,#283736,#283737,#283738,#283739,#283740,#283741,
#283742,#283743,#283744,#283745,#283746,#283747,#283748,#283749,#283750,
#283751,#283752,#283753,#283754,#283755,#283756,#283757,#283758,#283759,
#283760,#283761,#283762,#283763,#283764,#283765,#283766,#283767,#283768,
#283769,#283770,#283771,#283772,#283773,#283774,#283775,#283776,#283777,
#283778,#283779,#283780,#283781,#283782,#283783,#283784,#283785,#283786,
#283787,#283788,#283789,#283790,#283791,#283792,#283793,#283794,#283795,
#283796,#283797,#283798,#283799,#283800,#283801,#283802,#283803,#283804,
#283805,#283806,#283807,#283808,#283809,#283810,#283811,#283812,#283813,
#283814,#283815,#283816,#283817,#283818,#283819,#283820,#283821,#283822,
#283823,#283824,#283825,#283826,#283827,#283828,#283829,#283830,#283831,
#283832,#283833,#283834,#283835,#283836,#283837,#283838,#283839,#283840,
#283841,#283842,#283843,#283844,#283845,#283846,#283847,#283848,#283849,
#283850,#283851,#283852,#283853,#283854,#283855,#283856,#283857,#283858,
#283859,#283860,#283861,#283862,#283863,#283864,#283865,#283866,#283867,
#283868,#283869,#283870,#283871,#283872,#283873,#283874,#283875,#283876,
#283877,#283878,#283879,#283880,#283881,#283882,#283883,#283884,#283885,
#283886,#283887,#283888,#283889,#283890,#283891,#283892,#283893,#283894,
#283895,#283896,#283897,#283898,#283899,#283900,#283901,#283902,#283903,
#283904,#283905,#283906,#283907,#283908,#283909,#283910,#283911,#283912,
#283913,#283914,#283915,#283916,#283917,#283918,#283919,#283920,#283921,
#283922,#283923,#283924,#283925,#283926,#283927,#283928,#283929,#283930,
#283931,#283932,#283933,#283934,#283935,#283936,#283937,#283938,#283939,
#283940,#283941,#283942,#283943,#283944,#283945,#283946,#283947,#283948,
#283949,#283950,#283951,#283952,#283953,#283954,#283955,#283956,#283957,
#283958,#283959,#283960,#283961,#283962,#283963,#283964,#283965,#283966,
#283967,#283968,#283969,#283970,#283971,#283972,#283973,#283974,#283975,
#283976,#283977,#283978,#283979,#283980,#283981,#283982,#283983,#283984,
#283985,#283986,#283987,#283988,#283989,#283990,#283991,#283992,#283993,
#283994,#283995,#283996,#283997,#283998,#283999,#284000,#284001,#284002,
#284003,#284004,#284005,#284006,#284007,#284008,#284009,#284010,#284011,
#284012,#284013,#284014,#284015,#284016,#284017,#284018,#284019,#284020,
#284021,#284022,#284023,#284024,#284025,#284026,#284027,#284028,#284029,
#284030,#284031,#284032,#284033,#284034,#284035,#284036,#284037,#284038,
#284039,#284040,#284041,#284042,#284043,#284044,#284045,#284046,#284047,
#284048,#284049,#284050,#284051,#284052,#284053,#284054,#284055,#284056,
#284057,#284058,#284059,#284060,#284061,#284062,#284063,#284064,#284065,
#284066,#284067,#284068,#284069,#284070,#284071,#284072,#284073,#284074,
#284075,#284076,#284077,#284078,#284079,#284080,#284081,#284082,#284083,
#284084,#284085,#284086,#284087,#284088,#284089,#284090,#284091,#284092,
#284093,#284094,#284095,#284096,#284097,#284098,#284099,#284100,#284101,
#284102,#284103,#284104,#284105,#284106,#284107,#284108,#284109,#284110,
#284111,#284112,#284113,#284114,#284115,#284116,#284117,#284118,#284119,
#284120,#284121,#284122,#284123,#284124,#284125,#284126,#284127,#284128,
#284129,#284130,#284131,#284132,#284133,#284134,#284135,#284136,#284137,
#284138,#284139,#284140,#284141,#284142,#284143,#284144,#284145,#284146,
#284147,#284148,#284149,#284150,#284151,#284152,#284153,#284154,#284155,
#284156,#284157,#284158,#284159,#284160,#284161,#284162,#284163,#284164,
#284165,#284166,#284167,#284168,#284169,#284170,#284171,#284172,#284173,
#284174,#284175,#284176,#284177,#284178,#284179,#284180,#284181,#284182,
#284183,#284184,#284185,#284186,#284187,#284188,#284189,#284190,#284191,
#284192,#284193,#284194,#284195,#284196,#284197,#284198,#284199,#284200,
#284201,#284202,#284203,#284204,#284205,#284206,#284207,#284208,#284209,
#284210,#284211,#284212,#284213,#284214,#284215,#284216,#284217,#284218,
#284219,#284220,#284221,#284222,#284223,#284224,#284225,#284226,#284227,
#284228,#284229,#284230,#284231,#284232,#284233,#284234,#284235,#284236,
#284237,#284238,#284239,#284240,#284241,#284242,#284243,#284244,#284245,
#284246,#284247,#284248,#284249,#284250,#284251,#284252,#284253,#284254,
#284255,#284256,#284257,#284258,#284259,#284260,#284261,#284262,#284263,
#284264,#284265,#284266,#284267,#284268,#284269,#284270,#284271,#284272,
#284273,#284274,#284275,#284276,#284277,#284278,#284279,#284280,#284281,
#284282,#284283,#284284,#284285,#284286,#284287,#284288,#284289,#284290,
#284291,#284292,#284293,#284294,#284295,#284296,#284297,#284298,#284299,
#284300,#284301,#284302,#284303,#284304,#284305,#284306,#284307,#284308,
#284309,#284310,#284311,#284312,#284313,#284314,#284315,#284316,#284317,
#284318,#284319,#284320,#284321,#284322,#284323,#284324,#284325,#284326,
#284327,#284328,#284329,#284330,#284331,#284332,#284333,#284334,#284335,
#284336,#284337,#284338,#284339,#284340,#284341,#284342,#284343,#284344,
#284345,#284346,#284347,#284348,#284349,#284350,#284351,#284352,#284353,
#284354,#284355,#284356,#284357,#284358,#284359,#284360,#284361,#284362,
#284363,#284364,#284365,#284366,#284367,#284368,#284369,#284370,#284371,
#284372,#284373,#284374,#284375,#284376,#284377,#284378,#284379,#284380,
#284381,#284382,#284383,#284384,#284385,#284386,#284387,#284388,#284389,
#284390,#284391,#284392,#284393,#284394,#284395,#284396,#284397,#284398,
#284399,#284400,#284401,#284402,#284403,#284404,#284405,#284406,#284407,
#284408,#284409,#284410,#284411,#284412,#284413,#284414,#284415,#284416,
#284417,#284418,#284419,#284420,#284421,#284422,#284423,#284424,#284425,
#284426,#284427,#284428,#284429,#284430,#284431,#284432,#284433,#284434,
#284435,#284436,#284437,#284438,#284439,#284440,#284441,#284442,#284443,
#284444,#284445,#284446,#284447,#284448,#284449,#284450,#284451,#284452,
#284453,#284454,#284455,#284456,#284457,#284458,#284459,#284460,#284461,
#284462,#284463,#284464,#284465,#284466,#284467,#284468,#284469,#284470,
#284471,#284472,#284473,#284474,#284475,#284476,#284477,#284478,#284479,
#284480,#284481,#284482,#284483,#284484,#284485,#284486,#284487,#284488,
#284489,#284490,#284491,#284492,#284493,#284494,#284495,#284496,#284497,
#284498,#284499,#284500,#284501,#284502,#284503,#284504,#284505,#284506,
#284507,#284508,#284509,#284510,#284511,#284512,#284513,#284514,#284515,
#284516,#284517,#284518,#284519,#284520,#284521,#284522,#284523,#284524,
#284525,#284526,#284527,#284528,#284529,#284530,#284531,#284532,#284533,
#284534,#284535,#284536,#284537,#284538,#284539,#284540,#284541,#284542,
#284543,#284544,#284545,#284546,#284547,#284548,#284549,#284550,#284551,
#284552,#284553,#284554,#284555,#284556,#284557,#284558,#284559,#284560,
#284561,#284562,#284563,#284564,#284565,#284566,#284567,#284568,#284569,
#284570,#284571,#284572,#284573,#284574,#284575,#284576,#284577,#284578,
#284579,#284580,#284581,#284582,#284583,#284584,#284585,#284586,#284587,
#284588,#284589,#284590,#284591,#284592,#284593,#284594,#284595,#284596,
#284597,#284598,#284599,#284600,#284601,#284602,#284603,#284604,#284605,
#284606,#284607,#284608,#284609,#284610,#284611,#284612,#284613,#284614,
#284615,#284616,#284617,#284618,#284619,#284620,#284621,#284622,#284623,
#284624,#284625,#284626,#284627,#284628,#284629,#284630,#284631,#284632,
#284633,#284634,#284635,#284636,#284637,#284638,#284639,#284640,#284641,
#284642,#284643,#284644,#284645,#284646),(#284647,#284648,#284649,#284650,
#284651,#284652,#284653,#284654,#284655,#284656,#284657,#284658,#284659,
#284660,#284661,#284662,#284663,#284664,#284665,#284666,#284667,#284668,
#284669,#284670,#284671,#284672,#284673,#284674,#284675,#284676,#284677,
#284678,#284679,#284680,#284681,#284682,#284683,#284684,#284685,#284686,
#284687,#284688,#284689,#284690,#284691,#284692,#284693,#284694,#284695,
#284696,#284697,#284698,#284699,#284700,#284701,#284702,#284703,#284704,
#284705,#284706,#284707,#284708,#284709,#284710,#284711,#284712,#284713,
#284714,#284715,#284716,#284717,#284718,#284719,#284720,#284721,#284722,
#284723,#284724,#284725,#284726,#284727,#284728,#284729,#284730,#284731,
#284732,#284733,#284734,#284735,#284736,#284737,#284738,#284739,#284740,
#284741,#284742,#284743,#284744,#284745,#284746,#284747,#284748,#284749,
#284750,#284751,#284752,#284753,#284754,#284755,#284756,#284757,#284758,
#284759,#284760,#284761,#284762,#284763,#284764,#284765,#284766,#284767,
#284768,#284769,#284770,#284771,#284772,#284773,#284774,#284775,#284776,
#284777,#284778,#284779,#284780,#284781,#284782,#284783,#284784,#284785,
#284786,#284787,#284788,#284789,#284790,#284791,#284792,#284793,#284794,
#284795,#284796,#284797,#284798,#284799,#284800,#284801,#284802,#284803,
#284804,#284805,#284806,#284807,#284808,#284809,#284810,#284811,#284812,
#284813,#284814,#284815,#284816,#284817,#284818,#284819,#284820,#284821,
#284822,#284823,#284824,#284825,#284826,#284827,#284828,#284829,#284830,
#284831,#284832,#284833,#284834,#284835,#284836,#284837,#284838,#284839,
#284840,#284841,#284842,#284843,#284844,#284845,#284846,#284847,#284848,
#284849,#284850,#284851,#284852,#284853,#284854,#284855,#284856,#284857,
#284858,#284859,#284860,#284861,#284862,#284863,#284864,#284865,#284866,
#284867,#284868,#284869,#284870,#284871,#284872,#284873,#284874,#284875,
#284876,#284877,#284878,#284879,#284880,#284881,#284882,#284883,#284884,
#284885,#284886,#284887,#284888,#284889,#284890,#284891,#284892,#284893,
#284894,#284895,#284896,#284897,#284898,#284899,#284900,#284901,#284902,
#284903,#284904,#284905,#284906,#284907,#284908,#284909,#284910,#284911,
#284912,#284913,#284914,#284915,#284916,#284917,#284918,#284919,#284920,
#284921,#284922,#284923,#284924,#284925,#284926,#284927,#284928,#284929,
#284930,#284931,#284932,#284933,#284934,#284935,#284936,#284937,#284938,
#284939,#284940,#284941,#284942,#284943,#284944,#284945,#284946,#284947,
#284948,#284949,#284950,#284951,#284952,#284953,#284954,#284955,#284956,
#284957,#284958,#284959,#284960,#284961,#284962,#284963,#284964,#284965,
#284966,#284967,#284968,#284969,#284970,#284971,#284972,#284973,#284974,
#284975,#284976,#284977,#284978,#284979,#284980,#284981,#284982,#284983,
#284984,#284985,#284986,#284987,#284988,#284989,#284990,#284991,#284992,
#284993,#284994,#284995,#284996,#284997,#284998,#284999,#285000,#285001,
#285002,#285003,#285004,#285005,#285006,#285007,#285008,#285009,#285010,
#285011,#285012,#285013,#285014,#285015,#285016,#285017,#285018,#285019,
#285020,#285021,#285022,#285023,#285024,#285025,#285026,#285027,#285028,
#285029,#285030,#285031,#285032,#285033,#285034,#285035,#285036,#285037,
#285038,#285039,#285040,#285041,#285042,#285043,#285044,#285045,#285046,
#285047,#285048,#285049,#285050,#285051,#285052,#285053,#285054,#285055,
#285056,#285057,#285058,#285059,#285060,#285061,#285062,#285063,#285064,
#285065,#285066,#285067,#285068,#285069,#285070,#285071,#285072,#285073,
#285074,#285075,#285076,#285077,#285078,#285079,#285080,#285081,#285082,
#285083,#285084,#285085,#285086,#285087,#285088,#285089,#285090,#285091,
#285092,#285093,#285094,#285095,#285096,#285097,#285098,#285099,#285100,
#285101,#285102,#285103,#285104,#285105,#285106,#285107,#285108,#285109,
#285110,#285111,#285112,#285113,#285114,#285115,#285116,#285117,#285118,
#285119,#285120,#285121,#285122,#285123,#285124,#285125,#285126,#285127,
#285128,#285129,#285130,#285131,#285132,#285133,#285134,#285135,#285136,
#285137,#285138,#285139,#285140,#285141,#285142,#285143,#285144,#285145,
#285146,#285147,#285148,#285149,#285150,#285151,#285152,#285153,#285154,
#285155,#285156,#285157,#285158,#285159,#285160,#285161,#285162,#285163,
#285164,#285165,#285166,#285167,#285168,#285169,#285170,#285171,#285172,
#285173,#285174,#285175,#285176,#285177,#285178,#285179,#285180,#285181,
#285182,#285183,#285184,#285185,#285186,#285187,#285188,#285189,#285190,
#285191,#285192,#285193,#285194,#285195,#285196,#285197,#285198,#285199,
#285200,#285201,#285202,#285203,#285204,#285205,#285206,#285207,#285208,
#285209,#285210,#285211,#285212,#285213,#285214,#285215,#285216,#285217,
#285218,#285219,#285220,#285221,#285222,#285223,#285224,#285225,#285226,
#285227,#285228,#285229,#285230,#285231,#285232,#285233,#285234,#285235,
#285236,#285237,#285238,#285239,#285240,#285241,#285242,#285243,#285244,
#285245,#285246,#285247,#285248,#285249,#285250,#285251,#285252,#285253,
#285254,#285255,#285256,#285257,#285258,#285259,#285260,#285261,#285262,
#285263,#285264,#285265,#285266,#285267,#285268,#285269,#285270,#285271,
#285272,#285273,#285274,#285275,#285276,#285277,#285278,#285279,#285280,
#285281,#285282,#285283,#285284,#285285,#285286,#285287,#285288,#285289,
#285290,#285291,#285292,#285293,#285294,#285295,#285296,#285297,#285298,
#285299,#285300,#285301,#285302,#285303,#285304,#285305,#285306,#285307,
#285308,#285309,#285310,#285311,#285312,#285313,#285314,#285315,#285316,
#285317,#285318,#285319,#285320,#285321,#285322,#285323,#285324,#285325,
#285326,#285327,#285328,#285329,#285330,#285331,#285332,#285333,#285334,
#285335,#285336,#285337,#285338,#285339,#285340,#285341,#285342,#285343,
#285344,#285345,#285346,#285347,#285348,#285349,#285350,#285351,#285352,
#285353,#285354,#285355,#285356,#285357,#285358,#285359,#285360,#285361,
#285362,#285363,#285364,#285365,#285366,#285367,#285368,#285369,#285370,
#285371,#285372,#285373,#285374,#285375,#285376,#285377,#285378,#285379,
#285380,#285381,#285382,#285383,#285384,#285385,#285386,#285387,#285388,
#285389,#285390,#285391,#285392,#285393,#285394,#285395,#285396,#285397,
#285398,#285399,#285400,#285401,#285402,#285403,#285404,#285405,#285406,
#285407,#285408,#285409,#285410,#285411,#285412,#285413,#285414,#285415,
#285416,#285417,#285418,#285419,#285420,#285421,#285422,#285423,#285424,
#285425,#285426,#285427,#285428,#285429,#285430,#285431,#285432,#285433,
#285434,#285435,#285436,#285437,#285438,#285439,#285440,#285441,#285442,
#285443,#285444,#285445,#285446,#285447,#285448,#285449,#285450,#285451,
#285452,#285453,#285454,#285455,#285456,#285457,#285458,#285459,#285460,
#285461,#285462,#285463,#285464,#285465,#285466,#285467,#285468,#285469,
#285470,#285471,#285472,#285473,#285474,#285475,#285476,#285477,#285478,
#285479,#285480,#285481,#285482,#285483,#285484,#285485,#285486,#285487,
#285488,#285489,#285490,#285491,#285492,#285493,#285494,#285495,#285496,
#285497,#285498,#285499,#285500,#285501,#285502,#285503,#285504,#285505,
#285506,#285507,#285508,#285509,#285510,#285511,#285512,#285513,#285514,
#285515,#285516,#285517,#285518,#285519,#285520,#285521,#285522,#285523,
#285524,#285525,#285526,#285527,#285528,#285529,#285530,#285531,#285532,
#285533,#285534,#285535,#285536,#285537,#285538,#285539,#285540,#285541,
#285542,#285543,#285544,#285545,#285546,#285547,#285548,#285549,#285550,
#285551,#285552,#285553,#285554,#285555,#285556,#285557,#285558,#285559,
#285560,#285561,#285562,#285563,#285564,#285565,#285566,#285567,#285568,
#285569,#285570,#285571,#285572,#285573,#285574,#285575,#285576,#285577,
#285578,#285579,#285580,#285581,#285582,#285583,#285584,#285585,#285586,
#285587,#285588,#285589,#285590,#285591,#285592,#285593,#285594,#285595,
#285596,#285597,#285598,#285599,#285600,#285601,#285602,#285603,#285604,
#285605,#285606,#285607,#285608,#285609,#285610,#285611,#285612,#285613,
#285614,#285615,#285616,#285617,#285618,#285619,#285620,#285621,#285622,
#285623,#285624,#285625,#285626,#285627,#285628,#285629,#285630,#285631,
#285632,#285633,#285634,#285635,#285636,#285637,#285638,#285639,#285640,
#285641,#285642,#285643,#285644,#285645,#285646,#285647,#285648,#285649,
#285650,#285651,#285652,#285653,#285654,#285655,#285656,#285657,#285658,
#285659,#285660,#285661,#285662,#285663,#285664,#285665,#285666,#285667,
#285668,#285669,#285670,#285671,#285672,#285673,#285674,#285675,#285676,
#285677,#285678,#285679,#285680,#285681,#285682,#285683)),.UNSPECIFIED.,
 .F.,.F.,.F.)
B_SPLINE_SURFACE_WITH_KNOTS((2,2),(3,2,2,2,2,2,2,2,2,2,2,2,2,2,2,2,2,2,
2,2,2,2,2,2,2,2,2,2,2,2,2,2,2,2,2,2,2,2,2,2,2,2,2,2,2,2,2,2,2,2,2,2,2,2,
2,2,2,2,2,2,2,2,2,2,2,2,2,2,2,2,2,2,2,2,2,2,2,2,2,2,2,2,2,2,2,2,2,2,2,2,
2,2,2,2,2,2,2,2,2,2,2,2,2,2,2,2,2,2,2,2,2,2,2,2,2,2,2,2,2,2,2,2,2,2,2,2,
2,2,2,2,2,2,2,2,2,2,2,2,2,2,2,2,2,2,2,2,2,2,2,2,2,2,2,2,2,2,2,2,2,2,2,2,
2,2,2,2,2,2,2,2,2,2,2,2,2,2,2,2,2,2,2,2,2,2,2,2,2,2,2,2,2,2,2,2,2,2,2,2,
2,2,2,2,2,2,2,2,2,2,2,2,2,2,2,2,2,2,2,2,2,2,2,2,2,2,2,2,2,2,2,2,2,2,2,2,
2,2,2,2,2,2,2,2,2,2,2,2,2,2,2,2,2,2,2,2,2,2,2,2,2,2,2,2,2,2,2,2,2,2,2,2,
2,2,2,2,2,2,2,2,2,2,2,2,2,2,2,2,2,2,2,2,2,2,2,2,2,2,2,2,2,2,2,2,2,2,2,2,
2,2,2,2,2,2,2,2,2,2,2,2,2,2,2,2,2,2,2,2,2,2,2,2,2,2,2,2,2,2,2,2,2,2,2,2,
2,2,2,2,2,2,2,2,2,2,2,2,2,2,2,2,2,2,2,2,2,2,2,2,2,2,2,2,2,2,2,2,2,2,2,2,
2,2,2,2,2,2,2,2,2,2,2,2,2,2,2,2,2,2,2,2,2,2,2,2,2,2,2,2,2,2,2,2,2,2,2,2,
2,2,2,2,2,2,2,2,2,2,2,2,2,2,2,2,2,2,2,2,2,2,2,2,2,2,2,2,2,2,2,2,2,2,2,2,
2,2,2,2,2,2,2,2,2,2,2,2,2,2,2,2,2,2,2,2,2,2,2,2,2,2,2,2,2,2,2,2,2,2,2,2,
2,2,2,2,2,2,2,2,2,2,2,2,2,2,2,2,2,2,2,2,2,2,2,2,2,2,2,2,2,2,2,2,3),(0.,
1.00000449367228),(0.,0.00192307692307692,0.00384615384615385,0.00576923076923077,
0.00769230769230769,0.00961538461538462,0.0115384615384615,0.0134615384615385,
0.0153846153846154,0.0173076923076923,0.0192307692307692,0.0211538461538462,
0.0230769230769231,0.025,0.0269230769230769,0.0288461538461538,0.0307692307692308,
0.0326923076923077,0.0346153846153846,0.0365384615384615,0.0384615384615385,
0.0403846153846154,0.0423076923076923,0.0442307692307692,0.0461538461538462,
0.0480769230769231,0.05,0.0519230769230769,0.0538461538461538,0.0557692307692308,
0.0576923076923077,0.0596153846153846,0.0615384615384615,0.0634615384615385,
0.0653846153846154,0.0673076923076923,0.0692307692307692,0.0711538461538462,
0.0730769230769231,0.075,0.0769230769230769,0.0788461538461538,0.0807692307692308,
0.0826923076923077,0.0846153846153846,0.0865384615384615,0.0884615384615385,
0.0903846153846154,0.0923076923076923,0.0942307692307692,0.0961538461538462,
0.0980769230769231,0.1,0.101923076923077,0.103846153846154,0.105769230769231,
0.107692307692308,0.109615384615385,0.111538461538462,0.113461538461538,
0.115384615384615,0.117307692307692,0.119230769230769,0.121153846153846,
0.123076923076923,0.125,0.126923076923077,0.128846153846154,0.130769230769231,
0.132692307692308,0.134615384615385,0.136538461538462,0.138461538461538,
0.140384615384615,0.142307692307692,0.144230769230769,0.146153846153846,
0.148076923076923,0.15,0.151923076923077,0.153846153846154,0.155769230769231,
0.157692307692308,0.159615384615385,0.161538461538462,0.163461538461538,
0.165384615384615,0.167307692307692,0.169230769230769,0.171153846153846,
0.173076923076923,0.175,0.176923076923077,0.178846153846154,0.180769230769231,
0.182692307692308,0.184615384615385,0.186538461538462,0.188461538461538,
0.190384615384615,0.192307692307692,0.194230769230769,0.196153846153846,
0.198076923076923,0.2,0.201923076923077,0.203846153846154,0.205769230769231,
0.207692307692308,0.209615384615385,0.211538461538462,0.213461538461538,
0.215384615384615,0.217307692307692,0.219230769230769,0.221153846153846,
0.223076923076923,0.225,0.226923076923077,0.228846153846154,0.230769230769231,
0.232692307692308,0.234615384615385,0.236538461538462,0.238461538461538,
0.240384615384615,0.242307692307692,0.244230769230769,0.246153846153846,
0.248076923076923,0.25,0.251923076923077,0.253846153846154,0.255769230769231,
0.257692307692308,0.259615384615385,0.261538461538462,0.263461538461538,
0.265384615384615,0.267307692307692,0.269230769230769,0.271153846153846,
0.273076923076923,0.275,0.276923076923077,0.278846153846154,0.280769230769231,
0.282692307692308,0.284615384615385,0.286538461538462,0.288461538461538,
0.290384615384615,0.292307692307692,0.294230769230769,0.296153846153846,
0.298076923076923,0.3,0.301923076923077,0.303846153846154,0.305769230769231,
0.307692307692308,0.309615384615385,0.311538461538462,0.313461538461538,
0.315384615384615,0.317307692307692,0.319230769230769,0.321153846153846,
0.323076923076923,0.325,0.326923076923077,0.328846153846154,0.330769230769231,
0.332692307692308,0.334615384615385,0.336538461538462,0.338461538461538,
0.340384615384615,0.342307692307692,0.344230769230769,0.346153846153846,
0.348076923076923,0.35,0.351923076923077,0.353846153846154,0.355769230769231,
0.357692307692308,0.359615384615385,0.361538461538462,0.363461538461538,
0.365384615384615,0.367307692307692,0.369230769230769,0.371153846153846,
0.373076923076923,0.375,0.376923076923077,0.378846153846154,0.380769230769231,
0.382692307692308,0.384615384615385,0.386538461538462,0.388461538461538,
0.390384615384615,0.392307692307692,0.394230769230769,0.396153846153846,
0.398076923076923,0.4,0.401923076923077,0.403846153846154,0.405769230769231,
0.407692307692308,0.409615384615385,0.411538461538462,0.413461538461538,
0.415384615384615,0.417307692307692,0.419230769230769,0.421153846153846,
0.423076923076923,0.425,0.426923076923077,0.428846153846154,0.430769230769231,
0.432692307692308,0.434615384615385,0.436538461538462,0.438461538461538,
0.440384615384615,0.442307692307692,0.444230769230769,0.446153846153846,
0.448076923076923,0.45,0.451923076923077,0.453846153846154,0.455769230769231,
0.457692307692308,0.459615384615385,0.461538461538462,0.463461538461538,
0.465384615384615,0.467307692307692,0.469230769230769,0.471153846153846,
0.473076923076923,0.475,0.476923076923077,0.478846153846154,0.480769230769231,
0.482692307692308,0.484615384615385,0.486538461538462,0.488461538461538,
0.490384615384615,0.492307692307692,0.494230769230769,0.496153846153846,
0.498076923076923,0.5,0.501923076923077,0.503846153846154,0.505769230769231,
0.507692307692308,0.509615384615385,0.511538461538461,0.513461538461538,
0.515384615384615,0.517307692307692,0.519230769230769,0.521153846153846,
0.523076923076923,0.525,0.526923076923077,0.528846153846154,0.530769230769231,
0.532692307692308,0.534615384615385,0.536538461538462,0.538461538461538,
0.540384615384615,0.542307692307692,0.544230769230769,0.546153846153846,
0.548076923076923,0.55,0.551923076923077,0.553846153846154,0.555769230769231,
0.557692307692308,0.559615384615385,0.561538461538462,0.563461538461538,
0.565384615384615,0.567307692307692,0.569230769230769,0.571153846153846,
0.573076923076923,0.575,0.576923076923077,0.578846153846154,0.580769230769231,
0.582692307692308,0.584615384615385,0.586538461538462,0.588461538461538,
0.590384615384615,0.592307692307692,0.594230769230769,0.596153846153846,
0.598076923076923,0.6,0.601923076923077,0.603846153846154,0.605769230769231,
0.607692307692308,0.609615384615385,0.611538461538462,0.613461538461539,
0.615384615384615,0.617307692307692,0.619230769230769,0.621153846153846,
0.623076923076923,0.625,0.626923076923077,0.628846153846154,0.630769230769231,
0.632692307692308,0.634615384615385,0.636538461538461,0.638461538461538,
0.640384615384615,0.642307692307692,0.644230769230769,0.646153846153846,
0.648076923076923,0.65,0.651923076923077,0.653846153846154,0.655769230769231,
0.657692307692308,0.659615384615385,0.661538461538462,0.663461538461538,
0.665384615384615,0.667307692307692,0.669230769230769,0.671153846153846,
0.673076923076923,0.675,0.676923076923077,0.678846153846154,0.680769230769231,
0.682692307692308,0.684615384615385,0.686538461538462,0.688461538461538,
0.690384615384615,0.692307692307692,0.694230769230769,0.696153846153846,
0.698076923076923,0.7,0.701923076923077,0.703846153846154,0.705769230769231,
0.707692307692308,0.709615384615385,0.711538461538462,0.713461538461538,
0.715384615384615,0.717307692307692,0.719230769230769,0.721153846153846,
0.723076923076923,0.725,0.726923076923077,0.728846153846154,0.730769230769231,
0.732692307692308,0.734615384615385,0.736538461538462,0.738461538461539,
0.740384615384615,0.742307692307692,0.744230769230769,0.746153846153846,
0.748076923076923,0.75,0.751923076923077,0.753846153846154,0.755769230769231,
0.757692307692308,0.759615384615385,0.761538461538461,0.763461538461538,
0.765384615384615,0.767307692307692,0.769230769230769,0.771153846153846,
0.773076923076923,0.775,0.776923076923077,0.778846153846154,0.780769230769231,
0.782692307692308,0.784615384615385,0.786538461538462,0.788461538461538,
0.790384615384615,0.792307692307692,0.794230769230769,0.796153846153846,
0.798076923076923,0.8,0.801923076923077,0.803846153846154,0.805769230769231,
0.807692307692308,0.809615384615385,0.811538461538462,0.813461538461538,
0.815384615384615,0.817307692307692,0.819230769230769,0.821153846153846,
0.823076923076923,0.825,0.826923076923077,0.828846153846154,0.830769230769231,
0.832692307692308,0.834615384615385,0.836538461538462,0.838461538461538,
0.840384615384615,0.842307692307692,0.844230769230769,0.846153846153846,
0.848076923076923,0.85,0.851923076923077,0.853846153846154,0.855769230769231,
0.857692307692308,0.859615384615385,0.861538461538462,0.863461538461539,
0.865384615384615,0.867307692307692,0.869230769230769,0.871153846153846,
0.873076923076923,0.875,0.876923076923077,0.878846153846154,0.880769230769231,
0.882692307692308,0.884615384615385,0.886538461538461,0.888461538461538,
0.890384615384615,0.892307692307692,0.894230769230769,0.896153846153846,
0.898076923076923,0.9,0.901923076923077,0.903846153846154,0.905769230769231,
0.907692307692308,0.909615384615385,0.911538461538462,0.913461538461538,
0.915384615384615,0.917307692307692,0.919230769230769,0.921153846153846,
0.923076923076923,0.925,0.926923076923077,0.928846153846154,0.930769230769231,
0.932692307692308,0.934615384615385,0.936538461538462,0.938461538461538,
0.940384615384615,0.942307692307692,0.944230769230769,0.946153846153846,
0.948076923076923,0.95,0.951923076923077,0.953846153846154,0.955769230769231,
0.957692307692308,0.959615384615385,0.961538461538462,0.963461538461538,
0.965384615384615,0.967307692307692,0.969230769230769,0.971153846153846,
0.973076923076923,0.975,0.976923076923077,0.978846153846154,0.980769230769231,
0.982692307692308,0.984615384615385,0.986538461538462,0.988461538461539,
0.990384615384615,0.992307692307692,0.994230769230769,0.996153846153846),
 .UNSPECIFIED.)
GEOMETRIC_REPRESENTATION_ITEM()
RATIONAL_B_SPLINE_SURFACE(((1.,0.951056516295154,1.,0.951056516295154,1.,
0.951056516295154,1.,0.951056516295154,1.,0.951056516295154,1.,0.951056516295154,
1.,0.951056516295154,1.,0.951056516295154,1.,0.951056516295154,1.,0.951056516295154,
1.,0.951056516295154,1.,0.951056516295154,1.,0.951056516295154,1.,0.951056516295154,
1.,0.951056516295154,1.,0.951056516295154,1.,0.951056516295154,1.,0.951056516295154,
1.,0.951056516295154,1.,0.951056516295154,1.,0.951056516295154,1.,0.951056516295154,
1.,0.951056516295154,1.,0.951056516295154,1.,0.951056516295154,1.,0.951056516295154,
1.,0.951056516295154,1.,0.951056516295154,1.,0.951056516295154,1.,0.951056516295154,
1.,0.951056516295154,1.,0.951056516295154,1.,0.951056516295154,1.,0.951056516295154,
1.,0.951056516295154,1.,0.951056516295154,1.,0.951056516295154,1.,0.951056516295154,
1.,0.951056516295154,1.,0.951056516295154,1.,0.951056516295154,1.,0.951056516295154,
1.,0.951056516295154,1.,0.951056516295154,1.,0.951056516295154,1.,0.951056516295154,
1.,0.951056516295154,1.,0.951056516295154,1.,0.951056516295154,1.,0.951056516295154,
1.,0.951056516295154,1.,0.951056516295154,1.,0.951056516295154,1.,0.951056516295154,
1.,0.951056516295154,1.,0.951056516295154,1.,0.951056516295154,1.,0.951056516295154,
1.,0.951056516295154,1.,0.951056516295154,1.,0.951056516295154,1.,0.951056516295154,
1.,0.951056516295154,1.,0.951056516295154,1.,0.951056516295154,1.,0.951056516295154,
1.,0.951056516295154,1.,0.951056516295154,1.,0.951056516295154,1.,0.951056516295154,
1.,0.951056516295154,1.,0.951056516295154,1.,0.951056516295154,1.,0.951056516295154,
1.,0.951056516295154,1.,0.951056516295154,1.,0.951056516295154,1.,0.951056516295154,
1.,0.951056516295154,1.,0.951056516295154,1.,0.951056516295154,1.,0.951056516295154,
1.,0.951056516295154,1.,0.951056516295154,1.,0.951056516295154,1.,0.951056516295154,
1.,0.951056516295154,1.,0.951056516295154,1.,0.951056516295154,1.,0.951056516295154,
1.,0.951056516295154,1.,0.951056516295154,1.,0.951056516295154,1.,0.951056516295154,
1.,0.951056516295154,1.,0.951056516295154,1.,0.951056516295154,1.,0.951056516295154,
1.,0.951056516295154,1.,0.951056516295154,1.,0.951056516295154,1.,0.951056516295154,
1.,0.951056516295154,1.,0.951056516295154,1.,0.951056516295154,1.,0.951056516295154,
1.,0.951056516295154,1.,0.951056516295154,1.,0.951056516295154,1.,0.951056516295154,
1.,0.951056516295154,1.,0.951056516295154,1.,0.951056516295154,1.,0.951056516295154,
1.,0.951056516295154,1.,0.951056516295154,1.,0.951056516295154,1.,0.951056516295154,
1.,0.951056516295154,1.,0.951056516295154,1.,0.951056516295154,1.,0.951056516295154,
1.,0.951056516295154,1.,0.951056516295154,1.,0.951056516295154,1.,0.951056516295154,
1.,0.951056516295154,1.,0.951056516295154,1.,0.951056516295154,1.,0.951056516295154,
1.,0.951056516295154,1.,0.951056516295154,1.,0.951056516295154,1.,0.951056516295154,
1.,0.951056516295154,1.,0.951056516295154,1.,0.951056516295154,1.,0.951056516295154,
1.,0.951056516295154,1.,0.951056516295154,1.,0.951056516295154,1.,0.951056516295154,
1.,0.951056516295154,1.,0.951056516295154,1.,0.951056516295154,1.,0.951056516295154,
1.,0.951056516295154,1.,0.951056516295154,1.,0.951056516295154,1.,0.951056516295154,
1.,0.951056516295154,1.,0.951056516295154,1.,0.951056516295154,1.,0.951056516295154,
1.,0.951056516295154,1.,0.951056516295154,1.,0.951056516295154,1.,0.951056516295154,
1.,0.951056516295154,1.,0.951056516295154,1.,0.951056516295154,1.,0.951056516295154,
1.,0.951056516295154,1.,0.951056516295154,1.,0.951056516295154,1.,0.951056516295154,
1.,0.951056516295154,1.,0.951056516295154,1.,0.951056516295154,1.,0.951056516295154,
1.,0.951056516295154,1.,0.951056516295154,1.,0.951056516295154,1.,0.951056516295154,
1.,0.951056516295154,1.,0.951056516295154,1.,0.951056516295154,1.,0.951056516295154,
1.,0.951056516295154,1.,0.951056516295154,1.,0.951056516295154,1.,0.951056516295154,
1.,0.951056516295154,1.,0.951056516295154,1.,0.951056516295154,1.,0.951056516295154,
1.,0.951056516295154,1.,0.951056516295154,1.,0.951056516295154,1.,0.951056516295154,
1.,0.951056516295154,1.,0.951056516295154,1.,0.951056516295154,1.,0.951056516295154,
1.,0.951056516295154,1.,0.951056516295154,1.,0.951056516295154,1.,0.951056516295154,
1.,0.951056516295154,1.,0.951056516295154,1.,0.951056516295154,1.,0.951056516295154,
1.,0.951056516295154,1.,0.951056516295154,1.,0.951056516295154,1.,0.951056516295154,
1.,0.951056516295154,1.,0.951056516295154,1.,0.951056516295154,1.,0.951056516295154,
1.,0.951056516295154,1.,0.951056516295154,1.,0.951056516295154,1.,0.951056516295154,
1.,0.951056516295154,1.,0.951056516295154,1.,0.951056516295154,1.,0.951056516295154,
1.,0.951056516295154,1.,0.951056516295154,1.,0.951056516295154,1.,0.951056516295154,
1.,0.951056516295154,1.,0.951056516295154,1.,0.951056516295154,1.,0.951056516295154,
1.,0.951056516295154,1.,0.951056516295154,1.,0.951056516295154,1.,0.951056516295154,
1.,0.951056516295154,1.,0.951056516295154,1.,0.951056516295154,1.,0.951056516295154,
1.,0.951056516295154,1.,0.951056516295154,1.,0.951056516295154,1.,0.951056516295154,
1.,0.951056516295154,1.,0.951056516295154,1.,0.951056516295154,1.,0.951056516295154,
1.,0.951056516295154,1.,0.951056516295154,1.,0.951056516295154,1.,0.951056516295154,
1.,0.951056516295154,1.,0.951056516295154,1.,0.951056516295154,1.,0.951056516295154,
1.,0.951056516295154,1.,0.951056516295154,1.,0.951056516295154,1.,0.951056516295154,
1.,0.951056516295154,1.,0.951056516295154,1.,0.951056516295154,1.,0.951056516295154,
1.,0.951056516295154,1.,0.951056516295154,1.,0.951056516295154,1.,0.951056516295154,
1.,0.951056516295154,1.,0.951056516295154,1.,0.951056516295154,1.,0.951056516295154,
1.,0.951056516295154,1.,0.951056516295154,1.,0.951056516295154,1.,0.951056516295154,
1.,0.951056516295154,1.,0.951056516295154,1.,0.951056516295154,1.,0.951056516295154,
1.,0.951056516295154,1.,0.951056516295154,1.,0.951056516295154,1.,0.951056516295154,
1.,0.951056516295154,1.,0.951056516295154,1.,0.951056516295154,1.,0.951056516295154,
1.,0.951056516295154,1.,0.951056516295154,1.,0.951056516295154,1.,0.951056516295154,
1.,0.951056516295154,1.,0.951056516295154,1.,0.951056516295154,1.,0.951056516295154,
1.,0.951056516295154,1.,0.951056516295154,1.,0.951056516295154,1.,0.951056516295154,
1.,0.951056516295154,1.,0.951056516295154,1.,0.951056516295154,1.,0.951056516295154,
1.,0.951056516295154,1.,0.951056516295154,1.,0.951056516295154,1.,0.951056516295154,
1.,0.951056516295154,1.,0.951056516295154,1.,0.951056516295154,1.,0.951056516295154,
1.,0.951056516295154,1.,0.951056516295154,1.,0.951056516295154,1.,0.951056516295154,
1.,0.951056516295154,1.,0.951056516295154,1.,0.951056516295154,1.,0.951056516295154,
1.,0.951056516295154,1.,0.951056516295154,1.,0.951056516295154,1.,0.951056516295154,
1.,0.951056516295154,1.,0.951056516295154,1.,0.951056516295154,1.,0.951056516295154,
1.,0.951056516295154,1.,0.951056516295154,1.,0.951056516295154,1.,0.951056516295154,
1.,0.951056516295154,1.,0.951056516295154,1.,0.951056516295154,1.,0.951056516295154,
1.,0.951056516295154,1.,0.951056516295154,1.,0.951056516295154,1.,0.951056516295154,
1.,0.951056516295154,1.,0.951056516295154,1.,0.951056516295154,1.,0.951056516295154,
1.,0.951056516295154,1.,0.951056516295154,1.,0.951056516295154,1.,0.951056516295154,
1.,0.951056516295154,1.,0.951056516295154,1.,0.951056516295154,1.,0.951056516295154,
1.,0.951056516295154,1.,0.951056516295154,1.,0.951056516295154,1.,0.951056516295154,
1.,0.951056516295154,1.,0.951056516295154,1.,0.951056516295154,1.,0.951056516295154,
1.,0.951056516295154,1.,0.951056516295154,1.,0.951056516295154,1.,0.951056516295154,
1.,0.951056516295154,1.,0.951056516295154,1.,0.951056516295154,1.,0.951056516295154,
1.,0.951056516295154,1.,0.951056516295154,1.,0.951056516295154,1.,0.951056516295154,
1.,0.951056516295154,1.,0.951056516295154,1.,0.951056516295154,1.,0.951056516295154,
1.,0.951056516295154,1.,0.951056516295154,1.,0.951056516295154,1.,0.951056516295154,
1.,0.951056516295154,1.,0.951056516295154,1.,0.951056516295154,1.,0.951056516295154,
1.,0.951056516295154,1.,0.951056516295154,1.,0.951056516295154,1.,0.951056516295154,
1.,0.951056516295154,1.,0.951056516295154,1.,0.951056516295154,1.,0.951056516295154,
1.,0.951056516295154,1.,0.951056516295154,1.,0.951056516295154,1.,0.951056516295154,
1.,0.951056516295154,1.,0.951056516295154,1.,0.951056516295154,1.,0.951056516295154,
1.,0.951056516295154,1.,0.951056516295154,1.,0.951056516295154,1.,0.951056516295154,
1.,0.951056516295154,1.,0.951056516295154,1.,0.951056516295154,1.,0.951056516295154,
1.,0.951056516295154,1.,0.951056516295154,1.,0.951056516295154,1.,0.951056516295154,
1.,0.951056516295154,1.,0.951056516295154,1.,0.951056516295154,1.,0.951056516295154,
1.,0.951056516295154,1.,0.951056516295154,1.,0.951056516295154,1.,0.951056516295154,
1.,0.951056516295154,1.,0.951056516295154,1.,0.951056516295154,1.,0.951056516295154,
1.,0.951056516295154,1.,0.951056516295154,1.,0.951056516295154,1.,0.951056516295154,
1.,0.951056516295154,1.,0.951056516295154,1.,0.951056516295154,1.,0.951056516295154,
1.,0.951056516295154,1.,0.951056516295154,1.,0.951056516295154,1.,0.951056516295154,
1.,0.951056516295154,1.,0.951056516295154,1.,0.951056516295154,1.,0.951056516295154,
1.,0.951056516295154,1.,0.951056516295154,1.,0.951056516295154,1.,0.951056516295154,
1.,0.951056516295154,1.,0.951056516295154,1.,0.951056516295154,1.,0.951056516295154,
1.,0.951056516295154,1.,0.951056516295154,1.,0.951056516295154,1.,0.951056516295154,
1.,0.951056516295154,1.,0.951056516295154,1.,0.951056516295154,1.,0.951056516295154,
1.,0.951056516295154,1.,0.951056516295154,1.,0.951056516295154,1.,0.951056516295154,
1.,0.951056516295154,1.,0.951056516295154,1.,0.951056516295154,1.,0.951056516295154,
1.,0.951056516295154,1.,0.951056516295154,1.,0.951056516295154,1.,0.951056516295154,
1.,0.951056516295154,1.,0.951056516295154,1.,0.951056516295154,1.,0.951056516295154,
1.,0.951056516295154,1.,0.951056516295154,1.,0.951056516295154,1.,0.951056516295154,
1.,0.951056516295154,1.,0.951056516295154,1.,0.951056516295154,1.,0.951056516295154,
1.,0.951056516295154,1.,0.951056516295154,1.,0.951056516295154,1.,0.951056516295154,
1.,0.951056516295154,1.,0.951056516295154,1.,0.951056516295154,1.,0.951056516295154,
1.,0.951056516295154,1.,0.951056516295154,1.,0.951056516295154,1.,0.951056516295154,
1.,0.951056516295154,1.,0.951056516295154,1.,0.951056516295154,1.,0.951056516295154,
1.,0.951056516295154,1.,0.951056516295154,1.,0.951056516295154,1.,0.951056516295154,
1.,0.951056516295154,1.,0.951056516295154,1.,0.951056516295154,1.,0.951056516295154,
1.,0.951056516295154,1.,0.951056516295154,1.,0.951056516295154,1.,0.951056516295154,
1.,0.951056516295154,1.,0.951056516295154,1.,0.951056516295154,1.,0.951056516295154,
1.,0.951056516295154,1.,0.951056516295154,1.,0.951056516295154,1.,0.951056516295154,
1.,0.951056516295154,1.,0.951056516295154,1.,0.951056516295154,1.,0.951056516295154,
1.,0.951056516295154,1.,0.951056516295154,1.,0.951056516295154,1.,0.951056516295154,
1.),(1.,0.951056516295154,1.,0.951056516295154,1.,0.951056516295154,1.,
0.951056516295154,1.,0.951056516295154,1.,0.951056516295154,1.,0.951056516295154,
1.,0.951056516295154,1.,0.951056516295154,1.,0.951056516295154,1.,0.951056516295154,
1.,0.951056516295154,1.,0.951056516295154,1.,0.951056516295154,1.,0.951056516295154,
1.,0.951056516295154,1.,0.951056516295154,1.,0.951056516295154,1.,0.951056516295154,
1.,0.951056516295154,1.,0.951056516295154,1.,0.951056516295154,1.,0.951056516295154,
1.,0.951056516295154,1.,0.951056516295154,1.,0.951056516295154,1.,0.951056516295154,
1.,0.951056516295154,1.,0.951056516295154,1.,0.951056516295154,1.,0.951056516295154,
1.,0.951056516295154,1.,0.951056516295154,1.,0.951056516295154,1.,0.951056516295154,
1.,0.951056516295154,1.,0.951056516295154,1.,0.951056516295154,1.,0.951056516295154,
1.,0.951056516295154,1.,0.951056516295154,1.,0.951056516295154,1.,0.951056516295154,
1.,0.951056516295154,1.,0.951056516295154,1.,0.951056516295154,1.,0.951056516295154,
1.,0.951056516295154,1.,0.951056516295154,1.,0.951056516295154,1.,0.951056516295154,
1.,0.951056516295154,1.,0.951056516295154,1.,0.951056516295154,1.,0.951056516295154,
1.,0.951056516295154,1.,0.951056516295154,1.,0.951056516295154,1.,0.951056516295154,
1.,0.951056516295154,1.,0.951056516295154,1.,0.951056516295154,1.,0.951056516295154,
1.,0.951056516295154,1.,0.951056516295154,1.,0.951056516295154,1.,0.951056516295154,
1.,0.951056516295154,1.,0.951056516295154,1.,0.951056516295154,1.,0.951056516295154,
1.,0.951056516295154,1.,0.951056516295154,1.,0.951056516295154,1.,0.951056516295154,
1.,0.951056516295154,1.,0.951056516295154,1.,0.951056516295154,1.,0.951056516295154,
1.,0.951056516295154,1.,0.951056516295154,1.,0.951056516295154,1.,0.951056516295154,
1.,0.951056516295154,1.,0.951056516295154,1.,0.951056516295154,1.,0.951056516295154,
1.,0.951056516295154,1.,0.951056516295154,1.,0.951056516295154,1.,0.951056516295154,
1.,0.951056516295154,1.,0.951056516295154,1.,0.951056516295154,1.,0.951056516295154,
1.,0.951056516295154,1.,0.951056516295154,1.,0.951056516295154,1.,0.951056516295154,
1.,0.951056516295154,1.,0.951056516295154,1.,0.951056516295154,1.,0.951056516295154,
1.,0.951056516295154,1.,0.951056516295154,1.,0.951056516295154,1.,0.951056516295154,
1.,0.951056516295154,1.,0.951056516295154,1.,0.951056516295154,1.,0.951056516295154,
1.,0.951056516295154,1.,0.951056516295154,1.,0.951056516295154,1.,0.951056516295154,
1.,0.951056516295154,1.,0.951056516295154,1.,0.951056516295154,1.,0.951056516295154,
1.,0.951056516295154,1.,0.951056516295154,1.,0.951056516295154,1.,0.951056516295154,
1.,0.951056516295154,1.,0.951056516295154,1.,0.951056516295154,1.,0.951056516295154,
1.,0.951056516295154,1.,0.951056516295154,1.,0.951056516295154,1.,0.951056516295154,
1.,0.951056516295154,1.,0.951056516295154,1.,0.951056516295154,1.,0.951056516295154,
1.,0.951056516295154,1.,0.951056516295154,1.,0.951056516295154,1.,0.951056516295154,
1.,0.951056516295154,1.,0.951056516295154,1.,0.951056516295154,1.,0.951056516295154,
1.,0.951056516295154,1.,0.951056516295154,1.,0.951056516295154,1.,0.951056516295154,
1.,0.951056516295154,1.,0.951056516295154,1.,0.951056516295154,1.,0.951056516295154,
1.,0.951056516295154,1.,0.951056516295154,1.,0.951056516295154,1.,0.951056516295154,
1.,0.951056516295154,1.,0.951056516295154,1.,0.951056516295154,1.,0.951056516295154,
1.,0.951056516295154,1.,0.951056516295154,1.,0.951056516295154,1.,0.951056516295154,
1.,0.951056516295154,1.,0.951056516295154,1.,0.951056516295154,1.,0.951056516295154,
1.,0.951056516295154,1.,0.951056516295154,1.,0.951056516295154,1.,0.951056516295154,
1.,0.951056516295154,1.,0.951056516295154,1.,0.951056516295154,1.,0.951056516295154,
1.,0.951056516295154,1.,0.951056516295154,1.,0.951056516295154,1.,0.951056516295154,
1.,0.951056516295154,1.,0.951056516295154,1.,0.951056516295154,1.,0.951056516295154,
1.,0.951056516295154,1.,0.951056516295154,1.,0.951056516295154,1.,0.951056516295154,
1.,0.951056516295154,1.,0.951056516295154,1.,0.951056516295154,1.,0.951056516295154,
1.,0.951056516295154,1.,0.951056516295154,1.,0.951056516295154,1.,0.951056516295154,
1.,0.951056516295154,1.,0.951056516295154,1.,0.951056516295154,1.,0.951056516295154,
1.,0.951056516295154,1.,0.951056516295154,1.,0.951056516295154,1.,0.951056516295154,
1.,0.951056516295154,1.,0.951056516295154,1.,0.951056516295154,1.,0.951056516295154,
1.,0.951056516295154,1.,0.951056516295154,1.,0.951056516295154,1.,0.951056516295154,
1.,0.951056516295154,1.,0.951056516295154,1.,0.951056516295154,1.,0.951056516295154,
1.,0.951056516295154,1.,0.951056516295154,1.,0.951056516295154,1.,0.951056516295154,
1.,0.951056516295154,1.,0.951056516295154,1.,0.951056516295154,1.,0.951056516295154,
1.,0.951056516295154,1.,0.951056516295154,1.,0.951056516295154,1.,0.951056516295154,
1.,0.951056516295154,1.,0.951056516295154,1.,0.951056516295154,1.,0.951056516295154,
1.,0.951056516295154,1.,0.951056516295154,1.,0.951056516295154,1.,0.951056516295154,
1.,0.951056516295154,1.,0.951056516295154,1.,0.951056516295154,1.,0.951056516295154,
1.,0.951056516295154,1.,0.951056516295154,1.,0.951056516295154,1.,0.951056516295154,
1.,0.951056516295154,1.,0.951056516295154,1.,0.951056516295154,1.,0.951056516295154,
1.,0.951056516295154,1.,0.951056516295154,1.,0.951056516295154,1.,0.951056516295154,
1.,0.951056516295154,1.,0.951056516295154,1.,0.951056516295154,1.,0.951056516295154,
1.,0.951056516295154,1.,0.951056516295154,1.,0.951056516295154,1.,0.951056516295154,
1.,0.951056516295154,1.,0.951056516295154,1.,0.951056516295154,1.,0.951056516295154,
1.,0.951056516295154,1.,0.951056516295154,1.,0.951056516295154,1.,0.951056516295154,
1.,0.951056516295154,1.,0.951056516295154,1.,0.951056516295154,1.,0.951056516295154,
1.,0.951056516295154,1.,0.951056516295154,1.,0.951056516295154,1.,0.951056516295154,
1.,0.951056516295154,1.,0.951056516295154,1.,0.951056516295154,1.,0.951056516295154,
1.,0.951056516295154,1.,0.951056516295154,1.,0.951056516295154,1.,0.951056516295154,
1.,0.951056516295154,1.,0.951056516295154,1.,0.951056516295154,1.,0.951056516295154,
1.,0.951056516295154,1.,0.951056516295154,1.,0.951056516295154,1.,0.951056516295154,
1.,0.951056516295154,1.,0.951056516295154,1.,0.951056516295154,1.,0.951056516295154,
1.,0.951056516295154,1.,0.951056516295154,1.,0.951056516295154,1.,0.951056516295154,
1.,0.951056516295154,1.,0.951056516295154,1.,0.951056516295154,1.,0.951056516295154,
1.,0.951056516295154,1.,0.951056516295154,1.,0.951056516295154,1.,0.951056516295154,
1.,0.951056516295154,1.,0.951056516295154,1.,0.951056516295154,1.,0.951056516295154,
1.,0.951056516295154,1.,0.951056516295154,1.,0.951056516295154,1.,0.951056516295154,
1.,0.951056516295154,1.,0.951056516295154,1.,0.951056516295154,1.,0.951056516295154,
1.,0.951056516295154,1.,0.951056516295154,1.,0.951056516295154,1.,0.951056516295154,
1.,0.951056516295154,1.,0.951056516295154,1.,0.951056516295154,1.,0.951056516295154,
1.,0.951056516295154,1.,0.951056516295154,1.,0.951056516295154,1.,0.951056516295154,
1.,0.951056516295154,1.,0.951056516295154,1.,0.951056516295154,1.,0.951056516295154,
1.,0.951056516295154,1.,0.951056516295154,1.,0.951056516295154,1.,0.951056516295154,
1.,0.951056516295154,1.,0.951056516295154,1.,0.951056516295154,1.,0.951056516295154,
1.,0.951056516295154,1.,0.951056516295154,1.,0.951056516295154,1.,0.951056516295154,
1.,0.951056516295154,1.,0.951056516295154,1.,0.951056516295154,1.,0.951056516295154,
1.,0.951056516295154,1.,0.951056516295154,1.,0.951056516295154,1.,0.951056516295154,
1.,0.951056516295154,1.,0.951056516295154,1.,0.951056516295154,1.,0.951056516295154,
1.,0.951056516295154,1.,0.951056516295154,1.,0.951056516295154,1.,0.951056516295154,
1.,0.951056516295154,1.,0.951056516295154,1.,0.951056516295154,1.,0.951056516295154,
1.,0.951056516295154,1.,0.951056516295154,1.,0.951056516295154,1.,0.951056516295154,
1.,0.951056516295154,1.,0.951056516295154,1.,0.951056516295154,1.,0.951056516295154,
1.,0.951056516295154,1.,0.951056516295154,1.,0.951056516295154,1.,0.951056516295154,
1.,0.951056516295154,1.,0.951056516295154,1.,0.951056516295154,1.,0.951056516295154,
1.,0.951056516295154,1.,0.951056516295154,1.,0.951056516295154,1.,0.951056516295154,
1.,0.951056516295154,1.,0.951056516295154,1.,0.951056516295154,1.,0.951056516295154,
1.,0.951056516295154,1.,0.951056516295154,1.,0.951056516295154,1.,0.951056516295154,
1.,0.951056516295154,1.,0.951056516295154,1.,0.951056516295154,1.,0.951056516295154,
1.,0.951056516295154,1.,0.951056516295154,1.,0.951056516295154,1.,0.951056516295154,
1.,0.951056516295154,1.,0.951056516295154,1.,0.951056516295154,1.,0.951056516295154,
1.,0.951056516295154,1.,0.951056516295154,1.,0.951056516295154,1.,0.951056516295154,
1.,0.951056516295154,1.,0.951056516295154,1.,0.951056516295154,1.,0.951056516295154,
1.,0.951056516295154,1.,0.951056516295154,1.,0.951056516295154,1.,0.951056516295154,
1.,0.951056516295154,1.,0.951056516295154,1.,0.951056516295154,1.,0.951056516295154,
1.,0.951056516295154,1.,0.951056516295154,1.,0.951056516295154,1.,0.951056516295154,
1.,0.951056516295154,1.,0.951056516295154,1.,0.951056516295154,1.,0.951056516295154,
1.,0.951056516295154,1.,0.951056516295154,1.,0.951056516295154,1.,0.951056516295154,
1.,0.951056516295154,1.,0.951056516295154,1.,0.951056516295154,1.,0.951056516295154,
1.,0.951056516295154,1.,0.951056516295154,1.,0.951056516295154,1.,0.951056516295154,
1.,0.951056516295154,1.,0.951056516295154,1.,0.951056516295154,1.,0.951056516295154,
1.,0.951056516295154,1.,0.951056516295154,1.,0.951056516295154,1.,0.951056516295154,
1.,0.951056516295154,1.,0.951056516295154,1.,0.951056516295154,1.,0.951056516295154,
1.,0.951056516295154,1.,0.951056516295154,1.,0.951056516295154,1.,0.951056516295154,
1.,0.951056516295154,1.,0.951056516295154,1.,0.951056516295154,1.,0.951056516295154,
1.,0.951056516295154,1.,0.951056516295154,1.,0.951056516295154,1.,0.951056516295154,
1.,0.951056516295154,1.,0.951056516295154,1.,0.951056516295154,1.,0.951056516295154,
1.,0.951056516295154,1.,0.951056516295154,1.,0.951056516295154,1.,0.951056516295154,
1.,0.951056516295154,1.,0.951056516295154,1.,0.951056516295154,1.,0.951056516295154,
1.,0.951056516295154,1.,0.951056516295154,1.,0.951056516295154,1.,0.951056516295154,
1.,0.951056516295154,1.,0.951056516295154,1.,0.951056516295154,1.,0.951056516295154,
1.,0.951056516295154,1.,0.951056516295154,1.,0.951056516295154,1.,0.951056516295154,
1.,0.951056516295154,1.,0.951056516295154,1.,0.951056516295154,1.,0.951056516295154,
1.,0.951056516295154,1.,0.951056516295154,1.,0.951056516295154,1.,0.951056516295154,
1.,0.951056516295154,1.,0.951056516295154,1.,0.951056516295154,1.,0.951056516295154,
1.,0.951056516295154,1.,0.951056516295154,1.,0.951056516295154,1.,0.951056516295154,
1.,0.951056516295154,1.,0.951056516295154,1.,0.951056516295154,1.,0.951056516295154,
1.,0.951056516295154,1.,0.951056516295154,1.,0.951056516295154,1.,0.951056516295154,
1.,0.951056516295154,1.,0.951056516295154,1.,0.951056516295154,1.)))
REPRESENTATION_ITEM('')
SURFACE()
);
#3196=(
BOUNDED_SURFACE()
B_SPLINE_SURFACE(1,2,((#285828,#285829,#285830,#285831,#285832,#285833,
#285834,#285835,#285836,#285837,#285838,#285839,#285840,#285841,#285842,
#285843,#285844,#285845,#285846,#285847,#285848,#285849,#285850,#285851,
#285852,#285853,#285854,#285855,#285856,#285857,#285858,#285859,#285860,
#285861,#285862,#285863,#285864,#285865,#285866,#285867,#285868,#285869,
#285870,#285871,#285872,#285873,#285874,#285875,#285876,#285877,#285878,
#285879,#285880,#285881,#285882,#285883,#285884,#285885,#285886,#285887,
#285888,#285889,#285890,#285891,#285892,#285893,#285894,#285895,#285896,
#285897,#285898,#285899,#285900,#285901,#285902,#285903,#285904,#285905,
#285906,#285907,#285908,#285909,#285910,#285911,#285912,#285913,#285914,
#285915,#285916,#285917,#285918,#285919,#285920,#285921,#285922,#285923,
#285924,#285925,#285926,#285927,#285928,#285929,#285930,#285931,#285932,
#285933,#285934,#285935,#285936,#285937,#285938,#285939,#285940,#285941,
#285942,#285943,#285944,#285945,#285946,#285947,#285948,#285949,#285950,
#285951,#285952,#285953,#285954,#285955,#285956,#285957,#285958,#285959,
#285960,#285961,#285962,#285963,#285964,#285965,#285966,#285967,#285968,
#285969,#285970,#285971,#285972,#285973,#285974,#285975,#285976,#285977,
#285978,#285979,#285980,#285981,#285982,#285983,#285984,#285985,#285986,
#285987,#285988,#285989,#285990,#285991,#285992,#285993,#285994,#285995,
#285996,#285997,#285998,#285999,#286000,#286001,#286002,#286003,#286004,
#286005,#286006,#286007,#286008,#286009,#286010,#286011,#286012,#286013,
#286014,#286015,#286016,#286017,#286018,#286019,#286020,#286021,#286022,
#286023,#286024,#286025,#286026,#286027,#286028,#286029,#286030,#286031,
#286032,#286033,#286034,#286035,#286036,#286037,#286038,#286039,#286040,
#286041,#286042,#286043,#286044,#286045,#286046,#286047,#286048,#286049,
#286050,#286051,#286052,#286053,#286054,#286055,#286056,#286057,#286058,
#286059,#286060,#286061,#286062,#286063,#286064,#286065,#286066,#286067,
#286068,#286069,#286070,#286071,#286072,#286073,#286074,#286075,#286076,
#286077,#286078,#286079,#286080,#286081,#286082,#286083,#286084,#286085,
#286086,#286087,#286088,#286089,#286090,#286091,#286092,#286093,#286094,
#286095,#286096,#286097,#286098,#286099,#286100,#286101,#286102,#286103,
#286104,#286105,#286106,#286107,#286108,#286109,#286110,#286111,#286112,
#286113,#286114,#286115,#286116,#286117,#286118,#286119,#286120,#286121,
#286122,#286123,#286124,#286125,#286126,#286127,#286128,#286129,#286130,
#286131,#286132,#286133,#286134,#286135,#286136,#286137,#286138,#286139,
#286140,#286141,#286142,#286143,#286144,#286145,#286146,#286147,#286148,
#286149,#286150,#286151,#286152,#286153,#286154,#286155,#286156,#286157,
#286158,#286159,#286160,#286161,#286162,#286163,#286164,#286165,#286166,
#286167,#286168,#286169,#286170,#286171,#286172,#286173,#286174,#286175,
#286176,#286177,#286178,#286179,#286180,#286181,#286182,#286183,#286184,
#286185,#286186,#286187,#286188,#286189,#286190,#286191,#286192,#286193,
#286194,#286195,#286196,#286197,#286198,#286199,#286200,#286201,#286202,
#286203,#286204,#286205,#286206,#286207,#286208,#286209,#286210,#286211,
#286212,#286213,#286214,#286215,#286216,#286217,#286218,#286219,#286220,
#286221,#286222,#286223,#286224,#286225,#286226,#286227,#286228,#286229,
#286230,#286231,#286232,#286233,#286234,#286235,#286236,#286237,#286238,
#286239,#286240,#286241,#286242,#286243,#286244,#286245,#286246,#286247,
#286248,#286249,#286250,#286251,#286252,#286253,#286254,#286255,#286256,
#286257,#286258,#286259,#286260,#286261,#286262,#286263,#286264,#286265,
#286266,#286267,#286268,#286269,#286270,#286271,#286272,#286273,#286274,
#286275,#286276,#286277,#286278,#286279,#286280,#286281,#286282,#286283,
#286284,#286285,#286286,#286287,#286288,#286289,#286290,#286291,#286292,
#286293,#286294,#286295,#286296,#286297,#286298,#286299,#286300,#286301,
#286302,#286303,#286304,#286305,#286306,#286307,#286308,#286309,#286310,
#286311,#286312,#286313,#286314,#286315,#286316,#286317,#286318,#286319,
#286320,#286321,#286322,#286323,#286324,#286325,#286326,#286327,#286328,
#286329,#286330,#286331,#286332,#286333,#286334,#286335,#286336,#286337,
#286338,#286339,#286340,#286341,#286342,#286343,#286344,#286345,#286346,
#286347,#286348,#286349,#286350,#286351,#286352,#286353,#286354,#286355,
#286356,#286357,#286358,#286359,#286360,#286361,#286362,#286363,#286364,
#286365,#286366,#286367,#286368,#286369,#286370,#286371,#286372,#286373,
#286374,#286375,#286376,#286377,#286378,#286379,#286380,#286381,#286382,
#286383,#286384,#286385,#286386,#286387,#286388,#286389,#286390,#286391,
#286392,#286393,#286394,#286395,#286396,#286397,#286398,#286399,#286400,
#286401,#286402,#286403,#286404,#286405,#286406,#286407,#286408,#286409,
#286410,#286411,#286412,#286413,#286414,#286415,#286416,#286417,#286418,
#286419,#286420,#286421,#286422,#286423,#286424,#286425,#286426,#286427,
#286428,#286429,#286430,#286431,#286432,#286433,#286434,#286435,#286436,
#286437,#286438,#286439,#286440,#286441,#286442,#286443,#286444,#286445,
#286446,#286447,#286448,#286449,#286450,#286451,#286452,#286453,#286454,
#286455,#286456,#286457,#286458,#286459,#286460,#286461,#286462,#286463,
#286464,#286465,#286466,#286467,#286468,#286469,#286470,#286471,#286472,
#286473,#286474,#286475,#286476,#286477,#286478,#286479,#286480,#286481,
#286482,#286483,#286484,#286485,#286486,#286487,#286488,#286489,#286490,
#286491,#286492,#286493,#286494,#286495,#286496,#286497,#286498,#286499,
#286500,#286501,#286502,#286503,#286504,#286505,#286506,#286507,#286508,
#286509,#286510,#286511,#286512,#286513,#286514,#286515,#286516,#286517,
#286518,#286519,#286520,#286521,#286522,#286523,#286524,#286525,#286526,
#286527,#286528,#286529,#286530,#286531,#286532,#286533,#286534,#286535,
#286536,#286537,#286538,#286539,#286540,#286541,#286542,#286543,#286544,
#286545,#286546,#286547,#286548,#286549,#286550,#286551,#286552,#286553,
#286554,#286555,#286556,#286557,#286558,#286559,#286560,#286561,#286562,
#286563,#286564,#286565,#286566,#286567,#286568,#286569,#286570,#286571,
#286572,#286573,#286574,#286575,#286576,#286577,#286578,#286579,#286580,
#286581,#286582,#286583,#286584,#286585,#286586,#286587,#286588,#286589,
#286590,#286591,#286592,#286593,#286594,#286595,#286596,#286597,#286598,
#286599,#286600,#286601,#286602,#286603,#286604,#286605,#286606,#286607,
#286608,#286609,#286610,#286611,#286612,#286613,#286614,#286615,#286616,
#286617,#286618,#286619,#286620,#286621,#286622,#286623,#286624,#286625,
#286626,#286627,#286628,#286629,#286630,#286631,#286632,#286633,#286634,
#286635,#286636,#286637,#286638,#286639,#286640,#286641,#286642,#286643,
#286644,#286645,#286646,#286647,#286648,#286649,#286650,#286651,#286652,
#286653,#286654,#286655,#286656,#286657,#286658,#286659,#286660,#286661,
#286662,#286663,#286664,#286665,#286666,#286667,#286668,#286669,#286670,
#286671,#286672,#286673,#286674,#286675,#286676,#286677,#286678,#286679,
#286680,#286681,#286682,#286683,#286684,#286685,#286686,#286687,#286688,
#286689,#286690,#286691,#286692,#286693,#286694,#286695,#286696,#286697,
#286698,#286699,#286700,#286701,#286702,#286703,#286704,#286705,#286706,
#286707,#286708,#286709,#286710,#286711,#286712,#286713,#286714,#286715,
#286716,#286717,#286718,#286719,#286720,#286721,#286722,#286723,#286724,
#286725,#286726,#286727,#286728,#286729,#286730,#286731,#286732,#286733,
#286734,#286735,#286736,#286737,#286738,#286739,#286740,#286741,#286742,
#286743,#286744,#286745,#286746,#286747,#286748,#286749,#286750,#286751,
#286752,#286753,#286754,#286755,#286756,#286757,#286758,#286759,#286760,
#286761,#286762,#286763,#286764,#286765,#286766,#286767,#286768,#286769,
#286770,#286771,#286772,#286773,#286774,#286775,#286776,#286777,#286778,
#286779,#286780,#286781,#286782,#286783,#286784,#286785,#286786,#286787,
#286788,#286789,#286790,#286791,#286792,#286793,#286794,#286795,#286796,
#286797,#286798,#286799,#286800,#286801,#286802,#286803,#286804,#286805,
#286806,#286807,#286808,#286809,#286810,#286811,#286812,#286813,#286814,
#286815,#286816,#286817,#286818,#286819,#286820,#286821,#286822,#286823,
#286824,#286825,#286826,#286827,#286828,#286829,#286830,#286831,#286832,
#286833,#286834,#286835,#286836,#286837,#286838,#286839,#286840,#286841,
#286842,#286843,#286844,#286845,#286846,#286847,#286848,#286849,#286850,
#286851,#286852,#286853,#286854,#286855,#286856,#286857,#286858,#286859,
#286860,#286861,#286862,#286863,#286864),(#286865,#286866,#286867,#286868,
#286869,#286870,#286871,#286872,#286873,#286874,#286875,#286876,#286877,
#286878,#286879,#286880,#286881,#286882,#286883,#286884,#286885,#286886,
#286887,#286888,#286889,#286890,#286891,#286892,#286893,#286894,#286895,
#286896,#286897,#286898,#286899,#286900,#286901,#286902,#286903,#286904,
#286905,#286906,#286907,#286908,#286909,#286910,#286911,#286912,#286913,
#286914,#286915,#286916,#286917,#286918,#286919,#286920,#286921,#286922,
#286923,#286924,#286925,#286926,#286927,#286928,#286929,#286930,#286931,
#286932,#286933,#286934,#286935,#286936,#286937,#286938,#286939,#286940,
#286941,#286942,#286943,#286944,#286945,#286946,#286947,#286948,#286949,
#286950,#286951,#286952,#286953,#286954,#286955,#286956,#286957,#286958,
#286959,#286960,#286961,#286962,#286963,#286964,#286965,#286966,#286967,
#286968,#286969,#286970,#286971,#286972,#286973,#286974,#286975,#286976,
#286977,#286978,#286979,#286980,#286981,#286982,#286983,#286984,#286985,
#286986,#286987,#286988,#286989,#286990,#286991,#286992,#286993,#286994,
#286995,#286996,#286997,#286998,#286999,#287000,#287001,#287002,#287003,
#287004,#287005,#287006,#287007,#287008,#287009,#287010,#287011,#287012,
#287013,#287014,#287015,#287016,#287017,#287018,#287019,#287020,#287021,
#287022,#287023,#287024,#287025,#287026,#287027,#287028,#287029,#287030,
#287031,#287032,#287033,#287034,#287035,#287036,#287037,#287038,#287039,
#287040,#287041,#287042,#287043,#287044,#287045,#287046,#287047,#287048,
#287049,#287050,#287051,#287052,#287053,#287054,#287055,#287056,#287057,
#287058,#287059,#287060,#287061,#287062,#287063,#287064,#287065,#287066,
#287067,#287068,#287069,#287070,#287071,#287072,#287073,#287074,#287075,
#287076,#287077,#287078,#287079,#287080,#287081,#287082,#287083,#287084,
#287085,#287086,#287087,#287088,#287089,#287090,#287091,#287092,#287093,
#287094,#287095,#287096,#287097,#287098,#287099,#287100,#287101,#287102,
#287103,#287104,#287105,#287106,#287107,#287108,#287109,#287110,#287111,
#287112,#287113,#287114,#287115,#287116,#287117,#287118,#287119,#287120,
#287121,#287122,#287123,#287124,#287125,#287126,#287127,#287128,#287129,
#287130,#287131,#287132,#287133,#287134,#287135,#287136,#287137,#287138,
#287139,#287140,#287141,#287142,#287143,#287144,#287145,#287146,#287147,
#287148,#287149,#287150,#287151,#287152,#287153,#287154,#287155,#287156,
#287157,#287158,#287159,#287160,#287161,#287162,#287163,#287164,#287165,
#287166,#287167,#287168,#287169,#287170,#287171,#287172,#287173,#287174,
#287175,#287176,#287177,#287178,#287179,#287180,#287181,#287182,#287183,
#287184,#287185,#287186,#287187,#287188,#287189,#287190,#287191,#287192,
#287193,#287194,#287195,#287196,#287197,#287198,#287199,#287200,#287201,
#287202,#287203,#287204,#287205,#287206,#287207,#287208,#287209,#287210,
#287211,#287212,#287213,#287214,#287215,#287216,#287217,#287218,#287219,
#287220,#287221,#287222,#287223,#287224,#287225,#287226,#287227,#287228,
#287229,#287230,#287231,#287232,#287233,#287234,#287235,#287236,#287237,
#287238,#287239,#287240,#287241,#287242,#287243,#287244,#287245,#287246,
#287247,#287248,#287249,#287250,#287251,#287252,#287253,#287254,#287255,
#287256,#287257,#287258,#287259,#287260,#287261,#287262,#287263,#287264,
#287265,#287266,#287267,#287268,#287269,#287270,#287271,#287272,#287273,
#287274,#287275,#287276,#287277,#287278,#287279,#287280,#287281,#287282,
#287283,#287284,#287285,#287286,#287287,#287288,#287289,#287290,#287291,
#287292,#287293,#287294,#287295,#287296,#287297,#287298,#287299,#287300,
#287301,#287302,#287303,#287304,#287305,#287306,#287307,#287308,#287309,
#287310,#287311,#287312,#287313,#287314,#287315,#287316,#287317,#287318,
#287319,#287320,#287321,#287322,#287323,#287324,#287325,#287326,#287327,
#287328,#287329,#287330,#287331,#287332,#287333,#287334,#287335,#287336,
#287337,#287338,#287339,#287340,#287341,#287342,#287343,#287344,#287345,
#287346,#287347,#287348,#287349,#287350,#287351,#287352,#287353,#287354,
#287355,#287356,#287357,#287358,#287359,#287360,#287361,#287362,#287363,
#287364,#287365,#287366,#287367,#287368,#287369,#287370,#287371,#287372,
#287373,#287374,#287375,#287376,#287377,#287378,#287379,#287380,#287381,
#287382,#287383,#287384,#287385,#287386,#287387,#287388,#287389,#287390,
#287391,#287392,#287393,#287394,#287395,#287396,#287397,#287398,#287399,
#287400,#287401,#287402,#287403,#287404,#287405,#287406,#287407,#287408,
#287409,#287410,#287411,#287412,#287413,#287414,#287415,#287416,#287417,
#287418,#287419,#287420,#287421,#287422,#287423,#287424,#287425,#287426,
#287427,#287428,#287429,#287430,#287431,#287432,#287433,#287434,#287435,
#287436,#287437,#287438,#287439,#287440,#287441,#287442,#287443,#287444,
#287445,#287446,#287447,#287448,#287449,#287450,#287451,#287452,#287453,
#287454,#287455,#287456,#287457,#287458,#287459,#287460,#287461,#287462,
#287463,#287464,#287465,#287466,#287467,#287468,#287469,#287470,#287471,
#287472,#287473,#287474,#287475,#287476,#287477,#287478,#287479,#287480,
#287481,#287482,#287483,#287484,#287485,#287486,#287487,#287488,#287489,
#287490,#287491,#287492,#287493,#287494,#287495,#287496,#287497,#287498,
#287499,#287500,#287501,#287502,#287503,#287504,#287505,#287506,#287507,
#287508,#287509,#287510,#287511,#287512,#287513,#287514,#287515,#287516,
#287517,#287518,#287519,#287520,#287521,#287522,#287523,#287524,#287525,
#287526,#287527,#287528,#287529,#287530,#287531,#287532,#287533,#287534,
#287535,#287536,#287537,#287538,#287539,#287540,#287541,#287542,#287543,
#287544,#287545,#287546,#287547,#287548,#287549,#287550,#287551,#287552,
#287553,#287554,#287555,#287556,#287557,#287558,#287559,#287560,#287561,
#287562,#287563,#287564,#287565,#287566,#287567,#287568,#287569,#287570,
#287571,#287572,#287573,#287574,#287575,#287576,#287577,#287578,#287579,
#287580,#287581,#287582,#287583,#287584,#287585,#287586,#287587,#287588,
#287589,#287590,#287591,#287592,#287593,#287594,#287595,#287596,#287597,
#287598,#287599,#287600,#287601,#287602,#287603,#287604,#287605,#287606,
#287607,#287608,#287609,#287610,#287611,#287612,#287613,#287614,#287615,
#287616,#287617,#287618,#287619,#287620,#287621,#287622,#287623,#287624,
#287625,#287626,#287627,#287628,#287629,#287630,#287631,#287632,#287633,
#287634,#287635,#287636,#287637,#287638,#287639,#287640,#287641,#287642,
#287643,#287644,#287645,#287646,#287647,#287648,#287649,#287650,#287651,
#287652,#287653,#287654,#287655,#287656,#287657,#287658,#287659,#287660,
#287661,#287662,#287663,#287664,#287665,#287666,#287667,#287668,#287669,
#287670,#287671,#287672,#287673,#287674,#287675,#287676,#287677,#287678,
#287679,#287680,#287681,#287682,#287683,#287684,#287685,#287686,#287687,
#287688,#287689,#287690,#287691,#287692,#287693,#287694,#287695,#287696,
#287697,#287698,#287699,#287700,#287701,#287702,#287703,#287704,#287705,
#287706,#287707,#287708,#287709,#287710,#287711,#287712,#287713,#287714,
#287715,#287716,#287717,#287718,#287719,#287720,#287721,#287722,#287723,
#287724,#287725,#287726,#287727,#287728,#287729,#287730,#287731,#287732,
#287733,#287734,#287735,#287736,#287737,#287738,#287739,#287740,#287741,
#287742,#287743,#287744,#287745,#287746,#287747,#287748,#287749,#287750,
#287751,#287752,#287753,#287754,#287755,#287756,#287757,#287758,#287759,
#287760,#287761,#287762,#287763,#287764,#287765,#287766,#287767,#287768,
#287769,#287770,#287771,#287772,#287773,#287774,#287775,#287776,#287777,
#287778,#287779,#287780,#287781,#287782,#287783,#287784,#287785,#287786,
#287787,#287788,#287789,#287790,#287791,#287792,#287793,#287794,#287795,
#287796,#287797,#287798,#287799,#287800,#287801,#287802,#287803,#287804,
#287805,#287806,#287807,#287808,#287809,#287810,#287811,#287812,#287813,
#287814,#287815,#287816,#287817,#287818,#287819,#287820,#287821,#287822,
#287823,#287824,#287825,#287826,#287827,#287828,#287829,#287830,#287831,
#287832,#287833,#287834,#287835,#287836,#287837,#287838,#287839,#287840,
#287841,#287842,#287843,#287844,#287845,#287846,#287847,#287848,#287849,
#287850,#287851,#287852,#287853,#287854,#287855,#287856,#287857,#287858,
#287859,#287860,#287861,#287862,#287863,#287864,#287865,#287866,#287867,
#287868,#287869,#287870,#287871,#287872,#287873,#287874,#287875,#287876,
#287877,#287878,#287879,#287880,#287881,#287882,#287883,#287884,#287885,
#287886,#287887,#287888,#287889,#287890,#287891,#287892,#287893,#287894,
#287895,#287896,#287897,#287898,#287899,#287900,#287901)),.UNSPECIFIED.,
 .F.,.F.,.F.)
B_SPLINE_SURFACE_WITH_KNOTS((2,2),(3,2,2,2,2,2,2,2,2,2,2,2,2,2,2,2,2,2,
2,2,2,2,2,2,2,2,2,2,2,2,2,2,2,2,2,2,2,2,2,2,2,2,2,2,2,2,2,2,2,2,2,2,2,2,
2,2,2,2,2,2,2,2,2,2,2,2,2,2,2,2,2,2,2,2,2,2,2,2,2,2,2,2,2,2,2,2,2,2,2,2,
2,2,2,2,2,2,2,2,2,2,2,2,2,2,2,2,2,2,2,2,2,2,2,2,2,2,2,2,2,2,2,2,2,2,2,2,
2,2,2,2,2,2,2,2,2,2,2,2,2,2,2,2,2,2,2,2,2,2,2,2,2,2,2,2,2,2,2,2,2,2,2,2,
2,2,2,2,2,2,2,2,2,2,2,2,2,2,2,2,2,2,2,2,2,2,2,2,2,2,2,2,2,2,2,2,2,2,2,2,
2,2,2,2,2,2,2,2,2,2,2,2,2,2,2,2,2,2,2,2,2,2,2,2,2,2,2,2,2,2,2,2,2,2,2,2,
2,2,2,2,2,2,2,2,2,2,2,2,2,2,2,2,2,2,2,2,2,2,2,2,2,2,2,2,2,2,2,2,2,2,2,2,
2,2,2,2,2,2,2,2,2,2,2,2,2,2,2,2,2,2,2,2,2,2,2,2,2,2,2,2,2,2,2,2,2,2,2,2,
2,2,2,2,2,2,2,2,2,2,2,2,2,2,2,2,2,2,2,2,2,2,2,2,2,2,2,2,2,2,2,2,2,2,2,2,
2,2,2,2,2,2,2,2,2,2,2,2,2,2,2,2,2,2,2,2,2,2,2,2,2,2,2,2,2,2,2,2,2,2,2,2,
2,2,2,2,2,2,2,2,2,2,2,2,2,2,2,2,2,2,2,2,2,2,2,2,2,2,2,2,2,2,2,2,2,2,2,2,
2,2,2,2,2,2,2,2,2,2,2,2,2,2,2,2,2,2,2,2,2,2,2,2,2,2,2,2,2,2,2,2,2,2,2,2,
2,2,2,2,2,2,2,2,2,2,2,2,2,2,2,2,2,2,2,2,2,2,2,2,2,2,2,2,2,2,2,2,2,2,2,2,
2,2,2,2,2,2,2,2,2,2,2,2,2,2,2,2,2,2,2,2,2,2,2,2,2,2,2,2,2,2,2,2,3),(0.,
1.),(0.,0.00192307692307692,0.00384615384615385,0.00576923076923077,0.00769230769230769,
0.00961538461538462,0.0115384615384615,0.0134615384615385,0.0153846153846154,
0.0173076923076923,0.0192307692307692,0.0211538461538462,0.0230769230769231,
0.025,0.0269230769230769,0.0288461538461538,0.0307692307692308,0.0326923076923077,
0.0346153846153846,0.0365384615384615,0.0384615384615385,0.0403846153846154,
0.0423076923076923,0.0442307692307692,0.0461538461538462,0.0480769230769231,
0.05,0.0519230769230769,0.0538461538461538,0.0557692307692308,0.0576923076923077,
0.0596153846153846,0.0615384615384615,0.0634615384615385,0.0653846153846154,
0.0673076923076923,0.0692307692307692,0.0711538461538462,0.0730769230769231,
0.075,0.0769230769230769,0.0788461538461538,0.0807692307692308,0.0826923076923077,
0.0846153846153846,0.0865384615384615,0.0884615384615385,0.0903846153846154,
0.0923076923076923,0.0942307692307692,0.0961538461538462,0.0980769230769231,
0.1,0.101923076923077,0.103846153846154,0.105769230769231,0.107692307692308,
0.109615384615385,0.111538461538462,0.113461538461538,0.115384615384615,
0.117307692307692,0.119230769230769,0.121153846153846,0.123076923076923,
0.125,0.126923076923077,0.128846153846154,0.130769230769231,0.132692307692308,
0.134615384615385,0.136538461538462,0.138461538461538,0.140384615384615,
0.142307692307692,0.144230769230769,0.146153846153846,0.148076923076923,
0.15,0.151923076923077,0.153846153846154,0.155769230769231,0.157692307692308,
0.159615384615385,0.161538461538462,0.163461538461538,0.165384615384615,
0.167307692307692,0.169230769230769,0.171153846153846,0.173076923076923,
0.175,0.176923076923077,0.178846153846154,0.180769230769231,0.182692307692308,
0.184615384615385,0.186538461538462,0.188461538461538,0.190384615384615,
0.192307692307692,0.194230769230769,0.196153846153846,0.198076923076923,
0.2,0.201923076923077,0.203846153846154,0.205769230769231,0.207692307692308,
0.209615384615385,0.211538461538462,0.213461538461538,0.215384615384615,
0.217307692307692,0.219230769230769,0.221153846153846,0.223076923076923,
0.225,0.226923076923077,0.228846153846154,0.230769230769231,0.232692307692308,
0.234615384615385,0.236538461538462,0.238461538461538,0.240384615384615,
0.242307692307692,0.244230769230769,0.246153846153846,0.248076923076923,
0.25,0.251923076923077,0.253846153846154,0.255769230769231,0.257692307692308,
0.259615384615385,0.261538461538462,0.263461538461538,0.265384615384615,
0.267307692307692,0.269230769230769,0.271153846153846,0.273076923076923,
0.275,0.276923076923077,0.278846153846154,0.280769230769231,0.282692307692308,
0.284615384615385,0.286538461538462,0.288461538461538,0.290384615384615,
0.292307692307692,0.294230769230769,0.296153846153846,0.298076923076923,
0.3,0.301923076923077,0.303846153846154,0.305769230769231,0.307692307692308,
0.309615384615385,0.311538461538462,0.313461538461538,0.315384615384615,
0.317307692307692,0.319230769230769,0.321153846153846,0.323076923076923,
0.325,0.326923076923077,0.328846153846154,0.330769230769231,0.332692307692308,
0.334615384615385,0.336538461538462,0.338461538461538,0.340384615384615,
0.342307692307692,0.344230769230769,0.346153846153846,0.348076923076923,
0.35,0.351923076923077,0.353846153846154,0.355769230769231,0.357692307692308,
0.359615384615385,0.361538461538462,0.363461538461538,0.365384615384615,
0.367307692307692,0.369230769230769,0.371153846153846,0.373076923076923,
0.375,0.376923076923077,0.378846153846154,0.380769230769231,0.382692307692308,
0.384615384615385,0.386538461538462,0.388461538461538,0.390384615384615,
0.392307692307692,0.394230769230769,0.396153846153846,0.398076923076923,
0.4,0.401923076923077,0.403846153846154,0.405769230769231,0.407692307692308,
0.409615384615385,0.411538461538462,0.413461538461538,0.415384615384615,
0.417307692307692,0.419230769230769,0.421153846153846,0.423076923076923,
0.425,0.426923076923077,0.428846153846154,0.430769230769231,0.432692307692308,
0.434615384615385,0.436538461538462,0.438461538461538,0.440384615384615,
0.442307692307692,0.444230769230769,0.446153846153846,0.448076923076923,
0.45,0.451923076923077,0.453846153846154,0.455769230769231,0.457692307692308,
0.459615384615385,0.461538461538462,0.463461538461538,0.465384615384615,
0.467307692307692,0.469230769230769,0.471153846153846,0.473076923076923,
0.475,0.476923076923077,0.478846153846154,0.480769230769231,0.482692307692308,
0.484615384615385,0.486538461538462,0.488461538461538,0.490384615384615,
0.492307692307692,0.494230769230769,0.496153846153846,0.498076923076923,
0.5,0.501923076923077,0.503846153846154,0.505769230769231,0.507692307692308,
0.509615384615385,0.511538461538461,0.513461538461538,0.515384615384615,
0.517307692307692,0.519230769230769,0.521153846153846,0.523076923076923,
0.525,0.526923076923077,0.528846153846154,0.530769230769231,0.532692307692308,
0.534615384615385,0.536538461538462,0.538461538461538,0.540384615384615,
0.542307692307692,0.544230769230769,0.546153846153846,0.548076923076923,
0.55,0.551923076923077,0.553846153846154,0.555769230769231,0.557692307692308,
0.559615384615385,0.561538461538462,0.563461538461538,0.565384615384615,
0.567307692307692,0.569230769230769,0.571153846153846,0.573076923076923,
0.575,0.576923076923077,0.578846153846154,0.580769230769231,0.582692307692308,
0.584615384615385,0.586538461538462,0.588461538461538,0.590384615384615,
0.592307692307692,0.594230769230769,0.596153846153846,0.598076923076923,
0.6,0.601923076923077,0.603846153846154,0.605769230769231,0.607692307692308,
0.609615384615385,0.611538461538462,0.613461538461539,0.615384615384615,
0.617307692307692,0.619230769230769,0.621153846153846,0.623076923076923,
0.625,0.626923076923077,0.628846153846154,0.630769230769231,0.632692307692308,
0.634615384615385,0.636538461538461,0.638461538461538,0.640384615384615,
0.642307692307692,0.644230769230769,0.646153846153846,0.648076923076923,
0.65,0.651923076923077,0.653846153846154,0.655769230769231,0.657692307692308,
0.659615384615385,0.661538461538462,0.663461538461538,0.665384615384615,
0.667307692307692,0.669230769230769,0.671153846153846,0.673076923076923,
0.675,0.676923076923077,0.678846153846154,0.680769230769231,0.682692307692308,
0.684615384615385,0.686538461538462,0.688461538461538,0.690384615384615,
0.692307692307692,0.694230769230769,0.696153846153846,0.698076923076923,
0.7,0.701923076923077,0.703846153846154,0.705769230769231,0.707692307692308,
0.709615384615385,0.711538461538462,0.713461538461538,0.715384615384615,
0.717307692307692,0.719230769230769,0.721153846153846,0.723076923076923,
0.725,0.726923076923077,0.728846153846154,0.730769230769231,0.732692307692308,
0.734615384615385,0.736538461538462,0.738461538461539,0.740384615384615,
0.742307692307692,0.744230769230769,0.746153846153846,0.748076923076923,
0.75,0.751923076923077,0.753846153846154,0.755769230769231,0.757692307692308,
0.759615384615385,0.761538461538461,0.763461538461538,0.765384615384615,
0.767307692307692,0.769230769230769,0.771153846153846,0.773076923076923,
0.775,0.776923076923077,0.778846153846154,0.780769230769231,0.782692307692308,
0.784615384615385,0.786538461538462,0.788461538461538,0.790384615384615,
0.792307692307692,0.794230769230769,0.796153846153846,0.798076923076923,
0.8,0.801923076923077,0.803846153846154,0.805769230769231,0.807692307692308,
0.809615384615385,0.811538461538462,0.813461538461538,0.815384615384615,
0.817307692307692,0.819230769230769,0.821153846153846,0.823076923076923,
0.825,0.826923076923077,0.828846153846154,0.830769230769231,0.832692307692308,
0.834615384615385,0.836538461538462,0.838461538461538,0.840384615384615,
0.842307692307692,0.844230769230769,0.846153846153846,0.848076923076923,
0.85,0.851923076923077,0.853846153846154,0.855769230769231,0.857692307692308,
0.859615384615385,0.861538461538462,0.863461538461539,0.865384615384615,
0.867307692307692,0.869230769230769,0.871153846153846,0.873076923076923,
0.875,0.876923076923077,0.878846153846154,0.880769230769231,0.882692307692308,
0.884615384615385,0.886538461538461,0.888461538461538,0.890384615384615,
0.892307692307692,0.894230769230769,0.896153846153846,0.898076923076923,
0.9,0.901923076923077,0.903846153846154,0.905769230769231,0.907692307692308,
0.909615384615385,0.911538461538462,0.913461538461538,0.915384615384615,
0.917307692307692,0.919230769230769,0.921153846153846,0.923076923076923,
0.925,0.926923076923077,0.928846153846154,0.930769230769231,0.932692307692308,
0.934615384615385,0.936538461538462,0.938461538461538,0.940384615384615,
0.942307692307692,0.944230769230769,0.946153846153846,0.948076923076923,
0.95,0.951923076923077,0.953846153846154,0.955769230769231,0.957692307692308,
0.959615384615385,0.961538461538462,0.963461538461538,0.965384615384615,
0.967307692307692,0.969230769230769,0.971153846153846,0.973076923076923,
0.975,0.976923076923077,0.978846153846154,0.980769230769231,0.982692307692308,
0.984615384615385,0.986538461538462,0.988461538461539,0.990384615384615,
0.992307692307692,0.994230769230769,0.996153846153846),.UNSPECIFIED.)
GEOMETRIC_REPRESENTATION_ITEM()
RATIONAL_B_SPLINE_SURFACE(((1.,0.951056516295154,1.,0.951056516295154,1.,
0.951056516295154,1.,0.951056516295154,1.,0.951056516295154,1.,0.951056516295154,
1.,0.951056516295154,1.,0.951056516295154,1.,0.951056516295154,1.,0.951056516295154,
1.,0.951056516295154,1.,0.951056516295154,1.,0.951056516295154,1.,0.951056516295154,
1.,0.951056516295154,1.,0.951056516295154,1.,0.951056516295154,1.,0.951056516295154,
1.,0.951056516295154,1.,0.951056516295154,1.,0.951056516295154,1.,0.951056516295154,
1.,0.951056516295154,1.,0.951056516295154,1.,0.951056516295154,1.,0.951056516295154,
1.,0.951056516295154,1.,0.951056516295154,1.,0.951056516295154,1.,0.951056516295154,
1.,0.951056516295154,1.,0.951056516295154,1.,0.951056516295154,1.,0.951056516295154,
1.,0.951056516295154,1.,0.951056516295154,1.,0.951056516295154,1.,0.951056516295154,
1.,0.951056516295154,1.,0.951056516295154,1.,0.951056516295154,1.,0.951056516295154,
1.,0.951056516295154,1.,0.951056516295154,1.,0.951056516295154,1.,0.951056516295154,
1.,0.951056516295154,1.,0.951056516295154,1.,0.951056516295154,1.,0.951056516295154,
1.,0.951056516295154,1.,0.951056516295154,1.,0.951056516295154,1.,0.951056516295154,
1.,0.951056516295154,1.,0.951056516295154,1.,0.951056516295154,1.,0.951056516295154,
1.,0.951056516295154,1.,0.951056516295154,1.,0.951056516295154,1.,0.951056516295154,
1.,0.951056516295154,1.,0.951056516295154,1.,0.951056516295154,1.,0.951056516295154,
1.,0.951056516295154,1.,0.951056516295154,1.,0.951056516295154,1.,0.951056516295154,
1.,0.951056516295154,1.,0.951056516295154,1.,0.951056516295154,1.,0.951056516295154,
1.,0.951056516295154,1.,0.951056516295154,1.,0.951056516295154,1.,0.951056516295154,
1.,0.951056516295154,1.,0.951056516295154,1.,0.951056516295154,1.,0.951056516295154,
1.,0.951056516295154,1.,0.951056516295154,1.,0.951056516295154,1.,0.951056516295154,
1.,0.951056516295154,1.,0.951056516295154,1.,0.951056516295154,1.,0.951056516295154,
1.,0.951056516295154,1.,0.951056516295154,1.,0.951056516295154,1.,0.951056516295154,
1.,0.951056516295154,1.,0.951056516295154,1.,0.951056516295154,1.,0.951056516295154,
1.,0.951056516295154,1.,0.951056516295154,1.,0.951056516295154,1.,0.951056516295154,
1.,0.951056516295154,1.,0.951056516295154,1.,0.951056516295154,1.,0.951056516295154,
1.,0.951056516295154,1.,0.951056516295154,1.,0.951056516295154,1.,0.951056516295154,
1.,0.951056516295154,1.,0.951056516295154,1.,0.951056516295154,1.,0.951056516295154,
1.,0.951056516295154,1.,0.951056516295154,1.,0.951056516295154,1.,0.951056516295154,
1.,0.951056516295154,1.,0.951056516295154,1.,0.951056516295154,1.,0.951056516295154,
1.,0.951056516295154,1.,0.951056516295154,1.,0.951056516295154,1.,0.951056516295154,
1.,0.951056516295154,1.,0.951056516295154,1.,0.951056516295154,1.,0.951056516295154,
1.,0.951056516295154,1.,0.951056516295154,1.,0.951056516295154,1.,0.951056516295154,
1.,0.951056516295154,1.,0.951056516295154,1.,0.951056516295154,1.,0.951056516295154,
1.,0.951056516295154,1.,0.951056516295154,1.,0.951056516295154,1.,0.951056516295154,
1.,0.951056516295154,1.,0.951056516295154,1.,0.951056516295154,1.,0.951056516295154,
1.,0.951056516295154,1.,0.951056516295154,1.,0.951056516295154,1.,0.951056516295154,
1.,0.951056516295154,1.,0.951056516295154,1.,0.951056516295154,1.,0.951056516295154,
1.,0.951056516295154,1.,0.951056516295154,1.,0.951056516295154,1.,0.951056516295154,
1.,0.951056516295154,1.,0.951056516295154,1.,0.951056516295154,1.,0.951056516295154,
1.,0.951056516295154,1.,0.951056516295154,1.,0.951056516295154,1.,0.951056516295154,
1.,0.951056516295154,1.,0.951056516295154,1.,0.951056516295154,1.,0.951056516295154,
1.,0.951056516295154,1.,0.951056516295154,1.,0.951056516295154,1.,0.951056516295154,
1.,0.951056516295154,1.,0.951056516295154,1.,0.951056516295154,1.,0.951056516295154,
1.,0.951056516295154,1.,0.951056516295154,1.,0.951056516295154,1.,0.951056516295154,
1.,0.951056516295154,1.,0.951056516295154,1.,0.951056516295154,1.,0.951056516295154,
1.,0.951056516295154,1.,0.951056516295154,1.,0.951056516295154,1.,0.951056516295154,
1.,0.951056516295154,1.,0.951056516295154,1.,0.951056516295154,1.,0.951056516295154,
1.,0.951056516295154,1.,0.951056516295154,1.,0.951056516295154,1.,0.951056516295154,
1.,0.951056516295154,1.,0.951056516295154,1.,0.951056516295154,1.,0.951056516295154,
1.,0.951056516295154,1.,0.951056516295154,1.,0.951056516295154,1.,0.951056516295154,
1.,0.951056516295154,1.,0.951056516295154,1.,0.951056516295154,1.,0.951056516295154,
1.,0.951056516295154,1.,0.951056516295154,1.,0.951056516295154,1.,0.951056516295154,
1.,0.951056516295154,1.,0.951056516295154,1.,0.951056516295154,1.,0.951056516295154,
1.,0.951056516295154,1.,0.951056516295154,1.,0.951056516295154,1.,0.951056516295154,
1.,0.951056516295154,1.,0.951056516295154,1.,0.951056516295154,1.,0.951056516295154,
1.,0.951056516295154,1.,0.951056516295154,1.,0.951056516295154,1.,0.951056516295154,
1.,0.951056516295154,1.,0.951056516295154,1.,0.951056516295154,1.,0.951056516295154,
1.,0.951056516295154,1.,0.951056516295154,1.,0.951056516295154,1.,0.951056516295154,
1.,0.951056516295154,1.,0.951056516295154,1.,0.951056516295154,1.,0.951056516295154,
1.,0.951056516295154,1.,0.951056516295154,1.,0.951056516295154,1.,0.951056516295154,
1.,0.951056516295154,1.,0.951056516295154,1.,0.951056516295154,1.,0.951056516295154,
1.,0.951056516295154,1.,0.951056516295154,1.,0.951056516295154,1.,0.951056516295154,
1.,0.951056516295154,1.,0.951056516295154,1.,0.951056516295154,1.,0.951056516295154,
1.,0.951056516295154,1.,0.951056516295154,1.,0.951056516295154,1.,0.951056516295154,
1.,0.951056516295154,1.,0.951056516295154,1.,0.951056516295154,1.,0.951056516295154,
1.,0.951056516295154,1.,0.951056516295154,1.,0.951056516295154,1.,0.951056516295154,
1.,0.951056516295154,1.,0.951056516295154,1.,0.951056516295154,1.,0.951056516295154,
1.,0.951056516295154,1.,0.951056516295154,1.,0.951056516295154,1.,0.951056516295154,
1.,0.951056516295154,1.,0.951056516295154,1.,0.951056516295154,1.,0.951056516295154,
1.,0.951056516295154,1.,0.951056516295154,1.,0.951056516295154,1.,0.951056516295154,
1.,0.951056516295154,1.,0.951056516295154,1.,0.951056516295154,1.,0.951056516295154,
1.,0.951056516295154,1.,0.951056516295154,1.,0.951056516295154,1.,0.951056516295154,
1.,0.951056516295154,1.,0.951056516295154,1.,0.951056516295154,1.,0.951056516295154,
1.,0.951056516295154,1.,0.951056516295154,1.,0.951056516295154,1.,0.951056516295154,
1.,0.951056516295154,1.,0.951056516295154,1.,0.951056516295154,1.,0.951056516295154,
1.,0.951056516295154,1.,0.951056516295154,1.,0.951056516295154,1.,0.951056516295154,
1.,0.951056516295154,1.,0.951056516295154,1.,0.951056516295154,1.,0.951056516295154,
1.,0.951056516295154,1.,0.951056516295154,1.,0.951056516295154,1.,0.951056516295154,
1.,0.951056516295154,1.,0.951056516295154,1.,0.951056516295154,1.,0.951056516295154,
1.,0.951056516295154,1.,0.951056516295154,1.,0.951056516295154,1.,0.951056516295154,
1.,0.951056516295154,1.,0.951056516295154,1.,0.951056516295154,1.,0.951056516295154,
1.,0.951056516295154,1.,0.951056516295154,1.,0.951056516295154,1.,0.951056516295154,
1.,0.951056516295154,1.,0.951056516295154,1.,0.951056516295154,1.,0.951056516295154,
1.,0.951056516295154,1.,0.951056516295154,1.,0.951056516295154,1.,0.951056516295154,
1.,0.951056516295154,1.,0.951056516295154,1.,0.951056516295154,1.,0.951056516295154,
1.,0.951056516295154,1.,0.951056516295154,1.,0.951056516295154,1.,0.951056516295154,
1.,0.951056516295154,1.,0.951056516295154,1.,0.951056516295154,1.,0.951056516295154,
1.,0.951056516295154,1.,0.951056516295154,1.,0.951056516295154,1.,0.951056516295154,
1.,0.951056516295154,1.,0.951056516295154,1.,0.951056516295154,1.,0.951056516295154,
1.,0.951056516295154,1.,0.951056516295154,1.,0.951056516295154,1.,0.951056516295154,
1.,0.951056516295154,1.,0.951056516295154,1.,0.951056516295154,1.,0.951056516295154,
1.,0.951056516295154,1.,0.951056516295154,1.,0.951056516295154,1.,0.951056516295154,
1.,0.951056516295154,1.,0.951056516295154,1.,0.951056516295154,1.,0.951056516295154,
1.,0.951056516295154,1.,0.951056516295154,1.,0.951056516295154,1.,0.951056516295154,
1.,0.951056516295154,1.,0.951056516295154,1.,0.951056516295154,1.,0.951056516295154,
1.,0.951056516295154,1.,0.951056516295154,1.,0.951056516295154,1.,0.951056516295154,
1.,0.951056516295154,1.,0.951056516295154,1.,0.951056516295154,1.,0.951056516295154,
1.,0.951056516295154,1.,0.951056516295154,1.,0.951056516295154,1.,0.951056516295154,
1.,0.951056516295154,1.,0.951056516295154,1.,0.951056516295154,1.,0.951056516295154,
1.,0.951056516295154,1.,0.951056516295154,1.,0.951056516295154,1.,0.951056516295154,
1.,0.951056516295154,1.,0.951056516295154,1.,0.951056516295154,1.,0.951056516295154,
1.,0.951056516295154,1.,0.951056516295154,1.,0.951056516295154,1.,0.951056516295154,
1.,0.951056516295154,1.,0.951056516295154,1.,0.951056516295154,1.,0.951056516295154,
1.,0.951056516295154,1.,0.951056516295154,1.,0.951056516295154,1.,0.951056516295154,
1.,0.951056516295154,1.,0.951056516295154,1.,0.951056516295154,1.,0.951056516295154,
1.,0.951056516295154,1.,0.951056516295154,1.,0.951056516295154,1.,0.951056516295154,
1.,0.951056516295154,1.,0.951056516295154,1.,0.951056516295154,1.,0.951056516295154,
1.,0.951056516295154,1.,0.951056516295154,1.,0.951056516295154,1.,0.951056516295154,
1.,0.951056516295154,1.,0.951056516295154,1.,0.951056516295154,1.,0.951056516295154,
1.,0.951056516295154,1.,0.951056516295154,1.,0.951056516295154,1.,0.951056516295154,
1.,0.951056516295154,1.,0.951056516295154,1.,0.951056516295154,1.,0.951056516295154,
1.,0.951056516295154,1.,0.951056516295154,1.,0.951056516295154,1.,0.951056516295154,
1.,0.951056516295154,1.,0.951056516295154,1.,0.951056516295154,1.,0.951056516295154,
1.,0.951056516295154,1.,0.951056516295154,1.,0.951056516295154,1.,0.951056516295154,
1.,0.951056516295154,1.,0.951056516295154,1.,0.951056516295154,1.,0.951056516295154,
1.,0.951056516295154,1.,0.951056516295154,1.,0.951056516295154,1.,0.951056516295154,
1.,0.951056516295154,1.,0.951056516295154,1.,0.951056516295154,1.,0.951056516295154,
1.,0.951056516295154,1.,0.951056516295154,1.,0.951056516295154,1.,0.951056516295154,
1.,0.951056516295154,1.,0.951056516295154,1.,0.951056516295154,1.,0.951056516295154,
1.,0.951056516295154,1.,0.951056516295154,1.,0.951056516295154,1.,0.951056516295154,
1.,0.951056516295154,1.,0.951056516295154,1.,0.951056516295154,1.,0.951056516295154,
1.,0.951056516295154,1.,0.951056516295154,1.,0.951056516295154,1.,0.951056516295154,
1.,0.951056516295154,1.,0.951056516295154,1.,0.951056516295154,1.,0.951056516295154,
1.,0.951056516295154,1.,0.951056516295154,1.,0.951056516295154,1.,0.951056516295154,
1.,0.951056516295154,1.,0.951056516295154,1.,0.951056516295154,1.,0.951056516295154,
1.,0.951056516295154,1.,0.951056516295154,1.,0.951056516295154,1.,0.951056516295154,
1.,0.951056516295154,1.,0.951056516295154,1.,0.951056516295154,1.,0.951056516295154,
1.,0.951056516295154,1.,0.951056516295154,1.,0.951056516295154,1.,0.951056516295154,
1.),(1.,0.951056516295154,1.,0.951056516295154,1.,0.951056516295154,1.,
0.951056516295154,1.,0.951056516295154,1.,0.951056516295154,1.,0.951056516295154,
1.,0.951056516295154,1.,0.951056516295154,1.,0.951056516295154,1.,0.951056516295154,
1.,0.951056516295154,1.,0.951056516295154,1.,0.951056516295154,1.,0.951056516295154,
1.,0.951056516295154,1.,0.951056516295154,1.,0.951056516295154,1.,0.951056516295154,
1.,0.951056516295154,1.,0.951056516295154,1.,0.951056516295154,1.,0.951056516295154,
1.,0.951056516295154,1.,0.951056516295154,1.,0.951056516295154,1.,0.951056516295154,
1.,0.951056516295154,1.,0.951056516295154,1.,0.951056516295154,1.,0.951056516295154,
1.,0.951056516295154,1.,0.951056516295154,1.,0.951056516295154,1.,0.951056516295154,
1.,0.951056516295154,1.,0.951056516295154,1.,0.951056516295154,1.,0.951056516295154,
1.,0.951056516295154,1.,0.951056516295154,1.,0.951056516295154,1.,0.951056516295154,
1.,0.951056516295154,1.,0.951056516295154,1.,0.951056516295154,1.,0.951056516295154,
1.,0.951056516295154,1.,0.951056516295154,1.,0.951056516295154,1.,0.951056516295154,
1.,0.951056516295154,1.,0.951056516295154,1.,0.951056516295154,1.,0.951056516295154,
1.,0.951056516295154,1.,0.951056516295154,1.,0.951056516295154,1.,0.951056516295154,
1.,0.951056516295154,1.,0.951056516295154,1.,0.951056516295154,1.,0.951056516295154,
1.,0.951056516295154,1.,0.951056516295154,1.,0.951056516295154,1.,0.951056516295154,
1.,0.951056516295154,1.,0.951056516295154,1.,0.951056516295154,1.,0.951056516295154,
1.,0.951056516295154,1.,0.951056516295154,1.,0.951056516295154,1.,0.951056516295154,
1.,0.951056516295154,1.,0.951056516295154,1.,0.951056516295154,1.,0.951056516295154,
1.,0.951056516295154,1.,0.951056516295154,1.,0.951056516295154,1.,0.951056516295154,
1.,0.951056516295154,1.,0.951056516295154,1.,0.951056516295154,1.,0.951056516295154,
1.,0.951056516295154,1.,0.951056516295154,1.,0.951056516295154,1.,0.951056516295154,
1.,0.951056516295154,1.,0.951056516295154,1.,0.951056516295154,1.,0.951056516295154,
1.,0.951056516295154,1.,0.951056516295154,1.,0.951056516295154,1.,0.951056516295154,
1.,0.951056516295154,1.,0.951056516295154,1.,0.951056516295154,1.,0.951056516295154,
1.,0.951056516295154,1.,0.951056516295154,1.,0.951056516295154,1.,0.951056516295154,
1.,0.951056516295154,1.,0.951056516295154,1.,0.951056516295154,1.,0.951056516295154,
1.,0.951056516295154,1.,0.951056516295154,1.,0.951056516295154,1.,0.951056516295154,
1.,0.951056516295154,1.,0.951056516295154,1.,0.951056516295154,1.,0.951056516295154,
1.,0.951056516295154,1.,0.951056516295154,1.,0.951056516295154,1.,0.951056516295154,
1.,0.951056516295154,1.,0.951056516295154,1.,0.951056516295154,1.,0.951056516295154,
1.,0.951056516295154,1.,0.951056516295154,1.,0.951056516295154,1.,0.951056516295154,
1.,0.951056516295154,1.,0.951056516295154,1.,0.951056516295154,1.,0.951056516295154,
1.,0.951056516295154,1.,0.951056516295154,1.,0.951056516295154,1.,0.951056516295154,
1.,0.951056516295154,1.,0.951056516295154,1.,0.951056516295154,1.,0.951056516295154,
1.,0.951056516295154,1.,0.951056516295154,1.,0.951056516295154,1.,0.951056516295154,
1.,0.951056516295154,1.,0.951056516295154,1.,0.951056516295154,1.,0.951056516295154,
1.,0.951056516295154,1.,0.951056516295154,1.,0.951056516295154,1.,0.951056516295154,
1.,0.951056516295154,1.,0.951056516295154,1.,0.951056516295154,1.,0.951056516295154,
1.,0.951056516295154,1.,0.951056516295154,1.,0.951056516295154,1.,0.951056516295154,
1.,0.951056516295154,1.,0.951056516295154,1.,0.951056516295154,1.,0.951056516295154,
1.,0.951056516295154,1.,0.951056516295154,1.,0.951056516295154,1.,0.951056516295154,
1.,0.951056516295154,1.,0.951056516295154,1.,0.951056516295154,1.,0.951056516295154,
1.,0.951056516295154,1.,0.951056516295154,1.,0.951056516295154,1.,0.951056516295154,
1.,0.951056516295154,1.,0.951056516295154,1.,0.951056516295154,1.,0.951056516295154,
1.,0.951056516295154,1.,0.951056516295154,1.,0.951056516295154,1.,0.951056516295154,
1.,0.951056516295154,1.,0.951056516295154,1.,0.951056516295154,1.,0.951056516295154,
1.,0.951056516295154,1.,0.951056516295154,1.,0.951056516295154,1.,0.951056516295154,
1.,0.951056516295154,1.,0.951056516295154,1.,0.951056516295154,1.,0.951056516295154,
1.,0.951056516295154,1.,0.951056516295154,1.,0.951056516295154,1.,0.951056516295154,
1.,0.951056516295154,1.,0.951056516295154,1.,0.951056516295154,1.,0.951056516295154,
1.,0.951056516295154,1.,0.951056516295154,1.,0.951056516295154,1.,0.951056516295154,
1.,0.951056516295154,1.,0.951056516295154,1.,0.951056516295154,1.,0.951056516295154,
1.,0.951056516295154,1.,0.951056516295154,1.,0.951056516295154,1.,0.951056516295154,
1.,0.951056516295154,1.,0.951056516295154,1.,0.951056516295154,1.,0.951056516295154,
1.,0.951056516295154,1.,0.951056516295154,1.,0.951056516295154,1.,0.951056516295154,
1.,0.951056516295154,1.,0.951056516295154,1.,0.951056516295154,1.,0.951056516295154,
1.,0.951056516295154,1.,0.951056516295154,1.,0.951056516295154,1.,0.951056516295154,
1.,0.951056516295154,1.,0.951056516295154,1.,0.951056516295154,1.,0.951056516295154,
1.,0.951056516295154,1.,0.951056516295154,1.,0.951056516295154,1.,0.951056516295154,
1.,0.951056516295154,1.,0.951056516295154,1.,0.951056516295154,1.,0.951056516295154,
1.,0.951056516295154,1.,0.951056516295154,1.,0.951056516295154,1.,0.951056516295154,
1.,0.951056516295154,1.,0.951056516295154,1.,0.951056516295154,1.,0.951056516295154,
1.,0.951056516295154,1.,0.951056516295154,1.,0.951056516295154,1.,0.951056516295154,
1.,0.951056516295154,1.,0.951056516295154,1.,0.951056516295154,1.,0.951056516295154,
1.,0.951056516295154,1.,0.951056516295154,1.,0.951056516295154,1.,0.951056516295154,
1.,0.951056516295154,1.,0.951056516295154,1.,0.951056516295154,1.,0.951056516295154,
1.,0.951056516295154,1.,0.951056516295154,1.,0.951056516295154,1.,0.951056516295154,
1.,0.951056516295154,1.,0.951056516295154,1.,0.951056516295154,1.,0.951056516295154,
1.,0.951056516295154,1.,0.951056516295154,1.,0.951056516295154,1.,0.951056516295154,
1.,0.951056516295154,1.,0.951056516295154,1.,0.951056516295154,1.,0.951056516295154,
1.,0.951056516295154,1.,0.951056516295154,1.,0.951056516295154,1.,0.951056516295154,
1.,0.951056516295154,1.,0.951056516295154,1.,0.951056516295154,1.,0.951056516295154,
1.,0.951056516295154,1.,0.951056516295154,1.,0.951056516295154,1.,0.951056516295154,
1.,0.951056516295154,1.,0.951056516295154,1.,0.951056516295154,1.,0.951056516295154,
1.,0.951056516295154,1.,0.951056516295154,1.,0.951056516295154,1.,0.951056516295154,
1.,0.951056516295154,1.,0.951056516295154,1.,0.951056516295154,1.,0.951056516295154,
1.,0.951056516295154,1.,0.951056516295154,1.,0.951056516295154,1.,0.951056516295154,
1.,0.951056516295154,1.,0.951056516295154,1.,0.951056516295154,1.,0.951056516295154,
1.,0.951056516295154,1.,0.951056516295154,1.,0.951056516295154,1.,0.951056516295154,
1.,0.951056516295154,1.,0.951056516295154,1.,0.951056516295154,1.,0.951056516295154,
1.,0.951056516295154,1.,0.951056516295154,1.,0.951056516295154,1.,0.951056516295154,
1.,0.951056516295154,1.,0.951056516295154,1.,0.951056516295154,1.,0.951056516295154,
1.,0.951056516295154,1.,0.951056516295154,1.,0.951056516295154,1.,0.951056516295154,
1.,0.951056516295154,1.,0.951056516295154,1.,0.951056516295154,1.,0.951056516295154,
1.,0.951056516295154,1.,0.951056516295154,1.,0.951056516295154,1.,0.951056516295154,
1.,0.951056516295154,1.,0.951056516295154,1.,0.951056516295154,1.,0.951056516295154,
1.,0.951056516295154,1.,0.951056516295154,1.,0.951056516295154,1.,0.951056516295154,
1.,0.951056516295154,1.,0.951056516295154,1.,0.951056516295154,1.,0.951056516295154,
1.,0.951056516295154,1.,0.951056516295154,1.,0.951056516295154,1.,0.951056516295154,
1.,0.951056516295154,1.,0.951056516295154,1.,0.951056516295154,1.,0.951056516295154,
1.,0.951056516295154,1.,0.951056516295154,1.,0.951056516295154,1.,0.951056516295154,
1.,0.951056516295154,1.,0.951056516295154,1.,0.951056516295154,1.,0.951056516295154,
1.,0.951056516295154,1.,0.951056516295154,1.,0.951056516295154,1.,0.951056516295154,
1.,0.951056516295154,1.,0.951056516295154,1.,0.951056516295154,1.,0.951056516295154,
1.,0.951056516295154,1.,0.951056516295154,1.,0.951056516295154,1.,0.951056516295154,
1.,0.951056516295154,1.,0.951056516295154,1.,0.951056516295154,1.,0.951056516295154,
1.,0.951056516295154,1.,0.951056516295154,1.,0.951056516295154,1.,0.951056516295154,
1.,0.951056516295154,1.,0.951056516295154,1.,0.951056516295154,1.,0.951056516295154,
1.,0.951056516295154,1.,0.951056516295154,1.,0.951056516295154,1.,0.951056516295154,
1.,0.951056516295154,1.,0.951056516295154,1.,0.951056516295154,1.,0.951056516295154,
1.,0.951056516295154,1.,0.951056516295154,1.,0.951056516295154,1.,0.951056516295154,
1.,0.951056516295154,1.,0.951056516295154,1.,0.951056516295154,1.,0.951056516295154,
1.,0.951056516295154,1.,0.951056516295154,1.,0.951056516295154,1.,0.951056516295154,
1.,0.951056516295154,1.,0.951056516295154,1.,0.951056516295154,1.,0.951056516295154,
1.,0.951056516295154,1.,0.951056516295154,1.,0.951056516295154,1.,0.951056516295154,
1.,0.951056516295154,1.,0.951056516295154,1.,0.951056516295154,1.,0.951056516295154,
1.,0.951056516295154,1.,0.951056516295154,1.,0.951056516295154,1.,0.951056516295154,
1.,0.951056516295154,1.,0.951056516295154,1.,0.951056516295154,1.,0.951056516295154,
1.,0.951056516295154,1.,0.951056516295154,1.,0.951056516295154,1.,0.951056516295154,
1.,0.951056516295154,1.,0.951056516295154,1.,0.951056516295154,1.,0.951056516295154,
1.,0.951056516295154,1.,0.951056516295154,1.,0.951056516295154,1.,0.951056516295154,
1.,0.951056516295154,1.,0.951056516295154,1.,0.951056516295154,1.,0.951056516295154,
1.,0.951056516295154,1.,0.951056516295154,1.,0.951056516295154,1.,0.951056516295154,
1.,0.951056516295154,1.,0.951056516295154,1.,0.951056516295154,1.,0.951056516295154,
1.,0.951056516295154,1.,0.951056516295154,1.,0.951056516295154,1.,0.951056516295154,
1.,0.951056516295154,1.,0.951056516295154,1.,0.951056516295154,1.,0.951056516295154,
1.,0.951056516295154,1.,0.951056516295154,1.,0.951056516295154,1.,0.951056516295154,
1.,0.951056516295154,1.,0.951056516295154,1.,0.951056516295154,1.,0.951056516295154,
1.,0.951056516295154,1.,0.951056516295154,1.,0.951056516295154,1.,0.951056516295154,
1.,0.951056516295154,1.,0.951056516295154,1.,0.951056516295154,1.,0.951056516295154,
1.,0.951056516295154,1.,0.951056516295154,1.,0.951056516295154,1.,0.951056516295154,
1.,0.951056516295154,1.,0.951056516295154,1.,0.951056516295154,1.,0.951056516295154,
1.,0.951056516295154,1.,0.951056516295154,1.,0.951056516295154,1.,0.951056516295154,
1.,0.951056516295154,1.,0.951056516295154,1.,0.951056516295154,1.,0.951056516295154,
1.,0.951056516295154,1.,0.951056516295154,1.,0.951056516295154,1.,0.951056516295154,
1.,0.951056516295154,1.,0.951056516295154,1.,0.951056516295154,1.,0.951056516295154,
1.,0.951056516295154,1.,0.951056516295154,1.,0.951056516295154,1.,0.951056516295154,
1.,0.951056516295154,1.,0.951056516295154,1.,0.951056516295154,1.)))
REPRESENTATION_ITEM('')
SURFACE()
);
#3197=(
BOUNDED_SURFACE()
B_SPLINE_SURFACE(1,2,((#287932,#287933,#287934,#287935,#287936,#287937,
#287938,#287939,#287940,#287941,#287942,#287943,#287944,#287945,#287946,
#287947,#287948,#287949,#287950,#287951,#287952,#287953,#287954,#287955,
#287956,#287957,#287958,#287959,#287960,#287961,#287962,#287963,#287964,
#287965,#287966,#287967,#287968,#287969,#287970,#287971,#287972,#287973,
#287974,#287975,#287976,#287977,#287978,#287979,#287980,#287981,#287982,
#287983,#287984,#287985,#287986,#287987,#287988,#287989,#287990,#287991,
#287992,#287993,#287994,#287995,#287996,#287997,#287998,#287999,#288000,
#288001,#288002,#288003,#288004,#288005,#288006,#288007,#288008,#288009,
#288010,#288011,#288012,#288013,#288014,#288015,#288016,#288017,#288018,
#288019,#288020,#288021,#288022,#288023,#288024,#288025,#288026,#288027,
#288028,#288029,#288030,#288031,#288032,#288033,#288034,#288035,#288036,
#288037,#288038,#288039,#288040,#288041,#288042,#288043,#288044,#288045,
#288046,#288047,#288048,#288049,#288050,#288051,#288052,#288053,#288054,
#288055,#288056,#288057,#288058,#288059,#288060,#288061,#288062,#288063,
#288064,#288065,#288066,#288067,#288068,#288069,#288070,#288071,#288072,
#288073,#288074,#288075,#288076,#288077,#288078,#288079,#288080,#288081,
#288082,#288083,#288084,#288085,#288086,#288087,#288088,#288089,#288090,
#288091,#288092,#288093,#288094,#288095,#288096,#288097,#288098,#288099,
#288100,#288101,#288102,#288103,#288104,#288105,#288106,#288107,#288108,
#288109,#288110,#288111,#288112,#288113,#288114,#288115,#288116,#288117,
#288118,#288119,#288120,#288121,#288122,#288123,#288124,#288125,#288126,
#288127,#288128,#288129,#288130,#288131,#288132,#288133,#288134,#288135,
#288136,#288137,#288138,#288139,#288140,#288141,#288142,#288143,#288144,
#288145,#288146,#288147,#288148,#288149,#288150,#288151,#288152,#288153,
#288154,#288155,#288156,#288157,#288158,#288159,#288160,#288161,#288162,
#288163,#288164,#288165,#288166,#288167,#288168,#288169,#288170,#288171,
#288172,#288173,#288174,#288175,#288176,#288177,#288178,#288179,#288180,
#288181,#288182,#288183,#288184,#288185,#288186,#288187,#288188,#288189,
#288190,#288191,#288192,#288193,#288194,#288195,#288196,#288197,#288198,
#288199,#288200,#288201,#288202,#288203,#288204,#288205,#288206,#288207,
#288208,#288209,#288210,#288211,#288212,#288213,#288214,#288215,#288216,
#288217,#288218,#288219,#288220,#288221,#288222,#288223,#288224,#288225,
#288226,#288227,#288228,#288229,#288230,#288231,#288232,#288233,#288234,
#288235,#288236,#288237,#288238,#288239,#288240,#288241,#288242,#288243,
#288244,#288245,#288246,#288247,#288248,#288249,#288250,#288251,#288252,
#288253,#288254,#288255,#288256,#288257,#288258,#288259,#288260,#288261,
#288262,#288263,#288264,#288265,#288266,#288267,#288268,#288269,#288270,
#288271,#288272,#288273,#288274,#288275,#288276,#288277,#288278,#288279,
#288280,#288281,#288282,#288283,#288284,#288285,#288286,#288287,#288288,
#288289,#288290,#288291,#288292,#288293,#288294,#288295,#288296,#288297,
#288298,#288299,#288300,#288301,#288302,#288303,#288304,#288305,#288306,
#288307,#288308,#288309,#288310,#288311,#288312,#288313,#288314,#288315,
#288316,#288317,#288318,#288319,#288320,#288321,#288322,#288323,#288324,
#288325,#288326,#288327,#288328,#288329,#288330,#288331,#288332,#288333,
#288334,#288335,#288336,#288337,#288338,#288339,#288340,#288341,#288342,
#288343,#288344,#288345,#288346,#288347,#288348,#288349,#288350,#288351,
#288352,#288353,#288354,#288355,#288356,#288357,#288358,#288359,#288360,
#288361,#288362,#288363,#288364,#288365,#288366,#288367,#288368,#288369,
#288370,#288371,#288372,#288373,#288374,#288375,#288376,#288377,#288378,
#288379,#288380,#288381,#288382,#288383,#288384,#288385,#288386,#288387,
#288388,#288389,#288390,#288391,#288392,#288393,#288394,#288395,#288396,
#288397,#288398,#288399,#288400,#288401,#288402,#288403,#288404,#288405,
#288406,#288407,#288408,#288409,#288410,#288411,#288412,#288413,#288414,
#288415,#288416,#288417,#288418,#288419,#288420,#288421,#288422,#288423,
#288424,#288425,#288426,#288427,#288428,#288429,#288430,#288431,#288432,
#288433,#288434,#288435,#288436,#288437,#288438,#288439,#288440,#288441,
#288442,#288443,#288444,#288445,#288446,#288447,#288448,#288449,#288450,
#288451,#288452,#288453,#288454,#288455,#288456,#288457,#288458,#288459,
#288460,#288461,#288462,#288463,#288464,#288465,#288466,#288467,#288468,
#288469,#288470,#288471,#288472,#288473,#288474,#288475,#288476,#288477,
#288478,#288479,#288480,#288481,#288482,#288483,#288484,#288485,#288486,
#288487,#288488,#288489,#288490,#288491,#288492,#288493,#288494,#288495,
#288496,#288497,#288498,#288499,#288500,#288501,#288502,#288503,#288504,
#288505,#288506,#288507,#288508,#288509,#288510,#288511,#288512,#288513,
#288514,#288515,#288516,#288517,#288518,#288519,#288520,#288521,#288522,
#288523,#288524,#288525,#288526,#288527,#288528,#288529,#288530,#288531,
#288532,#288533,#288534,#288535,#288536,#288537,#288538,#288539,#288540,
#288541,#288542,#288543,#288544,#288545,#288546,#288547,#288548,#288549,
#288550,#288551,#288552,#288553,#288554,#288555,#288556,#288557,#288558,
#288559,#288560,#288561,#288562,#288563,#288564,#288565,#288566,#288567,
#288568,#288569,#288570,#288571,#288572,#288573,#288574,#288575,#288576,
#288577,#288578,#288579,#288580,#288581,#288582,#288583,#288584,#288585,
#288586,#288587,#288588,#288589,#288590,#288591,#288592,#288593,#288594,
#288595,#288596,#288597,#288598,#288599,#288600,#288601,#288602,#288603,
#288604,#288605,#288606,#288607,#288608,#288609,#288610,#288611,#288612,
#288613,#288614,#288615,#288616,#288617,#288618,#288619,#288620,#288621,
#288622,#288623,#288624,#288625,#288626,#288627,#288628,#288629,#288630,
#288631,#288632,#288633,#288634,#288635,#288636,#288637,#288638,#288639,
#288640,#288641,#288642,#288643,#288644,#288645,#288646,#288647,#288648,
#288649,#288650,#288651,#288652,#288653,#288654,#288655,#288656,#288657,
#288658,#288659,#288660,#288661,#288662,#288663,#288664,#288665,#288666,
#288667,#288668,#288669,#288670,#288671,#288672,#288673,#288674,#288675,
#288676,#288677,#288678,#288679,#288680,#288681,#288682,#288683,#288684,
#288685,#288686,#288687,#288688,#288689,#288690,#288691,#288692,#288693,
#288694,#288695,#288696,#288697,#288698,#288699,#288700,#288701,#288702,
#288703,#288704,#288705,#288706,#288707,#288708,#288709,#288710,#288711,
#288712,#288713,#288714,#288715,#288716,#288717,#288718,#288719,#288720,
#288721,#288722,#288723,#288724,#288725,#288726,#288727,#288728,#288729,
#288730,#288731,#288732,#288733,#288734,#288735,#288736,#288737,#288738,
#288739,#288740,#288741,#288742,#288743,#288744,#288745,#288746,#288747,
#288748,#288749,#288750,#288751,#288752,#288753,#288754,#288755,#288756,
#288757,#288758,#288759,#288760,#288761,#288762,#288763,#288764,#288765,
#288766,#288767,#288768,#288769,#288770,#288771,#288772,#288773,#288774,
#288775,#288776,#288777,#288778,#288779,#288780,#288781,#288782,#288783,
#288784,#288785,#288786,#288787,#288788,#288789,#288790,#288791,#288792,
#288793,#288794,#288795,#288796,#288797,#288798,#288799,#288800,#288801,
#288802,#288803,#288804,#288805,#288806,#288807,#288808,#288809,#288810,
#288811,#288812,#288813,#288814,#288815,#288816,#288817,#288818,#288819,
#288820,#288821,#288822,#288823,#288824,#288825,#288826,#288827,#288828,
#288829,#288830,#288831,#288832,#288833,#288834,#288835,#288836,#288837,
#288838,#288839,#288840,#288841,#288842,#288843,#288844,#288845,#288846,
#288847,#288848,#288849,#288850,#288851,#288852,#288853,#288854,#288855,
#288856,#288857,#288858,#288859,#288860,#288861,#288862,#288863,#288864,
#288865,#288866,#288867,#288868,#288869,#288870,#288871,#288872,#288873,
#288874,#288875,#288876,#288877,#288878,#288879,#288880,#288881,#288882,
#288883,#288884,#288885,#288886,#288887,#288888,#288889,#288890,#288891,
#288892,#288893,#288894,#288895,#288896,#288897,#288898,#288899,#288900,
#288901,#288902,#288903,#288904,#288905,#288906,#288907,#288908,#288909,
#288910,#288911,#288912,#288913,#288914,#288915,#288916,#288917,#288918,
#288919,#288920,#288921,#288922,#288923,#288924,#288925,#288926,#288927,
#288928,#288929,#288930,#288931,#288932,#288933,#288934,#288935,#288936,
#288937,#288938,#288939,#288940,#288941,#288942,#288943,#288944,#288945,
#288946,#288947,#288948,#288949,#288950,#288951,#288952,#288953,#288954,
#288955,#288956,#288957,#288958,#288959,#288960,#288961,#288962,#288963,
#288964,#288965,#288966,#288967,#288968),(#288969,#288970,#288971,#288972,
#288973,#288974,#288975,#288976,#288977,#288978,#288979,#288980,#288981,
#288982,#288983,#288984,#288985,#288986,#288987,#288988,#288989,#288990,
#288991,#288992,#288993,#288994,#288995,#288996,#288997,#288998,#288999,
#289000,#289001,#289002,#289003,#289004,#289005,#289006,#289007,#289008,
#289009,#289010,#289011,#289012,#289013,#289014,#289015,#289016,#289017,
#289018,#289019,#289020,#289021,#289022,#289023,#289024,#289025,#289026,
#289027,#289028,#289029,#289030,#289031,#289032,#289033,#289034,#289035,
#289036,#289037,#289038,#289039,#289040,#289041,#289042,#289043,#289044,
#289045,#289046,#289047,#289048,#289049,#289050,#289051,#289052,#289053,
#289054,#289055,#289056,#289057,#289058,#289059,#289060,#289061,#289062,
#289063,#289064,#289065,#289066,#289067,#289068,#289069,#289070,#289071,
#289072,#289073,#289074,#289075,#289076,#289077,#289078,#289079,#289080,
#289081,#289082,#289083,#289084,#289085,#289086,#289087,#289088,#289089,
#289090,#289091,#289092,#289093,#289094,#289095,#289096,#289097,#289098,
#289099,#289100,#289101,#289102,#289103,#289104,#289105,#289106,#289107,
#289108,#289109,#289110,#289111,#289112,#289113,#289114,#289115,#289116,
#289117,#289118,#289119,#289120,#289121,#289122,#289123,#289124,#289125,
#289126,#289127,#289128,#289129,#289130,#289131,#289132,#289133,#289134,
#289135,#289136,#289137,#289138,#289139,#289140,#289141,#289142,#289143,
#289144,#289145,#289146,#289147,#289148,#289149,#289150,#289151,#289152,
#289153,#289154,#289155,#289156,#289157,#289158,#289159,#289160,#289161,
#289162,#289163,#289164,#289165,#289166,#289167,#289168,#289169,#289170,
#289171,#289172,#289173,#289174,#289175,#289176,#289177,#289178,#289179,
#289180,#289181,#289182,#289183,#289184,#289185,#289186,#289187,#289188,
#289189,#289190,#289191,#289192,#289193,#289194,#289195,#289196,#289197,
#289198,#289199,#289200,#289201,#289202,#289203,#289204,#289205,#289206,
#289207,#289208,#289209,#289210,#289211,#289212,#289213,#289214,#289215,
#289216,#289217,#289218,#289219,#289220,#289221,#289222,#289223,#289224,
#289225,#289226,#289227,#289228,#289229,#289230,#289231,#289232,#289233,
#289234,#289235,#289236,#289237,#289238,#289239,#289240,#289241,#289242,
#289243,#289244,#289245,#289246,#289247,#289248,#289249,#289250,#289251,
#289252,#289253,#289254,#289255,#289256,#289257,#289258,#289259,#289260,
#289261,#289262,#289263,#289264,#289265,#289266,#289267,#289268,#289269,
#289270,#289271,#289272,#289273,#289274,#289275,#289276,#289277,#289278,
#289279,#289280,#289281,#289282,#289283,#289284,#289285,#289286,#289287,
#289288,#289289,#289290,#289291,#289292,#289293,#289294,#289295,#289296,
#289297,#289298,#289299,#289300,#289301,#289302,#289303,#289304,#289305,
#289306,#289307,#289308,#289309,#289310,#289311,#289312,#289313,#289314,
#289315,#289316,#289317,#289318,#289319,#289320,#289321,#289322,#289323,
#289324,#289325,#289326,#289327,#289328,#289329,#289330,#289331,#289332,
#289333,#289334,#289335,#289336,#289337,#289338,#289339,#289340,#289341,
#289342,#289343,#289344,#289345,#289346,#289347,#289348,#289349,#289350,
#289351,#289352,#289353,#289354,#289355,#289356,#289357,#289358,#289359,
#289360,#289361,#289362,#289363,#289364,#289365,#289366,#289367,#289368,
#289369,#289370,#289371,#289372,#289373,#289374,#289375,#289376,#289377,
#289378,#289379,#289380,#289381,#289382,#289383,#289384,#289385,#289386,
#289387,#289388,#289389,#289390,#289391,#289392,#289393,#289394,#289395,
#289396,#289397,#289398,#289399,#289400,#289401,#289402,#289403,#289404,
#289405,#289406,#289407,#289408,#289409,#289410,#289411,#289412,#289413,
#289414,#289415,#289416,#289417,#289418,#289419,#289420,#289421,#289422,
#289423,#289424,#289425,#289426,#289427,#289428,#289429,#289430,#289431,
#289432,#289433,#289434,#289435,#289436,#289437,#289438,#289439,#289440,
#289441,#289442,#289443,#289444,#289445,#289446,#289447,#289448,#289449,
#289450,#289451,#289452,#289453,#289454,#289455,#289456,#289457,#289458,
#289459,#289460,#289461,#289462,#289463,#289464,#289465,#289466,#289467,
#289468,#289469,#289470,#289471,#289472,#289473,#289474,#289475,#289476,
#289477,#289478,#289479,#289480,#289481,#289482,#289483,#289484,#289485,
#289486,#289487,#289488,#289489,#289490,#289491,#289492,#289493,#289494,
#289495,#289496,#289497,#289498,#289499,#289500,#289501,#289502,#289503,
#289504,#289505,#289506,#289507,#289508,#289509,#289510,#289511,#289512,
#289513,#289514,#289515,#289516,#289517,#289518,#289519,#289520,#289521,
#289522,#289523,#289524,#289525,#289526,#289527,#289528,#289529,#289530,
#289531,#289532,#289533,#289534,#289535,#289536,#289537,#289538,#289539,
#289540,#289541,#289542,#289543,#289544,#289545,#289546,#289547,#289548,
#289549,#289550,#289551,#289552,#289553,#289554,#289555,#289556,#289557,
#289558,#289559,#289560,#289561,#289562,#289563,#289564,#289565,#289566,
#289567,#289568,#289569,#289570,#289571,#289572,#289573,#289574,#289575,
#289576,#289577,#289578,#289579,#289580,#289581,#289582,#289583,#289584,
#289585,#289586,#289587,#289588,#289589,#289590,#289591,#289592,#289593,
#289594,#289595,#289596,#289597,#289598,#289599,#289600,#289601,#289602,
#289603,#289604,#289605,#289606,#289607,#289608,#289609,#289610,#289611,
#289612,#289613,#289614,#289615,#289616,#289617,#289618,#289619,#289620,
#289621,#289622,#289623,#289624,#289625,#289626,#289627,#289628,#289629,
#289630,#289631,#289632,#289633,#289634,#289635,#289636,#289637,#289638,
#289639,#289640,#289641,#289642,#289643,#289644,#289645,#289646,#289647,
#289648,#289649,#289650,#289651,#289652,#289653,#289654,#289655,#289656,
#289657,#289658,#289659,#289660,#289661,#289662,#289663,#289664,#289665,
#289666,#289667,#289668,#289669,#289670,#289671,#289672,#289673,#289674,
#289675,#289676,#289677,#289678,#289679,#289680,#289681,#289682,#289683,
#289684,#289685,#289686,#289687,#289688,#289689,#289690,#289691,#289692,
#289693,#289694,#289695,#289696,#289697,#289698,#289699,#289700,#289701,
#289702,#289703,#289704,#289705,#289706,#289707,#289708,#289709,#289710,
#289711,#289712,#289713,#289714,#289715,#289716,#289717,#289718,#289719,
#289720,#289721,#289722,#289723,#289724,#289725,#289726,#289727,#289728,
#289729,#289730,#289731,#289732,#289733,#289734,#289735,#289736,#289737,
#289738,#289739,#289740,#289741,#289742,#289743,#289744,#289745,#289746,
#289747,#289748,#289749,#289750,#289751,#289752,#289753,#289754,#289755,
#289756,#289757,#289758,#289759,#289760,#289761,#289762,#289763,#289764,
#289765,#289766,#289767,#289768,#289769,#289770,#289771,#289772,#289773,
#289774,#289775,#289776,#289777,#289778,#289779,#289780,#289781,#289782,
#289783,#289784,#289785,#289786,#289787,#289788,#289789,#289790,#289791,
#289792,#289793,#289794,#289795,#289796,#289797,#289798,#289799,#289800,
#289801,#289802,#289803,#289804,#289805,#289806,#289807,#289808,#289809,
#289810,#289811,#289812,#289813,#289814,#289815,#289816,#289817,#289818,
#289819,#289820,#289821,#289822,#289823,#289824,#289825,#289826,#289827,
#289828,#289829,#289830,#289831,#289832,#289833,#289834,#289835,#289836,
#289837,#289838,#289839,#289840,#289841,#289842,#289843,#289844,#289845,
#289846,#289847,#289848,#289849,#289850,#289851,#289852,#289853,#289854,
#289855,#289856,#289857,#289858,#289859,#289860,#289861,#289862,#289863,
#289864,#289865,#289866,#289867,#289868,#289869,#289870,#289871,#289872,
#289873,#289874,#289875,#289876,#289877,#289878,#289879,#289880,#289881,
#289882,#289883,#289884,#289885,#289886,#289887,#289888,#289889,#289890,
#289891,#289892,#289893,#289894,#289895,#289896,#289897,#289898,#289899,
#289900,#289901,#289902,#289903,#289904,#289905,#289906,#289907,#289908,
#289909,#289910,#289911,#289912,#289913,#289914,#289915,#289916,#289917,
#289918,#289919,#289920,#289921,#289922,#289923,#289924,#289925,#289926,
#289927,#289928,#289929,#289930,#289931,#289932,#289933,#289934,#289935,
#289936,#289937,#289938,#289939,#289940,#289941,#289942,#289943,#289944,
#289945,#289946,#289947,#289948,#289949,#289950,#289951,#289952,#289953,
#289954,#289955,#289956,#289957,#289958,#289959,#289960,#289961,#289962,
#289963,#289964,#289965,#289966,#289967,#289968,#289969,#289970,#289971,
#289972,#289973,#289974,#289975,#289976,#289977,#289978,#289979,#289980,
#289981,#289982,#289983,#289984,#289985,#289986,#289987,#289988,#289989,
#289990,#289991,#289992,#289993,#289994,#289995,#289996,#289997,#289998,
#289999,#290000,#290001,#290002,#290003,#290004,#290005)),.UNSPECIFIED.,
 .F.,.F.,.F.)
B_SPLINE_SURFACE_WITH_KNOTS((2,2),(3,2,2,2,2,2,2,2,2,2,2,2,2,2,2,2,2,2,
2,2,2,2,2,2,2,2,2,2,2,2,2,2,2,2,2,2,2,2,2,2,2,2,2,2,2,2,2,2,2,2,2,2,2,2,
2,2,2,2,2,2,2,2,2,2,2,2,2,2,2,2,2,2,2,2,2,2,2,2,2,2,2,2,2,2,2,2,2,2,2,2,
2,2,2,2,2,2,2,2,2,2,2,2,2,2,2,2,2,2,2,2,2,2,2,2,2,2,2,2,2,2,2,2,2,2,2,2,
2,2,2,2,2,2,2,2,2,2,2,2,2,2,2,2,2,2,2,2,2,2,2,2,2,2,2,2,2,2,2,2,2,2,2,2,
2,2,2,2,2,2,2,2,2,2,2,2,2,2,2,2,2,2,2,2,2,2,2,2,2,2,2,2,2,2,2,2,2,2,2,2,
2,2,2,2,2,2,2,2,2,2,2,2,2,2,2,2,2,2,2,2,2,2,2,2,2,2,2,2,2,2,2,2,2,2,2,2,
2,2,2,2,2,2,2,2,2,2,2,2,2,2,2,2,2,2,2,2,2,2,2,2,2,2,2,2,2,2,2,2,2,2,2,2,
2,2,2,2,2,2,2,2,2,2,2,2,2,2,2,2,2,2,2,2,2,2,2,2,2,2,2,2,2,2,2,2,2,2,2,2,
2,2,2,2,2,2,2,2,2,2,2,2,2,2,2,2,2,2,2,2,2,2,2,2,2,2,2,2,2,2,2,2,2,2,2,2,
2,2,2,2,2,2,2,2,2,2,2,2,2,2,2,2,2,2,2,2,2,2,2,2,2,2,2,2,2,2,2,2,2,2,2,2,
2,2,2,2,2,2,2,2,2,2,2,2,2,2,2,2,2,2,2,2,2,2,2,2,2,2,2,2,2,2,2,2,2,2,2,2,
2,2,2,2,2,2,2,2,2,2,2,2,2,2,2,2,2,2,2,2,2,2,2,2,2,2,2,2,2,2,2,2,2,2,2,2,
2,2,2,2,2,2,2,2,2,2,2,2,2,2,2,2,2,2,2,2,2,2,2,2,2,2,2,2,2,2,2,2,2,2,2,2,
2,2,2,2,2,2,2,2,2,2,2,2,2,2,2,2,2,2,2,2,2,2,2,2,2,2,2,2,2,2,2,2,3),(0.,
1.),(0.,0.00192307692307692,0.00384615384615385,0.00576923076923077,0.00769230769230769,
0.00961538461538462,0.0115384615384615,0.0134615384615385,0.0153846153846154,
0.0173076923076923,0.0192307692307692,0.0211538461538462,0.0230769230769231,
0.025,0.0269230769230769,0.0288461538461538,0.0307692307692308,0.0326923076923077,
0.0346153846153846,0.0365384615384615,0.0384615384615385,0.0403846153846154,
0.0423076923076923,0.0442307692307692,0.0461538461538462,0.0480769230769231,
0.05,0.0519230769230769,0.0538461538461538,0.0557692307692308,0.0576923076923077,
0.0596153846153846,0.0615384615384615,0.0634615384615385,0.0653846153846154,
0.0673076923076923,0.0692307692307692,0.0711538461538462,0.0730769230769231,
0.075,0.0769230769230769,0.0788461538461538,0.0807692307692308,0.0826923076923077,
0.0846153846153846,0.0865384615384615,0.0884615384615385,0.0903846153846154,
0.0923076923076923,0.0942307692307692,0.0961538461538462,0.0980769230769231,
0.1,0.101923076923077,0.103846153846154,0.105769230769231,0.107692307692308,
0.109615384615385,0.111538461538462,0.113461538461538,0.115384615384615,
0.117307692307692,0.119230769230769,0.121153846153846,0.123076923076923,
0.125,0.126923076923077,0.128846153846154,0.130769230769231,0.132692307692308,
0.134615384615385,0.136538461538462,0.138461538461538,0.140384615384615,
0.142307692307692,0.144230769230769,0.146153846153846,0.148076923076923,
0.15,0.151923076923077,0.153846153846154,0.155769230769231,0.157692307692308,
0.159615384615385,0.161538461538462,0.163461538461538,0.165384615384615,
0.167307692307692,0.169230769230769,0.171153846153846,0.173076923076923,
0.175,0.176923076923077,0.178846153846154,0.180769230769231,0.182692307692308,
0.184615384615385,0.186538461538462,0.188461538461538,0.190384615384615,
0.192307692307692,0.194230769230769,0.196153846153846,0.198076923076923,
0.2,0.201923076923077,0.203846153846154,0.205769230769231,0.207692307692308,
0.209615384615385,0.211538461538462,0.213461538461538,0.215384615384615,
0.217307692307692,0.219230769230769,0.221153846153846,0.223076923076923,
0.225,0.226923076923077,0.228846153846154,0.230769230769231,0.232692307692308,
0.234615384615385,0.236538461538462,0.238461538461538,0.240384615384615,
0.242307692307692,0.244230769230769,0.246153846153846,0.248076923076923,
0.25,0.251923076923077,0.253846153846154,0.255769230769231,0.257692307692308,
0.259615384615385,0.261538461538462,0.263461538461538,0.265384615384615,
0.267307692307692,0.269230769230769,0.271153846153846,0.273076923076923,
0.275,0.276923076923077,0.278846153846154,0.280769230769231,0.282692307692308,
0.284615384615385,0.286538461538462,0.288461538461538,0.290384615384615,
0.292307692307692,0.294230769230769,0.296153846153846,0.298076923076923,
0.3,0.301923076923077,0.303846153846154,0.305769230769231,0.307692307692308,
0.309615384615385,0.311538461538462,0.313461538461538,0.315384615384615,
0.317307692307692,0.319230769230769,0.321153846153846,0.323076923076923,
0.325,0.326923076923077,0.328846153846154,0.330769230769231,0.332692307692308,
0.334615384615385,0.336538461538462,0.338461538461538,0.340384615384615,
0.342307692307692,0.344230769230769,0.346153846153846,0.348076923076923,
0.35,0.351923076923077,0.353846153846154,0.355769230769231,0.357692307692308,
0.359615384615385,0.361538461538462,0.363461538461538,0.365384615384615,
0.367307692307692,0.369230769230769,0.371153846153846,0.373076923076923,
0.375,0.376923076923077,0.378846153846154,0.380769230769231,0.382692307692308,
0.384615384615385,0.386538461538462,0.388461538461538,0.390384615384615,
0.392307692307692,0.394230769230769,0.396153846153846,0.398076923076923,
0.4,0.401923076923077,0.403846153846154,0.405769230769231,0.407692307692308,
0.409615384615385,0.411538461538462,0.413461538461538,0.415384615384615,
0.417307692307692,0.419230769230769,0.421153846153846,0.423076923076923,
0.425,0.426923076923077,0.428846153846154,0.430769230769231,0.432692307692308,
0.434615384615385,0.436538461538462,0.438461538461538,0.440384615384615,
0.442307692307692,0.444230769230769,0.446153846153846,0.448076923076923,
0.45,0.451923076923077,0.453846153846154,0.455769230769231,0.457692307692308,
0.459615384615385,0.461538461538462,0.463461538461538,0.465384615384615,
0.467307692307692,0.469230769230769,0.471153846153846,0.473076923076923,
0.475,0.476923076923077,0.478846153846154,0.480769230769231,0.482692307692308,
0.484615384615385,0.486538461538462,0.488461538461538,0.490384615384615,
0.492307692307692,0.494230769230769,0.496153846153846,0.498076923076923,
0.5,0.501923076923077,0.503846153846154,0.505769230769231,0.507692307692308,
0.509615384615385,0.511538461538461,0.513461538461538,0.515384615384615,
0.517307692307692,0.519230769230769,0.521153846153846,0.523076923076923,
0.525,0.526923076923077,0.528846153846154,0.530769230769231,0.532692307692308,
0.534615384615385,0.536538461538462,0.538461538461538,0.540384615384615,
0.542307692307692,0.544230769230769,0.546153846153846,0.548076923076923,
0.55,0.551923076923077,0.553846153846154,0.555769230769231,0.557692307692308,
0.559615384615385,0.561538461538462,0.563461538461538,0.565384615384615,
0.567307692307692,0.569230769230769,0.571153846153846,0.573076923076923,
0.575,0.576923076923077,0.578846153846154,0.580769230769231,0.582692307692308,
0.584615384615385,0.586538461538462,0.588461538461538,0.590384615384615,
0.592307692307692,0.594230769230769,0.596153846153846,0.598076923076923,
0.6,0.601923076923077,0.603846153846154,0.605769230769231,0.607692307692308,
0.609615384615385,0.611538461538462,0.613461538461539,0.615384615384615,
0.617307692307692,0.619230769230769,0.621153846153846,0.623076923076923,
0.625,0.626923076923077,0.628846153846154,0.630769230769231,0.632692307692308,
0.634615384615385,0.636538461538461,0.638461538461538,0.640384615384615,
0.642307692307692,0.644230769230769,0.646153846153846,0.648076923076923,
0.65,0.651923076923077,0.653846153846154,0.655769230769231,0.657692307692308,
0.659615384615385,0.661538461538462,0.663461538461538,0.665384615384615,
0.667307692307692,0.669230769230769,0.671153846153846,0.673076923076923,
0.675,0.676923076923077,0.678846153846154,0.680769230769231,0.682692307692308,
0.684615384615385,0.686538461538462,0.688461538461538,0.690384615384615,
0.692307692307692,0.694230769230769,0.696153846153846,0.698076923076923,
0.7,0.701923076923077,0.703846153846154,0.705769230769231,0.707692307692308,
0.709615384615385,0.711538461538462,0.713461538461538,0.715384615384615,
0.717307692307692,0.719230769230769,0.721153846153846,0.723076923076923,
0.725,0.726923076923077,0.728846153846154,0.730769230769231,0.732692307692308,
0.734615384615385,0.736538461538462,0.738461538461539,0.740384615384615,
0.742307692307692,0.744230769230769,0.746153846153846,0.748076923076923,
0.75,0.751923076923077,0.753846153846154,0.755769230769231,0.757692307692308,
0.759615384615385,0.761538461538461,0.763461538461538,0.765384615384615,
0.767307692307692,0.769230769230769,0.771153846153846,0.773076923076923,
0.775,0.776923076923077,0.778846153846154,0.780769230769231,0.782692307692308,
0.784615384615385,0.786538461538462,0.788461538461538,0.790384615384615,
0.792307692307692,0.794230769230769,0.796153846153846,0.798076923076923,
0.8,0.801923076923077,0.803846153846154,0.805769230769231,0.807692307692308,
0.809615384615385,0.811538461538462,0.813461538461538,0.815384615384615,
0.817307692307692,0.819230769230769,0.821153846153846,0.823076923076923,
0.825,0.826923076923077,0.828846153846154,0.830769230769231,0.832692307692308,
0.834615384615385,0.836538461538462,0.838461538461538,0.840384615384615,
0.842307692307692,0.844230769230769,0.846153846153846,0.848076923076923,
0.85,0.851923076923077,0.853846153846154,0.855769230769231,0.857692307692308,
0.859615384615385,0.861538461538462,0.863461538461539,0.865384615384615,
0.867307692307692,0.869230769230769,0.871153846153846,0.873076923076923,
0.875,0.876923076923077,0.878846153846154,0.880769230769231,0.882692307692308,
0.884615384615385,0.886538461538461,0.888461538461538,0.890384615384615,
0.892307692307692,0.894230769230769,0.896153846153846,0.898076923076923,
0.9,0.901923076923077,0.903846153846154,0.905769230769231,0.907692307692308,
0.909615384615385,0.911538461538462,0.913461538461538,0.915384615384615,
0.917307692307692,0.919230769230769,0.921153846153846,0.923076923076923,
0.925,0.926923076923077,0.928846153846154,0.930769230769231,0.932692307692308,
0.934615384615385,0.936538461538462,0.938461538461538,0.940384615384615,
0.942307692307692,0.944230769230769,0.946153846153846,0.948076923076923,
0.95,0.951923076923077,0.953846153846154,0.955769230769231,0.957692307692308,
0.959615384615385,0.961538461538462,0.963461538461538,0.965384615384615,
0.967307692307692,0.969230769230769,0.971153846153846,0.973076923076923,
0.975,0.976923076923077,0.978846153846154,0.980769230769231,0.982692307692308,
0.984615384615385,0.986538461538462,0.988461538461539,0.990384615384615,
0.992307692307692,0.994230769230769,0.996153846153846),.UNSPECIFIED.)
GEOMETRIC_REPRESENTATION_ITEM()
RATIONAL_B_SPLINE_SURFACE(((1.,0.951056516295154,1.,0.951056516295154,1.,
0.951056516295154,1.,0.951056516295154,1.,0.951056516295154,1.,0.951056516295154,
1.,0.951056516295154,1.,0.951056516295154,1.,0.951056516295154,1.,0.951056516295154,
1.,0.951056516295154,1.,0.951056516295154,1.,0.951056516295154,1.,0.951056516295154,
1.,0.951056516295154,1.,0.951056516295154,1.,0.951056516295154,1.,0.951056516295154,
1.,0.951056516295154,1.,0.951056516295154,1.,0.951056516295154,1.,0.951056516295154,
1.,0.951056516295154,1.,0.951056516295154,1.,0.951056516295154,1.,0.951056516295154,
1.,0.951056516295154,1.,0.951056516295154,1.,0.951056516295154,1.,0.951056516295154,
1.,0.951056516295154,1.,0.951056516295154,1.,0.951056516295154,1.,0.951056516295154,
1.,0.951056516295154,1.,0.951056516295154,1.,0.951056516295154,1.,0.951056516295154,
1.,0.951056516295154,1.,0.951056516295154,1.,0.951056516295154,1.,0.951056516295154,
1.,0.951056516295154,1.,0.951056516295154,1.,0.951056516295154,1.,0.951056516295154,
1.,0.951056516295154,1.,0.951056516295154,1.,0.951056516295154,1.,0.951056516295154,
1.,0.951056516295154,1.,0.951056516295154,1.,0.951056516295154,1.,0.951056516295154,
1.,0.951056516295154,1.,0.951056516295154,1.,0.951056516295154,1.,0.951056516295154,
1.,0.951056516295154,1.,0.951056516295154,1.,0.951056516295154,1.,0.951056516295154,
1.,0.951056516295154,1.,0.951056516295154,1.,0.951056516295154,1.,0.951056516295154,
1.,0.951056516295154,1.,0.951056516295154,1.,0.951056516295154,1.,0.951056516295154,
1.,0.951056516295154,1.,0.951056516295154,1.,0.951056516295154,1.,0.951056516295154,
1.,0.951056516295154,1.,0.951056516295154,1.,0.951056516295154,1.,0.951056516295154,
1.,0.951056516295154,1.,0.951056516295154,1.,0.951056516295154,1.,0.951056516295154,
1.,0.951056516295154,1.,0.951056516295154,1.,0.951056516295154,1.,0.951056516295154,
1.,0.951056516295154,1.,0.951056516295154,1.,0.951056516295154,1.,0.951056516295154,
1.,0.951056516295154,1.,0.951056516295154,1.,0.951056516295154,1.,0.951056516295154,
1.,0.951056516295154,1.,0.951056516295154,1.,0.951056516295154,1.,0.951056516295154,
1.,0.951056516295154,1.,0.951056516295154,1.,0.951056516295154,1.,0.951056516295154,
1.,0.951056516295154,1.,0.951056516295154,1.,0.951056516295154,1.,0.951056516295154,
1.,0.951056516295154,1.,0.951056516295154,1.,0.951056516295154,1.,0.951056516295154,
1.,0.951056516295154,1.,0.951056516295154,1.,0.951056516295154,1.,0.951056516295154,
1.,0.951056516295154,1.,0.951056516295154,1.,0.951056516295154,1.,0.951056516295154,
1.,0.951056516295154,1.,0.951056516295154,1.,0.951056516295154,1.,0.951056516295154,
1.,0.951056516295154,1.,0.951056516295154,1.,0.951056516295154,1.,0.951056516295154,
1.,0.951056516295154,1.,0.951056516295154,1.,0.951056516295154,1.,0.951056516295154,
1.,0.951056516295154,1.,0.951056516295154,1.,0.951056516295154,1.,0.951056516295154,
1.,0.951056516295154,1.,0.951056516295154,1.,0.951056516295154,1.,0.951056516295154,
1.,0.951056516295154,1.,0.951056516295154,1.,0.951056516295154,1.,0.951056516295154,
1.,0.951056516295154,1.,0.951056516295154,1.,0.951056516295154,1.,0.951056516295154,
1.,0.951056516295154,1.,0.951056516295154,1.,0.951056516295154,1.,0.951056516295154,
1.,0.951056516295154,1.,0.951056516295154,1.,0.951056516295154,1.,0.951056516295154,
1.,0.951056516295154,1.,0.951056516295154,1.,0.951056516295154,1.,0.951056516295154,
1.,0.951056516295154,1.,0.951056516295154,1.,0.951056516295154,1.,0.951056516295154,
1.,0.951056516295154,1.,0.951056516295154,1.,0.951056516295154,1.,0.951056516295154,
1.,0.951056516295154,1.,0.951056516295154,1.,0.951056516295154,1.,0.951056516295154,
1.,0.951056516295154,1.,0.951056516295154,1.,0.951056516295154,1.,0.951056516295154,
1.,0.951056516295154,1.,0.951056516295154,1.,0.951056516295154,1.,0.951056516295154,
1.,0.951056516295154,1.,0.951056516295154,1.,0.951056516295154,1.,0.951056516295154,
1.,0.951056516295154,1.,0.951056516295154,1.,0.951056516295154,1.,0.951056516295154,
1.,0.951056516295154,1.,0.951056516295154,1.,0.951056516295154,1.,0.951056516295154,
1.,0.951056516295154,1.,0.951056516295154,1.,0.951056516295154,1.,0.951056516295154,
1.,0.951056516295154,1.,0.951056516295154,1.,0.951056516295154,1.,0.951056516295154,
1.,0.951056516295154,1.,0.951056516295154,1.,0.951056516295154,1.,0.951056516295154,
1.,0.951056516295154,1.,0.951056516295154,1.,0.951056516295154,1.,0.951056516295154,
1.,0.951056516295154,1.,0.951056516295154,1.,0.951056516295154,1.,0.951056516295154,
1.,0.951056516295154,1.,0.951056516295154,1.,0.951056516295154,1.,0.951056516295154,
1.,0.951056516295154,1.,0.951056516295154,1.,0.951056516295154,1.,0.951056516295154,
1.,0.951056516295154,1.,0.951056516295154,1.,0.951056516295154,1.,0.951056516295154,
1.,0.951056516295154,1.,0.951056516295154,1.,0.951056516295154,1.,0.951056516295154,
1.,0.951056516295154,1.,0.951056516295154,1.,0.951056516295154,1.,0.951056516295154,
1.,0.951056516295154,1.,0.951056516295154,1.,0.951056516295154,1.,0.951056516295154,
1.,0.951056516295154,1.,0.951056516295154,1.,0.951056516295154,1.,0.951056516295154,
1.,0.951056516295154,1.,0.951056516295154,1.,0.951056516295154,1.,0.951056516295154,
1.,0.951056516295154,1.,0.951056516295154,1.,0.951056516295154,1.,0.951056516295154,
1.,0.951056516295154,1.,0.951056516295154,1.,0.951056516295154,1.,0.951056516295154,
1.,0.951056516295154,1.,0.951056516295154,1.,0.951056516295154,1.,0.951056516295154,
1.,0.951056516295154,1.,0.951056516295154,1.,0.951056516295154,1.,0.951056516295154,
1.,0.951056516295154,1.,0.951056516295154,1.,0.951056516295154,1.,0.951056516295154,
1.,0.951056516295154,1.,0.951056516295154,1.,0.951056516295154,1.,0.951056516295154,
1.,0.951056516295154,1.,0.951056516295154,1.,0.951056516295154,1.,0.951056516295154,
1.,0.951056516295154,1.,0.951056516295154,1.,0.951056516295154,1.,0.951056516295154,
1.,0.951056516295154,1.,0.951056516295154,1.,0.951056516295154,1.,0.951056516295154,
1.,0.951056516295154,1.,0.951056516295154,1.,0.951056516295154,1.,0.951056516295154,
1.,0.951056516295154,1.,0.951056516295154,1.,0.951056516295154,1.,0.951056516295154,
1.,0.951056516295154,1.,0.951056516295154,1.,0.951056516295154,1.,0.951056516295154,
1.,0.951056516295154,1.,0.951056516295154,1.,0.951056516295154,1.,0.951056516295154,
1.,0.951056516295154,1.,0.951056516295154,1.,0.951056516295154,1.,0.951056516295154,
1.,0.951056516295154,1.,0.951056516295154,1.,0.951056516295154,1.,0.951056516295154,
1.,0.951056516295154,1.,0.951056516295154,1.,0.951056516295154,1.,0.951056516295154,
1.,0.951056516295154,1.,0.951056516295154,1.,0.951056516295154,1.,0.951056516295154,
1.,0.951056516295154,1.,0.951056516295154,1.,0.951056516295154,1.,0.951056516295154,
1.,0.951056516295154,1.,0.951056516295154,1.,0.951056516295154,1.,0.951056516295154,
1.,0.951056516295154,1.,0.951056516295154,1.,0.951056516295154,1.,0.951056516295154,
1.,0.951056516295154,1.,0.951056516295154,1.,0.951056516295154,1.,0.951056516295154,
1.,0.951056516295154,1.,0.951056516295154,1.,0.951056516295154,1.,0.951056516295154,
1.,0.951056516295154,1.,0.951056516295154,1.,0.951056516295154,1.,0.951056516295154,
1.,0.951056516295154,1.,0.951056516295154,1.,0.951056516295154,1.,0.951056516295154,
1.,0.951056516295154,1.,0.951056516295154,1.,0.951056516295154,1.,0.951056516295154,
1.,0.951056516295154,1.,0.951056516295154,1.,0.951056516295154,1.,0.951056516295154,
1.,0.951056516295154,1.,0.951056516295154,1.,0.951056516295154,1.,0.951056516295154,
1.,0.951056516295154,1.,0.951056516295154,1.,0.951056516295154,1.,0.951056516295154,
1.,0.951056516295154,1.,0.951056516295154,1.,0.951056516295154,1.,0.951056516295154,
1.,0.951056516295154,1.,0.951056516295154,1.,0.951056516295154,1.,0.951056516295154,
1.,0.951056516295154,1.,0.951056516295154,1.,0.951056516295154,1.,0.951056516295154,
1.,0.951056516295154,1.,0.951056516295154,1.,0.951056516295154,1.,0.951056516295154,
1.,0.951056516295154,1.,0.951056516295154,1.,0.951056516295154,1.,0.951056516295154,
1.,0.951056516295154,1.,0.951056516295154,1.,0.951056516295154,1.,0.951056516295154,
1.,0.951056516295154,1.,0.951056516295154,1.,0.951056516295154,1.,0.951056516295154,
1.,0.951056516295154,1.,0.951056516295154,1.,0.951056516295154,1.,0.951056516295154,
1.,0.951056516295154,1.,0.951056516295154,1.,0.951056516295154,1.,0.951056516295154,
1.,0.951056516295154,1.,0.951056516295154,1.,0.951056516295154,1.,0.951056516295154,
1.,0.951056516295154,1.,0.951056516295154,1.,0.951056516295154,1.,0.951056516295154,
1.,0.951056516295154,1.,0.951056516295154,1.,0.951056516295154,1.,0.951056516295154,
1.,0.951056516295154,1.,0.951056516295154,1.,0.951056516295154,1.,0.951056516295154,
1.,0.951056516295154,1.,0.951056516295154,1.,0.951056516295154,1.,0.951056516295154,
1.,0.951056516295154,1.,0.951056516295154,1.,0.951056516295154,1.,0.951056516295154,
1.,0.951056516295154,1.,0.951056516295154,1.,0.951056516295154,1.,0.951056516295154,
1.,0.951056516295154,1.,0.951056516295154,1.,0.951056516295154,1.,0.951056516295154,
1.,0.951056516295154,1.,0.951056516295154,1.,0.951056516295154,1.,0.951056516295154,
1.,0.951056516295154,1.,0.951056516295154,1.,0.951056516295154,1.,0.951056516295154,
1.,0.951056516295154,1.,0.951056516295154,1.,0.951056516295154,1.,0.951056516295154,
1.,0.951056516295154,1.,0.951056516295154,1.,0.951056516295154,1.,0.951056516295154,
1.,0.951056516295154,1.,0.951056516295154,1.,0.951056516295154,1.,0.951056516295154,
1.,0.951056516295154,1.,0.951056516295154,1.,0.951056516295154,1.,0.951056516295154,
1.,0.951056516295154,1.,0.951056516295154,1.,0.951056516295154,1.,0.951056516295154,
1.,0.951056516295154,1.,0.951056516295154,1.,0.951056516295154,1.,0.951056516295154,
1.,0.951056516295154,1.,0.951056516295154,1.,0.951056516295154,1.,0.951056516295154,
1.,0.951056516295154,1.,0.951056516295154,1.,0.951056516295154,1.,0.951056516295154,
1.,0.951056516295154,1.,0.951056516295154,1.,0.951056516295154,1.,0.951056516295154,
1.,0.951056516295154,1.,0.951056516295154,1.,0.951056516295154,1.,0.951056516295154,
1.,0.951056516295154,1.,0.951056516295154,1.,0.951056516295154,1.,0.951056516295154,
1.,0.951056516295154,1.,0.951056516295154,1.,0.951056516295154,1.,0.951056516295154,
1.,0.951056516295154,1.,0.951056516295154,1.,0.951056516295154,1.,0.951056516295154,
1.,0.951056516295154,1.,0.951056516295154,1.,0.951056516295154,1.,0.951056516295154,
1.,0.951056516295154,1.,0.951056516295154,1.,0.951056516295154,1.,0.951056516295154,
1.,0.951056516295154,1.,0.951056516295154,1.,0.951056516295154,1.,0.951056516295154,
1.,0.951056516295154,1.,0.951056516295154,1.,0.951056516295154,1.,0.951056516295154,
1.,0.951056516295154,1.,0.951056516295154,1.,0.951056516295154,1.,0.951056516295154,
1.,0.951056516295154,1.,0.951056516295154,1.,0.951056516295154,1.,0.951056516295154,
1.,0.951056516295154,1.,0.951056516295154,1.,0.951056516295154,1.,0.951056516295154,
1.,0.951056516295154,1.,0.951056516295154,1.,0.951056516295154,1.,0.951056516295154,
1.,0.951056516295154,1.,0.951056516295154,1.,0.951056516295154,1.,0.951056516295154,
1.),(1.,0.951056516295154,1.,0.951056516295154,1.,0.951056516295154,1.,
0.951056516295154,1.,0.951056516295154,1.,0.951056516295154,1.,0.951056516295154,
1.,0.951056516295154,1.,0.951056516295154,1.,0.951056516295154,1.,0.951056516295154,
1.,0.951056516295154,1.,0.951056516295154,1.,0.951056516295154,1.,0.951056516295154,
1.,0.951056516295154,1.,0.951056516295154,1.,0.951056516295154,1.,0.951056516295154,
1.,0.951056516295154,1.,0.951056516295154,1.,0.951056516295154,1.,0.951056516295154,
1.,0.951056516295154,1.,0.951056516295154,1.,0.951056516295154,1.,0.951056516295154,
1.,0.951056516295154,1.,0.951056516295154,1.,0.951056516295154,1.,0.951056516295154,
1.,0.951056516295154,1.,0.951056516295154,1.,0.951056516295154,1.,0.951056516295154,
1.,0.951056516295154,1.,0.951056516295154,1.,0.951056516295154,1.,0.951056516295154,
1.,0.951056516295154,1.,0.951056516295154,1.,0.951056516295154,1.,0.951056516295154,
1.,0.951056516295154,1.,0.951056516295154,1.,0.951056516295154,1.,0.951056516295154,
1.,0.951056516295154,1.,0.951056516295154,1.,0.951056516295154,1.,0.951056516295154,
1.,0.951056516295154,1.,0.951056516295154,1.,0.951056516295154,1.,0.951056516295154,
1.,0.951056516295154,1.,0.951056516295154,1.,0.951056516295154,1.,0.951056516295154,
1.,0.951056516295154,1.,0.951056516295154,1.,0.951056516295154,1.,0.951056516295154,
1.,0.951056516295154,1.,0.951056516295154,1.,0.951056516295154,1.,0.951056516295154,
1.,0.951056516295154,1.,0.951056516295154,1.,0.951056516295154,1.,0.951056516295154,
1.,0.951056516295154,1.,0.951056516295154,1.,0.951056516295154,1.,0.951056516295154,
1.,0.951056516295154,1.,0.951056516295154,1.,0.951056516295154,1.,0.951056516295154,
1.,0.951056516295154,1.,0.951056516295154,1.,0.951056516295154,1.,0.951056516295154,
1.,0.951056516295154,1.,0.951056516295154,1.,0.951056516295154,1.,0.951056516295154,
1.,0.951056516295154,1.,0.951056516295154,1.,0.951056516295154,1.,0.951056516295154,
1.,0.951056516295154,1.,0.951056516295154,1.,0.951056516295154,1.,0.951056516295154,
1.,0.951056516295154,1.,0.951056516295154,1.,0.951056516295154,1.,0.951056516295154,
1.,0.951056516295154,1.,0.951056516295154,1.,0.951056516295154,1.,0.951056516295154,
1.,0.951056516295154,1.,0.951056516295154,1.,0.951056516295154,1.,0.951056516295154,
1.,0.951056516295154,1.,0.951056516295154,1.,0.951056516295154,1.,0.951056516295154,
1.,0.951056516295154,1.,0.951056516295154,1.,0.951056516295154,1.,0.951056516295154,
1.,0.951056516295154,1.,0.951056516295154,1.,0.951056516295154,1.,0.951056516295154,
1.,0.951056516295154,1.,0.951056516295154,1.,0.951056516295154,1.,0.951056516295154,
1.,0.951056516295154,1.,0.951056516295154,1.,0.951056516295154,1.,0.951056516295154,
1.,0.951056516295154,1.,0.951056516295154,1.,0.951056516295154,1.,0.951056516295154,
1.,0.951056516295154,1.,0.951056516295154,1.,0.951056516295154,1.,0.951056516295154,
1.,0.951056516295154,1.,0.951056516295154,1.,0.951056516295154,1.,0.951056516295154,
1.,0.951056516295154,1.,0.951056516295154,1.,0.951056516295154,1.,0.951056516295154,
1.,0.951056516295154,1.,0.951056516295154,1.,0.951056516295154,1.,0.951056516295154,
1.,0.951056516295154,1.,0.951056516295154,1.,0.951056516295154,1.,0.951056516295154,
1.,0.951056516295154,1.,0.951056516295154,1.,0.951056516295154,1.,0.951056516295154,
1.,0.951056516295154,1.,0.951056516295154,1.,0.951056516295154,1.,0.951056516295154,
1.,0.951056516295154,1.,0.951056516295154,1.,0.951056516295154,1.,0.951056516295154,
1.,0.951056516295154,1.,0.951056516295154,1.,0.951056516295154,1.,0.951056516295154,
1.,0.951056516295154,1.,0.951056516295154,1.,0.951056516295154,1.,0.951056516295154,
1.,0.951056516295154,1.,0.951056516295154,1.,0.951056516295154,1.,0.951056516295154,
1.,0.951056516295154,1.,0.951056516295154,1.,0.951056516295154,1.,0.951056516295154,
1.,0.951056516295154,1.,0.951056516295154,1.,0.951056516295154,1.,0.951056516295154,
1.,0.951056516295154,1.,0.951056516295154,1.,0.951056516295154,1.,0.951056516295154,
1.,0.951056516295154,1.,0.951056516295154,1.,0.951056516295154,1.,0.951056516295154,
1.,0.951056516295154,1.,0.951056516295154,1.,0.951056516295154,1.,0.951056516295154,
1.,0.951056516295154,1.,0.951056516295154,1.,0.951056516295154,1.,0.951056516295154,
1.,0.951056516295154,1.,0.951056516295154,1.,0.951056516295154,1.,0.951056516295154,
1.,0.951056516295154,1.,0.951056516295154,1.,0.951056516295154,1.,0.951056516295154,
1.,0.951056516295154,1.,0.951056516295154,1.,0.951056516295154,1.,0.951056516295154,
1.,0.951056516295154,1.,0.951056516295154,1.,0.951056516295154,1.,0.951056516295154,
1.,0.951056516295154,1.,0.951056516295154,1.,0.951056516295154,1.,0.951056516295154,
1.,0.951056516295154,1.,0.951056516295154,1.,0.951056516295154,1.,0.951056516295154,
1.,0.951056516295154,1.,0.951056516295154,1.,0.951056516295154,1.,0.951056516295154,
1.,0.951056516295154,1.,0.951056516295154,1.,0.951056516295154,1.,0.951056516295154,
1.,0.951056516295154,1.,0.951056516295154,1.,0.951056516295154,1.,0.951056516295154,
1.,0.951056516295154,1.,0.951056516295154,1.,0.951056516295154,1.,0.951056516295154,
1.,0.951056516295154,1.,0.951056516295154,1.,0.951056516295154,1.,0.951056516295154,
1.,0.951056516295154,1.,0.951056516295154,1.,0.951056516295154,1.,0.951056516295154,
1.,0.951056516295154,1.,0.951056516295154,1.,0.951056516295154,1.,0.951056516295154,
1.,0.951056516295154,1.,0.951056516295154,1.,0.951056516295154,1.,0.951056516295154,
1.,0.951056516295154,1.,0.951056516295154,1.,0.951056516295154,1.,0.951056516295154,
1.,0.951056516295154,1.,0.951056516295154,1.,0.951056516295154,1.,0.951056516295154,
1.,0.951056516295154,1.,0.951056516295154,1.,0.951056516295154,1.,0.951056516295154,
1.,0.951056516295154,1.,0.951056516295154,1.,0.951056516295154,1.,0.951056516295154,
1.,0.951056516295154,1.,0.951056516295154,1.,0.951056516295154,1.,0.951056516295154,
1.,0.951056516295154,1.,0.951056516295154,1.,0.951056516295154,1.,0.951056516295154,
1.,0.951056516295154,1.,0.951056516295154,1.,0.951056516295154,1.,0.951056516295154,
1.,0.951056516295154,1.,0.951056516295154,1.,0.951056516295154,1.,0.951056516295154,
1.,0.951056516295154,1.,0.951056516295154,1.,0.951056516295154,1.,0.951056516295154,
1.,0.951056516295154,1.,0.951056516295154,1.,0.951056516295154,1.,0.951056516295154,
1.,0.951056516295154,1.,0.951056516295154,1.,0.951056516295154,1.,0.951056516295154,
1.,0.951056516295154,1.,0.951056516295154,1.,0.951056516295154,1.,0.951056516295154,
1.,0.951056516295154,1.,0.951056516295154,1.,0.951056516295154,1.,0.951056516295154,
1.,0.951056516295154,1.,0.951056516295154,1.,0.951056516295154,1.,0.951056516295154,
1.,0.951056516295154,1.,0.951056516295154,1.,0.951056516295154,1.,0.951056516295154,
1.,0.951056516295154,1.,0.951056516295154,1.,0.951056516295154,1.,0.951056516295154,
1.,0.951056516295154,1.,0.951056516295154,1.,0.951056516295154,1.,0.951056516295154,
1.,0.951056516295154,1.,0.951056516295154,1.,0.951056516295154,1.,0.951056516295154,
1.,0.951056516295154,1.,0.951056516295154,1.,0.951056516295154,1.,0.951056516295154,
1.,0.951056516295154,1.,0.951056516295154,1.,0.951056516295154,1.,0.951056516295154,
1.,0.951056516295154,1.,0.951056516295154,1.,0.951056516295154,1.,0.951056516295154,
1.,0.951056516295154,1.,0.951056516295154,1.,0.951056516295154,1.,0.951056516295154,
1.,0.951056516295154,1.,0.951056516295154,1.,0.951056516295154,1.,0.951056516295154,
1.,0.951056516295154,1.,0.951056516295154,1.,0.951056516295154,1.,0.951056516295154,
1.,0.951056516295154,1.,0.951056516295154,1.,0.951056516295154,1.,0.951056516295154,
1.,0.951056516295154,1.,0.951056516295154,1.,0.951056516295154,1.,0.951056516295154,
1.,0.951056516295154,1.,0.951056516295154,1.,0.951056516295154,1.,0.951056516295154,
1.,0.951056516295154,1.,0.951056516295154,1.,0.951056516295154,1.,0.951056516295154,
1.,0.951056516295154,1.,0.951056516295154,1.,0.951056516295154,1.,0.951056516295154,
1.,0.951056516295154,1.,0.951056516295154,1.,0.951056516295154,1.,0.951056516295154,
1.,0.951056516295154,1.,0.951056516295154,1.,0.951056516295154,1.,0.951056516295154,
1.,0.951056516295154,1.,0.951056516295154,1.,0.951056516295154,1.,0.951056516295154,
1.,0.951056516295154,1.,0.951056516295154,1.,0.951056516295154,1.,0.951056516295154,
1.,0.951056516295154,1.,0.951056516295154,1.,0.951056516295154,1.,0.951056516295154,
1.,0.951056516295154,1.,0.951056516295154,1.,0.951056516295154,1.,0.951056516295154,
1.,0.951056516295154,1.,0.951056516295154,1.,0.951056516295154,1.,0.951056516295154,
1.,0.951056516295154,1.,0.951056516295154,1.,0.951056516295154,1.,0.951056516295154,
1.,0.951056516295154,1.,0.951056516295154,1.,0.951056516295154,1.,0.951056516295154,
1.,0.951056516295154,1.,0.951056516295154,1.,0.951056516295154,1.,0.951056516295154,
1.,0.951056516295154,1.,0.951056516295154,1.,0.951056516295154,1.,0.951056516295154,
1.,0.951056516295154,1.,0.951056516295154,1.,0.951056516295154,1.,0.951056516295154,
1.,0.951056516295154,1.,0.951056516295154,1.,0.951056516295154,1.,0.951056516295154,
1.,0.951056516295154,1.,0.951056516295154,1.,0.951056516295154,1.,0.951056516295154,
1.,0.951056516295154,1.,0.951056516295154,1.,0.951056516295154,1.,0.951056516295154,
1.,0.951056516295154,1.,0.951056516295154,1.,0.951056516295154,1.,0.951056516295154,
1.,0.951056516295154,1.,0.951056516295154,1.,0.951056516295154,1.,0.951056516295154,
1.,0.951056516295154,1.,0.951056516295154,1.,0.951056516295154,1.,0.951056516295154,
1.,0.951056516295154,1.,0.951056516295154,1.,0.951056516295154,1.,0.951056516295154,
1.,0.951056516295154,1.,0.951056516295154,1.,0.951056516295154,1.,0.951056516295154,
1.,0.951056516295154,1.,0.951056516295154,1.,0.951056516295154,1.,0.951056516295154,
1.,0.951056516295154,1.,0.951056516295154,1.,0.951056516295154,1.,0.951056516295154,
1.,0.951056516295154,1.,0.951056516295154,1.,0.951056516295154,1.,0.951056516295154,
1.,0.951056516295154,1.,0.951056516295154,1.,0.951056516295154,1.,0.951056516295154,
1.,0.951056516295154,1.,0.951056516295154,1.,0.951056516295154,1.,0.951056516295154,
1.,0.951056516295154,1.,0.951056516295154,1.,0.951056516295154,1.,0.951056516295154,
1.,0.951056516295154,1.,0.951056516295154,1.,0.951056516295154,1.,0.951056516295154,
1.,0.951056516295154,1.,0.951056516295154,1.,0.951056516295154,1.,0.951056516295154,
1.,0.951056516295154,1.,0.951056516295154,1.,0.951056516295154,1.,0.951056516295154,
1.,0.951056516295154,1.,0.951056516295154,1.,0.951056516295154,1.,0.951056516295154,
1.,0.951056516295154,1.,0.951056516295154,1.,0.951056516295154,1.,0.951056516295154,
1.,0.951056516295154,1.,0.951056516295154,1.,0.951056516295154,1.,0.951056516295154,
1.,0.951056516295154,1.,0.951056516295154,1.,0.951056516295154,1.,0.951056516295154,
1.,0.951056516295154,1.,0.951056516295154,1.,0.951056516295154,1.,0.951056516295154,
1.,0.951056516295154,1.,0.951056516295154,1.,0.951056516295154,1.,0.951056516295154,
1.,0.951056516295154,1.,0.951056516295154,1.,0.951056516295154,1.,0.951056516295154,
1.,0.951056516295154,1.,0.951056516295154,1.,0.951056516295154,1.)))
REPRESENTATION_ITEM('')
SURFACE()
);
#3198=(
BOUNDED_SURFACE()
B_SPLINE_SURFACE(1,2,((#294054,#294055,#294056,#294057,#294058,#294059,
#294060,#294061,#294062,#294063,#294064,#294065,#294066,#294067,#294068,
#294069,#294070,#294071,#294072,#294073,#294074,#294075,#294076,#294077,
#294078,#294079,#294080,#294081,#294082,#294083,#294084,#294085,#294086,
#294087,#294088,#294089,#294090,#294091,#294092,#294093,#294094,#294095,
#294096,#294097,#294098,#294099,#294100,#294101,#294102,#294103,#294104,
#294105,#294106,#294107,#294108,#294109,#294110,#294111,#294112,#294113,
#294114,#294115,#294116,#294117,#294118,#294119,#294120,#294121,#294122,
#294123,#294124,#294125,#294126,#294127,#294128,#294129,#294130,#294131,
#294132,#294133,#294134,#294135,#294136,#294137,#294138,#294139,#294140,
#294141,#294142,#294143,#294144,#294145,#294146,#294147,#294148,#294149,
#294150,#294151,#294152,#294153,#294154,#294155,#294156,#294157,#294158,
#294159,#294160,#294161,#294162,#294163,#294164,#294165,#294166,#294167,
#294168,#294169,#294170,#294171,#294172,#294173,#294174,#294175,#294176,
#294177,#294178,#294179,#294180,#294181,#294182,#294183,#294184,#294185,
#294186,#294187,#294188,#294189,#294190,#294191,#294192,#294193,#294194,
#294195,#294196,#294197,#294198,#294199,#294200,#294201,#294202,#294203,
#294204,#294205,#294206,#294207,#294208,#294209,#294210,#294211,#294212,
#294213,#294214,#294215,#294216,#294217,#294218,#294219,#294220,#294221,
#294222,#294223,#294224,#294225,#294226,#294227,#294228,#294229,#294230,
#294231,#294232,#294233,#294234,#294235,#294236,#294237,#294238,#294239,
#294240,#294241,#294242,#294243,#294244,#294245,#294246,#294247,#294248,
#294249,#294250,#294251,#294252,#294253,#294254,#294255,#294256,#294257,
#294258,#294259,#294260,#294261,#294262,#294263,#294264,#294265,#294266,
#294267,#294268,#294269,#294270,#294271,#294272,#294273,#294274,#294275,
#294276,#294277,#294278,#294279,#294280,#294281,#294282,#294283,#294284,
#294285,#294286,#294287,#294288,#294289,#294290,#294291,#294292,#294293,
#294294,#294295,#294296,#294297,#294298,#294299,#294300,#294301,#294302,
#294303,#294304,#294305,#294306,#294307,#294308,#294309,#294310,#294311,
#294312,#294313,#294314,#294315,#294316,#294317,#294318,#294319,#294320,
#294321,#294322,#294323,#294324,#294325,#294326,#294327,#294328,#294329,
#294330,#294331,#294332,#294333,#294334,#294335,#294336,#294337,#294338,
#294339,#294340,#294341,#294342,#294343,#294344,#294345,#294346,#294347,
#294348,#294349,#294350,#294351,#294352,#294353,#294354,#294355,#294356,
#294357,#294358,#294359,#294360,#294361,#294362,#294363,#294364,#294365,
#294366,#294367,#294368,#294369,#294370,#294371,#294372,#294373,#294374,
#294375,#294376,#294377,#294378,#294379,#294380,#294381,#294382,#294383,
#294384,#294385,#294386,#294387,#294388,#294389,#294390,#294391,#294392,
#294393,#294394,#294395,#294396,#294397,#294398,#294399,#294400,#294401,
#294402,#294403,#294404,#294405,#294406,#294407,#294408,#294409,#294410,
#294411,#294412,#294413,#294414,#294415,#294416,#294417,#294418,#294419,
#294420,#294421,#294422,#294423,#294424,#294425,#294426,#294427,#294428,
#294429,#294430,#294431,#294432,#294433,#294434,#294435,#294436,#294437,
#294438,#294439,#294440,#294441,#294442,#294443,#294444,#294445,#294446,
#294447,#294448,#294449,#294450,#294451,#294452,#294453,#294454,#294455,
#294456,#294457,#294458,#294459,#294460,#294461,#294462,#294463,#294464,
#294465,#294466,#294467,#294468,#294469,#294470,#294471,#294472,#294473,
#294474,#294475,#294476,#294477,#294478,#294479,#294480,#294481,#294482,
#294483,#294484,#294485,#294486,#294487,#294488,#294489,#294490,#294491,
#294492,#294493,#294494,#294495,#294496,#294497,#294498,#294499,#294500,
#294501,#294502,#294503,#294504,#294505,#294506,#294507,#294508,#294509,
#294510,#294511,#294512,#294513,#294514,#294515,#294516,#294517,#294518,
#294519,#294520,#294521,#294522,#294523,#294524,#294525,#294526,#294527,
#294528,#294529,#294530,#294531,#294532,#294533,#294534,#294535,#294536,
#294537,#294538,#294539,#294540,#294541,#294542,#294543,#294544,#294545,
#294546,#294547,#294548,#294549,#294550,#294551,#294552,#294553,#294554,
#294555,#294556,#294557,#294558,#294559,#294560,#294561,#294562,#294563,
#294564,#294565,#294566,#294567,#294568,#294569,#294570,#294571,#294572,
#294573,#294574,#294575,#294576,#294577,#294578,#294579,#294580,#294581,
#294582,#294583,#294584,#294585,#294586,#294587,#294588,#294589,#294590,
#294591,#294592,#294593,#294594,#294595,#294596,#294597,#294598,#294599,
#294600,#294601,#294602,#294603,#294604,#294605,#294606,#294607,#294608,
#294609,#294610,#294611,#294612,#294613,#294614,#294615,#294616,#294617,
#294618,#294619,#294620,#294621,#294622,#294623,#294624,#294625,#294626,
#294627,#294628,#294629,#294630,#294631,#294632,#294633,#294634,#294635,
#294636,#294637,#294638,#294639,#294640,#294641,#294642,#294643,#294644,
#294645,#294646,#294647,#294648,#294649,#294650,#294651,#294652,#294653,
#294654,#294655,#294656,#294657,#294658,#294659,#294660,#294661,#294662,
#294663,#294664,#294665,#294666,#294667,#294668,#294669,#294670,#294671,
#294672,#294673,#294674,#294675,#294676,#294677,#294678,#294679,#294680,
#294681,#294682,#294683,#294684,#294685,#294686,#294687,#294688,#294689,
#294690,#294691,#294692,#294693,#294694,#294695,#294696,#294697,#294698,
#294699,#294700,#294701,#294702,#294703,#294704,#294705,#294706,#294707,
#294708,#294709,#294710,#294711,#294712,#294713,#294714,#294715,#294716,
#294717,#294718,#294719,#294720,#294721,#294722,#294723,#294724,#294725,
#294726,#294727,#294728,#294729,#294730,#294731,#294732,#294733,#294734,
#294735,#294736,#294737,#294738,#294739,#294740,#294741,#294742,#294743,
#294744,#294745,#294746,#294747,#294748,#294749,#294750,#294751,#294752,
#294753,#294754,#294755,#294756,#294757,#294758,#294759,#294760,#294761,
#294762,#294763,#294764,#294765,#294766,#294767,#294768,#294769,#294770,
#294771,#294772,#294773,#294774,#294775,#294776,#294777,#294778,#294779,
#294780,#294781,#294782,#294783,#294784,#294785,#294786,#294787,#294788,
#294789,#294790,#294791,#294792,#294793,#294794,#294795,#294796,#294797,
#294798,#294799,#294800,#294801,#294802,#294803,#294804,#294805,#294806,
#294807,#294808,#294809,#294810,#294811,#294812,#294813,#294814,#294815,
#294816,#294817,#294818,#294819,#294820,#294821,#294822,#294823,#294824,
#294825,#294826,#294827,#294828,#294829,#294830,#294831,#294832,#294833,
#294834,#294835,#294836,#294837,#294838,#294839,#294840,#294841,#294842,
#294843,#294844,#294845,#294846,#294847,#294848,#294849,#294850,#294851,
#294852,#294853,#294854,#294855,#294856,#294857,#294858,#294859,#294860,
#294861,#294862,#294863,#294864,#294865,#294866,#294867,#294868,#294869,
#294870,#294871,#294872,#294873,#294874,#294875,#294876,#294877,#294878,
#294879,#294880,#294881,#294882,#294883,#294884,#294885,#294886,#294887,
#294888,#294889,#294890,#294891,#294892,#294893,#294894,#294895,#294896,
#294897,#294898,#294899,#294900,#294901,#294902,#294903,#294904,#294905,
#294906,#294907,#294908,#294909,#294910,#294911,#294912,#294913,#294914,
#294915,#294916,#294917,#294918,#294919,#294920,#294921,#294922,#294923,
#294924,#294925,#294926,#294927,#294928,#294929,#294930,#294931,#294932,
#294933,#294934,#294935,#294936,#294937,#294938,#294939,#294940,#294941,
#294942,#294943,#294944,#294945,#294946,#294947,#294948,#294949,#294950,
#294951,#294952,#294953,#294954,#294955,#294956,#294957,#294958,#294959,
#294960,#294961,#294962,#294963,#294964,#294965,#294966,#294967,#294968,
#294969,#294970,#294971,#294972,#294973,#294974,#294975,#294976,#294977,
#294978,#294979,#294980,#294981,#294982,#294983,#294984,#294985,#294986,
#294987,#294988,#294989,#294990,#294991,#294992,#294993,#294994,#294995,
#294996,#294997,#294998,#294999,#295000,#295001,#295002,#295003,#295004,
#295005,#295006,#295007,#295008,#295009,#295010,#295011,#295012,#295013,
#295014,#295015,#295016,#295017,#295018,#295019,#295020,#295021,#295022,
#295023,#295024,#295025,#295026,#295027,#295028,#295029,#295030,#295031,
#295032,#295033,#295034,#295035,#295036,#295037,#295038,#295039,#295040,
#295041,#295042,#295043,#295044,#295045,#295046,#295047,#295048,#295049,
#295050,#295051,#295052,#295053,#295054,#295055,#295056,#295057,#295058,
#295059,#295060,#295061,#295062,#295063,#295064,#295065,#295066,#295067,
#295068,#295069,#295070,#295071,#295072,#295073,#295074,#295075,#295076,
#295077,#295078,#295079,#295080,#295081,#295082,#295083,#295084,#295085,
#295086,#295087,#295088,#295089,#295090),(#295091,#295092,#295093,#295094,
#295095,#295096,#295097,#295098,#295099,#295100,#295101,#295102,#295103,
#295104,#295105,#295106,#295107,#295108,#295109,#295110,#295111,#295112,
#295113,#295114,#295115,#295116,#295117,#295118,#295119,#295120,#295121,
#295122,#295123,#295124,#295125,#295126,#295127,#295128,#295129,#295130,
#295131,#295132,#295133,#295134,#295135,#295136,#295137,#295138,#295139,
#295140,#295141,#295142,#295143,#295144,#295145,#295146,#295147,#295148,
#295149,#295150,#295151,#295152,#295153,#295154,#295155,#295156,#295157,
#295158,#295159,#295160,#295161,#295162,#295163,#295164,#295165,#295166,
#295167,#295168,#295169,#295170,#295171,#295172,#295173,#295174,#295175,
#295176,#295177,#295178,#295179,#295180,#295181,#295182,#295183,#295184,
#295185,#295186,#295187,#295188,#295189,#295190,#295191,#295192,#295193,
#295194,#295195,#295196,#295197,#295198,#295199,#295200,#295201,#295202,
#295203,#295204,#295205,#295206,#295207,#295208,#295209,#295210,#295211,
#295212,#295213,#295214,#295215,#295216,#295217,#295218,#295219,#295220,
#295221,#295222,#295223,#295224,#295225,#295226,#295227,#295228,#295229,
#295230,#295231,#295232,#295233,#295234,#295235,#295236,#295237,#295238,
#295239,#295240,#295241,#295242,#295243,#295244,#295245,#295246,#295247,
#295248,#295249,#295250,#295251,#295252,#295253,#295254,#295255,#295256,
#295257,#295258,#295259,#295260,#295261,#295262,#295263,#295264,#295265,
#295266,#295267,#295268,#295269,#295270,#295271,#295272,#295273,#295274,
#295275,#295276,#295277,#295278,#295279,#295280,#295281,#295282,#295283,
#295284,#295285,#295286,#295287,#295288,#295289,#295290,#295291,#295292,
#295293,#295294,#295295,#295296,#295297,#295298,#295299,#295300,#295301,
#295302,#295303,#295304,#295305,#295306,#295307,#295308,#295309,#295310,
#295311,#295312,#295313,#295314,#295315,#295316,#295317,#295318,#295319,
#295320,#295321,#295322,#295323,#295324,#295325,#295326,#295327,#295328,
#295329,#295330,#295331,#295332,#295333,#295334,#295335,#295336,#295337,
#295338,#295339,#295340,#295341,#295342,#295343,#295344,#295345,#295346,
#295347,#295348,#295349,#295350,#295351,#295352,#295353,#295354,#295355,
#295356,#295357,#295358,#295359,#295360,#295361,#295362,#295363,#295364,
#295365,#295366,#295367,#295368,#295369,#295370,#295371,#295372,#295373,
#295374,#295375,#295376,#295377,#295378,#295379,#295380,#295381,#295382,
#295383,#295384,#295385,#295386,#295387,#295388,#295389,#295390,#295391,
#295392,#295393,#295394,#295395,#295396,#295397,#295398,#295399,#295400,
#295401,#295402,#295403,#295404,#295405,#295406,#295407,#295408,#295409,
#295410,#295411,#295412,#295413,#295414,#295415,#295416,#295417,#295418,
#295419,#295420,#295421,#295422,#295423,#295424,#295425,#295426,#295427,
#295428,#295429,#295430,#295431,#295432,#295433,#295434,#295435,#295436,
#295437,#295438,#295439,#295440,#295441,#295442,#295443,#295444,#295445,
#295446,#295447,#295448,#295449,#295450,#295451,#295452,#295453,#295454,
#295455,#295456,#295457,#295458,#295459,#295460,#295461,#295462,#295463,
#295464,#295465,#295466,#295467,#295468,#295469,#295470,#295471,#295472,
#295473,#295474,#295475,#295476,#295477,#295478,#295479,#295480,#295481,
#295482,#295483,#295484,#295485,#295486,#295487,#295488,#295489,#295490,
#295491,#295492,#295493,#295494,#295495,#295496,#295497,#295498,#295499,
#295500,#295501,#295502,#295503,#295504,#295505,#295506,#295507,#295508,
#295509,#295510,#295511,#295512,#295513,#295514,#295515,#295516,#295517,
#295518,#295519,#295520,#295521,#295522,#295523,#295524,#295525,#295526,
#295527,#295528,#295529,#295530,#295531,#295532,#295533,#295534,#295535,
#295536,#295537,#295538,#295539,#295540,#295541,#295542,#295543,#295544,
#295545,#295546,#295547,#295548,#295549,#295550,#295551,#295552,#295553,
#295554,#295555,#295556,#295557,#295558,#295559,#295560,#295561,#295562,
#295563,#295564,#295565,#295566,#295567,#295568,#295569,#295570,#295571,
#295572,#295573,#295574,#295575,#295576,#295577,#295578,#295579,#295580,
#295581,#295582,#295583,#295584,#295585,#295586,#295587,#295588,#295589,
#295590,#295591,#295592,#295593,#295594,#295595,#295596,#295597,#295598,
#295599,#295600,#295601,#295602,#295603,#295604,#295605,#295606,#295607,
#295608,#295609,#295610,#295611,#295612,#295613,#295614,#295615,#295616,
#295617,#295618,#295619,#295620,#295621,#295622,#295623,#295624,#295625,
#295626,#295627,#295628,#295629,#295630,#295631,#295632,#295633,#295634,
#295635,#295636,#295637,#295638,#295639,#295640,#295641,#295642,#295643,
#295644,#295645,#295646,#295647,#295648,#295649,#295650,#295651,#295652,
#295653,#295654,#295655,#295656,#295657,#295658,#295659,#295660,#295661,
#295662,#295663,#295664,#295665,#295666,#295667,#295668,#295669,#295670,
#295671,#295672,#295673,#295674,#295675,#295676,#295677,#295678,#295679,
#295680,#295681,#295682,#295683,#295684,#295685,#295686,#295687,#295688,
#295689,#295690,#295691,#295692,#295693,#295694,#295695,#295696,#295697,
#295698,#295699,#295700,#295701,#295702,#295703,#295704,#295705,#295706,
#295707,#295708,#295709,#295710,#295711,#295712,#295713,#295714,#295715,
#295716,#295717,#295718,#295719,#295720,#295721,#295722,#295723,#295724,
#295725,#295726,#295727,#295728,#295729,#295730,#295731,#295732,#295733,
#295734,#295735,#295736,#295737,#295738,#295739,#295740,#295741,#295742,
#295743,#295744,#295745,#295746,#295747,#295748,#295749,#295750,#295751,
#295752,#295753,#295754,#295755,#295756,#295757,#295758,#295759,#295760,
#295761,#295762,#295763,#295764,#295765,#295766,#295767,#295768,#295769,
#295770,#295771,#295772,#295773,#295774,#295775,#295776,#295777,#295778,
#295779,#295780,#295781,#295782,#295783,#295784,#295785,#295786,#295787,
#295788,#295789,#295790,#295791,#295792,#295793,#295794,#295795,#295796,
#295797,#295798,#295799,#295800,#295801,#295802,#295803,#295804,#295805,
#295806,#295807,#295808,#295809,#295810,#295811,#295812,#295813,#295814,
#295815,#295816,#295817,#295818,#295819,#295820,#295821,#295822,#295823,
#295824,#295825,#295826,#295827,#295828,#295829,#295830,#295831,#295832,
#295833,#295834,#295835,#295836,#295837,#295838,#295839,#295840,#295841,
#295842,#295843,#295844,#295845,#295846,#295847,#295848,#295849,#295850,
#295851,#295852,#295853,#295854,#295855,#295856,#295857,#295858,#295859,
#295860,#295861,#295862,#295863,#295864,#295865,#295866,#295867,#295868,
#295869,#295870,#295871,#295872,#295873,#295874,#295875,#295876,#295877,
#295878,#295879,#295880,#295881,#295882,#295883,#295884,#295885,#295886,
#295887,#295888,#295889,#295890,#295891,#295892,#295893,#295894,#295895,
#295896,#295897,#295898,#295899,#295900,#295901,#295902,#295903,#295904,
#295905,#295906,#295907,#295908,#295909,#295910,#295911,#295912,#295913,
#295914,#295915,#295916,#295917,#295918,#295919,#295920,#295921,#295922,
#295923,#295924,#295925,#295926,#295927,#295928,#295929,#295930,#295931,
#295932,#295933,#295934,#295935,#295936,#295937,#295938,#295939,#295940,
#295941,#295942,#295943,#295944,#295945,#295946,#295947,#295948,#295949,
#295950,#295951,#295952,#295953,#295954,#295955,#295956,#295957,#295958,
#295959,#295960,#295961,#295962,#295963,#295964,#295965,#295966,#295967,
#295968,#295969,#295970,#295971,#295972,#295973,#295974,#295975,#295976,
#295977,#295978,#295979,#295980,#295981,#295982,#295983,#295984,#295985,
#295986,#295987,#295988,#295989,#295990,#295991,#295992,#295993,#295994,
#295995,#295996,#295997,#295998,#295999,#296000,#296001,#296002,#296003,
#296004,#296005,#296006,#296007,#296008,#296009,#296010,#296011,#296012,
#296013,#296014,#296015,#296016,#296017,#296018,#296019,#296020,#296021,
#296022,#296023,#296024,#296025,#296026,#296027,#296028,#296029,#296030,
#296031,#296032,#296033,#296034,#296035,#296036,#296037,#296038,#296039,
#296040,#296041,#296042,#296043,#296044,#296045,#296046,#296047,#296048,
#296049,#296050,#296051,#296052,#296053,#296054,#296055,#296056,#296057,
#296058,#296059,#296060,#296061,#296062,#296063,#296064,#296065,#296066,
#296067,#296068,#296069,#296070,#296071,#296072,#296073,#296074,#296075,
#296076,#296077,#296078,#296079,#296080,#296081,#296082,#296083,#296084,
#296085,#296086,#296087,#296088,#296089,#296090,#296091,#296092,#296093,
#296094,#296095,#296096,#296097,#296098,#296099,#296100,#296101,#296102,
#296103,#296104,#296105,#296106,#296107,#296108,#296109,#296110,#296111,
#296112,#296113,#296114,#296115,#296116,#296117,#296118,#296119,#296120,
#296121,#296122,#296123,#296124,#296125,#296126,#296127)),.UNSPECIFIED.,
 .F.,.F.,.F.)
B_SPLINE_SURFACE_WITH_KNOTS((2,2),(3,2,2,2,2,2,2,2,2,2,2,2,2,2,2,2,2,2,
2,2,2,2,2,2,2,2,2,2,2,2,2,2,2,2,2,2,2,2,2,2,2,2,2,2,2,2,2,2,2,2,2,2,2,2,
2,2,2,2,2,2,2,2,2,2,2,2,2,2,2,2,2,2,2,2,2,2,2,2,2,2,2,2,2,2,2,2,2,2,2,2,
2,2,2,2,2,2,2,2,2,2,2,2,2,2,2,2,2,2,2,2,2,2,2,2,2,2,2,2,2,2,2,2,2,2,2,2,
2,2,2,2,2,2,2,2,2,2,2,2,2,2,2,2,2,2,2,2,2,2,2,2,2,2,2,2,2,2,2,2,2,2,2,2,
2,2,2,2,2,2,2,2,2,2,2,2,2,2,2,2,2,2,2,2,2,2,2,2,2,2,2,2,2,2,2,2,2,2,2,2,
2,2,2,2,2,2,2,2,2,2,2,2,2,2,2,2,2,2,2,2,2,2,2,2,2,2,2,2,2,2,2,2,2,2,2,2,
2,2,2,2,2,2,2,2,2,2,2,2,2,2,2,2,2,2,2,2,2,2,2,2,2,2,2,2,2,2,2,2,2,2,2,2,
2,2,2,2,2,2,2,2,2,2,2,2,2,2,2,2,2,2,2,2,2,2,2,2,2,2,2,2,2,2,2,2,2,2,2,2,
2,2,2,2,2,2,2,2,2,2,2,2,2,2,2,2,2,2,2,2,2,2,2,2,2,2,2,2,2,2,2,2,2,2,2,2,
2,2,2,2,2,2,2,2,2,2,2,2,2,2,2,2,2,2,2,2,2,2,2,2,2,2,2,2,2,2,2,2,2,2,2,2,
2,2,2,2,2,2,2,2,2,2,2,2,2,2,2,2,2,2,2,2,2,2,2,2,2,2,2,2,2,2,2,2,2,2,2,2,
2,2,2,2,2,2,2,2,2,2,2,2,2,2,2,2,2,2,2,2,2,2,2,2,2,2,2,2,2,2,2,2,2,2,2,2,
2,2,2,2,2,2,2,2,2,2,2,2,2,2,2,2,2,2,2,2,2,2,2,2,2,2,2,2,2,2,2,2,2,2,2,2,
2,2,2,2,2,2,2,2,2,2,2,2,2,2,2,2,2,2,2,2,2,2,2,2,2,2,2,2,2,2,2,2,3),(0.,
1.),(0.,0.00192307692307692,0.00384615384615385,0.00576923076923077,0.00769230769230769,
0.00961538461538462,0.0115384615384615,0.0134615384615385,0.0153846153846154,
0.0173076923076923,0.0192307692307692,0.0211538461538462,0.0230769230769231,
0.025,0.0269230769230769,0.0288461538461538,0.0307692307692308,0.0326923076923077,
0.0346153846153846,0.0365384615384615,0.0384615384615385,0.0403846153846154,
0.0423076923076923,0.0442307692307692,0.0461538461538462,0.0480769230769231,
0.05,0.0519230769230769,0.0538461538461538,0.0557692307692308,0.0576923076923077,
0.0596153846153846,0.0615384615384615,0.0634615384615385,0.0653846153846154,
0.0673076923076923,0.0692307692307692,0.0711538461538462,0.0730769230769231,
0.075,0.0769230769230769,0.0788461538461538,0.0807692307692308,0.0826923076923077,
0.0846153846153846,0.0865384615384615,0.0884615384615385,0.0903846153846154,
0.0923076923076923,0.0942307692307692,0.0961538461538462,0.0980769230769231,
0.1,0.101923076923077,0.103846153846154,0.105769230769231,0.107692307692308,
0.109615384615385,0.111538461538462,0.113461538461538,0.115384615384615,
0.117307692307692,0.119230769230769,0.121153846153846,0.123076923076923,
0.125,0.126923076923077,0.128846153846154,0.130769230769231,0.132692307692308,
0.134615384615385,0.136538461538462,0.138461538461538,0.140384615384615,
0.142307692307692,0.144230769230769,0.146153846153846,0.148076923076923,
0.15,0.151923076923077,0.153846153846154,0.155769230769231,0.157692307692308,
0.159615384615385,0.161538461538462,0.163461538461538,0.165384615384615,
0.167307692307692,0.169230769230769,0.171153846153846,0.173076923076923,
0.175,0.176923076923077,0.178846153846154,0.180769230769231,0.182692307692308,
0.184615384615385,0.186538461538462,0.188461538461538,0.190384615384615,
0.192307692307692,0.194230769230769,0.196153846153846,0.198076923076923,
0.2,0.201923076923077,0.203846153846154,0.205769230769231,0.207692307692308,
0.209615384615385,0.211538461538462,0.213461538461538,0.215384615384615,
0.217307692307692,0.219230769230769,0.221153846153846,0.223076923076923,
0.225,0.226923076923077,0.228846153846154,0.230769230769231,0.232692307692308,
0.234615384615385,0.236538461538462,0.238461538461538,0.240384615384615,
0.242307692307692,0.244230769230769,0.246153846153846,0.248076923076923,
0.25,0.251923076923077,0.253846153846154,0.255769230769231,0.257692307692308,
0.259615384615385,0.261538461538462,0.263461538461538,0.265384615384615,
0.267307692307692,0.269230769230769,0.271153846153846,0.273076923076923,
0.275,0.276923076923077,0.278846153846154,0.280769230769231,0.282692307692308,
0.284615384615385,0.286538461538462,0.288461538461538,0.290384615384615,
0.292307692307692,0.294230769230769,0.296153846153846,0.298076923076923,
0.3,0.301923076923077,0.303846153846154,0.305769230769231,0.307692307692308,
0.309615384615385,0.311538461538462,0.313461538461538,0.315384615384615,
0.317307692307692,0.319230769230769,0.321153846153846,0.323076923076923,
0.325,0.326923076923077,0.328846153846154,0.330769230769231,0.332692307692308,
0.334615384615385,0.336538461538462,0.338461538461538,0.340384615384615,
0.342307692307692,0.344230769230769,0.346153846153846,0.348076923076923,
0.35,0.351923076923077,0.353846153846154,0.355769230769231,0.357692307692308,
0.359615384615385,0.361538461538462,0.363461538461538,0.365384615384615,
0.367307692307692,0.369230769230769,0.371153846153846,0.373076923076923,
0.375,0.376923076923077,0.378846153846154,0.380769230769231,0.382692307692308,
0.384615384615385,0.386538461538462,0.388461538461538,0.390384615384615,
0.392307692307692,0.394230769230769,0.396153846153846,0.398076923076923,
0.4,0.401923076923077,0.403846153846154,0.405769230769231,0.407692307692308,
0.409615384615385,0.411538461538462,0.413461538461538,0.415384615384615,
0.417307692307692,0.419230769230769,0.421153846153846,0.423076923076923,
0.425,0.426923076923077,0.428846153846154,0.430769230769231,0.432692307692308,
0.434615384615385,0.436538461538462,0.438461538461538,0.440384615384615,
0.442307692307692,0.444230769230769,0.446153846153846,0.448076923076923,
0.45,0.451923076923077,0.453846153846154,0.455769230769231,0.457692307692308,
0.459615384615385,0.461538461538462,0.463461538461538,0.465384615384615,
0.467307692307692,0.469230769230769,0.471153846153846,0.473076923076923,
0.475,0.476923076923077,0.478846153846154,0.480769230769231,0.482692307692308,
0.484615384615385,0.486538461538462,0.488461538461538,0.490384615384615,
0.492307692307692,0.494230769230769,0.496153846153846,0.498076923076923,
0.5,0.501923076923077,0.503846153846154,0.505769230769231,0.507692307692308,
0.509615384615385,0.511538461538461,0.513461538461538,0.515384615384615,
0.517307692307692,0.519230769230769,0.521153846153846,0.523076923076923,
0.525,0.526923076923077,0.528846153846154,0.530769230769231,0.532692307692308,
0.534615384615385,0.536538461538462,0.538461538461538,0.540384615384615,
0.542307692307692,0.544230769230769,0.546153846153846,0.548076923076923,
0.55,0.551923076923077,0.553846153846154,0.555769230769231,0.557692307692308,
0.559615384615385,0.561538461538462,0.563461538461538,0.565384615384615,
0.567307692307692,0.569230769230769,0.571153846153846,0.573076923076923,
0.575,0.576923076923077,0.578846153846154,0.580769230769231,0.582692307692308,
0.584615384615385,0.586538461538462,0.588461538461538,0.590384615384615,
0.592307692307692,0.594230769230769,0.596153846153846,0.598076923076923,
0.6,0.601923076923077,0.603846153846154,0.605769230769231,0.607692307692308,
0.609615384615385,0.611538461538462,0.613461538461539,0.615384615384615,
0.617307692307692,0.619230769230769,0.621153846153846,0.623076923076923,
0.625,0.626923076923077,0.628846153846154,0.630769230769231,0.632692307692308,
0.634615384615385,0.636538461538461,0.638461538461538,0.640384615384615,
0.642307692307692,0.644230769230769,0.646153846153846,0.648076923076923,
0.65,0.651923076923077,0.653846153846154,0.655769230769231,0.657692307692308,
0.659615384615385,0.661538461538462,0.663461538461538,0.665384615384615,
0.667307692307692,0.669230769230769,0.671153846153846,0.673076923076923,
0.675,0.676923076923077,0.678846153846154,0.680769230769231,0.682692307692308,
0.684615384615385,0.686538461538462,0.688461538461538,0.690384615384615,
0.692307692307692,0.694230769230769,0.696153846153846,0.698076923076923,
0.7,0.701923076923077,0.703846153846154,0.705769230769231,0.707692307692308,
0.709615384615385,0.711538461538462,0.713461538461538,0.715384615384615,
0.717307692307692,0.719230769230769,0.721153846153846,0.723076923076923,
0.725,0.726923076923077,0.728846153846154,0.730769230769231,0.732692307692308,
0.734615384615385,0.736538461538462,0.738461538461539,0.740384615384615,
0.742307692307692,0.744230769230769,0.746153846153846,0.748076923076923,
0.75,0.751923076923077,0.753846153846154,0.755769230769231,0.757692307692308,
0.759615384615385,0.761538461538461,0.763461538461538,0.765384615384615,
0.767307692307692,0.769230769230769,0.771153846153846,0.773076923076923,
0.775,0.776923076923077,0.778846153846154,0.780769230769231,0.782692307692308,
0.784615384615385,0.786538461538462,0.788461538461538,0.790384615384615,
0.792307692307692,0.794230769230769,0.796153846153846,0.798076923076923,
0.8,0.801923076923077,0.803846153846154,0.805769230769231,0.807692307692308,
0.809615384615385,0.811538461538462,0.813461538461538,0.815384615384615,
0.817307692307692,0.819230769230769,0.821153846153846,0.823076923076923,
0.825,0.826923076923077,0.828846153846154,0.830769230769231,0.832692307692308,
0.834615384615385,0.836538461538462,0.838461538461538,0.840384615384615,
0.842307692307692,0.844230769230769,0.846153846153846,0.848076923076923,
0.85,0.851923076923077,0.853846153846154,0.855769230769231,0.857692307692308,
0.859615384615385,0.861538461538462,0.863461538461539,0.865384615384615,
0.867307692307692,0.869230769230769,0.871153846153846,0.873076923076923,
0.875,0.876923076923077,0.878846153846154,0.880769230769231,0.882692307692308,
0.884615384615385,0.886538461538461,0.888461538461538,0.890384615384615,
0.892307692307692,0.894230769230769,0.896153846153846,0.898076923076923,
0.9,0.901923076923077,0.903846153846154,0.905769230769231,0.907692307692308,
0.909615384615385,0.911538461538462,0.913461538461538,0.915384615384615,
0.917307692307692,0.919230769230769,0.921153846153846,0.923076923076923,
0.925,0.926923076923077,0.928846153846154,0.930769230769231,0.932692307692308,
0.934615384615385,0.936538461538462,0.938461538461538,0.940384615384615,
0.942307692307692,0.944230769230769,0.946153846153846,0.948076923076923,
0.95,0.951923076923077,0.953846153846154,0.955769230769231,0.957692307692308,
0.959615384615385,0.961538461538462,0.963461538461538,0.965384615384615,
0.967307692307692,0.969230769230769,0.971153846153846,0.973076923076923,
0.975,0.976923076923077,0.978846153846154,0.980769230769231,0.982692307692308,
0.984615384615385,0.986538461538462,0.988461538461539,0.990384615384615,
0.992307692307692,0.994230769230769,0.996153846153846),.UNSPECIFIED.)
GEOMETRIC_REPRESENTATION_ITEM()
RATIONAL_B_SPLINE_SURFACE(((1.,0.951056516295154,1.,0.951056516295154,1.,
0.951056516295154,1.,0.951056516295154,1.,0.951056516295154,1.,0.951056516295154,
1.,0.951056516295154,1.,0.951056516295154,1.,0.951056516295154,1.,0.951056516295154,
1.,0.951056516295154,1.,0.951056516295154,1.,0.951056516295154,1.,0.951056516295154,
1.,0.951056516295154,1.,0.951056516295154,1.,0.951056516295154,1.,0.951056516295154,
1.,0.951056516295154,1.,0.951056516295154,1.,0.951056516295154,1.,0.951056516295154,
1.,0.951056516295154,1.,0.951056516295154,1.,0.951056516295154,1.,0.951056516295154,
1.,0.951056516295154,1.,0.951056516295154,1.,0.951056516295154,1.,0.951056516295154,
1.,0.951056516295154,1.,0.951056516295154,1.,0.951056516295154,1.,0.951056516295154,
1.,0.951056516295154,1.,0.951056516295154,1.,0.951056516295154,1.,0.951056516295154,
1.,0.951056516295154,1.,0.951056516295154,1.,0.951056516295154,1.,0.951056516295154,
1.,0.951056516295154,1.,0.951056516295154,1.,0.951056516295154,1.,0.951056516295154,
1.,0.951056516295154,1.,0.951056516295154,1.,0.951056516295154,1.,0.951056516295154,
1.,0.951056516295154,1.,0.951056516295154,1.,0.951056516295154,1.,0.951056516295154,
1.,0.951056516295154,1.,0.951056516295154,1.,0.951056516295154,1.,0.951056516295154,
1.,0.951056516295154,1.,0.951056516295154,1.,0.951056516295154,1.,0.951056516295154,
1.,0.951056516295154,1.,0.951056516295154,1.,0.951056516295154,1.,0.951056516295154,
1.,0.951056516295154,1.,0.951056516295154,1.,0.951056516295154,1.,0.951056516295154,
1.,0.951056516295154,1.,0.951056516295154,1.,0.951056516295154,1.,0.951056516295154,
1.,0.951056516295154,1.,0.951056516295154,1.,0.951056516295154,1.,0.951056516295154,
1.,0.951056516295154,1.,0.951056516295154,1.,0.951056516295154,1.,0.951056516295154,
1.,0.951056516295154,1.,0.951056516295154,1.,0.951056516295154,1.,0.951056516295154,
1.,0.951056516295154,1.,0.951056516295154,1.,0.951056516295154,1.,0.951056516295154,
1.,0.951056516295154,1.,0.951056516295154,1.,0.951056516295154,1.,0.951056516295154,
1.,0.951056516295154,1.,0.951056516295154,1.,0.951056516295154,1.,0.951056516295154,
1.,0.951056516295154,1.,0.951056516295154,1.,0.951056516295154,1.,0.951056516295154,
1.,0.951056516295154,1.,0.951056516295154,1.,0.951056516295154,1.,0.951056516295154,
1.,0.951056516295154,1.,0.951056516295154,1.,0.951056516295154,1.,0.951056516295154,
1.,0.951056516295154,1.,0.951056516295154,1.,0.951056516295154,1.,0.951056516295154,
1.,0.951056516295154,1.,0.951056516295154,1.,0.951056516295154,1.,0.951056516295154,
1.,0.951056516295154,1.,0.951056516295154,1.,0.951056516295154,1.,0.951056516295154,
1.,0.951056516295154,1.,0.951056516295154,1.,0.951056516295154,1.,0.951056516295154,
1.,0.951056516295154,1.,0.951056516295154,1.,0.951056516295154,1.,0.951056516295154,
1.,0.951056516295154,1.,0.951056516295154,1.,0.951056516295154,1.,0.951056516295154,
1.,0.951056516295154,1.,0.951056516295154,1.,0.951056516295154,1.,0.951056516295154,
1.,0.951056516295154,1.,0.951056516295154,1.,0.951056516295154,1.,0.951056516295154,
1.,0.951056516295154,1.,0.951056516295154,1.,0.951056516295154,1.,0.951056516295154,
1.,0.951056516295154,1.,0.951056516295154,1.,0.951056516295154,1.,0.951056516295154,
1.,0.951056516295154,1.,0.951056516295154,1.,0.951056516295154,1.,0.951056516295154,
1.,0.951056516295154,1.,0.951056516295154,1.,0.951056516295154,1.,0.951056516295154,
1.,0.951056516295154,1.,0.951056516295154,1.,0.951056516295154,1.,0.951056516295154,
1.,0.951056516295154,1.,0.951056516295154,1.,0.951056516295154,1.,0.951056516295154,
1.,0.951056516295154,1.,0.951056516295154,1.,0.951056516295154,1.,0.951056516295154,
1.,0.951056516295154,1.,0.951056516295154,1.,0.951056516295154,1.,0.951056516295154,
1.,0.951056516295154,1.,0.951056516295154,1.,0.951056516295154,1.,0.951056516295154,
1.,0.951056516295154,1.,0.951056516295154,1.,0.951056516295154,1.,0.951056516295154,
1.,0.951056516295154,1.,0.951056516295154,1.,0.951056516295154,1.,0.951056516295154,
1.,0.951056516295154,1.,0.951056516295154,1.,0.951056516295154,1.,0.951056516295154,
1.,0.951056516295154,1.,0.951056516295154,1.,0.951056516295154,1.,0.951056516295154,
1.,0.951056516295154,1.,0.951056516295154,1.,0.951056516295154,1.,0.951056516295154,
1.,0.951056516295154,1.,0.951056516295154,1.,0.951056516295154,1.,0.951056516295154,
1.,0.951056516295154,1.,0.951056516295154,1.,0.951056516295154,1.,0.951056516295154,
1.,0.951056516295154,1.,0.951056516295154,1.,0.951056516295154,1.,0.951056516295154,
1.,0.951056516295154,1.,0.951056516295154,1.,0.951056516295154,1.,0.951056516295154,
1.,0.951056516295154,1.,0.951056516295154,1.,0.951056516295154,1.,0.951056516295154,
1.,0.951056516295154,1.,0.951056516295154,1.,0.951056516295154,1.,0.951056516295154,
1.,0.951056516295154,1.,0.951056516295154,1.,0.951056516295154,1.,0.951056516295154,
1.,0.951056516295154,1.,0.951056516295154,1.,0.951056516295154,1.,0.951056516295154,
1.,0.951056516295154,1.,0.951056516295154,1.,0.951056516295154,1.,0.951056516295154,
1.,0.951056516295154,1.,0.951056516295154,1.,0.951056516295154,1.,0.951056516295154,
1.,0.951056516295154,1.,0.951056516295154,1.,0.951056516295154,1.,0.951056516295154,
1.,0.951056516295154,1.,0.951056516295154,1.,0.951056516295154,1.,0.951056516295154,
1.,0.951056516295154,1.,0.951056516295154,1.,0.951056516295154,1.,0.951056516295154,
1.,0.951056516295154,1.,0.951056516295154,1.,0.951056516295154,1.,0.951056516295154,
1.,0.951056516295154,1.,0.951056516295154,1.,0.951056516295154,1.,0.951056516295154,
1.,0.951056516295154,1.,0.951056516295154,1.,0.951056516295154,1.,0.951056516295154,
1.,0.951056516295154,1.,0.951056516295154,1.,0.951056516295154,1.,0.951056516295154,
1.,0.951056516295154,1.,0.951056516295154,1.,0.951056516295154,1.,0.951056516295154,
1.,0.951056516295154,1.,0.951056516295154,1.,0.951056516295154,1.,0.951056516295154,
1.,0.951056516295154,1.,0.951056516295154,1.,0.951056516295154,1.,0.951056516295154,
1.,0.951056516295154,1.,0.951056516295154,1.,0.951056516295154,1.,0.951056516295154,
1.,0.951056516295154,1.,0.951056516295154,1.,0.951056516295154,1.,0.951056516295154,
1.,0.951056516295154,1.,0.951056516295154,1.,0.951056516295154,1.,0.951056516295154,
1.,0.951056516295154,1.,0.951056516295154,1.,0.951056516295154,1.,0.951056516295154,
1.,0.951056516295154,1.,0.951056516295154,1.,0.951056516295154,1.,0.951056516295154,
1.,0.951056516295154,1.,0.951056516295154,1.,0.951056516295154,1.,0.951056516295154,
1.,0.951056516295154,1.,0.951056516295154,1.,0.951056516295154,1.,0.951056516295154,
1.,0.951056516295154,1.,0.951056516295154,1.,0.951056516295154,1.,0.951056516295154,
1.,0.951056516295154,1.,0.951056516295154,1.,0.951056516295154,1.,0.951056516295154,
1.,0.951056516295154,1.,0.951056516295154,1.,0.951056516295154,1.,0.951056516295154,
1.,0.951056516295154,1.,0.951056516295154,1.,0.951056516295154,1.,0.951056516295154,
1.,0.951056516295154,1.,0.951056516295154,1.,0.951056516295154,1.,0.951056516295154,
1.,0.951056516295154,1.,0.951056516295154,1.,0.951056516295154,1.,0.951056516295154,
1.,0.951056516295154,1.,0.951056516295154,1.,0.951056516295154,1.,0.951056516295154,
1.,0.951056516295154,1.,0.951056516295154,1.,0.951056516295154,1.,0.951056516295154,
1.,0.951056516295154,1.,0.951056516295154,1.,0.951056516295154,1.,0.951056516295154,
1.,0.951056516295154,1.,0.951056516295154,1.,0.951056516295154,1.,0.951056516295154,
1.,0.951056516295154,1.,0.951056516295154,1.,0.951056516295154,1.,0.951056516295154,
1.,0.951056516295154,1.,0.951056516295154,1.,0.951056516295154,1.,0.951056516295154,
1.,0.951056516295154,1.,0.951056516295154,1.,0.951056516295154,1.,0.951056516295154,
1.,0.951056516295154,1.,0.951056516295154,1.,0.951056516295154,1.,0.951056516295154,
1.,0.951056516295154,1.,0.951056516295154,1.,0.951056516295154,1.,0.951056516295154,
1.,0.951056516295154,1.,0.951056516295154,1.,0.951056516295154,1.,0.951056516295154,
1.,0.951056516295154,1.,0.951056516295154,1.,0.951056516295154,1.,0.951056516295154,
1.,0.951056516295154,1.,0.951056516295154,1.,0.951056516295154,1.,0.951056516295154,
1.,0.951056516295154,1.,0.951056516295154,1.,0.951056516295154,1.,0.951056516295154,
1.,0.951056516295154,1.,0.951056516295154,1.,0.951056516295154,1.,0.951056516295154,
1.,0.951056516295154,1.,0.951056516295154,1.,0.951056516295154,1.,0.951056516295154,
1.,0.951056516295154,1.,0.951056516295154,1.,0.951056516295154,1.,0.951056516295154,
1.,0.951056516295154,1.,0.951056516295154,1.,0.951056516295154,1.,0.951056516295154,
1.,0.951056516295154,1.,0.951056516295154,1.,0.951056516295154,1.,0.951056516295154,
1.,0.951056516295154,1.,0.951056516295154,1.,0.951056516295154,1.,0.951056516295154,
1.,0.951056516295154,1.,0.951056516295154,1.,0.951056516295154,1.,0.951056516295154,
1.,0.951056516295154,1.,0.951056516295154,1.,0.951056516295154,1.,0.951056516295154,
1.,0.951056516295154,1.,0.951056516295154,1.,0.951056516295154,1.,0.951056516295154,
1.,0.951056516295154,1.,0.951056516295154,1.,0.951056516295154,1.,0.951056516295154,
1.,0.951056516295154,1.,0.951056516295154,1.,0.951056516295154,1.,0.951056516295154,
1.,0.951056516295154,1.,0.951056516295154,1.,0.951056516295154,1.,0.951056516295154,
1.,0.951056516295154,1.,0.951056516295154,1.,0.951056516295154,1.,0.951056516295154,
1.,0.951056516295154,1.,0.951056516295154,1.,0.951056516295154,1.,0.951056516295154,
1.,0.951056516295154,1.,0.951056516295154,1.,0.951056516295154,1.,0.951056516295154,
1.,0.951056516295154,1.,0.951056516295154,1.,0.951056516295154,1.,0.951056516295154,
1.,0.951056516295154,1.,0.951056516295154,1.,0.951056516295154,1.,0.951056516295154,
1.,0.951056516295154,1.,0.951056516295154,1.,0.951056516295154,1.,0.951056516295154,
1.,0.951056516295154,1.,0.951056516295154,1.,0.951056516295154,1.,0.951056516295154,
1.,0.951056516295154,1.,0.951056516295154,1.,0.951056516295154,1.,0.951056516295154,
1.,0.951056516295154,1.,0.951056516295154,1.,0.951056516295154,1.,0.951056516295154,
1.,0.951056516295154,1.,0.951056516295154,1.,0.951056516295154,1.,0.951056516295154,
1.,0.951056516295154,1.,0.951056516295154,1.,0.951056516295154,1.,0.951056516295154,
1.,0.951056516295154,1.,0.951056516295154,1.,0.951056516295154,1.,0.951056516295154,
1.,0.951056516295154,1.,0.951056516295154,1.,0.951056516295154,1.,0.951056516295154,
1.,0.951056516295154,1.,0.951056516295154,1.,0.951056516295154,1.,0.951056516295154,
1.,0.951056516295154,1.,0.951056516295154,1.,0.951056516295154,1.,0.951056516295154,
1.,0.951056516295154,1.,0.951056516295154,1.,0.951056516295154,1.,0.951056516295154,
1.,0.951056516295154,1.,0.951056516295154,1.,0.951056516295154,1.,0.951056516295154,
1.,0.951056516295154,1.,0.951056516295154,1.,0.951056516295154,1.,0.951056516295154,
1.,0.951056516295154,1.,0.951056516295154,1.,0.951056516295154,1.,0.951056516295154,
1.,0.951056516295154,1.,0.951056516295154,1.,0.951056516295154,1.,0.951056516295154,
1.,0.951056516295154,1.,0.951056516295154,1.,0.951056516295154,1.,0.951056516295154,
1.,0.951056516295154,1.,0.951056516295154,1.,0.951056516295154,1.,0.951056516295154,
1.),(1.,0.951056516295154,1.,0.951056516295154,1.,0.951056516295154,1.,
0.951056516295154,1.,0.951056516295154,1.,0.951056516295154,1.,0.951056516295154,
1.,0.951056516295154,1.,0.951056516295154,1.,0.951056516295154,1.,0.951056516295154,
1.,0.951056516295154,1.,0.951056516295154,1.,0.951056516295154,1.,0.951056516295154,
1.,0.951056516295154,1.,0.951056516295154,1.,0.951056516295154,1.,0.951056516295154,
1.,0.951056516295154,1.,0.951056516295154,1.,0.951056516295154,1.,0.951056516295154,
1.,0.951056516295154,1.,0.951056516295154,1.,0.951056516295154,1.,0.951056516295154,
1.,0.951056516295154,1.,0.951056516295154,1.,0.951056516295154,1.,0.951056516295154,
1.,0.951056516295154,1.,0.951056516295154,1.,0.951056516295154,1.,0.951056516295154,
1.,0.951056516295154,1.,0.951056516295154,1.,0.951056516295154,1.,0.951056516295154,
1.,0.951056516295154,1.,0.951056516295154,1.,0.951056516295154,1.,0.951056516295154,
1.,0.951056516295154,1.,0.951056516295154,1.,0.951056516295154,1.,0.951056516295154,
1.,0.951056516295154,1.,0.951056516295154,1.,0.951056516295154,1.,0.951056516295154,
1.,0.951056516295154,1.,0.951056516295154,1.,0.951056516295154,1.,0.951056516295154,
1.,0.951056516295154,1.,0.951056516295154,1.,0.951056516295154,1.,0.951056516295154,
1.,0.951056516295154,1.,0.951056516295154,1.,0.951056516295154,1.,0.951056516295154,
1.,0.951056516295154,1.,0.951056516295154,1.,0.951056516295154,1.,0.951056516295154,
1.,0.951056516295154,1.,0.951056516295154,1.,0.951056516295154,1.,0.951056516295154,
1.,0.951056516295154,1.,0.951056516295154,1.,0.951056516295154,1.,0.951056516295154,
1.,0.951056516295154,1.,0.951056516295154,1.,0.951056516295154,1.,0.951056516295154,
1.,0.951056516295154,1.,0.951056516295154,1.,0.951056516295154,1.,0.951056516295154,
1.,0.951056516295154,1.,0.951056516295154,1.,0.951056516295154,1.,0.951056516295154,
1.,0.951056516295154,1.,0.951056516295154,1.,0.951056516295154,1.,0.951056516295154,
1.,0.951056516295154,1.,0.951056516295154,1.,0.951056516295154,1.,0.951056516295154,
1.,0.951056516295154,1.,0.951056516295154,1.,0.951056516295154,1.,0.951056516295154,
1.,0.951056516295154,1.,0.951056516295154,1.,0.951056516295154,1.,0.951056516295154,
1.,0.951056516295154,1.,0.951056516295154,1.,0.951056516295154,1.,0.951056516295154,
1.,0.951056516295154,1.,0.951056516295154,1.,0.951056516295154,1.,0.951056516295154,
1.,0.951056516295154,1.,0.951056516295154,1.,0.951056516295154,1.,0.951056516295154,
1.,0.951056516295154,1.,0.951056516295154,1.,0.951056516295154,1.,0.951056516295154,
1.,0.951056516295154,1.,0.951056516295154,1.,0.951056516295154,1.,0.951056516295154,
1.,0.951056516295154,1.,0.951056516295154,1.,0.951056516295154,1.,0.951056516295154,
1.,0.951056516295154,1.,0.951056516295154,1.,0.951056516295154,1.,0.951056516295154,
1.,0.951056516295154,1.,0.951056516295154,1.,0.951056516295154,1.,0.951056516295154,
1.,0.951056516295154,1.,0.951056516295154,1.,0.951056516295154,1.,0.951056516295154,
1.,0.951056516295154,1.,0.951056516295154,1.,0.951056516295154,1.,0.951056516295154,
1.,0.951056516295154,1.,0.951056516295154,1.,0.951056516295154,1.,0.951056516295154,
1.,0.951056516295154,1.,0.951056516295154,1.,0.951056516295154,1.,0.951056516295154,
1.,0.951056516295154,1.,0.951056516295154,1.,0.951056516295154,1.,0.951056516295154,
1.,0.951056516295154,1.,0.951056516295154,1.,0.951056516295154,1.,0.951056516295154,
1.,0.951056516295154,1.,0.951056516295154,1.,0.951056516295154,1.,0.951056516295154,
1.,0.951056516295154,1.,0.951056516295154,1.,0.951056516295154,1.,0.951056516295154,
1.,0.951056516295154,1.,0.951056516295154,1.,0.951056516295154,1.,0.951056516295154,
1.,0.951056516295154,1.,0.951056516295154,1.,0.951056516295154,1.,0.951056516295154,
1.,0.951056516295154,1.,0.951056516295154,1.,0.951056516295154,1.,0.951056516295154,
1.,0.951056516295154,1.,0.951056516295154,1.,0.951056516295154,1.,0.951056516295154,
1.,0.951056516295154,1.,0.951056516295154,1.,0.951056516295154,1.,0.951056516295154,
1.,0.951056516295154,1.,0.951056516295154,1.,0.951056516295154,1.,0.951056516295154,
1.,0.951056516295154,1.,0.951056516295154,1.,0.951056516295154,1.,0.951056516295154,
1.,0.951056516295154,1.,0.951056516295154,1.,0.951056516295154,1.,0.951056516295154,
1.,0.951056516295154,1.,0.951056516295154,1.,0.951056516295154,1.,0.951056516295154,
1.,0.951056516295154,1.,0.951056516295154,1.,0.951056516295154,1.,0.951056516295154,
1.,0.951056516295154,1.,0.951056516295154,1.,0.951056516295154,1.,0.951056516295154,
1.,0.951056516295154,1.,0.951056516295154,1.,0.951056516295154,1.,0.951056516295154,
1.,0.951056516295154,1.,0.951056516295154,1.,0.951056516295154,1.,0.951056516295154,
1.,0.951056516295154,1.,0.951056516295154,1.,0.951056516295154,1.,0.951056516295154,
1.,0.951056516295154,1.,0.951056516295154,1.,0.951056516295154,1.,0.951056516295154,
1.,0.951056516295154,1.,0.951056516295154,1.,0.951056516295154,1.,0.951056516295154,
1.,0.951056516295154,1.,0.951056516295154,1.,0.951056516295154,1.,0.951056516295154,
1.,0.951056516295154,1.,0.951056516295154,1.,0.951056516295154,1.,0.951056516295154,
1.,0.951056516295154,1.,0.951056516295154,1.,0.951056516295154,1.,0.951056516295154,
1.,0.951056516295154,1.,0.951056516295154,1.,0.951056516295154,1.,0.951056516295154,
1.,0.951056516295154,1.,0.951056516295154,1.,0.951056516295154,1.,0.951056516295154,
1.,0.951056516295154,1.,0.951056516295154,1.,0.951056516295154,1.,0.951056516295154,
1.,0.951056516295154,1.,0.951056516295154,1.,0.951056516295154,1.,0.951056516295154,
1.,0.951056516295154,1.,0.951056516295154,1.,0.951056516295154,1.,0.951056516295154,
1.,0.951056516295154,1.,0.951056516295154,1.,0.951056516295154,1.,0.951056516295154,
1.,0.951056516295154,1.,0.951056516295154,1.,0.951056516295154,1.,0.951056516295154,
1.,0.951056516295154,1.,0.951056516295154,1.,0.951056516295154,1.,0.951056516295154,
1.,0.951056516295154,1.,0.951056516295154,1.,0.951056516295154,1.,0.951056516295154,
1.,0.951056516295154,1.,0.951056516295154,1.,0.951056516295154,1.,0.951056516295154,
1.,0.951056516295154,1.,0.951056516295154,1.,0.951056516295154,1.,0.951056516295154,
1.,0.951056516295154,1.,0.951056516295154,1.,0.951056516295154,1.,0.951056516295154,
1.,0.951056516295154,1.,0.951056516295154,1.,0.951056516295154,1.,0.951056516295154,
1.,0.951056516295154,1.,0.951056516295154,1.,0.951056516295154,1.,0.951056516295154,
1.,0.951056516295154,1.,0.951056516295154,1.,0.951056516295154,1.,0.951056516295154,
1.,0.951056516295154,1.,0.951056516295154,1.,0.951056516295154,1.,0.951056516295154,
1.,0.951056516295154,1.,0.951056516295154,1.,0.951056516295154,1.,0.951056516295154,
1.,0.951056516295154,1.,0.951056516295154,1.,0.951056516295154,1.,0.951056516295154,
1.,0.951056516295154,1.,0.951056516295154,1.,0.951056516295154,1.,0.951056516295154,
1.,0.951056516295154,1.,0.951056516295154,1.,0.951056516295154,1.,0.951056516295154,
1.,0.951056516295154,1.,0.951056516295154,1.,0.951056516295154,1.,0.951056516295154,
1.,0.951056516295154,1.,0.951056516295154,1.,0.951056516295154,1.,0.951056516295154,
1.,0.951056516295154,1.,0.951056516295154,1.,0.951056516295154,1.,0.951056516295154,
1.,0.951056516295154,1.,0.951056516295154,1.,0.951056516295154,1.,0.951056516295154,
1.,0.951056516295154,1.,0.951056516295154,1.,0.951056516295154,1.,0.951056516295154,
1.,0.951056516295154,1.,0.951056516295154,1.,0.951056516295154,1.,0.951056516295154,
1.,0.951056516295154,1.,0.951056516295154,1.,0.951056516295154,1.,0.951056516295154,
1.,0.951056516295154,1.,0.951056516295154,1.,0.951056516295154,1.,0.951056516295154,
1.,0.951056516295154,1.,0.951056516295154,1.,0.951056516295154,1.,0.951056516295154,
1.,0.951056516295154,1.,0.951056516295154,1.,0.951056516295154,1.,0.951056516295154,
1.,0.951056516295154,1.,0.951056516295154,1.,0.951056516295154,1.,0.951056516295154,
1.,0.951056516295154,1.,0.951056516295154,1.,0.951056516295154,1.,0.951056516295154,
1.,0.951056516295154,1.,0.951056516295154,1.,0.951056516295154,1.,0.951056516295154,
1.,0.951056516295154,1.,0.951056516295154,1.,0.951056516295154,1.,0.951056516295154,
1.,0.951056516295154,1.,0.951056516295154,1.,0.951056516295154,1.,0.951056516295154,
1.,0.951056516295154,1.,0.951056516295154,1.,0.951056516295154,1.,0.951056516295154,
1.,0.951056516295154,1.,0.951056516295154,1.,0.951056516295154,1.,0.951056516295154,
1.,0.951056516295154,1.,0.951056516295154,1.,0.951056516295154,1.,0.951056516295154,
1.,0.951056516295154,1.,0.951056516295154,1.,0.951056516295154,1.,0.951056516295154,
1.,0.951056516295154,1.,0.951056516295154,1.,0.951056516295154,1.,0.951056516295154,
1.,0.951056516295154,1.,0.951056516295154,1.,0.951056516295154,1.,0.951056516295154,
1.,0.951056516295154,1.,0.951056516295154,1.,0.951056516295154,1.,0.951056516295154,
1.,0.951056516295154,1.,0.951056516295154,1.,0.951056516295154,1.,0.951056516295154,
1.,0.951056516295154,1.,0.951056516295154,1.,0.951056516295154,1.,0.951056516295154,
1.,0.951056516295154,1.,0.951056516295154,1.,0.951056516295154,1.,0.951056516295154,
1.,0.951056516295154,1.,0.951056516295154,1.,0.951056516295154,1.,0.951056516295154,
1.,0.951056516295154,1.,0.951056516295154,1.,0.951056516295154,1.,0.951056516295154,
1.,0.951056516295154,1.,0.951056516295154,1.,0.951056516295154,1.,0.951056516295154,
1.,0.951056516295154,1.,0.951056516295154,1.,0.951056516295154,1.,0.951056516295154,
1.,0.951056516295154,1.,0.951056516295154,1.,0.951056516295154,1.,0.951056516295154,
1.,0.951056516295154,1.,0.951056516295154,1.,0.951056516295154,1.,0.951056516295154,
1.,0.951056516295154,1.,0.951056516295154,1.,0.951056516295154,1.,0.951056516295154,
1.,0.951056516295154,1.,0.951056516295154,1.,0.951056516295154,1.,0.951056516295154,
1.,0.951056516295154,1.,0.951056516295154,1.,0.951056516295154,1.,0.951056516295154,
1.,0.951056516295154,1.,0.951056516295154,1.,0.951056516295154,1.,0.951056516295154,
1.,0.951056516295154,1.,0.951056516295154,1.,0.951056516295154,1.,0.951056516295154,
1.,0.951056516295154,1.,0.951056516295154,1.,0.951056516295154,1.,0.951056516295154,
1.,0.951056516295154,1.,0.951056516295154,1.,0.951056516295154,1.,0.951056516295154,
1.,0.951056516295154,1.,0.951056516295154,1.,0.951056516295154,1.,0.951056516295154,
1.,0.951056516295154,1.,0.951056516295154,1.,0.951056516295154,1.,0.951056516295154,
1.,0.951056516295154,1.,0.951056516295154,1.,0.951056516295154,1.,0.951056516295154,
1.,0.951056516295154,1.,0.951056516295154,1.,0.951056516295154,1.,0.951056516295154,
1.,0.951056516295154,1.,0.951056516295154,1.,0.951056516295154,1.,0.951056516295154,
1.,0.951056516295154,1.,0.951056516295154,1.,0.951056516295154,1.,0.951056516295154,
1.,0.951056516295154,1.,0.951056516295154,1.,0.951056516295154,1.,0.951056516295154,
1.,0.951056516295154,1.,0.951056516295154,1.,0.951056516295154,1.,0.951056516295154,
1.,0.951056516295154,1.,0.951056516295154,1.,0.951056516295154,1.,0.951056516295154,
1.,0.951056516295154,1.,0.951056516295154,1.,0.951056516295154,1.,0.951056516295154,
1.,0.951056516295154,1.,0.951056516295154,1.,0.951056516295154,1.)))
REPRESENTATION_ITEM('')
SURFACE()
);
#3199=(
BOUNDED_SURFACE()
B_SPLINE_SURFACE(1,2,((#296159,#296160,#296161,#296162,#296163,#296164,
#296165,#296166,#296167,#296168,#296169,#296170,#296171,#296172,#296173,
#296174,#296175,#296176,#296177,#296178,#296179,#296180,#296181,#296182,
#296183,#296184,#296185,#296186,#296187,#296188,#296189,#296190,#296191,
#296192,#296193,#296194,#296195,#296196,#296197,#296198,#296199,#296200,
#296201,#296202,#296203,#296204,#296205,#296206,#296207,#296208,#296209,
#296210,#296211,#296212,#296213,#296214,#296215,#296216,#296217,#296218,
#296219,#296220,#296221,#296222,#296223,#296224,#296225,#296226,#296227,
#296228,#296229,#296230,#296231,#296232,#296233,#296234,#296235,#296236,
#296237,#296238,#296239,#296240,#296241,#296242,#296243,#296244,#296245,
#296246,#296247,#296248,#296249,#296250,#296251,#296252,#296253,#296254,
#296255,#296256,#296257,#296258,#296259,#296260,#296261,#296262,#296263,
#296264,#296265,#296266,#296267,#296268,#296269,#296270,#296271,#296272,
#296273,#296274,#296275,#296276,#296277,#296278,#296279,#296280,#296281,
#296282,#296283,#296284,#296285,#296286,#296287,#296288,#296289,#296290,
#296291,#296292,#296293,#296294,#296295,#296296,#296297,#296298,#296299,
#296300,#296301,#296302,#296303,#296304,#296305,#296306,#296307,#296308,
#296309,#296310,#296311,#296312,#296313,#296314,#296315,#296316,#296317,
#296318,#296319,#296320,#296321,#296322,#296323,#296324,#296325,#296326,
#296327,#296328,#296329,#296330,#296331,#296332,#296333,#296334,#296335,
#296336,#296337,#296338,#296339,#296340,#296341,#296342,#296343,#296344,
#296345,#296346,#296347,#296348,#296349,#296350,#296351,#296352,#296353,
#296354,#296355,#296356,#296357,#296358,#296359,#296360,#296361,#296362,
#296363,#296364,#296365,#296366,#296367,#296368,#296369,#296370,#296371,
#296372,#296373,#296374,#296375,#296376,#296377,#296378,#296379,#296380,
#296381,#296382,#296383,#296384,#296385,#296386,#296387,#296388,#296389,
#296390,#296391,#296392,#296393,#296394,#296395,#296396,#296397,#296398,
#296399,#296400,#296401,#296402,#296403,#296404,#296405,#296406,#296407,
#296408,#296409,#296410,#296411,#296412,#296413,#296414,#296415,#296416,
#296417,#296418,#296419,#296420,#296421,#296422,#296423,#296424,#296425,
#296426,#296427,#296428,#296429,#296430,#296431,#296432,#296433,#296434,
#296435,#296436,#296437,#296438,#296439,#296440,#296441,#296442,#296443,
#296444,#296445,#296446,#296447,#296448,#296449,#296450,#296451,#296452,
#296453,#296454,#296455,#296456,#296457,#296458,#296459,#296460,#296461,
#296462,#296463,#296464,#296465,#296466,#296467,#296468,#296469,#296470,
#296471,#296472,#296473,#296474,#296475,#296476,#296477,#296478,#296479,
#296480,#296481,#296482,#296483,#296484,#296485,#296486,#296487,#296488,
#296489,#296490,#296491,#296492,#296493,#296494,#296495,#296496,#296497,
#296498,#296499,#296500,#296501,#296502,#296503,#296504,#296505,#296506,
#296507,#296508,#296509,#296510,#296511,#296512,#296513,#296514,#296515,
#296516,#296517,#296518,#296519,#296520,#296521,#296522,#296523,#296524,
#296525,#296526,#296527,#296528,#296529,#296530,#296531,#296532,#296533,
#296534,#296535,#296536,#296537,#296538,#296539,#296540,#296541,#296542,
#296543,#296544,#296545,#296546,#296547,#296548,#296549,#296550,#296551,
#296552,#296553,#296554,#296555,#296556,#296557,#296558,#296559,#296560,
#296561,#296562,#296563,#296564,#296565,#296566,#296567,#296568,#296569,
#296570,#296571,#296572,#296573,#296574,#296575,#296576,#296577,#296578,
#296579,#296580,#296581,#296582,#296583,#296584,#296585,#296586,#296587,
#296588,#296589,#296590,#296591,#296592,#296593,#296594,#296595,#296596,
#296597,#296598,#296599,#296600,#296601,#296602,#296603,#296604,#296605,
#296606,#296607,#296608,#296609,#296610,#296611,#296612,#296613,#296614,
#296615,#296616,#296617,#296618,#296619,#296620,#296621,#296622,#296623,
#296624,#296625,#296626,#296627,#296628,#296629,#296630,#296631,#296632,
#296633,#296634,#296635,#296636,#296637,#296638,#296639,#296640,#296641,
#296642,#296643,#296644,#296645,#296646,#296647,#296648,#296649,#296650,
#296651,#296652,#296653,#296654,#296655,#296656,#296657,#296658,#296659,
#296660,#296661,#296662,#296663,#296664,#296665,#296666,#296667,#296668,
#296669,#296670,#296671,#296672,#296673,#296674,#296675,#296676,#296677,
#296678,#296679,#296680,#296681,#296682,#296683,#296684,#296685,#296686,
#296687,#296688,#296689,#296690,#296691,#296692,#296693,#296694,#296695,
#296696,#296697,#296698,#296699,#296700,#296701,#296702,#296703,#296704,
#296705,#296706,#296707,#296708,#296709,#296710,#296711,#296712,#296713,
#296714,#296715,#296716,#296717,#296718,#296719,#296720,#296721,#296722,
#296723,#296724,#296725,#296726,#296727,#296728,#296729,#296730,#296731,
#296732,#296733,#296734,#296735,#296736,#296737,#296738,#296739,#296740,
#296741,#296742,#296743,#296744,#296745,#296746,#296747,#296748,#296749,
#296750,#296751,#296752,#296753,#296754,#296755,#296756,#296757,#296758,
#296759,#296760,#296761,#296762,#296763,#296764,#296765,#296766,#296767,
#296768,#296769,#296770,#296771,#296772,#296773,#296774,#296775,#296776,
#296777,#296778,#296779,#296780,#296781,#296782,#296783,#296784,#296785,
#296786,#296787,#296788,#296789,#296790,#296791,#296792,#296793,#296794,
#296795,#296796,#296797,#296798,#296799,#296800,#296801,#296802,#296803,
#296804,#296805,#296806,#296807,#296808,#296809,#296810,#296811,#296812,
#296813,#296814,#296815,#296816,#296817,#296818,#296819,#296820,#296821,
#296822,#296823,#296824,#296825,#296826,#296827,#296828,#296829,#296830,
#296831,#296832,#296833,#296834,#296835,#296836,#296837,#296838,#296839,
#296840,#296841,#296842,#296843,#296844,#296845,#296846,#296847,#296848,
#296849,#296850,#296851,#296852,#296853,#296854,#296855,#296856,#296857,
#296858,#296859,#296860,#296861,#296862,#296863,#296864,#296865,#296866,
#296867,#296868,#296869,#296870,#296871,#296872,#296873,#296874,#296875,
#296876,#296877,#296878,#296879,#296880,#296881,#296882,#296883,#296884,
#296885,#296886,#296887,#296888,#296889,#296890,#296891,#296892,#296893,
#296894,#296895,#296896,#296897,#296898,#296899,#296900,#296901,#296902,
#296903,#296904,#296905,#296906,#296907,#296908,#296909,#296910,#296911,
#296912,#296913,#296914,#296915,#296916,#296917,#296918,#296919,#296920,
#296921,#296922,#296923,#296924,#296925,#296926,#296927,#296928,#296929,
#296930,#296931,#296932,#296933,#296934,#296935,#296936,#296937,#296938,
#296939,#296940,#296941,#296942,#296943,#296944,#296945,#296946,#296947,
#296948,#296949,#296950,#296951,#296952,#296953,#296954,#296955,#296956,
#296957,#296958,#296959,#296960,#296961,#296962,#296963,#296964,#296965,
#296966,#296967,#296968,#296969,#296970,#296971,#296972,#296973,#296974,
#296975,#296976,#296977,#296978,#296979,#296980,#296981,#296982,#296983,
#296984,#296985,#296986,#296987,#296988,#296989,#296990,#296991,#296992,
#296993,#296994,#296995,#296996,#296997,#296998,#296999,#297000,#297001,
#297002,#297003,#297004,#297005,#297006,#297007,#297008,#297009,#297010,
#297011,#297012,#297013,#297014,#297015,#297016,#297017,#297018,#297019,
#297020,#297021,#297022,#297023,#297024,#297025,#297026,#297027,#297028,
#297029,#297030,#297031,#297032,#297033,#297034,#297035,#297036,#297037,
#297038,#297039,#297040,#297041,#297042,#297043,#297044,#297045,#297046,
#297047,#297048,#297049,#297050,#297051,#297052,#297053,#297054,#297055,
#297056,#297057,#297058,#297059,#297060,#297061,#297062,#297063,#297064,
#297065,#297066,#297067,#297068,#297069,#297070,#297071,#297072,#297073,
#297074,#297075,#297076,#297077,#297078,#297079,#297080,#297081,#297082,
#297083,#297084,#297085,#297086,#297087,#297088,#297089,#297090,#297091,
#297092,#297093,#297094,#297095,#297096,#297097,#297098,#297099,#297100,
#297101,#297102,#297103,#297104,#297105,#297106,#297107,#297108,#297109,
#297110,#297111,#297112,#297113,#297114,#297115,#297116,#297117,#297118,
#297119,#297120,#297121,#297122,#297123,#297124,#297125,#297126,#297127,
#297128,#297129,#297130,#297131,#297132,#297133,#297134,#297135,#297136,
#297137,#297138,#297139,#297140,#297141,#297142,#297143,#297144,#297145,
#297146,#297147,#297148,#297149,#297150,#297151,#297152,#297153,#297154,
#297155,#297156,#297157,#297158,#297159,#297160,#297161,#297162,#297163,
#297164,#297165,#297166,#297167,#297168,#297169,#297170,#297171,#297172,
#297173,#297174,#297175,#297176,#297177,#297178,#297179,#297180,#297181,
#297182,#297183,#297184,#297185,#297186,#297187,#297188,#297189,#297190,
#297191,#297192,#297193,#297194,#297195),(#297196,#297197,#297198,#297199,
#297200,#297201,#297202,#297203,#297204,#297205,#297206,#297207,#297208,
#297209,#297210,#297211,#297212,#297213,#297214,#297215,#297216,#297217,
#297218,#297219,#297220,#297221,#297222,#297223,#297224,#297225,#297226,
#297227,#297228,#297229,#297230,#297231,#297232,#297233,#297234,#297235,
#297236,#297237,#297238,#297239,#297240,#297241,#297242,#297243,#297244,
#297245,#297246,#297247,#297248,#297249,#297250,#297251,#297252,#297253,
#297254,#297255,#297256,#297257,#297258,#297259,#297260,#297261,#297262,
#297263,#297264,#297265,#297266,#297267,#297268,#297269,#297270,#297271,
#297272,#297273,#297274,#297275,#297276,#297277,#297278,#297279,#297280,
#297281,#297282,#297283,#297284,#297285,#297286,#297287,#297288,#297289,
#297290,#297291,#297292,#297293,#297294,#297295,#297296,#297297,#297298,
#297299,#297300,#297301,#297302,#297303,#297304,#297305,#297306,#297307,
#297308,#297309,#297310,#297311,#297312,#297313,#297314,#297315,#297316,
#297317,#297318,#297319,#297320,#297321,#297322,#297323,#297324,#297325,
#297326,#297327,#297328,#297329,#297330,#297331,#297332,#297333,#297334,
#297335,#297336,#297337,#297338,#297339,#297340,#297341,#297342,#297343,
#297344,#297345,#297346,#297347,#297348,#297349,#297350,#297351,#297352,
#297353,#297354,#297355,#297356,#297357,#297358,#297359,#297360,#297361,
#297362,#297363,#297364,#297365,#297366,#297367,#297368,#297369,#297370,
#297371,#297372,#297373,#297374,#297375,#297376,#297377,#297378,#297379,
#297380,#297381,#297382,#297383,#297384,#297385,#297386,#297387,#297388,
#297389,#297390,#297391,#297392,#297393,#297394,#297395,#297396,#297397,
#297398,#297399,#297400,#297401,#297402,#297403,#297404,#297405,#297406,
#297407,#297408,#297409,#297410,#297411,#297412,#297413,#297414,#297415,
#297416,#297417,#297418,#297419,#297420,#297421,#297422,#297423,#297424,
#297425,#297426,#297427,#297428,#297429,#297430,#297431,#297432,#297433,
#297434,#297435,#297436,#297437,#297438,#297439,#297440,#297441,#297442,
#297443,#297444,#297445,#297446,#297447,#297448,#297449,#297450,#297451,
#297452,#297453,#297454,#297455,#297456,#297457,#297458,#297459,#297460,
#297461,#297462,#297463,#297464,#297465,#297466,#297467,#297468,#297469,
#297470,#297471,#297472,#297473,#297474,#297475,#297476,#297477,#297478,
#297479,#297480,#297481,#297482,#297483,#297484,#297485,#297486,#297487,
#297488,#297489,#297490,#297491,#297492,#297493,#297494,#297495,#297496,
#297497,#297498,#297499,#297500,#297501,#297502,#297503,#297504,#297505,
#297506,#297507,#297508,#297509,#297510,#297511,#297512,#297513,#297514,
#297515,#297516,#297517,#297518,#297519,#297520,#297521,#297522,#297523,
#297524,#297525,#297526,#297527,#297528,#297529,#297530,#297531,#297532,
#297533,#297534,#297535,#297536,#297537,#297538,#297539,#297540,#297541,
#297542,#297543,#297544,#297545,#297546,#297547,#297548,#297549,#297550,
#297551,#297552,#297553,#297554,#297555,#297556,#297557,#297558,#297559,
#297560,#297561,#297562,#297563,#297564,#297565,#297566,#297567,#297568,
#297569,#297570,#297571,#297572,#297573,#297574,#297575,#297576,#297577,
#297578,#297579,#297580,#297581,#297582,#297583,#297584,#297585,#297586,
#297587,#297588,#297589,#297590,#297591,#297592,#297593,#297594,#297595,
#297596,#297597,#297598,#297599,#297600,#297601,#297602,#297603,#297604,
#297605,#297606,#297607,#297608,#297609,#297610,#297611,#297612,#297613,
#297614,#297615,#297616,#297617,#297618,#297619,#297620,#297621,#297622,
#297623,#297624,#297625,#297626,#297627,#297628,#297629,#297630,#297631,
#297632,#297633,#297634,#297635,#297636,#297637,#297638,#297639,#297640,
#297641,#297642,#297643,#297644,#297645,#297646,#297647,#297648,#297649,
#297650,#297651,#297652,#297653,#297654,#297655,#297656,#297657,#297658,
#297659,#297660,#297661,#297662,#297663,#297664,#297665,#297666,#297667,
#297668,#297669,#297670,#297671,#297672,#297673,#297674,#297675,#297676,
#297677,#297678,#297679,#297680,#297681,#297682,#297683,#297684,#297685,
#297686,#297687,#297688,#297689,#297690,#297691,#297692,#297693,#297694,
#297695,#297696,#297697,#297698,#297699,#297700,#297701,#297702,#297703,
#297704,#297705,#297706,#297707,#297708,#297709,#297710,#297711,#297712,
#297713,#297714,#297715,#297716,#297717,#297718,#297719,#297720,#297721,
#297722,#297723,#297724,#297725,#297726,#297727,#297728,#297729,#297730,
#297731,#297732,#297733,#297734,#297735,#297736,#297737,#297738,#297739,
#297740,#297741,#297742,#297743,#297744,#297745,#297746,#297747,#297748,
#297749,#297750,#297751,#297752,#297753,#297754,#297755,#297756,#297757,
#297758,#297759,#297760,#297761,#297762,#297763,#297764,#297765,#297766,
#297767,#297768,#297769,#297770,#297771,#297772,#297773,#297774,#297775,
#297776,#297777,#297778,#297779,#297780,#297781,#297782,#297783,#297784,
#297785,#297786,#297787,#297788,#297789,#297790,#297791,#297792,#297793,
#297794,#297795,#297796,#297797,#297798,#297799,#297800,#297801,#297802,
#297803,#297804,#297805,#297806,#297807,#297808,#297809,#297810,#297811,
#297812,#297813,#297814,#297815,#297816,#297817,#297818,#297819,#297820,
#297821,#297822,#297823,#297824,#297825,#297826,#297827,#297828,#297829,
#297830,#297831,#297832,#297833,#297834,#297835,#297836,#297837,#297838,
#297839,#297840,#297841,#297842,#297843,#297844,#297845,#297846,#297847,
#297848,#297849,#297850,#297851,#297852,#297853,#297854,#297855,#297856,
#297857,#297858,#297859,#297860,#297861,#297862,#297863,#297864,#297865,
#297866,#297867,#297868,#297869,#297870,#297871,#297872,#297873,#297874,
#297875,#297876,#297877,#297878,#297879,#297880,#297881,#297882,#297883,
#297884,#297885,#297886,#297887,#297888,#297889,#297890,#297891,#297892,
#297893,#297894,#297895,#297896,#297897,#297898,#297899,#297900,#297901,
#297902,#297903,#297904,#297905,#297906,#297907,#297908,#297909,#297910,
#297911,#297912,#297913,#297914,#297915,#297916,#297917,#297918,#297919,
#297920,#297921,#297922,#297923,#297924,#297925,#297926,#297927,#297928,
#297929,#297930,#297931,#297932,#297933,#297934,#297935,#297936,#297937,
#297938,#297939,#297940,#297941,#297942,#297943,#297944,#297945,#297946,
#297947,#297948,#297949,#297950,#297951,#297952,#297953,#297954,#297955,
#297956,#297957,#297958,#297959,#297960,#297961,#297962,#297963,#297964,
#297965,#297966,#297967,#297968,#297969,#297970,#297971,#297972,#297973,
#297974,#297975,#297976,#297977,#297978,#297979,#297980,#297981,#297982,
#297983,#297984,#297985,#297986,#297987,#297988,#297989,#297990,#297991,
#297992,#297993,#297994,#297995,#297996,#297997,#297998,#297999,#298000,
#298001,#298002,#298003,#298004,#298005,#298006,#298007,#298008,#298009,
#298010,#298011,#298012,#298013,#298014,#298015,#298016,#298017,#298018,
#298019,#298020,#298021,#298022,#298023,#298024,#298025,#298026,#298027,
#298028,#298029,#298030,#298031,#298032,#298033,#298034,#298035,#298036,
#298037,#298038,#298039,#298040,#298041,#298042,#298043,#298044,#298045,
#298046,#298047,#298048,#298049,#298050,#298051,#298052,#298053,#298054,
#298055,#298056,#298057,#298058,#298059,#298060,#298061,#298062,#298063,
#298064,#298065,#298066,#298067,#298068,#298069,#298070,#298071,#298072,
#298073,#298074,#298075,#298076,#298077,#298078,#298079,#298080,#298081,
#298082,#298083,#298084,#298085,#298086,#298087,#298088,#298089,#298090,
#298091,#298092,#298093,#298094,#298095,#298096,#298097,#298098,#298099,
#298100,#298101,#298102,#298103,#298104,#298105,#298106,#298107,#298108,
#298109,#298110,#298111,#298112,#298113,#298114,#298115,#298116,#298117,
#298118,#298119,#298120,#298121,#298122,#298123,#298124,#298125,#298126,
#298127,#298128,#298129,#298130,#298131,#298132,#298133,#298134,#298135,
#298136,#298137,#298138,#298139,#298140,#298141,#298142,#298143,#298144,
#298145,#298146,#298147,#298148,#298149,#298150,#298151,#298152,#298153,
#298154,#298155,#298156,#298157,#298158,#298159,#298160,#298161,#298162,
#298163,#298164,#298165,#298166,#298167,#298168,#298169,#298170,#298171,
#298172,#298173,#298174,#298175,#298176,#298177,#298178,#298179,#298180,
#298181,#298182,#298183,#298184,#298185,#298186,#298187,#298188,#298189,
#298190,#298191,#298192,#298193,#298194,#298195,#298196,#298197,#298198,
#298199,#298200,#298201,#298202,#298203,#298204,#298205,#298206,#298207,
#298208,#298209,#298210,#298211,#298212,#298213,#298214,#298215,#298216,
#298217,#298218,#298219,#298220,#298221,#298222,#298223,#298224,#298225,
#298226,#298227,#298228,#298229,#298230,#298231,#298232)),.UNSPECIFIED.,
 .F.,.F.,.F.)
B_SPLINE_SURFACE_WITH_KNOTS((2,2),(3,2,2,2,2,2,2,2,2,2,2,2,2,2,2,2,2,2,
2,2,2,2,2,2,2,2,2,2,2,2,2,2,2,2,2,2,2,2,2,2,2,2,2,2,2,2,2,2,2,2,2,2,2,2,
2,2,2,2,2,2,2,2,2,2,2,2,2,2,2,2,2,2,2,2,2,2,2,2,2,2,2,2,2,2,2,2,2,2,2,2,
2,2,2,2,2,2,2,2,2,2,2,2,2,2,2,2,2,2,2,2,2,2,2,2,2,2,2,2,2,2,2,2,2,2,2,2,
2,2,2,2,2,2,2,2,2,2,2,2,2,2,2,2,2,2,2,2,2,2,2,2,2,2,2,2,2,2,2,2,2,2,2,2,
2,2,2,2,2,2,2,2,2,2,2,2,2,2,2,2,2,2,2,2,2,2,2,2,2,2,2,2,2,2,2,2,2,2,2,2,
2,2,2,2,2,2,2,2,2,2,2,2,2,2,2,2,2,2,2,2,2,2,2,2,2,2,2,2,2,2,2,2,2,2,2,2,
2,2,2,2,2,2,2,2,2,2,2,2,2,2,2,2,2,2,2,2,2,2,2,2,2,2,2,2,2,2,2,2,2,2,2,2,
2,2,2,2,2,2,2,2,2,2,2,2,2,2,2,2,2,2,2,2,2,2,2,2,2,2,2,2,2,2,2,2,2,2,2,2,
2,2,2,2,2,2,2,2,2,2,2,2,2,2,2,2,2,2,2,2,2,2,2,2,2,2,2,2,2,2,2,2,2,2,2,2,
2,2,2,2,2,2,2,2,2,2,2,2,2,2,2,2,2,2,2,2,2,2,2,2,2,2,2,2,2,2,2,2,2,2,2,2,
2,2,2,2,2,2,2,2,2,2,2,2,2,2,2,2,2,2,2,2,2,2,2,2,2,2,2,2,2,2,2,2,2,2,2,2,
2,2,2,2,2,2,2,2,2,2,2,2,2,2,2,2,2,2,2,2,2,2,2,2,2,2,2,2,2,2,2,2,2,2,2,2,
2,2,2,2,2,2,2,2,2,2,2,2,2,2,2,2,2,2,2,2,2,2,2,2,2,2,2,2,2,2,2,2,2,2,2,2,
2,2,2,2,2,2,2,2,2,2,2,2,2,2,2,2,2,2,2,2,2,2,2,2,2,2,2,2,2,2,2,2,3),(0.,
1.),(0.,0.00192307692307692,0.00384615384615385,0.00576923076923077,0.00769230769230769,
0.00961538461538462,0.0115384615384615,0.0134615384615385,0.0153846153846154,
0.0173076923076923,0.0192307692307692,0.0211538461538462,0.0230769230769231,
0.025,0.0269230769230769,0.0288461538461538,0.0307692307692308,0.0326923076923077,
0.0346153846153846,0.0365384615384615,0.0384615384615385,0.0403846153846154,
0.0423076923076923,0.0442307692307692,0.0461538461538462,0.0480769230769231,
0.05,0.0519230769230769,0.0538461538461538,0.0557692307692308,0.0576923076923077,
0.0596153846153846,0.0615384615384615,0.0634615384615385,0.0653846153846154,
0.0673076923076923,0.0692307692307692,0.0711538461538462,0.0730769230769231,
0.075,0.0769230769230769,0.0788461538461538,0.0807692307692308,0.0826923076923077,
0.0846153846153846,0.0865384615384615,0.0884615384615385,0.0903846153846154,
0.0923076923076923,0.0942307692307692,0.0961538461538462,0.0980769230769231,
0.1,0.101923076923077,0.103846153846154,0.105769230769231,0.107692307692308,
0.109615384615385,0.111538461538462,0.113461538461538,0.115384615384615,
0.117307692307692,0.119230769230769,0.121153846153846,0.123076923076923,
0.125,0.126923076923077,0.128846153846154,0.130769230769231,0.132692307692308,
0.134615384615385,0.136538461538462,0.138461538461538,0.140384615384615,
0.142307692307692,0.144230769230769,0.146153846153846,0.148076923076923,
0.15,0.151923076923077,0.153846153846154,0.155769230769231,0.157692307692308,
0.159615384615385,0.161538461538462,0.163461538461538,0.165384615384615,
0.167307692307692,0.169230769230769,0.171153846153846,0.173076923076923,
0.175,0.176923076923077,0.178846153846154,0.180769230769231,0.182692307692308,
0.184615384615385,0.186538461538462,0.188461538461538,0.190384615384615,
0.192307692307692,0.194230769230769,0.196153846153846,0.198076923076923,
0.2,0.201923076923077,0.203846153846154,0.205769230769231,0.207692307692308,
0.209615384615385,0.211538461538462,0.213461538461538,0.215384615384615,
0.217307692307692,0.219230769230769,0.221153846153846,0.223076923076923,
0.225,0.226923076923077,0.228846153846154,0.230769230769231,0.232692307692308,
0.234615384615385,0.236538461538462,0.238461538461538,0.240384615384615,
0.242307692307692,0.244230769230769,0.246153846153846,0.248076923076923,
0.25,0.251923076923077,0.253846153846154,0.255769230769231,0.257692307692308,
0.259615384615385,0.261538461538462,0.263461538461538,0.265384615384615,
0.267307692307692,0.269230769230769,0.271153846153846,0.273076923076923,
0.275,0.276923076923077,0.278846153846154,0.280769230769231,0.282692307692308,
0.284615384615385,0.286538461538462,0.288461538461538,0.290384615384615,
0.292307692307692,0.294230769230769,0.296153846153846,0.298076923076923,
0.3,0.301923076923077,0.303846153846154,0.305769230769231,0.307692307692308,
0.309615384615385,0.311538461538462,0.313461538461538,0.315384615384615,
0.317307692307692,0.319230769230769,0.321153846153846,0.323076923076923,
0.325,0.326923076923077,0.328846153846154,0.330769230769231,0.332692307692308,
0.334615384615385,0.336538461538462,0.338461538461538,0.340384615384615,
0.342307692307692,0.344230769230769,0.346153846153846,0.348076923076923,
0.35,0.351923076923077,0.353846153846154,0.355769230769231,0.357692307692308,
0.359615384615385,0.361538461538462,0.363461538461538,0.365384615384615,
0.367307692307692,0.369230769230769,0.371153846153846,0.373076923076923,
0.375,0.376923076923077,0.378846153846154,0.380769230769231,0.382692307692308,
0.384615384615385,0.386538461538462,0.388461538461538,0.390384615384615,
0.392307692307692,0.394230769230769,0.396153846153846,0.398076923076923,
0.4,0.401923076923077,0.403846153846154,0.405769230769231,0.407692307692308,
0.409615384615385,0.411538461538462,0.413461538461538,0.415384615384615,
0.417307692307692,0.419230769230769,0.421153846153846,0.423076923076923,
0.425,0.426923076923077,0.428846153846154,0.430769230769231,0.432692307692308,
0.434615384615385,0.436538461538462,0.438461538461538,0.440384615384615,
0.442307692307692,0.444230769230769,0.446153846153846,0.448076923076923,
0.45,0.451923076923077,0.453846153846154,0.455769230769231,0.457692307692308,
0.459615384615385,0.461538461538462,0.463461538461538,0.465384615384615,
0.467307692307692,0.469230769230769,0.471153846153846,0.473076923076923,
0.475,0.476923076923077,0.478846153846154,0.480769230769231,0.482692307692308,
0.484615384615385,0.486538461538462,0.488461538461538,0.490384615384615,
0.492307692307692,0.494230769230769,0.496153846153846,0.498076923076923,
0.5,0.501923076923077,0.503846153846154,0.505769230769231,0.507692307692308,
0.509615384615385,0.511538461538461,0.513461538461538,0.515384615384615,
0.517307692307692,0.519230769230769,0.521153846153846,0.523076923076923,
0.525,0.526923076923077,0.528846153846154,0.530769230769231,0.532692307692308,
0.534615384615385,0.536538461538462,0.538461538461538,0.540384615384615,
0.542307692307692,0.544230769230769,0.546153846153846,0.548076923076923,
0.55,0.551923076923077,0.553846153846154,0.555769230769231,0.557692307692308,
0.559615384615385,0.561538461538462,0.563461538461538,0.565384615384615,
0.567307692307692,0.569230769230769,0.571153846153846,0.573076923076923,
0.575,0.576923076923077,0.578846153846154,0.580769230769231,0.582692307692308,
0.584615384615385,0.586538461538462,0.588461538461538,0.590384615384615,
0.592307692307692,0.594230769230769,0.596153846153846,0.598076923076923,
0.6,0.601923076923077,0.603846153846154,0.605769230769231,0.607692307692308,
0.609615384615385,0.611538461538462,0.613461538461539,0.615384615384615,
0.617307692307692,0.619230769230769,0.621153846153846,0.623076923076923,
0.625,0.626923076923077,0.628846153846154,0.630769230769231,0.632692307692308,
0.634615384615385,0.636538461538461,0.638461538461538,0.640384615384615,
0.642307692307692,0.644230769230769,0.646153846153846,0.648076923076923,
0.65,0.651923076923077,0.653846153846154,0.655769230769231,0.657692307692308,
0.659615384615385,0.661538461538462,0.663461538461538,0.665384615384615,
0.667307692307692,0.669230769230769,0.671153846153846,0.673076923076923,
0.675,0.676923076923077,0.678846153846154,0.680769230769231,0.682692307692308,
0.684615384615385,0.686538461538462,0.688461538461538,0.690384615384615,
0.692307692307692,0.694230769230769,0.696153846153846,0.698076923076923,
0.7,0.701923076923077,0.703846153846154,0.705769230769231,0.707692307692308,
0.709615384615385,0.711538461538462,0.713461538461538,0.715384615384615,
0.717307692307692,0.719230769230769,0.721153846153846,0.723076923076923,
0.725,0.726923076923077,0.728846153846154,0.730769230769231,0.732692307692308,
0.734615384615385,0.736538461538462,0.738461538461539,0.740384615384615,
0.742307692307692,0.744230769230769,0.746153846153846,0.748076923076923,
0.75,0.751923076923077,0.753846153846154,0.755769230769231,0.757692307692308,
0.759615384615385,0.761538461538461,0.763461538461538,0.765384615384615,
0.767307692307692,0.769230769230769,0.771153846153846,0.773076923076923,
0.775,0.776923076923077,0.778846153846154,0.780769230769231,0.782692307692308,
0.784615384615385,0.786538461538462,0.788461538461538,0.790384615384615,
0.792307692307692,0.794230769230769,0.796153846153846,0.798076923076923,
0.8,0.801923076923077,0.803846153846154,0.805769230769231,0.807692307692308,
0.809615384615385,0.811538461538462,0.813461538461538,0.815384615384615,
0.817307692307692,0.819230769230769,0.821153846153846,0.823076923076923,
0.825,0.826923076923077,0.828846153846154,0.830769230769231,0.832692307692308,
0.834615384615385,0.836538461538462,0.838461538461538,0.840384615384615,
0.842307692307692,0.844230769230769,0.846153846153846,0.848076923076923,
0.85,0.851923076923077,0.853846153846154,0.855769230769231,0.857692307692308,
0.859615384615385,0.861538461538462,0.863461538461539,0.865384615384615,
0.867307692307692,0.869230769230769,0.871153846153846,0.873076923076923,
0.875,0.876923076923077,0.878846153846154,0.880769230769231,0.882692307692308,
0.884615384615385,0.886538461538461,0.888461538461538,0.890384615384615,
0.892307692307692,0.894230769230769,0.896153846153846,0.898076923076923,
0.9,0.901923076923077,0.903846153846154,0.905769230769231,0.907692307692308,
0.909615384615385,0.911538461538462,0.913461538461538,0.915384615384615,
0.917307692307692,0.919230769230769,0.921153846153846,0.923076923076923,
0.925,0.926923076923077,0.928846153846154,0.930769230769231,0.932692307692308,
0.934615384615385,0.936538461538462,0.938461538461538,0.940384615384615,
0.942307692307692,0.944230769230769,0.946153846153846,0.948076923076923,
0.95,0.951923076923077,0.953846153846154,0.955769230769231,0.957692307692308,
0.959615384615385,0.961538461538462,0.963461538461538,0.965384615384615,
0.967307692307692,0.969230769230769,0.971153846153846,0.973076923076923,
0.975,0.976923076923077,0.978846153846154,0.980769230769231,0.982692307692308,
0.984615384615385,0.986538461538462,0.988461538461539,0.990384615384615,
0.992307692307692,0.994230769230769,0.996153846153846),.UNSPECIFIED.)
GEOMETRIC_REPRESENTATION_ITEM()
RATIONAL_B_SPLINE_SURFACE(((1.,0.951056516295154,1.,0.951056516295154,1.,
0.951056516295154,1.,0.951056516295154,1.,0.951056516295154,1.,0.951056516295154,
1.,0.951056516295154,1.,0.951056516295154,1.,0.951056516295154,1.,0.951056516295154,
1.,0.951056516295154,1.,0.951056516295154,1.,0.951056516295154,1.,0.951056516295154,
1.,0.951056516295154,1.,0.951056516295154,1.,0.951056516295154,1.,0.951056516295154,
1.,0.951056516295154,1.,0.951056516295154,1.,0.951056516295154,1.,0.951056516295154,
1.,0.951056516295154,1.,0.951056516295154,1.,0.951056516295154,1.,0.951056516295154,
1.,0.951056516295154,1.,0.951056516295154,1.,0.951056516295154,1.,0.951056516295154,
1.,0.951056516295154,1.,0.951056516295154,1.,0.951056516295154,1.,0.951056516295154,
1.,0.951056516295154,1.,0.951056516295154,1.,0.951056516295154,1.,0.951056516295154,
1.,0.951056516295154,1.,0.951056516295154,1.,0.951056516295154,1.,0.951056516295154,
1.,0.951056516295154,1.,0.951056516295154,1.,0.951056516295154,1.,0.951056516295154,
1.,0.951056516295154,1.,0.951056516295154,1.,0.951056516295154,1.,0.951056516295154,
1.,0.951056516295154,1.,0.951056516295154,1.,0.951056516295154,1.,0.951056516295154,
1.,0.951056516295154,1.,0.951056516295154,1.,0.951056516295154,1.,0.951056516295154,
1.,0.951056516295154,1.,0.951056516295154,1.,0.951056516295154,1.,0.951056516295154,
1.,0.951056516295154,1.,0.951056516295154,1.,0.951056516295154,1.,0.951056516295154,
1.,0.951056516295154,1.,0.951056516295154,1.,0.951056516295154,1.,0.951056516295154,
1.,0.951056516295154,1.,0.951056516295154,1.,0.951056516295154,1.,0.951056516295154,
1.,0.951056516295154,1.,0.951056516295154,1.,0.951056516295154,1.,0.951056516295154,
1.,0.951056516295154,1.,0.951056516295154,1.,0.951056516295154,1.,0.951056516295154,
1.,0.951056516295154,1.,0.951056516295154,1.,0.951056516295154,1.,0.951056516295154,
1.,0.951056516295154,1.,0.951056516295154,1.,0.951056516295154,1.,0.951056516295154,
1.,0.951056516295154,1.,0.951056516295154,1.,0.951056516295154,1.,0.951056516295154,
1.,0.951056516295154,1.,0.951056516295154,1.,0.951056516295154,1.,0.951056516295154,
1.,0.951056516295154,1.,0.951056516295154,1.,0.951056516295154,1.,0.951056516295154,
1.,0.951056516295154,1.,0.951056516295154,1.,0.951056516295154,1.,0.951056516295154,
1.,0.951056516295154,1.,0.951056516295154,1.,0.951056516295154,1.,0.951056516295154,
1.,0.951056516295154,1.,0.951056516295154,1.,0.951056516295154,1.,0.951056516295154,
1.,0.951056516295154,1.,0.951056516295154,1.,0.951056516295154,1.,0.951056516295154,
1.,0.951056516295154,1.,0.951056516295154,1.,0.951056516295154,1.,0.951056516295154,
1.,0.951056516295154,1.,0.951056516295154,1.,0.951056516295154,1.,0.951056516295154,
1.,0.951056516295154,1.,0.951056516295154,1.,0.951056516295154,1.,0.951056516295154,
1.,0.951056516295154,1.,0.951056516295154,1.,0.951056516295154,1.,0.951056516295154,
1.,0.951056516295154,1.,0.951056516295154,1.,0.951056516295154,1.,0.951056516295154,
1.,0.951056516295154,1.,0.951056516295154,1.,0.951056516295154,1.,0.951056516295154,
1.,0.951056516295154,1.,0.951056516295154,1.,0.951056516295154,1.,0.951056516295154,
1.,0.951056516295154,1.,0.951056516295154,1.,0.951056516295154,1.,0.951056516295154,
1.,0.951056516295154,1.,0.951056516295154,1.,0.951056516295154,1.,0.951056516295154,
1.,0.951056516295154,1.,0.951056516295154,1.,0.951056516295154,1.,0.951056516295154,
1.,0.951056516295154,1.,0.951056516295154,1.,0.951056516295154,1.,0.951056516295154,
1.,0.951056516295154,1.,0.951056516295154,1.,0.951056516295154,1.,0.951056516295154,
1.,0.951056516295154,1.,0.951056516295154,1.,0.951056516295154,1.,0.951056516295154,
1.,0.951056516295154,1.,0.951056516295154,1.,0.951056516295154,1.,0.951056516295154,
1.,0.951056516295154,1.,0.951056516295154,1.,0.951056516295154,1.,0.951056516295154,
1.,0.951056516295154,1.,0.951056516295154,1.,0.951056516295154,1.,0.951056516295154,
1.,0.951056516295154,1.,0.951056516295154,1.,0.951056516295154,1.,0.951056516295154,
1.,0.951056516295154,1.,0.951056516295154,1.,0.951056516295154,1.,0.951056516295154,
1.,0.951056516295154,1.,0.951056516295154,1.,0.951056516295154,1.,0.951056516295154,
1.,0.951056516295154,1.,0.951056516295154,1.,0.951056516295154,1.,0.951056516295154,
1.,0.951056516295154,1.,0.951056516295154,1.,0.951056516295154,1.,0.951056516295154,
1.,0.951056516295154,1.,0.951056516295154,1.,0.951056516295154,1.,0.951056516295154,
1.,0.951056516295154,1.,0.951056516295154,1.,0.951056516295154,1.,0.951056516295154,
1.,0.951056516295154,1.,0.951056516295154,1.,0.951056516295154,1.,0.951056516295154,
1.,0.951056516295154,1.,0.951056516295154,1.,0.951056516295154,1.,0.951056516295154,
1.,0.951056516295154,1.,0.951056516295154,1.,0.951056516295154,1.,0.951056516295154,
1.,0.951056516295154,1.,0.951056516295154,1.,0.951056516295154,1.,0.951056516295154,
1.,0.951056516295154,1.,0.951056516295154,1.,0.951056516295154,1.,0.951056516295154,
1.,0.951056516295154,1.,0.951056516295154,1.,0.951056516295154,1.,0.951056516295154,
1.,0.951056516295154,1.,0.951056516295154,1.,0.951056516295154,1.,0.951056516295154,
1.,0.951056516295154,1.,0.951056516295154,1.,0.951056516295154,1.,0.951056516295154,
1.,0.951056516295154,1.,0.951056516295154,1.,0.951056516295154,1.,0.951056516295154,
1.,0.951056516295154,1.,0.951056516295154,1.,0.951056516295154,1.,0.951056516295154,
1.,0.951056516295154,1.,0.951056516295154,1.,0.951056516295154,1.,0.951056516295154,
1.,0.951056516295154,1.,0.951056516295154,1.,0.951056516295154,1.,0.951056516295154,
1.,0.951056516295154,1.,0.951056516295154,1.,0.951056516295154,1.,0.951056516295154,
1.,0.951056516295154,1.,0.951056516295154,1.,0.951056516295154,1.,0.951056516295154,
1.,0.951056516295154,1.,0.951056516295154,1.,0.951056516295154,1.,0.951056516295154,
1.,0.951056516295154,1.,0.951056516295154,1.,0.951056516295154,1.,0.951056516295154,
1.,0.951056516295154,1.,0.951056516295154,1.,0.951056516295154,1.,0.951056516295154,
1.,0.951056516295154,1.,0.951056516295154,1.,0.951056516295154,1.,0.951056516295154,
1.,0.951056516295154,1.,0.951056516295154,1.,0.951056516295154,1.,0.951056516295154,
1.,0.951056516295154,1.,0.951056516295154,1.,0.951056516295154,1.,0.951056516295154,
1.,0.951056516295154,1.,0.951056516295154,1.,0.951056516295154,1.,0.951056516295154,
1.,0.951056516295154,1.,0.951056516295154,1.,0.951056516295154,1.,0.951056516295154,
1.,0.951056516295154,1.,0.951056516295154,1.,0.951056516295154,1.,0.951056516295154,
1.,0.951056516295154,1.,0.951056516295154,1.,0.951056516295154,1.,0.951056516295154,
1.,0.951056516295154,1.,0.951056516295154,1.,0.951056516295154,1.,0.951056516295154,
1.,0.951056516295154,1.,0.951056516295154,1.,0.951056516295154,1.,0.951056516295154,
1.,0.951056516295154,1.,0.951056516295154,1.,0.951056516295154,1.,0.951056516295154,
1.,0.951056516295154,1.,0.951056516295154,1.,0.951056516295154,1.,0.951056516295154,
1.,0.951056516295154,1.,0.951056516295154,1.,0.951056516295154,1.,0.951056516295154,
1.,0.951056516295154,1.,0.951056516295154,1.,0.951056516295154,1.,0.951056516295154,
1.,0.951056516295154,1.,0.951056516295154,1.,0.951056516295154,1.,0.951056516295154,
1.,0.951056516295154,1.,0.951056516295154,1.,0.951056516295154,1.,0.951056516295154,
1.,0.951056516295154,1.,0.951056516295154,1.,0.951056516295154,1.,0.951056516295154,
1.,0.951056516295154,1.,0.951056516295154,1.,0.951056516295154,1.,0.951056516295154,
1.,0.951056516295154,1.,0.951056516295154,1.,0.951056516295154,1.,0.951056516295154,
1.,0.951056516295154,1.,0.951056516295154,1.,0.951056516295154,1.,0.951056516295154,
1.,0.951056516295154,1.,0.951056516295154,1.,0.951056516295154,1.,0.951056516295154,
1.,0.951056516295154,1.,0.951056516295154,1.,0.951056516295154,1.,0.951056516295154,
1.,0.951056516295154,1.,0.951056516295154,1.,0.951056516295154,1.,0.951056516295154,
1.,0.951056516295154,1.,0.951056516295154,1.,0.951056516295154,1.,0.951056516295154,
1.,0.951056516295154,1.,0.951056516295154,1.,0.951056516295154,1.,0.951056516295154,
1.,0.951056516295154,1.,0.951056516295154,1.,0.951056516295154,1.,0.951056516295154,
1.,0.951056516295154,1.,0.951056516295154,1.,0.951056516295154,1.,0.951056516295154,
1.,0.951056516295154,1.,0.951056516295154,1.,0.951056516295154,1.,0.951056516295154,
1.,0.951056516295154,1.,0.951056516295154,1.,0.951056516295154,1.,0.951056516295154,
1.,0.951056516295154,1.,0.951056516295154,1.,0.951056516295154,1.,0.951056516295154,
1.,0.951056516295154,1.,0.951056516295154,1.,0.951056516295154,1.,0.951056516295154,
1.,0.951056516295154,1.,0.951056516295154,1.,0.951056516295154,1.,0.951056516295154,
1.,0.951056516295154,1.,0.951056516295154,1.,0.951056516295154,1.,0.951056516295154,
1.,0.951056516295154,1.,0.951056516295154,1.,0.951056516295154,1.,0.951056516295154,
1.,0.951056516295154,1.,0.951056516295154,1.,0.951056516295154,1.,0.951056516295154,
1.,0.951056516295154,1.,0.951056516295154,1.,0.951056516295154,1.,0.951056516295154,
1.,0.951056516295154,1.,0.951056516295154,1.,0.951056516295154,1.,0.951056516295154,
1.,0.951056516295154,1.,0.951056516295154,1.,0.951056516295154,1.,0.951056516295154,
1.,0.951056516295154,1.,0.951056516295154,1.,0.951056516295154,1.,0.951056516295154,
1.,0.951056516295154,1.,0.951056516295154,1.,0.951056516295154,1.,0.951056516295154,
1.,0.951056516295154,1.,0.951056516295154,1.,0.951056516295154,1.,0.951056516295154,
1.,0.951056516295154,1.,0.951056516295154,1.,0.951056516295154,1.,0.951056516295154,
1.,0.951056516295154,1.,0.951056516295154,1.,0.951056516295154,1.,0.951056516295154,
1.,0.951056516295154,1.,0.951056516295154,1.,0.951056516295154,1.,0.951056516295154,
1.,0.951056516295154,1.,0.951056516295154,1.,0.951056516295154,1.,0.951056516295154,
1.,0.951056516295154,1.,0.951056516295154,1.,0.951056516295154,1.,0.951056516295154,
1.,0.951056516295154,1.,0.951056516295154,1.,0.951056516295154,1.,0.951056516295154,
1.,0.951056516295154,1.,0.951056516295154,1.,0.951056516295154,1.,0.951056516295154,
1.,0.951056516295154,1.,0.951056516295154,1.,0.951056516295154,1.,0.951056516295154,
1.,0.951056516295154,1.,0.951056516295154,1.,0.951056516295154,1.,0.951056516295154,
1.,0.951056516295154,1.,0.951056516295154,1.,0.951056516295154,1.,0.951056516295154,
1.,0.951056516295154,1.,0.951056516295154,1.,0.951056516295154,1.,0.951056516295154,
1.,0.951056516295154,1.,0.951056516295154,1.,0.951056516295154,1.,0.951056516295154,
1.,0.951056516295154,1.,0.951056516295154,1.,0.951056516295154,1.,0.951056516295154,
1.,0.951056516295154,1.,0.951056516295154,1.,0.951056516295154,1.,0.951056516295154,
1.,0.951056516295154,1.,0.951056516295154,1.,0.951056516295154,1.,0.951056516295154,
1.,0.951056516295154,1.,0.951056516295154,1.,0.951056516295154,1.,0.951056516295154,
1.,0.951056516295154,1.,0.951056516295154,1.,0.951056516295154,1.,0.951056516295154,
1.,0.951056516295154,1.,0.951056516295154,1.,0.951056516295154,1.,0.951056516295154,
1.,0.951056516295154,1.,0.951056516295154,1.,0.951056516295154,1.,0.951056516295154,
1.,0.951056516295154,1.,0.951056516295154,1.,0.951056516295154,1.,0.951056516295154,
1.),(1.,0.951056516295154,1.,0.951056516295154,1.,0.951056516295154,1.,
0.951056516295154,1.,0.951056516295154,1.,0.951056516295154,1.,0.951056516295154,
1.,0.951056516295154,1.,0.951056516295154,1.,0.951056516295154,1.,0.951056516295154,
1.,0.951056516295154,1.,0.951056516295154,1.,0.951056516295154,1.,0.951056516295154,
1.,0.951056516295154,1.,0.951056516295154,1.,0.951056516295154,1.,0.951056516295154,
1.,0.951056516295154,1.,0.951056516295154,1.,0.951056516295154,1.,0.951056516295154,
1.,0.951056516295154,1.,0.951056516295154,1.,0.951056516295154,1.,0.951056516295154,
1.,0.951056516295154,1.,0.951056516295154,1.,0.951056516295154,1.,0.951056516295154,
1.,0.951056516295154,1.,0.951056516295154,1.,0.951056516295154,1.,0.951056516295154,
1.,0.951056516295154,1.,0.951056516295154,1.,0.951056516295154,1.,0.951056516295154,
1.,0.951056516295154,1.,0.951056516295154,1.,0.951056516295154,1.,0.951056516295154,
1.,0.951056516295154,1.,0.951056516295154,1.,0.951056516295154,1.,0.951056516295154,
1.,0.951056516295154,1.,0.951056516295154,1.,0.951056516295154,1.,0.951056516295154,
1.,0.951056516295154,1.,0.951056516295154,1.,0.951056516295154,1.,0.951056516295154,
1.,0.951056516295154,1.,0.951056516295154,1.,0.951056516295154,1.,0.951056516295154,
1.,0.951056516295154,1.,0.951056516295154,1.,0.951056516295154,1.,0.951056516295154,
1.,0.951056516295154,1.,0.951056516295154,1.,0.951056516295154,1.,0.951056516295154,
1.,0.951056516295154,1.,0.951056516295154,1.,0.951056516295154,1.,0.951056516295154,
1.,0.951056516295154,1.,0.951056516295154,1.,0.951056516295154,1.,0.951056516295154,
1.,0.951056516295154,1.,0.951056516295154,1.,0.951056516295154,1.,0.951056516295154,
1.,0.951056516295154,1.,0.951056516295154,1.,0.951056516295154,1.,0.951056516295154,
1.,0.951056516295154,1.,0.951056516295154,1.,0.951056516295154,1.,0.951056516295154,
1.,0.951056516295154,1.,0.951056516295154,1.,0.951056516295154,1.,0.951056516295154,
1.,0.951056516295154,1.,0.951056516295154,1.,0.951056516295154,1.,0.951056516295154,
1.,0.951056516295154,1.,0.951056516295154,1.,0.951056516295154,1.,0.951056516295154,
1.,0.951056516295154,1.,0.951056516295154,1.,0.951056516295154,1.,0.951056516295154,
1.,0.951056516295154,1.,0.951056516295154,1.,0.951056516295154,1.,0.951056516295154,
1.,0.951056516295154,1.,0.951056516295154,1.,0.951056516295154,1.,0.951056516295154,
1.,0.951056516295154,1.,0.951056516295154,1.,0.951056516295154,1.,0.951056516295154,
1.,0.951056516295154,1.,0.951056516295154,1.,0.951056516295154,1.,0.951056516295154,
1.,0.951056516295154,1.,0.951056516295154,1.,0.951056516295154,1.,0.951056516295154,
1.,0.951056516295154,1.,0.951056516295154,1.,0.951056516295154,1.,0.951056516295154,
1.,0.951056516295154,1.,0.951056516295154,1.,0.951056516295154,1.,0.951056516295154,
1.,0.951056516295154,1.,0.951056516295154,1.,0.951056516295154,1.,0.951056516295154,
1.,0.951056516295154,1.,0.951056516295154,1.,0.951056516295154,1.,0.951056516295154,
1.,0.951056516295154,1.,0.951056516295154,1.,0.951056516295154,1.,0.951056516295154,
1.,0.951056516295154,1.,0.951056516295154,1.,0.951056516295154,1.,0.951056516295154,
1.,0.951056516295154,1.,0.951056516295154,1.,0.951056516295154,1.,0.951056516295154,
1.,0.951056516295154,1.,0.951056516295154,1.,0.951056516295154,1.,0.951056516295154,
1.,0.951056516295154,1.,0.951056516295154,1.,0.951056516295154,1.,0.951056516295154,
1.,0.951056516295154,1.,0.951056516295154,1.,0.951056516295154,1.,0.951056516295154,
1.,0.951056516295154,1.,0.951056516295154,1.,0.951056516295154,1.,0.951056516295154,
1.,0.951056516295154,1.,0.951056516295154,1.,0.951056516295154,1.,0.951056516295154,
1.,0.951056516295154,1.,0.951056516295154,1.,0.951056516295154,1.,0.951056516295154,
1.,0.951056516295154,1.,0.951056516295154,1.,0.951056516295154,1.,0.951056516295154,
1.,0.951056516295154,1.,0.951056516295154,1.,0.951056516295154,1.,0.951056516295154,
1.,0.951056516295154,1.,0.951056516295154,1.,0.951056516295154,1.,0.951056516295154,
1.,0.951056516295154,1.,0.951056516295154,1.,0.951056516295154,1.,0.951056516295154,
1.,0.951056516295154,1.,0.951056516295154,1.,0.951056516295154,1.,0.951056516295154,
1.,0.951056516295154,1.,0.951056516295154,1.,0.951056516295154,1.,0.951056516295154,
1.,0.951056516295154,1.,0.951056516295154,1.,0.951056516295154,1.,0.951056516295154,
1.,0.951056516295154,1.,0.951056516295154,1.,0.951056516295154,1.,0.951056516295154,
1.,0.951056516295154,1.,0.951056516295154,1.,0.951056516295154,1.,0.951056516295154,
1.,0.951056516295154,1.,0.951056516295154,1.,0.951056516295154,1.,0.951056516295154,
1.,0.951056516295154,1.,0.951056516295154,1.,0.951056516295154,1.,0.951056516295154,
1.,0.951056516295154,1.,0.951056516295154,1.,0.951056516295154,1.,0.951056516295154,
1.,0.951056516295154,1.,0.951056516295154,1.,0.951056516295154,1.,0.951056516295154,
1.,0.951056516295154,1.,0.951056516295154,1.,0.951056516295154,1.,0.951056516295154,
1.,0.951056516295154,1.,0.951056516295154,1.,0.951056516295154,1.,0.951056516295154,
1.,0.951056516295154,1.,0.951056516295154,1.,0.951056516295154,1.,0.951056516295154,
1.,0.951056516295154,1.,0.951056516295154,1.,0.951056516295154,1.,0.951056516295154,
1.,0.951056516295154,1.,0.951056516295154,1.,0.951056516295154,1.,0.951056516295154,
1.,0.951056516295154,1.,0.951056516295154,1.,0.951056516295154,1.,0.951056516295154,
1.,0.951056516295154,1.,0.951056516295154,1.,0.951056516295154,1.,0.951056516295154,
1.,0.951056516295154,1.,0.951056516295154,1.,0.951056516295154,1.,0.951056516295154,
1.,0.951056516295154,1.,0.951056516295154,1.,0.951056516295154,1.,0.951056516295154,
1.,0.951056516295154,1.,0.951056516295154,1.,0.951056516295154,1.,0.951056516295154,
1.,0.951056516295154,1.,0.951056516295154,1.,0.951056516295154,1.,0.951056516295154,
1.,0.951056516295154,1.,0.951056516295154,1.,0.951056516295154,1.,0.951056516295154,
1.,0.951056516295154,1.,0.951056516295154,1.,0.951056516295154,1.,0.951056516295154,
1.,0.951056516295154,1.,0.951056516295154,1.,0.951056516295154,1.,0.951056516295154,
1.,0.951056516295154,1.,0.951056516295154,1.,0.951056516295154,1.,0.951056516295154,
1.,0.951056516295154,1.,0.951056516295154,1.,0.951056516295154,1.,0.951056516295154,
1.,0.951056516295154,1.,0.951056516295154,1.,0.951056516295154,1.,0.951056516295154,
1.,0.951056516295154,1.,0.951056516295154,1.,0.951056516295154,1.,0.951056516295154,
1.,0.951056516295154,1.,0.951056516295154,1.,0.951056516295154,1.,0.951056516295154,
1.,0.951056516295154,1.,0.951056516295154,1.,0.951056516295154,1.,0.951056516295154,
1.,0.951056516295154,1.,0.951056516295154,1.,0.951056516295154,1.,0.951056516295154,
1.,0.951056516295154,1.,0.951056516295154,1.,0.951056516295154,1.,0.951056516295154,
1.,0.951056516295154,1.,0.951056516295154,1.,0.951056516295154,1.,0.951056516295154,
1.,0.951056516295154,1.,0.951056516295154,1.,0.951056516295154,1.,0.951056516295154,
1.,0.951056516295154,1.,0.951056516295154,1.,0.951056516295154,1.,0.951056516295154,
1.,0.951056516295154,1.,0.951056516295154,1.,0.951056516295154,1.,0.951056516295154,
1.,0.951056516295154,1.,0.951056516295154,1.,0.951056516295154,1.,0.951056516295154,
1.,0.951056516295154,1.,0.951056516295154,1.,0.951056516295154,1.,0.951056516295154,
1.,0.951056516295154,1.,0.951056516295154,1.,0.951056516295154,1.,0.951056516295154,
1.,0.951056516295154,1.,0.951056516295154,1.,0.951056516295154,1.,0.951056516295154,
1.,0.951056516295154,1.,0.951056516295154,1.,0.951056516295154,1.,0.951056516295154,
1.,0.951056516295154,1.,0.951056516295154,1.,0.951056516295154,1.,0.951056516295154,
1.,0.951056516295154,1.,0.951056516295154,1.,0.951056516295154,1.,0.951056516295154,
1.,0.951056516295154,1.,0.951056516295154,1.,0.951056516295154,1.,0.951056516295154,
1.,0.951056516295154,1.,0.951056516295154,1.,0.951056516295154,1.,0.951056516295154,
1.,0.951056516295154,1.,0.951056516295154,1.,0.951056516295154,1.,0.951056516295154,
1.,0.951056516295154,1.,0.951056516295154,1.,0.951056516295154,1.,0.951056516295154,
1.,0.951056516295154,1.,0.951056516295154,1.,0.951056516295154,1.,0.951056516295154,
1.,0.951056516295154,1.,0.951056516295154,1.,0.951056516295154,1.,0.951056516295154,
1.,0.951056516295154,1.,0.951056516295154,1.,0.951056516295154,1.,0.951056516295154,
1.,0.951056516295154,1.,0.951056516295154,1.,0.951056516295154,1.,0.951056516295154,
1.,0.951056516295154,1.,0.951056516295154,1.,0.951056516295154,1.,0.951056516295154,
1.,0.951056516295154,1.,0.951056516295154,1.,0.951056516295154,1.,0.951056516295154,
1.,0.951056516295154,1.,0.951056516295154,1.,0.951056516295154,1.,0.951056516295154,
1.,0.951056516295154,1.,0.951056516295154,1.,0.951056516295154,1.,0.951056516295154,
1.,0.951056516295154,1.,0.951056516295154,1.,0.951056516295154,1.,0.951056516295154,
1.,0.951056516295154,1.,0.951056516295154,1.,0.951056516295154,1.,0.951056516295154,
1.,0.951056516295154,1.,0.951056516295154,1.,0.951056516295154,1.,0.951056516295154,
1.,0.951056516295154,1.,0.951056516295154,1.,0.951056516295154,1.,0.951056516295154,
1.,0.951056516295154,1.,0.951056516295154,1.,0.951056516295154,1.,0.951056516295154,
1.,0.951056516295154,1.,0.951056516295154,1.,0.951056516295154,1.,0.951056516295154,
1.,0.951056516295154,1.,0.951056516295154,1.,0.951056516295154,1.,0.951056516295154,
1.,0.951056516295154,1.,0.951056516295154,1.,0.951056516295154,1.,0.951056516295154,
1.,0.951056516295154,1.,0.951056516295154,1.,0.951056516295154,1.,0.951056516295154,
1.,0.951056516295154,1.,0.951056516295154,1.,0.951056516295154,1.,0.951056516295154,
1.,0.951056516295154,1.,0.951056516295154,1.,0.951056516295154,1.,0.951056516295154,
1.,0.951056516295154,1.,0.951056516295154,1.,0.951056516295154,1.,0.951056516295154,
1.,0.951056516295154,1.,0.951056516295154,1.,0.951056516295154,1.,0.951056516295154,
1.,0.951056516295154,1.,0.951056516295154,1.,0.951056516295154,1.,0.951056516295154,
1.,0.951056516295154,1.,0.951056516295154,1.,0.951056516295154,1.,0.951056516295154,
1.,0.951056516295154,1.,0.951056516295154,1.,0.951056516295154,1.,0.951056516295154,
1.,0.951056516295154,1.,0.951056516295154,1.,0.951056516295154,1.,0.951056516295154,
1.,0.951056516295154,1.,0.951056516295154,1.,0.951056516295154,1.,0.951056516295154,
1.,0.951056516295154,1.,0.951056516295154,1.,0.951056516295154,1.,0.951056516295154,
1.,0.951056516295154,1.,0.951056516295154,1.,0.951056516295154,1.,0.951056516295154,
1.,0.951056516295154,1.,0.951056516295154,1.,0.951056516295154,1.,0.951056516295154,
1.,0.951056516295154,1.,0.951056516295154,1.,0.951056516295154,1.,0.951056516295154,
1.,0.951056516295154,1.,0.951056516295154,1.,0.951056516295154,1.,0.951056516295154,
1.,0.951056516295154,1.,0.951056516295154,1.,0.951056516295154,1.,0.951056516295154,
1.,0.951056516295154,1.,0.951056516295154,1.,0.951056516295154,1.,0.951056516295154,
1.,0.951056516295154,1.,0.951056516295154,1.,0.951056516295154,1.,0.951056516295154,
1.,0.951056516295154,1.,0.951056516295154,1.,0.951056516295154,1.,0.951056516295154,
1.,0.951056516295154,1.,0.951056516295154,1.,0.951056516295154,1.)))
REPRESENTATION_ITEM('')
SURFACE()
);
#3200=(
BOUNDED_SURFACE()
B_SPLINE_SURFACE(1,2,((#298462,#298463,#298464,#298465,#298466,#298467,
#298468,#298469,#298470,#298471,#298472,#298473,#298474,#298475,#298476,
#298477,#298478,#298479,#298480,#298481,#298482,#298483,#298484,#298485,
#298486,#298487,#298488,#298489,#298490,#298491,#298492,#298493,#298494,
#298495,#298496,#298497,#298498,#298499,#298500,#298501,#298502,#298503,
#298504,#298505,#298506,#298507,#298508,#298509,#298510,#298511,#298512,
#298513,#298514,#298515,#298516,#298517,#298518,#298519,#298520,#298521,
#298522,#298523,#298524,#298525,#298526,#298527,#298528,#298529,#298530,
#298531,#298532,#298533,#298534,#298535,#298536,#298537,#298538,#298539,
#298540,#298541,#298542,#298543,#298544,#298545,#298546,#298547,#298548,
#298549,#298550,#298551,#298552,#298553,#298554,#298555,#298556,#298557,
#298558,#298559,#298560,#298561,#298562,#298563,#298564,#298565,#298566,
#298567,#298568,#298569,#298570,#298571,#298572,#298573,#298574,#298575,
#298576,#298577,#298578,#298579,#298580,#298581,#298582,#298583,#298584,
#298585,#298586,#298587,#298588,#298589,#298590,#298591,#298592,#298593,
#298594,#298595,#298596,#298597,#298598,#298599,#298600,#298601,#298602,
#298603,#298604,#298605,#298606,#298607,#298608,#298609,#298610,#298611,
#298612,#298613,#298614,#298615,#298616,#298617,#298618,#298619,#298620,
#298621,#298622,#298623,#298624,#298625,#298626,#298627,#298628,#298629,
#298630,#298631,#298632,#298633,#298634,#298635,#298636,#298637,#298638,
#298639,#298640,#298641,#298642,#298643,#298644,#298645,#298646,#298647,
#298648,#298649,#298650,#298651,#298652,#298653,#298654,#298655,#298656,
#298657,#298658,#298659,#298660,#298661,#298662,#298663,#298664,#298665,
#298666,#298667,#298668,#298669,#298670,#298671,#298672,#298673,#298674,
#298675,#298676,#298677,#298678,#298679,#298680,#298681,#298682,#298683,
#298684,#298685,#298686,#298687,#298688,#298689,#298690,#298691,#298692,
#298693,#298694,#298695,#298696,#298697,#298698,#298699,#298700,#298701,
#298702,#298703,#298704,#298705,#298706,#298707,#298708,#298709,#298710,
#298711,#298712,#298713,#298714,#298715,#298716,#298717,#298718,#298719,
#298720,#298721,#298722,#298723,#298724,#298725,#298726,#298727,#298728,
#298729,#298730,#298731,#298732,#298733,#298734,#298735,#298736,#298737,
#298738,#298739,#298740,#298741,#298742,#298743,#298744,#298745,#298746,
#298747,#298748,#298749,#298750,#298751,#298752,#298753,#298754,#298755,
#298756,#298757,#298758,#298759,#298760,#298761,#298762,#298763,#298764,
#298765,#298766,#298767,#298768,#298769,#298770,#298771,#298772,#298773,
#298774,#298775,#298776,#298777,#298778,#298779,#298780,#298781,#298782,
#298783,#298784,#298785,#298786,#298787,#298788,#298789,#298790,#298791,
#298792,#298793,#298794,#298795,#298796,#298797,#298798,#298799,#298800,
#298801,#298802,#298803,#298804,#298805,#298806,#298807,#298808,#298809,
#298810,#298811,#298812,#298813,#298814,#298815,#298816,#298817,#298818,
#298819,#298820,#298821,#298822,#298823,#298824,#298825,#298826,#298827,
#298828,#298829,#298830,#298831,#298832,#298833,#298834,#298835,#298836,
#298837,#298838,#298839,#298840,#298841,#298842,#298843,#298844,#298845,
#298846,#298847,#298848,#298849,#298850,#298851,#298852,#298853,#298854,
#298855,#298856,#298857,#298858,#298859,#298860,#298861,#298862,#298863,
#298864,#298865,#298866,#298867,#298868,#298869,#298870,#298871,#298872,
#298873,#298874,#298875,#298876,#298877,#298878,#298879,#298880,#298881,
#298882,#298883,#298884,#298885,#298886,#298887,#298888,#298889,#298890,
#298891,#298892,#298893,#298894,#298895,#298896,#298897,#298898,#298899,
#298900,#298901,#298902,#298903,#298904,#298905,#298906,#298907,#298908,
#298909,#298910,#298911,#298912,#298913,#298914,#298915,#298916,#298917,
#298918,#298919,#298920,#298921,#298922,#298923,#298924,#298925,#298926,
#298927,#298928,#298929,#298930,#298931,#298932,#298933,#298934,#298935,
#298936,#298937,#298938,#298939,#298940,#298941,#298942,#298943,#298944,
#298945,#298946,#298947,#298948,#298949,#298950,#298951,#298952,#298953,
#298954,#298955,#298956,#298957,#298958,#298959,#298960,#298961,#298962,
#298963,#298964,#298965,#298966,#298967,#298968,#298969,#298970,#298971,
#298972,#298973,#298974,#298975,#298976,#298977,#298978,#298979,#298980,
#298981,#298982,#298983,#298984,#298985,#298986,#298987,#298988,#298989,
#298990,#298991,#298992,#298993,#298994,#298995,#298996,#298997,#298998,
#298999,#299000,#299001,#299002,#299003,#299004,#299005,#299006,#299007,
#299008,#299009,#299010,#299011,#299012,#299013,#299014,#299015,#299016,
#299017,#299018,#299019,#299020,#299021,#299022,#299023,#299024,#299025,
#299026,#299027,#299028,#299029,#299030,#299031,#299032,#299033,#299034,
#299035,#299036,#299037,#299038,#299039,#299040,#299041,#299042,#299043,
#299044,#299045,#299046,#299047,#299048,#299049,#299050,#299051,#299052,
#299053,#299054,#299055,#299056,#299057,#299058,#299059,#299060,#299061,
#299062,#299063,#299064,#299065,#299066,#299067,#299068,#299069,#299070,
#299071,#299072,#299073,#299074,#299075,#299076,#299077,#299078,#299079,
#299080,#299081,#299082,#299083,#299084,#299085,#299086,#299087,#299088,
#299089,#299090,#299091,#299092,#299093,#299094,#299095,#299096,#299097,
#299098,#299099,#299100,#299101,#299102,#299103,#299104,#299105,#299106,
#299107,#299108,#299109,#299110,#299111,#299112,#299113,#299114,#299115,
#299116,#299117,#299118,#299119,#299120,#299121,#299122,#299123,#299124,
#299125,#299126,#299127,#299128,#299129,#299130,#299131,#299132,#299133,
#299134,#299135,#299136,#299137,#299138,#299139,#299140,#299141,#299142,
#299143,#299144,#299145,#299146,#299147,#299148,#299149,#299150,#299151,
#299152,#299153,#299154,#299155,#299156,#299157,#299158,#299159,#299160,
#299161,#299162,#299163,#299164,#299165,#299166,#299167,#299168,#299169,
#299170,#299171,#299172,#299173,#299174,#299175,#299176,#299177,#299178,
#299179,#299180,#299181,#299182,#299183,#299184,#299185,#299186,#299187,
#299188,#299189,#299190,#299191,#299192,#299193,#299194,#299195,#299196,
#299197,#299198,#299199,#299200,#299201,#299202,#299203,#299204,#299205,
#299206,#299207,#299208,#299209,#299210,#299211,#299212,#299213,#299214,
#299215,#299216,#299217,#299218,#299219,#299220,#299221,#299222,#299223,
#299224,#299225,#299226,#299227,#299228,#299229,#299230,#299231,#299232,
#299233,#299234,#299235,#299236,#299237,#299238,#299239,#299240,#299241,
#299242,#299243,#299244,#299245,#299246,#299247,#299248,#299249,#299250,
#299251,#299252,#299253,#299254,#299255,#299256,#299257,#299258,#299259,
#299260,#299261,#299262,#299263,#299264,#299265,#299266,#299267,#299268,
#299269,#299270,#299271,#299272,#299273,#299274,#299275,#299276,#299277,
#299278,#299279,#299280,#299281,#299282,#299283,#299284,#299285,#299286,
#299287,#299288,#299289,#299290,#299291,#299292,#299293,#299294,#299295,
#299296,#299297,#299298,#299299,#299300,#299301,#299302,#299303,#299304,
#299305,#299306,#299307,#299308,#299309,#299310,#299311,#299312,#299313,
#299314,#299315,#299316,#299317,#299318,#299319,#299320,#299321,#299322,
#299323,#299324,#299325,#299326,#299327,#299328,#299329,#299330,#299331,
#299332,#299333,#299334,#299335,#299336,#299337,#299338,#299339,#299340,
#299341,#299342,#299343,#299344,#299345,#299346,#299347,#299348,#299349,
#299350,#299351,#299352,#299353,#299354,#299355,#299356,#299357,#299358,
#299359,#299360,#299361,#299362,#299363,#299364,#299365,#299366,#299367,
#299368,#299369,#299370,#299371,#299372,#299373,#299374,#299375,#299376,
#299377,#299378,#299379,#299380,#299381,#299382,#299383,#299384,#299385,
#299386,#299387,#299388,#299389,#299390,#299391,#299392,#299393,#299394,
#299395,#299396,#299397,#299398,#299399,#299400,#299401,#299402,#299403,
#299404,#299405,#299406,#299407,#299408,#299409,#299410,#299411,#299412,
#299413,#299414,#299415,#299416,#299417,#299418,#299419,#299420,#299421,
#299422,#299423,#299424,#299425,#299426,#299427,#299428,#299429,#299430,
#299431,#299432,#299433,#299434,#299435,#299436,#299437,#299438,#299439,
#299440,#299441,#299442,#299443,#299444,#299445,#299446,#299447,#299448,
#299449,#299450,#299451,#299452,#299453,#299454,#299455,#299456,#299457,
#299458,#299459,#299460,#299461,#299462,#299463,#299464,#299465,#299466,
#299467,#299468,#299469,#299470,#299471,#299472,#299473,#299474,#299475,
#299476,#299477,#299478,#299479,#299480,#299481,#299482,#299483,#299484,
#299485,#299486,#299487,#299488,#299489,#299490,#299491,#299492,#299493,
#299494,#299495,#299496,#299497,#299498),(#299499,#299500,#299501,#299502,
#299503,#299504,#299505,#299506,#299507,#299508,#299509,#299510,#299511,
#299512,#299513,#299514,#299515,#299516,#299517,#299518,#299519,#299520,
#299521,#299522,#299523,#299524,#299525,#299526,#299527,#299528,#299529,
#299530,#299531,#299532,#299533,#299534,#299535,#299536,#299537,#299538,
#299539,#299540,#299541,#299542,#299543,#299544,#299545,#299546,#299547,
#299548,#299549,#299550,#299551,#299552,#299553,#299554,#299555,#299556,
#299557,#299558,#299559,#299560,#299561,#299562,#299563,#299564,#299565,
#299566,#299567,#299568,#299569,#299570,#299571,#299572,#299573,#299574,
#299575,#299576,#299577,#299578,#299579,#299580,#299581,#299582,#299583,
#299584,#299585,#299586,#299587,#299588,#299589,#299590,#299591,#299592,
#299593,#299594,#299595,#299596,#299597,#299598,#299599,#299600,#299601,
#299602,#299603,#299604,#299605,#299606,#299607,#299608,#299609,#299610,
#299611,#299612,#299613,#299614,#299615,#299616,#299617,#299618,#299619,
#299620,#299621,#299622,#299623,#299624,#299625,#299626,#299627,#299628,
#299629,#299630,#299631,#299632,#299633,#299634,#299635,#299636,#299637,
#299638,#299639,#299640,#299641,#299642,#299643,#299644,#299645,#299646,
#299647,#299648,#299649,#299650,#299651,#299652,#299653,#299654,#299655,
#299656,#299657,#299658,#299659,#299660,#299661,#299662,#299663,#299664,
#299665,#299666,#299667,#299668,#299669,#299670,#299671,#299672,#299673,
#299674,#299675,#299676,#299677,#299678,#299679,#299680,#299681,#299682,
#299683,#299684,#299685,#299686,#299687,#299688,#299689,#299690,#299691,
#299692,#299693,#299694,#299695,#299696,#299697,#299698,#299699,#299700,
#299701,#299702,#299703,#299704,#299705,#299706,#299707,#299708,#299709,
#299710,#299711,#299712,#299713,#299714,#299715,#299716,#299717,#299718,
#299719,#299720,#299721,#299722,#299723,#299724,#299725,#299726,#299727,
#299728,#299729,#299730,#299731,#299732,#299733,#299734,#299735,#299736,
#299737,#299738,#299739,#299740,#299741,#299742,#299743,#299744,#299745,
#299746,#299747,#299748,#299749,#299750,#299751,#299752,#299753,#299754,
#299755,#299756,#299757,#299758,#299759,#299760,#299761,#299762,#299763,
#299764,#299765,#299766,#299767,#299768,#299769,#299770,#299771,#299772,
#299773,#299774,#299775,#299776,#299777,#299778,#299779,#299780,#299781,
#299782,#299783,#299784,#299785,#299786,#299787,#299788,#299789,#299790,
#299791,#299792,#299793,#299794,#299795,#299796,#299797,#299798,#299799,
#299800,#299801,#299802,#299803,#299804,#299805,#299806,#299807,#299808,
#299809,#299810,#299811,#299812,#299813,#299814,#299815,#299816,#299817,
#299818,#299819,#299820,#299821,#299822,#299823,#299824,#299825,#299826,
#299827,#299828,#299829,#299830,#299831,#299832,#299833,#299834,#299835,
#299836,#299837,#299838,#299839,#299840,#299841,#299842,#299843,#299844,
#299845,#299846,#299847,#299848,#299849,#299850,#299851,#299852,#299853,
#299854,#299855,#299856,#299857,#299858,#299859,#299860,#299861,#299862,
#299863,#299864,#299865,#299866,#299867,#299868,#299869,#299870,#299871,
#299872,#299873,#299874,#299875,#299876,#299877,#299878,#299879,#299880,
#299881,#299882,#299883,#299884,#299885,#299886,#299887,#299888,#299889,
#299890,#299891,#299892,#299893,#299894,#299895,#299896,#299897,#299898,
#299899,#299900,#299901,#299902,#299903,#299904,#299905,#299906,#299907,
#299908,#299909,#299910,#299911,#299912,#299913,#299914,#299915,#299916,
#299917,#299918,#299919,#299920,#299921,#299922,#299923,#299924,#299925,
#299926,#299927,#299928,#299929,#299930,#299931,#299932,#299933,#299934,
#299935,#299936,#299937,#299938,#299939,#299940,#299941,#299942,#299943,
#299944,#299945,#299946,#299947,#299948,#299949,#299950,#299951,#299952,
#299953,#299954,#299955,#299956,#299957,#299958,#299959,#299960,#299961,
#299962,#299963,#299964,#299965,#299966,#299967,#299968,#299969,#299970,
#299971,#299972,#299973,#299974,#299975,#299976,#299977,#299978,#299979,
#299980,#299981,#299982,#299983,#299984,#299985,#299986,#299987,#299988,
#299989,#299990,#299991,#299992,#299993,#299994,#299995,#299996,#299997,
#299998,#299999,#300000,#300001,#300002,#300003,#300004,#300005,#300006,
#300007,#300008,#300009,#300010,#300011,#300012,#300013,#300014,#300015,
#300016,#300017,#300018,#300019,#300020,#300021,#300022,#300023,#300024,
#300025,#300026,#300027,#300028,#300029,#300030,#300031,#300032,#300033,
#300034,#300035,#300036,#300037,#300038,#300039,#300040,#300041,#300042,
#300043,#300044,#300045,#300046,#300047,#300048,#300049,#300050,#300051,
#300052,#300053,#300054,#300055,#300056,#300057,#300058,#300059,#300060,
#300061,#300062,#300063,#300064,#300065,#300066,#300067,#300068,#300069,
#300070,#300071,#300072,#300073,#300074,#300075,#300076,#300077,#300078,
#300079,#300080,#300081,#300082,#300083,#300084,#300085,#300086,#300087,
#300088,#300089,#300090,#300091,#300092,#300093,#300094,#300095,#300096,
#300097,#300098,#300099,#300100,#300101,#300102,#300103,#300104,#300105,
#300106,#300107,#300108,#300109,#300110,#300111,#300112,#300113,#300114,
#300115,#300116,#300117,#300118,#300119,#300120,#300121,#300122,#300123,
#300124,#300125,#300126,#300127,#300128,#300129,#300130,#300131,#300132,
#300133,#300134,#300135,#300136,#300137,#300138,#300139,#300140,#300141,
#300142,#300143,#300144,#300145,#300146,#300147,#300148,#300149,#300150,
#300151,#300152,#300153,#300154,#300155,#300156,#300157,#300158,#300159,
#300160,#300161,#300162,#300163,#300164,#300165,#300166,#300167,#300168,
#300169,#300170,#300171,#300172,#300173,#300174,#300175,#300176,#300177,
#300178,#300179,#300180,#300181,#300182,#300183,#300184,#300185,#300186,
#300187,#300188,#300189,#300190,#300191,#300192,#300193,#300194,#300195,
#300196,#300197,#300198,#300199,#300200,#300201,#300202,#300203,#300204,
#300205,#300206,#300207,#300208,#300209,#300210,#300211,#300212,#300213,
#300214,#300215,#300216,#300217,#300218,#300219,#300220,#300221,#300222,
#300223,#300224,#300225,#300226,#300227,#300228,#300229,#300230,#300231,
#300232,#300233,#300234,#300235,#300236,#300237,#300238,#300239,#300240,
#300241,#300242,#300243,#300244,#300245,#300246,#300247,#300248,#300249,
#300250,#300251,#300252,#300253,#300254,#300255,#300256,#300257,#300258,
#300259,#300260,#300261,#300262,#300263,#300264,#300265,#300266,#300267,
#300268,#300269,#300270,#300271,#300272,#300273,#300274,#300275,#300276,
#300277,#300278,#300279,#300280,#300281,#300282,#300283,#300284,#300285,
#300286,#300287,#300288,#300289,#300290,#300291,#300292,#300293,#300294,
#300295,#300296,#300297,#300298,#300299,#300300,#300301,#300302,#300303,
#300304,#300305,#300306,#300307,#300308,#300309,#300310,#300311,#300312,
#300313,#300314,#300315,#300316,#300317,#300318,#300319,#300320,#300321,
#300322,#300323,#300324,#300325,#300326,#300327,#300328,#300329,#300330,
#300331,#300332,#300333,#300334,#300335,#300336,#300337,#300338,#300339,
#300340,#300341,#300342,#300343,#300344,#300345,#300346,#300347,#300348,
#300349,#300350,#300351,#300352,#300353,#300354,#300355,#300356,#300357,
#300358,#300359,#300360,#300361,#300362,#300363,#300364,#300365,#300366,
#300367,#300368,#300369,#300370,#300371,#300372,#300373,#300374,#300375,
#300376,#300377,#300378,#300379,#300380,#300381,#300382,#300383,#300384,
#300385,#300386,#300387,#300388,#300389,#300390,#300391,#300392,#300393,
#300394,#300395,#300396,#300397,#300398,#300399,#300400,#300401,#300402,
#300403,#300404,#300405,#300406,#300407,#300408,#300409,#300410,#300411,
#300412,#300413,#300414,#300415,#300416,#300417,#300418,#300419,#300420,
#300421,#300422,#300423,#300424,#300425,#300426,#300427,#300428,#300429,
#300430,#300431,#300432,#300433,#300434,#300435,#300436,#300437,#300438,
#300439,#300440,#300441,#300442,#300443,#300444,#300445,#300446,#300447,
#300448,#300449,#300450,#300451,#300452,#300453,#300454,#300455,#300456,
#300457,#300458,#300459,#300460,#300461,#300462,#300463,#300464,#300465,
#300466,#300467,#300468,#300469,#300470,#300471,#300472,#300473,#300474,
#300475,#300476,#300477,#300478,#300479,#300480,#300481,#300482,#300483,
#300484,#300485,#300486,#300487,#300488,#300489,#300490,#300491,#300492,
#300493,#300494,#300495,#300496,#300497,#300498,#300499,#300500,#300501,
#300502,#300503,#300504,#300505,#300506,#300507,#300508,#300509,#300510,
#300511,#300512,#300513,#300514,#300515,#300516,#300517,#300518,#300519,
#300520,#300521,#300522,#300523,#300524,#300525,#300526,#300527,#300528,
#300529,#300530,#300531,#300532,#300533,#300534,#300535)),.UNSPECIFIED.,
 .F.,.F.,.F.)
B_SPLINE_SURFACE_WITH_KNOTS((2,2),(3,2,2,2,2,2,2,2,2,2,2,2,2,2,2,2,2,2,
2,2,2,2,2,2,2,2,2,2,2,2,2,2,2,2,2,2,2,2,2,2,2,2,2,2,2,2,2,2,2,2,2,2,2,2,
2,2,2,2,2,2,2,2,2,2,2,2,2,2,2,2,2,2,2,2,2,2,2,2,2,2,2,2,2,2,2,2,2,2,2,2,
2,2,2,2,2,2,2,2,2,2,2,2,2,2,2,2,2,2,2,2,2,2,2,2,2,2,2,2,2,2,2,2,2,2,2,2,
2,2,2,2,2,2,2,2,2,2,2,2,2,2,2,2,2,2,2,2,2,2,2,2,2,2,2,2,2,2,2,2,2,2,2,2,
2,2,2,2,2,2,2,2,2,2,2,2,2,2,2,2,2,2,2,2,2,2,2,2,2,2,2,2,2,2,2,2,2,2,2,2,
2,2,2,2,2,2,2,2,2,2,2,2,2,2,2,2,2,2,2,2,2,2,2,2,2,2,2,2,2,2,2,2,2,2,2,2,
2,2,2,2,2,2,2,2,2,2,2,2,2,2,2,2,2,2,2,2,2,2,2,2,2,2,2,2,2,2,2,2,2,2,2,2,
2,2,2,2,2,2,2,2,2,2,2,2,2,2,2,2,2,2,2,2,2,2,2,2,2,2,2,2,2,2,2,2,2,2,2,2,
2,2,2,2,2,2,2,2,2,2,2,2,2,2,2,2,2,2,2,2,2,2,2,2,2,2,2,2,2,2,2,2,2,2,2,2,
2,2,2,2,2,2,2,2,2,2,2,2,2,2,2,2,2,2,2,2,2,2,2,2,2,2,2,2,2,2,2,2,2,2,2,2,
2,2,2,2,2,2,2,2,2,2,2,2,2,2,2,2,2,2,2,2,2,2,2,2,2,2,2,2,2,2,2,2,2,2,2,2,
2,2,2,2,2,2,2,2,2,2,2,2,2,2,2,2,2,2,2,2,2,2,2,2,2,2,2,2,2,2,2,2,2,2,2,2,
2,2,2,2,2,2,2,2,2,2,2,2,2,2,2,2,2,2,2,2,2,2,2,2,2,2,2,2,2,2,2,2,2,2,2,2,
2,2,2,2,2,2,2,2,2,2,2,2,2,2,2,2,2,2,2,2,2,2,2,2,2,2,2,2,2,2,2,2,3),(0.,
1.),(0.,0.00192307692307692,0.00384615384615385,0.00576923076923077,0.00769230769230769,
0.00961538461538462,0.0115384615384615,0.0134615384615385,0.0153846153846154,
0.0173076923076923,0.0192307692307692,0.0211538461538462,0.0230769230769231,
0.025,0.0269230769230769,0.0288461538461538,0.0307692307692308,0.0326923076923077,
0.0346153846153846,0.0365384615384615,0.0384615384615385,0.0403846153846154,
0.0423076923076923,0.0442307692307692,0.0461538461538462,0.0480769230769231,
0.05,0.0519230769230769,0.0538461538461538,0.0557692307692308,0.0576923076923077,
0.0596153846153846,0.0615384615384615,0.0634615384615385,0.0653846153846154,
0.0673076923076923,0.0692307692307692,0.0711538461538462,0.0730769230769231,
0.075,0.0769230769230769,0.0788461538461538,0.0807692307692308,0.0826923076923077,
0.0846153846153846,0.0865384615384615,0.0884615384615385,0.0903846153846154,
0.0923076923076923,0.0942307692307692,0.0961538461538462,0.0980769230769231,
0.1,0.101923076923077,0.103846153846154,0.105769230769231,0.107692307692308,
0.109615384615385,0.111538461538462,0.113461538461538,0.115384615384615,
0.117307692307692,0.119230769230769,0.121153846153846,0.123076923076923,
0.125,0.126923076923077,0.128846153846154,0.130769230769231,0.132692307692308,
0.134615384615385,0.136538461538462,0.138461538461538,0.140384615384615,
0.142307692307692,0.144230769230769,0.146153846153846,0.148076923076923,
0.15,0.151923076923077,0.153846153846154,0.155769230769231,0.157692307692308,
0.159615384615385,0.161538461538462,0.163461538461538,0.165384615384615,
0.167307692307692,0.169230769230769,0.171153846153846,0.173076923076923,
0.175,0.176923076923077,0.178846153846154,0.180769230769231,0.182692307692308,
0.184615384615385,0.186538461538462,0.188461538461538,0.190384615384615,
0.192307692307692,0.194230769230769,0.196153846153846,0.198076923076923,
0.2,0.201923076923077,0.203846153846154,0.205769230769231,0.207692307692308,
0.209615384615385,0.211538461538462,0.213461538461538,0.215384615384615,
0.217307692307692,0.219230769230769,0.221153846153846,0.223076923076923,
0.225,0.226923076923077,0.228846153846154,0.230769230769231,0.232692307692308,
0.234615384615385,0.236538461538462,0.238461538461538,0.240384615384615,
0.242307692307692,0.244230769230769,0.246153846153846,0.248076923076923,
0.25,0.251923076923077,0.253846153846154,0.255769230769231,0.257692307692308,
0.259615384615385,0.261538461538462,0.263461538461538,0.265384615384615,
0.267307692307692,0.269230769230769,0.271153846153846,0.273076923076923,
0.275,0.276923076923077,0.278846153846154,0.280769230769231,0.282692307692308,
0.284615384615385,0.286538461538462,0.288461538461538,0.290384615384615,
0.292307692307692,0.294230769230769,0.296153846153846,0.298076923076923,
0.3,0.301923076923077,0.303846153846154,0.305769230769231,0.307692307692308,
0.309615384615385,0.311538461538462,0.313461538461538,0.315384615384615,
0.317307692307692,0.319230769230769,0.321153846153846,0.323076923076923,
0.325,0.326923076923077,0.328846153846154,0.330769230769231,0.332692307692308,
0.334615384615385,0.336538461538462,0.338461538461538,0.340384615384615,
0.342307692307692,0.344230769230769,0.346153846153846,0.348076923076923,
0.35,0.351923076923077,0.353846153846154,0.355769230769231,0.357692307692308,
0.359615384615385,0.361538461538462,0.363461538461538,0.365384615384615,
0.367307692307692,0.369230769230769,0.371153846153846,0.373076923076923,
0.375,0.376923076923077,0.378846153846154,0.380769230769231,0.382692307692308,
0.384615384615385,0.386538461538462,0.388461538461538,0.390384615384615,
0.392307692307692,0.394230769230769,0.396153846153846,0.398076923076923,
0.4,0.401923076923077,0.403846153846154,0.405769230769231,0.407692307692308,
0.409615384615385,0.411538461538462,0.413461538461538,0.415384615384615,
0.417307692307692,0.419230769230769,0.421153846153846,0.423076923076923,
0.425,0.426923076923077,0.428846153846154,0.430769230769231,0.432692307692308,
0.434615384615385,0.436538461538462,0.438461538461538,0.440384615384615,
0.442307692307692,0.444230769230769,0.446153846153846,0.448076923076923,
0.45,0.451923076923077,0.453846153846154,0.455769230769231,0.457692307692308,
0.459615384615385,0.461538461538462,0.463461538461538,0.465384615384615,
0.467307692307692,0.469230769230769,0.471153846153846,0.473076923076923,
0.475,0.476923076923077,0.478846153846154,0.480769230769231,0.482692307692308,
0.484615384615385,0.486538461538462,0.488461538461538,0.490384615384615,
0.492307692307692,0.494230769230769,0.496153846153846,0.498076923076923,
0.5,0.501923076923077,0.503846153846154,0.505769230769231,0.507692307692308,
0.509615384615385,0.511538461538461,0.513461538461538,0.515384615384615,
0.517307692307692,0.519230769230769,0.521153846153846,0.523076923076923,
0.525,0.526923076923077,0.528846153846154,0.530769230769231,0.532692307692308,
0.534615384615385,0.536538461538462,0.538461538461538,0.540384615384615,
0.542307692307692,0.544230769230769,0.546153846153846,0.548076923076923,
0.55,0.551923076923077,0.553846153846154,0.555769230769231,0.557692307692308,
0.559615384615385,0.561538461538462,0.563461538461538,0.565384615384615,
0.567307692307692,0.569230769230769,0.571153846153846,0.573076923076923,
0.575,0.576923076923077,0.578846153846154,0.580769230769231,0.582692307692308,
0.584615384615385,0.586538461538462,0.588461538461538,0.590384615384615,
0.592307692307692,0.594230769230769,0.596153846153846,0.598076923076923,
0.6,0.601923076923077,0.603846153846154,0.605769230769231,0.607692307692308,
0.609615384615385,0.611538461538462,0.613461538461539,0.615384615384615,
0.617307692307692,0.619230769230769,0.621153846153846,0.623076923076923,
0.625,0.626923076923077,0.628846153846154,0.630769230769231,0.632692307692308,
0.634615384615385,0.636538461538461,0.638461538461538,0.640384615384615,
0.642307692307692,0.644230769230769,0.646153846153846,0.648076923076923,
0.65,0.651923076923077,0.653846153846154,0.655769230769231,0.657692307692308,
0.659615384615385,0.661538461538462,0.663461538461538,0.665384615384615,
0.667307692307692,0.669230769230769,0.671153846153846,0.673076923076923,
0.675,0.676923076923077,0.678846153846154,0.680769230769231,0.682692307692308,
0.684615384615385,0.686538461538462,0.688461538461538,0.690384615384615,
0.692307692307692,0.694230769230769,0.696153846153846,0.698076923076923,
0.7,0.701923076923077,0.703846153846154,0.705769230769231,0.707692307692308,
0.709615384615385,0.711538461538462,0.713461538461538,0.715384615384615,
0.717307692307692,0.719230769230769,0.721153846153846,0.723076923076923,
0.725,0.726923076923077,0.728846153846154,0.730769230769231,0.732692307692308,
0.734615384615385,0.736538461538462,0.738461538461539,0.740384615384615,
0.742307692307692,0.744230769230769,0.746153846153846,0.748076923076923,
0.75,0.751923076923077,0.753846153846154,0.755769230769231,0.757692307692308,
0.759615384615385,0.761538461538461,0.763461538461538,0.765384615384615,
0.767307692307692,0.769230769230769,0.771153846153846,0.773076923076923,
0.775,0.776923076923077,0.778846153846154,0.780769230769231,0.782692307692308,
0.784615384615385,0.786538461538462,0.788461538461538,0.790384615384615,
0.792307692307692,0.794230769230769,0.796153846153846,0.798076923076923,
0.8,0.801923076923077,0.803846153846154,0.805769230769231,0.807692307692308,
0.809615384615385,0.811538461538462,0.813461538461538,0.815384615384615,
0.817307692307692,0.819230769230769,0.821153846153846,0.823076923076923,
0.825,0.826923076923077,0.828846153846154,0.830769230769231,0.832692307692308,
0.834615384615385,0.836538461538462,0.838461538461538,0.840384615384615,
0.842307692307692,0.844230769230769,0.846153846153846,0.848076923076923,
0.85,0.851923076923077,0.853846153846154,0.855769230769231,0.857692307692308,
0.859615384615385,0.861538461538462,0.863461538461539,0.865384615384615,
0.867307692307692,0.869230769230769,0.871153846153846,0.873076923076923,
0.875,0.876923076923077,0.878846153846154,0.880769230769231,0.882692307692308,
0.884615384615385,0.886538461538461,0.888461538461538,0.890384615384615,
0.892307692307692,0.894230769230769,0.896153846153846,0.898076923076923,
0.9,0.901923076923077,0.903846153846154,0.905769230769231,0.907692307692308,
0.909615384615385,0.911538461538462,0.913461538461538,0.915384615384615,
0.917307692307692,0.919230769230769,0.921153846153846,0.923076923076923,
0.925,0.926923076923077,0.928846153846154,0.930769230769231,0.932692307692308,
0.934615384615385,0.936538461538462,0.938461538461538,0.940384615384615,
0.942307692307692,0.944230769230769,0.946153846153846,0.948076923076923,
0.95,0.951923076923077,0.953846153846154,0.955769230769231,0.957692307692308,
0.959615384615385,0.961538461538462,0.963461538461538,0.965384615384615,
0.967307692307692,0.969230769230769,0.971153846153846,0.973076923076923,
0.975,0.976923076923077,0.978846153846154,0.980769230769231,0.982692307692308,
0.984615384615385,0.986538461538462,0.988461538461539,0.990384615384615,
0.992307692307692,0.994230769230769,0.996153846153846),.UNSPECIFIED.)
GEOMETRIC_REPRESENTATION_ITEM()
RATIONAL_B_SPLINE_SURFACE(((1.,0.951056516295154,1.,0.951056516295154,1.,
0.951056516295154,1.,0.951056516295154,1.,0.951056516295154,1.,0.951056516295154,
1.,0.951056516295154,1.,0.951056516295154,1.,0.951056516295154,1.,0.951056516295154,
1.,0.951056516295154,1.,0.951056516295154,1.,0.951056516295154,1.,0.951056516295154,
1.,0.951056516295154,1.,0.951056516295154,1.,0.951056516295154,1.,0.951056516295154,
1.,0.951056516295154,1.,0.951056516295154,1.,0.951056516295154,1.,0.951056516295154,
1.,0.951056516295154,1.,0.951056516295154,1.,0.951056516295154,1.,0.951056516295154,
1.,0.951056516295154,1.,0.951056516295154,1.,0.951056516295154,1.,0.951056516295154,
1.,0.951056516295154,1.,0.951056516295154,1.,0.951056516295154,1.,0.951056516295154,
1.,0.951056516295154,1.,0.951056516295154,1.,0.951056516295154,1.,0.951056516295154,
1.,0.951056516295154,1.,0.951056516295154,1.,0.951056516295154,1.,0.951056516295154,
1.,0.951056516295154,1.,0.951056516295154,1.,0.951056516295154,1.,0.951056516295154,
1.,0.951056516295154,1.,0.951056516295154,1.,0.951056516295154,1.,0.951056516295154,
1.,0.951056516295154,1.,0.951056516295154,1.,0.951056516295154,1.,0.951056516295154,
1.,0.951056516295154,1.,0.951056516295154,1.,0.951056516295154,1.,0.951056516295154,
1.,0.951056516295154,1.,0.951056516295154,1.,0.951056516295154,1.,0.951056516295154,
1.,0.951056516295154,1.,0.951056516295154,1.,0.951056516295154,1.,0.951056516295154,
1.,0.951056516295154,1.,0.951056516295154,1.,0.951056516295154,1.,0.951056516295154,
1.,0.951056516295154,1.,0.951056516295154,1.,0.951056516295154,1.,0.951056516295154,
1.,0.951056516295154,1.,0.951056516295154,1.,0.951056516295154,1.,0.951056516295154,
1.,0.951056516295154,1.,0.951056516295154,1.,0.951056516295154,1.,0.951056516295154,
1.,0.951056516295154,1.,0.951056516295154,1.,0.951056516295154,1.,0.951056516295154,
1.,0.951056516295154,1.,0.951056516295154,1.,0.951056516295154,1.,0.951056516295154,
1.,0.951056516295154,1.,0.951056516295154,1.,0.951056516295154,1.,0.951056516295154,
1.,0.951056516295154,1.,0.951056516295154,1.,0.951056516295154,1.,0.951056516295154,
1.,0.951056516295154,1.,0.951056516295154,1.,0.951056516295154,1.,0.951056516295154,
1.,0.951056516295154,1.,0.951056516295154,1.,0.951056516295154,1.,0.951056516295154,
1.,0.951056516295154,1.,0.951056516295154,1.,0.951056516295154,1.,0.951056516295154,
1.,0.951056516295154,1.,0.951056516295154,1.,0.951056516295154,1.,0.951056516295154,
1.,0.951056516295154,1.,0.951056516295154,1.,0.951056516295154,1.,0.951056516295154,
1.,0.951056516295154,1.,0.951056516295154,1.,0.951056516295154,1.,0.951056516295154,
1.,0.951056516295154,1.,0.951056516295154,1.,0.951056516295154,1.,0.951056516295154,
1.,0.951056516295154,1.,0.951056516295154,1.,0.951056516295154,1.,0.951056516295154,
1.,0.951056516295154,1.,0.951056516295154,1.,0.951056516295154,1.,0.951056516295154,
1.,0.951056516295154,1.,0.951056516295154,1.,0.951056516295154,1.,0.951056516295154,
1.,0.951056516295154,1.,0.951056516295154,1.,0.951056516295154,1.,0.951056516295154,
1.,0.951056516295154,1.,0.951056516295154,1.,0.951056516295154,1.,0.951056516295154,
1.,0.951056516295154,1.,0.951056516295154,1.,0.951056516295154,1.,0.951056516295154,
1.,0.951056516295154,1.,0.951056516295154,1.,0.951056516295154,1.,0.951056516295154,
1.,0.951056516295154,1.,0.951056516295154,1.,0.951056516295154,1.,0.951056516295154,
1.,0.951056516295154,1.,0.951056516295154,1.,0.951056516295154,1.,0.951056516295154,
1.,0.951056516295154,1.,0.951056516295154,1.,0.951056516295154,1.,0.951056516295154,
1.,0.951056516295154,1.,0.951056516295154,1.,0.951056516295154,1.,0.951056516295154,
1.,0.951056516295154,1.,0.951056516295154,1.,0.951056516295154,1.,0.951056516295154,
1.,0.951056516295154,1.,0.951056516295154,1.,0.951056516295154,1.,0.951056516295154,
1.,0.951056516295154,1.,0.951056516295154,1.,0.951056516295154,1.,0.951056516295154,
1.,0.951056516295154,1.,0.951056516295154,1.,0.951056516295154,1.,0.951056516295154,
1.,0.951056516295154,1.,0.951056516295154,1.,0.951056516295154,1.,0.951056516295154,
1.,0.951056516295154,1.,0.951056516295154,1.,0.951056516295154,1.,0.951056516295154,
1.,0.951056516295154,1.,0.951056516295154,1.,0.951056516295154,1.,0.951056516295154,
1.,0.951056516295154,1.,0.951056516295154,1.,0.951056516295154,1.,0.951056516295154,
1.,0.951056516295154,1.,0.951056516295154,1.,0.951056516295154,1.,0.951056516295154,
1.,0.951056516295154,1.,0.951056516295154,1.,0.951056516295154,1.,0.951056516295154,
1.,0.951056516295154,1.,0.951056516295154,1.,0.951056516295154,1.,0.951056516295154,
1.,0.951056516295154,1.,0.951056516295154,1.,0.951056516295154,1.,0.951056516295154,
1.,0.951056516295154,1.,0.951056516295154,1.,0.951056516295154,1.,0.951056516295154,
1.,0.951056516295154,1.,0.951056516295154,1.,0.951056516295154,1.,0.951056516295154,
1.,0.951056516295154,1.,0.951056516295154,1.,0.951056516295154,1.,0.951056516295154,
1.,0.951056516295154,1.,0.951056516295154,1.,0.951056516295154,1.,0.951056516295154,
1.,0.951056516295154,1.,0.951056516295154,1.,0.951056516295154,1.,0.951056516295154,
1.,0.951056516295154,1.,0.951056516295154,1.,0.951056516295154,1.,0.951056516295154,
1.,0.951056516295154,1.,0.951056516295154,1.,0.951056516295154,1.,0.951056516295154,
1.,0.951056516295154,1.,0.951056516295154,1.,0.951056516295154,1.,0.951056516295154,
1.,0.951056516295154,1.,0.951056516295154,1.,0.951056516295154,1.,0.951056516295154,
1.,0.951056516295154,1.,0.951056516295154,1.,0.951056516295154,1.,0.951056516295154,
1.,0.951056516295154,1.,0.951056516295154,1.,0.951056516295154,1.,0.951056516295154,
1.,0.951056516295154,1.,0.951056516295154,1.,0.951056516295154,1.,0.951056516295154,
1.,0.951056516295154,1.,0.951056516295154,1.,0.951056516295154,1.,0.951056516295154,
1.,0.951056516295154,1.,0.951056516295154,1.,0.951056516295154,1.,0.951056516295154,
1.,0.951056516295154,1.,0.951056516295154,1.,0.951056516295154,1.,0.951056516295154,
1.,0.951056516295154,1.,0.951056516295154,1.,0.951056516295154,1.,0.951056516295154,
1.,0.951056516295154,1.,0.951056516295154,1.,0.951056516295154,1.,0.951056516295154,
1.,0.951056516295154,1.,0.951056516295154,1.,0.951056516295154,1.,0.951056516295154,
1.,0.951056516295154,1.,0.951056516295154,1.,0.951056516295154,1.,0.951056516295154,
1.,0.951056516295154,1.,0.951056516295154,1.,0.951056516295154,1.,0.951056516295154,
1.,0.951056516295154,1.,0.951056516295154,1.,0.951056516295154,1.,0.951056516295154,
1.,0.951056516295154,1.,0.951056516295154,1.,0.951056516295154,1.,0.951056516295154,
1.,0.951056516295154,1.,0.951056516295154,1.,0.951056516295154,1.,0.951056516295154,
1.,0.951056516295154,1.,0.951056516295154,1.,0.951056516295154,1.,0.951056516295154,
1.,0.951056516295154,1.,0.951056516295154,1.,0.951056516295154,1.,0.951056516295154,
1.,0.951056516295154,1.,0.951056516295154,1.,0.951056516295154,1.,0.951056516295154,
1.,0.951056516295154,1.,0.951056516295154,1.,0.951056516295154,1.,0.951056516295154,
1.,0.951056516295154,1.,0.951056516295154,1.,0.951056516295154,1.,0.951056516295154,
1.,0.951056516295154,1.,0.951056516295154,1.,0.951056516295154,1.,0.951056516295154,
1.,0.951056516295154,1.,0.951056516295154,1.,0.951056516295154,1.,0.951056516295154,
1.,0.951056516295154,1.,0.951056516295154,1.,0.951056516295154,1.,0.951056516295154,
1.,0.951056516295154,1.,0.951056516295154,1.,0.951056516295154,1.,0.951056516295154,
1.,0.951056516295154,1.,0.951056516295154,1.,0.951056516295154,1.,0.951056516295154,
1.,0.951056516295154,1.,0.951056516295154,1.,0.951056516295154,1.,0.951056516295154,
1.,0.951056516295154,1.,0.951056516295154,1.,0.951056516295154,1.,0.951056516295154,
1.,0.951056516295154,1.,0.951056516295154,1.,0.951056516295154,1.,0.951056516295154,
1.,0.951056516295154,1.,0.951056516295154,1.,0.951056516295154,1.,0.951056516295154,
1.,0.951056516295154,1.,0.951056516295154,1.,0.951056516295154,1.,0.951056516295154,
1.,0.951056516295154,1.,0.951056516295154,1.,0.951056516295154,1.,0.951056516295154,
1.,0.951056516295154,1.,0.951056516295154,1.,0.951056516295154,1.,0.951056516295154,
1.,0.951056516295154,1.,0.951056516295154,1.,0.951056516295154,1.,0.951056516295154,
1.,0.951056516295154,1.,0.951056516295154,1.,0.951056516295154,1.,0.951056516295154,
1.,0.951056516295154,1.,0.951056516295154,1.,0.951056516295154,1.,0.951056516295154,
1.,0.951056516295154,1.,0.951056516295154,1.,0.951056516295154,1.,0.951056516295154,
1.,0.951056516295154,1.,0.951056516295154,1.,0.951056516295154,1.,0.951056516295154,
1.,0.951056516295154,1.,0.951056516295154,1.,0.951056516295154,1.,0.951056516295154,
1.,0.951056516295154,1.,0.951056516295154,1.,0.951056516295154,1.,0.951056516295154,
1.,0.951056516295154,1.,0.951056516295154,1.,0.951056516295154,1.,0.951056516295154,
1.,0.951056516295154,1.,0.951056516295154,1.,0.951056516295154,1.,0.951056516295154,
1.,0.951056516295154,1.,0.951056516295154,1.,0.951056516295154,1.,0.951056516295154,
1.,0.951056516295154,1.,0.951056516295154,1.,0.951056516295154,1.,0.951056516295154,
1.,0.951056516295154,1.,0.951056516295154,1.,0.951056516295154,1.,0.951056516295154,
1.,0.951056516295154,1.,0.951056516295154,1.,0.951056516295154,1.,0.951056516295154,
1.,0.951056516295154,1.,0.951056516295154,1.,0.951056516295154,1.,0.951056516295154,
1.,0.951056516295154,1.,0.951056516295154,1.,0.951056516295154,1.,0.951056516295154,
1.,0.951056516295154,1.,0.951056516295154,1.,0.951056516295154,1.,0.951056516295154,
1.,0.951056516295154,1.,0.951056516295154,1.,0.951056516295154,1.,0.951056516295154,
1.,0.951056516295154,1.,0.951056516295154,1.,0.951056516295154,1.,0.951056516295154,
1.,0.951056516295154,1.,0.951056516295154,1.,0.951056516295154,1.,0.951056516295154,
1.,0.951056516295154,1.,0.951056516295154,1.,0.951056516295154,1.,0.951056516295154,
1.,0.951056516295154,1.,0.951056516295154,1.,0.951056516295154,1.,0.951056516295154,
1.,0.951056516295154,1.,0.951056516295154,1.,0.951056516295154,1.,0.951056516295154,
1.,0.951056516295154,1.,0.951056516295154,1.,0.951056516295154,1.,0.951056516295154,
1.,0.951056516295154,1.,0.951056516295154,1.,0.951056516295154,1.,0.951056516295154,
1.,0.951056516295154,1.,0.951056516295154,1.,0.951056516295154,1.,0.951056516295154,
1.,0.951056516295154,1.,0.951056516295154,1.,0.951056516295154,1.,0.951056516295154,
1.,0.951056516295154,1.,0.951056516295154,1.,0.951056516295154,1.,0.951056516295154,
1.,0.951056516295154,1.,0.951056516295154,1.,0.951056516295154,1.,0.951056516295154,
1.,0.951056516295154,1.,0.951056516295154,1.,0.951056516295154,1.,0.951056516295154,
1.,0.951056516295154,1.,0.951056516295154,1.,0.951056516295154,1.,0.951056516295154,
1.,0.951056516295154,1.,0.951056516295154,1.,0.951056516295154,1.,0.951056516295154,
1.,0.951056516295154,1.,0.951056516295154,1.,0.951056516295154,1.,0.951056516295154,
1.,0.951056516295154,1.,0.951056516295154,1.,0.951056516295154,1.,0.951056516295154,
1.,0.951056516295154,1.,0.951056516295154,1.,0.951056516295154,1.,0.951056516295154,
1.,0.951056516295154,1.,0.951056516295154,1.,0.951056516295154,1.,0.951056516295154,
1.),(1.,0.951056516295154,1.,0.951056516295154,1.,0.951056516295154,1.,
0.951056516295154,1.,0.951056516295154,1.,0.951056516295154,1.,0.951056516295154,
1.,0.951056516295154,1.,0.951056516295154,1.,0.951056516295154,1.,0.951056516295154,
1.,0.951056516295154,1.,0.951056516295154,1.,0.951056516295154,1.,0.951056516295154,
1.,0.951056516295154,1.,0.951056516295154,1.,0.951056516295154,1.,0.951056516295154,
1.,0.951056516295154,1.,0.951056516295154,1.,0.951056516295154,1.,0.951056516295154,
1.,0.951056516295154,1.,0.951056516295154,1.,0.951056516295154,1.,0.951056516295154,
1.,0.951056516295154,1.,0.951056516295154,1.,0.951056516295154,1.,0.951056516295154,
1.,0.951056516295154,1.,0.951056516295154,1.,0.951056516295154,1.,0.951056516295154,
1.,0.951056516295154,1.,0.951056516295154,1.,0.951056516295154,1.,0.951056516295154,
1.,0.951056516295154,1.,0.951056516295154,1.,0.951056516295154,1.,0.951056516295154,
1.,0.951056516295154,1.,0.951056516295154,1.,0.951056516295154,1.,0.951056516295154,
1.,0.951056516295154,1.,0.951056516295154,1.,0.951056516295154,1.,0.951056516295154,
1.,0.951056516295154,1.,0.951056516295154,1.,0.951056516295154,1.,0.951056516295154,
1.,0.951056516295154,1.,0.951056516295154,1.,0.951056516295154,1.,0.951056516295154,
1.,0.951056516295154,1.,0.951056516295154,1.,0.951056516295154,1.,0.951056516295154,
1.,0.951056516295154,1.,0.951056516295154,1.,0.951056516295154,1.,0.951056516295154,
1.,0.951056516295154,1.,0.951056516295154,1.,0.951056516295154,1.,0.951056516295154,
1.,0.951056516295154,1.,0.951056516295154,1.,0.951056516295154,1.,0.951056516295154,
1.,0.951056516295154,1.,0.951056516295154,1.,0.951056516295154,1.,0.951056516295154,
1.,0.951056516295154,1.,0.951056516295154,1.,0.951056516295154,1.,0.951056516295154,
1.,0.951056516295154,1.,0.951056516295154,1.,0.951056516295154,1.,0.951056516295154,
1.,0.951056516295154,1.,0.951056516295154,1.,0.951056516295154,1.,0.951056516295154,
1.,0.951056516295154,1.,0.951056516295154,1.,0.951056516295154,1.,0.951056516295154,
1.,0.951056516295154,1.,0.951056516295154,1.,0.951056516295154,1.,0.951056516295154,
1.,0.951056516295154,1.,0.951056516295154,1.,0.951056516295154,1.,0.951056516295154,
1.,0.951056516295154,1.,0.951056516295154,1.,0.951056516295154,1.,0.951056516295154,
1.,0.951056516295154,1.,0.951056516295154,1.,0.951056516295154,1.,0.951056516295154,
1.,0.951056516295154,1.,0.951056516295154,1.,0.951056516295154,1.,0.951056516295154,
1.,0.951056516295154,1.,0.951056516295154,1.,0.951056516295154,1.,0.951056516295154,
1.,0.951056516295154,1.,0.951056516295154,1.,0.951056516295154,1.,0.951056516295154,
1.,0.951056516295154,1.,0.951056516295154,1.,0.951056516295154,1.,0.951056516295154,
1.,0.951056516295154,1.,0.951056516295154,1.,0.951056516295154,1.,0.951056516295154,
1.,0.951056516295154,1.,0.951056516295154,1.,0.951056516295154,1.,0.951056516295154,
1.,0.951056516295154,1.,0.951056516295154,1.,0.951056516295154,1.,0.951056516295154,
1.,0.951056516295154,1.,0.951056516295154,1.,0.951056516295154,1.,0.951056516295154,
1.,0.951056516295154,1.,0.951056516295154,1.,0.951056516295154,1.,0.951056516295154,
1.,0.951056516295154,1.,0.951056516295154,1.,0.951056516295154,1.,0.951056516295154,
1.,0.951056516295154,1.,0.951056516295154,1.,0.951056516295154,1.,0.951056516295154,
1.,0.951056516295154,1.,0.951056516295154,1.,0.951056516295154,1.,0.951056516295154,
1.,0.951056516295154,1.,0.951056516295154,1.,0.951056516295154,1.,0.951056516295154,
1.,0.951056516295154,1.,0.951056516295154,1.,0.951056516295154,1.,0.951056516295154,
1.,0.951056516295154,1.,0.951056516295154,1.,0.951056516295154,1.,0.951056516295154,
1.,0.951056516295154,1.,0.951056516295154,1.,0.951056516295154,1.,0.951056516295154,
1.,0.951056516295154,1.,0.951056516295154,1.,0.951056516295154,1.,0.951056516295154,
1.,0.951056516295154,1.,0.951056516295154,1.,0.951056516295154,1.,0.951056516295154,
1.,0.951056516295154,1.,0.951056516295154,1.,0.951056516295154,1.,0.951056516295154,
1.,0.951056516295154,1.,0.951056516295154,1.,0.951056516295154,1.,0.951056516295154,
1.,0.951056516295154,1.,0.951056516295154,1.,0.951056516295154,1.,0.951056516295154,
1.,0.951056516295154,1.,0.951056516295154,1.,0.951056516295154,1.,0.951056516295154,
1.,0.951056516295154,1.,0.951056516295154,1.,0.951056516295154,1.,0.951056516295154,
1.,0.951056516295154,1.,0.951056516295154,1.,0.951056516295154,1.,0.951056516295154,
1.,0.951056516295154,1.,0.951056516295154,1.,0.951056516295154,1.,0.951056516295154,
1.,0.951056516295154,1.,0.951056516295154,1.,0.951056516295154,1.,0.951056516295154,
1.,0.951056516295154,1.,0.951056516295154,1.,0.951056516295154,1.,0.951056516295154,
1.,0.951056516295154,1.,0.951056516295154,1.,0.951056516295154,1.,0.951056516295154,
1.,0.951056516295154,1.,0.951056516295154,1.,0.951056516295154,1.,0.951056516295154,
1.,0.951056516295154,1.,0.951056516295154,1.,0.951056516295154,1.,0.951056516295154,
1.,0.951056516295154,1.,0.951056516295154,1.,0.951056516295154,1.,0.951056516295154,
1.,0.951056516295154,1.,0.951056516295154,1.,0.951056516295154,1.,0.951056516295154,
1.,0.951056516295154,1.,0.951056516295154,1.,0.951056516295154,1.,0.951056516295154,
1.,0.951056516295154,1.,0.951056516295154,1.,0.951056516295154,1.,0.951056516295154,
1.,0.951056516295154,1.,0.951056516295154,1.,0.951056516295154,1.,0.951056516295154,
1.,0.951056516295154,1.,0.951056516295154,1.,0.951056516295154,1.,0.951056516295154,
1.,0.951056516295154,1.,0.951056516295154,1.,0.951056516295154,1.,0.951056516295154,
1.,0.951056516295154,1.,0.951056516295154,1.,0.951056516295154,1.,0.951056516295154,
1.,0.951056516295154,1.,0.951056516295154,1.,0.951056516295154,1.,0.951056516295154,
1.,0.951056516295154,1.,0.951056516295154,1.,0.951056516295154,1.,0.951056516295154,
1.,0.951056516295154,1.,0.951056516295154,1.,0.951056516295154,1.,0.951056516295154,
1.,0.951056516295154,1.,0.951056516295154,1.,0.951056516295154,1.,0.951056516295154,
1.,0.951056516295154,1.,0.951056516295154,1.,0.951056516295154,1.,0.951056516295154,
1.,0.951056516295154,1.,0.951056516295154,1.,0.951056516295154,1.,0.951056516295154,
1.,0.951056516295154,1.,0.951056516295154,1.,0.951056516295154,1.,0.951056516295154,
1.,0.951056516295154,1.,0.951056516295154,1.,0.951056516295154,1.,0.951056516295154,
1.,0.951056516295154,1.,0.951056516295154,1.,0.951056516295154,1.,0.951056516295154,
1.,0.951056516295154,1.,0.951056516295154,1.,0.951056516295154,1.,0.951056516295154,
1.,0.951056516295154,1.,0.951056516295154,1.,0.951056516295154,1.,0.951056516295154,
1.,0.951056516295154,1.,0.951056516295154,1.,0.951056516295154,1.,0.951056516295154,
1.,0.951056516295154,1.,0.951056516295154,1.,0.951056516295154,1.,0.951056516295154,
1.,0.951056516295154,1.,0.951056516295154,1.,0.951056516295154,1.,0.951056516295154,
1.,0.951056516295154,1.,0.951056516295154,1.,0.951056516295154,1.,0.951056516295154,
1.,0.951056516295154,1.,0.951056516295154,1.,0.951056516295154,1.,0.951056516295154,
1.,0.951056516295154,1.,0.951056516295154,1.,0.951056516295154,1.,0.951056516295154,
1.,0.951056516295154,1.,0.951056516295154,1.,0.951056516295154,1.,0.951056516295154,
1.,0.951056516295154,1.,0.951056516295154,1.,0.951056516295154,1.,0.951056516295154,
1.,0.951056516295154,1.,0.951056516295154,1.,0.951056516295154,1.,0.951056516295154,
1.,0.951056516295154,1.,0.951056516295154,1.,0.951056516295154,1.,0.951056516295154,
1.,0.951056516295154,1.,0.951056516295154,1.,0.951056516295154,1.,0.951056516295154,
1.,0.951056516295154,1.,0.951056516295154,1.,0.951056516295154,1.,0.951056516295154,
1.,0.951056516295154,1.,0.951056516295154,1.,0.951056516295154,1.,0.951056516295154,
1.,0.951056516295154,1.,0.951056516295154,1.,0.951056516295154,1.,0.951056516295154,
1.,0.951056516295154,1.,0.951056516295154,1.,0.951056516295154,1.,0.951056516295154,
1.,0.951056516295154,1.,0.951056516295154,1.,0.951056516295154,1.,0.951056516295154,
1.,0.951056516295154,1.,0.951056516295154,1.,0.951056516295154,1.,0.951056516295154,
1.,0.951056516295154,1.,0.951056516295154,1.,0.951056516295154,1.,0.951056516295154,
1.,0.951056516295154,1.,0.951056516295154,1.,0.951056516295154,1.,0.951056516295154,
1.,0.951056516295154,1.,0.951056516295154,1.,0.951056516295154,1.,0.951056516295154,
1.,0.951056516295154,1.,0.951056516295154,1.,0.951056516295154,1.,0.951056516295154,
1.,0.951056516295154,1.,0.951056516295154,1.,0.951056516295154,1.,0.951056516295154,
1.,0.951056516295154,1.,0.951056516295154,1.,0.951056516295154,1.,0.951056516295154,
1.,0.951056516295154,1.,0.951056516295154,1.,0.951056516295154,1.,0.951056516295154,
1.,0.951056516295154,1.,0.951056516295154,1.,0.951056516295154,1.,0.951056516295154,
1.,0.951056516295154,1.,0.951056516295154,1.,0.951056516295154,1.,0.951056516295154,
1.,0.951056516295154,1.,0.951056516295154,1.,0.951056516295154,1.,0.951056516295154,
1.,0.951056516295154,1.,0.951056516295154,1.,0.951056516295154,1.,0.951056516295154,
1.,0.951056516295154,1.,0.951056516295154,1.,0.951056516295154,1.,0.951056516295154,
1.,0.951056516295154,1.,0.951056516295154,1.,0.951056516295154,1.,0.951056516295154,
1.,0.951056516295154,1.,0.951056516295154,1.,0.951056516295154,1.,0.951056516295154,
1.,0.951056516295154,1.,0.951056516295154,1.,0.951056516295154,1.,0.951056516295154,
1.,0.951056516295154,1.,0.951056516295154,1.,0.951056516295154,1.,0.951056516295154,
1.,0.951056516295154,1.,0.951056516295154,1.,0.951056516295154,1.,0.951056516295154,
1.,0.951056516295154,1.,0.951056516295154,1.,0.951056516295154,1.,0.951056516295154,
1.,0.951056516295154,1.,0.951056516295154,1.,0.951056516295154,1.,0.951056516295154,
1.,0.951056516295154,1.,0.951056516295154,1.,0.951056516295154,1.,0.951056516295154,
1.,0.951056516295154,1.,0.951056516295154,1.,0.951056516295154,1.,0.951056516295154,
1.,0.951056516295154,1.,0.951056516295154,1.,0.951056516295154,1.,0.951056516295154,
1.,0.951056516295154,1.,0.951056516295154,1.,0.951056516295154,1.,0.951056516295154,
1.,0.951056516295154,1.,0.951056516295154,1.,0.951056516295154,1.,0.951056516295154,
1.,0.951056516295154,1.,0.951056516295154,1.,0.951056516295154,1.,0.951056516295154,
1.,0.951056516295154,1.,0.951056516295154,1.,0.951056516295154,1.,0.951056516295154,
1.,0.951056516295154,1.,0.951056516295154,1.,0.951056516295154,1.,0.951056516295154,
1.,0.951056516295154,1.,0.951056516295154,1.,0.951056516295154,1.,0.951056516295154,
1.,0.951056516295154,1.,0.951056516295154,1.,0.951056516295154,1.,0.951056516295154,
1.,0.951056516295154,1.,0.951056516295154,1.,0.951056516295154,1.,0.951056516295154,
1.,0.951056516295154,1.,0.951056516295154,1.,0.951056516295154,1.,0.951056516295154,
1.,0.951056516295154,1.,0.951056516295154,1.,0.951056516295154,1.,0.951056516295154,
1.,0.951056516295154,1.,0.951056516295154,1.,0.951056516295154,1.,0.951056516295154,
1.,0.951056516295154,1.,0.951056516295154,1.,0.951056516295154,1.,0.951056516295154,
1.,0.951056516295154,1.,0.951056516295154,1.,0.951056516295154,1.,0.951056516295154,
1.,0.951056516295154,1.,0.951056516295154,1.,0.951056516295154,1.)))
REPRESENTATION_ITEM('')
SURFACE()
);
#3201=(
BOUNDED_SURFACE()
B_SPLINE_SURFACE(1,2,((#300541,#300542,#300543,#300544,#300545,#300546,
#300547,#300548,#300549,#300550,#300551,#300552,#300553,#300554,#300555,
#300556,#300557,#300558,#300559,#300560,#300561,#300562,#300563,#300564,
#300565,#300566,#300567,#300568,#300569,#300570,#300571,#300572,#300573,
#300574,#300575,#300576,#300577,#300578,#300579,#300580,#300581,#300582,
#300583,#300584,#300585,#300586,#300587,#300588,#300589,#300590,#300591,
#300592,#300593,#300594,#300595,#300596,#300597,#300598,#300599,#300600,
#300601,#300602,#300603,#300604,#300605,#300606,#300607,#300608,#300609,
#300610,#300611,#300612,#300613,#300614,#300615,#300616,#300617,#300618,
#300619,#300620,#300621,#300622,#300623,#300624,#300625,#300626,#300627,
#300628,#300629,#300630,#300631,#300632,#300633,#300634,#300635,#300636,
#300637,#300638,#300639,#300640,#300641,#300642,#300643,#300644,#300645,
#300646,#300647,#300648,#300649,#300650,#300651,#300652,#300653,#300654,
#300655,#300656,#300657,#300658,#300659,#300660,#300661,#300662,#300663,
#300664,#300665,#300666,#300667,#300668,#300669,#300670,#300671,#300672,
#300673,#300674,#300675,#300676,#300677,#300678,#300679,#300680,#300681,
#300682,#300683,#300684,#300685,#300686,#300687,#300688,#300689,#300690,
#300691,#300692,#300693,#300694,#300695,#300696,#300697,#300698,#300699,
#300700,#300701,#300702,#300703,#300704,#300705,#300706,#300707,#300708,
#300709,#300710,#300711,#300712,#300713,#300714,#300715,#300716,#300717,
#300718,#300719,#300720,#300721,#300722,#300723,#300724,#300725,#300726,
#300727,#300728,#300729,#300730,#300731,#300732,#300733,#300734,#300735,
#300736,#300737,#300738,#300739,#300740,#300741,#300742,#300743,#300744,
#300745,#300746,#300747,#300748,#300749,#300750,#300751,#300752,#300753,
#300754,#300755,#300756,#300757,#300758,#300759,#300760,#300761,#300762,
#300763,#300764,#300765,#300766,#300767,#300768,#300769,#300770,#300771,
#300772,#300773,#300774,#300775,#300776,#300777,#300778,#300779,#300780,
#300781,#300782,#300783,#300784,#300785,#300786,#300787,#300788,#300789,
#300790,#300791,#300792,#300793,#300794,#300795,#300796,#300797,#300798,
#300799,#300800,#300801,#300802,#300803,#300804,#300805,#300806,#300807,
#300808,#300809,#300810,#300811,#300812,#300813,#300814,#300815,#300816,
#300817,#300818,#300819,#300820,#300821,#300822,#300823,#300824,#300825,
#300826,#300827,#300828,#300829,#300830,#300831,#300832,#300833,#300834,
#300835,#300836,#300837,#300838,#300839,#300840,#300841,#300842,#300843,
#300844,#300845,#300846,#300847,#300848,#300849,#300850,#300851,#300852,
#300853,#300854,#300855,#300856,#300857,#300858,#300859,#300860,#300861,
#300862,#300863,#300864,#300865,#300866,#300867,#300868,#300869,#300870,
#300871,#300872,#300873,#300874,#300875,#300876,#300877,#300878,#300879,
#300880,#300881,#300882,#300883,#300884,#300885,#300886,#300887,#300888,
#300889,#300890,#300891,#300892,#300893,#300894,#300895,#300896,#300897,
#300898,#300899,#300900,#300901,#300902,#300903,#300904,#300905,#300906,
#300907,#300908,#300909,#300910,#300911,#300912,#300913,#300914,#300915,
#300916,#300917,#300918,#300919,#300920,#300921,#300922,#300923,#300924,
#300925,#300926,#300927,#300928,#300929,#300930,#300931,#300932,#300933,
#300934,#300935,#300936,#300937,#300938,#300939,#300940,#300941,#300942,
#300943,#300944,#300945,#300946,#300947,#300948,#300949,#300950,#300951,
#300952,#300953,#300954,#300955,#300956,#300957,#300958,#300959,#300960,
#300961,#300962,#300963,#300964,#300965,#300966,#300967,#300968,#300969,
#300970,#300971,#300972,#300973,#300974,#300975,#300976,#300977,#300978,
#300979,#300980,#300981,#300982,#300983,#300984,#300985,#300986,#300987,
#300988,#300989,#300990,#300991,#300992,#300993,#300994,#300995,#300996,
#300997,#300998,#300999,#301000,#301001,#301002,#301003,#301004,#301005,
#301006,#301007,#301008,#301009,#301010,#301011,#301012,#301013,#301014,
#301015,#301016,#301017,#301018,#301019,#301020,#301021,#301022,#301023,
#301024,#301025,#301026,#301027,#301028,#301029,#301030,#301031,#301032,
#301033,#301034,#301035,#301036,#301037,#301038,#301039,#301040,#301041,
#301042,#301043,#301044,#301045,#301046,#301047,#301048,#301049,#301050,
#301051,#301052,#301053,#301054,#301055,#301056,#301057,#301058,#301059,
#301060,#301061,#301062,#301063,#301064,#301065,#301066,#301067,#301068,
#301069,#301070,#301071,#301072,#301073,#301074,#301075,#301076,#301077,
#301078,#301079,#301080,#301081,#301082,#301083,#301084,#301085,#301086,
#301087,#301088,#301089,#301090,#301091,#301092,#301093,#301094,#301095,
#301096,#301097,#301098,#301099,#301100,#301101,#301102,#301103,#301104,
#301105,#301106,#301107,#301108,#301109,#301110,#301111,#301112,#301113,
#301114,#301115,#301116,#301117,#301118,#301119,#301120,#301121,#301122,
#301123,#301124,#301125,#301126,#301127,#301128,#301129,#301130,#301131,
#301132,#301133,#301134,#301135,#301136,#301137,#301138,#301139,#301140,
#301141,#301142,#301143,#301144,#301145,#301146,#301147,#301148,#301149,
#301150,#301151,#301152,#301153,#301154,#301155,#301156,#301157,#301158,
#301159,#301160,#301161,#301162,#301163,#301164,#301165,#301166,#301167,
#301168,#301169,#301170,#301171,#301172,#301173,#301174,#301175,#301176,
#301177,#301178,#301179,#301180,#301181,#301182,#301183,#301184,#301185,
#301186,#301187,#301188,#301189,#301190,#301191,#301192,#301193,#301194,
#301195,#301196,#301197,#301198,#301199,#301200,#301201,#301202,#301203,
#301204,#301205,#301206,#301207,#301208,#301209,#301210,#301211,#301212,
#301213,#301214,#301215,#301216,#301217,#301218,#301219,#301220,#301221,
#301222,#301223,#301224,#301225,#301226,#301227,#301228,#301229,#301230,
#301231,#301232,#301233,#301234,#301235,#301236,#301237,#301238,#301239,
#301240,#301241,#301242,#301243,#301244,#301245,#301246,#301247,#301248,
#301249,#301250,#301251,#301252,#301253,#301254,#301255,#301256,#301257,
#301258,#301259,#301260,#301261,#301262,#301263,#301264,#301265,#301266,
#301267,#301268,#301269,#301270,#301271,#301272,#301273,#301274,#301275,
#301276,#301277,#301278,#301279,#301280,#301281,#301282,#301283,#301284,
#301285,#301286,#301287,#301288,#301289,#301290,#301291,#301292,#301293,
#301294,#301295,#301296,#301297,#301298,#301299,#301300,#301301,#301302,
#301303,#301304,#301305,#301306,#301307,#301308,#301309,#301310,#301311,
#301312,#301313,#301314,#301315,#301316,#301317,#301318,#301319,#301320,
#301321,#301322,#301323,#301324,#301325,#301326,#301327,#301328,#301329,
#301330,#301331,#301332,#301333,#301334,#301335,#301336,#301337,#301338,
#301339,#301340,#301341,#301342,#301343,#301344,#301345,#301346,#301347,
#301348,#301349,#301350,#301351,#301352,#301353,#301354,#301355,#301356,
#301357,#301358,#301359,#301360,#301361,#301362,#301363,#301364,#301365,
#301366,#301367,#301368,#301369,#301370,#301371,#301372,#301373,#301374,
#301375,#301376,#301377,#301378,#301379,#301380,#301381,#301382,#301383,
#301384,#301385,#301386,#301387,#301388,#301389,#301390,#301391,#301392,
#301393,#301394,#301395,#301396,#301397,#301398,#301399,#301400,#301401,
#301402,#301403,#301404,#301405,#301406,#301407,#301408,#301409,#301410,
#301411,#301412,#301413,#301414,#301415,#301416,#301417,#301418,#301419,
#301420,#301421,#301422,#301423,#301424,#301425,#301426,#301427,#301428,
#301429,#301430,#301431,#301432,#301433,#301434,#301435,#301436,#301437,
#301438,#301439,#301440,#301441,#301442,#301443,#301444,#301445,#301446,
#301447,#301448,#301449,#301450,#301451,#301452,#301453,#301454,#301455,
#301456,#301457,#301458,#301459,#301460,#301461,#301462,#301463,#301464,
#301465,#301466,#301467,#301468,#301469,#301470,#301471,#301472,#301473,
#301474,#301475,#301476,#301477,#301478,#301479,#301480,#301481,#301482,
#301483,#301484,#301485,#301486,#301487,#301488,#301489,#301490,#301491,
#301492,#301493,#301494,#301495,#301496,#301497,#301498,#301499,#301500,
#301501,#301502,#301503,#301504,#301505,#301506,#301507,#301508,#301509,
#301510,#301511,#301512,#301513,#301514,#301515,#301516,#301517,#301518,
#301519,#301520,#301521,#301522,#301523,#301524,#301525,#301526,#301527,
#301528,#301529,#301530,#301531,#301532,#301533,#301534,#301535,#301536,
#301537,#301538,#301539,#301540,#301541,#301542,#301543,#301544,#301545,
#301546,#301547,#301548,#301549,#301550,#301551,#301552,#301553,#301554,
#301555,#301556,#301557,#301558,#301559,#301560,#301561,#301562,#301563,
#301564,#301565,#301566,#301567,#301568,#301569,#301570,#301571,#301572,
#301573,#301574,#301575,#301576,#301577),(#301578,#301579,#301580,#301581,
#301582,#301583,#301584,#301585,#301586,#301587,#301588,#301589,#301590,
#301591,#301592,#301593,#301594,#301595,#301596,#301597,#301598,#301599,
#301600,#301601,#301602,#301603,#301604,#301605,#301606,#301607,#301608,
#301609,#301610,#301611,#301612,#301613,#301614,#301615,#301616,#301617,
#301618,#301619,#301620,#301621,#301622,#301623,#301624,#301625,#301626,
#301627,#301628,#301629,#301630,#301631,#301632,#301633,#301634,#301635,
#301636,#301637,#301638,#301639,#301640,#301641,#301642,#301643,#301644,
#301645,#301646,#301647,#301648,#301649,#301650,#301651,#301652,#301653,
#301654,#301655,#301656,#301657,#301658,#301659,#301660,#301661,#301662,
#301663,#301664,#301665,#301666,#301667,#301668,#301669,#301670,#301671,
#301672,#301673,#301674,#301675,#301676,#301677,#301678,#301679,#301680,
#301681,#301682,#301683,#301684,#301685,#301686,#301687,#301688,#301689,
#301690,#301691,#301692,#301693,#301694,#301695,#301696,#301697,#301698,
#301699,#301700,#301701,#301702,#301703,#301704,#301705,#301706,#301707,
#301708,#301709,#301710,#301711,#301712,#301713,#301714,#301715,#301716,
#301717,#301718,#301719,#301720,#301721,#301722,#301723,#301724,#301725,
#301726,#301727,#301728,#301729,#301730,#301731,#301732,#301733,#301734,
#301735,#301736,#301737,#301738,#301739,#301740,#301741,#301742,#301743,
#301744,#301745,#301746,#301747,#301748,#301749,#301750,#301751,#301752,
#301753,#301754,#301755,#301756,#301757,#301758,#301759,#301760,#301761,
#301762,#301763,#301764,#301765,#301766,#301767,#301768,#301769,#301770,
#301771,#301772,#301773,#301774,#301775,#301776,#301777,#301778,#301779,
#301780,#301781,#301782,#301783,#301784,#301785,#301786,#301787,#301788,
#301789,#301790,#301791,#301792,#301793,#301794,#301795,#301796,#301797,
#301798,#301799,#301800,#301801,#301802,#301803,#301804,#301805,#301806,
#301807,#301808,#301809,#301810,#301811,#301812,#301813,#301814,#301815,
#301816,#301817,#301818,#301819,#301820,#301821,#301822,#301823,#301824,
#301825,#301826,#301827,#301828,#301829,#301830,#301831,#301832,#301833,
#301834,#301835,#301836,#301837,#301838,#301839,#301840,#301841,#301842,
#301843,#301844,#301845,#301846,#301847,#301848,#301849,#301850,#301851,
#301852,#301853,#301854,#301855,#301856,#301857,#301858,#301859,#301860,
#301861,#301862,#301863,#301864,#301865,#301866,#301867,#301868,#301869,
#301870,#301871,#301872,#301873,#301874,#301875,#301876,#301877,#301878,
#301879,#301880,#301881,#301882,#301883,#301884,#301885,#301886,#301887,
#301888,#301889,#301890,#301891,#301892,#301893,#301894,#301895,#301896,
#301897,#301898,#301899,#301900,#301901,#301902,#301903,#301904,#301905,
#301906,#301907,#301908,#301909,#301910,#301911,#301912,#301913,#301914,
#301915,#301916,#301917,#301918,#301919,#301920,#301921,#301922,#301923,
#301924,#301925,#301926,#301927,#301928,#301929,#301930,#301931,#301932,
#301933,#301934,#301935,#301936,#301937,#301938,#301939,#301940,#301941,
#301942,#301943,#301944,#301945,#301946,#301947,#301948,#301949,#301950,
#301951,#301952,#301953,#301954,#301955,#301956,#301957,#301958,#301959,
#301960,#301961,#301962,#301963,#301964,#301965,#301966,#301967,#301968,
#301969,#301970,#301971,#301972,#301973,#301974,#301975,#301976,#301977,
#301978,#301979,#301980,#301981,#301982,#301983,#301984,#301985,#301986,
#301987,#301988,#301989,#301990,#301991,#301992,#301993,#301994,#301995,
#301996,#301997,#301998,#301999,#302000,#302001,#302002,#302003,#302004,
#302005,#302006,#302007,#302008,#302009,#302010,#302011,#302012,#302013,
#302014,#302015,#302016,#302017,#302018,#302019,#302020,#302021,#302022,
#302023,#302024,#302025,#302026,#302027,#302028,#302029,#302030,#302031,
#302032,#302033,#302034,#302035,#302036,#302037,#302038,#302039,#302040,
#302041,#302042,#302043,#302044,#302045,#302046,#302047,#302048,#302049,
#302050,#302051,#302052,#302053,#302054,#302055,#302056,#302057,#302058,
#302059,#302060,#302061,#302062,#302063,#302064,#302065,#302066,#302067,
#302068,#302069,#302070,#302071,#302072,#302073,#302074,#302075,#302076,
#302077,#302078,#302079,#302080,#302081,#302082,#302083,#302084,#302085,
#302086,#302087,#302088,#302089,#302090,#302091,#302092,#302093,#302094,
#302095,#302096,#302097,#302098,#302099,#302100,#302101,#302102,#302103,
#302104,#302105,#302106,#302107,#302108,#302109,#302110,#302111,#302112,
#302113,#302114,#302115,#302116,#302117,#302118,#302119,#302120,#302121,
#302122,#302123,#302124,#302125,#302126,#302127,#302128,#302129,#302130,
#302131,#302132,#302133,#302134,#302135,#302136,#302137,#302138,#302139,
#302140,#302141,#302142,#302143,#302144,#302145,#302146,#302147,#302148,
#302149,#302150,#302151,#302152,#302153,#302154,#302155,#302156,#302157,
#302158,#302159,#302160,#302161,#302162,#302163,#302164,#302165,#302166,
#302167,#302168,#302169,#302170,#302171,#302172,#302173,#302174,#302175,
#302176,#302177,#302178,#302179,#302180,#302181,#302182,#302183,#302184,
#302185,#302186,#302187,#302188,#302189,#302190,#302191,#302192,#302193,
#302194,#302195,#302196,#302197,#302198,#302199,#302200,#302201,#302202,
#302203,#302204,#302205,#302206,#302207,#302208,#302209,#302210,#302211,
#302212,#302213,#302214,#302215,#302216,#302217,#302218,#302219,#302220,
#302221,#302222,#302223,#302224,#302225,#302226,#302227,#302228,#302229,
#302230,#302231,#302232,#302233,#302234,#302235,#302236,#302237,#302238,
#302239,#302240,#302241,#302242,#302243,#302244,#302245,#302246,#302247,
#302248,#302249,#302250,#302251,#302252,#302253,#302254,#302255,#302256,
#302257,#302258,#302259,#302260,#302261,#302262,#302263,#302264,#302265,
#302266,#302267,#302268,#302269,#302270,#302271,#302272,#302273,#302274,
#302275,#302276,#302277,#302278,#302279,#302280,#302281,#302282,#302283,
#302284,#302285,#302286,#302287,#302288,#302289,#302290,#302291,#302292,
#302293,#302294,#302295,#302296,#302297,#302298,#302299,#302300,#302301,
#302302,#302303,#302304,#302305,#302306,#302307,#302308,#302309,#302310,
#302311,#302312,#302313,#302314,#302315,#302316,#302317,#302318,#302319,
#302320,#302321,#302322,#302323,#302324,#302325,#302326,#302327,#302328,
#302329,#302330,#302331,#302332,#302333,#302334,#302335,#302336,#302337,
#302338,#302339,#302340,#302341,#302342,#302343,#302344,#302345,#302346,
#302347,#302348,#302349,#302350,#302351,#302352,#302353,#302354,#302355,
#302356,#302357,#302358,#302359,#302360,#302361,#302362,#302363,#302364,
#302365,#302366,#302367,#302368,#302369,#302370,#302371,#302372,#302373,
#302374,#302375,#302376,#302377,#302378,#302379,#302380,#302381,#302382,
#302383,#302384,#302385,#302386,#302387,#302388,#302389,#302390,#302391,
#302392,#302393,#302394,#302395,#302396,#302397,#302398,#302399,#302400,
#302401,#302402,#302403,#302404,#302405,#302406,#302407,#302408,#302409,
#302410,#302411,#302412,#302413,#302414,#302415,#302416,#302417,#302418,
#302419,#302420,#302421,#302422,#302423,#302424,#302425,#302426,#302427,
#302428,#302429,#302430,#302431,#302432,#302433,#302434,#302435,#302436,
#302437,#302438,#302439,#302440,#302441,#302442,#302443,#302444,#302445,
#302446,#302447,#302448,#302449,#302450,#302451,#302452,#302453,#302454,
#302455,#302456,#302457,#302458,#302459,#302460,#302461,#302462,#302463,
#302464,#302465,#302466,#302467,#302468,#302469,#302470,#302471,#302472,
#302473,#302474,#302475,#302476,#302477,#302478,#302479,#302480,#302481,
#302482,#302483,#302484,#302485,#302486,#302487,#302488,#302489,#302490,
#302491,#302492,#302493,#302494,#302495,#302496,#302497,#302498,#302499,
#302500,#302501,#302502,#302503,#302504,#302505,#302506,#302507,#302508,
#302509,#302510,#302511,#302512,#302513,#302514,#302515,#302516,#302517,
#302518,#302519,#302520,#302521,#302522,#302523,#302524,#302525,#302526,
#302527,#302528,#302529,#302530,#302531,#302532,#302533,#302534,#302535,
#302536,#302537,#302538,#302539,#302540,#302541,#302542,#302543,#302544,
#302545,#302546,#302547,#302548,#302549,#302550,#302551,#302552,#302553,
#302554,#302555,#302556,#302557,#302558,#302559,#302560,#302561,#302562,
#302563,#302564,#302565,#302566,#302567,#302568,#302569,#302570,#302571,
#302572,#302573,#302574,#302575,#302576,#302577,#302578,#302579,#302580,
#302581,#302582,#302583,#302584,#302585,#302586,#302587,#302588,#302589,
#302590,#302591,#302592,#302593,#302594,#302595,#302596,#302597,#302598,
#302599,#302600,#302601,#302602,#302603,#302604,#302605,#302606,#302607,
#302608,#302609,#302610,#302611,#302612,#302613,#302614)),.UNSPECIFIED.,
 .F.,.F.,.F.)
B_SPLINE_SURFACE_WITH_KNOTS((2,2),(3,2,2,2,2,2,2,2,2,2,2,2,2,2,2,2,2,2,
2,2,2,2,2,2,2,2,2,2,2,2,2,2,2,2,2,2,2,2,2,2,2,2,2,2,2,2,2,2,2,2,2,2,2,2,
2,2,2,2,2,2,2,2,2,2,2,2,2,2,2,2,2,2,2,2,2,2,2,2,2,2,2,2,2,2,2,2,2,2,2,2,
2,2,2,2,2,2,2,2,2,2,2,2,2,2,2,2,2,2,2,2,2,2,2,2,2,2,2,2,2,2,2,2,2,2,2,2,
2,2,2,2,2,2,2,2,2,2,2,2,2,2,2,2,2,2,2,2,2,2,2,2,2,2,2,2,2,2,2,2,2,2,2,2,
2,2,2,2,2,2,2,2,2,2,2,2,2,2,2,2,2,2,2,2,2,2,2,2,2,2,2,2,2,2,2,2,2,2,2,2,
2,2,2,2,2,2,2,2,2,2,2,2,2,2,2,2,2,2,2,2,2,2,2,2,2,2,2,2,2,2,2,2,2,2,2,2,
2,2,2,2,2,2,2,2,2,2,2,2,2,2,2,2,2,2,2,2,2,2,2,2,2,2,2,2,2,2,2,2,2,2,2,2,
2,2,2,2,2,2,2,2,2,2,2,2,2,2,2,2,2,2,2,2,2,2,2,2,2,2,2,2,2,2,2,2,2,2,2,2,
2,2,2,2,2,2,2,2,2,2,2,2,2,2,2,2,2,2,2,2,2,2,2,2,2,2,2,2,2,2,2,2,2,2,2,2,
2,2,2,2,2,2,2,2,2,2,2,2,2,2,2,2,2,2,2,2,2,2,2,2,2,2,2,2,2,2,2,2,2,2,2,2,
2,2,2,2,2,2,2,2,2,2,2,2,2,2,2,2,2,2,2,2,2,2,2,2,2,2,2,2,2,2,2,2,2,2,2,2,
2,2,2,2,2,2,2,2,2,2,2,2,2,2,2,2,2,2,2,2,2,2,2,2,2,2,2,2,2,2,2,2,2,2,2,2,
2,2,2,2,2,2,2,2,2,2,2,2,2,2,2,2,2,2,2,2,2,2,2,2,2,2,2,2,2,2,2,2,2,2,2,2,
2,2,2,2,2,2,2,2,2,2,2,2,2,2,2,2,2,2,2,2,2,2,2,2,2,2,2,2,2,2,2,2,3),(0.,
1.),(0.,0.00192307692307692,0.00384615384615385,0.00576923076923077,0.00769230769230769,
0.00961538461538462,0.0115384615384615,0.0134615384615385,0.0153846153846154,
0.0173076923076923,0.0192307692307692,0.0211538461538462,0.0230769230769231,
0.025,0.0269230769230769,0.0288461538461538,0.0307692307692308,0.0326923076923077,
0.0346153846153846,0.0365384615384615,0.0384615384615385,0.0403846153846154,
0.0423076923076923,0.0442307692307692,0.0461538461538462,0.0480769230769231,
0.05,0.0519230769230769,0.0538461538461538,0.0557692307692308,0.0576923076923077,
0.0596153846153846,0.0615384615384615,0.0634615384615385,0.0653846153846154,
0.0673076923076923,0.0692307692307692,0.0711538461538462,0.0730769230769231,
0.075,0.0769230769230769,0.0788461538461538,0.0807692307692308,0.0826923076923077,
0.0846153846153846,0.0865384615384615,0.0884615384615385,0.0903846153846154,
0.0923076923076923,0.0942307692307692,0.0961538461538462,0.0980769230769231,
0.1,0.101923076923077,0.103846153846154,0.105769230769231,0.107692307692308,
0.109615384615385,0.111538461538462,0.113461538461538,0.115384615384615,
0.117307692307692,0.119230769230769,0.121153846153846,0.123076923076923,
0.125,0.126923076923077,0.128846153846154,0.130769230769231,0.132692307692308,
0.134615384615385,0.136538461538462,0.138461538461538,0.140384615384615,
0.142307692307692,0.144230769230769,0.146153846153846,0.148076923076923,
0.15,0.151923076923077,0.153846153846154,0.155769230769231,0.157692307692308,
0.159615384615385,0.161538461538462,0.163461538461538,0.165384615384615,
0.167307692307692,0.169230769230769,0.171153846153846,0.173076923076923,
0.175,0.176923076923077,0.178846153846154,0.180769230769231,0.182692307692308,
0.184615384615385,0.186538461538462,0.188461538461538,0.190384615384615,
0.192307692307692,0.194230769230769,0.196153846153846,0.198076923076923,
0.2,0.201923076923077,0.203846153846154,0.205769230769231,0.207692307692308,
0.209615384615385,0.211538461538462,0.213461538461538,0.215384615384615,
0.217307692307692,0.219230769230769,0.221153846153846,0.223076923076923,
0.225,0.226923076923077,0.228846153846154,0.230769230769231,0.232692307692308,
0.234615384615385,0.236538461538462,0.238461538461538,0.240384615384615,
0.242307692307692,0.244230769230769,0.246153846153846,0.248076923076923,
0.25,0.251923076923077,0.253846153846154,0.255769230769231,0.257692307692308,
0.259615384615385,0.261538461538462,0.263461538461538,0.265384615384615,
0.267307692307692,0.269230769230769,0.271153846153846,0.273076923076923,
0.275,0.276923076923077,0.278846153846154,0.280769230769231,0.282692307692308,
0.284615384615385,0.286538461538462,0.288461538461538,0.290384615384615,
0.292307692307692,0.294230769230769,0.296153846153846,0.298076923076923,
0.3,0.301923076923077,0.303846153846154,0.305769230769231,0.307692307692308,
0.309615384615385,0.311538461538462,0.313461538461538,0.315384615384615,
0.317307692307692,0.319230769230769,0.321153846153846,0.323076923076923,
0.325,0.326923076923077,0.328846153846154,0.330769230769231,0.332692307692308,
0.334615384615385,0.336538461538462,0.338461538461538,0.340384615384615,
0.342307692307692,0.344230769230769,0.346153846153846,0.348076923076923,
0.35,0.351923076923077,0.353846153846154,0.355769230769231,0.357692307692308,
0.359615384615385,0.361538461538462,0.363461538461538,0.365384615384615,
0.367307692307692,0.369230769230769,0.371153846153846,0.373076923076923,
0.375,0.376923076923077,0.378846153846154,0.380769230769231,0.382692307692308,
0.384615384615385,0.386538461538462,0.388461538461538,0.390384615384615,
0.392307692307692,0.394230769230769,0.396153846153846,0.398076923076923,
0.4,0.401923076923077,0.403846153846154,0.405769230769231,0.407692307692308,
0.409615384615385,0.411538461538462,0.413461538461538,0.415384615384615,
0.417307692307692,0.419230769230769,0.421153846153846,0.423076923076923,
0.425,0.426923076923077,0.428846153846154,0.430769230769231,0.432692307692308,
0.434615384615385,0.436538461538462,0.438461538461538,0.440384615384615,
0.442307692307692,0.444230769230769,0.446153846153846,0.448076923076923,
0.45,0.451923076923077,0.453846153846154,0.455769230769231,0.457692307692308,
0.459615384615385,0.461538461538462,0.463461538461538,0.465384615384615,
0.467307692307692,0.469230769230769,0.471153846153846,0.473076923076923,
0.475,0.476923076923077,0.478846153846154,0.480769230769231,0.482692307692308,
0.484615384615385,0.486538461538462,0.488461538461538,0.490384615384615,
0.492307692307692,0.494230769230769,0.496153846153846,0.498076923076923,
0.5,0.501923076923077,0.503846153846154,0.505769230769231,0.507692307692308,
0.509615384615385,0.511538461538461,0.513461538461538,0.515384615384615,
0.517307692307692,0.519230769230769,0.521153846153846,0.523076923076923,
0.525,0.526923076923077,0.528846153846154,0.530769230769231,0.532692307692308,
0.534615384615385,0.536538461538462,0.538461538461538,0.540384615384615,
0.542307692307692,0.544230769230769,0.546153846153846,0.548076923076923,
0.55,0.551923076923077,0.553846153846154,0.555769230769231,0.557692307692308,
0.559615384615385,0.561538461538462,0.563461538461538,0.565384615384615,
0.567307692307692,0.569230769230769,0.571153846153846,0.573076923076923,
0.575,0.576923076923077,0.578846153846154,0.580769230769231,0.582692307692308,
0.584615384615385,0.586538461538462,0.588461538461538,0.590384615384615,
0.592307692307692,0.594230769230769,0.596153846153846,0.598076923076923,
0.6,0.601923076923077,0.603846153846154,0.605769230769231,0.607692307692308,
0.609615384615385,0.611538461538462,0.613461538461539,0.615384615384615,
0.617307692307692,0.619230769230769,0.621153846153846,0.623076923076923,
0.625,0.626923076923077,0.628846153846154,0.630769230769231,0.632692307692308,
0.634615384615385,0.636538461538461,0.638461538461538,0.640384615384615,
0.642307692307692,0.644230769230769,0.646153846153846,0.648076923076923,
0.65,0.651923076923077,0.653846153846154,0.655769230769231,0.657692307692308,
0.659615384615385,0.661538461538462,0.663461538461538,0.665384615384615,
0.667307692307692,0.669230769230769,0.671153846153846,0.673076923076923,
0.675,0.676923076923077,0.678846153846154,0.680769230769231,0.682692307692308,
0.684615384615385,0.686538461538462,0.688461538461538,0.690384615384615,
0.692307692307692,0.694230769230769,0.696153846153846,0.698076923076923,
0.7,0.701923076923077,0.703846153846154,0.705769230769231,0.707692307692308,
0.709615384615385,0.711538461538462,0.713461538461538,0.715384615384615,
0.717307692307692,0.719230769230769,0.721153846153846,0.723076923076923,
0.725,0.726923076923077,0.728846153846154,0.730769230769231,0.732692307692308,
0.734615384615385,0.736538461538462,0.738461538461539,0.740384615384615,
0.742307692307692,0.744230769230769,0.746153846153846,0.748076923076923,
0.75,0.751923076923077,0.753846153846154,0.755769230769231,0.757692307692308,
0.759615384615385,0.761538461538461,0.763461538461538,0.765384615384615,
0.767307692307692,0.769230769230769,0.771153846153846,0.773076923076923,
0.775,0.776923076923077,0.778846153846154,0.780769230769231,0.782692307692308,
0.784615384615385,0.786538461538462,0.788461538461538,0.790384615384615,
0.792307692307692,0.794230769230769,0.796153846153846,0.798076923076923,
0.8,0.801923076923077,0.803846153846154,0.805769230769231,0.807692307692308,
0.809615384615385,0.811538461538462,0.813461538461538,0.815384615384615,
0.817307692307692,0.819230769230769,0.821153846153846,0.823076923076923,
0.825,0.826923076923077,0.828846153846154,0.830769230769231,0.832692307692308,
0.834615384615385,0.836538461538462,0.838461538461538,0.840384615384615,
0.842307692307692,0.844230769230769,0.846153846153846,0.848076923076923,
0.85,0.851923076923077,0.853846153846154,0.855769230769231,0.857692307692308,
0.859615384615385,0.861538461538462,0.863461538461539,0.865384615384615,
0.867307692307692,0.869230769230769,0.871153846153846,0.873076923076923,
0.875,0.876923076923077,0.878846153846154,0.880769230769231,0.882692307692308,
0.884615384615385,0.886538461538461,0.888461538461538,0.890384615384615,
0.892307692307692,0.894230769230769,0.896153846153846,0.898076923076923,
0.9,0.901923076923077,0.903846153846154,0.905769230769231,0.907692307692308,
0.909615384615385,0.911538461538462,0.913461538461538,0.915384615384615,
0.917307692307692,0.919230769230769,0.921153846153846,0.923076923076923,
0.925,0.926923076923077,0.928846153846154,0.930769230769231,0.932692307692308,
0.934615384615385,0.936538461538462,0.938461538461538,0.940384615384615,
0.942307692307692,0.944230769230769,0.946153846153846,0.948076923076923,
0.95,0.951923076923077,0.953846153846154,0.955769230769231,0.957692307692308,
0.959615384615385,0.961538461538462,0.963461538461538,0.965384615384615,
0.967307692307692,0.969230769230769,0.971153846153846,0.973076923076923,
0.975,0.976923076923077,0.978846153846154,0.980769230769231,0.982692307692308,
0.984615384615385,0.986538461538462,0.988461538461539,0.990384615384615,
0.992307692307692,0.994230769230769,0.996153846153846),.UNSPECIFIED.)
GEOMETRIC_REPRESENTATION_ITEM()
RATIONAL_B_SPLINE_SURFACE(((1.,0.951056516295154,1.,0.951056516295154,1.,
0.951056516295154,1.,0.951056516295154,1.,0.951056516295154,1.,0.951056516295154,
1.,0.951056516295154,1.,0.951056516295154,1.,0.951056516295154,1.,0.951056516295154,
1.,0.951056516295154,1.,0.951056516295154,1.,0.951056516295154,1.,0.951056516295154,
1.,0.951056516295154,1.,0.951056516295154,1.,0.951056516295154,1.,0.951056516295154,
1.,0.951056516295154,1.,0.951056516295154,1.,0.951056516295154,1.,0.951056516295154,
1.,0.951056516295154,1.,0.951056516295154,1.,0.951056516295154,1.,0.951056516295154,
1.,0.951056516295154,1.,0.951056516295154,1.,0.951056516295154,1.,0.951056516295154,
1.,0.951056516295154,1.,0.951056516295154,1.,0.951056516295154,1.,0.951056516295154,
1.,0.951056516295154,1.,0.951056516295154,1.,0.951056516295154,1.,0.951056516295154,
1.,0.951056516295154,1.,0.951056516295154,1.,0.951056516295154,1.,0.951056516295154,
1.,0.951056516295154,1.,0.951056516295154,1.,0.951056516295154,1.,0.951056516295154,
1.,0.951056516295154,1.,0.951056516295154,1.,0.951056516295154,1.,0.951056516295154,
1.,0.951056516295154,1.,0.951056516295154,1.,0.951056516295154,1.,0.951056516295154,
1.,0.951056516295154,1.,0.951056516295154,1.,0.951056516295154,1.,0.951056516295154,
1.,0.951056516295154,1.,0.951056516295154,1.,0.951056516295154,1.,0.951056516295154,
1.,0.951056516295154,1.,0.951056516295154,1.,0.951056516295154,1.,0.951056516295154,
1.,0.951056516295154,1.,0.951056516295154,1.,0.951056516295154,1.,0.951056516295154,
1.,0.951056516295154,1.,0.951056516295154,1.,0.951056516295154,1.,0.951056516295154,
1.,0.951056516295154,1.,0.951056516295154,1.,0.951056516295154,1.,0.951056516295154,
1.,0.951056516295154,1.,0.951056516295154,1.,0.951056516295154,1.,0.951056516295154,
1.,0.951056516295154,1.,0.951056516295154,1.,0.951056516295154,1.,0.951056516295154,
1.,0.951056516295154,1.,0.951056516295154,1.,0.951056516295154,1.,0.951056516295154,
1.,0.951056516295154,1.,0.951056516295154,1.,0.951056516295154,1.,0.951056516295154,
1.,0.951056516295154,1.,0.951056516295154,1.,0.951056516295154,1.,0.951056516295154,
1.,0.951056516295154,1.,0.951056516295154,1.,0.951056516295154,1.,0.951056516295154,
1.,0.951056516295154,1.,0.951056516295154,1.,0.951056516295154,1.,0.951056516295154,
1.,0.951056516295154,1.,0.951056516295154,1.,0.951056516295154,1.,0.951056516295154,
1.,0.951056516295154,1.,0.951056516295154,1.,0.951056516295154,1.,0.951056516295154,
1.,0.951056516295154,1.,0.951056516295154,1.,0.951056516295154,1.,0.951056516295154,
1.,0.951056516295154,1.,0.951056516295154,1.,0.951056516295154,1.,0.951056516295154,
1.,0.951056516295154,1.,0.951056516295154,1.,0.951056516295154,1.,0.951056516295154,
1.,0.951056516295154,1.,0.951056516295154,1.,0.951056516295154,1.,0.951056516295154,
1.,0.951056516295154,1.,0.951056516295154,1.,0.951056516295154,1.,0.951056516295154,
1.,0.951056516295154,1.,0.951056516295154,1.,0.951056516295154,1.,0.951056516295154,
1.,0.951056516295154,1.,0.951056516295154,1.,0.951056516295154,1.,0.951056516295154,
1.,0.951056516295154,1.,0.951056516295154,1.,0.951056516295154,1.,0.951056516295154,
1.,0.951056516295154,1.,0.951056516295154,1.,0.951056516295154,1.,0.951056516295154,
1.,0.951056516295154,1.,0.951056516295154,1.,0.951056516295154,1.,0.951056516295154,
1.,0.951056516295154,1.,0.951056516295154,1.,0.951056516295154,1.,0.951056516295154,
1.,0.951056516295154,1.,0.951056516295154,1.,0.951056516295154,1.,0.951056516295154,
1.,0.951056516295154,1.,0.951056516295154,1.,0.951056516295154,1.,0.951056516295154,
1.,0.951056516295154,1.,0.951056516295154,1.,0.951056516295154,1.,0.951056516295154,
1.,0.951056516295154,1.,0.951056516295154,1.,0.951056516295154,1.,0.951056516295154,
1.,0.951056516295154,1.,0.951056516295154,1.,0.951056516295154,1.,0.951056516295154,
1.,0.951056516295154,1.,0.951056516295154,1.,0.951056516295154,1.,0.951056516295154,
1.,0.951056516295154,1.,0.951056516295154,1.,0.951056516295154,1.,0.951056516295154,
1.,0.951056516295154,1.,0.951056516295154,1.,0.951056516295154,1.,0.951056516295154,
1.,0.951056516295154,1.,0.951056516295154,1.,0.951056516295154,1.,0.951056516295154,
1.,0.951056516295154,1.,0.951056516295154,1.,0.951056516295154,1.,0.951056516295154,
1.,0.951056516295154,1.,0.951056516295154,1.,0.951056516295154,1.,0.951056516295154,
1.,0.951056516295154,1.,0.951056516295154,1.,0.951056516295154,1.,0.951056516295154,
1.,0.951056516295154,1.,0.951056516295154,1.,0.951056516295154,1.,0.951056516295154,
1.,0.951056516295154,1.,0.951056516295154,1.,0.951056516295154,1.,0.951056516295154,
1.,0.951056516295154,1.,0.951056516295154,1.,0.951056516295154,1.,0.951056516295154,
1.,0.951056516295154,1.,0.951056516295154,1.,0.951056516295154,1.,0.951056516295154,
1.,0.951056516295154,1.,0.951056516295154,1.,0.951056516295154,1.,0.951056516295154,
1.,0.951056516295154,1.,0.951056516295154,1.,0.951056516295154,1.,0.951056516295154,
1.,0.951056516295154,1.,0.951056516295154,1.,0.951056516295154,1.,0.951056516295154,
1.,0.951056516295154,1.,0.951056516295154,1.,0.951056516295154,1.,0.951056516295154,
1.,0.951056516295154,1.,0.951056516295154,1.,0.951056516295154,1.,0.951056516295154,
1.,0.951056516295154,1.,0.951056516295154,1.,0.951056516295154,1.,0.951056516295154,
1.,0.951056516295154,1.,0.951056516295154,1.,0.951056516295154,1.,0.951056516295154,
1.,0.951056516295154,1.,0.951056516295154,1.,0.951056516295154,1.,0.951056516295154,
1.,0.951056516295154,1.,0.951056516295154,1.,0.951056516295154,1.,0.951056516295154,
1.,0.951056516295154,1.,0.951056516295154,1.,0.951056516295154,1.,0.951056516295154,
1.,0.951056516295154,1.,0.951056516295154,1.,0.951056516295154,1.,0.951056516295154,
1.,0.951056516295154,1.,0.951056516295154,1.,0.951056516295154,1.,0.951056516295154,
1.,0.951056516295154,1.,0.951056516295154,1.,0.951056516295154,1.,0.951056516295154,
1.,0.951056516295154,1.,0.951056516295154,1.,0.951056516295154,1.,0.951056516295154,
1.,0.951056516295154,1.,0.951056516295154,1.,0.951056516295154,1.,0.951056516295154,
1.,0.951056516295154,1.,0.951056516295154,1.,0.951056516295154,1.,0.951056516295154,
1.,0.951056516295154,1.,0.951056516295154,1.,0.951056516295154,1.,0.951056516295154,
1.,0.951056516295154,1.,0.951056516295154,1.,0.951056516295154,1.,0.951056516295154,
1.,0.951056516295154,1.,0.951056516295154,1.,0.951056516295154,1.,0.951056516295154,
1.,0.951056516295154,1.,0.951056516295154,1.,0.951056516295154,1.,0.951056516295154,
1.,0.951056516295154,1.,0.951056516295154,1.,0.951056516295154,1.,0.951056516295154,
1.,0.951056516295154,1.,0.951056516295154,1.,0.951056516295154,1.,0.951056516295154,
1.,0.951056516295154,1.,0.951056516295154,1.,0.951056516295154,1.,0.951056516295154,
1.,0.951056516295154,1.,0.951056516295154,1.,0.951056516295154,1.,0.951056516295154,
1.,0.951056516295154,1.,0.951056516295154,1.,0.951056516295154,1.,0.951056516295154,
1.,0.951056516295154,1.,0.951056516295154,1.,0.951056516295154,1.,0.951056516295154,
1.,0.951056516295154,1.,0.951056516295154,1.,0.951056516295154,1.,0.951056516295154,
1.,0.951056516295154,1.,0.951056516295154,1.,0.951056516295154,1.,0.951056516295154,
1.,0.951056516295154,1.,0.951056516295154,1.,0.951056516295154,1.,0.951056516295154,
1.,0.951056516295154,1.,0.951056516295154,1.,0.951056516295154,1.,0.951056516295154,
1.,0.951056516295154,1.,0.951056516295154,1.,0.951056516295154,1.,0.951056516295154,
1.,0.951056516295154,1.,0.951056516295154,1.,0.951056516295154,1.,0.951056516295154,
1.,0.951056516295154,1.,0.951056516295154,1.,0.951056516295154,1.,0.951056516295154,
1.,0.951056516295154,1.,0.951056516295154,1.,0.951056516295154,1.,0.951056516295154,
1.,0.951056516295154,1.,0.951056516295154,1.,0.951056516295154,1.,0.951056516295154,
1.,0.951056516295154,1.,0.951056516295154,1.,0.951056516295154,1.,0.951056516295154,
1.,0.951056516295154,1.,0.951056516295154,1.,0.951056516295154,1.,0.951056516295154,
1.,0.951056516295154,1.,0.951056516295154,1.,0.951056516295154,1.,0.951056516295154,
1.,0.951056516295154,1.,0.951056516295154,1.,0.951056516295154,1.,0.951056516295154,
1.,0.951056516295154,1.,0.951056516295154,1.,0.951056516295154,1.,0.951056516295154,
1.,0.951056516295154,1.,0.951056516295154,1.,0.951056516295154,1.,0.951056516295154,
1.,0.951056516295154,1.,0.951056516295154,1.,0.951056516295154,1.,0.951056516295154,
1.,0.951056516295154,1.,0.951056516295154,1.,0.951056516295154,1.,0.951056516295154,
1.,0.951056516295154,1.,0.951056516295154,1.,0.951056516295154,1.,0.951056516295154,
1.,0.951056516295154,1.,0.951056516295154,1.,0.951056516295154,1.,0.951056516295154,
1.,0.951056516295154,1.,0.951056516295154,1.,0.951056516295154,1.,0.951056516295154,
1.,0.951056516295154,1.,0.951056516295154,1.,0.951056516295154,1.,0.951056516295154,
1.,0.951056516295154,1.,0.951056516295154,1.,0.951056516295154,1.,0.951056516295154,
1.,0.951056516295154,1.,0.951056516295154,1.,0.951056516295154,1.,0.951056516295154,
1.,0.951056516295154,1.,0.951056516295154,1.,0.951056516295154,1.,0.951056516295154,
1.,0.951056516295154,1.,0.951056516295154,1.,0.951056516295154,1.,0.951056516295154,
1.,0.951056516295154,1.,0.951056516295154,1.,0.951056516295154,1.,0.951056516295154,
1.,0.951056516295154,1.,0.951056516295154,1.,0.951056516295154,1.,0.951056516295154,
1.,0.951056516295154,1.,0.951056516295154,1.,0.951056516295154,1.,0.951056516295154,
1.,0.951056516295154,1.,0.951056516295154,1.,0.951056516295154,1.,0.951056516295154,
1.,0.951056516295154,1.,0.951056516295154,1.,0.951056516295154,1.,0.951056516295154,
1.,0.951056516295154,1.,0.951056516295154,1.,0.951056516295154,1.,0.951056516295154,
1.,0.951056516295154,1.,0.951056516295154,1.,0.951056516295154,1.,0.951056516295154,
1.,0.951056516295154,1.,0.951056516295154,1.,0.951056516295154,1.,0.951056516295154,
1.,0.951056516295154,1.,0.951056516295154,1.,0.951056516295154,1.,0.951056516295154,
1.,0.951056516295154,1.,0.951056516295154,1.,0.951056516295154,1.,0.951056516295154,
1.,0.951056516295154,1.,0.951056516295154,1.,0.951056516295154,1.,0.951056516295154,
1.,0.951056516295154,1.,0.951056516295154,1.,0.951056516295154,1.,0.951056516295154,
1.,0.951056516295154,1.,0.951056516295154,1.,0.951056516295154,1.,0.951056516295154,
1.,0.951056516295154,1.,0.951056516295154,1.,0.951056516295154,1.,0.951056516295154,
1.,0.951056516295154,1.,0.951056516295154,1.,0.951056516295154,1.,0.951056516295154,
1.,0.951056516295154,1.,0.951056516295154,1.,0.951056516295154,1.,0.951056516295154,
1.,0.951056516295154,1.,0.951056516295154,1.,0.951056516295154,1.,0.951056516295154,
1.,0.951056516295154,1.,0.951056516295154,1.,0.951056516295154,1.,0.951056516295154,
1.,0.951056516295154,1.,0.951056516295154,1.,0.951056516295154,1.,0.951056516295154,
1.,0.951056516295154,1.,0.951056516295154,1.,0.951056516295154,1.,0.951056516295154,
1.,0.951056516295154,1.,0.951056516295154,1.,0.951056516295154,1.,0.951056516295154,
1.,0.951056516295154,1.,0.951056516295154,1.,0.951056516295154,1.,0.951056516295154,
1.,0.951056516295154,1.,0.951056516295154,1.,0.951056516295154,1.,0.951056516295154,
1.),(1.,0.951056516295154,1.,0.951056516295154,1.,0.951056516295154,1.,
0.951056516295154,1.,0.951056516295154,1.,0.951056516295154,1.,0.951056516295154,
1.,0.951056516295154,1.,0.951056516295154,1.,0.951056516295154,1.,0.951056516295154,
1.,0.951056516295154,1.,0.951056516295154,1.,0.951056516295154,1.,0.951056516295154,
1.,0.951056516295154,1.,0.951056516295154,1.,0.951056516295154,1.,0.951056516295154,
1.,0.951056516295154,1.,0.951056516295154,1.,0.951056516295154,1.,0.951056516295154,
1.,0.951056516295154,1.,0.951056516295154,1.,0.951056516295154,1.,0.951056516295154,
1.,0.951056516295154,1.,0.951056516295154,1.,0.951056516295154,1.,0.951056516295154,
1.,0.951056516295154,1.,0.951056516295154,1.,0.951056516295154,1.,0.951056516295154,
1.,0.951056516295154,1.,0.951056516295154,1.,0.951056516295154,1.,0.951056516295154,
1.,0.951056516295154,1.,0.951056516295154,1.,0.951056516295154,1.,0.951056516295154,
1.,0.951056516295154,1.,0.951056516295154,1.,0.951056516295154,1.,0.951056516295154,
1.,0.951056516295154,1.,0.951056516295154,1.,0.951056516295154,1.,0.951056516295154,
1.,0.951056516295154,1.,0.951056516295154,1.,0.951056516295154,1.,0.951056516295154,
1.,0.951056516295154,1.,0.951056516295154,1.,0.951056516295154,1.,0.951056516295154,
1.,0.951056516295154,1.,0.951056516295154,1.,0.951056516295154,1.,0.951056516295154,
1.,0.951056516295154,1.,0.951056516295154,1.,0.951056516295154,1.,0.951056516295154,
1.,0.951056516295154,1.,0.951056516295154,1.,0.951056516295154,1.,0.951056516295154,
1.,0.951056516295154,1.,0.951056516295154,1.,0.951056516295154,1.,0.951056516295154,
1.,0.951056516295154,1.,0.951056516295154,1.,0.951056516295154,1.,0.951056516295154,
1.,0.951056516295154,1.,0.951056516295154,1.,0.951056516295154,1.,0.951056516295154,
1.,0.951056516295154,1.,0.951056516295154,1.,0.951056516295154,1.,0.951056516295154,
1.,0.951056516295154,1.,0.951056516295154,1.,0.951056516295154,1.,0.951056516295154,
1.,0.951056516295154,1.,0.951056516295154,1.,0.951056516295154,1.,0.951056516295154,
1.,0.951056516295154,1.,0.951056516295154,1.,0.951056516295154,1.,0.951056516295154,
1.,0.951056516295154,1.,0.951056516295154,1.,0.951056516295154,1.,0.951056516295154,
1.,0.951056516295154,1.,0.951056516295154,1.,0.951056516295154,1.,0.951056516295154,
1.,0.951056516295154,1.,0.951056516295154,1.,0.951056516295154,1.,0.951056516295154,
1.,0.951056516295154,1.,0.951056516295154,1.,0.951056516295154,1.,0.951056516295154,
1.,0.951056516295154,1.,0.951056516295154,1.,0.951056516295154,1.,0.951056516295154,
1.,0.951056516295154,1.,0.951056516295154,1.,0.951056516295154,1.,0.951056516295154,
1.,0.951056516295154,1.,0.951056516295154,1.,0.951056516295154,1.,0.951056516295154,
1.,0.951056516295154,1.,0.951056516295154,1.,0.951056516295154,1.,0.951056516295154,
1.,0.951056516295154,1.,0.951056516295154,1.,0.951056516295154,1.,0.951056516295154,
1.,0.951056516295154,1.,0.951056516295154,1.,0.951056516295154,1.,0.951056516295154,
1.,0.951056516295154,1.,0.951056516295154,1.,0.951056516295154,1.,0.951056516295154,
1.,0.951056516295154,1.,0.951056516295154,1.,0.951056516295154,1.,0.951056516295154,
1.,0.951056516295154,1.,0.951056516295154,1.,0.951056516295154,1.,0.951056516295154,
1.,0.951056516295154,1.,0.951056516295154,1.,0.951056516295154,1.,0.951056516295154,
1.,0.951056516295154,1.,0.951056516295154,1.,0.951056516295154,1.,0.951056516295154,
1.,0.951056516295154,1.,0.951056516295154,1.,0.951056516295154,1.,0.951056516295154,
1.,0.951056516295154,1.,0.951056516295154,1.,0.951056516295154,1.,0.951056516295154,
1.,0.951056516295154,1.,0.951056516295154,1.,0.951056516295154,1.,0.951056516295154,
1.,0.951056516295154,1.,0.951056516295154,1.,0.951056516295154,1.,0.951056516295154,
1.,0.951056516295154,1.,0.951056516295154,1.,0.951056516295154,1.,0.951056516295154,
1.,0.951056516295154,1.,0.951056516295154,1.,0.951056516295154,1.,0.951056516295154,
1.,0.951056516295154,1.,0.951056516295154,1.,0.951056516295154,1.,0.951056516295154,
1.,0.951056516295154,1.,0.951056516295154,1.,0.951056516295154,1.,0.951056516295154,
1.,0.951056516295154,1.,0.951056516295154,1.,0.951056516295154,1.,0.951056516295154,
1.,0.951056516295154,1.,0.951056516295154,1.,0.951056516295154,1.,0.951056516295154,
1.,0.951056516295154,1.,0.951056516295154,1.,0.951056516295154,1.,0.951056516295154,
1.,0.951056516295154,1.,0.951056516295154,1.,0.951056516295154,1.,0.951056516295154,
1.,0.951056516295154,1.,0.951056516295154,1.,0.951056516295154,1.,0.951056516295154,
1.,0.951056516295154,1.,0.951056516295154,1.,0.951056516295154,1.,0.951056516295154,
1.,0.951056516295154,1.,0.951056516295154,1.,0.951056516295154,1.,0.951056516295154,
1.,0.951056516295154,1.,0.951056516295154,1.,0.951056516295154,1.,0.951056516295154,
1.,0.951056516295154,1.,0.951056516295154,1.,0.951056516295154,1.,0.951056516295154,
1.,0.951056516295154,1.,0.951056516295154,1.,0.951056516295154,1.,0.951056516295154,
1.,0.951056516295154,1.,0.951056516295154,1.,0.951056516295154,1.,0.951056516295154,
1.,0.951056516295154,1.,0.951056516295154,1.,0.951056516295154,1.,0.951056516295154,
1.,0.951056516295154,1.,0.951056516295154,1.,0.951056516295154,1.,0.951056516295154,
1.,0.951056516295154,1.,0.951056516295154,1.,0.951056516295154,1.,0.951056516295154,
1.,0.951056516295154,1.,0.951056516295154,1.,0.951056516295154,1.,0.951056516295154,
1.,0.951056516295154,1.,0.951056516295154,1.,0.951056516295154,1.,0.951056516295154,
1.,0.951056516295154,1.,0.951056516295154,1.,0.951056516295154,1.,0.951056516295154,
1.,0.951056516295154,1.,0.951056516295154,1.,0.951056516295154,1.,0.951056516295154,
1.,0.951056516295154,1.,0.951056516295154,1.,0.951056516295154,1.,0.951056516295154,
1.,0.951056516295154,1.,0.951056516295154,1.,0.951056516295154,1.,0.951056516295154,
1.,0.951056516295154,1.,0.951056516295154,1.,0.951056516295154,1.,0.951056516295154,
1.,0.951056516295154,1.,0.951056516295154,1.,0.951056516295154,1.,0.951056516295154,
1.,0.951056516295154,1.,0.951056516295154,1.,0.951056516295154,1.,0.951056516295154,
1.,0.951056516295154,1.,0.951056516295154,1.,0.951056516295154,1.,0.951056516295154,
1.,0.951056516295154,1.,0.951056516295154,1.,0.951056516295154,1.,0.951056516295154,
1.,0.951056516295154,1.,0.951056516295154,1.,0.951056516295154,1.,0.951056516295154,
1.,0.951056516295154,1.,0.951056516295154,1.,0.951056516295154,1.,0.951056516295154,
1.,0.951056516295154,1.,0.951056516295154,1.,0.951056516295154,1.,0.951056516295154,
1.,0.951056516295154,1.,0.951056516295154,1.,0.951056516295154,1.,0.951056516295154,
1.,0.951056516295154,1.,0.951056516295154,1.,0.951056516295154,1.,0.951056516295154,
1.,0.951056516295154,1.,0.951056516295154,1.,0.951056516295154,1.,0.951056516295154,
1.,0.951056516295154,1.,0.951056516295154,1.,0.951056516295154,1.,0.951056516295154,
1.,0.951056516295154,1.,0.951056516295154,1.,0.951056516295154,1.,0.951056516295154,
1.,0.951056516295154,1.,0.951056516295154,1.,0.951056516295154,1.,0.951056516295154,
1.,0.951056516295154,1.,0.951056516295154,1.,0.951056516295154,1.,0.951056516295154,
1.,0.951056516295154,1.,0.951056516295154,1.,0.951056516295154,1.,0.951056516295154,
1.,0.951056516295154,1.,0.951056516295154,1.,0.951056516295154,1.,0.951056516295154,
1.,0.951056516295154,1.,0.951056516295154,1.,0.951056516295154,1.,0.951056516295154,
1.,0.951056516295154,1.,0.951056516295154,1.,0.951056516295154,1.,0.951056516295154,
1.,0.951056516295154,1.,0.951056516295154,1.,0.951056516295154,1.,0.951056516295154,
1.,0.951056516295154,1.,0.951056516295154,1.,0.951056516295154,1.,0.951056516295154,
1.,0.951056516295154,1.,0.951056516295154,1.,0.951056516295154,1.,0.951056516295154,
1.,0.951056516295154,1.,0.951056516295154,1.,0.951056516295154,1.,0.951056516295154,
1.,0.951056516295154,1.,0.951056516295154,1.,0.951056516295154,1.,0.951056516295154,
1.,0.951056516295154,1.,0.951056516295154,1.,0.951056516295154,1.,0.951056516295154,
1.,0.951056516295154,1.,0.951056516295154,1.,0.951056516295154,1.,0.951056516295154,
1.,0.951056516295154,1.,0.951056516295154,1.,0.951056516295154,1.,0.951056516295154,
1.,0.951056516295154,1.,0.951056516295154,1.,0.951056516295154,1.,0.951056516295154,
1.,0.951056516295154,1.,0.951056516295154,1.,0.951056516295154,1.,0.951056516295154,
1.,0.951056516295154,1.,0.951056516295154,1.,0.951056516295154,1.,0.951056516295154,
1.,0.951056516295154,1.,0.951056516295154,1.,0.951056516295154,1.,0.951056516295154,
1.,0.951056516295154,1.,0.951056516295154,1.,0.951056516295154,1.,0.951056516295154,
1.,0.951056516295154,1.,0.951056516295154,1.,0.951056516295154,1.,0.951056516295154,
1.,0.951056516295154,1.,0.951056516295154,1.,0.951056516295154,1.,0.951056516295154,
1.,0.951056516295154,1.,0.951056516295154,1.,0.951056516295154,1.,0.951056516295154,
1.,0.951056516295154,1.,0.951056516295154,1.,0.951056516295154,1.,0.951056516295154,
1.,0.951056516295154,1.,0.951056516295154,1.,0.951056516295154,1.,0.951056516295154,
1.,0.951056516295154,1.,0.951056516295154,1.,0.951056516295154,1.,0.951056516295154,
1.,0.951056516295154,1.,0.951056516295154,1.,0.951056516295154,1.,0.951056516295154,
1.,0.951056516295154,1.,0.951056516295154,1.,0.951056516295154,1.,0.951056516295154,
1.,0.951056516295154,1.,0.951056516295154,1.,0.951056516295154,1.,0.951056516295154,
1.,0.951056516295154,1.,0.951056516295154,1.,0.951056516295154,1.,0.951056516295154,
1.,0.951056516295154,1.,0.951056516295154,1.,0.951056516295154,1.,0.951056516295154,
1.,0.951056516295154,1.,0.951056516295154,1.,0.951056516295154,1.,0.951056516295154,
1.,0.951056516295154,1.,0.951056516295154,1.,0.951056516295154,1.,0.951056516295154,
1.,0.951056516295154,1.,0.951056516295154,1.,0.951056516295154,1.,0.951056516295154,
1.,0.951056516295154,1.,0.951056516295154,1.,0.951056516295154,1.,0.951056516295154,
1.,0.951056516295154,1.,0.951056516295154,1.,0.951056516295154,1.,0.951056516295154,
1.,0.951056516295154,1.,0.951056516295154,1.,0.951056516295154,1.,0.951056516295154,
1.,0.951056516295154,1.,0.951056516295154,1.,0.951056516295154,1.,0.951056516295154,
1.,0.951056516295154,1.,0.951056516295154,1.,0.951056516295154,1.,0.951056516295154,
1.,0.951056516295154,1.,0.951056516295154,1.,0.951056516295154,1.,0.951056516295154,
1.,0.951056516295154,1.,0.951056516295154,1.,0.951056516295154,1.,0.951056516295154,
1.,0.951056516295154,1.,0.951056516295154,1.,0.951056516295154,1.,0.951056516295154,
1.,0.951056516295154,1.,0.951056516295154,1.,0.951056516295154,1.,0.951056516295154,
1.,0.951056516295154,1.,0.951056516295154,1.,0.951056516295154,1.,0.951056516295154,
1.,0.951056516295154,1.,0.951056516295154,1.,0.951056516295154,1.,0.951056516295154,
1.,0.951056516295154,1.,0.951056516295154,1.,0.951056516295154,1.,0.951056516295154,
1.,0.951056516295154,1.,0.951056516295154,1.,0.951056516295154,1.,0.951056516295154,
1.,0.951056516295154,1.,0.951056516295154,1.,0.951056516295154,1.,0.951056516295154,
1.,0.951056516295154,1.,0.951056516295154,1.,0.951056516295154,1.,0.951056516295154,
1.,0.951056516295154,1.,0.951056516295154,1.,0.951056516295154,1.)))
REPRESENTATION_ITEM('')
SURFACE()
);
#3202=(
BOUNDED_SURFACE()
B_SPLINE_SURFACE(1,2,((#305134,#305135,#305136,#305137,#305138,#305139,
#305140,#305141,#305142,#305143,#305144,#305145,#305146,#305147,#305148,
#305149,#305150,#305151,#305152,#305153,#305154,#305155,#305156,#305157,
#305158,#305159,#305160,#305161,#305162,#305163,#305164,#305165,#305166,
#305167,#305168,#305169,#305170,#305171,#305172,#305173,#305174,#305175,
#305176,#305177,#305178,#305179,#305180,#305181,#305182,#305183,#305184,
#305185,#305186,#305187,#305188,#305189,#305190,#305191,#305192,#305193,
#305194,#305195,#305196,#305197,#305198,#305199,#305200,#305201,#305202,
#305203,#305204,#305205,#305206,#305207,#305208,#305209,#305210,#305211,
#305212,#305213,#305214,#305215,#305216,#305217,#305218,#305219,#305220,
#305221,#305222,#305223,#305224,#305225,#305226,#305227,#305228,#305229,
#305230,#305231,#305232,#305233,#305234,#305235,#305236,#305237,#305238,
#305239,#305240,#305241,#305242,#305243,#305244,#305245,#305246,#305247,
#305248,#305249,#305250,#305251,#305252,#305253,#305254,#305255,#305256,
#305257,#305258,#305259,#305260,#305261,#305262,#305263,#305264,#305265,
#305266,#305267,#305268,#305269,#305270,#305271,#305272,#305273,#305274,
#305275,#305276,#305277,#305278,#305279,#305280,#305281,#305282,#305283,
#305284,#305285,#305286,#305287,#305288,#305289,#305290,#305291,#305292,
#305293,#305294,#305295,#305296,#305297,#305298,#305299,#305300,#305301,
#305302,#305303,#305304,#305305,#305306,#305307,#305308,#305309,#305310,
#305311,#305312,#305313,#305314,#305315,#305316,#305317,#305318,#305319,
#305320,#305321,#305322,#305323,#305324,#305325,#305326,#305327,#305328,
#305329,#305330,#305331,#305332,#305333,#305334,#305335,#305336,#305337,
#305338,#305339,#305340,#305341,#305342,#305343,#305344,#305345,#305346,
#305347,#305348,#305349,#305350,#305351,#305352,#305353,#305354,#305355,
#305356,#305357,#305358,#305359,#305360,#305361,#305362,#305363,#305364,
#305365,#305366,#305367,#305368,#305369,#305370,#305371,#305372,#305373,
#305374,#305375,#305376,#305377,#305378,#305379,#305380,#305381,#305382,
#305383,#305384,#305385,#305386,#305387,#305388,#305389,#305390,#305391,
#305392,#305393,#305394,#305395,#305396,#305397,#305398,#305399,#305400,
#305401,#305402,#305403,#305404,#305405,#305406,#305407,#305408,#305409,
#305410,#305411,#305412,#305413,#305414,#305415,#305416,#305417,#305418,
#305419,#305420,#305421,#305422,#305423,#305424,#305425,#305426,#305427,
#305428,#305429,#305430,#305431,#305432,#305433,#305434,#305435,#305436,
#305437,#305438,#305439,#305440,#305441,#305442,#305443,#305444,#305445,
#305446,#305447,#305448,#305449,#305450,#305451,#305452,#305453,#305454,
#305455,#305456,#305457,#305458,#305459,#305460,#305461,#305462,#305463,
#305464,#305465,#305466,#305467,#305468,#305469,#305470,#305471,#305472,
#305473,#305474,#305475,#305476,#305477,#305478,#305479,#305480,#305481,
#305482,#305483,#305484,#305485,#305486,#305487,#305488,#305489,#305490,
#305491,#305492,#305493,#305494,#305495,#305496,#305497,#305498),(#305499,
#305500,#305501,#305502,#305503,#305504,#305505,#305506,#305507,#305508,
#305509,#305510,#305511,#305512,#305513,#305514,#305515,#305516,#305517,
#305518,#305519,#305520,#305521,#305522,#305523,#305524,#305525,#305526,
#305527,#305528,#305529,#305530,#305531,#305532,#305533,#305534,#305535,
#305536,#305537,#305538,#305539,#305540,#305541,#305542,#305543,#305544,
#305545,#305546,#305547,#305548,#305549,#305550,#305551,#305552,#305553,
#305554,#305555,#305556,#305557,#305558,#305559,#305560,#305561,#305562,
#305563,#305564,#305565,#305566,#305567,#305568,#305569,#305570,#305571,
#305572,#305573,#305574,#305575,#305576,#305577,#305578,#305579,#305580,
#305581,#305582,#305583,#305584,#305585,#305586,#305587,#305588,#305589,
#305590,#305591,#305592,#305593,#305594,#305595,#305596,#305597,#305598,
#305599,#305600,#305601,#305602,#305603,#305604,#305605,#305606,#305607,
#305608,#305609,#305610,#305611,#305612,#305613,#305614,#305615,#305616,
#305617,#305618,#305619,#305620,#305621,#305622,#305623,#305624,#305625,
#305626,#305627,#305628,#305629,#305630,#305631,#305632,#305633,#305634,
#305635,#305636,#305637,#305638,#305639,#305640,#305641,#305642,#305643,
#305644,#305645,#305646,#305647,#305648,#305649,#305650,#305651,#305652,
#305653,#305654,#305655,#305656,#305657,#305658,#305659,#305660,#305661,
#305662,#305663,#305664,#305665,#305666,#305667,#305668,#305669,#305670,
#305671,#305672,#305673,#305674,#305675,#305676,#305677,#305678,#305679,
#305680,#305681,#305682,#305683,#305684,#305685,#305686,#305687,#305688,
#305689,#305690,#305691,#305692,#305693,#305694,#305695,#305696,#305697,
#305698,#305699,#305700,#305701,#305702,#305703,#305704,#305705,#305706,
#305707,#305708,#305709,#305710,#305711,#305712,#305713,#305714,#305715,
#305716,#305717,#305718,#305719,#305720,#305721,#305722,#305723,#305724,
#305725,#305726,#305727,#305728,#305729,#305730,#305731,#305732,#305733,
#305734,#305735,#305736,#305737,#305738,#305739,#305740,#305741,#305742,
#305743,#305744,#305745,#305746,#305747,#305748,#305749,#305750,#305751,
#305752,#305753,#305754,#305755,#305756,#305757,#305758,#305759,#305760,
#305761,#305762,#305763,#305764,#305765,#305766,#305767,#305768,#305769,
#305770,#305771,#305772,#305773,#305774,#305775,#305776,#305777,#305778,
#305779,#305780,#305781,#305782,#305783,#305784,#305785,#305786,#305787,
#305788,#305789,#305790,#305791,#305792,#305793,#305794,#305795,#305796,
#305797,#305798,#305799,#305800,#305801,#305802,#305803,#305804,#305805,
#305806,#305807,#305808,#305809,#305810,#305811,#305812,#305813,#305814,
#305815,#305816,#305817,#305818,#305819,#305820,#305821,#305822,#305823,
#305824,#305825,#305826,#305827,#305828,#305829,#305830,#305831,#305832,
#305833,#305834,#305835,#305836,#305837,#305838,#305839,#305840,#305841,
#305842,#305843,#305844,#305845,#305846,#305847,#305848,#305849,#305850,
#305851,#305852,#305853,#305854,#305855,#305856,#305857,#305858,#305859,
#305860,#305861,#305862,#305863)),.UNSPECIFIED.,.F.,.F.,.F.)
B_SPLINE_SURFACE_WITH_KNOTS((2,2),(3,2,2,2,2,2,2,2,2,2,2,2,2,2,2,2,2,2,
2,2,2,2,2,2,2,2,2,2,2,2,2,2,2,2,2,2,2,2,2,2,2,2,2,2,2,2,2,2,2,2,2,2,2,2,
2,2,2,2,2,2,2,2,2,2,2,2,2,2,2,2,2,2,2,2,2,2,2,2,2,2,2,2,2,2,2,2,2,2,2,2,
2,2,2,2,2,2,2,2,2,2,2,2,2,2,2,2,2,2,2,2,2,2,2,2,2,2,2,2,2,2,2,2,2,2,2,2,
2,2,2,2,2,2,2,2,2,2,2,2,2,2,2,2,2,2,2,2,2,2,2,2,2,2,2,2,2,2,2,2,2,2,2,2,
2,2,2,2,2,2,2,2,2,2,2,2,2,2,2,2,2,2,2,2,3),(0.,1.00001329281699),(0.,0.00526315789473684,
0.0105263157894737,0.0157894736842105,0.0210526315789474,0.0263157894736842,
0.031578947368421,0.0368421052631579,0.0421052631578947,0.0473684210526316,
0.0526315789473684,0.0578947368421053,0.0631578947368421,0.068421052631579,
0.0736842105263158,0.0789473684210526,0.0842105263157895,0.0894736842105263,
0.0947368421052632,0.1,0.105263157894737,0.110526315789474,0.11578947368421,
0.121052631578947,0.126315789473684,0.131578947368421,0.136842105263158,
0.142105263157895,0.147368421052632,0.152631578947369,0.157894736842105,
0.163157894736842,0.168421052631579,0.173684210526316,0.178947368421052,
0.18421052631579,0.189473684210526,0.194736842105263,0.2,0.205263157894737,
0.210526315789474,0.215789473684211,0.221052631578948,0.226315789473684,
0.231578947368421,0.236842105263158,0.242105263157895,0.247368421052632,
0.252631578947369,0.257894736842106,0.263157894736842,0.268421052631579,
0.273684210526316,0.278947368421052,0.28421052631579,0.289473684210526,
0.294736842105263,0.3,0.305263157894737,0.310526315789473,0.315789473684211,
0.321052631578947,0.326315789473685,0.331578947368421,0.336842105263158,
0.342105263157895,0.347368421052631,0.352631578947369,0.357894736842105,
0.363157894736842,0.368421052631579,0.373684210526316,0.378947368421053,
0.38421052631579,0.389473684210526,0.394736842105263,0.4,0.405263157894737,
0.410526315789473,0.415789473684211,0.421052631578948,0.426315789473684,
0.431578947368421,0.436842105263158,0.442105263157895,0.447368421052632,
0.452631578947369,0.457894736842105,0.463157894736842,0.468421052631579,
0.473684210526316,0.478947368421053,0.48421052631579,0.489473684210526,
0.494736842105263,0.5,0.505263157894737,0.510526315789474,0.515789473684211,
0.521052631578947,0.526315789473684,0.531578947368421,0.536842105263158,
0.542105263157895,0.547368421052632,0.552631578947369,0.557894736842105,
0.563157894736842,0.568421052631579,0.573684210526316,0.578947368421053,
0.58421052631579,0.589473684210526,0.594736842105263,0.6,0.605263157894737,
0.610526315789474,0.615789473684211,0.621052631578947,0.626315789473684,
0.631578947368421,0.636842105263158,0.642105263157895,0.647368421052632,
0.652631578947369,0.657894736842105,0.663157894736842,0.668421052631579,
0.673684210526316,0.678947368421053,0.68421052631579,0.689473684210526,
0.694736842105263,0.7,0.705263157894737,0.710526315789474,0.715789473684211,
0.721052631578947,0.726315789473684,0.731578947368421,0.736842105263158,
0.742105263157895,0.747368421052632,0.752631578947368,0.757894736842105,
0.763157894736842,0.768421052631579,0.773684210526316,0.778947368421053,
0.78421052631579,0.789473684210526,0.794736842105263,0.8,0.805263157894737,
0.810526315789474,0.815789473684211,0.821052631578947,0.826315789473684,
0.831578947368421,0.836842105263158,0.842105263157895,0.847368421052632,
0.852631578947368,0.857894736842105,0.863157894736842,0.868421052631579,
0.873684210526316,0.878947368421053,0.884210526315789,0.889473684210526,
0.894736842105263,0.9,0.905263157894737,0.910526315789474,0.91578947368421,
0.921052631578947,0.926315789473684,0.931578947368421,0.936842105263158,
0.942105263157895,0.947368421052632,0.952631578947368,0.954890265398446),
 .UNSPECIFIED.)
GEOMETRIC_REPRESENTATION_ITEM()
RATIONAL_B_SPLINE_SURFACE(((1.,0.951056516295154,1.,0.951056516295154,1.,
0.951056516295154,1.,0.951056516295154,1.,0.951056516295154,1.,0.951056516295154,
1.,0.951056516295154,1.,0.951056516295154,1.,0.951056516295154,1.,0.951056516295154,
1.,0.951056516295154,1.,0.951056516295154,1.,0.951056516295154,1.,0.951056516295154,
1.,0.951056516295154,1.,0.951056516295154,1.,0.951056516295154,1.,0.951056516295154,
1.,0.951056516295154,1.,0.951056516295154,1.,0.951056516295154,1.,0.951056516295154,
1.,0.951056516295154,1.,0.951056516295154,1.,0.951056516295154,1.,0.951056516295154,
1.,0.951056516295154,1.,0.951056516295154,1.,0.951056516295154,1.,0.951056516295154,
1.,0.951056516295154,1.,0.951056516295154,1.,0.951056516295154,1.,0.951056516295154,
1.,0.951056516295154,1.,0.951056516295154,1.,0.951056516295154,1.,0.951056516295154,
1.,0.951056516295154,1.,0.951056516295154,1.,0.951056516295154,1.,0.951056516295154,
1.,0.951056516295154,1.,0.951056516295154,1.,0.951056516295154,1.,0.951056516295154,
1.,0.951056516295154,1.,0.951056516295154,1.,0.951056516295154,1.,0.951056516295154,
1.,0.951056516295154,1.,0.951056516295154,1.,0.951056516295154,1.,0.951056516295154,
1.,0.951056516295154,1.,0.951056516295154,1.,0.951056516295154,1.,0.951056516295154,
1.,0.951056516295154,1.,0.951056516295154,1.,0.951056516295154,1.,0.951056516295154,
1.,0.951056516295154,1.,0.951056516295154,1.,0.951056516295154,1.,0.951056516295154,
1.,0.951056516295154,1.,0.951056516295154,1.,0.951056516295154,1.,0.951056516295154,
1.,0.951056516295154,1.,0.951056516295154,1.,0.951056516295154,1.,0.951056516295154,
1.,0.951056516295154,1.,0.951056516295154,1.,0.951056516295154,1.,0.951056516295154,
1.,0.951056516295154,1.,0.951056516295154,1.,0.951056516295154,1.,0.951056516295154,
1.,0.951056516295154,1.,0.951056516295154,1.,0.951056516295154,1.,0.951056516295154,
1.,0.951056516295154,1.,0.951056516295154,1.,0.951056516295154,1.,0.951056516295154,
1.,0.951056516295154,1.,0.951056516295154,1.,0.951056516295154,1.,0.951056516295154,
1.,0.951056516295154,1.,0.951056516295154,1.,0.951056516295154,1.,0.951056516295154,
1.,0.951056516295154,1.,0.951056516295154,1.,0.951056516295154,1.,0.951056516295154,
1.,0.951056516295154,1.,0.951056516295154,1.,0.951056516295154,1.,0.951056516295154,
1.,0.951056516295154,1.,0.951056516295154,1.,0.951056516295154,1.,0.951056516295154,
1.,0.951056516295154,1.,0.951056516295154,1.,0.951056516295154,1.,0.951056516295154,
1.,0.951056516295154,1.,0.951056516295154,1.,0.951056516295154,1.,0.951056516295154,
1.,0.951056516295154,1.,0.951056516295154,1.,0.951056516295154,1.,0.951056516295154,
1.,0.951056516295154,1.,0.951056516295154,1.,0.951056516295154,1.,0.951056516295154,
1.,0.951056516295154,1.,0.951056516295154,1.,0.951056516295154,1.,0.951056516295154,
1.,0.951056516295154,1.,0.951056516295154,1.,0.951056516295154,1.,0.951056516295154,
1.,0.951056516295154,1.,0.951056516295154,1.,0.951056516295154,1.,0.951056516295154,
1.,0.951056516295154,1.,0.951056516295154,1.,0.951056516295154,1.,0.951056516295154,
1.,0.951056516295154,1.,0.951056516295154,1.,0.951056516295154,1.,0.951056516295154,
1.,0.951056516295154,1.,0.951056516295154,1.,0.951056516295154,1.,0.951056516295154,
1.,0.951056516295154,1.,0.951056516295154,1.,0.951056516295154,1.,0.951056516295154,
1.,0.951056516295154,1.,0.951056516295154,1.,0.951056516295154,1.,0.951056516295154,
1.,0.951056516295154,1.,0.951056516295154,1.,0.951056516295154,1.,0.951056516295154,
1.,0.951056516295154,1.,0.951056516295154,1.,0.951056516295154,1.,0.951056516295154,
1.,0.951056516295154,1.,0.951056516295154,1.,0.951056516295154,1.,0.951056516295154,
1.,0.951056516295154,1.,0.951056516295154,1.,0.951056516295154,1.,0.951056516295154,
1.,0.951056516295154,1.,0.951056516295154,1.,0.951056516295154,1.,0.951056516295154,
1.,0.951056516295154,1.,0.951056516295154,1.,0.951056516295154,1.,0.978995883132586,
0.976019617655583),(1.,0.951056516295154,1.,0.951056516295154,1.,0.951056516295154,
1.,0.951056516295154,1.,0.951056516295154,1.,0.951056516295154,1.,0.951056516295154,
1.,0.951056516295154,1.,0.951056516295154,1.,0.951056516295154,1.,0.951056516295154,
1.,0.951056516295154,1.,0.951056516295154,1.,0.951056516295154,1.,0.951056516295154,
1.,0.951056516295154,1.,0.951056516295154,1.,0.951056516295154,1.,0.951056516295154,
1.,0.951056516295154,1.,0.951056516295154,1.,0.951056516295154,1.,0.951056516295154,
1.,0.951056516295154,1.,0.951056516295154,1.,0.951056516295154,1.,0.951056516295154,
1.,0.951056516295154,1.,0.951056516295154,1.,0.951056516295154,1.,0.951056516295154,
1.,0.951056516295154,1.,0.951056516295154,1.,0.951056516295154,1.,0.951056516295154,
1.,0.951056516295154,1.,0.951056516295154,1.,0.951056516295154,1.,0.951056516295154,
1.,0.951056516295154,1.,0.951056516295154,1.,0.951056516295154,1.,0.951056516295154,
1.,0.951056516295154,1.,0.951056516295154,1.,0.951056516295154,1.,0.951056516295154,
1.,0.951056516295154,1.,0.951056516295154,1.,0.951056516295154,1.,0.951056516295154,
1.,0.951056516295154,1.,0.951056516295154,1.,0.951056516295154,1.,0.951056516295154,
1.,0.951056516295154,1.,0.951056516295154,1.,0.951056516295154,1.,0.951056516295154,
1.,0.951056516295154,1.,0.951056516295154,1.,0.951056516295154,1.,0.951056516295154,
1.,0.951056516295154,1.,0.951056516295154,1.,0.951056516295154,1.,0.951056516295154,
1.,0.951056516295154,1.,0.951056516295154,1.,0.951056516295154,1.,0.951056516295154,
1.,0.951056516295154,1.,0.951056516295154,1.,0.951056516295154,1.,0.951056516295154,
1.,0.951056516295154,1.,0.951056516295154,1.,0.951056516295154,1.,0.951056516295154,
1.,0.951056516295154,1.,0.951056516295154,1.,0.951056516295154,1.,0.951056516295154,
1.,0.951056516295154,1.,0.951056516295154,1.,0.951056516295154,1.,0.951056516295154,
1.,0.951056516295154,1.,0.951056516295154,1.,0.951056516295154,1.,0.951056516295154,
1.,0.951056516295154,1.,0.951056516295154,1.,0.951056516295154,1.,0.951056516295154,
1.,0.951056516295154,1.,0.951056516295154,1.,0.951056516295154,1.,0.951056516295154,
1.,0.951056516295154,1.,0.951056516295154,1.,0.951056516295154,1.,0.951056516295154,
1.,0.951056516295154,1.,0.951056516295154,1.,0.951056516295154,1.,0.951056516295154,
1.,0.951056516295154,1.,0.951056516295154,1.,0.951056516295154,1.,0.951056516295154,
1.,0.951056516295154,1.,0.951056516295154,1.,0.951056516295154,1.,0.951056516295154,
1.,0.951056516295154,1.,0.951056516295154,1.,0.951056516295154,1.,0.951056516295154,
1.,0.951056516295154,1.,0.951056516295154,1.,0.951056516295154,1.,0.951056516295154,
1.,0.951056516295154,1.,0.951056516295154,1.,0.951056516295154,1.,0.951056516295154,
1.,0.951056516295154,1.,0.951056516295154,1.,0.951056516295154,1.,0.951056516295154,
1.,0.951056516295154,1.,0.951056516295154,1.,0.951056516295154,1.,0.951056516295154,
1.,0.951056516295154,1.,0.951056516295154,1.,0.951056516295154,1.,0.951056516295154,
1.,0.951056516295154,1.,0.951056516295154,1.,0.951056516295154,1.,0.951056516295154,
1.,0.951056516295154,1.,0.951056516295154,1.,0.951056516295154,1.,0.951056516295154,
1.,0.951056516295154,1.,0.951056516295154,1.,0.951056516295154,1.,0.951056516295154,
1.,0.951056516295154,1.,0.951056516295154,1.,0.951056516295154,1.,0.951056516295154,
1.,0.951056516295154,1.,0.951056516295154,1.,0.951056516295154,1.,0.951056516295154,
1.,0.951056516295154,1.,0.951056516295154,1.,0.951056516295154,1.,0.951056516295154,
1.,0.951056516295154,1.,0.951056516295154,1.,0.951056516295154,1.,0.951056516295154,
1.,0.951056516295154,1.,0.951056516295154,1.,0.951056516295154,1.,0.951056516295154,
1.,0.951056516295154,1.,0.951056516295154,1.,0.951056516295154,1.,0.951056516295154,
1.,0.951056516295154,1.,0.951056516295154,1.,0.951056516295154,1.,0.951056516295154,
1.,0.951056516295154,1.,0.951056516295154,1.,0.978995883132586,0.976019617655583)))
REPRESENTATION_ITEM('')
SURFACE()
);
#3203=(
BOUNDED_SURFACE()
B_SPLINE_SURFACE(1,2,((#305903,#305904,#305905,#305906,#305907,#305908,
#305909,#305910,#305911,#305912,#305913,#305914,#305915,#305916,#305917,
#305918,#305919,#305920,#305921,#305922,#305923,#305924,#305925,#305926,
#305927,#305928,#305929,#305930,#305931,#305932,#305933,#305934,#305935,
#305936,#305937,#305938,#305939,#305940,#305941,#305942,#305943,#305944,
#305945,#305946,#305947,#305948,#305949,#305950,#305951,#305952,#305953,
#305954,#305955,#305956,#305957,#305958,#305959,#305960,#305961,#305962,
#305963,#305964,#305965,#305966,#305967,#305968,#305969,#305970,#305971,
#305972,#305973,#305974,#305975,#305976,#305977,#305978,#305979,#305980,
#305981,#305982,#305983,#305984,#305985,#305986,#305987,#305988,#305989,
#305990,#305991,#305992,#305993,#305994,#305995,#305996,#305997,#305998,
#305999,#306000,#306001,#306002,#306003,#306004,#306005,#306006,#306007,
#306008,#306009,#306010,#306011,#306012,#306013,#306014,#306015,#306016,
#306017,#306018,#306019,#306020,#306021,#306022,#306023,#306024,#306025,
#306026,#306027,#306028,#306029,#306030,#306031,#306032,#306033,#306034,
#306035,#306036,#306037,#306038,#306039,#306040,#306041,#306042,#306043,
#306044,#306045,#306046,#306047,#306048,#306049,#306050,#306051,#306052,
#306053,#306054,#306055,#306056,#306057,#306058,#306059,#306060,#306061,
#306062,#306063,#306064,#306065,#306066,#306067,#306068,#306069,#306070,
#306071,#306072,#306073,#306074,#306075,#306076,#306077,#306078,#306079,
#306080,#306081,#306082,#306083,#306084,#306085,#306086,#306087,#306088,
#306089,#306090,#306091,#306092,#306093,#306094,#306095,#306096,#306097,
#306098,#306099,#306100,#306101,#306102,#306103,#306104,#306105,#306106,
#306107,#306108,#306109,#306110,#306111,#306112,#306113,#306114,#306115,
#306116,#306117,#306118,#306119,#306120,#306121,#306122,#306123,#306124,
#306125,#306126,#306127,#306128,#306129,#306130,#306131,#306132,#306133,
#306134,#306135,#306136,#306137,#306138,#306139,#306140,#306141,#306142,
#306143,#306144,#306145,#306146,#306147,#306148,#306149,#306150,#306151,
#306152,#306153,#306154,#306155,#306156,#306157,#306158,#306159,#306160,
#306161,#306162,#306163,#306164,#306165,#306166,#306167,#306168,#306169,
#306170,#306171,#306172,#306173,#306174,#306175,#306176,#306177,#306178,
#306179,#306180,#306181,#306182,#306183,#306184,#306185,#306186,#306187,
#306188,#306189,#306190,#306191,#306192,#306193,#306194,#306195,#306196,
#306197,#306198,#306199,#306200,#306201,#306202,#306203,#306204,#306205,
#306206,#306207,#306208,#306209,#306210,#306211,#306212,#306213,#306214,
#306215,#306216,#306217,#306218,#306219,#306220,#306221,#306222,#306223,
#306224,#306225,#306226,#306227,#306228,#306229,#306230,#306231,#306232,
#306233,#306234,#306235,#306236,#306237,#306238,#306239,#306240,#306241,
#306242,#306243,#306244,#306245,#306246,#306247,#306248,#306249,#306250,
#306251,#306252,#306253,#306254,#306255,#306256,#306257,#306258,#306259,
#306260,#306261,#306262,#306263,#306264,#306265,#306266,#306267),(#306268,
#306269,#306270,#306271,#306272,#306273,#306274,#306275,#306276,#306277,
#306278,#306279,#306280,#306281,#306282,#306283,#306284,#306285,#306286,
#306287,#306288,#306289,#306290,#306291,#306292,#306293,#306294,#306295,
#306296,#306297,#306298,#306299,#306300,#306301,#306302,#306303,#306304,
#306305,#306306,#306307,#306308,#306309,#306310,#306311,#306312,#306313,
#306314,#306315,#306316,#306317,#306318,#306319,#306320,#306321,#306322,
#306323,#306324,#306325,#306326,#306327,#306328,#306329,#306330,#306331,
#306332,#306333,#306334,#306335,#306336,#306337,#306338,#306339,#306340,
#306341,#306342,#306343,#306344,#306345,#306346,#306347,#306348,#306349,
#306350,#306351,#306352,#306353,#306354,#306355,#306356,#306357,#306358,
#306359,#306360,#306361,#306362,#306363,#306364,#306365,#306366,#306367,
#306368,#306369,#306370,#306371,#306372,#306373,#306374,#306375,#306376,
#306377,#306378,#306379,#306380,#306381,#306382,#306383,#306384,#306385,
#306386,#306387,#306388,#306389,#306390,#306391,#306392,#306393,#306394,
#306395,#306396,#306397,#306398,#306399,#306400,#306401,#306402,#306403,
#306404,#306405,#306406,#306407,#306408,#306409,#306410,#306411,#306412,
#306413,#306414,#306415,#306416,#306417,#306418,#306419,#306420,#306421,
#306422,#306423,#306424,#306425,#306426,#306427,#306428,#306429,#306430,
#306431,#306432,#306433,#306434,#306435,#306436,#306437,#306438,#306439,
#306440,#306441,#306442,#306443,#306444,#306445,#306446,#306447,#306448,
#306449,#306450,#306451,#306452,#306453,#306454,#306455,#306456,#306457,
#306458,#306459,#306460,#306461,#306462,#306463,#306464,#306465,#306466,
#306467,#306468,#306469,#306470,#306471,#306472,#306473,#306474,#306475,
#306476,#306477,#306478,#306479,#306480,#306481,#306482,#306483,#306484,
#306485,#306486,#306487,#306488,#306489,#306490,#306491,#306492,#306493,
#306494,#306495,#306496,#306497,#306498,#306499,#306500,#306501,#306502,
#306503,#306504,#306505,#306506,#306507,#306508,#306509,#306510,#306511,
#306512,#306513,#306514,#306515,#306516,#306517,#306518,#306519,#306520,
#306521,#306522,#306523,#306524,#306525,#306526,#306527,#306528,#306529,
#306530,#306531,#306532,#306533,#306534,#306535,#306536,#306537,#306538,
#306539,#306540,#306541,#306542,#306543,#306544,#306545,#306546,#306547,
#306548,#306549,#306550,#306551,#306552,#306553,#306554,#306555,#306556,
#306557,#306558,#306559,#306560,#306561,#306562,#306563,#306564,#306565,
#306566,#306567,#306568,#306569,#306570,#306571,#306572,#306573,#306574,
#306575,#306576,#306577,#306578,#306579,#306580,#306581,#306582,#306583,
#306584,#306585,#306586,#306587,#306588,#306589,#306590,#306591,#306592,
#306593,#306594,#306595,#306596,#306597,#306598,#306599,#306600,#306601,
#306602,#306603,#306604,#306605,#306606,#306607,#306608,#306609,#306610,
#306611,#306612,#306613,#306614,#306615,#306616,#306617,#306618,#306619,
#306620,#306621,#306622,#306623,#306624,#306625,#306626,#306627,#306628,
#306629,#306630,#306631,#306632)),.UNSPECIFIED.,.F.,.F.,.F.)
B_SPLINE_SURFACE_WITH_KNOTS((2,2),(3,2,2,2,2,2,2,2,2,2,2,2,2,2,2,2,2,2,
2,2,2,2,2,2,2,2,2,2,2,2,2,2,2,2,2,2,2,2,2,2,2,2,2,2,2,2,2,2,2,2,2,2,2,2,
2,2,2,2,2,2,2,2,2,2,2,2,2,2,2,2,2,2,2,2,2,2,2,2,2,2,2,2,2,2,2,2,2,2,2,2,
2,2,2,2,2,2,2,2,2,2,2,2,2,2,2,2,2,2,2,2,2,2,2,2,2,2,2,2,2,2,2,2,2,2,2,2,
2,2,2,2,2,2,2,2,2,2,2,2,2,2,2,2,2,2,2,2,2,2,2,2,2,2,2,2,2,2,2,2,2,2,2,2,
2,2,2,2,2,2,2,2,2,2,2,2,2,2,2,2,2,2,2,2,3),(-9.0530534475071E-6,1.),(0.,
0.00526315789473684,0.0105263157894737,0.0157894736842105,0.0210526315789474,
0.0263157894736842,0.031578947368421,0.0368421052631579,0.0421052631578947,
0.0473684210526316,0.0526315789473684,0.0578947368421053,0.0631578947368421,
0.068421052631579,0.0736842105263158,0.0789473684210526,0.0842105263157895,
0.0894736842105263,0.0947368421052632,0.1,0.105263157894737,0.110526315789474,
0.11578947368421,0.121052631578947,0.126315789473684,0.131578947368421,
0.136842105263158,0.142105263157895,0.147368421052632,0.152631578947369,
0.157894736842105,0.163157894736842,0.168421052631579,0.173684210526316,
0.178947368421052,0.18421052631579,0.189473684210526,0.194736842105263,
0.2,0.205263157894737,0.210526315789474,0.215789473684211,0.221052631578948,
0.226315789473684,0.231578947368421,0.236842105263158,0.242105263157895,
0.247368421052632,0.252631578947369,0.257894736842106,0.263157894736842,
0.268421052631579,0.273684210526316,0.278947368421052,0.28421052631579,
0.289473684210526,0.294736842105263,0.3,0.305263157894737,0.310526315789473,
0.315789473684211,0.321052631578947,0.326315789473685,0.331578947368421,
0.336842105263158,0.342105263157895,0.347368421052631,0.352631578947369,
0.357894736842105,0.363157894736842,0.368421052631579,0.373684210526316,
0.378947368421053,0.38421052631579,0.389473684210526,0.394736842105263,
0.4,0.405263157894737,0.410526315789473,0.415789473684211,0.421052631578948,
0.426315789473684,0.431578947368421,0.436842105263158,0.442105263157895,
0.447368421052632,0.452631578947369,0.457894736842105,0.463157894736842,
0.468421052631579,0.473684210526316,0.478947368421053,0.48421052631579,
0.489473684210526,0.494736842105263,0.5,0.505263157894737,0.510526315789474,
0.515789473684211,0.521052631578947,0.526315789473684,0.531578947368421,
0.536842105263158,0.542105263157895,0.547368421052632,0.552631578947369,
0.557894736842105,0.563157894736842,0.568421052631579,0.573684210526316,
0.578947368421053,0.58421052631579,0.589473684210526,0.594736842105263,
0.6,0.605263157894737,0.610526315789474,0.615789473684211,0.621052631578947,
0.626315789473684,0.631578947368421,0.636842105263158,0.642105263157895,
0.647368421052632,0.652631578947369,0.657894736842105,0.663157894736842,
0.668421052631579,0.673684210526316,0.678947368421053,0.68421052631579,
0.689473684210526,0.694736842105263,0.7,0.705263157894737,0.710526315789474,
0.715789473684211,0.721052631578947,0.726315789473684,0.731578947368421,
0.736842105263158,0.742105263157895,0.747368421052632,0.752631578947368,
0.757894736842105,0.763157894736842,0.768421052631579,0.773684210526316,
0.778947368421053,0.78421052631579,0.789473684210526,0.794736842105263,
0.8,0.805263157894737,0.810526315789474,0.815789473684211,0.821052631578947,
0.826315789473684,0.831578947368421,0.836842105263158,0.842105263157895,
0.847368421052632,0.852631578947368,0.857894736842105,0.863157894736842,
0.868421052631579,0.873684210526316,0.878947368421053,0.884210526315789,
0.889473684210526,0.894736842105263,0.9,0.905263157894737,0.910526315789474,
0.91578947368421,0.921052631578947,0.926315789473684,0.931578947368421,
0.936842105263158,0.942105263157895,0.947368421052632,0.952631578947368,
0.954890272715098),.UNSPECIFIED.)
GEOMETRIC_REPRESENTATION_ITEM()
RATIONAL_B_SPLINE_SURFACE(((1.,0.951056516295154,1.,0.951056516295154,1.,
0.951056516295154,1.,0.951056516295154,1.,0.951056516295154,1.,0.951056516295154,
1.,0.951056516295154,1.,0.951056516295154,1.,0.951056516295154,1.,0.951056516295154,
1.,0.951056516295154,1.,0.951056516295154,1.,0.951056516295154,1.,0.951056516295154,
1.,0.951056516295154,1.,0.951056516295154,1.,0.951056516295154,1.,0.951056516295154,
1.,0.951056516295154,1.,0.951056516295154,1.,0.951056516295154,1.,0.951056516295154,
1.,0.951056516295154,1.,0.951056516295154,1.,0.951056516295154,1.,0.951056516295154,
1.,0.951056516295154,1.,0.951056516295154,1.,0.951056516295154,1.,0.951056516295154,
1.,0.951056516295154,1.,0.951056516295154,1.,0.951056516295154,1.,0.951056516295154,
1.,0.951056516295154,1.,0.951056516295154,1.,0.951056516295154,1.,0.951056516295154,
1.,0.951056516295154,1.,0.951056516295154,1.,0.951056516295154,1.,0.951056516295154,
1.,0.951056516295154,1.,0.951056516295154,1.,0.951056516295154,1.,0.951056516295154,
1.,0.951056516295154,1.,0.951056516295154,1.,0.951056516295154,1.,0.951056516295154,
1.,0.951056516295154,1.,0.951056516295154,1.,0.951056516295154,1.,0.951056516295154,
1.,0.951056516295154,1.,0.951056516295154,1.,0.951056516295154,1.,0.951056516295154,
1.,0.951056516295154,1.,0.951056516295154,1.,0.951056516295154,1.,0.951056516295154,
1.,0.951056516295154,1.,0.951056516295154,1.,0.951056516295154,1.,0.951056516295154,
1.,0.951056516295154,1.,0.951056516295154,1.,0.951056516295154,1.,0.951056516295154,
1.,0.951056516295154,1.,0.951056516295154,1.,0.951056516295154,1.,0.951056516295154,
1.,0.951056516295154,1.,0.951056516295154,1.,0.951056516295154,1.,0.951056516295154,
1.,0.951056516295154,1.,0.951056516295154,1.,0.951056516295154,1.,0.951056516295154,
1.,0.951056516295154,1.,0.951056516295154,1.,0.951056516295154,1.,0.951056516295154,
1.,0.951056516295154,1.,0.951056516295154,1.,0.951056516295154,1.,0.951056516295154,
1.,0.951056516295154,1.,0.951056516295154,1.,0.951056516295154,1.,0.951056516295154,
1.,0.951056516295154,1.,0.951056516295154,1.,0.951056516295154,1.,0.951056516295154,
1.,0.951056516295154,1.,0.951056516295154,1.,0.951056516295154,1.,0.951056516295154,
1.,0.951056516295154,1.,0.951056516295154,1.,0.951056516295154,1.,0.951056516295154,
1.,0.951056516295154,1.,0.951056516295154,1.,0.951056516295154,1.,0.951056516295154,
1.,0.951056516295154,1.,0.951056516295154,1.,0.951056516295154,1.,0.951056516295154,
1.,0.951056516295154,1.,0.951056516295154,1.,0.951056516295154,1.,0.951056516295154,
1.,0.951056516295154,1.,0.951056516295154,1.,0.951056516295154,1.,0.951056516295154,
1.,0.951056516295154,1.,0.951056516295154,1.,0.951056516295154,1.,0.951056516295154,
1.,0.951056516295154,1.,0.951056516295154,1.,0.951056516295154,1.,0.951056516295154,
1.,0.951056516295154,1.,0.951056516295154,1.,0.951056516295154,1.,0.951056516295154,
1.,0.951056516295154,1.,0.951056516295154,1.,0.951056516295154,1.,0.951056516295154,
1.,0.951056516295154,1.,0.951056516295154,1.,0.951056516295154,1.,0.951056516295154,
1.,0.951056516295154,1.,0.951056516295154,1.,0.951056516295154,1.,0.951056516295154,
1.,0.951056516295154,1.,0.951056516295154,1.,0.951056516295154,1.,0.951056516295154,
1.,0.951056516295154,1.,0.951056516295154,1.,0.951056516295154,1.,0.951056516295154,
1.,0.951056516295154,1.,0.951056516295154,1.,0.951056516295154,1.,0.951056516295154,
1.,0.951056516295154,1.,0.951056516295154,1.,0.951056516295154,1.,0.951056516295154,
1.,0.951056516295154,1.,0.951056516295154,1.,0.951056516295154,1.,0.951056516295154,
1.,0.951056516295154,1.,0.951056516295154,1.,0.951056516295154,1.,0.951056516295154,
1.,0.951056516295154,1.,0.951056516295154,1.,0.951056516295154,1.,0.951056516295154,
1.,0.951056516295154,1.,0.951056516295154,1.,0.951056516295154,1.,0.951056516295154,
1.,0.951056516295154,1.,0.951056516295154,1.,0.951056516295154,1.,0.978995815093128,
0.976019598373506),(1.,0.951056516295154,1.,0.951056516295154,1.,0.951056516295154,
1.,0.951056516295154,1.,0.951056516295154,1.,0.951056516295154,1.,0.951056516295154,
1.,0.951056516295154,1.,0.951056516295154,1.,0.951056516295154,1.,0.951056516295154,
1.,0.951056516295154,1.,0.951056516295154,1.,0.951056516295154,1.,0.951056516295154,
1.,0.951056516295154,1.,0.951056516295154,1.,0.951056516295154,1.,0.951056516295154,
1.,0.951056516295154,1.,0.951056516295154,1.,0.951056516295154,1.,0.951056516295154,
1.,0.951056516295154,1.,0.951056516295154,1.,0.951056516295154,1.,0.951056516295154,
1.,0.951056516295154,1.,0.951056516295154,1.,0.951056516295154,1.,0.951056516295154,
1.,0.951056516295154,1.,0.951056516295154,1.,0.951056516295154,1.,0.951056516295154,
1.,0.951056516295154,1.,0.951056516295154,1.,0.951056516295154,1.,0.951056516295154,
1.,0.951056516295154,1.,0.951056516295154,1.,0.951056516295154,1.,0.951056516295154,
1.,0.951056516295154,1.,0.951056516295154,1.,0.951056516295154,1.,0.951056516295154,
1.,0.951056516295154,1.,0.951056516295154,1.,0.951056516295154,1.,0.951056516295154,
1.,0.951056516295154,1.,0.951056516295154,1.,0.951056516295154,1.,0.951056516295154,
1.,0.951056516295154,1.,0.951056516295154,1.,0.951056516295154,1.,0.951056516295154,
1.,0.951056516295154,1.,0.951056516295154,1.,0.951056516295154,1.,0.951056516295154,
1.,0.951056516295154,1.,0.951056516295154,1.,0.951056516295154,1.,0.951056516295154,
1.,0.951056516295154,1.,0.951056516295154,1.,0.951056516295154,1.,0.951056516295154,
1.,0.951056516295154,1.,0.951056516295154,1.,0.951056516295154,1.,0.951056516295154,
1.,0.951056516295154,1.,0.951056516295154,1.,0.951056516295154,1.,0.951056516295154,
1.,0.951056516295154,1.,0.951056516295154,1.,0.951056516295154,1.,0.951056516295154,
1.,0.951056516295154,1.,0.951056516295154,1.,0.951056516295154,1.,0.951056516295154,
1.,0.951056516295154,1.,0.951056516295154,1.,0.951056516295154,1.,0.951056516295154,
1.,0.951056516295154,1.,0.951056516295154,1.,0.951056516295154,1.,0.951056516295154,
1.,0.951056516295154,1.,0.951056516295154,1.,0.951056516295154,1.,0.951056516295154,
1.,0.951056516295154,1.,0.951056516295154,1.,0.951056516295154,1.,0.951056516295154,
1.,0.951056516295154,1.,0.951056516295154,1.,0.951056516295154,1.,0.951056516295154,
1.,0.951056516295154,1.,0.951056516295154,1.,0.951056516295154,1.,0.951056516295154,
1.,0.951056516295154,1.,0.951056516295154,1.,0.951056516295154,1.,0.951056516295154,
1.,0.951056516295154,1.,0.951056516295154,1.,0.951056516295154,1.,0.951056516295154,
1.,0.951056516295154,1.,0.951056516295154,1.,0.951056516295154,1.,0.951056516295154,
1.,0.951056516295154,1.,0.951056516295154,1.,0.951056516295154,1.,0.951056516295154,
1.,0.951056516295154,1.,0.951056516295154,1.,0.951056516295154,1.,0.951056516295154,
1.,0.951056516295154,1.,0.951056516295154,1.,0.951056516295154,1.,0.951056516295154,
1.,0.951056516295154,1.,0.951056516295154,1.,0.951056516295154,1.,0.951056516295154,
1.,0.951056516295154,1.,0.951056516295154,1.,0.951056516295154,1.,0.951056516295154,
1.,0.951056516295154,1.,0.951056516295154,1.,0.951056516295154,1.,0.951056516295154,
1.,0.951056516295154,1.,0.951056516295154,1.,0.951056516295154,1.,0.951056516295154,
1.,0.951056516295154,1.,0.951056516295154,1.,0.951056516295154,1.,0.951056516295154,
1.,0.951056516295154,1.,0.951056516295154,1.,0.951056516295154,1.,0.951056516295154,
1.,0.951056516295154,1.,0.951056516295154,1.,0.951056516295154,1.,0.951056516295154,
1.,0.951056516295154,1.,0.951056516295154,1.,0.951056516295154,1.,0.951056516295154,
1.,0.951056516295154,1.,0.951056516295154,1.,0.951056516295154,1.,0.951056516295154,
1.,0.951056516295154,1.,0.951056516295154,1.,0.951056516295154,1.,0.951056516295154,
1.,0.951056516295154,1.,0.951056516295154,1.,0.951056516295154,1.,0.951056516295154,
1.,0.951056516295154,1.,0.951056516295154,1.,0.978995815093128,0.976019598373506)))
REPRESENTATION_ITEM('')
SURFACE()
);
#3204=(
BOUNDED_SURFACE()
B_SPLINE_SURFACE(1,2,((#309430,#309431,#309432,#309433,#309434,#309435,
#309436,#309437,#309438,#309439,#309440,#309441,#309442,#309443,#309444,
#309445,#309446,#309447,#309448,#309449,#309450,#309451,#309452,#309453,
#309454,#309455,#309456,#309457,#309458,#309459,#309460,#309461,#309462,
#309463,#309464,#309465,#309466,#309467,#309468,#309469,#309470,#309471,
#309472,#309473,#309474,#309475,#309476,#309477,#309478,#309479,#309480,
#309481,#309482,#309483,#309484,#309485,#309486,#309487,#309488,#309489,
#309490,#309491,#309492,#309493,#309494,#309495,#309496,#309497,#309498,
#309499,#309500,#309501,#309502,#309503,#309504,#309505,#309506,#309507,
#309508,#309509,#309510,#309511,#309512,#309513,#309514,#309515,#309516,
#309517,#309518,#309519,#309520,#309521,#309522,#309523,#309524,#309525,
#309526,#309527,#309528,#309529,#309530,#309531,#309532,#309533,#309534,
#309535,#309536,#309537,#309538,#309539,#309540,#309541,#309542,#309543,
#309544,#309545,#309546,#309547,#309548,#309549,#309550,#309551,#309552,
#309553,#309554,#309555,#309556,#309557,#309558,#309559,#309560,#309561,
#309562,#309563,#309564,#309565,#309566),(#309567,#309568,#309569,#309570,
#309571,#309572,#309573,#309574,#309575,#309576,#309577,#309578,#309579,
#309580,#309581,#309582,#309583,#309584,#309585,#309586,#309587,#309588,
#309589,#309590,#309591,#309592,#309593,#309594,#309595,#309596,#309597,
#309598,#309599,#309600,#309601,#309602,#309603,#309604,#309605,#309606,
#309607,#309608,#309609,#309610,#309611,#309612,#309613,#309614,#309615,
#309616,#309617,#309618,#309619,#309620,#309621,#309622,#309623,#309624,
#309625,#309626,#309627,#309628,#309629,#309630,#309631,#309632,#309633,
#309634,#309635,#309636,#309637,#309638,#309639,#309640,#309641,#309642,
#309643,#309644,#309645,#309646,#309647,#309648,#309649,#309650,#309651,
#309652,#309653,#309654,#309655,#309656,#309657,#309658,#309659,#309660,
#309661,#309662,#309663,#309664,#309665,#309666,#309667,#309668,#309669,
#309670,#309671,#309672,#309673,#309674,#309675,#309676,#309677,#309678,
#309679,#309680,#309681,#309682,#309683,#309684,#309685,#309686,#309687,
#309688,#309689,#309690,#309691,#309692,#309693,#309694,#309695,#309696,
#309697,#309698,#309699,#309700,#309701,#309702,#309703)),.UNSPECIFIED.,
 .F.,.F.,.F.)
B_SPLINE_SURFACE_WITH_KNOTS((2,2),(3,2,2,2,2,2,2,2,2,2,2,2,2,2,2,2,2,2,
2,2,2,2,2,2,2,2,2,2,2,2,2,2,2,2,2,2,2,2,2,2,2,2,2,2,2,2,2,2,2,2,2,2,2,2,
2,2,2,2,2,2,2,2,2,2,2,2,2,2,3),(0.,1.00001687186328),(0.,0.0142857142857143,
0.0285714285714285,0.0428571428571429,0.0571428571428571,0.0714285714285714,
0.0857142857142857,0.1,0.114285714285714,0.128571428571429,0.142857142857143,
0.157142857142857,0.171428571428572,0.185714285714285,0.2,0.214285714285714,
0.228571428571428,0.242857142857143,0.257142857142857,0.271428571428572,
0.285714285714286,0.3,0.314285714285715,0.328571428571429,0.342857142857143,
0.357142857142857,0.371428571428571,0.385714285714286,0.4,0.414285714285715,
0.428571428571428,0.442857142857143,0.457142857142857,0.471428571428571,
0.485714285714286,0.5,0.514285714285714,0.528571428571429,0.542857142857143,
0.557142857142857,0.571428571428571,0.585714285714286,0.6,0.614285714285714,
0.628571428571429,0.642857142857143,0.657142857142857,0.671428571428571,
0.685714285714286,0.7,0.714285714285714,0.728571428571428,0.742857142857143,
0.757142857142857,0.771428571428571,0.785714285714286,0.8,0.814285714285714,
0.828571428571429,0.842857142857143,0.857142857142857,0.871428571428571,
0.885714285714286,0.9,0.914285714285714,0.928571428571429,0.942857142857143,
0.957142857142857,0.95920445073468),.UNSPECIFIED.)
GEOMETRIC_REPRESENTATION_ITEM()
RATIONAL_B_SPLINE_SURFACE(((1.,0.951056516295154,1.,0.951056516295154,1.,
0.951056516295154,1.,0.951056516295154,1.,0.951056516295154,1.,0.951056516295154,
1.,0.951056516295154,1.,0.951056516295154,1.,0.951056516295154,1.,0.951056516295154,
1.,0.951056516295154,1.,0.951056516295154,1.,0.951056516295154,1.,0.951056516295154,
1.,0.951056516295154,1.,0.951056516295154,1.,0.951056516295154,1.,0.951056516295154,
1.,0.951056516295154,1.,0.951056516295154,1.,0.951056516295154,1.,0.951056516295154,
1.,0.951056516295154,1.,0.951056516295154,1.,0.951056516295154,1.,0.951056516295154,
1.,0.951056516295154,1.,0.951056516295154,1.,0.951056516295154,1.,0.951056516295154,
1.,0.951056516295154,1.,0.951056516295154,1.,0.951056516295154,1.,0.951056516295154,
1.,0.951056516295154,1.,0.951056516295154,1.,0.951056516295154,1.,0.951056516295154,
1.,0.951056516295154,1.,0.951056516295154,1.,0.951056516295154,1.,0.951056516295154,
1.,0.951056516295154,1.,0.951056516295154,1.,0.951056516295154,1.,0.951056516295154,
1.,0.951056516295154,1.,0.951056516295154,1.,0.951056516295154,1.,0.951056516295154,
1.,0.951056516295154,1.,0.951056516295154,1.,0.951056516295154,1.,0.951056516295154,
1.,0.951056516295154,1.,0.951056516295154,1.,0.951056516295154,1.,0.951056516295154,
1.,0.951056516295154,1.,0.951056516295154,1.,0.951056516295154,1.,0.951056516295154,
1.,0.951056516295154,1.,0.951056516295154,1.,0.951056516295154,1.,0.951056516295154,
1.,0.951056516295154,1.,0.99293688993428,0.987912356611537),(1.,0.951056516295154,
1.,0.951056516295154,1.,0.951056516295154,1.,0.951056516295154,1.,0.951056516295154,
1.,0.951056516295154,1.,0.951056516295154,1.,0.951056516295154,1.,0.951056516295154,
1.,0.951056516295154,1.,0.951056516295154,1.,0.951056516295154,1.,0.951056516295154,
1.,0.951056516295154,1.,0.951056516295154,1.,0.951056516295154,1.,0.951056516295154,
1.,0.951056516295154,1.,0.951056516295154,1.,0.951056516295154,1.,0.951056516295154,
1.,0.951056516295154,1.,0.951056516295154,1.,0.951056516295154,1.,0.951056516295154,
1.,0.951056516295154,1.,0.951056516295154,1.,0.951056516295154,1.,0.951056516295154,
1.,0.951056516295154,1.,0.951056516295154,1.,0.951056516295154,1.,0.951056516295154,
1.,0.951056516295154,1.,0.951056516295154,1.,0.951056516295154,1.,0.951056516295154,
1.,0.951056516295154,1.,0.951056516295154,1.,0.951056516295154,1.,0.951056516295154,
1.,0.951056516295154,1.,0.951056516295154,1.,0.951056516295154,1.,0.951056516295154,
1.,0.951056516295154,1.,0.951056516295154,1.,0.951056516295154,1.,0.951056516295154,
1.,0.951056516295154,1.,0.951056516295154,1.,0.951056516295154,1.,0.951056516295154,
1.,0.951056516295154,1.,0.951056516295154,1.,0.951056516295154,1.,0.951056516295154,
1.,0.951056516295154,1.,0.951056516295154,1.,0.951056516295154,1.,0.951056516295154,
1.,0.951056516295154,1.,0.951056516295154,1.,0.951056516295154,1.,0.951056516295154,
1.,0.951056516295154,1.,0.951056516295154,1.,0.99293688993428,0.987912356611537)))
REPRESENTATION_ITEM('')
SURFACE()
);
#3205=(
BOUNDED_SURFACE()
B_SPLINE_SURFACE(1,2,((#309842,#309843,#309844,#309845,#309846,#309847,
#309848,#309849,#309850,#309851,#309852,#309853,#309854,#309855,#309856,
#309857,#309858,#309859,#309860,#309861,#309862,#309863,#309864,#309865,
#309866,#309867,#309868,#309869,#309870,#309871,#309872,#309873,#309874,
#309875,#309876,#309877,#309878,#309879,#309880,#309881,#309882,#309883,
#309884,#309885,#309886,#309887,#309888,#309889,#309890,#309891,#309892,
#309893,#309894,#309895,#309896,#309897,#309898,#309899,#309900,#309901,
#309902,#309903,#309904,#309905,#309906,#309907,#309908,#309909,#309910,
#309911,#309912,#309913,#309914,#309915,#309916,#309917,#309918,#309919,
#309920,#309921,#309922,#309923,#309924,#309925,#309926,#309927,#309928,
#309929,#309930,#309931,#309932,#309933,#309934,#309935,#309936,#309937,
#309938,#309939,#309940,#309941,#309942,#309943,#309944,#309945,#309946,
#309947,#309948,#309949,#309950,#309951,#309952,#309953,#309954,#309955,
#309956,#309957,#309958,#309959,#309960,#309961,#309962,#309963,#309964,
#309965,#309966,#309967,#309968,#309969,#309970,#309971,#309972,#309973,
#309974,#309975,#309976,#309977,#309978),(#309979,#309980,#309981,#309982,
#309983,#309984,#309985,#309986,#309987,#309988,#309989,#309990,#309991,
#309992,#309993,#309994,#309995,#309996,#309997,#309998,#309999,#310000,
#310001,#310002,#310003,#310004,#310005,#310006,#310007,#310008,#310009,
#310010,#310011,#310012,#310013,#310014,#310015,#310016,#310017,#310018,
#310019,#310020,#310021,#310022,#310023,#310024,#310025,#310026,#310027,
#310028,#310029,#310030,#310031,#310032,#310033,#310034,#310035,#310036,
#310037,#310038,#310039,#310040,#310041,#310042,#310043,#310044,#310045,
#310046,#310047,#310048,#310049,#310050,#310051,#310052,#310053,#310054,
#310055,#310056,#310057,#310058,#310059,#310060,#310061,#310062,#310063,
#310064,#310065,#310066,#310067,#310068,#310069,#310070,#310071,#310072,
#310073,#310074,#310075,#310076,#310077,#310078,#310079,#310080,#310081,
#310082,#310083,#310084,#310085,#310086,#310087,#310088,#310089,#310090,
#310091,#310092,#310093,#310094,#310095,#310096,#310097,#310098,#310099,
#310100,#310101,#310102,#310103,#310104,#310105,#310106,#310107,#310108,
#310109,#310110,#310111,#310112,#310113,#310114,#310115)),.UNSPECIFIED.,
 .F.,.F.,.F.)
B_SPLINE_SURFACE_WITH_KNOTS((2,2),(3,2,2,2,2,2,2,2,2,2,2,2,2,2,2,2,2,2,
2,2,2,2,2,2,2,2,2,2,2,2,2,2,2,2,2,2,2,2,2,2,2,2,2,2,2,2,2,2,2,2,2,2,2,2,
2,2,2,2,2,2,2,2,2,2,2,2,2,2,3),(-5.49146708075157E-6,1.),(0.,0.0142857142857143,
0.0285714285714285,0.0428571428571429,0.0571428571428571,0.0714285714285714,
0.0857142857142857,0.1,0.114285714285714,0.128571428571429,0.142857142857143,
0.157142857142857,0.171428571428572,0.185714285714285,0.2,0.214285714285714,
0.228571428571428,0.242857142857143,0.257142857142857,0.271428571428572,
0.285714285714286,0.3,0.314285714285715,0.328571428571429,0.342857142857143,
0.357142857142857,0.371428571428571,0.385714285714286,0.4,0.414285714285715,
0.428571428571428,0.442857142857143,0.457142857142857,0.471428571428571,
0.485714285714286,0.5,0.514285714285714,0.528571428571429,0.542857142857143,
0.557142857142857,0.571428571428571,0.585714285714286,0.6,0.614285714285714,
0.628571428571429,0.642857142857143,0.657142857142857,0.671428571428571,
0.685714285714286,0.7,0.714285714285714,0.728571428571428,0.742857142857143,
0.757142857142857,0.771428571428571,0.785714285714286,0.8,0.814285714285714,
0.828571428571429,0.842857142857143,0.857142857142857,0.871428571428571,
0.885714285714286,0.9,0.914285714285714,0.928571428571429,0.942857142857143,
0.957142857142857,0.959204499671976),.UNSPECIFIED.)
GEOMETRIC_REPRESENTATION_ITEM()
RATIONAL_B_SPLINE_SURFACE(((1.,0.951056516295154,1.,0.951056516295154,1.,
0.951056516295154,1.,0.951056516295154,1.,0.951056516295154,1.,0.951056516295154,
1.,0.951056516295154,1.,0.951056516295154,1.,0.951056516295154,1.,0.951056516295154,
1.,0.951056516295154,1.,0.951056516295154,1.,0.951056516295154,1.,0.951056516295154,
1.,0.951056516295154,1.,0.951056516295154,1.,0.951056516295154,1.,0.951056516295154,
1.,0.951056516295154,1.,0.951056516295154,1.,0.951056516295154,1.,0.951056516295154,
1.,0.951056516295154,1.,0.951056516295154,1.,0.951056516295154,1.,0.951056516295154,
1.,0.951056516295154,1.,0.951056516295154,1.,0.951056516295154,1.,0.951056516295154,
1.,0.951056516295154,1.,0.951056516295154,1.,0.951056516295154,1.,0.951056516295154,
1.,0.951056516295154,1.,0.951056516295154,1.,0.951056516295154,1.,0.951056516295154,
1.,0.951056516295154,1.,0.951056516295154,1.,0.951056516295154,1.,0.951056516295154,
1.,0.951056516295154,1.,0.951056516295154,1.,0.951056516295154,1.,0.951056516295154,
1.,0.951056516295154,1.,0.951056516295154,1.,0.951056516295154,1.,0.951056516295154,
1.,0.951056516295154,1.,0.951056516295154,1.,0.951056516295154,1.,0.951056516295154,
1.,0.951056516295154,1.,0.951056516295154,1.,0.951056516295154,1.,0.951056516295154,
1.,0.951056516295154,1.,0.951056516295154,1.,0.951056516295154,1.,0.951056516295154,
1.,0.951056516295154,1.,0.951056516295154,1.,0.951056516295154,1.,0.951056516295154,
1.,0.951056516295154,1.,0.992936722272959,0.987912118071905),(1.,0.951056516295154,
1.,0.951056516295154,1.,0.951056516295154,1.,0.951056516295154,1.,0.951056516295154,
1.,0.951056516295154,1.,0.951056516295154,1.,0.951056516295154,1.,0.951056516295154,
1.,0.951056516295154,1.,0.951056516295154,1.,0.951056516295154,1.,0.951056516295154,
1.,0.951056516295154,1.,0.951056516295154,1.,0.951056516295154,1.,0.951056516295154,
1.,0.951056516295154,1.,0.951056516295154,1.,0.951056516295154,1.,0.951056516295154,
1.,0.951056516295154,1.,0.951056516295154,1.,0.951056516295154,1.,0.951056516295154,
1.,0.951056516295154,1.,0.951056516295154,1.,0.951056516295154,1.,0.951056516295154,
1.,0.951056516295154,1.,0.951056516295154,1.,0.951056516295154,1.,0.951056516295154,
1.,0.951056516295154,1.,0.951056516295154,1.,0.951056516295154,1.,0.951056516295154,
1.,0.951056516295154,1.,0.951056516295154,1.,0.951056516295154,1.,0.951056516295154,
1.,0.951056516295154,1.,0.951056516295154,1.,0.951056516295154,1.,0.951056516295154,
1.,0.951056516295154,1.,0.951056516295154,1.,0.951056516295154,1.,0.951056516295154,
1.,0.951056516295154,1.,0.951056516295154,1.,0.951056516295154,1.,0.951056516295154,
1.,0.951056516295154,1.,0.951056516295154,1.,0.951056516295154,1.,0.951056516295154,
1.,0.951056516295154,1.,0.951056516295154,1.,0.951056516295154,1.,0.951056516295154,
1.,0.951056516295154,1.,0.951056516295154,1.,0.951056516295154,1.,0.951056516295154,
1.,0.951056516295154,1.,0.951056516295154,1.,0.992936722272959,0.987912118071905)))
REPRESENTATION_ITEM('')
SURFACE()
);
#3206=TOROIDAL_SURFACE('',#94111,2.5,0.5);
#3207=TOROIDAL_SURFACE('',#94120,2.,1.);
#3208=TOROIDAL_SURFACE('',#94128,2.,1.);
#3209=TOROIDAL_SURFACE('',#94138,57.3875000000282,1.);
#3210=TOROIDAL_SURFACE('',#94155,57.3875000000282,1.);
#3211=TOROIDAL_SURFACE('',#94165,58.8875000000282,0.5);
#3212=TOROIDAL_SURFACE('',#94172,57.3875000000282,1.);
#3213=TOROIDAL_SURFACE('',#94181,58.8875000000282,0.5);
#3214=TOROIDAL_SURFACE('',#94186,57.3875000000282,1.);
#3215=TOROIDAL_SURFACE('',#94194,58.8875000000282,0.5);
#3216=TOROIDAL_SURFACE('',#94201,57.3875000000282,1.);
#3217=TOROIDAL_SURFACE('',#94216,57.3875000000282,1.);
#3218=TOROIDAL_SURFACE('',#94233,4.5,0.5);
#3219=TOROIDAL_SURFACE('',#94256,4.5,0.5);
#3220=TOROIDAL_SURFACE('',#94265,2.,1.);
#3221=TOROIDAL_SURFACE('',#94273,2.,1.);
#3222=TOROIDAL_SURFACE('',#94281,57.3875000000282,1.);
#3223=TOROIDAL_SURFACE('',#94289,58.8875000000282,0.5);
#3224=TOROIDAL_SURFACE('',#94295,57.3875000000282,1.);
#3225=TOROIDAL_SURFACE('',#94308,57.3875000000282,1.);
#3226=TOROIDAL_SURFACE('',#94321,57.3875000000282,1.);
#3227=TOROIDAL_SURFACE('',#94334,57.3875000000282,1.);
#3228=TOROIDAL_SURFACE('',#94342,58.8875000000282,0.5);
#3229=TOROIDAL_SURFACE('',#94348,57.3875000000282,1.);
#3230=TOROIDAL_SURFACE('',#94474,1.,0.5);
#3231=TOROIDAL_SURFACE('',#94486,1.,0.5);
#3232=TOROIDAL_SURFACE('',#94492,1.,0.5);
#3233=TOROIDAL_SURFACE('',#94498,45.1752328136335,1.);
#3234=TOROIDAL_SURFACE('',#94506,1.,0.5);
#3235=TOROIDAL_SURFACE('',#94512,1.,0.5);
#3236=TOROIDAL_SURFACE('',#94518,45.1752328136335,1.);
#3237=TOROIDAL_SURFACE('',#94528,1.,0.5);
#3238=TOROIDAL_SURFACE('',#94534,1.,0.5);
#3239=TOROIDAL_SURFACE('',#94546,1.,0.5);
#3240=TOROIDAL_SURFACE('',#94552,1.,0.5);
#3241=TOROIDAL_SURFACE('',#94566,4.5,0.5);
#3242=TOROIDAL_SURFACE('',#94575,5.25,0.25);
#3243=TOROIDAL_SURFACE('',#94581,2.75,0.25);
#3244=TOROIDAL_SURFACE('',#94585,67.25,0.25);
#3245=TOROIDAL_SURFACE('',#94589,2.75,0.25);
#3246=TOROIDAL_SURFACE('',#94595,5.25,0.25);
#3247=TOROIDAL_SURFACE('',#94599,58.25,0.25);
#3248=TOROIDAL_SURFACE('',#94603,5.25,0.25);
#3249=TOROIDAL_SURFACE('',#94609,2.75,0.25);
#3250=TOROIDAL_SURFACE('',#94613,67.25,0.25);
#3251=TOROIDAL_SURFACE('',#94617,2.75,0.25);
#3252=TOROIDAL_SURFACE('',#94623,3.25,0.25);
#3253=TOROIDAL_SURFACE('',#94640,57.5,1.);
#3254=TOROIDAL_SURFACE('',#94649,59.,0.5);
#3255=TOROIDAL_SURFACE('',#94656,57.5,1.);
#3256=TOROIDAL_SURFACE('',#94671,57.5,1.);
#3257=TOROIDAL_SURFACE('',#94683,59.,0.5);
#3258=TOROIDAL_SURFACE('',#94733,59.024570260837,1.);
#3259=TOROIDAL_SURFACE('',#94888,59.024570260837,1.);
#3260=TOROIDAL_SURFACE('',#94956,59.024570260837,1.);
#3261=TOROIDAL_SURFACE('',#94973,59.024570260837,1.);
#3262=TOROIDAL_SURFACE('',#95024,59.,0.5);
#3263=TOROIDAL_SURFACE('',#95044,2.5,0.5);
#3264=TOROIDAL_SURFACE('',#95052,3.5,0.5);
#3265=TOROIDAL_SURFACE('',#95199,2.5,0.5);
#3266=TOROIDAL_SURFACE('',#95204,2.5,0.5);
#3267=TOROIDAL_SURFACE('',#95208,2.5,0.5);
#3268=TOROIDAL_SURFACE('',#95217,2.5,0.5);
#3269=TOROIDAL_SURFACE('',#95224,2.5,0.5);
#3270=TOROIDAL_SURFACE('',#95229,2.5,0.5);
#3271=TOROIDAL_SURFACE('',#95236,2.5,0.5);
#3272=TOROIDAL_SURFACE('',#95240,2.5,0.5);
#3273=TOROIDAL_SURFACE('',#95245,2.5,0.5);
#3274=TOROIDAL_SURFACE('',#95250,2.5,0.5);
#3275=TOROIDAL_SURFACE('',#95252,2.5,0.5);
#3276=TOROIDAL_SURFACE('',#95257,2.5,0.5);
#3277=TOROIDAL_SURFACE('',#95273,2.5,0.5);
#3278=TOROIDAL_SURFACE('',#95287,2.5,0.5);
#3279=TOROIDAL_SURFACE('',#95292,2.5,0.5);
#3280=TOROIDAL_SURFACE('',#95296,2.5,0.5);
#3281=TOROIDAL_SURFACE('',#95301,2.5,0.5);
#3282=TOROIDAL_SURFACE('',#95403,2.5,0.5);
#3283=TOROIDAL_SURFACE('',#95409,2.5,0.5);
#3284=TOROIDAL_SURFACE('',#95413,2.5,0.5);
#3285=TOROIDAL_SURFACE('',#95418,2.5,0.5);
#3286=TOROIDAL_SURFACE('',#95439,2.5,0.5);
#3287=TOROIDAL_SURFACE('',#95452,59.024570260837,1.);
#3288=TOROIDAL_SURFACE('',#95461,2.5,0.5);
#3289=TOROIDAL_SURFACE('',#95466,2.5,0.5);
#3290=TOROIDAL_SURFACE('',#95479,2.5,0.5);
#3291=TOROIDAL_SURFACE('',#95491,2.5,0.5);
#3292=TOROIDAL_SURFACE('',#95511,2.5,0.5);
#3293=TOROIDAL_SURFACE('',#95531,2.5,0.5);
#3294=TOROIDAL_SURFACE('',#95536,2.5,0.5);
#3295=TOROIDAL_SURFACE('',#95540,2.5,0.5);
#3296=TOROIDAL_SURFACE('',#95559,2.5,0.5);
#3297=TOROIDAL_SURFACE('',#95561,59.024570260837,1.);
#3298=TOROIDAL_SURFACE('',#95571,2.5,0.5);
#3299=TOROIDAL_SURFACE('',#95575,2.5,0.5);
#3300=TOROIDAL_SURFACE('',#95582,2.5,0.5);
#3301=TOROIDAL_SURFACE('',#95586,2.5,0.5);
#3302=TOROIDAL_SURFACE('',#95591,59.024570260837,1.);
#3303=TOROIDAL_SURFACE('',#95604,2.5,0.5);
#3304=TOROIDAL_SURFACE('',#95609,2.5,0.5);
#3305=TOROIDAL_SURFACE('',#95622,2.5,0.5);
#3306=TOROIDAL_SURFACE('',#95627,2.5,0.5);
#3307=TOROIDAL_SURFACE('',#95655,2.5,0.5);
#3308=TOROIDAL_SURFACE('',#95675,2.5,0.5);
#3309=TOROIDAL_SURFACE('',#95680,2.5,0.5);
#3310=TOROIDAL_SURFACE('',#95684,2.5,0.5);
#3311=TOROIDAL_SURFACE('',#95703,2.5,0.5);
#3312=TOROIDAL_SURFACE('',#95716,2.5,0.5);
#3313=TOROIDAL_SURFACE('',#95733,2.5,0.5);
#3314=TOROIDAL_SURFACE('',#95738,2.5,0.5);
#3315=TOROIDAL_SURFACE('',#95748,2.5,0.5);
#3316=TOROIDAL_SURFACE('',#95770,2.5,0.5);
#3317=TOROIDAL_SURFACE('',#95772,59.024570260837,1.);
#3318=TOROIDAL_SURFACE('',#95791,2.5,0.5);
#3319=TOROIDAL_SURFACE('',#95796,2.5,0.5);
#3320=TOROIDAL_SURFACE('',#95800,2.5,0.5);
#3321=TOROIDAL_SURFACE('',#95820,2.5,0.5);
#3322=TOROIDAL_SURFACE('',#95829,2.,1.);
#3323=TOROIDAL_SURFACE('',#95831,66.5,1.);
#3324=TOROIDAL_SURFACE('',#95833,2.,1.);
#3325=TOROIDAL_SURFACE('',#95848,59.,0.5);
#3326=TOROIDAL_SURFACE('',#95851,57.5,1.);
#3327=TOROIDAL_SURFACE('',#95854,59.,0.5);
#3328=TOROIDAL_SURFACE('',#95858,57.5,1.);
#3329=TOROIDAL_SURFACE('',#95863,57.5,1.);
#3330=TOROIDAL_SURFACE('',#95868,57.5,1.);
#3331=TOROIDAL_SURFACE('',#95873,57.5,1.);
#3332=TOROIDAL_SURFACE('',#95877,59.,0.5);
#3333=TOROIDAL_SURFACE('',#95880,57.5,1.);
#3334=TOROIDAL_SURFACE('',#95883,59.,0.5);
#3335=TOROIDAL_SURFACE('',#95899,2.,1.);
#3336=TOROIDAL_SURFACE('',#95901,66.5,1.);
#3337=TOROIDAL_SURFACE('',#95903,2.,1.);
#3338=TOROIDAL_SURFACE('',#95916,59.1370702608075,1.);
#3339=TOROIDAL_SURFACE('',#95957,59.1370702608075,1.);
#3340=TOROIDAL_SURFACE('',#95976,59.1370702608075,1.);
#3341=TOROIDAL_SURFACE('',#95979,59.1370702608075,1.);
#3342=TOROIDAL_SURFACE('',#95991,59.1370702608075,1.);
#3343=TOROIDAL_SURFACE('',#95998,59.1370702608075,1.);
#3344=TOROIDAL_SURFACE('',#96019,59.1370702608075,1.);
#3345=TOROIDAL_SURFACE('',#96027,59.1370702608075,1.);
#3346=TOROIDAL_SURFACE('',#96042,59.1370702608075,1.);
#3347=TOROIDAL_SURFACE('',#96046,59.1370702608075,1.);
#3348=TOROIDAL_SURFACE('',#96077,59.1370702608075,1.);
#3349=TOROIDAL_SURFACE('',#96148,59.1370702608075,1.);
#3350=TOROIDAL_SURFACE('',#96174,2.,1.);
#3351=TOROIDAL_SURFACE('',#96178,66.5,1.);
#3352=TOROIDAL_SURFACE('',#96182,2.,1.);
#3353=TOROIDAL_SURFACE('',#96206,59.,0.5);
#3354=TOROIDAL_SURFACE('',#96210,57.5,1.);
#3355=TOROIDAL_SURFACE('',#96216,59.,0.5);
#3356=TOROIDAL_SURFACE('',#96222,57.5,1.);
#3357=TOROIDAL_SURFACE('',#96231,57.5,1.);
#3358=TOROIDAL_SURFACE('',#96240,57.5,1.);
#3359=TOROIDAL_SURFACE('',#96249,57.5,1.);
#3360=TOROIDAL_SURFACE('',#96256,59.,0.5);
#3361=TOROIDAL_SURFACE('',#96260,57.5,1.);
#3362=TOROIDAL_SURFACE('',#96266,59.,0.5);
#3363=TOROIDAL_SURFACE('',#96287,2.,1.);
#3364=TOROIDAL_SURFACE('',#96291,66.5,1.);
#3365=TOROIDAL_SURFACE('',#96295,2.,1.);
#3366=TOROIDAL_SURFACE('',#96309,2.5,0.5);
#3367=TOROIDAL_SURFACE('',#96332,2.5,0.5);
#3368=TOROIDAL_SURFACE('',#96338,2.5,0.5);
#3369=TOROIDAL_SURFACE('',#96344,2.5,0.5);
#3370=TOROIDAL_SURFACE('',#96363,59.024570260837,1.);
#3371=TOROIDAL_SURFACE('',#96365,2.5,0.5);
#3372=TOROIDAL_SURFACE('',#96388,2.5,0.5);
#3373=TOROIDAL_SURFACE('',#96402,2.5,0.5);
#3374=TOROIDAL_SURFACE('',#96408,2.5,0.5);
#3375=TOROIDAL_SURFACE('',#96425,2.5,0.5);
#3376=TOROIDAL_SURFACE('',#96436,2.5,0.5);
#3377=TOROIDAL_SURFACE('',#96456,2.5,0.5);
#3378=TOROIDAL_SURFACE('',#96462,2.5,0.5);
#3379=TOROIDAL_SURFACE('',#96468,2.5,0.5);
#3380=TOROIDAL_SURFACE('',#96489,2.5,0.5);
#3381=TOROIDAL_SURFACE('',#96520,2.5,0.5);
#3382=TOROIDAL_SURFACE('',#96529,2.5,0.5);
#3383=TOROIDAL_SURFACE('',#96546,2.5,0.5);
#3384=TOROIDAL_SURFACE('',#96552,2.5,0.5);
#3385=TOROIDAL_SURFACE('',#96563,59.024570260837,1.);
#3386=TOROIDAL_SURFACE('',#96571,2.5,0.5);
#3387=TOROIDAL_SURFACE('',#96578,2.5,0.5);
#3388=TOROIDAL_SURFACE('',#96590,2.5,0.5);
#3389=TOROIDAL_SURFACE('',#96597,2.5,0.5);
#3390=TOROIDAL_SURFACE('',#96611,59.024570260837,1.);
#3391=TOROIDAL_SURFACE('',#96613,2.5,0.5);
#3392=TOROIDAL_SURFACE('',#96633,2.5,0.5);
#3393=TOROIDAL_SURFACE('',#96639,2.5,0.5);
#3394=TOROIDAL_SURFACE('',#96645,2.5,0.5);
#3395=TOROIDAL_SURFACE('',#96666,2.5,0.5);
#3396=TOROIDAL_SURFACE('',#96690,2.5,0.5);
#3397=TOROIDAL_SURFACE('',#96701,2.5,0.5);
#3398=TOROIDAL_SURFACE('',#96717,2.5,0.5);
#3399=TOROIDAL_SURFACE('',#96723,2.5,0.5);
#3400=TOROIDAL_SURFACE('',#96730,59.024570260837,1.);
#3401=TOROIDAL_SURFACE('',#96746,2.5,0.5);
#3402=TOROIDAL_SURFACE('',#96765,2.5,0.5);
#3403=TOROIDAL_SURFACE('',#96771,2.5,0.5);
#3404=TOROIDAL_SURFACE('',#96777,2.5,0.5);
#3405=TOROIDAL_SURFACE('',#96783,2.5,0.5);
#3406=TOROIDAL_SURFACE('',#96892,2.5,0.5);
#3407=TOROIDAL_SURFACE('',#96898,2.5,0.5);
#3408=TOROIDAL_SURFACE('',#96904,2.5,0.5);
#3409=TOROIDAL_SURFACE('',#96910,2.5,0.5);
#3410=TOROIDAL_SURFACE('',#96924,2.5,0.5);
#3411=TOROIDAL_SURFACE('',#96941,2.5,0.5);
#3412=TOROIDAL_SURFACE('',#96947,2.5,0.5);
#3413=TOROIDAL_SURFACE('',#96950,2.5,0.5);
#3414=TOROIDAL_SURFACE('',#96956,2.5,0.5);
#3415=TOROIDAL_SURFACE('',#96972,2.5,0.5);
#3416=TOROIDAL_SURFACE('',#96979,2.5,0.5);
#3417=TOROIDAL_SURFACE('',#96994,2.5,0.5);
#3418=TOROIDAL_SURFACE('',#97001,2.5,0.5);
#3419=TOROIDAL_SURFACE('',#97011,2.5,0.5);
#3420=TOROIDAL_SURFACE('',#97024,2.5,0.5);
#3421=TOROIDAL_SURFACE('',#97030,2.5,0.5);
#3422=TOROIDAL_SURFACE('',#97036,2.5,0.5);
#3423=TOROIDAL_SURFACE('',#97212,3.5,0.5);
#3424=TOROIDAL_SURFACE('',#97220,2.5,0.5);
#3425=TOROIDAL_SURFACE('',#97242,59.,0.5);
#3426=TOROIDAL_SURFACE('',#97277,59.024570260837,1.);
#3427=TOROIDAL_SURFACE('',#97286,59.024570260837,1.);
#3428=TOROIDAL_SURFACE('',#97323,59.024570260837,1.);
#3429=TOROIDAL_SURFACE('',#97447,59.024570260837,1.);
#3430=TOROIDAL_SURFACE('',#97490,59.,0.5);
#3431=TOROIDAL_SURFACE('',#97499,57.5,1.);
#3432=TOROIDAL_SURFACE('',#97508,57.5,1.);
#3433=TOROIDAL_SURFACE('',#97513,59.,0.5);
#3434=TOROIDAL_SURFACE('',#97518,57.5,1.);
#3435=TOROIDAL_SURFACE('',#97526,3.25,0.25);
#3436=TOROIDAL_SURFACE('',#97532,2.75,0.25);
#3437=TOROIDAL_SURFACE('',#97535,67.25,0.25);
#3438=TOROIDAL_SURFACE('',#97538,2.75,0.25);
#3439=TOROIDAL_SURFACE('',#97543,5.25,0.25);
#3440=TOROIDAL_SURFACE('',#97546,58.25,0.25);
#3441=TOROIDAL_SURFACE('',#97549,5.25,0.25);
#3442=TOROIDAL_SURFACE('',#97554,2.75,0.25);
#3443=TOROIDAL_SURFACE('',#97557,67.25,0.25);
#3444=TOROIDAL_SURFACE('',#97560,2.75,0.25);
#3445=TOROIDAL_SURFACE('',#97565,5.25,0.25);
#3446=TOROIDAL_SURFACE('',#97573,4.5,0.5);
#3447=TOROIDAL_SURFACE('',#97584,1.,0.5);
#3448=TOROIDAL_SURFACE('',#97589,1.,0.5);
#3449=TOROIDAL_SURFACE('',#97596,1.,0.5);
#3450=TOROIDAL_SURFACE('',#97601,1.,0.5);
#3451=TOROIDAL_SURFACE('',#97608,45.1752328136335,1.);
#3452=TOROIDAL_SURFACE('',#97612,1.,0.5);
#3453=TOROIDAL_SURFACE('',#97617,1.,0.5);
#3454=TOROIDAL_SURFACE('',#97621,45.1752328136335,1.);
#3455=TOROIDAL_SURFACE('',#97625,1.,0.5);
#3456=TOROIDAL_SURFACE('',#97630,1.,0.5);
#3457=TOROIDAL_SURFACE('',#97639,1.,0.5);
#3458=TOROIDAL_SURFACE('',#97753,57.3875000000282,1.);
#3459=TOROIDAL_SURFACE('',#97758,58.8875000000282,0.5);
#3460=TOROIDAL_SURFACE('',#97763,57.3875000000282,1.);
#3461=TOROIDAL_SURFACE('',#97772,57.3875000000282,1.);
#3462=TOROIDAL_SURFACE('',#97781,57.3875000000282,1.);
#3463=TOROIDAL_SURFACE('',#97790,57.3875000000282,1.);
#3464=TOROIDAL_SURFACE('',#97795,58.8875000000282,0.5);
#3465=TOROIDAL_SURFACE('',#97800,57.3875000000282,1.);
#3466=TOROIDAL_SURFACE('',#97806,2.,1.);
#3467=TOROIDAL_SURFACE('',#97811,2.,1.);
#3468=TOROIDAL_SURFACE('',#97817,4.5,0.5);
#3469=TOROIDAL_SURFACE('',#97826,4.5,0.5);
#3470=TOROIDAL_SURFACE('',#97836,57.3875000000282,1.);
#3471=TOROIDAL_SURFACE('',#97845,57.3875000000282,1.);
#3472=TOROIDAL_SURFACE('',#97850,58.8875000000282,0.5);
#3473=TOROIDAL_SURFACE('',#97855,57.3875000000282,1.);
#3474=TOROIDAL_SURFACE('',#97859,58.8875000000282,0.5);
#3475=TOROIDAL_SURFACE('',#97865,57.3875000000282,1.);
#3476=TOROIDAL_SURFACE('',#97870,58.8875000000282,0.5);
#3477=TOROIDAL_SURFACE('',#97875,57.3875000000282,1.);
#3478=TOROIDAL_SURFACE('',#97885,57.3875000000282,1.);
#3479=TOROIDAL_SURFACE('',#97894,2.,1.);
#3480=TOROIDAL_SURFACE('',#97899,2.,1.);
#3481=TOROIDAL_SURFACE('',#97905,2.5,0.5);
#3482=TOROIDAL_SURFACE('',#97917,58.25,0.25);
#3483=TOROIDAL_SURFACE('',#97921,58.25,0.25);
#3484=TOROIDAL_SURFACE('',#97925,59.,0.5);
#3485=TOROIDAL_SURFACE('',#97931,45.1752328136335,1.);
#3486=TOROIDAL_SURFACE('',#97935,57.3875000000282,1.);
#3487=TOROIDAL_SURFACE('',#97961,3.,0.25);
#3488=TOROIDAL_SURFACE('',#97983,4.01589928084081,0.5);
#3489=TOROIDAL_SURFACE('',#97995,2.,0.5);
#3490=TOROIDAL_SURFACE('',#98000,74.3,0.5);
#3491=TOROIDAL_SURFACE('',#98005,2.,0.5);
#3492=TOROIDAL_SURFACE('',#98027,2.,0.5);
#3493=TOROIDAL_SURFACE('',#98034,74.3,0.5);
#3494=TOROIDAL_SURFACE('',#98039,2.,0.5);
#3495=TOROIDAL_SURFACE('',#98042,12.0057534629026,0.5);
#3496=TOROIDAL_SURFACE('',#98047,77.6552534828746,0.5);
#3497=TOROIDAL_SURFACE('',#98051,12.0057534629026,0.5);
#3498=TOROIDAL_SURFACE('',#98055,1067.5427534629,0.5);
#3499=TOROIDAL_SURFACE('',#98059,12.0057534629025,0.5);
#3500=TOROIDAL_SURFACE('',#98063,77.6552534828746,0.5);
#3501=TOROIDAL_SURFACE('',#98067,12.0057534629026,0.5);
#3502=TOROIDAL_SURFACE('',#98090,77.6139048513169,0.5);
#3503=TOROIDAL_SURFACE('',#98095,77.6139048513167,0.5);
#3504=TOROIDAL_SURFACE('',#98115,73.05,0.75);
#3505=TOROIDAL_SURFACE('',#98129,76.3639048513167,0.75);
#3506=TOROIDAL_SURFACE('',#98142,76.3639048513169,0.75);
#3507=TOROIDAL_SURFACE('',#98155,73.05,0.75);
#3508=TOROIDAL_SURFACE('',#98171,1.2,0.45);
#3509=TOROIDAL_SURFACE('',#98178,204.945690815561,0.45);
#3510=TOROIDAL_SURFACE('',#98182,1.2,0.45);
#3511=TOROIDAL_SURFACE('',#98186,1.45,0.45);
#3512=TOROIDAL_SURFACE('',#98192,48.45,0.45);
#3513=TOROIDAL_SURFACE('',#98196,1.2,0.45);
#3514=TOROIDAL_SURFACE('',#98200,1.2,0.45);
#3515=TOROIDAL_SURFACE('',#98205,1.2,0.45);
#3516=TOROIDAL_SURFACE('',#98212,204.945690815561,0.45);
#3517=TOROIDAL_SURFACE('',#98216,1.2,0.45);
#3518=TOROIDAL_SURFACE('',#98220,1.2,0.45);
#3519=TOROIDAL_SURFACE('',#98228,1.2,0.45);
#3520=TOROIDAL_SURFACE('',#98231,1.2,0.45);
#3521=TOROIDAL_SURFACE('',#98238,204.945690815561,0.45);
#3522=TOROIDAL_SURFACE('',#98242,1.2,0.45);
#3523=TOROIDAL_SURFACE('',#98246,1.2,0.45);
#3524=TOROIDAL_SURFACE('',#98254,1.2,0.45);
#3525=TOROIDAL_SURFACE('',#98257,1.2,0.45);
#3526=TOROIDAL_SURFACE('',#98266,1.2,0.45);
#3527=TOROIDAL_SURFACE('',#98270,1.2,0.45);
#3528=TOROIDAL_SURFACE('',#98278,1.2,0.45);
#3529=TOROIDAL_SURFACE('',#98281,1.2,0.45);
#3530=TOROIDAL_SURFACE('',#98290,1.2,0.45);
#3531=TOROIDAL_SURFACE('',#98294,1.2,0.45);
#3532=TOROIDAL_SURFACE('',#98298,12.6555395526668,0.45);
#3533=TOROIDAL_SURFACE('',#98304,10.45,0.45);
#3534=TOROIDAL_SURFACE('',#98308,1.2,0.45);
#3535=TOROIDAL_SURFACE('',#98311,1.2,0.45);
#3536=TOROIDAL_SURFACE('',#98320,1.2,0.45);
#3537=TOROIDAL_SURFACE('',#98324,1.2,0.45);
#3538=TOROIDAL_SURFACE('',#98332,1.2,0.45);
#3539=TOROIDAL_SURFACE('',#98335,1.2,0.45);
#3540=TOROIDAL_SURFACE('',#98344,1.2,0.45);
#3541=TOROIDAL_SURFACE('',#98348,1.2,0.45);
#3542=TOROIDAL_SURFACE('',#98356,1.2,0.45);
#3543=TOROIDAL_SURFACE('',#98359,1.2,0.45);
#3544=TOROIDAL_SURFACE('',#98368,1.2,0.45);
#3545=TOROIDAL_SURFACE('',#98372,1.2,0.45);
#3546=TOROIDAL_SURFACE('',#98380,1.2,0.45);
#3547=TOROIDAL_SURFACE('',#98383,1.2,0.45);
#3548=TOROIDAL_SURFACE('',#98392,1.2,0.45);
#3549=TOROIDAL_SURFACE('',#98396,1.2,0.45);
#3550=TOROIDAL_SURFACE('',#98404,1.2,0.45);
#3551=TOROIDAL_SURFACE('',#98407,1.2,0.45);
#3552=TOROIDAL_SURFACE('',#98416,1.2,0.45);
#3553=TOROIDAL_SURFACE('',#98420,1.2,0.45);
#3554=TOROIDAL_SURFACE('',#98426,677.884816028482,0.45);
#3555=TOROIDAL_SURFACE('',#98430,1.2,0.45);
#3556=TOROIDAL_SURFACE('',#98433,1.2,0.45);
#3557=TOROIDAL_SURFACE('',#98442,1.2,0.45);
#3558=TOROIDAL_SURFACE('',#98446,1.2,0.45);
#3559=TOROIDAL_SURFACE('',#98452,48.45,0.45);
#3560=TOROIDAL_SURFACE('',#98456,1.2,0.45);
#3561=TOROIDAL_SURFACE('',#98460,1.45,0.45);
#3562=TOROIDAL_SURFACE('',#98464,677.884816028482,0.45);
#3563=TOROIDAL_SURFACE('',#98467,1.2,0.45);
#3564=TOROIDAL_SURFACE('',#98476,1.2,0.45);
#3565=TOROIDAL_SURFACE('',#98480,1.2,0.45);
#3566=TOROIDAL_SURFACE('',#98486,677.884816028482,0.45);
#3567=TOROIDAL_SURFACE('',#98490,1.2,0.45);
#3568=TOROIDAL_SURFACE('',#98493,1.2,0.45);
#3569=TOROIDAL_SURFACE('',#98502,1.2,0.45);
#3570=TOROIDAL_SURFACE('',#98506,1.2,0.45);
#3571=TOROIDAL_SURFACE('',#98514,1.2,0.45);
#3572=TOROIDAL_SURFACE('',#98517,1.2,0.45);
#3573=TOROIDAL_SURFACE('',#98524,11.6555395526668,0.45);
#3574=TOROIDAL_SURFACE('',#98528,1.2,0.45);
#3575=TOROIDAL_SURFACE('',#98532,10.45,0.45);
#3576=TOROIDAL_SURFACE('',#98540,1.2,0.45);
#3577=TOROIDAL_SURFACE('',#98544,1.2,0.45);
#3578=TOROIDAL_SURFACE('',#98549,1.2,0.45);
#3579=TOROIDAL_SURFACE('',#98558,1.2,0.45);
#3580=TOROIDAL_SURFACE('',#98562,10.45,0.45);
#3581=TOROIDAL_SURFACE('',#98568,11.6555395526668,0.45);
#3582=TOROIDAL_SURFACE('',#98572,1.2,0.45);
#3583=TOROIDAL_SURFACE('',#98576,1.2,0.45);
#3584=TOROIDAL_SURFACE('',#98581,1.2,0.45);
#3585=TOROIDAL_SURFACE('',#98590,1.2,0.45);
#3586=TOROIDAL_SURFACE('',#98594,1.2,0.45);
#3587=TOROIDAL_SURFACE('',#98602,1.2,0.45);
#3588=TOROIDAL_SURFACE('',#98605,1.2,0.45);
#3589=TOROIDAL_SURFACE('',#98614,1.2,0.45);
#3590=TOROIDAL_SURFACE('',#98618,1.2,0.45);
#3591=TOROIDAL_SURFACE('',#98622,677.884816028482,0.45);
#3592=TOROIDAL_SURFACE('',#98628,1.2,0.45);
#3593=TOROIDAL_SURFACE('',#98631,1.2,0.45);
#3594=TOROIDAL_SURFACE('',#98640,1.2,0.45);
#3595=TOROIDAL_SURFACE('',#98644,1.2,0.45);
#3596=TOROIDAL_SURFACE('',#98652,1.2,0.45);
#3597=TOROIDAL_SURFACE('',#98655,1.2,0.45);
#3598=TOROIDAL_SURFACE('',#98664,1.2,0.45);
#3599=TOROIDAL_SURFACE('',#98668,1.2,0.45);
#3600=TOROIDAL_SURFACE('',#98676,1.2,0.45);
#3601=TOROIDAL_SURFACE('',#98679,1.2,0.45);
#3602=TOROIDAL_SURFACE('',#98688,1.2,0.45);
#3603=TOROIDAL_SURFACE('',#98692,1.2,0.45);
#3604=TOROIDAL_SURFACE('',#98698,12.6555395526668,0.45);
#3605=TOROIDAL_SURFACE('',#98702,1.2,0.45);
#3606=TOROIDAL_SURFACE('',#98706,10.45,0.45);
#3607=TOROIDAL_SURFACE('',#98709,1.2,0.45);
#3608=TOROIDAL_SURFACE('',#98718,1.2,0.45);
#3609=TOROIDAL_SURFACE('',#98722,1.2,0.45);
#3610=TOROIDAL_SURFACE('',#98726,677.884816028482,0.45);
#3611=TOROIDAL_SURFACE('',#98732,1.2,0.45);
#3612=TOROIDAL_SURFACE('',#98735,1.2,0.45);
#3613=TOROIDAL_SURFACE('',#98744,1.2,0.45);
#3614=TOROIDAL_SURFACE('',#98748,1.2,0.45);
#3615=TOROIDAL_SURFACE('',#98752,48.45,0.45);
#3616=TOROIDAL_SURFACE('',#98758,1.45,0.45);
#3617=TOROIDAL_SURFACE('',#98762,1.2,0.45);
#3618=TOROIDAL_SURFACE('',#98766,677.884816028482,0.45);
#3619=TOROIDAL_SURFACE('',#98769,1.2,0.45);
#3620=TOROIDAL_SURFACE('',#98778,1.2,0.45);
#3621=TOROIDAL_SURFACE('',#98782,1.2,0.45);
#3622=TOROIDAL_SURFACE('',#98790,1.2,0.45);
#3623=TOROIDAL_SURFACE('',#98793,1.2,0.45);
#3624=TOROIDAL_SURFACE('',#98802,1.2,0.45);
#3625=TOROIDAL_SURFACE('',#98806,1.2,0.45);
#3626=TOROIDAL_SURFACE('',#98812,48.45,0.45);
#3627=TOROIDAL_SURFACE('',#98816,1.2,0.45);
#3628=TOROIDAL_SURFACE('',#98820,1.44999999999996,0.45);
#3629=TOROIDAL_SURFACE('',#98824,677.884816028482,0.45);
#3630=TOROIDAL_SURFACE('',#98827,1.2,0.45);
#3631=TOROIDAL_SURFACE('',#98836,1.2,0.45);
#3632=TOROIDAL_SURFACE('',#98840,1.2,0.45);
#3633=TOROIDAL_SURFACE('',#98846,677.884816028482,0.45);
#3634=TOROIDAL_SURFACE('',#98850,1.2,0.45);
#3635=TOROIDAL_SURFACE('',#98853,1.2,0.45);
#3636=TOROIDAL_SURFACE('',#98862,1.2,0.45);
#3637=TOROIDAL_SURFACE('',#98866,1.2,0.45);
#3638=TOROIDAL_SURFACE('',#98874,1.2,0.45);
#3639=TOROIDAL_SURFACE('',#98877,1.2,0.45);
#3640=TOROIDAL_SURFACE('',#98886,1.2,0.45);
#3641=TOROIDAL_SURFACE('',#98890,1.2,0.45);
#3642=TOROIDAL_SURFACE('',#98896,677.884816028482,0.45);
#3643=TOROIDAL_SURFACE('',#98900,1.2,0.45);
#3644=TOROIDAL_SURFACE('',#98903,1.2,0.45);
#3645=TOROIDAL_SURFACE('',#98912,1.2,0.45);
#3646=TOROIDAL_SURFACE('',#98916,1.2,0.45);
#3647=TOROIDAL_SURFACE('',#98924,1.2,0.45);
#3648=TOROIDAL_SURFACE('',#98927,1.2,0.45);
#3649=TOROIDAL_SURFACE('',#98934,48.45,0.45);
#3650=TOROIDAL_SURFACE('',#98938,1.2,0.45);
#3651=TOROIDAL_SURFACE('',#98942,1.2,0.45);
#3652=TOROIDAL_SURFACE('',#98947,1.2,0.45);
#3653=TOROIDAL_SURFACE('',#98954,48.45,0.45);
#3654=TOROIDAL_SURFACE('',#98958,1.2,0.45);
#3655=TOROIDAL_SURFACE('',#98962,1.2,0.45);
#3656=TOROIDAL_SURFACE('',#98967,6.44999999999992,0.45);
#3657=TOROIDAL_SURFACE('',#98972,53.45,0.45);
#3658=TOROIDAL_SURFACE('',#98976,6.45,0.45);
#3659=TOROIDAL_SURFACE('',#98980,682.884816028482,0.45);
#3660=TOROIDAL_SURFACE('',#98984,6.45,0.45);
#3661=TOROIDAL_SURFACE('',#98988,53.45,0.45);
#3662=TOROIDAL_SURFACE('',#98992,6.45,0.45);
#3663=TOROIDAL_SURFACE('',#98996,4.34999999999995,0.45);
#3664=TOROIDAL_SURFACE('',#99001,51.35,0.45);
#3665=TOROIDAL_SURFACE('',#99005,4.35,0.45);
#3666=TOROIDAL_SURFACE('',#99009,680.784816028482,0.45);
#3667=TOROIDAL_SURFACE('',#99013,4.35,0.45);
#3668=TOROIDAL_SURFACE('',#99017,51.35,0.45);
#3669=TOROIDAL_SURFACE('',#99021,4.35,0.45);
#3670=TOROIDAL_SURFACE('',#99025,1.2,0.45);
#3671=TOROIDAL_SURFACE('',#99031,1.2,0.45);
#3672=TOROIDAL_SURFACE('',#99035,11.5555395526669,0.45);
#3673=TOROIDAL_SURFACE('',#99039,1.2,0.45);
#3674=TOROIDAL_SURFACE('',#99045,1.2,0.45);
#3675=TOROIDAL_SURFACE('',#99048,1.2,0.45);
#3676=TOROIDAL_SURFACE('',#99054,1.2,0.45);
#3677=TOROIDAL_SURFACE('',#99058,11.5555395526669,0.45);
#3678=TOROIDAL_SURFACE('',#99062,1.2,0.45);
#3679=TOROIDAL_SURFACE('',#99068,1.2,0.45);
#3680=TOROIDAL_SURFACE('',#99071,1.2,0.45);
#3681=TOROIDAL_SURFACE('',#99077,1.2,0.45);
#3682=TOROIDAL_SURFACE('',#99081,11.5555395526669,0.45);
#3683=TOROIDAL_SURFACE('',#99085,1.2,0.45);
#3684=TOROIDAL_SURFACE('',#99091,1.2,0.45);
#3685=TOROIDAL_SURFACE('',#99094,1.2,0.45);
#3686=TOROIDAL_SURFACE('',#99100,1.2,0.45);
#3687=TOROIDAL_SURFACE('',#99104,11.5555395526669,0.45);
#3688=TOROIDAL_SURFACE('',#99108,1.2,0.45);
#3689=TOROIDAL_SURFACE('',#99114,1.2,0.45);
#3690=TOROIDAL_SURFACE('',#99117,12.5403589366713,1.5);
#3691=TOROIDAL_SURFACE('',#99122,78.1898589566432,1.5);
#3692=TOROIDAL_SURFACE('',#99126,12.5403589366712,1.5);
#3693=TOROIDAL_SURFACE('',#99130,1068.07735893667,1.5);
#3694=TOROIDAL_SURFACE('',#99134,12.5403589366712,1.5);
#3695=TOROIDAL_SURFACE('',#99138,78.1898589566432,1.5);
#3696=TOROIDAL_SURFACE('',#99142,12.5403589366713,1.5);
#3697=TOROIDAL_SURFACE('',#99205,17.1605488438955,4.99999999963848);
#3698=TOROIDAL_SURFACE('',#99881,4.01589928084003,0.5);
#3699=TOROIDAL_SURFACE('',#99885,4.01589928084081,0.5);
#3700=TOROIDAL_SURFACE('',#99897,2.,0.5);
#3701=TOROIDAL_SURFACE('',#99902,74.3,0.5);
#3702=TOROIDAL_SURFACE('',#99907,2.,0.5);
#3703=TOROIDAL_SURFACE('',#99929,2.,0.5);
#3704=TOROIDAL_SURFACE('',#99936,74.3,0.5);
#3705=TOROIDAL_SURFACE('',#99941,2.,0.5);
#3706=TOROIDAL_SURFACE('',#99944,232.542753462903,0.5);
#3707=TOROIDAL_SURFACE('',#99948,12.0057534629026,0.5);
#3708=TOROIDAL_SURFACE('',#99952,77.6552534828746,0.5);
#3709=TOROIDAL_SURFACE('',#99956,12.0057534629026,0.5);
#3710=TOROIDAL_SURFACE('',#99960,1067.5427534629,0.5);
#3711=TOROIDAL_SURFACE('',#99964,12.0057534629025,0.5);
#3712=TOROIDAL_SURFACE('',#99968,77.6552534828746,0.5);
#3713=TOROIDAL_SURFACE('',#99972,12.0057534629026,0.5);
#3714=TOROIDAL_SURFACE('',#99976,1067.5427534629,0.5);
#3715=TOROIDAL_SURFACE('',#99998,77.6139048513169,0.5);
#3716=TOROIDAL_SURFACE('',#100003,77.6139048513167,0.5);
#3717=TOROIDAL_SURFACE('',#100023,73.05,0.75);
#3718=TOROIDAL_SURFACE('',#100037,76.3639048513167,0.75);
#3719=TOROIDAL_SURFACE('',#100050,76.3639048513169,0.75);
#3720=TOROIDAL_SURFACE('',#100063,73.05,0.75);
#3721=TOROIDAL_SURFACE('',#100079,1.2,0.45);
#3722=TOROIDAL_SURFACE('',#100086,204.945690815561,0.45);
#3723=TOROIDAL_SURFACE('',#100090,1.2,0.45);
#3724=TOROIDAL_SURFACE('',#100094,1.45,0.45);
#3725=TOROIDAL_SURFACE('',#100100,48.45,0.45);
#3726=TOROIDAL_SURFACE('',#100104,1.2,0.45);
#3727=TOROIDAL_SURFACE('',#100108,1.2,0.45);
#3728=TOROIDAL_SURFACE('',#100113,1.2,0.45);
#3729=TOROIDAL_SURFACE('',#100120,204.945690815561,0.45);
#3730=TOROIDAL_SURFACE('',#100124,1.2,0.45);
#3731=TOROIDAL_SURFACE('',#100128,1.2,0.45);
#3732=TOROIDAL_SURFACE('',#100136,1.2,0.45);
#3733=TOROIDAL_SURFACE('',#100139,1.2,0.45);
#3734=TOROIDAL_SURFACE('',#100146,204.945690815561,0.45);
#3735=TOROIDAL_SURFACE('',#100150,1.2,0.45);
#3736=TOROIDAL_SURFACE('',#100154,1.2,0.45);
#3737=TOROIDAL_SURFACE('',#100162,1.2,0.45);
#3738=TOROIDAL_SURFACE('',#100165,1.2,0.45);
#3739=TOROIDAL_SURFACE('',#100174,1.2,0.45);
#3740=TOROIDAL_SURFACE('',#100178,1.2,0.45);
#3741=TOROIDAL_SURFACE('',#100186,1.2,0.45);
#3742=TOROIDAL_SURFACE('',#100189,1.2,0.45);
#3743=TOROIDAL_SURFACE('',#100198,1.2,0.45);
#3744=TOROIDAL_SURFACE('',#100202,1.2,0.45);
#3745=TOROIDAL_SURFACE('',#100206,12.6555395526668,0.45);
#3746=TOROIDAL_SURFACE('',#100212,10.45,0.45);
#3747=TOROIDAL_SURFACE('',#100216,1.2,0.45);
#3748=TOROIDAL_SURFACE('',#100219,1.2,0.45);
#3749=TOROIDAL_SURFACE('',#100228,1.2,0.45);
#3750=TOROIDAL_SURFACE('',#100232,1.2,0.45);
#3751=TOROIDAL_SURFACE('',#100240,1.2,0.45);
#3752=TOROIDAL_SURFACE('',#100243,1.2,0.45);
#3753=TOROIDAL_SURFACE('',#100252,1.2,0.45);
#3754=TOROIDAL_SURFACE('',#100256,1.2,0.45);
#3755=TOROIDAL_SURFACE('',#100264,1.2,0.45);
#3756=TOROIDAL_SURFACE('',#100267,1.2,0.45);
#3757=TOROIDAL_SURFACE('',#100276,1.2,0.45);
#3758=TOROIDAL_SURFACE('',#100280,1.2,0.45);
#3759=TOROIDAL_SURFACE('',#100288,1.2,0.45);
#3760=TOROIDAL_SURFACE('',#100291,1.2,0.45);
#3761=TOROIDAL_SURFACE('',#100300,1.2,0.45);
#3762=TOROIDAL_SURFACE('',#100304,1.2,0.45);
#3763=TOROIDAL_SURFACE('',#100312,1.2,0.45);
#3764=TOROIDAL_SURFACE('',#100315,1.2,0.45);
#3765=TOROIDAL_SURFACE('',#100324,1.2,0.45);
#3766=TOROIDAL_SURFACE('',#100328,1.2,0.45);
#3767=TOROIDAL_SURFACE('',#100334,677.884816028482,0.45);
#3768=TOROIDAL_SURFACE('',#100338,1.2,0.45);
#3769=TOROIDAL_SURFACE('',#100341,1.2,0.45);
#3770=TOROIDAL_SURFACE('',#100350,1.2,0.45);
#3771=TOROIDAL_SURFACE('',#100354,1.2,0.45);
#3772=TOROIDAL_SURFACE('',#100360,48.45,0.45);
#3773=TOROIDAL_SURFACE('',#100364,1.2,0.45);
#3774=TOROIDAL_SURFACE('',#100368,1.45,0.45);
#3775=TOROIDAL_SURFACE('',#100372,677.884816028482,0.45);
#3776=TOROIDAL_SURFACE('',#100375,1.2,0.45);
#3777=TOROIDAL_SURFACE('',#100384,1.2,0.45);
#3778=TOROIDAL_SURFACE('',#100388,1.2,0.45);
#3779=TOROIDAL_SURFACE('',#100394,677.884816028482,0.45);
#3780=TOROIDAL_SURFACE('',#100398,1.2,0.45);
#3781=TOROIDAL_SURFACE('',#100401,1.2,0.45);
#3782=TOROIDAL_SURFACE('',#100410,1.2,0.45);
#3783=TOROIDAL_SURFACE('',#100414,1.2,0.45);
#3784=TOROIDAL_SURFACE('',#100422,1.2,0.45);
#3785=TOROIDAL_SURFACE('',#100425,1.2,0.45);
#3786=TOROIDAL_SURFACE('',#100432,11.6555395526668,0.45);
#3787=TOROIDAL_SURFACE('',#100436,1.2,0.45);
#3788=TOROIDAL_SURFACE('',#100440,10.45,0.45);
#3789=TOROIDAL_SURFACE('',#100448,1.2,0.45);
#3790=TOROIDAL_SURFACE('',#100452,1.2,0.45);
#3791=TOROIDAL_SURFACE('',#100457,1.2,0.45);
#3792=TOROIDAL_SURFACE('',#100466,1.2,0.45);
#3793=TOROIDAL_SURFACE('',#100470,10.45,0.45);
#3794=TOROIDAL_SURFACE('',#100476,11.6555395526668,0.45);
#3795=TOROIDAL_SURFACE('',#100480,1.2,0.45);
#3796=TOROIDAL_SURFACE('',#100484,1.2,0.45);
#3797=TOROIDAL_SURFACE('',#100489,1.2,0.45);
#3798=TOROIDAL_SURFACE('',#100498,1.2,0.45);
#3799=TOROIDAL_SURFACE('',#100502,1.2,0.45);
#3800=TOROIDAL_SURFACE('',#100510,1.2,0.45);
#3801=TOROIDAL_SURFACE('',#100513,1.2,0.45);
#3802=TOROIDAL_SURFACE('',#100522,1.2,0.45);
#3803=TOROIDAL_SURFACE('',#100526,1.2,0.45);
#3804=TOROIDAL_SURFACE('',#100530,677.884816028482,0.45);
#3805=TOROIDAL_SURFACE('',#100536,1.2,0.45);
#3806=TOROIDAL_SURFACE('',#100539,1.2,0.45);
#3807=TOROIDAL_SURFACE('',#100548,1.2,0.45);
#3808=TOROIDAL_SURFACE('',#100552,1.2,0.45);
#3809=TOROIDAL_SURFACE('',#100560,1.2,0.45);
#3810=TOROIDAL_SURFACE('',#100563,1.2,0.45);
#3811=TOROIDAL_SURFACE('',#100572,1.2,0.45);
#3812=TOROIDAL_SURFACE('',#100576,1.2,0.45);
#3813=TOROIDAL_SURFACE('',#100584,1.2,0.45);
#3814=TOROIDAL_SURFACE('',#100587,1.2,0.45);
#3815=TOROIDAL_SURFACE('',#100596,1.2,0.45);
#3816=TOROIDAL_SURFACE('',#100600,1.2,0.45);
#3817=TOROIDAL_SURFACE('',#100606,12.6555395526668,0.45);
#3818=TOROIDAL_SURFACE('',#100610,1.2,0.45);
#3819=TOROIDAL_SURFACE('',#100614,10.45,0.45);
#3820=TOROIDAL_SURFACE('',#100617,1.2,0.45);
#3821=TOROIDAL_SURFACE('',#100626,1.2,0.45);
#3822=TOROIDAL_SURFACE('',#100630,1.2,0.45);
#3823=TOROIDAL_SURFACE('',#100634,677.884816028482,0.45);
#3824=TOROIDAL_SURFACE('',#100640,1.2,0.45);
#3825=TOROIDAL_SURFACE('',#100643,1.2,0.45);
#3826=TOROIDAL_SURFACE('',#100652,1.2,0.45);
#3827=TOROIDAL_SURFACE('',#100656,1.2,0.45);
#3828=TOROIDAL_SURFACE('',#100660,48.45,0.45);
#3829=TOROIDAL_SURFACE('',#100666,1.45,0.45);
#3830=TOROIDAL_SURFACE('',#100670,1.2,0.45);
#3831=TOROIDAL_SURFACE('',#100674,677.884816028482,0.45);
#3832=TOROIDAL_SURFACE('',#100677,1.2,0.45);
#3833=TOROIDAL_SURFACE('',#100686,1.2,0.45);
#3834=TOROIDAL_SURFACE('',#100690,1.2,0.45);
#3835=TOROIDAL_SURFACE('',#100698,1.2,0.45);
#3836=TOROIDAL_SURFACE('',#100701,1.2,0.45);
#3837=TOROIDAL_SURFACE('',#100710,1.2,0.45);
#3838=TOROIDAL_SURFACE('',#100714,1.2,0.45);
#3839=TOROIDAL_SURFACE('',#100720,48.45,0.45);
#3840=TOROIDAL_SURFACE('',#100724,1.2,0.45);
#3841=TOROIDAL_SURFACE('',#100728,1.44999999999996,0.45);
#3842=TOROIDAL_SURFACE('',#100732,677.884816028482,0.45);
#3843=TOROIDAL_SURFACE('',#100735,1.2,0.45);
#3844=TOROIDAL_SURFACE('',#100744,1.2,0.45);
#3845=TOROIDAL_SURFACE('',#100748,1.2,0.45);
#3846=TOROIDAL_SURFACE('',#100754,677.884816028482,0.45);
#3847=TOROIDAL_SURFACE('',#100758,1.2,0.45);
#3848=TOROIDAL_SURFACE('',#100761,1.2,0.45);
#3849=TOROIDAL_SURFACE('',#100770,1.2,0.45);
#3850=TOROIDAL_SURFACE('',#100774,1.2,0.45);
#3851=TOROIDAL_SURFACE('',#100782,1.2,0.45);
#3852=TOROIDAL_SURFACE('',#100785,1.2,0.45);
#3853=TOROIDAL_SURFACE('',#100794,1.2,0.45);
#3854=TOROIDAL_SURFACE('',#100798,1.2,0.45);
#3855=TOROIDAL_SURFACE('',#100804,677.884816028482,0.45);
#3856=TOROIDAL_SURFACE('',#100808,1.2,0.45);
#3857=TOROIDAL_SURFACE('',#100811,1.2,0.45);
#3858=TOROIDAL_SURFACE('',#100820,1.2,0.45);
#3859=TOROIDAL_SURFACE('',#100824,1.2,0.45);
#3860=TOROIDAL_SURFACE('',#100832,1.2,0.45);
#3861=TOROIDAL_SURFACE('',#100835,1.2,0.45);
#3862=TOROIDAL_SURFACE('',#100842,48.45,0.45);
#3863=TOROIDAL_SURFACE('',#100846,1.2,0.45);
#3864=TOROIDAL_SURFACE('',#100850,1.2,0.45);
#3865=TOROIDAL_SURFACE('',#100855,1.2,0.45);
#3866=TOROIDAL_SURFACE('',#100862,48.45,0.45);
#3867=TOROIDAL_SURFACE('',#100866,1.2,0.45);
#3868=TOROIDAL_SURFACE('',#100870,1.2,0.45);
#3869=TOROIDAL_SURFACE('',#100875,7.65553955266686,0.45);
#3870=TOROIDAL_SURFACE('',#100879,5.07535,0.45);
#3871=TOROIDAL_SURFACE('',#100883,682.884816028482,0.45);
#3872=TOROIDAL_SURFACE('',#100887,6.44999999999992,0.45);
#3873=TOROIDAL_SURFACE('',#100891,53.45,0.45);
#3874=TOROIDAL_SURFACE('',#100895,6.45,0.45);
#3875=TOROIDAL_SURFACE('',#100899,682.884816028482,0.45);
#3876=TOROIDAL_SURFACE('',#100903,6.45,0.45);
#3877=TOROIDAL_SURFACE('',#100907,53.45,0.45);
#3878=TOROIDAL_SURFACE('',#100911,6.45,0.45);
#3879=TOROIDAL_SURFACE('',#100915,209.945690815561,0.45);
#3880=TOROIDAL_SURFACE('',#100918,680.784816028482,0.45);
#3881=TOROIDAL_SURFACE('',#100922,4.34999999999995,0.45);
#3882=TOROIDAL_SURFACE('',#100926,51.35,0.45);
#3883=TOROIDAL_SURFACE('',#100930,4.35,0.45);
#3884=TOROIDAL_SURFACE('',#100934,680.784816028482,0.45);
#3885=TOROIDAL_SURFACE('',#100938,4.35,0.45);
#3886=TOROIDAL_SURFACE('',#100942,51.35,0.45);
#3887=TOROIDAL_SURFACE('',#100946,4.35,0.45);
#3888=TOROIDAL_SURFACE('',#100950,207.845690815561,0.45);
#3889=TOROIDAL_SURFACE('',#100953,1.2,0.45);
#3890=TOROIDAL_SURFACE('',#100959,1.2,0.45);
#3891=TOROIDAL_SURFACE('',#100963,11.5555395526669,0.45);
#3892=TOROIDAL_SURFACE('',#100967,1.2,0.45);
#3893=TOROIDAL_SURFACE('',#100973,1.2,0.45);
#3894=TOROIDAL_SURFACE('',#100976,1.2,0.45);
#3895=TOROIDAL_SURFACE('',#100982,1.2,0.45);
#3896=TOROIDAL_SURFACE('',#100986,11.5555395526669,0.45);
#3897=TOROIDAL_SURFACE('',#100990,1.2,0.45);
#3898=TOROIDAL_SURFACE('',#100996,1.2,0.45);
#3899=TOROIDAL_SURFACE('',#100999,1.2,0.45);
#3900=TOROIDAL_SURFACE('',#101005,1.2,0.45);
#3901=TOROIDAL_SURFACE('',#101009,11.5555395526669,0.45);
#3902=TOROIDAL_SURFACE('',#101013,1.2,0.45);
#3903=TOROIDAL_SURFACE('',#101019,1.2,0.45);
#3904=TOROIDAL_SURFACE('',#101022,1.2,0.45);
#3905=TOROIDAL_SURFACE('',#101028,1.2,0.45);
#3906=TOROIDAL_SURFACE('',#101032,11.5555395526669,0.45);
#3907=TOROIDAL_SURFACE('',#101036,1.2,0.45);
#3908=TOROIDAL_SURFACE('',#101042,1.2,0.45);
#3909=TOROIDAL_SURFACE('',#101045,233.077358936672,1.5);
#3910=TOROIDAL_SURFACE('',#101049,12.5403589366713,1.5);
#3911=TOROIDAL_SURFACE('',#101053,78.1898589566432,1.5);
#3912=TOROIDAL_SURFACE('',#101057,12.5403589366712,1.5);
#3913=TOROIDAL_SURFACE('',#101061,1068.07735893667,1.5);
#3914=TOROIDAL_SURFACE('',#101065,12.5403589366712,1.5);
#3915=TOROIDAL_SURFACE('',#101069,78.1898589566432,1.5);
#3916=TOROIDAL_SURFACE('',#101073,12.5403589366713,1.5);
#3917=TOROIDAL_SURFACE('',#101077,1068.07735893667,1.5);
#3918=TOROIDAL_SURFACE('',#101141,17.1621953438396,5.00000000078575);
#3919=TOROIDAL_SURFACE('',#101878,4.01589928084003,0.5);
#3920=TOROIDAL_SURFACE('',#101898,3.,0.25);
#3921=TOROIDAL_SURFACE('',#101990,3.,0.25);
#3922=TOROIDAL_SURFACE('',#102003,8.55,0.25);
#3923=TOROIDAL_SURFACE('',#102007,8.55,0.25);
#3924=TOROIDAL_SURFACE('',#102036,6.5,0.5);
#3925=TOROIDAL_SURFACE('',#102045,6.5,0.5);
#3926=TOROIDAL_SURFACE('',#102049,6.5,0.5);
#3927=TOROIDAL_SURFACE('',#102057,6.5,0.5);
#3928=TOROIDAL_SURFACE('',#102068,5.,1.);
#3929=TOROIDAL_SURFACE('',#102075,5.,1.);
#3930=TOROIDAL_SURFACE('',#102081,3.,1.);
#3931=TOROIDAL_SURFACE('',#102085,3.,1.);
#3932=TOROIDAL_SURFACE('',#102098,3.,1.);
#3933=TOROIDAL_SURFACE('',#102101,3.,1.);
#3934=TOROIDAL_SURFACE('',#102107,5.,1.);
#3935=TOROIDAL_SURFACE('',#102113,5.,1.);
#3936=TOROIDAL_SURFACE('',#102141,8.55,0.25);
#3937=TOROIDAL_SURFACE('',#102145,8.55,0.25);
#3938=TOROIDAL_SURFACE('',#102165,1.,0.5);
#3939=TOROIDAL_SURFACE('',#102171,1.,0.5);
#3940=TOROIDAL_SURFACE('',#102179,1.,0.5);
#3941=TOROIDAL_SURFACE('',#102185,1.,0.5);
#3942=TOROIDAL_SURFACE('',#102193,2.5,0.5);
#3943=TOROIDAL_SURFACE('',#102199,1.,0.5);
#3944=TOROIDAL_SURFACE('',#102205,1.,0.5);
#3945=TOROIDAL_SURFACE('',#102211,2.5,0.5);
#3946=TOROIDAL_SURFACE('',#102220,2.5,0.5);
#3947=TOROIDAL_SURFACE('',#102226,1.,0.5);
#3948=TOROIDAL_SURFACE('',#102234,2.5,0.5);
#3949=TOROIDAL_SURFACE('',#102240,1.,0.5);
#3950=TOROIDAL_SURFACE('',#102244,5.5,0.5);
#3951=TOROIDAL_SURFACE('',#102250,1.,0.5);
#3952=TOROIDAL_SURFACE('',#102256,2.5,0.5);
#3953=TOROIDAL_SURFACE('',#102265,2.5,0.5);
#3954=TOROIDAL_SURFACE('',#102271,1.,0.5);
#3955=TOROIDAL_SURFACE('',#102275,58.,0.5);
#3956=TOROIDAL_SURFACE('',#102279,1.,0.5);
#3957=TOROIDAL_SURFACE('',#102285,2.5,0.5);
#3958=TOROIDAL_SURFACE('',#102294,2.5,0.5);
#3959=TOROIDAL_SURFACE('',#102300,1.,0.5);
#3960=TOROIDAL_SURFACE('',#102304,58.,0.5);
#3961=TOROIDAL_SURFACE('',#102308,1.,0.5);
#3962=TOROIDAL_SURFACE('',#102314,2.5,0.5);
#3963=TOROIDAL_SURFACE('',#102323,2.5,0.5);
#3964=TOROIDAL_SURFACE('',#102329,1.,0.5);
#3965=TOROIDAL_SURFACE('',#102333,58.,0.5);
#3966=TOROIDAL_SURFACE('',#102337,1.,0.5);
#3967=TOROIDAL_SURFACE('',#102343,2.5,0.5);
#3968=TOROIDAL_SURFACE('',#102352,2.5,0.5);
#3969=TOROIDAL_SURFACE('',#102358,1.,0.5);
#3970=TOROIDAL_SURFACE('',#102362,58.,0.5);
#3971=TOROIDAL_SURFACE('',#102366,1.,0.5);
#3972=TOROIDAL_SURFACE('',#102372,2.5,0.5);
#3973=TOROIDAL_SURFACE('',#102381,2.5,0.5);
#3974=TOROIDAL_SURFACE('',#102387,1.,0.5);
#3975=TOROIDAL_SURFACE('',#102391,58.,0.5);
#3976=TOROIDAL_SURFACE('',#102395,1.,0.5);
#3977=TOROIDAL_SURFACE('',#102401,2.5,0.5);
#3978=TOROIDAL_SURFACE('',#102410,2.5,0.5);
#3979=TOROIDAL_SURFACE('',#102416,1.,0.5);
#3980=TOROIDAL_SURFACE('',#102420,58.,0.5);
#3981=TOROIDAL_SURFACE('',#102424,1.,0.5);
#3982=TOROIDAL_SURFACE('',#102430,2.5,0.5);
#3983=TOROIDAL_SURFACE('',#102439,2.5,0.5);
#3984=TOROIDAL_SURFACE('',#102445,1.,0.5);
#3985=TOROIDAL_SURFACE('',#102451,5.5,0.5);
#3986=TOROIDAL_SURFACE('',#102455,1.,0.5);
#3987=TOROIDAL_SURFACE('',#102461,2.5,0.5);
#3988=TOROIDAL_SURFACE('',#102470,2.5,0.5);
#3989=TOROIDAL_SURFACE('',#102476,1.,0.5);
#3990=TOROIDAL_SURFACE('',#102482,1.,0.5);
#3991=TOROIDAL_SURFACE('',#102488,2.5,0.5);
#3992=TOROIDAL_SURFACE('',#102496,1.,0.5);
#3993=TOROIDAL_SURFACE('',#102502,2.5,0.5);
#3994=TOROIDAL_SURFACE('',#102728,3.,0.25);
#3995=TOROIDAL_SURFACE('',#102752,1.75,0.75);
#3996=TOROIDAL_SURFACE('',#102759,493.060657452016,0.75);
#3997=TOROIDAL_SURFACE('',#102761,493.060657452016,0.75);
#3998=TOROIDAL_SURFACE('',#102767,1.75,0.75);
#3999=TOROIDAL_SURFACE('',#102770,1.75,0.75);
#4000=TOROIDAL_SURFACE('',#102773,1.75,0.75);
#4001=TOROIDAL_SURFACE('',#102799,1.75,0.75);
#4002=TOROIDAL_SURFACE('',#102806,493.060657452016,0.75);
#4003=TOROIDAL_SURFACE('',#102808,493.060657452016,0.75);
#4004=TOROIDAL_SURFACE('',#102814,1.75,0.75);
#4005=TOROIDAL_SURFACE('',#102817,1.75,0.75);
#4006=TOROIDAL_SURFACE('',#102820,1.75,0.75);
#4007=TOROIDAL_SURFACE('',#102838,6.25,0.75);
#4008=TOROIDAL_SURFACE('',#102845,6.25,0.75);
#4009=TOROIDAL_SURFACE('',#102863,6.25,0.75);
#4010=TOROIDAL_SURFACE('',#102870,6.25,0.75);
#4011=TOROIDAL_SURFACE('',#103086,6.75,0.25);
#4012=TOROIDAL_SURFACE('',#103090,5.89644660940673,0.25);
#4013=TOROIDAL_SURFACE('',#103095,6.75,0.25);
#4014=TOROIDAL_SURFACE('',#103212,66.,1.5);
#4015=TOROIDAL_SURFACE('',#103214,66.,1.5);
#4016=TOROIDAL_SURFACE('',#103267,56.8875000000281,1.5);
#4017=TOROIDAL_SURFACE('',#103269,54.8875000000282,1.);
#4018=TOROIDAL_SURFACE('',#103272,55.3875000000282,1.5);
#4019=TOROIDAL_SURFACE('',#103274,56.8875000000281,1.5);
#4020=TOROIDAL_SURFACE('',#103276,56.8875000000281,1.5);
#4021=TOROIDAL_SURFACE('',#103278,66.,1.5);
#4022=TOROIDAL_SURFACE('',#103280,66.,1.5);
#4023=TOROIDAL_SURFACE('',#103287,56.8875000000281,1.5);
#4024=TOROIDAL_SURFACE('',#103341,32.976,0.576);
#4025=TOROIDAL_SURFACE('',#103396,40.6764810164406,18.288);
#4026=TOROIDAL_SURFACE('',#103398,40.6764810164406,18.288);
#4027=TOROIDAL_SURFACE('',#103400,40.6764810164406,18.288);
#4028=TOROIDAL_SURFACE('',#103402,40.6764810164406,18.288);
#4029=TOROIDAL_SURFACE('',#103404,40.6764810164406,18.288);
#4030=TOROIDAL_SURFACE('',#103406,40.6764810164406,18.288);
#4031=TOROIDAL_SURFACE('',#103408,40.6764810164406,18.288);
#4032=TOROIDAL_SURFACE('',#103410,40.6764810164406,18.288);
#4033=TOROIDAL_SURFACE('',#103412,40.6764810164406,18.288);
#4034=TOROIDAL_SURFACE('',#103414,40.6764810164406,18.288);
#4035=TOROIDAL_SURFACE('',#103416,40.6764810164406,18.288);
#4036=TOROIDAL_SURFACE('',#103418,40.6764810164406,18.288);
#4037=TOROIDAL_SURFACE('',#103420,40.6764810164406,18.288);
#4038=TOROIDAL_SURFACE('',#103422,40.6764810164406,18.288);
#4039=TOROIDAL_SURFACE('',#103452,40.6764810164406,18.288);
#4040=TOROIDAL_SURFACE('',#103454,40.6764810164406,18.288);
#4041=TOROIDAL_SURFACE('',#103456,40.6764810164406,18.288);
#4042=TOROIDAL_SURFACE('',#103458,40.6764810164406,18.288);
#4043=TOROIDAL_SURFACE('',#103460,40.6764810164406,18.288);
#4044=TOROIDAL_SURFACE('',#103462,40.6764810164406,18.288);
#4045=TOROIDAL_SURFACE('',#103464,40.6764810164406,18.288);
#4046=TOROIDAL_SURFACE('',#103466,40.6764810164406,18.288);
#4047=TOROIDAL_SURFACE('',#103468,40.6764810164406,18.288);
#4048=TOROIDAL_SURFACE('',#103470,40.6764810164406,18.288);
#4049=TOROIDAL_SURFACE('',#103472,40.6764810164406,18.288);
#4050=TOROIDAL_SURFACE('',#103474,40.6764810164406,18.288);
#4051=TOROIDAL_SURFACE('',#103476,40.6764810164406,18.288);
#4052=TOROIDAL_SURFACE('',#103478,40.6764810164406,18.288);
#4053=TOROIDAL_SURFACE('',#103480,40.6764810164406,18.288);
#4054=TOROIDAL_SURFACE('',#103484,40.6764810164406,18.288);
#4055=TOROIDAL_SURFACE('',#103548,25.536,0.336);
#4056=TOROIDAL_SURFACE('',#103592,49.1019873874548,10.668);
#4057=TOROIDAL_SURFACE('',#103597,49.1019873874548,10.668);
#4058=TOROIDAL_SURFACE('',#103651,49.1019873874548,10.668);
#4059=TOROIDAL_SURFACE('',#103653,49.1019873874548,10.668);
#4060=TOROIDAL_SURFACE('',#103655,49.1019873874548,10.668);
#4061=TOROIDAL_SURFACE('',#103657,49.1019873874548,10.668);
#4062=TOROIDAL_SURFACE('',#103659,49.1019873874548,10.668);
#4063=TOROIDAL_SURFACE('',#103661,49.1019873874548,10.668);
#4064=TOROIDAL_SURFACE('',#103663,49.1019873874548,10.668);
#4065=TOROIDAL_SURFACE('',#103665,49.1019873874548,10.668);
#4066=TOROIDAL_SURFACE('',#103667,49.1019873874548,10.668);
#4067=TOROIDAL_SURFACE('',#103669,49.1019873874548,10.668);
#4068=TOROIDAL_SURFACE('',#103671,49.1019873874548,10.668);
#4069=TOROIDAL_SURFACE('',#103673,49.1019873874548,10.668);
#4070=TOROIDAL_SURFACE('',#103675,49.1019873874548,10.668);
#4071=TOROIDAL_SURFACE('',#103677,49.1019873874548,10.668);
#4072=TOROIDAL_SURFACE('',#103679,49.1019873874548,10.668);
#4073=TOROIDAL_SURFACE('',#103681,49.1019873874548,10.668);
#4074=TOROIDAL_SURFACE('',#103683,49.1019873874548,10.668);
#4075=TOROIDAL_SURFACE('',#103685,49.1019873874548,10.668);
#4076=TOROIDAL_SURFACE('',#103687,49.1019873874548,10.668);
#4077=TOROIDAL_SURFACE('',#103689,49.1019873874548,10.668);
#4078=TOROIDAL_SURFACE('',#103691,49.1019873874548,10.668);
#4079=TOROIDAL_SURFACE('',#103693,49.1019873874548,10.668);
#4080=TOROIDAL_SURFACE('',#103695,49.1019873874548,10.668);
#4081=TOROIDAL_SURFACE('',#103697,49.1019873874548,10.668);
#4082=TOROIDAL_SURFACE('',#103699,49.1019873874548,10.668);
#4083=TOROIDAL_SURFACE('',#103701,49.1019873874548,10.668);
#4084=TOROIDAL_SURFACE('',#103703,49.1019873874548,10.668);
#4085=TOROIDAL_SURFACE('',#103705,49.1019873874548,10.668);
#4086=TOROIDAL_SURFACE('',#103763,49.1019873874548,10.668);
#4087=TOROIDAL_SURFACE('',#103765,49.1019873874548,10.668);
#4088=TOROIDAL_SURFACE('',#103767,49.1019873874548,10.668);
#4089=TOROIDAL_SURFACE('',#103769,49.1019873874548,10.668);
#4090=TOROIDAL_SURFACE('',#103771,49.1019873874548,10.668);
#4091=TOROIDAL_SURFACE('',#103773,49.1019873874548,10.668);
#4092=TOROIDAL_SURFACE('',#103775,49.1019873874548,10.668);
#4093=TOROIDAL_SURFACE('',#103777,49.1019873874548,10.668);
#4094=TOROIDAL_SURFACE('',#103779,49.1019873874548,10.668);
#4095=TOROIDAL_SURFACE('',#103781,49.1019873874548,10.668);
#4096=TOROIDAL_SURFACE('',#103783,49.1019873874548,10.668);
#4097=TOROIDAL_SURFACE('',#103785,49.1019873874548,10.668);
#4098=TOROIDAL_SURFACE('',#103787,49.1019873874548,10.668);
#4099=TOROIDAL_SURFACE('',#103789,49.1019873874548,10.668);
#4100=TOROIDAL_SURFACE('',#103791,49.1019873874548,10.668);
#4101=TOROIDAL_SURFACE('',#103793,49.1019873874548,10.668);
#4102=TOROIDAL_SURFACE('',#103795,49.1019873874548,10.668);
#4103=TOROIDAL_SURFACE('',#103797,49.1019873874548,10.668);
#4104=TOROIDAL_SURFACE('',#103799,49.1019873874548,10.668);
#4105=TOROIDAL_SURFACE('',#103801,49.1019873874548,10.668);
#4106=TOROIDAL_SURFACE('',#103803,49.1019873874548,10.668);
#4107=TOROIDAL_SURFACE('',#103805,49.1019873874548,10.668);
#4108=TOROIDAL_SURFACE('',#103807,49.1019873874548,10.668);
#4109=TOROIDAL_SURFACE('',#103809,49.1019873874548,10.668);
#4110=TOROIDAL_SURFACE('',#103811,49.1019873874548,10.668);
#4111=TOROIDAL_SURFACE('',#103813,49.1019873874548,10.668);
#4112=TOROIDAL_SURFACE('',#103815,49.1019873874548,10.668);
#4113=TOROIDAL_SURFACE('',#103817,49.1019873874548,10.668);
#4114=TOROIDAL_SURFACE('',#103819,49.1019873874548,10.668);
#4115=TOROIDAL_SURFACE('',#103823,49.1019873874548,10.668);
#4116=TOROIDAL_SURFACE('',#104130,16.0425342723895,1.);
#4117=TOROIDAL_SURFACE('',#104134,26.5598538869239,5.238);
#4118=TOROIDAL_SURFACE('',#104138,26.5598538869239,5.238);
#4119=TOROIDAL_SURFACE('',#104144,17.0841991774145,1.);
#4120=TOROIDAL_SURFACE('',#104147,22.4,1.);
#4121=TOROIDAL_SURFACE('',#104155,22.4,1.);
#4122=TOROIDAL_SURFACE('',#104164,35.,1.);
#4123=TOROIDAL_SURFACE('',#104170,35.,1.);
#4124=TOROIDAL_SURFACE('',#104514,44.9676630434783,0.396875);
#4125=TOROIDAL_SURFACE('',#104518,17.2301371659243,0.396875);
#4126=TOROIDAL_SURFACE('',#104524,43.9357880434783,0.635000000000001);
#4127=B_SPLINE_CURVE_WITH_KNOTS('',3,(#131356,#131357,#131358,#131359,#131360,
#131361,#131362),.UNSPECIFIED.,.F.,.F.,(4,3,4),(0.,0.00021456400433525,
0.000397824826383788),.UNSPECIFIED.);
#4128=B_SPLINE_CURVE_WITH_KNOTS('',3,(#131365,#131366,#131367,#131368),
 .UNSPECIFIED.,.F.,.F.,(4,4),(0.,1.),.UNSPECIFIED.);
#4129=B_SPLINE_CURVE_WITH_KNOTS('',3,(#131379,#131380,#131381,#131382),
 .UNSPECIFIED.,.F.,.F.,(4,4),(0.,1.),.UNSPECIFIED.);
#4130=B_SPLINE_CURVE_WITH_KNOTS('',3,(#131403,#131404,#131405,#131406,#131407,
#131408,#131409,#131410,#131411,#131412),.UNSPECIFIED.,.F.,.F.,(4,3,3,4),
(0.,0.360016030384402,0.739381400890229,1.),.UNSPECIFIED.);
#4131=B_SPLINE_CURVE_WITH_KNOTS('',3,(#131429,#131430,#131431,#131432,#131433,
#131434,#131435),.UNSPECIFIED.,.F.,.F.,(4,3,4),(1.57079632679491,2.35619449019235,
3.14159265358979),.UNSPECIFIED.);
#4132=B_SPLINE_CURVE_WITH_KNOTS('',3,(#131439,#131440,#131441,#131442,#131443,
#131444,#131445),.UNSPECIFIED.,.F.,.F.,(4,3,4),(-1.77635683940025E-15,0.785398163397447,
1.57079632679489),.UNSPECIFIED.);
#4133=B_SPLINE_CURVE_WITH_KNOTS('',3,(#131451,#131452,#131453,#131454,#131455,
#131456,#131457,#131458,#131459,#131460,#131461,#131462,#131463,#131464,
#131465,#131466,#131467,#131468,#131469),.UNSPECIFIED.,.F.,.F.,(4,3,3,3,
3,3,4),(0.00047266192456923,0.000857724029065683,0.00153872216954601,0.0018499707510604,
0.00201291034255504,0.00292749448068747,0.00355315876054085),
 .UNSPECIFIED.);
#4134=B_SPLINE_CURVE_WITH_KNOTS('',3,(#131472,#131473,#131474,#131475,#131476,
#131477,#131478,#131479,#131480,#131481,#131482,#131483,#131484,#131485,
#131486,#131487,#131488,#131489,#131490,#131491,#131492,#131493,#131494,
#131495,#131496,#131497,#131498,#131499,#131500,#131501,#131502,#131503,
#131504,#131505,#131506,#131507,#131508),.UNSPECIFIED.,.F.,.F.,(4,3,3,3,
3,3,3,3,3,3,3,3,4),(1.96820403583049,2.07447029970642,2.18239924823465,
2.29295513021916,2.40448289443547,2.51591247508908,2.55489944283297,2.66627384567102,
2.77787483330248,2.88775468513439,2.99605880939301,3.10223763839193,3.14159265358979),
 .UNSPECIFIED.);
#4135=B_SPLINE_CURVE_WITH_KNOTS('',3,(#131515,#131516,#131517,#131518,#131519,
#131520,#131521),.UNSPECIFIED.,.F.,.F.,(4,3,4),(4.7123889803847,5.49778714378215,
6.28318530717959),.UNSPECIFIED.);
#4136=B_SPLINE_CURVE_WITH_KNOTS('',3,(#131525,#131526,#131527,#131528,#131529,
#131530,#131531),.UNSPECIFIED.,.F.,.F.,(4,3,4),(-1.77635683940025E-15,0.785398163397447,
1.57079632679489),.UNSPECIFIED.);
#4137=B_SPLINE_CURVE_WITH_KNOTS('',3,(#131560,#131561,#131562,#131563,#131564,
#131565,#131566,#131567,#131568,#131569,#131570,#131571,#131572,#131573,
#131574,#131575,#131576,#131577,#131578),.UNSPECIFIED.,.F.,.F.,(4,3,3,3,
3,3,4),(0.,0.000905681138571635,0.00148255506350336,0.00163490147399828,
0.00222383259525504,0.00274053607505753,0.00296511012700672),
 .UNSPECIFIED.);
#4138=B_SPLINE_CURVE_WITH_KNOTS('',3,(#131584,#131585,#131586,#131587,#131588,
#131589,#131590),.UNSPECIFIED.,.F.,.F.,(4,3,4),(4.7123889803847,5.4977871437821,
6.28318530717959),.UNSPECIFIED.);
#4139=B_SPLINE_CURVE_WITH_KNOTS('',3,(#131594,#131595,#131596,#131597,#131598,
#131599,#131600),.UNSPECIFIED.,.F.,.F.,(4,3,4),(3.1415926535898,3.92699081698724,
4.71238898038469),.UNSPECIFIED.);
#4140=B_SPLINE_CURVE_WITH_KNOTS('',3,(#131608,#131609,#131610,#131611,#131612,
#131613,#131614),.UNSPECIFIED.,.F.,.F.,(4,3,4),(4.7123889803847,5.49778714378215,
6.28318530717959),.UNSPECIFIED.);
#4141=B_SPLINE_CURVE_WITH_KNOTS('',3,(#131618,#131619,#131620,#131621,#131622,
#131623,#131624),.UNSPECIFIED.,.F.,.F.,(4,3,4),(1.23467863058848E-16,0.785398163397455,
1.57079632679491),.UNSPECIFIED.);
#4142=B_SPLINE_CURVE_WITH_KNOTS('',3,(#131660,#131661,#131662,#131663,#131664,
#131665,#131666,#131667),.UNSPECIFIED.,.F.,.F.,(4,2,2,4),(9.50038252796028E-8,
0.5,0.75,1.),.UNSPECIFIED.);
#4143=B_SPLINE_CURVE_WITH_KNOTS('',3,(#131670,#131671,#131672,#131673,#131674,
#131675,#131676,#131677),.UNSPECIFIED.,.F.,.F.,(4,2,2,4),(0.,0.25,0.5,1.),
 .UNSPECIFIED.);
#4144=B_SPLINE_CURVE_WITH_KNOTS('',3,(#131735,#131736,#131737,#131738,#131739,
#131740,#131741,#131742,#131743,#131744,#131745,#131746,#131747,#131748,
#131749,#131750,#131751,#131752,#131753,#131754,#131755,#131756,#131757,
#131758,#131759,#131760,#131761,#131762,#131763,#131764,#131765,#131766,
#131767,#131768,#131769,#131770,#131771,#131772,#131773,#131774,#131775,
#131776,#131777,#131778,#131779,#131780),.UNSPECIFIED.,.F.,.F.,(4,3,3,3,
3,3,3,3,3,3,3,3,3,3,3,4),(0.,0.000143086625661407,0.000288513574061178,
0.000426569889101407,0.000433940522460948,0.000435486060835305,0.000709558652807024,
0.000867881044921896,0.000870195056295089,0.00115300716696448,0.00130182156738284,
0.00130356397838256,0.00142320462553202,0.00154203711262815,0.00165601506682433,
0.00173576208984379),.UNSPECIFIED.);
#4145=B_SPLINE_CURVE_WITH_KNOTS('',3,(#131783,#131784,#131785,#131786,#131787,
#131788,#131789,#131790,#131791,#131792),.UNSPECIFIED.,.F.,.F.,(4,2,2,2,
4),(0.,0.25,0.5,0.75,1.),.UNSPECIFIED.);
#4146=B_SPLINE_CURVE_WITH_KNOTS('',3,(#131841,#131842,#131843,#131844,#131845,
#131846,#131847,#131848,#131849,#131850,#131851,#131852,#131853,#131854,
#131855,#131856,#131857,#131858,#131859,#131860,#131861,#131862,#131863,
#131864,#131865,#131866,#131867,#131868,#131869,#131870,#131871,#131872,
#131873,#131874,#131875,#131876,#131877),.UNSPECIFIED.,.F.,.F.,(4,3,3,3,
3,3,3,3,3,3,3,3,4),(0.,0.000202328389738336,0.000393070531576854,0.000394637415448944,
0.000657523627602419,0.000787104044603762,0.000789274830897888,0.0010065772809709,
0.00118241998772925,0.00118391224634683,0.00131758895200357,0.00145591556828473,
0.00157854966179577),.UNSPECIFIED.);
#4147=B_SPLINE_CURVE_WITH_KNOTS('',3,(#131880,#131881,#131882,#131883,#131884,
#131885,#131886,#131887,#131888,#131889),.UNSPECIFIED.,.F.,.F.,(4,2,2,2,
4),(0.,0.25,0.500000000000001,0.75,1.),.UNSPECIFIED.);
#4148=B_SPLINE_CURVE_WITH_KNOTS('',3,(#131933,#131934,#131935,#131936,#131937,
#131938),.UNSPECIFIED.,.F.,.F.,(4,2,4),(0.,0.499999999999999,1.),
 .UNSPECIFIED.);
#4149=B_SPLINE_CURVE_WITH_KNOTS('',3,(#131941,#131942,#131943,#131944,#131945,
#131946),.UNSPECIFIED.,.F.,.F.,(4,2,4),(0.,0.500000000000001,1.),
 .UNSPECIFIED.);
#4150=B_SPLINE_CURVE_WITH_KNOTS('',3,(#131984,#131985,#131986,#131987,#131988,
#131989,#131990,#131991,#131992,#131993,#131994,#131995,#131996,#131997,
#131998,#131999,#132000,#132001,#132002,#132003,#132004,#132005,#132006,
#132007,#132008,#132009,#132010,#132011,#132012,#132013,#132014,#132015,
#132016,#132017,#132018,#132019,#132020,#132021,#132022,#132023,#132024,
#132025,#132026),.UNSPECIFIED.,.F.,.F.,(4,3,3,3,3,3,3,3,3,3,3,3,3,3,4),
(0.,0.000126914134949751,0.000262536143227196,0.000398158151504642,0.000399655746142223,
0.000648709723489428,0.000797160169367613,0.000799311492284445,0.00106908297786168,
0.00119740971470135,0.00119896723842667,0.00131358784144406,0.00142842585215498,
0.00154010419706602,0.00159862298456889),.UNSPECIFIED.);
#4151=B_SPLINE_CURVE_WITH_KNOTS('',3,(#132029,#132030,#132031,#132032,#132033,
#132034,#132035,#132036,#132037,#132038,#132039,#132040,#132041,#132042,
#132043,#132044,#132045,#132046,#132047,#132048,#132049,#132050,#132051,
#132052,#132053,#132054,#132055,#132056,#132057,#132058,#132059,#132060,
#132061,#132062,#132063,#132064,#132065),.UNSPECIFIED.,.F.,.F.,(4,3,3,3,
3,3,3,3,3,3,3,3,4),(0.,0.0847666443586869,0.169627705088856,0.25,0.337926927638317,
0.426118365859893,0.499999999999999,0.587394748316425,0.674958582364191,
0.749999999999999,0.835586424041094,0.921207988122376,1.),.UNSPECIFIED.);
#4152=B_SPLINE_CURVE_WITH_KNOTS('',3,(#132119,#132120,#132121,#132122,#132123,
#132124,#132125,#132126,#132127,#132128,#132129,#132130,#132131,#132132,
#132133,#132134,#132135,#132136,#132137,#132138,#132139,#132140,#132141,
#132142,#132143,#132144,#132145,#132146,#132147,#132148,#132149,#132150,
#132151,#132152,#132153,#132154,#132155,#132156,#132157,#132158,#132159,
#132160,#132161),.UNSPECIFIED.,.F.,.F.,(4,3,3,3,3,3,3,3,3,3,3,3,3,3,4),
(0.,0.000124096840872178,0.000249826409753251,0.000377706687950382,0.000412914062840745,
0.000414565512418997,0.000703661138433462,0.00082582812568149,0.000828047391046449,
0.0011074529067618,0.00123874218852223,0.00124024370669315,0.00141015471005694,
0.00158186346550348,0.00165165625136298),.UNSPECIFIED.);
#4153=B_SPLINE_CURVE_WITH_KNOTS('',3,(#132164,#132165,#132166,#132167,#132168,
#132169,#132170,#132171,#132172,#132173),.UNSPECIFIED.,.F.,.F.,(4,2,2,2,
4),(0.,0.25,0.5,0.75,1.),.UNSPECIFIED.);
#4154=B_SPLINE_CURVE_WITH_KNOTS('',3,(#132185,#132186,#132187,#132188,#132189,
#132190,#132191,#132192,#132193,#132194,#132195,#132196,#132197,#132198,
#132199,#132200,#132201,#132202,#132203),.UNSPECIFIED.,.F.,.F.,(4,3,3,3,
3,3,4),(0.,0.163601301030445,0.331800650515222,0.5,0.666788663885585,0.833394331942792,
1.),.UNSPECIFIED.);
#4155=B_SPLINE_CURVE_WITH_KNOTS('',3,(#132211,#132212,#132213,#132214),
 .UNSPECIFIED.,.F.,.F.,(4,4),(0.,1.),.UNSPECIFIED.);
#4156=B_SPLINE_CURVE_WITH_KNOTS('',3,(#132244,#132245,#132246,#132247,#132248,
#132249),.UNSPECIFIED.,.F.,.F.,(4,2,4),(0.,0.5,1.),.UNSPECIFIED.);
#4157=B_SPLINE_CURVE_WITH_KNOTS('',3,(#132250,#132251,#132252,#132253,#132254,
#132255),.UNSPECIFIED.,.F.,.F.,(4,2,4),(0.,0.5,1.),.UNSPECIFIED.);
#4158=B_SPLINE_CURVE_WITH_KNOTS('',3,(#132295,#132296,#132297,#132298,#132299,
#132300,#132301,#132302,#132303,#132304),.UNSPECIFIED.,.F.,.F.,(4,2,2,2,
4),(0.,0.25,0.5,0.75,1.),.UNSPECIFIED.);
#4159=B_SPLINE_CURVE_WITH_KNOTS('',3,(#132305,#132306,#132307,#132308,#132309,
#132310,#132311,#132312,#132313,#132314,#132315,#132316,#132317,#132318,
#132319,#132320,#132321,#132322,#132323,#132324,#132325,#132326,#132327,
#132328,#132329,#132330,#132331,#132332,#132333,#132334,#132335,#132336,
#132337,#132338,#132339,#132340,#132341,#132342,#132343,#132344,#132345,
#132346,#132347,#132348,#132349,#132350),.UNSPECIFIED.,.F.,.F.,(4,3,3,3,
3,3,3,3,3,3,3,3,3,3,3,4),(0.,0.000126520648339663,0.000255464746612453,
0.000383289319161181,0.000402202417173518,0.000403696977019687,0.000649443966577954,
0.000805221313633907,0.000807393954039373,0.00107833188461984,0.00120950149130569,
0.00121109093105906,0.0013247333581667,0.00143856386975717,0.00154897302143399,
0.00161478790807874),.UNSPECIFIED.);
#4160=B_SPLINE_CURVE_WITH_KNOTS('',3,(#132406,#132407,#132408,#132409,#132410,
#132411,#132412,#132413,#132414,#132415),.UNSPECIFIED.,.F.,.F.,(4,2,2,2,
4),(0.,0.25,0.5,0.750000000000001,1.),.UNSPECIFIED.);
#4161=B_SPLINE_CURVE_WITH_KNOTS('',3,(#132416,#132417,#132418,#132419,#132420,
#132421,#132422,#132423,#132424,#132425,#132426,#132427,#132428,#132429,
#132430,#132431,#132432,#132433,#132434,#132435,#132436,#132437,#132438,
#132439,#132440,#132441,#132442,#132443,#132444,#132445,#132446,#132447,
#132448,#132449,#132450,#132451,#132452,#132453,#132454,#132455,#132456,
#132457,#132458),.UNSPECIFIED.,.F.,.F.,(4,3,3,3,3,3,3,3,3,3,3,3,3,3,4),
(0.,0.000133466187697127,0.000269195218942899,0.000394210955663315,0.000395766414125755,
0.000656135621800232,0.000788421911326631,0.000790581154836762,0.00102610013257283,
0.00118263286698995,0.00118412769954352,0.0013056923112994,0.00142779909867113,
0.00154775473597367,0.00157684382265327),.UNSPECIFIED.);
#4162=B_SPLINE_CURVE_WITH_KNOTS('',3,(#132497,#132498,#132499,#132500,#132501,
#132502),.UNSPECIFIED.,.F.,.F.,(4,2,4),(0.000117319100397047,0.500000000000001,
1.),.UNSPECIFIED.);
#4163=B_SPLINE_CURVE_WITH_KNOTS('',3,(#132503,#132504,#132505,#132506,#132507,
#132508),.UNSPECIFIED.,.F.,.F.,(4,2,4),(0.,0.499999999999999,1.),
 .UNSPECIFIED.);
#4164=B_SPLINE_CURVE_WITH_KNOTS('',3,(#132564,#132565,#132566,#132567,#132568,
#132569,#132570,#132571,#132572,#132573),.UNSPECIFIED.,.F.,.F.,(4,2,2,2,
4),(0.,0.25,0.5,0.75,0.999996541004657),.UNSPECIFIED.);
#4165=B_SPLINE_CURVE_WITH_KNOTS('',3,(#132574,#132575,#132576,#132577,#132578,
#132579,#132580,#132581,#132582,#132583,#132584,#132585),.UNSPECIFIED.,
 .F.,.F.,(4,2,2,2,2,4),(0.,0.000425271195884802,0.000850542391769605,0.00127581358765441,
0.00148844918559681,0.00170108478353921),.UNSPECIFIED.);
#4166=B_SPLINE_CURVE_WITH_KNOTS('',3,(#132642,#132643,#132644,#132645,#132646,
#132647,#132648,#132649,#132650,#132651,#132652,#132653),.UNSPECIFIED.,
 .F.,.F.,(4,2,2,2,2,4),(0.,0.25,0.499999999999999,0.624999999999999,0.749999999999999,
1.),.UNSPECIFIED.);
#4167=B_SPLINE_CURVE_WITH_KNOTS('',3,(#132654,#132655,#132656,#132657,#132658,
#132659,#132660,#132661,#132662,#132663,#132664,#132665,#132666,#132667,
#132668,#132669,#132670,#132671,#132672,#132673,#132674,#132675,#132676,
#132677,#132678,#132679,#132680,#132681,#132682,#132683,#132684,#132685,
#132686,#132687,#132688,#132689,#132690,#132691,#132692,#132693,#132694,
#132695,#132696),.UNSPECIFIED.,.F.,.F.,(4,3,3,3,3,3,3,3,3,3,3,3,3,3,4),
(0.,0.000155846438314328,0.000318202659849571,0.000479330525642439,0.00048138854528345,
0.000719581971214066,0.000722082817925181,0.000946156964943833,0.000960283452349071,
0.000962777090566911,0.00127358059295693,0.00144265205691353,0.00144416563585035,
0.00187401285519362,0.0019255541811338),.UNSPECIFIED.);
#4168=B_SPLINE_CURVE_WITH_KNOTS('',3,(#132719,#132720,#132721,#132722),
 .UNSPECIFIED.,.F.,.F.,(4,4),(0.,1.),.UNSPECIFIED.);
#4169=B_SPLINE_CURVE_WITH_KNOTS('',3,(#132741,#132742,#132743,#132744,#132745,
#132746,#132747,#132748,#132749,#132750),.UNSPECIFIED.,.F.,.F.,(4,3,3,4),
(0.,0.361091546871882,0.717052845282562,1.),.UNSPECIFIED.);
#4170=B_SPLINE_CURVE_WITH_KNOTS('',3,(#132760,#132761,#132762,#132763,#132764,
#132765),.UNSPECIFIED.,.F.,.F.,(4,2,4),(0.,0.5,1.),.UNSPECIFIED.);
#4171=B_SPLINE_CURVE_WITH_KNOTS('',3,(#132772,#132773,#132774,#132775,#132776,
#132777,#132778,#132779),.UNSPECIFIED.,.F.,.F.,(4,2,2,4),(0.,0.25,0.5,1.),
 .UNSPECIFIED.);
#4172=B_SPLINE_CURVE_WITH_KNOTS('',3,(#132787,#132788,#132789,#132790,#132791,
#132792,#132793,#132794,#132795,#132796,#132797,#132798,#132799,#132800,
#132801,#132802,#132803,#132804,#132805,#132806,#132807,#132808,#132809,
#132810,#132811,#132812,#132813,#132814,#132815,#132816,#132817,#132818,
#132819,#132820,#132821,#132822,#132823,#132824,#132825,#132826,#132827,
#132828,#132829),.UNSPECIFIED.,.F.,.F.,(4,3,3,3,3,3,3,3,3,3,3,3,3,3,4),
(0.,0.000127008698005028,0.000262529185195807,0.000398049672386586,0.000399547425717595,
0.000648679298355362,0.000796943972592097,0.00079909485143519,0.00106876545795233,
0.00119708559701167,0.00119864227715278,0.0013133030862701,0.00142818443762435,
0.00153991729226742,0.00159818970287038),.UNSPECIFIED.);
#4173=B_SPLINE_CURVE_WITH_KNOTS('',3,(#132833,#132834,#132835,#132836,#132837,
#132838),.UNSPECIFIED.,.F.,.F.,(4,2,4),(0.,0.500000000000001,1.),
 .UNSPECIFIED.);
#4174=B_SPLINE_CURVE_WITH_KNOTS('',3,(#132846,#132847,#132848,#132849,#132850,
#132851,#132852,#132853),.UNSPECIFIED.,.F.,.F.,(4,2,2,4),(0.,0.5,0.75,1.),
 .UNSPECIFIED.);
#4175=B_SPLINE_CURVE_WITH_KNOTS('',3,(#132857,#132858,#132859,#132860,#132861,
#132862,#132863,#132864,#132865,#132866,#132867,#132868,#132869,#132870,
#132871,#132872,#132873,#132874,#132875,#132876,#132877,#132878,#132879,
#132880,#132881,#132882,#132883,#132884,#132885,#132886,#132887,#132888,
#132889,#132890,#132891,#132892,#132893,#132894,#132895,#132896,#132897,
#132898,#132899,#132900,#132901,#132902,#132903,#132904,#132905,#132906,
#132907,#132908),.UNSPECIFIED.,.F.,.F.,(4,3,3,3,3,3,3,3,3,3,3,3,3,3,3,3,
3,4),(0.,0.00016297400035178,0.000319609377590886,0.00044215652538248,0.000443701447435103,
0.000705760117587487,0.000884313050764961,0.000886662825918404,0.00117556448144828,
0.00132646957614744,0.00132826306101653,0.0014179261914274,0.00143700870749306,
0.00151991305600227,0.0015500272930556,0.00163724702277249,0.00172192727480442,
0.00176862610152992),.UNSPECIFIED.);
#4176=B_SPLINE_CURVE_WITH_KNOTS('',3,(#132916,#132917,#132918,#132919,#132920,
#132921,#132922,#132923,#132924,#132925),.UNSPECIFIED.,.F.,.F.,(4,2,2,2,
4),(0.,0.25,0.375000000000001,0.5,1.),.UNSPECIFIED.);
#4177=B_SPLINE_CURVE_WITH_KNOTS('',3,(#132929,#132930,#132931,#132932,#132933,
#132934,#132935,#132936,#132937,#132938,#132939,#132940,#132941,#132942,
#132943,#132944,#132945,#132946,#132947,#132948,#132949,#132950),
 .UNSPECIFIED.,.F.,.F.,(4,3,3,3,3,3,3,4),(0.,0.000360666935666808,0.000449610485509243,
0.000757497233646948,0.000899220971018486,0.00134883145652773,0.00157363669928234,
0.00179844194203696),.UNSPECIFIED.);
#4178=B_SPLINE_CURVE_WITH_KNOTS('',3,(#132958,#132959,#132960,#132961,#132962,
#132963,#132964,#132965,#132966,#132967,#132968,#132969,#132970,#132971,
#132972,#132973,#132974,#132975,#132976,#132977,#132978,#132979,#132980,
#132981,#132982,#132983,#132984,#132985,#132986,#132987,#132988,#132989,
#132990,#132991,#132992,#132993,#132994,#132995,#132996,#132997,#132998,
#132999,#133000),.UNSPECIFIED.,.F.,.F.,(4,3,3,3,3,3,3,3,3,3,3,3,3,3,4),
(0.,0.000195170703378013,0.000400502314394682,0.000446304927367807,0.000448134863283483,
0.000669908621781835,0.000672202294925215,0.000876863243054838,0.000893889262421614,
0.000896269726566947,0.00123667266509072,0.00134284656974637,0.00134440458985042,
0.00167688520284659,0.0017925394531339),.UNSPECIFIED.);
#4179=B_SPLINE_CURVE_WITH_KNOTS('',3,(#133004,#133005,#133006,#133007,#133008,
#133009,#133010,#133011,#133012,#133013,#133014,#133015,#133016,#133017,
#133018,#133019,#133020,#133021,#133022,#133023,#133024,#133025,#133026,
#133027,#133028,#133029,#133030,#133031,#133032,#133033,#133034,#133035,
#133036,#133037,#133038,#133039,#133040,#133041,#133042,#133043,#133044,
#133045,#133046,#133047,#133048,#133049),.UNSPECIFIED.,.F.,.F.,(4,3,3,3,
3,3,3,3,3,3,3,3,3,3,3,4),(0.,0.000125938335250217,0.000251511263370856,
0.000372362493801517,0.000393010036481153,0.000394487267106025,0.000650087135465414,
0.000786020072962305,0.00078818046791129,0.00103122780428863,0.00117903010944346,
0.0011805925563396,0.00129302327548806,0.00140596384630442,0.00151582795231503,
0.00157204014592461),.UNSPECIFIED.);
#4180=B_SPLINE_CURVE_WITH_KNOTS('',3,(#133057,#133058,#133059,#133060,#133061,
#133062,#133063,#133064,#133065,#133066,#133067,#133068,#133069,#133070,
#133071,#133072,#133073,#133074,#133075,#133076,#133077,#133078,#133079,
#133080,#133081,#133082,#133083,#133084,#133085,#133086,#133087,#133088,
#133089,#133090,#133091,#133092,#133093,#133094,#133095,#133096,#133097,
#133098,#133099),.UNSPECIFIED.,.F.,.F.,(4,3,3,3,3,3,3,3,3,3,3,3,3,3,4),
(0.,0.000128730917859202,0.000262886260532207,0.000397041603205213,0.000398543239038962,
0.00064756610669814,0.000794935814474575,0.000797086478077925,0.00106486773330264,
0.00119408026895391,0.00119562971711689,0.00131091067532176,0.0014265060792,
0.00153915940329535,0.00159417295615585),.UNSPECIFIED.);
#4181=B_SPLINE_CURVE_WITH_KNOTS('',3,(#133103,#133104,#133105,#133106,#133107,
#133108,#133109,#133110),.UNSPECIFIED.,.F.,.F.,(4,2,2,4),(0.,0.5,0.75,1.),
 .UNSPECIFIED.);
#4182=B_SPLINE_CURVE_WITH_KNOTS('',3,(#133117,#133118,#133119,#133120,#133121,
#133122),.UNSPECIFIED.,.F.,.F.,(4,2,4),(0.,0.5,1.),.UNSPECIFIED.);
#4183=B_SPLINE_CURVE_WITH_KNOTS('',3,(#133138,#133139,#133140,#133141),
 .UNSPECIFIED.,.F.,.F.,(4,4),(0.,6.88517764864569E-5),.UNSPECIFIED.);
#4184=B_SPLINE_CURVE_WITH_KNOTS('',3,(#133167,#133168,#133169,#133170,#133171,
#133172),.UNSPECIFIED.,.F.,.F.,(4,2,4),(0.,0.5,1.),.UNSPECIFIED.);
#4185=B_SPLINE_CURVE_WITH_KNOTS('',3,(#133189,#133190,#133191,#133192,#133193,
#133194,#133195),.UNSPECIFIED.,.F.,.F.,(4,3,4),(1.5707963267949,2.35619449019235,
3.1415926535898),.UNSPECIFIED.);
#4186=B_SPLINE_CURVE_WITH_KNOTS('',3,(#133199,#133200,#133201,#133202,#133203,
#133204,#133205),.UNSPECIFIED.,.F.,.F.,(4,3,4),(1.23467863058847E-16,0.785398163397447,
1.5707963267949),.UNSPECIFIED.);
#4187=B_SPLINE_CURVE_WITH_KNOTS('',3,(#133211,#133212,#133213,#133214,#133215,
#133216,#133217,#133218,#133219,#133220,#133221,#133222,#133223,#133224,
#133225,#133226,#133227,#133228,#133229),.UNSPECIFIED.,.F.,.F.,(4,3,3,3,
3,3,4),(0.000169216231991231,0.000729993311375969,0.000968460740699438,
0.00168309612079798,0.00176770524940811,0.00279102522271593,0.00336619426682546),
 .UNSPECIFIED.);
#4188=B_SPLINE_CURVE_WITH_KNOTS('',3,(#133239,#133240,#133241,#133242,#133243,
#133244,#133245),.UNSPECIFIED.,.F.,.F.,(4,3,4),(4.71238898038469,5.49778714378214,
6.28318530717959),.UNSPECIFIED.);
#4189=B_SPLINE_CURVE_WITH_KNOTS('',3,(#133249,#133250,#133251,#133252,#133253,
#133254,#133255),.UNSPECIFIED.,.F.,.F.,(4,3,4),(1.23467863058847E-16,0.785398163397447,
1.5707963267949),.UNSPECIFIED.);
#4190=B_SPLINE_CURVE_WITH_KNOTS('',3,(#133288,#133289,#133290,#133291,#133292,
#133293,#133294),.UNSPECIFIED.,.F.,.F.,(4,3,4),(1.5707963267949,2.35619449019234,
3.14159265358979),.UNSPECIFIED.);
#4191=B_SPLINE_CURVE_WITH_KNOTS('',3,(#133298,#133299,#133300,#133301,#133302,
#133303,#133304),.UNSPECIFIED.,.F.,.F.,(4,3,4),(3.14159265358979,3.92699081698724,
4.71238898038469),.UNSPECIFIED.);
#4192=B_SPLINE_CURVE_WITH_KNOTS('',3,(#133310,#133311,#133312,#133313,#133314,
#133315,#133316,#133317,#133318,#133319,#133320,#133321,#133322,#133323,
#133324,#133325),.UNSPECIFIED.,.F.,.F.,(4,3,3,3,3,4),(0.000244714080610449,
0.00121583023103576,0.00174053473821824,0.00180545417371792,0.00292276797843844,
0.00336619426682539),.UNSPECIFIED.);
#4193=B_SPLINE_CURVE_WITH_KNOTS('',3,(#133329,#133330,#133331,#133332,#133333,
#133334,#133335),.UNSPECIFIED.,.F.,.F.,(4,3,4),(1.5707963267949,2.35619449019232,
3.14159265358979),.UNSPECIFIED.);
#4194=B_SPLINE_CURVE_WITH_KNOTS('',3,(#133339,#133340,#133341,#133342,#133343,
#133344,#133345),.UNSPECIFIED.,.F.,.F.,(4,3,4),(-1.77635683940025E-15,0.785398163397447,
1.57079632679489),.UNSPECIFIED.);
#4195=B_SPLINE_CURVE_WITH_KNOTS('',3,(#133367,#133368,#133369,#133370,#133371,
#133372),.UNSPECIFIED.,.F.,.F.,(4,2,4),(0.,0.5,1.),.UNSPECIFIED.);
#4196=B_SPLINE_CURVE_WITH_KNOTS('',3,(#133415,#133416,#133417,#133418,#133419,
#133420,#133421,#133422),.UNSPECIFIED.,.F.,.F.,(4,2,2,4),(0.,0.25,0.5,1.),
 .UNSPECIFIED.);
#4197=B_SPLINE_CURVE_WITH_KNOTS('',3,(#133459,#133460,#133461,#133462,#133463,
#133464,#133465,#133466,#133467,#133468),.UNSPECIFIED.,.F.,.F.,(4,2,2,2,
4),(0.,0.25,0.5,0.749999999999999,1.),.UNSPECIFIED.);
#4198=B_SPLINE_CURVE_WITH_KNOTS('',3,(#133517,#133518,#133519,#133520,#133521,
#133522,#133523,#133524,#133525,#133526),.UNSPECIFIED.,.F.,.F.,(4,2,2,2,
4),(0.,0.25,0.500000000000001,0.750000000000001,1.),.UNSPECIFIED.);
#4199=B_SPLINE_CURVE_WITH_KNOTS('',3,(#133580,#133581,#133582,#133583,#133584,
#133585,#133586,#133587,#133588,#133589,#133590,#133591,#133592,#133593,
#133594,#133595,#133596,#133597,#133598,#133599,#133600,#133601,#133602,
#133603,#133604,#133605,#133606,#133607,#133608,#133609,#133610,#133611,
#133612,#133613,#133614,#133615,#133616,#133617,#133618,#133619,#133620,
#133621,#133622,#133623,#133624,#133625,#133626,#133627,#133628),
 .UNSPECIFIED.,.F.,.F.,(4,3,3,3,3,3,3,3,3,3,3,3,3,3,3,3,4),(0.,0.087564719729141,
0.168782359864571,0.245864630016523,0.25,0.354535950890996,0.447075382683936,
0.5,0.555980429743289,0.611777642915431,0.625,0.691371875377358,0.750000000000001,
0.82986450531225,0.906218926800638,0.979271353598852,1.),.UNSPECIFIED.);
#4200=B_SPLINE_CURVE_WITH_KNOTS('',3,(#133677,#133678,#133679,#133680,#133681,
#133682,#133683,#133684,#133685,#133686,#133687,#133688,#133689,#133690,
#133691,#133692,#133693,#133694,#133695,#133696,#133697,#133698,#133699,
#133700,#133701,#133702,#133703,#133704,#133705,#133706,#133707,#133708,
#133709,#133710,#133711,#133712,#133713,#133714,#133715,#133716,#133717,
#133718,#133719,#133720,#133721,#133722,#133723,#133724,#133725),
 .UNSPECIFIED.,.F.,.F.,(4,3,3,3,3,3,3,3,3,3,3,3,3,3,3,3,4),(0.,0.0673211146699331,
0.134715456033185,0.202659384537495,0.25,0.322758924734933,0.396441399379554,
0.471979834578492,0.5,0.575516106875766,0.652984132469324,0.733824490565147,
0.75,0.829223437699597,0.91178455799991,0.940509163793382,1.),
 .UNSPECIFIED.);
#4201=B_SPLINE_CURVE_WITH_KNOTS('',3,(#133773,#133774,#133775,#133776,#133777,
#133778,#133779,#133780,#133781,#133782,#133783,#133784,#133785,#133786,
#133787,#133788,#133789,#133790,#133791,#133792,#133793,#133794,#133795,
#133796,#133797,#133798,#133799,#133800,#133801,#133802,#133803,#133804,
#133805,#133806,#133807,#133808,#133809,#133810,#133811,#133812,#133813,
#133814,#133815,#133816,#133817,#133818,#133819,#133820,#133821),
 .UNSPECIFIED.,.F.,.F.,(4,3,3,3,3,3,3,3,3,3,3,3,3,3,3,3,4),(0.,0.0643187684459386,
0.151144143415235,0.238358107561426,0.317473279366759,0.394527907474398,
0.469118347726267,0.5,0.567041589025861,0.624999999999999,0.679259523694771,
0.733605072096865,0.75,0.821970997330374,0.892478293684135,0.961558653299543,
1.),.UNSPECIFIED.);
#4202=B_SPLINE_CURVE_WITH_KNOTS('',3,(#133870,#133871,#133872,#133873,#133874,
#133875,#133876,#133877,#133878,#133879),.UNSPECIFIED.,.F.,.F.,(4,2,2,2,
4),(0.,0.25,0.499999999999999,0.749999999999998,1.),.UNSPECIFIED.);
#4203=B_SPLINE_CURVE_WITH_KNOTS('',3,(#133921,#133922,#133923,#133924,#133925,
#133926,#133927,#133928),.UNSPECIFIED.,.F.,.F.,(4,2,2,4),(0.,0.25,0.5,1.),
 .UNSPECIFIED.);
#4204=B_SPLINE_CURVE_WITH_KNOTS('',3,(#133965,#133966,#133967,#133968,#133969,
#133970),.UNSPECIFIED.,.F.,.F.,(4,2,4),(0.,0.499999999999999,1.),
 .UNSPECIFIED.);
#4205=B_SPLINE_CURVE_WITH_KNOTS('',3,(#134007,#134008,#134009,#134010,#134011,
#134012,#134013,#134014,#134015,#134016,#134017,#134018,#134019,#134020,
#134021,#134022,#134023,#134024,#134025,#134026,#134027,#134028,#134029,
#134030,#134031,#134032,#134033,#134034,#134035,#134036,#134037,#134038,
#134039,#134040,#134041,#134042,#134043),.UNSPECIFIED.,.F.,.F.,(4,3,3,3,
3,3,3,3,3,3,3,3,4),(0.,0.0849060387652225,0.169905587248193,0.25,0.337991601382829,
0.426246250502731,0.499999999999999,0.587308431420735,0.674783689226744,
0.749999999999999,0.835530010300542,0.921094023848129,1.),.UNSPECIFIED.);
#4206=B_SPLINE_CURVE_WITH_KNOTS('',3,(#134084,#134085,#134086,#134087,#134088,
#134089,#134090,#134091),.UNSPECIFIED.,.F.,.F.,(4,2,2,4),(0.,0.5,0.75,1.),
 .UNSPECIFIED.);
#4207=B_SPLINE_CURVE_WITH_KNOTS('',3,(#134096,#134097,#134098,#134099,#134100,
#134101,#134102,#134103,#134104,#134105),.UNSPECIFIED.,.F.,.F.,(4,2,2,2,
4),(0.,0.250000000000004,0.5,0.750000000000003,1.),.UNSPECIFIED.);
#4208=B_SPLINE_CURVE_WITH_KNOTS('',3,(#134106,#134107,#134108,#134109,#134110,
#134111,#134112,#134113,#134114,#134115),.UNSPECIFIED.,.F.,.F.,(4,2,2,2,
4),(0.,0.250000000000001,0.500000000000001,0.75,1.),.UNSPECIFIED.);
#4209=B_SPLINE_CURVE_WITH_KNOTS('',3,(#134142,#134143,#134144,#134145,#134146,
#134147),.UNSPECIFIED.,.F.,.F.,(4,2,4),(0.,0.5,1.),.UNSPECIFIED.);
#4210=B_SPLINE_CURVE_WITH_KNOTS('',3,(#134172,#134173,#134174,#134175,#134176,
#134177),.UNSPECIFIED.,.F.,.F.,(4,2,4),(0.,0.5,1.),.UNSPECIFIED.);
#4211=B_SPLINE_CURVE_WITH_KNOTS('',3,(#134185,#134186,#134187,#134188,#134189,
#134190,#134191,#134192,#134193,#134194),.UNSPECIFIED.,.F.,.F.,(4,2,2,2,
4),(0.,0.250000000000004,0.5,0.749999999999997,1.),.UNSPECIFIED.);
#4212=B_SPLINE_CURVE_WITH_KNOTS('',3,(#134215,#134216,#134217,#134218,#134219,
#134220),.UNSPECIFIED.,.F.,.F.,(4,2,4),(0.,0.5,1.),.UNSPECIFIED.);
#4213=B_SPLINE_CURVE_WITH_KNOTS('',3,(#134246,#134247,#134248,#134249,#134250,
#134251),.UNSPECIFIED.,.F.,.F.,(4,2,4),(0.,0.502999491316249,1.),
 .UNSPECIFIED.);
#4214=B_SPLINE_CURVE_WITH_KNOTS('',3,(#134252,#134253,#134254,#134255,#134256,
#134257),.UNSPECIFIED.,.F.,.F.,(4,2,4),(0.,0.5,1.),.UNSPECIFIED.);
#4215=B_SPLINE_CURVE_WITH_KNOTS('',3,(#134261,#134262,#134263,#134264,#134265,
#134266,#134267,#134268,#134269,#134270),.UNSPECIFIED.,.F.,.F.,(4,2,2,2,
4),(0.,0.25,0.5,0.75,1.),.UNSPECIFIED.);
#4216=B_SPLINE_CURVE_WITH_KNOTS('',3,(#134297,#134298,#134299,#134300,#134301,
#134302),.UNSPECIFIED.,.F.,.F.,(4,2,4),(0.,0.5,1.),.UNSPECIFIED.);
#4217=B_SPLINE_CURVE_WITH_KNOTS('',3,(#134327,#134328,#134329,#134330,#134331,
#134332),.UNSPECIFIED.,.F.,.F.,(4,2,4),(0.,0.500000000000002,1.),
 .UNSPECIFIED.);
#4218=B_SPLINE_CURVE_WITH_KNOTS('',3,(#134359,#134360,#134361,#134362,#134363,
#134364),.UNSPECIFIED.,.F.,.F.,(4,2,4),(0.,0.5,1.),.UNSPECIFIED.);
#4219=B_SPLINE_CURVE_WITH_KNOTS('',3,(#134369,#134370,#134371,#134372,#134373,
#134374,#134375,#134376,#134377,#134378),.UNSPECIFIED.,.F.,.F.,(4,2,2,2,
4),(0.,0.250000000000001,0.499999999999999,0.749999999999999,1.),
 .UNSPECIFIED.);
#4220=B_SPLINE_CURVE_WITH_KNOTS('',3,(#134379,#134380,#134381,#134382,#134383,
#134384,#134385,#134386,#134387,#134388),.UNSPECIFIED.,.F.,.F.,(4,2,2,2,
4),(0.,0.250000000000001,0.500000000000002,0.750000000000002,1.),
 .UNSPECIFIED.);
#4221=B_SPLINE_CURVE_WITH_KNOTS('',3,(#134415,#134416,#134417,#134418,#134419,
#134420),.UNSPECIFIED.,.F.,.F.,(4,2,4),(0.,0.5,1.),.UNSPECIFIED.);
#4222=B_SPLINE_CURVE_WITH_KNOTS('',3,(#134445,#134446,#134447,#134448,#134449,
#134450),.UNSPECIFIED.,.F.,.F.,(4,2,4),(0.,0.500000000000002,1.),
 .UNSPECIFIED.);
#4223=B_SPLINE_CURVE_WITH_KNOTS('',3,(#134474,#134475,#134476,#134477,#134478,
#134479),.UNSPECIFIED.,.F.,.F.,(4,2,4),(0.,0.503000256250808,1.),
 .UNSPECIFIED.);
#4224=B_SPLINE_CURVE_WITH_KNOTS('',3,(#134480,#134481,#134482,#134483,#134484,
#134485,#134486,#134487,#134488,#134489,#134490,#134491),.UNSPECIFIED.,
 .F.,.F.,(4,2,2,2,2,4),(0.,0.250000000000001,0.375000000000002,0.499999999999998,
0.750000000000001,1.),.UNSPECIFIED.);
#4225=B_SPLINE_CURVE_WITH_KNOTS('',3,(#134495,#134496,#134497,#134498,#134499,
#134500,#134501,#134502,#134503,#134504),.UNSPECIFIED.,.F.,.F.,(4,2,2,2,
4),(0.,0.25,0.5,0.75,1.),.UNSPECIFIED.);
#4226=B_SPLINE_CURVE_WITH_KNOTS('',3,(#134531,#134532,#134533,#134534,#134535,
#134536),.UNSPECIFIED.,.F.,.F.,(4,2,4),(0.,0.499999999999998,1.),
 .UNSPECIFIED.);
#4227=B_SPLINE_CURVE_WITH_KNOTS('',3,(#134561,#134562,#134563,#134564,#134565,
#134566),.UNSPECIFIED.,.F.,.F.,(4,2,4),(0.,0.500000000000002,1.),
 .UNSPECIFIED.);
#4228=B_SPLINE_CURVE_WITH_KNOTS('',3,(#134577,#134578,#134579,#134580,#134581,
#134582,#134583,#134584,#134585,#134586),.UNSPECIFIED.,.F.,.F.,(4,2,2,2,
4),(0.,0.250000000000004,0.5,0.749999999999997,1.),.UNSPECIFIED.);
#4229=B_SPLINE_CURVE_WITH_KNOTS('',3,(#134587,#134588,#134589,#134590,#134591,
#134592,#134593,#134594,#134595,#134596),.UNSPECIFIED.,.F.,.F.,(4,2,2,2,
4),(0.,0.250000000000001,0.5,0.75,1.),.UNSPECIFIED.);
#4230=B_SPLINE_CURVE_WITH_KNOTS('',3,(#134623,#134624,#134625,#134626,#134627,
#134628),.UNSPECIFIED.,.F.,.F.,(4,2,4),(0.,0.5,1.),.UNSPECIFIED.);
#4231=B_SPLINE_CURVE_WITH_KNOTS('',3,(#134653,#134654,#134655,#134656,#134657,
#134658),.UNSPECIFIED.,.F.,.F.,(4,2,4),(0.,0.5,1.),.UNSPECIFIED.);
#4232=B_SPLINE_CURVE_WITH_KNOTS('',3,(#134666,#134667,#134668,#134669,#134670,
#134671,#134672,#134673,#134674,#134675),.UNSPECIFIED.,.F.,.F.,(4,2,2,2,
4),(0.,0.250000000000004,0.5,0.749999999999997,1.),.UNSPECIFIED.);
#4233=B_SPLINE_CURVE_WITH_KNOTS('',3,(#134724,#134725,#134726,#134727,#134728,
#134729,#134730,#134731,#134732,#134733,#134734,#134735,#134736),
 .UNSPECIFIED.,.F.,.F.,(4,3,3,3,4),(0.,0.269537008270268,0.544459888994111,
0.814598147393945,1.),.UNSPECIFIED.);
#4234=B_SPLINE_CURVE_WITH_KNOTS('',3,(#134740,#134741,#134742,#134743,#134744,
#134745,#134746,#134747,#134748,#134749),.UNSPECIFIED.,.F.,.F.,(4,2,2,2,
4),(0.,0.250000000000001,0.5,0.75,1.),.UNSPECIFIED.);
#4235=B_SPLINE_CURVE_WITH_KNOTS('',3,(#134776,#134777,#134778,#134779,#134780,
#134781),.UNSPECIFIED.,.F.,.F.,(4,2,4),(0.,0.5,1.),.UNSPECIFIED.);
#4236=B_SPLINE_CURVE_WITH_KNOTS('',3,(#134806,#134807,#134808,#134809,#134810,
#134811),.UNSPECIFIED.,.F.,.F.,(4,2,4),(0.,0.499999999999998,1.),
 .UNSPECIFIED.);
#4237=B_SPLINE_CURVE_WITH_KNOTS('',3,(#134836,#134837,#134838,#134839,#134840,
#134841),.UNSPECIFIED.,.F.,.F.,(4,2,4),(0.,0.497000288786711,1.),
 .UNSPECIFIED.);
#4238=B_SPLINE_CURVE_WITH_KNOTS('',3,(#134843,#134844,#134845,#134846,#134847,
#134848),.UNSPECIFIED.,.F.,.F.,(4,2,4),(0.,0.499999999999998,1.),
 .UNSPECIFIED.);
#4239=B_SPLINE_CURVE_WITH_KNOTS('',3,(#134871,#134872,#134873,#134874,#134875,
#134876,#134877,#134878,#134879,#134880),.UNSPECIFIED.,.F.,.F.,(4,2,2,2,
4),(0.,0.250000000000001,0.499999999999998,0.749999999999999,1.),
 .UNSPECIFIED.);
#4240=B_SPLINE_CURVE_WITH_KNOTS('',3,(#134907,#134908,#134909,#134910,#134911,
#134912),.UNSPECIFIED.,.F.,.F.,(4,2,4),(0.,0.5,1.),.UNSPECIFIED.);
#4241=B_SPLINE_CURVE_WITH_KNOTS('',3,(#134937,#134938,#134939,#134940,#134941,
#134942),.UNSPECIFIED.,.F.,.F.,(4,2,4),(0.,0.5,1.),.UNSPECIFIED.);
#4242=B_SPLINE_CURVE_WITH_KNOTS('',3,(#134951,#134952,#134953,#134954,#134955,
#134956,#134957,#134958,#134959,#134960),.UNSPECIFIED.,.F.,.F.,(4,2,2,2,
4),(0.,0.249999999999998,0.499999999999999,0.749999999999999,1.),
 .UNSPECIFIED.);
#4243=B_SPLINE_CURVE_WITH_KNOTS('',3,(#134961,#134962,#134963,#134964,#134965,
#134966,#134967,#134968,#134969,#134970),.UNSPECIFIED.,.F.,.F.,(4,2,2,2,
4),(0.,0.250000000000001,0.499999999999998,0.749999999999999,1.),
 .UNSPECIFIED.);
#4244=B_SPLINE_CURVE_WITH_KNOTS('',3,(#134997,#134998,#134999,#135000,#135001,
#135002),.UNSPECIFIED.,.F.,.F.,(4,2,4),(0.,0.5,1.),.UNSPECIFIED.);
#4245=B_SPLINE_CURVE_WITH_KNOTS('',3,(#135029,#135030,#135031,#135032,#135033,
#135034),.UNSPECIFIED.,.F.,.F.,(4,2,4),(0.,0.5,1.),.UNSPECIFIED.);
#4246=B_SPLINE_CURVE_WITH_KNOTS('',3,(#135044,#135045,#135046,#135047,#135048,
#135049,#135050,#135051,#135052,#135053),.UNSPECIFIED.,.F.,.F.,(4,2,2,2,
4),(0.,0.249999999999998,0.499999999999999,0.749999999999999,1.),
 .UNSPECIFIED.);
#4247=B_SPLINE_CURVE_WITH_KNOTS('',3,(#135116,#135117,#135118,#135119),
 .UNSPECIFIED.,.F.,.F.,(4,4),(0.,1.),.UNSPECIFIED.);
#4248=B_SPLINE_CURVE_WITH_KNOTS('',3,(#135122,#135123,#135124,#135125),
 .UNSPECIFIED.,.F.,.F.,(4,4),(0.,0.0331958858056162),.UNSPECIFIED.);
#4249=B_SPLINE_CURVE_WITH_KNOTS('',3,(#135169,#135170,#135171,#135172,#135173,
#135174,#135175,#135176,#135177,#135178,#135179,#135180,#135181,#135182,
#135183,#135184,#135185,#135186,#135187,#135188,#135189,#135190,#135191,
#135192,#135193,#135194,#135195,#135196,#135197,#135198,#135199,#135200,
#135201,#135202,#135203,#135204,#135205,#135206,#135207,#135208),
 .UNSPECIFIED.,.F.,.F.,(4,3,3,3,3,3,3,3,3,3,3,3,3,4),(0.,0.250000000000401,
0.37500000000056,0.437500000000597,0.468750000000618,0.484375000000582,
0.496808957139414,0.500000000000546,0.593872927450488,0.687778494940771,
0.781121765432879,0.873618088950425,0.964138621540856,1.),.UNSPECIFIED.);
#4250=B_SPLINE_CURVE_WITH_KNOTS('',3,(#135226,#135227,#135228,#135229,#135230,
#135231),.UNSPECIFIED.,.F.,.F.,(4,2,4),(0.,0.000500369188755688,0.00100073837751138),
 .UNSPECIFIED.);
#4251=B_SPLINE_CURVE_WITH_KNOTS('',3,(#135250,#135251,#135252,#135253,#135254,
#135255),.UNSPECIFIED.,.F.,.F.,(4,2,4),(0.,0.5,1.),.UNSPECIFIED.);
#4252=B_SPLINE_CURVE_WITH_KNOTS('',3,(#135257,#135258,#135259,#135260,#135261,
#135262),.UNSPECIFIED.,.F.,.F.,(4,2,4),(0.,0.5,1.),.UNSPECIFIED.);
#4253=B_SPLINE_CURVE_WITH_KNOTS('',3,(#135264,#135265,#135266,#135267),
 .UNSPECIFIED.,.F.,.F.,(4,4),(0.,1.),.UNSPECIFIED.);
#4254=B_SPLINE_CURVE_WITH_KNOTS('',3,(#135270,#135271,#135272,#135273,#135274,
#135275,#135276,#135277,#135278,#135279),.UNSPECIFIED.,.F.,.F.,(4,2,2,2,
4),(0.,0.25,0.5,0.75,1.),.UNSPECIFIED.);
#4255=B_SPLINE_CURVE_WITH_KNOTS('',3,(#135325,#135326,#135327,#135328,#135329,
#135330,#135331,#135332,#135333,#135334,#135335,#135336),.UNSPECIFIED.,
 .F.,.F.,(4,2,2,2,2,4),(0.,0.31912132670696,0.47868199006044,0.63824265341392,
0.95736398012088,1.),.UNSPECIFIED.);
#4256=B_SPLINE_CURVE_WITH_KNOTS('',3,(#135339,#135340,#135341,#135342,#135343,
#135344,#135345,#135346,#135347,#135348,#135349,#135350,#135351,#135352,
#135353,#135354,#135355,#135356,#135357,#135358,#135359,#135360,#135361,
#135362,#135363,#135364,#135365,#135366,#135367,#135368,#135369,#135370,
#135371,#135372,#135373,#135374,#135375,#135376,#135377,#135378,#135379,
#135380,#135381),.UNSPECIFIED.,.F.,.F.,(4,3,3,3,3,3,3,3,3,3,3,3,3,3,4),
(4.80131737206195E-10,0.0725092726268684,0.144994898707486,0.21754885026403,
0.250000000000001,0.322952563145093,0.395915689830995,0.468996449355532,
0.500000000000002,0.586371586023873,0.673119802689203,0.760419685943488,
0.847982202568464,0.935943610235565,1.),.UNSPECIFIED.);
#4257=B_SPLINE_CURVE_WITH_KNOTS('',3,(#135439,#135440,#135441,#135442,#135443,
#135444),.UNSPECIFIED.,.F.,.F.,(4,2,4),(0.000562946727309309,0.00236076329038739,
0.00415857985346548),.UNSPECIFIED.);
#4258=B_SPLINE_CURVE_WITH_KNOTS('',3,(#135448,#135449,#135450,#135451,#135452,
#135453),.UNSPECIFIED.,.F.,.F.,(4,2,4),(3.44768074808928E-6,0.516296525972948,
1.),.UNSPECIFIED.);
#4259=B_SPLINE_CURVE_WITH_KNOTS('',3,(#135454,#135455,#135456,#135457,#135458,
#135459,#135460,#135461,#135462,#135463),.UNSPECIFIED.,.F.,.F.,(4,2,2,2,
4),(0.,0.250000000000004,0.500000000000003,0.750000000000001,1.),
 .UNSPECIFIED.);
#4260=B_SPLINE_CURVE_WITH_KNOTS('',3,(#135578,#135579,#135580,#135581,#135582,
#135583,#135584,#135585,#135586,#135587,#135588,#135589,#135590,#135591,
#135592,#135593,#135594,#135595,#135596,#135597,#135598,#135599,#135600,
#135601,#135602,#135603,#135604,#135605,#135606,#135607,#135608),
 .UNSPECIFIED.,.F.,.F.,(4,3,3,3,3,3,3,3,3,3,4),(0.,0.000563737664817631,
0.000564164457966258,0.00104582443004183,0.00112760220035037,0.00112832891593252,
0.00161216721523005,0.00169210723432587,0.00169249337389877,0.00210946737364631,
0.00225665783186503),.UNSPECIFIED.);
#4261=B_SPLINE_CURVE_WITH_KNOTS('',3,(#135615,#135616,#135617,#135618,#135619,
#135620,#135621,#135622,#135623,#135624),.UNSPECIFIED.,.F.,.F.,(4,2,2,2,
4),(0.,0.25,0.499999999999999,0.749999999999998,1.),.UNSPECIFIED.);
#4262=B_SPLINE_CURVE_WITH_KNOTS('',3,(#135738,#135739,#135740,#135741,#135742,
#135743,#135744,#135745,#135746,#135747,#135748,#135749,#135750,#135751,
#135752,#135753,#135754,#135755,#135756,#135757,#135758,#135759,#135760,
#135761,#135762,#135763),.UNSPECIFIED.,.F.,.F.,(4,2,2,2,2,2,2,2,2,2,2,2,
4),(0.,0.0308819193977864,0.0647401130033729,0.0887784724846976,0.122010977791757,
0.141217536873128,0.14606144500119,0.164774918181124,0.172906057212047,
0.180478634267683,0.208285706582933,0.247371596054736,0.282492401339011),
 .UNSPECIFIED.);
#4263=B_SPLINE_CURVE_WITH_KNOTS('',3,(#135772,#135773,#135774,#135775,#135776,
#135777,#135778,#135779,#135780,#135781,#135782,#135783,#135784,#135785,
#135786,#135787,#135788,#135789),.UNSPECIFIED.,.F.,.F.,(4,2,2,2,2,2,2,2,
4),(-0.2325452866513,-0.202278856490703,-0.169720566967503,-0.147070875717209,
-0.116272702466171,-0.0854925566395962,-0.062837160360675,-0.0302640152403312,
0.),.UNSPECIFIED.);
#4264=B_SPLINE_CURVE_WITH_KNOTS('',3,(#135796,#135797,#135798,#135799,#135800,
#135801,#135802,#135803),.UNSPECIFIED.,.F.,.F.,(4,2,2,4),(-0.169530887591468,
-0.138792065251541,-0.106611941486663,-0.0847654430253264),
 .UNSPECIFIED.);
#4265=B_SPLINE_CURVE_WITH_KNOTS('',3,(#135808,#135809,#135810,#135811,#135812,
#135813,#135814,#135815),.UNSPECIFIED.,.F.,.F.,(4,2,2,4),(-0.0847650334136806,
-0.0629270182290063,-0.0307530884809931,0.),.UNSPECIFIED.);
#4266=B_SPLINE_CURVE_WITH_KNOTS('',3,(#135818,#135819,#135820,#135821,#135822,
#135823,#135824,#135825,#135826,#135827,#135828,#135829,#135830,#135831,
#135832,#135833,#135834,#135835),.UNSPECIFIED.,.F.,.F.,(4,2,2,2,2,2,2,2,
4),(-0.232545286657315,-0.202278856495331,-0.169720566970565,-0.14707087571913,
-0.116272702467069,-0.0854925566400001,-0.0628371603609857,-0.030264015240477,
0.),.UNSPECIFIED.);
#4267=B_SPLINE_CURVE_WITH_KNOTS('',3,(#135870,#135871,#135872,#135873,#135874,
#135875,#135876,#135877,#135878,#135879),.UNSPECIFIED.,.F.,.F.,(4,2,2,2,
4),(0.,0.250000000000001,0.5,0.75,1.),.UNSPECIFIED.);
#4268=B_SPLINE_CURVE_WITH_KNOTS('',3,(#135882,#135883,#135884,#135885,#135886,
#135887,#135888,#135889,#135890,#135891,#135892,#135893,#135894,#135895,
#135896,#135897,#135898,#135899,#135900,#135901,#135902,#135903,#135904,
#135905,#135906,#135907,#135908,#135909,#135910,#135911,#135912,#135913,
#135914,#135915,#135916,#135917,#135918,#135919,#135920,#135921,#135922,
#135923,#135924),.UNSPECIFIED.,.F.,.F.,(4,3,3,3,3,3,3,3,3,3,3,3,3,3,4),
(0.,0.000168850029785981,0.000336050047503145,0.000405527490133943,0.000407005029304983,
0.000682198964496424,0.000811826624698267,0.000814010058609966,0.00109897545099435,
0.00121939063721614,0.00122101508791495,0.00134692436003259,0.001471310831548,
0.00159335498692783,0.00162802011721993),.UNSPECIFIED.);
#4269=B_SPLINE_CURVE_WITH_KNOTS('',3,(#135980,#135981,#135982,#135983,#135984,
#135985,#135986,#135987,#135988,#135989,#135990,#135991,#135992,#135993,
#135994,#135995,#135996,#135997,#135998,#135999,#136000,#136001,#136002,
#136003,#136004,#136005,#136006,#136007,#136008,#136009,#136010,#136011,
#136012,#136013,#136014,#136015,#136016),.UNSPECIFIED.,.F.,.F.,(4,3,3,3,
3,3,3,3,3,3,3,3,4),(0.,0.0855690909158042,0.171174585040492,0.25,0.337530389879789,
0.42495453801557,0.5,0.588221947844027,0.676235883140647,0.75,0.834877270845738,
0.919731176821254,1.),.UNSPECIFIED.);
#4270=B_SPLINE_CURVE_WITH_KNOTS('',3,(#136017,#136018,#136019,#136020,#136021,
#136022,#136023,#136024,#136025,#136026,#136027,#136028,#136029,#136030,
#136031,#136032,#136033,#136034,#136035,#136036,#136037,#136038,#136039,
#136040,#136041,#136042,#136043,#136044,#136045,#136046,#136047,#136048,
#136049,#136050,#136051,#136052,#136053,#136054,#136055,#136056,#136057,
#136058,#136059,#136060,#136061,#136062),.UNSPECIFIED.,.F.,.F.,(4,3,3,3,
3,3,3,3,3,3,3,3,3,3,3,4),(0.,0.000111620791367541,0.000225473811195175,
0.000339302579903037,0.000397521249509077,0.000399067370002251,0.00066751766164224,
0.000795042499018153,0.000797178277617397,0.00104506031877337,0.00119256374852723,
0.00119405065366288,0.00132343586690882,0.00145676043247256,0.00158159308775804,
0.0015900849980363),.UNSPECIFIED.);
#4271=B_SPLINE_CURVE_WITH_KNOTS('',3,(#136088,#136089,#136090,#136091,#136092,
#136093),.UNSPECIFIED.,.F.,.F.,(4,2,4),(0.,0.500000000000001,1.),
 .UNSPECIFIED.);
#4272=B_SPLINE_CURVE_WITH_KNOTS('',3,(#136096,#136097,#136098,#136099,#136100,
#136101),.UNSPECIFIED.,.F.,.F.,(4,2,4),(0.,0.499999999999999,1.),
 .UNSPECIFIED.);
#4273=B_SPLINE_CURVE_WITH_KNOTS('',3,(#136151,#136152,#136153,#136154,#136155,
#136156,#136157,#136158),.UNSPECIFIED.,.F.,.F.,(4,2,2,4),(0.,0.499999999999999,
0.75,1.),.UNSPECIFIED.);
#4274=B_SPLINE_CURVE_WITH_KNOTS('',3,(#136159,#136160,#136161,#136162,#136163,
#136164,#136165,#136166),.UNSPECIFIED.,.F.,.F.,(4,2,2,4),(0.,0.25,0.500000000000001,
1.),.UNSPECIFIED.);
#4275=B_SPLINE_CURVE_WITH_KNOTS('',3,(#136215,#136216,#136217,#136218,#136219,
#136220,#136221,#136222,#136223,#136224,#136225,#136226,#136227,#136228,
#136229,#136230,#136231,#136232,#136233,#136234,#136235,#136236,#136237,
#136238,#136239,#136240,#136241,#136242,#136243,#136244,#136245,#136246,
#136247,#136248,#136249,#136250,#136251,#136252,#136253,#136254,#136255,
#136256,#136257,#136258,#136259,#136260,#136261,#136262,#136263,#136264,
#136265,#136266),.UNSPECIFIED.,.F.,.F.,(4,3,3,3,3,3,3,3,3,3,3,3,3,3,3,3,
3,4),(0.,8.48627990059856E-5,0.000110154370857281,0.000197555987869132,
0.00023405941935963,0.000330463112571844,0.000419877362193068,0.000438835738394215,
0.000440617483429125,0.000729065363181661,0.00087889719586762,0.00088123496685825,
0.00114445185849832,0.00132031265264404,0.00132185245028737,0.00147439999768875,
0.00163314747063781,0.0017624699337165),.UNSPECIFIED.);
#4276=B_SPLINE_CURVE_WITH_KNOTS('',3,(#136269,#136270,#136271,#136272,#136273,
#136274,#136275,#136276,#136277,#136278),.UNSPECIFIED.,.F.,.F.,(4,2,2,2,
4),(0.,0.249999999999999,0.5,0.75,1.),.UNSPECIFIED.);
#4277=B_SPLINE_CURVE_WITH_KNOTS('',3,(#136334,#136335,#136336,#136337,#136338,
#136339,#136340,#136341,#136342,#136343,#136344,#136345,#136346,#136347,
#136348,#136349,#136350,#136351,#136352,#136353,#136354,#136355,#136356,
#136357,#136358,#136359,#136360,#136361,#136362,#136363,#136364,#136365,
#136366,#136367,#136368,#136369,#136370,#136371,#136372,#136373,#136374,
#136375,#136376,#136377,#136378,#136379,#136380,#136381,#136382),
 .UNSPECIFIED.,.F.,.F.,(4,3,3,3,3,3,3,3,3,3,3,3,3,3,3,3,4),(0.,0.0694026021440636,
0.139645419416936,0.211930659092264,0.25,0.304387057659765,0.358678892493984,
0.375,0.44229150378928,0.500000000000001,0.574699847176716,0.651271982256802,
0.731430997765807,0.813937157578756,0.900570004879131,0.937863451189354,
1.),.UNSPECIFIED.);
#4278=B_SPLINE_CURVE_WITH_KNOTS('',3,(#136383,#136384,#136385,#136386,#136387,
#136388,#136389,#136390,#136391,#136392),.UNSPECIFIED.,.F.,.F.,(4,2,2,2,
4),(0.,0.499999999999999,0.625,0.75,1.),.UNSPECIFIED.);
#4279=B_SPLINE_CURVE_WITH_KNOTS('',3,(#136398,#136399,#136400,#136401),
 .UNSPECIFIED.,.F.,.F.,(4,4),(0.,1.),.UNSPECIFIED.);
#4280=B_SPLINE_CURVE_WITH_KNOTS('',3,(#136405,#136406,#136407,#136408,#136409,
#136410),.UNSPECIFIED.,.F.,.F.,(4,2,4),(0.,0.5,1.),.UNSPECIFIED.);
#4281=B_SPLINE_CURVE_WITH_KNOTS('',3,(#136427,#136428,#136429,#136430),
 .UNSPECIFIED.,.F.,.F.,(4,4),(0.,1.),.UNSPECIFIED.);
#4282=B_SPLINE_CURVE_WITH_KNOTS('',3,(#136432,#136433,#136434,#136435),
 .UNSPECIFIED.,.F.,.F.,(4,4),(0.,1.),.UNSPECIFIED.);
#4283=B_SPLINE_CURVE_WITH_KNOTS('',3,(#136482,#136483,#136484,#136485,#136486,
#136487,#136488,#136489,#136490,#136491,#136492,#136493,#136494,#136495,
#136496,#136497,#136498,#136499,#136500,#136501,#136502,#136503,#136504,
#136505,#136506,#136507,#136508,#136509),.UNSPECIFIED.,.F.,.F.,(4,3,3,3,
3,3,3,3,3,4),(0.,0.000418680346172109,0.000626513004308685,0.000899330166364171,
0.00105990140469318,0.00112416270795522,0.00125349750883986,0.00134899524954626,
0.00159071512184879,0.00179866033272836),.UNSPECIFIED.);
#4284=B_SPLINE_CURVE_WITH_KNOTS('',3,(#136552,#136553,#136554,#136555,#136556,
#136557,#136558,#136559,#136560,#136561,#136562,#136563,#136564,#136565,
#136566,#136567,#136568,#136569,#136570,#136571,#136572,#136573,#136574,
#136575,#136576,#136577,#136578,#136579,#136580,#136581,#136582,#136583,
#136584,#136585,#136586,#136587,#136588),.UNSPECIFIED.,.F.,.F.,(4,3,3,3,
3,3,3,3,3,3,3,3,4),(0.000628504292635843,0.00064025498632194,0.000837411769726014,
0.000877277691072229,0.00100166439029042,0.00112605108950862,0.0012996740600194,
0.00158178243882745,0.00162359788638139,0.00162947384441178,0.00195921469101129,
0.00212114468325416,0.00261869148012693),.UNSPECIFIED.);
#4285=B_SPLINE_CURVE_WITH_KNOTS('',3,(#136589,#136590,#136591,#136592,#136593,
#136594,#136595,#136596,#136597,#136598,#136599,#136600),.UNSPECIFIED.,
 .F.,.F.,(4,2,2,2,2,4),(0.,0.251509454663243,0.377264181994864,0.503018909326486,
0.754528363989729,1.),.UNSPECIFIED.);
#4286=B_SPLINE_CURVE_WITH_KNOTS('',3,(#136637,#136638,#136639,#136640,#136641,
#136642,#136643),.UNSPECIFIED.,.F.,.F.,(4,3,4),(0.,0.490447172337672,1.),
 .UNSPECIFIED.);
#4287=B_SPLINE_CURVE_WITH_KNOTS('',3,(#136644,#136645,#136646,#136647,#136648,
#136649,#136650,#136651,#136652,#136653,#136654,#136655),.UNSPECIFIED.,
 .F.,.F.,(4,2,3,3,4),(0.,0.00100000000000032,0.00500000000004302,0.0210000000041071,
0.0383173498474262),.UNSPECIFIED.);
#4288=B_SPLINE_CURVE_WITH_KNOTS('',3,(#136656,#136657,#136658,#136659),
 .UNSPECIFIED.,.F.,.F.,(4,4),(0.,1.),.UNSPECIFIED.);
#4289=B_SPLINE_CURVE_WITH_KNOTS('',3,(#136677,#136678,#136679,#136680,#136681,
#136682,#136683,#136684,#136685,#136686,#136687,#136688,#136689,#136690,
#136691,#136692,#136693,#136694,#136695,#136696,#136697,#136698,#136699,
#136700,#136701,#136702,#136703,#136704,#136705,#136706,#136707,#136708,
#136709,#136710,#136711,#136712,#136713),.UNSPECIFIED.,.F.,.F.,(4,3,3,3,
3,3,3,3,3,3,3,3,4),(0.,0.000308449407263107,0.000616898814526214,0.000757033039934092,
0.00113555144207261,0.00123379762905243,0.00151396810348857,0.00181929544894823,
0.00185069644357864,0.00189260692917409,0.00221146178004248,0.00227133710209361,
0.00246759525810486),.UNSPECIFIED.);
#4290=B_SPLINE_CURVE_WITH_KNOTS('',3,(#136716,#136717,#136718,#136719,#136720,
#136721,#136722,#136723,#136724,#136725,#136726,#136727,#136728,#136729,
#136730,#136731,#136732,#136733,#136734,#136735,#136736,#136737,#136738,
#136739,#136740,#136741,#136742,#136743,#136744,#136745,#136746,#136747,
#136748,#136749,#136750,#136751,#136752),.UNSPECIFIED.,.F.,.F.,(4,3,3,3,
3,3,3,3,3,3,3,3,4),(0.00064734234469968,0.000773679728910249,0.000794515777305426,
0.00111794174210909,0.00114512410810862,0.00123603607512266,0.00151649021309283,
0.00182472980554565,0.00188790100005034,0.00225930818373534,0.00241342353596863,
0.00270777040118012,0.00300211726639161),.UNSPECIFIED.);
#4291=B_SPLINE_CURVE_WITH_KNOTS('',3,(#136761,#136762,#136763,#136764,#136765,
#136766,#136767,#136768,#136769,#136770,#136771,#136772,#136773),
 .UNSPECIFIED.,.F.,.F.,(4,3,3,3,4),(0.,0.000680510137073302,0.00109976462606963,
0.002047167230467,0.00219952925213926),.UNSPECIFIED.);
#4292=B_SPLINE_CURVE_WITH_KNOTS('',3,(#136777,#136778,#136779,#136780,#136781,
#136782,#136783,#136784,#136785,#136786,#136787,#136788,#136789),
 .UNSPECIFIED.,.F.,.F.,(4,3,3,3,4),(0.,0.000627390790128563,0.00109987581267579,
0.00205656007244151,0.00219975162535158),.UNSPECIFIED.);
#4293=B_SPLINE_CURVE_WITH_KNOTS('',3,(#136865,#136866,#136867,#136868,#136869,
#136870,#136871,#136872,#136873,#136874,#136875,#136876),.UNSPECIFIED.,
 .F.,.F.,(4,2,2,2,2,4),(0.,0.253338275236372,0.506676550472745,0.633345688090933,
0.76001482570911,1.),.UNSPECIFIED.);
#4294=B_SPLINE_CURVE_WITH_KNOTS('',3,(#136877,#136878,#136879,#136880),
 .UNSPECIFIED.,.F.,.F.,(4,4),(0.0037358385977583,0.00423610566507283),
 .UNSPECIFIED.);
#4295=B_SPLINE_CURVE_WITH_KNOTS('',3,(#136918,#136919,#136920,#136921,#136922,
#136923,#136924,#136925,#136926,#136927,#136928,#136929,#136930,#136931,
#136932,#136933,#136934,#136935,#136936,#136937,#136938,#136939,#136940,
#136941,#136942,#136943,#136944,#136945,#136946,#136947,#136948,#136949,
#136950,#136951,#136952,#136953,#136954,#136955,#136956,#136957,#136958,
#136959,#136960,#136961,#136962,#136963),.UNSPECIFIED.,.F.,.F.,(4,3,3,3,
3,3,3,3,3,3,3,3,3,3,3,4),(0.000450499470650019,0.00054011395429817,0.000798583304346381,
0.000986883024373906,0.00116741533983523,0.00137527276208873,0.00169825994125939,
0.00176385446568028,0.00188433120902044,0.00210726599697033,0.00224278914361301,
0.00241357708828729,0.00254109024997701,0.0026012470782056,0.00316630230566398,
0.00331816294739075),.UNSPECIFIED.);
#4296=B_SPLINE_CURVE_WITH_KNOTS('',3,(#136982,#136983,#136984,#136985,#136986,
#136987,#136988,#136989,#136990,#136991,#136992,#136993,#136994,#136995,
#136996,#136997,#136998,#136999,#137000,#137001,#137002,#137003,#137004,
#137005,#137006,#137007,#137008,#137009,#137010,#137011,#137012,#137013,
#137014,#137015,#137016,#137017,#137018,#137019,#137020,#137021,#137022,
#137023,#137024,#137025,#137026,#137027,#137028,#137029,#137030),
 .UNSPECIFIED.,.F.,.F.,(4,3,3,3,3,3,3,3,3,3,3,3,3,3,3,3,4),(0.,0.000568992160114069,
0.000684369961878612,0.000753736971436074,0.000939442240058873,0.00102655494281796,
0.00113065957381952,0.00136873992375731,0.00150755451437509,0.00188444398402291,
0.00205310988563609,0.00222420237610578,0.002260801563485,0.00235252174395805,
0.00254500079573646,0.00264124032162566,0.00273747984751486),
 .UNSPECIFIED.);
#4297=B_SPLINE_CURVE_WITH_KNOTS('',3,(#137038,#137039,#137040,#137041,#137042,
#137043,#137044,#137045,#137046,#137047,#137048,#137049,#137050),
 .UNSPECIFIED.,.F.,.F.,(4,3,3,3,4),(0.,0.000962747670576822,0.00119082241359643,
0.00216097007597471,0.00238164482719285),.UNSPECIFIED.);
#4298=B_SPLINE_CURVE_WITH_KNOTS('',3,(#137054,#137055,#137056,#137057,#137058,
#137059,#137060,#137061,#137062,#137063,#137064,#137065,#137066),
 .UNSPECIFIED.,.F.,.F.,(4,3,3,3,4),(0.,0.000775847435672983,0.00119114916434495,
0.00218083968926337,0.00238229832868991),.UNSPECIFIED.);
#4299=B_SPLINE_CURVE_WITH_KNOTS('',3,(#137076,#137077,#137078,#137079,#137080,
#137081),.UNSPECIFIED.,.F.,.F.,(4,2,4),(0.,0.432355968717148,1.),
 .UNSPECIFIED.);
#4300=B_SPLINE_CURVE_WITH_KNOTS('',3,(#137086,#137087,#137088,#137089),
 .UNSPECIFIED.,.F.,.F.,(4,4),(0.,1.),.UNSPECIFIED.);
#4301=B_SPLINE_CURVE_WITH_KNOTS('',3,(#137118,#137119,#137120,#137121),
 .UNSPECIFIED.,.F.,.F.,(4,4),(0.,0.0322629186945109),.UNSPECIFIED.);
#4302=B_SPLINE_CURVE_WITH_KNOTS('',3,(#137123,#137124,#137125,#137126,#137127,
#137128,#137129,#137130,#137131,#137132,#137133,#137134,#137135,#137136,
#137137,#137138),.UNSPECIFIED.,.F.,.F.,(4,3,3,3,3,4),(0.,0.000549388570662942,
0.00110809797239399,0.00147175517552831,0.00249356706682249,0.00294351035105662),
 .UNSPECIFIED.);
#4303=B_SPLINE_CURVE_WITH_KNOTS('',3,(#137142,#137143,#137144,#137145,#137146,
#137147,#137148,#137149,#137150,#137151,#137152,#137153,#137154),
 .UNSPECIFIED.,.F.,.F.,(4,3,3,3,4),(0.,0.000882415156994226,0.00147346850157273,
0.00255877694108978,0.00294693700314546),.UNSPECIFIED.);
#4304=B_SPLINE_CURVE_WITH_KNOTS('',3,(#137155,#137156,#137157,#137158),
 .UNSPECIFIED.,.F.,.F.,(4,4),(0.,0.0319950621716304),.UNSPECIFIED.);
#4305=B_SPLINE_CURVE_WITH_KNOTS('',3,(#137195,#137196,#137197,#137198),
 .UNSPECIFIED.,.F.,.F.,(4,4),(0.,0.0298008594779328),.UNSPECIFIED.);
#4306=B_SPLINE_CURVE_WITH_KNOTS('',3,(#137200,#137201,#137202,#137203,#137204,
#137205,#137206,#137207,#137208,#137209,#137210,#137211,#137212,#137213,
#137214,#137215),.UNSPECIFIED.,.F.,.F.,(4,3,3,3,3,4),(0.,0.000531847314911702,
0.00107596315612957,0.00162007899734744,0.00266000146298276,0.00324015799469487),
 .UNSPECIFIED.);
#4307=B_SPLINE_CURVE_WITH_KNOTS('',3,(#137219,#137220,#137221,#137222,#137223,
#137224,#137225,#137226,#137227,#137228,#137229,#137230,#137231),
 .UNSPECIFIED.,.F.,.F.,(4,3,3,3,4),(0.,0.000817558298561711,0.00162295210526764,
0.00275577655347827,0.00324590421053527),.UNSPECIFIED.);
#4308=B_SPLINE_CURVE_WITH_KNOTS('',3,(#137233,#137234,#137235,#137236),
 .UNSPECIFIED.,.F.,.F.,(4,4),(0.,0.0300693678107436),.UNSPECIFIED.);
#4309=B_SPLINE_CURVE_WITH_KNOTS('',3,(#137241,#137242,#137243,#137244,#137245,
#137246,#137247),.UNSPECIFIED.,.F.,.F.,(4,3,4),(6.08671444000369E-7,0.379970146635923,
1.),.UNSPECIFIED.);
#4310=B_SPLINE_CURVE_WITH_KNOTS('',3,(#137252,#137253,#137254,#137255),
 .UNSPECIFIED.,.F.,.F.,(4,4),(0.,1.),.UNSPECIFIED.);
#4311=B_SPLINE_CURVE_WITH_KNOTS('',3,(#137284,#137285,#137286,#137287),
 .UNSPECIFIED.,.F.,.F.,(4,4),(0.,0.0240963563036403),.UNSPECIFIED.);
#4312=B_SPLINE_CURVE_WITH_KNOTS('',3,(#137289,#137290,#137291,#137292,#137293,
#137294,#137295,#137296,#137297,#137298,#137299,#137300,#137301,#137302,
#137303,#137304,#137305,#137306,#137307,#137308,#137309,#137310,#137311,
#137312,#137313),.UNSPECIFIED.,.F.,.F.,(4,3,3,3,3,3,3,3,4),(0.,0.000403252952291635,
0.000810273659956253,0.000991778862067342,0.0014336523721451,0.00187173698199313,
0.00198355772413468,0.00304641612721467,0.00396711544826929),
 .UNSPECIFIED.);
#4313=B_SPLINE_CURVE_WITH_KNOTS('',3,(#137317,#137318,#137319,#137320,#137321,
#137322,#137323,#137324,#137325,#137326,#137327,#137328,#137329,#137330,
#137331,#137332,#137333,#137334,#137335),.UNSPECIFIED.,.F.,.F.,(4,3,3,3,
3,3,4),(0.,0.000606703134123721,0.00123626357061692,0.00189155006086011,
0.00198795077588647,0.00324033736596706,0.00397590155177294),
 .UNSPECIFIED.);
#4314=B_SPLINE_CURVE_WITH_KNOTS('',3,(#137336,#137337,#137338,#137339),
 .UNSPECIFIED.,.F.,.F.,(4,4),(0.,0.0238258198664154),.UNSPECIFIED.);
#4315=B_SPLINE_CURVE_WITH_KNOTS('',3,(#137346,#137347,#137348,#137349,#137350,
#137351,#137352,#137353),.UNSPECIFIED.,.F.,.F.,(4,2,2,4),(0.,0.5,0.749999999999999,
1.),.UNSPECIFIED.);
#4316=B_SPLINE_CURVE_WITH_KNOTS('',3,(#137381,#137382,#137383,#137384,#137385,
#137386,#137387,#137388,#137389,#137390,#137391,#137392,#137393,#137394,
#137395,#137396),.UNSPECIFIED.,.F.,.F.,(4,3,3,3,3,4),(0.,0.000625284942165436,
0.00128905281997377,0.00194949793575932,0.00318811191752659,0.00389899587151865),
 .UNSPECIFIED.);
#4317=B_SPLINE_CURVE_WITH_KNOTS('',3,(#137398,#137399,#137400,#137401),
 .UNSPECIFIED.,.F.,.F.,(4,4),(0.,0.024690830875569),.UNSPECIFIED.);
#4318=B_SPLINE_CURVE_WITH_KNOTS('',3,(#137419,#137420,#137421,#137422),
 .UNSPECIFIED.,.F.,.F.,(4,4),(0.,0.0278605201857756),.UNSPECIFIED.);
#4319=B_SPLINE_CURVE_WITH_KNOTS('',3,(#137424,#137425,#137426,#137427,#137428,
#137429,#137430,#137431),.UNSPECIFIED.,.F.,.F.,(4,2,2,4),(0.,0.000890496769046365,
0.00178099353809273,0.0035619870761855),.UNSPECIFIED.);
#4320=B_SPLINE_CURVE_WITH_KNOTS('',3,(#137454,#137455,#137456,#137457,#137458,
#137459),.UNSPECIFIED.,.F.,.F.,(4,2,4),(0.,0.50310275859516,1.),
 .UNSPECIFIED.);
#4321=B_SPLINE_CURVE_WITH_KNOTS('',3,(#137460,#137461,#137462,#137463),
 .UNSPECIFIED.,.F.,.F.,(4,4),(0.,1.),.UNSPECIFIED.);
#4322=B_SPLINE_CURVE_WITH_KNOTS('',3,(#137485,#137486,#137487,#137488,#137489,
#137490,#137491,#137492,#137493,#137494,#137495,#137496,#137497,#137498,
#137499,#137500,#137501,#137502,#137503,#137504,#137505,#137506,#137507,
#137508,#137509,#137510,#137511,#137512,#137513,#137514,#137515,#137516,
#137517,#137518,#137519,#137520,#137521,#137522,#137523,#137524,#137525,
#137526,#137527,#137528,#137529,#137530,#137531,#137532,#137533,#137534,
#137535,#137536,#137537,#137538,#137539,#137540,#137541,#137542,#137543,
#137544,#137545,#137546,#137547,#137548),.UNSPECIFIED.,.F.,.F.,(4,3,3,3,
3,3,3,3,3,3,3,3,3,3,3,3,3,3,3,3,3,4),(0.,0.00024394307186977,0.000489165049879305,
0.000733924827046494,0.000899069239743237,0.000911316177023075,0.00119563029973435,
0.00134860385961487,0.00136698289390588,0.00175854423315568,0.0017981384794865,
0.00182264071786975,0.00224767309935813,0.00227830273883051,0.0025704401924202,
0.00269720771922976,0.00273398747333099,0.00295810023175185,0.0031467423391014,
0.00331012937356541,0.003472902617082,0.00359627695897302),
 .UNSPECIFIED.);
#4323=B_SPLINE_CURVE_WITH_KNOTS('',3,(#137553,#137554,#137555,#137556,#137557,
#137558,#137559,#137560,#137561,#137562,#137563,#137564,#137565,#137566,
#137567,#137568,#137569,#137570,#137571,#137572,#137573,#137574,#137575,
#137576,#137577,#137578,#137579,#137580,#137581,#137582,#137583,#137584,
#137585,#137586),.UNSPECIFIED.,.F.,.F.,(4,3,3,3,3,3,3,3,3,3,3,4),(0.,0.000121613272085654,
0.000230848939029442,0.000231076761054257,0.000462001643661034,0.000462153522108514,
0.000693154344712357,0.000693230283162771,0.000767002378129216,0.00084153649830509,
0.000913992773638304,0.000924307044217028),.UNSPECIFIED.);
#4324=B_SPLINE_CURVE_WITH_KNOTS('',3,(#137588,#137589,#137590,#137591),
 .UNSPECIFIED.,.F.,.F.,(4,4),(0.,9.64176041888327E-5),.UNSPECIFIED.);
#4325=B_SPLINE_CURVE_WITH_KNOTS('',3,(#137592,#137593,#137594,#137595),
 .UNSPECIFIED.,.F.,.F.,(4,4),(0.,0.0333345873458536),.UNSPECIFIED.);
#4326=B_SPLINE_CURVE_WITH_KNOTS('',3,(#137639,#137640,#137641,#137642,#137643,
#137644,#137645,#137646,#137647,#137648,#137649,#137650,#137651,#137652),
 .UNSPECIFIED.,.F.,.F.,(4,2,2,2,2,2,4),(0.,0.222921495031895,0.352434579193248,
0.481947663354594,0.611460747515947,0.740973831677298,1.),.UNSPECIFIED.);
#4327=B_SPLINE_CURVE_WITH_KNOTS('',3,(#137667,#137668,#137669,#137670,#137671,
#137672,#137673,#137674,#137675,#137676,#137677,#137678),.UNSPECIFIED.,
 .F.,.F.,(4,2,2,2,2,4),(0.,0.251487957710783,0.502975915421567,0.628719894276953,
0.754463873132351,1.),.UNSPECIFIED.);
#4328=B_SPLINE_CURVE_WITH_KNOTS('',3,(#137717,#137718,#137719,#137720,#137721,
#137722,#137723,#137724,#137725,#137726,#137727,#137728,#137729,#137730,
#137731,#137732,#137733,#137734,#137735,#137736,#137737,#137738,#137739,
#137740,#137741,#137742,#137743,#137744,#137745,#137746,#137747,#137748,
#137749,#137750,#137751,#137752,#137753,#137754,#137755,#137756,#137757,
#137758,#137759,#137760,#137761,#137762,#137763,#137764,#137765,#137766,
#137767,#137768,#137769,#137770,#137771,#137772,#137773,#137774,#137775,
#137776,#137777),.UNSPECIFIED.,.F.,.F.,(4,3,3,3,3,3,3,3,3,3,3,3,3,3,3,3,
3,3,3,3,4),(0.000632518815593833,0.000932214526663858,0.00101585454476649,
0.00107182189614632,0.00126737972551736,0.00139919027393915,0.00150973846725992,
0.00175129113716284,0.0017825260031118,0.00194741404639006,0.00209785990015682,
0.00215891919163232,0.00222254437895217,0.00246825757120489,0.00254919746145711,
0.00271487168756755,0.00282308344954008,0.00293253319062976,0.00318749230619625,
0.00344334847758565,0.00369920464897506),.UNSPECIFIED.);
#4329=B_SPLINE_CURVE_WITH_KNOTS('',3,(#137796,#137797,#137798,#137799),
 .UNSPECIFIED.,.F.,.F.,(4,4),(3.46944695195361E-18,0.0333425790106738),
 .UNSPECIFIED.);
#4330=B_SPLINE_CURVE_WITH_KNOTS('',3,(#137800,#137801,#137802,#137803,#137804,
#137805,#137806,#137807,#137808,#137809,#137810,#137811,#137812,#137813,
#137814,#137815,#137816,#137817,#137818,#137819,#137820,#137821,#137822,
#137823,#137824,#137825,#137826,#137827,#137828,#137829,#137830,#137831,
#137832,#137833),.UNSPECIFIED.,.F.,.F.,(4,3,3,3,3,3,3,3,3,3,3,4),(0.,7.30072795026687E-5,
0.000147770013513677,0.000221881916258645,0.000252597382995535,0.00050519476599107,
0.000631493458785095,0.000757792148986605,0.000834383528242275,0.000911454457737675,
0.000985554988538247,0.00101038953198214),.UNSPECIFIED.);
#4331=B_SPLINE_CURVE_WITH_KNOTS('',3,(#137836,#137837,#137838,#137839),
 .UNSPECIFIED.,.F.,.F.,(4,4),(0.,1.),.UNSPECIFIED.);
#4332=B_SPLINE_CURVE_WITH_KNOTS('',3,(#137840,#137841,#137842,#137843),
 .UNSPECIFIED.,.F.,.F.,(4,4),(0.,1.),.UNSPECIFIED.);
#4333=B_SPLINE_CURVE_WITH_KNOTS('',3,(#137861,#137862,#137863,#137864,#137865,
#137866,#137867,#137868,#137869,#137870,#137871,#137872,#137873,#137874,
#137875,#137876,#137877,#137878,#137879,#137880,#137881,#137882,#137883,
#137884,#137885,#137886,#137887,#137888,#137889,#137890,#137891),
 .UNSPECIFIED.,.F.,.F.,(4,3,3,3,3,3,3,3,3,3,4),(0.,0.000497569400086742,
0.000640953038946951,0.00096143126389141,0.000995138800173484,0.00128203532234786,
0.00149270820026023,0.00161710055028191,0.00180479162331791,0.00192302626316565,
0.00199027760034697),.UNSPECIFIED.);
#4334=B_SPLINE_CURVE_WITH_KNOTS('',3,(#137894,#137895,#137896,#137897,#137898,
#137899),.UNSPECIFIED.,.F.,.F.,(4,2,4),(0.,0.000501785580775435,0.00100357116155087),
 .UNSPECIFIED.);
#4335=B_SPLINE_CURVE_WITH_KNOTS('',3,(#137967,#137968,#137969,#137970,#137971,
#137972,#137973,#137974,#137975,#137976),.UNSPECIFIED.,.F.,.F.,(4,2,2,2,
4),(0.,0.25149977741346,0.502999554826924,0.754499332240389,1.),
 .UNSPECIFIED.);
#4336=B_SPLINE_CURVE_WITH_KNOTS('',3,(#137977,#137978,#137979,#137980),
 .UNSPECIFIED.,.F.,.F.,(4,4),(0.0171576436379621,0.0176580988602617),
 .UNSPECIFIED.);
#4337=B_SPLINE_CURVE_WITH_KNOTS('',3,(#138012,#138013,#138014,#138015,#138016,
#138017,#138018,#138019,#138020,#138021,#138022,#138023,#138024,#138025,
#138026,#138027,#138028,#138029,#138030,#138031,#138032,#138033,#138034,
#138035,#138036,#138037,#138038,#138039),.UNSPECIFIED.,.F.,.F.,(4,3,3,3,
3,3,3,3,3,4),(0.000712605368931889,0.00092646187873443,0.00114426125513566,
0.00117428487373109,0.00139094819074949,0.00157723429047313,0.00180778147057016,
0.0020948168670341,0.00237995362541881,0.00244186321201438),
 .UNSPECIFIED.);
#4338=B_SPLINE_CURVE_WITH_KNOTS('',3,(#138083,#138084,#138085,#138086,#138087,
#138088,#138089),.UNSPECIFIED.,.F.,.F.,(4,3,4),(0.,0.014563917689728,0.029127835379456),
 .UNSPECIFIED.);
#4339=B_SPLINE_CURVE_WITH_KNOTS('',3,(#138091,#138092,#138093,#138094,#138095,
#138096,#138097,#138098,#138099,#138100,#138101,#138102,#138103,#138104,
#138105,#138106,#138107,#138108,#138109,#138110,#138111,#138112,#138113,
#138114,#138115),.UNSPECIFIED.,.F.,.F.,(4,3,3,3,3,3,3,3,4),(0.,0.000422069097418792,
0.000847931637830459,0.00104448509574678,0.00149181651230618,0.00193535496126664,
0.00208897019149356,0.00315378543073329,0.00417794038298713),
 .UNSPECIFIED.);
#4340=B_SPLINE_CURVE_WITH_KNOTS('',3,(#138119,#138120,#138121,#138122,#138123,
#138124,#138125,#138126,#138127,#138128,#138129,#138130,#138131,#138132,
#138133,#138134,#138135,#138136,#138137,#138138,#138139,#138140),
 .UNSPECIFIED.,.F.,.F.,(4,3,3,3,3,3,3,4),(0.,0.000384591749546137,0.00078374926264035,
0.00104647183020208,0.00173887398624976,0.00209294366040415,0.00337921840659428,
0.00418588732080839),.UNSPECIFIED.);
#4341=B_SPLINE_CURVE_WITH_KNOTS('',3,(#138142,#138143,#138144,#138145,#138146,
#138147,#138148),.UNSPECIFIED.,.F.,.F.,(4,3,4),(0.,0.0146992078328598,0.0293984156657196),
 .UNSPECIFIED.);
#4342=B_SPLINE_CURVE_WITH_KNOTS('',3,(#138168,#138169,#138170,#138171,#138172,
#138173,#138174),.UNSPECIFIED.,.F.,.F.,(4,3,4),(0.,0.626599975159676,0.999999250966931),
 .UNSPECIFIED.);
#4343=B_SPLINE_CURVE_WITH_KNOTS('',3,(#138181,#138182,#138183,#138184,#138185,
#138186),.UNSPECIFIED.,.F.,.F.,(4,2,4),(0.,0.5,1.),.UNSPECIFIED.);
#4344=B_SPLINE_CURVE_WITH_KNOTS('',3,(#138218,#138219,#138220,#138221,#138222,
#138223,#138224),.UNSPECIFIED.,.F.,.F.,(4,3,4),(0.,0.0178323395635859,0.0356646791271718),
 .UNSPECIFIED.);
#4345=B_SPLINE_CURVE_WITH_KNOTS('',3,(#138226,#138227,#138228,#138229,#138230,
#138231,#138232,#138233),.UNSPECIFIED.,.F.,.F.,(4,2,2,4),(0.,0.000848531500815463,
0.00169706300163092,0.00339412600326177),.UNSPECIFIED.);
#4346=B_SPLINE_CURVE_WITH_KNOTS('',3,(#138237,#138238,#138239,#138240,#138241,
#138242,#138243,#138244,#138245,#138246,#138247,#138248,#138249,#138250,
#138251,#138252),.UNSPECIFIED.,.F.,.F.,(4,3,3,3,3,4),(0.,0.000761157739919989,
0.00156083390161768,0.00170051723463269,0.00285526923553587,0.00340103446926538),
 .UNSPECIFIED.);
#4347=B_SPLINE_CURVE_WITH_KNOTS('',3,(#138253,#138254,#138255,#138256,#138257,
#138258,#138259),.UNSPECIFIED.,.F.,.F.,(4,3,4),(0.,0.0176980703187956,0.0353961406375911),
 .UNSPECIFIED.);
#4348=B_SPLINE_CURVE_WITH_KNOTS('',3,(#138289,#138290,#138291,#138292,#138293,
#138294,#138295),.UNSPECIFIED.,.F.,.F.,(4,3,4),(0.,0.0188568492058762,0.0377136984117524),
 .UNSPECIFIED.);
#4349=B_SPLINE_CURVE_WITH_KNOTS('',3,(#138297,#138298,#138299,#138300,#138301,
#138302,#138303,#138304,#138305,#138306,#138307,#138308,#138309,#138310,
#138311,#138312),.UNSPECIFIED.,.F.,.F.,(4,3,3,3,3,4),(0.,0.000540889688193241,
0.00109121002634586,0.00153442409609832,0.00256481294069221,0.00306884819219665),
 .UNSPECIFIED.);
#4350=B_SPLINE_CURVE_WITH_KNOTS('',3,(#138316,#138317,#138318,#138319,#138320,
#138321,#138322,#138323,#138324,#138325,#138326,#138327,#138328),
 .UNSPECIFIED.,.F.,.F.,(4,3,3,3,4),(2.8609792490764E-17,0.000811916222427858,
0.00153648298481487,0.00264039900673925,0.0030729659696297),
 .UNSPECIFIED.);
#4351=B_SPLINE_CURVE_WITH_KNOTS('',3,(#138330,#138331,#138332,#138333,#138334,
#138335,#138336),.UNSPECIFIED.,.F.,.F.,(4,3,4),(0.,0.018990790064314,0.0379815801286281),
 .UNSPECIFIED.);
#4352=B_SPLINE_CURVE_WITH_KNOTS('',3,(#138349,#138350,#138351,#138352,#138353,
#138354,#138355,#138356,#138357,#138358),.UNSPECIFIED.,.F.,.F.,(4,3,3,4),
(0.,0.282541552346412,0.571946461065579,0.999999565238375),
 .UNSPECIFIED.);
#4353=B_SPLINE_CURVE_WITH_KNOTS('',3,(#138359,#138360,#138361,#138362,#138363,
#138364),.UNSPECIFIED.,.F.,.F.,(4,2,4),(0.,0.500000000000001,1.),
 .UNSPECIFIED.);
#4354=B_SPLINE_CURVE_WITH_KNOTS('',3,(#138386,#138387,#138388,#138389,#138390,
#138391,#138392,#138393,#138394,#138395,#138396,#138397,#138398,#138399,
#138400,#138401,#138402,#138403,#138404,#138405,#138406,#138407,#138408,
#138409,#138410,#138411,#138412,#138413,#138414,#138415,#138416,#138417,
#138418,#138419,#138420,#138421,#138422,#138423,#138424,#138425,#138426,
#138427,#138428,#138429,#138430,#138431,#138432,#138433,#138434,#138435,
#138436,#138437),.UNSPECIFIED.,.F.,.F.,(4,3,3,3,3,3,3,3,3,3,3,3,3,3,3,3,
3,4),(0.,0.000568167570465986,0.000689873068221808,0.000757350079825038,
0.000945020241884818,0.00103480960233271,0.0011360777163446,0.00136729697222306,
0.00137974613644361,0.00151477367390368,0.00189346791975904,0.0020696192046654,
0.00221265318267551,0.00227165379781723,0.00237143867201243,0.00256546547244981,
0.0026624788726685,0.00275949227288719),.UNSPECIFIED.);
#4355=B_SPLINE_CURVE_WITH_KNOTS('',3,(#138441,#138442,#138443,#138444,#138445,
#138446,#138447,#138448,#138449,#138450,#138451,#138452,#138453,#138454,
#138455,#138456,#138457,#138458,#138459,#138460,#138461,#138462,#138463,
#138464,#138465,#138466,#138467,#138468,#138469,#138470,#138471,#138472,
#138473,#138474,#138475,#138476,#138477),.UNSPECIFIED.,.F.,.F.,(4,3,3,3,
3,3,3,3,3,3,3,3,4),(0.000467059137334316,0.000632797502959653,0.000860961305648091,
0.000897131574002758,0.00113001259983567,0.00126720169019544,0.00163753656891932,
0.00179296606233701,0.00200786773946722,0.00237820352986643,0.00245591952483837,
0.00301621129961807,0.00311887298733972),.UNSPECIFIED.);
#4356=B_SPLINE_CURVE_WITH_KNOTS('',3,(#138483,#138484,#138485,#138486),
 .UNSPECIFIED.,.F.,.F.,(4,4),(0.,0.0420570108120997),.UNSPECIFIED.);
#4357=B_SPLINE_CURVE_WITH_KNOTS('',3,(#138488,#138489,#138490,#138491,#138492,
#138493,#138494,#138495,#138496,#138497,#138498,#138499,#138500),
 .UNSPECIFIED.,.F.,.F.,(4,3,3,3,4),(0.,0.000795137544056449,0.00122134837748785,
0.00219865189863128,0.0024426967549757),.UNSPECIFIED.);
#4358=B_SPLINE_CURVE_WITH_KNOTS('',3,(#138504,#138505,#138506,#138507,#138508,
#138509,#138510,#138511,#138512,#138513,#138514,#138515,#138516),
 .UNSPECIFIED.,.F.,.F.,(4,3,3,3,4),(0.,0.00089438056074498,0.00122171954771057,
0.00222146414309878,0.00244343909542114),.UNSPECIFIED.);
#4359=B_SPLINE_CURVE_WITH_KNOTS('',3,(#138517,#138518,#138519,#138520),
 .UNSPECIFIED.,.F.,.F.,(4,4),(0.,0.0417901757617078),.UNSPECIFIED.);
#4360=B_SPLINE_CURVE_WITH_KNOTS('',3,(#138564,#138565,#138566,#138567,#138568,
#138569,#138570,#138571,#138572,#138573,#138574,#138575,#138576,#138577),
 .UNSPECIFIED.,.F.,.F.,(4,2,2,2,2,2,4),(0.,0.240255593310268,0.366879661091889,
0.493503728873512,0.620127796655135,0.746751864436756,1.),.UNSPECIFIED.);
#4361=B_SPLINE_CURVE_WITH_KNOTS('',3,(#138592,#138593,#138594,#138595,#138596,
#138597,#138598,#138599,#138600,#138601,#138602,#138603,#138604,#138605),
 .UNSPECIFIED.,.F.,.F.,(4,2,2,2,2,2,4),(0.,0.251506213404696,0.377259320107042,
0.503012426809389,0.628765533511738,0.754518640214088,1.),.UNSPECIFIED.);
#4362=B_SPLINE_CURVE_WITH_KNOTS('',3,(#138606,#138607,#138608,#138609),
 .UNSPECIFIED.,.F.,.F.,(4,4),(0.0206793054465132,0.021179777605653),
 .UNSPECIFIED.);
#4363=B_SPLINE_CURVE_WITH_KNOTS('',3,(#138653,#138654,#138655,#138656,#138657,
#138658,#138659,#138660,#138661,#138662,#138663,#138664,#138665,#138666,
#138667,#138668,#138669,#138670,#138671,#138672,#138673,#138674,#138675,
#138676,#138677,#138678,#138679,#138680,#138681,#138682,#138683,#138684,
#138685,#138686,#138687,#138688,#138689),.UNSPECIFIED.,.F.,.F.,(4,3,3,3,
3,3,3,3,3,3,3,3,4),(0.000646102271931852,0.000780355288939442,0.000794331971528649,
0.00113223030154688,0.00115328378670241,0.00123902107032975,0.00152620034295103,
0.00183193986873122,0.00189906794388762,0.00227197283133226,0.00242485866713269,
0.00272131806633342,0.00301777746553416),.UNSPECIFIED.);
#4364=B_SPLINE_CURVE_WITH_KNOTS('',3,(#138709,#138710,#138711,#138712,#138713,
#138714,#138715,#138716,#138717,#138718,#138719,#138720,#138721,#138722,
#138723,#138724,#138725,#138726,#138727,#138728,#138729,#138730,#138731,
#138732,#138733,#138734,#138735,#138736,#138737,#138738,#138739,#138740,
#138741,#138742),.UNSPECIFIED.,.F.,.F.,(4,3,3,3,3,3,3,3,3,3,3,4),(0.,0.000275770613304119,
0.000551541226608238,0.000716520337534463,0.00107478390778079,0.00110308245321648,
0.00134771653693895,0.00143334685918384,0.00165462367982471,0.00179132390797124,
0.00214954043896842,0.00220616490643295),.UNSPECIFIED.);
#4365=B_SPLINE_CURVE_WITH_KNOTS('',3,(#138750,#138751,#138752,#138753,#138754,
#138755,#138756,#138757,#138758,#138759,#138760,#138761,#138762),
 .UNSPECIFIED.,.F.,.F.,(4,3,3,3,4),(0.,0.000727903814955585,0.00111811425806593,
0.00207062545858955,0.00223622851613186),.UNSPECIFIED.);
#4366=B_SPLINE_CURVE_WITH_KNOTS('',3,(#138766,#138767,#138768,#138769,#138770,
#138771,#138772,#138773,#138774,#138775,#138776,#138777,#138778),
 .UNSPECIFIED.,.F.,.F.,(4,3,3,3,4),(0.,0.000659089694864322,0.00111822884501791,
0.00208128371043693,0.00223645769003581),.UNSPECIFIED.);
#4367=B_SPLINE_CURVE_WITH_KNOTS('',3,(#138790,#138791,#138792,#138793,#138794,
#138795),.UNSPECIFIED.,.F.,.F.,(4,2,4),(0.,0.510991543129055,1.),
 .UNSPECIFIED.);
#4368=B_SPLINE_CURVE_WITH_KNOTS('',3,(#138800,#138801,#138802,#138803),
 .UNSPECIFIED.,.F.,.F.,(4,4),(0.,1.),.UNSPECIFIED.);
#4369=B_SPLINE_CURVE_WITH_KNOTS('',3,(#138821,#138822,#138823,#138824,#138825,
#138826,#138827,#138828,#138829,#138830,#138831,#138832,#138833,#138834,
#138835,#138836,#138837,#138838,#138839,#138840,#138841,#138842,#138843,
#138844,#138845,#138846,#138847,#138848),.UNSPECIFIED.,.F.,.F.,(4,3,3,3,
3,3,3,3,3,4),(0.,0.000434392388671951,0.000626649590030437,0.000901221465792679,
0.00106184511664083,0.00112652683224085,0.00125380565733159,0.00135183219868902,
0.00158807055660419,0.00180244293158534),.UNSPECIFIED.);
#4370=B_SPLINE_CURVE_WITH_KNOTS('',3,(#138852,#138853,#138854,#138855,#138856,
#138857,#138858,#138859,#138860,#138861,#138862,#138863,#138864,#138865,
#138866,#138867,#138868,#138869,#138870,#138871,#138872,#138873,#138874,
#138875,#138876),.UNSPECIFIED.,.F.,.F.,(4,3,3,3,3,3,3,3,4),(0.000689304848361576,
0.000906283726281564,0.00111364302895385,0.00133013985168632,0.00150801684530018,
0.0017199369438561,0.00199672649963737,0.00227140074390536,0.00232672884224074),
 .UNSPECIFIED.);
#4371=B_SPLINE_CURVE_WITH_KNOTS('',3,(#138993,#138994,#138995,#138996,#138997,
#138998,#138999,#139000,#139001,#139002,#139003,#139004,#139005,#139006,
#139007,#139008,#139009,#139010,#139011,#139012,#139013,#139014,#139015,
#139016,#139017,#139018,#139019,#139020),.UNSPECIFIED.,.F.,.F.,(4,3,3,3,
3,3,3,3,3,4),(0.000653658633860215,0.000901612111390036,0.00110350292160905,
0.00119693882169381,0.00132842506548346,0.00148931670393005,0.00155334720935788,
0.0018252077501562,0.00223261138725098,0.00245303578485557),
 .UNSPECIFIED.);
#4372=B_SPLINE_CURVE_WITH_KNOTS('',3,(#139050,#139051,#139052,#139053),
 .UNSPECIFIED.,.F.,.F.,(4,4),(0.,0.0447707136167657),.UNSPECIFIED.);
#4373=B_SPLINE_CURVE_WITH_KNOTS('',3,(#139059,#139060,#139061,#139062,#139063,
#139064,#139065,#139066,#139067,#139068,#139069,#139070,#139071,#139072,
#139073,#139074,#139075,#139076,#139077,#139078,#139079,#139080,#139081,
#139082,#139083),.UNSPECIFIED.,.F.,.F.,(4,3,3,3,3,3,3,3,4),(0.,0.000275481208481522,
0.000553063545339124,0.000602887330399936,0.000809845174226025,0.00102800957885635,
0.00120532901601379,0.00142404055844574,0.00161969034845205),
 .UNSPECIFIED.);
#4374=B_SPLINE_CURVE_WITH_KNOTS('',3,(#139096,#139097,#139098,#139099),
 .UNSPECIFIED.,.F.,.F.,(4,4),(0.,1.),.UNSPECIFIED.);
#4375=B_SPLINE_CURVE_WITH_KNOTS('',3,(#139121,#139122,#139123,#139124,#139125,
#139126,#139127,#139128,#139129,#139130,#139131,#139132,#139133,#139134,
#139135,#139136,#139137,#139138,#139139,#139140,#139141,#139142,#139143,
#139144,#139145,#139146,#139147,#139148,#139149,#139150,#139151,#139152,
#139153,#139154,#139155,#139156,#139157),.UNSPECIFIED.,.F.,.F.,(4,3,3,3,
3,3,3,3,3,3,3,3,4),(0.,0.000289456070004167,0.000578912140008334,0.000732555002063411,
0.00109883518473064,0.00115782428001667,0.00146516214354768,0.001736736420025,
0.00183135727517645,0.00202619249002917,0.00217092052503125,0.00219767702911212,
0.00231564856003333),.UNSPECIFIED.);
#4376=B_SPLINE_CURVE_WITH_KNOTS('',3,(#139161,#139162,#139163,#139164,#139165,
#139166,#139167,#139168,#139169,#139170,#139171,#139172,#139173,#139174,
#139175,#139176,#139177,#139178,#139179,#139180,#139181,#139182,#139183,
#139184,#139185,#139186,#139187,#139188,#139189,#139190,#139191,#139192,
#139193,#139194,#139195,#139196,#139197),.UNSPECIFIED.,.F.,.F.,(4,3,3,3,
3,3,3,3,3,3,3,3,4),(0.000672031760609077,0.000712854075812315,0.00100252198457116,
0.00107233830279969,0.0012216976510115,0.00143188803178762,0.00171092729228739,
0.00177136354141392,0.00179176783191224,0.00215141270034081,0.00232102943181635,
0.00259586237701756,0.00287069532221878),.UNSPECIFIED.);
#4377=B_SPLINE_CURVE_WITH_KNOTS('',3,(#139208,#139209,#139210,#139211,#139212,
#139213,#139214,#139215,#139216,#139217,#139218,#139219,#139220),
 .UNSPECIFIED.,.F.,.F.,(4,3,3,3,4),(0.,0.00070198654781531,0.00111013811990961,
0.00206054695802749,0.00222027623981921),.UNSPECIFIED.);
#4378=B_SPLINE_CURVE_WITH_KNOTS('',3,(#139224,#139225,#139226,#139227,#139228,
#139229,#139230,#139231,#139232,#139233,#139234,#139235,#139236),
 .UNSPECIFIED.,.F.,.F.,(4,3,3,3,4),(0.,0.000647478258305606,0.00111023907191622,
0.002070391292413,0.00222047814383243),.UNSPECIFIED.);
#4379=B_SPLINE_CURVE_WITH_KNOTS('',3,(#139312,#139313,#139314,#139315,#139316,
#139317,#139318,#139319,#139320,#139321,#139322,#139323,#139324,#139325),
 .UNSPECIFIED.,.F.,.F.,(4,2,2,2,2,2,4),(0.,0.253127110916779,0.379690666375168,
0.506254221833555,0.632817777291944,0.759381332750333,1.),.UNSPECIFIED.);
#4380=B_SPLINE_CURVE_WITH_KNOTS('',3,(#139326,#139327,#139328,#139329),
 .UNSPECIFIED.,.F.,.F.,(4,4),(0.00436813896256353,0.00486865237729894),
 .UNSPECIFIED.);
#4381=B_SPLINE_CURVE_WITH_KNOTS('',3,(#139373,#139374,#139375,#139376,#139377,
#139378,#139379,#139380,#139381,#139382,#139383,#139384,#139385,#139386,
#139387,#139388,#139389,#139390,#139391,#139392,#139393,#139394,#139395,
#139396,#139397,#139398,#139399,#139400,#139401,#139402,#139403,#139404,
#139405,#139406,#139407,#139408,#139409),.UNSPECIFIED.,.F.,.F.,(4,3,3,3,
3,3,3,3,3,3,3,3,4),(0.000461676008985161,0.000632546215505795,0.000848081241001053,
0.00093127816033473,0.0011451568350677,0.00130839695615338,0.00168583810655035,
0.00182863766115024,0.00206327508940322,0.00244071732574779,0.00251211848723277,
0.00307037767187467,0.00319559931331531),.UNSPECIFIED.);
#4382=B_SPLINE_CURVE_WITH_KNOTS('',3,(#139428,#139429,#139430,#139431),
 .UNSPECIFIED.,.F.,.F.,(4,4),(0.,0.0419168978153696),.UNSPECIFIED.);
#4383=B_SPLINE_CURVE_WITH_KNOTS('',3,(#139433,#139434,#139435,#139436,#139437,
#139438,#139439,#139440,#139441,#139442,#139443,#139444,#139445),
 .UNSPECIFIED.,.F.,.F.,(4,3,3,3,4),(0.,0.000842979772292327,0.00121101869920095,
0.00218603126583571,0.00242203739840189),.UNSPECIFIED.);
#4384=B_SPLINE_CURVE_WITH_KNOTS('',3,(#139449,#139450,#139451,#139452,#139453,
#139454,#139455,#139456,#139457,#139458,#139459,#139460,#139461),
 .UNSPECIFIED.,.F.,.F.,(4,3,3,3,4),(0.,0.000857870627763608,0.00121135746045287,
0.00220749552005158,0.00242271492090574),.UNSPECIFIED.);
#4385=B_SPLINE_CURVE_WITH_KNOTS('',3,(#139463,#139464,#139465,#139466),
 .UNSPECIFIED.,.F.,.F.,(4,4),(0.,0.0421837023697854),.UNSPECIFIED.);
#4386=B_SPLINE_CURVE_WITH_KNOTS('',3,(#139472,#139473,#139474,#139475,#139476,
#139477,#139478,#139479,#139480,#139481,#139482,#139483,#139484,#139485,
#139486,#139487,#139488,#139489,#139490,#139491,#139492,#139493,#139494,
#139495,#139496,#139497,#139498,#139499,#139500,#139501,#139502,#139503,
#139504,#139505,#139506,#139507,#139508,#139509,#139510,#139511),
 .UNSPECIFIED.,.F.,.F.,(4,3,3,3,3,3,3,3,3,3,3,3,3,4),(0.,0.000556259975663021,
0.000647586119897307,0.000728260191095084,0.00109239125585008,0.00129517223979461,
0.00145651805257901,0.00182064826297317,0.00194275835969192,0.00212625862851252,
0.00218441767336186,0.00226655141964057,0.00244042135138774,0.00259034447958922),
 .UNSPECIFIED.);
#4387=B_SPLINE_CURVE_WITH_KNOTS('',3,(#139516,#139517,#139518,#139519,#139520,
#139521,#139522,#139523),.UNSPECIFIED.,.F.,.F.,(4,2,2,4),(0.,0.141658916901159,
0.430052386440966,1.),.UNSPECIFIED.);
#4388=B_SPLINE_CURVE_WITH_KNOTS('',3,(#139528,#139529,#139530,#139531,#139532,
#139533),.UNSPECIFIED.,.F.,.F.,(4,2,4),(0.,0.5,1.),.UNSPECIFIED.);
#4389=B_SPLINE_CURVE_WITH_KNOTS('',3,(#139563,#139564,#139565,#139566,#139567,
#139568,#139569),.UNSPECIFIED.,.F.,.F.,(4,3,4),(6.93889390390723E-18,0.0190876722191456,
0.0381753444382913),.UNSPECIFIED.);
#4390=B_SPLINE_CURVE_WITH_KNOTS('',3,(#139571,#139572,#139573,#139574,#139575,
#139576,#139577,#139578,#139579,#139580,#139581,#139582,#139583,#139584,
#139585,#139586),.UNSPECIFIED.,.F.,.F.,(4,3,3,3,3,4),(0.,0.000542853834904753,
0.0010951883108263,0.00152034213881841,0.00254894911026828,0.00304068427763681),
 .UNSPECIFIED.);
#4391=B_SPLINE_CURVE_WITH_KNOTS('',3,(#139590,#139591,#139592,#139593,#139594,
#139595,#139596,#139597,#139598,#139599,#139600,#139601,#139602),
 .UNSPECIFIED.,.F.,.F.,(4,3,3,3,4),(0.,0.000817157754010372,0.00152229638412186,
0.00262171283977742,0.00304459276824371),.UNSPECIFIED.);
#4392=B_SPLINE_CURVE_WITH_KNOTS('',3,(#139603,#139604,#139605,#139606,#139607,
#139608,#139609),.UNSPECIFIED.,.F.,.F.,(4,3,4),(0.,0.0189537577590876,0.0379075155181752),
 .UNSPECIFIED.);
#4393=B_SPLINE_CURVE_WITH_KNOTS('',3,(#139639,#139640,#139641,#139642,#139643,
#139644,#139645),.UNSPECIFIED.,.F.,.F.,(4,3,4),(0.,0.0178083890192188,0.0356167780384377),
 .UNSPECIFIED.);
#4394=B_SPLINE_CURVE_WITH_KNOTS('',3,(#139647,#139648,#139649,#139650,#139651,
#139652,#139653,#139654),.UNSPECIFIED.,.F.,.F.,(4,2,2,4),(0.,0.000841011829491348,
0.00168202365898269,0.00336404731796539),.UNSPECIFIED.);
#4395=B_SPLINE_CURVE_WITH_KNOTS('',3,(#139658,#139659,#139660,#139661,#139662,
#139663,#139664,#139665,#139666,#139667,#139668,#139669,#139670,#139671,
#139672,#139673),.UNSPECIFIED.,.F.,.F.,(4,3,3,3,3,4),(0.,0.000762418881013546,
0.00156275687157928,0.00168533471950014,0.00283547033563459,0.00337066943900028),
 .UNSPECIFIED.);
#4396=B_SPLINE_CURVE_WITH_KNOTS('',3,(#139675,#139676,#139677,#139678,#139679,
#139680,#139681),.UNSPECIFIED.,.F.,.F.,(4,3,4),(0.,0.0179426259581151,0.0358852519162302),
 .UNSPECIFIED.);
#4397=B_SPLINE_CURVE_WITH_KNOTS('',3,(#139696,#139697,#139698,#139699,#139700,
#139701,#139702),.UNSPECIFIED.,.F.,.F.,(4,3,4),(7.55544064091613E-7,0.374830472019235,
1.),.UNSPECIFIED.);
#4398=B_SPLINE_CURVE_WITH_KNOTS('',3,(#139735,#139736,#139737,#139738,#139739,
#139740,#139741),.UNSPECIFIED.,.F.,.F.,(4,3,4),(0.,0.0148367096635454,0.0296734193270908),
 .UNSPECIFIED.);
#4399=B_SPLINE_CURVE_WITH_KNOTS('',3,(#139743,#139744,#139745,#139746,#139747,
#139748,#139749,#139750,#139751,#139752,#139753,#139754,#139755,#139756,
#139757,#139758,#139759,#139760,#139761,#139762,#139763,#139764,#139765,
#139766,#139767),.UNSPECIFIED.,.F.,.F.,(4,3,3,3,3,3,3,3,4),(0.,0.000418974782549054,
0.000841777476039438,0.00103655247459,0.00148268378394067,0.00192505831514581,
0.00207310494918,0.00313777887503632,0.00414620989836001),.UNSPECIFIED.);
#4400=B_SPLINE_CURVE_WITH_KNOTS('',3,(#139771,#139772,#139773,#139774,#139775,
#139776,#139777,#139778,#139779,#139780,#139781,#139782,#139783,#139784,
#139785,#139786,#139787,#139788,#139789,#139790,#139791,#139792),
 .UNSPECIFIED.,.F.,.F.,(4,3,3,3,3,3,3,4),(1.55158384577954E-17,0.000383789572585087,
0.000781910391030218,0.00103855983331611,0.00179575082686721,0.00207711966663221,
0.00335799595905766,0.00415423933326436),.UNSPECIFIED.);
#4401=B_SPLINE_CURVE_WITH_KNOTS('',3,(#139793,#139794,#139795,#139796,#139797,
#139798,#139799),.UNSPECIFIED.,.F.,.F.,(4,3,4),(0.,0.0147014688781887,0.0294029377563774),
 .UNSPECIFIED.);
#4402=B_SPLINE_CURVE_WITH_KNOTS('',3,(#139812,#139813,#139814,#139815),
 .UNSPECIFIED.,.F.,.F.,(4,4),(0.,8.25660289862869E-5),.UNSPECIFIED.);
#4403=B_SPLINE_CURVE_WITH_KNOTS('',3,(#139920,#139921,#139922,#139923),
 .UNSPECIFIED.,.F.,.F.,(4,4),(0.,0.000203650363220012),.UNSPECIFIED.);
#4404=B_SPLINE_CURVE_WITH_KNOTS('',3,(#139925,#139926,#139927,#139928,#139929,
#139930,#139931,#139932,#139933,#139934,#139935,#139936,#139937,#139938,
#139939,#139940,#139941,#139942,#139943,#139944,#139945,#139946,#139947,
#139948,#139949),.UNSPECIFIED.,.F.,.F.,(4,3,3,3,3,3,3,3,4),(0.,7.36083385132494E-5,
0.000151188117340887,0.000234018984647725,0.000250167431468888,0.000250705751451724,
0.000332906541326753,0.0004186952522917,0.000500334862937777),
 .UNSPECIFIED.);
#4405=B_SPLINE_CURVE_WITH_KNOTS('',3,(#139951,#139952,#139953,#139954,#139955,
#139956,#139957,#139958,#139959,#139960,#139961,#139962,#139963,#139964,
#139965,#139966),.UNSPECIFIED.,.F.,.F.,(4,3,3,3,3,4),(0.,0.0014169282635678,
0.00283385652713561,0.00425078479070341,0.00538743306805026,0.00566771305427122),
 .UNSPECIFIED.);
#4406=B_SPLINE_CURVE_WITH_KNOTS('',3,(#139970,#139971,#139972,#139973,#139974,
#139975,#139976,#139977,#139978,#139979,#139980,#139981,#139982),
 .UNSPECIFIED.,.F.,.F.,(4,3,3,3,4),(6.93889390390723E-18,0.00134873564674426,
0.00269747129348853,0.00432753805226678,0.00539494258697707),
 .UNSPECIFIED.);
#4407=B_SPLINE_CURVE_WITH_KNOTS('',3,(#139984,#139985,#139986,#139987,#139988,
#139989,#139990,#139991,#139992,#139993,#139994,#139995,#139996,#139997,
#139998,#139999,#140000,#140001,#140002),.UNSPECIFIED.,.F.,.F.,(4,3,3,3,
3,3,4),(0.,0.000151278709681427,0.000175639358542286,0.000320819121628032,
0.000351502905376566,0.000527285240968795,0.000703005810753132),
 .UNSPECIFIED.);
#4408=B_SPLINE_CURVE_WITH_KNOTS('',3,(#140030,#140031,#140032,#140033,#140034,
#140035,#140036,#140037,#140038,#140039,#140040,#140041,#140042,#140043,
#140044,#140045,#140046,#140047,#140048,#140049,#140050,#140051,#140052,
#140053,#140054,#140055,#140056,#140057,#140058,#140059,#140060),
 .UNSPECIFIED.,.F.,.F.,(4,3,3,3,3,3,3,3,3,3,4),(0.,0.000563737664817591,
0.000564164457966204,0.00104582442927209,0.0011276022003503,0.00112832891593241,
0.00161216721638057,0.00169210723432567,0.00169249337389861,0.00210946737344705,
0.00225665783186482),.UNSPECIFIED.);
#4409=B_SPLINE_CURVE_WITH_KNOTS('',3,(#140097,#140098,#140099,#140100,#140101,
#140102,#140103,#140104,#140105,#140106,#140107,#140108,#140109,#140110,
#140111,#140112,#140113,#140114,#140115,#140116,#140117,#140118,#140119,
#140120,#140121,#140122,#140123,#140124,#140125,#140126,#140127,#140128,
#140129,#140130,#140131,#140132,#140133),.UNSPECIFIED.,.F.,.F.,(4,3,3,3,
3,3,3,3,3,3,3,3,4),(0.,0.000231966620805442,0.000541763265449849,0.000565419069388556,
0.000565630623675328,0.00113073622792201,0.00113126124735066,0.00146429940364797,
0.00169659085207846,0.00169689187102598,0.00198522910629736,0.00223959723149682,
0.00226252249470131),.UNSPECIFIED.);
#4410=B_SPLINE_CURVE_WITH_KNOTS('',3,(#140190,#140191,#140192,#140193,#140194,
#140195,#140196,#140197,#140198,#140199,#140200,#140201,#140202,#140203,
#140204,#140205,#140206,#140207,#140208,#140209,#140210,#140211,#140212,
#140213,#140214,#140215,#140216,#140217,#140218,#140219,#140220),
 .UNSPECIFIED.,.F.,.F.,(4,3,3,3,3,3,3,3,3,3,4),(0.,0.00011822449235466,
0.000239962463540573,0.000354016906950293,0.000486351214789361,0.000618764034589224,
0.000708033813900585,0.000911280042633104,0.00111586864905152,0.00131545298208588,
0.00141606762780121),.UNSPECIFIED.);
#4411=B_SPLINE_CURVE_WITH_KNOTS('',3,(#140233,#140234,#140235,#140236),
 .UNSPECIFIED.,.F.,.F.,(4,4),(0.,0.0203430832871546),.UNSPECIFIED.);
#4412=B_SPLINE_CURVE_WITH_KNOTS('',3,(#140238,#140239,#140240,#140241,#140242,
#140243,#140244,#140245,#140246,#140247,#140248,#140249,#140250),
 .UNSPECIFIED.,.F.,.F.,(4,3,3,3,4),(0.,0.00107468821847175,0.0021493764369435,
0.00322406465541528,0.00429875287388706),.UNSPECIFIED.);
#4413=B_SPLINE_CURVE_WITH_KNOTS('',3,(#140254,#140255,#140256,#140257,#140258,
#140259,#140260,#140261,#140262,#140263,#140264,#140265,#140266,#140267,
#140268,#140269,#140270,#140271,#140272,#140273,#140274,#140275),
 .UNSPECIFIED.,.F.,.F.,(4,3,3,3,3,3,3,4),(0.,0.000387785729070444,0.000791054588127252,
0.00107666227523054,0.00167259937147553,0.00215332455046108,0.00346243334013028,
0.00430664910092208),.UNSPECIFIED.);
#4414=B_SPLINE_CURVE_WITH_KNOTS('',3,(#140277,#140278,#140279,#140280),
 .UNSPECIFIED.,.F.,.F.,(4,4),(0.,0.0206148669995797),.UNSPECIFIED.);
#4415=B_SPLINE_CURVE_WITH_KNOTS('',3,(#140282,#140283,#140284,#140285),
 .UNSPECIFIED.,.F.,.F.,(4,4),(0.,0.000103369667661668),.UNSPECIFIED.);
#4416=B_SPLINE_CURVE_WITH_KNOTS('',3,(#140287,#140288,#140289,#140290,#140291,
#140292,#140293,#140294,#140295,#140296,#140297,#140298,#140299),
 .UNSPECIFIED.,.F.,.F.,(4,3,3,3,4),(0.,0.000379823720135543,0.000488238270882253,
0.000734566123594352,0.000976476541764506),.UNSPECIFIED.);
#4417=B_SPLINE_CURVE_WITH_KNOTS('',3,(#140308,#140309,#140310,#140311,#140312,
#140313,#140314,#140315),.UNSPECIFIED.,.F.,.F.,(4,2,2,4),(0.,0.25,0.5,1.),
 .UNSPECIFIED.);
#4418=B_SPLINE_CURVE_WITH_KNOTS('',3,(#140387,#140388,#140389,#140390,#140391,
#140392,#140393,#140394,#140395,#140396,#140397,#140398,#140399,#140400,
#140401,#140402,#140403,#140404,#140405),.UNSPECIFIED.,.F.,.F.,(4,3,3,3,
3,3,4),(0.,0.000108392306331872,0.000159419175882384,0.000279017984019056,
0.000319155213741796,0.000478738661811072,0.000638310427483592),
 .UNSPECIFIED.);
#4419=B_SPLINE_CURVE_WITH_KNOTS('',3,(#140407,#140408,#140409,#140410),
 .UNSPECIFIED.,.F.,.F.,(4,4),(0.,0.01284355850178),.UNSPECIFIED.);
#4420=B_SPLINE_CURVE_WITH_KNOTS('',3,(#140412,#140413,#140414,#140415,#140416,
#140417,#140418,#140419,#140420,#140421,#140422,#140423,#140424,#140425,
#140426,#140427),.UNSPECIFIED.,.F.,.F.,(4,3,3,3,3,4),(0.,0.00125936773350451,
0.00251873546700902,0.00377810320051352,0.00490364900521194,0.00503747093401803),
 .UNSPECIFIED.);
#4421=B_SPLINE_CURVE_WITH_KNOTS('',3,(#140431,#140432,#140433,#140434,#140435,
#140436,#140437,#140438,#140439,#140440,#140441,#140442,#140443),
 .UNSPECIFIED.,.F.,.F.,(4,3,3,3,4),(0.,0.00126095469566737,0.00252190939133473,
0.00394829824261489,0.00504381878266947),.UNSPECIFIED.);
#4422=B_SPLINE_CURVE_WITH_KNOTS('',3,(#140445,#140446,#140447,#140448),
 .UNSPECIFIED.,.F.,.F.,(4,4),(0.,0.0125680158145827),.UNSPECIFIED.);
#4423=B_SPLINE_CURVE_WITH_KNOTS('',3,(#140450,#140451,#140452,#140453,#140454,
#140455,#140456,#140457,#140458,#140459,#140460,#140461,#140462),
 .UNSPECIFIED.,.F.,.F.,(4,3,3,3,4),(0.,0.000167806452110249,0.000320197614368795,
0.000480307701132281,0.000640395228737589),.UNSPECIFIED.);
#4424=B_SPLINE_CURVE_WITH_KNOTS('',3,(#140488,#140489,#140490,#140491,#140492,
#140493,#140494,#140495,#140496,#140497,#140498,#140499,#140500,#140501,
#140502,#140503,#140504,#140505,#140506,#140507,#140508,#140509),
 .UNSPECIFIED.,.F.,.F.,(4,3,3,3,3,3,3,4),(0.,0.00011032124306843,0.00023255444160577,
0.000327443278856643,0.000415696683397808,0.000505913400363213,0.000594574640422507,
0.000654886557713287),.UNSPECIFIED.);
#4425=B_SPLINE_CURVE_WITH_KNOTS('',3,(#140511,#140512,#140513,#140514),
 .UNSPECIFIED.,.F.,.F.,(4,4),(0.,0.00876509433037234),.UNSPECIFIED.);
#4426=B_SPLINE_CURVE_WITH_KNOTS('',3,(#140516,#140517,#140518,#140519,#140520,
#140521,#140522,#140523,#140524,#140525,#140526,#140527,#140528,#140529,
#140530,#140531,#140532,#140533,#140534,#140535,#140536,#140537,#140538,
#140539,#140540),.UNSPECIFIED.,.F.,.F.,(4,3,3,3,3,3,3,3,4),(0.,0.00066897147268262,
0.00133794294536524,0.00197188997955202,0.0025968969389697,0.00267588589073048,
0.00401382883609571,0.00511764383901403,0.00535177178146096),
 .UNSPECIFIED.);
#4427=B_SPLINE_CURVE_WITH_KNOTS('',3,(#140544,#140545,#140546,#140547,#140548,
#140549,#140550,#140551,#140552,#140553,#140554,#140555,#140556,#140557,
#140558,#140559),.UNSPECIFIED.,.F.,.F.,(4,3,3,3,3,4),(0.,0.00120908655042554,
0.00133938491136683,0.00267876982273365,0.0041514377188616,0.0053575396454673),
 .UNSPECIFIED.);
#4428=B_SPLINE_CURVE_WITH_KNOTS('',3,(#140561,#140562,#140563,#140564),
 .UNSPECIFIED.,.F.,.F.,(4,4),(0.,0.00904291806877093),.UNSPECIFIED.);
#4429=B_SPLINE_CURVE_WITH_KNOTS('',3,(#140566,#140567,#140568,#140569,#140570,
#140571,#140572,#140573,#140574,#140575,#140576,#140577,#140578,#140579,
#140580,#140581),.UNSPECIFIED.,.F.,.F.,(4,3,3,3,3,4),(0.,0.00019490585199519,
0.000327981152987957,0.000444921456705669,0.000551183314035708,0.000655962305975913),
 .UNSPECIFIED.);
#4430=B_SPLINE_CURVE_WITH_KNOTS('',3,(#140697,#140698,#140699,#140700,#140701,
#140702,#140703,#140704,#140705,#140706,#140707,#140708,#140709),
 .UNSPECIFIED.,.F.,.F.,(4,3,3,3,4),(0.,0.00125486684196805,0.0025097336839361,
0.00393224022465218,0.00501946736787221),.UNSPECIFIED.);
#4431=B_SPLINE_CURVE_WITH_KNOTS('',3,(#140711,#140712,#140713,#140714),
 .UNSPECIFIED.,.F.,.F.,(4,4),(0.,0.0135233968444946),.UNSPECIFIED.);
#4432=B_SPLINE_CURVE_WITH_KNOTS('',3,(#140716,#140717,#140718,#140719,#140720,
#140721,#140722,#140723,#140724,#140725,#140726,#140727,#140728,#140729,
#140730,#140731,#140732,#140733,#140734),.UNSPECIFIED.,.F.,.F.,(4,3,3,3,
3,3,4),(0.,0.000165241084431127,0.000319189981521249,0.000429288245408173,
0.000533834104225336,0.000631975129725757,0.000638379963042499),
 .UNSPECIFIED.);
#4433=B_SPLINE_CURVE_WITH_KNOTS('',3,(#140750,#140751,#140752,#140753,#140754,
#140755,#140756,#140757,#140758,#140759,#140760,#140761,#140762,#140763,
#140764,#140765,#140766,#140767,#140768,#140769,#140770,#140771,#140772,
#140773,#140774,#140775,#140776,#140777,#140778,#140779,#140780,#140781,
#140782,#140783,#140784,#140785,#140786,#140787,#140788,#140789),
 .UNSPECIFIED.,.F.,.F.,(4,3,3,3,3,3,3,3,3,3,3,3,3,4),(0.,0.00016104755367178,
0.000326655464486219,0.00049386305290849,0.000580621437699987,0.00058187576131232,
0.0011633223004275,0.00116375152262464,0.00145467271006653,0.00145468940328081,
0.00174562728393698,0.0017460231201541,0.00204798180553722,0.00232750304524933),
 .UNSPECIFIED.);
#4434=B_SPLINE_CURVE_WITH_KNOTS('',3,(#140791,#140792,#140793,#140794,#140795,
#140796,#140797,#140798,#140799,#140800,#140801,#140802,#140803,#140804,
#140805,#140806,#140807,#140808,#140809),.UNSPECIFIED.,.F.,.F.,(4,3,3,3,
3,3,4),(0.,0.000151109125705162,0.000302236517833045,0.000386300967573319,
0.000471902393705335,0.000555234376218938,0.000604473035666092),
 .UNSPECIFIED.);
#4435=B_SPLINE_CURVE_WITH_KNOTS('',3,(#140811,#140812,#140813,#140814),
 .UNSPECIFIED.,.F.,.F.,(4,4),(0.,0.0170848224870981),.UNSPECIFIED.);
#4436=B_SPLINE_CURVE_WITH_KNOTS('',3,(#140816,#140817,#140818,#140819,#140820,
#140821,#140822,#140823,#140824,#140825,#140826,#140827,#140828),
 .UNSPECIFIED.,.F.,.F.,(4,3,3,3,4),(0.,0.00117191361843274,0.00234382723686548,
0.00351574085529822,0.00468765447373096),.UNSPECIFIED.);
#4437=B_SPLINE_CURVE_WITH_KNOTS('',3,(#140904,#140905,#140906,#140907,#140908,
#140909,#140910,#140911,#140912,#140913,#140914,#140915,#140916),
 .UNSPECIFIED.,.F.,.F.,(4,3,3,3,4),(3.1415926535898,3.53429173528852,3.92699081698724,
4.31968989868597,4.71238898038469),.UNSPECIFIED.);
#4438=B_SPLINE_CURVE_WITH_KNOTS('',3,(#140948,#140949,#140950,#140951,#140952,
#140953,#140954,#140955,#140956,#140957,#140958,#140959,#140960,#140961,
#140962,#140963,#140964,#140965,#140966),.UNSPECIFIED.,.F.,.F.,(4,3,3,3,
3,3,4),(0.,0.000168652558320961,0.000337340594483331,0.000432590797837365,
0.000530250662249296,0.000626975088861455,0.000674681188966661),
 .UNSPECIFIED.);
#4439=B_SPLINE_CURVE_WITH_KNOTS('',3,(#140973,#140974,#140975,#140976,#140977,
#140978,#140979,#140980,#140981,#140982,#140983,#140984,#140985,#140986,
#140987,#140988),.UNSPECIFIED.,.F.,.F.,(4,3,3,3,3,4),(0.,0.00159103011507281,
0.00287711962167565,0.00431567943251345,0.00538763071254621,0.00575423924335125),
 .UNSPECIFIED.);
#4440=B_SPLINE_CURVE_WITH_KNOTS('',3,(#141098,#141099,#141100,#141101,#141102,
#141103,#141104,#141105,#141106,#141107,#141108,#141109,#141110,#141111,
#141112,#141113,#141114,#141115,#141116),.UNSPECIFIED.,.F.,.F.,(4,3,3,3,
3,3,4),(0.,0.000174255415100454,0.000348555105993215,0.00044998536948759,
0.000554229835728645,0.00065771924945466,0.000697110211986431),
 .UNSPECIFIED.);
#4441=B_SPLINE_CURVE_WITH_KNOTS('',3,(#141123,#141124,#141125,#141126,#141127,
#141128,#141129,#141130,#141131,#141132,#141133,#141134,#141135,#141136,
#141137,#141138,#141139,#141140,#141141),.UNSPECIFIED.,.F.,.F.,(4,3,3,3,
3,3,4),(0.,0.00156956785490461,0.00313913570980923,0.00392391963731218,
0.00470870356471384,0.00573336346877459,0.00627827141961845),
 .UNSPECIFIED.);
#4442=B_SPLINE_CURVE_WITH_KNOTS('',3,(#141145,#141146,#141147,#141148,#141149,
#141150,#141151,#141152,#141153,#141154,#141155,#141156,#141157,#141158,
#141159,#141160),.UNSPECIFIED.,.F.,.F.,(4,3,3,3,3,4),(0.,0.00104863959930094,
0.00157050793024954,0.00314101586049909,0.00471152379074863,0.00628203172099817),
 .UNSPECIFIED.);
#4443=B_SPLINE_CURVE_WITH_KNOTS('',3,(#141167,#141168,#141169,#141170,#141171,
#141172,#141173,#141174,#141175,#141176,#141177,#141178,#141179),
 .UNSPECIFIED.,.F.,.F.,(4,3,3,3,4),(0.,0.000174780063231097,0.000349568960659906,
0.000524372653650724,0.000699137921319812),.UNSPECIFIED.);
#4444=B_SPLINE_CURVE_WITH_KNOTS('',3,(#141253,#141254,#141255,#141256,#141257,
#141258,#141259,#141260,#141261,#141262,#141263,#141264,#141265,#141266,
#141267,#141268,#141269,#141270,#141271),.UNSPECIFIED.,.F.,.F.,(4,3,3,3,
3,3,4),(0.,0.000358645716708602,0.000416788078411026,0.000833987724853057,
0.000834068655632161,0.00125109176933023,0.00166813731126432),
 .UNSPECIFIED.);
#4445=B_SPLINE_CURVE_WITH_KNOTS('',3,(#141297,#141298,#141299,#141300,#141301,
#141302,#141303,#141304,#141305,#141306,#141307,#141308,#141309,#141310,
#141311,#141312,#141313,#141314,#141315),.UNSPECIFIED.,.F.,.F.,(4,3,3,3,
3,3,4),(0.,0.000417356154990511,0.000834652124500517,0.000834737818312929,
0.0012522269622177,0.00161112215869288,0.00166930424900103),
 .UNSPECIFIED.);
#4446=B_SPLINE_CURVE_WITH_KNOTS('',3,(#141337,#141338,#141339,#141340,#141341,
#141342,#141343),.UNSPECIFIED.,.F.,.F.,(4,3,4),(0.,0.0129055642122842,0.0258111284245685),
 .UNSPECIFIED.);
#4447=B_SPLINE_CURVE_WITH_KNOTS('',3,(#141345,#141346,#141347,#141348,#141349,
#141350,#141351,#141352,#141353,#141354,#141355,#141356,#141357,#141358,
#141359,#141360),.UNSPECIFIED.,.F.,.F.,(4,3,3,3,3,4),(0.,0.00112455173535831,
0.00224910347071663,0.00337365520607496,0.00439646903553278,0.0044982069414333),
 .UNSPECIFIED.);
#4448=B_SPLINE_CURVE_WITH_KNOTS('',3,(#141364,#141365,#141366,#141367,#141368,
#141369,#141370,#141371,#141372,#141373,#141374,#141375,#141376,#141377,
#141378,#141379,#141380,#141381,#141382,#141383,#141384,#141385,#141386,
#141387,#141388),.UNSPECIFIED.,.F.,.F.,(4,3,3,3,3,3,3,3,4),(0.,0.00039368558594612,
0.000804157569269251,0.00112634951454785,0.00164227212955535,0.00217802033014988,
0.0022526990290957,0.00359217050441368,0.00450539805819141),
 .UNSPECIFIED.);
#4449=B_SPLINE_CURVE_WITH_KNOTS('',3,(#141390,#141391,#141392,#141393,#141394,
#141395,#141396),.UNSPECIFIED.,.F.,.F.,(4,3,4),(0.,0.0130414224518927,0.0260828449037854),
 .UNSPECIFIED.);
#4450=B_SPLINE_CURVE_WITH_KNOTS('',3,(#141398,#141399,#141400,#141401),
 .UNSPECIFIED.,.F.,.F.,(4,4),(0.,0.000106239733749475),.UNSPECIFIED.);
#4451=B_SPLINE_CURVE_WITH_KNOTS('',3,(#141403,#141404,#141405,#141406,#141407,
#141408,#141409,#141410,#141411,#141412,#141413,#141414,#141415),
 .UNSPECIFIED.,.F.,.F.,(4,3,3,3,4),(0.,0.000360360286282916,0.000488761174293949,
0.000765042797522198,0.000977522348587897),.UNSPECIFIED.);
#4452=B_SPLINE_CURVE_WITH_KNOTS('',3,(#141443,#141444,#141445,#141446),
 .UNSPECIFIED.,.F.,.F.,(4,4),(1.7347234759768E-18,0.000135753226310594),
 .UNSPECIFIED.);
#4453=B_SPLINE_CURVE_WITH_KNOTS('',3,(#141447,#141448,#141449,#141450),
 .UNSPECIFIED.,.F.,.F.,(4,4),(0.,1.),.UNSPECIFIED.);
#4454=B_SPLINE_CURVE_WITH_KNOTS('',3,(#141458,#141459,#141460,#141461,#141462,
#141463,#141464,#141465),.UNSPECIFIED.,.F.,.F.,(4,2,2,4),(0.,0.25,0.5,1.),
 .UNSPECIFIED.);
#4455=B_SPLINE_CURVE_WITH_KNOTS('',3,(#141537,#141538,#141539,#141540,#141541,
#141542,#141543,#141544,#141545,#141546,#141547,#141548,#141549,#141550,
#141551,#141552,#141553,#141554,#141555),.UNSPECIFIED.,.F.,.F.,(4,3,3,3,
3,3,4),(0.,0.000108634712275121,0.000159257284564384,0.000279020961387413,
0.000318828120207844,0.000478248046436964,0.000637656240415689),
 .UNSPECIFIED.);
#4456=B_SPLINE_CURVE_WITH_KNOTS('',3,(#141557,#141558,#141559,#141560),
 .UNSPECIFIED.,.F.,.F.,(4,4),(0.,0.0180689587739334),.UNSPECIFIED.);
#4457=B_SPLINE_CURVE_WITH_KNOTS('',3,(#141562,#141563,#141564,#141565,#141566,
#141567,#141568,#141569,#141570,#141571,#141572,#141573,#141574,#141575,
#141576,#141577),.UNSPECIFIED.,.F.,.F.,(4,3,3,3,3,4),(0.,0.0013179209674593,
0.00263584193491861,0.00395376290237792,0.00506352109400701,0.00527168386983722),
 .UNSPECIFIED.);
#4458=B_SPLINE_CURVE_WITH_KNOTS('',3,(#141581,#141582,#141583,#141584,#141585,
#141586,#141587,#141588,#141589,#141590,#141591,#141592,#141593,#141594,
#141595,#141596),.UNSPECIFIED.,.F.,.F.,(4,3,3,3,3,4),(0.,0.00122256915433072,
0.0013193477680122,0.00263869553602439,0.00409736884770839,0.00527739107204874),
 .UNSPECIFIED.);
#4459=B_SPLINE_CURVE_WITH_KNOTS('',3,(#141598,#141599,#141600,#141601),
 .UNSPECIFIED.,.F.,.F.,(4,4),(0.,0.0177935197894076),.UNSPECIFIED.);
#4460=B_SPLINE_CURVE_WITH_KNOTS('',3,(#141603,#141604,#141605,#141606,#141607,
#141608,#141609,#141610,#141611,#141612,#141613,#141614,#141615),
 .UNSPECIFIED.,.F.,.F.,(4,3,3,3,4),(0.,0.000166958822901273,0.000319870924789836,
0.000479817604858626,0.000639741849579673),.UNSPECIFIED.);
#4461=B_SPLINE_CURVE_WITH_KNOTS('',3,(#141641,#141642,#141643,#141644,#141645,
#141646,#141647,#141648,#141649,#141650,#141651,#141652,#141653,#141654,
#141655,#141656,#141657,#141658,#141659,#141660,#141661,#141662),
 .UNSPECIFIED.,.F.,.F.,(4,3,3,3,3,3,3,4),(0.,0.000110683358086875,0.00023326550317951,
0.000327042610606244,0.000415140332124169,0.00050518854044065,0.000593686275838932,
0.000654085221212487),.UNSPECIFIED.);
#4462=B_SPLINE_CURVE_WITH_KNOTS('',3,(#141664,#141665,#141666,#141667),
 .UNSPECIFIED.,.F.,.F.,(4,4),(0.,0.0138879247081574),.UNSPECIFIED.);
#4463=B_SPLINE_CURVE_WITH_KNOTS('',3,(#141669,#141670,#141671,#141672,#141673,
#141674,#141675,#141676,#141677,#141678,#141679,#141680,#141681,#141682,
#141683,#141684,#141685,#141686,#141687),.UNSPECIFIED.,.F.,.F.,(4,3,3,3,
3,3,4),(0.,0.00107929064721465,0.00212940062359531,0.00279822589210569,
0.00419733883815853,0.0052823468058471,0.00559645178421137),
 .UNSPECIFIED.);
#4464=B_SPLINE_CURVE_WITH_KNOTS('',3,(#141691,#141692,#141693,#141694,#141695,
#141696,#141697,#141698,#141699,#141700,#141701,#141702,#141703,#141704,
#141705,#141706),.UNSPECIFIED.,.F.,.F.,(4,3,3,3,3,4),(0.,0.00116583085678931,
0.00140039358904036,0.00280078717808072,0.0043057456358814,0.00560157435616136),
 .UNSPECIFIED.);
#4465=B_SPLINE_CURVE_WITH_KNOTS('',3,(#141708,#141709,#141710,#141711),
 .UNSPECIFIED.,.F.,.F.,(4,4),(0.,0.0141656229616797),.UNSPECIFIED.);
#4466=B_SPLINE_CURVE_WITH_KNOTS('',3,(#141713,#141714,#141715,#141716,#141717,
#141718,#141719,#141720,#141721,#141722,#141723,#141724,#141725,#141726,
#141727,#141728),.UNSPECIFIED.,.F.,.F.,(4,3,3,3,3,4),(0.,0.000193094254409061,
0.000327589980483358,0.000444218816712202,0.000550274313876603,0.000655179960966716),
 .UNSPECIFIED.);
#4467=B_SPLINE_CURVE_WITH_KNOTS('',3,(#141748,#141749,#141750,#141751,#141752,
#141753,#141754,#141755,#141756,#141757),.UNSPECIFIED.,.F.,.F.,(4,2,2,2,
4),(0.,0.25,0.5,0.750000000000001,1.),.UNSPECIFIED.);
#4468=B_SPLINE_CURVE_WITH_KNOTS('',3,(#141779,#141780,#141781,#141782,#141783,
#141784,#141785,#141786,#141787,#141788,#141789,#141790,#141791,#141792,
#141793,#141794,#141795,#141796,#141797,#141798,#141799,#141800,#141801,
#141802,#141803,#141804,#141805,#141806,#141807,#141808,#141809),
 .UNSPECIFIED.,.F.,.F.,(4,3,3,3,3,3,3,3,3,3,4),(0.,0.000166652275730451,
0.000342276073641816,0.000519944361542555,0.000694209917748529,0.000732292525246715,
0.000732496372314207,0.000946324251635485,0.00115726770428045,0.0013594228398131,
0.00146458505049343),.UNSPECIFIED.);
#4469=B_SPLINE_CURVE_WITH_KNOTS('',3,(#141814,#141815,#141816,#141817,#141818,
#141819,#141820,#141821,#141822,#141823,#141824,#141825,#141826),
 .UNSPECIFIED.,.F.,.F.,(4,3,3,3,4),(0.,0.000259173930192671,0.000518347860385342,
0.00087729776681203,0.00103669572077068),.UNSPECIFIED.);
#4470=B_SPLINE_CURVE_WITH_KNOTS('',3,(#141828,#141829,#141830,#141831),
 .UNSPECIFIED.,.F.,.F.,(4,4),(0.,0.000120540380538642),.UNSPECIFIED.);
#4471=B_SPLINE_CURVE_WITH_KNOTS('',3,(#141833,#141834,#141835,#141836,#141837,
#141838,#141839),.UNSPECIFIED.,.F.,.F.,(4,3,4),(0.,0.0128929585057523,0.0257859170115047),
 .UNSPECIFIED.);
#4472=B_SPLINE_CURVE_WITH_KNOTS('',3,(#141841,#141842,#141843,#141844,#141845,
#141846,#141847,#141848,#141849,#141850,#141851,#141852,#141853,#141854,
#141855,#141856),.UNSPECIFIED.,.F.,.F.,(4,3,3,3,3,4),(0.,0.00113243548370091,
0.00226487096740181,0.00339730645110276,0.0044193232014814,0.00452974193480371),
 .UNSPECIFIED.);
#4473=B_SPLINE_CURVE_WITH_KNOTS('',3,(#141860,#141861,#141862,#141863,#141864,
#141865,#141866,#141867,#141868,#141869,#141870,#141871,#141872,#141873,
#141874,#141875,#141876,#141877,#141878,#141879,#141880,#141881,#141882,
#141883,#141884),.UNSPECIFIED.,.F.,.F.,(4,3,3,3,3,3,3,3,4),(0.,0.00039468403092862,
0.000806360979195845,0.00113421626089741,0.00164507477301071,0.00217582874625811,
0.00226843252179482,0.00361301771688345,0.00453686504358963),
 .UNSPECIFIED.);
#4474=B_SPLINE_CURVE_WITH_KNOTS('',3,(#141886,#141887,#141888,#141889,#141890,
#141891,#141892),.UNSPECIFIED.,.F.,.F.,(4,3,4),(0.,0.0127570403976527,0.0255140807953054),
 .UNSPECIFIED.);
#4475=B_SPLINE_CURVE_WITH_KNOTS('',3,(#141961,#141962,#141963,#141964,#141965,
#141966,#141967,#141968,#141969,#141970,#141971,#141972,#141973,#141974,
#141975,#141976,#141977,#141978,#141979,#141980,#141981,#141982,#141983,
#141984,#141985,#141986,#141987,#141988,#141989,#141990,#141991),
 .UNSPECIFIED.,.F.,.F.,(4,3,3,3,3,3,3,3,3,3,4),(0.,0.000366648609662479,
0.00067395652917383,0.00118123470620554,0.00134837711191729,0.00134840211582016,
0.00202256566787594,0.00202269623773767,0.00236849530085589,0.0026591601716747,
0.00269675422383458),.UNSPECIFIED.);
#4476=B_SPLINE_CURVE_WITH_KNOTS('',3,(#141999,#142000,#142001,#142002,#142003,
#142004,#142005,#142006,#142007,#142008,#142009,#142010,#142011,#142012,
#142013,#142014,#142015,#142016,#142017,#142018,#142019,#142020,#142021,
#142022,#142023,#142024,#142025,#142026),.UNSPECIFIED.,.F.,.F.,(4,3,3,3,
3,3,3,3,3,4),(0.,0.000297352361641283,0.000685187759872983,0.000685314779244029,
0.00137061382937429,0.00137062955848806,0.00183455251927366,0.00205619372744575,
0.00244930001359206,0.00274125911697611),.UNSPECIFIED.);
#4477=B_SPLINE_CURVE_WITH_KNOTS('',3,(#142074,#142075,#142076,#142077,#142078,
#142079,#142080,#142081,#142082,#142083,#142084,#142085,#142086,#142087,
#142088,#142089,#142090,#142091,#142092),.UNSPECIFIED.,.F.,.F.,(4,3,3,3,
3,3,4),(0.,0.000175073926804946,0.000350193522739415,0.000452577371514084,
0.000557835767991038,0.000662370656289191,0.000700387045478831),
 .UNSPECIFIED.);
#4478=B_SPLINE_CURVE_WITH_KNOTS('',3,(#142099,#142100,#142101,#142102,#142103,
#142104,#142105,#142106,#142107,#142108,#142109,#142110,#142111,#142112,
#142113,#142114,#142115,#142116,#142117),.UNSPECIFIED.,.F.,.F.,(4,3,3,3,
3,3,4),(0.,0.00157595519506122,0.00315191039012244,0.00393988798770612,
0.00472786558518367,0.00575007285733746,0.00630382078024489),
 .UNSPECIFIED.);
#4479=B_SPLINE_CURVE_WITH_KNOTS('',3,(#142121,#142122,#142123,#142124,#142125,
#142126,#142127,#142128,#142129,#142130,#142131,#142132,#142133,#142134,
#142135,#142136),.UNSPECIFIED.,.F.,.F.,(4,3,3,3,3,4),(0.,0.00104430221457033,
0.00157688090361367,0.00315376180722735,0.00473064271084103,0.00630752361445471),
 .UNSPECIFIED.);
#4480=B_SPLINE_CURVE_WITH_KNOTS('',3,(#142143,#142144,#142145,#142146,#142147,
#142148,#142149,#142150,#142151,#142152,#142153,#142154,#142155),
 .UNSPECIFIED.,.F.,.F.,(4,3,3,3,4),(0.,0.000175209888250476,0.000350428553470057,
0.000525662295915621,0.000700857106940114),.UNSPECIFIED.);
#4481=B_SPLINE_CURVE_WITH_KNOTS('',3,(#142239,#142240,#142241,#142242,#142243,
#142244,#142245,#142246,#142247,#142248,#142249,#142250,#142251),
 .UNSPECIFIED.,.F.,.F.,(4,3,3,3,4),(3.1415926535898,3.53429173528852,3.92699081698725,
4.31968989868597,4.7123889803847),.UNSPECIFIED.);
#4482=B_SPLINE_CURVE_WITH_KNOTS('',3,(#142279,#142280,#142281,#142282,#142283,
#142284,#142285,#142286,#142287,#142288,#142289,#142290,#142291,#142292,
#142293,#142294,#142295,#142296,#142297,#142298,#142299,#142300),
 .UNSPECIFIED.,.F.,.F.,(4,3,3,3,3,3,3,4),(0.,0.000110166739483085,0.000232250654979584,
0.000327614165524935,0.000415934063629714,0.000506222853831995,0.000594954171387644,
0.000655228331049871),.UNSPECIFIED.);
#4483=B_SPLINE_CURVE_WITH_KNOTS('',3,(#142302,#142303,#142304,#142305),
 .UNSPECIFIED.,.F.,.F.,(4,4),(0.,0.0138038180377133),.UNSPECIFIED.);
#4484=B_SPLINE_CURVE_WITH_KNOTS('',3,(#142307,#142308,#142309,#142310,#142311,
#142312,#142313,#142314,#142315,#142316,#142317,#142318,#142319,#142320,
#142321,#142322,#142323,#142324,#142325),.UNSPECIFIED.,.F.,.F.,(4,3,3,3,
3,3,4),(0.,0.00115159118172974,0.00227058783088812,0.00281251499795634,
0.00421877249693456,0.00530146752118551,0.00562502999591277),
 .UNSPECIFIED.);
#4485=B_SPLINE_CURVE_WITH_KNOTS('',3,(#142329,#142330,#142331,#142332,#142333,
#142334,#142335,#142336,#142337,#142338,#142339,#142340,#142341,#142342,
#142343,#142344),.UNSPECIFIED.,.F.,.F.,(4,3,3,3,3,4),(0.,0.00116086488264771,
0.0014075250438046,0.0028150500876092,0.00432397808187545,0.00563010017521834),
 .UNSPECIFIED.);
#4486=B_SPLINE_CURVE_WITH_KNOTS('',3,(#142346,#142347,#142348,#142349),
 .UNSPECIFIED.,.F.,.F.,(4,4),(0.,0.0135258923233721),.UNSPECIFIED.);
#4487=B_SPLINE_CURVE_WITH_KNOTS('',3,(#142351,#142352,#142353,#142354,#142355,
#142356,#142357,#142358,#142359,#142360,#142361,#142362,#142363,#142364,
#142365,#142366),.UNSPECIFIED.,.F.,.F.,(4,3,3,3,3,4),(0.,0.000197943176920928,
0.000328605151068823,0.000446042787173481,0.000552633627937305,0.000657210302137648),
 .UNSPECIFIED.);
#4488=B_SPLINE_CURVE_WITH_KNOTS('',3,(#142434,#142435,#142436,#142437,#142438,
#142439,#142440,#142441,#142442,#142443,#142444,#142445,#142446,#142447,
#142448,#142449,#142450,#142451,#142452),.UNSPECIFIED.,.F.,.F.,(4,3,3,3,
3,3,4),(0.,0.000108019327761152,0.000159670358772899,0.000279016064561992,
0.000319662760640411,0.000479499943955603,0.000639325521280822),
 .UNSPECIFIED.);
#4489=B_SPLINE_CURVE_WITH_KNOTS('',3,(#142454,#142455,#142456,#142457),
 .UNSPECIFIED.,.F.,.F.,(4,4),(0.,0.0174508326761739),.UNSPECIFIED.);
#4490=B_SPLINE_CURVE_WITH_KNOTS('',3,(#142459,#142460,#142461,#142462,#142463,
#142464,#142465,#142466,#142467,#142468,#142469,#142470,#142471,#142472,
#142473,#142474,#142475,#142476,#142477,#142478,#142479,#142480,#142481,
#142482,#142483,#142484,#142485,#142486),.UNSPECIFIED.,.F.,.F.,(4,3,3,3,
3,3,3,3,3,4),(0.,0.000662679024145193,0.00128919539297308,0.00132535804829039,
0.00193492508883213,0.00253635637125076,0.00265071609658077,0.00397607414487116,
0.00508368314709806,0.00530143219316154),.UNSPECIFIED.);
#4491=B_SPLINE_CURVE_WITH_KNOTS('',3,(#142490,#142491,#142492,#142493,#142494,
#142495,#142496,#142497,#142498,#142499,#142500,#142501,#142502,#142503,
#142504,#142505),.UNSPECIFIED.,.F.,.F.,(4,3,3,3,3,4),(0.,0.00121734210048524,
0.00132677154899614,0.00265354309799227,0.00411654704464283,0.00530708619598447),
 .UNSPECIFIED.);
#4492=B_SPLINE_CURVE_WITH_KNOTS('',3,(#142507,#142508,#142509,#142510),
 .UNSPECIFIED.,.F.,.F.,(4,4),(0.,0.0177264565684136),.UNSPECIFIED.);
#4493=B_SPLINE_CURVE_WITH_KNOTS('',3,(#142512,#142513,#142514,#142515,#142516,
#142517,#142518,#142519,#142520,#142521,#142522,#142523,#142524),
 .UNSPECIFIED.,.F.,.F.,(4,3,3,3,4),(0.,0.000168209862999138,0.000320350766922646,
0.000480537459018473,0.000640701533845293),.UNSPECIFIED.);
#4494=B_SPLINE_CURVE_WITH_KNOTS('',3,(#142555,#142556,#142557,#142558,#142559,
#142560,#142561,#142562),.UNSPECIFIED.,.F.,.F.,(4,2,2,4),(-0.0847651026480947,
-0.0629186902711198,-0.0307386998646501,0.),.UNSPECIFIED.);
#4495=B_SPLINE_CURVE_WITH_KNOTS('',3,(#142563,#142564,#142565,#142566,#142567,
#142568,#142569,#142570),.UNSPECIFIED.,.F.,.F.,(4,2,2,4),(-0.16953083368722,
-0.138777607634066,-0.106603528596837,-0.0847654169752063),
 .UNSPECIFIED.);
#4496=B_SPLINE_CURVE_WITH_KNOTS('',3,(#142616,#142617,#142618,#142619,#142620,
#142621,#142622,#142623,#142624,#142625,#142626,#142627,#142628,#142629,
#142630,#142631,#142632,#142633,#142634,#142635,#142636,#142637,#142638,
#142639,#142640,#142641),.UNSPECIFIED.,.F.,.F.,(4,2,2,2,2,2,2,2,2,2,2,2,
4),(0.,0.035098338728144,0.0741581944022324,0.101946776653776,0.109514391089664,
0.117640234446691,0.136341904849524,0.141182675691644,0.160390411163872,
0.193626235421715,0.217667420358703,0.251529378123532,0.282413954967513),
 .UNSPECIFIED.);
#4497=B_SPLINE_CURVE_WITH_KNOTS('',3,(#142644,#142645,#142646,#142647,#142648,
#142649,#142650,#142651,#142652,#142653,#142654,#142655,#142656,#142657,
#142658,#142659,#142660,#142661),.UNSPECIFIED.,.F.,.F.,(4,2,2,2,2,2,2,2,
4),(0.,0.0302664700381103,0.0628248024585381,0.085474523550968,0.116272737380296,
0.147052923761435,0.169708349890063,0.202281537927324,0.232545593042104),
 .UNSPECIFIED.);
#4498=B_SPLINE_CURVE_WITH_KNOTS('',3,(#142711,#142712,#142713,#142714,#142715,
#142716,#142717,#142718,#142719,#142720),.UNSPECIFIED.,.F.,.F.,(4,2,2,2,
4),(0.,0.25,0.5,0.75,1.),.UNSPECIFIED.);
#4499=B_SPLINE_CURVE_WITH_KNOTS('',3,(#142742,#142743,#142744,#142745,#142746,
#142747),.UNSPECIFIED.,.F.,.F.,(4,2,4),(0.,0.5,1.),.UNSPECIFIED.);
#4500=B_SPLINE_CURVE_WITH_KNOTS('',3,(#142766,#142767,#142768,#142769),
 .UNSPECIFIED.,.F.,.F.,(4,4),(0.,1.),.UNSPECIFIED.);
#4501=B_SPLINE_CURVE_WITH_KNOTS('',3,(#142788,#142789,#142790,#142791,#142792,
#142793),.UNSPECIFIED.,.F.,.F.,(4,2,4),(0.,0.5,1.),.UNSPECIFIED.);
#4502=B_SPLINE_CURVE_WITH_KNOTS('',3,(#142942,#142943,#142944,#142945,#142946,
#142947,#142948,#142949,#142950,#142951,#142952,#142953,#142954,#142955,
#142956,#142957,#142958,#142959,#142960,#142961,#142962,#142963,#142964,
#142965,#142966,#142967,#142968,#142969),.UNSPECIFIED.,.F.,.F.,(4,3,3,3,
3,3,3,3,3,4),(0.,0.096881526972298,0.197661145229223,0.299127849036553,
0.40238568979424,0.5,0.640715041917235,0.780973931021849,0.919960936066223,
0.999999999999993),.UNSPECIFIED.);
#4503=B_SPLINE_CURVE_WITH_KNOTS('',3,(#143007,#143008,#143009,#143010,#143011,
#143012,#143013,#143014,#143015,#143016,#143017,#143018,#143019,#143020,
#143021,#143022),.UNSPECIFIED.,.F.,.F.,(4,3,3,3,3,4),(0.000681462205008639,
0.00273329612790008,0.00491895821256213,0.00671017185179961,0.00912678453081515,
0.00930288319891504),.UNSPECIFIED.);
#4504=B_SPLINE_CURVE_WITH_KNOTS('',3,(#143058,#143059,#143060,#143061,#143062,
#143063,#143064,#143065,#143066,#143067,#143068,#143069,#143070),
 .UNSPECIFIED.,.F.,.F.,(4,3,3,3,4),(0.000775072234384454,0.00360015924840977,
0.00665118856909886,0.00786282367425579,0.0104581756611108),
 .UNSPECIFIED.);
#4505=B_SPLINE_CURVE_WITH_KNOTS('',3,(#143156,#143157,#143158,#143159,#143160,
#143161,#143162,#143163,#143164,#143165),.UNSPECIFIED.,.F.,.F.,(4,2,2,2,
4),(0.,0.250000000000004,0.5,0.750000000000003,1.),.UNSPECIFIED.);
#4506=B_SPLINE_CURVE_WITH_KNOTS('',3,(#143200,#143201,#143202,#143203,#143204,
#143205,#143206,#143207,#143208,#143209,#143210,#143211,#143212),
 .UNSPECIFIED.,.F.,.F.,(4,3,3,3,4),(4.71238898038469,5.10508806208342,5.49778714378214,
5.89048622548087,6.28318530717959),.UNSPECIFIED.);
#4507=B_SPLINE_CURVE_WITH_KNOTS('',3,(#143235,#143236,#143237,#143238,#143239,
#143240,#143241,#143242,#143243,#143244,#143245,#143246,#143247),
 .UNSPECIFIED.,.F.,.F.,(4,3,3,3,4),(0.,0.00157041135329281,0.00191432655883667,
0.00304584187046407,0.00382865311767335),.UNSPECIFIED.);
#4508=B_SPLINE_CURVE_WITH_KNOTS('',3,(#143253,#143254,#143255,#143256,#143257,
#143258,#143259),.UNSPECIFIED.,.F.,.F.,(4,3,4),(4.71238898038469,5.49778714378214,
6.28318530717959),.UNSPECIFIED.);
#4509=B_SPLINE_CURVE_WITH_KNOTS('',3,(#143263,#143264,#143265,#143266,#143267,
#143268,#143269),.UNSPECIFIED.,.F.,.F.,(4,3,4),(3.1415926535898,3.92699081698724,
4.71238898038469),.UNSPECIFIED.);
#4510=B_SPLINE_CURVE_WITH_KNOTS('',3,(#143277,#143278,#143279,#143280,#143281,
#143282,#143283),.UNSPECIFIED.,.F.,.F.,(4,3,4),(4.71238898038469,5.49778714378214,
6.28318530717959),.UNSPECIFIED.);
#4511=B_SPLINE_CURVE_WITH_KNOTS('',3,(#143287,#143288,#143289,#143290,#143291,
#143292,#143293),.UNSPECIFIED.,.F.,.F.,(4,3,4),(1.23467863058847E-16,0.785398163397447,
1.5707963267949),.UNSPECIFIED.);
#4512=B_SPLINE_CURVE_WITH_KNOTS('',3,(#143299,#143300,#143301,#143302),
 .UNSPECIFIED.,.F.,.F.,(4,4),(0.,1.),.UNSPECIFIED.);
#4513=B_SPLINE_CURVE_WITH_KNOTS('',3,(#143305,#143306,#143307,#143308,#143309,
#143310),.UNSPECIFIED.,.F.,.F.,(4,2,4),(0.,0.5,1.),.UNSPECIFIED.);
#4514=B_SPLINE_CURVE_WITH_KNOTS('',3,(#143319,#143320,#143321,#143322,#143323,
#143324,#143325,#143326,#143327,#143328,#143329,#143330,#143331,#143332,
#143333,#143334,#143335,#143336,#143337,#143338,#143339,#143340,#143341,
#143342,#143343,#143344,#143345,#143346,#143347,#143348,#143349,#143350,
#143351,#143352,#143353,#143354,#143355,#143356,#143357,#143358,#143359,
#143360,#143361,#143362,#143363,#143364),.UNSPECIFIED.,.F.,.F.,(4,3,3,3,
3,3,3,3,3,3,3,3,3,3,3,4),(0.,0.000109331983970022,0.000221348099123313,
0.000333853905447977,0.000407294015799104,0.000408910815664253,0.000676681051235422,
0.000814588031598208,0.000816767951597532,0.00106247378106521,0.00122188204739731,
0.00122336180785488,0.0013543902429315,0.00149178315306396,0.00162097073973742,
0.00162917606319641),.UNSPECIFIED.);
#4515=B_SPLINE_CURVE_WITH_KNOTS('',3,(#143372,#143373,#143374,#143375,#143376,
#143377,#143378,#143379),.UNSPECIFIED.,.F.,.F.,(4,2,2,4),(0.,0.25,0.5,1.),
 .UNSPECIFIED.);
#4516=B_SPLINE_CURVE_WITH_KNOTS('',3,(#143383,#143384,#143385,#143386,#143387,
#143388),.UNSPECIFIED.,.F.,.F.,(4,2,4),(0.,0.500000000000002,1.),
 .UNSPECIFIED.);
#4517=B_SPLINE_CURVE_WITH_KNOTS('',3,(#143398,#143399,#143400,#143401,#143402,
#143403,#143404,#143405,#143406,#143407,#143408,#143409,#143410,#143411,
#143412,#143413,#143414,#143415,#143416,#143417,#143418,#143419,#143420,
#143421,#143422,#143423,#143424,#143425,#143426,#143427,#143428,#143429,
#143430,#143431,#143432,#143433,#143434,#143435,#143436,#143437,#143438,
#143439,#143440),.UNSPECIFIED.,.F.,.F.,(4,3,3,3,3,3,3,3,3,3,3,3,3,3,4),
(0.,0.000108912497168548,0.000220164732383848,0.000331071157537683,0.000392199517465978,
0.000393776648066525,0.000641215708234082,0.000785392845861507,0.000787553296133051,
0.0010345334193873,0.00117987002828322,0.00118132994419958,0.00130742143740802,
0.00144126401483706,0.0015751065922661),.UNSPECIFIED.);
#4518=B_SPLINE_CURVE_WITH_KNOTS('',3,(#143444,#143445,#143446,#143447,#143448,
#143449,#143450,#143451),.UNSPECIFIED.,.F.,.F.,(4,2,2,4),(0.,0.499999999999999,
0.749999999999998,1.),.UNSPECIFIED.);
#4519=B_SPLINE_CURVE_WITH_KNOTS('',3,(#143459,#143460,#143461,#143462,#143463,
#143464,#143465,#143466),.UNSPECIFIED.,.F.,.F.,(4,2,2,4),(0.,0.25,0.5,1.),
 .UNSPECIFIED.);
#4520=B_SPLINE_CURVE_WITH_KNOTS('',3,(#143470,#143471,#143472,#143473,#143474,
#143475,#143476,#143477,#143478,#143479,#143480,#143481,#143482,#143483,
#143484,#143485,#143486,#143487,#143488,#143489,#143490,#143491,#143492,
#143493,#143494,#143495,#143496,#143497,#143498,#143499,#143500,#143501,
#143502,#143503,#143504,#143505,#143506,#143507,#143508,#143509),
 .UNSPECIFIED.,.F.,.F.,(4,3,3,3,3,3,3,3,3,3,3,3,3,4),(0.,0.000424781762265252,
0.000463398440131748,0.000464821262797085,0.000754099901313884,0.000926796880263496,
0.000929181095996172,0.0011584961003294,0.00116090942630384,0.00139019532039531,
0.00139219601406769,0.00155797632198516,0.00171877163857689,0.00185359376052713),
 .UNSPECIFIED.);
#4521=B_SPLINE_CURVE_WITH_KNOTS('',3,(#143517,#143518,#143519,#143520,#143521,
#143522,#143523,#143524,#143525,#143526,#143527,#143528,#143529,#143530,
#143531,#143532,#143533,#143534,#143535,#143536,#143537,#143538,#143539,
#143540,#143541,#143542,#143543,#143544,#143545,#143546,#143547,#143548,
#143549,#143550,#143551,#143552,#143553,#143554,#143555,#143556,#143557,
#143558,#143559,#143560,#143561,#143562,#143563,#143564,#143565),
 .UNSPECIFIED.,.F.,.F.,(4,3,3,3,3,3,3,3,3,3,3,3,3,3,3,3,4),(0.,8.46514984579067E-5,
0.000170997186917714,0.000221020978416691,0.00025513917286035,0.0003380084618147,
0.000429234945596046,0.000448835576014519,0.000450677949086267,0.000735348747775932,
0.000898977028079799,0.000901355898172495,0.0011519668249772,0.00135049620570088,
0.00135203384725872,0.00157737282180184,0.00180271179634495),
 .UNSPECIFIED.);
#4522=B_SPLINE_CURVE_WITH_KNOTS('',3,(#143569,#143570,#143571,#143572,#143573,
#143574),.UNSPECIFIED.,.F.,.F.,(4,2,4),(0.,0.499999999999999,1.),
 .UNSPECIFIED.);
#4523=B_SPLINE_CURVE_WITH_KNOTS('',3,(#143582,#143583,#143584,#143585),
 .UNSPECIFIED.,.F.,.F.,(4,4),(0.,1.),.UNSPECIFIED.);
#4524=B_SPLINE_CURVE_WITH_KNOTS('',3,(#143587,#143588,#143589,#143590),
 .UNSPECIFIED.,.F.,.F.,(4,4),(0.,1.),.UNSPECIFIED.);
#4525=B_SPLINE_CURVE_WITH_KNOTS('',3,(#143594,#143595,#143596,#143597,#143598,
#143599,#143600,#143601,#143602,#143603,#143604,#143605,#143606,#143607,
#143608,#143609,#143610,#143611,#143612,#143613,#143614,#143615,#143616,
#143617,#143618,#143619,#143620,#143621,#143622,#143623,#143624,#143625,
#143626,#143627,#143628,#143629,#143630,#143631,#143632,#143633,#143634,
#143635,#143636,#143637,#143638,#143639),.UNSPECIFIED.,.F.,.F.,(4,3,3,3,
3,3,3,3,3,3,3,3,3,3,3,4),(0.,0.00011167181015014,0.000225567853890617,0.000339431029143606,
0.000397399329631602,0.000398944559102931,0.000667283904097484,0.000794798659263204,
0.000796933919810637,0.00104488468555027,0.00119219798889481,0.00119368499584663,
0.00132317769579387,0.00145638750716014,0.00158130618071513,0.00158959731852641),
 .UNSPECIFIED.);
#4526=B_SPLINE_CURVE_WITH_KNOTS('',3,(#143647,#143648,#143649,#143650,#143651,
#143652,#143653,#143654,#143655,#143656,#143657,#143658,#143659,#143660,
#143661,#143662,#143663,#143664,#143665,#143666,#143667,#143668,#143669,
#143670,#143671,#143672,#143673,#143674,#143675,#143676,#143677,#143678,
#143679,#143680,#143681,#143682,#143683,#143684,#143685,#143686,#143687,
#143688,#143689),.UNSPECIFIED.,.F.,.F.,(4,3,3,3,3,3,3,3,3,3,3,3,3,3,4),
(0.,0.000167563212024588,0.000333534252401052,0.000405329103688545,0.000406806783530084,
0.000681033266852063,0.000811430892222414,0.000813613567060169,0.00109814343427173,
0.00121879730292854,0.00122042035059025,0.00134667139739561,0.00147140108610396,
0.00159377061182622,0.00162722713412034),.UNSPECIFIED.);
#4527=B_SPLINE_CURVE_WITH_KNOTS('',3,(#143692,#143693,#143694,#143695),
 .UNSPECIFIED.,.F.,.F.,(4,4),(0.,1.),.UNSPECIFIED.);
#4528=B_SPLINE_CURVE_WITH_KNOTS('',3,(#143700,#143701,#143702,#143703),
 .UNSPECIFIED.,.F.,.F.,(4,4),(0.,1.),.UNSPECIFIED.);
#4529=B_SPLINE_CURVE_WITH_KNOTS('',3,(#143706,#143707,#143708,#143709,#143710,
#143711),.UNSPECIFIED.,.F.,.F.,(4,2,4),(0.,0.5,1.),.UNSPECIFIED.);
#4530=B_SPLINE_CURVE_WITH_KNOTS('',3,(#143719,#143720,#143721,#143722,#143723,
#143724,#143725),.UNSPECIFIED.,.F.,.F.,(4,3,4),(1.5707963267949,2.35619449019235,
3.1415926535898),.UNSPECIFIED.);
#4531=B_SPLINE_CURVE_WITH_KNOTS('',3,(#143729,#143730,#143731,#143732,#143733,
#143734,#143735),.UNSPECIFIED.,.F.,.F.,(4,3,4),(1.23467863058848E-16,0.785398163397447,
1.5707963267949),.UNSPECIFIED.);
#4532=B_SPLINE_CURVE_WITH_KNOTS('',3,(#143740,#143741,#143742,#143743,#143744,
#143745,#143746,#143747,#143748,#143749,#143750,#143751,#143752),
 .UNSPECIFIED.,.F.,.F.,(4,3,3,3,4),(6.93889390390723E-18,0.00113151531066751,
0.00191432655883665,0.00348473784368841,0.00382865311767331),
 .UNSPECIFIED.);
#4533=B_SPLINE_CURVE_WITH_KNOTS('',3,(#143760,#143761,#143762,#143763,#143764,
#143765,#143766),.UNSPECIFIED.,.F.,.F.,(4,3,4),(4.71238898038468,5.49778714378213,
6.28318530717959),.UNSPECIFIED.);
#4534=B_SPLINE_CURVE_WITH_KNOTS('',3,(#143770,#143771,#143772,#143773,#143774,
#143775,#143776),.UNSPECIFIED.,.F.,.F.,(4,3,4),(1.23467863058848E-16,0.785398163397447,
1.5707963267949),.UNSPECIFIED.);
#4535=B_SPLINE_CURVE_WITH_KNOTS('',3,(#143794,#143795,#143796,#143797,#143798,
#143799,#143800,#143801,#143802,#143803,#143804,#143805,#143806),
 .UNSPECIFIED.,.F.,.F.,(4,3,3,3,4),(0.,0.0015008721912107,0.00207200756106571,
0.00310801134159857,0.00414401512213143),.UNSPECIFIED.);
#4536=B_SPLINE_CURVE_WITH_KNOTS('',3,(#143812,#143813,#143814,#143815,#143816,
#143817,#143818),.UNSPECIFIED.,.F.,.F.,(4,3,4),(4.71238898038468,5.49778714378214,
6.28318530717959),.UNSPECIFIED.);
#4537=B_SPLINE_CURVE_WITH_KNOTS('',3,(#143822,#143823,#143824,#143825,#143826,
#143827,#143828),.UNSPECIFIED.,.F.,.F.,(4,3,4),(3.14159265358979,3.92699081698724,
4.71238898038469),.UNSPECIFIED.);
#4538=B_SPLINE_CURVE_WITH_KNOTS('',3,(#143836,#143837,#143838,#143839,#143840,
#143841,#143842),.UNSPECIFIED.,.F.,.F.,(4,3,4),(4.71238898038469,5.49778714378214,
6.28318530717959),.UNSPECIFIED.);
#4539=B_SPLINE_CURVE_WITH_KNOTS('',3,(#143846,#143847,#143848,#143849,#143850,
#143851,#143852),.UNSPECIFIED.,.F.,.F.,(4,3,4),(-8.88178419700125E-16,0.78539816339745,
1.5707963267949),.UNSPECIFIED.);
#4540=B_SPLINE_CURVE_WITH_KNOTS('',3,(#144008,#144009,#144010,#144011,#144012,
#144013,#144014),.UNSPECIFIED.,.F.,.F.,(4,3,4),(0.,0.619995026988033,0.999999394204749),
 .UNSPECIFIED.);
#4541=B_SPLINE_CURVE_WITH_KNOTS('',3,(#144015,#144016,#144017,#144018),
 .UNSPECIFIED.,.F.,.F.,(4,4),(0.,1.),.UNSPECIFIED.);
#4542=B_SPLINE_CURVE_WITH_KNOTS('',3,(#144062,#144063,#144064,#144065,#144066,
#144067),.UNSPECIFIED.,.F.,.F.,(4,2,4),(0.,0.567644438072849,1.),
 .UNSPECIFIED.);
#4543=B_SPLINE_CURVE_WITH_KNOTS('',3,(#144068,#144069,#144070,#144071),
 .UNSPECIFIED.,.F.,.F.,(4,4),(0.,1.),.UNSPECIFIED.);
#4544=B_SPLINE_CURVE_WITH_KNOTS('',3,(#144128,#144129,#144130,#144131,#144132,
#144133,#144134,#144135,#144136,#144137,#144138,#144139,#144140,#144141),
 .UNSPECIFIED.,.F.,.F.,(4,2,2,2,2,2,4),(0.,0.240475312512509,0.367062760427093,
0.493650208341673,0.620237656256254,0.746825104170835,1.),.UNSPECIFIED.);
#4545=B_SPLINE_CURVE_WITH_KNOTS('',3,(#144156,#144157,#144158,#144159,#144160,
#144161,#144162,#144163,#144164,#144165,#144166,#144167,#144168,#144169),
 .UNSPECIFIED.,.F.,.F.,(4,2,2,2,2,2,4),(0.,0.251505324083449,0.377257986125173,
0.503010648166897,0.628763310208625,0.75451597225035,1.),.UNSPECIFIED.);
#4546=B_SPLINE_CURVE_WITH_KNOTS('',3,(#144170,#144171,#144172,#144173),
 .UNSPECIFIED.,.F.,.F.,(4,4),(0.020578988719059,0.0210794636037261),
 .UNSPECIFIED.);
#4547=B_SPLINE_CURVE_WITH_KNOTS('',3,(#144232,#144233,#144234,#144235,#144236,
#144237,#144238,#144239,#144240,#144241,#144242,#144243),.UNSPECIFIED.,
 .F.,.F.,(4,2,3,3,4),(0.,0.00100000000000208,0.00500000000023154,0.02100000001009,
0.0385835581099273),.UNSPECIFIED.);
#4548=B_SPLINE_CURVE_WITH_KNOTS('',3,(#144245,#144246,#144247,#144248,#144249,
#144250,#144251,#144252),.UNSPECIFIED.,.F.,.F.,(4,2,2,4),(0.,0.251717747068591,
0.509550086771184,1.),.UNSPECIFIED.);
#4549=B_SPLINE_CURVE_WITH_KNOTS('',3,(#144291,#144292,#144293,#144294,#144295,
#144296),.UNSPECIFIED.,.F.,.F.,(4,2,4),(0.,0.5,1.),.UNSPECIFIED.);
#4550=B_SPLINE_CURVE_WITH_KNOTS('',3,(#144316,#144317,#144318,#144319,#144320,
#144321),.UNSPECIFIED.,.F.,.F.,(4,2,4),(0.,0.5,1.),.UNSPECIFIED.);
#4551=B_SPLINE_CURVE_WITH_KNOTS('',3,(#144405,#144406,#144407,#144408,#144409,
#144410,#144411,#144412,#144413,#144414,#144415,#144416,#144417,#144418,
#144419,#144420,#144421,#144422,#144423,#144424,#144425,#144426,#144427,
#144428,#144429),.UNSPECIFIED.,.F.,.F.,(4,3,3,3,3,3,3,3,4),(0.000524342078796179,
0.00180901876828853,0.00304673005325099,0.00340077219985262,0.00411987972637406,
0.00482370949852814,0.00550912189802027,0.00616177752105426,0.00627720230593839),
 .UNSPECIFIED.);
#4552=B_SPLINE_CURVE_WITH_KNOTS('',3,(#144430,#144431,#144432,#144433,#144434,
#144435,#144436),.UNSPECIFIED.,.F.,.F.,(4,3,4),(0.,0.500000000000002,0.999999986878769),
 .UNSPECIFIED.);
#4553=B_SPLINE_CURVE_WITH_KNOTS('',3,(#144492,#144493,#144494,#144495,#144496,
#144497,#144498,#144499,#144500,#144501,#144502,#144503,#144504,#144505,
#144506,#144507,#144508,#144509,#144510,#144511,#144512,#144513,#144514,
#144515,#144516),.UNSPECIFIED.,.F.,.F.,(4,3,3,3,3,3,3,3,4),(0.,0.141656513734972,
0.284805721555512,0.429042216431012,0.499999999999999,0.655877906767802,
0.811014022503117,0.965340744220155,1.),.UNSPECIFIED.);
#4554=B_SPLINE_CURVE_WITH_KNOTS('',3,(#144580,#144581,#144582,#144583,#144584,
#144585,#144586,#144587,#144588,#144589,#144590,#144591,#144592,#144593,
#144594,#144595,#144596,#144597,#144598,#144599,#144600,#144601,#144602,
#144603,#144604),.UNSPECIFIED.,.F.,.F.,(4,3,3,3,3,3,3,3,4),(0.,0.135948715488849,
0.27312999148841,0.411116711101826,0.5,0.651860141828472,0.802504749805492,
0.951647349185892,1.),.UNSPECIFIED.);
#4555=B_SPLINE_CURVE_WITH_KNOTS('',3,(#144627,#144628,#144629,#144630,#144631,
#144632),.UNSPECIFIED.,.F.,.F.,(4,2,4),(0.,0.5,1.),.UNSPECIFIED.);
#4556=B_SPLINE_CURVE_WITH_KNOTS('',3,(#144652,#144653,#144654,#144655,#144656,
#144657,#144658,#144659,#144660,#144661,#144662,#144663,#144664,#144665,
#144666,#144667),.UNSPECIFIED.,.F.,.F.,(4,3,3,3,3,4),(0.000601267884717356,
0.00181647811677124,0.00299735824906937,0.00382211018819771,0.00557536121785049,
0.00704295249167806),.UNSPECIFIED.);
#4557=B_SPLINE_CURVE_WITH_KNOTS('',3,(#144729,#144730,#144731,#144732,#144733,
#144734,#144735,#144736,#144737,#144738,#144739,#144740,#144741,#144742,
#144743,#144744,#144745,#144746,#144747,#144748,#144749,#144750,#144751,
#144752,#144753,#144754,#144755,#144756),.UNSPECIFIED.,.F.,.F.,(4,3,3,3,
3,3,3,3,3,4),(0.,0.113371007866148,0.229897420767909,0.347745026578629,
0.466701720784187,0.5,0.642794296332829,0.784841419789057,0.925820243963234,
0.999999999999991),.UNSPECIFIED.);
#4558=B_SPLINE_CURVE_WITH_KNOTS('',3,(#144831,#144832,#144833,#144834,#144835,
#144836,#144837,#144838,#144839,#144840,#144841,#144842,#144843,#144844,
#144845,#144846,#144847,#144848,#144849,#144850,#144851,#144852,#144853,
#144854,#144855,#144856,#144857,#144858),.UNSPECIFIED.,.F.,.F.,(4,3,3,3,
3,3,3,3,3,4),(0.,0.113914306204002,0.229749700148325,0.34594430565268,0.461668871939815,
0.5,0.63174105075801,0.760423146797041,0.884931285751174,1.),
 .UNSPECIFIED.);
#4559=B_SPLINE_CURVE_WITH_KNOTS('',3,(#144881,#144882,#144883,#144884,#144885,
#144886),.UNSPECIFIED.,.F.,.F.,(4,2,4),(1.29812701169007E-5,0.500000000000001,
1.),.UNSPECIFIED.);
#4560=B_SPLINE_CURVE_WITH_KNOTS('',3,(#144912,#144913,#144914,#144915,#144916,
#144917,#144918,#144919,#144920,#144921,#144922,#144923,#144924,#144925,
#144926,#144927),.UNSPECIFIED.,.F.,.F.,(4,3,3,3,3,4),(0.000694356721436431,
0.00259637723191676,0.00305563622484014,0.00480503978353657,0.00647539340150566,
0.00814574701947475),.UNSPECIFIED.);
#4561=B_SPLINE_CURVE_WITH_KNOTS('',3,(#144989,#144990,#144991,#144992,#144993,
#144994,#144995,#144996,#144997,#144998,#144999,#145000,#145001,#145002,
#145003,#145004,#145005,#145006,#145007,#145008,#145009,#145010,#145011,
#145012,#145013,#145014,#145015,#145016,#145017,#145018,#145019),
 .UNSPECIFIED.,.F.,.F.,(4,3,3,3,3,3,3,3,3,3,4),(0.,0.0881043395261828,0.178030981308937,
0.270574666304827,0.364321258892522,0.459368561145583,0.500000000000001,
0.64789166764264,0.797396677123148,0.945384894755191,1.),.UNSPECIFIED.);
#4562=B_SPLINE_CURVE_WITH_KNOTS('',3,(#145043,#145044,#145045,#145046,#145047,
#145048,#145049),.UNSPECIFIED.,.F.,.F.,(4,3,4),(0.,0.640590439740815,0.999999469629731),
 .UNSPECIFIED.);
#4563=B_SPLINE_CURVE_WITH_KNOTS('',3,(#145050,#145051,#145052,#145053),
 .UNSPECIFIED.,.F.,.F.,(4,4),(0.,1.),.UNSPECIFIED.);
#4564=B_SPLINE_CURVE_WITH_KNOTS('',3,(#145128,#145129,#145130,#145131,#145132,
#145133,#145134,#145135,#145136,#145137,#145138,#145139,#145140,#145141,
#145142,#145143,#145144,#145145,#145146,#145147,#145148,#145149,#145150,
#145151,#145152,#145153,#145154,#145155,#145156,#145157,#145158),
 .UNSPECIFIED.,.F.,.F.,(4,3,3,3,3,3,3,3,3,3,4),(8.28401126087789E-15,0.103891034062219,
0.209333681833554,0.314870836921643,0.419526492710104,0.5,0.61507405516711,
0.725151653805686,0.832721765547754,0.937002679485264,1.),.UNSPECIFIED.);
#4565=B_SPLINE_CURVE_WITH_KNOTS('',3,(#145272,#145273,#145274,#145275,#145276,
#145277,#145278,#145279,#145280,#145281),.UNSPECIFIED.,.F.,.F.,(4,2,2,2,
4),(0.,0.25,0.5,0.75,1.),.UNSPECIFIED.);
#4566=B_SPLINE_CURVE_WITH_KNOTS('',3,(#145320,#145321,#145322,#145323,#145324,
#145325),.UNSPECIFIED.,.F.,.F.,(4,2,4),(0.,0.5,1.),.UNSPECIFIED.);
#4567=B_SPLINE_CURVE_WITH_KNOTS('',3,(#145346,#145347,#145348,#145349,#145350,
#145351),.UNSPECIFIED.,.F.,.F.,(4,2,4),(0.,0.5,0.999999988140019),
 .UNSPECIFIED.);
#4568=B_SPLINE_CURVE_WITH_KNOTS('',3,(#145375,#145376,#145377,#145378,#145379,
#145380,#145381,#145382,#145383,#145384,#145385,#145386,#145387,#145388,
#145389,#145390,#145391,#145392,#145393,#145394,#145395,#145396,#145397,
#145398,#145399,#145400,#145401,#145402,#145403,#145404,#145405),
 .UNSPECIFIED.,.F.,.F.,(4,3,3,3,3,3,3,3,3,3,4),(0.,0.0841106566558007,0.169966621792399,
0.258433889273308,0.348104167089326,0.439210954526272,0.500000000000001,
0.653513844289969,0.813728745872899,0.971758040989338,0.999999999999993),
 .UNSPECIFIED.);
#4569=B_SPLINE_CURVE_WITH_KNOTS('',3,(#145449,#145450,#145451,#145452,#145453,
#145454,#145455,#145456,#145457,#145458,#145459,#145460,#145461,#145462,
#145463,#145464,#145465,#145466,#145467),.UNSPECIFIED.,.F.,.F.,(4,3,3,3,
3,3,4),(0.000636256268971442,0.00222779634230967,0.003876291264432,0.0056280359891258,
0.00591708699638704,0.00780896916228463,0.00825282706815076),
 .UNSPECIFIED.);
#4570=B_SPLINE_CURVE_WITH_KNOTS('',3,(#145468,#145469,#145470,#145471,#145472,
#145473,#145474,#145475,#145476,#145477,#145478,#145479,#145480,#145481,
#145482,#145483,#145484,#145485,#145486,#145487,#145488,#145489,#145490,
#145491,#145492,#145493,#145494,#145495,#145496,#145497,#145498),
 .UNSPECIFIED.,.F.,.F.,(4,3,3,3,3,3,3,3,3,3,4),(4.68648016623899E-15,0.110926165634124,
0.223711806532316,0.336827055115305,0.449445226496388,0.5,0.627102535999364,
0.751142482631481,0.87557124131574,0.993677341969705,1.),.UNSPECIFIED.);
#4571=B_SPLINE_CURVE_WITH_KNOTS('',3,(#145561,#145562,#145563,#145564,#145565,
#145566),.UNSPECIFIED.,.F.,.F.,(4,2,4),(1.4856211342407E-5,0.5,1.),
 .UNSPECIFIED.);
#4572=B_SPLINE_CURVE_WITH_KNOTS('',3,(#145587,#145588,#145589,#145590,#145591,
#145592),.UNSPECIFIED.,.F.,.F.,(4,2,4),(0.,0.500000000000001,1.),
 .UNSPECIFIED.);
#4573=B_SPLINE_CURVE_WITH_KNOTS('',3,(#145614,#145615,#145616,#145617,#145618,
#145619,#145620,#145621),.UNSPECIFIED.,.F.,.F.,(4,2,2,4),(0.,0.5,0.75,1.),
 .UNSPECIFIED.);
#4574=B_SPLINE_CURVE_WITH_KNOTS('',3,(#145666,#145667,#145668,#145669),
 .UNSPECIFIED.,.F.,.F.,(4,4),(0.,1.),.UNSPECIFIED.);
#4575=B_SPLINE_CURVE_WITH_KNOTS('',3,(#145762,#145763,#145764,#145765,#145766,
#145767,#145768,#145769,#145770,#145771,#145772,#145773,#145774,#145775,
#145776,#145777,#145778,#145779,#145780,#145781,#145782,#145783,#145784,
#145785,#145786,#145787,#145788,#145789),.UNSPECIFIED.,.F.,.F.,(4,3,3,3,
3,3,3,3,3,4),(0.,0.109785608660835,0.222741427481541,0.337045865985497,
0.452594310492733,0.500000000000001,0.64133306133531,0.781868923872316,
0.921212099227518,1.),.UNSPECIFIED.);
#4576=B_SPLINE_CURVE_WITH_KNOTS('',3,(#145815,#145816,#145817,#145818,#145819,
#145820,#145821,#145822,#145823,#145824,#145825,#145826,#145827,#145828,
#145829,#145830,#145831,#145832,#145833),.UNSPECIFIED.,.F.,.F.,(4,3,3,3,
3,3,4),(0.000544979362130299,0.00239221479430278,0.00380801466457332,0.00469824400931087,
0.00578923755784658,0.00680407029599512,0.00707104996701635),
 .UNSPECIFIED.);
#4577=B_SPLINE_CURVE_WITH_KNOTS('',3,(#145834,#145835,#145836,#145837,#145838,
#145839,#145840,#145841,#145842,#145843,#145844,#145845,#145846,#145847,
#145848,#145849,#145850,#145851,#145852,#145853,#145854,#145855,#145856,
#145857,#145858),.UNSPECIFIED.,.F.,.F.,(4,3,3,3,3,3,3,3,4),(0.,0.133858617770367,
0.268928589573922,0.404818946884987,0.5,0.650059845006746,0.798865163431494,
0.946095668638004,1.),.UNSPECIFIED.);
#4578=B_SPLINE_CURVE_WITH_KNOTS('',3,(#145915,#145916,#145917,#145918,#145919,
#145920),.UNSPECIFIED.,.F.,.F.,(4,2,4),(0.,0.5,1.),.UNSPECIFIED.);
#4579=B_SPLINE_CURVE_WITH_KNOTS('',3,(#146000,#146001,#146002,#146003,#146004,
#146005,#146006,#146007,#146008,#146009,#146010,#146011,#146012,#146013),
 .UNSPECIFIED.,.F.,.F.,(4,2,2,2,2,2,4),(0.,0.25310390433008,0.379655856495117,
0.506207808660157,0.632759760825198,0.759311712990238,1.),.UNSPECIFIED.);
#4580=B_SPLINE_CURVE_WITH_KNOTS('',3,(#146014,#146015,#146016,#146017,#146018,
#146019,#146020,#146021,#146022,#146023),.UNSPECIFIED.,.F.,.F.,(4,2,2,2,
4),(0.,0.25,0.5,0.75,1.),.UNSPECIFIED.);
#4581=B_SPLINE_CURVE_WITH_KNOTS('',3,(#146029,#146030,#146031,#146032),
 .UNSPECIFIED.,.F.,.F.,(4,4),(0.00465289315641866,0.00515351125805147),
 .UNSPECIFIED.);
#4582=B_SPLINE_CURVE_WITH_KNOTS('',3,(#146105,#146106,#146107,#146108,#146109,
#146110,#146111,#146112,#146113,#146114,#146115,#146116,#146117,#146118,
#146119,#146120,#146121,#146122,#146123,#146124,#146125,#146126,#146127,
#146128,#146129,#146130,#146131,#146132,#146133,#146134,#146135,#146136,
#146137,#146138,#146139,#146140,#146141,#146142,#146143,#146144,#146145,
#146146,#146147),.UNSPECIFIED.,.F.,.F.,(4,3,3,3,3,3,3,3,3,3,3,3,3,3,4),
(0.,0.0632636272771733,0.127512975023493,0.193161069570627,0.250000000000002,
0.323161603585242,0.398727785487939,0.478054969239045,0.500000000000001,
0.583571175025073,0.670742277688246,0.764579159679674,0.862667985480895,
0.965751654555339,1.),.UNSPECIFIED.);
#4583=B_SPLINE_CURVE_WITH_KNOTS('',3,(#146204,#146205,#146206,#146207,#146208,
#146209,#146210),.UNSPECIFIED.,.F.,.F.,(4,3,4),(0.,0.500000000000006,1.),
 .UNSPECIFIED.);
#4584=B_SPLINE_CURVE_WITH_KNOTS('',3,(#146233,#146234,#146235,#146236,#146237,
#146238,#146239,#146240,#146241,#146242,#146243,#146244,#146245,#146246,
#146247,#146248,#146249,#146250,#146251,#146252,#146253,#146254,#146255,
#146256,#146257),.UNSPECIFIED.,.F.,.F.,(4,3,3,3,3,3,3,3,4),(0.,0.140179798979954,
0.281858061384262,0.424662898949861,0.499999999999999,0.654971604573252,
0.809174109715774,0.962522009696372,1.),.UNSPECIFIED.);
#4585=B_SPLINE_CURVE_WITH_KNOTS('',3,(#146277,#146278,#146279,#146280,#146281,
#146282,#146283,#146284,#146285,#146286,#146287,#146288,#146289,#146290,
#146291,#146292,#146293,#146294,#146295,#146296,#146297,#146298),
 .UNSPECIFIED.,.F.,.F.,(4,3,3,3,3,3,3,4),(0.000499308730788156,0.00146046002319833,
0.00243695586828934,0.00338583705476887,0.00376364965220018,0.00474984309182789,
0.00578812738994236,0.00627236538267016),.UNSPECIFIED.);
#4586=B_SPLINE_CURVE_WITH_KNOTS('',3,(#146359,#146360,#146361,#146362),
 .UNSPECIFIED.,.F.,.F.,(4,4),(0.,1.),.UNSPECIFIED.);
#4587=B_SPLINE_CURVE_WITH_KNOTS('',3,(#146422,#146423,#146424,#146425,#146426,
#146427,#146428,#146429,#146430,#146431,#146432,#146433,#146434,#146435,
#146436,#146437,#146438,#146439,#146440,#146441,#146442,#146443,#146444,
#146445,#146446,#146447,#146448,#146449,#146450,#146451,#146452,#146453,
#146454,#146455,#146456,#146457,#146458,#146459,#146460,#146461,#146462,
#146463,#146464,#146465,#146466,#146467),.UNSPECIFIED.,.F.,.F.,(4,3,3,3,
3,3,3,3,3,3,3,3,3,3,3,4),(0.,0.0915750010276041,0.131325095428788,0.212675685292389,
0.290151690513043,0.365784162784195,0.439131591082695,0.5,0.56919091022333,
0.637494190722665,0.705032480811157,0.75,0.816374271265617,0.882302233429591,
0.94798000078784,1.),.UNSPECIFIED.);
#4588=B_SPLINE_CURVE_WITH_KNOTS('',3,(#146530,#146531,#146532,#146533,#146534,
#146535,#146536,#146537,#146538,#146539,#146540,#146541),.UNSPECIFIED.,
 .F.,.F.,(4,2,2,2,2,4),(0.,0.25,0.375,0.5,0.75,1.),.UNSPECIFIED.);
#4589=B_SPLINE_CURVE_WITH_KNOTS('',3,(#146574,#146575,#146576,#146577),
 .UNSPECIFIED.,.F.,.F.,(4,4),(0.,1.),.UNSPECIFIED.);
#4590=B_SPLINE_CURVE_WITH_KNOTS('',3,(#146635,#146636,#146637,#146638,#146639,
#146640,#146641,#146642,#146643,#146644,#146645,#146646,#146647,#146648,
#146649,#146650,#146651,#146652,#146653,#146654,#146655,#146656,#146657,
#146658,#146659),.UNSPECIFIED.,.F.,.F.,(4,3,3,3,3,3,3,3,4),(0.000526414844798677,
0.0016264626269863,0.00270005642798455,0.00303445478718795,0.00340650091711803,
0.00424257270328544,0.00468441200509802,0.00552307032315886,0.0062865869894374),
 .UNSPECIFIED.);
#4591=B_SPLINE_CURVE_WITH_KNOTS('',3,(#146660,#146661,#146662,#146663,#146664,
#146665,#146666),.UNSPECIFIED.,.F.,.F.,(4,3,4),(0.,0.5,1.),
 .UNSPECIFIED.);
#4592=B_SPLINE_CURVE_WITH_KNOTS('',3,(#146723,#146724,#146725,#146726,#146727,
#146728,#146729,#146730,#146731,#146732,#146733,#146734,#146735,#146736,
#146737,#146738,#146739,#146740,#146741,#146742,#146743,#146744,#146745,
#146746,#146747),.UNSPECIFIED.,.F.,.F.,(4,3,3,3,3,3,3,3,4),(0.,0.140856133935696,
0.283205124587202,0.426655231031233,0.5,0.655301545313637,0.809843231900818,
0.963548210345928,1.),.UNSPECIFIED.);
#4593=B_SPLINE_CURVE_WITH_KNOTS('',3,(#146827,#146828,#146829,#146830,#146831,
#146832,#146833,#146834,#146835,#146836,#146837,#146838,#146839,#146840),
 .UNSPECIFIED.,.F.,.F.,(4,2,2,2,2,2,4),(0.,0.251497274344898,0.377245911517345,
0.502994548689796,0.628743185862243,0.754491823034691,1.),.UNSPECIFIED.);
#4594=B_SPLINE_CURVE_WITH_KNOTS('',3,(#146841,#146842,#146843,#146844,#146845,
#146846,#146847,#146848,#146849,#146850,#146851,#146852,#146853,#146854,
#146855,#146856,#146857,#146858,#146859,#146860,#146861,#146862,#146863,
#146864,#146865,#146866,#146867,#146868,#146869,#146870,#146871,#146872,
#146873,#146874,#146875,#146876,#146877,#146878,#146879,#146880,#146881,
#146882,#146883),.UNSPECIFIED.,.F.,.F.,(4,3,3,3,3,3,3,3,3,3,3,3,3,3,4),
(0.,0.0883066236689891,0.169881016966313,0.25,0.345565144469168,0.432992430689934,
0.5,0.579720574572057,0.657499747134168,0.73321670512183,0.75,0.821556884509131,
0.891976019923854,0.961324436963321,0.999999999999875),.UNSPECIFIED.);
#4595=B_SPLINE_CURVE_WITH_KNOTS('',3,(#146889,#146890,#146891,#146892),
 .UNSPECIFIED.,.F.,.F.,(4,4),(0.0209654295165786,0.0214659702660322),
 .UNSPECIFIED.);
#4596=B_SPLINE_CURVE_WITH_KNOTS('',3,(#146951,#146952,#146953,#146954,#146955,
#146956,#146957,#146958,#146959,#146960,#146961,#146962,#146963,#146964),
 .UNSPECIFIED.,.F.,.F.,(4,2,2,2,2,2,4),(0.,0.241136840065836,0.3676140333882,
0.49409122671056,0.62056842003292,0.74704561335528,1.),.UNSPECIFIED.);
#4597=B_SPLINE_CURVE_WITH_KNOTS('',3,(#146965,#146966,#146967,#146968,#146969,
#146970),.UNSPECIFIED.,.F.,.F.,(4,2,4),(0.,0.500000000000001,1.),
 .UNSPECIFIED.);
#4598=B_SPLINE_CURVE_WITH_KNOTS('',3,(#147027,#147028,#147029,#147030,#147031,
#147032,#147033,#147034,#147035,#147036,#147037,#147038,#147039,#147040,
#147041,#147042,#147043,#147044,#147045,#147046,#147047,#147048,#147049,
#147050,#147051),.UNSPECIFIED.,.F.,.F.,(4,3,3,3,3,3,3,3,4),(6.69029905996544E-15,
0.134488788622136,0.270199226691756,0.406736460097312,0.5,0.650772475386906,
0.800288993579067,0.9482361842095,1.),.UNSPECIFIED.);
#4599=B_SPLINE_CURVE_WITH_KNOTS('',3,(#147074,#147075,#147076,#147077,#147078,
#147079),.UNSPECIFIED.,.F.,.F.,(4,2,4),(0.,0.499999999999999,1.),
 .UNSPECIFIED.);
#4600=B_SPLINE_CURVE_WITH_KNOTS('',3,(#147105,#147106,#147107,#147108,#147109,
#147110,#147111,#147112,#147113,#147114,#147115,#147116,#147117,#147118,
#147119,#147120,#147121,#147122,#147123),.UNSPECIFIED.,.F.,.F.,(4,3,3,3,
3,3,4),(0.000609719129519901,0.00229610816230499,0.00296440479617456,0.00386266882834386,
0.00506716034621366,0.00622435639369392,0.00711561852716782),
 .UNSPECIFIED.);
#4601=B_SPLINE_CURVE_WITH_KNOTS('',3,(#147192,#147193,#147194,#147195,#147196,
#147197,#147198,#147199,#147200,#147201,#147202,#147203,#147204,#147205,
#147206,#147207,#147208,#147209,#147210,#147211,#147212,#147213,#147214,
#147215,#147216,#147217,#147218,#147219),.UNSPECIFIED.,.F.,.F.,(4,3,3,3,
3,3,3,3,3,4),(0.,0.110591919110538,0.224346970330222,0.339439967219989,
0.455737261262023,0.499999999999999,0.641794484661474,0.78280483557739,
0.922640336453395,1.),.UNSPECIFIED.);
#4602=B_SPLINE_CURVE_WITH_KNOTS('',3,(#147240,#147241,#147242,#147243,#147244,
#147245),.UNSPECIFIED.,.F.,.F.,(4,2,4),(0.,0.500000000000001,1.),
 .UNSPECIFIED.);
#4603=B_SPLINE_CURVE_WITH_KNOTS('',3,(#147269,#147270,#147271,#147272),
 .UNSPECIFIED.,.F.,.F.,(4,4),(0.,1.),.UNSPECIFIED.);
#4604=B_SPLINE_CURVE_WITH_KNOTS('',3,(#147315,#147316,#147317,#147318,#147319,
#147320,#147321,#147322,#147323,#147324,#147325,#147326,#147327,#147328,
#147329,#147330,#147331,#147332,#147333,#147334,#147335,#147336,#147337,
#147338,#147339,#147340,#147341,#147342,#147343,#147344,#147345,#147346,
#147347,#147348,#147349,#147350,#147351),.UNSPECIFIED.,.F.,.F.,(4,3,3,3,
3,3,3,3,3,3,3,3,4),(0.,0.0855121196768925,0.171061973228972,0.249999999999999,
0.337442080953179,0.424780528770959,0.499999999999999,0.588285009908279,
0.676363239585974,0.75,0.835015716367125,0.920008379189467,1.),
 .UNSPECIFIED.);
#4605=B_SPLINE_CURVE_WITH_KNOTS('',3,(#147390,#147391,#147392,#147393,#147394,
#147395),.UNSPECIFIED.,.F.,.F.,(4,2,4),(0.,0.5,1.),.UNSPECIFIED.);
#4606=B_SPLINE_CURVE_WITH_KNOTS('',3,(#147416,#147417,#147418,#147419,#147420,
#147421,#147422,#147423,#147424,#147425,#147426,#147427,#147428,#147429,
#147430,#147431,#147432,#147433,#147434,#147435,#147436,#147437,#147438,
#147439,#147440,#147441,#147442,#147443),.UNSPECIFIED.,.F.,.F.,(4,3,3,3,
3,3,3,3,3,4),(0.,0.111439972739101,0.224754294220322,0.338408661878299,
0.451580972885512,0.500000000000001,0.627994499207414,0.752939260132545,
0.876469630066272,1.),.UNSPECIFIED.);
#4607=B_SPLINE_CURVE_WITH_KNOTS('',3,(#147466,#147467,#147468,#147469,#147470,
#147471,#147472),.UNSPECIFIED.,.F.,.F.,(4,3,4),(1.50276431479551E-5,0.500000000000001,
1.),.UNSPECIFIED.);
#4608=B_SPLINE_CURVE_WITH_KNOTS('',3,(#147492,#147493,#147494,#147495,#147496,
#147497,#147498,#147499,#147500,#147501,#147502,#147503,#147504,#147505,
#147506,#147507,#147508,#147509,#147510),.UNSPECIFIED.,.F.,.F.,(4,3,3,3,
3,3,4),(0.000708752105543503,0.00258350608982207,0.00304683603862546,0.00476166896123969,
0.00640184829291217,0.00796195121144225,0.00830118856937974),
 .UNSPECIFIED.);
#4609=B_SPLINE_CURVE_WITH_KNOTS('',3,(#147511,#147512,#147513,#147514,#147515,
#147516),.UNSPECIFIED.,.F.,.F.,(4,2,4),(0.,0.500000000000001,0.999999987841376),
 .UNSPECIFIED.);
#4610=B_SPLINE_CURVE_WITH_KNOTS('',3,(#147559,#147560,#147561,#147562,#147563,
#147564,#147565,#147566,#147567,#147568),.UNSPECIFIED.,.F.,.F.,(4,2,2,2,
4),(0.,0.25,0.5,0.75,1.),.UNSPECIFIED.);
#4611=B_SPLINE_CURVE_WITH_KNOTS('',3,(#147618,#147619,#147620,#147621,#147622,
#147623,#147624,#147625,#147626,#147627,#147628,#147629,#147630,#147631,
#147632,#147633,#147634,#147635,#147636,#147637,#147638,#147639,#147640,
#147641,#147642,#147643,#147644,#147645,#147646,#147647,#147648),
 .UNSPECIFIED.,.F.,.F.,(4,3,3,3,3,3,3,3,3,3,4),(0.,0.0847040358914981,0.17116589808823,
0.260240904791955,0.350519080310786,0.442212155487767,0.500000000000001,
0.652840714424581,0.811062123407797,0.96706666050884,1.),.UNSPECIFIED.);
#4612=B_SPLINE_CURVE_WITH_KNOTS('',3,(#147667,#147668,#147669,#147670,#147671,
#147672),.UNSPECIFIED.,.F.,.F.,(4,2,4),(0.,0.500000000000001,1.),
 .UNSPECIFIED.);
#4613=B_SPLINE_CURVE_WITH_KNOTS('',3,(#147687,#147688,#147689,#147690),
 .UNSPECIFIED.,.F.,.F.,(4,4),(0.000932565055856382,0.00145387661961334),
 .UNSPECIFIED.);
#4614=B_SPLINE_CURVE_WITH_KNOTS('',3,(#147692,#147693,#147694,#147695,#147696,
#147697,#147698,#147699,#147700,#147701),.UNSPECIFIED.,.F.,.F.,(4,2,2,2,
4),(0.,0.25,0.5,0.750000000000001,0.999999175968697),.UNSPECIFIED.);
#4615=B_SPLINE_CURVE_WITH_KNOTS('',3,(#147709,#147710,#147711,#147712,#147713,
#147714),.UNSPECIFIED.,.F.,.F.,(4,2,4),(0.,0.5,1.),.UNSPECIFIED.);
#4616=B_SPLINE_CURVE_WITH_KNOTS('',3,(#147750,#147751,#147752,#147753,#147754,
#147755,#147756,#147757,#147758,#147759),.UNSPECIFIED.,.F.,.F.,(4,2,2,2,
4),(0.,0.25,0.5,0.75,1.),.UNSPECIFIED.);
#4617=B_SPLINE_CURVE_WITH_KNOTS('',3,(#147767,#147768,#147769,#147770,#147771,
#147772),.UNSPECIFIED.,.F.,.F.,(4,2,4),(0.,0.499999999999999,1.),
 .UNSPECIFIED.);
#4618=B_SPLINE_CURVE_WITH_KNOTS('',3,(#147840,#147841,#147842,#147843,#147844,
#147845,#147846,#147847,#147848,#147849),.UNSPECIFIED.,.F.,.F.,(4,3,3,4),
(0.,0.499999999999717,0.749999999999858,1.),.UNSPECIFIED.);
#4619=B_SPLINE_CURVE_WITH_KNOTS('',3,(#147886,#147887,#147888,#147889,#147890,
#147891,#147892,#147893,#147894,#147895,#147896,#147897,#147898,#147899,
#147900,#147901,#147902,#147903,#147904,#147905,#147906,#147907,#147908,
#147909,#147910,#147911,#147912,#147913,#147914,#147915,#147916,#147917,
#147918,#147919,#147920,#147921,#147922,#147923,#147924,#147925,#147926,
#147927,#147928),.UNSPECIFIED.,.F.,.F.,(4,3,3,3,3,3,3,3,3,3,3,3,3,3,4),
(0.,0.0625,0.123895355591394,0.186947677795697,0.25,0.326192612901303,0.403694113418718,
0.482847078444175,0.5,0.602353575542828,0.711321847725079,0.75,0.839036507722233,
0.928336927687806,1.),.UNSPECIFIED.);
#4620=B_SPLINE_CURVE_WITH_KNOTS('',3,(#147949,#147950,#147951,#147952,#147953,
#147954),.UNSPECIFIED.,.F.,.F.,(4,2,4),(0.,0.500000000000005,1.),
 .UNSPECIFIED.);
#4621=B_SPLINE_CURVE_WITH_KNOTS('',3,(#148029,#148030,#148031,#148032,#148033,
#148034),.UNSPECIFIED.,.F.,.F.,(4,2,4),(0.,0.5,1.),.UNSPECIFIED.);
#4622=B_SPLINE_CURVE_WITH_KNOTS('',3,(#148069,#148070,#148071,#148072,#148073,
#148074,#148075,#148076,#148077,#148078),.UNSPECIFIED.,.F.,.F.,(4,2,2,2,
4),(0.,0.250000000000001,0.500000000000002,0.749999999999999,1.),
 .UNSPECIFIED.);
#4623=B_SPLINE_CURVE_WITH_KNOTS('',3,(#148165,#148166,#148167,#148168,#148169,
#148170,#148171,#148172,#148173,#148174,#148175,#148176,#148177,#148178,
#148179,#148180,#148181,#148182,#148183,#148184,#148185,#148186,#148187,
#148188,#148189,#148190,#148191,#148192,#148193,#148194,#148195),
 .UNSPECIFIED.,.F.,.F.,(4,3,3,3,3,3,3,3,3,3,4),(0.,0.0990505281004008,0.199396658312436,
0.299649788385249,0.399824894192624,0.5,0.605387357037088,0.706111159001044,
0.804538030595637,0.902269015297818,1.),.UNSPECIFIED.);
#4624=B_SPLINE_CURVE_WITH_KNOTS('',3,(#148226,#148227,#148228,#148229,#148230,
#148231,#148232,#148233),.UNSPECIFIED.,.F.,.F.,(4,2,2,4),(3.81942240222894E-5,
0.5,0.75,1.),.UNSPECIFIED.);
#4625=B_SPLINE_CURVE_WITH_KNOTS('',3,(#148258,#148259,#148260,#148261),
 .UNSPECIFIED.,.F.,.F.,(4,4),(1.85554534979779E-6,1.),.UNSPECIFIED.);
#4626=B_SPLINE_CURVE_WITH_KNOTS('',3,(#148332,#148333,#148334,#148335,#148336,
#148337,#148338,#148339,#148340,#148341),.UNSPECIFIED.,.F.,.F.,(4,3,3,4),
(0.,0.499999999999922,0.749999999999962,0.999999984042409),
 .UNSPECIFIED.);
#4627=B_SPLINE_CURVE_WITH_KNOTS('',3,(#148378,#148379,#148380,#148381,#148382,
#148383,#148384,#148385,#148386,#148387,#148388,#148389,#148390,#148391,
#148392,#148393,#148394,#148395,#148396,#148397,#148398,#148399,#148400,
#148401,#148402,#148403,#148404,#148405,#148406,#148407,#148408,#148409,
#148410,#148411,#148412,#148413,#148414,#148415,#148416,#148417),
 .UNSPECIFIED.,.F.,.F.,(4,3,3,3,3,3,3,3,3,3,3,3,3,4),(0.,0.0663260948058646,
0.133685855257027,0.202613561710615,0.25,0.331751956472141,0.41587597823607,
0.499999999999999,0.611670400716575,0.728976448656423,0.75,0.841370986237791,
0.932703732962715,1.),.UNSPECIFIED.);
#4628=B_SPLINE_CURVE_WITH_KNOTS('',3,(#148468,#148469,#148470,#148471,#148472,
#148473,#148474,#148475,#148476,#148477),.UNSPECIFIED.,.F.,.F.,(4,2,2,2,
4),(0.,0.25,0.5,0.75,1.),.UNSPECIFIED.);
#4629=B_SPLINE_CURVE_WITH_KNOTS('',3,(#148513,#148514,#148515,#148516,#148517,
#148518,#148519,#148520,#148521,#148522),.UNSPECIFIED.,.F.,.F.,(4,2,2,2,
4),(0.,0.25,0.5,0.75,1.),.UNSPECIFIED.);
#4630=B_SPLINE_CURVE_WITH_KNOTS('',3,(#148530,#148531,#148532,#148533,#148534,
#148535),.UNSPECIFIED.,.F.,.F.,(4,2,4),(0.,0.499999999999999,1.),
 .UNSPECIFIED.);
#4631=B_SPLINE_CURVE_WITH_KNOTS('',3,(#148557,#148558,#148559,#148560,#148561,
#148562),.UNSPECIFIED.,.F.,.F.,(4,2,4),(0.,0.499999999999998,1.),
 .UNSPECIFIED.);
#4632=B_SPLINE_CURVE_WITH_KNOTS('',3,(#148598,#148599,#148600,#148601,#148602,
#148603,#148604,#148605,#148606,#148607),.UNSPECIFIED.,.F.,.F.,(4,2,2,2,
4),(0.,0.250000000000001,0.500000000000002,0.750000000000002,1.),
 .UNSPECIFIED.);
#4633=B_SPLINE_CURVE_WITH_KNOTS('',3,(#148632,#148633,#148634,#148635,#148636,
#148637),.UNSPECIFIED.,.F.,.F.,(4,2,4),(0.,0.500000000000001,1.),
 .UNSPECIFIED.);
#4634=B_SPLINE_CURVE_WITH_KNOTS('',3,(#148652,#148653,#148654,#148655),
 .UNSPECIFIED.,.F.,.F.,(4,4),(0.,1.),.UNSPECIFIED.);
#4635=B_SPLINE_CURVE_WITH_KNOTS('',3,(#148682,#148683,#148684,#148685,#148686,
#148687,#148688,#148689,#148690,#148691,#148692,#148693,#148694,#148695,
#148696,#148697,#148698,#148699,#148700,#148701,#148702,#148703,#148704,
#148705,#148706,#148707,#148708,#148709,#148710,#148711,#148712,#148713,
#148714,#148715,#148716,#148717,#148718,#148719,#148720,#148721),
 .UNSPECIFIED.,.F.,.F.,(4,3,3,3,3,3,3,3,3,3,3,3,3,4),(3.23711100202308E-15,
0.0890075956720996,0.178502409862928,0.267659454900732,0.355866780049122,
0.441950412840108,0.5,0.586691146881939,0.671658526049874,0.75,0.81604551378379,
0.881127848945156,0.944594173895109,1.),.UNSPECIFIED.);
#4636=B_SPLINE_CURVE_WITH_KNOTS('',3,(#148752,#148753,#148754,#148755,#148756,
#148757,#148758,#148759),.UNSPECIFIED.,.F.,.F.,(4,2,2,4),(2.50635257585442E-5,
0.25,0.5,1.),.UNSPECIFIED.);
#4637=B_SPLINE_CURVE_WITH_KNOTS('',3,(#148773,#148774,#148775,#148776),
 .UNSPECIFIED.,.F.,.F.,(4,4),(0.,1.),.UNSPECIFIED.);
#4638=B_SPLINE_CURVE_WITH_KNOTS('',3,(#148805,#148806,#148807,#148808,#148809,
#148810,#148811,#148812),.UNSPECIFIED.,.F.,.F.,(4,2,2,4),(0.,0.5,0.75,1.),
 .UNSPECIFIED.);
#4639=B_SPLINE_CURVE_WITH_KNOTS('',3,(#148813,#148814,#148815,#148816,#148817,
#148818),.UNSPECIFIED.,.F.,.F.,(4,2,4),(0.,0.5,1.),.UNSPECIFIED.);
#4640=B_SPLINE_CURVE_WITH_KNOTS('',3,(#148856,#148857,#148858,#148859),
 .UNSPECIFIED.,.F.,.F.,(4,4),(0.,1.),.UNSPECIFIED.);
#4641=B_SPLINE_CURVE_WITH_KNOTS('',3,(#148885,#148886,#148887,#148888,#148889,
#148890,#148891,#148892,#148893,#148894,#148895,#148896,#148897,#148898,
#148899,#148900,#148901,#148902,#148903,#148904,#148905,#148906,#148907,
#148908,#148909,#148910,#148911,#148912,#148913,#148914,#148915,#148916,
#148917,#148918,#148919,#148920,#148921,#148922,#148923,#148924),
 .UNSPECIFIED.,.F.,.F.,(4,3,3,3,3,3,3,3,3,3,3,3,3,4),(0.,0.0918748454737772,
0.184355396105487,0.276688554701798,0.36816212505023,0.457673897462644,
0.5,0.589889351053675,0.678272371100533,0.75,0.820588727807885,0.890157630216019,
0.958083323445281,1.),.UNSPECIFIED.);
#4642=B_SPLINE_CURVE_WITH_KNOTS('',3,(#148964,#148965,#148966,#148967,#148968,
#148969,#148970,#148971,#148972,#148973,#148974,#148975,#148976,#148977,
#148978,#148979,#148980,#148981,#148982,#148983,#148984,#148985,#148986,
#148987,#148988,#148989,#148990,#148991,#148992,#148993,#148994,#148995,
#148996,#148997,#148998,#148999,#149000,#149001,#149002,#149003),
 .UNSPECIFIED.,.F.,.F.,(4,3,3,3,3,3,3,3,3,3,3,3,3,4),(0.,0.0714747014717626,
0.14406512628289,0.218232697883806,0.25,0.336678327359007,0.425479051500161,
0.499999999999999,0.603940978333897,0.708843934985259,0.749999999999999,
0.844822927402583,0.939528967854887,1.),.UNSPECIFIED.);
#4643=B_SPLINE_CURVE_WITH_KNOTS('',3,(#149053,#149054,#149055,#149056,#149057,
#149058,#149059,#149060),.UNSPECIFIED.,.F.,.F.,(4,2,2,4),(5.22261572021516E-9,
0.25,0.5,1.),.UNSPECIFIED.);
#4644=B_SPLINE_CURVE_WITH_KNOTS('',3,(#149074,#149075,#149076,#149077),
 .UNSPECIFIED.,.F.,.F.,(4,4),(0.,0.00407596620376747),.UNSPECIFIED.);
#4645=B_SPLINE_CURVE_WITH_KNOTS('',3,(#149106,#149107,#149108,#149109,#149110,
#149111),.UNSPECIFIED.,.F.,.F.,(4,2,4),(0.,0.5,1.),.UNSPECIFIED.);
#4646=B_SPLINE_CURVE_WITH_KNOTS('',3,(#149112,#149113,#149114,#149115,#149116,
#149117,#149118,#149119,#149120,#149121),.UNSPECIFIED.,.F.,.F.,(4,2,2,2,
4),(0.,0.25,0.5,0.75,1.),.UNSPECIFIED.);
#4647=B_SPLINE_CURVE_WITH_KNOTS('',3,(#149161,#149162,#149163,#149164,#149165,
#149166,#149167,#149168,#149169,#149170),.UNSPECIFIED.,.F.,.F.,(4,2,2,2,
4),(0.,0.249999999999998,0.499999999999999,0.749999999999999,1.),
 .UNSPECIFIED.);
#4648=B_SPLINE_CURVE_WITH_KNOTS('',3,(#149178,#149179,#149180,#149181,#149182,
#149183),.UNSPECIFIED.,.F.,.F.,(4,2,4),(0.,0.5,1.),.UNSPECIFIED.);
#4649=B_SPLINE_CURVE_WITH_KNOTS('',3,(#149239,#149240,#149241,#149242),
 .UNSPECIFIED.,.F.,.F.,(4,4),(0.,0.00425966609677044),.UNSPECIFIED.);
#4650=B_SPLINE_CURVE_WITH_KNOTS('',3,(#149275,#149276,#149277,#149278,#149279,
#149280,#149281,#149282,#149283,#149284,#149285,#149286,#149287,#149288,
#149289,#149290,#149291,#149292,#149293,#149294,#149295,#149296,#149297,
#149298,#149299,#149300,#149301,#149302,#149303,#149304,#149305,#149306,
#149307,#149308,#149309,#149310,#149311,#149312,#149313,#149314,#149315,
#149316,#149317,#149318,#149319,#149320,#149321,#149322,#149323),
 .UNSPECIFIED.,.F.,.F.,(4,3,3,3,3,3,3,3,3,3,3,3,3,3,3,3,4),(0.,0.0816151725490495,
0.165807586274525,0.25,0.328615088456192,0.405988550271647,0.481325889494902,
0.5,0.578932430016132,0.656234385435454,0.731485876446147,0.75,0.805022411038226,
0.858733068040437,0.911617182774789,0.963210525378497,1.),.UNSPECIFIED.);
#4651=B_SPLINE_CURVE_WITH_KNOTS('',3,(#149366,#149367,#149368,#149369,#149370,
#149371,#149372,#149373,#149374,#149375,#149376,#149377,#149378,#149379,
#149380,#149381,#149382,#149383,#149384,#149385,#149386,#149387,#149388,
#149389,#149390,#149391,#149392,#149393,#149394,#149395,#149396,#149397,
#149398,#149399,#149400,#149401,#149402,#149403,#149404,#149405,#149406,
#149407,#149408,#149409,#149410,#149411,#149412,#149413,#149414),
 .UNSPECIFIED.,.F.,.F.,(4,3,3,3,3,3,3,3,3,3,3,3,3,3,3,3,4),(0.,0.0510981392875666,
0.103679684270398,0.157057814696616,0.211633657635973,0.25,0.315602833834227,
0.375,0.442162015238332,0.5,0.575392432169574,0.652181332108927,0.73067248504618,
0.750000000000001,0.831704547321132,0.915852273660566,1.),.UNSPECIFIED.);
#4652=B_SPLINE_CURVE_WITH_KNOTS('',3,(#149429,#149430,#149431,#149432),
 .UNSPECIFIED.,.F.,.F.,(4,4),(0.,0.00454447370442107),.UNSPECIFIED.);
#4653=B_SPLINE_CURVE_WITH_KNOTS('',3,(#149459,#149460,#149461,#149462,#149463,
#149464,#149465,#149466),.UNSPECIFIED.,.F.,.F.,(4,2,2,4),(0.,0.5,0.75,1.),
 .UNSPECIFIED.);
#4654=B_SPLINE_CURVE_WITH_KNOTS('',3,(#149518,#149519,#149520,#149521,#149522,
#149523),.UNSPECIFIED.,.F.,.F.,(4,2,4),(0.,0.5,1.),.UNSPECIFIED.);
#4655=B_SPLINE_CURVE_WITH_KNOTS('',3,(#149558,#149559,#149560,#149561,#149562,
#149563,#149564,#149565,#149566,#149567),.UNSPECIFIED.,.F.,.F.,(4,2,2,2,
4),(0.,0.250000000000001,0.500000000000002,0.749999999999999,1.),
 .UNSPECIFIED.);
#4656=B_SPLINE_CURVE_WITH_KNOTS('',3,(#149574,#149575,#149576,#149577,#149578,
#149579,#149580,#149581,#149582,#149583),.UNSPECIFIED.,.F.,.F.,(4,3,3,4),
(0.,0.366159133847531,0.707490766021897,1.),.UNSPECIFIED.);
#4657=B_SPLINE_CURVE_WITH_KNOTS('',3,(#149587,#149588,#149589,#149590,#149591,
#149592),.UNSPECIFIED.,.F.,.F.,(4,2,4),(0.,0.5,1.),.UNSPECIFIED.);
#4658=B_SPLINE_CURVE_WITH_KNOTS('',3,(#149616,#149617,#149618,#149619,#149620,
#149621,#149622,#149623,#149624,#149625,#149626,#149627,#149628,#149629,
#149630,#149631,#149632,#149633,#149634,#149635,#149636,#149637,#149638,
#149639,#149640),.UNSPECIFIED.,.F.,.F.,(4,3,3,3,3,3,3,3,4),(0.,0.153482428046558,
0.30779152303746,0.461567879573118,0.5,0.654327083157327,0.810904002598426,
0.96838512301851,1.),.UNSPECIFIED.);
#4659=B_SPLINE_CURVE_WITH_KNOTS('',3,(#149676,#149677,#149678,#149679,#149680,
#149681),.UNSPECIFIED.,.F.,.F.,(4,2,4),(0.,0.5,1.),.UNSPECIFIED.);
#4660=B_SPLINE_CURVE_WITH_KNOTS('',3,(#149702,#149703,#149704,#149705,#149706,
#149707,#149708,#149709,#149710,#149711,#149712,#149713,#149714,#149715,
#149716,#149717,#149718,#149719,#149720,#149721,#149722,#149723,#149724,
#149725,#149726,#149727,#149728,#149729,#149730,#149731,#149732,#149733,
#149734,#149735,#149736,#149737,#149738),.UNSPECIFIED.,.F.,.F.,(4,3,3,3,
3,3,3,3,3,3,3,3,4),(0.,0.0966473935252569,0.197485545143943,0.295141620703053,
0.392110161524986,0.487415820015577,0.5,0.600531670333472,0.700398752750104,
0.794302669238309,0.886236884590961,0.975690548447645,1.),.UNSPECIFIED.);
#4661=B_SPLINE_CURVE_WITH_KNOTS('',3,(#149769,#149770,#149771,#149772,#149773,
#149774,#149775,#149776,#149777,#149778),.UNSPECIFIED.,.F.,.F.,(4,3,3,4),
(7.90081955571743E-6,0.5,0.750000000000001,1.),.UNSPECIFIED.);
#4662=B_SPLINE_CURVE_WITH_KNOTS('',3,(#149837,#149838,#149839,#149840,#149841,
#149842,#149843),.UNSPECIFIED.,.F.,.F.,(4,3,4),(4.04098200660582E-7,0.327146603495783,
1.),.UNSPECIFIED.);
#4663=B_SPLINE_CURVE_WITH_KNOTS('',3,(#149844,#149845,#149846,#149847),
 .UNSPECIFIED.,.F.,.F.,(4,4),(0.,1.),.UNSPECIFIED.);
#4664=B_SPLINE_CURVE_WITH_KNOTS('',3,(#149914,#149915,#149916,#149917,#149918,
#149919,#149920,#149921,#149922,#149923),.UNSPECIFIED.,.F.,.F.,(4,3,3,4),
(0.,0.49999999999992,0.749999999999959,0.999999993899122),.UNSPECIFIED.);
#4665=B_SPLINE_CURVE_WITH_KNOTS('',3,(#149960,#149961,#149962,#149963,#149964,
#149965,#149966,#149967,#149968,#149969),.UNSPECIFIED.,.F.,.F.,(4,2,2,2,
4),(6.1213090326977E-9,0.25,0.499999999999999,0.75,1.),.UNSPECIFIED.);
#4666=B_SPLINE_CURVE_WITH_KNOTS('',3,(#149984,#149985,#149986,#149987),
 .UNSPECIFIED.,.F.,.F.,(4,4),(0.,1.),.UNSPECIFIED.);
#4667=B_SPLINE_CURVE_WITH_KNOTS('',3,(#150020,#150021,#150022,#150023,#150024,
#150025,#150026,#150027,#150028,#150029),.UNSPECIFIED.,.F.,.F.,(4,2,2,2,
4),(0.,0.25,0.5,0.749999999999999,1.),.UNSPECIFIED.);
#4668=B_SPLINE_CURVE_WITH_KNOTS('',3,(#150065,#150066,#150067,#150068,#150069,
#150070,#150071,#150072,#150073,#150074),.UNSPECIFIED.,.F.,.F.,(4,2,2,2,
4),(0.,0.249999999999998,0.499999999999999,0.749999999999999,1.),
 .UNSPECIFIED.);
#4669=B_SPLINE_CURVE_WITH_KNOTS('',3,(#150082,#150083,#150084,#150085,#150086,
#150087),.UNSPECIFIED.,.F.,.F.,(4,2,4),(0.,0.5,1.),.UNSPECIFIED.);
#4670=B_SPLINE_CURVE_WITH_KNOTS('',3,(#150109,#150110,#150111,#150112,#150113,
#150114),.UNSPECIFIED.,.F.,.F.,(4,2,4),(0.,0.5,1.),.UNSPECIFIED.);
#4671=B_SPLINE_CURVE_WITH_KNOTS('',3,(#150150,#150151,#150152,#150153,#150154,
#150155,#150156,#150157,#150158,#150159),.UNSPECIFIED.,.F.,.F.,(4,2,2,2,
4),(0.,0.250000000000001,0.500000000000002,0.749999999999999,1.),
 .UNSPECIFIED.);
#4672=B_SPLINE_CURVE_WITH_KNOTS('',3,(#150184,#150185,#150186,#150187,#150188,
#150189),.UNSPECIFIED.,.F.,.F.,(4,2,4),(0.,0.5,1.),.UNSPECIFIED.);
#4673=B_SPLINE_CURVE_WITH_KNOTS('',3,(#150204,#150205,#150206,#150207),
 .UNSPECIFIED.,.F.,.F.,(4,4),(0.,1.),.UNSPECIFIED.);
#4674=B_SPLINE_CURVE_WITH_KNOTS('',3,(#150234,#150235,#150236,#150237,#150238,
#150239,#150240,#150241,#150242,#150243,#150244,#150245,#150246,#150247,
#150248,#150249,#150250,#150251,#150252,#150253,#150254,#150255,#150256,
#150257,#150258,#150259,#150260,#150261,#150262,#150263,#150264,#150265,
#150266,#150267,#150268,#150269,#150270,#150271,#150272,#150273),
 .UNSPECIFIED.,.F.,.F.,(4,3,3,3,3,3,3,3,3,3,3,3,3,4),(3.06013101603585E-15,
0.0868770599546466,0.174176392221001,0.261052249862412,0.346949892959567,
0.430648677455611,0.5,0.584788005264847,0.667617697597973,0.75,0.812804103608978,
0.874691742956029,0.937345871478015,1.),.UNSPECIFIED.);
#4675=B_SPLINE_CURVE_WITH_KNOTS('',3,(#150304,#150305,#150306,#150307,#150308,
#150309,#150310,#150311,#150312,#150313,#150314,#150315,#150316,#150317,
#150318,#150319,#150320,#150321,#150322,#150323,#150324,#150325,#150326,
#150327,#150328,#150329,#150330,#150331,#150332,#150333,#150334,#150335,
#150336,#150337,#150338,#150339,#150340,#150341,#150342,#150343,#150344,
#150345,#150346,#150347,#150348,#150349),.UNSPECIFIED.,.F.,.F.,(4,3,3,3,
3,3,3,3,3,3,3,3,3,3,3,4),(0.,0.0588319507752074,0.119280604150712,0.18064195969371,
0.243181726830164,0.25,0.32489127172958,0.401033799041576,0.478740210308195,
0.5,0.584292661882019,0.670546056491487,0.759159439922366,0.848371083490158,
0.937600152938783,1.),.UNSPECIFIED.);
#4676=B_SPLINE_CURVE_WITH_KNOTS('',3,(#150363,#150364,#150365,#150366),
 .UNSPECIFIED.,.F.,.F.,(4,4),(0.,1.),.UNSPECIFIED.);
#4677=B_SPLINE_CURVE_WITH_KNOTS('',3,(#150394,#150395,#150396,#150397,#150398,
#150399,#150400),.UNSPECIFIED.,.F.,.F.,(4,3,4),(0.,0.674038033463522,0.999999605243852),
 .UNSPECIFIED.);
#4678=B_SPLINE_CURVE_WITH_KNOTS('',3,(#150401,#150402,#150403,#150404),
 .UNSPECIFIED.,.F.,.F.,(4,4),(0.,1.),.UNSPECIFIED.);
#4679=B_SPLINE_CURVE_WITH_KNOTS('',3,(#150405,#150406,#150407,#150408,#150409,
#150410),.UNSPECIFIED.,.F.,.F.,(4,2,4),(0.,0.5,1.),.UNSPECIFIED.);
#4680=B_SPLINE_CURVE_WITH_KNOTS('',3,(#150477,#150478,#150479,#150480,#150481,
#150482),.UNSPECIFIED.,.F.,.F.,(4,2,4),(0.,0.499999999999999,1.),
 .UNSPECIFIED.);
#4681=B_SPLINE_CURVE_WITH_KNOTS('',3,(#150487,#150488,#150489,#150490,#150491,
#150492),.UNSPECIFIED.,.F.,.F.,(4,2,4),(0.,0.5,1.),.UNSPECIFIED.);
#4682=B_SPLINE_CURVE_WITH_KNOTS('',3,(#150543,#150544,#150545,#150546,#150547,
#150548,#150549,#150550,#150551,#150552,#150553,#150554,#150555,#150556,
#150557,#150558,#150559,#150560,#150561,#150562,#150563,#150564,#150565,
#150566,#150567,#150568,#150569,#150570,#150571,#150572,#150573,#150574,
#150575,#150576,#150577,#150578,#150579),.UNSPECIFIED.,.F.,.F.,(4,3,3,3,
3,3,3,3,3,3,3,3,4),(0.,0.096322507088443,0.197241880316332,0.294537759139576,
0.39113272840702,0.486046208564947,0.5,0.599805200905989,0.699853900679492,
0.79306779554781,0.884327816606269,0.973109138977564,1.),.UNSPECIFIED.);
#4683=B_SPLINE_CURVE_WITH_KNOTS('',3,(#150610,#150611,#150612,#150613,#150614,
#150615,#150616,#150617,#150618,#150619),.UNSPECIFIED.,.F.,.F.,(4,3,3,4),
(7.73028779751986E-6,0.499999999999999,0.75,1.),.UNSPECIFIED.);
#4684=B_SPLINE_CURVE_WITH_KNOTS('',3,(#150691,#150692,#150693,#150694,#150695,
#150696,#150697,#150698,#150699,#150700),.UNSPECIFIED.,.F.,.F.,(4,2,2,2,
4),(0.,0.250000000000004,0.5,0.750000000000003,1.),.UNSPECIFIED.);
#4685=B_SPLINE_CURVE_WITH_KNOTS('',3,(#150708,#150709,#150710,#150711,#150712,
#150713),.UNSPECIFIED.,.F.,.F.,(4,2,4),(0.,0.5,1.),.UNSPECIFIED.);
#4686=B_SPLINE_CURVE_WITH_KNOTS('',3,(#150773,#150774,#150775,#150776,#150777,
#150778),.UNSPECIFIED.,.F.,.F.,(4,2,4),(0.,0.5,1.),.UNSPECIFIED.);
#4687=B_SPLINE_CURVE_WITH_KNOTS('',3,(#150816,#150817,#150818,#150819,#150820,
#150821,#150822,#150823,#150824,#150825),.UNSPECIFIED.,.F.,.F.,(4,2,2,2,
4),(0.,0.249999999999999,0.499999999999999,0.75,1.),.UNSPECIFIED.);
#4688=B_SPLINE_CURVE_WITH_KNOTS('',3,(#150862,#150863,#150864,#150865,#150866,
#150867,#150868,#150869,#150870,#150871),.UNSPECIFIED.,.F.,.F.,(4,2,2,2,
4),(0.,0.25,0.5,0.749999999999999,1.),.UNSPECIFIED.);
#4689=B_SPLINE_CURVE_WITH_KNOTS('',3,(#150886,#150887,#150888,#150889),
 .UNSPECIFIED.,.F.,.F.,(4,4),(0.,0.0041383639263312),.UNSPECIFIED.);
#4690=B_SPLINE_CURVE_WITH_KNOTS('',3,(#150922,#150923,#150924,#150925,#150926,
#150927,#150928,#150929,#150930,#150931,#150932,#150933,#150934,#150935,
#150936,#150937,#150938,#150939,#150940,#150941,#150942,#150943,#150944,
#150945,#150946,#150947,#150948,#150949,#150950,#150951,#150952,#150953,
#150954,#150955,#150956,#150957,#150958,#150959,#150960,#150961,#150962,
#150963,#150964,#150965,#150966,#150967,#150968,#150969,#150970),
 .UNSPECIFIED.,.F.,.F.,(4,3,3,3,3,3,3,3,3,3,3,3,3,3,3,3,4),(0.,0.0814682051398938,
0.165734102569947,0.25,0.328395291585389,0.405548538423333,0.480663972186547,
0.5,0.57867163212605,0.655704680829147,0.730672357703364,0.750000000000001,
0.804753401868345,0.858198891364756,0.910821998101223,0.962154755762754,
1.),.UNSPECIFIED.);
#4691=B_SPLINE_CURVE_WITH_KNOTS('',3,(#151013,#151014,#151015,#151016,#151017,
#151018,#151019,#151020,#151021,#151022,#151023,#151024,#151025,#151026,
#151027,#151028,#151029,#151030,#151031,#151032,#151033,#151034,#151035,
#151036,#151037,#151038,#151039,#151040,#151041,#151042,#151043,#151044,
#151045,#151046,#151047,#151048,#151049,#151050,#151051,#151052,#151053,
#151054,#151055,#151056,#151057,#151058,#151059,#151060,#151061),
 .UNSPECIFIED.,.F.,.F.,(4,3,3,3,3,3,3,3,3,3,3,3,3,3,3,3,4),(0.,0.0508457726259258,
0.103170761367999,0.15628866585067,0.210605274562482,0.25,0.315356401070316,
0.375,0.441638820974095,0.5,0.575194165397271,0.651783139678669,0.730078138175237,
0.749999999999999,0.83154071027051,0.915770355135255,1.),.UNSPECIFIED.);
#4692=B_SPLINE_CURVE_WITH_KNOTS('',3,(#151076,#151077,#151078,#151079),
 .UNSPECIFIED.,.F.,.F.,(4,4),(0.,0.00385317783226068),.UNSPECIFIED.);
#4693=B_SPLINE_CURVE_WITH_KNOTS('',3,(#151105,#151106,#151107,#151108,#151109,
#151110,#151111,#151112),.UNSPECIFIED.,.F.,.F.,(4,2,2,4),(0.,0.5,0.750000000000001,
1.),.UNSPECIFIED.);
#4694=B_SPLINE_CURVE_WITH_KNOTS('',3,(#151123,#151124,#151125,#151126,#151127,
#151128),.UNSPECIFIED.,.F.,.F.,(4,2,4),(0.,0.5,1.),.UNSPECIFIED.);
#4695=B_SPLINE_CURVE_WITH_KNOTS('',3,(#151164,#151165,#151166,#151167),
 .UNSPECIFIED.,.F.,.F.,(4,4),(0.,1.),.UNSPECIFIED.);
#4696=B_SPLINE_CURVE_WITH_KNOTS('',3,(#151194,#151195,#151196,#151197,#151198,
#151199,#151200,#151201,#151202,#151203,#151204,#151205,#151206,#151207,
#151208,#151209,#151210,#151211,#151212,#151213,#151214,#151215,#151216,
#151217,#151218,#151219,#151220,#151221,#151222,#151223,#151224,#151225,
#151226,#151227,#151228,#151229,#151230,#151231,#151232,#151233,#151234,
#151235,#151236),.UNSPECIFIED.,.F.,.F.,(4,3,3,3,3,3,3,3,3,3,3,3,3,3,4),
(3.00632357117456E-15,0.0866568870700394,0.173726346313476,0.260357383779208,
0.346004233647263,0.429440823274784,0.5,0.584571854059349,0.667285927029675,
0.75,0.8125,0.874021143077118,0.937010571538559,0.996237991481499,1.),
 .UNSPECIFIED.);
#4697=B_SPLINE_CURVE_WITH_KNOTS('',3,(#151267,#151268,#151269,#151270,#151271,
#151272,#151273,#151274,#151275,#151276,#151277,#151278,#151279,#151280,
#151281,#151282,#151283,#151284,#151285,#151286,#151287,#151288,#151289,
#151290,#151291,#151292,#151293,#151294,#151295,#151296,#151297,#151298,
#151299,#151300,#151301,#151302,#151303,#151304,#151305,#151306,#151307,
#151308,#151309,#151310,#151311,#151312),.UNSPECIFIED.,.F.,.F.,(4,3,3,3,
3,3,3,3,3,3,3,3,3,3,3,4),(0.,0.0584822194913625,0.118574901578209,0.179574980246278,
0.241754287190893,0.25,0.324564021641555,0.40037551082833,0.477754744932888,
0.5,0.583489443865849,0.66889279993803,0.75661190226229,0.844919580084762,
0.933262852347954,1.),.UNSPECIFIED.);
#4698=B_SPLINE_CURVE_WITH_KNOTS('',3,(#151327,#151328,#151329,#151330),
 .UNSPECIFIED.,.F.,.F.,(4,4),(0.,1.),.UNSPECIFIED.);
#4699=B_SPLINE_CURVE_WITH_KNOTS('',3,(#151351,#151352,#151353,#151354,#151355,
#151356),.UNSPECIFIED.,.F.,.F.,(4,2,4),(0.,0.5,1.),.UNSPECIFIED.);
#4700=B_SPLINE_CURVE_WITH_KNOTS('',3,(#151392,#151393,#151394,#151395,#151396,
#151397,#151398,#151399,#151400,#151401),.UNSPECIFIED.,.F.,.F.,(4,2,2,2,
4),(0.,0.250000000000004,0.5,0.750000000000003,1.),.UNSPECIFIED.);
#4701=B_SPLINE_CURVE_WITH_KNOTS('',3,(#151409,#151410,#151411,#151412,#151413,
#151414),.UNSPECIFIED.,.F.,.F.,(4,2,4),(0.,0.499999999999998,1.),
 .UNSPECIFIED.);
#4702=B_SPLINE_CURVE_WITH_KNOTS('',3,(#151437,#151438,#151439,#151440,#151441,
#151442),.UNSPECIFIED.,.F.,.F.,(4,2,4),(0.,0.5,1.),.UNSPECIFIED.);
#4703=B_SPLINE_CURVE_WITH_KNOTS('',3,(#151480,#151481,#151482,#151483,#151484,
#151485,#151486,#151487,#151488,#151489),.UNSPECIFIED.,.F.,.F.,(4,2,2,2,
4),(0.,0.249999999999999,0.499999999999999,0.75,1.),.UNSPECIFIED.);
#4704=B_SPLINE_CURVE_WITH_KNOTS('',3,(#151520,#151521,#151522,#151523,#151524,
#151525,#151526,#151527),.UNSPECIFIED.,.F.,.F.,(4,2,2,4),(0.,0.25,0.5,1.),
 .UNSPECIFIED.);
#4705=B_SPLINE_CURVE_WITH_KNOTS('',3,(#151542,#151543,#151544,#151545),
 .UNSPECIFIED.,.F.,.F.,(4,4),(0.,1.),.UNSPECIFIED.);
#4706=B_SPLINE_CURVE_WITH_KNOTS('',3,(#151572,#151573,#151574,#151575,#151576,
#151577,#151578,#151579,#151580,#151581),.UNSPECIFIED.,.F.,.F.,(4,3,3,4),
(0.,0.49999999999996,0.749999999999982,0.99999999401614),.UNSPECIFIED.);
#4707=B_SPLINE_CURVE_WITH_KNOTS('',3,(#151611,#151612,#151613,#151614,#151615,
#151616,#151617,#151618,#151619,#151620,#151621,#151622,#151623,#151624,
#151625,#151626,#151627,#151628,#151629,#151630,#151631,#151632,#151633,
#151634,#151635,#151636,#151637,#151638,#151639,#151640,#151641,#151642,
#151643,#151644,#151645,#151646,#151647,#151648,#151649,#151650,#151651,
#151652,#151653),.UNSPECIFIED.,.F.,.F.,(4,3,3,3,3,3,3,3,3,3,3,3,3,3,4),
(0.,0.0628142014478904,0.126607829830903,0.191964238766059,0.25,0.328385271386528,
0.408052842259139,0.48922860882376,0.5,0.593627159335556,0.68989241160167,
0.789176056525988,0.889186506003656,0.988920801147075,1.),.UNSPECIFIED.);
#4708=B_SPLINE_CURVE_WITH_KNOTS('',3,(#151713,#151714,#151715,#151716,#151717,
#151718,#151719),.UNSPECIFIED.,.F.,.F.,(4,3,4),(0.,0.680762826204378,0.999999809903877),
 .UNSPECIFIED.);
#4709=B_SPLINE_CURVE_WITH_KNOTS('',3,(#151973,#151974,#151975,#151976),
 .UNSPECIFIED.,.F.,.F.,(4,4),(0.,1.),.UNSPECIFIED.);
#4710=B_SPLINE_CURVE_WITH_KNOTS('',3,(#152237,#152238,#152239,#152240,#152241,
#152242),.UNSPECIFIED.,.F.,.F.,(4,2,4),(0.,0.499999999999998,1.),
 .UNSPECIFIED.);
#4711=B_SPLINE_CURVE_WITH_KNOTS('',3,(#152351,#152352,#152353,#152354),
 .UNSPECIFIED.,.F.,.F.,(4,4),(0.,1.),.UNSPECIFIED.);
#4712=B_SPLINE_CURVE_WITH_KNOTS('',3,(#152584,#152585,#152586,#152587,#152588,
#152589,#152590,#152591),.UNSPECIFIED.,.F.,.F.,(4,2,2,4),(0.,0.25,0.500000000000001,
1.),.UNSPECIFIED.);
#4713=B_SPLINE_CURVE_WITH_KNOTS('',3,(#152619,#152620,#152621,#152622,#152623,
#152624,#152625,#152626,#152627,#152628,#152629,#152630,#152631,#152632,
#152633,#152634,#152635,#152636,#152637),.UNSPECIFIED.,.F.,.F.,(4,3,3,3,
3,3,4),(0.000623203325049932,0.00219889325760151,0.00382915155670995,0.00555512420845626,
0.00571003463709915,0.00756817415875739,0.00806753801901704),
 .UNSPECIFIED.);
#4714=B_SPLINE_CURVE_WITH_KNOTS('',3,(#152658,#152659,#152660,#152661,#152662,
#152663,#152664,#152665,#152666,#152667,#152668,#152669,#152670,#152671,
#152672,#152673),.UNSPECIFIED.,.F.,.F.,(4,3,3,3,3,4),(0.000539871559505675,
0.00223531956681298,0.00375574051851002,0.00457928549922768,0.00579560462260938,
0.00697160947751434),.UNSPECIFIED.);
#4715=B_SPLINE_CURVE_WITH_KNOTS('',3,(#152698,#152699,#152700,#152701,#152702,
#152703,#152704,#152705,#152706,#152707,#152708,#152709,#152710,#152711,
#152712,#152713,#152714,#152715,#152716,#152717,#152718,#152719,#152720,
#152721,#152722),.UNSPECIFIED.,.F.,.F.,(4,3,3,3,3,3,3,3,4),(0.00049834301207312,
0.00231282934721122,0.00337277528899485,0.00370896758807423,0.00446136300849288,
0.00522125339640802,0.00534496249690202,0.00614439986206378,0.00624720756634296),
 .UNSPECIFIED.);
#4716=B_SPLINE_CURVE_WITH_KNOTS('',3,(#152738,#152739,#152740,#152741,#152742,
#152743,#152744),.UNSPECIFIED.,.F.,.F.,(4,3,4),(7.49040536136306E-7,0.373399908132615,
1.),.UNSPECIFIED.);
#4717=B_SPLINE_CURVE_WITH_KNOTS('',3,(#152763,#152764,#152765,#152766,#152767,
#152768,#152769,#152770,#152771,#152772,#152773,#152774,#152775,#152776,
#152777,#152778,#152779,#152780,#152781),.UNSPECIFIED.,.F.,.F.,(4,3,3,3,
3,3,4),(0.000711431901436798,0.00260509764013045,0.00304924424816995,0.00478266330430852,
0.00644043866289917,0.00801739908984626,0.00833474438776835),
 .UNSPECIFIED.);
#4718=B_SPLINE_CURVE_WITH_KNOTS('',3,(#152792,#152793,#152794,#152795,#152796,
#152797),.UNSPECIFIED.,.F.,.F.,(4,2,4),(0.,0.428102325431166,1.),
 .UNSPECIFIED.);
#4719=B_SPLINE_CURVE_WITH_KNOTS('',3,(#152816,#152817,#152818,#152819,#152820,
#152821,#152822,#152823,#152824,#152825,#152826,#152827,#152828,#152829,
#152830,#152831),.UNSPECIFIED.,.F.,.F.,(4,3,3,3,3,4),(0.00061266112179062,
0.00182296639992156,0.0029850620415817,0.00388203060349254,0.00558489832474133,
0.00715140008519447),.UNSPECIFIED.);
#4720=B_SPLINE_CURVE_WITH_KNOTS('',3,(#152878,#152879,#152880,#152881,#152882,
#152883,#152884,#152885,#152886,#152887,#152888,#152889,#152890,#152891,
#152892,#152893,#152894,#152895,#152896,#152897,#152898,#152899,#152900,
#152901,#152902),.UNSPECIFIED.,.F.,.F.,(4,3,3,3,3,3,3,3,4),(0.000528035090325194,
0.0016124914159346,0.0026700115184638,0.00302714454343539,0.00341353154252654,
0.00423239659979929,0.00468651457632683,0.00549911074687934,0.0062990279947279),
 .UNSPECIFIED.);
#4721=B_SPLINE_CURVE_WITH_KNOTS('',3,(#152917,#152918,#152919,#152920,#152921,
#152922),.UNSPECIFIED.,.F.,.F.,(4,2,4),(0.,0.509180994354165,1.),
 .UNSPECIFIED.);
#4722=B_SPLINE_CURVE_WITH_KNOTS('',3,(#152941,#152942,#152943,#152944,#152945,
#152946,#152947,#152948,#152949,#152950,#152951,#152952,#152953,#152954,
#152955,#152956,#152957,#152958,#152959),.UNSPECIFIED.,.F.,.F.,(4,3,3,3,
3,3,4),(0.00049889453195992,0.00225071250487917,0.00337891514771613,0.00374149706694668,
0.00465083407571109,0.00559677886660822,0.00625893576407251),
 .UNSPECIFIED.);
#4723=B_SPLINE_CURVE_WITH_KNOTS('',3,(#152974,#152975,#152976,#152977,#152978,
#152979,#152980,#152981),.UNSPECIFIED.,.F.,.F.,(4,2,2,4),(0.,0.570298119392456,
0.858868992686398,1.),.UNSPECIFIED.);
#4724=B_SPLINE_CURVE_WITH_KNOTS('',3,(#153006,#153007,#153008,#153009,#153010,
#153011,#153012,#153013,#153014,#153015,#153016,#153017,#153018,#153019,
#153020,#153021,#153022,#153023,#153024),.UNSPECIFIED.,.F.,.F.,(4,3,3,3,
3,3,4),(0.000543628862815408,0.00167393673136798,0.00258252559983906,0.00379688806421997,
0.00467674795200451,0.00601647986746607,0.00704595220449218),
 .UNSPECIFIED.);
#4725=B_SPLINE_CURVE_WITH_KNOTS('',3,(#153034,#153035,#153036,#153037,#153038,
#153039,#153040),.UNSPECIFIED.,.F.,.F.,(4,3,4),(0.,0.625174273651469,0.99999924413068),
 .UNSPECIFIED.);
#4726=B_SPLINE_CURVE_WITH_KNOTS('',3,(#153059,#153060,#153061,#153062,#153063,
#153064,#153065,#153066,#153067,#153068,#153069,#153070,#153071,#153072,
#153073,#153074,#153075,#153076,#153077),.UNSPECIFIED.,.F.,.F.,(4,3,3,3,
3,3,4),(0.000633514536432522,0.00221236722518429,0.00384759398055232,0.00558513688102114,
0.00588295359619705,0.00776048988119671,0.00821913918141333),
 .UNSPECIFIED.);
#4727=B_SPLINE_CURVE_WITH_KNOTS('',3,(#153094,#153095,#153096,#153097),
 .UNSPECIFIED.,.F.,.F.,(4,4),(0.000856775130582955,0.0102382230284107),
 .UNSPECIFIED.);
#4728=B_SPLINE_CURVE_WITH_KNOTS('',3,(#153098,#153099,#153100,#153101),
 .UNSPECIFIED.,.F.,.F.,(4,4),(1.21683837293175E-6,1.),.UNSPECIFIED.);
#4729=B_SPLINE_CURVE_WITH_KNOTS('',3,(#153109,#153110,#153111,#153112),
 .UNSPECIFIED.,.F.,.F.,(4,4),(0.000801783579032724,0.0101814026529808),
 .UNSPECIFIED.);
#4730=B_SPLINE_CURVE_WITH_KNOTS('',3,(#153127,#153128,#153129,#153130),
 .UNSPECIFIED.,.F.,.F.,(4,4),(0.,0.999998771610134),.UNSPECIFIED.);
#4731=B_SPLINE_CURVE_WITH_KNOTS('',3,(#153158,#153159,#153160,#153161),
 .UNSPECIFIED.,.F.,.F.,(4,4),(0.,0.999998144078028),.UNSPECIFIED.);
#4732=B_SPLINE_CURVE_WITH_KNOTS('',3,(#153174,#153175,#153176,#153177),
 .UNSPECIFIED.,.F.,.F.,(4,4),(0.000716623500636008,0.00919276877023496),
 .UNSPECIFIED.);
#4733=B_SPLINE_CURVE_WITH_KNOTS('',3,(#153179,#153180,#153181,#153182),
 .UNSPECIFIED.,.F.,.F.,(4,4),(0.00078229444191847,0.00926194220748866),
 .UNSPECIFIED.);
#4734=B_SPLINE_CURVE_WITH_KNOTS('',3,(#153204,#153205,#153206,#153207),
 .UNSPECIFIED.,.F.,.F.,(4,4),(1.30575596808862E-6,1.),.UNSPECIFIED.);
#4735=B_SPLINE_CURVE_WITH_KNOTS('',3,(#153225,#153226,#153227,#153228),
 .UNSPECIFIED.,.F.,.F.,(4,4),(0.000874668174674732,0.0104577126980746),
 .UNSPECIFIED.);
#4736=B_SPLINE_CURVE_WITH_KNOTS('',3,(#153230,#153231,#153232,#153233),
 .UNSPECIFIED.,.F.,.F.,(4,4),(0.000819410081741501,0.0104007046320713),
 .UNSPECIFIED.);
#4737=B_SPLINE_CURVE_WITH_KNOTS('',3,(#153246,#153247,#153248,#153249),
 .UNSPECIFIED.,.F.,.F.,(4,4),(0.,0.999998694225143),.UNSPECIFIED.);
#4738=B_SPLINE_CURVE_WITH_KNOTS('',3,(#153259,#153260,#153261,#153262,#153263,
#153264,#153265),.UNSPECIFIED.,.F.,.F.,(4,3,4),(0.,0.672852549108075,0.999999595945834),
 .UNSPECIFIED.);
#4739=B_SPLINE_CURVE_WITH_KNOTS('',3,(#153284,#153285,#153286,#153287,#153288,
#153289,#153290,#153291,#153292,#153293,#153294,#153295,#153296),
 .UNSPECIFIED.,.F.,.F.,(4,3,3,3,4),(0.000731998639840557,0.00321503108606918,
0.00587687390150681,0.00707184840840047,0.00939432936633357),
 .UNSPECIFIED.);
#4740=B_SPLINE_CURVE_WITH_KNOTS('',3,(#153298,#153299,#153300,#153301,#153302,
#153303,#153304,#153305,#153306,#153307,#153308,#153309,#153310),
 .UNSPECIFIED.,.F.,.F.,(4,3,3,3,4),(0.000799595655510347,0.00312305020211246,
0.00581514086609625,0.00831497793887529,0.00946542910228819),
 .UNSPECIFIED.);
#4741=B_SPLINE_CURVE_WITH_KNOTS('',3,(#153353,#153354,#153355,#153356,#153357,
#153358,#153359,#153360,#153361,#153362,#153363,#153364,#153365),
 .UNSPECIFIED.,.F.,.F.,(4,3,3,3,4),(0.000734608576009405,0.00325207345695062,
0.00595173535838772,0.00710294415665481,0.0094247370890218),
 .UNSPECIFIED.);
#4742=B_SPLINE_CURVE_WITH_KNOTS('',3,(#153367,#153368,#153369,#153370,#153371,
#153372,#153373,#153374,#153375,#153376,#153377,#153378,#153379),
 .UNSPECIFIED.,.F.,.F.,(4,3,3,3,4),(0.000801891157765995,0.00312464263181538,
0.00585483490545202,0.00838933971211676,0.00949544874465978),
 .UNSPECIFIED.);
#4743=B_SPLINE_CURVE_WITH_KNOTS('',3,(#153398,#153399,#153400,#153401,#153402,
#153403,#153404),.UNSPECIFIED.,.F.,.F.,(4,3,4),(3.94809455506897E-7,0.325960924204632,
1.),.UNSPECIFIED.);
#4744=B_SPLINE_CURVE_WITH_KNOTS('',3,(#153419,#153420,#153421,#153422),
 .UNSPECIFIED.,.F.,.F.,(4,4),(1.27679595912943E-6,1.),.UNSPECIFIED.);
#4745=B_SPLINE_CURVE_WITH_KNOTS('',3,(#153435,#153436,#153437,#153438),
 .UNSPECIFIED.,.F.,.F.,(4,4),(0.000876507471789284,0.010482245256776),
 .UNSPECIFIED.);
#4746=B_SPLINE_CURVE_WITH_KNOTS('',3,(#153440,#153441,#153442,#153443),
 .UNSPECIFIED.,.F.,.F.,(4,4),(0.000821546900565006,0.0104255562384257),
 .UNSPECIFIED.);
#4747=B_SPLINE_CURVE_WITH_KNOTS('',3,(#153456,#153457,#153458,#153459),
 .UNSPECIFIED.,.F.,.F.,(4,4),(0.,0.999998701161504),.UNSPECIFIED.);
#4748=B_SPLINE_CURVE_WITH_KNOTS('',3,(#153498,#153499,#153500,#153501,#153502,
#153503,#153504,#153505,#153506,#153507,#153508,#153509,#153510,#153511,
#153512,#153513),.UNSPECIFIED.,.F.,.F.,(4,3,3,3,3,4),(0.,0.234070507545302,
0.476434331275526,0.724187361959147,0.979964419025256,0.999998630096402),
 .UNSPECIFIED.);
#4749=B_SPLINE_CURVE_WITH_KNOTS('',3,(#153515,#153516,#153517,#153518,#153519,
#153520,#153521,#153522,#153523,#153524,#153525,#153526,#153527,#153528,
#153529,#153530),.UNSPECIFIED.,.F.,.F.,(4,3,3,3,3,4),(0.,0.25,0.495026107729062,
0.747513053864531,0.982920025273709,1.),.UNSPECIFIED.);
#4750=B_SPLINE_CURVE_WITH_KNOTS('',3,(#153533,#153534,#153535,#153536),
 .UNSPECIFIED.,.F.,.F.,(4,4),(0.,0.00385317783226068),.UNSPECIFIED.);
#4751=B_SPLINE_CURVE_WITH_KNOTS('',3,(#153551,#153552,#153553,#153554),
 .UNSPECIFIED.,.F.,.F.,(4,4),(0.000821546900565006,0.0104255562384257),
 .UNSPECIFIED.);
#4752=B_SPLINE_CURVE_WITH_KNOTS('',3,(#153555,#153556,#153557,#153558,#153559,
#153560,#153561,#153562,#153563,#153564,#153565,#153566,#153567,#153568,
#153569,#153570,#153571,#153572,#153573,#153574,#153575,#153576,#153577,
#153578,#153579,#153580,#153581,#153582,#153583,#153584,#153585,#153586,
#153587,#153588,#153589,#153590,#153591,#153592,#153593,#153594,#153595,
#153596,#153597,#153598,#153599,#153600,#153601,#153602,#153603,#153604,
#153605,#153606,#153607,#153608,#153609,#153610,#153611,#153612,#153613,
#153614,#153615,#153616,#153617,#153618,#153619,#153620,#153621,#153622,
#153623,#153624,#153625,#153626,#153627,#153628,#153629,#153630,#153631,
#153632,#153633,#153634,#153635,#153636,#153637,#153638,#153639,#153640,
#153641,#153642,#153643,#153644,#153645,#153646,#153647,#153648,#153649,
#153650,#153651,#153652,#153653,#153654,#153655,#153656,#153657,#153658,
#153659,#153660,#153661,#153662,#153663,#153664,#153665,#153666,#153667,
#153668,#153669,#153670,#153671,#153672,#153673,#153674,#153675,#153676,
#153677,#153678,#153679,#153680,#153681,#153682,#153683,#153684),
 .UNSPECIFIED.,.F.,.F.,(4,3,3,3,3,3,3,3,3,3,3,3,3,3,3,3,3,3,3,3,3,3,3,3,
3,3,3,3,3,3,3,3,3,3,3,3,3,3,3,3,3,3,3,4),(0.,0.0557300906452975,0.108669123630166,
0.16220672376782,0.206103361884435,0.228051680942743,0.239025840471897,
0.244512920236474,0.247256460118762,0.247942345089334,0.248143462518013,
0.25000000000105,0.28525026953172,0.319586978968953,0.35282166185891,0.375000000001453,
0.406706302027439,0.437500000001657,0.468750000001765,0.484375000001819,
0.492187500001848,0.496093750001873,0.496600762442034,0.498046875001885,
0.499023437501879,0.499267578126878,0.499450683595627,0.500000000001873,
0.548163509889134,0.598706375701685,0.625000000001358,0.679498466368399,
0.687500000001101,0.718750000000971,0.734375000000903,0.742187500000869,
0.746093750000855,0.74894953049805,0.750000000000842,0.806399791364996,
0.865484672157621,0.926633610120571,0.991716815566447,0.999967809902464),
 .UNSPECIFIED.);
#4753=B_SPLINE_CURVE_WITH_KNOTS('',3,(#153685,#153686,#153687,#153688,#153689,
#153690,#153691,#153692,#153693,#153694,#153695,#153696,#153697,#153698,
#153699,#153700,#153701,#153702,#153703,#153704,#153705,#153706,#153707,
#153708,#153709,#153710,#153711,#153712,#153713,#153714,#153715,#153716,
#153717,#153718,#153719,#153720,#153721,#153722,#153723,#153724,#153725,
#153726,#153727,#153728,#153729,#153730,#153731,#153732,#153733,#153734,
#153735,#153736,#153737,#153738,#153739,#153740,#153741,#153742,#153743,
#153744,#153745,#153746,#153747,#153748,#153749,#153750,#153751,#153752,
#153753,#153754,#153755,#153756,#153757,#153758,#153759,#153760,#153761,
#153762,#153763,#153764,#153765,#153766,#153767,#153768,#153769,#153770,
#153771,#153772,#153773,#153774,#153775,#153776,#153777,#153778,#153779,
#153780,#153781,#153782,#153783,#153784,#153785,#153786,#153787,#153788,
#153789,#153790),.UNSPECIFIED.,.F.,.F.,(4,3,3,3,3,3,3,3,3,3,3,3,3,3,3,3,
3,3,3,3,3,3,3,3,3,3,3,3,3,3,3,3,3,3,3,4),(1.17227643855583E-8,0.0584463886983609,
0.113231413189016,0.124999999993601,0.175293985242217,0.223827131926143,
0.248046874987312,0.249999999987212,0.253226722903014,0.327396670298302,
0.374999999980813,0.387436040596127,0.422635833669734,0.44231367500128,
0.498046874974511,0.499999999974409,0.503900809428433,0.556200109021788,
0.562499999970921,0.613653614494003,0.624511718717445,0.624999999967415,
0.643506073008206,0.662090682222471,0.680808883543099,0.699860002069781,
0.718997321555854,0.738880238098642,0.749023437478302,0.749999999978387,
0.751151936740845,0.80273675767465,0.854547924236456,0.906490674366243,
0.958653924668795,1.),.UNSPECIFIED.);
#4754=B_SPLINE_CURVE_WITH_KNOTS('',3,(#153794,#153795,#153796,#153797),
 .UNSPECIFIED.,.F.,.F.,(4,4),(0.000876507471789284,0.010482245256776),
 .UNSPECIFIED.);
#4755=B_SPLINE_CURVE_WITH_KNOTS('',3,(#153814,#153815,#153816,#153817,#153818,
#153819,#153820,#153821,#153822,#153823,#153824,#153825,#153826,#153827,
#153828,#153829),.UNSPECIFIED.,.F.,.F.,(4,3,3,3,3,4),(1.34720087857547E-6,
0.250001010400659,0.492522569244812,0.729567600587388,0.959631099383557,
1.),.UNSPECIFIED.);
#4756=B_SPLINE_CURVE_WITH_KNOTS('',3,(#153830,#153831,#153832,#153833,#153834,
#153835,#153836,#153837,#153838,#153839,#153840,#153841,#153842,#153843,
#153844,#153845,#153846,#153847,#153848,#153849,#153850,#153851,#153852,
#153853,#153854,#153855,#153856,#153857,#153858,#153859,#153860,#153861,
#153862,#153863,#153864,#153865,#153866,#153867,#153868,#153869,#153870,
#153871,#153872,#153873,#153874,#153875,#153876,#153877,#153878,#153879,
#153880,#153881,#153882,#153883,#153884,#153885,#153886,#153887,#153888,
#153889,#153890,#153891,#153892,#153893,#153894,#153895,#153896,#153897,
#153898,#153899,#153900,#153901,#153902,#153903,#153904,#153905,#153906,
#153907,#153908,#153909,#153910,#153911,#153912,#153913,#153914,#153915,
#153916,#153917,#153918,#153919,#153920,#153921,#153922,#153923,#153924,
#153925,#153926,#153927,#153928,#153929,#153930,#153931,#153932,#153933,
#153934,#153935,#153936,#153937,#153938,#153939,#153940,#153941,#153942,
#153943,#153944,#153945,#153946,#153947),.UNSPECIFIED.,.F.,.F.,(4,3,3,3,
3,3,3,3,3,3,3,3,3,3,3,3,3,3,3,3,3,3,3,3,3,3,3,3,3,3,3,3,3,3,3,3,3,3,3,4),
(3.18229911605046E-5,0.0312499999998296,0.0976865037949654,0.124999999999318,
0.182154808287466,0.187499999998977,0.218749999998807,0.234374999998721,
0.242187499998673,0.246093749998648,0.249795185825512,0.249999999998623,
0.25263968832415,0.345710027577214,0.374999999997752,0.437499999997316,
0.468749999997092,0.484374999996979,0.492187499996922,0.496093749996894,
0.499023437496878,0.499999999996877,0.510199912070258,0.541121704839755,
0.562499999997224,0.593749999997398,0.624999999997572,0.656249999997749,
0.687499999997927,0.718749999998099,0.73437499999819,0.742187499998239,
0.746093749998268,0.748046874998287,0.749999999998305,0.803805944723814,
0.858633463684494,0.914040237915491,0.97030630160842,1.),.UNSPECIFIED.);
#4757=B_SPLINE_CURVE_WITH_KNOTS('',3,(#153948,#153949,#153950,#153951,#153952,
#153953,#153954,#153955,#153956,#153957,#153958,#153959,#153960,#153961,
#153962,#153963,#153964,#153965,#153966,#153967,#153968,#153969,#153970,
#153971,#153972,#153973,#153974,#153975,#153976,#153977,#153978,#153979,
#153980,#153981,#153982,#153983,#153984,#153985,#153986,#153987,#153988,
#153989,#153990,#153991,#153992,#153993,#153994,#153995,#153996,#153997,
#153998,#153999,#154000,#154001,#154002,#154003,#154004,#154005,#154006,
#154007,#154008,#154009,#154010,#154011,#154012,#154013,#154014,#154015,
#154016,#154017,#154018,#154019,#154020,#154021,#154022,#154023,#154024,
#154025,#154026,#154027,#154028,#154029,#154030,#154031,#154032,#154033,
#154034,#154035,#154036,#154037,#154038,#154039,#154040,#154041,#154042,
#154043,#154044,#154045,#154046,#154047,#154048,#154049,#154050,#154051,
#154052,#154053,#154054,#154055,#154056,#154057,#154058,#154059,#154060,
#154061,#154062,#154063,#154064,#154065),.UNSPECIFIED.,.F.,.F.,(4,3,3,3,
3,3,3,3,3,3,3,3,3,3,3,3,3,3,3,3,3,3,3,3,3,3,3,3,3,3,3,3,3,3,3,3,3,3,3,4),
(8.34701282724942E-14,0.051104738268533,0.10144538171935,0.125000000000385,
0.177843714271829,0.187500000000577,0.218750000000668,0.234375000000713,
0.242187500000736,0.246093750000747,0.249259269767851,0.250000000000758,
0.312500000000785,0.375000000000812,0.437500000000845,0.468750000000868,
0.484375000000879,0.492187500000885,0.496093750000882,0.498901284980378,
0.500000000000879,0.548101422879337,0.598678455292358,0.625000000000582,
0.678879260280721,0.713530942889026,0.730856784193179,0.739519704845255,
0.743851165171293,0.746016895334312,0.747099760415822,0.747641192956576,
0.748033970104978,0.748182625497331,0.75000000000027,0.799033416400584,
0.850056418490652,0.902463987625779,0.957816263810161,0.99999998849761),
 .UNSPECIFIED.);
#4758=B_SPLINE_CURVE_WITH_KNOTS('',3,(#154070,#154071,#154072,#154073,#154074,
#154075,#154076,#154077,#154078,#154079,#154080,#154081,#154082,#154083,
#154084,#154085),.UNSPECIFIED.,.F.,.F.,(4,3,3,3,3,4),(0.,0.230911412126844,
0.468240019037909,0.709718394074353,0.957565639068108,1.),.UNSPECIFIED.);
#4759=B_SPLINE_CURVE_WITH_KNOTS('',3,(#154086,#154087,#154088,#154089),
 .UNSPECIFIED.,.F.,.F.,(4,4),(0.,0.0041383639263312),.UNSPECIFIED.);
#4760=B_SPLINE_CURVE_WITH_KNOTS('',3,(#154094,#154095,#154096,#154097,#154098,
#154099,#154100,#154101,#154102,#154103,#154104,#154105,#154106,#154107,
#154108,#154109,#154110,#154111,#154112,#154113,#154114,#154115,#154116,
#154117,#154118,#154119,#154120,#154121,#154122,#154123,#154124,#154125,
#154126,#154127,#154128,#154129,#154130,#154131,#154132,#154133,#154134,
#154135,#154136,#154137,#154138,#154139,#154140,#154141,#154142,#154143,
#154144,#154145,#154146,#154147,#154148),.UNSPECIFIED.,.F.,.F.,(4,3,3,3,
3,3,3,3,3,3,3,3,3,3,3,3,3,3,4),(0.,0.0632048838696367,0.127921929473124,
0.195281348929666,0.249999999999537,0.321563999196289,0.374999999999306,
0.437499999999191,0.468749999999113,0.484374999999066,0.492187499999073,
0.498658068589728,0.49999999999908,0.59334512646801,0.688354285547602,0.785958734092665,
0.885147124073086,0.986657689579597,0.999999999999993),.UNSPECIFIED.);
#4761=B_SPLINE_CURVE_WITH_KNOTS('',3,(#154149,#154150,#154151,#154152,#154153,
#154154,#154155,#154156,#154157,#154158,#154159,#154160,#154161,#154162,
#154163,#154164,#154165,#154166,#154167,#154168,#154169,#154170,#154171,
#154172,#154173,#154174,#154175,#154176,#154177,#154178,#154179,#154180,
#154181,#154182,#154183,#154184,#154185,#154186,#154187,#154188,#154189,
#154190,#154191,#154192,#154193,#154194,#154195,#154196,#154197,#154198,
#154199,#154200,#154201,#154202,#154203,#154204,#154205,#154206,#154207,
#154208,#154209,#154210,#154211,#154212,#154213,#154214,#154215,#154216,
#154217,#154218,#154219,#154220,#154221,#154222,#154223,#154224,#154225,
#154226,#154227),.UNSPECIFIED.,.F.,.F.,(4,3,3,3,3,3,3,3,3,3,3,3,3,3,3,3,
3,3,3,3,3,3,3,3,3,3,4),(0.,0.0822388323866184,0.125000000000039,0.203743158983877,
0.249314582772148,0.282486317967716,0.332958488475827,0.36498976178814,
0.394097477848506,0.473638989559932,0.48437500000016,0.494250955016996,
0.50000000000016,0.522888790187838,0.595779308163083,0.625000000000112,
0.697913150166242,0.734375000000034,0.742187500000031,0.748069533718682,
0.750000000000028,0.77031774650841,0.824713583203907,0.880483079532543,
0.937161849130565,0.99522645066287,1.),.UNSPECIFIED.);
#4762=B_SPLINE_CURVE_WITH_KNOTS('',3,(#154258,#154259,#154260,#154261,#154262,
#154263,#154264,#154265,#154266,#154267,#154268,#154269,#154270),
 .UNSPECIFIED.,.F.,.F.,(4,3,3,3,4),(0.,0.264159105979835,0.53472290465884,
0.816453844755532,1.),.UNSPECIFIED.);
#4763=B_SPLINE_CURVE_WITH_KNOTS('',3,(#154275,#154276,#154277,#154278,#154279,
#154280,#154281,#154282,#154283,#154284,#154285,#154286,#154287,#154288,
#154289,#154290,#154291,#154292,#154293,#154294,#154295,#154296,#154297,
#154298,#154299,#154300,#154301,#154302,#154303,#154304,#154305,#154306,
#154307,#154308,#154309,#154310,#154311,#154312,#154313,#154314,#154315,
#154316,#154317,#154318,#154319,#154320,#154321,#154322,#154323,#154324,
#154325,#154326,#154327,#154328,#154329,#154330,#154331,#154332,#154333,
#154334,#154335,#154336,#154337,#154338,#154339,#154340,#154341,#154342,
#154343,#154344,#154345,#154346,#154347,#154348,#154349,#154350),
 .UNSPECIFIED.,.F.,.F.,(4,3,3,3,3,3,3,3,3,3,3,3,3,3,3,3,3,3,3,3,3,3,3,3,
3,4),(0.,0.0869793228874166,0.124999999999851,0.199030619385428,0.245213138173373,
0.273061238771005,0.32653577523374,0.364990790896793,0.39936394258499,0.484374999999404,
0.494494116758885,0.499999999999391,0.514138283290129,0.599085378376048,
0.62499999999927,0.68749999999923,0.71874999999921,0.7343749999992,0.742187499999195,
0.748148077780528,0.74999999999919,0.804514066320572,0.85851274981487,0.911762507617596,
0.963252162150356,1.),.UNSPECIFIED.);
#4764=B_SPLINE_CURVE_WITH_KNOTS('',3,(#154351,#154352,#154353,#154354,#154355,
#154356,#154357,#154358,#154359,#154360,#154361,#154362,#154363,#154364,
#154365,#154366,#154367),.UNSPECIFIED.,.F.,.F.,(4,2,2,2,1,1,1,2,2,4),(0.,
0.250000000000024,0.375000000000034,0.437500000000038,0.468750000000039,
0.48437500000004,0.492187500000042,0.496093750000043,0.500000000000043,
1.),.UNSPECIFIED.);
#4765=B_SPLINE_CURVE_WITH_KNOTS('',3,(#154370,#154371,#154372,#154373,#154374,
#154375,#154376,#154377,#154378,#154379,#154380,#154381,#154382,#154383,
#154384,#154385,#154386,#154387,#154388,#154389,#154390,#154391,#154392,
#154393,#154394,#154395,#154396,#154397),.UNSPECIFIED.,.F.,.F.,(4,3,3,3,
3,3,3,3,3,4),(0.,0.163940541204184,0.333114778935776,0.498046874999602,
0.499999999999603,0.50003591612275,0.639284504482635,0.781135100020726,
0.927355971067516,1.),.UNSPECIFIED.);
#4766=B_SPLINE_CURVE_WITH_KNOTS('',3,(#154399,#154400,#154401,#154402,#154403,
#154404,#154405,#154406,#154407,#154408,#154409,#154410,#154411,#154412,
#154413,#154414),.UNSPECIFIED.,.F.,.F.,(4,3,3,3,3,4),(4.19542126215829E-7,
0.2338396427201,0.339508613309501,0.56969049637124,0.786423133885641,1.),
 .UNSPECIFIED.);
#4767=B_SPLINE_CURVE_WITH_KNOTS('',3,(#154415,#154416,#154417,#154418,#154419,
#154420,#154421,#154422,#154423,#154424,#154425,#154426,#154427,#154428,
#154429,#154430,#154431,#154432,#154433),.UNSPECIFIED.,.F.,.F.,(4,3,3,3,
3,3,4),(0.,0.206475863478243,0.405461434738878,0.600838474120482,0.800419237060241,
0.988221216743423,1.),.UNSPECIFIED.);
#4768=B_SPLINE_CURVE_WITH_KNOTS('',3,(#154453,#154454,#154455,#154456,#154457,
#154458,#154459,#154460,#154461,#154462,#154463,#154464,#154465,#154466,
#154467,#154468,#154469,#154470,#154471,#154472,#154473,#154474,#154475,
#154476,#154477,#154478,#154479,#154480,#154481,#154482,#154483,#154484,
#154485,#154486,#154487,#154488,#154489,#154490,#154491,#154492,#154493,
#154494,#154495,#154496,#154497,#154498,#154499,#154500,#154501,#154502,
#154503,#154504,#154505,#154506,#154507),.UNSPECIFIED.,.F.,.F.,(4,3,3,3,
3,3,3,3,3,3,3,3,3,3,3,3,3,3,4),(0.,0.0708860635919454,0.140367818135151,
0.207849069624002,0.249999999999808,0.315086127274307,0.378502885651149,
0.437499999999646,0.46874999999961,0.484374999999591,0.492187499999582,
0.496093749999571,0.49999999999956,0.592295283092291,0.685212828844724,
0.74999999999978,0.845125224808466,0.93995821969057,1.),.UNSPECIFIED.);
#4769=B_SPLINE_CURVE_WITH_KNOTS('',3,(#154509,#154510,#154511,#154512,#154513,
#154514,#154515,#154516,#154517,#154518,#154519,#154520,#154521),
 .UNSPECIFIED.,.F.,.F.,(4,3,3,3,4),(0.000801891157765995,0.00312464263181538,
0.00585483490544955,0.00838933971206778,0.00949544874465978),
 .UNSPECIFIED.);
#4770=B_SPLINE_CURVE_WITH_KNOTS('',3,(#154522,#154523,#154524,#154525,#154526,
#154527,#154528,#154529,#154530,#154531,#154532,#154533,#154534,#154535,
#154536,#154537,#154538,#154539,#154540,#154541,#154542,#154543,#154544,
#154545,#154546,#154547,#154548,#154549,#154550,#154551,#154552,#154553,
#154554,#154555,#154556,#154557,#154558,#154559,#154560,#154561,#154562,
#154563,#154564,#154565,#154566,#154567,#154568,#154569,#154570,#154571,
#154572,#154573,#154574,#154575,#154576,#154577,#154578,#154579,#154580,
#154581,#154582,#154583,#154584,#154585,#154586,#154587,#154588,#154589,
#154590,#154591,#154592,#154593,#154594,#154595,#154596,#154597,#154598,
#154599,#154600),.UNSPECIFIED.,.F.,.F.,(4,3,3,3,3,3,3,3,3,3,3,3,3,3,3,3,
3,3,3,3,3,3,3,3,3,3,4),(0.,0.0585857549643099,0.115353783315363,0.124999999999788,
0.179827236593527,0.187499999999675,0.218749999999618,0.234374999999589,
0.242187499999581,0.246093749999577,0.249999999999573,0.340405595850071,
0.374999999999441,0.437499999999376,0.468749999999343,0.484374999999334,
0.492187499999323,0.496093749999317,0.499999999999311,0.564089078061403,
0.628856738294988,0.694923673370365,0.749999999999655,0.818394393929608,
0.887854174965178,0.959138516319878,1.),.UNSPECIFIED.);
#4771=B_SPLINE_CURVE_WITH_KNOTS('',3,(#154605,#154606,#154607,#154608,#154609,
#154610,#154611,#154612,#154613,#154614,#154615,#154616,#154617),
 .UNSPECIFIED.,.F.,.F.,(4,3,3,3,4),(0.000734608576009405,0.00325207345693861,
0.00595173535833846,0.00710294415665481,0.0094247370890218),
 .UNSPECIFIED.);
#4772=B_SPLINE_CURVE_WITH_KNOTS('',3,(#154638,#154639,#154640,#154641,#154642,
#154643,#154644,#154645,#154646,#154647,#154648,#154649,#154650,#154651,
#154652,#154653,#154654,#154655,#154656,#154657,#154658,#154659,#154660,
#154661,#154662,#154663,#154664,#154665,#154666,#154667,#154668,#154669,
#154670,#154671,#154672,#154673,#154674,#154675,#154676,#154677,#154678,
#154679,#154680,#154681,#154682,#154683,#154684,#154685,#154686,#154687,
#154688,#154689,#154690,#154691,#154692,#154693,#154694,#154695,#154696,
#154697,#154698,#154699,#154700,#154701,#154702,#154703,#154704,#154705,
#154706,#154707,#154708,#154709,#154710,#154711,#154712,#154713,#154714,
#154715,#154716,#154717,#154718,#154719,#154720,#154721,#154722),
 .UNSPECIFIED.,.F.,.F.,(4,3,3,3,3,3,3,3,3,3,3,3,3,3,3,3,3,3,3,3,3,3,3,3,
3,3,3,3,4),(0.,0.0689593679009489,0.131763023438308,0.190881511719319,0.220440755859824,
0.235220377930077,0.23891528344764,0.241686462585813,0.242263277167448,
0.248759657469872,0.25000000000033,0.33324707772351,0.37500000000042,0.406250000000441,
0.437500000000461,0.468750000000477,0.484375000000485,0.492187500000485,
0.49609375000048,0.499458273983288,0.500000000000475,0.562500000000416,
0.609375000000371,0.679687500000304,0.750000000000238,0.825469442525012,
0.875000000000119,0.957373830350825,0.999990011221892),.UNSPECIFIED.);
#4773=B_SPLINE_CURVE_WITH_KNOTS('',3,(#154724,#154725,#154726,#154727,#154728,
#154729,#154730,#154731,#154732,#154733,#154734,#154735,#154736,#154737,
#154738,#154739),.UNSPECIFIED.,.F.,.F.,(4,3,3,3,3,4),(0.,0.215215032325329,
0.443136127796081,0.660489501790431,0.894219532612502,0.999999580511107),
 .UNSPECIFIED.);
#4774=B_SPLINE_CURVE_WITH_KNOTS('',3,(#154740,#154741,#154742,#154743,#154744,
#154745,#154746,#154747,#154748,#154749,#154750,#154751,#154752,#154753,
#154754,#154755,#154756,#154757,#154758,#154759,#154760,#154761,#154762,
#154763,#154764,#154765,#154766,#154767,#154768,#154769,#154770,#154771,
#154772,#154773,#154774,#154775,#154776,#154777,#154778,#154779,#154780,
#154781,#154782,#154783,#154784,#154785,#154786,#154787,#154788,#154789,
#154790,#154791,#154792,#154793,#154794,#154795,#154796,#154797,#154798,
#154799,#154800,#154801,#154802,#154803,#154804,#154805,#154806),
 .UNSPECIFIED.,.F.,.F.,(4,3,3,3,3,3,3,3,3,3,3,3,3,3,3,3,3,3,3,3,3,3,4),
(6.92056175195316E-9,0.0702731195301449,0.124999999999889,0.18554687499984,
0.246093749999791,0.249999999999789,0.252383107672787,0.351045659631276,
0.374999999999917,0.4417236941113,0.496093750000031,0.500000000000033,0.5024909590578,
0.581475430365078,0.625000000000024,0.656250000000022,0.68750000000002,
0.723520265942537,0.750000000000016,0.812500000000012,0.859375000000009,
0.968403554298818,1.),.UNSPECIFIED.);
#4775=B_SPLINE_CURVE_WITH_KNOTS('',3,(#154855,#154856,#154857,#154858,#154859,
#154860,#154861,#154862,#154863,#154864,#154865,#154866,#154867),
 .UNSPECIFIED.,.F.,.F.,(4,3,3,3,4),(0.000799595655510347,0.00312305020211246,
0.00581514086608832,0.00831497793897699,0.00946542910228819),
 .UNSPECIFIED.);
#4776=B_SPLINE_CURVE_WITH_KNOTS('',3,(#154869,#154870,#154871,#154872,#154873,
#154874,#154875,#154876,#154877,#154878,#154879,#154880,#154881,#154882,
#154883,#154884,#154885,#154886,#154887,#154888,#154889,#154890,#154891,
#154892,#154893,#154894,#154895,#154896,#154897,#154898,#154899,#154900,
#154901,#154902,#154903,#154904,#154905,#154906,#154907,#154908,#154909,
#154910,#154911,#154912,#154913,#154914,#154915,#154916,#154917,#154918,
#154919,#154920,#154921,#154922,#154923,#154924,#154925,#154926,#154927,
#154928,#154929,#154930,#154931,#154932,#154933,#154934,#154935,#154936,
#154937,#154938,#154939,#154940,#154941,#154942,#154943,#154944),
 .UNSPECIFIED.,.F.,.F.,(4,3,3,3,3,3,3,3,3,3,3,3,3,3,3,3,3,3,3,3,3,3,3,3,
3,4),(2.00063521920002E-13,0.0591216028065502,0.117082720868845,0.125000000000246,
0.187500000000369,0.21875000000043,0.234375000000461,0.242187500000477,
0.246093750000481,0.250000000000486,0.346565173458337,0.375000000000604,
0.46785306768388,0.496093750000721,0.499268681857144,0.500000000000721,
0.552855316954113,0.562500000000631,0.609375000000563,0.666076030952446,
0.722777061904329,0.75000000000036,0.821201537843276,0.87500000000018,0.954964862982302,
0.999999992138103),.UNSPECIFIED.);
#4777=B_SPLINE_CURVE_WITH_KNOTS('',3,(#154946,#154947,#154948,#154949,#154950,
#154951,#154952,#154953,#154954,#154955,#154956,#154957,#154958,#154959,
#154960,#154961),.UNSPECIFIED.,.F.,.F.,(4,3,3,3,3,4),(4.29492375686315E-7,
0.233750383144039,0.340769128367464,0.569821997539196,0.785318576880101,
1.),.UNSPECIFIED.);
#4778=B_SPLINE_CURVE_WITH_KNOTS('',3,(#154962,#154963,#154964,#154965,#154966,
#154967,#154968,#154969,#154970,#154971,#154972,#154973,#154974,#154975,
#154976,#154977,#154978,#154979,#154980),.UNSPECIFIED.,.F.,.F.,(4,2,2,2,
1,1,1,2,2,2,4),(1.10457472515728E-5,0.249999999999914,0.374999999999875,
0.437499999999855,0.468749999999841,0.48437499999983,0.492187499999825,
0.496093749999822,0.49999999999982,0.74999999999991,1.),.UNSPECIFIED.);
#4779=B_SPLINE_CURVE_WITH_KNOTS('',3,(#154984,#154985,#154986,#154987,#154988,
#154989,#154990,#154991,#154992,#154993,#154994,#154995,#154996),
 .UNSPECIFIED.,.F.,.F.,(4,3,3,3,4),(0.000731998639840557,0.00321503108606633,
0.00587687390152188,0.00707184840840047,0.00939432936633357),
 .UNSPECIFIED.);
#4780=B_SPLINE_CURVE_WITH_KNOTS('',3,(#155019,#155020,#155021,#155022,#155023,
#155024,#155025,#155026,#155027,#155028,#155029,#155030,#155031,#155032,
#155033,#155034),.UNSPECIFIED.,.F.,.F.,(4,3,3,3,3,4),(0.,0.213825330538362,
0.440424504941056,0.659229336836956,0.892889616266567,0.999999570551571),
 .UNSPECIFIED.);
#4781=B_SPLINE_CURVE_WITH_KNOTS('',3,(#155035,#155036,#155037,#155038,#155039,
#155040,#155041,#155042,#155043,#155044,#155045,#155046,#155047,#155048,
#155049,#155050,#155051,#155052,#155053,#155054,#155055,#155056,#155057,
#155058,#155059,#155060,#155061,#155062,#155063,#155064,#155065,#155066,
#155067,#155068,#155069,#155070,#155071,#155072,#155073,#155074,#155075,
#155076,#155077,#155078,#155079,#155080,#155081,#155082,#155083,#155084,
#155085,#155086,#155087,#155088,#155089,#155090,#155091,#155092,#155093,
#155094,#155095,#155096,#155097,#155098,#155099,#155100,#155101,#155102,
#155103,#155104,#155105,#155106,#155107,#155108,#155109,#155110,#155111,
#155112,#155113,#155114,#155115,#155116,#155117,#155118,#155119,#155120,
#155121,#155122,#155123,#155124,#155125,#155126,#155127,#155128,#155129,
#155130,#155131,#155132,#155133,#155134,#155135,#155136,#155137,#155138,
#155139,#155140,#155141,#155142,#155143,#155144,#155145,#155146,#155147,
#155148,#155149),.UNSPECIFIED.,.F.,.F.,(4,3,3,3,3,3,3,3,3,3,3,3,3,3,3,3,
3,3,3,3,3,3,3,3,3,3,3,3,3,3,3,3,3,3,3,3,3,3,4),(7.04705196002291E-9,0.0707966831419206,
0.124999999999487,0.185546874999241,0.246093749998995,0.249999999998986,
0.252359143174423,0.349332373867497,0.374999999998765,0.441778173658313,
0.498046874998564,0.499999999998558,0.503193747522868,0.544115575223839,
0.562499999998729,0.59374999999881,0.609374999998851,0.617187499998871,
0.621093749998881,0.623046874998886,0.624999999998891,0.648786262364636,
0.67299328259835,0.687499999998841,0.712035681312914,0.718749999998816,
0.734374999998814,0.742187499998798,0.746093749998791,0.748046874998788,
0.749023437498787,0.749267578123787,0.749633789061286,0.749999999998785,
0.751100775325356,0.815360308562951,0.879496436852205,0.943465428441742,
1.),.UNSPECIFIED.);
#4782=B_SPLINE_CURVE_WITH_KNOTS('',3,(#155150,#155151,#155152,#155153,#155154,
#155155,#155156,#155157,#155158,#155159,#155160,#155161,#155162,#155163,
#155164,#155165,#155166,#155167,#155168,#155169,#155170,#155171,#155172,
#155173,#155174,#155175,#155176,#155177,#155178,#155179,#155180,#155181,
#155182,#155183,#155184,#155185,#155186,#155187,#155188,#155189,#155190,
#155191,#155192,#155193,#155194,#155195,#155196,#155197,#155198,#155199,
#155200,#155201,#155202,#155203,#155204,#155205,#155206,#155207,#155208,
#155209,#155210,#155211,#155212,#155213,#155214,#155215,#155216,#155217,
#155218,#155219,#155220,#155221,#155222,#155223,#155224,#155225,#155226,
#155227,#155228,#155229,#155230,#155231,#155232,#155233,#155234,#155235,
#155236,#155237),.UNSPECIFIED.,.F.,.F.,(4,3,3,3,3,3,3,3,3,3,3,3,3,3,3,3,
3,3,3,3,3,3,3,3,3,3,3,3,3,4),(0.,0.069441977607991,0.132550750715234,0.191275375357326,
0.220637687678371,0.235318843838894,0.238989132879025,0.241741849659123,
0.242574401393792,0.249103102141126,0.249999999999417,0.333593575490244,
0.374999999999471,0.406249999999485,0.437499999999498,0.468749999999512,
0.48437499999951,0.4921874999995,0.496093749999504,0.49946576207654,0.499999999999507,
0.562499999999569,0.609374999999615,0.679687499999684,0.749999999999754,
0.812499999999815,0.891008696034271,0.906249999999908,0.989050414896488,
0.999989783729688),.UNSPECIFIED.);
#4783=B_SPLINE_CURVE_WITH_KNOTS('',3,(#155242,#155243,#155244,#155245,#155246,
#155247,#155248,#155249,#155250,#155251,#155252,#155253,#155254,#155255,
#155256,#155257,#155258,#155259,#155260),.UNSPECIFIED.,.F.,.F.,(4,3,3,3,
3,3,4),(0.,0.185535625540095,0.37453758023397,0.569181963234827,0.767518059616989,
0.971532910971265,1.),.UNSPECIFIED.);
#4784=B_SPLINE_CURVE_WITH_KNOTS('',3,(#155261,#155262,#155263,#155264,#155265,
#155266,#155267,#155268,#155269,#155270,#155271,#155272,#155273,#155274,
#155275,#155276,#155277,#155278,#155279,#155280,#155281,#155282,#155283,
#155284,#155285,#155286,#155287,#155288),.UNSPECIFIED.,.F.,.F.,(4,3,3,3,
3,3,3,3,3,4),(0.,0.144905414369803,0.28628718158065,0.424070029202907,0.49804687499993,
0.4999598944088,0.499999999999929,0.669838342253323,0.834919171126662,1.),
 .UNSPECIFIED.);
#4785=B_SPLINE_CURVE_WITH_KNOTS('',3,(#155290,#155291,#155292,#155293,#155294,
#155295,#155296,#155297,#155298,#155299,#155300,#155301,#155302,#155303,
#155304,#155305),.UNSPECIFIED.,.F.,.F.,(4,2,2,2,1,1,2,2,4),(0.,0.249999999999503,
0.374999999999255,0.437499999999149,0.46874999999912,0.484374999999104,
0.492187499999097,0.499999999999091,1.),.UNSPECIFIED.);
#4786=B_SPLINE_CURVE_WITH_KNOTS('',3,(#155309,#155310,#155311,#155312,#155313,
#155314,#155315,#155316,#155317,#155318,#155319,#155320,#155321,#155322,
#155323,#155324),.UNSPECIFIED.,.F.,.F.,(4,3,3,3,3,4),(0.,0.227672506314025,
0.443584943305661,0.653737655502801,0.855842244026882,1.),.UNSPECIFIED.);
#4787=B_SPLINE_CURVE_WITH_KNOTS('',3,(#155325,#155326,#155327,#155328,#155329,
#155330,#155331,#155332,#155333,#155334,#155335,#155336,#155337,#155338,
#155339,#155340,#155341,#155342,#155343,#155344,#155345,#155346,#155347,
#155348,#155349,#155350,#155351,#155352,#155353,#155354,#155355,#155356,
#155357,#155358,#155359,#155360,#155361,#155362,#155363,#155364,#155365,
#155366,#155367),.UNSPECIFIED.,.F.,.F.,(4,3,3,3,3,3,3,3,3,3,3,3,3,3,4),
(0.,0.13007938114654,0.249999999999951,0.363303681175031,0.461966998162734,
0.496093749999904,0.499999999999904,0.500099040742567,0.58565984718958,
0.670743841464584,0.749999999999952,0.825272702193343,0.900311502331646,
0.975559281692812,1.),.UNSPECIFIED.);
#4788=B_SPLINE_CURVE_WITH_KNOTS('',3,(#155379,#155380,#155381,#155382,#155383,
#155384,#155385,#155386,#155387,#155388,#155389,#155390,#155391,#155392,
#155393,#155394,#155395,#155396,#155397,#155398,#155399,#155400,#155401,
#155402,#155403,#155404,#155405,#155406,#155407,#155408,#155409,#155410,
#155411,#155412,#155413,#155414,#155415,#155416,#155417,#155418,#155419,
#155420,#155421,#155422,#155423,#155424,#155425,#155426,#155427,#155428,
#155429,#155430,#155431,#155432,#155433,#155434,#155435,#155436,#155437,
#155438,#155439,#155440,#155441,#155442,#155443,#155444,#155445,#155446,
#155447,#155448),.UNSPECIFIED.,.F.,.F.,(4,3,3,3,3,3,3,3,3,3,3,3,3,3,3,3,
3,3,3,3,3,3,3,4),(0.,0.0468252282105052,0.0625000000000385,0.111671414475211,
0.161991880251615,0.215493244493045,0.234375000000112,0.242187500000095,
0.248559869936323,0.250000000000078,0.328196609751316,0.374999999999974,
0.432074481984959,0.469350116156201,0.478281110394449,0.484374999999853,
0.494498947188093,0.499999999999825,0.575316649815483,0.654093366024209,
0.717727187058543,0.806910800011888,0.905137785263374,1.),.UNSPECIFIED.);
#4789=B_SPLINE_CURVE_WITH_KNOTS('',3,(#155451,#155452,#155453,#155454,#155455,
#155456,#155457,#155458,#155459,#155460,#155461,#155462,#155463,#155464,
#155465,#155466,#155467,#155468,#155469,#155470,#155471,#155472,#155473,
#155474,#155475,#155476,#155477,#155478,#155479,#155480,#155481,#155482,
#155483,#155484,#155485,#155486,#155487,#155488,#155489,#155490,#155491,
#155492,#155493,#155494,#155495,#155496,#155497,#155498,#155499,#155500,
#155501,#155502,#155503,#155504,#155505,#155506,#155507,#155508,#155509,
#155510,#155511,#155512,#155513,#155514,#155515,#155516,#155517),
 .UNSPECIFIED.,.F.,.F.,(4,3,3,3,3,3,3,3,3,3,3,3,3,3,3,3,3,3,3,3,3,3,4),
(0.,0.100728557328594,0.199752664823961,0.29623824427798,0.375000000000072,
0.437500000000091,0.468750000000082,0.484375000000094,0.49448394416446,
0.500000000000106,0.581634289657116,0.660418077435017,0.687500000000417,
0.718750000000468,0.734375000000501,0.742187500000507,0.748155000660193,
0.750000000000513,0.803598400947262,0.856014092687743,0.907470928865847,
0.957106875072136,1.),.UNSPECIFIED.);
#4790=B_SPLINE_CURVE_WITH_KNOTS('',3,(#155520,#155521,#155522,#155523),
 .UNSPECIFIED.,.F.,.F.,(4,4),(0.,0.00454447370442107),.UNSPECIFIED.);
#4791=B_SPLINE_CURVE_WITH_KNOTS('',3,(#155525,#155526,#155527,#155528,#155529,
#155530,#155531,#155532,#155533,#155534,#155535,#155536,#155537,#155538,
#155539,#155540),.UNSPECIFIED.,.F.,.F.,(4,3,3,3,3,4),(0.,0.228718000314846,
0.465913558148734,0.708585998597329,0.959609200667992,0.999998621928069),
 .UNSPECIFIED.);
#4792=B_SPLINE_CURVE_WITH_KNOTS('',3,(#155541,#155542,#155543,#155544,#155545,
#155546,#155547,#155548,#155549,#155550,#155551,#155552,#155553,#155554,
#155555,#155556),.UNSPECIFIED.,.F.,.F.,(4,3,3,3,3,4),(0.,0.25,0.485591974112626,
0.71711850744027,0.943391881004635,1.),.UNSPECIFIED.);
#4793=B_SPLINE_CURVE_WITH_KNOTS('',3,(#155570,#155571,#155572,#155573,#155574,
#155575,#155576,#155577,#155578,#155579,#155580,#155581,#155582,#155583,
#155584,#155585,#155586,#155587,#155588,#155589,#155590,#155591,#155592,
#155593,#155594,#155595,#155596,#155597,#155598,#155599,#155600,#155601,
#155602,#155603,#155604,#155605,#155606,#155607,#155608,#155609,#155610,
#155611,#155612,#155613,#155614,#155615,#155616,#155617,#155618,#155619,
#155620,#155621,#155622,#155623,#155624,#155625,#155626,#155627,#155628,
#155629,#155630,#155631,#155632,#155633,#155634,#155635,#155636,#155637,
#155638,#155639,#155640,#155641,#155642,#155643,#155644,#155645,#155646,
#155647,#155648,#155649,#155650,#155651,#155652,#155653,#155654,#155655,
#155656,#155657,#155658,#155659,#155660,#155661,#155662,#155663,#155664,
#155665,#155666,#155667,#155668,#155669,#155670,#155671,#155672),
 .UNSPECIFIED.,.F.,.F.,(4,3,3,3,3,3,3,3,3,3,3,3,3,3,3,3,3,3,3,3,3,3,3,3,
3,3,3,3,3,3,3,3,3,3,4),(1.17970694753713E-8,0.0587741274153463,0.113845507635111,
0.124999999999931,0.175544805271069,0.224300881613421,0.248046874999881,
0.24999999999988,0.253204771838808,0.328016123646574,0.374999999999958,
0.387439460343596,0.422619984926577,0.442478326522261,0.498046875000016,
0.500000000000013,0.503886071361003,0.555745869040186,0.562500000000114,
0.593750000000165,0.609375000000191,0.617187500000204,0.62109375000021,
0.625000000000216,0.687500000000337,0.718750000000397,0.734375000000433,
0.742187500000451,0.746093750000454,0.750000000000456,0.751226796212957,
0.81468448368076,0.875000000000228,0.938570202129679,1.),.UNSPECIFIED.);
#4794=B_SPLINE_CURVE_WITH_KNOTS('',3,(#155674,#155675,#155676,#155677),
 .UNSPECIFIED.,.F.,.F.,(4,4),(0.000819410081741501,0.0104007046320713),
 .UNSPECIFIED.);
#4795=B_SPLINE_CURVE_WITH_KNOTS('',3,(#155678,#155679,#155680,#155681,#155682,
#155683,#155684,#155685,#155686,#155687,#155688,#155689,#155690,#155691,
#155692,#155693,#155694,#155695,#155696,#155697,#155698,#155699,#155700,
#155701,#155702,#155703,#155704,#155705,#155706,#155707,#155708,#155709,
#155710,#155711,#155712,#155713,#155714,#155715,#155716,#155717,#155718,
#155719,#155720,#155721,#155722,#155723,#155724,#155725,#155726,#155727,
#155728,#155729,#155730,#155731,#155732,#155733,#155734,#155735,#155736,
#155737,#155738,#155739,#155740,#155741,#155742,#155743,#155744,#155745,
#155746,#155747,#155748,#155749,#155750,#155751,#155752,#155753,#155754,
#155755,#155756,#155757,#155758,#155759,#155760,#155761,#155762,#155763,
#155764,#155765,#155766,#155767,#155768,#155769,#155770,#155771,#155772,
#155773,#155774,#155775,#155776,#155777,#155778,#155779,#155780,#155781,
#155782,#155783,#155784,#155785,#155786,#155787,#155788,#155789,#155790,
#155791,#155792,#155793,#155794,#155795,#155796,#155797,#155798,#155799,
#155800,#155801,#155802,#155803,#155804,#155805,#155806,#155807),
 .UNSPECIFIED.,.F.,.F.,(4,3,3,3,3,3,3,3,3,3,3,3,3,3,3,3,3,3,3,3,3,3,3,3,
3,3,3,3,3,3,3,3,3,3,3,3,3,3,3,3,3,3,3,4),(0.,0.0560216703334645,0.109196961913243,
0.163091705635906,0.206545852817787,0.228272926408728,0.239136463204198,
0.244568231601933,0.247284115800801,0.247963086850518,0.248140226278139,
0.249999999999668,0.284700972192902,0.318528987481047,0.351288118199589,
0.374999999998669,0.406284954267776,0.437499999998176,0.46874999999793,
0.484374999997806,0.492187499997762,0.496093749997764,0.496366305327242,
0.498046874997764,0.499023437497763,0.499267578122763,0.499450683591513,
0.499999999997763,0.548181491589199,0.598745345927553,0.624999999998493,
0.67952017226536,0.687499999998851,0.718749999999024,0.73437499999911,0.742187499999145,
0.746093749999162,0.748968852511644,0.74999999999918,0.806751404285961,
0.866224004565218,0.927798228713741,0.993361011423219,0.999967748998623),
 .UNSPECIFIED.);
#4796=B_SPLINE_CURVE_WITH_KNOTS('',3,(#155812,#155813,#155814,#155815),
 .UNSPECIFIED.,.F.,.F.,(4,4),(0.000874668174674732,0.0104577126980746),
 .UNSPECIFIED.);
#4797=B_SPLINE_CURVE_WITH_KNOTS('',3,(#155830,#155831,#155832,#155833,#155834,
#155835,#155836,#155837,#155838,#155839,#155840,#155841,#155842,#155843,
#155844,#155845,#155846,#155847,#155848,#155849,#155850,#155851,#155852,
#155853,#155854,#155855,#155856,#155857,#155858,#155859,#155860,#155861,
#155862,#155863,#155864,#155865,#155866,#155867,#155868,#155869,#155870,
#155871,#155872,#155873,#155874,#155875,#155876,#155877,#155878,#155879,
#155880,#155881,#155882,#155883,#155884,#155885,#155886,#155887,#155888,
#155889,#155890,#155891,#155892,#155893,#155894,#155895,#155896,#155897,
#155898,#155899,#155900,#155901,#155902,#155903,#155904,#155905,#155906,
#155907,#155908,#155909,#155910,#155911,#155912,#155913,#155914,#155915,
#155916,#155917,#155918,#155919,#155920,#155921,#155922,#155923,#155924,
#155925,#155926,#155927,#155928,#155929,#155930,#155931,#155932,#155933,
#155934,#155935,#155936,#155937,#155938,#155939,#155940,#155941,#155942,
#155943,#155944,#155945,#155946,#155947,#155948,#155949,#155950),
 .UNSPECIFIED.,.F.,.F.,(4,3,3,3,3,3,3,3,3,3,3,3,3,3,3,3,3,3,3,3,3,3,3,3,
3,3,3,3,3,3,3,3,3,3,3,3,3,3,3,3,4),(0.,0.0513261920791295,0.101891051484157,
0.125000000000127,0.178106823792157,0.187500000000194,0.218750000000228,
0.234375000000247,0.242187500000254,0.24609375000026,0.249264080962771,
0.250000000000267,0.312500000000385,0.375000000000502,0.437500000000617,
0.468750000000675,0.484375000000701,0.492187500000714,0.496093750000717,
0.498911066758421,0.500000000000721,0.548095655335943,0.598666505518088,
0.625000000000672,0.678884598604091,0.713546942576494,0.730878114562696,
0.739543700555797,0.743876493552347,0.746042890050623,0.74712608829976,
0.747667687424329,0.747967116726168,0.748168766823433,0.748209286548898,
0.750000000000624,0.79929200859889,0.850588465705387,0.903284387505033,
0.958942755428889,0.999999988259552),.UNSPECIFIED.);
#4798=B_SPLINE_CURVE_WITH_KNOTS('',3,(#155952,#155953,#155954,#155955,#155956,
#155957,#155958,#155959,#155960,#155961,#155962,#155963,#155964,#155965,
#155966,#155967),.UNSPECIFIED.,.F.,.F.,(4,3,3,3,3,4),(1.37805369294038E-6,
0.25000103354027,0.491490606329696,0.727506144562777,0.956522966635118,
1.),.UNSPECIFIED.);
#4799=B_SPLINE_CURVE_WITH_KNOTS('',3,(#155968,#155969,#155970,#155971,#155972,
#155973,#155974,#155975,#155976,#155977,#155978,#155979,#155980,#155981,
#155982,#155983,#155984,#155985,#155986,#155987,#155988,#155989,#155990,
#155991,#155992,#155993,#155994,#155995,#155996,#155997,#155998,#155999,
#156000,#156001,#156002,#156003,#156004,#156005,#156006,#156007,#156008,
#156009,#156010,#156011,#156012,#156013,#156014,#156015,#156016,#156017,
#156018,#156019,#156020,#156021,#156022,#156023,#156024,#156025,#156026,
#156027,#156028,#156029,#156030,#156031,#156032,#156033,#156034,#156035,
#156036,#156037,#156038,#156039,#156040,#156041,#156042,#156043,#156044,
#156045,#156046,#156047,#156048,#156049,#156050,#156051,#156052,#156053,
#156054,#156055,#156056,#156057,#156058,#156059,#156060,#156061,#156062,
#156063,#156064,#156065,#156066,#156067,#156068,#156069,#156070,#156071,
#156072,#156073,#156074,#156075,#156076,#156077,#156078,#156079,#156080,
#156081,#156082,#156083,#156084,#156085,#156086,#156087,#156088,#156089,
#156090,#156091,#156092,#156093,#156094,#156095,#156096,#156097,#156098,
#156099,#156100,#156101,#156102,#156103,#156104,#156105,#156106,#156107,
#156108,#156109,#156110,#156111,#156112,#156113,#156114,#156115,#156116,
#156117,#156118,#156119,#156120,#156121,#156122,#156123,#156124),
 .UNSPECIFIED.,.F.,.F.,(4,3,3,3,3,3,3,3,3,3,3,3,3,3,3,3,3,3,3,3,3,3,3,3,
3,3,3,3,3,3,3,3,3,3,3,3,3,3,3,3,3,3,3,3,3,3,3,3,3,3,3,3,4),(0.000325310152520073,
0.00195312500001419,0.00207519531251508,0.00230407714845424,0.00390625000002838,
0.00585937500004257,0.00683593750004902,0.00781250000005548,0.0156250000001289,
0.0285965136258737,0.0312500000002777,0.0468750000004264,0.0580811522582563,
0.0625000000005752,0.0937500000008728,0.109375000001022,0.117187500001095,
0.123820195931982,0.125000000001169,0.187500000001785,0.218750000002089,
0.234375000002238,0.242187500002309,0.246093750002341,0.250000000002374,
0.252616048242064,0.344815548524214,0.375000000003363,0.437500000003857,
0.468750000004101,0.484375000004223,0.492187500004284,0.496093750004315,
0.499023437504339,0.500000000004347,0.51082228289493,0.541375719978749,
0.56250000000385,0.593750000003602,0.625000000003353,0.656250000003104,
0.687500000002855,0.718750000002607,0.734375000002485,0.742187500002423,
0.746093750002393,0.748046875002378,0.750000000002362,0.804086151359939,
0.859205844316772,0.914912172240495,0.971483295233683,1.),.UNSPECIFIED.);
#4800=B_SPLINE_CURVE_WITH_KNOTS('',3,(#156148,#156149,#156150,#156151),
 .UNSPECIFIED.,.F.,.F.,(4,4),(0.,0.00425966609677044),.UNSPECIFIED.);
#4801=B_SPLINE_CURVE_WITH_KNOTS('',3,(#156154,#156155,#156156,#156157,#156158,
#156159,#156160,#156161,#156162,#156163,#156164,#156165,#156166,#156167,
#156168,#156169),.UNSPECIFIED.,.F.,.F.,(4,3,3,3,3,4),(0.,0.230186031233572,
0.466791142229912,0.707543496522388,0.954682760211977,1.),.UNSPECIFIED.);
#4802=B_SPLINE_CURVE_WITH_KNOTS('',3,(#156173,#156174,#156175,#156176,#156177,
#156178,#156179,#156180,#156181,#156182,#156183,#156184,#156185,#156186,
#156187,#156188),.UNSPECIFIED.,.F.,.F.,(4,3,3,3,3,4),(0.,0.236247566825257,
0.482337922300788,0.667935821043213,0.875614812669031,0.999999798365662),
 .UNSPECIFIED.);
#4803=B_SPLINE_CURVE_WITH_KNOTS('',3,(#156190,#156191,#156192,#156193,#156194,
#156195,#156196,#156197,#156198,#156199,#156200,#156201,#156202),
 .UNSPECIFIED.,.F.,.F.,(4,3,3,3,4),(0.,0.274763476845488,0.544290520349838,
0.806409249078579,1.),.UNSPECIFIED.);
#4804=B_SPLINE_CURVE_WITH_KNOTS('',3,(#156205,#156206,#156207,#156208),
 .UNSPECIFIED.,.F.,.F.,(4,4),(0.,0.00407596620376747),.UNSPECIFIED.);
#4805=B_SPLINE_CURVE_WITH_KNOTS('',3,(#156212,#156213,#156214,#156215,#156216,
#156217,#156218,#156219,#156220,#156221,#156222,#156223,#156224),
 .UNSPECIFIED.,.F.,.F.,(4,3,3,3,4),(0.,0.237145647143792,0.483293389898376,
0.74164604880973,0.999998707721084),.UNSPECIFIED.);
#4806=B_SPLINE_CURVE_WITH_KNOTS('',3,(#156226,#156227,#156228,#156229,#156230,
#156231,#156232,#156233,#156234,#156235),.UNSPECIFIED.,.F.,.F.,(4,3,3,4),
(0.,0.384739188680616,0.759105290249364,1.),.UNSPECIFIED.);
#4807=B_SPLINE_CURVE_WITH_KNOTS('',3,(#156279,#156280,#156281,#156282),
 .UNSPECIFIED.,.F.,.F.,(4,4),(0.00078229444191847,0.00926194220748866),
 .UNSPECIFIED.);
#4808=B_SPLINE_CURVE_WITH_KNOTS('',3,(#156284,#156285,#156286,#156287,#156288,
#156289,#156290,#156291,#156292,#156293,#156294,#156295,#156296,#156297,
#156298,#156299,#156300,#156301,#156302,#156303,#156304,#156305,#156306,
#156307,#156308,#156309,#156310,#156311,#156312,#156313,#156314,#156315,
#156316,#156317,#156318,#156319,#156320,#156321,#156322,#156323,#156324,
#156325,#156326,#156327,#156328,#156329,#156330,#156331,#156332,#156333,
#156334,#156335,#156336,#156337,#156338,#156339,#156340,#156341,#156342,
#156343,#156344,#156345,#156346,#156347,#156348,#156349,#156350,#156351,
#156352,#156353,#156354,#156355,#156356),.UNSPECIFIED.,.F.,.F.,(4,3,3,3,
3,3,3,3,3,3,3,3,3,3,3,3,3,3,3,3,3,3,3,3,4),(8.44091860321908E-14,0.0624999999999906,
0.124999999999897,0.187499999999841,0.218749999999817,0.234374999999809,
0.242187499999805,0.246093749999806,0.249999999999808,0.347890901443095,
0.37499999999986,0.469604033890482,0.496093749999897,0.499305817827702,
0.499999999999895,0.55402564985833,0.562499999999909,0.609374999999918,
0.667671420454354,0.723088971645676,0.749999999999948,0.825882492417378,
0.874999999999974,0.960462506686326,0.999999979523105),.UNSPECIFIED.);
#4809=B_SPLINE_CURVE_WITH_KNOTS('',3,(#156358,#156359,#156360,#156361,#156362,
#156363,#156364,#156365,#156366,#156367,#156368,#156369,#156370,#156371,
#156372,#156373,#156374,#156375,#156376),.UNSPECIFIED.,.F.,.F.,(4,3,3,3,
3,3,4),(1.9687011228103E-6,0.214511984278332,0.415074732621236,0.60922528181149,
0.804612640905745,0.985865888199921,1.),.UNSPECIFIED.);
#4810=B_SPLINE_CURVE_WITH_KNOTS('',3,(#156377,#156378,#156379,#156380,#156381,
#156382,#156383,#156384,#156385,#156386,#156387,#156388,#156389,#156390,
#156391,#156392,#156393,#156394,#156395,#156396,#156397,#156398,#156399,
#156400,#156401,#156402,#156403,#156404,#156405,#156406,#156407,#156408,
#156409,#156410,#156411,#156412,#156413,#156414,#156415,#156416,#156417,
#156418,#156419),.UNSPECIFIED.,.F.,.F.,(4,2,1,1,2,2,2,2,1,2,2,2,1,1,1,2,
2,2,2,1,1,1,2,2,2,4),(0.000601430764826355,0.00781249999997516,0.0117187499999639,
0.0136718749999563,0.0146484374999525,0.0156249999999487,0.0312499999999361,
0.0624999999999109,0.0937499999998857,0.109374999999876,0.124999999999867,
0.187499999999835,0.218749999999818,0.23437499999981,0.242187499999802,
0.246093749999798,0.249999999999794,0.374999999999919,0.437499999999986,
0.468750000000016,0.484375000000032,0.492187500000039,0.496093750000039,
0.500000000000038,0.750000000000019,1.),.UNSPECIFIED.);
#4811=B_SPLINE_CURVE_WITH_KNOTS('',3,(#156423,#156424,#156425,#156426),
 .UNSPECIFIED.,.F.,.F.,(4,4),(0.000716623500636008,0.00919276877023496),
 .UNSPECIFIED.);
#4812=B_SPLINE_CURVE_WITH_KNOTS('',3,(#156443,#156444,#156445,#156446,#156447,
#156448,#156449,#156450,#156451,#156452,#156453,#156454,#156455,#156456,
#156457,#156458,#156459,#156460,#156461),.UNSPECIFIED.,.F.,.F.,(4,3,3,3,
3,3,4),(0.,0.182234855225268,0.370330240564428,0.568260122897141,0.772901042897791,
0.988056605769259,0.999998030911719),.UNSPECIFIED.);
#4813=B_SPLINE_CURVE_WITH_KNOTS('',3,(#156462,#156463,#156464,#156465,#156466,
#156467,#156468,#156469,#156470,#156471,#156472,#156473,#156474,#156475,
#156476,#156477,#156478,#156479,#156480,#156481,#156482,#156483,#156484,
#156485,#156486,#156487,#156488,#156489,#156490,#156491,#156492,#156493,
#156494,#156495,#156496,#156497,#156498,#156499,#156500,#156501,#156502,
#156503,#156504,#156505,#156506,#156507,#156508,#156509,#156510,#156511,
#156512,#156513,#156514,#156515,#156516,#156517,#156518,#156519,#156520,
#156521,#156522,#156523,#156524,#156525,#156526,#156527,#156528,#156529,
#156530,#156531,#156532,#156533,#156534,#156535,#156536,#156537,#156538,
#156539,#156540,#156541,#156542,#156543,#156544,#156545,#156546,#156547,
#156548,#156549,#156550,#156551,#156552,#156553,#156554,#156555,#156556,
#156557,#156558,#156559,#156560,#156561,#156562,#156563,#156564,#156565,
#156566,#156567),.UNSPECIFIED.,.F.,.F.,(4,3,3,3,3,3,3,3,3,3,3,3,3,3,3,3,
3,3,3,3,3,3,3,3,3,3,3,3,3,3,3,3,3,3,3,4),(1.82991911842132E-8,0.0751759264972593,
0.124999999999493,0.187805693540276,0.246093749998999,0.249999999998986,
0.252178981767012,0.342801458928556,0.374999999998785,0.443052550002119,
0.498046874998592,0.499999999998585,0.503012031054894,0.54307955855884,
0.56249999999841,0.602710083228639,0.617187499998271,0.621093749998255,
0.624999999998238,0.650878840433193,0.677324037255935,0.687499999998016,
0.714364448746321,0.718749999997905,0.734374999997839,0.742187499997806,
0.746093749997789,0.748046874997766,0.74902343749777,0.749511718747773,
0.749999999997775,0.751100566896097,0.817288275153847,0.88330529692333,
0.94908639453054,1.),.UNSPECIFIED.);
#4814=B_SPLINE_CURVE_WITH_KNOTS('',3,(#156568,#156569,#156570,#156571,#156572,
#156573,#156574,#156575,#156576,#156577,#156578,#156579,#156580,#156581,
#156582,#156583,#156584,#156585,#156586,#156587,#156588,#156589,#156590,
#156591,#156592,#156593,#156594,#156595,#156596,#156597,#156598,#156599,
#156600,#156601,#156602,#156603,#156604,#156605,#156606,#156607,#156608,
#156609,#156610,#156611,#156612,#156613,#156614,#156615,#156616,#156617,
#156618,#156619,#156620,#156621,#156622,#156623,#156624,#156625,#156626,
#156627,#156628,#156629,#156630,#156631,#156632,#156633,#156634,#156635,
#156636,#156637,#156638,#156639,#156640,#156641,#156642,#156643,#156644,
#156645,#156646,#156647,#156648,#156649,#156650,#156651,#156652,#156653,
#156654,#156655),.UNSPECIFIED.,.F.,.F.,(4,3,3,3,3,3,3,3,3,3,3,3,3,3,3,3,
3,3,3,3,3,3,3,3,3,3,3,3,3,4),(0.,0.0706981254337144,0.134756746486677,0.19237837324321,
0.221189186621476,0.235594593310609,0.239195944982892,0.241896958737105,
0.242572531958201,0.249192599119759,0.249999999999742,0.335864630298422,
0.374999999999788,0.4062499999998,0.437499999999812,0.468749999999815,0.488648139108568,
0.499415549493787,0.499999999999818,0.562499999999833,0.675822191009255,
0.718749999999872,0.734374999999877,0.746329099519318,0.749999999999882,
0.833428133033808,0.874999999999941,0.906249999999956,0.953124999999978,
0.999960672072946),.UNSPECIFIED.);
#4815=B_SPLINE_CURVE_WITH_KNOTS('',3,(#156660,#156661,#156662,#156663,#156664,
#156665,#156666,#156667,#156668,#156669,#156670,#156671,#156672),
 .UNSPECIFIED.,.F.,.F.,(4,3,3,3,4),(0.,0.275945685186237,0.556684630972288,
0.845469782669404,1.),.UNSPECIFIED.);
#4816=B_SPLINE_CURVE_WITH_KNOTS('',3,(#156673,#156674,#156675,#156676,#156677,
#156678,#156679,#156680,#156681,#156682,#156683,#156684,#156685,#156686,
#156687,#156688),.UNSPECIFIED.,.F.,.F.,(4,3,3,3,3,4),(0.,0.210999634175483,
0.413457389674863,0.611835729512844,0.805917864756422,1.),.UNSPECIFIED.);
#4817=B_SPLINE_CURVE_WITH_KNOTS('',3,(#156719,#156720,#156721,#156722,#156723,
#156724,#156725,#156726,#156727,#156728,#156729,#156730,#156731,#156732,
#156733,#156734,#156735,#156736,#156737,#156738,#156739,#156740,#156741,
#156742,#156743,#156744,#156745,#156746,#156747,#156748,#156749,#156750,
#156751,#156752,#156753,#156754,#156755,#156756,#156757,#156758,#156759,
#156760,#156761,#156762,#156763,#156764,#156765,#156766,#156767,#156768,
#156769,#156770,#156771,#156772,#156773,#156774,#156775,#156776,#156777,
#156778,#156779,#156780,#156781,#156782,#156783,#156784,#156785),
 .UNSPECIFIED.,.F.,.F.,(4,3,3,3,3,3,3,3,3,3,3,3,3,3,3,3,3,3,3,3,3,3,4),
(0.,0.100713214097213,0.199722071073913,0.296192282820578,0.375000000000224,
0.437500000000288,0.468750000000316,0.48437500000034,0.494481346924202,
0.500000000000365,0.581133205728252,0.625000000000431,0.687500000000466,
0.718750000000492,0.7343750000005,0.742187500000495,0.748154667016358,0.750000000000489,
0.803589729788625,0.855998067274474,0.907448277355546,0.957078195684321,
1.),.UNSPECIFIED.);
#4818=B_SPLINE_CURVE_WITH_KNOTS('',3,(#156799,#156800,#156801,#156802,#156803,
#156804,#156805,#156806,#156807,#156808,#156809,#156810,#156811,#156812,
#156813,#156814,#156815,#156816,#156817,#156818,#156819,#156820,#156821,
#156822,#156823,#156824,#156825,#156826,#156827,#156828,#156829,#156830,
#156831,#156832,#156833,#156834,#156835,#156836,#156837,#156838,#156839,
#156840,#156841,#156842,#156843,#156844,#156845,#156846,#156847,#156848,
#156849,#156850),.UNSPECIFIED.,.F.,.F.,(4,3,3,3,3,3,3,3,3,3,3,3,3,3,3,3,
3,4),(0.,0.0915574244606729,0.18774925655722,0.264441926099368,0.370387398191383,
0.423360134237391,0.449846502260395,0.463946416685409,0.46859215699834,
0.471131668249386,0.476332870283398,0.493787055659413,0.500000000000326,
0.605248837029928,0.712774761887522,0.821859923323834,0.933891888691301,
0.999999999999318),.UNSPECIFIED.);
#4819=B_SPLINE_CURVE_WITH_KNOTS('',3,(#156865,#156866,#156867,#156868,#156869,
#156870,#156871,#156872,#156873,#156874,#156875,#156876,#156877,#156878,
#156879,#156880,#156881,#156882,#156883,#156884,#156885,#156886,#156887,
#156888,#156889,#156890,#156891,#156892,#156893,#156894,#156895,#156896,
#156897,#156898,#156899,#156900,#156901,#156902,#156903,#156904,#156905,
#156906,#156907,#156908,#156909,#156910,#156911,#156912,#156913,#156914,
#156915,#156916,#156917,#156918,#156919,#156920,#156921,#156922,#156923,
#156924,#156925,#156926,#156927,#156928,#156929,#156930,#156931,#156932,
#156933,#156934,#156935,#156936,#156937,#156938,#156939,#156940,#156941,
#156942,#156943,#156944,#156945,#156946,#156947,#156948,#156949,#156950,
#156951,#156952,#156953,#156954,#156955),.UNSPECIFIED.,.F.,.F.,(4,3,3,3,
3,3,3,3,3,3,3,3,3,3,3,3,3,3,3,3,3,3,3,3,3,3,3,3,3,3,4),(0.,0.0665803261300661,
0.124999999999229,0.185546874998862,0.241891523992033,0.246093749998496,
0.24999999999848,0.252377916984439,0.374999999997735,0.441988271863787,
0.498046874997,0.49999999999699,0.503010835744694,0.549750791226953,0.562499999997204,
0.593749999997324,0.609374999997384,0.617187499997414,0.621093749997429,
0.624999999997444,0.687499999997845,0.718749999998051,0.734374999998155,
0.742187499998214,0.746093749998243,0.749999999998272,0.751172933773213,
0.822437083828853,0.874999999999136,0.945792987000676,1.),.UNSPECIFIED.);
#4820=B_SPLINE_CURVE_WITH_KNOTS('',3,(#156957,#156958,#156959,#156960),
 .UNSPECIFIED.,.F.,.F.,(4,4),(0.000801783579032724,0.0101814026529808),
 .UNSPECIFIED.);
#4821=B_SPLINE_CURVE_WITH_KNOTS('',3,(#156961,#156962,#156963,#156964,#156965,
#156966,#156967,#156968,#156969,#156970,#156971,#156972,#156973,#156974,
#156975,#156976,#156977,#156978,#156979,#156980,#156981,#156982,#156983,
#156984,#156985,#156986,#156987,#156988,#156989,#156990,#156991,#156992,
#156993,#156994,#156995,#156996,#156997,#156998,#156999,#157000,#157001,
#157002,#157003,#157004,#157005,#157006,#157007,#157008,#157009,#157010,
#157011,#157012,#157013,#157014,#157015,#157016,#157017,#157018,#157019,
#157020,#157021,#157022,#157023,#157024,#157025,#157026,#157027,#157028,
#157029,#157030,#157031,#157032,#157033,#157034,#157035,#157036,#157037,
#157038,#157039,#157040,#157041,#157042,#157043,#157044,#157045,#157046,
#157047,#157048,#157049,#157050,#157051,#157052,#157053,#157054,#157055,
#157056,#157057,#157058,#157059,#157060,#157061,#157062,#157063,#157064,
#157065,#157066,#157067,#157068,#157069,#157070,#157071,#157072,#157073,
#157074,#157075,#157076,#157077,#157078,#157079,#157080,#157081,#157082,
#157083,#157084,#157085,#157086,#157087),.UNSPECIFIED.,.F.,.F.,(4,3,3,3,
3,3,3,3,3,3,3,3,3,3,3,3,3,3,3,3,3,3,3,3,3,3,3,3,3,3,3,3,3,3,3,3,3,3,3,3,
3,3,4),(0.,0.0575336852850224,0.11198525032856,0.167849108085092,0.208924554042927,
0.229462277021845,0.239731138511304,0.244865569256033,0.247432784628398,
0.247753686549944,0.247945857259859,0.248138049254024,0.250000000000763,
0.282925510948109,0.315143228875522,0.346441281795087,0.375000000001455,
0.406250000001632,0.437500000001809,0.468750000001998,0.484375000002073,
0.492187500002108,0.4950791904349,0.496093750002159,0.498046875002222,0.499023437502213,
0.499511718752208,0.500000000002203,0.548747958738085,0.599908063232395,
0.625000000001634,0.680103968548825,0.687500000001349,0.718750000001199,
0.734375000001116,0.742187500001066,0.746093750001048,0.749103884050622,
0.75000000000103,0.812492512889779,0.875564869958435,0.943003068446462,
0.999970051556025),.UNSPECIFIED.);
#4822=B_SPLINE_CURVE_WITH_KNOTS('',3,(#157092,#157093,#157094,#157095),
 .UNSPECIFIED.,.F.,.F.,(4,4),(0.000856775130582955,0.0102382230284107),
 .UNSPECIFIED.);
#4823=B_SPLINE_CURVE_WITH_KNOTS('',3,(#157123,#157124,#157125,#157126,#157127,
#157128,#157129,#157130,#157131,#157132),.UNSPECIFIED.,.F.,.F.,(4,3,3,4),
(0.,0.384406684848453,0.779039496016362,1.),.UNSPECIFIED.);
#4824=B_SPLINE_CURVE_WITH_KNOTS('',3,(#157133,#157134,#157135,#157136,#157137,
#157138,#157139,#157140,#157141,#157142,#157143,#157144,#157145),
 .UNSPECIFIED.,.F.,.F.,(4,3,3,3,4),(1.27819991133542E-6,0.264022670170208,
0.521486442313197,0.769264763105439,1.),.UNSPECIFIED.);
#4825=B_SPLINE_CURVE_WITH_KNOTS('',3,(#157159,#157160,#157161,#157162,#157163,
#157164,#157165,#157166,#157167,#157168,#157169,#157170,#157171,#157172,
#157173,#157174,#157175,#157176,#157177,#157178,#157179,#157180,#157181,
#157182,#157183,#157184,#157185,#157186,#157187,#157188,#157189,#157190,
#157191,#157192,#157193,#157194,#157195,#157196,#157197,#157198,#157199,
#157200,#157201,#157202,#157203,#157204,#157205,#157206,#157207,#157208,
#157209,#157210,#157211,#157212,#157213,#157214,#157215,#157216,#157217,
#157218,#157219,#157220,#157221,#157222,#157223,#157224,#157225,#157226,
#157227,#157228,#157229,#157230,#157231,#157232,#157233,#157234,#157235,
#157236,#157237,#157238,#157239,#157240,#157241,#157242,#157243,#157244,
#157245,#157246,#157247,#157248,#157249,#157250,#157251,#157252,#157253,
#157254,#157255,#157256,#157257,#157258,#157259,#157260,#157261,#157262,
#157263,#157264,#157265,#157266,#157267,#157268,#157269,#157270,#157271,
#157272,#157273,#157274,#157275,#157276),.UNSPECIFIED.,.F.,.F.,(4,3,3,3,
3,3,3,3,3,3,3,3,3,3,3,3,3,3,3,3,3,3,3,3,3,3,3,3,3,3,3,3,3,3,3,3,3,3,3,4),
(0.,0.0590683228806878,0.116947001900935,0.12500000000061,0.187500000000918,
0.218750000001069,0.234375000001147,0.242187500001189,0.246093750001211,
0.249023437501223,0.250000000001225,0.28125000000129,0.311332831951185,
0.341061141711148,0.370364786792094,0.375000000001484,0.403715310671607,
0.432254350266244,0.460813536183436,0.487361700983429,0.496093750001687,
0.49804687500169,0.499023437501685,0.499511718751682,0.500000000001679,
0.552231180312084,0.60711677393185,0.625000000001268,0.683312841681498,
0.687500000001066,0.718750000000961,0.734375000000912,0.742187500000887,
0.746093750000875,0.74924093922361,0.750000000000863,0.814480974141558,
0.880798950734992,0.951107468086681,1.),.UNSPECIFIED.);
#4826=B_SPLINE_CURVE_WITH_KNOTS('',3,(#157277,#157278,#157279,#157280),
 .UNSPECIFIED.,.F.,.F.,(4,4),(0.000932565055856382,0.00145387661961335),
 .UNSPECIFIED.);
#4827=B_SPLINE_CURVE_WITH_KNOTS('',3,(#157281,#157282,#157283,#157284,#157285,
#157286,#157287,#157288,#157289,#157290,#157291,#157292,#157293,#157294,
#157295,#157296,#157297,#157298,#157299,#157300,#157301,#157302,#157303,
#157304,#157305,#157306,#157307,#157308,#157309,#157310,#157311,#157312,
#157313,#157314,#157315,#157316,#157317,#157318,#157319,#157320,#157321,
#157322,#157323,#157324,#157325,#157326,#157327,#157328,#157329,#157330,
#157331,#157332,#157333,#157334,#157335,#157336,#157337,#157338,#157339,
#157340),.UNSPECIFIED.,.F.,.F.,(4,2,1,2,2,2,2,2,2,1,1,2,2,2,1,1,1,2,2,2,
2,1,1,1,1,2,2,2,2,2,1,1,1,1,2,2,4),(0.000325542589491421,0.00390625000006981,
0.00585937500010367,0.00683593750012059,0.00781250000013752,0.0156250000002675,
0.0312500000005256,0.0468750000007837,0.0625000000010418,0.0937500000015648,
0.109375000001826,0.117187500001961,0.125000000002096,0.187500000003154,
0.218750000003686,0.234375000003956,0.242187500004087,0.24609375000415,
0.250000000004212,0.375000000006297,0.437500000007336,0.468750000007856,
0.484375000008115,0.492187500008246,0.496093750008311,0.49902343750836,
0.500000000008378,0.625000000006009,0.687500000004824,0.718750000004232,
0.734375000003934,0.742187500003785,0.746093750003708,0.748046875003672,
0.749023437503654,0.750000000003636,1.),.UNSPECIFIED.);
#4828=B_SPLINE_CURVE_WITH_KNOTS('',3,(#157359,#157360,#157361,#157362,#157363,
#157364,#157365,#157366,#157367,#157368,#157369,#157370,#157371,#157372,
#157373,#157374,#157375,#157376,#157377),.UNSPECIFIED.,.F.,.F.,(4,3,3,3,
3,3,4),(0.000633514536432522,0.00221236722518767,0.0038475939806142,0.0055851368810824,
0.00588295359619696,0.00776048988122894,0.00821913918141333),
 .UNSPECIFIED.);
#4829=B_SPLINE_CURVE_WITH_KNOTS('',3,(#157381,#157382,#157383,#157384,#157385,
#157386,#157387,#157388,#157389,#157390,#157391,#157392,#157393,#157394,
#157395,#157396,#157397,#157398,#157399),.UNSPECIFIED.,.F.,.F.,(4,3,3,3,
3,3,4),(0.000708752105543503,0.00258350608964089,0.00304683603862555,0.00476166896126371,
0.00640184829314115,0.00796195121168144,0.00830118856937974),
 .UNSPECIFIED.);
#4830=B_SPLINE_CURVE_WITH_KNOTS('',3,(#157421,#157422,#157423,#157424,#157425,
#157426,#157427,#157428,#157429,#157430,#157431,#157432,#157433,#157434,
#157435,#157436),.UNSPECIFIED.,.F.,.F.,(4,3,3,3,3,4),(0.,0.191851125007783,
0.406480624881621,0.608561884440055,0.854526014883085,0.999999191020381),
 .UNSPECIFIED.);
#4831=B_SPLINE_CURVE_WITH_KNOTS('',3,(#157437,#157438,#157439,#157440,#157441,
#157442,#157443,#157444,#157445,#157446,#157447,#157448,#157449,#157450,
#157451,#157452,#157453,#157454,#157455,#157456,#157457,#157458,#157459,
#157460,#157461,#157462,#157463,#157464,#157465,#157466,#157467,#157468,
#157469,#157470,#157471,#157472,#157473,#157474,#157475,#157476,#157477),
 .UNSPECIFIED.,.F.,.F.,(4,2,2,1,1,1,2,2,2,2,1,1,1,1,2,2,2,2,2,1,1,1,1,2,
2,4),(1.37021161665357E-8,0.125000000001154,0.187500000001739,0.218750000002024,
0.234375000002165,0.242187500002236,0.246093750002262,0.250000000002289,
0.375000000003502,0.437500000004118,0.468750000004426,0.48437500000458,
0.492187500004649,0.496093750004684,0.498046875004701,0.500000000004718,
0.62500000000551,0.687500000005905,0.718750000006103,0.734375000006183,
0.742187500006222,0.746093750006241,0.748046875006277,0.749023437506266,
0.750000000006256,1.),.UNSPECIFIED.);
#4832=B_SPLINE_CURVE_WITH_KNOTS('',3,(#157478,#157479,#157480,#157481,#157482,
#157483,#157484,#157485,#157486,#157487,#157488,#157489,#157490,#157491,
#157492,#157493,#157494,#157495,#157496,#157497,#157498,#157499,#157500,
#157501,#157502,#157503,#157504,#157505,#157506,#157507,#157508,#157509,
#157510,#157511,#157512,#157513,#157514,#157515,#157516,#157517,#157518,
#157519,#157520,#157521,#157522,#157523,#157524,#157525,#157526,#157527,
#157528,#157529,#157530,#157531,#157532,#157533,#157534,#157535,#157536,
#157537,#157538,#157539,#157540,#157541,#157542,#157543,#157544,#157545,
#157546,#157547,#157548,#157549,#157550,#157551,#157552,#157553,#157554,
#157555,#157556,#157557,#157558,#157559,#157560,#157561,#157562,#157563,
#157564,#157565,#157566,#157567,#157568),.UNSPECIFIED.,.F.,.F.,(4,3,3,3,
3,3,3,3,3,3,3,3,3,3,3,3,3,3,3,3,3,3,3,3,3,3,3,3,3,3,4),(0.,0.0942187049135352,
0.172109352457099,0.211054676228881,0.230527338114772,0.240263669057718,
0.245131834529191,0.24584290831596,0.246288773375984,0.250000000000663,
0.310546875000763,0.368000688459125,0.430094094230093,0.49218750000106,
0.499784370190774,0.500000000001073,0.547046753073244,0.595404792786901,
0.62500000000146,0.674219419647568,0.687500000001642,0.718750000001735,
0.734375000001779,0.742187500001802,0.746093750001812,0.748046875001799,
0.750000000001786,0.824413102467963,0.901016120596062,0.980588302632023,
0.999982499870738),.UNSPECIFIED.);
#4833=B_SPLINE_CURVE_WITH_KNOTS('',3,(#157573,#157574,#157575,#157576,#157577,
#157578,#157579,#157580,#157581,#157582,#157583,#157584,#157585,#157586,
#157587,#157588,#157589,#157590,#157591,#157592,#157593,#157594,#157595,
#157596,#157597,#157598,#157599,#157600,#157601,#157602,#157603,#157604,
#157605,#157606,#157607,#157608,#157609,#157610,#157611,#157612),
 .UNSPECIFIED.,.F.,.F.,(4,3,3,3,3,3,3,3,3,3,3,3,3,4),(0.,0.152110083047855,
0.249999999999927,0.37499999999989,0.437499999999873,0.468749999999866,
0.484374999999861,0.499023437499852,0.49999999999985,0.500032662678491,
0.628278229772928,0.75903464790435,0.894326952680693,1.),.UNSPECIFIED.);
#4834=B_SPLINE_CURVE_WITH_KNOTS('',3,(#157613,#157614,#157615,#157616,#157617,
#157618,#157619,#157620,#157621,#157622,#157623,#157624,#157625,#157626,
#157627,#157628,#157629,#157630,#157631,#157632,#157633,#157634,#157635,
#157636,#157637,#157638,#157639,#157640,#157641,#157642,#157643),
 .UNSPECIFIED.,.F.,.F.,(4,3,3,3,3,3,3,3,3,3,4),(0.,0.13024412390066,0.256700429361413,
0.378760361967859,0.499023437500028,0.49997472214385,0.500000000000029,
0.659213532399644,0.814240717125258,0.964146097215223,1.),.UNSPECIFIED.);
#4835=B_SPLINE_CURVE_WITH_KNOTS('',3,(#157668,#157669,#157670,#157671,#157672,
#157673,#157674,#157675,#157676,#157677,#157678,#157679,#157680,#157681,
#157682,#157683,#157684,#157685,#157686,#157687,#157688,#157689,#157690,
#157691,#157692,#157693,#157694,#157695,#157696,#157697,#157698),
 .UNSPECIFIED.,.F.,.F.,(4,3,3,3,3,3,3,3,3,3,4),(0.,0.163914497973559,0.250000000000003,
0.312500000000004,0.347315553940031,0.375000000000005,0.500000000000005,
0.632160630087504,0.76037903141579,0.882749786044512,1.),.UNSPECIFIED.);
#4836=B_SPLINE_CURVE_WITH_KNOTS('',3,(#157702,#157703,#157704,#157705,#157706,
#157707,#157708,#157709,#157710,#157711,#157712,#157713,#157714,#157715,
#157716,#157717,#157718,#157719,#157720),.UNSPECIFIED.,.F.,.F.,(4,3,3,3,
3,3,4),(0.000609719129519901,0.00229610816233235,0.00296440479617455,0.00386266882834386,
0.00506716034621368,0.00622435639369075,0.00711561852716782),
 .UNSPECIFIED.);
#4837=B_SPLINE_CURVE_WITH_KNOTS('',3,(#157724,#157725,#157726,#157727,#157728,
#157729,#157730,#157731,#157732,#157733,#157734,#157735,#157736,#157737,
#157738,#157739,#157740,#157741,#157742),.UNSPECIFIED.,.F.,.F.,(4,3,3,3,
3,3,4),(0.000543628862815408,0.00167393673136745,0.00258252559983906,0.00379688806421983,
0.00467674795200451,0.0060164798674652,0.00704595220449218),
 .UNSPECIFIED.);
#4838=B_SPLINE_CURVE_WITH_KNOTS('',3,(#157770,#157771,#157772,#157773,#157774,
#157775,#157776,#157777,#157778,#157779,#157780,#157781,#157782,#157783,
#157784,#157785,#157786,#157787,#157788,#157789,#157790,#157791),
 .UNSPECIFIED.,.F.,.F.,(4,3,3,3,3,3,3,4),(0.,0.209978546231012,0.516853342342681,
0.55334059960295,0.677766711290302,0.809718518620088,0.850799142123614,
0.999999957313844),.UNSPECIFIED.);
#4839=B_SPLINE_CURVE_WITH_KNOTS('',3,(#157792,#157793,#157794,#157795,#157796,
#157797,#157798,#157799,#157800,#157801,#157802,#157803,#157804,#157805,
#157806,#157807,#157808,#157809,#157810,#157811,#157812,#157813,#157814,
#157815,#157816,#157817,#157818,#157819,#157820,#157821,#157822,#157823,
#157824,#157825,#157826,#157827,#157828,#157829,#157830,#157831,#157832,
#157833,#157834,#157835,#157836,#157837,#157838,#157839,#157840,#157841,
#157842,#157843,#157844,#157845,#157846,#157847,#157848,#157849,#157850,
#157851,#157852,#157853,#157854,#157855,#157856,#157857,#157858,#157859,
#157860,#157861,#157862,#157863,#157864,#157865,#157866,#157867,#157868,
#157869,#157870),.UNSPECIFIED.,.F.,.F.,(4,3,3,3,3,3,3,3,3,3,3,3,3,3,3,3,
3,3,3,3,3,3,3,3,3,3,4),(2.68021967053581E-8,0.0901737464676206,0.125000000004943,
0.187500000007436,0.218750000008682,0.234375000009306,0.242187500009617,
0.246093750009773,0.248046875009851,0.250000000009929,0.284837518478703,
0.319813158669615,0.354999270488202,0.388272574435471,0.424332270935315,
0.461189572970983,0.49804687500665,0.500000000006616,0.500285687694454,
0.569196019485871,0.625000000004962,0.700368074597989,0.750000000003308,
0.828257149063034,0.908768627880029,0.992262118086699,1.),.UNSPECIFIED.);
#4840=B_SPLINE_CURVE_WITH_KNOTS('',3,(#157871,#157872,#157873,#157874,#157875,
#157876,#157877,#157878,#157879,#157880,#157881,#157882,#157883,#157884,
#157885,#157886,#157887,#157888,#157889,#157890,#157891,#157892,#157893,
#157894,#157895,#157896,#157897,#157898,#157899,#157900,#157901,#157902,
#157903,#157904,#157905,#157906,#157907,#157908,#157909,#157910,#157911,
#157912,#157913,#157914,#157915,#157916,#157917,#157918,#157919,#157920,
#157921,#157922,#157923,#157924,#157925,#157926,#157927,#157928,#157929,
#157930,#157931,#157932,#157933,#157934),.UNSPECIFIED.,.F.,.F.,(4,3,3,3,
3,3,3,3,3,3,3,3,3,3,3,3,3,3,3,3,3,4),(0.,0.118271603684389,0.213215421513922,
0.276599705427053,0.378014263819111,0.476502100417059,0.498046875002522,
0.500000000002524,0.500226658109365,0.543785052858866,0.587308456982946,
0.625000000001855,0.668197289819432,0.71031813419112,0.734375000001243,
0.742187500001194,0.74609375000118,0.750000000001165,0.815058929541337,
0.88140492073318,0.94923986208531,0.999998612059214),.UNSPECIFIED.);
#4841=B_SPLINE_CURVE_WITH_KNOTS('',3,(#157939,#157940,#157941,#157942,#157943,
#157944,#157945,#157946,#157947,#157948,#157949,#157950,#157951,#157952,
#157953,#157954,#157955,#157956,#157957,#157958,#157959,#157960,#157961,
#157962,#157963,#157964,#157965,#157966,#157967,#157968,#157969,#157970,
#157971,#157972,#157973,#157974,#157975,#157976,#157977,#157978,#157979,
#157980,#157981),.UNSPECIFIED.,.F.,.F.,(4,3,3,3,3,3,3,3,3,3,3,3,3,3,4),
(0.,0.152629020565605,0.249999999999822,0.374999999999733,0.43749999999969,
0.468749999999669,0.484374999999659,0.492187499999655,0.49902343749965,
0.499999999999649,0.500016866394184,0.625012649795638,0.752170083217449,
0.885031771841597,1.),.UNSPECIFIED.);
#4842=B_SPLINE_CURVE_WITH_KNOTS('',3,(#157982,#157983,#157984,#157985,#157986,
#157987,#157988,#157989,#157990,#157991,#157992,#157993,#157994,#157995,
#157996,#157997),.UNSPECIFIED.,.F.,.F.,(4,2,2,1,1,1,1,2,2,4),(0.,0.249999999999634,
0.374999999999451,0.43749999999936,0.468749999999314,0.484374999999291,
0.49218749999928,0.499511718749273,0.499999999999273,1.),.UNSPECIFIED.);
#4843=B_SPLINE_CURVE_WITH_KNOTS('',3,(#158012,#158013,#158014,#158015,#158016,
#158017,#158018,#158019,#158020,#158021,#158022,#158023,#158024,#158025,
#158026,#158027,#158028,#158029,#158030,#158031,#158032,#158033,#158034,
#158035,#158036,#158037,#158038,#158039,#158040,#158041,#158042,#158043,
#158044,#158045,#158046,#158047,#158048,#158049,#158050,#158051,#158052,
#158053,#158054,#158055,#158056,#158057,#158058,#158059,#158060,#158061,
#158062,#158063,#158064,#158065,#158066,#158067,#158068,#158069,#158070,
#158071,#158072,#158073,#158074,#158075,#158076,#158077,#158078,#158079,
#158080,#158081,#158082,#158083,#158084,#158085,#158086,#158087,#158088,
#158089,#158090,#158091,#158092,#158093,#158094,#158095,#158096,#158097,
#158098,#158099,#158100,#158101,#158102,#158103,#158104,#158105,#158106,
#158107,#158108,#158109,#158110,#158111,#158112,#158113,#158114,#158115,
#158116,#158117,#158118,#158119,#158120,#158121,#158122,#158123),
 .UNSPECIFIED.,.F.,.F.,(4,3,3,3,3,3,3,3,3,3,3,3,3,3,3,3,3,3,3,3,3,3,3,3,
3,3,3,3,3,3,3,3,3,3,3,3,3,4),(0.,0.0312499999998062,0.0605342632990558,
0.0894827504846968,0.118001403536209,0.124999999999225,0.153278974298353,
0.18129948503294,0.187499999998837,0.216951734368515,0.218749999998643,
0.234374999998554,0.242187499998502,0.246093749998477,0.248046874998471,
0.249999999998465,0.251315421686666,0.287025254902491,0.323897744396542,
0.362533590707892,0.365329311803758,0.374999999998303,0.435546874998244,
0.486640465010263,0.496093749998184,0.499801280154157,0.499999999998196,
0.502837829566728,0.557028783578141,0.612188173491773,0.618785031193608,
0.707396936947145,0.740020308462563,0.749999999999098,0.808109157563208,
0.868876091672364,0.934438045836177,0.999999999999991),.UNSPECIFIED.);
#4844=B_SPLINE_CURVE_WITH_KNOTS('',3,(#158127,#158128,#158129,#158130,#158131,
#158132,#158133,#158134,#158135,#158136,#158137,#158138,#158139,#158140,
#158141,#158142,#158143,#158144,#158145,#158146,#158147,#158148,#158149,
#158150,#158151,#158152,#158153,#158154,#158155,#158156,#158157,#158158,
#158159,#158160,#158161,#158162,#158163,#158164,#158165,#158166,#158167,
#158168,#158169,#158170,#158171,#158172,#158173,#158174,#158175,#158176,
#158177,#158178,#158179,#158180,#158181,#158182,#158183,#158184,#158185,
#158186,#158187,#158188,#158189,#158190,#158191,#158192,#158193,#158194,
#158195,#158196,#158197,#158198,#158199,#158200,#158201,#158202,#158203,
#158204,#158205,#158206,#158207,#158208,#158209,#158210,#158211,#158212,
#158213,#158214,#158215,#158216,#158217,#158218,#158219,#158220,#158221,
#158222,#158223,#158224,#158225,#158226),.UNSPECIFIED.,.F.,.F.,(4,3,3,3,
3,3,3,3,3,3,3,3,3,3,3,3,3,3,3,3,3,3,3,3,3,3,3,3,3,3,3,3,3,4),(0.,0.0648910438044147,
0.128717958621191,0.191025514880074,0.250000000000982,0.31045583673544,
0.370223161889096,0.429183251024718,0.437500000001725,0.46875000000185,
0.484375000001905,0.492187500001924,0.496093750001933,0.499608596766509,
0.500000000001942,0.547658410706032,0.594339973290379,0.640919986645954,
0.687500000001529,0.718750000001471,0.734375000001432,0.742187500001413,
0.746093750001393,0.748046875001384,0.750000000001374,0.775181875051039,
0.801125965610821,0.828252261465758,0.856100708458129,0.884636130316055,
0.91411422298605,0.944011866396523,0.974420019927077,1.),.UNSPECIFIED.);
#4845=B_SPLINE_CURVE_WITH_KNOTS('',3,(#158227,#158228,#158229,#158230),
 .UNSPECIFIED.,.F.,.F.,(4,4),(0.0209654295165786,0.0214659702660322),
 .UNSPECIFIED.);
#4846=B_SPLINE_CURVE_WITH_KNOTS('',3,(#158234,#158235,#158236,#158237,#158238,
#158239,#158240,#158241,#158242,#158243,#158244,#158245,#158246,#158247,
#158248,#158249,#158250,#158251,#158252),.UNSPECIFIED.,.F.,.F.,(4,3,3,3,
3,3,4),(0.000498894531959924,0.00225071250488168,0.00337891514771613,0.00374149706694668,
0.00465083407571407,0.00559677886661334,0.00625893576407251),
 .UNSPECIFIED.);
#4847=B_SPLINE_CURVE_WITH_KNOTS('',3,(#158256,#158257,#158258,#158259,#158260,
#158261,#158262,#158263,#158264,#158265,#158266,#158267,#158268,#158269,
#158270,#158271,#158272,#158273,#158274,#158275,#158276,#158277,#158278,
#158279,#158280),.UNSPECIFIED.,.F.,.F.,(4,3,3,3,3,3,3,3,4),(0.000526414844798677,
0.00162646262698099,0.00270005642797546,0.00303445478718795,0.00340650091711803,
0.00424257270328492,0.00468441200509802,0.00552307032315888,0.0062865869894374),
 .UNSPECIFIED.);
#4848=B_SPLINE_CURVE_WITH_KNOTS('',3,(#158302,#158303,#158304,#158305,#158306,
#158307,#158308,#158309,#158310,#158311,#158312,#158313,#158314,#158315,
#158316,#158317,#158318,#158319,#158320,#158321,#158322,#158323,#158324,
#158325,#158326),.UNSPECIFIED.,.F.,.F.,(4,3,3,3,3,3,3,3,4),(7.55472550129836E-12,
0.249999999999995,0.374999999999993,0.437499999999994,0.468749999999996,
0.484374999999998,0.499999999999999,0.75,1.),.UNSPECIFIED.);
#4849=B_SPLINE_CURVE_WITH_KNOTS('',3,(#158327,#158328,#158329,#158330,#158331,
#158332,#158333,#158334,#158335,#158336,#158337,#158338,#158339,#158340,
#158341,#158342,#158343,#158344,#158345,#158346,#158347,#158348,#158349,
#158350,#158351,#158352,#158353,#158354,#158355,#158356,#158357,#158358,
#158359,#158360,#158361,#158362,#158363,#158364,#158365,#158366,#158367,
#158368,#158369,#158370,#158371,#158372,#158373,#158374,#158375,#158376,
#158377,#158378,#158379,#158380,#158381,#158382,#158383,#158384,#158385,
#158386,#158387,#158388,#158389,#158390),.UNSPECIFIED.,.F.,.F.,(4,3,3,3,
3,3,3,3,3,3,3,3,3,3,3,3,3,3,3,3,3,4),(0.,0.062499999999913,0.121268938782561,
0.124999999999826,0.182866167131341,0.187499999999739,0.221010185130871,
0.249999999999652,0.30930397539579,0.369343026326928,0.430208840841633,
0.437499999999391,0.468749999999367,0.484374999999355,0.492187499999348,
0.49609374999937,0.499999999999391,0.599290847525026,0.701894875544265,
0.806426977227526,0.914331950747426,1.),.UNSPECIFIED.);
#4850=B_SPLINE_CURVE_WITH_KNOTS('',3,(#158396,#158397,#158398,#158399,#158400,
#158401,#158402,#158403,#158404,#158405,#158406,#158407,#158408,#158409,
#158410),.UNSPECIFIED.,.F.,.F.,(4,2,2,1,1,1,2,2,4),(0.,0.250000000000126,
0.375000000000189,0.437500000000219,0.468750000000235,0.484375000000243,
0.499511718750253,0.500000000000252,1.),.UNSPECIFIED.);
#4851=B_SPLINE_CURVE_WITH_KNOTS('',3,(#158411,#158412,#158413,#158414,#158415,
#158416,#158417,#158418,#158419,#158420),.UNSPECIFIED.,.F.,.F.,(4,3,3,4),
(1.28225413371019E-15,0.448593385958983,0.838218300237572,1.),
 .UNSPECIFIED.);
#4852=B_SPLINE_CURVE_WITH_KNOTS('',3,(#158435,#158436,#158437,#158438,#158439,
#158440,#158441,#158442,#158443,#158444,#158445,#158446,#158447,#158448,
#158449,#158450,#158451,#158452,#158453,#158454,#158455,#158456,#158457,
#158458,#158459,#158460,#158461,#158462,#158463,#158464,#158465,#158466,
#158467,#158468,#158469,#158470,#158471,#158472,#158473,#158474,#158475,
#158476,#158477,#158478,#158479,#158480,#158481,#158482,#158483,#158484,
#158485,#158486,#158487,#158488,#158489,#158490,#158491,#158492,#158493,
#158494,#158495),.UNSPECIFIED.,.F.,.F.,(4,3,3,3,3,3,3,3,3,3,3,3,3,3,3,3,
3,3,3,3,4),(0.,0.0502633235240096,0.101045843377086,0.152970535449028,0.189102546852238,
0.238178111545533,0.25,0.304377708692877,0.358316326919491,0.399399448923178,
0.459255053387673,0.5,0.560867125063224,0.62437046877712,0.652851120149406,
0.729686322421556,0.75,0.830074596814701,0.910059278387214,0.989928126244262,
1.),.UNSPECIFIED.);
#4853=B_SPLINE_CURVE_WITH_KNOTS('',3,(#158499,#158500,#158501,#158502,#158503,
#158504,#158505,#158506,#158507,#158508,#158509,#158510,#158511,#158512,
#158513,#158514,#158515,#158516,#158517,#158518,#158519,#158520,#158521,
#158522,#158523,#158524,#158525,#158526,#158527,#158528,#158529,#158530,
#158531,#158532,#158533,#158534,#158535,#158536,#158537,#158538),
 .UNSPECIFIED.,.F.,.F.,(4,3,3,3,3,3,3,3,3,3,3,3,3,4),(0.,0.0800261451261139,
0.159426517805461,0.238333591819812,0.316877881690732,0.395188406678548,
0.473451575133888,0.55177676839471,0.630277038124919,0.709065913000149,
0.788573007004716,0.868542366834391,0.949461691917387,1.),.UNSPECIFIED.);
#4854=B_SPLINE_CURVE_WITH_KNOTS('',3,(#158543,#158544,#158545,#158546,#158547,
#158548,#158549,#158550,#158551,#158552,#158553,#158554,#158555,#158556,
#158557,#158558,#158559,#158560,#158561,#158562,#158563,#158564,#158565,
#158566,#158567),.UNSPECIFIED.,.F.,.F.,(4,3,3,3,3,3,3,3,4),(0.000528035090325194,
0.0016124914159284,0.00267001151846031,0.00302714454343539,0.00341353154252654,
0.00423239659979752,0.00468651457632683,0.00549911074687931,0.0062990279947279),
 .UNSPECIFIED.);
#4855=B_SPLINE_CURVE_WITH_KNOTS('',3,(#158571,#158572,#158573,#158574,#158575,
#158576,#158577,#158578,#158579,#158580,#158581,#158582,#158583,#158584,
#158585,#158586,#158587,#158588,#158589,#158590,#158591,#158592),
 .UNSPECIFIED.,.F.,.F.,(4,3,3,3,3,3,3,4),(0.000499308730788174,0.00146046002320121,
0.00243695586829252,0.00338583705476887,0.00376364965220018,0.00474984309182762,
0.00578812738994436,0.00627236538267016),.UNSPECIFIED.);
#4856=B_SPLINE_CURVE_WITH_KNOTS('',3,(#158620,#158621,#158622,#158623,#158624,
#158625,#158626,#158627,#158628,#158629,#158630,#158631,#158632,#158633,
#158634,#158635,#158636,#158637,#158638,#158639,#158640,#158641,#158642,
#158643,#158644,#158645,#158646,#158647,#158648,#158649,#158650,#158651,
#158652,#158653,#158654,#158655,#158656,#158657,#158658,#158659,#158660,
#158661,#158662),.UNSPECIFIED.,.F.,.F.,(4,3,3,3,3,3,3,3,3,3,3,3,3,3,4),
(0.,0.101173413162297,0.202391851056343,0.23209554217457,0.334240321391055,
0.431696971553665,0.49004936393671,0.499999999999992,0.562499999999993,
0.59262152003138,0.618082675029418,0.622918819150938,0.627640870459847,
0.845903088419632,1.),.UNSPECIFIED.);
#4857=B_SPLINE_CURVE_WITH_KNOTS('',3,(#158664,#158665,#158666,#158667,#158668,
#158669,#158670,#158671,#158672,#158673,#158674,#158675,#158676,#158677,
#158678,#158679,#158680,#158681,#158682,#158683,#158684,#158685,#158686,
#158687,#158688,#158689,#158690,#158691,#158692,#158693,#158694,#158695,
#158696,#158697,#158698,#158699,#158700,#158701,#158702,#158703,#158704,
#158705,#158706,#158707,#158708,#158709,#158710,#158711,#158712,#158713,
#158714,#158715,#158716,#158717,#158718,#158719,#158720,#158721,#158722,
#158723,#158724),.UNSPECIFIED.,.F.,.F.,(4,3,3,3,3,3,3,3,3,3,3,3,3,3,3,3,
3,3,3,3,4),(0.,0.107509121767451,0.212828833412304,0.315061928584091,0.374999999999339,
0.437499999999212,0.468749999999133,0.484374999999095,0.492187499999061,
0.496093749999059,0.499999999999056,0.562499999999177,0.624999999999298,
0.673320118680395,0.719243863834343,0.749999999999539,0.806482839148098,
0.864299406979082,0.922736798740935,0.98187500024349,1.),.UNSPECIFIED.);
#4858=B_SPLINE_CURVE_WITH_KNOTS('',3,(#158729,#158730,#158731,#158732,#158733,
#158734,#158735,#158736,#158737,#158738,#158739,#158740,#158741,#158742,
#158743,#158744,#158745,#158746,#158747,#158748,#158749,#158750,#158751,
#158752,#158753,#158754,#158755,#158756),.UNSPECIFIED.,.F.,.F.,(4,3,3,3,
3,3,3,3,3,4),(0.,0.249999999999957,0.374999999999935,0.437499999999924,
0.468749999999919,0.484374999999917,0.499511718749913,0.499999999999911,
0.882725836403091,1.),.UNSPECIFIED.);
#4859=B_SPLINE_CURVE_WITH_KNOTS('',3,(#158757,#158758,#158759,#158760,#158761,
#158762,#158763,#158764,#158765,#158766,#158767,#158768,#158769,#158770,
#158771,#158772),.UNSPECIFIED.,.F.,.F.,(4,2,2,1,1,1,1,2,2,4),(0.,0.249999999999903,
0.374999999999855,0.437499999999831,0.468749999999819,0.484374999999812,
0.492187499999809,0.499511718749801,0.4999999999998,1.),.UNSPECIFIED.);
#4860=B_SPLINE_CURVE_WITH_KNOTS('',3,(#158787,#158788,#158789,#158790,#158791,
#158792,#158793,#158794,#158795,#158796,#158797,#158798,#158799,#158800,
#158801,#158802,#158803,#158804,#158805,#158806,#158807,#158808,#158809,
#158810,#158811,#158812,#158813,#158814,#158815,#158816),.UNSPECIFIED.,
 .F.,.F.,(4,2,2,2,1,1,1,2,2,2,2,1,1,1,2,2,2,4),(0.,0.124999999999242,0.187499999998862,
0.218749999998682,0.2343749999986,0.242187499998551,0.246093749998534,0.248046874998532,
0.24999999999853,0.374999999998953,0.437499999999164,0.468749999999281,
0.484374999999338,0.492187499999366,0.496093749999368,0.49999999999937,
0.749999999999685,1.),.UNSPECIFIED.);
#4861=B_SPLINE_CURVE_WITH_KNOTS('',3,(#158820,#158821,#158822,#158823,#158824,
#158825,#158826,#158827,#158828,#158829,#158830,#158831,#158832,#158833,
#158834,#158835,#158836,#158837,#158838,#158839,#158840,#158841,#158842,
#158843,#158844,#158845,#158846,#158847,#158848,#158849,#158850,#158851,
#158852,#158853,#158854,#158855,#158856,#158857,#158858,#158859,#158860,
#158861,#158862,#158863,#158864,#158865,#158866,#158867,#158868,#158869,
#158870,#158871,#158872,#158873,#158874,#158875,#158876,#158877,#158878,
#158879,#158880,#158881,#158882,#158883,#158884,#158885,#158886,#158887,
#158888,#158889,#158890,#158891,#158892,#158893,#158894,#158895,#158896,
#158897,#158898,#158899,#158900,#158901,#158902,#158903,#158904,#158905,
#158906,#158907,#158908,#158909,#158910,#158911,#158912,#158913,#158914,
#158915,#158916,#158917,#158918,#158919,#158920,#158921,#158922,#158923,
#158924,#158925,#158926,#158927,#158928,#158929,#158930,#158931,#158932,
#158933,#158934,#158935,#158936,#158937,#158938,#158939,#158940,#158941,
#158942,#158943,#158944,#158945,#158946,#158947,#158948,#158949),
 .UNSPECIFIED.,.F.,.F.,(4,3,3,3,3,3,3,3,3,3,3,3,3,3,3,3,3,3,3,3,3,3,3,3,
3,3,3,3,3,3,3,3,3,3,3,3,3,3,3,3,3,3,3,4),(0.,0.0626020078314224,0.12324694439226,
0.182080107324034,0.238598266130295,0.250000000000055,0.259982465184285,
0.314824665619934,0.354767132150864,0.380835408119498,0.430687988199657,
0.463893449524915,0.480496180187545,0.488797545518859,0.492948228184517,
0.495142943523771,0.495701691310286,0.496087181651465,0.496422077430329,
0.497098910850174,0.499250141665798,0.499899244790537,0.500161408362611,
0.567469545706375,0.601123614378257,0.618828367313947,0.633430720214261,
0.634777683050139,0.671858037763955,0.690862597687715,0.729912399485414,
0.74804687500011,0.748759759105555,0.750000000000109,0.779470645992731,
0.808817315775199,0.838104849358379,0.867326644519458,0.875000000000055,
0.903673998781796,0.932886331005841,0.962446376948863,0.992551691206423,
1.),.UNSPECIFIED.);
#4862=B_SPLINE_CURVE_WITH_KNOTS('',3,(#158950,#158951,#158952,#158953),
 .UNSPECIFIED.,.F.,.F.,(4,4),(0.00465289315641866,0.00515351125805147),
 .UNSPECIFIED.);
#4863=B_SPLINE_CURVE_WITH_KNOTS('',3,(#158957,#158958,#158959,#158960,#158961,
#158962,#158963,#158964,#158965,#158966,#158967,#158968,#158969,#158970,
#158971,#158972),.UNSPECIFIED.,.F.,.F.,(4,3,3,3,3,4),(0.00061266112179062,
0.00182296639992346,0.00298506204158171,0.00388203060349254,0.00558489832474453,
0.00715140008519447),.UNSPECIFIED.);
#4864=B_SPLINE_CURVE_WITH_KNOTS('',3,(#158976,#158977,#158978,#158979,#158980,
#158981,#158982,#158983,#158984,#158985,#158986,#158987,#158988,#158989,
#158990,#158991,#158992,#158993,#158994),.UNSPECIFIED.,.F.,.F.,(4,3,3,3,
3,3,4),(0.000544979362130299,0.00239221479429946,0.00380801466457332,0.00469824400931087,
0.00578923755784715,0.00680407029599512,0.00707104996701635),
 .UNSPECIFIED.);
#4865=B_SPLINE_CURVE_WITH_KNOTS('',3,(#159016,#159017,#159018,#159019,#159020,
#159021,#159022,#159023,#159024,#159025,#159026,#159027,#159028,#159029,
#159030,#159031,#159032,#159033,#159034),.UNSPECIFIED.,.F.,.F.,(4,3,3,3,
3,3,4),(4.13078214559669E-7,0.173852294489811,0.36677856517358,0.445174356588884,
0.722587178294442,0.929452460433655,1.),.UNSPECIFIED.);
#4866=B_SPLINE_CURVE_WITH_KNOTS('',3,(#159035,#159036,#159037,#159038,#159039,
#159040,#159041,#159042,#159043,#159044,#159045,#159046,#159047,#159048,
#159049,#159050,#159051,#159052,#159053,#159054,#159055,#159056,#159057,
#159058,#159059,#159060,#159061,#159062,#159063,#159064,#159065,#159066,
#159067,#159068,#159069,#159070,#159071,#159072,#159073,#159074,#159075,
#159076,#159077,#159078,#159079,#159080,#159081,#159082,#159083,#159084,
#159085,#159086,#159087,#159088,#159089,#159090,#159091,#159092,#159093,
#159094,#159095,#159096,#159097,#159098,#159099,#159100,#159101,#159102,
#159103,#159104,#159105,#159106,#159107,#159108,#159109,#159110),
 .UNSPECIFIED.,.F.,.F.,(4,3,3,3,3,3,3,3,3,3,3,3,3,3,3,3,3,3,3,3,3,3,3,3,
3,4),(0.,0.0690701057454117,0.125000000000561,0.187500000000856,0.21875000000099,
0.23437500000107,0.242187500001099,0.246093750001112,0.250000000001125,
0.289133934492208,0.328724352958703,0.368791285218157,0.409021034277532,
0.449394661938092,0.468750000001254,0.484375000001259,0.492187500001262,
0.496093750001307,0.49804687500128,0.500000000001253,0.590549171677946,
0.683067489715376,0.778781322937074,0.876449024523388,0.977044229356509,
1.),.UNSPECIFIED.);
#4867=B_SPLINE_CURVE_WITH_KNOTS('',3,(#159111,#159112,#159113,#159114,#159115,
#159116,#159117,#159118,#159119,#159120,#159121,#159122,#159123,#159124,
#159125,#159126,#159127,#159128,#159129,#159130,#159131,#159132,#159133,
#159134,#159135,#159136,#159137,#159138,#159139,#159140,#159141,#159142,
#159143,#159144,#159145,#159146,#159147,#159148,#159149,#159150,#159151,
#159152,#159153,#159154,#159155,#159156,#159157,#159158,#159159,#159160,
#159161,#159162,#159163,#159164,#159165,#159166,#159167,#159168,#159169,
#159170,#159171,#159172,#159173,#159174,#159175,#159176,#159177,#159178,
#159179,#159180,#159181,#159182,#159183,#159184,#159185,#159186,#159187,
#159188,#159189,#159190,#159191,#159192,#159193,#159194,#159195,#159196,
#159197,#159198,#159199,#159200,#159201,#159202,#159203,#159204,#159205,
#159206,#159207,#159208,#159209,#159210),.UNSPECIFIED.,.F.,.F.,(4,3,3,3,
3,3,3,3,3,3,3,3,3,3,3,3,3,3,3,3,3,3,3,3,3,3,3,3,3,3,3,3,3,4),(0.,0.0892180981438803,
0.125000000000199,0.187500000000311,0.218750000000367,0.234375000000406,
0.242187500000414,0.246093750000407,0.2500000000004,0.318440736490326,0.384858698678957,
0.437499999999504,0.468749999999366,0.484374999999297,0.492187499999262,
0.496093749999246,0.498046874999247,0.499999999999249,0.534729265670756,
0.569880614318735,0.605480155084377,0.641236534437177,0.677123723783148,
0.68749999999937,0.718749999999408,0.734374999999456,0.742187499999477,
0.746093749999491,0.748046874999498,0.749999999999506,0.822639083758781,
0.896597809459177,0.972564265462607,1.),.UNSPECIFIED.);
#4868=B_SPLINE_CURVE_WITH_KNOTS('',3,(#159215,#159216,#159217,#159218,#159219,
#159220,#159221,#159222,#159223,#159224,#159225,#159226,#159227,#159228,
#159229,#159230),.UNSPECIFIED.,.F.,.F.,(4,2,2,1,1,1,1,2,2,4),(0.,0.250000000000162,
0.375000000000243,0.437500000000284,0.468750000000303,0.484375000000312,
0.492187500000317,0.499511718750325,0.500000000000325,1.),.UNSPECIFIED.);
#4869=B_SPLINE_CURVE_WITH_KNOTS('',3,(#159231,#159232,#159233,#159234,#159235,
#159236,#159237,#159238,#159239,#159240,#159241,#159242,#159243,#159244,
#159245,#159246),.UNSPECIFIED.,.F.,.F.,(4,2,2,1,1,1,1,2,2,4),(0.,0.249999999999989,
0.374999999999983,0.43749999999998,0.468749999999979,0.48437499999998,0.49218749999998,
0.499023437499977,0.499999999999976,1.),.UNSPECIFIED.);
#4870=B_SPLINE_CURVE_WITH_KNOTS('',3,(#159252,#159253,#159254,#159255,#159256,
#159257,#159258,#159259,#159260,#159261,#159262,#159263,#159264,#159265),
 .UNSPECIFIED.,.F.,.F.,(4,2,2,1,1,2,2,4),(0.,0.250000000000154,0.375000000000264,
0.437500000000318,0.468750000000337,0.484375000000338,0.500000000000339,
1.),.UNSPECIFIED.);
#4871=B_SPLINE_CURVE_WITH_KNOTS('',3,(#159297,#159298,#159299,#159300,#159301,
#159302,#159303,#159304,#159305,#159306,#159307,#159308,#159309,#159310,
#159311,#159312,#159313,#159314,#159315),.UNSPECIFIED.,.F.,.F.,(4,3,3,3,
3,3,4),(0.000636256268971442,0.00222779634231115,0.00387629126444982,0.00562803598926337,
0.00591708699638702,0.0078089691620698,0.00825282706815076),
 .UNSPECIFIED.);
#4872=B_SPLINE_CURVE_WITH_KNOTS('',3,(#159319,#159320,#159321,#159322,#159323,
#159324,#159325,#159326,#159327,#159328,#159329,#159330,#159331,#159332,
#159333,#159334,#159335,#159336,#159337),.UNSPECIFIED.,.F.,.F.,(4,3,3,3,
3,3,4),(0.000711431901436798,0.00260509764011623,0.00304924424816995,0.00478266330431027,
0.00644043866278196,0.00801739908969177,0.00833474438776835),
 .UNSPECIFIED.);
#4873=B_SPLINE_CURVE_WITH_KNOTS('',3,(#159359,#159360,#159361,#159362,#159363,
#159364,#159365,#159366,#159367,#159368,#159369,#159370,#159371,#159372,
#159373,#159374),.UNSPECIFIED.,.F.,.F.,(4,3,3,3,3,4),(8.01577071537318E-7,
0.262495050804752,0.389947950402742,0.611074818510006,0.806599097074307,
1.),.UNSPECIFIED.);
#4874=B_SPLINE_CURVE_WITH_KNOTS('',3,(#159375,#159376,#159377,#159378,#159379,
#159380,#159381,#159382,#159383,#159384,#159385,#159386,#159387,#159388,
#159389,#159390,#159391,#159392,#159393,#159394,#159395,#159396,#159397,
#159398,#159399,#159400,#159401,#159402,#159403,#159404,#159405,#159406,
#159407,#159408,#159409,#159410,#159411,#159412,#159413,#159414,#159415,
#159416,#159417,#159418,#159419,#159420,#159421,#159422,#159423,#159424,
#159425,#159426,#159427,#159428,#159429,#159430,#159431,#159432,#159433,
#159434,#159435,#159436,#159437,#159438,#159439,#159440,#159441,#159442,
#159443,#159444,#159445,#159446,#159447,#159448,#159449,#159450,#159451,
#159452,#159453,#159454,#159455,#159456,#159457,#159458,#159459),
 .UNSPECIFIED.,.F.,.F.,(4,3,3,3,3,3,3,3,3,3,3,3,3,3,3,3,3,3,3,3,3,3,3,3,
3,3,3,3,4),(1.71570245437392E-5,0.0625000000005735,0.125000000001147,0.18750000000171,
0.218750000001983,0.234375000002118,0.242187500002177,0.246093750002206,
0.24804687500222,0.250000000002234,0.300092256335661,0.351162113591053,
0.375000000001859,0.430234827802864,0.43750000000167,0.468750000001586,
0.484375000001535,0.4965639918839,0.500000000001485,0.500516815631294,0.55935025332849,
0.620369079944048,0.625000000001113,0.695027282812789,0.744902136073919,
0.776223206194934,0.847905243539548,0.923952621769774,1.),.UNSPECIFIED.);
#4875=B_SPLINE_CURVE_WITH_KNOTS('',3,(#159460,#159461,#159462,#159463,#159464,
#159465,#159466,#159467,#159468,#159469,#159470,#159471,#159472,#159473,
#159474,#159475,#159476,#159477,#159478,#159479,#159480,#159481,#159482,
#159483,#159484,#159485,#159486,#159487,#159488,#159489,#159490,#159491,
#159492,#159493,#159494,#159495,#159496,#159497,#159498,#159499),
 .UNSPECIFIED.,.F.,.F.,(4,2,2,1,1,1,1,2,2,2,2,2,1,1,1,2,2,2,2,1,1,1,2,2,
4),(0.,0.125000000002992,0.187500000004488,0.218750000005237,0.234375000005619,
0.242187500005819,0.246093750005911,0.249023437505987,0.250000000006018,
0.375000000004521,0.437500000003772,0.468750000003398,0.484375000003211,
0.492187500003117,0.496093750003077,0.498046875003056,0.500000000003036,
0.625000000002027,0.687500000001514,0.718750000001247,0.734375000001123,
0.742187500001071,0.746093750001047,0.750000000001022,0.999999986537213),
 .UNSPECIFIED.);
#4876=B_SPLINE_CURVE_WITH_KNOTS('',3,(#159504,#159505,#159506,#159507,#159508,
#159509,#159510,#159511,#159512,#159513,#159514,#159515,#159516,#159517,
#159518,#159519,#159520,#159521,#159522,#159523,#159524,#159525,#159526,
#159527,#159528,#159529,#159530,#159531,#159532,#159533,#159534),
 .UNSPECIFIED.,.F.,.F.,(4,3,3,3,3,3,3,3,3,3,4),(0.,0.150663464397143,0.304609114316041,
0.464152105860527,0.499023437500262,0.500000000000263,0.500022138851066,
0.6250166041383,0.749963007430494,0.880076354371466,1.),.UNSPECIFIED.);
#4877=B_SPLINE_CURVE_WITH_KNOTS('',3,(#159535,#159536,#159537,#159538,#159539,
#159540,#159541,#159542,#159543,#159544,#159545,#159546,#159547,#159548,
#159549,#159550),.UNSPECIFIED.,.F.,.F.,(4,2,2,1,1,1,1,2,2,4),(0.,0.249999999999979,
0.374999999999969,0.437499999999965,0.468749999999961,0.484374999999959,
0.492187499999957,0.499023437499959,0.499999999999959,1.),.UNSPECIFIED.);
#4878=B_SPLINE_CURVE_WITH_KNOTS('',3,(#159572,#159573,#159574,#159575,#159576,
#159577,#159578,#159579,#159580,#159581,#159582,#159583,#159584,#159585,
#159586,#159587,#159588,#159589,#159590),.UNSPECIFIED.,.F.,.F.,(4,3,3,3,
3,3,4),(0.000623203325049932,0.00219889325760342,0.00382915155667807,0.00555512420839928,
0.00571003463709915,0.00756817415875732,0.00806753801901704),
 .UNSPECIFIED.);
#4879=B_SPLINE_CURVE_WITH_KNOTS('',3,(#159594,#159595,#159596,#159597,#159598,
#159599,#159600,#159601,#159602,#159603,#159604,#159605,#159606,#159607,
#159608,#159609),.UNSPECIFIED.,.F.,.F.,(4,3,3,3,3,4),(0.000694356721436431,
0.00259637723166065,0.00305563622484018,0.00480503978353614,0.00647539340150544,
0.00814574701947475),.UNSPECIFIED.);
#4880=B_SPLINE_CURVE_WITH_KNOTS('',3,(#159623,#159624,#159625,#159626,#159627,
#159628,#159629,#159630,#159631,#159632,#159633,#159634,#159635,#159636,
#159637,#159638),.UNSPECIFIED.,.F.,.F.,(4,3,3,3,3,4),(0.000539871559505675,
0.00223531956680388,0.00375574051851002,0.00457928549922769,0.00579560462260641,
0.00697160947751436),.UNSPECIFIED.);
#4881=B_SPLINE_CURVE_WITH_KNOTS('',3,(#159642,#159643,#159644,#159645,#159646,
#159647,#159648,#159649,#159650,#159651,#159652,#159653,#159654,#159655,
#159656,#159657),.UNSPECIFIED.,.F.,.F.,(4,3,3,3,3,4),(0.000601267884717356,
0.00181647811676878,0.00299735824906937,0.00382211018819771,0.00557536121784445,
0.00704295249167806),.UNSPECIFIED.);
#4882=B_SPLINE_CURVE_WITH_KNOTS('',3,(#159662,#159663,#159664,#159665,#159666,
#159667,#159668,#159669,#159670,#159671,#159672,#159673,#159674,#159675,
#159676,#159677,#159678,#159679,#159680,#159681,#159682,#159683,#159684,
#159685,#159686),.UNSPECIFIED.,.F.,.F.,(4,3,3,3,3,3,3,3,4),(0.000498343012073112,
0.00231282934720829,0.00337277528899485,0.00370896758807423,0.00446136300849209,
0.00522125339641071,0.00534496249690202,0.00614439986206087,0.00624720756634296),
 .UNSPECIFIED.);
#4883=B_SPLINE_CURVE_WITH_KNOTS('',3,(#159690,#159691,#159692,#159693,#159694,
#159695,#159696,#159697,#159698,#159699,#159700,#159701,#159702,#159703,
#159704,#159705,#159706,#159707,#159708,#159709,#159710,#159711,#159712,
#159713,#159714),.UNSPECIFIED.,.F.,.F.,(4,3,3,3,3,3,3,3,4),(0.000524342078796179,
0.0018090187682887,0.00304673005325099,0.00340077219985262,0.00411987972637411,
0.00482370949852624,0.00550912189800533,0.00616177752105068,0.00627720230593858),
 .UNSPECIFIED.);
#4884=B_SPLINE_CURVE_WITH_KNOTS('',3,(#159726,#159727,#159728,#159729,#159730,
#159731,#159732,#159733,#159734,#159735,#159736,#159737,#159738,#159739,
#159740,#159741),.UNSPECIFIED.,.F.,.F.,(4,2,2,2,1,1,2,2,4),(0.,0.250000000000448,
0.375000000000645,0.437500000000763,0.468750000000802,0.484375000000844,
0.492187500000843,0.500000000000842,1.),.UNSPECIFIED.);
#4885=B_SPLINE_CURVE_WITH_KNOTS('',3,(#159745,#159746,#159747,#159748,#159749,
#159750,#159751,#159752,#159753,#159754,#159755,#159756,#159757),
 .UNSPECIFIED.,.F.,.F.,(4,3,3,3,4),(0.,0.282022506904398,0.55577415031973,
0.81819454057582,1.),.UNSPECIFIED.);
#4886=B_SPLINE_CURVE_WITH_KNOTS('',3,(#159758,#159759,#159760,#159761,#159762,
#159763,#159764,#159765,#159766,#159767,#159768,#159769,#159770,#159771,
#159772,#159773,#159774,#159775,#159776,#159777,#159778,#159779,#159780,
#159781,#159782,#159783,#159784,#159785,#159786,#159787,#159788,#159789,
#159790,#159791,#159792,#159793,#159794,#159795,#159796,#159797,#159798,
#159799,#159800,#159801,#159802,#159803,#159804,#159805,#159806),
 .UNSPECIFIED.,.F.,.F.,(4,3,3,3,3,3,3,3,3,3,3,3,3,3,3,3,4),(0.,0.115464076706584,
0.204631414112565,0.249999999999961,0.288081633301557,0.398618541405039,
0.498046874999928,0.499807527138215,0.499999999999929,0.569629412683859,
0.624999999999946,0.693718017752262,0.749999999999964,0.813244782606989,
0.876468684100435,0.940110360346619,1.),.UNSPECIFIED.);
#4887=B_SPLINE_CURVE_WITH_KNOTS('',3,(#159833,#159834,#159835,#159836,#159837,
#159838,#159839,#159840,#159841,#159842,#159843,#159844),.UNSPECIFIED.,
 .F.,.F.,(4,2,1,1,2,2,4),(0.,0.250000000000003,0.375000000000005,0.437500000000007,
0.468750000000007,0.500000000000006,1.),.UNSPECIFIED.);
#4888=B_SPLINE_CURVE_WITH_KNOTS('',3,(#159845,#159846,#159847,#159848,#159849,
#159850,#159851,#159852,#159853,#159854,#159855,#159856,#159857,#159858,
#159859,#159860,#159861,#159862,#159863,#159864,#159865,#159866,#159867,
#159868,#159869,#159870,#159871,#159872,#159873,#159874,#159875,#159876,
#159877,#159878,#159879,#159880,#159881,#159882,#159883,#159884,#159885,
#159886,#159887,#159888,#159889,#159890,#159891,#159892,#159893,#159894,
#159895,#159896,#159897,#159898,#159899,#159900,#159901,#159902,#159903,
#159904,#159905,#159906,#159907,#159908),.UNSPECIFIED.,.F.,.F.,(4,3,3,3,
3,3,3,3,3,3,3,3,3,3,3,3,3,3,3,3,3,4),(0.,0.06478051091971,0.124999999999183,
0.187499999998777,0.218749999998586,0.23437499999849,0.24633111659959,0.249999999998394,
0.303541233291795,0.357640266150352,0.412373093698651,0.437499999997239,
0.468749999997027,0.484374999996945,0.492187499996904,0.496093749996909,
0.499999999996914,0.597546155193341,0.698418193262823,0.801205662027104,
0.90739104893303,1.),.UNSPECIFIED.);
#4889=B_SPLINE_CURVE_WITH_KNOTS('',3,(#159930,#159931,#159932,#159933,#159934,
#159935,#159936,#159937,#159938,#159939,#159940,#159941,#159942,#159943,
#159944,#159945,#159946,#159947,#159948),.UNSPECIFIED.,.F.,.F.,(4,3,3,3,
3,3,4),(0.,0.244850538777774,0.488158489871772,0.552096889019018,0.73851462781602,
0.910728935155691,0.999999749632916),.UNSPECIFIED.);
#4890=B_SPLINE_CURVE_WITH_KNOTS('',3,(#159949,#159950,#159951,#159952,#159953,
#159954,#159955,#159956,#159957,#159958,#159959,#159960,#159961,#159962,
#159963,#159964,#159965,#159966,#159967,#159968,#159969,#159970,#159971,
#159972,#159973,#159974,#159975,#159976,#159977,#159978,#159979,#159980,
#159981,#159982,#159983,#159984,#159985,#159986,#159987,#159988,#159989,
#159990,#159991,#159992,#159993,#159994,#159995,#159996,#159997,#159998,
#159999,#160000,#160001,#160002,#160003,#160004,#160005,#160006,#160007,
#160008,#160009,#160010,#160011,#160012,#160013,#160014,#160015,#160016,
#160017,#160018,#160019,#160020,#160021,#160022,#160023,#160024,#160025,
#160026,#160027,#160028,#160029,#160030),.UNSPECIFIED.,.F.,.F.,(4,3,3,3,
3,3,3,3,3,3,3,3,3,3,3,3,3,3,3,3,3,3,3,3,3,3,3,4),(2.533555643913E-8,0.0910320813626261,
0.125000000001408,0.187500000002101,0.218750000002447,0.23437500000262,
0.242187500002707,0.24609375000275,0.248046875002772,0.250000000002794,
0.286382660441103,0.32291484838725,0.359669340739657,0.394628946654578,
0.431903778620834,0.470456940434937,0.496093750001528,0.499668058076043,
0.500000000001504,0.500264737842257,0.569725175841976,0.625000000001128,
0.700983068432055,0.750000000000752,0.82894421112137,0.910139370401911,
0.994278938005407,1.),.UNSPECIFIED.);
#4891=B_SPLINE_CURVE_WITH_KNOTS('',3,(#160031,#160032,#160033,#160034,#160035,
#160036,#160037,#160038,#160039,#160040,#160041,#160042,#160043,#160044,
#160045,#160046,#160047,#160048,#160049,#160050,#160051,#160052,#160053,
#160054,#160055,#160056,#160057,#160058,#160059,#160060,#160061,#160062,
#160063,#160064,#160065,#160066,#160067,#160068,#160069,#160070,#160071,
#160072,#160073,#160074,#160075,#160076,#160077,#160078,#160079,#160080,
#160081,#160082,#160083,#160084,#160085,#160086,#160087,#160088,#160089,
#160090,#160091,#160092,#160093,#160094,#160095,#160096,#160097,#160098,
#160099,#160100),.UNSPECIFIED.,.F.,.F.,(4,3,3,3,3,3,3,3,3,3,3,3,3,3,3,3,
3,3,3,3,3,3,3,4),(0.,0.115241963249706,0.210943191186066,0.272629228253125,
0.375456875050642,0.473607625967427,0.498046874995147,0.499999999995132,
0.500407886731958,0.537881861244917,0.575395554961941,0.612898174107899,
0.624999999996623,0.662411153773846,0.699072930188149,0.734374999997964,
0.742187499998073,0.746093749998126,0.749691223502617,0.749999999998179,
0.817036471811887,0.88546296533256,0.955529737150269,0.999991171984779),
 .UNSPECIFIED.);
#4892=B_SPLINE_CURVE_WITH_KNOTS('',3,(#160127,#160128,#160129,#160130,#160131,
#160132,#160133,#160134,#160135,#160136,#160137,#160138,#160139,#160140,
#160141,#160142),.UNSPECIFIED.,.F.,.F.,(4,3,3,3,3,4),(0.,0.200694999329658,
0.427247628482963,0.604195087233359,0.885229128579841,0.999999354109336),
 .UNSPECIFIED.);
#4893=B_SPLINE_CURVE_WITH_KNOTS('',3,(#160143,#160144,#160145,#160146,#160147,
#160148,#160149,#160150,#160151,#160152,#160153,#160154,#160155,#160156,
#160157,#160158,#160159,#160160,#160161,#160162,#160163,#160164,#160165,
#160166,#160167,#160168,#160169,#160170,#160171,#160172,#160173,#160174,
#160175,#160176,#160177,#160178,#160179,#160180,#160181,#160182,#160183,
#160184,#160185,#160186,#160187,#160188,#160189,#160190,#160191,#160192,
#160193,#160194,#160195,#160196,#160197,#160198,#160199,#160200,#160201,
#160202,#160203,#160204,#160205,#160206,#160207,#160208,#160209,#160210,
#160211,#160212,#160213,#160214,#160215,#160216,#160217,#160218,#160219,
#160220,#160221,#160222,#160223,#160224,#160225,#160226,#160227,#160228,
#160229,#160230,#160231,#160232,#160233,#160234,#160235,#160236,#160237,
#160238,#160239,#160240,#160241,#160242,#160243,#160244,#160245),
 .UNSPECIFIED.,.F.,.F.,(4,3,3,3,3,3,3,3,3,3,3,3,3,3,3,3,3,3,3,3,3,3,3,3,
3,3,3,3,3,3,3,3,3,3,4),(1.5402703012166E-8,0.125000000000293,0.208446749922841,
0.244646765557539,0.245773986165532,0.246072415283787,0.246368383987472,
0.248334622198511,0.249310060686018,0.249836852332955,0.250148121466892,
0.315972242753915,0.373760882794706,0.444714699846058,0.498046875000427,
0.500000000000431,0.500779867134539,0.53444283139843,0.562500000000715,
0.598013518121477,0.625000000000999,0.66129218269956,0.687500000001273,
0.718750000001425,0.734375000001481,0.742187500001509,0.746093750001524,
0.748046875001505,0.7485351562515,0.749267578126493,0.750000000001485,0.818372711897459,
0.888509784935343,0.961434487868489,1.),.UNSPECIFIED.);
#4894=B_SPLINE_CURVE_WITH_KNOTS('',3,(#160246,#160247,#160248,#160249,#160250,
#160251,#160252,#160253,#160254,#160255,#160256,#160257,#160258,#160259,
#160260,#160261,#160262,#160263,#160264,#160265,#160266,#160267,#160268,
#160269,#160270,#160271,#160272,#160273,#160274,#160275,#160276,#160277,
#160278,#160279,#160280,#160281,#160282,#160283,#160284,#160285,#160286,
#160287,#160288,#160289,#160290,#160291,#160292,#160293,#160294,#160295,
#160296,#160297,#160298,#160299,#160300,#160301,#160302,#160303,#160304,
#160305,#160306,#160307,#160308,#160309,#160310,#160311,#160312,#160313,
#160314,#160315,#160316,#160317,#160318,#160319,#160320,#160321,#160322,
#160323,#160324,#160325,#160326,#160327,#160328,#160329,#160330,#160331,
#160332,#160333,#160334,#160335,#160336,#160337,#160338,#160339,#160340,
#160341,#160342,#160343,#160344,#160345,#160346,#160347,#160348,#160349,
#160350,#160351,#160352,#160353,#160354),.UNSPECIFIED.,.F.,.F.,(4,3,3,3,
3,3,3,3,3,3,3,3,3,3,3,3,3,3,3,3,3,3,3,3,3,3,3,3,3,3,3,3,3,3,3,3,4),(0.,
0.0953370365995093,0.176698850256003,0.215158368973863,0.231984408412927,
0.239871614399988,0.243691979799971,0.245572315895275,0.246091243916352,
0.2463897663404,0.248249025978357,0.249171393064374,0.249740342882374,0.249997511217146,
0.250204522741881,0.310264212512982,0.368061028373041,0.428066686248988,
0.484374999998885,0.495112152105643,0.499805054424163,0.499999999998881,
0.547749307420529,0.596812594126604,0.624999999998827,0.674967800891608,
0.6874999999988,0.718749999998787,0.73437499999878,0.742187499998761,0.746093749998768,
0.748046874998789,0.749999999998811,0.825517565210902,0.903222315217755,
0.983862504053623,0.999984984351931),.UNSPECIFIED.);
#4895=B_SPLINE_CURVE_WITH_KNOTS('',3,(#160400,#160401,#160402,#160403,#160404,
#160405,#160406,#160407,#160408,#160409,#160410,#160411,#160412),
 .UNSPECIFIED.,.F.,.F.,(4,3,3,3,4),(0.,0.00150087219104035,0.00207200756106571,
0.00310801134159857,0.00414401512213143),.UNSPECIFIED.);
#4896=B_SPLINE_CURVE_WITH_KNOTS('',3,(#160416,#160417,#160418,#160419,#160420,
#160421,#160422,#160423,#160424,#160425,#160426,#160427,#160428,#160429,
#160430,#160431,#160432,#160433,#160434,#160435,#160436,#160437,#160438,
#160439,#160440,#160441,#160442,#160443,#160444,#160445,#160446,#160447,
#160448,#160449,#160450,#160451,#160452,#160453,#160454,#160455,#160456,
#160457,#160458,#160459,#160460,#160461,#160462,#160463,#160464,#160465,
#160466,#160467,#160468,#160469,#160470,#160471,#160472,#160473,#160474,
#160475,#160476,#160477,#160478,#160479,#160480,#160481,#160482,#160483,
#160484,#160485,#160486,#160487,#160488),.UNSPECIFIED.,.F.,.F.,(4,3,3,3,
3,3,3,3,3,3,3,3,3,3,3,3,3,3,3,3,3,3,3,3,4),(0.,0.0827800474306258,0.164476544804415,
0.244653694889878,0.323963103854387,0.402053885677088,0.437500000000753,
0.468750000000797,0.482808608553153,0.497325464085628,0.500000000000842,
0.563666376687189,0.625583188344086,0.687500000000982,0.718750000001013,
0.734375000001029,0.742187500001028,0.746930764484763,0.750000000001027,
0.798770062773211,0.846466169814649,0.892304506589185,0.936986645493463,
0.979989519943143,1.),.UNSPECIFIED.);
#4897=B_SPLINE_CURVE_WITH_KNOTS('',3,(#160510,#160511,#160512,#160513,#160514,
#160515,#160516,#160517,#160518,#160519,#160520,#160521,#160522,#160523,
#160524,#160525,#160526,#160527,#160528,#160529,#160530,#160531,#160532,
#160533,#160534,#160535,#160536,#160537,#160538,#160539,#160540,#160541,
#160542,#160543,#160544,#160545,#160546,#160547,#160548,#160549,#160550,
#160551,#160552,#160553,#160554,#160555,#160556,#160557,#160558,#160559,
#160560,#160561,#160562,#160563,#160564),.UNSPECIFIED.,.F.,.F.,(4,3,3,3,
3,3,3,3,3,3,3,3,3,3,3,3,3,3,4),(0.,0.104715580701354,0.210383985033992,
0.249999999999817,0.354011981377643,0.374999999999734,0.437499999999696,
0.468749999999665,0.484374999999646,0.493439254443789,0.499999999999626,
0.577747102581383,0.652041765361407,0.721927843697446,0.749999999999813,
0.814470107593342,0.877192615710051,0.938596307855025,1.),.UNSPECIFIED.);
#4898=B_SPLINE_CURVE_WITH_KNOTS('',3,(#160567,#160568,#160569,#160570,#160571,
#160572,#160573),.UNSPECIFIED.,.F.,.F.,(4,3,4),(4.71238898038468,5.49778714378214,
6.28318530717959),.UNSPECIFIED.);
#4899=B_SPLINE_CURVE_WITH_KNOTS('',3,(#160597,#160598,#160599,#160600,#160601,
#160602,#160603),.UNSPECIFIED.,.F.,.F.,(4,3,4),(3.14159265358979,3.92699081698724,
4.71238898038469),.UNSPECIFIED.);
#4900=B_SPLINE_CURVE_WITH_KNOTS('',3,(#160606,#160607,#160608,#160609,#160610,
#160611,#160612,#160613,#160614,#160615,#160616,#160617,#160618,#160619,
#160620,#160621,#160622,#160623,#160624,#160625,#160626,#160627,#160628,
#160629,#160630,#160631,#160632,#160633,#160634,#160635,#160636,#160637,
#160638,#160639,#160640,#160641,#160642,#160643,#160644,#160645,#160646,
#160647,#160648,#160649,#160650,#160651),.UNSPECIFIED.,.F.,.F.,(4,3,3,3,
3,3,3,3,3,3,3,3,3,3,3,4),(0.,0.0605468750000088,0.122426142584879,0.186284753089235,
0.245362452615264,0.322247692375512,0.398189409304048,0.475083017862261,
0.484375000000071,0.493930247608612,0.500000000000069,0.605247959003852,
0.710628641082224,0.816191187900766,0.922233554824866,1.),.UNSPECIFIED.);
#4901=B_SPLINE_CURVE_WITH_KNOTS('',3,(#160656,#160657,#160658,#160659,#160660,
#160661,#160662,#160663,#160664,#160665,#160666,#160667,#160668,#160669,
#160670,#160671,#160672,#160673,#160674,#160675,#160676,#160677,#160678,
#160679,#160680,#160681,#160682,#160683,#160684,#160685,#160686,#160687,
#160688,#160689,#160690,#160691,#160692,#160693,#160694,#160695,#160696,
#160697,#160698,#160699,#160700,#160701,#160702,#160703,#160704,#160705,
#160706,#160707,#160708,#160709,#160710,#160711,#160712,#160713,#160714,
#160715,#160716,#160717,#160718,#160719,#160720,#160721,#160722,#160723,
#160724,#160725,#160726,#160727,#160728),.UNSPECIFIED.,.F.,.F.,(4,3,3,3,
3,3,3,3,3,3,3,3,3,3,3,3,3,3,3,3,3,3,3,3,4),(0.,0.0827800472710771,0.164476544468573,
0.244653694362582,0.323963103155625,0.402053884755395,0.437500000000487,
0.468750000000525,0.482808608365209,0.497325463721906,0.500000000000563,
0.563666376083932,0.625583188042332,0.687500000000732,0.718750000000761,
0.734375000000765,0.742187500000777,0.746930764471125,0.75000000000079,
0.79877006272679,0.846466169726166,0.892304506462131,0.936986645329322,
0.979989519741638,1.),.UNSPECIFIED.);
#4902=B_SPLINE_CURVE_WITH_KNOTS('',3,(#160729,#160730,#160731,#160732,#160733,
#160734,#160735,#160736,#160737,#160738,#160739,#160740,#160741,#160742,
#160743,#160744,#160745,#160746,#160747,#160748,#160749,#160750,#160751,
#160752,#160753,#160754,#160755,#160756,#160757,#160758,#160759,#160760,
#160761,#160762,#160763,#160764,#160765,#160766,#160767,#160768,#160769,
#160770,#160771,#160772,#160773,#160774,#160775,#160776,#160777,#160778,
#160779,#160780,#160781,#160782,#160783,#160784,#160785,#160786,#160787,
#160788,#160789,#160790,#160791,#160792,#160793,#160794,#160795,#160796,
#160797,#160798),.UNSPECIFIED.,.F.,.F.,(4,3,3,3,3,3,3,3,3,3,3,3,3,3,3,3,
3,3,3,3,3,3,3,4),(0.,0.0417433063302083,0.0856783502063842,0.125000000000064,
0.172058636966678,0.221141673751301,0.242187500000112,0.247530062035886,
0.25000000000012,0.258757699077574,0.318098755622358,0.375000000000093,
0.438761223505778,0.468750000000083,0.483267071906232,0.497350908759363,
0.500000000000075,0.586409574409656,0.674221064481857,0.743171333762874,
0.750000000000038,0.839284683635661,0.929619546314489,1.),.UNSPECIFIED.);
#4903=B_SPLINE_CURVE_WITH_KNOTS('',3,(#160821,#160822,#160823,#160824,#160825,
#160826,#160827),.UNSPECIFIED.,.F.,.F.,(4,3,4),(4.71238898038469,5.49778714378214,
6.28318530717959),.UNSPECIFIED.);
#4904=B_SPLINE_CURVE_WITH_KNOTS('',3,(#160829,#160830,#160831,#160832,#160833,
#160834,#160835,#160836,#160837,#160838,#160839,#160840,#160841,#160842,
#160843,#160844,#160845,#160846,#160847,#160848,#160849,#160850,#160851,
#160852,#160853,#160854,#160855,#160856,#160857,#160858,#160859,#160860,
#160861,#160862,#160863,#160864,#160865,#160866,#160867,#160868,#160869,
#160870,#160871,#160872,#160873,#160874,#160875,#160876,#160877,#160878,
#160879,#160880,#160881,#160882,#160883),.UNSPECIFIED.,.F.,.F.,(4,3,3,3,
3,3,3,3,3,3,3,3,3,3,3,3,3,3,4),(0.,0.1047155801347,0.210383983761551,0.249999999998705,
0.354011980517942,0.374999999998113,0.437499999997821,0.468749999997671,
0.484374999997637,0.49343925441085,0.499999999997603,0.577747102421286,
0.65204176505497,0.721927843234957,0.749999999998801,0.814470107408982,
0.877192615336184,0.938596307668092,1.),.UNSPECIFIED.);
#4905=B_SPLINE_CURVE_WITH_KNOTS('',3,(#160907,#160908,#160909,#160910,#160911,
#160912,#160913),.UNSPECIFIED.,.F.,.F.,(4,3,4),(-8.88178419700125E-16,0.78539816339745,
1.5707963267949),.UNSPECIFIED.);
#4906=B_SPLINE_CURVE_WITH_KNOTS('',3,(#160916,#160917,#160918,#160919,#160920,
#160921,#160922,#160923,#160924,#160925,#160926,#160927,#160928,#160929,
#160930,#160931,#160932,#160933,#160934,#160935,#160936,#160937,#160938,
#160939,#160940,#160941,#160942,#160943,#160944,#160945,#160946,#160947,
#160948,#160949,#160950,#160951,#160952,#160953,#160954,#160955,#160956,
#160957,#160958,#160959,#160960,#160961),.UNSPECIFIED.,.F.,.F.,(4,3,3,3,
3,3,3,3,3,3,3,3,3,3,3,4),(0.,0.060546874999865,0.122426142580309,0.186284753080097,
0.245362452602329,0.322247692345566,0.398189409215696,0.475083013998846,
0.48437499999892,0.49393024760668,0.499999999998935,0.605247958974294,0.710628641027629,
0.816191187822136,0.922233554723543,1.),.UNSPECIFIED.);
#4907=B_SPLINE_CURVE_WITH_KNOTS('',3,(#160967,#160968,#160969,#160970,#160971,
#160972,#160973,#160974,#160975,#160976,#160977,#160978,#160979,#160980,
#160981,#160982,#160983,#160984,#160985,#160986,#160987,#160988,#160989,
#160990,#160991,#160992,#160993,#160994,#160995,#160996,#160997,#160998,
#160999,#161000,#161001,#161002,#161003,#161004,#161005,#161006,#161007,
#161008,#161009,#161010,#161011,#161012,#161013,#161014,#161015,#161016,
#161017,#161018,#161019,#161020,#161021,#161022,#161023,#161024,#161025,
#161026,#161027,#161028,#161029,#161030,#161031,#161032,#161033,#161034,
#161035,#161036),.UNSPECIFIED.,.F.,.F.,(4,3,3,3,3,3,3,3,3,3,3,3,3,3,3,3,
3,3,3,3,3,3,3,4),(0.,0.0417433067437773,0.085678351037766,0.125000000000076,
0.172058637390442,0.221141674281389,0.242187500000128,0.247530062059483,
0.250000000000119,0.258757699107327,0.318098756280707,0.375000000000195,
0.438761224377743,0.46875000000021,0.483267072005296,0.497350908963462,
0.500000000000197,0.586409574334292,0.67422106433992,0.743171333738989,
0.750000000000099,0.839284683557368,0.929619546162419,1.),.UNSPECIFIED.);
#4908=B_SPLINE_CURVE_WITH_KNOTS('',3,(#161079,#161080,#161081,#161082,#161083,
#161084,#161085,#161086,#161087,#161088,#161089,#161090,#161091,#161092,
#161093,#161094,#161095,#161096,#161097,#161098,#161099,#161100,#161101,
#161102,#161103,#161104,#161105,#161106,#161107,#161108,#161109,#161110,
#161111,#161112,#161113,#161114,#161115,#161116,#161117,#161118,#161119,
#161120,#161121,#161122,#161123,#161124,#161125,#161126,#161127),
 .UNSPECIFIED.,.F.,.F.,(4,3,3,3,3,3,3,3,3,3,3,3,3,3,3,3,4),(0.,0.104472515273559,
0.209822727893399,0.24999999999986,0.35418712941254,0.438820809815404,0.484374999999763,
0.493439281928252,0.49999999999974,0.577466051600214,0.651600365001254,
0.721481777027291,0.74999999999987,0.814614317509502,0.877383216253357,
0.938691608126678,1.),.UNSPECIFIED.);
#4909=B_SPLINE_CURVE_WITH_KNOTS('',3,(#161130,#161131,#161132,#161133,#161134,
#161135,#161136),.UNSPECIFIED.,.F.,.F.,(4,3,4),(1.5707963267949,2.35619449019235,
3.1415926535898),.UNSPECIFIED.);
#4910=B_SPLINE_CURVE_WITH_KNOTS('',3,(#161160,#161161,#161162,#161163,#161164,
#161165,#161166),.UNSPECIFIED.,.F.,.F.,(4,3,4),(1.23467863058848E-16,0.785398163397447,
1.5707963267949),.UNSPECIFIED.);
#4911=B_SPLINE_CURVE_WITH_KNOTS('',3,(#161169,#161170,#161171,#161172,#161173,
#161174,#161175,#161176,#161177,#161178,#161179,#161180,#161181,#161182,
#161183,#161184,#161185,#161186,#161187,#161188,#161189,#161190,#161191,
#161192,#161193,#161194,#161195,#161196,#161197,#161198,#161199,#161200,
#161201,#161202,#161203,#161204,#161205,#161206,#161207,#161208,#161209,
#161210,#161211,#161212,#161213,#161214,#161215,#161216,#161217,#161218,
#161219,#161220),.UNSPECIFIED.,.F.,.F.,(4,3,3,3,3,3,3,3,3,3,3,3,3,3,3,3,
3,4),(0.,0.0625000000000772,0.124900823545415,0.190034230928347,0.250000000000309,
0.319870182296621,0.375000000000471,0.437500000000552,0.468750000000589,
0.48437500000056,0.494074303447769,0.50000000000053,0.591975494567463,0.685251275132029,
0.780573779584712,0.877101419355448,0.975445333692385,1.),.UNSPECIFIED.);
#4912=B_SPLINE_CURVE_WITH_KNOTS('',3,(#161223,#161224,#161225,#161226,#161227,
#161228,#161229,#161230,#161231,#161232,#161233,#161234,#161235,#161236,
#161237,#161238,#161239,#161240,#161241,#161242,#161243,#161244,#161245,
#161246,#161247,#161248,#161249,#161250,#161251,#161252,#161253,#161254,
#161255,#161256,#161257,#161258,#161259,#161260,#161261,#161262,#161263,
#161264,#161265,#161266,#161267,#161268,#161269,#161270,#161271,#161272,
#161273,#161274,#161275,#161276,#161277,#161278,#161279,#161280,#161281,
#161282,#161283,#161284,#161285,#161286,#161287,#161288,#161289,#161290,
#161291,#161292,#161293,#161294,#161295,#161296,#161297,#161298),
 .UNSPECIFIED.,.F.,.F.,(4,3,3,3,3,3,3,3,3,3,3,3,3,3,3,3,3,3,3,3,3,3,3,3,
3,4),(0.,0.0427401092012923,0.0873804166631017,0.13313759505412,0.180399662455455,
0.187500000000028,0.218750000000024,0.234375000000025,0.242187500000029,
0.247546297842306,0.250000000000033,0.309158131845126,0.369865863968725,
0.375000000000126,0.437500000000172,0.46875000000019,0.483324530441297,
0.497499574224517,0.500000000000208,0.577335497435133,0.655589023587681,
0.734790128085894,0.815464874684637,0.897007690809156,0.979843823811218,
1.),.UNSPECIFIED.);
#4913=B_SPLINE_CURVE_WITH_KNOTS('',3,(#161321,#161322,#161323,#161324,#161325,
#161326,#161327,#161328,#161329,#161330,#161331,#161332,#161333),
 .UNSPECIFIED.,.F.,.F.,(4,3,3,3,4),(6.93889390390723E-18,0.00113151531066505,
0.00191432655883665,0.00348473784371938,0.00382865311767331),
 .UNSPECIFIED.);
#4914=B_SPLINE_CURVE_WITH_KNOTS('',3,(#161339,#161340,#161341,#161342,#161343,
#161344,#161345,#161346,#161347,#161348,#161349,#161350,#161351,#161352,
#161353,#161354,#161355,#161356,#161357,#161358,#161359,#161360,#161361,
#161362,#161363,#161364,#161365,#161366,#161367,#161368,#161369,#161370,
#161371,#161372,#161373,#161374,#161375,#161376,#161377,#161378,#161379,
#161380,#161381,#161382,#161383,#161384,#161385,#161386,#161387,#161388,
#161389,#161390,#161391,#161392,#161393,#161394,#161395,#161396,#161397,
#161398,#161399,#161400,#161401,#161402,#161403,#161404,#161405,#161406,
#161407,#161408),.UNSPECIFIED.,.F.,.F.,(4,3,3,3,3,3,3,3,3,3,3,3,3,3,3,3,
3,3,3,3,3,3,3,4),(0.,0.0904805863956041,0.179890948435827,0.24999999999996,
0.256840728572676,0.344945742334393,0.429509229332709,0.468749999999929,
0.482752596495082,0.497175643681866,0.499999999999926,0.56298906712764,
0.6249999999999,0.68399450346291,0.741245408299592,0.74218749999991,0.746913732826963,
0.749999999999906,0.799311389349656,0.849483542012242,0.894712088324863,
0.938468707059143,0.980197893115309,1.),.UNSPECIFIED.);
#4915=B_SPLINE_CURVE_WITH_KNOTS('',3,(#161432,#161433,#161434,#161435,#161436,
#161437,#161438),.UNSPECIFIED.,.F.,.F.,(4,3,4),(4.71238898038468,5.49778714378213,
6.28318530717959),.UNSPECIFIED.);
#4916=B_SPLINE_CURVE_WITH_KNOTS('',3,(#161440,#161441,#161442,#161443,#161444,
#161445,#161446,#161447,#161448,#161449,#161450,#161451,#161452,#161453,
#161454,#161455,#161456,#161457,#161458,#161459,#161460,#161461,#161462,
#161463,#161464,#161465,#161466,#161467,#161468,#161469,#161470,#161471,
#161472,#161473,#161474,#161475,#161476,#161477,#161478,#161479,#161480,
#161481,#161482,#161483,#161484,#161485,#161486,#161487,#161488),
 .UNSPECIFIED.,.F.,.F.,(4,3,3,3,3,3,3,3,3,3,3,3,3,3,3,3,4),(0.,0.104472515277785,
0.209822727901897,0.25000000000095,0.354187129412535,0.438820810898927,
0.484375000001802,0.493439281930502,0.500000000001818,0.577466051602124,
0.65160036500341,0.721481777029761,0.750000000000909,0.814614317510989,
0.87738321625524,0.93869160812762,1.),.UNSPECIFIED.);
#4917=B_SPLINE_CURVE_WITH_KNOTS('',3,(#161512,#161513,#161514,#161515,#161516,
#161517,#161518),.UNSPECIFIED.,.F.,.F.,(4,3,4),(1.23467863058848E-16,0.785398163397447,
1.5707963267949),.UNSPECIFIED.);
#4918=B_SPLINE_CURVE_WITH_KNOTS('',3,(#161521,#161522,#161523,#161524,#161525,
#161526,#161527,#161528,#161529,#161530,#161531,#161532,#161533,#161534,
#161535,#161536,#161537,#161538,#161539,#161540,#161541,#161542,#161543,
#161544,#161545,#161546,#161547,#161548,#161549,#161550,#161551,#161552,
#161553,#161554,#161555,#161556,#161557,#161558,#161559,#161560,#161561,
#161562,#161563,#161564,#161565,#161566,#161567,#161568,#161569,#161570,
#161571,#161572),.UNSPECIFIED.,.F.,.F.,(4,3,3,3,3,3,3,3,3,3,3,3,3,3,3,3,
3,4),(0.,0.0625000000000519,0.124900823545418,0.190034230928422,0.250000000000208,
0.319870182295419,0.375000000000326,0.437500000000372,0.468750000000392,
0.484375000000367,0.494074303447496,0.500000000000342,0.591975494567397,
0.685251275132125,0.780573779585023,0.87710141935604,0.97544533369326,1.),
 .UNSPECIFIED.);
#4919=B_SPLINE_CURVE_WITH_KNOTS('',3,(#161577,#161578,#161579,#161580,#161581,
#161582,#161583,#161584,#161585,#161586,#161587,#161588,#161589,#161590,
#161591,#161592,#161593,#161594,#161595,#161596,#161597,#161598,#161599,
#161600,#161601,#161602,#161603,#161604,#161605,#161606,#161607,#161608,
#161609,#161610,#161611,#161612,#161613,#161614,#161615,#161616,#161617,
#161618,#161619,#161620,#161621,#161622,#161623,#161624,#161625,#161626,
#161627,#161628,#161629,#161630,#161631,#161632,#161633,#161634,#161635,
#161636,#161637,#161638,#161639,#161640,#161641,#161642,#161643,#161644,
#161645,#161646),.UNSPECIFIED.,.F.,.F.,(4,3,3,3,3,3,3,3,3,3,3,3,3,3,3,3,
3,3,3,3,3,3,3,4),(0.,0.0904805863645094,0.179890948371529,0.249999999999614,
0.25684072858258,0.344945742312153,0.42950922919613,0.468749999999293,0.482752596421625,
0.497175643541116,0.499999999999244,0.562989066800544,0.624999999999167,
0.683994503499725,0.741245408316608,0.742187499999101,0.746913732804136,
0.749999999999098,0.799311389113812,0.849483541835359,0.894712087957233,
0.938468706507326,0.980197892375734,1.),.UNSPECIFIED.);
#4920=B_SPLINE_CURVE_WITH_KNOTS('',3,(#161647,#161648,#161649,#161650,#161651,
#161652,#161653,#161654,#161655,#161656,#161657,#161658,#161659,#161660,
#161661,#161662,#161663,#161664,#161665,#161666,#161667,#161668,#161669,
#161670,#161671,#161672,#161673,#161674,#161675,#161676,#161677,#161678,
#161679,#161680,#161681,#161682,#161683,#161684,#161685,#161686,#161687,
#161688,#161689,#161690,#161691,#161692,#161693,#161694,#161695,#161696,
#161697,#161698,#161699,#161700,#161701,#161702,#161703,#161704,#161705,
#161706,#161707,#161708,#161709,#161710,#161711,#161712,#161713,#161714,
#161715,#161716,#161717,#161718,#161719,#161720,#161721,#161722),
 .UNSPECIFIED.,.F.,.F.,(4,3,3,3,3,3,3,3,3,3,3,3,3,3,3,3,3,3,3,3,3,3,3,3,
3,4),(0.,0.0427401094863224,0.0873804172404971,0.133137595941066,0.180399663654732,
0.18749999999992,0.218749999999916,0.234374999999926,0.242187499999936,
0.247546297862462,0.249999999999946,0.309158132445463,0.36986586515317,
0.374999999999943,0.437499999999942,0.468749999999964,0.483324530559454,
0.497499574469254,0.499999999999985,0.577335497496591,0.655589023707543,
0.734790128260523,0.815464874927968,0.897007691098662,0.979843824141047,
1.),.UNSPECIFIED.);
#4921=B_SPLINE_CURVE_WITH_KNOTS('',3,(#161736,#161737,#161738,#161739,#161740,
#161741,#161742,#161743,#161744,#161745,#161746,#161747,#161748,#161749,
#161750,#161751,#161752,#161753,#161754,#161755,#161756,#161757,#161758,
#161759,#161760,#161761,#161762,#161763,#161764,#161765,#161766,#161767,
#161768,#161769,#161770,#161771,#161772),.UNSPECIFIED.,.F.,.F.,(4,3,3,3,
3,3,3,3,3,3,3,3,4),(1.70755612180505E-6,0.218048820966207,0.413536615724655,
0.450190577241864,0.467372121703056,0.470177992009516,0.486734929759218,
0.494754696481731,0.498886349000283,0.501099101143529,0.683464306546563,
0.847789526356529,1.),.UNSPECIFIED.);
#4922=B_SPLINE_CURVE_WITH_KNOTS('',3,(#161773,#161774,#161775,#161776,#161777,
#161778,#161779,#161780,#161781,#161782,#161783,#161784,#161785,#161786,
#161787,#161788,#161789,#161790,#161791,#161792,#161793,#161794,#161795,
#161796,#161797,#161798,#161799,#161800,#161801,#161802,#161803,#161804,
#161805,#161806),.UNSPECIFIED.,.F.,.F.,(4,3,3,3,3,3,3,3,3,3,3,4),(2.03157429207824E-5,
0.14867142041905,0.273762375268916,0.374999999999955,0.429438237983039,
0.484372693795509,0.499999999999939,0.506412229479512,0.639519611027661,
0.770764026496447,0.900223227858203,1.),.UNSPECIFIED.);
#4923=B_SPLINE_CURVE_WITH_KNOTS('',3,(#161829,#161830,#161831,#161832,#161833,
#161834,#161835,#161836,#161837,#161838,#161839,#161840,#161841,#161842),
 .UNSPECIFIED.,.F.,.F.,(4,2,2,2,2,2,4),(0.,0.250000000000022,0.375000000000029,
0.43750000000005,0.500000000000072,0.750000000000036,1.),.UNSPECIFIED.);
#4924=B_SPLINE_CURVE_WITH_KNOTS('',3,(#161845,#161846,#161847,#161848,#161849,
#161850,#161851,#161852,#161853,#161854,#161855,#161856,#161857,#161858,
#161859,#161860,#161861,#161862,#161863,#161864,#161865,#161866,#161867,
#161868,#161869,#161870,#161871,#161872),.UNSPECIFIED.,.F.,.F.,(4,3,3,3,
3,3,3,3,3,4),(0.,0.138160071953523,0.28057569199304,0.430296839593711,0.491456739356699,
0.5,0.653325725654778,0.78125,0.967247952047853,1.),.UNSPECIFIED.);
#4925=B_SPLINE_CURVE_WITH_KNOTS('',3,(#161926,#161927,#161928,#161929,#161930,
#161931,#161932,#161933,#161934,#161935,#161936,#161937,#161938,#161939,
#161940,#161941,#161942,#161943,#161944,#161945,#161946,#161947,#161948,
#161949,#161950,#161951,#161952,#161953,#161954,#161955,#161956,#161957,
#161958,#161959,#161960,#161961,#161962,#161963,#161964,#161965,#161966,
#161967,#161968,#161969,#161970,#161971,#161972,#161973,#161974,#161975,
#161976,#161977,#161978,#161979,#161980,#161981,#161982,#161983,#161984,
#161985,#161986),.UNSPECIFIED.,.F.,.F.,(4,3,3,3,3,3,3,3,3,3,3,3,3,3,3,3,
3,3,3,3,4),(0.,0.0624999999999682,0.124999999999936,0.187499999999898,0.21874999999989,
0.234374999999906,0.244323266293418,0.249999999999922,0.332208918070905,
0.37500000000021,0.437500000000337,0.468750000000369,0.484375000000366,
0.494186090879374,0.500000000000364,0.584475175928334,0.670102559384199,
0.757636314324216,0.846235385908535,0.936632476909697,1.),.UNSPECIFIED.);
#4926=B_SPLINE_CURVE_WITH_KNOTS('',3,(#161987,#161988,#161989,#161990,#161991,
#161992,#161993,#161994,#161995,#161996,#161997,#161998,#161999,#162000,
#162001,#162002,#162003,#162004,#162005,#162006,#162007,#162008,#162009,
#162010,#162011,#162012,#162013,#162014,#162015,#162016,#162017,#162018,
#162019,#162020,#162021,#162022,#162023,#162024,#162025,#162026,#162027,
#162028,#162029,#162030,#162031,#162032),.UNSPECIFIED.,.F.,.F.,(4,3,3,3,
3,3,3,3,3,3,3,3,3,3,3,4),(0.,0.000109331983970333,0.000221348099123991,
0.000333853905449093,0.000407294015799104,0.00040891081566422,0.000676681051257162,
0.000814588031598208,0.000816767951597528,0.00106247378106637,0.00122188204739731,
0.00122336180785488,0.00135439024293119,0.0014917831530638,0.00162097073973685,
0.00162917606319641),.UNSPECIFIED.);
#4927=B_SPLINE_CURVE_WITH_KNOTS('',3,(#162066,#162067,#162068,#162069,#162070,
#162071,#162072,#162073,#162074,#162075,#162076,#162077,#162078,#162079,
#162080,#162081,#162082,#162083,#162084,#162085,#162086,#162087,#162088,
#162089,#162090,#162091,#162092,#162093,#162094,#162095,#162096,#162097,
#162098,#162099,#162100,#162101,#162102,#162103,#162104,#162105,#162106,
#162107,#162108,#162109,#162110,#162111,#162112,#162113,#162114,#162115,
#162116,#162117,#162118,#162119,#162120,#162121,#162122,#162123,#162124,
#162125,#162126,#162127,#162128,#162129,#162130,#162131,#162132,#162133,
#162134,#162135,#162136,#162137,#162138),.UNSPECIFIED.,.F.,.F.,(4,3,3,3,
3,3,3,3,3,3,3,3,3,3,3,3,3,3,3,3,3,3,3,3,4),(0.,0.0886343067351491,0.17728465402347,
0.250000000000028,0.339768627519797,0.419803528705912,0.484375000000132,
0.484817009440956,0.494431768800152,0.500000000000148,0.579374625844902,
0.625000000000001,0.68749999999995,0.718749999999931,0.734374999999927,
0.74037936111593,0.74218749999993,0.747622414733742,0.749999999999932,0.797680859480093,
0.84531438956593,0.891837596509057,0.93715800399846,0.980323118936031,1.),
 .UNSPECIFIED.);
#4928=B_SPLINE_CURVE_WITH_KNOTS('',3,(#162141,#162142,#162143,#162144,#162145,
#162146,#162147,#162148,#162149,#162150),.UNSPECIFIED.,.F.,.F.,(4,2,2,2,
4),(0.,0.25,0.5,0.75,1.),.UNSPECIFIED.);
#4929=B_SPLINE_CURVE_WITH_KNOTS('',3,(#162175,#162176,#162177,#162178,#162179,
#162180,#162181,#162182,#162183,#162184,#162185,#162186,#162187,#162188,
#162189,#162190,#162191,#162192,#162193,#162194,#162195,#162196,#162197,
#162198,#162199,#162200,#162201,#162202,#162203,#162204,#162205),
 .UNSPECIFIED.,.F.,.F.,(4,3,3,3,3,3,3,3,3,3,4),(0.,0.140771014207785,0.2827542070083,
0.419250990292061,0.5,0.500558885625981,0.612546529858198,0.728431346217552,
0.844245046450148,0.956707375096577,1.),.UNSPECIFIED.);
#4930=B_SPLINE_CURVE_WITH_KNOTS('',3,(#162221,#162222,#162223,#162224,#162225,
#162226,#162227,#162228,#162229,#162230),.UNSPECIFIED.,.F.,.F.,(4,3,3,4),
(0.,0.324689572914811,0.662344786457405,1.),.UNSPECIFIED.);
#4931=B_SPLINE_CURVE_WITH_KNOTS('',3,(#162271,#162272,#162273,#162274,#162275,
#162276,#162277,#162278,#162279,#162280,#162281,#162282,#162283,#162284,
#162285,#162286,#162287,#162288,#162289,#162290,#162291,#162292,#162293,
#162294,#162295,#162296,#162297,#162298,#162299,#162300,#162301,#162302,
#162303,#162304,#162305,#162306,#162307,#162308,#162309,#162310,#162311,
#162312,#162313,#162314,#162315,#162316,#162317,#162318,#162319,#162320,
#162321,#162322,#162323,#162324,#162325,#162326,#162327,#162328,#162329,
#162330,#162331,#162332,#162333,#162334),.UNSPECIFIED.,.F.,.F.,(4,3,3,3,
3,3,3,3,3,3,3,3,3,3,3,3,3,3,3,3,3,4),(0.,0.124999999999932,0.187499999999894,
0.212470944414348,0.236430927507225,0.249999999999857,0.282985586965997,
0.374999999999872,0.415041056558414,0.454731726716648,0.49308919967899,
0.499999999999889,0.535211298208892,0.608652493243637,0.624999999999905,
0.668556878124494,0.711950889580769,0.749999999999921,0.769948319789834,
0.843818367415393,0.921909183395617,0.99999999937584),.UNSPECIFIED.);
#4932=B_SPLINE_CURVE_WITH_KNOTS('',3,(#162337,#162338,#162339,#162340,#162341,
#162342,#162343,#162344,#162345,#162346,#162347,#162348,#162349,#162350,
#162351,#162352,#162353,#162354,#162355,#162356,#162357,#162358,#162359,
#162360,#162361,#162362,#162363,#162364,#162365,#162366,#162367,#162368,
#162369,#162370,#162371,#162372,#162373,#162374,#162375,#162376,#162377,
#162378,#162379),.UNSPECIFIED.,.F.,.F.,(4,3,3,3,3,3,3,3,3,3,3,3,3,3,4),
(0.,0.000108912497168437,0.000220164732383741,0.000331071157537523,0.000392199517465982,
0.000393776648066525,0.000641215708209299,0.000785392845861483,0.000787553296133051,
0.00103453341935802,0.00117987002828324,0.00118132994419958,0.00130742143740821,
0.00144126401483716,0.0015751065922661),.UNSPECIFIED.);
#4933=B_SPLINE_CURVE_WITH_KNOTS('',3,(#162420,#162421,#162422,#162423,#162424,
#162425,#162426,#162427,#162428,#162429,#162430,#162431,#162432,#162433,
#162434,#162435,#162436,#162437,#162438,#162439,#162440,#162441,#162442,
#162443,#162444,#162445,#162446,#162447,#162448,#162449,#162450,#162451,
#162452,#162453,#162454,#162455,#162456,#162457,#162458,#162459,#162460,
#162461,#162462,#162463,#162464,#162465,#162466,#162467,#162468,#162469,
#162470,#162471,#162472,#162473,#162474,#162475,#162476,#162477,#162478,
#162479,#162480,#162481,#162482,#162483,#162484,#162485,#162486,#162487,
#162488,#162489,#162490,#162491,#162492,#162493,#162494,#162495,#162496,
#162497,#162498,#162499,#162500,#162501),.UNSPECIFIED.,.F.,.F.,(4,3,3,3,
3,3,3,3,3,3,3,3,3,3,3,3,3,3,3,3,3,3,3,3,3,3,3,4),(0.,0.0665796625644221,
0.124999999999965,0.194730242247893,0.210359162922861,0.216044757699717,
0.219049295426768,0.236001069080282,0.248594752262763,0.251421853354319,
0.320964043791546,0.391760595068546,0.437499999999978,0.46162556726757,
0.485139651704675,0.499999999999965,0.501282997982719,0.567072139505908,
0.624999999999971,0.687499999999976,0.711787277249982,0.735596853593493,
0.749999999999982,0.750995459618546,0.818462588046628,0.885485905599099,
0.951384278224423,1.),.UNSPECIFIED.);
#4934=B_SPLINE_CURVE_WITH_KNOTS('',3,(#162504,#162505,#162506,#162507,#162508,
#162509,#162510,#162511,#162512,#162513,#162514,#162515,#162516,#162517,
#162518),.UNSPECIFIED.,.F.,.F.,(4,2,2,2,1,2,2,4),(0.,0.250000000000107,
0.375000000000158,0.437500000000159,0.468750000000162,0.484375000000163,
0.500000000000164,1.),.UNSPECIFIED.);
#4935=B_SPLINE_CURVE_WITH_KNOTS('',3,(#162552,#162553,#162554,#162555,#162556,
#162557,#162558,#162559,#162560,#162561,#162562,#162563,#162564,#162565,
#162566,#162567,#162568,#162569,#162570,#162571,#162572,#162573,#162574,
#162575,#162576,#162577,#162578,#162579,#162580,#162581,#162582,#162583,
#162584,#162585,#162586,#162587,#162588,#162589,#162590,#162591,#162592,
#162593,#162594,#162595,#162596,#162597,#162598,#162599,#162600,#162601,
#162602,#162603,#162604,#162605,#162606,#162607,#162608,#162609,#162610,
#162611,#162612,#162613,#162614,#162615,#162616,#162617,#162618,#162619,
#162620,#162621,#162622,#162623,#162624,#162625,#162626,#162627),
 .UNSPECIFIED.,.F.,.F.,(4,3,3,3,3,3,3,3,3,3,3,3,3,3,3,3,3,3,3,3,3,3,3,3,
3,4),(0.,0.12499999999987,0.23628510341623,0.24999999999974,0.312499999999692,
0.374999999999645,0.4374999999996,0.468749999999579,0.484374999999532,0.493831417688319,
0.499999999999485,0.562499999999428,0.568696020518362,0.5937499999994,0.624999999999372,
0.687499999999315,0.718749999999315,0.734374999999345,0.742908936105005,
0.749999999999375,0.798369290592606,0.812499999999531,0.877723444080328,
0.929687499999824,0.995541758473931,1.),.UNSPECIFIED.);
#4936=B_SPLINE_CURVE_WITH_KNOTS('',3,(#162630,#162631,#162632,#162633,#162634,
#162635,#162636,#162637,#162638,#162639,#162640,#162641,#162642,#162643,
#162644,#162645,#162646),.UNSPECIFIED.,.F.,.F.,(4,1,1,2,2,1,1,1,2,2,4),
(0.,0.124999999999952,0.187499999999928,0.218749999999915,0.249999999999903,
0.37499999999986,0.437499999999854,0.468749999999833,0.484374999999823,
0.499999999999812,1.),.UNSPECIFIED.);
#4937=B_SPLINE_CURVE_WITH_KNOTS('',3,(#162699,#162700,#162701,#162702,#162703,
#162704,#162705,#162706,#162707,#162708,#162709,#162710,#162711,#162712,
#162713,#162714,#162715,#162716,#162717,#162718,#162719,#162720,#162721,
#162722,#162723,#162724,#162725,#162726,#162727,#162728,#162729,#162730,
#162731,#162732,#162733,#162734,#162735,#162736,#162737,#162738),
 .UNSPECIFIED.,.F.,.F.,(4,3,3,3,3,3,3,3,3,3,3,3,3,4),(0.,0.000424781762269412,
0.000463398440131748,0.000464821262797086,0.000754099901314684,0.000926796880263496,
0.000929181095996172,0.0011584961003294,0.00116090942630379,0.00139019532039531,
0.00139219601406769,0.00155797632182194,0.00171877163871738,0.00185359376052713),
 .UNSPECIFIED.);
#4938=B_SPLINE_CURVE_WITH_KNOTS('',3,(#162741,#162742,#162743,#162744,#162745,
#162746,#162747,#162748,#162749,#162750,#162751,#162752,#162753,#162754,
#162755,#162756,#162757,#162758,#162759,#162760,#162761,#162762,#162763,
#162764,#162765,#162766,#162767,#162768,#162769,#162770,#162771,#162772,
#162773,#162774,#162775,#162776,#162777,#162778,#162779,#162780,#162781,
#162782,#162783,#162784,#162785,#162786,#162787,#162788,#162789,#162790,
#162791,#162792,#162793,#162794,#162795,#162796,#162797,#162798,#162799,
#162800,#162801,#162802,#162803,#162804,#162805,#162806,#162807,#162808,
#162809,#162810,#162811,#162812,#162813,#162814,#162815,#162816,#162817,
#162818,#162819,#162820,#162821,#162822,#162823,#162824,#162825,#162826,
#162827,#162828),.UNSPECIFIED.,.F.,.F.,(4,3,3,3,3,3,3,3,3,3,3,3,3,3,3,3,
3,3,3,3,3,3,3,3,3,3,3,3,3,4),(0.,0.0471813589526015,0.062500000000042,0.111599854246627,
0.156868243243704,0.183319433108903,0.202136632240781,0.219600693186217,
0.23121412579211,0.23427767967472,0.235710755256672,0.243779701571778,0.248075229850627,
0.249694423524974,0.250682693256269,0.312508154033365,0.372068646189272,
0.386851020524303,0.43162913834518,0.437500000000381,0.468750000000386,
0.484375000000387,0.493500360972887,0.500000000000388,0.591105250217313,
0.686862723351654,0.710255118648367,0.819587104644768,0.932825248138224,
1.),.UNSPECIFIED.);
#4939=B_SPLINE_CURVE_WITH_KNOTS('',3,(#162868,#162869,#162870,#162871,#162872,
#162873,#162874,#162875,#162876,#162877,#162878,#162879,#162880,#162881,
#162882,#162883,#162884,#162885,#162886,#162887,#162888,#162889,#162890,
#162891,#162892,#162893,#162894,#162895,#162896,#162897,#162898,#162899,
#162900,#162901,#162902,#162903,#162904,#162905,#162906,#162907,#162908,
#162909,#162910,#162911,#162912,#162913,#162914,#162915,#162916,#162917,
#162918,#162919,#162920,#162921,#162922,#162923,#162924,#162925,#162926,
#162927,#162928,#162929,#162930,#162931,#162932,#162933,#162934,#162935,
#162936,#162937),.UNSPECIFIED.,.F.,.F.,(4,3,3,3,3,3,3,3,3,3,3,3,3,3,3,3,
3,3,3,3,3,3,3,4),(0.,0.0823663764173504,0.163873434652409,0.219525593901905,
0.255715741026493,0.274015070266574,0.371382535133357,0.409594292583447,
0.46875000000014,0.484375000000129,0.49436143907224,0.500000000000117,0.549262840412801,
0.624999999999946,0.687499999999886,0.718749999999881,0.732850340412289,
0.746266055559976,0.749999999999877,0.784242342539938,0.850134833448856,
0.914122650155725,0.975785622000229,1.),.UNSPECIFIED.);
#4940=B_SPLINE_CURVE_WITH_KNOTS('',3,(#162940,#162941,#162942,#162943,#162944,
#162945,#162946,#162947,#162948,#162949,#162950,#162951,#162952,#162953,
#162954,#162955,#162956,#162957,#162958,#162959,#162960,#162961,#162962,
#162963,#162964,#162965,#162966,#162967,#162968,#162969,#162970,#162971,
#162972,#162973,#162974,#162975,#162976,#162977,#162978,#162979,#162980,
#162981,#162982,#162983,#162984,#162985,#162986,#162987,#162988),
 .UNSPECIFIED.,.F.,.F.,(4,3,3,3,3,3,3,3,3,3,3,3,3,3,3,3,4),(0.,8.46514984578604E-5,
0.000170997186917751,0.000221020978418102,0.00025513917286212,0.0003380084618147,
0.000429234945598969,0.000448835576014525,0.000450677949086267,0.000735348747783541,
0.000898977028079808,0.000901355898172495,0.00115196682498163,0.00135049620570087,
0.00135203384725872,0.00157737282180184,0.00180271179634495),
 .UNSPECIFIED.);
#4941=B_SPLINE_CURVE_WITH_KNOTS('',3,(#163023,#163024,#163025,#163026,#163027,
#163028,#163029,#163030,#163031,#163032,#163033,#163034,#163035,#163036,
#163037,#163038,#163039,#163040,#163041,#163042,#163043,#163044,#163045,
#163046,#163047,#163048,#163049,#163050),.UNSPECIFIED.,.F.,.F.,(4,3,3,3,
3,3,3,3,3,4),(0.,0.125000000000083,0.187500000000098,0.250000000000114,
0.375000000000096,0.437500000000064,0.500000000000032,0.686608408121615,
0.750000000000016,1.),.UNSPECIFIED.);
#4942=B_SPLINE_CURVE_WITH_KNOTS('',3,(#163053,#163054,#163055,#163056,#163057,
#163058,#163059,#163060,#163061,#163062,#163063,#163064,#163065,#163066,
#163067,#163068,#163069,#163070,#163071,#163072,#163073,#163074,#163075,
#163076,#163077,#163078,#163079,#163080,#163081,#163082,#163083,#163084,
#163085,#163086,#163087,#163088,#163089,#163090,#163091,#163092,#163093,
#163094,#163095,#163096,#163097,#163098,#163099,#163100,#163101),
 .UNSPECIFIED.,.F.,.F.,(4,3,3,3,3,3,3,3,3,3,3,3,3,3,3,3,4),(1.05484258504493E-9,
0.191534277963448,0.259654838607526,0.331309849098388,0.397663184819074,
0.435861255746886,0.46401652053976,0.468749999999952,0.484374999999957,
0.499999999999962,0.526357797460517,0.61505709794376,0.705276548341834,
0.798422422273867,0.893550910308075,0.991493363605814,1.),.UNSPECIFIED.);
#4943=B_SPLINE_CURVE_WITH_KNOTS('',3,(#163123,#163124,#163125,#163126,#163127,
#163128),.UNSPECIFIED.,.F.,.F.,(4,2,4),(0.,0.5,1.),.UNSPECIFIED.);
#4944=B_SPLINE_CURVE_WITH_KNOTS('',3,(#163131,#163132,#163133,#163134,#163135,
#163136,#163137,#163138,#163139,#163140,#163141,#163142,#163143,#163144,
#163145,#163146,#163147,#163148,#163149,#163150,#163151,#163152,#163153,
#163154,#163155,#163156,#163157,#163158,#163159,#163160,#163161,#163162,
#163163,#163164,#163165,#163166,#163167),.UNSPECIFIED.,.F.,.F.,(4,3,3,3,
3,3,3,3,3,3,3,3,4),(0.,0.120708757094103,0.243232014226317,0.365509787471685,
0.477257340603764,0.497653150606378,0.514241701439531,0.6359369624296,0.758974043423795,
0.8125,0.90625,0.953125,1.),.UNSPECIFIED.);
#4945=B_SPLINE_CURVE_WITH_KNOTS('',3,(#163182,#163183,#163184,#163185,#163186,
#163187,#163188,#163189,#163190,#163191,#163192,#163193,#163194,#163195,
#163196,#163197,#163198,#163199,#163200,#163201,#163202,#163203,#163204,
#163205,#163206,#163207,#163208,#163209),.UNSPECIFIED.,.F.,.F.,(4,3,3,3,
3,3,3,3,3,4),(0.,0.11665693587126,0.231069038396355,0.345034028170232,0.457575140319161,
0.5,0.626037841254244,0.752522996696677,0.877297259197685,1.),
 .UNSPECIFIED.);
#4946=B_SPLINE_CURVE_WITH_KNOTS('',3,(#163247,#163248,#163249,#163250,#163251,
#163252,#163253,#163254,#163255,#163256,#163257,#163258,#163259,#163260,
#163261,#163262),.UNSPECIFIED.,.F.,.F.,(4,2,2,2,1,1,2,2,4),(0.,0.250000000000283,
0.375000000000425,0.437500000000534,0.46875000000058,0.484375000000603,
0.492187500000607,0.50000000000061,1.),.UNSPECIFIED.);
#4947=B_SPLINE_CURVE_WITH_KNOTS('',3,(#163263,#163264,#163265,#163266,#163267,
#163268,#163269,#163270,#163271,#163272,#163273,#163274,#163275,#163276,
#163277,#163278,#163279,#163280,#163281,#163282,#163283,#163284,#163285,
#163286,#163287,#163288,#163289,#163290,#163291,#163292,#163293,#163294,
#163295,#163296,#163297,#163298,#163299,#163300,#163301,#163302,#163303,
#163304,#163305,#163306,#163307,#163308),.UNSPECIFIED.,.F.,.F.,(4,3,3,3,
3,3,3,3,3,3,3,3,3,3,3,4),(0.,0.00011167181015012,0.000225567853890619,0.000339431029143628,
0.000397399329631602,0.00039894455910293,0.000667283904094347,0.000794798659263204,
0.000796933919810636,0.00104488468554081,0.00119219798889481,0.0011936849958466,
0.00132317769579385,0.00145638750716013,0.00158130618071587,0.00158959731852641),
 .UNSPECIFIED.);
#4948=B_SPLINE_CURVE_WITH_KNOTS('',3,(#163349,#163350,#163351,#163352,#163353,
#163354,#163355,#163356,#163357,#163358,#163359,#163360,#163361,#163362,
#163363,#163364,#163365,#163366,#163367,#163368,#163369,#163370,#163371,
#163372,#163373,#163374,#163375,#163376,#163377,#163378,#163379,#163380,
#163381,#163382,#163383,#163384,#163385,#163386,#163387,#163388,#163389,
#163390,#163391),.UNSPECIFIED.,.F.,.F.,(4,3,3,3,3,3,3,3,3,3,3,3,3,3,4),
(0.,0.00016756321202441,0.000333534252400233,0.000405329103688545,0.000406806783530084,
0.000681033266856812,0.00081143089222242,0.000813613567060169,0.00109814343430376,
0.00121879730292857,0.00122042035059025,0.00134667139739562,0.00147140108610384,
0.00159377061182578,0.00162722713412034),.UNSPECIFIED.);
#4949=B_SPLINE_CURVE_WITH_KNOTS('',3,(#163393,#163394,#163395,#163396,#163397,
#163398,#163399,#163400,#163401,#163402,#163403,#163404,#163405,#163406,
#163407,#163408,#163409,#163410,#163411,#163412,#163413,#163414,#163415,
#163416,#163417,#163418,#163419,#163420,#163421,#163422,#163423,#163424,
#163425,#163426,#163427,#163428,#163429,#163430,#163431,#163432,#163433,
#163434,#163435,#163436,#163437,#163438,#163439,#163440,#163441,#163442,
#163443,#163444,#163445,#163446,#163447,#163448,#163449,#163450,#163451,
#163452,#163453,#163454,#163455,#163456,#163457,#163458,#163459,#163460,
#163461,#163462),.UNSPECIFIED.,.F.,.F.,(4,3,3,3,3,3,3,3,3,3,3,3,3,3,3,3,
3,3,3,3,3,3,3,4),(0.,0.077221954709809,0.155942297777895,0.237205163639056,
0.245892449851707,0.249999999999969,0.327737648600097,0.374999999999958,
0.437499999999981,0.468749999999967,0.472685944192633,0.484374999999935,
0.492187499999947,0.497991200093118,0.499999999999958,0.61072165925943,
0.708652887979474,0.749999999999979,0.769114755462166,0.781249999999982,
0.858290325115874,0.890624999999991,0.970567820080817,1.),.UNSPECIFIED.);
#4950=B_SPLINE_CURVE_WITH_KNOTS('',3,(#163480,#163481,#163482,#163483,#163484,
#163485,#163486),.UNSPECIFIED.,.F.,.F.,(4,3,4),(0.,0.5,1.),
 .UNSPECIFIED.);
#4951=B_SPLINE_CURVE_WITH_KNOTS('',3,(#163489,#163490,#163491,#163492,#163493,
#163494,#163495,#163496,#163497,#163498,#163499,#163500,#163501,#163502,
#163503,#163504,#163505,#163506,#163507,#163508,#163509,#163510,#163511,
#163512,#163513,#163514,#163515,#163516,#163517,#163518,#163519,#163520,
#163521,#163522,#163523,#163524,#163525),.UNSPECIFIED.,.F.,.F.,(4,3,3,3,
3,3,3,3,3,3,3,3,4),(0.,0.100588965941516,0.213435253911614,0.321668078608275,
0.37500000000007,0.437500000000022,0.468749999999998,0.484374999999996,
0.492187499999995,0.499999999999994,0.684746090436115,0.879413380072057,
1.),.UNSPECIFIED.);
#4952=B_SPLINE_CURVE_WITH_KNOTS('',3,(#163539,#163540,#163541,#163542,#163543,
#163544,#163545,#163546,#163547,#163548,#163549,#163550,#163551,#163552,
#163553,#163554,#163555,#163556,#163557,#163558,#163559,#163560,#163561,
#163562,#163563,#163564,#163565,#163566,#163567,#163568,#163569,#163570,
#163571,#163572),.UNSPECIFIED.,.F.,.F.,(4,3,3,3,3,3,3,3,3,3,3,4),(0.,0.125443689754645,
0.249999999999871,0.383895651702588,0.437499999999815,0.468602955116825,
0.499115673875061,0.499999999999761,0.639475850377752,0.780204293879566,
0.923774089074692,0.999989478723035),.UNSPECIFIED.);
#4953=B_SPLINE_CURVE_WITH_KNOTS('',3,(#163574,#163575,#163576,#163577,#163578,
#163579,#163580,#163581,#163582,#163583,#163584,#163585,#163586,#163587,
#163588,#163589,#163590,#163591,#163592,#163593,#163594,#163595,#163596,
#163597,#163598,#163599,#163600,#163601,#163602,#163603,#163604,#163605,
#163606,#163607,#163608,#163609,#163610),.UNSPECIFIED.,.F.,.F.,(4,3,3,3,
3,3,3,3,3,3,3,3,4),(0.,0.118442531101612,0.242864853287292,0.378342680351954,
0.437499999999567,0.468749999999536,0.484374999999537,0.499215229757745,
0.499999999999537,0.656694403675684,0.817828302438324,0.986303070645228,
0.999999565360524),.UNSPECIFIED.);
#4954=B_SPLINE_CURVE_WITH_KNOTS('',3,(#163633,#163634,#163635,#163636,#163637,
#163638),.UNSPECIFIED.,.F.,.F.,(4,2,4),(0.,0.5,1.),.UNSPECIFIED.);
#4955=B_SPLINE_CURVE_WITH_KNOTS('',3,(#163639,#163640,#163641,#163642,#163643,
#163644,#163645,#163646,#163647,#163648,#163649,#163650),.UNSPECIFIED.,
 .F.,.F.,(4,2,2,2,2,4),(0.,0.249999999999836,0.374999999999753,0.437499999999745,
0.499999999999737,1.),.UNSPECIFIED.);
#4956=B_SPLINE_CURVE_WITH_KNOTS('',3,(#163671,#163672,#163673,#163674,#163675,
#163676,#163677,#163678,#163679,#163680,#163681,#163682,#163683),
 .UNSPECIFIED.,.F.,.F.,(4,3,3,3,4),(0.,0.00157041135329187,0.00191432655883667,
0.00304584187045998,0.00382865311767335),.UNSPECIFIED.);
#4957=B_SPLINE_CURVE_WITH_KNOTS('',3,(#163687,#163688,#163689,#163690,#163691,
#163692,#163693,#163694,#163695,#163696,#163697,#163698,#163699,#163700,
#163701,#163702,#163703,#163704,#163705,#163706,#163707,#163708,#163709,
#163710,#163711,#163712,#163713,#163714,#163715,#163716,#163717,#163718,
#163719,#163720,#163721,#163722,#163723,#163724,#163725,#163726,#163727,
#163728,#163729,#163730,#163731,#163732,#163733,#163734,#163735,#163736,
#163737,#163738,#163739,#163740,#163741,#163742,#163743,#163744,#163745,
#163746,#163747,#163748,#163749,#163750,#163751,#163752,#163753,#163754,
#163755,#163756,#163757,#163758,#163759),.UNSPECIFIED.,.F.,.F.,(4,3,3,3,
3,3,3,3,3,3,3,3,3,3,3,3,3,3,3,3,3,3,3,3,4),(0.,0.082780047467355,0.164476544882018,
0.244653695027588,0.323963104070488,0.402053886069737,0.437500000000005,
0.468750000000019,0.48280860858439,0.497325464146971,0.500000000000034,
0.563238185116385,0.624999999999974,0.687499999999944,0.718749999999934,
0.73437499999992,0.742187499999908,0.746930764488159,0.749999999999896,
0.798770062739853,0.846466169752031,0.892304506499701,0.936986645378172,
0.979989519801786,1.),.UNSPECIFIED.);
#4958=B_SPLINE_CURVE_WITH_KNOTS('',3,(#163781,#163782,#163783,#163784,#163785,
#163786,#163787,#163788,#163789,#163790,#163791,#163792,#163793,#163794,
#163795,#163796,#163797,#163798,#163799,#163800,#163801,#163802,#163803,
#163804,#163805,#163806,#163807,#163808,#163809,#163810,#163811,#163812,
#163813,#163814,#163815,#163816,#163817,#163818,#163819,#163820,#163821,
#163822,#163823,#163824,#163825,#163826,#163827,#163828,#163829,#163830,
#163831,#163832,#163833,#163834,#163835),.UNSPECIFIED.,.F.,.F.,(4,3,3,3,
3,3,3,3,3,3,3,3,3,3,3,3,3,3,4),(0.,0.104715580142832,0.210383983783548,
0.249999999999323,0.354011980528842,0.374999999999033,0.437499999998846,
0.468749999998796,0.484374999998733,0.493439254411786,0.49999999999867,
0.577747102422539,0.652041765056392,0.721927843236613,0.749999999999335,
0.814470107409843,0.877192615337485,0.938596307668742,1.),.UNSPECIFIED.);
#4959=B_SPLINE_CURVE_WITH_KNOTS('',3,(#163838,#163839,#163840,#163841,#163842,
#163843,#163844),.UNSPECIFIED.,.F.,.F.,(4,3,4),(4.71238898038469,5.49778714378214,
6.28318530717959),.UNSPECIFIED.);
#4960=B_SPLINE_CURVE_WITH_KNOTS('',3,(#163868,#163869,#163870,#163871,#163872,
#163873,#163874),.UNSPECIFIED.,.F.,.F.,(4,3,4),(3.1415926535898,3.92699081698724,
4.71238898038469),.UNSPECIFIED.);
#4961=B_SPLINE_CURVE_WITH_KNOTS('',3,(#163877,#163878,#163879,#163880,#163881,
#163882,#163883,#163884,#163885,#163886,#163887,#163888,#163889,#163890,
#163891,#163892,#163893,#163894,#163895,#163896,#163897,#163898,#163899,
#163900,#163901,#163902,#163903,#163904,#163905,#163906,#163907,#163908,
#163909,#163910,#163911,#163912,#163913,#163914,#163915,#163916,#163917,
#163918,#163919,#163920,#163921,#163922),.UNSPECIFIED.,.F.,.F.,(4,3,3,3,
3,3,3,3,3,3,3,3,3,3,3,4),(0.,0.0605468750000136,0.122426142767112,0.186284753451113,
0.245362453102209,0.322247693278209,0.398189410474041,0.475083019593307,
0.484375000000109,0.493930247632433,0.500000000000104,0.605247959968731,
0.710628642835913,0.816191190373723,0.9222335579368,1.),.UNSPECIFIED.);
#4962=B_SPLINE_CURVE_WITH_KNOTS('',3,(#163927,#163928,#163929,#163930,#163931,
#163932,#163933,#163934,#163935,#163936,#163937,#163938,#163939,#163940,
#163941,#163942,#163943,#163944,#163945,#163946,#163947,#163948,#163949,
#163950,#163951,#163952,#163953,#163954,#163955,#163956,#163957,#163958,
#163959,#163960,#163961,#163962,#163963,#163964,#163965,#163966,#163967,
#163968,#163969,#163970,#163971,#163972,#163973,#163974,#163975,#163976,
#163977,#163978,#163979,#163980,#163981,#163982,#163983,#163984,#163985,
#163986,#163987,#163988,#163989,#163990,#163991,#163992,#163993,#163994,
#163995,#163996,#163997,#163998,#163999),.UNSPECIFIED.,.F.,.F.,(4,3,3,3,
3,3,3,3,3,3,3,3,3,3,3,3,3,3,3,3,3,3,3,3,4),(0.,0.0828931975148567,0.164185746816491,
0.244579641303135,0.323662152922592,0.375000000000147,0.437500000000148,
0.468750000000125,0.482808608613976,0.497325464204033,0.500000000000102,
0.563666376881648,0.625583188440782,0.687499999999916,0.718749999999873,
0.734374999999842,0.742187499999841,0.746930764461493,0.74999999999984,
0.798770062779461,0.846466169827735,0.892304506608502,0.936986645518803,
0.979989519974505,1.),.UNSPECIFIED.);
#4963=B_SPLINE_CURVE_WITH_KNOTS('',3,(#164000,#164001,#164002,#164003,#164004,
#164005,#164006,#164007,#164008,#164009,#164010,#164011,#164012,#164013,
#164014,#164015,#164016,#164017,#164018,#164019,#164020,#164021,#164022,
#164023,#164024,#164025,#164026,#164027,#164028,#164029,#164030,#164031,
#164032,#164033,#164034,#164035,#164036,#164037,#164038,#164039,#164040,
#164041,#164042,#164043,#164044,#164045,#164046,#164047,#164048,#164049,
#164050,#164051,#164052,#164053,#164054,#164055,#164056,#164057,#164058,
#164059,#164060,#164061,#164062,#164063,#164064,#164065,#164066,#164067,
#164068,#164069),.UNSPECIFIED.,.F.,.F.,(4,3,3,3,3,3,3,3,3,3,3,3,3,3,3,3,
3,3,3,3,3,3,3,4),(0.,0.0417433064021318,0.0856783503512316,0.125000000000202,
0.172058637042935,0.221141673238027,0.242187500000332,0.247530062045159,
0.250000000000331,0.258757699094845,0.318098755992443,0.375000000000289,
0.438761223626928,0.468750000000226,0.483267071980795,0.497350908913188,
0.500000000000198,0.586409574598886,0.674221064847019,0.743171333827662,
0.750000000000099,0.839284683852181,0.929619546736012,1.),.UNSPECIFIED.);
#4964=B_SPLINE_CURVE_WITH_KNOTS('',3,(#164092,#164093,#164094,#164095,#164096,
#164097,#164098),.UNSPECIFIED.,.F.,.F.,(4,3,4),(4.71238898038469,5.49778714378214,
6.28318530717959),.UNSPECIFIED.);
#4965=B_SPLINE_CURVE_WITH_KNOTS('',3,(#164100,#164101,#164102,#164103,#164104,
#164105,#164106,#164107,#164108,#164109,#164110,#164111,#164112,#164113,
#164114,#164115,#164116,#164117,#164118,#164119,#164120,#164121,#164122,
#164123,#164124,#164125,#164126,#164127,#164128,#164129,#164130,#164131,
#164132,#164133,#164134,#164135,#164136,#164137,#164138,#164139,#164140,
#164141,#164142,#164143,#164144,#164145,#164146,#164147,#164148,#164149,
#164150,#164151,#164152,#164153,#164154),.UNSPECIFIED.,.F.,.F.,(4,3,3,3,
3,3,3,3,3,3,3,3,3,3,3,3,3,3,4),(0.,0.104715580048555,0.210383983573989,
0.250000000000528,0.354011980382662,0.375000000000741,0.43750000000089,
0.468750000000963,0.484375000000993,0.49343925440917,0.500000000001023,
0.577747102398773,0.652041765008489,0.721927843163034,0.750000000000512,
0.814470107381001,0.877192615277638,0.938596307638819,1.),.UNSPECIFIED.);
#4966=B_SPLINE_CURVE_WITH_KNOTS('',3,(#164178,#164179,#164180,#164181,#164182,
#164183,#164184),.UNSPECIFIED.,.F.,.F.,(4,3,4),(1.23467863058847E-16,0.785398163397447,
1.5707963267949),.UNSPECIFIED.);
#4967=B_SPLINE_CURVE_WITH_KNOTS('',3,(#164187,#164188,#164189,#164190,#164191,
#164192,#164193,#164194,#164195,#164196,#164197,#164198,#164199,#164200,
#164201,#164202,#164203,#164204,#164205,#164206,#164207,#164208,#164209,
#164210,#164211,#164212,#164213,#164214,#164215,#164216,#164217,#164218,
#164219,#164220,#164221,#164222,#164223,#164224,#164225,#164226,#164227,
#164228,#164229,#164230,#164231,#164232),.UNSPECIFIED.,.F.,.F.,(4,3,3,3,
3,3,3,3,3,3,3,3,3,3,3,4),(0.,0.060546874999967,0.122426142535212,0.186284752990579,
0.245362452470406,0.322247692137301,0.39818940892974,0.475083013899954,
0.484374999999736,0.493930247601759,0.499999999999743,0.605247958737039,
0.71062864059231,0.816191187206391,0.922233553949779,1.),.UNSPECIFIED.);
#4968=B_SPLINE_CURVE_WITH_KNOTS('',3,(#164238,#164239,#164240,#164241,#164242,
#164243,#164244,#164245,#164246,#164247,#164248,#164249,#164250,#164251,
#164252,#164253,#164254,#164255,#164256,#164257,#164258,#164259,#164260,
#164261,#164262,#164263,#164264,#164265,#164266,#164267,#164268,#164269,
#164270,#164271,#164272,#164273,#164274,#164275,#164276,#164277,#164278,
#164279,#164280,#164281,#164282,#164283,#164284,#164285,#164286,#164287,
#164288,#164289,#164290,#164291,#164292,#164293,#164294,#164295,#164296,
#164297,#164298,#164299,#164300,#164301,#164302,#164303,#164304,#164305,
#164306,#164307),.UNSPECIFIED.,.F.,.F.,(4,3,3,3,3,3,3,3,3,3,3,3,3,3,3,3,
3,3,3,3,3,3,3,4),(0.,0.0417041814131079,0.0849340865860686,0.13082840629655,
0.178067342047349,0.227196348247942,0.242187499999745,0.247530062045447,
0.24999999999975,0.258757699094019,0.318098755985604,0.374999999999687,
0.438761223875019,0.468749999999677,0.483267071975172,0.497350908902079,
0.499999999999685,0.586409574537516,0.674221064733702,0.74317133380861,
0.749999999999842,0.839284683789798,0.929619546616256,1.),.UNSPECIFIED.);
#4969=B_SPLINE_CURVE_WITH_KNOTS('',3,(#164333,#164334,#164335,#164336,#164337,
#164338,#164339,#164340,#164341,#164342,#164343,#164344,#164345,#164346,
#164347,#164348,#164349,#164350,#164351,#164352,#164353,#164354,#164355,
#164356,#164357,#164358,#164359,#164360,#164361,#164362,#164363,#164364,
#164365,#164366,#164367,#164368,#164369,#164370,#164371,#164372,#164373,
#164374,#164375,#164376,#164377,#164378,#164379,#164380,#164381,#164382,
#164383,#164384,#164385,#164386,#164387,#164388,#164389,#164390,#164391,
#164392,#164393,#164394,#164395,#164396,#164397,#164398,#164399,#164400,
#164401,#164402),.UNSPECIFIED.,.F.,.F.,(4,3,3,3,3,3,3,3,3,3,3,3,3,3,3,3,
3,3,3,3,3,3,3,4),(0.,0.0904805865747593,0.179890948794643,0.250000000000156,
0.256840728511668,0.344945742473561,0.429509229825221,0.468750000000257,
0.482752596547783,0.497175643783503,0.500000000000261,0.56298906728729,
0.625000000000418,0.683994503650316,0.741245408290876,0.742187500000548,
0.746913732889895,0.750000000000554,0.799311389337984,0.849483542003488,
0.894712088307748,0.938468707034261,0.980197893082773,1.),.UNSPECIFIED.);
#4970=B_SPLINE_CURVE_WITH_KNOTS('',3,(#164431,#164432,#164433,#164434,#164435,
#164436,#164437,#164438,#164439,#164440,#164441,#164442,#164443),
 .UNSPECIFIED.,.F.,.F.,(4,3,3,3,4),(0.000775072234384454,0.00360015924840042,
0.0066511885691017,0.00786282367425579,0.0104581756611108),
 .UNSPECIFIED.);
#4971=B_SPLINE_CURVE_WITH_KNOTS('',3,(#164444,#164445,#164446,#164447,#164448,
#164449,#164450,#164451,#164452,#164453,#164454,#164455,#164456,#164457,
#164458,#164459,#164460,#164461,#164462,#164463,#164464,#164465,#164466,
#164467,#164468,#164469,#164470,#164471,#164472,#164473,#164474,#164475,
#164476,#164477,#164478,#164479,#164480,#164481,#164482,#164483,#164484,
#164485,#164486,#164487,#164488,#164489,#164490,#164491,#164492,#164493,
#164494,#164495,#164496,#164497,#164498,#164499,#164500,#164501,#164502,
#164503,#164504,#164505,#164506,#164507,#164508,#164509,#164510,#164511,
#164512,#164513,#164514,#164515,#164516,#164517,#164518,#164519,#164520,
#164521,#164522,#164523,#164524,#164525,#164526,#164527,#164528,#164529,
#164530,#164531,#164532,#164533,#164534),.UNSPECIFIED.,.F.,.F.,(4,3,3,3,
3,3,3,3,3,3,3,3,3,3,3,3,3,3,3,3,3,3,3,3,3,3,3,3,3,3,4),(0.,0.0625000000000528,
0.119882029542211,0.181191318326517,0.215595659163364,0.232797829581788,
0.241398914790999,0.245699457395605,0.246075569668044,0.246422124286298,
0.250000000000211,0.328341414165092,0.37500000000021,0.406250000000209,
0.437500000000209,0.468750000000208,0.484375000000208,0.492187500000204,
0.496093750000202,0.499312791455558,0.5000000000002,0.553910651984701,0.562500000000175,
0.609375000000156,0.67005767057599,0.723432332910554,0.7500000000001,0.823678063759278,
0.87500000000005,0.96075141168338,0.999994499179906),.UNSPECIFIED.);
#4972=B_SPLINE_CURVE_WITH_KNOTS('',3,(#164535,#164536,#164537,#164538,#164539,
#164540,#164541,#164542,#164543,#164544,#164545,#164546,#164547,#164548,
#164549,#164550,#164551,#164552,#164553,#164554,#164555,#164556,#164557,
#164558,#164559,#164560,#164561,#164562,#164563,#164564,#164565,#164566,
#164567,#164568,#164569,#164570,#164571,#164572,#164573,#164574,#164575,
#164576,#164577,#164578,#164579,#164580,#164581,#164582,#164583,#164584,
#164585,#164586,#164587,#164588,#164589,#164590,#164591,#164592,#164593,
#164594,#164595,#164596,#164597,#164598,#164599,#164600,#164601,#164602,
#164603,#164604,#164605,#164606,#164607,#164608,#164609,#164610,#164611,
#164612,#164613,#164614,#164615,#164616,#164617,#164618,#164619,#164620,
#164621,#164622,#164623,#164624,#164625,#164626,#164627,#164628,#164629,
#164630,#164631,#164632,#164633,#164634,#164635,#164636,#164637,#164638,
#164639,#164640),.UNSPECIFIED.,.F.,.F.,(4,3,3,3,3,3,3,3,3,3,3,3,3,3,3,3,
3,3,3,3,3,3,3,3,3,3,3,3,3,3,3,3,3,3,3,4),(6.04008760640985E-9,0.0631615253640654,
0.125000000000745,0.181057237407362,0.234824141910246,0.246093750001476,
0.249787108631666,0.250000000001502,0.252757249528496,0.360659948060548,
0.375000000002354,0.439765134614748,0.499023437503205,0.500000000003212,
0.507860695079115,0.541007150026823,0.574249368414924,0.607699600826058,
0.625000000002433,0.659336202062174,0.691632909124592,0.726096190864088,
0.743215178935082,0.747227441764222,0.747721138167026,0.748023769356437,
0.748174988831839,0.749158680281715,0.74964860473429,0.749947616638847,
0.750081406970028,0.802195408057856,0.855320680231657,0.909014588024604,
0.963580917838172,1.),.UNSPECIFIED.);
#4973=B_SPLINE_CURVE_WITH_KNOTS('',3,(#164661,#164662,#164663,#164664,#164665,
#164666,#164667,#164668,#164669,#164670,#164671,#164672,#164673,#164674,
#164675,#164676),.UNSPECIFIED.,.F.,.F.,(4,3,3,3,3,4),(0.000681462205008639,
0.00273329612790433,0.00491895821255326,0.00671017185179961,0.00912678453082223,
0.00930288319891504),.UNSPECIFIED.);
#4974=B_SPLINE_CURVE_WITH_KNOTS('',3,(#164678,#164679,#164680,#164681,#164682,
#164683,#164684,#164685,#164686,#164687,#164688,#164689,#164690,#164691,
#164692,#164693,#164694,#164695,#164696,#164697,#164698,#164699,#164700,
#164701,#164702,#164703,#164704,#164705,#164706,#164707,#164708,#164709,
#164710,#164711,#164712,#164713,#164714,#164715,#164716,#164717,#164718,
#164719,#164720,#164721,#164722,#164723,#164724,#164725,#164726,#164727,
#164728,#164729,#164730,#164731,#164732,#164733,#164734,#164735,#164736,
#164737,#164738,#164739,#164740,#164741,#164742,#164743,#164744,#164745,
#164746,#164747,#164748,#164749,#164750,#164751,#164752,#164753,#164754,
#164755,#164756,#164757,#164758,#164759,#164760,#164761,#164762,#164763,
#164764,#164765,#164766,#164767,#164768,#164769,#164770,#164771,#164772,
#164773,#164774,#164775,#164776,#164777,#164778,#164779,#164780,#164781,
#164782,#164783),.UNSPECIFIED.,.F.,.F.,(4,3,3,3,3,3,3,3,3,3,3,3,3,3,3,3,
3,3,3,3,3,3,3,3,3,3,3,3,3,3,3,3,3,3,3,4),(0.,0.0786487036192077,0.140954525450891,
0.195477262726112,0.222738631363722,0.236369315682527,0.24318465784193,
0.246592328921631,0.247444246691557,0.247763715855279,0.24797366756617,
0.2481420722479,0.250000000001332,0.28832882578824,0.326567472140649,0.364722818248368,
0.402831690846228,0.440266729938598,0.478356316773867,0.496093750000979,
0.499612062949285,0.50000000000097,0.554876643694226,0.611930537520896,
0.625000000000741,0.684310971889722,0.687500000000626,0.718750000000563,
0.734375000000532,0.742187500000516,0.746093750000507,0.750000000000499,
0.823764329859907,0.899903185373135,0.979642186186956,0.999986903780746),
 .UNSPECIFIED.);
#4975=B_SPLINE_CURVE_WITH_KNOTS('',3,(#164785,#164786,#164787,#164788,#164789,
#164790,#164791,#164792,#164793,#164794,#164795,#164796,#164797,#164798,
#164799,#164800),.UNSPECIFIED.,.F.,.F.,(4,3,3,3,3,4),(0.,0.199145041073045,
0.413635430144668,0.625526552290449,0.851258415695788,0.999999434617583),
 .UNSPECIFIED.);
#4976=B_SPLINE_CURVE_WITH_KNOTS('',3,(#164801,#164802,#164803,#164804,#164805,
#164806,#164807,#164808,#164809,#164810,#164811,#164812,#164813,#164814,
#164815,#164816,#164817,#164818,#164819,#164820,#164821,#164822,#164823,
#164824,#164825,#164826,#164827,#164828,#164829,#164830,#164831,#164832,
#164833,#164834,#164835,#164836,#164837,#164838,#164839,#164840,#164841,
#164842,#164843,#164844,#164845,#164846,#164847,#164848,#164849,#164850,
#164851,#164852,#164853,#164854,#164855,#164856,#164857,#164858,#164859,
#164860,#164861,#164862,#164863,#164864,#164865,#164866,#164867,#164868,
#164869,#164870,#164871,#164872,#164873,#164874,#164875,#164876,#164877,
#164878,#164879,#164880,#164881,#164882,#164883,#164884,#164885,#164886,
#164887,#164888),.UNSPECIFIED.,.F.,.F.,(4,3,3,3,3,3,3,3,3,3,3,3,3,3,3,3,
3,3,3,3,3,3,3,3,3,3,3,3,3,4),(1.10570935039285E-8,0.0831077289908478,0.125000000000325,
0.192214037137834,0.246093750000652,0.250000000000664,0.251900676065446,
0.332426051101153,0.375000000000854,0.443871170179604,0.49804687500106,
0.500000000001065,0.502961890600083,0.537631002255159,0.562500000000996,
0.599948155247652,0.625000000000926,0.658190763311687,0.687500000000856,
0.718750000000822,0.734375000000804,0.742187500000796,0.746093750000792,
0.74804687500079,0.750000000000787,0.751057688908144,0.823026195316543,
0.8946442291177,0.965792345222205,1.),.UNSPECIFIED.);
#4977=B_SPLINE_CURVE_WITH_KNOTS('',3,(#164900,#164901,#164902,#164903,#164904,
#164905,#164906,#164907,#164908,#164909,#164910,#164911,#164912,#164913,
#164914,#164915,#164916,#164917,#164918,#164919,#164920,#164921,#164922,
#164923,#164924,#164925,#164926,#164927,#164928,#164929,#164930,#164931,
#164932,#164933,#164934,#164935,#164936,#164937,#164938,#164939),
 .UNSPECIFIED.,.F.,.F.,(4,3,3,3,3,3,3,3,3,3,3,3,3,4),(0.,0.125000000000011,
0.250000000000021,0.37500000000003,0.437500000000033,0.468750000000031,
0.487324584826517,0.500000000000029,0.500520266105271,0.602937076851582,
0.707582462658716,0.811875894948651,0.913121167622829,1.),.UNSPECIFIED.);
#4978=B_SPLINE_CURVE_WITH_KNOTS('',3,(#164974,#164975,#164976,#164977,#164978,
#164979,#164980,#164981,#164982,#164983,#164984,#164985,#164986,#164987,
#164988,#164989),.UNSPECIFIED.,.F.,.F.,(4,3,3,3,3,4),(0.,0.19107940674639,
0.393309555059792,0.593827441197275,0.800859069985332,1.),.UNSPECIFIED.);
#4979=B_SPLINE_CURVE_WITH_KNOTS('',3,(#164992,#164993,#164994,#164995),
 .UNSPECIFIED.,.F.,.F.,(4,4),(0.,0.0174508326761739),.UNSPECIFIED.);
#4980=B_SPLINE_CURVE_WITH_KNOTS('',3,(#165022,#165023,#165024,#165025,#165026,
#165027,#165028,#165029,#165030,#165031,#165032,#165033,#165034,#165035,
#165036,#165037,#165038,#165039,#165040,#165041,#165042,#165043,#165044,
#165045,#165046,#165047,#165048,#165049),.UNSPECIFIED.,.F.,.F.,(4,3,3,3,
3,3,3,3,3,4),(0.,0.000662679024145193,0.00128919539297031,0.00132535804829039,
0.0019349250888321,0.00253635637124923,0.00265071609658077,0.00397607414487116,
0.00508368314703509,0.00530143219316154),.UNSPECIFIED.);
#4981=B_SPLINE_CURVE_WITH_KNOTS('',3,(#165080,#165081,#165082,#165083,#165084,
#165085,#165086,#165087,#165088,#165089,#165090,#165091,#165092,#165093,
#165094,#165095),.UNSPECIFIED.,.F.,.F.,(4,3,3,3,3,4),(0.,0.00121734210059923,
0.00132677154899614,0.00265354309799227,0.00411654704464365,0.00530708619598447),
 .UNSPECIFIED.);
#4982=B_SPLINE_CURVE_WITH_KNOTS('',3,(#165110,#165111,#165112,#165113),
 .UNSPECIFIED.,.F.,.F.,(4,4),(0.,0.0177264565684136),.UNSPECIFIED.);
#4983=B_SPLINE_CURVE_WITH_KNOTS('',3,(#165140,#165141,#165142,#165143,#165144,
#165145,#165146,#165147,#165148,#165149,#165150,#165151,#165152),
 .UNSPECIFIED.,.F.,.F.,(4,3,3,3,4),(0.,0.000168209862994577,0.000320350766922646,
0.000480537459018489,0.000640701533845293),.UNSPECIFIED.);
#4984=B_SPLINE_CURVE_WITH_KNOTS('',3,(#165311,#165312,#165313,#165314,#165315,
#165316,#165317,#165318,#165319,#165320,#165321,#165322,#165323,#165324,
#165325,#165326,#165327,#165328,#165329,#165330,#165331,#165332),
 .UNSPECIFIED.,.F.,.F.,(4,3,3,3,3,3,3,4),(0.,0.000110166739482577,0.000232250654978379,
0.000327614165524935,0.000415934063629706,0.000506222853831825,0.000594954171387356,
0.000655228331049871),.UNSPECIFIED.);
#4985=B_SPLINE_CURVE_WITH_KNOTS('',3,(#165347,#165348,#165349,#165350),
 .UNSPECIFIED.,.F.,.F.,(4,4),(0.,0.0138038180377133),.UNSPECIFIED.);
#4986=B_SPLINE_CURVE_WITH_KNOTS('',3,(#165377,#165378,#165379,#165380,#165381,
#165382,#165383,#165384,#165385,#165386,#165387,#165388,#165389,#165390,
#165391,#165392,#165393,#165394,#165395),.UNSPECIFIED.,.F.,.F.,(4,3,3,3,
3,3,4),(0.,0.00115159118172271,0.00227058783087512,0.00281251499795634,
0.00421877249693456,0.00530146752106949,0.00562502999591277),
 .UNSPECIFIED.);
#4987=B_SPLINE_CURVE_WITH_KNOTS('',3,(#165426,#165427,#165428,#165429,#165430,
#165431,#165432,#165433,#165434,#165435,#165436,#165437,#165438,#165439,
#165440,#165441),.UNSPECIFIED.,.F.,.F.,(4,3,3,3,3,4),(0.,0.00116086488263883,
0.0014075250438046,0.0028150500876092,0.00432397808186733,0.00563010017521834),
 .UNSPECIFIED.);
#4988=B_SPLINE_CURVE_WITH_KNOTS('',3,(#165456,#165457,#165458,#165459),
 .UNSPECIFIED.,.F.,.F.,(4,4),(0.,0.0135258923233721),.UNSPECIFIED.);
#4989=B_SPLINE_CURVE_WITH_KNOTS('',3,(#165480,#165481,#165482,#165483,#165484,
#165485,#165486,#165487,#165488,#165489,#165490,#165491,#165492,#165493,
#165494,#165495),.UNSPECIFIED.,.F.,.F.,(4,3,3,3,3,4),(0.,0.00019794317692089,
0.000328605151068823,0.000446042787173756,0.000552633627937672,0.000657210302137648),
 .UNSPECIFIED.);
#4990=B_SPLINE_CURVE_WITH_KNOTS('',3,(#165498,#165499,#165500,#165501,#165502,
#165503,#165504,#165505,#165506,#165507,#165508,#165509,#165510,#165511,
#165512,#165513,#165514,#165515,#165516,#165517,#165518,#165519,#165520,
#165521,#165522,#165523,#165524,#165525,#165526,#165527,#165528,#165529,
#165530,#165531,#165532,#165533,#165534,#165535,#165536,#165537,#165538,
#165539,#165540,#165541,#165542,#165543,#165544,#165545,#165546,#165547,
#165548,#165549,#165550,#165551,#165552,#165553,#165554,#165555,#165556,
#165557,#165558,#165559,#165560,#165561,#165562,#165563,#165564,#165565,
#165566,#165567,#165568,#165569,#165570,#165571,#165572,#165573),
 .UNSPECIFIED.,.F.,.F.,(4,3,3,3,3,3,3,3,3,3,3,3,3,3,3,3,3,3,3,3,3,3,3,3,
3,4),(0.,0.0971694717327587,0.124999999999839,0.187499999999759,0.249999999999678,
0.337621660100129,0.374999999999518,0.437499999999443,0.468749999999418,
0.484374999999408,0.494411509442002,0.499999999999398,0.516541470396192,
0.603517981247307,0.624999999999403,0.687499999999395,0.718749999999381,
0.734374999999381,0.742187499999374,0.748133238950809,0.749999999999367,
0.804479122806833,0.85884481476214,0.912694297575866,0.965054460214556,
1.),.UNSPECIFIED.);
#4991=B_SPLINE_CURVE_WITH_KNOTS('',3,(#165583,#165584,#165585,#165586,#165587,
#165588,#165589,#165590,#165591,#165592,#165593,#165594,#165595,#165596,
#165597,#165598,#165599,#165600,#165601,#165602,#165603,#165604,#165605,
#165606,#165607,#165608,#165609,#165610,#165611,#165612,#165613,#165614,
#165615,#165616,#165617,#165618,#165619,#165620,#165621,#165622,#165623,
#165624,#165625,#165626,#165627,#165628,#165629,#165630,#165631,#165632,
#165633,#165634,#165635,#165636,#165637,#165638,#165639,#165640,#165641,
#165642,#165643,#165644,#165645,#165646,#165647,#165648,#165649,#165650,
#165651,#165652),.UNSPECIFIED.,.F.,.F.,(4,3,3,3,3,3,3,3,3,3,3,3,3,3,3,3,
3,3,3,3,3,3,3,4),(0.,0.0468928010521469,0.0624999999999663,0.11173734352247,
0.162092700602332,0.215593455071074,0.234374999999845,0.242187499999848,
0.248562191291075,0.24999999999985,0.328344811834936,0.374999999999854,
0.431665597222767,0.468940652178127,0.478556608155973,0.484374999999853,
0.494460980872878,0.499999999999851,0.57484627083378,0.653167719012279,
0.717622076559044,0.805768836993062,0.902884418496531,1.),.UNSPECIFIED.);
#4992=B_SPLINE_CURVE_WITH_KNOTS('',3,(#165696,#165697,#165698,#165699,#165700,
#165701,#165702,#165703,#165704,#165705,#165706,#165707,#165708,#165709,
#165710,#165711,#165712,#165713,#165714),.UNSPECIFIED.,.F.,.F.,(4,3,3,3,
3,3,4),(0.,0.00017507392680495,0.000350193522739415,0.000452577371514132,
0.000557835767991203,0.000662370656289507,0.000700387045478831),
 .UNSPECIFIED.);
#4993=B_SPLINE_CURVE_WITH_KNOTS('',3,(#165771,#165772,#165773,#165774,#165775,
#165776,#165777,#165778,#165779,#165780,#165781,#165782,#165783,#165784,
#165785,#165786,#165787,#165788,#165789),.UNSPECIFIED.,.F.,.F.,(4,3,3,3,
3,3,4),(0.,0.00157595519506122,0.00315191039012244,0.00393988798770612,
0.00472786558518367,0.00575007285732184,0.00630382078024489),
 .UNSPECIFIED.);
#4994=B_SPLINE_CURVE_WITH_KNOTS('',3,(#165827,#165828,#165829,#165830,#165831,
#165832,#165833,#165834,#165835,#165836,#165837,#165838,#165839,#165840,
#165841,#165842),.UNSPECIFIED.,.F.,.F.,(4,3,3,3,3,4),(0.,0.00104430221452871,
0.00157688090361367,0.00315376180722735,0.00473064271084103,0.00630752361445471),
 .UNSPECIFIED.);
#4995=B_SPLINE_CURVE_WITH_KNOTS('',3,(#165893,#165894,#165895,#165896,#165897,
#165898,#165899,#165900,#165901,#165902,#165903,#165904,#165905),
 .UNSPECIFIED.,.F.,.F.,(4,3,3,3,4),(0.,0.000175209888250467,0.000350428553470057,
0.000525662295915607,0.000700857106940114),.UNSPECIFIED.);
#4996=B_SPLINE_CURVE_WITH_KNOTS('',3,(#166018,#166019,#166020,#166021,#166022,
#166023,#166024,#166025,#166026,#166027,#166028,#166029,#166030,#166031,
#166032,#166033,#166034,#166035,#166036,#166037,#166038,#166039,#166040,
#166041,#166042,#166043,#166044,#166045),.UNSPECIFIED.,.F.,.F.,(4,3,3,3,
3,3,3,3,3,4),(0.,0.000297352361641552,0.000685187759872985,0.000685314779244029,
0.00137061382937429,0.00137062955848806,0.00183455251928066,0.00205619372744575,
0.00244930001359525,0.00274125911697611),.UNSPECIFIED.);
#4997=B_SPLINE_CURVE_WITH_KNOTS('',3,(#166048,#166049,#166050,#166051,#166052,
#166053,#166054,#166055,#166056,#166057,#166058,#166059,#166060,#166061,
#166062,#166063,#166064,#166065,#166066,#166067,#166068,#166069,#166070,
#166071,#166072,#166073),.UNSPECIFIED.,.F.,.F.,(4,2,2,2,2,2,2,2,2,2,2,2,
4),(0.,0.0308819193980004,0.0647401130039136,0.0887784724853781,0.122010977792549,
0.1412175368743,0.146061445002154,0.16477491817878,0.172906057208515,0.180478634262882,
0.208285706571513,0.24737159603407,0.282492401310004),.UNSPECIFIED.);
#4998=B_SPLINE_CURVE_WITH_KNOTS('',3,(#166151,#166152,#166153,#166154),
 .UNSPECIFIED.,.F.,.F.,(4,4),(0.,0.000120540380538642),.UNSPECIFIED.);
#4999=B_SPLINE_CURVE_WITH_KNOTS('',3,(#166175,#166176,#166177,#166178,#166179,
#166180,#166181),.UNSPECIFIED.,.F.,.F.,(4,3,4),(0.,0.0128929585057523,0.0257859170115047),
 .UNSPECIFIED.);
#5000=B_SPLINE_CURVE_WITH_KNOTS('',3,(#166208,#166209,#166210,#166211,#166212,
#166213,#166214,#166215,#166216,#166217,#166218,#166219,#166220,#166221,
#166222,#166223),.UNSPECIFIED.,.F.,.F.,(4,3,3,3,3,4),(0.,0.00113243548370091,
0.00226487096740181,0.00339730645110275,0.00441932320149626,0.0045297419348037),
 .UNSPECIFIED.);
#5001=B_SPLINE_CURVE_WITH_KNOTS('',3,(#166248,#166249,#166250,#166251,#166252,
#166253,#166254,#166255,#166256,#166257,#166258,#166259,#166260,#166261,
#166262,#166263,#166264,#166265,#166266,#166267,#166268,#166269,#166270,
#166271,#166272),.UNSPECIFIED.,.F.,.F.,(4,3,3,3,3,3,3,3,4),(0.,0.000394684030928064,
0.000806360979195566,0.00113421626089741,0.0016450747730102,0.00217582874625842,
0.00226843252179482,0.0036130177168745,0.00453686504358963),
 .UNSPECIFIED.);
#5002=B_SPLINE_CURVE_WITH_KNOTS('',3,(#166294,#166295,#166296,#166297,#166298,
#166299,#166300,#166301,#166302,#166303,#166304,#166305,#166306,#166307,
#166308,#166309,#166310,#166311,#166312,#166313,#166314,#166315,#166316,
#166317,#166318,#166319,#166320,#166321),.UNSPECIFIED.,.F.,.F.,(4,3,3,3,
3,3,3,3,3,4),(0.,0.147232559566058,0.290903059743303,0.430985431195598,
0.498046874999703,0.499959580131913,0.499999999999702,0.672084672956296,
0.838421918110885,1.),.UNSPECIFIED.);
#5003=B_SPLINE_CURVE_WITH_KNOTS('',3,(#166322,#166323,#166324,#166325,#166326,
#166327,#166328),.UNSPECIFIED.,.F.,.F.,(4,3,4),(0.,0.0127570403976527,0.0255140807953054),
 .UNSPECIFIED.);
#5004=B_SPLINE_CURVE_WITH_KNOTS('',3,(#166364,#166365,#166366,#166367,#166368,
#166369,#166370,#166371,#166372,#166373,#166374,#166375,#166376),
 .UNSPECIFIED.,.F.,.F.,(4,3,3,3,4),(0.,0.000259173930192671,0.000518347860385342,
0.000877297766812356,0.00103669572077068),.UNSPECIFIED.);
#5005=B_SPLINE_CURVE_WITH_KNOTS('',3,(#166407,#166408,#166409,#166410,#166411,
#166412,#166413,#166414,#166415,#166416,#166417,#166418,#166419,#166420,
#166421,#166422),.UNSPECIFIED.,.F.,.F.,(4,2,2,2,1,1,2,2,4),(0.,0.249999999999956,
0.374999999999936,0.437499999999936,0.468749999999936,0.484374999999931,
0.492187499999936,0.49999999999994,1.),.UNSPECIFIED.);
#5006=B_SPLINE_CURVE_WITH_KNOTS('',3,(#166423,#166424,#166425,#166426,#166427,
#166428,#166429,#166430,#166431,#166432,#166433,#166434,#166435,#166436,
#166437,#166438,#166439,#166440,#166441),.UNSPECIFIED.,.F.,.F.,(4,3,3,3,
3,3,4),(0.,0.000108019327761347,0.000159670358772896,0.000279016064561974,
0.000319662760640411,0.000479499943955599,0.000639325521280822),
 .UNSPECIFIED.);
#5007=B_SPLINE_CURVE_WITH_KNOTS('',3,(#166492,#166493,#166494,#166495,#166496,
#166497,#166498,#166499,#166500,#166501,#166502,#166503,#166504,#166505,
#166506,#166507,#166508,#166509,#166510,#166511,#166512,#166513,#166514,
#166515,#166516,#166517,#166518,#166519,#166520,#166521,#166522,#166523,
#166524,#166525,#166526,#166527,#166528,#166529,#166530,#166531,#166532,
#166533,#166534,#166535,#166536,#166537,#166538,#166539,#166540,#166541,
#166542,#166543,#166544,#166545,#166546),.UNSPECIFIED.,.F.,.F.,(4,3,3,3,
3,3,3,3,3,3,3,3,3,3,3,3,3,3,4),(0.,0.0629468896977532,0.127653253164506,
0.194231548280777,0.263838668437689,0.335209452936689,0.40915172120043,
0.437500000000475,0.4687500000005,0.484375000000496,0.492187500000494,0.498659258613318,
0.500000000000492,0.593366456738352,0.68839728589612,0.786023585231411,
0.885234101519568,0.986766500565735,1.),.UNSPECIFIED.);
#5008=B_SPLINE_CURVE_WITH_KNOTS('',3,(#166549,#166550,#166551,#166552,#166553,
#166554,#166555,#166556,#166557,#166558,#166559,#166560,#166561,#166562,
#166563,#166564,#166565,#166566,#166567,#166568,#166569,#166570),
 .UNSPECIFIED.,.F.,.F.,(4,3,3,3,3,3,3,4),(0.,0.00011068335808725,0.000233265503180217,
0.000327042610606244,0.000415140332124215,0.000505188540440904,0.000593686275839362,
0.000654085221212487),.UNSPECIFIED.);
#5009=B_SPLINE_CURVE_WITH_KNOTS('',3,(#166585,#166586,#166587,#166588),
 .UNSPECIFIED.,.F.,.F.,(4,4),(0.,0.0138879247081574),.UNSPECIFIED.);
#5010=B_SPLINE_CURVE_WITH_KNOTS('',3,(#166615,#166616,#166617,#166618,#166619,
#166620,#166621,#166622,#166623,#166624,#166625,#166626,#166627,#166628,
#166629,#166630,#166631,#166632,#166633),.UNSPECIFIED.,.F.,.F.,(4,3,3,3,
3,3,4),(0.,0.00107929064721622,0.00212940062359847,0.00279822589210569,
0.00419733883815853,0.00528234680577585,0.00559645178421137),
 .UNSPECIFIED.);
#5011=B_SPLINE_CURVE_WITH_KNOTS('',3,(#166664,#166665,#166666,#166667,#166668,
#166669,#166670,#166671,#166672,#166673,#166674,#166675,#166676,#166677,
#166678,#166679),.UNSPECIFIED.,.F.,.F.,(4,3,3,3,3,4),(0.,0.00116583085671967,
0.00140039358904036,0.00280078717808072,0.00430574563588143,0.00560157435616136),
 .UNSPECIFIED.);
#5012=B_SPLINE_CURVE_WITH_KNOTS('',3,(#166694,#166695,#166696,#166697),
 .UNSPECIFIED.,.F.,.F.,(4,4),(0.,0.0141656229616797),.UNSPECIFIED.);
#5013=B_SPLINE_CURVE_WITH_KNOTS('',3,(#166718,#166719,#166720,#166721,#166722,
#166723,#166724,#166725,#166726,#166727,#166728,#166729,#166730,#166731,
#166732,#166733),.UNSPECIFIED.,.F.,.F.,(4,3,3,3,3,4),(0.,0.000193094254403281,
0.000327589980483358,0.000444218816713235,0.000550274313879027,0.000655179960966716),
 .UNSPECIFIED.);
#5014=B_SPLINE_CURVE_WITH_KNOTS('',3,(#166893,#166894,#166895,#166896,#166897,
#166898,#166899,#166900,#166901,#166902,#166903,#166904,#166905,#166906,
#166907,#166908,#166909,#166910,#166911),.UNSPECIFIED.,.F.,.F.,(4,3,3,3,
3,3,4),(0.,0.000108634712274956,0.000159257284564388,0.000279020961387661,
0.000318828120207844,0.000478248046436968,0.000637656240415689),
 .UNSPECIFIED.);
#5015=B_SPLINE_CURVE_WITH_KNOTS('',3,(#166926,#166927,#166928,#166929),
 .UNSPECIFIED.,.F.,.F.,(4,4),(0.,0.0180689587739334),.UNSPECIFIED.);
#5016=B_SPLINE_CURVE_WITH_KNOTS('',3,(#166962,#166963,#166964,#166965,#166966,
#166967,#166968,#166969,#166970,#166971,#166972,#166973,#166974,#166975,
#166976,#166977),.UNSPECIFIED.,.F.,.F.,(4,3,3,3,3,4),(0.,0.0013179209674593,
0.00263584193491861,0.00395376290237792,0.00506352109384539,0.00527168386983722),
 .UNSPECIFIED.);
#5017=B_SPLINE_CURVE_WITH_KNOTS('',3,(#167008,#167009,#167010,#167011,#167012,
#167013,#167014,#167015,#167016,#167017,#167018,#167019,#167020,#167021,
#167022,#167023),.UNSPECIFIED.,.F.,.F.,(4,3,3,3,3,4),(0.,0.00122256915433042,
0.0013193477680122,0.00263869553602439,0.00409736884770778,0.00527739107204874),
 .UNSPECIFIED.);
#5018=B_SPLINE_CURVE_WITH_KNOTS('',3,(#167038,#167039,#167040,#167041),
 .UNSPECIFIED.,.F.,.F.,(4,4),(0.,0.0177935197894076),.UNSPECIFIED.);
#5019=B_SPLINE_CURVE_WITH_KNOTS('',3,(#167044,#167045,#167046,#167047,#167048,
#167049,#167050,#167051,#167052,#167053,#167054,#167055,#167056,#167057,
#167058,#167059,#167060,#167061,#167062),.UNSPECIFIED.,.F.,.F.,(4,3,3,3,
3,3,4),(0.,0.206413742690837,0.405311323110467,0.600590525300877,0.800295262650439,
0.987977524790166,1.),.UNSPECIFIED.);
#5020=B_SPLINE_CURVE_WITH_KNOTS('',3,(#167096,#167097,#167098,#167099,#167100,
#167101,#167102,#167103,#167104,#167105,#167106,#167107,#167108),
 .UNSPECIFIED.,.F.,.F.,(4,3,3,3,4),(0.,0.000166958822900708,0.000319870924789836,
0.000479817604858628,0.000639741849579673),.UNSPECIFIED.);
#5021=B_SPLINE_CURVE_WITH_KNOTS('',3,(#167109,#167110,#167111,#167112,#167113,
#167114,#167115,#167116,#167117,#167118,#167119,#167120,#167121,#167122,
#167123,#167124,#167125,#167126,#167127,#167128,#167129,#167130,#167131,
#167132,#167133,#167134,#167135,#167136,#167137,#167138,#167139,#167140,
#167141,#167142,#167143,#167144,#167145,#167146,#167147,#167148,#167149,
#167150,#167151,#167152,#167153,#167154,#167155,#167156,#167157,#167158,
#167159,#167160,#167161,#167162,#167163,#167164,#167165,#167166,#167167,
#167168,#167169,#167170,#167171,#167172,#167173,#167174,#167175,#167176,
#167177,#167178,#167179,#167180,#167181,#167182,#167183,#167184),
 .UNSPECIFIED.,.F.,.F.,(4,3,3,3,3,3,3,3,3,3,3,3,3,3,3,3,3,3,3,3,3,3,3,3,
3,4),(0.,0.087049194558667,0.124999999999871,0.198958822720699,0.245113667123151,
0.272917645441527,0.326518624903113,0.365109832712131,0.399526497461392,
0.484374999999516,0.49449736054903,0.499999999999496,0.513989113488382,
0.598906346294231,0.62499999999941,0.687499999999356,0.718749999999328,
0.734374999999315,0.742187499999308,0.748148548384524,0.749999999999301,
0.804506513683484,0.858475482518048,0.911683608185878,0.963118260439554,
1.),.UNSPECIFIED.);
#5022=B_SPLINE_CURVE_WITH_KNOTS('',3,(#167188,#167189,#167190,#167191,#167192,
#167193,#167194,#167195,#167196,#167197,#167198,#167199,#167200,#167201,
#167202,#167203,#167204,#167205,#167206,#167207,#167208,#167209,#167210,
#167211,#167212,#167213,#167214,#167215),.UNSPECIFIED.,.F.,.F.,(4,3,3,3,
3,3,3,3,3,4),(0.,0.164413128193527,0.334088671484012,0.498046875000089,
0.500000000000089,0.500035489066017,0.639686048889431,0.781957047690301,
0.928621019402901,1.),.UNSPECIFIED.);
#5023=B_SPLINE_CURVE_WITH_KNOTS('',3,(#167245,#167246,#167247,#167248,#167249,
#167250,#167251,#167252,#167253,#167254,#167255,#167256,#167257),
 .UNSPECIFIED.,.F.,.F.,(4,3,3,3,4),(0.,0.287427955658528,0.570428246820337,
0.848327210027682,1.),.UNSPECIFIED.);
#5024=B_SPLINE_CURVE_WITH_KNOTS('',3,(#167293,#167294,#167295,#167296,#167297,
#167298,#167299),.UNSPECIFIED.,.F.,.F.,(4,3,4),(0.,0.0129055642122842,0.0258111284245685),
 .UNSPECIFIED.);
#5025=B_SPLINE_CURVE_WITH_KNOTS('',3,(#167326,#167327,#167328,#167329,#167330,
#167331,#167332,#167333,#167334,#167335,#167336,#167337,#167338,#167339,
#167340,#167341),.UNSPECIFIED.,.F.,.F.,(4,3,3,3,3,4),(0.,0.00112455173535831,
0.00224910347071663,0.00337365520607496,0.00439646903552834,0.0044982069414333),
 .UNSPECIFIED.);
#5026=B_SPLINE_CURVE_WITH_KNOTS('',3,(#167366,#167367,#167368,#167369,#167370,
#167371,#167372,#167373,#167374,#167375,#167376,#167377,#167378,#167379,
#167380,#167381,#167382,#167383,#167384,#167385,#167386,#167387,#167388,
#167389,#167390),.UNSPECIFIED.,.F.,.F.,(4,3,3,3,3,3,3,3,4),(0.,0.000393685585946579,
0.000804157569269683,0.00112634951454785,0.00164227212955572,0.00217802033015107,
0.0022526990290957,0.0035921705044767,0.00450539805819141),
 .UNSPECIFIED.);
#5027=B_SPLINE_CURVE_WITH_KNOTS('',3,(#167411,#167412,#167413,#167414,#167415,
#167416,#167417),.UNSPECIFIED.,.F.,.F.,(4,3,4),(0.,0.0130414224518927,0.0260828449037854),
 .UNSPECIFIED.);
#5028=B_SPLINE_CURVE_WITH_KNOTS('',3,(#167432,#167433,#167434,#167435),
 .UNSPECIFIED.,.F.,.F.,(4,4),(0.,0.000106239733749475),.UNSPECIFIED.);
#5029=B_SPLINE_CURVE_WITH_KNOTS('',3,(#167456,#167457,#167458,#167459,#167460,
#167461,#167462,#167463,#167464,#167465,#167466,#167467,#167468),
 .UNSPECIFIED.,.F.,.F.,(4,3,3,3,4),(0.,0.000360360286228923,0.000488761174293949,
0.000765042797560336,0.000977522348587897),.UNSPECIFIED.);
#5030=B_SPLINE_CURVE_WITH_KNOTS('',3,(#167580,#167581,#167582,#167583,#167584,
#167585,#167586,#167587,#167588,#167589,#167590,#167591,#167592,#167593,
#167594,#167595,#167596,#167597,#167598),.UNSPECIFIED.,.F.,.F.,(4,3,3,3,
3,3,4),(0.,0.000417356154990511,0.000834652124500517,0.000834737818312929,
0.00125222696221769,0.00161112215869395,0.00166930424900103),
 .UNSPECIFIED.);
#5031=B_SPLINE_CURVE_WITH_KNOTS('',3,(#167602,#167603,#167604,#167605,#167606,
#167607,#167608,#167609),.UNSPECIFIED.,.F.,.F.,(4,2,2,4),(0.,0.0307530884815225,
0.0629270182301273,0.0847650334152431),.UNSPECIFIED.);
#5032=B_SPLINE_CURVE_WITH_KNOTS('',3,(#167610,#167611,#167612,#167613,#167614,
#167615,#167616,#167617),.UNSPECIFIED.,.F.,.F.,(4,2,2,4),(0.0847654430259031,
0.106611941487456,0.138792065252627,0.169530887592823),.UNSPECIFIED.);
#5033=B_SPLINE_CURVE_WITH_KNOTS('',3,(#167622,#167623,#167624,#167625,#167626,
#167627,#167628,#167629,#167630,#167631,#167632,#167633,#167634,#167635,
#167636,#167637,#167638,#167639,#167640,#167641,#167642,#167643,#167644,
#167645,#167646,#167647,#167648,#167649,#167650,#167651,#167652,#167653,
#167654,#167655,#167656,#167657,#167658),.UNSPECIFIED.,.F.,.F.,(4,3,3,3,
3,3,3,3,3,3,3,3,4),(0.,0.11441361461611,0.227673917164459,0.343130048663463,
0.437499999999992,0.465087007106255,0.496480388221911,0.499999999999997,
0.590811089022654,0.685064677202165,0.785221931931703,0.892701183249464,
1.),.UNSPECIFIED.);
#5034=B_SPLINE_CURVE_WITH_KNOTS('',3,(#167702,#167703,#167704,#167705,#167706,
#167707,#167708,#167709,#167710,#167711,#167712,#167713,#167714,#167715,
#167716,#167717,#167718,#167719,#167720),.UNSPECIFIED.,.F.,.F.,(4,3,3,3,
3,3,4),(0.,0.000174255415100464,0.000348555105993215,0.000449985369487469,
0.000554229835728735,0.000657719249454963,0.000697110211986431),
 .UNSPECIFIED.);
#5035=B_SPLINE_CURVE_WITH_KNOTS('',3,(#167777,#167778,#167779,#167780,#167781,
#167782,#167783,#167784,#167785,#167786,#167787,#167788,#167789,#167790,
#167791,#167792,#167793,#167794,#167795),.UNSPECIFIED.,.F.,.F.,(4,3,3,3,
3,3,4),(0.,0.00156956785490461,0.00313913570980923,0.00392391963731218,
0.00470870356471384,0.00573336346876343,0.00627827141961845),
 .UNSPECIFIED.);
#5036=B_SPLINE_CURVE_WITH_KNOTS('',3,(#167832,#167833,#167834,#167835,#167836,
#167837,#167838,#167839,#167840,#167841,#167842,#167843,#167844,#167845,
#167846,#167847),.UNSPECIFIED.,.F.,.F.,(4,3,3,3,3,4),(0.,0.00104863959929747,
0.00157050793024954,0.00314101586049909,0.00471152379074863,0.00628203172099817),
 .UNSPECIFIED.);
#5037=B_SPLINE_CURVE_WITH_KNOTS('',3,(#167899,#167900,#167901,#167902,#167903,
#167904,#167905,#167906,#167907,#167908,#167909,#167910,#167911,#167912,
#167913,#167914,#167915,#167916,#167917,#167918,#167919,#167920,#167921,
#167922,#167923,#167924,#167925,#167926,#167927,#167928,#167929,#167930,
#167931,#167932,#167933,#167934,#167935,#167936,#167937,#167938,#167939,
#167940,#167941,#167942,#167943,#167944,#167945,#167946,#167947,#167948,
#167949,#167950,#167951,#167952,#167953,#167954,#167955,#167956,#167957,
#167958,#167959,#167960,#167961,#167962,#167963,#167964,#167965,#167966,
#167967,#167968,#167969,#167970,#167971,#167972,#167973,#167974,#167975,
#167976,#167977),.UNSPECIFIED.,.F.,.F.,(4,3,3,3,3,3,3,3,3,3,3,3,3,3,3,3,
3,3,3,3,3,3,3,3,3,3,4),(0.,0.0823558144348623,0.12499999999997,0.203651427244223,
0.249243429408674,0.282302854488475,0.332820890866331,0.364919347441214,
0.394174559507633,0.47403885817937,0.484374999999898,0.494257434932484,
0.499999999999903,0.522744871728982,0.595589883701348,0.624999999999984,
0.697813020501469,0.734375000000044,0.74218750000005,0.748069745909579,
0.750000000000057,0.770214559218657,0.82461903965541,0.880397897679706,
0.937085248067258,0.995155836674171,1.),.UNSPECIFIED.);
#5038=B_SPLINE_CURVE_WITH_KNOTS('',3,(#167978,#167979,#167980,#167981,#167982,
#167983,#167984,#167985,#167986,#167987,#167988,#167989,#167990),
 .UNSPECIFIED.,.F.,.F.,(4,3,3,3,4),(0.,0.000174780063231096,0.000349568960659906,
0.00052437265365072,0.000699137921319812),.UNSPECIFIED.);
#5039=B_SPLINE_CURVE_WITH_KNOTS('',3,(#168096,#168097,#168098,#168099,#168100,
#168101,#168102,#168103,#168104,#168105,#168106,#168107,#168108,#168109,
#168110,#168111,#168112,#168113,#168114),.UNSPECIFIED.,.F.,.F.,(4,3,3,3,
3,3,4),(0.,0.000168652558320961,0.000337340594483331,0.000432590797837398,
0.000530250662249359,0.000626975088861563,0.000674681188966661),
 .UNSPECIFIED.);
#5040=B_SPLINE_CURVE_WITH_KNOTS('',3,(#168116,#168117,#168118,#168119,#168120,
#168121,#168122,#168123,#168124,#168125,#168126,#168127,#168128,#168129,
#168130,#168131,#168132,#168133,#168134,#168135,#168136,#168137,#168138,
#168139,#168140,#168141,#168142,#168143,#168144,#168145,#168146,#168147,
#168148,#168149,#168150,#168151,#168152,#168153,#168154,#168155,#168156,
#168157,#168158,#168159,#168160,#168161,#168162,#168163,#168164,#168165,
#168166,#168167,#168168,#168169,#168170,#168171,#168172,#168173,#168174,
#168175,#168176,#168177,#168178,#168179,#168180,#168181,#168182,#168183,
#168184,#168185,#168186,#168187,#168188),.UNSPECIFIED.,.F.,.F.,(4,3,3,3,
3,3,3,3,3,3,3,3,3,3,3,3,3,3,3,3,3,3,3,3,4),(0.,0.0466130745701607,0.0624999999999758,
0.110609695998509,0.161358773789719,0.214918577626033,0.218749999999909,
0.23437499999991,0.242187499999898,0.248565636806847,0.249999999999886,
0.327720997850909,0.374999999999767,0.438264832152717,0.476586654637605,
0.480754066517823,0.484374999999699,0.494592854670677,0.499999999999701,
0.578329040666612,0.660059923923264,0.720472595197765,0.817502903971575,
0.924488968621202,1.),.UNSPECIFIED.);
#5041=B_SPLINE_CURVE_WITH_KNOTS('',3,(#168232,#168233,#168234,#168235,#168236,
#168237,#168238,#168239,#168240,#168241,#168242,#168243,#168244,#168245,
#168246,#168247),.UNSPECIFIED.,.F.,.F.,(4,3,3,3,3,4),(0.,0.00159103011504873,
0.00287711962167565,0.00431567943251345,0.00538763071251274,0.00575423924335125),
 .UNSPECIFIED.);
#5042=B_SPLINE_CURVE_WITH_KNOTS('',3,(#168280,#168281,#168282,#168283,#168284,
#168285,#168286,#168287,#168288,#168289,#168290,#168291,#168292,#168293,
#168294,#168295,#168296,#168297,#168298,#168299,#168300,#168301,#168302,
#168303,#168304,#168305,#168306,#168307,#168308,#168309,#168310,#168311,
#168312,#168313,#168314,#168315,#168316,#168317,#168318,#168319,#168320,
#168321,#168322,#168323,#168324,#168325,#168326,#168327,#168328,#168329,
#168330,#168331,#168332,#168333,#168334,#168335,#168336,#168337,#168338,
#168339,#168340,#168341,#168342,#168343,#168344,#168345,#168346,#168347,
#168348,#168349,#168350,#168351,#168352,#168353,#168354,#168355,#168356,
#168357,#168358,#168359,#168360,#168361,#168362,#168363,#168364,#168365,
#168366,#168367,#168368,#168369,#168370,#168371,#168372,#168373),
 .UNSPECIFIED.,.F.,.F.,(4,3,3,3,3,3,3,3,3,3,3,3,3,3,3,3,3,3,3,3,3,3,3,3,
3,3,3,3,3,3,3,4),(0.,0.0762493613834967,0.125000000000117,0.18628438331924,
0.216926574978801,0.232247670808581,0.233849499850804,0.235177693318918,
0.243766448203366,0.247568766638362,0.249645155900695,0.250597019269575,
0.30766327935826,0.367620699912883,0.40625000000014,0.453125000000129,0.497645716780995,
0.500000000000118,0.500538290361993,0.531250000000111,0.587063744180494,
0.640625000000085,0.695312500000072,0.717781622680416,0.722656250000066,
0.736328125000062,0.750000000000059,0.812500000000044,0.87500000000003,
0.937500000000015,0.968750000000007,1.),.UNSPECIFIED.);
#5043=B_SPLINE_CURVE_WITH_KNOTS('',3,(#168377,#168378,#168379,#168380,#168381,
#168382,#168383,#168384,#168385,#168386,#168387,#168388,#168389,#168390,
#168391,#168392,#168393,#168394,#168395),.UNSPECIFIED.,.F.,.F.,(4,3,3,3,
3,3,4),(0.,0.194046007642795,0.397883063949626,0.5,0.676457301204358,0.848320696951666,
1.),.UNSPECIFIED.);
#5044=B_SPLINE_CURVE_WITH_KNOTS('',3,(#168415,#168416,#168417,#168418),
 .UNSPECIFIED.,.F.,.F.,(4,4),(0.,0.0170848224870981),.UNSPECIFIED.);
#5045=B_SPLINE_CURVE_WITH_KNOTS('',3,(#168420,#168421,#168422,#168423,#168424,
#168425,#168426,#168427,#168428,#168429,#168430,#168431,#168432,#168433,
#168434,#168435),.UNSPECIFIED.,.F.,.F.,(4,3,3,3,3,4),(0.,0.216031740979677,
0.438702468406263,0.665600341454978,0.899498011354753,1.),.UNSPECIFIED.);
#5046=B_SPLINE_CURVE_WITH_KNOTS('',3,(#168467,#168468,#168469,#168470,#168471,
#168472,#168473,#168474,#168475,#168476,#168477,#168478,#168479),
 .UNSPECIFIED.,.F.,.F.,(4,3,3,3,4),(0.,0.00117191361843274,0.00234382723686548,
0.00351574085529822,0.00468765447373096),.UNSPECIFIED.);
#5047=B_SPLINE_CURVE_WITH_KNOTS('',3,(#168542,#168543,#168544,#168545,#168546,
#168547,#168548,#168549,#168550,#168551,#168552,#168553,#168554),
 .UNSPECIFIED.,.F.,.F.,(4,3,3,3,4),(0.,0.00125486684196805,0.0025097336839361,
0.00393224022465245,0.00501946736787221),.UNSPECIFIED.);
#5048=B_SPLINE_CURVE_WITH_KNOTS('',3,(#168569,#168570,#168571,#168572),
 .UNSPECIFIED.,.F.,.F.,(4,4),(0.,0.0135233968444946),.UNSPECIFIED.);
#5049=B_SPLINE_CURVE_WITH_KNOTS('',3,(#168594,#168595,#168596,#168597,#168598,
#168599,#168600,#168601,#168602,#168603,#168604,#168605,#168606,#168607,
#168608,#168609,#168610,#168611,#168612,#168613,#168614,#168615,#168616,
#168617,#168618,#168619,#168620,#168621,#168622,#168623,#168624,#168625,
#168626,#168627,#168628,#168629,#168630,#168631,#168632,#168633,#168634,
#168635,#168636,#168637,#168638,#168639,#168640,#168641,#168642,#168643,
#168644,#168645,#168646,#168647,#168648,#168649,#168650,#168651,#168652,
#168653,#168654,#168655,#168656,#168657,#168658,#168659,#168660,#168661,
#168662,#168663,#168664,#168665,#168666,#168667,#168668,#168669),
 .UNSPECIFIED.,.F.,.F.,(4,3,3,3,3,3,3,3,3,3,3,3,3,3,3,3,3,3,3,3,3,3,3,3,
3,4),(0.,0.0971655280396629,0.125000000000066,0.221059690008173,0.250000000000131,
0.339606682262106,0.375000000000198,0.437500000000225,0.468750000000233,
0.484375000000243,0.494471091409305,0.500000000000253,0.513777078434529,
0.599578820798521,0.625000000000219,0.687500000000208,0.718750000000209,
0.734375000000208,0.742187500000215,0.748149663075622,0.750000000000222,
0.804508551754479,0.858449558770446,0.911613486215102,0.962986872288349,
1.),.UNSPECIFIED.);
#5050=B_SPLINE_CURVE_WITH_KNOTS('',3,(#168670,#168671,#168672,#168673,#168674,
#168675,#168676,#168677,#168678,#168679,#168680,#168681,#168682,#168683,
#168684,#168685,#168686,#168687,#168688),.UNSPECIFIED.,.F.,.F.,(4,3,3,3,
3,3,4),(0.,0.000165241084431759,0.000319189981521249,0.000429288245407915,
0.000533834104225207,0.000631975129725552,0.000638379963042499),
 .UNSPECIFIED.);
#5051=B_SPLINE_CURVE_WITH_KNOTS('',3,(#168734,#168735,#168736,#168737,#168738,
#168739,#168740,#168741,#168742,#168743,#168744,#168745,#168746,#168747,
#168748,#168749,#168750,#168751,#168752,#168753,#168754,#168755,#168756,
#168757,#168758,#168759,#168760,#168761,#168762,#168763,#168764,#168765,
#168766,#168767,#168768,#168769,#168770,#168771,#168772,#168773,#168774,
#168775,#168776,#168777,#168778,#168779,#168780,#168781,#168782,#168783,
#168784,#168785,#168786,#168787,#168788),.UNSPECIFIED.,.F.,.F.,(4,3,3,3,
3,3,3,3,3,3,3,3,3,3,3,3,3,3,4),(0.,0.0626986305266445,0.127141358331606,
0.194501704871004,0.263573954919851,0.335355949256235,0.37500000000041,
0.437500000000472,0.46875000000049,0.484375000000489,0.492187500000474,
0.498658321176073,0.500000000000459,0.593349888207087,0.688363929203977,
0.785973373274766,0.885166870466393,0.986682553086995,1.),.UNSPECIFIED.);
#5052=B_SPLINE_CURVE_WITH_KNOTS('',3,(#168791,#168792,#168793,#168794,#168795,
#168796,#168797,#168798,#168799,#168800,#168801,#168802,#168803,#168804,
#168805,#168806,#168807,#168808,#168809,#168810,#168811,#168812),
 .UNSPECIFIED.,.F.,.F.,(4,3,3,3,3,3,3,4),(0.,0.00011032124306877,0.000232554441606406,
0.000327443278856643,0.000415696683397815,0.000505913400363394,0.000594574640422778,
0.000654886557713287),.UNSPECIFIED.);
#5053=B_SPLINE_CURVE_WITH_KNOTS('',3,(#168827,#168828,#168829,#168830),
 .UNSPECIFIED.,.F.,.F.,(4,4),(0.,0.00876509433037234),.UNSPECIFIED.);
#5054=B_SPLINE_CURVE_WITH_KNOTS('',3,(#168857,#168858,#168859,#168860,#168861,
#168862,#168863,#168864,#168865,#168866,#168867,#168868,#168869,#168870,
#168871,#168872,#168873,#168874,#168875,#168876,#168877,#168878,#168879,
#168880,#168881),.UNSPECIFIED.,.F.,.F.,(4,3,3,3,3,3,3,3,4),(0.,0.00066897147268262,
0.00133794294536524,0.00197188997954967,0.00259689693896644,0.00267588589073048,
0.00401382883609571,0.00511764383917763,0.00535177178146096),
 .UNSPECIFIED.);
#5055=B_SPLINE_CURVE_WITH_KNOTS('',3,(#168912,#168913,#168914,#168915,#168916,
#168917,#168918,#168919,#168920,#168921,#168922,#168923,#168924,#168925,
#168926,#168927),.UNSPECIFIED.,.F.,.F.,(4,3,3,3,3,4),(0.,0.0012090865501967,
0.00133938491136683,0.00267876982273365,0.00415143771886329,0.0053575396454673),
 .UNSPECIFIED.);
#5056=B_SPLINE_CURVE_WITH_KNOTS('',3,(#168942,#168943,#168944,#168945),
 .UNSPECIFIED.,.F.,.F.,(4,4),(0.,0.00904291806877093),.UNSPECIFIED.);
#5057=B_SPLINE_CURVE_WITH_KNOTS('',3,(#168966,#168967,#168968,#168969,#168970,
#168971,#168972,#168973,#168974,#168975,#168976,#168977,#168978,#168979,
#168980,#168981),.UNSPECIFIED.,.F.,.F.,(4,3,3,3,3,4),(0.,0.00019490585198886,
0.000327981152987957,0.000444921456706714,0.000551183314037962,0.000655962305975913),
 .UNSPECIFIED.);
#5058=B_SPLINE_CURVE_WITH_KNOTS('',3,(#169141,#169142,#169143,#169144,#169145,
#169146,#169147,#169148,#169149,#169150,#169151,#169152,#169153,#169154,
#169155,#169156,#169157,#169158,#169159),.UNSPECIFIED.,.F.,.F.,(4,3,3,3,
3,3,4),(0.,0.000108392306331539,0.000159419175882383,0.000279017984019912,
0.000319155213741796,0.000478738661811073,0.000638310427483592),
 .UNSPECIFIED.);
#5059=B_SPLINE_CURVE_WITH_KNOTS('',3,(#169174,#169175,#169176,#169177),
 .UNSPECIFIED.,.F.,.F.,(4,4),(0.,0.01284355850178),.UNSPECIFIED.);
#5060=B_SPLINE_CURVE_WITH_KNOTS('',3,(#169210,#169211,#169212,#169213,#169214,
#169215,#169216,#169217,#169218,#169219,#169220,#169221,#169222,#169223,
#169224,#169225),.UNSPECIFIED.,.F.,.F.,(4,3,3,3,3,4),(0.,0.00125936773350451,
0.00251873546700902,0.00377810320051352,0.00490364900505264,0.00503747093401803),
 .UNSPECIFIED.);
#5061=B_SPLINE_CURVE_WITH_KNOTS('',3,(#169256,#169257,#169258,#169259,#169260,
#169261,#169262,#169263,#169264,#169265,#169266,#169267,#169268),
 .UNSPECIFIED.,.F.,.F.,(4,3,3,3,4),(0.,0.00126095469566737,0.00252190939133473,
0.00394829824261256,0.00504381878266947),.UNSPECIFIED.);
#5062=B_SPLINE_CURVE_WITH_KNOTS('',3,(#169283,#169284,#169285,#169286),
 .UNSPECIFIED.,.F.,.F.,(4,4),(0.,0.0125680158145827),.UNSPECIFIED.);
#5063=B_SPLINE_CURVE_WITH_KNOTS('',3,(#169289,#169290,#169291,#169292,#169293,
#169294,#169295,#169296,#169297,#169298,#169299,#169300,#169301),
 .UNSPECIFIED.,.F.,.F.,(4,3,3,3,4),(0.,0.293726063052163,0.581913693472172,
0.862643124884957,1.),.UNSPECIFIED.);
#5064=B_SPLINE_CURVE_WITH_KNOTS('',3,(#169335,#169336,#169337,#169338,#169339,
#169340,#169341,#169342,#169343,#169344,#169345,#169346,#169347),
 .UNSPECIFIED.,.F.,.F.,(4,3,3,3,4),(0.,0.000167806452105701,0.000320197614368795,
0.000480307701132286,0.000640395228737589),.UNSPECIFIED.);
#5065=B_SPLINE_CURVE_WITH_KNOTS('',3,(#169348,#169349,#169350,#169351,#169352,
#169353,#169354,#169355,#169356,#169357,#169358,#169359,#169360,#169361,
#169362,#169363,#169364,#169365,#169366,#169367,#169368,#169369,#169370,
#169371,#169372,#169373,#169374,#169375,#169376,#169377,#169378,#169379,
#169380,#169381,#169382,#169383,#169384,#169385,#169386,#169387,#169388,
#169389,#169390,#169391,#169392,#169393,#169394,#169395,#169396,#169397,
#169398,#169399,#169400,#169401,#169402,#169403,#169404,#169405,#169406,
#169407,#169408,#169409,#169410,#169411,#169412,#169413,#169414,#169415,
#169416,#169417,#169418,#169419,#169420,#169421,#169422,#169423),
 .UNSPECIFIED.,.F.,.F.,(4,3,3,3,3,3,3,3,3,3,3,3,3,3,3,3,3,3,3,3,3,3,3,3,
3,4),(0.,0.0870023380906959,0.124999999999938,0.19900805061357,0.245182333562838,
0.273016101227201,0.326530647858571,0.365028892168486,0.399414806094218,
0.484374999999772,0.494494956765455,0.499999999999771,0.514090654941682,
0.599026190945531,0.624999999999764,0.687499999999756,0.718749999999752,
0.73437499999975,0.74218749999975,0.748147972438602,0.749999999999749,0.804505950346522,
0.858489911214372,0.911721504923935,0.963189048359122,1.),.UNSPECIFIED.);
#5066=B_SPLINE_CURVE_WITH_KNOTS('',3,(#169427,#169428,#169429,#169430,#169431,
#169432,#169433,#169434,#169435,#169436,#169437,#169438,#169439,#169440,
#169441,#169442),.UNSPECIFIED.,.F.,.F.,(4,3,3,3,3,4),(0.,0.193117490837313,
0.394838118127984,0.598407779512051,0.809334151745404,1.),.UNSPECIFIED.);
#5067=B_SPLINE_CURVE_WITH_KNOTS('',3,(#169469,#169470,#169471,#169472),
 .UNSPECIFIED.,.F.,.F.,(4,4),(0.,0.0203430832871546),.UNSPECIFIED.);
#5068=B_SPLINE_CURVE_WITH_KNOTS('',3,(#169499,#169500,#169501,#169502,#169503,
#169504,#169505,#169506,#169507,#169508,#169509,#169510,#169511),
 .UNSPECIFIED.,.F.,.F.,(4,3,3,3,4),(0.,0.00107468821847175,0.0021493764369435,
0.00322406465541528,0.00429875287388706),.UNSPECIFIED.);
#5069=B_SPLINE_CURVE_WITH_KNOTS('',3,(#169536,#169537,#169538,#169539,#169540,
#169541,#169542,#169543,#169544,#169545,#169546,#169547,#169548,#169549,
#169550,#169551,#169552,#169553,#169554,#169555,#169556,#169557),
 .UNSPECIFIED.,.F.,.F.,(4,3,3,3,3,3,3,4),(0.,0.000387785729069979,0.000791054588126119,
0.00107666227523054,0.00167259937146367,0.00215332455046108,0.00346243334011356,
0.00430664910092208),.UNSPECIFIED.);
#5070=B_SPLINE_CURVE_WITH_KNOTS('',3,(#169572,#169573,#169574,#169575),
 .UNSPECIFIED.,.F.,.F.,(4,4),(0.,0.0206148669995797),.UNSPECIFIED.);
#5071=B_SPLINE_CURVE_WITH_KNOTS('',3,(#169590,#169591,#169592,#169593),
 .UNSPECIFIED.,.F.,.F.,(4,4),(0.,0.000103369667661668),.UNSPECIFIED.);
#5072=B_SPLINE_CURVE_WITH_KNOTS('',3,(#169615,#169616,#169617,#169618,#169619,
#169620,#169621,#169622,#169623,#169624,#169625,#169626,#169627,#169628,
#169629,#169630,#169631,#169632,#169633,#169634,#169635,#169636,#169637,
#169638,#169639,#169640,#169641,#169642,#169643,#169644,#169645,#169646,
#169647,#169648),.UNSPECIFIED.,.F.,.F.,(4,3,3,3,3,3,3,3,3,3,3,4),(3.96777284137604E-14,
0.124999999999938,0.249999999999836,0.379017862416308,0.468749999999687,
0.488635543023418,0.497380093045793,0.499999999999651,0.6544631322486,0.810594430460327,
0.970117896208719,0.999999999092843),.UNSPECIFIED.);
#5073=B_SPLINE_CURVE_WITH_KNOTS('',3,(#169649,#169650,#169651,#169652,#169653,
#169654,#169655,#169656,#169657,#169658,#169659,#169660,#169661),
 .UNSPECIFIED.,.F.,.F.,(4,3,3,3,4),(0.,0.000379823720134918,0.000488238270882253,
0.000734566123585685,0.000976476541764506),.UNSPECIFIED.);
#5074=B_SPLINE_CURVE_WITH_KNOTS('',3,(#169675,#169676,#169677,#169678,#169679,
#169680,#169681,#169682,#169683,#169684,#169685,#169686,#169687),
 .UNSPECIFIED.,.F.,.F.,(4,3,3,3,4),(0.,0.256134514950837,0.516016641878448,
0.782357628273516,1.),.UNSPECIFIED.);
#5075=B_SPLINE_CURVE_WITH_KNOTS('',3,(#169790,#169791,#169792,#169793,#169794,
#169795,#169796,#169797,#169798,#169799,#169800,#169801,#169802,#169803,
#169804,#169805,#169806,#169807,#169808,#169809,#169810,#169811,#169812,
#169813,#169814,#169815,#169816,#169817,#169818,#169819,#169820,#169821,
#169822,#169823,#169824,#169825,#169826),.UNSPECIFIED.,.F.,.F.,(4,3,3,3,
3,3,3,3,3,3,3,3,4),(0.,0.000231966620805271,0.000541763265450615,0.000565419069388565,
0.000565630623675328,0.00113073622792203,0.00113126124735066,0.00146429940365072,
0.00169659085207846,0.00169689187102598,0.00198522910630028,0.00223959723150185,
0.00226252249470131),.UNSPECIFIED.);
#5076=B_SPLINE_CURVE_WITH_KNOTS('',3,(#169828,#169829,#169830,#169831,#169832,
#169833,#169834,#169835,#169836,#169837,#169838,#169839,#169840,#169841,
#169842,#169843,#169844,#169845),.UNSPECIFIED.,.F.,.F.,(4,2,2,2,2,2,2,2,
4),(-0.232545286649255,-0.202278856488963,-0.169720566966038,-0.147070875715933,
-0.116272702465016,-0.0854925566385012,-0.0628371603598658,-0.0302640152400447,
0.),.UNSPECIFIED.);
#5077=B_SPLINE_CURVE_WITH_KNOTS('',3,(#169887,#169888,#169889,#169890),
 .UNSPECIFIED.,.F.,.F.,(4,4),(0.,0.000203650363220012),.UNSPECIFIED.);
#5078=B_SPLINE_CURVE_WITH_KNOTS('',3,(#169911,#169912,#169913,#169914,#169915,
#169916,#169917,#169918,#169919,#169920,#169921,#169922,#169923,#169924,
#169925,#169926,#169927,#169928,#169929,#169930,#169931,#169932,#169933,
#169934,#169935),.UNSPECIFIED.,.F.,.F.,(4,3,3,3,3,3,3,3,4),(0.,7.36083385127449E-5,
0.000151188117339882,0.000234018984645761,0.000250167431468888,0.000250705751451749,
0.000332906541327113,0.000418695252292313,0.000500334862937777),
 .UNSPECIFIED.);
#5079=B_SPLINE_CURVE_WITH_KNOTS('',3,(#169968,#169969,#169970,#169971,#169972,
#169973,#169974,#169975,#169976,#169977,#169978,#169979,#169980,#169981,
#169982,#169983),.UNSPECIFIED.,.F.,.F.,(4,3,3,3,3,4),(0.,0.0014169282635678,
0.00283385652713561,0.00425078479070341,0.00538743306816435,0.00566771305427122),
 .UNSPECIFIED.);
#5080=B_SPLINE_CURVE_WITH_KNOTS('',3,(#170013,#170014,#170015,#170016,#170017,
#170018,#170019,#170020,#170021,#170022,#170023,#170024,#170025),
 .UNSPECIFIED.,.F.,.F.,(4,3,3,3,4),(6.93889390390723E-18,0.00134873564674426,
0.00269747129348853,0.00432753805226364,0.00539494258697707),
 .UNSPECIFIED.);
#5081=B_SPLINE_CURVE_WITH_KNOTS('',3,(#170058,#170059,#170060,#170061,#170062,
#170063,#170064,#170065,#170066,#170067,#170068,#170069,#170070,#170071,
#170072,#170073,#170074,#170075,#170076),.UNSPECIFIED.,.F.,.F.,(4,3,3,3,
3,3,4),(0.,0.000151278709680665,0.000175639358542291,0.00032081912162696,
0.000351502905376566,0.000527285240968804,0.000703005810753132),
 .UNSPECIFIED.);
#5082=B_SPLINE_CURVE_WITH_KNOTS('',3,(#170079,#170080,#170081,#170082,#170083,
#170084,#170085,#170086,#170087,#170088,#170089,#170090,#170091,#170092,
#170093,#170094,#170095,#170096,#170097,#170098,#170099,#170100,#170101,
#170102,#170103),.UNSPECIFIED.,.F.,.F.,(4,2,2,2,1,2,2,2,2,1,1,2,2,4),(0.,
0.249999999999732,0.37499999999959,0.437499999999521,0.468749999999492,
0.484374999999488,0.499999999999485,0.624999999999589,0.687499999999633,
0.718749999999655,0.734374999999666,0.742187499999676,0.749999999999686,
0.999999477481404),.UNSPECIFIED.);
#5083=B_SPLINE_CURVE_WITH_KNOTS('',3,(#170195,#170196,#170197,#170198),
 .UNSPECIFIED.,.F.,.F.,(4,4),(0.,8.25660289862869E-5),.UNSPECIFIED.);
#5084=B_SPLINE_CURVE_WITH_KNOTS('',3,(#170221,#170222,#170223,#170224,#170225,
#170226,#170227),.UNSPECIFIED.,.F.,.F.,(4,3,4),(0.,0.0148367096635454,0.0296734193270908),
 .UNSPECIFIED.);
#5085=B_SPLINE_CURVE_WITH_KNOTS('',3,(#170248,#170249,#170250,#170251,#170252,
#170253,#170254,#170255,#170256,#170257,#170258,#170259,#170260,#170261,
#170262,#170263,#170264,#170265,#170266,#170267,#170268,#170269,#170270,
#170271,#170272),.UNSPECIFIED.,.F.,.F.,(4,3,3,3,3,3,3,3,4),(0.,0.000418974782548372,
0.000841777476037116,0.00103655247459,0.00148268378393581,0.0019250583151384,
0.00207310494918,0.00313777887502721,0.00414620989836001),.UNSPECIFIED.);
#5086=B_SPLINE_CURVE_WITH_KNOTS('',3,(#170298,#170299,#170300,#170301,#170302,
#170303,#170304,#170305,#170306,#170307,#170308,#170309,#170310,#170311,
#170312,#170313,#170314,#170315,#170316,#170317,#170318,#170319,#170320,
#170321,#170322,#170323,#170324,#170325,#170326,#170327,#170328,#170329,
#170330,#170331,#170332,#170333,#170334,#170335,#170336),.UNSPECIFIED.,
 .F.,.F.,(4,2,2,1,1,1,1,2,2,2,2,2,1,1,2,2,2,2,1,1,1,2,2,4),(0.,0.124999999999703,
0.187499999999554,0.218749999999476,0.234374999999437,0.242187499999421,
0.246093749999413,0.248046874999405,0.249999999999396,0.374999999999367,
0.437499999999356,0.468749999999351,0.484374999999349,0.492187499999348,
0.496093749999347,0.499999999999347,0.624999999999361,0.687499999999364,
0.718749999999365,0.734374999999367,0.742187499999368,0.746093749999375,
0.749999999999382,0.999999986192015),.UNSPECIFIED.);
#5087=B_SPLINE_CURVE_WITH_KNOTS('',3,(#170337,#170338,#170339,#170340,#170341,
#170342,#170343,#170344,#170345,#170346,#170347,#170348,#170349,#170350,
#170351,#170352,#170353,#170354,#170355,#170356,#170357,#170358),
 .UNSPECIFIED.,.F.,.F.,(4,3,3,3,3,3,3,4),(1.55158384577954E-17,0.000383789572583399,
0.000781910391026632,0.00103855983331611,0.00179575082696553,0.00207711966663221,
0.00335799595902739,0.00415423933326436),.UNSPECIFIED.);
#5088=B_SPLINE_CURVE_WITH_KNOTS('',3,(#170410,#170411,#170412,#170413,#170414,
#170415,#170416,#170417,#170418,#170419,#170420,#170421,#170422,#170423,
#170424,#170425),.UNSPECIFIED.,.F.,.F.,(4,2,2,1,1,1,1,2,2,4),(0.,0.24999999999986,
0.37499999999979,0.437499999999754,0.468749999999737,0.484374999999728,
0.492187499999723,0.49902343749972,0.499999999999719,1.),.UNSPECIFIED.);
#5089=B_SPLINE_CURVE_WITH_KNOTS('',3,(#170426,#170427,#170428,#170429,#170430,
#170431,#170432),.UNSPECIFIED.,.F.,.F.,(4,3,4),(0.,0.0147014688781887,0.0294029377563774),
 .UNSPECIFIED.);
#5090=B_SPLINE_CURVE_WITH_KNOTS('',3,(#170452,#170453,#170454,#170455,#170456,
#170457,#170458,#170459,#170460,#170461,#170462,#170463,#170464,#170465,
#170466,#170467),.UNSPECIFIED.,.F.,.F.,(4,3,3,3,3,4),(8.08667809653667E-7,
0.261781280773483,0.391444635181636,0.617402649693561,0.814980261808023,
1.),.UNSPECIFIED.);
#5091=B_SPLINE_CURVE_WITH_KNOTS('',3,(#170468,#170469,#170470,#170471,#170472,
#170473,#170474,#170475,#170476,#170477,#170478,#170479,#170480,#170481,
#170482,#170483,#170484,#170485,#170486,#170487,#170488,#170489,#170490,
#170491,#170492,#170493,#170494,#170495,#170496,#170497,#170498,#170499,
#170500,#170501,#170502,#170503,#170504,#170505,#170506,#170507,#170508,
#170509,#170510,#170511,#170512,#170513,#170514,#170515,#170516,#170517,
#170518,#170519,#170520,#170521,#170522,#170523,#170524,#170525,#170526,
#170527,#170528,#170529,#170530,#170531,#170532,#170533,#170534,#170535,
#170536,#170537,#170538,#170539,#170540,#170541,#170542,#170543,#170544,
#170545,#170546,#170547,#170548,#170549),.UNSPECIFIED.,.F.,.F.,(4,3,3,3,
3,3,3,3,3,3,3,3,3,3,3,3,3,3,3,3,3,3,3,3,3,3,3,4),(1.73784017987518E-5,0.0624999999999309,
0.124999999999862,0.187499999999794,0.21874999999976,0.234374999999738,
0.242187499999727,0.246093749999722,0.248046874999723,0.249999999999724,
0.299242278960943,0.349392080063728,0.374999999999775,0.429018671543615,
0.4374999999998,0.468749999999814,0.48437499999982,0.49577510820138,0.499999999999827,
0.500495595336202,0.562747797668036,0.62499999999987,0.696123920530156,
0.74666554161023,0.782709136401979,0.855162490063989,0.930474985780909,
1.),.UNSPECIFIED.);
#5092=B_SPLINE_CURVE_WITH_KNOTS('',3,(#170572,#170573,#170574,#170575,#170576,
#170577,#170578,#170579),.UNSPECIFIED.,.F.,.F.,(4,2,2,4),(0.,0.000841011829491348,
0.00168202365898269,0.00336404731796539),.UNSPECIFIED.);
#5093=B_SPLINE_CURVE_WITH_KNOTS('',3,(#170603,#170604,#170605,#170606,#170607,
#170608,#170609,#170610,#170611,#170612,#170613,#170614,#170615,#170616,
#170617,#170618),.UNSPECIFIED.,.F.,.F.,(4,3,3,3,3,4),(0.,0.000762418881005378,
0.00156275687156247,0.00168533471950014,0.00283547033566749,0.00337066943900028),
 .UNSPECIFIED.);
#5094=B_SPLINE_CURVE_WITH_KNOTS('',3,(#170639,#170640,#170641,#170642,#170643,
#170644,#170645),.UNSPECIFIED.,.F.,.F.,(4,3,4),(0.,0.0179426259581151,0.0358852519162302),
 .UNSPECIFIED.);
#5095=B_SPLINE_CURVE_WITH_KNOTS('',3,(#170696,#170697,#170698,#170699,#170700,
#170701,#170702,#170703,#170704,#170705,#170706,#170707,#170708,#170709,
#170710,#170711,#170712,#170713,#170714,#170715,#170716,#170717,#170718,
#170719,#170720,#170721,#170722,#170723,#170724,#170725,#170726),
 .UNSPECIFIED.,.F.,.F.,(4,3,3,3,3,3,3,3,3,3,4),(0.,0.151691911771996,0.306710028502103,
0.467372294165444,0.499023437500016,0.500000000000016,0.500021673300866,
0.625016254975649,0.750863508401593,0.881927831571319,1.),.UNSPECIFIED.);
#5096=B_SPLINE_CURVE_WITH_KNOTS('',3,(#170729,#170730,#170731,#170732,#170733,
#170734,#170735),.UNSPECIFIED.,.F.,.F.,(4,3,4),(0.,0.0178083890192188,0.0356167780384377),
 .UNSPECIFIED.);
#5097=B_SPLINE_CURVE_WITH_KNOTS('',3,(#170797,#170798,#170799,#170800,#170801,
#170802,#170803),.UNSPECIFIED.,.F.,.F.,(4,3,4),(6.93889390390723E-18,0.0190876722191456,
0.0381753444382913),.UNSPECIFIED.);
#5098=B_SPLINE_CURVE_WITH_KNOTS('',3,(#170824,#170825,#170826,#170827,#170828,
#170829,#170830,#170831,#170832,#170833,#170834,#170835,#170836,#170837,
#170838,#170839),.UNSPECIFIED.,.F.,.F.,(4,3,3,3,3,4),(0.,0.000542853834905746,
0.00109518831082765,0.00152034213881841,0.00254894911026922,0.00304068427763681),
 .UNSPECIFIED.);
#5099=B_SPLINE_CURVE_WITH_KNOTS('',3,(#170866,#170867,#170868,#170869,#170870,
#170871,#170872,#170873,#170874,#170875,#170876,#170877,#170878,#170879,
#170880,#170881,#170882,#170883,#170884,#170885,#170886,#170887,#170888,
#170889,#170890,#170891,#170892,#170893,#170894,#170895,#170896,#170897,
#170898,#170899,#170900,#170901,#170902,#170903,#170904,#170905,#170906,
#170907,#170908,#170909,#170910,#170911,#170912,#170913,#170914,#170915,
#170916,#170917,#170918,#170919,#170920,#170921,#170922,#170923,#170924,
#170925,#170926,#170927,#170928,#170929,#170930,#170931,#170932,#170933,
#170934,#170935,#170936,#170937,#170938,#170939,#170940,#170941,#170942,
#170943,#170944,#170945,#170946,#170947,#170948,#170949,#170950,#170951,
#170952,#170953,#170954,#170955,#170956,#170957,#170958,#170959,#170960,
#170961,#170962,#170963,#170964,#170965,#170966,#170967,#170968),
 .UNSPECIFIED.,.F.,.F.,(4,3,3,3,3,3,3,3,3,3,3,3,3,3,3,3,3,3,3,3,3,3,3,3,
3,3,3,3,3,3,3,3,3,3,4),(0.,0.0900245051711857,0.12500000000326,0.187500000004897,
0.218750000005709,0.234375000006121,0.242187500006326,0.246093750006424,
0.250000000006521,0.319655504681364,0.387239150766509,0.437500000011095,
0.468750000011866,0.484375000012251,0.492187500012445,0.496093750012541,
0.498046875012584,0.500000000012627,0.532507155583111,0.565381440866807,
0.598529785335568,0.631930879298941,0.66539941633402,0.698913886443443,
0.718750000017358,0.734375000017693,0.742187500017856,0.746093750017937,
0.748046875017916,0.749023437517847,0.750000000017778,0.821623578614083,
0.894552114764428,0.969478886559688,1.),.UNSPECIFIED.);
#5100=B_SPLINE_CURVE_WITH_KNOTS('',3,(#170969,#170970,#170971,#170972,#170973,
#170974,#170975,#170976,#170977,#170978,#170979,#170980,#170981),
 .UNSPECIFIED.,.F.,.F.,(4,3,3,3,4),(0.,0.000817157754010358,0.00152229638412186,
0.00262171283977965,0.00304459276824371),.UNSPECIFIED.);
#5101=B_SPLINE_CURVE_WITH_KNOTS('',3,(#171003,#171004,#171005,#171006,#171007,
#171008,#171009,#171010,#171011,#171012,#171013,#171014,#171015,#171016,
#171017,#171018),.UNSPECIFIED.,.F.,.F.,(4,2,2,1,1,1,1,2,2,4),(0.,0.249999999999946,
0.374999999999919,0.437499999999904,0.468749999999897,0.484374999999893,
0.492187499999891,0.499023437499889,0.499999999999889,1.),.UNSPECIFIED.);
#5102=B_SPLINE_CURVE_WITH_KNOTS('',3,(#171019,#171020,#171021,#171022,#171023,
#171024,#171025),.UNSPECIFIED.,.F.,.F.,(4,3,4),(0.,0.0189537577590876,0.0379075155181752),
 .UNSPECIFIED.);
#5103=B_SPLINE_CURVE_WITH_KNOTS('',3,(#171051,#171052,#171053,#171054,#171055,
#171056,#171057,#171058,#171059,#171060,#171061,#171062,#171063,#171064,
#171065,#171066,#171067,#171068,#171069,#171070,#171071,#171072),
 .UNSPECIFIED.,.F.,.F.,(4,3,3,3,3,3,3,4),(4.13152027403574E-8,0.150452793181179,
0.265782575349523,0.374279137552784,0.44848875244278,0.72424437622139,0.921304556955205,
1.),.UNSPECIFIED.);
#5104=B_SPLINE_CURVE_WITH_KNOTS('',3,(#171073,#171074,#171075,#171076,#171077,
#171078,#171079,#171080,#171081,#171082,#171083,#171084,#171085,#171086,
#171087,#171088,#171089,#171090,#171091,#171092,#171093,#171094,#171095,
#171096,#171097,#171098,#171099,#171100,#171101,#171102,#171103,#171104,
#171105,#171106,#171107,#171108,#171109,#171110,#171111,#171112,#171113,
#171114,#171115,#171116,#171117,#171118,#171119,#171120,#171121,#171122,
#171123,#171124,#171125,#171126,#171127,#171128,#171129,#171130,#171131,
#171132,#171133,#171134,#171135,#171136,#171137,#171138,#171139,#171140,
#171141,#171142,#171143,#171144,#171145,#171146,#171147,#171148,#171149,
#171150,#171151,#171152,#171153,#171154),.UNSPECIFIED.,.F.,.F.,(4,3,3,3,
3,3,3,3,3,3,3,3,3,3,3,3,3,3,3,3,3,3,3,3,3,3,3,4),(1.312206885811E-6,0.0698966901337594,
0.125000000000195,0.187500000000286,0.218750000000339,0.234375000000365,
0.242187500000377,0.246093750000384,0.250000000000391,0.290090360663461,
0.330650857430358,0.371698509928867,0.412916364884191,0.454282110705438,
0.468750000000707,0.484375000000744,0.492187500000784,0.496093750000782,
0.498046875000781,0.498535156250781,0.498901367188281,0.500000000000781,
0.590487268190957,0.682955872901068,0.77862973559014,0.876261101941014,
0.97682566140977,0.999999999999992),.UNSPECIFIED.);
#5105=B_SPLINE_CURVE_WITH_KNOTS('',3,(#171177,#171178,#171179,#171180,#171181,
#171182,#171183,#171184,#171185,#171186,#171187,#171188,#171189),
 .UNSPECIFIED.,.F.,.F.,(4,3,3,3,4),(0.,0.000842979772258894,0.00121101869920095,
0.00218603126581974,0.00242203739840189),.UNSPECIFIED.);
#5106=B_SPLINE_CURVE_WITH_KNOTS('',3,(#171214,#171215,#171216,#171217,#171218,
#171219,#171220,#171221,#171222,#171223,#171224,#171225,#171226),
 .UNSPECIFIED.,.F.,.F.,(4,3,3,3,4),(0.,0.000857870627796964,0.00121135746045287,
0.00220749552011028,0.00242271492090574),.UNSPECIFIED.);
#5107=B_SPLINE_CURVE_WITH_KNOTS('',3,(#171241,#171242,#171243,#171244),
 .UNSPECIFIED.,.F.,.F.,(4,4),(0.,0.0421837023697854),.UNSPECIFIED.);
#5108=B_SPLINE_CURVE_WITH_KNOTS('',3,(#171306,#171307,#171308,#171309,#171310,
#171311,#171312,#171313,#171314,#171315,#171316,#171317,#171318,#171319,
#171320,#171321,#171322,#171323,#171324,#171325,#171326,#171327,#171328,
#171329,#171330,#171331,#171332,#171333,#171334,#171335,#171336,#171337,
#171338,#171339,#171340,#171341,#171342,#171343,#171344,#171345),
 .UNSPECIFIED.,.F.,.F.,(4,3,3,3,3,3,3,3,3,3,3,3,3,4),(0.,0.000556259975763551,
0.000647586119897307,0.000728260191095046,0.00109239125585009,0.00129517223979461,
0.00145651805257904,0.00182064826297319,0.00194275835969192,0.00212625862851037,
0.00218441767336186,0.00226655141964057,0.00244042135138738,0.00259034447958922),
 .UNSPECIFIED.);
#5109=B_SPLINE_CURVE_WITH_KNOTS('',3,(#171360,#171361,#171362,#171363,#171364,
#171365,#171366,#171367,#171368,#171369,#171370,#171371,#171372,#171373,
#171374,#171375),.UNSPECIFIED.,.F.,.F.,(4,2,2,1,1,1,1,2,2,4),(0.,0.250000000000176,
0.375000000000264,0.437500000000308,0.46875000000033,0.484375000000341,
0.492187500000346,0.499511718750351,0.500000000000351,1.),.UNSPECIFIED.);
#5110=B_SPLINE_CURVE_WITH_KNOTS('',3,(#171378,#171379,#171380,#171381),
 .UNSPECIFIED.,.F.,.F.,(4,4),(0.,0.0419168978153696),.UNSPECIFIED.);
#5111=B_SPLINE_CURVE_WITH_KNOTS('',3,(#171390,#171391,#171392,#171393),
 .UNSPECIFIED.,.F.,.F.,(4,4),(0.00436813896256353,0.00486865237729894),
 .UNSPECIFIED.);
#5112=B_SPLINE_CURVE_WITH_KNOTS('',3,(#171443,#171444,#171445,#171446,#171447,
#171448,#171449,#171450,#171451,#171452,#171453,#171454,#171455,#171456,
#171457,#171458,#171459,#171460,#171461,#171462,#171463,#171464,#171465,
#171466,#171467,#171468,#171469,#171470,#171471,#171472,#171473,#171474,
#171475,#171476,#171477,#171478,#171479),.UNSPECIFIED.,.F.,.F.,(4,3,3,3,
3,3,3,3,3,3,3,3,4),(0.000672031760609077,0.000712854075812315,0.00100252198456931,
0.00107233830279968,0.0012216976510115,0.00143188803178761,0.00171092729228638,
0.00177136354141392,0.00179176783191222,0.00215141270034081,0.00232102943181635,
0.00259586237701756,0.00287069532221878),.UNSPECIFIED.);
#5113=B_SPLINE_CURVE_WITH_KNOTS('',3,(#171537,#171538,#171539,#171540,#171541,
#171542,#171543,#171544,#171545,#171546,#171547,#171548,#171549),
 .UNSPECIFIED.,.F.,.F.,(4,3,3,3,4),(0.,0.000701986547780456,0.00111013811990961,
0.00206054695785466,0.00222027623981923),.UNSPECIFIED.);
#5114=B_SPLINE_CURVE_WITH_KNOTS('',3,(#171574,#171575,#171576,#171577,#171578,
#171579,#171580,#171581,#171582,#171583,#171584,#171585,#171586),
 .UNSPECIFIED.,.F.,.F.,(4,3,3,3,4),(0.,0.000647478258315285,0.00111023907191622,
0.00207039129249102,0.00222047814383243),.UNSPECIFIED.);
#5115=B_SPLINE_CURVE_WITH_KNOTS('',3,(#171589,#171590,#171591,#171592,#171593,
#171594,#171595,#171596,#171597,#171598,#171599,#171600,#171601,#171602,
#171603,#171604,#171605,#171606,#171607,#171608,#171609,#171610,#171611,
#171612,#171613,#171614,#171615,#171616,#171617,#171618,#171619,#171620,
#171621,#171622,#171623,#171624,#171625,#171626,#171627,#171628,#171629,
#171630,#171631,#171632,#171633,#171634,#171635,#171636,#171637,#171638,
#171639,#171640,#171641,#171642,#171643,#171644,#171645,#171646,#171647,
#171648,#171649,#171650,#171651,#171652),.UNSPECIFIED.,.F.,.F.,(4,3,3,3,
3,3,3,3,3,3,3,3,3,3,3,3,3,3,3,3,3,4),(0.,0.137315011687963,0.249999999999215,
0.374999999998815,0.437499999998613,0.46874999999852,0.48437499999848,0.49218749999846,
0.496093749998458,0.499999999998455,0.500132617240959,0.562566308619912,
0.624999999998865,0.687499999999072,0.718749999999174,0.73987160258027,
0.749999999999276,0.805747260200159,0.863072799323141,0.921013881125668,
0.979478145917718,0.999999974089565),.UNSPECIFIED.);
#5116=B_SPLINE_CURVE_WITH_KNOTS('',3,(#171672,#171673,#171674,#171675,#171676,
#171677,#171678,#171679,#171680,#171681,#171682,#171683,#171684,#171685,
#171686,#171687),.UNSPECIFIED.,.F.,.F.,(4,2,2,1,1,1,1,2,2,4),(0.,0.249999999999879,
0.37499999999982,0.43749999999979,0.468749999999775,0.484374999999767,0.492187499999763,
0.499511718749759,0.499999999999759,1.),.UNSPECIFIED.);
#5117=B_SPLINE_CURVE_WITH_KNOTS('',3,(#171713,#171714,#171715,#171716,#171717,
#171718,#171719,#171720,#171721,#171722,#171723,#171724,#171725,#171726,
#171727,#171728,#171729,#171730,#171731,#171732,#171733,#171734,#171735,
#171736,#171737,#171738,#171739,#171740,#171741,#171742,#171743,#171744,
#171745,#171746,#171747,#171748,#171749,#171750,#171751,#171752),
 .UNSPECIFIED.,.F.,.F.,(4,3,3,3,3,3,3,3,3,3,3,3,3,4),(0.,0.179991932872247,
0.233369732025158,0.249999999999994,0.338178756215747,0.374999999999992,
0.437499999999991,0.46874999999999,0.484374999999989,0.490038899812079,
0.499999999999989,0.749999999999994,0.96759783696102,1.),.UNSPECIFIED.);
#5118=B_SPLINE_CURVE_WITH_KNOTS('',3,(#171804,#171805,#171806,#171807),
 .UNSPECIFIED.,.F.,.F.,(4,4),(0.,0.0447707136167657),.UNSPECIFIED.);
#5119=B_SPLINE_CURVE_WITH_KNOTS('',3,(#171857,#171858,#171859,#171860,#171861,
#171862,#171863,#171864,#171865,#171866,#171867,#171868,#171869,#171870,
#171871,#171872,#171873,#171874,#171875,#171876,#171877,#171878,#171879,
#171880,#171881),.UNSPECIFIED.,.F.,.F.,(4,3,3,3,3,3,3,3,4),(0.,0.000275481208481403,
0.000553063545339304,0.000602887330399936,0.000809845174226025,0.00102800957885645,
0.00120532901601379,0.00142404055844572,0.00161969034845205),
 .UNSPECIFIED.);
#5120=B_SPLINE_CURVE_WITH_KNOTS('',3,(#171896,#171897,#171898,#171899,#171900,
#171901,#171902,#171903,#171904,#171905),.UNSPECIFIED.,.F.,.F.,(4,3,3,4),
(0.,0.389160316713121,0.830817831506134,1.),.UNSPECIFIED.);
#5121=B_SPLINE_CURVE_WITH_KNOTS('',3,(#171958,#171959,#171960,#171961,#171962,
#171963,#171964,#171965,#171966,#171967,#171968,#171969,#171970,#171971,
#171972,#171973,#171974,#171975,#171976,#171977,#171978,#171979,#171980,
#171981,#171982),.UNSPECIFIED.,.F.,.F.,(4,3,3,3,3,3,3,3,4),(0.000689304848359617,
0.00090628372627929,0.00111364302895387,0.00133013985168599,0.00150801684530018,
0.00171993694385612,0.00199672649963881,0.00227140074390808,0.00232672884224074),
 .UNSPECIFIED.);
#5122=B_SPLINE_CURVE_WITH_KNOTS('',3,(#172076,#172077,#172078,#172079,#172080,
#172081,#172082,#172083,#172084,#172085,#172086,#172087,#172088,#172089,
#172090,#172091,#172092,#172093,#172094,#172095,#172096,#172097,#172098,
#172099,#172100),.UNSPECIFIED.,.F.,.F.,(4,3,3,3,3,3,3,3,4),(0.,0.374999999999775,
0.437499999999737,0.468749999999718,0.484374999999709,0.499511718749699,
0.499999999999699,0.888987273624248,1.),.UNSPECIFIED.);
#5123=B_SPLINE_CURVE_WITH_KNOTS('',3,(#172120,#172121,#172122,#172123,#172124,
#172125,#172126,#172127,#172128,#172129,#172130,#172131,#172132,#172133,
#172134,#172135,#172136,#172137,#172138,#172139,#172140,#172141,#172142,
#172143,#172144,#172145,#172146,#172147,#172148,#172149,#172150),
 .UNSPECIFIED.,.F.,.F.,(4,3,3,3,3,3,3,3,3,3,4),(0.,0.184213842299516,0.384184423243072,
0.484375000000021,0.498581836652927,0.500000000000022,0.512531515748722,
0.644734984770559,0.776535034074271,0.907370191348794,1.),.UNSPECIFIED.);
#5124=B_SPLINE_CURVE_WITH_KNOTS('',3,(#172151,#172152,#172153,#172154,#172155,
#172156,#172157,#172158,#172159,#172160,#172161,#172162,#172163,#172164,
#172165,#172166,#172167,#172168,#172169,#172170,#172171,#172172,#172173,
#172174,#172175,#172176,#172177,#172178,#172179,#172180,#172181,#172182,
#172183,#172184,#172185,#172186,#172187,#172188,#172189,#172190,#172191,
#172192,#172193,#172194,#172195,#172196,#172197,#172198,#172199,#172200,
#172201,#172202,#172203,#172204,#172205,#172206,#172207,#172208),
 .UNSPECIFIED.,.F.,.F.,(4,3,3,3,3,3,3,3,3,3,3,3,3,3,3,3,3,3,3,4),(0.,0.0625000000000331,
0.125000000000066,0.175859082344618,0.224397356720149,0.250000000000132,
0.307328937444154,0.365341671430271,0.424129973950711,0.437500000000222,
0.468750000000235,0.484375000000231,0.492187500000216,0.496093750000209,
0.500000000000202,0.59834670848804,0.700014659932125,0.803605996460746,
0.910590148948139,1.),.UNSPECIFIED.);
#5125=B_SPLINE_CURVE_WITH_KNOTS('',3,(#172231,#172232,#172233,#172234,#172235,
#172236,#172237,#172238,#172239,#172240,#172241,#172242,#172243),
 .UNSPECIFIED.,.F.,.F.,(4,3,3,3,4),(0.,0.000727903814955922,0.00111811425806593,
0.00207062545858035,0.00223622851613186),.UNSPECIFIED.);
#5126=B_SPLINE_CURVE_WITH_KNOTS('',3,(#172268,#172269,#172270,#172271,#172272,
#172273,#172274,#172275,#172276,#172277,#172278,#172279,#172280),
 .UNSPECIFIED.,.F.,.F.,(4,3,3,3,4),(0.,0.000659089694855302,0.00111822884501791,
0.002081283710365,0.00223645769003581),.UNSPECIFIED.);
#5127=B_SPLINE_CURVE_WITH_KNOTS('',3,(#172360,#172361,#172362,#172363,#172364,
#172365,#172366,#172367,#172368,#172369,#172370,#172371,#172372,#172373,
#172374,#172375,#172376,#172377,#172378,#172379,#172380,#172381,#172382,
#172383,#172384,#172385,#172386,#172387,#172388,#172389,#172390,#172391,
#172392,#172393),.UNSPECIFIED.,.F.,.F.,(4,3,3,3,3,3,3,3,3,3,3,4),(0.,0.000275770613304119,
0.000551541226608238,0.000716520337534457,0.0010747839077808,0.00110308245321648,
0.00134771653693952,0.00143334685918384,0.00165462367982471,0.00179132390797124,
0.00214954043896842,0.00220616490643295),.UNSPECIFIED.);
#5128=B_SPLINE_CURVE_WITH_KNOTS('',3,(#172408,#172409,#172410,#172411,#172412,
#172413,#172414,#172415,#172416,#172417,#172418,#172419,#172420,#172421,
#172422),.UNSPECIFIED.,.F.,.F.,(4,2,2,1,1,1,2,2,4),(0.,0.250000000000171,
0.375000000000256,0.437500000000298,0.46875000000032,0.484375000000331,
0.499511718750343,0.500000000000343,1.),.UNSPECIFIED.);
#5129=B_SPLINE_CURVE_WITH_KNOTS('',3,(#172437,#172438,#172439,#172440),
 .UNSPECIFIED.,.F.,.F.,(4,4),(0.0206793054465132,0.021179777605653),
 .UNSPECIFIED.);
#5130=B_SPLINE_CURVE_WITH_KNOTS('',3,(#172490,#172491,#172492,#172493,#172494,
#172495,#172496,#172497,#172498,#172499,#172500,#172501,#172502,#172503,
#172504,#172505,#172506,#172507,#172508,#172509,#172510,#172511,#172512,
#172513,#172514,#172515,#172516,#172517,#172518,#172519,#172520,#172521,
#172522,#172523,#172524,#172525,#172526),.UNSPECIFIED.,.F.,.F.,(4,3,3,3,
3,3,3,3,3,3,3,3,4),(0.000467059137334316,0.000632797502959653,0.00086096130564352,
0.000897131574002738,0.00113001259983567,0.00126720169019539,0.00163753656891931,
0.00179296606233701,0.00200786773946722,0.00237820352986643,0.00245591952483837,
0.0030162112996301,0.00311887298733972),.UNSPECIFIED.);
#5131=B_SPLINE_CURVE_WITH_KNOTS('',3,(#172560,#172561,#172562,#172563),
 .UNSPECIFIED.,.F.,.F.,(4,4),(0.,0.0420570108120997),.UNSPECIFIED.);
#5132=B_SPLINE_CURVE_WITH_KNOTS('',3,(#172584,#172585,#172586,#172587,#172588,
#172589,#172590,#172591,#172592,#172593,#172594,#172595,#172596),
 .UNSPECIFIED.,.F.,.F.,(4,3,3,3,4),(0.,0.000795137544078952,0.00122134837748785,
0.00219865189862556,0.00244269675497567),.UNSPECIFIED.);
#5133=B_SPLINE_CURVE_WITH_KNOTS('',3,(#172621,#172622,#172623,#172624,#172625,
#172626,#172627,#172628,#172629,#172630,#172631,#172632,#172633),
 .UNSPECIFIED.,.F.,.F.,(4,3,3,3,4),(0.,0.000894380560743248,0.00122171954771057,
0.00222146414309688,0.00244343909542114),.UNSPECIFIED.);
#5134=B_SPLINE_CURVE_WITH_KNOTS('',3,(#172636,#172637,#172638,#172639,#172640,
#172641,#172642,#172643,#172644,#172645,#172646,#172647,#172648,#172649,
#172650,#172651,#172652,#172653,#172654,#172655,#172656,#172657,#172658,
#172659,#172660,#172661,#172662,#172663,#172664,#172665,#172666,#172667,
#172668,#172669,#172670,#172671,#172672,#172673,#172674,#172675,#172676,
#172677,#172678,#172679,#172680,#172681,#172682,#172683,#172684,#172685,
#172686,#172687,#172688,#172689,#172690,#172691,#172692,#172693,#172694,
#172695,#172696,#172697,#172698,#172699),.UNSPECIFIED.,.F.,.F.,(4,3,3,3,
3,3,3,3,3,3,3,3,3,3,3,3,3,3,3,3,3,4),(0.,0.117678986907631,0.212770958931128,
0.274508663183841,0.376875434432681,0.475298330914508,0.49804687500162,
0.500000000001621,0.500228117075086,0.54311799305188,0.585976806827622,
0.62500000000116,0.667538069824397,0.709029432927037,0.73437500000076,0.742187500000732,
0.746093750000722,0.750000000000712,0.814123113213129,0.87948779349594,
0.946280975523161,0.999984983959274),.UNSPECIFIED.);
#5135=B_SPLINE_CURVE_WITH_KNOTS('',3,(#172713,#172714,#172715,#172716),
 .UNSPECIFIED.,.F.,.F.,(4,4),(0.,0.0417901757617078),.UNSPECIFIED.);
#5136=B_SPLINE_CURVE_WITH_KNOTS('',3,(#172719,#172720,#172721,#172722,#172723,
#172724,#172725,#172726,#172727,#172728,#172729,#172730,#172731,#172732,
#172733,#172734),.UNSPECIFIED.,.F.,.F.,(4,2,2,1,1,1,1,2,2,4),(0.,0.249999999999767,
0.374999999999651,0.437499999999593,0.468749999999564,0.484374999999549,
0.492187499999542,0.499511718749537,0.499999999999538,1.),.UNSPECIFIED.);
#5137=B_SPLINE_CURVE_WITH_KNOTS('',3,(#172760,#172761,#172762,#172763,#172764,
#172765,#172766,#172767,#172768,#172769,#172770,#172771,#172772,#172773,
#172774,#172775,#172776,#172777,#172778,#172779,#172780,#172781,#172782,
#172783,#172784),.UNSPECIFIED.,.F.,.F.,(4,3,3,3,3,3,3,3,4),(0.,0.234918010763658,
0.268228507342618,0.382645199292437,0.503001406327853,0.555176579325945,
0.757548181588527,0.935344993134881,0.999999537405455),.UNSPECIFIED.);
#5138=B_SPLINE_CURVE_WITH_KNOTS('',3,(#172785,#172786,#172787,#172788,#172789,
#172790,#172791,#172792,#172793,#172794,#172795,#172796,#172797,#172798,
#172799,#172800,#172801,#172802,#172803,#172804,#172805,#172806,#172807,
#172808,#172809,#172810,#172811,#172812,#172813,#172814,#172815,#172816,
#172817,#172818,#172819,#172820,#172821,#172822,#172823,#172824,#172825,
#172826,#172827,#172828,#172829,#172830,#172831,#172832,#172833,#172834,
#172835,#172836,#172837,#172838,#172839,#172840,#172841,#172842,#172843,
#172844,#172845,#172846,#172847,#172848,#172849,#172850,#172851,#172852,
#172853,#172854,#172855,#172856,#172857,#172858,#172859,#172860,#172861,
#172862,#172863),.UNSPECIFIED.,.F.,.F.,(4,3,3,3,3,3,3,3,3,3,3,3,3,3,3,3,
3,3,3,3,3,3,3,3,3,3,4),(8.70442931586916E-9,0.0902335702297538,0.125000000001714,
0.187500000002585,0.21875000000302,0.234375000003238,0.242187500003347,
0.246093750003401,0.248046875003428,0.250000000003456,0.285027994706698,
0.320202466330442,0.355598103085239,0.388926552204718,0.425197759906794,
0.462045466695683,0.498046875001628,0.500000000001617,0.500299813510911,
0.568943255332965,0.625000000001213,0.700077040250471,0.750000000000809,
0.827937432249017,0.9081222359888,0.991289142222388,1.),.UNSPECIFIED.);
#5139=B_SPLINE_CURVE_WITH_KNOTS('',3,(#172886,#172887,#172888,#172889,#172890,
#172891,#172892,#172893,#172894,#172895,#172896,#172897,#172898,#172899,
#172900,#172901),.UNSPECIFIED.,.F.,.F.,(4,3,3,3,3,4),(0.,0.000540889688193889,
0.00109121002634669,0.00153442409609832,0.00256481294069276,0.00306884819219665),
 .UNSPECIFIED.);
#5140=B_SPLINE_CURVE_WITH_KNOTS('',3,(#172925,#172926,#172927,#172928,#172929,
#172930,#172931,#172932,#172933,#172934,#172935,#172936,#172937),
 .UNSPECIFIED.,.F.,.F.,(4,3,3,3,4),(2.8609792490764E-17,0.000811916222429989,
0.00153648298481487,0.00264039900673923,0.0030729659696297),
 .UNSPECIFIED.);
#5141=B_SPLINE_CURVE_WITH_KNOTS('',3,(#172958,#172959,#172960,#172961,#172962,
#172963,#172964),.UNSPECIFIED.,.F.,.F.,(4,3,4),(0.,0.018990790064314,0.0379815801286281),
 .UNSPECIFIED.);
#5142=B_SPLINE_CURVE_WITH_KNOTS('',3,(#173011,#173012,#173013,#173014,#173015,
#173016,#173017,#173018,#173019,#173020,#173021,#173022,#173023,#173024,
#173025,#173026,#173027,#173028,#173029,#173030,#173031,#173032,#173033,
#173034,#173035,#173036,#173037,#173038,#173039,#173040,#173041,#173042,
#173043,#173044,#173045,#173046,#173047,#173048,#173049,#173050,#173051,
#173052,#173053),.UNSPECIFIED.,.F.,.F.,(4,3,3,3,3,3,3,3,3,3,3,3,3,3,4),
(0.,0.152946157858152,0.249999999999975,0.374999999999963,0.437499999999957,
0.468749999999955,0.484374999999953,0.492187499999951,0.499023437499951,
0.499999999999952,0.500017274533875,0.625012955900406,0.75266030275651,
0.885972940012859,1.),.UNSPECIFIED.);
#5143=B_SPLINE_CURVE_WITH_KNOTS('',3,(#173056,#173057,#173058,#173059,#173060,
#173061,#173062),.UNSPECIFIED.,.F.,.F.,(4,3,4),(0.,0.0188568492058762,0.0377136984117524),
 .UNSPECIFIED.);
#5144=B_SPLINE_CURVE_WITH_KNOTS('',3,(#173128,#173129,#173130,#173131,#173132,
#173133,#173134),.UNSPECIFIED.,.F.,.F.,(4,3,4),(0.,0.0178323395635859,0.0356646791271718),
 .UNSPECIFIED.);
#5145=B_SPLINE_CURVE_WITH_KNOTS('',3,(#173155,#173156,#173157,#173158,#173159,
#173160,#173161,#173162),.UNSPECIFIED.,.F.,.F.,(4,2,2,4),(0.,0.000848531500815463,
0.00169706300163092,0.00339412600326177),.UNSPECIFIED.);
#5146=B_SPLINE_CURVE_WITH_KNOTS('',3,(#173189,#173190,#173191,#173192,#173193,
#173194,#173195,#173196,#173197,#173198,#173199,#173200,#173201,#173202,
#173203,#173204,#173205,#173206,#173207,#173208,#173209,#173210,#173211,
#173212,#173213,#173214,#173215,#173216,#173217,#173218,#173219,#173220,
#173221,#173222,#173223,#173224,#173225,#173226,#173227,#173228,#173229,
#173230,#173231,#173232,#173233,#173234,#173235,#173236,#173237,#173238,
#173239,#173240,#173241,#173242,#173243,#173244,#173245,#173246,#173247,
#173248,#173249,#173250,#173251,#173252,#173253,#173254,#173255,#173256,
#173257,#173258,#173259,#173260,#173261,#173262,#173263,#173264,#173265,
#173266,#173267,#173268,#173269,#173270,#173271,#173272,#173273,#173274,
#173275,#173276,#173277,#173278,#173279,#173280,#173281,#173282,#173283,
#173284,#173285),.UNSPECIFIED.,.F.,.F.,(4,3,3,3,3,3,3,3,3,3,3,3,3,3,3,3,
3,3,3,3,3,3,3,3,3,3,3,3,3,3,3,3,4),(0.,0.0932635068722853,0.173120445513539,
0.212027264824284,0.246070731721185,0.246374889451879,0.248234265315532,
0.24923556874209,0.249694825443765,0.249937243565367,0.250147139192889,
0.308730107077419,0.365357971714009,0.424866485856754,0.484374999999498,
0.49535871603758,0.499770916189278,0.499999999999506,0.547691012729422,
0.596740786897328,0.624999999999556,0.674962700199832,0.687499999999575,
0.718749999999584,0.734374999999581,0.742187499999577,0.746093749999584,
0.748046874999589,0.749999999999594,0.824471881370616,0.901151261803454,
0.980838602588325,0.999982733045328),.UNSPECIFIED.);
#5147=B_SPLINE_CURVE_WITH_KNOTS('',3,(#173286,#173287,#173288,#173289,#173290,
#173291,#173292,#173293,#173294,#173295,#173296,#173297,#173298,#173299,
#173300,#173301),.UNSPECIFIED.,.F.,.F.,(4,3,3,3,3,4),(0.,0.000761157739917319,
0.00156083390161805,0.00170051723463269,0.00285526923554342,0.00340103446926538),
 .UNSPECIFIED.);
#5148=B_SPLINE_CURVE_WITH_KNOTS('',3,(#173323,#173324,#173325,#173326,#173327,
#173328,#173329,#173330,#173331,#173332,#173333,#173334,#173335,#173336,
#173337,#173338,#173339,#173340,#173341,#173342,#173343,#173344,#173345,
#173346,#173347,#173348,#173349,#173350,#173351,#173352,#173353),
 .UNSPECIFIED.,.F.,.F.,(4,3,3,3,3,3,3,3,3,3,4),(0.,0.131009823433625,0.258234932379081,
0.38109330009218,0.499023437500229,0.499974366980884,0.500000000000229,
0.659817335393859,0.815466379844275,0.966024828559954,1.),.UNSPECIFIED.);
#5149=B_SPLINE_CURVE_WITH_KNOTS('',3,(#173354,#173355,#173356,#173357,#173358,
#173359,#173360),.UNSPECIFIED.,.F.,.F.,(4,3,4),(0.,0.0176980703187956,0.0353961406375911),
 .UNSPECIFIED.);
#5150=B_SPLINE_CURVE_WITH_KNOTS('',3,(#173380,#173381,#173382,#173383,#173384,
#173385,#173386,#173387,#173388,#173389,#173390,#173391,#173392,#173393,
#173394,#173395),.UNSPECIFIED.,.F.,.F.,(4,3,3,3,3,4),(0.,0.192339441584989,
0.407181235959237,0.610051883739392,0.855180865457149,0.999999198430051),
 .UNSPECIFIED.);
#5151=B_SPLINE_CURVE_WITH_KNOTS('',3,(#173396,#173397,#173398,#173399,#173400,
#173401,#173402,#173403,#173404,#173405,#173406,#173407,#173408,#173409,
#173410,#173411,#173412,#173413,#173414,#173415,#173416,#173417,#173418,
#173419,#173420,#173421,#173422,#173423,#173424,#173425,#173426,#173427,
#173428,#173429,#173430,#173431,#173432,#173433,#173434,#173435,#173436,
#173437,#173438,#173439,#173440,#173441,#173442,#173443,#173444,#173445,
#173446,#173447,#173448,#173449,#173450,#173451,#173452,#173453,#173454,
#173455,#173456,#173457,#173458,#173459,#173460,#173461,#173462,#173463,
#173464,#173465,#173466,#173467,#173468,#173469,#173470,#173471,#173472,
#173473,#173474,#173475,#173476,#173477,#173478,#173479,#173480,#173481,
#173482,#173483,#173484,#173485,#173486,#173487,#173488,#173489,#173490,
#173491,#173492,#173493,#173494,#173495,#173496,#173497,#173498,#173499,
#173500,#173501),.UNSPECIFIED.,.F.,.F.,(4,3,3,3,3,3,3,3,3,3,3,3,3,3,3,3,
3,3,3,3,3,3,3,3,3,3,3,3,3,3,3,3,3,3,3,4),(0.,0.0751687560234797,0.124999999999828,
0.187499999999744,0.218749999999701,0.23437499999968,0.24218749999967,0.246093749999667,
0.249999999999665,0.306700379523328,0.362571924844633,0.417147083320517,
0.437500000000012,0.468750000000065,0.484375000000091,0.492187500000101,
0.496093750000106,0.498046875000108,0.500000000000111,0.532145122746275,
0.564912906759694,0.598491128155236,0.632424031668225,0.666766974875665,
0.68750000000056,0.718750000000641,0.734375000000671,0.742187500000699,
0.746093750000697,0.748046875000696,0.749023437500695,0.750000000000694,
0.817229294988516,0.885907714625437,0.956984553878538,1.),.UNSPECIFIED.);
#5152=B_SPLINE_CURVE_WITH_KNOTS('',3,(#173534,#173535,#173536,#173537,#173538,
#173539,#173540),.UNSPECIFIED.,.F.,.F.,(4,3,4),(0.,0.014563917689728,0.029127835379456),
 .UNSPECIFIED.);
#5153=B_SPLINE_CURVE_WITH_KNOTS('',3,(#173542,#173543,#173544,#173545,#173546,
#173547,#173548,#173549,#173550,#173551,#173552,#173553,#173554,#173555,
#173556,#173557,#173558,#173559,#173560,#173561,#173562,#173563,#173564,
#173565,#173566,#173567,#173568,#173569,#173570,#173571,#173572,#173573,
#173574,#173575,#173576,#173577,#173578,#173579,#173580,#173581),
 .UNSPECIFIED.,.F.,.F.,(4,3,3,3,3,3,3,3,3,3,3,3,3,4),(0.,0.153641825342759,
0.249999999999996,0.374999999999994,0.437499999999993,0.468749999999993,
0.484374999999993,0.49902343749999,0.499999999999989,0.500006129759065,
0.629863266340263,0.762254527670502,0.899175022789813,1.),.UNSPECIFIED.);
#5154=B_SPLINE_CURVE_WITH_KNOTS('',3,(#173601,#173602,#173603,#173604,#173605,
#173606,#173607,#173608,#173609,#173610,#173611,#173612,#173613,#173614,
#173615,#173616,#173617,#173618,#173619,#173620,#173621,#173622,#173623,
#173624,#173625),.UNSPECIFIED.,.F.,.F.,(4,3,3,3,3,3,3,3,4),(0.,0.000422069097417445,
0.000847931637827783,0.00104448509574678,0.00149181651230484,0.00193535496126402,
0.00208897019149356,0.00315378543072143,0.00417794038298713),
 .UNSPECIFIED.);
#5155=B_SPLINE_CURVE_WITH_KNOTS('',3,(#173650,#173651,#173652,#173653,#173654,
#173655,#173656,#173657,#173658,#173659,#173660,#173661,#173662,#173663,
#173664,#173665,#173666,#173667,#173668,#173669,#173670,#173671),
 .UNSPECIFIED.,.F.,.F.,(4,3,3,3,3,3,3,4),(0.,0.000384591749545137,0.00078374926263879,
0.00104647183020208,0.00173887398626118,0.00209294366040415,0.00337921840668196,
0.00418588732080839),.UNSPECIFIED.);
#5156=B_SPLINE_CURVE_WITH_KNOTS('',3,(#173692,#173693,#173694,#173695,#173696,
#173697,#173698),.UNSPECIFIED.,.F.,.F.,(4,3,4),(0.,0.0146992078328598,0.0293984156657196),
 .UNSPECIFIED.);
#5157=B_SPLINE_CURVE_WITH_KNOTS('',3,(#173764,#173765,#173766,#173767,#173768,
#173769,#173770,#173771,#173772,#173773,#173774,#173775,#173776,#173777),
 .UNSPECIFIED.,.F.,.F.,(4,2,1,1,1,1,2,2,4),(0.,0.249999999999965,0.374999999999947,
0.437499999999939,0.468749999999935,0.484374999999932,0.49902343749993,
0.49999999999993,1.),.UNSPECIFIED.);
#5158=B_SPLINE_CURVE_WITH_KNOTS('',3,(#173800,#173801,#173802,#173803),
 .UNSPECIFIED.,.F.,.F.,(4,4),(3.46944695195361E-18,0.0333425790106738),
 .UNSPECIFIED.);
#5159=B_SPLINE_CURVE_WITH_KNOTS('',3,(#173806,#173807,#173808,#173809,#173810,
#173811,#173812,#173813,#173814,#173815,#173816,#173817,#173818,#173819),
 .UNSPECIFIED.,.F.,.F.,(4,2,1,1,1,1,2,2,4),(0.,0.250000000000072,0.375000000000108,
0.437500000000126,0.468750000000135,0.484375000000139,0.499023437500143,
0.500000000000143,1.),.UNSPECIFIED.);
#5160=B_SPLINE_CURVE_WITH_KNOTS('',3,(#173839,#173840,#173841,#173842),
 .UNSPECIFIED.,.F.,.F.,(4,4),(0.,9.64176041888327E-5),.UNSPECIFIED.);
#5161=B_SPLINE_CURVE_WITH_KNOTS('',3,(#173858,#173859,#173860,#173861,#173862,
#173863,#173864,#173865,#173866,#173867,#173868,#173869,#173870,#173871,
#173872,#173873,#173874,#173875,#173876),.UNSPECIFIED.,.F.,.F.,(4,3,3,3,
3,3,4),(0.,0.190207366592191,0.372524918669027,0.545027215306253,0.713431358990858,
0.875775939334647,1.),.UNSPECIFIED.);
#5162=B_SPLINE_CURVE_WITH_KNOTS('',3,(#173877,#173878,#173879,#173880),
 .UNSPECIFIED.,.F.,.F.,(4,4),(0.,0.0333345873458536),.UNSPECIFIED.);
#5163=B_SPLINE_CURVE_WITH_KNOTS('',3,(#173897,#173898,#173899,#173900),
 .UNSPECIFIED.,.F.,.F.,(4,4),(0.,0.0278605201857756),.UNSPECIFIED.);
#5164=B_SPLINE_CURVE_WITH_KNOTS('',3,(#173903,#173904,#173905,#173906,#173907,
#173908,#173909,#173910,#173911,#173912,#173913,#173914,#173915,#173916,
#173917,#173918,#173919,#173920,#173921),.UNSPECIFIED.,.F.,.F.,(4,3,3,3,
3,3,4),(0.,0.161013821218371,0.325610113125001,0.496657244829195,0.671778199953257,
0.854525113432085,1.),.UNSPECIFIED.);
#5165=B_SPLINE_CURVE_WITH_KNOTS('',3,(#173941,#173942,#173943,#173944,#173945,
#173946,#173947,#173948),.UNSPECIFIED.,.F.,.F.,(4,2,2,4),(0.,0.000890496769046365,
0.00178099353809273,0.0035619870761855),.UNSPECIFIED.);
#5166=B_SPLINE_CURVE_WITH_KNOTS('',3,(#173951,#173952,#173953,#173954,#173955,
#173956,#173957,#173958,#173959,#173960,#173961,#173962,#173963,#173964,
#173965,#173966,#173967,#173968,#173969,#173970,#173971,#173972,#173973,
#173974,#173975,#173976,#173977,#173978,#173979,#173980,#173981,#173982,
#173983,#173984,#173985,#173986,#173987,#173988,#173989,#173990,#173991,
#173992,#173993,#173994,#173995,#173996,#173997,#173998,#173999,#174000,
#174001,#174002,#174003,#174004,#174005,#174006,#174007,#174008,#174009,
#174010,#174011,#174012,#174013,#174014,#174015,#174016,#174017,#174018,
#174019,#174020,#174021,#174022,#174023,#174024,#174025,#174026,#174027,
#174028,#174029,#174030,#174031,#174032,#174033,#174034,#174035,#174036,
#174037,#174038,#174039,#174040,#174041,#174042,#174043,#174044,#174045,
#174046,#174047,#174048,#174049,#174050,#174051,#174052,#174053),
 .UNSPECIFIED.,.F.,.F.,(4,3,3,3,3,3,3,3,3,3,3,3,3,3,3,3,3,3,3,3,3,3,3,3,
3,3,3,3,3,3,3,3,3,3,4),(1.57528194328481E-8,0.113390184051606,0.125000000000386,
0.208213799444507,0.242733949514119,0.244621770221051,0.24555830627488,
0.246025309240556,0.246288313900857,0.248148366136017,0.249993886713091,
0.250183242419508,0.305303406015141,0.358943150387979,0.415198367832281,
0.470499806007569,0.484375000001403,0.496707221246892,0.500000000001438,
0.500644507573531,0.545230766738762,0.591400861254902,0.625000000001714,
0.672876488128917,0.687500000001858,0.71875000000193,0.734375000001958,
0.742187500001965,0.746093750001959,0.748046875001948,0.750000000001936,
0.823877912198341,0.899739373902168,0.97859232774702,1.),.UNSPECIFIED.);
#5167=B_SPLINE_CURVE_WITH_KNOTS('',3,(#174109,#174110,#174111,#174112,#174113,
#174114,#174115,#174116,#174117,#174118,#174119,#174120,#174121,#174122,
#174123,#174124),.UNSPECIFIED.,.F.,.F.,(4,3,3,3,3,4),(0.,0.000625284942165368,
0.0012890528199733,0.00194949793575932,0.00318811191752231,0.00389899587151865),
 .UNSPECIFIED.);
#5168=B_SPLINE_CURVE_WITH_KNOTS('',3,(#174140,#174141,#174142,#174143,#174144,
#174145,#174146,#174147,#174148,#174149,#174150,#174151,#174152,#174153,
#174154,#174155,#174156,#174157,#174158),.UNSPECIFIED.,.F.,.F.,(4,3,3,3,
3,3,4),(0.,0.19217742618272,0.378585784323496,0.557722246321134,0.733231503446162,
0.903822311654046,1.),.UNSPECIFIED.);
#5169=B_SPLINE_CURVE_WITH_KNOTS('',3,(#174159,#174160,#174161,#174162),
 .UNSPECIFIED.,.F.,.F.,(4,4),(0.,0.024690830875569),.UNSPECIFIED.);
#5170=B_SPLINE_CURVE_WITH_KNOTS('',3,(#174190,#174191,#174192,#174193,#174194,
#174195,#174196,#174197,#174198,#174199,#174200,#174201,#174202,#174203,
#174204,#174205,#174206,#174207,#174208),.UNSPECIFIED.,.F.,.F.,(4,3,3,3,
3,3,4),(0.,0.000151109125705162,0.000302236517833045,0.000386300967573271,
0.000471902393705294,0.00055523437621895,0.000604473035666092),
 .UNSPECIFIED.);
#5171=B_SPLINE_CURVE_WITH_KNOTS('',3,(#174209,#174210,#174211,#174212,#174213,
#174214,#174215,#174216,#174217,#174218,#174219,#174220,#174221,#174222,
#174223,#174224,#174225,#174226,#174227,#174228,#174229,#174230,#174231,
#174232,#174233,#174234,#174235,#174236,#174237,#174238,#174239,#174240,
#174241,#174242,#174243,#174244,#174245,#174246,#174247,#174248,#174249,
#174250,#174251,#174252,#174253,#174254,#174255,#174256,#174257,#174258,
#174259,#174260,#174261,#174262,#174263),.UNSPECIFIED.,.F.,.F.,(4,3,3,3,
3,3,3,3,3,3,3,3,3,3,3,3,3,3,4),(0.,0.0579960117174044,0.118910654037608,
0.125000000000006,0.215056456326176,0.247031472716539,0.282964889031184,
0.361398792416325,0.433567066284115,0.476592509119368,0.485225825304686,
0.492187500000023,0.49881285509328,0.500000000000011,0.586335878991574,
0.6759254922935,0.728649541045074,0.876166749959378,1.),.UNSPECIFIED.);
#5172=B_SPLINE_CURVE_WITH_KNOTS('',3,(#174315,#174316,#174317,#174318),
 .UNSPECIFIED.,.F.,.F.,(4,4),(0.,0.0240963563036403),.UNSPECIFIED.);
#5173=B_SPLINE_CURVE_WITH_KNOTS('',3,(#174320,#174321,#174322,#174323,#174324,
#174325,#174326,#174327,#174328,#174329,#174330,#174331,#174332,#174333,
#174334,#174335,#174336,#174337,#174338),.UNSPECIFIED.,.F.,.F.,(4,3,3,3,
3,3,4),(0.,0.172866351701051,0.349384406750267,0.532176733764,0.719026799190666,
0.912787151767933,1.),.UNSPECIFIED.);
#5174=B_SPLINE_CURVE_WITH_KNOTS('',3,(#174358,#174359,#174360,#174361,#174362,
#174363,#174364,#174365,#174366,#174367,#174368,#174369,#174370,#174371,
#174372,#174373,#174374,#174375,#174376,#174377,#174378,#174379,#174380,
#174381,#174382),.UNSPECIFIED.,.F.,.F.,(4,3,3,3,3,3,3,3,4),(0.,0.000403252952291858,
0.000810273659957097,0.000991778862067342,0.00143365237214696,0.00187173698199696,
0.00198355772413468,0.00304641612723371,0.00396711544826929),
 .UNSPECIFIED.);
#5175=B_SPLINE_CURVE_WITH_KNOTS('',3,(#174407,#174408,#174409,#174410,#174411,
#174412,#174413,#174414,#174415,#174416,#174417,#174418,#174419,#174420,
#174421,#174422,#174423,#174424,#174425),.UNSPECIFIED.,.F.,.F.,(4,3,3,3,
3,3,4),(0.,0.000606703134123652,0.00123626357061655,0.00189155006086063,
0.00198795077588647,0.0032403373659691,0.00397590155177294),
 .UNSPECIFIED.);
#5176=B_SPLINE_CURVE_WITH_KNOTS('',3,(#174428,#174429,#174430,#174431,#174432,
#174433,#174434,#174435,#174436,#174437,#174438,#174439,#174440,#174441,
#174442,#174443,#174444,#174445,#174446,#174447,#174448,#174449,#174450,
#174451,#174452,#174453,#174454,#174455,#174456,#174457,#174458,#174459,
#174460,#174461,#174462,#174463,#174464,#174465,#174466),.UNSPECIFIED.,
 .F.,.F.,(4,2,2,1,1,1,1,2,2,2,2,2,1,1,2,2,2,2,1,1,1,2,2,4),(0.,0.124999999999855,
0.187499999999778,0.218749999999739,0.23437499999972,0.242187499999711,
0.246093749999706,0.248046874999704,0.249999999999701,0.374999999999798,
0.437499999999845,0.468749999999869,0.484374999999881,0.492187499999884,
0.496093749999882,0.499999999999881,0.624999999999869,0.687499999999859,
0.718749999999854,0.734374999999848,0.742187499999838,0.74609374999984,
0.749999999999841,0.999999987824138),.UNSPECIFIED.);
#5177=B_SPLINE_CURVE_WITH_KNOTS('',3,(#174480,#174481,#174482,#174483),
 .UNSPECIFIED.,.F.,.F.,(4,4),(0.,0.0238258198664154),.UNSPECIFIED.);
#5178=B_SPLINE_CURVE_WITH_KNOTS('',3,(#174486,#174487,#174488,#174489,#174490,
#174491,#174492,#174493,#174494,#174495,#174496,#174497,#174498,#174499,
#174500,#174501,#174502,#174503,#174504),.UNSPECIFIED.,.F.,.F.,(4,3,3,3,
3,3,4),(0.,0.196095667009585,0.386442595766244,0.569588535581485,0.749087760231935,
0.923761630375088,1.),.UNSPECIFIED.);
#5179=B_SPLINE_CURVE_WITH_KNOTS('',3,(#174524,#174525,#174526,#174527,#174528,
#174529,#174530,#174531,#174532,#174533,#174534,#174535,#174536,#174537,
#174538,#174539,#174540,#174541,#174542),.UNSPECIFIED.,.F.,.F.,(4,3,3,3,
3,3,4),(6.48727906844412E-7,0.345786654980507,0.395757238724258,0.59010138294459,
0.774910284816947,0.948267161783481,1.),.UNSPECIFIED.);
#5180=B_SPLINE_CURVE_WITH_KNOTS('',3,(#174543,#174544,#174545,#174546,#174547,
#174548,#174549,#174550,#174551,#174552,#174553,#174554,#174555,#174556,
#174557,#174558,#174559,#174560,#174561,#174562,#174563,#174564,#174565,
#174566,#174567,#174568,#174569,#174570,#174571,#174572,#174573,#174574,
#174575,#174576,#174577,#174578),.UNSPECIFIED.,.F.,.F.,(4,2,2,1,1,1,1,2,
2,2,2,1,2,2,2,2,2,2,1,2,4),(1.49874026637454E-5,0.124999999999844,0.187499999999766,
0.218749999999723,0.234374999999695,0.242187499999681,0.246093749999674,
0.248046874999672,0.249999999999669,0.374999999999717,0.437499999999741,
0.468749999999749,0.484374999999748,0.499999999999747,0.749999999999862,
0.812499999999884,0.828124999999901,0.83593749999991,0.843749999999918,
0.87499999999993,1.),.UNSPECIFIED.);
#5181=B_SPLINE_CURVE_WITH_KNOTS('',3,(#174611,#174612,#174613,#174614,#174615,
#174616,#174617,#174618,#174619,#174620,#174621,#174622,#174623,#174624,
#174625,#174626),.UNSPECIFIED.,.F.,.F.,(4,3,3,3,3,4),(0.,0.000531847314912768,
0.0010759631561301,0.00162007899734744,0.00266000146296125,0.00324015799469487),
 .UNSPECIFIED.);
#5182=B_SPLINE_CURVE_WITH_KNOTS('',3,(#174651,#174652,#174653,#174654,#174655,
#174656,#174657,#174658,#174659,#174660,#174661,#174662,#174663),
 .UNSPECIFIED.,.F.,.F.,(4,3,3,3,4),(0.,0.000817558298551379,0.00162295210526764,
0.00275577655351122,0.00324590421053527),.UNSPECIFIED.);
#5183=B_SPLINE_CURVE_WITH_KNOTS('',3,(#174679,#174680,#174681,#174682,#174683,
#174684,#174685,#174686,#174687,#174688,#174689,#174690,#174691,#174692,
#174693,#174694,#174695,#174696,#174697),.UNSPECIFIED.,.F.,.F.,(4,3,3,3,
3,3,4),(0.,0.185664878352089,0.364657978690721,0.534856302418504,0.701562136952496,
0.862722007449341,1.),.UNSPECIFIED.);
#5184=B_SPLINE_CURVE_WITH_KNOTS('',3,(#174698,#174699,#174700,#174701),
 .UNSPECIFIED.,.F.,.F.,(4,4),(0.,0.0300693678107436),.UNSPECIFIED.);
#5185=B_SPLINE_CURVE_WITH_KNOTS('',3,(#174715,#174716,#174717,#174718,#174719,
#174720,#174721,#174722,#174723,#174724,#174725,#174726,#174727,#174728,
#174729,#174730,#174731,#174732,#174733),.UNSPECIFIED.,.F.,.F.,(4,3,3,3,
3,3,4),(0.,0.161837694415199,0.327487306305213,0.499540509367366,0.675600434337124,
0.860932038423597,1.),.UNSPECIFIED.);
#5186=B_SPLINE_CURVE_WITH_KNOTS('',3,(#174736,#174737,#174738,#174739),
 .UNSPECIFIED.,.F.,.F.,(4,4),(0.,0.0298008594779328),.UNSPECIFIED.);
#5187=B_SPLINE_CURVE_WITH_KNOTS('',3,(#174780,#174781,#174782,#174783),
 .UNSPECIFIED.,.F.,.F.,(4,4),(0.,0.0322629186945109),.UNSPECIFIED.);
#5188=B_SPLINE_CURVE_WITH_KNOTS('',3,(#174785,#174786,#174787,#174788,#174789,
#174790,#174791,#174792,#174793,#174794,#174795,#174796,#174797,#174798,
#174799,#174800,#174801,#174802,#174803),.UNSPECIFIED.,.F.,.F.,(4,3,3,3,
3,3,4),(0.,0.159102637702074,0.329551318851037,0.5,0.684750559143937,0.882446988411837,
1.),.UNSPECIFIED.);
#5189=B_SPLINE_CURVE_WITH_KNOTS('',3,(#174823,#174824,#174825,#174826,#174827,
#174828,#174829,#174830,#174831,#174832,#174833,#174834,#174835,#174836,
#174837,#174838),.UNSPECIFIED.,.F.,.F.,(4,3,3,3,3,4),(0.,0.000549388570659784,
0.00110809797237947,0.00147175517552831,0.00249356706683659,0.0029435103510566),
 .UNSPECIFIED.);
#5190=B_SPLINE_CURVE_WITH_KNOTS('',3,(#174863,#174864,#174865,#174866,#174867,
#174868,#174869,#174870,#174871,#174872,#174873,#174874,#174875),
 .UNSPECIFIED.,.F.,.F.,(4,3,3,3,4),(0.,0.000882415156986212,0.00147346850157273,
0.00255877694109341,0.00294693700314546),.UNSPECIFIED.);
#5191=B_SPLINE_CURVE_WITH_KNOTS('',3,(#174878,#174879,#174880,#174881,#174882,
#174883,#174884,#174885,#174886,#174887,#174888,#174889,#174890,#174891,
#174892,#174893,#174894,#174895,#174896,#174897,#174898,#174899,#174900,
#174901,#174902,#174903,#174904,#174905,#174906,#174907,#174908,#174909,
#174910,#174911,#174912,#174913,#174914,#174915,#174916,#174917,#174918,
#174919,#174920,#174921,#174922,#174923,#174924,#174925,#174926,#174927,
#174928,#174929,#174930,#174931,#174932,#174933,#174934,#174935,#174936,
#174937,#174938,#174939,#174940,#174941,#174942,#174943,#174944,#174945,
#174946,#174947,#174948,#174949,#174950,#174951,#174952,#174953,#174954,
#174955,#174956,#174957,#174958,#174959,#174960,#174961,#174962,#174963,
#174964,#174965,#174966,#174967,#174968,#174969,#174970,#174971,#174972,
#174973,#174974),.UNSPECIFIED.,.F.,.F.,(4,3,3,3,3,3,3,3,3,3,3,3,3,3,3,3,
3,3,3,3,3,3,3,3,3,3,3,3,3,3,3,3,4),(0.,0.0905528058390064,0.124999999999613,
0.18749999999942,0.218749999999329,0.23437499999929,0.24218749999927,0.24609374999926,
0.24999999999925,0.319163806059011,0.386358508937325,0.437499999998957,
0.468749999998914,0.484374999998893,0.492187499998883,0.496093749998882,
0.498046874998882,0.499999999998882,0.535697174154708,0.571806572205483,
0.608542429153761,0.645244164743076,0.682070032970534,0.718749999998596,
0.734374999998572,0.742187499998564,0.746093749998559,0.748046874998577,
0.749999999998595,0.824061086681612,0.89946952859405,0.976878755501281,
1.),.UNSPECIFIED.);
#5192=B_SPLINE_CURVE_WITH_KNOTS('',3,(#174988,#174989,#174990,#174991),
 .UNSPECIFIED.,.F.,.F.,(4,4),(0.,0.0319950621716304),.UNSPECIFIED.);
#5193=B_SPLINE_CURVE_WITH_KNOTS('',3,(#174994,#174995,#174996,#174997,#174998,
#174999,#175000,#175001,#175002,#175003,#175004,#175005,#175006,#175007,
#175008,#175009,#175010,#175011,#175012),.UNSPECIFIED.,.F.,.F.,(4,3,3,3,
3,3,4),(0.,0.201044054442995,0.388350105070278,0.5,0.666356063422891,0.833178031711445,
1.),.UNSPECIFIED.);
#5194=B_SPLINE_CURVE_WITH_KNOTS('',3,(#175032,#175033,#175034,#175035,#175036,
#175037,#175038,#175039,#175040,#175041,#175042,#175043,#175044,#175045,
#175046,#175047,#175048,#175049,#175050),.UNSPECIFIED.,.F.,.F.,(4,3,3,3,
3,3,4),(2.6071439595974E-7,0.171040742442568,0.354898569694402,0.447899270646099,
0.681237843610931,0.939818966220111,1.),.UNSPECIFIED.);
#5195=B_SPLINE_CURVE_WITH_KNOTS('',3,(#175051,#175052,#175053,#175054,#175055,
#175056,#175057,#175058,#175059,#175060,#175061,#175062,#175063,#175064,
#175065,#175066,#175067,#175068,#175069,#175070,#175071,#175072,#175073,
#175074,#175075,#175076,#175077,#175078,#175079,#175080,#175081,#175082,
#175083,#175084,#175085,#175086,#175087,#175088,#175089,#175090,#175091,
#175092,#175093,#175094,#175095,#175096,#175097,#175098,#175099,#175100,
#175101,#175102,#175103,#175104,#175105,#175106,#175107,#175108,#175109,
#175110,#175111,#175112,#175113,#175114,#175115,#175116,#175117,#175118,
#175119,#175120,#175121,#175122,#175123,#175124,#175125,#175126,#175127,
#175128,#175129,#175130,#175131,#175132),.UNSPECIFIED.,.F.,.F.,(4,3,3,3,
3,3,3,3,3,3,3,3,3,3,3,3,3,3,3,3,3,3,3,3,3,3,3,4),(0.,0.0718965045218442,
0.124999999999785,0.187499999999686,0.218749999999637,0.234374999999614,
0.242187499999603,0.246093749999598,0.248046874999596,0.249999999999595,
0.284793264427814,0.319965488512714,0.355518433439908,0.391200908602362,
0.426991239961754,0.437499999999188,0.468749999999136,0.484374999999107,
0.492187499999093,0.496093749999086,0.49804687499909,0.499999999999095,
0.59050135792091,0.682969730017932,0.778626353234705,0.87622436996633,0.976719140644226,
1.),.UNSPECIFIED.);
#5196=B_SPLINE_CURVE_WITH_KNOTS('',3,(#175155,#175156,#175157,#175158,#175159,
#175160,#175161,#175162,#175163,#175164,#175165,#175166,#175167),
 .UNSPECIFIED.,.F.,.F.,(4,3,3,3,4),(0.,0.000962747670504001,0.00119082241359643,
0.00216097007606112,0.00238164482719285),.UNSPECIFIED.);
#5197=B_SPLINE_CURVE_WITH_KNOTS('',3,(#175192,#175193,#175194,#175195,#175196,
#175197,#175198,#175199,#175200,#175201,#175202,#175203,#175204),
 .UNSPECIFIED.,.F.,.F.,(4,3,3,3,4),(0.,0.000775847435696327,0.00119114916434495,
0.00218083968933889,0.00238229832868991),.UNSPECIFIED.);
#5198=B_SPLINE_CURVE_WITH_KNOTS('',3,(#175220,#175221,#175222,#175223,#175224,
#175225,#175226,#175227,#175228,#175229,#175230,#175231,#175232,#175233,
#175234,#175235),.UNSPECIFIED.,.F.,.F.,(4,2,2,1,1,1,1,2,2,4),(0.,0.250000000000137,
0.375000000000206,0.43750000000024,0.468750000000256,0.484375000000264,
0.492187500000269,0.499023437500275,0.500000000000276,1.),.UNSPECIFIED.);
#5199=B_SPLINE_CURVE_WITH_KNOTS('',3,(#175253,#175254,#175255,#175256,#175257,
#175258,#175259,#175260,#175261,#175262,#175263,#175264,#175265,#175266,
#175267),.UNSPECIFIED.,.F.,.F.,(4,2,2,1,1,1,2,2,4),(0.,0.250000000000068,
0.375000000000102,0.437500000000119,0.468750000000127,0.484375000000131,
0.499023437500133,0.500000000000132,1.),.UNSPECIFIED.);
#5200=B_SPLINE_CURVE_WITH_KNOTS('',3,(#175285,#175286,#175287,#175288),
 .UNSPECIFIED.,.F.,.F.,(4,4),(0.0037358385977583,0.00423610566507283),
 .UNSPECIFIED.);
#5201=B_SPLINE_CURVE_WITH_KNOTS('',3,(#175291,#175292,#175293,#175294),
 .UNSPECIFIED.,.F.,.F.,(4,4),(0.020578988719059,0.0210794636037261),
 .UNSPECIFIED.);
#5202=B_SPLINE_CURVE_WITH_KNOTS('',3,(#175322,#175323,#175324,#175325,#175326,
#175327,#175328,#175329,#175330,#175331,#175332,#175333,#175334,#175335),
 .UNSPECIFIED.,.F.,.F.,(4,2,1,1,1,1,2,2,4),(0.,0.249999999999876,0.374999999999813,
0.437499999999783,0.468749999999766,0.484374999999757,0.499023437499747,
0.499999999999747,1.),.UNSPECIFIED.);
#5203=B_SPLINE_CURVE_WITH_KNOTS('',3,(#175355,#175356,#175357,#175358,#175359,
#175360,#175361,#175362,#175363,#175364,#175365,#175366,#175367),
 .UNSPECIFIED.,.F.,.F.,(4,3,3,3,4),(0.,0.00068051013705706,0.00109976462606963,
0.00204716723038797,0.00219952925213926),.UNSPECIFIED.);
#5204=B_SPLINE_CURVE_WITH_KNOTS('',3,(#175392,#175393,#175394,#175395,#175396,
#175397,#175398,#175399,#175400,#175401,#175402,#175403,#175404),
 .UNSPECIFIED.,.F.,.F.,(4,3,3,3,4),(0.,0.000627390790120107,0.00109987581267579,
0.00205656007236013,0.00219975162535158),.UNSPECIFIED.);
#5205=B_SPLINE_CURVE_WITH_KNOTS('',3,(#175407,#175408,#175409,#175410,#175411,
#175412,#175413,#175414,#175415,#175416,#175417,#175418,#175419,#175420,
#175421,#175422,#175423,#175424,#175425,#175426,#175427,#175428,#175429,
#175430,#175431,#175432,#175433,#175434,#175435,#175436,#175437,#175438,
#175439,#175440,#175441,#175442,#175443,#175444,#175445,#175446,#175447,
#175448,#175449,#175450,#175451,#175452,#175453,#175454,#175455,#175456,
#175457,#175458,#175459,#175460,#175461,#175462,#175463,#175464,#175465,
#175466,#175467,#175468,#175469,#175470,#175471,#175472,#175473,#175474,
#175475,#175476),.UNSPECIFIED.,.F.,.F.,(4,3,3,3,3,3,3,3,3,3,3,3,3,3,3,3,
3,3,3,3,3,3,3,4),(0.,0.130518220707149,0.25000000000017,0.375000000000256,
0.437500000000298,0.468750000000328,0.484375000000343,0.492187500000358,
0.496093750000372,0.500000000000385,0.500118514677062,0.555615849833377,
0.610869328165162,0.625000000000319,0.67976455378678,0.687500000000294,
0.718750000000282,0.734375000000276,0.746581455128004,0.75000000000027,
0.812499999925157,0.874854647535847,0.938420259612278,0.99999999969982),
 .UNSPECIFIED.);
#5206=B_SPLINE_CURVE_WITH_KNOTS('',3,(#175496,#175497,#175498,#175499,#175500,
#175501,#175502,#175503,#175504,#175505,#175506,#175507,#175508,#175509,
#175510,#175511,#175512,#175513,#175514,#175515,#175516,#175517,#175518,
#175519,#175520,#175521,#175522,#175523,#175524,#175525,#175526,#175527,
#175528,#175529,#175530,#175531,#175532,#175533,#175534,#175535,#175536,
#175537,#175538,#175539,#175540,#175541,#175542,#175543,#175544,#175545,
#175546,#175547,#175548,#175549,#175550,#175551,#175552,#175553),
 .UNSPECIFIED.,.F.,.F.,(4,3,3,3,3,3,3,3,3,3,3,3,3,3,3,3,3,3,3,4),(0.,0.249999999999903,
0.374999999999853,0.437499999999828,0.468749999999815,0.484374999999808,
0.492431640624811,0.49639701843243,0.498364217579178,0.498854096272949,
0.498972243282005,0.499071824544578,0.499561012215921,0.499805367190425,
0.499913587130118,0.499995666848597,0.500051933987096,0.732986788196755,
0.954689120223703,1.),.UNSPECIFIED.);
#5207=B_SPLINE_CURVE_WITH_KNOTS('',3,(#175573,#175574,#175575,#175576,#175577,
#175578,#175579,#175580,#175581,#175582,#175583,#175584,#175585),
 .UNSPECIFIED.,.F.,.F.,(4,2,1,1,1,2,2,4),(0.,0.250000000000011,0.375000000000015,
0.437500000000018,0.468750000000018,0.484375000000018,0.500000000000018,
1.),.UNSPECIFIED.);
#5208=B_SPLINE_CURVE_WITH_KNOTS('',3,(#175638,#175639,#175640,#175641,#175642,
#175643,#175644,#175645,#175646,#175647,#175648,#175649),.UNSPECIFIED.,
 .F.,.F.,(4,2,3,3,4),(0.,0.00100000000000208,0.00500000000023154,0.02100000001009,
0.0385835581099273),.UNSPECIFIED.);
#5209=B_SPLINE_CURVE_WITH_KNOTS('',3,(#175667,#175668,#175669,#175670,#175671,
#175672,#175673,#175674,#175675,#175676,#175677,#175678),.UNSPECIFIED.,
 .F.,.F.,(4,2,3,3,4),(0.,0.00100000000000032,0.00500000000004302,0.0210000000041071,
0.0383173498474262),.UNSPECIFIED.);
#5210=B_SPLINE_CURVE_WITH_KNOTS('',3,(#175693,#175694,#175695,#175696,#175697,
#175698,#175699,#175700,#175701,#175702,#175703,#175704,#175705,#175706,
#175707,#175708,#175709,#175710,#175711,#175712,#175713,#175714,#175715,
#175716,#175717,#175718,#175719,#175720,#175721,#175722,#175723,#175724,
#175725,#175726,#175727,#175728,#175729,#175730,#175731,#175732,#175733,
#175734,#175735,#175736,#175737,#175738),.UNSPECIFIED.,.F.,.F.,(4,3,3,3,
3,3,3,3,3,3,3,3,3,3,3,4),(0.,0.0830546620592719,0.125000000000492,0.229571060394868,
0.250000000000983,0.348011454012246,0.375000000001503,0.437500000001736,
0.468750000001785,0.484375000001759,0.492187500001746,0.500000000001733,
0.6250000000013,0.771819373948562,0.923348618181731,1.),.UNSPECIFIED.);
#5211=B_SPLINE_CURVE_WITH_KNOTS('',3,(#175740,#175741,#175742,#175743,#175744,
#175745),.UNSPECIFIED.,.F.,.F.,(4,2,4),(0.,0.5,1.),.UNSPECIFIED.);
#5212=B_SPLINE_CURVE_WITH_KNOTS('',3,(#175759,#175760,#175761,#175762,#175763,
#175764,#175765,#175766,#175767,#175768,#175769),.UNSPECIFIED.,.F.,.F.,
(4,2,1,2,2,4),(0.,0.250000000000047,0.375000000000077,0.43750000000009,
0.500000000000103,1.),.UNSPECIFIED.);
#5213=B_SPLINE_CURVE_WITH_KNOTS('',3,(#175791,#175792,#175793,#175794,#175795,
#175796,#175797,#175798,#175799,#175800,#175801,#175802),.UNSPECIFIED.,
 .F.,.F.,(4,2,2,2,2,4),(0.,0.25000000000007,0.375000000000103,0.437500000000076,
0.500000000000049,1.),.UNSPECIFIED.);
#5214=B_SPLINE_CURVE_WITH_KNOTS('',3,(#175886,#175887,#175888,#175889,#175890,
#175891,#175892,#175893,#175894,#175895,#175896,#175897,#175898,#175899,
#175900,#175901,#175902,#175903,#175904,#175905,#175906,#175907,#175908,
#175909,#175910,#175911,#175912,#175913,#175914,#175915,#175916,#175917,
#175918,#175919,#175920,#175921,#175922),.UNSPECIFIED.,.F.,.F.,(4,3,3,3,
3,3,3,3,3,3,3,3,4),(0.00064734234469968,0.000773679728910273,0.000794515777305426,
0.00111794174211916,0.00114512410810862,0.00123603607512266,0.00151649021309282,
0.00182472980554565,0.00188790100005033,0.00225930818373536,0.00241342353596863,
0.00270777040118012,0.00300211726639161),.UNSPECIFIED.);
#5215=B_SPLINE_CURVE_WITH_KNOTS('',3,(#175924,#175925,#175926,#175927,#175928,
#175929,#175930,#175931,#175932,#175933,#175934,#175935,#175936,#175937,
#175938,#175939,#175940,#175941,#175942,#175943,#175944,#175945,#175946,
#175947,#175948,#175949,#175950,#175951,#175952,#175953,#175954,#175955,
#175956,#175957,#175958,#175959,#175960,#175961,#175962,#175963,#175964,
#175965,#175966,#175967,#175968,#175969,#175970,#175971,#175972,#175973,
#175974,#175975,#175976,#175977,#175978,#175979,#175980,#175981,#175982,
#175983,#175984,#175985,#175986,#175987,#175988,#175989,#175990,#175991,
#175992,#175993),.UNSPECIFIED.,.F.,.F.,(4,3,3,3,3,3,3,3,3,3,3,3,3,3,3,3,
3,3,3,3,3,3,3,4),(0.,0.0909637694368515,0.178799587602911,0.24999999999992,
0.269286037251739,0.320475373835143,0.406735621633324,0.46874999999988,
0.484374999999908,0.494411073072455,0.499999999999934,0.544308918389705,
0.616362009200579,0.624999999999929,0.687499999999932,0.718749999999958,
0.733555217110215,0.747697754998785,0.749999999999984,0.780356397068987,
0.849170048020548,0.916030064764027,0.980468771416945,1.),.UNSPECIFIED.);
#5216=B_SPLINE_CURVE_WITH_KNOTS('',3,(#175994,#175995,#175996,#175997,#175998,
#175999,#176000,#176001,#176002,#176003,#176004,#176005,#176006,#176007,
#176008,#176009,#176010,#176011,#176012,#176013,#176014,#176015,#176016,
#176017,#176018,#176019,#176020,#176021,#176022,#176023),.UNSPECIFIED.,
 .F.,.F.,(4,2,2,2,1,1,1,2,2,2,2,1,1,1,2,2,2,4),(0.,0.125000000000031,0.187500000000059,
0.218750000000073,0.234375000000079,0.242187500000088,0.246093750000099,
0.248046875000105,0.25000000000011,0.374999999999913,0.437499999999804,
0.468749999999764,0.484374999999732,0.492187499999724,0.496093749999717,
0.499999999999709,0.749999999999854,1.),.UNSPECIFIED.);
#5217=B_SPLINE_CURVE_WITH_KNOTS('',3,(#176038,#176039,#176040,#176041,#176042,
#176043,#176044,#176045,#176046,#176047,#176048,#176049,#176050,#176051,
#176052,#176053,#176054,#176055,#176056,#176057,#176058,#176059,#176060,
#176061,#176062,#176063,#176064,#176065,#176066,#176067,#176068,#176069),
 .UNSPECIFIED.,.F.,.F.,(4,2,2,2,1,1,1,2,2,2,2,2,1,1,1,2,2,2,4),(0.,0.249999999999737,
0.374999999999601,0.437499999999541,0.46874999999952,0.4843749999995,0.492187499999488,
0.496093749999487,0.499999999999486,0.624999999999202,0.68749999999906,
0.718749999999,0.734374999998961,0.742187499998943,0.746093749998934,0.748046874998939,
0.749999999998944,0.874999999999472,1.),.UNSPECIFIED.);
#5218=B_SPLINE_CURVE_WITH_KNOTS('',3,(#176113,#176114,#176115,#176116,#176117,
#176118,#176119,#176120,#176121,#176122,#176123,#176124,#176125,#176126,
#176127,#176128,#176129,#176130,#176131,#176132,#176133,#176134,#176135,
#176136,#176137,#176138,#176139,#176140,#176141,#176142,#176143,#176144,
#176145,#176146,#176147,#176148,#176149,#176150,#176151,#176152,#176153,
#176154,#176155,#176156,#176157,#176158,#176159,#176160,#176161),
 .UNSPECIFIED.,.F.,.F.,(4,3,3,3,3,3,3,3,3,3,3,3,3,3,3,3,4),(0.,0.0684875562747417,
0.136659016526091,0.204808625883849,0.250000000000048,0.318760027576873,
0.375000000000071,0.414532745911366,0.454363518454273,0.495640942979285,
0.500000000000095,0.584838655976972,0.66918100853855,0.753595793198019,
0.83822364534784,0.923951954929328,1.),.UNSPECIFIED.);
#5219=B_SPLINE_CURVE_WITH_KNOTS('',3,(#176162,#176163,#176164,#176165,#176166,
#176167,#176168,#176169,#176170,#176171,#176172,#176173,#176174,#176175,
#176176,#176177,#176178,#176179,#176180,#176181,#176182,#176183,#176184,
#176185,#176186,#176187,#176188,#176189,#176190,#176191,#176192,#176193,
#176194,#176195,#176196,#176197,#176198,#176199,#176200,#176201,#176202,
#176203,#176204,#176205,#176206,#176207,#176208,#176209,#176210),
 .UNSPECIFIED.,.F.,.F.,(4,3,3,3,3,3,3,3,3,3,3,3,3,3,3,3,4),(0.,0.000568992160183443,
0.000684369961878612,0.000753736971436056,0.000939442240060596,0.00102655494281796,
0.00113065957381952,0.00136873992375731,0.00150755451437507,0.00188444398402289,
0.00205310988563609,0.00222420237610578,0.00226080156348499,0.00235252174395805,
0.00254500079573646,0.00264124032162566,0.00273747984751486),
 .UNSPECIFIED.);
#5220=B_SPLINE_CURVE_WITH_KNOTS('',3,(#176251,#176252,#176253,#176254,#176255,
#176256,#176257,#176258,#176259,#176260,#176261,#176262,#176263,#176264,
#176265,#176266),.UNSPECIFIED.,.F.,.F.,(4,2,2,1,1,2,2,2,4),(0.,0.249999999999916,
0.374999999999924,0.437499999999896,0.468749999999911,0.484374999999942,
0.499999999999973,0.749999999999986,1.),.UNSPECIFIED.);
#5221=B_SPLINE_CURVE_WITH_KNOTS('',3,(#176274,#176275,#176276,#176277,#176278,
#176279,#176280,#176281,#176282,#176283,#176284,#176285,#176286,#176287,
#176288,#176289),.UNSPECIFIED.,.F.,.F.,(4,2,2,2,1,1,2,2,4),(0.,0.249999999999886,
0.374999999999848,0.437499999999797,0.46874999999974,0.484374999999751,
0.492187499999733,0.499999999999715,1.),.UNSPECIFIED.);
#5222=B_SPLINE_CURVE_WITH_KNOTS('',3,(#176330,#176331,#176332,#176333,#176334,
#176335,#176336,#176337,#176338,#176339,#176340,#176341,#176342,#176343,
#176344,#176345,#176346,#176347,#176348,#176349,#176350,#176351,#176352,
#176353,#176354,#176355,#176356,#176357,#176358,#176359,#176360,#176361,
#176362,#176363,#176364,#176365,#176366,#176367,#176368,#176369,#176370,
#176371,#176372,#176373,#176374,#176375,#176376,#176377,#176378,#176379,
#176380,#176381,#176382,#176383,#176384,#176385,#176386,#176387,#176388,
#176389,#176390,#176391,#176392,#176393,#176394,#176395,#176396,#176397,
#176398,#176399),.UNSPECIFIED.,.F.,.F.,(4,3,3,3,3,3,3,3,3,3,3,3,3,3,3,3,
3,3,3,3,3,3,3,4),(0.,0.076883980804006,0.155236173506771,0.236099575550264,
0.245845450188085,0.250000000001421,0.327307321279621,0.375000000002082,
0.437500000002376,0.468750000002516,0.472513732477007,0.484375000002586,
0.492187500002609,0.497985201456684,0.500000000002632,0.612018993597418,
0.710669180284392,0.750000000001316,0.769020159477365,0.781250000001152,
0.858443094492983,0.890625000000576,0.970594010184165,1.),.UNSPECIFIED.);
#5223=B_SPLINE_CURVE_WITH_KNOTS('',3,(#176439,#176440,#176441,#176442,#176443,
#176444,#176445,#176446),.UNSPECIFIED.,.F.,.F.,(4,2,2,4),(0.,0.0307386998643325,
0.0629186902704779,0.0847651026474671),.UNSPECIFIED.);
#5224=B_SPLINE_CURVE_WITH_KNOTS('',3,(#176447,#176448,#176449,#176450,#176451,
#176452,#176453,#176454),.UNSPECIFIED.,.F.,.F.,(4,2,2,4),(0.0847654169755104,
0.106603528597414,0.138777607634753,0.16953083368799),.UNSPECIFIED.);
#5225=B_SPLINE_CURVE_WITH_KNOTS('',3,(#176455,#176456,#176457,#176458,#176459,
#176460,#176461,#176462,#176463,#176464,#176465,#176466,#176467,#176468,
#176469,#176470,#176471,#176472,#176473),.UNSPECIFIED.,.F.,.F.,(4,3,3,3,
3,3,4),(0.,0.000358645716711148,0.000416788078411022,0.000833987724853048,
0.000834068655632161,0.00125109176933023,0.00166813731126432),
 .UNSPECIFIED.);
#5226=B_SPLINE_CURVE_WITH_KNOTS('',3,(#176506,#176507,#176508,#176509,#176510,
#176511,#176512,#176513,#176514,#176515,#176516,#176517,#176518,#176519,
#176520,#176521,#176522,#176523,#176524,#176525,#176526,#176527,#176528,
#176529,#176530,#176531),.UNSPECIFIED.,.F.,.F.,(4,2,2,2,2,2,2,2,2,2,2,2,
4),(0.,0.0350983387286775,0.0741581944032339,0.101946776655108,0.109514391091077,
0.11764023444793,0.136341904849521,0.141182675692268,0.160390411168246,
0.193626235432022,0.217667420373208,0.251529378143752,0.2824139549931),
 .UNSPECIFIED.);
#5227=B_SPLINE_CURVE_WITH_KNOTS('',3,(#176532,#176533,#176534,#176535,#176536,
#176537,#176538,#176539,#176540,#176541,#176542,#176543,#176544,#176545,
#176546,#176547,#176548,#176549,#176550,#176551,#176552,#176553,#176554,
#176555,#176556,#176557,#176558,#176559,#176560,#176561,#176562),
 .UNSPECIFIED.,.F.,.F.,(4,3,3,3,3,3,3,3,3,3,4),(0.,0.000366648609668148,
0.000673956529173827,0.00118123470619227,0.00134837711191729,0.00134840211582016,
0.00202256566787594,0.00202269623773768,0.0023684953008591,0.00265916017167732,
0.00269675422383458),.UNSPECIFIED.);
#5228=B_SPLINE_CURVE_WITH_KNOTS('',3,(#176597,#176598,#176599,#176600,#176601,
#176602,#176603,#176604,#176605,#176606,#176607,#176608,#176609,#176610,
#176611,#176612,#176613,#176614),.UNSPECIFIED.,.F.,.F.,(4,2,2,2,2,2,2,2,
4),(0.,0.0302664700381998,0.0628248024586328,0.0854745235510308,0.116272737380146,
0.147052923761063,0.169708349889542,0.202281537926532,0.232545593041181),
 .UNSPECIFIED.);
#5229=B_SPLINE_CURVE_WITH_KNOTS('',3,(#176615,#176616,#176617,#176618,#176619,
#176620,#176621,#176622,#176623,#176624,#176625,#176626,#176627,#176628,
#176629,#176630,#176631,#176632,#176633,#176634,#176635,#176636,#176637,
#176638,#176639,#176640,#176641,#176642,#176643,#176644,#176645),
 .UNSPECIFIED.,.F.,.F.,(4,3,3,3,3,3,3,3,3,3,4),(0.,0.000563737664817588,
0.000564164457966204,0.00104582442932934,0.00112760220035029,0.00112832891593241,
0.00161216721635697,0.00169210723432566,0.00169249337389861,0.00210946737344097,
0.00225665783186482),.UNSPECIFIED.);
#5230=B_SPLINE_CURVE_WITH_KNOTS('',3,(#176703,#176704,#176705,#176706,#176707,
#176708,#176709,#176710,#176711,#176712,#176713,#176714,#176715),
 .UNSPECIFIED.,.F.,.F.,(4,3,3,3,4),(4.71238898038469,5.10508806208342,5.49778714378214,
5.89048622548087,6.28318530717959),.UNSPECIFIED.);
#5231=B_SPLINE_CURVE_WITH_KNOTS('',3,(#176752,#176753,#176754,#176755,#176756,
#176757,#176758,#176759,#176760,#176761,#176762,#176763,#176764,#176765,
#176766,#176767,#176768,#176769,#176770,#176771,#176772,#176773,#176774,
#176775,#176776,#176777,#176778,#176779,#176780,#176781,#176782,#176783,
#176784,#176785,#176786,#176787,#176788,#176789,#176790,#176791,#176792,
#176793,#176794,#176795,#176796,#176797,#176798,#176799,#176800,#176801,
#176802,#176803,#176804,#176805,#176806,#176807,#176808,#176809,#176810,
#176811,#176812,#176813,#176814,#176815,#176816,#176817,#176818,#176819,
#176820,#176821,#176822,#176823,#176824,#176825,#176826,#176827,#176828,
#176829,#176830,#176831,#176832,#176833,#176834,#176835,#176836,#176837,
#176838,#176839,#176840,#176841,#176842,#176843,#176844,#176845),
 .UNSPECIFIED.,.F.,.F.,(4,3,3,3,3,3,3,3,3,3,3,3,3,3,3,3,3,3,3,3,3,3,3,3,
3,3,3,3,3,3,3,4),(0.,0.0848538873601167,0.124999999999949,0.187499999999932,
0.21134842114964,0.234943711617932,0.249999999999915,0.260068072866973,
0.318500635089809,0.374999999999881,0.433593749999855,0.485685382805016,
0.492187499999828,0.497237166982873,0.499999999999823,0.548708184837966,
0.596046174884053,0.624999999999797,0.670698621118158,0.715864692245719,
0.74124433963234,0.746093749999775,0.748046874999775,0.749999999999775,
0.787508057868778,0.824345378943297,0.860001761682919,0.874999999999888,
0.908764508078463,0.941702858531229,0.973398294005402,1.),.UNSPECIFIED.);
#5232=B_SPLINE_CURVE_WITH_KNOTS('',3,(#176928,#176929,#176930,#176931,#176932,
#176933,#176934,#176935,#176936,#176937,#176938,#176939,#176940,#176941,
#176942,#176943,#176944,#176945),.UNSPECIFIED.,.F.,.F.,(4,2,2,2,2,2,2,2,
4),(0.,0.0302664700381639,0.0628248024586889,0.0854745235512447,0.116272737380081,
0.147052923760174,0.169708349887848,0.202281537923779,0.232545593037369),
 .UNSPECIFIED.);
#5233=B_SPLINE_CURVE_WITH_KNOTS('',3,(#176946,#176947,#176948,#176949,#176950,
#176951,#176952,#176953,#176954,#176955,#176956,#176957,#176958,#176959,
#176960,#176961,#176962,#176963,#176964,#176965,#176966,#176967,#176968,
#176969,#176970,#176971,#176972,#176973,#176974,#176975,#176976),
 .UNSPECIFIED.,.F.,.F.,(4,3,3,3,3,3,3,3,3,3,4),(0.,0.000563737664817634,
0.000564164457966258,0.00104582442998829,0.00112760220035038,0.00112832891593252,
0.00161216721525258,0.00169210723432587,0.00169249337389877,0.00210946737362081,
0.00225665783186503),.UNSPECIFIED.);
#5234=B_SPLINE_CURVE_WITH_KNOTS('',3,(#177109,#177110,#177111,#177112,#177113,
#177114,#177115,#177116,#177117,#177118,#177119,#177120,#177121,#177122,
#177123,#177124,#177125,#177126,#177127,#177128,#177129,#177130,#177131,
#177132,#177133,#177134,#177135,#177136,#177137,#177138,#177139,#177140,
#177141,#177142,#177143,#177144,#177145,#177146,#177147,#177148,#177149,
#177150,#177151,#177152,#177153,#177154,#177155,#177156,#177157),
 .UNSPECIFIED.,.F.,.F.,(4,3,3,3,3,3,3,3,3,3,3,3,3,3,3,3,4),(4.25657365665928E-6,
0.0813278485490425,0.124999999999948,0.187499999999922,0.218749999999908,
0.2343749999999,0.242187499999898,0.249999999999898,0.384939308991726,0.492187499999907,
0.499607739469523,0.499999999999908,0.514870101102984,0.669487794470102,
0.749999999999954,0.879941940443589,1.),.UNSPECIFIED.);
#5235=B_SPLINE_CURVE_WITH_KNOTS('',3,(#177158,#177159,#177160,#177161,#177162,
#177163,#177164,#177165,#177166,#177167,#177168,#177169,#177170,#177171,
#177172,#177173,#177174,#177175,#177176,#177177,#177178,#177179),
 .UNSPECIFIED.,.F.,.F.,(4,3,3,3,3,3,3,4),(0.,0.197532150015397,0.462790841234246,
0.484806537167571,0.629594317573962,0.780867938240718,0.942621022464376,
1.),.UNSPECIFIED.);
#5236=B_SPLINE_CURVE_WITH_KNOTS('',3,(#177211,#177212,#177213,#177214,#177215,
#177216,#177217,#177218,#177219,#177220,#177221,#177222,#177223,#177224,
#177225,#177226,#177227,#177228,#177229,#177230,#177231,#177232,#177233,
#177234,#177235,#177236,#177237,#177238,#177239,#177240,#177241,#177242,
#177243,#177244,#177245,#177246,#177247,#177248,#177249,#177250,#177251,
#177252,#177253,#177254,#177255,#177256,#177257,#177258,#177259,#177260,
#177261,#177262,#177263,#177264,#177265,#177266,#177267,#177268,#177269,
#177270,#177271,#177272,#177273,#177274,#177275,#177276,#177277,#177278,
#177279,#177280,#177281,#177282,#177283,#177284,#177285,#177286,#177287,
#177288,#177289,#177290,#177291,#177292,#177293,#177294,#177295,#177296,
#177297,#177298,#177299,#177300,#177301,#177302,#177303,#177304,#177305,
#177306,#177307,#177308,#177309,#177310),.UNSPECIFIED.,.F.,.F.,(4,3,3,3,
3,3,3,3,3,3,3,3,3,3,3,3,3,3,3,3,3,3,3,3,3,3,3,3,3,3,3,3,3,4),(0.,0.0343791361047495,
0.0625000000001909,0.0937500000002863,0.109375000000334,0.125000000000382,
0.163294442145796,0.18750000000058,0.218750000000676,0.234375000000738,
0.241645237443817,0.242187500000769,0.246093750000772,0.248046875000773,
0.250000000000775,0.306559060440209,0.362191713414393,0.375000000000652,
0.431342405906489,0.437500000000599,0.468750000000571,0.482664534375719,
0.494988196652662,0.500000000000543,0.563130724290198,0.625155813819059,
0.6862883583218,0.747420902824542,0.750000000000271,0.801992080489307,0.854451944080758,
0.907057823204673,0.959601903223852,0.99999893160244),.UNSPECIFIED.);
#5237=B_SPLINE_CURVE_WITH_KNOTS('',3,(#177313,#177314,#177315,#177316,#177317,
#177318,#177319,#177320,#177321,#177322,#177323,#177324,#177325,#177326,
#177327,#177328,#177329,#177330,#177331,#177332,#177333,#177334,#177335,
#177336,#177337,#177338,#177339,#177340,#177341,#177342,#177343,#177344,
#177345,#177346),.UNSPECIFIED.,.F.,.F.,(4,3,3,3,3,3,3,3,3,3,3,4),(0.,0.000121613272085656,
0.000230848939029442,0.000231076761054257,0.000462001643661032,0.000462153522108514,
0.000693154344712357,0.000693230283162771,0.000767002378129274,0.000841536498305322,
0.000913992773638785,0.000924307044217028),.UNSPECIFIED.);
#5238=B_SPLINE_CURVE_WITH_KNOTS('',3,(#177422,#177423,#177424,#177425,#177426,
#177427,#177428,#177429,#177430,#177431,#177432,#177433,#177434,#177435,
#177436,#177437,#177438,#177439,#177440,#177441,#177442,#177443,#177444,
#177445,#177446,#177447,#177448,#177449,#177450,#177451,#177452,#177453,
#177454,#177455),.UNSPECIFIED.,.F.,.F.,(4,3,3,3,3,3,3,3,3,3,3,4),(0.,7.30072795026847E-5,
0.000147770013513584,0.000221881916258506,0.000252597382995535,0.00050519476599107,
0.000631493458785083,0.000757792148986605,0.000834383528241785,0.000911454457736763,
0.00098555498853702,0.00101038953198214),.UNSPECIFIED.);
#5239=B_SPLINE_CURVE_WITH_KNOTS('',3,(#177459,#177460,#177461,#177462,#177463,
#177464,#177465,#177466,#177467,#177468,#177469,#177470,#177471,#177472,
#177473,#177474,#177475,#177476),.UNSPECIFIED.,.F.,.F.,(4,2,2,2,1,1,2,2,
2,4),(0.,0.250000000000059,0.375000000000088,0.4375000000001,0.468750000000106,
0.484375000000098,0.492187500000103,0.500000000000108,0.750000000000054,
1.),.UNSPECIFIED.);
#5240=B_SPLINE_CURVE_WITH_KNOTS('',3,(#177517,#177518,#177519,#177520,#177521,
#177522,#177523,#177524,#177525,#177526,#177527,#177528,#177529,#177530,
#177531,#177532,#177533,#177534,#177535,#177536,#177537,#177538,#177539,
#177540,#177541,#177542,#177543,#177544,#177545,#177546,#177547,#177548,
#177549,#177550,#177551,#177552,#177553,#177554,#177555,#177556,#177557,
#177558,#177559,#177560,#177561,#177562,#177563,#177564,#177565,#177566,
#177567,#177568,#177569,#177570,#177571,#177572,#177573,#177574,#177575,
#177576,#177577),.UNSPECIFIED.,.F.,.F.,(4,3,3,3,3,3,3,3,3,3,3,3,3,3,3,3,
3,3,3,3,4),(0.,0.0495055255292412,0.100209542104456,0.152193164617286,0.207894873463021,
0.263458555812716,0.321344960646642,0.375000000000226,0.43750000000027,
0.46875000000028,0.484375000000273,0.492187500000252,0.497889045411213,
0.500000000000231,0.576744445667211,0.654433500550048,0.733098323656875,
0.813288233486846,0.894374265212616,0.976809019714828,0.99999999957007),
 .UNSPECIFIED.);
#5241=B_SPLINE_CURVE_WITH_KNOTS('',3,(#177580,#177581,#177582,#177583,#177584,
#177585),.UNSPECIFIED.,.F.,.F.,(4,2,4),(0.,0.000501785580775435,0.00100357116155087),
 .UNSPECIFIED.);
#5242=B_SPLINE_CURVE_WITH_KNOTS('',3,(#177600,#177601,#177602,#177603),
 .UNSPECIFIED.,.F.,.F.,(4,4),(0.0171576436379621,0.0176580988602617),
 .UNSPECIFIED.);
#5243=B_SPLINE_CURVE_WITH_KNOTS('',3,(#177632,#177633,#177634,#177635,#177636,
#177637,#177638,#177639,#177640,#177641,#177642,#177643,#177644,#177645,
#177646,#177647,#177648,#177649,#177650,#177651,#177652,#177653,#177654,
#177655,#177656,#177657,#177658,#177659,#177660,#177661,#177662,#177663,
#177664,#177665,#177666,#177667,#177668,#177669,#177670,#177671,#177672,
#177673,#177674,#177675,#177676,#177677),.UNSPECIFIED.,.F.,.F.,(4,3,3,3,
3,3,3,3,3,3,3,3,3,3,3,4),(0.,0.0785956779669218,0.160354336421304,0.24882607911666,
0.305407052180528,0.42271380724194,0.49218749999989,0.498963544975227,0.499999999999892,
0.503499840825533,0.594170920862958,0.685885083834807,0.779934809548503,
0.875859615671826,0.975510441703396,1.),.UNSPECIFIED.);
#5244=B_SPLINE_CURVE_WITH_KNOTS('',3,(#177692,#177693,#177694,#177695,#177696,
#177697,#177698,#177699,#177700,#177701,#177702,#177703,#177704,#177705,
#177706,#177707,#177708,#177709,#177710,#177711,#177712,#177713,#177714,
#177715,#177716,#177717,#177718,#177719,#177720,#177721,#177722,#177723,
#177724,#177725),.UNSPECIFIED.,.F.,.F.,(4,3,3,3,3,3,3,3,3,3,3,4),(0.,0.0625000000000025,
0.203210009066382,0.25000000000001,0.339585721546707,0.427987553177131,
0.50000000000002,0.625000000000015,0.718750000000011,0.859375000000006,
0.929687500000003,1.),.UNSPECIFIED.);
#5245=B_SPLINE_CURVE_WITH_KNOTS('',3,(#177754,#177755,#177756,#177757,#177758,
#177759,#177760,#177761,#177762,#177763,#177764,#177765,#177766,#177767,
#177768,#177769,#177770,#177771,#177772,#177773,#177774,#177775,#177776,
#177777,#177778,#177779,#177780,#177781,#177782,#177783,#177784,#177785,
#177786,#177787),.UNSPECIFIED.,.F.,.F.,(4,3,3,3,3,3,3,3,3,3,3,4),(0.,0.124999999999929,
0.245408262930441,0.357304671146824,0.468749999999767,0.487553083205154,
0.499999999999741,0.504270157601894,0.642179092659868,0.774946277671523,
0.90129593860598,1.),.UNSPECIFIED.);
#5246=B_SPLINE_CURVE_WITH_KNOTS('',3,(#177820,#177821,#177822,#177823,#177824,
#177825,#177826,#177827,#177828,#177829,#177830,#177831,#177832,#177833,
#177834,#177835),.UNSPECIFIED.,.F.,.F.,(4,2,2,2,2,2,2,4),(0.,0.249999999999971,
0.374999999999958,0.437499999999955,0.499999999999952,0.624999999999961,
0.74999999999997,1.),.UNSPECIFIED.);
#5247=B_SPLINE_CURVE_WITH_KNOTS('',3,(#177985,#177986,#177987,#177988,#177989,
#177990,#177991,#177992,#177993,#177994,#177995,#177996,#177997,#177998,
#177999,#178000,#178001,#178002,#178003,#178004,#178005,#178006,#178007,
#178008,#178009,#178010,#178011,#178012,#178013,#178014,#178015,#178016,
#178017,#178018,#178019,#178020,#178021,#178022,#178023,#178024,#178025,
#178026,#178027,#178028,#178029,#178030,#178031,#178032,#178033,#178034,
#178035,#178036,#178037,#178038,#178039,#178040,#178041,#178042,#178043,
#178044,#178045,#178046,#178047,#178048,#178049,#178050,#178051,#178052,
#178053,#178054,#178055,#178056,#178057),.UNSPECIFIED.,.F.,.F.,(4,3,3,3,
3,3,3,3,3,3,3,3,3,3,3,3,3,3,3,3,3,3,3,3,4),(0.,0.082779980612263,0.164476403995074,
0.244653469516663,0.323962788611773,0.402053471713434,0.437499999999713,
0.468749999999689,0.482808502334718,0.497325258698629,0.499999999999665,
0.563666004332427,0.625583002165994,0.687499999999561,0.718749999999545,
0.734374999999534,0.742187499999531,0.746930749075681,0.749999999999528,
0.798769943401674,0.84646594186107,0.892304179059618,0.936986222417194,
0.979989000405518,1.),.UNSPECIFIED.);
#5248=B_SPLINE_CURVE_WITH_KNOTS('',3,(#178063,#178064,#178065,#178066,#178067,
#178068,#178069,#178070,#178071,#178072,#178073,#178074,#178075,#178076,
#178077,#178078,#178079,#178080,#178081,#178082,#178083,#178084,#178085,
#178086,#178087,#178088,#178089,#178090,#178091,#178092,#178093,#178094,
#178095,#178096,#178097,#178098,#178099,#178100,#178101,#178102,#178103,
#178104,#178105,#178106,#178107,#178108,#178109,#178110,#178111,#178112,
#178113,#178114,#178115,#178116,#178117),.UNSPECIFIED.,.F.,.F.,(4,3,3,3,
3,3,3,3,3,3,3,3,3,3,3,3,3,3,4),(0.,0.104765563683224,0.210444272545764,
0.25000000000008,0.354080737998022,0.375000000000133,0.437500000000166,
0.468750000000186,0.484375000000179,0.493467332381432,0.500000000000171,
0.577628367609106,0.651921806122704,0.721921630140622,0.750000000000086,
0.814799791967406,0.877825876853573,0.938912938426786,1.),.UNSPECIFIED.);
#5249=B_SPLINE_CURVE_WITH_KNOTS('',3,(#178125,#178126,#178127,#178128,#178129,
#178130,#178131,#178132,#178133,#178134,#178135,#178136,#178137,#178138,
#178139,#178140,#178141,#178142,#178143,#178144,#178145,#178146,#178147,
#178148,#178149,#178150,#178151,#178152,#178153,#178154,#178155,#178156,
#178157,#178158,#178159,#178160,#178161,#178162,#178163,#178164,#178165,
#178166,#178167,#178168,#178169,#178170),.UNSPECIFIED.,.F.,.F.,(4,3,3,3,
3,3,3,3,3,3,3,3,3,3,3,4),(0.,0.0625000000000026,0.124542361690346,0.189407379068573,
0.25000000000001,0.320392682405879,0.396093817100428,0.473112575495438,
0.484375000000034,0.493957180840421,0.500000000000055,0.60537483706371,
0.710879749792983,0.81656475508876,0.922725793047527,1.),.UNSPECIFIED.);
#5250=B_SPLINE_CURVE_WITH_KNOTS('',3,(#178175,#178176,#178177,#178178,#178179,
#178180,#178181,#178182,#178183,#178184,#178185,#178186,#178187),
 .UNSPECIFIED.,.F.,.F.,(4,3,3,3,4),(3.1415926535898,3.53429173528852,3.92699081698725,
4.31968989868597,4.7123889803847),.UNSPECIFIED.);
#5251=B_SPLINE_CURVE_WITH_KNOTS('',3,(#178220,#178221,#178222,#178223,#178224,
#178225,#178226,#178227,#178228,#178229,#178230,#178231,#178232,#178233,
#178234,#178235,#178236,#178237,#178238,#178239,#178240,#178241,#178242,
#178243,#178244,#178245,#178246,#178247,#178248,#178249,#178250,#178251,
#178252,#178253,#178254,#178255,#178256,#178257,#178258,#178259,#178260,
#178261,#178262,#178263,#178264,#178265,#178266,#178267,#178268,#178269,
#178270,#178271,#178272,#178273,#178274,#178275,#178276,#178277,#178278,
#178279,#178280,#178281,#178282,#178283,#178284,#178285,#178286,#178287,
#178288,#178289),.UNSPECIFIED.,.F.,.F.,(4,3,3,3,3,3,3,3,3,3,3,3,3,3,3,3,
3,3,3,3,3,3,3,4),(0.,0.0418556349283318,0.085887226797697,0.125000000000002,
0.172074981291823,0.221103566867858,0.242187500000009,0.247532486206105,
0.250000000000003,0.258757700059768,0.31821086461791,0.374999999999964,
0.438770544658119,0.468749999999953,0.48328939377611,0.497396607321518,
0.499999999999955,0.586546601545785,0.674398018105785,0.743166321732782,
0.749999999999978,0.839281118802835,0.929643700148846,1.),.UNSPECIFIED.);
#5252=B_SPLINE_CURVE_WITH_KNOTS('',3,(#178335,#178336,#178337,#178338,#178339,
#178340,#178341,#178342,#178343,#178344,#178345,#178346,#178347,#178348,
#178349,#178350,#178351,#178352,#178353,#178354,#178355,#178356,#178357,
#178358,#178359,#178360,#178361,#178362,#178363,#178364,#178365,#178366,
#178367,#178368,#178369,#178370,#178371,#178372,#178373,#178374,#178375,
#178376,#178377,#178378,#178379,#178380,#178381,#178382,#178383,#178384,
#178385,#178386,#178387,#178388,#178389,#178390,#178391,#178392,#178393,
#178394,#178395,#178396,#178397,#178398,#178399,#178400,#178401,#178402,
#178403,#178404,#178405,#178406,#178407),.UNSPECIFIED.,.F.,.F.,(4,3,3,3,
3,3,3,3,3,3,3,3,3,3,3,3,3,3,3,3,3,3,3,3,4),(0.,0.082893131556343,0.164185603605923,
0.244579415150671,0.32366183441379,0.374999999999872,0.437499999999848,
0.468749999999836,0.482808502022526,0.497325258097958,0.499999999999824,
0.563666002926397,0.625583001463082,0.687499999999767,0.71874999999976,
0.734374999999749,0.742187499999748,0.746930748996793,0.749999999999748,
0.798769942118381,0.84646593941013,0.892304175537976,0.936986217868166,
0.979988994819292,1.),.UNSPECIFIED.);
#5253=B_SPLINE_CURVE_WITH_KNOTS('',3,(#178414,#178415,#178416,#178417,#178418,
#178419,#178420,#178421,#178422,#178423,#178424,#178425,#178426,#178427,
#178428,#178429,#178430,#178431,#178432,#178433,#178434,#178435,#178436,
#178437,#178438,#178439,#178440,#178441,#178442,#178443,#178444,#178445,
#178446,#178447,#178448,#178449,#178450,#178451,#178452,#178453,#178454,
#178455,#178456,#178457,#178458,#178459,#178460,#178461,#178462,#178463,
#178464,#178465,#178466,#178467,#178468),.UNSPECIFIED.,.F.,.F.,(4,3,3,3,
3,3,3,3,3,3,3,3,3,3,3,3,3,3,4),(0.,0.104765562818283,0.210444270602352,
0.249999999999833,0.354080736731079,0.374999999999737,0.437499999999706,
0.468749999999691,0.484374999999682,0.493467332336236,0.499999999999673,
0.577628367388466,0.651921805693988,0.721921629485197,0.749999999999836,
0.814799791699761,0.877825876310641,0.938912938155321,1.),.UNSPECIFIED.);
#5254=B_SPLINE_CURVE_WITH_KNOTS('',3,(#178476,#178477,#178478,#178479,#178480,
#178481,#178482,#178483,#178484,#178485,#178486,#178487,#178488,#178489,
#178490,#178491,#178492,#178493,#178494,#178495,#178496,#178497,#178498,
#178499,#178500,#178501,#178502,#178503,#178504,#178505,#178506,#178507,
#178508,#178509,#178510,#178511,#178512,#178513,#178514,#178515,#178516,
#178517,#178518,#178519,#178520,#178521),.UNSPECIFIED.,.F.,.F.,(4,3,3,3,
3,3,3,3,3,3,3,3,3,3,3,4),(0.,0.0625000000000706,0.124542361511373,0.189407378720157,
0.250000000000282,0.320392682263235,0.396093816754809,0.473112577400942,
0.48437500000048,0.493957180817966,0.500000000000473,0.605374836123673,
0.710879748053809,0.816564752616696,0.922725789936784,1.),.UNSPECIFIED.);
#5255=B_SPLINE_CURVE_WITH_KNOTS('',3,(#178568,#178569,#178570,#178571,#178572,
#178573,#178574,#178575,#178576,#178577,#178578,#178579,#178580,#178581,
#178582,#178583,#178584,#178585,#178586,#178587,#178588,#178589,#178590,
#178591,#178592,#178593,#178594,#178595,#178596,#178597,#178598,#178599,
#178600,#178601,#178602,#178603,#178604,#178605,#178606,#178607,#178608,
#178609,#178610,#178611,#178612,#178613,#178614,#178615,#178616,#178617,
#178618,#178619,#178620,#178621,#178622,#178623,#178624,#178625,#178626,
#178627,#178628,#178629,#178630,#178631,#178632,#178633,#178634,#178635,
#178636,#178637),.UNSPECIFIED.,.F.,.F.,(4,3,3,3,3,3,3,3,3,3,3,3,3,3,3,3,
3,3,3,3,3,3,3,4),(0.,0.0418556342384494,0.0858872254110088,0.12499999999993,
0.172074980585341,0.221103564965063,0.242187499999858,0.247532486136659,
0.249999999999857,0.258757699937542,0.318210861887775,0.374999999999913,
0.438770542085752,0.468749999999938,0.483289393255924,0.497396606247191,
0.499999999999944,0.586546600221947,0.674398015536128,0.74316632133627,
0.749999999999972,0.83928111752282,0.929643697667232,1.),.UNSPECIFIED.);
#5256=B_SPLINE_CURVE_WITH_KNOTS('',3,(#178643,#178644,#178645,#178646,#178647,
#178648,#178649,#178650,#178651,#178652,#178653,#178654,#178655,#178656,
#178657,#178658,#178659,#178660,#178661,#178662,#178663,#178664,#178665,
#178666,#178667,#178668,#178669,#178670,#178671,#178672,#178673),
 .UNSPECIFIED.,.F.,.F.,(4,3,3,3,3,3,3,3,3,3,4),(0.,0.000166652275730501,
0.000342276073641851,0.000519944361542677,0.000694209917748756,0.000732292525246715,
0.000732496372314203,0.000946324251635091,0.0011572677042798,0.00135942283981261,
0.00146458505049343),.UNSPECIFIED.);
#5257=B_SPLINE_CURVE_WITH_KNOTS('',3,(#178694,#178695,#178696,#178697,#178698,
#178699,#178700,#178701,#178702,#178703,#178704,#178705,#178706,#178707,
#178708,#178709,#178710,#178711,#178712,#178713,#178714,#178715,#178716,
#178717,#178718,#178719,#178720,#178721,#178722,#178723,#178724,#178725,
#178726,#178727,#178728,#178729,#178730,#178731,#178732,#178733,#178734,
#178735,#178736,#178737,#178738,#178739,#178740,#178741,#178742,#178743,
#178744,#178745,#178746,#178747,#178748,#178749,#178750,#178751,#178752,
#178753,#178754,#178755,#178756,#178757,#178758,#178759,#178760,#178761,
#178762,#178763),.UNSPECIFIED.,.F.,.F.,(4,3,3,3,3,3,3,3,3,3,3,3,3,3,3,3,
3,3,3,3,3,3,3,4),(1.89239362219216E-7,0.109656192603923,0.214471642067222,
0.250000000000101,0.350954415556579,0.44027528545044,0.48437500000021,0.494567477383746,
0.495748146752598,0.500000000000218,0.584905953245314,0.625000000000277,
0.687500000000317,0.718750000000337,0.734375000000348,0.742187500000354,
0.747999956706539,0.75000000000036,0.801011505835862,0.850758629376896,
0.899080436624542,0.945809460694209,0.990195448603225,1.),.UNSPECIFIED.);
#5258=B_SPLINE_CURVE_WITH_KNOTS('',3,(#178765,#178766,#178767,#178768,#178769,
#178770,#178771,#178772,#178773,#178774,#178775,#178776,#178777,#178778,
#178779,#178780,#178781,#178782,#178783,#178784,#178785,#178786,#178787,
#178788,#178789,#178790,#178791,#178792,#178793,#178794,#178795,#178796,
#178797,#178798,#178799,#178800,#178801,#178802,#178803,#178804,#178805,
#178806,#178807,#178808,#178809,#178810,#178811,#178812,#178813,#178814,
#178815,#178816,#178817,#178818,#178819),.UNSPECIFIED.,.F.,.F.,(4,3,3,3,
3,3,3,3,3,3,3,3,3,3,3,3,3,3,4),(3.58447939321108E-8,0.140119837080351,0.271105288786313,
0.384337543497189,0.440953670852627,0.469261734530347,0.483415766369206,
0.490492782288636,0.494031290248351,0.495800544228208,0.496350538320295,
0.497569798208066,0.499532416183815,0.499974395152803,0.500257543470681,
0.662105397139048,0.822253299281346,0.98089203121495,1.),.UNSPECIFIED.);
#5259=B_SPLINE_CURVE_WITH_KNOTS('',3,(#178837,#178838,#178839,#178840,#178841,
#178842,#178843,#178844,#178845,#178846,#178847,#178848,#178849,#178850,
#178851,#178852,#178853,#178854,#178855,#178856,#178857,#178858,#178859,
#178860,#178861,#178862,#178863,#178864,#178865,#178866,#178867,#178868,
#178869,#178870,#178871,#178872,#178873,#178874,#178875,#178876,#178877,
#178878,#178879,#178880,#178881,#178882,#178883,#178884,#178885),
 .UNSPECIFIED.,.F.,.F.,(4,3,3,3,3,3,3,3,3,3,3,3,3,3,3,3,4),(0.,0.104670426468367,
0.210224880572374,0.249999999999829,0.354199578347449,0.438725565324252,
0.484374999999684,0.493467343025674,0.499999999999679,0.577519175226156,
0.651750918301883,0.721751437166635,0.74999999999984,0.814856950659882,
0.877899885674253,0.938949942837126,1.),.UNSPECIFIED.);
#5260=B_SPLINE_CURVE_WITH_KNOTS('',3,(#178893,#178894,#178895,#178896,#178897,
#178898,#178899,#178900,#178901,#178902,#178903,#178904,#178905,#178906,
#178907,#178908,#178909,#178910,#178911,#178912,#178913,#178914,#178915,
#178916,#178917,#178918,#178919,#178920,#178921,#178922,#178923,#178924,
#178925,#178926,#178927,#178928,#178929,#178930,#178931,#178932,#178933,
#178934,#178935,#178936,#178937,#178938,#178939,#178940,#178941,#178942,
#178943,#178944),.UNSPECIFIED.,.F.,.F.,(4,3,3,3,3,3,3,3,3,3,3,3,3,3,3,3,
3,4),(0.,0.0624999999999843,0.124900823539908,0.19003423091758,0.249999999999937,
0.319870182290624,0.374999999999898,0.437499999999879,0.468749999999869,
0.484374999999867,0.494074303446313,0.499999999999866,0.591975494556334,
0.685251275110955,0.780573779554895,0.877101419317664,0.97544533364762,
1.),.UNSPECIFIED.);
#5261=B_SPLINE_CURVE_WITH_KNOTS('',3,(#178991,#178992,#178993,#178994,#178995,
#178996,#178997,#178998,#178999,#179000,#179001,#179002,#179003,#179004,
#179005,#179006,#179007,#179008,#179009,#179010,#179011,#179012,#179013,
#179014,#179015,#179016,#179017,#179018,#179019,#179020,#179021,#179022,
#179023,#179024,#179025,#179026,#179027,#179028,#179029,#179030,#179031,
#179032,#179033,#179034,#179035,#179036,#179037,#179038,#179039,#179040,
#179041,#179042,#179043,#179044,#179045,#179046,#179047,#179048,#179049,
#179050,#179051,#179052,#179053,#179054,#179055,#179056,#179057,#179058,
#179059,#179060,#179061,#179062,#179063,#179064,#179065,#179066),
 .UNSPECIFIED.,.F.,.F.,(4,3,3,3,3,3,3,3,3,3,3,3,3,3,3,3,3,3,3,3,3,3,3,3,
3,4),(0.,0.0427402135105615,0.0873806279031941,0.133137916968273,0.180400098768673,
0.187499999999966,0.218749999999969,0.234374999999968,0.242187499999964,
0.247546309647879,0.249999999999959,0.309558526821291,0.370252346988014,
0.432604522742537,0.437499999999955,0.468749999999956,0.483324625619423,
0.497499771299632,0.499999999999956,0.577335604024361,0.655589231504514,
0.734790431766,0.815465264185707,0.897008160634072,0.979844363470657,1.),
 .UNSPECIFIED.);
#5262=B_SPLINE_CURVE_WITH_KNOTS('',3,(#179073,#179074,#179075,#179076,#179077,
#179078,#179079,#179080,#179081,#179082,#179083,#179084,#179085,#179086,
#179087,#179088,#179089,#179090,#179091,#179092,#179093),.UNSPECIFIED.,
 .F.,.F.,(4,2,1,1,1,2,2,1,1,1,1,2,2,4),(0.,0.124999999999982,0.187499999999972,
0.218749999999967,0.234374999999965,0.242187499999963,0.249999999999962,
0.374999999999944,0.437499999999935,0.46874999999993,0.484374999999928,
0.492187499999928,0.499999999999928,1.),.UNSPECIFIED.);
#5263=B_SPLINE_CURVE_WITH_KNOTS('',3,(#179094,#179095,#179096,#179097),
 .UNSPECIFIED.,.F.,.F.,(4,4),(1.7347234759768E-18,0.000135753226310594),
 .UNSPECIFIED.);
#5264=B_SPLINE_CURVE_WITH_KNOTS('',3,(#179127,#179128,#179129,#179130,#179131,
#179132,#179133,#179134,#179135,#179136,#179137,#179138,#179139,#179140,
#179141,#179142,#179143,#179144,#179145,#179146,#179147,#179148,#179149,
#179150,#179151,#179152,#179153,#179154,#179155,#179156,#179157,#179158,
#179159,#179160,#179161,#179162,#179163,#179164,#179165,#179166,#179167,
#179168,#179169),.UNSPECIFIED.,.F.,.F.,(4,3,3,3,3,3,3,3,3,3,3,3,3,3,4),
(0.,0.101744188003888,0.124999999999806,0.210937499999683,0.263804240260239,
0.356835436800772,0.448994247360205,0.468749999999312,0.484374999999354,
0.488281249999364,0.492187499999375,0.499999999999396,0.720215862423713,
0.94347057076842,1.),.UNSPECIFIED.);
#5265=B_SPLINE_CURVE_WITH_KNOTS('',3,(#179220,#179221,#179222,#179223,#179224,
#179225,#179226,#179227,#179228,#179229,#179230,#179231,#179232,#179233,
#179234,#179235,#179236,#179237,#179238,#179239,#179240,#179241,#179242,
#179243,#179244,#179245,#179246,#179247,#179248,#179249,#179250,#179251,
#179252,#179253,#179254,#179255,#179256,#179257,#179258,#179259,#179260,
#179261,#179262,#179263,#179264,#179265,#179266,#179267,#179268,#179269,
#179270,#179271,#179272,#179273,#179274,#179275,#179276,#179277,#179278,
#179279,#179280,#179281,#179282,#179283,#179284,#179285,#179286,#179287,
#179288,#179289),.UNSPECIFIED.,.F.,.F.,(4,3,3,3,3,3,3,3,3,3,3,3,3,3,3,3,
3,3,3,3,3,3,3,4),(0.,0.0905130979426558,0.179924323869351,0.249999999999846,
0.256845940090264,0.344978647123152,0.429175620757808,0.468749999999701,
0.482777958801453,0.497225251801371,0.49999999999968,0.563069736113812,
0.624999999999634,0.683922647535721,0.74124546623732,0.742187499999593,
0.746915985771409,0.749999999999596,0.799322866456926,0.849492149842694,
0.894781080106962,0.938608217041727,0.980419225683544,1.),.UNSPECIFIED.);
#5266=B_SPLINE_CURVE_WITH_KNOTS('',3,(#179293,#179294,#179295,#179296,#179297,
#179298,#179299,#179300,#179301,#179302,#179303,#179304,#179305,#179306,
#179307,#179308,#179309,#179310,#179311,#179312,#179313,#179314,#179315,
#179316,#179317,#179318,#179319,#179320,#179321,#179322,#179323,#179324,
#179325,#179326,#179327,#179328,#179329,#179330,#179331,#179332,#179333,
#179334,#179335,#179336,#179337,#179338,#179339,#179340,#179341),
 .UNSPECIFIED.,.F.,.F.,(4,3,3,3,3,3,3,3,3,3,3,3,3,3,3,3,4),(0.,0.104670426730792,
0.210224881162747,0.250000000000034,0.354199578725455,0.438725566300584,
0.484375000000055,0.493467343039256,0.500000000000053,0.577519175286133,
0.65175091842001,0.721751437351517,0.750000000000026,0.814856950739285,
0.877899885834773,0.938949942917387,1.),.UNSPECIFIED.);
#5267=B_SPLINE_CURVE_WITH_KNOTS('',3,(#179349,#179350,#179351,#179352,#179353,
#179354,#179355,#179356,#179357,#179358,#179359,#179360,#179361,#179362,
#179363,#179364,#179365,#179366,#179367,#179368,#179369,#179370,#179371,
#179372,#179373,#179374,#179375,#179376,#179377,#179378,#179379,#179380,
#179381,#179382,#179383,#179384,#179385,#179386,#179387,#179388,#179389,
#179390,#179391,#179392,#179393,#179394,#179395,#179396,#179397,#179398,
#179399,#179400),.UNSPECIFIED.,.F.,.F.,(4,3,3,3,3,3,3,3,3,3,3,3,3,3,3,3,
3,4),(0.,0.0625000000000074,0.12490082348445,0.190034230807917,0.25000000000003,
0.319870182241521,0.375000000000042,0.437500000000057,0.468750000000049,
0.484375000000045,0.494074303438786,0.500000000000041,0.591975494447328,
0.685251274899277,0.780573779252049,0.877101418930033,0.975445333187664,
1.),.UNSPECIFIED.);
#5268=B_SPLINE_CURVE_WITH_KNOTS('',3,(#179446,#179447,#179448,#179449,#179450,
#179451,#179452,#179453,#179454,#179455,#179456,#179457,#179458,#179459,
#179460,#179461,#179462,#179463,#179464,#179465,#179466,#179467,#179468,
#179469,#179470,#179471,#179472,#179473,#179474,#179475,#179476,#179477,
#179478,#179479,#179480,#179481,#179482,#179483,#179484,#179485,#179486,
#179487,#179488,#179489,#179490,#179491,#179492,#179493,#179494,#179495,
#179496,#179497,#179498,#179499,#179500,#179501,#179502,#179503,#179504,
#179505,#179506,#179507,#179508,#179509,#179510,#179511,#179512,#179513,
#179514,#179515),.UNSPECIFIED.,.F.,.F.,(4,3,3,3,3,3,3,3,3,3,3,3,3,3,3,3,
3,3,3,3,3,3,3,4),(0.,0.0905130975136295,0.179924322983699,0.249999999999951,
0.256845940234234,0.344978646792586,0.429175619853906,0.468749999999914,
0.482777958649709,0.497225251507927,0.499999999999913,0.563069735586386,
0.624999999999939,0.683922647435557,0.741245466266932,0.742187499999951,
0.74691598574573,0.749999999999955,0.799322866380848,0.849492149785636,
0.894781079988712,0.938608216864493,0.980419225446453,1.),.UNSPECIFIED.);
#5269=B_SPLINE_CURVE_WITH_KNOTS('',3,(#179549,#179550,#179551,#179552,#179553,
#179554,#179555,#179556,#179557,#179558,#179559,#179560,#179561,#179562,
#179563,#179564,#179565,#179566,#179567,#179568,#179569,#179570,#179571,
#179572,#179573,#179574,#179575,#179576,#179577,#179578,#179579,#179580,
#179581,#179582,#179583,#179584,#179585,#179586,#179587,#179588,#179589,
#179590,#179591,#179592,#179593,#179594,#179595,#179596,#179597,#179598,
#179599,#179600,#179601,#179602,#179603,#179604,#179605,#179606,#179607,
#179608,#179609,#179610,#179611,#179612,#179613,#179614,#179615,#179616,
#179617,#179618,#179619,#179620,#179621,#179622,#179623,#179624),
 .UNSPECIFIED.,.F.,.F.,(4,3,3,3,3,3,3,3,3,3,3,3,3,3,3,3,3,3,3,3,3,3,3,3,
3,4),(0.,0.0430097483234137,0.0878255518128777,0.124999999999833,0.172143318494293,
0.187499999999742,0.218749999999705,0.234374999999686,0.242187499999689,
0.247546309656834,0.249999999999692,0.309158559883821,0.36986670864448,
0.374999999999702,0.43749999999971,0.468749999999719,0.483324625655138,
0.497499771373716,0.499999999999727,0.577335604004243,0.655589231465469,
0.734790431709053,0.815465264114797,0.897008160548024,0.979844363371395,
1.),.UNSPECIFIED.);
#5270=B_SPLINE_CURVE_WITH_KNOTS('',3,(#179645,#179646,#179647,#179648,#179649,
#179650,#179651,#179652,#179653,#179654,#179655,#179656,#179657,#179658,
#179659,#179660,#179661,#179662,#179663,#179664,#179665,#179666,#179667,
#179668,#179669,#179670,#179671,#179672,#179673,#179674,#179675,#179676,
#179677,#179678,#179679,#179680,#179681,#179682,#179683,#179684,#179685,
#179686,#179687,#179688,#179689,#179690,#179691,#179692,#179693,#179694,
#179695,#179696,#179697,#179698,#179699),.UNSPECIFIED.,.F.,.F.,(4,3,3,3,
3,3,3,3,3,3,3,3,3,3,3,3,3,3,4),(0.,0.104765563478566,0.210444272083717,
0.250000000000343,0.354080737693078,0.375000000000532,0.437500000000626,
0.468750000000673,0.484375000000687,0.493467332371258,0.500000000000701,
0.577628367556246,0.651921806019438,0.721921629982362,0.75000000000035,
0.814799791902674,0.877825876721737,0.938912938360868,1.),.UNSPECIFIED.);
#5271=B_SPLINE_CURVE_WITH_KNOTS('',3,(#179707,#179708,#179709,#179710,#179711,
#179712,#179713,#179714,#179715,#179716,#179717,#179718,#179719,#179720,
#179721,#179722,#179723,#179724,#179725,#179726,#179727,#179728,#179729,
#179730,#179731,#179732,#179733,#179734,#179735,#179736,#179737,#179738,
#179739,#179740,#179741,#179742,#179743,#179744,#179745,#179746,#179747,
#179748,#179749,#179750,#179751,#179752),.UNSPECIFIED.,.F.,.F.,(4,3,3,3,
3,3,3,3,3,3,3,3,3,3,3,4),(0.,0.0625000000000197,0.124542361697189,0.189407379081926,
0.250000000000079,0.320392682411276,0.396093817089821,0.473112577633271,
0.484375000000176,0.493957180841483,0.500000000000194,0.605374837099206,
0.710879749859165,0.816564755183575,0.922725793167858,1.),.UNSPECIFIED.);
#5272=B_SPLINE_CURVE_WITH_KNOTS('',3,(#179757,#179758,#179759,#179760,#179761,
#179762,#179763,#179764,#179765,#179766,#179767,#179768,#179769),
 .UNSPECIFIED.,.F.,.F.,(4,3,3,3,4),(3.1415926535898,3.53429173528852,3.92699081698724,
4.31968989868597,4.71238898038469),.UNSPECIFIED.);
#5273=B_SPLINE_CURVE_WITH_KNOTS('',3,(#179802,#179803,#179804,#179805,#179806,
#179807,#179808,#179809,#179810,#179811,#179812,#179813,#179814,#179815,
#179816,#179817,#179818,#179819,#179820,#179821,#179822,#179823,#179824,
#179825,#179826,#179827,#179828,#179829,#179830,#179831,#179832,#179833,
#179834,#179835,#179836,#179837,#179838,#179839,#179840,#179841,#179842,
#179843,#179844,#179845,#179846,#179847,#179848,#179849,#179850,#179851,
#179852,#179853,#179854,#179855,#179856,#179857,#179858,#179859,#179860,
#179861,#179862,#179863,#179864,#179865,#179866,#179867,#179868,#179869,
#179870,#179871),.UNSPECIFIED.,.F.,.F.,(4,3,3,3,3,3,3,3,3,3,3,3,3,3,3,3,
3,3,3,3,3,3,3,4),(0.,0.0418556347635635,0.0858872264664174,0.12499999999986,
0.172074981123076,0.221103566406418,0.242187499999732,0.247532486182558,
0.249999999999724,0.258757700014179,0.318210863601387,0.374999999999747,
0.438770543659797,0.468749999999766,0.483289393572595,0.497396606901275,
0.499999999999779,0.586546600897368,0.674398016851886,0.743166321541273,
0.749999999999889,0.839281118186762,0.929643698954937,1.),.UNSPECIFIED.);
#5274=B_SPLINE_CURVE_WITH_KNOTS('',3,(#179911,#179912,#179913,#179914,#179915,
#179916,#179917,#179918,#179919,#179920,#179921,#179922,#179923,#179924,
#179925,#179926,#179927,#179928,#179929,#179930,#179931,#179932,#179933,
#179934,#179935,#179936,#179937,#179938,#179939,#179940,#179941,#179942,
#179943,#179944,#179945,#179946,#179947,#179948,#179949,#179950),
 .UNSPECIFIED.,.F.,.F.,(4,3,3,3,3,3,3,3,3,3,3,3,3,4),(0.,0.000161047553671253,
0.00032665546448548,0.000493863052907836,0.000580621437699987,0.00058187576131232,
0.0011633223004275,0.00116375152262464,0.00145467271006653,0.00145468940328081,
0.00174562728393698,0.0017460231201541,0.00204798180553644,0.00232750304524933),
 .UNSPECIFIED.);
#5275=B_SPLINE_CURVE_WITH_KNOTS('',3,(#179951,#179952,#179953,#179954,#179955,
#179956,#179957,#179958,#179959,#179960,#179961,#179962,#179963,#179964,
#179965,#179966,#179967,#179968,#179969,#179970,#179971,#179972,#179973,
#179974,#179975,#179976,#179977,#179978,#179979,#179980,#179981,#179982,
#179983,#179984,#179985,#179986,#179987,#179988,#179989,#179990,#179991,
#179992,#179993,#179994,#179995,#179996,#179997,#179998,#179999,#180000,
#180001,#180002,#180003,#180004,#180005,#180006,#180007,#180008,#180009,
#180010,#180011,#180012,#180013,#180014,#180015,#180016,#180017,#180018,
#180019,#180020),.UNSPECIFIED.,.F.,.F.,(4,3,3,3,3,3,3,3,3,3,3,3,3,3,3,3,
3,3,3,3,3,3,3,4),(0.,0.0645978303967565,0.128839691720708,0.192883319322283,
0.249999999999887,0.314290451368615,0.374999999999836,0.437499999999809,
0.468749999999795,0.484374999999779,0.492187499999781,0.497804168442645,
0.499999999999782,0.555878234310221,0.609222458807199,0.661110211917442,
0.710954042038781,0.749999999999891,0.797583166200646,0.844123803798507,
0.88948355346123,0.934266047761903,0.978456173795685,1.),.UNSPECIFIED.);
#5276=B_SPLINE_CURVE_WITH_KNOTS('',3,(#180028,#180029,#180030,#180031,#180032,
#180033,#180034,#180035,#180036,#180037,#180038,#180039,#180040,#180041,
#180042,#180043,#180044,#180045,#180046,#180047,#180048,#180049,#180050,
#180051,#180052,#180053,#180054,#180055,#180056,#180057,#180058,#180059,
#180060,#180061,#180062,#180063,#180064,#180065,#180066,#180067,#180068,
#180069,#180070,#180071,#180072,#180073,#180074,#180075,#180076,#180077,
#180078,#180079,#180080,#180081,#180082),.UNSPECIFIED.,.F.,.F.,(4,3,3,3,
3,3,3,3,3,3,3,3,3,3,3,3,3,3,4),(0.,0.104765563474887,0.210444272078553,
0.250000000000062,0.35408073770077,0.375000000000105,0.437500000000124,
0.468750000000142,0.484375000000157,0.493467332370735,0.500000000000172,
0.577628367556476,0.651921806020633,0.721921629984373,0.750000000000086,
0.814799791903652,0.877825876724308,0.938912938362154,1.),.UNSPECIFIED.);
#5277=B_SPLINE_CURVE_WITH_KNOTS('',3,(#180090,#180091,#180092,#180093,#180094,
#180095,#180096,#180097,#180098,#180099,#180100,#180101,#180102,#180103,
#180104,#180105,#180106,#180107,#180108,#180109,#180110,#180111,#180112,
#180113,#180114,#180115,#180116,#180117,#180118,#180119,#180120,#180121,
#180122,#180123,#180124,#180125,#180126,#180127,#180128,#180129,#180130,
#180131,#180132,#180133,#180134,#180135),.UNSPECIFIED.,.F.,.F.,(4,3,3,3,
3,3,3,3,3,3,3,3,3,3,3,4),(0.,0.0625000000000364,0.124542361523147,0.189407378742922,
0.250000000000146,0.32039268227165,0.39609381677263,0.473112576960276,0.484375000000262,
0.493957180819043,0.500000000000255,0.605374836184627,0.710879748162737,
0.816564752767341,0.922725790120419,1.),.UNSPECIFIED.);
#5278=B_SPLINE_CURVE_WITH_KNOTS('',3,(#180183,#180184,#180185,#180186,#180187,
#180188,#180189,#180190,#180191,#180192,#180193,#180194,#180195,#180196,
#180197,#180198,#180199,#180200,#180201,#180202,#180203,#180204,#180205,
#180206,#180207,#180208,#180209,#180210,#180211,#180212,#180213,#180214,
#180215,#180216,#180217,#180218,#180219,#180220,#180221,#180222,#180223,
#180224,#180225,#180226,#180227,#180228,#180229,#180230,#180231,#180232,
#180233,#180234,#180235,#180236,#180237,#180238,#180239,#180240,#180241,
#180242,#180243,#180244,#180245,#180246,#180247,#180248,#180249,#180250,
#180251,#180252,#180253,#180254,#180255),.UNSPECIFIED.,.F.,.F.,(4,3,3,3,
3,3,3,3,3,3,3,3,3,3,3,3,3,3,3,3,3,3,3,3,4),(0.,0.0828931316413898,0.16418560379089,
0.244579415455065,0.323661834828471,0.374999999999967,0.437499999999958,
0.468749999999954,0.4828085023222,0.497325258675924,0.49999999999995,0.563237806906317,
0.624999999999955,0.687499999999966,0.718749999999971,0.734374999999977,
0.742187499999976,0.746930749059886,0.749999999999976,0.798769942866912,
0.846465940839484,0.892304177591545,0.936986220520651,0.979988998076433,
1.),.UNSPECIFIED.);
#5279=B_SPLINE_CURVE_WITH_KNOTS('',3,(#180288,#180289,#180290,#180291,#180292,
#180293,#180294,#180295,#180296,#180297,#180298,#180299,#180300,#180301,
#180302,#180303,#180304,#180305,#180306,#180307,#180308,#180309,#180310,
#180311,#180312,#180313,#180314,#180315,#180316,#180317,#180318,#180319,
#180320,#180321,#180322,#180323,#180324,#180325,#180326,#180327,#180328,
#180329,#180330,#180331,#180332,#180333,#180334,#180335,#180336,#180337,
#180338,#180339,#180340,#180341,#180342,#180343,#180344,#180345,#180346,
#180347,#180348,#180349,#180350,#180351,#180352,#180353,#180354,#180355,
#180356,#180357),.UNSPECIFIED.,.F.,.F.,(4,3,3,3,3,3,3,3,3,3,3,3,3,3,3,3,
3,3,3,3,3,3,3,4),(0.,0.0418167934441984,0.085151181427437,0.130899470147945,
0.178154905267451,0.227239765683116,0.24218750000028,0.247532486200105,
0.250000000000283,0.258757700046366,0.318210864309325,0.375000000000234,
0.438770544391353,0.468750000000198,0.483289393711794,0.497396607188351,
0.500000000000183,0.586546601298008,0.674398017630146,0.743166321661521,
0.750000000000092,0.839281118572534,0.92964369970189,1.),.UNSPECIFIED.);
#5280=B_SPLINE_CURVE_WITH_KNOTS('',3,(#180377,#180378,#180379,#180380,#180381,
#180382,#180383,#180384,#180385,#180386,#180387,#180388,#180389,#180390,
#180391,#180392,#180393,#180394,#180395,#180396,#180397,#180398,#180399,
#180400,#180401,#180402,#180403,#180404,#180405,#180406,#180407,#180408,
#180409,#180410,#180411,#180412,#180413,#180414,#180415,#180416,#180417,
#180418,#180419,#180420,#180421,#180422,#180423,#180424,#180425),
 .UNSPECIFIED.,.F.,.F.,(4,3,3,3,3,3,3,3,3,3,3,3,3,3,3,3,4),(0.,0.104670426541109,
0.210224880734563,0.249999999999775,0.354199578449117,0.438725567291639,
0.484374999999608,0.493467343029225,0.499999999999603,0.577519175242144,
0.651750918333578,0.721751437216418,0.749999999999802,0.814856950681533,
0.877899885718081,0.93894994285904,1.),.UNSPECIFIED.);
#5281=B_SPLINE_CURVE_WITH_KNOTS('',3,(#180433,#180434,#180435,#180436,#180437,
#180438,#180439,#180440,#180441,#180442,#180443,#180444,#180445,#180446,
#180447,#180448,#180449,#180450,#180451,#180452,#180453,#180454,#180455,
#180456,#180457,#180458,#180459,#180460,#180461,#180462,#180463,#180464,
#180465,#180466,#180467,#180468,#180469,#180470,#180471,#180472,#180473,
#180474,#180475,#180476,#180477,#180478,#180479,#180480,#180481,#180482,
#180483,#180484),.UNSPECIFIED.,.F.,.F.,(4,3,3,3,3,3,3,3,3,3,3,3,3,3,3,3,
3,4),(0.,0.0603576848723925,0.122428434116216,0.187494850857853,0.254338193740552,
0.324292162869377,0.37500000000018,0.4375000000002,0.468750000000182,0.484375000000177,
0.494074303427759,0.500000000000172,0.591975494289549,0.685251274592972,
0.780573778813809,0.877101418369239,0.975445332522005,1.),.UNSPECIFIED.);
#5282=B_SPLINE_CURVE_WITH_KNOTS('',3,(#180531,#180532,#180533,#180534,#180535,
#180536,#180537,#180538,#180539,#180540,#180541,#180542,#180543,#180544,
#180545,#180546,#180547,#180548,#180549,#180550,#180551,#180552,#180553,
#180554,#180555,#180556,#180557,#180558,#180559,#180560,#180561,#180562,
#180563,#180564,#180565,#180566,#180567,#180568,#180569,#180570,#180571,
#180572,#180573,#180574,#180575,#180576,#180577,#180578,#180579,#180580,
#180581,#180582,#180583,#180584,#180585,#180586,#180587,#180588,#180589,
#180590,#180591,#180592,#180593,#180594,#180595,#180596,#180597,#180598,
#180599,#180600,#180601,#180602,#180603,#180604,#180605,#180606),
 .UNSPECIFIED.,.F.,.F.,(4,3,3,3,3,3,3,3,3,3,3,3,3,3,3,3,3,3,3,3,3,3,3,3,
3,4),(0.,0.0430097487356867,0.0878255526448179,0.124999999999681,0.172143318924996,
0.187499999999521,0.218749999999441,0.234374999999418,0.242187499999425,
0.247546309684307,0.249999999999432,0.309158560680158,0.369866710216006,
0.374999999999513,0.437499999999554,0.468749999999584,0.483324625807977,
0.497499771690094,0.499999999999615,0.577335604065574,0.65558923158524,
0.734790431884213,0.815465264338645,0.897008160817874,0.979844363681157,
1.),.UNSPECIFIED.);
#5283=B_SPLINE_CURVE_WITH_KNOTS('',3,(#180612,#180613,#180614,#180615,#180616,
#180617,#180618,#180619,#180620,#180621,#180622,#180623,#180624,#180625,
#180626,#180627,#180628,#180629,#180630,#180631,#180632),.UNSPECIFIED.,
 .F.,.F.,(4,2,1,1,1,2,2,1,1,1,1,2,2,4),(0.,0.125000000000008,0.18750000000001,
0.218750000000008,0.234375000000006,0.242187500000008,0.250000000000009,
0.375000000000036,0.437500000000049,0.468750000000053,0.484375000000051,
0.492187500000049,0.500000000000047,1.),.UNSPECIFIED.);
#5284=B_SPLINE_CURVE_WITH_KNOTS('',3,(#180635,#180636,#180637,#180638,#180639,
#180640,#180641,#180642,#180643,#180644,#180645,#180646,#180647,#180648,
#180649,#180650,#180651,#180652,#180653,#180654,#180655,#180656,#180657,
#180658,#180659,#180660,#180661,#180662,#180663,#180664,#180665),
 .UNSPECIFIED.,.F.,.F.,(4,3,3,3,3,3,3,3,3,3,4),(0.,0.000118224492354554,
0.000239962463540374,0.000354016906950293,0.000486351214795248,0.000618764034602114,
0.000708033813900585,0.000911280042592202,0.00111586864896652,0.00131545298196076,
0.00141606762780121),.UNSPECIFIED.);
#5285=B_SPLINE_CURVE_WITH_KNOTS('',3,(#180688,#180689,#180690,#180691,#180692,
#180693,#180694,#180695,#180696,#180697,#180698,#180699,#180700,#180701,
#180702,#180703),.UNSPECIFIED.,.F.,.F.,(4,2,2,2,1,1,2,2,4),(0.,0.25000000000023,
0.375000000000355,0.437500000000406,0.468750000000446,0.484375000000451,
0.492187500000452,0.500000000000452,1.),.UNSPECIFIED.);
#5286=B_SPLINE_CURVE_WITH_KNOTS('',3,(#180748,#180749,#180750,#180751,#180752,
#180753,#180754,#180755,#180756,#180757,#180758,#180759,#180760,#180761,
#180762,#180763,#180764,#180765,#180766,#180767,#180768,#180769,#180770,
#180771,#180772,#180773,#180774,#180775,#180776,#180777,#180778,#180779,
#180780,#180781,#180782,#180783,#180784,#180785,#180786,#180787,#180788,
#180789,#180790,#180791,#180792,#180793,#180794,#180795,#180796,#180797,
#180798,#180799,#180800,#180801,#180802,#180803,#180804,#180805,#180806,
#180807,#180808,#180809,#180810,#180811,#180812,#180813,#180814,#180815,
#180816,#180817),.UNSPECIFIED.,.F.,.F.,(4,3,3,3,3,3,3,3,3,3,3,3,3,3,3,3,
3,3,3,3,3,3,3,4),(0.,0.0905130970652387,0.179924322055766,0.250000000000042,
0.25684594038563,0.344978646443199,0.429175619074524,0.468750000000064,
0.4827779584993,0.497225251216987,0.500000000000063,0.563069735064877,0.625,
0.683922646620614,0.741245466295442,0.742187499999971,0.746915985725626,
0.749999999999977,0.799322866332637,0.849492149749478,0.894781079909806,
0.938608216744346,0.980419225283251,1.),.UNSPECIFIED.);
#5287=B_SPLINE_CURVE_WITH_KNOTS('',3,(#180824,#180825,#180826,#180827,#180828,
#180829,#180830,#180831,#180832,#180833,#180834,#180835,#180836,#180837,
#180838,#180839,#180840,#180841,#180842,#180843,#180844,#180845,#180846,
#180847,#180848,#180849,#180850,#180851,#180852,#180853,#180854,#180855,
#180856,#180857,#180858,#180859,#180860,#180861,#180862,#180863,#180864,
#180865,#180866,#180867,#180868,#180869,#180870,#180871,#180872),
 .UNSPECIFIED.,.F.,.F.,(4,3,3,3,3,3,3,3,3,3,3,3,3,3,3,3,4),(0.,0.104670426476868,
0.210224880592324,0.250000000000098,0.354199578363952,0.438725565774003,
0.484375000000191,0.493467343026711,0.500000000000194,0.577519175228676,
0.651750918306284,0.721751437173546,0.750000000000097,0.814856950663166,
0.877899885680621,0.93894994284031,1.),.UNSPECIFIED.);
#5288=B_SPLINE_CURVE_WITH_KNOTS('',3,(#180880,#180881,#180882,#180883,#180884,
#180885,#180886,#180887,#180888,#180889,#180890,#180891,#180892,#180893,
#180894,#180895,#180896,#180897,#180898,#180899,#180900,#180901,#180902,
#180903,#180904,#180905,#180906,#180907,#180908,#180909,#180910,#180911,
#180912,#180913,#180914,#180915,#180916,#180917,#180918,#180919,#180920,
#180921,#180922,#180923,#180924,#180925,#180926,#180927,#180928,#180929,
#180930,#180931),.UNSPECIFIED.,.F.,.F.,(4,3,3,3,3,3,3,3,3,3,3,3,3,3,3,3,
3,4),(0.,0.0625000000000059,0.124900823533827,0.190034230905517,0.250000000000024,
0.319870182285393,0.375000000000043,0.43750000000004,0.468750000000034,
0.484375000000031,0.494074303445622,0.500000000000028,0.591975494544407,
0.685251275087606,0.780573779521403,0.877101419274667,0.975445333596583,
1.),.UNSPECIFIED.);
#5289=B_SPLINE_CURVE_WITH_KNOTS('',3,(#180977,#180978,#180979,#180980,#180981,
#180982,#180983,#180984,#180985,#180986,#180987,#180988,#180989,#180990,
#180991,#180992,#180993,#180994,#180995,#180996,#180997,#180998,#180999,
#181000,#181001,#181002,#181003,#181004,#181005,#181006,#181007,#181008,
#181009,#181010,#181011,#181012,#181013,#181014,#181015,#181016,#181017,
#181018,#181019,#181020,#181021,#181022,#181023,#181024,#181025,#181026,
#181027,#181028,#181029,#181030,#181031,#181032,#181033,#181034,#181035,
#181036,#181037,#181038,#181039,#181040,#181041,#181042,#181043,#181044,
#181045,#181046),.UNSPECIFIED.,.F.,.F.,(4,3,3,3,3,3,3,3,3,3,3,3,3,3,3,3,
3,3,3,3,3,3,3,4),(0.,0.0905130976711778,0.179924323296518,0.2500000000002,
0.256845940181976,0.344978646915006,0.429175619818899,0.46875000000037,
0.482777958797654,0.497225251792372,0.500000000000387,0.563069736211347,
0.625000000000415,0.683922647615147,0.741245466233434,0.742187500000435,
0.746915985752997,0.750000000000441,0.799322866751923,0.849492150063943,
0.894781080567531,0.938608217733336,0.980419226610287,1.),.UNSPECIFIED.);
#5290=B_SPLINE_CURVE_WITH_KNOTS('',3,(#181080,#181081,#181082,#181083,#181084,
#181085,#181086,#181087,#181088,#181089,#181090,#181091,#181092,#181093,
#181094,#181095,#181096,#181097,#181098,#181099,#181100,#181101,#181102,
#181103,#181104,#181105,#181106,#181107,#181108,#181109,#181110,#181111,
#181112,#181113,#181114,#181115,#181116,#181117,#181118,#181119,#181120,
#181121,#181122,#181123,#181124,#181125,#181126,#181127,#181128,#181129,
#181130,#181131,#181132,#181133,#181134,#181135,#181136,#181137,#181138,
#181139,#181140,#181141,#181142,#181143,#181144,#181145,#181146,#181147,
#181148,#181149,#181150,#181151,#181152,#181153,#181154,#181155),
 .UNSPECIFIED.,.F.,.F.,(4,3,3,3,3,3,3,3,3,3,3,3,3,3,3,3,3,3,3,3,3,3,3,3,
3,4),(0.,0.0430097489401156,0.0878255530574435,0.125000000000092,0.172143319139764,
0.187500000000139,0.21875000000016,0.234375000000171,0.242187500000173,
0.247546309687597,0.250000000000175,0.309158560547553,0.369866709953412,
0.375000000000161,0.437851735660631,0.468750000000141,0.483324625752687,
0.497499771574761,0.500000000000134,0.577335603884166,0.65558923123085,
0.734790431366338,0.81546526367158,0.897008160014305,0.979844362759134,
1.),.UNSPECIFIED.);
#5291=B_SPLINE_CURVE_WITH_KNOTS('',3,(#181204,#181205,#181206,#181207,#181208,
#181209,#181210,#181211,#181212,#181213,#181214,#181215,#181216,#181217,
#181218,#181219,#181220,#181221),.UNSPECIFIED.,.F.,.F.,(4,2,2,2,1,1,2,2,
2,4),(0.,0.249999999999941,0.374999999999907,0.437499999999891,0.468749999999884,
0.484374999999875,0.492187499999875,0.499999999999874,0.749999999999937,
1.),.UNSPECIFIED.);
#5292=B_SPLINE_CURVE_WITH_KNOTS('',3,(#181229,#181230,#181231,#181232,#181233,
#181234,#181235,#181236,#181237,#181238,#181239,#181240,#181241,#181242,
#181243,#181244,#181245,#181246,#181247,#181248,#181249,#181250,#181251,
#181252,#181253,#181254,#181255,#181256,#181257,#181258,#181259,#181260,
#181261,#181262,#181263,#181264,#181265,#181266,#181267,#181268,#181269,
#181270,#181271,#181272,#181273,#181274,#181275,#181276,#181277,#181278,
#181279,#181280),.UNSPECIFIED.,.F.,.F.,(4,3,3,3,3,3,3,3,3,3,3,3,3,3,3,3,
3,4),(0.,0.0670765920356927,0.13598231875245,0.207892462939091,0.28167954349829,
0.358370245208511,0.374999999999787,0.437499999999752,0.468749999999743,
0.484374999999756,0.49392515163699,0.499999999999768,0.589682112064697,
0.680498948238462,0.773128091633332,0.866800460343817,0.962105139368486,
1.),.UNSPECIFIED.);
#5293=B_SPLINE_CURVE_WITH_KNOTS('',3,(#181308,#181309,#181310,#181311,#181312,
#181313,#181314,#181315,#181316,#181317,#181318,#181319,#181320,#181321,
#181322,#181323,#181324,#181325,#181326,#181327,#181328,#181329,#181330,
#181331,#181332,#181333,#181334,#181335,#181336,#181337,#181338,#181339,
#181340,#181341,#181342,#181343,#181344),.UNSPECIFIED.,.F.,.F.,(4,3,3,3,
3,3,3,3,3,3,3,3,4),(0.000461676008985161,0.000632546215505795,0.00084808124100127,
0.000931278160334732,0.0011451568350677,0.00130839695615338,0.00168583810655035,
0.00182863766115024,0.00206327508940322,0.0024407173257478,0.00251211848723277,
0.00307037767189825,0.00319559931331531),.UNSPECIFIED.);
#5294=B_SPLINE_CURVE_WITH_KNOTS('',3,(#181403,#181404,#181405,#181406,#181407,
#181408,#181409,#181410,#181411,#181412,#181413,#181414,#181415,#181416),
 .UNSPECIFIED.,.F.,.F.,(4,2,2,2,2,2,4),(0.,0.249999999999991,0.374999999999987,
0.437499999999983,0.499999999999979,0.749999999999989,1.),.UNSPECIFIED.);
#5295=B_SPLINE_CURVE_WITH_KNOTS('',3,(#181417,#181418,#181419,#181420,#181421,
#181422,#181423,#181424,#181425,#181426,#181427,#181428,#181429,#181430,
#181431,#181432,#181433,#181434,#181435,#181436,#181437,#181438,#181439,
#181440,#181441,#181442,#181443,#181444,#181445,#181446),.UNSPECIFIED.,
 .F.,.F.,(4,2,2,2,1,1,1,2,2,2,2,1,1,1,2,2,2,4),(0.,0.125000000000023,0.187500000000034,
0.218750000000039,0.234375000000041,0.242187500000045,0.246093750000045,
0.248046875000043,0.250000000000041,0.374999999999938,0.437499999999886,
0.468749999999863,0.48437499999985,0.492187499999843,0.496093749999843,
0.499999999999843,0.749999999999921,1.),.UNSPECIFIED.);
#5296=B_SPLINE_CURVE_WITH_KNOTS('',3,(#181461,#181462,#181463,#181464,#181465,
#181466,#181467,#181468,#181469,#181470,#181471,#181472,#181473,#181474,
#181475,#181476,#181477,#181478,#181479,#181480,#181481,#181482,#181483,
#181484,#181485,#181486,#181487,#181488,#181489,#181490,#181491,#181492,
#181493,#181494,#181495,#181496,#181497,#181498,#181499,#181500,#181501,
#181502,#181503,#181504,#181505,#181506,#181507,#181508,#181509,#181510,
#181511,#181512,#181513,#181514,#181515,#181516,#181517,#181518,#181519,
#181520,#181521,#181522,#181523,#181524,#181525,#181526,#181527,#181528,
#181529,#181530,#181531,#181532,#181533,#181534,#181535,#181536,#181537,
#181538,#181539,#181540,#181541,#181542,#181543,#181544,#181545,#181546,
#181547,#181548,#181549,#181550,#181551,#181552,#181553,#181554,#181555,
#181556,#181557,#181558,#181559,#181560,#181561,#181562,#181563,#181564,
#181565,#181566,#181567,#181568,#181569,#181570,#181571,#181572,#181573,
#181574,#181575,#181576,#181577,#181578,#181579,#181580,#181581,#181582,
#181583,#181584,#181585,#181586,#181587,#181588,#181589,#181590),
 .UNSPECIFIED.,.F.,.F.,(4,3,3,3,3,3,3,3,3,3,3,3,3,3,3,3,3,3,3,3,3,3,3,3,
3,3,3,3,3,3,3,3,3,3,3,3,3,3,3,3,3,3,3,4),(0.,0.062499999999966,0.120656530897949,
0.176870757385599,0.230542201431043,0.249999999999864,0.259793340669136,
0.313569339020365,0.35253241852512,0.371529541832909,0.380609090930782,
0.425963310764886,0.461524220485096,0.479304675345201,0.488194902775253,
0.49264001649028,0.495270859962502,0.495839588709159,0.496320627056616,
0.497085130205306,0.499236772471531,0.499899226174417,0.5001602572298,0.567475246236759,
0.601132740740238,0.61841473872259,0.633624637649322,0.634790235243718,
0.671680165287415,0.690752079936576,0.730043729761344,0.748046874999687,
0.748752498895434,0.749999999999691,0.779220977126903,0.808330934535299,
0.837387447374634,0.86638313108366,0.874999999999846,0.903412282810721,
0.93238433174654,0.961715718964714,0.991613901781098,1.),.UNSPECIFIED.);
#5297=B_SPLINE_CURVE_WITH_KNOTS('',3,(#181634,#181635,#181636,#181637,#181638,
#181639,#181640,#181641,#181642,#181643,#181644,#181645,#181646,#181647,
#181648,#181649,#181650,#181651,#181652,#181653,#181654,#181655,#181656,
#181657,#181658,#181659,#181660,#181661,#181662,#181663,#181664,#181665,
#181666,#181667,#181668,#181669,#181670,#181671,#181672,#181673,#181674,
#181675,#181676,#181677,#181678,#181679,#181680,#181681,#181682,#181683,
#181684,#181685,#181686,#181687,#181688,#181689,#181690,#181691),
 .UNSPECIFIED.,.F.,.F.,(4,3,3,3,3,3,3,3,3,3,3,3,3,3,3,3,3,3,3,4),(0.,0.0624999999999946,
0.132935195695894,0.187179787252051,0.220234134189882,0.236211803414422,
0.26695249642912,0.339621823531675,0.395049568810745,0.445404134727815,
0.458833950506198,0.484374999999953,0.493493076075797,0.499999999999957,
0.585514487699712,0.672074572499599,0.730941551546193,0.820268275761333,
0.912558465070212,1.),.UNSPECIFIED.);
#5298=B_SPLINE_CURVE_WITH_KNOTS('',3,(#181692,#181693,#181694,#181695,#181696,
#181697,#181698,#181699,#181700,#181701,#181702,#181703,#181704,#181705,
#181706,#181707,#181708,#181709,#181710,#181711,#181712,#181713,#181714,
#181715,#181716,#181717,#181718,#181719,#181720,#181721,#181722,#181723,
#181724,#181725,#181726,#181727,#181728),.UNSPECIFIED.,.F.,.F.,(4,3,3,3,
3,3,3,3,3,3,3,3,4),(0.,0.000289456070004167,0.000578912140008334,0.000732555002063405,
0.00109883518473064,0.00115782428001667,0.00146516214354768,0.001736736420025,
0.00183135727517645,0.00202619249002917,0.00217092052503125,0.00219767702911212,
0.00231564856003333),.UNSPECIFIED.);
#5299=B_SPLINE_CURVE_WITH_KNOTS('',3,(#181755,#181756,#181757,#181758,#181759,
#181760,#181761,#181762,#181763,#181764,#181765,#181766,#181767,#181768,
#181769,#181770,#181771,#181772,#181773,#181774,#181775,#181776,#181777,
#181778,#181779,#181780,#181781,#181782),.UNSPECIFIED.,.F.,.F.,(4,3,3,3,
3,3,3,3,3,4),(0.000653658633860215,0.000901612111392076,0.00110350292160905,
0.00119693882169383,0.00132842506548346,0.00148931670393185,0.00155334720935788,
0.0018252077501562,0.00223261138725129,0.00245303578485557),
 .UNSPECIFIED.);
#5300=B_SPLINE_CURVE_WITH_KNOTS('',3,(#181829,#181830,#181831,#181832,#181833,
#181834,#181835,#181836,#181837,#181838,#181839,#181840,#181841,#181842,
#181843,#181844,#181845,#181846,#181847,#181848,#181849,#181850,#181851,
#181852,#181853,#181854,#181855,#181856,#181857,#181858,#181859,#181860,
#181861,#181862,#181863,#181864,#181865,#181866,#181867,#181868,#181869,
#181870,#181871,#181872,#181873,#181874,#181875,#181876,#181877,#181878,
#181879,#181880,#181881,#181882,#181883,#181884,#181885,#181886,#181887,
#181888,#181889,#181890,#181891,#181892,#181893,#181894,#181895,#181896,
#181897,#181898,#181899,#181900,#181901),.UNSPECIFIED.,.F.,.F.,(4,3,3,3,
3,3,3,3,3,3,3,3,3,3,3,3,3,3,3,3,3,3,3,3,4),(8.44303797994522E-15,0.135144161881906,
0.24999999999991,0.349909277361936,0.374999999999867,0.437499999999847,
0.46874999999984,0.484374999999842,0.493921148051312,0.499999999999845,
0.562216067098283,0.565498317572536,0.624999999999914,0.67538814217395,
0.683242331719054,0.687499999999947,0.718749999999953,0.73193993458769,
0.744411742542878,0.749999999999959,0.795268362209216,0.848575988791016,
0.901164076236429,0.952422125938682,1.),.UNSPECIFIED.);
#5301=B_SPLINE_CURVE_WITH_KNOTS('',3,(#181902,#181903,#181904,#181905,#181906,
#181907,#181908,#181909,#181910,#181911,#181912,#181913,#181914,#181915,
#181916,#181917,#181918,#181919,#181920,#181921,#181922,#181923,#181924,
#181925,#181926,#181927,#181928,#181929,#181930,#181931,#181932,#181933,
#181934,#181935,#181936,#181937,#181938,#181939,#181940,#181941),
 .UNSPECIFIED.,.F.,.F.,(4,3,3,3,3,3,3,3,3,3,3,3,3,4),(0.,0.0779250053195204,
0.155057508641545,0.231528329066271,0.307465716646408,0.382995817637975,
0.460121340433228,0.535227647548595,0.610339521074979,0.685565358678351,
0.764174019008763,0.840195626431609,0.920097813215804,1.),.UNSPECIFIED.);
#5302=B_SPLINE_CURVE_WITH_KNOTS('',3,(#181956,#181957,#181958,#181959,#181960,
#181961,#181962,#181963,#181964,#181965,#181966,#181967,#181968,#181969,
#181970,#181971,#181972,#181973,#181974,#181975,#181976,#181977,#181978,
#181979,#181980,#181981,#181982,#181983,#181984,#181985,#181986,#181987,
#181988,#181989,#181990,#181991,#181992,#181993,#181994,#181995,#181996,
#181997,#181998,#181999,#182000,#182001,#182002,#182003,#182004,#182005,
#182006,#182007,#182008,#182009,#182010,#182011,#182012,#182013,#182014,
#182015,#182016),.UNSPECIFIED.,.F.,.F.,(4,3,3,3,3,3,3,3,3,3,3,3,3,3,3,3,
3,3,3,3,4),(0.,0.0773791158424523,0.154909736797379,0.232737497421732,0.25,
0.333103137439076,0.348714047736977,0.408234656906365,0.465438190403892,
0.5,0.554799431810658,0.601556608085492,0.65460625822029,0.708180619658644,
0.75,0.798278525182264,0.811109335356995,0.861461000849684,0.911120449252677,
0.959993731055844,1.),.UNSPECIFIED.);
#5303=B_SPLINE_CURVE_WITH_KNOTS('',3,(#182048,#182049,#182050,#182051,#182052,
#182053,#182054,#182055,#182056,#182057,#182058,#182059,#182060,#182061,
#182062,#182063,#182064,#182065,#182066,#182067,#182068,#182069,#182070,
#182071,#182072,#182073,#182074,#182075,#182076,#182077,#182078,#182079,
#182080,#182081,#182082,#182083,#182084,#182085,#182086,#182087,#182088,
#182089,#182090,#182091,#182092,#182093,#182094,#182095,#182096,#182097,
#182098,#182099,#182100,#182101,#182102,#182103,#182104,#182105,#182106,
#182107,#182108,#182109,#182110,#182111,#182112,#182113,#182114,#182115,
#182116,#182117),.UNSPECIFIED.,.F.,.F.,(4,3,3,3,3,3,3,3,3,3,3,3,3,3,3,3,
3,3,3,3,3,3,3,4),(2.30429796095351E-13,0.0653635991916027,0.124999999999902,
0.172311751454373,0.201820164413576,0.204919298358608,0.218749999999829,
0.230991507982218,0.243867579297171,0.249999999999807,0.312499999999765,
0.374999999999722,0.435313808412958,0.437499999999674,0.468749999999655,
0.484374999999648,0.493599726240859,0.49999999999964,0.591487052058411,
0.685705265585678,0.714514960993195,0.818813520304589,0.926648756273366,
1.),.UNSPECIFIED.);
#5304=B_SPLINE_CURVE_WITH_KNOTS('',3,(#182118,#182119,#182120,#182121,#182122,
#182123,#182124,#182125,#182126,#182127,#182128,#182129,#182130,#182131,
#182132,#182133,#182134,#182135,#182136,#182137,#182138,#182139,#182140,
#182141,#182142,#182143,#182144,#182145),.UNSPECIFIED.,.F.,.F.,(4,3,3,3,
3,3,3,3,3,4),(0.,0.000434392388669906,0.000626649590030441,0.000901221465792679,
0.00106184511664208,0.00112652683224085,0.00125380565733158,0.00135183219868902,
0.00158807055660732,0.00180244293158536),.UNSPECIFIED.);
#5305=B_SPLINE_CURVE_WITH_KNOTS('',3,(#182172,#182173,#182174,#182175,#182176,
#182177,#182178,#182179,#182180,#182181,#182182,#182183,#182184,#182185,
#182186,#182187,#182188,#182189,#182190,#182191,#182192,#182193,#182194,
#182195,#182196,#182197,#182198,#182199,#182200,#182201,#182202,#182203,
#182204,#182205,#182206,#182207,#182208),.UNSPECIFIED.,.F.,.F.,(4,3,3,3,
3,3,3,3,3,3,3,3,4),(0.000646102271928282,0.000780355288939433,0.000794331971528649,
0.00113223030152275,0.00115328378670241,0.00123902107032975,0.00152620034295103,
0.00183193986873122,0.00189906794388761,0.00227197283133227,0.00242485866713269,
0.00272131806633342,0.00301777746553416),.UNSPECIFIED.);
#5306=B_SPLINE_CURVE_WITH_KNOTS('',3,(#182267,#182268,#182269,#182270,#182271,
#182272,#182273,#182274,#182275,#182276,#182277,#182278,#182279,#182280,
#182281,#182282,#182283,#182284,#182285,#182286,#182287,#182288,#182289,
#182290,#182291,#182292,#182293,#182294,#182295,#182296,#182297,#182298,
#182299,#182300,#182301,#182302,#182303,#182304,#182305,#182306,#182307,
#182308,#182309,#182310,#182311,#182312,#182313,#182314,#182315,#182316,
#182317,#182318,#182319,#182320,#182321,#182322,#182323,#182324,#182325,
#182326,#182327,#182328,#182329,#182330,#182331,#182332,#182333,#182334,
#182335,#182336,#182337,#182338,#182339,#182340,#182341,#182342),
 .UNSPECIFIED.,.F.,.F.,(4,3,3,3,3,3,3,3,3,3,3,3,3,3,3,3,3,3,3,3,3,3,3,3,
3,4),(0.,0.0747149608966636,0.149327349717458,0.224017940702021,0.249999999999885,
0.267379393754175,0.368064696876988,0.403285137580062,0.468749999999801,
0.484374999999806,0.494437622037064,0.499999999999811,0.542078850476596,
0.617551256841197,0.624999999999861,0.661231284595247,0.715848897344134,
0.718749999999887,0.734374999999892,0.748641071841499,0.749999999999896,
0.778559801946971,0.844934573565376,0.910167849387285,0.973985577236299,
1.),.UNSPECIFIED.);
#5307=B_SPLINE_CURVE_WITH_KNOTS('',3,(#182343,#182344,#182345,#182346,#182347,
#182348,#182349,#182350,#182351,#182352,#182353,#182354,#182355,#182356,
#182357,#182358,#182359,#182360,#182361,#182362,#182363,#182364,#182365,
#182366,#182367,#182368,#182369,#182370,#182371,#182372),.UNSPECIFIED.,
 .F.,.F.,(4,2,2,2,1,1,1,2,2,2,2,1,1,1,2,2,2,4),(0.,0.124999999999883,0.187499999999825,
0.218749999999798,0.234374999999784,0.242187499999776,0.246093749999774,
0.248046874999774,0.249999999999774,0.374999999999773,0.43749999999977,
0.468749999999767,0.484374999999767,0.492187499999767,0.496093749999768,
0.499999999999768,0.749999999999884,1.),.UNSPECIFIED.);
#5308=B_SPLINE_CURVE_WITH_KNOTS('',3,(#182387,#182388,#182389,#182390,#182391,
#182392,#182393,#182394,#182395,#182396,#182397,#182398,#182399,#182400,
#182401,#182402,#182403,#182404,#182405,#182406,#182407,#182408,#182409,
#182410,#182411,#182412,#182413,#182414,#182415,#182416,#182417,#182418),
 .UNSPECIFIED.,.F.,.F.,(4,2,2,2,1,1,1,2,2,2,2,2,1,1,1,2,2,2,4),(0.,0.249999999999888,
0.374999999999834,0.437499999999805,0.468749999999789,0.484374999999781,
0.492187499999776,0.496093749999774,0.499999999999773,0.624999999999617,
0.687499999999539,0.718749999999501,0.734374999999485,0.742187499999479,
0.746093749999476,0.748046874999477,0.749999999999478,0.874999999999739,
1.),.UNSPECIFIED.);
#5309=B_SPLINE_CURVE_WITH_KNOTS('',3,(#182462,#182463,#182464,#182465,#182466,
#182467,#182468,#182469,#182470,#182471,#182472,#182473,#182474,#182475,
#182476,#182477,#182478,#182479,#182480,#182481,#182482,#182483,#182484,
#182485,#182486,#182487,#182488,#182489,#182490,#182491,#182492,#182493,
#182494,#182495,#182496,#182497,#182498,#182499,#182500,#182501,#182502,
#182503,#182504,#182505,#182506,#182507,#182508,#182509,#182510,#182511,
#182512,#182513,#182514,#182515,#182516,#182517,#182518,#182519,#182520,
#182521,#182522,#182523,#182524,#182525),.UNSPECIFIED.,.F.,.F.,(4,3,3,3,
3,3,3,3,3,3,3,3,3,3,3,3,3,3,3,3,3,4),(6.93365572599307E-10,0.0799018607364408,
0.124999999999984,0.16590247381775,0.206515416690505,0.23522651337888,0.249999999999967,
0.308568145931547,0.367273300160574,0.425754288427686,0.470393849025489,
0.499999999999945,0.60399947981351,0.624999999999934,0.687499999999939,
0.711940888291548,0.72132830679594,0.746951441711128,0.749999999999944,
0.863504722177636,0.982906462376687,1.),.UNSPECIFIED.);
#5310=B_SPLINE_CURVE_WITH_KNOTS('',3,(#182526,#182527,#182528,#182529,#182530,
#182531,#182532,#182533,#182534,#182535,#182536,#182537,#182538,#182539,
#182540,#182541,#182542,#182543,#182544,#182545,#182546,#182547,#182548,
#182549,#182550,#182551,#182552,#182553,#182554,#182555,#182556,#182557,
#182558,#182559,#182560,#182561,#182562,#182563,#182564,#182565,#182566,
#182567,#182568,#182569,#182570,#182571,#182572,#182573,#182574,#182575,
#182576,#182577),.UNSPECIFIED.,.F.,.F.,(4,3,3,3,3,3,3,3,3,3,3,3,3,3,3,3,
3,4),(0.,0.000568167570453903,0.000689873068221808,0.000757350079825042,
0.000945020241885804,0.00103480960233271,0.0011360777163446,0.00136729697222071,
0.00137974613644361,0.00151477367390368,0.00189346791975904,0.0020696192046654,
0.00221265318266025,0.00227165379781724,0.00237143867201243,0.00256546547244981,
0.0026624788726685,0.00275949227288719),.UNSPECIFIED.);
#5311=B_SPLINE_CURVE_WITH_KNOTS('',3,(#182622,#182623,#182624,#182625,#182626,
#182627,#182628,#182629,#182630,#182631,#182632,#182633,#182634,#182635,
#182636,#182637,#182638,#182639,#182640,#182641,#182642,#182643,#182644,
#182645,#182646,#182647,#182648,#182649,#182650,#182651,#182652,#182653,
#182654,#182655,#182656,#182657,#182658,#182659,#182660,#182661,#182662,
#182663,#182664,#182665,#182666,#182667,#182668,#182669,#182670),
 .UNSPECIFIED.,.F.,.F.,(4,3,3,3,3,3,3,3,3,3,3,3,3,3,3,3,4),(0.,0.0948667215790916,
0.188589440506681,0.28179472025342,0.37500000000016,0.437500000000192,0.468750000000196,
0.484375000000191,0.493434737105491,0.500000000000186,0.580918025814847,
0.659023039321664,0.734520568710628,0.806482846270357,0.876608217979102,
0.944078406641015,1.),.UNSPECIFIED.);
#5312=B_SPLINE_CURVE_WITH_KNOTS('',3,(#182678,#182679,#182680,#182681,#182682,
#182683,#182684,#182685,#182686,#182687,#182688,#182689,#182690,#182691,
#182692,#182693,#182694,#182695,#182696,#182697,#182698,#182699,#182700,
#182701,#182702,#182703,#182704,#182705,#182706,#182707,#182708,#182709,
#182710,#182711,#182712,#182713,#182714,#182715,#182716,#182717,#182718,
#182719,#182720,#182721,#182722,#182723,#182724,#182725,#182726,#182727,
#182728,#182729,#182730,#182731,#182732,#182733,#182734,#182735,#182736,
#182737,#182738,#182739,#182740,#182741,#182742,#182743,#182744,#182745,
#182746,#182747,#182748,#182749,#182750,#182751,#182752,#182753),
 .UNSPECIFIED.,.F.,.F.,(4,3,3,3,3,3,3,3,3,3,3,3,3,3,3,3,3,3,3,3,3,3,3,3,
3,4),(0.,0.0421877665880278,0.0918529461680548,0.121595727119581,0.156341218045798,
0.187500000000267,0.2187500000003,0.234375000000331,0.242187500000325,0.246093750000323,
0.25000000000032,0.259656373146243,0.33431792746277,0.375000000000227,0.437500000000185,
0.48437500000018,0.494310480798385,0.500000000000185,0.515232119733451,
0.593015658117578,0.675285422265481,0.712991994452306,0.801479119446512,
0.856495997226153,0.935184420368532,1.),.UNSPECIFIED.);
#5313=B_SPLINE_CURVE_WITH_KNOTS('',3,(#182792,#182793,#182794,#182795,#182796,
#182797,#182798,#182799,#182800,#182801,#182802,#182803,#182804),
 .UNSPECIFIED.,.F.,.F.,(4,3,3,3,4),(0.,0.304005884126683,0.606187253193727,
0.905860933135587,1.),.UNSPECIFIED.);
#5314=B_SPLINE_CURVE_WITH_KNOTS('',3,(#182811,#182812,#182813,#182814,#182815,
#182816,#182817,#182818,#182819,#182820,#182821,#182822,#182823,#182824,
#182825,#182826,#182827,#182828,#182829,#182830,#182831,#182832,#182833,
#182834,#182835,#182836,#182837,#182838,#182839,#182840,#182841,#182842,
#182843,#182844,#182845,#182846,#182847,#182848,#182849,#182850,#182851,
#182852,#182853),.UNSPECIFIED.,.F.,.F.,(4,3,3,3,3,3,3,3,3,3,3,3,3,3,4),
(0.,0.114160776840688,0.232043703654348,0.249999999999881,0.374999999999845,
0.437499999999821,0.468749999999809,0.47471823218372,0.489504435425131,
0.499999999999797,0.613342917066077,0.721572740801358,0.827582465287451,
0.930897765172478,1.),.UNSPECIFIED.);
#5315=B_SPLINE_CURVE_WITH_KNOTS('',3,(#182855,#182856,#182857,#182858),
 .UNSPECIFIED.,.F.,.F.,(4,4),(0.,1.),.UNSPECIFIED.);
#5316=B_SPLINE_CURVE_WITH_KNOTS('',3,(#182866,#182867,#182868,#182869,#182870,
#182871,#182872,#182873,#182874,#182875,#182876,#182877,#182878),
 .UNSPECIFIED.,.F.,.F.,(4,3,3,3,4),(0.,0.25,0.496827497839013,0.750275035845233,
1.),.UNSPECIFIED.);
#5317=B_SPLINE_CURVE_WITH_KNOTS('',3,(#182884,#182885,#182886,#182887,#182888,
#182889,#182890,#182891,#182892,#182893,#182894,#182895,#182896,#182897,
#182898,#182899,#182900,#182901,#182902,#182903,#182904,#182905,#182906,
#182907,#182908,#182909,#182910,#182911,#182912,#182913,#182914,#182915,
#182916,#182917),.UNSPECIFIED.,.F.,.F.,(4,3,3,3,3,3,3,3,3,3,3,4),(0.,0.106653491061592,
0.219036071567704,0.250000000000003,0.334704087655355,0.420584442640105,
0.486614479419915,0.500000000000006,0.660932422463628,0.818357566951526,
0.966974096514476,1.),.UNSPECIFIED.);
#5318=B_SPLINE_CURVE_WITH_KNOTS('',3,(#182925,#182926,#182927,#182928),
 .UNSPECIFIED.,.F.,.F.,(4,4),(0.,6.88517764864569E-5),.UNSPECIFIED.);
#5319=B_SPLINE_CURVE_WITH_KNOTS('',3,(#182929,#182930,#182931,#182932,#182933,
#182934,#182935,#182936,#182937,#182938,#182939,#182940,#182941,#182942,
#182943,#182944,#182945,#182946,#182947,#182948,#182949,#182950,#182951,
#182952,#182953,#182954,#182955,#182956,#182957,#182958,#182959,#182960,
#182961,#182962,#182963,#182964,#182965,#182966,#182967,#182968,#182969,
#182970,#182971,#182972,#182973,#182974,#182975,#182976,#182977),
 .UNSPECIFIED.,.F.,.F.,(4,3,3,3,3,3,3,3,3,3,3,3,3,3,3,3,4),(0.,0.0789809457866306,
0.161285417776234,0.245599696437801,0.333230417767524,0.37499999999985,
0.437499999999833,0.46874999999983,0.484374999999829,0.49397464410552,0.499999999999828,
0.591682610550623,0.684555700018607,0.779305938640673,0.875152751961459,
0.972664363097949,1.),.UNSPECIFIED.);
#5320=B_SPLINE_CURVE_WITH_KNOTS('',3,(#182984,#182985,#182986,#182987,#182988,
#182989,#182990,#182991,#182992,#182993,#182994,#182995,#182996,#182997,
#182998,#182999,#183000,#183001,#183002,#183003,#183004,#183005,#183006,
#183007,#183008,#183009,#183010,#183011),.UNSPECIFIED.,.F.,.F.,(4,3,3,3,
3,3,3,3,3,4),(0.000712605368931889,0.000926461878734654,0.00114426125513561,
0.00117428487373109,0.00139094819074976,0.00157723429047313,0.00180778147057016,
0.00209481686703422,0.00237995362541951,0.00244186321201438),
 .UNSPECIFIED.);
#5321=B_SPLINE_CURVE_WITH_KNOTS('',3,(#183015,#183016,#183017,#183018,#183019,
#183020),.UNSPECIFIED.,.F.,.F.,(4,2,4),(0.,0.000500369188755688,0.00100073837751138),
 .UNSPECIFIED.);
#5322=B_SPLINE_CURVE_WITH_KNOTS('',3,(#183021,#183022,#183023,#183024),
 .UNSPECIFIED.,.F.,.F.,(4,4),(0.,0.0331958858056162),.UNSPECIFIED.);
#5323=B_SPLINE_CURVE_WITH_KNOTS('',3,(#183056,#183057,#183058,#183059,#183060,
#183061,#183062,#183063,#183064,#183065,#183066,#183067,#183068,#183069,
#183070,#183071,#183072,#183073,#183074,#183075,#183076,#183077,#183078,
#183079,#183080,#183081,#183082,#183083,#183084,#183085,#183086,#183087,
#183088,#183089,#183090,#183091,#183092,#183093,#183094,#183095,#183096,
#183097,#183098,#183099,#183100,#183101,#183102,#183103,#183104,#183105,
#183106,#183107,#183108,#183109,#183110,#183111,#183112,#183113,#183114,
#183115,#183116,#183117,#183118,#183119,#183120,#183121,#183122,#183123,
#183124,#183125),.UNSPECIFIED.,.F.,.F.,(4,3,3,3,3,3,3,3,3,3,3,3,3,3,3,3,
3,3,3,3,3,3,3,4),(0.,0.102857470141467,0.125000000000026,0.220263138689686,
0.250000000000052,0.284634156633098,0.375000000000079,0.4375000000001,0.468750000000111,
0.484375000000114,0.493913132672327,0.500000000000116,0.563704176814045,
0.62500000000009,0.682712478891769,0.699894434445292,0.734375000000072,
0.743077120945512,0.750000000000067,0.794106423027594,0.849243360995836,
0.903603919149664,0.957011397681897,0.999999993037464),.UNSPECIFIED.);
#5324=B_SPLINE_CURVE_WITH_KNOTS('',3,(#183126,#183127,#183128,#183129,#183130,
#183131,#183132,#183133,#183134,#183135,#183136,#183137,#183138,#183139,
#183140,#183141,#183142,#183143,#183144,#183145,#183146,#183147,#183148,
#183149,#183150,#183151,#183152,#183153,#183154,#183155,#183156,#183157,
#183158,#183159,#183160,#183161,#183162,#183163,#183164,#183165,#183166,
#183167,#183168,#183169,#183170,#183171,#183172,#183173,#183174,#183175,
#183176,#183177,#183178,#183179,#183180,#183181,#183182,#183183,#183184,
#183185,#183186,#183187,#183188,#183189,#183190,#183191,#183192,#183193,
#183194,#183195,#183196,#183197,#183198,#183199,#183200,#183201,#183202,
#183203,#183204,#183205,#183206,#183207,#183208,#183209,#183210),
 .UNSPECIFIED.,.F.,.F.,(4,3,3,3,3,3,3,3,3,3,3,3,3,3,3,3,3,3,3,3,3,3,3,3,
3,3,3,3,4),(0.,0.0312894328292875,0.0622354553383098,0.0936177276691337,
0.124999999999958,0.156249999999947,0.187499999999937,0.194792789675713,
0.202551490020127,0.203124999999931,0.218749999999926,0.242527406522679,
0.282862122212415,0.329320663124785,0.380198846483021,0.431355268401253,
0.485129013232248,0.496093749999816,0.499999999999818,0.502687086598598,
0.566609075637323,0.632182148458018,0.70053635082894,0.740544135088561,
0.749999999999909,0.823221108105435,0.897670430593762,0.974675815205079,
0.999999999970395),.UNSPECIFIED.);
#5325=B_SPLINE_CURVE_WITH_KNOTS('',3,(#183225,#183226,#183227,#183228,#183229,
#183230,#183231,#183232,#183233,#183234,#183235,#183236,#183237,#183238,
#183239,#183240,#183241,#183242,#183243,#183244,#183245,#183246,#183247,
#183248,#183249,#183250,#183251,#183252,#183253,#183254,#183255,#183256,
#183257,#183258,#183259,#183260,#183261,#183262,#183263,#183264,#183265,
#183266,#183267,#183268,#183269,#183270,#183271,#183272,#183273,#183274,
#183275,#183276,#183277,#183278,#183279,#183280,#183281,#183282,#183283,
#183284,#183285,#183286,#183287,#183288,#183289,#183290,#183291,#183292,
#183293,#183294,#183295,#183296,#183297,#183298,#183299,#183300,#183301,
#183302,#183303,#183304,#183305,#183306,#183307,#183308,#183309,#183310,
#183311,#183312,#183313,#183314,#183315,#183316,#183317,#183318),
 .UNSPECIFIED.,.F.,.F.,(4,3,3,3,3,3,3,3,3,3,3,3,3,3,3,3,3,3,3,3,3,3,3,3,
3,3,3,3,3,3,3,4),(0.,0.07198248742987,0.142766259275923,0.211951276696239,
0.250000000000095,0.317389348407017,0.383564948093474,0.437500000000164,
0.468750000000174,0.484375000000181,0.492187500000187,0.496093750000192,
0.49978162785641,0.500000000000198,0.553158315085203,0.604461352990886,
0.654731630643987,0.703470233159367,0.750000000000084,0.781250000000072,
0.78515625000007,0.788461425907795,0.789062500000069,0.796875000000065,
0.812500000000058,0.840059259163279,0.86829920100936,0.89716635807548,0.926821656402351,
0.956825743880503,0.987204115019961,1.),.UNSPECIFIED.);
#5326=B_SPLINE_CURVE_WITH_KNOTS('',3,(#183356,#183357,#183358,#183359,#183360,
#183361,#183362,#183363,#183364,#183365,#183366,#183367,#183368,#183369,
#183370,#183371,#183372,#183373,#183374,#183375,#183376,#183377,#183378,
#183379,#183380,#183381,#183382,#183383,#183384,#183385,#183386,#183387,
#183388,#183389,#183390,#183391,#183392,#183393,#183394,#183395,#183396,
#183397,#183398,#183399,#183400,#183401,#183402,#183403,#183404,#183405,
#183406,#183407,#183408,#183409,#183410,#183411,#183412,#183413,#183414,
#183415,#183416,#183417,#183418,#183419,#183420,#183421,#183422,#183423,
#183424,#183425),.UNSPECIFIED.,.F.,.F.,(4,3,3,3,3,3,3,3,3,3,3,3,3,3,3,3,
3,3,3,3,3,3,3,4),(3.27359973213996E-13,0.0857365026607216,0.124999999999915,
0.174375612862638,0.204585644336071,0.209083762348739,0.218749999999854,
0.232924773331302,0.247673015334756,0.249999999999833,0.312499999999785,
0.374999999999736,0.437499999999679,0.43884535386112,0.468749999999659,
0.484374999999656,0.493704288796288,0.499999999999654,0.59264919846013,
0.688070810914995,0.716212286393592,0.820643696798982,0.928592372305829,
0.999996088506396),.UNSPECIFIED.);
#5327=B_SPLINE_CURVE_WITH_KNOTS('',3,(#183426,#183427,#183428,#183429,#183430,
#183431,#183432,#183433,#183434,#183435,#183436,#183437,#183438,#183439,
#183440,#183441,#183442,#183443,#183444,#183445,#183446,#183447,#183448,
#183449,#183450,#183451,#183452,#183453,#183454,#183455,#183456),
 .UNSPECIFIED.,.F.,.F.,(4,3,3,3,3,3,3,3,3,3,4),(0.,0.000497569400086742,
0.000640953038946957,0.0009614312638914,0.000995138800173484,0.00128203532234786,
0.00149270820026023,0.00161710055028191,0.00180479162331784,0.00192302626316565,
0.00199027760034697),.UNSPECIFIED.);
#5328=B_SPLINE_CURVE_WITH_KNOTS('',3,(#183485,#183486,#183487,#183488,#183489,
#183490,#183491,#183492,#183493,#183494,#183495,#183496,#183497,#183498,
#183499,#183500,#183501,#183502,#183503,#183504,#183505,#183506,#183507,
#183508,#183509,#183510,#183511,#183512,#183513,#183514,#183515,#183516,
#183517,#183518,#183519,#183520,#183521,#183522,#183523,#183524,#183525,
#183526,#183527,#183528,#183529,#183530,#183531,#183532,#183533,#183534,
#183535,#183536,#183537,#183538,#183539,#183540,#183541,#183542,#183543,
#183544,#183545),.UNSPECIFIED.,.F.,.F.,(4,3,3,3,3,3,3,3,3,3,3,3,3,3,3,3,
3,3,3,3,4),(0.000632518815593833,0.000932214526658406,0.00101585454476649,
0.00107182189614633,0.00126737972551708,0.00139919027393915,0.00150973846725992,
0.00175129113716496,0.0017825260031118,0.00194741404639007,0.00209785990015683,
0.00215891919182298,0.00222254437896024,0.00246825757121381,0.00254919746145711,
0.00271487168756702,0.0028230834495401,0.00293253319062976,0.00318749230619698,
0.00344334847758602,0.00369920464897506),.UNSPECIFIED.);
#5329=B_SPLINE_CURVE_WITH_KNOTS('',3,(#183599,#183600,#183601,#183602,#183603,
#183604,#183605,#183606,#183607,#183608,#183609,#183610,#183611,#183612,
#183613,#183614,#183615,#183616,#183617,#183618,#183619,#183620,#183621,
#183622,#183623,#183624,#183625,#183626,#183627,#183628,#183629,#183630,
#183631,#183632,#183633,#183634,#183635,#183636,#183637,#183638,#183639,
#183640,#183641,#183642,#183643,#183644,#183645,#183646,#183647,#183648,
#183649,#183650,#183651,#183652,#183653,#183654,#183655,#183656,#183657,
#183658,#183659,#183660,#183661,#183662,#183663,#183664,#183665,#183666,
#183667,#183668,#183669,#183670,#183671,#183672,#183673,#183674,#183675,
#183676,#183677,#183678,#183679,#183680),.UNSPECIFIED.,.F.,.F.,(4,3,3,3,
3,3,3,3,3,3,3,3,3,3,3,3,3,3,3,3,3,3,3,3,3,3,3,4),(0.,0.0347059239069192,
0.0702944863998228,0.107079974258399,0.125000000000524,0.162191772866572,
0.187500000000781,0.218750000000929,0.234375000001002,0.242187500000992,
0.249424935941155,0.250000000000981,0.301248065768145,0.352433147510947,
0.375000000000836,0.437500000000757,0.468750000000713,0.484375000000691,
0.498608696187955,0.50000000000067,0.569611194950186,0.639357942877805,
0.709783596290922,0.750000000000335,0.822081078895063,0.895102993899266,
0.969950340120507,1.),.UNSPECIFIED.);
#5330=B_SPLINE_CURVE_WITH_KNOTS('',3,(#183681,#183682,#183683,#183684,#183685,
#183686,#183687,#183688,#183689,#183690,#183691,#183692,#183693,#183694,
#183695,#183696,#183697,#183698,#183699,#183700,#183701,#183702,#183703,
#183704,#183705,#183706,#183707,#183708,#183709,#183710,#183711,#183712,
#183713,#183714,#183715,#183716,#183717,#183718,#183719,#183720,#183721,
#183722,#183723,#183724,#183725,#183726,#183727,#183728,#183729,#183730,
#183731,#183732,#183733,#183734,#183735,#183736,#183737,#183738,#183739,
#183740,#183741,#183742,#183743,#183744,#183745,#183746,#183747,#183748,
#183749,#183750,#183751,#183752,#183753,#183754,#183755,#183756,#183757,
#183758,#183759,#183760,#183761,#183762,#183763,#183764,#183765,#183766,
#183767,#183768),.UNSPECIFIED.,.F.,.F.,(4,3,3,3,3,3,3,3,3,3,3,3,3,3,3,3,
3,3,3,3,3,3,3,3,3,3,3,3,3,4),(0.,0.0551115055721159,0.108953779567591,0.162273305591977,
0.21144363860674,0.236028805114121,0.248602245718417,0.256548955259473,
0.260613971621503,0.318507353716111,0.361927390287068,0.376413794214911,
0.423796678888208,0.471178079428924,0.492187499999938,0.497822391426295,
0.499999999999937,0.503298936899024,0.556038805749608,0.608145796234962,
0.635679690970773,0.685905062891556,0.737189132830948,0.749999999999968,
0.761847144546501,0.808861184933272,0.856645888699954,0.902952577790402,
0.951476288895201,1.),.UNSPECIFIED.);
#5331=B_SPLINE_CURVE_WITH_KNOTS('',3,(#183783,#183784,#183785,#183786,#183787,
#183788,#183789,#183790,#183791,#183792,#183793,#183794,#183795,#183796,
#183797,#183798,#183799,#183800,#183801,#183802,#183803,#183804,#183805,
#183806,#183807,#183808,#183809,#183810,#183811,#183812,#183813,#183814,
#183815,#183816,#183817,#183818,#183819,#183820,#183821,#183822,#183823,
#183824,#183825,#183826,#183827,#183828,#183829,#183830,#183831,#183832,
#183833,#183834,#183835,#183836,#183837,#183838,#183839,#183840,#183841,
#183842,#183843,#183844,#183845,#183846,#183847,#183848,#183849,#183850,
#183851,#183852,#183853,#183854,#183855,#183856,#183857,#183858,#183859,
#183860,#183861,#183862,#183863,#183864),.UNSPECIFIED.,.F.,.F.,(4,3,3,3,
3,3,3,3,3,3,3,3,3,3,3,3,3,3,3,3,3,3,3,3,3,3,3,4),(1.34985451482093E-13,
0.056751333121689,0.111716230590216,0.165601173577879,0.217745992585657,
0.250000000000001,0.300400507324752,0.350801014649504,0.389142445556312,
0.426377110084194,0.462057538976088,0.488683010340457,0.500000000000003,
0.54693009782314,0.591723632592143,0.606245868675057,0.625000000000002,
0.660743347771245,0.696577628491914,0.712544338223846,0.750000000000001,
0.811350030058359,0.866771747342932,0.875000000000001,0.911268783979688,
0.947507821305827,0.983698341291556,1.),.UNSPECIFIED.);
#5332=B_SPLINE_CURVE_WITH_KNOTS('',3,(#183908,#183909,#183910,#183911,#183912,
#183913,#183914,#183915,#183916,#183917,#183918,#183919,#183920,#183921,
#183922,#183923,#183924,#183925,#183926,#183927,#183928,#183929,#183930,
#183931,#183932,#183933,#183934,#183935,#183936,#183937,#183938,#183939,
#183940,#183941,#183942,#183943,#183944,#183945,#183946,#183947,#183948,
#183949,#183950,#183951,#183952,#183953,#183954,#183955,#183956,#183957,
#183958,#183959,#183960,#183961,#183962,#183963,#183964,#183965,#183966,
#183967,#183968,#183969,#183970,#183971),.UNSPECIFIED.,.F.,.F.,(4,3,3,3,
3,3,3,3,3,3,3,3,3,3,3,3,3,3,3,3,3,4),(8.59038016877541E-10,0.0733303750771787,
0.125000000000027,0.190074946227628,0.22888061590917,0.294022873922094,
0.36021312493933,0.430448645641966,0.484375000000101,0.493741968173762,
0.500000000000104,0.504812740617916,0.587025088775253,0.625000000000078,
0.681677197130213,0.715381499528901,0.736543530082876,0.766480294100765,
0.838951501085421,0.875000000000026,0.954886761461704,1.),.UNSPECIFIED.);
#5333=B_SPLINE_CURVE_WITH_KNOTS('',3,(#183972,#183973,#183974,#183975,#183976,
#183977,#183978,#183979,#183980,#183981,#183982,#183983,#183984,#183985,
#183986,#183987,#183988,#183989,#183990,#183991,#183992,#183993,#183994,
#183995,#183996,#183997,#183998,#183999,#184000,#184001,#184002,#184003,
#184004,#184005,#184006,#184007,#184008,#184009,#184010,#184011,#184012,
#184013,#184014,#184015,#184016,#184017,#184018,#184019,#184020,#184021,
#184022,#184023,#184024,#184025,#184026,#184027,#184028,#184029,#184030,
#184031,#184032,#184033,#184034,#184035),.UNSPECIFIED.,.F.,.F.,(4,3,3,3,
3,3,3,3,3,3,3,3,3,3,3,3,3,3,3,3,3,4),(0.,0.000243943071869819,0.000489165049879495,
0.000733924827046607,0.000899069239743237,0.000911316177023075,0.00119563029973622,
0.00134860385961487,0.00136698289390588,0.00175854423317811,0.0017981384794865,
0.00182264071786974,0.00224767309935813,0.00227830273883051,0.00257044019241884,
0.00269720771922976,0.002733987473331,0.00295810023175296,0.0031467423391014,
0.00331012937356572,0.00347290261708232,0.00359627695897302),
 .UNSPECIFIED.);
#5334=B_SPLINE_CURVE_WITH_KNOTS('',3,(#184082,#184083,#184084,#184085,#184086,
#184087,#184088,#184089,#184090,#184091,#184092,#184093,#184094,#184095,
#184096,#184097,#184098,#184099,#184100,#184101,#184102,#184103,#184104,
#184105,#184106,#184107,#184108,#184109,#184110,#184111,#184112,#184113,
#184114,#184115,#184116,#184117,#184118,#184119,#184120,#184121,#184122,
#184123,#184124,#184125,#184126,#184127,#184128,#184129,#184130,#184131,
#184132,#184133,#184134,#184135,#184136,#184137,#184138,#184139,#184140,
#184141,#184142,#184143,#184144,#184145,#184146,#184147,#184148,#184149,
#184150,#184151,#184152,#184153,#184154,#184155,#184156,#184157,#184158,
#184159,#184160,#184161,#184162,#184163),.UNSPECIFIED.,.F.,.F.,(4,3,3,3,
3,3,3,3,3,3,3,3,3,3,3,3,3,3,3,3,3,3,3,3,3,3,3,4),(0.,0.0863130095180163,
0.124999999999993,0.187499999999993,0.218749999999993,0.232144860506862,
0.247931741713982,0.249999999999992,0.333313232249592,0.37499999999993,
0.437499999999906,0.468749999999902,0.476693585153444,0.491282462856874,
0.499999999999898,0.57747845846861,0.624999999999936,0.68749999999994,0.718749999999944,
0.734374999999939,0.735025645679648,0.744357247627351,0.749999999999935,
0.812499999999951,0.87138267660412,0.927432801000241,0.979960253731857,
1.),.UNSPECIFIED.);
#5335=B_SPLINE_CURVE_WITH_KNOTS('',3,(#184171,#184172,#184173,#184174,#184175,
#184176,#184177,#184178,#184179,#184180,#184181,#184182,#184183,#184184,
#184185,#184186),.UNSPECIFIED.,.F.,.F.,(4,2,2,2,1,1,2,2,4),(0.,0.249999999999856,
0.374999999999799,0.437499999999791,0.468749999999786,0.484374999999784,
0.492187499999798,0.499999999999811,1.),.UNSPECIFIED.);
#5336=B_SPLINE_CURVE_WITH_KNOTS('',3,(#184207,#184208,#184209,#184210,#184211,
#184212,#184213,#184214,#184215,#184216,#184217,#184218,#184219,#184220,
#184221,#184222),.UNSPECIFIED.,.F.,.F.,(4,3,3,3,3,4),(0.,0.228004650890224,
0.457585570846926,0.688183484414605,0.920419006980701,1.),.UNSPECIFIED.);
#5337=B_SPLINE_CURVE_WITH_KNOTS('',3,(#184227,#184228,#184229,#184230,#184231,
#184232,#184233,#184234,#184235,#184236,#184237,#184238,#184239,#184240,
#184241,#184242,#184243,#184244,#184245,#184246,#184247,#184248,#184249,
#184250,#184251,#184252,#184253,#184254,#184255,#184256,#184257,#184258,
#184259,#184260),.UNSPECIFIED.,.F.,.F.,(4,3,3,3,3,3,3,3,3,3,3,4),(0.,0.137126090839981,
0.258934713814541,0.410851602161014,0.468750000000055,0.490339286585085,
0.500000000000056,0.513599342481747,0.6455154402161,0.774520962955583,0.899340216824067,
1.),.UNSPECIFIED.);
#5338=B_SPLINE_CURVE_WITH_KNOTS('',3,(#184261,#184262,#184263,#184264,#184265,
#184266,#184267,#184268,#184269,#184270,#184271,#184272,#184273,#184274,
#184275,#184276,#184277,#184278,#184279,#184280,#184281,#184282,#184283,
#184284,#184285,#184286,#184287,#184288,#184289,#184290,#184291),
 .UNSPECIFIED.,.F.,.F.,(4,3,3,3,3,3,3,3,3,3,4),(0.,0.0729993287143241,0.1205082445585,
0.219240574404831,0.349365992062872,0.499876044794966,0.502870118528192,
0.562504597086005,0.749896118500103,0.887412448086525,1.),.UNSPECIFIED.);
#5339=B_SPLINE_CURVE_WITH_KNOTS('',3,(#184296,#184297,#184298,#184299,#184300,
#184301,#184302,#184303,#184304,#184305,#184306,#184307,#184308,#184309,
#184310,#184311,#184312,#184313,#184314,#184315,#184316,#184317,#184318,
#184319,#184320,#184321,#184322,#184323,#184324,#184325,#184326,#184327,
#184328,#184329,#184330,#184331,#184332,#184333,#184334,#184335,#184336,
#184337,#184338,#184339,#184340,#184341,#184342,#184343,#184344,#184345,
#184346,#184347,#184348,#184349,#184350,#184351,#184352,#184353,#184354,
#184355,#184356,#184357,#184358,#184359,#184360,#184361,#184362,#184363,
#184364,#184365),.UNSPECIFIED.,.F.,.F.,(4,3,3,3,3,3,3,3,3,3,3,3,3,3,3,3,
3,3,3,3,3,3,3,4),(0.,0.0795438263529059,0.124999999999882,0.187499999999824,
0.218749999999794,0.231135975157282,0.249999999999765,0.342939196677063,
0.374999999999647,0.437499999999583,0.468749999999534,0.484374999999514,
0.492187499999508,0.498391551397716,0.499999999999502,0.527623760044591,
0.604845273664748,0.683741209693796,0.714465797142799,0.754800912699018,
0.84727383837472,0.8572328985714,0.930360007098205,1.),.UNSPECIFIED.);
#5340=B_SPLINE_CURVE_WITH_KNOTS('',3,(#184413,#184414,#184415,#184416,#184417,
#184418,#184419,#184420,#184421,#184422,#184423,#184424,#184425,#184426,
#184427,#184428,#184429,#184430),.UNSPECIFIED.,.F.,.F.,(4,2,2,2,1,1,2,2,
2,4),(0.,0.250000000000419,0.375000000000626,0.437500000000725,0.468750000000762,
0.484375000000761,0.492187500000745,0.500000000000729,0.750000000000364,
1.),.UNSPECIFIED.);
#5341=B_SPLINE_CURVE_WITH_KNOTS('',3,(#184438,#184439,#184440,#184441,#184442,
#184443,#184444,#184445,#184446,#184447,#184448,#184449,#184450,#184451,
#184452,#184453,#184454,#184455,#184456,#184457,#184458,#184459,#184460,
#184461,#184462,#184463,#184464,#184465,#184466,#184467,#184468,#184469,
#184470,#184471,#184472,#184473,#184474,#184475,#184476,#184477,#184478,
#184479,#184480,#184481,#184482,#184483,#184484,#184485,#184486,#184487,
#184488,#184489),.UNSPECIFIED.,.F.,.F.,(4,3,3,3,3,3,3,3,3,3,3,3,3,3,3,3,
3,4),(0.,0.0670799139916658,0.13599024748976,0.207907147469578,0.281702493042214,
0.358403426941099,0.374999999999999,0.437499999999991,0.468749999999991,
0.48437499999998,0.493917046584479,0.49999999999997,0.589612381791532,0.680360224688852,
0.772922373758745,0.866528534163224,0.961769826620013,1.),.UNSPECIFIED.);
#5342=B_SPLINE_CURVE_WITH_KNOTS('',3,(#184521,#184522,#184523,#184524,#184525,
#184526,#184527,#184528,#184529,#184530,#184531,#184532,#184533,#184534,
#184535,#184536,#184537,#184538,#184539,#184540,#184541,#184542,#184543,
#184544,#184545,#184546,#184547,#184548,#184549,#184550,#184551,#184552,
#184553,#184554,#184555,#184556,#184557,#184558,#184559,#184560,#184561,
#184562,#184563,#184564,#184565,#184566),.UNSPECIFIED.,.F.,.F.,(4,3,3,3,
3,3,3,3,3,3,3,3,3,3,3,4),(0.000450499470650019,0.00054011395429817,0.000798583304342707,
0.000986883024373894,0.00116741533983523,0.00137527276208874,0.00169825994125316,
0.00176385446568028,0.00188433120902044,0.00210726599696856,0.00224278914361301,
0.00241357708828738,0.00254109024997703,0.0026012470782056,0.00316630230572219,
0.00331816294739075),.UNSPECIFIED.);
#5343=B_SPLINE_CURVE_WITH_KNOTS('',3,(#184619,#184620,#184621,#184622,#184623,
#184624,#184625,#184626,#184627,#184628,#184629,#184630,#184631,#184632,
#184633,#184634,#184635,#184636,#184637,#184638,#184639,#184640,#184641,
#184642,#184643,#184644,#184645,#184646,#184647,#184648,#184649,#184650,
#184651,#184652,#184653,#184654,#184655,#184656,#184657,#184658,#184659,
#184660,#184661,#184662,#184663,#184664,#184665,#184666,#184667,#184668,
#184669,#184670,#184671,#184672,#184673,#184674,#184675,#184676,#184677,
#184678,#184679,#184680,#184681,#184682),.UNSPECIFIED.,.F.,.F.,(4,3,3,3,
3,3,3,3,3,3,3,3,3,3,3,3,3,3,3,3,3,4),(0.,0.0922518249521236,0.124999999999966,
0.187499999999968,0.21401656664708,0.239789942133961,0.24999999999997,0.275182709279866,
0.401192886020697,0.499999999999992,0.524820514521064,0.618210322834091,
0.624999999999993,0.662910196285119,0.700740355222286,0.739058341955884,
0.749999999999994,0.762750903735254,0.832354637129329,0.902472607068448,
0.972781141742723,0.999999847268213),.UNSPECIFIED.);
#5344=B_SPLINE_CURVE_WITH_KNOTS('',3,(#184683,#184684,#184685,#184686,#184687,
#184688,#184689,#184690,#184691,#184692,#184693,#184694,#184695,#184696,
#184697,#184698,#184699,#184700,#184701,#184702,#184703,#184704,#184705,
#184706,#184707,#184708,#184709,#184710,#184711,#184712,#184713,#184714,
#184715,#184716,#184717,#184718,#184719,#184720,#184721,#184722,#184723,
#184724,#184725,#184726,#184727,#184728,#184729,#184730,#184731,#184732,
#184733,#184734,#184735,#184736,#184737,#184738,#184739,#184740,#184741,
#184742,#184743,#184744,#184745,#184746,#184747,#184748,#184749,#184750,
#184751,#184752,#184753,#184754,#184755,#184756,#184757,#184758,#184759,
#184760,#184761,#184762,#184763,#184764),.UNSPECIFIED.,.F.,.F.,(4,3,3,3,
3,3,3,3,3,3,3,3,3,3,3,3,3,3,3,3,3,3,3,3,3,3,3,4),(0.,0.0569576591821558,
0.112755151148855,0.168107128830785,0.223066017844343,0.249999999999972,
0.260222583084969,0.335298290313108,0.374999999999957,0.431109645708327,
0.437499999999951,0.468749999999948,0.484374999999947,0.493293930533613,
0.499999999999946,0.507115891968341,0.561313062720312,0.611963343037344,
0.624999999999959,0.639766051419202,0.691395847196872,0.736848157965738,
0.761599820846938,0.766283550877083,0.84574998738632,0.922874993617906,
0.995168128022229,0.999999999849491),.UNSPECIFIED.);
#5345=B_SPLINE_CURVE_WITH_KNOTS('',3,(#184779,#184780,#184781,#184782,#184783,
#184784,#184785,#184786,#184787,#184788,#184789,#184790,#184791,#184792,
#184793,#184794,#184795,#184796,#184797,#184798,#184799,#184800,#184801,
#184802,#184803,#184804,#184805,#184806,#184807,#184808,#184809,#184810,
#184811,#184812,#184813,#184814,#184815,#184816,#184817,#184818,#184819,
#184820,#184821,#184822,#184823,#184824,#184825,#184826,#184827,#184828,
#184829,#184830,#184831,#184832,#184833,#184834,#184835,#184836,#184837,
#184838,#184839,#184840,#184841,#184842,#184843,#184844,#184845,#184846,
#184847,#184848,#184849,#184850,#184851,#184852,#184853,#184854,#184855,
#184856,#184857,#184858,#184859,#184860,#184861,#184862,#184863,#184864,
#184865,#184866),.UNSPECIFIED.,.F.,.F.,(4,3,3,3,3,3,3,3,3,3,3,3,3,3,3,3,
3,3,3,3,3,3,3,3,3,3,3,3,3,4),(4.79077677789156E-15,0.0625000000000102,0.119437937333093,
0.174434651404281,0.226856935996688,0.250000000000027,0.259607248156974,
0.31248276171328,0.346461802787087,0.369037373645423,0.380440843860894,
0.418757995092361,0.442888681175932,0.469986336276138,0.483535163826241,
0.485333141233566,0.495430448048758,0.497083991376344,0.50000000000005,
0.56320260393989,0.618434035218326,0.68012401263361,0.738312181743081,0.741813990048893,
0.750000000000025,0.805848380212432,0.862121697127147,0.918811408327095,
0.976432987956455,1.),.UNSPECIFIED.);
#5346=B_SPLINE_CURVE_WITH_KNOTS('',3,(#184910,#184911,#184912,#184913,#184914,
#184915,#184916,#184917,#184918,#184919,#184920,#184921,#184922,#184923,
#184924,#184925,#184926,#184927,#184928,#184929,#184930,#184931,#184932,
#184933,#184934,#184935,#184936,#184937,#184938,#184939,#184940,#184941,
#184942,#184943,#184944,#184945,#184946,#184947,#184948,#184949,#184950,
#184951,#184952,#184953,#184954,#184955,#184956,#184957,#184958,#184959,
#184960,#184961,#184962,#184963,#184964,#184965,#184966,#184967,#184968,
#184969,#184970,#184971,#184972,#184973),.UNSPECIFIED.,.F.,.F.,(4,3,3,3,
3,3,3,3,3,3,3,3,3,3,3,3,3,3,3,3,3,4),(0.,0.0691966740878807,0.125000000000041,
0.185982401655162,0.227879315918833,0.238353522132354,0.267545001222266,
0.342870914442811,0.407678156640436,0.452094475638223,0.463461622214131,
0.484375000000144,0.493645266144116,0.500000000000138,0.562500000000121,
0.649447035395343,0.713513413029987,0.736394070790565,0.750000000000069,
0.840743294607341,0.935248128666082,1.),.UNSPECIFIED.);
#5347=B_SPLINE_CURVE_WITH_KNOTS('',3,(#184974,#184975,#184976,#184977,#184978,
#184979,#184980,#184981,#184982,#184983,#184984,#184985,#184986,#184987,
#184988,#184989,#184990,#184991,#184992,#184993,#184994,#184995,#184996,
#184997,#184998,#184999,#185000,#185001,#185002,#185003,#185004,#185005,
#185006,#185007,#185008,#185009,#185010),.UNSPECIFIED.,.F.,.F.,(4,3,3,3,
3,3,3,3,3,3,3,3,4),(0.,0.000308449407263107,0.000616898814526214,0.000757033039934084,
0.00113555144207261,0.00123379762905243,0.00151396810348859,0.00181929544895182,
0.00185069644357864,0.00189260692917412,0.00221146178004545,0.00227133710209363,
0.00246759525810486),.UNSPECIFIED.);
#5348=B_SPLINE_CURVE_WITH_KNOTS('',3,(#185038,#185039,#185040,#185041,#185042,
#185043,#185044,#185045,#185046,#185047,#185048,#185049,#185050,#185051,
#185052,#185053,#185054,#185055,#185056,#185057,#185058,#185059,#185060,
#185061,#185062,#185063,#185064,#185065),.UNSPECIFIED.,.F.,.F.,(4,3,3,3,
3,3,3,3,3,4),(0.,0.000418680346171866,0.000626513004308685,0.000899330166364171,
0.00105990140469727,0.00112416270795522,0.00125349750883986,0.00134899524954626,
0.0015907151218419,0.00179866033272836),.UNSPECIFIED.);
#5349=B_SPLINE_CURVE_WITH_KNOTS('',3,(#185072,#185073,#185074,#185075,#185076,
#185077,#185078,#185079,#185080,#185081,#185082,#185083,#185084,#185085,
#185086,#185087,#185088,#185089,#185090,#185091,#185092,#185093,#185094,
#185095,#185096,#185097,#185098,#185099,#185100,#185101,#185102,#185103,
#185104,#185105,#185106,#185107,#185108),.UNSPECIFIED.,.F.,.F.,(4,3,3,3,
3,3,3,3,3,3,3,3,4),(0.000628504292635843,0.000640254986321947,0.000837411769728766,
0.000877277691072229,0.00100166439029042,0.00112605108950862,0.00129967406001939,
0.00158178243883092,0.00162359788638139,0.00162947384441178,0.00195921469101131,
0.00212114468325416,0.00261869148012693),.UNSPECIFIED.);
#5350=B_SPLINE_CURVE_WITH_KNOTS('',3,(#185162,#185163,#185164,#185165,#185166,
#185167,#185168,#185169,#185170,#185171,#185172,#185173,#185174,#185175,
#185176,#185177,#185178,#185179,#185180,#185181,#185182,#185183,#185184,
#185185,#185186,#185187,#185188,#185189,#185190,#185191,#185192,#185193,
#185194,#185195,#185196,#185197,#185198,#185199,#185200,#185201,#185202,
#185203,#185204,#185205,#185206,#185207,#185208,#185209,#185210,#185211,
#185212,#185213,#185214,#185215,#185216,#185217,#185218,#185219,#185220,
#185221,#185222,#185223,#185224,#185225),.UNSPECIFIED.,.F.,.F.,(4,3,3,3,
3,3,3,3,3,3,3,3,3,3,3,3,3,3,3,3,3,4),(1.06711334784298E-7,0.162604295707322,
0.250000000000111,0.346235688365917,0.37500000000017,0.437500000000205,
0.468750000000223,0.484375000000228,0.494029099182314,0.500000000000232,
0.562024892877923,0.625000000000202,0.686304312199343,0.718750000000151,
0.732744455805283,0.746155904384784,0.750000000000127,0.791548708438476,
0.845340878863513,0.898737355231329,0.951745167827004,1.),.UNSPECIFIED.);
#5351=B_SPLINE_CURVE_WITH_KNOTS('',3,(#185227,#185228,#185229,#185230,#185231,
#185232,#185233,#185234,#185235,#185236,#185237,#185238,#185239,#185240,
#185241,#185242,#185243,#185244,#185245,#185246,#185247,#185248,#185249,
#185250,#185251,#185252,#185253,#185254,#185255,#185256,#185257,#185258,
#185259,#185260,#185261,#185262,#185263,#185264,#185265,#185266,#185267,
#185268,#185269),.UNSPECIFIED.,.F.,.F.,(4,3,3,3,3,3,3,3,3,3,3,3,3,3,4),
(6.03724857329268E-15,0.0751859964940513,0.1495754148425,0.223294821152985,
0.29646818908788,0.369217351735024,0.441662438840354,0.51393127270104,0.586176148411227,
0.658501301088192,0.731011174783843,0.804060525502846,0.877464812066976,
0.951640239520033,1.),.UNSPECIFIED.);
#5352=B_SPLINE_CURVE_WITH_KNOTS('',3,(#185306,#185307,#185308,#185309,#185310,
#185311,#185312,#185313,#185314,#185315,#185316,#185317,#185318,#185319,
#185320,#185321,#185322,#185323,#185324,#185325,#185326,#185327,#185328,
#185329,#185330,#185331,#185332,#185333,#185334,#185335,#185336,#185337,
#185338,#185339,#185340,#185341,#185342,#185343,#185344,#185345),
 .UNSPECIFIED.,.F.,.F.,(4,3,3,3,3,3,3,3,3,3,3,3,3,4),(0.,0.0769432907447413,
0.153258768055538,0.229074002309316,0.304514589970782,0.379704601656095,
0.457241526449082,0.532396464239891,0.607701562850284,0.683265685333108,
0.762449263999828,0.839174120767956,0.919587060383972,0.999999999999988),
 .UNSPECIFIED.);
#5353=B_SPLINE_CURVE_WITH_KNOTS('',3,(#185346,#185347,#185348,#185349,#185350,
#185351,#185352,#185353,#185354,#185355,#185356,#185357,#185358,#185359,
#185360,#185361,#185362,#185363,#185364,#185365,#185366,#185367,#185368,
#185369,#185370,#185371,#185372,#185373,#185374,#185375,#185376,#185377,
#185378,#185379,#185380,#185381,#185382,#185383,#185384,#185385,#185386,
#185387,#185388,#185389,#185390,#185391,#185392,#185393,#185394,#185395,
#185396,#185397,#185398,#185399,#185400,#185401,#185402,#185403,#185404,
#185405,#185406,#185407,#185408,#185409,#185410,#185411,#185412,#185413,
#185414,#185415,#185416,#185417,#185418),.UNSPECIFIED.,.F.,.F.,(4,3,3,3,
3,3,3,3,3,3,3,3,3,3,3,3,3,3,3,3,3,3,3,3,4),(0.,0.053066835316157,0.107443152978828,
0.12499999999975,0.164971619184019,0.190888873117842,0.204943238368287,
0.218749999999565,0.230944613269073,0.243881742710735,0.249999999999505,
0.3086696401951,0.31701739205347,0.374999999999218,0.43499167648113,0.437499999999049,
0.46874999999896,0.484374999998946,0.493605897327227,0.499999999998931,
0.562499999999065,0.672531769754724,0.785034592397643,0.90313919621424,
1.),.UNSPECIFIED.);
#5354=B_SPLINE_CURVE_WITH_KNOTS('',3,(#185437,#185438,#185439,#185440,#185441,
#185442,#185443,#185444,#185445,#185446,#185447,#185448,#185449,#185450,
#185451,#185452,#185453,#185454,#185455,#185456,#185457,#185458,#185459,
#185460,#185461,#185462,#185463,#185464,#185465,#185466,#185467),
 .UNSPECIFIED.,.F.,.F.,(4,3,3,3,3,3,3,3,3,3,4),(0.,0.133384645899484,0.241711565162048,
0.265234332982687,0.367395294896058,0.446470883034051,0.501816373465676,
0.633825505921846,0.766458015306425,0.897442561934306,1.),.UNSPECIFIED.);
#5355=B_SPLINE_CURVE_WITH_KNOTS('',3,(#185505,#185506,#185507,#185508,#185509,
#185510,#185511,#185512,#185513,#185514,#185515,#185516,#185517,#185518,
#185519,#185520,#185521,#185522),.UNSPECIFIED.,.F.,.F.,(4,2,1,1,1,2,2,1,
2,2,4),(0.,0.250000000000277,0.375000000000416,0.437500000000485,0.468750000000498,
0.484375000000484,0.500000000000469,0.625000000000387,0.68750000000033,
0.750000000000273,1.),.UNSPECIFIED.);
#5356=B_SPLINE_CURVE_WITH_KNOTS('',3,(#185564,#185565,#185566,#185567,#185568,
#185569,#185570,#185571,#185572,#185573,#185574,#185575,#185576,#185577,
#185578,#185579,#185580,#185581,#185582,#185583,#185584,#185585,#185586,
#185587,#185588,#185589,#185590,#185591,#185592,#185593,#185594,#185595,
#185596,#185597,#185598,#185599,#185600,#185601,#185602,#185603,#185604,
#185605,#185606,#185607,#185608,#185609,#185610,#185611,#185612,#185613,
#185614,#185615),.UNSPECIFIED.,.F.,.F.,(4,3,3,3,3,3,3,3,3,3,3,3,3,3,3,3,
3,4),(0.,8.48627990060068E-5,0.000110154370857281,0.000197555987869283,
0.00023405941937725,0.000330463112571844,0.000419877362193912,0.000438835738394224,
0.000440617483429125,0.000729065363264048,0.000878897195867667,0.00088123496685825,
0.00114445185852502,0.00132031265264404,0.00132185245028737,0.00147439999768883,
0.00163314747063792,0.0017624699337165),.UNSPECIFIED.);
#5357=B_SPLINE_CURVE_WITH_KNOTS('',3,(#185656,#185657,#185658,#185659,#185660,
#185661,#185662,#185663,#185664,#185665,#185666,#185667,#185668,#185669,
#185670,#185671,#185672,#185673,#185674,#185675,#185676,#185677,#185678,
#185679,#185680),.UNSPECIFIED.,.F.,.F.,(4,3,3,3,3,3,3,3,4),(0.,0.124999999999963,
0.187499999999945,0.249999999999927,0.374999999999939,0.499999999999951,
0.696720148433668,0.749999999999976,1.),.UNSPECIFIED.);
#5358=B_SPLINE_CURVE_WITH_KNOTS('',3,(#185710,#185711,#185712,#185713,#185714,
#185715,#185716,#185717,#185718,#185719,#185720,#185721,#185722,#185723,
#185724,#185725,#185726,#185727,#185728,#185729,#185730,#185731),
 .UNSPECIFIED.,.F.,.F.,(4,3,3,3,3,3,3,4),(0.,0.22646738217556,0.25,0.5,
0.689823042701396,0.75,0.923487802122837,1.),.UNSPECIFIED.);
#5359=B_SPLINE_CURVE_WITH_KNOTS('',3,(#185767,#185768,#185769,#185770,#185771,
#185772,#185773,#185774,#185775,#185776,#185777,#185778,#185779,#185780,
#185781,#185782,#185783,#185784,#185785,#185786,#185787,#185788,#185789,
#185790,#185791,#185792,#185793,#185794,#185795,#185796,#185797,#185798,
#185799,#185800,#185801,#185802,#185803,#185804,#185805,#185806,#185807,
#185808,#185809,#185810,#185811,#185812),.UNSPECIFIED.,.F.,.F.,(4,3,3,3,
3,3,3,3,3,3,3,3,3,3,3,4),(0.,0.000111620791367575,0.000225473811195191,
0.000339302579903024,0.000397521249509077,0.000399067370002251,0.000667517661644283,
0.000795042499018153,0.000797178277617395,0.00104506031877655,0.00119256374852723,
0.00119405065366289,0.0013234358669085,0.0014567604324724,0.00158159308775795,
0.0015900849980363),.UNSPECIFIED.);
#5360=B_SPLINE_CURVE_WITH_KNOTS('',3,(#185852,#185853,#185854,#185855,#185856,
#185857,#185858,#185859,#185860,#185861,#185862,#185863,#185864,#185865,
#185866,#185867,#185868,#185869,#185870,#185871,#185872,#185873,#185874,
#185875,#185876,#185877,#185878,#185879,#185880,#185881,#185882,#185883,
#185884,#185885,#185886,#185887,#185888,#185889,#185890,#185891,#185892,
#185893,#185894),.UNSPECIFIED.,.F.,.F.,(4,3,3,3,3,3,3,3,3,3,3,3,3,3,4),
(0.,0.000168850029785425,0.000336050047502259,0.000405527490133955,0.000407005029304983,
0.000682198964448582,0.000811826624698246,0.000814010058609966,0.00109897545099617,
0.00121939063721615,0.00122101508791495,0.00134692436003165,0.00147131083154616,
0.00159335498692557,0.0016280201172199),.UNSPECIFIED.);
#5361=B_SPLINE_CURVE_WITH_KNOTS('',3,(#186057,#186058,#186059,#186060,#186061,
#186062),.UNSPECIFIED.,.F.,.F.,(4,2,4),(0.000562946727309309,0.00236076329038739,
0.00415857985346548),.UNSPECIFIED.);
#5362=B_SPLINE_CURVE_WITH_KNOTS('',3,(#186160,#186161,#186162,#186163,#186164,
#186165,#186166,#186167,#186168,#186169,#186170,#186171,#186172,#186173,
#186174,#186175,#186176,#186177,#186178,#186179,#186180,#186181,#186182,
#186183,#186184,#186185,#186186,#186187,#186188,#186189,#186190,#186191,
#186192,#186193,#186194,#186195,#186196,#186197,#186198,#186199,#186200,
#186201,#186202,#186203,#186204,#186205,#186206,#186207,#186208,#186209,
#186210,#186211,#186212,#186213,#186214,#186215,#186216,#186217,#186218,
#186219,#186220,#186221,#186222,#186223,#186224,#186225,#186226,#186227,
#186228,#186229,#186230,#186231,#186232),.UNSPECIFIED.,.F.,.F.,(4,3,3,3,
3,3,3,3,3,3,3,3,3,3,3,3,3,3,3,3,3,3,3,3,4),(5.59106843353732E-9,0.0443629897048473,
0.119873585712499,0.190502577283635,0.209068196859206,0.249999999999805,
0.321582585084567,0.367287555228283,0.381990119969657,0.441953706375988,
0.492187499999601,0.497575926912646,0.499999999999598,0.531254057232031,
0.585370887938339,0.637190770031103,0.685890707754348,0.723267035789511,
0.749999999999799,0.802882641837966,0.854604290016104,0.8749999999999,0.920965954037863,
0.964332381888369,1.),.UNSPECIFIED.);
#5363=B_SPLINE_CURVE_WITH_KNOTS('',3,(#186248,#186249,#186250,#186251,#186252,
#186253,#186254,#186255,#186256,#186257),.UNSPECIFIED.,.F.,.F.,(4,3,3,4),
(0.,0.371377520235629,0.776879610669599,1.),.UNSPECIFIED.);
#5364=B_SPLINE_CURVE_WITH_KNOTS('',3,(#186275,#186276,#186277,#186278,#186279,
#186280,#186281,#186282,#186283,#186284,#186285,#186286,#186287,#186288,
#186289,#186290,#186291,#186292,#186293,#186294,#186295,#186296,#186297,
#186298,#186299,#186300,#186301,#186302,#186303,#186304,#186305,#186306,
#186307,#186308,#186309,#186310,#186311),.UNSPECIFIED.,.F.,.F.,(4,3,3,3,
3,3,3,3,3,3,3,3,4),(0.,0.152151913276676,0.25000000000001,0.386714368335732,
0.437499999999995,0.463570378436081,0.490496823135862,0.499999999999993,
0.614091604002371,0.723372130571636,0.830296728032007,0.934020703510205,
1.),.UNSPECIFIED.);
#5365=B_SPLINE_CURVE_WITH_KNOTS('',3,(#186313,#186314,#186315,#186316,#186317,
#186318,#186319,#186320,#186321,#186322,#186323,#186324,#186325),
 .UNSPECIFIED.,.F.,.F.,(4,3,3,3,4),(0.,0.306533919199522,0.613513205477452,
0.921258276490977,1.),.UNSPECIFIED.);
#5366=B_SPLINE_CURVE_WITH_KNOTS('',3,(#186381,#186382,#186383,#186384,#186385,
#186386,#186387),.UNSPECIFIED.,.F.,.F.,(4,3,4),(4.7123889803847,5.4977871437821,
6.28318530717959),.UNSPECIFIED.);
#5367=B_SPLINE_CURVE_WITH_KNOTS('',3,(#186412,#186413,#186414,#186415,#186416,
#186417,#186418),.UNSPECIFIED.,.F.,.F.,(4,3,4),(3.1415926535898,3.92699081698724,
4.71238898038469),.UNSPECIFIED.);
#5368=B_SPLINE_CURVE_WITH_KNOTS('',3,(#186447,#186448,#186449,#186450,#186451,
#186452,#186453),.UNSPECIFIED.,.F.,.F.,(4,3,4),(4.7123889803847,5.49778714378215,
6.28318530717959),.UNSPECIFIED.);
#5369=B_SPLINE_CURVE_WITH_KNOTS('',3,(#186478,#186479,#186480,#186481,#186482,
#186483,#186484),.UNSPECIFIED.,.F.,.F.,(4,3,4),(1.23467863058848E-16,0.785398163397455,
1.57079632679491),.UNSPECIFIED.);
#5370=B_SPLINE_CURVE_WITH_KNOTS('',3,(#186528,#186529,#186530,#186531,#186532,
#186533,#186534,#186535,#186536,#186537,#186538,#186539,#186540,#186541,
#186542,#186543,#186544,#186545,#186546),.UNSPECIFIED.,.F.,.F.,(4,3,3,3,
3,3,4),(0.,0.000905681138562551,0.00148255506350336,0.00163490147399828,
0.00222383259525504,0.00274053607504981,0.00296511012700672),
 .UNSPECIFIED.);
#5371=B_SPLINE_CURVE_WITH_KNOTS('',3,(#186571,#186572,#186573,#186574,#186575,
#186576,#186577),.UNSPECIFIED.,.F.,.F.,(4,3,4),(1.5707963267949,2.35619449019235,
3.1415926535898),.UNSPECIFIED.);
#5372=B_SPLINE_CURVE_WITH_KNOTS('',3,(#186602,#186603,#186604,#186605,#186606,
#186607,#186608),.UNSPECIFIED.,.F.,.F.,(4,3,4),(1.23467863058847E-16,0.785398163397447,
1.5707963267949),.UNSPECIFIED.);
#5373=B_SPLINE_CURVE_WITH_KNOTS('',3,(#186633,#186634,#186635,#186636,#186637,
#186638,#186639,#186640,#186641,#186642,#186643,#186644,#186645,#186646,
#186647,#186648,#186649,#186650,#186651),.UNSPECIFIED.,.F.,.F.,(4,3,3,3,
3,3,4),(0.000169216231990766,0.000729993311367161,0.000968460740699438,
0.00168309612079798,0.00176770524940811,0.00279102522271382,0.00336619426682546),
 .UNSPECIFIED.);
#5374=B_SPLINE_CURVE_WITH_KNOTS('',3,(#186698,#186699,#186700,#186701,#186702,
#186703,#186704),.UNSPECIFIED.,.F.,.F.,(4,3,4),(4.71238898038469,5.49778714378214,
6.28318530717959),.UNSPECIFIED.);
#5375=B_SPLINE_CURVE_WITH_KNOTS('',3,(#186729,#186730,#186731,#186732,#186733,
#186734,#186735),.UNSPECIFIED.,.F.,.F.,(4,3,4),(1.23467863058847E-16,0.785398163397447,
1.5707963267949),.UNSPECIFIED.);
#5376=B_SPLINE_CURVE_WITH_KNOTS('',3,(#186771,#186772,#186773,#186774,#186775,
#186776,#186777),.UNSPECIFIED.,.F.,.F.,(4,3,4),(1.5707963267949,2.35619449019234,
3.14159265358979),.UNSPECIFIED.);
#5377=B_SPLINE_CURVE_WITH_KNOTS('',3,(#186802,#186803,#186804,#186805,#186806,
#186807,#186808),.UNSPECIFIED.,.F.,.F.,(4,3,4),(3.14159265358979,3.92699081698724,
4.71238898038469),.UNSPECIFIED.);
#5378=B_SPLINE_CURVE_WITH_KNOTS('',3,(#186834,#186835,#186836,#186837,#186838,
#186839,#186840,#186841,#186842,#186843,#186844,#186845,#186846,#186847,
#186848,#186849),.UNSPECIFIED.,.F.,.F.,(4,3,3,3,3,4),(0.000244714080610449,
0.00121583023104281,0.00174053473821824,0.00180545417371792,0.00292276797849773,
0.00336619426682539),.UNSPECIFIED.);
#5379=B_SPLINE_CURVE_WITH_KNOTS('',3,(#186874,#186875,#186876,#186877,#186878,
#186879,#186880),.UNSPECIFIED.,.F.,.F.,(4,3,4),(1.5707963267949,2.35619449019232,
3.14159265358979),.UNSPECIFIED.);
#5380=B_SPLINE_CURVE_WITH_KNOTS('',3,(#186905,#186906,#186907,#186908,#186909,
#186910,#186911),.UNSPECIFIED.,.F.,.F.,(4,3,4),(-1.77635683940025E-15,0.785398163397447,
1.57079632679489),.UNSPECIFIED.);
#5381=B_SPLINE_CURVE_WITH_KNOTS('',3,(#186937,#186938,#186939,#186940,#186941,
#186942,#186943,#186944,#186945,#186946,#186947,#186948,#186949,#186950,
#186951,#186952,#186953,#186954,#186955,#186956,#186957,#186958,#186959,
#186960,#186961,#186962,#186963,#186964,#186965,#186966,#186967,#186968,
#186969,#186970,#186971,#186972,#186973,#186974,#186975,#186976,#186977,
#186978,#186979,#186980,#186981,#186982,#186983,#186984,#186985,#186986,
#186987,#186988,#186989,#186990,#186991,#186992,#186993,#186994),
 .UNSPECIFIED.,.F.,.F.,(4,3,3,3,3,3,3,3,3,3,3,3,3,3,3,3,3,3,3,4),(0.,0.0574313460779371,
0.117800031813472,0.183766052524469,0.218749999999997,0.234374999999995,
0.242187499999999,0.250000000000002,0.336658026235113,0.375000000000007,
0.466327390959677,0.484375000000006,0.496043375977593,0.500000000000006,
0.502720832074079,0.59984784615854,0.7048612171632,0.815201166331238,0.93528875928782,
1.),.UNSPECIFIED.);
#5382=B_SPLINE_CURVE_WITH_KNOTS('',3,(#187025,#187026,#187027,#187028,#187029,
#187030,#187031),.UNSPECIFIED.,.F.,.F.,(4,3,4),(1.57079632679491,2.35619449019235,
3.14159265358979),.UNSPECIFIED.);
#5383=B_SPLINE_CURVE_WITH_KNOTS('',3,(#187056,#187057,#187058,#187059,#187060,
#187061,#187062),.UNSPECIFIED.,.F.,.F.,(4,3,4),(-1.77635683940025E-15,0.785398163397447,
1.57079632679489),.UNSPECIFIED.);
#5384=B_SPLINE_CURVE_WITH_KNOTS('',3,(#187087,#187088,#187089,#187090,#187091,
#187092,#187093,#187094,#187095,#187096,#187097,#187098,#187099,#187100,
#187101,#187102,#187103,#187104,#187105),.UNSPECIFIED.,.F.,.F.,(4,3,3,3,
3,3,4),(0.00047266192456923,0.000857724029065683,0.00153872216956474,0.0018499707510604,
0.00201291034255504,0.00292749448069884,0.00355315876054085),
 .UNSPECIFIED.);
#5385=B_SPLINE_CURVE_WITH_KNOTS('',3,(#187130,#187131,#187132,#187133,#187134,
#187135,#187136,#187137,#187138,#187139,#187140,#187141,#187142,#187143,
#187144,#187145,#187146,#187147,#187148,#187149,#187150,#187151,#187152,
#187153,#187154,#187155,#187156,#187157,#187158,#187159,#187160,#187161,
#187162,#187163,#187164,#187165,#187166),.UNSPECIFIED.,.F.,.F.,(4,3,3,3,
3,3,3,3,3,3,3,3,4),(1.96820403583049,2.07447029970642,2.18239924823465,
2.29295513021916,2.40448289443547,2.51591247508908,2.55489944283297,2.66627384567102,
2.77787483330248,2.88775468513439,2.99605880939301,3.10223763839193,3.14159265358979),
 .UNSPECIFIED.);
#5386=B_SPLINE_CURVE_WITH_KNOTS('',3,(#187195,#187196,#187197,#187198,#187199,
#187200,#187201),.UNSPECIFIED.,.F.,.F.,(4,3,4),(4.7123889803847,5.49778714378215,
6.28318530717959),.UNSPECIFIED.);
#5387=B_SPLINE_CURVE_WITH_KNOTS('',3,(#187226,#187227,#187228,#187229,#187230,
#187231,#187232),.UNSPECIFIED.,.F.,.F.,(4,3,4),(-1.77635683940025E-15,0.785398163397447,
1.57079632679489),.UNSPECIFIED.);
#5388=B_SPLINE_CURVE_WITH_KNOTS('',3,(#187264,#187265,#187266,#187267,#187268,
#187269,#187270,#187271,#187272,#187273,#187274,#187275,#187276,#187277,
#187278,#187279,#187280,#187281,#187282,#187283,#187284,#187285,#187286,
#187287,#187288,#187289,#187290,#187291,#187292,#187293,#187294,#187295,
#187296,#187297,#187298,#187299,#187300,#187301,#187302,#187303,#187304,
#187305,#187306,#187307,#187308,#187309,#187310,#187311,#187312,#187313,
#187314,#187315,#187316,#187317,#187318,#187319,#187320,#187321,#187322,
#187323,#187324,#187325,#187326,#187327,#187328,#187329,#187330),
 .UNSPECIFIED.,.F.,.F.,(4,3,3,3,3,3,3,3,3,3,3,3,3,3,3,3,3,3,3,3,3,3,4),
(0.,0.103658513321288,0.125,0.169018534161299,0.213461877707459,0.250000000000001,
0.250951766798841,0.335698253700407,0.375000000000001,0.416829400350235,
0.459227774972107,0.500000000000001,0.501310898730185,0.571535494191993,
0.625000000000002,0.672446050926232,0.687500000000002,0.735320212679162,
0.750000000000002,0.819805912927389,0.890142978787528,0.960075009265078,
1.),.UNSPECIFIED.);
#5389=B_SPLINE_CURVE_WITH_KNOTS('',3,(#187371,#187372,#187373,#187374,#187375,
#187376,#187377,#187378,#187379,#187380,#187381,#187382,#187383,#187384,
#187385,#187386,#187387,#187388,#187389,#187390,#187391,#187392,#187393,
#187394,#187395,#187396,#187397,#187398,#187399,#187400,#187401,#187402,
#187403,#187404,#187405,#187406,#187407,#187408,#187409,#187410,#187411,
#187412,#187413),.UNSPECIFIED.,.F.,.F.,(4,3,3,3,3,3,3,3,3,3,3,3,3,3,4),
(0.,0.000127008698005063,0.000262529185195825,0.000398049672386588,0.000399547425717595,
0.00064867929835264,0.000796943972592095,0.00079909485143519,0.00106876545795213,
0.00119708559701166,0.00119864227715278,0.00131330308627002,0.00142818443762419,
0.00153991729226719,0.00159818970287038),.UNSPECIFIED.);
#5390=B_SPLINE_CURVE_WITH_KNOTS('',3,(#187438,#187439,#187440,#187441,#187442,
#187443,#187444,#187445,#187446,#187447,#187448,#187449,#187450,#187451,
#187452,#187453,#187454,#187455,#187456),.UNSPECIFIED.,.F.,.F.,(4,3,3,3,
3,3,4),(0.,0.176003355398739,0.25,0.442266421325595,0.5,0.75,1.),
 .UNSPECIFIED.);
#5391=B_SPLINE_CURVE_WITH_KNOTS('',3,(#187492,#187493,#187494,#187495,#187496,
#187497,#187498,#187499,#187500,#187501,#187502,#187503,#187504,#187505,
#187506,#187507,#187508,#187509,#187510,#187511,#187512,#187513,#187514,
#187515,#187516,#187517,#187518,#187519),.UNSPECIFIED.,.F.,.F.,(4,3,3,3,
3,3,3,3,3,4),(0.,0.231192918218893,0.249999999999998,0.374999999999998,
0.499999999999999,0.624999999999999,0.687499999999999,0.749999999999999,
0.943972933317676,1.),.UNSPECIFIED.);
#5392=B_SPLINE_CURVE_WITH_KNOTS('',3,(#187567,#187568,#187569,#187570,#187571,
#187572,#187573,#187574,#187575,#187576,#187577,#187578,#187579,#187580,
#187581,#187582,#187583,#187584,#187585,#187586,#187587,#187588,#187589,
#187590,#187591,#187592,#187593,#187594,#187595,#187596,#187597,#187598,
#187599,#187600,#187601,#187602,#187603,#187604,#187605,#187606,#187607,
#187608,#187609,#187610,#187611,#187612,#187613,#187614,#187615,#187616,
#187617,#187618),.UNSPECIFIED.,.F.,.F.,(4,3,3,3,3,3,3,3,3,3,3,3,3,3,3,3,
3,4),(0.,0.000162974000351715,0.000319609377590832,0.00044215652538248,
0.000443701447435103,0.000705760117587417,0.000884313050764961,0.000886662825918405,
0.00117556448146201,0.00132646957614744,0.00132826306101653,0.00141792619142879,
0.00143700870749306,0.00151991305600227,0.00155002729305631,0.00163724702277407,
0.0017219272748049,0.00176862610152992),.UNSPECIFIED.);
#5393=B_SPLINE_CURVE_WITH_KNOTS('',3,(#187659,#187660,#187661,#187662,#187663,
#187664,#187665,#187666,#187667,#187668,#187669,#187670,#187671,#187672,
#187673,#187674,#187675),.UNSPECIFIED.,.F.,.F.,(4,1,1,2,2,1,1,1,2,2,4),
(0.,0.125000000000005,0.187500000000007,0.218750000000008,0.250000000000009,
0.375000000000011,0.437500000000013,0.46875000000001,0.484375000000014,
0.500000000000017,1.),.UNSPECIFIED.);
#5394=B_SPLINE_CURVE_WITH_KNOTS('',3,(#187723,#187724,#187725,#187726,#187727,
#187728,#187729,#187730,#187731,#187732,#187733,#187734,#187735,#187736,
#187737,#187738,#187739,#187740,#187741,#187742,#187743,#187744),
 .UNSPECIFIED.,.F.,.F.,(4,3,3,3,3,3,3,4),(0.,0.000360666935666808,0.000449610485509243,
0.000757497233646948,0.000899220971018486,0.00134883145652773,0.00157363669928234,
0.00179844194203696),.UNSPECIFIED.);
#5395=B_SPLINE_CURVE_WITH_KNOTS('',3,(#187791,#187792,#187793,#187794,#187795,
#187796,#187797,#187798,#187799,#187800,#187801,#187802,#187803,#187804,
#187805,#187806,#187807,#187808,#187809,#187810,#187811,#187812,#187813,
#187814,#187815,#187816,#187817,#187818,#187819,#187820,#187821,#187822,
#187823,#187824,#187825,#187826,#187827,#187828,#187829,#187830,#187831,
#187832,#187833),.UNSPECIFIED.,.F.,.F.,(4,3,3,3,3,3,3,3,3,3,3,3,3,3,4),
(0.,0.000195170703352208,0.000400502314359219,0.000446304927367807,0.000448134863283483,
0.000669908621781837,0.000672202294925215,0.000876863243061371,0.000893889262421621,
0.000896269726566947,0.00123667266508701,0.00134284656974638,0.00134440458985042,
0.00167688520284754,0.0017925394531339),.UNSPECIFIED.);
#5396=B_SPLINE_CURVE_WITH_KNOTS('',3,(#187881,#187882,#187883,#187884,#187885,
#187886,#187887,#187888,#187889,#187890,#187891,#187892,#187893,#187894,
#187895,#187896,#187897,#187898,#187899,#187900,#187901,#187902,#187903,
#187904,#187905,#187906,#187907,#187908,#187909,#187910,#187911,#187912,
#187913,#187914,#187915,#187916,#187917,#187918,#187919,#187920,#187921,
#187922,#187923,#187924,#187925,#187926),.UNSPECIFIED.,.F.,.F.,(4,3,3,3,
3,3,3,3,3,3,3,3,3,3,3,4),(0.,0.000125938335250352,0.000251511263371068,
0.000372362493801798,0.000393010036481153,0.000394487267106017,0.000650087135459798,
0.000786020072962305,0.000788180467911298,0.00103122780428417,0.00117903010944346,
0.00118059255633961,0.00129302327548811,0.00140596384630459,0.00151582795231526,
0.00157204014592461),.UNSPECIFIED.);
#5397=B_SPLINE_CURVE_WITH_KNOTS('',3,(#187966,#187967,#187968,#187969,#187970,
#187971,#187972,#187973,#187974,#187975,#187976,#187977,#187978,#187979,
#187980,#187981,#187982,#187983,#187984,#187985,#187986,#187987,#187988,
#187989,#187990,#187991,#187992,#187993,#187994,#187995,#187996,#187997,
#187998,#187999,#188000,#188001,#188002,#188003,#188004,#188005,#188006,
#188007,#188008),.UNSPECIFIED.,.F.,.F.,(4,3,3,3,3,3,3,3,3,3,3,3,3,3,4),
(0.,0.00012873091785914,0.000262886260532174,0.000397041603205207,0.000398543239038962,
0.000647566106702508,0.00079493581447458,0.000797086478077925,0.0010648677332478,
0.0011940802689539,0.00119562971711689,0.00131091067532157,0.00142650607919961,
0.00153915940329476,0.00159417295615585),.UNSPECIFIED.);
#5398=B_SPLINE_CURVE_WITH_KNOTS('',3,(#188039,#188040,#188041,#188042,#188043,
#188044,#188045,#188046,#188047,#188048,#188049,#188050,#188051,#188052,
#188053,#188054,#188055,#188056,#188057,#188058,#188059,#188060,#188061,
#188062,#188063,#188064,#188065,#188066,#188067,#188068,#188069,#188070,
#188071,#188072,#188073,#188074,#188075,#188076,#188077,#188078,#188079,
#188080,#188081,#188082,#188083,#188084,#188085,#188086,#188087,#188088,
#188089,#188090,#188091,#188092,#188093,#188094,#188095,#188096,#188097,
#188098,#188099),.UNSPECIFIED.,.F.,.F.,(4,3,3,3,3,3,3,3,3,3,3,3,3,3,3,3,
3,3,3,3,4),(0.,0.0625,0.139972153586169,0.15625,0.203125,0.25,0.3125,0.373286324414759,
0.43664316220738,0.496400222194438,0.5,0.501338831661234,0.571965089366115,
0.643232621636668,0.714229744959872,0.75,0.750926094557218,0.816401548475787,
0.88227904244363,0.947752342475233,1.),.UNSPECIFIED.);
#5399=B_SPLINE_CURVE_WITH_KNOTS('',3,(#188129,#188130,#188131,#188132,#188133,
#188134,#188135,#188136,#188137,#188138,#188139,#188140,#188141,#188142,
#188143,#188144,#188145,#188146,#188147,#188148,#188149,#188150,#188151,
#188152,#188153,#188154,#188155,#188156,#188157,#188158,#188159,#188160,
#188161,#188162,#188163,#188164,#188165,#188166,#188167,#188168,#188169,
#188170,#188171,#188172,#188173,#188174,#188175,#188176,#188177,#188178,
#188179,#188180),.UNSPECIFIED.,.F.,.F.,(4,3,3,3,3,3,3,3,3,3,3,3,3,3,3,3,
3,4),(0.,0.0644560924807926,0.128938108510493,0.192301428483669,0.25,0.31621626382761,
0.382182203805898,0.446812923850572,0.49888213793019,0.5,0.564513527455447,
0.629270711991716,0.693229549254467,0.75,0.825671875473234,0.901486212188946,
0.976405679522825,1.),.UNSPECIFIED.);
#5400=B_SPLINE_CURVE_WITH_KNOTS('',3,(#188227,#188228,#188229,#188230,#188231,
#188232,#188233,#188234,#188235,#188236,#188237),.UNSPECIFIED.,.F.,.F.,
(4,2,1,2,2,4),(0.,0.250000000000002,0.375000000000004,0.437500000000004,
0.500000000000005,1.),.UNSPECIFIED.);
#5401=B_SPLINE_CURVE_WITH_KNOTS('',3,(#188277,#188278,#188279,#188280,#188281,
#188282,#188283),.UNSPECIFIED.,.F.,.F.,(4,3,4),(0.,0.000214564004336314,
0.000397824826383788),.UNSPECIFIED.);
#5402=B_SPLINE_CURVE_WITH_KNOTS('',3,(#188300,#188301,#188302,#188303,#188304,
#188305,#188306,#188307,#188308,#188309,#188310,#188311,#188312,#188313,
#188314,#188315,#188316,#188317,#188318,#188319,#188320,#188321,#188322,
#188323,#188324,#188325,#188326,#188327,#188328,#188329,#188330),
 .UNSPECIFIED.,.F.,.F.,(4,3,3,3,3,3,3,3,3,3,4),(0.,0.148641184291234,0.250000000000006,
0.345102558943317,0.426964739075402,0.498594146690977,0.519796210982841,
0.671896501503741,0.824299079636482,0.974619845594587,1.),.UNSPECIFIED.);
#5403=B_SPLINE_CURVE_WITH_KNOTS('',3,(#188372,#188373,#188374,#188375,#188376,
#188377,#188378,#188379,#188380,#188381,#188382,#188383,#188384,#188385,
#188386,#188387,#188388,#188389,#188390,#188391,#188392,#188393,#188394,
#188395,#188396,#188397,#188398,#188399,#188400,#188401,#188402,#188403,
#188404,#188405,#188406,#188407,#188408,#188409,#188410,#188411,#188412,
#188413,#188414),.UNSPECIFIED.,.F.,.F.,(4,3,3,3,3,3,3,3,3,3,3,3,3,3,4),
(0.,0.00015584643830928,0.000318202659845265,0.000479330525642436,0.00048138854528345,
0.000719581971214055,0.000722082817925181,0.000946156964932637,0.000960283452349063,
0.000962777090566911,0.0012735805929567,0.00144265205691352,0.00144416563585035,
0.00187401285515416,0.0019255541811338),.UNSPECIFIED.);
#5404=B_SPLINE_CURVE_WITH_KNOTS('',3,(#188462,#188463,#188464,#188465,#188466,
#188467,#188468,#188469,#188470,#188471,#188472,#188473),.UNSPECIFIED.,
 .F.,.F.,(4,2,2,2,2,4),(0.,0.000425271195884802,0.000850542391769605,0.00127581358765441,
0.00148844918559681,0.00170108478353921),.UNSPECIFIED.);
#5405=B_SPLINE_CURVE_WITH_KNOTS('',3,(#188502,#188503,#188504,#188505,#188506,
#188507,#188508,#188509,#188510,#188511,#188512,#188513),.UNSPECIFIED.,
 .F.,.F.,(4,2,2,2,2,4),(0.,0.125,0.25,0.5,0.75,1.),.UNSPECIFIED.);
#5406=B_SPLINE_CURVE_WITH_KNOTS('',3,(#188561,#188562,#188563,#188564,#188565,
#188566,#188567,#188568,#188569,#188570,#188571,#188572,#188573,#188574,
#188575,#188576,#188577,#188578,#188579,#188580,#188581,#188582,#188583,
#188584,#188585,#188586,#188587,#188588,#188589,#188590,#188591,#188592,
#188593,#188594,#188595,#188596,#188597,#188598,#188599,#188600,#188601,
#188602,#188603),.UNSPECIFIED.,.F.,.F.,(4,3,3,3,3,3,3,3,3,3,3,3,3,3,4),
(0.,0.000133466187697468,0.000269195218943483,0.000394210955663315,0.000395766414125746,
0.000656135621812108,0.000788421911326631,0.000790581154836762,0.00102610013258057,
0.00118263286698995,0.00118412769954352,0.00130569231129943,0.00142779909867114,
0.00154775473597367,0.00157684382265327),.UNSPECIFIED.);
#5407=B_SPLINE_CURVE_WITH_KNOTS('',3,(#188644,#188645,#188646,#188647,#188648,
#188649,#188650,#188651,#188652,#188653,#188654,#188655,#188656,#188657,
#188658,#188659,#188660,#188661,#188662,#188663,#188664,#188665,#188666,
#188667,#188668,#188669,#188670,#188671,#188672,#188673,#188674,#188675,
#188676,#188677,#188678,#188679,#188680,#188681,#188682,#188683,#188684,
#188685,#188686,#188687,#188688,#188689),.UNSPECIFIED.,.F.,.F.,(4,3,3,3,
3,3,3,3,3,3,3,3,3,3,3,4),(0.,0.000126520648339655,0.000255464746612705,
0.000383289319161563,0.000402202417173513,0.000403696977019687,0.000649443966573114,
0.000805221313633904,0.000807393954039373,0.00107833188460959,0.00120950149130568,
0.00121109093105906,0.00132473335816662,0.00143856386975698,0.00154897302143375,
0.00161478790807874),.UNSPECIFIED.);
#5408=B_SPLINE_CURVE_WITH_KNOTS('',3,(#188714,#188715,#188716,#188717,#188718,
#188719,#188720,#188721,#188722,#188723,#188724,#188725,#188726,#188727),
 .UNSPECIFIED.,.F.,.F.,(4,2,2,2,2,2,4),(0.,0.124999999999998,0.249999999999996,
0.374999999999994,0.499999999999992,0.749999999999996,1.),.UNSPECIFIED.);
#5409=B_SPLINE_CURVE_WITH_KNOTS('',3,(#188775,#188776,#188777,#188778,#188779,
#188780,#188781,#188782,#188783,#188784,#188785,#188786,#188787,#188788,
#188789,#188790,#188791,#188792,#188793,#188794,#188795,#188796,#188797,
#188798,#188799,#188800,#188801,#188802,#188803,#188804,#188805,#188806,
#188807,#188808,#188809,#188810,#188811,#188812,#188813,#188814,#188815,
#188816,#188817),.UNSPECIFIED.,.F.,.F.,(4,3,3,3,3,3,3,3,3,3,3,3,3,3,4),
(0.,0.000124096840872279,0.000249826409753379,0.000377706687950511,0.000412914062840745,
0.000414565512418999,0.000703661138430754,0.00082582812568149,0.000828047391046449,
0.00110745290673328,0.00123874218852223,0.00124024370669316,0.00141015471005652,
0.00158186346550297,0.00165165625136298),.UNSPECIFIED.);
#5410=B_SPLINE_CURVE_WITH_KNOTS('',3,(#188858,#188859,#188860,#188861,#188862,
#188863,#188864,#188865,#188866,#188867,#188868,#188869,#188870,#188871,
#188872,#188873,#188874,#188875,#188876,#188877,#188878,#188879,#188880,
#188881,#188882,#188883,#188884,#188885,#188886,#188887,#188888,#188889,
#188890,#188891,#188892,#188893,#188894,#188895,#188896,#188897,#188898,
#188899,#188900),.UNSPECIFIED.,.F.,.F.,(4,3,3,3,3,3,3,3,3,3,3,3,3,3,4),
(0.,0.000126914134949833,0.000262536143227239,0.000398158151504644,0.000399655746142223,
0.000648709723487763,0.000797160169367609,0.000799311492284445,0.00106908297786263,
0.00119740971470136,0.00119896723842667,0.00131358784144415,0.00142842585215519,
0.0015401041970663,0.00159862298456889),.UNSPECIFIED.);
#5411=B_SPLINE_CURVE_WITH_KNOTS('',3,(#188925,#188926,#188927,#188928,#188929,
#188930,#188931,#188932,#188933,#188934,#188935,#188936,#188937,#188938,
#188939,#188940,#188941,#188942,#188943),.UNSPECIFIED.,.F.,.F.,(4,3,3,3,
3,3,4),(0.,0.175945370266497,0.249999999999999,0.442549347776631,0.499999999999999,
0.749999999999998,1.),.UNSPECIFIED.);
#5412=B_SPLINE_CURVE_WITH_KNOTS('',3,(#188984,#188985,#188986,#188987,#188988,
#188989,#188990,#188991,#188992,#188993,#188994,#188995,#188996,#188997,
#188998,#188999,#189000,#189001,#189002,#189003,#189004,#189005,#189006,
#189007,#189008,#189009,#189010,#189011,#189012,#189013,#189014,#189015,
#189016,#189017,#189018,#189019,#189020),.UNSPECIFIED.,.F.,.F.,(4,3,3,3,
3,3,3,3,3,3,3,3,4),(0.,0.000202328389737709,0.00039307053157685,0.000394637415448944,
0.000657523627630533,0.000787104044603751,0.000789274830897888,0.00100657728096933,
0.00118241998772925,0.00118391224634683,0.00131758895200345,0.00145591556828444,
0.00157854966179577),.UNSPECIFIED.);
#5413=B_SPLINE_CURVE_WITH_KNOTS('',3,(#189070,#189071,#189072,#189073,#189074,
#189075,#189076,#189077,#189078,#189079,#189080,#189081,#189082,#189083,
#189084,#189085,#189086,#189087,#189088,#189089,#189090,#189091,#189092,
#189093,#189094,#189095,#189096,#189097,#189098,#189099,#189100,#189101,
#189102,#189103,#189104,#189105,#189106,#189107,#189108,#189109,#189110,
#189111,#189112,#189113,#189114,#189115),.UNSPECIFIED.,.F.,.F.,(4,3,3,3,
3,3,3,3,3,3,3,3,3,3,3,4),(0.,0.00014308662566148,0.000288513574061214,0.00042656988910148,
0.000433940522460948,0.000435486060835305,0.000709558652808421,0.000867881044921896,
0.000870195056295086,0.00115300716696084,0.00130182156738284,0.00130356397838256,
0.00142320462553198,0.00154203711262811,0.00165601506682426,0.00173576208984379),
 .UNSPECIFIED.);
#5414=B_SPLINE_CURVE_WITH_KNOTS('',3,(#189149,#189150,#189151,#189152,#189153,
#189154,#189155,#189156,#189157,#189158,#189159,#189160,#189161,#189162,
#189163),.UNSPECIFIED.,.F.,.F.,(4,1,2,2,1,1,2,2,4),(0.,0.124999999999991,
0.187499999999987,0.249999999999983,0.374999999999974,0.437499999999969,
0.468749999999972,0.499999999999974,1.),.UNSPECIFIED.);
#5415=B_SPLINE_CURVE_WITH_KNOTS('',3,(#189210,#189211,#189212,#189213,#189214,
#189215,#189216,#189217,#189218,#189219,#189220,#189221,#189222),
 .UNSPECIFIED.,.F.,.F.,(4,3,3,3,4),(0.,0.306929728150734,0.616198997155632,
0.925384154814288,1.),.UNSPECIFIED.);
#5416=B_SPLINE_CURVE_WITH_KNOTS('',3,(#189440,#189441,#189442,#189443,#189444,
#189445),.UNSPECIFIED.,.F.,.F.,(4,2,4),(0.,0.5,1.),.UNSPECIFIED.);
#5417=B_SPLINE_CURVE_WITH_KNOTS('',3,(#189496,#189497,#189498,#189499,#189500,
#189501,#189502,#189503,#189504,#189505,#189506,#189507,#189508,#189509,
#189510,#189511,#189512,#189513,#189514,#189515,#189516,#189517,#189518,
#189519,#189520,#189521,#189522,#189523,#189524,#189525,#189526),
 .UNSPECIFIED.,.F.,.F.,(4,3,3,3,3,3,3,3,3,3,4),(2.72268262058649E-15,0.000200725121679123,
0.000415654200899631,0.000612812743333638,0.000613704338138227,0.00122637007266604,
0.00122740867627373,0.00180004332072134,0.0018404606068653,0.00184111301440923,
0.00245481735254474),.UNSPECIFIED.);
#5418=B_SPLINE_CURVE_WITH_KNOTS('',3,(#189529,#189530,#189531,#189532,#189533,
#189534,#189535,#189536,#189537,#189538),.UNSPECIFIED.,.F.,.F.,(4,2,2,2,
4),(0.,0.25,0.5,0.749999999999999,1.),.UNSPECIFIED.);
#5419=B_SPLINE_CURVE_WITH_KNOTS('',3,(#189554,#189555,#189556,#189557),
 .UNSPECIFIED.,.F.,.F.,(4,4),(0.,0.0105146476282051),.UNSPECIFIED.);
#5420=B_SPLINE_CURVE_WITH_KNOTS('',3,(#189558,#189559,#189560,#189561,#189562,
#189563,#189564,#189565,#189566,#189567,#189568,#189569,#189570,#189571,
#189572,#189573,#189574,#189575,#189576),.UNSPECIFIED.,.F.,.F.,(4,3,3,3,
3,3,4),(0.,0.213104637861165,0.407982689360979,0.589084311419952,0.696008383904322,
0.866070542392472,1.),.UNSPECIFIED.);
#5421=B_SPLINE_CURVE_WITH_KNOTS('',3,(#189614,#189615,#189616,#189617,#189618,
#189619,#189620,#189621,#189622,#189623,#189624,#189625,#189626,#189627,
#189628,#189629,#189630,#189631,#189632,#189633,#189634,#189635,#189636,
#189637,#189638,#189639,#189640,#189641,#189642,#189643,#189644,#189645,
#189646,#189647,#189648,#189649,#189650,#189651,#189652,#189653,#189654,
#189655,#189656,#189657,#189658,#189659,#189660,#189661,#189662,#189663,
#189664,#189665),.UNSPECIFIED.,.F.,.F.,(4,3,3,3,3,3,3,3,3,3,3,3,3,3,3,3,
3,4),(0.,0.0577449572001592,0.115760673898661,0.173966397974882,0.232612154939909,
0.25,0.317701909767158,0.387380567559864,0.460298498604314,0.5,0.576716836363912,
0.655971198986622,0.738743908648322,0.750000000000001,0.828430140854719,
0.908165239695145,0.988685556276332,0.999999999999989),.UNSPECIFIED.);
#5422=B_SPLINE_CURVE_WITH_KNOTS('',3,(#189666,#189667,#189668,#189669,#189670,
#189671,#189672,#189673,#189674,#189675),.UNSPECIFIED.,.F.,.F.,(4,2,2,2,
4),(0.,0.249999999999999,0.5,0.75,1.),.UNSPECIFIED.);
#5423=B_SPLINE_CURVE_WITH_KNOTS('',3,(#189703,#189704,#189705,#189706,#189707,
#189708,#189709),.UNSPECIFIED.,.F.,.F.,(4,3,4),(9.81307786677359E-18,0.00416048285086259,
0.00832096570172518),.UNSPECIFIED.);
#5424=B_SPLINE_CURVE_WITH_KNOTS('',3,(#189710,#189711,#189712,#189713,#189714,
#189715),.UNSPECIFIED.,.F.,.F.,(4,2,4),(0.,0.5,1.),.UNSPECIFIED.);
#5425=B_SPLINE_CURVE_WITH_KNOTS('',3,(#189755,#189756,#189757,#189758,#189759,
#189760,#189761,#189762,#189763,#189764,#189765,#189766,#189767,#189768,
#189769,#189770,#189771,#189772,#189773,#189774,#189775,#189776,#189777,
#189778,#189779,#189780,#189781,#189782,#189783,#189784,#189785,#189786,
#189787,#189788,#189789,#189790,#189791,#189792,#189793,#189794,#189795,
#189796,#189797,#189798,#189799,#189800,#189801,#189802,#189803),
 .UNSPECIFIED.,.F.,.F.,(4,3,3,3,3,3,3,3,3,3,3,3,3,3,3,3,4),(1.38012332775335E-14,
0.0812387813843933,0.165619390692197,0.244281834991246,0.25,0.337320583840223,
0.420544762023585,0.5,0.571921750742126,0.641679642600622,0.708356570658027,
0.75,0.8125,0.872346811049028,0.931984514842584,0.991450954272749,1.),
 .UNSPECIFIED.);
#5426=B_SPLINE_CURVE_WITH_KNOTS('',3,(#189804,#189805,#189806,#189807,#189808,
#189809,#189810,#189811,#189812,#189813),.UNSPECIFIED.,.F.,.F.,(4,2,2,2,
4),(0.,0.25,0.5,0.75,1.),.UNSPECIFIED.);
#5427=B_SPLINE_CURVE_WITH_KNOTS('',3,(#189835,#189836,#189837,#189838),
 .UNSPECIFIED.,.F.,.F.,(4,4),(0.,0.0107001581246114),.UNSPECIFIED.);
#5428=B_SPLINE_CURVE_WITH_KNOTS('',3,(#189839,#189840,#189841,#189842),
 .UNSPECIFIED.,.F.,.F.,(4,4),(0.,1.),.UNSPECIFIED.);
#5429=B_SPLINE_CURVE_WITH_KNOTS('',3,(#189858,#189859,#189860,#189861),
 .UNSPECIFIED.,.F.,.F.,(4,4),(0.,1.),.UNSPECIFIED.);
#5430=B_SPLINE_CURVE_WITH_KNOTS('',3,(#189862,#189863,#189864,#189865),
 .UNSPECIFIED.,.F.,.F.,(4,4),(0.,1.),.UNSPECIFIED.);
#5431=B_SPLINE_CURVE_WITH_KNOTS('',3,(#189888,#189889,#189890,#189891,#189892,
#189893,#189894,#189895,#189896,#189897,#189898,#189899,#189900,#189901,
#189902,#189903,#189904,#189905,#189906,#189907,#189908,#189909,#189910,
#189911,#189912),.UNSPECIFIED.,.F.,.F.,(4,3,3,3,3,3,3,3,4),(0.,0.122312447861915,
0.247147624918063,0.375895981289337,0.424647071101479,0.558508838421222,
0.69921940889293,0.849609704446465,1.),.UNSPECIFIED.);
#5432=B_SPLINE_CURVE_WITH_KNOTS('',3,(#189913,#189914,#189915,#189916,#189917,
#189918),.UNSPECIFIED.,.F.,.F.,(4,2,4),(0.,0.5,1.),.UNSPECIFIED.);
#5433=B_SPLINE_CURVE_WITH_KNOTS('',3,(#189961,#189962,#189963,#189964,#189965,
#189966,#189967,#189968,#189969,#189970,#189971,#189972),.UNSPECIFIED.,
 .F.,.F.,(4,2,2,2,2,4),(0.,0.249999999999999,0.375,0.500000000000001,0.75,
1.),.UNSPECIFIED.);
#5434=B_SPLINE_CURVE_WITH_KNOTS('',3,(#189975,#189976,#189977,#189978,#189979,
#189980,#189981,#189982,#189983,#189984,#189985,#189986,#189987,#189988,
#189989,#189990,#189991,#189992,#189993,#189994,#189995,#189996,#189997,
#189998,#189999,#190000,#190001,#190002,#190003,#190004,#190005,#190006,
#190007,#190008,#190009,#190010,#190011,#190012,#190013,#190014,#190015,
#190016,#190017,#190018,#190019,#190020,#190021,#190022,#190023,#190024,
#190025,#190026,#190027,#190028,#190029),.UNSPECIFIED.,.F.,.F.,(4,3,3,3,
3,3,3,3,3,3,3,3,3,3,3,3,3,3,4),(0.,0.0789176820769353,0.157127159397805,
0.233367179050978,0.25,0.325562808086822,0.399246594459274,0.469841989659592,
0.499999999999999,0.577528901441685,0.625,0.678393373561975,0.731135413249808,
0.750000000000001,0.806829802933232,0.863252623549527,0.919502567920812,
0.975672037690016,1.),.UNSPECIFIED.);
#5435=B_SPLINE_CURVE_WITH_KNOTS('',3,(#190045,#190046,#190047,#190048),
 .UNSPECIFIED.,.F.,.F.,(4,4),(4.04603565571183E-17,0.00980967348625103),
 .UNSPECIFIED.);
#5436=B_SPLINE_CURVE_WITH_KNOTS('',3,(#190049,#190050,#190051,#190052,#190053,
#190054,#190055,#190056,#190057,#190058,#190059,#190060,#190061),
 .UNSPECIFIED.,.F.,.F.,(4,3,3,3,4),(0.,0.268855438291974,0.55495113409128,
0.863752202872325,1.),.UNSPECIFIED.);
#5437=B_SPLINE_CURVE_WITH_KNOTS('',3,(#190083,#190084,#190085,#190086,#190087,
#190088,#190089,#190090,#190091,#190092,#190093,#190094,#190095,#190096,
#190097,#190098,#190099,#190100,#190101,#190102,#190103,#190104,#190105,
#190106,#190107),.UNSPECIFIED.,.F.,.F.,(4,3,3,3,3,3,3,3,4),(0.,0.152876067585667,
0.30639781432929,0.373021274914802,0.5,0.656092103689984,0.810004975183274,
0.95906628874972,1.),.UNSPECIFIED.);
#5438=B_SPLINE_CURVE_WITH_KNOTS('',3,(#190108,#190109,#190110,#190111,#190112,
#190113,#190114),.UNSPECIFIED.,.F.,.F.,(4,3,4),(0.,0.00416021787251447,
0.00832043574502893),.UNSPECIFIED.);
#5439=B_SPLINE_CURVE_WITH_KNOTS('',3,(#190136,#190137,#190138,#190139,#190140,
#190141),.UNSPECIFIED.,.F.,.F.,(4,2,4),(0.,0.5,1.),.UNSPECIFIED.);
#5440=B_SPLINE_CURVE_WITH_KNOTS('',3,(#190142,#190143,#190144,#190145,#190146,
#190147),.UNSPECIFIED.,.F.,.F.,(4,2,4),(0.,0.5,1.),.UNSPECIFIED.);
#5441=B_SPLINE_CURVE_WITH_KNOTS('',3,(#190181,#190182,#190183,#190184,#190185,
#190186,#190187,#190188,#190189,#190190),.UNSPECIFIED.,.F.,.F.,(4,2,2,2,
4),(0.,0.249999999999999,0.499999999999999,0.75,1.),.UNSPECIFIED.);
#5442=B_SPLINE_CURVE_WITH_KNOTS('',3,(#190191,#190192,#190193,#190194,#190195,
#190196,#190197,#190198,#190199,#190200,#190201,#190202,#190203,#190204,
#190205,#190206,#190207,#190208,#190209,#190210,#190211,#190212,#190213,
#190214,#190215,#190216,#190217,#190218,#190219,#190220,#190221,#190222,
#190223,#190224,#190225,#190226,#190227,#190228,#190229,#190230,#190231,
#190232,#190233,#190234,#190235,#190236,#190237,#190238,#190239,#190240,
#190241,#190242),.UNSPECIFIED.,.F.,.F.,(4,3,3,3,3,3,3,3,3,3,3,3,3,3,3,3,
3,4),(0.,0.0582415495970998,0.116663503047352,0.175224355996429,0.234148749404122,
0.25,0.322580824057758,0.396872773529455,0.473813539319455,0.500000000000001,
0.572660400761366,0.647461247395867,0.725045015722337,0.750000000000002,
0.826854309093119,0.904998593137059,0.98393508435569,1.),.UNSPECIFIED.);
#5443=B_SPLINE_CURVE_WITH_KNOTS('',3,(#190262,#190263,#190264,#190265,#190266,
#190267,#190268,#190269,#190270,#190271,#190272,#190273,#190274,#190275,
#190276,#190277,#190278,#190279,#190280),.UNSPECIFIED.,.F.,.F.,(4,3,3,3,
3,3,4),(0.,0.195941169472998,0.290434549960185,0.500144896478958,0.700717460267629,
0.890960745354147,1.),.UNSPECIFIED.);
#5444=B_SPLINE_CURVE_WITH_KNOTS('',3,(#190281,#190282,#190283,#190284),
 .UNSPECIFIED.,.F.,.F.,(4,4),(0.,0.00972938600277915),.UNSPECIFIED.);
#5445=B_SPLINE_CURVE_WITH_KNOTS('',3,(#190300,#190301,#190302,#190303),
 .UNSPECIFIED.,.F.,.F.,(4,4),(0.,2.59869381596583E-5),.UNSPECIFIED.);
#5446=B_SPLINE_CURVE_WITH_KNOTS('',3,(#190304,#190305,#190306,#190307),
 .UNSPECIFIED.,.F.,.F.,(4,4),(0.,3.23803390124219E-5),.UNSPECIFIED.);
#5447=B_SPLINE_CURVE_WITH_KNOTS('',3,(#190335,#190336,#190337,#190338,#190339,
#190340,#190341,#190342),.UNSPECIFIED.,.F.,.F.,(4,2,2,4),(0.,0.249999999999999,
0.5,1.),.UNSPECIFIED.);
#5448=B_SPLINE_CURVE_WITH_KNOTS('',3,(#190343,#190344,#190345,#190346,#190347,
#190348,#190349,#190350),.UNSPECIFIED.,.F.,.F.,(4,2,2,4),(0.,0.5,0.750000000000001,
1.),.UNSPECIFIED.);
#5449=B_SPLINE_CURVE_WITH_KNOTS('',3,(#190382,#190383,#190384,#190385),
 .UNSPECIFIED.,.F.,.F.,(4,4),(6.93889390390723E-18,2.09370149851292E-5),
 .UNSPECIFIED.);
#5450=B_SPLINE_CURVE_WITH_KNOTS('',3,(#190386,#190387,#190388,#190389),
 .UNSPECIFIED.,.F.,.F.,(4,4),(0.,1.68205588696557E-5),.UNSPECIFIED.);
#5451=B_SPLINE_CURVE_WITH_KNOTS('',3,(#190471,#190472,#190473,#190474),
 .UNSPECIFIED.,.F.,.F.,(4,4),(0.,0.000210836370419721),.UNSPECIFIED.);
#5452=B_SPLINE_CURVE_WITH_KNOTS('',3,(#190512,#190513,#190514,#190515,#190516,
#190517,#190518,#190519,#190520,#190521,#190522,#190523),.UNSPECIFIED.,
 .F.,.F.,(4,2,2,2,2,4),(0.,0.125,0.249999999999999,0.5,0.75,1.),
 .UNSPECIFIED.);
#5453=B_SPLINE_CURVE_WITH_KNOTS('',3,(#190526,#190527,#190528,#190529,#190530,
#190531,#190532,#190533,#190534,#190535,#190536,#190537),.UNSPECIFIED.,
 .F.,.F.,(4,2,2,2,2,4),(0.,0.25,0.500000000000001,0.750000000000001,0.875,
1.),.UNSPECIFIED.);
#5454=B_SPLINE_CURVE_WITH_KNOTS('',3,(#190577,#190578,#190579,#190580,#190581,
#190582,#190583,#190584,#190585,#190586,#190587,#190588,#190589,#190590,
#190591,#190592,#190593,#190594,#190595,#190596,#190597,#190598,#190599,
#190600,#190601,#190602,#190603,#190604,#190605,#190606,#190607,#190608,
#190609,#190610),.UNSPECIFIED.,.F.,.F.,(4,3,3,3,3,3,3,3,3,3,3,4),(0.,0.146910620412476,
0.25,0.391211209956079,0.5,0.583892307870227,0.625,0.706893805446917,0.75,
0.85002508516687,0.938030549136298,1.),.UNSPECIFIED.);
#5455=B_SPLINE_CURVE_WITH_KNOTS('',3,(#190611,#190612,#190613,#190614,#190615,
#190616,#190617,#190618,#190619,#190620,#190621,#190622),.UNSPECIFIED.,
 .F.,.F.,(4,2,2,2,2,4),(0.,0.25,0.375,0.5,0.75,1.),.UNSPECIFIED.);
#5456=B_SPLINE_CURVE_WITH_KNOTS('',3,(#190672,#190673,#190674,#190675,#190676,
#190677,#190678,#190679,#190680,#190681),.UNSPECIFIED.,.F.,.F.,(4,3,3,4),
(6.93889390390723E-18,0.000636015601018232,0.00129844965740646,0.00158760011419448),
 .UNSPECIFIED.);
#5457=B_SPLINE_CURVE_WITH_KNOTS('',3,(#190682,#190683,#190684,#190685,#190686,
#190687,#190688,#190689,#190690,#190691,#190692,#190693,#190694),
 .UNSPECIFIED.,.F.,.F.,(4,3,3,3,4),(0.,0.25669998202569,0.50808588571949,
0.754042942859745,1.),.UNSPECIFIED.);
#5458=B_SPLINE_CURVE_WITH_KNOTS('',3,(#190710,#190711,#190712,#190713,#190714,
#190715,#190716,#190717,#190718,#190719,#190720,#190721,#190722),
 .UNSPECIFIED.,.F.,.F.,(4,3,3,3,4),(0.,0.253266620399936,0.51240411680184,
0.78046435058956,1.),.UNSPECIFIED.);
#5459=B_SPLINE_CURVE_WITH_KNOTS('',3,(#190723,#190724,#190725,#190726,#190727,
#190728,#190729,#190730,#190731,#190732),.UNSPECIFIED.,.F.,.F.,(4,3,3,4),
(0.,0.000679723972679124,0.00133201311756995,0.0015185374894695),
 .UNSPECIFIED.);
#5460=B_SPLINE_CURVE_WITH_KNOTS('',3,(#190760,#190761,#190762,#190763,#190764,
#190765,#190766,#190767),.UNSPECIFIED.,.F.,.F.,(4,2,2,4),(0.,0.25,0.5,1.),
 .UNSPECIFIED.);
#5461=B_SPLINE_CURVE_WITH_KNOTS('',3,(#190768,#190769,#190770,#190771,#190772,
#190773,#190774,#190775),.UNSPECIFIED.,.F.,.F.,(4,2,2,4),(5.09829085353129E-9,
0.5,0.75,1.),.UNSPECIFIED.);
#5462=B_SPLINE_CURVE_WITH_KNOTS('',3,(#190803,#190804,#190805,#190806,#190807,
#190808,#190809,#190810),.UNSPECIFIED.,.F.,.F.,(4,2,2,4),(0.,0.25,0.5,0.999999992626662),
 .UNSPECIFIED.);
#5463=B_SPLINE_CURVE_WITH_KNOTS('',3,(#190811,#190812,#190813,#190814,#190815,
#190816,#190817,#190818),.UNSPECIFIED.,.F.,.F.,(4,2,2,4),(0.,0.5,0.75,1.),
 .UNSPECIFIED.);
#5464=B_SPLINE_CURVE_WITH_KNOTS('',3,(#190876,#190877,#190878,#190879,#190880,
#190881,#190882,#190883,#190884,#190885,#190886,#190887,#190888,#190889,
#190890,#190891,#190892,#190893),.UNSPECIFIED.,.F.,.F.,(4,2,2,2,2,2,2,2,
4),(0.,0.00781250000000114,0.0156250000000006,0.0312500000000013,0.0625000000000006,
0.125,0.250000000000001,0.5,1.),.UNSPECIFIED.);
#5465=B_SPLINE_CURVE_WITH_KNOTS('',3,(#190894,#190895,#190896,#190897,#190898,
#190899,#190900,#190901,#190902,#190903,#190904,#190905,#190906,#190907,
#190908,#190909,#190910,#190911),.UNSPECIFIED.,.F.,.F.,(4,2,2,2,2,2,2,2,
4),(9.19004041809617E-16,0.00254332115550819,0.00381498173326183,0.00445081202213868,
0.00476872716657715,0.00492768473879635,0.00500716352490594,0.00504690291796077,
0.0050866423110156),.UNSPECIFIED.);
#5466=B_SPLINE_CURVE_WITH_KNOTS('',3,(#190969,#190970,#190971,#190972,#190973,
#190974,#190975,#190976,#190977,#190978,#190979,#190980,#190981,#190982,
#190983,#190984,#190985,#190986,#190987,#190988,#190989,#190990,#190991,
#190992,#190993),.UNSPECIFIED.,.F.,.F.,(4,3,3,3,3,3,3,3,4),(0.,4.03932117393399E-5,
8.08651294214249E-5,0.000161907626915798,0.000324108918069935,0.000648595245071396,
0.00129766017874913,0.00259586603175177,0.00519236941687791),
 .UNSPECIFIED.);
#5467=B_SPLINE_CURVE_WITH_KNOTS('',3,(#190994,#190995,#190996,#190997,#190998,
#190999,#191000,#191001,#191002,#191003,#191004,#191005,#191006,#191007,
#191008,#191009,#191010,#191011),.UNSPECIFIED.,.F.,.F.,(4,2,2,2,2,2,2,2,
4),(0.,0.5,0.75,0.875,0.9375,0.96875,0.984375,0.9921875,1.),
 .UNSPECIFIED.);
#5468=B_SPLINE_CURVE_WITH_KNOTS('',3,(#191073,#191074,#191075,#191076,#191077,
#191078,#191079,#191080,#191081,#191082,#191083,#191084,#191085,#191086,
#191087,#191088,#191089,#191090),.UNSPECIFIED.,.F.,.F.,(4,2,2,2,2,2,2,2,
4),(0.,0.00262931855771754,0.00394397783657636,0.00460130747600577,0.00492997229572051,
0.00509430470557792,0.00517647091050667,0.00521755401297108,0.00525863711543548),
 .UNSPECIFIED.);
#5469=B_SPLINE_CURVE_WITH_KNOTS('',3,(#191093,#191094,#191095,#191096,#191097,
#191098,#191099,#191100,#191101,#191102,#191103,#191104,#191105,#191106,
#191107,#191108,#191109,#191110),.UNSPECIFIED.,.F.,.F.,(4,2,2,2,2,2,2,2,
4),(0.,0.00781250000000008,0.0156250000000003,0.0312500000000008,0.0624999999999995,
0.124999999999999,0.250000000000001,0.5,1.),.UNSPECIFIED.);
#5470=B_SPLINE_CURVE_WITH_KNOTS('',3,(#191144,#191145,#191146,#191147,#191148,
#191149,#191150,#191151),.UNSPECIFIED.,.F.,.F.,(4,2,2,4),(6.90105437428163E-9,
0.500000000000001,0.75,1.),.UNSPECIFIED.);
#5471=B_SPLINE_CURVE_WITH_KNOTS('',3,(#191152,#191153,#191154,#191155,#191156,
#191157,#191158,#191159),.UNSPECIFIED.,.F.,.F.,(4,2,2,4),(0.,0.25,0.499999999999999,
1.),.UNSPECIFIED.);
#5472=B_SPLINE_CURVE_WITH_KNOTS('',3,(#191217,#191218,#191219,#191220,#191221,
#191222,#191223,#191224,#191225,#191226,#191227,#191228,#191229,#191230,
#191231,#191232,#191233,#191234),.UNSPECIFIED.,.F.,.F.,(4,2,2,2,2,2,2,2,
4),(0.,0.5,0.75,0.875,0.9375,0.96875,0.984375,0.9921875,1.),
 .UNSPECIFIED.);
#5473=B_SPLINE_CURVE_WITH_KNOTS('',3,(#191235,#191236,#191237,#191238,#191239,
#191240,#191241,#191242,#191243,#191244,#191245,#191246,#191247,#191248,
#191249,#191250,#191251,#191252,#191253,#191254,#191255,#191256,#191257,
#191258,#191259),.UNSPECIFIED.,.F.,.F.,(4,3,3,3,3,3,3,3,4),(4.9065389333868E-17,
4.15775196007892E-5,8.32361282030658E-5,0.000166653476908059,0.000333604410320719,
0.000667590055213201,0.00133565310169655,0.00267185549873087,0.0053443518360984),
 .UNSPECIFIED.);
#5474=B_SPLINE_CURVE_WITH_KNOTS('',3,(#191275,#191276,#191277,#191278,#191279,
#191280,#191281,#191282,#191283,#191284,#191285,#191286,#191287),
 .UNSPECIFIED.,.F.,.F.,(4,3,3,3,4),(0.,0.327766562741204,0.663883281370602,
0.973924754667621,1.),.UNSPECIFIED.);
#5475=B_SPLINE_CURVE_WITH_KNOTS('',3,(#191288,#191289,#191290,#191291,#191292,
#191293,#191294),.UNSPECIFIED.,.F.,.F.,(4,3,4),(0.,0.000722422580495128,
0.00123518557486524),.UNSPECIFIED.);
#5476=B_SPLINE_CURVE_WITH_KNOTS('',3,(#191323,#191324,#191325,#191326),
 .UNSPECIFIED.,.F.,.F.,(4,4),(0.,1.),.UNSPECIFIED.);
#5477=B_SPLINE_CURVE_WITH_KNOTS('',3,(#191327,#191328,#191329,#191330,#191331,
#191332,#191333,#191334,#191335,#191336,#191337,#191338,#191339),
 .UNSPECIFIED.,.F.,.F.,(4,3,3,3,4),(3.67744356508555E-9,0.288281482145314,
0.499999999999999,0.644141111476281,1.),.UNSPECIFIED.);
#5478=B_SPLINE_CURVE_WITH_KNOTS('',3,(#191340,#191341,#191342,#191343,#191344,
#191345,#191346,#191347),.UNSPECIFIED.,.F.,.F.,(4,2,2,4),(0.,0.25,0.499999999999999,
1.),.UNSPECIFIED.);
#5479=B_SPLINE_CURVE_WITH_KNOTS('',3,(#191380,#191381,#191382,#191383,#191384,
#191385,#191386),.UNSPECIFIED.,.F.,.F.,(4,3,4),(0.,0.000727844608945735,
0.00121469382512387),.UNSPECIFIED.);
#5480=B_SPLINE_CURVE_WITH_KNOTS('',3,(#191387,#191388,#191389,#191390,#191391,
#191392,#191393,#191394,#191395,#191396),.UNSPECIFIED.,.F.,.F.,(4,3,3,4),
(0.,0.318581264575039,0.659290632287519,1.),.UNSPECIFIED.);
#5481=B_SPLINE_CURVE_WITH_KNOTS('',3,(#191439,#191440,#191441,#191442,#191443,
#191444,#191445,#191446,#191447,#191448,#191449,#191450,#191451,#191452,
#191453,#191454,#191455,#191456,#191457,#191458,#191459,#191460,#191461,
#191462,#191463,#191464,#191465,#191466,#191467,#191468,#191469,#191470,
#191471,#191472,#191473,#191474,#191475),.UNSPECIFIED.,.F.,.F.,(4,3,3,3,
3,3,3,3,3,3,3,3,4),(0.,0.0917080761850634,0.193847311803682,0.25,0.338811353118771,
0.375,0.45988080137128,0.5,0.608296703387408,0.625,0.75,0.923180341345264,
1.),.UNSPECIFIED.);
#5482=B_SPLINE_CURVE_WITH_KNOTS('',3,(#191476,#191477,#191478,#191479,#191480,
#191481,#191482,#191483,#191484,#191485,#191486,#191487,#191488,#191489,
#191490,#191491,#191492,#191493,#191494,#191495,#191496,#191497,#191498,
#191499,#191500,#191501,#191502,#191503,#191504,#191505,#191506,#191507,
#191508,#191509,#191510,#191511,#191512,#191513,#191514,#191515,#191516,
#191517,#191518,#191519,#191520,#191521,#191522,#191523,#191524,#191525,
#191526,#191527,#191528,#191529,#191530,#191531,#191532,#191533,#191534,
#191535,#191536),.UNSPECIFIED.,.F.,.F.,(4,3,3,3,3,3,3,3,3,3,3,3,3,3,3,3,
3,3,3,3,4),(0.,0.0735852225213234,0.145541216767293,0.214668449408842,0.25,
0.325070225880086,0.375,0.4375,0.496212771549303,0.5,0.548323841680636,
0.595853929305818,0.625,0.667359798109466,0.709665698884139,0.75,0.80690825694747,
0.864567180132038,0.92279287238488,0.982204606290843,1.),.UNSPECIFIED.);
#5483=B_SPLINE_CURVE_WITH_KNOTS('',3,(#191590,#191591,#191592,#191593,#191594,
#191595,#191596,#191597,#191598,#191599,#191600,#191601),.UNSPECIFIED.,
 .F.,.F.,(4,2,2,2,2,4),(0.,0.25,0.375,0.499999999999999,0.75,1.),
 .UNSPECIFIED.);
#5484=B_SPLINE_CURVE_WITH_KNOTS('',3,(#191602,#191603,#191604,#191605,#191606,
#191607,#191608,#191609,#191610,#191611,#191612,#191613,#191614,#191615,
#191616,#191617,#191618,#191619,#191620,#191621,#191622,#191623,#191624,
#191625,#191626,#191627,#191628,#191629,#191630,#191631,#191632,#191633,
#191634,#191635),.UNSPECIFIED.,.F.,.F.,(4,3,3,3,3,3,3,3,3,3,3,4),(0.,0.159857018254139,
0.25,0.393133814716374,0.500000000000001,0.586072065778788,0.625,0.711030211262596,
0.75,0.860251075790316,0.958533798021047,1.),.UNSPECIFIED.);
#5485=B_SPLINE_CURVE_WITH_KNOTS('',3,(#193430,#193431,#193432,#193433,#193434,
#193435,#193436,#193437,#193438,#193439),.UNSPECIFIED.,.F.,.F.,(4,2,2,2,
4),(-0.0951055308727295,-0.0757879150760358,-0.0421208524807574,0.,0.00038304003494894),
 .UNSPECIFIED.);
#5486=B_SPLINE_CURVE_WITH_KNOTS('',3,(#193474,#193475,#193476,#193477,#193478,
#193479,#193480,#193481,#193482,#193483),.UNSPECIFIED.,.F.,.F.,(4,2,2,2,
4),(-0.324953678743299,-0.324570638701253,-0.28244978588071,-0.248782723015611,
-0.229465107064107),.UNSPECIFIED.);
#5487=B_SPLINE_CURVE_WITH_KNOTS('',3,(#193493,#193494,#193495,#193496,#193497,
#193498,#193499,#193500,#193501,#193502),.UNSPECIFIED.,.F.,.F.,(4,2,2,2,
4),(-0.0951055274869706,-0.0757879123768078,-0.0421208509780448,-1.08246744900953E-15,
0.000383040004758421),.UNSPECIFIED.);
#5488=B_SPLINE_CURVE_WITH_KNOTS('',3,(#193537,#193538,#193539,#193540,#193541,
#193542,#193543,#193544,#193545,#193546),.UNSPECIFIED.,.F.,.F.,(4,2,2,2,
4),(-0.324953682197493,-0.324570642147117,-0.282449788877878,-0.248782725655785,
-0.229465109499444),.UNSPECIFIED.);
#5489=B_SPLINE_CURVE_WITH_KNOTS('',3,(#193556,#193557,#193558,#193559,#193560,
#193561,#193562,#193563,#193564,#193565),.UNSPECIFIED.,.F.,.F.,(4,2,2,2,
4),(-0.0951055284907788,-0.0757879131770604,-0.0421208514235227,0.,0.000383040013518366),
 .UNSPECIFIED.);
#5490=B_SPLINE_CURVE_WITH_KNOTS('',3,(#193600,#193601,#193602,#193603,#193604,
#193605,#193606,#193607,#193608,#193609),.UNSPECIFIED.,.F.,.F.,(4,2,2,2,
4),(-0.324953664307694,-0.324570624303572,-0.282449773358066,-0.248782711984591,
-0.22946509688894),.UNSPECIFIED.);
#5491=B_SPLINE_CURVE_WITH_KNOTS('',3,(#193615,#193616,#193617,#193618,#193619,
#193620,#193621,#193622,#193623,#193624),.UNSPECIFIED.,.F.,.F.,(4,2,2,2,
4),(-0.0003830399169838,0.,0.042120846642674,0.0757879045921621,0.095105517723294),
 .UNSPECIFIED.);
#5492=B_SPLINE_CURVE_WITH_KNOTS('',3,(#193663,#193664,#193665,#193666,#193667,
#193668,#193669,#193670,#193671,#193672),.UNSPECIFIED.,.F.,.F.,(4,2,2,2,
4),(-0.324953631774432,-0.324570591855723,-0.28244974513484,-0.248782687123421,
-0.229465073956758),.UNSPECIFIED.);
#5493=B_SPLINE_CURVE_WITH_KNOTS('',3,(#193866,#193867,#193868,#193869,#193870,
#193871,#193872,#193873,#193874,#193875,#193876,#193877,#193878,#193879,
#193880,#193881,#193882,#193883,#193884,#193885,#193886,#193887),
 .UNSPECIFIED.,.F.,.F.,(4,2,1,1,2,2,2,2,2,2,2,4),(0.,0.0156250000000012,
0.0312500000000023,0.0625000000000033,0.125000000000004,0.250000000000003,
0.500000000000002,0.750000000000001,0.875,0.9375,0.96875,1.),
 .UNSPECIFIED.);
#5494=B_SPLINE_CURVE_WITH_KNOTS('',3,(#193889,#193890,#193891,#193892,#193893,
#193894,#193895,#193896,#193897,#193898,#193899,#193900,#193901,#193902,
#193903,#193904,#193905,#193906,#193907,#193908,#193909,#193910,#193911,
#193912,#193913,#193914),.UNSPECIFIED.,.F.,.F.,(4,2,2,2,2,2,2,2,2,2,2,2,
4),(0.,0.00459330644835038,0.0094020344365217,0.0190194904128667,0.0382544023655542,
0.0767242262709338,0.384482817513955,0.538362113135469,0.61530176094622,
0.634536672898912,0.653771584851599,0.692241408756977,1.),.UNSPECIFIED.);
#5495=B_SPLINE_CURVE_WITH_KNOTS('',3,(#193918,#193919,#193920,#193921,#193922,
#193923,#193924,#193925,#193926,#193927,#193928,#193929,#193930,#193931,
#193932,#193933,#193934,#193935,#193936,#193937,#193938,#193939,#193940,
#193941,#193942,#193943,#193944,#193945,#193946,#193947,#193948,#193949,
#193950,#193951,#193952,#193953,#193954,#193955,#193956,#193957,#193958,
#193959,#193960,#193961,#193962,#193963,#193964,#193965,#193966,#193967,
#193968,#193969,#193970,#193971,#193972,#193973,#193974,#193975,#193976,
#193977,#193978,#193979,#193980,#193981,#193982,#193983,#193984,#193985,
#193986,#193987,#193988,#193989,#193990,#193991,#193992,#193993,#193994,
#193995,#193996,#193997,#193998,#193999,#194000,#194001,#194002,#194003,
#194004,#194005,#194006,#194007,#194008,#194009,#194010,#194011,#194012,
#194013,#194014,#194015,#194016,#194017,#194018,#194019,#194020,#194021,
#194022,#194023,#194024,#194025,#194026,#194027,#194028,#194029),
 .UNSPECIFIED.,.F.,.F.,(4,3,3,3,3,3,3,3,3,3,3,3,3,3,3,3,3,3,3,3,3,3,3,3,
3,3,3,3,3,3,3,3,3,3,3,3,3,4),(4.87707812168843E-13,0.00106872162737289,
0.00213668903088859,0.00293590036890479,0.0029378487127682,0.00330316625056856,
0.00348679919079069,0.00367043213192709,0.00367231089096026,0.00440496389379973,
0.0044067730691523,0.00587402741748767,0.0058756974255364,0.00881215446495341,
0.00881354613830458,0.00917942034579961,0.00936305328639039,0.00945486975663566,
0.00950077799173426,0.00954668622681246,0.00954800831649663,0.0102812179886621,
0.0102824704946887,0.0117502815123831,0.0117513948510728,0.0146884085598291,
0.0146892435638409,0.0154229402826017,0.015790206158568,0.0159738391130884,
0.0160656555960944,0.0161115638392354,0.016157472083545,0.016158167920225,
0.0176265356072484,0.0176270922766091,0.0205649409893773,0.0235027897021455),
 .UNSPECIFIED.);
#5496=B_SPLINE_CURVE_WITH_KNOTS('',3,(#194032,#194033,#194034,#194035,#194036,
#194037,#194038,#194039,#194040,#194041,#194042),.UNSPECIFIED.,.F.,.F.,
(4,1,2,2,2,4),(0.,0.500000000000001,0.750000000000002,0.875000000000003,
0.984375000000001,1.),.UNSPECIFIED.);
#5497=B_SPLINE_CURVE_WITH_KNOTS('',3,(#194058,#194059,#194060,#194061),
 .UNSPECIFIED.,.F.,.F.,(4,4),(0.,1.),.UNSPECIFIED.);
#5498=B_SPLINE_CURVE_WITH_KNOTS('',3,(#194062,#194063,#194064,#194065),
 .UNSPECIFIED.,.F.,.F.,(4,4),(0.,0.000322395538615397),.UNSPECIFIED.);
#5499=B_SPLINE_CURVE_WITH_KNOTS('',3,(#194164,#194165,#194166,#194167,#194168,
#194169,#194170,#194171,#194172,#194173,#194174,#194175,#194176,#194177,
#194178,#194179,#194180,#194181,#194182,#194183,#194184,#194185,#194186,
#194187,#194188,#194189),.UNSPECIFIED.,.F.,.F.,(4,2,2,2,2,2,2,2,2,2,2,2,
4),(0.,0.125000000000001,0.156250000000001,0.187500000000002,0.250000000000001,
0.375000000000001,0.5,0.562500000000001,0.625,0.75,0.8125,0.875,1.),
 .UNSPECIFIED.);
#5500=B_SPLINE_CURVE_WITH_KNOTS('',3,(#194190,#194191,#194192,#194193,#194194,
#194195,#194196,#194197,#194198,#194199,#194200,#194201,#194202,#194203,
#194204,#194205,#194206,#194207,#194208,#194209,#194210,#194211,#194212,
#194213,#194214,#194215,#194216,#194217,#194218,#194219,#194220,#194221,
#194222,#194223,#194224,#194225,#194226),.UNSPECIFIED.,.F.,.F.,(4,3,3,3,
3,3,3,3,3,3,3,3,4),(0.,0.000191440270420746,0.000287160692730017,0.000382881236840892,
0.000574322481675384,0.000670043078002301,0.00076576358733981,0.000957204470373581,
0.00114864534416313,0.00124436578623716,0.00129222601008214,0.00134008623637552,
0.00153152717467962),.UNSPECIFIED.);
#5501=B_SPLINE_CURVE_WITH_KNOTS('',3,(#194266,#194267,#194268,#194269,#194270,
#194271,#194272,#194273,#194274,#194275,#194276,#194277,#194278,#194279,
#194280,#194281,#194282,#194283,#194284,#194285,#194286,#194287,#194288,
#194289,#194290,#194291,#194292,#194293,#194294,#194295,#194296,#194297,
#194298,#194299,#194300,#194301,#194302,#194303,#194304,#194305,#194306,
#194307,#194308,#194309,#194310,#194311,#194312,#194313,#194314,#194315,
#194316,#194317,#194318,#194319,#194320,#194321,#194322,#194323,#194324,
#194325,#194326,#194327,#194328,#194329,#194330,#194331,#194332,#194333,
#194334,#194335,#194336,#194337,#194338,#194339,#194340,#194341,#194342,
#194343,#194344,#194345,#194346,#194347),.UNSPECIFIED.,.F.,.F.,(4,3,3,3,
3,3,3,3,3,3,3,3,3,3,3,3,3,3,3,3,3,3,3,3,3,3,3,4),(0.,0.0401050357347157,
0.0812206026238641,0.123882732875838,0.167390541414787,0.212077250701923,
0.238079056359111,0.25,0.292319902552325,0.336625084595829,0.374999999999999,
0.420046787969305,0.466533956719877,0.495505970383118,0.5,0.545041357418745,
0.590377250465255,0.63449200813962,0.677383348177903,0.718184700217024,
0.75,0.756613713052315,0.8004091838459,0.84325569019173,0.884513955801954,
0.924879177580128,0.963805079356448,1.),.UNSPECIFIED.);
#5502=B_SPLINE_CURVE_WITH_KNOTS('',3,(#194348,#194349,#194350,#194351,#194352,
#194353,#194354,#194355,#194356,#194357,#194358,#194359,#194360,#194361,
#194362,#194363,#194364,#194365,#194366),.UNSPECIFIED.,.F.,.F.,(4,3,3,3,
3,3,4),(0.,0.00503761689939749,0.00646885457540687,0.0129377091508137,0.0161721364385172,
0.0194065637262206,0.0258754183016275),.UNSPECIFIED.);
#5503=B_SPLINE_CURVE_WITH_KNOTS('',3,(#194472,#194473,#194474,#194475,#194476,
#194477,#194478,#194479,#194480,#194481,#194482,#194483,#194484,#194485,
#194486,#194487,#194488,#194489,#194490,#194491,#194492,#194493,#194494,
#194495,#194496,#194497,#194498,#194499,#194500,#194501,#194502,#194503,
#194504,#194505),.UNSPECIFIED.,.F.,.F.,(4,2,2,2,2,2,2,2,2,2,2,2,2,2,2,2,
4),(0.,0.125000000000002,0.187500000000001,0.250000000000001,0.3125,0.375,
0.4375,0.500000000000001,0.5625,0.625,0.6875,0.75,0.8125,0.84375,0.875,
0.9375,1.),.UNSPECIFIED.);
#5504=B_SPLINE_CURVE_WITH_KNOTS('',3,(#194506,#194507,#194508,#194509,#194510,
#194511,#194512,#194513,#194514,#194515,#194516,#194517,#194518,#194519,
#194520,#194521,#194522,#194523,#194524,#194525,#194526,#194527,#194528,
#194529,#194530,#194531,#194532,#194533,#194534,#194535,#194536,#194537,
#194538,#194539,#194540,#194541,#194542,#194543,#194544,#194545,#194546,
#194547,#194548,#194549,#194550,#194551,#194552,#194553,#194554),
 .UNSPECIFIED.,.F.,.F.,(4,3,3,3,3,3,3,3,3,3,3,3,3,3,3,3,4),(0.,0.000127303360486361,
0.000254607331807631,0.000318259502487228,0.000381911773022019,0.000509216543183179,
0.000636521501341121,0.000763826506543775,0.000891131417838548,0.00101843609427484,
0.00114573874978534,0.00127303875321421,0.00140033769575051,0.00152763716845166,
0.00165493876244132,0.00178224406910835,0.00203687218854967),
 .UNSPECIFIED.);
#5505=B_SPLINE_CURVE_WITH_KNOTS('',3,(#194587,#194588,#194589,#194590),
 .UNSPECIFIED.,.F.,.F.,(4,4),(0.,1.),.UNSPECIFIED.);
#5506=B_SPLINE_CURVE_WITH_KNOTS('',3,(#194591,#194592,#194593,#194594),
 .UNSPECIFIED.,.F.,.F.,(4,4),(6.93889390390723E-18,0.000463834979289304),
 .UNSPECIFIED.);
#5507=B_SPLINE_CURVE_WITH_KNOTS('',3,(#194911,#194912,#194913,#194914,#194915,
#194916,#194917,#194918,#194919,#194920,#194921,#194922,#194923,#194924,
#194925,#194926,#194927,#194928,#194929,#194930,#194931,#194932,#194933,
#194934,#194935,#194936,#194937,#194938,#194939,#194940,#194941,#194942,
#194943,#194944,#194945,#194946,#194947,#194948,#194949,#194950,#194951,
#194952,#194953,#194954,#194955,#194956,#194957,#194958,#194959,#194960,
#194961,#194962),.UNSPECIFIED.,.F.,.F.,(4,3,3,3,3,3,3,3,3,3,3,3,3,3,3,3,
3,4),(0.,0.118561059956462,0.193296673546538,0.311563674713324,0.428677054200604,
0.467557845905428,0.500000000000002,0.618691112431543,0.730136570084834,
0.737382224863085,0.750000000000003,0.860639773248037,0.875000000000003,
0.937500000000003,0.968750000000002,0.984375000000001,0.995689543360724,
1.),.UNSPECIFIED.);
#5508=B_SPLINE_CURVE_WITH_KNOTS('',3,(#194964,#194965,#194966,#194967,#194968,
#194969,#194970,#194971,#194972,#194973,#194974,#194975,#194976,#194977,
#194978,#194979,#194980,#194981,#194982,#194983,#194984,#194985,#194986,
#194987,#194988,#194989,#194990,#194991,#194992,#194993,#194994,#194995,
#194996,#194997,#194998,#194999,#195000,#195001,#195002,#195003),
 .UNSPECIFIED.,.F.,.F.,(4,3,3,3,3,3,3,3,3,3,3,3,3,4),(0.,0.00505175093915313,
0.015625000000001,0.0212638638717959,0.031250000000002,0.0625000000000022,
0.125000000000002,0.150960766387526,0.66974837608655,0.929142180936068,
0.937500000000002,0.984375000000001,0.993990629527285,1.),.UNSPECIFIED.);
#5509=B_SPLINE_CURVE_WITH_KNOTS('',3,(#195005,#195006,#195007,#195008,#195009,
#195010,#195011,#195012,#195013,#195014,#195015,#195016,#195017,#195018,
#195019,#195020,#195021,#195022,#195023,#195024,#195025,#195026,#195027,
#195028,#195029,#195030,#195031,#195032,#195033,#195034,#195035,#195036,
#195037,#195038,#195039,#195040,#195041,#195042,#195043,#195044,#195045,
#195046,#195047,#195048),.UNSPECIFIED.,.F.,.F.,(4,2,2,2,2,2,2,2,2,2,2,2,
2,2,2,2,2,2,2,2,2,4),(1.21542793577394E-6,0.000926751404419985,0.0045096865781495,
0.0116755569256177,0.0260072976205485,0.0833342604002824,0.312642111519209,
0.427296037078671,0.484622999858401,0.513286481248267,0.527618221943199,
0.531201157116932,0.534784092290667,0.54194996263813,0.771257813757056,
0.885911739316519,0.943238702096252,0.971902183486115,0.986233924181051,
0.993399794528514,0.996982729702248,1.),.UNSPECIFIED.);
#5510=B_SPLINE_CURVE_WITH_KNOTS('',3,(#195050,#195051,#195052,#195053,#195054,
#195055,#195056,#195057,#195058,#195059,#195060,#195061,#195062,#195063,
#195064,#195065),.UNSPECIFIED.,.F.,.F.,(4,2,2,2,2,2,2,4),(0.,0.00107945262646427,
0.438665331950596,0.65745827161266,0.876251211274724,0.985647681105758,
0.999322239834636,1.),.UNSPECIFIED.);
#5511=B_SPLINE_CURVE_WITH_KNOTS('',3,(#195067,#195068,#195069,#195070,#195071,
#195072,#195073,#195074,#195075,#195076,#195077,#195078,#195079,#195080,
#195081,#195082,#195083,#195084,#195085,#195086,#195087,#195088,#195089,
#195090,#195091,#195092,#195093,#195094,#195095,#195096,#195097,#195098,
#195099,#195100,#195101,#195102,#195103,#195104,#195105,#195106,#195107,
#195108,#195109,#195110,#195111,#195112,#195113,#195114,#195115,#195116,
#195117,#195118,#195119,#195120,#195121,#195122,#195123,#195124,#195125,
#195126,#195127),.UNSPECIFIED.,.F.,.F.,(4,3,3,3,3,3,3,3,3,3,3,3,3,3,3,3,
3,3,3,3,4),(0.,0.00781249999999971,0.0156249999999994,0.0312499999999994,
0.0624999999999994,0.124999999999999,0.249129116160185,0.249999999999999,
0.350754550530283,0.451829475765032,0.497596952377019,0.499999999999999,
0.653289414190925,0.74797126632589,0.749999999999999,0.875,0.9375,0.96875,
0.984375,0.996876914777217,0.999999999247695),.UNSPECIFIED.);
#5512=B_SPLINE_CURVE_WITH_KNOTS('',3,(#195128,#195129,#195130,#195131,#195132,
#195133,#195134,#195135,#195136,#195137,#195138,#195139,#195140,#195141,
#195142,#195143),.UNSPECIFIED.,.F.,.F.,(4,3,3,3,3,4),(0.,0.00802457780095953,
0.0982041616372357,0.278563329309788,0.639281664654894,1.),
 .UNSPECIFIED.);
#5513=B_SPLINE_CURVE_WITH_KNOTS('',3,(#195144,#195145,#195146,#195147,#195148,
#195149,#195150,#195151,#195152,#195153,#195154,#195155,#195156,#195157,
#195158,#195159,#195160,#195161,#195162,#195163,#195164,#195165,#195166,
#195167,#195168,#195169,#195170,#195171,#195172,#195173,#195174,#195175,
#195176,#195177,#195178,#195179,#195180,#195181,#195182,#195183,#195184,
#195185,#195186,#195187,#195188,#195189,#195190,#195191,#195192,#195193,
#195194,#195195,#195196,#195197,#195198,#195199,#195200,#195201,#195202,
#195203,#195204,#195205,#195206,#195207,#195208,#195209,#195210,#195211,
#195212,#195213,#195214,#195215,#195216,#195217,#195218,#195219,#195220,
#195221,#195222,#195223,#195224,#195225,#195226,#195227,#195228,#195229,
#195230,#195231,#195232,#195233,#195234,#195235,#195236,#195237,#195238,
#195239,#195240,#195241,#195242,#195243,#195244,#195245,#195246,#195247,
#195248,#195249,#195250,#195251,#195252,#195253,#195254,#195255,#195256,
#195257,#195258,#195259,#195260,#195261,#195262,#195263,#195264,#195265,
#195266,#195267,#195268,#195269,#195270,#195271,#195272,#195273,#195274,
#195275,#195276,#195277,#195278,#195279,#195280,#195281,#195282,#195283,
#195284,#195285,#195286,#195287,#195288,#195289,#195290,#195291,#195292,
#195293,#195294,#195295,#195296,#195297),.UNSPECIFIED.,.F.,.F.,(4,3,3,3,
3,3,3,3,3,3,3,3,3,3,3,3,3,3,3,3,3,3,3,3,3,3,3,3,3,3,3,3,3,3,3,3,3,3,3,3,
3,3,3,3,3,3,3,3,3,3,3,4),(1.04083408558608E-17,0.00250327328955152,0.00500654657910303,
0.00625818322387879,0.00688400154626667,0.00696222883656844,0.00704045612686793,
0.00719691070746254,0.00750981986865454,0.010013093158206,0.0112647298029818,
0.011577638964179,0.0117340935447715,0.0117732071899202,0.0118123208350694,
0.0118905481253697,0.0125163664477576,0.0137680030925333,0.015019639737309,
0.0175229130268605,0.0175620266720094,0.0176011403171581,0.0176793676074551,
0.0178358221880486,0.0181487313492361,0.0187745496716364,0.0200261863164121,
0.0225294596059636,0.0226076868962739,0.022646800541427,0.0226859141865788,
0.0228423687671764,0.0231552779283514,0.0237810962507394,0.0250327328955151,
0.0275360061850667,0.0281618245074545,0.0283182790880578,0.028396506378356,
0.0284356200235045,0.0284747336686529,0.0287876428298423,0.0300392794746181,
0.0325425527641696,0.0331683710865575,0.0332465983768559,0.0333248256671528,
0.033481280247746,0.0337941894089454,0.0350458260537211,0.0375490993432726,
0.0400523726328241),.UNSPECIFIED.);
#5514=B_SPLINE_CURVE_WITH_KNOTS('',3,(#195313,#195314,#195315,#195316),
 .UNSPECIFIED.,.F.,.F.,(4,4),(0.,1.),.UNSPECIFIED.);
#5515=B_SPLINE_CURVE_WITH_KNOTS('',3,(#195317,#195318,#195319,#195320),
 .UNSPECIFIED.,.F.,.F.,(4,4),(0.,0.000517487663021482),.UNSPECIFIED.);
#5516=B_SPLINE_CURVE_WITH_KNOTS('',3,(#195437,#195438,#195439,#195440,#195441,
#195442,#195443,#195444,#195445,#195446,#195447,#195448,#195449,#195450,
#195451,#195452,#195453,#195454,#195455,#195456,#195457,#195458,#195459,
#195460,#195461,#195462,#195463,#195464,#195465,#195466,#195467,#195468),
 .UNSPECIFIED.,.F.,.F.,(4,2,2,2,2,2,2,2,2,2,2,2,2,2,2,4),(0.,0.0625000000000002,
0.125,0.15625,0.1875,0.25,0.3125,0.375,0.5,0.5625,0.625,0.6875,0.75,0.8125,
0.875,1.),.UNSPECIFIED.);
#5517=B_SPLINE_CURVE_WITH_KNOTS('',3,(#195469,#195470,#195471,#195472,#195473,
#195474,#195475,#195476,#195477,#195478,#195479,#195480,#195481,#195482,
#195483,#195484,#195485,#195486,#195487,#195488,#195489,#195490,#195491,
#195492,#195493,#195494,#195495,#195496,#195497,#195498,#195499,#195500,
#195501,#195502,#195503,#195504,#195505,#195506,#195507,#195508,#195509,
#195510,#195511,#195512,#195513,#195514),.UNSPECIFIED.,.F.,.F.,(4,3,3,3,
3,3,3,3,3,3,3,3,3,3,3,4),(6.93889390390723E-18,0.000249844530040023,0.000374757201987746,
0.000499665804996624,0.00062457208312752,0.000749477780116716,0.000874384639619363,
0.000999294405453595,0.00124911879765638,0.00137403129062446,0.00149894371772633,
0.0016238558811297,0.0016863118021229,0.00174876758300643,0.00187367862553572,
0.00199858881090719),.UNSPECIFIED.);
#5518=B_SPLINE_CURVE_WITH_KNOTS('',3,(#195554,#195555,#195556,#195557,#195558,
#195559,#195560,#195561,#195562,#195563,#195564,#195565,#195566,#195567,
#195568,#195569,#195570,#195571,#195572,#195573,#195574,#195575,#195576,
#195577,#195578,#195579,#195580,#195581,#195582,#195583,#195584,#195585,
#195586,#195587,#195588,#195589,#195590,#195591,#195592,#195593,#195594,
#195595,#195596,#195597,#195598,#195599,#195600,#195601,#195602,#195603,
#195604,#195605,#195606,#195607,#195608,#195609,#195610,#195611,#195612,
#195613,#195614,#195615,#195616,#195617,#195618,#195619,#195620,#195621,
#195622,#195623,#195624,#195625,#195626,#195627,#195628,#195629,#195630,
#195631,#195632,#195633,#195634,#195635,#195636,#195637,#195638,#195639,
#195640,#195641),.UNSPECIFIED.,.F.,.F.,(4,3,3,3,3,3,3,3,3,3,3,3,3,3,3,3,
3,3,3,3,3,3,3,3,3,3,3,3,3,4),(0.,0.0368559176034455,0.0746437033404335,
0.113370738808261,0.153426274720315,0.196061576008915,0.238696877297516,
0.249999999999999,0.291411119211606,0.334741693441388,0.374999999999999,
0.416196373054901,0.458658881793208,0.497478515250967,0.499999999999999,
0.541479495018386,0.583190607592968,0.624892955694726,0.664441000977951,
0.702841807290668,0.739636661690415,0.75,0.759103064710313,0.799902601459033,
0.839924725486378,0.879943544114783,0.917760112553561,0.954791160548494,
0.990723248093471,1.),.UNSPECIFIED.);
#5519=B_SPLINE_CURVE_WITH_KNOTS('',3,(#195642,#195643,#195644,#195645,#195646,
#195647,#195648,#195649,#195650,#195651,#195652,#195653,#195654,#195655,
#195656,#195657,#195658,#195659,#195660,#195661,#195662,#195663),
 .UNSPECIFIED.,.F.,.F.,(4,3,3,3,3,3,3,4),(9.81307786677359E-18,0.00542754419072061,
0.00715193125010651,0.014303862500213,0.0178798281252662,0.0214557937503195,
0.0280312223938407,0.028607725000426),.UNSPECIFIED.);
#5520=B_SPLINE_CURVE_WITH_KNOTS('',3,(#195769,#195770,#195771,#195772,#195773,
#195774,#195775,#195776,#195777,#195778,#195779,#195780,#195781,#195782,
#195783,#195784,#195785,#195786,#195787,#195788,#195789,#195790,#195791,
#195792,#195793,#195794,#195795,#195796,#195797,#195798,#195799,#195800,
#195801,#195802),.UNSPECIFIED.,.F.,.F.,(4,2,2,2,2,2,2,2,2,2,2,2,2,2,2,2,
4),(0.,0.0624999999999985,0.124999999999999,0.187499999999999,0.25,0.312499999999998,
0.374999999999999,0.4375,0.46875,0.499999999999999,0.624999999999999,0.6875,
0.75,0.8125,0.84375,0.875,1.),.UNSPECIFIED.);
#5521=B_SPLINE_CURVE_WITH_KNOTS('',3,(#195803,#195804,#195805,#195806,#195807,
#195808,#195809,#195810,#195811,#195812,#195813,#195814,#195815,#195816,
#195817,#195818,#195819,#195820,#195821,#195822,#195823,#195824,#195825,
#195826,#195827,#195828,#195829,#195830,#195831,#195832,#195833,#195834,
#195835,#195836,#195837,#195838,#195839,#195840,#195841,#195842,#195843,
#195844,#195845,#195846,#195847,#195848,#195849,#195850,#195851),
 .UNSPECIFIED.,.F.,.F.,(4,3,3,3,3,3,3,3,3,3,3,3,3,3,3,3,4),(0.,0.000209907523070278,
0.000262386427442229,0.000314865930148693,0.000419826308247615,0.000524787812645559,
0.000629749598530388,0.000839670635464471,0.000892150044011657,0.000944629442448278,
0.00104958821836654,0.00115454698196066,0.00125950575196963,0.00136446454713245,
0.00146942338618815,0.00157438228787588,0.00167934127092895),
 .UNSPECIFIED.);
#5522=B_SPLINE_CURVE_WITH_KNOTS('',3,(#195884,#195885,#195886,#195887),
 .UNSPECIFIED.,.F.,.F.,(4,4),(0.,0.999999715020008),.UNSPECIFIED.);
#5523=B_SPLINE_CURVE_WITH_KNOTS('',3,(#195888,#195889,#195890,#195891),
 .UNSPECIFIED.,.F.,.F.,(4,4),(3.46944695195361E-18,0.000487799384074577),
 .UNSPECIFIED.);
#5524=B_SPLINE_CURVE_WITH_KNOTS('',3,(#196010,#196011,#196012,#196013,#196014,
#196015,#196016,#196017,#196018,#196019,#196020,#196021,#196022,#196023,
#196024,#196025,#196026,#196027,#196028,#196029,#196030,#196031,#196032,
#196033,#196034,#196035),.UNSPECIFIED.,.F.,.F.,(4,2,2,2,2,2,2,2,2,2,2,2,
4),(0.,0.124999999999997,0.249999999999993,0.374999999999989,0.499999999999999,
0.562499999999991,0.624999999999996,0.749999999999993,0.812499999999998,
0.87499999999999,0.906249999999992,0.937499999999995,1.),.UNSPECIFIED.);
#5525=B_SPLINE_CURVE_WITH_KNOTS('',3,(#196036,#196037,#196038,#196039,#196040,
#196041,#196042,#196043,#196044,#196045,#196046,#196047,#196048,#196049,
#196050,#196051,#196052,#196053,#196054,#196055,#196056,#196057,#196058,
#196059,#196060,#196061),.UNSPECIFIED.,.F.,.F.,(4,2,2,2,2,2,2,2,2,2,2,2,
4),(0.,0.0625000000000051,0.0937500000000081,0.12500000000001,0.187500000000002,
0.250000000000007,0.375000000000004,0.437500000000009,0.500000000000001,
0.625000000000011,0.750000000000007,0.875000000000003,1.),.UNSPECIFIED.);
#5526=B_SPLINE_CURVE_WITH_KNOTS('',3,(#196089,#196090,#196091,#196092,#196093,
#196094,#196095,#196096,#196097,#196098,#196099,#196100,#196101,#196102,
#196103,#196104,#196105,#196106,#196107,#196108,#196109,#196110,#196111,
#196112,#196113,#196114,#196115,#196116,#196117,#196118,#196119,#196120,
#196121),.UNSPECIFIED.,.F.,.F.,(4,2,2,2,2,2,2,2,2,2,2,2,2,2,2,1,4),(0.,
0.125000000000071,0.156250000000092,0.187500000000113,0.250000000000138,
0.312500000000162,0.343750000000175,0.359375000000185,0.375000000000194,
0.406250000000208,0.437500000000221,0.500000000000248,0.562500000000275,
0.570312500000275,0.578125000000274,0.625000000000249,1.),.UNSPECIFIED.);
#5527=B_SPLINE_CURVE_WITH_KNOTS('',3,(#196122,#196123,#196124,#196125,#196126,
#196127,#196128,#196129,#196130,#196131,#196132,#196133,#196134),
 .UNSPECIFIED.,.F.,.F.,(4,3,3,3,4),(6.93889390390723E-18,0.000381255515696972,
0.000469255885429327,0.000705402670132244,0.000942818873534133),
 .UNSPECIFIED.);
#5528=B_SPLINE_CURVE_WITH_KNOTS('',3,(#196149,#196150,#196151,#196152,#196153,
#196154),.UNSPECIFIED.,.F.,.F.,(4,2,4),(0.,0.5,0.999992304477323),
 .UNSPECIFIED.);
#5529=B_SPLINE_CURVE_WITH_KNOTS('',3,(#196156,#196157,#196158,#196159),
 .UNSPECIFIED.,.F.,.F.,(4,4),(0.,1.),.UNSPECIFIED.);
#5530=B_SPLINE_CURVE_WITH_KNOTS('',3,(#196176,#196177,#196178,#196179,#196180,
#196181,#196182,#196183,#196184,#196185),.UNSPECIFIED.,.F.,.F.,(4,3,3,4),
(0.,7.57680559097057E-5,0.000160273670968369,0.000194799519911097),
 .UNSPECIFIED.);
#5531=B_SPLINE_CURVE_WITH_KNOTS('',3,(#196206,#196207,#196208,#196209,#196210,
#196211,#196212,#196213,#196214,#196215,#196216,#196217,#196218,#196219,
#196220,#196221,#196222,#196223,#196224,#196225,#196226,#196227,#196228,
#196229,#196230,#196231,#196232,#196233,#196234,#196235,#196236,#196237,
#196238,#196239,#196240,#196241,#196242,#196243,#196244,#196245,#196246,
#196247,#196248,#196249,#196250,#196251,#196252,#196253,#196254,#196255,
#196256,#196257,#196258,#196259,#196260,#196261,#196262,#196263),
 .UNSPECIFIED.,.F.,.F.,(4,3,3,3,3,3,3,3,3,3,3,3,3,3,3,3,3,3,3,4),(7.10667107881632E-12,
0.0777967911957834,0.155397709641609,0.232815426199448,0.25000000000003,
0.333850548679027,0.389419000752951,0.437500000000041,0.466951073723059,
0.496142061056067,0.500000000000037,0.500265459427049,0.567807557951046,
0.636514506183817,0.707974454992009,0.750000000000018,0.8217273781834,0.894665117182011,
0.968437096835554,0.999990298090105),.UNSPECIFIED.);
#5532=B_SPLINE_CURVE_WITH_KNOTS('',3,(#196668,#196669,#196670,#196671,#196672,
#196673,#196674,#196675,#196676,#196677,#196678,#196679,#196680,#196681,
#196682,#196683,#196684,#196685,#196686,#196687,#196688,#196689,#196690,
#196691,#196692),.UNSPECIFIED.,.F.,.F.,(4,3,3,3,3,3,3,3,4),(2.28823383841608E-11,
0.128993498150867,0.259210238149049,0.390210937649005,0.500000000000001,
0.625000000000001,0.745864344071094,0.872932172035547,1.),.UNSPECIFIED.);
#5533=B_SPLINE_CURVE_WITH_KNOTS('',3,(#196694,#196695,#196696,#196697,#196698,
#196699,#196700,#196701,#196702,#196703,#196704,#196705,#196706,#196707,
#196708,#196709,#196710,#196711,#196712,#196713,#196714,#196715,#196716,
#196717,#196718,#196719,#196720,#196721,#196722,#196723,#196724,#196725,
#196726,#196727,#196728,#196729,#196730,#196731,#196732,#196733,#196734,
#196735,#196736),.UNSPECIFIED.,.F.,.F.,(4,3,3,3,3,3,3,3,3,3,3,3,3,3,4),
(0.,0.125,0.137817678947238,0.307927954228248,0.478038229509258,0.64814850479027,
0.874999999999999,0.968749999999999,0.984374999999999,0.988369053825107,
0.9921875,0.99609375,0.9970703125,0.99853515625,0.999999999623881),
 .UNSPECIFIED.);
#5534=B_SPLINE_CURVE_WITH_KNOTS('',3,(#196738,#196739,#196740,#196741,#196742,
#196743,#196744,#196745,#196746,#196747,#196748,#196749,#196750,#196751,
#196752,#196753,#196754,#196755,#196756,#196757,#196758,#196759,#196760,
#196761,#196762,#196763,#196764,#196765),.UNSPECIFIED.,.F.,.F.,(4,2,2,2,
2,2,2,2,2,2,2,2,2,4),(0.,0.0069548877073492,0.0155193349966718,0.0497771241539778,
0.11829270246859,0.255323859097813,0.529386172356271,0.666417328985494,
0.803448485614717,0.94047964224394,0.974737431401246,0.991866325979906,
0.996148549624567,1.),.UNSPECIFIED.);
#5535=B_SPLINE_CURVE_WITH_KNOTS('',3,(#196767,#196768,#196769,#196770,#196771,
#196772,#196773,#196774,#196775,#196776,#196777,#196778,#196779,#196780,
#196781,#196782,#196783,#196784,#196785,#196786),.UNSPECIFIED.,.F.,.F.,
(4,2,2,2,2,2,2,2,2,4),(0.,0.000334191767478362,0.00697844754728855,0.0601324937857085,
0.485364863693081,0.910597233600454,0.963751279838875,0.990328302958084,
0.996972558737885,1.),.UNSPECIFIED.);
#5536=B_SPLINE_CURVE_WITH_KNOTS('',3,(#196788,#196789,#196790,#196791,#196792,
#196793,#196794,#196795,#196796,#196797,#196798,#196799,#196800,#196801,
#196802,#196803,#196804,#196805,#196806,#196807,#196808,#196809,#196810,
#196811,#196812,#196813,#196814,#196815,#196816),.UNSPECIFIED.,.F.,.F.,
(4,2,2,2,2,2,2,2,2,2,2,2,1,2,4),(0.,0.000388754147012465,0.0047713452534302,
0.0223017096791179,0.162544625084547,0.302787540489991,0.44303045589542,
0.72351628670628,0.863759202111711,0.933880659814438,0.968941388665797,
0.986471753091468,0.995236935304305,0.999619526410721,1.),.UNSPECIFIED.);
#5537=B_SPLINE_CURVE_WITH_KNOTS('',3,(#196818,#196819,#196820,#196821,#196822,
#196823,#196824,#196825,#196826,#196827,#196828,#196829,#196830,#196831,
#196832,#196833,#196834,#196835,#196836,#196837,#196838,#196839,#196840,
#196841,#196842),.UNSPECIFIED.,.F.,.F.,(4,2,1,1,1,2,2,2,2,2,2,1,1,2,4),
(0.,0.00390625000000159,0.0312500000000058,0.0625000000000054,0.125000000000005,
0.250000000000003,0.500000000000001,0.749999999999999,0.874999999999999,
0.937499999999999,0.968749999999998,0.984374999999997,0.992187499999998,
0.996093749999999,1.),.UNSPECIFIED.);
#5538=B_SPLINE_CURVE_WITH_KNOTS('',3,(#196844,#196845,#196846,#196847,#196848,
#196849,#196850,#196851,#196852,#196853,#196854,#196855,#196856,#196857,
#196858,#196859,#196860,#196861,#196862,#196863,#196864,#196865,#196866,
#196867),.UNSPECIFIED.,.F.,.F.,(4,2,1,1,1,1,2,2,2,1,2,2,1,2,4),(0.,0.00390624999999841,
0.00781249999999682,0.015624999999997,0.0312499999999974,0.062499999999997,
0.124999999999999,0.25,0.500000000000001,0.750000000000002,0.937500000000003,
0.968750000000002,0.984375000000001,0.9921875,0.99999999134495),
 .UNSPECIFIED.);
#5539=B_SPLINE_CURVE_WITH_KNOTS('',3,(#196868,#196869,#196870,#196871,#196872,
#196873,#196874,#196875,#196876,#196877,#196878,#196879,#196880,#196881,
#196882,#196883,#196884,#196885,#196886,#196887,#196888,#196889,#196890,
#196891,#196892,#196893,#196894,#196895,#196896,#196897,#196898,#196899,
#196900,#196901,#196902,#196903,#196904,#196905,#196906,#196907,#196908,
#196909,#196910,#196911,#196912,#196913,#196914,#196915,#196916),
 .UNSPECIFIED.,.F.,.F.,(4,3,3,3,3,3,3,3,3,3,3,3,3,3,3,3,4),(1.60377085177131E-7,
0.00257403723325268,0.00390624999999833,0.00781249999999667,0.0136608742270577,
0.0156249999999971,0.0312499999999979,0.0580082231262107,0.146702920920664,
0.324092316509571,0.501481712098478,0.590176409892927,0.678871107687397,
0.8562605032763,0.875000000000001,0.944955187638308,1.),.UNSPECIFIED.);
#5540=B_SPLINE_CURVE_WITH_KNOTS('',3,(#196917,#196918,#196919,#196920,#196921,
#196922,#196923,#196924,#196925,#196926,#196927,#196928,#196929,#196930,
#196931,#196932,#196933,#196934,#196935,#196936,#196937,#196938,#196939,
#196940,#196941,#196942,#196943,#196944,#196945,#196946,#196947,#196948,
#196949,#196950,#196951,#196952,#196953,#196954,#196955,#196956,#196957,
#196958,#196959,#196960,#196961,#196962,#196963,#196964,#196965,#196966,
#196967,#196968,#196969,#196970,#196971,#196972,#196973,#196974,#196975,
#196976,#196977,#196978,#196979,#196980,#196981,#196982,#196983,#196984,
#196985,#196986,#196987,#196988,#196989,#196990,#196991,#196992,#196993,
#196994,#196995,#196996,#196997,#196998,#196999,#197000,#197001,#197002,
#197003,#197004,#197005,#197006,#197007,#197008,#197009,#197010,#197011,
#197012,#197013,#197014,#197015,#197016,#197017,#197018,#197019,#197020,
#197021,#197022,#197023,#197024,#197025,#197026,#197027,#197028,#197029,
#197030,#197031,#197032,#197033,#197034,#197035,#197036,#197037,#197038,
#197039,#197040,#197041,#197042,#197043,#197044,#197045,#197046,#197047,
#197048,#197049,#197050,#197051,#197052,#197053,#197054,#197055,#197056,
#197057,#197058,#197059,#197060,#197061,#197062,#197063,#197064,#197065,
#197066,#197067,#197068,#197069,#197070,#197071,#197072,#197073,#197074,
#197075,#197076,#197077,#197078,#197079,#197080,#197081,#197082,#197083,
#197084,#197085,#197086,#197087,#197088,#197089,#197090,#197091,#197092,
#197093,#197094,#197095,#197096,#197097,#197098,#197099,#197100,#197101,
#197102,#197103,#197104,#197105,#197106,#197107,#197108,#197109,#197110,
#197111,#197112,#197113,#197114,#197115,#197116,#197117,#197118,#197119,
#197120,#197121,#197122,#197123,#197124,#197125,#197126,#197127,#197128,
#197129,#197130,#197131,#197132,#197133,#197134,#197135,#197136,#197137,
#197138,#197139,#197140,#197141,#197142,#197143,#197144,#197145,#197146,
#197147,#197148,#197149,#197150,#197151,#197152,#197153,#197154,#197155,
#197156,#197157,#197158,#197159,#197160,#197161,#197162,#197163,#197164,
#197165,#197166,#197167,#197168,#197169,#197170,#197171,#197172,#197173,
#197174,#197175,#197176,#197177,#197178,#197179,#197180,#197181,#197182,
#197183,#197184,#197185,#197186,#197187,#197188,#197189,#197190,#197191,
#197192,#197193,#197194,#197195,#197196,#197197,#197198,#197199,#197200,
#197201,#197202,#197203,#197204,#197205,#197206,#197207,#197208,#197209,
#197210,#197211,#197212,#197213,#197214,#197215,#197216,#197217,#197218,
#197219,#197220,#197221,#197222,#197223,#197224,#197225,#197226,#197227,
#197228,#197229,#197230,#197231,#197232,#197233,#197234,#197235,#197236,
#197237,#197238,#197239,#197240,#197241,#197242,#197243,#197244,#197245,
#197246,#197247,#197248,#197249,#197250,#197251,#197252,#197253,#197254,
#197255,#197256,#197257,#197258,#197259,#197260,#197261,#197262,#197263,
#197264,#197265,#197266,#197267,#197268),.UNSPECIFIED.,.F.,.F.,(4,3,3,3,
3,3,3,3,3,3,3,3,3,3,3,3,3,3,3,3,3,3,3,3,3,3,3,3,3,3,3,3,3,3,3,3,3,3,3,3,
3,3,3,3,3,3,3,3,3,3,3,3,3,3,3,3,3,3,3,3,3,3,3,3,3,3,3,3,3,3,3,3,3,3,3,3,
3,3,3,3,3,3,3,3,3,3,3,3,3,3,3,3,3,3,3,3,3,3,3,3,3,3,3,3,3,3,3,3,3,3,3,3,
3,3,3,3,3,4),(0.,0.000458642979612002,0.00148039975907437,0.00155548413886127,
0.00215808125410714,0.00351929604547634,0.00375138748260762,0.00431616250821427,
0.00485043313466948,0.00595000606436429,0.00647424376232141,0.00814921412206644,
0.00863232501642855,0.0103483019189537,0.0107904062705357,0.0114478221282345,
0.0118694468975892,0.0119975520112361,0.0121349909920248,0.0121693507398585,
0.0122037104862784,0.0122724299699395,0.012408967211116,0.0125473080812304,
0.0129484875246428,0.0164016794277588,0.0169452741711578,0.0172646500328571,
0.0191441895986679,0.0194227312869643,0.0196939101106087,0.0198313397462589,
0.0198485184451409,0.0198656971433598,0.019900054538499,0.0199622516004911,
0.0199687693285922,0.0202436289341201,0.0205017719140178,0.0213430827748702,
0.0215808125410714,0.0236608084713611,0.0257408044016508,0.0258969750492855,
0.027059011742913,0.0280550563033925,0.0289136017549235,0.0291340969304461,
0.0301383324656715,0.0301726862499191,0.0302070399948121,0.0302131375574996,
0.0302757474855599,0.0304131631667517,0.0306879973674717,0.0312376772927355,
0.0323370846027418,0.0345293000657137,0.0345360999801471,0.0356083406927672,
0.0356357138934573,0.0366115735239252,0.0366873813198207,0.036735364064563,
0.0376935360434091,0.0377664219468742,0.037834874245495,0.03797230394085,
0.0380066611974582,0.0380410184323685,0.0381097329274824,0.038305942260401,
0.0383845939060418,0.0388454625739277,0.0389343227662998,0.0416287480698856,
0.0431616250821419,0.0433319227699236,0.0455053529354623,0.0474777875903559,
0.0477291370890009,0.0480173079038827,0.0482787598919225,0.0483474623355813,
0.048381813564519,0.0484161648055658,0.0485535700013955,0.0485568282174095,
0.0488283820820523,0.049635868844463,0.0499276530066707,0.0510269469116911,
0.05179395009857,0.0521261923582727,0.054324468909372,0.0554235143696246,
0.0559730160990559,0.056110112606784,0.0562477622140428,0.0563164484206554,
0.0563851344750846,0.0565225060213207,0.0566496329203107,0.0571891532338374,
0.0582681938608909,0.0599454964430044,0.0604262751149979,0.0609187453906406,
0.0623709320634497,0.0625843563691049,0.0631171315120633,0.0647424376232119,
0.065315179230263,0.0669005188773189,0.0675129021160854,0.0679795595043724,
0.068863383040997,0.0690586001314259),.UNSPECIFIED.);
#5541=B_SPLINE_CURVE_WITH_KNOTS('',3,(#197289,#197290,#197291,#197292,#197293,
#197294,#197295,#197296,#197297,#197298,#197299,#197300,#197301,#197302),
 .UNSPECIFIED.,.F.,.F.,(4,2,2,1,1,2,2,4),(0.,0.249999999999831,0.374999999999745,
0.437499999999717,0.468749999999702,0.484374999999696,0.49999999999969,
0.999968793306949),.UNSPECIFIED.);
#5542=B_SPLINE_CURVE_WITH_KNOTS('',3,(#197318,#197319,#197320,#197321,#197322,
#197323,#197324),.UNSPECIFIED.,.F.,.F.,(4,3,4),(3.39934988877629E-17,8.80333896086783E-5,
0.000139297820505393),.UNSPECIFIED.);
#5543=B_SPLINE_CURVE_WITH_KNOTS('',3,(#197325,#197326,#197327,#197328),
 .UNSPECIFIED.,.F.,.F.,(4,4),(1.05519109601004E-16,0.000332772401868219),
 .UNSPECIFIED.);
#5544=B_SPLINE_CURVE_WITH_KNOTS('',3,(#197367,#197368,#197369,#197370,#197371,
#197372),.UNSPECIFIED.,.F.,.F.,(4,2,4),(0.,0.5,1.),.UNSPECIFIED.);
#5545=B_SPLINE_CURVE_WITH_KNOTS('',3,(#197373,#197374,#197375,#197376,#197377,
#197378,#197379),.UNSPECIFIED.,.F.,.F.,(4,3,4),(0.,0.000376539260809641,
0.00075440118473929),.UNSPECIFIED.);
#5546=B_SPLINE_CURVE_WITH_KNOTS('',3,(#197461,#197462,#197463,#197464,#197465,
#197466,#197467,#197468,#197469,#197470,#197471,#197472,#197473,#197474,
#197475,#197476,#197477,#197478,#197479,#197480,#197481,#197482,#197483,
#197484,#197485,#197486,#197487,#197488,#197489,#197490,#197491,#197492,
#197493,#197494,#197495,#197496,#197497,#197498,#197499,#197500,#197501,
#197502,#197503,#197504,#197505,#197506,#197507,#197508,#197509,#197510,
#197511,#197512,#197513,#197514,#197515,#197516,#197517,#197518,#197519,
#197520,#197521,#197522,#197523,#197524,#197525,#197526,#197527,#197528,
#197529,#197530,#197531,#197532,#197533,#197534,#197535,#197536,#197537,
#197538,#197539,#197540,#197541,#197542,#197543,#197544,#197545,#197546,
#197547,#197548,#197549,#197550,#197551,#197552,#197553,#197554,#197555,
#197556,#197557,#197558,#197559,#197560,#197561,#197562,#197563,#197564,
#197565,#197566,#197567,#197568,#197569,#197570,#197571,#197572,#197573,
#197574,#197575,#197576,#197577,#197578,#197579,#197580,#197581,#197582,
#197583,#197584,#197585,#197586,#197587,#197588,#197589,#197590,#197591,
#197592,#197593),.UNSPECIFIED.,.F.,.F.,(4,3,3,3,3,3,3,3,3,3,3,3,3,3,3,3,
3,3,3,3,3,3,3,3,3,3,3,3,3,3,3,3,3,3,3,3,3,3,3,3,3,3,3,3,4),(0.,0.0202204421099624,
0.0395451483058804,0.0582377862400879,0.0624999999999951,0.0875613665156572,
0.0937499999999927,0.105792877064545,0.119535285750553,0.124999999999989,
0.143266369710153,0.160852989255863,0.177878328056101,0.187499999999999,
0.216630220683948,0.233848186590877,0.249999999999994,0.270617506030971,
0.292475272788992,0.316626262912307,0.342458186784713,0.370975671115348,
0.374999999999997,0.399246099196213,0.403095241035769,0.429234253193885,
0.437499999999992,0.476973357033904,0.5,0.544412193223352,0.580280434548985,
0.62499999999999,0.668486704216791,0.711205001631657,0.749999999999993,
0.753891896102902,0.789218995972688,0.826185861752328,0.861325504709182,
0.874999999999997,0.910862553258451,0.928894079945525,0.964447039972762,
0.99809894552016,1.),.UNSPECIFIED.);
#5547=B_SPLINE_CURVE_WITH_KNOTS('',3,(#197594,#197595,#197596,#197597,#197598,
#197599,#197600,#197601,#197602,#197603,#197604,#197605,#197606,#197607,
#197608,#197609,#197610,#197611,#197612,#197613,#197614,#197615,#197616,
#197617,#197618,#197619),.UNSPECIFIED.,.F.,.F.,(4,2,2,2,2,2,2,2,2,2,2,2,
4),(0.,0.125000000000003,0.250000000000007,0.37500000000001,0.5,0.562500000000008,
0.625000000000003,0.750000000000007,0.812500000000001,0.875000000000011,
0.906250000000007,0.937500000000005,1.),.UNSPECIFIED.);
#5548=B_SPLINE_CURVE_WITH_KNOTS('',3,(#197650,#197651,#197652,#197653),
 .UNSPECIFIED.,.F.,.F.,(4,4),(0.,1.),.UNSPECIFIED.);
#5549=B_SPLINE_CURVE_WITH_KNOTS('',3,(#197670,#197671,#197672,#197673,#197674,
#197675,#197676,#197677,#197678,#197679,#197680,#197681,#197682,#197683,
#197684,#197685,#197686,#197687,#197688),.UNSPECIFIED.,.F.,.F.,(4,3,3,3,
3,3,4),(0.,0.185533700348248,0.389150275261186,0.586067466801276,0.777142226369554,
0.956993746407619,1.),.UNSPECIFIED.);
#5550=B_SPLINE_CURVE_WITH_KNOTS('',3,(#197689,#197690,#197691,#197692,#197693,
#197694,#197695,#197696,#197697,#197698,#197699,#197700,#197701,#197702,
#197703,#197704,#197705,#197706,#197707,#197708,#197709,#197710,#197711,
#197712,#197713,#197714,#197715,#197716,#197717,#197718,#197719,#197720,
#197721,#197722,#197723,#197724,#197725,#197726,#197727,#197728,#197729,
#197730,#197731,#197732,#197733,#197734),.UNSPECIFIED.,.F.,.F.,(4,3,3,3,
3,3,3,3,3,3,3,3,3,3,3,4),(3.82465140600628E-12,0.080165926001864,0.159888411076935,
0.238758088141874,0.25,0.3272825015128,0.40328844376453,0.47787089026108,
0.550149874260245,0.621091964466054,0.689969931524664,0.75,0.815939883785364,
0.880799348024208,0.944115505909337,1.),.UNSPECIFIED.);
#5551=B_SPLINE_CURVE_WITH_KNOTS('',3,(#197802,#197803,#197804,#197805,#197806,
#197807,#197808,#197809,#197810,#197811),.UNSPECIFIED.,.F.,.F.,(4,2,2,2,
4),(0.,0.25,0.5,0.75,1.),.UNSPECIFIED.);
#5552=B_SPLINE_CURVE_WITH_KNOTS('',3,(#197812,#197813,#197814,#197815,#197816,
#197817,#197818,#197819,#197820,#197821,#197822,#197823,#197824),
 .UNSPECIFIED.,.F.,.F.,(4,3,3,3,4),(0.,0.000262347006055043,0.000525082323798981,
0.000788127838504804,0.00105144790336124),.UNSPECIFIED.);
#5553=B_SPLINE_CURVE_WITH_KNOTS('',3,(#197906,#197907,#197908,#197909,#197910,
#197911,#197912,#197913,#197914,#197915,#197916,#197917,#197918,#197919,
#197920,#197921,#197922,#197923,#197924,#197925,#197926,#197927,#197928,
#197929,#197930,#197931),.UNSPECIFIED.,.F.,.F.,(4,2,2,2,2,2,2,2,2,2,2,2,
4),(0.,0.0624999999999995,0.0937500000000063,0.124999999999998,0.187499999999997,
0.249999999999997,0.374999999999995,0.437499999999993,0.499999999999993,
0.624999999999991,0.749999999999989,0.874999999999988,1.),.UNSPECIFIED.);
#5554=B_SPLINE_CURVE_WITH_KNOTS('',3,(#197932,#197933,#197934,#197935,#197936,
#197937,#197938,#197939,#197940,#197941,#197942,#197943,#197944,#197945,
#197946,#197947,#197948,#197949,#197950,#197951,#197952,#197953,#197954,
#197955,#197956,#197957),.UNSPECIFIED.,.F.,.F.,(4,2,2,2,2,2,2,2,2,2,2,2,
4),(0.,0.125000000000012,0.250000000000011,0.375000000000009,0.500000000000007,
0.562500000000007,0.625000000000005,0.750000000000003,0.812500000000003,
0.875000000000002,0.906249999999994,0.937500000000001,1.),.UNSPECIFIED.);
#5555=B_SPLINE_CURVE_WITH_KNOTS('',3,(#197973,#197974,#197975,#197976,#197977,
#197978,#197979,#197980,#197981,#197982),.UNSPECIFIED.,.F.,.F.,(4,3,3,4),
(0.,0.000342739114726225,0.000689887212155792,0.000728014676542687),
 .UNSPECIFIED.);
#5556=B_SPLINE_CURVE_WITH_KNOTS('',3,(#197997,#197998,#197999,#198000),
 .UNSPECIFIED.,.F.,.F.,(4,4),(0.,1.),.UNSPECIFIED.);
#5557=B_SPLINE_CURVE_WITH_KNOTS('',3,(#198198,#198199,#198200,#198201,#198202,
#198203,#198204,#198205,#198206,#198207,#198208,#198209,#198210,#198211,
#198212,#198213,#198214,#198215,#198216,#198217,#198218,#198219,#198220),
 .UNSPECIFIED.,.F.,.F.,(4,2,1,2,2,2,2,2,2,2,2,4),(0.,0.00283826710419251,
0.00633276476528107,0.0133217600874583,0.0412777413761679,0.0971897039535873,
0.209013629108426,0.432661479418103,0.879957180037457,0.991781105192296,
0.998770100514473,0.99999981607236),.UNSPECIFIED.);
#5558=B_SPLINE_CURVE_WITH_KNOTS('',3,(#198222,#198223,#198224,#198225,#198226,
#198227,#198228,#198229,#198230,#198231,#198232,#198233,#198234,#198235,
#198236,#198237,#198238,#198239,#198240,#198241,#198242,#198243,#198244,
#198245,#198246,#198247,#198248,#198249,#198250,#198251,#198252,#198253,
#198254,#198255),.UNSPECIFIED.,.F.,.F.,(4,3,3,3,3,3,3,3,3,3,3,4),(0.,0.00620530037449982,
0.0212662809590181,0.0513882421280549,0.11163216446613,0.352607853818434,
0.834559232523038,0.955047077199191,0.985169038368228,0.992699528660487,
0.996464773806616,1.),.UNSPECIFIED.);
#5559=B_SPLINE_CURVE_WITH_KNOTS('',3,(#198257,#198258,#198259,#198260,#198261,
#198262,#198263,#198264,#198265,#198266,#198267,#198268,#198269,#198270,
#198271,#198272,#198273,#198274),.UNSPECIFIED.,.F.,.F.,(4,2,2,2,2,2,2,2,
4),(1.98733438466738E-7,0.000182929632426367,0.0121606367275007,0.0600714651078031,
0.251714778628998,0.443358092150197,0.539179748910797,0.635001405671392,
1.),.UNSPECIFIED.);
#5560=B_SPLINE_CURVE_WITH_KNOTS('',3,(#198276,#198277,#198278,#198279,#198280,
#198281,#198282,#198283,#198284,#198285,#198286,#198287,#198288,#198289,
#198290,#198291,#198292,#198293,#198294,#198295,#198296,#198297,#198298,
#198299,#198300,#198301,#198302,#198303),.UNSPECIFIED.,.F.,.F.,(4,3,3,3,
3,3,3,3,3,4),(0.,0.117306771483226,0.234396839308952,0.351440364191732,
0.468658786203015,0.5,0.625,0.748613077229995,0.874306538614997,1.),
 .UNSPECIFIED.);
#5561=B_SPLINE_CURVE_WITH_KNOTS('',3,(#198304,#198305,#198306,#198307,#198308,
#198309,#198310,#198311,#198312,#198313,#198314,#198315,#198316,#198317,
#198318,#198319,#198320,#198321,#198322,#198323,#198324,#198325,#198326,
#198327,#198328,#198329,#198330,#198331,#198332,#198333,#198334,#198335,
#198336,#198337,#198338,#198339,#198340,#198341,#198342,#198343,#198344,
#198345,#198346,#198347,#198348,#198349,#198350,#198351,#198352,#198353,
#198354,#198355,#198356,#198357,#198358,#198359,#198360,#198361,#198362,
#198363,#198364,#198365,#198366,#198367,#198368,#198369,#198370,#198371,
#198372,#198373,#198374,#198375,#198376,#198377,#198378,#198379,#198380,
#198381,#198382,#198383,#198384,#198385,#198386,#198387,#198388,#198389,
#198390,#198391,#198392,#198393,#198394,#198395,#198396,#198397,#198398,
#198399,#198400,#198401,#198402,#198403,#198404,#198405,#198406,#198407,
#198408,#198409,#198410,#198411,#198412,#198413,#198414,#198415,#198416,
#198417,#198418,#198419,#198420,#198421,#198422,#198423,#198424,#198425,
#198426,#198427,#198428,#198429,#198430,#198431,#198432,#198433,#198434,
#198435,#198436,#198437,#198438,#198439,#198440,#198441,#198442,#198443,
#198444,#198445,#198446,#198447,#198448,#198449,#198450,#198451,#198452,
#198453,#198454,#198455,#198456,#198457,#198458,#198459,#198460,#198461,
#198462,#198463,#198464,#198465,#198466,#198467,#198468,#198469),
 .UNSPECIFIED.,.F.,.F.,(4,3,3,3,3,3,3,3,3,3,3,3,3,3,3,3,3,3,3,3,3,3,3,3,
3,3,3,3,3,3,3,3,3,3,3,3,3,3,3,3,3,3,3,3,3,3,3,3,3,3,3,3,3,3,3,4),(3.0340749909216E-15,
0.00129418773529668,0.00218682165402767,0.00327794725358747,0.00398945644969675,
0.00437364330805532,0.00509766529618652,0.00620616680139718,0.0079538318987134,
0.00842283797271616,0.00874728661611061,0.0106381507815725,0.0109341082701383,
0.0111918496720615,0.011330267843016,0.0113648723663157,0.0113994769397398,
0.0114686863527641,0.0114808136836452,0.0117455395577677,0.0120275190971521,
0.0128530198691994,0.0131209299241659,0.0165925219296371,0.0172816770907989,
0.0174945732322213,0.0194950733089173,0.019681394886249,0.0200483162030301,
0.0202281002997558,0.0203249209658281,0.0204632190439244,0.0205323676346262,
0.0206015162605049,0.0207748057132628,0.0217079731878835,0.0218682165402766,
0.0241483525471447,0.026134520310489,0.0262418598483319,0.0275481788415811,
0.0283480821017152,0.0284286815023595,0.0293305776083927,0.0294547291211144,
0.0295220923293734,0.0300079248057878,0.0300687977428803,0.0302844849745068,
0.0303536218586848,0.0303881901705513,0.0304227584828617,0.0305610330454479,
0.0306155031563872,0.0335427501364283,0.0349891464644424),.UNSPECIFIED.);
#5562=B_SPLINE_CURVE_WITH_KNOTS('',3,(#198470,#198471,#198472,#198473,#198474,
#198475,#198476,#198477,#198478,#198479),.UNSPECIFIED.,.F.,.F.,(4,2,2,2,
4),(4.18095462764722E-18,0.00255445063423646,0.00383167595135469,0.00447028860991381,
0.00510890126847292),.UNSPECIFIED.);
#5563=B_SPLINE_CURVE_WITH_KNOTS('',3,(#198499,#198500,#198501,#198502,#198503,
#198504,#198505,#198506,#198507,#198508,#198509,#198510,#198511,#198512,
#198513,#198514,#198515,#198516,#198517,#198518,#198519,#198520,#198521,
#198522,#198523,#198524,#198525,#198526,#198527,#198528,#198529),
 .UNSPECIFIED.,.F.,.F.,(4,3,3,3,3,3,3,3,3,3,4),(0.,0.124999999999992,0.249999999999984,
0.374999999999976,0.426911475280936,0.479016552299178,0.499999999999968,
0.624999999999976,0.749774040198044,0.874887020099022,1.),.UNSPECIFIED.);
#5564=B_SPLINE_CURVE_WITH_KNOTS('',3,(#198566,#198567,#198568,#198569,#198570,
#198571,#198572),.UNSPECIFIED.,.F.,.F.,(4,3,4),(0.,5.20100073045258E-5,
8.99378298105574E-5),.UNSPECIFIED.);
#5565=B_SPLINE_CURVE_WITH_KNOTS('',3,(#198607,#198608,#198609,#198610,#198611,
#198612,#198613,#198614,#198615,#198616,#198617,#198618,#198619),
 .UNSPECIFIED.,.F.,.F.,(4,3,3,3,4),(1.38777878078145E-17,0.000218644279498117,
0.000437193341875465,0.000655638180355839,0.000873969830693171),
 .UNSPECIFIED.);
#5566=B_SPLINE_CURVE_WITH_KNOTS('',3,(#198620,#198621,#198622,#198623,#198624,
#198625,#198626,#198627,#198628,#198629,#198630,#198631,#198632,#198633,
#198634,#198635,#198636,#198637,#198638,#198639,#198640,#198641,#198642,
#198643,#198644,#198645,#198646,#198647,#198648,#198649,#198650,#198651,
#198652,#198653,#198654,#198655,#198656,#198657,#198658,#198659,#198660,
#198661,#198662,#198663,#198664,#198665,#198666,#198667,#198668,#198669,
#198670,#198671,#198672,#198673,#198674,#198675,#198676,#198677,#198678,
#198679,#198680,#198681,#198682,#198683,#198684,#198685,#198686,#198687,
#198688,#198689,#198690,#198691,#198692,#198693,#198694,#198695,#198696,
#198697,#198698,#198699,#198700,#198701),.UNSPECIFIED.,.F.,.F.,(4,3,3,3,
3,3,3,3,3,3,3,3,3,3,3,3,3,3,3,3,3,3,3,3,3,3,3,4),(0.,0.0518784908944668,
0.0929898358507259,0.12499999999993,0.159020278629369,0.187499999999899,
0.234066953854059,0.249999999999868,0.258856206327037,0.281249999999866,
0.289062499999863,0.296874999999861,0.312499999999857,0.345889511569537,
0.374999999999793,0.406249999999761,0.421874999999748,0.427424553674678,
0.429687499999741,0.437499999999734,0.496169719132871,0.49999999999976,
0.531650206071813,0.562499999999787,0.578124999999789,0.749999999999881,
0.75959960473149,1.),.UNSPECIFIED.);
#5567=B_SPLINE_CURVE_WITH_KNOTS('',3,(#198785,#198786,#198787,#198788,#198789,
#198790,#198791,#198792,#198793,#198794,#198795,#198796,#198797,#198798,
#198799,#198800,#198801,#198802,#198803,#198804,#198805,#198806,#198807,
#198808,#198809,#198810,#198811,#198812,#198813,#198814,#198815,#198816,
#198817,#198818,#198819,#198820,#198821,#198822,#198823,#198824,#198825,
#198826,#198827,#198828,#198829,#198830,#198831,#198832,#198833,#198834,
#198835,#198836,#198837,#198838,#198839,#198840,#198841,#198842,#198843,
#198844,#198845,#198846,#198847,#198848,#198849,#198850,#198851,#198852,
#198853,#198854,#198855,#198856,#198857,#198858,#198859,#198860,#198861,
#198862,#198863,#198864,#198865,#198866,#198867,#198868,#198869,#198870,
#198871,#198872,#198873,#198874,#198875,#198876,#198877,#198878,#198879,
#198880,#198881,#198882,#198883,#198884,#198885,#198886,#198887,#198888,
#198889,#198890,#198891,#198892,#198893,#198894,#198895,#198896,#198897,
#198898,#198899,#198900,#198901,#198902,#198903,#198904,#198905,#198906,
#198907,#198908,#198909,#198910,#198911),.UNSPECIFIED.,.F.,.F.,(4,3,3,3,
3,3,3,3,3,3,3,3,3,3,3,3,3,3,3,3,3,3,3,3,3,3,3,3,3,3,3,3,3,3,3,3,3,3,3,3,
3,3,4),(0.,0.00781250000000299,0.0148064814531594,0.015625000000006,0.031250000000012,
0.0502697957749594,0.0625000000000225,0.0828125223056203,0.0864099718511293,
0.107941083662414,0.130513449180188,0.15512947215691,0.18135251250197,0.21073819198987,
0.21360810907109,0.250000000000073,0.281250000000074,0.305550632363911,
0.312500000000075,0.35152559275442,0.390681933501771,0.429805112351713,
0.44018428138064,0.46498154374185,0.487905034853124,0.509922052039041,0.530846691221498,
0.539373330825481,0.551742955240353,0.562500000000056,0.570312500000056,
0.574429310563791,0.578125000000056,0.57886137870164,0.593750000000054,
0.625000000000051,0.638851379824668,0.725746931047932,0.759003379547896,
0.82678271683287,0.879385809313665,0.93750000000001,1.),.UNSPECIFIED.);
#5568=B_SPLINE_CURVE_WITH_KNOTS('',3,(#198945,#198946,#198947,#198948),
 .UNSPECIFIED.,.F.,.F.,(4,4),(0.,0.999997872858114),.UNSPECIFIED.);
#5569=B_SPLINE_CURVE_WITH_KNOTS('',3,(#198967,#198968,#198969,#198970,#198971,
#198972,#198973,#198974,#198975,#198976,#198977,#198978,#198979,#198980,
#198981,#198982,#198983,#198984,#198985,#198986,#198987,#198988),
 .UNSPECIFIED.,.F.,.F.,(4,3,3,3,3,3,3,4),(0.,0.163501572963403,0.330250786373319,
0.496999999783234,0.657493800287202,0.817444914178316,0.976787577632667,
1.),.UNSPECIFIED.);
#5570=B_SPLINE_CURVE_WITH_KNOTS('',3,(#198989,#198990,#198991,#198992,#198993,
#198994,#198995),.UNSPECIFIED.,.F.,.F.,(4,3,4),(0.00166725821467356,0.0142672384485507,
0.0264527075460118),.UNSPECIFIED.);
#5571=B_SPLINE_CURVE_WITH_KNOTS('',3,(#199008,#199009,#199010,#199011),
 .UNSPECIFIED.,.F.,.F.,(4,4),(0.,1.),.UNSPECIFIED.);
#5572=B_SPLINE_CURVE_WITH_KNOTS('',3,(#199012,#199013,#199014,#199015,#199016,
#199017,#199018,#199019,#199020,#199021,#199022,#199023,#199024,#199025,
#199026,#199027,#199028,#199029,#199030,#199031,#199032,#199033,#199034,
#199035,#199036),.UNSPECIFIED.,.F.,.F.,(4,3,3,3,3,3,3,3,4),(0.,0.136592041997272,
0.273213474352422,0.40987042422622,0.546568921813974,0.683339210013659,
0.820155615618192,0.957042445426518,1.),.UNSPECIFIED.);
#5573=B_SPLINE_CURVE_WITH_KNOTS('',3,(#199049,#199050,#199051,#199052,#199053,
#199054,#199055,#199056,#199057,#199058,#199059,#199060,#199061,#199062,
#199063,#199064,#199065,#199066,#199067,#199068,#199069,#199070,#199071,
#199072,#199073),.UNSPECIFIED.,.F.,.F.,(4,3,3,3,3,3,3,3,4),(1.1294748534261E-15,
0.138879076413939,0.277696122602223,0.416455864927007,0.562341898695256,
0.700986033244264,0.839599984102251,0.978180893530377,1.),.UNSPECIFIED.);
#5574=B_SPLINE_CURVE_WITH_KNOTS('',3,(#199074,#199075,#199076,#199077),
 .UNSPECIFIED.,.F.,.F.,(4,4),(0.,1.),.UNSPECIFIED.);
#5575=B_SPLINE_CURVE_WITH_KNOTS('',3,(#199102,#199103,#199104,#199105,#199106,
#199107),.UNSPECIFIED.,.F.,.F.,(4,2,4),(0.,0.502999982291435,1.),
 .UNSPECIFIED.);
#5576=B_SPLINE_CURVE_WITH_KNOTS('',3,(#200138,#200139,#200140,#200141,#200142,
#200143),.UNSPECIFIED.,.F.,.F.,(4,2,4),(-0.478433280045229,-0.243107720536295,
-3.73666282285079E-6),.UNSPECIFIED.);
#5577=B_SPLINE_CURVE_WITH_KNOTS('',3,(#200146,#200147,#200148,#200149,#200150,
#200151),.UNSPECIFIED.,.F.,.F.,(4,2,4),(-0.11270920227521,-0.0563552908536106,
-1.55324366682301E-6),.UNSPECIFIED.);
#5578=B_SPLINE_CURVE_WITH_KNOTS('',3,(#200158,#200159,#200160,#200161,#200162,
#200163),.UNSPECIFIED.,.F.,.F.,(4,2,4),(-0.0955355300118146,-0.0477684952643569,
-2.39971101840152E-6),.UNSPECIFIED.);
#5579=B_SPLINE_CURVE_WITH_KNOTS('',3,(#200167,#200168,#200169,#200170,#200171,
#200172),.UNSPECIFIED.,.F.,.F.,(4,2,4),(-0.0524683090000949,-0.0262347766775936,
-1.35358985086397E-6),.UNSPECIFIED.);
#5580=B_SPLINE_CURVE_WITH_KNOTS('',3,(#200184,#200185,#200186,#200187,#200188,
#200189),.UNSPECIFIED.,.F.,.F.,(4,2,4),(-0.253936238094734,-0.126979219567194,
-2.10375784686121E-6),.UNSPECIFIED.);
#5581=B_SPLINE_CURVE_WITH_KNOTS('',3,(#200197,#200198,#200199,#200200,#200201,
#200202),.UNSPECIFIED.,.F.,.F.,(4,2,4),(-0.258394873018348,-0.130229816210363,
-7.22354834947758E-7),.UNSPECIFIED.);
#5582=B_SPLINE_CURVE_WITH_KNOTS('',3,(#200216,#200217,#200218,#200219,#200220,
#200221),.UNSPECIFIED.,.F.,.F.,(4,2,4),(-0.228463041876464,-0.114227664573105,
-1.02920038175703E-6),.UNSPECIFIED.);
#5583=B_SPLINE_CURVE_WITH_KNOTS('',3,(#200235,#200236,#200237,#200238,#200239,
#200240),.UNSPECIFIED.,.F.,.F.,(4,2,4),(-0.227406176455065,-0.113706766455299,
-2.53502892005267E-6),.UNSPECIFIED.);
#5584=B_SPLINE_CURVE_WITH_KNOTS('',3,(#200277,#200278,#200279,#200280,#200281,
#200282),.UNSPECIFIED.,.F.,.F.,(4,2,4),(0.000194400838126528,0.116630356892709,
0.234421206579217),.UNSPECIFIED.);
#5585=B_SPLINE_CURVE_WITH_KNOTS('',3,(#200663,#200664,#200665,#200666,#200667,
#200668,#200669,#200670,#200671,#200672,#200673,#200674,#200675,#200676,
#200677,#200678,#200679,#200680,#200681,#200682),.UNSPECIFIED.,.F.,.F.,
(4,2,2,2,2,2,2,2,2,4),(0.,0.017536475393927,0.0219930830442672,0.0365274377738634,
0.070751261917734,0.0870574187505271,0.108664084129225,0.116991567530894,
0.121015033558203,0.127334633238972),.UNSPECIFIED.);
#5586=B_SPLINE_CURVE_WITH_KNOTS('',3,(#200684,#200685,#200686,#200687),
 .UNSPECIFIED.,.F.,.F.,(4,4),(0.0542180481640577,0.969015107905792),
 .UNSPECIFIED.);
#5587=B_SPLINE_CURVE_WITH_KNOTS('',3,(#200689,#200690,#200691,#200692,#200693,
#200694),.UNSPECIFIED.,.F.,.F.,(4,2,4),(4.76787336209101E-6,0.023593931008308,
0.0467878966544116),.UNSPECIFIED.);
#5588=B_SPLINE_CURVE_WITH_KNOTS('',3,(#200696,#200697,#200698,#200699,#200700,
#200701,#200702,#200703,#200704,#200705,#200706,#200707,#200708,#200709,
#200710,#200711,#200712,#200713,#200714,#200715,#200716,#200717),
 .UNSPECIFIED.,.F.,.F.,(4,2,2,2,2,2,2,2,2,2,4),(-0.555900774455164,-0.502035745496051,
-0.442390038983038,-0.424393273850783,-0.278932745293561,-0.233572033726155,
-0.156253627001661,-0.103501888368127,-0.0719169619346684,-0.032299277465137,
-2.45584905744778E-8),.UNSPECIFIED.);
#5589=B_SPLINE_CURVE_WITH_KNOTS('',3,(#200718,#200719,#200720,#200721,#200722,
#200723),.UNSPECIFIED.,.F.,.F.,(4,2,4),(0.,0.499006624679324,1.),
 .UNSPECIFIED.);
#5590=B_SPLINE_CURVE_WITH_KNOTS('',3,(#201285,#201286,#201287,#201288,#201289,
#201290,#201291,#201292,#201293,#201294,#201295,#201296,#201297,#201298,
#201299,#201300,#201301,#201302,#201303,#201304,#201305,#201306,#201307,
#201308),.UNSPECIFIED.,.F.,.F.,(4,2,2,2,2,2,2,2,2,2,2,4),(2.76063624704878E-7,
0.0103153193883155,0.0162903958553272,0.030872917071823,0.0697465314854658,
0.105053549140273,0.131809427696887,0.166538084415886,0.179730168174984,
0.220760236727318,0.242652969759649,0.273632513734802),.UNSPECIFIED.);
#5591=B_SPLINE_CURVE_WITH_KNOTS('',3,(#201310,#201311,#201312,#201313,#201314,
#201315,#201316,#201317,#201318,#201319),.UNSPECIFIED.,.F.,.F.,(4,2,2,2,
4),(0.,0.121284653603274,0.248608377129924,0.503255824183223,1.),
 .UNSPECIFIED.);
#5592=B_SPLINE_CURVE_WITH_KNOTS('',3,(#201321,#201322,#201323,#201324,#201325,
#201326,#201327,#201328,#201329,#201330,#201331,#201332,#201333,#201334,
#201335,#201336,#201337,#201338,#201339,#201340,#201341,#201342,#201343,
#201344),.UNSPECIFIED.,.F.,.F.,(4,2,2,2,2,2,2,2,2,2,2,4),(-0.542815827090465,
-0.505700033297898,-0.491406398135943,-0.426347230473485,-0.367919935175952,
-0.332652097482442,-0.313415302389993,-0.269024583259606,-0.128804589688154,
-0.09423657526446,-0.0693837256095411,-9.80508876202713E-7),
 .UNSPECIFIED.);
#5593=B_SPLINE_CURVE_WITH_KNOTS('',3,(#201346,#201347,#201348,#201349,#201350,
#201351,#201352,#201353,#201354,#201355),.UNSPECIFIED.,.F.,.F.,(4,2,2,2,
4),(-0.0740026973086748,-0.0369819514200437,-0.0179638246492492,-0.00888021376129463,
-1.00929457245466E-6),.UNSPECIFIED.);
#5594=B_SPLINE_CURVE_WITH_KNOTS('',3,(#201356,#201357,#201358,#201359),
 .UNSPECIFIED.,.F.,.F.,(4,4),(0.0559227492896294,0.969509810868811),
 .UNSPECIFIED.);
#5595=B_SPLINE_CURVE_WITH_KNOTS('',3,(#201726,#201727,#201728,#201729,#201730,
#201731,#201732,#201733,#201734,#201735,#201736,#201737,#201738,#201739,
#201740,#201741,#201742,#201743),.UNSPECIFIED.,.F.,.F.,(4,2,2,2,2,2,2,2,
4),(0.,0.02720791312337,0.0372043347179621,0.0718760780183553,0.0851663596652269,
0.0954636286661527,0.105386974740314,0.122140097830235,0.143001526856776),
 .UNSPECIFIED.);
#5596=B_SPLINE_CURVE_WITH_KNOTS('',3,(#201745,#201746,#201747,#201748,#201749,
#201750,#201751,#201752,#201753,#201754,#201755,#201756,#201757),
 .UNSPECIFIED.,.F.,.F.,(4,3,3,3,4),(2.3630439517094E-9,0.205079086868114,
0.455501131081411,0.728640752439003,1.),.UNSPECIFIED.);
#5597=B_SPLINE_CURVE_WITH_KNOTS('',3,(#201759,#201760,#201761,#201762,#201763,
#201764),.UNSPECIFIED.,.F.,.F.,(4,2,4),(1.40358012628945E-6,0.0217472883131899,
0.0430970546722853),.UNSPECIFIED.);
#5598=B_SPLINE_CURVE_WITH_KNOTS('',3,(#201766,#201767,#201768,#201769,#201770,
#201771,#201772,#201773,#201774,#201775,#201776,#201777,#201778,#201779,
#201780,#201781,#201782,#201783,#201784,#201785,#201786,#201787,#201788,
#201789),.UNSPECIFIED.,.F.,.F.,(4,2,2,2,2,2,2,2,2,2,2,4),(-0.412088451451376,
-0.372529944186826,-0.32964743775779,-0.299376123190801,-0.259218195736909,
-0.205822994030569,-0.172572535791612,-0.116278410061126,-0.0779939860474743,
-0.0546435191146628,-0.0247676692703238,-1.32710811784342E-8),
 .UNSPECIFIED.);
#5599=B_SPLINE_CURVE_WITH_KNOTS('',3,(#201790,#201791,#201792,#201793,#201794,
#201795),.UNSPECIFIED.,.F.,.F.,(4,2,4),(0.,0.49886621310506,1.),
 .UNSPECIFIED.);
#5600=B_SPLINE_CURVE_WITH_KNOTS('',3,(#202318,#202319,#202320,#202321,#202322,
#202323,#202324,#202325,#202326,#202327,#202328,#202329,#202330,#202331,
#202332,#202333),.UNSPECIFIED.,.F.,.F.,(4,2,2,2,2,2,2,4),(9.90112058791825E-7,
0.0138330094252819,0.0228535045364718,0.0434251080287075,0.0559716654418013,
0.0911264005088734,0.114270201886057,0.155254267708859),.UNSPECIFIED.);
#5601=B_SPLINE_CURVE_WITH_KNOTS('',3,(#202335,#202336,#202337,#202338,#202339,
#202340,#202341),.UNSPECIFIED.,.F.,.F.,(4,3,4),(1.19928029072876E-8,0.499701190314832,
0.999999995466719),.UNSPECIFIED.);
#5602=B_SPLINE_CURVE_WITH_KNOTS('',3,(#202343,#202344,#202345,#202346,#202347,
#202348,#202349,#202350,#202351,#202352,#202353,#202354,#202355,#202356,
#202357,#202358,#202359,#202360,#202361,#202362,#202363,#202364,#202365,
#202366,#202367,#202368),.UNSPECIFIED.,.F.,.F.,(4,2,2,2,2,2,2,2,2,2,2,2,
4),(-0.557432688185859,-0.539947613481655,-0.522228990190384,-0.481224242184197,
-0.449055525828226,-0.397089859289312,-0.32199400192039,-0.278105986122691,
-0.204825331566453,-0.177237377052104,-0.128621503496169,-0.0603607907826898,
-9.84241908086325E-7),.UNSPECIFIED.);
#5603=B_SPLINE_CURVE_WITH_KNOTS('',3,(#202370,#202371,#202372,#202373,#202374,
#202375,#202376,#202377),.UNSPECIFIED.,.F.,.F.,(4,2,2,4),(-0.0542958923388243,
-0.0270296190498593,-0.0132206493661975,-1.0001819469588E-6),
 .UNSPECIFIED.);
#5604=B_SPLINE_CURVE_WITH_KNOTS('',3,(#202378,#202379,#202380,#202381),
 .UNSPECIFIED.,.F.,.F.,(4,4),(0.0408435581858421,0.955362835047561),
 .UNSPECIFIED.);
#5605=B_SPLINE_CURVE_WITH_KNOTS('',3,(#202388,#202389,#202390,#202391,#202392,
#202393),.UNSPECIFIED.,.F.,.F.,(4,2,4),(-0.0363835945027032,-0.0181194609557856,
-1.32631589895571E-6),.UNSPECIFIED.);
#5606=B_SPLINE_CURVE_WITH_KNOTS('',3,(#202396,#202397,#202398,#202399,#202400,
#202401,#202402,#202403),.UNSPECIFIED.,.F.,.F.,(4,2,2,4),(-0.501368889131238,
-0.378312632595403,-0.251119784430402,-9.99947370461385E-7),
 .UNSPECIFIED.);
#5607=B_SPLINE_CURVE_WITH_KNOTS('',3,(#202405,#202406,#202407,#202408,#202409,
#202410),.UNSPECIFIED.,.F.,.F.,(4,2,4),(-0.50276667251833,-0.250728203604819,
-1.64858791458983E-6),.UNSPECIFIED.);
#5608=B_SPLINE_CURVE_WITH_KNOTS('',3,(#202429,#202430,#202431,#202432,#202433,
#202434,#202435,#202436),.UNSPECIFIED.,.F.,.F.,(4,2,2,4),(-0.519837304219326,
-0.24805813049356,-0.122424589346183,-1.86609418195765E-6),
 .UNSPECIFIED.);
#5609=B_SPLINE_CURVE_WITH_KNOTS('',3,(#202440,#202441,#202442,#202443,#202444,
#202445,#202446,#202447),.UNSPECIFIED.,.F.,.F.,(4,2,2,4),(-0.517963944857837,
-0.397262600557783,-0.272934034479511,-1.00033364894634E-6),
 .UNSPECIFIED.);
#5610=B_SPLINE_CURVE_WITH_KNOTS('',3,(#202515,#202516,#202517,#202518,#202519,
#202520),.UNSPECIFIED.,.F.,.F.,(4,2,4),(2.38553191273868E-5,0.38451969589073,
0.769032294646552),.UNSPECIFIED.);
#5611=B_SPLINE_CURVE_WITH_KNOTS('',3,(#202522,#202523,#202524,#202525,#202526,
#202527),.UNSPECIFIED.,.F.,.F.,(4,2,4),(1.50356860986035E-5,1.25241012483363,
2.53999779295726),.UNSPECIFIED.);
#5612=B_SPLINE_CURVE_WITH_KNOTS('',3,(#202528,#202529,#202530,#202531,#202532,
#202533),.UNSPECIFIED.,.F.,.F.,(4,2,4),(-0.779389334694245,-0.389697685223124,
-5.55355428311088E-10),.UNSPECIFIED.);
#5613=B_SPLINE_CURVE_WITH_KNOTS('',3,(#202551,#202552,#202553,#202554,#202555,
#202556),.UNSPECIFIED.,.F.,.F.,(4,2,4),(-0.78359241345728,-0.391796250396355,
-5.76655713470621E-6),.UNSPECIFIED.);
#5614=B_SPLINE_CURVE_WITH_KNOTS('',3,(#202558,#202559,#202560,#202561,#202562,
#202563),.UNSPECIFIED.,.F.,.F.,(4,2,4),(5.52446895573059E-7,1.19166141028964,
2.34466320735633),.UNSPECIFIED.);
#5615=B_SPLINE_CURVE_WITH_KNOTS('',3,(#202564,#202565,#202566,#202567,#202568,
#202569),.UNSPECIFIED.,.F.,.F.,(4,2,4),(7.27550329604178E-10,0.387014349072472,
0.774020170091024),.UNSPECIFIED.);
#5616=B_SPLINE_CURVE_WITH_KNOTS('',3,(#202571,#202572,#202573,#202574,#202575,
#202576,#202577,#202578,#202579,#202580,#202581,#202582,#202583,#202584,
#202585,#202586,#202587,#202588,#202589,#202590,#202591,#202592,#202593,
#202594,#202595,#202596,#202597,#202598,#202599,#202600,#202601,#202602,
#202603,#202604,#202605,#202606,#202607,#202608,#202609,#202610,#202611,
#202612,#202613,#202614,#202615,#202616,#202617,#202618,#202619,#202620,
#202621,#202622,#202623,#202624,#202625,#202626,#202627,#202628,#202629,
#202630,#202631,#202632,#202633,#202634,#202635,#202636,#202637,#202638,
#202639,#202640,#202641,#202642,#202643,#202644,#202645,#202646,#202647,
#202648,#202649,#202650,#202651,#202652,#202653,#202654,#202655,#202656,
#202657,#202658,#202659,#202660,#202661,#202662,#202663,#202664,#202665,
#202666,#202667,#202668,#202669,#202670,#202671,#202672,#202673,#202674,
#202675,#202676,#202677,#202678,#202679,#202680,#202681,#202682,#202683,
#202684,#202685,#202686,#202687,#202688,#202689,#202690,#202691,#202692,
#202693,#202694,#202695,#202696,#202697,#202698,#202699,#202700,#202701,
#202702,#202703,#202704,#202705,#202706,#202707,#202708,#202709,#202710,
#202711,#202712,#202713,#202714,#202715,#202716,#202717,#202718,#202719,
#202720,#202721,#202722,#202723,#202724,#202725,#202726,#202727,#202728,
#202729,#202730,#202731,#202732,#202733,#202734,#202735,#202736,#202737,
#202738,#202739,#202740,#202741,#202742,#202743,#202744,#202745,#202746,
#202747,#202748,#202749,#202750,#202751),.UNSPECIFIED.,.F.,.F.,(4,3,3,3,
3,3,3,3,3,3,3,3,3,3,3,3,3,3,3,3,3,3,3,3,3,3,3,3,3,3,3,3,3,3,3,3,3,3,3,3,
3,3,3,3,3,3,3,3,3,3,3,3,3,3,3,3,3,3,3,3,4),(-24.3791246898611,-21.9390511734847,
-21.587247653096,-20.9141411659479,-20.6749811972056,-20.3837713733337,
-20.3467231118568,-20.3139855512779,-20.2510876320262,-20.1280178699515,
-19.6785227528667,-18.0213957458283,-17.1910657827344,-16.6732915992545,
-16.606389804286,-16.5376226319807,-16.3841689273798,-16.0983915481674,
-15.4288562409009,-14.0828994997063,-13.0642722748157,-12.5402964114879,
-12.2266745209215,-12.1849575357879,-12.1642539264969,-12.1461887234912,
-12.0737332692285,-11.929579766766,-11.3129407028397,-10.16778088186,-9.03949592610626,
-8.47302954415004,-8.41915480146032,-8.2767480703946,-8.20384374683888,
-8.16718304435154,-8.12582623258736,-7.79810494513167,-7.2698798002026,
-6.31526529078602,-4.47499777521626,-4.24042728411652,-4.11506543944821,
-4.0830927553645,-4.06936168313156,-4.05586885160344,-4.00154868216668,
-3.56567492147755,-2.85831957756782,-2.36821257735992,-1.74323718478967,
-1.44214112090375,-1.36520157105012,-1.33001001266006,-1.31371874445417,
-1.30574819406026,-1.29669997244628,-1.1739315159141,-0.840135585432776,
-0.462288295934132,0.),.UNSPECIFIED.);
#5617=B_SPLINE_CURVE_WITH_KNOTS('',3,(#202772,#202773,#202774,#202775,#202776,
#202777,#202778,#202779,#202780,#202781,#202782,#202783,#202784,#202785,
#202786,#202787,#202788,#202789,#202790,#202791,#202792,#202793,#202794,
#202795,#202796,#202797,#202798,#202799,#202800,#202801,#202802,#202803,
#202804,#202805,#202806,#202807,#202808,#202809,#202810,#202811,#202812,
#202813,#202814,#202815,#202816,#202817,#202818,#202819,#202820,#202821,
#202822,#202823,#202824,#202825,#202826,#202827,#202828,#202829,#202830,
#202831,#202832,#202833,#202834,#202835,#202836,#202837,#202838,#202839,
#202840,#202841,#202842,#202843,#202844,#202845,#202846,#202847),
 .UNSPECIFIED.,.F.,.F.,(4,3,3,3,3,3,3,3,3,3,3,3,3,3,3,3,3,3,3,3,3,3,3,3,
3,4),(6.34981825321816E-8,0.0989503026875498,0.125000000000009,0.187500000000015,
0.218750000000019,0.234375000000023,0.242187500000026,0.248046875000028,
0.250000000000029,0.359531791882742,0.375000000000205,0.437500000000292,
0.468750000000336,0.484375000000357,0.492187500000366,0.498046875000372,
0.500000000000373,0.625000000000412,0.687500000000433,0.718750000000443,
0.734375000000447,0.742187500000449,0.74804687500045,0.750000000000449,
0.888290218203772,1.),.UNSPECIFIED.);
#5618=B_SPLINE_CURVE_WITH_KNOTS('',3,(#202848,#202849,#202850,#202851,#202852,
#202853),.UNSPECIFIED.,.F.,.F.,(4,2,4),(-0.920999101727438,-0.460499463349185,
0.),.UNSPECIFIED.);
#5619=B_SPLINE_CURVE_WITH_KNOTS('',3,(#202857,#202858,#202859,#202860,#202861,
#202862),.UNSPECIFIED.,.F.,.F.,(4,2,4),(8.97768736117609E-5,0.0361831683940628,
0.072357762392722),.UNSPECIFIED.);
#5620=B_SPLINE_CURVE_WITH_KNOTS('',3,(#202863,#202864,#202865,#202866,#202867,
#202868,#202869,#202870,#202871,#202872,#202873,#202874,#202875,#202876,
#202877,#202878),.UNSPECIFIED.,.F.,.F.,(4,2,2,2,2,2,2,4),(0.,0.0840900735190167,
0.170079589631641,0.345597941878049,0.709772911470069,1.47183879031424,
2.24214841760652,3.28470623629705),.UNSPECIFIED.);
#5621=B_SPLINE_CURVE_WITH_KNOTS('',3,(#202882,#202883,#202884,#202885,#202886,
#202887),.UNSPECIFIED.,.F.,.F.,(4,2,4),(1.16230659145506E-5,0.0315626968355423,
0.0631239559511615),.UNSPECIFIED.);
#5622=B_SPLINE_CURVE_WITH_KNOTS('',3,(#202906,#202907,#202908,#202909,#202910,
#202911,#202912,#202913,#202914,#202915,#202916,#202917,#202918,#202919,
#202920,#202921,#202922,#202923,#202924,#202925,#202926,#202927,#202928,
#202929,#202930,#202931,#202932,#202933,#202934,#202935,#202936,#202937,
#202938,#202939,#202940,#202941,#202942,#202943,#202944,#202945),
 .UNSPECIFIED.,.F.,.F.,(4,3,3,3,3,3,3,3,3,3,3,3,3,4),(1.46398934889516E-7,
0.132682753700099,0.250000000000049,0.375000000000075,0.437500000000089,
0.468750000000096,0.484375000000098,0.492187500000101,0.499511718750102,
0.500000000000101,0.629789774175571,0.756495566402389,0.878945558600266,
1.),.UNSPECIFIED.);
#5623=B_SPLINE_CURVE_WITH_KNOTS('',3,(#202946,#202947,#202948,#202949,#202950,
#202951),.UNSPECIFIED.,.F.,.F.,(4,2,4),(-0.78909387311141,-0.394547649846113,
-2.83084323799167E-6),.UNSPECIFIED.);
#5624=B_SPLINE_CURVE_WITH_KNOTS('',3,(#202954,#202955,#202956,#202957,#202958,
#202959),.UNSPECIFIED.,.F.,.F.,(4,2,4),(-0.144999030706854,-0.0722850858966769,
-1.08948736717993E-6),.UNSPECIFIED.);
#5625=B_SPLINE_CURVE_WITH_KNOTS('',3,(#202961,#202962,#202963,#202964,#202965,
#202966),.UNSPECIFIED.,.F.,.F.,(4,2,4),(-0.145062519279745,-0.0717246702272529,
-2.04904239573723E-6),.UNSPECIFIED.);
#5626=B_SPLINE_CURVE_WITH_KNOTS('',3,(#203165,#203166,#203167,#203168,#203169,
#203170,#203171,#203172,#203173,#203174,#203175,#203176,#203177,#203178),
 .UNSPECIFIED.,.F.,.F.,(4,2,2,2,2,2,4),(-1.33017036243567,-1.18625647343036,
-1.01397324567186,-0.691555155250063,-0.300153323254672,-0.150122339964719,
-3.71851020656187E-6),.UNSPECIFIED.);
#5627=B_SPLINE_CURVE_WITH_KNOTS('',3,(#203179,#203180,#203181,#203182,#203183,
#203184,#203185,#203186,#203187,#203188,#203189,#203190,#203191,#203192,
#203193,#203194),.UNSPECIFIED.,.F.,.F.,(4,2,2,2,2,2,2,4),(0.,0.0775932728882868,
0.156868688544549,0.318279132560059,0.651367894554687,1.34248027769519,
2.03705495700613,2.68811868112204),.UNSPECIFIED.);
#5628=B_SPLINE_CURVE_WITH_KNOTS('',3,(#203195,#203196,#203197,#203198,#203199,
#203200,#203201,#203202,#203203,#203204,#203205,#203206,#203207,#203208),
 .UNSPECIFIED.,.F.,.F.,(4,2,2,2,2,2,4),(4.21885373736936E-6,0.150120351661493,
0.335800964668187,0.716383852778975,1.16414712511149,1.32805324237018,1.49332401797822),
 .UNSPECIFIED.);
#5629=B_SPLINE_CURVE_WITH_KNOTS('',3,(#203210,#203211,#203212,#203213,#203214,
#203215),.UNSPECIFIED.,.F.,.F.,(4,2,4),(-0.288938372418224,-0.144350861152813,
-2.02154080876134E-6),.UNSPECIFIED.);
#5630=B_SPLINE_CURVE_WITH_KNOTS('',3,(#203217,#203218,#203219,#203220,#203221,
#203222),.UNSPECIFIED.,.F.,.F.,(4,2,4),(-0.106301599642394,-0.0531518973430255,
0.),.UNSPECIFIED.);
#5631=B_SPLINE_CURVE_WITH_KNOTS('',3,(#203223,#203224,#203225,#203226,#203227,
#203228),.UNSPECIFIED.,.F.,.F.,(4,2,4),(-0.0594936343766405,-0.0297474281548696,
-1.17962743812669E-6),.UNSPECIFIED.);
#5632=B_SPLINE_CURVE_WITH_KNOTS('',3,(#203231,#203232,#203233,#203234,#203235,
#203236),.UNSPECIFIED.,.F.,.F.,(4,2,4),(0.,0.0596783514028972,0.119718248687109),
 .UNSPECIFIED.);
#5633=B_SPLINE_CURVE_WITH_KNOTS('',3,(#203239,#203240,#203241,#203242,#203243,
#203244),.UNSPECIFIED.,.F.,.F.,(4,2,4),(1.76072677471803E-6,0.0155815452526277,
0.031165071681481),.UNSPECIFIED.);
#5634=B_SPLINE_CURVE_WITH_KNOTS('',3,(#203526,#203527,#203528,#203529,#203530,
#203531,#203532,#203533,#203534,#203535,#203536,#203537,#203538,#203539,
#203540,#203541),.UNSPECIFIED.,.F.,.F.,(4,2,2,2,2,2,2,4),(-1.38384890716764,
-1.29505750437121,-1.20010459148349,-1.01223063363571,-0.713348009009054,
-0.327085141772229,-0.164588178759744,-3.61030969499539E-6),
 .UNSPECIFIED.);
#5635=B_SPLINE_CURVE_WITH_KNOTS('',3,(#203542,#203543,#203544,#203545,#203546,
#203547,#203548,#203549,#203550,#203551,#203552,#203553,#203554,#203555,
#203556,#203557),.UNSPECIFIED.,.F.,.F.,(4,2,2,2,2,2,2,4),(9.99999998611766E-7,
0.0993759126941353,0.203266326829571,0.419074165587955,0.737922963129613,
1.15644233100818,1.36237389456797,1.52406811373926),.UNSPECIFIED.);
#5636=B_SPLINE_CURVE_WITH_KNOTS('',3,(#203558,#203559,#203560,#203561),
 .UNSPECIFIED.,.F.,.F.,(4,4),(0.,1.),.UNSPECIFIED.);
#5637=B_SPLINE_CURVE_WITH_KNOTS('',3,(#203566,#203567,#203568,#203569,#203570,
#203571),.UNSPECIFIED.,.F.,.F.,(4,2,4),(9.87884185704088E-7,0.256849336223313,
0.514256161629985),.UNSPECIFIED.);
#5638=B_SPLINE_CURVE_WITH_KNOTS('',3,(#203573,#203574,#203575,#203576,#203577,
#203578),.UNSPECIFIED.,.F.,.F.,(4,2,4),(0.,0.0346991781454662,0.069353995647711),
 .UNSPECIFIED.);
#5639=B_SPLINE_CURVE_WITH_KNOTS('',3,(#203581,#203582,#203583,#203584,#203585,
#203586),.UNSPECIFIED.,.F.,.F.,(4,2,4),(0.,0.0363145822537585,0.0726180231601224),
 .UNSPECIFIED.);
#5640=B_SPLINE_CURVE_WITH_KNOTS('',3,(#203591,#203592,#203593,#203594,#203595,
#203596),.UNSPECIFIED.,.F.,.F.,(4,2,4),(4.78770270599075E-8,0.128060743206973,
0.256048544261365),.UNSPECIFIED.);
#5641=B_SPLINE_CURVE_WITH_KNOTS('',3,(#203601,#203602,#203603,#203604,#203605,
#203606),.UNSPECIFIED.,.F.,.F.,(4,2,4),(4.98277165604429E-5,0.167649620755388,
0.334882293597469),.UNSPECIFIED.);
#5642=B_SPLINE_CURVE_WITH_KNOTS('',3,(#203611,#203612,#203613,#203614,#203615,
#203616),.UNSPECIFIED.,.F.,.F.,(4,2,4),(3.03081736350241E-7,0.129774103732234,
0.259677566733192),.UNSPECIFIED.);
#5643=B_SPLINE_CURVE_WITH_KNOTS('',3,(#203620,#203621,#203622,#203623,#203624,
#203625),.UNSPECIFIED.,.F.,.F.,(4,2,4),(1.63384903984051E-6,0.172602040902318,
0.345633561259572),.UNSPECIFIED.);
#5644=B_SPLINE_CURVE_WITH_KNOTS('',3,(#203633,#203634,#203635,#203636,#203637,
#203638,#203639,#203640),.UNSPECIFIED.,.F.,.F.,(4,2,2,4),(4.10708027676161E-7,
0.142324182994593,0.242655243240103,0.336291803605073),.UNSPECIFIED.);
#5645=B_SPLINE_CURVE_WITH_KNOTS('',3,(#203643,#203644,#203645,#203646,#203647,
#203648,#203649,#203650),.UNSPECIFIED.,.F.,.F.,(4,2,2,4),(-0.233723723416541,
-0.134753236172302,-0.0639786247876465,0.),.UNSPECIFIED.);
#5646=B_SPLINE_CURVE_WITH_KNOTS('',3,(#203655,#203656,#203657,#203658,#203659,
#203660,#203661,#203662),.UNSPECIFIED.,.F.,.F.,(4,2,2,4),(-0.212938364160185,
-0.137840855028458,-0.114290139265485,-2.81167466484031E-6),
 .UNSPECIFIED.);
#5647=B_SPLINE_CURVE_WITH_KNOTS('',3,(#203663,#203664,#203665,#203666,#203667,
#203668),.UNSPECIFIED.,.F.,.F.,(4,2,4),(-0.274300204892665,-0.138756656361396,
0.),.UNSPECIFIED.);
#5648=B_SPLINE_CURVE_WITH_KNOTS('',3,(#203672,#203673,#203674,#203675,#203676,
#203677),.UNSPECIFIED.,.F.,.F.,(4,2,4),(-0.234582769559139,-0.113404422883209,
0.),.UNSPECIFIED.);
#5649=B_SPLINE_CURVE_WITH_KNOTS('',3,(#203682,#203683,#203684,#203685,#203686,
#203687),.UNSPECIFIED.,.F.,.F.,(4,2,4),(-0.333867148600103,-0.169761706315603,
-1.67365979304573E-6),.UNSPECIFIED.);
#5650=B_SPLINE_CURVE_WITH_KNOTS('',3,(#203688,#203689,#203690,#203691,#203692,
#203693,#203694,#203695,#203696,#203697),.UNSPECIFIED.,.F.,.F.,(4,2,2,2,
4),(-0.26114851459812,-0.219345918382166,-0.211987678333995,-0.164711934999612,
-1.00032645433914E-6),.UNSPECIFIED.);
#5651=B_SPLINE_CURVE_WITH_KNOTS('',3,(#203699,#203700,#203701,#203702,#203703,
#203704,#203705,#203706,#203707,#203708,#203709,#203710,#203711,#203712,
#203713,#203714,#203715,#203716,#203717,#203718),.UNSPECIFIED.,.F.,.F.,
(4,2,2,2,2,2,2,2,2,4),(-0.673428088960982,-0.645968473599191,-0.63864640624558,
-0.636802786602354,-0.632872979199508,-0.569476839505419,-0.344878488981366,
-0.18144254201973,-0.0902078250720447,0.),.UNSPECIFIED.);
#5652=B_SPLINE_CURVE_WITH_KNOTS('',3,(#203720,#203721,#203722,#203723,#203724,
#203725),.UNSPECIFIED.,.F.,.F.,(4,2,4),(3.82662946478662E-7,0.114173063341795,
0.229641536291977),.UNSPECIFIED.);
#5653=B_SPLINE_CURVE_WITH_KNOTS('',3,(#204832,#204833,#204834,#204835,#204836,
#204837),.UNSPECIFIED.,.F.,.F.,(4,2,4),(0.,0.130029291827762,0.259524252867855),
 .UNSPECIFIED.);
#5654=B_SPLINE_CURVE_WITH_KNOTS('',3,(#204838,#204839,#204840,#204841),
 .UNSPECIFIED.,.F.,.F.,(4,4),(-2.59791985233575E-6,0.),.UNSPECIFIED.);
#5655=B_SPLINE_CURVE_WITH_KNOTS('',3,(#204843,#204844,#204845,#204846),
 .UNSPECIFIED.,.F.,.F.,(4,4),(-5.76565361003733E-6,0.),.UNSPECIFIED.);
#5656=B_SPLINE_CURVE_WITH_KNOTS('',3,(#204847,#204848,#204849,#204850,#204851,
#204852),.UNSPECIFIED.,.F.,.F.,(4,2,4),(9.99590034037455E-7,0.121785421623563,
0.24403732646739),.UNSPECIFIED.);
#5657=B_SPLINE_CURVE_WITH_KNOTS('',3,(#204853,#204854,#204855,#204856,#204857,
#204858),.UNSPECIFIED.,.F.,.F.,(4,2,4),(1.60537344364761E-6,0.13325159691034,
0.266722953368679),.UNSPECIFIED.);
#5658=B_SPLINE_CURVE_WITH_KNOTS('',3,(#204859,#204860,#204861,#204862,#204863,
#204864),.UNSPECIFIED.,.F.,.F.,(4,2,4),(7.42837984032087E-6,0.13590839804954,
0.271773150673492),.UNSPECIFIED.);
#5659=B_SPLINE_CURVE_WITH_KNOTS('',3,(#205145,#205146,#205147,#205148),
 .UNSPECIFIED.,.F.,.F.,(4,4),(0.0216968151072032,0.926937308587682),
 .UNSPECIFIED.);
#5660=B_SPLINE_CURVE_WITH_KNOTS('',3,(#205249,#205250,#205251,#205252),
 .UNSPECIFIED.,.F.,.F.,(4,4),(0.0222286199771242,0.926269849314919),
 .UNSPECIFIED.);
#5661=B_SPLINE_CURVE_WITH_KNOTS('',3,(#205330,#205331,#205332,#205333),
 .UNSPECIFIED.,.F.,.F.,(4,4),(0.0248339691417604,0.928145544482466),
 .UNSPECIFIED.);
#5662=B_SPLINE_CURVE_WITH_KNOTS('',3,(#205455,#205456,#205457,#205458),
 .UNSPECIFIED.,.F.,.F.,(4,4),(0.0238586497886119,0.928715545244436),
 .UNSPECIFIED.);
#5663=B_SPLINE_CURVE_WITH_KNOTS('',3,(#207120,#207121,#207122,#207123,#207124,
#207125,#207126,#207127,#207128,#207129,#207130,#207131,#207132,#207133,
#207134,#207135,#207136,#207137,#207138,#207139,#207140,#207141,#207142,
#207143,#207144,#207145,#207146,#207147,#207148,#207149,#207150,#207151,
#207152,#207153,#207154,#207155,#207156,#207157,#207158,#207159,#207160,
#207161,#207162,#207163,#207164,#207165,#207166,#207167,#207168,#207169,
#207170,#207171),.UNSPECIFIED.,.F.,.F.,(4,3,3,3,3,3,3,3,3,3,3,3,3,3,3,3,
3,4),(0.,0.0806048268663761,0.158714022235957,0.232021283797936,0.25,0.324001677230945,
0.401282678539864,0.48204973327551,0.5,0.500003584331971,0.580215606076185,
0.657617727195775,0.729959718881743,0.75,0.823833465567288,0.901157686681193,
0.982168573173414,1.),.UNSPECIFIED.);
#5664=B_SPLINE_CURVE_WITH_KNOTS('',3,(#207174,#207175,#207176,#207177,#207178,
#207179,#207180,#207181,#207182,#207183,#207184,#207185,#207186,#207187,
#207188,#207189,#207190,#207191,#207192,#207193,#207194,#207195,#207196,
#207197,#207198),.UNSPECIFIED.,.F.,.F.,(4,3,3,3,3,3,3,3,4),(0.,0.153526582008217,
0.311669465590391,0.422907894812392,0.494875521969546,0.500438042996234,
0.723275285884918,0.95807330633445,1.),.UNSPECIFIED.);
#5665=B_SPLINE_CURVE_WITH_KNOTS('',3,(#207246,#207247,#207248,#207249,#207250,
#207251,#207252,#207253,#207254,#207255,#207256,#207257,#207258,#207259,
#207260,#207261,#207262,#207263,#207264,#207265,#207266,#207267,#207268,
#207269,#207270,#207271,#207272,#207273,#207274,#207275,#207276,#207277,
#207278,#207279,#207280,#207281,#207282,#207283,#207284,#207285,#207286,
#207287,#207288,#207289,#207290,#207291,#207292,#207293,#207294,#207295,
#207296,#207297,#207298,#207299,#207300,#207301,#207302,#207303,#207304,
#207305,#207306,#207307,#207308,#207309,#207310,#207311,#207312,#207313,
#207314,#207315,#207316,#207317,#207318,#207319,#207320,#207321,#207322,
#207323,#207324),.UNSPECIFIED.,.F.,.F.,(4,3,3,3,3,3,3,3,3,3,3,3,3,3,3,3,
3,3,3,3,3,3,3,3,3,3,4),(0.,0.114629667334485,0.125000000000061,0.206386555414009,
0.242187500000125,0.249216553086816,0.250000000000131,0.255775387823804,
0.323300862474338,0.375000000000178,0.461187437204239,0.468750000000189,
0.484375000000195,0.494659013330622,0.500000000000202,0.509467435940447,
0.588597252522088,0.625000000000096,0.705669214159792,0.734375000000023,
0.744075465277332,0.750000000000004,0.758228559601408,0.826291788767228,
0.897548314370709,0.974137440758978,1.),.UNSPECIFIED.);
#5666=B_SPLINE_CURVE_WITH_KNOTS('',3,(#207327,#207328,#207329,#207330,#207331,
#207332,#207333,#207334,#207335,#207336,#207337,#207338,#207339,#207340,
#207341,#207342,#207343,#207344,#207345,#207346,#207347,#207348,#207349,
#207350,#207351,#207352,#207353,#207354,#207355,#207356,#207357),
 .UNSPECIFIED.,.F.,.F.,(4,3,3,3,3,3,3,3,3,3,4),(2.72268262058649E-15,0.000200725121439935,
0.000415654200400088,0.00061281274333361,0.000613704338138227,0.00122637007266609,
0.00122740867627373,0.00180004332875768,0.00184046060686526,0.00184111301440923,
0.00245481735254474),.UNSPECIFIED.);
#5667=B_SPLINE_CURVE_WITH_KNOTS('',3,(#207373,#207374,#207375,#207376,#207377,
#207378,#207379,#207380,#207381,#207382,#207383,#207384,#207385,#207386,
#207387,#207388,#207389,#207390,#207391,#207392,#207393,#207394,#207395,
#207396,#207397,#207398,#207399,#207400,#207401,#207402,#207403,#207404,
#207405,#207406,#207407,#207408,#207409,#207410,#207411,#207412,#207413,
#207414,#207415,#207416,#207417,#207418),.UNSPECIFIED.,.F.,.F.,(4,3,3,3,
3,3,3,3,3,3,3,3,3,3,3,4),(0.,0.25,0.4375,0.47265625,0.4891357421875,0.49312686920166,
0.49519146587179,0.495762776265408,0.496086078670549,0.496404892001326,
0.498372060391946,0.499351802461493,0.499918280627807,0.500154192246593,
0.796879510224575,1.),.UNSPECIFIED.);
#5668=B_SPLINE_CURVE_WITH_KNOTS('',3,(#207419,#207420,#207421,#207422),
 .UNSPECIFIED.,.F.,.F.,(4,4),(0.,0.0105146476282051),.UNSPECIFIED.);
#5669=B_SPLINE_CURVE_WITH_KNOTS('',3,(#207460,#207461,#207462,#207463,#207464,
#207465,#207466,#207467,#207468,#207469,#207470,#207471,#207472,#207473,
#207474,#207475,#207476,#207477,#207478,#207479,#207480,#207481,#207482,
#207483,#207484,#207485,#207486,#207487,#207488),.UNSPECIFIED.,.F.,.F.,
(4,1,1,2,2,2,1,1,2,2,2,1,2,2,2,2,4),(0.,0.125000000000098,0.187500000000144,
0.218750000000156,0.250000000000167,0.37500000000017,0.437500000000172,
0.468750000000185,0.484375000000191,0.500000000000197,0.625000000000202,
0.687500000000194,0.718750000000179,0.750000000000163,0.812500000000127,
0.875000000000091,1.),.UNSPECIFIED.);
#5670=B_SPLINE_CURVE_WITH_KNOTS('',3,(#207489,#207490,#207491,#207492,#207493,
#207494,#207495,#207496,#207497,#207498,#207499,#207500,#207501,#207502,
#207503,#207504,#207505,#207506,#207507,#207508,#207509,#207510,#207511,
#207512,#207513,#207514,#207515,#207516,#207517,#207518,#207519,#207520,
#207521,#207522),.UNSPECIFIED.,.F.,.F.,(4,2,2,1,1,2,2,2,2,1,1,2,2,2,2,1,
1,2,2,4),(0.,0.124999999999803,0.187499999999708,0.218749999999656,0.234374999999626,
0.242187499999614,0.249999999999602,0.374999999999714,0.437499999999765,
0.468749999999791,0.484374999999798,0.492187499999795,0.499999999999793,
0.624999999999634,0.687499999999566,0.71874999999953,0.734374999999508,
0.742187499999501,0.749999999999494,1.),.UNSPECIFIED.);
#5671=B_SPLINE_CURVE_WITH_KNOTS('',3,(#207550,#207551,#207552,#207553,#207554,
#207555,#207556,#207557,#207558,#207559,#207560,#207561,#207562,#207563,
#207564,#207565,#207566,#207567,#207568,#207569,#207570,#207571,#207572,
#207573,#207574),.UNSPECIFIED.,.F.,.F.,(4,3,3,3,3,3,3,3,4),(0.,0.169713712399116,
0.334856856199558,0.5,0.507353484491204,0.653685075739568,0.800970657233946,
0.950008965085336,1.),.UNSPECIFIED.);
#5672=B_SPLINE_CURVE_WITH_KNOTS('',3,(#207575,#207576,#207577,#207578,#207579,
#207580,#207581),.UNSPECIFIED.,.F.,.F.,(4,3,4),(9.81307786677359E-18,0.00416048285086259,
0.00832096570172518),.UNSPECIFIED.);
#5673=B_SPLINE_CURVE_WITH_KNOTS('',3,(#207621,#207622,#207623,#207624,#207625,
#207626,#207627,#207628,#207629,#207630,#207631,#207632,#207633,#207634,
#207635,#207636,#207637,#207638,#207639,#207640,#207641,#207642,#207643,
#207644,#207645,#207646,#207647,#207648,#207649,#207650,#207651,#207652,
#207653,#207654,#207655,#207656,#207657,#207658,#207659,#207660,#207661,
#207662,#207663,#207664,#207665,#207666,#207667,#207668,#207669,#207670,
#207671,#207672,#207673,#207674,#207675,#207676,#207677,#207678,#207679,
#207680,#207681,#207682,#207683,#207684,#207685,#207686,#207687,#207688,
#207689,#207690,#207691,#207692,#207693,#207694,#207695,#207696,#207697,
#207698,#207699,#207700,#207701,#207702,#207703,#207704,#207705,#207706,
#207707,#207708),.UNSPECIFIED.,.F.,.F.,(4,3,3,3,3,3,3,3,3,3,3,3,3,3,3,3,
3,3,3,3,3,3,3,3,3,3,3,3,3,4),(0.,0.0425126216922903,0.0624999999999267,
0.0846170699876459,0.09374999999989,0.109374999999872,0.124999999999853,
0.165041622176756,0.18749999999978,0.218749999999743,0.231263054308858,
0.244025736157331,0.249115753962458,0.249999999999707,0.312499999999637,
0.367366877870503,0.420962374636525,0.47656605752872,0.484374999999499,
0.493186960475905,0.499012025841205,0.499999999999505,0.56249999999956,
0.627138290432272,0.689890516986081,0.718749999999689,0.734644169494065,
0.749415530119711,0.749999999999721,1.),.UNSPECIFIED.);
#5674=B_SPLINE_CURVE_WITH_KNOTS('',3,(#207709,#207710,#207711,#207712,#207713,
#207714,#207715,#207716,#207717,#207718,#207719,#207720,#207721,#207722,
#207723,#207724,#207725,#207726,#207727,#207728,#207729,#207730,#207731,
#207732,#207733,#207734,#207735,#207736,#207737,#207738,#207739,#207740,
#207741,#207742),.UNSPECIFIED.,.F.,.F.,(4,2,2,1,1,2,2,2,2,1,1,2,2,2,2,1,
1,2,2,4),(0.,0.125000000000029,0.187500000000059,0.21875000000007,0.234375000000061,
0.242187500000052,0.250000000000042,0.374999999999973,0.437499999999958,
0.468749999999966,0.484374999999972,0.492187499999981,0.499999999999989,
0.625000000000122,0.687500000000187,0.718750000000232,0.734375000000254,
0.742187500000259,0.750000000000263,1.),.UNSPECIFIED.);
#5675=B_SPLINE_CURVE_WITH_KNOTS('',3,(#207764,#207765,#207766,#207767,#207768,
#207769,#207770,#207771,#207772,#207773,#207774,#207775,#207776,#207777,
#207778),.UNSPECIFIED.,.F.,.F.,(4,2,1,1,1,1,1,2,2,4),(0.,0.250000000000044,
0.375000000000067,0.437500000000079,0.468750000000085,0.484375000000087,
0.492187500000093,0.496093750000094,0.500000000000094,1.),.UNSPECIFIED.);
#5676=B_SPLINE_CURVE_WITH_KNOTS('',3,(#207779,#207780,#207781,#207782),
 .UNSPECIFIED.,.F.,.F.,(4,4),(0.,0.0107001581246114),.UNSPECIFIED.);
#5677=B_SPLINE_CURVE_WITH_KNOTS('',3,(#207798,#207799,#207800,#207801,#207802,
#207803,#207804,#207805,#207806,#207807,#207808,#207809,#207810,#207811,
#207812,#207813,#207814,#207815,#207816,#207817,#207818,#207819,#207820,
#207821,#207822,#207823,#207824,#207825,#207826,#207827,#207828,#207829,
#207830,#207831),.UNSPECIFIED.,.F.,.F.,(4,3,3,3,3,3,3,3,3,3,3,4),(0.,0.22396800402836,
0.249999999999856,0.374999999999772,0.43749999999973,0.468749999999695,
0.492663034070687,0.49999999999966,0.671520232782927,0.835760116391464,
0.986566865590623,1.),.UNSPECIFIED.);
#5678=B_SPLINE_CURVE_WITH_KNOTS('',3,(#207832,#207833,#207834,#207835),
 .UNSPECIFIED.,.F.,.F.,(4,4),(0.,1.),.UNSPECIFIED.);
#5679=B_SPLINE_CURVE_WITH_KNOTS('',3,(#207856,#207857,#207858,#207859,#207860,
#207861,#207862,#207863,#207864,#207865,#207866,#207867,#207868,#207869,
#207870,#207871,#207872,#207873,#207874,#207875,#207876,#207877,#207878,
#207879,#207880,#207881,#207882,#207883,#207884,#207885,#207886,#207887,
#207888,#207889,#207890,#207891,#207892,#207893,#207894,#207895,#207896,
#207897,#207898,#207899,#207900,#207901,#207902,#207903,#207904),
 .UNSPECIFIED.,.F.,.F.,(4,3,3,3,3,3,3,3,3,3,3,3,3,3,3,3,4),(0.,0.110193348836804,
0.226300572156345,0.347525286078198,0.468750000000051,0.486260581590066,
0.500000000000042,0.50052681277108,0.578360302839722,0.625000000000001,
0.687499999999979,0.71874999999998,0.735487941433878,0.749999999999982,
0.836356690732367,0.924217807330732,1.),.UNSPECIFIED.);
#5680=B_SPLINE_CURVE_WITH_KNOTS('',3,(#207906,#207907,#207908,#207909,#207910,
#207911,#207912,#207913,#207914,#207915,#207916,#207917,#207918,#207919,
#207920,#207921,#207922,#207923,#207924,#207925,#207926,#207927,#207928,
#207929,#207930,#207931,#207932,#207933,#207934,#207935,#207936,#207937,
#207938,#207939,#207940,#207941,#207942,#207943,#207944,#207945,#207946,
#207947,#207948,#207949,#207950,#207951,#207952,#207953,#207954,#207955,
#207956,#207957,#207958,#207959,#207960),.UNSPECIFIED.,.F.,.F.,(4,3,3,3,
3,3,3,3,3,3,3,3,3,3,3,3,3,3,4),(2.53418446955826E-6,0.0998044898858354,
0.193933366124132,0.269558082684436,0.348527825145383,0.397466750068292,
0.42749756760633,0.457698304529386,0.478849152264081,0.489424576131429,
0.492068432098266,0.492601765237038,0.499268082446897,0.499999999998776,
0.616033678583699,0.725387395575726,0.830726652989945,0.930602413285796,
1.),.UNSPECIFIED.);
#5681=B_SPLINE_CURVE_WITH_KNOTS('',3,(#208004,#208005,#208006,#208007,#208008,
#208009,#208010,#208011,#208012,#208013,#208014,#208015,#208016,#208017,
#208018,#208019,#208020,#208021,#208022,#208023,#208024,#208025,#208026,
#208027,#208028,#208029,#208030,#208031,#208032,#208033,#208034,#208035,
#208036,#208037),.UNSPECIFIED.,.F.,.F.,(4,2,2,1,1,2,2,2,2,1,1,2,2,2,2,1,
1,2,2,4),(0.,0.124999999999678,0.187499999999503,0.21874999999941,0.23437499999937,
0.242187499999368,0.249999999999367,0.374999999999121,0.437499999999018,
0.468749999998965,0.484374999998937,0.49218749999893,0.499999999998922,
0.624999999999086,0.687499999999163,0.718749999999202,0.734374999999215,
0.742187499999228,0.749999999999241,1.),.UNSPECIFIED.);
#5682=B_SPLINE_CURVE_WITH_KNOTS('',3,(#208040,#208041,#208042,#208043,#208044,
#208045,#208046,#208047,#208048,#208049,#208050,#208051,#208052,#208053,
#208054,#208055,#208056,#208057,#208058,#208059,#208060,#208061,#208062,
#208063,#208064,#208065,#208066),.UNSPECIFIED.,.F.,.F.,(4,2,1,1,2,2,2,1,
1,2,2,2,1,2,2,4),(0.,0.124999999999879,0.187499999999819,0.218749999999792,
0.23437499999979,0.249999999999788,0.3749999999998,0.437499999999805,0.468749999999808,
0.484374999999806,0.499999999999804,0.62499999999983,0.68749999999983,0.718749999999846,
0.749999999999862,1.),.UNSPECIFIED.);
#5683=B_SPLINE_CURVE_WITH_KNOTS('',3,(#208082,#208083,#208084,#208085),
 .UNSPECIFIED.,.F.,.F.,(4,4),(0.,1.),.UNSPECIFIED.);
#5684=B_SPLINE_CURVE_WITH_KNOTS('',3,(#208086,#208087,#208088,#208089),
 .UNSPECIFIED.,.F.,.F.,(4,4),(4.04603565571183E-17,0.00980967348625103),
 .UNSPECIFIED.);
#5685=B_SPLINE_CURVE_WITH_KNOTS('',3,(#208111,#208112,#208113,#208114,#208115,
#208116,#208117),.UNSPECIFIED.,.F.,.F.,(4,3,4),(0.,0.00416021787251447,
0.00832043574502893),.UNSPECIFIED.);
#5686=B_SPLINE_CURVE_WITH_KNOTS('',3,(#208118,#208119,#208120,#208121,#208122,
#208123,#208124,#208125,#208126,#208127,#208128,#208129,#208130,#208131,
#208132,#208133,#208134,#208135,#208136,#208137,#208138,#208139),
 .UNSPECIFIED.,.F.,.F.,(4,3,3,3,3,3,3,4),(0.,0.174023413314913,0.343412686965267,
0.51280196061562,0.661616188253227,0.810426910260397,0.959545980295111,
1.),.UNSPECIFIED.);
#5687=B_SPLINE_CURVE_WITH_KNOTS('',3,(#208161,#208162,#208163,#208164,#208165,
#208166,#208167,#208168,#208169,#208170,#208171,#208172,#208173,#208174,
#208175,#208176,#208177,#208178,#208179,#208180,#208181,#208182,#208183,
#208184,#208185,#208186,#208187,#208188,#208189,#208190,#208191,#208192,
#208193,#208194,#208195,#208196,#208197,#208198,#208199,#208200,#208201,
#208202,#208203,#208204,#208205,#208206,#208207,#208208,#208209,#208210,
#208211,#208212,#208213,#208214,#208215,#208216,#208217,#208218),
 .UNSPECIFIED.,.F.,.F.,(4,3,3,3,3,3,3,3,3,3,3,3,3,3,3,3,3,3,3,4),(0.,0.0969945238812358,
0.200908355313719,0.288417201918382,0.395108792074533,0.484375000000186,
0.496161411879799,0.500000000000187,0.500467577071174,0.574698071762265,
0.625000000000102,0.687500000000059,0.718750000000036,0.734375000000025,
0.74523453307188,0.750000000000014,0.812500000000011,0.900353222249502,
0.989751398368336,1.),.UNSPECIFIED.);
#5688=B_SPLINE_CURVE_WITH_KNOTS('',3,(#208219,#208220,#208221,#208222,#208223,
#208224,#208225,#208226,#208227,#208228,#208229,#208230,#208231,#208232,
#208233,#208234,#208235,#208236,#208237,#208238,#208239,#208240,#208241,
#208242,#208243,#208244,#208245,#208246,#208247,#208248,#208249,#208250,
#208251,#208252,#208253,#208254,#208255,#208256,#208257,#208258,#208259,
#208260,#208261,#208262,#208263,#208264,#208265,#208266,#208267,#208268,
#208269,#208270,#208271,#208272,#208273,#208274,#208275,#208276,#208277,
#208278,#208279,#208280,#208281,#208282,#208283,#208284,#208285,#208286,
#208287,#208288,#208289,#208290,#208291,#208292,#208293,#208294,#208295,
#208296,#208297,#208298,#208299,#208300),.UNSPECIFIED.,.F.,.F.,(4,3,3,3,
3,3,3,3,3,3,3,3,3,3,3,3,3,3,3,3,3,3,3,3,3,3,3,4),(0.,0.0771005613023838,
0.125000000000185,0.216511745445919,0.286309253196597,0.356488197815171,
0.423767589799145,0.45981549070489,0.484747979915122,0.491046981783119,
0.491844143094684,0.492573845881986,0.496712163198199,0.49871666064824,
0.499810910719285,0.50025674181692,0.594269001722782,0.625000000000811,
0.687500000000829,0.718750000000836,0.734375000000824,0.742187500000821,
0.748946705574376,0.750000000000817,0.8270954483746,0.901599505899295,0.972126634077241,
1.),.UNSPECIFIED.);
#5689=B_SPLINE_CURVE_WITH_KNOTS('',3,(#208334,#208335,#208336,#208337,#208338,
#208339,#208340,#208341,#208342,#208343,#208344,#208345,#208346,#208347,
#208348,#208349,#208350,#208351,#208352,#208353,#208354,#208355,#208356,
#208357,#208358,#208359,#208360,#208361,#208362,#208363,#208364,#208365,
#208366,#208367),.UNSPECIFIED.,.F.,.F.,(4,2,2,1,1,2,2,2,2,1,1,2,2,2,2,1,
1,2,2,4),(0.,0.124999999999397,0.187499999999094,0.218749999998944,0.234374999998861,
0.242187499998828,0.249999999998795,0.374999999998407,0.437499999998207,
0.468749999998112,0.484374999998075,0.492187499998049,0.499999999998023,
0.624999999998236,0.687499999998338,0.718749999998405,0.734374999998451,
0.742187499998474,0.749999999998497,1.),.UNSPECIFIED.);
#5690=B_SPLINE_CURVE_WITH_KNOTS('',3,(#208368,#208369,#208370,#208371,#208372,
#208373,#208374,#208375,#208376,#208377,#208378,#208379,#208380,#208381,
#208382,#208383,#208384,#208385,#208386,#208387,#208388,#208389,#208390,
#208391,#208392,#208393,#208394,#208395,#208396),.UNSPECIFIED.,.F.,.F.,
(4,1,1,2,2,2,1,1,2,2,2,1,2,2,2,2,4),(0.,0.124999999999937,0.187499999999906,
0.218749999999893,0.24999999999988,0.374999999999836,0.437499999999826,
0.468749999999805,0.484374999999804,0.499999999999802,0.624999999999829,
0.687499999999847,0.718749999999856,0.749999999999865,0.812499999999898,
0.87499999999993,1.),.UNSPECIFIED.);
#5691=B_SPLINE_CURVE_WITH_KNOTS('',3,(#208416,#208417,#208418,#208419),
 .UNSPECIFIED.,.F.,.F.,(4,4),(0.,0.00972938600277915),.UNSPECIFIED.);
#5692=B_SPLINE_CURVE_WITH_KNOTS('',3,(#208420,#208421,#208422,#208423,#208424,
#208425,#208426,#208427,#208428,#208429,#208430,#208431,#208432,#208433,
#208434),.UNSPECIFIED.,.F.,.F.,(4,2,2,1,1,1,2,2,4),(0.,0.250000000000011,
0.375000000000019,0.437500000000025,0.468750000000028,0.484375000000027,
0.492187500000026,0.500000000000025,1.),.UNSPECIFIED.);
#5693=B_SPLINE_CURVE_WITH_KNOTS('',3,(#208450,#208451,#208452,#208453),
 .UNSPECIFIED.,.F.,.F.,(4,4),(0.,3.23803390124219E-5),.UNSPECIFIED.);
#5694=B_SPLINE_CURVE_WITH_KNOTS('',3,(#208454,#208455,#208456,#208457),
 .UNSPECIFIED.,.F.,.F.,(4,4),(0.,2.59869381596583E-5),.UNSPECIFIED.);
#5695=B_SPLINE_CURVE_WITH_KNOTS('',3,(#208485,#208486,#208487,#208488,#208489,
#208490,#208491,#208492,#208493,#208494,#208495,#208496,#208497,#208498,
#208499,#208500,#208501,#208502,#208503,#208504,#208505,#208506,#208507,
#208508,#208509,#208510,#208511,#208512,#208513,#208514,#208515,#208516,
#208517,#208518,#208519,#208520,#208521,#208522,#208523,#208524,#208525,
#208526,#208527,#208528,#208529,#208530),.UNSPECIFIED.,.F.,.F.,(4,3,3,3,
3,3,3,3,3,3,3,3,3,3,3,4),(0.,0.0906629207478083,0.188650654775597,0.249999999999092,
0.373046874998603,0.467058712523105,0.496093749998114,0.499999999998105,
0.508669898665942,0.586164263608202,0.66828506364852,0.733205222480325,
0.795419535562799,0.860569483442956,0.930284741721478,1.),.UNSPECIFIED.);
#5696=B_SPLINE_CURVE_WITH_KNOTS('',3,(#208531,#208532,#208533,#208534,#208535,
#208536,#208537,#208538,#208539,#208540,#208541,#208542,#208543,#208544,
#208545,#208546,#208547,#208548,#208549,#208550,#208551,#208552,#208553,
#208554,#208555,#208556,#208557,#208558,#208559,#208560,#208561,#208562,
#208563,#208564,#208565,#208566,#208567,#208568,#208569,#208570,#208571,
#208572,#208573,#208574,#208575,#208576,#208577,#208578,#208579,#208580,
#208581,#208582,#208583,#208584,#208585,#208586,#208587,#208588),
 .UNSPECIFIED.,.F.,.F.,(4,3,3,3,3,3,3,3,3,3,3,3,3,3,3,3,3,3,3,4),(0.,0.0689082811774419,
0.137184580919919,0.20664499924701,0.234374999999953,0.244741122741839,
0.249594660540849,0.249999999999948,0.361641502564665,0.374999999999894,
0.437499999999878,0.468749999999856,0.484374999999857,0.495706414317134,
0.499537692650688,0.499999999999857,0.638127812197921,0.774660191713116,
0.909042522090822,1.),.UNSPECIFIED.);
#5697=B_SPLINE_CURVE_WITH_KNOTS('',3,(#208620,#208621,#208622,#208623),
 .UNSPECIFIED.,.F.,.F.,(4,4),(0.,1.68205588696557E-5),.UNSPECIFIED.);
#5698=B_SPLINE_CURVE_WITH_KNOTS('',3,(#208624,#208625,#208626,#208627),
 .UNSPECIFIED.,.F.,.F.,(4,4),(6.93889390390723E-18,2.09370149851292E-5),
 .UNSPECIFIED.);
#5699=B_SPLINE_CURVE_WITH_KNOTS('',3,(#208714,#208715,#208716,#208717),
 .UNSPECIFIED.,.F.,.F.,(4,4),(0.,0.000210836370419721),.UNSPECIFIED.);
#5700=B_SPLINE_CURVE_WITH_KNOTS('',3,(#208756,#208757,#208758,#208759,#208760,
#208761,#208762,#208763,#208764,#208765,#208766,#208767,#208768,#208769,
#208770,#208771,#208772,#208773,#208774,#208775,#208776,#208777,#208778,
#208779,#208780,#208781,#208782,#208783,#208784,#208785,#208786,#208787),
 .UNSPECIFIED.,.F.,.F.,(4,2,2,1,2,2,1,2,2,1,1,2,2,2,1,1,2,2,4),(0.,0.0624999999999714,
0.124999999999943,0.187499999999914,0.218749999999901,0.249999999999887,
0.312499999999844,0.343749999999822,0.3749999999998,0.437499999999771,0.468749999999757,
0.484374999999755,0.499999999999754,0.624999999999732,0.687499999999739,
0.718749999999749,0.734374999999755,0.74999999999976,1.),.UNSPECIFIED.);
#5701=B_SPLINE_CURVE_WITH_KNOTS('',3,(#208789,#208790,#208791,#208792,#208793,
#208794,#208795,#208796,#208797,#208798,#208799,#208800,#208801,#208802,
#208803,#208804,#208805,#208806,#208807,#208808,#208809,#208810,#208811),
 .UNSPECIFIED.,.F.,.F.,(4,2,2,1,1,1,2,2,2,1,1,2,2,4),(0.,0.25000000000007,
0.375000000000092,0.437500000000124,0.468750000000127,0.484375000000116,
0.492187500000111,0.500000000000106,0.625000000000092,0.687500000000093,
0.718750000000093,0.734375000000072,0.750000000000051,1.),.UNSPECIFIED.);
#5702=B_SPLINE_CURVE_WITH_KNOTS('',3,(#208852,#208853,#208854,#208855,#208856,
#208857,#208858,#208859,#208860,#208861,#208862,#208863,#208864,#208865,
#208866,#208867,#208868),.UNSPECIFIED.,.F.,.F.,(4,2,2,2,1,1,1,2,2,4),(0.,
0.250000000001027,0.375000000001554,0.437500000001813,0.468750000001952,
0.48437500000201,0.492187500002025,0.496093750002033,0.50000000000204,1.),
 .UNSPECIFIED.);
#5703=B_SPLINE_CURVE_WITH_KNOTS('',3,(#208869,#208870,#208871,#208872,#208873,
#208874,#208875,#208876,#208877,#208878,#208879,#208880,#208881,#208882,
#208883,#208884,#208885,#208886,#208887,#208888,#208889,#208890,#208891,
#208892,#208893,#208894,#208895,#208896,#208897,#208898,#208899,#208900,
#208901,#208902,#208903,#208904,#208905,#208906,#208907,#208908,#208909,
#208910,#208911,#208912,#208913,#208914,#208915,#208916,#208917,#208918,
#208919,#208920,#208921,#208922,#208923,#208924,#208925,#208926,#208927,
#208928,#208929,#208930,#208931,#208932,#208933,#208934,#208935,#208936,
#208937,#208938,#208939,#208940,#208941,#208942,#208943,#208944,#208945,
#208946,#208947,#208948,#208949,#208950,#208951,#208952,#208953,#208954,
#208955,#208956,#208957,#208958,#208959,#208960,#208961,#208962,#208963,
#208964,#208965,#208966,#208967,#208968,#208969,#208970,#208971,#208972,
#208973,#208974,#208975,#208976,#208977,#208978,#208979,#208980,#208981,
#208982,#208983,#208984,#208985,#208986,#208987,#208988,#208989,#208990,
#208991,#208992,#208993,#208994,#208995,#208996,#208997,#208998),
 .UNSPECIFIED.,.F.,.F.,(4,3,3,3,3,3,3,3,3,3,3,3,3,3,3,3,3,3,3,3,3,3,3,3,
3,3,3,3,3,3,3,3,3,3,3,3,3,3,3,3,3,3,3,4),(0.,0.0823270774102905,0.125000000000094,
0.187500000000141,0.218750000000155,0.234375000000162,0.243570804458758,
0.25000000000017,0.250186396125238,0.295692350820031,0.346719906813076,
0.375000000000246,0.457188321893283,0.468750000000302,0.484375000000294,
0.492442181687317,0.500000000000287,0.50058849156398,0.537417390281148,
0.562500000000271,0.593750000000251,0.606558538060083,0.61892440865582,
0.625000000000231,0.625785934282743,0.656250000000211,0.680095796146748,
0.687004607525639,0.69277546770298,0.70312500000018,0.726562500000165,0.732421875000161,
0.75000000000015,0.750800803251414,0.792958838704499,0.81250000000011,0.843750000000093,
0.855813090863169,0.868300478426156,0.875000000000077,0.916195051773411,
0.958097525886705,0.997217794971731,1.),.UNSPECIFIED.);
#5704=B_SPLINE_CURVE_WITH_KNOTS('',3,(#209048,#209049,#209050,#209051,#209052,
#209053,#209054,#209055,#209056,#209057,#209058,#209059,#209060,#209061,
#209062,#209063,#209064,#209065,#209066,#209067,#209068,#209069,#209070,
#209071,#209072,#209073,#209074,#209075,#209076,#209077,#209078,#209079,
#209080,#209081,#209082,#209083,#209084,#209085,#209086,#209087,#209088,
#209089,#209090,#209091,#209092,#209093,#209094,#209095,#209096),
 .UNSPECIFIED.,.F.,.F.,(4,3,3,3,3,3,3,3,3,3,3,3,3,3,3,3,4),(0.,0.0467203140673268,
0.093322248216158,0.125000000000416,0.171247762433252,0.187500000000625,
0.218750000000742,0.234375000000792,0.242187500000816,0.246093750000817,
0.250000000000818,0.375000000000667,0.437500000000608,0.478869108686064,
0.50000000000055,0.75000000000027,0.999999999999991),.UNSPECIFIED.);
#5705=B_SPLINE_CURVE_WITH_KNOTS('',3,(#209097,#209098,#209099,#209100,#209101,
#209102,#209103,#209104,#209105,#209106),.UNSPECIFIED.,.F.,.F.,(4,3,3,4),
(6.93889390390723E-18,0.000636015601019443,0.00129844965740935,0.00158760011419448),
 .UNSPECIFIED.);
#5706=B_SPLINE_CURVE_WITH_KNOTS('',3,(#209122,#209123,#209124,#209125,#209126,
#209127,#209128,#209129,#209130,#209131),.UNSPECIFIED.,.F.,.F.,(4,3,3,4),
(0.,0.000679723972684053,0.00133201311757647,0.0015185374894695),
 .UNSPECIFIED.);
#5707=B_SPLINE_CURVE_WITH_KNOTS('',3,(#209132,#209133,#209134,#209135,#209136,
#209137,#209138,#209139,#209140,#209141,#209142,#209143,#209144,#209145,
#209146,#209147,#209148,#209149,#209150,#209151,#209152,#209153,#209154,
#209155,#209156,#209157,#209158,#209159,#209160,#209161,#209162,#209163,
#209164,#209165,#209166,#209167,#209168,#209169,#209170,#209171,#209172,
#209173,#209174,#209175,#209176,#209177,#209178,#209179,#209180,#209181,
#209182,#209183),.UNSPECIFIED.,.F.,.F.,(4,3,3,3,3,3,3,3,3,3,3,3,3,3,3,3,
3,4),(1.7719643363079E-14,0.249999999999962,0.374999999999965,0.437499999999957,
0.479463228974921,0.49999999999995,0.624999999999912,0.687499999999895,
0.718749999999885,0.734374999999887,0.746093749999895,0.749999999999911,
0.796573030417351,0.843551162119774,0.89092801606667,0.938447913903747,
0.986074086976133,1.),.UNSPECIFIED.);
#5708=B_SPLINE_CURVE_WITH_KNOTS('',3,(#209211,#209212,#209213,#209214,#209215,
#209216,#209217,#209218,#209219,#209220,#209221,#209222,#209223,#209224,
#209225,#209226,#209227,#209228,#209229,#209230,#209231,#209232,#209233,
#209234,#209235,#209236,#209237,#209238,#209239,#209240,#209241,#209242,
#209243,#209244,#209245,#209246,#209247,#209248,#209249,#209250,#209251,
#209252),.UNSPECIFIED.,.F.,.F.,(4,2,1,1,1,1,2,2,2,2,1,1,2,2,2,2,1,1,1,2,
2,2,2,2,1,4),(7.98944320809248E-8,0.125000000000703,0.187500000001066,0.218750000001238,
0.234375000001325,0.242187500001355,0.248046875001389,0.250000000001407,
0.375000000001313,0.437500000001265,0.468750000001242,0.48437500000123,
0.492187500001225,0.500000000001219,0.625000000001405,0.687500000001511,
0.718750000001579,0.734375000001613,0.742187500001628,0.746093750001613,
0.750000000001599,0.875000000000742,0.906250000000527,0.921875000000435,
0.937500000000343,1.),.UNSPECIFIED.);
#5709=B_SPLINE_CURVE_WITH_KNOTS('',3,(#209253,#209254,#209255,#209256,#209257,
#209258,#209259,#209260,#209261,#209262,#209263,#209264,#209265,#209266,
#209267,#209268,#209269,#209270,#209271,#209272,#209273,#209274,#209275,
#209276,#209277,#209278,#209279,#209280,#209281,#209282,#209283,#209284,
#209285,#209286,#209287,#209288,#209289,#209290,#209291,#209292,#209293,
#209294,#209295,#209296,#209297,#209298,#209299,#209300,#209301,#209302,
#209303,#209304,#209305,#209306,#209307,#209308,#209309,#209310,#209311,
#209312,#209313,#209314,#209315,#209316,#209317,#209318,#209319,#209320,
#209321,#209322,#209323,#209324,#209325,#209326,#209327,#209328,#209329,
#209330,#209331,#209332,#209333,#209334,#209335,#209336,#209337,#209338,
#209339,#209340,#209341,#209342,#209343,#209344,#209345,#209346,#209347,
#209348,#209349,#209350,#209351,#209352),.UNSPECIFIED.,.F.,.F.,(4,3,3,3,
3,3,3,3,3,3,3,3,3,3,3,3,3,3,3,3,3,3,3,3,3,3,3,3,3,3,3,3,3,4),(0.,0.0156249999999717,
0.0624999999998867,0.09374999999983,0.109374999999802,0.117187499999775,
0.123461617059797,0.124999999999748,0.140624999999709,0.181612062947922,
0.18749999999959,0.21874999999951,0.234374999999459,0.242187499999445,0.248785718386343,
0.249999999999431,0.259946689298152,0.26562499999941,0.322561688284792,
0.374999999999263,0.429126579721212,0.437499999999179,0.468749999999148,
0.484374999999132,0.492187499999136,0.49999999999914,0.510027340931445,
0.608514426712397,0.624999999999355,0.713539679447043,0.74999999999957,
0.857165949068296,0.962181280863057,1.),.UNSPECIFIED.);
#5710=B_SPLINE_CURVE_WITH_KNOTS('',3,(#209380,#209381,#209382,#209383,#209384,
#209385,#209386,#209387,#209388,#209389,#209390,#209391,#209392,#209393,
#209394,#209395,#209396,#209397,#209398,#209399,#209400,#209401,#209402,
#209403,#209404,#209405,#209406,#209407,#209408,#209409,#209410,#209411,
#209412,#209413,#209414,#209415,#209416,#209417,#209418,#209419,#209420,
#209421,#209422,#209423,#209424,#209425,#209426,#209427,#209428,#209429,
#209430,#209431,#209432,#209433,#209434,#209435,#209436,#209437,#209438,
#209439,#209440,#209441,#209442,#209443,#209444,#209445,#209446,#209447,
#209448,#209449,#209450,#209451,#209452,#209453,#209454,#209455,#209456,
#209457,#209458,#209459,#209460,#209461,#209462,#209463,#209464,#209465,
#209466,#209467,#209468,#209469,#209470,#209471,#209472,#209473),
 .UNSPECIFIED.,.F.,.F.,(4,3,3,3,3,3,3,3,3,3,3,3,3,3,3,3,3,3,3,3,3,3,3,3,
3,3,3,3,3,3,3,4),(0.,0.110965913270212,0.227650776136299,0.249999999999794,
0.376459127159745,0.484374999999595,0.489891538603025,0.499999999999583,
0.551168547591977,0.562499999999553,0.617114766859165,0.624999999999523,
0.681846022228115,0.687499999999481,0.718749999999474,0.734374999999471,
0.739546449428334,0.742187499999469,0.748939833770959,0.749999999999468,
0.791295688660075,0.81249999999959,0.843749999999639,0.859374999999662,
0.867187499999687,0.873635825536526,0.874999999999712,0.920254653271175,
0.937499999999856,0.968749999999928,0.984374999999964,1.),.UNSPECIFIED.);
#5711=B_SPLINE_CURVE_WITH_KNOTS('',3,(#209474,#209475,#209476,#209477,#209478,
#209479,#209480,#209481,#209482,#209483,#209484,#209485,#209486,#209487,
#209488,#209489,#209490,#209491,#209492,#209493,#209494,#209495,#209496,
#209497,#209498,#209499,#209500,#209501,#209502,#209503,#209504,#209505,
#209506,#209507,#209508),.UNSPECIFIED.,.F.,.F.,(4,2,2,1,1,1,2,2,2,2,1,2,
2,2,2,1,1,1,2,2,4),(0.,0.125000000000223,0.187500000000349,0.218750000000401,
0.234375000000438,0.242187500000456,0.246093750000454,0.250000000000453,
0.375000000000397,0.437500000000356,0.468750000000339,0.48437500000034,
0.500000000000341,0.625000000000326,0.687500000000331,0.718750000000338,
0.734375000000342,0.74218750000035,0.746093750000347,0.750000000000345,
0.999999939294813),.UNSPECIFIED.);
#5712=B_SPLINE_CURVE_WITH_KNOTS('',3,(#209566,#209567,#209568,#209569,#209570,
#209571,#209572,#209573,#209574,#209575,#209576,#209577,#209578,#209579,
#209580,#209581,#209582,#209583),.UNSPECIFIED.,.F.,.F.,(4,2,2,2,2,2,2,2,
4),(9.19004041809617E-16,0.00254332115550819,0.00381498173326183,0.00445081202213868,
0.00476872716657715,0.00492768473879635,0.00500716352490594,0.00504690291796077,
0.0050866423110156),.UNSPECIFIED.);
#5713=B_SPLINE_CURVE_WITH_KNOTS('',3,(#209584,#209585,#209586,#209587,#209588,
#209589,#209590,#209591,#209592,#209593,#209594,#209595,#209596,#209597,
#209598,#209599,#209600,#209601,#209602,#209603,#209604,#209605,#209606,
#209607,#209608,#209609,#209610,#209611,#209612,#209613,#209614,#209615,
#209616,#209617,#209618,#209619,#209620,#209621,#209622,#209623,#209624,
#209625,#209626,#209627,#209628,#209629,#209630,#209631,#209632,#209633,
#209634,#209635,#209636,#209637,#209638,#209639,#209640,#209641,#209642,
#209643,#209644,#209645,#209646,#209647,#209648,#209649,#209650,#209651,
#209652,#209653,#209654,#209655,#209656,#209657,#209658,#209659,#209660,
#209661,#209662,#209663,#209664,#209665,#209666,#209667,#209668,#209669,
#209670,#209671,#209672,#209673,#209674,#209675,#209676,#209677,#209678,
#209679,#209680),.UNSPECIFIED.,.F.,.F.,(4,3,3,3,3,3,3,3,3,3,3,3,3,3,3,3,
3,3,3,3,3,3,3,3,3,3,3,3,3,3,3,3,4),(0.,0.0138775285159946,0.0263638591569942,
0.0379447519617947,0.0486412646310953,0.0508344497447169,0.0653856475986571,
0.0787319799100734,0.0858260410294844,0.105561629787405,0.123439328425312,
0.138689316605115,0.165941329943547,0.19093791381173,0.214525800517685,
0.215934497679913,0.252600765134276,0.286679270362538,0.318148735572388,
0.326400669130735,0.374710481742207,0.419592700784505,0.460839040374595,
0.482156546551197,0.54530149924857,0.603918811955974,0.657495913758009,
0.699491765232357,0.780512945753581,0.855736405104934,0.927868202552467,
0.994072321442603,1.),.UNSPECIFIED.);
#5714=B_SPLINE_CURVE_WITH_KNOTS('',3,(#209738,#209739,#209740,#209741,#209742,
#209743,#209744,#209745,#209746,#209747,#209748,#209749,#209750,#209751,
#209752,#209753,#209754,#209755,#209756,#209757,#209758,#209759,#209760,
#209761,#209762,#209763,#209764,#209765,#209766,#209767,#209768,#209769,
#209770,#209771,#209772,#209773,#209774,#209775,#209776,#209777,#209778,
#209779,#209780,#209781,#209782,#209783,#209784,#209785,#209786,#209787,
#209788,#209789,#209790,#209791,#209792,#209793,#209794,#209795,#209796,
#209797,#209798,#209799,#209800,#209801,#209802,#209803,#209804,#209805,
#209806,#209807,#209808,#209809,#209810,#209811,#209812,#209813,#209814,
#209815,#209816,#209817,#209818,#209819,#209820,#209821,#209822,#209823,
#209824,#209825,#209826,#209827,#209828,#209829,#209830,#209831),
 .UNSPECIFIED.,.F.,.F.,(4,3,3,3,3,3,3,3,3,3,3,3,3,3,3,3,3,3,3,3,3,3,3,3,
3,3,3,3,3,3,3,4),(0.,0.0660388479518842,0.137757862277712,0.213874090227569,
0.300378565075664,0.354680588111974,0.411594223257197,0.47485576477693,
0.517586657220905,0.559251985910025,0.603199515032552,0.651841152392032,
0.673245241820224,0.705425371021804,0.739431720776586,0.776992864370152,
0.783656785143308,0.807195660453429,0.832000104243301,0.859138712389666,
0.86089437271487,0.878999038648541,0.898863662967972,0.91379488830539,0.926782431890997,
0.940841839198321,0.948858179523771,0.959313204820475,0.970816466407867,
0.983181220337405,0.997538681807663,1.),.UNSPECIFIED.);
#5715=B_SPLINE_CURVE_WITH_KNOTS('',3,(#209832,#209833,#209834,#209835,#209836,
#209837,#209838,#209839,#209840,#209841,#209842,#209843,#209844,#209845,
#209846,#209847,#209848,#209849,#209850,#209851,#209852,#209853,#209854,
#209855,#209856),.UNSPECIFIED.,.F.,.F.,(4,3,3,3,3,3,3,3,4),(0.,4.03932117393399E-5,
8.08651294214249E-5,0.000161907626915798,0.000324108918069935,0.000648595245071396,
0.00129766017874913,0.00259586603175174,0.00519236941687791),
 .UNSPECIFIED.);
#5716=B_SPLINE_CURVE_WITH_KNOTS('',3,(#209918,#209919,#209920,#209921,#209922,
#209923,#209924,#209925,#209926,#209927,#209928,#209929,#209930,#209931,
#209932,#209933,#209934,#209935,#209936,#209937,#209938,#209939,#209940,
#209941,#209942,#209943,#209944,#209945,#209946,#209947,#209948,#209949,
#209950,#209951,#209952,#209953,#209954,#209955,#209956,#209957,#209958,
#209959,#209960,#209961,#209962,#209963,#209964,#209965,#209966,#209967,
#209968,#209969,#209970,#209971,#209972,#209973,#209974,#209975,#209976,
#209977,#209978,#209979,#209980,#209981,#209982,#209983,#209984,#209985,
#209986,#209987,#209988,#209989,#209990,#209991,#209992,#209993,#209994,
#209995,#209996,#209997,#209998,#209999,#210000,#210001,#210002,#210003,
#210004,#210005,#210006,#210007,#210008,#210009,#210010,#210011,#210012,
#210013,#210014),.UNSPECIFIED.,.F.,.F.,(4,3,3,3,3,3,3,3,3,3,3,3,3,3,3,3,
3,3,3,3,3,3,3,3,3,3,3,3,3,3,3,3,4),(0.,0.0135707811258087,0.0257973618116296,
0.0371444834848967,0.0476053919484337,0.0512894550931262,0.0663694894719871,
0.0801408578431507,0.0863831089251375,0.106233188646732,0.124191482070428,
0.139294493982615,0.166374253731966,0.191446547086697,0.214889264756252,
0.216518840441428,0.253015854179144,0.286946529617756,0.318281048146731,
0.326893697308868,0.37512471145545,0.419927206528289,0.461095796836194,
0.482498445678343,0.545340922048112,0.603700223197135,0.657049883728935,
0.699650410399617,0.780317183144115,0.85523809456008,0.92761904728004,0.993565053861809,
1.),.UNSPECIFIED.);
#5717=B_SPLINE_CURVE_WITH_KNOTS('',3,(#210017,#210018,#210019,#210020,#210021,
#210022,#210023,#210024,#210025,#210026,#210027,#210028,#210029,#210030,
#210031,#210032,#210033,#210034),.UNSPECIFIED.,.F.,.F.,(4,2,2,2,2,2,2,2,
4),(0.,0.00262931855771754,0.00394397783657636,0.00460130747600577,0.00492997229572051,
0.00509430470557792,0.00517647091050667,0.00521755401297108,0.00525863711543548),
 .UNSPECIFIED.);
#5718=B_SPLINE_CURVE_WITH_KNOTS('',3,(#210068,#210069,#210070,#210071,#210072,
#210073,#210074,#210075,#210076,#210077,#210078,#210079,#210080,#210081,
#210082,#210083,#210084,#210085,#210086,#210087,#210088,#210089,#210090,
#210091,#210092,#210093,#210094,#210095,#210096,#210097,#210098,#210099,
#210100,#210101,#210102,#210103,#210104,#210105,#210106,#210107,#210108,
#210109,#210110,#210111,#210112,#210113,#210114,#210115,#210116,#210117,
#210118,#210119,#210120,#210121,#210122,#210123,#210124,#210125,#210126,
#210127,#210128,#210129,#210130,#210131,#210132,#210133,#210134,#210135,
#210136,#210137,#210138,#210139,#210140,#210141,#210142,#210143,#210144,
#210145,#210146,#210147,#210148,#210149,#210150,#210151,#210152,#210153,
#210154,#210155,#210156,#210157,#210158,#210159,#210160,#210161,#210162,
#210163,#210164,#210165,#210166,#210167),.UNSPECIFIED.,.F.,.F.,(4,3,3,3,
3,3,3,3,3,3,3,3,3,3,3,3,3,3,3,3,3,3,3,3,3,3,3,3,3,3,3,3,3,4),(0.,0.0156250000000012,
0.0625000000000047,0.0937500000000208,0.109375000000029,0.117187500000046,
0.123521240792477,0.125000000000063,0.140625000000092,0.182242701318326,
0.187500000000178,0.218750000000236,0.234375000000265,0.242187500000279,
0.248811697549323,0.250000000000293,0.259894607749493,0.265625000000329,
0.322815512042762,0.375000000000577,0.429301576080171,0.437500000000718,
0.468750000000776,0.484375000000792,0.492187500000788,0.500000000000784,
0.510043502713035,0.612883296558313,0.625000000000588,0.717261013975742,
0.750000000000392,0.857991169889234,0.963554025874452,1.),.UNSPECIFIED.);
#5719=B_SPLINE_CURVE_WITH_KNOTS('',3,(#210168,#210169,#210170,#210171,#210172,
#210173,#210174,#210175,#210176,#210177,#210178,#210179,#210180,#210181,
#210182,#210183,#210184,#210185,#210186,#210187,#210188,#210189,#210190,
#210191,#210192,#210193,#210194,#210195,#210196,#210197,#210198,#210199,
#210200,#210201,#210202),.UNSPECIFIED.,.F.,.F.,(4,2,1,1,1,1,2,2,2,2,1,1,
2,2,2,2,1,1,1,2,2,4),(1.1089353930245E-7,0.125000000000895,0.187500000001354,
0.218750000001597,0.23437500000172,0.242187500001771,0.248046875001825,
0.250000000001843,0.375000000001895,0.437500000001909,0.468750000001917,
0.484375000001913,0.492187500001903,0.500000000001893,0.62500000000167,
0.687500000001546,0.718750000001486,0.734375000001438,0.742187500001393,
0.74609375000137,0.750000000001347,1.),.UNSPECIFIED.);
#5720=B_SPLINE_CURVE_WITH_KNOTS('',3,(#210260,#210261,#210262,#210263,#210264,
#210265,#210266,#210267,#210268,#210269,#210270,#210271,#210272,#210273,
#210274,#210275,#210276,#210277,#210278,#210279,#210280,#210281,#210282,
#210283,#210284),.UNSPECIFIED.,.F.,.F.,(4,3,3,3,3,3,3,3,4),(4.9065389333868E-17,
4.15775196007892E-5,8.32361282030658E-5,0.000166653476908059,0.000333604410320719,
0.000667590055213201,0.00133565310169655,0.00267185549873086,0.0053443518360984),
 .UNSPECIFIED.);
#5721=B_SPLINE_CURVE_WITH_KNOTS('',3,(#210285,#210286,#210287,#210288,#210289,
#210290,#210291,#210292,#210293,#210294,#210295,#210296,#210297,#210298,
#210299,#210300,#210301,#210302,#210303,#210304,#210305,#210306,#210307,
#210308,#210309,#210310,#210311,#210312,#210313,#210314,#210315,#210316,
#210317,#210318,#210319,#210320,#210321,#210322,#210323,#210324,#210325,
#210326,#210327,#210328,#210329,#210330,#210331,#210332,#210333,#210334,
#210335,#210336,#210337,#210338,#210339,#210340,#210341,#210342,#210343,
#210344,#210345,#210346,#210347,#210348,#210349,#210350,#210351,#210352,
#210353,#210354,#210355,#210356,#210357,#210358,#210359,#210360,#210361,
#210362,#210363,#210364,#210365,#210366,#210367,#210368,#210369,#210370,
#210371,#210372,#210373,#210374,#210375,#210376,#210377,#210378),
 .UNSPECIFIED.,.F.,.F.,(4,3,3,3,3,3,3,3,3,3,3,3,3,3,3,3,3,3,3,3,3,3,3,3,
3,3,3,3,3,3,3,4),(0.,0.065834090762222,0.137306570430488,0.213134649886981,
0.300236631091948,0.354496304796746,0.411178610110194,0.474156885636163,
0.517275325911139,0.558829344637946,0.602654437698862,0.65115886647553,
0.672792203999343,0.70485168831114,0.73872438206961,0.776133779531016,0.783116707833807,
0.806639447972133,0.831430832553541,0.858566765699478,0.860332482558115,
0.8783845180258,0.898197506292583,0.913275454353936,0.926158161133152,0.940105356609658,
0.948432049893693,0.958705571236069,0.970008019291287,0.982144963325018,
0.996260037816924,1.),.UNSPECIFIED.);
#5722=B_SPLINE_CURVE_WITH_KNOTS('',3,(#210394,#210395,#210396,#210397,#210398,
#210399,#210400),.UNSPECIFIED.,.F.,.F.,(4,3,4),(0.,0.000722422580495111,
0.00123518557486524),.UNSPECIFIED.);
#5723=B_SPLINE_CURVE_WITH_KNOTS('',3,(#210401,#210402,#210403,#210404,#210405,
#210406,#210407,#210408,#210409,#210410,#210411,#210412,#210413,#210414,
#210415,#210416,#210417,#210418,#210419,#210420,#210421,#210422,#210423,
#210424,#210425,#210426,#210427,#210428,#210429,#210430,#210431,#210432,
#210433,#210434,#210435,#210436,#210437,#210438,#210439,#210440,#210441,
#210442,#210443,#210444,#210445,#210446),.UNSPECIFIED.,.F.,.F.,(4,3,3,3,
3,3,3,3,3,3,3,3,3,3,3,4),(0.,0.052742842989654,0.105378129680294,0.125000000000152,
0.177350919706812,0.187500000000203,0.218750000000212,0.234375000000214,
0.242187500000217,0.246093750000209,0.2500000000002,0.375000000000174,0.445646917646005,
0.500000000000147,0.806305246709664,1.),.UNSPECIFIED.);
#5724=B_SPLINE_CURVE_WITH_KNOTS('',3,(#210474,#210475,#210476,#210477,#210478,
#210479,#210480,#210481,#210482,#210483,#210484,#210485,#210486,#210487,
#210488,#210489,#210490,#210491,#210492,#210493,#210494,#210495,#210496,
#210497,#210498,#210499,#210500,#210501,#210502,#210503,#210504,#210505,
#210506,#210507,#210508),.UNSPECIFIED.,.F.,.F.,(4,2,2,1,1,1,2,2,2,2,1,2,
2,2,2,1,1,1,2,2,4),(0.,0.124999999999531,0.18749999999931,0.218749999999199,
0.234374999999143,0.242187499999117,0.246093749999103,0.24999999999909,
0.374999999999434,0.437499999999608,0.468749999999694,0.484374999999727,
0.49999999999976,0.624999999999942,0.687500000000033,0.718750000000096,
0.734375000000149,0.742187500000195,0.746093750000197,0.7500000000002,0.999999975394086),
 .UNSPECIFIED.);
#5725=B_SPLINE_CURVE_WITH_KNOTS('',3,(#210510,#210511,#210512,#210513,#210514,
#210515,#210516,#210517,#210518,#210519,#210520,#210521,#210522,#210523,
#210524,#210525,#210526,#210527,#210528),.UNSPECIFIED.,.F.,.F.,(4,2,2,2,
1,2,2,2,2,4),(6.19941202265524E-9,0.249999999999908,0.374999999999861,0.406249999999859,
0.437499999999856,0.499999999999882,0.624999999999895,0.687499999999901,
0.749999999999908,1.),.UNSPECIFIED.);
#5726=B_SPLINE_CURVE_WITH_KNOTS('',3,(#210529,#210530,#210531,#210532,#210533,
#210534,#210535,#210536,#210537,#210538,#210539,#210540,#210541),
 .UNSPECIFIED.,.F.,.F.,(4,3,3,3,4),(0.,0.350293314944234,0.5,0.75,1.),
 .UNSPECIFIED.);
#5727=B_SPLINE_CURVE_WITH_KNOTS('',3,(#210574,#210575,#210576,#210577,#210578,
#210579,#210580,#210581,#210582,#210583,#210584,#210585,#210586,#210587,
#210588,#210589,#210590,#210591,#210592,#210593,#210594,#210595,#210596,
#210597,#210598,#210599,#210600,#210601,#210602,#210603,#210604,#210605,
#210606,#210607,#210608,#210609,#210610,#210611,#210612,#210613,#210614,
#210615,#210616,#210617,#210618,#210619),.UNSPECIFIED.,.F.,.F.,(4,3,3,3,
3,3,3,3,3,3,3,3,3,3,3,4),(0.,0.249999999999783,0.374999999999653,0.445711246785852,
0.499999999999523,0.624999999999394,0.687499999999349,0.718749999999327,
0.734374999999336,0.746093749999319,0.749999999999331,0.802225425262499,
0.854956889811044,0.907864634104767,0.960922572191772,1.),.UNSPECIFIED.);
#5728=B_SPLINE_CURVE_WITH_KNOTS('',3,(#210620,#210621,#210622,#210623,#210624,
#210625,#210626),.UNSPECIFIED.,.F.,.F.,(4,3,4),(0.,0.000727844608904283,
0.00121469382512387),.UNSPECIFIED.);
#5729=B_SPLINE_CURVE_WITH_KNOTS('',3,(#210669,#210670,#210671,#210672,#210673,
#210674,#210675,#210676,#210677,#210678,#210679,#210680,#210681,#210682,
#210683,#210684,#210685,#210686,#210687,#210688,#210689,#210690,#210691,
#210692,#210693,#210694,#210695),.UNSPECIFIED.,.F.,.F.,(4,2,1,2,2,2,1,1,
2,2,2,1,1,2,2,4),(0.,0.124999999999888,0.187499999999837,0.218749999999819,
0.249999999999801,0.374999999999777,0.437499999999764,0.468749999999755,
0.48437499999975,0.499999999999746,0.6249999999998,0.687499999999827,0.718749999999827,
0.734374999999829,0.749999999999832,1.),.UNSPECIFIED.);
#5730=B_SPLINE_CURVE_WITH_KNOTS('',3,(#210696,#210697,#210698,#210699,#210700,
#210701,#210702,#210703,#210704,#210705,#210706,#210707,#210708,#210709,
#210710,#210711,#210712,#210713,#210714,#210715,#210716,#210717,#210718,
#210719),.UNSPECIFIED.,.F.,.F.,(4,2,2,1,1,1,1,2,2,2,2,2,2,4),(0.,0.250000000000058,
0.375000000000071,0.437500000000069,0.468750000000072,0.484375000000074,
0.492187500000075,0.49609375000008,0.500000000000086,0.62500000000011,0.687500000000122,
0.718750000000128,0.750000000000135,1.),.UNSPECIFIED.);
#5731=B_SPLINE_CURVE_WITH_KNOTS('',3,(#210773,#210774,#210775,#210776,#210777,
#210778,#210779,#210780,#210781,#210782,#210783,#210784,#210785,#210786,
#210787,#210788,#210789,#210790,#210791,#210792,#210793,#210794,#210795),
 .UNSPECIFIED.,.F.,.F.,(4,2,2,2,2,2,2,1,1,1,2,2,4),(0.,0.125000000000141,
0.187500000000215,0.218750000000266,0.250000000000316,0.375000000000535,
0.43750000000064,0.468750000000692,0.484375000000707,0.492187500000705,
0.496093750000704,0.500000000000703,1.),.UNSPECIFIED.);
#5732=B_SPLINE_CURVE_WITH_KNOTS('',3,(#210796,#210797,#210798,#210799,#210800,
#210801,#210802,#210803,#210804,#210805,#210806,#210807,#210808,#210809,
#210810,#210811,#210812,#210813,#210814,#210815,#210816,#210817,#210818,
#210819,#210820,#210821,#210822,#210823,#210824,#210825,#210826,#210827,
#210828),.UNSPECIFIED.,.F.,.F.,(4,2,1,1,2,2,2,1,1,2,2,2,2,2,2,1,2,2,4),
(0.,0.125000000000212,0.187500000000329,0.218750000000376,0.234375000000397,
0.250000000000419,0.375000000000466,0.437500000000487,0.468750000000496,
0.484375000000501,0.500000000000505,0.562500000000444,0.625000000000383,
0.687500000000321,0.75000000000026,0.812500000000199,0.84375000000017,0.87500000000014,
1.),.UNSPECIFIED.);
#5733=B_SPLINE_CURVE_WITH_KNOTS('',3,(#212647,#212648,#212649,#212650,#212651,
#212652,#212653,#212654,#212655,#212656),.UNSPECIFIED.,.F.,.F.,(4,2,2,2,
4),(0.229465105224976,0.24878272102183,0.282449783617402,0.324570636098563,
0.324953676133515),.UNSPECIFIED.);
#5734=B_SPLINE_CURVE_WITH_KNOTS('',3,(#212691,#212692,#212693,#212694,#212695,
#212696,#212697,#212698,#212699,#212700),.UNSPECIFIED.,.F.,.F.,(4,2,2,2,
4),(-0.000383040042044683,0.,0.0421208528204372,0.0757879156854754,0.0951055316369486),
 .UNSPECIFIED.);
#5735=B_SPLINE_CURVE_WITH_KNOTS('',3,(#212710,#212711,#212712,#212713,#212714,
#212715,#212716,#212717,#212718,#212719),.UNSPECIFIED.,.F.,.F.,(4,2,2,2,
4),(0.229465097061585,0.248782712171685,0.282449773570366,0.324570624548349,
0.324953664553108),.UNSPECIFIED.);
#5736=B_SPLINE_CURVE_WITH_KNOTS('',3,(#212754,#212755,#212756,#212757,#212758,
#212759,#212760,#212761,#212762,#212763),.UNSPECIFIED.,.F.,.F.,(4,2,2,2,
4),(-0.000383040050378712,1.21072856601456E-15,0.0421208532697368,0.0757879164922472,
0.0951055326488294),.UNSPECIFIED.);
#5737=B_SPLINE_CURVE_WITH_KNOTS('',3,(#212773,#212774,#212775,#212776,#212777,
#212778,#212779,#212780,#212781,#212782),.UNSPECIFIED.,.F.,.F.,(4,2,2,2,
4),(0.229465099488756,0.248782714803057,0.282449776557603,0.324570627982376,
0.324953667995646),.UNSPECIFIED.);
#5738=B_SPLINE_CURVE_WITH_KNOTS('',3,(#212817,#212818,#212819,#212820,#212821,
#212822,#212823,#212824,#212825,#212826),.UNSPECIFIED.,.F.,.F.,(4,2,2,2,
4),(-0.000383039996431936,0.,0.0421208505751745,0.0757879116535588,0.095105526579897),
 .UNSPECIFIED.);
#5739=B_SPLINE_CURVE_WITH_KNOTS('',3,(#212832,#212833,#212834,#212835,#212836,
#212837,#212838,#212839,#212840,#212841),.UNSPECIFIED.,.F.,.F.,(4,2,2,2,
4),(0.229465073530738,0.248782686661591,0.282449744610596,0.324570591252679,
0.324953631169658),.UNSPECIFIED.);
#5740=B_SPLINE_CURVE_WITH_KNOTS('',3,(#212880,#212881,#212882,#212883,#212884,
#212885,#212886,#212887,#212888,#212889),.UNSPECIFIED.,.F.,.F.,(4,2,2,2,
4),(-0.000383039917846548,0.,0.042120846689148,0.075787904675495,0.0951055178277825),
 .UNSPECIFIED.);
#5741=B_SPLINE_CURVE_WITH_KNOTS('',3,(#213089,#213090,#213091,#213092,#213093,
#213094,#213095,#213096,#213097,#213098,#213099,#213100,#213101,#213102,
#213103,#213104,#213105,#213106,#213107,#213108,#213109,#213110,#213111,
#213112,#213113,#213114,#213115,#213116,#213117,#213118,#213119,#213120,
#213121,#213122,#213123,#213124,#213125,#213126,#213127,#213128,#213129,
#213130,#213131,#213132,#213133,#213134,#213135,#213136,#213137,#213138,
#213139,#213140),.UNSPECIFIED.,.F.,.F.,(4,3,3,3,3,3,3,3,3,3,3,3,3,3,3,3,
3,4),(0.,0.00570218474091234,0.0124164787169346,0.0258456091874862,0.052708361918506,
0.106470460366992,0.214291739632625,0.317553434342842,0.421799620076628,
0.5,0.590995103774971,0.656293369359574,0.748411394066377,0.839734838233114,
0.885082497885734,0.97491039354239,0.999679933047398,1.),.UNSPECIFIED.);
#5742=B_SPLINE_CURVE_WITH_KNOTS('',3,(#213142,#213143,#213144,#213145,#213146,
#213147,#213148,#213149,#213150,#213151,#213152,#213153,#213154,#213155,
#213156,#213157,#213158,#213159,#213160,#213161,#213162,#213163,#213164,
#213165,#213166,#213167,#213168,#213169,#213170,#213171,#213172,#213173,
#213174,#213175),.UNSPECIFIED.,.F.,.F.,(4,3,3,3,3,3,3,3,3,3,3,4),(0.,0.137478057277644,
0.273420104059381,0.407374454225706,0.5,0.620341176999436,0.739318733841433,
0.80587229841711,0.896219091184997,0.9990234375,0.999068147311954,1.),
 .UNSPECIFIED.);
#5743=B_SPLINE_CURVE_WITH_KNOTS('',3,(#213178,#213179,#213180,#213181,#213182,
#213183,#213184,#213185,#213186,#213187,#213188,#213189,#213190,#213191,
#213192,#213193,#213194,#213195,#213196,#213197,#213198,#213199,#213200,
#213201,#213202,#213203,#213204,#213205,#213206,#213207,#213208,#213209,
#213210,#213211,#213212,#213213,#213214,#213215,#213216,#213217,#213218,
#213219,#213220,#213221,#213222,#213223,#213224,#213225,#213226,#213227,
#213228,#213229,#213230,#213231,#213232,#213233,#213234,#213235,#213236,
#213237,#213238,#213239,#213240,#213241,#213242,#213243,#213244,#213245,
#213246,#213247,#213248,#213249,#213250,#213251,#213252,#213253,#213254,
#213255,#213256,#213257,#213258,#213259,#213260,#213261,#213262,#213263,
#213264,#213265,#213266,#213267,#213268,#213269,#213270,#213271,#213272,
#213273,#213274,#213275,#213276,#213277,#213278,#213279,#213280,#213281,
#213282,#213283,#213284,#213285,#213286,#213287,#213288,#213289),
 .UNSPECIFIED.,.F.,.F.,(4,3,3,3,3,3,3,3,3,3,3,3,3,3,3,3,3,3,3,3,3,3,3,3,
3,3,3,3,3,3,3,3,3,3,3,3,3,4),(0.,0.00106872167482631,0.00213668912630082,
0.00293590036761761,0.0029378487127682,0.00330316624931786,0.00348679918954151,
0.00367043213068583,0.00367231089096026,0.0044049638926048,0.0044067730691523,
0.00587402741638414,0.0058756974255364,0.0088121544640339,0.00881354613830458,
0.00917942034489251,0.00936305328548731,0.00945486975574288,0.00950077799084981,
0.00954668622593886,0.00954800831649663,0.0102812179878345,0.0102824704946887,
0.0117502815116473,0.0117513948510728,0.0146884085592774,0.0146892435638409,
0.0154229402821364,0.0157902061581132,0.0159738391126328,0.0160656555956372,
0.0161115638387771,0.0161574720830854,0.016158167920225,0.0176265356068806,
0.0176270922766091,0.0205649409893773,0.0235027897021455),.UNSPECIFIED.);
#5744=B_SPLINE_CURVE_WITH_KNOTS('',3,(#213290,#213291,#213292,#213293,#213294,
#213295,#213296,#213297,#213298,#213299,#213300,#213301,#213302,#213303,
#213304,#213305,#213306,#213307,#213308,#213309,#213310,#213311,#213312,
#213313,#213314,#213315,#213316,#213317,#213318,#213319,#213320,#213321,
#213322,#213323,#213324,#213325,#213326,#213327,#213328,#213329,#213330,
#213331,#213332,#213333,#213334,#213335,#213336,#213337,#213338,#213339,
#213340,#213341,#213342,#213343,#213344,#213345,#213346,#213347,#213348,
#213349,#213350,#213351,#213352,#213353,#213354,#213355,#213356,#213357,
#213358,#213359,#213360,#213361,#213362,#213363,#213364,#213365,#213366,
#213367,#213368,#213369,#213370,#213371,#213372,#213373,#213374,#213375,
#213376,#213377,#213378,#213379,#213380,#213381,#213382,#213383,#213384,
#213385,#213386,#213387,#213388,#213389,#213390,#213391,#213392,#213393,
#213394,#213395),.UNSPECIFIED.,.F.,.F.,(4,3,3,3,3,3,3,3,3,3,3,3,3,3,3,3,
3,3,3,3,3,3,3,3,3,3,3,3,3,3,3,3,3,3,3,4),(7.33112690889359E-11,0.00447014585407084,
0.00914986570716556,0.0185087890749796,0.0372224668762703,0.0746163803537859,
0.148246793986367,0.203469604210804,0.244886711879131,0.255815311626838,
0.330322389164154,0.369138034884112,0.375000000000005,0.437500000000005,
0.468750000000006,0.484375000000006,0.492187500000006,0.499138724547647,
0.500000000000006,0.516108728237381,0.555120919008716,0.593622058561214,
0.612985630693563,0.623334726960567,0.625000000000005,0.631597432104248,
0.632529868687029,0.65830781467943,0.674061695699477,0.70060922959337,0.727034623063786,
0.750000000000003,0.819699069590602,0.888646808802703,0.956324027361056,
1.),.UNSPECIFIED.);
#5745=B_SPLINE_CURVE_WITH_KNOTS('',3,(#213411,#213412,#213413,#213414),
 .UNSPECIFIED.,.F.,.F.,(4,4),(0.,0.000322395538615397),.UNSPECIFIED.);
#5746=B_SPLINE_CURVE_WITH_KNOTS('',3,(#213514,#213515,#213516,#213517,#213518,
#213519,#213520,#213521,#213522,#213523,#213524,#213525,#213526,#213527,
#213528,#213529,#213530,#213531,#213532,#213533,#213534,#213535,#213536,
#213537,#213538,#213539,#213540,#213541,#213542,#213543,#213544,#213545,
#213546,#213547,#213548,#213549,#213550),.UNSPECIFIED.,.F.,.F.,(4,3,3,3,
3,3,3,3,3,3,3,3,4),(0.,0.000191440270420746,0.000287160692730018,0.000382881236840893,
0.000574322481675385,0.000670043078002303,0.00076576358733981,0.000957204470373583,
0.00114864534416313,0.00124436578623717,0.00129222601008214,0.00134008623637552,
0.00153152717467962),.UNSPECIFIED.);
#5747=B_SPLINE_CURVE_WITH_KNOTS('',3,(#213551,#213552,#213553,#213554,#213555,
#213556,#213557,#213558,#213559,#213560,#213561,#213562,#213563,#213564,
#213565,#213566,#213567,#213568,#213569,#213570,#213571,#213572,#213573,
#213574,#213575,#213576,#213577,#213578,#213579,#213580,#213581,#213582,
#213583,#213584,#213585,#213586,#213587,#213588,#213589,#213590,#213591,
#213592,#213593,#213594,#213595,#213596,#213597,#213598,#213599,#213600,
#213601,#213602,#213603,#213604,#213605,#213606,#213607,#213608,#213609,
#213610,#213611,#213612,#213613,#213614,#213615,#213616,#213617,#213618,
#213619,#213620,#213621,#213622,#213623,#213624,#213625),.UNSPECIFIED.,
 .F.,.F.,(4,2,2,2,1,2,2,2,2,2,1,1,1,2,2,2,2,2,2,1,2,2,2,1,1,2,2,2,2,1,1,
2,2,2,2,1,1,2,2,2,2,2,4),(0.,0.0624999999999565,0.0937499999999354,0.109374999999925,
0.117187499999921,0.121093749999922,0.124999999999922,0.156250000000006,
0.171875000000048,0.18750000000009,0.218750000000164,0.2343750000002,0.242187500000218,
0.246093750000224,0.25000000000023,0.281250000000224,0.312500000000217,
0.34375000000021,0.35937500000021,0.367187500000206,0.371093750000201,0.375000000000196,
0.437500000000105,0.468750000000063,0.484375000000042,0.492187500000031,
0.50000000000002,0.562499999999868,0.593749999999794,0.609374999999759,
0.617187499999741,0.621093749999737,0.624999999999734,0.687499999999692,
0.718749999999674,0.734374999999663,0.742187499999661,0.746093749999661,
0.74999999999966,0.812499999999755,0.843749999999799,0.874999999999842,
1.),.UNSPECIFIED.);
#5748=B_SPLINE_CURVE_WITH_KNOTS('',3,(#213665,#213666,#213667,#213668,#213669,
#213670,#213671,#213672,#213673,#213674,#213675,#213676,#213677,#213678,
#213679,#213680,#213681,#213682,#213683),.UNSPECIFIED.,.F.,.F.,(4,3,3,3,
3,3,4),(0.,0.00503761689941682,0.00646885457540687,0.0129377091508137,0.0161721364385172,
0.0194065637262206,0.0258754183016275),.UNSPECIFIED.);
#5749=B_SPLINE_CURVE_WITH_KNOTS('',3,(#213684,#213685,#213686,#213687,#213688,
#213689,#213690,#213691,#213692,#213693,#213694,#213695,#213696,#213697,
#213698,#213699,#213700,#213701,#213702,#213703,#213704,#213705,#213706,
#213707,#213708,#213709,#213710,#213711,#213712,#213713,#213714,#213715,
#213716,#213717,#213718,#213719,#213720,#213721,#213722,#213723,#213724,
#213725,#213726,#213727,#213728,#213729,#213730,#213731,#213732,#213733,
#213734,#213735,#213736,#213737,#213738,#213739,#213740,#213741,#213742,
#213743,#213744,#213745,#213746,#213747,#213748,#213749,#213750,#213751,
#213752,#213753,#213754,#213755,#213756,#213757,#213758,#213759,#213760,
#213761,#213762,#213763,#213764,#213765,#213766,#213767,#213768,#213769,
#213770,#213771,#213772,#213773,#213774,#213775,#213776,#213777,#213778,
#213779,#213780,#213781,#213782,#213783,#213784,#213785,#213786,#213787,
#213788,#213789,#213790,#213791,#213792),.UNSPECIFIED.,.F.,.F.,(4,3,3,3,
3,3,3,3,3,3,3,3,3,3,3,3,3,3,3,3,3,3,3,3,3,3,3,3,3,3,3,3,3,3,3,3,4),(0.,
0.0624999999999447,0.124999999999889,0.187011718749834,0.218110068264968,
0.241135819705506,0.249023437499779,0.249999999999779,0.251447098061137,
0.292027665321456,0.333513832660559,0.372044971928076,0.374999999999662,
0.38487225586242,0.437499999999604,0.468749999999575,0.48437499999956,0.492187499999552,
0.496093749999549,0.498046874999547,0.499023437499547,0.499511718749547,
0.499999999999547,0.501761858639276,0.563380929319468,0.62499999999966,
0.675786892642834,0.723600741712145,0.749999999999773,0.778068207596557,
0.822278116509677,0.86523298278097,0.874999999999887,0.912812998100895,
0.950228509081889,0.987192663426709,1.),.UNSPECIFIED.);
#5750=B_SPLINE_CURVE_WITH_KNOTS('',3,(#213898,#213899,#213900,#213901,#213902,
#213903,#213904,#213905,#213906,#213907,#213908,#213909,#213910,#213911,
#213912,#213913,#213914,#213915,#213916,#213917,#213918,#213919,#213920,
#213921,#213922,#213923,#213924,#213925,#213926,#213927,#213928,#213929,
#213930,#213931,#213932,#213933,#213934,#213935,#213936,#213937,#213938,
#213939,#213940,#213941,#213942,#213943,#213944,#213945,#213946),
 .UNSPECIFIED.,.F.,.F.,(4,3,3,3,3,3,3,3,3,3,3,3,3,3,3,3,4),(0.,0.000127303360486361,
0.000254607331807631,0.000318259502487228,0.000381911773022019,0.000509216543183179,
0.000636521501341121,0.000763826506543775,0.000891131417838548,0.00101843609427484,
0.00114573874978534,0.00127303875321421,0.00140033769575051,0.00152763716845166,
0.00165493876244132,0.00178224406910835,0.00203687218854967),
 .UNSPECIFIED.);
#5751=B_SPLINE_CURVE_WITH_KNOTS('',3,(#213947,#213948,#213949,#213950,#213951,
#213952,#213953,#213954,#213955,#213956,#213957,#213958,#213959,#213960,
#213961,#213962,#213963,#213964,#213965,#213966,#213967,#213968,#213969,
#213970,#213971,#213972,#213973,#213974,#213975,#213976,#213977,#213978,
#213979,#213980,#213981,#213982,#213983,#213984,#213985,#213986,#213987,
#213988,#213989,#213990,#213991,#213992,#213993,#213994,#213995,#213996,
#213997,#213998,#213999,#214000,#214001,#214002,#214003,#214004,#214005,
#214006,#214007,#214008,#214009,#214010,#214011,#214012,#214013,#214014,
#214015,#214016,#214017,#214018,#214019,#214020,#214021,#214022,#214023,
#214024,#214025,#214026,#214027,#214028,#214029,#214030,#214031,#214032,
#214033,#214034,#214035,#214036,#214037,#214038,#214039),.UNSPECIFIED.,
 .F.,.F.,(4,2,2,2,1,1,2,2,2,2,2,2,2,2,2,2,2,2,1,1,1,2,2,1,2,2,2,1,2,2,2,
2,1,2,2,2,2,1,1,2,2,2,2,1,1,2,2,2,2,1,2,2,4),(0.,0.0624999999999063,0.0937499999998621,
0.109374999999839,0.117187499999827,0.121093749999825,0.123046874999823,
0.124999999999822,0.187499999999776,0.218749999999753,0.24999999999973,
0.31249999999968,0.320312499999672,0.328124999999663,0.343749999999657,
0.374999999999638,0.390624999999631,0.394531249999628,0.398437499999625,
0.406249999999626,0.437499999999632,0.468749999999639,0.484374999999646,
0.492187499999651,0.496093749999649,0.499999999999647,0.531249999999644,
0.546874999999642,0.554687499999642,0.562499999999642,0.593749999999643,
0.609374999999644,0.617187499999646,0.621093749999647,0.624999999999648,
0.687499999999675,0.718749999999691,0.734374999999699,0.742187499999701,
0.748046874999702,0.749999999999703,0.781249999999769,0.796874999999803,
0.804687499999818,0.808593749999826,0.810546874999831,0.812499999999835,
0.843749999999876,0.859374999999898,0.867187499999907,0.871093749999913,
0.874999999999919,1.),.UNSPECIFIED.);
#5752=B_SPLINE_CURVE_WITH_KNOTS('',3,(#214072,#214073,#214074,#214075),
 .UNSPECIFIED.,.F.,.F.,(4,4),(6.93889390390723E-18,0.000463834979289304),
 .UNSPECIFIED.);
#5753=B_SPLINE_CURVE_WITH_KNOTS('',3,(#214076,#214077,#214078,#214079,#214080,
#214081,#214082,#214083,#214084,#214085,#214086,#214087,#214088),
 .UNSPECIFIED.,.F.,.F.,(4,3,3,3,4),(3.53293614125829E-14,0.25717577121601,
0.517057560954111,0.782215252408013,1.),.UNSPECIFIED.);
#5754=B_SPLINE_CURVE_WITH_KNOTS('',3,(#214404,#214405,#214406,#214407,#214408,
#214409,#214410,#214411,#214412,#214413,#214414,#214415,#214416,#214417,
#214418,#214419,#214420,#214421,#214422,#214423,#214424,#214425,#214426,
#214427,#214428,#214429,#214430,#214431,#214432,#214433,#214434,#214435,
#214436,#214437,#214438,#214439,#214440,#214441,#214442,#214443,#214444,
#214445,#214446,#214447,#214448,#214449,#214450,#214451,#214452,#214453,
#214454,#214455,#214456,#214457,#214458,#214459,#214460,#214461,#214462,
#214463,#214464,#214465,#214466,#214467,#214468,#214469,#214470,#214471,
#214472,#214473,#214474,#214475,#214476,#214477,#214478,#214479,#214480,
#214481,#214482,#214483,#214484,#214485,#214486,#214487,#214488,#214489,
#214490,#214491,#214492,#214493,#214494,#214495,#214496,#214497,#214498,
#214499,#214500,#214501,#214502,#214503,#214504,#214505,#214506,#214507,
#214508,#214509,#214510,#214511,#214512,#214513,#214514,#214515,#214516,
#214517,#214518,#214519,#214520,#214521,#214522,#214523,#214524,#214525,
#214526,#214527,#214528,#214529,#214530,#214531,#214532,#214533,#214534,
#214535,#214536,#214537,#214538,#214539,#214540,#214541,#214542,#214543,
#214544,#214545,#214546,#214547,#214548,#214549,#214550,#214551,#214552,
#214553,#214554,#214555,#214556,#214557),.UNSPECIFIED.,.F.,.F.,(4,3,3,3,
3,3,3,3,3,3,3,3,3,3,3,3,3,3,3,3,3,3,3,3,3,3,3,3,3,3,3,3,3,3,3,3,3,3,3,3,
3,3,3,3,3,3,3,3,3,3,3,4),(1.04083408558608E-17,0.00250327328955152,0.00500654657910303,
0.00625818322387879,0.00688400154626667,0.00696222883656844,0.00704045612686793,
0.00719691070746254,0.00750981986865454,0.010013093158206,0.0112647298029818,
0.011577638964179,0.0117340935447715,0.0117732071899202,0.0118123208350694,
0.0118905481253697,0.0125163664477576,0.0137680030925333,0.015019639737309,
0.0175229130268605,0.0175620266720094,0.0176011403171581,0.0176793676074551,
0.0178358221880486,0.0181487313492361,0.0187745496716364,0.0200261863164121,
0.0225294596059636,0.0226076868962739,0.022646800541427,0.0226859141865788,
0.0228423687671764,0.0231552779283514,0.0237810962507394,0.0250327328955151,
0.0275360061850667,0.0281618245074545,0.0283182790880578,0.028396506378356,
0.0284356200235045,0.0284747336686529,0.0287876428298423,0.0300392794746181,
0.0325425527641696,0.0331683710865575,0.0332465983768559,0.0333248256671528,
0.033481280247746,0.0337941894089454,0.0350458260537211,0.0375490993432726,
0.0400523726328241),.UNSPECIFIED.);
#5755=B_SPLINE_CURVE_WITH_KNOTS('',3,(#214559,#214560,#214561,#214562,#214563,
#214564,#214565,#214566,#214567,#214568,#214569,#214570,#214571,#214572,
#214573,#214574,#214575,#214576,#214577,#214578,#214579,#214580,#214581,
#214582,#214583,#214584,#214585,#214586,#214587,#214588,#214589,#214590,
#214591,#214592),.UNSPECIFIED.,.F.,.F.,(4,3,3,3,3,3,3,3,3,3,3,4),(3.16237554060526E-11,
0.00769621628560935,0.0942246885002856,0.188514052913123,0.268067768599901,
0.366694922218767,0.467383535651208,0.5,0.624300582161452,0.746194067844642,
0.873097033922321,1.),.UNSPECIFIED.);
#5756=B_SPLINE_CURVE_WITH_KNOTS('',3,(#214594,#214595,#214596,#214597,#214598,
#214599),.UNSPECIFIED.,.F.,.F.,(4,2,4),(0.,0.5,1.),.UNSPECIFIED.);
#5757=B_SPLINE_CURVE_WITH_KNOTS('',3,(#214601,#214602,#214603,#214604,#214605,
#214606,#214607,#214608,#214609,#214610,#214611,#214612,#214613,#214614,
#214615,#214616,#214617,#214618,#214619,#214620,#214621,#214622,#214623,
#214624,#214625),.UNSPECIFIED.,.F.,.F.,(4,3,3,3,3,3,3,3,4),(3.07872546239425E-8,
0.205970371403195,0.247195775727949,0.449140217199346,0.496232918574816,
0.695053534951905,0.747153201208519,0.943375398914435,1.),.UNSPECIFIED.);
#5758=B_SPLINE_CURVE_WITH_KNOTS('',3,(#214627,#214628,#214629,#214630,#214631,
#214632,#214633,#214634,#214635,#214636,#214637,#214638,#214639,#214640,
#214641,#214642,#214643,#214644,#214645,#214646,#214647,#214648,#214649,
#214650,#214651,#214652,#214653,#214654,#214655,#214656,#214657,#214658,
#214659,#214660,#214661,#214662,#214663,#214664,#214665,#214666,#214667,
#214668,#214669,#214670,#214671,#214672,#214673,#214674,#214675,#214676,
#214677,#214678,#214679,#214680,#214681,#214682,#214683,#214684,#214685,
#214686,#214687,#214688,#214689,#214690,#214691,#214692,#214693,#214694,
#214695,#214696,#214697,#214698,#214699,#214700,#214701,#214702,#214703,
#214704,#214705,#214706,#214707,#214708,#214709,#214710,#214711,#214712,
#214713,#214714,#214715,#214716,#214717,#214718,#214719,#214720,#214721,
#214722,#214723,#214724,#214725,#214726,#214727,#214728,#214729,#214730,
#214731,#214732,#214733,#214734,#214735,#214736,#214737,#214738,#214739,
#214740,#214741,#214742,#214743,#214744,#214745,#214746,#214747,#214748,
#214749,#214750,#214751,#214752,#214753,#214754,#214755,#214756,#214757,
#214758,#214759,#214760,#214761,#214762,#214763,#214764,#214765,#214766,
#214767,#214768,#214769,#214770,#214771,#214772,#214773,#214774,#214775,
#214776,#214777,#214778,#214779,#214780,#214781,#214782,#214783,#214784,
#214785,#214786,#214787,#214788,#214789,#214790,#214791,#214792,#214793,
#214794,#214795,#214796,#214797,#214798,#214799,#214800,#214801),
 .UNSPECIFIED.,.F.,.F.,(4,3,3,3,3,3,3,3,3,3,3,3,3,3,3,3,3,3,3,3,3,3,3,3,
3,3,3,3,3,3,3,3,3,3,3,3,3,3,3,3,3,3,3,3,3,3,3,3,3,3,3,3,3,3,3,3,3,3,4),
(5.11034703543556E-8,0.000873397419564922,0.0042500144715355,0.0110025729195959,
0.0245010336941165,0.0640615231347867,0.0782432330913535,0.117418545504279,
0.124999999999962,0.187499999999943,0.234374999999928,0.244074093365877,
0.249999999999923,0.28691180927552,0.312499999999901,0.343749999999891,
0.359374999999886,0.367187499999884,0.371093749999882,0.373046874999882,
0.374999999999882,0.389263941687661,0.421832640387145,0.437499999999877,
0.438011301743273,0.465579486605632,0.468749999999874,0.480420548010491,
0.484293531293508,0.484374999999873,0.485520093773314,0.486781273444035,
0.488347437529155,0.488715417527697,0.49104828189574,0.492091101543253,
0.492494932064152,0.498046874999872,0.498383440689722,0.499999999999872,
0.54381309779903,0.587574177420254,0.624999999999904,0.672300987356324,
0.720762729405673,0.749999999999936,0.780535590518307,0.800739932311164,
0.828389269516647,0.854590150943252,0.874999999999968,0.904680252492238,
0.936356112347426,0.952858265257535,0.97669791610675,0.988587589368534,
0.994528743976525,0.997498877793861,0.99999999333144),.UNSPECIFIED.);
#5759=B_SPLINE_CURVE_WITH_KNOTS('',3,(#214803,#214804,#214805,#214806,#214807,
#214808,#214809,#214810,#214811,#214812,#214813,#214814,#214815,#214816,
#214817,#214818,#214819,#214820,#214821,#214822,#214823,#214824,#214825,
#214826,#214827,#214828,#214829,#214830,#214831,#214832,#214833,#214834,
#214835,#214836,#214837,#214838,#214839,#214840,#214841,#214842,#214843,
#214844,#214845),.UNSPECIFIED.,.F.,.F.,(4,3,3,3,3,3,3,3,3,3,3,3,3,3,4),
(0.,0.00521624725809631,0.0219557443112584,0.127779125462104,0.155680996700394,
0.266876415174393,0.378071833648393,0.5,0.652665472244447,0.678222244348951,
0.841762036962165,0.931561558766766,0.972431017039262,0.994218849932195,
1.),.UNSPECIFIED.);
#5760=B_SPLINE_CURVE_WITH_KNOTS('',3,(#214846,#214847,#214848,#214849,#214850,
#214851,#214852,#214853,#214854,#214855,#214856,#214857,#214858,#214859,
#214860,#214861,#214862,#214863,#214864,#214865,#214866,#214867,#214868,
#214869,#214870,#214871,#214872,#214873,#214874,#214875,#214876,#214877,
#214878,#214879,#214880,#214881,#214882,#214883,#214884,#214885,#214886,
#214887,#214888,#214889,#214890,#214891,#214892,#214893,#214894,#214895,
#214896,#214897,#214898,#214899,#214900,#214901,#214902,#214903,#214904,
#214905,#214906,#214907,#214908,#214909,#214910,#214911,#214912),
 .UNSPECIFIED.,.F.,.F.,(4,3,3,3,3,3,3,3,3,3,3,3,3,3,3,3,3,3,3,3,3,3,4),
(0.,0.127017155003427,0.250000000000004,0.364050961127173,0.373592405032721,
0.375000000000005,0.437500000000007,0.468750000000006,0.484375000000006,
0.492187500000006,0.500000000000006,0.61402579368828,0.725538073484568,
0.742827926521692,0.853717851291447,0.92478861938177,0.969729339656795,
0.975,0.985309039289484,0.992130828740079,0.99375,0.997042240357058,1.),
 .UNSPECIFIED.);
#5761=B_SPLINE_CURVE_WITH_KNOTS('',3,(#214928,#214929,#214930,#214931),
 .UNSPECIFIED.,.F.,.F.,(4,4),(0.,0.000517487663021482),.UNSPECIFIED.);
#5762=B_SPLINE_CURVE_WITH_KNOTS('',3,(#214932,#214933,#214934,#214935,#214936,
#214937,#214938,#214939,#214940,#214941,#214942,#214943,#214944,#214945,
#214946,#214947),.UNSPECIFIED.,.F.,.F.,(4,3,3,3,3,4),(0.,0.25,0.492721003519506,
0.732246481544643,0.967977404015073,1.),.UNSPECIFIED.);
#5763=B_SPLINE_CURVE_WITH_KNOTS('',3,(#215064,#215065,#215066,#215067,#215068,
#215069,#215070,#215071,#215072,#215073,#215074,#215075,#215076,#215077,
#215078,#215079,#215080,#215081,#215082,#215083,#215084,#215085,#215086,
#215087,#215088,#215089,#215090,#215091,#215092,#215093,#215094,#215095,
#215096,#215097,#215098,#215099,#215100,#215101,#215102,#215103,#215104,
#215105,#215106,#215107,#215108,#215109),.UNSPECIFIED.,.F.,.F.,(4,3,3,3,
3,3,3,3,3,3,3,3,3,3,3,4),(6.93889390390723E-18,0.000249844530040024,0.000374757201987747,
0.000499665804996625,0.000624572083127522,0.000749477780116718,0.000874384639619365,
0.000999294405453595,0.00124911879765639,0.00137403129062446,0.00149894371772633,
0.0016238558811297,0.00168631180212291,0.00174876758300643,0.00187367862553572,
0.00199858881090719),.UNSPECIFIED.);
#5764=B_SPLINE_CURVE_WITH_KNOTS('',3,(#215110,#215111,#215112,#215113,#215114,
#215115,#215116,#215117,#215118,#215119,#215120,#215121,#215122,#215123,
#215124,#215125,#215126,#215127,#215128,#215129,#215130,#215131,#215132,
#215133,#215134,#215135,#215136,#215137,#215138,#215139,#215140,#215141,
#215142,#215143,#215144,#215145,#215146,#215147,#215148,#215149,#215150,
#215151,#215152,#215153,#215154,#215155,#215156,#215157,#215158,#215159,
#215160,#215161,#215162,#215163,#215164,#215165,#215166,#215167,#215168,
#215169,#215170,#215171,#215172,#215173,#215174,#215175,#215176,#215177,
#215178,#215179,#215180,#215181,#215182,#215183,#215184,#215185,#215186,
#215187,#215188,#215189,#215190,#215191,#215192,#215193,#215194,#215195,
#215196,#215197,#215198,#215199,#215200,#215201,#215202,#215203,#215204,
#215205,#215206,#215207,#215208,#215209,#215210,#215211,#215212,#215213,
#215214,#215215,#215216,#215217,#215218,#215219,#215220,#215221,#215222,
#215223,#215224,#215225,#215226,#215227,#215228,#215229,#215230,#215231,
#215232,#215233,#215234,#215235,#215236,#215237,#215238,#215239,#215240,
#215241,#215242,#215243,#215244,#215245,#215246,#215247,#215248,#215249,
#215250,#215251,#215252,#215253,#215254,#215255,#215256,#215257,#215258,
#215259,#215260,#215261,#215262,#215263,#215264,#215265,#215266,#215267,
#215268,#215269,#215270,#215271,#215272,#215273,#215274,#215275,#215276,
#215277,#215278,#215279,#215280,#215281,#215282,#215283,#215284,#215285,
#215286,#215287,#215288,#215289,#215290,#215291,#215292,#215293,#215294,
#215295,#215296,#215297,#215298,#215299,#215300,#215301,#215302,#215303,
#215304,#215305,#215306,#215307,#215308,#215309,#215310,#215311,#215312,
#215313,#215314,#215315,#215316,#215317,#215318,#215319,#215320,#215321,
#215322,#215323,#215324,#215325,#215326,#215327,#215328,#215329,#215330,
#215331,#215332,#215333,#215334,#215335,#215336,#215337,#215338,#215339,
#215340,#215341,#215342,#215343,#215344,#215345,#215346,#215347,#215348,
#215349,#215350,#215351,#215352,#215353),.UNSPECIFIED.,.F.,.F.,(4,3,3,3,
3,3,3,3,3,3,3,3,3,3,3,3,3,3,3,3,3,3,3,3,3,3,3,3,3,3,3,3,3,3,3,3,3,3,3,3,
3,3,3,3,3,3,3,3,3,3,3,3,3,3,3,3,3,3,3,3,3,3,3,3,3,3,3,3,3,3,3,3,3,3,3,3,
3,3,3,3,3,4),(0.,0.0176762168154105,0.0369288430396893,0.0625000000000662,
0.0804000847057079,0.0937500000001003,0.108534387348399,0.109375000000121,
0.117187500000132,0.121093750000141,0.123592830383238,0.125000000000149,
0.140625000000149,0.155299847822507,0.156250000000149,0.169812069115432,
0.171875000000153,0.175781156354155,0.179687500000153,0.186769743781012,
0.187500000000153,0.218750000000149,0.234375000000148,0.242187500000148,
0.246093750000152,0.249721061039022,0.250000000000157,0.267171415929118,
0.283690610775299,0.299270948687442,0.30601050866871,0.31250000000016,0.32812500000016,
0.344367416171609,0.362170588585856,0.375000000000162,0.396143546472783,
0.406250000000162,0.421425997586886,0.421875000000158,0.429687500000155,
0.436857136050967,0.437500000000152,0.464627815166797,0.468750000000132,
0.484375000000125,0.496966596898197,0.500000000000118,0.522165361571699,
0.530572459240834,0.531250000000112,0.548581690940993,0.562500000000106,
0.5837268904211,0.593750000000099,0.609375000000098,0.617187500000094,0.624043972239538,
0.62500000000009,0.631234248578734,0.687500000000071,0.718750000000065,
0.734375000000063,0.740976426461612,0.750000000000061,0.812500000000059,
0.843750000000054,0.85937500000005,0.860151897939662,0.867187500000048,
0.871093750000046,0.873046875000039,0.875000000000032,0.894490298314019,
0.912568234704668,0.928964010240284,0.937500000000016,0.953125000000012,
0.967043443278746,0.98046419054641,0.993247432378915,1.),.UNSPECIFIED.);
#5765=B_SPLINE_CURVE_WITH_KNOTS('',3,(#215393,#215394,#215395,#215396,#215397,
#215398,#215399,#215400,#215401,#215402,#215403,#215404,#215405,#215406,
#215407,#215408,#215409,#215410,#215411,#215412,#215413,#215414),
 .UNSPECIFIED.,.F.,.F.,(4,3,3,3,3,3,3,4),(9.81307786677359E-18,0.00542754419074161,
0.00715193125010651,0.014303862500213,0.0178798281252662,0.0214557937503195,
0.0280312223938665,0.028607725000426),.UNSPECIFIED.);
#5766=B_SPLINE_CURVE_WITH_KNOTS('',3,(#215415,#215416,#215417,#215418,#215419,
#215420,#215421,#215422,#215423,#215424,#215425,#215426,#215427,#215428,
#215429,#215430,#215431,#215432,#215433,#215434,#215435,#215436,#215437,
#215438,#215439,#215440,#215441,#215442,#215443,#215444,#215445,#215446,
#215447,#215448,#215449,#215450,#215451,#215452,#215453,#215454,#215455,
#215456,#215457,#215458,#215459,#215460,#215461,#215462,#215463,#215464,
#215465,#215466,#215467,#215468,#215469,#215470,#215471,#215472,#215473,
#215474,#215475,#215476,#215477,#215478,#215479,#215480,#215481,#215482,
#215483,#215484,#215485,#215486,#215487,#215488,#215489,#215490,#215491,
#215492,#215493,#215494,#215495,#215496,#215497,#215498,#215499,#215500,
#215501,#215502,#215503,#215504,#215505,#215506,#215507,#215508,#215509,
#215510,#215511,#215512,#215513,#215514,#215515,#215516,#215517,#215518,
#215519,#215520,#215521,#215522,#215523,#215524,#215525,#215526,#215527,
#215528,#215529,#215530,#215531,#215532),.UNSPECIFIED.,.F.,.F.,(4,3,3,3,
3,3,3,3,3,3,3,3,3,3,3,3,3,3,3,3,3,3,3,3,3,3,3,3,3,3,3,3,3,3,3,3,3,3,3,4),
(0.,0.0588562399508839,0.116099365452458,0.125000000000124,0.180790191521428,
0.215150955135839,0.237429157520627,0.24951171875025,0.25000000000025,0.251302670656806,
0.285017840611363,0.317872441773445,0.349454566382291,0.375000000000254,
0.388817631691855,0.426956164769927,0.437500000000256,0.468750000000257,
0.484375000000258,0.492187500000258,0.496093750000257,0.498046875000257,
0.499023437500257,0.499755859375256,0.500000000000256,0.501787124098895,
0.555536630444185,0.612771063976521,0.625000000000192,0.671073302300544,
0.71439559262535,0.750000000000128,0.779782388171214,0.819625737711521,
0.858392751693001,0.875000000000064,0.909733146934382,0.944132077001742,
0.978130950313487,1.),.UNSPECIFIED.);
#5767=B_SPLINE_CURVE_WITH_KNOTS('',3,(#215638,#215639,#215640,#215641,#215642,
#215643,#215644,#215645,#215646,#215647,#215648,#215649,#215650,#215651,
#215652,#215653,#215654,#215655,#215656,#215657,#215658,#215659,#215660,
#215661,#215662,#215663,#215664,#215665,#215666,#215667,#215668,#215669,
#215670,#215671,#215672,#215673,#215674,#215675,#215676,#215677,#215678,
#215679,#215680,#215681,#215682,#215683,#215684,#215685,#215686),
 .UNSPECIFIED.,.F.,.F.,(4,3,3,3,3,3,3,3,3,3,3,3,3,3,3,3,4),(0.,0.000209907523070278,
0.000262386427442229,0.000314865930148693,0.000419826308247615,0.000524787812645559,
0.000629749598530388,0.000839670635464471,0.000892150044011657,0.000944629442448278,
0.00104958821836654,0.00115454698196066,0.00125950575196963,0.00136446454713245,
0.00146942338618816,0.00157438228787588,0.00167934127092895),
 .UNSPECIFIED.);
#5768=B_SPLINE_CURVE_WITH_KNOTS('',3,(#215687,#215688,#215689,#215690,#215691,
#215692,#215693,#215694,#215695,#215696,#215697,#215698,#215699,#215700,
#215701,#215702,#215703,#215704,#215705,#215706,#215707,#215708,#215709,
#215710,#215711,#215712,#215713,#215714,#215715,#215716,#215717,#215718,
#215719,#215720,#215721,#215722,#215723,#215724,#215725,#215726,#215727,
#215728,#215729,#215730,#215731,#215732,#215733,#215734,#215735,#215736,
#215737,#215738,#215739,#215740,#215741,#215742,#215743,#215744,#215745,
#215746,#215747,#215748,#215749,#215750,#215751,#215752,#215753,#215754,
#215755,#215756,#215757,#215758,#215759,#215760),.UNSPECIFIED.,.F.,.F.,
(4,2,2,2,2,2,2,1,2,2,2,2,1,1,2,2,2,2,2,1,1,2,2,2,2,1,2,2,2,2,2,2,2,2,2,
2,2,2,2,4),(0.,0.0625000000001367,0.125000000000273,0.18750000000041,0.250000000000547,
0.281250000000612,0.289062500000624,0.296875000000636,0.31250000000065,
0.375000000000693,0.390625000000707,0.398437500000714,0.406250000000721,
0.437500000000757,0.468750000000793,0.484375000000813,0.492187500000822,
0.500000000000831,0.531250000000825,0.546875000000818,0.554687500000816,
0.558593750000814,0.562500000000813,0.593750000000799,0.609375000000795,
0.617187500000788,0.621093750000784,0.62500000000078,0.656250000000682,
0.67187500000064,0.679687500000624,0.687500000000607,0.718750000000543,
0.734375000000509,0.742187500000493,0.750000000000478,0.812500000000359,
0.875000000000239,0.93750000000012,1.),.UNSPECIFIED.);
#5769=B_SPLINE_CURVE_WITH_KNOTS('',3,(#215793,#215794,#215795,#215796),
 .UNSPECIFIED.,.F.,.F.,(4,4),(3.46944695195361E-18,0.000487799384074577),
 .UNSPECIFIED.);
#5770=B_SPLINE_CURVE_WITH_KNOTS('',3,(#215797,#215798,#215799,#215800,#215801,
#215802,#215803,#215804,#215805,#215806,#215807,#215808,#215809),
 .UNSPECIFIED.,.F.,.F.,(4,3,3,3,4),(0.,0.252285837043446,0.507554797966739,
0.768599643387901,1.),.UNSPECIFIED.);
#5771=B_SPLINE_CURVE_WITH_KNOTS('',3,(#216124,#216125,#216126,#216127,#216128,
#216129,#216130,#216131,#216132,#216133,#216134,#216135,#216136,#216137,
#216138,#216139,#216140,#216141,#216142,#216143,#216144,#216145,#216146,
#216147,#216148,#216149,#216150,#216151,#216152,#216153,#216154,#216155,
#216156,#216157,#216158,#216159,#216160,#216161,#216162,#216163,#216164,
#216165,#216166,#216167,#216168,#216169,#216170,#216171,#216172,#216173,
#216174,#216175,#216176,#216177,#216178,#216179,#216180,#216181,#216182,
#216183,#216184,#216185,#216186,#216187,#216188,#216189,#216190,#216191,
#216192,#216193,#216194,#216195,#216196,#216197,#216198,#216199,#216200,
#216201,#216202,#216203,#216204,#216205,#216206,#216207,#216208,#216209,
#216210,#216211,#216212,#216213,#216214,#216215,#216216,#216217,#216218,
#216219,#216220,#216221,#216222,#216223),.UNSPECIFIED.,.F.,.F.,(4,3,3,3,
3,3,3,3,3,3,3,3,3,3,3,3,3,3,3,3,3,3,3,3,3,3,3,3,3,3,3,3,3,4),(0.,0.0779136589103248,
0.0882485852908278,0.162928798217767,0.173223837107886,0.187500000000003,
0.218750000000004,0.234375000000004,0.242187500000003,0.246093750000003,
0.248046875000003,0.250000000000003,0.256564631049091,0.29210193516486,
0.326726692869407,0.343750000000017,0.344829642597288,0.359375000000018,
0.36718750000002,0.37109375000002,0.374620536182301,0.375000000000021,0.424706860044605,
0.474200684446832,0.500000000000017,0.503570887679342,0.596730160309364,
0.66791097260569,0.718750000000011,0.736275753263558,0.750000000000009,
0.834360354991451,0.983724571879412,0.999998925899605),.UNSPECIFIED.);
#5772=B_SPLINE_CURVE_WITH_KNOTS('',3,(#216225,#216226,#216227,#216228,#216229,
#216230,#216231,#216232,#216233,#216234,#216235,#216236,#216237,#216238,
#216239,#216240,#216241,#216242,#216243,#216244,#216245,#216246,#216247,
#216248,#216249,#216250,#216251,#216252,#216253,#216254,#216255,#216256,
#216257,#216258,#216259,#216260,#216261,#216262,#216263,#216264,#216265,
#216266,#216267,#216268,#216269,#216270),.UNSPECIFIED.,.F.,.F.,(4,3,3,3,
3,3,3,3,3,3,3,3,3,3,3,4),(0.,0.00545528971435915,0.280220483963937,0.288806896284233,
0.293100102444383,0.297393308604534,0.314566133245131,0.348911782526331,
0.417603081088726,0.554985678213514,0.829750872463092,0.967133469587875,
0.984306294228478,0.992892706548774,0.996446353274387,0.999999999838516),
 .UNSPECIFIED.);
#5773=B_SPLINE_CURVE_WITH_KNOTS('',3,(#216272,#216273,#216274,#216275,#216276,
#216277,#216278,#216279,#216280,#216281,#216282,#216283,#216284,#216285,
#216286,#216287,#216288,#216289,#216290,#216291,#216292),.UNSPECIFIED.,
 .F.,.F.,(4,2,1,1,2,2,2,2,1,1,1,2,4),(0.,0.0156250000000005,0.0312500000000011,
0.0625000000000017,0.125000000000002,0.250000000000001,0.5,0.749999999999998,
0.874999999999998,0.937499999999999,0.968749999999999,0.984375,1.),
 .UNSPECIFIED.);
#5774=B_SPLINE_CURVE_WITH_KNOTS('',3,(#216293,#216294,#216295,#216296,#216297,
#216298,#216299,#216300,#216301,#216302,#216303,#216304,#216305,#216306,
#216307,#216308,#216309,#216310,#216311,#216312,#216313,#216314,#216315,
#216316,#216317,#216318,#216319,#216320,#216321,#216322,#216323),
 .UNSPECIFIED.,.F.,.F.,(4,3,3,3,3,3,3,3,3,3,4),(0.,0.00474675381323911,
0.00781250000000027,0.0156250000000005,0.030266067385407,0.0625000000000007,
0.0813046945943531,0.125,0.18338195186464,0.591690975932319,1.),
 .UNSPECIFIED.);
#5775=B_SPLINE_CURVE_WITH_KNOTS('',3,(#216324,#216325,#216326,#216327,#216328,
#216329,#216330,#216331,#216332,#216333,#216334,#216335,#216336,#216337,
#216338,#216339,#216340,#216341,#216342,#216343,#216344,#216345,#216346,
#216347,#216348,#216349,#216350,#216351,#216352,#216353,#216354,#216355,
#216356,#216357,#216358,#216359,#216360,#216361,#216362,#216363,#216364,
#216365,#216366,#216367,#216368,#216369,#216370,#216371,#216372,#216373,
#216374,#216375,#216376,#216377,#216378,#216379,#216380,#216381,#216382,
#216383,#216384,#216385,#216386,#216387,#216388,#216389,#216390,#216391,
#216392,#216393,#216394,#216395,#216396,#216397,#216398,#216399,#216400,
#216401,#216402,#216403,#216404,#216405,#216406,#216407,#216408,#216409,
#216410,#216411,#216412,#216413,#216414,#216415,#216416,#216417,#216418,
#216419,#216420,#216421,#216422,#216423,#216424,#216425,#216426,#216427,
#216428,#216429,#216430,#216431,#216432,#216433,#216434,#216435,#216436,
#216437,#216438,#216439,#216440,#216441,#216442,#216443,#216444,#216445,
#216446,#216447,#216448,#216449,#216450,#216451,#216452,#216453,#216454,
#216455,#216456,#216457,#216458,#216459,#216460,#216461,#216462,#216463,
#216464,#216465,#216466,#216467,#216468,#216469,#216470,#216471,#216472,
#216473,#216474,#216475,#216476,#216477,#216478,#216479,#216480,#216481,
#216482,#216483,#216484,#216485,#216486,#216487,#216488,#216489,#216490,
#216491,#216492,#216493,#216494,#216495,#216496,#216497,#216498,#216499,
#216500,#216501,#216502,#216503,#216504,#216505,#216506,#216507,#216508,
#216509,#216510,#216511,#216512,#216513,#216514,#216515,#216516,#216517,
#216518,#216519,#216520,#216521,#216522,#216523,#216524,#216525,#216526,
#216527,#216528,#216529,#216530,#216531,#216532,#216533,#216534,#216535,
#216536,#216537,#216538,#216539,#216540,#216541,#216542,#216543,#216544,
#216545,#216546,#216547,#216548,#216549,#216550,#216551,#216552,#216553,
#216554,#216555,#216556,#216557,#216558,#216559,#216560,#216561,#216562,
#216563,#216564,#216565,#216566,#216567,#216568,#216569,#216570,#216571,
#216572,#216573,#216574,#216575,#216576,#216577,#216578,#216579,#216580,
#216581,#216582,#216583,#216584,#216585,#216586,#216587,#216588,#216589,
#216590,#216591,#216592,#216593,#216594,#216595,#216596,#216597,#216598,
#216599,#216600,#216601,#216602,#216603),.UNSPECIFIED.,.F.,.F.,(4,3,3,3,
3,3,3,3,3,3,3,3,3,3,3,3,3,3,3,3,3,3,3,3,3,3,3,3,3,3,3,3,3,3,3,3,3,3,3,3,
3,3,3,3,3,3,3,3,3,3,3,3,3,3,3,3,3,3,3,3,3,3,3,3,3,3,3,3,3,3,3,3,3,3,3,3,
3,3,3,3,3,3,3,3,3,3,3,3,3,3,3,3,3,4),(3.46944695195361E-18,0.00251321548397822,
0.00252618216605191,0.00431652351870221,0.00502643096795645,0.0050523631196123,
0.00628303870994556,0.00631545541643819,0.00639439869545078,0.00647334192364792,
0.00663122827834575,0.00691134258094011,0.0069470009329515,0.00753964645193465,
0.00757854646468453,0.0100528619359129,0.0101047288113934,0.0106811658069074,
0.0107362741734552,0.0109953177424047,0.0110520469397126,0.0111309901351074,
0.0111704617311478,0.0112099333265805,0.011309469677902,0.0113678197142864,
0.0125660774198911,0.0126309107307065,0.0149188987799849,0.0150792929038693,
0.0151570929628482,0.0163359006458585,0.0164201840296525,0.016964204516853,
0.0170517295614678,0.0172783564523502,0.0173675023312846,0.0174464455249122,
0.0174859171210369,0.017525388716906,0.0175925083878475,0.0176832737054695,
0.0182566011601652,0.0188331435913378,0.018943209217914,0.0195351789828337,
0.0201057238718258,0.0201875071813319,0.0211909991553901,0.0221894422408006,
0.0226189393558041,0.0226772058573312,0.0227557547052305,0.0227950386486702,
0.0228343240121577,0.0229330912913013,0.0229914102955462,0.0232472432267986,
0.0233051459757238,0.0238755470977931,0.0239316652744055,0.0251321548397822,
0.0251846404969728,0.0276453703237604,0.0276905921486432,0.0289019780657495,
0.0289435691951432,0.0291001957684129,0.0291785065739474,0.0292568164041345,
0.029530281936744,0.0295700559705409,0.0301585858077386,0.0301965438884586,
0.0326718012917168,0.0327024956320061,0.0339284090337059,0.0339554719475575,
0.0340337845090096,0.0340729398943169,0.0341120949376171,0.0342425609692031,
0.0342687153965129,0.0345567129047004,0.0345819593578056,0.035185016775695,
0.0352084472800867,0.0376982322596731,0.0377143994811302,0.0383006441491539,
0.0388957484754305,0.0394801741002239,0.0400377689422836,0.0402114477436513),
 .UNSPECIFIED.);
#5776=B_SPLINE_CURVE_WITH_KNOTS('',3,(#216605,#216606,#216607,#216608,#216609,
#216610,#216611,#216612,#216613,#216614,#216615,#216616,#216617,#216618,
#216619,#216620,#216621,#216622,#216623,#216624,#216625,#216626,#216627,
#216628,#216629,#216630,#216631,#216632,#216633,#216634,#216635,#216636,
#216637,#216638,#216639,#216640,#216641,#216642,#216643,#216644,#216645,
#216646,#216647,#216648,#216649,#216650,#216651,#216652,#216653),
 .UNSPECIFIED.,.F.,.F.,(4,3,3,3,3,3,3,3,3,3,3,3,3,3,3,3,4),(0.,0.00265415439005135,
0.102720312462561,0.20133059727198,0.249999999999989,0.353342179378799,
0.374999999999984,0.43749999999998,0.468749999999978,0.484374999999978,
0.496753448869959,0.499999999999978,0.601051550778275,0.702354920594771,
0.804823358871256,0.909563908684595,1.),.UNSPECIFIED.);
#5777=B_SPLINE_CURVE_WITH_KNOTS('',3,(#216654,#216655,#216656,#216657,#216658,
#216659,#216660,#216661,#216662,#216663,#216664,#216665,#216666,#216667,
#216668,#216669,#216670,#216671,#216672,#216673,#216674,#216675,#216676,
#216677,#216678,#216679,#216680,#216681,#216682,#216683,#216684,#216685,
#216686,#216687,#216688,#216689,#216690,#216691,#216692,#216693,#216694,
#216695,#216696,#216697,#216698,#216699,#216700,#216701,#216702,#216703,
#216704,#216705,#216706,#216707,#216708,#216709,#216710,#216711,#216712,
#216713,#216714,#216715,#216716,#216717,#216718,#216719,#216720,#216721,
#216722,#216723,#216724,#216725,#216726),.UNSPECIFIED.,.F.,.F.,(4,3,3,3,
3,3,3,3,3,3,3,3,3,3,3,3,3,3,3,3,3,3,3,3,4),(4.05198363567377E-7,0.00787298863610522,
0.0273567818531982,0.0781878140360392,0.104285438977262,0.154412767520936,
0.203500430496265,0.24678211002478,0.250000000000018,0.33637967744521,0.375000000000026,
0.43750000000003,0.468750000000032,0.484375000000032,0.492187500000033,
0.496093750000033,0.500000000000032,0.647718153766782,0.745632761495269,
0.874942760220384,0.939328417322223,0.971461269619396,0.974303379404863,
0.987472851275835,1.),.UNSPECIFIED.);
#5778=B_SPLINE_CURVE_WITH_KNOTS('',3,(#216740,#216741,#216742,#216743,#216744,
#216745,#216746,#216747,#216748,#216749,#216750,#216751,#216752,#216753,
#216754,#216755,#216756,#216757,#216758,#216759,#216760,#216761),
 .UNSPECIFIED.,.F.,.F.,(4,3,3,3,3,3,3,4),(0.,0.176890528384024,0.345636984164273,
0.509227738123205,0.660395309268134,0.806605995633615,0.946450892839879,
1.),.UNSPECIFIED.);
#5779=B_SPLINE_CURVE_WITH_KNOTS('',3,(#216863,#216864,#216865,#216866,#216867,
#216868,#216869,#216870,#216871,#216872,#216873,#216874,#216875,#216876,
#216877,#216878,#216879,#216880,#216881,#216882,#216883,#216884,#216885,
#216886,#216887,#216888,#216889,#216890,#216891,#216892,#216893,#216894,
#216895,#216896,#216897,#216898,#216899,#216900,#216901,#216902,#216903,
#216904,#216905,#216906,#216907,#216908,#216909,#216910,#216911,#216912,
#216913,#216914,#216915,#216916,#216917,#216918,#216919,#216920,#216921,
#216922,#216923,#216924,#216925,#216926,#216927,#216928,#216929,#216930,
#216931,#216932,#216933,#216934,#216935,#216936,#216937,#216938,#216939,
#216940,#216941),.UNSPECIFIED.,.F.,.F.,(4,3,3,3,3,3,3,3,3,3,3,3,3,3,3,3,
3,3,3,3,3,3,3,3,3,3,4),(0.,0.0699362617129251,0.103904228120223,0.124999999999995,
0.137268630045529,0.20235451817345,0.249999999999989,0.265485387458136,
0.326032873596611,0.374999999999986,0.38653728259255,0.43428842418918,0.437499999999984,
0.444547027425897,0.473935618526858,0.492187499999978,0.498537282033062,
0.499999999999977,0.500942948294706,0.592037747362571,0.625127000188452,
0.717273178183023,0.749301981791401,0.840484550520233,0.87405473528525,
0.964870050196674,1.),.UNSPECIFIED.);
#5780=B_SPLINE_CURVE_WITH_KNOTS('',3,(#216942,#216943,#216944,#216945,#216946,
#216947,#216948,#216949,#216950,#216951,#216952,#216953,#216954,#216955,
#216956,#216957,#216958,#216959,#216960,#216961,#216962,#216963,#216964,
#216965,#216966,#216967,#216968,#216969,#216970,#216971,#216972,#216973,
#216974,#216975,#216976,#216977,#216978,#216979,#216980,#216981,#216982,
#216983,#216984,#216985,#216986,#216987,#216988,#216989,#216990,#216991,
#216992,#216993,#216994,#216995,#216996,#216997,#216998,#216999,#217000,
#217001,#217002,#217003,#217004,#217005,#217006,#217007,#217008,#217009,
#217010,#217011,#217012,#217013,#217014,#217015,#217016,#217017,#217018,
#217019,#217020,#217021,#217022,#217023,#217024,#217025,#217026,#217027,
#217028,#217029,#217030,#217031,#217032,#217033,#217034,#217035,#217036,
#217037,#217038,#217039,#217040,#217041,#217042,#217043,#217044,#217045,
#217046,#217047,#217048,#217049,#217050,#217051,#217052,#217053,#217054,
#217055,#217056,#217057,#217058,#217059,#217060,#217061,#217062,#217063,
#217064,#217065,#217066,#217067,#217068,#217069,#217070,#217071,#217072,
#217073,#217074,#217075,#217076,#217077,#217078,#217079,#217080,#217081,
#217082,#217083,#217084,#217085,#217086,#217087,#217088,#217089,#217090,
#217091,#217092,#217093,#217094,#217095,#217096,#217097,#217098,#217099,
#217100,#217101,#217102,#217103,#217104,#217105,#217106,#217107,#217108,
#217109,#217110,#217111,#217112,#217113,#217114,#217115,#217116,#217117,
#217118,#217119,#217120,#217121,#217122,#217123,#217124,#217125,#217126,
#217127,#217128,#217129,#217130,#217131,#217132,#217133,#217134,#217135,
#217136,#217137,#217138,#217139,#217140,#217141,#217142,#217143,#217144,
#217145,#217146,#217147,#217148,#217149,#217150,#217151,#217152,#217153,
#217154,#217155,#217156,#217157,#217158,#217159,#217160,#217161,#217162,
#217163,#217164,#217165,#217166,#217167,#217168,#217169,#217170,#217171,
#217172,#217173,#217174,#217175,#217176,#217177,#217178,#217179,#217180,
#217181,#217182,#217183,#217184,#217185,#217186,#217187,#217188),
 .UNSPECIFIED.,.F.,.F.,(4,3,3,3,3,3,3,3,3,3,3,3,3,3,3,3,3,3,3,3,3,3,3,3,
3,3,3,3,3,3,3,3,3,3,3,3,3,3,3,3,3,3,3,3,3,3,3,3,3,3,3,3,3,3,3,3,3,3,3,3,
3,3,3,3,3,3,3,3,3,3,3,3,3,3,3,3,3,3,3,3,3,3,4),(0.,0.0137545866432384,0.0492401835094905,
0.0625000000000268,0.0937500000000405,0.109375000000047,0.11718750000005,
0.123875958867671,0.125000000000053,0.174156395228104,0.20291116071406,
0.218750000000069,0.234375000000071,0.242187500000073,0.246093750000075,
0.250000000000078,0.281848408221954,0.312500000000087,0.34375000000009,
0.35937500000009,0.367187500000089,0.371093750000089,0.375000000000089,
0.397346070709233,0.437500000000074,0.468750000000068,0.484375000000062,
0.498046875000063,0.500000000000065,0.52073830350297,0.531250000000054,
0.54687500000005,0.554687500000049,0.558593750000048,0.560546875000049,
0.562500000000049,0.577571866921682,0.581137214692785,0.593750000000042,
0.608462325772321,0.609375000000036,0.617187500000037,0.621093750000035,
0.623046875000043,0.62402343750004,0.625000000000037,0.666535878910816,
0.687499999999788,0.718749999999663,0.7343749999996,0.74218749999957,0.749023437499547,
0.749999999999541,0.760356549744039,0.770430402015572,0.780504254287105,
0.792502672640471,0.796874999999502,0.804687499999497,0.808593749999494,
0.810546874999492,0.812115977136946,0.81249999999949,0.828352802307223,
0.843749999999467,0.859374999999458,0.867187499999452,0.871093749999448,
0.87384301473899,0.874999999999443,0.898739986678005,0.90624999999941,0.921874999999392,
0.929687499999384,0.93359374999938,0.936523437499377,0.937499999999376,
0.947583425348786,0.958066165670755,0.969573174789762,0.984786587394881,
0.995666532359992,1.),.UNSPECIFIED.);
#5781=B_SPLINE_CURVE_WITH_KNOTS('',3,(#217216,#217217,#217218,#217219,#217220,
#217221,#217222,#217223,#217224,#217225,#217226,#217227,#217228),
 .UNSPECIFIED.,.F.,.F.,(4,3,3,3,4),(6.93889390390723E-18,0.000381255516945798,
0.000469255885454269,0.000705402670155963,0.000942818873534133),
 .UNSPECIFIED.);
#5782=B_SPLINE_CURVE_WITH_KNOTS('',3,(#217229,#217230,#217231,#217232,#217233,
#217234,#217235,#217236,#217237,#217238,#217239,#217240,#217241,#217242,
#217243,#217244,#217245,#217246,#217247),.UNSPECIFIED.,.F.,.F.,(4,2,2,1,
1,1,2,2,2,2,4),(0.,0.124999999999029,0.187499999998545,0.21874999999831,
0.234374999998192,0.242187499998133,0.246093749998135,0.249999999998136,
0.374999999998442,0.499999999998747,1.),.UNSPECIFIED.);
#5783=B_SPLINE_CURVE_WITH_KNOTS('',3,(#217262,#217263,#217264,#217265,#217266,
#217267,#217268,#217269,#217270,#217271,#217272,#217273,#217274,#217275,
#217276),.UNSPECIFIED.,.F.,.F.,(4,2,2,1,1,1,2,2,4),(0.,0.250000000000346,
0.375000000000519,0.437500000000606,0.468750000000651,0.484375000000672,
0.492187500000683,0.500000000000693,0.99998999934417),.UNSPECIFIED.);
#5784=B_SPLINE_CURVE_WITH_KNOTS('',3,(#217295,#217296,#217297,#217298,#217299,
#217300,#217301,#217302,#217303,#217304),.UNSPECIFIED.,.F.,.F.,(4,3,3,4),
(1.04998151009522E-15,7.57680534135841E-5,0.000160273665463363,0.000194799519911097),
 .UNSPECIFIED.);
#5785=B_SPLINE_CURVE_WITH_KNOTS('',3,(#217325,#217326,#217327,#217328,#217329,
#217330,#217331,#217332,#217333,#217334,#217335,#217336,#217337,#217338,
#217339,#217340,#217341,#217342,#217343,#217344,#217345,#217346,#217347,
#217348,#217349),.UNSPECIFIED.,.F.,.F.,(4,3,3,3,3,3,3,3,4),(1.42699696935763E-12,
0.134118179434847,0.269533840744077,0.405806590660504,0.5,0.627124388053351,
0.754010818070997,0.880892917577905,1.),.UNSPECIFIED.);
#5786=B_SPLINE_CURVE_WITH_KNOTS('',3,(#217754,#217755,#217756,#217757,#217758,
#217759,#217760,#217761,#217762,#217763,#217764,#217765,#217766,#217767,
#217768,#217769,#217770,#217771,#217772,#217773,#217774,#217775,#217776,
#217777,#217778,#217779,#217780,#217781,#217782,#217783,#217784,#217785,
#217786,#217787,#217788,#217789,#217790,#217791,#217792,#217793,#217794,
#217795,#217796,#217797,#217798,#217799,#217800,#217801,#217802,#217803,
#217804,#217805),.UNSPECIFIED.,.F.,.F.,(4,3,3,3,3,3,3,3,3,3,3,3,3,3,3,3,
3,4),(4.34856172578496E-12,0.0825964622752124,0.166298231137607,0.250000000000002,
0.34372743266562,0.401376017787723,0.468749999999996,0.486596533951206,
0.499999999999986,0.500286464469699,0.562714848352273,0.625720242594846,
0.691315601603277,0.749999999999993,0.81758269229801,0.886453217052764,
0.956347341619819,0.999958634704665),.UNSPECIFIED.);
#5787=B_SPLINE_CURVE_WITH_KNOTS('',3,(#217806,#217807,#217808,#217809,#217810,
#217811,#217812,#217813,#217814,#217815,#217816,#217817,#217818,#217819,
#217820,#217821,#217822,#217823,#217824,#217825,#217826,#217827,#217828,
#217829,#217830,#217831,#217832,#217833,#217834,#217835,#217836,#217837,
#217838,#217839,#217840,#217841,#217842,#217843,#217844,#217845,#217846,
#217847,#217848,#217849,#217850,#217851,#217852,#217853,#217854,#217855,
#217856,#217857,#217858,#217859,#217860,#217861,#217862,#217863,#217864,
#217865,#217866,#217867,#217868,#217869,#217870,#217871,#217872,#217873,
#217874,#217875,#217876,#217877,#217878,#217879,#217880,#217881,#217882,
#217883,#217884,#217885,#217886,#217887,#217888,#217889,#217890,#217891,
#217892,#217893,#217894,#217895,#217896,#217897,#217898,#217899,#217900,
#217901,#217902,#217903,#217904,#217905,#217906,#217907,#217908,#217909,
#217910,#217911,#217912,#217913,#217914,#217915,#217916,#217917,#217918,
#217919,#217920,#217921,#217922,#217923,#217924,#217925,#217926,#217927,
#217928,#217929,#217930,#217931,#217932,#217933,#217934,#217935,#217936,
#217937,#217938,#217939,#217940,#217941,#217942,#217943,#217944,#217945,
#217946,#217947,#217948,#217949,#217950,#217951,#217952,#217953,#217954,
#217955,#217956,#217957,#217958,#217959,#217960,#217961,#217962,#217963,
#217964,#217965,#217966,#217967,#217968,#217969,#217970,#217971,#217972,
#217973,#217974,#217975,#217976,#217977,#217978,#217979,#217980,#217981,
#217982,#217983,#217984,#217985,#217986,#217987,#217988,#217989,#217990,
#217991,#217992,#217993,#217994,#217995,#217996,#217997,#217998,#217999,
#218000,#218001,#218002,#218003,#218004,#218005,#218006,#218007,#218008,
#218009,#218010,#218011,#218012,#218013,#218014,#218015,#218016,#218017,
#218018,#218019,#218020,#218021,#218022,#218023,#218024,#218025,#218026,
#218027,#218028,#218029,#218030,#218031,#218032,#218033,#218034,#218035,
#218036,#218037,#218038,#218039,#218040,#218041,#218042,#218043,#218044,
#218045,#218046,#218047,#218048,#218049,#218050,#218051,#218052,#218053,
#218054,#218055,#218056,#218057,#218058,#218059,#218060,#218061,#218062,
#218063,#218064,#218065,#218066,#218067,#218068,#218069,#218070,#218071,
#218072,#218073,#218074,#218075,#218076,#218077,#218078,#218079,#218080,
#218081,#218082,#218083,#218084,#218085,#218086,#218087,#218088,#218089,
#218090,#218091,#218092,#218093,#218094,#218095,#218096,#218097,#218098,
#218099,#218100,#218101,#218102,#218103,#218104,#218105,#218106,#218107,
#218108,#218109,#218110,#218111,#218112,#218113,#218114,#218115,#218116,
#218117,#218118,#218119,#218120,#218121,#218122,#218123,#218124,#218125,
#218126,#218127,#218128,#218129,#218130,#218131,#218132,#218133,#218134,
#218135,#218136,#218137,#218138,#218139,#218140,#218141,#218142,#218143,
#218144,#218145,#218146,#218147,#218148,#218149,#218150,#218151,#218152,
#218153,#218154,#218155,#218156,#218157),.UNSPECIFIED.,.F.,.F.,(4,3,3,3,
3,3,3,3,3,3,3,3,3,3,3,3,3,3,3,3,3,3,3,3,3,3,3,3,3,3,3,3,3,3,3,3,3,3,3,3,
3,3,3,3,3,3,3,3,3,3,3,3,3,3,3,3,3,3,3,3,3,3,3,3,3,3,3,3,3,3,3,3,3,3,3,3,
3,3,3,3,3,3,3,3,3,3,3,3,3,3,3,3,3,3,3,3,3,3,3,3,3,3,3,3,3,3,3,3,3,3,3,3,
3,3,3,3,3,4),(7.6340784608749E-10,0.000458642979624075,0.00148039977483381,
0.00155548413886924,0.00215808125410714,0.00351929599465174,0.00375138748261493,
0.00431616250821427,0.00485043313467506,0.00595000606436421,0.00647424376232141,
0.00814921412208154,0.00863232501642855,0.0103483019189587,0.0107904062705357,
0.0114478221282486,0.0118694468975892,0.011997552011241,0.0121349909920189,
0.0121693507398505,0.0122037104862686,0.0122724299699281,0.012408967211116,
0.0125473080812288,0.0129484875246428,0.0164016813619231,0.0169452741711653,
0.0172646500328571,0.019144189598669,0.0194227312869643,0.0196939101106168,
0.0198313397462725,0.0198485184451541,0.0198656971433723,0.0199000545385089,
0.0199622516004911,0.019968769328592,0.0202436289341077,0.0205017719140178,
0.0213430827748677,0.0215808125410714,0.023660808471361,0.0257408044016506,
0.0258969750492855,0.0270590117429158,0.0280550563033925,0.0289136017549253,
0.0291340969304461,0.0301383324656715,0.030172686249919,0.0302070399948121,
0.0302131375574996,0.0302757474855599,0.0304131631667517,0.0306879973674717,
0.0312376772927354,0.0323370846027418,0.0345293000657137,0.0345360999801471,
0.0356083406927672,0.0356357138934573,0.0366115735239226,0.0366873813198207,
0.036735364064563,0.0376935360434175,0.0377664219468742,0.037834874245495,
0.03797230394085,0.0380066611974582,0.0380410184323685,0.0381097329274824,
0.038305942260401,0.0383845939060418,0.0388454625739277,0.0389343227662998,
0.0416287480698926,0.0431616250821419,0.0433319227699236,0.0455053529354617,
0.0474777875903559,0.0477291370889975,0.0480173079038827,0.0482787598919197,
0.0483474623355832,0.0483818135645227,0.0484161648055707,0.0485535700013951,
0.0485568282174095,0.048828382082034,0.049635868844463,0.0499276530066721,
0.0510269469117059,0.05179395009857,0.0521261923582703,0.0543244689093608,
0.0554235143696222,0.0559730160990558,0.056110112606784,0.0562477622140428,
0.0563164484206554,0.0563851344750846,0.0565225060213207,0.0566496329203107,
0.0571891532338374,0.0582681938608909,0.0599454964430095,0.0604262751149979,
0.06091874539064,0.0623709320756,0.0625843563691049,0.0631171315120619,
0.0647424376232119,0.0653151792302629,0.0669005188773189,0.0675129021160856,
0.0679795595043724,0.0688633830386992,0.0690586001314259),.UNSPECIFIED.);
#5788=B_SPLINE_CURVE_WITH_KNOTS('',3,(#218159,#218160,#218161,#218162,#218163,
#218164,#218165,#218166,#218167,#218168,#218169,#218170,#218171,#218172,
#218173,#218174,#218175,#218176,#218177,#218178,#218179,#218180,#218181,
#218182,#218183,#218184,#218185,#218186,#218187,#218188,#218189,#218190,
#218191,#218192,#218193,#218194,#218195,#218196,#218197,#218198,#218199,
#218200,#218201,#218202,#218203,#218204,#218205,#218206,#218207,#218208,
#218209,#218210,#218211,#218212,#218213,#218214,#218215,#218216,#218217,
#218218,#218219,#218220,#218221,#218222,#218223,#218224,#218225,#218226,
#218227,#218228,#218229,#218230,#218231,#218232,#218233,#218234,#218235,
#218236,#218237),.UNSPECIFIED.,.F.,.F.,(4,3,3,3,3,3,3,3,3,3,3,3,3,3,3,3,
3,3,3,3,3,3,3,3,3,3,4),(4.77884326448819E-11,0.00202028309269962,0.0039176051110123,
0.00783365280887212,0.0156653625435356,0.0313274786564338,0.0626484630366808,
0.125294063429656,0.188446065875006,0.250307838177388,0.302395984903941,
0.3779647184045,0.445740485537048,0.499645843896646,0.561681656144702,0.577853278825029,
0.622127447016507,0.680957127046811,0.738153985517249,0.79371261558945,
0.822603609701943,0.847641311410194,0.899965028869779,0.938213647190648,
0.950728580880526,0.981074031663759,1.),.UNSPECIFIED.);
#5789=B_SPLINE_CURVE_WITH_KNOTS('',3,(#218239,#218240,#218241,#218242,#218243,
#218244,#218245,#218246,#218247,#218248,#218249,#218250,#218251,#218252,
#218253,#218254,#218255,#218256,#218257,#218258,#218259,#218260,#218261,
#218262,#218263,#218264,#218265,#218266,#218267,#218268,#218269,#218270,
#218271,#218272,#218273,#218274,#218275,#218276,#218277,#218278,#218279,
#218280,#218281,#218282,#218283,#218284,#218285,#218286,#218287,#218288,
#218289,#218290,#218291,#218292,#218293,#218294,#218295,#218296,#218297,
#218298,#218299,#218300,#218301,#218302,#218303,#218304,#218305),
 .UNSPECIFIED.,.F.,.F.,(4,3,3,3,3,3,3,3,3,3,3,3,3,3,3,3,3,3,3,3,3,3,4),
(0.,0.0312499999999975,0.0468749999999962,0.0546874999999938,0.0585937499999938,
0.0624999999999939,0.0977910955042792,0.124999999999995,0.187499999999997,
0.218749999999998,0.237790831202695,0.25,0.375000000000006,0.437500000000008,
0.46875000000001,0.482748988899476,0.484375000000011,0.492187500000011,
0.500000000000012,0.6282098955093,0.740654930187649,0.870327465093825,1.),
 .UNSPECIFIED.);
#5790=B_SPLINE_CURVE_WITH_KNOTS('',3,(#218307,#218308,#218309,#218310,#218311,
#218312,#218313,#218314,#218315,#218316,#218317,#218318,#218319,#218320,
#218321,#218322,#218323,#218324,#218325,#218326,#218327,#218328,#218329,
#218330,#218331,#218332,#218333,#218334,#218335,#218336,#218337,#218338,
#218339,#218340,#218341,#218342,#218343,#218344),.UNSPECIFIED.,.F.,.F.,
(4,1,1,2,2,2,1,1,2,2,2,2,2,1,2,2,2,1,1,1,2,2,4),(0.,0.00390625000009151,
0.00585937500013782,0.00732421875017266,0.00781250000018431,0.0117187500001906,
0.0136718750001931,0.0146484375001943,0.0151367187501945,0.0156250000001947,
0.0312500000001926,0.0625000000001896,0.12500000000018,0.187500000000171,
0.218750000000165,0.250000000000159,0.375000000000137,0.437500000000125,
0.46875000000012,0.484375000000117,0.492187500000115,0.500000000000114,
1.),.UNSPECIFIED.);
#5791=B_SPLINE_CURVE_WITH_KNOTS('',3,(#218346,#218347,#218348,#218349,#218350,
#218351,#218352,#218353,#218354,#218355,#218356,#218357,#218358,#218359,
#218360,#218361,#218362,#218363,#218364,#218365,#218366,#218367,#218368,
#218369,#218370,#218371,#218372,#218373,#218374,#218375,#218376,#218377),
 .UNSPECIFIED.,.F.,.F.,(4,2,1,1,1,2,2,2,2,2,2,1,2,2,2,2,2,4),(0.,0.0156250000000023,
0.0234375000000034,0.0273437500000047,0.0292968750000052,0.0302734375000052,
0.0312500000000052,0.0625000000000046,0.125000000000005,0.250000000000005,
0.375000000000005,0.437500000000005,0.468750000000005,0.500000000000005,
0.625000000000004,0.687500000000004,0.750000000000003,1.),.UNSPECIFIED.);
#5792=B_SPLINE_CURVE_WITH_KNOTS('',3,(#218379,#218380,#218381,#218382,#218383,
#218384,#218385,#218386,#218387,#218388,#218389,#218390,#218391,#218392,
#218393,#218394,#218395,#218396,#218397,#218398,#218399,#218400,#218401,
#218402,#218403,#218404,#218405,#218406,#218407,#218408,#218409,#218410,
#218411,#218412,#218413,#218414,#218415,#218416,#218417,#218418,#218419,
#218420,#218421,#218422,#218423,#218424,#218425,#218426,#218427,#218428,
#218429,#218430,#218431,#218432,#218433,#218434,#218435,#218436,#218437,
#218438,#218439,#218440,#218441,#218442,#218443,#218444,#218445,#218446,
#218447,#218448,#218449,#218450,#218451,#218452,#218453,#218454,#218455,
#218456,#218457,#218458,#218459,#218460,#218461,#218462,#218463,#218464,
#218465,#218466,#218467,#218468,#218469,#218470,#218471,#218472,#218473,
#218474,#218475,#218476,#218477,#218478,#218479,#218480,#218481,#218482,
#218483,#218484,#218485,#218486,#218487,#218488,#218489,#218490,#218491,
#218492,#218493,#218494,#218495,#218496,#218497,#218498,#218499,#218500,
#218501,#218502),.UNSPECIFIED.,.F.,.F.,(4,3,3,3,3,3,3,3,3,3,3,3,3,3,3,3,
3,3,3,3,3,3,3,3,3,3,3,3,3,3,3,3,3,3,3,3,3,3,3,3,3,4),(0.,0.00032758361939681,
0.00676055619332624,0.0229628150776129,0.039310820342462,0.0564454475397725,
0.0583030570676846,0.0625000000000044,0.0683593750000044,0.0698013305664106,
0.0702138167440786,0.0705630656159106,0.0762964552156621,0.0777123116125716,
0.0786023886535299,0.0929693901461635,0.0960501440206557,0.117390760019365,
0.122790494671226,0.125341744964798,0.175764617567141,0.187228865205509,
0.191986365790403,0.222675570066603,0.249528623808278,0.252764358890674,
0.336698626740585,0.421722401430846,0.437500000000002,0.468750000000002,
0.482174841649079,0.500000000000002,0.589596724551366,0.6784245448769,0.766897797949448,
0.854958523913957,0.909319437118939,0.963183385534347,0.967483243263316,
0.990177312386673,0.99692531213621,0.999999948688291),.UNSPECIFIED.);
#5793=B_SPLINE_CURVE_WITH_KNOTS('',3,(#218504,#218505,#218506,#218507,#218508,
#218509,#218510,#218511,#218512,#218513,#218514,#218515,#218516,#218517,
#218518,#218519,#218520,#218521,#218522,#218523,#218524,#218525,#218526,
#218527,#218528,#218529,#218530,#218531,#218532,#218533,#218534,#218535,
#218536),.UNSPECIFIED.,.F.,.F.,(4,2,2,2,1,2,2,2,2,1,1,2,2,2,1,1,2,2,4),
(0.,0.0312499999999877,0.0351562499999857,0.0371093749999851,0.0390624999999845,
0.0468749999999845,0.0624999999999847,0.0937499999999842,0.124999999999984,
0.187499999999982,0.218749999999982,0.234374999999983,0.249999999999983,
0.374999999999987,0.437499999999989,0.46874999999999,0.48437499999999,0.49999999999999,
0.999999981795557),.UNSPECIFIED.);
#5794=B_SPLINE_CURVE_WITH_KNOTS('',3,(#218537,#218538,#218539,#218540,#218541,
#218542,#218543,#218544,#218545,#218546,#218547,#218548,#218549,#218550,
#218551,#218552),.UNSPECIFIED.,.F.,.F.,(4,2,2,1,1,1,1,2,2,4),(0.,0.249999999999993,
0.37499999999999,0.437499999999989,0.468749999999988,0.484374999999988,
0.492187499999988,0.498046874999989,0.499999999999989,1.),.UNSPECIFIED.);
#5795=B_SPLINE_CURVE_WITH_KNOTS('',3,(#218573,#218574,#218575,#218576,#218577,
#218578),.UNSPECIFIED.,.F.,.F.,(4,2,4),(0.,0.500000000000001,0.999968221947089),
 .UNSPECIFIED.);
#5796=B_SPLINE_CURVE_WITH_KNOTS('',3,(#218594,#218595,#218596,#218597),
 .UNSPECIFIED.,.F.,.F.,(4,4),(1.05519109601004E-16,0.000332772401868219),
 .UNSPECIFIED.);
#5797=B_SPLINE_CURVE_WITH_KNOTS('',3,(#218598,#218599,#218600,#218601,#218602,
#218603,#218604),.UNSPECIFIED.,.F.,.F.,(4,3,4),(3.39934988877629E-17,8.80333921656039E-5,
0.000139297820483867),.UNSPECIFIED.);
#5798=B_SPLINE_CURVE_WITH_KNOTS('',3,(#218643,#218644,#218645,#218646,#218647,
#218648,#218649),.UNSPECIFIED.,.F.,.F.,(4,3,4),(0.,0.00037653926080856,
0.00075440118473929),.UNSPECIFIED.);
#5799=B_SPLINE_CURVE_WITH_KNOTS('',3,(#218650,#218651,#218652,#218653,#218654,
#218655,#218656,#218657,#218658,#218659,#218660,#218661,#218662),
 .UNSPECIFIED.,.F.,.F.,(4,2,2,1,2,2,4),(0.,0.249999999999973,0.374999999999955,
0.437499999999942,0.468749999999936,0.49999999999993,1.),.UNSPECIFIED.);
#5800=B_SPLINE_CURVE_WITH_KNOTS('',3,(#218744,#218745,#218746,#218747,#218748,
#218749,#218750,#218751,#218752,#218753,#218754,#218755,#218756,#218757,
#218758,#218759,#218760,#218761,#218762,#218763,#218764,#218765,#218766,
#218767,#218768,#218769,#218770,#218771,#218772,#218773,#218774,#218775,
#218776,#218777,#218778,#218779,#218780,#218781,#218782,#218783,#218784,
#218785,#218786,#218787,#218788,#218789,#218790,#218791,#218792,#218793,
#218794,#218795,#218796,#218797,#218798,#218799,#218800,#218801,#218802,
#218803,#218804,#218805,#218806,#218807,#218808,#218809,#218810,#218811,
#218812,#218813,#218814,#218815,#218816,#218817,#218818,#218819,#218820,
#218821,#218822),.UNSPECIFIED.,.F.,.F.,(4,3,3,3,3,3,3,3,3,3,3,3,3,3,3,3,
3,3,3,3,3,3,3,3,3,3,4),(0.,0.0844654919461902,0.122470941342419,0.207003614964972,
0.245798182809739,0.249999999999935,0.333296210281669,0.370668428198448,
0.374999999999902,0.441433008969332,0.496093749999876,0.497619617625721,
0.499999999999877,0.547503235522682,0.553623071983059,0.610885110373799,
0.702888851910236,0.730748815474926,0.749999999999938,0.793828402446633,
0.855095787109683,0.859466281586824,0.874999999999969,0.893379318442533,
0.928115077845369,0.972989979546055,0.999999999999993),.UNSPECIFIED.);
#5801=B_SPLINE_CURVE_WITH_KNOTS('',3,(#218823,#218824,#218825,#218826,#218827,
#218828,#218829,#218830,#218831,#218832,#218833,#218834,#218835,#218836,
#218837,#218838,#218839,#218840,#218841,#218842,#218843,#218844,#218845,
#218846,#218847,#218848,#218849,#218850,#218851,#218852,#218853,#218854,
#218855,#218856,#218857,#218858,#218859,#218860,#218861,#218862,#218863,
#218864,#218865,#218866,#218867,#218868,#218869,#218870,#218871,#218872,
#218873,#218874,#218875,#218876,#218877,#218878,#218879,#218880,#218881,
#218882,#218883,#218884,#218885,#218886,#218887,#218888,#218889,#218890,
#218891,#218892,#218893,#218894,#218895,#218896,#218897,#218898,#218899,
#218900,#218901,#218902,#218903,#218904,#218905,#218906,#218907,#218908,
#218909,#218910,#218911,#218912,#218913,#218914,#218915,#218916,#218917,
#218918,#218919,#218920,#218921,#218922,#218923,#218924,#218925,#218926,
#218927,#218928,#218929,#218930,#218931,#218932,#218933,#218934,#218935,
#218936,#218937,#218938,#218939,#218940,#218941,#218942,#218943,#218944,
#218945,#218946,#218947,#218948,#218949,#218950,#218951,#218952,#218953,
#218954,#218955,#218956,#218957,#218958,#218959,#218960,#218961,#218962,
#218963,#218964,#218965,#218966,#218967,#218968,#218969,#218970,#218971,
#218972,#218973,#218974,#218975,#218976,#218977,#218978,#218979,#218980,
#218981,#218982,#218983,#218984,#218985,#218986,#218987,#218988,#218989,
#218990,#218991,#218992,#218993,#218994,#218995,#218996,#218997,#218998,
#218999,#219000,#219001,#219002,#219003),.UNSPECIFIED.,.F.,.F.,(4,3,3,3,
3,3,3,3,3,3,3,3,3,3,3,3,3,3,3,3,3,3,3,3,3,3,3,3,3,3,3,3,3,3,3,3,3,3,3,3,
3,3,3,3,3,3,3,3,3,3,3,3,3,3,3,3,3,3,3,3,4),(0.,0.00666408113292331,0.0129639075512711,
0.0156250000000025,0.021368878326581,0.0234375000000028,0.027343750000003,
0.0312500000000032,0.0412694451432147,0.0468750000000061,0.0568048710303721,
0.0625000000000091,0.0766768025718624,0.090160869705112,0.0937500000000153,
0.0971456960406208,0.0989180593347306,0.101562500000017,0.109375000000019,
0.12500000000002,0.144362575322191,0.16321779851779,0.181421980887489,0.187500000000014,
0.195312500000014,0.199218750000013,0.201823967502558,0.203125000000012,
0.218750000000006,0.228153442731374,0.249999999999999,0.312499999999983,
0.343749999999977,0.348147427493963,0.351562499999975,0.359374999999974,
0.37499999999998,0.391144204108983,0.401883223401621,0.406249999999994,
0.421875000000003,0.430859737207603,0.437500000000011,0.457620056656504,
0.468750000000032,0.484375000000043,0.492187500000048,0.496093750000049,
0.50000000000005,0.550509377734149,0.579051287512532,0.636233117757933,
0.692439018597193,0.747357765783153,0.764210507176442,0.80695746796269,
0.849189186907056,0.890619527408069,0.930878773987873,0.975556510704755,
1.),.UNSPECIFIED.);
#5802=B_SPLINE_CURVE_WITH_KNOTS('',3,(#219033,#219034,#219035,#219036,#219037,
#219038,#219039,#219040,#219041,#219042,#219043,#219044,#219045,#219046,
#219047,#219048,#219049,#219050,#219051,#219052,#219053,#219054,#219055,
#219056,#219057,#219058,#219059,#219060,#219061,#219062,#219063,#219064,
#219065,#219066),.UNSPECIFIED.,.F.,.F.,(4,3,3,3,3,3,3,3,3,3,3,4),(0.,0.0896986624636303,
0.182830915896643,0.281579891583428,0.383870416571602,0.490905478463475,
0.5,0.612068495674318,0.726057759562033,0.839966626268522,0.953108020681144,
1.),.UNSPECIFIED.);
#5803=B_SPLINE_CURVE_WITH_KNOTS('',3,(#219448,#219449,#219450,#219451,#219452,
#219453,#219454,#219455,#219456,#219457,#219458,#219459,#219460,#219461),
 .UNSPECIFIED.,.F.,.F.,(4,2,2,1,1,2,2,4),(0.,0.249999999999997,0.374999999999996,
0.437499999999996,0.468749999999995,0.484374999999995,0.499999999999994,
1.),.UNSPECIFIED.);
#5804=B_SPLINE_CURVE_WITH_KNOTS('',3,(#219463,#219464,#219465,#219466,#219467,
#219468,#219469,#219470,#219471,#219472,#219473,#219474,#219475,#219476,
#219477,#219478),.UNSPECIFIED.,.F.,.F.,(4,2,2,1,1,1,1,2,2,4),(0.,0.24999999999999,
0.374999999999987,0.437499999999985,0.468749999999984,0.484374999999982,
0.492187499999983,0.496093749999983,0.499999999999983,1.),.UNSPECIFIED.);
#5805=B_SPLINE_CURVE_WITH_KNOTS('',3,(#219480,#219481,#219482,#219483,#219484,
#219485),.UNSPECIFIED.,.F.,.F.,(4,2,4),(0.,0.5,0.999993881110035),
 .UNSPECIFIED.);
#5806=B_SPLINE_CURVE_WITH_KNOTS('',3,(#219486,#219487,#219488,#219489,#219490,
#219491,#219492,#219493,#219494,#219495,#219496,#219497,#219498,#219499,
#219500,#219501,#219502,#219503,#219504,#219505,#219506,#219507,#219508,
#219509,#219510,#219511,#219512,#219513,#219514,#219515,#219516,#219517,
#219518,#219519,#219520,#219521,#219522,#219523,#219524,#219525,#219526,
#219527,#219528,#219529,#219530,#219531,#219532,#219533,#219534,#219535,
#219536,#219537,#219538,#219539,#219540,#219541,#219542,#219543,#219544,
#219545,#219546,#219547,#219548,#219549,#219550,#219551,#219552,#219553,
#219554,#219555,#219556,#219557,#219558,#219559,#219560,#219561,#219562,
#219563,#219564,#219565,#219566,#219567,#219568,#219569,#219570,#219571,
#219572,#219573,#219574,#219575,#219576,#219577,#219578,#219579,#219580,
#219581,#219582,#219583,#219584,#219585,#219586,#219587,#219588,#219589,
#219590,#219591,#219592,#219593,#219594,#219595,#219596,#219597,#219598,
#219599,#219600,#219601,#219602,#219603,#219604,#219605,#219606,#219607,
#219608,#219609,#219610,#219611,#219612,#219613,#219614,#219615,#219616,
#219617,#219618,#219619,#219620,#219621,#219622,#219623,#219624,#219625,
#219626,#219627,#219628,#219629,#219630,#219631,#219632,#219633,#219634,
#219635,#219636,#219637,#219638,#219639,#219640,#219641,#219642,#219643,
#219644,#219645,#219646,#219647,#219648,#219649,#219650,#219651,#219652,
#219653,#219654,#219655,#219656,#219657,#219658,#219659,#219660,#219661,
#219662,#219663,#219664,#219665,#219666,#219667,#219668,#219669,#219670,
#219671,#219672,#219673,#219674,#219675,#219676,#219677,#219678,#219679,
#219680,#219681,#219682,#219683,#219684,#219685,#219686,#219687,#219688,
#219689,#219690,#219691,#219692,#219693,#219694,#219695,#219696,#219697,
#219698,#219699,#219700,#219701,#219702,#219703,#219704,#219705,#219706,
#219707,#219708,#219709,#219710,#219711,#219712,#219713,#219714,#219715,
#219716,#219717,#219718,#219719,#219720,#219721,#219722,#219723,#219724,
#219725,#219726,#219727,#219728,#219729,#219730,#219731,#219732,#219733,
#219734,#219735,#219736,#219737,#219738,#219739,#219740,#219741,#219742,
#219743,#219744,#219745,#219746,#219747,#219748,#219749,#219750,#219751,
#219752,#219753,#219754,#219755,#219756,#219757,#219758,#219759,#219760,
#219761,#219762,#219763,#219764,#219765,#219766,#219767,#219768,#219769,
#219770,#219771,#219772,#219773,#219774,#219775,#219776,#219777,#219778,
#219779,#219780,#219781,#219782,#219783,#219784,#219785,#219786,#219787,
#219788,#219789,#219790,#219791,#219792,#219793,#219794,#219795,#219796,
#219797,#219798,#219799,#219800,#219801,#219802,#219803,#219804,#219805,
#219806,#219807,#219808,#219809,#219810,#219811,#219812,#219813,#219814,
#219815,#219816,#219817,#219818,#219819,#219820,#219821,#219822,#219823,
#219824,#219825),.UNSPECIFIED.,.F.,.F.,(4,3,3,3,3,3,3,3,3,3,3,3,3,3,3,3,
3,3,3,3,3,3,3,3,3,3,3,3,3,3,3,3,3,3,3,3,3,3,3,3,3,3,3,3,3,3,3,3,3,3,3,3,
3,3,3,3,3,3,3,3,3,3,3,3,3,3,3,3,3,3,3,3,3,3,3,3,3,3,3,3,3,3,3,3,3,3,3,3,
3,3,3,3,3,3,3,3,3,3,3,3,3,3,3,3,3,3,3,3,3,3,3,3,3,4),(-0.0339772660920509,
-0.0325203430581518,-0.032386048693209,-0.0318780990992314,-0.0306598615635381,
-0.0302573909015708,-0.0297789321064117,-0.0276581536141349,-0.0259928474480018,
-0.0255805981207726,-0.0249267022358351,-0.0245310146243628,-0.0243936296904867,
-0.024326995626826,-0.0242603615617803,-0.024127093428565,-0.023860557156862,
-0.0234814311279529,-0.0217282650368408,-0.0213822641351333,-0.0190428209661952,
-0.0174636751340817,-0.0171839301494941,-0.0166591384012892,-0.016397507911909,
-0.0162642461309164,-0.0161976136106437,-0.0161343466530843,-0.0161309799318905,
-0.0158644424540839,-0.0153313628316309,-0.0150847631566745,-0.013198990770689,
-0.0129855961638549,-0.0106966589063659,-0.00893402822640652,-0.00878726217821559,
-0.0071484990754369,-0.00680141898440107,-0.00668809518539594,-0.00573515795867427,
-0.00563851168898612,-0.00520205258212156,-0.00511371994078121,-0.00506876286241163,
-0.00500210501706407,-0.00496877348718764,-0.00493544103430002,-0.00466882155644317,
-0.0045889281925763,-0.00312096876785597,-0.00254453035286046,-0.00248976119975661,
-0.00148840346537639,-0.000436339145097795,-0.000390594206936927,0.00046358534986054,
0.000613822975248156,0.00141916260425755,0.00166725247387988,0.00170857278588276,
0.00317162738240526,0.00379103467916695,0.00380773977870245,0.00463539969377852,
0.00485732327511229,0.00485907394948943,0.00492583309157905,0.00495921266595899,
0.00499259224328974,0.00512611059303194,0.00539314760000376,0.00590690677152213,
0.00592722382056531,0.00800607376434179,0.00806356257284219,0.0111178351121071,
0.0122044077499811,0.0123363966390162,0.0143035747428008,0.0144728977439664,
0.0153531582392106,0.0155411644433074,0.0158779499874155,0.0160752947519555,
0.0161086774948306,0.016142060232708,0.0161754429719895,0.0162088257190771,
0.0163423569135267,0.0164027417356204,0.0166094212137446,0.0187054832686268,
0.0206010757212598,0.0208827465629589,0.0227002427140795,0.0230196099239667,
0.0235538292510131,0.0237498262104893,0.0238209047714043,0.0239544298768528,
0.0240211910330551,0.0240879522750274,0.0242746179586943,0.0247994097068993,
0.0251563789301884,0.0273038426614853,0.0289977436925387,0.0294352127171892,
0.0310969106853584,0.0315785446359996,0.0322002513430661,0.0327863759675397,
0.033196077678178),.UNSPECIFIED.);
#5807=B_SPLINE_CURVE_WITH_KNOTS('',3,(#219827,#219828,#219829,#219830,#219831,
#219832,#219833,#219834,#219835,#219836,#219837,#219838,#219839,#219840),
 .UNSPECIFIED.,.F.,.F.,(4,2,2,2,2,2,4),(0.,0.177361653110089,0.396250772308705,
0.834029010705937,0.943473570305246,0.9981958501049,1.),.UNSPECIFIED.);
#5808=B_SPLINE_CURVE_WITH_KNOTS('',3,(#219842,#219843,#219844,#219845,#219846,
#219847,#219848,#219849,#219850,#219851,#219852,#219853,#219854,#219855,
#219856,#219857,#219858,#219859,#219860,#219861,#219862,#219863,#219864,
#219865,#219866),.UNSPECIFIED.,.F.,.F.,(4,2,1,1,2,1,2,2,2,2,2,2,2,4),(0.,
0.00781250000000103,0.0156250000000021,0.0312500000000029,0.0625000000000033,
0.125000000000004,0.250000000000004,0.500000000000004,0.750000000000003,
0.875000000000004,0.968750000000004,0.984375000000003,0.992187500000002,
1.),.UNSPECIFIED.);
#5809=B_SPLINE_CURVE_WITH_KNOTS('',3,(#219868,#219869,#219870,#219871,#219872,
#219873,#219874,#219875,#219876,#219877,#219878,#219879,#219880,#219881,
#219882,#219883,#219884,#219885,#219886,#219887,#219888,#219889,#219890,
#219891,#219892,#219893,#219894,#219895,#219896,#219897,#219898,#219899,
#219900,#219901,#219902,#219903,#219904,#219905,#219906,#219907,#219908,
#219909,#219910,#219911,#219912,#219913,#219914,#219915,#219916,#219917,
#219918,#219919,#219920,#219921,#219922,#219923,#219924,#219925,#219926,
#219927,#219928,#219929,#219930,#219931),.UNSPECIFIED.,.F.,.F.,(4,3,3,3,
3,3,3,3,3,3,3,3,3,3,3,3,3,3,3,3,3,4),(0.,0.00477412889230797,0.00781250000000079,
0.0106654879371521,0.0156250000000016,0.0312500000000015,0.0342309236257492,
0.0625000000000014,0.0813617964285784,0.26988528574785,0.646932264386396,
0.835455753705669,0.929717498365307,0.96875,0.976848370695126,0.984375,
0.988631089346493,0.9921875,0.994522449578665,0.99609375,0.997468127244565,
1.),.UNSPECIFIED.);
#5810=B_SPLINE_CURVE_WITH_KNOTS('',3,(#219933,#219934,#219935,#219936,#219937,
#219938,#219939,#219940,#219941,#219942,#219943,#219944,#219945,#219946,
#219947,#219948,#219949,#219950,#219951,#219952,#219953,#219954,#219955,
#219956,#219957,#219958,#219959,#219960,#219961,#219962,#219963,#219964,
#219965,#219966),.UNSPECIFIED.,.F.,.F.,(4,3,3,3,3,3,3,3,3,3,3,4),(0.,0.000940021348058807,
0.0156250000000013,0.0312500000000026,0.0544722738485389,0.0625000000000029,
0.125000000000003,0.48273015832635,0.69685910820713,0.750000000000001,0.910988091716797,
1.),.UNSPECIFIED.);
#5811=B_SPLINE_CURVE_WITH_KNOTS('',3,(#219968,#219969,#219970,#219971,#219972,
#219973,#219974,#219975,#219976,#219977,#219978,#219979,#219980,#219981,
#219982,#219983,#219984,#219985,#219986,#219987,#219988,#219989,#219990,
#219991,#219992,#219993,#219994,#219995,#219996,#219997,#219998,#219999,
#220000,#220001,#220002,#220003,#220004,#220005,#220006,#220007),
 .UNSPECIFIED.,.F.,.F.,(4,3,3,3,3,3,3,3,3,3,3,3,3,4),(0.,0.000267216601111374,
0.0131577248626226,0.120048731344561,0.225313165495544,0.329701106959535,
0.433524683977464,0.5,0.648342485904365,0.664128121681686,0.771050593343276,
0.877973065004865,0.967295544654949,0.999999999999711),.UNSPECIFIED.);
#5812=B_SPLINE_CURVE_WITH_KNOTS('',3,(#220008,#220009,#220010,#220011,#220012,
#220013,#220014,#220015,#220016,#220017,#220018,#220019,#220020,#220021,
#220022,#220023,#220024,#220025,#220026,#220027,#220028,#220029,#220030,
#220031,#220032,#220033,#220034,#220035,#220036,#220037,#220038,#220039,
#220040,#220041,#220042,#220043,#220044,#220045,#220046,#220047,#220048,
#220049,#220050,#220051,#220052,#220053,#220054,#220055,#220056,#220057,
#220058,#220059,#220060,#220061,#220062,#220063,#220064,#220065,#220066,
#220067,#220068,#220069,#220070,#220071,#220072,#220073,#220074,#220075,
#220076,#220077,#220078,#220079,#220080,#220081,#220082,#220083,#220084,
#220085,#220086,#220087,#220088,#220089,#220090,#220091,#220092,#220093,
#220094,#220095,#220096,#220097,#220098,#220099,#220100,#220101),
 .UNSPECIFIED.,.F.,.F.,(4,3,3,3,3,3,3,3,3,3,3,3,3,3,3,3,3,3,3,3,3,3,3,3,
3,3,3,3,3,3,3,4),(0.,2.26241632322562E-6,0.00248004559774673,0.0035223755445969,
0.00701329037683304,0.0422709661520407,0.0597479664257431,0.0938229732817104,
0.12793820187041,0.155552859161154,0.190169805986124,0.22547721974652,0.25,
0.330973628752631,0.342469754057526,0.375,0.4375,0.46875,0.484375,0.4921875,
0.5,0.591257092400212,0.683349188310747,0.719815403392367,0.815155205598429,
0.910495007804491,0.9582618981018,0.962510291841565,0.982178193347656,0.994141900010685,
0.997133062479398,0.999999999936109),.UNSPECIFIED.);
#5813=B_SPLINE_CURVE_WITH_KNOTS('',3,(#220184,#220185,#220186,#220187,#220188,
#220189,#220190,#220191,#220192,#220193,#220194,#220195,#220196),
 .UNSPECIFIED.,.F.,.F.,(4,3,3,3,4),(0.,0.000262347006043535,0.00052508232379868,
0.000788127838510806,0.00105144790336124),.UNSPECIFIED.);
#5814=B_SPLINE_CURVE_WITH_KNOTS('',3,(#220197,#220198,#220199,#220200,#220201,
#220202,#220203,#220204,#220205,#220206,#220207,#220208,#220209,#220210,
#220211,#220212,#220213,#220214,#220215,#220216,#220217,#220218,#220219,
#220220,#220221,#220222,#220223,#220224,#220225,#220226,#220227,#220228,
#220229,#220230,#220231,#220232,#220233,#220234,#220235,#220236,#220237,
#220238,#220239,#220240,#220241,#220242,#220243,#220244,#220245,#220246,
#220247,#220248,#220249,#220250,#220251,#220252,#220253,#220254,#220255,
#220256,#220257,#220258,#220259,#220260,#220261,#220262,#220263,#220264,
#220265,#220266,#220267,#220268,#220269,#220270,#220271,#220272,#220273,
#220274,#220275,#220276,#220277,#220278,#220279,#220280,#220281,#220282,
#220283,#220284,#220285,#220286,#220287,#220288,#220289,#220290,#220291,
#220292,#220293,#220294,#220295,#220296,#220297,#220298,#220299,#220300,
#220301,#220302,#220303,#220304,#220305,#220306,#220307,#220308,#220309,
#220310,#220311,#220312,#220313,#220314,#220315,#220316,#220317),
 .UNSPECIFIED.,.F.,.F.,(4,3,3,3,3,3,3,3,3,3,3,3,3,3,3,3,3,3,3,3,3,3,3,3,
3,3,3,3,3,3,3,3,3,3,3,3,3,3,3,3,4),(0.,0.0481141113853886,0.0922200232969331,
0.124999999999905,0.164962385534248,0.187499999999854,0.218749999999828,
0.234374999999811,0.236646032545267,0.249999999999793,0.318804263020611,
0.374999999999725,0.437499999999693,0.466954438082284,0.46874999999968,
0.484374999999679,0.498424907910557,0.499999999999678,0.562499999999683,
0.620664099512309,0.624999999999687,0.687499999999698,0.718749999999709,
0.721406653442237,0.734374999999714,0.742187499999717,0.746337890624721,
0.748348236083708,0.749380988230567,0.749974461597412,0.750497174889094,
0.790225960908271,0.832612980454062,0.853806490226957,0.859104867670181,
0.860293591729929,0.874999999999853,0.902852200787948,0.935747746931192,
0.975590086367635,1.),.UNSPECIFIED.);
#5815=B_SPLINE_CURVE_WITH_KNOTS('',3,(#220399,#220400,#220401,#220402,#220403,
#220404,#220405,#220406,#220407,#220408,#220409,#220410,#220411,#220412,
#220413,#220414,#220415,#220416,#220417,#220418,#220419,#220420,#220421,
#220422,#220423,#220424,#220425,#220426,#220427,#220428,#220429,#220430,
#220431,#220432,#220433,#220434,#220435,#220436,#220437,#220438,#220439,
#220440,#220441,#220442,#220443,#220444,#220445,#220446,#220447,#220448,
#220449,#220450,#220451,#220452,#220453,#220454,#220455,#220456,#220457,
#220458,#220459,#220460,#220461,#220462,#220463,#220464,#220465,#220466,
#220467,#220468,#220469,#220470,#220471,#220472,#220473,#220474,#220475,
#220476,#220477,#220478,#220479,#220480,#220481,#220482,#220483,#220484,
#220485,#220486,#220487,#220488,#220489,#220490,#220491,#220492,#220493,
#220494,#220495,#220496,#220497,#220498,#220499,#220500,#220501,#220502,
#220503,#220504,#220505,#220506,#220507,#220508,#220509,#220510,#220511,
#220512,#220513),.UNSPECIFIED.,.F.,.F.,(4,3,3,3,3,3,3,3,3,3,3,3,3,3,3,3,
3,3,3,3,3,3,3,3,3,3,3,3,3,3,3,3,3,3,3,3,3,3,4),(0.,0.125000000000075,0.129138910233674,
0.187500000000111,0.218750000000129,0.234375000000138,0.245584641133974,
0.248410569305501,0.250000000000148,0.336537419726474,0.371504451325829,
0.375000000000245,0.437500000000291,0.468750000000316,0.484375000000329,
0.492187500000333,0.496093750000332,0.498211359913546,0.500000000000331,
0.55551957851444,0.603575446450059,0.615889256785246,0.625000000000302,
0.687500000000288,0.718750000000278,0.734375000000271,0.742187500000269,
0.746093750000268,0.748046875000267,0.748826280767137,0.750000000000266,
0.794921440761665,0.80172102164972,0.840711183572136,0.859490017116372,
0.890874071151793,0.924376073377366,0.980784458226199,1.),.UNSPECIFIED.);
#5816=B_SPLINE_CURVE_WITH_KNOTS('',3,(#220514,#220515,#220516,#220517,#220518,
#220519,#220520,#220521,#220522,#220523,#220524,#220525,#220526,#220527,
#220528,#220529,#220530,#220531,#220532,#220533,#220534,#220535,#220536,
#220537,#220538,#220539,#220540,#220541,#220542,#220543,#220544,#220545,
#220546,#220547,#220548,#220549,#220550,#220551,#220552,#220553,#220554,
#220555,#220556,#220557,#220558,#220559,#220560,#220561,#220562,#220563,
#220564,#220565,#220566,#220567,#220568,#220569,#220570,#220571,#220572,
#220573,#220574,#220575,#220576,#220577,#220578,#220579,#220580,#220581,
#220582,#220583,#220584,#220585,#220586,#220587,#220588,#220589,#220590,
#220591,#220592,#220593),.UNSPECIFIED.,.F.,.F.,(4,2,2,2,1,2,2,2,2,2,2,2,
1,1,2,2,1,1,1,2,2,2,2,1,2,2,2,2,1,1,2,2,2,2,2,1,1,2,2,2,2,2,1,2,2,4),(0.,
0.062500000000062,0.0937500000000954,0.10937500000011,0.117187500000119,
0.123046875000124,0.125000000000124,0.156250000000161,0.171875000000177,
0.187500000000193,0.218750000000225,0.234375000000241,0.242187500000252,
0.246093750000255,0.248046875000261,0.250000000000266,0.312500000000522,
0.343750000000647,0.35937500000071,0.373046875000764,0.37500000000077,0.406250000000778,
0.421875000000782,0.429687500000782,0.433593750000785,0.437500000000788,
0.46875000000079,0.484375000000792,0.492187500000789,0.496093750000792,
0.498046875000789,0.500000000000786,0.625000000000577,0.640625000000551,
0.644531250000544,0.648437500000537,0.656250000000529,0.687500000000512,
0.750000000000475,0.781250000000457,0.785156250000452,0.789062500000447,
0.796875000000434,0.812500000000401,0.875000000000267,1.),.UNSPECIFIED.);
#5817=B_SPLINE_CURVE_WITH_KNOTS('',3,(#220610,#220611,#220612,#220613,#220614,
#220615,#220616,#220617,#220618,#220619),.UNSPECIFIED.,.F.,.F.,(4,3,3,4),
(0.,0.000342739116435002,0.000689887215256671,0.000728014676542687),
 .UNSPECIFIED.);
#5818=B_SPLINE_CURVE_WITH_KNOTS('',3,(#220633,#220634,#220635,#220636,#220637,
#220638,#220639,#220640,#220641,#220642),.UNSPECIFIED.,.F.,.F.,(4,3,3,4),
(0.,0.331792271676137,0.665896135838068,1.),.UNSPECIFIED.);
#5819=B_SPLINE_CURVE_WITH_KNOTS('',3,(#220837,#220838,#220839,#220840,#220841,
#220842,#220843,#220844,#220845,#220846,#220847,#220848,#220849,#220850,
#220851,#220852,#220853,#220854,#220855,#220856,#220857,#220858,#220859,
#220860,#220861,#220862,#220863,#220864,#220865,#220866,#220867,#220868,
#220869,#220870),.UNSPECIFIED.,.F.,.F.,(4,1,1,2,2,2,1,1,2,2,2,2,2,2,2,1,
1,2,2,4),(0.,0.00781250000002213,0.0117187500000346,0.0146484375000462,
0.0156250000000499,0.0234375000000586,0.027343750000063,0.029296875000065,
0.030273437500066,0.0312500000000671,0.0625000000000648,0.12500000000006,
0.187500000000056,0.250000000000051,0.375000000000042,0.437500000000038,
0.468750000000035,0.484375000000034,0.500000000000032,0.999999868413402),
 .UNSPECIFIED.);
#5820=B_SPLINE_CURVE_WITH_KNOTS('',3,(#220871,#220872,#220873,#220874,#220875,
#220876,#220877,#220878,#220879,#220880),.UNSPECIFIED.,.F.,.F.,(4,2,2,2,
4),(4.18095462764722E-18,0.00255445063423646,0.00383167595135469,0.00447028860991381,
0.00510890126847292),.UNSPECIFIED.);
#5821=B_SPLINE_CURVE_WITH_KNOTS('',3,(#220882,#220883,#220884,#220885,#220886,
#220887,#220888,#220889,#220890,#220891,#220892,#220893,#220894,#220895,
#220896,#220897,#220898,#220899,#220900,#220901,#220902,#220903,#220904,
#220905,#220906,#220907,#220908,#220909,#220910,#220911,#220912,#220913,
#220914,#220915,#220916,#220917,#220918,#220919,#220920,#220921,#220922,
#220923,#220924,#220925,#220926,#220927,#220928,#220929,#220930,#220931,
#220932,#220933,#220934,#220935,#220936,#220937,#220938,#220939,#220940,
#220941,#220942,#220943,#220944,#220945,#220946,#220947,#220948,#220949,
#220950,#220951,#220952,#220953,#220954,#220955,#220956,#220957,#220958,
#220959,#220960,#220961,#220962,#220963,#220964,#220965,#220966,#220967,
#220968,#220969,#220970,#220971,#220972,#220973,#220974,#220975,#220976,
#220977,#220978,#220979,#220980,#220981,#220982,#220983,#220984,#220985,
#220986,#220987,#220988,#220989,#220990,#220991,#220992,#220993,#220994,
#220995,#220996,#220997,#220998,#220999,#221000,#221001,#221002,#221003,
#221004,#221005,#221006,#221007,#221008,#221009,#221010,#221011,#221012,
#221013,#221014,#221015,#221016,#221017,#221018,#221019,#221020,#221021,
#221022,#221023,#221024,#221025,#221026,#221027,#221028,#221029,#221030,
#221031,#221032,#221033,#221034,#221035,#221036,#221037,#221038,#221039,
#221040,#221041,#221042,#221043,#221044,#221045,#221046,#221047),
 .UNSPECIFIED.,.F.,.F.,(4,3,3,3,3,3,3,3,3,3,3,3,3,3,3,3,3,3,3,3,3,3,3,3,
3,3,3,3,3,3,3,3,3,3,3,3,3,3,3,3,3,3,3,3,3,3,3,3,3,3,3,3,3,3,3,4),(3.84474371945078E-15,
0.00129418777048261,0.00218682165402767,0.00327794728486691,0.00398945644969312,
0.00437364330805532,0.0050976652962974,0.00620616680151919,0.00795383201123593,
0.00842283797271545,0.00874728661611061,0.0106381507815742,0.0109341082701383,
0.0111918496720621,0.0113302678430169,0.0113648723663165,0.0113994769397404,
0.0114686863527641,0.0114808136836452,0.0117455395577679,0.0120275190971521,
0.0128530198691882,0.0131209299241659,0.0165925164204044,0.0172816770907965,
0.0174945732322213,0.019495073308936,0.019681394886249,0.0200483162030429,
0.0202281002997558,0.0203249209658382,0.0204632190439302,0.0205323676346298,
0.0206015162605072,0.0207748057132628,0.0217079731878734,0.0218682165402766,
0.0241483517759356,0.0261345203104882,0.0262418598483319,0.0275481788415872,
0.0283480821017152,0.0284286815023595,0.0293305775946609,0.0294547291211152,
0.0295220923293734,0.0300079248057894,0.0300687977428803,0.0302844849745231,
0.0303536218586976,0.0303881901705619,0.0304227584828701,0.0305610330454487,
0.0306155031563872,0.0335427501364484,0.0349891464644424),.UNSPECIFIED.);
#5822=B_SPLINE_CURVE_WITH_KNOTS('',3,(#221049,#221050,#221051,#221052,#221053,
#221054,#221055,#221056,#221057,#221058,#221059,#221060,#221061,#221062,
#221063,#221064,#221065,#221066,#221067,#221068,#221069,#221070,#221071,
#221072,#221073,#221074,#221075,#221076,#221077,#221078,#221079,#221080,
#221081,#221082,#221083,#221084,#221085,#221086,#221087,#221088,#221089,
#221090,#221091,#221092,#221093,#221094,#221095,#221096,#221097,#221098,
#221099,#221100,#221101,#221102,#221103,#221104,#221105,#221106,#221107,
#221108,#221109,#221110,#221111,#221112),.UNSPECIFIED.,.F.,.F.,(4,3,3,3,
3,3,3,3,3,3,3,3,3,3,3,3,3,3,3,3,3,4),(3.94435119578486E-14,0.0661070715252713,
0.131240897937816,0.140624999999884,0.187499999999846,0.249999999999794,
0.308921024725339,0.365490856280017,0.374999999999676,0.428753346904277,
0.437499999999626,0.46874999999959,0.484374999999562,0.492187499999558,
0.4984488684236,0.499662271028205,0.499999999999553,0.664758583825297,0.749999999999777,
0.838636570956166,0.926879967465366,0.999999999865913),.UNSPECIFIED.);
#5823=B_SPLINE_CURVE_WITH_KNOTS('',3,(#221114,#221115,#221116,#221117,#221118,
#221119,#221120,#221121,#221122,#221123,#221124,#221125,#221126,#221127,
#221128,#221129,#221130,#221131,#221132,#221133,#221134,#221135,#221136,
#221137,#221138,#221139,#221140,#221141,#221142,#221143,#221144,#221145,
#221146,#221147,#221148,#221149,#221150,#221151,#221152,#221153,#221154,
#221155,#221156),.UNSPECIFIED.,.F.,.F.,(4,1,1,2,2,2,1,1,2,2,2,2,2,2,1,1,
1,2,2,2,1,1,1,1,2,2,4),(0.,0.00390624999994919,0.00585937499992379,0.00732421874990716,
0.00781249999990194,0.0117187499999027,0.013671874999902,0.0146484374999016,
0.0151367187499008,0.0156249999998999,0.0312499999998973,0.0624999999998953,
0.0937499999998933,0.124999999999891,0.187499999999888,0.218749999999886,
0.234374999999886,0.242187499999887,0.249999999999888,0.374999999999892,
0.437499999999895,0.468749999999897,0.484374999999897,0.492187499999897,
0.496093749999898,0.499999999999899,1.),.UNSPECIFIED.);
#5824=B_SPLINE_CURVE_WITH_KNOTS('',3,(#221157,#221158,#221159,#221160,#221161,
#221162,#221163,#221164,#221165,#221166,#221167,#221168,#221169,#221170,
#221171,#221172,#221173,#221174,#221175,#221176,#221177,#221178,#221179,
#221180,#221181,#221182,#221183,#221184,#221185,#221186,#221187,#221188,
#221189,#221190,#221191,#221192,#221193,#221194,#221195,#221196,#221197,
#221198,#221199,#221200,#221201,#221202,#221203,#221204,#221205,#221206,
#221207,#221208,#221209,#221210,#221211,#221212,#221213,#221214,#221215,
#221216,#221217,#221218,#221219,#221220,#221221,#221222,#221223,#221224,
#221225,#221226,#221227,#221228,#221229,#221230,#221231,#221232,#221233,
#221234,#221235,#221236,#221237,#221238,#221239,#221240,#221241,#221242,
#221243,#221244,#221245,#221246,#221247,#221248,#221249,#221250,#221251,
#221252,#221253,#221254,#221255,#221256,#221257,#221258,#221259,#221260,
#221261,#221262,#221263,#221264,#221265,#221266,#221267,#221268),
 .UNSPECIFIED.,.F.,.F.,(4,3,3,3,3,3,3,3,3,3,3,3,3,3,3,3,3,3,3,3,3,3,3,3,
3,3,3,3,3,3,3,3,3,3,3,3,3,4),(0.,0.00282254399121512,0.00586614516938873,
0.00651606421840167,0.0228133545141081,0.0388819768075745,0.054179413201791,
0.0625000000000008,0.0703124999999999,0.0762984211550201,0.078124999999999,
0.0937499999999989,0.113221577872514,0.124999999999998,0.187499999999997,
0.221409998208068,0.238251470487989,0.249614071096417,0.253335824028494,
0.356141776447435,0.396642919128224,0.448321459564108,0.47416072978205,
0.480620547336536,0.483496454516943,0.485164620119042,0.496996851944816,
0.499999999999993,0.641721524748589,0.788214551204109,0.838614676791042,
0.924794957777326,0.953285960601031,0.956447955489975,0.985643664365405,
0.992933726435535,0.996578250210837,0.999999904445776),.UNSPECIFIED.);
#5825=B_SPLINE_CURVE_WITH_KNOTS('',3,(#221288,#221289,#221290,#221291,#221292,
#221293,#221294,#221295,#221296,#221297,#221298,#221299,#221300,#221301,
#221302,#221303,#221304,#221305,#221306,#221307,#221308,#221309,#221310,
#221311,#221312,#221313,#221314,#221315),.UNSPECIFIED.,.F.,.F.,(4,3,3,3,
3,3,3,3,3,4),(0.,0.117448719031058,0.23465352743689,0.35179443705116,0.469085047802828,
0.5,0.625,0.748726478170368,0.874363239085184,1.),.UNSPECIFIED.);
#5826=B_SPLINE_CURVE_WITH_KNOTS('',3,(#221331,#221332,#221333,#221334,#221335,
#221336,#221337,#221338,#221339,#221340),.UNSPECIFIED.,.F.,.F.,(4,3,3,4),
(0.,0.406538901690834,0.808488591965978,0.999999999958054),
 .UNSPECIFIED.);
#5827=B_SPLINE_CURVE_WITH_KNOTS('',3,(#221359,#221360,#221361,#221362,#221363,
#221364,#221365),.UNSPECIFIED.,.F.,.F.,(4,3,4),(0.,5.20100074843796E-5,
8.9937829810603E-5),.UNSPECIFIED.);
#5828=B_SPLINE_CURVE_WITH_KNOTS('',3,(#221399,#221400,#221401,#221402,#221403,
#221404,#221405,#221406,#221407,#221408,#221409,#221410,#221411,#221412,
#221413,#221414,#221415,#221416,#221417,#221418,#221419,#221420,#221421,
#221422,#221423,#221424,#221425),.UNSPECIFIED.,.F.,.F.,(4,2,2,1,1,2,2,2,
2,2,2,1,2,2,4),(0.,0.125000000000187,0.187500000000272,0.218750000000309,
0.234375000000323,0.242187500000315,0.250000000000307,0.375000000000268,
0.437500000000258,0.500000000000248,0.62500000000022,0.687500000000207,
0.718750000000191,0.750000000000176,1.),.UNSPECIFIED.);
#5829=B_SPLINE_CURVE_WITH_KNOTS('',3,(#221426,#221427,#221428,#221429,#221430,
#221431,#221432,#221433,#221434,#221435,#221436,#221437,#221438),
 .UNSPECIFIED.,.F.,.F.,(4,3,3,3,4),(1.38777878078145E-17,0.000218644279510345,
0.000437193341879142,0.000655638180349197,0.000873969830693171),
 .UNSPECIFIED.);
#5830=B_SPLINE_CURVE_WITH_KNOTS('',3,(#221502,#221503,#221504,#221505,#221506,
#221507,#221508,#221509,#221510,#221511,#221512,#221513,#221514,#221515,
#221516,#221517,#221518,#221519,#221520,#221521,#221522,#221523,#221524,
#221525,#221526,#221527,#221528,#221529,#221530,#221531,#221532,#221533,
#221534,#221535,#221536,#221537,#221538,#221539,#221540,#221541,#221542,
#221543,#221544,#221545,#221546,#221547,#221548,#221549,#221550,#221551,
#221552,#221553,#221554,#221555,#221556,#221557,#221558,#221559,#221560,
#221561,#221562,#221563,#221564,#221565,#221566,#221567,#221568,#221569,
#221570,#221571,#221572,#221573,#221574,#221575,#221576,#221577,#221578,
#221579,#221580,#221581,#221582,#221583,#221584,#221585,#221586,#221587,
#221588,#221589,#221590,#221591,#221592,#221593,#221594,#221595,#221596,
#221597,#221598,#221599,#221600,#221601,#221602,#221603,#221604,#221605,
#221606,#221607,#221608,#221609,#221610,#221611,#221612,#221613,#221614,
#221615,#221616,#221617,#221618,#221619,#221620,#221621,#221622,#221623,
#221624,#221625,#221626,#221627,#221628,#221629,#221630,#221631,#221632,
#221633,#221634,#221635,#221636,#221637,#221638,#221639,#221640,#221641,
#221642,#221643,#221644,#221645,#221646,#221647,#221648,#221649,#221650,
#221651,#221652,#221653,#221654,#221655,#221656,#221657,#221658,#221659,
#221660,#221661,#221662,#221663,#221664,#221665,#221666,#221667,#221668,
#221669,#221670,#221671,#221672,#221673,#221674,#221675,#221676,#221677,
#221678,#221679,#221680,#221681,#221682,#221683,#221684,#221685,#221686,
#221687,#221688,#221689,#221690,#221691,#221692,#221693,#221694,#221695,
#221696,#221697,#221698,#221699,#221700,#221701,#221702,#221703,#221704,
#221705,#221706,#221707,#221708,#221709,#221710,#221711,#221712,#221713,
#221714,#221715,#221716,#221717,#221718,#221719,#221720,#221721,#221722,
#221723,#221724,#221725,#221726,#221727,#221728,#221729,#221730,#221731,
#221732,#221733,#221734,#221735,#221736,#221737,#221738,#221739,#221740,
#221741,#221742,#221743,#221744,#221745,#221746,#221747,#221748),
 .UNSPECIFIED.,.F.,.F.,(4,3,3,3,3,3,3,3,3,3,3,3,3,3,3,3,3,3,3,3,3,3,3,3,
3,3,3,3,3,3,3,3,3,3,3,3,3,3,3,3,3,3,3,3,3,3,3,3,3,3,3,3,3,3,3,3,3,3,3,3,
3,3,3,3,3,3,3,3,3,3,3,3,3,3,3,3,3,3,3,3,3,3,4),(0.,0.0312499999999464,0.0468749999999195,
0.0546874999999061,0.0585937499999004,0.0624999999998947,0.0816944959084324,
0.0937499999998461,0.109374999999822,0.117187499999809,0.1210937499998,
0.123046874999798,0.124999999999796,0.151338478147273,0.187499999999701,
0.218749999999654,0.234374999999631,0.246093749999614,0.24999999999961,
0.283734989216096,0.312499999999641,0.343749999999659,0.359374999999667,
0.359919964895214,0.367187499999673,0.371093749999678,0.374999999999682,
0.39459606244507,0.416671189759111,0.437499999999733,0.463193895153147,
0.468749999999759,0.484374999999766,0.49218749999977,0.496093749999766,
0.498046874999753,0.49999999999974,0.534110585575294,0.558950115148432,
0.562499999999334,0.593749999999131,0.609374999999031,0.617187499998981,
0.621093749998958,0.623046874998947,0.624999999998935,0.64207191973391,
0.656249999998824,0.671874999998769,0.679687499998743,0.68496404906836,
0.687499999998717,0.711490137633078,0.718749999998614,0.734374999998562,
0.742187499998539,0.74609374999853,0.746669664934028,0.749686729299358,
0.749999999998521,0.769789557229922,0.790340500844122,0.812121449595702,
0.834784976813535,0.860334536496689,0.874999999998234,0.888476593882743,
0.90624999999816,0.921874999998121,0.929687499998103,0.935546874998086,
0.937252953214231,0.937499999998081,0.945466322826954,0.953124999998562,
0.960937499998805,0.964843749998927,0.966796874998987,0.968405695614136,
0.968749999999048,0.982751356553703,0.997765223026701,1.),.UNSPECIFIED.);
#5831=B_SPLINE_CURVE_WITH_KNOTS('',3,(#221749,#221750,#221751,#221752,#221753,
#221754,#221755,#221756,#221757,#221758,#221759,#221760,#221761,#221762,
#221763,#221764,#221765,#221766,#221767,#221768,#221769,#221770,#221771,
#221772,#221773,#221774,#221775,#221776,#221777,#221778,#221779,#221780,
#221781,#221782,#221783,#221784,#221785,#221786,#221787,#221788,#221789,
#221790,#221791,#221792,#221793,#221794,#221795,#221796,#221797,#221798,
#221799,#221800,#221801,#221802,#221803,#221804,#221805,#221806,#221807,
#221808,#221809,#221810,#221811,#221812),.UNSPECIFIED.,.F.,.F.,(4,3,3,3,
3,3,3,3,3,3,3,3,3,3,3,3,3,3,3,3,3,4),(0.,0.104472712536878,0.143833362593174,
0.221616793428957,0.249999999999996,0.272765207700177,0.364018417806752,
0.374999999999994,0.390898624571728,0.437499999999996,0.446744971466346,
0.468749999999998,0.484375,0.492187500000001,0.499298442314967,0.500000000000002,
0.500701252711277,0.623020578288952,0.746999029313984,0.855597812446925,
0.872653871556337,1.),.UNSPECIFIED.);
#5832=B_SPLINE_CURVE_WITH_KNOTS('',3,(#221828,#221829,#221830,#221831,#221832,
#221833,#221834,#221835,#221836,#221837,#221838,#221839,#221840),
 .UNSPECIFIED.,.F.,.F.,(4,3,3,3,4),(0.,0.378104296523149,0.5,0.866163286535829,
1.),.UNSPECIFIED.);
#5833=B_SPLINE_CURVE_WITH_KNOTS('',3,(#221854,#221855,#221856,#221857,#221858,
#221859,#221860,#221861,#221862,#221863,#221864,#221865,#221866),
 .UNSPECIFIED.,.F.,.F.,(4,3,3,3,4),(0.,0.230076523236993,0.47903074115821,
0.750119827238623,0.999997761900286),.UNSPECIFIED.);
#5834=B_SPLINE_CURVE_WITH_KNOTS('',3,(#221867,#221868,#221869,#221870,#221871,
#221872,#221873,#221874,#221875,#221876,#221877,#221878,#221879,#221880,
#221881,#221882,#221883,#221884,#221885),.UNSPECIFIED.,.F.,.F.,(4,3,3,3,
3,3,4),(0.,0.188673283403314,0.369161567333252,0.538899468433716,0.703430166255707,
0.860489953582614,1.),.UNSPECIFIED.);
#5835=B_SPLINE_CURVE_WITH_KNOTS('',3,(#221904,#221905,#221906,#221907,#221908,
#221909,#221910,#221911,#221912,#221913,#221914,#221915,#221916,#221917,
#221918,#221919,#221920,#221921,#221922,#221923,#221924,#221925,#221926,
#221927,#221928,#221929,#221930,#221931,#221932,#221933,#221934),
 .UNSPECIFIED.,.F.,.F.,(4,3,3,3,3,3,3,3,3,3,4),(0.,0.20570874903028,0.249999999999735,
0.442981918132296,0.497264694230287,0.499023437499477,0.499999999999478,
0.649996181070983,0.79237661029201,0.925792371617293,1.),.UNSPECIFIED.);
#5836=B_SPLINE_CURVE_WITH_KNOTS('',3,(#221935,#221936,#221937,#221938,#221939,
#221940,#221941),.UNSPECIFIED.,.F.,.F.,(4,3,4),(0.00166725821467356,0.014267238448545,
0.0264527075460118),.UNSPECIFIED.);
#5837=B_SPLINE_CURVE_WITH_KNOTS('',3,(#221954,#221955,#221956,#221957,#221958,
#221959,#221960,#221961,#221962,#221963,#221964,#221965,#221966,#221967,
#221968,#221969,#221970,#221971,#221972,#221973,#221974,#221975,#221976,
#221977,#221978,#221979,#221980,#221981,#221982,#221983,#221984,#221985,
#221986,#221987,#221988,#221989,#221990,#221991,#221992,#221993,#221994,
#221995,#221996,#221997,#221998,#221999,#222000,#222001,#222002,#222003,
#222004,#222005,#222006,#222007,#222008),.UNSPECIFIED.,.F.,.F.,(4,3,3,3,
3,3,3,3,3,3,3,3,3,3,3,3,3,3,4),(0.,0.214315851661325,0.249999999999893,
0.37499999999984,0.45312499999986,0.487304687499869,0.495315551757683,0.49728697538363,
0.498268836759834,0.498758808598935,0.499018361648366,0.499101930796815,
0.499591089067522,0.499835429356063,0.499982229064921,0.500040936858297,
0.750020468429149,0.975872543910639,1.),.UNSPECIFIED.);
#5838=B_SPLINE_CURVE_WITH_KNOTS('',3,(#222009,#222010,#222011,#222012,#222013,
#222014,#222015,#222016,#222017,#222018,#222019,#222020,#222021,#222022,
#222023,#222024,#222025,#222026,#222027,#222028,#222029,#222030,#222031,
#222032,#222033,#222034,#222035,#222036),.UNSPECIFIED.,.F.,.F.,(4,3,3,3,
3,3,3,3,3,4),(0.,0.24999999999984,0.37499999999976,0.437499999999719,0.468749999999699,
0.48437499999969,0.499023437499683,0.499999999999684,0.76071527755839,1.),
 .UNSPECIFIED.);
#5839=B_SPLINE_CURVE_WITH_KNOTS('',3,(#222049,#222050,#222051,#222052,#222053,
#222054,#222055,#222056,#222057,#222058,#222059,#222060,#222061,#222062,
#222063),.UNSPECIFIED.,.F.,.F.,(4,2,2,1,1,1,2,2,4),(0.,0.250000000000125,
0.375000000000188,0.437500000000219,0.468750000000234,0.484375000000242,
0.499023437500251,0.500000000000251,1.),.UNSPECIFIED.);
#5840=B_SPLINE_CURVE_WITH_KNOTS('',3,(#222064,#222065,#222066,#222067,#222068,
#222069,#222070,#222071,#222072,#222073,#222074,#222075,#222076,#222077,
#222078,#222079,#222080,#222081,#222082,#222083,#222084,#222085,#222086,
#222087,#222088,#222089,#222090,#222091,#222092,#222093,#222094,#222095,
#222096,#222097,#222098,#222099,#222100,#222101,#222102,#222103,#222104,
#222105,#222106,#222107,#222108,#222109,#222110,#222111,#222112,#222113,
#222114,#222115,#222116,#222117,#222118),.UNSPECIFIED.,.F.,.F.,(4,3,3,3,
3,3,3,3,3,3,3,3,3,3,3,3,3,3,4),(0.,0.234963913086287,0.250000000000182,
0.375000000000272,0.453125000000238,0.487304687500223,0.495315551758032,
0.497286975383978,0.498268836760181,0.498758808599282,0.499021790751283,
0.499105006360904,0.499594161628129,0.499838500416397,0.499987953667902,
0.50004752798089,0.724683195181892,0.965177174746084,1.),.UNSPECIFIED.);
#5841=B_SPLINE_CURVE_WITH_KNOTS('',3,(#222137,#222138,#222139,#222140,#222141,
#222142,#222143,#222144,#222145,#222146,#222147,#222148,#222149,#222150,
#222151,#222152,#222153,#222154,#222155,#222156,#222157,#222158,#222159,
#222160,#222161,#222162,#222163,#222164,#222165,#222166,#222167,#222168,
#222169,#222170,#222171),.UNSPECIFIED.,.F.,.F.,(4,2,2,1,1,1,2,2,2,1,1,1,
1,2,2,2,1,1,1,1,2,2,4),(0.,0.124999999999923,0.187499999999883,0.218749999999863,
0.234374999999853,0.242187499999848,0.248046874999843,0.24999999999984,
0.374999999999744,0.437499999999695,0.46874999999967,0.484374999999657,
0.492187499999651,0.498046874999649,0.49999999999965,0.624999999999703,
0.687499999999729,0.718749999999742,0.734374999999749,0.742187499999752,
0.748046874999756,0.749999999999758,1.),.UNSPECIFIED.);
#5842=B_SPLINE_CURVE_WITH_KNOTS('',3,(#222172,#222173,#222174,#222175,#222176,
#222177,#222178,#222179,#222180,#222181,#222182,#222183,#222184,#222185,
#222186,#222187),.UNSPECIFIED.,.F.,.F.,(4,2,2,1,1,1,1,2,2,4),(0.,0.249999999999839,
0.374999999999757,0.437499999999716,0.468749999999695,0.484374999999687,
0.492187499999682,0.499023437499678,0.499999999999678,1.),.UNSPECIFIED.);
#5843=B_SPLINE_CURVE_WITH_KNOTS('',3,(#223329,#223330,#223331,#223332,#223333,
#223334),.UNSPECIFIED.,.F.,.F.,(4,2,4),(4.10724833792282E-6,0.241237590782085,
0.483186237929456),.UNSPECIFIED.);
#5844=B_SPLINE_CURVE_WITH_KNOTS('',3,(#223348,#223349,#223350,#223351,#223352,
#223353),.UNSPECIFIED.,.F.,.F.,(4,2,4),(0.,0.0477670349008267,0.0955331274490537),
 .UNSPECIFIED.);
#5845=B_SPLINE_CURVE_WITH_KNOTS('',3,(#223356,#223357,#223358,#223359,#223360,
#223361),.UNSPECIFIED.,.F.,.F.,(4,2,4),(1.13358908630587E-6,0.0262346930665884,
0.0524681434362511),.UNSPECIFIED.);
#5846=B_SPLINE_CURVE_WITH_KNOTS('',3,(#223370,#223371,#223372,#223373,#223374,
#223375),.UNSPECIFIED.,.F.,.F.,(4,2,4),(9.82188160298338E-7,0.126873328128178,
0.25376575794151),.UNSPECIFIED.);
#5847=B_SPLINE_CURVE_WITH_KNOTS('',3,(#223389,#223390,#223391,#223392,#223393,
#223394),.UNSPECIFIED.,.F.,.F.,(4,2,4),(2.15646689644485E-6,0.125624403775893,
0.258424816795553),.UNSPECIFIED.);
#5848=B_SPLINE_CURVE_WITH_KNOTS('',3,(#223408,#223409,#223410,#223411,#223412,
#223413),.UNSPECIFIED.,.F.,.F.,(4,2,4),(2.32100271924243E-6,0.114258712352594,
0.228506360165928),.UNSPECIFIED.);
#5849=B_SPLINE_CURVE_WITH_KNOTS('',3,(#223421,#223422,#223423,#223424,#223425,
#223426),.UNSPECIFIED.,.F.,.F.,(4,2,4),(1.02478977306241E-6,0.113688459278625,
0.227380714685831),.UNSPECIFIED.);
#5850=B_SPLINE_CURVE_WITH_KNOTS('',3,(#224660,#224661,#224662,#224663,#224664,
#224665,#224666,#224667,#224668,#224669,#224670,#224671,#224672,#224673),
 .UNSPECIFIED.,.F.,.F.,(4,2,2,2,2,2,4),(2.93038070849918E-6,0.0527238910564628,
0.0983357876907069,0.104035629430328,0.107433622421913,0.173175220318963,
0.608688061649262),.UNSPECIFIED.);
#5851=B_SPLINE_CURVE_WITH_KNOTS('',3,(#224675,#224676,#224677,#224678,#224679,
#224680),.UNSPECIFIED.,.F.,.F.,(4,2,4),(-0.352164527632873,-0.175885968938167,
0.),.UNSPECIFIED.);
#5852=B_SPLINE_CURVE_WITH_KNOTS('',3,(#224682,#224683,#224684,#224685,#224686,
#224687,#224688,#224689,#224690,#224691,#224692,#224693,#224694,#224695),
 .UNSPECIFIED.,.F.,.F.,(4,2,2,2,2,2,4),(-0.146050691310393,-0.133401168786229,
-0.122457304257569,-0.121089707324725,-0.120274395422017,-0.104500136704916,
-1.85098674576232E-6),.UNSPECIFIED.);
#5853=B_SPLINE_CURVE_WITH_KNOTS('',3,(#224696,#224697,#224698,#224699,#224700,
#224701),.UNSPECIFIED.,.F.,.F.,(4,2,4),(1.20017331883328E-7,0.235767253078328,
0.473063078352785),.UNSPECIFIED.);
#5854=B_SPLINE_CURVE_WITH_KNOTS('',3,(#224703,#224704,#224705,#224706,#224707,
#224708,#224709,#224710,#224711,#224712,#224713,#224714,#224715,#224716,
#224717,#224718,#224719,#224720,#224721,#224722,#224723,#224724,#224725,
#224726,#224727,#224728,#224729,#224730,#224731,#224732,#224733,#224734,
#224735,#224736,#224737,#224738,#224739,#224740,#224741,#224742,#224743,
#224744,#224745,#224746,#224747,#224748,#224749,#224750,#224751,#224752,
#224753,#224754,#224755,#224756,#224757,#224758,#224759,#224760,#224761,
#224762,#224763,#224764,#224765,#224766,#224767,#224768,#224769,#224770,
#224771,#224772,#224773,#224774,#224775,#224776,#224777,#224778,#224779,
#224780,#224781,#224782,#224783,#224784,#224785,#224786,#224787,#224788,
#224789,#224790,#224791,#224792,#224793,#224794,#224795,#224796,#224797,
#224798,#224799,#224800,#224801,#224802,#224803,#224804,#224805,#224806,
#224807,#224808,#224809,#224810,#224811,#224812,#224813,#224814,#224815,
#224816,#224817,#224818,#224819,#224820,#224821,#224822,#224823,#224824,
#224825,#224826,#224827,#224828,#224829,#224830,#224831,#224832,#224833,
#224834,#224835,#224836,#224837,#224838,#224839,#224840,#224841,#224842,
#224843,#224844,#224845,#224846,#224847,#224848,#224849,#224850,#224851,
#224852,#224853,#224854,#224855,#224856,#224857,#224858,#224859,#224860,
#224861,#224862,#224863,#224864,#224865,#224866,#224867,#224868,#224869,
#224870,#224871,#224872,#224873,#224874,#224875,#224876,#224877,#224878,
#224879,#224880,#224881,#224882,#224883,#224884,#224885,#224886,#224887,
#224888,#224889,#224890,#224891,#224892,#224893,#224894,#224895,#224896,
#224897,#224898),.UNSPECIFIED.,.F.,.F.,(4,3,3,3,3,3,3,3,3,3,3,3,3,3,3,3,
3,3,3,3,3,3,3,3,3,3,3,3,3,3,3,3,3,3,3,3,3,3,3,3,3,3,3,3,3,3,3,3,3,3,3,3,
3,3,3,3,3,3,3,3,3,3,3,3,3,4),(1.78689916273263E-6,0.349245406790117,0.705619403193492,
0.847493897628981,1.09071672564526,1.11694270883417,1.13031122083896,1.14453449936953,
1.20207522753681,1.31684392925775,1.54514481618978,2.44434146799478,4.19003111005039,
4.62046391575794,4.834341084108,4.93927480926269,4.96407578134244,4.99172316125023,
5.04802388301726,6.11997279598932,8.51952615505129,9.48378467016358,9.76391566762591,
10.5357861585198,10.5621467631509,10.5882563452092,10.6358557074836,10.7311025900593,
10.9200281613937,11.2796932852465,12.4465964798207,13.553746576423,14.6336841515732,
15.5822098205818,15.7876476637103,16.1401718470435,16.3220955100764,16.4133639203428,
16.4589226555197,16.4839070143489,16.5091312288925,17.2592565921019,18.2148053264092,
18.4712765951995,20.7885640811388,21.9649409448773,22.0549091144489,22.1009150614603,
22.1430542625552,22.312830378863,22.6646547127049,23.3174872351635,23.9964420606342,
24.6435854565312,25.0185833917038,25.8245931816792,26.0254191587144,26.1198119705167,
26.1655357658906,26.1768238193963,26.1882756857331,26.2133954469193,26.5759403027651,
27.3712415078498,27.6069804389702,28.3229150078202),.UNSPECIFIED.);
#5855=B_SPLINE_CURVE_WITH_KNOTS('',3,(#224900,#224901,#224902,#224903,#224904,
#224905,#224906,#224907,#224908,#224909,#224910,#224911,#224912,#224913,
#224914,#224915,#224916,#224917,#224918,#224919,#224920,#224921,#224922,
#224923,#224924,#224925,#224926,#224927,#224928,#224929,#224930,#224931,
#224932,#224933,#224934,#224935,#224936,#224937,#224938,#224939),
 .UNSPECIFIED.,.F.,.F.,(4,3,3,3,3,3,3,3,3,3,3,3,3,4),(1.49278976973505E-7,
0.141377231663466,0.249999999999955,0.374999999999933,0.437499999999923,
0.468749999999918,0.484374999999916,0.492187499999915,0.499023437499913,
0.499999999999912,0.518810985931556,0.696449207513925,0.858128319650762,
1.),.UNSPECIFIED.);
#5856=B_SPLINE_CURVE_WITH_KNOTS('',3,(#224941,#224942,#224943,#224944,#224945,
#224946),.UNSPECIFIED.,.F.,.F.,(4,2,4),(-0.0631146096128023,-0.0315634825964837,
-2.17021022817649E-6),.UNSPECIFIED.);
#5857=B_SPLINE_CURVE_WITH_KNOTS('',3,(#224948,#224949,#224950,#224951,#224952,
#224953,#224954,#224955,#224956,#224957,#224958,#224959,#224960,#224961,
#224962,#224963,#224964,#224965,#224966,#224967),.UNSPECIFIED.,.F.,.F.,
(4,2,2,2,2,2,2,2,2,4),(9.54272002648276E-7,0.039668729271524,0.0502460852682275,
0.0529093523368603,0.0585862970221902,0.150167472119632,0.47461910179334,
0.71071638044721,0.842512773974448,0.972825733893553),.UNSPECIFIED.);
#5858=B_SPLINE_CURVE_WITH_KNOTS('',3,(#224969,#224970,#224971,#224972,#224973,
#224974),.UNSPECIFIED.,.F.,.F.,(4,2,4),(-0.348032286208327,-0.174233719491681,
-1.04624545273724E-6),.UNSPECIFIED.);
#5859=B_SPLINE_CURVE_WITH_KNOTS('',3,(#224976,#224977,#224978,#224979,#224980,
#224981),.UNSPECIFIED.,.F.,.F.,(4,2,4),(-0.181030043604558,-0.0910312711858393,
-1.10663912709387E-5),.UNSPECIFIED.);
#5860=B_SPLINE_CURVE_WITH_KNOTS('',3,(#224982,#224983,#224984,#224985,#224986,
#224987),.UNSPECIFIED.,.F.,.F.,(4,2,4),(-0.472029599120786,-0.236764162407715,
0.),.UNSPECIFIED.);
#5861=B_SPLINE_CURVE_WITH_KNOTS('',3,(#225594,#225595,#225596,#225597,#225598,
#225599),.UNSPECIFIED.,.F.,.F.,(4,2,4),(-0.0726217219155311,-0.0363071423916649,
-3.64731715070445E-6),.UNSPECIFIED.);
#5862=B_SPLINE_CURVE_WITH_KNOTS('',3,(#225601,#225602,#225603,#225604,#225605,
#225606,#225607,#225608,#225609,#225610,#225611,#225612,#225613,#225614,
#225615,#225616,#225617,#225618,#225619,#225620,#225621,#225622,#225623,
#225624,#225625,#225626,#225627,#225628,#225629,#225630,#225631,#225632,
#225633,#225634,#225635,#225636,#225637,#225638,#225639,#225640,#225641,
#225642,#225643,#225644,#225645,#225646,#225647,#225648,#225649,#225650,
#225651,#225652,#225653,#225654,#225655,#225656,#225657,#225658,#225659,
#225660,#225661),.UNSPECIFIED.,.F.,.F.,(4,3,3,3,3,3,3,3,3,3,3,3,3,3,3,3,
3,3,3,3,4),(6.55221773018224E-8,0.198533780132414,0.249999999999826,0.374999999999739,
0.437499999999696,0.468749999999675,0.484374999999665,0.492187499999661,
0.499023437499656,0.499999999999657,0.608653468230123,0.624999999999709,
0.687499999999737,0.71874999999975,0.734374999999758,0.742187499999761,
0.748046874999763,0.749999999999764,0.857427266285853,0.964048886395737,
1.),.UNSPECIFIED.);
#5863=B_SPLINE_CURVE_WITH_KNOTS('',3,(#225662,#225663,#225664,#225665,#225666,
#225667,#225668,#225669,#225670,#225671,#225672,#225673,#225674,#225675,
#225676,#225677,#225678,#225679,#225680,#225681,#225682,#225683,#225684,
#225685,#225686,#225687,#225688,#225689,#225690,#225691,#225692,#225693,
#225694,#225695,#225696,#225697,#225698,#225699,#225700,#225701,#225702,
#225703,#225704,#225705,#225706,#225707,#225708,#225709,#225710,#225711,
#225712,#225713,#225714,#225715,#225716,#225717,#225718,#225719,#225720,
#225721,#225722,#225723,#225724,#225725,#225726,#225727,#225728,#225729,
#225730,#225731,#225732,#225733,#225734,#225735,#225736,#225737,#225738,
#225739,#225740,#225741,#225742,#225743,#225744,#225745,#225746,#225747,
#225748,#225749,#225750,#225751,#225752,#225753,#225754,#225755,#225756,
#225757,#225758,#225759,#225760,#225761,#225762,#225763,#225764,#225765,
#225766,#225767,#225768,#225769,#225770,#225771,#225772,#225773,#225774,
#225775,#225776,#225777,#225778,#225779,#225780,#225781,#225782,#225783,
#225784,#225785,#225786,#225787,#225788,#225789,#225790,#225791,#225792,
#225793,#225794,#225795,#225796,#225797,#225798,#225799,#225800,#225801,
#225802,#225803,#225804,#225805,#225806,#225807,#225808,#225809,#225810,
#225811,#225812,#225813,#225814,#225815,#225816,#225817,#225818,#225819,
#225820,#225821,#225822,#225823,#225824,#225825,#225826,#225827,#225828,
#225829,#225830,#225831,#225832,#225833),.UNSPECIFIED.,.F.,.F.,(4,3,3,3,
3,3,3,3,3,3,3,3,3,3,3,3,3,3,3,3,3,3,3,3,3,3,3,3,3,3,3,3,3,3,3,3,3,3,3,3,
3,3,3,3,3,3,3,3,3,3,3,3,3,3,3,3,3,4),(-10.0118009515725,-9.380144348375,
-9.28193689793529,-9.22251029152007,-9.19147789919078,-9.17779037797217,
-9.16464451434807,-9.13017042783428,-8.99160305605499,-8.68736646402747,
-8.52180373132443,-8.41041892963837,-8.3758072763443,-8.35673588517422,
-8.35173647900018,-8.34601909497381,-8.33358519993068,-8.21883901831532,
-7.28686586998718,-7.16008381787202,-6.80650500239442,-6.50180850406331,
-6.46109833741843,-6.44123587433924,-6.42379799474065,-6.35522340568956,
-6.22668897461121,-5.92002477860756,-5.3247417048503,-4.86206937746766,
-4.42610453669277,-4.30346091911995,-4.23870089998684,-4.22228697144672,
-4.20361062602334,-4.16537895898503,-3.87762847487079,-3.76886371593885,
-3.42827377469716,-2.92395744537593,-2.56497067190565,-2.45214102185328,
-2.43752731019248,-2.43051889000834,-2.42424270775226,-2.39905523317864,
-2.3485592868193,-2.15607432218952,-1.86312912747339,-1.70318514070286,
-1.39379233399322,-1.14178495836116,-1.12409212545336,-1.10568452874485,
-1.06389214424081,-0.982911261414093,-0.846211153564692,-6.66741710329381E-6),
 .UNSPECIFIED.);
#5864=B_SPLINE_CURVE_WITH_KNOTS('',3,(#225834,#225835,#225836,#225837,#225838,
#225839,#225840,#225841,#225842,#225843,#225844,#225845,#225846,#225847,
#225848,#225849,#225850,#225851,#225852,#225853,#225854,#225855,#225856,
#225857,#225858,#225859,#225860,#225861),.UNSPECIFIED.,.F.,.F.,(4,3,3,3,
3,3,3,3,3,4),(2.47031549411892E-5,0.330322577512475,0.531914497354827,0.575033270917861,
0.692616065858012,0.756752965780754,0.790033944881865,0.804313961995532,
0.818107734326963,0.901208376257383),.UNSPECIFIED.);
#5865=B_SPLINE_CURVE_WITH_KNOTS('',3,(#225863,#225864,#225865,#225866,#225867,
#225868,#225869,#225870,#225871,#225872),.UNSPECIFIED.,.F.,.F.,(4,2,2,2,
4),(1.01154219413529E-6,0.197911925947378,0.383079900974823,0.578872967472904,
0.753869196345672),.UNSPECIFIED.);
#5866=B_SPLINE_CURVE_WITH_KNOTS('',3,(#225874,#225875,#225876,#225877,#225878,
#225879),.UNSPECIFIED.,.F.,.F.,(4,2,4),(-0.52032371085874,-0.260164299656232,
-1.26885779850293E-6),.UNSPECIFIED.);
#5867=B_SPLINE_CURVE_WITH_KNOTS('',3,(#225881,#225882,#225883,#225884,#225885,
#225886,#225887,#225888,#225889,#225890),.UNSPECIFIED.,.F.,.F.,(4,2,2,2,
4),(-0.808794323077665,-0.596464192824083,-0.397805427063807,-0.187747447983837,
-1.59820013576218E-6),.UNSPECIFIED.);
#5868=B_SPLINE_CURVE_WITH_KNOTS('',3,(#225892,#225893,#225894,#225895,#225896,
#225897),.UNSPECIFIED.,.F.,.F.,(4,2,4),(-0.512833689847384,-0.262850347931808,
-2.73829768859812E-8),.UNSPECIFIED.);
#5869=B_SPLINE_CURVE_WITH_KNOTS('',3,(#225898,#225899,#225900,#225901,#225902,
#225903,#225904,#225905,#225906,#225907,#225908,#225909,#225910,#225911,
#225912,#225913,#225914,#225915,#225916,#225917,#225918,#225919,#225920,
#225921,#225922),.UNSPECIFIED.,.F.,.F.,(4,3,3,3,3,3,3,3,4),(-0.582199554717882,
-0.346112236555124,-0.210722915399725,-0.134760117007276,-0.0933253284297944,
-0.0718245964311411,-0.0625992031160378,-0.0536879216367247,-1.96467184541608E-6),
 .UNSPECIFIED.);
#5870=B_SPLINE_CURVE_WITH_KNOTS('',3,(#225965,#225966,#225967,#225968,#225969,
#225970),.UNSPECIFIED.,.F.,.F.,(4,2,4),(-0.234147853965519,-0.114087724688498,
0.),.UNSPECIFIED.);
#5871=B_SPLINE_CURVE_WITH_KNOTS('',3,(#226350,#226351,#226352,#226353,#226354,
#226355,#226356,#226357,#226358,#226359,#226360,#226361,#226362,#226363,
#226364,#226365,#226366,#226367,#226368,#226369),.UNSPECIFIED.,.F.,.F.,
(4,2,2,2,2,2,2,2,2,4),(-0.238232821898405,-0.205423492378447,-0.197085539277143,
-0.169892934987575,-0.105862923175614,-0.0753554195472226,-0.0349310916978768,
-0.0193510418585195,-0.0118234613898232,0.),.UNSPECIFIED.);
#5872=B_SPLINE_CURVE_WITH_KNOTS('',3,(#226371,#226372,#226373,#226374,#226375,
#226376,#226377,#226378,#226379,#226380,#226381,#226382,#226383),
 .UNSPECIFIED.,.F.,.F.,(4,3,3,3,4),(0.,0.248409226325233,0.499006625537372,
0.502852684896152,1.),.UNSPECIFIED.);
#5873=B_SPLINE_CURVE_WITH_KNOTS('',3,(#226385,#226386,#226387,#226388,#226389,
#226390,#226391,#226392,#226393,#226394,#226395,#226396,#226397,#226398,
#226399,#226400,#226401,#226402,#226403,#226404,#226405,#226406),
 .UNSPECIFIED.,.F.,.F.,(4,2,2,2,2,2,2,2,2,2,4),(4.11923473698837E-6,0.0532044237289185,
0.112114067677964,0.129888742302041,0.273554203521723,0.318355137795804,
0.394719390871768,0.446820142683063,0.478015292941828,0.517144072378212,
0.549044733910222),.UNSPECIFIED.);
#5874=B_SPLINE_CURVE_WITH_KNOTS('',3,(#226408,#226409,#226410,#226411,#226412,
#226413),.UNSPECIFIED.,.F.,.F.,(4,2,4),(-0.0469583750615504,-0.0233153845128203,
0.),.UNSPECIFIED.);
#5875=B_SPLINE_CURVE_WITH_KNOTS('',3,(#226414,#226415,#226416,#226417),
 .UNSPECIFIED.,.F.,.F.,(4,4),(0.0542180481640577,0.969015107905792),
 .UNSPECIFIED.);
#5876=B_SPLINE_CURVE_WITH_KNOTS('',3,(#226979,#226980,#226981,#226982,#226983,
#226984,#226985,#226986,#226987,#226988,#226989,#226990,#226991,#226992,
#226993,#226994,#226995,#226996,#226997,#226998,#226999,#227000),
 .UNSPECIFIED.,.F.,.F.,(4,2,2,2,2,2,2,2,2,2,4),(-0.0469823194624915,-0.0448779513354515,
-0.043871616538125,-0.0417699201921335,-0.0365670119809625,-0.0349794965192584,
-0.029838901311014,-0.0234761972380763,-0.0131803115290423,-0.00771050065983768,
-9.96545261977566E-7),.UNSPECIFIED.);
#5877=B_SPLINE_CURVE_WITH_KNOTS('',3,(#227002,#227003,#227004,#227005),
 .UNSPECIFIED.,.F.,.F.,(4,4),(0.0559227492896307,0.969509810868812),
 .UNSPECIFIED.);
#5878=B_SPLINE_CURVE_WITH_KNOTS('',3,(#227007,#227008,#227009,#227010,#227011,
#227012,#227013,#227014,#227015,#227016),.UNSPECIFIED.,.F.,.F.,(4,2,2,2,
4),(1.01948866288982E-6,0.0265245583807015,0.039717133035126,0.0460199136553313,
0.0521877159679606),.UNSPECIFIED.);
#5879=B_SPLINE_CURVE_WITH_KNOTS('',3,(#227018,#227019,#227020,#227021,#227022,
#227023,#227024,#227025,#227026,#227027,#227028,#227029,#227030,#227031,
#227032,#227033,#227034,#227035,#227036,#227037,#227038,#227039,#227040,
#227041),.UNSPECIFIED.,.F.,.F.,(4,2,2,2,2,2,2,2,2,2,2,4),(8.74098857277626E-8,
0.0345413375471952,0.0478434921558638,0.108389819035251,0.162764294558867,
0.195585772394031,0.213488203760146,0.254799752738697,0.385293361542727,
0.417463559505062,0.440592486828372,0.505162485488175),.UNSPECIFIED.);
#5880=B_SPLINE_CURVE_WITH_KNOTS('',3,(#227042,#227043,#227044,#227045,#227046,
#227047,#227048,#227049,#227050,#227051,#227052,#227053,#227054),
 .UNSPECIFIED.,.F.,.F.,(4,3,3,3,4),(0.,0.121286618183145,0.248611887968643,
0.503260702170736,1.),.UNSPECIFIED.);
#5881=B_SPLINE_CURVE_WITH_KNOTS('',3,(#227421,#227422,#227423,#227424,#227425,
#227426,#227427,#227428,#227429,#227430,#227431,#227432,#227433,#227434,
#227435,#227436,#227437,#227438,#227439,#227440),.UNSPECIFIED.,.F.,.F.,
(4,2,2,2,2,2,2,2,2,4),(-0.115918278885804,-0.0892169661896314,-0.0795730255112448,
-0.0500602494615251,-0.0402734344922609,-0.0327836602742112,-0.0258163526316461,
-0.0148454000357724,-0.00934050276061678,0.),.UNSPECIFIED.);
#5882=B_SPLINE_CURVE_WITH_KNOTS('',3,(#227442,#227443,#227444,#227445,#227446,
#227447,#227448,#227449,#227450,#227451,#227452,#227453,#227454),
 .UNSPECIFIED.,.F.,.F.,(4,3,3,3,4),(0.,0.248207134125547,0.498866213704792,
0.502443591376185,1.),.UNSPECIFIED.);
#5883=B_SPLINE_CURVE_WITH_KNOTS('',3,(#227456,#227457,#227458,#227459,#227460,
#227461,#227462,#227463,#227464,#227465,#227466,#227467,#227468,#227469,
#227470,#227471,#227472,#227473,#227474,#227475,#227476,#227477,#227478,
#227479),.UNSPECIFIED.,.F.,.F.,(4,2,2,2,2,2,2,2,2,2,2,4),(1.34129012567919E-6,
0.0388365429884076,0.0809349663735409,0.110652786603789,0.150076448441442,
0.202495348256536,0.235137840136492,0.290402658704084,0.327987073052442,
0.350910589522497,0.380240175864255,0.404554968880074),.UNSPECIFIED.);
#5884=B_SPLINE_CURVE_WITH_KNOTS('',3,(#227481,#227482,#227483,#227484,#227485,
#227486),.UNSPECIFIED.,.F.,.F.,(4,2,4),(-0.0432556987863833,-0.0214374711513382,
0.),.UNSPECIFIED.);
#5885=B_SPLINE_CURVE_WITH_KNOTS('',3,(#227487,#227488,#227489,#227490),
 .UNSPECIFIED.,.F.,.F.,(4,4),(0.,1.),.UNSPECIFIED.);
#5886=B_SPLINE_CURVE_WITH_KNOTS('',3,(#228013,#228014,#228015,#228016,#228017,
#228018,#228019,#228020,#228021,#228022,#228023,#228024,#228025,#228026,
#228027,#228028),.UNSPECIFIED.,.F.,.F.,(4,2,2,2,2,2,2,4),(-0.0532039057008744,
-0.0485064898699985,-0.0454445922183713,-0.0383797315059074,-0.0340621721264607,
-0.0219073807078276,-0.0140093117094523,-9.96369002963238E-7),
 .UNSPECIFIED.);
#5887=B_SPLINE_CURVE_WITH_KNOTS('',3,(#228030,#228031,#228032,#228033),
 .UNSPECIFIED.,.F.,.F.,(4,4),(0.0408435581858526,0.955362835047561),
 .UNSPECIFIED.);
#5888=B_SPLINE_CURVE_WITH_KNOTS('',3,(#228035,#228036,#228037,#228038,#228039,
#228040,#228041,#228042),.UNSPECIFIED.,.F.,.F.,(4,2,2,4),(1.01576402050443E-6,
0.0186922722070423,0.028158435435005,0.0372206145737922),.UNSPECIFIED.);
#5889=B_SPLINE_CURVE_WITH_KNOTS('',3,(#228044,#228045,#228046,#228047,#228048,
#228049,#228050,#228051,#228052,#228053,#228054,#228055,#228056,#228057,
#228058,#228059,#228060,#228061,#228062,#228063,#228064,#228065,#228066,
#228067,#228068,#228069),.UNSPECIFIED.,.F.,.F.,(4,2,2,2,2,2,2,2,2,2,2,2,
4),(1.00349669506866E-6,0.0149902028524071,0.0301796168541512,0.0653312244747095,
0.0929080820335093,0.137456013888724,0.20183246394693,0.239455773090012,
0.30227612781367,0.325926095178214,0.367602393520655,0.426119367916936,
0.477863235121803),.UNSPECIFIED.);
#5890=B_SPLINE_CURVE_WITH_KNOTS('',3,(#228070,#228071,#228072,#228073,#228074,
#228075),.UNSPECIFIED.,.F.,.F.,(4,2,4),(1.21996442589897E-8,0.499703627209769,
0.999999992717194),.UNSPECIFIED.);
#5891=B_SPLINE_CURVE_WITH_KNOTS('',3,(#228082,#228083,#228084,#228085,#228086,
#228087),.UNSPECIFIED.,.F.,.F.,(4,2,4),(1.00005279208342E-6,0.0180894029160134,
0.0360332116186634),.UNSPECIFIED.);
#5892=B_SPLINE_CURVE_WITH_KNOTS('',3,(#228090,#228091,#228092,#228093,#228094,
#228095,#228096,#228097),.UNSPECIFIED.,.F.,.F.,(4,2,2,4),(1.68023398205945E-6,
0.123369994045964,0.250885389419846,0.502640983753045),.UNSPECIFIED.);
#5893=B_SPLINE_CURVE_WITH_KNOTS('',3,(#228102,#228103,#228104,#228105,#228106,
#228107),.UNSPECIFIED.,.F.,.F.,(4,2,4),(9.99995512679503E-7,0.251122560205324,
0.500936979469621),.UNSPECIFIED.);
#5894=B_SPLINE_CURVE_WITH_KNOTS('',3,(#228122,#228123,#228124,#228125,#228126,
#228127),.UNSPECIFIED.,.F.,.F.,(4,2,4),(1.74474206022349E-6,0.259610843491103,
0.519873535593903),.UNSPECIFIED.);
#5895=B_SPLINE_CURVE_WITH_KNOTS('',3,(#228132,#228133,#228134,#228135,#228136,
#228137,#228138,#228139),.UNSPECIFIED.,.F.,.F.,(4,2,2,4),(9.99996049876919E-7,
0.25935475971615,0.390604083523162,0.518299611782085),.UNSPECIFIED.);
#5896=B_SPLINE_CURVE_WITH_KNOTS('',3,(#228147,#228148,#228149,#228150,#228151,
#228152),.UNSPECIFIED.,.F.,.F.,(4,2,4),(5.20898920908954E-7,0.394546120022865,
0.789090255646932),.UNSPECIFIED.);
#5897=B_SPLINE_CURVE_WITH_KNOTS('',3,(#228224,#228225,#228226,#228227,#228228,
#228229),.UNSPECIFIED.,.F.,.F.,(4,2,4),(-0.768987117999718,-0.384501938178755,
-6.39808872548997E-10),.UNSPECIFIED.);
#5898=B_SPLINE_CURVE_WITH_KNOTS('',3,(#228231,#228232,#228233,#228234,#228235,
#228236),.UNSPECIFIED.,.F.,.F.,(4,2,4),(7.16885188820924E-6,0.389700990930307,
0.77940084823311),.UNSPECIFIED.);
#5899=B_SPLINE_CURVE_WITH_KNOTS('',3,(#228237,#228238,#228239,#228240,#228241,
#228242),.UNSPECIFIED.,.F.,.F.,(4,2,4),(-2.50574735670183,-1.27023285791173,
-1.26197706507014E-7),.UNSPECIFIED.);
#5900=B_SPLINE_CURVE_WITH_KNOTS('',3,(#228260,#228261,#228262,#228263,#228264,
#228265),.UNSPECIFIED.,.F.,.F.,(4,2,4),(5.46905462932057E-7,0.391794447842365,
0.783582614970145),.UNSPECIFIED.);
#5901=B_SPLINE_CURVE_WITH_KNOTS('',3,(#228267,#228268,#228269,#228270,#228271,
#228272),.UNSPECIFIED.,.F.,.F.,(4,2,4),(-0.774055471160218,-0.387030382163849,
-1.38207304385376E-5),.UNSPECIFIED.);
#5902=B_SPLINE_CURVE_WITH_KNOTS('',3,(#228273,#228274,#228275,#228276,#228277,
#228278),.UNSPECIFIED.,.F.,.F.,(4,2,4),(-2.41443710174894,-1.18731782863127,
-8.04546614600221E-6),.UNSPECIFIED.);
#5903=B_SPLINE_CURVE_WITH_KNOTS('',3,(#228280,#228281,#228282,#228283,#228284,
#228285,#228286,#228287,#228288,#228289,#228290,#228291,#228292,#228293,
#228294,#228295,#228296,#228297,#228298,#228299,#228300,#228301,#228302,
#228303,#228304,#228305,#228306,#228307,#228308,#228309,#228310,#228311,
#228312,#228313,#228314,#228315,#228316,#228317,#228318,#228319,#228320,
#228321,#228322,#228323,#228324,#228325,#228326,#228327,#228328,#228329,
#228330,#228331,#228332,#228333,#228334,#228335,#228336,#228337,#228338,
#228339,#228340,#228341,#228342,#228343,#228344,#228345,#228346,#228347,
#228348,#228349,#228350,#228351,#228352,#228353,#228354,#228355,#228356,
#228357,#228358,#228359,#228360,#228361,#228362,#228363,#228364,#228365,
#228366,#228367,#228368,#228369,#228370,#228371,#228372,#228373,#228374,
#228375,#228376,#228377,#228378,#228379,#228380,#228381,#228382,#228383,
#228384,#228385,#228386,#228387,#228388,#228389,#228390,#228391,#228392,
#228393,#228394,#228395,#228396,#228397,#228398,#228399,#228400,#228401,
#228402,#228403,#228404,#228405,#228406,#228407,#228408,#228409,#228410,
#228411,#228412,#228413,#228414,#228415,#228416,#228417,#228418,#228419,
#228420,#228421,#228422,#228423,#228424,#228425,#228426,#228427,#228428,
#228429,#228430,#228431,#228432,#228433,#228434,#228435,#228436,#228437,
#228438,#228439,#228440,#228441,#228442,#228443,#228444,#228445,#228446,
#228447,#228448,#228449,#228450,#228451,#228452,#228453,#228454,#228455,
#228456,#228457,#228458,#228459,#228460),.UNSPECIFIED.,.F.,.F.,(4,3,3,3,
3,3,3,3,3,3,3,3,3,3,3,3,3,3,3,3,3,3,3,3,3,3,3,3,3,3,3,3,3,3,3,3,3,3,3,3,
3,3,3,3,3,3,3,3,3,3,3,3,3,3,3,3,3,3,3,3,4),(0.,0.101652515081683,0.840095270426277,
0.951350449593331,1.11460256910622,1.20222962321025,1.21337770183555,1.22322866068737,
1.24215508047792,1.27918762477272,1.41444382060503,1.91308482137222,2.16293686170842,
2.31873870184034,2.3388699155934,2.35956243431462,2.40573771750418,2.49173011142808,
2.50522275730167,2.72512517847504,3.09820563685861,3.40471762826703,3.56238559688252,
3.65675659727303,3.66930952721422,3.67553938673372,3.68097533151684,3.70277767984807,
3.74615446777659,3.93440481248742,4.2762919621573,4.4629569057448,4.80246566838423,
4.84531684069589,4.86725425690884,4.87828571635999,4.89073026763831,4.98934387426452,
5.14829048116897,5.43554060290253,5.98928985210521,6.05987373854709,6.09759598641818,
6.10721678864328,6.11134856344036,6.11540864995827,6.1317539654039,6.26291140079336,
6.47575952606869,6.58219308214426,6.81129554606021,6.90189743840945,6.92504908218588,
6.935638466,6.94054062150879,6.9429390153616,6.94566168795314,6.98260356735261,
7.08304507613446,7.15822821963323,7.33584769615335),.UNSPECIFIED.);
#5904=B_SPLINE_CURVE_WITH_KNOTS('',3,(#228478,#228479,#228480,#228481,#228482,
#228483),.UNSPECIFIED.,.F.,.F.,(4,2,4),(2.70771998432966E-6,0.460501033060921,
0.921000224556805),.UNSPECIFIED.);
#5905=B_SPLINE_CURVE_WITH_KNOTS('',3,(#228490,#228491,#228492,#228493,#228494,
#228495,#228496,#228497,#228498,#228499,#228500,#228501,#228502,#228503,
#228504,#228505),.UNSPECIFIED.,.F.,.F.,(4,2,2,2,2,2,2,4),(-0.982605045330243,
-0.957450000265146,-0.931726665878099,-0.879221227191873,-0.770280103416555,
-0.542311900866116,-0.311877616829005,-1.70255117412049E-6),
 .UNSPECIFIED.);
#5906=B_SPLINE_CURVE_WITH_KNOTS('',3,(#228506,#228507,#228508,#228509,#228510,
#228511),.UNSPECIFIED.,.F.,.F.,(4,2,4),(-0.0722680566464597,-0.0361746296017969,
0.),.UNSPECIFIED.);
#5907=B_SPLINE_CURVE_WITH_KNOTS('',3,(#228530,#228531,#228532,#228533,#228534,
#228535),.UNSPECIFIED.,.F.,.F.,(4,2,4),(1.77148721322176E-6,0.0720279028463182,
0.144150482966194),.UNSPECIFIED.);
#5908=B_SPLINE_CURVE_WITH_KNOTS('',3,(#228538,#228539,#228540,#228541,#228542,
#228543),.UNSPECIFIED.,.F.,.F.,(4,2,4),(2.79355861066373E-6,0.0720991492051481,
0.143966171702797),.UNSPECIFIED.);
#5909=B_SPLINE_CURVE_WITH_KNOTS('',3,(#228741,#228742,#228743,#228744,#228745,
#228746,#228747,#228748,#228749,#228750,#228751,#228752,#228753,#228754),
 .UNSPECIFIED.,.F.,.F.,(4,2,2,2,2,2,4),(8.79576979640004E-7,0.161091039185441,
0.353936447289158,0.714835470723924,1.15295148424327,1.32088879345487,1.48892420048076),
 .UNSPECIFIED.);
#5910=B_SPLINE_CURVE_WITH_KNOTS('',3,(#228756,#228757,#228758,#228759,#228760,
#228761),.UNSPECIFIED.,.F.,.F.,(4,2,4),(1.48538090247618E-6,0.0297476815236481,
0.059493920780927),.UNSPECIFIED.);
#5911=B_SPLINE_CURVE_WITH_KNOTS('',3,(#228763,#228764,#228765,#228766,#228767,
#228768),.UNSPECIFIED.,.F.,.F.,(4,2,4),(2.90466498097714E-6,0.053152581148337,
0.106304452166784),.UNSPECIFIED.);
#5912=B_SPLINE_CURVE_WITH_KNOTS('',3,(#228769,#228770,#228771,#228772,#228773,
#228774),.UNSPECIFIED.,.F.,.F.,(4,2,4),(5.00463248281416E-6,0.14458386001298,
0.288882060685716),.UNSPECIFIED.);
#5913=B_SPLINE_CURVE_WITH_KNOTS('',3,(#228775,#228776,#228777,#228778,#228779,
#228780,#228781,#228782,#228783,#228784,#228785,#228786,#228787,#228788),
 .UNSPECIFIED.,.F.,.F.,(4,2,2,2,2,2,4),(-1.33002773489275,-1.19632686097329,
-1.0309504969832,-0.691984499274297,-0.293184319134546,-0.147201401084202,
-3.05059735880904E-6),.UNSPECIFIED.);
#5914=B_SPLINE_CURVE_WITH_KNOTS('',3,(#228789,#228790,#228791,#228792,#228793,
#228794,#228795,#228796,#228797,#228798,#228799,#228800,#228801,#228802,
#228803,#228804),.UNSPECIFIED.,.F.,.F.,(4,2,2,2,2,2,2,4),(-2.53746494961163,
-2.46422033767662,-2.38938785749608,-2.23702354943545,-1.92260251519736,
-1.27022304439062,-0.614575319391794,-8.39797342777615E-9),
 .UNSPECIFIED.);
#5915=B_SPLINE_CURVE_WITH_KNOTS('',3,(#228807,#228808,#228809,#228810,#228811,
#228812),.UNSPECIFIED.,.F.,.F.,(4,2,4),(-0.0311640358773885,-0.0155842549001969,
-7.32013339722184E-7),.UNSPECIFIED.);
#5916=B_SPLINE_CURVE_WITH_KNOTS('',3,(#228815,#228816,#228817,#228818,#228819,
#228820),.UNSPECIFIED.,.F.,.F.,(4,2,4),(-0.118814653628038,-0.0594775620868716,
-8.25559444165143E-6),.UNSPECIFIED.);
#5917=B_SPLINE_CURVE_WITH_KNOTS('',3,(#229102,#229103,#229104,#229105,#229106,
#229107,#229108,#229109,#229110,#229111,#229112,#229113,#229114,#229115,
#229116,#229117),.UNSPECIFIED.,.F.,.F.,(4,2,2,2,2,2,2,4),(1.31319461189347E-5,
0.0969398305739712,0.200592571707003,0.40568002081205,0.731947033912492,
1.15360029034027,1.33098563964491,1.51064986605988),.UNSPECIFIED.);
#5918=B_SPLINE_CURVE_WITH_KNOTS('',3,(#229118,#229119,#229120,#229121),
 .UNSPECIFIED.,.F.,.F.,(4,4),(0.,1.),.UNSPECIFIED.);
#5919=B_SPLINE_CURVE_WITH_KNOTS('',3,(#229122,#229123,#229124,#229125,#229126,
#229127,#229128,#229129,#229130,#229131,#229132,#229133,#229134,#229135,
#229136,#229137),.UNSPECIFIED.,.F.,.F.,(4,2,2,2,2,2,2,4),(1.00000001008263E-6,
0.147548369920231,0.335441273894288,0.717509453274639,1.00870782358177,
1.20577091648481,1.30068851548524,1.39147288337523),.UNSPECIFIED.);
#5920=B_SPLINE_CURVE_WITH_KNOTS('',3,(#229141,#229142,#229143,#229144,#229145,
#229146),.UNSPECIFIED.,.F.,.F.,(4,2,4),(-0.0694028841990137,-0.0347037380359889,
-4.89524744334324E-5),.UNSPECIFIED.);
#5921=B_SPLINE_CURVE_WITH_KNOTS('',3,(#229151,#229152,#229153,#229154,#229155,
#229156),.UNSPECIFIED.,.F.,.F.,(4,2,4),(-0.256260280232773,-0.128094391485911,
-2.91397728446885E-7),.UNSPECIFIED.);
#5922=B_SPLINE_CURVE_WITH_KNOTS('',3,(#229161,#229162,#229163,#229164,#229165,
#229166),.UNSPECIFIED.,.F.,.F.,(4,2,4),(-0.335038423290503,-0.16756094841115,
-4.64089220713822E-5),.UNSPECIFIED.);
#5923=B_SPLINE_CURVE_WITH_KNOTS('',3,(#229171,#229172,#229173,#229174,#229175,
#229176),.UNSPECIFIED.,.F.,.F.,(4,2,4),(-0.259482172087391,-0.12980603886175,
-3.40862289005539E-7),.UNSPECIFIED.);
#5924=B_SPLINE_CURVE_WITH_KNOTS('',3,(#229186,#229187,#229188,#229189,#229190,
#229191,#229192,#229193),.UNSPECIFIED.,.F.,.F.,(4,2,2,4),(-0.240357308665275,
-0.138634339792356,-0.0669247924035088,0.),.UNSPECIFIED.);
#5925=B_SPLINE_CURVE_WITH_KNOTS('',3,(#229195,#229196,#229197,#229198,#229199,
#229200,#229201,#229202),.UNSPECIFIED.,.F.,.F.,(4,2,2,4),(4.59252772077989E-7,
0.137071464030345,0.235092069952917,0.323700448386457),.UNSPECIFIED.);
#5926=B_SPLINE_CURVE_WITH_KNOTS('',3,(#229208,#229209,#229210,#229211,#229212,
#229213),.UNSPECIFIED.,.F.,.F.,(4,2,4),(1.6862576013651E-6,0.176160467008657,
0.356495154469502),.UNSPECIFIED.);
#5927=B_SPLINE_CURVE_WITH_KNOTS('',3,(#229214,#229215,#229216,#229217,#229218,
#229219,#229220,#229221),.UNSPECIFIED.,.F.,.F.,(4,2,2,4),(1.58031091229498E-6,
0.158410018331858,0.208087193257185,0.449161461367469),.UNSPECIFIED.);
#5928=B_SPLINE_CURVE_WITH_KNOTS('',3,(#229224,#229225,#229226,#229227,#229228,
#229229),.UNSPECIFIED.,.F.,.F.,(4,2,4),(0.000426112405584672,0.120709745014509,
0.235106063097469),.UNSPECIFIED.);
#5929=B_SPLINE_CURVE_WITH_KNOTS('',3,(#229235,#229236,#229237,#229238,#229239,
#229240,#229241,#229242,#229243,#229244),.UNSPECIFIED.,.F.,.F.,(4,2,2,2,
4),(2.26014760912018E-6,0.103733355677681,0.121992468029059,0.239304910920547,
0.648027032476922),.UNSPECIFIED.);
#5930=B_SPLINE_CURVE_WITH_KNOTS('',3,(#229245,#229246,#229247,#229248,#229249,
#229250),.UNSPECIFIED.,.F.,.F.,(4,2,4),(0.,0.135475174046834,0.275618423023284),
 .UNSPECIFIED.);
#5931=B_SPLINE_CURVE_WITH_KNOTS('',3,(#230358,#230359,#230360,#230361,#230362,
#230363),.UNSPECIFIED.,.F.,.F.,(4,2,4),(-0.259382230541658,-0.131398743270302,
-4.17832249355321E-7),.UNSPECIFIED.);
#5932=B_SPLINE_CURVE_WITH_KNOTS('',3,(#230364,#230365,#230366,#230367,#230368,
#230369),.UNSPECIFIED.,.F.,.F.,(4,2,4),(-0.27137277077401,-0.135669107685874,
-1.55628221640116E-6),.UNSPECIFIED.);
#5933=B_SPLINE_CURVE_WITH_KNOTS('',3,(#230370,#230371,#230372,#230373,#230374,
#230375),.UNSPECIFIED.,.F.,.F.,(4,2,4),(-0.267093811957073,-0.133661308819734,
-7.086251292861E-6),.UNSPECIFIED.);
#5934=B_SPLINE_CURVE_WITH_KNOTS('',3,(#230377,#230378,#230379,#230380,#230381,
#230382),.UNSPECIFIED.,.F.,.F.,(4,2,4),(-0.24460605653258,-0.120778493079658,
0.),.UNSPECIFIED.);
#5935=B_SPLINE_CURVE_WITH_KNOTS('',3,(#230383,#230384,#230385,#230386),
 .UNSPECIFIED.,.F.,.F.,(4,4),(-5.76565965941832E-6,0.),.UNSPECIFIED.);
#5936=B_SPLINE_CURVE_WITH_KNOTS('',3,(#230387,#230388,#230389,#230390),
 .UNSPECIFIED.,.F.,.F.,(4,4),(0.,2.59792363940038E-6),.UNSPECIFIED.);
#5937=B_SPLINE_CURVE_WITH_KNOTS('',3,(#230914,#230915,#230916,#230917),
 .UNSPECIFIED.,.F.,.F.,(4,4),(0.0216968151072032,0.926937308587682),
 .UNSPECIFIED.);
#5938=B_SPLINE_CURVE_WITH_KNOTS('',3,(#231018,#231019,#231020,#231021),
 .UNSPECIFIED.,.F.,.F.,(4,4),(0.0222286199771242,0.926269849314919),
 .UNSPECIFIED.);
#5939=B_SPLINE_CURVE_WITH_KNOTS('',3,(#231099,#231100,#231101,#231102),
 .UNSPECIFIED.,.F.,.F.,(4,4),(0.0248339691417604,0.928145544482466),
 .UNSPECIFIED.);
#5940=B_SPLINE_CURVE_WITH_KNOTS('',3,(#231224,#231225,#231226,#231227),
 .UNSPECIFIED.,.F.,.F.,(4,4),(0.0238586497886119,0.928715545244436),
 .UNSPECIFIED.);
#5941=B_SPLINE_CURVE_WITH_KNOTS('',3,(#233265,#233266,#233267,#233268,#233269,
#233270,#233271,#233272,#233273,#233274,#233275,#233276,#233277,#233278,
#233279,#233280,#233281,#233282),.UNSPECIFIED.,.F.,.F.,(4,2,2,2,2,2,2,2,
4),(0.250531060456585,0.281923860175215,0.313316659893845,0.343787122861574,
0.374257585829303,0.404728048797032,0.435198511764761,0.466591311483391,
0.497984111202021),.UNSPECIFIED.);
#5942=B_SPLINE_CURVE_WITH_KNOTS('',3,(#233285,#233286,#233287,#233288,#233289,
#233290,#233291,#233292,#233293,#233294,#233295,#233296,#233297,#233298,
#233299,#233300,#233301,#233302),.UNSPECIFIED.,.F.,.F.,(4,2,2,2,2,2,2,2,
4),(-0.497984111202022,-0.466591311483392,-0.435198511764761,-0.404728048797032,
-0.374257585829303,-0.343787122861574,-0.313316659893845,-0.281923860175215,
-0.250531060456585),.UNSPECIFIED.);
#5943=B_SPLINE_CURVE_WITH_KNOTS('',3,(#233577,#233578,#233579,#233580,#233581,
#233582,#233583,#233584,#233585,#233586,#233587,#233588,#233589,#233590,
#233591,#233592,#233593,#233594),.UNSPECIFIED.,.F.,.F.,(4,2,2,2,2,2,2,2,
4),(0.250531060456585,0.281923860175215,0.313316659893845,0.343787122861574,
0.374257585829303,0.404728048797032,0.435198511764761,0.466591311483391,
0.497984111202021),.UNSPECIFIED.);
#5944=B_SPLINE_CURVE_WITH_KNOTS('',3,(#233597,#233598,#233599,#233600,#233601,
#233602,#233603,#233604,#233605,#233606,#233607,#233608,#233609,#233610,
#233611,#233612,#233613,#233614),.UNSPECIFIED.,.F.,.F.,(4,2,2,2,2,2,2,2,
4),(-0.497984111202022,-0.466591311483392,-0.435198511764761,-0.404728048797032,
-0.374257585829303,-0.343787122861574,-0.313316659893845,-0.281923860175215,
-0.250531060456585),.UNSPECIFIED.);
#5945=B_SPLINE_CURVE_WITH_KNOTS('',3,(#233663,#233664,#233665,#233666,#233667,
#233668,#233669,#233670,#233671,#233672),.UNSPECIFIED.,.F.,.F.,(4,2,2,2,
4),(-0.151069834593804,-0.13224008360155,-0.113410332609297,-0.0944672174322318,
-0.0755241022551671),.UNSPECIFIED.);
#5946=B_SPLINE_CURVE_WITH_KNOTS('',3,(#233695,#233696,#233697,#233698,#233699,
#233700,#233701,#233702,#233703,#233704),.UNSPECIFIED.,.F.,.F.,(4,2,2,2,
4),(-0.22769072019282,-0.20856051537961,-0.1894303105664,-0.170609998467856,
-0.151789686369312),.UNSPECIFIED.);
#5947=B_SPLINE_CURVE_WITH_KNOTS('',3,(#233737,#233738,#233739,#233740,#233741,
#233742,#233743,#233744,#233745,#233746),.UNSPECIFIED.,.F.,.F.,(4,2,2,2,
4),(-0.226527604643677,-0.207600143540642,-0.188672682437608,-0.16984222009878,
-0.151011757759953),.UNSPECIFIED.);
#5948=B_SPLINE_CURVE_WITH_KNOTS('',3,(#233836,#233837,#233838,#233839,#233840,
#233841,#233842,#233843,#233844,#233845),.UNSPECIFIED.,.F.,.F.,(4,2,2,2,
4),(-0.150991595557356,-0.132160886570981,-0.113330177584607,-0.0944081585608019,
-0.0754861395369968),.UNSPECIFIED.);
#5949=B_SPLINE_CURVE_WITH_KNOTS('',3,(#234376,#234377,#234378,#234379,#234380,
#234381,#234382,#234383,#234384,#234385),.UNSPECIFIED.,.F.,.F.,(4,2,2,2,
4),(-0.226530961978678,-0.207602903031429,-0.188674844084179,-0.169844408864107,
-0.151013973644034),.UNSPECIFIED.);
#5950=B_SPLINE_CURVE_WITH_KNOTS('',3,(#235141,#235142,#235143,#235144),
 .UNSPECIFIED.,.F.,.F.,(4,4),(0.463715801913011,0.551217064825118),
 .UNSPECIFIED.);
#5951=B_SPLINE_CURVE_WITH_KNOTS('',3,(#235155,#235156,#235157,#235158,#235159,
#235160),.UNSPECIFIED.,.F.,.F.,(4,2,4),(3.73929755316747,4.16560560244743,
4.26808174572346),.UNSPECIFIED.);
#5952=B_SPLINE_CURVE_WITH_KNOTS('',3,(#235166,#235167,#235168,#235169,#235170,
#235171),.UNSPECIFIED.,.F.,.F.,(4,2,4),(0.414971574747897,0.517447718023913,
0.943755767303881),.UNSPECIFIED.);
#5953=B_SPLINE_CURVE_WITH_KNOTS('',3,(#235181,#235182,#235183,#235184),
 .UNSPECIFIED.,.F.,.F.,(4,4),(0.,0.0875012629120985),.UNSPECIFIED.);
#5954=B_SPLINE_CURVE_WITH_KNOTS('',3,(#235191,#235192,#235193,#235194,#235195,
#235196),.UNSPECIFIED.,.F.,.F.,(4,2,4),(0.,0.0957509671557199,0.156185454533133),
 .UNSPECIFIED.);
#5955=B_SPLINE_CURVE_WITH_KNOTS('',3,(#235200,#235201,#235202,#235203),
 .UNSPECIFIED.,.F.,.F.,(4,4),(0.460964693240806,0.551217064825115),
 .UNSPECIFIED.);
#5956=B_SPLINE_CURVE_WITH_KNOTS('',3,(#235223,#235224,#235225,#235226,#235227,
#235228,#235229,#235230,#235231,#235232),.UNSPECIFIED.,.F.,.F.,(4,2,2,2,
4),(0.,0.250000000000004,0.5,0.750000000000003,1.),.UNSPECIFIED.);
#5957=B_SPLINE_CURVE_WITH_KNOTS('',3,(#235286,#235287,#235288,#235289),
 .UNSPECIFIED.,.F.,.F.,(4,4),(0.,0.087501262912106),.UNSPECIFIED.);
#5958=B_SPLINE_CURVE_WITH_KNOTS('',3,(#235299,#235300,#235301,#235302,#235303,
#235304),.UNSPECIFIED.,.F.,.F.,(4,2,4),(0.414971574747878,0.517447718023913,
0.943755767303879),.UNSPECIFIED.);
#5959=B_SPLINE_CURVE_WITH_KNOTS('',3,(#235311,#235312,#235313,#235314,#235315,
#235316),.UNSPECIFIED.,.F.,.F.,(4,2,4),(3.73945461705751,4.16576266633748,
4.2682388096135),.UNSPECIFIED.);
#5960=B_SPLINE_CURVE_WITH_KNOTS('',3,(#235324,#235325,#235326,#235327),
 .UNSPECIFIED.,.F.,.F.,(4,4),(0.463715801913015,0.551217064825115),
 .UNSPECIFIED.);
#5961=B_SPLINE_CURVE_WITH_KNOTS('',3,(#235336,#235337,#235338,#235339,#235340,
#235341),.UNSPECIFIED.,.F.,.F.,(4,2,4),(0.395031610291999,0.455466097669405,
0.551217064825116),.UNSPECIFIED.);
#5962=B_SPLINE_CURVE_WITH_KNOTS('',3,(#235347,#235348,#235349,#235350),
 .UNSPECIFIED.,.F.,.F.,(4,4),(0.,0.0902523715843086),.UNSPECIFIED.);
#5963=B_SPLINE_CURVE_WITH_KNOTS('',3,(#235368,#235369,#235370,#235371,#235372,
#235373,#235374,#235375,#235376,#235377,#235378,#235379,#235380,#235381,
#235382,#235383,#235384,#235385,#235386,#235387,#235388,#235389,#235390,
#235391,#235392,#235393,#235394,#235395,#235396,#235397,#235398,#235399,
#235400,#235401,#235402,#235403,#235404,#235405,#235406,#235407,#235408,
#235409,#235410,#235411,#235412,#235413,#235414,#235415,#235416,#235417,
#235418,#235419,#235420,#235421,#235422,#235423,#235424,#235425,#235426,
#235427,#235428,#235429,#235430,#235431,#235432,#235433,#235434,#235435,
#235436,#235437,#235438,#235439,#235440,#235441,#235442,#235443),
 .UNSPECIFIED.,.F.,.F.,(4,3,3,3,3,3,3,3,3,3,3,3,3,3,3,3,3,3,3,3,3,3,3,3,
3,4),(0.,0.0631673587290824,0.126547835356396,0.189564804454163,0.250000000000068,
0.260069163320057,0.344083184009803,0.375000000000095,0.460278096077198,
0.468750000000068,0.482531787683698,0.496942193289613,0.500000000000047,
0.566043536818633,0.624999999999914,0.692784513998588,0.741244196317371,
0.742187499999759,0.747855634183151,0.749999999999754,0.807209377839192,
0.858244761980869,0.906405690497173,0.953202845248587,0.996323746112527,
1.),.UNSPECIFIED.);
#5964=B_SPLINE_CURVE_WITH_KNOTS('',3,(#235643,#235644,#235645,#235646,#235647,
#235648,#235649,#235650,#235651,#235652,#235653,#235654,#235655,#235656,
#235657,#235658,#235659,#235660,#235661,#235662),.UNSPECIFIED.,.F.,.F.,
(4,2,2,2,2,2,2,2,2,4),(-23.538612912682,-23.492751629174,-23.4452708186545,
-23.3654723554788,-23.2889368147367,-23.2112691912892,-23.1318212040186,
-23.0559652009404,-22.9774384343871,-22.9093233420168),.UNSPECIFIED.);
#5965=B_SPLINE_CURVE_WITH_KNOTS('',3,(#235665,#235666,#235667,#235668,#235669,
#235670,#235671,#235672,#235673,#235674,#235675,#235676,#235677,#235678,
#235679,#235680,#235681,#235682,#235683,#235684,#235685,#235686,#235687,
#235688,#235689,#235690,#235691,#235692),.UNSPECIFIED.,.F.,.F.,(4,2,2,2,
2,2,2,2,2,2,2,2,2,4),(-0.919201423751235,-0.863947826486626,-0.784692530174886,
-0.708354325422247,-0.628658366861542,-0.550251814512154,-0.473954549019739,
-0.393359509391264,-0.315854735569516,-0.238120045391477,-0.158534522064103,
-0.0819365090807384,-0.0416788465054895,-9.999999992516E-7),
 .UNSPECIFIED.);
#5966=B_SPLINE_CURVE_WITH_KNOTS('',3,(#235697,#235698,#235699,#235700,#235701,
#235702,#235703,#235704,#235705,#235706,#235707,#235708,#235709,#235710,
#235711,#235712,#235713,#235714,#235715,#235716,#235717,#235718,#235719,
#235720,#235721,#235722,#235723,#235724,#235725,#235726,#235727,#235728,
#235729,#235730,#235731,#235732),.UNSPECIFIED.,.F.,.F.,(4,2,2,2,2,2,2,2,
2,2,2,2,2,2,2,2,2,4),(-22.9093233420168,-22.8980081380999,-22.8214383480908,
-22.7418667046431,-22.6649521723812,-22.5874864184619,-22.5080154533073,
-22.4321155129901,-22.3537860381917,-22.2735454894312,-22.1971278635793,
-22.1177268304184,-22.0403427308672,-21.9630230720725,-21.883490552651,
-21.8074370746856,-21.729248955998,-21.6498054932123),.UNSPECIFIED.);
#5967=B_SPLINE_CURVE_WITH_KNOTS('',3,(#235733,#235734,#235735,#235736,#235737,
#235738,#235739,#235740,#235741,#235742,#235743,#235744,#235745,#235746,
#235747,#235748,#235749,#235750,#235751,#235752,#235753,#235754,#235755,
#235756,#235757,#235758,#235759,#235760,#235761,#235762,#235763,#235764,
#235765,#235766,#235767,#235768),.UNSPECIFIED.,.F.,.F.,(4,2,2,2,2,2,2,2,
2,2,2,2,2,2,2,2,2,4),(-2.18087056096665,-2.11334107330462,-2.03463289979668,
-1.95862454259661,-1.87902018720997,-1.80117228584085,-1.72452337235938,
-1.64453746915212,-1.56758510758694,-1.48881063002582,-1.4098497250647,
-1.33374220758123,-1.25411458432869,-1.17600877123226,-1.09960383018546,
-1.01933486542919,-0.942126422073293,-0.919201423751235),.UNSPECIFIED.);
#5968=B_SPLINE_CURVE_WITH_KNOTS('',3,(#235773,#235774,#235775,#235776,#235777,
#235778,#235779,#235780,#235781,#235782,#235783,#235784,#235785,#235786,
#235787,#235788,#235789,#235790,#235791,#235792,#235793,#235794,#235795,
#235796,#235797,#235798,#235799,#235800,#235801,#235802,#235803,#235804,
#235805,#235806,#235807,#235808,#235809,#235810),.UNSPECIFIED.,.F.,.F.,
(4,2,2,2,2,2,2,2,2,2,2,2,2,2,2,2,2,2,4),(-21.6498054932123,-21.6497464036347,
-21.5734775119496,-21.4942444230556,-21.4161627634651,-21.3389785571066,
-21.2587331926262,-21.1823927786933,-21.1043114670783,-21.0247306584986,
-20.9486563934726,-20.8697210600931,-20.7910568722386,-20.714132461226,
-20.6341741471182,-20.5576019018695,-20.4797824951719,-20.4002288768587,
-20.3887331680916),.UNSPECIFIED.);
#5969=B_SPLINE_CURVE_WITH_KNOTS('',3,(#235811,#235812,#235813,#235814,#235815,
#235816,#235817,#235818,#235819,#235820,#235821,#235822,#235823,#235824,
#235825,#235826,#235827,#235828,#235829,#235830,#235831,#235832,#235833,
#235834,#235835,#235836,#235837,#235838,#235839,#235840,#235841,#235842,
#235843,#235844,#235845,#235846),.UNSPECIFIED.,.F.,.F.,(4,2,2,2,2,2,2,2,
2,2,2,2,2,2,2,2,2,4),(-3.44277235542014,-3.36378726174833,-3.28543153234955,
-3.20925143282931,-3.1295715636847,-3.05208541691551,-2.97460818332899,
-2.89503370211843,-2.81845045220135,-2.73815053652911,-2.65964627644047,
-2.58360826692366,-2.50398561017137,-2.42634623254457,-2.34933057724823,
-2.26957822067693,-2.19283610748922,-2.18087056096665),.UNSPECIFIED.);
#5970=B_SPLINE_CURVE_WITH_KNOTS('',3,(#235851,#235852,#235853,#235854,#235855,
#235856,#235857,#235858,#235859,#235860,#235861,#235862,#235863,#235864,
#235865,#235866,#235867,#235868,#235869,#235870,#235871,#235872,#235873,
#235874,#235875,#235876,#235877,#235878,#235879,#235880,#235881,#235882,
#235883,#235884,#235885,#235886),.UNSPECIFIED.,.F.,.F.,(4,2,2,2,2,2,2,2,
2,2,2,2,2,2,2,2,2,4),(-20.3887331680916,-20.324265763245,-20.2455870739102,
-20.1662125920531,-20.0895026903313,-20.0097825331845,-19.93285402267,-19.8552477503529,
-19.7756794908763,-19.6996979335461,-19.6212277463401,-19.5410546843959,
-19.464508413356,-19.3849712910484,-19.3075886648593,-19.2301407428766,
-19.150518751006,-19.1278936731383),.UNSPECIFIED.);
#5971=B_SPLINE_CURVE_WITH_KNOTS('',3,(#235887,#235888,#235889,#235890,#235891,
#235892,#235893,#235894,#235895,#235896,#235897,#235898,#235899,#235900,
#235901,#235902,#235903,#235904,#235905,#235906,#235907,#235908,#235909,
#235910,#235911,#235912,#235913,#235914,#235915,#235916,#235917,#235918,
#235919,#235920,#235921,#235922,#235923,#235924),.UNSPECIFIED.,.F.,.F.,
(4,2,2,2,2,2,2,2,2,2,2,2,2,2,2,2,2,2,4),(-4.7060737882392,-4.69519937299706,
-4.61551026078769,-4.53753270632772,-4.46086272369519,-4.380739889656,-4.30365892107839,
-4.22493237909333,-4.14583270082916,-4.06960942142222,-3.9898882750686,
-3.91164341996169,-3.83519103093889,-3.7547756928784,-3.67742986449246,
-3.5992709523531,-3.51986889045247,-3.44343853969079,-3.44277235542014),
 .UNSPECIFIED.);
#5972=B_SPLINE_CURVE_WITH_KNOTS('',3,(#235929,#235930,#235931,#235932,#235933,
#235934,#235935,#235936,#235937,#235938,#235939,#235940,#235941,#235942,
#235943,#235944,#235945,#235946,#235947,#235948,#235949,#235950,#235951,
#235952,#235953,#235954,#235955,#235956,#235957,#235958,#235959,#235960,
#235961,#235962,#235963,#235964),.UNSPECIFIED.,.F.,.F.,(4,2,2,2,2,2,2,2,
2,2,2,2,2,2,2,2,2,4),(-19.1278936731383,-19.0744044534855,-18.996087951931,
-18.9164933593102,-18.8401028125983,-18.7607411272415,-18.6826906925281,
-18.6053864788049,-18.5250128810173,-18.4486382082739,-18.3704354020229,
-18.2907776589607,-18.214602649211,-18.1355462654448,-18.0569413086003,
-17.9799052983999,-17.8998277847766,-17.8656348671598),.UNSPECIFIED.);
#5973=B_SPLINE_CURVE_WITH_KNOTS('',3,(#235965,#235966,#235967,#235968,#235969,
#235970,#235971,#235972,#235973,#235974,#235975,#235976,#235977,#235978,
#235979,#235980,#235981,#235982,#235983,#235984,#235985,#235986,#235987,
#235988,#235989,#235990,#235991,#235992,#235993,#235994,#235995,#235996,
#235997,#235998,#235999,#236000),.UNSPECIFIED.,.F.,.F.,(4,2,2,2,2,2,2,2,
2,2,2,2,2,2,2,2,2,4),(-5.96899237092104,-5.94689777629729,-5.86714879464217,
-5.78955527581653,-5.71209524525375,-5.63240631532895,-5.55571520757411,
-5.47549701610858,-5.39687374256572,-5.3207715990157,-5.2410722589028,-5.16331386417817,
-5.08629968512605,-5.00642109254712,-4.92956024459656,-4.85013448804389,
-4.77129673291419,-4.7060737882392),.UNSPECIFIED.);
#5974=B_SPLINE_CURVE_WITH_KNOTS('',3,(#236005,#236006,#236007,#236008,#236009,
#236010,#236011,#236012,#236013,#236014,#236015,#236016,#236017,#236018,
#236019,#236020,#236021,#236022,#236023,#236024,#236025,#236026,#236027,
#236028,#236029,#236030,#236031,#236032,#236033,#236034,#236035,#236036,
#236037,#236038,#236039,#236040),.UNSPECIFIED.,.F.,.F.,(4,2,2,2,2,2,2,2,
2,2,2,2,2,2,2,2,2,4),(-17.8656348671598,-17.8232472448269,-17.7453153279261,
-17.6656933743908,-17.5896555747679,-17.5108646186686,-17.43157097449,-17.3547589518092,
-17.2749298588699,-17.1980155426997,-17.1203069744517,-17.0406782951708,
-16.9646465413014,-16.886074223839,-16.8059950689099,-16.7293571613581,
-16.6497224659435,-16.6038873599052),.UNSPECIFIED.);
#5975=B_SPLINE_CURVE_WITH_KNOTS('',3,(#236041,#236042,#236043,#236044,#236045,
#236046,#236047,#236048,#236049,#236050,#236051,#236052,#236053,#236054,
#236055,#236056,#236057,#236058,#236059,#236060,#236061,#236062,#236063,
#236064,#236065,#236066,#236067,#236068,#236069,#236070,#236071,#236072,
#236073,#236074,#236075,#236076),.UNSPECIFIED.,.F.,.F.,(4,2,2,2,2,2,2,2,
2,2,2,2,2,2,2,2,2,4),(-7.23318841533112,-7.19957470382814,-7.11935355932711,
-7.0421810608984,-6.96352897163342,-6.88432908237977,-6.80802291954084,
-6.72824482451805,-6.64989908822763,-6.57342887176945,-6.49290657182504,
-6.41546114839076,-6.33734862206539,-6.25783914264643,-6.18130749664818,
-6.10158446177322,-6.02312142516336,-5.96899237092104),.UNSPECIFIED.);
#5976=B_SPLINE_CURVE_WITH_KNOTS('',3,(#236081,#236082,#236083,#236084,#236085,
#236086,#236087,#236088,#236089,#236090,#236091,#236092,#236093,#236094,
#236095,#236096,#236097,#236098,#236099,#236100,#236101,#236102,#236103,
#236104,#236105,#236106,#236107,#236108,#236109,#236110,#236111,#236112,
#236113,#236114,#236115,#236116),.UNSPECIFIED.,.F.,.F.,(4,2,2,2,2,2,2,2,
2,2,2,2,2,2,2,2,2,4),(-16.6038873599052,-16.5723700238927,-16.4948310453186,
-16.4151560532357,-16.3390120605727,-16.2606047195213,-16.1809544208964,
-16.1044785091047,-16.0250259669085,-15.9470346001031,-15.8696467819783,
-15.789182869367,-15.7128037003227,-15.6345161629282,-15.554817361204,-15.4785735840658,
-15.3994333255414,-15.3409628745653),.UNSPECIFIED.);
#5977=B_SPLINE_CURVE_WITH_KNOTS('',3,(#236117,#236118,#236119,#236120,#236121,
#236122,#236123,#236124,#236125,#236126,#236127,#236128,#236129,#236130,
#236131,#236132,#236133,#236134,#236135,#236136,#236137,#236138,#236139,
#236140,#236141,#236142,#236143,#236144,#236145,#236146,#236147,#236148,
#236149,#236150,#236151,#236152),.UNSPECIFIED.,.F.,.F.,(4,2,2,2,2,2,2,2,
2,2,2,2,2,2,2,2,2,4),(-8.49672659742791,-8.45141042511854,-8.37164403540904,
-8.29488064960835,-8.2147729910192,-8.13606764451279,-8.05993239453284,
-7.98019242317436,-7.90235158161355,-7.82536795780181,-7.74540092188602,
-7.66845766152962,-7.58912849400417,-7.51019892410252,-7.43404417168783,
-7.3543066092219,-7.27623678020524,-7.23318841533112),.UNSPECIFIED.);
#5978=B_SPLINE_CURVE_WITH_KNOTS('',3,(#236157,#236158,#236159,#236160,#236161,
#236162,#236163,#236164,#236165,#236166,#236167,#236168,#236169,#236170,
#236171,#236172,#236173,#236174,#236175,#236176,#236177,#236178,#236179,
#236180,#236181,#236182,#236183,#236184,#236185,#236186,#236187,#236188,
#236189,#236190,#236191,#236192),.UNSPECIFIED.,.F.,.F.,(4,2,2,2,2,2,2,2,
2,2,2,2,2,2,2,2,2,4),(-15.3409628745653,-15.3209156696805,-15.2438038964523,
-15.1636444677601,-15.0870850956638,-15.0090768059695,-14.9294222582231,
-14.8533408497659,-14.7744741587621,-14.6952904569345,-14.6184115554974,
-14.5385101569848,-14.4616398790464,-14.3838645152729,-14.3042110278374,
-14.2281598966633,-14.149521329459,-14.0787866057879),.UNSPECIFIED.);
#5979=B_SPLINE_CURVE_WITH_KNOTS('',3,(#236193,#236194,#236195,#236196,#236197,
#236198,#236199,#236200,#236201,#236202,#236203,#236204,#236205,#236206,
#236207,#236208,#236209,#236210,#236211,#236212,#236213,#236214,#236215,
#236216,#236217,#236218,#236219,#236220,#236221,#236222,#236223,#236224,
#236225,#236226,#236227,#236228),.UNSPECIFIED.,.F.,.F.,(4,2,2,2,2,2,2,2,
2,2,2,2,2,2,2,2,2,4),(-9.76130517536905,-9.70340846015941,-9.62414431736556,
-9.54778645507806,-9.46798686882107,-9.38957577756636,-9.31311791274687,
-9.23252523276213,-9.15501539013617,-9.0769787310619,-8.99739820703599,
-8.92080027718151,-8.84104113619735,-8.7625069471703,-8.6862708056307,-8.60648851823689,
-8.52882343306893,-8.49672659742791),.UNSPECIFIED.);
#5980=B_SPLINE_CURVE_WITH_KNOTS('',3,(#236233,#236234,#236235,#236236,#236237,
#236238,#236239,#236240,#236241,#236242,#236243,#236244,#236245,#236246,
#236247,#236248,#236249,#236250,#236251,#236252,#236253,#236254,#236255,
#236256,#236257,#236258,#236259,#236260,#236261,#236262,#236263,#236264,
#236265,#236266,#236267,#236268,#236269,#236270),.UNSPECIFIED.,.F.,.F.,
(4,2,2,2,2,2,2,2,2,2,2,2,2,2,2,2,2,2,4),(-14.0787866057879,-14.0695668038531,
-13.9928719303782,-13.9131756726274,-13.8358841817083,-13.7582890624203,
-13.6785965537892,-13.6024539769723,-13.5239910721253,-13.4443203751484,
-13.3677933054043,-13.2882854129754,-13.2103839518074,-13.129881596516,
-13.0524588825429,-12.9745208657521,-12.8950294193056,-12.8185173950185,
-12.815698709465),.UNSPECIFIED.);
#5981=B_SPLINE_CURVE_WITH_KNOTS('',3,(#236271,#236272,#236273,#236274,#236275,
#236276,#236277,#236278,#236279,#236280,#236281,#236282,#236283,#236284,
#236285,#236286,#236287,#236288,#236289,#236290,#236291,#236292,#236293,
#236294,#236295,#236296,#236297,#236298,#236299,#236300,#236301,#236302,
#236303,#236304,#236305,#236306),.UNSPECIFIED.,.F.,.F.,(4,2,2,2,2,2,2,2,
2,2,2,2,2,2,2,2,2,4),(-11.0249860124619,-10.9547951692771,-10.8760427721033,
-10.7999052685861,-10.7201601701575,-10.6422715072435,-10.56534947872,-10.4853296583778,
-10.4083383410507,-10.3291372920938,-10.2501513951993,-10.1739699629713,
-10.0942194333807,-10.0160924019212,-9.93946853215564,-9.85918519782063,
-9.78195594007543,-9.76130517536905),.UNSPECIFIED.);
#5982=B_SPLINE_CURVE_WITH_KNOTS('',3,(#236311,#236312,#236313,#236314,#236315,
#236316,#236317,#236318,#236319,#236320,#236321,#236322,#236323,#236324,
#236325,#236326,#236327,#236328,#236329,#236330,#236331,#236332,#236333,
#236334,#236335,#236336,#236337,#236338,#236339,#236340,#236341,#236342,
#236343,#236344,#236345,#236346),.UNSPECIFIED.,.F.,.F.,(4,2,2,2,2,2,2,2,
2,2,2,2,2,2,2,2,2,4),(-12.815698709465,-12.7388502838186,-12.6604039289512,
-12.5842573753116,-12.5045673723298,-12.426989055931,-12.3496716860682,
-12.2699941073719,-12.1933163681172,-12.1133125021989,-12.0346943554925,
-11.958646940508,-11.8789986323752,-11.8012439329055,-11.7243541098449,
-11.6444752807082,-11.5676171032067,-11.5534578894946),.UNSPECIFIED.);
#5983=B_SPLINE_CURVE_WITH_KNOTS('',3,(#236347,#236348,#236349,#236350,#236351,
#236352,#236353,#236354,#236355,#236356,#236357,#236358,#236359,#236360,
#236361,#236362,#236363,#236364,#236365,#236366,#236367,#236368,#236369,
#236370,#236371,#236372,#236373,#236374,#236375,#236376,#236377,#236378,
#236379,#236380,#236381,#236382,#236383,#236384),.UNSPECIFIED.,.F.,.F.,
(4,2,2,2,2,2,2,2,2,2,2,2,2,2,2,2,2,2,4),(-12.2894458654892,-12.2877187485206,
-12.2079332513791,-12.1294910114847,-12.053076894753,-11.9724489486166,
-11.8949085570648,-11.816980570571,-11.7373638662537,-11.6607332796557,
-11.5809733408869,-11.5024026205688,-11.4261854709585,-11.3464053946431,
-11.2687029874123,-11.1913692300601,-11.1115606273989,-11.0347589397308,
-11.0249860124619),.UNSPECIFIED.);
#5984=B_SPLINE_CURVE_WITH_KNOTS('',3,(#236389,#236390,#236391,#236392,#236393,
#236394,#236395,#236396,#236397,#236398,#236399,#236400,#236401,#236402,
#236403,#236404,#236405,#236406,#236407,#236408,#236409,#236410,#236411,
#236412,#236413,#236414,#236415,#236416,#236417,#236418,#236419,#236420,
#236421,#236422,#236423,#236424),.UNSPECIFIED.,.F.,.F.,(4,2,2,2,2,2,2,2,
2,2,2,2,2,2,2,2,2,4),(-11.5534578894946,-11.4883896521,-11.4095468044081,
-11.3334780090213,-11.2538314964982,-11.1758473301944,-11.09927687961,-11.0191434895105,
-10.9420556489546,-10.8635026982174,-10.7843892130607,-10.7081672155377,
-10.6284795542192,-10.5502191518199,-10.47383832356,-10.3934034755595,-10.3160424178526,
-10.2909000381992),.UNSPECIFIED.);
#5985=B_SPLINE_CURVE_WITH_KNOTS('',3,(#236425,#236426,#236427,#236428,#236429,
#236430,#236431,#236432,#236433,#236434,#236435,#236436,#236437,#236438,
#236439,#236440,#236441,#236442,#236443,#236444,#236445,#236446,#236447,
#236448,#236449,#236450,#236451,#236452,#236453,#236454,#236455,#236456,
#236457,#236458,#236459,#236460),.UNSPECIFIED.,.F.,.F.,(4,2,2,2,2,2,2,2,
2,2,2,2,2,2,2,2,2,4),(-13.5529028614626,-13.5366310611161,-13.4596134279343,
-13.3795630232731,-13.3027330821113,-13.2248185416059,-13.1450960915604,
-13.0689795559661,-12.9899718253951,-12.9137942828532,-12.8340666894434,
-12.7559164845886,-12.6793631199568,-12.599052526635,-12.5218002367153,
-12.4433917233644,-12.3640980140278,-12.2894458654892),.UNSPECIFIED.);
#5986=B_SPLINE_CURVE_WITH_KNOTS('',3,(#236465,#236466,#236467,#236468,#236469,
#236470,#236471,#236472,#236473,#236474,#236475,#236476,#236477,#236478,
#236479,#236480,#236481,#236482,#236483,#236484,#236485,#236486,#236487,
#236488,#236489,#236490,#236491,#236492,#236493,#236494,#236495,#236496,
#236497,#236498,#236499,#236500),.UNSPECIFIED.,.F.,.F.,(4,2,2,2,2,2,2,2,
2,2,2,2,2,2,2,2,2,4),(-10.2909000381992,-10.2380261799054,-10.1586029228117,
-10.082154433658,-10.0025206211922,-9.92414258171931,-9.84800606350118,
-9.76834654803807,-9.69083698889078,-9.61347022104288,-9.53386720169178,
-9.45725895014511,-9.37714223779883,-9.29860326982443,-9.22258650707221,
-9.14297599529373,-9.06530087798291,-9.02890583393059),.UNSPECIFIED.);
#5987=B_SPLINE_CURVE_WITH_KNOTS('',3,(#236501,#236502,#236503,#236504,#236505,
#236506,#236507,#236508,#236509,#236510,#236511,#236512,#236513,#236514,
#236515,#236516,#236517,#236518,#236519,#236520,#236521,#236522,#236523,
#236524,#236525,#236526,#236527,#236528,#236529,#236530,#236531,#236532,
#236533,#236534,#236535,#236536),.UNSPECIFIED.,.F.,.F.,(4,2,2,2,2,2,2,2,
2,2,2,2,2,2,2,2,2,4),(-14.8171068447876,-14.7898947256491,-14.7123410728569,
-14.6316990445303,-14.5552778459057,-14.4768221679673,-14.3970268053498,
-14.3206350511274,-14.2413279210765,-14.1629199795842,-14.0856550865695,
-14.0053311123276,-13.9287728850427,-13.8506099370316,-13.7708732308644,
-13.6946853232978,-13.6156648455926,-13.5529028614626),.UNSPECIFIED.);
#5988=B_SPLINE_CURVE_WITH_KNOTS('',3,(#236541,#236542,#236543,#236544,#236545,
#236546,#236547,#236548,#236549,#236550,#236551,#236552,#236553,#236554,
#236555,#236556,#236557,#236558,#236559,#236560,#236561,#236562,#236563,
#236564,#236565,#236566,#236567,#236568,#236569,#236570,#236571,#236572,
#236573,#236574,#236575,#236576),.UNSPECIFIED.,.F.,.F.,(4,2,2,2,2,2,2,2,
2,2,2,2,2,2,2,2,2,4),(-9.02890583393059,-8.98837818038564,-8.9085848357724,
-8.83180622648821,-8.75247998524822,-8.67372599849014,-8.5977120980958,
-8.51811118370627,-8.44021636866933,-8.36363570047745,-8.28359760205359,
-8.20659839258143,-8.12796884716024,-8.04895256139842,-7.97281085546684,
-7.89317727237044,-7.81501477128926,-7.76734335477425),.UNSPECIFIED.);
#5989=B_SPLINE_CURVE_WITH_KNOTS('',3,(#236577,#236578,#236579,#236580,#236581,
#236582,#236583,#236584,#236585,#236586,#236587,#236588,#236589,#236590,
#236591,#236592,#236593,#236594,#236595,#236596,#236597,#236598,#236599,
#236600,#236601,#236602,#236603,#236604,#236605,#236606,#236607,#236608,
#236609,#236610,#236611,#236612),.UNSPECIFIED.,.F.,.F.,(4,2,2,2,2,2,2,2,
2,2,2,2,2,2,2,2,2,4),(-16.0812642602168,-16.0427033691111,-15.9648000015417,
-15.8850434578948,-15.8088951087731,-15.7301279517022,-15.6501648691772,
-15.5733494034149,-15.4935262820714,-15.4161882581257,-15.3384720230956,
-15.2586811009834,-15.1824548683918,-15.1038702650408,-15.0240992276322,
-14.9474553393011,-14.8678246263304,-14.8171068447876),.UNSPECIFIED.);
#5990=B_SPLINE_CURVE_WITH_KNOTS('',3,(#236617,#236618,#236619,#236620,#236621,
#236622,#236623,#236624,#236625,#236626,#236627,#236628,#236629,#236630,
#236631,#236632,#236633,#236634,#236635,#236636,#236637,#236638,#236639,
#236640,#236641,#236642,#236643,#236644,#236645,#236646,#236647,#236648,
#236649,#236650,#236651,#236652),.UNSPECIFIED.,.F.,.F.,(4,2,2,2,2,2,2,2,
2,2,2,2,2,2,2,2,2,4),(-7.76734335477425,-7.73864941116114,-7.65831844901966,
-7.58105403612982,-7.50298926113532,-7.42367035955319,-7.34732022310147,
-7.26775524759053,-7.18948146926026,-7.11338601140779,-7.0337926806513,
-6.95638747398355,-6.87900125726489,-6.79950955808733,-6.7230061602176,
-6.64280571406996,-6.56438262228941,-6.50606900159132),.UNSPECIFIED.);
#5991=B_SPLINE_CURVE_WITH_KNOTS('',3,(#236653,#236654,#236655,#236656,#236657,
#236658,#236659,#236660,#236661,#236662,#236663,#236664,#236665,#236666,
#236667,#236668,#236669,#236670,#236671,#236672,#236673,#236674,#236675,
#236676,#236677,#236678,#236679,#236680,#236681,#236682,#236683,#236684,
#236685,#236686,#236687,#236688),.UNSPECIFIED.,.F.,.F.,(4,2,2,2,2,2,2,2,
2,2,2,2,2,2,2,2,2,4),(-17.3455030680058,-17.2955931490807,-17.2171658662611,
-17.137353476371,-17.060980682749,-16.9817003234495,-16.9031503849096,-16.8259057966854,
-16.7456062623404,-16.6689747781945,-16.5908322516153,-16.5110696292502,
-16.4348753299627,-16.3558738930773,-16.2766722752647,-16.1996663634789,
-16.1196311389729,-16.0812642602168),.UNSPECIFIED.);
#5992=B_SPLINE_CURVE_WITH_KNOTS('',3,(#236693,#236694,#236695,#236696,#236697,
#236698,#236699,#236700,#236701,#236702,#236703,#236704,#236705,#236706,
#236707,#236708,#236709,#236710,#236711,#236712,#236713,#236714,#236715,
#236716,#236717,#236718,#236719,#236720,#236721,#236722,#236723,#236724,
#236725,#236726,#236727,#236728),.UNSPECIFIED.,.F.,.F.,(4,2,2,2,2,2,2,2,
2,2,2,2,2,2,2,2,2,4),(-6.50606900159132,-6.48842746165265,-6.40889066737013,
-6.33133145822056,-6.25440506460236,-6.17473473444485,-6.09807176978359,
-6.01867433671648,-5.94004670161983,-5.86411917020774,-5.78460000677712,
-5.70683164491114,-5.6302697856161,-5.55036530368567,-5.47349152610902,
-5.39481215007952,-5.31593132099885,-5.24598146676954),.UNSPECIFIED.);
#5993=B_SPLINE_CURVE_WITH_KNOTS('',3,(#236729,#236730,#236731,#236732,#236733,
#236734,#236735,#236736,#236737,#236738,#236739,#236740,#236741,#236742,
#236743,#236744,#236745,#236746,#236747,#236748,#236749,#236750,#236751,
#236752,#236753,#236754,#236755,#236756,#236757,#236758,#236759,#236760,
#236761,#236762,#236763,#236764),.UNSPECIFIED.,.F.,.F.,(4,2,2,2,2,2,2,2,
2,2,2,2,2,2,2,2,2,4),(-18.6099778127053,-18.5493148479147,-18.4705919470025,
-18.390482017717,-18.3137021311011,-18.2339184021079,-18.1564983637494,
-18.0788167044097,-17.999020658113,-17.9227728263697,-17.8442219756113,
-17.7644488433926,-17.6878349083277,-17.6082375764479,-17.5301961468915,
-17.4526703162838,-17.3720607330546,-17.3455030680058),.UNSPECIFIED.);
#5994=B_SPLINE_CURVE_WITH_KNOTS('',3,(#236769,#236770,#236771,#236772,#236773,
#236774,#236775,#236776,#236777,#236778,#236779,#236780,#236781,#236782,
#236783,#236784,#236785,#236786,#236787,#236788,#236789,#236790,#236791,
#236792,#236793,#236794,#236795,#236796,#236797,#236798,#236799,#236800,
#236801,#236802,#236803,#236804,#236805,#236806),.UNSPECIFIED.,.F.,.F.,
(4,2,2,2,2,2,2,2,2,2,2,2,2,2,2,2,2,2,4),(-5.24598146676954,-5.23990258087749,
-5.16035947250977,-5.08233272728431,-5.00601244460324,-4.92582445436964,
-4.84869417225652,-4.77060768728586,-4.69143207223894,-4.61517073377482,
-4.53555851063403,-4.45723061749692,-4.38101556066038,-4.30132492142305,
-4.22386755581104,-4.14629439014171,-4.06675367644276,-3.99020072545403,
-3.98436239557673),.UNSPECIFIED.);
#5995=B_SPLINE_CURVE_WITH_KNOTS('',3,(#236807,#236808,#236809,#236810,#236811,
#236812,#236813,#236814,#236815,#236816,#236817,#236818,#236819,#236820,
#236821,#236822,#236823,#236824,#236825,#236826,#236827,#236828,#236829,
#236830,#236831,#236832,#236833,#236834,#236835,#236836,#236837,#236838,
#236839,#236840,#236841,#236842),.UNSPECIFIED.,.F.,.F.,(4,2,2,2,2,2,2,2,
2,2,2,2,2,2,2,2,2,4),(-19.8737805950392,-19.8012842880796,-19.7220653407672,
-19.6434081509384,-19.5662175651196,-19.4859773616869,-19.4093051239936,
-19.3312170184939,-19.2514644782548,-19.175294381749,-19.0963464545443,
-19.0170139310546,-18.9400533385336,-18.8600680614421,-18.7830760907932,
-18.7052177840403,-18.6254634676243,-18.6099778127053),.UNSPECIFIED.);
#5996=B_SPLINE_CURVE_WITH_KNOTS('',3,(#236847,#236848,#236849,#236850,#236851,
#236852,#236853,#236854,#236855,#236856,#236857,#236858,#236859,#236860,
#236861,#236862,#236863,#236864,#236865,#236866,#236867,#236868,#236869,
#236870,#236871,#236872,#236873,#236874,#236875,#236876,#236877,#236878,
#236879,#236880,#236881,#236882),.UNSPECIFIED.,.F.,.F.,(4,2,2,2,2,2,2,2,
2,2,2,2,2,2,2,2,2,4),(-3.98436239557673,-3.91058816835304,-3.8320914425044,
-3.75604716698683,-3.67642092649783,-3.5987893352205,-3.52175035472291,
-3.44200702890818,-3.36527291528161,-3.28573643693738,-3.20703850423459,
-3.13103018768841,-3.05142431534688,-2.97358691830964,-2.89692041149797,
-2.81694626637145,-2.74000442254937,-2.72287955455984),.UNSPECIFIED.);
#5997=B_SPLINE_CURVE_WITH_KNOTS('',3,(#236883,#236884,#236885,#236886,#236887,
#236888,#236889,#236890,#236891,#236892,#236893,#236894,#236895,#236896,
#236897,#236898,#236899,#236900,#236901,#236902,#236903,#236904,#236905,
#236906,#236907,#236908,#236909,#236910,#236911,#236912,#236913,#236914,
#236915,#236916,#236917,#236918,#236919,#236920),.UNSPECIFIED.,.F.,.F.,
(4,2,2,2,2,2,2,2,2,2,2,2,2,2,2,2,2,2,4),(-21.1380887072673,-21.1301824628563,
-21.0534720598587,-20.973762889165,-20.8962932999746,-20.8186803921204,
-20.7389147745979,-20.6626769042768,-20.5841943615403,-20.5044544735613,
-20.427904062833,-20.348374912106,-20.2702550696609,-20.1927908814288,-20.1122487957223,
-20.0357663606382,-19.9574016283348,-19.8776078608383,-19.8737805950392),
 .UNSPECIFIED.);
#5998=B_SPLINE_CURVE_WITH_KNOTS('',3,(#236925,#236926,#236927,#236928,#236929,
#236930,#236931,#236932,#236933,#236934,#236935,#236936,#236937,#236938,
#236939,#236940,#236941,#236942,#236943,#236944,#236945,#236946,#236947,
#236948,#236949,#236950,#236951,#236952,#236953,#236954,#236955,#236956,
#236957,#236958,#236959,#236960),.UNSPECIFIED.,.F.,.F.,(4,2,2,2,2,2,2,2,
2,2,2,2,2,2,2,2,2,4),(-2.72287955455984,-2.6611939409923,-2.58224561704119,
-2.50614498809059,-2.42651807456794,-2.34842515143559,-2.27200938659411,
-2.19175457142759,-2.11455886794221,-2.03635146652478,-1.95711065417433,
-1.88078587379711,-1.80109296697817,-1.7227012773198,-1.64640027132008,
-1.56582136420733,-1.48833119993793,-1.4603242851032),.UNSPECIFIED.);
#5999=B_SPLINE_CURVE_WITH_KNOTS('',3,(#236961,#236962,#236963,#236964,#236965,
#236966,#236967,#236968,#236969,#236970,#236971,#236972,#236973,#236974,
#236975,#236976,#236977,#236978,#236979,#236980,#236981,#236982,#236983,
#236984,#236985,#236986,#236987,#236988,#236989,#236990,#236991,#236992,
#236993,#236994,#236995,#236996),.UNSPECIFIED.,.F.,.F.,(4,2,2,2,2,2,2,2,
2,2,2,2,2,2,2,2,2,4),(-22.4011363767123,-22.3825091502153,-22.3054072138646,
-22.2252623253679,-22.1485797733878,-22.0705810376521,-21.9908740563847,
-21.9147588411359,-21.8358997915956,-21.7564682633744,-21.6795872469303,
-21.5996874662663,-21.522662492958,-21.4448837755089,-21.3651672061648,
-21.2890491931534,-21.2104054765067,-21.1380887072673),.UNSPECIFIED.);
#6000=B_SPLINE_CURVE_WITH_KNOTS('',3,(#237002,#237003,#237004,#237005,#237006,
#237007,#237008,#237009),.UNSPECIFIED.,.F.,.F.,(4,2,2,4),(-0.790626080807867,
-0.749696276559816,-0.708676254523423,-0.640412608621221),.UNSPECIFIED.);
#6001=B_SPLINE_CURVE_WITH_KNOTS('',3,(#237011,#237012,#237013,#237014,#237015,
#237016),.UNSPECIFIED.,.F.,.F.,(4,2,4),(0.,0.0243519941209903,0.0487062313865143),
 .UNSPECIFIED.);
#6002=B_SPLINE_CURVE_WITH_KNOTS('',3,(#237017,#237018,#237019,#237020,#237021,
#237022,#237023,#237024),.UNSPECIFIED.,.F.,.F.,(4,2,2,4),(-0.197604024225048,
-0.160169062454954,-0.0801828347949093,-1.0183968231669E-6),
 .UNSPECIFIED.);
#6003=B_SPLINE_CURVE_WITH_KNOTS('',3,(#237030,#237031,#237032,#237033,#237034,
#237035,#237036,#237037,#237038,#237039,#237040,#237041),.UNSPECIFIED.,
 .F.,.F.,(4,2,2,2,2,4),(-23.5722065003637,-23.497693055354,-23.4210054488723,
-23.342379146909,-23.2652626317729,-23.2565691746208),.UNSPECIFIED.);
#6004=B_SPLINE_CURVE_WITH_KNOTS('',3,(#237044,#237045,#237046,#237047,#237048,
#237049,#237050,#237051,#237052,#237053,#237054,#237055,#237056,#237057,
#237058,#237059,#237060,#237061),.UNSPECIFIED.,.F.,.F.,(4,2,2,2,2,2,2,2,
4),(-0.602752842964723,-0.541077168469372,-0.464578035407547,-0.384478668278887,
-0.307424763205198,-0.228970812045174,-0.149889767174645,-0.0750970133704404,
-9.99999999695689E-7),.UNSPECIFIED.);
#6005=B_SPLINE_CURVE_WITH_KNOTS('',3,(#237066,#237067,#237068,#237069,#237070,
#237071,#237072,#237073,#237074,#237075,#237076,#237077,#237078,#237079,
#237080,#237081,#237082,#237083,#237084,#237085,#237086,#237087,#237088,
#237089,#237090,#237091,#237092,#237093,#237094,#237095,#237096,#237097,
#237098,#237099,#237100,#237101),.UNSPECIFIED.,.F.,.F.,(4,2,2,2,2,2,2,2,
2,2,2,2,2,2,2,2,2,4),(-23.2565691746208,-23.1851002816822,-23.1084754817438,
-23.0304622347963,-22.9507738401723,-22.8746683922162,-22.7957957470848,
-22.7164884410324,-22.6395993516767,-22.5596891465343,-22.4827386348412,
-22.4049524313817,-22.3252601513637,-22.2491695959833,-22.1705192500891,
-22.090431095132,-22.0137198994339,-21.993829988038),.UNSPECIFIED.);
#6006=B_SPLINE_CURVE_WITH_KNOTS('',3,(#237102,#237103,#237104,#237105,#237106,
#237107,#237108,#237109,#237110,#237111,#237112,#237113,#237114,#237115,
#237116,#237117,#237118,#237119,#237120,#237121,#237122,#237123,#237124,
#237125,#237126,#237127,#237128,#237129,#237130,#237131,#237132,#237133,
#237134,#237135,#237136,#237137),.UNSPECIFIED.,.F.,.F.,(4,2,2,2,2,2,2,2,
2,2,2,2,2,2,2,2,2,4),(-1.86395731614265,-1.79131469143525,-1.71408508177727,
-1.63444898401876,-1.55781207307748,-1.47792338108508,-1.39934401643668,
-1.32335141532464,-1.24375914507094,-1.16604229617437,-1.08923305708754,
-1.00939166539875,-0.932570581095492,-0.853451657054535,-0.774644071183091,
-0.698620497957606,-0.619026937738768,-0.602752842964723),.UNSPECIFIED.);
#6007=B_SPLINE_CURVE_WITH_KNOTS('',3,(#237142,#237143,#237144,#237145,#237146,
#237147,#237148,#237149,#237150,#237151,#237152,#237153,#237154,#237155,
#237156,#237157,#237158,#237159,#237160,#237161,#237162,#237163,#237164,
#237165,#237166,#237167,#237168,#237169,#237170,#237171,#237172,#237173,
#237174,#237175,#237176,#237177),.UNSPECIFIED.,.F.,.F.,(4,2,2,2,2,2,2,2,
2,2,2,2,2,2,2,2,2,4),(-21.993829988038,-21.9340081905832,-21.8566253226136,
-21.7790127559565,-21.6992767985655,-21.6230814628004,-21.5446001511914,
-21.4648878735189,-21.3883409400274,-21.308813815213,-21.2308021377538,
-21.1533434094453,-21.0728045264707,-20.9963828996738,-20.9180235568831,
-20.8382680744993,-20.7619585762964,-20.7299620242508),.UNSPECIFIED.);
#6008=B_SPLINE_CURVE_WITH_KNOTS('',3,(#237178,#237179,#237180,#237181,#237182,
#237183,#237184,#237185,#237186,#237187,#237188,#237189,#237190,#237191,
#237192,#237193,#237194,#237195,#237196,#237197,#237198,#237199,#237200,
#237201,#237202,#237203,#237204,#237205,#237206,#237207,#237208,#237209,
#237210,#237211,#237212,#237213,#237214,#237215),.UNSPECIFIED.,.F.,.F.,
(4,2,2,2,2,2,2,2,2,2,2,2,2,2,2,2,2,2,4),(-3.12604785474054,-3.11916406014114,
-3.04206941199171,-2.96373543201984,-2.88460664086586,-2.80838290395217,
-2.72874018594438,-2.65046210727937,-2.57416915143261,-2.49371165741852,
-2.41633340568906,-2.33849516052129,-2.25904746070068,-2.18257839052104,
-2.10296905145572,-2.02456552352352,-1.94848217127368,-1.86885112563732,
-1.86395731614265),.UNSPECIFIED.);
#6009=B_SPLINE_CURVE_WITH_KNOTS('',3,(#237220,#237221,#237222,#237223,#237224,
#237225,#237226,#237227,#237228,#237229,#237230,#237231,#237232,#237233,
#237234,#237235,#237236,#237237,#237238,#237239,#237240,#237241,#237242,
#237243,#237244,#237245,#237246,#237247,#237248,#237249,#237250,#237251,
#237252,#237253,#237254,#237255),.UNSPECIFIED.,.F.,.F.,(4,2,2,2,2,2,2,2,
2,2,2,2,2,2,2,2,2,4),(-20.7299620242508,-20.6827463946196,-20.6042186226985,
-20.5270388935432,-20.4468076578971,-20.3702151620859,-20.2921382009833,
-20.2124301153876,-20.1362922046833,-20.0573566378915,-19.9781710469159,
-19.9012274967379,-19.8212578690367,-19.7443628476554,-19.6665223661209,
-19.5868182062698,-19.5107195193131,-19.4668934640671),.UNSPECIFIED.);
#6010=B_SPLINE_CURVE_WITH_KNOTS('',3,(#237256,#237257,#237258,#237259,#237260,
#237261,#237262,#237263,#237264,#237265,#237266,#237267,#237268,#237269,
#237270,#237271,#237272,#237273,#237274,#237275,#237276,#237277,#237278,
#237279,#237280,#237281,#237282,#237283,#237284,#237285,#237286,#237287,
#237288,#237289,#237290,#237291),.UNSPECIFIED.,.F.,.F.,(4,2,2,2,2,2,2,2,
2,2,2,2,2,2,2,2,2,4),(-4.38713111494036,-4.36896197353506,-4.2923027086423,
-4.21257525484536,-4.13396520723424,-4.05798513071122,-3.97840472490161,
-3.90065622254177,-3.82392384525069,-3.74404628396318,-3.66719317659379,
-3.58821871314422,-3.50937129947931,-3.43333555020512,-3.35374592435993,
-3.27575513813943,-3.19930900911089,-3.12604785474054),.UNSPECIFIED.);
#6011=B_SPLINE_CURVE_WITH_KNOTS('',3,(#237296,#237297,#237298,#237299,#237300,
#237301,#237302,#237303,#237304,#237305,#237306,#237307,#237308,#237309,
#237310,#237311,#237312,#237313,#237314,#237315,#237316,#237317,#237318,
#237319,#237320,#237321,#237322,#237323,#237324,#237325,#237326,#237327,
#237328,#237329,#237330,#237331),.UNSPECIFIED.,.F.,.F.,(4,2,2,2,2,2,2,2,
2,2,2,2,2,2,2,2,2,4),(-19.4668934640671,-19.4320155876266,-19.3520645278124,
-19.2753086679126,-19.1955481533192,-19.1182381534648,-19.0405818480038,
-18.9608413232741,-18.8846589211247,-18.8061345868867,-18.7264147794134,
-18.6498288754341,-18.5702590313714,-18.4923494476519,-18.4148538038223,
-18.3342730653254,-18.2578890735217,-18.2031408914352),.UNSPECIFIED.);
#6012=B_SPLINE_CURVE_WITH_KNOTS('',3,(#237332,#237333,#237334,#237335,#237336,
#237337,#237338,#237339,#237340,#237341,#237342,#237343,#237344,#237345,
#237346,#237347,#237348,#237349,#237350,#237351,#237352,#237353,#237354,
#237355,#237356,#237357,#237358,#237359,#237360,#237361,#237362,#237363,
#237364,#237365,#237366,#237367),.UNSPECIFIED.,.F.,.F.,(4,2,2,2,2,2,2,2,
2,2,2,2,2,2,2,2,2,4),(-5.64892676185118,-5.6188978192691,-5.54266696049746,
-5.46305555514589,-5.38476245669672,-5.30852869070133,-5.22805245343415,
-5.15065962464527,-5.07294679429705,-4.99347930984184,-4.91699341878228,
-4.83740023522811,-4.75897645240369,-4.68292735856954,-4.60331559595368,
-4.52575792609574,-4.44862376378175,-4.38713111494036),.UNSPECIFIED.);
#6013=B_SPLINE_CURVE_WITH_KNOTS('',3,(#237372,#237373,#237374,#237375,#237376,
#237377,#237378,#237379,#237380,#237381,#237382,#237383,#237384,#237385,
#237386,#237387,#237388,#237389,#237390,#237391,#237392,#237393,#237394,
#237395,#237396,#237397,#237398,#237399,#237400,#237401,#237402,#237403,
#237404,#237405,#237406,#237407),.UNSPECIFIED.,.F.,.F.,(4,2,2,2,2,2,2,2,
2,2,2,2,2,2,2,2,2,4),(-18.2031408914352,-18.179492152848,-18.0997439313982,
-18.0234073251507,-17.9441590506585,-17.8657632814858,-17.7885541573198,
-17.7082890833817,-17.631760730409,-17.5536541757552,-17.4739621076796,
-17.3978222587249,-17.3188583449362,-17.2398298963329,-17.1628655277294,
-17.0828713188359,-17.0060645825577,-16.9401280371148),.UNSPECIFIED.);
#6014=B_SPLINE_CURVE_WITH_KNOTS('',3,(#237408,#237409,#237410,#237411,#237412,
#237413,#237414,#237415,#237416,#237417,#237418,#237419,#237420,#237421,
#237422,#237423,#237424,#237425,#237426,#237427,#237428,#237429,#237430,
#237431,#237432,#237433,#237434,#237435,#237436,#237437,#237438,#237439,
#237440,#237441,#237442,#237443),.UNSPECIFIED.,.F.,.F.,(4,2,2,2,2,2,2,2,
2,2,2,2,2,2,2,2,2,4),(-6.90946184483317,-6.86760642961369,-6.7916708400602,
-6.7121392179253,-6.63439293140309,-6.55777252826709,-6.47789349608262,
-6.40104193860036,-6.32225111214459,-6.24339822683304,-6.16738099587715,
-6.08783178147495,-6.00983394361517,-5.93347443663795,-5.85331874214117,
-5.77621703982064,-5.69803979876399,-5.64892676185118),.UNSPECIFIED.);
#6015=B_SPLINE_CURVE_WITH_KNOTS('',3,(#237448,#237449,#237450,#237451,#237452,
#237453,#237454,#237455,#237456,#237457,#237458,#237459,#237460,#237461,
#237462,#237463,#237464,#237465,#237466,#237467,#237468,#237469,#237470,
#237471,#237472,#237473,#237474,#237475,#237476,#237477,#237478,#237479,
#237480,#237481,#237482,#237483),.UNSPECIFIED.,.F.,.F.,(4,2,2,2,2,2,2,2,
2,2,2,2,2,2,2,2,2,4),(-16.9401280371148,-16.9282037503213,-16.8485236627961,
-16.7724481057347,-16.6937249444493,-16.6139486511616,-16.537181650428,
-16.4574070398215,-16.3802047121582,-16.3025384902836,-16.222829570132,
-16.1466925369983,-16.0681594104423,-15.9884679751763,-15.9118764226213,
-15.8322983428692,-15.7545270051868,-15.6771758708029),.UNSPECIFIED.);
#6016=B_SPLINE_CURVE_WITH_KNOTS('',3,(#237484,#237485,#237486,#237487,#237488,
#237489,#237490,#237491,#237492,#237493,#237494,#237495,#237496,#237497,
#237498,#237499,#237500,#237501,#237502,#237503,#237504,#237505,#237506,
#237507,#237508,#237509,#237510,#237511,#237512,#237513,#237514,#237515,
#237516,#237517,#237518,#237519),.UNSPECIFIED.,.F.,.F.,(4,2,2,2,2,2,2,2,
2,2,2,2,2,2,2,2,2,4),(-8.17021312579191,-8.11747034451843,-8.04133415108175,
-7.96171687108957,-7.88431742195717,-7.80684514073046,-7.72736245062139,
-7.65086608992251,-7.5705299105957,-7.49212030099125,-7.41613911530324,
-7.33658395835915,-7.25903903962238,-7.18203779924169,-7.10238510837754,
-7.02573715227108,-6.94621282645275,-6.90946184483317),.UNSPECIFIED.);
#6017=B_SPLINE_CURVE_WITH_KNOTS('',3,(#237524,#237525,#237526,#237527,#237528,
#237529,#237530,#237531,#237532,#237533,#237534,#237535,#237536,#237537,
#237538,#237539,#237540,#237541,#237542,#237543,#237544,#237545,#237546,
#237547,#237548,#237549,#237550,#237551,#237552,#237553,#237554,#237555,
#237556,#237557,#237558,#237559,#237560,#237561),.UNSPECIFIED.,.F.,.F.,
(4,2,2,2,2,2,2,2,2,2,2,2,2,2,2,2,2,2,4),(-15.6771758708029,-15.6770280684428,
-15.5964402318874,-15.5201268390809,-15.4417262916037,-15.3620219047567,
-15.2856882575655,-15.2064383814064,-15.1282131561966,-15.0510083229075,
-14.9707442012106,-14.8943145632693,-14.81621240392,-14.7365735239284,-14.6604627016941,
-14.5815049486408,-14.5026750732159,-14.4257236808457,-14.4146492123929),
 .UNSPECIFIED.);
#6018=B_SPLINE_CURVE_WITH_KNOTS('',3,(#237562,#237563,#237564,#237565,#237566,
#237567,#237568,#237569,#237570,#237571,#237572,#237573,#237574,#237575,
#237576,#237577,#237578,#237579,#237580,#237581,#237582,#237583,#237584,
#237585,#237586,#237587,#237588,#237589,#237590,#237591,#237592,#237593,
#237594,#237595,#237596,#237597),.UNSPECIFIED.,.F.,.F.,(4,2,2,2,2,2,2,2,
2,2,2,2,2,2,2,2,2,4),(-9.42971000722909,-9.3658882895704,-9.28942247658091,
-9.20958233406318,-9.1327714201309,-9.05421232368468,-8.97539387085022,
-8.8994311344934,-8.81996532926532,-8.74199974137761,-8.66576704950347,
-8.58564082857867,-8.50857101307976,-8.43059536142831,-8.35148004581058,
-8.27527702862697,-8.19573923437247,-8.17021312579191),.UNSPECIFIED.);
#6019=B_SPLINE_CURVE_WITH_KNOTS('',3,(#237602,#237603,#237604,#237605,#237606,
#237607,#237608,#237609,#237610,#237611,#237612,#237613,#237614,#237615,
#237616,#237617,#237618,#237619,#237620,#237621,#237622,#237623,#237624,
#237625,#237626,#237627,#237628,#237629,#237630,#237631,#237632,#237633,
#237634,#237635,#237636,#237637),.UNSPECIFIED.,.F.,.F.,(4,2,2,2,2,2,2,2,
2,2,2,2,2,2,2,2,2,4),(-14.4146492123929,-14.3457397794975,-14.2690579791201,
-14.1912108935331,-14.1115926026985,-14.0355727044255,-13.9568648986143,
-13.8773078146962,-13.7976881026888,-13.7198092566215,-13.643166601816,
-13.5631476297004,-13.4861645139395,-13.4074202264935,-13.3284254156655,
-13.2522917794569,-13.1726458279891,-13.1529000929986),.UNSPECIFIED.);
#6020=B_SPLINE_CURVE_WITH_KNOTS('',3,(#237638,#237639,#237640,#237641,#237642,
#237643,#237644,#237645,#237646,#237647,#237648,#237649,#237650,#237651,
#237652,#237653,#237654,#237655,#237656,#237657,#237658,#237659,#237660,
#237661,#237662,#237663,#237664,#237665,#237666,#237667,#237668,#237669,
#237670,#237671,#237672,#237673),.UNSPECIFIED.,.F.,.F.,(4,2,2,2,2,2,2,2,
2,2,2,2,2,2,2,2,2,4),(-10.6886668367708,-10.6141171329505,-10.5368397267788,
-10.4574188227709,-10.3809842606412,-10.3009163157618,-10.2225611611604,
-10.1466878558215,-10.0672335555996,-9.98974112954057,-9.91291816909027,
-9.83331520225674,-9.75671789916803,-9.677448188703,-9.59888546489566,-9.52303209351768,
-9.44359290672304,-9.42971000722909),.UNSPECIFIED.);
#6021=B_SPLINE_CURVE_WITH_KNOTS('',3,(#237678,#237679,#237680,#237681,#237682,
#237683,#237684,#237685,#237686,#237687,#237688,#237689,#237690,#237691,
#237692,#237693,#237694,#237695,#237696,#237697,#237698,#237699,#237700,
#237701,#237702,#237703,#237704,#237705,#237706,#237707,#237708,#237709,
#237710,#237711,#237712,#237713),.UNSPECIFIED.,.F.,.F.,(4,2,2,2,2,2,2,2,
2,2,2,2,2,2,2,2,2,4),(-13.1529000929986,-13.0945058791895,-13.0180982140432,
-12.9377929757886,-12.8605508001914,-12.7823927291035,-12.7031007650497,
-12.626727585356,-12.5470099608498,-12.4685664186318,-12.3922568723288,
-12.3124597685296,-12.234887676826,-12.1572356575688,-12.0775759124685,
-12.0009090277532,-11.9203829768641,-11.8894930626961),.UNSPECIFIED.);
#6022=B_SPLINE_CURVE_WITH_KNOTS('',3,(#237714,#237715,#237716,#237717,#237718,
#237719,#237720,#237721,#237722,#237723,#237724,#237725,#237726,#237727,
#237728,#237729,#237730,#237731,#237732,#237733,#237734,#237735,#237736,
#237737,#237738,#237739,#237740,#237741,#237742,#237743,#237744,#237745,
#237746,#237747,#237748,#237749,#237750,#237751),.UNSPECIFIED.,.F.,.F.,
(4,2,2,2,2,2,2,2,2,2,2,2,2,2,2,2,2,2,4),(-11.949044188699,-11.9399073283772,
-11.8629827014429,-11.7844811604486,-11.7055394645275,-11.6294741132395,
-11.5499292488032,-11.4718399984583,-11.3955712959968,-11.3153146061308,
-11.2381226360676,-11.1601765604512,-11.0809304220309,-11.004650968641,
-10.9251700697058,-10.8469676740098,-10.7709605586456,-10.6914521379874,
-10.6886668367708),.UNSPECIFIED.);
#6023=B_SPLINE_CURVE_WITH_KNOTS('',3,(#237756,#237757,#237758,#237759,#237760,
#237761,#237762,#237763,#237764,#237765,#237766,#237767,#237768,#237769,
#237770,#237771,#237772,#237773,#237774,#237775,#237776,#237777,#237778,
#237779,#237780,#237781,#237782,#237783,#237784,#237785,#237786,#237787,
#237788,#237789,#237790,#237791),.UNSPECIFIED.,.F.,.F.,(4,2,2,2,2,2,2,2,
2,2,2,2,2,2,2,2,2,4),(-11.8894930626961,-11.8417990530921,-11.7656459491589,
-11.6859115275326,-11.6081942888121,-11.5310151799915,-11.4511857098612,
-11.3743674966686,-11.294655740804,-11.2158751815502,-11.1397691168386,
-11.0600587262734,-10.9821402628285,-10.9053440481854,-10.8252883261443,
-10.7482666060734,-10.6692911183768,-10.6263497039737),.UNSPECIFIED.);
#6024=B_SPLINE_CURVE_WITH_KNOTS('',3,(#237792,#237793,#237794,#237795,#237796,
#237797,#237798,#237799,#237800,#237801,#237802,#237803,#237804,#237805,
#237806,#237807,#237808,#237809,#237810,#237811,#237812,#237813,#237814,
#237815,#237816,#237817,#237818,#237819,#237820,#237821,#237822,#237823,
#237824,#237825,#237826,#237827),.UNSPECIFIED.,.F.,.F.,(4,2,2,2,2,2,2,2,
2,2,2,2,2,2,2,2,2,4),(-13.2089732113637,-13.188699892793,-13.1121716476065,
-13.0321957518606,-12.9537363504872,-12.8778110294063,-12.7982941966592,
-12.7206973807655,-12.643886836538,-12.5641727738037,-12.4874712705778,
-12.4082806472394,-12.3296035017028,-12.2536736195776,-12.1741639788225,
-12.0963447205716,-12.0198688686453,-11.949044188699),.UNSPECIFIED.);
#6025=B_SPLINE_CURVE_WITH_KNOTS('',3,(#237832,#237833,#237834,#237835,#237836,
#237837,#237838,#237839,#237840,#237841,#237842,#237843,#237844,#237845,
#237846,#237847,#237848,#237849,#237850,#237851,#237852,#237853,#237854,
#237855,#237856,#237857,#237858,#237859,#237860,#237861,#237862,#237863,
#237864,#237865,#237866,#237867),.UNSPECIFIED.,.F.,.F.,(4,2,2,2,2,2,2,2,
2,2,2,2,2,2,2,2,2,4),(-10.6263497039737,-10.590264032485,-10.5140776179666,
-10.4343500724478,-10.3561800171732,-10.2796467264391,-10.1993142464524,
-10.1220423076596,-10.0436833142805,-9.96436692329861,-9.88796784593152,
-9.80817848973431,-9.72971296377646,-9.65330724382957,-9.57265395682767,
-9.49509066675103,-9.41719889463007,-9.36205618767461),.UNSPECIFIED.);
#6026=B_SPLINE_CURVE_WITH_KNOTS('',3,(#237868,#237869,#237870,#237871,#237872,
#237873,#237874,#237875,#237876,#237877,#237878,#237879,#237880,#237881,
#237882,#237883,#237884,#237885,#237886,#237887,#237888,#237889,#237890,
#237891,#237892,#237893,#237894,#237895,#237896,#237897,#237898,#237899,
#237900,#237901,#237902,#237903),.UNSPECIFIED.,.F.,.F.,(4,2,2,2,2,2,2,2,
2,2,2,2,2,2,2,2,2,4),(-14.4685414185229,-14.4371861006538,-14.3570666160918,
-14.2806911965607,-14.201333110894,-14.1240417499958,-14.046765531488,-13.9672936809693,
-13.8913078705452,-13.8131641808844,-13.73372132699,-13.6574971431671,-13.5783096732641,
-13.5003327647789,-13.4231949969096,-13.3429966170248,-13.2667342522707,
-13.2089732113637),.UNSPECIFIED.);
#6027=B_SPLINE_CURVE_WITH_KNOTS('',3,(#237908,#237909,#237910,#237911,#237912,
#237913,#237914,#237915,#237916,#237917,#237918,#237919,#237920,#237921,
#237922,#237923,#237924,#237925,#237926,#237927,#237928,#237929,#237930,
#237931,#237932,#237933,#237934,#237935,#237936,#237937,#237938,#237939,
#237940,#237941,#237942,#237943),.UNSPECIFIED.,.F.,.F.,(4,2,2,2,2,2,2,2,
2,2,2,2,2,2,2,2,2,4),(-9.36205618767461,-9.33755664571965,-9.26090242145497,
-9.18113217965199,-9.10253596259969,-9.02631670802215,-8.94652766712044,
-8.86879953456162,-8.79148939019274,-8.71165272718738,-8.63482504688624,
-8.55491220288934,-8.47612988204783,-8.3999810243187,-8.32022382374916,
-8.24230500962556,-8.16539861414471,-8.09802537957356),.UNSPECIFIED.);
#6028=B_SPLINE_CURVE_WITH_KNOTS('',3,(#237944,#237945,#237946,#237947,#237948,
#237949,#237950,#237951,#237952,#237953,#237954,#237955,#237956,#237957,
#237958,#237959,#237960,#237961,#237962,#237963,#237964,#237965,#237966,
#237967,#237968,#237969,#237970,#237971,#237972,#237973,#237974,#237975,
#237976,#237977,#237978,#237979),.UNSPECIFIED.,.F.,.F.,(4,2,2,2,2,2,2,2,
2,2,2,2,2,2,2,2,2,4),(-15.7266574265448,-15.6832398993101,-15.6046482364568,
-15.5279086562263,-15.4481445412296,-15.371686569013,-15.2940538243071,
-15.2146602981345,-15.1388543838039,-15.0603634600351,-14.9810490749452,
-14.9045172989487,-14.8249840679432,-14.7481560310107,-14.6707292209604,
-14.5913158937944,-14.515475679086,-14.4685414185229),.UNSPECIFIED.);
#6029=B_SPLINE_CURVE_WITH_KNOTS('',3,(#237984,#237985,#237986,#237987,#237988,
#237989,#237990,#237991,#237992,#237993,#237994,#237995,#237996,#237997,
#237998,#237999,#238000,#238001,#238002,#238003,#238004,#238005,#238006,
#238007,#238008,#238009,#238010,#238011,#238012,#238013,#238014,#238015,
#238016,#238017,#238018,#238019),.UNSPECIFIED.,.F.,.F.,(4,2,2,2,2,2,2,2,
2,2,2,2,2,2,2,2,2,4),(-8.09802537957356,-8.08534627872566,-8.00832485868984,
-7.92916764555054,-7.8501479341364,-7.7739446603837,-7.69417866279333,-7.61601753652654,
-7.53939934799904,-7.45907954203661,-7.38181651819004,-7.30330259097503,
-7.22400130531918,-7.14761101036681,-7.06779228564878,-6.98934367034265,
-6.91288045049293,-6.83360317581237),.UNSPECIFIED.);
#6030=B_SPLINE_CURVE_WITH_KNOTS('',3,(#238020,#238021,#238022,#238023,#238024,
#238025,#238026,#238027,#238028,#238029,#238030,#238031,#238032,#238033,
#238034,#238035,#238036,#238037,#238038,#238039,#238040,#238041,#238042,
#238043,#238044,#238045,#238046,#238047,#238048,#238049,#238050,#238051,
#238052,#238053,#238054,#238055),.UNSPECIFIED.,.F.,.F.,(4,2,2,2,2,2,2,2,
2,2,2,2,2,2,2,2,2,4),(-16.9860676137287,-16.9305459155631,-16.8530028103589,
-16.775715329367,-16.6953469507869,-16.6192500471932,-16.5410633784241,
-16.4615818946196,-16.3854570106574,-16.3064235736138,-16.2284315885244,
-16.1514382709984,-16.0713936373972,-15.9951840612662,-15.9172958763925,
-15.8378808126566,-15.7619811309377,-15.7266574265448),.UNSPECIFIED.);
#6031=B_SPLINE_CURVE_WITH_KNOTS('',3,(#238060,#238061,#238062,#238063,#238064,
#238065,#238066,#238067,#238068,#238069,#238070,#238071,#238072,#238073,
#238074,#238075,#238076,#238077,#238078,#238079,#238080,#238081,#238082,
#238083,#238084,#238085,#238086,#238087,#238088,#238089,#238090,#238091,
#238092,#238093,#238094,#238095,#238096,#238097),.UNSPECIFIED.,.F.,.F.,
(4,2,2,2,2,2,2,2,2,2,2,2,2,2,2,2,2,2,4),(-6.83360317581237,-6.83224784905331,
-6.75470100800845,-6.67668555636461,-6.5970650214824,-6.52042947802374,
-6.4406450177057,-6.36207097203192,-6.28581916926094,-6.2060127908259,-6.12830778993307,
-6.05090391849408,-5.9710949013656,-5.8942914568354,-5.81421912317929,-5.73546942914718,
-5.65930973552131,-5.57954261838186,-5.56913783942761),.UNSPECIFIED.);
#6032=B_SPLINE_CURVE_WITH_KNOTS('',3,(#238098,#238099,#238100,#238101,#238102,
#238103,#238104,#238105,#238106,#238107,#238108,#238109,#238110,#238111,
#238112,#238113,#238114,#238115,#238116,#238117,#238118,#238119,#238120,
#238121,#238122,#238123,#238124,#238125,#238126,#238127,#238128,#238129,
#238130,#238131,#238132,#238133),.UNSPECIFIED.,.F.,.F.,(4,2,2,2,2,2,2,2,
2,2,2,2,2,2,2,2,2,4),(-18.2453522235663,-18.1776525209244,-18.1010656003546,
-18.0234153086571,-17.9439557986802,-17.8680906548125,-17.7895805206712,
-17.7100420811292,-17.6334836692764,-17.5539255287679,-17.476946377409,
-17.3994913336737,-17.3200039291733,-17.2440800453835,-17.1657605948636,
-17.0862902489563,-17.0099074139525,-16.9860676137287),.UNSPECIFIED.);
#6033=B_SPLINE_CURVE_WITH_KNOTS('',3,(#238138,#238139,#238140,#238141,#238142,
#238143,#238144,#238145,#238146,#238147,#238148,#238149,#238150,#238151,
#238152,#238153,#238154,#238155,#238156,#238157,#238158,#238159,#238160,
#238161,#238162,#238163,#238164,#238165,#238166,#238167,#238168,#238169,
#238170,#238171,#238172,#238173),.UNSPECIFIED.,.F.,.F.,(4,2,2,2,2,2,2,2,
2,2,2,2,2,2,2,2,2,4),(-5.56913783942761,-5.50165737991348,-5.42467576492216,
-5.34466158022702,-5.26767409052678,-5.1883740752882,-5.10939616535199,
-5.03320676482875,-4.95343878279698,-4.87532052203619,-4.79865084377856,
-4.71837849729253,-4.64115802239225,-4.56252559337156,-4.48327392493462,
-4.40692255332495,-4.32711046819931,-4.30497396562869),.UNSPECIFIED.);
#6034=B_SPLINE_CURVE_WITH_KNOTS('',3,(#238174,#238175,#238176,#238177,#238178,
#238179,#238180,#238181,#238182,#238183,#238184,#238185,#238186,#238187,
#238188,#238189,#238190,#238191,#238192,#238193,#238194,#238195,#238196,
#238197,#238198,#238199,#238200,#238201,#238202,#238203,#238204,#238205,
#238206,#238207,#238208,#238209),.UNSPECIFIED.,.F.,.F.,(4,2,2,2,2,2,2,2,
2,2,2,2,2,2,2,2,2,4),(-19.5051615199427,-19.4256178472367,-19.3494467260214,
-19.2712598891341,-19.1917305088467,-19.1155993348017,-19.0365636442837,
-18.958396927912,-18.8813955586696,-18.8013460874971,-18.7250340151242,
-18.6471376406698,-18.5676652621586,-18.4917331427441,-18.412981897987,
-18.334187158106,-18.2574308338498,-18.2453522235663),.UNSPECIFIED.);
#6035=B_SPLINE_CURVE_WITH_KNOTS('',3,(#238214,#238215,#238216,#238217,#238218,
#238219,#238220,#238221,#238222,#238223,#238224,#238225,#238226,#238227,
#238228,#238229,#238230,#238231,#238232,#238233,#238234,#238235,#238236,
#238237,#238238,#238239,#238240,#238241,#238242,#238243,#238244,#238245,
#238246,#238247,#238248,#238249),.UNSPECIFIED.,.F.,.F.,(4,2,2,2,2,2,2,2,
2,2,2,2,2,2,2,2,2,4),(-4.30497396562869,-4.24871276630561,-4.17222419819763,
-4.09164713925734,-4.01415041814135,-3.93604575143311,-3.85648152440021,
-3.77989805921464,-3.70013491408271,-3.62161738401807,-3.54536495412576,
-3.46557701007066,-3.38792909310605,-3.31046498954944,-3.23071851119358,
-3.15397297029016,-3.07377666013053,-3.0404377993062),.UNSPECIFIED.);
#6036=B_SPLINE_CURVE_WITH_KNOTS('',3,(#238250,#238251,#238252,#238253,#238254,
#238255,#238256,#238257,#238258,#238259,#238260,#238261,#238262,#238263,
#238264,#238265,#238266,#238267,#238268,#238269,#238270,#238271,#238272,
#238273,#238274,#238275,#238276,#238277,#238278,#238279,#238280,#238281,
#238282,#238283,#238284,#238285,#238286,#238287),.UNSPECIFIED.,.F.,.F.,
(4,2,2,2,2,2,2,2,2,2,2,2,2,2,2,2,2,2,4),(-20.7651480509305,-20.7542372169798,
-20.6747496324084,-20.5988578946382,-20.5203631373555,-20.4406458485752,
-20.364094824007,-20.2845468918017,-20.2074562622594,-20.1300073492215,
-20.0504843172495,-19.9745114843353,-19.896196995271,-19.8166942811889,
-19.7403133680385,-19.6609562476344,-19.5832709603124,-19.5059830142488,
-19.5051615199427),.UNSPECIFIED.);
#6037=B_SPLINE_CURVE_WITH_KNOTS('',3,(#238292,#238293,#238294,#238295,#238296,
#238297,#238298,#238299,#238300,#238301,#238302,#238303,#238304,#238305,
#238306,#238307,#238308,#238309,#238310,#238311,#238312,#238313,#238314,
#238315,#238316,#238317,#238318,#238319,#238320,#238321,#238322,#238323,
#238324,#238325,#238326,#238327),.UNSPECIFIED.,.F.,.F.,(4,2,2,2,2,2,2,2,
2,2,2,2,2,2,2,2,2,4),(-3.0404377993062,-2.99509419358038,-2.91895468092827,
-2.83921330030169,-2.7613958259546,-2.68437088706612,-2.60443001067381,
-2.52751036167285,-2.44810103283402,-2.3691998612149,-2.29305490552806,
-2.21332045711987,-2.13527956318884,-2.05858944660127,-1.9784000437842,
-1.90125631748013,-1.82253721525056,-1.77693741255607),.UNSPECIFIED.);
#6038=B_SPLINE_CURVE_WITH_KNOTS('',3,(#238328,#238329,#238330,#238331,#238332,
#238333,#238334,#238335,#238336,#238337,#238338,#238339,#238340,#238341,
#238342,#238343,#238344,#238345,#238346,#238347,#238348,#238349,#238350,
#238351,#238352,#238353,#238354,#238355,#238356,#238357,#238358,#238359,
#238360,#238361,#238362,#238363),.UNSPECIFIED.,.F.,.F.,(4,2,2,2,2,2,2,2,
2,2,2,2,2,2,2,2,2,4),(-22.0249622838298,-22.0023547571536,-21.922814161715,
-21.8467066862456,-21.7677031731419,-21.6894008143267,-21.6124250410366,
-21.5324054689352,-21.4560257497192,-21.3781551357414,-21.29866276063,-21.2227291775328,
-21.1440023962923,-21.0650466736007,-20.9883073940863,-20.9085497524053,
-20.8318709630664,-20.7651480509305),.UNSPECIFIED.);
#6039=B_SPLINE_CURVE_WITH_KNOTS('',3,(#238369,#238370,#238371,#238372,#238373,
#238374,#238375,#238376,#238377,#238378,#238379,#238380,#238381,#238382,
#238383,#238384),.UNSPECIFIED.,.F.,.F.,(4,2,2,2,2,2,2,4),(0.324863770283186,
0.395667134570481,0.472791225099944,0.552555445808509,0.629311039769859,
0.708734538016899,0.749777571670018,0.790730601234904),.UNSPECIFIED.);
#6040=B_SPLINE_CURVE_WITH_KNOTS('',3,(#238386,#238387,#238388,#238389,#238390,
#238391),.UNSPECIFIED.,.F.,.F.,(4,2,4),(1.00022081805299E-6,0.0243479089776584,
0.0486953353237867),.UNSPECIFIED.);
#6041=B_SPLINE_CURVE_WITH_KNOTS('',3,(#238392,#238393,#238394,#238395,#238396,
#238397,#238398,#238399,#238400,#238401,#238402,#238403,#238404,#238405,
#238406,#238407,#238408,#238409),.UNSPECIFIED.,.F.,.F.,(4,2,2,2,2,2,2,2,
4),(-0.513010840582583,-0.491707909785119,-0.415055184345757,-0.334765707541337,
-0.256186603725737,-0.180098289337284,-0.100418478920529,-0.0495366954217494,
-1.00000008074197E-6),.UNSPECIFIED.);
#6042=B_SPLINE_CURVE_WITH_KNOTS('',3,(#238419,#238420,#238421,#238422,#238423,
#238424),.UNSPECIFIED.,.F.,.F.,(4,2,4),(-0.0520203312674702,-0.0267861740298943,
-1.0000000459226E-6),.UNSPECIFIED.);
#6043=B_SPLINE_CURVE_WITH_KNOTS('',3,(#238441,#238442,#238443,#238444,#238445,
#238446,#238447,#238448,#238449,#238450,#238451,#238452),.UNSPECIFIED.,
 .F.,.F.,(4,2,2,2,2,4),(-0.179361978655781,-0.134721706620385,-0.0896676871854849,
-0.0448235819521571,-0.0392550189488239,-1.00000011879486E-6),
 .UNSPECIFIED.);
#6044=B_SPLINE_CURVE_WITH_KNOTS('',3,(#238969,#238970,#238971,#238972,#238973,
#238974,#238975,#238976,#238977,#238978,#238979,#238980,#238981,#238982,
#238983,#238984,#238985,#238986,#238987,#238988,#238989,#238990,#238991,
#238992,#238993,#238994,#238995,#238996),.UNSPECIFIED.,.F.,.F.,(4,2,2,2,
2,2,2,2,2,2,2,2,2,4),(22.6236748723828,22.6407093081193,22.7173617942293,
22.7968830932907,22.8754944544741,22.9514332474403,23.0309680597223,23.1087193135484,
23.1853402255204,23.2652245118562,23.3420810027936,23.4208695790923,23.4959114338434,
23.5687658403324),.UNSPECIFIED.);
#6045=B_SPLINE_CURVE_WITH_KNOTS('',3,(#238999,#239000,#239001,#239002,#239003,
#239004,#239005,#239006,#239007,#239008,#239009,#239010,#239011,#239012,
#239013,#239014,#239015,#239016,#239017,#239018,#239019,#239020,#239021,
#239022,#239023,#239024,#239025,#239026,#239027,#239028,#239029,#239030,
#239031,#239032,#239033,#239034),.UNSPECIFIED.,.F.,.F.,(4,2,2,2,2,2,2,2,
2,2,2,2,2,2,2,2,2,4),(9.99999999717517E-7,0.0462547190314567,0.0908553254087972,
0.167757479715614,0.247681226172906,0.324646289047548,0.40244572157152,
0.482152132491632,0.558256242839576,0.636919981793369,0.717024322840535,
0.793748683042598,0.873474040064272,0.950871759823262,1.02849766570582,
1.10824785849813,1.18445704254395,1.23484507369462),.UNSPECIFIED.);
#6046=B_SPLINE_CURVE_WITH_KNOTS('',3,(#239039,#239040,#239041,#239042,#239043,
#239044,#239045,#239046,#239047,#239048,#239049,#239050,#239051,#239052,
#239053,#239054,#239055,#239056,#239057,#239058,#239059,#239060,#239061,
#239062,#239063,#239064,#239065,#239066,#239067,#239068,#239069,#239070,
#239071,#239072,#239073,#239074),.UNSPECIFIED.,.F.,.F.,(4,2,2,2,2,2,2,2,
2,2,2,2,2,2,2,2,2,4),(21.3625688139077,21.3913787543729,21.4677304856353,
21.5473202777439,21.625593224373,21.7017308865875,21.7813507414309,21.8587542522225,
21.9362256297425,22.0157126587402,22.0922131081633,22.1725458477689,22.2509599885555,
22.3269434172786,22.4065014473729,22.4840508988643,22.5610518004103,22.6236748723828),
 .UNSPECIFIED.);
#6047=B_SPLINE_CURVE_WITH_KNOTS('',3,(#239075,#239076,#239077,#239078,#239079,
#239080,#239081,#239082,#239083,#239084,#239085,#239086,#239087,#239088,
#239089,#239090,#239091,#239092,#239093,#239094,#239095,#239096,#239097,
#239098,#239099,#239100,#239101,#239102,#239103,#239104,#239105,#239106,
#239107,#239108,#239109,#239110),.UNSPECIFIED.,.F.,.F.,(4,2,2,2,2,2,2,2,
2,2,2,2,2,2,2,2,2,4),(1.23484507369462,1.26295188142383,1.34267841695845,
1.41923862457627,1.49877951130816,1.57680660074797,1.65427879563786,1.73483163550077,
1.81126754077481,1.88964050402294,1.96941044583165,2.04573335376308,2.12495932843831,
2.20350299174566,2.28069623673453,2.36094148010891,2.43754863000376,2.49897999942429),
 .UNSPECIFIED.);
#6048=B_SPLINE_CURVE_WITH_KNOTS('',3,(#239115,#239116,#239117,#239118,#239119,
#239120,#239121,#239122,#239123,#239124,#239125,#239126,#239127,#239128,
#239129,#239130,#239131,#239132,#239133,#239134,#239135,#239136,#239137,
#239138,#239139,#239140,#239141,#239142,#239143,#239144,#239145,#239146,
#239147,#239148,#239149,#239150),.UNSPECIFIED.,.F.,.F.,(4,2,2,2,2,2,2,2,
2,2,2,2,2,2,2,2,2,4),(20.1001536081644,20.1407906125954,20.2168374619708,
20.2964789771982,20.3743832097966,20.4510415586,20.5310869382233,20.6080951883912,
20.6868495520353,20.765870747754,20.8420282128573,20.9216967326681,20.9998629340078,
21.0762885379599,21.1566210589077,21.2338891810234,21.3120596620606,21.3625688139077),
 .UNSPECIFIED.);
#6049=B_SPLINE_CURVE_WITH_KNOTS('',3,(#239151,#239152,#239153,#239154,#239155,
#239156,#239157,#239158,#239159,#239160,#239161,#239162,#239163,#239164,
#239165,#239166,#239167,#239168,#239169,#239170,#239171,#239172,#239173,
#239174,#239175,#239176,#239177,#239178,#239179,#239180,#239181,#239182,
#239183,#239184,#239185,#239186),.UNSPECIFIED.,.F.,.F.,(4,2,2,2,2,2,2,2,
2,2,2,2,2,2,2,2,2,4),(2.49897999942429,2.51563926655626,2.59536191643896,
2.67151353631666,2.7504629491092,2.82966487001291,2.90662200693993,2.98660571779551,
3.06351576270205,3.14136999944524,3.22108882729151,3.29720154164607,3.37591939849584,
3.45588714541026,3.53265668598561,3.61243138446563,3.68975672333244,3.76219964214866),
 .UNSPECIFIED.);
#6050=B_SPLINE_CURVE_WITH_KNOTS('',3,(#239191,#239192,#239193,#239194,#239195,
#239196,#239197,#239198,#239199,#239200,#239201,#239202,#239203,#239204,
#239205,#239206,#239207,#239208,#239209,#239210,#239211,#239212,#239213,
#239214,#239215,#239216,#239217,#239218,#239219,#239220,#239221,#239222,
#239223,#239224,#239225,#239226),.UNSPECIFIED.,.F.,.F.,(4,2,2,2,2,2,2,2,
2,2,2,2,2,2,2,2,2,4),(18.8378147773619,18.8895407867648,18.9657401122406,
19.045450464741,19.1229833437424,19.2004539326094,19.2800782003355,19.3567083962423,
19.4369741709152,19.5155301835049,19.5915961112866,19.6712524836123,19.7489436039846,
19.8259591767686,19.905766394743,19.9825601373105,20.0620261236383,20.1001536081644),
 .UNSPECIFIED.);
#6051=B_SPLINE_CURVE_WITH_KNOTS('',3,(#239227,#239228,#239229,#239230,#239231,
#239232,#239233,#239234,#239235,#239236,#239237,#239238,#239239,#239240,
#239241,#239242,#239243,#239244,#239245,#239246,#239247,#239248,#239249,
#239250,#239251,#239252,#239253,#239254,#239255,#239256,#239257,#239258,
#239259,#239260,#239261,#239262,#239263,#239264),.UNSPECIFIED.,.F.,.F.,
(4,2,2,2,2,2,2,2,2,2,2,2,2,2,2,2,2,2,4),(3.76219964214866,3.76742688845616,
3.84718218555019,3.92337891552651,4.00191728040496,4.08165181563963,4.15825144289695,
4.23783551467587,4.31576094089768,4.39327050359559,4.47386566806185,4.55026435353068,
4.62867535147353,4.7084385050342,4.78478892495954,4.86405145560046,4.94246356555156,
5.01968665557928,5.02622452893907),.UNSPECIFIED.);
#6052=B_SPLINE_CURVE_WITH_KNOTS('',3,(#239269,#239270,#239271,#239272,#239273,
#239274,#239275,#239276,#239277,#239278,#239279,#239280,#239281,#239282,
#239283,#239284,#239285,#239286,#239287,#239288,#239289,#239290,#239291,
#239292,#239293,#239294,#239295,#239296,#239297,#239298,#239299,#239300,
#239301,#239302,#239303,#239304),.UNSPECIFIED.,.F.,.F.,(4,2,2,2,2,2,2,2,
2,2,2,2,2,2,2,2,2,4),(17.5740980330669,17.6369933046161,17.7136606695414,
17.7938263393176,17.8709472323695,17.9496429457457,18.0287862833124,18.1050454201912,
18.1847918646659,18.2630806427599,18.3395412734652,18.4200031485925,18.4973923493336,
18.5755322223201,18.6549810287802,18.7314554867318,18.811138344041,18.8378147773619),
 .UNSPECIFIED.);
#6053=B_SPLINE_CURVE_WITH_KNOTS('',3,(#239305,#239306,#239307,#239308,#239309,
#239310,#239311,#239312,#239313,#239314,#239315,#239316,#239317,#239318,
#239319,#239320,#239321,#239322,#239323,#239324,#239325,#239326,#239327,
#239328,#239329,#239330,#239331,#239332,#239333,#239334,#239335,#239336,
#239337,#239338,#239339,#239340),.UNSPECIFIED.,.F.,.F.,(4,2,2,2,2,2,2,2,
2,2,2,2,2,2,2,2,2,4),(5.02622452893907,5.09996620350271,5.17650963611587,
5.25463032028455,5.33433742926195,5.4104913933453,5.48946961334628,5.56851486802525,
5.64549327134522,5.7255020272037,5.80232422478868,5.88019926400631,5.95989449979103,
6.03598450046676,6.11472204449212,6.19451553182695,6.27129665989664,6.28915126608589),
 .UNSPECIFIED.);
#6054=B_SPLINE_CURVE_WITH_KNOTS('',3,(#239345,#239346,#239347,#239348,#239349,
#239350,#239351,#239352,#239353,#239354,#239355,#239356,#239357,#239358,
#239359,#239360,#239361,#239362,#239363,#239364,#239365,#239366,#239367,
#239368,#239369,#239370,#239371,#239372,#239373,#239374,#239375,#239376,
#239377,#239378,#239379,#239380),.UNSPECIFIED.,.F.,.F.,(4,2,2,2,2,2,2,2,
2,2,2,2,2,2,2,2,2,4),(16.3109364258552,16.3847150284939,16.4621561301153,
16.541878995712,16.6186018112264,16.698774275327,16.777433447177,16.8535503932859,
16.9332681431273,17.0110625795403,17.088064655456,17.1679818672716,17.2448787446325,
17.3242644681819,17.4031422854142,17.4792646858285,17.5589755096573,17.5740980330669),
 .UNSPECIFIED.);
#6055=B_SPLINE_CURVE_WITH_KNOTS('',3,(#239381,#239382,#239383,#239384,#239385,
#239386,#239387,#239388,#239389,#239390,#239391,#239392,#239393,#239394,
#239395,#239396,#239397,#239398,#239399,#239400,#239401,#239402,#239403,
#239404,#239405,#239406,#239407,#239408,#239409,#239410,#239411,#239412,
#239413,#239414,#239415,#239416),.UNSPECIFIED.,.F.,.F.,(4,2,2,2,2,2,2,2,
2,2,2,2,2,2,2,2,2,4),(6.28915126608589,6.35108591673579,6.42830404984285,
6.50598458202569,6.58570875809415,6.66186055160458,6.74040816495516,6.82011480794906,
6.896720527872,6.9763132947808,7.05410096033775,7.13161426404932,7.21221698959725,
7.28854551609797,7.3669605933149,7.44668040181184,7.52302826097822,7.55270818716772),
 .UNSPECIFIED.);
#6056=B_SPLINE_CURVE_WITH_KNOTS('',3,(#239421,#239422,#239423,#239424,#239425,
#239426,#239427,#239428,#239429,#239430,#239431,#239432,#239433,#239434,
#239435,#239436,#239437,#239438,#239439,#239440,#239441,#239442,#239443,
#239444,#239445,#239446,#239447,#239448,#239449,#239450,#239451,#239452,
#239453,#239454,#239455,#239456,#239457,#239458),.UNSPECIFIED.,.F.,.F.,
(4,2,2,2,2,2,2,2,2,2,2,2,2,2,2,2,2,2,4),(15.0466193961525,15.0546599548629,
15.1318575552455,15.210466605289,15.2896948007098,15.3660235527781,15.4458119759886,
15.5241864587444,15.600652332661,15.6812055287019,15.7586792974288,15.8367607569033,
15.9163014218172,15.9928622064941,16.0726017119744,16.1510959904507,16.2273258093889,
16.3070901049585,16.3109364258552),.UNSPECIFIED.);
#6057=B_SPLINE_CURVE_WITH_KNOTS('',3,(#239459,#239460,#239461,#239462,#239463,
#239464,#239465,#239466,#239467,#239468,#239469,#239470,#239471,#239472,
#239473,#239474,#239475,#239476,#239477,#239478,#239479,#239480,#239481,
#239482,#239483,#239484,#239485,#239486,#239487,#239488,#239489,#239490,
#239491,#239492,#239493,#239494),.UNSPECIFIED.,.F.,.F.,(4,2,2,2,2,2,2,2,
2,2,2,2,2,2,2,2,2,4),(7.55270818716772,7.60229285314904,7.68053493798863,
7.75775418641584,7.8380332458771,7.91447842599388,7.9925951681434,8.07224958728399,
8.14837493544016,8.22734745510189,8.30619469613861,8.38316057429433,8.46315948803179,
8.53985724263922,8.61771899026031,8.69735293570344,8.77338771037036,8.81490714031691),
 .UNSPECIFIED.);
#6058=B_SPLINE_CURVE_WITH_KNOTS('',3,(#239499,#239500,#239501,#239502,#239503,
#239504,#239505,#239506,#239507,#239508,#239509,#239510,#239511,#239512,
#239513,#239514,#239515,#239516,#239517,#239518,#239519,#239520,#239521,
#239522,#239523,#239524,#239525,#239526,#239527,#239528,#239529,#239530,
#239531,#239532,#239533,#239534),.UNSPECIFIED.,.F.,.F.,(4,2,2,2,2,2,2,2,
2,2,2,2,2,2,2,2,2,4),(13.7830271212104,13.8023150783772,13.8790957622896,
13.9591442691831,14.0378706299548,14.1140077346993,14.1937511946023,14.2716133566261,
14.3485721051306,14.4285625845395,14.505527264209,14.584803690052,14.6637582039623,
14.7399250197211,14.8196693484089,14.8977644685878,14.9744113852441,15.0466193961525),
 .UNSPECIFIED.);
#6059=B_SPLINE_CURVE_WITH_KNOTS('',3,(#239535,#239536,#239537,#239538,#239539,
#239540,#239541,#239542,#239543,#239544,#239545,#239546,#239547,#239548,
#239549,#239550,#239551,#239552,#239553,#239554,#239555,#239556,#239557,
#239558,#239559,#239560,#239561,#239562,#239563,#239564,#239565,#239566,
#239567,#239568,#239569,#239570),.UNSPECIFIED.,.F.,.F.,(4,2,2,2,2,2,2,2,
2,2,2,2,2,2,2,2,2,4),(8.81490714031691,8.85211036064628,8.9316852408578,
9.008443970894,9.08821269376554,9.16528452273819,9.24294109920656,9.32259595371586,
9.39866832476149,9.47719040174472,9.55683132445173,9.63340918913478,9.71297561297174,
9.79058398860146,9.86806671460512,9.94545247074768,10.0232994383367,10.07726006159),
 .UNSPECIFIED.);
#6060=B_SPLINE_CURVE_WITH_KNOTS('',3,(#239575,#239576,#239577,#239578,#239579,
#239580,#239581,#239582,#239583,#239584,#239585,#239586,#239587,#239588,
#239589,#239590,#239591,#239592,#239593,#239594,#239595,#239596,#239597,
#239598,#239599,#239600,#239601,#239602,#239603,#239604,#239605,#239606,
#239607,#239608,#239609,#239610),.UNSPECIFIED.,.F.,.F.,(4,2,2,2,2,2,2,2,
2,2,2,2,2,2,2,2,2,4),(12.5184563203764,12.5497802836604,12.6261479314363,
12.7059429734401,12.7843683363411,12.8608088529379,12.9414175563509,13.0189414121536,
13.0969336657911,13.1765306033314,13.2531434329733,13.3329042286112,13.4114549875406,
13.4876841628844,13.5674668685525,13.6451488408897,13.7225297112902,13.7830271212104),
 .UNSPECIFIED.);
#6061=B_SPLINE_CURVE_WITH_KNOTS('',3,(#239611,#239612,#239613,#239614,#239615,
#239616,#239617,#239618,#239619,#239620,#239621,#239622,#239623,#239624,
#239625,#239626,#239627,#239628,#239629,#239630,#239631,#239632,#239633,
#239634,#239635,#239636,#239637,#239638,#239639,#239640,#239641,#239642,
#239643,#239644,#239645,#239646),.UNSPECIFIED.,.F.,.F.,(4,2,2,2,2,2,2,2,
2,2,2,2,2,2,2,2,2,4),(10.07726006159,10.1027548027335,10.1792312683471,
10.2588485858205,10.3372596705821,10.4133508147372,10.4929898662385,10.5705337636431,
10.6477717871671,10.7274155175606,10.8040597932003,10.8839577096872,10.9625445602035,
11.0385447654803,11.1181449759676,11.1958692177396,11.2726866802344,11.3388557888326),
 .UNSPECIFIED.);
#6062=B_SPLINE_CURVE_WITH_KNOTS('',3,(#239651,#239652,#239653,#239654,#239655,
#239656,#239657,#239658,#239659,#239660,#239661,#239662,#239663,#239664,
#239665,#239666,#239667,#239668,#239669,#239670,#239671,#239672,#239673,
#239674,#239675,#239676,#239677,#239678,#239679,#239680,#239681,#239682,
#239683,#239684,#239685,#239686),.UNSPECIFIED.,.F.,.F.,(4,2,2,2,2,2,2,2,
2,2,2,2,2,2,2,2,2,4),(11.2548510467115,11.2980233086365,11.3741495640617,
11.4538830912037,11.5317788009478,11.6086623347247,11.6886909350883,11.7656895172056,
11.8448231642113,11.923819448896,12.0000001175665,12.0797424434144,12.1578803983245,
12.2344758235014,12.3147718199753,12.3920119387833,12.4705025041557,12.5184563203764),
 .UNSPECIFIED.);
#6063=B_SPLINE_CURVE_WITH_KNOTS('',3,(#239687,#239688,#239689,#239690,#239691,
#239692,#239693,#239694,#239695,#239696,#239697,#239698,#239699,#239700,
#239701,#239702,#239703,#239704,#239705,#239706,#239707,#239708,#239709,
#239710,#239711,#239712,#239713,#239714,#239715,#239716,#239717,#239718,
#239719,#239720,#239721,#239722),.UNSPECIFIED.,.F.,.F.,(4,2,2,2,2,2,2,2,
2,2,2,2,2,2,2,2,2,4),(11.3388557888326,11.3525356361157,11.4293640214325,
11.5084919604289,11.5873069769148,11.6633379518827,11.7429393865072,11.8208965953283,
11.8974038509132,11.9775108617879,12.0545721457777,12.1330349777865,12.2121235451364,
12.288317305646,12.3679631434665,12.4461995842588,12.5225273003769,12.6005934315007),
 .UNSPECIFIED.);
#6064=B_SPLINE_CURVE_WITH_KNOTS('',3,(#239727,#239728,#239729,#239730,#239731,
#239732,#239733,#239734,#239735,#239736,#239737,#239738,#239739,#239740,
#239741,#239742,#239743,#239744,#239745,#239746,#239747,#239748,#239749,
#239750,#239751,#239752,#239753,#239754,#239755,#239756,#239757,#239758,
#239759,#239760,#239761,#239762),.UNSPECIFIED.,.F.,.F.,(4,2,2,2,2,2,2,2,
2,2,2,2,2,2,2,2,2,4),(9.99071847554691,10.0448123826062,10.1211953987327,
10.2018247631317,10.2793650452417,10.3572336365993,10.4368522634336,10.513483750659,
10.5932303128834,10.6718032184567,10.7479998379628,10.8277651919765,10.9054702711791,
10.9827574236387,11.0625704099994,11.1393753047155,11.2192643489391,11.2548510467115),
 .UNSPECIFIED.);
#6065=B_SPLINE_CURVE_WITH_KNOTS('',3,(#239763,#239764,#239765,#239766,#239767,
#239768,#239769,#239770,#239771,#239772,#239773,#239774,#239775,#239776,
#239777,#239778,#239779,#239780,#239781,#239782,#239783,#239784,#239785,
#239786,#239787,#239788,#239789,#239790,#239791,#239792,#239793,#239794,
#239795,#239796,#239797,#239798,#239799,#239800),.UNSPECIFIED.,.F.,.F.,
(4,2,2,2,2,2,2,2,2,2,2,2,2,2,2,2,2,2,4),(12.6005934315007,12.602938763315,
12.6802760682319,12.7582135669689,12.8376143514832,12.9140404005903,12.9936380748357,
13.0719943611852,13.1480875810128,13.2277098734604,13.3051983880356,13.3824979963671,
13.4620809471436,13.5386690096921,13.6186921682012,13.6972135502531,13.7731950393595,
13.8527712040441,13.8621232120524),.UNSPECIFIED.);
#6066=B_SPLINE_CURVE_WITH_KNOTS('',3,(#239805,#239806,#239807,#239808,#239809,
#239810,#239811,#239812,#239813,#239814,#239815,#239816,#239817,#239818,
#239819,#239820,#239821,#239822,#239823,#239824,#239825,#239826,#239827,
#239828,#239829,#239830,#239831,#239832,#239833,#239834,#239835,#239836,
#239837,#239838,#239839,#239840),.UNSPECIFIED.,.F.,.F.,(4,2,2,2,2,2,2,2,
2,2,2,2,2,2,2,2,2,4),(8.72728889099367,8.79501613456367,8.87186385542684,
8.94976017855893,9.02947910082415,9.10559165966755,9.18435078087881,9.26417432599307,
9.34097681421297,9.42078815997437,9.49803277374631,9.57573497112963,9.65548316171832,
9.73165848498506,9.8102280573935,9.88660446939589,9.96637013208894,9.99071847554691),
 .UNSPECIFIED.);
#6067=B_SPLINE_CURVE_WITH_KNOTS('',3,(#239841,#239842,#239843,#239844,#239845,
#239846,#239847,#239848,#239849,#239850,#239851,#239852,#239853,#239854,
#239855,#239856,#239857,#239858,#239859,#239860,#239861,#239862,#239863,
#239864,#239865,#239866,#239867,#239868,#239869,#239870,#239871,#239872,
#239873,#239874,#239875,#239876),.UNSPECIFIED.,.F.,.F.,(4,2,2,2,2,2,2,2,
2,2,2,2,2,2,2,2,2,4),(13.8621232120524,13.9304294236307,14.0072915450429,
14.0870689942372,14.1638312685282,14.243069734594,14.3218098137758,14.3977978550319,
14.4773674628283,14.5552490882758,14.6317781328063,14.7118040439196,14.7887903475489,
14.8673410523001,14.9463465581447,15.0224722538337,15.1020778057827,15.1231092357584),
 .UNSPECIFIED.);
#6068=B_SPLINE_CURVE_WITH_KNOTS('',3,(#239881,#239882,#239883,#239884,#239885,
#239886,#239887,#239888,#239889,#239890,#239891,#239892,#239893,#239894,
#239895,#239896,#239897,#239898,#239899,#239900,#239901,#239902,#239903,
#239904,#239905,#239906,#239907,#239908,#239909,#239910,#239911,#239912,
#239913,#239914,#239915,#239916),.UNSPECIFIED.,.F.,.F.,(4,2,2,2,2,2,2,2,
2,2,2,2,2,2,2,2,2,4),(7.46340241241562,7.54301805341094,7.61943998793248,
7.69787170413151,7.77765784819711,7.85402877837828,7.93331233352954,8.0117522463032,
8.08899605949032,8.16929701121815,8.24586485699811,8.32400650944155,8.40373696570717,
8.47991244175215,8.55891192768175,8.63798625095867,8.71498566581844,8.72728889099367),
 .UNSPECIFIED.);
#6069=B_SPLINE_CURVE_WITH_KNOTS('',3,(#239917,#239918,#239919,#239920,#239921,
#239922,#239923,#239924,#239925,#239926,#239927,#239928,#239929,#239930,
#239931,#239932,#239933,#239934,#239935,#239936,#239937,#239938,#239939,
#239940,#239941,#239942,#239943,#239944,#239945,#239946,#239947,#239948,
#239949,#239950,#239951,#239952),.UNSPECIFIED.,.F.,.F.,(4,2,2,2,2,2,2,2,
2,2,2,2,2,2,2,2,2,4),(15.1231092357584,15.1802303202402,15.2565541765279,
15.3368761555168,15.4141306527047,15.4921277966692,15.5714385512177,15.6477800297023,
15.7273227850391,15.8055890541803,15.881653251365,15.9612233321017,16.0386216052047,
16.1159520022845,16.1954382244697,16.2719354612956,16.3520530655929,16.3842164827505),
 .UNSPECIFIED.);
#6070=B_SPLINE_CURVE_WITH_KNOTS('',3,(#239957,#239958,#239959,#239960,#239961,
#239962,#239963,#239964,#239965,#239966,#239967,#239968,#239969,#239970,
#239971,#239972,#239973,#239974,#239975,#239976,#239977,#239978,#239979,
#239980,#239981,#239982,#239983,#239984,#239985,#239986,#239987,#239988,
#239989,#239990,#239991,#239992,#239993,#239994),.UNSPECIFIED.,.F.,.F.,
(4,2,2,2,2,2,2,2,2,2,2,2,2,2,2,2,2,2,4),(6.19938299209805,6.21014794327352,
6.28988894821445,6.36602291168288,6.44476091855524,6.5247570910379,6.60154659665179,
6.68134194060473,6.75869227209202,6.83638269450315,6.9161604845104,6.9923793783196,
7.07093827717526,7.1506951720957,7.22731494863593,7.30691986016907,7.38487167598359,
7.46240172944621,7.46340241241562),.UNSPECIFIED.);
#6071=B_SPLINE_CURVE_WITH_KNOTS('',3,(#239995,#239996,#239997,#239998,#239999,
#240000,#240001,#240002,#240003,#240004,#240005,#240006,#240007,#240008,
#240009,#240010,#240011,#240012,#240013,#240014,#240015,#240016,#240017,
#240018,#240019,#240020,#240021,#240022,#240023,#240024,#240025,#240026,
#240027,#240028,#240029,#240030),.UNSPECIFIED.,.F.,.F.,(4,2,2,2,2,2,2,2,
2,2,2,2,2,2,2,2,2,4),(16.3842164827505,16.4304731640843,16.5064051428445,
16.5859216865821,16.6634784492848,16.7403553652435,16.820024748001,16.8966857350638,
16.9760055552314,17.054634238895,17.1305483096494,17.2100503919758,17.2878203704037,
17.364341733933,17.4442493394675,17.5211249001405,17.5997353506844,17.6440450612851),
 .UNSPECIFIED.);
#6072=B_SPLINE_CURVE_WITH_KNOTS('',3,(#240035,#240036,#240037,#240038,#240039,
#240040,#240041,#240042,#240043,#240044,#240045,#240046,#240047,#240048,
#240049,#240050,#240051,#240052,#240053,#240054,#240055,#240056,#240057,
#240058,#240059,#240060,#240061,#240062,#240063,#240064,#240065,#240066,
#240067,#240068,#240069,#240070),.UNSPECIFIED.,.F.,.F.,(4,2,2,2,2,2,2,2,
2,2,2,2,2,2,2,2,2,4),(4.93557907506006,4.95807649474067,5.03786794568686,
5.11421010640617,5.1934556653646,5.27202569037795,5.34923825762195,5.42950345425129,
5.50613366843463,5.58424385977541,5.66398836103944,5.74016022249727,5.81912946818321,
5.89835892633256,5.97533567811949,6.05533965656332,6.13227383133234,6.19938299209805),
 .UNSPECIFIED.);
#6073=B_SPLINE_CURVE_WITH_KNOTS('',3,(#240071,#240072,#240073,#240074,#240075,
#240076,#240077,#240078,#240079,#240080,#240081,#240082,#240083,#240084,
#240085,#240086,#240087,#240088,#240089,#240090,#240091,#240092,#240093,
#240094,#240095,#240096,#240097,#240098,#240099,#240100,#240101,#240102,
#240103,#240104,#240105,#240106),.UNSPECIFIED.,.F.,.F.,(4,2,2,2,2,2,2,2,
2,2,2,2,2,2,2,2,2,4),(17.6440450612851,17.6786207001756,17.7546464114692,
17.8341758503396,17.91220775608,17.9884979989117,18.068692661484,18.145828028411,
18.2238569341798,18.3030400062917,18.3792607066525,18.4587122680853,18.5368510646172,
18.6128551439165,18.6923365995457,18.7696075127427,18.8469399687415,18.9040360682104),
 .UNSPECIFIED.);
#6074=B_SPLINE_CURVE_WITH_KNOTS('',3,(#240111,#240112,#240113,#240114,#240115,
#240116,#240117,#240118,#240119,#240120,#240121,#240122,#240123,#240124,
#240125,#240126,#240127,#240128,#240129,#240130,#240131,#240132,#240133,
#240134,#240135,#240136,#240137,#240138,#240139,#240140,#240141,#240142,
#240143,#240144,#240145,#240146),.UNSPECIFIED.,.F.,.F.,(4,2,2,2,2,2,2,2,
2,2,2,2,2,2,2,2,2,4),(3.6713151088133,3.7050232003142,3.78515463088442,
3.86189760876706,3.94164221384685,4.01906364102073,4.0967084462536,4.17647971918973,
4.25270981752711,4.33122379458765,4.41097122102382,4.48755018224877,4.56711046192888,
4.64516256671576,4.7226538463442,4.80322638839784,4.87968423324783,4.93557907506006),
 .UNSPECIFIED.);
#6075=B_SPLINE_CURVE_WITH_KNOTS('',3,(#240147,#240148,#240149,#240150,#240151,
#240152,#240153,#240154,#240155,#240156,#240157,#240158,#240159,#240160,
#240161,#240162,#240163,#240164,#240165,#240166,#240167,#240168,#240169,
#240170,#240171,#240172,#240173,#240174,#240175,#240176,#240177,#240178,
#240179,#240180,#240181,#240182),.UNSPECIFIED.,.F.,.F.,(4,2,2,2,2,2,2,2,
2,2,2,2,2,2,2,2,2,4),(18.9040360682104,18.9262910406328,19.0026605322289,
19.0828460907298,19.1611264225512,19.2369775122534,19.3163976259115,19.3938148083998,
19.4706783340212,19.5502001780755,19.6267219868126,19.706098068117,19.7845758100659,
19.8603835447724,19.9397808781415,20.0174000463419,20.0938853198427,20.1622975463945),
 .UNSPECIFIED.);
#6076=B_SPLINE_CURVE_WITH_KNOTS('',3,(#240187,#240188,#240189,#240190,#240191,
#240192,#240193,#240194,#240195,#240196,#240197,#240198,#240199,#240200,
#240201,#240202,#240203,#240204,#240205,#240206,#240207,#240208,#240209,
#240210,#240211,#240212,#240213,#240214,#240215,#240216,#240217,#240218,
#240219,#240220,#240221,#240222),.UNSPECIFIED.,.F.,.F.,(4,2,2,2,2,2,2,2,
2,2,2,2,2,2,2,2,2,4),(2.40800177534909,2.45399201896089,2.53265891076704,
2.60980635838972,2.69000068997139,2.76666154078788,2.84470609564807,2.9244289591419,
3.0005666709432,3.07947104951592,3.15882048506469,3.23574089239875,3.31568349328153,
3.39267145052468,3.47048938577085,3.55021656235879,3.62634069975032,3.6713151088133),
 .UNSPECIFIED.);
#6077=B_SPLINE_CURVE_WITH_KNOTS('',3,(#240223,#240224,#240225,#240226,#240227,
#240228,#240229,#240230,#240231,#240232,#240233,#240234,#240235,#240236,
#240237,#240238,#240239,#240240,#240241,#240242,#240243,#240244,#240245,
#240246,#240247,#240248,#240249,#240250,#240251,#240252,#240253,#240254,
#240255,#240256,#240257,#240258),.UNSPECIFIED.,.F.,.F.,(4,2,2,2,2,2,2,2,
2,2,2,2,2,2,2,2,2,4),(20.1622975463945,20.1736340848943,20.2503600390948,
20.3290056748752,20.4077303181208,20.4836219336482,20.5630375985878,20.6409087371531,
20.7171358811133,20.7971616872148,20.8741381490283,20.9521737072777,21.0311876618635,
21.1072948695045,21.1867734591295,21.2649400887203,21.3410441964928,21.4212632201289),
 .UNSPECIFIED.);
#6078=B_SPLINE_CURVE_WITH_KNOTS('',3,(#240264,#240265,#240266,#240267,#240268,
#240269),.UNSPECIFIED.,.F.,.F.,(4,2,4),(22.6805778338202,22.7225346851399,
22.7746249205198),.UNSPECIFIED.);
#6079=B_SPLINE_CURVE_WITH_KNOTS('',3,(#240271,#240272,#240273,#240274,#240275,
#240276,#240277,#240278,#240279,#240280),.UNSPECIFIED.,.F.,.F.,(4,2,2,2,
4),(0.,0.0529987112262313,0.105968001362697,0.158971646797024,0.21203675183673),
 .UNSPECIFIED.);
#6080=B_SPLINE_CURVE_WITH_KNOTS('',3,(#240282,#240283,#240284,#240285,#240286,
#240287,#240288,#240289,#240290,#240291,#240292,#240293,#240294,#240295,
#240296,#240297,#240298,#240299,#240300,#240301,#240302,#240303,#240304,
#240305,#240306,#240307),.UNSPECIFIED.,.F.,.F.,(4,2,2,2,2,2,2,2,2,2,2,2,
4),(-0.790728037067121,-0.749775115806686,-0.708732159090347,-0.62930879973315,
-0.552553327511713,-0.472789234158408,-0.395665227958601,-0.31556998695274,
-0.238516351993173,-0.159861788318521,-0.080788503022024,-0.0396943940909934,
-9.95303702788775E-7),.UNSPECIFIED.);
#6081=B_SPLINE_CURVE_WITH_KNOTS('',3,(#240310,#240311,#240312,#240313,#240314,
#240315,#240316,#240317,#240318,#240319,#240320,#240321,#240322,#240323,
#240324,#240325,#240326,#240327,#240328,#240329,#240330,#240331,#240332,
#240333,#240334,#240335,#240336,#240337,#240338,#240339,#240340,#240341,
#240342,#240343),.UNSPECIFIED.,.F.,.F.,(4,2,2,2,2,2,2,2,2,2,2,2,2,2,2,2,
4),(1.00510724934941E-6,0.0525834672969985,0.106573631372961,0.186239291839903,
0.262311996105734,0.341115594311459,0.42055455516659,0.497383903920253,
0.577229073521196,0.654240311296405,0.731967090606045,0.811644918579921,
0.887728407406906,0.966320033313811,1.04655454272418,1.12321674093992,1.14417183100891),
 .UNSPECIFIED.);
#6082=B_SPLINE_CURVE_WITH_KNOTS('',3,(#240353,#240354,#240355,#240356,#240357,
#240358,#240359,#240360,#240361,#240362,#240363,#240364,#240365,#240366,
#240367,#240368),.UNSPECIFIED.,.F.,.F.,(4,3,3,3,3,4),(0.,0.144328413863221,
0.303472318230778,0.628464617347887,0.963059075130798,1.),.UNSPECIFIED.);
#6083=B_SPLINE_CURVE_WITH_KNOTS('',3,(#240385,#240386,#240387,#240388,#240389,
#240390,#240391,#240392,#240393,#240394,#240395,#240396),.UNSPECIFIED.,
 .F.,.F.,(4,2,2,2,2,4),(1.00000010121019E-6,0.0446394239019562,0.0896993921078784,
0.134509378723331,0.140080640396739,0.179359231239673),.UNSPECIFIED.);
#6084=B_SPLINE_CURVE_WITH_KNOTS('',3,(#240914,#240915,#240916,#240917,#240918,
#240919,#240920,#240921,#240922,#240923),.UNSPECIFIED.,.F.,.F.,(4,2,2,2,
4),(9.99999999774313E-7,0.0674884200460847,0.133887544817669,0.212371065462948,
0.287372916582337),.UNSPECIFIED.);
#6085=B_SPLINE_CURVE_WITH_KNOTS('',3,(#240928,#240929,#240930,#240931,#240932,
#240933,#240934,#240935,#240936,#240937,#240938,#240939,#240940,#240941,
#240942,#240943,#240944,#240945,#240946,#240947,#240948,#240949,#240950,
#240951,#240952,#240953,#240954,#240955,#240956,#240957,#240958,#240959,
#240960,#240961,#240962,#240963),.UNSPECIFIED.,.F.,.F.,(4,2,2,2,2,2,2,2,
2,2,2,2,2,2,2,2,2,4),(22.2691796383917,22.2806866530766,22.3601873799206,
22.4379542915872,22.5144766103392,22.5943809263863,22.671253438802,22.7498674627958,
22.8287494305076,22.9047725585822,22.9843003162939,23.062328811022,23.1386190219282,
23.2188100493447,23.2959420465468,23.3739734639397,23.4527575968905,23.5294112994357),
 .UNSPECIFIED.);
#6086=B_SPLINE_CURVE_WITH_KNOTS('',3,(#240964,#240965,#240966,#240967,#240968,
#240969,#240970,#240971,#240972,#240973,#240974,#240975,#240976,#240977,
#240978,#240979,#240980,#240981,#240982,#240983,#240984,#240985,#240986,
#240987,#240988,#240989,#240990,#240991,#240992,#240993,#240994,#240995,
#240996,#240997,#240998,#240999,#241000,#241001),.UNSPECIFIED.,.F.,.F.,
(4,2,2,2,2,2,2,2,2,2,2,2,2,2,2,2,2,2,4),(0.287372916582337,0.292012075113482,
0.368555506568093,0.448083595544,0.52580567198518,0.603255911016295,0.683793119295233,
0.760058356770533,0.838409640892086,0.918063811525401,0.994349480776281,
1.07354955396753,1.15172514075825,1.22888144004619,1.30909511453487,1.38547644460694,
1.46352950583805,1.54311818413994,1.54965533150543),.UNSPECIFIED.);
#6087=B_SPLINE_CURVE_WITH_KNOTS('',3,(#241006,#241007,#241008,#241009,#241010,
#241011,#241012,#241013,#241014,#241015,#241016,#241017,#241018,#241019,
#241020,#241021,#241022,#241023,#241024,#241025,#241026,#241027,#241028,
#241029,#241030,#241031,#241032,#241033,#241034,#241035,#241036,#241037,
#241038,#241039,#241040,#241041),.UNSPECIFIED.,.F.,.F.,(4,2,2,2,2,2,2,2,
2,2,2,2,2,2,2,2,2,4),(21.0091763975789,21.0318031777429,21.1113724869712,
21.1887685156285,21.2661013080159,21.3455850694411,21.4220800230878,21.5022024880104,
21.580619931206,21.6565512470235,21.7360667361565,21.8136208238973,21.8904995412877,
21.970166027991,22.0468243300758,22.1261485322222,22.2047741711635,22.2691796383917),
 .UNSPECIFIED.);
#6088=B_SPLINE_CURVE_WITH_KNOTS('',3,(#241042,#241043,#241044,#241045,#241046,
#241047,#241048,#241049,#241050,#241051,#241052,#241053,#241054,#241055,
#241056,#241057,#241058,#241059,#241060,#241061,#241062,#241063,#241064,
#241065,#241066,#241067,#241068,#241069,#241070,#241071,#241072,#241073,
#241074,#241075,#241076,#241077),.UNSPECIFIED.,.F.,.F.,(4,2,2,2,2,2,2,2,
2,2,2,2,2,2,2,2,2,4),(1.54965533150543,1.6191810954755,1.69808920760654,
1.77686898372047,1.85377197718216,1.93370558140581,2.01033884039764,2.08813696215977,
2.1677050397341,2.24367700877286,2.32233530521275,2.40184177204162,2.47853762445349,
2.55824105027393,2.63524770661228,2.71284064966069,2.79242948533891,2.81051496707889),
 .UNSPECIFIED.);
#6089=B_SPLINE_CURVE_WITH_KNOTS('',3,(#241082,#241083,#241084,#241085,#241086,
#241087,#241088,#241089,#241090,#241091,#241092,#241093,#241094,#241095,
#241096,#241097,#241098,#241099,#241100,#241101,#241102,#241103,#241104,
#241105,#241106,#241107,#241108,#241109,#241110,#241111,#241112,#241113,
#241114,#241115,#241116,#241117),.UNSPECIFIED.,.F.,.F.,(4,2,2,2,2,2,2,2,
2,2,2,2,2,2,2,2,2,4),(19.7477505345541,19.7819394034219,19.8619634678305,
19.9389481080936,20.0175033641031,20.0965069290084,20.1726312691743,20.2522365031935,
20.3303870326243,20.4067119579603,20.4870317747689,20.5642843143553,20.6422849545906,
20.7215935067328,20.7979329433488,20.8774748285065,20.9557388752909,21.0091763975789),
 .UNSPECIFIED.);
#6090=B_SPLINE_CURVE_WITH_KNOTS('',3,(#241118,#241119,#241120,#241121,#241122,
#241123,#241124,#241125,#241126,#241127,#241128,#241129,#241130,#241131,
#241132,#241133,#241134,#241135,#241136,#241137,#241138,#241139,#241140,
#241141,#241142,#241143,#241144,#241145,#241146,#241147,#241148,#241149,
#241150,#241151,#241152,#241153),.UNSPECIFIED.,.F.,.F.,(4,2,2,2,2,2,2,2,
2,2,2,2,2,2,2,2,2,4),(2.81051496707889,2.86843861292801,2.94689632536739,
3.02721101822537,3.1037514070629,3.18328064150779,3.26075337113605,3.33819671505569,
3.41784506617566,3.49400238700364,3.57231522265173,3.65193423432565,3.72832380273608,
3.80768284665575,3.88584597194112,3.96315144920267,4.04352381654236,4.07266414291054),
 .UNSPECIFIED.);
#6091=B_SPLINE_CURVE_WITH_KNOTS('',3,(#241158,#241159,#241160,#241161,#241162,
#241163,#241164,#241165,#241166,#241167,#241168,#241169,#241170,#241171,
#241172,#241173,#241174,#241175,#241176,#241177,#241178,#241179,#241180,
#241181,#241182,#241183,#241184,#241185,#241186,#241187,#241188,#241189,
#241190,#241191,#241192,#241193),.UNSPECIFIED.,.F.,.F.,(4,2,2,2,2,2,2,2,
2,2,2,2,2,2,2,2,2,4),(18.4868313729185,18.5326534242109,18.6122352945202,
18.6888224014101,18.7688514808402,18.8473715865055,18.9233535675701,19.002930020034,
19.0805869298598,19.1574519297428,19.2372278940146,19.3139888393418,19.3932326930507,
19.4719711381632,19.5479587690643,19.6275283739101,19.7054083287184,19.7477505345541),
 .UNSPECIFIED.);
#6092=B_SPLINE_CURVE_WITH_KNOTS('',3,(#241194,#241195,#241196,#241197,#241198,
#241199,#241200,#241201,#241202,#241203,#241204,#241205,#241206,#241207,
#241208,#241209,#241210,#241211,#241212,#241213,#241214,#241215,#241216,
#241217,#241218,#241219,#241220,#241221,#241222,#241223,#241224,#241225,
#241226,#241227,#241228,#241229),.UNSPECIFIED.,.F.,.F.,(4,2,2,2,2,2,2,2,
2,2,2,2,2,2,2,2,2,4),(4.07266414291054,4.11996124283415,4.19816525237173,
4.27785857376779,4.35404733303679,4.43310623910865,4.51184517608608,4.58888829036109,
4.6689708373675,4.74563347273896,4.82357284926374,4.90323666539291,4.97930718285682,
5.05810677448008,5.13755120139774,5.2143770041859,5.29421835227979,5.33520243665533),
 .UNSPECIFIED.);
#6093=B_SPLINE_CURVE_WITH_KNOTS('',3,(#241234,#241235,#241236,#241237,#241238,
#241239,#241240,#241241,#241242,#241243,#241244,#241245,#241246,#241247,
#241248,#241249,#241250,#241251,#241252,#241253,#241254,#241255,#241256,
#241257,#241258,#241259,#241260,#241261,#241262,#241263,#241264,#241265,
#241266,#241267,#241268,#241269),.UNSPECIFIED.,.F.,.F.,(4,2,2,2,2,2,2,2,
2,2,2,2,2,2,2,2,2,4),(17.2247319659337,17.283183116068,17.3622710832688,
17.438464650737,17.518111489222,17.5963472698658,17.6726771747172,17.7530878399949,
17.8304244991097,17.9083665824597,17.9877665213978,18.0641918344984,18.1437899655652,
18.222145378313,18.2982398577519,18.3778627113094,18.4553503172739,18.4868313729185),
 .UNSPECIFIED.);
#6094=B_SPLINE_CURVE_WITH_KNOTS('',3,(#241270,#241271,#241272,#241273,#241274,
#241275,#241276,#241277,#241278,#241279,#241280,#241281,#241282,#241283,
#241284,#241285,#241286,#241287,#241288,#241289,#241290,#241291,#241292,
#241293,#241294,#241295,#241296,#241297,#241298,#241299,#241300,#241301,
#241302,#241303,#241304,#241305),.UNSPECIFIED.,.F.,.F.,(4,2,2,2,2,2,2,2,
2,2,2,2,2,2,2,2,2,4),(5.33520243665533,5.37123175487558,5.44895499788664,
5.52863136770331,5.60471386189317,5.68330197566796,5.76354258712913,5.84020175081883,
5.91985679742295,5.99732069529608,6.07488238510482,6.15461057457674,6.23082057603543,
6.30925179094805,6.38895324573563,6.46545480897963,6.54493239908358,6.59826968210442),
 .UNSPECIFIED.);
#6095=B_SPLINE_CURVE_WITH_KNOTS('',3,(#241310,#241311,#241312,#241313,#241314,
#241315,#241316,#241317,#241318,#241319,#241320,#241321,#241322,#241323,
#241324,#241325,#241326,#241327,#241328,#241329,#241330,#241331,#241332,
#241333,#241334,#241335,#241336,#241337,#241338,#241339,#241340,#241341,
#241342,#241343,#241344,#241345),.UNSPECIFIED.,.F.,.F.,(4,2,2,2,2,2,2,2,
2,2,2,2,2,2,2,2,2,4),(15.9633759832345,16.0340829053594,16.1126697840488,
16.1886716274734,16.2682734445992,16.3459976665135,16.4228191552351,16.5026679549044,
16.5794962911535,16.6586307779,16.7374454828078,16.8134771903943,16.893079940854,
16.9710367863344,17.0475471941891,17.1276537050312,17.2047146217245,17.2247319659337),
 .UNSPECIFIED.);
#6096=B_SPLINE_CURVE_WITH_KNOTS('',3,(#241346,#241347,#241348,#241349,#241350,
#241351,#241352,#241353,#241354,#241355,#241356,#241357,#241358,#241359,
#241360,#241361,#241362,#241363,#241364,#241365,#241366,#241367,#241368,
#241369,#241370,#241371,#241372,#241373,#241374,#241375,#241376,#241377,
#241378,#241379,#241380,#241381),.UNSPECIFIED.,.F.,.F.,(4,2,2,2,2,2,2,2,
2,2,2,2,2,2,2,2,2,4),(6.59826968210442,6.62305723184909,6.70047303463833,
6.78096354367303,6.85742750785752,6.93574323524729,7.01550404527384,7.09178510173153,
7.17095517546818,7.24962779957794,7.32677300079539,7.40696484447098,7.48362817734374,
7.5616704738598,7.64139323350021,7.71753027422718,7.79643244085222,7.86199738742149),
 .UNSPECIFIED.);
#6097=B_SPLINE_CURVE_WITH_KNOTS('',3,(#241386,#241387,#241388,#241389,#241390,
#241391,#241392,#241393,#241394,#241395,#241396,#241397,#241398,#241399,
#241400,#241401,#241402,#241403,#241404,#241405,#241406,#241407,#241408,
#241409,#241410,#241411,#241412,#241413,#241414,#241415,#241416,#241417,
#241418,#241419,#241420,#241421,#241422,#241423),.UNSPECIFIED.,.F.,.F.,
(4,2,2,2,2,2,2,2,2,2,2,2,2,2,2,2,2,2,4),(14.701099149603,14.7034557678201,
14.7831089134017,14.8613951944832,14.9376995229283,15.0181652998994,15.0955516706383,
15.1734044319978,15.2528602486155,15.3293372297621,15.4089563152068,15.4873678151406,
15.5634613867607,15.6431023180422,15.7206465816924,15.7978892940474,15.8775332564797,
15.9541778414377,15.9633759832345),.UNSPECIFIED.);
#6098=B_SPLINE_CURVE_WITH_KNOTS('',3,(#241424,#241425,#241426,#241427,#241428,
#241429,#241430,#241431,#241432,#241433,#241434,#241435,#241436,#241437,
#241438,#241439,#241440,#241441,#241442,#241443,#241444,#241445,#241446,
#241447,#241448,#241449,#241450,#241451,#241452,#241453,#241454,#241455,
#241456,#241457,#241458,#241459),.UNSPECIFIED.,.F.,.F.,(4,2,2,2,2,2,2,2,
2,2,2,2,2,2,2,2,2,4),(7.86199738742149,7.87578870684037,7.95270729700455,
8.03264787424434,8.10963942101754,8.18745556104782,8.26718301070552,8.34330764872676,
8.42198839637052,8.50212736795937,8.57886900849719,8.6586121098341,8.73603794343607,
8.81368146932958,8.89345336931947,8.96968497119851,9.04819771303439,9.12550391178119),
 .UNSPECIFIED.);
#6099=B_SPLINE_CURVE_WITH_KNOTS('',3,(#241464,#241465,#241466,#241467,#241468,
#241469,#241470,#241471,#241472,#241473,#241474,#241475,#241476,#241477,
#241478,#241479,#241480,#241481,#241482,#241483,#241484,#241485,#241486,
#241487,#241488,#241489,#241490,#241491,#241492,#241493,#241494,#241495,
#241496,#241497,#241498,#241499),.UNSPECIFIED.,.F.,.F.,(4,2,2,2,2,2,2,2,
2,2,2,2,2,2,2,2,2,4),(13.4396934393828,13.4536847447015,13.5332763419421,
13.6110337656732,13.6877798940162,13.7676664530154,13.8445283476067,13.9235200048667,
14.0023761148105,14.0784213926254,14.1580218413539,14.236021157819,14.3124798944769,
14.3926334525682,14.4697365270538,14.5480864601419,14.6272236300065,14.701099149603),
 .UNSPECIFIED.);
#6100=B_SPLINE_CURVE_WITH_KNOTS('',3,(#241500,#241501,#241502,#241503,#241504,
#241505,#241506,#241507,#241508,#241509,#241510,#241511,#241512,#241513,
#241514,#241515,#241516,#241517,#241518,#241519,#241520,#241521,#241522,
#241523,#241524,#241525,#241526,#241527,#241528,#241529,#241530,#241531,
#241532,#241533,#241534,#241535,#241536,#241537),.UNSPECIFIED.,.F.,.F.,
(4,2,2,2,2,2,2,2,2,2,2,2,2,2,2,2,2,2,4),(9.12550391178119,9.12794562854735,
9.20452353347352,9.28408260990182,9.36214053189483,9.43963086875648,9.52020226565107,
9.59666281547,9.67505411358347,9.75177793909778,9.83235205988809,9.91099486481556,
9.98720176193357,10.0669933113407,10.1447688600247,10.221998524202,10.3018881334216,
10.378764057835,10.3900588862096),.UNSPECIFIED.);
#6101=B_SPLINE_CURVE_WITH_KNOTS('',3,(#241542,#241543,#241544,#241545,#241546,
#241547,#241548,#241549,#241550,#241551,#241552,#241553,#241554,#241555,
#241556,#241557,#241558,#241559,#241560,#241561,#241562,#241563,#241564,
#241565,#241566,#241567,#241568,#241569,#241570,#241571,#241572,#241573,
#241574,#241575,#241576,#241577),.UNSPECIFIED.,.F.,.F.,(4,2,2,2,2,2,2,2,
2,2,2,2,2,2,2,2,2,4),(12.1779611485506,12.2029615970869,12.2834477046188,
12.3608501882395,12.4385791971972,12.5180563732016,12.5945516971524,12.6741562699566,
12.7525895879676,12.8286503860145,12.9082736895974,12.9858407333286,13.0629895967305,
13.1426608362597,13.2193293058411,13.2990748665947,13.3776939963258,13.4396934393828),
 .UNSPECIFIED.);
#6102=B_SPLINE_CURVE_WITH_KNOTS('',3,(#241578,#241579,#241580,#241581,#241582,
#241583,#241584,#241585,#241586,#241587,#241588,#241589,#241590,#241591,
#241592,#241593,#241594,#241595,#241596,#241597,#241598,#241599,#241600,
#241601,#241602,#241603,#241604,#241605,#241606,#241607,#241608,#241609,
#241610,#241611,#241612,#241613),.UNSPECIFIED.,.F.,.F.,(4,2,2,2,2,2,2,2,
2,2,2,2,2,2,2,2,2,4),(10.3900588862096,10.4585239664231,10.5373641952025,
10.613525477726,10.6932934610687,10.7712710279127,10.8481188279578,10.9282355033061,
11.0053156823111,11.0843400095939,11.163427504345,11.2396707996032,11.3194564691121,
11.3976863806327,11.4742726349846,11.5546668407259,11.6319979505454,11.6542522257011),
 .UNSPECIFIED.);
#6103=B_SPLINE_CURVE_WITH_KNOTS('',3,(#241618,#241619,#241620,#241621,#241622,
#241623,#241624,#241625,#241626,#241627,#241628,#241629,#241630,#241631,
#241632,#241633,#241634,#241635,#241636,#241637,#241638,#241639,#241640,
#241641,#241642,#241643,#241644,#241645,#241646,#241647,#241648,#241649,
#241650,#241651,#241652,#241653),.UNSPECIFIED.,.F.,.F.,(4,2,2,2,2,2,2,2,
2,2,2,2,2,2,2,2,2,4),(10.9168245999786,10.9535273517243,11.0334169764488,
11.1102788663099,11.1890887960723,11.26795195487,11.3439801294688,11.4235418699849,
11.5015497913461,11.5779234924823,11.6580893856383,11.7352010537127,11.8133960223397,
11.8925479562904,11.968788588237,12.048412096038,12.1267149477204,12.1779611485506),
 .UNSPECIFIED.);
#6104=B_SPLINE_CURVE_WITH_KNOTS('',3,(#241654,#241655,#241656,#241657,#241658,
#241659,#241660,#241661,#241662,#241663,#241664,#241665,#241666,#241667,
#241668,#241669,#241670,#241671,#241672,#241673,#241674,#241675,#241676,
#241677,#241678,#241679,#241680,#241681,#241682,#241683,#241684,#241685,
#241686,#241687,#241688,#241689),.UNSPECIFIED.,.F.,.F.,(4,2,2,2,2,2,2,2,
2,2,2,2,2,2,2,2,2,4),(11.6542522257011,11.710407002519,11.7897844888648,
11.8662421728206,11.9460902634938,12.0246163526226,12.1010766272691,12.1817923681703,
12.2594155071029,12.3373589223573,12.4170629140417,12.4937764276779,12.5736063166663,
12.6522635035179,12.7285386772514,12.8083871849551,12.886175686978,12.9197561116359),
 .UNSPECIFIED.);
#6105=B_SPLINE_CURVE_WITH_KNOTS('',3,(#241694,#241695,#241696,#241697,#241698,
#241699,#241700,#241701,#241702,#241703,#241704,#241705,#241706,#241707,
#241708,#241709,#241710,#241711,#241712,#241713,#241714,#241715,#241716,
#241717,#241718,#241719,#241720,#241721,#241722,#241723,#241724,#241725,
#241726,#241727,#241728,#241729),.UNSPECIFIED.,.F.,.F.,(4,2,2,2,2,2,2,2,
2,2,2,2,2,2,2,2,2,4),(9.65613189117811,9.70510400601994,9.78456788722448,
9.86104801334814,9.94060117886638,10.0190219155385,10.0950163875207,10.1745848390524,
10.2521407022053,10.329158445023,10.4088221904792,10.4854809063298,10.5650253891295,
10.6436424495944,10.7195901998136,10.7991347429344,10.8768915098314,10.9168245999786),
 .UNSPECIFIED.);
#6106=B_SPLINE_CURVE_WITH_KNOTS('',3,(#241730,#241731,#241732,#241733,#241734,
#241735,#241736,#241737,#241738,#241739,#241740,#241741,#241742,#241743,
#241744,#241745,#241746,#241747,#241748,#241749,#241750,#241751,#241752,
#241753,#241754,#241755,#241756,#241757,#241758,#241759,#241760,#241761,
#241762,#241763,#241764,#241765),.UNSPECIFIED.,.F.,.F.,(4,2,2,2,2,2,2,2,
2,2,2,2,2,2,2,2,2,4),(12.9197561116359,12.9635388590835,13.0434377626046,
13.1203251920892,13.2002890507829,13.2791331064625,13.3553391645683,13.4351562582792,
13.5131362104416,13.5900964960459,13.6702118626848,13.7472937576194,13.8265024709751,
13.9055846424562,13.9818466592195,14.0616730390502,14.1398960400751,14.1845909974411),
 .UNSPECIFIED.);
#6107=B_SPLINE_CURVE_WITH_KNOTS('',3,(#241770,#241771,#241772,#241773,#241774,
#241775,#241776,#241777,#241778,#241779,#241780,#241781,#241782,#241783,
#241784,#241785,#241786,#241787,#241788,#241789,#241790,#241791,#241792,
#241793,#241794,#241795,#241796,#241797,#241798,#241799,#241800,#241801,
#241802,#241803,#241804,#241805),.UNSPECIFIED.,.F.,.F.,(4,2,2,2,2,2,2,2,
2,2,2,2,2,2,2,2,2,4),(8.39571461391817,8.45407111577228,8.53244461553089,
8.6125792647267,8.6890336707027,8.76847463807125,8.84580191678438,8.92315742029522,
9.00269660548283,9.07873856353393,9.15696198687568,9.23647302573939,9.31277379135651,
9.39204156144936,9.47004475002984,9.54725898117665,9.62753801892365,9.65613189117811),
 .UNSPECIFIED.);
#6108=B_SPLINE_CURVE_WITH_KNOTS('',3,(#241806,#241807,#241808,#241809,#241810,
#241811,#241812,#241813,#241814,#241815,#241816,#241817,#241818,#241819,
#241820,#241821,#241822,#241823,#241824,#241825,#241826,#241827,#241828,
#241829,#241830,#241831,#241832,#241833,#241834,#241835,#241836,#241837,
#241838,#241839,#241840,#241841),.UNSPECIFIED.,.F.,.F.,(4,2,2,2,2,2,2,2,
2,2,2,2,2,2,2,2,2,4),(14.1845909974411,14.2165693414243,14.2969529355151,
14.3742771308546,14.4528435761911,14.5322079993234,14.6086586834019,14.6885383554083,
14.7670495417927,14.8435693412187,14.9242664485727,15.0018751272443,15.0799445063026,
15.1596288186321,15.2363256200211,15.3161718844887,15.3948089191141,15.4504769545923),
 .UNSPECIFIED.);
#6109=B_SPLINE_CURVE_WITH_KNOTS('',3,(#241846,#241847,#241848,#241849,#241850,
#241851,#241852,#241853,#241854,#241855,#241856,#241857,#241858,#241859,
#241860,#241861,#241862,#241863,#241864,#241865,#241866,#241867,#241868,
#241869,#241870,#241871,#241872,#241873,#241874,#241875,#241876,#241877,
#241878,#241879,#241880,#241881),.UNSPECIFIED.,.F.,.F.,(4,2,2,2,2,2,2,2,
2,2,2,2,2,2,2,2,2,4),(7.13646531059583,7.20645785952193,7.28529023825674,
7.36390735835512,7.44073341990602,7.52058854397155,7.59709484904002,7.67481490273967,
7.75428113144242,7.83015861471465,7.90873729764548,7.98807040244311,8.06468506885083,
8.14430541451292,8.2211743405915,8.29868460094256,8.37816785133338,8.39571461391817),
 .UNSPECIFIED.);
#6110=B_SPLINE_CURVE_WITH_KNOTS('',3,(#241882,#241883,#241884,#241885,#241886,
#241887,#241888,#241889,#241890,#241891,#241892,#241893,#241894,#241895,
#241896,#241897,#241898,#241899,#241900,#241901,#241902,#241903,#241904,
#241905,#241906,#241907,#241908,#241909,#241910,#241911,#241912,#241913,
#241914,#241915,#241916,#241917),.UNSPECIFIED.,.F.,.F.,(4,2,2,2,2,2,2,2,
2,2,2,2,2,2,2,2,2,4),(15.4504769545923,15.4711186088728,15.5509866302239,
15.6287539943615,15.7062130664185,15.7860863660806,15.8629515346015,15.9430772952779,
16.0218907399634,16.0981095094446,16.1779386748971,16.2558870405988,16.3329245748492,
16.4130038296978,16.4900537660969,16.5694075427569,16.6484499320012,16.7154590663106),
 .UNSPECIFIED.);
#6111=B_SPLINE_CURVE_WITH_KNOTS('',3,(#241922,#241923,#241924,#241925,#241926,
#241927,#241928,#241929,#241930,#241931,#241932,#241933,#241934,#241935,
#241936,#241937,#241938,#241939,#241940,#241941,#241942,#241943,#241944,
#241945,#241946,#241947,#241948,#241949,#241950,#241951,#241952,#241953,
#241954,#241955,#241956,#241957,#241958,#241959),.UNSPECIFIED.,.F.,.F.,
(4,2,2,2,2,2,2,2,2,2,2,2,2,2,2,2,2,2,4),(5.87566374904269,5.88157874395125,
5.95808562271841,6.03757865154077,6.11509465883298,6.19250524853729,6.2721444610133,
6.34830821943425,6.42658870612222,6.50614928028767,6.58236422400605,6.66149176274634,
6.73951849537886,6.81660152826874,6.89674065773059,6.97300750773828,7.05098645673024,
7.13047725888505,7.13646531059583),.UNSPECIFIED.);
#6112=B_SPLINE_CURVE_WITH_KNOTS('',3,(#241960,#241961,#241962,#241963,#241964,
#241965,#241966,#241967,#241968,#241969,#241970,#241971,#241972,#241973,
#241974,#241975,#241976,#241977,#241978,#241979,#241980,#241981,#241982,
#241983,#241984,#241985,#241986,#241987,#241988,#241989,#241990,#241991,
#241992,#241993,#241994,#241995,#241996,#241997),.UNSPECIFIED.,.F.,.F.,
(4,2,2,2,2,2,2,2,2,2,2,2,2,2,2,2,2,2,4),(16.7154590663106,16.7246998818893,
16.8045303784101,16.8827125049289,16.9594392487068,17.0397774247768,17.1170610444518,
17.195748111439,17.2750649428163,17.3514784766028,17.4313536164282,17.509815885501,
17.5863629146892,17.6670065264203,17.744567061855,17.8227276640817,17.9023577000694,
17.9790043840932,17.9812155694434),.UNSPECIFIED.);
#6113=B_SPLINE_CURVE_WITH_KNOTS('',3,(#242002,#242003,#242004,#242005,#242006,
#242007,#242008,#242009,#242010,#242011,#242012,#242013,#242014,#242015,
#242016,#242017,#242018,#242019,#242020,#242021,#242022,#242023,#242024,
#242025,#242026,#242027,#242028,#242029,#242030,#242031,#242032,#242033,
#242034,#242035,#242036,#242037),.UNSPECIFIED.,.F.,.F.,(4,2,2,2,2,2,2,2,
2,2,2,2,2,2,2,2,2,4),(4.61497841375817,4.63217000394447,4.70906659679136,
4.78899393182726,4.86560768946728,4.94339927105396,5.02295495299878,5.09891572879304,
5.17756723650798,5.2570426907455,5.33373099645916,5.41342691260482,5.49041135868395,
5.56799652190477,5.64757199748644,5.72356699798226,5.80201668627962,5.87566374904269),
 .UNSPECIFIED.);
#6114=B_SPLINE_CURVE_WITH_KNOTS('',3,(#242038,#242039,#242040,#242041,#242042,
#242043,#242044,#242045,#242046,#242047,#242048,#242049,#242050,#242051,
#242052,#242053,#242054,#242055,#242056,#242057,#242058,#242059,#242060,
#242061,#242062,#242063,#242064,#242065,#242066,#242067,#242068,#242069,
#242070,#242071,#242072,#242073),.UNSPECIFIED.,.F.,.F.,(4,2,2,2,2,2,2,2,
2,2,2,2,2,2,2,2,2,4),(17.9812155694434,18.0588314147492,18.1374139506599,
18.2137261374055,18.2935778201302,18.3712900944934,18.4488113528749,18.5286241637414,
18.6054334063077,18.6856852076825,18.7644334583262,18.8406338650887,18.9204393841381,
18.9983219952603,19.0754047258784,19.1554127395687,19.2323968287287,19.2459664568064),
 .UNSPECIFIED.);
#6115=B_SPLINE_CURVE_WITH_KNOTS('',3,(#242078,#242079,#242080,#242081,#242082,
#242083,#242084,#242085,#242086,#242087,#242088,#242089,#242090,#242091,
#242092,#242093,#242094,#242095,#242096,#242097,#242098,#242099,#242100,
#242101,#242102,#242103,#242104,#242105,#242106,#242107,#242108,#242109,
#242110,#242111,#242112,#242113),.UNSPECIFIED.,.F.,.F.,(4,2,2,2,2,2,2,2,
2,2,2,2,2,2,2,2,2,4),(3.35320138787495,3.3812638703186,3.45870958005293,
3.53924251659103,3.61549479037889,3.6938415306858,3.77348545760913,3.84976616653828,
3.92896139623998,4.00711204191994,4.08426294194264,4.164471424109,4.24083643470692,
4.31888403362048,4.39846134862252,4.47451624184274,4.55341862304842,4.61497841375817),
 .UNSPECIFIED.);
#6116=B_SPLINE_CURVE_WITH_KNOTS('',3,(#242114,#242115,#242116,#242117,#242118,
#242119,#242120,#242121,#242122,#242123,#242124,#242125,#242126,#242127,
#242128,#242129,#242130,#242131,#242132,#242133,#242134,#242135,#242136,
#242137,#242138,#242139,#242140,#242141,#242142,#242143,#242144,#242145,
#242146,#242147,#242148,#242149),.UNSPECIFIED.,.F.,.F.,(4,2,2,2,2,2,2,2,
2,2,2,2,2,2,2,2,2,4),(19.2459664568064,19.311861864962,19.3908295702844,
19.4670368686963,19.5468359152358,19.6249427044891,19.7016916993731,19.7819490198206,
19.8591579029915,19.9379334922596,20.0171674984929,20.0935131839074,20.1733483901513,
20.2517269610892,20.3282705175368,20.4088248715252,20.4863028260136,20.5108796016852),
 .UNSPECIFIED.);
#6117=B_SPLINE_CURVE_WITH_KNOTS('',3,(#242154,#242155,#242156,#242157,#242158,
#242159,#242160,#242161,#242162,#242163,#242164,#242165,#242166,#242167,
#242168,#242169,#242170,#242171,#242172,#242173,#242174,#242175,#242176,
#242177,#242178,#242179,#242180,#242181,#242182,#242183,#242184,#242185,
#242186,#242187,#242188,#242189),.UNSPECIFIED.,.F.,.F.,(4,2,2,2,2,2,2,2,
2,2,2,2,2,2,2,2,2,4),(2.09124089524434,2.1306490107864,2.20845837087744,
2.28808039431898,2.36410071092841,2.44277166696175,2.52247191422365,2.59918710644569,
2.67890818519645,2.75604429529321,2.83365794816793,2.91330787937623,2.98938692491842,
3.06786674749038,3.14749960455273,3.2240388295728,3.30356283068734,3.35320138787495),
 .UNSPECIFIED.);
#6118=B_SPLINE_CURVE_WITH_KNOTS('',3,(#242190,#242191,#242192,#242193,#242194,
#242195,#242196,#242197,#242198,#242199,#242200,#242201,#242202,#242203,
#242204,#242205,#242206,#242207,#242208,#242209,#242210,#242211,#242212,
#242213,#242214,#242215,#242216,#242217,#242218,#242219,#242220,#242221,
#242222,#242223,#242224,#242225),.UNSPECIFIED.,.F.,.F.,(4,2,2,2,2,2,2,2,
2,2,2,2,2,2,2,2,2,4),(20.5108796016852,20.5645236332566,20.644063861161,
20.720626194123,20.8003986187961,20.878891356537,20.9551748472087,21.0349746409647,
21.1125968876481,21.190149416361,21.2698657094522,21.346584335433,21.4269312331983,
21.5055783974057,21.5817295613149,21.6614757641737,21.7392571101579,21.7750720110093),
 .UNSPECIFIED.);
#6119=B_SPLINE_CURVE_WITH_KNOTS('',3,(#242231,#242232,#242233,#242234,#242235,
#242236,#242237,#242238,#242239,#242240,#242241,#242242,#242243,#242244,
#242245,#242246,#242247,#242248,#242249,#242250,#242251,#242252,#242253,
#242254,#242255,#242256),.UNSPECIFIED.,.F.,.F.,(4,2,2,2,2,2,2,2,2,2,2,2,
4),(0.00950822744729325,0.0410482442676837,0.0835736901067871,0.162757220120456,
0.241102173023232,0.318248671367356,0.398448377125879,0.474921972698114,
0.552965181657624,0.632596307645776,0.708676431490648,0.749696686020115,
0.790626617481797),.UNSPECIFIED.);
#6120=B_SPLINE_CURVE_WITH_KNOTS('',3,(#242258,#242259,#242260,#242261,#242262,
#242263),.UNSPECIFIED.,.F.,.F.,(4,2,4),(9.99824055476731E-7,0.0243498221505662,
0.0486954662228403),.UNSPECIFIED.);
#6121=B_SPLINE_CURVE_WITH_KNOTS('',3,(#242264,#242265,#242266,#242267,#242268,
#242269,#242270,#242271,#242272,#242273,#242274,#242275,#242276,#242277,
#242278,#242279,#242280,#242281,#242282,#242283,#242284,#242285,#242286,
#242287,#242288,#242289),.UNSPECIFIED.,.F.,.F.,(4,2,2,2,2,2,2,2,2,2,2,2,
4),(1.00000007505208E-6,0.0481217371548365,0.0975555807269073,0.177241325850779,
0.253369517923901,0.331844467981179,0.411509871161699,0.488047266994232,
0.567566980440415,0.645410620509902,0.722856893712002,0.803386711797282,
0.828975078082139),.UNSPECIFIED.);
#6122=B_SPLINE_CURVE_WITH_KNOTS('',3,(#242299,#242300,#242301,#242302,#242303,
#242304),.UNSPECIFIED.,.F.,.F.,(4,2,4),(1.00000004082002E-6,0.0254438039575916,
0.0520246360988654),.UNSPECIFIED.);
#6123=B_SPLINE_CURVE_WITH_KNOTS('',3,(#242321,#242322,#242323,#242324,#242325,
#242326,#242327,#242328,#242329,#242330,#242331,#242332),.UNSPECIFIED.,
 .F.,.F.,(4,2,2,2,2,4),(1.00000007766482E-6,0.0445461052973873,0.0896481038803835,
0.134464834369227,0.140040820732742,0.179234915771338),.UNSPECIFIED.);
#6124=B_SPLINE_CURVE_WITH_KNOTS('',3,(#242853,#242854,#242855,#242856,#242857,
#242858),.UNSPECIFIED.,.F.,.F.,(4,2,4),(-0.052023619808277,-0.0259934271027802,
-1.00000004377848E-6),.UNSPECIFIED.);
#6125=B_SPLINE_CURVE_WITH_KNOTS('',3,(#242875,#242876,#242877,#242878,#242879,
#242880,#242881,#242882,#242883,#242884,#242885,#242886),.UNSPECIFIED.,
 .F.,.F.,(4,2,2,2,2,4),(-0.17929919968084,-0.134583984746606,-0.0896249144840832,
-0.0448429285044394,-0.0392636416192798,-1.00000009822798E-6),
 .UNSPECIFIED.);
#6126=B_SPLINE_CURVE_WITH_KNOTS('',3,(#243428,#243429,#243430,#243431,#243432,
#243433,#243434,#243435,#243436,#243437,#243438,#243439,#243440,#243441,
#243442,#243443,#243444,#243445,#243446,#243447,#243448,#243449,#243450,
#243451,#243452,#243453,#243454,#243455,#243456,#243457,#243458,#243459,
#243460,#243461,#243462,#243463,#243464,#243465,#243466,#243467),
 .UNSPECIFIED.,.F.,.F.,(4,3,3,3,3,3,3,3,3,3,3,3,3,4),(1.96246868729215E-28,
0.000438443356248491,0.00067092441681323,0.00110918484354966,0.00134856915744274,
0.00189097627470433,0.00203013834973696,0.00270986824049021,0.00271266901570489,
0.00339379571613445,0.00406480236073532,0.00407250537600557,0.00481439427282875,
0.00541973648098043),.UNSPECIFIED.);
#6127=B_SPLINE_CURVE_WITH_KNOTS('',3,(#243475,#243476,#243477,#243478,#243479,
#243480,#243481,#243482,#243483,#243484,#243485,#243486,#243487,#243488,
#243489,#243490,#243491,#243492,#243493,#243494,#243495,#243496,#243497,
#243498,#243499,#243500,#243501,#243502,#243503,#243504,#243505,#243506,
#243507,#243508,#243509,#243510,#243511,#243512,#243513,#243514,#243515,
#243516,#243517),.UNSPECIFIED.,.F.,.F.,(4,3,3,3,3,3,3,3,3,3,3,3,3,3,4),
(0.,0.000627149038362586,0.0012879482962516,0.00134802948058203,0.00135592142842901,
0.00202680625468173,0.00270776094006554,0.00271184285685801,0.00338988085637128,
0.0039809874146687,0.00407131269878862,0.00454781218229871,0.00474992819159083,
0.00522421399683384,0.00542368571371602),.UNSPECIFIED.);
#6128=B_SPLINE_CURVE_WITH_KNOTS('',3,(#243560,#243561,#243562,#243563,#243564,
#243565,#243566,#243567,#243568,#243569,#243570,#243571,#243572,#243573),
 .UNSPECIFIED.,.F.,.F.,(4,2,2,2,2,2,4),(-0.31539760291967,-0.309659972902578,
-0.305224290839027,-0.30075945665783,-0.294897994554676,-0.282601216297714,
-0.259650109440469),.UNSPECIFIED.);
#6129=B_SPLINE_CURVE_WITH_KNOTS('',3,(#243577,#243578,#243579,#243580,#243581,
#243582),.UNSPECIFIED.,.F.,.F.,(4,2,4),(0.,0.000518432414188003,0.00103686532124488),
 .UNSPECIFIED.);
#6130=B_SPLINE_CURVE_WITH_KNOTS('',3,(#243584,#243585,#243586,#243587,#243588,
#243589),.UNSPECIFIED.,.F.,.F.,(4,2,4),(0.,0.0400464786590225,0.088560968632653),
 .UNSPECIFIED.);
#6131=B_SPLINE_CURVE_WITH_KNOTS('',3,(#243591,#243592,#243593,#243594,#243595,
#243596,#243597,#243598,#243599,#243600,#243601,#243602,#243603,#243604,
#243605,#243606,#243607,#243608,#243609,#243610,#243611,#243612,#243613,
#243614,#243615,#243616,#243617,#243618,#243619,#243620,#243621,#243622,
#243623,#243624,#243625,#243626,#243627,#243628,#243629,#243630,#243631,
#243632,#243633,#243634,#243635,#243636,#243637,#243638,#243639,#243640,
#243641,#243642,#243643,#243644,#243645,#243646,#243647,#243648,#243649,
#243650,#243651,#243652,#243653,#243654,#243655,#243656,#243657,#243658,
#243659,#243660,#243661,#243662,#243663,#243664,#243665,#243666,#243667,
#243668,#243669,#243670,#243671,#243672,#243673,#243674,#243675,#243676,
#243677,#243678,#243679,#243680,#243681,#243682,#243683,#243684,#243685,
#243686,#243687,#243688,#243689,#243690,#243691,#243692,#243693,#243694,
#243695,#243696,#243697,#243698,#243699,#243700,#243701,#243702,#243703,
#243704,#243705,#243706,#243707,#243708,#243709,#243710,#243711,#243712,
#243713,#243714,#243715,#243716,#243717,#243718,#243719,#243720,#243721,
#243722,#243723),.UNSPECIFIED.,.F.,.F.,(4,3,3,3,3,3,3,3,3,3,3,3,3,3,3,3,
3,3,3,3,3,3,3,3,3,3,3,3,3,3,3,3,3,3,3,3,3,3,3,3,3,3,3,3,4),(1.45587086745827E-6,
0.00205325642694755,0.00478261105644799,0.00781250000000508,0.00957936860333274,
0.0129445313449779,0.0156250000000102,0.0181089234731001,0.0234375000000152,
0.0286242003934857,0.0312500000000203,0.0384097547368286,0.0468750000000305,
0.05811776116225,0.0625000000000406,0.0751447560520765,0.0892613199263578,
0.0937500000000388,0.10683528115677,0.121344253798209,0.125000000000037,
0.145340107425858,0.151594249264444,0.170677873925115,0.187500000000033,
0.21121939936984,0.235769851684623,0.25000000000003,0.293640925185931,0.375000000000023,
0.437500000000023,0.465862845666036,0.49410987334067,0.500000000000023,
0.556532034001133,0.625000000000014,0.674164735985126,0.7249035415464,0.750000000000004,
0.8125,0.838218536984945,0.864879862610272,0.874999999999995,0.939619921550813,
1.),.UNSPECIFIED.);
#6132=B_SPLINE_CURVE_WITH_KNOTS('',3,(#243731,#243732,#243733,#243734,#243735,
#243736,#243737,#243738,#243739,#243740,#243741,#243742,#243743,#243744,
#243745,#243746,#243747,#243748,#243749,#243750,#243751,#243752,#243753,
#243754,#243755,#243756,#243757,#243758,#243759,#243760,#243761,#243762,
#243763,#243764,#243765,#243766,#243767,#243768,#243769,#243770,#243771,
#243772,#243773,#243774,#243775,#243776,#243777,#243778,#243779,#243780,
#243781,#243782,#243783,#243784,#243785,#243786,#243787,#243788,#243789,
#243790,#243791,#243792,#243793,#243794,#243795,#243796,#243797,#243798,
#243799,#243800),.UNSPECIFIED.,.F.,.F.,(4,3,3,3,3,3,3,3,3,3,3,3,3,3,3,3,
3,3,3,3,3,3,3,4),(0.,0.0625000000000169,0.125000000000034,0.250000000000057,
0.37500000000008,0.437500000000086,0.500000000000093,0.625000000000091,
0.687500000000086,0.750000000000081,0.781250000000077,0.812500000000074,
0.84375000000007,0.859375000000062,0.875000000000054,0.906250000000033,
0.921875000000018,0.937500000000004,0.953124999999989,0.960937499999993,
0.968749999999996,0.9765625,0.984375000000003,0.999999989277624),
 .UNSPECIFIED.);
#6133=B_SPLINE_CURVE_WITH_KNOTS('',3,(#243802,#243803,#243804,#243805,#243806,
#243807),.UNSPECIFIED.,.F.,.F.,(4,2,4),(0.,0.0364844625194263,0.0729123026181721),
 .UNSPECIFIED.);
#6134=B_SPLINE_CURVE_WITH_KNOTS('',3,(#243809,#243810,#243811,#243812,#243813,
#243814),.UNSPECIFIED.,.F.,.F.,(4,2,4),(0.,0.000518419907319716,0.00103683901965123),
 .UNSPECIFIED.);
#6135=B_SPLINE_CURVE_WITH_KNOTS('',3,(#243818,#243819,#243820,#243821,#243822,
#243823,#243824,#243825,#243826,#243827,#243828,#243829,#243830,#243831),
 .UNSPECIFIED.,.F.,.F.,(4,2,2,2,2,2,4),(-0.0557474934792282,-0.0327963866219729,
-0.020499608365005,-0.0146381462618493,-0.0101733120806503,-0.00573763001709685,
-1.87350135405495E-15),.UNSPECIFIED.);
#6136=B_SPLINE_CURVE_WITH_KNOTS('',3,(#243868,#243869,#243870,#243871,#243872,
#243873,#243874,#243875,#243876,#243877,#243878,#243879,#243880,#243881,
#243882,#243883,#243884,#243885),.UNSPECIFIED.,.F.,.F.,(4,2,2,2,2,2,2,2,
4),(-3.75036220066221,-3.57763083092397,-3.34575392115624,-3.06826697792209,
-2.79078003468794,-2.45898956740662,-2.29309433376597,-2.21014671694564,
-2.12719910012531),.UNSPECIFIED.);
#6137=B_SPLINE_CURVE_WITH_KNOTS('',3,(#243887,#243888,#243889,#243890,#243891,
#243892,#243893,#243894,#243895,#243896,#243897,#243898,#243899,#243900,
#243901,#243902,#243903,#243904),.UNSPECIFIED.,.F.,.F.,(4,2,2,2,2,2,2,2,
4),(-2.12719910012531,-2.0512596972242,-1.97532029432308,-1.82344148852086,
-1.51968387691641,-1.21823046919714,-0.916777061477878,-0.68747239865552,
-0.512363412091961),.UNSPECIFIED.);
#6138=B_SPLINE_CURVE_WITH_KNOTS('',3,(#244376,#244377,#244378,#244379,#244380,
#244381,#244382,#244383,#244384,#244385,#244386,#244387,#244388,#244389,
#244390,#244391,#244392,#244393,#244394,#244395,#244396,#244397,#244398,
#244399,#244400,#244401,#244402,#244403,#244404,#244405,#244406,#244407,
#244408,#244409,#244410,#244411,#244412,#244413,#244414,#244415,#244416,
#244417,#244418,#244419,#244420,#244421,#244422,#244423,#244424),
 .UNSPECIFIED.,.F.,.F.,(4,3,3,3,3,3,3,3,3,3,3,3,3,3,3,3,4),(0.670958968253536,
0.671875,0.6796875,0.6875,0.69140625,0.6953125,0.703125,0.71875,0.734375,
0.7421875,0.75,0.7578125,0.765625,0.7734375,0.78125,0.7890625,0.795736939319615),
 .UNSPECIFIED.);
#6139=B_SPLINE_CURVE_WITH_KNOTS('',3,(#244425,#244426,#244427,#244428,#244429,
#244430,#244431,#244432,#244433,#244434,#244435,#244436,#244437,#244438),
 .UNSPECIFIED.,.F.,.F.,(4,2,2,2,2,2,4),(9.86350491042899E-7,0.0393479876408068,
0.0757501092296844,0.0769070276303121,0.0792997502710887,0.115445556288863,
0.157977332025505),.UNSPECIFIED.);
#6140=B_SPLINE_CURVE_WITH_KNOTS('',3,(#244993,#244994,#244995,#244996,#244997,
#244998,#244999,#245000,#245001,#245002,#245003,#245004,#245005,#245006,
#245007,#245008,#245009,#245010,#245011,#245012,#245013,#245014,#245015,
#245016,#245017,#245018,#245019,#245020,#245021,#245022,#245023),
 .UNSPECIFIED.,.F.,.F.,(4,3,3,3,3,3,3,3,3,3,4),(0.106516886763067,0.107092942250384,
0.107670887972796,0.108254131185161,0.10884090238149,0.109435073327893,
0.109760614783791,0.110353705997288,0.110941670818037,0.111523726510257,
0.112049065484215),.UNSPECIFIED.);
#6141=B_SPLINE_CURVE_WITH_KNOTS('',3,(#245376,#245377,#245378,#245379,#245380,
#245381,#245382,#245383,#245384,#245385,#245386,#245387,#245388,#245389,
#245390,#245391,#245392,#245393,#245394,#245395,#245396,#245397,#245398,
#245399,#245400,#245401,#245402,#245403,#245404,#245405,#245406,#245407,
#245408,#245409,#245410,#245411,#245412,#245413,#245414,#245415,#245416,
#245417,#245418,#245419,#245420,#245421),.UNSPECIFIED.,.F.,.F.,(4,3,3,3,
3,3,3,3,3,3,3,3,3,3,3,4),(0.610561088386796,0.61718750038455,0.625,0.6328125,
0.640625,0.6484375,0.65625,0.671874995282168,0.679687492655973,0.6875,0.69140625,
0.6953125,0.703125,0.71875,0.734375,0.735482731103291),.UNSPECIFIED.);
#6142=B_SPLINE_CURVE_WITH_KNOTS('',3,(#245422,#245423,#245424,#245425,#245426,
#245427,#245428,#245429,#245430,#245431,#245432,#245433,#245434,#245435),
 .UNSPECIFIED.,.F.,.F.,(4,2,2,2,2,2,4),(-0.159353996056155,-0.120185717626862,
-0.0828817665727692,-0.0817045553496745,-0.0792736925960643,-0.0432511430807235,
-1.00011724153364E-6),.UNSPECIFIED.);
#6143=B_SPLINE_CURVE_WITH_KNOTS('',3,(#245990,#245991,#245992,#245993,#245994,
#245995,#245996,#245997,#245998,#245999,#246000,#246001,#246002,#246003,
#246004,#246005,#246006,#246007,#246008,#246009,#246010,#246011,#246012,
#246013,#246014,#246015,#246016,#246017,#246018,#246019,#246020),
 .UNSPECIFIED.,.F.,.F.,(4,3,3,3,3,3,3,3,3,3,4),(0.106516884683353,0.107092939699245,
0.107670885152251,0.108254128432155,0.108840899894406,0.10943507143996,
0.109760614783791,0.110353692948115,0.110941647902085,0.111523698461363,
0.112049172840853),.UNSPECIFIED.);
#6144=B_SPLINE_CURVE_WITH_KNOTS('',3,(#246084,#246085,#246086,#246087,#246088,
#246089,#246090,#246091,#246092,#246093,#246094,#246095,#246096,#246097,
#246098,#246099,#246100,#246101,#246102,#246103,#246104,#246105,#246106,
#246107,#246108,#246109,#246110,#246111,#246112,#246113,#246114,#246115,
#246116,#246117,#246118,#246119,#246120,#246121,#246122,#246123,#246124,
#246125,#246126,#246127,#246128,#246129,#246130,#246131,#246132,#246133,
#246134,#246135,#246136,#246137,#246138,#246139,#246140,#246141,#246142,
#246143,#246144,#246145,#246146,#246147,#246148,#246149,#246150,#246151,
#246152,#246153,#246154,#246155,#246156,#246157,#246158,#246159,#246160,
#246161,#246162,#246163,#246164,#246165,#246166,#246167,#246168,#246169,
#246170,#246171,#246172,#246173,#246174),.UNSPECIFIED.,.F.,.F.,(4,3,3,3,
3,3,3,3,3,3,3,3,3,3,3,3,3,3,3,3,3,3,3,3,3,3,3,3,3,3,4),(4.21395407591397E-15,
0.0513337499264628,0.102587935188955,0.125000000000031,0.176343801200056,
0.187500000000046,0.218750000000049,0.234375000000048,0.244041897155707,
0.250000000000047,0.309672654416341,0.369105698372573,0.428395485970964,
0.43750000000001,0.468750000000009,0.484375000000006,0.492187500000005,
0.497814922027182,0.500000000000003,0.573415958268157,0.625000000000011,
0.687500000000019,0.718750000000022,0.734375000000019,0.742187500000021,
0.748509676604922,0.750000000000022,0.831491304930903,0.915745652465452,
0.995687255361179,1.),.UNSPECIFIED.);
#6145=B_SPLINE_CURVE_WITH_KNOTS('',3,(#246176,#246177,#246178,#246179,#246180,
#246181,#246182,#246183,#246184,#246185,#246186,#246187,#246188,#246189,
#246190,#246191,#246192,#246193,#246194,#246195,#246196,#246197,#246198,
#246199,#246200,#246201),.UNSPECIFIED.,.F.,.F.,(4,2,2,2,2,2,2,2,2,2,2,2,
4),(-0.0336607847350189,-0.0252529472090739,-0.0183080555179268,-0.0146735416284525,
-0.0131510496302063,-0.0124740531690606,-0.0121414421254511,-0.0119752048891003,
-0.0118919360214624,-0.0118502431729518,-0.00873986850434003,-0.00356796757225184,
0.),.UNSPECIFIED.);
#6146=B_SPLINE_CURVE_WITH_KNOTS('',3,(#246203,#246204,#246205,#246206,#246207,
#246208,#246209,#246210,#246211,#246212),.UNSPECIFIED.,.F.,.F.,(4,3,3,4),
(1.23506593368833E-9,0.383469765022769,0.771748903020239,0.999982570836687),
 .UNSPECIFIED.);
#6147=B_SPLINE_CURVE_WITH_KNOTS('',3,(#246213,#246214,#246215,#246216,#246217,
#246218,#246219,#246220,#246221,#246222,#246223,#246224,#246225,#246226,
#246227,#246228,#246229,#246230,#246231,#246232,#246233,#246234,#246235),
 .UNSPECIFIED.,.F.,.F.,(4,2,1,1,1,1,2,2,2,1,1,1,2,2,4),(0.,0.250000000000111,
0.375000000000166,0.437500000000193,0.468750000000216,0.484375000000238,
0.49218750000024,0.500000000000242,0.62500000000017,0.687500000000123,0.718750000000091,
0.734375000000072,0.742187500000063,0.750000000000053,1.),.UNSPECIFIED.);
#6148=B_SPLINE_CURVE_WITH_KNOTS('',3,(#246268,#246269,#246270,#246271,#246272,
#246273,#246274,#246275,#246276,#246277,#246278,#246279,#246280,#246281,
#246282,#246283),.UNSPECIFIED.,.F.,.F.,(4,3,3,3,3,4),(0.,0.205474320931334,
0.405512720698626,0.603462068588223,0.801731034294112,1.),.UNSPECIFIED.);
#6149=B_SPLINE_CURVE_WITH_KNOTS('',3,(#246284,#246285,#246286,#246287,#246288,
#246289,#246290,#246291,#246292,#246293,#246294,#246295,#246296),
 .UNSPECIFIED.,.F.,.F.,(4,3,3,3,4),(0.,0.313781217437814,0.626723184051377,
0.938079360646063,1.),.UNSPECIFIED.);
#6150=B_SPLINE_CURVE_WITH_KNOTS('',3,(#246330,#246331,#246332,#246333,#246334,
#246335,#246336,#246337,#246338,#246339,#246340,#246341,#246342,#246343,
#246344,#246345,#246346,#246347,#246348,#246349,#246350,#246351,#246352,
#246353,#246354,#246355,#246356,#246357,#246358,#246359,#246360,#246361,
#246362,#246363,#246364,#246365,#246366,#246367,#246368,#246369,#246370,
#246371,#246372,#246373,#246374,#246375,#246376,#246377,#246378,#246379,
#246380,#246381,#246382,#246383,#246384),.UNSPECIFIED.,.F.,.F.,(4,3,3,3,
3,3,3,3,3,3,3,3,3,3,3,3,3,3,4),(0.,0.138504284258626,0.25,0.374999999999999,
0.437499999999998,0.470325698801164,0.499999999999997,0.500138551474872,
0.549028602637725,0.597465662805955,0.624999999999997,0.62596050941851,
0.681158301184605,0.718749999999996,0.736589248328212,0.749999999999997,
0.750154530180252,0.886556322996174,1.),.UNSPECIFIED.);
#6151=B_SPLINE_CURVE_WITH_KNOTS('',3,(#246385,#246386,#246387,#246388,#246389,
#246390,#246391,#246392,#246393,#246394,#246395,#246396,#246397,#246398,
#246399,#246400,#246401,#246402,#246403,#246404,#246405,#246406,#246407,
#246408,#246409,#246410,#246411,#246412,#246413,#246414,#246415,#246416,
#246417,#246418,#246419,#246420,#246421,#246422,#246423,#246424,#246425,
#246426,#246427,#246428,#246429,#246430,#246431,#246432,#246433,#246434,
#246435,#246436,#246437,#246438,#246439,#246440,#246441,#246442),
 .UNSPECIFIED.,.F.,.F.,(4,3,3,3,3,3,3,3,3,3,3,3,3,3,3,3,3,3,3,4),(0.,0.080558140948196,
0.16278162914552,0.245005117342845,0.286012425338604,0.360319101235246,
0.37102880065776,0.381960157756901,0.431472826356726,0.484375000000007,
0.495385439719595,0.500000000000006,0.500151948917147,0.581487373177427,
0.662653965760947,0.74699047432071,0.828040801997895,0.909144794487731,
0.990409652328597,1.),.UNSPECIFIED.);
#6152=B_SPLINE_CURVE_WITH_KNOTS('',3,(#246463,#246464,#246465,#246466,#246467,
#246468),.UNSPECIFIED.,.F.,.F.,(4,2,4),(-0.00572418575854378,-0.00286323169356134,
0.),.UNSPECIFIED.);
#6153=B_SPLINE_CURVE_WITH_KNOTS('',3,(#246469,#246470,#246471,#246472,#246473,
#246474,#246475,#246476,#246477,#246478,#246479,#246480,#246481,#246482,
#246483,#246484,#246485,#246486,#246487,#246488,#246489,#246490,#246491,
#246492,#246493,#246494,#246495,#246496,#246497,#246498,#246499),
 .UNSPECIFIED.,.F.,.F.,(4,3,3,3,3,3,3,3,3,3,4),(0.,0.11761557917262,0.239211453690796,
0.368222332867088,0.442407161882584,0.537154674978954,0.634968309816214,
0.73831066301708,0.845453355624249,0.959390767423322,0.999998837624099),
 .UNSPECIFIED.);
#6154=B_SPLINE_CURVE_WITH_KNOTS('',3,(#246501,#246502,#246503,#246504,#246505,
#246506,#246507,#246508,#246509,#246510,#246511,#246512,#246513,#246514,
#246515,#246516),.UNSPECIFIED.,.F.,.F.,(4,3,3,3,3,4),(0.,0.160379797404396,
0.25,0.526438124442171,0.791916875509661,1.),.UNSPECIFIED.);
#6155=B_SPLINE_CURVE_WITH_KNOTS('',3,(#246517,#246518,#246519,#246520,#246521,
#246522),.UNSPECIFIED.,.F.,.F.,(4,2,4),(-0.0615356806447155,-0.0307265379384587,
0.),.UNSPECIFIED.);
#6156=B_SPLINE_CURVE_WITH_KNOTS('',3,(#246584,#246585,#246586,#246587,#246588,
#246589,#246590,#246591,#246592,#246593,#246594,#246595,#246596,#246597,
#246598,#246599),.UNSPECIFIED.,.F.,.F.,(4,2,2,2,2,2,2,4),(3.3017407839461E-5,
0.249999999999985,0.374999999999977,0.437499999999978,0.468749999999975,
0.499999999999972,0.749999999999986,0.999999937134297),.UNSPECIFIED.);
#6157=B_SPLINE_CURVE_WITH_KNOTS('',3,(#246621,#246622,#246623,#246624,#246625,
#246626,#246627,#246628,#246629,#246630,#246631,#246632,#246633,#246634,
#246635,#246636,#246637,#246638,#246639,#246640,#246641,#246642,#246643,
#246644,#246645,#246646,#246647,#246648,#246649,#246650,#246651,#246652,
#246653,#246654,#246655,#246656,#246657,#246658,#246659,#246660,#246661,
#246662,#246663,#246664,#246665,#246666,#246667,#246668,#246669,#246670,
#246671,#246672,#246673,#246674,#246675),.UNSPECIFIED.,.F.,.F.,(4,3,3,3,
3,3,3,3,3,3,3,3,3,3,3,3,3,3,4),(0.,0.136293856989282,0.250000000000071,
0.375000000000084,0.437500000000081,0.472971764724835,0.500000000000077,
0.625000000000053,0.679526483168007,0.734502976449291,0.750000000000029,
0.815145744893402,0.875000000000005,0.901444261501065,0.92472577106741,
0.937500000000002,0.96396693827555,0.990694659952347,1.),.UNSPECIFIED.);
#6158=B_SPLINE_CURVE_WITH_KNOTS('',3,(#246724,#246725,#246726,#246727,#246728,
#246729,#246730,#246731,#246732,#246733,#246734,#246735,#246736,#246737,
#246738,#246739,#246740,#246741,#246742,#246743,#246744,#246745,#246746,
#246747,#246748,#246749,#246750,#246751,#246752,#246753,#246754,#246755,
#246756,#246757,#246758,#246759,#246760,#246761,#246762,#246763,#246764,
#246765,#246766,#246767,#246768,#246769,#246770,#246771,#246772,#246773,
#246774,#246775),.UNSPECIFIED.,.F.,.F.,(4,3,3,3,3,3,3,3,3,3,3,3,3,3,3,3,
3,4),(0.,0.0264122776644583,0.0525704699845341,0.0624999999999952,0.0830347144030536,
0.106647415780136,0.12499999999999,0.180884076821772,0.236293420895041,
0.249999999999977,0.374999999999964,0.437499999999959,0.473333285050837,
0.499999999999955,0.633762556066951,0.768082693942593,0.904334277462089,
1.),.UNSPECIFIED.);
#6159=B_SPLINE_CURVE_WITH_KNOTS('',3,(#246836,#246837,#246838,#246839,#246840,
#246841,#246842,#246843,#246844,#246845,#246846,#246847,#246848,#246849,
#246850,#246851),.UNSPECIFIED.,.F.,.F.,(4,2,2,2,2,2,2,4),(4.71302443996447E-8,
0.249999999999948,0.374999999999924,0.437499999999912,0.46874999999991,
0.499999999999908,0.749999999999954,0.999999958685833),.UNSPECIFIED.);
#6160=B_SPLINE_CURVE_WITH_KNOTS('',3,(#246865,#246866,#246867,#246868),
 .UNSPECIFIED.,.F.,.F.,(4,4),(0.000150513941758003,0.00194200748227624),
 .UNSPECIFIED.);
#6161=B_SPLINE_CURVE_WITH_KNOTS('',3,(#246870,#246871,#246872,#246873,#246874,
#246875),.UNSPECIFIED.,.F.,.F.,(4,2,4),(2.80044314047858E-9,0.0954464079467005,
0.190095771623502),.UNSPECIFIED.);
#6162=B_SPLINE_CURVE_WITH_KNOTS('',3,(#246878,#246879,#246880,#246881,#246882,
#246883),.UNSPECIFIED.,.F.,.F.,(4,2,4),(-0.050445736393907,-0.0244802048333361,
-5.52363958843116E-7),.UNSPECIFIED.);
#6163=B_SPLINE_CURVE_WITH_KNOTS('',3,(#246930,#246931,#246932,#246933,#246934,
#246935,#246936,#246937,#246938,#246939,#246940,#246941,#246942,#246943,
#246944,#246945,#246946,#246947,#246948,#246949,#246950,#246951,#246952,
#246953,#246954,#246955,#246956,#246957,#246958,#246959,#246960,#246961,
#246962,#246963,#246964,#246965,#246966,#246967,#246968,#246969,#246970,
#246971,#246972,#246973,#246974,#246975,#246976,#246977,#246978,#246979,
#246980,#246981,#246982,#246983,#246984,#246985,#246986,#246987,#246988,
#246989,#246990,#246991,#246992,#246993,#246994,#246995,#246996,#246997,
#246998,#246999,#247000,#247001,#247002,#247003,#247004,#247005,#247006,
#247007,#247008,#247009,#247010,#247011,#247012,#247013,#247014,#247015,
#247016,#247017,#247018,#247019,#247020,#247021,#247022,#247023,#247024,
#247025,#247026),.UNSPECIFIED.,.F.,.F.,(4,3,3,3,3,3,3,3,3,3,3,3,3,3,3,3,
3,3,3,3,3,3,3,3,3,3,3,3,3,3,3,3,4),(4.90643966544258E-10,0.0484929148260123,
0.0624999999999239,0.0937499999998868,0.109374999999871,0.117187499999864,
0.121917492028509,0.124999999999858,0.156249999999857,0.187499999999855,
0.215117790312726,0.234374999999851,0.242144940602164,0.246418240190107,
0.249999999999851,0.292416118246735,0.337195875190666,0.361094236029373,
0.374999999999876,0.419241773384761,0.465335153524285,0.497676368738863,
0.499999999999902,0.555006865257746,0.61025570631107,0.63852067128082,0.718028377305788,
0.749999999999951,0.765547908324208,0.826638203583669,0.887847641427647,
0.949089724737531,1.),.UNSPECIFIED.);
#6164=B_SPLINE_CURVE_WITH_KNOTS('',3,(#247027,#247028,#247029,#247030,#247031,
#247032,#247033,#247034,#247035,#247036,#247037,#247038,#247039,#247040,
#247041,#247042,#247043,#247044,#247045,#247046,#247047,#247048,#247049,
#247050,#247051,#247052,#247053,#247054,#247055,#247056,#247057,#247058,
#247059,#247060,#247061,#247062,#247063,#247064,#247065,#247066,#247067,
#247068,#247069,#247070,#247071,#247072,#247073,#247074,#247075,#247076,
#247077,#247078,#247079,#247080,#247081,#247082,#247083,#247084,#247085,
#247086,#247087,#247088,#247089,#247090,#247091,#247092,#247093,#247094,
#247095,#247096,#247097,#247098,#247099,#247100,#247101,#247102,#247103,
#247104,#247105,#247106,#247107,#247108),.UNSPECIFIED.,.F.,.F.,(4,3,3,3,
3,3,3,3,3,3,3,3,3,3,3,3,3,3,3,3,3,3,3,3,3,3,3,4),(0.,0.0707256112310334,
0.143494179479758,0.17045670394154,0.244355170384741,0.249999999999997,
0.326199977717216,0.374999999999996,0.415486708305964,0.437499999999992,
0.46874999999999,0.484950527153161,0.499999999999987,0.572299455137252,
0.624999999999996,0.635472223482649,0.687500000000006,0.718750000000013,
0.734375000000019,0.742187500000023,0.748402724993224,0.750000000000026,
0.802194690059772,0.851646017502705,0.898368266629995,0.944112234320723,
0.990046607588191,0.999999999831502),.UNSPECIFIED.);
#6165=B_SPLINE_CURVE_WITH_KNOTS('',3,(#247148,#247149,#247150,#247151,#247152,
#247153,#247154,#247155,#247156,#247157,#247158,#247159,#247160,#247161,
#247162,#247163,#247164,#247165,#247166,#247167,#247168,#247169,#247170,
#247171,#247172,#247173,#247174,#247175),.UNSPECIFIED.,.F.,.F.,(4,3,3,3,
3,3,3,3,3,4),(0.838474295473316,0.930058057517816,1.02271627966907,1.11634472529987,
1.17837075498859,1.27647714794017,1.37034540944472,1.46344152971751,1.55490687474701,
1.5707963267949),.UNSPECIFIED.);
#6166=B_SPLINE_CURVE_WITH_KNOTS('',3,(#247176,#247177,#247178,#247179,#247180,
#247181,#247182,#247183,#247184,#247185,#247186,#247187,#247188,#247189,
#247190,#247191,#247192,#247193,#247194,#247195,#247196,#247197,#247198,
#247199,#247200,#247201,#247202,#247203,#247204,#247205,#247206,#247207,
#247208,#247209,#247210,#247211,#247212,#247213,#247214,#247215,#247216,
#247217,#247218,#247219,#247220,#247221,#247222,#247223,#247224,#247225,
#247226,#247227,#247228,#247229,#247230,#247231,#247232,#247233,#247234,
#247235,#247236,#247237,#247238,#247239,#247240,#247241,#247242,#247243,
#247244,#247245,#247246,#247247,#247248),.UNSPECIFIED.,.F.,.F.,(4,3,3,3,
3,3,3,3,3,3,3,3,3,3,3,3,3,3,3,3,3,3,3,3,4),(0.,0.0401919312141592,0.0819963404705172,
0.129529840467209,0.176267374973055,0.225909382758087,0.242187499999802,
0.246093749999801,0.249999999999799,0.25875764645275,0.316878823226282,
0.374999999999814,0.43851508519816,0.484374999999833,0.493696347244718,
0.499999999999837,0.573948265789786,0.624999999999878,0.666613401443068,
0.708142799438681,0.739741591291496,0.74999999999992,0.858692239174755,
0.96742933190215,1.),.UNSPECIFIED.);
#6167=B_SPLINE_CURVE_WITH_KNOTS('',3,(#247292,#247293,#247294,#247295,#247296,
#247297,#247298,#247299,#247300,#247301,#247302,#247303,#247304,#247305,
#247306,#247307,#247308,#247309,#247310,#247311,#247312,#247313,#247314,
#247315,#247316,#247317,#247318,#247319,#247320,#247321,#247322,#247323,
#247324,#247325,#247326,#247327,#247328,#247329,#247330,#247331,#247332,
#247333,#247334,#247335,#247336,#247337,#247338,#247339,#247340,#247341,
#247342,#247343,#247344,#247345,#247346,#247347,#247348,#247349,#247350,
#247351,#247352,#247353,#247354,#247355,#247356,#247357,#247358,#247359,
#247360,#247361,#247362,#247363,#247364,#247365,#247366,#247367),
 .UNSPECIFIED.,.F.,.F.,(4,3,3,3,3,3,3,3,3,3,3,3,3,3,3,3,3,3,3,3,3,3,3,3,
3,4),(0.,0.0556216394818239,0.114786080727818,0.125000000000148,0.170750843532883,
0.187500000000216,0.218750000000247,0.234375000000262,0.242187500000269,
0.250000000000276,0.307005920394933,0.367744726360799,0.375000000000249,
0.400758159320508,0.437500000000244,0.468750000000244,0.484375000000236,
0.492187500000229,0.500000000000223,0.579547472665855,0.63240430891721,
0.709879787609452,0.79182759636595,0.881990335411978,0.905051170989505,
0.999999999999986),.UNSPECIFIED.);
#6168=B_SPLINE_CURVE_WITH_KNOTS('',3,(#247369,#247370,#247371,#247372,#247373,
#247374,#247375,#247376,#247377,#247378,#247379,#247380,#247381,#247382,
#247383,#247384,#247385,#247386,#247387,#247388,#247389,#247390,#247391,
#247392,#247393,#247394,#247395,#247396,#247397,#247398,#247399,#247400,
#247401,#247402,#247403,#247404,#247405,#247406,#247407,#247408,#247409,
#247410,#247411,#247412,#247413,#247414,#247415,#247416,#247417,#247418,
#247419,#247420,#247421,#247422,#247423,#247424,#247425,#247426,#247427,
#247428,#247429,#247430,#247431,#247432,#247433,#247434,#247435,#247436,
#247437,#247438,#247439,#247440,#247441,#247442,#247443,#247444,#247445,
#247446,#247447,#247448,#247449,#247450,#247451,#247452,#247453,#247454,
#247455,#247456,#247457,#247458,#247459,#247460,#247461,#247462,#247463,
#247464,#247465,#247466,#247467,#247468,#247469,#247470,#247471,#247472,
#247473,#247474),.UNSPECIFIED.,.F.,.F.,(4,3,3,3,3,3,3,3,3,3,3,3,3,3,3,3,
3,3,3,3,3,3,3,3,3,3,3,3,3,3,3,3,3,3,3,4),(0.,0.031249999999987,0.0609011661437237,
0.0900742302575725,0.116500739893332,0.139847180987321,0.167385385740464,
0.19228716190139,0.216441510703671,0.233220755351783,0.241610377675839,
0.245805188837868,0.246124074157174,0.248829591534349,0.249999999999896,
0.25307350048546,0.303563924576077,0.356881390395021,0.368339324261443,
0.374999999999939,0.417741125365788,0.437499999999959,0.468749999999971,
0.484374999999979,0.493079053533789,0.499999999999986,0.505683401295463,
0.580643685324135,0.624064275299452,0.690096059492877,0.745168072966554,
0.749999999999993,0.820916344647453,0.892677383913134,0.965739469496175,
1.),.UNSPECIFIED.);
#6169=B_SPLINE_CURVE_WITH_KNOTS('',3,(#247479,#247480,#247481,#247482,#247483,
#247484),.UNSPECIFIED.,.F.,.F.,(4,2,4),(-0.0269664855274713,-0.0134828803856389,
-9.31064075733457E-8),.UNSPECIFIED.);
#6170=B_SPLINE_CURVE_WITH_KNOTS('',3,(#247521,#247522,#247523,#247524,#247525,
#247526,#247527,#247528,#247529,#247530,#247531,#247532,#247533,#247534,
#247535,#247536,#247537,#247538,#247539,#247540,#247541,#247542,#247543,
#247544,#247545,#247546,#247547,#247548,#247549,#247550,#247551,#247552,
#247553,#247554,#247555,#247556,#247557,#247558,#247559,#247560,#247561,
#247562,#247563,#247564,#247565,#247566,#247567,#247568,#247569,#247570,
#247571,#247572,#247573,#247574,#247575,#247576,#247577,#247578,#247579,
#247580,#247581,#247582,#247583,#247584,#247585,#247586,#247587,#247588,
#247589,#247590,#247591,#247592,#247593,#247594,#247595,#247596,#247597,
#247598,#247599,#247600,#247601,#247602),.UNSPECIFIED.,.F.,.F.,(4,3,3,3,
3,3,3,3,3,3,3,3,3,3,3,3,3,3,3,3,3,3,3,3,3,3,3,4),(2.56487959041513E-5,0.0937141008831449,
0.125000000000051,0.167506357101888,0.209606233741686,0.250000000000101,
0.255551994916339,0.331355837399193,0.375000000000152,0.446289040401504,
0.484375000000202,0.493412876541942,0.496956676406121,0.500000000000213,
0.562500000000231,0.625000000000249,0.685483798309844,0.739929054069917,
0.742187500000292,0.746093750000291,0.749589802703738,0.750000000000291,
0.799105712593443,0.846444987881696,0.890808069977353,0.933559317031731,
0.974096720592753,1.),.UNSPECIFIED.);
#6171=B_SPLINE_CURVE_WITH_KNOTS('',3,(#247603,#247604,#247605,#247606,#247607,
#247608,#247609,#247610,#247611,#247612,#247613,#247614,#247615,#247616,
#247617,#247618,#247619,#247620,#247621,#247622,#247623,#247624,#247625,
#247626,#247627,#247628,#247629,#247630),.UNSPECIFIED.,.F.,.F.,(4,3,3,3,
3,3,3,3,3,4),(1.5707963267949,1.66216581219747,1.7554915464119,1.8494444653613,
1.94323589460212,1.96555277811107,2.05915766062388,2.15220658922426,2.24364798476046,
2.30311835811648),.UNSPECIFIED.);
#6172=B_SPLINE_CURVE_WITH_KNOTS('',3,(#247713,#247714,#247715,#247716,#247717,
#247718,#247719,#247720,#247721,#247722,#247723,#247724,#247725,#247726,
#247727,#247728,#247729,#247730,#247731,#247732,#247733,#247734,#247735,
#247736,#247737,#247738,#247739,#247740,#247741,#247742,#247743,#247744,
#247745,#247746,#247747,#247748,#247749,#247750,#247751,#247752,#247753,
#247754,#247755,#247756,#247757,#247758,#247759,#247760,#247761,#247762,
#247763,#247764,#247765,#247766,#247767,#247768,#247769,#247770,#247771,
#247772,#247773,#247774,#247775,#247776,#247777,#247778,#247779,#247780,
#247781,#247782,#247783,#247784,#247785,#247786,#247787,#247788,#247789,
#247790,#247791,#247792,#247793,#247794,#247795,#247796,#247797,#247798,
#247799,#247800),.UNSPECIFIED.,.F.,.F.,(4,3,3,3,3,3,3,3,3,3,3,3,3,3,3,3,
3,3,3,3,3,3,3,3,3,3,3,3,3,4),(0.,0.0794481524643703,0.156768214864146,0.231339825995753,
0.249999999999803,0.259044933609346,0.317022466804525,0.374999999999703,
0.382132705216096,0.432682584624564,0.437499999999653,0.468749999999628,
0.484374999999614,0.492187499999605,0.496093749999601,0.499514900518553,
0.499999999999598,0.503507170613991,0.558938703049898,0.610863177296971,
0.66100706983879,0.708568267760028,0.749999999999799,0.792248812129508,
0.812499999999849,0.859374999999887,0.902003267191604,0.943270081246986,
0.982693916806458,1.),.UNSPECIFIED.);
#6173=B_SPLINE_CURVE_WITH_KNOTS('',3,(#247801,#247802,#247803,#247804,#247805,
#247806,#247807,#247808,#247809,#247810,#247811,#247812,#247813,#247814,
#247815,#247816,#247817,#247818,#247819,#247820,#247821,#247822,#247823,
#247824,#247825,#247826,#247827,#247828,#247829,#247830,#247831,#247832,
#247833,#247834,#247835,#247836,#247837),.UNSPECIFIED.,.F.,.F.,(4,3,3,3,
3,3,3,3,3,3,3,3,4),(0.,0.000111500026751792,0.000198033010607759,0.000314017729824417,
0.000396641361730405,0.000472439313739977,0.000496099573318823,0.000572015964014575,
0.000578662087025262,0.000595420430124543,0.000632317246134149,0.000714137978067164,
0.00079328272346081),.UNSPECIFIED.);
#6174=B_SPLINE_CURVE_WITH_KNOTS('',3,(#247905,#247906,#247907,#247908,#247909,
#247910,#247911,#247912,#247913,#247914,#247915,#247916,#247917,#247918,
#247919,#247920,#247921,#247922,#247923,#247924,#247925,#247926,#247927,
#247928,#247929,#247930,#247931,#247932,#247933,#247934,#247935,#247936,
#247937,#247938,#247939,#247940,#247941),.UNSPECIFIED.,.F.,.F.,(4,3,3,3,
3,3,3,3,3,3,3,3,4),(0.,8.15311101657598E-5,0.000163591288741779,0.00017635437994511,
0.00019860108990148,0.000231640871620125,0.000308214802536355,0.000385145785492459,
0.000397500346645172,0.000497039263014267,0.000596687155864874,0.000699642509595148,
0.000795000693290343),.UNSPECIFIED.);
#6175=B_SPLINE_CURVE_WITH_KNOTS('',3,(#247942,#247943,#247944,#247945,#247946,
#247947,#247948,#247949,#247950,#247951,#247952,#247953,#247954,#247955,
#247956,#247957,#247958,#247959,#247960),.UNSPECIFIED.,.F.,.F.,(4,2,2,2,
1,1,1,2,2,2,4),(0.,0.249999999999961,0.374999999999946,0.437499999999938,
0.468749999999932,0.484374999999921,0.492187499999909,0.49609374999991,
0.49999999999991,0.749999999999955,1.),.UNSPECIFIED.);
#6176=B_SPLINE_CURVE_WITH_KNOTS('',3,(#247980,#247981,#247982,#247983,#247984,
#247985,#247986,#247987,#247988,#247989,#247990,#247991,#247992,#247993,
#247994,#247995),.UNSPECIFIED.,.F.,.F.,(4,3,3,3,3,4),(0.,0.211457556634167,
0.425375488930141,0.639024931200921,0.850118550185379,1.),.UNSPECIFIED.);
#6177=B_SPLINE_CURVE_WITH_KNOTS('',3,(#248004,#248005,#248006,#248007,#248008,
#248009,#248010,#248011,#248012,#248013,#248014,#248015,#248016,#248017,
#248018,#248019),.UNSPECIFIED.,.F.,.F.,(4,3,3,3,3,4),(0.,0.211457556638465,
0.42537548893837,0.639024931212968,0.850118550201083,1.),.UNSPECIFIED.);
#6178=B_SPLINE_CURVE_WITH_KNOTS('',3,(#248028,#248029,#248030,#248031,#248032,
#248033,#248034,#248035,#248036,#248037,#248038,#248039,#248040,#248041,
#248042,#248043),.UNSPECIFIED.,.F.,.F.,(4,3,3,3,3,4),(0.,0.210153564503388,
0.423721788860115,0.637632960030634,0.849873129905918,1.),.UNSPECIFIED.);
#6179=B_SPLINE_CURVE_WITH_KNOTS('',3,(#248060,#248061,#248062,#248063,#248064,
#248065,#248066,#248067,#248068,#248069,#248070,#248071,#248072),
 .UNSPECIFIED.,.F.,.F.,(4,3,3,3,4),(0.,0.000473404920692545,0.000946160257514461,
0.0014172553414947,0.00169753871027588),.UNSPECIFIED.);
#6180=B_SPLINE_CURVE_WITH_KNOTS('',3,(#248081,#248082,#248083,#248084,#248085,
#248086),.UNSPECIFIED.,.F.,.F.,(4,2,4),(0.,0.5,1.),.UNSPECIFIED.);
#6181=B_SPLINE_CURVE_WITH_KNOTS('',3,(#248103,#248104,#248105,#248106),
 .UNSPECIFIED.,.F.,.F.,(4,4),(0.,0.0169301343956772),.UNSPECIFIED.);
#6182=B_SPLINE_CURVE_WITH_KNOTS('',3,(#248129,#248130,#248131,#248132,#248133,
#248134,#248135,#248136,#248137,#248138,#248139,#248140,#248141,#248142,
#248143,#248144),.UNSPECIFIED.,.F.,.F.,(4,3,3,3,3,4),(0.,0.000357599365643427,
0.000494441238575043,0.000494698486827334,0.000823483292681039,0.000988882477150085),
 .UNSPECIFIED.);
#6183=B_SPLINE_CURVE_WITH_KNOTS('',3,(#248170,#248171,#248172,#248173,#248174,
#248175,#248176,#248177,#248178,#248179,#248180,#248181,#248182,#248183,
#248184,#248185),.UNSPECIFIED.,.F.,.F.,(4,3,3,3,3,4),(0.,0.000351072004839477,
0.000494230507537995,0.000494489082053731,0.000752353626049509,0.000988978164107462),
 .UNSPECIFIED.);
#6184=B_SPLINE_CURVE_WITH_KNOTS('',3,(#248188,#248189,#248190,#248191),
 .UNSPECIFIED.,.F.,.F.,(4,4),(0.,0.0169301343956772),.UNSPECIFIED.);
#6185=B_SPLINE_CURVE_WITH_KNOTS('',3,(#248208,#248209,#248210,#248211,#248212,
#248213,#248214,#248215,#248216,#248217,#248218,#248219,#248220),
 .UNSPECIFIED.,.F.,.F.,(4,3,3,3,4),(0.,0.000471266058852581,0.000943667138230186,
0.00141714356512851,0.00169753871027587),.UNSPECIFIED.);
#6186=B_SPLINE_CURVE_WITH_KNOTS('',3,(#248229,#248230,#248231,#248232,#248233,
#248234),.UNSPECIFIED.,.F.,.F.,(4,2,4),(0.,0.499999999999999,1.),
 .UNSPECIFIED.);
#6187=B_SPLINE_CURVE_WITH_KNOTS('',3,(#248250,#248251,#248252,#248253),
 .UNSPECIFIED.,.F.,.F.,(4,4),(0.00345714931441652,0.0169301343956773),
 .UNSPECIFIED.);
#6188=B_SPLINE_CURVE_WITH_KNOTS('',3,(#248279,#248280,#248281,#248282,#248283,
#248284,#248285,#248286,#248287,#248288,#248289,#248290,#248291,#248292,
#248293,#248294),.UNSPECIFIED.,.F.,.F.,(4,3,3,3,3,4),(0.,0.000357599364445761,
0.000494441238575047,0.000494698486827312,0.000823483291488249,0.000988882477150094),
 .UNSPECIFIED.);
#6189=B_SPLINE_CURVE_WITH_KNOTS('',3,(#248320,#248321,#248322,#248323,#248324,
#248325,#248326,#248327,#248328,#248329,#248330,#248331,#248332,#248333,
#248334,#248335),.UNSPECIFIED.,.F.,.F.,(4,3,3,3,3,4),(0.,0.000351072006453831,
0.000494230507538011,0.000494489082053725,0.000752353626509348,0.00098897816410745),
 .UNSPECIFIED.);
#6190=B_SPLINE_CURVE_WITH_KNOTS('',3,(#248338,#248339,#248340,#248341),
 .UNSPECIFIED.,.F.,.F.,(4,4),(0.,0.0169301343956772),.UNSPECIFIED.);
#6191=B_SPLINE_CURVE_WITH_KNOTS('',3,(#248358,#248359,#248360,#248361,#248362,
#248363,#248364,#248365,#248366,#248367,#248368,#248369,#248370),
 .UNSPECIFIED.,.F.,.F.,(4,3,3,3,4),(0.,0.000471266059312478,0.000943667139110938,
0.00141714356637207,0.00169753871027587),.UNSPECIFIED.);
#6192=B_SPLINE_CURVE_WITH_KNOTS('',3,(#248383,#248384,#248385,#248386,#248387,
#248388,#248389,#248390,#248391,#248392,#248393,#248394,#248395,#248396,
#248397,#248398,#248399,#248400,#248401,#248402,#248403,#248404,#248405,
#248406,#248407,#248408,#248409,#248410),.UNSPECIFIED.,.F.,.F.,(4,3,3,3,
3,3,3,3,3,4),(0.,0.109615221367934,0.221368175865868,0.334395344060503,
0.448689930122853,0.564253205982057,0.681798912079819,0.800474133367955,
0.92099033968873,1.),.UNSPECIFIED.);
#6193=B_SPLINE_CURVE_WITH_KNOTS('',3,(#248425,#248426,#248427,#248428,#248429,
#248430,#248431,#248432,#248433,#248434,#248435,#248436,#248437,#248438,
#248439,#248440,#248441,#248442,#248443,#248444,#248445,#248446,#248447,
#248448,#248449,#248450,#248451,#248452),.UNSPECIFIED.,.F.,.F.,(4,3,3,3,
3,3,3,3,3,4),(0.,0.109615221365806,0.221368175853348,0.334395344045476,
0.448689930098025,0.564253205940007,0.681798912032425,0.800474133326316,
0.920990339655845,1.),.UNSPECIFIED.);
#6194=B_SPLINE_CURVE_WITH_KNOTS('',3,(#248467,#248468,#248469,#248470,#248471,
#248472,#248473,#248474,#248475,#248476,#248477,#248478,#248479,#248480,
#248481,#248482,#248483,#248484,#248485,#248486,#248487,#248488,#248489,
#248490,#248491,#248492,#248493,#248494),.UNSPECIFIED.,.F.,.F.,(4,3,3,3,
3,3,3,3,3,4),(0.,0.125,0.243735787420882,0.361132522922663,0.477221946749902,
0.592021254917456,0.704884640467779,0.816636758371523,0.926654827500873,
1.),.UNSPECIFIED.);
#6195=B_SPLINE_CURVE_WITH_KNOTS('',3,(#248500,#248501,#248502,#248503,#248504,
#248505,#248506,#248507,#248508,#248509,#248510,#248511,#248512,#248513,
#248514,#248515,#248516,#248517,#248518),.UNSPECIFIED.,.F.,.F.,(4,3,3,3,
3,3,4),(0.,0.193537780414673,0.395153335311005,0.588509404331274,0.782367954940123,
0.977488548866527,1.),.UNSPECIFIED.);
#6196=B_SPLINE_CURVE_WITH_KNOTS('',3,(#248527,#248528,#248529,#248530,#248531,
#248532,#248533,#248534,#248535,#248536,#248537,#248538,#248539,#248540,
#248541,#248542,#248543,#248544,#248545),.UNSPECIFIED.,.F.,.F.,(4,3,3,3,
3,3,4),(0.,0.194999919104645,0.396249939328484,0.589433349910318,0.782576073903087,
0.976165346307675,1.),.UNSPECIFIED.);
#6197=B_SPLINE_CURVE_WITH_KNOTS('',3,(#248554,#248555,#248556,#248557,#248558,
#248559,#248560,#248561,#248562,#248563,#248564,#248565,#248566,#248567,
#248568,#248569,#248570,#248571,#248572),.UNSPECIFIED.,.F.,.F.,(4,3,3,3,
3,3,4),(0.,0.193537780417685,0.395153335313264,0.588509404336086,0.78236795494766,
0.977488548876437,1.),.UNSPECIFIED.);
#6198=B_SPLINE_CURVE_WITH_KNOTS('',3,(#248581,#248582,#248583,#248584,#248585,
#248586,#248587,#248588,#248589,#248590,#248591,#248592,#248593,#248594,
#248595,#248596,#248597,#248598,#248599),.UNSPECIFIED.,.F.,.F.,(4,3,3,3,
3,3,4),(0.,0.194999919126221,0.396249939344666,0.589433349950878,0.782576073968802,
0.976165346399302,1.),.UNSPECIFIED.);
#6199=B_SPLINE_CURVE_WITH_KNOTS('',3,(#248621,#248622,#248623,#248624,#248625,
#248626,#248627,#248628,#248629,#248630,#248631,#248632,#248633),
 .UNSPECIFIED.,.F.,.F.,(4,3,3,3,4),(0.,0.000473404920692537,0.000946160257514427,
0.00141725534149459,0.00169753871027588),.UNSPECIFIED.);
#6200=B_SPLINE_CURVE_WITH_KNOTS('',3,(#248640,#248641,#248642,#248643,#248644,
#248645,#248646,#248647,#248648,#248649,#248650,#248651,#248652,#248653,
#248654,#248655,#248656,#248657,#248658,#248659,#248660,#248661),
 .UNSPECIFIED.,.F.,.F.,(4,3,3,3,3,3,3,4),(0.,0.151764361358548,0.302277176656851,
0.451566165387974,0.599064031232558,0.745556092124806,0.890528328351801,
1.),.UNSPECIFIED.);
#6201=B_SPLINE_CURVE_WITH_KNOTS('',3,(#248670,#248671,#248672,#248673,#248674,
#248675,#248676,#248677,#248678,#248679,#248680,#248681,#248682,#248683,
#248684,#248685,#248686,#248687,#248688,#248689,#248690,#248691),
 .UNSPECIFIED.,.F.,.F.,(4,3,3,3,3,3,3,4),(0.,0.14495178916051,0.291012358970586,
0.438205967951544,0.587224233824978,0.737255355597419,0.888962473623652,
1.),.UNSPECIFIED.);
#6202=B_SPLINE_CURVE_WITH_KNOTS('',3,(#248696,#248697,#248698,#248699),
 .UNSPECIFIED.,.F.,.F.,(4,4),(0.,0.0169301343956772),.UNSPECIFIED.);
#6203=B_SPLINE_CURVE_WITH_KNOTS('',3,(#248722,#248723,#248724,#248725,#248726,
#248727,#248728,#248729,#248730,#248731,#248732,#248733,#248734,#248735,
#248736,#248737),.UNSPECIFIED.,.F.,.F.,(4,3,3,3,3,4),(0.,0.000357599365646066,
0.000494441238575043,0.000494698486827332,0.000823483292682126,0.000988882477150085),
 .UNSPECIFIED.);
#6204=B_SPLINE_CURVE_WITH_KNOTS('',3,(#248763,#248764,#248765,#248766,#248767,
#248768,#248769,#248770,#248771,#248772,#248773,#248774,#248775,#248776,
#248777,#248778),.UNSPECIFIED.,.F.,.F.,(4,3,3,3,3,4),(0.,0.000351072004843104,
0.000494230507537992,0.000494489082053731,0.00075235362604859,0.000988978164107462),
 .UNSPECIFIED.);
#6205=B_SPLINE_CURVE_WITH_KNOTS('',3,(#248781,#248782,#248783,#248784),
 .UNSPECIFIED.,.F.,.F.,(4,4),(0.,0.0169301343956772),.UNSPECIFIED.);
#6206=B_SPLINE_CURVE_WITH_KNOTS('',3,(#248801,#248802,#248803,#248804,#248805,
#248806,#248807,#248808,#248809,#248810,#248811,#248812,#248813),
 .UNSPECIFIED.,.F.,.F.,(4,3,3,3,4),(0.,0.000471266058852855,0.000943667138229705,
0.00141714356512824,0.00169753871027587),.UNSPECIFIED.);
#6207=B_SPLINE_CURVE_WITH_KNOTS('',3,(#248833,#248834,#248835,#248836,#248837,
#248838,#248839,#248840,#248841,#248842,#248843,#248844,#248845),
 .UNSPECIFIED.,.F.,.F.,(4,3,3,3,4),(0.,0.000473404921390372,0.000946160258865428,
0.00141725534343648,0.00169753871027587),.UNSPECIFIED.);
#6208=B_SPLINE_CURVE_WITH_KNOTS('',3,(#248852,#248853,#248854,#248855,#248856,
#248857,#248858,#248859,#248860,#248861,#248862,#248863,#248864,#248865,
#248866,#248867,#248868,#248869,#248870,#248871,#248872,#248873),
 .UNSPECIFIED.,.F.,.F.,(4,3,3,3,3,3,3,4),(0.,0.151764361358931,0.302277176656673,
0.451566165387056,0.599064031230457,0.74555609212193,0.890528328348514,
1.),.UNSPECIFIED.);
#6209=B_SPLINE_CURVE_WITH_KNOTS('',3,(#248882,#248883,#248884,#248885,#248886,
#248887,#248888,#248889,#248890,#248891,#248892,#248893,#248894,#248895,
#248896,#248897,#248898,#248899,#248900,#248901,#248902,#248903),
 .UNSPECIFIED.,.F.,.F.,(4,3,3,3,3,3,3,4),(0.,0.144951789160898,0.291012358971132,
0.438205967951823,0.587224233825539,0.737255355598683,0.888962473625554,
1.),.UNSPECIFIED.);
#6210=B_SPLINE_CURVE_WITH_KNOTS('',3,(#248908,#248909,#248910,#248911),
 .UNSPECIFIED.,.F.,.F.,(4,4),(0.,0.0169301343956773),.UNSPECIFIED.);
#6211=B_SPLINE_CURVE_WITH_KNOTS('',3,(#248934,#248935,#248936,#248937,#248938,
#248939,#248940,#248941,#248942,#248943,#248944,#248945,#248946,#248947,
#248948,#248949),.UNSPECIFIED.,.F.,.F.,(4,3,3,3,3,4),(0.,0.000357599364441133,
0.000494441238575047,0.000494698486827317,0.000823483291485574,0.000988882477150094),
 .UNSPECIFIED.);
#6212=B_SPLINE_CURVE_WITH_KNOTS('',3,(#248975,#248976,#248977,#248978,#248979,
#248980,#248981,#248982,#248983,#248984,#248985,#248986,#248987,#248988,
#248989,#248990),.UNSPECIFIED.,.F.,.F.,(4,3,3,3,3,4),(0.,0.000351072006454456,
0.000494230507538008,0.000494489082053725,0.000752353626508291,0.00098897816410745),
 .UNSPECIFIED.);
#6213=B_SPLINE_CURVE_WITH_KNOTS('',3,(#248993,#248994,#248995,#248996),
 .UNSPECIFIED.,.F.,.F.,(4,4),(0.,0.0169301343956772),.UNSPECIFIED.);
#6214=B_SPLINE_CURVE_WITH_KNOTS('',3,(#249013,#249014,#249015,#249016,#249017,
#249018,#249019,#249020,#249021,#249022,#249023,#249024,#249025),
 .UNSPECIFIED.,.F.,.F.,(4,3,3,3,4),(0.,0.000471266059312478,0.000943667139110938,
0.00141714356637207,0.00169753871027587),.UNSPECIFIED.);
#6215=B_SPLINE_CURVE_WITH_KNOTS('',3,(#249053,#249054,#249055,#249056,#249057,
#249058,#249059,#249060,#249061,#249062,#249063,#249064,#249065,#249066,
#249067,#249068),.UNSPECIFIED.,.F.,.F.,(4,3,3,3,3,4),(0.,0.203691748333807,
0.402768811250355,0.498651532784128,0.778653969973165,1.),.UNSPECIFIED.);
#6216=B_SPLINE_CURVE_WITH_KNOTS('',3,(#249083,#249084,#249085,#249086,#249087,
#249088,#249089,#249090,#249091,#249092,#249093,#249094,#249095,#249096,
#249097,#249098,#249099,#249100,#249101),.UNSPECIFIED.,.F.,.F.,(4,3,3,3,
3,3,4),(0.,0.25440556101236,0.44080417075927,0.527162630963832,0.750951239011533,
0.954610616175962,1.),.UNSPECIFIED.);
#6217=B_SPLINE_CURVE_WITH_KNOTS('',3,(#249114,#249115,#249116,#249117,#249118,
#249119,#249120,#249121,#249122,#249123,#249124,#249125,#249126,#249127,
#249128,#249129),.UNSPECIFIED.,.F.,.F.,(4,3,3,3,3,4),(0.,0.203691748342557,
0.402768811256918,0.498651532789133,0.778653969972626,1.),.UNSPECIFIED.);
#6218=B_SPLINE_CURVE_WITH_KNOTS('',3,(#249144,#249145,#249146,#249147,#249148,
#249149,#249150,#249151,#249152,#249153,#249154,#249155,#249156,#249157,
#249158,#249159,#249160,#249161,#249162),.UNSPECIFIED.,.F.,.F.,(4,3,3,3,
3,3,4),(0.,0.254405561026845,0.440804170770133,0.527162630968293,0.750951238968695,
0.954610616116233,1.),.UNSPECIFIED.);
#6219=B_SPLINE_CURVE_WITH_KNOTS('',3,(#249184,#249185,#249186,#249187),
 .UNSPECIFIED.,.F.,.F.,(4,4),(0.,1.),.UNSPECIFIED.);
#6220=B_SPLINE_CURVE_WITH_KNOTS('',3,(#249548,#249549,#249550,#249551,#249552,
#249553,#249554,#249555,#249556,#249557,#249558,#249559,#249560,#249561,
#249562,#249563,#249564,#249565,#249566,#249567,#249568,#249569,#249570,
#249571,#249572,#249573,#249574,#249575,#249576,#249577,#249578,#249579,
#249580,#249581,#249582,#249583,#249584,#249585,#249586,#249587),
 .UNSPECIFIED.,.F.,.F.,(4,3,3,3,3,3,3,3,3,3,3,3,3,4),(0.595270229260643,
0.601562499850747,0.609375000000292,0.617187498808339,0.624999995264159,
0.632812500000061,0.636718750000023,0.640624999999984,0.65624999999983,
0.671874999999676,0.687499999999522,0.703124999999369,0.718749999999215,
0.720233735124377),.UNSPECIFIED.);
#6221=B_SPLINE_CURVE_WITH_KNOTS('',3,(#249588,#249589,#249590,#249591,#249592,
#249593,#249594,#249595,#249596,#249597,#249598,#249599,#249600,#249601),
 .UNSPECIFIED.,.F.,.F.,(4,2,2,2,2,2,4),(-0.159234538760931,-0.11979722499102,
-0.0828045251107409,-0.0816375126728872,-0.0792258592190679,-0.0429042526546323,
-1.00001016328255E-6),.UNSPECIFIED.);
#6222=B_SPLINE_CURVE_WITH_KNOTS('',3,(#250156,#250157,#250158,#250159,#250160,
#250161,#250162,#250163,#250164,#250165,#250166,#250167,#250168,#250169,
#250170,#250171,#250172,#250173,#250174,#250175,#250176,#250177,#250178,
#250179,#250180,#250181,#250182,#250183,#250184,#250185,#250186),
 .UNSPECIFIED.,.F.,.F.,(4,3,3,3,3,3,3,3,3,3,4),(0.881769399096963,0.882351628344185,
0.882937092487587,0.883530275652419,0.884057971014493,0.884652700978261,
0.885241428493491,0.88582365002593,0.886402716932186,0.886978997726707,
0.887301779570027),.UNSPECIFIED.);
#6223=B_SPLINE_CURVE_WITH_KNOTS('',3,(#250189,#250190,#250191,#250192,#250193,
#250194,#250195,#250196,#250197,#250198,#250199,#250200,#250201,#250202,
#250203,#250204,#250205,#250206,#250207,#250208,#250209,#250210,#250211,
#250212,#250213,#250214,#250215,#250216,#250217,#250218,#250219),
 .UNSPECIFIED.,.F.,.F.,(4,3,3,3,3,3,3,3,3,3,4),(0.,0.0937364629817202,0.20846275873661,
0.322150628458144,0.434851188691642,0.546612363950819,0.657479176507349,
0.767494003890456,0.876696808412568,0.985125342372657,1.),.UNSPECIFIED.);
#6224=B_SPLINE_CURVE_WITH_KNOTS('',3,(#250221,#250222,#250223,#250224,#250225,
#250226,#250227,#250228,#250229,#250230,#250231,#250232,#250233,#250234,
#250235,#250236,#250237,#250238,#250239,#250240,#250241,#250242,#250243,
#250244,#250245,#250246,#250247,#250248,#250249,#250250,#250251,#250252,
#250253,#250254,#250255,#250256,#250257,#250258,#250259,#250260,#250261,
#250262,#250263,#250264,#250265,#250266,#250267,#250268,#250269,#250270,
#250271,#250272,#250273,#250274,#250275,#250276,#250277,#250278,#250279,
#250280,#250281,#250282,#250283,#250284),.UNSPECIFIED.,.F.,.F.,(4,3,3,3,
3,3,3,3,3,3,3,3,3,3,3,3,3,3,3,3,3,4),(0.146962374419461,0.147547046336026,
0.148127472789239,0.148704825740929,0.149280291284793,0.149855398739328,
0.150431147356518,0.151008540254158,0.151591055410951,0.152176891110784,
0.152770353285494,0.153238785047258,0.15383405187594,0.154422885444334,
0.155004864618472,0.155583500875027,0.156159817034624,0.156734823245514,
0.157310355761555,0.157886625174272,0.15846634810946,0.158932774246921),
 .UNSPECIFIED.);
#6225=B_SPLINE_CURVE_WITH_KNOTS('',3,(#250285,#250286,#250287,#250288,#250289,
#250290,#250291,#250292,#250293,#250294,#250295,#250296,#250297,#250298,
#250299,#250300,#250301,#250302,#250303,#250304,#250305,#250306,#250307,
#250308,#250309,#250310,#250311,#250312,#250313,#250314,#250315,#250316,
#250317,#250318,#250319,#250320,#250321),.UNSPECIFIED.,.F.,.F.,(4,3,3,3,
3,3,3,3,3,3,3,3,4),(0.,0.00148484200664636,0.0905231864990854,0.181211845999667,
0.273638712259328,0.367899711438529,0.562354567719848,0.662791026196378,
0.765550077502759,0.863546828921589,0.870788292842745,0.978680556821164,
1.),.UNSPECIFIED.);
#6226=B_SPLINE_CURVE_WITH_KNOTS('',3,(#250680,#250681,#250682,#250683,#250684,
#250685,#250686,#250687,#250688,#250689,#250690,#250691,#250692,#250693,
#250694,#250695,#250696,#250697,#250698,#250699,#250700,#250701,#250702,
#250703),.UNSPECIFIED.,.F.,.F.,(4,2,2,2,2,2,2,2,2,2,2,4),(-0.191299715244794,
-0.157661652097922,-0.125069220643887,-0.10269082405758,-0.102057729196898,
-0.10142671334636,-0.10017288684426,-0.0988724155437573,-0.0962033280839491,
-0.0705045556846333,-0.0201379948223164,0.),.UNSPECIFIED.);
#6227=B_SPLINE_CURVE_WITH_KNOTS('',3,(#251066,#251067,#251068,#251069,#251070,
#251071,#251072,#251073,#251074,#251075,#251076,#251077,#251078,#251079,
#251080,#251081,#251082,#251083,#251084,#251085,#251086,#251087,#251088,
#251089,#251090,#251091,#251092,#251093,#251094,#251095),.UNSPECIFIED.,
 .F.,.F.,(4,2,2,1,1,1,2,2,2,2,2,1,2,2,2,2,4),(0.,0.00781249999999989,0.015625,
0.0234375,0.03125,0.046875,0.0546875,0.0625,0.06640625,0.0703125,0.078125,
0.09375,0.109375,0.1171875,0.121093749999999,0.125,0.13856539019169),
 .UNSPECIFIED.);
#6228=B_SPLINE_CURVE_WITH_KNOTS('',3,(#251096,#251097,#251098,#251099,#251100,
#251101,#251102,#251103,#251104,#251105),.UNSPECIFIED.,.F.,.F.,(4,2,2,2,
4),(-0.173949783400974,-0.127702308831258,-0.0869385908804911,-0.0411391376925877,
-1.00000012467905E-6),.UNSPECIFIED.);
#6229=B_SPLINE_CURVE_WITH_KNOTS('',3,(#251468,#251469,#251470,#251471,#251472,
#251473,#251474,#251475,#251476,#251477,#251478,#251479,#251480,#251481,
#251482,#251483,#251484,#251485),.UNSPECIFIED.,.F.,.F.,(4,2,2,2,2,2,2,2,
4),(-0.333980240161851,-0.278002895178562,-0.207048595661841,-0.167393086348014,
-0.160091762120317,-0.159200052079505,-0.128005285823074,-0.0810446390995098,
-9.65957239584814E-7),.UNSPECIFIED.);
#6230=B_SPLINE_CURVE_WITH_KNOTS('',3,(#251486,#251487,#251488,#251489,#251490,
#251491,#251492,#251493,#251494,#251495,#251496,#251497,#251498,#251499,
#251500,#251501,#251502,#251503,#251504,#251505,#251506,#251507,#251508,
#251509,#251510,#251511,#251512,#251513,#251514,#251515,#251516,#251517,
#251518,#251519,#251520,#251521,#251522,#251523,#251524,#251525,#251526,
#251527,#251528,#251529,#251530,#251531,#251532,#251533,#251534),
 .UNSPECIFIED.,.F.,.F.,(4,3,3,3,3,3,3,3,3,3,3,3,3,3,3,3,4),(0.790138930296763,
0.792968750000001,0.796875,0.8125,0.828125,0.8359375,0.84375,0.8515625,
0.859375,0.875,0.890625,0.89453125,0.8984375,0.90625,0.9140625,0.921875,
0.932216014912642),.UNSPECIFIED.);
#6231=B_SPLINE_CURVE_WITH_KNOTS('',3,(#251535,#251536,#251537,#251538,#251539,
#251540,#251541,#251542,#251543,#251544,#251545,#251546,#251547,#251548,
#251549,#251550,#251551,#251552,#251553,#251554,#251555,#251556,#251557,
#251558,#251559,#251560),.UNSPECIFIED.,.F.,.F.,(4,2,2,2,2,2,2,2,2,2,2,2,
4),(-0.866661855593407,-0.708970781836436,-0.558780900260934,-0.401558682989752,
-0.298232076935225,-0.215863746327597,-0.199487234948257,-0.19136087774753,
-0.187332094114913,-0.185319962216916,-0.124545068875862,-0.062491088958267,
-1.00000010871959E-6),.UNSPECIFIED.);
#6232=B_SPLINE_CURVE_WITH_KNOTS('',3,(#252016,#252017,#252018,#252019,#252020,
#252021,#252022,#252023,#252024,#252025,#252026,#252027,#252028,#252029,
#252030,#252031,#252032,#252033,#252034,#252035),.UNSPECIFIED.,.F.,.F.,
(4,2,2,2,2,2,2,2,2,4),(-0.737343996452552,-0.644050018112871,-0.549473453853603,
-0.457744561332403,-0.36907523507599,-0.280277933358412,-0.193344737919196,
-0.105307046015033,-0.0528181412185139,0.),.UNSPECIFIED.);
#6233=B_SPLINE_CURVE_WITH_KNOTS('',3,(#253173,#253174,#253175,#253176,#253177,
#253178),.UNSPECIFIED.,.F.,.F.,(4,2,4),(-0.0951753096986671,-0.0475925862889819,
-1.05240395974435E-6),.UNSPECIFIED.);
#6234=B_SPLINE_CURVE_WITH_KNOTS('',3,(#253179,#253180,#253181,#253182,#253183,
#253184,#253185,#253186,#253187,#253188,#253189,#253190,#253191,#253192),
 .UNSPECIFIED.,.F.,.F.,(4,2,2,2,2,2,4),(0.,0.0445367209370214,0.0852877077239505,
0.158230060143529,0.214173442983221,0.243463509223617,0.271164771184466),
 .UNSPECIFIED.);
#6235=B_SPLINE_CURVE_WITH_KNOTS('',3,(#253193,#253194,#253195,#253196,#253197,
#253198,#253199,#253200,#253201,#253202,#253203,#253204,#253205,#253206,
#253207,#253208,#253209,#253210,#253211,#253212,#253213,#253214,#253215,
#253216,#253217,#253218,#253219,#253220,#253221,#253222,#253223,#253224,
#253225,#253226,#253227,#253228),.UNSPECIFIED.,.F.,.F.,(4,2,2,2,2,2,2,2,
2,2,2,2,2,2,2,2,2,4),(-1.4603242851032,-1.41057592975987,-1.33100660979353,
-1.25442360789161,-1.1747428461744,-1.09621833622064,-1.02009237475002,
-0.940394301350014,-0.862736537925816,-0.785548626949009,-0.705782504629548,
-0.62902379887815,-0.549265680452016,-0.470550628024444,-0.394484973247153,
-0.314815339999637,-0.236962458486878,-0.197604024225048),.UNSPECIFIED.);
#6236=B_SPLINE_CURVE_WITH_KNOTS('',3,(#253784,#253785,#253786,#253787,#253788,
#253789,#253790,#253791,#253792,#253793,#253794,#253795,#253796,#253797,
#253798,#253799,#253800,#253801,#253802,#253803,#253804,#253805),
 .UNSPECIFIED.,.F.,.F.,(4,2,2,2,2,2,2,2,2,2,4),(-0.640412608621221,-0.632596141832508,
-0.552965143807485,-0.474922049306285,-0.398448588061734,-0.318248999100166,
-0.241102613874202,-0.162757814574324,-0.0835743992560574,-0.0410491015749916,
-9.99999716144728E-7),.UNSPECIFIED.);
#6237=B_SPLINE_CURVE_WITH_KNOTS('',3,(#253806,#253807,#253808,#253809,#253810,
#253811,#253812,#253813,#253814,#253815),.UNSPECIFIED.,.F.,.F.,(4,2,2,2,
4),(-0.240375949776406,-0.18190588491853,-0.119969355086001,-0.0632948344662496,
-1.01531671729965E-6),.UNSPECIFIED.);
#6238=B_SPLINE_CURVE_WITH_KNOTS('',3,(#254370,#254371,#254372,#254373,#254374,
#254375,#254376,#254377,#254378,#254379,#254380,#254381,#254382,#254383),
 .UNSPECIFIED.,.F.,.F.,(4,2,2,2,2,2,4),(0.,0.0475788933783159,0.0933534150844901,
0.157993829184702,0.243152490202414,0.307867924694747,0.372920208810498),
 .UNSPECIFIED.);
#6239=B_SPLINE_CURVE_WITH_KNOTS('',3,(#254384,#254385,#254386,#254387,#254388,
#254389),.UNSPECIFIED.,.F.,.F.,(4,2,4),(-0.0551872851809273,-0.0258550695504278,
0.),.UNSPECIFIED.);
#6240=B_SPLINE_CURVE_WITH_KNOTS('',3,(#254390,#254391,#254392,#254393,#254394,
#254395,#254396,#254397,#254398,#254399,#254400,#254401,#254402,#254403),
 .UNSPECIFIED.,.F.,.F.,(4,2,2,2,2,2,4),(-22.8114091378978,-22.7546556945913,
-22.6963478192231,-22.6166081018008,-22.5403648384663,-22.4612431166947,
-22.4011363767123),.UNSPECIFIED.);
#6241=B_SPLINE_CURVE_WITH_KNOTS('',3,(#254407,#254408,#254409,#254410,#254411,
#254412,#254413,#254414,#254415,#254416,#254417,#254418,#254419,#254420,
#254421,#254422,#254423,#254424,#254425,#254426,#254427,#254428,#254429,
#254430,#254431,#254432,#254433,#254434,#254435,#254436,#254437,#254438,
#254439,#254440,#254441,#254442,#254443,#254444,#254445,#254446,#254447,
#254448,#254449,#254450,#254451,#254452,#254453,#254454,#254455,#254456,
#254457,#254458,#254459,#254460,#254461,#254462,#254463,#254464,#254465,
#254466,#254467,#254468,#254469,#254470,#254471,#254472,#254473,#254474,
#254475,#254476,#254477,#254478,#254479,#254480,#254481,#254482,#254483,
#254484,#254485,#254486,#254487,#254488,#254489,#254490,#254491,#254492,
#254493,#254494,#254495,#254496,#254497,#254498,#254499,#254500,#254501,
#254502,#254503),.UNSPECIFIED.,.F.,.F.,(4,3,3,3,3,3,3,3,3,3,3,3,3,3,3,3,
3,3,3,3,3,3,3,3,3,3,3,3,3,3,3,3,4),(0.585665352728702,0.58593750000017,
0.593750000000174,0.601562500000179,0.609375000000184,0.617187500000188,
0.625000000000193,0.632812500000197,0.636718750000199,0.640625000000202,
0.656250000000211,0.67187500000022,0.687500000000229,0.703125000000238,
0.718750000000247,0.726562500000251,0.734375000000256,0.742187500000261,
0.750000000000265,0.75781250000027,0.765625000000274,0.773437500000279,
0.781250000000283,0.789062500000288,0.79296875000029,0.796875000000292,
0.812500000000301,0.82812500000031,0.835937500000315,0.84375000000032,0.851562500000324,
0.859375000000329,0.860346605686114),.UNSPECIFIED.);
#6242=B_SPLINE_CURVE_WITH_KNOTS('',3,(#254504,#254505,#254506,#254507,#254508,
#254509,#254510,#254511,#254512,#254513,#254514,#254515,#254516,#254517,
#254518,#254519,#254520,#254521,#254522,#254523,#254524,#254525,#254526,
#254527,#254528,#254529,#254530,#254531,#254532,#254533,#254534,#254535,
#254536,#254537,#254538,#254539,#254540,#254541,#254542,#254543,#254544,
#254545,#254546,#254547,#254548,#254549,#254550,#254551,#254552,#254553,
#254554,#254555,#254556,#254557,#254558,#254559,#254560,#254561,#254562,
#254563,#254564,#254565,#254566,#254567),.UNSPECIFIED.,.F.,.F.,(4,3,3,3,
3,3,3,3,3,3,3,3,3,3,3,3,3,3,3,3,3,4),(0.146962376116165,0.147547047946169,
0.148127474319873,0.148704827199106,0.149280292681386,0.149855400081028,
0.150431148650181,0.151008541506803,0.151591056632366,0.152176892307433,
0.15277035446366,0.153238785047258,0.153834051806347,0.154422885335194,
0.155004864512828,0.155583500799316,0.156159817014816,0.156734823307263,
0.15731035594623,0.15788662550386,0.158466348626833,0.158932777953849),
 .UNSPECIFIED.);
#6243=B_SPLINE_CURVE_WITH_KNOTS('',3,(#254926,#254927,#254928,#254929,#254930,
#254931,#254932,#254933,#254934,#254935,#254936,#254937,#254938,#254939,
#254940,#254941,#254942,#254943,#254944,#254945,#254946,#254947),
 .UNSPECIFIED.,.F.,.F.,(4,2,2,2,2,2,2,2,2,2,4),(0.,0.0414487749299163,0.0701930279287442,
0.0896240078608044,0.090185540254589,0.0913147136737188,0.0936095790942993,
0.0959463008528485,0.118254097601967,0.162358043499866,0.197736906325247),
 .UNSPECIFIED.);
#6244=B_SPLINE_CURVE_WITH_KNOTS('',3,(#255307,#255308,#255309,#255310,#255311,
#255312,#255313,#255314,#255315,#255316,#255317,#255318,#255319,#255320,
#255321,#255322,#255323,#255324,#255325,#255326,#255327,#255328,#255329,
#255330,#255331,#255332,#255333,#255334,#255335,#255336,#255337,#255338,
#255339,#255340,#255341),.UNSPECIFIED.,.F.,.F.,(4,1,2,2,2,1,1,2,2,2,2,2,
2,2,2,2,2,1,1,4),(0.594033433120655,0.609374999999978,0.617187499999968,
0.624999999999957,0.632812499999947,0.640624999999936,0.656249999999915,
0.664062499999905,0.671874999999895,0.675781249999889,0.679687499999884,
0.687499999999874,0.703124999999853,0.718749999999832,0.722656249999827,
0.726562499999822,0.734374999999811,0.74999999999979,0.75781249999978,0.762507688533689),
 .UNSPECIFIED.);
#6245=B_SPLINE_CURVE_WITH_KNOTS('',3,(#255342,#255343,#255344,#255345,#255346,
#255347,#255348,#255349,#255350,#255351),.UNSPECIFIED.,.F.,.F.,(4,2,2,2,
4),(9.46482055419996E-7,0.0627301013079089,0.114566930226501,0.175834122904311,
0.228935107620853),.UNSPECIFIED.);
#6246=B_SPLINE_CURVE_WITH_KNOTS('',3,(#255352,#255353,#255354,#255355,#255356,
#255357),.UNSPECIFIED.,.F.,.F.,(4,2,4),(0.,0.0475563832059397,0.0951278725828074),
 .UNSPECIFIED.);
#6247=B_SPLINE_CURVE_WITH_KNOTS('',3,(#255720,#255721,#255722,#255723,#255724,
#255725),.UNSPECIFIED.,.F.,.F.,(4,2,4),(9.97452242539264E-7,0.0364245031687067,
0.072772555381456),.UNSPECIFIED.);
#6248=B_SPLINE_CURVE_WITH_KNOTS('',3,(#255961,#255962,#255963,#255964,#255965,
#255966,#255967,#255968,#255969,#255970,#255971,#255972,#255973,#255974,
#255975,#255976,#255977,#255978,#255979,#255980,#255981,#255982,#255983,
#255984,#255985,#255986,#255987,#255988,#255989,#255990,#255991,#255992,
#255993,#255994,#255995,#255996,#255997,#255998,#255999,#256000,#256001,
#256002,#256003,#256004,#256005,#256006,#256007,#256008,#256009,#256010,
#256011,#256012,#256013,#256014,#256015,#256016,#256017,#256018,#256019,
#256020,#256021,#256022,#256023,#256024,#256025,#256026,#256027,#256028,
#256029,#256030,#256031,#256032,#256033,#256034,#256035,#256036,#256037,
#256038,#256039,#256040,#256041,#256042,#256043,#256044,#256045,#256046,
#256047,#256048,#256049,#256050,#256051,#256052,#256053,#256054,#256055,
#256056,#256057,#256058,#256059,#256060,#256061,#256062,#256063,#256064,
#256065,#256066,#256067,#256068,#256069,#256070,#256071,#256072,#256073,
#256074,#256075,#256076),.UNSPECIFIED.,.F.,.F.,(4,2,2,2,2,2,2,2,2,2,2,2,
2,2,2,2,2,2,2,2,2,2,2,2,2,2,2,2,2,2,2,2,2,2,2,2,2,2,2,2,2,2,2,2,2,2,2,2,
2,2,2,2,2,2,2,2,2,4),(0.5,0.5078125,0.515625,0.53125,0.546875,0.5546875,
0.5625,0.5703125,0.578125,0.59375,0.6015625,0.609375,0.6171875,0.625,0.6328125,
0.640625,0.65625,0.6640625,0.671875,0.67578125,0.6796875,0.6875,0.703125,
0.71875,0.72265625,0.7265625,0.734375,0.7421875,0.75,0.7578125,0.765625,
0.7734375,0.78125,0.7890625,0.796875,0.8125,0.8203125,0.828125,0.8359375,
0.84375,0.859375,0.875,0.87890625,0.8828125,0.890625,0.8984375,0.90625,
0.921875,0.9296875,0.93359375,0.9375,0.9453125,0.953125,0.96875,0.9765625,
0.984375,0.9921875,1.),.UNSPECIFIED.);
#6249=B_SPLINE_CURVE_WITH_KNOTS('',3,(#256080,#256081,#256082,#256083,#256084,
#256085,#256086,#256087,#256088,#256089,#256090,#256091,#256092,#256093,
#256094,#256095,#256096,#256097,#256098),.UNSPECIFIED.,.F.,.F.,(4,2,2,2,
2,1,1,1,2,2,4),(0.928243302054433,0.9296875,0.933593749999999,0.9375,0.9453125,
0.953125,0.96875,0.9765625,0.984375,0.9921875,1.),.UNSPECIFIED.);
#6250=B_SPLINE_CURVE_WITH_KNOTS('',3,(#256099,#256100,#256101,#256102,#256103,
#256104,#256105,#256106,#256107,#256108,#256109,#256110,#256111,#256112,
#256113,#256114,#256115,#256116,#256117,#256118,#256119,#256120,#256121,
#256122,#256123,#256124,#256125,#256126,#256127,#256128,#256129,#256130,
#256131,#256132,#256133,#256134,#256135,#256136,#256137,#256138),
 .UNSPECIFIED.,.F.,.F.,(4,2,2,2,2,2,2,2,2,2,2,2,2,2,2,2,2,2,2,4),(0.0717572711999334,
0.0781250000000086,0.0937500000000291,0.101562500000039,0.10937500000005,
0.11718750000006,0.121093750000065,0.12500000000007,0.140625000000091,0.156250000000111,
0.164062500000122,0.171875000000132,0.179687500000142,0.187500000000153,
0.203125000000174,0.210937500000184,0.218750000000194,0.226562500000205,
0.234375000000214,0.237493805076694),.UNSPECIFIED.);
#6251=B_SPLINE_CURVE_WITH_KNOTS('',3,(#256720,#256721,#256722,#256723,#256724,
#256725,#256726,#256727,#256728,#256729,#256730,#256731,#256732,#256733,
#256734,#256735,#256736,#256737,#256738,#256739,#256740,#256741),
 .UNSPECIFIED.,.F.,.F.,(4,2,2,2,2,2,2,2,2,2,4),(9.08424390484079E-7,0.0696685016542001,
0.132515655806531,0.167139005391392,0.173548401015734,0.174327936224742,
0.175107609363997,0.202506476161798,0.243347745195621,0.326904360471616,
0.335458527233704),.UNSPECIFIED.);
#6252=B_SPLINE_CURVE_WITH_KNOTS('',3,(#257296,#257297,#257298,#257299,#257300,
#257301,#257302,#257303,#257304,#257305,#257306,#257307,#257308,#257309),
 .UNSPECIFIED.,.F.,.F.,(4,2,2,2,2,2,4),(0.,0.0445367209381238,0.0852877077272262,
0.158230060150209,0.214173442992252,0.243463509233813,0.271164771195753),
 .UNSPECIFIED.);
#6253=B_SPLINE_CURVE_WITH_KNOTS('',3,(#257310,#257311,#257312,#257313,#257314,
#257315,#257316,#257317,#257318,#257319,#257320,#257321,#257322,#257323,
#257324,#257325,#257326,#257327,#257328,#257329,#257330,#257331,#257332,
#257333,#257334,#257335,#257336,#257337,#257338,#257339,#257340,#257341,
#257342,#257343,#257344,#257345),.UNSPECIFIED.,.F.,.F.,(4,2,2,2,2,2,2,2,
2,2,2,2,2,2,2,2,2,4),(-1.77693741255607,-1.74337044899102,-1.66708872982112,
-1.58731865470844,-1.50900670182408,-1.43252339445671,-1.35203770301058,
-1.27462559370405,-1.19646251166751,-1.11699018971931,-1.04049309552052,
-0.96078663431139,-0.882360986508158,-0.806139075597756,-0.726405109641131,
-0.648849283597101,-0.571355699778421,-0.513010840582583),.UNSPECIFIED.);
#6254=B_SPLINE_CURVE_WITH_KNOTS('',3,(#257900,#257901,#257902,#257903,#257904,
#257905,#257906,#257907,#257908,#257909,#257910,#257911,#257912,#257913),
 .UNSPECIFIED.,.F.,.F.,(4,2,2,2,2,2,4),(9.99999933537955E-7,0.0396954777717048,
0.0807907164979224,0.159863856633394,0.238518326425717,0.315571821712752,
0.324863770283186),.UNSPECIFIED.);
#6255=B_SPLINE_CURVE_WITH_KNOTS('',3,(#257915,#257916,#257917,#257918,#257919,
#257920),.UNSPECIFIED.,.F.,.F.,(4,2,4),(0.,0.0473068317072604,0.0914569630334385),
 .UNSPECIFIED.);
#6256=B_SPLINE_CURVE_WITH_KNOTS('',3,(#257921,#257922,#257923,#257924,#257925,
#257926,#257927,#257928,#257929,#257930,#257931,#257932,#257933,#257934,
#257935,#257936,#257937,#257938,#257939,#257940,#257941,#257942,#257943,
#257944,#257945,#257946),.UNSPECIFIED.,.F.,.F.,(4,2,2,2,2,2,2,2,2,2,2,2,
4),(1.00000010012831E-6,0.0641700687511304,0.1509137744414,0.264210362010751,
0.330507922832673,0.332373878134189,0.334242797798112,0.338007256168076,
0.415092030263758,0.550891681219715,0.683444154698735,0.793447320497175,
0.915560088311105),.UNSPECIFIED.);
#6257=B_SPLINE_CURVE_WITH_KNOTS('',3,(#258501,#258502,#258503,#258504,#258505,
#258506,#258507,#258508,#258509,#258510,#258511,#258512,#258513,#258514),
 .UNSPECIFIED.,.F.,.F.,(4,2,2,2,2,2,4),(0.,0.0475788933774115,0.0933534150825772,
0.157993829182703,0.243152490201031,0.307867924694816,0.372920208811896),
 .UNSPECIFIED.);
#6258=B_SPLINE_CURVE_WITH_KNOTS('',3,(#258515,#258516,#258517,#258518,#258519,
#258520,#258521,#258522,#258523,#258524,#258525,#258526,#258527,#258528,
#258529,#258530,#258531,#258532,#258533,#258534,#258535,#258536),
 .UNSPECIFIED.,.F.,.F.,(4,2,2,2,2,2,2,2,2,2,4),(-22.7495119090184,-22.6891751763705,
-22.6272563246175,-22.5477571954083,-22.4714114519975,-22.3920931070546,
-22.3143022160145,-22.2370473604176,-22.1567200784823,-22.0805078797818,
-22.0249622838298),.UNSPECIFIED.);
#6259=B_SPLINE_CURVE_WITH_KNOTS('',3,(#258539,#258540,#258541,#258542,#258543,
#258544,#258545,#258546,#258547,#258548,#258549,#258550,#258551,#258552,
#258553,#258554,#258555,#258556,#258557,#258558),.UNSPECIFIED.,.F.,.F.,
(4,2,2,2,2,2,2,2,2,4),(0.600895783241409,0.601562500000476,0.609375000000422,
0.617187500000369,0.625000000000315,0.632812500000261,0.640625000000208,
0.648437500000154,0.6562500000001,0.670958963198009),.UNSPECIFIED.);
#6260=B_SPLINE_CURVE_WITH_KNOTS('',3,(#258560,#258561,#258562,#258563,#258564,
#258565,#258566,#258567,#258568,#258569,#258570,#258571,#258572,#258573,
#258574,#258575,#258576,#258577,#258578,#258579,#258580,#258581,#258582,
#258583,#258584,#258585,#258586,#258587,#258588,#258589,#258590,#258591,
#258592,#258593,#258594,#258595,#258596,#258597,#258598,#258599,#258600,
#258601,#258602,#258603,#258604,#258605,#258606,#258607,#258608,#258609,
#258610,#258611,#258612,#258613,#258614,#258615,#258616,#258617,#258618,
#258619,#258620,#258621,#258622,#258623),.UNSPECIFIED.,.F.,.F.,(4,3,3,3,
3,3,3,3,3,3,3,3,3,3,3,3,3,3,3,3,3,4),(0.146962336060241,0.147547010031667,
0.148127438310315,0.148704792860876,0.149280259664182,0.149855368171419,
0.150431117633161,0.151008511164717,0.151591026661658,0.15217686251404,
0.152770324644434,0.153238785047258,0.153834050607704,0.15442288381429,
0.155004863907804,0.155583501870188,0.156159820503461,0.156734829941232,
0.157310366903482,0.157886641401883,0.158466370708173,0.158932909601972),
 .UNSPECIFIED.);
#6261=B_SPLINE_CURVE_WITH_KNOTS('',3,(#258624,#258625,#258626,#258627,#258628,
#258629,#258630,#258631,#258632,#258633,#258634,#258635,#258636,#258637,
#258638,#258639,#258640,#258641,#258642,#258643,#258644,#258645,#258646,
#258647,#258648,#258649,#258650,#258651),.UNSPECIFIED.,.F.,.F.,(4,3,3,3,
3,3,3,3,3,4),(0.795736943641777,0.796875,0.8046875,0.8125,0.828124999999984,
0.835937499999979,0.843749999999974,0.851562499999969,0.859374999999964,
0.87563910993131),.UNSPECIFIED.);
#6262=B_SPLINE_CURVE_WITH_KNOTS('',3,(#258653,#258654,#258655,#258656,#258657,
#258658,#258659,#258660,#258661,#258662,#258663,#258664,#258665,#258666,
#258667,#258668,#258669,#258670,#258671,#258672,#258673,#258674,#258675,
#258676,#258677,#258678,#258679,#258680,#258681,#258682,#258683,#258684,
#258685,#258686,#258687,#258688),.UNSPECIFIED.,.F.,.F.,(4,2,2,2,2,2,2,2,
2,2,2,2,2,2,2,2,2,4),(0.828975078082139,0.879713519041278,0.958060620508997,
1.03775275544132,1.11403993721078,1.19323762107853,1.27156359459928,1.34872275498068,
1.42893628260974,1.50540420656939,1.58346020570364,1.66309517102489,1.73918274620376,
1.81809535814628,1.89705049108488,1.9739640560586,2.05390581774317,2.09124089524434),
 .UNSPECIFIED.);
#6263=B_SPLINE_CURVE_WITH_KNOTS('',3,(#258690,#258691,#258692,#258693,#258694,
#258695,#258696,#258697,#258698,#258699,#258700,#258701,#258702,#258703,
#258704,#258705,#258706,#258707,#258708,#258709,#258710,#258711,#258712,
#258713,#258714,#258715,#258716,#258717,#258718,#258719),.UNSPECIFIED.,
 .F.,.F.,(4,2,2,2,2,2,2,2,2,2,2,2,2,2,4),(21.7750720110093,21.8163550216855,
21.8962550811618,21.9731379982383,22.0526849055576,22.1315413187615,22.2076747786694,
22.2874065086602,22.3654017492244,22.4421433496673,22.5222824581149,22.5993806961363,
22.6782164764829,22.7484162072171,22.8170734816833),.UNSPECIFIED.);
#6264=B_SPLINE_CURVE_WITH_KNOTS('',3,(#258721,#258722,#258723,#258724,#258725,
#258726,#258727,#258728,#258729,#258730,#258731,#258732,#258733,#258734,
#258735,#258736,#258737,#258738,#258739,#258740,#258741,#258742,#258743,
#258744,#258745,#258746,#258747,#258748,#258749,#258750,#258751,#258752,
#258753,#258754,#258755,#258756,#258757,#258758,#258759,#258760,#258761,
#258762),.UNSPECIFIED.,.F.,.F.,(4,2,2,2,2,2,2,2,2,2,2,2,2,2,2,2,2,2,2,2,
4),(0.087011959968012,0.0937500000000087,0.101562500000008,0.109375000000007,
0.117187500000007,0.125000000000006,0.132812500000006,0.140625000000005,
0.156250000000003,0.164062500000003,0.171875000000002,0.175781250000002,
0.1796875,0.1875,0.203125,0.21875,0.2265625,0.234374999999998,0.242187499999997,
0.249999999999997,0.252776195245581),.UNSPECIFIED.);
#6265=B_SPLINE_CURVE_WITH_KNOTS('',3,(#258763,#258764,#258765,#258766),
 .UNSPECIFIED.,.F.,.F.,(4,4),(1.00000019201407E-6,0.00950822744729325),
 .UNSPECIFIED.);
#6266=B_SPLINE_CURVE_WITH_KNOTS('',3,(#259117,#259118,#259119,#259120,#259121,
#259122,#259123,#259124,#259125,#259126,#259127,#259128,#259129,#259130,
#259131,#259132,#259133,#259134,#259135,#259136,#259137,#259138),
 .UNSPECIFIED.,.F.,.F.,(4,2,2,2,2,2,2,2,2,2,4),(0.,0.0407060625625224,0.0695287735504407,
0.0890141598140192,0.0901238371088544,0.0912415302284534,0.0935209638282502,
0.0958498997334589,0.118224510663079,0.161531293622999,0.199451543342295),
 .UNSPECIFIED.);
#6267=B_SPLINE_CURVE_WITH_KNOTS('',3,(#259489,#259490,#259491,#259492,#259493,
#259494,#259495,#259496,#259497,#259498,#259499,#259500,#259501,#259502,
#259503,#259504,#259505,#259506,#259507,#259508,#259509,#259510,#259511,
#259512,#259513,#259514,#259515,#259516,#259517,#259518,#259519),
 .UNSPECIFIED.,.F.,.F.,(4,1,1,2,2,2,2,1,2,2,2,1,1,2,2,2,1,1,4),(0.578748721371666,
0.59375,0.6015625,0.609375,0.6171875,0.625,0.640625,0.65625,0.6640625,0.671875,
0.6796875,0.6875,0.703125,0.7109375,0.71875,0.7265625,0.734375,0.7421875,
0.747223819417002),.UNSPECIFIED.);
#6268=B_SPLINE_CURVE_WITH_KNOTS('',3,(#259520,#259521,#259522,#259523,#259524,
#259525,#259526,#259527,#259528,#259529),.UNSPECIFIED.,.F.,.F.,(4,2,2,2,
4),(1.0000844347723E-6,0.0627354187718775,0.114609893887245,0.175887326420162,
0.228995408318134),.UNSPECIFIED.);
#6269=B_SPLINE_CURVE_WITH_KNOTS('',3,(#259530,#259531,#259532,#259533,#259534,
#259535),.UNSPECIFIED.,.F.,.F.,(4,2,4),(0.,0.0474595169994712,0.0948138149984923),
 .UNSPECIFIED.);
#6270=B_SPLINE_CURVE_WITH_KNOTS('',3,(#259890,#259891,#259892,#259893,#259894,
#259895),.UNSPECIFIED.,.F.,.F.,(4,2,4),(1.03839813943911E-6,0.0231962182546486,
0.0535038699466261),.UNSPECIFIED.);
#6271=B_SPLINE_CURVE_WITH_KNOTS('',3,(#260127,#260128,#260129,#260130,#260131,
#260132,#260133,#260134,#260135,#260136,#260137,#260138,#260139,#260140,
#260141,#260142,#260143,#260144,#260145,#260146,#260147,#260148,#260149,
#260150,#260151,#260152,#260153,#260154,#260155,#260156,#260157,#260158,
#260159,#260160,#260161,#260162,#260163,#260164,#260165,#260166,#260167,
#260168,#260169,#260170,#260171,#260172,#260173,#260174,#260175,#260176,
#260177,#260178,#260179,#260180,#260181,#260182,#260183,#260184,#260185,
#260186,#260187,#260188,#260189,#260190,#260191,#260192,#260193,#260194,
#260195,#260196,#260197,#260198,#260199,#260200,#260201,#260202,#260203,
#260204,#260205,#260206,#260207,#260208,#260209,#260210,#260211,#260212,
#260213,#260214,#260215,#260216,#260217,#260218,#260219,#260220,#260221,
#260222,#260223,#260224,#260225,#260226,#260227,#260228,#260229,#260230,
#260231,#260232,#260233,#260234,#260235,#260236,#260237,#260238,#260239,
#260240),.UNSPECIFIED.,.F.,.F.,(4,2,2,2,2,2,2,2,2,2,2,2,2,2,2,2,2,2,2,2,
2,2,2,2,2,2,2,2,2,2,2,2,2,2,2,2,2,2,2,2,2,2,2,2,2,2,2,2,2,2,2,2,2,2,2,2,
4),(0.5,0.5078125,0.515625,0.53125,0.546875,0.5546875,0.5625,0.56640625,
0.5703125,0.578125,0.59375,0.6015625,0.609375,0.6171875,0.625,0.640625,
0.65625,0.6640625,0.671875,0.6796875,0.6875,0.703125,0.7109375,0.71875,
0.7265625,0.734375,0.7421875,0.75,0.7578125,0.765625,0.7734375,0.78125,
0.796875,0.8125,0.8203125,0.82421875,0.828125,0.8359375,0.84375,0.859375,
0.8671875,0.875,0.8828125,0.890625,0.8984375,0.90625,0.921875,0.9296875,
0.93359375,0.9375,0.9453125,0.953125,0.96875,0.984375,0.98828125,0.9921875,
1.),.UNSPECIFIED.);
#6272=B_SPLINE_CURVE_WITH_KNOTS('',3,(#260243,#260244,#260245,#260246,#260247,
#260248,#260249,#260250,#260251,#260252,#260253,#260254,#260255,#260256,
#260257,#260258,#260259,#260260,#260261,#260262,#260263,#260264,#260265,
#260266,#260267,#260268,#260269,#260270,#260271,#260272,#260273,#260274,
#260275,#260276),.UNSPECIFIED.,.F.,.F.,(4,3,3,3,3,3,3,3,3,3,3,4),(0.912988518764536,
0.921875,0.9296875,0.933593749999993,0.9375,0.945312519622535,0.953125,
0.96875,0.984375,0.988281249999999,0.9921875,1.),.UNSPECIFIED.);
#6273=B_SPLINE_CURVE_WITH_KNOTS('',3,(#260858,#260859,#260860,#260861,#260862,
#260863,#260864,#260865,#260866,#260867,#260868,#260869,#260870,#260871,
#260872,#260873,#260874,#260875,#260876,#260877,#260878,#260879),
 .UNSPECIFIED.,.F.,.F.,(4,2,2,2,2,2,2,2,2,2,4),(9.99997572121511E-7,0.0698852730817763,
0.132684785041426,0.167356797468204,0.173651470712272,0.174417517076423,
0.175184206163386,0.202554827937819,0.242523180847451,0.332118763813277,
0.335590797498318),.UNSPECIFIED.);
#6274=B_SPLINE_CURVE_WITH_KNOTS('',3,(#261434,#261435,#261436,#261437,#261438,
#261439,#261440,#261441,#261442,#261443,#261444,#261445,#261446,#261447),
 .UNSPECIFIED.,.F.,.F.,(4,2,2,2,2,2,4),(0.,0.0445367209372115,0.0852877077244626,
0.158230060144531,0.214173442984663,0.243463509225319,0.271164771186406),
 .UNSPECIFIED.);
#6275=B_SPLINE_CURVE_WITH_KNOTS('',3,(#262003,#262004,#262005,#262006,#262007,
#262008),.UNSPECIFIED.,.F.,.F.,(4,2,4),(1.00000011194028E-6,0.057300026554469,
0.11061517160577),.UNSPECIFIED.);
#6276=B_SPLINE_CURVE_WITH_KNOTS('',3,(#262009,#262010,#262011,#262012,#262013,
#262014,#262015,#262016,#262017,#262018,#262019,#262020,#262021,#262022,
#262023,#262024,#262025,#262026,#262027,#262028,#262029,#262030,#262031,
#262032,#262033,#262034,#262035,#262036),.UNSPECIFIED.,.F.,.F.,(4,2,2,2,
2,2,2,2,2,2,2,2,2,4),(1.00000011188427E-6,0.0832221019749246,0.173855357223232,
0.285282254196699,0.350899698372918,0.352769583200478,0.356527952715664,
0.364166049206607,0.380007478352134,0.401208730960821,0.52557169063662,
0.65515458631013,0.741483348095175,0.817065929829985),.UNSPECIFIED.);
#6277=B_SPLINE_CURVE_WITH_KNOTS('',3,(#262591,#262592,#262593,#262594,#262595,
#262596,#262597,#262598,#262599,#262600,#262601,#262602,#262603,#262604),
 .UNSPECIFIED.,.F.,.F.,(4,2,2,2,2,2,4),(0.,0.0475788933775829,0.0933534150829525,
0.157993829183029,0.243152490201361,0.307867924693099,0.372920208808051),
 .UNSPECIFIED.);
#6278=B_SPLINE_CURVE_WITH_KNOTS('',3,(#262607,#262608,#262609,#262610,#262611,
#262612,#262613,#262614),.UNSPECIFIED.,.F.,.F.,(4,2,2,4),(-0.102619939297055,
-0.0761483982920385,-0.0380341424800056,-1.07959900090539E-6),
 .UNSPECIFIED.);
#6279=B_SPLINE_CURVE_WITH_KNOTS('',3,(#262616,#262617,#262618,#262619,#262620,
#262621,#262622,#262623,#262624,#262625,#262626,#262627,#262628,#262629,
#262630,#262631,#262632,#262633,#262634,#262635,#262636,#262637,#262638,
#262639,#262640,#262641,#262642,#262643),.UNSPECIFIED.,.F.,.F.,(4,3,3,3,
3,3,3,3,3,4),(5.74832516592867E-8,0.100019677399835,0.215425485139183,0.32964672174934,
0.44270341057891,0.554615368045972,0.665402183763977,0.775083203425616,
0.88367751419001,0.99999990291026),.UNSPECIFIED.);
#6280=B_SPLINE_CURVE_WITH_KNOTS('',3,(#262644,#262645,#262646,#262647,#262648,
#262649,#262650,#262651,#262652,#262653,#262654,#262655,#262656,#262657),
 .UNSPECIFIED.,.F.,.F.,(4,2,2,2,2,2,4),(9.94972903414894E-7,0.0412659037688975,
0.0833228578270448,0.163008146711966,0.239131811149326,0.317616589247055,
0.349058981567732),.UNSPECIFIED.);
#6281=B_SPLINE_CURVE_WITH_KNOTS('',3,(#262659,#262660,#262661,#262662,#262663,
#262664,#262665,#262666,#262667,#262668,#262669,#262670,#262671,#262672,
#262673,#262674,#262675,#262676,#262677,#262678,#262679,#262680,#262681,
#262682,#262683,#262684,#262685,#262686,#262687,#262688,#262689,#262690,
#262691,#262692,#262693,#262694),.UNSPECIFIED.,.F.,.F.,(4,2,2,2,2,2,2,2,
2,2,2,2,2,2,2,2,2,4),(1.14417183100891,1.20287505491137,1.28033601080281,
1.35790068856985,1.4376299732138,1.51383997385877,1.59227414974943,1.67197682977705,
1.74848112168798,1.82796165173032,1.90608212512207,1.98350055193403,2.06399395345673,
2.14045668174614,2.21877507056622,2.29853639318799,2.37481934054265,2.40800177534909),
 .UNSPECIFIED.);
#6282=B_SPLINE_CURVE_WITH_KNOTS('',3,(#262695,#262696,#262697,#262698,#262699,
#262700,#262701,#262702,#262703,#262704,#262705,#262706,#262707,#262708,
#262709,#262710,#262711,#262712,#262713,#262714,#262715,#262716,#262717,
#262718,#262719,#262720,#262721,#262722,#262723,#262724,#262725,#262726,
#262727,#262728,#262729,#262730,#262731,#262732),.UNSPECIFIED.,.F.,.F.,
(4,2,2,2,2,2,2,2,2,2,2,2,2,2,2,2,2,2,4),(21.4212632201289,21.4213907374562,
21.4986585247935,21.5762333053668,21.6555728240449,21.7319353477459,21.8113971171506,
21.8896946695694,21.9656166308523,22.0450966603124,22.122529601833,22.1995293602665,
22.2790633827883,22.3555994802065,22.4351823980347,22.513666830597,22.5895218629738,
22.6689712527135,22.6805778338202),.UNSPECIFIED.);
#6283=B_SPLINE_CURVE_WITH_KNOTS('',3,(#263083,#263084,#263085,#263086,#263087,
#263088,#263089,#263090,#263091,#263092,#263093,#263094,#263095,#263096,
#263097,#263098,#263099,#263100,#263101,#263102,#263103,#263104,#263105,
#263106),.UNSPECIFIED.,.F.,.F.,(4,2,2,2,2,2,2,2,2,2,2,4),(-0.166809588212098,
-0.148843254996767,-0.125453562572242,-0.102931760276549,-0.102285580484546,
-0.101637831913971,-0.100331074316472,-0.099014130685927,-0.0963279314427469,
-0.0707416722561485,-0.0202992977557707,0.),.UNSPECIFIED.);
#6284=B_SPLINE_CURVE_WITH_KNOTS('',3,(#263460,#263461,#263462,#263463,#263464,
#263465,#263466,#263467,#263468,#263469,#263470,#263471,#263472,#263473,
#263474,#263475,#263476,#263477,#263478,#263479,#263480,#263481,#263482,
#263483,#263484,#263485,#263486,#263487,#263488,#263489,#263490),
 .UNSPECIFIED.,.F.,.F.,(4,2,2,2,2,1,2,2,2,2,2,1,2,2,2,1,4),(0.,0.00781249999998982,
0.0117187499999848,0.0156249999999797,0.0312499999999596,0.0468749999999394,
0.0624999999999192,0.0664062499999142,0.0703124999999091,0.0781249999998989,
0.0937499999998787,0.101562499999869,0.117187499999848,0.124999999999838,
0.132812499999828,0.140624999999818,0.153862286619807),.UNSPECIFIED.);
#6285=B_SPLINE_CURVE_WITH_KNOTS('',3,(#263491,#263492,#263493,#263494,#263495,
#263496,#263497,#263498,#263499,#263500),.UNSPECIFIED.,.F.,.F.,(4,2,2,2,
4),(-0.103716212520426,-0.0778648817986832,-0.0553429806067814,-0.0297234386418945,
-9.99979852549906E-7),.UNSPECIFIED.);
#6286=B_SPLINE_CURVE_WITH_KNOTS('',3,(#263855,#263856,#263857,#263858,#263859,
#263860,#263861,#263862,#263863,#263864,#263865,#263866,#263867,#263868,
#263869,#263870,#263871,#263872,#263873,#263874),.UNSPECIFIED.,.F.,.F.,
(4,2,2,2,2,2,2,2,2,4),(-0.286833505370044,-0.256117950648564,-0.206802564626801,
-0.16737932509528,-0.16372205833922,-0.160109502717139,-0.159218025502164,
-0.1276378189132,-0.0816572572313796,-9.901146603708E-7),.UNSPECIFIED.);
#6287=B_SPLINE_CURVE_WITH_KNOTS('',3,(#263875,#263876,#263877,#263878,#263879,
#263880,#263881,#263882,#263883,#263884,#263885,#263886,#263887,#263888,
#263889,#263890,#263891,#263892,#263893,#263894,#263895,#263896,#263897),
 .UNSPECIFIED.,.F.,.F.,(4,1,1,2,2,2,2,1,2,2,1,1,1,1,4),(0.805330004638041,
0.8125,0.828125,0.8359375,0.84375,0.8515625,0.859375,0.875,0.890625,0.8984375,
0.90625,0.9140625,0.921875,0.9375,0.947453465595126),.UNSPECIFIED.);
#6288=B_SPLINE_CURVE_WITH_KNOTS('',3,(#263898,#263899,#263900,#263901,#263902,
#263903,#263904,#263905,#263906,#263907,#263908,#263909,#263910,#263911,
#263912,#263913,#263914,#263915,#263916,#263917,#263918,#263919,#263920,
#263921,#263922,#263923,#263924,#263925),.UNSPECIFIED.,.F.,.F.,(4,2,2,2,
2,2,2,2,2,2,2,2,2,4),(-0.57555153577955,-0.481403152518014,-0.391518410394815,
-0.304012543115108,-0.248875154314629,-0.20331457493217,-0.193640973353304,
-0.192462380537007,-0.191871804250229,-0.172674099621673,-0.162424596047124,
-0.0875987710768544,-0.0434789311703104,-1.00000008174117E-6),
 .UNSPECIFIED.);
#6289=B_SPLINE_CURVE_WITH_KNOTS('',3,(#264377,#264378,#264379,#264380,#264381,
#264382,#264383,#264384,#264385,#264386,#264387,#264388,#264389,#264390,
#264391,#264392,#264393,#264394,#264395,#264396),.UNSPECIFIED.,.F.,.F.,
(4,2,2,2,2,2,2,2,2,4),(-0.737111713840115,-0.641804134708795,-0.547885152214752,
-0.45702238184443,-0.368891693747479,-0.280602623811107,-0.193827199088049,
-0.105057099212705,-0.0527008074164365,0.),.UNSPECIFIED.);
#6290=B_SPLINE_CURVE_WITH_KNOTS('',3,(#264400,#264401,#264402,#264403,#264404,
#264405,#264406,#264407,#264408,#264409,#264410,#264411,#264412,#264413),
 .UNSPECIFIED.,.F.,.F.,(4,2,2,2,2,2,4),(0.,0.0475788933774156,0.0933534150825965,
0.157993829182779,0.243152490201106,0.307867924695236,0.372920208812621),
 .UNSPECIFIED.);
#6291=B_SPLINE_CURVE_WITH_KNOTS('',3,(#264414,#264415,#264416,#264417,#264418,
#264419,#264420,#264421,#264422,#264423,#264424,#264425,#264426,#264427),
 .UNSPECIFIED.,.F.,.F.,(4,2,2,2,2,2,4),(0.,0.0445367209371377,0.0852877077243032,
0.158230060144259,0.214173442984407,0.243463509225075,0.271164771186191),
 .UNSPECIFIED.);
#6292=B_SPLINE_CURVE_WITH_KNOTS('',3,(#265563,#265564,#265565,#265566,#265567,
#265568),.UNSPECIFIED.,.F.,.F.,(4,2,4),(-0.0951503607589064,-0.0475879046034892,
-1.01889197450439E-6),.UNSPECIFIED.);
#6293=B_SPLINE_CURVE_WITH_KNOTS('',3,(#266123,#266124,#266125,#266126,#266127,
#266128,#266129,#266130,#266131,#266132),.UNSPECIFIED.,.F.,.F.,(4,2,2,2,
4),(-0.222459738018975,-0.168926717083018,-0.11127636113476,-0.0584376614951339,
-9.93245333813508E-7),.UNSPECIFIED.);
#6294=B_SPLINE_CURVE_WITH_KNOTS('',3,(#266687,#266688,#266689,#266690,#266691,
#266692),.UNSPECIFIED.,.F.,.F.,(4,2,4),(-0.0369392618720219,-0.0184680082272592,
0.),.UNSPECIFIED.);
#6295=B_SPLINE_CURVE_WITH_KNOTS('',3,(#266695,#266696,#266697,#266698,#266699,
#266700,#266701,#266702,#266703,#266704),.UNSPECIFIED.,.F.,.F.,(4,2,2,2,
4),(2.44533830141617E-8,0.0529928666678925,0.105880759966484,0.158840335145018,
0.211973983367163),.UNSPECIFIED.);
#6296=B_SPLINE_CURVE_WITH_KNOTS('',3,(#266706,#266707,#266708,#266709,#266710,
#266711,#266712,#266713,#266714,#266715,#266716,#266717,#266718,#266719,
#266720,#266721,#266722,#266723,#266724,#266725,#266726,#266727,#266728,
#266729,#266730,#266731,#266732,#266733,#266734,#266735,#266736,#266737,
#266738,#266739,#266740,#266741,#266742,#266743,#266744,#266745,#266746,
#266747,#266748,#266749,#266750,#266751,#266752,#266753,#266754,#266755,
#266756,#266757,#266758,#266759,#266760,#266761,#266762,#266763,#266764,
#266765,#266766,#266767,#266768,#266769,#266770,#266771,#266772,#266773,
#266774,#266775,#266776,#266777,#266778,#266779,#266780,#266781,#266782,
#266783,#266784,#266785,#266786,#266787,#266788,#266789,#266790,#266791,
#266792,#266793,#266794,#266795,#266796,#266797,#266798,#266799,#266800,
#266801,#266802,#266803,#266804,#266805,#266806,#266807,#266808,#266809,
#266810,#266811,#266812,#266813,#266814,#266815,#266816,#266817),
 .UNSPECIFIED.,.F.,.F.,(4,2,2,2,2,2,2,2,2,2,2,2,2,2,2,2,2,2,2,2,2,2,2,2,
2,2,2,2,2,2,2,2,2,2,2,2,2,2,2,2,2,2,2,2,2,2,2,2,2,2,2,2,2,2,2,4),(0.,0.0078125,
0.015625,0.03125,0.046875,0.0625,0.078125,0.0859375,0.09375,0.1015625,0.109375,
0.1171875,0.125,0.140625,0.1484375,0.15625,0.1640625,0.171875,0.1875,0.1953125,
0.203125,0.2109375,0.21875,0.2265625,0.234375,0.2421875,0.25,0.2578125,
0.265625,0.28125,0.296875,0.3046875,0.30859375,0.3125,0.3203125,0.328125,
0.34375,0.3515625,0.359375,0.3671875,0.375,0.3828125,0.390625,0.3984375,
0.40625,0.4140625,0.421875,0.4296875,0.4375,0.453125,0.4609375,0.46875,
0.4765625,0.484375,0.4921875,0.5),.UNSPECIFIED.);
#6297=B_SPLINE_CURVE_WITH_KNOTS('',3,(#266818,#266819,#266820,#266821,#266822,
#266823,#266824,#266825,#266826,#266827,#266828,#266829,#266830,#266831,
#266832,#266833,#266834,#266835,#266836,#266837),.UNSPECIFIED.,.F.,.F.,
(4,2,2,2,2,2,2,2,2,4),(-0.737771146043194,-0.6422087309344,-0.548787649635823,
-0.457895273356038,-0.369025600510949,-0.28011278264437,-0.191911802745247,
-0.102744293435205,-0.0513522263156295,0.),.UNSPECIFIED.);
#6298=B_SPLINE_CURVE_WITH_KNOTS('',3,(#266838,#266839,#266840,#266841,#266842,
#266843,#266844,#266845,#266846,#266847,#266848,#266849,#266850,#266851,
#266852,#266853,#266854,#266855,#266856,#266857),.UNSPECIFIED.,.F.,.F.,
(4,2,2,2,2,2,2,2,2,4),(-0.738072505252876,-0.643967634208436,-0.550034248922507,
-0.458427614573009,-0.369107138036355,-0.279727670045679,-0.191507430126554,
-0.102692762879055,-0.0513175343902644,0.),.UNSPECIFIED.);
#6299=B_SPLINE_CURVE_WITH_KNOTS('',3,(#266858,#266859,#266860,#266861,#266862,
#266863,#266864,#266865,#266866,#266867,#266868,#266869,#266870,#266871,
#266872,#266873,#266874,#266875,#266876,#266877,#266878,#266879,#266880,
#266881,#266882,#266883,#266884,#266885,#266886,#266887,#266888,#266889,
#266890,#266891,#266892,#266893,#266894,#266895,#266896,#266897,#266898,
#266899,#266900,#266901,#266902,#266903,#266904,#266905,#266906,#266907,
#266908,#266909,#266910,#266911,#266912,#266913,#266914,#266915,#266916,
#266917,#266918,#266919,#266920,#266921,#266922,#266923,#266924,#266925,
#266926,#266927,#266928,#266929,#266930,#266931,#266932,#266933,#266934,
#266935,#266936,#266937,#266938,#266939,#266940,#266941,#266942,#266943,
#266944,#266945,#266946,#266947,#266948,#266949,#266950,#266951,#266952,
#266953,#266954,#266955,#266956,#266957,#266958,#266959,#266960,#266961,
#266962,#266963,#266964,#266965,#266966,#266967,#266968,#266969),
 .UNSPECIFIED.,.F.,.F.,(4,2,2,2,2,2,2,2,2,2,2,2,2,2,2,2,2,2,2,2,2,2,2,2,
2,2,2,2,2,2,2,2,2,2,2,2,2,2,2,2,2,2,2,2,2,2,2,2,2,2,2,2,2,2,2,4),(0.,0.0078125,
0.015625,0.03125,0.0390625,0.046875,0.0546875,0.0625,0.078125,0.0859375,
0.09375,0.1015625,0.10546875,0.109375,0.125,0.140625,0.1484375,0.15625,
0.1640625,0.171875,0.1875,0.203125,0.20703125,0.2109375,0.21875,0.2265625,
0.234375,0.2421875,0.25,0.2578125,0.265625,0.2734375,0.28125,0.296875,0.3125,
0.328125,0.34375,0.359375,0.36328125,0.3671875,0.375,0.3828125,0.390625,
0.3984375,0.40625,0.4140625,0.421875,0.4296875,0.4375,0.453125,0.4609375,
0.46875,0.4765625,0.484375,0.4921875,0.5),.UNSPECIFIED.);
#6300=B_SPLINE_CURVE_WITH_KNOTS('',3,(#267419,#267420,#267421,#267422,#267423,
#267424,#267425,#267426,#267427,#267428,#267429,#267430,#267431,#267432,
#267433,#267434,#267435,#267436,#267437,#267438,#267439,#267440,#267441,
#267442,#267443,#267444,#267445,#267446,#267447,#267448,#267449,#267450,
#267451,#267452,#267453,#267454,#267455,#267456,#267457,#267458,#267459,
#267460,#267461,#267462,#267463,#267464,#267465,#267466,#267467,#267468,
#267469,#267470,#267471,#267472,#267473,#267474,#267475,#267476,#267477,
#267478,#267479),.UNSPECIFIED.,.F.,.F.,(4,3,3,3,3,3,3,3,3,3,3,3,3,3,3,3,
3,3,3,3,4),(0.31954923250906,0.3203125,0.328125,0.3359375,0.34375,0.359375,
0.375,0.3828125,0.390625,0.3984375,0.40625,0.421875,0.4296875,0.43359375,
0.4375,0.4453125,0.453125,0.46875,0.484375,0.4921875,0.5),.UNSPECIFIED.);
#6301=B_SPLINE_CURVE_WITH_KNOTS('',3,(#268404,#268405,#268406,#268407,#268408,
#268409,#268410,#268411,#268412,#268413,#268414,#268415,#268416,#268417,
#268418,#268419,#268420,#268421,#268422,#268423),.UNSPECIFIED.,.F.,.F.,
(4,1,2,2,2,1,1,1,2,2,2,4),(0.399104234309458,0.406249999999556,0.414062499999593,
0.42187499999963,0.429687499999667,0.437499999999704,0.453124999999778,
0.460937499999815,0.468749999999852,0.476562499999889,0.484374999999926,
0.5),.UNSPECIFIED.);
#6302=B_SPLINE_CURVE_WITH_KNOTS('',3,(#268424,#268425,#268426,#268427,#268428,
#268429,#268430,#268431,#268432,#268433,#268434,#268435,#268436,#268437,
#268438,#268439),.UNSPECIFIED.,.F.,.F.,(4,1,1,2,1,1,1,1,2,2,4),(0.,0.0156250000000065,
0.031250000000013,0.0468750000000195,0.062500000000026,0.0781250000000325,
0.0859375000000357,0.0937500000000389,0.101562500000042,0.109375000000045,
0.12436089589415),.UNSPECIFIED.);
#6303=B_SPLINE_CURVE_WITH_KNOTS('',3,(#269365,#269366,#269367,#269368,#269369,
#269370,#269371,#269372,#269373,#269374,#269375,#269376,#269377,#269378,
#269379,#269380,#269381,#269382,#269383,#269384,#269385,#269386,#269387,
#269388,#269389,#269390,#269391,#269392,#269393,#269394,#269395),
 .UNSPECIFIED.,.F.,.F.,(4,3,3,3,3,3,3,3,3,3,4),(0.414335116362591,0.421874999999847,
0.429687494127349,0.437499994567745,0.453124999999908,0.460937499999924,
0.468749999999939,0.476562499999954,0.484374999999969,0.492187500000011,
0.5),.UNSPECIFIED.);
#6304=B_SPLINE_CURVE_WITH_KNOTS('',3,(#269396,#269397,#269398,#269399,#269400,
#269401,#269402,#269403,#269404,#269405,#269406,#269407,#269408,#269409,
#269410,#269411,#269412,#269413,#269414,#269415,#269416,#269417,#269418,
#269419,#269420,#269421,#269422,#269423,#269424,#269425,#269426,#269427,
#269428,#269429,#269430,#269431,#269432,#269433,#269434,#269435,#269436,
#269437,#269438,#269439,#269440,#269441),.UNSPECIFIED.,.F.,.F.,(4,3,3,3,
3,3,3,3,3,3,3,3,3,3,3,4),(0.,0.00781249973784698,0.0156249998843613,0.0312499999999252,
0.0390624999999065,0.0468749999998878,0.0546874999998691,0.0624999999998504,
0.0781249961571057,0.0859374423201947,0.0937499720252506,0.101562499999757,
0.105468749999748,0.109374999999738,0.124999992316058,0.139651873775064),
 .UNSPECIFIED.);
#6305=B_SPLINE_CURVE_WITH_KNOTS('',3,(#270291,#270292,#270293,#270294,#270295,
#270296,#270297,#270298,#270299,#270300,#270301,#270302,#270303,#270304,
#270305,#270306,#270307,#270308,#270309,#270310,#270311,#270312,#270313,
#270314,#270315,#270316,#270317,#270318,#270319,#270320,#270321,#270322,
#270323,#270324,#270325,#270326,#270327,#270328,#270329,#270330,#270331,
#270332,#270333,#270334,#270335,#270336,#270337,#270338,#270339,#270340,
#270341,#270342,#270343,#270344,#270345,#270346,#270347,#270348,#270349,
#270350,#270351,#270352,#270353,#270354,#270355,#270356,#270357),
 .UNSPECIFIED.,.F.,.F.,(4,3,3,3,3,3,3,3,3,3,3,3,3,3,3,3,3,3,3,3,3,3,4),
(0.304282083218851,0.3125,0.3203125,0.32421875,0.328125,0.3359375,0.34374999988077,
0.359375,0.3671875,0.375,0.3828125,0.390625,0.39843756172038,0.40625,0.421875,
0.4296875,0.4375,0.4453125,0.453125,0.46875,0.484375,0.4921875,0.5),
 .UNSPECIFIED.);
#6306=B_SPLINE_CURVE_WITH_KNOTS('',3,(#271237,#271238,#271239,#271240,#271241,
#271242,#271243,#271244),.UNSPECIFIED.,.F.,.F.,(4,2,2,4),(-8.98049293427854,
-8.97889171867458,-8.34884827602697,-8.12983481855878),.UNSPECIFIED.);
#6307=B_SPLINE_CURVE_WITH_KNOTS('',3,(#271248,#271249,#271250,#271251,#271252,
#271253),.UNSPECIFIED.,.F.,.F.,(4,2,4),(-2.68771546706156,-2.29799156778152,
-1.97285776109994),.UNSPECIFIED.);
#6308=B_SPLINE_CURVE_WITH_KNOTS('',3,(#271258,#271259,#271260,#271261,#271262,
#271263),.UNSPECIFIED.,.F.,.F.,(4,2,4),(0.518273427329016,0.647448708132802,
0.677306880099543),.UNSPECIFIED.);
#6309=B_SPLINE_CURVE_WITH_KNOTS('',3,(#271267,#271268,#271269,#271270),
 .UNSPECIFIED.,.F.,.F.,(4,4),(1.16920248436213,1.3284621703947),
 .UNSPECIFIED.);
#6310=B_SPLINE_CURVE_WITH_KNOTS('',3,(#271274,#271275,#271276,#271277,#271278,
#271279),.UNSPECIFIED.,.F.,.F.,(4,2,4),(2.36444145730686,2.40335316097516,
2.52343865872206),.UNSPECIFIED.);
#6311=B_SPLINE_CURVE_WITH_KNOTS('',3,(#271283,#271284,#271285,#271286,#271287,
#271288),.UNSPECIFIED.,.F.,.F.,(4,2,4),(3.01719559991105,3.07732160469005,
3.17624638273508),.UNSPECIFIED.);
#6312=B_SPLINE_CURVE_WITH_KNOTS('',3,(#271295,#271296,#271297,#271298,#271299,
#271300),.UNSPECIFIED.,.F.,.F.,(4,2,4),(0.51827342732949,0.647448708132718,
0.677306880099455),.UNSPECIFIED.);
#6313=B_SPLINE_CURVE_WITH_KNOTS('',3,(#271304,#271305,#271306,#271307),
 .UNSPECIFIED.,.F.,.F.,(4,4),(1.16920248460095,1.3284621706712),
 .UNSPECIFIED.);
#6314=B_SPLINE_CURVE_WITH_KNOTS('',3,(#271311,#271312,#271313,#271314,#271315,
#271316),.UNSPECIFIED.,.F.,.F.,(4,2,4),(2.36444145785531,2.40335316153482,
2.5234386593167),.UNSPECIFIED.);
#6315=B_SPLINE_CURVE_WITH_KNOTS('',3,(#271319,#271320,#271321,#271322,#271323,
#271324),.UNSPECIFIED.,.F.,.F.,(4,2,4),(3.01719559991067,3.07732160468965,
3.17624638273467),.UNSPECIFIED.);
#6316=B_SPLINE_CURVE_WITH_KNOTS('',3,(#271330,#271331,#271332,#271333,#271334,
#271335),.UNSPECIFIED.,.F.,.F.,(4,2,4),(0.51827342732973,0.647448708133012,
0.677306880099766),.UNSPECIFIED.);
#6317=B_SPLINE_CURVE_WITH_KNOTS('',3,(#271339,#271340,#271341,#271342),
 .UNSPECIFIED.,.F.,.F.,(4,4),(1.16920248436227,1.32846217039502),
 .UNSPECIFIED.);
#6318=B_SPLINE_CURVE_WITH_KNOTS('',3,(#271346,#271347,#271348,#271349,#271350,
#271351),.UNSPECIFIED.,.F.,.F.,(4,2,4),(2.36444145730766,2.40335316097597,
2.523438658723),.UNSPECIFIED.);
#6319=B_SPLINE_CURVE_WITH_KNOTS('',3,(#271354,#271355,#271356,#271357,#271358,
#271359),.UNSPECIFIED.,.F.,.F.,(4,2,4),(3.0171955999124,3.07732160469143,
3.1762463827365),.UNSPECIFIED.);
#6320=B_SPLINE_CURVE_WITH_KNOTS('',3,(#271363,#271364,#271365,#271366,#271367,
#271368),.UNSPECIFIED.,.F.,.F.,(4,2,4),(3.01719559991218,3.07732160469121,
3.17624638273563),.UNSPECIFIED.);
#6321=B_SPLINE_CURVE_WITH_KNOTS('',3,(#271372,#271373,#271374,#271375,#271376,
#271377),.UNSPECIFIED.,.F.,.F.,(4,2,4),(0.518273427329665,0.647448708132928,
0.677306880099671),.UNSPECIFIED.);
#6322=B_SPLINE_CURVE_WITH_KNOTS('',3,(#271381,#271382,#271383,#271384),
 .UNSPECIFIED.,.F.,.F.,(4,4),(1.1692024843613,1.32846217039385),
 .UNSPECIFIED.);
#6323=B_SPLINE_CURVE_WITH_KNOTS('',3,(#271388,#271389,#271390,#271391,#271392,
#271393),.UNSPECIFIED.,.F.,.F.,(4,2,4),(2.36444145730499,2.40335316097287,
2.52343865871962),.UNSPECIFIED.);
#6324=B_SPLINE_CURVE_WITH_KNOTS('',3,(#271400,#271401,#271402,#271403,#271404,
#271405),.UNSPECIFIED.,.F.,.F.,(4,2,4),(0.518273427329571,0.647448708132802,
0.677306880099541),.UNSPECIFIED.);
#6325=B_SPLINE_CURVE_WITH_KNOTS('',3,(#271409,#271410,#271411,#271412),
 .UNSPECIFIED.,.F.,.F.,(4,4),(1.16920248412223,1.32846217011725),
 .UNSPECIFIED.);
#6326=B_SPLINE_CURVE_WITH_KNOTS('',3,(#271416,#271417,#271418,#271419,#271420,
#271421),.UNSPECIFIED.,.F.,.F.,(4,2,4),(2.3644414567562,2.40335316041326,
2.52343865812509),.UNSPECIFIED.);
#6327=B_SPLINE_CURVE_WITH_KNOTS('',3,(#271424,#271425,#271426,#271427,#271428,
#271429),.UNSPECIFIED.,.F.,.F.,(4,2,4),(3.01719559991075,3.07732160468976,
3.17624638273476),.UNSPECIFIED.);
#6328=B_SPLINE_CURVE_WITH_KNOTS('',3,(#271435,#271436,#271437,#271438,#271439,
#271440),.UNSPECIFIED.,.F.,.F.,(4,2,4),(0.518273427329574,0.647448708132822,
0.677306880099564),.UNSPECIFIED.);
#6329=B_SPLINE_CURVE_WITH_KNOTS('',3,(#271444,#271445,#271446,#271447),
 .UNSPECIFIED.,.F.,.F.,(4,4),(1.16920248436231,1.32846217039508),
 .UNSPECIFIED.);
#6330=B_SPLINE_CURVE_WITH_KNOTS('',3,(#271451,#271452,#271453,#271454,#271455,
#271456),.UNSPECIFIED.,.F.,.F.,(4,2,4),(2.3644414573074,2.40335316097572,
2.52343865872264),.UNSPECIFIED.);
#6331=B_SPLINE_CURVE_WITH_KNOTS('',3,(#271459,#271460,#271461,#271462,#271463,
#271464),.UNSPECIFIED.,.F.,.F.,(4,2,4),(3.01719559991156,3.07732160469059,
3.17624638273566),.UNSPECIFIED.);
#6332=B_SPLINE_CURVE_WITH_KNOTS('',3,(#271468,#271469,#271470,#271471,#271472,
#271473),.UNSPECIFIED.,.F.,.F.,(4,2,4),(-2.68771546706066,-2.29799156778083,
-1.9728577610994),.UNSPECIFIED.);
#6333=B_SPLINE_CURVE_WITH_KNOTS('',3,(#271477,#271478,#271479,#271480,#271481,
#271482,#271483,#271484),.UNSPECIFIED.,.F.,.F.,(4,2,2,4),(-8.98049293427925,
-8.97889171867529,-8.34884827602781,-8.12983481855968),.UNSPECIFIED.);
#6334=B_SPLINE_CURVE_WITH_KNOTS('',3,(#271552,#271553,#271554,#271555,#271556,
#271557,#271558,#271559),.UNSPECIFIED.,.F.,.F.,(4,2,2,4),(-8.98049293427854,
-8.97889171867458,-8.34884827602725,-8.12983481855919),.UNSPECIFIED.);
#6335=B_SPLINE_CURVE_WITH_KNOTS('',3,(#271563,#271564,#271565,#271566,#271567,
#271568),.UNSPECIFIED.,.F.,.F.,(4,2,4),(-2.68771546706143,-2.29799156778143,
-1.97285776109989),.UNSPECIFIED.);
#6336=B_SPLINE_CURVE_WITH_KNOTS('',3,(#271569,#271570,#271571,#271572,#271573,
#271574),.UNSPECIFIED.,.F.,.F.,(4,2,4),(0.51827342732961,0.64744870813287,
0.677306880099612),.UNSPECIFIED.);
#6337=B_SPLINE_CURVE_WITH_KNOTS('',3,(#271575,#271576,#271577,#271578,#271579,
#271580),.UNSPECIFIED.,.F.,.F.,(4,2,4),(3.0171955999114,3.07732160469042,
3.17624638273548),.UNSPECIFIED.);
#6338=B_SPLINE_CURVE_WITH_KNOTS('',3,(#271583,#271584,#271585,#271586,#271587,
#271588),.UNSPECIFIED.,.F.,.F.,(4,2,4),(0.518273427329597,0.647448708132832,
0.677306880099573),.UNSPECIFIED.);
#6339=B_SPLINE_CURVE_WITH_KNOTS('',3,(#271590,#271591,#271592,#271593,#271594,
#271595),.UNSPECIFIED.,.F.,.F.,(4,2,4),(3.01719559990933,3.07732160468829,
3.17624638273323),.UNSPECIFIED.);
#6340=B_SPLINE_CURVE_WITH_KNOTS('',3,(#271597,#271598,#271599,#271600,#271601,
#271602,#271603,#271604),.UNSPECIFIED.,.F.,.F.,(4,2,2,4),(-8.98049293427795,
-8.97889171867398,-8.3488482760265,-8.12983481855838),.UNSPECIFIED.);
#6341=B_SPLINE_CURVE_WITH_KNOTS('',3,(#271607,#271608,#271609,#271610,#271611,
#271612),.UNSPECIFIED.,.F.,.F.,(4,2,4),(-2.6877154670615,-2.29799156778146,
-1.97285776109988),.UNSPECIFIED.);
#6342=B_SPLINE_CURVE_WITH_KNOTS('',3,(#271615,#271616,#271617,#271618,#271619,
#271620),.UNSPECIFIED.,.F.,.F.,(4,2,4),(0.518273427329312,0.647448708132468,
0.677306880099178),.UNSPECIFIED.);
#6343=B_SPLINE_CURVE_WITH_KNOTS('',3,(#271622,#271623,#271624,#271625,#271626,
#271627),.UNSPECIFIED.,.F.,.F.,(4,2,4),(3.0171955999108,3.0773216046898,
3.1762463827348),.UNSPECIFIED.);
#6344=B_SPLINE_CURVE_WITH_KNOTS('',3,(#271629,#271630,#271631,#271632,#271633,
#271634,#271635,#271636),.UNSPECIFIED.,.F.,.F.,(4,2,2,4),(-8.98049293427752,
-8.97889171867356,-8.34884827602617,-8.12983481855807),.UNSPECIFIED.);
#6345=B_SPLINE_CURVE_WITH_KNOTS('',3,(#271639,#271640,#271641,#271642,#271643,
#271644),.UNSPECIFIED.,.F.,.F.,(4,2,4),(-2.68771546706155,-2.29799156778148,
-1.9728577610999),.UNSPECIFIED.);
#6346=B_SPLINE_CURVE_WITH_KNOTS('',3,(#271647,#271648,#271649,#271650,#271651,
#271652),.UNSPECIFIED.,.F.,.F.,(4,2,4),(0.518273427329541,0.647448708132767,
0.6773068800995),.UNSPECIFIED.);
#6347=B_SPLINE_CURVE_WITH_KNOTS('',3,(#271654,#271655,#271656,#271657,#271658,
#271659),.UNSPECIFIED.,.F.,.F.,(4,2,4),(3.01719559991074,3.07732160468976,
3.17624638273482),.UNSPECIFIED.);
#6348=B_SPLINE_CURVE_WITH_KNOTS('',3,(#271661,#271662,#271663,#271664,#271665,
#271666,#271667,#271668),.UNSPECIFIED.,.F.,.F.,(4,2,2,4),(-8.98049293427772,
-8.97889171867376,-8.34884827602598,-8.12983481855773),.UNSPECIFIED.);
#6349=B_SPLINE_CURVE_WITH_KNOTS('',3,(#271671,#271672,#271673,#271674,#271675,
#271676),.UNSPECIFIED.,.F.,.F.,(4,2,4),(-2.68771546706066,-2.29799156778086,
-1.97285776109946),.UNSPECIFIED.);
#6350=B_SPLINE_CURVE_WITH_KNOTS('',3,(#271681,#271682,#271683,#271684,#271685,
#271686),.UNSPECIFIED.,.F.,.F.,(4,2,4),(-2.68771546706142,-2.29799156778141,
-1.97285776109986),.UNSPECIFIED.);
#6351=B_SPLINE_CURVE_WITH_KNOTS('',3,(#271687,#271688,#271689,#271690,#271691,
#271692),.UNSPECIFIED.,.F.,.F.,(4,2,4),(0.518273427329233,0.647448708132411,
0.677306880099119),.UNSPECIFIED.);
#6352=B_SPLINE_CURVE_WITH_KNOTS('',3,(#271693,#271694,#271695,#271696,#271697,
#271698),.UNSPECIFIED.,.F.,.F.,(4,2,4),(3.01719559991029,3.0773216046893,
3.17624638273431),.UNSPECIFIED.);
#6353=B_SPLINE_CURVE_WITH_KNOTS('',3,(#271701,#271702,#271703,#271704,#271705,
#271706),.UNSPECIFIED.,.F.,.F.,(4,2,4),(0.518273427329369,0.647448708132555,
0.677306880099271),.UNSPECIFIED.);
#6354=B_SPLINE_CURVE_WITH_KNOTS('',3,(#271708,#271709,#271710,#271711,#271712,
#271713),.UNSPECIFIED.,.F.,.F.,(4,2,4),(3.01719559991216,3.07732160469119,
3.17624638273627),.UNSPECIFIED.);
#6355=B_SPLINE_CURVE_WITH_KNOTS('',3,(#271715,#271716,#271717,#271718,#271719,
#271720,#271721,#271722),.UNSPECIFIED.,.F.,.F.,(4,2,2,4),(-8.98049293427722,
-8.97889171867326,-8.34884827602583,-8.1298348185577),.UNSPECIFIED.);
#6356=B_SPLINE_CURVE_WITH_KNOTS('',3,(#271725,#271726,#271727,#271728,#271729,
#271730),.UNSPECIFIED.,.F.,.F.,(4,2,4),(-2.68771546706111,-2.29799156778117,
-1.97285776109968),.UNSPECIFIED.);
#6357=B_SPLINE_CURVE_WITH_KNOTS('',3,(#271734,#271735,#271736,#271737,#271738,
#271739,#271740,#271741),.UNSPECIFIED.,.F.,.F.,(4,2,2,4),(-8.98049293427961,
-8.97889171867565,-8.34884827602804,-8.12983481855986),.UNSPECIFIED.);
#6358=B_SPLINE_CURVE_WITH_KNOTS('',3,(#271745,#271746,#271747,#271748,#271749,
#271750),.UNSPECIFIED.,.F.,.F.,(4,2,4),(-2.68771546706186,-2.29799156778171,
-1.97285776110007),.UNSPECIFIED.);
#6359=B_SPLINE_CURVE_WITH_KNOTS('',3,(#271751,#271752,#271753,#271754,#271755,
#271756),.UNSPECIFIED.,.F.,.F.,(4,2,4),(0.51827342732934,0.647448708132526,
0.677306880099254),.UNSPECIFIED.);
#6360=B_SPLINE_CURVE_WITH_KNOTS('',3,(#271757,#271758,#271759,#271760,#271761,
#271762),.UNSPECIFIED.,.F.,.F.,(4,2,4),(3.01719559990916,3.07732160468812,
3.17624638273306),.UNSPECIFIED.);
#6361=B_SPLINE_CURVE_WITH_KNOTS('',3,(#271765,#271766,#271767,#271768,#271769,
#271770,#271771,#271772),.UNSPECIFIED.,.F.,.F.,(4,2,2,4),(-8.98049293427778,
-8.97889171867381,-8.34884827602637,-8.12983481855824),.UNSPECIFIED.);
#6362=B_SPLINE_CURVE_WITH_KNOTS('',3,(#271775,#271776,#271777,#271778,#271779,
#271780),.UNSPECIFIED.,.F.,.F.,(4,2,4),(-2.68771546706139,-2.29799156778137,
-1.97285776109982),.UNSPECIFIED.);
#6363=B_SPLINE_CURVE_WITH_KNOTS('',3,(#271783,#271784,#271785,#271786,#271787,
#271788),.UNSPECIFIED.,.F.,.F.,(4,2,4),(3.01719559990971,3.07732160468868,
3.17624638273366),.UNSPECIFIED.);
#6364=B_SPLINE_CURVE_WITH_KNOTS('',3,(#271790,#271791,#271792,#271793,#271794,
#271795,#271796,#271797),.UNSPECIFIED.,.F.,.F.,(4,2,2,4),(-8.98049293427817,
-8.97889171867421,-8.34884827602685,-8.12983481855876),.UNSPECIFIED.);
#6365=B_SPLINE_CURVE_WITH_KNOTS('',3,(#271800,#271801,#271802,#271803,#271804,
#271805),.UNSPECIFIED.,.F.,.F.,(4,2,4),(-2.68771546706148,-2.29799156778145,
-1.97285776109989),.UNSPECIFIED.);
#6366=B_SPLINE_CURVE_WITH_KNOTS('',3,(#271808,#271809,#271810,#271811,#271812,
#271813,#271814,#271815),.UNSPECIFIED.,.F.,.F.,(4,2,2,4),(-8.98049293427992,
-8.97889171867596,-8.34884827602816,-8.12983481855992),.UNSPECIFIED.);
#6367=B_SPLINE_CURVE_WITH_KNOTS('',3,(#271818,#271819,#271820,#271821,#271822,
#271823),.UNSPECIFIED.,.F.,.F.,(4,2,4),(-2.68771546706129,-2.29799156778129,
-1.97285776109976),.UNSPECIFIED.);
#6368=B_SPLINE_CURVE_WITH_KNOTS('',3,(#271826,#271827,#271828,#271829,#271830,
#271831,#271832,#271833),.UNSPECIFIED.,.F.,.F.,(4,2,2,4),(-8.98049293428024,
-8.97889171867627,-8.34884827602869,-8.12983481856052),.UNSPECIFIED.);
#6369=B_SPLINE_CURVE_WITH_KNOTS('',3,(#271836,#271837,#271838,#271839,#271840,
#271841),.UNSPECIFIED.,.F.,.F.,(4,2,4),(-2.68771546706172,-2.29799156778164,
-1.97285776110006),.UNSPECIFIED.);
#6370=B_SPLINE_CURVE_WITH_KNOTS('',3,(#271844,#271845,#271846,#271847,#271848,
#271849,#271850,#271851),.UNSPECIFIED.,.F.,.F.,(4,2,2,4),(-8.98049293427857,
-8.97889171867461,-8.34884827602675,-8.12983481855846),.UNSPECIFIED.);
#6371=B_SPLINE_CURVE_WITH_KNOTS('',3,(#271854,#271855,#271856,#271857,#271858,
#271859),.UNSPECIFIED.,.F.,.F.,(4,2,4),(-2.68771546706135,-2.29799156778136,
-1.97285776109983),.UNSPECIFIED.);
#6372=B_SPLINE_CURVE_WITH_KNOTS('',3,(#271862,#271863,#271864,#271865,#271866,
#271867,#271868,#271869),.UNSPECIFIED.,.F.,.F.,(4,2,2,4),(-8.98049293428122,
-8.97889171867726,-8.34884827602979,-8.12983481856169),.UNSPECIFIED.);
#6373=B_SPLINE_CURVE_WITH_KNOTS('',3,(#271873,#271874,#271875,#271876,#271877,
#271878),.UNSPECIFIED.,.F.,.F.,(4,2,4),(-2.68771546706168,-2.29799156778158,
-1.97285776109999),.UNSPECIFIED.);
#6374=B_SPLINE_CURVE_WITH_KNOTS('',3,(#271879,#271880,#271881,#271882,#271883,
#271884),.UNSPECIFIED.,.F.,.F.,(4,2,4),(0.518273427329314,0.647448708132495,
0.677306880099206),.UNSPECIFIED.);
#6375=B_SPLINE_CURVE_WITH_KNOTS('',3,(#271887,#271888,#271889,#271890,#271891,
#271892,#271893,#271894),.UNSPECIFIED.,.F.,.F.,(4,2,2,4),(-8.98049293427992,
-8.97889171867595,-8.34884827602839,-8.12983481856025),.UNSPECIFIED.);
#6376=B_SPLINE_CURVE_WITH_KNOTS('',3,(#271897,#271898,#271899,#271900,#271901,
#271902),.UNSPECIFIED.,.F.,.F.,(4,2,4),(-2.68771546706109,-2.29799156778117,
-1.97285776109969),.UNSPECIFIED.);
#6377=B_SPLINE_CURVE_WITH_KNOTS('',3,(#271987,#271988,#271989,#271990,#271991,
#271992),.UNSPECIFIED.,.F.,.F.,(4,2,4),(-2.68771546706178,-2.29799156778168,
-1.97285776110008),.UNSPECIFIED.);
#6378=B_SPLINE_CURVE_WITH_KNOTS('',3,(#271994,#271995,#271996,#271997,#271998,
#271999),.UNSPECIFIED.,.F.,.F.,(4,2,4),(2.36444145730966,2.403353160978,
2.52343865872509),.UNSPECIFIED.);
#6379=B_SPLINE_CURVE_WITH_KNOTS('',3,(#272003,#272004,#272005,#272006),
 .UNSPECIFIED.,.F.,.F.,(4,4),(1.16920248436245,1.32846217039523),
 .UNSPECIFIED.);
#6380=B_SPLINE_CURVE_WITH_KNOTS('',3,(#272007,#272008,#272009,#272010,#272011,
#272012,#272013,#272014),.UNSPECIFIED.,.F.,.F.,(4,2,2,4),(-8.98049293428071,
-8.97889171867675,-8.34884827602921,-8.12983481856106),.UNSPECIFIED.);
#6381=B_SPLINE_CURVE_WITH_KNOTS('',3,(#272018,#272019,#272020,#272021),
 .UNSPECIFIED.,.F.,.F.,(4,4),(1.16920248436348,1.32846217039639),
 .UNSPECIFIED.);
#6382=B_SPLINE_CURVE_WITH_KNOTS('',3,(#272022,#272023,#272024,#272025,#272026,
#272027,#272028,#272029),.UNSPECIFIED.,.F.,.F.,(4,2,2,4),(-8.98049293427966,
-8.97889171867569,-8.34884827602823,-8.12983481856012),.UNSPECIFIED.);
#6383=B_SPLINE_CURVE_WITH_KNOTS('',3,(#272031,#272032,#272033,#272034,#272035,
#272036),.UNSPECIFIED.,.F.,.F.,(4,2,4),(-2.68771546706079,-2.29799156778091,
-1.97285776109946),.UNSPECIFIED.);
#6384=B_SPLINE_CURVE_WITH_KNOTS('',3,(#272038,#272039,#272040,#272041,#272042,
#272043),.UNSPECIFIED.,.F.,.F.,(4,2,4),(2.36444145731017,2.40335316097854,
2.52343865872566),.UNSPECIFIED.);
#6385=B_SPLINE_CURVE_WITH_KNOTS('',3,(#272048,#272049,#272050,#272051),
 .UNSPECIFIED.,.F.,.F.,(4,4),(1.16920248436344,1.32846217039637),
 .UNSPECIFIED.);
#6386=B_SPLINE_CURVE_WITH_KNOTS('',3,(#272052,#272053,#272054,#272055,#272056,
#272057,#272058,#272059),.UNSPECIFIED.,.F.,.F.,(4,2,2,4),(-8.98049293427945,
-8.97889171867549,-8.34884827602783,-8.12983481855963),.UNSPECIFIED.);
#6387=B_SPLINE_CURVE_WITH_KNOTS('',3,(#272061,#272062,#272063,#272064,#272065,
#272066),.UNSPECIFIED.,.F.,.F.,(4,2,4),(-2.68771546706122,-2.29799156778128,
-1.97285776109977),.UNSPECIFIED.);
#6388=B_SPLINE_CURVE_WITH_KNOTS('',3,(#272068,#272069,#272070,#272071,#272072,
#272073),.UNSPECIFIED.,.F.,.F.,(4,2,4),(2.36444145675313,2.40335316041008,
2.52343865812168),.UNSPECIFIED.);
#6389=B_SPLINE_CURVE_WITH_KNOTS('',3,(#272078,#272079,#272080,#272081),
 .UNSPECIFIED.,.F.,.F.,(4,4),(1.16920248412103,1.32846217011589),
 .UNSPECIFIED.);
#6390=B_SPLINE_CURVE_WITH_KNOTS('',3,(#272082,#272083,#272084,#272085,#272086,
#272087,#272088,#272089),.UNSPECIFIED.,.F.,.F.,(4,2,2,4),(-8.98049293427762,
-8.97889171867365,-8.34884827602598,-8.12983481855776),.UNSPECIFIED.);
#6391=B_SPLINE_CURVE_WITH_KNOTS('',3,(#272091,#272092,#272093,#272094,#272095,
#272096),.UNSPECIFIED.,.F.,.F.,(4,2,4),(-2.68771546706239,-2.29799156778215,
-1.97285776110044),.UNSPECIFIED.);
#6392=B_SPLINE_CURVE_WITH_KNOTS('',3,(#272098,#272099,#272100,#272101,#272102,
#272103),.UNSPECIFIED.,.F.,.F.,(4,2,4),(2.36444145730695,2.40335316097526,
2.5234386587222),.UNSPECIFIED.);
#6393=B_SPLINE_CURVE_WITH_KNOTS('',3,(#272107,#272108,#272109,#272110,#272111,
#272112),.UNSPECIFIED.,.F.,.F.,(4,2,4),(2.36444145785125,2.4033531615307,
2.52343865931237),.UNSPECIFIED.);
#6394=B_SPLINE_CURVE_WITH_KNOTS('',3,(#272116,#272117,#272118,#272119),
 .UNSPECIFIED.,.F.,.F.,(4,4),(1.16920248436207,1.3284621703948),
 .UNSPECIFIED.);
#6395=B_SPLINE_CURVE_WITH_KNOTS('',3,(#272120,#272121,#272122,#272123,#272124,
#272125,#272126,#272127),.UNSPECIFIED.,.F.,.F.,(4,2,2,4),(-8.98049293427944,
-8.97889171867548,-8.34884827602771,-8.12983481855948),.UNSPECIFIED.);
#6396=B_SPLINE_CURVE_WITH_KNOTS('',3,(#272131,#272132,#272133,#272134),
 .UNSPECIFIED.,.F.,.F.,(4,4),(1.16920248459907,1.32846217066903),
 .UNSPECIFIED.);
#6397=B_SPLINE_CURVE_WITH_KNOTS('',3,(#272135,#272136,#272137,#272138,#272139,
#272140,#272141,#272142),.UNSPECIFIED.,.F.,.F.,(4,2,2,4),(-8.98049293428055,
-8.97889171867659,-8.34884827602886,-8.12983481856065),.UNSPECIFIED.);
#6398=B_SPLINE_CURVE_WITH_KNOTS('',3,(#272144,#272145,#272146,#272147,#272148,
#272149),.UNSPECIFIED.,.F.,.F.,(4,2,4),(-2.68771546706087,-2.297991567781,
-1.97285776109955),.UNSPECIFIED.);
#6399=B_SPLINE_CURVE_WITH_KNOTS('',3,(#272151,#272152,#272153,#272154,#272155,
#272156),.UNSPECIFIED.,.F.,.F.,(4,2,4),(2.36444145730775,2.4033531609761,
2.5234386587231),.UNSPECIFIED.);
#6400=B_SPLINE_CURVE_WITH_KNOTS('',3,(#272160,#272161,#272162,#272163,#272164,
#272165),.UNSPECIFIED.,.F.,.F.,(4,2,4),(-2.68771546706131,-2.29799156778135,
-1.97285776109984),.UNSPECIFIED.);
#6401=B_SPLINE_CURVE_WITH_KNOTS('',3,(#272167,#272168,#272169,#272170,#272171,
#272172),.UNSPECIFIED.,.F.,.F.,(4,2,4),(2.36444145730746,2.40335316097579,
2.52343865872281),.UNSPECIFIED.);
#6402=B_SPLINE_CURVE_WITH_KNOTS('',3,(#272176,#272177,#272178,#272179),
 .UNSPECIFIED.,.F.,.F.,(4,4),(1.16920248412219,1.32846217011718),
 .UNSPECIFIED.);
#6403=B_SPLINE_CURVE_WITH_KNOTS('',3,(#272180,#272181,#272182,#272183,#272184,
#272185,#272186,#272187),.UNSPECIFIED.,.F.,.F.,(4,2,2,4),(-8.98049293428066,
-8.9788917186767,-8.34884827602938,-8.12983481856134),.UNSPECIFIED.);
#6404=B_SPLINE_CURVE_WITH_KNOTS('',3,(#272189,#272190,#272191,#272192,#272193,
#272194),.UNSPECIFIED.,.F.,.F.,(4,2,4),(-2.68771546706095,-2.29799156778107,
-1.97285776109961),.UNSPECIFIED.);
#6405=B_SPLINE_CURVE_WITH_KNOTS('',3,(#272196,#272197,#272198,#272199,#272200,
#272201,#272202,#272203),.UNSPECIFIED.,.F.,.F.,(4,2,2,4),(-8.98049293427952,
-8.97889171867556,-8.34884827602786,-8.12983481855966),.UNSPECIFIED.);
#6406=B_SPLINE_CURVE_WITH_KNOTS('',3,(#272205,#272206,#272207,#272208,#272209,
#272210,#272211,#272212),.UNSPECIFIED.,.F.,.F.,(4,2,2,4),(-8.98049293428018,
-8.97889171867621,-8.34884827602859,-8.12983481856041),.UNSPECIFIED.);
#6407=B_SPLINE_CURVE_WITH_KNOTS('',3,(#272214,#272215,#272216,#272217,#272218,
#272219),.UNSPECIFIED.,.F.,.F.,(4,2,4),(-2.68771546706135,-2.29799156778134,
-1.9728577610998),.UNSPECIFIED.);
#6408=B_SPLINE_CURVE_WITH_KNOTS('',3,(#272221,#272222,#272223,#272224,#272225,
#272226),.UNSPECIFIED.,.F.,.F.,(4,2,4),(2.36444145675532,2.40335316041232,
2.52343865812401),.UNSPECIFIED.);
#6409=B_SPLINE_CURVE_WITH_KNOTS('',3,(#272229,#272230,#272231,#272232,#272233,
#272234),.UNSPECIFIED.,.F.,.F.,(4,2,4),(-2.68771546706153,-2.2979915677815,
-1.97285776109994),.UNSPECIFIED.);
#6410=B_SPLINE_CURVE_WITH_KNOTS('',3,(#272236,#272237,#272238,#272239,#272240,
#272241,#272242,#272243),.UNSPECIFIED.,.F.,.F.,(4,2,2,4),(-8.98049293427927,
-8.97889171867531,-8.34884827602772,-8.12983481855955),.UNSPECIFIED.);
#6411=B_SPLINE_CURVE_WITH_KNOTS('',3,(#272245,#272246,#272247,#272248,#272249,
#272250),.UNSPECIFIED.,.F.,.F.,(4,2,4),(-2.68771546706105,-2.29799156778115,
-1.97285776109967),.UNSPECIFIED.);
#6412=B_SPLINE_CURVE_WITH_KNOTS('',3,(#272252,#272253,#272254,#272255,#272256,
#272257,#272258,#272259),.UNSPECIFIED.,.F.,.F.,(4,2,2,4),(-8.98049293428103,
-8.97889171867707,-8.34884827602985,-8.12983481856184),.UNSPECIFIED.);
#6413=B_SPLINE_CURVE_WITH_KNOTS('',3,(#272261,#272262,#272263,#272264,#272265,
#272266,#272267,#272268),.UNSPECIFIED.,.F.,.F.,(4,2,2,4),(-8.98049293428005,
-8.97889171867609,-8.34884827602866,-8.12983481856055),.UNSPECIFIED.);
#6414=B_SPLINE_CURVE_WITH_KNOTS('',3,(#272269,#272270,#272271,#272272,#272273,
#272274),.UNSPECIFIED.,.F.,.F.,(4,2,4),(-2.68771546706036,-2.29799156778066,
-1.97285776109931),.UNSPECIFIED.);
#6415=B_SPLINE_CURVE_WITH_KNOTS('',3,(#272277,#272278,#272279,#272280,#272281,
#272282),.UNSPECIFIED.,.F.,.F.,(4,2,4),(-2.68771546706178,-2.2979915677817,
-1.9728577611001),.UNSPECIFIED.);
#6416=B_SPLINE_CURVE_WITH_KNOTS('',3,(#272286,#272287,#272288,#272289),
 .UNSPECIFIED.,.F.,.F.,(4,4),(1.16920248412169,1.32846217011663),
 .UNSPECIFIED.);
#6417=B_SPLINE_CURVE_WITH_KNOTS('',3,(#272290,#272291,#272292,#272293,#272294,
#272295,#272296,#272297),.UNSPECIFIED.,.F.,.F.,(4,2,2,4),(-8.98049293427827,
-8.9788917186743,-8.34884827602666,-8.12983481855847),.UNSPECIFIED.);
#6418=B_SPLINE_CURVE_WITH_KNOTS('',3,(#272299,#272300,#272301,#272302,#272303,
#272304,#272305,#272306),.UNSPECIFIED.,.F.,.F.,(4,2,2,4),(-8.98049293428091,
-8.97889171867695,-8.34884827602936,-8.12983481856121),.UNSPECIFIED.);
#6419=B_SPLINE_CURVE_WITH_KNOTS('',3,(#272307,#272308,#272309,#272310,#272311,
#272312),.UNSPECIFIED.,.F.,.F.,(4,2,4),(-2.68771546706137,-2.29799156778137,
-1.97285776109986),.UNSPECIFIED.);
#6420=B_SPLINE_CURVE_WITH_KNOTS('',3,(#272315,#272316,#272317,#272318,#272319,
#272320),.UNSPECIFIED.,.F.,.F.,(4,2,4),(0.518273427329387,0.647448708132598,
0.677306880099315),.UNSPECIFIED.);
#6421=B_SPLINE_CURVE_WITH_KNOTS('',3,(#272322,#272323,#272324,#272325,#272326,
#272327),.UNSPECIFIED.,.F.,.F.,(4,2,4),(3.01719559990939,3.07732160468838,
3.17624638273335),.UNSPECIFIED.);
#6422=B_SPLINE_CURVE_WITH_KNOTS('',3,(#272329,#272330,#272331,#272332,#272333,
#272334,#272335,#272336),.UNSPECIFIED.,.F.,.F.,(4,2,2,4),(-8.98049293428025,
-8.97889171867629,-8.34884827602915,-8.12983481856118),.UNSPECIFIED.);
#6423=B_SPLINE_CURVE_WITH_KNOTS('',3,(#272344,#272345,#272346,#272347),
 .UNSPECIFIED.,.F.,.F.,(4,4),(1.16920248436201,1.32846217039475),
 .UNSPECIFIED.);
#6424=B_SPLINE_CURVE_WITH_KNOTS('',3,(#272349,#272350,#272351,#272352,#272353,
#272354),.UNSPECIFIED.,.F.,.F.,(4,2,4),(-2.68771546706102,-2.29799156778106,
-1.97285776109958),.UNSPECIFIED.);
#6425=B_SPLINE_CURVE_WITH_KNOTS('',3,(#272356,#272357,#272358,#272359,#272360,
#272361),.UNSPECIFIED.,.F.,.F.,(4,2,4),(2.36444145675474,2.40335316041175,
2.5234386581235),.UNSPECIFIED.);
#6426=B_SPLINE_CURVE_WITH_KNOTS('',3,(#272477,#272478,#272479,#272480,#272481,
#272482),.UNSPECIFIED.,.F.,.F.,(4,2,4),(-1.6873876187543,-1.63190661744399,
-1.18678936119335),.UNSPECIFIED.);
#6427=B_SPLINE_CURVE_WITH_KNOTS('',3,(#272486,#272487,#272488,#272489,#272490,
#272491,#272492,#272493),.UNSPECIFIED.,.F.,.F.,(4,2,2,4),(-5.73653316281924,
-5.72047347154335,-5.28796112447222,-5.23617773822564),.UNSPECIFIED.);
#6428=B_SPLINE_CURVE_WITH_KNOTS('',3,(#272498,#272499,#272500,#272501,#272502,
#272503,#272504,#272505),.UNSPECIFIED.,.F.,.F.,(4,2,2,4),(-5.73653316281959,
-5.72047347154369,-5.28796112447255,-5.23617773822598),.UNSPECIFIED.);
#6429=B_SPLINE_CURVE_WITH_KNOTS('',3,(#272509,#272510,#272511,#272512,#272513,
#272514),.UNSPECIFIED.,.F.,.F.,(4,2,4),(-1.68738761875429,-1.63190661744397,
-1.18678936119331),.UNSPECIFIED.);
#6430=B_SPLINE_CURVE_WITH_KNOTS('',3,(#272521,#272522,#272523,#272524,#272525,
#272526,#272527,#272528,#272529,#272530),.UNSPECIFIED.,.F.,.F.,(4,3,3,4),
(0.00710274596862205,0.00747376540688557,0.00783502386845829,0.00801837063754701),
 .UNSPECIFIED.);
#6431=B_SPLINE_CURVE_WITH_KNOTS('',3,(#272534,#272535,#272536,#272537),
 .UNSPECIFIED.,.F.,.F.,(4,4),(0.673390429668365,0.765903724821262),
 .UNSPECIFIED.);
#6432=B_SPLINE_CURVE_WITH_KNOTS('',3,(#272541,#272542,#272543,#272544,#272545,
#272546,#272547,#272548,#272549,#272550),.UNSPECIFIED.,.F.,.F.,(4,3,3,4),
(0.00710284094402589,0.00747383068998922,0.00783505699281219,0.0080184642589637),
 .UNSPECIFIED.);
#6433=B_SPLINE_CURVE_WITH_KNOTS('',3,(#272553,#272554,#272555,#272556,#272557,
#272558),.UNSPECIFIED.,.F.,.F.,(4,2,4),(1.75167822390513,1.82489845087556,
1.84415950245262),.UNSPECIFIED.);
#6434=B_SPLINE_CURVE_WITH_KNOTS('',3,(#272564,#272565,#272566,#272567,#272568,
#272569,#272570,#272571,#272572,#272573),.UNSPECIFIED.,.F.,.F.,(4,3,3,4),
(0.00710274294853988,0.00747376648681281,0.00783502929878955,0.00801836762245747),
 .UNSPECIFIED.);
#6435=B_SPLINE_CURVE_WITH_KNOTS('',3,(#272577,#272578,#272579,#272580),
 .UNSPECIFIED.,.F.,.F.,(4,4),(0.673390429683384,0.765903724839824),
 .UNSPECIFIED.);
#6436=B_SPLINE_CURVE_WITH_KNOTS('',3,(#272584,#272585,#272586,#272587,#272588,
#272589,#272590,#272591,#272592,#272593),.UNSPECIFIED.,.F.,.F.,(4,3,3,4),
(0.0071027909646029,0.00747379949023628,0.00783504604208146,0.00801841495400679),
 .UNSPECIFIED.);
#6437=B_SPLINE_CURVE_WITH_KNOTS('',3,(#272596,#272597,#272598,#272599,#272600,
#272601),.UNSPECIFIED.,.F.,.F.,(4,2,4),(1.7516782239595,1.82489845093397,
1.84415950251209),.UNSPECIFIED.);
#6438=B_SPLINE_CURVE_WITH_KNOTS('',3,(#272607,#272608,#272609,#272610,#272611,
#272612,#272613,#272614,#272615,#272616),.UNSPECIFIED.,.F.,.F.,(4,3,3,4),
(0.00710274848401425,0.00747377224143413,0.00783503523508107,0.00801837305550075),
 .UNSPECIFIED.);
#6439=B_SPLINE_CURVE_WITH_KNOTS('',3,(#272620,#272621,#272622,#272623),
 .UNSPECIFIED.,.F.,.F.,(4,4),(0.673390432198586,0.765903727898388),
 .UNSPECIFIED.);
#6440=B_SPLINE_CURVE_WITH_KNOTS('',3,(#272627,#272628,#272629,#272630,#272631,
#272632,#272633,#272634,#272635,#272636),.UNSPECIFIED.,.F.,.F.,(4,3,3,4),
(0.00710275267632021,0.00747377512290787,0.00783503669679513,0.00801837718804213),
 .UNSPECIFIED.);
#6441=B_SPLINE_CURVE_WITH_KNOTS('',3,(#272639,#272640,#272641,#272642,#272643,
#272644),.UNSPECIFIED.,.F.,.F.,(4,2,4),(1.75167822396455,1.82489845093931,
1.84415950251752),.UNSPECIFIED.);
#6442=B_SPLINE_CURVE_WITH_KNOTS('',3,(#272650,#272651,#272652,#272653,#272654,
#272655,#272656,#272657,#272658,#272659),.UNSPECIFIED.,.F.,.F.,(4,3,3,4),
(0.00710274372650064,0.00747376845075347,0.00783503250649641,0.00801836837208912),
 .UNSPECIFIED.);
#6443=B_SPLINE_CURVE_WITH_KNOTS('',3,(#272663,#272664,#272665,#272666),
 .UNSPECIFIED.,.F.,.F.,(4,4),(0.673390432227944,0.765903727934262),
 .UNSPECIFIED.);
#6444=B_SPLINE_CURVE_WITH_KNOTS('',3,(#272670,#272671,#272672,#272673,#272674,
#272675,#272676,#272677,#272678,#272679),.UNSPECIFIED.,.F.,.F.,(4,3,3,4),
(0.00710276617990407,0.00747378388366959,0.00783504033541444,0.00801839050540093),
 .UNSPECIFIED.);
#6445=B_SPLINE_CURVE_WITH_KNOTS('',3,(#272682,#272683,#272684,#272685,#272686,
#272687),.UNSPECIFIED.,.F.,.F.,(4,2,4),(1.7516782239634,1.82489845093825,
1.84415950251648),.UNSPECIFIED.);
#6446=B_SPLINE_CURVE_WITH_KNOTS('',3,(#272691,#272692,#272693,#272694,#272695,
#272696),.UNSPECIFIED.,.F.,.F.,(4,2,4),(0.311414679923399,0.386708223984938,
0.403787209257592),.UNSPECIFIED.);
#6447=B_SPLINE_CURVE_WITH_KNOTS('',3,(#272700,#272701,#272702,#272703),
 .UNSPECIFIED.,.F.,.F.,(4,4),(0.673390427100202,0.765903721697738),
 .UNSPECIFIED.);
#6448=B_SPLINE_CURVE_WITH_KNOTS('',3,(#272707,#272708,#272709,#272710,#272711,
#272712,#272713,#272714,#272715,#272716),.UNSPECIFIED.,.F.,.F.,(4,3,3,4),
(0.00710274287152855,0.00747376729113706,0.00783503103327042,0.00801836753620372),
 .UNSPECIFIED.);
#6449=B_SPLINE_CURVE_WITH_KNOTS('',3,(#272720,#272721,#272722,#272723,#272724,
#272725),.UNSPECIFIED.,.F.,.F.,(4,2,4),(1.75167822395949,1.82489845093397,
1.8441595025121),.UNSPECIFIED.);
#6450=B_SPLINE_CURVE_WITH_KNOTS('',3,(#272730,#272731,#272732,#272733,#272734,
#272735),.UNSPECIFIED.,.F.,.F.,(4,2,4),(0.311414679921635,0.386708223982506,
0.403787209254994),.UNSPECIFIED.);
#6451=B_SPLINE_CURVE_WITH_KNOTS('',3,(#272739,#272740,#272741,#272742),
 .UNSPECIFIED.,.F.,.F.,(4,4),(0.67339042968077,0.765903724836084),
 .UNSPECIFIED.);
#6452=B_SPLINE_CURVE_WITH_KNOTS('',3,(#272746,#272747,#272748,#272749,#272750,
#272751,#272752,#272753,#272754,#272755),.UNSPECIFIED.,.F.,.F.,(4,3,3,4),
(0.00710274556156679,0.00747377006444483,0.00783503387032176,0.00801837017674505),
 .UNSPECIFIED.);
#6453=B_SPLINE_CURVE_WITH_KNOTS('',3,(#272759,#272760,#272761,#272762,#272763,
#272764),.UNSPECIFIED.,.F.,.F.,(4,2,4),(1.75167822393186,1.82489845090426,
1.84415950248185),.UNSPECIFIED.);
#6454=B_SPLINE_CURVE_WITH_KNOTS('',3,(#272769,#272770,#272771,#272772,#272773,
#272774),.UNSPECIFIED.,.F.,.F.,(4,2,4),(1.75167822396114,1.82489845093575,
1.84415950251343),.UNSPECIFIED.);
#6455=B_SPLINE_CURVE_WITH_KNOTS('',3,(#272778,#272779,#272780,#272781,#272782,
#272783,#272784,#272785,#272786,#272787),.UNSPECIFIED.,.F.,.F.,(4,3,3,4),
(0.00710274556156676,0.00747377006444954,0.00783503387033569,0.00801837017674508),
 .UNSPECIFIED.);
#6456=B_SPLINE_CURVE_WITH_KNOTS('',3,(#272791,#272792,#272793,#272794),
 .UNSPECIFIED.,.F.,.F.,(4,4),(0.673390429683286,0.765903724839261),
 .UNSPECIFIED.);
#6457=B_SPLINE_CURVE_WITH_KNOTS('',3,(#272798,#272799,#272800,#272801,#272802,
#272803),.UNSPECIFIED.,.F.,.F.,(4,2,4),(1.38841536190411,1.44431919666813,
1.480702891614),.UNSPECIFIED.);
#6458=B_SPLINE_CURVE_WITH_KNOTS('',3,(#272810,#272811,#272812,#272813,#272814,
#272815,#272816,#272817,#272818,#272819),.UNSPECIFIED.,.F.,.F.,(4,3,3,4),
(0.00710275267632017,0.00747377512292421,0.00783503669676932,0.00801837718804213),
 .UNSPECIFIED.);
#6459=B_SPLINE_CURVE_WITH_KNOTS('',3,(#272823,#272824,#272825,#272826),
 .UNSPECIFIED.,.F.,.F.,(4,4),(0.673390429659051,0.765903724809687),
 .UNSPECIFIED.);
#6460=B_SPLINE_CURVE_WITH_KNOTS('',3,(#272830,#272831,#272832,#272833,#272834,
#272835,#272836,#272837,#272838,#272839),.UNSPECIFIED.,.F.,.F.,(4,3,3,4),
(0.00710274848401431,0.00747377224144616,0.00783503523508854,0.00801837305550078),
 .UNSPECIFIED.);
#6461=B_SPLINE_CURVE_WITH_KNOTS('',3,(#272842,#272843,#272844,#272845,#272846,
#272847),.UNSPECIFIED.,.F.,.F.,(4,2,4),(1.75167822393867,1.82489845091149,
1.8441595024892),.UNSPECIFIED.);
#6462=B_SPLINE_CURVE_WITH_KNOTS('',3,(#272851,#272852,#272853,#272854,#272855,
#272856),.UNSPECIFIED.,.F.,.F.,(4,2,4),(1.75167822389203,1.8248984508612,
1.84415950243739),.UNSPECIFIED.);
#6463=B_SPLINE_CURVE_WITH_KNOTS('',3,(#272860,#272861,#272862,#272863,#272864,
#272865,#272866,#272867,#272868,#272869),.UNSPECIFIED.,.F.,.F.,(4,3,3,4),
(0.00710274287152849,0.00747376729116317,0.00783503103329361,0.00801836753620371),
 .UNSPECIFIED.);
#6464=B_SPLINE_CURVE_WITH_KNOTS('',3,(#272873,#272874,#272875,#272876),
 .UNSPECIFIED.,.F.,.F.,(4,4),(0.673390429665128,0.765903724817488),
 .UNSPECIFIED.);
#6465=B_SPLINE_CURVE_WITH_KNOTS('',3,(#272880,#272881,#272882,#272883,#272884,
#272885),.UNSPECIFIED.,.F.,.F.,(4,2,4),(1.38841536184886,1.444319196609,
1.48070289155233),.UNSPECIFIED.);
#6466=B_SPLINE_CURVE_WITH_KNOTS('',3,(#272892,#272893,#272894,#272895,#272896,
#272897,#272898,#272899,#272900,#272901),.UNSPECIFIED.,.F.,.F.,(4,3,3,4),
(0.00710276617990401,0.00747378388366924,0.00783504033542184,0.00801839050540089),
 .UNSPECIFIED.);
#6467=B_SPLINE_CURVE_WITH_KNOTS('',3,(#272905,#272906,#272907,#272908),
 .UNSPECIFIED.,.F.,.F.,(4,4),(0.673390432231233,0.765903727938084),
 .UNSPECIFIED.);
#6468=B_SPLINE_CURVE_WITH_KNOTS('',3,(#272912,#272913,#272914,#272915,#272916,
#272917,#272918,#272919,#272920,#272921),.UNSPECIFIED.,.F.,.F.,(4,3,3,4),
(0.00710274372650068,0.00747376845078837,0.00783503250653971,0.00801836837208909),
 .UNSPECIFIED.);
#6469=B_SPLINE_CURVE_WITH_KNOTS('',3,(#272924,#272925,#272926,#272927,#272928,
#272929),.UNSPECIFIED.,.F.,.F.,(4,2,4),(1.75167822389501,1.82489845086412,
1.84415950244083),.UNSPECIFIED.);
#6470=B_SPLINE_CURVE_WITH_KNOTS('',3,(#272935,#272936,#272937,#272938,#272939,
#272940,#272941,#272942,#272943,#272944),.UNSPECIFIED.,.F.,.F.,(4,3,3,4),
(0.00710279096460286,0.00747379949026601,0.00783504604209238,0.0080184149540068),
 .UNSPECIFIED.);
#6471=B_SPLINE_CURVE_WITH_KNOTS('',3,(#272948,#272949,#272950,#272951),
 .UNSPECIFIED.,.F.,.F.,(4,4),(0.673390429675743,0.765903724830226),
 .UNSPECIFIED.);
#6472=B_SPLINE_CURVE_WITH_KNOTS('',3,(#272955,#272956,#272957,#272958,#272959,
#272960,#272961,#272962,#272963,#272964),.UNSPECIFIED.,.F.,.F.,(4,3,3,4),
(0.00710274294853991,0.0074737664867412,0.0078350292986902,0.00801836762245745),
 .UNSPECIFIED.);
#6473=B_SPLINE_CURVE_WITH_KNOTS('',3,(#272967,#272968,#272969,#272970,#272971,
#272972),.UNSPECIFIED.,.F.,.F.,(4,2,4),(1.75167822398024,1.82489845095654,
1.8441595025352),.UNSPECIFIED.);
#6474=B_SPLINE_CURVE_WITH_KNOTS('',3,(#272978,#272979,#272980,#272981,#272982,
#272983,#272984,#272985,#272986,#272987),.UNSPECIFIED.,.F.,.F.,(4,3,3,4),
(0.00710284094402584,0.00747383069000615,0.00783505699282562,0.00801846425896367),
 .UNSPECIFIED.);
#6475=B_SPLINE_CURVE_WITH_KNOTS('',3,(#272991,#272992,#272993,#272994),
 .UNSPECIFIED.,.F.,.F.,(4,4),(0.673390429692054,0.765903724850254),
 .UNSPECIFIED.);
#6476=B_SPLINE_CURVE_WITH_KNOTS('',3,(#272998,#272999,#273000,#273001,#273002,
#273003,#273004,#273005,#273006,#273007),.UNSPECIFIED.,.F.,.F.,(4,3,3,4),
(0.00710274596862209,0.00747376540702079,0.00783502386859213,0.00801837063754698),
 .UNSPECIFIED.);
#6477=B_SPLINE_CURVE_WITH_KNOTS('',3,(#273010,#273011,#273012,#273013,#273014,
#273015),.UNSPECIFIED.,.F.,.F.,(4,2,4),(1.75167822394042,1.82489845091343,
1.84415950249118),.UNSPECIFIED.);
#6478=B_SPLINE_CURVE_WITH_KNOTS('',3,(#273021,#273022,#273023,#273024,#273025,
#273026),.UNSPECIFIED.,.F.,.F.,(4,2,4),(-1.68738761875423,-1.63190661744391,
-1.18678936119335),.UNSPECIFIED.);
#6479=B_SPLINE_CURVE_WITH_KNOTS('',3,(#273028,#273029,#273030,#273031,#273032,
#273033,#273034,#273035,#273036,#273037),.UNSPECIFIED.,.F.,.F.,(4,3,3,4),
(0.00710284094402589,0.00747383068999436,0.00783505699281514,0.0080184642589637),
 .UNSPECIFIED.);
#6480=B_SPLINE_CURVE_WITH_KNOTS('',3,(#273041,#273042,#273043,#273044),
 .UNSPECIFIED.,.F.,.F.,(4,4),(0.673390429666604,0.7659037248194),
 .UNSPECIFIED.);
#6481=B_SPLINE_CURVE_WITH_KNOTS('',3,(#273045,#273046,#273047,#273048,#273049,
#273050,#273051,#273052),.UNSPECIFIED.,.F.,.F.,(4,2,2,4),(-5.73653316281647,
-5.7204734715406,-5.28796112446986,-5.23617773822333),.UNSPECIFIED.);
#6482=B_SPLINE_CURVE_WITH_KNOTS('',3,(#273064,#273065,#273066,#273067,#273068,
#273069),.UNSPECIFIED.,.F.,.F.,(4,2,4),(1.75167822396951,1.82489845094498,
1.84415950252339),.UNSPECIFIED.);
#6483=B_SPLINE_CURVE_WITH_KNOTS('',3,(#273070,#273071,#273072,#273073,#273074,
#273075,#273076,#273077),.UNSPECIFIED.,.F.,.F.,(4,2,2,4),(-5.73653316281843,
-5.72047347154254,-5.28796112447152,-5.23617773822495),.UNSPECIFIED.);
#6484=B_SPLINE_CURVE_WITH_KNOTS('',3,(#273079,#273080,#273081,#273082,#273083,
#273084),.UNSPECIFIED.,.F.,.F.,(4,2,4),(-1.68738761875408,-1.63190661744377,
-1.18678936119326),.UNSPECIFIED.);
#6485=B_SPLINE_CURVE_WITH_KNOTS('',3,(#273085,#273086,#273087,#273088,#273089,
#273090,#273091,#273092,#273093,#273094),.UNSPECIFIED.,.F.,.F.,(4,3,3,4),
(0.00710284094402584,0.00747383068999716,0.00783505699282223,0.00801846425896371),
 .UNSPECIFIED.);
#6486=B_SPLINE_CURVE_WITH_KNOTS('',3,(#273200,#273201,#273202,#273203,#273204,
#273205,#273206,#273207),.UNSPECIFIED.,.F.,.F.,(4,2,2,4),(-5.73653316281843,
-5.72047347154255,-5.28796112447153,-5.23617773822497),.UNSPECIFIED.);
#6487=B_SPLINE_CURVE_WITH_KNOTS('',3,(#273211,#273212,#273213,#273214,#273215,
#273216),.UNSPECIFIED.,.F.,.F.,(4,2,4),(-1.68738761875411,-1.6319066174438,
-1.18678936119328),.UNSPECIFIED.);
#6488=B_SPLINE_CURVE_WITH_KNOTS('',3,(#273217,#273218,#273219,#273220,#273221,
#273222,#273223,#273224,#273225,#273226),.UNSPECIFIED.,.F.,.F.,(4,3,3,4),
(0.00710279096460287,0.00747379949022753,0.00783504604206607,0.00801841495400678),
 .UNSPECIFIED.);
#6489=B_SPLINE_CURVE_WITH_KNOTS('',3,(#273227,#273228,#273229,#273230,#273231,
#273232),.UNSPECIFIED.,.F.,.F.,(4,2,4),(1.75167822397008,1.82489845094558,
1.84415950252402),.UNSPECIFIED.);
#6490=B_SPLINE_CURVE_WITH_KNOTS('',3,(#273235,#273236,#273237,#273238,#273239,
#273240,#273241,#273242,#273243,#273244),.UNSPECIFIED.,.F.,.F.,(4,3,3,4),
(0.00710274596862205,0.00747376540693236,0.00783502386849402,0.00801837063754702),
 .UNSPECIFIED.);
#6491=B_SPLINE_CURVE_WITH_KNOTS('',3,(#273246,#273247,#273248,#273249,#273250,
#273251),.UNSPECIFIED.,.F.,.F.,(4,2,4),(1.75167822396416,1.82489845093897,
1.84415950251715),.UNSPECIFIED.);
#6492=B_SPLINE_CURVE_WITH_KNOTS('',3,(#273253,#273254,#273255,#273256,#273257,
#273258,#273259,#273260),.UNSPECIFIED.,.F.,.F.,(4,2,2,4),(-5.73653316281831,
-5.72047347154243,-5.28796112447143,-5.23617773822487),.UNSPECIFIED.);
#6493=B_SPLINE_CURVE_WITH_KNOTS('',3,(#273263,#273264,#273265,#273266,#273267,
#273268),.UNSPECIFIED.,.F.,.F.,(4,2,4),(-1.68738761875401,-1.63190661744371,
-1.18678936119322),.UNSPECIFIED.);
#6494=B_SPLINE_CURVE_WITH_KNOTS('',3,(#273271,#273272,#273273,#273274,#273275,
#273276,#273277,#273278,#273279,#273280),.UNSPECIFIED.,.F.,.F.,(4,3,3,4),
(0.00710274294853987,0.00747376648670428,0.00783502929868148,0.00801836762245748),
 .UNSPECIFIED.);
#6495=B_SPLINE_CURVE_WITH_KNOTS('',3,(#273282,#273283,#273284,#273285,#273286,
#273287),.UNSPECIFIED.,.F.,.F.,(4,2,4),(1.75167822398049,1.82489845095657,
1.84415950253511),.UNSPECIFIED.);
#6496=B_SPLINE_CURVE_WITH_KNOTS('',3,(#273289,#273290,#273291,#273292,#273293,
#273294,#273295,#273296),.UNSPECIFIED.,.F.,.F.,(4,2,2,4),(-5.73653316281822,
-5.72047347154233,-5.28796112447135,-5.23617773822479),.UNSPECIFIED.);
#6497=B_SPLINE_CURVE_WITH_KNOTS('',3,(#273299,#273300,#273301,#273302,#273303,
#273304),.UNSPECIFIED.,.F.,.F.,(4,2,4),(-1.68738761875411,-1.6319066174438,
-1.18678936119327),.UNSPECIFIED.);
#6498=B_SPLINE_CURVE_WITH_KNOTS('',3,(#273307,#273308,#273309,#273310,#273311,
#273312,#273313,#273314,#273315,#273316),.UNSPECIFIED.,.F.,.F.,(4,3,3,4),
(0.00710274372650065,0.00747376845074211,0.00783503250649763,0.00801836837208913),
 .UNSPECIFIED.);
#6499=B_SPLINE_CURVE_WITH_KNOTS('',3,(#273318,#273319,#273320,#273321,#273322,
#273323),.UNSPECIFIED.,.F.,.F.,(4,2,4),(1.75167822398513,1.82489845096143,
1.84415950254005),.UNSPECIFIED.);
#6500=B_SPLINE_CURVE_WITH_KNOTS('',3,(#273325,#273326,#273327,#273328,#273329,
#273330,#273331,#273332),.UNSPECIFIED.,.F.,.F.,(4,2,2,4),(-5.73653316281763,
-5.72047347154175,-5.2879611244708,-5.23617773822424),.UNSPECIFIED.);
#6501=B_SPLINE_CURVE_WITH_KNOTS('',3,(#273335,#273336,#273337,#273338,#273339,
#273340),.UNSPECIFIED.,.F.,.F.,(4,2,4),(-1.68738761875406,-1.63190661744375,
-1.18678936119324),.UNSPECIFIED.);
#6502=B_SPLINE_CURVE_WITH_KNOTS('',3,(#273344,#273345,#273346,#273347,#273348,
#273349,#273350,#273351),.UNSPECIFIED.,.F.,.F.,(4,2,2,4),(-5.73653316281763,
-5.72047347154175,-5.28796112447086,-5.2361777382243),.UNSPECIFIED.);
#6503=B_SPLINE_CURVE_WITH_KNOTS('',3,(#273355,#273356,#273357,#273358,#273359,
#273360),.UNSPECIFIED.,.F.,.F.,(4,2,4),(-1.6873876187539,-1.6319066174436,
-1.18678936119314),.UNSPECIFIED.);
#6504=B_SPLINE_CURVE_WITH_KNOTS('',3,(#273361,#273362,#273363,#273364,#273365,
#273366,#273367,#273368,#273369,#273370),.UNSPECIFIED.,.F.,.F.,(4,3,3,4),
(0.00710275842609582,0.00747377890657602,0.00783503835572276,0.00801838285788017),
 .UNSPECIFIED.);
#6505=B_SPLINE_CURVE_WITH_KNOTS('',3,(#273371,#273372,#273373,#273374,#273375,
#273376),.UNSPECIFIED.,.F.,.F.,(4,2,4),(1.75167822396027,1.82489845093474,
1.84415950251286),.UNSPECIFIED.);
#6506=B_SPLINE_CURVE_WITH_KNOTS('',3,(#273378,#273379,#273380,#273381,#273382,
#273383,#273384,#273385,#273386,#273387),.UNSPECIFIED.,.F.,.F.,(4,3,3,4),
(0.00710277664195228,0.00747379050272964,0.00783504280851268,0.00801840082520104),
 .UNSPECIFIED.);
#6507=B_SPLINE_CURVE_WITH_KNOTS('',3,(#273389,#273390,#273391,#273392,#273393,
#273394),.UNSPECIFIED.,.F.,.F.,(4,2,4),(1.75167822402901,1.82489845100883,
1.84415950258839),.UNSPECIFIED.);
#6508=B_SPLINE_CURVE_WITH_KNOTS('',3,(#273396,#273397,#273398,#273399,#273400,
#273401,#273402,#273403),.UNSPECIFIED.,.F.,.F.,(4,2,2,4),(-5.73653316281821,
-5.72047347154232,-5.28796112447134,-5.23617773822477),.UNSPECIFIED.);
#6509=B_SPLINE_CURVE_WITH_KNOTS('',3,(#273407,#273408,#273409,#273410,#273411,
#273412,#273413,#273414,#273415,#273416),.UNSPECIFIED.,.F.,.F.,(4,3,3,4),
(0.00710274848401426,0.00747377224139712,0.00783503523503374,0.00801837305550079),
 .UNSPECIFIED.);
#6510=B_SPLINE_CURVE_WITH_KNOTS('',3,(#273418,#273419,#273420,#273421,#273422,
#273423),.UNSPECIFIED.,.F.,.F.,(4,2,4),(1.75167822392663,1.82489845089845,
1.84415950247588),.UNSPECIFIED.);
#6511=B_SPLINE_CURVE_WITH_KNOTS('',3,(#273425,#273426,#273427,#273428,#273429,
#273430,#273431,#273432),.UNSPECIFIED.,.F.,.F.,(4,2,2,4),(-5.73653316281796,
-5.72047347154208,-5.28796112447113,-5.23617773822457),.UNSPECIFIED.);
#6512=B_SPLINE_CURVE_WITH_KNOTS('',3,(#273435,#273436,#273437,#273438,#273439,
#273440),.UNSPECIFIED.,.F.,.F.,(4,2,4),(-1.68738761875412,-1.63190661744382,
-1.1867893611933),.UNSPECIFIED.);
#6513=B_SPLINE_CURVE_WITH_KNOTS('',3,(#273444,#273445,#273446,#273447,#273448,
#273449,#273450,#273451),.UNSPECIFIED.,.F.,.F.,(4,2,2,4),(-5.73653316281711,
-5.72047347154123,-5.28796112447036,-5.23617773822381),.UNSPECIFIED.);
#6514=B_SPLINE_CURVE_WITH_KNOTS('',3,(#273455,#273456,#273457,#273458,#273459,
#273460),.UNSPECIFIED.,.F.,.F.,(4,2,4),(-1.68738761875405,-1.63190661744374,
-1.18678936119325),.UNSPECIFIED.);
#6515=B_SPLINE_CURVE_WITH_KNOTS('',3,(#273461,#273462,#273463,#273464,#273465,
#273466,#273467,#273468,#273469,#273470),.UNSPECIFIED.,.F.,.F.,(4,3,3,4),
(0.00710281114521604,0.00747381210003836,0.00783505048827464,0.00801843486213954),
 .UNSPECIFIED.);
#6516=B_SPLINE_CURVE_WITH_KNOTS('',3,(#273471,#273472,#273473,#273474,#273475,
#273476),.UNSPECIFIED.,.F.,.F.,(4,2,4),(1.75167822397278,1.8248984509485,
1.84415950252695),.UNSPECIFIED.);
#6517=B_SPLINE_CURVE_WITH_KNOTS('',3,(#273479,#273480,#273481,#273482,#273483,
#273484,#273485,#273486,#273487,#273488),.UNSPECIFIED.,.F.,.F.,(4,3,3,4),
(0.0071027490873384,0.00747377283389233,0.0078350358106713,0.00801837364807993),
 .UNSPECIFIED.);
#6518=B_SPLINE_CURVE_WITH_KNOTS('',3,(#273490,#273491,#273492,#273493,#273494,
#273495),.UNSPECIFIED.,.F.,.F.,(4,2,4),(1.75167822393089,1.82489845090296,
1.84415950248043),.UNSPECIFIED.);
#6519=B_SPLINE_CURVE_WITH_KNOTS('',3,(#273497,#273498,#273499,#273500,#273501,
#273502,#273503,#273504),.UNSPECIFIED.,.F.,.F.,(4,2,2,4),(-5.73653316281819,
-5.7204734715423,-5.2879611244713,-5.23617773822474),.UNSPECIFIED.);
#6520=B_SPLINE_CURVE_WITH_KNOTS('',3,(#273507,#273508,#273509,#273510,#273511,
#273512),.UNSPECIFIED.,.F.,.F.,(4,2,4),(-1.68738761875405,-1.63190661744374,
-1.18678936119326),.UNSPECIFIED.);
#6521=B_SPLINE_CURVE_WITH_KNOTS('',3,(#273515,#273516,#273517,#273518,#273519,
#273520,#273521,#273522,#273523,#273524),.UNSPECIFIED.,.F.,.F.,(4,3,3,4),
(0.00710274396181581,0.00747376592129383,0.00783502705943546,0.00801836863650809),
 .UNSPECIFIED.);
#6522=B_SPLINE_CURVE_WITH_KNOTS('',3,(#273525,#273526,#273527,#273528,#273529,
#273530),.UNSPECIFIED.,.F.,.F.,(4,2,4),(1.75167822392141,1.82489845089256,
1.84415950246982),.UNSPECIFIED.);
#6523=B_SPLINE_CURVE_WITH_KNOTS('',3,(#273533,#273534,#273535,#273536,#273537,
#273538),.UNSPECIFIED.,.F.,.F.,(4,2,4),(-1.68738761875407,-1.63190661744377,
-1.18678936119326),.UNSPECIFIED.);
#6524=B_SPLINE_CURVE_WITH_KNOTS('',3,(#273542,#273543,#273544,#273545,#273546,
#273547,#273548,#273549),.UNSPECIFIED.,.F.,.F.,(4,2,2,4),(-5.73653316281851,
-5.72047347154262,-5.2879611244716,-5.23617773822503),.UNSPECIFIED.);
#6525=B_SPLINE_CURVE_WITH_KNOTS('',3,(#273553,#273554,#273555,#273556,#273557,
#273558),.UNSPECIFIED.,.F.,.F.,(4,2,4),(-1.68738761875428,-1.63190661744396,
-1.18678936119339),.UNSPECIFIED.);
#6526=B_SPLINE_CURVE_WITH_KNOTS('',3,(#273559,#273560,#273561,#273562,#273563,
#273564,#273565,#273566,#273567,#273568),.UNSPECIFIED.,.F.,.F.,(4,3,3,4),
(0.00710274287152851,0.00747376729109832,0.00783503103323433,0.00801836753620372),
 .UNSPECIFIED.);
#6527=B_SPLINE_CURVE_WITH_KNOTS('',3,(#273569,#273570,#273571,#273572,#273573,
#273574),.UNSPECIFIED.,.F.,.F.,(4,2,4),(1.75167822396654,1.8248984509415,
1.84415950251975),.UNSPECIFIED.);
#6528=B_SPLINE_CURVE_WITH_KNOTS('',3,(#273577,#273578,#273579,#273580,#273581,
#273582,#273583,#273584,#273585,#273586),.UNSPECIFIED.,.F.,.F.,(4,3,3,4),
(0.00710274556156676,0.00747377006442299,0.00783503387029698,0.00801837017674507),
 .UNSPECIFIED.);
#6529=B_SPLINE_CURVE_WITH_KNOTS('',3,(#273588,#273589,#273590,#273591,#273592,
#273593),.UNSPECIFIED.,.F.,.F.,(4,2,4),(1.75167822394173,1.82489845091482,
1.84415950249256),.UNSPECIFIED.);
#6530=B_SPLINE_CURVE_WITH_KNOTS('',3,(#273595,#273596,#273597,#273598,#273599,
#273600,#273601,#273602),.UNSPECIFIED.,.F.,.F.,(4,2,2,4),(-5.73653316281893,
-5.72047347154304,-5.28796112447197,-5.23617773822539),.UNSPECIFIED.);
#6531=B_SPLINE_CURVE_WITH_KNOTS('',3,(#273605,#273606,#273607,#273608,#273609,
#273610),.UNSPECIFIED.,.F.,.F.,(4,2,4),(-1.68738761875412,-1.63190661744381,
-1.1867893611933),.UNSPECIFIED.);
#6532=B_SPLINE_CURVE_WITH_KNOTS('',3,(#273614,#273615,#273616,#273617,#273618,
#273619,#273620,#273621),.UNSPECIFIED.,.F.,.F.,(4,2,2,4),(-5.73653316281756,
-5.72047347154168,-5.28796112447075,-5.2361777382242),.UNSPECIFIED.);
#6533=B_SPLINE_CURVE_WITH_KNOTS('',3,(#273625,#273626,#273627,#273628,#273629,
#273630),.UNSPECIFIED.,.F.,.F.,(4,2,4),(-1.68738761875423,-1.63190661744392,
-1.18678936119336),.UNSPECIFIED.);
#6534=B_SPLINE_CURVE_WITH_KNOTS('',3,(#273631,#273632,#273633,#273634,#273635,
#273636,#273637,#273638,#273639,#273640),.UNSPECIFIED.,.F.,.F.,(4,3,3,4),
(0.00710275267632017,0.00747377512286913,0.00783503669672892,0.00801837718804214),
 .UNSPECIFIED.);
#6535=B_SPLINE_CURVE_WITH_KNOTS('',3,(#273641,#273642,#273643,#273644,#273645,
#273646),.UNSPECIFIED.,.F.,.F.,(4,2,4),(1.75167822394468,1.82489845091785,
1.84415950249561),.UNSPECIFIED.);
#6536=B_SPLINE_CURVE_WITH_KNOTS('',3,(#273649,#273650,#273651,#273652,#273653,
#273654,#273655,#273656,#273657,#273658),.UNSPECIFIED.,.F.,.F.,(4,3,3,4),
(0.00710276617990402,0.00747378388367883,0.00783504033543201,0.00801839050540095),
 .UNSPECIFIED.);
#6537=B_SPLINE_CURVE_WITH_KNOTS('',3,(#273660,#273661,#273662,#273663,#273664,
#273665),.UNSPECIFIED.,.F.,.F.,(4,2,4),(1.75167822395908,1.82489845093353,
1.84415950251173),.UNSPECIFIED.);
#6538=B_SPLINE_CURVE_WITH_KNOTS('',3,(#273667,#273668,#273669,#273670,#273671,
#273672,#273673,#273674),.UNSPECIFIED.,.F.,.F.,(4,2,2,4),(-5.73653316281958,
-5.72047347154368,-5.28796112447252,-5.23617773822594),.UNSPECIFIED.);
#6539=B_SPLINE_CURVE_WITH_KNOTS('',3,(#273677,#273678,#273679,#273680,#273681,
#273682),.UNSPECIFIED.,.F.,.F.,(4,2,4),(-1.68738761875405,-1.63190661744374,
-1.18678936119325),.UNSPECIFIED.);
#6540=B_SPLINE_CURVE_WITH_KNOTS('',3,(#273685,#273686,#273687,#273688,#273689,
#273690,#273691,#273692),.UNSPECIFIED.,.F.,.F.,(4,2,2,4),(-5.73653316281852,
-5.72047347154263,-5.28796112447155,-5.23617773822497),.UNSPECIFIED.);
#6541=B_SPLINE_CURVE_WITH_KNOTS('',3,(#273695,#273696,#273697,#273698,#273699,
#273700),.UNSPECIFIED.,.F.,.F.,(4,2,4),(-1.68738761875409,-1.63190661744378,
-1.18678936119328),.UNSPECIFIED.);
#6542=B_SPLINE_CURVE_WITH_KNOTS('',3,(#273703,#273704,#273705,#273706,#273707,
#273708,#273709,#273710),.UNSPECIFIED.,.F.,.F.,(4,2,2,4),(-5.73653316281855,
-5.72047347154266,-5.28796112447163,-5.23617773822506),.UNSPECIFIED.);
#6543=B_SPLINE_CURVE_WITH_KNOTS('',3,(#273713,#273714,#273715,#273716,#273717,
#273718),.UNSPECIFIED.,.F.,.F.,(4,2,4),(-1.68738761875414,-1.63190661744383,
-1.18678936119329),.UNSPECIFIED.);
#6544=B_SPLINE_CURVE_WITH_KNOTS('',3,(#273721,#273722,#273723,#273724,#273725,
#273726,#273727,#273728),.UNSPECIFIED.,.F.,.F.,(4,2,2,4),(-5.73653316281849,
-5.7204734715426,-5.28796112447158,-5.23617773822501),.UNSPECIFIED.);
#6545=B_SPLINE_CURVE_WITH_KNOTS('',3,(#273731,#273732,#273733,#273734,#273735,
#273736),.UNSPECIFIED.,.F.,.F.,(4,2,4),(-1.68738761875438,-1.63190661744405,
-1.18678936119344),.UNSPECIFIED.);
#6546=B_SPLINE_CURVE_WITH_KNOTS('',3,(#273739,#273740,#273741,#273742,#273743,
#273744,#273745,#273746),.UNSPECIFIED.,.F.,.F.,(4,2,2,4),(-5.73653316281912,
-5.72047347154323,-5.28796112447213,-5.23617773822555),.UNSPECIFIED.);
#6547=B_SPLINE_CURVE_WITH_KNOTS('',3,(#273749,#273750,#273751,#273752,#273753,
#273754),.UNSPECIFIED.,.F.,.F.,(4,2,4),(-1.68738761875427,-1.63190661744396,
-1.18678936119339),.UNSPECIFIED.);
#6548=B_SPLINE_CURVE_WITH_KNOTS('',3,(#273757,#273758,#273759,#273760,#273761,
#273762,#273763,#273764),.UNSPECIFIED.,.F.,.F.,(4,2,2,4),(-5.73653316281971,
-5.72047347154382,-5.28796112447267,-5.23617773822609),.UNSPECIFIED.);
#6549=B_SPLINE_CURVE_WITH_KNOTS('',3,(#273767,#273768,#273769,#273770,#273771,
#273772),.UNSPECIFIED.,.F.,.F.,(4,2,4),(-1.68738761875429,-1.63190661744397,
-1.18678936119339),.UNSPECIFIED.);
#6550=B_SPLINE_CURVE_WITH_KNOTS('',3,(#273775,#273776,#273777,#273778,#273779,
#273780,#273781,#273782),.UNSPECIFIED.,.F.,.F.,(4,2,2,4),(-5.73653316281998,
-5.72047347154409,-5.28796112447289,-5.2361777382263),.UNSPECIFIED.);
#6551=B_SPLINE_CURVE_WITH_KNOTS('',3,(#273785,#273786,#273787,#273788,#273789,
#273790),.UNSPECIFIED.,.F.,.F.,(4,2,4),(-1.68738761875409,-1.63190661744378,
-1.18678936119326),.UNSPECIFIED.);
#6552=B_SPLINE_CURVE_WITH_KNOTS('',3,(#273793,#273794,#273795,#273796,#273797,
#273798),.UNSPECIFIED.,.F.,.F.,(4,2,4),(1.75167822400724,1.82489845098526,
1.84415950256435),.UNSPECIFIED.);
#6553=B_SPLINE_CURVE_WITH_KNOTS('',3,(#273800,#273801,#273802,#273803,#273804,
#273805,#273806,#273807),.UNSPECIFIED.,.F.,.F.,(4,2,2,4),(-5.73653316281915,
-5.72047347154326,-5.28796112447218,-5.2361777382256),.UNSPECIFIED.);
#6554=B_SPLINE_CURVE_WITH_KNOTS('',3,(#273810,#273811,#273812,#273813,#273814,
#273815),.UNSPECIFIED.,.F.,.F.,(4,2,4),(-1.68738761875405,-1.63190661744374,
-1.18678936119324),.UNSPECIFIED.);
#6555=B_SPLINE_CURVE_WITH_KNOTS('',3,(#273818,#273819,#273820,#273821,#273822,
#273823,#273824,#273825),.UNSPECIFIED.,.F.,.F.,(4,2,2,4),(-5.73653316281814,
-5.72047347154225,-5.28796112447131,-5.23617773822475),.UNSPECIFIED.);
#6556=B_SPLINE_CURVE_WITH_KNOTS('',3,(#273828,#273829,#273830,#273831,#273832,
#273833),.UNSPECIFIED.,.F.,.F.,(4,2,4),(-1.68738761875419,-1.63190661744387,
-1.1867893611933),.UNSPECIFIED.);
#6557=B_SPLINE_CURVE_WITH_KNOTS('',3,(#273836,#273837,#273838,#273839,#273840,
#273841,#273842,#273843),.UNSPECIFIED.,.F.,.F.,(4,2,2,4),(-5.73653316281769,
-5.7204734715418,-5.28796112447084,-5.23617773822428),.UNSPECIFIED.);
#6558=B_SPLINE_CURVE_WITH_KNOTS('',3,(#273846,#273847,#273848,#273849,#273850,
#273851),.UNSPECIFIED.,.F.,.F.,(4,2,4),(-1.68738761875417,-1.63190661744386,
-1.18678936119329),.UNSPECIFIED.);
#6559=B_SPLINE_CURVE_WITH_KNOTS('',3,(#273854,#273855,#273856,#273857,#273858,
#273859,#273860,#273861),.UNSPECIFIED.,.F.,.F.,(4,2,2,4),(-5.73653316281814,
-5.72047347154225,-5.2879611244713,-5.23617773822474),.UNSPECIFIED.);
#6560=B_SPLINE_CURVE_WITH_KNOTS('',3,(#273864,#273865,#273866,#273867,#273868,
#273869),.UNSPECIFIED.,.F.,.F.,(4,2,4),(-1.6873876187541,-1.63190661744379,
-1.18678936119325),.UNSPECIFIED.);
#6561=B_SPLINE_CURVE_WITH_KNOTS('',3,(#273872,#273873,#273874,#273875,#273876,
#273877,#273878,#273879),.UNSPECIFIED.,.F.,.F.,(4,2,2,4),(-5.73653316281885,
-5.72047347154296,-5.28796112447182,-5.23617773822524),.UNSPECIFIED.);
#6562=B_SPLINE_CURVE_WITH_KNOTS('',3,(#273883,#273884,#273885,#273886,#273887,
#273888),.UNSPECIFIED.,.F.,.F.,(4,2,4),(-1.68738761875405,-1.63190661744374,
-1.18678936119323),.UNSPECIFIED.);
#6563=B_SPLINE_CURVE_WITH_KNOTS('',3,(#273889,#273890,#273891,#273892,#273893,
#273894,#273895,#273896,#273897,#273898),.UNSPECIFIED.,.F.,.F.,(4,3,3,4),
(0.00710274396181582,0.00747376592129673,0.0078350270594336,0.0080183686365081),
 .UNSPECIFIED.);
#6564=B_SPLINE_CURVE_WITH_KNOTS('',3,(#273902,#273903,#273904,#273905,#273906,
#273907,#273908,#273909),.UNSPECIFIED.,.F.,.F.,(4,2,2,4),(-5.73653316281769,
-5.7204734715418,-5.2879611244709,-5.23617773822434),.UNSPECIFIED.);
#6565=B_SPLINE_CURVE_WITH_KNOTS('',3,(#273913,#273914,#273915,#273916,#273917,
#273918),.UNSPECIFIED.,.F.,.F.,(4,2,4),(-1.68738761875409,-1.63190661744378,
-1.18678936119327),.UNSPECIFIED.);
#6566=B_SPLINE_CURVE_WITH_KNOTS('',3,(#273919,#273920,#273921,#273922,#273923,
#273924,#273925,#273926,#273927,#273928),.UNSPECIFIED.,.F.,.F.,(4,3,3,4),
(0.00710274908733836,0.00747377283388781,0.00783503581067877,0.00801837364807989),
 .UNSPECIFIED.);
#6567=B_SPLINE_CURVE_WITH_KNOTS('',3,(#273929,#273930,#273931,#273932,#273933,
#273934),.UNSPECIFIED.,.F.,.F.,(4,2,4),(1.75167822398879,1.82489845096549,
1.84415950254423),.UNSPECIFIED.);
#6568=B_SPLINE_CURVE_WITH_KNOTS('',3,(#273937,#273938,#273939,#273940,#273941,
#273942,#273943,#273944),.UNSPECIFIED.,.F.,.F.,(4,2,2,4),(-5.73653316281731,
-5.72047347154143,-5.28796112447051,-5.23617773822395),.UNSPECIFIED.);
#6569=B_SPLINE_CURVE_WITH_KNOTS('',3,(#273947,#273948,#273949,#273950,#273951,
#273952),.UNSPECIFIED.,.F.,.F.,(4,2,4),(-1.68738761875397,-1.63190661744366,
-1.18678936119318),.UNSPECIFIED.);
#6570=B_SPLINE_CURVE_WITH_KNOTS('',3,(#273955,#273956,#273957,#273958,#273959,
#273960,#273961,#273962),.UNSPECIFIED.,.F.,.F.,(4,2,2,4),(-5.73653316281751,
-5.72047347154163,-5.28796112447074,-5.23617773822419),.UNSPECIFIED.);
#6571=B_SPLINE_CURVE_WITH_KNOTS('',3,(#273965,#273966,#273967,#273968,#273969,
#273970),.UNSPECIFIED.,.F.,.F.,(4,2,4),(-1.6873876187541,-1.63190661744379,
-1.18678936119324),.UNSPECIFIED.);
#6572=B_SPLINE_CURVE_WITH_KNOTS('',3,(#274137,#274138,#274139,#274140,#274141,
#274142),.UNSPECIFIED.,.F.,.F.,(4,2,4),(-1.68738761875416,-1.63190661744385,
-1.18678936119333),.UNSPECIFIED.);
#6573=B_SPLINE_CURVE_WITH_KNOTS('',3,(#274144,#274145,#274146,#274147,#274148,
#274149,#274150,#274151,#274152,#274153),.UNSPECIFIED.,.F.,.F.,(4,3,3,4),
(0.00710274596862211,0.00747376540693313,0.00783502386849516,0.00801837063754701),
 .UNSPECIFIED.);
#6574=B_SPLINE_CURVE_WITH_KNOTS('',3,(#274157,#274158,#274159,#274160),
 .UNSPECIFIED.,.F.,.F.,(4,4),(0.673390429676812,0.765903724831544),
 .UNSPECIFIED.);
#6575=B_SPLINE_CURVE_WITH_KNOTS('',3,(#274161,#274162,#274163,#274164,#274165,
#274166,#274167,#274168),.UNSPECIFIED.,.F.,.F.,(4,2,2,4),(-5.73653316281784,
-5.72047347154196,-5.287961124471,-5.23617773822444),.UNSPECIFIED.);
#6576=B_SPLINE_CURVE_WITH_KNOTS('',3,(#274172,#274173,#274174,#274175),
 .UNSPECIFIED.,.F.,.F.,(4,4),(0.673390429666292,0.765903724818824),
 .UNSPECIFIED.);
#6577=B_SPLINE_CURVE_WITH_KNOTS('',3,(#274176,#274177,#274178,#274179,#274180,
#274181,#274182,#274183),.UNSPECIFIED.,.F.,.F.,(4,2,2,4),(-5.73653316281748,
-5.7204734715416,-5.28796112447073,-5.23617773822417),.UNSPECIFIED.);
#6578=B_SPLINE_CURVE_WITH_KNOTS('',3,(#274185,#274186,#274187,#274188,#274189,
#274190),.UNSPECIFIED.,.F.,.F.,(4,2,4),(-1.68738761875411,-1.63190661744379,
-1.18678936119327),.UNSPECIFIED.);
#6579=B_SPLINE_CURVE_WITH_KNOTS('',3,(#274192,#274193,#274194,#274195,#274196,
#274197,#274198,#274199,#274200,#274201),.UNSPECIFIED.,.F.,.F.,(4,3,3,4),
(0.0071027909646029,0.00747379949021994,0.00783504604206349,0.00801841495400679),
 .UNSPECIFIED.);
#6580=B_SPLINE_CURVE_WITH_KNOTS('',3,(#274206,#274207,#274208,#274209),
 .UNSPECIFIED.,.F.,.F.,(4,4),(0.673390429691577,0.765903724849725),
 .UNSPECIFIED.);
#6581=B_SPLINE_CURVE_WITH_KNOTS('',3,(#274210,#274211,#274212,#274213,#274214,
#274215,#274216,#274217),.UNSPECIFIED.,.F.,.F.,(4,2,2,4),(-5.73653316281866,
-5.72047347154278,-5.28796112447173,-5.23617773822516),.UNSPECIFIED.);
#6582=B_SPLINE_CURVE_WITH_KNOTS('',3,(#274219,#274220,#274221,#274222,#274223,
#274224),.UNSPECIFIED.,.F.,.F.,(4,2,4),(-1.68738761875417,-1.63190661744386,
-1.18678936119332),.UNSPECIFIED.);
#6583=B_SPLINE_CURVE_WITH_KNOTS('',3,(#274226,#274227,#274228,#274229,#274230,
#274231,#274232,#274233,#274234,#274235),.UNSPECIFIED.,.F.,.F.,(4,3,3,4),
(0.00710276617990406,0.00747378388368516,0.00783504033543666,0.00801839050540092),
 .UNSPECIFIED.);
#6584=B_SPLINE_CURVE_WITH_KNOTS('',3,(#274240,#274241,#274242,#274243),
 .UNSPECIFIED.,.F.,.F.,(4,4),(0.673390429669713,0.765903724823031),
 .UNSPECIFIED.);
#6585=B_SPLINE_CURVE_WITH_KNOTS('',3,(#274244,#274245,#274246,#274247,#274248,
#274249,#274250,#274251),.UNSPECIFIED.,.F.,.F.,(4,2,2,4),(-5.73653316281874,
-5.72047347154286,-5.2879611244718,-5.23617773822523),.UNSPECIFIED.);
#6586=B_SPLINE_CURVE_WITH_KNOTS('',3,(#274253,#274254,#274255,#274256,#274257,
#274258),.UNSPECIFIED.,.F.,.F.,(4,2,4),(-1.68738761875415,-1.63190661744384,
-1.1867893611933),.UNSPECIFIED.);
#6587=B_SPLINE_CURVE_WITH_KNOTS('',3,(#274260,#274261,#274262,#274263,#274264,
#274265,#274266,#274267,#274268,#274269),.UNSPECIFIED.,.F.,.F.,(4,3,3,4),
(0.00710275267632021,0.0074737751228719,0.00783503669673661,0.00801837718804212),
 .UNSPECIFIED.);
#6588=B_SPLINE_CURVE_WITH_KNOTS('',3,(#274273,#274274,#274275,#274276,#274277,
#274278),.UNSPECIFIED.,.F.,.F.,(4,2,4),(-1.68738761875413,-1.63190661744382,
-1.18678936119329),.UNSPECIFIED.);
#6589=B_SPLINE_CURVE_WITH_KNOTS('',3,(#274280,#274281,#274282,#274283,#274284,
#274285,#274286,#274287,#274288,#274289),.UNSPECIFIED.,.F.,.F.,(4,3,3,4),
(0.00710274287152854,0.00747376729108694,0.00783503103322807,0.00801836753620372),
 .UNSPECIFIED.);
#6590=B_SPLINE_CURVE_WITH_KNOTS('',3,(#274293,#274294,#274295,#274296),
 .UNSPECIFIED.,.F.,.F.,(4,4),(0.673390429683854,0.765903724840037),
 .UNSPECIFIED.);
#6591=B_SPLINE_CURVE_WITH_KNOTS('',3,(#274297,#274298,#274299,#274300,#274301,
#274302,#274303,#274304),.UNSPECIFIED.,.F.,.F.,(4,2,2,4),(-5.73653316281854,
-5.72047347154266,-5.28796112447161,-5.23617773822503),.UNSPECIFIED.);
#6592=B_SPLINE_CURVE_WITH_KNOTS('',3,(#274307,#274308,#274309,#274310),
 .UNSPECIFIED.,.F.,.F.,(4,4),(0.673390429668841,0.765903724822033),
 .UNSPECIFIED.);
#6593=B_SPLINE_CURVE_WITH_KNOTS('',3,(#274312,#274313,#274314,#274315,#274316,
#274317),.UNSPECIFIED.,.F.,.F.,(4,2,4),(-1.68738761875431,-1.63190661744399,
-1.18678936119339),.UNSPECIFIED.);
#6594=B_SPLINE_CURVE_WITH_KNOTS('',3,(#274319,#274320,#274321,#274322,#274323,
#274324,#274325,#274326,#274327,#274328),.UNSPECIFIED.,.F.,.F.,(4,3,3,4),
(0.00710274396181585,0.00747376592127879,0.00783502705942774,0.00801836863650806),
 .UNSPECIFIED.);
#6595=B_SPLINE_CURVE_WITH_KNOTS('',3,(#274333,#274334,#274335,#274336),
 .UNSPECIFIED.,.F.,.F.,(4,4),(0.673390429663607,0.765903724815473),
 .UNSPECIFIED.);
#6596=B_SPLINE_CURVE_WITH_KNOTS('',3,(#274337,#274338,#274339,#274340,#274341,
#274342,#274343,#274344),.UNSPECIFIED.,.F.,.F.,(4,2,2,4),(-5.73653316281882,
-5.72047347154294,-5.28796112447192,-5.23617773822535),.UNSPECIFIED.);
#6597=B_SPLINE_CURVE_WITH_KNOTS('',3,(#274346,#274347,#274348,#274349,#274350,
#274351),.UNSPECIFIED.,.F.,.F.,(4,2,4),(-1.68738761875414,-1.63190661744383,
-1.18678936119329),.UNSPECIFIED.);
#6598=B_SPLINE_CURVE_WITH_KNOTS('',3,(#274353,#274354,#274355,#274356,#274357,
#274358,#274359,#274360,#274361,#274362),.UNSPECIFIED.,.F.,.F.,(4,3,3,4),
(0.0071027455615668,0.0074737700644107,0.00783503387028777,0.00801837017674507),
 .UNSPECIFIED.);
#6599=B_SPLINE_CURVE_WITH_KNOTS('',3,(#274366,#274367,#274368,#274369,#274370,
#274371),.UNSPECIFIED.,.F.,.F.,(4,2,4),(-1.68738761875419,-1.63190661744387,
-1.18678936119332),.UNSPECIFIED.);
#6600=B_SPLINE_CURVE_WITH_KNOTS('',3,(#274373,#274374,#274375,#274376,#274377,
#274378,#274379,#274380,#274381,#274382),.UNSPECIFIED.,.F.,.F.,(4,3,3,4),
(0.00710274908733838,0.00747377283384765,0.00783503581062305,0.00801837364807991),
 .UNSPECIFIED.);
#6601=B_SPLINE_CURVE_WITH_KNOTS('',3,(#274386,#274387,#274388,#274389),
 .UNSPECIFIED.,.F.,.F.,(4,4),(0.673390429687081,0.765903724844288),
 .UNSPECIFIED.);
#6602=B_SPLINE_CURVE_WITH_KNOTS('',3,(#274390,#274391,#274392,#274393,#274394,
#274395,#274396,#274397),.UNSPECIFIED.,.F.,.F.,(4,2,2,4),(-5.73653316281885,
-5.72047347154297,-5.28796112447191,-5.23617773822534),.UNSPECIFIED.);
#6603=B_SPLINE_CURVE_WITH_KNOTS('',3,(#274401,#274402,#274403,#274404),
 .UNSPECIFIED.,.F.,.F.,(4,4),(0.673390432246977,0.765903727957335),
 .UNSPECIFIED.);
#6604=B_SPLINE_CURVE_WITH_KNOTS('',3,(#274405,#274406,#274407,#274408,#274409,
#274410,#274411,#274412),.UNSPECIFIED.,.F.,.F.,(4,2,2,4),(-5.73653316281879,
-5.72047347154291,-5.28796112447184,-5.23617773822526),.UNSPECIFIED.);
#6605=B_SPLINE_CURVE_WITH_KNOTS('',3,(#274414,#274415,#274416,#274417,#274418,
#274419),.UNSPECIFIED.,.F.,.F.,(4,2,4),(-1.68738761875414,-1.63190661744383,
-1.1867893611933),.UNSPECIFIED.);
#6606=B_SPLINE_CURVE_WITH_KNOTS('',3,(#274421,#274422,#274423,#274424,#274425,
#274426,#274427,#274428,#274429,#274430),.UNSPECIFIED.,.F.,.F.,(4,3,3,4),
(0.00710281114521608,0.00747381210005874,0.00783505048828664,0.00801843486213951),
 .UNSPECIFIED.);
#6607=B_SPLINE_CURVE_WITH_KNOTS('',3,(#274435,#274436,#274437,#274438),
 .UNSPECIFIED.,.F.,.F.,(4,4),(0.673390429686447,0.765903724843666),
 .UNSPECIFIED.);
#6608=B_SPLINE_CURVE_WITH_KNOTS('',3,(#274439,#274440,#274441,#274442,#274443,
#274444,#274445,#274446),.UNSPECIFIED.,.F.,.F.,(4,2,2,4),(-5.7365331628184,
-5.72047347154252,-5.28796112447152,-5.23617773822495),.UNSPECIFIED.);
#6609=B_SPLINE_CURVE_WITH_KNOTS('',3,(#274448,#274449,#274450,#274451,#274452,
#274453,#274454,#274455,#274456,#274457),.UNSPECIFIED.,.F.,.F.,(4,3,3,4),
(0.00710277664195233,0.00747379050279132,0.00783504280857186,0.00801840082520103),
 .UNSPECIFIED.);
#6610=B_SPLINE_CURVE_WITH_KNOTS('',3,(#274461,#274462,#274463,#274464,#274465,
#274466),.UNSPECIFIED.,.F.,.F.,(4,2,4),(-1.68738761875411,-1.6319066174438,
-1.18678936119329),.UNSPECIFIED.);
#6611=B_SPLINE_CURVE_WITH_KNOTS('',3,(#274468,#274469,#274470,#274471,#274472,
#274473,#274474,#274475,#274476,#274477),.UNSPECIFIED.,.F.,.F.,(4,3,3,4),
(0.00710275842609585,0.00747377890659939,0.0078350383557556,0.00801838285788014),
 .UNSPECIFIED.);
#6612=B_SPLINE_CURVE_WITH_KNOTS('',3,(#274481,#274482,#274483,#274484),
 .UNSPECIFIED.,.F.,.F.,(4,4),(0.673390432223755,0.765903727929032),
 .UNSPECIFIED.);
#6613=B_SPLINE_CURVE_WITH_KNOTS('',3,(#274485,#274486,#274487,#274488,#274489,
#274490,#274491,#274492),.UNSPECIFIED.,.F.,.F.,(4,2,2,4),(-5.73653316281933,
-5.72047347154344,-5.28796112447234,-5.23617773822576),.UNSPECIFIED.);
#6614=B_SPLINE_CURVE_WITH_KNOTS('',3,(#274496,#274497,#274498,#274499),
 .UNSPECIFIED.,.F.,.F.,(4,4),(0.673390429678433,0.765903724833911),
 .UNSPECIFIED.);
#6615=B_SPLINE_CURVE_WITH_KNOTS('',3,(#274500,#274501,#274502,#274503,#274504,
#274505,#274506,#274507),.UNSPECIFIED.,.F.,.F.,(4,2,2,4),(-5.73653316281869,
-5.7204734715428,-5.28796112447175,-5.23617773822517),.UNSPECIFIED.);
#6616=B_SPLINE_CURVE_WITH_KNOTS('',3,(#274509,#274510,#274511,#274512,#274513,
#274514),.UNSPECIFIED.,.F.,.F.,(4,2,4),(-1.68738761875428,-1.63190661744396,
-1.1867893611934),.UNSPECIFIED.);
#6617=B_SPLINE_CURVE_WITH_KNOTS('',3,(#274516,#274517,#274518,#274519,#274520,
#274521,#274522,#274523,#274524,#274525),.UNSPECIFIED.,.F.,.F.,(4,3,3,4),
(0.00710274848401432,0.00747377224140442,0.00783503523505279,0.00801837305550079),
 .UNSPECIFIED.);
#6618=B_SPLINE_CURVE_WITH_KNOTS('',3,(#274529,#274530,#274531,#274532,#274533,
#274534),.UNSPECIFIED.,.F.,.F.,(4,2,4),(-1.68738761875434,-1.63190661744402,
-1.18678936119343),.UNSPECIFIED.);
#6619=B_SPLINE_CURVE_WITH_KNOTS('',3,(#274536,#274537,#274538,#274539,#274540,
#274541,#274542,#274543,#274544,#274545),.UNSPECIFIED.,.F.,.F.,(4,3,3,4),
(0.00710274372650068,0.00747376845073826,0.00783503250649141,0.0080183683720891),
 .UNSPECIFIED.);
#6620=B_SPLINE_CURVE_WITH_KNOTS('',3,(#274549,#274550,#274551,#274552),
 .UNSPECIFIED.,.F.,.F.,(4,4),(0.673390427101013,0.765903721698924),
 .UNSPECIFIED.);
#6621=B_SPLINE_CURVE_WITH_KNOTS('',3,(#274553,#274554,#274555,#274556,#274557,
#274558,#274559,#274560),.UNSPECIFIED.,.F.,.F.,(4,2,2,4),(-5.73653316281909,
-5.7204734715432,-5.28796112447211,-5.23617773822553),.UNSPECIFIED.);
#6622=B_SPLINE_CURVE_WITH_KNOTS('',3,(#274564,#274565,#274566,#274567),
 .UNSPECIFIED.,.F.,.F.,(4,4),(0.673390429693342,0.765903724851547),
 .UNSPECIFIED.);
#6623=B_SPLINE_CURVE_WITH_KNOTS('',3,(#274568,#274569,#274570,#274571,#274572,
#274573,#274574,#274575),.UNSPECIFIED.,.F.,.F.,(4,2,2,4),(-5.73653316281968,
-5.72047347154379,-5.28796112447263,-5.23617773822604),.UNSPECIFIED.);
#6624=B_SPLINE_CURVE_WITH_KNOTS('',3,(#274577,#274578,#274579,#274580,#274581,
#274582),.UNSPECIFIED.,.F.,.F.,(4,2,4),(-1.68738761875421,-1.6319066174439,
-1.18678936119335),.UNSPECIFIED.);
#6625=B_SPLINE_CURVE_WITH_KNOTS('',3,(#274584,#274585,#274586,#274587,#274588,
#274589,#274590,#274591,#274592,#274593),.UNSPECIFIED.,.F.,.F.,(4,3,3,4),
(0.00710274294853989,0.00747376648671073,0.0078350292986873,0.00801836762245744),
 .UNSPECIFIED.);
#6626=B_SPLINE_CURVE_WITH_KNOTS('',3,(#274596,#274597,#274598,#274599,#274600,
#274601),.UNSPECIFIED.,.F.,.F.,(4,2,4),(-1.68738761875434,-1.63190661744402,
-1.18678936119342),.UNSPECIFIED.);
#6627=B_SPLINE_CURVE_WITH_KNOTS('',3,(#274603,#274604,#274605,#274606,#274607,
#274608,#274609,#274610),.UNSPECIFIED.,.F.,.F.,(4,2,2,4),(-5.73653316282004,
-5.72047347154415,-5.28796112447295,-5.23617773822635),.UNSPECIFIED.);
#6628=B_SPLINE_CURVE_WITH_KNOTS('',3,(#274612,#274613,#274614,#274615,#274616,
#274617,#274618,#274619),.UNSPECIFIED.,.F.,.F.,(4,2,2,4),(-5.73653316281866,
-5.72047347154277,-5.28796112447173,-5.23617773822515),.UNSPECIFIED.);
#6629=B_SPLINE_CURVE_WITH_KNOTS('',3,(#274620,#274621,#274622,#274623,#274624,
#274625),.UNSPECIFIED.,.F.,.F.,(4,2,4),(-1.68738761875433,-1.63190661744401,
-1.18678936119343),.UNSPECIFIED.);
#6630=B_SPLINE_CURVE_WITH_KNOTS('',3,(#274628,#274629,#274630,#274631,#274632,
#274633,#274634,#274635),.UNSPECIFIED.,.F.,.F.,(4,2,2,4),(-5.73653316281802,
-5.72047347154213,-5.28796112447117,-5.23617773822461),.UNSPECIFIED.);
#6631=B_SPLINE_CURVE_WITH_KNOTS('',3,(#274636,#274637,#274638,#274639,#274640,
#274641),.UNSPECIFIED.,.F.,.F.,(4,2,4),(-1.68738761875432,-1.631906617444,
-1.18678936119341),.UNSPECIFIED.);
#6632=B_SPLINE_CURVE_WITH_KNOTS('',3,(#274644,#274645,#274646,#274647,#274648,
#274649),.UNSPECIFIED.,.F.,.F.,(4,2,4),(-1.68738761875423,-1.63190661744392,
-1.18678936119335),.UNSPECIFIED.);
#6633=B_SPLINE_CURVE_WITH_KNOTS('',3,(#274651,#274652,#274653,#274654,#274655,
#274656,#274657,#274658),.UNSPECIFIED.,.F.,.F.,(4,2,2,4),(-5.73653316281873,
-5.72047347154284,-5.2879611244718,-5.23617773822523),.UNSPECIFIED.);
#6634=B_SPLINE_CURVE_WITH_KNOTS('',3,(#274660,#274661,#274662,#274663,#274664,
#274665,#274666,#274667),.UNSPECIFIED.,.F.,.F.,(4,2,2,4),(-5.7365331628187,
-5.72047347154281,-5.28796112447176,-5.2361777382252),.UNSPECIFIED.);
#6635=B_SPLINE_CURVE_WITH_KNOTS('',3,(#274668,#274669,#274670,#274671,#274672,
#274673),.UNSPECIFIED.,.F.,.F.,(4,2,4),(-1.6873876187541,-1.63190661744378,
-1.18678936119327),.UNSPECIFIED.);
#6636=B_SPLINE_CURVE_WITH_KNOTS('',3,(#274676,#274677,#274678,#274679,#274680,
#274681),.UNSPECIFIED.,.F.,.F.,(4,2,4),(-1.68738761875444,-1.63190661744411,
-1.18678936119347),.UNSPECIFIED.);
#6637=B_SPLINE_CURVE_WITH_KNOTS('',3,(#274683,#274684,#274685,#274686,#274687,
#274688,#274689,#274690),.UNSPECIFIED.,.F.,.F.,(4,2,2,4),(-5.73653316281952,
-5.72047347154364,-5.2879611244725,-5.23617773822591),.UNSPECIFIED.);
#6638=B_SPLINE_CURVE_WITH_KNOTS('',3,(#274692,#274693,#274694,#274695,#274696,
#274697,#274698,#274699),.UNSPECIFIED.,.F.,.F.,(4,2,2,4),(-5.73653316281812,
-5.72047347154224,-5.28796112447125,-5.23617773822468),.UNSPECIFIED.);
#6639=B_SPLINE_CURVE_WITH_KNOTS('',3,(#274701,#274702,#274703,#274704,#274705,
#274706),.UNSPECIFIED.,.F.,.F.,(4,2,4),(-1.68738761875419,-1.63190661744387,
-1.18678936119332),.UNSPECIFIED.);
#6640=B_SPLINE_CURVE_WITH_KNOTS('',3,(#274708,#274709,#274710,#274711,#274712,
#274713,#274714,#274715,#274716,#274717),.UNSPECIFIED.,.F.,.F.,(4,3,3,4),
(0.00710274396181585,0.0074737659213073,0.00783502705945658,0.00801836863650807),
 .UNSPECIFIED.);
#6641=B_SPLINE_CURVE_WITH_KNOTS('',3,(#274720,#274721,#274722,#274723,#274724,
#274725),.UNSPECIFIED.,.F.,.F.,(4,2,4),(-1.68738761875417,-1.63190661744386,
-1.18678936119332),.UNSPECIFIED.);
#6642=B_SPLINE_CURVE_WITH_KNOTS('',3,(#274727,#274728,#274729,#274730,#274731,
#274732,#274733,#274734),.UNSPECIFIED.,.F.,.F.,(4,2,2,4),(-5.73653316282042,
-5.72047347154453,-5.28796112447321,-5.2361777382266),.UNSPECIFIED.);
#6643=B_SPLINE_CURVE_WITH_KNOTS('',3,(#274736,#274737,#274738,#274739,#274740,
#274741,#274742,#274743),.UNSPECIFIED.,.F.,.F.,(4,2,2,4),(-5.73653316281903,
-5.72047347154315,-5.28796112447213,-5.23617773822556),.UNSPECIFIED.);
#6644=B_SPLINE_CURVE_WITH_KNOTS('',3,(#274744,#274745,#274746,#274747,#274748,
#274749),.UNSPECIFIED.,.F.,.F.,(4,2,4),(-1.68738761875402,-1.63190661744372,
-1.18678936119324),.UNSPECIFIED.);
#6645=B_SPLINE_CURVE_WITH_KNOTS('',3,(#274752,#274753,#274754,#274755,#274756,
#274757,#274758,#274759),.UNSPECIFIED.,.F.,.F.,(4,2,2,4),(-5.73653316282014,
-5.72047347154425,-5.28796112447299,-5.23617773822639),.UNSPECIFIED.);
#6646=B_SPLINE_CURVE_WITH_KNOTS('',3,(#274760,#274761,#274762,#274763,#274764,
#274765),.UNSPECIFIED.,.F.,.F.,(4,2,4),(-1.68738761875435,-1.63190661744403,
-1.18678936119343),.UNSPECIFIED.);
#6647=B_SPLINE_CURVE_WITH_KNOTS('',3,(#274768,#274769,#274770,#274771,#274772,
#274773),.UNSPECIFIED.,.F.,.F.,(4,2,4),(-1.6873876187543,-1.63190661744398,
-1.1867893611934),.UNSPECIFIED.);
#6648=B_SPLINE_CURVE_WITH_KNOTS('',3,(#274777,#274778,#274779,#274780),
 .UNSPECIFIED.,.F.,.F.,(4,4),(0.673390429688366,0.765903724845993),
 .UNSPECIFIED.);
#6649=B_SPLINE_CURVE_WITH_KNOTS('',3,(#274781,#274782,#274783,#274784,#274785,
#274786,#274787,#274788),.UNSPECIFIED.,.F.,.F.,(4,2,2,4),(-5.73653316281831,
-5.72047347154242,-5.28796112447148,-5.23617773822492),.UNSPECIFIED.);
#6650=B_SPLINE_CURVE_WITH_KNOTS('',3,(#274791,#274792,#274793,#274794,#274795,
#274796),.UNSPECIFIED.,.F.,.F.,(4,2,4),(-1.68738761875411,-1.6319066174438,
-1.18678936119327),.UNSPECIFIED.);
#6651=B_SPLINE_CURVE_WITH_KNOTS('',3,(#274798,#274799,#274800,#274801,#274802,
#274803,#274804,#274805,#274806,#274807),.UNSPECIFIED.,.F.,.F.,(4,3,3,4),
(0.00710281114521606,0.00747381210002463,0.00783505048825559,0.00801843486213951),
 .UNSPECIFIED.);
#6652=B_SPLINE_CURVE_WITH_KNOTS('',3,(#274811,#274812,#274813,#274814),
 .UNSPECIFIED.,.F.,.F.,(4,4),(0.673390429663033,0.765903724814501),
 .UNSPECIFIED.);
#6653=B_SPLINE_CURVE_WITH_KNOTS('',3,(#274815,#274816,#274817,#274818,#274819,
#274820,#274821,#274822),.UNSPECIFIED.,.F.,.F.,(4,2,2,4),(-5.73653316281795,
-5.72047347154207,-5.2879611244711,-5.23617773822453),.UNSPECIFIED.);
#6654=B_SPLINE_CURVE_WITH_KNOTS('',3,(#274824,#274825,#274826,#274827,#274828,
#274829,#274830,#274831),.UNSPECIFIED.,.F.,.F.,(4,2,2,4),(-5.73653316281885,
-5.72047347154296,-5.28796112447191,-5.23617773822534),.UNSPECIFIED.);
#6655=B_SPLINE_CURVE_WITH_KNOTS('',3,(#274832,#274833,#274834,#274835,#274836,
#274837),.UNSPECIFIED.,.F.,.F.,(4,2,4),(-1.68738761875433,-1.63190661744402,
-1.18678936119343),.UNSPECIFIED.);
#6656=B_SPLINE_CURVE_WITH_KNOTS('',3,(#274840,#274841,#274842,#274843,#274844,
#274845,#274846,#274847),.UNSPECIFIED.,.F.,.F.,(4,2,2,4),(-5.73653316281845,
-5.72047347154257,-5.28796112447156,-5.23617773822498),.UNSPECIFIED.);
#6657=B_SPLINE_CURVE_WITH_KNOTS('',3,(#274848,#274849,#274850,#274851,#274852,
#274853),.UNSPECIFIED.,.F.,.F.,(4,2,4),(-1.6873876187544,-1.63190661744407,
-1.18678936119345),.UNSPECIFIED.);
#6658=B_SPLINE_CURVE_WITH_KNOTS('',3,(#274857,#274858,#274859,#274860,#274861,
#274862,#274863,#274864,#274865,#274866),.UNSPECIFIED.,.F.,.F.,(4,3,3,4),
(0.00710281114521603,0.00747381210002846,0.00783505048825458,0.00801843486213948),
 .UNSPECIFIED.);
#6659=B_SPLINE_CURVE_WITH_KNOTS('',3,(#274868,#274869,#274870,#274871,#274872,
#274873),.UNSPECIFIED.,.F.,.F.,(4,2,4),(1.75167822400075,1.82489845097847,
1.84415950255741),.UNSPECIFIED.);
#6660=B_SPLINE_CURVE_WITH_KNOTS('',3,(#274875,#274876,#274877,#274878,#274879,
#274880,#274881,#274882),.UNSPECIFIED.,.F.,.F.,(4,2,2,4),(-5.73653316281845,
-5.72047347154257,-5.28796112447152,-5.23617773822495),.UNSPECIFIED.);
#6661=B_SPLINE_CURVE_WITH_KNOTS('',3,(#274885,#274886,#274887,#274888,#274889,
#274890),.UNSPECIFIED.,.F.,.F.,(4,2,4),(-1.68738761875408,-1.63190661744377,
-1.18678936119327),.UNSPECIFIED.);
#6662=B_SPLINE_CURVE_WITH_KNOTS('',3,(#274900,#274901,#274902,#274903),
 .UNSPECIFIED.,.F.,.F.,(4,4),(0.673390429683733,0.765903724840068),
 .UNSPECIFIED.);
#6663=B_SPLINE_CURVE_WITH_KNOTS('',3,(#274904,#274905,#274906,#274907,#274908,
#274909,#274910,#274911),.UNSPECIFIED.,.F.,.F.,(4,2,2,4),(-5.73653316281842,
-5.72047347154254,-5.28796112447156,-5.236177738225),.UNSPECIFIED.);
#6664=B_SPLINE_CURVE_WITH_KNOTS('',3,(#274913,#274914,#274915,#274916,#274917,
#274918),.UNSPECIFIED.,.F.,.F.,(4,2,4),(-1.68738761875398,-1.63190661744368,
-1.18678936119318),.UNSPECIFIED.);
#6665=B_SPLINE_CURVE_WITH_KNOTS('',3,(#274920,#274921,#274922,#274923,#274924,
#274925,#274926,#274927,#274928,#274929),.UNSPECIFIED.,.F.,.F.,(4,3,3,4),
(0.00710274908733839,0.0074737728338415,0.00783503581060294,0.00801837364807991),
 .UNSPECIFIED.);
#6666=B_SPLINE_CURVE_WITH_KNOTS('',3,(#275737,#275738,#275739,#275740,#275741,
#275742,#275743,#275744),.UNSPECIFIED.,.F.,.F.,(4,2,2,4),(1.00000116132204E-6,
0.429497510617222,1.0120430239264,1.11775283487271),.UNSPECIFIED.);
#6667=B_SPLINE_CURVE_WITH_KNOTS('',3,(#275749,#275750,#275751,#275752),
 .UNSPECIFIED.,.F.,.F.,(4,4),(7.34352906207753,7.64557688708348),
 .UNSPECIFIED.);
#6668=B_SPLINE_CURVE_WITH_KNOTS('',3,(#275753,#275754,#275755,#275756,#275757,
#275758,#275759,#275760,#275761,#275762),.UNSPECIFIED.,.F.,.F.,(4,2,2,2,
4),(9.99999987588035E-7,0.202811370610722,0.414120939581438,0.71227877903909,
0.886181891443318),.UNSPECIFIED.);
#6669=B_SPLINE_CURVE_WITH_KNOTS('',3,(#275769,#275770,#275771,#275772,#275773,
#275774,#275775,#275776),.UNSPECIFIED.,.F.,.F.,(4,2,2,4),(-42.6556224181082,
-42.3393783982178,-42.0192508568443,-41.8325669335184),.UNSPECIFIED.);
#6670=B_SPLINE_CURVE_WITH_KNOTS('',3,(#275782,#275783,#275784,#275785,#275786,
#275787,#275788,#275789,#275790,#275791,#275792,#275793,#275794,#275795,
#275796,#275797,#275798,#275799,#275800,#275801,#275802,#275803,#275804,
#275805,#275806,#275807,#275808,#275809,#275810,#275811,#275812,#275813,
#275814,#275815,#275816,#275817),.UNSPECIFIED.,.F.,.F.,(4,2,2,2,2,2,2,2,
2,2,2,2,2,2,2,2,2,4),(-7.44116305045028,-7.17785504943678,-6.70990825692069,
-6.23401157001746,-5.76981930737753,-5.29794385498397,-4.82877043864304,
-4.36346848183658,-3.88740222504434,-3.4220963637296,-2.95310502793577,
-2.47931294698886,-2.01512664441116,-1.54211434015112,-1.0743024235615,
-0.608146386189052,-0.304927951315456,-9.99999993922529E-7),
 .UNSPECIFIED.);
#6671=B_SPLINE_CURVE_WITH_KNOTS('',3,(#275819,#275820,#275821,#275822,#275823,
#275824,#275825,#275826,#275827,#275828,#275829,#275830,#275831,#275832,
#275833,#275834,#275835,#275836,#275837,#275838,#275839,#275840,#275841,
#275842,#275843,#275844,#275845,#275846,#275847,#275848,#275849,#275850,
#275851,#275852,#275853,#275854),.UNSPECIFIED.,.F.,.F.,(4,2,2,2,2,2,2,2,
2,2,2,2,2,2,2,2,2,4),(-41.8325669335184,-41.5544565596035,-41.0761168548913,
-40.6089639671417,-40.1417104354557,-39.6676250020063,-39.2030407552377,
-38.7303486447156,-38.2603417146062,-37.7952178460956,-37.3180877048775,
-36.8519799622467,-36.3835773668435,-35.9106696866344,-35.4462857267773,
-34.9716819551014,-34.5027722391319,-34.2597187473986),.UNSPECIFIED.);
#6672=B_SPLINE_CURVE_WITH_KNOTS('',3,(#275859,#275860,#275861,#275862,#275863,
#275864,#275865,#275866,#275867,#275868,#275869,#275870,#275871,#275872,
#275873,#275874,#275875,#275876,#275877,#275878,#275879,#275880,#275881,
#275882,#275883,#275884,#275885,#275886,#275887,#275888,#275889,#275890,
#275891,#275892,#275893,#275894),.UNSPECIFIED.,.F.,.F.,(4,2,2,2,2,2,2,2,
2,2,2,2,2,2,2,2,2,4),(-15.0095788972105,-14.6891053876878,-14.2233099603447,
-13.7464994065718,-13.2816878142172,-12.8119957222621,-12.33962154027,-11.8753488433553,
-11.4015809522423,-10.9346413573587,-10.4678013743225,-9.98978205441938,
-9.52529968492163,-9.05446969804222,-8.58368061459515,-8.11893603960459,
-7.64396665170116,-7.44116305045028),.UNSPECIFIED.);
#6673=B_SPLINE_CURVE_WITH_KNOTS('',3,(#275895,#275896,#275897,#275898,#275899,
#275900,#275901,#275902,#275903,#275904,#275905,#275906,#275907,#275908,
#275909,#275910,#275911,#275912,#275913,#275914,#275915,#275916,#275917,
#275918,#275919,#275920,#275921,#275922,#275923,#275924,#275925,#275926,
#275927,#275928,#275929,#275930),.UNSPECIFIED.,.F.,.F.,(4,2,2,2,2,2,2,2,
2,2,2,2,2,2,2,2,2,4),(-34.2597187473986,-34.0370343829147,-33.5610627724172,
-33.0957264046361,-32.6258819919018,-32.1540895486335,-31.6896159949956,
-31.2128397783498,-30.7449484402703,-30.2783319795283,-29.8034272201055,
-29.338560671758,-28.8670395861306,-28.3962594537798,-27.9314186621211,
-27.4534667216445,-26.986674673592,-26.6867050296319),.UNSPECIFIED.);
#6674=B_SPLINE_CURVE_WITH_KNOTS('',3,(#275935,#275936,#275937,#275938,#275939,
#275940,#275941,#275942,#275943,#275944,#275945,#275946,#275947,#275948,
#275949,#275950,#275951,#275952,#275953,#275954,#275955,#275956,#275957,
#275958,#275959,#275960,#275961,#275962,#275963,#275964,#275965,#275966,
#275967,#275968,#275969,#275970),.UNSPECIFIED.,.F.,.F.,(4,2,2,2,2,2,2,2,
2,2,2,2,2,2,2,2,2,4),(-22.5771816796688,-22.1974829039796,-21.7329281055567,
-21.2583415224104,-20.792038573969,-20.3244607251778,-19.8480054086097,
-19.3838435875952,-18.9123672043351,-18.4428387263217,-17.9778142873194,
-17.502161518784,-17.0367364757151,-16.5681408884267,-16.0938564613078,
-15.6297840447666,-15.1571931357626,-15.0095788972105),.UNSPECIFIED.);
#6675=B_SPLINE_CURVE_WITH_KNOTS('',3,(#275971,#275972,#275973,#275974,#275975,
#275976,#275977,#275978,#275979,#275980,#275981,#275982,#275983,#275984,
#275985,#275986,#275987,#275988,#275989,#275990,#275991,#275992,#275993,
#275994,#275995,#275996,#275997,#275998,#275999,#276000,#276001,#276002,
#276003,#276004,#276005,#276006),.UNSPECIFIED.,.F.,.F.,(4,2,2,2,2,2,2,2,
2,2,2,2,2,2,2,2,2,4),(-26.6867050296319,-26.5191327937425,-26.0454265438289,
-25.5809543455129,-25.1077448664485,-24.6380946277012,-24.1728388918026,
-23.6960853050495,-23.2302611865729,-22.7658976619046,-22.2929524044554,
-21.8246432184248,-21.3585099790374,-20.8813404908684,-20.4162654100928,
-19.9462223577016,-19.4736481649645,-19.1145570626869),.UNSPECIFIED.);
#6676=B_SPLINE_CURVE_WITH_KNOTS('',3,(#276011,#276012,#276013,#276014,#276015,
#276016,#276017,#276018,#276019,#276020,#276021,#276022,#276023,#276024,
#276025,#276026,#276027,#276028,#276029,#276030,#276031,#276032,#276033,
#276034,#276035,#276036,#276037,#276038,#276039,#276040,#276041,#276042,
#276043,#276044,#276045,#276046),.UNSPECIFIED.,.F.,.F.,(4,2,2,2,2,2,2,2,
2,2,2,2,2,2,2,2,2,4),(-30.1445044786768,-29.7083751129182,-29.2402785855838,
-28.7677009365716,-28.3036318874976,-27.8293319784653,-27.3607488282678,
-26.8953199234704,-26.4196801308044,-25.9546641419191,-25.4851244920146,
-25.0136606183757,-24.5494995786249,-24.0730268352487,-23.6054605373483,
-23.1391515381628,-22.6686868414385,-22.5771816796688),.UNSPECIFIED.);
#6677=B_SPLINE_CURVE_WITH_KNOTS('',3,(#276047,#276048,#276049,#276050,#276051,
#276052,#276053,#276054,#276055,#276056,#276057,#276058,#276059,#276060,
#276061,#276062,#276063,#276064,#276065,#276066,#276067,#276068,#276069,
#276070,#276071,#276072,#276073,#276074,#276075,#276076,#276077,#276078,
#276079,#276080,#276081,#276082),.UNSPECIFIED.,.F.,.F.,(4,2,2,2,2,2,2,2,
2,2,2,2,2,2,2,2,2,4),(-19.1145570626869,-19.009069084107,-18.5349439065439,
-18.0677669735219,-17.6006289446376,-17.1224651546171,-16.6579203640066,
-16.1869539705083,-15.7161685208132,-15.2513185292807,-14.7762090591503,
-14.3100610165697,-13.8419777248235,-13.3661095595253,-12.901840724189,
-12.4298228977916,-11.9606418459535,-11.5438063668984),.UNSPECIFIED.);
#6678=B_SPLINE_CURVE_WITH_KNOTS('',3,(#276088,#276089,#276090,#276091,#276092,
#276093,#276094,#276095,#276096,#276097,#276098,#276099,#276100,#276101,
#276102,#276103,#276104,#276105,#276106,#276107),.UNSPECIFIED.,.F.,.F.,
(4,2,2,2,2,2,2,2,2,4),(-3.97345641689582,-3.50426059056884,-3.03988191488275,
-2.56866935179826,-2.09844180121526,-1.63350787928118,-1.15813639803468,
-0.692307299664475,-0.343901369245436,-9.999999992516E-7),.UNSPECIFIED.);
#6679=B_SPLINE_CURVE_WITH_KNOTS('',3,(#276110,#276111,#276112,#276113,#276114,
#276115,#276116,#276117,#276118,#276119,#276120,#276121,#276122,#276123,
#276124,#276125,#276126,#276127,#276128,#276129,#276130,#276131,#276132,
#276133),.UNSPECIFIED.,.F.,.F.,(4,2,2,2,2,2,2,2,2,2,2,4),(-42.6297087861989,
-42.2733922661027,-41.918043823783,-41.4442399042521,-40.975262620631,-40.5099558642212,
-40.0339042317455,-39.5686130984597,-39.0994318314099,-38.6275705716374,
-38.1633818297147,-37.7128902237401),.UNSPECIFIED.);
#6680=B_SPLINE_CURVE_WITH_KNOTS('',3,(#276135,#276136,#276137,#276138,#276139,
#276140,#276141,#276142,#276143,#276144,#276145,#276146,#276147,#276148,
#276149,#276150,#276151,#276152,#276153,#276154,#276155,#276156,#276157,
#276158,#276159,#276160,#276161,#276162,#276163,#276164,#276165,#276166,
#276167,#276168,#276169,#276170,#276171,#276172),.UNSPECIFIED.,.F.,.F.,
(4,2,2,2,2,2,2,2,2,2,2,2,2,2,2,2,2,2,4),(-37.7128902237401,-37.6874712538429,
-37.2195376691207,-36.7534229318995,-36.2784672722019,-35.8137309018735,
-35.3429320891482,-34.8721153061919,-34.4076341220623,-33.9296287163475,
-33.4628020605409,-32.9958564735305,-32.5221022327873,-32.0578354653717,
-31.5854484593393,-31.1157693469819,-30.6509563925439,-30.1741594603652,
-30.1445044786768),.UNSPECIFIED.);
#6681=B_SPLINE_CURVE_WITH_KNOTS('',3,(#276173,#276174,#276175,#276176,#276177,
#276178,#276179,#276180,#276181,#276182,#276183,#276184,#276185,#276186,
#276187,#276188,#276189,#276190,#276191,#276192,#276193,#276194,#276195,
#276196,#276197,#276198,#276199,#276200,#276201,#276202,#276203,#276204,
#276205,#276206,#276207,#276208,#276209,#276210),.UNSPECIFIED.,.F.,.F.,
(4,2,2,2,2,2,2,2,2,2,2,2,2,2,2,2,2,2,4),(-11.5438063668984,-11.4952185482997,
-11.0190068049884,-10.5536512371283,-10.0845187618387,-9.61074282219137,
-9.1464648778113,-8.67330637301754,-8.2054723003753,-7.73918014733004,-7.26178842260406,
-6.79695068115107,-6.32670321892208,-5.85473342556063,-5.39015939398363,
-4.91581118919752,-4.44901839880879,-3.98166664151097,-3.97345641689582),
 .UNSPECIFIED.);
#6682=B_SPLINE_CURVE_WITH_KNOTS('',3,(#276212,#276213,#276214,#276215,#276216,
#276217,#276218,#276219),.UNSPECIFIED.,.F.,.F.,(4,2,2,4),(0.886181891443318,
1.00363319154204,1.25505529473825,1.52001564473151),.UNSPECIFIED.);
#6683=B_SPLINE_CURVE_WITH_KNOTS('',3,(#276223,#276224,#276225,#276226,#276227,
#276228,#276229,#276230,#276231,#276232,#276233,#276234,#276235,#276236,
#276237,#276238,#276239,#276240,#276241,#276242,#276243,#276244,#276245,
#276246,#276247,#276248,#276249,#276250,#276251,#276252,#276253,#276254,
#276255,#276256,#276257,#276258,#276259,#276260),.UNSPECIFIED.,.F.,.F.,
(4,2,2,2,2,2,2,2,2,2,2,2,2,2,2,2,2,2,4),(1.00000002956069E-6,0.376972969184724,
0.75799918633037,1.21242033240789,1.43740179078372,1.88669535644621,2.30937841181643,
2.68597888099499,3.12649045709018,3.62482966496969,4.11196706709142,4.60170487876917,
4.84231053032182,5.29690378277065,5.76750323625794,6.27455902097634,6.7799859159262,
7.21138329694587,7.34352906207753),.UNSPECIFIED.);
#6684=B_SPLINE_CURVE_WITH_KNOTS('',3,(#276262,#276263,#276264,#276265,#276266,
#276267,#276268,#276269,#276270,#276271),.UNSPECIFIED.,.F.,.F.,(4,2,2,2,
4),(1.11775283487271,1.3201344337092,1.98402684478003,2.41673859827204,
2.92708277165291),.UNSPECIFIED.);
#6685=B_SPLINE_CURVE_WITH_KNOTS('',3,(#276273,#276274,#276275,#276276),
 .UNSPECIFIED.,.F.,.F.,(4,4),(9.99999986243288E-7,0.188629584531221),
 .UNSPECIFIED.);
#6686=B_SPLINE_CURVE_WITH_KNOTS('',3,(#276280,#276281,#276282,#276283,#276284,
#276285,#276286,#276287,#276288,#276289,#276290,#276291,#276292,#276293,
#276294,#276295,#276296,#276297,#276298,#276299,#276300,#276301,#276302,
#276303,#276304,#276305,#276306,#276307,#276308,#276309,#276310,#276311,
#276312,#276313,#276314,#276315,#276316,#276317),.UNSPECIFIED.,.F.,.F.,
(4,2,2,2,2,2,2,2,2,2,2,2,2,2,2,2,2,2,4),(0.188629584531221,0.394123083444476,
0.775094908203116,1.00161149469956,1.45530454079207,1.88145272689184,2.26155886735503,
2.69362881864141,3.16125461205091,3.61936691473805,4.07995327375831,4.56161966164196,
5.04003114519772,5.5043665714204,5.92302774285437,6.13173895340881,6.53854095434356,
6.91901551588997,7.29112327722061),.UNSPECIFIED.);
#6687=B_SPLINE_CURVE_WITH_KNOTS('',3,(#280873,#280874,#280875,#280876,#280877,
#280878,#280879,#280880),.UNSPECIFIED.,.F.,.F.,(4,2,2,4),(-46.6217887874376,
-46.2578454585251,-45.8892323703203,-45.6738876706438),.UNSPECIFIED.);
#6688=B_SPLINE_CURVE_WITH_KNOTS('',3,(#280885,#280886,#280887,#280888,#280889,
#280890,#280891,#280892,#280893,#280894,#280895,#280896,#280897,#280898,
#280899,#280900,#280901,#280902,#280903,#280904,#280905,#280906,#280907,
#280908,#280909,#280910,#280911,#280912,#280913,#280914,#280915,#280916,
#280917,#280918,#280919,#280920),.UNSPECIFIED.,.F.,.F.,(4,2,2,2,2,2,2,2,
2,2,2,2,2,2,2,2,2,4),(-7.56876057602163,-7.35729635649663,-6.88731803123374,
-6.41494627125509,-5.95046718064394,-5.47640437326289,-5.00939178691373,
-4.54231615347622,-4.06438205582116,-3.59996445059252,-3.12905565079213,
-2.658464871178,-2.19369990895879,-1.71864614164823,-1.25265148999412,-0.784624653178984,
-0.392650910730672,-1.00000001790335E-6),.UNSPECIFIED.);
#6689=B_SPLINE_CURVE_WITH_KNOTS('',3,(#280921,#280922,#280923,#280924,#280925,
#280926,#280927,#280928,#280929,#280930,#280931,#280932,#280933,#280934,
#280935,#280936,#280937,#280938,#280939,#280940,#280941,#280942,#280943,
#280944,#280945,#280946,#280947,#280948,#280949,#280950,#280951,#280952,
#280953,#280954,#280955,#280956),.UNSPECIFIED.,.F.,.F.,(4,2,2,2,2,2,2,2,
2,2,2,2,2,2,2,2,2,4),(-45.6738876706438,-45.4241622385571,-44.9471446938412,
-44.4811383037189,-44.0127611847923,-43.539964174791,-43.0756517655993,
-42.6010485658741,-42.132245850907,-41.6665520052273,-41.1906903497208,
-40.7254451393306,-40.2556172366779,-39.7839324263573,-39.3195205227013,
-38.8427377357185,-38.3749498540981,-38.1024403174797),.UNSPECIFIED.);
#6690=B_SPLINE_CURVE_WITH_KNOTS('',3,(#280961,#280962,#280963,#280964,#280965,
#280966,#280967,#280968,#280969,#280970,#280971,#280972,#280973,#280974,
#280975,#280976,#280977,#280978,#280979,#280980,#280981,#280982,#280983,
#280984,#280985,#280986,#280987,#280988,#280989,#280990,#280991,#280992,
#280993,#280994,#280995,#280996),.UNSPECIFIED.,.F.,.F.,(4,2,2,2,2,2,2,2,
2,2,2,2,2,2,2,2,2,4),(-15.1390134568254,-14.8703711811418,-14.4025233596478,
-13.9261219694299,-13.4618117547277,-12.9900535016762,-12.5205100985779,
-12.0552503764082,-11.5793093004391,-11.1137879339429,-10.6449122869091,
-10.1706599895591,-9.70640996906313,-9.23352862264522,-8.76539906730381,
-8.29933862556263,-7.82223236481082,-7.56876057602163),.UNSPECIFIED.);
#6691=B_SPLINE_CURVE_WITH_KNOTS('',3,(#280997,#280998,#280999,#281000,#281001,
#281002,#281003,#281004,#281005,#281006,#281007,#281008,#281009,#281010,
#281011,#281012,#281013,#281014,#281015,#281016,#281017,#281018,#281019,
#281020,#281021,#281022,#281023,#281024,#281025,#281026,#281027,#281028,
#281029,#281030,#281031,#281032),.UNSPECIFIED.,.F.,.F.,(4,2,2,2,2,2,2,2,
2,2,2,2,2,2,2,2,2,4),(-38.1024403174797,-37.908369141637,-37.4335703060707,
-36.9687843751113,-36.4972733014153,-36.0265964184819,-35.5618083565122,
-35.0839631626955,-34.6172720333329,-34.1497547127705,-33.6761535978443,
-33.2117526390136,-32.7385416715103,-32.2689933140818,-31.8037803554565,
-31.3271318265374,-30.8613991691482,-30.5307647496651),.UNSPECIFIED.);
#6692=B_SPLINE_CURVE_WITH_KNOTS('',3,(#281037,#281038,#281039,#281040,#281041,
#281042,#281043,#281044,#281045,#281046,#281047,#281048,#281049,#281050,
#281051,#281052,#281053,#281054,#281055,#281056,#281057,#281058,#281059,
#281060,#281061,#281062,#281063,#281064,#281065,#281066,#281067,#281068,
#281069,#281070,#281071,#281072),.UNSPECIFIED.,.F.,.F.,(4,2,2,2,2,2,2,2,
2,2,2,2,2,2,2,2,2,4),(-22.7092124132459,-22.382818915422,-21.9170703529098,
-21.4403616643235,-20.9753261216896,-20.5057249837587,-20.0328733432699,
-19.5685359670655,-19.0948722977256,-18.627606354345,-18.1608627726006,
-17.6829518794475,-17.2183013266551,-16.7475673180964,-16.2763682436002,
-15.8116091528861,-15.3367457660718,-15.1390134568254),.UNSPECIFIED.);
#6693=B_SPLINE_CURVE_WITH_KNOTS('',3,(#281073,#281074,#281075,#281076,#281077,
#281078,#281079,#281080,#281081,#281082,#281083,#281084,#281085,#281086,
#281087,#281088,#281089,#281090,#281091,#281092,#281093,#281094,#281095,
#281096,#281097,#281098,#281099,#281100,#281101,#281102,#281103,#281104,
#281105,#281106,#281107,#281108),.UNSPECIFIED.,.F.,.F.,(4,2,2,2,2,2,2,2,
2,2,2,2,2,2,2,2,2,4),(-30.5307647496651,-30.3926305138291,-29.9201905225812,
-29.4558935047261,-28.9806754193057,-28.5122020231605,-28.0462831131032,
-27.5707668457713,-27.105706206466,-26.6411884352463,-26.1670855034839,
-25.7000350708087,-25.2329199200806,-24.7549480979426,-24.2904922625418,
-23.819543534539,-23.3489150935619,-22.9601719025343),.UNSPECIFIED.);
#6694=B_SPLINE_CURVE_WITH_KNOTS('',3,(#281113,#281114,#281115,#281116,#281117,
#281118,#281119,#281120,#281121,#281122,#281123,#281124,#281125,#281126,
#281127,#281128,#281129,#281130,#281131,#281132,#281133,#281134,#281135,
#281136,#281137,#281138,#281139,#281140,#281141,#281142,#281143,#281144,
#281145,#281146,#281147,#281148),.UNSPECIFIED.,.F.,.F.,(4,2,2,2,2,2,2,2,
2,2,2,2,2,2,2,2,2,4),(-30.27910381554,-29.8960477742315,-29.4249957993259,
-28.954161031348,-28.4895402681035,-28.0115217593285,-27.5446786938516,
-27.0775194213598,-26.6037507201956,-26.1393927796599,-25.6667207227057,
-25.1970215589772,-24.73131825619,-24.2628015575025,-23.7879822109015,-23.3237890760973,
-22.8512936595655,-22.7092124132459),.UNSPECIFIED.);
#6695=B_SPLINE_CURVE_WITH_KNOTS('',3,(#281149,#281150,#281151,#281152,#281153,
#281154,#281155,#281156,#281157,#281158,#281159,#281160,#281161,#281162,
#281163,#281164,#281165,#281166,#281167,#281168,#281169,#281170,#281171,
#281172,#281173,#281174,#281175,#281176,#281177,#281178,#281179,#281180,
#281181,#281182,#281183,#281184),.UNSPECIFIED.,.F.,.F.,(4,2,2,2,2,2,2,2,
2,2,2,2,2,2,2,2,2,4),(-22.9601719025343,-22.8841111809573,-22.4090170950461,
-21.9429845050713,-21.4749179720702,-20.9992332900195,-20.5350391956014,
-20.0630335999792,-19.5939976673447,-19.128604847174,-18.65240363536,-18.187149951532,
-17.718030056841,-17.24442435561,-16.7802061331413,-16.3070565274049,-15.8393525332099,
-15.3912550272859),.UNSPECIFIED.);
#6696=B_SPLINE_CURVE_WITH_KNOTS('',3,(#281189,#281190,#281191,#281192,#281193,
#281194,#281195,#281196,#281197,#281198,#281199,#281200,#281201,#281202,
#281203,#281204,#281205,#281206,#281207,#281208,#281209,#281210,#281211,
#281212,#281213,#281214,#281215,#281216,#281217,#281218,#281219,#281220,
#281221,#281222,#281223,#281224),.UNSPECIFIED.,.F.,.F.,(4,2,2,2,2,2,2,2,
2,2,2,2,2,2,2,2,2,4),(-37.8493859968929,-37.4070914074001,-36.9390646224457,
-36.466064763649,-36.0017935798579,-35.5277130470903,-35.058726900269,-34.5932584637534,
-34.1172014784137,-33.6518686415785,-33.1824532454847,-32.71058352461,-32.2462786662642,
-31.7700701952743,-31.3021203457283,-30.8358216690874,-30.3608520954614,
-30.27910381554),.UNSPECIFIED.);
#6697=B_SPLINE_CURVE_WITH_KNOTS('',3,(#281225,#281226,#281227,#281228,#281229,
#281230,#281231,#281232,#281233,#281234,#281235,#281236,#281237,#281238,
#281239,#281240,#281241,#281242,#281243,#281244,#281245,#281246,#281247,
#281248,#281249,#281250,#281251,#281252,#281253,#281254,#281255,#281256,
#281257,#281258,#281259,#281260,#281261,#281262),.UNSPECIFIED.,.F.,.F.,
(4,2,2,2,2,2,2,2,2,2,2,2,2,2,2,2,2,2,4),(-15.3912550272859,-15.3730765213189,
-14.8956926027671,-14.4309419924448,-13.9607049000054,-13.4888885828601,
-13.0243600322952,-12.5500194056437,-12.0833400442585,-11.6159969274629,
-11.1387717209122,-10.6744669851398,-10.2032577033738,-9.73317433233838,
-9.26826994282085,-8.79289947084361,-8.32717155512522,-7.85884267836123,
-7.82217132368041),.UNSPECIFIED.);
#6698=B_SPLINE_CURVE_WITH_KNOTS('',3,(#281268,#281269,#281270,#281271),
 .UNSPECIFIED.,.F.,.F.,(4,4),(-0.254027045710766,-1.00000002078993E-6),
 .UNSPECIFIED.);
#6699=B_SPLINE_CURVE_WITH_KNOTS('',3,(#281274,#281275,#281276,#281277,#281278,
#281279,#281280,#281281),.UNSPECIFIED.,.F.,.F.,(4,2,2,4),(-46.6160574698286,
-46.238612042811,-45.8638054928735,-45.419398246854),.UNSPECIFIED.);
#6700=B_SPLINE_CURVE_WITH_KNOTS('',3,(#281283,#281284,#281285,#281286,#281287,
#281288,#281289,#281290,#281291,#281292,#281293,#281294,#281295,#281296,
#281297,#281298,#281299,#281300,#281301,#281302,#281303,#281304,#281305,
#281306,#281307,#281308,#281309,#281310,#281311,#281312,#281313,#281314,
#281315,#281316,#281317,#281318,#281319,#281320),.UNSPECIFIED.,.F.,.F.,
(4,2,2,2,2,2,2,2,2,2,2,2,2,2,2,2,2,2,4),(-45.419398246854,-45.388335458859,
-44.9201788529334,-44.4542375100199,-43.9790489160334,-43.5142083505892,
-43.0437468660947,-42.5727088239309,-42.1082957172573,-41.6305539035994,
-41.1633599487675,-40.6964212557151,-40.2222364592212,-39.7577103098546,
-39.2854822068615,-38.8153883474286,-38.3504794784601,-37.8732513328493,
-37.8493859968929),.UNSPECIFIED.);
#6701=B_SPLINE_CURVE_WITH_KNOTS('',3,(#281321,#281322,#281323,#281324,#281325,
#281326,#281327,#281328,#281329,#281330,#281331,#281332,#281333,#281334,
#281335,#281336,#281337,#281338,#281339,#281340,#281341,#281342,#281343,
#281344,#281345,#281346,#281347,#281348,#281349,#281350,#281351,#281352,
#281353,#281354,#281355,#281356),.UNSPECIFIED.,.F.,.F.,(4,2,2,2,2,2,2,2,
2,2,2,2,2,2,2,2,2,4),(-7.82217132368041,-7.38385187621001,-6.91972506820527,
-6.44742865870557,-5.97886619559227,-5.51328243212834,-5.03677797532993,
-4.57174887967328,-4.10234361258054,-3.62935221798109,-3.16511416248466,
-2.69165565360192,-2.22433643981363,-1.75778780089319,-1.28008600548505,
-0.815474412442063,-0.405490990239572,-0.254027045710766),.UNSPECIFIED.);
#6702=B_SPLINE_CURVE_WITH_KNOTS('',3,(#281409,#281410,#281411,#281412,#281413,
#281414,#281415,#281416,#281417,#281418,#281419,#281420),.UNSPECIFIED.,
 .F.,.F.,(4,2,2,2,2,4),(9.99999999029508E-7,0.392467864625591,0.772803552303566,
1.20676402389129,1.59513819877189,1.97927314617369),.UNSPECIFIED.);
#6703=B_SPLINE_CURVE_WITH_KNOTS('',3,(#281424,#281425,#281426,#281427,#281428,
#281429,#281430,#281431,#281432,#281433,#281434,#281435,#281436,#281437,
#281438,#281439,#281440,#281441,#281442,#281443,#281444,#281445,#281446,
#281447,#281448,#281449,#281450,#281451,#281452,#281453),.UNSPECIFIED.,
 .F.,.F.,(4,2,2,2,2,2,2,2,2,2,2,2,2,2,4),(1.97927314617369,2.02730718991295,
2.48197895053455,2.92990213883089,3.38495238463682,3.85815130246585,4.33242573779402,
4.79625192402839,5.21479621725514,5.42409530491494,5.83033362431084,6.24041628338956,
6.44209040988607,6.81263411618772,7.17194255907665),.UNSPECIFIED.);
#6704=B_SPLINE_CURVE_WITH_KNOTS('',3,(#281454,#281455,#281456,#281457,#281458,
#281459,#281460,#281461,#281462,#281463,#281464,#281465,#281466,#281467),
 .UNSPECIFIED.,.F.,.F.,(4,2,2,2,2,2,4),(0.,0.303989670039342,0.666040902826767,
1.36264560499374,2.25979709302026,2.777868489948,3.29723672060596),
 .UNSPECIFIED.);
#6705=B_SPLINE_CURVE_WITH_KNOTS('',3,(#281483,#281484,#281485,#281486,#281487,
#281488,#281489,#281490,#281491,#281492,#281493,#281494,#281495,#281496,
#281497,#281498),.UNSPECIFIED.,.F.,.F.,(4,2,2,2,2,2,2,4),(0.,0.238087952519387,
0.476113544168717,1.01011910515244,1.73799046632944,2.30408220983986,2.86072831234553,
3.43288601470779),.UNSPECIFIED.);
#6706=B_SPLINE_CURVE_WITH_KNOTS('',3,(#281499,#281500,#281501,#281502,#281503,
#281504,#281505,#281506,#281507,#281508,#281509,#281510,#281511,#281512,
#281513,#281514),.UNSPECIFIED.,.F.,.F.,(4,2,2,2,2,2,2,4),(1.00000044233709E-6,
0.539370132359783,1.28481747817566,1.98442658665292,2.48325218307673,2.95253551271824,
3.30333512017195,3.64287608445345),.UNSPECIFIED.);
#6707=B_SPLINE_CURVE_WITH_KNOTS('',3,(#285740,#285741,#285742,#285743,#285744,
#285745,#285746,#285747,#285748,#285749,#285750,#285751,#285752,#285753,
#285754,#285755,#285756,#285757,#285758,#285759,#285760,#285761,#285762,
#285763),.UNSPECIFIED.,.F.,.F.,(4,2,2,2,2,2,2,2,2,2,2,4),(1.00000001673761E-6,
0.323039742323442,0.634605365470257,1.07005687139309,1.45978725204872,1.89383348337783,
2.35103053579564,2.80133004158489,3.25887862097597,3.72872917648254,4.27536018155541,
4.56129717631177),.UNSPECIFIED.);
#6708=B_SPLINE_CURVE_WITH_KNOTS('',3,(#285767,#285768,#285769,#285770,#285771,
#285772,#285773,#285774,#285775,#285776,#285777,#285778,#285779,#285780,
#285781,#285782,#285783,#285784,#285785,#285786),.UNSPECIFIED.,.F.,.F.,
(4,2,2,2,2,2,2,2,2,4),(4.56129717631177,4.78025138948249,5.24019813332798,
5.47080497646155,5.91680419253928,6.36814416866029,6.58957679463825,7.00642309193714,
7.22277354918002,7.44333948969208),.UNSPECIFIED.);
#6709=B_SPLINE_CURVE_WITH_KNOTS('',3,(#285788,#285789,#285790,#285791,#285792,
#285793,#285794,#285795,#285796,#285797,#285798,#285799),.UNSPECIFIED.,
 .F.,.F.,(4,2,2,2,2,4),(-3.21369901094688,-2.40395999881897,-1.62924044691679,
-0.911220628324192,-0.414117520413494,0.),.UNSPECIFIED.);
#6710=B_SPLINE_CURVE_WITH_KNOTS('',3,(#285814,#285815,#285816,#285817,#285818,
#285819,#285820,#285821,#285822,#285823,#285824,#285825,#285826,#285827),
 .UNSPECIFIED.,.F.,.F.,(4,2,2,2,2,2,4),(-2.64506467679378,-2.30500727703039,
-1.84084072046588,-1.36787613459182,-0.900047765262215,-0.450187418519317,
-9.99999997031153E-7),.UNSPECIFIED.);
#6711=B_SPLINE_CURVE_WITH_KNOTS('',3,(#287914,#287915,#287916,#287917,#287918,
#287919,#287920,#287921,#287922,#287923,#287924,#287925,#287926,#287927,
#287928,#287929,#287930,#287931),.UNSPECIFIED.,.F.,.F.,(4,2,2,2,2,2,2,2,
4),(0.,0.226844249939865,0.465043591920983,0.874045242019083,1.423867627709,
2.24701645815008,2.92758088609289,3.21943913627986,3.52521182016246),
 .UNSPECIFIED.);
#6712=B_SPLINE_CURVE_WITH_KNOTS('',3,(#290007,#290008,#290009,#290010,#290011,
#290012,#290013,#290014,#290015,#290016,#290017,#290018,#290019,#290020,
#290021,#290022),.UNSPECIFIED.,.F.,.F.,(4,2,2,2,2,2,2,4),(9.99999979533284E-7,
0.442518894276843,1.00228459757929,1.78979762641102,2.54504033256861,3.08734332574651,
3.32519808039208,3.56352063065413),.UNSPECIFIED.);
#6713=B_SPLINE_CURVE_WITH_KNOTS('',3,(#291512,#291513,#291514,#291515,#291516,
#291517,#291518,#291519),.UNSPECIFIED.,.F.,.F.,(4,2,2,4),(93.9993055949368,
94.3962462510942,94.7498463849653,95.1031006473574),.UNSPECIFIED.);
#6714=B_SPLINE_CURVE_WITH_KNOTS('',3,(#291522,#291523,#291524,#291525),
 .UNSPECIFIED.,.F.,.F.,(4,4),(1.00000001485023E-6,0.159782552535823),
 .UNSPECIFIED.);
#6715=B_SPLINE_CURVE_WITH_KNOTS('',3,(#291530,#291531,#291532,#291533,#291534,
#291535,#291536,#291537,#291538,#291539,#291540,#291541,#291542,#291543,
#291544,#291545,#291546,#291547,#291548,#291549,#291550,#291551,#291552,
#291553,#291554,#291555,#291556,#291557,#291558,#291559,#291560,#291561,
#291562,#291563,#291564,#291565),.UNSPECIFIED.,.F.,.F.,(4,2,2,2,2,2,2,2,
2,2,2,2,2,2,2,2,2,4),(86.4283032330504,86.8841446466063,87.3485119173072,
87.820329195308,88.289929201456,88.7552467982501,89.2312474538849,89.6968255999065,
90.1657599095305,90.6400689963987,91.1043763025996,91.5773168767035,92.0455030850787,
92.5116217372129,92.9887877759706,93.4537807497936,93.9238179812892,93.9993055949368),
 .UNSPECIFIED.);
#6716=B_SPLINE_CURVE_WITH_KNOTS('',3,(#291566,#291567,#291568,#291569,#291570,
#291571,#291572,#291573,#291574,#291575,#291576,#291577,#291578,#291579,
#291580,#291581,#291582,#291583,#291584,#291585,#291586,#291587,#291588,
#291589,#291590,#291591,#291592,#291593,#291594,#291595,#291596,#291597,
#291598,#291599,#291600,#291601,#291602,#291603),.UNSPECIFIED.,.F.,.F.,
(4,2,2,2,2,2,2,2,2,2,2,2,2,2,2,2,2,2,4),(0.159782552535823,0.252910728987131,
0.508836642406898,0.981847476572238,1.45142846116938,1.91654378355729,2.3932291166619,
2.85897304032226,3.32757846013873,3.80005253365681,4.26429331421471,4.7392892518596,
5.20778983727417,5.67358966710173,6.14913633685796,6.61418480437811,7.08429819311843,
7.55567986130047,7.72908631110027),.UNSPECIFIED.);
#6717=B_SPLINE_CURVE_WITH_KNOTS('',3,(#291608,#291609,#291610,#291611,#291612,
#291613,#291614,#291615,#291616,#291617,#291618,#291619,#291620,#291621,
#291622,#291623,#291624,#291625,#291626,#291627,#291628,#291629,#291630,
#291631,#291632,#291633,#291634,#291635,#291636,#291637,#291638,#291639,
#291640,#291641,#291642,#291643,#291644,#291645),.UNSPECIFIED.,.F.,.F.,
(4,2,2,2,2,2,2,2,2,2,2,2,2,2,2,2,2,2,4),(78.8571778264449,78.8922125296406,
79.3689807828779,79.8340730116635,80.3037327862311,80.7766409809457,81.2410356474547,
81.7147585162183,82.1820809757828,82.6488828483276,83.1268534867744,83.5915609200449,
84.0623537302704,84.5336094434342,84.99842609755,85.4733488429337,85.939780108239,
86.4076863886255,86.4283032330504),.UNSPECIFIED.);
#6718=B_SPLINE_CURVE_WITH_KNOTS('',3,(#291646,#291647,#291648,#291649,#291650,
#291651,#291652,#291653,#291654,#291655,#291656,#291657,#291658,#291659,
#291660,#291661,#291662,#291663,#291664,#291665,#291666,#291667,#291668,
#291669,#291670,#291671,#291672,#291673,#291674,#291675,#291676,#291677,
#291678,#291679,#291680,#291681),.UNSPECIFIED.,.F.,.F.,(4,2,2,2,2,2,2,2,
2,2,2,2,2,2,2,2,2,4),(7.72908631110027,8.02008352434038,8.49730419371805,
8.96481300151504,9.43155223815228,9.9060622753284,10.3707187452509,10.8425562258666,
11.3129584062321,11.7777947823367,12.2553490830901,12.7217834663287,13.1895307642473,
13.6628480915371,14.1271797316805,14.600790093664,15.0700725120836,15.3003047236943),
 .UNSPECIFIED.);
#6719=B_SPLINE_CURVE_WITH_KNOTS('',3,(#291686,#291687,#291688,#291689,#291690,
#291691,#291692,#291693,#291694,#291695,#291696,#291697,#291698,#291699,
#291700,#291701,#291702,#291703,#291704,#291705,#291706,#291707,#291708,
#291709,#291710,#291711,#291712,#291713,#291714,#291715,#291716,#291717,
#291718,#291719,#291720,#291721),.UNSPECIFIED.,.F.,.F.,(4,2,2,2,2,2,2,2,
2,2,2,2,2,2,2,2,2,4),(71.286676879443,71.3793362999404,71.853916807073,
72.3206016385598,72.7881784157484,73.265266886318,73.7296623484898,74.201118681301,
74.6711421432683,75.1362347817962,75.6118593900078,76.0776192284145,76.546194373815,
77.0210702754228,77.4853204386284,77.9578748686566,78.426406018764,78.8571778264449),
 .UNSPECIFIED.);
#6720=B_SPLINE_CURVE_WITH_KNOTS('',3,(#291722,#291723,#291724,#291725,#291726,
#291727,#291728,#291729,#291730,#291731,#291732,#291733,#291734,#291735,
#291736,#291737,#291738,#291739,#291740,#291741,#291742,#291743,#291744,
#291745,#291746,#291747,#291748,#291749,#291750,#291751,#291752,#291753,
#291754,#291755,#291756,#291757),.UNSPECIFIED.,.F.,.F.,(4,2,2,2,2,2,2,2,
2,2,2,2,2,2,2,2,2,4),(15.3003047236943,15.5353971469736,16.0117656400808,
16.4773020474794,16.9463663727299,17.4185359888615,17.8828282335684,18.3585046724596,
18.8267291967529,19.2928191356463,19.7680752712759,20.2330067249166,20.7036518752658,
21.1747588162273,21.6392983776734,22.1172539198714,22.5845205862061,22.8714706980816),
 .UNSPECIFIED.);
#6721=B_SPLINE_CURVE_WITH_KNOTS('',3,(#291762,#291763,#291764,#291765,#291766,
#291767,#291768,#291769,#291770,#291771,#291772,#291773,#291774,#291775,
#291776,#291777,#291778,#291779,#291780,#291781,#291782,#291783,#291784,
#291785,#291786,#291787,#291788,#291789,#291790,#291791,#291792,#291793,
#291794,#291795,#291796,#291797),.UNSPECIFIED.,.F.,.F.,(4,2,2,2,2,2,2,2,
2,2,2,2,2,2,2,2,2,4),(63.7157748578674,63.8667739613376,64.3390086392791,
64.8079809218208,65.2735610187678,65.749997216052,66.2152806166965,66.6846270421634,
67.1581164959717,67.622456849824,68.0958431164314,68.5635163180422,69.0300112888132,
69.5076364615024,69.9724490797265,70.4429178387003,70.9146543577095,71.286676879443),
 .UNSPECIFIED.);
#6722=B_SPLINE_CURVE_WITH_KNOTS('',3,(#291798,#291799,#291800,#291801,#291802,
#291803,#291804,#291805,#291806,#291807,#291808,#291809,#291810,#291811,
#291812,#291813,#291814,#291815,#291816,#291817,#291818,#291819,#291820,
#291821,#291822,#291823,#291824,#291825,#291826,#291827,#291828,#291829,
#291830,#291831,#291832,#291833),.UNSPECIFIED.,.F.,.F.,(4,2,2,2,2,2,2,2,
2,2,2,2,2,2,2,2,2,4),(22.8714706980816,23.051617364947,23.525875102884,
23.9905047761518,24.4629235046836,24.9330920693315,25.3981376396358,25.875439535867,
26.3416800031223,26.8098780475167,27.2829520142995,27.7473381575111,28.2216223900459,
28.6906851247604,29.1563019249832,29.6324349705965,30.0978598595751,30.4439313175857),
 .UNSPECIFIED.);
#6723=B_SPLINE_CURVE_WITH_KNOTS('',3,(#291838,#291839,#291840,#291841,#291842,
#291843,#291844,#291845,#291846,#291847,#291848,#291849,#291850,#291851,
#291852,#291853,#291854,#291855,#291856,#291857,#291858,#291859,#291860,
#291861,#291862,#291863,#291864,#291865,#291866,#291867,#291868,#291869,
#291870,#291871,#291872,#291873),.UNSPECIFIED.,.F.,.F.,(4,2,2,2,2,2,2,2,
2,2,2,2,2,2,2,2,2,4),(56.144083628874,56.3525198790904,56.8227384992186,
57.2950413906242,57.7596779166521,58.2339896093383,58.7010155850834,59.1683341887742,
59.6461425436081,60.1106559537008,60.5818215910562,61.0523603629285,61.5173169435704,
61.9926351088461,62.4586675805972,62.9269512318712,63.4024908375553,63.7157748578674),
 .UNSPECIFIED.);
#6724=B_SPLINE_CURVE_WITH_KNOTS('',3,(#291874,#291875,#291876,#291877,#291878,
#291879,#291880,#291881,#291882,#291883,#291884,#291885,#291886,#291887,
#291888,#291889,#291890,#291891,#291892,#291893,#291894,#291895,#291896,
#291897,#291898,#291899,#291900,#291901,#291902,#291903,#291904,#291905,
#291906,#291907,#291908,#291909),.UNSPECIFIED.,.F.,.F.,(4,2,2,2,2,2,2,2,
2,2,2,2,2,2,2,2,2,4),(30.4439313175857,30.5674582054022,31.0394048318556,
31.5038365004404,31.9802587733485,32.4482886730917,32.914746234382,33.3897958731133,
33.8547045464092,34.3259485102396,34.7968646444142,35.2616232427546,35.7397219718357,
36.2066456605547,36.6739778191192,37.1478267439181,37.6122999116294,38.016360947702),
 .UNSPECIFIED.);
#6725=B_SPLINE_CURVE_WITH_KNOTS('',3,(#291914,#291915,#291916,#291917,#291918,
#291919,#291920,#291921,#291922,#291923,#291924,#291925,#291926,#291927,
#291928,#291929,#291930,#291931,#291932,#291933,#291934,#291935,#291936,
#291937,#291938,#291939,#291940,#291941,#291942,#291943,#291944,#291945,
#291946,#291947,#291948,#291949),.UNSPECIFIED.,.F.,.F.,(4,2,2,2,2,2,2,2,
2,2,2,2,2,2,2,2,2,4),(48.5719605686275,48.8375787381526,49.3056503252136,
49.7819246755741,50.2463296313892,50.718323774952,51.1878163381561,51.6532648716521,
52.1294480473886,52.5950075109716,53.0641172410405,53.5382674171041,54.002643888761,
54.4757697545506,54.9438783970752,55.4101593272649,55.8875150473913,56.144083628874),
 .UNSPECIFIED.);
#6726=B_SPLINE_CURVE_WITH_KNOTS('',3,(#291950,#291951,#291952,#291953,#291954,
#291955,#291956,#291957,#291958,#291959,#291960,#291961,#291962,#291963,
#291964,#291965,#291966,#291967,#291968,#291969,#291970,#291971,#291972,
#291973,#291974,#291975,#291976,#291977,#291978,#291979,#291980,#291981,
#291982,#291983,#291984,#291985),.UNSPECIFIED.,.F.,.F.,(4,2,2,2,2,2,2,2,
2,2,2,2,2,2,2,2,2,4),(38.016360947702,38.0851789736651,38.5606918019714,
39.0266489381757,39.4951197018306,39.9704047728814,40.4347225522676,40.9071580162034,
41.3759772432034,41.8417118872276,42.3183551619773,42.7836004036095,43.2531445841241,
43.7264164718864,44.1908318584271,44.664427268518,45.1319885476618,45.5876503801449),
 .UNSPECIFIED.);
#6727=B_SPLINE_CURVE_WITH_KNOTS('',3,(#291990,#291991,#291992,#291993,#291994,
#291995,#291996,#291997,#291998,#291999,#292000,#292001,#292002,#292003,
#292004,#292005,#292006,#292007,#292008,#292009,#292010,#292011,#292012,
#292013,#292014,#292015,#292016,#292017,#292018,#292019,#292020,#292021,
#292022,#292023,#292024,#292025),.UNSPECIFIED.,.F.,.F.,(4,2,2,2,2,2,2,2,
2,2,2,2,2,2,2,2,2,4),(41.0001199248139,41.3231774301242,41.78911725615,
42.2660541939051,42.7311229051682,43.2009434587001,43.6736831387611,44.1381462914927,
44.6120386288035,45.0792786949266,45.5462430113534,46.0243865775315,46.4891026897119,
46.9600595973249,47.4311852824456,47.8960997290458,48.3711933932353,48.5719605686275),
 .UNSPECIFIED.);
#6728=B_SPLINE_CURVE_WITH_KNOTS('',3,(#292026,#292027,#292028,#292029,#292030,
#292031,#292032,#292033,#292034,#292035,#292036,#292037,#292038,#292039,
#292040,#292041,#292042,#292043,#292044,#292045,#292046,#292047,#292048,
#292049,#292050,#292051,#292052,#292053,#292054,#292055,#292056,#292057,
#292058,#292059,#292060,#292061,#292062,#292063),.UNSPECIFIED.,.F.,.F.,
(4,2,2,2,2,2,2,2,2,2,2,2,2,2,2,2,2,2,4),(45.5876503801449,45.5986758559509,
46.0765148693568,46.5413289532617,47.0120009270319,47.4835655594758,47.9483600945364,
48.4231528636811,48.8897704410641,49.3575529036341,49.8344003044135,50.2988326237114,
50.7705098865814,51.2403871160248,51.7056343950673,52.1814875721346,52.6472130277606,
53.1160082110126,53.1596619246187),.UNSPECIFIED.);
#6729=B_SPLINE_CURVE_WITH_KNOTS('',3,(#292068,#292069,#292070,#292071,#292072,
#292073,#292074,#292075,#292076,#292077,#292078,#292079,#292080,#292081,
#292082,#292083,#292084,#292085,#292086,#292087,#292088,#292089,#292090,
#292091,#292092,#292093,#292094,#292095,#292096,#292097,#292098,#292099,
#292100,#292101,#292102,#292103),.UNSPECIFIED.,.F.,.F.,(4,2,2,2,2,2,2,2,
2,2,2,2,2,2,2,2,2,4),(33.4289203540015,33.8017623441053,34.2734695384679,
34.7439861866962,35.2088049428035,35.6864802632978,36.1530204914359,36.6206766322363,
37.0941120115672,37.5584735418785,38.0319244250421,38.5013175525154,38.9665989988937,
39.4430838829474,39.9177587985401,40.3820449298253,40.8547633332481,41.0001199248139),
 .UNSPECIFIED.);
#6730=B_SPLINE_CURVE_WITH_KNOTS('',3,(#292104,#292105,#292106,#292107,#292108,
#292109,#292110,#292111,#292112,#292113,#292114,#292115,#292116,#292117,
#292118,#292119,#292120,#292121,#292122,#292123,#292124,#292125,#292126,
#292127,#292128,#292129,#292130,#292131,#292132,#292133,#292134,#292135,
#292136,#292137,#292138,#292139),.UNSPECIFIED.,.F.,.F.,(4,2,2,2,2,2,2,2,
2,2,2,2,2,2,2,2,2,4),(53.1596619246187,53.590671333377,54.0549979571361,
54.5277856350263,54.9962063209033,55.4622084789415,55.9392160136559,56.4043119711095,
56.8742008482708,57.3469359753347,57.8114468705411,58.2854097230149,58.7526640946325,
59.2196972269946,59.6979123556361,60.1626628717794,60.6336888645837,60.7316199823971),
 .UNSPECIFIED.);
#6731=B_SPLINE_CURVE_WITH_KNOTS('',3,(#292144,#292145,#292146,#292147,#292148,
#292149,#292150,#292151,#292152,#292153,#292154,#292155,#292156,#292157,
#292158,#292159,#292160,#292161,#292162,#292163,#292164,#292165,#292166,
#292167,#292168,#292169,#292170,#292171,#292172,#292173,#292174,#292175,
#292176,#292177,#292178,#292179),.UNSPECIFIED.,.F.,.F.,(4,2,2,2,2,2,2,2,
2,2,2,2,2,2,2,2,2,4),(25.8580916349655,26.2897324013408,26.7582466058542,
27.2308552574274,27.6951268991933,28.1699649318621,28.638591500359,29.1043500637385,
29.580027924796,30.0451581297893,30.5151573988414,30.9866653386247,31.4510741532502,
31.9281191055042,32.39574427877,32.862421157186,33.3370514851652,33.4289203540015),
 .UNSPECIFIED.);
#6732=B_SPLINE_CURVE_WITH_KNOTS('',3,(#292180,#292181,#292182,#292183,#292184,
#292185,#292186,#292187,#292188,#292189,#292190,#292191,#292192,#292193,
#292194,#292195,#292196,#292197,#292198,#292199,#292200,#292201,#292202,
#292203,#292204,#292205,#292206,#292207,#292208,#292209,#292210,#292211,
#292212,#292213,#292214,#292215),.UNSPECIFIED.,.F.,.F.,(4,2,2,2,2,2,2,2,
2,2,2,2,2,2,2,2,2,4),(60.7316199823971,61.1048185437779,61.5697872371334,
62.0449517676864,62.5113595052275,62.9795002075708,63.4557669984041,63.9202128194296,
64.3922788870764,64.8617804579765,65.3272906155987,65.8035472390145,66.2691351401704,
66.738316236739,67.2124643837799,67.6768887040922,68.1500883737649,68.3044870520947),
 .UNSPECIFIED.);
#6733=B_SPLINE_CURVE_WITH_KNOTS('',3,(#292220,#292221,#292222,#292223,#292224,
#292225,#292226,#292227,#292228,#292229,#292230,#292231,#292232,#292233,
#292234,#292235,#292236,#292237,#292238,#292239,#292240,#292241,#292242,
#292243,#292244,#292245,#292246,#292247,#292248,#292249,#292250,#292251,
#292252,#292253,#292254,#292255,#292256,#292257),.UNSPECIFIED.,.F.,.F.,
(4,2,2,2,2,2,2,2,2,2,2,2,2,2,2,2,2,2,4),(18.2865751343784,18.3079357785441,
18.7758965839359,19.2423287253566,19.7173075924809,20.1821613811676,20.6533968732839,
21.1242439543697,21.5889660187706,22.0669933427192,22.5338486997724,23.0011628723484,
23.4749414259118,23.9393657833007,24.4122441508144,24.8819572888962,25.3470560430857,
25.823879834484,25.8580916349655),.UNSPECIFIED.);
#6734=B_SPLINE_CURVE_WITH_KNOTS('',3,(#292258,#292259,#292260,#292261,#292262,
#292263,#292264,#292265,#292266,#292267,#292268,#292269,#292270,#292271,
#292272,#292273,#292274,#292275,#292276,#292277,#292278,#292279,#292280,
#292281,#292282,#292283,#292284,#292285,#292286,#292287,#292288,#292289,
#292290,#292291,#292292,#292293),.UNSPECIFIED.,.F.,.F.,(4,2,2,2,2,2,2,2,
2,2,2,2,2,2,2,2,2,4),(68.3044870520947,68.6182126328683,69.0845621343954,
69.5619929048661,70.0270329255262,70.4973242517696,70.9696324304201,71.4343235782796,
71.9087100116139,72.3757591231006,72.8431508542522,73.3209523395419,73.7855068821371,
74.2567488157943,74.7272966253318,75.1923153308094,75.6677115997742,75.8772668463336),
 .UNSPECIFIED.);
#6735=B_SPLINE_CURVE_WITH_KNOTS('',3,(#292298,#292299,#292300,#292301,#292302,
#292303,#292304,#292305,#292306,#292307,#292308,#292309,#292310,#292311,
#292312,#292313,#292314,#292315,#292316,#292317,#292318,#292319,#292320,
#292321,#292322,#292323,#292324,#292325,#292326,#292327,#292328,#292329,
#292330,#292331,#292332,#292333),.UNSPECIFIED.,.F.,.F.,(4,2,2,2,2,2,2,2,
2,2,2,2,2,2,2,2,2,4),(10.7151222517789,10.7913599012759,11.2614558718779,
11.7264642452055,12.203691307493,12.6698634933475,13.138042532141,13.611042890141,
14.0753800813121,14.5496616010084,15.0186530670319,15.4842389138994,15.960298702674,
16.4256618397833,16.8952472113547,17.3671220636508,17.8315112596137,18.2865751343784),
 .UNSPECIFIED.);
#6736=B_SPLINE_CURVE_WITH_KNOTS('',3,(#292334,#292335,#292336,#292337,#292338,
#292339,#292340,#292341,#292342,#292343,#292344,#292345,#292346,#292347,
#292348,#292349,#292350,#292351,#292352,#292353,#292354,#292355,#292356,
#292357,#292358,#292359,#292360,#292361,#292362,#292363,#292364,#292365,
#292366,#292367,#292368,#292369),.UNSPECIFIED.,.F.,.F.,(4,2,2,2,2,2,2,2,
2,2,2,2,2,2,2,2,2,4),(75.8772668463336,76.1337725928702,76.6021323698784,
77.0776691799798,77.5420003802429,78.014314023934,78.4833010889462,78.9489509317474,
79.4254676248807,79.8907861158707,80.3602107320054,80.833703738573,81.2980994399929,
81.7715663367368,82.2392615376057,82.705833195356,83.1835402439425,83.4488930554441),
 .UNSPECIFIED.);
#6737=B_SPLINE_CURVE_WITH_KNOTS('',3,(#292374,#292375,#292376,#292377,#292378,
#292379,#292380,#292381,#292382,#292383,#292384,#292385,#292386,#292387,
#292388,#292389,#292390,#292391,#292392,#292393,#292394,#292395,#292396,
#292397,#292398,#292399,#292400,#292401,#292402,#292403,#292404,#292405,
#292406,#292407,#292408,#292409),.UNSPECIFIED.,.F.,.F.,(4,2,2,2,2,2,2,2,
2,2,2,2,2,2,2,2,2,4),(3.14443208990716,3.27554668679239,3.74763766305925,
4.2118807700592,4.68755559513844,5.15570421655467,5.62176327704835,6.09694161106962,
6.56181075862647,7.03244318834201,7.50347408717017,7.96797097464197,8.44592850904672,
8.91312216961858,9.38019300365707,9.85437618111417,10.3189505589872,10.7151222517789),
 .UNSPECIFIED.);
#6738=B_SPLINE_CURVE_WITH_KNOTS('',3,(#292410,#292411,#292412,#292413,#292414,
#292415,#292416,#292417,#292418,#292419,#292420,#292421,#292422,#292423,
#292424,#292425,#292426,#292427,#292428,#292429,#292430,#292431,#292432,
#292433,#292434,#292435,#292436,#292437,#292438,#292439,#292440,#292441,
#292442,#292443,#292444,#292445),.UNSPECIFIED.,.F.,.F.,(4,2,2,2,2,2,2,2,
2,2,2,2,2,2,2,2,2,4),(83.4488930554441,83.6483950281211,84.1189431117052,
84.5906911700159,85.0554352920183,85.5300971477342,85.9968119055917,86.4644682251567,
86.9415561790123,87.4060001152473,87.877539120961,88.3475784949245,88.8127409501058,
89.2884500085642,89.754245569256,90.2229029989712,90.6977831716255,91.0207492930948),
 .UNSPECIFIED.);
#6739=B_SPLINE_CURVE_WITH_KNOTS('',3,(#292451,#292452,#292453,#292454,#292455,
#292456,#292457,#292458,#292459,#292460,#292461,#292462,#292463,#292464,
#292465,#292466,#292467,#292468,#292469,#292470,#292471,#292472),
 .UNSPECIFIED.,.F.,.F.,(4,2,2,2,2,2,2,2,2,2,4),(136.24403458457,136.622483679541,
137.087116542782,137.561813612369,138.028135240898,138.495820731345,138.972238243539,
139.436453120851,139.908042383763,140.37046393164,140.833986548193),
 .UNSPECIFIED.);
#6740=B_SPLINE_CURVE_WITH_KNOTS('',3,(#292475,#292476,#292477,#292478,#292479,
#292480,#292481,#292482,#292483,#292484,#292485,#292486,#292487,#292488,
#292489,#292490,#292491,#292492),.UNSPECIFIED.,.F.,.F.,(4,2,2,2,2,2,2,2,
4),(1.00000002595246E-6,0.432220701825413,0.859903589947374,1.3366986521,
1.80250598802853,2.27083750612852,2.74341592545933,3.20758955595405,3.63988072813663),
 .UNSPECIFIED.);
#6741=B_SPLINE_CURVE_WITH_KNOTS('',3,(#292497,#292498,#292499,#292500,#292501,
#292502,#292503,#292504,#292505,#292506,#292507,#292508,#292509,#292510,
#292511,#292512,#292513,#292514,#292515,#292516,#292517,#292518,#292519,
#292520,#292521,#292522,#292523,#292524,#292525,#292526,#292527,#292528,
#292529,#292530,#292531,#292532),.UNSPECIFIED.,.F.,.F.,(4,2,2,2,2,2,2,2,
2,2,2,2,2,2,2,2,2,4),(128.675938040482,129.112558893719,129.576657723443,
130.048991214851,130.517448780484,130.983053196247,131.459596796231,131.924568127943,
132.394009334762,132.866869411823,133.331095846395,133.804594400205,134.271825895138,
134.738410083798,135.216153340899,135.680723343159,136.151295376315,136.24403458457),
 .UNSPECIFIED.);
#6742=B_SPLINE_CURVE_WITH_KNOTS('',3,(#292533,#292534,#292535,#292536,#292537,
#292538,#292539,#292540,#292541,#292542,#292543,#292544,#292545,#292546,
#292547,#292548,#292549,#292550,#292551,#292552,#292553,#292554,#292555,
#292556,#292557,#292558,#292559,#292560,#292561,#292562,#292563,#292564,
#292565,#292566,#292567,#292568,#292569,#292570),.UNSPECIFIED.,.F.,.F.,
(4,2,2,2,2,2,2,2,2,2,2,2,2,2,2,2,2,2,4),(3.63988072813663,3.68219744944784,
4.15078913768896,4.61639991622148,5.09204469600563,5.55711167641085,6.02691203047307,
6.49838465537246,6.96267787157272,7.43947959951173,7.9070637451659,8.37357792866613,
8.84816816756442,9.31279714879658,9.78429353632221,10.2547672182533,10.7194544807213,
11.1970895372671,11.2094799248909),.UNSPECIFIED.);
#6743=B_SPLINE_CURVE_WITH_KNOTS('',3,(#292575,#292576,#292577,#292578,#292579,
#292580,#292581,#292582,#292583,#292584,#292585,#292586,#292587,#292588,
#292589,#292590,#292591,#292592,#292593,#292594,#292595,#292596,#292597,
#292598,#292599,#292600,#292601,#292602,#292603,#292604,#292605,#292606,
#292607,#292608,#292609,#292610,#292611,#292612),.UNSPECIFIED.,.F.,.F.,
(4,2,2,2,2,2,2,2,2,2,2,2,2,2,2,2,2,2,4),(121.107364429924,121.123955006208,
121.60136663952,122.066059079849,122.536320554389,123.008007747065,123.472523016408,
123.94689130063,124.413484347362,124.880853415232,125.35792043923,125.822181143827,
126.293422250453,126.763386474281,127.228294640259,127.703699650335,128.169354359971,
128.637715264481,128.675938040482),.UNSPECIFIED.);
#6744=B_SPLINE_CURVE_WITH_KNOTS('',3,(#292613,#292614,#292615,#292616,#292617,
#292618,#292619,#292620,#292621,#292622,#292623,#292624,#292625,#292626,
#292627,#292628,#292629,#292630,#292631,#292632,#292633,#292634,#292635,
#292636,#292637,#292638,#292639,#292640,#292641,#292642,#292643,#292644,
#292645,#292646,#292647,#292648),.UNSPECIFIED.,.F.,.F.,(4,2,2,2,2,2,2,2,
2,2,2,2,2,2,2,2,2,4),(11.2094799248909,11.6635829376649,12.1310561877189,
12.6044504052173,13.0687133826433,13.5419326181211,14.011280641485,14.4764127911059,
14.9528547084907,15.418408801106,15.887154115734,16.3593915318822,16.8235710185186,
17.298815974715,17.7670945040135,18.2329514101939,18.7082674324183,18.7784627545738),
 .UNSPECIFIED.);
#6745=B_SPLINE_CURVE_WITH_KNOTS('',3,(#292653,#292654,#292655,#292656,#292657,
#292658,#292659,#292660,#292661,#292662,#292663,#292664,#292665,#292666,
#292667,#292668,#292669,#292670,#292671,#292672,#292673,#292674,#292675,
#292676,#292677,#292678,#292679,#292680,#292681,#292682,#292683,#292684,
#292685,#292686,#292687,#292688),.UNSPECIFIED.,.F.,.F.,(4,2,2,2,2,2,2,2,
2,2,2,2,2,2,2,2,2,4),(113.539080310834,113.613535836383,114.088649521034,
114.554593310473,115.022677384666,115.498200419705,115.962349691178,116.434377971026,
116.903293351852,117.368689275545,117.844915288929,118.31009488851,118.779236801359,
119.252695251587,119.71688487643,120.190060730064,120.657660459202,121.107364429924),
 .UNSPECIFIED.);
#6746=B_SPLINE_CURVE_WITH_KNOTS('',3,(#292689,#292690,#292691,#292692,#292693,
#292694,#292695,#292696,#292697,#292698,#292699,#292700,#292701,#292702,
#292703,#292704,#292705,#292706,#292707,#292708,#292709,#292710,#292711,
#292712,#292713,#292714,#292715,#292716,#292717,#292718,#292719,#292720,
#292721,#292722,#292723,#292724),.UNSPECIFIED.,.F.,.F.,(4,2,2,2,2,2,2,2,
2,2,2,2,2,2,2,2,2,4),(18.7784627545738,19.1731708477413,19.6434607197414,
20.1146201965419,20.5790046301623,21.056501945035,21.5238052639034,21.9906354266554,
22.4649335203834,22.9294898734969,23.4015289871598,23.8717291250978,24.3365830363145,
24.8139245228879,25.28017495983,25.7480597722722,26.2211694508468,26.3486586062954),
 .UNSPECIFIED.);
#6747=B_SPLINE_CURVE_WITH_KNOTS('',3,(#292729,#292730,#292731,#292732,#292733,
#292734,#292735,#292736,#292737,#292738,#292739,#292740,#292741,#292742,
#292743,#292744,#292745,#292746,#292747,#292748,#292749,#292750,#292751,
#292752,#292753,#292754,#292755,#292756,#292757,#292758,#292759,#292760,
#292761,#292762,#292763,#292764),.UNSPECIFIED.,.F.,.F.,(4,2,2,2,2,2,2,2,
2,2,2,2,2,2,2,2,2,4),(105.969272897385,106.100976102842,106.573907730878,
107.041957253409,107.508056840031,107.985215205638,108.4501158598,108.920142879015,
109.392410355181,109.856897820666,110.331012971347,110.797962572073,111.265088687778,
111.742889573364,112.20728516231,112.67825074303,113.148745691294,113.539080310834),
 .UNSPECIFIED.);
#6748=B_SPLINE_CURVE_WITH_KNOTS('',3,(#292765,#292766,#292767,#292768,#292769,
#292770,#292771,#292772,#292773,#292774,#292775,#292776,#292777,#292778,
#292779,#292780,#292781,#292782,#292783,#292784,#292785,#292786,#292787,
#292788,#292789,#292790,#292791,#292792,#292793,#292794,#292795,#292796,
#292797,#292798,#292799,#292800),.UNSPECIFIED.,.F.,.F.,(4,2,2,2,2,2,2,2,
2,2,2,2,2,2,2,2,2,4),(26.3486586062954,26.6854413743924,27.1592999290633,
27.6283870794954,28.0937707301691,28.5699346677542,29.0353280725909,29.5045718253718,
29.9765437467173,30.4408187574263,30.916779883259,31.3848214438468,31.8510084094083,
32.3260742260102,32.7909070779018,33.2617645498638,33.7326896544931,33.9189878766126),
 .UNSPECIFIED.);
#6749=B_SPLINE_CURVE_WITH_KNOTS('',3,(#292805,#292806,#292807,#292808,#292809,
#292810,#292811,#292812,#292813,#292814,#292815,#292816,#292817,#292818,
#292819,#292820,#292821,#292822,#292823,#292824,#292825,#292826,#292827,
#292828,#292829,#292830,#292831,#292832,#292833,#292834,#292835,#292836,
#292837,#292838,#292839,#292840),.UNSPECIFIED.,.F.,.F.,(4,2,2,2,2,2,2,2,
2,2,2,2,2,2,2,2,2,4),(98.3990302152714,98.5893892664047,99.0601631139654,
99.5312560680723,99.9960223863912,100.470928647386,100.937239158569,101.405127708902,
101.881395775322,102.34568347646,102.817487868981,103.286936380357,103.752219724559,
104.228209394403,104.693680205075,105.162601564527,105.636732990254,105.969272897385),
 .UNSPECIFIED.);
#6750=B_SPLINE_CURVE_WITH_KNOTS('',3,(#292841,#292842,#292843,#292844,#292845,
#292846,#292847,#292848,#292849,#292850,#292851,#292852,#292853,#292854,
#292855,#292856,#292857,#292858,#292859,#292860,#292861,#292862,#292863,
#292864,#292865,#292866,#292867,#292868,#292869,#292870,#292871,#292872,
#292873,#292874,#292875,#292876),.UNSPECIFIED.,.F.,.F.,(4,2,2,2,2,2,2,2,
2,2,2,2,2,2,2,2,2,4),(33.9189878766126,34.1972520714663,34.6753685555233,
35.1423031461174,35.6093148345641,36.0831788632793,36.5475371071326,37.0199763319678,
37.4897630905891,37.9546518147693,38.4315589904034,38.8974462320601,39.3656030133063,
39.8382894090536,40.3024443511905,40.7767910367888,41.2454804759632,41.4881001708513),
 .UNSPECIFIED.);
#6751=B_SPLINE_CURVE_WITH_KNOTS('',3,(#292881,#292882,#292883,#292884,#292885,
#292886,#292887,#292888,#292889,#292890,#292891,#292892,#292893,#292894,
#292895,#292896,#292897,#292898,#292899,#292900,#292901,#292902,#292903,
#292904,#292905,#292906,#292907,#292908,#292909,#292910,#292911,#292912,
#292913,#292914,#292915,#292916),.UNSPECIFIED.,.F.,.F.,(4,2,2,2,2,2,2,2,
2,2,2,2,2,2,2,2,2,4),(90.8296974779451,91.0766374667577,91.5451887830606,
92.0198667981449,92.4840365654737,92.9565715147367,93.424946900688,93.8907200849939,
94.3674702844793,94.8324529999625,95.3020923813277,95.7748187956589,96.2391488853637,
96.7128547646713,97.1800385313284,97.6468211298733,98.1247755874545,98.3990302152714),
 .UNSPECIFIED.);
#6752=B_SPLINE_CURVE_WITH_KNOTS('',3,(#292917,#292918,#292919,#292920,#292921,
#292922,#292923,#292924,#292925,#292926,#292927,#292928,#292929,#292930,
#292931,#292932,#292933,#292934,#292935,#292936,#292937,#292938,#292939,
#292940,#292941,#292942,#292943,#292944,#292945,#292946,#292947,#292948,
#292949,#292950,#292951,#292952),.UNSPECIFIED.,.F.,.F.,(4,2,2,2,2,2,2,2,
2,2,2,2,2,2,2,2,2,4),(41.4881001708513,41.7109798361461,42.1867282812913,
42.6518413385742,43.1214362960486,43.5930071060109,44.0572484489647,44.5337641130283,
45.0014346112672,45.4678094666162,45.9424903699166,46.4071305173474,46.8783991571689,
47.3489568235663,47.8135623653808,48.2912890647894,48.7578601251999,49.0573549288453),
 .UNSPECIFIED.);
#6753=B_SPLINE_CURVE_WITH_KNOTS('',3,(#292957,#292958,#292959,#292960,#292961,
#292962,#292963,#292964,#292965,#292966,#292967,#292968,#292969,#292970,
#292971,#292972,#292973,#292974,#292975,#292976,#292977,#292978,#292979,
#292980,#292981,#292982,#292983,#292984,#292985,#292986,#292987,#292988,
#292989,#292990,#292991,#292992),.UNSPECIFIED.,.F.,.F.,(4,2,2,2,2,2,2,2,
2,2,2,2,2,2,2,2,2,4),(83.2599065759065,83.5638785446524,84.0303385225607,
84.5079350778034,84.9726374682993,85.4430751168375,85.9146310054686,86.379246812249,
86.8537988530033,87.3203457237915,87.787893113324,88.2647721317994,88.7290714467532,
89.2005035658084,89.6703568226975,90.1353999365597,90.6110024064959,90.8296974779451),
 .UNSPECIFIED.);
#6754=B_SPLINE_CURVE_WITH_KNOTS('',3,(#292993,#292994,#292995,#292996,#292997,
#292998,#292999,#293000,#293001,#293002,#293003,#293004,#293005,#293006,
#293007,#293008,#293009,#293010,#293011,#293012,#293013,#293014,#293015,
#293016,#293017,#293018,#293019,#293020,#293021,#293022,#293023,#293024,
#293025,#293026,#293027,#293028),.UNSPECIFIED.,.F.,.F.,(4,2,2,2,2,2,2,2,
2,2,2,2,2,2,2,2,2,4),(49.0573549288453,49.2251563365931,49.6986391379984,
50.1628821752712,50.6358346231852,51.105262582369,51.5702796770147,52.0468081452395,
52.5124088045048,52.980941975819,53.4532615481695,53.9173873063535,54.3923333888046,
54.8606834805659,55.3263937313117,55.8017864800737,56.2667015279438,56.6256830979513),
 .UNSPECIFIED.);
#6755=B_SPLINE_CURVE_WITH_KNOTS('',3,(#293033,#293034,#293035,#293036,#293037,
#293038,#293039,#293040,#293041,#293042,#293043,#293044,#293045,#293046,
#293047,#293048,#293049,#293050,#293051,#293052,#293053,#293054,#293055,
#293056,#293057,#293058,#293059,#293060,#293061,#293062,#293063,#293064,
#293065,#293066,#293067,#293068),.UNSPECIFIED.,.F.,.F.,(4,2,2,2,2,2,2,2,
2,2,2,2,2,2,2,2,2,4),(75.6907199874016,76.0542240558732,76.5191143039749,
76.9943966225301,77.4602882622359,77.9285347773458,78.4038604257591,78.8680465700418,
79.3402486234638,79.8090485605776,80.2745788198699,80.7509839140138,81.216141299872,
81.6854546385995,82.1587450732675,82.6230044270935,83.0963611965978,83.2599065759065),
 .UNSPECIFIED.);
#6756=B_SPLINE_CURVE_WITH_KNOTS('',3,(#293069,#293070,#293071,#293072,#293073,
#293074,#293075,#293076,#293077,#293078,#293079,#293080,#293081,#293082,
#293083,#293084,#293085,#293086,#293087,#293088,#293089,#293090,#293091,
#293092,#293093,#293094,#293095,#293096,#293097,#293098,#293099,#293100,
#293101,#293102,#293103,#293104),.UNSPECIFIED.,.F.,.F.,(4,2,2,2,2,2,2,2,
2,2,2,2,2,2,2,2,2,4),(56.6256830979513,56.7367504130986,57.2079808841007,
57.6722786679109,58.1494551797369,58.6168172394204,59.0813134132729,59.5522332371109,
60.0229669193424,60.4877698659642,60.9628324484622,61.4289307276113,61.8969677657921,
62.3727826769255,62.8370034526151,63.308974812071,63.7781046940472,64.1949548606005),
 .UNSPECIFIED.);
#6757=B_SPLINE_CURVE_WITH_KNOTS('',3,(#293109,#293110,#293111,#293112,#293113,
#293114,#293115,#293116,#293117,#293118,#293119,#293120,#293121,#293122,
#293123,#293124,#293125,#293126,#293127,#293128,#293129,#293130,#293131,
#293132,#293133,#293134,#293135,#293136,#293137,#293138,#293139,#293140,
#293141,#293142,#293143,#293144),.UNSPECIFIED.,.F.,.F.,(4,2,2,2,2,2,2,2,
2,2,2,2,2,2,2,2,2,4),(68.1203183363462,68.5417873876646,69.0060663283817,
69.4791478952628,69.9470862950396,70.4133145452217,70.8906268551915,71.3555059566908,
71.8256791140487,72.2977871709703,72.7623409711255,73.2366098835529,73.7034826895161,
74.1707580079406,74.6483423631239,75.1127433836254,75.5838710201412,75.6907199874016),
 .UNSPECIFIED.);
#6758=B_SPLINE_CURVE_WITH_KNOTS('',3,(#293145,#293146,#293147,#293148,#293149,
#293150,#293151,#293152,#293153,#293154,#293155,#293156,#293157,#293158,
#293159,#293160,#293161,#293162,#293163,#293164,#293165,#293166,#293167,
#293168,#293169,#293170,#293171,#293172,#293173,#293174,#293175,#293176,
#293177,#293178,#293179,#293180,#293181,#293182),.UNSPECIFIED.,.F.,.F.,
(4,2,2,2,2,2,2,2,2,2,2,2,2,2,2,2,2,2,4),(64.1949548606005,64.2434814748872,
64.7196464066227,65.1849527935229,65.6540390711369,66.1277624520122,66.5919928976285,
67.0651049508879,67.5328885452889,67.9991346350153,68.476479537035,68.9412686999514,
69.4114699402805,69.8833879753948,70.3479150134625,70.8222167019006,71.2889597376057,
71.7562656212209,71.7645272101572),.UNSPECIFIED.);
#6759=B_SPLINE_CURVE_WITH_KNOTS('',3,(#293187,#293188,#293189,#293190,#293191,
#293192,#293193,#293194,#293195,#293196,#293197,#293198,#293199,#293200,
#293201,#293202,#293203,#293204,#293205,#293206,#293207,#293208,#293209,
#293210,#293211,#293212,#293213,#293214,#293215,#293216,#293217,#293218,
#293219,#293220,#293221,#293222,#293223,#293224),.UNSPECIFIED.,.F.,.F.,
(4,2,2,2,2,2,2,2,2,2,2,2,2,2,2,2,2,2,4),(60.5498333392294,60.5516208768603,
61.029713077203,61.4943018268745,61.9652050391113,62.4361334285903,62.9009642299098,
63.3760063085563,63.8422370545959,64.310256257033,64.7863055900214,65.2505975962196,
65.7225438217246,66.1918509203695,66.6572318432376,67.1333686185619,67.5987872086308,
68.0678490351813,68.1203183363462),.UNSPECIFIED.);
#6760=B_SPLINE_CURVE_WITH_KNOTS('',3,(#293225,#293226,#293227,#293228,#293229,
#293230,#293231,#293232,#293233,#293234,#293235,#293236,#293237,#293238,
#293239,#293240,#293241,#293242,#293243,#293244,#293245,#293246,#293247,
#293248,#293249,#293250,#293251,#293252,#293253,#293254,#293255,#293256,
#293257,#293258,#293259,#293260),.UNSPECIFIED.,.F.,.F.,(4,2,2,2,2,2,2,2,
2,2,2,2,2,2,2,2,2,4),(71.7645272101572,72.2336184703587,72.6979492173401,
73.1691158463344,73.6392922669799,74.1041798706507,74.5795050993304,75.0452851065681,
75.5135711699015,75.9886800701136,76.4528185565236,76.9250674549146,77.3937104149963,
77.8592621871405,78.3357171236383,78.8007845612436,79.2701433689272,79.3329795049996),
 .UNSPECIFIED.);
#6761=B_SPLINE_CURVE_WITH_KNOTS('',3,(#293265,#293266,#293267,#293268,#293269,
#293270,#293271,#293272,#293273,#293274,#293275,#293276,#293277,#293278,
#293279,#293280,#293281,#293282,#293283,#293284,#293285,#293286,#293287,
#293288,#293289,#293290,#293291,#293292,#293293,#293294,#293295,#293296,
#293297,#293298,#293299,#293300),.UNSPECIFIED.,.F.,.F.,(4,2,2,2,2,2,2,2,
2,2,2,2,2,2,2,2,2,4),(52.9806944783428,53.0476758259382,53.5172526200669,
53.9822867329294,54.4589700451137,54.9246978883063,55.3931826697128,55.8656533421869,
56.3298377489955,56.8046773546697,57.2731706643284,57.7388763386877,58.2144173370291,
58.679435794573,59.1438011651963,59.6176416939812,60.0847089200864,60.5498333392294),
 .UNSPECIFIED.);
#6762=B_SPLINE_CURVE_WITH_KNOTS('',3,(#293301,#293302,#293303,#293304,#293305,
#293306,#293307,#293308,#293309,#293310,#293311,#293312,#293313,#293314,
#293315,#293316,#293317,#293318,#293319,#293320,#293321,#293322,#293323,
#293324,#293325,#293326,#293327,#293328,#293329,#293330,#293331,#293332,
#293333,#293334,#293335,#293336),.UNSPECIFIED.,.F.,.F.,(4,2,2,2,2,2,2,2,
2,2,2,2,2,2,2,2,2,4),(79.3329795049996,79.7432389050355,80.2074739405494,
80.6808821375356,81.1482665820861,81.6147697069897,82.092419760985,82.5570552029074,
83.0275412408173,83.4989290104156,83.9635421064772,84.4381471318181,84.9045871045244,
85.3721846846847,85.8488549269602,86.313107852614,86.7845983573231,86.9020880596309),
 .UNSPECIFIED.);
#6763=B_SPLINE_CURVE_WITH_KNOTS('',3,(#293341,#293342,#293343,#293344,#293345,
#293346,#293347,#293348,#293349,#293350,#293351,#293352,#293353,#293354,
#293355,#293356,#293357,#293358,#293359,#293360,#293361,#293362,#293363,
#293364,#293365,#293366,#293367,#293368,#293369,#293370,#293371,#293372,
#293373,#293374,#293375,#293376),.UNSPECIFIED.,.F.,.F.,(4,2,2,2,2,2,2,2,
2,2,2,2,2,2,2,2,2,4),(45.4104974364304,45.5321719174255,46.0039037540315,
46.4682050210216,46.9446247162805,47.4124476030884,47.8788235312033,48.3536612318455,
48.8184039399149,49.2896146811765,49.7603238968664,50.2249690616266,50.702854011143,
51.1695732360491,51.6368449971586,52.1104831991918,52.5748078362504,52.9806944783428),
 .UNSPECIFIED.);
#6764=B_SPLINE_CURVE_WITH_KNOTS('',3,(#293377,#293378,#293379,#293380,#293381,
#293382,#293383,#293384,#293385,#293386,#293387,#293388,#293389,#293390,
#293391,#293392,#293393,#293394,#293395,#293396,#293397,#293398,#293399,
#293400,#293401,#293402,#293403,#293404,#293405,#293406,#293407,#293408,
#293409,#293410,#293411,#293412),.UNSPECIFIED.,.F.,.F.,(4,2,2,2,2,2,2,2,
2,2,2,2,2,2,2,2,2,4),(86.9020880596309,87.2542987090969,87.7193633179202,
88.1950279435794,88.6605753005546,89.1291848608632,89.6036709318418,90.0678172046687,
90.5404173981671,91.0086608535846,91.4744790277654,91.9512973083383,92.4162144467835,
92.8859170622057,93.3584748655669,93.8228043442849,94.2965791009012,94.4707808282852),
 .UNSPECIFIED.);
#6765=B_SPLINE_CURVE_WITH_KNOTS('',3,(#293417,#293418,#293419,#293420,#293421,
#293422,#293423,#293424,#293425,#293426,#293427,#293428,#293429,#293430,
#293431,#293432,#293433,#293434,#293435,#293436,#293437,#293438,#293439,
#293440,#293441,#293442,#293443,#293444,#293445,#293446,#293447,#293448,
#293449,#293450,#293451,#293452),.UNSPECIFIED.,.F.,.F.,(4,2,2,2,2,2,2,2,
2,2,2,2,2,2,2,2,2,4),(37.8404050120038,38.0187279036585,38.4927627146799,
38.9572252071081,39.4296082914203,39.8995596682351,40.3644899534552,40.8415681146096,
41.3076041454195,41.7757390083765,42.2485928495683,42.7128300300082,43.1870976300135,
43.6559470476141,44.1214664273962,44.5973803361899,45.0626195647578,45.4104974364304),
 .UNSPECIFIED.);
#6766=B_SPLINE_CURVE_WITH_KNOTS('',3,(#293453,#293454,#293455,#293456,#293457,
#293458,#293459,#293460,#293461,#293462,#293463,#293464,#293465,#293466,
#293467,#293468,#293469,#293470,#293471,#293472,#293473,#293474,#293475,
#293476,#293477,#293478,#293479,#293480,#293481,#293482,#293483,#293484,
#293485,#293486,#293487,#293488),.UNSPECIFIED.,.F.,.F.,(4,2,2,2,2,2,2,2,
2,2,2,2,2,2,2,2,2,4),(94.4707808282852,94.763655618974,95.230503489999,
95.7085287786169,96.1730996219083,96.6439388214966,97.1148906048698,97.5796768167616,
98.0546527520435,98.5208818428841,98.9888368347847,99.4649253819484,99.9291907564215,
100.40106925086,100.870392847739,101.33571930717,101.811786571165,102.040885959867),
 .UNSPECIFIED.);
#6767=B_SPLINE_CURVE_WITH_KNOTS('',3,(#293493,#293494,#293495,#293496,#293497,
#293498,#293499,#293500,#293501,#293502,#293503,#293504,#293505,#293506,
#293507,#293508,#293509,#293510,#293511,#293512,#293513,#293514,#293515,
#293516,#293517,#293518,#293519,#293520,#293521,#293522,#293523,#293524,
#293525,#293526,#293527,#293528),.UNSPECIFIED.,.F.,.F.,(4,2,2,2,2,2,2,2,
2,2,2,2,2,2,2,2,2,4),(30.2717430383538,30.5048631953018,30.9809925676507,
31.4463209930157,31.9153253368422,32.3872602441844,32.8514030187422,33.3270662479309,
33.7950640259182,34.2610568702298,34.7360806920456,35.2008248414998,35.6714249241691,
36.1423047011262,36.6067133213153,37.0846658279564,37.5517141448292,37.8404050120038),
 .UNSPECIFIED.);
#6768=B_SPLINE_CURVE_WITH_KNOTS('',3,(#293529,#293530,#293531,#293532,#293533,
#293534,#293535,#293536,#293537,#293538,#293539,#293540,#293541,#293542,
#293543,#293544,#293545,#293546,#293547,#293548,#293549,#293550,#293551,
#293552,#293553,#293554,#293555,#293556,#293557,#293558,#293559,#293560,
#293561,#293562,#293563,#293564),.UNSPECIFIED.,.F.,.F.,(4,2,2,2,2,2,2,2,
2,2,2,2,2,2,2,2,2,4),(102.040885959867,102.277195302756,102.746189989452,
103.220159927948,103.684402850689,104.157414263722,104.625360157971,105.09152469262,
105.568765443022,106.033625572829,106.503729888608,106.975859544708,107.440368265367,
107.914565867975,108.381435986137,108.848641741376,109.326264303091,109.610952863519),
 .UNSPECIFIED.);
#6769=B_SPLINE_CURVE_WITH_KNOTS('',3,(#293569,#293570,#293571,#293572,#293573,
#293574,#293575,#293576,#293577,#293578,#293579,#293580,#293581,#293582,
#293583,#293584,#293585,#293586,#293587,#293588,#293589,#293590,#293591,
#293592,#293593,#293594,#293595,#293596,#293597,#293598,#293599,#293600,
#293601,#293602,#293603,#293604),.UNSPECIFIED.,.F.,.F.,(4,2,2,2,2,2,2,2,
2,2,2,2,2,2,2,2,2,4),(22.7031707982564,22.99208933736,23.4692920572669,
23.9365641978222,24.403203099421,24.8774713373835,25.3419400064753,25.8137267074878,
26.2838928645293,26.7485956743227,27.2259067851868,27.692114101337,28.1597823250655,
28.632860104015,29.0970226309293,29.570603328209,30.0396530967059,30.2717430383538),
 .UNSPECIFIED.);
#6770=B_SPLINE_CURVE_WITH_KNOTS('',3,(#293605,#293606,#293607,#293608,#293609,
#293610,#293611,#293612,#293613,#293614,#293615,#293616,#293617,#293618,
#293619,#293620,#293621,#293622,#293623,#293624,#293625,#293626,#293627,
#293628,#293629,#293630,#293631,#293632,#293633,#293634,#293635,#293636,
#293637,#293638,#293639,#293640),.UNSPECIFIED.,.F.,.F.,(4,2,2,2,2,2,2,2,
2,2,2,2,2,2,2,2,2,4),(109.610952863519,109.790638320685,110.261692394934,
110.732061827133,111.19689695249,111.672103550742,112.137985181828,112.60615820867,
113.081516385384,113.545666191462,114.017791207714,114.486599692481,114.952064672917,
115.428390947034,115.893529453424,116.362766636795,116.836080905819,117.179557539184),
 .UNSPECIFIED.);
#6771=B_SPLINE_CURVE_WITH_KNOTS('',3,(#293645,#293646,#293647,#293648,#293649,
#293650,#293651,#293652,#293653,#293654,#293655,#293656,#293657,#293658,
#293659,#293660,#293661,#293662,#293663,#293664,#293665,#293666,#293667,
#293668,#293669,#293670,#293671,#293672,#293673,#293674,#293675,#293676,
#293677,#293678,#293679,#293680),.UNSPECIFIED.,.F.,.F.,(4,2,2,2,2,2,2,2,
2,2,2,2,2,2,2,2,2,4),(15.1357479359638,15.483569442746,15.9565317531947,
16.4258630167518,16.8908441963327,17.3672728159874,17.8327873664142,18.3013141843795,
18.7735358974931,19.2376068561131,19.7125725507048,20.1808286512787,20.6465127188702,
21.1218087780823,21.5866486252242,22.0566999630034,22.5278361424121,22.7031707982564),
 .UNSPECIFIED.);
#6772=B_SPLINE_CURVE_WITH_KNOTS('',3,(#293681,#293682,#293683,#293684,#293685,
#293686,#293687,#293688,#293689,#293690,#293691,#293692,#293693,#293694,
#293695,#293696,#293697,#293698,#293699,#293700,#293701,#293702,#293703,
#293704,#293705,#293706,#293707,#293708,#293709,#293710,#293711,#293712,
#293713,#293714,#293715,#293716),.UNSPECIFIED.,.F.,.F.,(4,2,2,2,2,2,2,2,
2,2,2,2,2,2,2,2,2,4),(117.179557539184,117.300294191774,117.77357180019,
118.241087915831,118.707473413946,119.184989407627,119.649663411256,120.12002348497,
120.591592365583,121.056153005238,121.53062502556,121.997159979772,122.464629349127,
122.941537765749,123.405800210544,123.877150376116,124.347010613714,124.748512061832),
 .UNSPECIFIED.);
#6773=B_SPLINE_CURVE_WITH_KNOTS('',3,(#293721,#293722,#293723,#293724,#293725,
#293726,#293727,#293728,#293729,#293730,#293731,#293732,#293733,#293734,
#293735,#293736,#293737,#293738,#293739,#293740,#293741,#293742,#293743,
#293744,#293745,#293746,#293747,#293748,#293749,#293750,#293751,#293752,
#293753,#293754,#293755,#293756),.UNSPECIFIED.,.F.,.F.,(4,2,2,2,2,2,2,2,
2,2,2,2,2,2,2,2,2,4),(7.56765982270858,7.97350892375056,8.44309508726157,
8.91456334139144,9.37874929116443,9.85528007747227,10.3228522472463,10.7891984448817,
11.2637785971085,11.7283438168659,12.1996104140286,12.6700700074204,13.1346293640203,
13.6122545095522,14.0787297444021,14.5460088545426,15.0193916841404,15.1357479359638),
 .UNSPECIFIED.);
#6774=B_SPLINE_CURVE_WITH_KNOTS('',3,(#293757,#293758,#293759,#293760,#293761,
#293762,#293763,#293764,#293765,#293766,#293767,#293768,#293769,#293770,
#293771,#293772,#293773,#293774,#293775,#293776,#293777,#293778,#293779,
#293780,#293781,#293782,#293783,#293784,#293785,#293786,#293787,#293788,
#293789,#293790,#293791,#293792),.UNSPECIFIED.,.F.,.F.,(4,2,2,2,2,2,2,2,
2,2,2,2,2,2,2,2,2,4),(124.748512061832,124.811988382779,125.287506788249,
125.753122095665,126.221591824151,126.6962926315,127.16041598402,127.632865894423,
128.101239772114,128.56693763404,129.043601068422,129.50855488633,129.978110384247,
130.450850185154,130.915124226038,131.388743327773,131.855915452059,132.31674072404),
 .UNSPECIFIED.);
#6775=B_SPLINE_CURVE_WITH_KNOTS('',3,(#293797,#293798,#293799,#293800,#293801,
#293802,#293803,#293804,#293805,#293806,#293807,#293808,#293809,#293810,
#293811,#293812,#293813,#293814,#293815,#293816,#293817,#293818,#293819,
#293820,#293821,#293822,#293823,#293824,#293825,#293826,#293827,#293828,
#293829,#293830,#293831,#293832),.UNSPECIFIED.,.F.,.F.,(4,2,2,2,2,2,2,2,
2,2,2,2,2,2,2,2,2,4),(9.99999998750232E-7,0.467334061734382,0.932035384281994,
1.40579202308201,1.87007446664982,2.3425110483518,2.81219352801155,3.27703519012564,
3.75383474865014,4.21962567702159,4.68776432105674,5.16034500528953,5.62443429016073,
6.0987886077358,6.56737603804431,7.0328381371557,7.50848165018001,7.56765982270858),
 .UNSPECIFIED.);
#6776=B_SPLINE_CURVE_WITH_KNOTS('',3,(#293833,#293834,#293835,#293836,#293837,
#293838,#293839,#293840,#293841,#293842,#293843,#293844,#293845,#293846,
#293847,#293848,#293849,#293850,#293851,#293852,#293853,#293854,#293855,
#293856,#293857,#293858,#293859,#293860,#293861,#293862,#293863,#293864,
#293865,#293866,#293867,#293868,#293869,#293870),.UNSPECIFIED.,.F.,.F.,
(4,2,2,2,2,2,2,2,2,2,2,2,2,2,2,2,2,2,4),(132.31674072404,132.322614006903,
132.800480328936,133.265055617999,133.73574449305,134.206839604717,134.671541151825,
135.14636009418,135.612648248539,136.080451677917,136.556737472824,137.020978236111,
137.492693772341,137.962137920711,138.427346634022,138.903245442099,139.368685915427,
139.837519056432,139.886098987271),.UNSPECIFIED.);
#6777=B_SPLINE_CURVE_WITH_KNOTS('',3,(#293873,#293874,#293875,#293876,#293877,
#293878,#293879,#293880),.UNSPECIFIED.,.F.,.F.,(4,2,2,4),(139.886098987271,
140.311661019487,140.573832875075,140.83351486988),.UNSPECIFIED.);
#6778=B_SPLINE_CURVE_WITH_KNOTS('',3,(#293884,#293885,#293886,#293887,#293888,
#293889,#293890,#293891,#293892,#293893,#293894,#293895,#293896,#293897,
#293898,#293899,#293900,#293901),.UNSPECIFIED.,.F.,.F.,(4,2,2,2,2,2,2,2,
4),(9.99999997069479E-7,0.291089014559669,0.5781604735274,0.773666909719169,
1.23141972216497,1.66182200097359,2.04579418676715,2.48304347384049,2.8013006831538),
 .UNSPECIFIED.);
#6779=B_SPLINE_CURVE_WITH_KNOTS('',3,(#293906,#293907,#293908,#293909,#293910,
#293911,#293912,#293913,#293914,#293915,#293916,#293917,#293918,#293919,
#293920,#293921,#293922,#293923,#293924,#293925,#293926,#293927,#293928,
#293929,#293930,#293931),.UNSPECIFIED.,.F.,.F.,(4,2,2,2,2,2,2,2,2,2,2,2,
4),(2.8013006831538,2.95750567567089,3.42207211239295,3.6534557788092,4.11157474291367,
4.54312783084037,4.99497502157467,5.49320161115939,6.01905209027688,6.51964999377779,
7.02384354840784,7.35807870641489,7.69625303519648),.UNSPECIFIED.);
#6780=B_SPLINE_CURVE_WITH_KNOTS('',3,(#293934,#293935,#293936,#293937,#293938,
#293939,#293940,#293941,#293942,#293943,#293944,#293945),.UNSPECIFIED.,
 .F.,.F.,(4,2,2,2,2,4),(0.,0.283334890257164,0.52169392280916,0.820631417753867,
1.09721857907454,1.42693465649552),.UNSPECIFIED.);
#6781=B_SPLINE_CURVE_WITH_KNOTS('',3,(#293949,#293950,#293951,#293952,#293953,
#293954,#293955,#293956,#293957,#293958),.UNSPECIFIED.,.F.,.F.,(4,2,2,2,
4),(6.45298424781494,6.58701147725645,7.0135559745479,7.32969503217713,
7.63409751686082),.UNSPECIFIED.);
#6782=B_SPLINE_CURVE_WITH_KNOTS('',3,(#293961,#293962,#293963,#293964,#293965,
#293966,#293967,#293968,#293969,#293970,#293971,#293972,#293973,#293974),
 .UNSPECIFIED.,.F.,.F.,(4,2,2,2,2,2,4),(-2.13428009774412,-1.60549823782287,
-1.17695770942762,-0.961094502946938,-0.74633863203622,-0.362979450140088,
0.),.UNSPECIFIED.);
#6783=B_SPLINE_CURVE_WITH_KNOTS('',3,(#293975,#293976,#293977,#293978,#293979,
#293980,#293981,#293982,#293983,#293984,#293985,#293986,#293987,#293988,
#293989,#293990,#293991,#293992,#293993,#293994,#293995,#293996,#293997,
#293998,#293999,#294000,#294001,#294002,#294003,#294004,#294005,#294006,
#294007,#294008),.UNSPECIFIED.,.F.,.F.,(4,2,2,2,2,2,2,2,2,2,2,2,2,2,2,2,
4),(9.99999953768269E-7,0.370257533413155,0.742867260998573,1.22246490552703,
1.7557170645661,2.25159185055114,2.4791417967581,2.93209432879808,3.15576838975421,
3.59500286984314,4.03092164371551,4.46885846514905,4.94125635881584,5.43523086524786,
5.92378997433212,6.3646784653317,6.45298424781494),.UNSPECIFIED.);
#6784=B_SPLINE_CURVE_WITH_KNOTS('',3,(#294014,#294015,#294016,#294017,#294018,
#294019,#294020,#294021,#294022,#294023,#294024,#294025,#294026,#294027,
#294028,#294029,#294030,#294031,#294032,#294033,#294034,#294035),
 .UNSPECIFIED.,.F.,.F.,(4,2,2,2,2,2,2,2,2,2,4),(91.0207492930948,91.1620889064705,
91.6347282811689,92.1032814796637,92.5691652146226,93.0460199029874,93.5111545444713,
93.9808982819425,94.4538175435407,94.7823719061299,95.1098199853164),
 .UNSPECIFIED.);
#6785=B_SPLINE_CURVE_WITH_KNOTS('',3,(#294038,#294039,#294040,#294041,#294042,
#294043,#294044,#294045,#294046,#294047,#294048,#294049,#294050,#294051,
#294052,#294053),.UNSPECIFIED.,.F.,.F.,(4,2,2,2,2,2,2,4),(9.99999994972016E-7,
0.464678467060016,0.930253604102473,1.399457943134,1.86474545923474,2.34103365921871,
2.80650042650129,3.14443208990716),.UNSPECIFIED.);
#6786=B_SPLINE_CURVE_WITH_KNOTS('',3,(#296128,#296129,#296130,#296131,#296132,
#296133,#296134,#296135,#296136,#296137,#296138,#296139,#296140,#296141,
#296142,#296143),.UNSPECIFIED.,.F.,.F.,(4,2,2,2,2,2,2,4),(0.,0.225987015547473,
0.464252847533295,0.875453617456248,1.4357921506269,2.26570179526748,2.85663059455104,
3.35180761336525),.UNSPECIFIED.);
#6787=B_SPLINE_CURVE_WITH_KNOTS('',3,(#298233,#298234,#298235,#298236,#298237,
#298238,#298239,#298240,#298241,#298242,#298243,#298244,#298245,#298246,
#298247,#298248,#298249,#298250),.UNSPECIFIED.,.F.,.F.,(4,2,2,2,2,2,2,2,
4),(9.99999986121495E-7,0.329680585623105,0.669907801738523,0.890088500101439,
1.29558589654613,1.65011885938668,1.91244034489391,2.02969065103336,2.13124206648743),
 .UNSPECIFIED.);
#6788=B_SPLINE_CURVE_WITH_KNOTS('',3,(#298430,#298431,#298432,#298433,#298434,
#298435,#298436,#298437,#298438,#298439,#298440,#298441,#298442,#298443,
#298444,#298445),.UNSPECIFIED.,.F.,.F.,(4,2,2,2,2,2,2,4),(1.00000044233709E-6,
0.539370132359783,1.28481747817566,1.98442658665292,2.48325218307673,2.95253551271824,
3.30333512017195,3.64287608445345),.UNSPECIFIED.);
#6789=B_SPLINE_CURVE_WITH_KNOTS('',3,(#298446,#298447,#298448,#298449,#298450,
#298451,#298452,#298453,#298454,#298455,#298456,#298457,#298458,#298459,
#298460,#298461),.UNSPECIFIED.,.F.,.F.,(4,2,2,2,2,2,2,4),(0.,0.238087952519387,
0.476113544168717,1.01011910515244,1.73799046632944,2.30408220983986,2.86072831234553,
3.43288601470779),.UNSPECIFIED.);
#6790=B_SPLINE_CURVE_WITH_KNOTS('',3,(#303022,#303023,#303024,#303025,#303026,
#303027,#303028,#303029,#303030,#303031,#303032,#303033,#303034,#303035,
#303036,#303037),.UNSPECIFIED.,.F.,.F.,(4,2,2,2,2,2,2,4),(1.2412134266385,
1.30125065201544,1.44881001361766,1.57542683632653,1.63813614188284,1.76112334826837,
1.8383565168018,1.91232314425083),.UNSPECIFIED.);
#6791=B_SPLINE_CURVE_WITH_KNOTS('',3,(#303042,#303043,#303044,#303045,#303046,
#303047,#303048,#303049,#303050,#303051,#303052,#303053),.UNSPECIFIED.,
 .F.,.F.,(4,2,2,2,2,4),(-0.602485002785239,-0.56859078279277,-0.367777547037733,
-0.175807956195899,-0.0864773397713831,-9.9999999780831E-7),
 .UNSPECIFIED.);
#6792=B_SPLINE_CURVE_WITH_KNOTS('',3,(#303060,#303061,#303062,#303063,#303064,
#303065,#303066,#303067,#303068,#303069,#303070,#303071,#303072,#303073,
#303074,#303075,#303076,#303077,#303078,#303079),.UNSPECIFIED.,.F.,.F.,
(4,2,2,2,2,2,2,2,2,4),(9.9999999701418E-7,0.0982828162925184,0.198026929183757,
0.38987455053706,0.594158820502547,0.77621883872625,0.866427631156547,1.04319620045318,
1.12898218312396,1.2412134266385),.UNSPECIFIED.);
#6793=B_SPLINE_CURVE_WITH_KNOTS('',3,(#303080,#303081,#303082,#303083,#303084,
#303085,#303086,#303087,#303088,#303089,#303090,#303091,#303092,#303093,
#303094,#303095,#303096,#303097,#303098,#303099,#303100,#303101,#303102,
#303103,#303104,#303105,#303106,#303107,#303108,#303109,#303110,#303111,
#303112,#303113,#303114,#303115,#303116,#303117,#303118,#303119),
 .UNSPECIFIED.,.F.,.F.,(4,2,2,2,2,2,2,2,2,2,2,2,2,2,2,2,2,2,2,4),(-3.42352177914162,
-3.36362658540771,-3.17690405027184,-2.99916395534607,-2.81491387816524,
-2.63585257564751,-2.45959577200563,-2.37188103111418,-2.19724000665655,
-2.02164462696103,-1.84975793686824,-1.76568449365736,-1.59640410954265,
-1.51180981583268,-1.34684855225214,-1.26283489210883,-1.10262428644002,
-0.938110474064238,-0.759074924884252,-0.602485002785239),.UNSPECIFIED.);
#6794=B_SPLINE_CURVE_WITH_KNOTS('',3,(#303125,#303126,#303127,#303128,#303129,
#303130,#303131,#303132,#303133,#303134,#303135,#303136,#303137,#303138,
#303139,#303140),.UNSPECIFIED.,.F.,.F.,(4,2,2,2,2,2,2,4),(9.99999999548357E-7,
0.139379921907621,0.277528623112359,0.510933121482433,0.744693179008006,
0.981547966045232,1.21378437584703,1.41773894915106),.UNSPECIFIED.);
#6795=B_SPLINE_CURVE_WITH_KNOTS('',3,(#303143,#303144,#303145,#303146,#303147,
#303148,#303149,#303150,#303151,#303152,#303153,#303154),.UNSPECIFIED.,
 .F.,.F.,(4,2,2,2,2,4),(61.0968842008273,61.0995937956945,61.3385697502591,
61.5709030970278,61.8062941894517,62.0430454361303),.UNSPECIFIED.);
#6796=B_SPLINE_CURVE_WITH_KNOTS('',3,(#303159,#303160,#303161,#303162,#303163,
#303164,#303165,#303166,#303167,#303168,#303169,#303170,#303171,#303172,
#303173,#303174,#303175,#303176,#303177,#303178,#303179,#303180,#303181,
#303182,#303183,#303184,#303185,#303186,#303187,#303188,#303189,#303190,
#303191,#303192,#303193,#303194),.UNSPECIFIED.,.F.,.F.,(4,2,2,2,2,2,2,2,
2,2,2,2,2,2,2,2,2,4),(1.41773894915106,1.45035486160213,1.6851967078116,
1.9178182494756,2.15620987025867,2.38913584240912,2.62348141723324,2.85976986412203,
3.0919410577353,3.32946420051038,3.56378499678541,3.79673459079611,4.03457860182644,
4.26716989015402,4.50224336087877,4.73801127084836,4.97026347926577,5.20262344011782),
 .UNSPECIFIED.);
#6797=B_SPLINE_CURVE_WITH_KNOTS('',3,(#303195,#303196,#303197,#303198,#303199,
#303200,#303201,#303202,#303203,#303204,#303205,#303206,#303207,#303208,
#303209,#303210,#303211,#303212,#303213,#303214,#303215,#303216,#303217,
#303218,#303219,#303220,#303221,#303222,#303223,#303224,#303225,#303226,
#303227,#303228,#303229,#303230),.UNSPECIFIED.,.F.,.F.,(4,2,2,2,2,2,2,2,
2,2,2,2,2,2,2,2,2,4),(57.3134340037929,57.3438788675244,57.5817073246283,
57.8145114738983,58.0488146074359,58.2861002964137,58.5181826423711,58.7544597317251,
58.9886213519691,59.2215184693227,59.4599014470676,59.6923979942522,59.9272282660549,
60.1635828267512,60.3957516150036,60.6326001141031,60.8661989335085,61.0968842008273),
 .UNSPECIFIED.);
#6798=B_SPLINE_CURVE_WITH_KNOTS('',3,(#303235,#303236,#303237,#303238,#303239,
#303240,#303241,#303242,#303243,#303244,#303245,#303246,#303247,#303248,
#303249,#303250,#303251,#303252,#303253,#303254,#303255,#303256,#303257,
#303258,#303259,#303260,#303261,#303262,#303263,#303264,#303265,#303266,
#303267,#303268,#303269,#303270,#303271,#303272),.UNSPECIFIED.,.F.,.F.,
(4,2,2,2,2,2,2,2,2,2,2,2,2,2,2,2,2,2,4),(5.20262344011782,5.20886345742205,
5.44271682375074,5.67612586248115,5.91348234838391,6.14589222000662,6.38180674084541,
6.61711861249481,6.84958963116392,7.08847725119523,7.32180057772338,7.55566394593537,
7.79242943844311,8.02465593652442,8.2613946873114,8.49615433278052,8.7288349619442,
8.96713950524592,8.98804835001342),.UNSPECIFIED.);
#6799=B_SPLINE_CURVE_WITH_KNOTS('',3,(#303273,#303274,#303275,#303276,#303277,
#303278,#303279,#303280,#303281,#303282,#303283,#303284,#303285,#303286,
#303287,#303288,#303289,#303290,#303291,#303292,#303293,#303294,#303295,
#303296,#303297,#303298,#303299,#303300,#303301,#303302,#303303,#303304,
#303305,#303306,#303307,#303308),.UNSPECIFIED.,.F.,.F.,(4,2,2,2,2,2,2,2,
2,2,2,2,2,2,2,2,2,4),(53.5296384471268,53.5876019606723,53.8243393699444,
54.0580154468014,54.2913052178265,54.5301667613154,54.7625089863747,54.9977916571498,
55.2334884215121,55.4658257577282,55.7031570515923,55.9364027204056,56.1702297701125,
56.4085764206654,56.640718837193,56.8764677959731,57.1113380070465,57.3134340037929),
 .UNSPECIFIED.);
#6800=B_SPLINE_CURVE_WITH_KNOTS('',3,(#303313,#303314,#303315,#303316,#303317,
#303318,#303319,#303320,#303321,#303322,#303323,#303324,#303325,#303326,
#303327,#303328,#303329,#303330,#303331,#303332,#303333,#303334,#303335,
#303336,#303337,#303338,#303339,#303340,#303341,#303342,#303343,#303344,
#303345,#303346,#303347,#303348),.UNSPECIFIED.,.F.,.F.,(4,2,2,2,2,2,2,2,
2,2,2,2,2,2,2,2,2,4),(8.98804835001342,9.20000803763523,9.43448334015654,
9.67068900303869,9.90287577614595,10.140591592428,10.3748382650961,10.6078712165112,
10.8456372745515,11.0781976407607,11.3134230786598,11.5491181338964,11.7814110000215,
12.0202212096964,12.2540116065607,12.4875248599571,12.7248157635537,12.7733801753947),
 .UNSPECIFIED.);
#6801=B_SPLINE_CURVE_WITH_KNOTS('',3,(#303349,#303350,#303351,#303352,#303353,
#303354,#303355,#303356,#303357,#303358,#303359,#303360,#303361,#303362,
#303363,#303364,#303365,#303366,#303367,#303368,#303369,#303370,#303371,
#303372,#303373,#303374,#303375,#303376,#303377,#303378,#303379,#303380,
#303381,#303382,#303383,#303384),.UNSPECIFIED.,.F.,.F.,(4,2,2,2,2,2,2,2,
2,2,2,2,2,2,2,2,2,4),(49.746329667915,49.8327292191111,50.0683827642741,
50.30337982278,50.5358649718823,50.7735928734603,51.0064554122485,51.2406622802839,
51.4781147625736,51.7101878221121,51.9463600519697,52.1806257300522,52.4134409835382,
52.6517147664406,52.8842452908403,53.1189716647374,53.3554678492974,53.5296384471268),
 .UNSPECIFIED.);
#6802=B_SPLINE_CURVE_WITH_KNOTS('',3,(#303389,#303390,#303391,#303392,#303393,
#303394,#303395,#303396,#303397,#303398,#303399,#303400,#303401,#303402,
#303403,#303404,#303405,#303406,#303407,#303408,#303409,#303410,#303411,
#303412,#303413,#303414,#303415,#303416,#303417,#303418,#303419,#303420,
#303421,#303422,#303423,#303424),.UNSPECIFIED.,.F.,.F.,(4,2,2,2,2,2,2,2,
2,2,2,2,2,2,2,2,2,4),(12.7733801753947,12.9572214265519,13.1933040723328,
13.4285561614687,13.6610902013302,13.8999129782384,14.1331853642295,14.3671810276077,
14.6038850340275,14.8361313833642,15.073066783886,15.3077721416732,15.5405409570327,
15.778786945767,16.0116287043582,16.2462620388275,16.4824132974095,16.5591900771066),
 .UNSPECIFIED.);
#6803=B_SPLINE_CURVE_WITH_KNOTS('',3,(#303425,#303426,#303427,#303428,#303429,
#303430,#303431,#303432,#303433,#303434,#303435,#303436,#303437,#303438,
#303439,#303440,#303441,#303442,#303443,#303444,#303445,#303446,#303447,
#303448,#303449,#303450,#303451,#303452,#303453,#303454,#303455,#303456,
#303457,#303458,#303459,#303460),.UNSPECIFIED.,.F.,.F.,(4,2,2,2,2,2,2,2,
2,2,2,2,2,2,2,2,2,4),(45.9623756797133,46.0761295473086,46.3107783205002,
46.5474476123326,46.7795766717039,47.0162292218167,47.2500134623971,47.4832269185953,
47.7220001181863,47.9543809031078,48.1895807664551,48.425421304983,48.6577296129388,
48.8949722396374,49.1282975779197,49.3620390544388,49.6005709483308,49.746329667915),
 .UNSPECIFIED.);
#6804=B_SPLINE_CURVE_WITH_KNOTS('',3,(#303465,#303466,#303467,#303468,#303469,
#303470,#303471,#303472,#303473,#303474,#303475,#303476,#303477,#303478,
#303479,#303480,#303481,#303482,#303483,#303484,#303485,#303486,#303487,
#303488,#303489,#303490,#303491,#303492,#303493,#303494,#303495,#303496,
#303497,#303498,#303499,#303500),.UNSPECIFIED.,.F.,.F.,(4,2,2,2,2,2,2,2,
2,2,2,2,2,2,2,2,2,4),(16.5591900771066,16.7146453262928,16.9525810732934,
17.1867819106692,17.4199266177265,17.6576436449791,17.8902036038456,18.1256081763627,
18.3612591412948,18.593621717838,18.8326679852899,19.0664240237015,19.30006893957,
19.5373235019442,19.7697549242191,20.0060316137086,20.24125296691,20.3456492025429),
 .UNSPECIFIED.);
#6805=B_SPLINE_CURVE_WITH_KNOTS('',3,(#303501,#303502,#303503,#303504,#303505,
#303506,#303507,#303508,#303509,#303510,#303511,#303512,#303513,#303514,
#303515,#303516,#303517,#303518,#303519,#303520,#303521,#303522,#303523,
#303524,#303525,#303526,#303527,#303528,#303529,#303530,#303531,#303532,
#303533,#303534,#303535,#303536),.UNSPECIFIED.,.F.,.F.,(4,2,2,2,2,2,2,2,
2,2,2,2,2,2,2,2,2,4),(42.178594420686,42.3197673512826,42.5534505985734,
42.7921972991454,43.0244011651343,43.2599866101189,43.4951403754128,43.7275997075312,
43.9652544313537,44.1982051996161,44.4323426165456,44.669992571529,44.9020862234648,
45.1381803472536,45.3725806597471,45.6053435710459,45.8435349737313,45.9623756797133),
 .UNSPECIFIED.);
#6806=B_SPLINE_CURVE_WITH_KNOTS('',3,(#303541,#303542,#303543,#303544,#303545,
#303546,#303547,#303548,#303549,#303550,#303551,#303552,#303553,#303554,
#303555,#303556,#303557,#303558,#303559,#303560,#303561,#303562,#303563,
#303564,#303565,#303566,#303567,#303568,#303569,#303570,#303571,#303572,
#303573,#303574,#303575,#303576),.UNSPECIFIED.,.F.,.F.,(4,2,2,2,2,2,2,2,
2,2,2,2,2,2,2,2,2,4),(20.3456492025429,20.4738781967648,20.7126658502402,
20.9459188409693,21.1800731686911,21.4167451846275,21.6490409199683,21.886197356947,
22.120877696677,22.3537619853571,22.5919793857185,22.8248255987001,23.0596419467705,
23.2957685294054,23.5280745178391,23.7662528620981,24.0004373054574,24.1324102092935),
 .UNSPECIFIED.);
#6807=B_SPLINE_CURVE_WITH_KNOTS('',3,(#303577,#303578,#303579,#303580,#303581,
#303582,#303583,#303584,#303585,#303586,#303587,#303588,#303589,#303590,
#303591,#303592,#303593,#303594,#303595,#303596,#303597,#303598,#303599,
#303600,#303601,#303602,#303603,#303604,#303605,#303606,#303607,#303608,
#303609,#303610,#303611,#303612),.UNSPECIFIED.,.F.,.F.,(4,2,2,2,2,2,2,2,
2,2,2,2,2,2,2,2,2,4),(38.3941558264512,38.5636470016297,38.7963883805231,
39.0345262052207,39.2672136511948,39.501812999719,39.7386832552294,39.9708371668894,
40.2074331234577,40.441354242262,40.674522022043,40.9132353048738,41.145683924188,
41.3808288230391,41.6168420311341,41.8491511752046,42.0863330635504,42.178594420686),
 .UNSPECIFIED.);
#6808=B_SPLINE_CURVE_WITH_KNOTS('',3,(#303617,#303618,#303619,#303620,#303621,
#303622,#303623,#303624,#303625,#303626,#303627,#303628,#303629,#303630,
#303631,#303632,#303633,#303634,#303635,#303636,#303637,#303638,#303639,
#303640,#303641,#303642,#303643,#303644,#303645,#303646,#303647,#303648,
#303649,#303650,#303651,#303652),.UNSPECIFIED.,.F.,.F.,(4,2,2,2,2,2,2,2,
2,2,2,2,2,2,2,2,2,4),(24.1324102092935,24.2337198206622,24.471417950881,
24.7040079669973,24.9396151150109,25.1752518518046,25.407711692159,25.6469416011285,
25.8805802095303,26.1142355494829,26.3513329821338,26.5836726675167,26.8200187049054,
27.055089591229,27.2876863097957,27.5263175344745,27.7594348383616,27.9188908085219),
 .UNSPECIFIED.);
#6809=B_SPLINE_CURVE_WITH_KNOTS('',3,(#303653,#303654,#303655,#303656,#303657,
#303658,#303659,#303660,#303661,#303662,#303663,#303664,#303665,#303666,
#303667,#303668,#303669,#303670,#303671,#303672,#303673,#303674,#303675,
#303676,#303677,#303678,#303679,#303680,#303681,#303682,#303683,#303684,
#303685,#303686,#303687,#303688),.UNSPECIFIED.,.F.,.F.,(4,2,2,2,2,2,2,2,
2,2,2,2,2,2,2,2,2,4),(34.6093522571136,34.8069208845197,35.0392607700812,
35.2764113533711,35.5099816017935,35.743635416534,35.9826219414602,36.2149002384306,
36.4504465708585,36.6857836018368,36.9182476700206,37.1558583806587,37.388925411623,
37.6230218964636,37.8608958248006,38.0930396222172,38.3290842831678,38.3941558264512),
 .UNSPECIFIED.);
#6810=B_SPLINE_CURVE_WITH_KNOTS('',3,(#303693,#303694,#303695,#303696,#303697,
#303698,#303699,#303700,#303701,#303702,#303703,#303704,#303705,#303706,
#303707,#303708,#303709,#303710,#303711,#303712,#303713,#303714,#303715,
#303716,#303717,#303718,#303719,#303720,#303721,#303722,#303723,#303724,
#303725,#303726,#303727,#303728),.UNSPECIFIED.,.F.,.F.,(4,2,2,2,2,2,2,2,
2,2,2,2,2,2,2,2,2,4),(27.9188908085219,27.9936250793838,28.2301448958016,
28.4623720202115,28.6996226455423,28.9341587490645,29.1670376320634,29.4051056835644,
29.6378398263206,29.8727145737872,30.1086967810473,30.3409577709205,30.5792495072044,
30.8132987490559,31.0465966730789,31.281962442723,31.5178689194523,31.7047302987816),
 .UNSPECIFIED.);
#6811=B_SPLINE_CURVE_WITH_KNOTS('',3,(#303729,#303730,#303731,#303732,#303733,
#303734,#303735,#303736,#303737,#303738,#303739,#303740,#303741,#303742,
#303743,#303744,#303745,#303746,#303747,#303748,#303749,#303750,#303751,
#303752,#303753,#303754,#303755,#303756,#303757,#303758,#303759,#303760,
#303761,#303762,#303763,#303764),.UNSPECIFIED.,.F.,.F.,(4,2,2,2,2,2,2,2,
2,2,2,2,2,2,2,2,2,4),(30.8240674906406,31.0500044124221,31.2822268132115,
31.5182518810668,31.7530013759189,31.9857524436451,32.2238668135051,32.4566740448876,
32.6912533841055,32.9283482461933,33.1605563897487,33.397125421422,33.6312092555386,
33.8643629938688,34.1030462650625,34.3355905929265,34.5707097441297,34.6093522571136),
 .UNSPECIFIED.);
#6812=B_SPLINE_CURVE_WITH_KNOTS('',3,(#303769,#303770,#303771,#303772,#303773,
#303774,#303775,#303776,#303777,#303778,#303779,#303780,#303781,#303782,
#303783,#303784,#303785,#303786,#303787,#303788,#303789,#303790,#303791,
#303792,#303793,#303794,#303795,#303796,#303797,#303798,#303799,#303800,
#303801,#303802,#303803,#303804),.UNSPECIFIED.,.F.,.F.,(4,2,2,2,2,2,2,2,
2,2,2,2,2,2,2,2,2,4),(31.7047302987816,31.7503174680194,31.9877297342918,
32.2211478923376,32.455055736683,32.6936366675314,32.925915263179,33.1617406103227,
33.396810498696,33.6294477866019,33.8673509262892,34.1003153669239,34.3346936583478,
34.5722025916434,34.8044070310837,35.0407555989327,35.2751036862081,35.4902881150602),
 .UNSPECIFIED.);
#6813=B_SPLINE_CURVE_WITH_KNOTS('',3,(#303805,#303806,#303807,#303808,#303809,
#303810,#303811,#303812,#303813,#303814,#303815,#303816,#303817,#303818,
#303819,#303820,#303821,#303822,#303823,#303824,#303825,#303826,#303827,
#303828,#303829,#303830,#303831,#303832,#303833,#303834,#303835,#303836,
#303837,#303838,#303839,#303840,#303841,#303842),.UNSPECIFIED.,.F.,.F.,
(4,2,2,2,2,2,2,2,2,2,2,2,2,2,2,2,2,2,4),(27.0389051345726,27.0577126469844,
27.2919955443905,27.5249424930835,27.7627474109057,27.9953103836241,28.2303964626859,
28.4661265986034,28.6983666265183,28.931906239097,29.1710343343977,29.4034142910445,
29.6389514703502,29.8744945422313,30.106993707325,30.3445906542744,30.5777995450349,
30.8118846482967,30.8240674906406),.UNSPECIFIED.);
#6814=B_SPLINE_CURVE_WITH_KNOTS('',3,(#303847,#303848,#303849,#303850,#303851,
#303852,#303853,#303854,#303855,#303856,#303857,#303858,#303859,#303860,
#303861,#303862,#303863,#303864,#303865,#303866,#303867,#303868,#303869,
#303870,#303871,#303872,#303873,#303874,#303875,#303876,#303877,#303878,
#303879,#303880,#303881,#303882,#303883,#303884),.UNSPECIFIED.,.F.,.F.,
(4,2,2,2,2,2,2,2,2,2,2,2,2,2,2,2,2,2,4),(35.4902881150602,35.5080828782027,
35.7465360959528,35.9791791042568,36.2140806323327,36.4506437626019,36.682920550086,
36.9198374361597,37.1536074034736,37.3870717465179,37.6261155342257,37.8585813647829,
38.0940416659604,38.3298180144348,38.5623085529083,38.7998212119301,39.0331731001541,
39.2671780065184,39.2762581355268),.UNSPECIFIED.);
#6815=B_SPLINE_CURVE_WITH_KNOTS('',3,(#303885,#303886,#303887,#303888,#303889,
#303890,#303891,#303892,#303893,#303894,#303895,#303896,#303897,#303898,
#303899,#303900,#303901,#303902,#303903,#303904,#303905,#303906,#303907,
#303908,#303909,#303910,#303911,#303912,#303913,#303914,#303915,#303916,
#303917,#303918,#303919,#303920),.UNSPECIFIED.,.F.,.F.,(4,2,2,2,2,2,2,2,
2,2,2,2,2,2,2,2,2,4),(23.2541689376758,23.2992951913372,23.5346535319949,
23.7670771733799,24.0060152939412,24.2393803367821,24.4731422028082,24.7099556569758,
24.9421686528967,25.1787552585656,25.4135573935473,25.6461708383038,25.8845213198659,
26.1174130189436,26.3517661968063,26.5880146450337,26.8201680131357,27.0389051345726),
 .UNSPECIFIED.);
#6816=B_SPLINE_CURVE_WITH_KNOTS('',3,(#303925,#303926,#303927,#303928,#303929,
#303930,#303931,#303932,#303933,#303934,#303935,#303936,#303937,#303938,
#303939,#303940,#303941,#303942,#303943,#303944,#303945,#303946,#303947,
#303948,#303949,#303950,#303951,#303952,#303953,#303954,#303955,#303956,
#303957,#303958,#303959,#303960),.UNSPECIFIED.,.F.,.F.,(4,2,2,2,2,2,2,2,
2,2,2,2,2,2,2,2,2,4),(39.2762581355268,39.505587894306,39.7378638237339,
39.9737959988975,40.2087529896849,40.4414587798656,40.6794738873387,40.9123934347045,
41.1468791851678,41.3842358822747,41.6164626815893,41.8529272269335,42.087185358293,
42.3202588625291,42.558832393382,42.7914548517187,43.0264712043312,43.0619965343569),
 .UNSPECIFIED.);
#6817=B_SPLINE_CURVE_WITH_KNOTS('',3,(#303961,#303962,#303963,#303964,#303965,
#303966,#303967,#303968,#303969,#303970,#303971,#303972,#303973,#303974,
#303975,#303976,#303977,#303978,#303979,#303980,#303981,#303982,#303983,
#303984,#303985,#303986,#303987,#303988,#303989,#303990,#303991,#303992,
#303993,#303994,#303995,#303996),.UNSPECIFIED.,.F.,.F.,(4,2,2,2,2,2,2,2,
2,2,2,2,2,2,2,2,2,4),(19.4692315614832,19.5413390779448,19.7776909728097,
20.009851950902,20.2472279055292,20.4816056446896,20.7144924661023,20.9523964880157,
21.1850135373671,21.4199709659037,21.6557950630017,21.8880175434394,22.1264558874441,
22.360357963883,22.5936876630703,22.8310950019613,23.0635099516054,23.2541689376758),
 .UNSPECIFIED.);
#6818=B_SPLINE_CURVE_WITH_KNOTS('',3,(#304001,#304002,#304003,#304004,#304005,
#304006,#304007,#304008,#304009,#304010,#304011,#304012,#304013,#304014,
#304015,#304016,#304017,#304018,#304019,#304020,#304021,#304022,#304023,
#304024,#304025,#304026,#304027,#304028,#304029,#304030,#304031,#304032,
#304033,#304034,#304035,#304036),.UNSPECIFIED.,.F.,.F.,(4,2,2,2,2,2,2,2,
2,2,2,2,2,2,2,2,2,4),(43.0619965343569,43.2629074392662,43.4952316912758,
43.7322705239129,43.9659772908775,44.1995586969195,44.4387280250369,44.6711984122979,
44.9067780999182,45.1424571928423,45.3750181490638,45.6126559706163,45.8459728161458,
46.0800990840976,46.3183727020659,46.5506756306829,46.786738618415,46.8485936589711),
 .UNSPECIFIED.);
#6819=B_SPLINE_CURVE_WITH_KNOTS('',3,(#304037,#304038,#304039,#304040,#304041,
#304042,#304043,#304044,#304045,#304046,#304047,#304048,#304049,#304050,
#304051,#304052,#304053,#304054,#304055,#304056,#304057,#304058,#304059,
#304060,#304061,#304062,#304063,#304064,#304065,#304066,#304067,#304068,
#304069,#304070,#304071,#304072),.UNSPECIFIED.,.F.,.F.,(4,2,2,2,2,2,2,2,
2,2,2,2,2,2,2,2,2,4),(15.6839332892533,15.782821791999,16.0203422716166,
16.2528136896479,16.4884851004376,16.7239507514617,16.9563640658718,17.1954154699755,
17.4288840826316,17.6625668779205,17.8994900438865,18.1317360792813,18.3681791547866,
18.6030837995683,18.8356615401653,19.0741198043588,19.3070917790011,19.4692315614832),
 .UNSPECIFIED.);
#6820=B_SPLINE_CURVE_WITH_KNOTS('',3,(#304077,#304078,#304079,#304080,#304081,
#304082,#304083,#304084,#304085,#304086,#304087,#304088,#304089,#304090,
#304091,#304092,#304093,#304094,#304095,#304096,#304097,#304098,#304099,
#304100,#304101,#304102,#304103,#304104,#304105,#304106,#304107,#304108,
#304109,#304110,#304111,#304112),.UNSPECIFIED.,.F.,.F.,(4,2,2,2,2,2,2,2,
2,2,2,2,2,2,2,2,2,4),(46.8485936589711,47.0216159195647,47.2544177903005,
47.4925687723112,47.725474467191,47.9600911742096,48.1973308216091,48.429608940541,
48.666212658611,48.9004139398187,49.1336081306584,49.3723251234082,49.6049574755668,
49.84011146838,50.0764558850996,50.308855490733,50.5460388328585,50.6352088804023),
 .UNSPECIFIED.);
#6821=B_SPLINE_CURVE_WITH_KNOTS('',3,(#304113,#304114,#304115,#304116,#304117,
#304118,#304119,#304120,#304121,#304122,#304123,#304124,#304125,#304126,
#304127,#304128,#304129,#304130,#304131,#304132,#304133,#304134,#304135,
#304136,#304137,#304138,#304139,#304140,#304141,#304142,#304143,#304144,
#304145,#304146,#304147,#304148),.UNSPECIFIED.,.F.,.F.,(4,2,2,2,2,2,2,2,
2,2,2,2,2,2,2,2,2,4),(11.8986040158769,12.0243613207986,12.2629518588974,
12.4960317159484,12.7302055983916,12.9666854476523,13.1988834932273,13.436124648461,
13.6706219597039,13.9034794829757,14.1415078050586,14.374207473683,14.6090685279858,
14.8450118149834,15.0772466276201,15.315531095212,15.5495427343885,15.6839332892533),
 .UNSPECIFIED.);
#6822=B_SPLINE_CURVE_WITH_KNOTS('',3,(#304153,#304154,#304155,#304156,#304157,
#304158,#304159,#304160,#304161,#304162,#304163,#304164,#304165,#304166,
#304167,#304168,#304169,#304170,#304171,#304172,#304173,#304174,#304175,
#304176,#304177,#304178,#304179,#304180,#304181,#304182,#304183,#304184,
#304185,#304186,#304187,#304188),.UNSPECIFIED.,.F.,.F.,(4,2,2,2,2,2,2,2,
2,2,2,2,2,2,2,2,2,4),(50.6352088804023,50.779714911507,51.0134015677832,
51.2525403684392,51.4848974847376,51.7204727123849,51.9559367579735,52.1884492079589,
52.4260870153873,52.6592513558619,52.8933755513534,53.1313949888071,53.3636070129719,
53.5996759364621,53.8343566499005,54.0671348611935,54.3052954975556,54.4208364023182),
 .UNSPECIFIED.);
#6823=B_SPLINE_CURVE_WITH_KNOTS('',3,(#304189,#304190,#304191,#304192,#304193,
#304194,#304195,#304196,#304197,#304198,#304199,#304200,#304201,#304202,
#304203,#304204,#304205,#304206,#304207,#304208,#304209,#304210,#304211,
#304212,#304213,#304214,#304215,#304216,#304217,#304218,#304219,#304220,
#304221,#304222,#304223,#304224),.UNSPECIFIED.,.F.,.F.,(4,2,2,2,2,2,2,2,
2,2,2,2,2,2,2,2,2,4),(8.11239459364437,8.26523226792941,8.50339890780251,
8.73754315172981,8.97080303206172,9.2084601167785,9.44101557047308,9.67660692827371,
9.91220348953535,10.1446362929211,10.3838249059144,10.6174234764245,10.8510593839814,
11.0881161592483,11.3204238869832,11.5567575241936,11.7917887714086,11.8986040158769),
 .UNSPECIFIED.);
#6824=B_SPLINE_CURVE_WITH_KNOTS('',3,(#304229,#304230,#304231,#304232,#304233,
#304234,#304235,#304236,#304237,#304238,#304239,#304240,#304241,#304242,
#304243,#304244,#304245,#304246,#304247,#304248,#304249,#304250,#304251,
#304252,#304253,#304254,#304255,#304256,#304257,#304258,#304259,#304260,
#304261,#304262,#304263,#304264),.UNSPECIFIED.,.F.,.F.,(4,2,2,2,2,2,2,2,
2,2,2,2,2,2,2,2,2,4),(54.4208364023182,54.5380700593176,54.7726933116663,
55.0096991104518,55.2419101196175,55.4785271334105,55.7125550932901,55.9457489905472,
56.1844822360332,56.4170069289476,56.6521732458631,56.8883096099332,57.1206651900448,
57.3578662747796,57.5913950898769,57.825097912479,58.0639871623955,58.2062941786064),
 .UNSPECIFIED.);
#6825=B_SPLINE_CURVE_WITH_KNOTS('',3,(#304265,#304266,#304267,#304268,#304269,
#304270,#304271,#304272,#304273,#304274,#304275,#304276,#304277,#304278,
#304279,#304280,#304281,#304282,#304283,#304284,#304285,#304286,#304287,
#304288,#304289,#304290,#304291,#304292,#304293,#304294,#304295,#304296,
#304297,#304298,#304299,#304300),.UNSPECIFIED.,.F.,.F.,(4,2,2,2,2,2,2,2,
2,2,2,2,2,2,2,2,2,4),(4.32614092106817,4.5074264780588,4.74368643906955,
4.97886575266752,5.21146326404075,5.45020780664062,5.6834205406393,5.9175544876609,
6.15418409958964,6.38644747818929,6.62359002635956,6.85822908616689,7.09108833089345,
7.32926347972645,7.56207220923553,7.79687076043539,8.03295588228145,8.11239459364437),
 .UNSPECIFIED.);
#6826=B_SPLINE_CURVE_WITH_KNOTS('',3,(#304309,#304310,#304311,#304312),
 .UNSPECIFIED.,.F.,.F.,(4,4),(61.9907935238473,62.0594966999548),
 .UNSPECIFIED.);
#6827=B_SPLINE_CURVE_WITH_KNOTS('',3,(#304315,#304316,#304317,#304318,#304319,
#304320,#304321,#304322,#304323,#304324),.UNSPECIFIED.,.F.,.F.,(4,2,2,2,
4),(9.99999995233633E-7,0.139869391385364,0.278811600184122,0.517011378301891,
0.54061986447261),.UNSPECIFIED.);
#6828=B_SPLINE_CURVE_WITH_KNOTS('',3,(#305074,#305075,#305076,#305077,#305078,
#305079,#305080,#305081,#305082,#305083,#305084,#305085,#305086,#305087),
 .UNSPECIFIED.,.F.,.F.,(4,2,2,2,2,2,4),(-0.78047807977081,-0.695301881662505,
-0.593639893486405,-0.425675928226966,-0.218826818693263,-0.10960289024564,
-9.99999999806711E-7),.UNSPECIFIED.);
#6829=B_SPLINE_CURVE_WITH_KNOTS('',3,(#305089,#305090,#305091,#305092,#305093,
#305094,#305095,#305096,#305097,#305098,#305099,#305100,#305101,#305102,
#305103,#305104,#305105,#305106,#305107,#305108,#305109,#305110,#305111,
#305112,#305113,#305114),.UNSPECIFIED.,.F.,.F.,(4,2,2,2,2,2,2,2,2,2,2,2,
4),(-4.05239234980258,-3.93862550091755,-3.82743496185452,-3.59617522122579,
-3.30037507154232,-3.02929753430978,-2.90428875735206,-2.65825727750779,
-2.41593958732872,-2.17055900710192,-1.91716465057545,-1.61902945081212,
-1.46516536274864),.UNSPECIFIED.);
#6830=B_SPLINE_CURVE_WITH_KNOTS('',3,(#305116,#305117,#305118,#305119,#305120,
#305121,#305122,#305123,#305124,#305125,#305126,#305127,#305128,#305129,
#305130,#305131,#305132,#305133),.UNSPECIFIED.,.F.,.F.,(4,2,2,2,2,2,2,2,
4),(-1.46516536274864,-1.34971750991573,-1.10796030676733,-0.986694312735197,
-0.753300167825488,-0.517085622070828,-0.401640164419751,-0.188272205565867,
-9.99999999695689E-7),.UNSPECIFIED.);
#6831=B_SPLINE_CURVE_WITH_KNOTS('',3,(#305864,#305865,#305866,#305867,#305868,
#305869,#305870,#305871,#305872,#305873,#305874,#305875,#305876,#305877,
#305878,#305879,#305880,#305881,#305882,#305883,#305884,#305885,#305886,
#305887,#305888,#305889,#305890,#305891,#305892,#305893,#305894,#305895,
#305896,#305897,#305898,#305899),.UNSPECIFIED.,.F.,.F.,(4,2,2,2,2,2,2,2,
2,2,2,2,2,2,2,2,2,4),(0.54061986447261,0.74981201493592,0.98442493645702,
1.22053124981613,1.45273047421174,1.69065225033218,1.92480945062251,2.15792871651212,
2.39560117799006,2.62812310862901,2.8635094758593,3.09911678414555,3.3314492881675,
3.57048314820672,3.80419695742923,4.03781856148348,4.27503010720451,4.32614092106817),
 .UNSPECIFIED.);
#6832=B_SPLINE_CURVE_WITH_KNOTS('',3,(#306633,#306634,#306635,#306636,#306637,
#306638,#306639,#306640,#306641,#306642,#306643,#306644,#306645,#306646,
#306647,#306648,#306649,#306650,#306651,#306652,#306653,#306654,#306655,
#306656,#306657,#306658,#306659,#306660,#306661,#306662,#306663,#306664,
#306665,#306666,#306667,#306668),.UNSPECIFIED.,.F.,.F.,(4,2,2,2,2,2,2,2,
2,2,2,2,2,2,2,2,2,4),(58.2062941786064,58.2962573272515,58.531858244201,
58.7671282443229,58.9996221986813,59.2372904797072,59.4703266701106,59.7044785679362,
59.9422635556724,60.1744124212493,60.4105174589839,60.6450243103711,60.8778099818224,
61.1160107455192,61.3486800137014,61.5833395502273,61.8201331537292,61.9907935238473),
 .UNSPECIFIED.);
#6833=B_SPLINE_CURVE_WITH_KNOTS('',3,(#306669,#306670,#306671,#306672,#306673,
#306674,#306675,#306676,#306677,#306678,#306679,#306680,#306681,#306682),
 .UNSPECIFIED.,.F.,.F.,(4,2,2,2,2,2,4),(-4.24206895984873,-4.08128650184182,
-3.92521410894753,-3.82989233455649,-3.64245446409652,-3.5499952935536,
-3.42352177914162),.UNSPECIFIED.);
#6834=B_SPLINE_CURVE_WITH_KNOTS('',3,(#306687,#306688,#306689,#306690,#306691,
#306692,#306693,#306694,#306695,#306696,#306697,#306698,#306699,#306700,
#306701,#306702,#306703,#306704,#306705),.UNSPECIFIED.,.F.,.F.,(4,1,1,1,
1,1,1,1,1,1,1,1,1,1,1,1,4),(0.,0.0577170366867072,0.113994474768008,0.16893758423175,
0.224179487123504,0.279968804571931,0.337633163696686,0.397092193126611,
0.459041827583877,0.522525900750905,0.586121573329079,0.650102352916103,
0.71540731027663,0.782762550840158,0.852275272320573,0.924507298607219,
1.),.UNSPECIFIED.);
#6835=B_SPLINE_CURVE_WITH_KNOTS('',3,(#306707,#306708,#306709,#306710,#306711,
#306712,#306713,#306714,#306715,#306716,#306717,#306718,#306719,#306720,
#306721,#306722,#306723,#306724,#306725),.UNSPECIFIED.,.F.,.F.,(4,1,1,1,
1,1,1,1,1,1,1,1,1,1,1,1,4),(0.,0.0768723536038944,0.150603343572851,0.220876273582275,
0.288315870518755,0.35395225660761,0.418604106617997,0.481972048717606,
0.545247561534372,0.606993813632933,0.665860906234417,0.723420981486814,
0.778433488719744,0.833552283298071,0.88813757158342,0.943362448943921,
1.),.UNSPECIFIED.);
#6836=B_SPLINE_CURVE_WITH_KNOTS('',3,(#306727,#306728,#306729,#306730,#306731,
#306732,#306733,#306734,#306735,#306736,#306737,#306738,#306739,#306740,
#306741,#306742,#306743,#306744,#306745),.UNSPECIFIED.,.F.,.F.,(4,1,1,1,
1,1,1,1,1,1,1,1,1,1,1,1,4),(0.,0.0580692684342556,0.114001303445375,0.169772099070702,
0.224674954494909,0.280054150165824,0.336957215314267,0.395112576113712,
0.456649482459617,0.519182398591372,0.582165728137028,0.645753825355143,
0.710908012329458,0.778341319290106,0.848949505917864,0.922850140892551,
1.),.UNSPECIFIED.);
#6837=B_SPLINE_CURVE_WITH_KNOTS('',3,(#306746,#306747,#306748,#306749,#306750,
#306751,#306752,#306753,#306754,#306755,#306756,#306757,#306758,#306759,
#306760,#306761,#306762,#306763,#306764),.UNSPECIFIED.,.F.,.F.,(4,1,1,1,
1,1,1,1,1,1,1,1,1,1,1,1,4),(0.,0.0766164418639844,0.150101977842741,0.220268821680907,
0.287483908975341,0.35290178839726,0.417338409308383,0.480866360224848,
0.543808187325834,0.605854592868513,0.665047756996982,0.722013651121557,
0.777789178028364,0.832724479504672,0.887128050755955,0.942855781853261,
1.),.UNSPECIFIED.);
#6838=B_SPLINE_CURVE_WITH_KNOTS('',3,(#306768,#306769,#306770,#306771,#306772,
#306773,#306774,#306775,#306776,#306777,#306778),.UNSPECIFIED.,.F.,.F.,
(4,1,1,1,1,1,1,1,4),(0.,0.113035127206385,0.22352787461649,0.337812984577189,
0.462304974001557,0.590889524052717,0.720496476039469,0.855414628911259,
1.),.UNSPECIFIED.);
#6839=B_SPLINE_CURVE_WITH_KNOTS('',3,(#306780,#306781,#306782,#306783,#306784,
#306785,#306786,#306787,#306788,#306789,#306790),.UNSPECIFIED.,.F.,.F.,
(4,1,1,1,1,1,1,1,4),(0.,0.153975786043391,0.294620990206987,0.425952943236339,
0.551063084753368,0.669883873511439,0.780296648018842,0.888858324162197,
1.),.UNSPECIFIED.);
#6840=B_SPLINE_CURVE_WITH_KNOTS('',3,(#306792,#306793,#306794,#306795,#306796,
#306797,#306798,#306799,#306800,#306801,#306802),.UNSPECIFIED.,.F.,.F.,
(4,1,1,1,1,1,1,1,4),(0.,0.113008663357688,0.223447121007772,0.335763095333029,
0.457240997711765,0.584219963833153,0.714811315114105,0.851997802140335,
1.),.UNSPECIFIED.);
#6841=B_SPLINE_CURVE_WITH_KNOTS('',3,(#306803,#306804,#306805,#306806,#306807,
#306808,#306809,#306810,#306811,#306812,#306813),.UNSPECIFIED.,.F.,.F.,
(4,1,1,1,1,1,1,1,4),(0.,0.149379665294656,0.288273014687601,0.418942648167458,
0.547753389590675,0.670496533301504,0.782663672045753,0.890203158268387,
1.),.UNSPECIFIED.);
#6842=B_SPLINE_CURVE_WITH_KNOTS('',3,(#306817,#306818,#306819,#306820,#306821,
#306822,#306823,#306824,#306825,#306826,#306827,#306828,#306829,#306830,
#306831,#306832,#306833,#306834,#306835),.UNSPECIFIED.,.F.,.F.,(4,1,1,1,
1,1,1,1,1,1,1,1,1,1,1,1,4),(0.,0.0577170366867072,0.113994474768008,0.16893758423175,
0.224179487123505,0.279968804571931,0.337633163696686,0.397092193126611,
0.459041827583877,0.522525900750905,0.586121573329079,0.650102352916103,
0.71540731027663,0.782762550840158,0.852275272320572,0.924507298607219,
1.),.UNSPECIFIED.);
#6843=B_SPLINE_CURVE_WITH_KNOTS('',3,(#306837,#306838,#306839,#306840,#306841,
#306842,#306843,#306844,#306845,#306846,#306847,#306848,#306849,#306850,
#306851,#306852,#306853,#306854,#306855),.UNSPECIFIED.,.F.,.F.,(4,1,1,1,
1,1,1,1,1,1,1,1,1,1,1,1,4),(0.,0.0768723536038944,0.150603343572851,0.220876273582275,
0.288315870518755,0.35395225660761,0.418604106617997,0.481972048717605,
0.545247561534372,0.606993813632933,0.665860906234417,0.723420981486814,
0.778433488719744,0.833552283298071,0.88813757158342,0.943362448943921,
1.),.UNSPECIFIED.);
#6844=B_SPLINE_CURVE_WITH_KNOTS('',3,(#306857,#306858,#306859,#306860,#306861,
#306862,#306863,#306864,#306865,#306866,#306867,#306868,#306869,#306870,
#306871,#306872,#306873,#306874,#306875),.UNSPECIFIED.,.F.,.F.,(4,1,1,1,
1,1,1,1,1,1,1,1,1,1,1,1,4),(0.,0.0580692684342556,0.114001303445375,0.169772099070702,
0.224674954494909,0.280054150165824,0.336957215314267,0.395112576113712,
0.456649482459617,0.519182398591372,0.582165728137028,0.645753825355143,
0.710908012329458,0.778341319290106,0.848949505917864,0.922850140892551,
1.),.UNSPECIFIED.);
#6845=B_SPLINE_CURVE_WITH_KNOTS('',3,(#306876,#306877,#306878,#306879,#306880,
#306881,#306882,#306883,#306884,#306885,#306886,#306887,#306888,#306889,
#306890,#306891,#306892,#306893,#306894),.UNSPECIFIED.,.F.,.F.,(4,1,1,1,
1,1,1,1,1,1,1,1,1,1,1,1,4),(0.,0.0766164418639844,0.150101977842741,0.220268821680907,
0.287483908975341,0.35290178839726,0.417338409308383,0.480866360224848,
0.543808187325834,0.605854592868513,0.665047756996982,0.722013651121557,
0.777789178028364,0.832724479504672,0.887128050755955,0.942855781853261,
1.),.UNSPECIFIED.);
#6846=B_SPLINE_CURVE_WITH_KNOTS('',3,(#306898,#306899,#306900,#306901,#306902,
#306903,#306904,#306905,#306906,#306907,#306908),.UNSPECIFIED.,.F.,.F.,
(4,1,1,1,1,1,1,1,4),(0.,0.113035127206385,0.22352787461649,0.337812984577189,
0.462304974001557,0.590889524052717,0.720496476039469,0.855414628911259,
1.),.UNSPECIFIED.);
#6847=B_SPLINE_CURVE_WITH_KNOTS('',3,(#306910,#306911,#306912,#306913,#306914,
#306915,#306916,#306917,#306918,#306919,#306920),.UNSPECIFIED.,.F.,.F.,
(4,1,1,1,1,1,1,1,4),(0.,0.153975786043391,0.294620990206987,0.42595294323634,
0.551063084753368,0.669883873511439,0.780296648018842,0.888858324162197,
1.),.UNSPECIFIED.);
#6848=B_SPLINE_CURVE_WITH_KNOTS('',3,(#306922,#306923,#306924,#306925,#306926,
#306927,#306928,#306929,#306930,#306931,#306932),.UNSPECIFIED.,.F.,.F.,
(4,1,1,1,1,1,1,1,4),(0.,0.113008663357688,0.223447121007772,0.335763095333029,
0.457240997711765,0.584219963833153,0.714811315114105,0.851997802140335,
1.),.UNSPECIFIED.);
#6849=B_SPLINE_CURVE_WITH_KNOTS('',3,(#306933,#306934,#306935,#306936,#306937,
#306938,#306939,#306940,#306941,#306942,#306943),.UNSPECIFIED.,.F.,.F.,
(4,1,1,1,1,1,1,1,4),(0.,0.149379665294656,0.288273014687601,0.418942648167458,
0.547753389590675,0.670496533301504,0.782663672045753,0.890203158268387,
1.),.UNSPECIFIED.);
#6850=B_SPLINE_CURVE_WITH_KNOTS('',3,(#306985,#306986,#306987,#306988,#306989,
#306990,#306991,#306992,#306993,#306994,#306995,#306996,#306997,#306998,
#306999,#307000,#307001,#307002,#307003),.UNSPECIFIED.,.F.,.F.,(4,1,1,1,
1,1,1,1,1,1,1,1,1,1,1,1,4),(0.,0.0771498591074487,0.151050494082136,0.221658680709894,
0.289091987670543,0.354246174644858,0.417834271862972,0.480817601408628,
0.543350517540383,0.604887423886288,0.663042784685733,0.719945849834176,
0.775325045505091,0.830227900929299,0.885998696554625,0.941930731565744,
1.),.UNSPECIFIED.);
#6851=B_SPLINE_CURVE_WITH_KNOTS('',3,(#307044,#307045,#307046,#307047,#307048,
#307049,#307050,#307051,#307052,#307053,#307054,#307055,#307056,#307057,
#307058,#307059,#307060,#307061,#307062),.UNSPECIFIED.,.F.,.F.,(4,1,1,1,
1,1,1,1,1,1,1,1,1,1,1,1,4),(-1.,-0.942855781853261,-0.887128050755955,-0.832724479504672,
-0.777789178028364,-0.722013651121557,-0.665047756996982,-0.605854592868513,
-0.543808187325834,-0.480866360224848,-0.417338409308383,-0.35290178839726,
-0.287483908975341,-0.220268821680907,-0.150101977842741,-0.0766164418639844,
0.),.UNSPECIFIED.);
#6852=B_SPLINE_CURVE_WITH_KNOTS('',3,(#307103,#307104,#307105,#307106,#307107,
#307108,#307109,#307110,#307111,#307112,#307113,#307114,#307115,#307116,
#307117,#307118,#307119,#307120,#307121),.UNSPECIFIED.,.F.,.F.,(4,1,1,1,
1,1,1,1,1,1,1,1,1,1,1,1,4),(0.,0.075492701392781,0.147724727679427,0.217237449159842,
0.284592689723369,0.349897647083897,0.413878426670921,0.477474099249095,
0.540958172416123,0.602907806873388,0.662366836303314,0.72003119542807,
0.775820512876496,0.83106241576825,0.886005525231993,0.942282963313293,
1.),.UNSPECIFIED.);
#6853=B_SPLINE_CURVE_WITH_KNOTS('',3,(#307161,#307162,#307163,#307164,#307165,
#307166,#307167,#307168,#307169,#307170,#307171,#307172,#307173,#307174,
#307175,#307176,#307177,#307178,#307179),.UNSPECIFIED.,.F.,.F.,(4,1,1,1,
1,1,1,1,1,1,1,1,1,1,1,1,4),(0.,0.0566375510560788,0.11186242841658,0.166447716701929,
0.221566511280256,0.276579018513186,0.334139093765582,0.393006186367067,
0.454752438465628,0.518027951282394,0.581395893382003,0.646047743392391,
0.711684129481244,0.779123726417726,0.849396656427148,0.923127646396106,
1.),.UNSPECIFIED.);
#6854=B_SPLINE_CURVE_WITH_KNOTS('',3,(#307205,#307206,#307207,#307208,#307209,
#307210,#307211,#307212,#307213,#307214,#307215),.UNSPECIFIED.,.F.,.F.,
(4,1,1,1,1,1,1,1,4),(0.,0.148002197859665,0.285188684885895,0.415780036166847,
0.542759002288235,0.664236904666971,0.776552878992228,0.886991336642312,
1.),.UNSPECIFIED.);
#6855=B_SPLINE_CURVE_WITH_KNOTS('',3,(#307240,#307241,#307242,#307243,#307244,
#307245,#307246,#307247,#307248,#307249,#307250),.UNSPECIFIED.,.F.,.F.,
(4,1,1,1,1,1,1,1,4),(0.,0.109796841731613,0.217336327954247,0.329503466698497,
0.452246610409325,0.581057351832542,0.711726985312399,0.850620334705344,
1.),.UNSPECIFIED.);
#6856=B_SPLINE_CURVE_WITH_KNOTS('',3,(#307275,#307276,#307277,#307278,#307279,
#307280,#307281,#307282,#307283,#307284,#307285),.UNSPECIFIED.,.F.,.F.,
(4,1,1,1,1,1,1,1,4),(0.,0.144585371088741,0.279503523960531,0.409110475947283,
0.537695025998443,0.662187015422811,0.77647212538351,0.886964872793615,
1.),.UNSPECIFIED.);
#6857=B_SPLINE_CURVE_WITH_KNOTS('',3,(#307309,#307310,#307311,#307312,#307313,
#307314,#307315,#307316,#307317,#307318,#307319),.UNSPECIFIED.,.F.,.F.,
(4,1,1,1,1,1,1,1,4),(0.,0.111141675837803,0.219703351981158,0.330116126488561,
0.448936915246632,0.57404705676366,0.705379009793014,0.846024213956609,
1.),.UNSPECIFIED.);
#6858=B_SPLINE_CURVE_WITH_KNOTS('',3,(#307361,#307362,#307363,#307364,#307365,
#307366,#307367,#307368,#307369,#307370,#307371,#307372,#307373,#307374,
#307375,#307376,#307377,#307378,#307379),.UNSPECIFIED.,.F.,.F.,(4,1,1,1,
1,1,1,1,1,1,1,1,1,1,1,1,4),(0.,0.0771498591074487,0.151050494082136,0.221658680709894,
0.289091987670542,0.354246174644858,0.417834271862972,0.480817601408628,
0.543350517540383,0.604887423886288,0.663042784685733,0.719945849834176,
0.775325045505091,0.830227900929299,0.885998696554625,0.941930731565744,
1.),.UNSPECIFIED.);
#6859=B_SPLINE_CURVE_WITH_KNOTS('',3,(#307420,#307421,#307422,#307423,#307424,
#307425,#307426,#307427,#307428,#307429,#307430,#307431,#307432,#307433,
#307434,#307435,#307436,#307437,#307438),.UNSPECIFIED.,.F.,.F.,(4,1,1,1,
1,1,1,1,1,1,1,1,1,1,1,1,4),(-1.,-0.942855781853261,-0.887128050755955,-0.832724479504672,
-0.777789178028364,-0.722013651121557,-0.665047756996982,-0.605854592868513,
-0.543808187325834,-0.480866360224848,-0.417338409308383,-0.35290178839726,
-0.287483908975341,-0.220268821680907,-0.150101977842741,-0.0766164418639844,
0.),.UNSPECIFIED.);
#6860=B_SPLINE_CURVE_WITH_KNOTS('',3,(#307479,#307480,#307481,#307482,#307483,
#307484,#307485,#307486,#307487,#307488,#307489,#307490,#307491,#307492,
#307493,#307494,#307495,#307496,#307497),.UNSPECIFIED.,.F.,.F.,(4,1,1,1,
1,1,1,1,1,1,1,1,1,1,1,1,4),(0.,0.075492701392781,0.147724727679427,0.217237449159842,
0.284592689723369,0.349897647083897,0.413878426670921,0.477474099249095,
0.540958172416123,0.602907806873388,0.662366836303314,0.72003119542807,
0.775820512876496,0.83106241576825,0.886005525231992,0.942282963313293,
1.),.UNSPECIFIED.);
#6861=B_SPLINE_CURVE_WITH_KNOTS('',3,(#307537,#307538,#307539,#307540,#307541,
#307542,#307543,#307544,#307545,#307546,#307547,#307548,#307549,#307550,
#307551,#307552,#307553,#307554,#307555),.UNSPECIFIED.,.F.,.F.,(4,1,1,1,
1,1,1,1,1,1,1,1,1,1,1,1,4),(0.,0.0566375510560786,0.11186242841658,0.16644771670193,
0.221566511280256,0.276579018513186,0.334139093765582,0.393006186367067,
0.454752438465629,0.518027951282395,0.581395893382003,0.646047743392391,
0.711684129481244,0.779123726417726,0.849396656427148,0.923127646396106,
1.),.UNSPECIFIED.);
#6862=B_SPLINE_CURVE_WITH_KNOTS('',3,(#307581,#307582,#307583,#307584,#307585,
#307586,#307587,#307588,#307589,#307590,#307591),.UNSPECIFIED.,.F.,.F.,
(4,1,1,1,1,1,1,1,4),(0.,0.148002197859665,0.285188684885895,0.415780036166847,
0.542759002288235,0.664236904666971,0.776552878992228,0.886991336642312,
1.),.UNSPECIFIED.);
#6863=B_SPLINE_CURVE_WITH_KNOTS('',3,(#307616,#307617,#307618,#307619,#307620,
#307621,#307622,#307623,#307624,#307625,#307626),.UNSPECIFIED.,.F.,.F.,
(4,1,1,1,1,1,1,1,4),(0.,0.109796841731613,0.217336327954247,0.329503466698497,
0.452246610409325,0.581057351832542,0.711726985312399,0.850620334705344,
1.),.UNSPECIFIED.);
#6864=B_SPLINE_CURVE_WITH_KNOTS('',3,(#307651,#307652,#307653,#307654,#307655,
#307656,#307657,#307658,#307659,#307660,#307661),.UNSPECIFIED.,.F.,.F.,
(4,1,1,1,1,1,1,1,4),(0.,0.144585371088741,0.279503523960531,0.409110475947283,
0.537695025998443,0.662187015422811,0.77647212538351,0.886964872793615,
1.),.UNSPECIFIED.);
#6865=B_SPLINE_CURVE_WITH_KNOTS('',3,(#307685,#307686,#307687,#307688,#307689,
#307690,#307691,#307692,#307693,#307694,#307695),.UNSPECIFIED.,.F.,.F.,
(4,1,1,1,1,1,1,1,4),(0.,0.111141675837803,0.219703351981158,0.330116126488562,
0.448936915246632,0.57404705676366,0.705379009793014,0.846024213956609,
1.),.UNSPECIFIED.);
#6866=B_SPLINE_CURVE_WITH_KNOTS('',3,(#307699,#307700,#307701,#307702,#307703,
#307704,#307705,#307706,#307707,#307708,#307709),.UNSPECIFIED.,.F.,.F.,
(4,1,1,1,1,1,1,1,4),(0.,0.14381860843526,0.276720184060535,0.40139659054717,
0.520594774062884,0.637293245567233,0.75409807560852,0.873962190826757,
1.),.UNSPECIFIED.);
#6867=B_SPLINE_CURVE_WITH_KNOTS('',3,(#307711,#307712,#307713,#307714,#307715,
#307716,#307717,#307718,#307719,#307720,#307721,#307722,#307723,#307724,
#307725,#307726,#307727,#307728,#307729),.UNSPECIFIED.,.F.,.F.,(4,1,1,1,
1,1,1,1,1,1,1,1,1,1,1,1,4),(-1.,-0.940276800846585,-0.882061797546221,-0.824126149789293,
-0.767064167323289,-0.71022527848224,-0.653190706601446,-0.595069793647295,
-0.535395707628871,-0.475131662182092,-0.41333034849776,-0.350394511043543,
-0.285894163869826,-0.218686839383758,-0.148475385165302,-0.0756779287595513,
0.),.UNSPECIFIED.);
#6868=B_SPLINE_CURVE_WITH_KNOTS('',3,(#307731,#307732,#307733,#307734,#307735,
#307736,#307737,#307738,#307739,#307740,#307741,#307742,#307743,#307744,
#307745,#307746,#307747,#307748,#307749),.UNSPECIFIED.,.F.,.F.,(4,1,1,1,
1,1,1,1,1,1,1,1,1,1,1,1,4),(0.,0.0735593902167768,0.144406880522386,0.212035000612302,
0.277455182895964,0.341240831122113,0.403615225713777,0.465772853725949,
0.527839405900435,0.589271108646648,0.648485061002809,0.706313491571885,
0.763897708792844,0.820995580197687,0.879024456534409,0.938439191447014,
1.),.UNSPECIFIED.);
#6869=B_SPLINE_CURVE_WITH_KNOTS('',3,(#307751,#307752,#307753,#307754,#307755,
#307756,#307757,#307758,#307759,#307760,#307761,#307762,#307763,#307764,
#307765,#307766,#307767,#307768,#307769),.UNSPECIFIED.,.F.,.F.,(4,1,1,1,
1,1,1,1,1,1,1,1,1,1,1,1,4),(0.,0.0612675560073353,0.120821287104165,0.178985698366598,
0.236645059586719,0.294395620729497,0.352792725296381,0.412241000299045,
0.474276810949433,0.536953714018934,0.599593467559458,0.66197417732883,
0.725552076032239,0.790752056360384,0.857809975221741,0.927515627061441,
1.),.UNSPECIFIED.);
#6870=B_SPLINE_CURVE_WITH_KNOTS('',3,(#307771,#307772,#307773,#307774,#307775,
#307776,#307777,#307778,#307779,#307780,#307781,#307782,#307783,#307784,
#307785,#307786,#307787,#307788,#307789),.UNSPECIFIED.,.F.,.F.,(4,1,1,1,
1,1,1,1,1,1,1,1,1,1,1,1,4),(0.,0.0737198727326366,0.143946935064662,0.212133747062962,
0.277912671008997,0.34156704167165,0.403626619899118,0.464825448444965,
0.524706702690351,0.583602784640957,0.642223378321782,0.700523711411864,
0.758512105377773,0.816969451940464,0.876419241746809,0.937592570779656,
1.),.UNSPECIFIED.);
#6871=B_SPLINE_CURVE_WITH_KNOTS('',3,(#307791,#307792,#307793,#307794,#307795,
#307796,#307797,#307798,#307799,#307800,#307801),.UNSPECIFIED.,.F.,.F.,
(4,1,1,1,1,1,1,1,4),(0.,0.129460777681808,0.251364758465844,0.369750478112862,
0.48633159458772,0.605179466580234,0.728807707522854,0.859213949280771,
1.),.UNSPECIFIED.);
#6872=B_SPLINE_CURVE_WITH_KNOTS('',3,(#307803,#307804,#307805,#307806,#307807,
#307808,#307809,#307810,#307811,#307812,#307813,#307814,#307815,#307816,
#307817,#307818,#307819,#307820,#307821),.UNSPECIFIED.,.F.,.F.,(4,1,1,1,
1,1,1,1,1,1,1,1,1,1,1,1,4),(0.,0.0724915710472832,0.142248636949713,0.209709388595723,
0.274857515432795,0.338249555361619,0.400730922620109,0.462891931966943,
0.525566461597643,0.587484469713601,0.64667511935087,0.705219765007066,
0.762798326707908,0.820199705010802,0.878348632650845,0.938420716788534,
1.),.UNSPECIFIED.);
#6873=B_SPLINE_CURVE_WITH_KNOTS('',3,(#307822,#307823,#307824,#307825,#307826,
#307827,#307828,#307829,#307830,#307831,#307832,#307833,#307834,#307835,
#307836,#307837,#307838,#307839,#307840),.UNSPECIFIED.,.F.,.F.,(4,1,1,1,
1,1,1,1,1,1,1,1,1,1,1,1,4),(0.,0.0618009710281554,0.122005337166018,0.18035060128547,
0.237956680350668,0.295993496555078,0.354224180223643,0.413796608373368,
0.475344905905867,0.537628047311842,0.600103014912843,0.662388390250829,
0.725572014773438,0.790351843146754,0.857597742298064,0.927154440774627,
1.),.UNSPECIFIED.);
#6874=B_SPLINE_CURVE_WITH_KNOTS('',3,(#307844,#307845,#307846,#307847,#307848,
#307849,#307850,#307851,#307852,#307853,#307854),.UNSPECIFIED.,.F.,.F.,
(4,1,1,1,1,1,1,1,4),(0.,0.14381860843526,0.276720184060535,0.40139659054717,
0.520594774062884,0.637293245567233,0.75409807560852,0.873962190826756,
1.),.UNSPECIFIED.);
#6875=B_SPLINE_CURVE_WITH_KNOTS('',3,(#307856,#307857,#307858,#307859,#307860,
#307861,#307862,#307863,#307864,#307865,#307866,#307867,#307868,#307869,
#307870,#307871,#307872,#307873,#307874),.UNSPECIFIED.,.F.,.F.,(4,1,1,1,
1,1,1,1,1,1,1,1,1,1,1,1,4),(-1.,-0.940276800846584,-0.882061797546221,-0.824126149789293,
-0.767064167323289,-0.71022527848224,-0.653190706601445,-0.595069793647295,
-0.535395707628871,-0.475131662182092,-0.41333034849776,-0.350394511043543,
-0.285894163869826,-0.218686839383758,-0.148475385165302,-0.0756779287595513,
0.),.UNSPECIFIED.);
#6876=B_SPLINE_CURVE_WITH_KNOTS('',3,(#307876,#307877,#307878,#307879,#307880,
#307881,#307882,#307883,#307884,#307885,#307886,#307887,#307888,#307889,
#307890,#307891,#307892,#307893,#307894),.UNSPECIFIED.,.F.,.F.,(4,1,1,1,
1,1,1,1,1,1,1,1,1,1,1,1,4),(0.,0.0735593902167768,0.144406880522386,0.212035000612302,
0.277455182895964,0.341240831122113,0.403615225713777,0.465772853725949,
0.527839405900435,0.589271108646648,0.648485061002809,0.706313491571885,
0.763897708792844,0.820995580197687,0.879024456534409,0.938439191447014,
1.),.UNSPECIFIED.);
#6877=B_SPLINE_CURVE_WITH_KNOTS('',3,(#307896,#307897,#307898,#307899,#307900,
#307901,#307902,#307903,#307904,#307905,#307906,#307907,#307908,#307909,
#307910,#307911,#307912,#307913,#307914),.UNSPECIFIED.,.F.,.F.,(4,1,1,1,
1,1,1,1,1,1,1,1,1,1,1,1,4),(0.,0.0612675560073353,0.120821287104165,0.178985698366598,
0.236645059586719,0.294395620729497,0.352792725296381,0.412241000299045,
0.474276810949433,0.536953714018934,0.599593467559457,0.66197417732883,
0.725552076032239,0.790752056360384,0.857809975221741,0.927515627061441,
1.),.UNSPECIFIED.);
#6878=B_SPLINE_CURVE_WITH_KNOTS('',3,(#307916,#307917,#307918,#307919,#307920,
#307921,#307922,#307923,#307924,#307925,#307926,#307927,#307928,#307929,
#307930,#307931,#307932,#307933,#307934),.UNSPECIFIED.,.F.,.F.,(4,1,1,1,
1,1,1,1,1,1,1,1,1,1,1,1,4),(0.,0.0737198727326366,0.143946935064662,0.212133747062962,
0.277912671008997,0.34156704167165,0.403626619899117,0.464825448444965,
0.524706702690351,0.583602784640957,0.642223378321781,0.700523711411864,
0.758512105377773,0.816969451940464,0.876419241746809,0.937592570779656,
1.),.UNSPECIFIED.);
#6879=B_SPLINE_CURVE_WITH_KNOTS('',3,(#307936,#307937,#307938,#307939,#307940,
#307941,#307942,#307943,#307944,#307945,#307946),.UNSPECIFIED.,.F.,.F.,
(4,1,1,1,1,1,1,1,4),(0.,0.129460777681808,0.251364758465844,0.369750478112862,
0.48633159458772,0.605179466580234,0.728807707522854,0.859213949280771,
1.),.UNSPECIFIED.);
#6880=B_SPLINE_CURVE_WITH_KNOTS('',3,(#307948,#307949,#307950,#307951,#307952,
#307953,#307954,#307955,#307956,#307957,#307958,#307959,#307960,#307961,
#307962,#307963,#307964,#307965,#307966),.UNSPECIFIED.,.F.,.F.,(4,1,1,1,
1,1,1,1,1,1,1,1,1,1,1,1,4),(0.,0.0724915710472832,0.142248636949713,0.209709388595723,
0.274857515432795,0.33824955536162,0.400730922620109,0.462891931966943,
0.525566461597643,0.587484469713601,0.64667511935087,0.705219765007066,
0.762798326707908,0.820199705010802,0.878348632650845,0.938420716788534,
1.),.UNSPECIFIED.);
#6881=B_SPLINE_CURVE_WITH_KNOTS('',3,(#307967,#307968,#307969,#307970,#307971,
#307972,#307973,#307974,#307975,#307976,#307977,#307978,#307979,#307980,
#307981,#307982,#307983,#307984,#307985),.UNSPECIFIED.,.F.,.F.,(4,1,1,1,
1,1,1,1,1,1,1,1,1,1,1,1,4),(0.,0.0618009710281554,0.122005337166018,0.18035060128547,
0.237956680350668,0.295993496555078,0.354224180223643,0.413796608373368,
0.475344905905867,0.537628047311842,0.600103014912843,0.662388390250829,
0.725572014773438,0.790351843146754,0.857597742298064,0.927154440774627,
1.),.UNSPECIFIED.);
#6882=B_SPLINE_CURVE_WITH_KNOTS('',3,(#308037,#308038,#308039,#308040,#308041,
#308042,#308043,#308044,#308045,#308046,#308047,#308048,#308049,#308050,
#308051,#308052,#308053,#308054,#308055),.UNSPECIFIED.,.F.,.F.,(4,1,1,1,
1,1,1,1,1,1,1,1,1,1,1,1,4),(0.,0.0624074292203441,0.123580758253191,0.183030548059535,
0.241487894622227,0.299476288588136,0.357776621678218,0.416397215359044,
0.475293297309649,0.535174551555035,0.596373380100883,0.65843295832835,
0.722087328991003,0.787866252937039,0.856053064935337,0.926280127267363,
1.),.UNSPECIFIED.);
#6883=B_SPLINE_CURVE_WITH_KNOTS('',3,(#308080,#308081,#308082,#308083,#308084,
#308085,#308086,#308087,#308088,#308089,#308090),.UNSPECIFIED.,.F.,.F.,
(4,1,1,1,1,1,1,1,4),(0.,0.140786050719229,0.271192292477146,0.394820533419766,
0.51366840541228,0.630249521887138,0.748635241534156,0.870539222318192,
1.),.UNSPECIFIED.);
#6884=B_SPLINE_CURVE_WITH_KNOTS('',3,(#308131,#308132,#308133,#308134,#308135,
#308136,#308137,#308138,#308139,#308140,#308141,#308142,#308143,#308144,
#308145,#308146,#308147,#308148,#308149),.UNSPECIFIED.,.F.,.F.,(4,1,1,1,
1,1,1,1,1,1,1,1,1,1,1,1,4),(0.,0.061579283211466,0.121651367349155,0.179800294989198,
0.237201673292092,0.294780234992934,0.353324880649131,0.412515530286399,
0.474433538402357,0.537108068033057,0.599269077379891,0.66175044463838,
0.725142484567205,0.790290611404277,0.857751363050287,0.927508428952717,
1.),.UNSPECIFIED.);
#6885=B_SPLINE_CURVE_WITH_KNOTS('',3,(#308190,#308191,#308192,#308193,#308194,
#308195,#308196,#308197,#308198,#308199,#308200,#308201,#308202,#308203,
#308204,#308205,#308206,#308207,#308208),.UNSPECIFIED.,.F.,.F.,(4,1,1,1,
1,1,1,1,1,1,1,1,1,1,1,1,4),(0.,0.0728455592253727,0.142402257701936,0.209648156853246,
0.274427985226561,0.337611609749171,0.399896985087157,0.462371952688158,
0.524655094094133,0.586203391626632,0.645775819776357,0.704006503444922,
0.762043319649332,0.81964939871453,0.877994662833982,0.938199028971844,
1.),.UNSPECIFIED.);
#6886=B_SPLINE_CURVE_WITH_KNOTS('',3,(#308233,#308234,#308235,#308236,#308237,
#308238,#308239,#308240,#308241,#308242,#308243),.UNSPECIFIED.,.F.,.F.,
(4,1,1,1,1,1,1,1,4),(0.,0.126037809173243,0.24590192439148,0.362706754432767,
0.479405225937116,0.59860340945283,0.723279815939465,0.85618139156474,1.),
 .UNSPECIFIED.);
#6887=B_SPLINE_CURVE_WITH_KNOTS('',3,(#308284,#308285,#308286,#308287,#308288,
#308289,#308290,#308291,#308292,#308293,#308294,#308295,#308296,#308297,
#308298,#308299,#308300,#308301,#308302),.UNSPECIFIED.,.F.,.F.,(4,1,1,1,
1,1,1,1,1,1,1,1,1,1,1,1,4),(0.,0.0756779287595513,0.148475385165302,0.218686839383758,
0.285894163869826,0.350394511043543,0.41333034849776,0.475131662182092,
0.535395707628871,0.595069793647295,0.653190706601446,0.71022527848224,
0.767064167323289,0.824126149789293,0.882061797546221,0.940276800846585,
1.),.UNSPECIFIED.);
#6888=B_SPLINE_CURVE_WITH_KNOTS('',3,(#308343,#308344,#308345,#308346,#308347,
#308348,#308349,#308350,#308351,#308352,#308353,#308354,#308355,#308356,
#308357,#308358,#308359,#308360,#308361),.UNSPECIFIED.,.F.,.F.,(4,1,1,1,
1,1,1,1,1,1,1,1,1,1,1,1,4),(0.,0.061560808552986,0.120975543465591,0.179004419802313,
0.236102291207156,0.293686508428115,0.351514938997191,0.410728891353352,
0.472160594099565,0.534227146274051,0.596384774286223,0.658759168877887,
0.722544817104037,0.787964999387698,0.855593119477614,0.926440609783223,
1.),.UNSPECIFIED.);
#6889=B_SPLINE_CURVE_WITH_KNOTS('',3,(#308400,#308401,#308402,#308403,#308404,
#308405,#308406,#308407,#308408,#308409,#308410,#308411,#308412,#308413,
#308414,#308415,#308416,#308417,#308418),.UNSPECIFIED.,.F.,.F.,(4,1,1,1,
1,1,1,1,1,1,1,1,1,1,1,1,4),(0.,0.0724843729385586,0.142190024778259,0.209247943639616,
0.274447923967761,0.33802582267117,0.400406532440542,0.463046285981066,
0.525723189050567,0.587758999700955,0.647207274703619,0.705604379270503,
0.76335494041328,0.821014301633402,0.879178712895835,0.938732443992665,
1.),.UNSPECIFIED.);
#6890=B_SPLINE_CURVE_WITH_KNOTS('',3,(#308461,#308462,#308463,#308464,#308465,
#308466,#308467,#308468,#308469,#308470,#308471,#308472,#308473,#308474,
#308475,#308476,#308477,#308478,#308479),.UNSPECIFIED.,.F.,.F.,(4,1,1,1,
1,1,1,1,1,1,1,1,1,1,1,1,4),(0.,0.0624074292203441,0.123580758253191,0.183030548059535,
0.241487894622227,0.299476288588135,0.357776621678218,0.416397215359044,
0.475293297309649,0.535174551555035,0.596373380100883,0.65843295832835,
0.722087328991003,0.787866252937039,0.856053064935338,0.926280127267363,
1.),.UNSPECIFIED.);
#6891=B_SPLINE_CURVE_WITH_KNOTS('',3,(#308504,#308505,#308506,#308507,#308508,
#308509,#308510,#308511,#308512,#308513,#308514),.UNSPECIFIED.,.F.,.F.,
(4,1,1,1,1,1,1,1,4),(0.,0.140786050719229,0.271192292477146,0.394820533419766,
0.51366840541228,0.630249521887138,0.748635241534156,0.870539222318192,
1.),.UNSPECIFIED.);
#6892=B_SPLINE_CURVE_WITH_KNOTS('',3,(#308555,#308556,#308557,#308558,#308559,
#308560,#308561,#308562,#308563,#308564,#308565,#308566,#308567,#308568,
#308569,#308570,#308571,#308572,#308573),.UNSPECIFIED.,.F.,.F.,(4,1,1,1,
1,1,1,1,1,1,1,1,1,1,1,1,4),(0.,0.061579283211466,0.121651367349155,0.179800294989198,
0.237201673292092,0.294780234992934,0.353324880649131,0.412515530286399,
0.474433538402357,0.537108068033057,0.599269077379891,0.66175044463838,
0.725142484567205,0.790290611404277,0.857751363050287,0.927508428952717,
1.),.UNSPECIFIED.);
#6893=B_SPLINE_CURVE_WITH_KNOTS('',3,(#308614,#308615,#308616,#308617,#308618,
#308619,#308620,#308621,#308622,#308623,#308624,#308625,#308626,#308627,
#308628,#308629,#308630,#308631,#308632),.UNSPECIFIED.,.F.,.F.,(4,1,1,1,
1,1,1,1,1,1,1,1,1,1,1,1,4),(0.,0.0728455592253727,0.142402257701936,0.209648156853246,
0.274427985226561,0.337611609749171,0.399896985087157,0.462371952688158,
0.524655094094133,0.586203391626633,0.645775819776357,0.704006503444922,
0.762043319649332,0.81964939871453,0.877994662833982,0.938199028971844,
1.),.UNSPECIFIED.);
#6894=B_SPLINE_CURVE_WITH_KNOTS('',3,(#308657,#308658,#308659,#308660,#308661,
#308662,#308663,#308664,#308665,#308666,#308667),.UNSPECIFIED.,.F.,.F.,
(4,1,1,1,1,1,1,1,4),(0.,0.126037809173244,0.24590192439148,0.362706754432767,
0.479405225937116,0.59860340945283,0.723279815939465,0.85618139156474,1.),
 .UNSPECIFIED.);
#6895=B_SPLINE_CURVE_WITH_KNOTS('',3,(#308708,#308709,#308710,#308711,#308712,
#308713,#308714,#308715,#308716,#308717,#308718,#308719,#308720,#308721,
#308722,#308723,#308724,#308725,#308726),.UNSPECIFIED.,.F.,.F.,(4,1,1,1,
1,1,1,1,1,1,1,1,1,1,1,1,4),(0.,0.0756779287595513,0.148475385165302,0.218686839383758,
0.285894163869826,0.350394511043543,0.41333034849776,0.475131662182092,
0.535395707628871,0.595069793647295,0.653190706601445,0.71022527848224,
0.767064167323289,0.824126149789293,0.882061797546221,0.940276800846584,
1.),.UNSPECIFIED.);
#6896=B_SPLINE_CURVE_WITH_KNOTS('',3,(#308767,#308768,#308769,#308770,#308771,
#308772,#308773,#308774,#308775,#308776,#308777,#308778,#308779,#308780,
#308781,#308782,#308783,#308784,#308785),.UNSPECIFIED.,.F.,.F.,(4,1,1,1,
1,1,1,1,1,1,1,1,1,1,1,1,4),(0.,0.061560808552986,0.120975543465591,0.179004419802313,
0.236102291207156,0.293686508428115,0.351514938997191,0.410728891353352,
0.472160594099565,0.534227146274051,0.596384774286223,0.658759168877887,
0.722544817104037,0.787964999387698,0.855593119477614,0.926440609783223,
1.),.UNSPECIFIED.);
#6897=B_SPLINE_CURVE_WITH_KNOTS('',3,(#308824,#308825,#308826,#308827,#308828,
#308829,#308830,#308831,#308832,#308833,#308834,#308835,#308836,#308837,
#308838,#308839,#308840,#308841,#308842),.UNSPECIFIED.,.F.,.F.,(4,1,1,1,
1,1,1,1,1,1,1,1,1,1,1,1,4),(0.,0.0724843729385586,0.142190024778259,0.209247943639616,
0.274447923967761,0.33802582267117,0.400406532440542,0.463046285981066,
0.525723189050567,0.587758999700955,0.647207274703619,0.705604379270503,
0.76335494041328,0.821014301633402,0.879178712895835,0.938732443992665,
1.),.UNSPECIFIED.);
#6898=B_SPLINE_CURVE_WITH_KNOTS('',3,(#308953,#308954,#308955,#308956,#308957,
#308958,#308959,#308960),.UNSPECIFIED.,.F.,.F.,(4,2,2,4),(9.9999999767032E-7,
0.0999956551432425,0.200882472133143,0.263234170060192),.UNSPECIFIED.);
#6899=B_SPLINE_CURVE_WITH_KNOTS('',3,(#308963,#308964,#308965,#308966,#308967,
#308968,#308969,#308970,#308971,#308972,#308973,#308974,#308975,#308976),
 .UNSPECIFIED.,.F.,.F.,(4,2,2,2,2,2,4),(0.173683564667831,0.259058622119751,
0.290413783825993,0.354637717539737,0.477856124224731,0.523001497040519,
0.557151695094327),.UNSPECIFIED.);
#6900=B_SPLINE_CURVE_WITH_KNOTS('',3,(#308982,#308983,#308984,#308985,#308986,
#308987,#308988,#308989,#308990,#308991,#308992,#308993,#308994,#308995,
#308996,#308997),.UNSPECIFIED.,.F.,.F.,(4,2,2,2,2,2,2,4),(-18.6044232501874,
-18.4152204113709,-18.2260245198036,-17.9923887330122,-17.7587449034554,
-17.5216133328485,-17.2892573593602,-17.2798161593979),.UNSPECIFIED.);
#6901=B_SPLINE_CURVE_WITH_KNOTS('',3,(#309000,#309001,#309002,#309003,#309004,
#309005,#309006,#309007,#309008,#309009,#309010,#309011,#309012,#309013,
#309014,#309015,#309016,#309017,#309018,#309019),.UNSPECIFIED.,.F.,.F.,
(4,2,2,2,2,2,2,2,2,4),(-1.79914710673844,-1.71083038040228,-1.47755135902926,
-1.24339398648431,-1.00520383669562,-0.772910845791891,-0.536812809995226,
-0.301993255983215,-0.150081981195142,-1.00000002722922E-6),
 .UNSPECIFIED.);
#6902=B_SPLINE_CURVE_WITH_KNOTS('',3,(#309024,#309025,#309026,#309027,#309028,
#309029,#309030,#309031,#309032,#309033,#309034,#309035,#309036,#309037,
#309038,#309039,#309040,#309041,#309042,#309043,#309044,#309045,#309046,
#309047,#309048,#309049,#309050,#309051,#309052,#309053,#309054,#309055,
#309056,#309057,#309058,#309059),.UNSPECIFIED.,.F.,.F.,(4,2,2,2,2,2,2,2,
2,2,2,2,2,2,2,2,2,4),(-17.2798161593979,-17.052938737066,-16.8178352897546,
-16.5852392730586,-16.3465740061095,-16.1134283553821,-15.8792563449518,
-15.6427035707161,-15.4104662708811,-15.1732497436008,-14.9386827923542,
-14.7058108627647,-14.4677107158127,-14.2349546508748,-14.0001041866954,
-13.7640911714114,-13.5318263968762,-13.4939982929491),.UNSPECIFIED.);
#6903=B_SPLINE_CURVE_WITH_KNOTS('',3,(#309060,#309061,#309062,#309063,#309064,
#309065,#309066,#309067,#309068,#309069,#309070,#309071,#309072,#309073,
#309074,#309075,#309076,#309077,#309078,#309079,#309080,#309081,#309082,
#309083,#309084,#309085,#309086,#309087,#309088,#309089,#309090,#309091,
#309092,#309093,#309094,#309095),.UNSPECIFIED.,.F.,.F.,(4,2,2,2,2,2,2,2,
2,2,2,2,2,2,2,2,2,4),(-5.58533174762334,-5.47049549570421,-5.23630005753687,
-5.00320609709793,-4.76460194975688,-4.53201074387952,-4.29696593781882,
-4.06060911752499,-3.82828546976905,-3.59121525458418,-3.35755892023313,
-3.12394708830492,-2.88474500970487,-2.65229456245123,-2.41668456425235,
-2.18107128571481,-1.94850078969714,-1.79914710673844),.UNSPECIFIED.);
#6904=B_SPLINE_CURVE_WITH_KNOTS('',3,(#309100,#309101,#309102,#309103,#309104,
#309105,#309106,#309107,#309108,#309109,#309110,#309111,#309112,#309113,
#309114,#309115,#309116,#309117,#309118,#309119,#309120,#309121,#309122,
#309123,#309124,#309125,#309126,#309127,#309128,#309129,#309130,#309131,
#309132,#309133,#309134,#309135),.UNSPECIFIED.,.F.,.F.,(4,2,2,2,2,2,2,2,
2,2,2,2,2,2,2,2,2,4),(-13.4939982929491,-13.2935738952139,-13.0594962824575,
-12.82621091684,-12.5886227052581,-12.3561047086897,-12.1204506023339,-11.8849195874974,
-11.6524849000808,-11.4133654689514,-11.1798323235161,-10.9461539830993,
-10.7091643355172,-10.4768804983775,-10.2404660644835,-10.0054978175092,
-9.77290831091157,-9.70804701379833),.UNSPECIFIED.);
#6905=B_SPLINE_CURVE_WITH_KNOTS('',3,(#309136,#309137,#309138,#309139,#309140,
#309141,#309142,#309143,#309144,#309145,#309146,#309147,#309148,#309149,
#309150,#309151,#309152,#309153,#309154,#309155,#309156,#309157,#309158,
#309159,#309160,#309161,#309162,#309163,#309164,#309165,#309166,#309167,
#309168,#309169,#309170,#309171),.UNSPECIFIED.,.F.,.F.,(4,2,2,2,2,2,2,2,
2,2,2,2,2,2,2,2,2,4),(-9.37108296243015,-9.22906033338744,-8.99336556927607,
-8.76087801275906,-8.5233432522494,-8.29004361701075,-8.0560178270479,-7.81770817391695,
-7.58545544178997,-7.34949823768963,-7.11461462448207,-6.88189986296259,
-6.64385766283799,-6.41098047501652,-6.17646937131389,-5.93920391259217,
-5.70698895911159,-5.58533174762334),.UNSPECIFIED.);
#6906=B_SPLINE_CURVE_WITH_KNOTS('',3,(#309176,#309177,#309178,#309179,#309180,
#309181,#309182,#309183,#309184,#309185,#309186,#309187,#309188,#309189,
#309190,#309191,#309192,#309193,#309194,#309195,#309196,#309197,#309198,
#309199,#309200,#309201,#309202,#309203,#309204,#309205,#309206,#309207,
#309208,#309209,#309210,#309211),.UNSPECIFIED.,.F.,.F.,(4,2,2,2,2,2,2,2,
2,2,2,2,2,2,2,2,2,4),(-9.70804701379833,-9.5343840344758,-9.30135623596084,
-9.06916727008946,-8.83282972254009,-8.59850286837222,-8.36553560893589,
-8.12709334075291,-7.8944679782875,-7.65957741824112,-7.42303753393001,
-7.19077496732653,-6.95386883099392,-6.7201187307232,-6.48666520198793,
-6.2476321327511,-6.01518268074078,-5.9226637994781),.UNSPECIFIED.);
#6907=B_SPLINE_CURVE_WITH_KNOTS('',3,(#309212,#309213,#309214,#309215,#309216,
#309217,#309218,#309219,#309220,#309221,#309222,#309223,#309224,#309225,
#309226,#309227,#309228,#309229,#309230,#309231,#309232,#309233,#309234,
#309235,#309236,#309237,#309238,#309239,#309240,#309241,#309242,#309243,
#309244,#309245,#309246,#309247),.UNSPECIFIED.,.F.,.F.,(4,2,2,2,2,2,2,2,
2,2,2,2,2,2,2,2,2,4),(-13.1564141152525,-12.9837710456499,-12.7507729137427,
-12.516492005001,-12.2801143778626,-12.0479245003057,-11.8105120712351,
-11.5761085159543,-11.3431900419091,-11.1052599297713,-10.872615747501,
-10.6376237109982,-10.4017735871133,-10.1695212094451,-9.93603831046464,
-9.6969725154889,-9.46454033645112,-9.37108296243015),.UNSPECIFIED.);
#6908=B_SPLINE_CURVE_WITH_KNOTS('',3,(#309253,#309254,#309255,#309256,#309257,
#309258,#309259,#309260,#309261,#309262,#309263,#309264,#309265,#309266,
#309267,#309268,#309269,#309270),.UNSPECIFIED.,.F.,.F.,(4,2,2,2,2,2,2,2,
4),(-18.6041766476204,-18.3879254158768,-18.1550376114361,-17.9169842730623,
-17.6842586928035,-17.4493644967635,-17.2133962593625,-16.9811328612893,
-16.9423174515002),.UNSPECIFIED.);
#6909=B_SPLINE_CURVE_WITH_KNOTS('',3,(#309275,#309276,#309277,#309278,#309279,
#309280,#309281,#309282,#309283,#309284,#309285,#309286,#309287,#309288,
#309289,#309290,#309291,#309292,#309293,#309294,#309295,#309296),
 .UNSPECIFIED.,.F.,.F.,(4,2,2,2,2,2,2,2,2,2,4),(-2.13687759585315,-2.0210882487643,
-1.78684984563254,-1.55378702616903,-1.31522335637624,-1.08261714125924,
-0.847610685706001,-0.611196108780494,-0.37888477337317,-0.188471738845002,
-9.99999997475243E-7),.UNSPECIFIED.);
#6910=B_SPLINE_CURVE_WITH_KNOTS('',3,(#309704,#309705,#309706,#309707,#309708,
#309709,#309710,#309711,#309712,#309713,#309714,#309715,#309716,#309717,
#309718,#309719,#309720,#309721,#309722,#309723,#309724,#309725,#309726,
#309727,#309728,#309729,#309730,#309731,#309732,#309733,#309734,#309735,
#309736,#309737,#309738,#309739),.UNSPECIFIED.,.F.,.F.,(4,2,2,2,2,2,2,2,
2,2,2,2,2,2,2,2,2,4),(-5.9226637994781,-5.77973314889478,-5.54397852289478,
-5.3115010616718,-5.07399902404122,-4.84066556806495,-4.6066712207202,-4.36828521464463,
-4.13602452995896,-3.90010256975103,-3.66516638126514,-3.43247239015531,
-3.19446738741631,-2.96156518684184,-2.72708953409623,-2.48975570213967,
-2.25754292115493,-2.13687759585315),.UNSPECIFIED.);
#6911=B_SPLINE_CURVE_WITH_KNOTS('',3,(#309740,#309741,#309742,#309743,#309744,
#309745),.UNSPECIFIED.,.F.,.F.,(4,2,4),(9.99997409965433E-7,0.146501658577725,
0.173683564667831),.UNSPECIFIED.);
#6912=B_SPLINE_CURVE_WITH_KNOTS('',3,(#309768,#309769,#309770,#309771,#309772,
#309773,#309774,#309775,#309776,#309777,#309778,#309779,#309780,#309781,
#309782,#309783,#309784,#309785,#309786,#309787,#309788,#309789,#309790,
#309791,#309792,#309793,#309794,#309795,#309796,#309797),.UNSPECIFIED.,
 .F.,.F.,(4,2,2,2,2,2,2,2,2,2,2,2,2,2,4),(9.99999999726749E-7,0.130707839264569,
0.259991147819482,0.472998818331275,0.696716416745347,0.814147340124016,
1.04649848427486,1.30651726561565,1.57149762551086,1.7131254536093,1.85156786432642,
2.15668396285832,2.483222578382,2.64892396867161,2.83146336233688),
 .UNSPECIFIED.);
#6913=B_SPLINE_CURVE_WITH_KNOTS('',3,(#309798,#309799,#309800,#309801,#309802,
#309803,#309804,#309805,#309806,#309807,#309808,#309809,#309810,#309811,
#309812,#309813,#309814,#309815,#309816,#309817),.UNSPECIFIED.,.F.,.F.,
(4,2,2,2,2,2,2,2,2,4),(2.83146336233688,2.98157423495795,3.32273775251514,
3.49495675413182,3.87338751477843,4.28823841167863,4.37710950869524,4.68170098346783,
4.83417108518993,4.99060309891423),.UNSPECIFIED.);
#6914=B_SPLINE_CURVE_WITH_KNOTS('',3,(#310116,#310117,#310118,#310119,#310120,
#310121,#310122,#310123,#310124,#310125,#310126,#310127,#310128,#310129,
#310130,#310131,#310132,#310133,#310134,#310135,#310136,#310137,#310138,
#310139,#310140,#310141,#310142,#310143,#310144,#310145,#310146,#310147,
#310148,#310149,#310150,#310151,#310152,#310153,#310154,#310155,#310156,
#310157),.UNSPECIFIED.,.F.,.F.,(4,2,2,2,2,2,2,2,2,2,2,2,2,2,2,2,2,2,2,2,
4),(0.263234170060192,0.387368656471732,0.436487962699596,0.633460506504842,
0.855015445306774,0.974732004315266,1.24137222287131,1.52351378413127,1.67243408083146,
1.96519939944981,2.28406876404804,2.45461478920459,2.83048775636771,3.24439250987047,
3.34640175008835,3.7582012400543,4.2159969589176,4.71750949992909,4.90457358104075,
5.17859562204822,5.45614014826222),.UNSPECIFIED.);
#6915=B_SPLINE_CURVE_WITH_KNOTS('',3,(#310158,#310159,#310160,#310161,#310162,
#310163,#310164,#310165,#310166,#310167,#310168,#310169,#310170,#310171,
#310172,#310173,#310174,#310175,#310176,#310177,#310178,#310179,#310180,
#310181,#310182,#310183,#310184,#310185,#310186,#310187,#310188,#310189,
#310190,#310191,#310192,#310193),.UNSPECIFIED.,.F.,.F.,(4,2,2,2,2,2,2,2,
2,2,2,2,2,2,2,2,2,4),(-16.9423174515002,-16.7428124565089,-16.5087755987168,
-16.2754652275235,-16.0379192294675,-15.8054207736165,-15.5697152811951,
-15.3342241467486,-15.1017811964504,-14.8627040923319,-14.6292101590594,
-14.3954948845505,-14.1585461493712,-13.9262721968018,-13.6897937684499,
-13.4548635315576,-13.2222551407783,-13.1564141152525),.UNSPECIFIED.);
#6916=B_SPLINE_CURVE_WITH_KNOTS('',3,(#310194,#310195,#310196,#310197,#310198,
#310199,#310200,#310201,#310202,#310203,#310204,#310205,#310206,#310207,
#310208,#310209),.UNSPECIFIED.,.F.,.F.,(4,2,2,2,2,2,2,4),(9.99998665002523E-7,
0.17925540834401,0.324372801233075,0.360565347733573,0.497288613301502,
0.54664963487918,0.61356551678679,0.671648570926337),.UNSPECIFIED.);
#6917=B_SPLINE_CURVE_WITH_KNOTS('',3,(#310213,#310214,#310215,#310216,#310217,
#310218,#310219,#310220,#310221,#310222),.UNSPECIFIED.,.F.,.F.,(4,2,2,2,
4),(-0.0616936784912174,-0.0584304026796343,-0.0471362732342459,-0.0358421437888575,
-0.0325788679773239),.UNSPECIFIED.);
#6918=B_SPLINE_CURVE_WITH_KNOTS('',3,(#310226,#310227,#310228,#310229,#310230,
#310231,#310232,#310233,#310234,#310235),.UNSPECIFIED.,.F.,.F.,(4,2,2,2,
4),(-0.152743320152561,-0.149480044341046,-0.138185914895657,-0.126891785450269,
-0.123628509639395),.UNSPECIFIED.);
#6919=B_SPLINE_CURVE_WITH_KNOTS('',3,(#310240,#310241,#310242,#310243,#310244,
#310245,#310246,#310247,#310248,#310249),.UNSPECIFIED.,.F.,.F.,(4,2,2,2,
4),(-0.0616936784912628,-0.0584304026796342,-0.0471362732342458,-0.0358421437888575,
-0.0325788679773241),.UNSPECIFIED.);
#6920=B_SPLINE_CURVE_WITH_KNOTS('',3,(#310253,#310254,#310255,#310256,#310257,
#310258,#310259,#310260,#310261,#310262),.UNSPECIFIED.,.F.,.F.,(4,2,2,2,
4),(-0.152743320152561,-0.149480044341046,-0.138185914895657,-0.126891785450269,
-0.123628509639806),.UNSPECIFIED.);
#6921=B_SPLINE_CURVE_WITH_KNOTS('',3,(#310267,#310268,#310269,#310270,#310271,
#310272,#310273,#310274,#310275,#310276),.UNSPECIFIED.,.F.,.F.,(4,2,2,2,
4),(-0.061693678491264,-0.0584304026796342,-0.0471362732342458,-0.0358421437888574,
-0.0325788679773307),.UNSPECIFIED.);
#6922=B_SPLINE_CURVE_WITH_KNOTS('',3,(#310280,#310281,#310282,#310283,#310284,
#310285,#310286,#310287,#310288,#310289),.UNSPECIFIED.,.F.,.F.,(4,2,2,2,
4),(-0.152743320152482,-0.149480044341046,-0.138185914895657,-0.126891785450269,
-0.123628509639806),.UNSPECIFIED.);
#6923=B_SPLINE_CURVE_WITH_KNOTS('',3,(#310294,#310295,#310296,#310297,#310298,
#310299,#310300,#310301,#310302,#310303),.UNSPECIFIED.,.F.,.F.,(4,2,2,2,
4),(-0.0616936784912173,-0.0584304026796343,-0.0471362732342459,-0.0358421437888575,
-0.032578867977324),.UNSPECIFIED.);
#6924=B_SPLINE_CURVE_WITH_KNOTS('',3,(#310307,#310308,#310309,#310310,#310311,
#310312,#310313,#310314,#310315,#310316),.UNSPECIFIED.,.F.,.F.,(4,2,2,2,
4),(-0.152743320152561,-0.149480044341046,-0.138185914895657,-0.126891785450269,
-0.123628509639395),.UNSPECIFIED.);
#6925=B_SPLINE_CURVE_WITH_KNOTS('',3,(#310321,#310322,#310323,#310324,#310325,
#310326,#310327,#310328,#310329,#310330),.UNSPECIFIED.,.F.,.F.,(4,2,2,2,
4),(-0.0616936784912626,-0.0584304026796342,-0.0471362732342458,-0.0358421437888574,
-0.032578867977324),.UNSPECIFIED.);
#6926=B_SPLINE_CURVE_WITH_KNOTS('',3,(#310334,#310335,#310336,#310337,#310338,
#310339,#310340,#310341,#310342,#310343),.UNSPECIFIED.,.F.,.F.,(4,2,2,2,
4),(-0.152743320152561,-0.149480044341046,-0.138185914895657,-0.126891785450269,
-0.123628509639806),.UNSPECIFIED.);
#6927=B_SPLINE_CURVE_WITH_KNOTS('',3,(#310348,#310349,#310350,#310351,#310352,
#310353,#310354,#310355,#310356,#310357),.UNSPECIFIED.,.F.,.F.,(4,2,2,2,
4),(-0.0616936784912639,-0.0584304026796342,-0.0471362732342458,-0.0358421437888574,
-0.0325788679773305),.UNSPECIFIED.);
#6928=B_SPLINE_CURVE_WITH_KNOTS('',3,(#310361,#310362,#310363,#310364,#310365,
#310366,#310367,#310368,#310369,#310370),.UNSPECIFIED.,.F.,.F.,(4,2,2,2,
4),(-0.152743320152481,-0.149480044341046,-0.138185914895657,-0.126891785450269,
-0.123628509639806),.UNSPECIFIED.);
#6929=CONICAL_SURFACE('',#94083,1.47499999999998,0.785398163397455);
#6930=CONICAL_SURFACE('',#94094,1.47499999999998,0.785398163397455);
#6931=CONICAL_SURFACE('',#94695,58.3875000000295,0.436332312998583);
#6932=CONICAL_SURFACE('',#94706,58.3875000000295,0.436332312998583);
#6933=CONICAL_SURFACE('',#94724,58.3875000000295,0.436332312998583);
#6934=CONICAL_SURFACE('',#94752,58.3875000000295,0.436332312998583);
#6935=CONICAL_SURFACE('',#94763,58.3875000000295,0.436332312998583);
#6936=CONICAL_SURFACE('',#94786,58.3875000000295,0.436332312998583);
#6937=CONICAL_SURFACE('',#94804,58.3875000000295,0.436332312998583);
#6938=CONICAL_SURFACE('',#94815,58.3875000000295,0.436332312998583);
#6939=CONICAL_SURFACE('',#94831,58.3875000000295,0.436332312998583);
#6940=CONICAL_SURFACE('',#94842,58.3875000000295,0.436332312998583);
#6941=CONICAL_SURFACE('',#94860,58.3875000000295,0.436332312998583);
#6942=CONICAL_SURFACE('',#95152,58.5,0.436332312998583);
#6943=CONICAL_SURFACE('',#95160,58.5,0.436332312998583);
#6944=CONICAL_SURFACE('',#95165,58.5,0.436332312998583);
#6945=CONICAL_SURFACE('',#95230,58.3875000000295,0.436332312998583);
#6946=CONICAL_SURFACE('',#95513,58.3875000000295,0.436332312998583);
#6947=CONICAL_SURFACE('',#95657,58.3875000000295,0.436332312998583);
#6948=CONICAL_SURFACE('',#95705,58.3875000000295,0.436332312998583);
#6949=CONICAL_SURFACE('',#95927,58.5,0.436332312998583);
#6950=CONICAL_SURFACE('',#95934,58.5,0.436332312998583);
#6951=CONICAL_SURFACE('',#95936,58.5,0.436332312998583);
#6952=CONICAL_SURFACE('',#95938,58.5,0.436332312998583);
#6953=CONICAL_SURFACE('',#95940,58.5,0.436332312998583);
#6954=CONICAL_SURFACE('',#95946,58.5,0.436332312998583);
#6955=CONICAL_SURFACE('',#95950,58.3875000000295,0.436332312998583);
#6956=CONICAL_SURFACE('',#95961,58.5,0.436332312998583);
#6957=CONICAL_SURFACE('',#95967,58.5,0.436332312998583);
#6958=CONICAL_SURFACE('',#95968,58.3875000000295,0.436332312998583);
#6959=CONICAL_SURFACE('',#95969,58.3875000000295,0.436332312998583);
#6960=CONICAL_SURFACE('',#95974,58.5,0.436332312998583);
#6961=CONICAL_SURFACE('',#95982,58.5,0.436332312998583);
#6962=CONICAL_SURFACE('',#95989,58.5,0.436332312998583);
#6963=CONICAL_SURFACE('',#96000,58.5,0.436332312998583);
#6964=CONICAL_SURFACE('',#96002,58.3875000000295,0.436332312998583);
#6965=CONICAL_SURFACE('',#96014,58.3875000000295,0.436332312998583);
#6966=CONICAL_SURFACE('',#96017,58.5,0.436332312998583);
#6967=CONICAL_SURFACE('',#96030,58.5,0.436332312998583);
#6968=CONICAL_SURFACE('',#96040,58.5,0.436332312998583);
#6969=CONICAL_SURFACE('',#96048,58.5,0.436332312998583);
#6970=CONICAL_SURFACE('',#96055,58.3875000000295,0.436332312998583);
#6971=CONICAL_SURFACE('',#96057,58.3875000000295,0.436332312998583);
#6972=CONICAL_SURFACE('',#96059,58.5,0.436332312998583);
#6973=CONICAL_SURFACE('',#96069,58.5,0.436332312998583);
#6974=CONICAL_SURFACE('',#96087,58.3875000000295,0.436332312998583);
#6975=CONICAL_SURFACE('',#96095,58.5,0.436332312998583);
#6976=CONICAL_SURFACE('',#96106,58.5,0.436332312998583);
#6977=CONICAL_SURFACE('',#96111,58.5,0.436332312998583);
#6978=CONICAL_SURFACE('',#96117,58.5,0.436332312998583);
#6979=CONICAL_SURFACE('',#96121,58.5,0.436332312998583);
#6980=CONICAL_SURFACE('',#96135,58.5,0.436332312998583);
#6981=CONICAL_SURFACE('',#96434,58.3875000000295,0.436332312998583);
#6982=CONICAL_SURFACE('',#96487,58.3875000000295,0.436332312998583);
#6983=CONICAL_SURFACE('',#96664,58.3875000000295,0.436332312998583);
#6984=CONICAL_SURFACE('',#96992,58.3875000000295,0.436332312998583);
#6985=CONICAL_SURFACE('',#97086,58.5,0.436332312998583);
#6986=CONICAL_SURFACE('',#97095,58.5,0.436332312998583);
#6987=CONICAL_SURFACE('',#97107,58.5,0.436332312998583);
#6988=CONICAL_SURFACE('',#97339,58.3875000000295,0.436332312998583);
#6989=CONICAL_SURFACE('',#97353,58.3875000000295,0.436332312998583);
#6990=CONICAL_SURFACE('',#97364,58.3875000000295,0.436332312998583);
#6991=CONICAL_SURFACE('',#97375,58.3875000000295,0.436332312998583);
#6992=CONICAL_SURFACE('',#97386,58.3875000000295,0.436332312998583);
#6993=CONICAL_SURFACE('',#97400,58.3875000000295,0.436332312998583);
#6994=CONICAL_SURFACE('',#97422,58.3875000000295,0.436332312998583);
#6995=CONICAL_SURFACE('',#97434,58.3875000000295,0.436332312998583);
#6996=CONICAL_SURFACE('',#97454,58.3875000000295,0.436332312998583);
#6997=CONICAL_SURFACE('',#97469,58.3875000000295,0.436332312998583);
#6998=CONICAL_SURFACE('',#97481,58.3875000000295,0.436332312998583);
#6999=CONICAL_SURFACE('',#97933,58.3875000000295,0.436332312998583);
#7000=CONICAL_SURFACE('',#97948,2.,1.0471975511966);
#7001=CONICAL_SURFACE('',#97949,1.73205080756888,0.78539816339745);
#7002=CONICAL_SURFACE('',#97951,1.73205080756888,0.78539816339745);
#7003=CONICAL_SURFACE('',#97953,1.73205080756888,0.78539816339745);
#7004=CONICAL_SURFACE('',#97955,1.73205080756888,0.78539816339745);
#7005=CONICAL_SURFACE('',#97957,1.73205080756888,0.78539816339745);
#7006=CONICAL_SURFACE('',#97959,1.73205080756888,0.78539816339745);
#7007=CONICAL_SURFACE('',#97970,1.47499999999998,0.785398163397455);
#7008=CONICAL_SURFACE('',#99631,9.01478559345382,0.0174532925199415);
#7009=CONICAL_SURFACE('',#99633,74.6642856134258,0.0174532925199415);
#7010=CONICAL_SURFACE('',#99635,9.01478559345372,0.0174532925199415);
#7011=CONICAL_SURFACE('',#99638,9.01478559345379,0.0174532925199415);
#7012=CONICAL_SURFACE('',#99641,74.6642856134258,0.0174532925199415);
#7013=CONICAL_SURFACE('',#99643,9.01478559345383,0.0174532925199415);
#7014=CONICAL_SURFACE('',#99646,1067.50038076211,0.0174532925199415);
#7015=CONICAL_SURFACE('',#99649,11.963380762109,0.0174532925199415);
#7016=CONICAL_SURFACE('',#99652,77.6128807820809,0.0174532925199415);
#7017=CONICAL_SURFACE('',#99655,11.963380762109,0.0174532925199415);
#7018=CONICAL_SURFACE('',#99658,11.963380762109,0.0174532925199415);
#7019=CONICAL_SURFACE('',#99661,77.6128807820809,0.0174532925199415);
#7020=CONICAL_SURFACE('',#99664,11.963380762109,0.0174532925199415);
#7021=CONICAL_SURFACE('',#99667,1064.55178559345,0.0174532925199415);
#7022=CONICAL_SURFACE('',#99703,5.84961923789098,0.0174532925199415);
#7023=CONICAL_SURFACE('',#99705,5.84961923789177,0.0174532925199415);
#7024=CONICAL_SURFACE('',#99722,3.35,0.0174532925199415);
#7025=CONICAL_SURFACE('',#99727,3.35000000000079,0.0174532925199415);
#7026=CONICAL_SURFACE('',#99771,11.5144048313448,0.0174532925199415);
#7027=CONICAL_SURFACE('',#99772,77.1639048513167,0.0174532925199415);
#7028=CONICAL_SURFACE('',#99773,11.5144048313447,0.0174532925199415);
#7029=CONICAL_SURFACE('',#99774,11.5144048313448,0.0174532925199415);
#7030=CONICAL_SURFACE('',#99775,77.1639048513167,0.0174532925199415);
#7031=CONICAL_SURFACE('',#99776,11.5144048313448,0.0174532925199415);
#7032=CONICAL_SURFACE('',#99777,1070.,0.0174532925199415);
#7033=CONICAL_SURFACE('',#99779,14.463,0.0174532925199415);
#7034=CONICAL_SURFACE('',#99781,80.1125000199719,0.0174532925199415);
#7035=CONICAL_SURFACE('',#99783,14.463,0.0174532925199415);
#7036=CONICAL_SURFACE('',#99785,14.463,0.0174532925199415);
#7037=CONICAL_SURFACE('',#99787,80.1125000199719,0.0174532925199415);
#7038=CONICAL_SURFACE('',#99789,14.463,0.0174532925199415);
#7039=CONICAL_SURFACE('',#99791,1067.05140483134,0.0174532925199415);
#7040=CONICAL_SURFACE('',#101623,9.01478559345382,0.0174532925199415);
#7041=CONICAL_SURFACE('',#101625,74.6642856134258,0.0174532925199415);
#7042=CONICAL_SURFACE('',#101627,9.01478559345372,0.0174532925199415);
#7043=CONICAL_SURFACE('',#101630,9.01478559345379,0.0174532925199415);
#7044=CONICAL_SURFACE('',#101633,74.6642856134258,0.0174532925199415);
#7045=CONICAL_SURFACE('',#101635,9.01478559345383,0.0174532925199415);
#7046=CONICAL_SURFACE('',#101638,1064.55178559345,0.0174532925199415);
#7047=CONICAL_SURFACE('',#101652,1067.50038076211,0.0174532925199415);
#7048=CONICAL_SURFACE('',#101654,11.963380762109,0.0174532925199415);
#7049=CONICAL_SURFACE('',#101656,77.6128807820809,0.0174532925199415);
#7050=CONICAL_SURFACE('',#101658,11.963380762109,0.0174532925199415);
#7051=CONICAL_SURFACE('',#101660,232.500380762109,0.0174532925199415);
#7052=CONICAL_SURFACE('',#101662,1067.50038076211,0.0174532925199415);
#7053=CONICAL_SURFACE('',#101664,11.963380762109,0.0174532925199415);
#7054=CONICAL_SURFACE('',#101666,77.6128807820809,0.0174532925199415);
#7055=CONICAL_SURFACE('',#101668,11.963380762109,0.0174532925199415);
#7056=CONICAL_SURFACE('',#101670,1064.55178559345,0.0174532925199415);
#7057=CONICAL_SURFACE('',#101672,229.551785593454,0.0174532925199415);
#7058=CONICAL_SURFACE('',#101706,5.84961923789098,0.0174532925199415);
#7059=CONICAL_SURFACE('',#101708,5.84961923789177,0.0174532925199415);
#7060=CONICAL_SURFACE('',#101718,3.35,0.0174532925199415);
#7061=CONICAL_SURFACE('',#101721,3.35000000000079,0.0174532925199415);
#7062=CONICAL_SURFACE('',#101774,11.5144048313448,0.0174532925199415);
#7063=CONICAL_SURFACE('',#101775,77.1639048513167,0.0174532925199415);
#7064=CONICAL_SURFACE('',#101776,11.5144048313447,0.0174532925199415);
#7065=CONICAL_SURFACE('',#101777,11.5144048313448,0.0174532925199415);
#7066=CONICAL_SURFACE('',#101778,77.1639048513167,0.0174532925199415);
#7067=CONICAL_SURFACE('',#101779,11.5144048313448,0.0174532925199415);
#7068=CONICAL_SURFACE('',#101780,1067.05140483134,0.0174532925199415);
#7069=CONICAL_SURFACE('',#101792,1070.,0.0174532925199415);
#7070=CONICAL_SURFACE('',#101793,14.463,0.0174532925199415);
#7071=CONICAL_SURFACE('',#101794,80.1125000199719,0.0174532925199415);
#7072=CONICAL_SURFACE('',#101795,14.463,0.0174532925199415);
#7073=CONICAL_SURFACE('',#101796,235.,0.0174532925199415);
#7074=CONICAL_SURFACE('',#101797,1070.,0.0174532925199415);
#7075=CONICAL_SURFACE('',#101798,14.463,0.0174532925199415);
#7076=CONICAL_SURFACE('',#101799,80.1125000199719,0.0174532925199415);
#7077=CONICAL_SURFACE('',#101800,14.463,0.0174532925199415);
#7078=CONICAL_SURFACE('',#101801,1067.05140483134,0.0174532925199415);
#7079=CONICAL_SURFACE('',#101802,232.051404831345,0.0174532925199415);
#7080=CONICAL_SURFACE('',#101885,2.,1.0471975511966);
#7081=CONICAL_SURFACE('',#101886,1.73205080756888,0.78539816339745);
#7082=CONICAL_SURFACE('',#101888,1.73205080756888,0.78539816339745);
#7083=CONICAL_SURFACE('',#101890,1.73205080756888,0.78539816339745);
#7084=CONICAL_SURFACE('',#101892,1.73205080756888,0.78539816339745);
#7085=CONICAL_SURFACE('',#101894,1.73205080756888,0.78539816339745);
#7086=CONICAL_SURFACE('',#101896,1.73205080756888,0.78539816339745);
#7087=CONICAL_SURFACE('',#101914,5.,0.78539816339745);
#7088=CONICAL_SURFACE('',#101915,5.,0.78539816339745);
#7089=CONICAL_SURFACE('',#101916,5.,0.78539816339745);
#7090=CONICAL_SURFACE('',#101917,5.,0.78539816339745);
#7091=CONICAL_SURFACE('',#101918,5.,0.78539816339745);
#7092=CONICAL_SURFACE('',#101919,5.,0.78539816339745);
#7093=CONICAL_SURFACE('',#101927,5.,1.0471975511966);
#7094=CONICAL_SURFACE('',#101928,5.,1.0471975511966);
#7095=CONICAL_SURFACE('',#101929,5.,1.0471975511966);
#7096=CONICAL_SURFACE('',#101930,5.,1.0471975511966);
#7097=CONICAL_SURFACE('',#101931,5.,1.0471975511966);
#7098=CONICAL_SURFACE('',#101932,5.,1.0471975511966);
#7099=CONICAL_SURFACE('',#101946,5.,0.78539816339745);
#7100=CONICAL_SURFACE('',#101947,5.,0.78539816339745);
#7101=CONICAL_SURFACE('',#101948,5.,0.78539816339745);
#7102=CONICAL_SURFACE('',#101949,5.,0.78539816339745);
#7103=CONICAL_SURFACE('',#101950,5.,0.78539816339745);
#7104=CONICAL_SURFACE('',#101951,5.,0.78539816339745);
#7105=CONICAL_SURFACE('',#101959,5.,1.0471975511966);
#7106=CONICAL_SURFACE('',#101960,5.,1.0471975511966);
#7107=CONICAL_SURFACE('',#101961,5.,1.0471975511966);
#7108=CONICAL_SURFACE('',#101962,5.,1.0471975511966);
#7109=CONICAL_SURFACE('',#101963,5.,1.0471975511966);
#7110=CONICAL_SURFACE('',#101964,5.,1.0471975511966);
#7111=CONICAL_SURFACE('',#101977,2.,1.0471975511966);
#7112=CONICAL_SURFACE('',#101978,1.73205080756888,0.78539816339745);
#7113=CONICAL_SURFACE('',#101980,1.73205080756888,0.78539816339745);
#7114=CONICAL_SURFACE('',#101982,1.73205080756888,0.78539816339745);
#7115=CONICAL_SURFACE('',#101984,1.73205080756888,0.78539816339745);
#7116=CONICAL_SURFACE('',#101986,1.73205080756888,0.78539816339745);
#7117=CONICAL_SURFACE('',#101988,1.73205080756888,0.78539816339745);
#7118=CONICAL_SURFACE('',#102016,0.750000000000001,0.0436332312998574);
#7119=CONICAL_SURFACE('',#102018,0.750000000000001,0.0436332312998574);
#7120=CONICAL_SURFACE('',#102025,1.47499999999998,0.785398163397455);
#7121=CONICAL_SURFACE('',#102154,0.750000000000001,0.0436332312998574);
#7122=CONICAL_SURFACE('',#102156,0.750000000000001,0.0436332312998574);
#7123=CONICAL_SURFACE('',#102652,5.,0.78539816339745);
#7124=CONICAL_SURFACE('',#102653,5.,0.78539816339745);
#7125=CONICAL_SURFACE('',#102654,5.,0.78539816339745);
#7126=CONICAL_SURFACE('',#102655,5.,0.78539816339745);
#7127=CONICAL_SURFACE('',#102656,5.,0.78539816339745);
#7128=CONICAL_SURFACE('',#102657,5.,0.78539816339745);
#7129=CONICAL_SURFACE('',#102665,5.,1.0471975511966);
#7130=CONICAL_SURFACE('',#102666,5.,1.0471975511966);
#7131=CONICAL_SURFACE('',#102667,5.,1.0471975511966);
#7132=CONICAL_SURFACE('',#102668,5.,1.0471975511966);
#7133=CONICAL_SURFACE('',#102669,5.,1.0471975511966);
#7134=CONICAL_SURFACE('',#102670,5.,1.0471975511966);
#7135=CONICAL_SURFACE('',#102684,5.,0.78539816339745);
#7136=CONICAL_SURFACE('',#102685,5.,0.78539816339745);
#7137=CONICAL_SURFACE('',#102686,5.,0.78539816339745);
#7138=CONICAL_SURFACE('',#102687,5.,0.78539816339745);
#7139=CONICAL_SURFACE('',#102688,5.,0.78539816339745);
#7140=CONICAL_SURFACE('',#102689,5.,0.78539816339745);
#7141=CONICAL_SURFACE('',#102697,5.,1.0471975511966);
#7142=CONICAL_SURFACE('',#102698,5.,1.0471975511966);
#7143=CONICAL_SURFACE('',#102699,5.,1.0471975511966);
#7144=CONICAL_SURFACE('',#102700,5.,1.0471975511966);
#7145=CONICAL_SURFACE('',#102701,5.,1.0471975511966);
#7146=CONICAL_SURFACE('',#102702,5.,1.0471975511966);
#7147=CONICAL_SURFACE('',#102715,2.,1.0471975511966);
#7148=CONICAL_SURFACE('',#102716,1.73205080756888,0.78539816339745);
#7149=CONICAL_SURFACE('',#102718,1.73205080756888,0.78539816339745);
#7150=CONICAL_SURFACE('',#102720,1.73205080756888,0.78539816339745);
#7151=CONICAL_SURFACE('',#102722,1.73205080756888,0.78539816339745);
#7152=CONICAL_SURFACE('',#102724,1.73205080756888,0.78539816339745);
#7153=CONICAL_SURFACE('',#102726,1.73205080756888,0.78539816339745);
#7154=CONICAL_SURFACE('',#103107,3.,1.0471975511966);
#7155=CONICAL_SURFACE('',#103108,2.88675134594813,0.78539816339745);
#7156=CONICAL_SURFACE('',#103110,2.88675134594813,0.78539816339745);
#7157=CONICAL_SURFACE('',#103112,2.88675134594813,0.78539816339745);
#7158=CONICAL_SURFACE('',#103114,2.88675134594813,0.78539816339745);
#7159=CONICAL_SURFACE('',#103116,2.88675134594813,0.78539816339745);
#7160=CONICAL_SURFACE('',#103118,2.88675134594813,0.78539816339745);
#7161=CONICAL_SURFACE('',#103120,6.,0.785398163397452);
#7162=CONICAL_SURFACE('',#103308,58.3875000000282,1.3264502315157);
#7163=CONICAL_SURFACE('',#104142,16.0850661013937,0.0416425087550466);
#7164=CONICAL_SURFACE('',#104257,12.,0.785398163397447);
#7165=CONICAL_SURFACE('',#104258,13.05,0.785398163397443);
#7166=CONICAL_SURFACE('',#104269,13.05,0.785398163397443);
#7167=CONICAL_SURFACE('',#104271,12.,0.785398163397447);
#7168=CONICAL_SURFACE('',#104293,18.,1.0471975511966);
#7169=CONICAL_SURFACE('',#104294,18.,1.0471975511966);
#7170=CONICAL_SURFACE('',#104295,18.,1.0471975511966);
#7171=CONICAL_SURFACE('',#104296,18.,1.0471975511966);
#7172=CONICAL_SURFACE('',#104297,18.,1.0471975511966);
#7173=CONICAL_SURFACE('',#104298,18.,1.0471975511966);
#7174=CONICAL_SURFACE('',#104299,18.,1.0471975511966);
#7175=CONICAL_SURFACE('',#104300,18.,1.0471975511966);
#7176=CONICAL_SURFACE('',#104301,18.,1.0471975511966);
#7177=CONICAL_SURFACE('',#104302,18.,1.0471975511966);
#7178=CONICAL_SURFACE('',#104303,18.,1.0471975511966);
#7179=CONICAL_SURFACE('',#104304,18.,1.0471975511966);
#7180=CONICAL_SURFACE('',#104334,12.9453125,0.610865238198017);
#7181=CONICAL_SURFACE('',#104336,12.,0.785398163397456);
#7182=CONICAL_SURFACE('',#104350,12.,0.785398163397447);
#7183=CONICAL_SURFACE('',#104429,13.05,0.785398163397443);
#7184=CONICAL_SURFACE('',#104432,9.90000000000002,0.785398163397447);
#7185=CONICAL_SURFACE('',#104464,18.,1.0471975511966);
#7186=CONICAL_SURFACE('',#104465,18.,1.0471975511966);
#7187=CONICAL_SURFACE('',#104466,18.,1.0471975511966);
#7188=CONICAL_SURFACE('',#104467,18.,1.0471975511966);
#7189=CONICAL_SURFACE('',#104468,18.,1.0471975511966);
#7190=CONICAL_SURFACE('',#104469,18.,1.0471975511966);
#7191=CONICAL_SURFACE('',#104470,18.,1.0471975511966);
#7192=CONICAL_SURFACE('',#104471,18.,1.0471975511966);
#7193=CONICAL_SURFACE('',#104472,18.,1.0471975511966);
#7194=CONICAL_SURFACE('',#104473,18.,1.0471975511966);
#7195=CONICAL_SURFACE('',#104474,18.,1.0471975511966);
#7196=CONICAL_SURFACE('',#104475,18.,1.0471975511966);
#7197=CONICAL_SURFACE('',#104638,6.,0.539306738866249);
#7198=CONICAL_SURFACE('',#104641,6.,0.539306738866249);
#7199=CONICAL_SURFACE('',#104684,4.6875,0.785398163397456);
#7200=CONICAL_SURFACE('',#104705,9.5,1.0471975511966);
#7201=CONICAL_SURFACE('',#104706,9.5,1.0471975511966);
#7202=CONICAL_SURFACE('',#104707,9.5,1.0471975511966);
#7203=CONICAL_SURFACE('',#104708,9.5,1.0471975511966);
#7204=CONICAL_SURFACE('',#104709,9.5,1.0471975511966);
#7205=CONICAL_SURFACE('',#104710,9.5,1.0471975511966);
#7206=CONICAL_SURFACE('',#104719,6.,0.539306738866249);
#7207=CONICAL_SURFACE('',#104721,6.,0.785398163397452);
#7208=CONICAL_SURFACE('',#104744,9.5,1.0471975511966);
#7209=CONICAL_SURFACE('',#104746,9.5,1.0471975511966);
#7210=CONICAL_SURFACE('',#104748,9.5,1.0471975511966);
#7211=CONICAL_SURFACE('',#104750,9.5,1.0471975511966);
#7212=CONICAL_SURFACE('',#104752,9.5,1.0471975511966);
#7213=CONICAL_SURFACE('',#104754,9.5,1.0471975511966);
#7214=CONICAL_SURFACE('',#104756,9.5,1.0471975511966);
#7215=CONICAL_SURFACE('',#104758,9.5,1.0471975511966);
#7216=CONICAL_SURFACE('',#104760,9.5,1.0471975511966);
#7217=CONICAL_SURFACE('',#104762,9.5,1.0471975511966);
#7218=CONICAL_SURFACE('',#104764,9.5,1.0471975511966);
#7219=CONICAL_SURFACE('',#104766,9.5,1.0471975511966);
#7220=CONICAL_SURFACE('',#104779,6.7,0.785398163397448);
#7221=CONICAL_SURFACE('',#104780,6.,0.785398163397452);
#7222=SHAPE_REPRESENTATION_RELATIONSHIP('SRR','None',#310894,#7239);
#7223=SHAPE_REPRESENTATION_RELATIONSHIP('SRR','None',#310895,#7240);
#7224=SHAPE_REPRESENTATION_RELATIONSHIP('SRR','None',#310896,#7241);
#7225=SHAPE_REPRESENTATION_RELATIONSHIP('SRR','None',#310897,#7242);
#7226=SHAPE_REPRESENTATION_RELATIONSHIP('SRR','None',#310899,#7243);
#7227=SHAPE_REPRESENTATION_RELATIONSHIP('SRR','None',#310900,#7244);
#7228=SHAPE_REPRESENTATION_RELATIONSHIP('SRR','None',#310901,#7245);
#7229=SHAPE_REPRESENTATION_RELATIONSHIP('SRR','None',#310902,#7246);
#7230=SHAPE_REPRESENTATION_RELATIONSHIP('SRR','None',#310903,#7247);
#7231=SHAPE_REPRESENTATION_RELATIONSHIP('SRR','None',#310904,#7248);
#7232=SHAPE_REPRESENTATION_RELATIONSHIP('SRR','None',#310905,#7249);
#7233=SHAPE_REPRESENTATION_RELATIONSHIP('SRR','None',#310906,#7250);
#7234=SHAPE_REPRESENTATION_RELATIONSHIP('SRR','None',#310907,#7251);
#7235=SHAPE_REPRESENTATION_RELATIONSHIP('SRR','None',#310909,#7252);
#7236=SHAPE_REPRESENTATION_RELATIONSHIP('SRR','None',#310910,#7253);
#7237=SHAPE_REPRESENTATION_RELATIONSHIP('SRR','None',#310912,#7254);
#7238=SHAPE_REPRESENTATION_RELATIONSHIP('SRR','None',#310913,#7255);
#7239=ADVANCED_BREP_SHAPE_REPRESENTATION('',(#7324),#310603);
#7240=ADVANCED_BREP_SHAPE_REPRESENTATION('',(#7325),#310604);
#7241=ADVANCED_BREP_SHAPE_REPRESENTATION('',(#7326,#7327,#7328,#7329,#7330,
#7331,#7332,#7333,#7334,#7335,#7336,#7337,#7338,#7339,#7340,#7341,#7342,
#7343,#7344,#7345),#310605);
#7242=ADVANCED_BREP_SHAPE_REPRESENTATION('',(#7346),#310606);
#7243=ADVANCED_BREP_SHAPE_REPRESENTATION('',(#7347,#7348),#310608);
#7244=ADVANCED_BREP_SHAPE_REPRESENTATION('',(#7349),#310609);
#7245=ADVANCED_BREP_SHAPE_REPRESENTATION('',(#7350,#7351,#7352,#7353),#310610);
#7246=ADVANCED_BREP_SHAPE_REPRESENTATION('',(#7354),#310611);
#7247=ADVANCED_BREP_SHAPE_REPRESENTATION('',(#7355,#7356,#7357,#7358,#7359,
#7360,#7361,#7362,#7363,#7364,#7365,#7366,#7367,#7368,#7369,#7370,#7371,
#7372,#7373,#7374,#7375,#7376,#7377,#7378,#7379,#7380),#310612);
#7248=ADVANCED_BREP_SHAPE_REPRESENTATION('',(#7381),#310613);
#7249=ADVANCED_BREP_SHAPE_REPRESENTATION('',(#7382,#7383,#12,#7384),#310614);
#7250=ADVANCED_BREP_SHAPE_REPRESENTATION('',(#7385),#310615);
#7251=ADVANCED_BREP_SHAPE_REPRESENTATION('',(#7386),#310616);
#7252=ADVANCED_BREP_SHAPE_REPRESENTATION('',(#7387),#310618);
#7253=ADVANCED_BREP_SHAPE_REPRESENTATION('',(#7388),#310619);
#7254=ADVANCED_BREP_SHAPE_REPRESENTATION('',(#7389),#310621);
#7255=ADVANCED_BREP_SHAPE_REPRESENTATION('',(#7390),#310622);
#7256=STYLED_ITEM('',(#311003),#7324);
#7257=STYLED_ITEM('',(#311004),#7325);
#7258=STYLED_ITEM('',(#311005),#7326);
#7259=STYLED_ITEM('',(#311005),#7327);
#7260=STYLED_ITEM('',(#311005),#7328);
#7261=STYLED_ITEM('',(#311005),#7329);
#7262=STYLED_ITEM('',(#311005),#7330);
#7263=STYLED_ITEM('',(#311005),#7331);
#7264=STYLED_ITEM('',(#311005),#7332);
#7265=STYLED_ITEM('',(#311005),#7333);
#7266=STYLED_ITEM('',(#311005),#7334);
#7267=STYLED_ITEM('',(#311005),#7335);
#7268=STYLED_ITEM('',(#311005),#7336);
#7269=STYLED_ITEM('',(#311005),#7337);
#7270=STYLED_ITEM('',(#311005),#7338);
#7271=STYLED_ITEM('',(#311005),#7339);
#7272=STYLED_ITEM('',(#311005),#7340);
#7273=STYLED_ITEM('',(#311005),#7341);
#7274=STYLED_ITEM('',(#311005),#7342);
#7275=STYLED_ITEM('',(#311005),#7343);
#7276=STYLED_ITEM('',(#311005),#7344);
#7277=STYLED_ITEM('',(#311005),#7345);
#7278=STYLED_ITEM('',(#311006),#7346);
#7279=STYLED_ITEM('',(#311003),#7347);
#7280=STYLED_ITEM('',(#311003),#7348);
#7281=STYLED_ITEM('',(#311003),#7349);
#7282=STYLED_ITEM('',(#311007),#7350);
#7283=STYLED_ITEM('',(#311007),#7351);
#7284=STYLED_ITEM('',(#311007),#7352);
#7285=STYLED_ITEM('',(#311007),#7353);
#7286=STYLED_ITEM('',(#311003),#7354);
#7287=STYLED_ITEM('',(#311007),#7355);
#7288=STYLED_ITEM('',(#311007),#7356);
#7289=STYLED_ITEM('',(#311007),#7357);
#7290=STYLED_ITEM('',(#311007),#7358);
#7291=STYLED_ITEM('',(#311007),#7359);
#7292=STYLED_ITEM('',(#311007),#7360);
#7293=STYLED_ITEM('',(#311007),#7361);
#7294=STYLED_ITEM('',(#311007),#7362);
#7295=STYLED_ITEM('',(#311007),#7363);
#7296=STYLED_ITEM('',(#311007),#7364);
#7297=STYLED_ITEM('',(#311007),#7365);
#7298=STYLED_ITEM('',(#311007),#7366);
#7299=STYLED_ITEM('',(#311007),#7367);
#7300=STYLED_ITEM('',(#311007),#7368);
#7301=STYLED_ITEM('',(#311007),#7369);
#7302=STYLED_ITEM('',(#311007),#7370);
#7303=STYLED_ITEM('',(#311007),#7371);
#7304=STYLED_ITEM('',(#311007),#7372);
#7305=STYLED_ITEM('',(#311007),#7373);
#7306=STYLED_ITEM('',(#311007),#7374);
#7307=STYLED_ITEM('',(#311007),#7375);
#7308=STYLED_ITEM('',(#311007),#7376);
#7309=STYLED_ITEM('',(#311007),#7377);
#7310=STYLED_ITEM('',(#311007),#7378);
#7311=STYLED_ITEM('',(#311007),#7379);
#7312=STYLED_ITEM('',(#311007),#7380);
#7313=STYLED_ITEM('',(#311007),#7381);
#7314=STYLED_ITEM('',(#311005),#7382);
#7315=STYLED_ITEM('',(#311005),#7383);
#7316=STYLED_ITEM('',(#311005),#12);
#7317=STYLED_ITEM('',(#311005),#7384);
#7318=STYLED_ITEM('',(#311004),#7385);
#7319=STYLED_ITEM('',(#311004),#7386);
#7320=STYLED_ITEM('',(#311004),#7387);
#7321=STYLED_ITEM('',(#311003),#7388);
#7322=STYLED_ITEM('',(#311008),#7389);
#7323=STYLED_ITEM('',(#311008),#7390);
#7324=MANIFOLD_SOLID_BREP('Body1',#93706);
#7325=MANIFOLD_SOLID_BREP('Body1',#93707);
#7326=MANIFOLD_SOLID_BREP('Body1',#93708);
#7327=MANIFOLD_SOLID_BREP('Body2',#93709);
#7328=MANIFOLD_SOLID_BREP('Body3',#93710);
#7329=MANIFOLD_SOLID_BREP('Body4',#93711);
#7330=MANIFOLD_SOLID_BREP('Body5',#93712);
#7331=MANIFOLD_SOLID_BREP('Body6',#93713);
#7332=MANIFOLD_SOLID_BREP('Body7',#93714);
#7333=MANIFOLD_SOLID_BREP('Body8',#93715);
#7334=MANIFOLD_SOLID_BREP('Body9',#93716);
#7335=MANIFOLD_SOLID_BREP('Body10',#93717);
#7336=MANIFOLD_SOLID_BREP('Body11',#93718);
#7337=MANIFOLD_SOLID_BREP('Body12',#93719);
#7338=MANIFOLD_SOLID_BREP('Body13',#93720);
#7339=MANIFOLD_SOLID_BREP('Body14',#93721);
#7340=MANIFOLD_SOLID_BREP('Body15',#93722);
#7341=MANIFOLD_SOLID_BREP('Body16',#93723);
#7342=MANIFOLD_SOLID_BREP('Body17',#93724);
#7343=MANIFOLD_SOLID_BREP('Body18',#93725);
#7344=MANIFOLD_SOLID_BREP('Body19',#93726);
#7345=MANIFOLD_SOLID_BREP('Body20',#93727);
#7346=MANIFOLD_SOLID_BREP('Body1',#93728);
#7347=MANIFOLD_SOLID_BREP('Body1',#93729);
#7348=MANIFOLD_SOLID_BREP('Body2',#93730);
#7349=MANIFOLD_SOLID_BREP('Body1',#93731);
#7350=MANIFOLD_SOLID_BREP('Body1',#93732);
#7351=MANIFOLD_SOLID_BREP('Body2',#93733);
#7352=MANIFOLD_SOLID_BREP('Body3',#93734);
#7353=MANIFOLD_SOLID_BREP('Body4',#93735);
#7354=MANIFOLD_SOLID_BREP('Body1',#93736);
#7355=MANIFOLD_SOLID_BREP('Body1',#93737);
#7356=MANIFOLD_SOLID_BREP('Body2',#93738);
#7357=MANIFOLD_SOLID_BREP('Body3',#93739);
#7358=MANIFOLD_SOLID_BREP('Body4',#93740);
#7359=MANIFOLD_SOLID_BREP('Body5',#93741);
#7360=MANIFOLD_SOLID_BREP('Body6',#93742);
#7361=MANIFOLD_SOLID_BREP('Body7',#93743);
#7362=MANIFOLD_SOLID_BREP('Body8',#93744);
#7363=MANIFOLD_SOLID_BREP('Body9',#93745);
#7364=MANIFOLD_SOLID_BREP('Body10',#93746);
#7365=MANIFOLD_SOLID_BREP('Body11',#93747);
#7366=MANIFOLD_SOLID_BREP('Body12',#93748);
#7367=MANIFOLD_SOLID_BREP('Body13',#93749);
#7368=MANIFOLD_SOLID_BREP('Body14',#93750);
#7369=MANIFOLD_SOLID_BREP('Body15',#93751);
#7370=MANIFOLD_SOLID_BREP('Body16',#93752);
#7371=MANIFOLD_SOLID_BREP('Body17',#93753);
#7372=MANIFOLD_SOLID_BREP('Body18',#93754);
#7373=MANIFOLD_SOLID_BREP('Body19',#93755);
#7374=MANIFOLD_SOLID_BREP('Body20',#93756);
#7375=MANIFOLD_SOLID_BREP('Body21',#93757);
#7376=MANIFOLD_SOLID_BREP('Body22',#93758);
#7377=MANIFOLD_SOLID_BREP('Body23',#93759);
#7378=MANIFOLD_SOLID_BREP('Body24',#93760);
#7379=MANIFOLD_SOLID_BREP('Body25',#93761);
#7380=MANIFOLD_SOLID_BREP('Body26',#93762);
#7381=MANIFOLD_SOLID_BREP('Body1',#93763);
#7382=MANIFOLD_SOLID_BREP('Body1',#93764);
#7383=MANIFOLD_SOLID_BREP('Body2',#93765);
#7384=MANIFOLD_SOLID_BREP('Body4',#93768);
#7385=MANIFOLD_SOLID_BREP('Body1',#93769);
#7386=MANIFOLD_SOLID_BREP('Body1',#93770);
#7387=MANIFOLD_SOLID_BREP('Body1',#93771);
#7388=MANIFOLD_SOLID_BREP('Body1',#93772);
#7389=MANIFOLD_SOLID_BREP('Body1',#93773);
#7390=MANIFOLD_SOLID_BREP('Body1',#93774);
#7391=FACE_BOUND('',#14442,.T.);
#7392=FACE_BOUND('',#14443,.T.);
#7393=FACE_BOUND('',#14444,.T.);
#7394=FACE_BOUND('',#14445,.T.);
#7395=FACE_BOUND('',#14446,.T.);
#7396=FACE_BOUND('',#14447,.T.);
#7397=FACE_BOUND('',#14448,.T.);
#7398=FACE_BOUND('',#14449,.T.);
#7399=FACE_BOUND('',#14450,.T.);
#7400=FACE_BOUND('',#14451,.T.);
#7401=FACE_BOUND('',#14452,.T.);
#7402=FACE_BOUND('',#14453,.T.);
#7403=FACE_BOUND('',#14458,.T.);
#7404=FACE_BOUND('',#14459,.T.);
#7405=FACE_BOUND('',#14460,.T.);
#7406=FACE_BOUND('',#14461,.T.);
#7407=FACE_BOUND('',#14462,.T.);
#7408=FACE_BOUND('',#14463,.T.);
#7409=FACE_BOUND('',#14464,.T.);
#7410=FACE_BOUND('',#14465,.T.);
#7411=FACE_BOUND('',#14466,.T.);
#7412=FACE_BOUND('',#14467,.T.);
#7413=FACE_BOUND('',#14468,.T.);
#7414=FACE_BOUND('',#14469,.T.);
#7415=FACE_BOUND('',#14492,.T.);
#7416=FACE_BOUND('',#14493,.T.);
#7417=FACE_BOUND('',#14494,.T.);
#7418=FACE_BOUND('',#14495,.T.);
#7419=FACE_BOUND('',#14496,.T.);
#7420=FACE_BOUND('',#14497,.T.);
#7421=FACE_BOUND('',#14498,.T.);
#7422=FACE_BOUND('',#14499,.T.);
#7423=FACE_BOUND('',#14500,.T.);
#7424=FACE_BOUND('',#14501,.T.);
#7425=FACE_BOUND('',#14502,.T.);
#7426=FACE_BOUND('',#14503,.T.);
#7427=FACE_BOUND('',#14508,.T.);
#7428=FACE_BOUND('',#14509,.T.);
#7429=FACE_BOUND('',#14510,.T.);
#7430=FACE_BOUND('',#14511,.T.);
#7431=FACE_BOUND('',#14512,.T.);
#7432=FACE_BOUND('',#14513,.T.);
#7433=FACE_BOUND('',#14514,.T.);
#7434=FACE_BOUND('',#14515,.T.);
#7435=FACE_BOUND('',#14516,.T.);
#7436=FACE_BOUND('',#14517,.T.);
#7437=FACE_BOUND('',#14518,.T.);
#7438=FACE_BOUND('',#14519,.T.);
#7439=FACE_BOUND('',#14531,.T.);
#7440=FACE_BOUND('',#14538,.T.);
#7441=FACE_BOUND('',#14957,.T.);
#7442=FACE_BOUND('',#14967,.T.);
#7443=FACE_BOUND('',#16361,.T.);
#7444=FACE_BOUND('',#16371,.T.);
#7445=FACE_BOUND('',#16795,.T.);
#7446=FACE_BOUND('',#16796,.T.);
#7447=FACE_BOUND('',#16797,.T.);
#7448=FACE_BOUND('',#16798,.T.);
#7449=FACE_BOUND('',#16811,.T.);
#7450=FACE_BOUND('',#16812,.T.);
#7451=FACE_BOUND('',#16813,.T.);
#7452=FACE_BOUND('',#16814,.T.);
#7453=FACE_BOUND('',#16831,.T.);
#7454=FACE_BOUND('',#16837,.T.);
#7455=FACE_BOUND('',#17565,.T.);
#7456=FACE_BOUND('',#18280,.T.);
#7457=FACE_BOUND('',#18352,.T.);
#7458=FACE_BOUND('',#18353,.T.);
#7459=FACE_BOUND('',#18354,.T.);
#7460=FACE_BOUND('',#18355,.T.);
#7461=FACE_BOUND('',#18356,.T.);
#7462=FACE_BOUND('',#18357,.T.);
#7463=FACE_BOUND('',#18358,.T.);
#7464=FACE_BOUND('',#18359,.T.);
#7465=FACE_BOUND('',#18360,.T.);
#7466=FACE_BOUND('',#18361,.T.);
#7467=FACE_BOUND('',#18362,.T.);
#7468=FACE_BOUND('',#18363,.T.);
#7469=FACE_BOUND('',#18364,.T.);
#7470=FACE_BOUND('',#18365,.T.);
#7471=FACE_BOUND('',#18366,.T.);
#7472=FACE_BOUND('',#18367,.T.);
#7473=FACE_BOUND('',#18368,.T.);
#7474=FACE_BOUND('',#18369,.T.);
#7475=FACE_BOUND('',#18370,.T.);
#7476=FACE_BOUND('',#18371,.T.);
#7477=FACE_BOUND('',#18372,.T.);
#7478=FACE_BOUND('',#18373,.T.);
#7479=FACE_BOUND('',#18374,.T.);
#7480=FACE_BOUND('',#18375,.T.);
#7481=FACE_BOUND('',#18376,.T.);
#7482=FACE_BOUND('',#18377,.T.);
#7483=FACE_BOUND('',#18378,.T.);
#7484=FACE_BOUND('',#18379,.T.);
#7485=FACE_BOUND('',#18380,.T.);
#7486=FACE_BOUND('',#18381,.T.);
#7487=FACE_BOUND('',#18382,.T.);
#7488=FACE_BOUND('',#18383,.T.);
#7489=FACE_BOUND('',#18384,.T.);
#7490=FACE_BOUND('',#18385,.T.);
#7491=FACE_BOUND('',#18386,.T.);
#7492=FACE_BOUND('',#18387,.T.);
#7493=FACE_BOUND('',#18388,.T.);
#7494=FACE_BOUND('',#18389,.T.);
#7495=FACE_BOUND('',#18390,.T.);
#7496=FACE_BOUND('',#18391,.T.);
#7497=FACE_BOUND('',#18392,.T.);
#7498=FACE_BOUND('',#18393,.T.);
#7499=FACE_BOUND('',#18394,.T.);
#7500=FACE_BOUND('',#18395,.T.);
#7501=FACE_BOUND('',#18396,.T.);
#7502=FACE_BOUND('',#18397,.T.);
#7503=FACE_BOUND('',#18398,.T.);
#7504=FACE_BOUND('',#18399,.T.);
#7505=FACE_BOUND('',#18400,.T.);
#7506=FACE_BOUND('',#18401,.T.);
#7507=FACE_BOUND('',#18402,.T.);
#7508=FACE_BOUND('',#18403,.T.);
#7509=FACE_BOUND('',#18404,.T.);
#7510=FACE_BOUND('',#18405,.T.);
#7511=FACE_BOUND('',#18406,.T.);
#7512=FACE_BOUND('',#18407,.T.);
#7513=FACE_BOUND('',#18408,.T.);
#7514=FACE_BOUND('',#18409,.T.);
#7515=FACE_BOUND('',#18410,.T.);
#7516=FACE_BOUND('',#18411,.T.);
#7517=FACE_BOUND('',#18412,.T.);
#7518=FACE_BOUND('',#18413,.T.);
#7519=FACE_BOUND('',#18414,.T.);
#7520=FACE_BOUND('',#18415,.T.);
#7521=FACE_BOUND('',#18416,.T.);
#7522=FACE_BOUND('',#18417,.T.);
#7523=FACE_BOUND('',#18418,.T.);
#7524=FACE_BOUND('',#18419,.T.);
#7525=FACE_BOUND('',#18461,.T.);
#7526=FACE_BOUND('',#18513,.T.);
#7527=FACE_BOUND('',#18531,.T.);
#7528=FACE_BOUND('',#18532,.T.);
#7529=FACE_BOUND('',#18533,.T.);
#7530=FACE_BOUND('',#18534,.T.);
#7531=FACE_BOUND('',#18535,.T.);
#7532=FACE_BOUND('',#18536,.T.);
#7533=FACE_BOUND('',#18537,.T.);
#7534=FACE_BOUND('',#18538,.T.);
#7535=FACE_BOUND('',#18539,.T.);
#7536=FACE_BOUND('',#18540,.T.);
#7537=FACE_BOUND('',#18541,.T.);
#7538=FACE_BOUND('',#18542,.T.);
#7539=FACE_BOUND('',#18543,.T.);
#7540=FACE_BOUND('',#18544,.T.);
#7541=FACE_BOUND('',#18545,.T.);
#7542=FACE_BOUND('',#18546,.T.);
#7543=FACE_BOUND('',#18547,.T.);
#7544=FACE_BOUND('',#18548,.T.);
#7545=FACE_BOUND('',#18549,.T.);
#7546=FACE_BOUND('',#18550,.T.);
#7547=FACE_BOUND('',#18551,.T.);
#7548=FACE_BOUND('',#18552,.T.);
#7549=FACE_BOUND('',#18553,.T.);
#7550=FACE_BOUND('',#18554,.T.);
#7551=FACE_BOUND('',#18555,.T.);
#7552=FACE_BOUND('',#18556,.T.);
#7553=FACE_BOUND('',#18557,.T.);
#7554=FACE_BOUND('',#18558,.T.);
#7555=FACE_BOUND('',#18559,.T.);
#7556=FACE_BOUND('',#18560,.T.);
#7557=FACE_BOUND('',#18561,.T.);
#7558=FACE_BOUND('',#18562,.T.);
#7559=FACE_BOUND('',#18563,.T.);
#7560=FACE_BOUND('',#18564,.T.);
#7561=FACE_BOUND('',#18565,.T.);
#7562=FACE_BOUND('',#18566,.T.);
#7563=FACE_BOUND('',#18567,.T.);
#7564=FACE_BOUND('',#18568,.T.);
#7565=FACE_BOUND('',#18569,.T.);
#7566=FACE_BOUND('',#18570,.T.);
#7567=FACE_BOUND('',#18571,.T.);
#7568=FACE_BOUND('',#18572,.T.);
#7569=FACE_BOUND('',#18573,.T.);
#7570=FACE_BOUND('',#18574,.T.);
#7571=FACE_BOUND('',#18575,.T.);
#7572=FACE_BOUND('',#18576,.T.);
#7573=FACE_BOUND('',#18577,.T.);
#7574=FACE_BOUND('',#18578,.T.);
#7575=FACE_BOUND('',#18579,.T.);
#7576=FACE_BOUND('',#18580,.T.);
#7577=FACE_BOUND('',#18581,.T.);
#7578=FACE_BOUND('',#18582,.T.);
#7579=FACE_BOUND('',#18583,.T.);
#7580=FACE_BOUND('',#18584,.T.);
#7581=FACE_BOUND('',#18585,.T.);
#7582=FACE_BOUND('',#18586,.T.);
#7583=FACE_BOUND('',#18587,.T.);
#7584=FACE_BOUND('',#18588,.T.);
#7585=FACE_BOUND('',#18589,.T.);
#7586=FACE_BOUND('',#18590,.T.);
#7587=FACE_BOUND('',#18591,.T.);
#7588=FACE_BOUND('',#18602,.T.);
#7589=FACE_BOUND('',#18624,.T.);
#7590=FACE_BOUND('',#18626,.T.);
#7591=FACE_BOUND('',#18642,.T.);
#7592=FACE_BOUND('',#18668,.T.);
#7593=FACE_BOUND('',#18736,.T.);
#7594=FACE_BOUND('',#18794,.T.);
#7595=FACE_BOUND('',#18797,.T.);
#7596=FACE_BOUND('',#18809,.T.);
#7597=FACE_BOUND('',#18814,.T.);
#7598=FACE_BOUND('',#18829,.T.);
#7599=FACE_BOUND('',#18830,.T.);
#7600=FACE_BOUND('',#18848,.T.);
#7601=FACE_BOUND('',#18849,.T.);
#7602=FACE_BOUND('',#18860,.T.);
#7603=FACE_BOUND('',#18868,.T.);
#7604=FACE_BOUND('',#18880,.T.);
#7605=FACE_BOUND('',#19146,.T.);
#7606=FACE_BOUND('',#19370,.T.);
#7607=FACE_BOUND('',#19371,.T.);
#7608=FACE_BOUND('',#19372,.T.);
#7609=FACE_BOUND('',#19374,.T.);
#7610=FACE_BOUND('',#19379,.T.);
#7611=FACE_BOUND('',#19384,.T.);
#7612=FACE_BOUND('',#19389,.T.);
#7613=FACE_BOUND('',#19411,.T.);
#7614=FACE_BOUND('',#19557,.T.);
#7615=FACE_BOUND('',#19558,.T.);
#7616=FACE_BOUND('',#19559,.T.);
#7617=FACE_BOUND('',#19560,.T.);
#7618=FACE_BOUND('',#19569,.T.);
#7619=FACE_BOUND('',#19570,.T.);
#7620=FACE_BOUND('',#19571,.T.);
#7621=FACE_BOUND('',#19572,.T.);
#7622=FACE_BOUND('',#19617,.T.);
#7623=FACE_BOUND('',#19619,.T.);
#7624=FACE_BOUND('',#19666,.T.);
#7625=FACE_BOUND('',#19713,.T.);
#7626=FACE_BOUND('',#19715,.T.);
#7627=FACE_BOUND('',#19737,.T.);
#7628=FACE_BOUND('',#19739,.T.);
#7629=FACE_BOUND('',#19828,.T.);
#7630=FACE_BOUND('',#19915,.T.);
#7631=FACE_BOUND('',#19916,.T.);
#7632=FACE_BOUND('',#19918,.T.);
#7633=FACE_BOUND('',#19919,.T.);
#7634=FACE_BOUND('',#19924,.T.);
#7635=FACE_BOUND('',#19925,.T.);
#7636=FACE_BOUND('',#19927,.T.);
#7637=FACE_BOUND('',#19928,.T.);
#7638=FACE_BOUND('',#19943,.T.);
#7639=FACE_BOUND('',#19945,.T.);
#7640=FACE_BOUND('',#19947,.T.);
#7641=FACE_BOUND('',#19949,.T.);
#7642=FACE_BOUND('',#19961,.T.);
#7643=FACE_BOUND('',#19963,.T.);
#7644=FACE_BOUND('',#19965,.T.);
#7645=FACE_BOUND('',#19966,.T.);
#7646=FACE_BOUND('',#19971,.T.);
#7647=FACE_BOUND('',#19973,.T.);
#7648=FACE_BOUND('',#20009,.T.);
#7649=FACE_BOUND('',#20011,.T.);
#7650=FACE_BOUND('',#20013,.T.);
#7651=FACE_BOUND('',#20016,.T.);
#7652=FACE_BOUND('',#20035,.T.);
#7653=FACE_BOUND('',#20043,.T.);
#7654=FACE_BOUND('',#20075,.T.);
#7655=FACE_BOUND('',#20079,.T.);
#7656=FACE_BOUND('',#20087,.T.);
#7657=FACE_BOUND('',#20099,.T.);
#7658=FACE_BOUND('',#20174,.T.);
#7659=FACE_BOUND('',#20176,.T.);
#7660=FACE_BOUND('',#20188,.T.);
#7661=FACE_BOUND('',#20217,.T.);
#7662=FACE_BOUND('',#20224,.T.);
#7663=FACE_BOUND('',#20226,.T.);
#7664=FACE_BOUND('',#20229,.T.);
#7665=FACE_BOUND('',#20240,.T.);
#7666=FACE_BOUND('',#20241,.T.);
#7667=FACE_BOUND('',#20242,.T.);
#7668=FACE_BOUND('',#20243,.T.);
#7669=FACE_BOUND('',#20244,.T.);
#7670=FACE_BOUND('',#20245,.T.);
#7671=FACE_BOUND('',#20246,.T.);
#7672=FACE_BOUND('',#20247,.T.);
#7673=FACE_BOUND('',#20248,.T.);
#7674=FACE_BOUND('',#20250,.T.);
#7675=FACE_BOUND('',#20252,.T.);
#7676=FACE_BOUND('',#20280,.T.);
#7677=FACE_BOUND('',#20281,.T.);
#7678=FACE_BOUND('',#20283,.T.);
#7679=FACE_BOUND('',#20284,.T.);
#7680=FACE_BOUND('',#20285,.T.);
#7681=FACE_BOUND('',#20287,.T.);
#7682=FACE_BOUND('',#20288,.T.);
#7683=FACE_BOUND('',#20289,.T.);
#7684=FACE_BOUND('',#20291,.T.);
#7685=FACE_BOUND('',#20292,.T.);
#7686=FACE_BOUND('',#20293,.T.);
#7687=FACE_BOUND('',#20295,.T.);
#7688=FACE_BOUND('',#20296,.T.);
#7689=FACE_BOUND('',#20298,.T.);
#7690=FACE_BOUND('',#20299,.T.);
#7691=FACE_BOUND('',#20300,.T.);
#7692=FACE_BOUND('',#20319,.T.);
#7693=FACE_BOUND('',#20320,.T.);
#7694=FACE_BOUND('',#20324,.T.);
#7695=FACE_BOUND('',#20325,.T.);
#7696=FACE_BOUND('',#20391,.T.);
#7697=FACE_BOUND('',#20392,.T.);
#7698=FACE_BOUND('',#20394,.T.);
#7699=FACE_BOUND('',#20395,.T.);
#7700=FACE_BOUND('',#20418,.T.);
#7701=FACE_BOUND('',#20419,.T.);
#7702=FACE_BOUND('',#20420,.T.);
#7703=FACE_BOUND('',#20434,.T.);
#7704=FACE_BOUND('',#20476,.T.);
#7705=FACE_BOUND('',#20478,.T.);
#7706=PLANE('',#94001);
#7707=PLANE('',#94002);
#7708=PLANE('',#94003);
#7709=PLANE('',#94004);
#7710=PLANE('',#94005);
#7711=PLANE('',#94006);
#7712=PLANE('',#94007);
#7713=PLANE('',#94008);
#7714=PLANE('',#94009);
#7715=PLANE('',#94014);
#7716=PLANE('',#94060);
#7717=PLANE('',#94061);
#7718=PLANE('',#94062);
#7719=PLANE('',#94063);
#7720=PLANE('',#94064);
#7721=PLANE('',#94065);
#7722=PLANE('',#94066);
#7723=PLANE('',#94067);
#7724=PLANE('',#94068);
#7725=PLANE('',#94073);
#7726=PLANE('',#94086);
#7727=PLANE('',#94089);
#7728=PLANE('',#94093);
#7729=PLANE('',#94097);
#7730=PLANE('',#94100);
#7731=PLANE('',#94104);
#7732=PLANE('',#94119);
#7733=PLANE('',#94127);
#7734=PLANE('',#94132);
#7735=PLANE('',#94263);
#7736=PLANE('',#94272);
#7737=PLANE('',#94277);
#7738=PLANE('',#94458);
#7739=PLANE('',#94463);
#7740=PLANE('',#94466);
#7741=PLANE('',#94563);
#7742=PLANE('',#94691);
#7743=PLANE('',#94698);
#7744=PLANE('',#94704);
#7745=PLANE('',#94709);
#7746=PLANE('',#94715);
#7747=PLANE('',#94720);
#7748=PLANE('',#94727);
#7749=PLANE('',#94738);
#7750=PLANE('',#94744);
#7751=PLANE('',#94747);
#7752=PLANE('',#94755);
#7753=PLANE('',#94762);
#7754=PLANE('',#94766);
#7755=PLANE('',#94769);
#7756=PLANE('',#94772);
#7757=PLANE('',#94777);
#7758=PLANE('',#94780);
#7759=PLANE('',#94789);
#7760=PLANE('',#94795);
#7761=PLANE('',#94800);
#7762=PLANE('',#94807);
#7763=PLANE('',#94813);
#7764=PLANE('',#94818);
#7765=PLANE('',#94827);
#7766=PLANE('',#94834);
#7767=PLANE('',#94840);
#7768=PLANE('',#94845);
#7769=PLANE('',#94851);
#7770=PLANE('',#94856);
#7771=PLANE('',#94863);
#7772=PLANE('',#94867);
#7773=PLANE('',#94871);
#7774=PLANE('',#94876);
#7775=PLANE('',#94879);
#7776=PLANE('',#94884);
#7777=PLANE('',#94892);
#7778=PLANE('',#94894);
#7779=PLANE('',#94899);
#7780=PLANE('',#94902);
#7781=PLANE('',#94905);
#7782=PLANE('',#94909);
#7783=PLANE('',#94914);
#7784=PLANE('',#94917);
#7785=PLANE('',#94922);
#7786=PLANE('',#94926);
#7787=PLANE('',#94929);
#7788=PLANE('',#94932);
#7789=PLANE('',#94936);
#7790=PLANE('',#94941);
#7791=PLANE('',#94945);
#7792=PLANE('',#94949);
#7793=PLANE('',#94960);
#7794=PLANE('',#94962);
#7795=PLANE('',#94967);
#7796=PLANE('',#94970);
#7797=PLANE('',#94978);
#7798=PLANE('',#94983);
#7799=PLANE('',#94988);
#7800=PLANE('',#94991);
#7801=PLANE('',#94995);
#7802=PLANE('',#94998);
#7803=PLANE('',#95003);
#7804=PLANE('',#95007);
#7805=PLANE('',#95010);
#7806=PLANE('',#95016);
#7807=PLANE('',#95035);
#7808=PLANE('',#95048);
#7809=PLANE('',#95058);
#7810=PLANE('',#95063);
#7811=PLANE('',#95069);
#7812=PLANE('',#95073);
#7813=PLANE('',#95077);
#7814=PLANE('',#95081);
#7815=PLANE('',#95085);
#7816=PLANE('',#95098);
#7817=PLANE('',#95105);
#7818=PLANE('',#95124);
#7819=PLANE('',#95131);
#7820=PLANE('',#95134);
#7821=PLANE('',#95140);
#7822=PLANE('',#95144);
#7823=PLANE('',#95148);
#7824=PLANE('',#95156);
#7825=PLANE('',#95173);
#7826=PLANE('',#95187);
#7827=PLANE('',#95325);
#7828=PLANE('',#95352);
#7829=PLANE('',#95380);
#7830=PLANE('',#95822);
#7831=PLANE('',#95825);
#7832=PLANE('',#95920);
#7833=PLANE('',#95921);
#7834=PLANE('',#95922);
#7835=PLANE('',#95923);
#7836=PLANE('',#95924);
#7837=PLANE('',#95925);
#7838=PLANE('',#95926);
#7839=PLANE('',#95928);
#7840=PLANE('',#95930);
#7841=PLANE('',#95932);
#7842=PLANE('',#95935);
#7843=PLANE('',#95937);
#7844=PLANE('',#95939);
#7845=PLANE('',#95941);
#7846=PLANE('',#95944);
#7847=PLANE('',#95945);
#7848=PLANE('',#95947);
#7849=PLANE('',#95948);
#7850=PLANE('',#95951);
#7851=PLANE('',#95953);
#7852=PLANE('',#95954);
#7853=PLANE('',#95960);
#7854=PLANE('',#95962);
#7855=PLANE('',#95963);
#7856=PLANE('',#95964);
#7857=PLANE('',#95966);
#7858=PLANE('',#95970);
#7859=PLANE('',#95972);
#7860=PLANE('',#95973);
#7861=PLANE('',#95978);
#7862=PLANE('',#95983);
#7863=PLANE('',#95984);
#7864=PLANE('',#95985);
#7865=PLANE('',#95987);
#7866=PLANE('',#95988);
#7867=PLANE('',#95993);
#7868=PLANE('',#95995);
#7869=PLANE('',#95996);
#7870=PLANE('',#96001);
#7871=PLANE('',#96003);
#7872=PLANE('',#96005);
#7873=PLANE('',#96006);
#7874=PLANE('',#96007);
#7875=PLANE('',#96009);
#7876=PLANE('',#96013);
#7877=PLANE('',#96016);
#7878=PLANE('',#96021);
#7879=PLANE('',#96022);
#7880=PLANE('',#96026);
#7881=PLANE('',#96031);
#7882=PLANE('',#96032);
#7883=PLANE('',#96036);
#7884=PLANE('',#96037);
#7885=PLANE('',#96039);
#7886=PLANE('',#96044);
#7887=PLANE('',#96049);
#7888=PLANE('',#96050);
#7889=PLANE('',#96054);
#7890=PLANE('',#96061);
#7891=PLANE('',#96065);
#7892=PLANE('',#96066);
#7893=PLANE('',#96068);
#7894=PLANE('',#96075);
#7895=PLANE('',#96081);
#7896=PLANE('',#96082);
#7897=PLANE('',#96086);
#7898=PLANE('',#96092);
#7899=PLANE('',#96094);
#7900=PLANE('',#96097);
#7901=PLANE('',#96099);
#7902=PLANE('',#96105);
#7903=PLANE('',#96109);
#7904=PLANE('',#96115);
#7905=PLANE('',#96120);
#7906=PLANE('',#96125);
#7907=PLANE('',#96129);
#7908=PLANE('',#96134);
#7909=PLANE('',#96137);
#7910=PLANE('',#96139);
#7911=PLANE('',#96140);
#7912=PLANE('',#96141);
#7913=PLANE('',#96142);
#7914=PLANE('',#96143);
#7915=PLANE('',#96144);
#7916=PLANE('',#96304);
#7917=PLANE('',#96307);
#7918=PLANE('',#96808);
#7919=PLANE('',#96838);
#7920=PLANE('',#96869);
#7921=PLANE('',#97056);
#7922=PLANE('',#97077);
#7923=PLANE('',#97101);
#7924=PLANE('',#97113);
#7925=PLANE('',#97115);
#7926=PLANE('',#97117);
#7927=PLANE('',#97119);
#7928=PLANE('',#97122);
#7929=PLANE('',#97129);
#7930=PLANE('',#97136);
#7931=PLANE('',#97143);
#7932=PLANE('',#97158);
#7933=PLANE('',#97164);
#7934=PLANE('',#97170);
#7935=PLANE('',#97176);
#7936=PLANE('',#97182);
#7937=PLANE('',#97191);
#7938=PLANE('',#97203);
#7939=PLANE('',#97217);
#7940=PLANE('',#97231);
#7941=PLANE('',#97251);
#7942=PLANE('',#97257);
#7943=PLANE('',#97259);
#7944=PLANE('',#97263);
#7945=PLANE('',#97265);
#7946=PLANE('',#97267);
#7947=PLANE('',#97269);
#7948=PLANE('',#97271);
#7949=PLANE('',#97273);
#7950=PLANE('',#97275);
#7951=PLANE('',#97278);
#7952=PLANE('',#97280);
#7953=PLANE('',#97282);
#7954=PLANE('',#97284);
#7955=PLANE('',#97290);
#7956=PLANE('',#97291);
#7957=PLANE('',#97294);
#7958=PLANE('',#97296);
#7959=PLANE('',#97299);
#7960=PLANE('',#97300);
#7961=PLANE('',#97302);
#7962=PLANE('',#97304);
#7963=PLANE('',#97307);
#7964=PLANE('',#97309);
#7965=PLANE('',#97311);
#7966=PLANE('',#97314);
#7967=PLANE('',#97315);
#7968=PLANE('',#97317);
#7969=PLANE('',#97319);
#7970=PLANE('',#97321);
#7971=PLANE('',#97324);
#7972=PLANE('',#97327);
#7973=PLANE('',#97329);
#7974=PLANE('',#97331);
#7975=PLANE('',#97334);
#7976=PLANE('',#97335);
#7977=PLANE('',#97341);
#7978=PLANE('',#97346);
#7979=PLANE('',#97349);
#7980=PLANE('',#97355);
#7981=PLANE('',#97360);
#7982=PLANE('',#97366);
#7983=PLANE('',#97371);
#7984=PLANE('',#97377);
#7985=PLANE('',#97382);
#7986=PLANE('',#97388);
#7987=PLANE('',#97393);
#7988=PLANE('',#97396);
#7989=PLANE('',#97404);
#7990=PLANE('',#97406);
#7991=PLANE('',#97412);
#7992=PLANE('',#97415);
#7993=PLANE('',#97418);
#7994=PLANE('',#97425);
#7995=PLANE('',#97430);
#7996=PLANE('',#97439);
#7997=PLANE('',#97441);
#7998=PLANE('',#97444);
#7999=PLANE('',#97450);
#8000=PLANE('',#97456);
#8001=PLANE('',#97461);
#8002=PLANE('',#97464);
#8003=PLANE('',#97471);
#8004=PLANE('',#97476);
#8005=PLANE('',#97483);
#8006=PLANE('',#97578);
#8007=PLANE('',#97647);
#8008=PLANE('',#97650);
#8009=PLANE('',#97653);
#8010=PLANE('',#97805);
#8011=PLANE('',#97808);
#8012=PLANE('',#97813);
#8013=PLANE('',#97893);
#8014=PLANE('',#97896);
#8015=PLANE('',#97901);
#8016=PLANE('',#97911);
#8017=PLANE('',#97919);
#8018=PLANE('',#97927);
#8019=PLANE('',#97928);
#8020=PLANE('',#97929);
#8021=PLANE('',#97941);
#8022=PLANE('',#97942);
#8023=PLANE('',#97943);
#8024=PLANE('',#97944);
#8025=PLANE('',#97945);
#8026=PLANE('',#97946);
#8027=PLANE('',#97947);
#8028=PLANE('',#97966);
#8029=PLANE('',#97968);
#8030=PLANE('',#97973);
#8031=PLANE('',#97976);
#8032=PLANE('',#97980);
#8033=PLANE('',#99502);
#8034=PLANE('',#99503);
#8035=PLANE('',#99510);
#8036=PLANE('',#99511);
#8037=PLANE('',#99516);
#8038=PLANE('',#99517);
#8039=PLANE('',#99518);
#8040=PLANE('',#99519);
#8041=PLANE('',#99520);
#8042=PLANE('',#99521);
#8043=PLANE('',#99522);
#8044=PLANE('',#99523);
#8045=PLANE('',#99524);
#8046=PLANE('',#99525);
#8047=PLANE('',#99526);
#8048=PLANE('',#99527);
#8049=PLANE('',#99528);
#8050=PLANE('',#99529);
#8051=PLANE('',#99530);
#8052=PLANE('',#99531);
#8053=PLANE('',#99532);
#8054=PLANE('',#99533);
#8055=PLANE('',#99534);
#8056=PLANE('',#99535);
#8057=PLANE('',#99536);
#8058=PLANE('',#99537);
#8059=PLANE('',#99538);
#8060=PLANE('',#99539);
#8061=PLANE('',#99540);
#8062=PLANE('',#99541);
#8063=PLANE('',#99542);
#8064=PLANE('',#99543);
#8065=PLANE('',#99544);
#8066=PLANE('',#99545);
#8067=PLANE('',#99546);
#8068=PLANE('',#99547);
#8069=PLANE('',#99548);
#8070=PLANE('',#99549);
#8071=PLANE('',#99550);
#8072=PLANE('',#99551);
#8073=PLANE('',#99552);
#8074=PLANE('',#99553);
#8075=PLANE('',#99554);
#8076=PLANE('',#99555);
#8077=PLANE('',#99556);
#8078=PLANE('',#99557);
#8079=PLANE('',#99558);
#8080=PLANE('',#99559);
#8081=PLANE('',#99560);
#8082=PLANE('',#99561);
#8083=PLANE('',#99562);
#8084=PLANE('',#99563);
#8085=PLANE('',#99564);
#8086=PLANE('',#99565);
#8087=PLANE('',#99566);
#8088=PLANE('',#99567);
#8089=PLANE('',#99568);
#8090=PLANE('',#99569);
#8091=PLANE('',#99570);
#8092=PLANE('',#99571);
#8093=PLANE('',#99572);
#8094=PLANE('',#99594);
#8095=PLANE('',#99596);
#8096=PLANE('',#99597);
#8097=PLANE('',#99599);
#8098=PLANE('',#99600);
#8099=PLANE('',#99601);
#8100=PLANE('',#99605);
#8101=PLANE('',#99606);
#8102=PLANE('',#99670);
#8103=PLANE('',#99674);
#8104=PLANE('',#99676);
#8105=PLANE('',#99678);
#8106=PLANE('',#99680);
#8107=PLANE('',#99682);
#8108=PLANE('',#99684);
#8109=PLANE('',#99686);
#8110=PLANE('',#99688);
#8111=PLANE('',#99690);
#8112=PLANE('',#99702);
#8113=PLANE('',#99704);
#8114=PLANE('',#99720);
#8115=PLANE('',#99725);
#8116=PLANE('',#99728);
#8117=PLANE('',#99729);
#8118=PLANE('',#99730);
#8119=PLANE('',#99732);
#8120=PLANE('',#99734);
#8121=PLANE('',#99735);
#8122=PLANE('',#99737);
#8123=PLANE('',#99738);
#8124=PLANE('',#99740);
#8125=PLANE('',#99741);
#8126=PLANE('',#99792);
#8127=PLANE('',#99793);
#8128=PLANE('',#99804);
#8129=PLANE('',#99805);
#8130=PLANE('',#99806);
#8131=PLANE('',#99807);
#8132=PLANE('',#99808);
#8133=PLANE('',#99809);
#8134=PLANE('',#99810);
#8135=PLANE('',#99811);
#8136=PLANE('',#99812);
#8137=PLANE('',#99813);
#8138=PLANE('',#99821);
#8139=PLANE('',#99822);
#8140=PLANE('',#99823);
#8141=PLANE('',#99824);
#8142=PLANE('',#99825);
#8143=PLANE('',#99826);
#8144=PLANE('',#99827);
#8145=PLANE('',#99828);
#8146=PLANE('',#99829);
#8147=PLANE('',#99830);
#8148=PLANE('',#99831);
#8149=PLANE('',#99832);
#8150=PLANE('',#99833);
#8151=PLANE('',#99834);
#8152=PLANE('',#99851);
#8153=PLANE('',#99852);
#8154=PLANE('',#99853);
#8155=PLANE('',#99854);
#8156=PLANE('',#99855);
#8157=PLANE('',#99856);
#8158=PLANE('',#99857);
#8159=PLANE('',#99858);
#8160=PLANE('',#99859);
#8161=PLANE('',#99860);
#8162=PLANE('',#99861);
#8163=PLANE('',#99862);
#8164=PLANE('',#99863);
#8165=PLANE('',#99864);
#8166=PLANE('',#99865);
#8167=PLANE('',#99866);
#8168=PLANE('',#99867);
#8169=PLANE('',#99868);
#8170=PLANE('',#99869);
#8171=PLANE('',#99870);
#8172=PLANE('',#99871);
#8173=PLANE('',#99872);
#8174=PLANE('',#99873);
#8175=PLANE('',#99874);
#8176=PLANE('',#99875);
#8177=PLANE('',#99876);
#8178=PLANE('',#99877);
#8179=PLANE('',#99878);
#8180=PLANE('',#101430);
#8181=PLANE('',#101433);
#8182=PLANE('',#101458);
#8183=PLANE('',#101459);
#8184=PLANE('',#101466);
#8185=PLANE('',#101467);
#8186=PLANE('',#101472);
#8187=PLANE('',#101473);
#8188=PLANE('',#101474);
#8189=PLANE('',#101475);
#8190=PLANE('',#101476);
#8191=PLANE('',#101477);
#8192=PLANE('',#101478);
#8193=PLANE('',#101479);
#8194=PLANE('',#101480);
#8195=PLANE('',#101481);
#8196=PLANE('',#101482);
#8197=PLANE('',#101483);
#8198=PLANE('',#101484);
#8199=PLANE('',#101485);
#8200=PLANE('',#101486);
#8201=PLANE('',#101487);
#8202=PLANE('',#101488);
#8203=PLANE('',#101489);
#8204=PLANE('',#101490);
#8205=PLANE('',#101491);
#8206=PLANE('',#101492);
#8207=PLANE('',#101493);
#8208=PLANE('',#101494);
#8209=PLANE('',#101495);
#8210=PLANE('',#101496);
#8211=PLANE('',#101497);
#8212=PLANE('',#101498);
#8213=PLANE('',#101499);
#8214=PLANE('',#101500);
#8215=PLANE('',#101501);
#8216=PLANE('',#101502);
#8217=PLANE('',#101503);
#8218=PLANE('',#101504);
#8219=PLANE('',#101505);
#8220=PLANE('',#101506);
#8221=PLANE('',#101507);
#8222=PLANE('',#101508);
#8223=PLANE('',#101509);
#8224=PLANE('',#101510);
#8225=PLANE('',#101511);
#8226=PLANE('',#101512);
#8227=PLANE('',#101513);
#8228=PLANE('',#101514);
#8229=PLANE('',#101515);
#8230=PLANE('',#101516);
#8231=PLANE('',#101517);
#8232=PLANE('',#101518);
#8233=PLANE('',#101519);
#8234=PLANE('',#101520);
#8235=PLANE('',#101521);
#8236=PLANE('',#101522);
#8237=PLANE('',#101523);
#8238=PLANE('',#101524);
#8239=PLANE('',#101525);
#8240=PLANE('',#101526);
#8241=PLANE('',#101527);
#8242=PLANE('',#101528);
#8243=PLANE('',#101529);
#8244=PLANE('',#101578);
#8245=PLANE('',#101580);
#8246=PLANE('',#101581);
#8247=PLANE('',#101583);
#8248=PLANE('',#101584);
#8249=PLANE('',#101585);
#8250=PLANE('',#101589);
#8251=PLANE('',#101590);
#8252=PLANE('',#101640);
#8253=PLANE('',#101673);
#8254=PLANE('',#101677);
#8255=PLANE('',#101679);
#8256=PLANE('',#101681);
#8257=PLANE('',#101682);
#8258=PLANE('',#101683);
#8259=PLANE('',#101684);
#8260=PLANE('',#101686);
#8261=PLANE('',#101688);
#8262=PLANE('',#101690);
#8263=PLANE('',#101691);
#8264=PLANE('',#101693);
#8265=PLANE('',#101705);
#8266=PLANE('',#101707);
#8267=PLANE('',#101716);
#8268=PLANE('',#101719);
#8269=PLANE('',#101722);
#8270=PLANE('',#101723);
#8271=PLANE('',#101724);
#8272=PLANE('',#101726);
#8273=PLANE('',#101727);
#8274=PLANE('',#101728);
#8275=PLANE('',#101730);
#8276=PLANE('',#101731);
#8277=PLANE('',#101733);
#8278=PLANE('',#101734);
#8279=PLANE('',#101736);
#8280=PLANE('',#101755);
#8281=PLANE('',#101781);
#8282=PLANE('',#101791);
#8283=PLANE('',#101803);
#8284=PLANE('',#101804);
#8285=PLANE('',#101805);
#8286=PLANE('',#101811);
#8287=PLANE('',#101812);
#8288=PLANE('',#101813);
#8289=PLANE('',#101814);
#8290=PLANE('',#101815);
#8291=PLANE('',#101816);
#8292=PLANE('',#101817);
#8293=PLANE('',#101818);
#8294=PLANE('',#101819);
#8295=PLANE('',#101820);
#8296=PLANE('',#101827);
#8297=PLANE('',#101828);
#8298=PLANE('',#101829);
#8299=PLANE('',#101830);
#8300=PLANE('',#101831);
#8301=PLANE('',#101832);
#8302=PLANE('',#101833);
#8303=PLANE('',#101834);
#8304=PLANE('',#101835);
#8305=PLANE('',#101836);
#8306=PLANE('',#101837);
#8307=PLANE('',#101838);
#8308=PLANE('',#101839);
#8309=PLANE('',#101840);
#8310=PLANE('',#101841);
#8311=PLANE('',#101850);
#8312=PLANE('',#101851);
#8313=PLANE('',#101852);
#8314=PLANE('',#101853);
#8315=PLANE('',#101854);
#8316=PLANE('',#101855);
#8317=PLANE('',#101856);
#8318=PLANE('',#101857);
#8319=PLANE('',#101858);
#8320=PLANE('',#101859);
#8321=PLANE('',#101860);
#8322=PLANE('',#101861);
#8323=PLANE('',#101862);
#8324=PLANE('',#101863);
#8325=PLANE('',#101864);
#8326=PLANE('',#101865);
#8327=PLANE('',#101866);
#8328=PLANE('',#101867);
#8329=PLANE('',#101868);
#8330=PLANE('',#101869);
#8331=PLANE('',#101870);
#8332=PLANE('',#101871);
#8333=PLANE('',#101872);
#8334=PLANE('',#101873);
#8335=PLANE('',#101874);
#8336=PLANE('',#101875);
#8337=PLANE('',#101876);
#8338=PLANE('',#101877);
#8339=PLANE('',#101879);
#8340=PLANE('',#101880);
#8341=PLANE('',#101881);
#8342=PLANE('',#101882);
#8343=PLANE('',#101883);
#8344=PLANE('',#101884);
#8345=PLANE('',#101903);
#8346=PLANE('',#101905);
#8347=PLANE('',#101907);
#8348=PLANE('',#101920);
#8349=PLANE('',#101933);
#8350=PLANE('',#101934);
#8351=PLANE('',#101935);
#8352=PLANE('',#101936);
#8353=PLANE('',#101937);
#8354=PLANE('',#101938);
#8355=PLANE('',#101939);
#8356=PLANE('',#101952);
#8357=PLANE('',#101965);
#8358=PLANE('',#101966);
#8359=PLANE('',#101967);
#8360=PLANE('',#101968);
#8361=PLANE('',#101969);
#8362=PLANE('',#101970);
#8363=PLANE('',#101971);
#8364=PLANE('',#101972);
#8365=PLANE('',#101973);
#8366=PLANE('',#101974);
#8367=PLANE('',#101975);
#8368=PLANE('',#101976);
#8369=PLANE('',#101995);
#8370=PLANE('',#101997);
#8371=PLANE('',#102012);
#8372=PLANE('',#102015);
#8373=PLANE('',#102017);
#8374=PLANE('',#102019);
#8375=PLANE('',#102024);
#8376=PLANE('',#102028);
#8377=PLANE('',#102031);
#8378=PLANE('',#102035);
#8379=PLANE('',#102060);
#8380=PLANE('',#102065);
#8381=PLANE('',#102116);
#8382=PLANE('',#102124);
#8383=PLANE('',#102126);
#8384=PLANE('',#102128);
#8385=PLANE('',#102130);
#8386=PLANE('',#102131);
#8387=PLANE('',#102132);
#8388=PLANE('',#102135);
#8389=PLANE('',#102136);
#8390=PLANE('',#102150);
#8391=PLANE('',#102153);
#8392=PLANE('',#102155);
#8393=PLANE('',#102157);
#8394=PLANE('',#102162);
#8395=PLANE('',#102560);
#8396=PLANE('',#102564);
#8397=PLANE('',#102567);
#8398=PLANE('',#102568);
#8399=PLANE('',#102569);
#8400=PLANE('',#102570);
#8401=PLANE('',#102571);
#8402=PLANE('',#102572);
#8403=PLANE('',#102573);
#8404=PLANE('',#102574);
#8405=PLANE('',#102575);
#8406=PLANE('',#102576);
#8407=PLANE('',#102577);
#8408=PLANE('',#102578);
#8409=PLANE('',#102579);
#8410=PLANE('',#102580);
#8411=PLANE('',#102584);
#8412=PLANE('',#102585);
#8413=PLANE('',#102586);
#8414=PLANE('',#102590);
#8415=PLANE('',#102591);
#8416=PLANE('',#102592);
#8417=PLANE('',#102596);
#8418=PLANE('',#102597);
#8419=PLANE('',#102598);
#8420=PLANE('',#102602);
#8421=PLANE('',#102603);
#8422=PLANE('',#102604);
#8423=PLANE('',#102606);
#8424=PLANE('',#102609);
#8425=PLANE('',#102612);
#8426=PLANE('',#102613);
#8427=PLANE('',#102618);
#8428=PLANE('',#102619);
#8429=PLANE('',#102621);
#8430=PLANE('',#102623);
#8431=PLANE('',#102625);
#8432=PLANE('',#102627);
#8433=PLANE('',#102630);
#8434=PLANE('',#102632);
#8435=PLANE('',#102634);
#8436=PLANE('',#102635);
#8437=PLANE('',#102636);
#8438=PLANE('',#102637);
#8439=PLANE('',#102638);
#8440=PLANE('',#102639);
#8441=PLANE('',#102641);
#8442=PLANE('',#102642);
#8443=PLANE('',#102643);
#8444=PLANE('',#102645);
#8445=PLANE('',#102658);
#8446=PLANE('',#102671);
#8447=PLANE('',#102672);
#8448=PLANE('',#102673);
#8449=PLANE('',#102674);
#8450=PLANE('',#102675);
#8451=PLANE('',#102676);
#8452=PLANE('',#102677);
#8453=PLANE('',#102690);
#8454=PLANE('',#102703);
#8455=PLANE('',#102704);
#8456=PLANE('',#102705);
#8457=PLANE('',#102706);
#8458=PLANE('',#102707);
#8459=PLANE('',#102708);
#8460=PLANE('',#102709);
#8461=PLANE('',#102710);
#8462=PLANE('',#102711);
#8463=PLANE('',#102712);
#8464=PLANE('',#102713);
#8465=PLANE('',#102714);
#8466=PLANE('',#102733);
#8467=PLANE('',#102735);
#8468=PLANE('',#102781);
#8469=PLANE('',#102782);
#8470=PLANE('',#102783);
#8471=PLANE('',#102828);
#8472=PLANE('',#102829);
#8473=PLANE('',#102830);
#8474=PLANE('',#102831);
#8475=PLANE('',#102832);
#8476=PLANE('',#102854);
#8477=PLANE('',#102875);
#8478=PLANE('',#102876);
#8479=PLANE('',#102877);
#8480=PLANE('',#103040);
#8481=PLANE('',#103041);
#8482=PLANE('',#103044);
#8483=PLANE('',#103045);
#8484=PLANE('',#103046);
#8485=PLANE('',#103047);
#8486=PLANE('',#103048);
#8487=PLANE('',#103049);
#8488=PLANE('',#103056);
#8489=PLANE('',#103062);
#8490=PLANE('',#103063);
#8491=PLANE('',#103069);
#8492=PLANE('',#103070);
#8493=PLANE('',#103076);
#8494=PLANE('',#103077);
#8495=PLANE('',#103085);
#8496=PLANE('',#103101);
#8497=PLANE('',#103102);
#8498=PLANE('',#103103);
#8499=PLANE('',#103104);
#8500=PLANE('',#103105);
#8501=PLANE('',#103106);
#8502=PLANE('',#103121);
#8503=PLANE('',#103168);
#8504=PLANE('',#103171);
#8505=PLANE('',#103172);
#8506=PLANE('',#103173);
#8507=PLANE('',#103186);
#8508=PLANE('',#103194);
#8509=PLANE('',#103201);
#8510=PLANE('',#103209);
#8511=PLANE('',#103233);
#8512=PLANE('',#103241);
#8513=PLANE('',#103253);
#8514=PLANE('',#103261);
#8515=PLANE('',#103304);
#8516=PLANE('',#103310);
#8517=PLANE('',#103311);
#8518=PLANE('',#103333);
#8519=PLANE('',#103334);
#8520=PLANE('',#103335);
#8521=PLANE('',#103336);
#8522=PLANE('',#103337);
#8523=PLANE('',#103338);
#8524=PLANE('',#103370);
#8525=PLANE('',#103395);
#8526=PLANE('',#103486);
#8527=PLANE('',#103533);
#8528=PLANE('',#103534);
#8529=PLANE('',#103535);
#8530=PLANE('',#103542);
#8531=PLANE('',#103543);
#8532=PLANE('',#103544);
#8533=PLANE('',#103545);
#8534=PLANE('',#103546);
#8535=PLANE('',#103602);
#8536=PLANE('',#103650);
#8537=PLANE('',#103825);
#8538=PLANE('',#103920);
#8539=PLANE('',#103921);
#8540=PLANE('',#103922);
#8541=PLANE('',#103942);
#8542=PLANE('',#103943);
#8543=PLANE('',#103953);
#8544=PLANE('',#103957);
#8545=PLANE('',#103967);
#8546=PLANE('',#103968);
#8547=PLANE('',#103972);
#8548=PLANE('',#103973);
#8549=PLANE('',#104125);
#8550=PLANE('',#104126);
#8551=PLANE('',#104127);
#8552=PLANE('',#104128);
#8553=PLANE('',#104158);
#8554=PLANE('',#104159);
#8555=PLANE('',#104173);
#8556=PLANE('',#104174);
#8557=PLANE('',#104236);
#8558=PLANE('',#104237);
#8559=PLANE('',#104238);
#8560=PLANE('',#104239);
#8561=PLANE('',#104240);
#8562=PLANE('',#104241);
#8563=PLANE('',#104242);
#8564=PLANE('',#104243);
#8565=PLANE('',#104244);
#8566=PLANE('',#104245);
#8567=PLANE('',#104246);
#8568=PLANE('',#104247);
#8569=PLANE('',#104273);
#8570=PLANE('',#104280);
#8571=PLANE('',#104281);
#8572=PLANE('',#104282);
#8573=PLANE('',#104283);
#8574=PLANE('',#104284);
#8575=PLANE('',#104285);
#8576=PLANE('',#104286);
#8577=PLANE('',#104338);
#8578=PLANE('',#104339);
#8579=PLANE('',#104340);
#8580=PLANE('',#104341);
#8581=PLANE('',#104342);
#8582=PLANE('',#104343);
#8583=PLANE('',#104344);
#8584=PLANE('',#104345);
#8585=PLANE('',#104346);
#8586=PLANE('',#104357);
#8587=PLANE('',#104438);
#8588=PLANE('',#104439);
#8589=PLANE('',#104440);
#8590=PLANE('',#104447);
#8591=PLANE('',#104448);
#8592=PLANE('',#104449);
#8593=PLANE('',#104450);
#8594=PLANE('',#104451);
#8595=PLANE('',#104452);
#8596=PLANE('',#104453);
#8597=PLANE('',#104454);
#8598=PLANE('',#104455);
#8599=PLANE('',#104456);
#8600=PLANE('',#104457);
#8601=PLANE('',#104476);
#8602=PLANE('',#104529);
#8603=PLANE('',#104530);
#8604=PLANE('',#104531);
#8605=PLANE('',#104532);
#8606=PLANE('',#104533);
#8607=PLANE('',#104534);
#8608=PLANE('',#104535);
#8609=PLANE('',#104536);
#8610=PLANE('',#104537);
#8611=PLANE('',#104538);
#8612=PLANE('',#104539);
#8613=PLANE('',#104540);
#8614=PLANE('',#104541);
#8615=PLANE('',#104542);
#8616=PLANE('',#104544);
#8617=PLANE('',#104545);
#8618=PLANE('',#104546);
#8619=PLANE('',#104547);
#8620=PLANE('',#104548);
#8621=PLANE('',#104549);
#8622=PLANE('',#104550);
#8623=PLANE('',#104551);
#8624=PLANE('',#104552);
#8625=PLANE('',#104553);
#8626=PLANE('',#104555);
#8627=PLANE('',#104556);
#8628=PLANE('',#104557);
#8629=PLANE('',#104558);
#8630=PLANE('',#104559);
#8631=PLANE('',#104560);
#8632=PLANE('',#104587);
#8633=PLANE('',#104588);
#8634=PLANE('',#104589);
#8635=PLANE('',#104590);
#8636=PLANE('',#104591);
#8637=PLANE('',#104592);
#8638=PLANE('',#104593);
#8639=PLANE('',#104594);
#8640=PLANE('',#104595);
#8641=PLANE('',#104596);
#8642=PLANE('',#104604);
#8643=PLANE('',#104605);
#8644=PLANE('',#104606);
#8645=PLANE('',#104607);
#8646=PLANE('',#104608);
#8647=PLANE('',#104609);
#8648=PLANE('',#104610);
#8649=PLANE('',#104611);
#8650=PLANE('',#104612);
#8651=PLANE('',#104615);
#8652=PLANE('',#104616);
#8653=PLANE('',#104619);
#8654=PLANE('',#104622);
#8655=PLANE('',#104625);
#8656=PLANE('',#104627);
#8657=PLANE('',#104630);
#8658=PLANE('',#104632);
#8659=PLANE('',#104633);
#8660=PLANE('',#104682);
#8661=PLANE('',#104687);
#8662=PLANE('',#104688);
#8663=PLANE('',#104689);
#8664=PLANE('',#104690);
#8665=PLANE('',#104691);
#8666=PLANE('',#104692);
#8667=PLANE('',#104693);
#8668=PLANE('',#104694);
#8669=PLANE('',#104695);
#8670=PLANE('',#104696);
#8671=PLANE('',#104697);
#8672=PLANE('',#104698);
#8673=PLANE('',#104711);
#8674=PLANE('',#104712);
#8675=PLANE('',#104713);
#8676=PLANE('',#104714);
#8677=PLANE('',#104715);
#8678=PLANE('',#104716);
#8679=PLANE('',#104717);
#8680=PLANE('',#104769);
#8681=PLANE('',#104770);
#8682=PLANE('',#104771);
#8683=PLANE('',#104772);
#8684=PLANE('',#104773);
#8685=PLANE('',#104774);
#8686=PLANE('',#104775);
#8687=PLANE('',#104777);
#8688=FACE_OUTER_BOUND('',#14427,.T.);
#8689=FACE_OUTER_BOUND('',#14428,.T.);
#8690=FACE_OUTER_BOUND('',#14429,.T.);
#8691=FACE_OUTER_BOUND('',#14430,.T.);
#8692=FACE_OUTER_BOUND('',#14431,.T.);
#8693=FACE_OUTER_BOUND('',#14432,.T.);
#8694=FACE_OUTER_BOUND('',#14433,.T.);
#8695=FACE_OUTER_BOUND('',#14434,.T.);
#8696=FACE_OUTER_BOUND('',#14435,.T.);
#8697=FACE_OUTER_BOUND('',#14436,.T.);
#8698=FACE_OUTER_BOUND('',#14437,.T.);
#8699=FACE_OUTER_BOUND('',#14438,.T.);
#8700=FACE_OUTER_BOUND('',#14439,.T.);
#8701=FACE_OUTER_BOUND('',#14440,.T.);
#8702=FACE_OUTER_BOUND('',#14441,.T.);
#8703=FACE_OUTER_BOUND('',#14454,.T.);
#8704=FACE_OUTER_BOUND('',#14455,.T.);
#8705=FACE_OUTER_BOUND('',#14456,.T.);
#8706=FACE_OUTER_BOUND('',#14457,.T.);
#8707=FACE_OUTER_BOUND('',#14470,.T.);
#8708=FACE_OUTER_BOUND('',#14471,.T.);
#8709=FACE_OUTER_BOUND('',#14472,.T.);
#8710=FACE_OUTER_BOUND('',#14473,.T.);
#8711=FACE_OUTER_BOUND('',#14474,.T.);
#8712=FACE_OUTER_BOUND('',#14475,.T.);
#8713=FACE_OUTER_BOUND('',#14476,.T.);
#8714=FACE_OUTER_BOUND('',#14477,.T.);
#8715=FACE_OUTER_BOUND('',#14478,.T.);
#8716=FACE_OUTER_BOUND('',#14479,.T.);
#8717=FACE_OUTER_BOUND('',#14480,.T.);
#8718=FACE_OUTER_BOUND('',#14481,.T.);
#8719=FACE_OUTER_BOUND('',#14482,.T.);
#8720=FACE_OUTER_BOUND('',#14483,.T.);
#8721=FACE_OUTER_BOUND('',#14484,.T.);
#8722=FACE_OUTER_BOUND('',#14485,.T.);
#8723=FACE_OUTER_BOUND('',#14486,.T.);
#8724=FACE_OUTER_BOUND('',#14487,.T.);
#8725=FACE_OUTER_BOUND('',#14488,.T.);
#8726=FACE_OUTER_BOUND('',#14489,.T.);
#8727=FACE_OUTER_BOUND('',#14490,.T.);
#8728=FACE_OUTER_BOUND('',#14491,.T.);
#8729=FACE_OUTER_BOUND('',#14504,.T.);
#8730=FACE_OUTER_BOUND('',#14505,.T.);
#8731=FACE_OUTER_BOUND('',#14506,.T.);
#8732=FACE_OUTER_BOUND('',#14507,.T.);
#8733=FACE_OUTER_BOUND('',#14520,.T.);
#8734=FACE_OUTER_BOUND('',#14521,.T.);
#8735=FACE_OUTER_BOUND('',#14522,.T.);
#8736=FACE_OUTER_BOUND('',#14523,.T.);
#8737=FACE_OUTER_BOUND('',#14524,.T.);
#8738=FACE_OUTER_BOUND('',#14525,.T.);
#8739=FACE_OUTER_BOUND('',#14526,.T.);
#8740=FACE_OUTER_BOUND('',#14527,.T.);
#8741=FACE_OUTER_BOUND('',#14528,.T.);
#8742=FACE_OUTER_BOUND('',#14529,.T.);
#8743=FACE_OUTER_BOUND('',#14530,.T.);
#8744=FACE_OUTER_BOUND('',#14532,.T.);
#8745=FACE_OUTER_BOUND('',#14533,.T.);
#8746=FACE_OUTER_BOUND('',#14534,.T.);
#8747=FACE_OUTER_BOUND('',#14535,.T.);
#8748=FACE_OUTER_BOUND('',#14536,.T.);
#8749=FACE_OUTER_BOUND('',#14537,.T.);
#8750=FACE_OUTER_BOUND('',#14539,.T.);
#8751=FACE_OUTER_BOUND('',#14540,.T.);
#8752=FACE_OUTER_BOUND('',#14541,.T.);
#8753=FACE_OUTER_BOUND('',#14542,.T.);
#8754=FACE_OUTER_BOUND('',#14543,.T.);
#8755=FACE_OUTER_BOUND('',#14544,.T.);
#8756=FACE_OUTER_BOUND('',#14545,.T.);
#8757=FACE_OUTER_BOUND('',#14546,.T.);
#8758=FACE_OUTER_BOUND('',#14547,.T.);
#8759=FACE_OUTER_BOUND('',#14548,.T.);
#8760=FACE_OUTER_BOUND('',#14549,.T.);
#8761=FACE_OUTER_BOUND('',#14550,.T.);
#8762=FACE_OUTER_BOUND('',#14551,.T.);
#8763=FACE_OUTER_BOUND('',#14552,.T.);
#8764=FACE_OUTER_BOUND('',#14553,.T.);
#8765=FACE_OUTER_BOUND('',#14554,.T.);
#8766=FACE_OUTER_BOUND('',#14555,.T.);
#8767=FACE_OUTER_BOUND('',#14556,.T.);
#8768=FACE_OUTER_BOUND('',#14557,.T.);
#8769=FACE_OUTER_BOUND('',#14558,.T.);
#8770=FACE_OUTER_BOUND('',#14559,.T.);
#8771=FACE_OUTER_BOUND('',#14560,.T.);
#8772=FACE_OUTER_BOUND('',#14561,.T.);
#8773=FACE_OUTER_BOUND('',#14562,.T.);
#8774=FACE_OUTER_BOUND('',#14563,.T.);
#8775=FACE_OUTER_BOUND('',#14564,.T.);
#8776=FACE_OUTER_BOUND('',#14565,.T.);
#8777=FACE_OUTER_BOUND('',#14566,.T.);
#8778=FACE_OUTER_BOUND('',#14567,.T.);
#8779=FACE_OUTER_BOUND('',#14568,.T.);
#8780=FACE_OUTER_BOUND('',#14569,.T.);
#8781=FACE_OUTER_BOUND('',#14570,.T.);
#8782=FACE_OUTER_BOUND('',#14571,.T.);
#8783=FACE_OUTER_BOUND('',#14572,.T.);
#8784=FACE_OUTER_BOUND('',#14573,.T.);
#8785=FACE_OUTER_BOUND('',#14574,.T.);
#8786=FACE_OUTER_BOUND('',#14575,.T.);
#8787=FACE_OUTER_BOUND('',#14576,.T.);
#8788=FACE_OUTER_BOUND('',#14577,.T.);
#8789=FACE_OUTER_BOUND('',#14578,.T.);
#8790=FACE_OUTER_BOUND('',#14579,.T.);
#8791=FACE_OUTER_BOUND('',#14580,.T.);
#8792=FACE_OUTER_BOUND('',#14581,.T.);
#8793=FACE_OUTER_BOUND('',#14582,.T.);
#8794=FACE_OUTER_BOUND('',#14583,.T.);
#8795=FACE_OUTER_BOUND('',#14584,.T.);
#8796=FACE_OUTER_BOUND('',#14585,.T.);
#8797=FACE_OUTER_BOUND('',#14586,.T.);
#8798=FACE_OUTER_BOUND('',#14587,.T.);
#8799=FACE_OUTER_BOUND('',#14588,.T.);
#8800=FACE_OUTER_BOUND('',#14589,.T.);
#8801=FACE_OUTER_BOUND('',#14590,.T.);
#8802=FACE_OUTER_BOUND('',#14591,.T.);
#8803=FACE_OUTER_BOUND('',#14592,.T.);
#8804=FACE_OUTER_BOUND('',#14593,.T.);
#8805=FACE_OUTER_BOUND('',#14594,.T.);
#8806=FACE_OUTER_BOUND('',#14595,.T.);
#8807=FACE_OUTER_BOUND('',#14596,.T.);
#8808=FACE_OUTER_BOUND('',#14597,.T.);
#8809=FACE_OUTER_BOUND('',#14598,.T.);
#8810=FACE_OUTER_BOUND('',#14599,.T.);
#8811=FACE_OUTER_BOUND('',#14600,.T.);
#8812=FACE_OUTER_BOUND('',#14601,.T.);
#8813=FACE_OUTER_BOUND('',#14602,.T.);
#8814=FACE_OUTER_BOUND('',#14603,.T.);
#8815=FACE_OUTER_BOUND('',#14604,.T.);
#8816=FACE_OUTER_BOUND('',#14605,.T.);
#8817=FACE_OUTER_BOUND('',#14606,.T.);
#8818=FACE_OUTER_BOUND('',#14607,.T.);
#8819=FACE_OUTER_BOUND('',#14608,.T.);
#8820=FACE_OUTER_BOUND('',#14609,.T.);
#8821=FACE_OUTER_BOUND('',#14610,.T.);
#8822=FACE_OUTER_BOUND('',#14611,.T.);
#8823=FACE_OUTER_BOUND('',#14612,.T.);
#8824=FACE_OUTER_BOUND('',#14613,.T.);
#8825=FACE_OUTER_BOUND('',#14614,.T.);
#8826=FACE_OUTER_BOUND('',#14615,.T.);
#8827=FACE_OUTER_BOUND('',#14616,.T.);
#8828=FACE_OUTER_BOUND('',#14617,.T.);
#8829=FACE_OUTER_BOUND('',#14618,.T.);
#8830=FACE_OUTER_BOUND('',#14619,.T.);
#8831=FACE_OUTER_BOUND('',#14620,.T.);
#8832=FACE_OUTER_BOUND('',#14621,.T.);
#8833=FACE_OUTER_BOUND('',#14622,.T.);
#8834=FACE_OUTER_BOUND('',#14623,.T.);
#8835=FACE_OUTER_BOUND('',#14624,.T.);
#8836=FACE_OUTER_BOUND('',#14625,.T.);
#8837=FACE_OUTER_BOUND('',#14626,.T.);
#8838=FACE_OUTER_BOUND('',#14627,.T.);
#8839=FACE_OUTER_BOUND('',#14628,.T.);
#8840=FACE_OUTER_BOUND('',#14629,.T.);
#8841=FACE_OUTER_BOUND('',#14630,.T.);
#8842=FACE_OUTER_BOUND('',#14631,.T.);
#8843=FACE_OUTER_BOUND('',#14632,.T.);
#8844=FACE_OUTER_BOUND('',#14633,.T.);
#8845=FACE_OUTER_BOUND('',#14634,.T.);
#8846=FACE_OUTER_BOUND('',#14635,.T.);
#8847=FACE_OUTER_BOUND('',#14636,.T.);
#8848=FACE_OUTER_BOUND('',#14637,.T.);
#8849=FACE_OUTER_BOUND('',#14638,.T.);
#8850=FACE_OUTER_BOUND('',#14639,.T.);
#8851=FACE_OUTER_BOUND('',#14640,.T.);
#8852=FACE_OUTER_BOUND('',#14641,.T.);
#8853=FACE_OUTER_BOUND('',#14642,.T.);
#8854=FACE_OUTER_BOUND('',#14643,.T.);
#8855=FACE_OUTER_BOUND('',#14644,.T.);
#8856=FACE_OUTER_BOUND('',#14645,.T.);
#8857=FACE_OUTER_BOUND('',#14646,.T.);
#8858=FACE_OUTER_BOUND('',#14647,.T.);
#8859=FACE_OUTER_BOUND('',#14648,.T.);
#8860=FACE_OUTER_BOUND('',#14649,.T.);
#8861=FACE_OUTER_BOUND('',#14650,.T.);
#8862=FACE_OUTER_BOUND('',#14651,.T.);
#8863=FACE_OUTER_BOUND('',#14652,.T.);
#8864=FACE_OUTER_BOUND('',#14653,.T.);
#8865=FACE_OUTER_BOUND('',#14654,.T.);
#8866=FACE_OUTER_BOUND('',#14655,.T.);
#8867=FACE_OUTER_BOUND('',#14656,.T.);
#8868=FACE_OUTER_BOUND('',#14657,.T.);
#8869=FACE_OUTER_BOUND('',#14658,.T.);
#8870=FACE_OUTER_BOUND('',#14659,.T.);
#8871=FACE_OUTER_BOUND('',#14660,.T.);
#8872=FACE_OUTER_BOUND('',#14661,.T.);
#8873=FACE_OUTER_BOUND('',#14662,.T.);
#8874=FACE_OUTER_BOUND('',#14663,.T.);
#8875=FACE_OUTER_BOUND('',#14664,.T.);
#8876=FACE_OUTER_BOUND('',#14665,.T.);
#8877=FACE_OUTER_BOUND('',#14666,.T.);
#8878=FACE_OUTER_BOUND('',#14667,.T.);
#8879=FACE_OUTER_BOUND('',#14668,.T.);
#8880=FACE_OUTER_BOUND('',#14669,.T.);
#8881=FACE_OUTER_BOUND('',#14670,.T.);
#8882=FACE_OUTER_BOUND('',#14671,.T.);
#8883=FACE_OUTER_BOUND('',#14672,.T.);
#8884=FACE_OUTER_BOUND('',#14673,.T.);
#8885=FACE_OUTER_BOUND('',#14674,.T.);
#8886=FACE_OUTER_BOUND('',#14675,.T.);
#8887=FACE_OUTER_BOUND('',#14676,.T.);
#8888=FACE_OUTER_BOUND('',#14677,.T.);
#8889=FACE_OUTER_BOUND('',#14678,.T.);
#8890=FACE_OUTER_BOUND('',#14679,.T.);
#8891=FACE_OUTER_BOUND('',#14680,.T.);
#8892=FACE_OUTER_BOUND('',#14681,.T.);
#8893=FACE_OUTER_BOUND('',#14682,.T.);
#8894=FACE_OUTER_BOUND('',#14683,.T.);
#8895=FACE_OUTER_BOUND('',#14684,.T.);
#8896=FACE_OUTER_BOUND('',#14685,.T.);
#8897=FACE_OUTER_BOUND('',#14686,.T.);
#8898=FACE_OUTER_BOUND('',#14687,.T.);
#8899=FACE_OUTER_BOUND('',#14688,.T.);
#8900=FACE_OUTER_BOUND('',#14689,.T.);
#8901=FACE_OUTER_BOUND('',#14690,.T.);
#8902=FACE_OUTER_BOUND('',#14691,.T.);
#8903=FACE_OUTER_BOUND('',#14692,.T.);
#8904=FACE_OUTER_BOUND('',#14693,.T.);
#8905=FACE_OUTER_BOUND('',#14694,.T.);
#8906=FACE_OUTER_BOUND('',#14695,.T.);
#8907=FACE_OUTER_BOUND('',#14696,.T.);
#8908=FACE_OUTER_BOUND('',#14697,.T.);
#8909=FACE_OUTER_BOUND('',#14698,.T.);
#8910=FACE_OUTER_BOUND('',#14699,.T.);
#8911=FACE_OUTER_BOUND('',#14700,.T.);
#8912=FACE_OUTER_BOUND('',#14701,.T.);
#8913=FACE_OUTER_BOUND('',#14702,.T.);
#8914=FACE_OUTER_BOUND('',#14703,.T.);
#8915=FACE_OUTER_BOUND('',#14704,.T.);
#8916=FACE_OUTER_BOUND('',#14705,.T.);
#8917=FACE_OUTER_BOUND('',#14706,.T.);
#8918=FACE_OUTER_BOUND('',#14707,.T.);
#8919=FACE_OUTER_BOUND('',#14708,.T.);
#8920=FACE_OUTER_BOUND('',#14709,.T.);
#8921=FACE_OUTER_BOUND('',#14710,.T.);
#8922=FACE_OUTER_BOUND('',#14711,.T.);
#8923=FACE_OUTER_BOUND('',#14712,.T.);
#8924=FACE_OUTER_BOUND('',#14713,.T.);
#8925=FACE_OUTER_BOUND('',#14714,.T.);
#8926=FACE_OUTER_BOUND('',#14715,.T.);
#8927=FACE_OUTER_BOUND('',#14716,.T.);
#8928=FACE_OUTER_BOUND('',#14717,.T.);
#8929=FACE_OUTER_BOUND('',#14718,.T.);
#8930=FACE_OUTER_BOUND('',#14719,.T.);
#8931=FACE_OUTER_BOUND('',#14720,.T.);
#8932=FACE_OUTER_BOUND('',#14721,.T.);
#8933=FACE_OUTER_BOUND('',#14722,.T.);
#8934=FACE_OUTER_BOUND('',#14723,.T.);
#8935=FACE_OUTER_BOUND('',#14724,.T.);
#8936=FACE_OUTER_BOUND('',#14725,.T.);
#8937=FACE_OUTER_BOUND('',#14726,.T.);
#8938=FACE_OUTER_BOUND('',#14727,.T.);
#8939=FACE_OUTER_BOUND('',#14728,.T.);
#8940=FACE_OUTER_BOUND('',#14729,.T.);
#8941=FACE_OUTER_BOUND('',#14730,.T.);
#8942=FACE_OUTER_BOUND('',#14731,.T.);
#8943=FACE_OUTER_BOUND('',#14732,.T.);
#8944=FACE_OUTER_BOUND('',#14733,.T.);
#8945=FACE_OUTER_BOUND('',#14734,.T.);
#8946=FACE_OUTER_BOUND('',#14735,.T.);
#8947=FACE_OUTER_BOUND('',#14736,.T.);
#8948=FACE_OUTER_BOUND('',#14737,.T.);
#8949=FACE_OUTER_BOUND('',#14738,.T.);
#8950=FACE_OUTER_BOUND('',#14739,.T.);
#8951=FACE_OUTER_BOUND('',#14740,.T.);
#8952=FACE_OUTER_BOUND('',#14741,.T.);
#8953=FACE_OUTER_BOUND('',#14742,.T.);
#8954=FACE_OUTER_BOUND('',#14743,.T.);
#8955=FACE_OUTER_BOUND('',#14744,.T.);
#8956=FACE_OUTER_BOUND('',#14745,.T.);
#8957=FACE_OUTER_BOUND('',#14746,.T.);
#8958=FACE_OUTER_BOUND('',#14747,.T.);
#8959=FACE_OUTER_BOUND('',#14748,.T.);
#8960=FACE_OUTER_BOUND('',#14749,.T.);
#8961=FACE_OUTER_BOUND('',#14750,.T.);
#8962=FACE_OUTER_BOUND('',#14751,.T.);
#8963=FACE_OUTER_BOUND('',#14752,.T.);
#8964=FACE_OUTER_BOUND('',#14753,.T.);
#8965=FACE_OUTER_BOUND('',#14754,.T.);
#8966=FACE_OUTER_BOUND('',#14755,.T.);
#8967=FACE_OUTER_BOUND('',#14756,.T.);
#8968=FACE_OUTER_BOUND('',#14757,.T.);
#8969=FACE_OUTER_BOUND('',#14758,.T.);
#8970=FACE_OUTER_BOUND('',#14759,.T.);
#8971=FACE_OUTER_BOUND('',#14760,.T.);
#8972=FACE_OUTER_BOUND('',#14761,.T.);
#8973=FACE_OUTER_BOUND('',#14762,.T.);
#8974=FACE_OUTER_BOUND('',#14763,.T.);
#8975=FACE_OUTER_BOUND('',#14764,.T.);
#8976=FACE_OUTER_BOUND('',#14765,.T.);
#8977=FACE_OUTER_BOUND('',#14766,.T.);
#8978=FACE_OUTER_BOUND('',#14767,.T.);
#8979=FACE_OUTER_BOUND('',#14768,.T.);
#8980=FACE_OUTER_BOUND('',#14769,.T.);
#8981=FACE_OUTER_BOUND('',#14770,.T.);
#8982=FACE_OUTER_BOUND('',#14771,.T.);
#8983=FACE_OUTER_BOUND('',#14772,.T.);
#8984=FACE_OUTER_BOUND('',#14773,.T.);
#8985=FACE_OUTER_BOUND('',#14774,.T.);
#8986=FACE_OUTER_BOUND('',#14775,.T.);
#8987=FACE_OUTER_BOUND('',#14776,.T.);
#8988=FACE_OUTER_BOUND('',#14777,.T.);
#8989=FACE_OUTER_BOUND('',#14778,.T.);
#8990=FACE_OUTER_BOUND('',#14779,.T.);
#8991=FACE_OUTER_BOUND('',#14780,.T.);
#8992=FACE_OUTER_BOUND('',#14781,.T.);
#8993=FACE_OUTER_BOUND('',#14782,.T.);
#8994=FACE_OUTER_BOUND('',#14783,.T.);
#8995=FACE_OUTER_BOUND('',#14784,.T.);
#8996=FACE_OUTER_BOUND('',#14785,.T.);
#8997=FACE_OUTER_BOUND('',#14786,.T.);
#8998=FACE_OUTER_BOUND('',#14787,.T.);
#8999=FACE_OUTER_BOUND('',#14788,.T.);
#9000=FACE_OUTER_BOUND('',#14789,.T.);
#9001=FACE_OUTER_BOUND('',#14790,.T.);
#9002=FACE_OUTER_BOUND('',#14791,.T.);
#9003=FACE_OUTER_BOUND('',#14792,.T.);
#9004=FACE_OUTER_BOUND('',#14793,.T.);
#9005=FACE_OUTER_BOUND('',#14794,.T.);
#9006=FACE_OUTER_BOUND('',#14795,.T.);
#9007=FACE_OUTER_BOUND('',#14796,.T.);
#9008=FACE_OUTER_BOUND('',#14797,.T.);
#9009=FACE_OUTER_BOUND('',#14798,.T.);
#9010=FACE_OUTER_BOUND('',#14799,.T.);
#9011=FACE_OUTER_BOUND('',#14800,.T.);
#9012=FACE_OUTER_BOUND('',#14801,.T.);
#9013=FACE_OUTER_BOUND('',#14802,.T.);
#9014=FACE_OUTER_BOUND('',#14803,.T.);
#9015=FACE_OUTER_BOUND('',#14804,.T.);
#9016=FACE_OUTER_BOUND('',#14805,.T.);
#9017=FACE_OUTER_BOUND('',#14806,.T.);
#9018=FACE_OUTER_BOUND('',#14807,.T.);
#9019=FACE_OUTER_BOUND('',#14808,.T.);
#9020=FACE_OUTER_BOUND('',#14809,.T.);
#9021=FACE_OUTER_BOUND('',#14810,.T.);
#9022=FACE_OUTER_BOUND('',#14811,.T.);
#9023=FACE_OUTER_BOUND('',#14812,.T.);
#9024=FACE_OUTER_BOUND('',#14813,.T.);
#9025=FACE_OUTER_BOUND('',#14814,.T.);
#9026=FACE_OUTER_BOUND('',#14815,.T.);
#9027=FACE_OUTER_BOUND('',#14816,.T.);
#9028=FACE_OUTER_BOUND('',#14817,.T.);
#9029=FACE_OUTER_BOUND('',#14818,.T.);
#9030=FACE_OUTER_BOUND('',#14819,.T.);
#9031=FACE_OUTER_BOUND('',#14820,.T.);
#9032=FACE_OUTER_BOUND('',#14821,.T.);
#9033=FACE_OUTER_BOUND('',#14822,.T.);
#9034=FACE_OUTER_BOUND('',#14823,.T.);
#9035=FACE_OUTER_BOUND('',#14824,.T.);
#9036=FACE_OUTER_BOUND('',#14825,.T.);
#9037=FACE_OUTER_BOUND('',#14826,.T.);
#9038=FACE_OUTER_BOUND('',#14827,.T.);
#9039=FACE_OUTER_BOUND('',#14828,.T.);
#9040=FACE_OUTER_BOUND('',#14829,.T.);
#9041=FACE_OUTER_BOUND('',#14830,.T.);
#9042=FACE_OUTER_BOUND('',#14831,.T.);
#9043=FACE_OUTER_BOUND('',#14832,.T.);
#9044=FACE_OUTER_BOUND('',#14833,.T.);
#9045=FACE_OUTER_BOUND('',#14834,.T.);
#9046=FACE_OUTER_BOUND('',#14835,.T.);
#9047=FACE_OUTER_BOUND('',#14836,.T.);
#9048=FACE_OUTER_BOUND('',#14837,.T.);
#9049=FACE_OUTER_BOUND('',#14838,.T.);
#9050=FACE_OUTER_BOUND('',#14839,.T.);
#9051=FACE_OUTER_BOUND('',#14840,.T.);
#9052=FACE_OUTER_BOUND('',#14841,.T.);
#9053=FACE_OUTER_BOUND('',#14842,.T.);
#9054=FACE_OUTER_BOUND('',#14843,.T.);
#9055=FACE_OUTER_BOUND('',#14844,.T.);
#9056=FACE_OUTER_BOUND('',#14845,.T.);
#9057=FACE_OUTER_BOUND('',#14846,.T.);
#9058=FACE_OUTER_BOUND('',#14847,.T.);
#9059=FACE_OUTER_BOUND('',#14848,.T.);
#9060=FACE_OUTER_BOUND('',#14849,.T.);
#9061=FACE_OUTER_BOUND('',#14850,.T.);
#9062=FACE_OUTER_BOUND('',#14851,.T.);
#9063=FACE_OUTER_BOUND('',#14852,.T.);
#9064=FACE_OUTER_BOUND('',#14853,.T.);
#9065=FACE_OUTER_BOUND('',#14854,.T.);
#9066=FACE_OUTER_BOUND('',#14855,.T.);
#9067=FACE_OUTER_BOUND('',#14856,.T.);
#9068=FACE_OUTER_BOUND('',#14857,.T.);
#9069=FACE_OUTER_BOUND('',#14858,.T.);
#9070=FACE_OUTER_BOUND('',#14859,.T.);
#9071=FACE_OUTER_BOUND('',#14860,.T.);
#9072=FACE_OUTER_BOUND('',#14861,.T.);
#9073=FACE_OUTER_BOUND('',#14862,.T.);
#9074=FACE_OUTER_BOUND('',#14863,.T.);
#9075=FACE_OUTER_BOUND('',#14864,.T.);
#9076=FACE_OUTER_BOUND('',#14865,.T.);
#9077=FACE_OUTER_BOUND('',#14866,.T.);
#9078=FACE_OUTER_BOUND('',#14867,.T.);
#9079=FACE_OUTER_BOUND('',#14868,.T.);
#9080=FACE_OUTER_BOUND('',#14869,.T.);
#9081=FACE_OUTER_BOUND('',#14870,.T.);
#9082=FACE_OUTER_BOUND('',#14871,.T.);
#9083=FACE_OUTER_BOUND('',#14872,.T.);
#9084=FACE_OUTER_BOUND('',#14873,.T.);
#9085=FACE_OUTER_BOUND('',#14874,.T.);
#9086=FACE_OUTER_BOUND('',#14875,.T.);
#9087=FACE_OUTER_BOUND('',#14876,.T.);
#9088=FACE_OUTER_BOUND('',#14877,.T.);
#9089=FACE_OUTER_BOUND('',#14878,.T.);
#9090=FACE_OUTER_BOUND('',#14879,.T.);
#9091=FACE_OUTER_BOUND('',#14880,.T.);
#9092=FACE_OUTER_BOUND('',#14881,.T.);
#9093=FACE_OUTER_BOUND('',#14882,.T.);
#9094=FACE_OUTER_BOUND('',#14883,.T.);
#9095=FACE_OUTER_BOUND('',#14884,.T.);
#9096=FACE_OUTER_BOUND('',#14885,.T.);
#9097=FACE_OUTER_BOUND('',#14886,.T.);
#9098=FACE_OUTER_BOUND('',#14887,.T.);
#9099=FACE_OUTER_BOUND('',#14888,.T.);
#9100=FACE_OUTER_BOUND('',#14889,.T.);
#9101=FACE_OUTER_BOUND('',#14890,.T.);
#9102=FACE_OUTER_BOUND('',#14891,.T.);
#9103=FACE_OUTER_BOUND('',#14892,.T.);
#9104=FACE_OUTER_BOUND('',#14893,.T.);
#9105=FACE_OUTER_BOUND('',#14894,.T.);
#9106=FACE_OUTER_BOUND('',#14895,.T.);
#9107=FACE_OUTER_BOUND('',#14896,.T.);
#9108=FACE_OUTER_BOUND('',#14897,.T.);
#9109=FACE_OUTER_BOUND('',#14898,.T.);
#9110=FACE_OUTER_BOUND('',#14899,.T.);
#9111=FACE_OUTER_BOUND('',#14900,.T.);
#9112=FACE_OUTER_BOUND('',#14901,.T.);
#9113=FACE_OUTER_BOUND('',#14902,.T.);
#9114=FACE_OUTER_BOUND('',#14903,.T.);
#9115=FACE_OUTER_BOUND('',#14904,.T.);
#9116=FACE_OUTER_BOUND('',#14905,.T.);
#9117=FACE_OUTER_BOUND('',#14906,.T.);
#9118=FACE_OUTER_BOUND('',#14907,.T.);
#9119=FACE_OUTER_BOUND('',#14908,.T.);
#9120=FACE_OUTER_BOUND('',#14909,.T.);
#9121=FACE_OUTER_BOUND('',#14910,.T.);
#9122=FACE_OUTER_BOUND('',#14911,.T.);
#9123=FACE_OUTER_BOUND('',#14912,.T.);
#9124=FACE_OUTER_BOUND('',#14913,.T.);
#9125=FACE_OUTER_BOUND('',#14914,.T.);
#9126=FACE_OUTER_BOUND('',#14915,.T.);
#9127=FACE_OUTER_BOUND('',#14916,.T.);
#9128=FACE_OUTER_BOUND('',#14917,.T.);
#9129=FACE_OUTER_BOUND('',#14918,.T.);
#9130=FACE_OUTER_BOUND('',#14919,.T.);
#9131=FACE_OUTER_BOUND('',#14920,.T.);
#9132=FACE_OUTER_BOUND('',#14921,.T.);
#9133=FACE_OUTER_BOUND('',#14922,.T.);
#9134=FACE_OUTER_BOUND('',#14923,.T.);
#9135=FACE_OUTER_BOUND('',#14924,.T.);
#9136=FACE_OUTER_BOUND('',#14925,.T.);
#9137=FACE_OUTER_BOUND('',#14926,.T.);
#9138=FACE_OUTER_BOUND('',#14927,.T.);
#9139=FACE_OUTER_BOUND('',#14928,.T.);
#9140=FACE_OUTER_BOUND('',#14929,.T.);
#9141=FACE_OUTER_BOUND('',#14930,.T.);
#9142=FACE_OUTER_BOUND('',#14931,.T.);
#9143=FACE_OUTER_BOUND('',#14932,.T.);
#9144=FACE_OUTER_BOUND('',#14933,.T.);
#9145=FACE_OUTER_BOUND('',#14934,.T.);
#9146=FACE_OUTER_BOUND('',#14935,.T.);
#9147=FACE_OUTER_BOUND('',#14936,.T.);
#9148=FACE_OUTER_BOUND('',#14937,.T.);
#9149=FACE_OUTER_BOUND('',#14938,.T.);
#9150=FACE_OUTER_BOUND('',#14939,.T.);
#9151=FACE_OUTER_BOUND('',#14940,.T.);
#9152=FACE_OUTER_BOUND('',#14941,.T.);
#9153=FACE_OUTER_BOUND('',#14942,.T.);
#9154=FACE_OUTER_BOUND('',#14943,.T.);
#9155=FACE_OUTER_BOUND('',#14944,.T.);
#9156=FACE_OUTER_BOUND('',#14945,.T.);
#9157=FACE_OUTER_BOUND('',#14946,.T.);
#9158=FACE_OUTER_BOUND('',#14947,.T.);
#9159=FACE_OUTER_BOUND('',#14948,.T.);
#9160=FACE_OUTER_BOUND('',#14949,.T.);
#9161=FACE_OUTER_BOUND('',#14950,.T.);
#9162=FACE_OUTER_BOUND('',#14951,.T.);
#9163=FACE_OUTER_BOUND('',#14952,.T.);
#9164=FACE_OUTER_BOUND('',#14953,.T.);
#9165=FACE_OUTER_BOUND('',#14954,.T.);
#9166=FACE_OUTER_BOUND('',#14955,.T.);
#9167=FACE_OUTER_BOUND('',#14956,.T.);
#9168=FACE_OUTER_BOUND('',#14958,.T.);
#9169=FACE_OUTER_BOUND('',#14959,.T.);
#9170=FACE_OUTER_BOUND('',#14960,.T.);
#9171=FACE_OUTER_BOUND('',#14961,.T.);
#9172=FACE_OUTER_BOUND('',#14962,.T.);
#9173=FACE_OUTER_BOUND('',#14963,.T.);
#9174=FACE_OUTER_BOUND('',#14964,.T.);
#9175=FACE_OUTER_BOUND('',#14965,.T.);
#9176=FACE_OUTER_BOUND('',#14966,.T.);
#9177=FACE_OUTER_BOUND('',#14968,.T.);
#9178=FACE_OUTER_BOUND('',#14969,.T.);
#9179=FACE_OUTER_BOUND('',#14970,.T.);
#9180=FACE_OUTER_BOUND('',#14971,.T.);
#9181=FACE_OUTER_BOUND('',#14972,.T.);
#9182=FACE_OUTER_BOUND('',#14973,.T.);
#9183=FACE_OUTER_BOUND('',#14974,.T.);
#9184=FACE_OUTER_BOUND('',#14975,.T.);
#9185=FACE_OUTER_BOUND('',#14976,.T.);
#9186=FACE_OUTER_BOUND('',#14977,.T.);
#9187=FACE_OUTER_BOUND('',#14978,.T.);
#9188=FACE_OUTER_BOUND('',#14979,.T.);
#9189=FACE_OUTER_BOUND('',#14980,.T.);
#9190=FACE_OUTER_BOUND('',#14981,.T.);
#9191=FACE_OUTER_BOUND('',#14982,.T.);
#9192=FACE_OUTER_BOUND('',#14983,.T.);
#9193=FACE_OUTER_BOUND('',#14984,.T.);
#9194=FACE_OUTER_BOUND('',#14985,.T.);
#9195=FACE_OUTER_BOUND('',#14986,.T.);
#9196=FACE_OUTER_BOUND('',#14987,.T.);
#9197=FACE_OUTER_BOUND('',#14988,.T.);
#9198=FACE_OUTER_BOUND('',#14989,.T.);
#9199=FACE_OUTER_BOUND('',#14990,.T.);
#9200=FACE_OUTER_BOUND('',#14991,.T.);
#9201=FACE_OUTER_BOUND('',#14992,.T.);
#9202=FACE_OUTER_BOUND('',#14993,.T.);
#9203=FACE_OUTER_BOUND('',#14994,.T.);
#9204=FACE_OUTER_BOUND('',#14995,.T.);
#9205=FACE_OUTER_BOUND('',#14996,.T.);
#9206=FACE_OUTER_BOUND('',#14997,.T.);
#9207=FACE_OUTER_BOUND('',#14998,.T.);
#9208=FACE_OUTER_BOUND('',#14999,.T.);
#9209=FACE_OUTER_BOUND('',#15000,.T.);
#9210=FACE_OUTER_BOUND('',#15001,.T.);
#9211=FACE_OUTER_BOUND('',#15002,.T.);
#9212=FACE_OUTER_BOUND('',#15003,.T.);
#9213=FACE_OUTER_BOUND('',#15004,.T.);
#9214=FACE_OUTER_BOUND('',#15005,.T.);
#9215=FACE_OUTER_BOUND('',#15006,.T.);
#9216=FACE_OUTER_BOUND('',#15007,.T.);
#9217=FACE_OUTER_BOUND('',#15008,.T.);
#9218=FACE_OUTER_BOUND('',#15009,.T.);
#9219=FACE_OUTER_BOUND('',#15010,.T.);
#9220=FACE_OUTER_BOUND('',#15011,.T.);
#9221=FACE_OUTER_BOUND('',#15012,.T.);
#9222=FACE_OUTER_BOUND('',#15013,.T.);
#9223=FACE_OUTER_BOUND('',#15014,.T.);
#9224=FACE_OUTER_BOUND('',#15015,.T.);
#9225=FACE_OUTER_BOUND('',#15016,.T.);
#9226=FACE_OUTER_BOUND('',#15017,.T.);
#9227=FACE_OUTER_BOUND('',#15018,.T.);
#9228=FACE_OUTER_BOUND('',#15019,.T.);
#9229=FACE_OUTER_BOUND('',#15020,.T.);
#9230=FACE_OUTER_BOUND('',#15021,.T.);
#9231=FACE_OUTER_BOUND('',#15022,.T.);
#9232=FACE_OUTER_BOUND('',#15023,.T.);
#9233=FACE_OUTER_BOUND('',#15024,.T.);
#9234=FACE_OUTER_BOUND('',#15025,.T.);
#9235=FACE_OUTER_BOUND('',#15026,.T.);
#9236=FACE_OUTER_BOUND('',#15027,.T.);
#9237=FACE_OUTER_BOUND('',#15028,.T.);
#9238=FACE_OUTER_BOUND('',#15029,.T.);
#9239=FACE_OUTER_BOUND('',#15030,.T.);
#9240=FACE_OUTER_BOUND('',#15031,.T.);
#9241=FACE_OUTER_BOUND('',#15032,.T.);
#9242=FACE_OUTER_BOUND('',#15033,.T.);
#9243=FACE_OUTER_BOUND('',#15034,.T.);
#9244=FACE_OUTER_BOUND('',#15035,.T.);
#9245=FACE_OUTER_BOUND('',#15036,.T.);
#9246=FACE_OUTER_BOUND('',#15037,.T.);
#9247=FACE_OUTER_BOUND('',#15038,.T.);
#9248=FACE_OUTER_BOUND('',#15039,.T.);
#9249=FACE_OUTER_BOUND('',#15040,.T.);
#9250=FACE_OUTER_BOUND('',#15041,.T.);
#9251=FACE_OUTER_BOUND('',#15042,.T.);
#9252=FACE_OUTER_BOUND('',#15043,.T.);
#9253=FACE_OUTER_BOUND('',#15044,.T.);
#9254=FACE_OUTER_BOUND('',#15045,.T.);
#9255=FACE_OUTER_BOUND('',#15046,.T.);
#9256=FACE_OUTER_BOUND('',#15047,.T.);
#9257=FACE_OUTER_BOUND('',#15048,.T.);
#9258=FACE_OUTER_BOUND('',#15049,.T.);
#9259=FACE_OUTER_BOUND('',#15050,.T.);
#9260=FACE_OUTER_BOUND('',#15051,.T.);
#9261=FACE_OUTER_BOUND('',#15052,.T.);
#9262=FACE_OUTER_BOUND('',#15053,.T.);
#9263=FACE_OUTER_BOUND('',#15054,.T.);
#9264=FACE_OUTER_BOUND('',#15055,.T.);
#9265=FACE_OUTER_BOUND('',#15056,.T.);
#9266=FACE_OUTER_BOUND('',#15057,.T.);
#9267=FACE_OUTER_BOUND('',#15058,.T.);
#9268=FACE_OUTER_BOUND('',#15059,.T.);
#9269=FACE_OUTER_BOUND('',#15060,.T.);
#9270=FACE_OUTER_BOUND('',#15061,.T.);
#9271=FACE_OUTER_BOUND('',#15062,.T.);
#9272=FACE_OUTER_BOUND('',#15063,.T.);
#9273=FACE_OUTER_BOUND('',#15064,.T.);
#9274=FACE_OUTER_BOUND('',#15065,.T.);
#9275=FACE_OUTER_BOUND('',#15066,.T.);
#9276=FACE_OUTER_BOUND('',#15067,.T.);
#9277=FACE_OUTER_BOUND('',#15068,.T.);
#9278=FACE_OUTER_BOUND('',#15069,.T.);
#9279=FACE_OUTER_BOUND('',#15070,.T.);
#9280=FACE_OUTER_BOUND('',#15071,.T.);
#9281=FACE_OUTER_BOUND('',#15072,.T.);
#9282=FACE_OUTER_BOUND('',#15073,.T.);
#9283=FACE_OUTER_BOUND('',#15074,.T.);
#9284=FACE_OUTER_BOUND('',#15075,.T.);
#9285=FACE_OUTER_BOUND('',#15076,.T.);
#9286=FACE_OUTER_BOUND('',#15077,.T.);
#9287=FACE_OUTER_BOUND('',#15078,.T.);
#9288=FACE_OUTER_BOUND('',#15079,.T.);
#9289=FACE_OUTER_BOUND('',#15080,.T.);
#9290=FACE_OUTER_BOUND('',#15081,.T.);
#9291=FACE_OUTER_BOUND('',#15082,.T.);
#9292=FACE_OUTER_BOUND('',#15083,.T.);
#9293=FACE_OUTER_BOUND('',#15084,.T.);
#9294=FACE_OUTER_BOUND('',#15085,.T.);
#9295=FACE_OUTER_BOUND('',#15086,.T.);
#9296=FACE_OUTER_BOUND('',#15087,.T.);
#9297=FACE_OUTER_BOUND('',#15088,.T.);
#9298=FACE_OUTER_BOUND('',#15089,.T.);
#9299=FACE_OUTER_BOUND('',#15090,.T.);
#9300=FACE_OUTER_BOUND('',#15091,.T.);
#9301=FACE_OUTER_BOUND('',#15092,.T.);
#9302=FACE_OUTER_BOUND('',#15093,.T.);
#9303=FACE_OUTER_BOUND('',#15094,.T.);
#9304=FACE_OUTER_BOUND('',#15095,.T.);
#9305=FACE_OUTER_BOUND('',#15096,.T.);
#9306=FACE_OUTER_BOUND('',#15097,.T.);
#9307=FACE_OUTER_BOUND('',#15098,.T.);
#9308=FACE_OUTER_BOUND('',#15099,.T.);
#9309=FACE_OUTER_BOUND('',#15100,.T.);
#9310=FACE_OUTER_BOUND('',#15101,.T.);
#9311=FACE_OUTER_BOUND('',#15102,.T.);
#9312=FACE_OUTER_BOUND('',#15103,.T.);
#9313=FACE_OUTER_BOUND('',#15104,.T.);
#9314=FACE_OUTER_BOUND('',#15105,.T.);
#9315=FACE_OUTER_BOUND('',#15106,.T.);
#9316=FACE_OUTER_BOUND('',#15107,.T.);
#9317=FACE_OUTER_BOUND('',#15108,.T.);
#9318=FACE_OUTER_BOUND('',#15109,.T.);
#9319=FACE_OUTER_BOUND('',#15110,.T.);
#9320=FACE_OUTER_BOUND('',#15111,.T.);
#9321=FACE_OUTER_BOUND('',#15112,.T.);
#9322=FACE_OUTER_BOUND('',#15113,.T.);
#9323=FACE_OUTER_BOUND('',#15114,.T.);
#9324=FACE_OUTER_BOUND('',#15115,.T.);
#9325=FACE_OUTER_BOUND('',#15116,.T.);
#9326=FACE_OUTER_BOUND('',#15117,.T.);
#9327=FACE_OUTER_BOUND('',#15118,.T.);
#9328=FACE_OUTER_BOUND('',#15119,.T.);
#9329=FACE_OUTER_BOUND('',#15120,.T.);
#9330=FACE_OUTER_BOUND('',#15121,.T.);
#9331=FACE_OUTER_BOUND('',#15122,.T.);
#9332=FACE_OUTER_BOUND('',#15123,.T.);
#9333=FACE_OUTER_BOUND('',#15124,.T.);
#9334=FACE_OUTER_BOUND('',#15125,.T.);
#9335=FACE_OUTER_BOUND('',#15126,.T.);
#9336=FACE_OUTER_BOUND('',#15127,.T.);
#9337=FACE_OUTER_BOUND('',#15128,.T.);
#9338=FACE_OUTER_BOUND('',#15129,.T.);
#9339=FACE_OUTER_BOUND('',#15130,.T.);
#9340=FACE_OUTER_BOUND('',#15131,.T.);
#9341=FACE_OUTER_BOUND('',#15132,.T.);
#9342=FACE_OUTER_BOUND('',#15133,.T.);
#9343=FACE_OUTER_BOUND('',#15134,.T.);
#9344=FACE_OUTER_BOUND('',#15135,.T.);
#9345=FACE_OUTER_BOUND('',#15136,.T.);
#9346=FACE_OUTER_BOUND('',#15137,.T.);
#9347=FACE_OUTER_BOUND('',#15138,.T.);
#9348=FACE_OUTER_BOUND('',#15139,.T.);
#9349=FACE_OUTER_BOUND('',#15140,.T.);
#9350=FACE_OUTER_BOUND('',#15141,.T.);
#9351=FACE_OUTER_BOUND('',#15142,.T.);
#9352=FACE_OUTER_BOUND('',#15143,.T.);
#9353=FACE_OUTER_BOUND('',#15144,.T.);
#9354=FACE_OUTER_BOUND('',#15145,.T.);
#9355=FACE_OUTER_BOUND('',#15146,.T.);
#9356=FACE_OUTER_BOUND('',#15147,.T.);
#9357=FACE_OUTER_BOUND('',#15148,.T.);
#9358=FACE_OUTER_BOUND('',#15149,.T.);
#9359=FACE_OUTER_BOUND('',#15150,.T.);
#9360=FACE_OUTER_BOUND('',#15151,.T.);
#9361=FACE_OUTER_BOUND('',#15152,.T.);
#9362=FACE_OUTER_BOUND('',#15153,.T.);
#9363=FACE_OUTER_BOUND('',#15154,.T.);
#9364=FACE_OUTER_BOUND('',#15155,.T.);
#9365=FACE_OUTER_BOUND('',#15156,.T.);
#9366=FACE_OUTER_BOUND('',#15157,.T.);
#9367=FACE_OUTER_BOUND('',#15158,.T.);
#9368=FACE_OUTER_BOUND('',#15159,.T.);
#9369=FACE_OUTER_BOUND('',#15160,.T.);
#9370=FACE_OUTER_BOUND('',#15161,.T.);
#9371=FACE_OUTER_BOUND('',#15162,.T.);
#9372=FACE_OUTER_BOUND('',#15163,.T.);
#9373=FACE_OUTER_BOUND('',#15164,.T.);
#9374=FACE_OUTER_BOUND('',#15165,.T.);
#9375=FACE_OUTER_BOUND('',#15166,.T.);
#9376=FACE_OUTER_BOUND('',#15167,.T.);
#9377=FACE_OUTER_BOUND('',#15168,.T.);
#9378=FACE_OUTER_BOUND('',#15169,.T.);
#9379=FACE_OUTER_BOUND('',#15170,.T.);
#9380=FACE_OUTER_BOUND('',#15171,.T.);
#9381=FACE_OUTER_BOUND('',#15172,.T.);
#9382=FACE_OUTER_BOUND('',#15173,.T.);
#9383=FACE_OUTER_BOUND('',#15174,.T.);
#9384=FACE_OUTER_BOUND('',#15175,.T.);
#9385=FACE_OUTER_BOUND('',#15176,.T.);
#9386=FACE_OUTER_BOUND('',#15177,.T.);
#9387=FACE_OUTER_BOUND('',#15178,.T.);
#9388=FACE_OUTER_BOUND('',#15179,.T.);
#9389=FACE_OUTER_BOUND('',#15180,.T.);
#9390=FACE_OUTER_BOUND('',#15181,.T.);
#9391=FACE_OUTER_BOUND('',#15182,.T.);
#9392=FACE_OUTER_BOUND('',#15183,.T.);
#9393=FACE_OUTER_BOUND('',#15184,.T.);
#9394=FACE_OUTER_BOUND('',#15185,.T.);
#9395=FACE_OUTER_BOUND('',#15186,.T.);
#9396=FACE_OUTER_BOUND('',#15187,.T.);
#9397=FACE_OUTER_BOUND('',#15188,.T.);
#9398=FACE_OUTER_BOUND('',#15189,.T.);
#9399=FACE_OUTER_BOUND('',#15190,.T.);
#9400=FACE_OUTER_BOUND('',#15191,.T.);
#9401=FACE_OUTER_BOUND('',#15192,.T.);
#9402=FACE_OUTER_BOUND('',#15193,.T.);
#9403=FACE_OUTER_BOUND('',#15194,.T.);
#9404=FACE_OUTER_BOUND('',#15195,.T.);
#9405=FACE_OUTER_BOUND('',#15196,.T.);
#9406=FACE_OUTER_BOUND('',#15197,.T.);
#9407=FACE_OUTER_BOUND('',#15198,.T.);
#9408=FACE_OUTER_BOUND('',#15199,.T.);
#9409=FACE_OUTER_BOUND('',#15200,.T.);
#9410=FACE_OUTER_BOUND('',#15201,.T.);
#9411=FACE_OUTER_BOUND('',#15202,.T.);
#9412=FACE_OUTER_BOUND('',#15203,.T.);
#9413=FACE_OUTER_BOUND('',#15204,.T.);
#9414=FACE_OUTER_BOUND('',#15205,.T.);
#9415=FACE_OUTER_BOUND('',#15206,.T.);
#9416=FACE_OUTER_BOUND('',#15207,.T.);
#9417=FACE_OUTER_BOUND('',#15208,.T.);
#9418=FACE_OUTER_BOUND('',#15209,.T.);
#9419=FACE_OUTER_BOUND('',#15210,.T.);
#9420=FACE_OUTER_BOUND('',#15211,.T.);
#9421=FACE_OUTER_BOUND('',#15212,.T.);
#9422=FACE_OUTER_BOUND('',#15213,.T.);
#9423=FACE_OUTER_BOUND('',#15214,.T.);
#9424=FACE_OUTER_BOUND('',#15215,.T.);
#9425=FACE_OUTER_BOUND('',#15216,.T.);
#9426=FACE_OUTER_BOUND('',#15217,.T.);
#9427=FACE_OUTER_BOUND('',#15218,.T.);
#9428=FACE_OUTER_BOUND('',#15219,.T.);
#9429=FACE_OUTER_BOUND('',#15220,.T.);
#9430=FACE_OUTER_BOUND('',#15221,.T.);
#9431=FACE_OUTER_BOUND('',#15222,.T.);
#9432=FACE_OUTER_BOUND('',#15223,.T.);
#9433=FACE_OUTER_BOUND('',#15224,.T.);
#9434=FACE_OUTER_BOUND('',#15225,.T.);
#9435=FACE_OUTER_BOUND('',#15226,.T.);
#9436=FACE_OUTER_BOUND('',#15227,.T.);
#9437=FACE_OUTER_BOUND('',#15228,.T.);
#9438=FACE_OUTER_BOUND('',#15229,.T.);
#9439=FACE_OUTER_BOUND('',#15230,.T.);
#9440=FACE_OUTER_BOUND('',#15231,.T.);
#9441=FACE_OUTER_BOUND('',#15232,.T.);
#9442=FACE_OUTER_BOUND('',#15233,.T.);
#9443=FACE_OUTER_BOUND('',#15234,.T.);
#9444=FACE_OUTER_BOUND('',#15235,.T.);
#9445=FACE_OUTER_BOUND('',#15236,.T.);
#9446=FACE_OUTER_BOUND('',#15237,.T.);
#9447=FACE_OUTER_BOUND('',#15238,.T.);
#9448=FACE_OUTER_BOUND('',#15239,.T.);
#9449=FACE_OUTER_BOUND('',#15240,.T.);
#9450=FACE_OUTER_BOUND('',#15241,.T.);
#9451=FACE_OUTER_BOUND('',#15242,.T.);
#9452=FACE_OUTER_BOUND('',#15243,.T.);
#9453=FACE_OUTER_BOUND('',#15244,.T.);
#9454=FACE_OUTER_BOUND('',#15245,.T.);
#9455=FACE_OUTER_BOUND('',#15246,.T.);
#9456=FACE_OUTER_BOUND('',#15247,.T.);
#9457=FACE_OUTER_BOUND('',#15248,.T.);
#9458=FACE_OUTER_BOUND('',#15249,.T.);
#9459=FACE_OUTER_BOUND('',#15250,.T.);
#9460=FACE_OUTER_BOUND('',#15251,.T.);
#9461=FACE_OUTER_BOUND('',#15252,.T.);
#9462=FACE_OUTER_BOUND('',#15253,.T.);
#9463=FACE_OUTER_BOUND('',#15254,.T.);
#9464=FACE_OUTER_BOUND('',#15255,.T.);
#9465=FACE_OUTER_BOUND('',#15256,.T.);
#9466=FACE_OUTER_BOUND('',#15257,.T.);
#9467=FACE_OUTER_BOUND('',#15258,.T.);
#9468=FACE_OUTER_BOUND('',#15259,.T.);
#9469=FACE_OUTER_BOUND('',#15260,.T.);
#9470=FACE_OUTER_BOUND('',#15261,.T.);
#9471=FACE_OUTER_BOUND('',#15262,.T.);
#9472=FACE_OUTER_BOUND('',#15263,.T.);
#9473=FACE_OUTER_BOUND('',#15264,.T.);
#9474=FACE_OUTER_BOUND('',#15265,.T.);
#9475=FACE_OUTER_BOUND('',#15266,.T.);
#9476=FACE_OUTER_BOUND('',#15267,.T.);
#9477=FACE_OUTER_BOUND('',#15268,.T.);
#9478=FACE_OUTER_BOUND('',#15269,.T.);
#9479=FACE_OUTER_BOUND('',#15270,.T.);
#9480=FACE_OUTER_BOUND('',#15271,.T.);
#9481=FACE_OUTER_BOUND('',#15272,.T.);
#9482=FACE_OUTER_BOUND('',#15273,.T.);
#9483=FACE_OUTER_BOUND('',#15274,.T.);
#9484=FACE_OUTER_BOUND('',#15275,.T.);
#9485=FACE_OUTER_BOUND('',#15276,.T.);
#9486=FACE_OUTER_BOUND('',#15277,.T.);
#9487=FACE_OUTER_BOUND('',#15278,.T.);
#9488=FACE_OUTER_BOUND('',#15279,.T.);
#9489=FACE_OUTER_BOUND('',#15280,.T.);
#9490=FACE_OUTER_BOUND('',#15281,.T.);
#9491=FACE_OUTER_BOUND('',#15282,.T.);
#9492=FACE_OUTER_BOUND('',#15283,.T.);
#9493=FACE_OUTER_BOUND('',#15284,.T.);
#9494=FACE_OUTER_BOUND('',#15285,.T.);
#9495=FACE_OUTER_BOUND('',#15286,.T.);
#9496=FACE_OUTER_BOUND('',#15287,.T.);
#9497=FACE_OUTER_BOUND('',#15288,.T.);
#9498=FACE_OUTER_BOUND('',#15289,.T.);
#9499=FACE_OUTER_BOUND('',#15290,.T.);
#9500=FACE_OUTER_BOUND('',#15291,.T.);
#9501=FACE_OUTER_BOUND('',#15292,.T.);
#9502=FACE_OUTER_BOUND('',#15293,.T.);
#9503=FACE_OUTER_BOUND('',#15294,.T.);
#9504=FACE_OUTER_BOUND('',#15295,.T.);
#9505=FACE_OUTER_BOUND('',#15296,.T.);
#9506=FACE_OUTER_BOUND('',#15297,.T.);
#9507=FACE_OUTER_BOUND('',#15298,.T.);
#9508=FACE_OUTER_BOUND('',#15299,.T.);
#9509=FACE_OUTER_BOUND('',#15300,.T.);
#9510=FACE_OUTER_BOUND('',#15301,.T.);
#9511=FACE_OUTER_BOUND('',#15302,.T.);
#9512=FACE_OUTER_BOUND('',#15303,.T.);
#9513=FACE_OUTER_BOUND('',#15304,.T.);
#9514=FACE_OUTER_BOUND('',#15305,.T.);
#9515=FACE_OUTER_BOUND('',#15306,.T.);
#9516=FACE_OUTER_BOUND('',#15307,.T.);
#9517=FACE_OUTER_BOUND('',#15308,.T.);
#9518=FACE_OUTER_BOUND('',#15309,.T.);
#9519=FACE_OUTER_BOUND('',#15310,.T.);
#9520=FACE_OUTER_BOUND('',#15311,.T.);
#9521=FACE_OUTER_BOUND('',#15312,.T.);
#9522=FACE_OUTER_BOUND('',#15313,.T.);
#9523=FACE_OUTER_BOUND('',#15314,.T.);
#9524=FACE_OUTER_BOUND('',#15315,.T.);
#9525=FACE_OUTER_BOUND('',#15316,.T.);
#9526=FACE_OUTER_BOUND('',#15317,.T.);
#9527=FACE_OUTER_BOUND('',#15318,.T.);
#9528=FACE_OUTER_BOUND('',#15319,.T.);
#9529=FACE_OUTER_BOUND('',#15320,.T.);
#9530=FACE_OUTER_BOUND('',#15321,.T.);
#9531=FACE_OUTER_BOUND('',#15322,.T.);
#9532=FACE_OUTER_BOUND('',#15323,.T.);
#9533=FACE_OUTER_BOUND('',#15324,.T.);
#9534=FACE_OUTER_BOUND('',#15325,.T.);
#9535=FACE_OUTER_BOUND('',#15326,.T.);
#9536=FACE_OUTER_BOUND('',#15327,.T.);
#9537=FACE_OUTER_BOUND('',#15328,.T.);
#9538=FACE_OUTER_BOUND('',#15329,.T.);
#9539=FACE_OUTER_BOUND('',#15330,.T.);
#9540=FACE_OUTER_BOUND('',#15331,.T.);
#9541=FACE_OUTER_BOUND('',#15332,.T.);
#9542=FACE_OUTER_BOUND('',#15333,.T.);
#9543=FACE_OUTER_BOUND('',#15334,.T.);
#9544=FACE_OUTER_BOUND('',#15335,.T.);
#9545=FACE_OUTER_BOUND('',#15336,.T.);
#9546=FACE_OUTER_BOUND('',#15337,.T.);
#9547=FACE_OUTER_BOUND('',#15338,.T.);
#9548=FACE_OUTER_BOUND('',#15339,.T.);
#9549=FACE_OUTER_BOUND('',#15340,.T.);
#9550=FACE_OUTER_BOUND('',#15341,.T.);
#9551=FACE_OUTER_BOUND('',#15342,.T.);
#9552=FACE_OUTER_BOUND('',#15343,.T.);
#9553=FACE_OUTER_BOUND('',#15344,.T.);
#9554=FACE_OUTER_BOUND('',#15345,.T.);
#9555=FACE_OUTER_BOUND('',#15346,.T.);
#9556=FACE_OUTER_BOUND('',#15347,.T.);
#9557=FACE_OUTER_BOUND('',#15348,.T.);
#9558=FACE_OUTER_BOUND('',#15349,.T.);
#9559=FACE_OUTER_BOUND('',#15350,.T.);
#9560=FACE_OUTER_BOUND('',#15351,.T.);
#9561=FACE_OUTER_BOUND('',#15352,.T.);
#9562=FACE_OUTER_BOUND('',#15353,.T.);
#9563=FACE_OUTER_BOUND('',#15354,.T.);
#9564=FACE_OUTER_BOUND('',#15355,.T.);
#9565=FACE_OUTER_BOUND('',#15356,.T.);
#9566=FACE_OUTER_BOUND('',#15357,.T.);
#9567=FACE_OUTER_BOUND('',#15358,.T.);
#9568=FACE_OUTER_BOUND('',#15359,.T.);
#9569=FACE_OUTER_BOUND('',#15360,.T.);
#9570=FACE_OUTER_BOUND('',#15361,.T.);
#9571=FACE_OUTER_BOUND('',#15362,.T.);
#9572=FACE_OUTER_BOUND('',#15363,.T.);
#9573=FACE_OUTER_BOUND('',#15364,.T.);
#9574=FACE_OUTER_BOUND('',#15365,.T.);
#9575=FACE_OUTER_BOUND('',#15366,.T.);
#9576=FACE_OUTER_BOUND('',#15367,.T.);
#9577=FACE_OUTER_BOUND('',#15368,.T.);
#9578=FACE_OUTER_BOUND('',#15369,.T.);
#9579=FACE_OUTER_BOUND('',#15370,.T.);
#9580=FACE_OUTER_BOUND('',#15371,.T.);
#9581=FACE_OUTER_BOUND('',#15372,.T.);
#9582=FACE_OUTER_BOUND('',#15373,.T.);
#9583=FACE_OUTER_BOUND('',#15374,.T.);
#9584=FACE_OUTER_BOUND('',#15375,.T.);
#9585=FACE_OUTER_BOUND('',#15376,.T.);
#9586=FACE_OUTER_BOUND('',#15377,.T.);
#9587=FACE_OUTER_BOUND('',#15378,.T.);
#9588=FACE_OUTER_BOUND('',#15379,.T.);
#9589=FACE_OUTER_BOUND('',#15380,.T.);
#9590=FACE_OUTER_BOUND('',#15381,.T.);
#9591=FACE_OUTER_BOUND('',#15382,.T.);
#9592=FACE_OUTER_BOUND('',#15383,.T.);
#9593=FACE_OUTER_BOUND('',#15384,.T.);
#9594=FACE_OUTER_BOUND('',#15385,.T.);
#9595=FACE_OUTER_BOUND('',#15386,.T.);
#9596=FACE_OUTER_BOUND('',#15387,.T.);
#9597=FACE_OUTER_BOUND('',#15388,.T.);
#9598=FACE_OUTER_BOUND('',#15389,.T.);
#9599=FACE_OUTER_BOUND('',#15390,.T.);
#9600=FACE_OUTER_BOUND('',#15391,.T.);
#9601=FACE_OUTER_BOUND('',#15392,.T.);
#9602=FACE_OUTER_BOUND('',#15393,.T.);
#9603=FACE_OUTER_BOUND('',#15394,.T.);
#9604=FACE_OUTER_BOUND('',#15395,.T.);
#9605=FACE_OUTER_BOUND('',#15396,.T.);
#9606=FACE_OUTER_BOUND('',#15397,.T.);
#9607=FACE_OUTER_BOUND('',#15398,.T.);
#9608=FACE_OUTER_BOUND('',#15399,.T.);
#9609=FACE_OUTER_BOUND('',#15400,.T.);
#9610=FACE_OUTER_BOUND('',#15401,.T.);
#9611=FACE_OUTER_BOUND('',#15402,.T.);
#9612=FACE_OUTER_BOUND('',#15403,.T.);
#9613=FACE_OUTER_BOUND('',#15404,.T.);
#9614=FACE_OUTER_BOUND('',#15405,.T.);
#9615=FACE_OUTER_BOUND('',#15406,.T.);
#9616=FACE_OUTER_BOUND('',#15407,.T.);
#9617=FACE_OUTER_BOUND('',#15408,.T.);
#9618=FACE_OUTER_BOUND('',#15409,.T.);
#9619=FACE_OUTER_BOUND('',#15410,.T.);
#9620=FACE_OUTER_BOUND('',#15411,.T.);
#9621=FACE_OUTER_BOUND('',#15412,.T.);
#9622=FACE_OUTER_BOUND('',#15413,.T.);
#9623=FACE_OUTER_BOUND('',#15414,.T.);
#9624=FACE_OUTER_BOUND('',#15415,.T.);
#9625=FACE_OUTER_BOUND('',#15416,.T.);
#9626=FACE_OUTER_BOUND('',#15417,.T.);
#9627=FACE_OUTER_BOUND('',#15418,.T.);
#9628=FACE_OUTER_BOUND('',#15419,.T.);
#9629=FACE_OUTER_BOUND('',#15420,.T.);
#9630=FACE_OUTER_BOUND('',#15421,.T.);
#9631=FACE_OUTER_BOUND('',#15422,.T.);
#9632=FACE_OUTER_BOUND('',#15423,.T.);
#9633=FACE_OUTER_BOUND('',#15424,.T.);
#9634=FACE_OUTER_BOUND('',#15425,.T.);
#9635=FACE_OUTER_BOUND('',#15426,.T.);
#9636=FACE_OUTER_BOUND('',#15427,.T.);
#9637=FACE_OUTER_BOUND('',#15428,.T.);
#9638=FACE_OUTER_BOUND('',#15429,.T.);
#9639=FACE_OUTER_BOUND('',#15430,.T.);
#9640=FACE_OUTER_BOUND('',#15431,.T.);
#9641=FACE_OUTER_BOUND('',#15432,.T.);
#9642=FACE_OUTER_BOUND('',#15433,.T.);
#9643=FACE_OUTER_BOUND('',#15434,.T.);
#9644=FACE_OUTER_BOUND('',#15435,.T.);
#9645=FACE_OUTER_BOUND('',#15436,.T.);
#9646=FACE_OUTER_BOUND('',#15437,.T.);
#9647=FACE_OUTER_BOUND('',#15438,.T.);
#9648=FACE_OUTER_BOUND('',#15439,.T.);
#9649=FACE_OUTER_BOUND('',#15440,.T.);
#9650=FACE_OUTER_BOUND('',#15441,.T.);
#9651=FACE_OUTER_BOUND('',#15442,.T.);
#9652=FACE_OUTER_BOUND('',#15443,.T.);
#9653=FACE_OUTER_BOUND('',#15444,.T.);
#9654=FACE_OUTER_BOUND('',#15445,.T.);
#9655=FACE_OUTER_BOUND('',#15446,.T.);
#9656=FACE_OUTER_BOUND('',#15447,.T.);
#9657=FACE_OUTER_BOUND('',#15448,.T.);
#9658=FACE_OUTER_BOUND('',#15449,.T.);
#9659=FACE_OUTER_BOUND('',#15450,.T.);
#9660=FACE_OUTER_BOUND('',#15451,.T.);
#9661=FACE_OUTER_BOUND('',#15452,.T.);
#9662=FACE_OUTER_BOUND('',#15453,.T.);
#9663=FACE_OUTER_BOUND('',#15454,.T.);
#9664=FACE_OUTER_BOUND('',#15455,.T.);
#9665=FACE_OUTER_BOUND('',#15456,.T.);
#9666=FACE_OUTER_BOUND('',#15457,.T.);
#9667=FACE_OUTER_BOUND('',#15458,.T.);
#9668=FACE_OUTER_BOUND('',#15459,.T.);
#9669=FACE_OUTER_BOUND('',#15460,.T.);
#9670=FACE_OUTER_BOUND('',#15461,.T.);
#9671=FACE_OUTER_BOUND('',#15462,.T.);
#9672=FACE_OUTER_BOUND('',#15463,.T.);
#9673=FACE_OUTER_BOUND('',#15464,.T.);
#9674=FACE_OUTER_BOUND('',#15465,.T.);
#9675=FACE_OUTER_BOUND('',#15466,.T.);
#9676=FACE_OUTER_BOUND('',#15467,.T.);
#9677=FACE_OUTER_BOUND('',#15468,.T.);
#9678=FACE_OUTER_BOUND('',#15469,.T.);
#9679=FACE_OUTER_BOUND('',#15470,.T.);
#9680=FACE_OUTER_BOUND('',#15471,.T.);
#9681=FACE_OUTER_BOUND('',#15472,.T.);
#9682=FACE_OUTER_BOUND('',#15473,.T.);
#9683=FACE_OUTER_BOUND('',#15474,.T.);
#9684=FACE_OUTER_BOUND('',#15475,.T.);
#9685=FACE_OUTER_BOUND('',#15476,.T.);
#9686=FACE_OUTER_BOUND('',#15477,.T.);
#9687=FACE_OUTER_BOUND('',#15478,.T.);
#9688=FACE_OUTER_BOUND('',#15479,.T.);
#9689=FACE_OUTER_BOUND('',#15480,.T.);
#9690=FACE_OUTER_BOUND('',#15481,.T.);
#9691=FACE_OUTER_BOUND('',#15482,.T.);
#9692=FACE_OUTER_BOUND('',#15483,.T.);
#9693=FACE_OUTER_BOUND('',#15484,.T.);
#9694=FACE_OUTER_BOUND('',#15485,.T.);
#9695=FACE_OUTER_BOUND('',#15486,.T.);
#9696=FACE_OUTER_BOUND('',#15487,.T.);
#9697=FACE_OUTER_BOUND('',#15488,.T.);
#9698=FACE_OUTER_BOUND('',#15489,.T.);
#9699=FACE_OUTER_BOUND('',#15490,.T.);
#9700=FACE_OUTER_BOUND('',#15491,.T.);
#9701=FACE_OUTER_BOUND('',#15492,.T.);
#9702=FACE_OUTER_BOUND('',#15493,.T.);
#9703=FACE_OUTER_BOUND('',#15494,.T.);
#9704=FACE_OUTER_BOUND('',#15495,.T.);
#9705=FACE_OUTER_BOUND('',#15496,.T.);
#9706=FACE_OUTER_BOUND('',#15497,.T.);
#9707=FACE_OUTER_BOUND('',#15498,.T.);
#9708=FACE_OUTER_BOUND('',#15499,.T.);
#9709=FACE_OUTER_BOUND('',#15500,.T.);
#9710=FACE_OUTER_BOUND('',#15501,.T.);
#9711=FACE_OUTER_BOUND('',#15502,.T.);
#9712=FACE_OUTER_BOUND('',#15503,.T.);
#9713=FACE_OUTER_BOUND('',#15504,.T.);
#9714=FACE_OUTER_BOUND('',#15505,.T.);
#9715=FACE_OUTER_BOUND('',#15506,.T.);
#9716=FACE_OUTER_BOUND('',#15507,.T.);
#9717=FACE_OUTER_BOUND('',#15508,.T.);
#9718=FACE_OUTER_BOUND('',#15509,.T.);
#9719=FACE_OUTER_BOUND('',#15510,.T.);
#9720=FACE_OUTER_BOUND('',#15511,.T.);
#9721=FACE_OUTER_BOUND('',#15512,.T.);
#9722=FACE_OUTER_BOUND('',#15513,.T.);
#9723=FACE_OUTER_BOUND('',#15514,.T.);
#9724=FACE_OUTER_BOUND('',#15515,.T.);
#9725=FACE_OUTER_BOUND('',#15516,.T.);
#9726=FACE_OUTER_BOUND('',#15517,.T.);
#9727=FACE_OUTER_BOUND('',#15518,.T.);
#9728=FACE_OUTER_BOUND('',#15519,.T.);
#9729=FACE_OUTER_BOUND('',#15520,.T.);
#9730=FACE_OUTER_BOUND('',#15521,.T.);
#9731=FACE_OUTER_BOUND('',#15522,.T.);
#9732=FACE_OUTER_BOUND('',#15523,.T.);
#9733=FACE_OUTER_BOUND('',#15524,.T.);
#9734=FACE_OUTER_BOUND('',#15525,.T.);
#9735=FACE_OUTER_BOUND('',#15526,.T.);
#9736=FACE_OUTER_BOUND('',#15527,.T.);
#9737=FACE_OUTER_BOUND('',#15528,.T.);
#9738=FACE_OUTER_BOUND('',#15529,.T.);
#9739=FACE_OUTER_BOUND('',#15530,.T.);
#9740=FACE_OUTER_BOUND('',#15531,.T.);
#9741=FACE_OUTER_BOUND('',#15532,.T.);
#9742=FACE_OUTER_BOUND('',#15533,.T.);
#9743=FACE_OUTER_BOUND('',#15534,.T.);
#9744=FACE_OUTER_BOUND('',#15535,.T.);
#9745=FACE_OUTER_BOUND('',#15536,.T.);
#9746=FACE_OUTER_BOUND('',#15537,.T.);
#9747=FACE_OUTER_BOUND('',#15538,.T.);
#9748=FACE_OUTER_BOUND('',#15539,.T.);
#9749=FACE_OUTER_BOUND('',#15540,.T.);
#9750=FACE_OUTER_BOUND('',#15541,.T.);
#9751=FACE_OUTER_BOUND('',#15542,.T.);
#9752=FACE_OUTER_BOUND('',#15543,.T.);
#9753=FACE_OUTER_BOUND('',#15544,.T.);
#9754=FACE_OUTER_BOUND('',#15545,.T.);
#9755=FACE_OUTER_BOUND('',#15546,.T.);
#9756=FACE_OUTER_BOUND('',#15547,.T.);
#9757=FACE_OUTER_BOUND('',#15548,.T.);
#9758=FACE_OUTER_BOUND('',#15549,.T.);
#9759=FACE_OUTER_BOUND('',#15550,.T.);
#9760=FACE_OUTER_BOUND('',#15551,.T.);
#9761=FACE_OUTER_BOUND('',#15552,.T.);
#9762=FACE_OUTER_BOUND('',#15553,.T.);
#9763=FACE_OUTER_BOUND('',#15554,.T.);
#9764=FACE_OUTER_BOUND('',#15555,.T.);
#9765=FACE_OUTER_BOUND('',#15556,.T.);
#9766=FACE_OUTER_BOUND('',#15557,.T.);
#9767=FACE_OUTER_BOUND('',#15558,.T.);
#9768=FACE_OUTER_BOUND('',#15559,.T.);
#9769=FACE_OUTER_BOUND('',#15560,.T.);
#9770=FACE_OUTER_BOUND('',#15561,.T.);
#9771=FACE_OUTER_BOUND('',#15562,.T.);
#9772=FACE_OUTER_BOUND('',#15563,.T.);
#9773=FACE_OUTER_BOUND('',#15564,.T.);
#9774=FACE_OUTER_BOUND('',#15565,.T.);
#9775=FACE_OUTER_BOUND('',#15566,.T.);
#9776=FACE_OUTER_BOUND('',#15567,.T.);
#9777=FACE_OUTER_BOUND('',#15568,.T.);
#9778=FACE_OUTER_BOUND('',#15569,.T.);
#9779=FACE_OUTER_BOUND('',#15570,.T.);
#9780=FACE_OUTER_BOUND('',#15571,.T.);
#9781=FACE_OUTER_BOUND('',#15572,.T.);
#9782=FACE_OUTER_BOUND('',#15573,.T.);
#9783=FACE_OUTER_BOUND('',#15574,.T.);
#9784=FACE_OUTER_BOUND('',#15575,.T.);
#9785=FACE_OUTER_BOUND('',#15576,.T.);
#9786=FACE_OUTER_BOUND('',#15577,.T.);
#9787=FACE_OUTER_BOUND('',#15578,.T.);
#9788=FACE_OUTER_BOUND('',#15579,.T.);
#9789=FACE_OUTER_BOUND('',#15580,.T.);
#9790=FACE_OUTER_BOUND('',#15581,.T.);
#9791=FACE_OUTER_BOUND('',#15582,.T.);
#9792=FACE_OUTER_BOUND('',#15583,.T.);
#9793=FACE_OUTER_BOUND('',#15584,.T.);
#9794=FACE_OUTER_BOUND('',#15585,.T.);
#9795=FACE_OUTER_BOUND('',#15586,.T.);
#9796=FACE_OUTER_BOUND('',#15587,.T.);
#9797=FACE_OUTER_BOUND('',#15588,.T.);
#9798=FACE_OUTER_BOUND('',#15589,.T.);
#9799=FACE_OUTER_BOUND('',#15590,.T.);
#9800=FACE_OUTER_BOUND('',#15591,.T.);
#9801=FACE_OUTER_BOUND('',#15592,.T.);
#9802=FACE_OUTER_BOUND('',#15593,.T.);
#9803=FACE_OUTER_BOUND('',#15594,.T.);
#9804=FACE_OUTER_BOUND('',#15595,.T.);
#9805=FACE_OUTER_BOUND('',#15596,.T.);
#9806=FACE_OUTER_BOUND('',#15597,.T.);
#9807=FACE_OUTER_BOUND('',#15598,.T.);
#9808=FACE_OUTER_BOUND('',#15599,.T.);
#9809=FACE_OUTER_BOUND('',#15600,.T.);
#9810=FACE_OUTER_BOUND('',#15601,.T.);
#9811=FACE_OUTER_BOUND('',#15602,.T.);
#9812=FACE_OUTER_BOUND('',#15603,.T.);
#9813=FACE_OUTER_BOUND('',#15604,.T.);
#9814=FACE_OUTER_BOUND('',#15605,.T.);
#9815=FACE_OUTER_BOUND('',#15606,.T.);
#9816=FACE_OUTER_BOUND('',#15607,.T.);
#9817=FACE_OUTER_BOUND('',#15608,.T.);
#9818=FACE_OUTER_BOUND('',#15609,.T.);
#9819=FACE_OUTER_BOUND('',#15610,.T.);
#9820=FACE_OUTER_BOUND('',#15611,.T.);
#9821=FACE_OUTER_BOUND('',#15612,.T.);
#9822=FACE_OUTER_BOUND('',#15613,.T.);
#9823=FACE_OUTER_BOUND('',#15614,.T.);
#9824=FACE_OUTER_BOUND('',#15615,.T.);
#9825=FACE_OUTER_BOUND('',#15616,.T.);
#9826=FACE_OUTER_BOUND('',#15617,.T.);
#9827=FACE_OUTER_BOUND('',#15618,.T.);
#9828=FACE_OUTER_BOUND('',#15619,.T.);
#9829=FACE_OUTER_BOUND('',#15620,.T.);
#9830=FACE_OUTER_BOUND('',#15621,.T.);
#9831=FACE_OUTER_BOUND('',#15622,.T.);
#9832=FACE_OUTER_BOUND('',#15623,.T.);
#9833=FACE_OUTER_BOUND('',#15624,.T.);
#9834=FACE_OUTER_BOUND('',#15625,.T.);
#9835=FACE_OUTER_BOUND('',#15626,.T.);
#9836=FACE_OUTER_BOUND('',#15627,.T.);
#9837=FACE_OUTER_BOUND('',#15628,.T.);
#9838=FACE_OUTER_BOUND('',#15629,.T.);
#9839=FACE_OUTER_BOUND('',#15630,.T.);
#9840=FACE_OUTER_BOUND('',#15631,.T.);
#9841=FACE_OUTER_BOUND('',#15632,.T.);
#9842=FACE_OUTER_BOUND('',#15633,.T.);
#9843=FACE_OUTER_BOUND('',#15634,.T.);
#9844=FACE_OUTER_BOUND('',#15635,.T.);
#9845=FACE_OUTER_BOUND('',#15636,.T.);
#9846=FACE_OUTER_BOUND('',#15637,.T.);
#9847=FACE_OUTER_BOUND('',#15638,.T.);
#9848=FACE_OUTER_BOUND('',#15639,.T.);
#9849=FACE_OUTER_BOUND('',#15640,.T.);
#9850=FACE_OUTER_BOUND('',#15641,.T.);
#9851=FACE_OUTER_BOUND('',#15642,.T.);
#9852=FACE_OUTER_BOUND('',#15643,.T.);
#9853=FACE_OUTER_BOUND('',#15644,.T.);
#9854=FACE_OUTER_BOUND('',#15645,.T.);
#9855=FACE_OUTER_BOUND('',#15646,.T.);
#9856=FACE_OUTER_BOUND('',#15647,.T.);
#9857=FACE_OUTER_BOUND('',#15648,.T.);
#9858=FACE_OUTER_BOUND('',#15649,.T.);
#9859=FACE_OUTER_BOUND('',#15650,.T.);
#9860=FACE_OUTER_BOUND('',#15651,.T.);
#9861=FACE_OUTER_BOUND('',#15652,.T.);
#9862=FACE_OUTER_BOUND('',#15653,.T.);
#9863=FACE_OUTER_BOUND('',#15654,.T.);
#9864=FACE_OUTER_BOUND('',#15655,.T.);
#9865=FACE_OUTER_BOUND('',#15656,.T.);
#9866=FACE_OUTER_BOUND('',#15657,.T.);
#9867=FACE_OUTER_BOUND('',#15658,.T.);
#9868=FACE_OUTER_BOUND('',#15659,.T.);
#9869=FACE_OUTER_BOUND('',#15660,.T.);
#9870=FACE_OUTER_BOUND('',#15661,.T.);
#9871=FACE_OUTER_BOUND('',#15662,.T.);
#9872=FACE_OUTER_BOUND('',#15663,.T.);
#9873=FACE_OUTER_BOUND('',#15664,.T.);
#9874=FACE_OUTER_BOUND('',#15665,.T.);
#9875=FACE_OUTER_BOUND('',#15666,.T.);
#9876=FACE_OUTER_BOUND('',#15667,.T.);
#9877=FACE_OUTER_BOUND('',#15668,.T.);
#9878=FACE_OUTER_BOUND('',#15669,.T.);
#9879=FACE_OUTER_BOUND('',#15670,.T.);
#9880=FACE_OUTER_BOUND('',#15671,.T.);
#9881=FACE_OUTER_BOUND('',#15672,.T.);
#9882=FACE_OUTER_BOUND('',#15673,.T.);
#9883=FACE_OUTER_BOUND('',#15674,.T.);
#9884=FACE_OUTER_BOUND('',#15675,.T.);
#9885=FACE_OUTER_BOUND('',#15676,.T.);
#9886=FACE_OUTER_BOUND('',#15677,.T.);
#9887=FACE_OUTER_BOUND('',#15678,.T.);
#9888=FACE_OUTER_BOUND('',#15679,.T.);
#9889=FACE_OUTER_BOUND('',#15680,.T.);
#9890=FACE_OUTER_BOUND('',#15681,.T.);
#9891=FACE_OUTER_BOUND('',#15682,.T.);
#9892=FACE_OUTER_BOUND('',#15683,.T.);
#9893=FACE_OUTER_BOUND('',#15684,.T.);
#9894=FACE_OUTER_BOUND('',#15685,.T.);
#9895=FACE_OUTER_BOUND('',#15686,.T.);
#9896=FACE_OUTER_BOUND('',#15687,.T.);
#9897=FACE_OUTER_BOUND('',#15688,.T.);
#9898=FACE_OUTER_BOUND('',#15689,.T.);
#9899=FACE_OUTER_BOUND('',#15690,.T.);
#9900=FACE_OUTER_BOUND('',#15691,.T.);
#9901=FACE_OUTER_BOUND('',#15692,.T.);
#9902=FACE_OUTER_BOUND('',#15693,.T.);
#9903=FACE_OUTER_BOUND('',#15694,.T.);
#9904=FACE_OUTER_BOUND('',#15695,.T.);
#9905=FACE_OUTER_BOUND('',#15696,.T.);
#9906=FACE_OUTER_BOUND('',#15697,.T.);
#9907=FACE_OUTER_BOUND('',#15698,.T.);
#9908=FACE_OUTER_BOUND('',#15699,.T.);
#9909=FACE_OUTER_BOUND('',#15700,.T.);
#9910=FACE_OUTER_BOUND('',#15701,.T.);
#9911=FACE_OUTER_BOUND('',#15702,.T.);
#9912=FACE_OUTER_BOUND('',#15703,.T.);
#9913=FACE_OUTER_BOUND('',#15704,.T.);
#9914=FACE_OUTER_BOUND('',#15705,.T.);
#9915=FACE_OUTER_BOUND('',#15706,.T.);
#9916=FACE_OUTER_BOUND('',#15707,.T.);
#9917=FACE_OUTER_BOUND('',#15708,.T.);
#9918=FACE_OUTER_BOUND('',#15709,.T.);
#9919=FACE_OUTER_BOUND('',#15710,.T.);
#9920=FACE_OUTER_BOUND('',#15711,.T.);
#9921=FACE_OUTER_BOUND('',#15712,.T.);
#9922=FACE_OUTER_BOUND('',#15713,.T.);
#9923=FACE_OUTER_BOUND('',#15714,.T.);
#9924=FACE_OUTER_BOUND('',#15715,.T.);
#9925=FACE_OUTER_BOUND('',#15716,.T.);
#9926=FACE_OUTER_BOUND('',#15717,.T.);
#9927=FACE_OUTER_BOUND('',#15718,.T.);
#9928=FACE_OUTER_BOUND('',#15719,.T.);
#9929=FACE_OUTER_BOUND('',#15720,.T.);
#9930=FACE_OUTER_BOUND('',#15721,.T.);
#9931=FACE_OUTER_BOUND('',#15722,.T.);
#9932=FACE_OUTER_BOUND('',#15723,.T.);
#9933=FACE_OUTER_BOUND('',#15724,.T.);
#9934=FACE_OUTER_BOUND('',#15725,.T.);
#9935=FACE_OUTER_BOUND('',#15726,.T.);
#9936=FACE_OUTER_BOUND('',#15727,.T.);
#9937=FACE_OUTER_BOUND('',#15728,.T.);
#9938=FACE_OUTER_BOUND('',#15729,.T.);
#9939=FACE_OUTER_BOUND('',#15730,.T.);
#9940=FACE_OUTER_BOUND('',#15731,.T.);
#9941=FACE_OUTER_BOUND('',#15732,.T.);
#9942=FACE_OUTER_BOUND('',#15733,.T.);
#9943=FACE_OUTER_BOUND('',#15734,.T.);
#9944=FACE_OUTER_BOUND('',#15735,.T.);
#9945=FACE_OUTER_BOUND('',#15736,.T.);
#9946=FACE_OUTER_BOUND('',#15737,.T.);
#9947=FACE_OUTER_BOUND('',#15738,.T.);
#9948=FACE_OUTER_BOUND('',#15739,.T.);
#9949=FACE_OUTER_BOUND('',#15740,.T.);
#9950=FACE_OUTER_BOUND('',#15741,.T.);
#9951=FACE_OUTER_BOUND('',#15742,.T.);
#9952=FACE_OUTER_BOUND('',#15743,.T.);
#9953=FACE_OUTER_BOUND('',#15744,.T.);
#9954=FACE_OUTER_BOUND('',#15745,.T.);
#9955=FACE_OUTER_BOUND('',#15746,.T.);
#9956=FACE_OUTER_BOUND('',#15747,.T.);
#9957=FACE_OUTER_BOUND('',#15748,.T.);
#9958=FACE_OUTER_BOUND('',#15749,.T.);
#9959=FACE_OUTER_BOUND('',#15750,.T.);
#9960=FACE_OUTER_BOUND('',#15751,.T.);
#9961=FACE_OUTER_BOUND('',#15752,.T.);
#9962=FACE_OUTER_BOUND('',#15753,.T.);
#9963=FACE_OUTER_BOUND('',#15754,.T.);
#9964=FACE_OUTER_BOUND('',#15755,.T.);
#9965=FACE_OUTER_BOUND('',#15756,.T.);
#9966=FACE_OUTER_BOUND('',#15757,.T.);
#9967=FACE_OUTER_BOUND('',#15758,.T.);
#9968=FACE_OUTER_BOUND('',#15759,.T.);
#9969=FACE_OUTER_BOUND('',#15760,.T.);
#9970=FACE_OUTER_BOUND('',#15761,.T.);
#9971=FACE_OUTER_BOUND('',#15762,.T.);
#9972=FACE_OUTER_BOUND('',#15763,.T.);
#9973=FACE_OUTER_BOUND('',#15764,.T.);
#9974=FACE_OUTER_BOUND('',#15765,.T.);
#9975=FACE_OUTER_BOUND('',#15766,.T.);
#9976=FACE_OUTER_BOUND('',#15767,.T.);
#9977=FACE_OUTER_BOUND('',#15768,.T.);
#9978=FACE_OUTER_BOUND('',#15769,.T.);
#9979=FACE_OUTER_BOUND('',#15770,.T.);
#9980=FACE_OUTER_BOUND('',#15771,.T.);
#9981=FACE_OUTER_BOUND('',#15772,.T.);
#9982=FACE_OUTER_BOUND('',#15773,.T.);
#9983=FACE_OUTER_BOUND('',#15774,.T.);
#9984=FACE_OUTER_BOUND('',#15775,.T.);
#9985=FACE_OUTER_BOUND('',#15776,.T.);
#9986=FACE_OUTER_BOUND('',#15777,.T.);
#9987=FACE_OUTER_BOUND('',#15778,.T.);
#9988=FACE_OUTER_BOUND('',#15779,.T.);
#9989=FACE_OUTER_BOUND('',#15780,.T.);
#9990=FACE_OUTER_BOUND('',#15781,.T.);
#9991=FACE_OUTER_BOUND('',#15782,.T.);
#9992=FACE_OUTER_BOUND('',#15783,.T.);
#9993=FACE_OUTER_BOUND('',#15784,.T.);
#9994=FACE_OUTER_BOUND('',#15785,.T.);
#9995=FACE_OUTER_BOUND('',#15786,.T.);
#9996=FACE_OUTER_BOUND('',#15787,.T.);
#9997=FACE_OUTER_BOUND('',#15788,.T.);
#9998=FACE_OUTER_BOUND('',#15789,.T.);
#9999=FACE_OUTER_BOUND('',#15790,.T.);
#10000=FACE_OUTER_BOUND('',#15791,.T.);
#10001=FACE_OUTER_BOUND('',#15792,.T.);
#10002=FACE_OUTER_BOUND('',#15793,.T.);
#10003=FACE_OUTER_BOUND('',#15794,.T.);
#10004=FACE_OUTER_BOUND('',#15795,.T.);
#10005=FACE_OUTER_BOUND('',#15796,.T.);
#10006=FACE_OUTER_BOUND('',#15797,.T.);
#10007=FACE_OUTER_BOUND('',#15798,.T.);
#10008=FACE_OUTER_BOUND('',#15799,.T.);
#10009=FACE_OUTER_BOUND('',#15800,.T.);
#10010=FACE_OUTER_BOUND('',#15801,.T.);
#10011=FACE_OUTER_BOUND('',#15802,.T.);
#10012=FACE_OUTER_BOUND('',#15803,.T.);
#10013=FACE_OUTER_BOUND('',#15804,.T.);
#10014=FACE_OUTER_BOUND('',#15805,.T.);
#10015=FACE_OUTER_BOUND('',#15806,.T.);
#10016=FACE_OUTER_BOUND('',#15807,.T.);
#10017=FACE_OUTER_BOUND('',#15808,.T.);
#10018=FACE_OUTER_BOUND('',#15809,.T.);
#10019=FACE_OUTER_BOUND('',#15810,.T.);
#10020=FACE_OUTER_BOUND('',#15811,.T.);
#10021=FACE_OUTER_BOUND('',#15812,.T.);
#10022=FACE_OUTER_BOUND('',#15813,.T.);
#10023=FACE_OUTER_BOUND('',#15814,.T.);
#10024=FACE_OUTER_BOUND('',#15815,.T.);
#10025=FACE_OUTER_BOUND('',#15816,.T.);
#10026=FACE_OUTER_BOUND('',#15817,.T.);
#10027=FACE_OUTER_BOUND('',#15818,.T.);
#10028=FACE_OUTER_BOUND('',#15819,.T.);
#10029=FACE_OUTER_BOUND('',#15820,.T.);
#10030=FACE_OUTER_BOUND('',#15821,.T.);
#10031=FACE_OUTER_BOUND('',#15822,.T.);
#10032=FACE_OUTER_BOUND('',#15823,.T.);
#10033=FACE_OUTER_BOUND('',#15824,.T.);
#10034=FACE_OUTER_BOUND('',#15825,.T.);
#10035=FACE_OUTER_BOUND('',#15826,.T.);
#10036=FACE_OUTER_BOUND('',#15827,.T.);
#10037=FACE_OUTER_BOUND('',#15828,.T.);
#10038=FACE_OUTER_BOUND('',#15829,.T.);
#10039=FACE_OUTER_BOUND('',#15830,.T.);
#10040=FACE_OUTER_BOUND('',#15831,.T.);
#10041=FACE_OUTER_BOUND('',#15832,.T.);
#10042=FACE_OUTER_BOUND('',#15833,.T.);
#10043=FACE_OUTER_BOUND('',#15834,.T.);
#10044=FACE_OUTER_BOUND('',#15835,.T.);
#10045=FACE_OUTER_BOUND('',#15836,.T.);
#10046=FACE_OUTER_BOUND('',#15837,.T.);
#10047=FACE_OUTER_BOUND('',#15838,.T.);
#10048=FACE_OUTER_BOUND('',#15839,.T.);
#10049=FACE_OUTER_BOUND('',#15840,.T.);
#10050=FACE_OUTER_BOUND('',#15841,.T.);
#10051=FACE_OUTER_BOUND('',#15842,.T.);
#10052=FACE_OUTER_BOUND('',#15843,.T.);
#10053=FACE_OUTER_BOUND('',#15844,.T.);
#10054=FACE_OUTER_BOUND('',#15845,.T.);
#10055=FACE_OUTER_BOUND('',#15846,.T.);
#10056=FACE_OUTER_BOUND('',#15847,.T.);
#10057=FACE_OUTER_BOUND('',#15848,.T.);
#10058=FACE_OUTER_BOUND('',#15849,.T.);
#10059=FACE_OUTER_BOUND('',#15850,.T.);
#10060=FACE_OUTER_BOUND('',#15851,.T.);
#10061=FACE_OUTER_BOUND('',#15852,.T.);
#10062=FACE_OUTER_BOUND('',#15853,.T.);
#10063=FACE_OUTER_BOUND('',#15854,.T.);
#10064=FACE_OUTER_BOUND('',#15855,.T.);
#10065=FACE_OUTER_BOUND('',#15856,.T.);
#10066=FACE_OUTER_BOUND('',#15857,.T.);
#10067=FACE_OUTER_BOUND('',#15858,.T.);
#10068=FACE_OUTER_BOUND('',#15859,.T.);
#10069=FACE_OUTER_BOUND('',#15860,.T.);
#10070=FACE_OUTER_BOUND('',#15861,.T.);
#10071=FACE_OUTER_BOUND('',#15862,.T.);
#10072=FACE_OUTER_BOUND('',#15863,.T.);
#10073=FACE_OUTER_BOUND('',#15864,.T.);
#10074=FACE_OUTER_BOUND('',#15865,.T.);
#10075=FACE_OUTER_BOUND('',#15866,.T.);
#10076=FACE_OUTER_BOUND('',#15867,.T.);
#10077=FACE_OUTER_BOUND('',#15868,.T.);
#10078=FACE_OUTER_BOUND('',#15869,.T.);
#10079=FACE_OUTER_BOUND('',#15870,.T.);
#10080=FACE_OUTER_BOUND('',#15871,.T.);
#10081=FACE_OUTER_BOUND('',#15872,.T.);
#10082=FACE_OUTER_BOUND('',#15873,.T.);
#10083=FACE_OUTER_BOUND('',#15874,.T.);
#10084=FACE_OUTER_BOUND('',#15875,.T.);
#10085=FACE_OUTER_BOUND('',#15876,.T.);
#10086=FACE_OUTER_BOUND('',#15877,.T.);
#10087=FACE_OUTER_BOUND('',#15878,.T.);
#10088=FACE_OUTER_BOUND('',#15879,.T.);
#10089=FACE_OUTER_BOUND('',#15880,.T.);
#10090=FACE_OUTER_BOUND('',#15881,.T.);
#10091=FACE_OUTER_BOUND('',#15882,.T.);
#10092=FACE_OUTER_BOUND('',#15883,.T.);
#10093=FACE_OUTER_BOUND('',#15884,.T.);
#10094=FACE_OUTER_BOUND('',#15885,.T.);
#10095=FACE_OUTER_BOUND('',#15886,.T.);
#10096=FACE_OUTER_BOUND('',#15887,.T.);
#10097=FACE_OUTER_BOUND('',#15888,.T.);
#10098=FACE_OUTER_BOUND('',#15889,.T.);
#10099=FACE_OUTER_BOUND('',#15890,.T.);
#10100=FACE_OUTER_BOUND('',#15891,.T.);
#10101=FACE_OUTER_BOUND('',#15892,.T.);
#10102=FACE_OUTER_BOUND('',#15893,.T.);
#10103=FACE_OUTER_BOUND('',#15894,.T.);
#10104=FACE_OUTER_BOUND('',#15895,.T.);
#10105=FACE_OUTER_BOUND('',#15896,.T.);
#10106=FACE_OUTER_BOUND('',#15897,.T.);
#10107=FACE_OUTER_BOUND('',#15898,.T.);
#10108=FACE_OUTER_BOUND('',#15899,.T.);
#10109=FACE_OUTER_BOUND('',#15900,.T.);
#10110=FACE_OUTER_BOUND('',#15901,.T.);
#10111=FACE_OUTER_BOUND('',#15902,.T.);
#10112=FACE_OUTER_BOUND('',#15903,.T.);
#10113=FACE_OUTER_BOUND('',#15904,.T.);
#10114=FACE_OUTER_BOUND('',#15905,.T.);
#10115=FACE_OUTER_BOUND('',#15906,.T.);
#10116=FACE_OUTER_BOUND('',#15907,.T.);
#10117=FACE_OUTER_BOUND('',#15908,.T.);
#10118=FACE_OUTER_BOUND('',#15909,.T.);
#10119=FACE_OUTER_BOUND('',#15910,.T.);
#10120=FACE_OUTER_BOUND('',#15911,.T.);
#10121=FACE_OUTER_BOUND('',#15912,.T.);
#10122=FACE_OUTER_BOUND('',#15913,.T.);
#10123=FACE_OUTER_BOUND('',#15914,.T.);
#10124=FACE_OUTER_BOUND('',#15915,.T.);
#10125=FACE_OUTER_BOUND('',#15916,.T.);
#10126=FACE_OUTER_BOUND('',#15917,.T.);
#10127=FACE_OUTER_BOUND('',#15918,.T.);
#10128=FACE_OUTER_BOUND('',#15919,.T.);
#10129=FACE_OUTER_BOUND('',#15920,.T.);
#10130=FACE_OUTER_BOUND('',#15921,.T.);
#10131=FACE_OUTER_BOUND('',#15922,.T.);
#10132=FACE_OUTER_BOUND('',#15923,.T.);
#10133=FACE_OUTER_BOUND('',#15924,.T.);
#10134=FACE_OUTER_BOUND('',#15925,.T.);
#10135=FACE_OUTER_BOUND('',#15926,.T.);
#10136=FACE_OUTER_BOUND('',#15927,.T.);
#10137=FACE_OUTER_BOUND('',#15928,.T.);
#10138=FACE_OUTER_BOUND('',#15929,.T.);
#10139=FACE_OUTER_BOUND('',#15930,.T.);
#10140=FACE_OUTER_BOUND('',#15931,.T.);
#10141=FACE_OUTER_BOUND('',#15932,.T.);
#10142=FACE_OUTER_BOUND('',#15933,.T.);
#10143=FACE_OUTER_BOUND('',#15934,.T.);
#10144=FACE_OUTER_BOUND('',#15935,.T.);
#10145=FACE_OUTER_BOUND('',#15936,.T.);
#10146=FACE_OUTER_BOUND('',#15937,.T.);
#10147=FACE_OUTER_BOUND('',#15938,.T.);
#10148=FACE_OUTER_BOUND('',#15939,.T.);
#10149=FACE_OUTER_BOUND('',#15940,.T.);
#10150=FACE_OUTER_BOUND('',#15941,.T.);
#10151=FACE_OUTER_BOUND('',#15942,.T.);
#10152=FACE_OUTER_BOUND('',#15943,.T.);
#10153=FACE_OUTER_BOUND('',#15944,.T.);
#10154=FACE_OUTER_BOUND('',#15945,.T.);
#10155=FACE_OUTER_BOUND('',#15946,.T.);
#10156=FACE_OUTER_BOUND('',#15947,.T.);
#10157=FACE_OUTER_BOUND('',#15948,.T.);
#10158=FACE_OUTER_BOUND('',#15949,.T.);
#10159=FACE_OUTER_BOUND('',#15950,.T.);
#10160=FACE_OUTER_BOUND('',#15951,.T.);
#10161=FACE_OUTER_BOUND('',#15952,.T.);
#10162=FACE_OUTER_BOUND('',#15953,.T.);
#10163=FACE_OUTER_BOUND('',#15954,.T.);
#10164=FACE_OUTER_BOUND('',#15955,.T.);
#10165=FACE_OUTER_BOUND('',#15956,.T.);
#10166=FACE_OUTER_BOUND('',#15957,.T.);
#10167=FACE_OUTER_BOUND('',#15958,.T.);
#10168=FACE_OUTER_BOUND('',#15959,.T.);
#10169=FACE_OUTER_BOUND('',#15960,.T.);
#10170=FACE_OUTER_BOUND('',#15961,.T.);
#10171=FACE_OUTER_BOUND('',#15962,.T.);
#10172=FACE_OUTER_BOUND('',#15963,.T.);
#10173=FACE_OUTER_BOUND('',#15964,.T.);
#10174=FACE_OUTER_BOUND('',#15965,.T.);
#10175=FACE_OUTER_BOUND('',#15966,.T.);
#10176=FACE_OUTER_BOUND('',#15967,.T.);
#10177=FACE_OUTER_BOUND('',#15968,.T.);
#10178=FACE_OUTER_BOUND('',#15969,.T.);
#10179=FACE_OUTER_BOUND('',#15970,.T.);
#10180=FACE_OUTER_BOUND('',#15971,.T.);
#10181=FACE_OUTER_BOUND('',#15972,.T.);
#10182=FACE_OUTER_BOUND('',#15973,.T.);
#10183=FACE_OUTER_BOUND('',#15974,.T.);
#10184=FACE_OUTER_BOUND('',#15975,.T.);
#10185=FACE_OUTER_BOUND('',#15976,.T.);
#10186=FACE_OUTER_BOUND('',#15977,.T.);
#10187=FACE_OUTER_BOUND('',#15978,.T.);
#10188=FACE_OUTER_BOUND('',#15979,.T.);
#10189=FACE_OUTER_BOUND('',#15980,.T.);
#10190=FACE_OUTER_BOUND('',#15981,.T.);
#10191=FACE_OUTER_BOUND('',#15982,.T.);
#10192=FACE_OUTER_BOUND('',#15983,.T.);
#10193=FACE_OUTER_BOUND('',#15984,.T.);
#10194=FACE_OUTER_BOUND('',#15985,.T.);
#10195=FACE_OUTER_BOUND('',#15986,.T.);
#10196=FACE_OUTER_BOUND('',#15987,.T.);
#10197=FACE_OUTER_BOUND('',#15988,.T.);
#10198=FACE_OUTER_BOUND('',#15989,.T.);
#10199=FACE_OUTER_BOUND('',#15990,.T.);
#10200=FACE_OUTER_BOUND('',#15991,.T.);
#10201=FACE_OUTER_BOUND('',#15992,.T.);
#10202=FACE_OUTER_BOUND('',#15993,.T.);
#10203=FACE_OUTER_BOUND('',#15994,.T.);
#10204=FACE_OUTER_BOUND('',#15995,.T.);
#10205=FACE_OUTER_BOUND('',#15996,.T.);
#10206=FACE_OUTER_BOUND('',#15997,.T.);
#10207=FACE_OUTER_BOUND('',#15998,.T.);
#10208=FACE_OUTER_BOUND('',#15999,.T.);
#10209=FACE_OUTER_BOUND('',#16000,.T.);
#10210=FACE_OUTER_BOUND('',#16001,.T.);
#10211=FACE_OUTER_BOUND('',#16002,.T.);
#10212=FACE_OUTER_BOUND('',#16003,.T.);
#10213=FACE_OUTER_BOUND('',#16004,.T.);
#10214=FACE_OUTER_BOUND('',#16005,.T.);
#10215=FACE_OUTER_BOUND('',#16006,.T.);
#10216=FACE_OUTER_BOUND('',#16007,.T.);
#10217=FACE_OUTER_BOUND('',#16008,.T.);
#10218=FACE_OUTER_BOUND('',#16009,.T.);
#10219=FACE_OUTER_BOUND('',#16010,.T.);
#10220=FACE_OUTER_BOUND('',#16011,.T.);
#10221=FACE_OUTER_BOUND('',#16012,.T.);
#10222=FACE_OUTER_BOUND('',#16013,.T.);
#10223=FACE_OUTER_BOUND('',#16014,.T.);
#10224=FACE_OUTER_BOUND('',#16015,.T.);
#10225=FACE_OUTER_BOUND('',#16016,.T.);
#10226=FACE_OUTER_BOUND('',#16017,.T.);
#10227=FACE_OUTER_BOUND('',#16018,.T.);
#10228=FACE_OUTER_BOUND('',#16019,.T.);
#10229=FACE_OUTER_BOUND('',#16020,.T.);
#10230=FACE_OUTER_BOUND('',#16021,.T.);
#10231=FACE_OUTER_BOUND('',#16022,.T.);
#10232=FACE_OUTER_BOUND('',#16023,.T.);
#10233=FACE_OUTER_BOUND('',#16024,.T.);
#10234=FACE_OUTER_BOUND('',#16025,.T.);
#10235=FACE_OUTER_BOUND('',#16026,.T.);
#10236=FACE_OUTER_BOUND('',#16027,.T.);
#10237=FACE_OUTER_BOUND('',#16028,.T.);
#10238=FACE_OUTER_BOUND('',#16029,.T.);
#10239=FACE_OUTER_BOUND('',#16030,.T.);
#10240=FACE_OUTER_BOUND('',#16031,.T.);
#10241=FACE_OUTER_BOUND('',#16032,.T.);
#10242=FACE_OUTER_BOUND('',#16033,.T.);
#10243=FACE_OUTER_BOUND('',#16034,.T.);
#10244=FACE_OUTER_BOUND('',#16035,.T.);
#10245=FACE_OUTER_BOUND('',#16036,.T.);
#10246=FACE_OUTER_BOUND('',#16037,.T.);
#10247=FACE_OUTER_BOUND('',#16038,.T.);
#10248=FACE_OUTER_BOUND('',#16039,.T.);
#10249=FACE_OUTER_BOUND('',#16040,.T.);
#10250=FACE_OUTER_BOUND('',#16041,.T.);
#10251=FACE_OUTER_BOUND('',#16042,.T.);
#10252=FACE_OUTER_BOUND('',#16043,.T.);
#10253=FACE_OUTER_BOUND('',#16044,.T.);
#10254=FACE_OUTER_BOUND('',#16045,.T.);
#10255=FACE_OUTER_BOUND('',#16046,.T.);
#10256=FACE_OUTER_BOUND('',#16047,.T.);
#10257=FACE_OUTER_BOUND('',#16048,.T.);
#10258=FACE_OUTER_BOUND('',#16049,.T.);
#10259=FACE_OUTER_BOUND('',#16050,.T.);
#10260=FACE_OUTER_BOUND('',#16051,.T.);
#10261=FACE_OUTER_BOUND('',#16052,.T.);
#10262=FACE_OUTER_BOUND('',#16053,.T.);
#10263=FACE_OUTER_BOUND('',#16054,.T.);
#10264=FACE_OUTER_BOUND('',#16055,.T.);
#10265=FACE_OUTER_BOUND('',#16056,.T.);
#10266=FACE_OUTER_BOUND('',#16057,.T.);
#10267=FACE_OUTER_BOUND('',#16058,.T.);
#10268=FACE_OUTER_BOUND('',#16059,.T.);
#10269=FACE_OUTER_BOUND('',#16060,.T.);
#10270=FACE_OUTER_BOUND('',#16061,.T.);
#10271=FACE_OUTER_BOUND('',#16062,.T.);
#10272=FACE_OUTER_BOUND('',#16063,.T.);
#10273=FACE_OUTER_BOUND('',#16064,.T.);
#10274=FACE_OUTER_BOUND('',#16065,.T.);
#10275=FACE_OUTER_BOUND('',#16066,.T.);
#10276=FACE_OUTER_BOUND('',#16067,.T.);
#10277=FACE_OUTER_BOUND('',#16068,.T.);
#10278=FACE_OUTER_BOUND('',#16069,.T.);
#10279=FACE_OUTER_BOUND('',#16070,.T.);
#10280=FACE_OUTER_BOUND('',#16071,.T.);
#10281=FACE_OUTER_BOUND('',#16072,.T.);
#10282=FACE_OUTER_BOUND('',#16073,.T.);
#10283=FACE_OUTER_BOUND('',#16074,.T.);
#10284=FACE_OUTER_BOUND('',#16075,.T.);
#10285=FACE_OUTER_BOUND('',#16076,.T.);
#10286=FACE_OUTER_BOUND('',#16077,.T.);
#10287=FACE_OUTER_BOUND('',#16078,.T.);
#10288=FACE_OUTER_BOUND('',#16079,.T.);
#10289=FACE_OUTER_BOUND('',#16080,.T.);
#10290=FACE_OUTER_BOUND('',#16081,.T.);
#10291=FACE_OUTER_BOUND('',#16082,.T.);
#10292=FACE_OUTER_BOUND('',#16083,.T.);
#10293=FACE_OUTER_BOUND('',#16084,.T.);
#10294=FACE_OUTER_BOUND('',#16085,.T.);
#10295=FACE_OUTER_BOUND('',#16086,.T.);
#10296=FACE_OUTER_BOUND('',#16087,.T.);
#10297=FACE_OUTER_BOUND('',#16088,.T.);
#10298=FACE_OUTER_BOUND('',#16089,.T.);
#10299=FACE_OUTER_BOUND('',#16090,.T.);
#10300=FACE_OUTER_BOUND('',#16091,.T.);
#10301=FACE_OUTER_BOUND('',#16092,.T.);
#10302=FACE_OUTER_BOUND('',#16093,.T.);
#10303=FACE_OUTER_BOUND('',#16094,.T.);
#10304=FACE_OUTER_BOUND('',#16095,.T.);
#10305=FACE_OUTER_BOUND('',#16096,.T.);
#10306=FACE_OUTER_BOUND('',#16097,.T.);
#10307=FACE_OUTER_BOUND('',#16098,.T.);
#10308=FACE_OUTER_BOUND('',#16099,.T.);
#10309=FACE_OUTER_BOUND('',#16100,.T.);
#10310=FACE_OUTER_BOUND('',#16101,.T.);
#10311=FACE_OUTER_BOUND('',#16102,.T.);
#10312=FACE_OUTER_BOUND('',#16103,.T.);
#10313=FACE_OUTER_BOUND('',#16104,.T.);
#10314=FACE_OUTER_BOUND('',#16105,.T.);
#10315=FACE_OUTER_BOUND('',#16106,.T.);
#10316=FACE_OUTER_BOUND('',#16107,.T.);
#10317=FACE_OUTER_BOUND('',#16108,.T.);
#10318=FACE_OUTER_BOUND('',#16109,.T.);
#10319=FACE_OUTER_BOUND('',#16110,.T.);
#10320=FACE_OUTER_BOUND('',#16111,.T.);
#10321=FACE_OUTER_BOUND('',#16112,.T.);
#10322=FACE_OUTER_BOUND('',#16113,.T.);
#10323=FACE_OUTER_BOUND('',#16114,.T.);
#10324=FACE_OUTER_BOUND('',#16115,.T.);
#10325=FACE_OUTER_BOUND('',#16116,.T.);
#10326=FACE_OUTER_BOUND('',#16117,.T.);
#10327=FACE_OUTER_BOUND('',#16118,.T.);
#10328=FACE_OUTER_BOUND('',#16119,.T.);
#10329=FACE_OUTER_BOUND('',#16120,.T.);
#10330=FACE_OUTER_BOUND('',#16121,.T.);
#10331=FACE_OUTER_BOUND('',#16122,.T.);
#10332=FACE_OUTER_BOUND('',#16123,.T.);
#10333=FACE_OUTER_BOUND('',#16124,.T.);
#10334=FACE_OUTER_BOUND('',#16125,.T.);
#10335=FACE_OUTER_BOUND('',#16126,.T.);
#10336=FACE_OUTER_BOUND('',#16127,.T.);
#10337=FACE_OUTER_BOUND('',#16128,.T.);
#10338=FACE_OUTER_BOUND('',#16129,.T.);
#10339=FACE_OUTER_BOUND('',#16130,.T.);
#10340=FACE_OUTER_BOUND('',#16131,.T.);
#10341=FACE_OUTER_BOUND('',#16132,.T.);
#10342=FACE_OUTER_BOUND('',#16133,.T.);
#10343=FACE_OUTER_BOUND('',#16134,.T.);
#10344=FACE_OUTER_BOUND('',#16135,.T.);
#10345=FACE_OUTER_BOUND('',#16136,.T.);
#10346=FACE_OUTER_BOUND('',#16137,.T.);
#10347=FACE_OUTER_BOUND('',#16138,.T.);
#10348=FACE_OUTER_BOUND('',#16139,.T.);
#10349=FACE_OUTER_BOUND('',#16140,.T.);
#10350=FACE_OUTER_BOUND('',#16141,.T.);
#10351=FACE_OUTER_BOUND('',#16142,.T.);
#10352=FACE_OUTER_BOUND('',#16143,.T.);
#10353=FACE_OUTER_BOUND('',#16144,.T.);
#10354=FACE_OUTER_BOUND('',#16145,.T.);
#10355=FACE_OUTER_BOUND('',#16146,.T.);
#10356=FACE_OUTER_BOUND('',#16147,.T.);
#10357=FACE_OUTER_BOUND('',#16148,.T.);
#10358=FACE_OUTER_BOUND('',#16149,.T.);
#10359=FACE_OUTER_BOUND('',#16150,.T.);
#10360=FACE_OUTER_BOUND('',#16151,.T.);
#10361=FACE_OUTER_BOUND('',#16152,.T.);
#10362=FACE_OUTER_BOUND('',#16153,.T.);
#10363=FACE_OUTER_BOUND('',#16154,.T.);
#10364=FACE_OUTER_BOUND('',#16155,.T.);
#10365=FACE_OUTER_BOUND('',#16156,.T.);
#10366=FACE_OUTER_BOUND('',#16157,.T.);
#10367=FACE_OUTER_BOUND('',#16158,.T.);
#10368=FACE_OUTER_BOUND('',#16159,.T.);
#10369=FACE_OUTER_BOUND('',#16160,.T.);
#10370=FACE_OUTER_BOUND('',#16161,.T.);
#10371=FACE_OUTER_BOUND('',#16162,.T.);
#10372=FACE_OUTER_BOUND('',#16163,.T.);
#10373=FACE_OUTER_BOUND('',#16164,.T.);
#10374=FACE_OUTER_BOUND('',#16165,.T.);
#10375=FACE_OUTER_BOUND('',#16166,.T.);
#10376=FACE_OUTER_BOUND('',#16167,.T.);
#10377=FACE_OUTER_BOUND('',#16168,.T.);
#10378=FACE_OUTER_BOUND('',#16169,.T.);
#10379=FACE_OUTER_BOUND('',#16170,.T.);
#10380=FACE_OUTER_BOUND('',#16171,.T.);
#10381=FACE_OUTER_BOUND('',#16172,.T.);
#10382=FACE_OUTER_BOUND('',#16173,.T.);
#10383=FACE_OUTER_BOUND('',#16174,.T.);
#10384=FACE_OUTER_BOUND('',#16175,.T.);
#10385=FACE_OUTER_BOUND('',#16176,.T.);
#10386=FACE_OUTER_BOUND('',#16177,.T.);
#10387=FACE_OUTER_BOUND('',#16178,.T.);
#10388=FACE_OUTER_BOUND('',#16179,.T.);
#10389=FACE_OUTER_BOUND('',#16180,.T.);
#10390=FACE_OUTER_BOUND('',#16181,.T.);
#10391=FACE_OUTER_BOUND('',#16182,.T.);
#10392=FACE_OUTER_BOUND('',#16183,.T.);
#10393=FACE_OUTER_BOUND('',#16184,.T.);
#10394=FACE_OUTER_BOUND('',#16185,.T.);
#10395=FACE_OUTER_BOUND('',#16186,.T.);
#10396=FACE_OUTER_BOUND('',#16187,.T.);
#10397=FACE_OUTER_BOUND('',#16188,.T.);
#10398=FACE_OUTER_BOUND('',#16189,.T.);
#10399=FACE_OUTER_BOUND('',#16190,.T.);
#10400=FACE_OUTER_BOUND('',#16191,.T.);
#10401=FACE_OUTER_BOUND('',#16192,.T.);
#10402=FACE_OUTER_BOUND('',#16193,.T.);
#10403=FACE_OUTER_BOUND('',#16194,.T.);
#10404=FACE_OUTER_BOUND('',#16195,.T.);
#10405=FACE_OUTER_BOUND('',#16196,.T.);
#10406=FACE_OUTER_BOUND('',#16197,.T.);
#10407=FACE_OUTER_BOUND('',#16198,.T.);
#10408=FACE_OUTER_BOUND('',#16199,.T.);
#10409=FACE_OUTER_BOUND('',#16200,.T.);
#10410=FACE_OUTER_BOUND('',#16201,.T.);
#10411=FACE_OUTER_BOUND('',#16202,.T.);
#10412=FACE_OUTER_BOUND('',#16203,.T.);
#10413=FACE_OUTER_BOUND('',#16204,.T.);
#10414=FACE_OUTER_BOUND('',#16205,.T.);
#10415=FACE_OUTER_BOUND('',#16206,.T.);
#10416=FACE_OUTER_BOUND('',#16207,.T.);
#10417=FACE_OUTER_BOUND('',#16208,.T.);
#10418=FACE_OUTER_BOUND('',#16209,.T.);
#10419=FACE_OUTER_BOUND('',#16210,.T.);
#10420=FACE_OUTER_BOUND('',#16211,.T.);
#10421=FACE_OUTER_BOUND('',#16212,.T.);
#10422=FACE_OUTER_BOUND('',#16213,.T.);
#10423=FACE_OUTER_BOUND('',#16214,.T.);
#10424=FACE_OUTER_BOUND('',#16215,.T.);
#10425=FACE_OUTER_BOUND('',#16216,.T.);
#10426=FACE_OUTER_BOUND('',#16217,.T.);
#10427=FACE_OUTER_BOUND('',#16218,.T.);
#10428=FACE_OUTER_BOUND('',#16219,.T.);
#10429=FACE_OUTER_BOUND('',#16220,.T.);
#10430=FACE_OUTER_BOUND('',#16221,.T.);
#10431=FACE_OUTER_BOUND('',#16222,.T.);
#10432=FACE_OUTER_BOUND('',#16223,.T.);
#10433=FACE_OUTER_BOUND('',#16224,.T.);
#10434=FACE_OUTER_BOUND('',#16225,.T.);
#10435=FACE_OUTER_BOUND('',#16226,.T.);
#10436=FACE_OUTER_BOUND('',#16227,.T.);
#10437=FACE_OUTER_BOUND('',#16228,.T.);
#10438=FACE_OUTER_BOUND('',#16229,.T.);
#10439=FACE_OUTER_BOUND('',#16230,.T.);
#10440=FACE_OUTER_BOUND('',#16231,.T.);
#10441=FACE_OUTER_BOUND('',#16232,.T.);
#10442=FACE_OUTER_BOUND('',#16233,.T.);
#10443=FACE_OUTER_BOUND('',#16234,.T.);
#10444=FACE_OUTER_BOUND('',#16235,.T.);
#10445=FACE_OUTER_BOUND('',#16236,.T.);
#10446=FACE_OUTER_BOUND('',#16237,.T.);
#10447=FACE_OUTER_BOUND('',#16238,.T.);
#10448=FACE_OUTER_BOUND('',#16239,.T.);
#10449=FACE_OUTER_BOUND('',#16240,.T.);
#10450=FACE_OUTER_BOUND('',#16241,.T.);
#10451=FACE_OUTER_BOUND('',#16242,.T.);
#10452=FACE_OUTER_BOUND('',#16243,.T.);
#10453=FACE_OUTER_BOUND('',#16244,.T.);
#10454=FACE_OUTER_BOUND('',#16245,.T.);
#10455=FACE_OUTER_BOUND('',#16246,.T.);
#10456=FACE_OUTER_BOUND('',#16247,.T.);
#10457=FACE_OUTER_BOUND('',#16248,.T.);
#10458=FACE_OUTER_BOUND('',#16249,.T.);
#10459=FACE_OUTER_BOUND('',#16250,.T.);
#10460=FACE_OUTER_BOUND('',#16251,.T.);
#10461=FACE_OUTER_BOUND('',#16252,.T.);
#10462=FACE_OUTER_BOUND('',#16253,.T.);
#10463=FACE_OUTER_BOUND('',#16254,.T.);
#10464=FACE_OUTER_BOUND('',#16255,.T.);
#10465=FACE_OUTER_BOUND('',#16256,.T.);
#10466=FACE_OUTER_BOUND('',#16257,.T.);
#10467=FACE_OUTER_BOUND('',#16258,.T.);
#10468=FACE_OUTER_BOUND('',#16259,.T.);
#10469=FACE_OUTER_BOUND('',#16260,.T.);
#10470=FACE_OUTER_BOUND('',#16261,.T.);
#10471=FACE_OUTER_BOUND('',#16262,.T.);
#10472=FACE_OUTER_BOUND('',#16263,.T.);
#10473=FACE_OUTER_BOUND('',#16264,.T.);
#10474=FACE_OUTER_BOUND('',#16265,.T.);
#10475=FACE_OUTER_BOUND('',#16266,.T.);
#10476=FACE_OUTER_BOUND('',#16267,.T.);
#10477=FACE_OUTER_BOUND('',#16268,.T.);
#10478=FACE_OUTER_BOUND('',#16269,.T.);
#10479=FACE_OUTER_BOUND('',#16270,.T.);
#10480=FACE_OUTER_BOUND('',#16271,.T.);
#10481=FACE_OUTER_BOUND('',#16272,.T.);
#10482=FACE_OUTER_BOUND('',#16273,.T.);
#10483=FACE_OUTER_BOUND('',#16274,.T.);
#10484=FACE_OUTER_BOUND('',#16275,.T.);
#10485=FACE_OUTER_BOUND('',#16276,.T.);
#10486=FACE_OUTER_BOUND('',#16277,.T.);
#10487=FACE_OUTER_BOUND('',#16278,.T.);
#10488=FACE_OUTER_BOUND('',#16279,.T.);
#10489=FACE_OUTER_BOUND('',#16280,.T.);
#10490=FACE_OUTER_BOUND('',#16281,.T.);
#10491=FACE_OUTER_BOUND('',#16282,.T.);
#10492=FACE_OUTER_BOUND('',#16283,.T.);
#10493=FACE_OUTER_BOUND('',#16284,.T.);
#10494=FACE_OUTER_BOUND('',#16285,.T.);
#10495=FACE_OUTER_BOUND('',#16286,.T.);
#10496=FACE_OUTER_BOUND('',#16287,.T.);
#10497=FACE_OUTER_BOUND('',#16288,.T.);
#10498=FACE_OUTER_BOUND('',#16289,.T.);
#10499=FACE_OUTER_BOUND('',#16290,.T.);
#10500=FACE_OUTER_BOUND('',#16291,.T.);
#10501=FACE_OUTER_BOUND('',#16292,.T.);
#10502=FACE_OUTER_BOUND('',#16293,.T.);
#10503=FACE_OUTER_BOUND('',#16294,.T.);
#10504=FACE_OUTER_BOUND('',#16295,.T.);
#10505=FACE_OUTER_BOUND('',#16296,.T.);
#10506=FACE_OUTER_BOUND('',#16297,.T.);
#10507=FACE_OUTER_BOUND('',#16298,.T.);
#10508=FACE_OUTER_BOUND('',#16299,.T.);
#10509=FACE_OUTER_BOUND('',#16300,.T.);
#10510=FACE_OUTER_BOUND('',#16301,.T.);
#10511=FACE_OUTER_BOUND('',#16302,.T.);
#10512=FACE_OUTER_BOUND('',#16303,.T.);
#10513=FACE_OUTER_BOUND('',#16304,.T.);
#10514=FACE_OUTER_BOUND('',#16305,.T.);
#10515=FACE_OUTER_BOUND('',#16306,.T.);
#10516=FACE_OUTER_BOUND('',#16307,.T.);
#10517=FACE_OUTER_BOUND('',#16308,.T.);
#10518=FACE_OUTER_BOUND('',#16309,.T.);
#10519=FACE_OUTER_BOUND('',#16310,.T.);
#10520=FACE_OUTER_BOUND('',#16311,.T.);
#10521=FACE_OUTER_BOUND('',#16312,.T.);
#10522=FACE_OUTER_BOUND('',#16313,.T.);
#10523=FACE_OUTER_BOUND('',#16314,.T.);
#10524=FACE_OUTER_BOUND('',#16315,.T.);
#10525=FACE_OUTER_BOUND('',#16316,.T.);
#10526=FACE_OUTER_BOUND('',#16317,.T.);
#10527=FACE_OUTER_BOUND('',#16318,.T.);
#10528=FACE_OUTER_BOUND('',#16319,.T.);
#10529=FACE_OUTER_BOUND('',#16320,.T.);
#10530=FACE_OUTER_BOUND('',#16321,.T.);
#10531=FACE_OUTER_BOUND('',#16322,.T.);
#10532=FACE_OUTER_BOUND('',#16323,.T.);
#10533=FACE_OUTER_BOUND('',#16324,.T.);
#10534=FACE_OUTER_BOUND('',#16325,.T.);
#10535=FACE_OUTER_BOUND('',#16326,.T.);
#10536=FACE_OUTER_BOUND('',#16327,.T.);
#10537=FACE_OUTER_BOUND('',#16328,.T.);
#10538=FACE_OUTER_BOUND('',#16329,.T.);
#10539=FACE_OUTER_BOUND('',#16330,.T.);
#10540=FACE_OUTER_BOUND('',#16331,.T.);
#10541=FACE_OUTER_BOUND('',#16332,.T.);
#10542=FACE_OUTER_BOUND('',#16333,.T.);
#10543=FACE_OUTER_BOUND('',#16334,.T.);
#10544=FACE_OUTER_BOUND('',#16335,.T.);
#10545=FACE_OUTER_BOUND('',#16336,.T.);
#10546=FACE_OUTER_BOUND('',#16337,.T.);
#10547=FACE_OUTER_BOUND('',#16338,.T.);
#10548=FACE_OUTER_BOUND('',#16339,.T.);
#10549=FACE_OUTER_BOUND('',#16340,.T.);
#10550=FACE_OUTER_BOUND('',#16341,.T.);
#10551=FACE_OUTER_BOUND('',#16342,.T.);
#10552=FACE_OUTER_BOUND('',#16343,.T.);
#10553=FACE_OUTER_BOUND('',#16344,.T.);
#10554=FACE_OUTER_BOUND('',#16345,.T.);
#10555=FACE_OUTER_BOUND('',#16346,.T.);
#10556=FACE_OUTER_BOUND('',#16347,.T.);
#10557=FACE_OUTER_BOUND('',#16348,.T.);
#10558=FACE_OUTER_BOUND('',#16349,.T.);
#10559=FACE_OUTER_BOUND('',#16350,.T.);
#10560=FACE_OUTER_BOUND('',#16351,.T.);
#10561=FACE_OUTER_BOUND('',#16352,.T.);
#10562=FACE_OUTER_BOUND('',#16353,.T.);
#10563=FACE_OUTER_BOUND('',#16354,.T.);
#10564=FACE_OUTER_BOUND('',#16355,.T.);
#10565=FACE_OUTER_BOUND('',#16356,.T.);
#10566=FACE_OUTER_BOUND('',#16357,.T.);
#10567=FACE_OUTER_BOUND('',#16358,.T.);
#10568=FACE_OUTER_BOUND('',#16359,.T.);
#10569=FACE_OUTER_BOUND('',#16360,.T.);
#10570=FACE_OUTER_BOUND('',#16362,.T.);
#10571=FACE_OUTER_BOUND('',#16363,.T.);
#10572=FACE_OUTER_BOUND('',#16364,.T.);
#10573=FACE_OUTER_BOUND('',#16365,.T.);
#10574=FACE_OUTER_BOUND('',#16366,.T.);
#10575=FACE_OUTER_BOUND('',#16367,.T.);
#10576=FACE_OUTER_BOUND('',#16368,.T.);
#10577=FACE_OUTER_BOUND('',#16369,.T.);
#10578=FACE_OUTER_BOUND('',#16370,.T.);
#10579=FACE_OUTER_BOUND('',#16372,.T.);
#10580=FACE_OUTER_BOUND('',#16373,.T.);
#10581=FACE_OUTER_BOUND('',#16374,.T.);
#10582=FACE_OUTER_BOUND('',#16375,.T.);
#10583=FACE_OUTER_BOUND('',#16376,.T.);
#10584=FACE_OUTER_BOUND('',#16377,.T.);
#10585=FACE_OUTER_BOUND('',#16378,.T.);
#10586=FACE_OUTER_BOUND('',#16379,.T.);
#10587=FACE_OUTER_BOUND('',#16380,.T.);
#10588=FACE_OUTER_BOUND('',#16381,.T.);
#10589=FACE_OUTER_BOUND('',#16382,.T.);
#10590=FACE_OUTER_BOUND('',#16383,.T.);
#10591=FACE_OUTER_BOUND('',#16384,.T.);
#10592=FACE_OUTER_BOUND('',#16385,.T.);
#10593=FACE_OUTER_BOUND('',#16386,.T.);
#10594=FACE_OUTER_BOUND('',#16387,.T.);
#10595=FACE_OUTER_BOUND('',#16388,.T.);
#10596=FACE_OUTER_BOUND('',#16389,.T.);
#10597=FACE_OUTER_BOUND('',#16390,.T.);
#10598=FACE_OUTER_BOUND('',#16391,.T.);
#10599=FACE_OUTER_BOUND('',#16392,.T.);
#10600=FACE_OUTER_BOUND('',#16393,.T.);
#10601=FACE_OUTER_BOUND('',#16394,.T.);
#10602=FACE_OUTER_BOUND('',#16395,.T.);
#10603=FACE_OUTER_BOUND('',#16396,.T.);
#10604=FACE_OUTER_BOUND('',#16397,.T.);
#10605=FACE_OUTER_BOUND('',#16398,.T.);
#10606=FACE_OUTER_BOUND('',#16399,.T.);
#10607=FACE_OUTER_BOUND('',#16400,.T.);
#10608=FACE_OUTER_BOUND('',#16401,.T.);
#10609=FACE_OUTER_BOUND('',#16402,.T.);
#10610=FACE_OUTER_BOUND('',#16403,.T.);
#10611=FACE_OUTER_BOUND('',#16404,.T.);
#10612=FACE_OUTER_BOUND('',#16405,.T.);
#10613=FACE_OUTER_BOUND('',#16406,.T.);
#10614=FACE_OUTER_BOUND('',#16407,.T.);
#10615=FACE_OUTER_BOUND('',#16408,.T.);
#10616=FACE_OUTER_BOUND('',#16409,.T.);
#10617=FACE_OUTER_BOUND('',#16410,.T.);
#10618=FACE_OUTER_BOUND('',#16411,.T.);
#10619=FACE_OUTER_BOUND('',#16412,.T.);
#10620=FACE_OUTER_BOUND('',#16413,.T.);
#10621=FACE_OUTER_BOUND('',#16414,.T.);
#10622=FACE_OUTER_BOUND('',#16415,.T.);
#10623=FACE_OUTER_BOUND('',#16416,.T.);
#10624=FACE_OUTER_BOUND('',#16417,.T.);
#10625=FACE_OUTER_BOUND('',#16418,.T.);
#10626=FACE_OUTER_BOUND('',#16419,.T.);
#10627=FACE_OUTER_BOUND('',#16420,.T.);
#10628=FACE_OUTER_BOUND('',#16421,.T.);
#10629=FACE_OUTER_BOUND('',#16422,.T.);
#10630=FACE_OUTER_BOUND('',#16423,.T.);
#10631=FACE_OUTER_BOUND('',#16424,.T.);
#10632=FACE_OUTER_BOUND('',#16425,.T.);
#10633=FACE_OUTER_BOUND('',#16426,.T.);
#10634=FACE_OUTER_BOUND('',#16427,.T.);
#10635=FACE_OUTER_BOUND('',#16428,.T.);
#10636=FACE_OUTER_BOUND('',#16429,.T.);
#10637=FACE_OUTER_BOUND('',#16430,.T.);
#10638=FACE_OUTER_BOUND('',#16431,.T.);
#10639=FACE_OUTER_BOUND('',#16432,.T.);
#10640=FACE_OUTER_BOUND('',#16433,.T.);
#10641=FACE_OUTER_BOUND('',#16434,.T.);
#10642=FACE_OUTER_BOUND('',#16435,.T.);
#10643=FACE_OUTER_BOUND('',#16436,.T.);
#10644=FACE_OUTER_BOUND('',#16437,.T.);
#10645=FACE_OUTER_BOUND('',#16438,.T.);
#10646=FACE_OUTER_BOUND('',#16439,.T.);
#10647=FACE_OUTER_BOUND('',#16440,.T.);
#10648=FACE_OUTER_BOUND('',#16441,.T.);
#10649=FACE_OUTER_BOUND('',#16442,.T.);
#10650=FACE_OUTER_BOUND('',#16443,.T.);
#10651=FACE_OUTER_BOUND('',#16444,.T.);
#10652=FACE_OUTER_BOUND('',#16445,.T.);
#10653=FACE_OUTER_BOUND('',#16446,.T.);
#10654=FACE_OUTER_BOUND('',#16447,.T.);
#10655=FACE_OUTER_BOUND('',#16448,.T.);
#10656=FACE_OUTER_BOUND('',#16449,.T.);
#10657=FACE_OUTER_BOUND('',#16450,.T.);
#10658=FACE_OUTER_BOUND('',#16451,.T.);
#10659=FACE_OUTER_BOUND('',#16452,.T.);
#10660=FACE_OUTER_BOUND('',#16453,.T.);
#10661=FACE_OUTER_BOUND('',#16454,.T.);
#10662=FACE_OUTER_BOUND('',#16455,.T.);
#10663=FACE_OUTER_BOUND('',#16456,.T.);
#10664=FACE_OUTER_BOUND('',#16457,.T.);
#10665=FACE_OUTER_BOUND('',#16458,.T.);
#10666=FACE_OUTER_BOUND('',#16459,.T.);
#10667=FACE_OUTER_BOUND('',#16460,.T.);
#10668=FACE_OUTER_BOUND('',#16461,.T.);
#10669=FACE_OUTER_BOUND('',#16462,.T.);
#10670=FACE_OUTER_BOUND('',#16463,.T.);
#10671=FACE_OUTER_BOUND('',#16464,.T.);
#10672=FACE_OUTER_BOUND('',#16465,.T.);
#10673=FACE_OUTER_BOUND('',#16466,.T.);
#10674=FACE_OUTER_BOUND('',#16467,.T.);
#10675=FACE_OUTER_BOUND('',#16468,.T.);
#10676=FACE_OUTER_BOUND('',#16469,.T.);
#10677=FACE_OUTER_BOUND('',#16470,.T.);
#10678=FACE_OUTER_BOUND('',#16471,.T.);
#10679=FACE_OUTER_BOUND('',#16472,.T.);
#10680=FACE_OUTER_BOUND('',#16473,.T.);
#10681=FACE_OUTER_BOUND('',#16474,.T.);
#10682=FACE_OUTER_BOUND('',#16475,.T.);
#10683=FACE_OUTER_BOUND('',#16476,.T.);
#10684=FACE_OUTER_BOUND('',#16477,.T.);
#10685=FACE_OUTER_BOUND('',#16478,.T.);
#10686=FACE_OUTER_BOUND('',#16479,.T.);
#10687=FACE_OUTER_BOUND('',#16480,.T.);
#10688=FACE_OUTER_BOUND('',#16481,.T.);
#10689=FACE_OUTER_BOUND('',#16482,.T.);
#10690=FACE_OUTER_BOUND('',#16483,.T.);
#10691=FACE_OUTER_BOUND('',#16484,.T.);
#10692=FACE_OUTER_BOUND('',#16485,.T.);
#10693=FACE_OUTER_BOUND('',#16486,.T.);
#10694=FACE_OUTER_BOUND('',#16487,.T.);
#10695=FACE_OUTER_BOUND('',#16488,.T.);
#10696=FACE_OUTER_BOUND('',#16489,.T.);
#10697=FACE_OUTER_BOUND('',#16490,.T.);
#10698=FACE_OUTER_BOUND('',#16491,.T.);
#10699=FACE_OUTER_BOUND('',#16492,.T.);
#10700=FACE_OUTER_BOUND('',#16493,.T.);
#10701=FACE_OUTER_BOUND('',#16494,.T.);
#10702=FACE_OUTER_BOUND('',#16495,.T.);
#10703=FACE_OUTER_BOUND('',#16496,.T.);
#10704=FACE_OUTER_BOUND('',#16497,.T.);
#10705=FACE_OUTER_BOUND('',#16498,.T.);
#10706=FACE_OUTER_BOUND('',#16499,.T.);
#10707=FACE_OUTER_BOUND('',#16500,.T.);
#10708=FACE_OUTER_BOUND('',#16501,.T.);
#10709=FACE_OUTER_BOUND('',#16502,.T.);
#10710=FACE_OUTER_BOUND('',#16503,.T.);
#10711=FACE_OUTER_BOUND('',#16504,.T.);
#10712=FACE_OUTER_BOUND('',#16505,.T.);
#10713=FACE_OUTER_BOUND('',#16506,.T.);
#10714=FACE_OUTER_BOUND('',#16507,.T.);
#10715=FACE_OUTER_BOUND('',#16508,.T.);
#10716=FACE_OUTER_BOUND('',#16509,.T.);
#10717=FACE_OUTER_BOUND('',#16510,.T.);
#10718=FACE_OUTER_BOUND('',#16511,.T.);
#10719=FACE_OUTER_BOUND('',#16512,.T.);
#10720=FACE_OUTER_BOUND('',#16513,.T.);
#10721=FACE_OUTER_BOUND('',#16514,.T.);
#10722=FACE_OUTER_BOUND('',#16515,.T.);
#10723=FACE_OUTER_BOUND('',#16516,.T.);
#10724=FACE_OUTER_BOUND('',#16517,.T.);
#10725=FACE_OUTER_BOUND('',#16518,.T.);
#10726=FACE_OUTER_BOUND('',#16519,.T.);
#10727=FACE_OUTER_BOUND('',#16520,.T.);
#10728=FACE_OUTER_BOUND('',#16521,.T.);
#10729=FACE_OUTER_BOUND('',#16522,.T.);
#10730=FACE_OUTER_BOUND('',#16523,.T.);
#10731=FACE_OUTER_BOUND('',#16524,.T.);
#10732=FACE_OUTER_BOUND('',#16525,.T.);
#10733=FACE_OUTER_BOUND('',#16526,.T.);
#10734=FACE_OUTER_BOUND('',#16527,.T.);
#10735=FACE_OUTER_BOUND('',#16528,.T.);
#10736=FACE_OUTER_BOUND('',#16529,.T.);
#10737=FACE_OUTER_BOUND('',#16530,.T.);
#10738=FACE_OUTER_BOUND('',#16531,.T.);
#10739=FACE_OUTER_BOUND('',#16532,.T.);
#10740=FACE_OUTER_BOUND('',#16533,.T.);
#10741=FACE_OUTER_BOUND('',#16534,.T.);
#10742=FACE_OUTER_BOUND('',#16535,.T.);
#10743=FACE_OUTER_BOUND('',#16536,.T.);
#10744=FACE_OUTER_BOUND('',#16537,.T.);
#10745=FACE_OUTER_BOUND('',#16538,.T.);
#10746=FACE_OUTER_BOUND('',#16539,.T.);
#10747=FACE_OUTER_BOUND('',#16540,.T.);
#10748=FACE_OUTER_BOUND('',#16541,.T.);
#10749=FACE_OUTER_BOUND('',#16542,.T.);
#10750=FACE_OUTER_BOUND('',#16543,.T.);
#10751=FACE_OUTER_BOUND('',#16544,.T.);
#10752=FACE_OUTER_BOUND('',#16545,.T.);
#10753=FACE_OUTER_BOUND('',#16546,.T.);
#10754=FACE_OUTER_BOUND('',#16547,.T.);
#10755=FACE_OUTER_BOUND('',#16548,.T.);
#10756=FACE_OUTER_BOUND('',#16549,.T.);
#10757=FACE_OUTER_BOUND('',#16550,.T.);
#10758=FACE_OUTER_BOUND('',#16551,.T.);
#10759=FACE_OUTER_BOUND('',#16552,.T.);
#10760=FACE_OUTER_BOUND('',#16553,.T.);
#10761=FACE_OUTER_BOUND('',#16554,.T.);
#10762=FACE_OUTER_BOUND('',#16555,.T.);
#10763=FACE_OUTER_BOUND('',#16556,.T.);
#10764=FACE_OUTER_BOUND('',#16557,.T.);
#10765=FACE_OUTER_BOUND('',#16558,.T.);
#10766=FACE_OUTER_BOUND('',#16559,.T.);
#10767=FACE_OUTER_BOUND('',#16560,.T.);
#10768=FACE_OUTER_BOUND('',#16561,.T.);
#10769=FACE_OUTER_BOUND('',#16562,.T.);
#10770=FACE_OUTER_BOUND('',#16563,.T.);
#10771=FACE_OUTER_BOUND('',#16564,.T.);
#10772=FACE_OUTER_BOUND('',#16565,.T.);
#10773=FACE_OUTER_BOUND('',#16566,.T.);
#10774=FACE_OUTER_BOUND('',#16567,.T.);
#10775=FACE_OUTER_BOUND('',#16568,.T.);
#10776=FACE_OUTER_BOUND('',#16569,.T.);
#10777=FACE_OUTER_BOUND('',#16570,.T.);
#10778=FACE_OUTER_BOUND('',#16571,.T.);
#10779=FACE_OUTER_BOUND('',#16572,.T.);
#10780=FACE_OUTER_BOUND('',#16573,.T.);
#10781=FACE_OUTER_BOUND('',#16574,.T.);
#10782=FACE_OUTER_BOUND('',#16575,.T.);
#10783=FACE_OUTER_BOUND('',#16576,.T.);
#10784=FACE_OUTER_BOUND('',#16577,.T.);
#10785=FACE_OUTER_BOUND('',#16578,.T.);
#10786=FACE_OUTER_BOUND('',#16579,.T.);
#10787=FACE_OUTER_BOUND('',#16580,.T.);
#10788=FACE_OUTER_BOUND('',#16581,.T.);
#10789=FACE_OUTER_BOUND('',#16582,.T.);
#10790=FACE_OUTER_BOUND('',#16583,.T.);
#10791=FACE_OUTER_BOUND('',#16584,.T.);
#10792=FACE_OUTER_BOUND('',#16585,.T.);
#10793=FACE_OUTER_BOUND('',#16586,.T.);
#10794=FACE_OUTER_BOUND('',#16587,.T.);
#10795=FACE_OUTER_BOUND('',#16588,.T.);
#10796=FACE_OUTER_BOUND('',#16589,.T.);
#10797=FACE_OUTER_BOUND('',#16590,.T.);
#10798=FACE_OUTER_BOUND('',#16591,.T.);
#10799=FACE_OUTER_BOUND('',#16592,.T.);
#10800=FACE_OUTER_BOUND('',#16593,.T.);
#10801=FACE_OUTER_BOUND('',#16594,.T.);
#10802=FACE_OUTER_BOUND('',#16595,.T.);
#10803=FACE_OUTER_BOUND('',#16596,.T.);
#10804=FACE_OUTER_BOUND('',#16597,.T.);
#10805=FACE_OUTER_BOUND('',#16598,.T.);
#10806=FACE_OUTER_BOUND('',#16599,.T.);
#10807=FACE_OUTER_BOUND('',#16600,.T.);
#10808=FACE_OUTER_BOUND('',#16601,.T.);
#10809=FACE_OUTER_BOUND('',#16602,.T.);
#10810=FACE_OUTER_BOUND('',#16603,.T.);
#10811=FACE_OUTER_BOUND('',#16604,.T.);
#10812=FACE_OUTER_BOUND('',#16605,.T.);
#10813=FACE_OUTER_BOUND('',#16606,.T.);
#10814=FACE_OUTER_BOUND('',#16607,.T.);
#10815=FACE_OUTER_BOUND('',#16608,.T.);
#10816=FACE_OUTER_BOUND('',#16609,.T.);
#10817=FACE_OUTER_BOUND('',#16610,.T.);
#10818=FACE_OUTER_BOUND('',#16611,.T.);
#10819=FACE_OUTER_BOUND('',#16612,.T.);
#10820=FACE_OUTER_BOUND('',#16613,.T.);
#10821=FACE_OUTER_BOUND('',#16614,.T.);
#10822=FACE_OUTER_BOUND('',#16615,.T.);
#10823=FACE_OUTER_BOUND('',#16616,.T.);
#10824=FACE_OUTER_BOUND('',#16617,.T.);
#10825=FACE_OUTER_BOUND('',#16618,.T.);
#10826=FACE_OUTER_BOUND('',#16619,.T.);
#10827=FACE_OUTER_BOUND('',#16620,.T.);
#10828=FACE_OUTER_BOUND('',#16621,.T.);
#10829=FACE_OUTER_BOUND('',#16622,.T.);
#10830=FACE_OUTER_BOUND('',#16623,.T.);
#10831=FACE_OUTER_BOUND('',#16624,.T.);
#10832=FACE_OUTER_BOUND('',#16625,.T.);
#10833=FACE_OUTER_BOUND('',#16626,.T.);
#10834=FACE_OUTER_BOUND('',#16627,.T.);
#10835=FACE_OUTER_BOUND('',#16628,.T.);
#10836=FACE_OUTER_BOUND('',#16629,.T.);
#10837=FACE_OUTER_BOUND('',#16630,.T.);
#10838=FACE_OUTER_BOUND('',#16631,.T.);
#10839=FACE_OUTER_BOUND('',#16632,.T.);
#10840=FACE_OUTER_BOUND('',#16633,.T.);
#10841=FACE_OUTER_BOUND('',#16634,.T.);
#10842=FACE_OUTER_BOUND('',#16635,.T.);
#10843=FACE_OUTER_BOUND('',#16636,.T.);
#10844=FACE_OUTER_BOUND('',#16637,.T.);
#10845=FACE_OUTER_BOUND('',#16638,.T.);
#10846=FACE_OUTER_BOUND('',#16639,.T.);
#10847=FACE_OUTER_BOUND('',#16640,.T.);
#10848=FACE_OUTER_BOUND('',#16641,.T.);
#10849=FACE_OUTER_BOUND('',#16642,.T.);
#10850=FACE_OUTER_BOUND('',#16643,.T.);
#10851=FACE_OUTER_BOUND('',#16644,.T.);
#10852=FACE_OUTER_BOUND('',#16645,.T.);
#10853=FACE_OUTER_BOUND('',#16646,.T.);
#10854=FACE_OUTER_BOUND('',#16647,.T.);
#10855=FACE_OUTER_BOUND('',#16648,.T.);
#10856=FACE_OUTER_BOUND('',#16649,.T.);
#10857=FACE_OUTER_BOUND('',#16650,.T.);
#10858=FACE_OUTER_BOUND('',#16651,.T.);
#10859=FACE_OUTER_BOUND('',#16652,.T.);
#10860=FACE_OUTER_BOUND('',#16653,.T.);
#10861=FACE_OUTER_BOUND('',#16654,.T.);
#10862=FACE_OUTER_BOUND('',#16655,.T.);
#10863=FACE_OUTER_BOUND('',#16656,.T.);
#10864=FACE_OUTER_BOUND('',#16657,.T.);
#10865=FACE_OUTER_BOUND('',#16658,.T.);
#10866=FACE_OUTER_BOUND('',#16659,.T.);
#10867=FACE_OUTER_BOUND('',#16660,.T.);
#10868=FACE_OUTER_BOUND('',#16661,.T.);
#10869=FACE_OUTER_BOUND('',#16662,.T.);
#10870=FACE_OUTER_BOUND('',#16663,.T.);
#10871=FACE_OUTER_BOUND('',#16664,.T.);
#10872=FACE_OUTER_BOUND('',#16665,.T.);
#10873=FACE_OUTER_BOUND('',#16666,.T.);
#10874=FACE_OUTER_BOUND('',#16667,.T.);
#10875=FACE_OUTER_BOUND('',#16668,.T.);
#10876=FACE_OUTER_BOUND('',#16669,.T.);
#10877=FACE_OUTER_BOUND('',#16670,.T.);
#10878=FACE_OUTER_BOUND('',#16671,.T.);
#10879=FACE_OUTER_BOUND('',#16672,.T.);
#10880=FACE_OUTER_BOUND('',#16673,.T.);
#10881=FACE_OUTER_BOUND('',#16674,.T.);
#10882=FACE_OUTER_BOUND('',#16675,.T.);
#10883=FACE_OUTER_BOUND('',#16676,.T.);
#10884=FACE_OUTER_BOUND('',#16677,.T.);
#10885=FACE_OUTER_BOUND('',#16678,.T.);
#10886=FACE_OUTER_BOUND('',#16679,.T.);
#10887=FACE_OUTER_BOUND('',#16680,.T.);
#10888=FACE_OUTER_BOUND('',#16681,.T.);
#10889=FACE_OUTER_BOUND('',#16682,.T.);
#10890=FACE_OUTER_BOUND('',#16683,.T.);
#10891=FACE_OUTER_BOUND('',#16684,.T.);
#10892=FACE_OUTER_BOUND('',#16685,.T.);
#10893=FACE_OUTER_BOUND('',#16686,.T.);
#10894=FACE_OUTER_BOUND('',#16687,.T.);
#10895=FACE_OUTER_BOUND('',#16688,.T.);
#10896=FACE_OUTER_BOUND('',#16689,.T.);
#10897=FACE_OUTER_BOUND('',#16690,.T.);
#10898=FACE_OUTER_BOUND('',#16691,.T.);
#10899=FACE_OUTER_BOUND('',#16692,.T.);
#10900=FACE_OUTER_BOUND('',#16693,.T.);
#10901=FACE_OUTER_BOUND('',#16694,.T.);
#10902=FACE_OUTER_BOUND('',#16695,.T.);
#10903=FACE_OUTER_BOUND('',#16696,.T.);
#10904=FACE_OUTER_BOUND('',#16697,.T.);
#10905=FACE_OUTER_BOUND('',#16698,.T.);
#10906=FACE_OUTER_BOUND('',#16699,.T.);
#10907=FACE_OUTER_BOUND('',#16700,.T.);
#10908=FACE_OUTER_BOUND('',#16701,.T.);
#10909=FACE_OUTER_BOUND('',#16702,.T.);
#10910=FACE_OUTER_BOUND('',#16703,.T.);
#10911=FACE_OUTER_BOUND('',#16704,.T.);
#10912=FACE_OUTER_BOUND('',#16705,.T.);
#10913=FACE_OUTER_BOUND('',#16706,.T.);
#10914=FACE_OUTER_BOUND('',#16707,.T.);
#10915=FACE_OUTER_BOUND('',#16708,.T.);
#10916=FACE_OUTER_BOUND('',#16709,.T.);
#10917=FACE_OUTER_BOUND('',#16710,.T.);
#10918=FACE_OUTER_BOUND('',#16711,.T.);
#10919=FACE_OUTER_BOUND('',#16712,.T.);
#10920=FACE_OUTER_BOUND('',#16713,.T.);
#10921=FACE_OUTER_BOUND('',#16714,.T.);
#10922=FACE_OUTER_BOUND('',#16715,.T.);
#10923=FACE_OUTER_BOUND('',#16716,.T.);
#10924=FACE_OUTER_BOUND('',#16717,.T.);
#10925=FACE_OUTER_BOUND('',#16718,.T.);
#10926=FACE_OUTER_BOUND('',#16719,.T.);
#10927=FACE_OUTER_BOUND('',#16720,.T.);
#10928=FACE_OUTER_BOUND('',#16721,.T.);
#10929=FACE_OUTER_BOUND('',#16722,.T.);
#10930=FACE_OUTER_BOUND('',#16723,.T.);
#10931=FACE_OUTER_BOUND('',#16724,.T.);
#10932=FACE_OUTER_BOUND('',#16725,.T.);
#10933=FACE_OUTER_BOUND('',#16726,.T.);
#10934=FACE_OUTER_BOUND('',#16727,.T.);
#10935=FACE_OUTER_BOUND('',#16728,.T.);
#10936=FACE_OUTER_BOUND('',#16729,.T.);
#10937=FACE_OUTER_BOUND('',#16730,.T.);
#10938=FACE_OUTER_BOUND('',#16731,.T.);
#10939=FACE_OUTER_BOUND('',#16732,.T.);
#10940=FACE_OUTER_BOUND('',#16733,.T.);
#10941=FACE_OUTER_BOUND('',#16734,.T.);
#10942=FACE_OUTER_BOUND('',#16735,.T.);
#10943=FACE_OUTER_BOUND('',#16736,.T.);
#10944=FACE_OUTER_BOUND('',#16737,.T.);
#10945=FACE_OUTER_BOUND('',#16738,.T.);
#10946=FACE_OUTER_BOUND('',#16739,.T.);
#10947=FACE_OUTER_BOUND('',#16740,.T.);
#10948=FACE_OUTER_BOUND('',#16741,.T.);
#10949=FACE_OUTER_BOUND('',#16742,.T.);
#10950=FACE_OUTER_BOUND('',#16743,.T.);
#10951=FACE_OUTER_BOUND('',#16744,.T.);
#10952=FACE_OUTER_BOUND('',#16745,.T.);
#10953=FACE_OUTER_BOUND('',#16746,.T.);
#10954=FACE_OUTER_BOUND('',#16747,.T.);
#10955=FACE_OUTER_BOUND('',#16748,.T.);
#10956=FACE_OUTER_BOUND('',#16749,.T.);
#10957=FACE_OUTER_BOUND('',#16750,.T.);
#10958=FACE_OUTER_BOUND('',#16751,.T.);
#10959=FACE_OUTER_BOUND('',#16752,.T.);
#10960=FACE_OUTER_BOUND('',#16753,.T.);
#10961=FACE_OUTER_BOUND('',#16754,.T.);
#10962=FACE_OUTER_BOUND('',#16755,.T.);
#10963=FACE_OUTER_BOUND('',#16756,.T.);
#10964=FACE_OUTER_BOUND('',#16757,.T.);
#10965=FACE_OUTER_BOUND('',#16758,.T.);
#10966=FACE_OUTER_BOUND('',#16759,.T.);
#10967=FACE_OUTER_BOUND('',#16760,.T.);
#10968=FACE_OUTER_BOUND('',#16761,.T.);
#10969=FACE_OUTER_BOUND('',#16762,.T.);
#10970=FACE_OUTER_BOUND('',#16763,.T.);
#10971=FACE_OUTER_BOUND('',#16764,.T.);
#10972=FACE_OUTER_BOUND('',#16765,.T.);
#10973=FACE_OUTER_BOUND('',#16766,.T.);
#10974=FACE_OUTER_BOUND('',#16767,.T.);
#10975=FACE_OUTER_BOUND('',#16768,.T.);
#10976=FACE_OUTER_BOUND('',#16769,.T.);
#10977=FACE_OUTER_BOUND('',#16770,.T.);
#10978=FACE_OUTER_BOUND('',#16771,.T.);
#10979=FACE_OUTER_BOUND('',#16772,.T.);
#10980=FACE_OUTER_BOUND('',#16773,.T.);
#10981=FACE_OUTER_BOUND('',#16774,.T.);
#10982=FACE_OUTER_BOUND('',#16775,.T.);
#10983=FACE_OUTER_BOUND('',#16776,.T.);
#10984=FACE_OUTER_BOUND('',#16777,.T.);
#10985=FACE_OUTER_BOUND('',#16778,.T.);
#10986=FACE_OUTER_BOUND('',#16779,.T.);
#10987=FACE_OUTER_BOUND('',#16780,.T.);
#10988=FACE_OUTER_BOUND('',#16781,.T.);
#10989=FACE_OUTER_BOUND('',#16782,.T.);
#10990=FACE_OUTER_BOUND('',#16783,.T.);
#10991=FACE_OUTER_BOUND('',#16784,.T.);
#10992=FACE_OUTER_BOUND('',#16785,.T.);
#10993=FACE_OUTER_BOUND('',#16786,.T.);
#10994=FACE_OUTER_BOUND('',#16787,.T.);
#10995=FACE_OUTER_BOUND('',#16788,.T.);
#10996=FACE_OUTER_BOUND('',#16789,.T.);
#10997=FACE_OUTER_BOUND('',#16790,.T.);
#10998=FACE_OUTER_BOUND('',#16791,.T.);
#10999=FACE_OUTER_BOUND('',#16792,.T.);
#11000=FACE_OUTER_BOUND('',#16793,.T.);
#11001=FACE_OUTER_BOUND('',#16794,.T.);
#11002=FACE_OUTER_BOUND('',#16799,.T.);
#11003=FACE_OUTER_BOUND('',#16800,.T.);
#11004=FACE_OUTER_BOUND('',#16801,.T.);
#11005=FACE_OUTER_BOUND('',#16802,.T.);
#11006=FACE_OUTER_BOUND('',#16803,.T.);
#11007=FACE_OUTER_BOUND('',#16804,.T.);
#11008=FACE_OUTER_BOUND('',#16805,.T.);
#11009=FACE_OUTER_BOUND('',#16806,.T.);
#11010=FACE_OUTER_BOUND('',#16807,.T.);
#11011=FACE_OUTER_BOUND('',#16808,.T.);
#11012=FACE_OUTER_BOUND('',#16809,.T.);
#11013=FACE_OUTER_BOUND('',#16810,.T.);
#11014=FACE_OUTER_BOUND('',#16815,.T.);
#11015=FACE_OUTER_BOUND('',#16816,.T.);
#11016=FACE_OUTER_BOUND('',#16817,.T.);
#11017=FACE_OUTER_BOUND('',#16818,.T.);
#11018=FACE_OUTER_BOUND('',#16819,.T.);
#11019=FACE_OUTER_BOUND('',#16820,.T.);
#11020=FACE_OUTER_BOUND('',#16821,.T.);
#11021=FACE_OUTER_BOUND('',#16822,.T.);
#11022=FACE_OUTER_BOUND('',#16823,.T.);
#11023=FACE_OUTER_BOUND('',#16824,.T.);
#11024=FACE_OUTER_BOUND('',#16825,.T.);
#11025=FACE_OUTER_BOUND('',#16826,.T.);
#11026=FACE_OUTER_BOUND('',#16827,.T.);
#11027=FACE_OUTER_BOUND('',#16828,.T.);
#11028=FACE_OUTER_BOUND('',#16829,.T.);
#11029=FACE_OUTER_BOUND('',#16830,.T.);
#11030=FACE_OUTER_BOUND('',#16832,.T.);
#11031=FACE_OUTER_BOUND('',#16833,.T.);
#11032=FACE_OUTER_BOUND('',#16834,.T.);
#11033=FACE_OUTER_BOUND('',#16835,.T.);
#11034=FACE_OUTER_BOUND('',#16836,.T.);
#11035=FACE_OUTER_BOUND('',#16838,.T.);
#11036=FACE_OUTER_BOUND('',#16839,.T.);
#11037=FACE_OUTER_BOUND('',#16840,.T.);
#11038=FACE_OUTER_BOUND('',#16841,.T.);
#11039=FACE_OUTER_BOUND('',#16842,.T.);
#11040=FACE_OUTER_BOUND('',#16843,.T.);
#11041=FACE_OUTER_BOUND('',#16844,.T.);
#11042=FACE_OUTER_BOUND('',#16845,.T.);
#11043=FACE_OUTER_BOUND('',#16846,.T.);
#11044=FACE_OUTER_BOUND('',#16847,.T.);
#11045=FACE_OUTER_BOUND('',#16848,.T.);
#11046=FACE_OUTER_BOUND('',#16849,.T.);
#11047=FACE_OUTER_BOUND('',#16850,.T.);
#11048=FACE_OUTER_BOUND('',#16851,.T.);
#11049=FACE_OUTER_BOUND('',#16852,.T.);
#11050=FACE_OUTER_BOUND('',#16853,.T.);
#11051=FACE_OUTER_BOUND('',#16854,.T.);
#11052=FACE_OUTER_BOUND('',#16855,.T.);
#11053=FACE_OUTER_BOUND('',#16856,.T.);
#11054=FACE_OUTER_BOUND('',#16857,.T.);
#11055=FACE_OUTER_BOUND('',#16858,.T.);
#11056=FACE_OUTER_BOUND('',#16859,.T.);
#11057=FACE_OUTER_BOUND('',#16860,.T.);
#11058=FACE_OUTER_BOUND('',#16861,.T.);
#11059=FACE_OUTER_BOUND('',#16862,.T.);
#11060=FACE_OUTER_BOUND('',#16863,.T.);
#11061=FACE_OUTER_BOUND('',#16864,.T.);
#11062=FACE_OUTER_BOUND('',#16865,.T.);
#11063=FACE_OUTER_BOUND('',#16866,.T.);
#11064=FACE_OUTER_BOUND('',#16867,.T.);
#11065=FACE_OUTER_BOUND('',#16868,.T.);
#11066=FACE_OUTER_BOUND('',#16869,.T.);
#11067=FACE_OUTER_BOUND('',#16870,.T.);
#11068=FACE_OUTER_BOUND('',#16871,.T.);
#11069=FACE_OUTER_BOUND('',#16872,.T.);
#11070=FACE_OUTER_BOUND('',#16873,.T.);
#11071=FACE_OUTER_BOUND('',#16874,.T.);
#11072=FACE_OUTER_BOUND('',#16875,.T.);
#11073=FACE_OUTER_BOUND('',#16876,.T.);
#11074=FACE_OUTER_BOUND('',#16877,.T.);
#11075=FACE_OUTER_BOUND('',#16878,.T.);
#11076=FACE_OUTER_BOUND('',#16879,.T.);
#11077=FACE_OUTER_BOUND('',#16880,.T.);
#11078=FACE_OUTER_BOUND('',#16881,.T.);
#11079=FACE_OUTER_BOUND('',#16882,.T.);
#11080=FACE_OUTER_BOUND('',#16883,.T.);
#11081=FACE_OUTER_BOUND('',#16884,.T.);
#11082=FACE_OUTER_BOUND('',#16885,.T.);
#11083=FACE_OUTER_BOUND('',#16886,.T.);
#11084=FACE_OUTER_BOUND('',#16887,.T.);
#11085=FACE_OUTER_BOUND('',#16888,.T.);
#11086=FACE_OUTER_BOUND('',#16889,.T.);
#11087=FACE_OUTER_BOUND('',#16890,.T.);
#11088=FACE_OUTER_BOUND('',#16891,.T.);
#11089=FACE_OUTER_BOUND('',#16892,.T.);
#11090=FACE_OUTER_BOUND('',#16893,.T.);
#11091=FACE_OUTER_BOUND('',#16894,.T.);
#11092=FACE_OUTER_BOUND('',#16895,.T.);
#11093=FACE_OUTER_BOUND('',#16896,.T.);
#11094=FACE_OUTER_BOUND('',#16897,.T.);
#11095=FACE_OUTER_BOUND('',#16898,.T.);
#11096=FACE_OUTER_BOUND('',#16899,.T.);
#11097=FACE_OUTER_BOUND('',#16900,.T.);
#11098=FACE_OUTER_BOUND('',#16901,.T.);
#11099=FACE_OUTER_BOUND('',#16902,.T.);
#11100=FACE_OUTER_BOUND('',#16903,.T.);
#11101=FACE_OUTER_BOUND('',#16904,.T.);
#11102=FACE_OUTER_BOUND('',#16905,.T.);
#11103=FACE_OUTER_BOUND('',#16906,.T.);
#11104=FACE_OUTER_BOUND('',#16907,.T.);
#11105=FACE_OUTER_BOUND('',#16908,.T.);
#11106=FACE_OUTER_BOUND('',#16909,.T.);
#11107=FACE_OUTER_BOUND('',#16910,.T.);
#11108=FACE_OUTER_BOUND('',#16911,.T.);
#11109=FACE_OUTER_BOUND('',#16912,.T.);
#11110=FACE_OUTER_BOUND('',#16913,.T.);
#11111=FACE_OUTER_BOUND('',#16914,.T.);
#11112=FACE_OUTER_BOUND('',#16915,.T.);
#11113=FACE_OUTER_BOUND('',#16916,.T.);
#11114=FACE_OUTER_BOUND('',#16917,.T.);
#11115=FACE_OUTER_BOUND('',#16918,.T.);
#11116=FACE_OUTER_BOUND('',#16919,.T.);
#11117=FACE_OUTER_BOUND('',#16920,.T.);
#11118=FACE_OUTER_BOUND('',#16921,.T.);
#11119=FACE_OUTER_BOUND('',#16922,.T.);
#11120=FACE_OUTER_BOUND('',#16923,.T.);
#11121=FACE_OUTER_BOUND('',#16924,.T.);
#11122=FACE_OUTER_BOUND('',#16925,.T.);
#11123=FACE_OUTER_BOUND('',#16926,.T.);
#11124=FACE_OUTER_BOUND('',#16927,.T.);
#11125=FACE_OUTER_BOUND('',#16928,.T.);
#11126=FACE_OUTER_BOUND('',#16929,.T.);
#11127=FACE_OUTER_BOUND('',#16930,.T.);
#11128=FACE_OUTER_BOUND('',#16931,.T.);
#11129=FACE_OUTER_BOUND('',#16932,.T.);
#11130=FACE_OUTER_BOUND('',#16933,.T.);
#11131=FACE_OUTER_BOUND('',#16934,.T.);
#11132=FACE_OUTER_BOUND('',#16935,.T.);
#11133=FACE_OUTER_BOUND('',#16936,.T.);
#11134=FACE_OUTER_BOUND('',#16937,.T.);
#11135=FACE_OUTER_BOUND('',#16938,.T.);
#11136=FACE_OUTER_BOUND('',#16939,.T.);
#11137=FACE_OUTER_BOUND('',#16940,.T.);
#11138=FACE_OUTER_BOUND('',#16941,.T.);
#11139=FACE_OUTER_BOUND('',#16942,.T.);
#11140=FACE_OUTER_BOUND('',#16943,.T.);
#11141=FACE_OUTER_BOUND('',#16944,.T.);
#11142=FACE_OUTER_BOUND('',#16945,.T.);
#11143=FACE_OUTER_BOUND('',#16946,.T.);
#11144=FACE_OUTER_BOUND('',#16947,.T.);
#11145=FACE_OUTER_BOUND('',#16948,.T.);
#11146=FACE_OUTER_BOUND('',#16949,.T.);
#11147=FACE_OUTER_BOUND('',#16950,.T.);
#11148=FACE_OUTER_BOUND('',#16951,.T.);
#11149=FACE_OUTER_BOUND('',#16952,.T.);
#11150=FACE_OUTER_BOUND('',#16953,.T.);
#11151=FACE_OUTER_BOUND('',#16954,.T.);
#11152=FACE_OUTER_BOUND('',#16955,.T.);
#11153=FACE_OUTER_BOUND('',#16956,.T.);
#11154=FACE_OUTER_BOUND('',#16957,.T.);
#11155=FACE_OUTER_BOUND('',#16958,.T.);
#11156=FACE_OUTER_BOUND('',#16959,.T.);
#11157=FACE_OUTER_BOUND('',#16960,.T.);
#11158=FACE_OUTER_BOUND('',#16961,.T.);
#11159=FACE_OUTER_BOUND('',#16962,.T.);
#11160=FACE_OUTER_BOUND('',#16963,.T.);
#11161=FACE_OUTER_BOUND('',#16964,.T.);
#11162=FACE_OUTER_BOUND('',#16965,.T.);
#11163=FACE_OUTER_BOUND('',#16966,.T.);
#11164=FACE_OUTER_BOUND('',#16967,.T.);
#11165=FACE_OUTER_BOUND('',#16968,.T.);
#11166=FACE_OUTER_BOUND('',#16969,.T.);
#11167=FACE_OUTER_BOUND('',#16970,.T.);
#11168=FACE_OUTER_BOUND('',#16971,.T.);
#11169=FACE_OUTER_BOUND('',#16972,.T.);
#11170=FACE_OUTER_BOUND('',#16973,.T.);
#11171=FACE_OUTER_BOUND('',#16974,.T.);
#11172=FACE_OUTER_BOUND('',#16975,.T.);
#11173=FACE_OUTER_BOUND('',#16976,.T.);
#11174=FACE_OUTER_BOUND('',#16977,.T.);
#11175=FACE_OUTER_BOUND('',#16978,.T.);
#11176=FACE_OUTER_BOUND('',#16979,.T.);
#11177=FACE_OUTER_BOUND('',#16980,.T.);
#11178=FACE_OUTER_BOUND('',#16981,.T.);
#11179=FACE_OUTER_BOUND('',#16982,.T.);
#11180=FACE_OUTER_BOUND('',#16983,.T.);
#11181=FACE_OUTER_BOUND('',#16984,.T.);
#11182=FACE_OUTER_BOUND('',#16985,.T.);
#11183=FACE_OUTER_BOUND('',#16986,.T.);
#11184=FACE_OUTER_BOUND('',#16987,.T.);
#11185=FACE_OUTER_BOUND('',#16988,.T.);
#11186=FACE_OUTER_BOUND('',#16989,.T.);
#11187=FACE_OUTER_BOUND('',#16990,.T.);
#11188=FACE_OUTER_BOUND('',#16991,.T.);
#11189=FACE_OUTER_BOUND('',#16992,.T.);
#11190=FACE_OUTER_BOUND('',#16993,.T.);
#11191=FACE_OUTER_BOUND('',#16994,.T.);
#11192=FACE_OUTER_BOUND('',#16995,.T.);
#11193=FACE_OUTER_BOUND('',#16996,.T.);
#11194=FACE_OUTER_BOUND('',#16997,.T.);
#11195=FACE_OUTER_BOUND('',#16998,.T.);
#11196=FACE_OUTER_BOUND('',#16999,.T.);
#11197=FACE_OUTER_BOUND('',#17000,.T.);
#11198=FACE_OUTER_BOUND('',#17001,.T.);
#11199=FACE_OUTER_BOUND('',#17002,.T.);
#11200=FACE_OUTER_BOUND('',#17003,.T.);
#11201=FACE_OUTER_BOUND('',#17004,.T.);
#11202=FACE_OUTER_BOUND('',#17005,.T.);
#11203=FACE_OUTER_BOUND('',#17006,.T.);
#11204=FACE_OUTER_BOUND('',#17007,.T.);
#11205=FACE_OUTER_BOUND('',#17008,.T.);
#11206=FACE_OUTER_BOUND('',#17009,.T.);
#11207=FACE_OUTER_BOUND('',#17010,.T.);
#11208=FACE_OUTER_BOUND('',#17011,.T.);
#11209=FACE_OUTER_BOUND('',#17012,.T.);
#11210=FACE_OUTER_BOUND('',#17013,.T.);
#11211=FACE_OUTER_BOUND('',#17014,.T.);
#11212=FACE_OUTER_BOUND('',#17015,.T.);
#11213=FACE_OUTER_BOUND('',#17016,.T.);
#11214=FACE_OUTER_BOUND('',#17017,.T.);
#11215=FACE_OUTER_BOUND('',#17018,.T.);
#11216=FACE_OUTER_BOUND('',#17019,.T.);
#11217=FACE_OUTER_BOUND('',#17020,.T.);
#11218=FACE_OUTER_BOUND('',#17021,.T.);
#11219=FACE_OUTER_BOUND('',#17022,.T.);
#11220=FACE_OUTER_BOUND('',#17023,.T.);
#11221=FACE_OUTER_BOUND('',#17024,.T.);
#11222=FACE_OUTER_BOUND('',#17025,.T.);
#11223=FACE_OUTER_BOUND('',#17026,.T.);
#11224=FACE_OUTER_BOUND('',#17027,.T.);
#11225=FACE_OUTER_BOUND('',#17028,.T.);
#11226=FACE_OUTER_BOUND('',#17029,.T.);
#11227=FACE_OUTER_BOUND('',#17030,.T.);
#11228=FACE_OUTER_BOUND('',#17031,.T.);
#11229=FACE_OUTER_BOUND('',#17032,.T.);
#11230=FACE_OUTER_BOUND('',#17033,.T.);
#11231=FACE_OUTER_BOUND('',#17034,.T.);
#11232=FACE_OUTER_BOUND('',#17035,.T.);
#11233=FACE_OUTER_BOUND('',#17036,.T.);
#11234=FACE_OUTER_BOUND('',#17037,.T.);
#11235=FACE_OUTER_BOUND('',#17038,.T.);
#11236=FACE_OUTER_BOUND('',#17039,.T.);
#11237=FACE_OUTER_BOUND('',#17040,.T.);
#11238=FACE_OUTER_BOUND('',#17041,.T.);
#11239=FACE_OUTER_BOUND('',#17042,.T.);
#11240=FACE_OUTER_BOUND('',#17043,.T.);
#11241=FACE_OUTER_BOUND('',#17044,.T.);
#11242=FACE_OUTER_BOUND('',#17045,.T.);
#11243=FACE_OUTER_BOUND('',#17046,.T.);
#11244=FACE_OUTER_BOUND('',#17047,.T.);
#11245=FACE_OUTER_BOUND('',#17048,.T.);
#11246=FACE_OUTER_BOUND('',#17049,.T.);
#11247=FACE_OUTER_BOUND('',#17050,.T.);
#11248=FACE_OUTER_BOUND('',#17051,.T.);
#11249=FACE_OUTER_BOUND('',#17052,.T.);
#11250=FACE_OUTER_BOUND('',#17053,.T.);
#11251=FACE_OUTER_BOUND('',#17054,.T.);
#11252=FACE_OUTER_BOUND('',#17055,.T.);
#11253=FACE_OUTER_BOUND('',#17056,.T.);
#11254=FACE_OUTER_BOUND('',#17057,.T.);
#11255=FACE_OUTER_BOUND('',#17058,.T.);
#11256=FACE_OUTER_BOUND('',#17059,.T.);
#11257=FACE_OUTER_BOUND('',#17060,.T.);
#11258=FACE_OUTER_BOUND('',#17061,.T.);
#11259=FACE_OUTER_BOUND('',#17062,.T.);
#11260=FACE_OUTER_BOUND('',#17063,.T.);
#11261=FACE_OUTER_BOUND('',#17064,.T.);
#11262=FACE_OUTER_BOUND('',#17065,.T.);
#11263=FACE_OUTER_BOUND('',#17066,.T.);
#11264=FACE_OUTER_BOUND('',#17067,.T.);
#11265=FACE_OUTER_BOUND('',#17068,.T.);
#11266=FACE_OUTER_BOUND('',#17069,.T.);
#11267=FACE_OUTER_BOUND('',#17070,.T.);
#11268=FACE_OUTER_BOUND('',#17071,.T.);
#11269=FACE_OUTER_BOUND('',#17072,.T.);
#11270=FACE_OUTER_BOUND('',#17073,.T.);
#11271=FACE_OUTER_BOUND('',#17074,.T.);
#11272=FACE_OUTER_BOUND('',#17075,.T.);
#11273=FACE_OUTER_BOUND('',#17076,.T.);
#11274=FACE_OUTER_BOUND('',#17077,.T.);
#11275=FACE_OUTER_BOUND('',#17078,.T.);
#11276=FACE_OUTER_BOUND('',#17079,.T.);
#11277=FACE_OUTER_BOUND('',#17080,.T.);
#11278=FACE_OUTER_BOUND('',#17081,.T.);
#11279=FACE_OUTER_BOUND('',#17082,.T.);
#11280=FACE_OUTER_BOUND('',#17083,.T.);
#11281=FACE_OUTER_BOUND('',#17084,.T.);
#11282=FACE_OUTER_BOUND('',#17085,.T.);
#11283=FACE_OUTER_BOUND('',#17086,.T.);
#11284=FACE_OUTER_BOUND('',#17087,.T.);
#11285=FACE_OUTER_BOUND('',#17088,.T.);
#11286=FACE_OUTER_BOUND('',#17089,.T.);
#11287=FACE_OUTER_BOUND('',#17090,.T.);
#11288=FACE_OUTER_BOUND('',#17091,.T.);
#11289=FACE_OUTER_BOUND('',#17092,.T.);
#11290=FACE_OUTER_BOUND('',#17093,.T.);
#11291=FACE_OUTER_BOUND('',#17094,.T.);
#11292=FACE_OUTER_BOUND('',#17095,.T.);
#11293=FACE_OUTER_BOUND('',#17096,.T.);
#11294=FACE_OUTER_BOUND('',#17097,.T.);
#11295=FACE_OUTER_BOUND('',#17098,.T.);
#11296=FACE_OUTER_BOUND('',#17099,.T.);
#11297=FACE_OUTER_BOUND('',#17100,.T.);
#11298=FACE_OUTER_BOUND('',#17101,.T.);
#11299=FACE_OUTER_BOUND('',#17102,.T.);
#11300=FACE_OUTER_BOUND('',#17103,.T.);
#11301=FACE_OUTER_BOUND('',#17104,.T.);
#11302=FACE_OUTER_BOUND('',#17105,.T.);
#11303=FACE_OUTER_BOUND('',#17106,.T.);
#11304=FACE_OUTER_BOUND('',#17107,.T.);
#11305=FACE_OUTER_BOUND('',#17108,.T.);
#11306=FACE_OUTER_BOUND('',#17109,.T.);
#11307=FACE_OUTER_BOUND('',#17110,.T.);
#11308=FACE_OUTER_BOUND('',#17111,.T.);
#11309=FACE_OUTER_BOUND('',#17112,.T.);
#11310=FACE_OUTER_BOUND('',#17113,.T.);
#11311=FACE_OUTER_BOUND('',#17114,.T.);
#11312=FACE_OUTER_BOUND('',#17115,.T.);
#11313=FACE_OUTER_BOUND('',#17116,.T.);
#11314=FACE_OUTER_BOUND('',#17117,.T.);
#11315=FACE_OUTER_BOUND('',#17118,.T.);
#11316=FACE_OUTER_BOUND('',#17119,.T.);
#11317=FACE_OUTER_BOUND('',#17120,.T.);
#11318=FACE_OUTER_BOUND('',#17121,.T.);
#11319=FACE_OUTER_BOUND('',#17122,.T.);
#11320=FACE_OUTER_BOUND('',#17123,.T.);
#11321=FACE_OUTER_BOUND('',#17124,.T.);
#11322=FACE_OUTER_BOUND('',#17125,.T.);
#11323=FACE_OUTER_BOUND('',#17126,.T.);
#11324=FACE_OUTER_BOUND('',#17127,.T.);
#11325=FACE_OUTER_BOUND('',#17128,.T.);
#11326=FACE_OUTER_BOUND('',#17129,.T.);
#11327=FACE_OUTER_BOUND('',#17130,.T.);
#11328=FACE_OUTER_BOUND('',#17131,.T.);
#11329=FACE_OUTER_BOUND('',#17132,.T.);
#11330=FACE_OUTER_BOUND('',#17133,.T.);
#11331=FACE_OUTER_BOUND('',#17134,.T.);
#11332=FACE_OUTER_BOUND('',#17135,.T.);
#11333=FACE_OUTER_BOUND('',#17136,.T.);
#11334=FACE_OUTER_BOUND('',#17137,.T.);
#11335=FACE_OUTER_BOUND('',#17138,.T.);
#11336=FACE_OUTER_BOUND('',#17139,.T.);
#11337=FACE_OUTER_BOUND('',#17140,.T.);
#11338=FACE_OUTER_BOUND('',#17141,.T.);
#11339=FACE_OUTER_BOUND('',#17142,.T.);
#11340=FACE_OUTER_BOUND('',#17143,.T.);
#11341=FACE_OUTER_BOUND('',#17144,.T.);
#11342=FACE_OUTER_BOUND('',#17145,.T.);
#11343=FACE_OUTER_BOUND('',#17146,.T.);
#11344=FACE_OUTER_BOUND('',#17147,.T.);
#11345=FACE_OUTER_BOUND('',#17148,.T.);
#11346=FACE_OUTER_BOUND('',#17149,.T.);
#11347=FACE_OUTER_BOUND('',#17150,.T.);
#11348=FACE_OUTER_BOUND('',#17151,.T.);
#11349=FACE_OUTER_BOUND('',#17152,.T.);
#11350=FACE_OUTER_BOUND('',#17153,.T.);
#11351=FACE_OUTER_BOUND('',#17154,.T.);
#11352=FACE_OUTER_BOUND('',#17155,.T.);
#11353=FACE_OUTER_BOUND('',#17156,.T.);
#11354=FACE_OUTER_BOUND('',#17157,.T.);
#11355=FACE_OUTER_BOUND('',#17158,.T.);
#11356=FACE_OUTER_BOUND('',#17159,.T.);
#11357=FACE_OUTER_BOUND('',#17160,.T.);
#11358=FACE_OUTER_BOUND('',#17161,.T.);
#11359=FACE_OUTER_BOUND('',#17162,.T.);
#11360=FACE_OUTER_BOUND('',#17163,.T.);
#11361=FACE_OUTER_BOUND('',#17164,.T.);
#11362=FACE_OUTER_BOUND('',#17165,.T.);
#11363=FACE_OUTER_BOUND('',#17166,.T.);
#11364=FACE_OUTER_BOUND('',#17167,.T.);
#11365=FACE_OUTER_BOUND('',#17168,.T.);
#11366=FACE_OUTER_BOUND('',#17169,.T.);
#11367=FACE_OUTER_BOUND('',#17170,.T.);
#11368=FACE_OUTER_BOUND('',#17171,.T.);
#11369=FACE_OUTER_BOUND('',#17172,.T.);
#11370=FACE_OUTER_BOUND('',#17173,.T.);
#11371=FACE_OUTER_BOUND('',#17174,.T.);
#11372=FACE_OUTER_BOUND('',#17175,.T.);
#11373=FACE_OUTER_BOUND('',#17176,.T.);
#11374=FACE_OUTER_BOUND('',#17177,.T.);
#11375=FACE_OUTER_BOUND('',#17178,.T.);
#11376=FACE_OUTER_BOUND('',#17179,.T.);
#11377=FACE_OUTER_BOUND('',#17180,.T.);
#11378=FACE_OUTER_BOUND('',#17181,.T.);
#11379=FACE_OUTER_BOUND('',#17182,.T.);
#11380=FACE_OUTER_BOUND('',#17183,.T.);
#11381=FACE_OUTER_BOUND('',#17184,.T.);
#11382=FACE_OUTER_BOUND('',#17185,.T.);
#11383=FACE_OUTER_BOUND('',#17186,.T.);
#11384=FACE_OUTER_BOUND('',#17187,.T.);
#11385=FACE_OUTER_BOUND('',#17188,.T.);
#11386=FACE_OUTER_BOUND('',#17189,.T.);
#11387=FACE_OUTER_BOUND('',#17190,.T.);
#11388=FACE_OUTER_BOUND('',#17191,.T.);
#11389=FACE_OUTER_BOUND('',#17192,.T.);
#11390=FACE_OUTER_BOUND('',#17193,.T.);
#11391=FACE_OUTER_BOUND('',#17194,.T.);
#11392=FACE_OUTER_BOUND('',#17195,.T.);
#11393=FACE_OUTER_BOUND('',#17196,.T.);
#11394=FACE_OUTER_BOUND('',#17197,.T.);
#11395=FACE_OUTER_BOUND('',#17198,.T.);
#11396=FACE_OUTER_BOUND('',#17199,.T.);
#11397=FACE_OUTER_BOUND('',#17200,.T.);
#11398=FACE_OUTER_BOUND('',#17201,.T.);
#11399=FACE_OUTER_BOUND('',#17202,.T.);
#11400=FACE_OUTER_BOUND('',#17203,.T.);
#11401=FACE_OUTER_BOUND('',#17204,.T.);
#11402=FACE_OUTER_BOUND('',#17205,.T.);
#11403=FACE_OUTER_BOUND('',#17206,.T.);
#11404=FACE_OUTER_BOUND('',#17207,.T.);
#11405=FACE_OUTER_BOUND('',#17208,.T.);
#11406=FACE_OUTER_BOUND('',#17209,.T.);
#11407=FACE_OUTER_BOUND('',#17210,.T.);
#11408=FACE_OUTER_BOUND('',#17211,.T.);
#11409=FACE_OUTER_BOUND('',#17212,.T.);
#11410=FACE_OUTER_BOUND('',#17213,.T.);
#11411=FACE_OUTER_BOUND('',#17214,.T.);
#11412=FACE_OUTER_BOUND('',#17215,.T.);
#11413=FACE_OUTER_BOUND('',#17216,.T.);
#11414=FACE_OUTER_BOUND('',#17217,.T.);
#11415=FACE_OUTER_BOUND('',#17218,.T.);
#11416=FACE_OUTER_BOUND('',#17219,.T.);
#11417=FACE_OUTER_BOUND('',#17220,.T.);
#11418=FACE_OUTER_BOUND('',#17221,.T.);
#11419=FACE_OUTER_BOUND('',#17222,.T.);
#11420=FACE_OUTER_BOUND('',#17223,.T.);
#11421=FACE_OUTER_BOUND('',#17224,.T.);
#11422=FACE_OUTER_BOUND('',#17225,.T.);
#11423=FACE_OUTER_BOUND('',#17226,.T.);
#11424=FACE_OUTER_BOUND('',#17227,.T.);
#11425=FACE_OUTER_BOUND('',#17228,.T.);
#11426=FACE_OUTER_BOUND('',#17229,.T.);
#11427=FACE_OUTER_BOUND('',#17230,.T.);
#11428=FACE_OUTER_BOUND('',#17231,.T.);
#11429=FACE_OUTER_BOUND('',#17232,.T.);
#11430=FACE_OUTER_BOUND('',#17233,.T.);
#11431=FACE_OUTER_BOUND('',#17234,.T.);
#11432=FACE_OUTER_BOUND('',#17235,.T.);
#11433=FACE_OUTER_BOUND('',#17236,.T.);
#11434=FACE_OUTER_BOUND('',#17237,.T.);
#11435=FACE_OUTER_BOUND('',#17238,.T.);
#11436=FACE_OUTER_BOUND('',#17239,.T.);
#11437=FACE_OUTER_BOUND('',#17240,.T.);
#11438=FACE_OUTER_BOUND('',#17241,.T.);
#11439=FACE_OUTER_BOUND('',#17242,.T.);
#11440=FACE_OUTER_BOUND('',#17243,.T.);
#11441=FACE_OUTER_BOUND('',#17244,.T.);
#11442=FACE_OUTER_BOUND('',#17245,.T.);
#11443=FACE_OUTER_BOUND('',#17246,.T.);
#11444=FACE_OUTER_BOUND('',#17247,.T.);
#11445=FACE_OUTER_BOUND('',#17248,.T.);
#11446=FACE_OUTER_BOUND('',#17249,.T.);
#11447=FACE_OUTER_BOUND('',#17250,.T.);
#11448=FACE_OUTER_BOUND('',#17251,.T.);
#11449=FACE_OUTER_BOUND('',#17252,.T.);
#11450=FACE_OUTER_BOUND('',#17253,.T.);
#11451=FACE_OUTER_BOUND('',#17254,.T.);
#11452=FACE_OUTER_BOUND('',#17255,.T.);
#11453=FACE_OUTER_BOUND('',#17256,.T.);
#11454=FACE_OUTER_BOUND('',#17257,.T.);
#11455=FACE_OUTER_BOUND('',#17258,.T.);
#11456=FACE_OUTER_BOUND('',#17259,.T.);
#11457=FACE_OUTER_BOUND('',#17260,.T.);
#11458=FACE_OUTER_BOUND('',#17261,.T.);
#11459=FACE_OUTER_BOUND('',#17262,.T.);
#11460=FACE_OUTER_BOUND('',#17263,.T.);
#11461=FACE_OUTER_BOUND('',#17264,.T.);
#11462=FACE_OUTER_BOUND('',#17265,.T.);
#11463=FACE_OUTER_BOUND('',#17266,.T.);
#11464=FACE_OUTER_BOUND('',#17267,.T.);
#11465=FACE_OUTER_BOUND('',#17268,.T.);
#11466=FACE_OUTER_BOUND('',#17269,.T.);
#11467=FACE_OUTER_BOUND('',#17270,.T.);
#11468=FACE_OUTER_BOUND('',#17271,.T.);
#11469=FACE_OUTER_BOUND('',#17272,.T.);
#11470=FACE_OUTER_BOUND('',#17273,.T.);
#11471=FACE_OUTER_BOUND('',#17274,.T.);
#11472=FACE_OUTER_BOUND('',#17275,.T.);
#11473=FACE_OUTER_BOUND('',#17276,.T.);
#11474=FACE_OUTER_BOUND('',#17277,.T.);
#11475=FACE_OUTER_BOUND('',#17278,.T.);
#11476=FACE_OUTER_BOUND('',#17279,.T.);
#11477=FACE_OUTER_BOUND('',#17280,.T.);
#11478=FACE_OUTER_BOUND('',#17281,.T.);
#11479=FACE_OUTER_BOUND('',#17282,.T.);
#11480=FACE_OUTER_BOUND('',#17283,.T.);
#11481=FACE_OUTER_BOUND('',#17284,.T.);
#11482=FACE_OUTER_BOUND('',#17285,.T.);
#11483=FACE_OUTER_BOUND('',#17286,.T.);
#11484=FACE_OUTER_BOUND('',#17287,.T.);
#11485=FACE_OUTER_BOUND('',#17288,.T.);
#11486=FACE_OUTER_BOUND('',#17289,.T.);
#11487=FACE_OUTER_BOUND('',#17290,.T.);
#11488=FACE_OUTER_BOUND('',#17291,.T.);
#11489=FACE_OUTER_BOUND('',#17292,.T.);
#11490=FACE_OUTER_BOUND('',#17293,.T.);
#11491=FACE_OUTER_BOUND('',#17294,.T.);
#11492=FACE_OUTER_BOUND('',#17295,.T.);
#11493=FACE_OUTER_BOUND('',#17296,.T.);
#11494=FACE_OUTER_BOUND('',#17297,.T.);
#11495=FACE_OUTER_BOUND('',#17298,.T.);
#11496=FACE_OUTER_BOUND('',#17299,.T.);
#11497=FACE_OUTER_BOUND('',#17300,.T.);
#11498=FACE_OUTER_BOUND('',#17301,.T.);
#11499=FACE_OUTER_BOUND('',#17302,.T.);
#11500=FACE_OUTER_BOUND('',#17303,.T.);
#11501=FACE_OUTER_BOUND('',#17304,.T.);
#11502=FACE_OUTER_BOUND('',#17305,.T.);
#11503=FACE_OUTER_BOUND('',#17306,.T.);
#11504=FACE_OUTER_BOUND('',#17307,.T.);
#11505=FACE_OUTER_BOUND('',#17308,.T.);
#11506=FACE_OUTER_BOUND('',#17309,.T.);
#11507=FACE_OUTER_BOUND('',#17310,.T.);
#11508=FACE_OUTER_BOUND('',#17311,.T.);
#11509=FACE_OUTER_BOUND('',#17312,.T.);
#11510=FACE_OUTER_BOUND('',#17313,.T.);
#11511=FACE_OUTER_BOUND('',#17314,.T.);
#11512=FACE_OUTER_BOUND('',#17315,.T.);
#11513=FACE_OUTER_BOUND('',#17316,.T.);
#11514=FACE_OUTER_BOUND('',#17317,.T.);
#11515=FACE_OUTER_BOUND('',#17318,.T.);
#11516=FACE_OUTER_BOUND('',#17319,.T.);
#11517=FACE_OUTER_BOUND('',#17320,.T.);
#11518=FACE_OUTER_BOUND('',#17321,.T.);
#11519=FACE_OUTER_BOUND('',#17322,.T.);
#11520=FACE_OUTER_BOUND('',#17323,.T.);
#11521=FACE_OUTER_BOUND('',#17324,.T.);
#11522=FACE_OUTER_BOUND('',#17325,.T.);
#11523=FACE_OUTER_BOUND('',#17326,.T.);
#11524=FACE_OUTER_BOUND('',#17327,.T.);
#11525=FACE_OUTER_BOUND('',#17328,.T.);
#11526=FACE_OUTER_BOUND('',#17329,.T.);
#11527=FACE_OUTER_BOUND('',#17330,.T.);
#11528=FACE_OUTER_BOUND('',#17331,.T.);
#11529=FACE_OUTER_BOUND('',#17332,.T.);
#11530=FACE_OUTER_BOUND('',#17333,.T.);
#11531=FACE_OUTER_BOUND('',#17334,.T.);
#11532=FACE_OUTER_BOUND('',#17335,.T.);
#11533=FACE_OUTER_BOUND('',#17336,.T.);
#11534=FACE_OUTER_BOUND('',#17337,.T.);
#11535=FACE_OUTER_BOUND('',#17338,.T.);
#11536=FACE_OUTER_BOUND('',#17339,.T.);
#11537=FACE_OUTER_BOUND('',#17340,.T.);
#11538=FACE_OUTER_BOUND('',#17341,.T.);
#11539=FACE_OUTER_BOUND('',#17342,.T.);
#11540=FACE_OUTER_BOUND('',#17343,.T.);
#11541=FACE_OUTER_BOUND('',#17344,.T.);
#11542=FACE_OUTER_BOUND('',#17345,.T.);
#11543=FACE_OUTER_BOUND('',#17346,.T.);
#11544=FACE_OUTER_BOUND('',#17347,.T.);
#11545=FACE_OUTER_BOUND('',#17348,.T.);
#11546=FACE_OUTER_BOUND('',#17349,.T.);
#11547=FACE_OUTER_BOUND('',#17350,.T.);
#11548=FACE_OUTER_BOUND('',#17351,.T.);
#11549=FACE_OUTER_BOUND('',#17352,.T.);
#11550=FACE_OUTER_BOUND('',#17353,.T.);
#11551=FACE_OUTER_BOUND('',#17354,.T.);
#11552=FACE_OUTER_BOUND('',#17355,.T.);
#11553=FACE_OUTER_BOUND('',#17356,.T.);
#11554=FACE_OUTER_BOUND('',#17357,.T.);
#11555=FACE_OUTER_BOUND('',#17358,.T.);
#11556=FACE_OUTER_BOUND('',#17359,.T.);
#11557=FACE_OUTER_BOUND('',#17360,.T.);
#11558=FACE_OUTER_BOUND('',#17361,.T.);
#11559=FACE_OUTER_BOUND('',#17362,.T.);
#11560=FACE_OUTER_BOUND('',#17363,.T.);
#11561=FACE_OUTER_BOUND('',#17364,.T.);
#11562=FACE_OUTER_BOUND('',#17365,.T.);
#11563=FACE_OUTER_BOUND('',#17366,.T.);
#11564=FACE_OUTER_BOUND('',#17367,.T.);
#11565=FACE_OUTER_BOUND('',#17368,.T.);
#11566=FACE_OUTER_BOUND('',#17369,.T.);
#11567=FACE_OUTER_BOUND('',#17370,.T.);
#11568=FACE_OUTER_BOUND('',#17371,.T.);
#11569=FACE_OUTER_BOUND('',#17372,.T.);
#11570=FACE_OUTER_BOUND('',#17373,.T.);
#11571=FACE_OUTER_BOUND('',#17374,.T.);
#11572=FACE_OUTER_BOUND('',#17375,.T.);
#11573=FACE_OUTER_BOUND('',#17376,.T.);
#11574=FACE_OUTER_BOUND('',#17377,.T.);
#11575=FACE_OUTER_BOUND('',#17378,.T.);
#11576=FACE_OUTER_BOUND('',#17379,.T.);
#11577=FACE_OUTER_BOUND('',#17380,.T.);
#11578=FACE_OUTER_BOUND('',#17381,.T.);
#11579=FACE_OUTER_BOUND('',#17382,.T.);
#11580=FACE_OUTER_BOUND('',#17383,.T.);
#11581=FACE_OUTER_BOUND('',#17384,.T.);
#11582=FACE_OUTER_BOUND('',#17385,.T.);
#11583=FACE_OUTER_BOUND('',#17386,.T.);
#11584=FACE_OUTER_BOUND('',#17387,.T.);
#11585=FACE_OUTER_BOUND('',#17388,.T.);
#11586=FACE_OUTER_BOUND('',#17389,.T.);
#11587=FACE_OUTER_BOUND('',#17390,.T.);
#11588=FACE_OUTER_BOUND('',#17391,.T.);
#11589=FACE_OUTER_BOUND('',#17392,.T.);
#11590=FACE_OUTER_BOUND('',#17393,.T.);
#11591=FACE_OUTER_BOUND('',#17394,.T.);
#11592=FACE_OUTER_BOUND('',#17395,.T.);
#11593=FACE_OUTER_BOUND('',#17396,.T.);
#11594=FACE_OUTER_BOUND('',#17397,.T.);
#11595=FACE_OUTER_BOUND('',#17398,.T.);
#11596=FACE_OUTER_BOUND('',#17399,.T.);
#11597=FACE_OUTER_BOUND('',#17400,.T.);
#11598=FACE_OUTER_BOUND('',#17401,.T.);
#11599=FACE_OUTER_BOUND('',#17402,.T.);
#11600=FACE_OUTER_BOUND('',#17403,.T.);
#11601=FACE_OUTER_BOUND('',#17404,.T.);
#11602=FACE_OUTER_BOUND('',#17405,.T.);
#11603=FACE_OUTER_BOUND('',#17406,.T.);
#11604=FACE_OUTER_BOUND('',#17407,.T.);
#11605=FACE_OUTER_BOUND('',#17408,.T.);
#11606=FACE_OUTER_BOUND('',#17409,.T.);
#11607=FACE_OUTER_BOUND('',#17410,.T.);
#11608=FACE_OUTER_BOUND('',#17411,.T.);
#11609=FACE_OUTER_BOUND('',#17412,.T.);
#11610=FACE_OUTER_BOUND('',#17413,.T.);
#11611=FACE_OUTER_BOUND('',#17414,.T.);
#11612=FACE_OUTER_BOUND('',#17415,.T.);
#11613=FACE_OUTER_BOUND('',#17416,.T.);
#11614=FACE_OUTER_BOUND('',#17417,.T.);
#11615=FACE_OUTER_BOUND('',#17418,.T.);
#11616=FACE_OUTER_BOUND('',#17419,.T.);
#11617=FACE_OUTER_BOUND('',#17420,.T.);
#11618=FACE_OUTER_BOUND('',#17421,.T.);
#11619=FACE_OUTER_BOUND('',#17422,.T.);
#11620=FACE_OUTER_BOUND('',#17423,.T.);
#11621=FACE_OUTER_BOUND('',#17424,.T.);
#11622=FACE_OUTER_BOUND('',#17425,.T.);
#11623=FACE_OUTER_BOUND('',#17426,.T.);
#11624=FACE_OUTER_BOUND('',#17427,.T.);
#11625=FACE_OUTER_BOUND('',#17428,.T.);
#11626=FACE_OUTER_BOUND('',#17429,.T.);
#11627=FACE_OUTER_BOUND('',#17430,.T.);
#11628=FACE_OUTER_BOUND('',#17431,.T.);
#11629=FACE_OUTER_BOUND('',#17432,.T.);
#11630=FACE_OUTER_BOUND('',#17433,.T.);
#11631=FACE_OUTER_BOUND('',#17434,.T.);
#11632=FACE_OUTER_BOUND('',#17435,.T.);
#11633=FACE_OUTER_BOUND('',#17436,.T.);
#11634=FACE_OUTER_BOUND('',#17437,.T.);
#11635=FACE_OUTER_BOUND('',#17438,.T.);
#11636=FACE_OUTER_BOUND('',#17439,.T.);
#11637=FACE_OUTER_BOUND('',#17440,.T.);
#11638=FACE_OUTER_BOUND('',#17441,.T.);
#11639=FACE_OUTER_BOUND('',#17442,.T.);
#11640=FACE_OUTER_BOUND('',#17443,.T.);
#11641=FACE_OUTER_BOUND('',#17444,.T.);
#11642=FACE_OUTER_BOUND('',#17445,.T.);
#11643=FACE_OUTER_BOUND('',#17446,.T.);
#11644=FACE_OUTER_BOUND('',#17447,.T.);
#11645=FACE_OUTER_BOUND('',#17448,.T.);
#11646=FACE_OUTER_BOUND('',#17449,.T.);
#11647=FACE_OUTER_BOUND('',#17450,.T.);
#11648=FACE_OUTER_BOUND('',#17451,.T.);
#11649=FACE_OUTER_BOUND('',#17452,.T.);
#11650=FACE_OUTER_BOUND('',#17453,.T.);
#11651=FACE_OUTER_BOUND('',#17454,.T.);
#11652=FACE_OUTER_BOUND('',#17455,.T.);
#11653=FACE_OUTER_BOUND('',#17456,.T.);
#11654=FACE_OUTER_BOUND('',#17457,.T.);
#11655=FACE_OUTER_BOUND('',#17458,.T.);
#11656=FACE_OUTER_BOUND('',#17459,.T.);
#11657=FACE_OUTER_BOUND('',#17460,.T.);
#11658=FACE_OUTER_BOUND('',#17461,.T.);
#11659=FACE_OUTER_BOUND('',#17462,.T.);
#11660=FACE_OUTER_BOUND('',#17463,.T.);
#11661=FACE_OUTER_BOUND('',#17464,.T.);
#11662=FACE_OUTER_BOUND('',#17465,.T.);
#11663=FACE_OUTER_BOUND('',#17466,.T.);
#11664=FACE_OUTER_BOUND('',#17467,.T.);
#11665=FACE_OUTER_BOUND('',#17468,.T.);
#11666=FACE_OUTER_BOUND('',#17469,.T.);
#11667=FACE_OUTER_BOUND('',#17470,.T.);
#11668=FACE_OUTER_BOUND('',#17471,.T.);
#11669=FACE_OUTER_BOUND('',#17472,.T.);
#11670=FACE_OUTER_BOUND('',#17473,.T.);
#11671=FACE_OUTER_BOUND('',#17474,.T.);
#11672=FACE_OUTER_BOUND('',#17475,.T.);
#11673=FACE_OUTER_BOUND('',#17476,.T.);
#11674=FACE_OUTER_BOUND('',#17477,.T.);
#11675=FACE_OUTER_BOUND('',#17478,.T.);
#11676=FACE_OUTER_BOUND('',#17479,.T.);
#11677=FACE_OUTER_BOUND('',#17480,.T.);
#11678=FACE_OUTER_BOUND('',#17481,.T.);
#11679=FACE_OUTER_BOUND('',#17482,.T.);
#11680=FACE_OUTER_BOUND('',#17483,.T.);
#11681=FACE_OUTER_BOUND('',#17484,.T.);
#11682=FACE_OUTER_BOUND('',#17485,.T.);
#11683=FACE_OUTER_BOUND('',#17486,.T.);
#11684=FACE_OUTER_BOUND('',#17487,.T.);
#11685=FACE_OUTER_BOUND('',#17488,.T.);
#11686=FACE_OUTER_BOUND('',#17489,.T.);
#11687=FACE_OUTER_BOUND('',#17490,.T.);
#11688=FACE_OUTER_BOUND('',#17491,.T.);
#11689=FACE_OUTER_BOUND('',#17492,.T.);
#11690=FACE_OUTER_BOUND('',#17493,.T.);
#11691=FACE_OUTER_BOUND('',#17494,.T.);
#11692=FACE_OUTER_BOUND('',#17495,.T.);
#11693=FACE_OUTER_BOUND('',#17496,.T.);
#11694=FACE_OUTER_BOUND('',#17497,.T.);
#11695=FACE_OUTER_BOUND('',#17498,.T.);
#11696=FACE_OUTER_BOUND('',#17499,.T.);
#11697=FACE_OUTER_BOUND('',#17500,.T.);
#11698=FACE_OUTER_BOUND('',#17501,.T.);
#11699=FACE_OUTER_BOUND('',#17502,.T.);
#11700=FACE_OUTER_BOUND('',#17503,.T.);
#11701=FACE_OUTER_BOUND('',#17504,.T.);
#11702=FACE_OUTER_BOUND('',#17505,.T.);
#11703=FACE_OUTER_BOUND('',#17506,.T.);
#11704=FACE_OUTER_BOUND('',#17507,.T.);
#11705=FACE_OUTER_BOUND('',#17508,.T.);
#11706=FACE_OUTER_BOUND('',#17509,.T.);
#11707=FACE_OUTER_BOUND('',#17510,.T.);
#11708=FACE_OUTER_BOUND('',#17511,.T.);
#11709=FACE_OUTER_BOUND('',#17512,.T.);
#11710=FACE_OUTER_BOUND('',#17513,.T.);
#11711=FACE_OUTER_BOUND('',#17514,.T.);
#11712=FACE_OUTER_BOUND('',#17515,.T.);
#11713=FACE_OUTER_BOUND('',#17516,.T.);
#11714=FACE_OUTER_BOUND('',#17517,.T.);
#11715=FACE_OUTER_BOUND('',#17518,.T.);
#11716=FACE_OUTER_BOUND('',#17519,.T.);
#11717=FACE_OUTER_BOUND('',#17520,.T.);
#11718=FACE_OUTER_BOUND('',#17521,.T.);
#11719=FACE_OUTER_BOUND('',#17522,.T.);
#11720=FACE_OUTER_BOUND('',#17523,.T.);
#11721=FACE_OUTER_BOUND('',#17524,.T.);
#11722=FACE_OUTER_BOUND('',#17525,.T.);
#11723=FACE_OUTER_BOUND('',#17526,.T.);
#11724=FACE_OUTER_BOUND('',#17527,.T.);
#11725=FACE_OUTER_BOUND('',#17528,.T.);
#11726=FACE_OUTER_BOUND('',#17529,.T.);
#11727=FACE_OUTER_BOUND('',#17530,.T.);
#11728=FACE_OUTER_BOUND('',#17531,.T.);
#11729=FACE_OUTER_BOUND('',#17532,.T.);
#11730=FACE_OUTER_BOUND('',#17533,.T.);
#11731=FACE_OUTER_BOUND('',#17534,.T.);
#11732=FACE_OUTER_BOUND('',#17535,.T.);
#11733=FACE_OUTER_BOUND('',#17536,.T.);
#11734=FACE_OUTER_BOUND('',#17537,.T.);
#11735=FACE_OUTER_BOUND('',#17538,.T.);
#11736=FACE_OUTER_BOUND('',#17539,.T.);
#11737=FACE_OUTER_BOUND('',#17540,.T.);
#11738=FACE_OUTER_BOUND('',#17541,.T.);
#11739=FACE_OUTER_BOUND('',#17542,.T.);
#11740=FACE_OUTER_BOUND('',#17543,.T.);
#11741=FACE_OUTER_BOUND('',#17544,.T.);
#11742=FACE_OUTER_BOUND('',#17545,.T.);
#11743=FACE_OUTER_BOUND('',#17546,.T.);
#11744=FACE_OUTER_BOUND('',#17547,.T.);
#11745=FACE_OUTER_BOUND('',#17548,.T.);
#11746=FACE_OUTER_BOUND('',#17549,.T.);
#11747=FACE_OUTER_BOUND('',#17550,.T.);
#11748=FACE_OUTER_BOUND('',#17551,.T.);
#11749=FACE_OUTER_BOUND('',#17552,.T.);
#11750=FACE_OUTER_BOUND('',#17553,.T.);
#11751=FACE_OUTER_BOUND('',#17554,.T.);
#11752=FACE_OUTER_BOUND('',#17555,.T.);
#11753=FACE_OUTER_BOUND('',#17556,.T.);
#11754=FACE_OUTER_BOUND('',#17557,.T.);
#11755=FACE_OUTER_BOUND('',#17558,.T.);
#11756=FACE_OUTER_BOUND('',#17559,.T.);
#11757=FACE_OUTER_BOUND('',#17560,.T.);
#11758=FACE_OUTER_BOUND('',#17561,.T.);
#11759=FACE_OUTER_BOUND('',#17562,.T.);
#11760=FACE_OUTER_BOUND('',#17563,.T.);
#11761=FACE_OUTER_BOUND('',#17564,.T.);
#11762=FACE_OUTER_BOUND('',#17566,.T.);
#11763=FACE_OUTER_BOUND('',#17567,.T.);
#11764=FACE_OUTER_BOUND('',#17568,.T.);
#11765=FACE_OUTER_BOUND('',#17569,.T.);
#11766=FACE_OUTER_BOUND('',#17570,.T.);
#11767=FACE_OUTER_BOUND('',#17571,.T.);
#11768=FACE_OUTER_BOUND('',#17572,.T.);
#11769=FACE_OUTER_BOUND('',#17573,.T.);
#11770=FACE_OUTER_BOUND('',#17574,.T.);
#11771=FACE_OUTER_BOUND('',#17575,.T.);
#11772=FACE_OUTER_BOUND('',#17576,.T.);
#11773=FACE_OUTER_BOUND('',#17577,.T.);
#11774=FACE_OUTER_BOUND('',#17578,.T.);
#11775=FACE_OUTER_BOUND('',#17579,.T.);
#11776=FACE_OUTER_BOUND('',#17580,.T.);
#11777=FACE_OUTER_BOUND('',#17581,.T.);
#11778=FACE_OUTER_BOUND('',#17582,.T.);
#11779=FACE_OUTER_BOUND('',#17583,.T.);
#11780=FACE_OUTER_BOUND('',#17584,.T.);
#11781=FACE_OUTER_BOUND('',#17585,.T.);
#11782=FACE_OUTER_BOUND('',#17586,.T.);
#11783=FACE_OUTER_BOUND('',#17587,.T.);
#11784=FACE_OUTER_BOUND('',#17588,.T.);
#11785=FACE_OUTER_BOUND('',#17589,.T.);
#11786=FACE_OUTER_BOUND('',#17590,.T.);
#11787=FACE_OUTER_BOUND('',#17591,.T.);
#11788=FACE_OUTER_BOUND('',#17592,.T.);
#11789=FACE_OUTER_BOUND('',#17593,.T.);
#11790=FACE_OUTER_BOUND('',#17594,.T.);
#11791=FACE_OUTER_BOUND('',#17595,.T.);
#11792=FACE_OUTER_BOUND('',#17596,.T.);
#11793=FACE_OUTER_BOUND('',#17597,.T.);
#11794=FACE_OUTER_BOUND('',#17598,.T.);
#11795=FACE_OUTER_BOUND('',#17599,.T.);
#11796=FACE_OUTER_BOUND('',#17600,.T.);
#11797=FACE_OUTER_BOUND('',#17601,.T.);
#11798=FACE_OUTER_BOUND('',#17602,.T.);
#11799=FACE_OUTER_BOUND('',#17603,.T.);
#11800=FACE_OUTER_BOUND('',#17604,.T.);
#11801=FACE_OUTER_BOUND('',#17605,.T.);
#11802=FACE_OUTER_BOUND('',#17606,.T.);
#11803=FACE_OUTER_BOUND('',#17607,.T.);
#11804=FACE_OUTER_BOUND('',#17608,.T.);
#11805=FACE_OUTER_BOUND('',#17609,.T.);
#11806=FACE_OUTER_BOUND('',#17610,.T.);
#11807=FACE_OUTER_BOUND('',#17611,.T.);
#11808=FACE_OUTER_BOUND('',#17612,.T.);
#11809=FACE_OUTER_BOUND('',#17613,.T.);
#11810=FACE_OUTER_BOUND('',#17614,.T.);
#11811=FACE_OUTER_BOUND('',#17615,.T.);
#11812=FACE_OUTER_BOUND('',#17616,.T.);
#11813=FACE_OUTER_BOUND('',#17617,.T.);
#11814=FACE_OUTER_BOUND('',#17618,.T.);
#11815=FACE_OUTER_BOUND('',#17619,.T.);
#11816=FACE_OUTER_BOUND('',#17620,.T.);
#11817=FACE_OUTER_BOUND('',#17621,.T.);
#11818=FACE_OUTER_BOUND('',#17622,.T.);
#11819=FACE_OUTER_BOUND('',#17623,.T.);
#11820=FACE_OUTER_BOUND('',#17624,.T.);
#11821=FACE_OUTER_BOUND('',#17625,.T.);
#11822=FACE_OUTER_BOUND('',#17626,.T.);
#11823=FACE_OUTER_BOUND('',#17627,.T.);
#11824=FACE_OUTER_BOUND('',#17628,.T.);
#11825=FACE_OUTER_BOUND('',#17629,.T.);
#11826=FACE_OUTER_BOUND('',#17630,.T.);
#11827=FACE_OUTER_BOUND('',#17631,.T.);
#11828=FACE_OUTER_BOUND('',#17632,.T.);
#11829=FACE_OUTER_BOUND('',#17633,.T.);
#11830=FACE_OUTER_BOUND('',#17634,.T.);
#11831=FACE_OUTER_BOUND('',#17635,.T.);
#11832=FACE_OUTER_BOUND('',#17636,.T.);
#11833=FACE_OUTER_BOUND('',#17637,.T.);
#11834=FACE_OUTER_BOUND('',#17638,.T.);
#11835=FACE_OUTER_BOUND('',#17639,.T.);
#11836=FACE_OUTER_BOUND('',#17640,.T.);
#11837=FACE_OUTER_BOUND('',#17641,.T.);
#11838=FACE_OUTER_BOUND('',#17642,.T.);
#11839=FACE_OUTER_BOUND('',#17643,.T.);
#11840=FACE_OUTER_BOUND('',#17644,.T.);
#11841=FACE_OUTER_BOUND('',#17645,.T.);
#11842=FACE_OUTER_BOUND('',#17646,.T.);
#11843=FACE_OUTER_BOUND('',#17647,.T.);
#11844=FACE_OUTER_BOUND('',#17648,.T.);
#11845=FACE_OUTER_BOUND('',#17649,.T.);
#11846=FACE_OUTER_BOUND('',#17650,.T.);
#11847=FACE_OUTER_BOUND('',#17651,.T.);
#11848=FACE_OUTER_BOUND('',#17652,.T.);
#11849=FACE_OUTER_BOUND('',#17653,.T.);
#11850=FACE_OUTER_BOUND('',#17654,.T.);
#11851=FACE_OUTER_BOUND('',#17655,.T.);
#11852=FACE_OUTER_BOUND('',#17656,.T.);
#11853=FACE_OUTER_BOUND('',#17657,.T.);
#11854=FACE_OUTER_BOUND('',#17658,.T.);
#11855=FACE_OUTER_BOUND('',#17659,.T.);
#11856=FACE_OUTER_BOUND('',#17660,.T.);
#11857=FACE_OUTER_BOUND('',#17661,.T.);
#11858=FACE_OUTER_BOUND('',#17662,.T.);
#11859=FACE_OUTER_BOUND('',#17663,.T.);
#11860=FACE_OUTER_BOUND('',#17664,.T.);
#11861=FACE_OUTER_BOUND('',#17665,.T.);
#11862=FACE_OUTER_BOUND('',#17666,.T.);
#11863=FACE_OUTER_BOUND('',#17667,.T.);
#11864=FACE_OUTER_BOUND('',#17668,.T.);
#11865=FACE_OUTER_BOUND('',#17669,.T.);
#11866=FACE_OUTER_BOUND('',#17670,.T.);
#11867=FACE_OUTER_BOUND('',#17671,.T.);
#11868=FACE_OUTER_BOUND('',#17672,.T.);
#11869=FACE_OUTER_BOUND('',#17673,.T.);
#11870=FACE_OUTER_BOUND('',#17674,.T.);
#11871=FACE_OUTER_BOUND('',#17675,.T.);
#11872=FACE_OUTER_BOUND('',#17676,.T.);
#11873=FACE_OUTER_BOUND('',#17677,.T.);
#11874=FACE_OUTER_BOUND('',#17678,.T.);
#11875=FACE_OUTER_BOUND('',#17679,.T.);
#11876=FACE_OUTER_BOUND('',#17680,.T.);
#11877=FACE_OUTER_BOUND('',#17681,.T.);
#11878=FACE_OUTER_BOUND('',#17682,.T.);
#11879=FACE_OUTER_BOUND('',#17683,.T.);
#11880=FACE_OUTER_BOUND('',#17684,.T.);
#11881=FACE_OUTER_BOUND('',#17685,.T.);
#11882=FACE_OUTER_BOUND('',#17686,.T.);
#11883=FACE_OUTER_BOUND('',#17687,.T.);
#11884=FACE_OUTER_BOUND('',#17688,.T.);
#11885=FACE_OUTER_BOUND('',#17689,.T.);
#11886=FACE_OUTER_BOUND('',#17690,.T.);
#11887=FACE_OUTER_BOUND('',#17691,.T.);
#11888=FACE_OUTER_BOUND('',#17692,.T.);
#11889=FACE_OUTER_BOUND('',#17693,.T.);
#11890=FACE_OUTER_BOUND('',#17694,.T.);
#11891=FACE_OUTER_BOUND('',#17695,.T.);
#11892=FACE_OUTER_BOUND('',#17696,.T.);
#11893=FACE_OUTER_BOUND('',#17697,.T.);
#11894=FACE_OUTER_BOUND('',#17698,.T.);
#11895=FACE_OUTER_BOUND('',#17699,.T.);
#11896=FACE_OUTER_BOUND('',#17700,.T.);
#11897=FACE_OUTER_BOUND('',#17701,.T.);
#11898=FACE_OUTER_BOUND('',#17702,.T.);
#11899=FACE_OUTER_BOUND('',#17703,.T.);
#11900=FACE_OUTER_BOUND('',#17704,.T.);
#11901=FACE_OUTER_BOUND('',#17705,.T.);
#11902=FACE_OUTER_BOUND('',#17706,.T.);
#11903=FACE_OUTER_BOUND('',#17707,.T.);
#11904=FACE_OUTER_BOUND('',#17708,.T.);
#11905=FACE_OUTER_BOUND('',#17709,.T.);
#11906=FACE_OUTER_BOUND('',#17710,.T.);
#11907=FACE_OUTER_BOUND('',#17711,.T.);
#11908=FACE_OUTER_BOUND('',#17712,.T.);
#11909=FACE_OUTER_BOUND('',#17713,.T.);
#11910=FACE_OUTER_BOUND('',#17714,.T.);
#11911=FACE_OUTER_BOUND('',#17715,.T.);
#11912=FACE_OUTER_BOUND('',#17716,.T.);
#11913=FACE_OUTER_BOUND('',#17717,.T.);
#11914=FACE_OUTER_BOUND('',#17718,.T.);
#11915=FACE_OUTER_BOUND('',#17719,.T.);
#11916=FACE_OUTER_BOUND('',#17720,.T.);
#11917=FACE_OUTER_BOUND('',#17721,.T.);
#11918=FACE_OUTER_BOUND('',#17722,.T.);
#11919=FACE_OUTER_BOUND('',#17723,.T.);
#11920=FACE_OUTER_BOUND('',#17724,.T.);
#11921=FACE_OUTER_BOUND('',#17725,.T.);
#11922=FACE_OUTER_BOUND('',#17726,.T.);
#11923=FACE_OUTER_BOUND('',#17727,.T.);
#11924=FACE_OUTER_BOUND('',#17728,.T.);
#11925=FACE_OUTER_BOUND('',#17729,.T.);
#11926=FACE_OUTER_BOUND('',#17730,.T.);
#11927=FACE_OUTER_BOUND('',#17731,.T.);
#11928=FACE_OUTER_BOUND('',#17732,.T.);
#11929=FACE_OUTER_BOUND('',#17733,.T.);
#11930=FACE_OUTER_BOUND('',#17734,.T.);
#11931=FACE_OUTER_BOUND('',#17735,.T.);
#11932=FACE_OUTER_BOUND('',#17736,.T.);
#11933=FACE_OUTER_BOUND('',#17737,.T.);
#11934=FACE_OUTER_BOUND('',#17738,.T.);
#11935=FACE_OUTER_BOUND('',#17739,.T.);
#11936=FACE_OUTER_BOUND('',#17740,.T.);
#11937=FACE_OUTER_BOUND('',#17741,.T.);
#11938=FACE_OUTER_BOUND('',#17742,.T.);
#11939=FACE_OUTER_BOUND('',#17743,.T.);
#11940=FACE_OUTER_BOUND('',#17744,.T.);
#11941=FACE_OUTER_BOUND('',#17745,.T.);
#11942=FACE_OUTER_BOUND('',#17746,.T.);
#11943=FACE_OUTER_BOUND('',#17747,.T.);
#11944=FACE_OUTER_BOUND('',#17748,.T.);
#11945=FACE_OUTER_BOUND('',#17749,.T.);
#11946=FACE_OUTER_BOUND('',#17750,.T.);
#11947=FACE_OUTER_BOUND('',#17751,.T.);
#11948=FACE_OUTER_BOUND('',#17752,.T.);
#11949=FACE_OUTER_BOUND('',#17753,.T.);
#11950=FACE_OUTER_BOUND('',#17754,.T.);
#11951=FACE_OUTER_BOUND('',#17755,.T.);
#11952=FACE_OUTER_BOUND('',#17756,.T.);
#11953=FACE_OUTER_BOUND('',#17757,.T.);
#11954=FACE_OUTER_BOUND('',#17758,.T.);
#11955=FACE_OUTER_BOUND('',#17759,.T.);
#11956=FACE_OUTER_BOUND('',#17760,.T.);
#11957=FACE_OUTER_BOUND('',#17761,.T.);
#11958=FACE_OUTER_BOUND('',#17762,.T.);
#11959=FACE_OUTER_BOUND('',#17763,.T.);
#11960=FACE_OUTER_BOUND('',#17764,.T.);
#11961=FACE_OUTER_BOUND('',#17765,.T.);
#11962=FACE_OUTER_BOUND('',#17766,.T.);
#11963=FACE_OUTER_BOUND('',#17767,.T.);
#11964=FACE_OUTER_BOUND('',#17768,.T.);
#11965=FACE_OUTER_BOUND('',#17769,.T.);
#11966=FACE_OUTER_BOUND('',#17770,.T.);
#11967=FACE_OUTER_BOUND('',#17771,.T.);
#11968=FACE_OUTER_BOUND('',#17772,.T.);
#11969=FACE_OUTER_BOUND('',#17773,.T.);
#11970=FACE_OUTER_BOUND('',#17774,.T.);
#11971=FACE_OUTER_BOUND('',#17775,.T.);
#11972=FACE_OUTER_BOUND('',#17776,.T.);
#11973=FACE_OUTER_BOUND('',#17777,.T.);
#11974=FACE_OUTER_BOUND('',#17778,.T.);
#11975=FACE_OUTER_BOUND('',#17779,.T.);
#11976=FACE_OUTER_BOUND('',#17780,.T.);
#11977=FACE_OUTER_BOUND('',#17781,.T.);
#11978=FACE_OUTER_BOUND('',#17782,.T.);
#11979=FACE_OUTER_BOUND('',#17783,.T.);
#11980=FACE_OUTER_BOUND('',#17784,.T.);
#11981=FACE_OUTER_BOUND('',#17785,.T.);
#11982=FACE_OUTER_BOUND('',#17786,.T.);
#11983=FACE_OUTER_BOUND('',#17787,.T.);
#11984=FACE_OUTER_BOUND('',#17788,.T.);
#11985=FACE_OUTER_BOUND('',#17789,.T.);
#11986=FACE_OUTER_BOUND('',#17790,.T.);
#11987=FACE_OUTER_BOUND('',#17791,.T.);
#11988=FACE_OUTER_BOUND('',#17792,.T.);
#11989=FACE_OUTER_BOUND('',#17793,.T.);
#11990=FACE_OUTER_BOUND('',#17794,.T.);
#11991=FACE_OUTER_BOUND('',#17795,.T.);
#11992=FACE_OUTER_BOUND('',#17796,.T.);
#11993=FACE_OUTER_BOUND('',#17797,.T.);
#11994=FACE_OUTER_BOUND('',#17798,.T.);
#11995=FACE_OUTER_BOUND('',#17799,.T.);
#11996=FACE_OUTER_BOUND('',#17800,.T.);
#11997=FACE_OUTER_BOUND('',#17801,.T.);
#11998=FACE_OUTER_BOUND('',#17802,.T.);
#11999=FACE_OUTER_BOUND('',#17803,.T.);
#12000=FACE_OUTER_BOUND('',#17804,.T.);
#12001=FACE_OUTER_BOUND('',#17805,.T.);
#12002=FACE_OUTER_BOUND('',#17806,.T.);
#12003=FACE_OUTER_BOUND('',#17807,.T.);
#12004=FACE_OUTER_BOUND('',#17808,.T.);
#12005=FACE_OUTER_BOUND('',#17809,.T.);
#12006=FACE_OUTER_BOUND('',#17810,.T.);
#12007=FACE_OUTER_BOUND('',#17811,.T.);
#12008=FACE_OUTER_BOUND('',#17812,.T.);
#12009=FACE_OUTER_BOUND('',#17813,.T.);
#12010=FACE_OUTER_BOUND('',#17814,.T.);
#12011=FACE_OUTER_BOUND('',#17815,.T.);
#12012=FACE_OUTER_BOUND('',#17816,.T.);
#12013=FACE_OUTER_BOUND('',#17817,.T.);
#12014=FACE_OUTER_BOUND('',#17818,.T.);
#12015=FACE_OUTER_BOUND('',#17819,.T.);
#12016=FACE_OUTER_BOUND('',#17820,.T.);
#12017=FACE_OUTER_BOUND('',#17821,.T.);
#12018=FACE_OUTER_BOUND('',#17822,.T.);
#12019=FACE_OUTER_BOUND('',#17823,.T.);
#12020=FACE_OUTER_BOUND('',#17824,.T.);
#12021=FACE_OUTER_BOUND('',#17825,.T.);
#12022=FACE_OUTER_BOUND('',#17826,.T.);
#12023=FACE_OUTER_BOUND('',#17827,.T.);
#12024=FACE_OUTER_BOUND('',#17828,.T.);
#12025=FACE_OUTER_BOUND('',#17829,.T.);
#12026=FACE_OUTER_BOUND('',#17830,.T.);
#12027=FACE_OUTER_BOUND('',#17831,.T.);
#12028=FACE_OUTER_BOUND('',#17832,.T.);
#12029=FACE_OUTER_BOUND('',#17833,.T.);
#12030=FACE_OUTER_BOUND('',#17834,.T.);
#12031=FACE_OUTER_BOUND('',#17835,.T.);
#12032=FACE_OUTER_BOUND('',#17836,.T.);
#12033=FACE_OUTER_BOUND('',#17837,.T.);
#12034=FACE_OUTER_BOUND('',#17838,.T.);
#12035=FACE_OUTER_BOUND('',#17839,.T.);
#12036=FACE_OUTER_BOUND('',#17840,.T.);
#12037=FACE_OUTER_BOUND('',#17841,.T.);
#12038=FACE_OUTER_BOUND('',#17842,.T.);
#12039=FACE_OUTER_BOUND('',#17843,.T.);
#12040=FACE_OUTER_BOUND('',#17844,.T.);
#12041=FACE_OUTER_BOUND('',#17845,.T.);
#12042=FACE_OUTER_BOUND('',#17846,.T.);
#12043=FACE_OUTER_BOUND('',#17847,.T.);
#12044=FACE_OUTER_BOUND('',#17848,.T.);
#12045=FACE_OUTER_BOUND('',#17849,.T.);
#12046=FACE_OUTER_BOUND('',#17850,.T.);
#12047=FACE_OUTER_BOUND('',#17851,.T.);
#12048=FACE_OUTER_BOUND('',#17852,.T.);
#12049=FACE_OUTER_BOUND('',#17853,.T.);
#12050=FACE_OUTER_BOUND('',#17854,.T.);
#12051=FACE_OUTER_BOUND('',#17855,.T.);
#12052=FACE_OUTER_BOUND('',#17856,.T.);
#12053=FACE_OUTER_BOUND('',#17857,.T.);
#12054=FACE_OUTER_BOUND('',#17858,.T.);
#12055=FACE_OUTER_BOUND('',#17859,.T.);
#12056=FACE_OUTER_BOUND('',#17860,.T.);
#12057=FACE_OUTER_BOUND('',#17861,.T.);
#12058=FACE_OUTER_BOUND('',#17862,.T.);
#12059=FACE_OUTER_BOUND('',#17863,.T.);
#12060=FACE_OUTER_BOUND('',#17864,.T.);
#12061=FACE_OUTER_BOUND('',#17865,.T.);
#12062=FACE_OUTER_BOUND('',#17866,.T.);
#12063=FACE_OUTER_BOUND('',#17867,.T.);
#12064=FACE_OUTER_BOUND('',#17868,.T.);
#12065=FACE_OUTER_BOUND('',#17869,.T.);
#12066=FACE_OUTER_BOUND('',#17870,.T.);
#12067=FACE_OUTER_BOUND('',#17871,.T.);
#12068=FACE_OUTER_BOUND('',#17872,.T.);
#12069=FACE_OUTER_BOUND('',#17873,.T.);
#12070=FACE_OUTER_BOUND('',#17874,.T.);
#12071=FACE_OUTER_BOUND('',#17875,.T.);
#12072=FACE_OUTER_BOUND('',#17876,.T.);
#12073=FACE_OUTER_BOUND('',#17877,.T.);
#12074=FACE_OUTER_BOUND('',#17878,.T.);
#12075=FACE_OUTER_BOUND('',#17879,.T.);
#12076=FACE_OUTER_BOUND('',#17880,.T.);
#12077=FACE_OUTER_BOUND('',#17881,.T.);
#12078=FACE_OUTER_BOUND('',#17882,.T.);
#12079=FACE_OUTER_BOUND('',#17883,.T.);
#12080=FACE_OUTER_BOUND('',#17884,.T.);
#12081=FACE_OUTER_BOUND('',#17885,.T.);
#12082=FACE_OUTER_BOUND('',#17886,.T.);
#12083=FACE_OUTER_BOUND('',#17887,.T.);
#12084=FACE_OUTER_BOUND('',#17888,.T.);
#12085=FACE_OUTER_BOUND('',#17889,.T.);
#12086=FACE_OUTER_BOUND('',#17890,.T.);
#12087=FACE_OUTER_BOUND('',#17891,.T.);
#12088=FACE_OUTER_BOUND('',#17892,.T.);
#12089=FACE_OUTER_BOUND('',#17893,.T.);
#12090=FACE_OUTER_BOUND('',#17894,.T.);
#12091=FACE_OUTER_BOUND('',#17895,.T.);
#12092=FACE_OUTER_BOUND('',#17896,.T.);
#12093=FACE_OUTER_BOUND('',#17897,.T.);
#12094=FACE_OUTER_BOUND('',#17898,.T.);
#12095=FACE_OUTER_BOUND('',#17899,.T.);
#12096=FACE_OUTER_BOUND('',#17900,.T.);
#12097=FACE_OUTER_BOUND('',#17901,.T.);
#12098=FACE_OUTER_BOUND('',#17902,.T.);
#12099=FACE_OUTER_BOUND('',#17903,.T.);
#12100=FACE_OUTER_BOUND('',#17904,.T.);
#12101=FACE_OUTER_BOUND('',#17905,.T.);
#12102=FACE_OUTER_BOUND('',#17906,.T.);
#12103=FACE_OUTER_BOUND('',#17907,.T.);
#12104=FACE_OUTER_BOUND('',#17908,.T.);
#12105=FACE_OUTER_BOUND('',#17909,.T.);
#12106=FACE_OUTER_BOUND('',#17910,.T.);
#12107=FACE_OUTER_BOUND('',#17911,.T.);
#12108=FACE_OUTER_BOUND('',#17912,.T.);
#12109=FACE_OUTER_BOUND('',#17913,.T.);
#12110=FACE_OUTER_BOUND('',#17914,.T.);
#12111=FACE_OUTER_BOUND('',#17915,.T.);
#12112=FACE_OUTER_BOUND('',#17916,.T.);
#12113=FACE_OUTER_BOUND('',#17917,.T.);
#12114=FACE_OUTER_BOUND('',#17918,.T.);
#12115=FACE_OUTER_BOUND('',#17919,.T.);
#12116=FACE_OUTER_BOUND('',#17920,.T.);
#12117=FACE_OUTER_BOUND('',#17921,.T.);
#12118=FACE_OUTER_BOUND('',#17922,.T.);
#12119=FACE_OUTER_BOUND('',#17923,.T.);
#12120=FACE_OUTER_BOUND('',#17924,.T.);
#12121=FACE_OUTER_BOUND('',#17925,.T.);
#12122=FACE_OUTER_BOUND('',#17926,.T.);
#12123=FACE_OUTER_BOUND('',#17927,.T.);
#12124=FACE_OUTER_BOUND('',#17928,.T.);
#12125=FACE_OUTER_BOUND('',#17929,.T.);
#12126=FACE_OUTER_BOUND('',#17930,.T.);
#12127=FACE_OUTER_BOUND('',#17931,.T.);
#12128=FACE_OUTER_BOUND('',#17932,.T.);
#12129=FACE_OUTER_BOUND('',#17933,.T.);
#12130=FACE_OUTER_BOUND('',#17934,.T.);
#12131=FACE_OUTER_BOUND('',#17935,.T.);
#12132=FACE_OUTER_BOUND('',#17936,.T.);
#12133=FACE_OUTER_BOUND('',#17937,.T.);
#12134=FACE_OUTER_BOUND('',#17938,.T.);
#12135=FACE_OUTER_BOUND('',#17939,.T.);
#12136=FACE_OUTER_BOUND('',#17940,.T.);
#12137=FACE_OUTER_BOUND('',#17941,.T.);
#12138=FACE_OUTER_BOUND('',#17942,.T.);
#12139=FACE_OUTER_BOUND('',#17943,.T.);
#12140=FACE_OUTER_BOUND('',#17944,.T.);
#12141=FACE_OUTER_BOUND('',#17945,.T.);
#12142=FACE_OUTER_BOUND('',#17946,.T.);
#12143=FACE_OUTER_BOUND('',#17947,.T.);
#12144=FACE_OUTER_BOUND('',#17948,.T.);
#12145=FACE_OUTER_BOUND('',#17949,.T.);
#12146=FACE_OUTER_BOUND('',#17950,.T.);
#12147=FACE_OUTER_BOUND('',#17951,.T.);
#12148=FACE_OUTER_BOUND('',#17952,.T.);
#12149=FACE_OUTER_BOUND('',#17953,.T.);
#12150=FACE_OUTER_BOUND('',#17954,.T.);
#12151=FACE_OUTER_BOUND('',#17955,.T.);
#12152=FACE_OUTER_BOUND('',#17956,.T.);
#12153=FACE_OUTER_BOUND('',#17957,.T.);
#12154=FACE_OUTER_BOUND('',#17958,.T.);
#12155=FACE_OUTER_BOUND('',#17959,.T.);
#12156=FACE_OUTER_BOUND('',#17960,.T.);
#12157=FACE_OUTER_BOUND('',#17961,.T.);
#12158=FACE_OUTER_BOUND('',#17962,.T.);
#12159=FACE_OUTER_BOUND('',#17963,.T.);
#12160=FACE_OUTER_BOUND('',#17964,.T.);
#12161=FACE_OUTER_BOUND('',#17965,.T.);
#12162=FACE_OUTER_BOUND('',#17966,.T.);
#12163=FACE_OUTER_BOUND('',#17967,.T.);
#12164=FACE_OUTER_BOUND('',#17968,.T.);
#12165=FACE_OUTER_BOUND('',#17969,.T.);
#12166=FACE_OUTER_BOUND('',#17970,.T.);
#12167=FACE_OUTER_BOUND('',#17971,.T.);
#12168=FACE_OUTER_BOUND('',#17972,.T.);
#12169=FACE_OUTER_BOUND('',#17973,.T.);
#12170=FACE_OUTER_BOUND('',#17974,.T.);
#12171=FACE_OUTER_BOUND('',#17975,.T.);
#12172=FACE_OUTER_BOUND('',#17976,.T.);
#12173=FACE_OUTER_BOUND('',#17977,.T.);
#12174=FACE_OUTER_BOUND('',#17978,.T.);
#12175=FACE_OUTER_BOUND('',#17979,.T.);
#12176=FACE_OUTER_BOUND('',#17980,.T.);
#12177=FACE_OUTER_BOUND('',#17981,.T.);
#12178=FACE_OUTER_BOUND('',#17982,.T.);
#12179=FACE_OUTER_BOUND('',#17983,.T.);
#12180=FACE_OUTER_BOUND('',#17984,.T.);
#12181=FACE_OUTER_BOUND('',#17985,.T.);
#12182=FACE_OUTER_BOUND('',#17986,.T.);
#12183=FACE_OUTER_BOUND('',#17987,.T.);
#12184=FACE_OUTER_BOUND('',#17988,.T.);
#12185=FACE_OUTER_BOUND('',#17989,.T.);
#12186=FACE_OUTER_BOUND('',#17990,.T.);
#12187=FACE_OUTER_BOUND('',#17991,.T.);
#12188=FACE_OUTER_BOUND('',#17992,.T.);
#12189=FACE_OUTER_BOUND('',#17993,.T.);
#12190=FACE_OUTER_BOUND('',#17994,.T.);
#12191=FACE_OUTER_BOUND('',#17995,.T.);
#12192=FACE_OUTER_BOUND('',#17996,.T.);
#12193=FACE_OUTER_BOUND('',#17997,.T.);
#12194=FACE_OUTER_BOUND('',#17998,.T.);
#12195=FACE_OUTER_BOUND('',#17999,.T.);
#12196=FACE_OUTER_BOUND('',#18000,.T.);
#12197=FACE_OUTER_BOUND('',#18001,.T.);
#12198=FACE_OUTER_BOUND('',#18002,.T.);
#12199=FACE_OUTER_BOUND('',#18003,.T.);
#12200=FACE_OUTER_BOUND('',#18004,.T.);
#12201=FACE_OUTER_BOUND('',#18005,.T.);
#12202=FACE_OUTER_BOUND('',#18006,.T.);
#12203=FACE_OUTER_BOUND('',#18007,.T.);
#12204=FACE_OUTER_BOUND('',#18008,.T.);
#12205=FACE_OUTER_BOUND('',#18009,.T.);
#12206=FACE_OUTER_BOUND('',#18010,.T.);
#12207=FACE_OUTER_BOUND('',#18011,.T.);
#12208=FACE_OUTER_BOUND('',#18012,.T.);
#12209=FACE_OUTER_BOUND('',#18013,.T.);
#12210=FACE_OUTER_BOUND('',#18014,.T.);
#12211=FACE_OUTER_BOUND('',#18015,.T.);
#12212=FACE_OUTER_BOUND('',#18016,.T.);
#12213=FACE_OUTER_BOUND('',#18017,.T.);
#12214=FACE_OUTER_BOUND('',#18018,.T.);
#12215=FACE_OUTER_BOUND('',#18019,.T.);
#12216=FACE_OUTER_BOUND('',#18020,.T.);
#12217=FACE_OUTER_BOUND('',#18021,.T.);
#12218=FACE_OUTER_BOUND('',#18022,.T.);
#12219=FACE_OUTER_BOUND('',#18023,.T.);
#12220=FACE_OUTER_BOUND('',#18024,.T.);
#12221=FACE_OUTER_BOUND('',#18025,.T.);
#12222=FACE_OUTER_BOUND('',#18026,.T.);
#12223=FACE_OUTER_BOUND('',#18027,.T.);
#12224=FACE_OUTER_BOUND('',#18028,.T.);
#12225=FACE_OUTER_BOUND('',#18029,.T.);
#12226=FACE_OUTER_BOUND('',#18030,.T.);
#12227=FACE_OUTER_BOUND('',#18031,.T.);
#12228=FACE_OUTER_BOUND('',#18032,.T.);
#12229=FACE_OUTER_BOUND('',#18033,.T.);
#12230=FACE_OUTER_BOUND('',#18034,.T.);
#12231=FACE_OUTER_BOUND('',#18035,.T.);
#12232=FACE_OUTER_BOUND('',#18036,.T.);
#12233=FACE_OUTER_BOUND('',#18037,.T.);
#12234=FACE_OUTER_BOUND('',#18038,.T.);
#12235=FACE_OUTER_BOUND('',#18039,.T.);
#12236=FACE_OUTER_BOUND('',#18040,.T.);
#12237=FACE_OUTER_BOUND('',#18041,.T.);
#12238=FACE_OUTER_BOUND('',#18042,.T.);
#12239=FACE_OUTER_BOUND('',#18043,.T.);
#12240=FACE_OUTER_BOUND('',#18044,.T.);
#12241=FACE_OUTER_BOUND('',#18045,.T.);
#12242=FACE_OUTER_BOUND('',#18046,.T.);
#12243=FACE_OUTER_BOUND('',#18047,.T.);
#12244=FACE_OUTER_BOUND('',#18048,.T.);
#12245=FACE_OUTER_BOUND('',#18049,.T.);
#12246=FACE_OUTER_BOUND('',#18050,.T.);
#12247=FACE_OUTER_BOUND('',#18051,.T.);
#12248=FACE_OUTER_BOUND('',#18052,.T.);
#12249=FACE_OUTER_BOUND('',#18053,.T.);
#12250=FACE_OUTER_BOUND('',#18054,.T.);
#12251=FACE_OUTER_BOUND('',#18055,.T.);
#12252=FACE_OUTER_BOUND('',#18056,.T.);
#12253=FACE_OUTER_BOUND('',#18057,.T.);
#12254=FACE_OUTER_BOUND('',#18058,.T.);
#12255=FACE_OUTER_BOUND('',#18059,.T.);
#12256=FACE_OUTER_BOUND('',#18060,.T.);
#12257=FACE_OUTER_BOUND('',#18061,.T.);
#12258=FACE_OUTER_BOUND('',#18062,.T.);
#12259=FACE_OUTER_BOUND('',#18063,.T.);
#12260=FACE_OUTER_BOUND('',#18064,.T.);
#12261=FACE_OUTER_BOUND('',#18065,.T.);
#12262=FACE_OUTER_BOUND('',#18066,.T.);
#12263=FACE_OUTER_BOUND('',#18067,.T.);
#12264=FACE_OUTER_BOUND('',#18068,.T.);
#12265=FACE_OUTER_BOUND('',#18069,.T.);
#12266=FACE_OUTER_BOUND('',#18070,.T.);
#12267=FACE_OUTER_BOUND('',#18071,.T.);
#12268=FACE_OUTER_BOUND('',#18072,.T.);
#12269=FACE_OUTER_BOUND('',#18073,.T.);
#12270=FACE_OUTER_BOUND('',#18074,.T.);
#12271=FACE_OUTER_BOUND('',#18075,.T.);
#12272=FACE_OUTER_BOUND('',#18076,.T.);
#12273=FACE_OUTER_BOUND('',#18077,.T.);
#12274=FACE_OUTER_BOUND('',#18078,.T.);
#12275=FACE_OUTER_BOUND('',#18079,.T.);
#12276=FACE_OUTER_BOUND('',#18080,.T.);
#12277=FACE_OUTER_BOUND('',#18081,.T.);
#12278=FACE_OUTER_BOUND('',#18082,.T.);
#12279=FACE_OUTER_BOUND('',#18083,.T.);
#12280=FACE_OUTER_BOUND('',#18084,.T.);
#12281=FACE_OUTER_BOUND('',#18085,.T.);
#12282=FACE_OUTER_BOUND('',#18086,.T.);
#12283=FACE_OUTER_BOUND('',#18087,.T.);
#12284=FACE_OUTER_BOUND('',#18088,.T.);
#12285=FACE_OUTER_BOUND('',#18089,.T.);
#12286=FACE_OUTER_BOUND('',#18090,.T.);
#12287=FACE_OUTER_BOUND('',#18091,.T.);
#12288=FACE_OUTER_BOUND('',#18092,.T.);
#12289=FACE_OUTER_BOUND('',#18093,.T.);
#12290=FACE_OUTER_BOUND('',#18094,.T.);
#12291=FACE_OUTER_BOUND('',#18095,.T.);
#12292=FACE_OUTER_BOUND('',#18096,.T.);
#12293=FACE_OUTER_BOUND('',#18097,.T.);
#12294=FACE_OUTER_BOUND('',#18098,.T.);
#12295=FACE_OUTER_BOUND('',#18099,.T.);
#12296=FACE_OUTER_BOUND('',#18100,.T.);
#12297=FACE_OUTER_BOUND('',#18101,.T.);
#12298=FACE_OUTER_BOUND('',#18102,.T.);
#12299=FACE_OUTER_BOUND('',#18103,.T.);
#12300=FACE_OUTER_BOUND('',#18104,.T.);
#12301=FACE_OUTER_BOUND('',#18105,.T.);
#12302=FACE_OUTER_BOUND('',#18106,.T.);
#12303=FACE_OUTER_BOUND('',#18107,.T.);
#12304=FACE_OUTER_BOUND('',#18108,.T.);
#12305=FACE_OUTER_BOUND('',#18109,.T.);
#12306=FACE_OUTER_BOUND('',#18110,.T.);
#12307=FACE_OUTER_BOUND('',#18111,.T.);
#12308=FACE_OUTER_BOUND('',#18112,.T.);
#12309=FACE_OUTER_BOUND('',#18113,.T.);
#12310=FACE_OUTER_BOUND('',#18114,.T.);
#12311=FACE_OUTER_BOUND('',#18115,.T.);
#12312=FACE_OUTER_BOUND('',#18116,.T.);
#12313=FACE_OUTER_BOUND('',#18117,.T.);
#12314=FACE_OUTER_BOUND('',#18118,.T.);
#12315=FACE_OUTER_BOUND('',#18119,.T.);
#12316=FACE_OUTER_BOUND('',#18120,.T.);
#12317=FACE_OUTER_BOUND('',#18121,.T.);
#12318=FACE_OUTER_BOUND('',#18122,.T.);
#12319=FACE_OUTER_BOUND('',#18123,.T.);
#12320=FACE_OUTER_BOUND('',#18124,.T.);
#12321=FACE_OUTER_BOUND('',#18125,.T.);
#12322=FACE_OUTER_BOUND('',#18126,.T.);
#12323=FACE_OUTER_BOUND('',#18127,.T.);
#12324=FACE_OUTER_BOUND('',#18128,.T.);
#12325=FACE_OUTER_BOUND('',#18129,.T.);
#12326=FACE_OUTER_BOUND('',#18130,.T.);
#12327=FACE_OUTER_BOUND('',#18131,.T.);
#12328=FACE_OUTER_BOUND('',#18132,.T.);
#12329=FACE_OUTER_BOUND('',#18133,.T.);
#12330=FACE_OUTER_BOUND('',#18134,.T.);
#12331=FACE_OUTER_BOUND('',#18135,.T.);
#12332=FACE_OUTER_BOUND('',#18136,.T.);
#12333=FACE_OUTER_BOUND('',#18137,.T.);
#12334=FACE_OUTER_BOUND('',#18138,.T.);
#12335=FACE_OUTER_BOUND('',#18139,.T.);
#12336=FACE_OUTER_BOUND('',#18140,.T.);
#12337=FACE_OUTER_BOUND('',#18141,.T.);
#12338=FACE_OUTER_BOUND('',#18142,.T.);
#12339=FACE_OUTER_BOUND('',#18143,.T.);
#12340=FACE_OUTER_BOUND('',#18144,.T.);
#12341=FACE_OUTER_BOUND('',#18145,.T.);
#12342=FACE_OUTER_BOUND('',#18146,.T.);
#12343=FACE_OUTER_BOUND('',#18147,.T.);
#12344=FACE_OUTER_BOUND('',#18148,.T.);
#12345=FACE_OUTER_BOUND('',#18149,.T.);
#12346=FACE_OUTER_BOUND('',#18150,.T.);
#12347=FACE_OUTER_BOUND('',#18151,.T.);
#12348=FACE_OUTER_BOUND('',#18152,.T.);
#12349=FACE_OUTER_BOUND('',#18153,.T.);
#12350=FACE_OUTER_BOUND('',#18154,.T.);
#12351=FACE_OUTER_BOUND('',#18155,.T.);
#12352=FACE_OUTER_BOUND('',#18156,.T.);
#12353=FACE_OUTER_BOUND('',#18157,.T.);
#12354=FACE_OUTER_BOUND('',#18158,.T.);
#12355=FACE_OUTER_BOUND('',#18159,.T.);
#12356=FACE_OUTER_BOUND('',#18160,.T.);
#12357=FACE_OUTER_BOUND('',#18161,.T.);
#12358=FACE_OUTER_BOUND('',#18162,.T.);
#12359=FACE_OUTER_BOUND('',#18163,.T.);
#12360=FACE_OUTER_BOUND('',#18164,.T.);
#12361=FACE_OUTER_BOUND('',#18165,.T.);
#12362=FACE_OUTER_BOUND('',#18166,.T.);
#12363=FACE_OUTER_BOUND('',#18167,.T.);
#12364=FACE_OUTER_BOUND('',#18168,.T.);
#12365=FACE_OUTER_BOUND('',#18169,.T.);
#12366=FACE_OUTER_BOUND('',#18170,.T.);
#12367=FACE_OUTER_BOUND('',#18171,.T.);
#12368=FACE_OUTER_BOUND('',#18172,.T.);
#12369=FACE_OUTER_BOUND('',#18173,.T.);
#12370=FACE_OUTER_BOUND('',#18174,.T.);
#12371=FACE_OUTER_BOUND('',#18175,.T.);
#12372=FACE_OUTER_BOUND('',#18176,.T.);
#12373=FACE_OUTER_BOUND('',#18177,.T.);
#12374=FACE_OUTER_BOUND('',#18178,.T.);
#12375=FACE_OUTER_BOUND('',#18179,.T.);
#12376=FACE_OUTER_BOUND('',#18180,.T.);
#12377=FACE_OUTER_BOUND('',#18181,.T.);
#12378=FACE_OUTER_BOUND('',#18182,.T.);
#12379=FACE_OUTER_BOUND('',#18183,.T.);
#12380=FACE_OUTER_BOUND('',#18184,.T.);
#12381=FACE_OUTER_BOUND('',#18185,.T.);
#12382=FACE_OUTER_BOUND('',#18186,.T.);
#12383=FACE_OUTER_BOUND('',#18187,.T.);
#12384=FACE_OUTER_BOUND('',#18188,.T.);
#12385=FACE_OUTER_BOUND('',#18189,.T.);
#12386=FACE_OUTER_BOUND('',#18190,.T.);
#12387=FACE_OUTER_BOUND('',#18191,.T.);
#12388=FACE_OUTER_BOUND('',#18192,.T.);
#12389=FACE_OUTER_BOUND('',#18193,.T.);
#12390=FACE_OUTER_BOUND('',#18194,.T.);
#12391=FACE_OUTER_BOUND('',#18195,.T.);
#12392=FACE_OUTER_BOUND('',#18196,.T.);
#12393=FACE_OUTER_BOUND('',#18197,.T.);
#12394=FACE_OUTER_BOUND('',#18198,.T.);
#12395=FACE_OUTER_BOUND('',#18199,.T.);
#12396=FACE_OUTER_BOUND('',#18200,.T.);
#12397=FACE_OUTER_BOUND('',#18201,.T.);
#12398=FACE_OUTER_BOUND('',#18202,.T.);
#12399=FACE_OUTER_BOUND('',#18203,.T.);
#12400=FACE_OUTER_BOUND('',#18204,.T.);
#12401=FACE_OUTER_BOUND('',#18205,.T.);
#12402=FACE_OUTER_BOUND('',#18206,.T.);
#12403=FACE_OUTER_BOUND('',#18207,.T.);
#12404=FACE_OUTER_BOUND('',#18208,.T.);
#12405=FACE_OUTER_BOUND('',#18209,.T.);
#12406=FACE_OUTER_BOUND('',#18210,.T.);
#12407=FACE_OUTER_BOUND('',#18211,.T.);
#12408=FACE_OUTER_BOUND('',#18212,.T.);
#12409=FACE_OUTER_BOUND('',#18213,.T.);
#12410=FACE_OUTER_BOUND('',#18214,.T.);
#12411=FACE_OUTER_BOUND('',#18215,.T.);
#12412=FACE_OUTER_BOUND('',#18216,.T.);
#12413=FACE_OUTER_BOUND('',#18217,.T.);
#12414=FACE_OUTER_BOUND('',#18218,.T.);
#12415=FACE_OUTER_BOUND('',#18219,.T.);
#12416=FACE_OUTER_BOUND('',#18220,.T.);
#12417=FACE_OUTER_BOUND('',#18221,.T.);
#12418=FACE_OUTER_BOUND('',#18222,.T.);
#12419=FACE_OUTER_BOUND('',#18223,.T.);
#12420=FACE_OUTER_BOUND('',#18224,.T.);
#12421=FACE_OUTER_BOUND('',#18225,.T.);
#12422=FACE_OUTER_BOUND('',#18226,.T.);
#12423=FACE_OUTER_BOUND('',#18227,.T.);
#12424=FACE_OUTER_BOUND('',#18228,.T.);
#12425=FACE_OUTER_BOUND('',#18229,.T.);
#12426=FACE_OUTER_BOUND('',#18230,.T.);
#12427=FACE_OUTER_BOUND('',#18231,.T.);
#12428=FACE_OUTER_BOUND('',#18232,.T.);
#12429=FACE_OUTER_BOUND('',#18233,.T.);
#12430=FACE_OUTER_BOUND('',#18234,.T.);
#12431=FACE_OUTER_BOUND('',#18235,.T.);
#12432=FACE_OUTER_BOUND('',#18236,.T.);
#12433=FACE_OUTER_BOUND('',#18237,.T.);
#12434=FACE_OUTER_BOUND('',#18238,.T.);
#12435=FACE_OUTER_BOUND('',#18239,.T.);
#12436=FACE_OUTER_BOUND('',#18240,.T.);
#12437=FACE_OUTER_BOUND('',#18241,.T.);
#12438=FACE_OUTER_BOUND('',#18242,.T.);
#12439=FACE_OUTER_BOUND('',#18243,.T.);
#12440=FACE_OUTER_BOUND('',#18244,.T.);
#12441=FACE_OUTER_BOUND('',#18245,.T.);
#12442=FACE_OUTER_BOUND('',#18246,.T.);
#12443=FACE_OUTER_BOUND('',#18247,.T.);
#12444=FACE_OUTER_BOUND('',#18248,.T.);
#12445=FACE_OUTER_BOUND('',#18249,.T.);
#12446=FACE_OUTER_BOUND('',#18250,.T.);
#12447=FACE_OUTER_BOUND('',#18251,.T.);
#12448=FACE_OUTER_BOUND('',#18252,.T.);
#12449=FACE_OUTER_BOUND('',#18253,.T.);
#12450=FACE_OUTER_BOUND('',#18254,.T.);
#12451=FACE_OUTER_BOUND('',#18255,.T.);
#12452=FACE_OUTER_BOUND('',#18256,.T.);
#12453=FACE_OUTER_BOUND('',#18257,.T.);
#12454=FACE_OUTER_BOUND('',#18258,.T.);
#12455=FACE_OUTER_BOUND('',#18259,.T.);
#12456=FACE_OUTER_BOUND('',#18260,.T.);
#12457=FACE_OUTER_BOUND('',#18261,.T.);
#12458=FACE_OUTER_BOUND('',#18262,.T.);
#12459=FACE_OUTER_BOUND('',#18263,.T.);
#12460=FACE_OUTER_BOUND('',#18264,.T.);
#12461=FACE_OUTER_BOUND('',#18265,.T.);
#12462=FACE_OUTER_BOUND('',#18266,.T.);
#12463=FACE_OUTER_BOUND('',#18267,.T.);
#12464=FACE_OUTER_BOUND('',#18268,.T.);
#12465=FACE_OUTER_BOUND('',#18269,.T.);
#12466=FACE_OUTER_BOUND('',#18270,.T.);
#12467=FACE_OUTER_BOUND('',#18271,.T.);
#12468=FACE_OUTER_BOUND('',#18272,.T.);
#12469=FACE_OUTER_BOUND('',#18273,.T.);
#12470=FACE_OUTER_BOUND('',#18274,.T.);
#12471=FACE_OUTER_BOUND('',#18275,.T.);
#12472=FACE_OUTER_BOUND('',#18276,.T.);
#12473=FACE_OUTER_BOUND('',#18277,.T.);
#12474=FACE_OUTER_BOUND('',#18278,.T.);
#12475=FACE_OUTER_BOUND('',#18279,.T.);
#12476=FACE_OUTER_BOUND('',#18281,.T.);
#12477=FACE_OUTER_BOUND('',#18282,.T.);
#12478=FACE_OUTER_BOUND('',#18283,.T.);
#12479=FACE_OUTER_BOUND('',#18284,.T.);
#12480=FACE_OUTER_BOUND('',#18285,.T.);
#12481=FACE_OUTER_BOUND('',#18286,.T.);
#12482=FACE_OUTER_BOUND('',#18287,.T.);
#12483=FACE_OUTER_BOUND('',#18288,.T.);
#12484=FACE_OUTER_BOUND('',#18289,.T.);
#12485=FACE_OUTER_BOUND('',#18290,.T.);
#12486=FACE_OUTER_BOUND('',#18291,.T.);
#12487=FACE_OUTER_BOUND('',#18292,.T.);
#12488=FACE_OUTER_BOUND('',#18293,.T.);
#12489=FACE_OUTER_BOUND('',#18294,.T.);
#12490=FACE_OUTER_BOUND('',#18295,.T.);
#12491=FACE_OUTER_BOUND('',#18296,.T.);
#12492=FACE_OUTER_BOUND('',#18297,.T.);
#12493=FACE_OUTER_BOUND('',#18298,.T.);
#12494=FACE_OUTER_BOUND('',#18299,.T.);
#12495=FACE_OUTER_BOUND('',#18300,.T.);
#12496=FACE_OUTER_BOUND('',#18301,.T.);
#12497=FACE_OUTER_BOUND('',#18302,.T.);
#12498=FACE_OUTER_BOUND('',#18303,.T.);
#12499=FACE_OUTER_BOUND('',#18304,.T.);
#12500=FACE_OUTER_BOUND('',#18305,.T.);
#12501=FACE_OUTER_BOUND('',#18306,.T.);
#12502=FACE_OUTER_BOUND('',#18307,.T.);
#12503=FACE_OUTER_BOUND('',#18308,.T.);
#12504=FACE_OUTER_BOUND('',#18309,.T.);
#12505=FACE_OUTER_BOUND('',#18310,.T.);
#12506=FACE_OUTER_BOUND('',#18311,.T.);
#12507=FACE_OUTER_BOUND('',#18312,.T.);
#12508=FACE_OUTER_BOUND('',#18313,.T.);
#12509=FACE_OUTER_BOUND('',#18314,.T.);
#12510=FACE_OUTER_BOUND('',#18315,.T.);
#12511=FACE_OUTER_BOUND('',#18316,.T.);
#12512=FACE_OUTER_BOUND('',#18317,.T.);
#12513=FACE_OUTER_BOUND('',#18318,.T.);
#12514=FACE_OUTER_BOUND('',#18319,.T.);
#12515=FACE_OUTER_BOUND('',#18320,.T.);
#12516=FACE_OUTER_BOUND('',#18321,.T.);
#12517=FACE_OUTER_BOUND('',#18322,.T.);
#12518=FACE_OUTER_BOUND('',#18323,.T.);
#12519=FACE_OUTER_BOUND('',#18324,.T.);
#12520=FACE_OUTER_BOUND('',#18325,.T.);
#12521=FACE_OUTER_BOUND('',#18326,.T.);
#12522=FACE_OUTER_BOUND('',#18327,.T.);
#12523=FACE_OUTER_BOUND('',#18328,.T.);
#12524=FACE_OUTER_BOUND('',#18329,.T.);
#12525=FACE_OUTER_BOUND('',#18330,.T.);
#12526=FACE_OUTER_BOUND('',#18331,.T.);
#12527=FACE_OUTER_BOUND('',#18332,.T.);
#12528=FACE_OUTER_BOUND('',#18333,.T.);
#12529=FACE_OUTER_BOUND('',#18334,.T.);
#12530=FACE_OUTER_BOUND('',#18335,.T.);
#12531=FACE_OUTER_BOUND('',#18336,.T.);
#12532=FACE_OUTER_BOUND('',#18337,.T.);
#12533=FACE_OUTER_BOUND('',#18338,.T.);
#12534=FACE_OUTER_BOUND('',#18339,.T.);
#12535=FACE_OUTER_BOUND('',#18340,.T.);
#12536=FACE_OUTER_BOUND('',#18341,.T.);
#12537=FACE_OUTER_BOUND('',#18342,.T.);
#12538=FACE_OUTER_BOUND('',#18343,.T.);
#12539=FACE_OUTER_BOUND('',#18344,.T.);
#12540=FACE_OUTER_BOUND('',#18345,.T.);
#12541=FACE_OUTER_BOUND('',#18346,.T.);
#12542=FACE_OUTER_BOUND('',#18347,.T.);
#12543=FACE_OUTER_BOUND('',#18348,.T.);
#12544=FACE_OUTER_BOUND('',#18349,.T.);
#12545=FACE_OUTER_BOUND('',#18350,.T.);
#12546=FACE_OUTER_BOUND('',#18351,.T.);
#12547=FACE_OUTER_BOUND('',#18420,.T.);
#12548=FACE_OUTER_BOUND('',#18421,.T.);
#12549=FACE_OUTER_BOUND('',#18422,.T.);
#12550=FACE_OUTER_BOUND('',#18423,.T.);
#12551=FACE_OUTER_BOUND('',#18424,.T.);
#12552=FACE_OUTER_BOUND('',#18425,.T.);
#12553=FACE_OUTER_BOUND('',#18426,.T.);
#12554=FACE_OUTER_BOUND('',#18427,.T.);
#12555=FACE_OUTER_BOUND('',#18428,.T.);
#12556=FACE_OUTER_BOUND('',#18429,.T.);
#12557=FACE_OUTER_BOUND('',#18430,.T.);
#12558=FACE_OUTER_BOUND('',#18431,.T.);
#12559=FACE_OUTER_BOUND('',#18432,.T.);
#12560=FACE_OUTER_BOUND('',#18433,.T.);
#12561=FACE_OUTER_BOUND('',#18434,.T.);
#12562=FACE_OUTER_BOUND('',#18435,.T.);
#12563=FACE_OUTER_BOUND('',#18436,.T.);
#12564=FACE_OUTER_BOUND('',#18437,.T.);
#12565=FACE_OUTER_BOUND('',#18438,.T.);
#12566=FACE_OUTER_BOUND('',#18439,.T.);
#12567=FACE_OUTER_BOUND('',#18440,.T.);
#12568=FACE_OUTER_BOUND('',#18441,.T.);
#12569=FACE_OUTER_BOUND('',#18442,.T.);
#12570=FACE_OUTER_BOUND('',#18443,.T.);
#12571=FACE_OUTER_BOUND('',#18444,.T.);
#12572=FACE_OUTER_BOUND('',#18445,.T.);
#12573=FACE_OUTER_BOUND('',#18446,.T.);
#12574=FACE_OUTER_BOUND('',#18447,.T.);
#12575=FACE_OUTER_BOUND('',#18448,.T.);
#12576=FACE_OUTER_BOUND('',#18449,.T.);
#12577=FACE_OUTER_BOUND('',#18450,.T.);
#12578=FACE_OUTER_BOUND('',#18451,.T.);
#12579=FACE_OUTER_BOUND('',#18452,.T.);
#12580=FACE_OUTER_BOUND('',#18453,.T.);
#12581=FACE_OUTER_BOUND('',#18454,.T.);
#12582=FACE_OUTER_BOUND('',#18455,.T.);
#12583=FACE_OUTER_BOUND('',#18456,.T.);
#12584=FACE_OUTER_BOUND('',#18457,.T.);
#12585=FACE_OUTER_BOUND('',#18458,.T.);
#12586=FACE_OUTER_BOUND('',#18459,.T.);
#12587=FACE_OUTER_BOUND('',#18460,.T.);
#12588=FACE_OUTER_BOUND('',#18462,.T.);
#12589=FACE_OUTER_BOUND('',#18463,.T.);
#12590=FACE_OUTER_BOUND('',#18464,.T.);
#12591=FACE_OUTER_BOUND('',#18465,.T.);
#12592=FACE_OUTER_BOUND('',#18466,.T.);
#12593=FACE_OUTER_BOUND('',#18467,.T.);
#12594=FACE_OUTER_BOUND('',#18468,.T.);
#12595=FACE_OUTER_BOUND('',#18469,.T.);
#12596=FACE_OUTER_BOUND('',#18470,.T.);
#12597=FACE_OUTER_BOUND('',#18471,.T.);
#12598=FACE_OUTER_BOUND('',#18472,.T.);
#12599=FACE_OUTER_BOUND('',#18473,.T.);
#12600=FACE_OUTER_BOUND('',#18474,.T.);
#12601=FACE_OUTER_BOUND('',#18475,.T.);
#12602=FACE_OUTER_BOUND('',#18476,.T.);
#12603=FACE_OUTER_BOUND('',#18477,.T.);
#12604=FACE_OUTER_BOUND('',#18478,.T.);
#12605=FACE_OUTER_BOUND('',#18479,.T.);
#12606=FACE_OUTER_BOUND('',#18480,.T.);
#12607=FACE_OUTER_BOUND('',#18481,.T.);
#12608=FACE_OUTER_BOUND('',#18482,.T.);
#12609=FACE_OUTER_BOUND('',#18483,.T.);
#12610=FACE_OUTER_BOUND('',#18484,.T.);
#12611=FACE_OUTER_BOUND('',#18485,.T.);
#12612=FACE_OUTER_BOUND('',#18486,.T.);
#12613=FACE_OUTER_BOUND('',#18487,.T.);
#12614=FACE_OUTER_BOUND('',#18488,.T.);
#12615=FACE_OUTER_BOUND('',#18489,.T.);
#12616=FACE_OUTER_BOUND('',#18490,.T.);
#12617=FACE_OUTER_BOUND('',#18491,.T.);
#12618=FACE_OUTER_BOUND('',#18492,.T.);
#12619=FACE_OUTER_BOUND('',#18493,.T.);
#12620=FACE_OUTER_BOUND('',#18494,.T.);
#12621=FACE_OUTER_BOUND('',#18495,.T.);
#12622=FACE_OUTER_BOUND('',#18496,.T.);
#12623=FACE_OUTER_BOUND('',#18497,.T.);
#12624=FACE_OUTER_BOUND('',#18498,.T.);
#12625=FACE_OUTER_BOUND('',#18499,.T.);
#12626=FACE_OUTER_BOUND('',#18500,.T.);
#12627=FACE_OUTER_BOUND('',#18501,.T.);
#12628=FACE_OUTER_BOUND('',#18502,.T.);
#12629=FACE_OUTER_BOUND('',#18503,.T.);
#12630=FACE_OUTER_BOUND('',#18504,.T.);
#12631=FACE_OUTER_BOUND('',#18505,.T.);
#12632=FACE_OUTER_BOUND('',#18506,.T.);
#12633=FACE_OUTER_BOUND('',#18507,.T.);
#12634=FACE_OUTER_BOUND('',#18508,.T.);
#12635=FACE_OUTER_BOUND('',#18509,.T.);
#12636=FACE_OUTER_BOUND('',#18510,.T.);
#12637=FACE_OUTER_BOUND('',#18511,.T.);
#12638=FACE_OUTER_BOUND('',#18512,.T.);
#12639=FACE_OUTER_BOUND('',#18514,.T.);
#12640=FACE_OUTER_BOUND('',#18515,.T.);
#12641=FACE_OUTER_BOUND('',#18516,.T.);
#12642=FACE_OUTER_BOUND('',#18517,.T.);
#12643=FACE_OUTER_BOUND('',#18518,.T.);
#12644=FACE_OUTER_BOUND('',#18519,.T.);
#12645=FACE_OUTER_BOUND('',#18520,.T.);
#12646=FACE_OUTER_BOUND('',#18521,.T.);
#12647=FACE_OUTER_BOUND('',#18522,.T.);
#12648=FACE_OUTER_BOUND('',#18523,.T.);
#12649=FACE_OUTER_BOUND('',#18524,.T.);
#12650=FACE_OUTER_BOUND('',#18525,.T.);
#12651=FACE_OUTER_BOUND('',#18526,.T.);
#12652=FACE_OUTER_BOUND('',#18527,.T.);
#12653=FACE_OUTER_BOUND('',#18528,.T.);
#12654=FACE_OUTER_BOUND('',#18529,.T.);
#12655=FACE_OUTER_BOUND('',#18530,.T.);
#12656=FACE_OUTER_BOUND('',#18592,.T.);
#12657=FACE_OUTER_BOUND('',#18593,.T.);
#12658=FACE_OUTER_BOUND('',#18594,.T.);
#12659=FACE_OUTER_BOUND('',#18595,.T.);
#12660=FACE_OUTER_BOUND('',#18596,.T.);
#12661=FACE_OUTER_BOUND('',#18597,.T.);
#12662=FACE_OUTER_BOUND('',#18598,.T.);
#12663=FACE_OUTER_BOUND('',#18599,.T.);
#12664=FACE_OUTER_BOUND('',#18600,.T.);
#12665=FACE_OUTER_BOUND('',#18601,.T.);
#12666=FACE_OUTER_BOUND('',#18603,.T.);
#12667=FACE_OUTER_BOUND('',#18604,.T.);
#12668=FACE_OUTER_BOUND('',#18605,.T.);
#12669=FACE_OUTER_BOUND('',#18606,.T.);
#12670=FACE_OUTER_BOUND('',#18607,.T.);
#12671=FACE_OUTER_BOUND('',#18608,.T.);
#12672=FACE_OUTER_BOUND('',#18609,.T.);
#12673=FACE_OUTER_BOUND('',#18610,.T.);
#12674=FACE_OUTER_BOUND('',#18611,.T.);
#12675=FACE_OUTER_BOUND('',#18612,.T.);
#12676=FACE_OUTER_BOUND('',#18613,.T.);
#12677=FACE_OUTER_BOUND('',#18614,.T.);
#12678=FACE_OUTER_BOUND('',#18615,.T.);
#12679=FACE_OUTER_BOUND('',#18616,.T.);
#12680=FACE_OUTER_BOUND('',#18617,.T.);
#12681=FACE_OUTER_BOUND('',#18618,.T.);
#12682=FACE_OUTER_BOUND('',#18619,.T.);
#12683=FACE_OUTER_BOUND('',#18620,.T.);
#12684=FACE_OUTER_BOUND('',#18621,.T.);
#12685=FACE_OUTER_BOUND('',#18622,.T.);
#12686=FACE_OUTER_BOUND('',#18623,.T.);
#12687=FACE_OUTER_BOUND('',#18625,.T.);
#12688=FACE_OUTER_BOUND('',#18627,.T.);
#12689=FACE_OUTER_BOUND('',#18628,.T.);
#12690=FACE_OUTER_BOUND('',#18629,.T.);
#12691=FACE_OUTER_BOUND('',#18630,.T.);
#12692=FACE_OUTER_BOUND('',#18631,.T.);
#12693=FACE_OUTER_BOUND('',#18632,.T.);
#12694=FACE_OUTER_BOUND('',#18633,.T.);
#12695=FACE_OUTER_BOUND('',#18634,.T.);
#12696=FACE_OUTER_BOUND('',#18635,.T.);
#12697=FACE_OUTER_BOUND('',#18636,.T.);
#12698=FACE_OUTER_BOUND('',#18637,.T.);
#12699=FACE_OUTER_BOUND('',#18638,.T.);
#12700=FACE_OUTER_BOUND('',#18639,.T.);
#12701=FACE_OUTER_BOUND('',#18640,.T.);
#12702=FACE_OUTER_BOUND('',#18641,.T.);
#12703=FACE_OUTER_BOUND('',#18643,.T.);
#12704=FACE_OUTER_BOUND('',#18644,.T.);
#12705=FACE_OUTER_BOUND('',#18645,.T.);
#12706=FACE_OUTER_BOUND('',#18646,.T.);
#12707=FACE_OUTER_BOUND('',#18647,.T.);
#12708=FACE_OUTER_BOUND('',#18648,.T.);
#12709=FACE_OUTER_BOUND('',#18649,.T.);
#12710=FACE_OUTER_BOUND('',#18650,.T.);
#12711=FACE_OUTER_BOUND('',#18651,.T.);
#12712=FACE_OUTER_BOUND('',#18652,.T.);
#12713=FACE_OUTER_BOUND('',#18653,.T.);
#12714=FACE_OUTER_BOUND('',#18654,.T.);
#12715=FACE_OUTER_BOUND('',#18655,.T.);
#12716=FACE_OUTER_BOUND('',#18656,.T.);
#12717=FACE_OUTER_BOUND('',#18657,.T.);
#12718=FACE_OUTER_BOUND('',#18658,.T.);
#12719=FACE_OUTER_BOUND('',#18659,.T.);
#12720=FACE_OUTER_BOUND('',#18660,.T.);
#12721=FACE_OUTER_BOUND('',#18661,.T.);
#12722=FACE_OUTER_BOUND('',#18662,.T.);
#12723=FACE_OUTER_BOUND('',#18663,.T.);
#12724=FACE_OUTER_BOUND('',#18664,.T.);
#12725=FACE_OUTER_BOUND('',#18665,.T.);
#12726=FACE_OUTER_BOUND('',#18666,.T.);
#12727=FACE_OUTER_BOUND('',#18667,.T.);
#12728=FACE_OUTER_BOUND('',#18669,.T.);
#12729=FACE_OUTER_BOUND('',#18670,.T.);
#12730=FACE_OUTER_BOUND('',#18671,.T.);
#12731=FACE_OUTER_BOUND('',#18672,.T.);
#12732=FACE_OUTER_BOUND('',#18673,.T.);
#12733=FACE_OUTER_BOUND('',#18674,.T.);
#12734=FACE_OUTER_BOUND('',#18675,.T.);
#12735=FACE_OUTER_BOUND('',#18676,.T.);
#12736=FACE_OUTER_BOUND('',#18677,.T.);
#12737=FACE_OUTER_BOUND('',#18678,.T.);
#12738=FACE_OUTER_BOUND('',#18679,.T.);
#12739=FACE_OUTER_BOUND('',#18680,.T.);
#12740=FACE_OUTER_BOUND('',#18681,.T.);
#12741=FACE_OUTER_BOUND('',#18682,.T.);
#12742=FACE_OUTER_BOUND('',#18683,.T.);
#12743=FACE_OUTER_BOUND('',#18684,.T.);
#12744=FACE_OUTER_BOUND('',#18685,.T.);
#12745=FACE_OUTER_BOUND('',#18686,.T.);
#12746=FACE_OUTER_BOUND('',#18687,.T.);
#12747=FACE_OUTER_BOUND('',#18688,.T.);
#12748=FACE_OUTER_BOUND('',#18689,.T.);
#12749=FACE_OUTER_BOUND('',#18690,.T.);
#12750=FACE_OUTER_BOUND('',#18691,.T.);
#12751=FACE_OUTER_BOUND('',#18692,.T.);
#12752=FACE_OUTER_BOUND('',#18693,.T.);
#12753=FACE_OUTER_BOUND('',#18694,.T.);
#12754=FACE_OUTER_BOUND('',#18695,.T.);
#12755=FACE_OUTER_BOUND('',#18696,.T.);
#12756=FACE_OUTER_BOUND('',#18697,.T.);
#12757=FACE_OUTER_BOUND('',#18698,.T.);
#12758=FACE_OUTER_BOUND('',#18699,.T.);
#12759=FACE_OUTER_BOUND('',#18700,.T.);
#12760=FACE_OUTER_BOUND('',#18701,.T.);
#12761=FACE_OUTER_BOUND('',#18702,.T.);
#12762=FACE_OUTER_BOUND('',#18703,.T.);
#12763=FACE_OUTER_BOUND('',#18704,.T.);
#12764=FACE_OUTER_BOUND('',#18705,.T.);
#12765=FACE_OUTER_BOUND('',#18706,.T.);
#12766=FACE_OUTER_BOUND('',#18707,.T.);
#12767=FACE_OUTER_BOUND('',#18708,.T.);
#12768=FACE_OUTER_BOUND('',#18709,.T.);
#12769=FACE_OUTER_BOUND('',#18710,.T.);
#12770=FACE_OUTER_BOUND('',#18711,.T.);
#12771=FACE_OUTER_BOUND('',#18712,.T.);
#12772=FACE_OUTER_BOUND('',#18713,.T.);
#12773=FACE_OUTER_BOUND('',#18714,.T.);
#12774=FACE_OUTER_BOUND('',#18715,.T.);
#12775=FACE_OUTER_BOUND('',#18716,.T.);
#12776=FACE_OUTER_BOUND('',#18717,.T.);
#12777=FACE_OUTER_BOUND('',#18718,.T.);
#12778=FACE_OUTER_BOUND('',#18719,.T.);
#12779=FACE_OUTER_BOUND('',#18720,.T.);
#12780=FACE_OUTER_BOUND('',#18721,.T.);
#12781=FACE_OUTER_BOUND('',#18722,.T.);
#12782=FACE_OUTER_BOUND('',#18723,.T.);
#12783=FACE_OUTER_BOUND('',#18724,.T.);
#12784=FACE_OUTER_BOUND('',#18725,.T.);
#12785=FACE_OUTER_BOUND('',#18726,.T.);
#12786=FACE_OUTER_BOUND('',#18727,.T.);
#12787=FACE_OUTER_BOUND('',#18728,.T.);
#12788=FACE_OUTER_BOUND('',#18729,.T.);
#12789=FACE_OUTER_BOUND('',#18730,.T.);
#12790=FACE_OUTER_BOUND('',#18731,.T.);
#12791=FACE_OUTER_BOUND('',#18732,.T.);
#12792=FACE_OUTER_BOUND('',#18733,.T.);
#12793=FACE_OUTER_BOUND('',#18734,.T.);
#12794=FACE_OUTER_BOUND('',#18735,.T.);
#12795=FACE_OUTER_BOUND('',#18737,.T.);
#12796=FACE_OUTER_BOUND('',#18738,.T.);
#12797=FACE_OUTER_BOUND('',#18739,.T.);
#12798=FACE_OUTER_BOUND('',#18740,.T.);
#12799=FACE_OUTER_BOUND('',#18741,.T.);
#12800=FACE_OUTER_BOUND('',#18742,.T.);
#12801=FACE_OUTER_BOUND('',#18743,.T.);
#12802=FACE_OUTER_BOUND('',#18744,.T.);
#12803=FACE_OUTER_BOUND('',#18745,.T.);
#12804=FACE_OUTER_BOUND('',#18746,.T.);
#12805=FACE_OUTER_BOUND('',#18747,.T.);
#12806=FACE_OUTER_BOUND('',#18748,.T.);
#12807=FACE_OUTER_BOUND('',#18749,.T.);
#12808=FACE_OUTER_BOUND('',#18750,.T.);
#12809=FACE_OUTER_BOUND('',#18751,.T.);
#12810=FACE_OUTER_BOUND('',#18752,.T.);
#12811=FACE_OUTER_BOUND('',#18753,.T.);
#12812=FACE_OUTER_BOUND('',#18754,.T.);
#12813=FACE_OUTER_BOUND('',#18755,.T.);
#12814=FACE_OUTER_BOUND('',#18756,.T.);
#12815=FACE_OUTER_BOUND('',#18757,.T.);
#12816=FACE_OUTER_BOUND('',#18758,.T.);
#12817=FACE_OUTER_BOUND('',#18759,.T.);
#12818=FACE_OUTER_BOUND('',#18760,.T.);
#12819=FACE_OUTER_BOUND('',#18761,.T.);
#12820=FACE_OUTER_BOUND('',#18762,.T.);
#12821=FACE_OUTER_BOUND('',#18763,.T.);
#12822=FACE_OUTER_BOUND('',#18764,.T.);
#12823=FACE_OUTER_BOUND('',#18765,.T.);
#12824=FACE_OUTER_BOUND('',#18766,.T.);
#12825=FACE_OUTER_BOUND('',#18767,.T.);
#12826=FACE_OUTER_BOUND('',#18768,.T.);
#12827=FACE_OUTER_BOUND('',#18769,.T.);
#12828=FACE_OUTER_BOUND('',#18770,.T.);
#12829=FACE_OUTER_BOUND('',#18771,.T.);
#12830=FACE_OUTER_BOUND('',#18772,.T.);
#12831=FACE_OUTER_BOUND('',#18773,.T.);
#12832=FACE_OUTER_BOUND('',#18774,.T.);
#12833=FACE_OUTER_BOUND('',#18775,.T.);
#12834=FACE_OUTER_BOUND('',#18776,.T.);
#12835=FACE_OUTER_BOUND('',#18777,.T.);
#12836=FACE_OUTER_BOUND('',#18778,.T.);
#12837=FACE_OUTER_BOUND('',#18779,.T.);
#12838=FACE_OUTER_BOUND('',#18780,.T.);
#12839=FACE_OUTER_BOUND('',#18781,.T.);
#12840=FACE_OUTER_BOUND('',#18782,.T.);
#12841=FACE_OUTER_BOUND('',#18783,.T.);
#12842=FACE_OUTER_BOUND('',#18784,.T.);
#12843=FACE_OUTER_BOUND('',#18785,.T.);
#12844=FACE_OUTER_BOUND('',#18786,.T.);
#12845=FACE_OUTER_BOUND('',#18787,.T.);
#12846=FACE_OUTER_BOUND('',#18788,.T.);
#12847=FACE_OUTER_BOUND('',#18789,.T.);
#12848=FACE_OUTER_BOUND('',#18790,.T.);
#12849=FACE_OUTER_BOUND('',#18791,.T.);
#12850=FACE_OUTER_BOUND('',#18792,.T.);
#12851=FACE_OUTER_BOUND('',#18793,.T.);
#12852=FACE_OUTER_BOUND('',#18795,.T.);
#12853=FACE_OUTER_BOUND('',#18796,.T.);
#12854=FACE_OUTER_BOUND('',#18798,.T.);
#12855=FACE_OUTER_BOUND('',#18799,.T.);
#12856=FACE_OUTER_BOUND('',#18800,.T.);
#12857=FACE_OUTER_BOUND('',#18801,.T.);
#12858=FACE_OUTER_BOUND('',#18802,.T.);
#12859=FACE_OUTER_BOUND('',#18803,.T.);
#12860=FACE_OUTER_BOUND('',#18804,.T.);
#12861=FACE_OUTER_BOUND('',#18805,.T.);
#12862=FACE_OUTER_BOUND('',#18806,.T.);
#12863=FACE_OUTER_BOUND('',#18807,.T.);
#12864=FACE_OUTER_BOUND('',#18808,.T.);
#12865=FACE_OUTER_BOUND('',#18810,.T.);
#12866=FACE_OUTER_BOUND('',#18811,.T.);
#12867=FACE_OUTER_BOUND('',#18812,.T.);
#12868=FACE_OUTER_BOUND('',#18813,.T.);
#12869=FACE_OUTER_BOUND('',#18815,.T.);
#12870=FACE_OUTER_BOUND('',#18816,.T.);
#12871=FACE_OUTER_BOUND('',#18817,.T.);
#12872=FACE_OUTER_BOUND('',#18818,.T.);
#12873=FACE_OUTER_BOUND('',#18819,.T.);
#12874=FACE_OUTER_BOUND('',#18820,.T.);
#12875=FACE_OUTER_BOUND('',#18821,.T.);
#12876=FACE_OUTER_BOUND('',#18822,.T.);
#12877=FACE_OUTER_BOUND('',#18823,.T.);
#12878=FACE_OUTER_BOUND('',#18824,.T.);
#12879=FACE_OUTER_BOUND('',#18825,.T.);
#12880=FACE_OUTER_BOUND('',#18826,.T.);
#12881=FACE_OUTER_BOUND('',#18827,.T.);
#12882=FACE_OUTER_BOUND('',#18828,.T.);
#12883=FACE_OUTER_BOUND('',#18831,.T.);
#12884=FACE_OUTER_BOUND('',#18832,.T.);
#12885=FACE_OUTER_BOUND('',#18833,.T.);
#12886=FACE_OUTER_BOUND('',#18834,.T.);
#12887=FACE_OUTER_BOUND('',#18835,.T.);
#12888=FACE_OUTER_BOUND('',#18836,.T.);
#12889=FACE_OUTER_BOUND('',#18837,.T.);
#12890=FACE_OUTER_BOUND('',#18838,.T.);
#12891=FACE_OUTER_BOUND('',#18839,.T.);
#12892=FACE_OUTER_BOUND('',#18840,.T.);
#12893=FACE_OUTER_BOUND('',#18841,.T.);
#12894=FACE_OUTER_BOUND('',#18842,.T.);
#12895=FACE_OUTER_BOUND('',#18843,.T.);
#12896=FACE_OUTER_BOUND('',#18844,.T.);
#12897=FACE_OUTER_BOUND('',#18845,.T.);
#12898=FACE_OUTER_BOUND('',#18846,.T.);
#12899=FACE_OUTER_BOUND('',#18847,.T.);
#12900=FACE_OUTER_BOUND('',#18850,.T.);
#12901=FACE_OUTER_BOUND('',#18851,.T.);
#12902=FACE_OUTER_BOUND('',#18852,.T.);
#12903=FACE_OUTER_BOUND('',#18853,.T.);
#12904=FACE_OUTER_BOUND('',#18854,.T.);
#12905=FACE_OUTER_BOUND('',#18855,.T.);
#12906=FACE_OUTER_BOUND('',#18856,.T.);
#12907=FACE_OUTER_BOUND('',#18857,.T.);
#12908=FACE_OUTER_BOUND('',#18858,.T.);
#12909=FACE_OUTER_BOUND('',#18859,.T.);
#12910=FACE_OUTER_BOUND('',#18861,.T.);
#12911=FACE_OUTER_BOUND('',#18862,.T.);
#12912=FACE_OUTER_BOUND('',#18863,.T.);
#12913=FACE_OUTER_BOUND('',#18864,.T.);
#12914=FACE_OUTER_BOUND('',#18865,.T.);
#12915=FACE_OUTER_BOUND('',#18866,.T.);
#12916=FACE_OUTER_BOUND('',#18867,.T.);
#12917=FACE_OUTER_BOUND('',#18869,.T.);
#12918=FACE_OUTER_BOUND('',#18870,.T.);
#12919=FACE_OUTER_BOUND('',#18871,.T.);
#12920=FACE_OUTER_BOUND('',#18872,.T.);
#12921=FACE_OUTER_BOUND('',#18873,.T.);
#12922=FACE_OUTER_BOUND('',#18874,.T.);
#12923=FACE_OUTER_BOUND('',#18875,.T.);
#12924=FACE_OUTER_BOUND('',#18876,.T.);
#12925=FACE_OUTER_BOUND('',#18877,.T.);
#12926=FACE_OUTER_BOUND('',#18878,.T.);
#12927=FACE_OUTER_BOUND('',#18879,.T.);
#12928=FACE_OUTER_BOUND('',#18881,.T.);
#12929=FACE_OUTER_BOUND('',#18882,.T.);
#12930=FACE_OUTER_BOUND('',#18883,.T.);
#12931=FACE_OUTER_BOUND('',#18884,.T.);
#12932=FACE_OUTER_BOUND('',#18885,.T.);
#12933=FACE_OUTER_BOUND('',#18886,.T.);
#12934=FACE_OUTER_BOUND('',#18887,.T.);
#12935=FACE_OUTER_BOUND('',#18888,.T.);
#12936=FACE_OUTER_BOUND('',#18889,.T.);
#12937=FACE_OUTER_BOUND('',#18890,.T.);
#12938=FACE_OUTER_BOUND('',#18891,.T.);
#12939=FACE_OUTER_BOUND('',#18892,.T.);
#12940=FACE_OUTER_BOUND('',#18893,.T.);
#12941=FACE_OUTER_BOUND('',#18894,.T.);
#12942=FACE_OUTER_BOUND('',#18895,.T.);
#12943=FACE_OUTER_BOUND('',#18896,.T.);
#12944=FACE_OUTER_BOUND('',#18897,.T.);
#12945=FACE_OUTER_BOUND('',#18898,.T.);
#12946=FACE_OUTER_BOUND('',#18899,.T.);
#12947=FACE_OUTER_BOUND('',#18900,.T.);
#12948=FACE_OUTER_BOUND('',#18901,.T.);
#12949=FACE_OUTER_BOUND('',#18902,.T.);
#12950=FACE_OUTER_BOUND('',#18903,.T.);
#12951=FACE_OUTER_BOUND('',#18904,.T.);
#12952=FACE_OUTER_BOUND('',#18905,.T.);
#12953=FACE_OUTER_BOUND('',#18906,.T.);
#12954=FACE_OUTER_BOUND('',#18907,.T.);
#12955=FACE_OUTER_BOUND('',#18908,.T.);
#12956=FACE_OUTER_BOUND('',#18909,.T.);
#12957=FACE_OUTER_BOUND('',#18910,.T.);
#12958=FACE_OUTER_BOUND('',#18911,.T.);
#12959=FACE_OUTER_BOUND('',#18912,.T.);
#12960=FACE_OUTER_BOUND('',#18913,.T.);
#12961=FACE_OUTER_BOUND('',#18914,.T.);
#12962=FACE_OUTER_BOUND('',#18915,.T.);
#12963=FACE_OUTER_BOUND('',#18916,.T.);
#12964=FACE_OUTER_BOUND('',#18917,.T.);
#12965=FACE_OUTER_BOUND('',#18918,.T.);
#12966=FACE_OUTER_BOUND('',#18919,.T.);
#12967=FACE_OUTER_BOUND('',#18920,.T.);
#12968=FACE_OUTER_BOUND('',#18921,.T.);
#12969=FACE_OUTER_BOUND('',#18922,.T.);
#12970=FACE_OUTER_BOUND('',#18923,.T.);
#12971=FACE_OUTER_BOUND('',#18924,.T.);
#12972=FACE_OUTER_BOUND('',#18925,.T.);
#12973=FACE_OUTER_BOUND('',#18926,.T.);
#12974=FACE_OUTER_BOUND('',#18927,.T.);
#12975=FACE_OUTER_BOUND('',#18928,.T.);
#12976=FACE_OUTER_BOUND('',#18929,.T.);
#12977=FACE_OUTER_BOUND('',#18930,.T.);
#12978=FACE_OUTER_BOUND('',#18931,.T.);
#12979=FACE_OUTER_BOUND('',#18932,.T.);
#12980=FACE_OUTER_BOUND('',#18933,.T.);
#12981=FACE_OUTER_BOUND('',#18934,.T.);
#12982=FACE_OUTER_BOUND('',#18935,.T.);
#12983=FACE_OUTER_BOUND('',#18936,.T.);
#12984=FACE_OUTER_BOUND('',#18937,.T.);
#12985=FACE_OUTER_BOUND('',#18938,.T.);
#12986=FACE_OUTER_BOUND('',#18939,.T.);
#12987=FACE_OUTER_BOUND('',#18940,.T.);
#12988=FACE_OUTER_BOUND('',#18941,.T.);
#12989=FACE_OUTER_BOUND('',#18942,.T.);
#12990=FACE_OUTER_BOUND('',#18943,.T.);
#12991=FACE_OUTER_BOUND('',#18944,.T.);
#12992=FACE_OUTER_BOUND('',#18945,.T.);
#12993=FACE_OUTER_BOUND('',#18946,.T.);
#12994=FACE_OUTER_BOUND('',#18947,.T.);
#12995=FACE_OUTER_BOUND('',#18948,.T.);
#12996=FACE_OUTER_BOUND('',#18949,.T.);
#12997=FACE_OUTER_BOUND('',#18950,.T.);
#12998=FACE_OUTER_BOUND('',#18951,.T.);
#12999=FACE_OUTER_BOUND('',#18952,.T.);
#13000=FACE_OUTER_BOUND('',#18953,.T.);
#13001=FACE_OUTER_BOUND('',#18954,.T.);
#13002=FACE_OUTER_BOUND('',#18955,.T.);
#13003=FACE_OUTER_BOUND('',#18956,.T.);
#13004=FACE_OUTER_BOUND('',#18957,.T.);
#13005=FACE_OUTER_BOUND('',#18958,.T.);
#13006=FACE_OUTER_BOUND('',#18959,.T.);
#13007=FACE_OUTER_BOUND('',#18960,.T.);
#13008=FACE_OUTER_BOUND('',#18961,.T.);
#13009=FACE_OUTER_BOUND('',#18962,.T.);
#13010=FACE_OUTER_BOUND('',#18963,.T.);
#13011=FACE_OUTER_BOUND('',#18964,.T.);
#13012=FACE_OUTER_BOUND('',#18965,.T.);
#13013=FACE_OUTER_BOUND('',#18966,.T.);
#13014=FACE_OUTER_BOUND('',#18967,.T.);
#13015=FACE_OUTER_BOUND('',#18968,.T.);
#13016=FACE_OUTER_BOUND('',#18969,.T.);
#13017=FACE_OUTER_BOUND('',#18970,.T.);
#13018=FACE_OUTER_BOUND('',#18971,.T.);
#13019=FACE_OUTER_BOUND('',#18972,.T.);
#13020=FACE_OUTER_BOUND('',#18973,.T.);
#13021=FACE_OUTER_BOUND('',#18974,.T.);
#13022=FACE_OUTER_BOUND('',#18975,.T.);
#13023=FACE_OUTER_BOUND('',#18976,.T.);
#13024=FACE_OUTER_BOUND('',#18977,.T.);
#13025=FACE_OUTER_BOUND('',#18978,.T.);
#13026=FACE_OUTER_BOUND('',#18979,.T.);
#13027=FACE_OUTER_BOUND('',#18980,.T.);
#13028=FACE_OUTER_BOUND('',#18981,.T.);
#13029=FACE_OUTER_BOUND('',#18982,.T.);
#13030=FACE_OUTER_BOUND('',#18983,.T.);
#13031=FACE_OUTER_BOUND('',#18984,.T.);
#13032=FACE_OUTER_BOUND('',#18985,.T.);
#13033=FACE_OUTER_BOUND('',#18986,.T.);
#13034=FACE_OUTER_BOUND('',#18987,.T.);
#13035=FACE_OUTER_BOUND('',#18988,.T.);
#13036=FACE_OUTER_BOUND('',#18989,.T.);
#13037=FACE_OUTER_BOUND('',#18990,.T.);
#13038=FACE_OUTER_BOUND('',#18991,.T.);
#13039=FACE_OUTER_BOUND('',#18992,.T.);
#13040=FACE_OUTER_BOUND('',#18993,.T.);
#13041=FACE_OUTER_BOUND('',#18994,.T.);
#13042=FACE_OUTER_BOUND('',#18995,.T.);
#13043=FACE_OUTER_BOUND('',#18996,.T.);
#13044=FACE_OUTER_BOUND('',#18997,.T.);
#13045=FACE_OUTER_BOUND('',#18998,.T.);
#13046=FACE_OUTER_BOUND('',#18999,.T.);
#13047=FACE_OUTER_BOUND('',#19000,.T.);
#13048=FACE_OUTER_BOUND('',#19001,.T.);
#13049=FACE_OUTER_BOUND('',#19002,.T.);
#13050=FACE_OUTER_BOUND('',#19003,.T.);
#13051=FACE_OUTER_BOUND('',#19004,.T.);
#13052=FACE_OUTER_BOUND('',#19005,.T.);
#13053=FACE_OUTER_BOUND('',#19006,.T.);
#13054=FACE_OUTER_BOUND('',#19007,.T.);
#13055=FACE_OUTER_BOUND('',#19008,.T.);
#13056=FACE_OUTER_BOUND('',#19009,.T.);
#13057=FACE_OUTER_BOUND('',#19010,.T.);
#13058=FACE_OUTER_BOUND('',#19011,.T.);
#13059=FACE_OUTER_BOUND('',#19012,.T.);
#13060=FACE_OUTER_BOUND('',#19013,.T.);
#13061=FACE_OUTER_BOUND('',#19014,.T.);
#13062=FACE_OUTER_BOUND('',#19015,.T.);
#13063=FACE_OUTER_BOUND('',#19016,.T.);
#13064=FACE_OUTER_BOUND('',#19017,.T.);
#13065=FACE_OUTER_BOUND('',#19018,.T.);
#13066=FACE_OUTER_BOUND('',#19019,.T.);
#13067=FACE_OUTER_BOUND('',#19020,.T.);
#13068=FACE_OUTER_BOUND('',#19021,.T.);
#13069=FACE_OUTER_BOUND('',#19022,.T.);
#13070=FACE_OUTER_BOUND('',#19023,.T.);
#13071=FACE_OUTER_BOUND('',#19024,.T.);
#13072=FACE_OUTER_BOUND('',#19025,.T.);
#13073=FACE_OUTER_BOUND('',#19026,.T.);
#13074=FACE_OUTER_BOUND('',#19027,.T.);
#13075=FACE_OUTER_BOUND('',#19028,.T.);
#13076=FACE_OUTER_BOUND('',#19029,.T.);
#13077=FACE_OUTER_BOUND('',#19030,.T.);
#13078=FACE_OUTER_BOUND('',#19031,.T.);
#13079=FACE_OUTER_BOUND('',#19032,.T.);
#13080=FACE_OUTER_BOUND('',#19033,.T.);
#13081=FACE_OUTER_BOUND('',#19034,.T.);
#13082=FACE_OUTER_BOUND('',#19035,.T.);
#13083=FACE_OUTER_BOUND('',#19036,.T.);
#13084=FACE_OUTER_BOUND('',#19037,.T.);
#13085=FACE_OUTER_BOUND('',#19038,.T.);
#13086=FACE_OUTER_BOUND('',#19039,.T.);
#13087=FACE_OUTER_BOUND('',#19040,.T.);
#13088=FACE_OUTER_BOUND('',#19041,.T.);
#13089=FACE_OUTER_BOUND('',#19042,.T.);
#13090=FACE_OUTER_BOUND('',#19043,.T.);
#13091=FACE_OUTER_BOUND('',#19044,.T.);
#13092=FACE_OUTER_BOUND('',#19045,.T.);
#13093=FACE_OUTER_BOUND('',#19046,.T.);
#13094=FACE_OUTER_BOUND('',#19047,.T.);
#13095=FACE_OUTER_BOUND('',#19048,.T.);
#13096=FACE_OUTER_BOUND('',#19049,.T.);
#13097=FACE_OUTER_BOUND('',#19050,.T.);
#13098=FACE_OUTER_BOUND('',#19051,.T.);
#13099=FACE_OUTER_BOUND('',#19052,.T.);
#13100=FACE_OUTER_BOUND('',#19053,.T.);
#13101=FACE_OUTER_BOUND('',#19054,.T.);
#13102=FACE_OUTER_BOUND('',#19055,.T.);
#13103=FACE_OUTER_BOUND('',#19056,.T.);
#13104=FACE_OUTER_BOUND('',#19057,.T.);
#13105=FACE_OUTER_BOUND('',#19058,.T.);
#13106=FACE_OUTER_BOUND('',#19059,.T.);
#13107=FACE_OUTER_BOUND('',#19060,.T.);
#13108=FACE_OUTER_BOUND('',#19061,.T.);
#13109=FACE_OUTER_BOUND('',#19062,.T.);
#13110=FACE_OUTER_BOUND('',#19063,.T.);
#13111=FACE_OUTER_BOUND('',#19064,.T.);
#13112=FACE_OUTER_BOUND('',#19065,.T.);
#13113=FACE_OUTER_BOUND('',#19066,.T.);
#13114=FACE_OUTER_BOUND('',#19067,.T.);
#13115=FACE_OUTER_BOUND('',#19068,.T.);
#13116=FACE_OUTER_BOUND('',#19069,.T.);
#13117=FACE_OUTER_BOUND('',#19070,.T.);
#13118=FACE_OUTER_BOUND('',#19071,.T.);
#13119=FACE_OUTER_BOUND('',#19072,.T.);
#13120=FACE_OUTER_BOUND('',#19073,.T.);
#13121=FACE_OUTER_BOUND('',#19074,.T.);
#13122=FACE_OUTER_BOUND('',#19075,.T.);
#13123=FACE_OUTER_BOUND('',#19076,.T.);
#13124=FACE_OUTER_BOUND('',#19077,.T.);
#13125=FACE_OUTER_BOUND('',#19078,.T.);
#13126=FACE_OUTER_BOUND('',#19079,.T.);
#13127=FACE_OUTER_BOUND('',#19080,.T.);
#13128=FACE_OUTER_BOUND('',#19081,.T.);
#13129=FACE_OUTER_BOUND('',#19082,.T.);
#13130=FACE_OUTER_BOUND('',#19083,.T.);
#13131=FACE_OUTER_BOUND('',#19084,.T.);
#13132=FACE_OUTER_BOUND('',#19085,.T.);
#13133=FACE_OUTER_BOUND('',#19086,.T.);
#13134=FACE_OUTER_BOUND('',#19087,.T.);
#13135=FACE_OUTER_BOUND('',#19088,.T.);
#13136=FACE_OUTER_BOUND('',#19089,.T.);
#13137=FACE_OUTER_BOUND('',#19090,.T.);
#13138=FACE_OUTER_BOUND('',#19091,.T.);
#13139=FACE_OUTER_BOUND('',#19092,.T.);
#13140=FACE_OUTER_BOUND('',#19093,.T.);
#13141=FACE_OUTER_BOUND('',#19094,.T.);
#13142=FACE_OUTER_BOUND('',#19095,.T.);
#13143=FACE_OUTER_BOUND('',#19096,.T.);
#13144=FACE_OUTER_BOUND('',#19097,.T.);
#13145=FACE_OUTER_BOUND('',#19098,.T.);
#13146=FACE_OUTER_BOUND('',#19099,.T.);
#13147=FACE_OUTER_BOUND('',#19100,.T.);
#13148=FACE_OUTER_BOUND('',#19101,.T.);
#13149=FACE_OUTER_BOUND('',#19102,.T.);
#13150=FACE_OUTER_BOUND('',#19103,.T.);
#13151=FACE_OUTER_BOUND('',#19104,.T.);
#13152=FACE_OUTER_BOUND('',#19105,.T.);
#13153=FACE_OUTER_BOUND('',#19106,.T.);
#13154=FACE_OUTER_BOUND('',#19107,.T.);
#13155=FACE_OUTER_BOUND('',#19108,.T.);
#13156=FACE_OUTER_BOUND('',#19109,.T.);
#13157=FACE_OUTER_BOUND('',#19110,.T.);
#13158=FACE_OUTER_BOUND('',#19111,.T.);
#13159=FACE_OUTER_BOUND('',#19112,.T.);
#13160=FACE_OUTER_BOUND('',#19113,.T.);
#13161=FACE_OUTER_BOUND('',#19114,.T.);
#13162=FACE_OUTER_BOUND('',#19115,.T.);
#13163=FACE_OUTER_BOUND('',#19116,.T.);
#13164=FACE_OUTER_BOUND('',#19117,.T.);
#13165=FACE_OUTER_BOUND('',#19118,.T.);
#13166=FACE_OUTER_BOUND('',#19119,.T.);
#13167=FACE_OUTER_BOUND('',#19120,.T.);
#13168=FACE_OUTER_BOUND('',#19121,.T.);
#13169=FACE_OUTER_BOUND('',#19122,.T.);
#13170=FACE_OUTER_BOUND('',#19123,.T.);
#13171=FACE_OUTER_BOUND('',#19124,.T.);
#13172=FACE_OUTER_BOUND('',#19125,.T.);
#13173=FACE_OUTER_BOUND('',#19126,.T.);
#13174=FACE_OUTER_BOUND('',#19127,.T.);
#13175=FACE_OUTER_BOUND('',#19128,.T.);
#13176=FACE_OUTER_BOUND('',#19129,.T.);
#13177=FACE_OUTER_BOUND('',#19130,.T.);
#13178=FACE_OUTER_BOUND('',#19131,.T.);
#13179=FACE_OUTER_BOUND('',#19132,.T.);
#13180=FACE_OUTER_BOUND('',#19133,.T.);
#13181=FACE_OUTER_BOUND('',#19134,.T.);
#13182=FACE_OUTER_BOUND('',#19135,.T.);
#13183=FACE_OUTER_BOUND('',#19136,.T.);
#13184=FACE_OUTER_BOUND('',#19137,.T.);
#13185=FACE_OUTER_BOUND('',#19138,.T.);
#13186=FACE_OUTER_BOUND('',#19139,.T.);
#13187=FACE_OUTER_BOUND('',#19140,.T.);
#13188=FACE_OUTER_BOUND('',#19141,.T.);
#13189=FACE_OUTER_BOUND('',#19142,.T.);
#13190=FACE_OUTER_BOUND('',#19143,.T.);
#13191=FACE_OUTER_BOUND('',#19144,.T.);
#13192=FACE_OUTER_BOUND('',#19145,.T.);
#13193=FACE_OUTER_BOUND('',#19147,.T.);
#13194=FACE_OUTER_BOUND('',#19148,.T.);
#13195=FACE_OUTER_BOUND('',#19149,.T.);
#13196=FACE_OUTER_BOUND('',#19150,.T.);
#13197=FACE_OUTER_BOUND('',#19151,.T.);
#13198=FACE_OUTER_BOUND('',#19152,.T.);
#13199=FACE_OUTER_BOUND('',#19153,.T.);
#13200=FACE_OUTER_BOUND('',#19154,.T.);
#13201=FACE_OUTER_BOUND('',#19155,.T.);
#13202=FACE_OUTER_BOUND('',#19156,.T.);
#13203=FACE_OUTER_BOUND('',#19157,.T.);
#13204=FACE_OUTER_BOUND('',#19158,.T.);
#13205=FACE_OUTER_BOUND('',#19159,.T.);
#13206=FACE_OUTER_BOUND('',#19160,.T.);
#13207=FACE_OUTER_BOUND('',#19161,.T.);
#13208=FACE_OUTER_BOUND('',#19162,.T.);
#13209=FACE_OUTER_BOUND('',#19163,.T.);
#13210=FACE_OUTER_BOUND('',#19164,.T.);
#13211=FACE_OUTER_BOUND('',#19165,.T.);
#13212=FACE_OUTER_BOUND('',#19166,.T.);
#13213=FACE_OUTER_BOUND('',#19167,.T.);
#13214=FACE_OUTER_BOUND('',#19168,.T.);
#13215=FACE_OUTER_BOUND('',#19169,.T.);
#13216=FACE_OUTER_BOUND('',#19170,.T.);
#13217=FACE_OUTER_BOUND('',#19171,.T.);
#13218=FACE_OUTER_BOUND('',#19172,.T.);
#13219=FACE_OUTER_BOUND('',#19173,.T.);
#13220=FACE_OUTER_BOUND('',#19174,.T.);
#13221=FACE_OUTER_BOUND('',#19175,.T.);
#13222=FACE_OUTER_BOUND('',#19176,.T.);
#13223=FACE_OUTER_BOUND('',#19177,.T.);
#13224=FACE_OUTER_BOUND('',#19178,.T.);
#13225=FACE_OUTER_BOUND('',#19179,.T.);
#13226=FACE_OUTER_BOUND('',#19180,.T.);
#13227=FACE_OUTER_BOUND('',#19181,.T.);
#13228=FACE_OUTER_BOUND('',#19182,.T.);
#13229=FACE_OUTER_BOUND('',#19183,.T.);
#13230=FACE_OUTER_BOUND('',#19184,.T.);
#13231=FACE_OUTER_BOUND('',#19185,.T.);
#13232=FACE_OUTER_BOUND('',#19186,.T.);
#13233=FACE_OUTER_BOUND('',#19187,.T.);
#13234=FACE_OUTER_BOUND('',#19188,.T.);
#13235=FACE_OUTER_BOUND('',#19189,.T.);
#13236=FACE_OUTER_BOUND('',#19190,.T.);
#13237=FACE_OUTER_BOUND('',#19191,.T.);
#13238=FACE_OUTER_BOUND('',#19192,.T.);
#13239=FACE_OUTER_BOUND('',#19193,.T.);
#13240=FACE_OUTER_BOUND('',#19194,.T.);
#13241=FACE_OUTER_BOUND('',#19195,.T.);
#13242=FACE_OUTER_BOUND('',#19196,.T.);
#13243=FACE_OUTER_BOUND('',#19197,.T.);
#13244=FACE_OUTER_BOUND('',#19198,.T.);
#13245=FACE_OUTER_BOUND('',#19199,.T.);
#13246=FACE_OUTER_BOUND('',#19200,.T.);
#13247=FACE_OUTER_BOUND('',#19201,.T.);
#13248=FACE_OUTER_BOUND('',#19202,.T.);
#13249=FACE_OUTER_BOUND('',#19203,.T.);
#13250=FACE_OUTER_BOUND('',#19204,.T.);
#13251=FACE_OUTER_BOUND('',#19205,.T.);
#13252=FACE_OUTER_BOUND('',#19206,.T.);
#13253=FACE_OUTER_BOUND('',#19207,.T.);
#13254=FACE_OUTER_BOUND('',#19208,.T.);
#13255=FACE_OUTER_BOUND('',#19209,.T.);
#13256=FACE_OUTER_BOUND('',#19210,.T.);
#13257=FACE_OUTER_BOUND('',#19211,.T.);
#13258=FACE_OUTER_BOUND('',#19212,.T.);
#13259=FACE_OUTER_BOUND('',#19213,.T.);
#13260=FACE_OUTER_BOUND('',#19214,.T.);
#13261=FACE_OUTER_BOUND('',#19215,.T.);
#13262=FACE_OUTER_BOUND('',#19216,.T.);
#13263=FACE_OUTER_BOUND('',#19217,.T.);
#13264=FACE_OUTER_BOUND('',#19218,.T.);
#13265=FACE_OUTER_BOUND('',#19219,.T.);
#13266=FACE_OUTER_BOUND('',#19220,.T.);
#13267=FACE_OUTER_BOUND('',#19221,.T.);
#13268=FACE_OUTER_BOUND('',#19222,.T.);
#13269=FACE_OUTER_BOUND('',#19223,.T.);
#13270=FACE_OUTER_BOUND('',#19224,.T.);
#13271=FACE_OUTER_BOUND('',#19225,.T.);
#13272=FACE_OUTER_BOUND('',#19226,.T.);
#13273=FACE_OUTER_BOUND('',#19227,.T.);
#13274=FACE_OUTER_BOUND('',#19228,.T.);
#13275=FACE_OUTER_BOUND('',#19229,.T.);
#13276=FACE_OUTER_BOUND('',#19230,.T.);
#13277=FACE_OUTER_BOUND('',#19231,.T.);
#13278=FACE_OUTER_BOUND('',#19232,.T.);
#13279=FACE_OUTER_BOUND('',#19233,.T.);
#13280=FACE_OUTER_BOUND('',#19234,.T.);
#13281=FACE_OUTER_BOUND('',#19235,.T.);
#13282=FACE_OUTER_BOUND('',#19236,.T.);
#13283=FACE_OUTER_BOUND('',#19237,.T.);
#13284=FACE_OUTER_BOUND('',#19238,.T.);
#13285=FACE_OUTER_BOUND('',#19239,.T.);
#13286=FACE_OUTER_BOUND('',#19240,.T.);
#13287=FACE_OUTER_BOUND('',#19241,.T.);
#13288=FACE_OUTER_BOUND('',#19242,.T.);
#13289=FACE_OUTER_BOUND('',#19243,.T.);
#13290=FACE_OUTER_BOUND('',#19244,.T.);
#13291=FACE_OUTER_BOUND('',#19245,.T.);
#13292=FACE_OUTER_BOUND('',#19246,.T.);
#13293=FACE_OUTER_BOUND('',#19247,.T.);
#13294=FACE_OUTER_BOUND('',#19248,.T.);
#13295=FACE_OUTER_BOUND('',#19249,.T.);
#13296=FACE_OUTER_BOUND('',#19250,.T.);
#13297=FACE_OUTER_BOUND('',#19251,.T.);
#13298=FACE_OUTER_BOUND('',#19252,.T.);
#13299=FACE_OUTER_BOUND('',#19253,.T.);
#13300=FACE_OUTER_BOUND('',#19254,.T.);
#13301=FACE_OUTER_BOUND('',#19255,.T.);
#13302=FACE_OUTER_BOUND('',#19256,.T.);
#13303=FACE_OUTER_BOUND('',#19257,.T.);
#13304=FACE_OUTER_BOUND('',#19258,.T.);
#13305=FACE_OUTER_BOUND('',#19259,.T.);
#13306=FACE_OUTER_BOUND('',#19260,.T.);
#13307=FACE_OUTER_BOUND('',#19261,.T.);
#13308=FACE_OUTER_BOUND('',#19262,.T.);
#13309=FACE_OUTER_BOUND('',#19263,.T.);
#13310=FACE_OUTER_BOUND('',#19264,.T.);
#13311=FACE_OUTER_BOUND('',#19265,.T.);
#13312=FACE_OUTER_BOUND('',#19266,.T.);
#13313=FACE_OUTER_BOUND('',#19267,.T.);
#13314=FACE_OUTER_BOUND('',#19268,.T.);
#13315=FACE_OUTER_BOUND('',#19269,.T.);
#13316=FACE_OUTER_BOUND('',#19270,.T.);
#13317=FACE_OUTER_BOUND('',#19271,.T.);
#13318=FACE_OUTER_BOUND('',#19272,.T.);
#13319=FACE_OUTER_BOUND('',#19273,.T.);
#13320=FACE_OUTER_BOUND('',#19274,.T.);
#13321=FACE_OUTER_BOUND('',#19275,.T.);
#13322=FACE_OUTER_BOUND('',#19276,.T.);
#13323=FACE_OUTER_BOUND('',#19277,.T.);
#13324=FACE_OUTER_BOUND('',#19278,.T.);
#13325=FACE_OUTER_BOUND('',#19279,.T.);
#13326=FACE_OUTER_BOUND('',#19280,.T.);
#13327=FACE_OUTER_BOUND('',#19281,.T.);
#13328=FACE_OUTER_BOUND('',#19282,.T.);
#13329=FACE_OUTER_BOUND('',#19283,.T.);
#13330=FACE_OUTER_BOUND('',#19284,.T.);
#13331=FACE_OUTER_BOUND('',#19285,.T.);
#13332=FACE_OUTER_BOUND('',#19286,.T.);
#13333=FACE_OUTER_BOUND('',#19287,.T.);
#13334=FACE_OUTER_BOUND('',#19288,.T.);
#13335=FACE_OUTER_BOUND('',#19289,.T.);
#13336=FACE_OUTER_BOUND('',#19290,.T.);
#13337=FACE_OUTER_BOUND('',#19291,.T.);
#13338=FACE_OUTER_BOUND('',#19292,.T.);
#13339=FACE_OUTER_BOUND('',#19293,.T.);
#13340=FACE_OUTER_BOUND('',#19294,.T.);
#13341=FACE_OUTER_BOUND('',#19295,.T.);
#13342=FACE_OUTER_BOUND('',#19296,.T.);
#13343=FACE_OUTER_BOUND('',#19297,.T.);
#13344=FACE_OUTER_BOUND('',#19298,.T.);
#13345=FACE_OUTER_BOUND('',#19299,.T.);
#13346=FACE_OUTER_BOUND('',#19300,.T.);
#13347=FACE_OUTER_BOUND('',#19301,.T.);
#13348=FACE_OUTER_BOUND('',#19302,.T.);
#13349=FACE_OUTER_BOUND('',#19303,.T.);
#13350=FACE_OUTER_BOUND('',#19304,.T.);
#13351=FACE_OUTER_BOUND('',#19305,.T.);
#13352=FACE_OUTER_BOUND('',#19306,.T.);
#13353=FACE_OUTER_BOUND('',#19307,.T.);
#13354=FACE_OUTER_BOUND('',#19308,.T.);
#13355=FACE_OUTER_BOUND('',#19309,.T.);
#13356=FACE_OUTER_BOUND('',#19310,.T.);
#13357=FACE_OUTER_BOUND('',#19311,.T.);
#13358=FACE_OUTER_BOUND('',#19312,.T.);
#13359=FACE_OUTER_BOUND('',#19313,.T.);
#13360=FACE_OUTER_BOUND('',#19314,.T.);
#13361=FACE_OUTER_BOUND('',#19315,.T.);
#13362=FACE_OUTER_BOUND('',#19316,.T.);
#13363=FACE_OUTER_BOUND('',#19317,.T.);
#13364=FACE_OUTER_BOUND('',#19318,.T.);
#13365=FACE_OUTER_BOUND('',#19319,.T.);
#13366=FACE_OUTER_BOUND('',#19320,.T.);
#13367=FACE_OUTER_BOUND('',#19321,.T.);
#13368=FACE_OUTER_BOUND('',#19322,.T.);
#13369=FACE_OUTER_BOUND('',#19323,.T.);
#13370=FACE_OUTER_BOUND('',#19324,.T.);
#13371=FACE_OUTER_BOUND('',#19325,.T.);
#13372=FACE_OUTER_BOUND('',#19326,.T.);
#13373=FACE_OUTER_BOUND('',#19327,.T.);
#13374=FACE_OUTER_BOUND('',#19328,.T.);
#13375=FACE_OUTER_BOUND('',#19329,.T.);
#13376=FACE_OUTER_BOUND('',#19330,.T.);
#13377=FACE_OUTER_BOUND('',#19331,.T.);
#13378=FACE_OUTER_BOUND('',#19332,.T.);
#13379=FACE_OUTER_BOUND('',#19333,.T.);
#13380=FACE_OUTER_BOUND('',#19334,.T.);
#13381=FACE_OUTER_BOUND('',#19335,.T.);
#13382=FACE_OUTER_BOUND('',#19336,.T.);
#13383=FACE_OUTER_BOUND('',#19337,.T.);
#13384=FACE_OUTER_BOUND('',#19338,.T.);
#13385=FACE_OUTER_BOUND('',#19339,.T.);
#13386=FACE_OUTER_BOUND('',#19340,.T.);
#13387=FACE_OUTER_BOUND('',#19341,.T.);
#13388=FACE_OUTER_BOUND('',#19342,.T.);
#13389=FACE_OUTER_BOUND('',#19343,.T.);
#13390=FACE_OUTER_BOUND('',#19344,.T.);
#13391=FACE_OUTER_BOUND('',#19345,.T.);
#13392=FACE_OUTER_BOUND('',#19346,.T.);
#13393=FACE_OUTER_BOUND('',#19347,.T.);
#13394=FACE_OUTER_BOUND('',#19348,.T.);
#13395=FACE_OUTER_BOUND('',#19349,.T.);
#13396=FACE_OUTER_BOUND('',#19350,.T.);
#13397=FACE_OUTER_BOUND('',#19351,.T.);
#13398=FACE_OUTER_BOUND('',#19352,.T.);
#13399=FACE_OUTER_BOUND('',#19353,.T.);
#13400=FACE_OUTER_BOUND('',#19354,.T.);
#13401=FACE_OUTER_BOUND('',#19355,.T.);
#13402=FACE_OUTER_BOUND('',#19356,.T.);
#13403=FACE_OUTER_BOUND('',#19357,.T.);
#13404=FACE_OUTER_BOUND('',#19358,.T.);
#13405=FACE_OUTER_BOUND('',#19359,.T.);
#13406=FACE_OUTER_BOUND('',#19360,.T.);
#13407=FACE_OUTER_BOUND('',#19361,.T.);
#13408=FACE_OUTER_BOUND('',#19362,.T.);
#13409=FACE_OUTER_BOUND('',#19363,.T.);
#13410=FACE_OUTER_BOUND('',#19364,.T.);
#13411=FACE_OUTER_BOUND('',#19365,.T.);
#13412=FACE_OUTER_BOUND('',#19366,.T.);
#13413=FACE_OUTER_BOUND('',#19367,.T.);
#13414=FACE_OUTER_BOUND('',#19368,.T.);
#13415=FACE_OUTER_BOUND('',#19369,.T.);
#13416=FACE_OUTER_BOUND('',#19373,.T.);
#13417=FACE_OUTER_BOUND('',#19375,.T.);
#13418=FACE_OUTER_BOUND('',#19376,.T.);
#13419=FACE_OUTER_BOUND('',#19377,.T.);
#13420=FACE_OUTER_BOUND('',#19378,.T.);
#13421=FACE_OUTER_BOUND('',#19380,.T.);
#13422=FACE_OUTER_BOUND('',#19381,.T.);
#13423=FACE_OUTER_BOUND('',#19382,.T.);
#13424=FACE_OUTER_BOUND('',#19383,.T.);
#13425=FACE_OUTER_BOUND('',#19385,.T.);
#13426=FACE_OUTER_BOUND('',#19386,.T.);
#13427=FACE_OUTER_BOUND('',#19387,.T.);
#13428=FACE_OUTER_BOUND('',#19388,.T.);
#13429=FACE_OUTER_BOUND('',#19390,.T.);
#13430=FACE_OUTER_BOUND('',#19391,.T.);
#13431=FACE_OUTER_BOUND('',#19392,.T.);
#13432=FACE_OUTER_BOUND('',#19393,.T.);
#13433=FACE_OUTER_BOUND('',#19394,.T.);
#13434=FACE_OUTER_BOUND('',#19395,.T.);
#13435=FACE_OUTER_BOUND('',#19396,.T.);
#13436=FACE_OUTER_BOUND('',#19397,.T.);
#13437=FACE_OUTER_BOUND('',#19398,.T.);
#13438=FACE_OUTER_BOUND('',#19399,.T.);
#13439=FACE_OUTER_BOUND('',#19400,.T.);
#13440=FACE_OUTER_BOUND('',#19401,.T.);
#13441=FACE_OUTER_BOUND('',#19402,.T.);
#13442=FACE_OUTER_BOUND('',#19403,.T.);
#13443=FACE_OUTER_BOUND('',#19404,.T.);
#13444=FACE_OUTER_BOUND('',#19405,.T.);
#13445=FACE_OUTER_BOUND('',#19406,.T.);
#13446=FACE_OUTER_BOUND('',#19407,.T.);
#13447=FACE_OUTER_BOUND('',#19408,.T.);
#13448=FACE_OUTER_BOUND('',#19409,.T.);
#13449=FACE_OUTER_BOUND('',#19410,.T.);
#13450=FACE_OUTER_BOUND('',#19412,.T.);
#13451=FACE_OUTER_BOUND('',#19413,.T.);
#13452=FACE_OUTER_BOUND('',#19414,.T.);
#13453=FACE_OUTER_BOUND('',#19415,.T.);
#13454=FACE_OUTER_BOUND('',#19416,.T.);
#13455=FACE_OUTER_BOUND('',#19417,.T.);
#13456=FACE_OUTER_BOUND('',#19418,.T.);
#13457=FACE_OUTER_BOUND('',#19419,.T.);
#13458=FACE_OUTER_BOUND('',#19420,.T.);
#13459=FACE_OUTER_BOUND('',#19421,.T.);
#13460=FACE_OUTER_BOUND('',#19422,.T.);
#13461=FACE_OUTER_BOUND('',#19423,.T.);
#13462=FACE_OUTER_BOUND('',#19424,.T.);
#13463=FACE_OUTER_BOUND('',#19425,.T.);
#13464=FACE_OUTER_BOUND('',#19426,.T.);
#13465=FACE_OUTER_BOUND('',#19427,.T.);
#13466=FACE_OUTER_BOUND('',#19428,.T.);
#13467=FACE_OUTER_BOUND('',#19429,.T.);
#13468=FACE_OUTER_BOUND('',#19430,.T.);
#13469=FACE_OUTER_BOUND('',#19431,.T.);
#13470=FACE_OUTER_BOUND('',#19432,.T.);
#13471=FACE_OUTER_BOUND('',#19433,.T.);
#13472=FACE_OUTER_BOUND('',#19434,.T.);
#13473=FACE_OUTER_BOUND('',#19435,.T.);
#13474=FACE_OUTER_BOUND('',#19436,.T.);
#13475=FACE_OUTER_BOUND('',#19437,.T.);
#13476=FACE_OUTER_BOUND('',#19438,.T.);
#13477=FACE_OUTER_BOUND('',#19439,.T.);
#13478=FACE_OUTER_BOUND('',#19440,.T.);
#13479=FACE_OUTER_BOUND('',#19441,.T.);
#13480=FACE_OUTER_BOUND('',#19442,.T.);
#13481=FACE_OUTER_BOUND('',#19443,.T.);
#13482=FACE_OUTER_BOUND('',#19444,.T.);
#13483=FACE_OUTER_BOUND('',#19445,.T.);
#13484=FACE_OUTER_BOUND('',#19446,.T.);
#13485=FACE_OUTER_BOUND('',#19447,.T.);
#13486=FACE_OUTER_BOUND('',#19448,.T.);
#13487=FACE_OUTER_BOUND('',#19449,.T.);
#13488=FACE_OUTER_BOUND('',#19450,.T.);
#13489=FACE_OUTER_BOUND('',#19451,.T.);
#13490=FACE_OUTER_BOUND('',#19452,.T.);
#13491=FACE_OUTER_BOUND('',#19453,.T.);
#13492=FACE_OUTER_BOUND('',#19454,.T.);
#13493=FACE_OUTER_BOUND('',#19455,.T.);
#13494=FACE_OUTER_BOUND('',#19456,.T.);
#13495=FACE_OUTER_BOUND('',#19457,.T.);
#13496=FACE_OUTER_BOUND('',#19458,.T.);
#13497=FACE_OUTER_BOUND('',#19459,.T.);
#13498=FACE_OUTER_BOUND('',#19460,.T.);
#13499=FACE_OUTER_BOUND('',#19461,.T.);
#13500=FACE_OUTER_BOUND('',#19462,.T.);
#13501=FACE_OUTER_BOUND('',#19463,.T.);
#13502=FACE_OUTER_BOUND('',#19464,.T.);
#13503=FACE_OUTER_BOUND('',#19465,.T.);
#13504=FACE_OUTER_BOUND('',#19466,.T.);
#13505=FACE_OUTER_BOUND('',#19467,.T.);
#13506=FACE_OUTER_BOUND('',#19468,.T.);
#13507=FACE_OUTER_BOUND('',#19469,.T.);
#13508=FACE_OUTER_BOUND('',#19470,.T.);
#13509=FACE_OUTER_BOUND('',#19471,.T.);
#13510=FACE_OUTER_BOUND('',#19472,.T.);
#13511=FACE_OUTER_BOUND('',#19473,.T.);
#13512=FACE_OUTER_BOUND('',#19474,.T.);
#13513=FACE_OUTER_BOUND('',#19475,.T.);
#13514=FACE_OUTER_BOUND('',#19476,.T.);
#13515=FACE_OUTER_BOUND('',#19477,.T.);
#13516=FACE_OUTER_BOUND('',#19478,.T.);
#13517=FACE_OUTER_BOUND('',#19479,.T.);
#13518=FACE_OUTER_BOUND('',#19480,.T.);
#13519=FACE_OUTER_BOUND('',#19481,.T.);
#13520=FACE_OUTER_BOUND('',#19482,.T.);
#13521=FACE_OUTER_BOUND('',#19483,.T.);
#13522=FACE_OUTER_BOUND('',#19484,.T.);
#13523=FACE_OUTER_BOUND('',#19485,.T.);
#13524=FACE_OUTER_BOUND('',#19486,.T.);
#13525=FACE_OUTER_BOUND('',#19487,.T.);
#13526=FACE_OUTER_BOUND('',#19488,.T.);
#13527=FACE_OUTER_BOUND('',#19489,.T.);
#13528=FACE_OUTER_BOUND('',#19490,.T.);
#13529=FACE_OUTER_BOUND('',#19491,.T.);
#13530=FACE_OUTER_BOUND('',#19492,.T.);
#13531=FACE_OUTER_BOUND('',#19493,.T.);
#13532=FACE_OUTER_BOUND('',#19494,.T.);
#13533=FACE_OUTER_BOUND('',#19495,.T.);
#13534=FACE_OUTER_BOUND('',#19496,.T.);
#13535=FACE_OUTER_BOUND('',#19497,.T.);
#13536=FACE_OUTER_BOUND('',#19498,.T.);
#13537=FACE_OUTER_BOUND('',#19499,.T.);
#13538=FACE_OUTER_BOUND('',#19500,.T.);
#13539=FACE_OUTER_BOUND('',#19501,.T.);
#13540=FACE_OUTER_BOUND('',#19502,.T.);
#13541=FACE_OUTER_BOUND('',#19503,.T.);
#13542=FACE_OUTER_BOUND('',#19504,.T.);
#13543=FACE_OUTER_BOUND('',#19505,.T.);
#13544=FACE_OUTER_BOUND('',#19506,.T.);
#13545=FACE_OUTER_BOUND('',#19507,.T.);
#13546=FACE_OUTER_BOUND('',#19508,.T.);
#13547=FACE_OUTER_BOUND('',#19509,.T.);
#13548=FACE_OUTER_BOUND('',#19510,.T.);
#13549=FACE_OUTER_BOUND('',#19511,.T.);
#13550=FACE_OUTER_BOUND('',#19512,.T.);
#13551=FACE_OUTER_BOUND('',#19513,.T.);
#13552=FACE_OUTER_BOUND('',#19514,.T.);
#13553=FACE_OUTER_BOUND('',#19515,.T.);
#13554=FACE_OUTER_BOUND('',#19516,.T.);
#13555=FACE_OUTER_BOUND('',#19517,.T.);
#13556=FACE_OUTER_BOUND('',#19518,.T.);
#13557=FACE_OUTER_BOUND('',#19519,.T.);
#13558=FACE_OUTER_BOUND('',#19520,.T.);
#13559=FACE_OUTER_BOUND('',#19521,.T.);
#13560=FACE_OUTER_BOUND('',#19522,.T.);
#13561=FACE_OUTER_BOUND('',#19523,.T.);
#13562=FACE_OUTER_BOUND('',#19524,.T.);
#13563=FACE_OUTER_BOUND('',#19525,.T.);
#13564=FACE_OUTER_BOUND('',#19526,.T.);
#13565=FACE_OUTER_BOUND('',#19527,.T.);
#13566=FACE_OUTER_BOUND('',#19528,.T.);
#13567=FACE_OUTER_BOUND('',#19529,.T.);
#13568=FACE_OUTER_BOUND('',#19530,.T.);
#13569=FACE_OUTER_BOUND('',#19531,.T.);
#13570=FACE_OUTER_BOUND('',#19532,.T.);
#13571=FACE_OUTER_BOUND('',#19533,.T.);
#13572=FACE_OUTER_BOUND('',#19534,.T.);
#13573=FACE_OUTER_BOUND('',#19535,.T.);
#13574=FACE_OUTER_BOUND('',#19536,.T.);
#13575=FACE_OUTER_BOUND('',#19537,.T.);
#13576=FACE_OUTER_BOUND('',#19538,.T.);
#13577=FACE_OUTER_BOUND('',#19539,.T.);
#13578=FACE_OUTER_BOUND('',#19540,.T.);
#13579=FACE_OUTER_BOUND('',#19541,.T.);
#13580=FACE_OUTER_BOUND('',#19542,.T.);
#13581=FACE_OUTER_BOUND('',#19543,.T.);
#13582=FACE_OUTER_BOUND('',#19544,.T.);
#13583=FACE_OUTER_BOUND('',#19545,.T.);
#13584=FACE_OUTER_BOUND('',#19546,.T.);
#13585=FACE_OUTER_BOUND('',#19547,.T.);
#13586=FACE_OUTER_BOUND('',#19548,.T.);
#13587=FACE_OUTER_BOUND('',#19549,.T.);
#13588=FACE_OUTER_BOUND('',#19550,.T.);
#13589=FACE_OUTER_BOUND('',#19551,.T.);
#13590=FACE_OUTER_BOUND('',#19552,.T.);
#13591=FACE_OUTER_BOUND('',#19553,.T.);
#13592=FACE_OUTER_BOUND('',#19554,.T.);
#13593=FACE_OUTER_BOUND('',#19555,.T.);
#13594=FACE_OUTER_BOUND('',#19556,.T.);
#13595=FACE_OUTER_BOUND('',#19561,.T.);
#13596=FACE_OUTER_BOUND('',#19562,.T.);
#13597=FACE_OUTER_BOUND('',#19563,.T.);
#13598=FACE_OUTER_BOUND('',#19564,.T.);
#13599=FACE_OUTER_BOUND('',#19565,.T.);
#13600=FACE_OUTER_BOUND('',#19566,.T.);
#13601=FACE_OUTER_BOUND('',#19567,.T.);
#13602=FACE_OUTER_BOUND('',#19568,.T.);
#13603=FACE_OUTER_BOUND('',#19573,.T.);
#13604=FACE_OUTER_BOUND('',#19574,.T.);
#13605=FACE_OUTER_BOUND('',#19575,.T.);
#13606=FACE_OUTER_BOUND('',#19576,.T.);
#13607=FACE_OUTER_BOUND('',#19577,.T.);
#13608=FACE_OUTER_BOUND('',#19578,.T.);
#13609=FACE_OUTER_BOUND('',#19579,.T.);
#13610=FACE_OUTER_BOUND('',#19580,.T.);
#13611=FACE_OUTER_BOUND('',#19581,.T.);
#13612=FACE_OUTER_BOUND('',#19582,.T.);
#13613=FACE_OUTER_BOUND('',#19583,.T.);
#13614=FACE_OUTER_BOUND('',#19584,.T.);
#13615=FACE_OUTER_BOUND('',#19585,.T.);
#13616=FACE_OUTER_BOUND('',#19586,.T.);
#13617=FACE_OUTER_BOUND('',#19587,.T.);
#13618=FACE_OUTER_BOUND('',#19588,.T.);
#13619=FACE_OUTER_BOUND('',#19589,.T.);
#13620=FACE_OUTER_BOUND('',#19590,.T.);
#13621=FACE_OUTER_BOUND('',#19591,.T.);
#13622=FACE_OUTER_BOUND('',#19592,.T.);
#13623=FACE_OUTER_BOUND('',#19593,.T.);
#13624=FACE_OUTER_BOUND('',#19594,.T.);
#13625=FACE_OUTER_BOUND('',#19595,.T.);
#13626=FACE_OUTER_BOUND('',#19596,.T.);
#13627=FACE_OUTER_BOUND('',#19597,.T.);
#13628=FACE_OUTER_BOUND('',#19598,.T.);
#13629=FACE_OUTER_BOUND('',#19599,.T.);
#13630=FACE_OUTER_BOUND('',#19600,.T.);
#13631=FACE_OUTER_BOUND('',#19601,.T.);
#13632=FACE_OUTER_BOUND('',#19602,.T.);
#13633=FACE_OUTER_BOUND('',#19603,.T.);
#13634=FACE_OUTER_BOUND('',#19604,.T.);
#13635=FACE_OUTER_BOUND('',#19605,.T.);
#13636=FACE_OUTER_BOUND('',#19606,.T.);
#13637=FACE_OUTER_BOUND('',#19607,.T.);
#13638=FACE_OUTER_BOUND('',#19608,.T.);
#13639=FACE_OUTER_BOUND('',#19609,.T.);
#13640=FACE_OUTER_BOUND('',#19610,.T.);
#13641=FACE_OUTER_BOUND('',#19611,.T.);
#13642=FACE_OUTER_BOUND('',#19612,.T.);
#13643=FACE_OUTER_BOUND('',#19613,.T.);
#13644=FACE_OUTER_BOUND('',#19614,.T.);
#13645=FACE_OUTER_BOUND('',#19615,.T.);
#13646=FACE_OUTER_BOUND('',#19616,.T.);
#13647=FACE_OUTER_BOUND('',#19618,.T.);
#13648=FACE_OUTER_BOUND('',#19620,.T.);
#13649=FACE_OUTER_BOUND('',#19621,.T.);
#13650=FACE_OUTER_BOUND('',#19622,.T.);
#13651=FACE_OUTER_BOUND('',#19623,.T.);
#13652=FACE_OUTER_BOUND('',#19624,.T.);
#13653=FACE_OUTER_BOUND('',#19625,.T.);
#13654=FACE_OUTER_BOUND('',#19626,.T.);
#13655=FACE_OUTER_BOUND('',#19627,.T.);
#13656=FACE_OUTER_BOUND('',#19628,.T.);
#13657=FACE_OUTER_BOUND('',#19629,.T.);
#13658=FACE_OUTER_BOUND('',#19630,.T.);
#13659=FACE_OUTER_BOUND('',#19631,.T.);
#13660=FACE_OUTER_BOUND('',#19632,.T.);
#13661=FACE_OUTER_BOUND('',#19633,.T.);
#13662=FACE_OUTER_BOUND('',#19634,.T.);
#13663=FACE_OUTER_BOUND('',#19635,.T.);
#13664=FACE_OUTER_BOUND('',#19636,.T.);
#13665=FACE_OUTER_BOUND('',#19637,.T.);
#13666=FACE_OUTER_BOUND('',#19638,.T.);
#13667=FACE_OUTER_BOUND('',#19639,.T.);
#13668=FACE_OUTER_BOUND('',#19640,.T.);
#13669=FACE_OUTER_BOUND('',#19641,.T.);
#13670=FACE_OUTER_BOUND('',#19642,.T.);
#13671=FACE_OUTER_BOUND('',#19643,.T.);
#13672=FACE_OUTER_BOUND('',#19644,.T.);
#13673=FACE_OUTER_BOUND('',#19645,.T.);
#13674=FACE_OUTER_BOUND('',#19646,.T.);
#13675=FACE_OUTER_BOUND('',#19647,.T.);
#13676=FACE_OUTER_BOUND('',#19648,.T.);
#13677=FACE_OUTER_BOUND('',#19649,.T.);
#13678=FACE_OUTER_BOUND('',#19650,.T.);
#13679=FACE_OUTER_BOUND('',#19651,.T.);
#13680=FACE_OUTER_BOUND('',#19652,.T.);
#13681=FACE_OUTER_BOUND('',#19653,.T.);
#13682=FACE_OUTER_BOUND('',#19654,.T.);
#13683=FACE_OUTER_BOUND('',#19655,.T.);
#13684=FACE_OUTER_BOUND('',#19656,.T.);
#13685=FACE_OUTER_BOUND('',#19657,.T.);
#13686=FACE_OUTER_BOUND('',#19658,.T.);
#13687=FACE_OUTER_BOUND('',#19659,.T.);
#13688=FACE_OUTER_BOUND('',#19660,.T.);
#13689=FACE_OUTER_BOUND('',#19661,.T.);
#13690=FACE_OUTER_BOUND('',#19662,.T.);
#13691=FACE_OUTER_BOUND('',#19663,.T.);
#13692=FACE_OUTER_BOUND('',#19664,.T.);
#13693=FACE_OUTER_BOUND('',#19665,.T.);
#13694=FACE_OUTER_BOUND('',#19667,.T.);
#13695=FACE_OUTER_BOUND('',#19668,.T.);
#13696=FACE_OUTER_BOUND('',#19669,.T.);
#13697=FACE_OUTER_BOUND('',#19670,.T.);
#13698=FACE_OUTER_BOUND('',#19671,.T.);
#13699=FACE_OUTER_BOUND('',#19672,.T.);
#13700=FACE_OUTER_BOUND('',#19673,.T.);
#13701=FACE_OUTER_BOUND('',#19674,.T.);
#13702=FACE_OUTER_BOUND('',#19675,.T.);
#13703=FACE_OUTER_BOUND('',#19676,.T.);
#13704=FACE_OUTER_BOUND('',#19677,.T.);
#13705=FACE_OUTER_BOUND('',#19678,.T.);
#13706=FACE_OUTER_BOUND('',#19679,.T.);
#13707=FACE_OUTER_BOUND('',#19680,.T.);
#13708=FACE_OUTER_BOUND('',#19681,.T.);
#13709=FACE_OUTER_BOUND('',#19682,.T.);
#13710=FACE_OUTER_BOUND('',#19683,.T.);
#13711=FACE_OUTER_BOUND('',#19684,.T.);
#13712=FACE_OUTER_BOUND('',#19685,.T.);
#13713=FACE_OUTER_BOUND('',#19686,.T.);
#13714=FACE_OUTER_BOUND('',#19687,.T.);
#13715=FACE_OUTER_BOUND('',#19688,.T.);
#13716=FACE_OUTER_BOUND('',#19689,.T.);
#13717=FACE_OUTER_BOUND('',#19690,.T.);
#13718=FACE_OUTER_BOUND('',#19691,.T.);
#13719=FACE_OUTER_BOUND('',#19692,.T.);
#13720=FACE_OUTER_BOUND('',#19693,.T.);
#13721=FACE_OUTER_BOUND('',#19694,.T.);
#13722=FACE_OUTER_BOUND('',#19695,.T.);
#13723=FACE_OUTER_BOUND('',#19696,.T.);
#13724=FACE_OUTER_BOUND('',#19697,.T.);
#13725=FACE_OUTER_BOUND('',#19698,.T.);
#13726=FACE_OUTER_BOUND('',#19699,.T.);
#13727=FACE_OUTER_BOUND('',#19700,.T.);
#13728=FACE_OUTER_BOUND('',#19701,.T.);
#13729=FACE_OUTER_BOUND('',#19702,.T.);
#13730=FACE_OUTER_BOUND('',#19703,.T.);
#13731=FACE_OUTER_BOUND('',#19704,.T.);
#13732=FACE_OUTER_BOUND('',#19705,.T.);
#13733=FACE_OUTER_BOUND('',#19706,.T.);
#13734=FACE_OUTER_BOUND('',#19707,.T.);
#13735=FACE_OUTER_BOUND('',#19708,.T.);
#13736=FACE_OUTER_BOUND('',#19709,.T.);
#13737=FACE_OUTER_BOUND('',#19710,.T.);
#13738=FACE_OUTER_BOUND('',#19711,.T.);
#13739=FACE_OUTER_BOUND('',#19712,.T.);
#13740=FACE_OUTER_BOUND('',#19714,.T.);
#13741=FACE_OUTER_BOUND('',#19716,.T.);
#13742=FACE_OUTER_BOUND('',#19717,.T.);
#13743=FACE_OUTER_BOUND('',#19718,.T.);
#13744=FACE_OUTER_BOUND('',#19719,.T.);
#13745=FACE_OUTER_BOUND('',#19720,.T.);
#13746=FACE_OUTER_BOUND('',#19721,.T.);
#13747=FACE_OUTER_BOUND('',#19722,.T.);
#13748=FACE_OUTER_BOUND('',#19723,.T.);
#13749=FACE_OUTER_BOUND('',#19724,.T.);
#13750=FACE_OUTER_BOUND('',#19725,.T.);
#13751=FACE_OUTER_BOUND('',#19726,.T.);
#13752=FACE_OUTER_BOUND('',#19727,.T.);
#13753=FACE_OUTER_BOUND('',#19728,.T.);
#13754=FACE_OUTER_BOUND('',#19729,.T.);
#13755=FACE_OUTER_BOUND('',#19730,.T.);
#13756=FACE_OUTER_BOUND('',#19731,.T.);
#13757=FACE_OUTER_BOUND('',#19732,.T.);
#13758=FACE_OUTER_BOUND('',#19733,.T.);
#13759=FACE_OUTER_BOUND('',#19734,.T.);
#13760=FACE_OUTER_BOUND('',#19735,.T.);
#13761=FACE_OUTER_BOUND('',#19736,.T.);
#13762=FACE_OUTER_BOUND('',#19738,.T.);
#13763=FACE_OUTER_BOUND('',#19740,.T.);
#13764=FACE_OUTER_BOUND('',#19741,.T.);
#13765=FACE_OUTER_BOUND('',#19742,.T.);
#13766=FACE_OUTER_BOUND('',#19743,.T.);
#13767=FACE_OUTER_BOUND('',#19744,.T.);
#13768=FACE_OUTER_BOUND('',#19745,.T.);
#13769=FACE_OUTER_BOUND('',#19746,.T.);
#13770=FACE_OUTER_BOUND('',#19747,.T.);
#13771=FACE_OUTER_BOUND('',#19748,.T.);
#13772=FACE_OUTER_BOUND('',#19749,.T.);
#13773=FACE_OUTER_BOUND('',#19750,.T.);
#13774=FACE_OUTER_BOUND('',#19751,.T.);
#13775=FACE_OUTER_BOUND('',#19752,.T.);
#13776=FACE_OUTER_BOUND('',#19753,.T.);
#13777=FACE_OUTER_BOUND('',#19754,.T.);
#13778=FACE_OUTER_BOUND('',#19755,.T.);
#13779=FACE_OUTER_BOUND('',#19756,.T.);
#13780=FACE_OUTER_BOUND('',#19757,.T.);
#13781=FACE_OUTER_BOUND('',#19758,.T.);
#13782=FACE_OUTER_BOUND('',#19759,.T.);
#13783=FACE_OUTER_BOUND('',#19760,.T.);
#13784=FACE_OUTER_BOUND('',#19761,.T.);
#13785=FACE_OUTER_BOUND('',#19762,.T.);
#13786=FACE_OUTER_BOUND('',#19763,.T.);
#13787=FACE_OUTER_BOUND('',#19764,.T.);
#13788=FACE_OUTER_BOUND('',#19765,.T.);
#13789=FACE_OUTER_BOUND('',#19766,.T.);
#13790=FACE_OUTER_BOUND('',#19767,.T.);
#13791=FACE_OUTER_BOUND('',#19768,.T.);
#13792=FACE_OUTER_BOUND('',#19769,.T.);
#13793=FACE_OUTER_BOUND('',#19770,.T.);
#13794=FACE_OUTER_BOUND('',#19771,.T.);
#13795=FACE_OUTER_BOUND('',#19772,.T.);
#13796=FACE_OUTER_BOUND('',#19773,.T.);
#13797=FACE_OUTER_BOUND('',#19774,.T.);
#13798=FACE_OUTER_BOUND('',#19775,.T.);
#13799=FACE_OUTER_BOUND('',#19776,.T.);
#13800=FACE_OUTER_BOUND('',#19777,.T.);
#13801=FACE_OUTER_BOUND('',#19778,.T.);
#13802=FACE_OUTER_BOUND('',#19779,.T.);
#13803=FACE_OUTER_BOUND('',#19780,.T.);
#13804=FACE_OUTER_BOUND('',#19781,.T.);
#13805=FACE_OUTER_BOUND('',#19782,.T.);
#13806=FACE_OUTER_BOUND('',#19783,.T.);
#13807=FACE_OUTER_BOUND('',#19784,.T.);
#13808=FACE_OUTER_BOUND('',#19785,.T.);
#13809=FACE_OUTER_BOUND('',#19786,.T.);
#13810=FACE_OUTER_BOUND('',#19787,.T.);
#13811=FACE_OUTER_BOUND('',#19788,.T.);
#13812=FACE_OUTER_BOUND('',#19789,.T.);
#13813=FACE_OUTER_BOUND('',#19790,.T.);
#13814=FACE_OUTER_BOUND('',#19791,.T.);
#13815=FACE_OUTER_BOUND('',#19792,.T.);
#13816=FACE_OUTER_BOUND('',#19793,.T.);
#13817=FACE_OUTER_BOUND('',#19794,.T.);
#13818=FACE_OUTER_BOUND('',#19795,.T.);
#13819=FACE_OUTER_BOUND('',#19796,.T.);
#13820=FACE_OUTER_BOUND('',#19797,.T.);
#13821=FACE_OUTER_BOUND('',#19798,.T.);
#13822=FACE_OUTER_BOUND('',#19799,.T.);
#13823=FACE_OUTER_BOUND('',#19800,.T.);
#13824=FACE_OUTER_BOUND('',#19801,.T.);
#13825=FACE_OUTER_BOUND('',#19802,.T.);
#13826=FACE_OUTER_BOUND('',#19803,.T.);
#13827=FACE_OUTER_BOUND('',#19804,.T.);
#13828=FACE_OUTER_BOUND('',#19805,.T.);
#13829=FACE_OUTER_BOUND('',#19806,.T.);
#13830=FACE_OUTER_BOUND('',#19807,.T.);
#13831=FACE_OUTER_BOUND('',#19808,.T.);
#13832=FACE_OUTER_BOUND('',#19809,.T.);
#13833=FACE_OUTER_BOUND('',#19810,.T.);
#13834=FACE_OUTER_BOUND('',#19811,.T.);
#13835=FACE_OUTER_BOUND('',#19812,.T.);
#13836=FACE_OUTER_BOUND('',#19813,.T.);
#13837=FACE_OUTER_BOUND('',#19814,.T.);
#13838=FACE_OUTER_BOUND('',#19815,.T.);
#13839=FACE_OUTER_BOUND('',#19816,.T.);
#13840=FACE_OUTER_BOUND('',#19817,.T.);
#13841=FACE_OUTER_BOUND('',#19818,.T.);
#13842=FACE_OUTER_BOUND('',#19819,.T.);
#13843=FACE_OUTER_BOUND('',#19820,.T.);
#13844=FACE_OUTER_BOUND('',#19821,.T.);
#13845=FACE_OUTER_BOUND('',#19822,.T.);
#13846=FACE_OUTER_BOUND('',#19823,.T.);
#13847=FACE_OUTER_BOUND('',#19824,.T.);
#13848=FACE_OUTER_BOUND('',#19825,.T.);
#13849=FACE_OUTER_BOUND('',#19826,.T.);
#13850=FACE_OUTER_BOUND('',#19827,.T.);
#13851=FACE_OUTER_BOUND('',#19829,.T.);
#13852=FACE_OUTER_BOUND('',#19830,.T.);
#13853=FACE_OUTER_BOUND('',#19831,.T.);
#13854=FACE_OUTER_BOUND('',#19832,.T.);
#13855=FACE_OUTER_BOUND('',#19833,.T.);
#13856=FACE_OUTER_BOUND('',#19834,.T.);
#13857=FACE_OUTER_BOUND('',#19835,.T.);
#13858=FACE_OUTER_BOUND('',#19836,.T.);
#13859=FACE_OUTER_BOUND('',#19837,.T.);
#13860=FACE_OUTER_BOUND('',#19838,.T.);
#13861=FACE_OUTER_BOUND('',#19839,.T.);
#13862=FACE_OUTER_BOUND('',#19840,.T.);
#13863=FACE_OUTER_BOUND('',#19841,.T.);
#13864=FACE_OUTER_BOUND('',#19842,.T.);
#13865=FACE_OUTER_BOUND('',#19843,.T.);
#13866=FACE_OUTER_BOUND('',#19844,.T.);
#13867=FACE_OUTER_BOUND('',#19845,.T.);
#13868=FACE_OUTER_BOUND('',#19846,.T.);
#13869=FACE_OUTER_BOUND('',#19847,.T.);
#13870=FACE_OUTER_BOUND('',#19848,.T.);
#13871=FACE_OUTER_BOUND('',#19849,.T.);
#13872=FACE_OUTER_BOUND('',#19850,.T.);
#13873=FACE_OUTER_BOUND('',#19851,.T.);
#13874=FACE_OUTER_BOUND('',#19852,.T.);
#13875=FACE_OUTER_BOUND('',#19853,.T.);
#13876=FACE_OUTER_BOUND('',#19854,.T.);
#13877=FACE_OUTER_BOUND('',#19855,.T.);
#13878=FACE_OUTER_BOUND('',#19856,.T.);
#13879=FACE_OUTER_BOUND('',#19857,.T.);
#13880=FACE_OUTER_BOUND('',#19858,.T.);
#13881=FACE_OUTER_BOUND('',#19859,.T.);
#13882=FACE_OUTER_BOUND('',#19860,.T.);
#13883=FACE_OUTER_BOUND('',#19861,.T.);
#13884=FACE_OUTER_BOUND('',#19862,.T.);
#13885=FACE_OUTER_BOUND('',#19863,.T.);
#13886=FACE_OUTER_BOUND('',#19864,.T.);
#13887=FACE_OUTER_BOUND('',#19865,.T.);
#13888=FACE_OUTER_BOUND('',#19866,.T.);
#13889=FACE_OUTER_BOUND('',#19867,.T.);
#13890=FACE_OUTER_BOUND('',#19868,.T.);
#13891=FACE_OUTER_BOUND('',#19869,.T.);
#13892=FACE_OUTER_BOUND('',#19870,.T.);
#13893=FACE_OUTER_BOUND('',#19871,.T.);
#13894=FACE_OUTER_BOUND('',#19872,.T.);
#13895=FACE_OUTER_BOUND('',#19873,.T.);
#13896=FACE_OUTER_BOUND('',#19874,.T.);
#13897=FACE_OUTER_BOUND('',#19875,.T.);
#13898=FACE_OUTER_BOUND('',#19876,.T.);
#13899=FACE_OUTER_BOUND('',#19877,.T.);
#13900=FACE_OUTER_BOUND('',#19878,.T.);
#13901=FACE_OUTER_BOUND('',#19879,.T.);
#13902=FACE_OUTER_BOUND('',#19880,.T.);
#13903=FACE_OUTER_BOUND('',#19881,.T.);
#13904=FACE_OUTER_BOUND('',#19882,.T.);
#13905=FACE_OUTER_BOUND('',#19883,.T.);
#13906=FACE_OUTER_BOUND('',#19884,.T.);
#13907=FACE_OUTER_BOUND('',#19885,.T.);
#13908=FACE_OUTER_BOUND('',#19886,.T.);
#13909=FACE_OUTER_BOUND('',#19887,.T.);
#13910=FACE_OUTER_BOUND('',#19888,.T.);
#13911=FACE_OUTER_BOUND('',#19889,.T.);
#13912=FACE_OUTER_BOUND('',#19890,.T.);
#13913=FACE_OUTER_BOUND('',#19891,.T.);
#13914=FACE_OUTER_BOUND('',#19892,.T.);
#13915=FACE_OUTER_BOUND('',#19893,.T.);
#13916=FACE_OUTER_BOUND('',#19894,.T.);
#13917=FACE_OUTER_BOUND('',#19895,.T.);
#13918=FACE_OUTER_BOUND('',#19896,.T.);
#13919=FACE_OUTER_BOUND('',#19897,.T.);
#13920=FACE_OUTER_BOUND('',#19898,.T.);
#13921=FACE_OUTER_BOUND('',#19899,.T.);
#13922=FACE_OUTER_BOUND('',#19900,.T.);
#13923=FACE_OUTER_BOUND('',#19901,.T.);
#13924=FACE_OUTER_BOUND('',#19902,.T.);
#13925=FACE_OUTER_BOUND('',#19903,.T.);
#13926=FACE_OUTER_BOUND('',#19904,.T.);
#13927=FACE_OUTER_BOUND('',#19905,.T.);
#13928=FACE_OUTER_BOUND('',#19906,.T.);
#13929=FACE_OUTER_BOUND('',#19907,.T.);
#13930=FACE_OUTER_BOUND('',#19908,.T.);
#13931=FACE_OUTER_BOUND('',#19909,.T.);
#13932=FACE_OUTER_BOUND('',#19910,.T.);
#13933=FACE_OUTER_BOUND('',#19911,.T.);
#13934=FACE_OUTER_BOUND('',#19912,.T.);
#13935=FACE_OUTER_BOUND('',#19913,.T.);
#13936=FACE_OUTER_BOUND('',#19914,.T.);
#13937=FACE_OUTER_BOUND('',#19917,.T.);
#13938=FACE_OUTER_BOUND('',#19920,.T.);
#13939=FACE_OUTER_BOUND('',#19921,.T.);
#13940=FACE_OUTER_BOUND('',#19922,.T.);
#13941=FACE_OUTER_BOUND('',#19923,.T.);
#13942=FACE_OUTER_BOUND('',#19926,.T.);
#13943=FACE_OUTER_BOUND('',#19929,.T.);
#13944=FACE_OUTER_BOUND('',#19930,.T.);
#13945=FACE_OUTER_BOUND('',#19931,.T.);
#13946=FACE_OUTER_BOUND('',#19932,.T.);
#13947=FACE_OUTER_BOUND('',#19933,.T.);
#13948=FACE_OUTER_BOUND('',#19934,.T.);
#13949=FACE_OUTER_BOUND('',#19935,.T.);
#13950=FACE_OUTER_BOUND('',#19936,.T.);
#13951=FACE_OUTER_BOUND('',#19937,.T.);
#13952=FACE_OUTER_BOUND('',#19938,.T.);
#13953=FACE_OUTER_BOUND('',#19939,.T.);
#13954=FACE_OUTER_BOUND('',#19940,.T.);
#13955=FACE_OUTER_BOUND('',#19941,.T.);
#13956=FACE_OUTER_BOUND('',#19942,.T.);
#13957=FACE_OUTER_BOUND('',#19944,.T.);
#13958=FACE_OUTER_BOUND('',#19946,.T.);
#13959=FACE_OUTER_BOUND('',#19948,.T.);
#13960=FACE_OUTER_BOUND('',#19950,.T.);
#13961=FACE_OUTER_BOUND('',#19951,.T.);
#13962=FACE_OUTER_BOUND('',#19952,.T.);
#13963=FACE_OUTER_BOUND('',#19953,.T.);
#13964=FACE_OUTER_BOUND('',#19954,.T.);
#13965=FACE_OUTER_BOUND('',#19955,.T.);
#13966=FACE_OUTER_BOUND('',#19956,.T.);
#13967=FACE_OUTER_BOUND('',#19957,.T.);
#13968=FACE_OUTER_BOUND('',#19958,.T.);
#13969=FACE_OUTER_BOUND('',#19959,.T.);
#13970=FACE_OUTER_BOUND('',#19960,.T.);
#13971=FACE_OUTER_BOUND('',#19962,.T.);
#13972=FACE_OUTER_BOUND('',#19964,.T.);
#13973=FACE_OUTER_BOUND('',#19967,.T.);
#13974=FACE_OUTER_BOUND('',#19968,.T.);
#13975=FACE_OUTER_BOUND('',#19969,.T.);
#13976=FACE_OUTER_BOUND('',#19970,.T.);
#13977=FACE_OUTER_BOUND('',#19972,.T.);
#13978=FACE_OUTER_BOUND('',#19974,.T.);
#13979=FACE_OUTER_BOUND('',#19975,.T.);
#13980=FACE_OUTER_BOUND('',#19976,.T.);
#13981=FACE_OUTER_BOUND('',#19977,.T.);
#13982=FACE_OUTER_BOUND('',#19978,.T.);
#13983=FACE_OUTER_BOUND('',#19979,.T.);
#13984=FACE_OUTER_BOUND('',#19980,.T.);
#13985=FACE_OUTER_BOUND('',#19981,.T.);
#13986=FACE_OUTER_BOUND('',#19982,.T.);
#13987=FACE_OUTER_BOUND('',#19983,.T.);
#13988=FACE_OUTER_BOUND('',#19984,.T.);
#13989=FACE_OUTER_BOUND('',#19985,.T.);
#13990=FACE_OUTER_BOUND('',#19986,.T.);
#13991=FACE_OUTER_BOUND('',#19987,.T.);
#13992=FACE_OUTER_BOUND('',#19988,.T.);
#13993=FACE_OUTER_BOUND('',#19989,.T.);
#13994=FACE_OUTER_BOUND('',#19990,.T.);
#13995=FACE_OUTER_BOUND('',#19991,.T.);
#13996=FACE_OUTER_BOUND('',#19992,.T.);
#13997=FACE_OUTER_BOUND('',#19993,.T.);
#13998=FACE_OUTER_BOUND('',#19994,.T.);
#13999=FACE_OUTER_BOUND('',#19995,.T.);
#14000=FACE_OUTER_BOUND('',#19996,.T.);
#14001=FACE_OUTER_BOUND('',#19997,.T.);
#14002=FACE_OUTER_BOUND('',#19998,.T.);
#14003=FACE_OUTER_BOUND('',#19999,.T.);
#14004=FACE_OUTER_BOUND('',#20000,.T.);
#14005=FACE_OUTER_BOUND('',#20001,.T.);
#14006=FACE_OUTER_BOUND('',#20002,.T.);
#14007=FACE_OUTER_BOUND('',#20003,.T.);
#14008=FACE_OUTER_BOUND('',#20004,.T.);
#14009=FACE_OUTER_BOUND('',#20005,.T.);
#14010=FACE_OUTER_BOUND('',#20006,.T.);
#14011=FACE_OUTER_BOUND('',#20007,.T.);
#14012=FACE_OUTER_BOUND('',#20008,.T.);
#14013=FACE_OUTER_BOUND('',#20010,.T.);
#14014=FACE_OUTER_BOUND('',#20012,.T.);
#14015=FACE_OUTER_BOUND('',#20014,.T.);
#14016=FACE_OUTER_BOUND('',#20015,.T.);
#14017=FACE_OUTER_BOUND('',#20017,.T.);
#14018=FACE_OUTER_BOUND('',#20018,.T.);
#14019=FACE_OUTER_BOUND('',#20019,.T.);
#14020=FACE_OUTER_BOUND('',#20020,.T.);
#14021=FACE_OUTER_BOUND('',#20021,.T.);
#14022=FACE_OUTER_BOUND('',#20022,.T.);
#14023=FACE_OUTER_BOUND('',#20023,.T.);
#14024=FACE_OUTER_BOUND('',#20024,.T.);
#14025=FACE_OUTER_BOUND('',#20025,.T.);
#14026=FACE_OUTER_BOUND('',#20026,.T.);
#14027=FACE_OUTER_BOUND('',#20027,.T.);
#14028=FACE_OUTER_BOUND('',#20028,.T.);
#14029=FACE_OUTER_BOUND('',#20029,.T.);
#14030=FACE_OUTER_BOUND('',#20030,.T.);
#14031=FACE_OUTER_BOUND('',#20031,.T.);
#14032=FACE_OUTER_BOUND('',#20032,.T.);
#14033=FACE_OUTER_BOUND('',#20033,.T.);
#14034=FACE_OUTER_BOUND('',#20034,.T.);
#14035=FACE_OUTER_BOUND('',#20036,.T.);
#14036=FACE_OUTER_BOUND('',#20037,.T.);
#14037=FACE_OUTER_BOUND('',#20038,.T.);
#14038=FACE_OUTER_BOUND('',#20039,.T.);
#14039=FACE_OUTER_BOUND('',#20040,.T.);
#14040=FACE_OUTER_BOUND('',#20041,.T.);
#14041=FACE_OUTER_BOUND('',#20042,.T.);
#14042=FACE_OUTER_BOUND('',#20044,.T.);
#14043=FACE_OUTER_BOUND('',#20045,.T.);
#14044=FACE_OUTER_BOUND('',#20046,.T.);
#14045=FACE_OUTER_BOUND('',#20047,.T.);
#14046=FACE_OUTER_BOUND('',#20048,.T.);
#14047=FACE_OUTER_BOUND('',#20049,.T.);
#14048=FACE_OUTER_BOUND('',#20050,.T.);
#14049=FACE_OUTER_BOUND('',#20051,.T.);
#14050=FACE_OUTER_BOUND('',#20052,.T.);
#14051=FACE_OUTER_BOUND('',#20053,.T.);
#14052=FACE_OUTER_BOUND('',#20054,.T.);
#14053=FACE_OUTER_BOUND('',#20055,.T.);
#14054=FACE_OUTER_BOUND('',#20056,.T.);
#14055=FACE_OUTER_BOUND('',#20057,.T.);
#14056=FACE_OUTER_BOUND('',#20058,.T.);
#14057=FACE_OUTER_BOUND('',#20059,.T.);
#14058=FACE_OUTER_BOUND('',#20060,.T.);
#14059=FACE_OUTER_BOUND('',#20061,.T.);
#14060=FACE_OUTER_BOUND('',#20062,.T.);
#14061=FACE_OUTER_BOUND('',#20063,.T.);
#14062=FACE_OUTER_BOUND('',#20064,.T.);
#14063=FACE_OUTER_BOUND('',#20065,.T.);
#14064=FACE_OUTER_BOUND('',#20066,.T.);
#14065=FACE_OUTER_BOUND('',#20067,.T.);
#14066=FACE_OUTER_BOUND('',#20068,.T.);
#14067=FACE_OUTER_BOUND('',#20069,.T.);
#14068=FACE_OUTER_BOUND('',#20070,.T.);
#14069=FACE_OUTER_BOUND('',#20071,.T.);
#14070=FACE_OUTER_BOUND('',#20072,.T.);
#14071=FACE_OUTER_BOUND('',#20073,.T.);
#14072=FACE_OUTER_BOUND('',#20074,.T.);
#14073=FACE_OUTER_BOUND('',#20076,.T.);
#14074=FACE_OUTER_BOUND('',#20077,.T.);
#14075=FACE_OUTER_BOUND('',#20078,.T.);
#14076=FACE_OUTER_BOUND('',#20080,.T.);
#14077=FACE_OUTER_BOUND('',#20081,.T.);
#14078=FACE_OUTER_BOUND('',#20082,.T.);
#14079=FACE_OUTER_BOUND('',#20083,.T.);
#14080=FACE_OUTER_BOUND('',#20084,.T.);
#14081=FACE_OUTER_BOUND('',#20085,.T.);
#14082=FACE_OUTER_BOUND('',#20086,.T.);
#14083=FACE_OUTER_BOUND('',#20088,.T.);
#14084=FACE_OUTER_BOUND('',#20089,.T.);
#14085=FACE_OUTER_BOUND('',#20090,.T.);
#14086=FACE_OUTER_BOUND('',#20091,.T.);
#14087=FACE_OUTER_BOUND('',#20092,.T.);
#14088=FACE_OUTER_BOUND('',#20093,.T.);
#14089=FACE_OUTER_BOUND('',#20094,.T.);
#14090=FACE_OUTER_BOUND('',#20095,.T.);
#14091=FACE_OUTER_BOUND('',#20096,.T.);
#14092=FACE_OUTER_BOUND('',#20097,.T.);
#14093=FACE_OUTER_BOUND('',#20098,.T.);
#14094=FACE_OUTER_BOUND('',#20100,.T.);
#14095=FACE_OUTER_BOUND('',#20101,.T.);
#14096=FACE_OUTER_BOUND('',#20102,.T.);
#14097=FACE_OUTER_BOUND('',#20103,.T.);
#14098=FACE_OUTER_BOUND('',#20104,.T.);
#14099=FACE_OUTER_BOUND('',#20105,.T.);
#14100=FACE_OUTER_BOUND('',#20106,.T.);
#14101=FACE_OUTER_BOUND('',#20107,.T.);
#14102=FACE_OUTER_BOUND('',#20108,.T.);
#14103=FACE_OUTER_BOUND('',#20109,.T.);
#14104=FACE_OUTER_BOUND('',#20110,.T.);
#14105=FACE_OUTER_BOUND('',#20111,.T.);
#14106=FACE_OUTER_BOUND('',#20112,.T.);
#14107=FACE_OUTER_BOUND('',#20113,.T.);
#14108=FACE_OUTER_BOUND('',#20114,.T.);
#14109=FACE_OUTER_BOUND('',#20115,.T.);
#14110=FACE_OUTER_BOUND('',#20116,.T.);
#14111=FACE_OUTER_BOUND('',#20117,.T.);
#14112=FACE_OUTER_BOUND('',#20118,.T.);
#14113=FACE_OUTER_BOUND('',#20119,.T.);
#14114=FACE_OUTER_BOUND('',#20120,.T.);
#14115=FACE_OUTER_BOUND('',#20121,.T.);
#14116=FACE_OUTER_BOUND('',#20122,.T.);
#14117=FACE_OUTER_BOUND('',#20123,.T.);
#14118=FACE_OUTER_BOUND('',#20124,.T.);
#14119=FACE_OUTER_BOUND('',#20125,.T.);
#14120=FACE_OUTER_BOUND('',#20126,.T.);
#14121=FACE_OUTER_BOUND('',#20127,.T.);
#14122=FACE_OUTER_BOUND('',#20128,.T.);
#14123=FACE_OUTER_BOUND('',#20129,.T.);
#14124=FACE_OUTER_BOUND('',#20130,.T.);
#14125=FACE_OUTER_BOUND('',#20131,.T.);
#14126=FACE_OUTER_BOUND('',#20132,.T.);
#14127=FACE_OUTER_BOUND('',#20133,.T.);
#14128=FACE_OUTER_BOUND('',#20134,.T.);
#14129=FACE_OUTER_BOUND('',#20135,.T.);
#14130=FACE_OUTER_BOUND('',#20136,.T.);
#14131=FACE_OUTER_BOUND('',#20137,.T.);
#14132=FACE_OUTER_BOUND('',#20138,.T.);
#14133=FACE_OUTER_BOUND('',#20139,.T.);
#14134=FACE_OUTER_BOUND('',#20140,.T.);
#14135=FACE_OUTER_BOUND('',#20141,.T.);
#14136=FACE_OUTER_BOUND('',#20142,.T.);
#14137=FACE_OUTER_BOUND('',#20143,.T.);
#14138=FACE_OUTER_BOUND('',#20144,.T.);
#14139=FACE_OUTER_BOUND('',#20145,.T.);
#14140=FACE_OUTER_BOUND('',#20146,.T.);
#14141=FACE_OUTER_BOUND('',#20147,.T.);
#14142=FACE_OUTER_BOUND('',#20148,.T.);
#14143=FACE_OUTER_BOUND('',#20149,.T.);
#14144=FACE_OUTER_BOUND('',#20150,.T.);
#14145=FACE_OUTER_BOUND('',#20151,.T.);
#14146=FACE_OUTER_BOUND('',#20152,.T.);
#14147=FACE_OUTER_BOUND('',#20153,.T.);
#14148=FACE_OUTER_BOUND('',#20154,.T.);
#14149=FACE_OUTER_BOUND('',#20155,.T.);
#14150=FACE_OUTER_BOUND('',#20156,.T.);
#14151=FACE_OUTER_BOUND('',#20157,.T.);
#14152=FACE_OUTER_BOUND('',#20158,.T.);
#14153=FACE_OUTER_BOUND('',#20159,.T.);
#14154=FACE_OUTER_BOUND('',#20160,.T.);
#14155=FACE_OUTER_BOUND('',#20161,.T.);
#14156=FACE_OUTER_BOUND('',#20162,.T.);
#14157=FACE_OUTER_BOUND('',#20163,.T.);
#14158=FACE_OUTER_BOUND('',#20164,.T.);
#14159=FACE_OUTER_BOUND('',#20165,.T.);
#14160=FACE_OUTER_BOUND('',#20166,.T.);
#14161=FACE_OUTER_BOUND('',#20167,.T.);
#14162=FACE_OUTER_BOUND('',#20168,.T.);
#14163=FACE_OUTER_BOUND('',#20169,.T.);
#14164=FACE_OUTER_BOUND('',#20170,.T.);
#14165=FACE_OUTER_BOUND('',#20171,.T.);
#14166=FACE_OUTER_BOUND('',#20172,.T.);
#14167=FACE_OUTER_BOUND('',#20173,.T.);
#14168=FACE_OUTER_BOUND('',#20175,.T.);
#14169=FACE_OUTER_BOUND('',#20177,.T.);
#14170=FACE_OUTER_BOUND('',#20178,.T.);
#14171=FACE_OUTER_BOUND('',#20179,.T.);
#14172=FACE_OUTER_BOUND('',#20180,.T.);
#14173=FACE_OUTER_BOUND('',#20181,.T.);
#14174=FACE_OUTER_BOUND('',#20182,.T.);
#14175=FACE_OUTER_BOUND('',#20183,.T.);
#14176=FACE_OUTER_BOUND('',#20184,.T.);
#14177=FACE_OUTER_BOUND('',#20185,.T.);
#14178=FACE_OUTER_BOUND('',#20186,.T.);
#14179=FACE_OUTER_BOUND('',#20187,.T.);
#14180=FACE_OUTER_BOUND('',#20189,.T.);
#14181=FACE_OUTER_BOUND('',#20190,.T.);
#14182=FACE_OUTER_BOUND('',#20191,.T.);
#14183=FACE_OUTER_BOUND('',#20192,.T.);
#14184=FACE_OUTER_BOUND('',#20193,.T.);
#14185=FACE_OUTER_BOUND('',#20194,.T.);
#14186=FACE_OUTER_BOUND('',#20195,.T.);
#14187=FACE_OUTER_BOUND('',#20196,.T.);
#14188=FACE_OUTER_BOUND('',#20197,.T.);
#14189=FACE_OUTER_BOUND('',#20198,.T.);
#14190=FACE_OUTER_BOUND('',#20199,.T.);
#14191=FACE_OUTER_BOUND('',#20200,.T.);
#14192=FACE_OUTER_BOUND('',#20201,.T.);
#14193=FACE_OUTER_BOUND('',#20202,.T.);
#14194=FACE_OUTER_BOUND('',#20203,.T.);
#14195=FACE_OUTER_BOUND('',#20204,.T.);
#14196=FACE_OUTER_BOUND('',#20205,.T.);
#14197=FACE_OUTER_BOUND('',#20206,.T.);
#14198=FACE_OUTER_BOUND('',#20207,.T.);
#14199=FACE_OUTER_BOUND('',#20208,.T.);
#14200=FACE_OUTER_BOUND('',#20209,.T.);
#14201=FACE_OUTER_BOUND('',#20210,.T.);
#14202=FACE_OUTER_BOUND('',#20211,.T.);
#14203=FACE_OUTER_BOUND('',#20212,.T.);
#14204=FACE_OUTER_BOUND('',#20213,.T.);
#14205=FACE_OUTER_BOUND('',#20214,.T.);
#14206=FACE_OUTER_BOUND('',#20215,.T.);
#14207=FACE_OUTER_BOUND('',#20216,.T.);
#14208=FACE_OUTER_BOUND('',#20218,.T.);
#14209=FACE_OUTER_BOUND('',#20219,.T.);
#14210=FACE_OUTER_BOUND('',#20220,.T.);
#14211=FACE_OUTER_BOUND('',#20221,.T.);
#14212=FACE_OUTER_BOUND('',#20222,.T.);
#14213=FACE_OUTER_BOUND('',#20223,.T.);
#14214=FACE_OUTER_BOUND('',#20225,.T.);
#14215=FACE_OUTER_BOUND('',#20227,.T.);
#14216=FACE_OUTER_BOUND('',#20228,.T.);
#14217=FACE_OUTER_BOUND('',#20230,.T.);
#14218=FACE_OUTER_BOUND('',#20231,.T.);
#14219=FACE_OUTER_BOUND('',#20232,.T.);
#14220=FACE_OUTER_BOUND('',#20233,.T.);
#14221=FACE_OUTER_BOUND('',#20234,.T.);
#14222=FACE_OUTER_BOUND('',#20235,.T.);
#14223=FACE_OUTER_BOUND('',#20236,.T.);
#14224=FACE_OUTER_BOUND('',#20237,.T.);
#14225=FACE_OUTER_BOUND('',#20238,.T.);
#14226=FACE_OUTER_BOUND('',#20239,.T.);
#14227=FACE_OUTER_BOUND('',#20249,.T.);
#14228=FACE_OUTER_BOUND('',#20251,.T.);
#14229=FACE_OUTER_BOUND('',#20253,.T.);
#14230=FACE_OUTER_BOUND('',#20254,.T.);
#14231=FACE_OUTER_BOUND('',#20255,.T.);
#14232=FACE_OUTER_BOUND('',#20256,.T.);
#14233=FACE_OUTER_BOUND('',#20257,.T.);
#14234=FACE_OUTER_BOUND('',#20258,.T.);
#14235=FACE_OUTER_BOUND('',#20259,.T.);
#14236=FACE_OUTER_BOUND('',#20260,.T.);
#14237=FACE_OUTER_BOUND('',#20261,.T.);
#14238=FACE_OUTER_BOUND('',#20262,.T.);
#14239=FACE_OUTER_BOUND('',#20263,.T.);
#14240=FACE_OUTER_BOUND('',#20264,.T.);
#14241=FACE_OUTER_BOUND('',#20265,.T.);
#14242=FACE_OUTER_BOUND('',#20266,.T.);
#14243=FACE_OUTER_BOUND('',#20267,.T.);
#14244=FACE_OUTER_BOUND('',#20268,.T.);
#14245=FACE_OUTER_BOUND('',#20269,.T.);
#14246=FACE_OUTER_BOUND('',#20270,.T.);
#14247=FACE_OUTER_BOUND('',#20271,.T.);
#14248=FACE_OUTER_BOUND('',#20272,.T.);
#14249=FACE_OUTER_BOUND('',#20273,.T.);
#14250=FACE_OUTER_BOUND('',#20274,.T.);
#14251=FACE_OUTER_BOUND('',#20275,.T.);
#14252=FACE_OUTER_BOUND('',#20276,.T.);
#14253=FACE_OUTER_BOUND('',#20277,.T.);
#14254=FACE_OUTER_BOUND('',#20278,.T.);
#14255=FACE_OUTER_BOUND('',#20279,.T.);
#14256=FACE_OUTER_BOUND('',#20282,.T.);
#14257=FACE_OUTER_BOUND('',#20286,.T.);
#14258=FACE_OUTER_BOUND('',#20290,.T.);
#14259=FACE_OUTER_BOUND('',#20294,.T.);
#14260=FACE_OUTER_BOUND('',#20297,.T.);
#14261=FACE_OUTER_BOUND('',#20301,.T.);
#14262=FACE_OUTER_BOUND('',#20302,.T.);
#14263=FACE_OUTER_BOUND('',#20303,.T.);
#14264=FACE_OUTER_BOUND('',#20304,.T.);
#14265=FACE_OUTER_BOUND('',#20305,.T.);
#14266=FACE_OUTER_BOUND('',#20306,.T.);
#14267=FACE_OUTER_BOUND('',#20307,.T.);
#14268=FACE_OUTER_BOUND('',#20308,.T.);
#14269=FACE_OUTER_BOUND('',#20309,.T.);
#14270=FACE_OUTER_BOUND('',#20310,.T.);
#14271=FACE_OUTER_BOUND('',#20311,.T.);
#14272=FACE_OUTER_BOUND('',#20312,.T.);
#14273=FACE_OUTER_BOUND('',#20313,.T.);
#14274=FACE_OUTER_BOUND('',#20314,.T.);
#14275=FACE_OUTER_BOUND('',#20315,.T.);
#14276=FACE_OUTER_BOUND('',#20316,.T.);
#14277=FACE_OUTER_BOUND('',#20317,.T.);
#14278=FACE_OUTER_BOUND('',#20318,.T.);
#14279=FACE_OUTER_BOUND('',#20321,.T.);
#14280=FACE_OUTER_BOUND('',#20322,.T.);
#14281=FACE_OUTER_BOUND('',#20323,.T.);
#14282=FACE_OUTER_BOUND('',#20326,.T.);
#14283=FACE_OUTER_BOUND('',#20327,.T.);
#14284=FACE_OUTER_BOUND('',#20328,.T.);
#14285=FACE_OUTER_BOUND('',#20329,.T.);
#14286=FACE_OUTER_BOUND('',#20330,.T.);
#14287=FACE_OUTER_BOUND('',#20331,.T.);
#14288=FACE_OUTER_BOUND('',#20332,.T.);
#14289=FACE_OUTER_BOUND('',#20333,.T.);
#14290=FACE_OUTER_BOUND('',#20334,.T.);
#14291=FACE_OUTER_BOUND('',#20335,.T.);
#14292=FACE_OUTER_BOUND('',#20336,.T.);
#14293=FACE_OUTER_BOUND('',#20337,.T.);
#14294=FACE_OUTER_BOUND('',#20338,.T.);
#14295=FACE_OUTER_BOUND('',#20339,.T.);
#14296=FACE_OUTER_BOUND('',#20340,.T.);
#14297=FACE_OUTER_BOUND('',#20341,.T.);
#14298=FACE_OUTER_BOUND('',#20342,.T.);
#14299=FACE_OUTER_BOUND('',#20343,.T.);
#14300=FACE_OUTER_BOUND('',#20344,.T.);
#14301=FACE_OUTER_BOUND('',#20345,.T.);
#14302=FACE_OUTER_BOUND('',#20346,.T.);
#14303=FACE_OUTER_BOUND('',#20347,.T.);
#14304=FACE_OUTER_BOUND('',#20348,.T.);
#14305=FACE_OUTER_BOUND('',#20349,.T.);
#14306=FACE_OUTER_BOUND('',#20350,.T.);
#14307=FACE_OUTER_BOUND('',#20351,.T.);
#14308=FACE_OUTER_BOUND('',#20352,.T.);
#14309=FACE_OUTER_BOUND('',#20353,.T.);
#14310=FACE_OUTER_BOUND('',#20354,.T.);
#14311=FACE_OUTER_BOUND('',#20355,.T.);
#14312=FACE_OUTER_BOUND('',#20356,.T.);
#14313=FACE_OUTER_BOUND('',#20357,.T.);
#14314=FACE_OUTER_BOUND('',#20358,.T.);
#14315=FACE_OUTER_BOUND('',#20359,.T.);
#14316=FACE_OUTER_BOUND('',#20360,.T.);
#14317=FACE_OUTER_BOUND('',#20361,.T.);
#14318=FACE_OUTER_BOUND('',#20362,.T.);
#14319=FACE_OUTER_BOUND('',#20363,.T.);
#14320=FACE_OUTER_BOUND('',#20364,.T.);
#14321=FACE_OUTER_BOUND('',#20365,.T.);
#14322=FACE_OUTER_BOUND('',#20366,.T.);
#14323=FACE_OUTER_BOUND('',#20367,.T.);
#14324=FACE_OUTER_BOUND('',#20368,.T.);
#14325=FACE_OUTER_BOUND('',#20369,.T.);
#14326=FACE_OUTER_BOUND('',#20370,.T.);
#14327=FACE_OUTER_BOUND('',#20371,.T.);
#14328=FACE_OUTER_BOUND('',#20372,.T.);
#14329=FACE_OUTER_BOUND('',#20373,.T.);
#14330=FACE_OUTER_BOUND('',#20374,.T.);
#14331=FACE_OUTER_BOUND('',#20375,.T.);
#14332=FACE_OUTER_BOUND('',#20376,.T.);
#14333=FACE_OUTER_BOUND('',#20377,.T.);
#14334=FACE_OUTER_BOUND('',#20378,.T.);
#14335=FACE_OUTER_BOUND('',#20379,.T.);
#14336=FACE_OUTER_BOUND('',#20380,.T.);
#14337=FACE_OUTER_BOUND('',#20381,.T.);
#14338=FACE_OUTER_BOUND('',#20382,.T.);
#14339=FACE_OUTER_BOUND('',#20383,.T.);
#14340=FACE_OUTER_BOUND('',#20384,.T.);
#14341=FACE_OUTER_BOUND('',#20385,.T.);
#14342=FACE_OUTER_BOUND('',#20386,.T.);
#14343=FACE_OUTER_BOUND('',#20387,.T.);
#14344=FACE_OUTER_BOUND('',#20388,.T.);
#14345=FACE_OUTER_BOUND('',#20389,.T.);
#14346=FACE_OUTER_BOUND('',#20390,.T.);
#14347=FACE_OUTER_BOUND('',#20393,.T.);
#14348=FACE_OUTER_BOUND('',#20396,.T.);
#14349=FACE_OUTER_BOUND('',#20397,.T.);
#14350=FACE_OUTER_BOUND('',#20398,.T.);
#14351=FACE_OUTER_BOUND('',#20399,.T.);
#14352=FACE_OUTER_BOUND('',#20400,.T.);
#14353=FACE_OUTER_BOUND('',#20401,.T.);
#14354=FACE_OUTER_BOUND('',#20402,.T.);
#14355=FACE_OUTER_BOUND('',#20403,.T.);
#14356=FACE_OUTER_BOUND('',#20404,.T.);
#14357=FACE_OUTER_BOUND('',#20405,.T.);
#14358=FACE_OUTER_BOUND('',#20406,.T.);
#14359=FACE_OUTER_BOUND('',#20407,.T.);
#14360=FACE_OUTER_BOUND('',#20408,.T.);
#14361=FACE_OUTER_BOUND('',#20409,.T.);
#14362=FACE_OUTER_BOUND('',#20410,.T.);
#14363=FACE_OUTER_BOUND('',#20411,.T.);
#14364=FACE_OUTER_BOUND('',#20412,.T.);
#14365=FACE_OUTER_BOUND('',#20413,.T.);
#14366=FACE_OUTER_BOUND('',#20414,.T.);
#14367=FACE_OUTER_BOUND('',#20415,.T.);
#14368=FACE_OUTER_BOUND('',#20416,.T.);
#14369=FACE_OUTER_BOUND('',#20417,.T.);
#14370=FACE_OUTER_BOUND('',#20421,.T.);
#14371=FACE_OUTER_BOUND('',#20422,.T.);
#14372=FACE_OUTER_BOUND('',#20423,.T.);
#14373=FACE_OUTER_BOUND('',#20424,.T.);
#14374=FACE_OUTER_BOUND('',#20425,.T.);
#14375=FACE_OUTER_BOUND('',#20426,.T.);
#14376=FACE_OUTER_BOUND('',#20427,.T.);
#14377=FACE_OUTER_BOUND('',#20428,.T.);
#14378=FACE_OUTER_BOUND('',#20429,.T.);
#14379=FACE_OUTER_BOUND('',#20430,.T.);
#14380=FACE_OUTER_BOUND('',#20431,.T.);
#14381=FACE_OUTER_BOUND('',#20432,.T.);
#14382=FACE_OUTER_BOUND('',#20433,.T.);
#14383=FACE_OUTER_BOUND('',#20435,.T.);
#14384=FACE_OUTER_BOUND('',#20436,.T.);
#14385=FACE_OUTER_BOUND('',#20437,.T.);
#14386=FACE_OUTER_BOUND('',#20438,.T.);
#14387=FACE_OUTER_BOUND('',#20439,.T.);
#14388=FACE_OUTER_BOUND('',#20440,.T.);
#14389=FACE_OUTER_BOUND('',#20441,.T.);
#14390=FACE_OUTER_BOUND('',#20442,.T.);
#14391=FACE_OUTER_BOUND('',#20443,.T.);
#14392=FACE_OUTER_BOUND('',#20444,.T.);
#14393=FACE_OUTER_BOUND('',#20445,.T.);
#14394=FACE_OUTER_BOUND('',#20446,.T.);
#14395=FACE_OUTER_BOUND('',#20447,.T.);
#14396=FACE_OUTER_BOUND('',#20448,.T.);
#14397=FACE_OUTER_BOUND('',#20449,.T.);
#14398=FACE_OUTER_BOUND('',#20450,.T.);
#14399=FACE_OUTER_BOUND('',#20451,.T.);
#14400=FACE_OUTER_BOUND('',#20452,.T.);
#14401=FACE_OUTER_BOUND('',#20453,.T.);
#14402=FACE_OUTER_BOUND('',#20454,.T.);
#14403=FACE_OUTER_BOUND('',#20455,.T.);
#14404=FACE_OUTER_BOUND('',#20456,.T.);
#14405=FACE_OUTER_BOUND('',#20457,.T.);
#14406=FACE_OUTER_BOUND('',#20458,.T.);
#14407=FACE_OUTER_BOUND('',#20459,.T.);
#14408=FACE_OUTER_BOUND('',#20460,.T.);
#14409=FACE_OUTER_BOUND('',#20461,.T.);
#14410=FACE_OUTER_BOUND('',#20462,.T.);
#14411=FACE_OUTER_BOUND('',#20463,.T.);
#14412=FACE_OUTER_BOUND('',#20464,.T.);
#14413=FACE_OUTER_BOUND('',#20465,.T.);
#14414=FACE_OUTER_BOUND('',#20466,.T.);
#14415=FACE_OUTER_BOUND('',#20467,.T.);
#14416=FACE_OUTER_BOUND('',#20468,.T.);
#14417=FACE_OUTER_BOUND('',#20469,.T.);
#14418=FACE_OUTER_BOUND('',#20470,.T.);
#14419=FACE_OUTER_BOUND('',#20471,.T.);
#14420=FACE_OUTER_BOUND('',#20472,.T.);
#14421=FACE_OUTER_BOUND('',#20473,.T.);
#14422=FACE_OUTER_BOUND('',#20474,.T.);
#14423=FACE_OUTER_BOUND('',#20475,.T.);
#14424=FACE_OUTER_BOUND('',#20477,.T.);
#14425=FACE_OUTER_BOUND('',#20479,.T.);
#14426=FACE_OUTER_BOUND('',#20480,.T.);
#14427=EDGE_LOOP('',(#57657,#57658,#57659,#57660));
#14428=EDGE_LOOP('',(#57661,#57662,#57663,#57664));
#14429=EDGE_LOOP('',(#57665,#57666,#57667,#57668));
#14430=EDGE_LOOP('',(#57669,#57670,#57671,#57672));
#14431=EDGE_LOOP('',(#57673,#57674,#57675,#57676));
#14432=EDGE_LOOP('',(#57677,#57678,#57679,#57680));
#14433=EDGE_LOOP('',(#57681,#57682,#57683,#57684));
#14434=EDGE_LOOP('',(#57685,#57686,#57687,#57688));
#14435=EDGE_LOOP('',(#57689,#57690,#57691,#57692));
#14436=EDGE_LOOP('',(#57693,#57694,#57695,#57696));
#14437=EDGE_LOOP('',(#57697,#57698,#57699,#57700));
#14438=EDGE_LOOP('',(#57701,#57702,#57703,#57704));
#14439=EDGE_LOOP('',(#57705,#57706,#57707,#57708));
#14440=EDGE_LOOP('',(#57709,#57710,#57711,#57712));
#14441=EDGE_LOOP('',(#57713,#57714,#57715,#57716));
#14442=EDGE_LOOP('',(#57717));
#14443=EDGE_LOOP('',(#57718));
#14444=EDGE_LOOP('',(#57719));
#14445=EDGE_LOOP('',(#57720));
#14446=EDGE_LOOP('',(#57721));
#14447=EDGE_LOOP('',(#57722));
#14448=EDGE_LOOP('',(#57723));
#14449=EDGE_LOOP('',(#57724));
#14450=EDGE_LOOP('',(#57725));
#14451=EDGE_LOOP('',(#57726));
#14452=EDGE_LOOP('',(#57727));
#14453=EDGE_LOOP('',(#57728));
#14454=EDGE_LOOP('',(#57729,#57730,#57731,#57732));
#14455=EDGE_LOOP('',(#57733,#57734,#57735,#57736));
#14456=EDGE_LOOP('',(#57737,#57738,#57739,#57740));
#14457=EDGE_LOOP('',(#57741,#57742,#57743,#57744));
#14458=EDGE_LOOP('',(#57745));
#14459=EDGE_LOOP('',(#57746));
#14460=EDGE_LOOP('',(#57747));
#14461=EDGE_LOOP('',(#57748));
#14462=EDGE_LOOP('',(#57749));
#14463=EDGE_LOOP('',(#57750));
#14464=EDGE_LOOP('',(#57751));
#14465=EDGE_LOOP('',(#57752));
#14466=EDGE_LOOP('',(#57753));
#14467=EDGE_LOOP('',(#57754));
#14468=EDGE_LOOP('',(#57755));
#14469=EDGE_LOOP('',(#57756));
#14470=EDGE_LOOP('',(#57757,#57758,#57759,#57760));
#14471=EDGE_LOOP('',(#57761,#57762,#57763,#57764,#57765,#57766,#57767,#57768,
#57769,#57770,#57771,#57772));
#14472=EDGE_LOOP('',(#57773,#57774,#57775,#57776,#57777,#57778,#57779,#57780,
#57781,#57782,#57783,#57784));
#14473=EDGE_LOOP('',(#57785,#57786,#57787,#57788));
#14474=EDGE_LOOP('',(#57789,#57790,#57791,#57792));
#14475=EDGE_LOOP('',(#57793,#57794,#57795,#57796));
#14476=EDGE_LOOP('',(#57797,#57798,#57799,#57800));
#14477=EDGE_LOOP('',(#57801,#57802,#57803,#57804));
#14478=EDGE_LOOP('',(#57805,#57806,#57807,#57808));
#14479=EDGE_LOOP('',(#57809,#57810,#57811,#57812));
#14480=EDGE_LOOP('',(#57813,#57814,#57815,#57816));
#14481=EDGE_LOOP('',(#57817,#57818,#57819,#57820));
#14482=EDGE_LOOP('',(#57821,#57822,#57823,#57824));
#14483=EDGE_LOOP('',(#57825,#57826,#57827,#57828));
#14484=EDGE_LOOP('',(#57829,#57830,#57831,#57832));
#14485=EDGE_LOOP('',(#57833,#57834,#57835,#57836));
#14486=EDGE_LOOP('',(#57837,#57838,#57839,#57840));
#14487=EDGE_LOOP('',(#57841,#57842,#57843,#57844));
#14488=EDGE_LOOP('',(#57845,#57846,#57847,#57848));
#14489=EDGE_LOOP('',(#57849,#57850,#57851,#57852));
#14490=EDGE_LOOP('',(#57853,#57854,#57855,#57856));
#14491=EDGE_LOOP('',(#57857,#57858,#57859,#57860));
#14492=EDGE_LOOP('',(#57861));
#14493=EDGE_LOOP('',(#57862));
#14494=EDGE_LOOP('',(#57863));
#14495=EDGE_LOOP('',(#57864));
#14496=EDGE_LOOP('',(#57865));
#14497=EDGE_LOOP('',(#57866));
#14498=EDGE_LOOP('',(#57867));
#14499=EDGE_LOOP('',(#57868));
#14500=EDGE_LOOP('',(#57869));
#14501=EDGE_LOOP('',(#57870));
#14502=EDGE_LOOP('',(#57871));
#14503=EDGE_LOOP('',(#57872));
#14504=EDGE_LOOP('',(#57873,#57874,#57875,#57876));
#14505=EDGE_LOOP('',(#57877,#57878,#57879,#57880));
#14506=EDGE_LOOP('',(#57881,#57882,#57883,#57884));
#14507=EDGE_LOOP('',(#57885,#57886,#57887,#57888));
#14508=EDGE_LOOP('',(#57889));
#14509=EDGE_LOOP('',(#57890));
#14510=EDGE_LOOP('',(#57891));
#14511=EDGE_LOOP('',(#57892));
#14512=EDGE_LOOP('',(#57893));
#14513=EDGE_LOOP('',(#57894));
#14514=EDGE_LOOP('',(#57895));
#14515=EDGE_LOOP('',(#57896));
#14516=EDGE_LOOP('',(#57897));
#14517=EDGE_LOOP('',(#57898));
#14518=EDGE_LOOP('',(#57899));
#14519=EDGE_LOOP('',(#57900));
#14520=EDGE_LOOP('',(#57901,#57902,#57903,#57904));
#14521=EDGE_LOOP('',(#57905,#57906,#57907,#57908,#57909,#57910,#57911,#57912,
#57913,#57914,#57915,#57916));
#14522=EDGE_LOOP('',(#57917,#57918,#57919,#57920,#57921,#57922,#57923,#57924,
#57925,#57926,#57927,#57928));
#14523=EDGE_LOOP('',(#57929,#57930,#57931,#57932));
#14524=EDGE_LOOP('',(#57933,#57934,#57935,#57936));
#14525=EDGE_LOOP('',(#57937,#57938,#57939,#57940));
#14526=EDGE_LOOP('',(#57941,#57942,#57943,#57944));
#14527=EDGE_LOOP('',(#57945,#57946,#57947,#57948));
#14528=EDGE_LOOP('',(#57949));
#14529=EDGE_LOOP('',(#57950,#57951,#57952,#57953));
#14530=EDGE_LOOP('',(#57954));
#14531=EDGE_LOOP('',(#57955));
#14532=EDGE_LOOP('',(#57956,#57957,#57958,#57959));
#14533=EDGE_LOOP('',(#57960));
#14534=EDGE_LOOP('',(#57961,#57962,#57963,#57964));
#14535=EDGE_LOOP('',(#57965));
#14536=EDGE_LOOP('',(#57966,#57967,#57968,#57969));
#14537=EDGE_LOOP('',(#57970));
#14538=EDGE_LOOP('',(#57971));
#14539=EDGE_LOOP('',(#57972,#57973,#57974,#57975));
#14540=EDGE_LOOP('',(#57976));
#14541=EDGE_LOOP('',(#57977,#57978,#57979,#57980,#57981,#57982));
#14542=EDGE_LOOP('',(#57983,#57984,#57985,#57986,#57987));
#14543=EDGE_LOOP('',(#57988,#57989,#57990,#57991));
#14544=EDGE_LOOP('',(#57992,#57993,#57994,#57995));
#14545=EDGE_LOOP('',(#57996,#57997,#57998,#57999));
#14546=EDGE_LOOP('',(#58000,#58001,#58002,#58003,#58004,#58005,#58006,#58007,
#58008,#58009,#58010,#58011,#58012,#58013,#58014,#58015,#58016,#58017,#58018));
#14547=EDGE_LOOP('',(#58019,#58020,#58021,#58022));
#14548=EDGE_LOOP('',(#58023,#58024,#58025,#58026));
#14549=EDGE_LOOP('',(#58027,#58028,#58029,#58030));
#14550=EDGE_LOOP('',(#58031,#58032,#58033,#58034));
#14551=EDGE_LOOP('',(#58035,#58036,#58037,#58038,#58039,#58040,#58041,#58042,
#58043,#58044,#58045,#58046,#58047,#58048,#58049,#58050,#58051,#58052,#58053));
#14552=EDGE_LOOP('',(#58054,#58055,#58056,#58057));
#14553=EDGE_LOOP('',(#58058,#58059,#58060,#58061));
#14554=EDGE_LOOP('',(#58062,#58063,#58064,#58065));
#14555=EDGE_LOOP('',(#58066,#58067,#58068,#58069,#58070,#58071));
#14556=EDGE_LOOP('',(#58072,#58073,#58074,#58075,#58076));
#14557=EDGE_LOOP('',(#58077,#58078,#58079,#58080));
#14558=EDGE_LOOP('',(#58081,#58082,#58083,#58084));
#14559=EDGE_LOOP('',(#58085,#58086,#58087,#58088));
#14560=EDGE_LOOP('',(#58089,#58090,#58091,#58092));
#14561=EDGE_LOOP('',(#58093,#58094,#58095,#58096,#58097));
#14562=EDGE_LOOP('',(#58098,#58099,#58100,#58101));
#14563=EDGE_LOOP('',(#58102,#58103,#58104,#58105));
#14564=EDGE_LOOP('',(#58106,#58107,#58108,#58109));
#14565=EDGE_LOOP('',(#58110,#58111,#58112,#58113));
#14566=EDGE_LOOP('',(#58114,#58115,#58116,#58117));
#14567=EDGE_LOOP('',(#58118,#58119,#58120,#58121));
#14568=EDGE_LOOP('',(#58122,#58123,#58124,#58125));
#14569=EDGE_LOOP('',(#58126,#58127,#58128,#58129));
#14570=EDGE_LOOP('',(#58130,#58131,#58132,#58133));
#14571=EDGE_LOOP('',(#58134,#58135,#58136,#58137));
#14572=EDGE_LOOP('',(#58138,#58139,#58140,#58141));
#14573=EDGE_LOOP('',(#58142,#58143,#58144,#58145));
#14574=EDGE_LOOP('',(#58146,#58147,#58148,#58149));
#14575=EDGE_LOOP('',(#58150,#58151,#58152,#58153));
#14576=EDGE_LOOP('',(#58154,#58155,#58156,#58157));
#14577=EDGE_LOOP('',(#58158,#58159,#58160,#58161));
#14578=EDGE_LOOP('',(#58162,#58163,#58164,#58165));
#14579=EDGE_LOOP('',(#58166,#58167,#58168,#58169));
#14580=EDGE_LOOP('',(#58170,#58171,#58172,#58173));
#14581=EDGE_LOOP('',(#58174,#58175,#58176,#58177));
#14582=EDGE_LOOP('',(#58178,#58179,#58180,#58181));
#14583=EDGE_LOOP('',(#58182,#58183,#58184,#58185));
#14584=EDGE_LOOP('',(#58186,#58187,#58188,#58189));
#14585=EDGE_LOOP('',(#58190,#58191,#58192,#58193));
#14586=EDGE_LOOP('',(#58194,#58195,#58196,#58197));
#14587=EDGE_LOOP('',(#58198,#58199,#58200,#58201));
#14588=EDGE_LOOP('',(#58202,#58203,#58204,#58205));
#14589=EDGE_LOOP('',(#58206,#58207,#58208,#58209));
#14590=EDGE_LOOP('',(#58210,#58211,#58212,#58213));
#14591=EDGE_LOOP('',(#58214,#58215,#58216,#58217));
#14592=EDGE_LOOP('',(#58218,#58219,#58220,#58221,#58222,#58223));
#14593=EDGE_LOOP('',(#58224,#58225,#58226,#58227,#58228,#58229,#58230,#58231,
#58232,#58233,#58234,#58235,#58236,#58237,#58238,#58239,#58240,#58241,#58242,
#58243,#58244,#58245,#58246,#58247,#58248,#58249,#58250,#58251,#58252,#58253,
#58254,#58255,#58256,#58257,#58258,#58259,#58260,#58261));
#14594=EDGE_LOOP('',(#58262,#58263,#58264,#58265));
#14595=EDGE_LOOP('',(#58266,#58267,#58268,#58269));
#14596=EDGE_LOOP('',(#58270,#58271,#58272,#58273));
#14597=EDGE_LOOP('',(#58274,#58275,#58276,#58277));
#14598=EDGE_LOOP('',(#58278,#58279,#58280,#58281,#58282,#58283,#58284,#58285,
#58286,#58287,#58288,#58289,#58290,#58291,#58292,#58293,#58294,#58295,#58296));
#14599=EDGE_LOOP('',(#58297,#58298,#58299,#58300));
#14600=EDGE_LOOP('',(#58301,#58302,#58303,#58304));
#14601=EDGE_LOOP('',(#58305,#58306,#58307,#58308));
#14602=EDGE_LOOP('',(#58309,#58310,#58311,#58312));
#14603=EDGE_LOOP('',(#58313,#58314,#58315,#58316,#58317,#58318,#58319,#58320,
#58321,#58322,#58323,#58324,#58325,#58326,#58327,#58328));
#14604=EDGE_LOOP('',(#58329,#58330,#58331,#58332));
#14605=EDGE_LOOP('',(#58333,#58334,#58335,#58336));
#14606=EDGE_LOOP('',(#58337,#58338,#58339,#58340));
#14607=EDGE_LOOP('',(#58341,#58342,#58343,#58344));
#14608=EDGE_LOOP('',(#58345,#58346,#58347,#58348));
#14609=EDGE_LOOP('',(#58349,#58350,#58351,#58352));
#14610=EDGE_LOOP('',(#58353,#58354,#58355,#58356));
#14611=EDGE_LOOP('',(#58357,#58358,#58359,#58360));
#14612=EDGE_LOOP('',(#58361,#58362,#58363,#58364));
#14613=EDGE_LOOP('',(#58365,#58366,#58367,#58368));
#14614=EDGE_LOOP('',(#58369,#58370,#58371,#58372));
#14615=EDGE_LOOP('',(#58373,#58374,#58375,#58376));
#14616=EDGE_LOOP('',(#58377,#58378,#58379,#58380));
#14617=EDGE_LOOP('',(#58381,#58382,#58383,#58384));
#14618=EDGE_LOOP('',(#58385,#58386,#58387,#58388));
#14619=EDGE_LOOP('',(#58389,#58390,#58391,#58392));
#14620=EDGE_LOOP('',(#58393,#58394,#58395,#58396));
#14621=EDGE_LOOP('',(#58397,#58398,#58399,#58400));
#14622=EDGE_LOOP('',(#58401,#58402,#58403,#58404));
#14623=EDGE_LOOP('',(#58405,#58406,#58407,#58408));
#14624=EDGE_LOOP('',(#58409,#58410,#58411,#58412));
#14625=EDGE_LOOP('',(#58413,#58414,#58415,#58416));
#14626=EDGE_LOOP('',(#58417,#58418,#58419,#58420));
#14627=EDGE_LOOP('',(#58421,#58422,#58423,#58424));
#14628=EDGE_LOOP('',(#58425,#58426,#58427,#58428));
#14629=EDGE_LOOP('',(#58429,#58430,#58431,#58432));
#14630=EDGE_LOOP('',(#58433,#58434,#58435,#58436));
#14631=EDGE_LOOP('',(#58437,#58438,#58439,#58440));
#14632=EDGE_LOOP('',(#58441,#58442,#58443,#58444));
#14633=EDGE_LOOP('',(#58445,#58446,#58447,#58448));
#14634=EDGE_LOOP('',(#58449,#58450,#58451,#58452));
#14635=EDGE_LOOP('',(#58453,#58454,#58455,#58456));
#14636=EDGE_LOOP('',(#58457,#58458,#58459,#58460));
#14637=EDGE_LOOP('',(#58461,#58462,#58463,#58464));
#14638=EDGE_LOOP('',(#58465,#58466,#58467,#58468));
#14639=EDGE_LOOP('',(#58469,#58470,#58471,#58472));
#14640=EDGE_LOOP('',(#58473,#58474,#58475,#58476));
#14641=EDGE_LOOP('',(#58477,#58478,#58479,#58480));
#14642=EDGE_LOOP('',(#58481,#58482,#58483,#58484));
#14643=EDGE_LOOP('',(#58485,#58486,#58487,#58488));
#14644=EDGE_LOOP('',(#58489,#58490,#58491,#58492));
#14645=EDGE_LOOP('',(#58493,#58494,#58495,#58496));
#14646=EDGE_LOOP('',(#58497,#58498,#58499,#58500));
#14647=EDGE_LOOP('',(#58501,#58502,#58503,#58504));
#14648=EDGE_LOOP('',(#58505,#58506,#58507,#58508));
#14649=EDGE_LOOP('',(#58509,#58510,#58511,#58512));
#14650=EDGE_LOOP('',(#58513,#58514,#58515,#58516));
#14651=EDGE_LOOP('',(#58517,#58518,#58519,#58520));
#14652=EDGE_LOOP('',(#58521,#58522,#58523,#58524));
#14653=EDGE_LOOP('',(#58525,#58526,#58527,#58528));
#14654=EDGE_LOOP('',(#58529,#58530,#58531,#58532));
#14655=EDGE_LOOP('',(#58533,#58534,#58535,#58536));
#14656=EDGE_LOOP('',(#58537,#58538,#58539,#58540));
#14657=EDGE_LOOP('',(#58541,#58542,#58543,#58544));
#14658=EDGE_LOOP('',(#58545,#58546,#58547,#58548));
#14659=EDGE_LOOP('',(#58549,#58550,#58551,#58552));
#14660=EDGE_LOOP('',(#58553,#58554,#58555,#58556));
#14661=EDGE_LOOP('',(#58557,#58558,#58559,#58560));
#14662=EDGE_LOOP('',(#58561,#58562,#58563,#58564));
#14663=EDGE_LOOP('',(#58565,#58566,#58567,#58568));
#14664=EDGE_LOOP('',(#58569,#58570,#58571,#58572));
#14665=EDGE_LOOP('',(#58573,#58574,#58575,#58576));
#14666=EDGE_LOOP('',(#58577,#58578,#58579,#58580));
#14667=EDGE_LOOP('',(#58581,#58582,#58583,#58584));
#14668=EDGE_LOOP('',(#58585,#58586,#58587,#58588));
#14669=EDGE_LOOP('',(#58589,#58590,#58591,#58592));
#14670=EDGE_LOOP('',(#58593,#58594,#58595,#58596));
#14671=EDGE_LOOP('',(#58597,#58598,#58599,#58600));
#14672=EDGE_LOOP('',(#58601,#58602,#58603,#58604));
#14673=EDGE_LOOP('',(#58605,#58606,#58607,#58608));
#14674=EDGE_LOOP('',(#58609,#58610,#58611,#58612));
#14675=EDGE_LOOP('',(#58613,#58614,#58615,#58616));
#14676=EDGE_LOOP('',(#58617,#58618,#58619,#58620));
#14677=EDGE_LOOP('',(#58621,#58622,#58623,#58624));
#14678=EDGE_LOOP('',(#58625,#58626,#58627,#58628));
#14679=EDGE_LOOP('',(#58629,#58630,#58631,#58632));
#14680=EDGE_LOOP('',(#58633,#58634,#58635,#58636,#58637));
#14681=EDGE_LOOP('',(#58638,#58639,#58640,#58641));
#14682=EDGE_LOOP('',(#58642,#58643,#58644,#58645));
#14683=EDGE_LOOP('',(#58646,#58647,#58648,#58649));
#14684=EDGE_LOOP('',(#58650,#58651,#58652,#58653));
#14685=EDGE_LOOP('',(#58654,#58655,#58656,#58657));
#14686=EDGE_LOOP('',(#58658,#58659,#58660,#58661));
#14687=EDGE_LOOP('',(#58662,#58663,#58664,#58665));
#14688=EDGE_LOOP('',(#58666,#58667,#58668,#58669));
#14689=EDGE_LOOP('',(#58670,#58671,#58672,#58673));
#14690=EDGE_LOOP('',(#58674,#58675,#58676,#58677));
#14691=EDGE_LOOP('',(#58678,#58679,#58680,#58681));
#14692=EDGE_LOOP('',(#58682,#58683,#58684,#58685));
#14693=EDGE_LOOP('',(#58686,#58687,#58688,#58689));
#14694=EDGE_LOOP('',(#58690,#58691,#58692,#58693));
#14695=EDGE_LOOP('',(#58694,#58695,#58696,#58697));
#14696=EDGE_LOOP('',(#58698,#58699,#58700,#58701));
#14697=EDGE_LOOP('',(#58702,#58703,#58704,#58705));
#14698=EDGE_LOOP('',(#58706,#58707,#58708,#58709));
#14699=EDGE_LOOP('',(#58710,#58711,#58712,#58713));
#14700=EDGE_LOOP('',(#58714,#58715,#58716,#58717,#58718));
#14701=EDGE_LOOP('',(#58719,#58720,#58721,#58722,#58723,#58724));
#14702=EDGE_LOOP('',(#58725,#58726,#58727,#58728));
#14703=EDGE_LOOP('',(#58729,#58730,#58731,#58732,#58733,#58734,#58735,#58736,
#58737,#58738,#58739,#58740));
#14704=EDGE_LOOP('',(#58741,#58742,#58743,#58744,#58745,#58746,#58747,#58748,
#58749));
#14705=EDGE_LOOP('',(#58750,#58751,#58752,#58753,#58754));
#14706=EDGE_LOOP('',(#58755,#58756,#58757,#58758,#58759));
#14707=EDGE_LOOP('',(#58760,#58761,#58762,#58763));
#14708=EDGE_LOOP('',(#58764,#58765,#58766,#58767));
#14709=EDGE_LOOP('',(#58768,#58769,#58770,#58771,#58772));
#14710=EDGE_LOOP('',(#58773,#58774,#58775,#58776));
#14711=EDGE_LOOP('',(#58777,#58778,#58779,#58780));
#14712=EDGE_LOOP('',(#58781,#58782,#58783,#58784,#58785,#58786,#58787,#58788,
#58789));
#14713=EDGE_LOOP('',(#58790,#58791,#58792,#58793));
#14714=EDGE_LOOP('',(#58794,#58795,#58796,#58797));
#14715=EDGE_LOOP('',(#58798,#58799,#58800,#58801));
#14716=EDGE_LOOP('',(#58802,#58803,#58804,#58805));
#14717=EDGE_LOOP('',(#58806,#58807,#58808,#58809));
#14718=EDGE_LOOP('',(#58810,#58811,#58812,#58813,#58814,#58815));
#14719=EDGE_LOOP('',(#58816,#58817,#58818,#58819));
#14720=EDGE_LOOP('',(#58820,#58821,#58822,#58823));
#14721=EDGE_LOOP('',(#58824,#58825,#58826,#58827));
#14722=EDGE_LOOP('',(#58828,#58829,#58830,#58831));
#14723=EDGE_LOOP('',(#58832,#58833,#58834,#58835));
#14724=EDGE_LOOP('',(#58836,#58837,#58838));
#14725=EDGE_LOOP('',(#58839,#58840,#58841,#58842,#58843));
#14726=EDGE_LOOP('',(#58844,#58845,#58846,#58847));
#14727=EDGE_LOOP('',(#58848,#58849,#58850,#58851));
#14728=EDGE_LOOP('',(#58852,#58853,#58854,#58855));
#14729=EDGE_LOOP('',(#58856,#58857,#58858,#58859));
#14730=EDGE_LOOP('',(#58860,#58861,#58862,#58863));
#14731=EDGE_LOOP('',(#58864,#58865,#58866,#58867));
#14732=EDGE_LOOP('',(#58868,#58869,#58870,#58871));
#14733=EDGE_LOOP('',(#58872,#58873,#58874,#58875));
#14734=EDGE_LOOP('',(#58876,#58877,#58878,#58879));
#14735=EDGE_LOOP('',(#58880,#58881,#58882,#58883));
#14736=EDGE_LOOP('',(#58884,#58885,#58886,#58887));
#14737=EDGE_LOOP('',(#58888,#58889,#58890,#58891));
#14738=EDGE_LOOP('',(#58892,#58893,#58894,#58895));
#14739=EDGE_LOOP('',(#58896,#58897,#58898,#58899));
#14740=EDGE_LOOP('',(#58900,#58901,#58902,#58903,#58904,#58905,#58906,#58907,
#58908));
#14741=EDGE_LOOP('',(#58909,#58910,#58911,#58912));
#14742=EDGE_LOOP('',(#58913,#58914,#58915,#58916));
#14743=EDGE_LOOP('',(#58917,#58918,#58919,#58920));
#14744=EDGE_LOOP('',(#58921,#58922,#58923,#58924));
#14745=EDGE_LOOP('',(#58925,#58926,#58927,#58928));
#14746=EDGE_LOOP('',(#58929,#58930,#58931,#58932));
#14747=EDGE_LOOP('',(#58933,#58934,#58935,#58936));
#14748=EDGE_LOOP('',(#58937,#58938,#58939,#58940));
#14749=EDGE_LOOP('',(#58941,#58942,#58943,#58944));
#14750=EDGE_LOOP('',(#58945,#58946,#58947,#58948));
#14751=EDGE_LOOP('',(#58949,#58950,#58951,#58952));
#14752=EDGE_LOOP('',(#58953,#58954,#58955,#58956));
#14753=EDGE_LOOP('',(#58957,#58958,#58959,#58960));
#14754=EDGE_LOOP('',(#58961,#58962,#58963,#58964));
#14755=EDGE_LOOP('',(#58965,#58966,#58967,#58968));
#14756=EDGE_LOOP('',(#58969,#58970,#58971,#58972));
#14757=EDGE_LOOP('',(#58973,#58974,#58975,#58976));
#14758=EDGE_LOOP('',(#58977,#58978,#58979,#58980));
#14759=EDGE_LOOP('',(#58981,#58982,#58983,#58984));
#14760=EDGE_LOOP('',(#58985,#58986,#58987,#58988,#58989,#58990,#58991,#58992));
#14761=EDGE_LOOP('',(#58993,#58994,#58995,#58996,#58997,#58998,#58999,#59000));
#14762=EDGE_LOOP('',(#59001,#59002,#59003,#59004));
#14763=EDGE_LOOP('',(#59005,#59006,#59007,#59008));
#14764=EDGE_LOOP('',(#59009,#59010,#59011,#59012));
#14765=EDGE_LOOP('',(#59013,#59014,#59015,#59016));
#14766=EDGE_LOOP('',(#59017,#59018,#59019,#59020));
#14767=EDGE_LOOP('',(#59021,#59022,#59023,#59024));
#14768=EDGE_LOOP('',(#59025,#59026,#59027,#59028));
#14769=EDGE_LOOP('',(#59029,#59030,#59031,#59032));
#14770=EDGE_LOOP('',(#59033,#59034,#59035,#59036));
#14771=EDGE_LOOP('',(#59037,#59038,#59039,#59040));
#14772=EDGE_LOOP('',(#59041,#59042,#59043,#59044));
#14773=EDGE_LOOP('',(#59045,#59046,#59047,#59048));
#14774=EDGE_LOOP('',(#59049,#59050,#59051,#59052));
#14775=EDGE_LOOP('',(#59053,#59054,#59055,#59056));
#14776=EDGE_LOOP('',(#59057,#59058,#59059,#59060));
#14777=EDGE_LOOP('',(#59061,#59062,#59063,#59064));
#14778=EDGE_LOOP('',(#59065,#59066,#59067,#59068));
#14779=EDGE_LOOP('',(#59069,#59070,#59071,#59072,#59073,#59074));
#14780=EDGE_LOOP('',(#59075,#59076,#59077,#59078));
#14781=EDGE_LOOP('',(#59079,#59080,#59081,#59082));
#14782=EDGE_LOOP('',(#59083,#59084,#59085,#59086));
#14783=EDGE_LOOP('',(#59087,#59088,#59089,#59090));
#14784=EDGE_LOOP('',(#59091,#59092,#59093,#59094));
#14785=EDGE_LOOP('',(#59095,#59096,#59097,#59098));
#14786=EDGE_LOOP('',(#59099,#59100,#59101,#59102,#59103,#59104,#59105,#59106,
#59107,#59108,#59109,#59110));
#14787=EDGE_LOOP('',(#59111,#59112,#59113,#59114));
#14788=EDGE_LOOP('',(#59115,#59116,#59117,#59118,#59119));
#14789=EDGE_LOOP('',(#59120,#59121,#59122,#59123,#59124,#59125,#59126,#59127,
#59128,#59129,#59130,#59131));
#14790=EDGE_LOOP('',(#59132,#59133,#59134,#59135));
#14791=EDGE_LOOP('',(#59136,#59137,#59138,#59139));
#14792=EDGE_LOOP('',(#59140,#59141,#59142,#59143));
#14793=EDGE_LOOP('',(#59144,#59145,#59146,#59147));
#14794=EDGE_LOOP('',(#59148,#59149,#59150,#59151,#59152,#59153,#59154,#59155,
#59156,#59157,#59158,#59159));
#14795=EDGE_LOOP('',(#59160,#59161,#59162,#59163));
#14796=EDGE_LOOP('',(#59164,#59165,#59166,#59167,#59168));
#14797=EDGE_LOOP('',(#59169,#59170,#59171,#59172,#59173,#59174,#59175,#59176,
#59177,#59178,#59179,#59180,#59181,#59182));
#14798=EDGE_LOOP('',(#59183,#59184,#59185,#59186));
#14799=EDGE_LOOP('',(#59187,#59188,#59189,#59190));
#14800=EDGE_LOOP('',(#59191,#59192,#59193,#59194));
#14801=EDGE_LOOP('',(#59195,#59196,#59197,#59198));
#14802=EDGE_LOOP('',(#59199,#59200,#59201,#59202,#59203,#59204,#59205,#59206,
#59207,#59208,#59209,#59210,#59211,#59212));
#14803=EDGE_LOOP('',(#59213,#59214,#59215,#59216));
#14804=EDGE_LOOP('',(#59217,#59218,#59219,#59220));
#14805=EDGE_LOOP('',(#59221,#59222,#59223,#59224,#59225,#59226,#59227,#59228,
#59229,#59230,#59231,#59232,#59233,#59234));
#14806=EDGE_LOOP('',(#59235,#59236,#59237,#59238));
#14807=EDGE_LOOP('',(#59239,#59240,#59241,#59242,#59243,#59244));
#14808=EDGE_LOOP('',(#59245,#59246,#59247,#59248));
#14809=EDGE_LOOP('',(#59249,#59250,#59251,#59252,#59253,#59254,#59255,#59256,
#59257,#59258,#59259));
#14810=EDGE_LOOP('',(#59260,#59261,#59262,#59263));
#14811=EDGE_LOOP('',(#59264,#59265,#59266,#59267));
#14812=EDGE_LOOP('',(#59268,#59269,#59270,#59271));
#14813=EDGE_LOOP('',(#59272,#59273,#59274,#59275,#59276,#59277,#59278,#59279,
#59280,#59281));
#14814=EDGE_LOOP('',(#59282,#59283,#59284,#59285));
#14815=EDGE_LOOP('',(#59286,#59287,#59288,#59289));
#14816=EDGE_LOOP('',(#59290,#59291,#59292,#59293));
#14817=EDGE_LOOP('',(#59294,#59295,#59296,#59297,#59298,#59299,#59300,#59301,
#59302));
#14818=EDGE_LOOP('',(#59303,#59304,#59305,#59306));
#14819=EDGE_LOOP('',(#59307,#59308,#59309,#59310));
#14820=EDGE_LOOP('',(#59311,#59312,#59313,#59314));
#14821=EDGE_LOOP('',(#59315,#59316,#59317,#59318));
#14822=EDGE_LOOP('',(#59319,#59320,#59321,#59322,#59323,#59324,#59325));
#14823=EDGE_LOOP('',(#59326,#59327,#59328,#59329));
#14824=EDGE_LOOP('',(#59330,#59331,#59332,#59333));
#14825=EDGE_LOOP('',(#59334,#59335,#59336,#59337,#59338,#59339,#59340));
#14826=EDGE_LOOP('',(#59341,#59342,#59343,#59344));
#14827=EDGE_LOOP('',(#59345,#59346,#59347,#59348));
#14828=EDGE_LOOP('',(#59349,#59350,#59351,#59352));
#14829=EDGE_LOOP('',(#59353,#59354,#59355,#59356,#59357,#59358,#59359));
#14830=EDGE_LOOP('',(#59360,#59361,#59362,#59363,#59364));
#14831=EDGE_LOOP('',(#59365,#59366,#59367,#59368));
#14832=EDGE_LOOP('',(#59369,#59370,#59371,#59372,#59373));
#14833=EDGE_LOOP('',(#59374,#59375,#59376,#59377,#59378));
#14834=EDGE_LOOP('',(#59379,#59380,#59381,#59382));
#14835=EDGE_LOOP('',(#59383,#59384,#59385,#59386,#59387));
#14836=EDGE_LOOP('',(#59388,#59389,#59390,#59391,#59392,#59393,#59394,#59395,
#59396,#59397,#59398,#59399,#59400,#59401));
#14837=EDGE_LOOP('',(#59402,#59403,#59404,#59405));
#14838=EDGE_LOOP('',(#59406,#59407,#59408,#59409));
#14839=EDGE_LOOP('',(#59410,#59411,#59412,#59413));
#14840=EDGE_LOOP('',(#59414,#59415,#59416,#59417,#59418,#59419,#59420,#59421,
#59422,#59423,#59424,#59425,#59426,#59427));
#14841=EDGE_LOOP('',(#59428,#59429,#59430,#59431));
#14842=EDGE_LOOP('',(#59432,#59433,#59434,#59435));
#14843=EDGE_LOOP('',(#59436,#59437,#59438,#59439));
#14844=EDGE_LOOP('',(#59440,#59441,#59442,#59443));
#14845=EDGE_LOOP('',(#59444,#59445,#59446,#59447,#59448,#59449,#59450,#59451,
#59452,#59453,#59454,#59455,#59456));
#14846=EDGE_LOOP('',(#59457,#59458,#59459,#59460));
#14847=EDGE_LOOP('',(#59461,#59462,#59463,#59464));
#14848=EDGE_LOOP('',(#59465,#59466,#59467,#59468,#59469,#59470,#59471,#59472,
#59473,#59474,#59475,#59476));
#14849=EDGE_LOOP('',(#59477,#59478,#59479,#59480));
#14850=EDGE_LOOP('',(#59481,#59482,#59483,#59484));
#14851=EDGE_LOOP('',(#59485,#59486,#59487,#59488));
#14852=EDGE_LOOP('',(#59489,#59490,#59491,#59492));
#14853=EDGE_LOOP('',(#59493,#59494,#59495,#59496,#59497,#59498,#59499,#59500,
#59501,#59502,#59503,#59504));
#14854=EDGE_LOOP('',(#59505,#59506,#59507,#59508));
#14855=EDGE_LOOP('',(#59509,#59510,#59511,#59512));
#14856=EDGE_LOOP('',(#59513,#59514,#59515,#59516,#59517,#59518,#59519,#59520,
#59521,#59522,#59523,#59524));
#14857=EDGE_LOOP('',(#59525,#59526,#59527,#59528));
#14858=EDGE_LOOP('',(#59529,#59530,#59531,#59532));
#14859=EDGE_LOOP('',(#59533,#59534,#59535,#59536));
#14860=EDGE_LOOP('',(#59537,#59538,#59539,#59540));
#14861=EDGE_LOOP('',(#59541,#59542,#59543,#59544,#59545,#59546,#59547,#59548,
#59549,#59550,#59551,#59552));
#14862=EDGE_LOOP('',(#59553,#59554,#59555,#59556));
#14863=EDGE_LOOP('',(#59557,#59558,#59559,#59560));
#14864=EDGE_LOOP('',(#59561,#59562,#59563,#59564,#59565,#59566,#59567,#59568,
#59569,#59570,#59571,#59572));
#14865=EDGE_LOOP('',(#59573,#59574,#59575,#59576));
#14866=EDGE_LOOP('',(#59577,#59578,#59579,#59580));
#14867=EDGE_LOOP('',(#59581,#59582,#59583,#59584));
#14868=EDGE_LOOP('',(#59585,#59586,#59587,#59588));
#14869=EDGE_LOOP('',(#59589,#59590,#59591,#59592,#59593,#59594,#59595,#59596,
#59597,#59598,#59599,#59600));
#14870=EDGE_LOOP('',(#59601,#59602,#59603,#59604));
#14871=EDGE_LOOP('',(#59605,#59606,#59607,#59608));
#14872=EDGE_LOOP('',(#59609,#59610,#59611,#59612,#59613,#59614,#59615,#59616,
#59617,#59618,#59619,#59620,#59621));
#14873=EDGE_LOOP('',(#59622,#59623,#59624,#59625));
#14874=EDGE_LOOP('',(#59626,#59627,#59628,#59629));
#14875=EDGE_LOOP('',(#59630,#59631,#59632,#59633));
#14876=EDGE_LOOP('',(#59634,#59635,#59636,#59637));
#14877=EDGE_LOOP('',(#59638,#59639,#59640,#59641,#59642,#59643,#59644,#59645,
#59646,#59647,#59648,#59649,#59650,#59651));
#14878=EDGE_LOOP('',(#59652,#59653,#59654,#59655));
#14879=EDGE_LOOP('',(#59656,#59657,#59658,#59659));
#14880=EDGE_LOOP('',(#59660,#59661,#59662,#59663,#59664,#59665,#59666,#59667,
#59668,#59669,#59670,#59671,#59672,#59673));
#14881=EDGE_LOOP('',(#59674,#59675,#59676,#59677,#59678));
#14882=EDGE_LOOP('',(#59679,#59680,#59681,#59682));
#14883=EDGE_LOOP('',(#59683,#59684,#59685,#59686));
#14884=EDGE_LOOP('',(#59687,#59688,#59689,#59690,#59691,#59692,#59693,#59694,
#59695,#59696,#59697,#59698,#59699,#59700,#59701,#59702,#59703));
#14885=EDGE_LOOP('',(#59704,#59705,#59706,#59707));
#14886=EDGE_LOOP('',(#59708,#59709,#59710,#59711));
#14887=EDGE_LOOP('',(#59712,#59713,#59714,#59715));
#14888=EDGE_LOOP('',(#59716,#59717,#59718,#59719,#59720,#59721,#59722,#59723,
#59724,#59725,#59726,#59727,#59728,#59729,#59730,#59731));
#14889=EDGE_LOOP('',(#59732,#59733,#59734,#59735));
#14890=EDGE_LOOP('',(#59736,#59737,#59738,#59739));
#14891=EDGE_LOOP('',(#59740,#59741,#59742,#59743,#59744,#59745,#59746,#59747,
#59748,#59749,#59750,#59751,#59752,#59753,#59754,#59755));
#14892=EDGE_LOOP('',(#59756,#59757,#59758,#59759,#59760));
#14893=EDGE_LOOP('',(#59761,#59762,#59763));
#14894=EDGE_LOOP('',(#59764,#59765,#59766,#59767));
#14895=EDGE_LOOP('',(#59768,#59769,#59770,#59771,#59772,#59773,#59774,#59775,
#59776,#59777,#59778,#59779,#59780,#59781,#59782,#59783,#59784,#59785));
#14896=EDGE_LOOP('',(#59786,#59787,#59788,#59789));
#14897=EDGE_LOOP('',(#59790,#59791,#59792,#59793));
#14898=EDGE_LOOP('',(#59794,#59795,#59796,#59797));
#14899=EDGE_LOOP('',(#59798,#59799,#59800,#59801,#59802,#59803,#59804,#59805,
#59806,#59807,#59808,#59809,#59810,#59811,#59812,#59813,#59814,#59815));
#14900=EDGE_LOOP('',(#59816,#59817,#59818,#59819));
#14901=EDGE_LOOP('',(#59820,#59821,#59822,#59823));
#14902=EDGE_LOOP('',(#59824,#59825,#59826,#59827));
#14903=EDGE_LOOP('',(#59828,#59829,#59830,#59831,#59832,#59833,#59834,#59835,
#59836,#59837,#59838,#59839));
#14904=EDGE_LOOP('',(#59840,#59841,#59842,#59843));
#14905=EDGE_LOOP('',(#59844,#59845,#59846,#59847));
#14906=EDGE_LOOP('',(#59848,#59849,#59850,#59851));
#14907=EDGE_LOOP('',(#59852,#59853,#59854,#59855,#59856,#59857,#59858,#59859,
#59860,#59861,#59862));
#14908=EDGE_LOOP('',(#59863,#59864,#59865,#59866));
#14909=EDGE_LOOP('',(#59867,#59868,#59869,#59870));
#14910=EDGE_LOOP('',(#59871,#59872,#59873,#59874,#59875,#59876,#59877,#59878));
#14911=EDGE_LOOP('',(#59879,#59880,#59881,#59882));
#14912=EDGE_LOOP('',(#59883,#59884,#59885,#59886));
#14913=EDGE_LOOP('',(#59887,#59888,#59889,#59890));
#14914=EDGE_LOOP('',(#59891,#59892,#59893,#59894,#59895,#59896,#59897,#59898,
#59899,#59900,#59901,#59902));
#14915=EDGE_LOOP('',(#59903,#59904,#59905,#59906));
#14916=EDGE_LOOP('',(#59907,#59908,#59909,#59910));
#14917=EDGE_LOOP('',(#59911,#59912,#59913,#59914));
#14918=EDGE_LOOP('',(#59915,#59916,#59917,#59918,#59919,#59920,#59921,#59922,
#59923,#59924,#59925,#59926,#59927,#59928,#59929,#59930,#59931,#59932));
#14919=EDGE_LOOP('',(#59933,#59934,#59935,#59936));
#14920=EDGE_LOOP('',(#59937,#59938,#59939,#59940));
#14921=EDGE_LOOP('',(#59941,#59942,#59943,#59944));
#14922=EDGE_LOOP('',(#59945,#59946,#59947,#59948));
#14923=EDGE_LOOP('',(#59949,#59950,#59951,#59952,#59953,#59954,#59955,#59956,
#59957,#59958,#59959,#59960,#59961,#59962,#59963,#59964,#59965,#59966));
#14924=EDGE_LOOP('',(#59967,#59968,#59969,#59970,#59971,#59972,#59973,#59974,
#59975,#59976,#59977,#59978,#59979,#59980,#59981,#59982,#59983));
#14925=EDGE_LOOP('',(#59984,#59985,#59986,#59987));
#14926=EDGE_LOOP('',(#59988,#59989,#59990));
#14927=EDGE_LOOP('',(#59991,#59992,#59993,#59994,#59995,#59996));
#14928=EDGE_LOOP('',(#59997,#59998,#59999));
#14929=EDGE_LOOP('',(#60000,#60001,#60002,#60003));
#14930=EDGE_LOOP('',(#60004,#60005,#60006,#60007,#60008,#60009,#60010,#60011,
#60012,#60013,#60014,#60015,#60016,#60017,#60018,#60019,#60020,#60021));
#14931=EDGE_LOOP('',(#60022,#60023,#60024,#60025));
#14932=EDGE_LOOP('',(#60026,#60027,#60028,#60029));
#14933=EDGE_LOOP('',(#60030,#60031,#60032,#60033));
#14934=EDGE_LOOP('',(#60034,#60035,#60036,#60037,#60038,#60039,#60040,#60041,
#60042,#60043,#60044,#60045,#60046,#60047,#60048,#60049,#60050,#60051));
#14935=EDGE_LOOP('',(#60052,#60053,#60054,#60055,#60056));
#14936=EDGE_LOOP('',(#60057,#60058,#60059,#60060));
#14937=EDGE_LOOP('',(#60061,#60062,#60063,#60064,#60065,#60066,#60067,#60068,
#60069,#60070,#60071,#60072,#60073,#60074,#60075,#60076));
#14938=EDGE_LOOP('',(#60077,#60078,#60079,#60080));
#14939=EDGE_LOOP('',(#60081,#60082,#60083,#60084,#60085,#60086,#60087,#60088,
#60089,#60090,#60091,#60092,#60093,#60094,#60095,#60096));
#14940=EDGE_LOOP('',(#60097,#60098,#60099,#60100));
#14941=EDGE_LOOP('',(#60101,#60102,#60103,#60104));
#14942=EDGE_LOOP('',(#60105,#60106,#60107,#60108));
#14943=EDGE_LOOP('',(#60109,#60110,#60111,#60112,#60113,#60114,#60115,#60116,
#60117,#60118,#60119,#60120,#60121,#60122,#60123,#60124,#60125,#60126));
#14944=EDGE_LOOP('',(#60127,#60128,#60129,#60130));
#14945=EDGE_LOOP('',(#60131,#60132,#60133,#60134));
#14946=EDGE_LOOP('',(#60135,#60136,#60137,#60138));
#14947=EDGE_LOOP('',(#60139,#60140,#60141,#60142,#60143,#60144,#60145,#60146,
#60147,#60148,#60149,#60150,#60151,#60152,#60153,#60154,#60155,#60156));
#14948=EDGE_LOOP('',(#60157,#60158,#60159,#60160));
#14949=EDGE_LOOP('',(#60161,#60162,#60163,#60164));
#14950=EDGE_LOOP('',(#60165,#60166,#60167,#60168));
#14951=EDGE_LOOP('',(#60169,#60170,#60171,#60172,#60173));
#14952=EDGE_LOOP('',(#60174,#60175,#60176,#60177,#60178,#60179,#60180,#60181,
#60182,#60183,#60184,#60185,#60186,#60187,#60188,#60189,#60190,#60191));
#14953=EDGE_LOOP('',(#60192,#60193,#60194));
#14954=EDGE_LOOP('',(#60195,#60196,#60197,#60198));
#14955=EDGE_LOOP('',(#60199,#60200,#60201,#60202));
#14956=EDGE_LOOP('',(#60203));
#14957=EDGE_LOOP('',(#60204));
#14958=EDGE_LOOP('',(#60205,#60206,#60207,#60208,#60209,#60210));
#14959=EDGE_LOOP('',(#60211,#60212,#60213,#60214));
#14960=EDGE_LOOP('',(#60215,#60216,#60217,#60218));
#14961=EDGE_LOOP('',(#60219,#60220,#60221,#60222));
#14962=EDGE_LOOP('',(#60223,#60224,#60225,#60226));
#14963=EDGE_LOOP('',(#60227,#60228,#60229,#60230));
#14964=EDGE_LOOP('',(#60231,#60232,#60233,#60234));
#14965=EDGE_LOOP('',(#60235,#60236,#60237,#60238));
#14966=EDGE_LOOP('',(#60239));
#14967=EDGE_LOOP('',(#60240));
#14968=EDGE_LOOP('',(#60241,#60242,#60243,#60244,#60245,#60246,#60247,#60248));
#14969=EDGE_LOOP('',(#60249,#60250,#60251,#60252));
#14970=EDGE_LOOP('',(#60253,#60254,#60255,#60256));
#14971=EDGE_LOOP('',(#60257,#60258,#60259,#60260));
#14972=EDGE_LOOP('',(#60261,#60262,#60263,#60264));
#14973=EDGE_LOOP('',(#60265,#60266,#60267,#60268));
#14974=EDGE_LOOP('',(#60269,#60270,#60271,#60272));
#14975=EDGE_LOOP('',(#60273,#60274,#60275,#60276));
#14976=EDGE_LOOP('',(#60277,#60278,#60279,#60280));
#14977=EDGE_LOOP('',(#60281,#60282,#60283,#60284));
#14978=EDGE_LOOP('',(#60285,#60286,#60287,#60288));
#14979=EDGE_LOOP('',(#60289,#60290,#60291,#60292));
#14980=EDGE_LOOP('',(#60293,#60294,#60295,#60296));
#14981=EDGE_LOOP('',(#60297,#60298,#60299,#60300));
#14982=EDGE_LOOP('',(#60301,#60302,#60303,#60304));
#14983=EDGE_LOOP('',(#60305,#60306,#60307,#60308,#60309));
#14984=EDGE_LOOP('',(#60310,#60311,#60312,#60313,#60314));
#14985=EDGE_LOOP('',(#60315,#60316,#60317,#60318));
#14986=EDGE_LOOP('',(#60319,#60320,#60321,#60322));
#14987=EDGE_LOOP('',(#60323,#60324,#60325,#60326));
#14988=EDGE_LOOP('',(#60327,#60328,#60329,#60330));
#14989=EDGE_LOOP('',(#60331,#60332,#60333,#60334));
#14990=EDGE_LOOP('',(#60335,#60336,#60337,#60338,#60339));
#14991=EDGE_LOOP('',(#60340,#60341,#60342));
#14992=EDGE_LOOP('',(#60343,#60344,#60345,#60346));
#14993=EDGE_LOOP('',(#60347,#60348,#60349,#60350));
#14994=EDGE_LOOP('',(#60351,#60352,#60353,#60354));
#14995=EDGE_LOOP('',(#60355,#60356,#60357,#60358));
#14996=EDGE_LOOP('',(#60359,#60360,#60361,#60362));
#14997=EDGE_LOOP('',(#60363,#60364,#60365,#60366));
#14998=EDGE_LOOP('',(#60367,#60368,#60369,#60370));
#14999=EDGE_LOOP('',(#60371,#60372,#60373,#60374));
#15000=EDGE_LOOP('',(#60375,#60376,#60377,#60378));
#15001=EDGE_LOOP('',(#60379,#60380,#60381,#60382));
#15002=EDGE_LOOP('',(#60383,#60384,#60385,#60386));
#15003=EDGE_LOOP('',(#60387,#60388,#60389,#60390));
#15004=EDGE_LOOP('',(#60391,#60392,#60393,#60394));
#15005=EDGE_LOOP('',(#60395,#60396,#60397,#60398));
#15006=EDGE_LOOP('',(#60399,#60400,#60401,#60402));
#15007=EDGE_LOOP('',(#60403,#60404,#60405,#60406));
#15008=EDGE_LOOP('',(#60407,#60408,#60409,#60410));
#15009=EDGE_LOOP('',(#60411,#60412,#60413,#60414));
#15010=EDGE_LOOP('',(#60415,#60416,#60417,#60418));
#15011=EDGE_LOOP('',(#60419,#60420,#60421,#60422));
#15012=EDGE_LOOP('',(#60423,#60424,#60425,#60426,#60427,#60428,#60429));
#15013=EDGE_LOOP('',(#60430,#60431,#60432,#60433));
#15014=EDGE_LOOP('',(#60434,#60435,#60436,#60437));
#15015=EDGE_LOOP('',(#60438,#60439,#60440,#60441));
#15016=EDGE_LOOP('',(#60442,#60443,#60444,#60445,#60446,#60447,#60448,#60449,
#60450,#60451,#60452,#60453,#60454,#60455,#60456,#60457,#60458));
#15017=EDGE_LOOP('',(#60459,#60460,#60461,#60462,#60463,#60464));
#15018=EDGE_LOOP('',(#60465,#60466,#60467,#60468,#60469,#60470,#60471,#60472,
#60473,#60474,#60475,#60476,#60477,#60478,#60479,#60480,#60481,#60482,#60483,
#60484,#60485,#60486,#60487,#60488,#60489,#60490,#60491,#60492,#60493,#60494,
#60495,#60496,#60497,#60498,#60499,#60500,#60501,#60502,#60503,#60504,#60505,
#60506,#60507,#60508));
#15019=EDGE_LOOP('',(#60509,#60510,#60511,#60512,#60513,#60514));
#15020=EDGE_LOOP('',(#60515,#60516,#60517,#60518,#60519,#60520,#60521,#60522,
#60523,#60524,#60525,#60526,#60527,#60528,#60529,#60530,#60531));
#15021=EDGE_LOOP('',(#60532,#60533,#60534,#60535));
#15022=EDGE_LOOP('',(#60536,#60537,#60538,#60539));
#15023=EDGE_LOOP('',(#60540,#60541,#60542,#60543));
#15024=EDGE_LOOP('',(#60544,#60545,#60546,#60547,#60548,#60549,#60550,#60551,
#60552,#60553,#60554,#60555,#60556,#60557,#60558,#60559,#60560));
#15025=EDGE_LOOP('',(#60561,#60562,#60563,#60564));
#15026=EDGE_LOOP('',(#60565,#60566,#60567,#60568,#60569,#60570,#60571,#60572,
#60573));
#15027=EDGE_LOOP('',(#60574,#60575,#60576,#60577));
#15028=EDGE_LOOP('',(#60578,#60579,#60580,#60581));
#15029=EDGE_LOOP('',(#60582,#60583,#60584,#60585,#60586));
#15030=EDGE_LOOP('',(#60587,#60588,#60589,#60590,#60591,#60592,#60593,#60594));
#15031=EDGE_LOOP('',(#60595,#60596,#60597));
#15032=EDGE_LOOP('',(#60598,#60599,#60600,#60601));
#15033=EDGE_LOOP('',(#60602,#60603,#60604,#60605));
#15034=EDGE_LOOP('',(#60606,#60607,#60608,#60609));
#15035=EDGE_LOOP('',(#60610,#60611,#60612,#60613));
#15036=EDGE_LOOP('',(#60614,#60615,#60616,#60617));
#15037=EDGE_LOOP('',(#60618,#60619,#60620,#60621));
#15038=EDGE_LOOP('',(#60622,#60623,#60624,#60625));
#15039=EDGE_LOOP('',(#60626,#60627,#60628,#60629));
#15040=EDGE_LOOP('',(#60630,#60631,#60632,#60633));
#15041=EDGE_LOOP('',(#60634,#60635,#60636,#60637));
#15042=EDGE_LOOP('',(#60638,#60639,#60640,#60641));
#15043=EDGE_LOOP('',(#60642,#60643,#60644,#60645));
#15044=EDGE_LOOP('',(#60646,#60647,#60648,#60649));
#15045=EDGE_LOOP('',(#60650,#60651,#60652,#60653));
#15046=EDGE_LOOP('',(#60654,#60655,#60656,#60657));
#15047=EDGE_LOOP('',(#60658,#60659,#60660,#60661));
#15048=EDGE_LOOP('',(#60662,#60663,#60664,#60665));
#15049=EDGE_LOOP('',(#60666,#60667,#60668,#60669));
#15050=EDGE_LOOP('',(#60670,#60671,#60672,#60673));
#15051=EDGE_LOOP('',(#60674,#60675,#60676,#60677,#60678));
#15052=EDGE_LOOP('',(#60679,#60680,#60681,#60682));
#15053=EDGE_LOOP('',(#60683,#60684,#60685,#60686));
#15054=EDGE_LOOP('',(#60687,#60688,#60689,#60690));
#15055=EDGE_LOOP('',(#60691,#60692,#60693,#60694));
#15056=EDGE_LOOP('',(#60695,#60696,#60697,#60698));
#15057=EDGE_LOOP('',(#60699,#60700,#60701,#60702));
#15058=EDGE_LOOP('',(#60703,#60704,#60705,#60706));
#15059=EDGE_LOOP('',(#60707,#60708,#60709,#60710));
#15060=EDGE_LOOP('',(#60711,#60712,#60713,#60714));
#15061=EDGE_LOOP('',(#60715,#60716,#60717,#60718));
#15062=EDGE_LOOP('',(#60719,#60720,#60721,#60722));
#15063=EDGE_LOOP('',(#60723,#60724,#60725,#60726));
#15064=EDGE_LOOP('',(#60727,#60728,#60729,#60730));
#15065=EDGE_LOOP('',(#60731,#60732,#60733,#60734));
#15066=EDGE_LOOP('',(#60735,#60736,#60737,#60738));
#15067=EDGE_LOOP('',(#60739,#60740,#60741,#60742));
#15068=EDGE_LOOP('',(#60743,#60744,#60745,#60746));
#15069=EDGE_LOOP('',(#60747,#60748,#60749,#60750));
#15070=EDGE_LOOP('',(#60751,#60752,#60753,#60754));
#15071=EDGE_LOOP('',(#60755,#60756,#60757,#60758));
#15072=EDGE_LOOP('',(#60759,#60760,#60761,#60762));
#15073=EDGE_LOOP('',(#60763,#60764,#60765,#60766));
#15074=EDGE_LOOP('',(#60767,#60768,#60769,#60770));
#15075=EDGE_LOOP('',(#60771,#60772,#60773,#60774));
#15076=EDGE_LOOP('',(#60775,#60776,#60777,#60778));
#15077=EDGE_LOOP('',(#60779,#60780,#60781,#60782));
#15078=EDGE_LOOP('',(#60783,#60784,#60785,#60786));
#15079=EDGE_LOOP('',(#60787,#60788,#60789,#60790));
#15080=EDGE_LOOP('',(#60791,#60792,#60793,#60794));
#15081=EDGE_LOOP('',(#60795,#60796,#60797,#60798));
#15082=EDGE_LOOP('',(#60799,#60800,#60801,#60802));
#15083=EDGE_LOOP('',(#60803,#60804,#60805,#60806));
#15084=EDGE_LOOP('',(#60807,#60808,#60809,#60810));
#15085=EDGE_LOOP('',(#60811,#60812,#60813,#60814));
#15086=EDGE_LOOP('',(#60815,#60816,#60817,#60818));
#15087=EDGE_LOOP('',(#60819,#60820,#60821,#60822));
#15088=EDGE_LOOP('',(#60823,#60824,#60825,#60826));
#15089=EDGE_LOOP('',(#60827,#60828,#60829,#60830));
#15090=EDGE_LOOP('',(#60831,#60832,#60833,#60834));
#15091=EDGE_LOOP('',(#60835,#60836,#60837,#60838));
#15092=EDGE_LOOP('',(#60839,#60840,#60841,#60842));
#15093=EDGE_LOOP('',(#60843,#60844,#60845,#60846));
#15094=EDGE_LOOP('',(#60847,#60848,#60849,#60850));
#15095=EDGE_LOOP('',(#60851,#60852,#60853,#60854));
#15096=EDGE_LOOP('',(#60855,#60856,#60857,#60858));
#15097=EDGE_LOOP('',(#60859,#60860,#60861,#60862));
#15098=EDGE_LOOP('',(#60863,#60864,#60865,#60866));
#15099=EDGE_LOOP('',(#60867,#60868,#60869,#60870));
#15100=EDGE_LOOP('',(#60871,#60872,#60873,#60874));
#15101=EDGE_LOOP('',(#60875,#60876,#60877,#60878));
#15102=EDGE_LOOP('',(#60879,#60880,#60881,#60882));
#15103=EDGE_LOOP('',(#60883,#60884,#60885,#60886));
#15104=EDGE_LOOP('',(#60887,#60888,#60889,#60890));
#15105=EDGE_LOOP('',(#60891,#60892,#60893,#60894));
#15106=EDGE_LOOP('',(#60895,#60896,#60897,#60898));
#15107=EDGE_LOOP('',(#60899,#60900,#60901,#60902));
#15108=EDGE_LOOP('',(#60903,#60904,#60905,#60906));
#15109=EDGE_LOOP('',(#60907,#60908,#60909,#60910));
#15110=EDGE_LOOP('',(#60911,#60912,#60913,#60914));
#15111=EDGE_LOOP('',(#60915,#60916,#60917,#60918));
#15112=EDGE_LOOP('',(#60919,#60920,#60921,#60922));
#15113=EDGE_LOOP('',(#60923,#60924,#60925,#60926));
#15114=EDGE_LOOP('',(#60927,#60928,#60929,#60930));
#15115=EDGE_LOOP('',(#60931,#60932,#60933,#60934));
#15116=EDGE_LOOP('',(#60935,#60936,#60937,#60938));
#15117=EDGE_LOOP('',(#60939,#60940,#60941,#60942));
#15118=EDGE_LOOP('',(#60943,#60944,#60945,#60946));
#15119=EDGE_LOOP('',(#60947,#60948,#60949,#60950));
#15120=EDGE_LOOP('',(#60951,#60952,#60953,#60954));
#15121=EDGE_LOOP('',(#60955,#60956,#60957,#60958));
#15122=EDGE_LOOP('',(#60959,#60960,#60961,#60962));
#15123=EDGE_LOOP('',(#60963,#60964,#60965,#60966));
#15124=EDGE_LOOP('',(#60967,#60968,#60969,#60970));
#15125=EDGE_LOOP('',(#60971,#60972,#60973,#60974));
#15126=EDGE_LOOP('',(#60975,#60976,#60977,#60978));
#15127=EDGE_LOOP('',(#60979,#60980,#60981,#60982));
#15128=EDGE_LOOP('',(#60983,#60984,#60985,#60986));
#15129=EDGE_LOOP('',(#60987,#60988,#60989,#60990));
#15130=EDGE_LOOP('',(#60991,#60992,#60993,#60994));
#15131=EDGE_LOOP('',(#60995,#60996,#60997,#60998));
#15132=EDGE_LOOP('',(#60999,#61000,#61001,#61002));
#15133=EDGE_LOOP('',(#61003,#61004,#61005,#61006));
#15134=EDGE_LOOP('',(#61007,#61008,#61009,#61010));
#15135=EDGE_LOOP('',(#61011,#61012,#61013,#61014));
#15136=EDGE_LOOP('',(#61015,#61016,#61017,#61018));
#15137=EDGE_LOOP('',(#61019,#61020,#61021,#61022));
#15138=EDGE_LOOP('',(#61023,#61024,#61025,#61026));
#15139=EDGE_LOOP('',(#61027,#61028,#61029,#61030));
#15140=EDGE_LOOP('',(#61031,#61032,#61033,#61034));
#15141=EDGE_LOOP('',(#61035,#61036,#61037,#61038));
#15142=EDGE_LOOP('',(#61039,#61040,#61041,#61042));
#15143=EDGE_LOOP('',(#61043,#61044,#61045,#61046));
#15144=EDGE_LOOP('',(#61047,#61048,#61049,#61050));
#15145=EDGE_LOOP('',(#61051,#61052,#61053,#61054));
#15146=EDGE_LOOP('',(#61055,#61056,#61057,#61058));
#15147=EDGE_LOOP('',(#61059,#61060,#61061,#61062,#61063));
#15148=EDGE_LOOP('',(#61064,#61065,#61066,#61067));
#15149=EDGE_LOOP('',(#61068,#61069,#61070,#61071));
#15150=EDGE_LOOP('',(#61072,#61073,#61074,#61075));
#15151=EDGE_LOOP('',(#61076,#61077,#61078,#61079));
#15152=EDGE_LOOP('',(#61080,#61081,#61082,#61083));
#15153=EDGE_LOOP('',(#61084,#61085,#61086,#61087));
#15154=EDGE_LOOP('',(#61088,#61089,#61090,#61091));
#15155=EDGE_LOOP('',(#61092,#61093,#61094,#61095));
#15156=EDGE_LOOP('',(#61096,#61097,#61098,#61099));
#15157=EDGE_LOOP('',(#61100,#61101,#61102,#61103));
#15158=EDGE_LOOP('',(#61104,#61105,#61106,#61107));
#15159=EDGE_LOOP('',(#61108,#61109,#61110,#61111));
#15160=EDGE_LOOP('',(#61112,#61113,#61114,#61115));
#15161=EDGE_LOOP('',(#61116,#61117,#61118,#61119));
#15162=EDGE_LOOP('',(#61120,#61121,#61122,#61123));
#15163=EDGE_LOOP('',(#61124,#61125,#61126,#61127));
#15164=EDGE_LOOP('',(#61128,#61129,#61130,#61131));
#15165=EDGE_LOOP('',(#61132,#61133,#61134,#61135));
#15166=EDGE_LOOP('',(#61136,#61137,#61138,#61139));
#15167=EDGE_LOOP('',(#61140,#61141,#61142,#61143));
#15168=EDGE_LOOP('',(#61144,#61145,#61146,#61147));
#15169=EDGE_LOOP('',(#61148,#61149,#61150,#61151));
#15170=EDGE_LOOP('',(#61152,#61153,#61154,#61155));
#15171=EDGE_LOOP('',(#61156,#61157,#61158,#61159));
#15172=EDGE_LOOP('',(#61160,#61161,#61162,#61163));
#15173=EDGE_LOOP('',(#61164,#61165,#61166,#61167));
#15174=EDGE_LOOP('',(#61168,#61169,#61170,#61171));
#15175=EDGE_LOOP('',(#61172,#61173,#61174,#61175));
#15176=EDGE_LOOP('',(#61176,#61177,#61178,#61179));
#15177=EDGE_LOOP('',(#61180,#61181,#61182,#61183));
#15178=EDGE_LOOP('',(#61184,#61185,#61186,#61187));
#15179=EDGE_LOOP('',(#61188,#61189,#61190,#61191));
#15180=EDGE_LOOP('',(#61192,#61193,#61194,#61195));
#15181=EDGE_LOOP('',(#61196,#61197,#61198,#61199));
#15182=EDGE_LOOP('',(#61200,#61201,#61202,#61203));
#15183=EDGE_LOOP('',(#61204,#61205,#61206,#61207));
#15184=EDGE_LOOP('',(#61208,#61209,#61210,#61211));
#15185=EDGE_LOOP('',(#61212,#61213,#61214,#61215));
#15186=EDGE_LOOP('',(#61216,#61217,#61218,#61219));
#15187=EDGE_LOOP('',(#61220,#61221,#61222,#61223));
#15188=EDGE_LOOP('',(#61224,#61225,#61226,#61227));
#15189=EDGE_LOOP('',(#61228,#61229,#61230,#61231));
#15190=EDGE_LOOP('',(#61232,#61233,#61234,#61235));
#15191=EDGE_LOOP('',(#61236,#61237,#61238,#61239));
#15192=EDGE_LOOP('',(#61240,#61241,#61242,#61243));
#15193=EDGE_LOOP('',(#61244,#61245,#61246,#61247));
#15194=EDGE_LOOP('',(#61248,#61249,#61250,#61251));
#15195=EDGE_LOOP('',(#61252,#61253,#61254,#61255));
#15196=EDGE_LOOP('',(#61256,#61257,#61258,#61259));
#15197=EDGE_LOOP('',(#61260,#61261,#61262,#61263));
#15198=EDGE_LOOP('',(#61264,#61265,#61266,#61267));
#15199=EDGE_LOOP('',(#61268,#61269,#61270,#61271));
#15200=EDGE_LOOP('',(#61272,#61273,#61274,#61275));
#15201=EDGE_LOOP('',(#61276,#61277,#61278,#61279));
#15202=EDGE_LOOP('',(#61280,#61281,#61282,#61283));
#15203=EDGE_LOOP('',(#61284,#61285,#61286,#61287));
#15204=EDGE_LOOP('',(#61288,#61289,#61290,#61291));
#15205=EDGE_LOOP('',(#61292,#61293,#61294,#61295));
#15206=EDGE_LOOP('',(#61296,#61297,#61298,#61299));
#15207=EDGE_LOOP('',(#61300,#61301,#61302,#61303));
#15208=EDGE_LOOP('',(#61304,#61305,#61306,#61307));
#15209=EDGE_LOOP('',(#61308,#61309,#61310,#61311));
#15210=EDGE_LOOP('',(#61312,#61313,#61314,#61315));
#15211=EDGE_LOOP('',(#61316,#61317,#61318,#61319));
#15212=EDGE_LOOP('',(#61320,#61321,#61322,#61323));
#15213=EDGE_LOOP('',(#61324,#61325,#61326,#61327));
#15214=EDGE_LOOP('',(#61328,#61329,#61330,#61331));
#15215=EDGE_LOOP('',(#61332,#61333,#61334,#61335));
#15216=EDGE_LOOP('',(#61336,#61337,#61338,#61339));
#15217=EDGE_LOOP('',(#61340,#61341,#61342,#61343));
#15218=EDGE_LOOP('',(#61344,#61345,#61346,#61347));
#15219=EDGE_LOOP('',(#61348,#61349,#61350,#61351));
#15220=EDGE_LOOP('',(#61352,#61353,#61354,#61355));
#15221=EDGE_LOOP('',(#61356,#61357,#61358,#61359));
#15222=EDGE_LOOP('',(#61360,#61361,#61362,#61363,#61364));
#15223=EDGE_LOOP('',(#61365,#61366,#61367,#61368));
#15224=EDGE_LOOP('',(#61369,#61370,#61371,#61372));
#15225=EDGE_LOOP('',(#61373,#61374,#61375,#61376));
#15226=EDGE_LOOP('',(#61377,#61378,#61379,#61380));
#15227=EDGE_LOOP('',(#61381,#61382,#61383,#61384));
#15228=EDGE_LOOP('',(#61385,#61386,#61387,#61388));
#15229=EDGE_LOOP('',(#61389,#61390,#61391,#61392));
#15230=EDGE_LOOP('',(#61393,#61394,#61395,#61396));
#15231=EDGE_LOOP('',(#61397,#61398,#61399,#61400));
#15232=EDGE_LOOP('',(#61401,#61402,#61403,#61404));
#15233=EDGE_LOOP('',(#61405,#61406,#61407,#61408));
#15234=EDGE_LOOP('',(#61409,#61410,#61411,#61412));
#15235=EDGE_LOOP('',(#61413,#61414,#61415,#61416));
#15236=EDGE_LOOP('',(#61417,#61418,#61419,#61420));
#15237=EDGE_LOOP('',(#61421,#61422,#61423,#61424));
#15238=EDGE_LOOP('',(#61425,#61426,#61427,#61428));
#15239=EDGE_LOOP('',(#61429,#61430,#61431,#61432));
#15240=EDGE_LOOP('',(#61433,#61434,#61435,#61436));
#15241=EDGE_LOOP('',(#61437,#61438,#61439,#61440));
#15242=EDGE_LOOP('',(#61441,#61442,#61443,#61444));
#15243=EDGE_LOOP('',(#61445,#61446,#61447,#61448));
#15244=EDGE_LOOP('',(#61449,#61450,#61451,#61452));
#15245=EDGE_LOOP('',(#61453,#61454,#61455,#61456));
#15246=EDGE_LOOP('',(#61457,#61458,#61459,#61460));
#15247=EDGE_LOOP('',(#61461,#61462,#61463,#61464));
#15248=EDGE_LOOP('',(#61465,#61466,#61467,#61468));
#15249=EDGE_LOOP('',(#61469,#61470,#61471,#61472));
#15250=EDGE_LOOP('',(#61473,#61474,#61475,#61476));
#15251=EDGE_LOOP('',(#61477,#61478,#61479,#61480));
#15252=EDGE_LOOP('',(#61481,#61482,#61483,#61484,#61485));
#15253=EDGE_LOOP('',(#61486,#61487,#61488,#61489,#61490));
#15254=EDGE_LOOP('',(#61491,#61492,#61493,#61494));
#15255=EDGE_LOOP('',(#61495,#61496,#61497,#61498));
#15256=EDGE_LOOP('',(#61499,#61500,#61501,#61502));
#15257=EDGE_LOOP('',(#61503,#61504,#61505,#61506));
#15258=EDGE_LOOP('',(#61507,#61508,#61509,#61510));
#15259=EDGE_LOOP('',(#61511,#61512,#61513,#61514));
#15260=EDGE_LOOP('',(#61515,#61516,#61517,#61518));
#15261=EDGE_LOOP('',(#61519,#61520,#61521,#61522));
#15262=EDGE_LOOP('',(#61523,#61524,#61525,#61526));
#15263=EDGE_LOOP('',(#61527,#61528,#61529,#61530));
#15264=EDGE_LOOP('',(#61531,#61532,#61533,#61534));
#15265=EDGE_LOOP('',(#61535,#61536,#61537,#61538));
#15266=EDGE_LOOP('',(#61539,#61540,#61541,#61542));
#15267=EDGE_LOOP('',(#61543,#61544,#61545,#61546));
#15268=EDGE_LOOP('',(#61547,#61548,#61549,#61550));
#15269=EDGE_LOOP('',(#61551,#61552,#61553,#61554));
#15270=EDGE_LOOP('',(#61555,#61556,#61557,#61558));
#15271=EDGE_LOOP('',(#61559,#61560,#61561,#61562));
#15272=EDGE_LOOP('',(#61563,#61564,#61565,#61566));
#15273=EDGE_LOOP('',(#61567,#61568,#61569,#61570));
#15274=EDGE_LOOP('',(#61571,#61572,#61573,#61574));
#15275=EDGE_LOOP('',(#61575,#61576,#61577,#61578));
#15276=EDGE_LOOP('',(#61579,#61580,#61581,#61582));
#15277=EDGE_LOOP('',(#61583,#61584,#61585,#61586));
#15278=EDGE_LOOP('',(#61587,#61588,#61589,#61590));
#15279=EDGE_LOOP('',(#61591,#61592,#61593,#61594));
#15280=EDGE_LOOP('',(#61595,#61596,#61597,#61598));
#15281=EDGE_LOOP('',(#61599,#61600,#61601,#61602));
#15282=EDGE_LOOP('',(#61603,#61604,#61605,#61606));
#15283=EDGE_LOOP('',(#61607,#61608,#61609,#61610));
#15284=EDGE_LOOP('',(#61611,#61612,#61613,#61614));
#15285=EDGE_LOOP('',(#61615,#61616,#61617,#61618));
#15286=EDGE_LOOP('',(#61619,#61620,#61621,#61622));
#15287=EDGE_LOOP('',(#61623,#61624,#61625,#61626));
#15288=EDGE_LOOP('',(#61627,#61628,#61629,#61630));
#15289=EDGE_LOOP('',(#61631,#61632,#61633,#61634));
#15290=EDGE_LOOP('',(#61635,#61636,#61637,#61638));
#15291=EDGE_LOOP('',(#61639,#61640,#61641,#61642));
#15292=EDGE_LOOP('',(#61643,#61644,#61645,#61646));
#15293=EDGE_LOOP('',(#61647,#61648,#61649,#61650));
#15294=EDGE_LOOP('',(#61651,#61652,#61653,#61654));
#15295=EDGE_LOOP('',(#61655,#61656,#61657,#61658));
#15296=EDGE_LOOP('',(#61659,#61660,#61661,#61662));
#15297=EDGE_LOOP('',(#61663,#61664,#61665,#61666));
#15298=EDGE_LOOP('',(#61667,#61668,#61669,#61670));
#15299=EDGE_LOOP('',(#61671,#61672,#61673,#61674));
#15300=EDGE_LOOP('',(#61675,#61676,#61677,#61678));
#15301=EDGE_LOOP('',(#61679,#61680,#61681,#61682));
#15302=EDGE_LOOP('',(#61683,#61684,#61685,#61686));
#15303=EDGE_LOOP('',(#61687,#61688,#61689,#61690));
#15304=EDGE_LOOP('',(#61691,#61692,#61693,#61694));
#15305=EDGE_LOOP('',(#61695,#61696,#61697,#61698));
#15306=EDGE_LOOP('',(#61699,#61700,#61701,#61702));
#15307=EDGE_LOOP('',(#61703,#61704,#61705,#61706));
#15308=EDGE_LOOP('',(#61707,#61708,#61709,#61710));
#15309=EDGE_LOOP('',(#61711,#61712,#61713,#61714));
#15310=EDGE_LOOP('',(#61715,#61716,#61717,#61718));
#15311=EDGE_LOOP('',(#61719,#61720,#61721,#61722));
#15312=EDGE_LOOP('',(#61723,#61724,#61725,#61726));
#15313=EDGE_LOOP('',(#61727,#61728,#61729,#61730));
#15314=EDGE_LOOP('',(#61731,#61732,#61733,#61734));
#15315=EDGE_LOOP('',(#61735,#61736,#61737,#61738));
#15316=EDGE_LOOP('',(#61739,#61740,#61741,#61742));
#15317=EDGE_LOOP('',(#61743,#61744,#61745,#61746));
#15318=EDGE_LOOP('',(#61747,#61748,#61749,#61750));
#15319=EDGE_LOOP('',(#61751,#61752,#61753,#61754));
#15320=EDGE_LOOP('',(#61755,#61756,#61757,#61758));
#15321=EDGE_LOOP('',(#61759,#61760,#61761,#61762));
#15322=EDGE_LOOP('',(#61763,#61764,#61765,#61766));
#15323=EDGE_LOOP('',(#61767,#61768,#61769,#61770));
#15324=EDGE_LOOP('',(#61771,#61772,#61773,#61774));
#15325=EDGE_LOOP('',(#61775,#61776,#61777,#61778));
#15326=EDGE_LOOP('',(#61779,#61780,#61781,#61782));
#15327=EDGE_LOOP('',(#61783,#61784,#61785,#61786));
#15328=EDGE_LOOP('',(#61787,#61788,#61789,#61790));
#15329=EDGE_LOOP('',(#61791,#61792,#61793,#61794));
#15330=EDGE_LOOP('',(#61795,#61796,#61797,#61798));
#15331=EDGE_LOOP('',(#61799,#61800,#61801,#61802));
#15332=EDGE_LOOP('',(#61803,#61804,#61805,#61806));
#15333=EDGE_LOOP('',(#61807,#61808,#61809,#61810));
#15334=EDGE_LOOP('',(#61811,#61812,#61813,#61814));
#15335=EDGE_LOOP('',(#61815,#61816,#61817,#61818));
#15336=EDGE_LOOP('',(#61819,#61820,#61821,#61822));
#15337=EDGE_LOOP('',(#61823,#61824,#61825,#61826));
#15338=EDGE_LOOP('',(#61827,#61828,#61829,#61830));
#15339=EDGE_LOOP('',(#61831,#61832,#61833,#61834));
#15340=EDGE_LOOP('',(#61835,#61836,#61837,#61838));
#15341=EDGE_LOOP('',(#61839,#61840,#61841,#61842));
#15342=EDGE_LOOP('',(#61843,#61844,#61845,#61846));
#15343=EDGE_LOOP('',(#61847,#61848,#61849,#61850,#61851));
#15344=EDGE_LOOP('',(#61852,#61853,#61854,#61855,#61856));
#15345=EDGE_LOOP('',(#61857,#61858,#61859,#61860));
#15346=EDGE_LOOP('',(#61861,#61862,#61863,#61864));
#15347=EDGE_LOOP('',(#61865,#61866,#61867,#61868));
#15348=EDGE_LOOP('',(#61869,#61870,#61871,#61872));
#15349=EDGE_LOOP('',(#61873,#61874,#61875,#61876));
#15350=EDGE_LOOP('',(#61877,#61878,#61879,#61880));
#15351=EDGE_LOOP('',(#61881,#61882,#61883,#61884));
#15352=EDGE_LOOP('',(#61885,#61886,#61887,#61888));
#15353=EDGE_LOOP('',(#61889,#61890,#61891,#61892));
#15354=EDGE_LOOP('',(#61893,#61894,#61895,#61896));
#15355=EDGE_LOOP('',(#61897,#61898,#61899,#61900));
#15356=EDGE_LOOP('',(#61901,#61902,#61903,#61904));
#15357=EDGE_LOOP('',(#61905,#61906,#61907,#61908));
#15358=EDGE_LOOP('',(#61909,#61910,#61911,#61912));
#15359=EDGE_LOOP('',(#61913,#61914,#61915,#61916));
#15360=EDGE_LOOP('',(#61917,#61918,#61919,#61920,#61921));
#15361=EDGE_LOOP('',(#61922,#61923,#61924,#61925));
#15362=EDGE_LOOP('',(#61926,#61927,#61928,#61929));
#15363=EDGE_LOOP('',(#61930,#61931,#61932,#61933));
#15364=EDGE_LOOP('',(#61934,#61935,#61936,#61937));
#15365=EDGE_LOOP('',(#61938,#61939,#61940,#61941));
#15366=EDGE_LOOP('',(#61942,#61943,#61944,#61945));
#15367=EDGE_LOOP('',(#61946,#61947,#61948,#61949));
#15368=EDGE_LOOP('',(#61950,#61951,#61952,#61953,#61954));
#15369=EDGE_LOOP('',(#61955,#61956,#61957,#61958));
#15370=EDGE_LOOP('',(#61959,#61960,#61961,#61962));
#15371=EDGE_LOOP('',(#61963,#61964,#61965,#61966));
#15372=EDGE_LOOP('',(#61967,#61968,#61969,#61970));
#15373=EDGE_LOOP('',(#61971,#61972,#61973,#61974));
#15374=EDGE_LOOP('',(#61975,#61976,#61977,#61978));
#15375=EDGE_LOOP('',(#61979,#61980,#61981,#61982));
#15376=EDGE_LOOP('',(#61983,#61984,#61985,#61986));
#15377=EDGE_LOOP('',(#61987,#61988,#61989,#61990));
#15378=EDGE_LOOP('',(#61991,#61992,#61993,#61994));
#15379=EDGE_LOOP('',(#61995,#61996,#61997,#61998));
#15380=EDGE_LOOP('',(#61999,#62000,#62001,#62002));
#15381=EDGE_LOOP('',(#62003,#62004,#62005,#62006));
#15382=EDGE_LOOP('',(#62007,#62008,#62009,#62010));
#15383=EDGE_LOOP('',(#62011,#62012,#62013,#62014));
#15384=EDGE_LOOP('',(#62015,#62016,#62017,#62018));
#15385=EDGE_LOOP('',(#62019,#62020,#62021,#62022));
#15386=EDGE_LOOP('',(#62023,#62024,#62025,#62026));
#15387=EDGE_LOOP('',(#62027,#62028,#62029,#62030));
#15388=EDGE_LOOP('',(#62031,#62032,#62033,#62034));
#15389=EDGE_LOOP('',(#62035,#62036,#62037,#62038));
#15390=EDGE_LOOP('',(#62039,#62040,#62041,#62042));
#15391=EDGE_LOOP('',(#62043,#62044,#62045,#62046));
#15392=EDGE_LOOP('',(#62047,#62048,#62049,#62050));
#15393=EDGE_LOOP('',(#62051,#62052,#62053,#62054));
#15394=EDGE_LOOP('',(#62055,#62056,#62057,#62058));
#15395=EDGE_LOOP('',(#62059,#62060,#62061,#62062));
#15396=EDGE_LOOP('',(#62063,#62064,#62065,#62066));
#15397=EDGE_LOOP('',(#62067,#62068,#62069,#62070));
#15398=EDGE_LOOP('',(#62071,#62072,#62073,#62074));
#15399=EDGE_LOOP('',(#62075,#62076,#62077,#62078));
#15400=EDGE_LOOP('',(#62079,#62080,#62081,#62082));
#15401=EDGE_LOOP('',(#62083,#62084,#62085,#62086));
#15402=EDGE_LOOP('',(#62087,#62088,#62089,#62090));
#15403=EDGE_LOOP('',(#62091,#62092,#62093,#62094));
#15404=EDGE_LOOP('',(#62095,#62096,#62097,#62098));
#15405=EDGE_LOOP('',(#62099,#62100,#62101,#62102));
#15406=EDGE_LOOP('',(#62103,#62104,#62105,#62106));
#15407=EDGE_LOOP('',(#62107,#62108,#62109,#62110));
#15408=EDGE_LOOP('',(#62111,#62112,#62113,#62114));
#15409=EDGE_LOOP('',(#62115,#62116,#62117,#62118));
#15410=EDGE_LOOP('',(#62119,#62120,#62121,#62122));
#15411=EDGE_LOOP('',(#62123,#62124,#62125,#62126));
#15412=EDGE_LOOP('',(#62127,#62128,#62129,#62130));
#15413=EDGE_LOOP('',(#62131,#62132,#62133,#62134));
#15414=EDGE_LOOP('',(#62135,#62136,#62137,#62138));
#15415=EDGE_LOOP('',(#62139,#62140,#62141,#62142));
#15416=EDGE_LOOP('',(#62143,#62144,#62145,#62146));
#15417=EDGE_LOOP('',(#62147,#62148,#62149,#62150,#62151));
#15418=EDGE_LOOP('',(#62152,#62153,#62154,#62155));
#15419=EDGE_LOOP('',(#62156,#62157,#62158,#62159));
#15420=EDGE_LOOP('',(#62160,#62161,#62162,#62163));
#15421=EDGE_LOOP('',(#62164,#62165,#62166,#62167));
#15422=EDGE_LOOP('',(#62168,#62169,#62170,#62171));
#15423=EDGE_LOOP('',(#62172,#62173,#62174,#62175));
#15424=EDGE_LOOP('',(#62176,#62177,#62178,#62179));
#15425=EDGE_LOOP('',(#62180,#62181,#62182,#62183));
#15426=EDGE_LOOP('',(#62184,#62185,#62186,#62187));
#15427=EDGE_LOOP('',(#62188,#62189,#62190,#62191));
#15428=EDGE_LOOP('',(#62192,#62193,#62194,#62195));
#15429=EDGE_LOOP('',(#62196,#62197,#62198,#62199));
#15430=EDGE_LOOP('',(#62200,#62201,#62202,#62203));
#15431=EDGE_LOOP('',(#62204,#62205,#62206,#62207));
#15432=EDGE_LOOP('',(#62208,#62209,#62210,#62211));
#15433=EDGE_LOOP('',(#62212,#62213,#62214,#62215));
#15434=EDGE_LOOP('',(#62216,#62217,#62218,#62219));
#15435=EDGE_LOOP('',(#62220,#62221,#62222,#62223));
#15436=EDGE_LOOP('',(#62224,#62225,#62226,#62227));
#15437=EDGE_LOOP('',(#62228,#62229,#62230,#62231));
#15438=EDGE_LOOP('',(#62232,#62233,#62234,#62235));
#15439=EDGE_LOOP('',(#62236,#62237,#62238,#62239,#62240));
#15440=EDGE_LOOP('',(#62241,#62242,#62243,#62244,#62245));
#15441=EDGE_LOOP('',(#62246,#62247,#62248,#62249));
#15442=EDGE_LOOP('',(#62250,#62251,#62252,#62253));
#15443=EDGE_LOOP('',(#62254,#62255,#62256,#62257));
#15444=EDGE_LOOP('',(#62258,#62259,#62260,#62261));
#15445=EDGE_LOOP('',(#62262,#62263,#62264,#62265));
#15446=EDGE_LOOP('',(#62266,#62267,#62268,#62269));
#15447=EDGE_LOOP('',(#62270,#62271,#62272,#62273));
#15448=EDGE_LOOP('',(#62274,#62275,#62276,#62277));
#15449=EDGE_LOOP('',(#62278,#62279,#62280,#62281));
#15450=EDGE_LOOP('',(#62282,#62283,#62284,#62285));
#15451=EDGE_LOOP('',(#62286,#62287,#62288,#62289));
#15452=EDGE_LOOP('',(#62290,#62291,#62292,#62293));
#15453=EDGE_LOOP('',(#62294,#62295,#62296,#62297));
#15454=EDGE_LOOP('',(#62298,#62299,#62300,#62301));
#15455=EDGE_LOOP('',(#62302,#62303,#62304,#62305));
#15456=EDGE_LOOP('',(#62306,#62307,#62308,#62309));
#15457=EDGE_LOOP('',(#62310,#62311,#62312,#62313));
#15458=EDGE_LOOP('',(#62314,#62315,#62316,#62317));
#15459=EDGE_LOOP('',(#62318,#62319,#62320,#62321));
#15460=EDGE_LOOP('',(#62322,#62323,#62324,#62325));
#15461=EDGE_LOOP('',(#62326,#62327,#62328,#62329));
#15462=EDGE_LOOP('',(#62330,#62331,#62332,#62333));
#15463=EDGE_LOOP('',(#62334,#62335,#62336,#62337));
#15464=EDGE_LOOP('',(#62338,#62339,#62340,#62341));
#15465=EDGE_LOOP('',(#62342,#62343,#62344,#62345));
#15466=EDGE_LOOP('',(#62346,#62347,#62348,#62349));
#15467=EDGE_LOOP('',(#62350,#62351,#62352,#62353));
#15468=EDGE_LOOP('',(#62354,#62355,#62356,#62357));
#15469=EDGE_LOOP('',(#62358,#62359,#62360,#62361));
#15470=EDGE_LOOP('',(#62362,#62363,#62364,#62365));
#15471=EDGE_LOOP('',(#62366,#62367,#62368,#62369));
#15472=EDGE_LOOP('',(#62370,#62371,#62372,#62373,#62374));
#15473=EDGE_LOOP('',(#62375,#62376,#62377,#62378,#62379));
#15474=EDGE_LOOP('',(#62380,#62381,#62382,#62383));
#15475=EDGE_LOOP('',(#62384,#62385,#62386,#62387));
#15476=EDGE_LOOP('',(#62388,#62389,#62390,#62391));
#15477=EDGE_LOOP('',(#62392,#62393,#62394,#62395));
#15478=EDGE_LOOP('',(#62396,#62397,#62398,#62399));
#15479=EDGE_LOOP('',(#62400,#62401,#62402,#62403));
#15480=EDGE_LOOP('',(#62404,#62405,#62406,#62407));
#15481=EDGE_LOOP('',(#62408,#62409,#62410,#62411));
#15482=EDGE_LOOP('',(#62412,#62413,#62414,#62415));
#15483=EDGE_LOOP('',(#62416,#62417,#62418,#62419));
#15484=EDGE_LOOP('',(#62420,#62421,#62422,#62423));
#15485=EDGE_LOOP('',(#62424,#62425,#62426,#62427));
#15486=EDGE_LOOP('',(#62428,#62429,#62430,#62431));
#15487=EDGE_LOOP('',(#62432,#62433,#62434,#62435));
#15488=EDGE_LOOP('',(#62436,#62437,#62438));
#15489=EDGE_LOOP('',(#62439,#62440,#62441,#62442));
#15490=EDGE_LOOP('',(#62443,#62444,#62445,#62446));
#15491=EDGE_LOOP('',(#62447,#62448,#62449,#62450));
#15492=EDGE_LOOP('',(#62451,#62452,#62453,#62454));
#15493=EDGE_LOOP('',(#62455,#62456,#62457,#62458));
#15494=EDGE_LOOP('',(#62459,#62460,#62461,#62462));
#15495=EDGE_LOOP('',(#62463,#62464,#62465,#62466));
#15496=EDGE_LOOP('',(#62467,#62468,#62469,#62470));
#15497=EDGE_LOOP('',(#62471,#62472,#62473,#62474));
#15498=EDGE_LOOP('',(#62475,#62476,#62477,#62478));
#15499=EDGE_LOOP('',(#62479,#62480,#62481,#62482));
#15500=EDGE_LOOP('',(#62483,#62484,#62485,#62486));
#15501=EDGE_LOOP('',(#62487,#62488,#62489,#62490));
#15502=EDGE_LOOP('',(#62491,#62492,#62493,#62494));
#15503=EDGE_LOOP('',(#62495,#62496,#62497,#62498));
#15504=EDGE_LOOP('',(#62499,#62500,#62501,#62502));
#15505=EDGE_LOOP('',(#62503,#62504,#62505,#62506));
#15506=EDGE_LOOP('',(#62507,#62508,#62509,#62510));
#15507=EDGE_LOOP('',(#62511,#62512,#62513,#62514));
#15508=EDGE_LOOP('',(#62515,#62516,#62517,#62518));
#15509=EDGE_LOOP('',(#62519,#62520,#62521,#62522));
#15510=EDGE_LOOP('',(#62523,#62524,#62525,#62526));
#15511=EDGE_LOOP('',(#62527,#62528,#62529,#62530));
#15512=EDGE_LOOP('',(#62531,#62532,#62533,#62534));
#15513=EDGE_LOOP('',(#62535,#62536,#62537,#62538));
#15514=EDGE_LOOP('',(#62539,#62540,#62541,#62542));
#15515=EDGE_LOOP('',(#62543,#62544,#62545,#62546));
#15516=EDGE_LOOP('',(#62547,#62548,#62549,#62550));
#15517=EDGE_LOOP('',(#62551,#62552,#62553,#62554));
#15518=EDGE_LOOP('',(#62555,#62556,#62557,#62558));
#15519=EDGE_LOOP('',(#62559,#62560,#62561,#62562));
#15520=EDGE_LOOP('',(#62563,#62564,#62565,#62566));
#15521=EDGE_LOOP('',(#62567,#62568,#62569,#62570));
#15522=EDGE_LOOP('',(#62571,#62572,#62573,#62574));
#15523=EDGE_LOOP('',(#62575,#62576,#62577,#62578));
#15524=EDGE_LOOP('',(#62579,#62580,#62581,#62582));
#15525=EDGE_LOOP('',(#62583,#62584,#62585,#62586));
#15526=EDGE_LOOP('',(#62587,#62588,#62589,#62590));
#15527=EDGE_LOOP('',(#62591,#62592,#62593,#62594));
#15528=EDGE_LOOP('',(#62595,#62596,#62597,#62598));
#15529=EDGE_LOOP('',(#62599,#62600,#62601,#62602));
#15530=EDGE_LOOP('',(#62603,#62604,#62605,#62606));
#15531=EDGE_LOOP('',(#62607,#62608,#62609,#62610));
#15532=EDGE_LOOP('',(#62611,#62612,#62613,#62614));
#15533=EDGE_LOOP('',(#62615,#62616,#62617,#62618));
#15534=EDGE_LOOP('',(#62619,#62620,#62621,#62622));
#15535=EDGE_LOOP('',(#62623,#62624,#62625,#62626));
#15536=EDGE_LOOP('',(#62627,#62628,#62629,#62630));
#15537=EDGE_LOOP('',(#62631,#62632,#62633,#62634));
#15538=EDGE_LOOP('',(#62635,#62636,#62637,#62638));
#15539=EDGE_LOOP('',(#62639,#62640,#62641,#62642));
#15540=EDGE_LOOP('',(#62643,#62644,#62645,#62646));
#15541=EDGE_LOOP('',(#62647,#62648,#62649,#62650));
#15542=EDGE_LOOP('',(#62651,#62652,#62653,#62654));
#15543=EDGE_LOOP('',(#62655,#62656,#62657,#62658));
#15544=EDGE_LOOP('',(#62659,#62660,#62661,#62662));
#15545=EDGE_LOOP('',(#62663,#62664,#62665,#62666));
#15546=EDGE_LOOP('',(#62667,#62668,#62669,#62670));
#15547=EDGE_LOOP('',(#62671,#62672,#62673,#62674));
#15548=EDGE_LOOP('',(#62675,#62676,#62677,#62678));
#15549=EDGE_LOOP('',(#62679,#62680,#62681,#62682));
#15550=EDGE_LOOP('',(#62683,#62684,#62685,#62686));
#15551=EDGE_LOOP('',(#62687,#62688,#62689,#62690));
#15552=EDGE_LOOP('',(#62691,#62692,#62693,#62694));
#15553=EDGE_LOOP('',(#62695,#62696,#62697,#62698));
#15554=EDGE_LOOP('',(#62699,#62700,#62701,#62702));
#15555=EDGE_LOOP('',(#62703,#62704,#62705,#62706));
#15556=EDGE_LOOP('',(#62707,#62708,#62709,#62710));
#15557=EDGE_LOOP('',(#62711,#62712,#62713,#62714));
#15558=EDGE_LOOP('',(#62715,#62716,#62717,#62718));
#15559=EDGE_LOOP('',(#62719,#62720,#62721,#62722));
#15560=EDGE_LOOP('',(#62723,#62724,#62725,#62726));
#15561=EDGE_LOOP('',(#62727,#62728,#62729,#62730));
#15562=EDGE_LOOP('',(#62731,#62732,#62733,#62734));
#15563=EDGE_LOOP('',(#62735,#62736,#62737,#62738));
#15564=EDGE_LOOP('',(#62739,#62740,#62741,#62742,#62743,#62744));
#15565=EDGE_LOOP('',(#62745,#62746,#62747,#62748));
#15566=EDGE_LOOP('',(#62749,#62750,#62751,#62752));
#15567=EDGE_LOOP('',(#62753,#62754,#62755,#62756));
#15568=EDGE_LOOP('',(#62757,#62758,#62759,#62760));
#15569=EDGE_LOOP('',(#62761,#62762,#62763,#62764));
#15570=EDGE_LOOP('',(#62765,#62766,#62767,#62768));
#15571=EDGE_LOOP('',(#62769,#62770,#62771,#62772));
#15572=EDGE_LOOP('',(#62773,#62774,#62775,#62776));
#15573=EDGE_LOOP('',(#62777,#62778,#62779,#62780));
#15574=EDGE_LOOP('',(#62781,#62782,#62783,#62784));
#15575=EDGE_LOOP('',(#62785,#62786,#62787,#62788));
#15576=EDGE_LOOP('',(#62789,#62790,#62791,#62792));
#15577=EDGE_LOOP('',(#62793,#62794,#62795,#62796));
#15578=EDGE_LOOP('',(#62797,#62798,#62799,#62800));
#15579=EDGE_LOOP('',(#62801,#62802,#62803,#62804));
#15580=EDGE_LOOP('',(#62805,#62806,#62807));
#15581=EDGE_LOOP('',(#62808,#62809,#62810,#62811));
#15582=EDGE_LOOP('',(#62812,#62813,#62814,#62815));
#15583=EDGE_LOOP('',(#62816,#62817,#62818,#62819));
#15584=EDGE_LOOP('',(#62820,#62821,#62822,#62823));
#15585=EDGE_LOOP('',(#62824,#62825,#62826,#62827));
#15586=EDGE_LOOP('',(#62828,#62829,#62830,#62831));
#15587=EDGE_LOOP('',(#62832,#62833,#62834,#62835));
#15588=EDGE_LOOP('',(#62836,#62837,#62838,#62839));
#15589=EDGE_LOOP('',(#62840,#62841,#62842,#62843));
#15590=EDGE_LOOP('',(#62844,#62845,#62846,#62847));
#15591=EDGE_LOOP('',(#62848,#62849,#62850,#62851));
#15592=EDGE_LOOP('',(#62852,#62853,#62854,#62855));
#15593=EDGE_LOOP('',(#62856,#62857,#62858,#62859));
#15594=EDGE_LOOP('',(#62860,#62861,#62862,#62863));
#15595=EDGE_LOOP('',(#62864,#62865,#62866,#62867));
#15596=EDGE_LOOP('',(#62868,#62869,#62870));
#15597=EDGE_LOOP('',(#62871,#62872,#62873,#62874));
#15598=EDGE_LOOP('',(#62875,#62876,#62877,#62878));
#15599=EDGE_LOOP('',(#62879,#62880,#62881,#62882));
#15600=EDGE_LOOP('',(#62883,#62884,#62885,#62886));
#15601=EDGE_LOOP('',(#62887,#62888,#62889,#62890));
#15602=EDGE_LOOP('',(#62891,#62892,#62893,#62894));
#15603=EDGE_LOOP('',(#62895,#62896,#62897,#62898));
#15604=EDGE_LOOP('',(#62899,#62900,#62901,#62902));
#15605=EDGE_LOOP('',(#62903,#62904,#62905,#62906,#62907));
#15606=EDGE_LOOP('',(#62908,#62909,#62910));
#15607=EDGE_LOOP('',(#62911,#62912,#62913,#62914));
#15608=EDGE_LOOP('',(#62915,#62916,#62917,#62918));
#15609=EDGE_LOOP('',(#62919,#62920,#62921,#62922));
#15610=EDGE_LOOP('',(#62923,#62924,#62925,#62926));
#15611=EDGE_LOOP('',(#62927,#62928,#62929,#62930,#62931));
#15612=EDGE_LOOP('',(#62932,#62933,#62934));
#15613=EDGE_LOOP('',(#62935,#62936,#62937,#62938,#62939));
#15614=EDGE_LOOP('',(#62940,#62941,#62942,#62943));
#15615=EDGE_LOOP('',(#62944,#62945,#62946,#62947));
#15616=EDGE_LOOP('',(#62948,#62949,#62950,#62951));
#15617=EDGE_LOOP('',(#62952,#62953,#62954,#62955));
#15618=EDGE_LOOP('',(#62956,#62957,#62958,#62959));
#15619=EDGE_LOOP('',(#62960,#62961,#62962,#62963));
#15620=EDGE_LOOP('',(#62964,#62965,#62966));
#15621=EDGE_LOOP('',(#62967,#62968,#62969,#62970));
#15622=EDGE_LOOP('',(#62971,#62972,#62973,#62974));
#15623=EDGE_LOOP('',(#62975,#62976,#62977,#62978));
#15624=EDGE_LOOP('',(#62979,#62980,#62981));
#15625=EDGE_LOOP('',(#62982,#62983,#62984,#62985));
#15626=EDGE_LOOP('',(#62986,#62987,#62988,#62989));
#15627=EDGE_LOOP('',(#62990,#62991,#62992,#62993));
#15628=EDGE_LOOP('',(#62994,#62995,#62996,#62997));
#15629=EDGE_LOOP('',(#62998,#62999,#63000,#63001));
#15630=EDGE_LOOP('',(#63002,#63003,#63004,#63005));
#15631=EDGE_LOOP('',(#63006,#63007,#63008,#63009));
#15632=EDGE_LOOP('',(#63010,#63011,#63012,#63013));
#15633=EDGE_LOOP('',(#63014,#63015,#63016,#63017));
#15634=EDGE_LOOP('',(#63018,#63019,#63020,#63021));
#15635=EDGE_LOOP('',(#63022,#63023,#63024,#63025));
#15636=EDGE_LOOP('',(#63026,#63027,#63028,#63029,#63030,#63031));
#15637=EDGE_LOOP('',(#63032,#63033,#63034,#63035));
#15638=EDGE_LOOP('',(#63036,#63037,#63038,#63039));
#15639=EDGE_LOOP('',(#63040,#63041,#63042,#63043));
#15640=EDGE_LOOP('',(#63044,#63045,#63046,#63047));
#15641=EDGE_LOOP('',(#63048,#63049,#63050));
#15642=EDGE_LOOP('',(#63051,#63052,#63053,#63054));
#15643=EDGE_LOOP('',(#63055,#63056,#63057,#63058));
#15644=EDGE_LOOP('',(#63059,#63060,#63061,#63062));
#15645=EDGE_LOOP('',(#63063,#63064,#63065,#63066));
#15646=EDGE_LOOP('',(#63067,#63068,#63069,#63070));
#15647=EDGE_LOOP('',(#63071,#63072,#63073,#63074));
#15648=EDGE_LOOP('',(#63075,#63076,#63077,#63078));
#15649=EDGE_LOOP('',(#63079,#63080,#63081,#63082,#63083,#63084));
#15650=EDGE_LOOP('',(#63085,#63086,#63087,#63088));
#15651=EDGE_LOOP('',(#63089,#63090,#63091,#63092));
#15652=EDGE_LOOP('',(#63093,#63094,#63095,#63096));
#15653=EDGE_LOOP('',(#63097,#63098,#63099,#63100));
#15654=EDGE_LOOP('',(#63101,#63102,#63103,#63104));
#15655=EDGE_LOOP('',(#63105,#63106,#63107,#63108));
#15656=EDGE_LOOP('',(#63109,#63110,#63111,#63112));
#15657=EDGE_LOOP('',(#63113,#63114,#63115,#63116));
#15658=EDGE_LOOP('',(#63117,#63118,#63119,#63120));
#15659=EDGE_LOOP('',(#63121,#63122,#63123,#63124));
#15660=EDGE_LOOP('',(#63125,#63126,#63127,#63128));
#15661=EDGE_LOOP('',(#63129,#63130,#63131,#63132));
#15662=EDGE_LOOP('',(#63133,#63134,#63135,#63136));
#15663=EDGE_LOOP('',(#63137,#63138,#63139));
#15664=EDGE_LOOP('',(#63140,#63141,#63142));
#15665=EDGE_LOOP('',(#63143,#63144,#63145,#63146));
#15666=EDGE_LOOP('',(#63147,#63148,#63149,#63150));
#15667=EDGE_LOOP('',(#63151,#63152,#63153,#63154));
#15668=EDGE_LOOP('',(#63155,#63156,#63157,#63158));
#15669=EDGE_LOOP('',(#63159,#63160,#63161,#63162));
#15670=EDGE_LOOP('',(#63163,#63164,#63165,#63166));
#15671=EDGE_LOOP('',(#63167,#63168,#63169,#63170));
#15672=EDGE_LOOP('',(#63171,#63172,#63173,#63174));
#15673=EDGE_LOOP('',(#63175,#63176,#63177,#63178));
#15674=EDGE_LOOP('',(#63179,#63180,#63181,#63182));
#15675=EDGE_LOOP('',(#63183,#63184,#63185,#63186));
#15676=EDGE_LOOP('',(#63187,#63188,#63189,#63190));
#15677=EDGE_LOOP('',(#63191,#63192,#63193,#63194));
#15678=EDGE_LOOP('',(#63195,#63196,#63197,#63198,#63199,#63200));
#15679=EDGE_LOOP('',(#63201,#63202,#63203,#63204));
#15680=EDGE_LOOP('',(#63205,#63206,#63207,#63208));
#15681=EDGE_LOOP('',(#63209,#63210,#63211,#63212));
#15682=EDGE_LOOP('',(#63213,#63214,#63215,#63216));
#15683=EDGE_LOOP('',(#63217,#63218,#63219,#63220));
#15684=EDGE_LOOP('',(#63221,#63222,#63223,#63224));
#15685=EDGE_LOOP('',(#63225,#63226,#63227,#63228));
#15686=EDGE_LOOP('',(#63229,#63230,#63231));
#15687=EDGE_LOOP('',(#63232,#63233,#63234,#63235));
#15688=EDGE_LOOP('',(#63236,#63237,#63238,#63239));
#15689=EDGE_LOOP('',(#63240,#63241,#63242,#63243));
#15690=EDGE_LOOP('',(#63244,#63245,#63246,#63247));
#15691=EDGE_LOOP('',(#63248,#63249,#63250,#63251,#63252,#63253));
#15692=EDGE_LOOP('',(#63254,#63255,#63256,#63257));
#15693=EDGE_LOOP('',(#63258,#63259,#63260,#63261));
#15694=EDGE_LOOP('',(#63262,#63263,#63264,#63265));
#15695=EDGE_LOOP('',(#63266,#63267,#63268,#63269));
#15696=EDGE_LOOP('',(#63270,#63271,#63272,#63273));
#15697=EDGE_LOOP('',(#63274,#63275,#63276,#63277));
#15698=EDGE_LOOP('',(#63278,#63279,#63280,#63281));
#15699=EDGE_LOOP('',(#63282,#63283,#63284,#63285));
#15700=EDGE_LOOP('',(#63286,#63287,#63288,#63289));
#15701=EDGE_LOOP('',(#63290,#63291,#63292,#63293));
#15702=EDGE_LOOP('',(#63294,#63295,#63296,#63297));
#15703=EDGE_LOOP('',(#63298,#63299,#63300));
#15704=EDGE_LOOP('',(#63301,#63302,#63303,#63304));
#15705=EDGE_LOOP('',(#63305,#63306,#63307,#63308));
#15706=EDGE_LOOP('',(#63309,#63310,#63311,#63312));
#15707=EDGE_LOOP('',(#63313,#63314,#63315));
#15708=EDGE_LOOP('',(#63316,#63317,#63318,#63319));
#15709=EDGE_LOOP('',(#63320,#63321,#63322,#63323));
#15710=EDGE_LOOP('',(#63324,#63325,#63326,#63327));
#15711=EDGE_LOOP('',(#63328,#63329,#63330,#63331));
#15712=EDGE_LOOP('',(#63332,#63333,#63334,#63335));
#15713=EDGE_LOOP('',(#63336,#63337,#63338,#63339));
#15714=EDGE_LOOP('',(#63340,#63341,#63342,#63343,#63344));
#15715=EDGE_LOOP('',(#63345,#63346,#63347));
#15716=EDGE_LOOP('',(#63348,#63349,#63350,#63351,#63352));
#15717=EDGE_LOOP('',(#63353,#63354,#63355,#63356));
#15718=EDGE_LOOP('',(#63357,#63358,#63359,#63360));
#15719=EDGE_LOOP('',(#63361,#63362,#63363,#63364));
#15720=EDGE_LOOP('',(#63365,#63366,#63367,#63368));
#15721=EDGE_LOOP('',(#63369,#63370,#63371));
#15722=EDGE_LOOP('',(#63372,#63373,#63374,#63375,#63376));
#15723=EDGE_LOOP('',(#63377,#63378,#63379,#63380));
#15724=EDGE_LOOP('',(#63381,#63382,#63383,#63384));
#15725=EDGE_LOOP('',(#63385,#63386,#63387,#63388));
#15726=EDGE_LOOP('',(#63389,#63390,#63391,#63392));
#15727=EDGE_LOOP('',(#63393,#63394,#63395,#63396));
#15728=EDGE_LOOP('',(#63397,#63398,#63399,#63400));
#15729=EDGE_LOOP('',(#63401,#63402,#63403,#63404));
#15730=EDGE_LOOP('',(#63405,#63406,#63407,#63408));
#15731=EDGE_LOOP('',(#63409,#63410,#63411));
#15732=EDGE_LOOP('',(#63412,#63413,#63414,#63415));
#15733=EDGE_LOOP('',(#63416,#63417,#63418,#63419));
#15734=EDGE_LOOP('',(#63420,#63421,#63422,#63423));
#15735=EDGE_LOOP('',(#63424,#63425,#63426,#63427));
#15736=EDGE_LOOP('',(#63428,#63429,#63430,#63431));
#15737=EDGE_LOOP('',(#63432,#63433,#63434,#63435));
#15738=EDGE_LOOP('',(#63436,#63437,#63438,#63439));
#15739=EDGE_LOOP('',(#63440,#63441,#63442,#63443));
#15740=EDGE_LOOP('',(#63444,#63445,#63446,#63447));
#15741=EDGE_LOOP('',(#63448,#63449,#63450,#63451));
#15742=EDGE_LOOP('',(#63452,#63453,#63454,#63455));
#15743=EDGE_LOOP('',(#63456,#63457,#63458,#63459));
#15744=EDGE_LOOP('',(#63460,#63461,#63462,#63463));
#15745=EDGE_LOOP('',(#63464,#63465,#63466,#63467));
#15746=EDGE_LOOP('',(#63468,#63469,#63470,#63471));
#15747=EDGE_LOOP('',(#63472,#63473,#63474));
#15748=EDGE_LOOP('',(#63475,#63476,#63477,#63478));
#15749=EDGE_LOOP('',(#63479,#63480,#63481,#63482));
#15750=EDGE_LOOP('',(#63483,#63484,#63485,#63486));
#15751=EDGE_LOOP('',(#63487,#63488,#63489,#63490));
#15752=EDGE_LOOP('',(#63491,#63492,#63493,#63494));
#15753=EDGE_LOOP('',(#63495,#63496,#63497,#63498));
#15754=EDGE_LOOP('',(#63499,#63500,#63501,#63502));
#15755=EDGE_LOOP('',(#63503,#63504,#63505,#63506));
#15756=EDGE_LOOP('',(#63507,#63508,#63509,#63510));
#15757=EDGE_LOOP('',(#63511,#63512,#63513,#63514));
#15758=EDGE_LOOP('',(#63515,#63516,#63517,#63518));
#15759=EDGE_LOOP('',(#63519,#63520,#63521,#63522));
#15760=EDGE_LOOP('',(#63523,#63524,#63525,#63526));
#15761=EDGE_LOOP('',(#63527,#63528,#63529,#63530));
#15762=EDGE_LOOP('',(#63531,#63532,#63533,#63534));
#15763=EDGE_LOOP('',(#63535,#63536,#63537,#63538,#63539,#63540));
#15764=EDGE_LOOP('',(#63541,#63542,#63543,#63544));
#15765=EDGE_LOOP('',(#63545,#63546,#63547,#63548));
#15766=EDGE_LOOP('',(#63549,#63550,#63551,#63552));
#15767=EDGE_LOOP('',(#63553,#63554,#63555,#63556));
#15768=EDGE_LOOP('',(#63557,#63558,#63559,#63560));
#15769=EDGE_LOOP('',(#63561,#63562,#63563,#63564));
#15770=EDGE_LOOP('',(#63565,#63566,#63567,#63568));
#15771=EDGE_LOOP('',(#63569,#63570,#63571,#63572));
#15772=EDGE_LOOP('',(#63573,#63574,#63575,#63576));
#15773=EDGE_LOOP('',(#63577,#63578,#63579,#63580));
#15774=EDGE_LOOP('',(#63581,#63582,#63583,#63584));
#15775=EDGE_LOOP('',(#63585,#63586,#63587,#63588));
#15776=EDGE_LOOP('',(#63589,#63590,#63591,#63592));
#15777=EDGE_LOOP('',(#63593,#63594,#63595,#63596));
#15778=EDGE_LOOP('',(#63597,#63598,#63599,#63600));
#15779=EDGE_LOOP('',(#63601,#63602,#63603,#63604));
#15780=EDGE_LOOP('',(#63605,#63606,#63607,#63608));
#15781=EDGE_LOOP('',(#63609,#63610,#63611,#63612));
#15782=EDGE_LOOP('',(#63613,#63614,#63615,#63616));
#15783=EDGE_LOOP('',(#63617,#63618,#63619,#63620));
#15784=EDGE_LOOP('',(#63621,#63622,#63623,#63624));
#15785=EDGE_LOOP('',(#63625,#63626,#63627,#63628));
#15786=EDGE_LOOP('',(#63629,#63630,#63631,#63632));
#15787=EDGE_LOOP('',(#63633,#63634,#63635,#63636));
#15788=EDGE_LOOP('',(#63637,#63638,#63639,#63640));
#15789=EDGE_LOOP('',(#63641,#63642,#63643,#63644));
#15790=EDGE_LOOP('',(#63645,#63646,#63647,#63648));
#15791=EDGE_LOOP('',(#63649,#63650,#63651,#63652));
#15792=EDGE_LOOP('',(#63653,#63654,#63655,#63656));
#15793=EDGE_LOOP('',(#63657,#63658,#63659,#63660));
#15794=EDGE_LOOP('',(#63661,#63662,#63663,#63664));
#15795=EDGE_LOOP('',(#63665,#63666,#63667,#63668));
#15796=EDGE_LOOP('',(#63669,#63670,#63671,#63672));
#15797=EDGE_LOOP('',(#63673,#63674,#63675,#63676));
#15798=EDGE_LOOP('',(#63677,#63678,#63679,#63680));
#15799=EDGE_LOOP('',(#63681,#63682,#63683,#63684));
#15800=EDGE_LOOP('',(#63685,#63686,#63687,#63688));
#15801=EDGE_LOOP('',(#63689,#63690,#63691,#63692));
#15802=EDGE_LOOP('',(#63693,#63694,#63695,#63696));
#15803=EDGE_LOOP('',(#63697,#63698,#63699,#63700));
#15804=EDGE_LOOP('',(#63701,#63702,#63703,#63704));
#15805=EDGE_LOOP('',(#63705,#63706,#63707,#63708));
#15806=EDGE_LOOP('',(#63709,#63710,#63711,#63712));
#15807=EDGE_LOOP('',(#63713,#63714,#63715,#63716));
#15808=EDGE_LOOP('',(#63717,#63718,#63719,#63720));
#15809=EDGE_LOOP('',(#63721,#63722,#63723,#63724));
#15810=EDGE_LOOP('',(#63725,#63726,#63727,#63728));
#15811=EDGE_LOOP('',(#63729,#63730,#63731,#63732));
#15812=EDGE_LOOP('',(#63733,#63734,#63735,#63736));
#15813=EDGE_LOOP('',(#63737,#63738,#63739,#63740));
#15814=EDGE_LOOP('',(#63741,#63742,#63743,#63744));
#15815=EDGE_LOOP('',(#63745,#63746,#63747,#63748));
#15816=EDGE_LOOP('',(#63749,#63750,#63751,#63752));
#15817=EDGE_LOOP('',(#63753,#63754,#63755,#63756));
#15818=EDGE_LOOP('',(#63757,#63758,#63759,#63760));
#15819=EDGE_LOOP('',(#63761,#63762,#63763,#63764));
#15820=EDGE_LOOP('',(#63765,#63766,#63767,#63768));
#15821=EDGE_LOOP('',(#63769,#63770,#63771,#63772));
#15822=EDGE_LOOP('',(#63773,#63774,#63775,#63776));
#15823=EDGE_LOOP('',(#63777,#63778,#63779,#63780));
#15824=EDGE_LOOP('',(#63781,#63782,#63783,#63784));
#15825=EDGE_LOOP('',(#63785,#63786,#63787,#63788));
#15826=EDGE_LOOP('',(#63789,#63790,#63791,#63792));
#15827=EDGE_LOOP('',(#63793,#63794,#63795,#63796));
#15828=EDGE_LOOP('',(#63797,#63798,#63799,#63800));
#15829=EDGE_LOOP('',(#63801,#63802,#63803,#63804));
#15830=EDGE_LOOP('',(#63805,#63806,#63807,#63808));
#15831=EDGE_LOOP('',(#63809,#63810,#63811,#63812));
#15832=EDGE_LOOP('',(#63813,#63814,#63815,#63816));
#15833=EDGE_LOOP('',(#63817,#63818,#63819,#63820));
#15834=EDGE_LOOP('',(#63821,#63822,#63823,#63824));
#15835=EDGE_LOOP('',(#63825,#63826,#63827,#63828));
#15836=EDGE_LOOP('',(#63829,#63830,#63831,#63832));
#15837=EDGE_LOOP('',(#63833,#63834,#63835,#63836));
#15838=EDGE_LOOP('',(#63837,#63838,#63839,#63840));
#15839=EDGE_LOOP('',(#63841,#63842,#63843));
#15840=EDGE_LOOP('',(#63844,#63845,#63846,#63847));
#15841=EDGE_LOOP('',(#63848,#63849,#63850,#63851));
#15842=EDGE_LOOP('',(#63852,#63853,#63854,#63855));
#15843=EDGE_LOOP('',(#63856,#63857,#63858,#63859));
#15844=EDGE_LOOP('',(#63860,#63861,#63862,#63863));
#15845=EDGE_LOOP('',(#63864,#63865,#63866,#63867));
#15846=EDGE_LOOP('',(#63868,#63869,#63870,#63871));
#15847=EDGE_LOOP('',(#63872,#63873,#63874,#63875));
#15848=EDGE_LOOP('',(#63876,#63877,#63878,#63879));
#15849=EDGE_LOOP('',(#63880,#63881,#63882,#63883));
#15850=EDGE_LOOP('',(#63884,#63885,#63886,#63887));
#15851=EDGE_LOOP('',(#63888,#63889,#63890,#63891));
#15852=EDGE_LOOP('',(#63892,#63893,#63894,#63895));
#15853=EDGE_LOOP('',(#63896,#63897,#63898,#63899));
#15854=EDGE_LOOP('',(#63900,#63901,#63902,#63903,#63904));
#15855=EDGE_LOOP('',(#63905,#63906,#63907,#63908,#63909));
#15856=EDGE_LOOP('',(#63910,#63911,#63912,#63913));
#15857=EDGE_LOOP('',(#63914,#63915,#63916,#63917));
#15858=EDGE_LOOP('',(#63918,#63919,#63920,#63921));
#15859=EDGE_LOOP('',(#63922,#63923,#63924,#63925));
#15860=EDGE_LOOP('',(#63926,#63927,#63928,#63929));
#15861=EDGE_LOOP('',(#63930,#63931,#63932,#63933));
#15862=EDGE_LOOP('',(#63934,#63935,#63936,#63937));
#15863=EDGE_LOOP('',(#63938,#63939,#63940,#63941));
#15864=EDGE_LOOP('',(#63942,#63943,#63944,#63945));
#15865=EDGE_LOOP('',(#63946,#63947,#63948,#63949));
#15866=EDGE_LOOP('',(#63950,#63951,#63952,#63953));
#15867=EDGE_LOOP('',(#63954,#63955,#63956,#63957));
#15868=EDGE_LOOP('',(#63958,#63959,#63960,#63961));
#15869=EDGE_LOOP('',(#63962,#63963,#63964,#63965));
#15870=EDGE_LOOP('',(#63966,#63967,#63968,#63969));
#15871=EDGE_LOOP('',(#63970,#63971,#63972,#63973));
#15872=EDGE_LOOP('',(#63974,#63975,#63976,#63977));
#15873=EDGE_LOOP('',(#63978,#63979,#63980,#63981));
#15874=EDGE_LOOP('',(#63982,#63983,#63984,#63985));
#15875=EDGE_LOOP('',(#63986,#63987,#63988,#63989));
#15876=EDGE_LOOP('',(#63990,#63991,#63992,#63993));
#15877=EDGE_LOOP('',(#63994,#63995,#63996,#63997));
#15878=EDGE_LOOP('',(#63998,#63999,#64000,#64001));
#15879=EDGE_LOOP('',(#64002,#64003,#64004,#64005));
#15880=EDGE_LOOP('',(#64006,#64007,#64008,#64009));
#15881=EDGE_LOOP('',(#64010,#64011,#64012,#64013));
#15882=EDGE_LOOP('',(#64014,#64015,#64016,#64017));
#15883=EDGE_LOOP('',(#64018,#64019,#64020,#64021));
#15884=EDGE_LOOP('',(#64022,#64023,#64024,#64025));
#15885=EDGE_LOOP('',(#64026,#64027,#64028,#64029));
#15886=EDGE_LOOP('',(#64030,#64031,#64032,#64033));
#15887=EDGE_LOOP('',(#64034,#64035,#64036,#64037,#64038));
#15888=EDGE_LOOP('',(#64039,#64040,#64041,#64042,#64043));
#15889=EDGE_LOOP('',(#64044,#64045,#64046,#64047));
#15890=EDGE_LOOP('',(#64048,#64049,#64050,#64051));
#15891=EDGE_LOOP('',(#64052,#64053,#64054,#64055));
#15892=EDGE_LOOP('',(#64056,#64057,#64058,#64059));
#15893=EDGE_LOOP('',(#64060,#64061,#64062,#64063));
#15894=EDGE_LOOP('',(#64064,#64065,#64066,#64067));
#15895=EDGE_LOOP('',(#64068,#64069,#64070,#64071));
#15896=EDGE_LOOP('',(#64072,#64073,#64074,#64075));
#15897=EDGE_LOOP('',(#64076,#64077,#64078,#64079));
#15898=EDGE_LOOP('',(#64080,#64081,#64082,#64083));
#15899=EDGE_LOOP('',(#64084,#64085,#64086,#64087));
#15900=EDGE_LOOP('',(#64088,#64089,#64090,#64091));
#15901=EDGE_LOOP('',(#64092,#64093,#64094,#64095));
#15902=EDGE_LOOP('',(#64096,#64097,#64098,#64099));
#15903=EDGE_LOOP('',(#64100,#64101,#64102,#64103));
#15904=EDGE_LOOP('',(#64104,#64105,#64106,#64107));
#15905=EDGE_LOOP('',(#64108,#64109,#64110,#64111));
#15906=EDGE_LOOP('',(#64112,#64113,#64114,#64115));
#15907=EDGE_LOOP('',(#64116,#64117,#64118,#64119));
#15908=EDGE_LOOP('',(#64120,#64121,#64122,#64123));
#15909=EDGE_LOOP('',(#64124,#64125,#64126,#64127));
#15910=EDGE_LOOP('',(#64128,#64129,#64130,#64131,#64132));
#15911=EDGE_LOOP('',(#64133,#64134,#64135,#64136));
#15912=EDGE_LOOP('',(#64137,#64138,#64139,#64140));
#15913=EDGE_LOOP('',(#64141,#64142,#64143,#64144));
#15914=EDGE_LOOP('',(#64145,#64146,#64147,#64148));
#15915=EDGE_LOOP('',(#64149,#64150,#64151,#64152));
#15916=EDGE_LOOP('',(#64153,#64154,#64155,#64156));
#15917=EDGE_LOOP('',(#64157,#64158,#64159,#64160));
#15918=EDGE_LOOP('',(#64161,#64162,#64163,#64164));
#15919=EDGE_LOOP('',(#64165,#64166,#64167,#64168));
#15920=EDGE_LOOP('',(#64169,#64170,#64171,#64172));
#15921=EDGE_LOOP('',(#64173,#64174,#64175,#64176));
#15922=EDGE_LOOP('',(#64177,#64178,#64179,#64180));
#15923=EDGE_LOOP('',(#64181,#64182,#64183,#64184));
#15924=EDGE_LOOP('',(#64185,#64186,#64187,#64188));
#15925=EDGE_LOOP('',(#64189,#64190,#64191,#64192));
#15926=EDGE_LOOP('',(#64193,#64194,#64195,#64196));
#15927=EDGE_LOOP('',(#64197,#64198,#64199,#64200));
#15928=EDGE_LOOP('',(#64201,#64202,#64203,#64204));
#15929=EDGE_LOOP('',(#64205,#64206,#64207,#64208));
#15930=EDGE_LOOP('',(#64209,#64210,#64211,#64212));
#15931=EDGE_LOOP('',(#64213,#64214,#64215,#64216));
#15932=EDGE_LOOP('',(#64217,#64218,#64219,#64220));
#15933=EDGE_LOOP('',(#64221,#64222,#64223,#64224));
#15934=EDGE_LOOP('',(#64225,#64226,#64227,#64228));
#15935=EDGE_LOOP('',(#64229,#64230,#64231,#64232));
#15936=EDGE_LOOP('',(#64233,#64234,#64235,#64236));
#15937=EDGE_LOOP('',(#64237,#64238,#64239,#64240));
#15938=EDGE_LOOP('',(#64241,#64242,#64243,#64244));
#15939=EDGE_LOOP('',(#64245,#64246,#64247,#64248));
#15940=EDGE_LOOP('',(#64249,#64250,#64251,#64252));
#15941=EDGE_LOOP('',(#64253,#64254,#64255,#64256));
#15942=EDGE_LOOP('',(#64257,#64258,#64259,#64260));
#15943=EDGE_LOOP('',(#64261,#64262,#64263,#64264));
#15944=EDGE_LOOP('',(#64265,#64266,#64267,#64268));
#15945=EDGE_LOOP('',(#64269,#64270,#64271,#64272));
#15946=EDGE_LOOP('',(#64273,#64274,#64275,#64276));
#15947=EDGE_LOOP('',(#64277,#64278,#64279,#64280));
#15948=EDGE_LOOP('',(#64281,#64282,#64283,#64284));
#15949=EDGE_LOOP('',(#64285,#64286,#64287,#64288));
#15950=EDGE_LOOP('',(#64289,#64290,#64291,#64292));
#15951=EDGE_LOOP('',(#64293,#64294,#64295,#64296));
#15952=EDGE_LOOP('',(#64297,#64298,#64299,#64300));
#15953=EDGE_LOOP('',(#64301,#64302,#64303,#64304));
#15954=EDGE_LOOP('',(#64305,#64306,#64307,#64308));
#15955=EDGE_LOOP('',(#64309,#64310,#64311,#64312));
#15956=EDGE_LOOP('',(#64313,#64314,#64315,#64316));
#15957=EDGE_LOOP('',(#64317,#64318,#64319,#64320));
#15958=EDGE_LOOP('',(#64321,#64322,#64323,#64324));
#15959=EDGE_LOOP('',(#64325,#64326,#64327,#64328,#64329));
#15960=EDGE_LOOP('',(#64330,#64331,#64332,#64333));
#15961=EDGE_LOOP('',(#64334,#64335,#64336,#64337));
#15962=EDGE_LOOP('',(#64338,#64339,#64340,#64341));
#15963=EDGE_LOOP('',(#64342,#64343,#64344,#64345));
#15964=EDGE_LOOP('',(#64346,#64347,#64348,#64349));
#15965=EDGE_LOOP('',(#64350,#64351,#64352,#64353));
#15966=EDGE_LOOP('',(#64354,#64355,#64356,#64357));
#15967=EDGE_LOOP('',(#64358,#64359,#64360,#64361,#64362));
#15968=EDGE_LOOP('',(#64363,#64364,#64365,#64366));
#15969=EDGE_LOOP('',(#64367,#64368,#64369,#64370));
#15970=EDGE_LOOP('',(#64371,#64372,#64373,#64374));
#15971=EDGE_LOOP('',(#64375,#64376,#64377,#64378));
#15972=EDGE_LOOP('',(#64379,#64380,#64381,#64382));
#15973=EDGE_LOOP('',(#64383,#64384,#64385,#64386));
#15974=EDGE_LOOP('',(#64387,#64388,#64389,#64390));
#15975=EDGE_LOOP('',(#64391,#64392,#64393,#64394));
#15976=EDGE_LOOP('',(#64395,#64396,#64397,#64398));
#15977=EDGE_LOOP('',(#64399,#64400,#64401,#64402));
#15978=EDGE_LOOP('',(#64403,#64404,#64405,#64406));
#15979=EDGE_LOOP('',(#64407,#64408,#64409,#64410));
#15980=EDGE_LOOP('',(#64411,#64412,#64413,#64414));
#15981=EDGE_LOOP('',(#64415,#64416,#64417,#64418));
#15982=EDGE_LOOP('',(#64419,#64420,#64421,#64422));
#15983=EDGE_LOOP('',(#64423,#64424,#64425,#64426,#64427));
#15984=EDGE_LOOP('',(#64428,#64429,#64430,#64431,#64432));
#15985=EDGE_LOOP('',(#64433,#64434,#64435,#64436));
#15986=EDGE_LOOP('',(#64437,#64438,#64439,#64440));
#15987=EDGE_LOOP('',(#64441,#64442,#64443,#64444));
#15988=EDGE_LOOP('',(#64445,#64446,#64447,#64448));
#15989=EDGE_LOOP('',(#64449,#64450,#64451,#64452));
#15990=EDGE_LOOP('',(#64453,#64454,#64455,#64456));
#15991=EDGE_LOOP('',(#64457,#64458,#64459,#64460));
#15992=EDGE_LOOP('',(#64461,#64462,#64463,#64464));
#15993=EDGE_LOOP('',(#64465,#64466,#64467,#64468));
#15994=EDGE_LOOP('',(#64469,#64470,#64471,#64472));
#15995=EDGE_LOOP('',(#64473,#64474,#64475,#64476));
#15996=EDGE_LOOP('',(#64477,#64478,#64479,#64480));
#15997=EDGE_LOOP('',(#64481,#64482,#64483,#64484));
#15998=EDGE_LOOP('',(#64485,#64486,#64487,#64488));
#15999=EDGE_LOOP('',(#64489,#64490,#64491,#64492));
#16000=EDGE_LOOP('',(#64493,#64494,#64495,#64496));
#16001=EDGE_LOOP('',(#64497,#64498,#64499,#64500));
#16002=EDGE_LOOP('',(#64501,#64502,#64503,#64504));
#16003=EDGE_LOOP('',(#64505,#64506,#64507,#64508));
#16004=EDGE_LOOP('',(#64509,#64510,#64511,#64512));
#16005=EDGE_LOOP('',(#64513,#64514,#64515,#64516));
#16006=EDGE_LOOP('',(#64517,#64518,#64519,#64520));
#16007=EDGE_LOOP('',(#64521,#64522,#64523,#64524));
#16008=EDGE_LOOP('',(#64525,#64526,#64527,#64528));
#16009=EDGE_LOOP('',(#64529,#64530,#64531,#64532));
#16010=EDGE_LOOP('',(#64533,#64534,#64535,#64536));
#16011=EDGE_LOOP('',(#64537,#64538,#64539,#64540));
#16012=EDGE_LOOP('',(#64541,#64542,#64543,#64544));
#16013=EDGE_LOOP('',(#64545,#64546,#64547,#64548));
#16014=EDGE_LOOP('',(#64549,#64550,#64551,#64552));
#16015=EDGE_LOOP('',(#64553,#64554,#64555,#64556));
#16016=EDGE_LOOP('',(#64557,#64558,#64559,#64560));
#16017=EDGE_LOOP('',(#64561,#64562,#64563,#64564));
#16018=EDGE_LOOP('',(#64565,#64566,#64567,#64568));
#16019=EDGE_LOOP('',(#64569,#64570,#64571,#64572));
#16020=EDGE_LOOP('',(#64573,#64574,#64575,#64576));
#16021=EDGE_LOOP('',(#64577,#64578,#64579,#64580));
#16022=EDGE_LOOP('',(#64581,#64582,#64583,#64584));
#16023=EDGE_LOOP('',(#64585,#64586,#64587,#64588));
#16024=EDGE_LOOP('',(#64589,#64590,#64591,#64592));
#16025=EDGE_LOOP('',(#64593,#64594,#64595,#64596));
#16026=EDGE_LOOP('',(#64597,#64598,#64599,#64600));
#16027=EDGE_LOOP('',(#64601,#64602,#64603,#64604));
#16028=EDGE_LOOP('',(#64605,#64606,#64607,#64608));
#16029=EDGE_LOOP('',(#64609,#64610,#64611,#64612));
#16030=EDGE_LOOP('',(#64613,#64614,#64615,#64616));
#16031=EDGE_LOOP('',(#64617,#64618,#64619,#64620));
#16032=EDGE_LOOP('',(#64621,#64622,#64623,#64624));
#16033=EDGE_LOOP('',(#64625,#64626,#64627,#64628));
#16034=EDGE_LOOP('',(#64629,#64630,#64631,#64632));
#16035=EDGE_LOOP('',(#64633,#64634,#64635,#64636));
#16036=EDGE_LOOP('',(#64637,#64638,#64639,#64640));
#16037=EDGE_LOOP('',(#64641,#64642,#64643,#64644));
#16038=EDGE_LOOP('',(#64645,#64646,#64647,#64648));
#16039=EDGE_LOOP('',(#64649,#64650,#64651,#64652));
#16040=EDGE_LOOP('',(#64653,#64654,#64655,#64656));
#16041=EDGE_LOOP('',(#64657,#64658,#64659,#64660));
#16042=EDGE_LOOP('',(#64661,#64662,#64663,#64664));
#16043=EDGE_LOOP('',(#64665,#64666,#64667,#64668));
#16044=EDGE_LOOP('',(#64669,#64670,#64671,#64672));
#16045=EDGE_LOOP('',(#64673,#64674,#64675,#64676));
#16046=EDGE_LOOP('',(#64677,#64678,#64679,#64680));
#16047=EDGE_LOOP('',(#64681,#64682,#64683,#64684));
#16048=EDGE_LOOP('',(#64685,#64686,#64687,#64688));
#16049=EDGE_LOOP('',(#64689,#64690,#64691,#64692));
#16050=EDGE_LOOP('',(#64693,#64694,#64695,#64696));
#16051=EDGE_LOOP('',(#64697,#64698,#64699,#64700));
#16052=EDGE_LOOP('',(#64701,#64702,#64703,#64704));
#16053=EDGE_LOOP('',(#64705,#64706,#64707,#64708));
#16054=EDGE_LOOP('',(#64709,#64710,#64711,#64712));
#16055=EDGE_LOOP('',(#64713,#64714,#64715,#64716));
#16056=EDGE_LOOP('',(#64717,#64718,#64719,#64720));
#16057=EDGE_LOOP('',(#64721,#64722,#64723,#64724));
#16058=EDGE_LOOP('',(#64725,#64726,#64727,#64728));
#16059=EDGE_LOOP('',(#64729,#64730,#64731,#64732));
#16060=EDGE_LOOP('',(#64733,#64734,#64735,#64736));
#16061=EDGE_LOOP('',(#64737,#64738,#64739,#64740));
#16062=EDGE_LOOP('',(#64741,#64742,#64743,#64744));
#16063=EDGE_LOOP('',(#64745,#64746,#64747,#64748));
#16064=EDGE_LOOP('',(#64749,#64750,#64751,#64752));
#16065=EDGE_LOOP('',(#64753,#64754,#64755,#64756));
#16066=EDGE_LOOP('',(#64757,#64758,#64759,#64760));
#16067=EDGE_LOOP('',(#64761,#64762,#64763,#64764));
#16068=EDGE_LOOP('',(#64765,#64766,#64767,#64768));
#16069=EDGE_LOOP('',(#64769,#64770,#64771,#64772));
#16070=EDGE_LOOP('',(#64773,#64774,#64775,#64776));
#16071=EDGE_LOOP('',(#64777,#64778,#64779,#64780));
#16072=EDGE_LOOP('',(#64781,#64782,#64783,#64784));
#16073=EDGE_LOOP('',(#64785,#64786,#64787,#64788));
#16074=EDGE_LOOP('',(#64789,#64790,#64791,#64792,#64793));
#16075=EDGE_LOOP('',(#64794,#64795,#64796,#64797,#64798));
#16076=EDGE_LOOP('',(#64799,#64800,#64801,#64802));
#16077=EDGE_LOOP('',(#64803,#64804,#64805,#64806));
#16078=EDGE_LOOP('',(#64807,#64808,#64809,#64810));
#16079=EDGE_LOOP('',(#64811,#64812,#64813,#64814));
#16080=EDGE_LOOP('',(#64815,#64816,#64817,#64818));
#16081=EDGE_LOOP('',(#64819,#64820,#64821,#64822));
#16082=EDGE_LOOP('',(#64823,#64824,#64825,#64826));
#16083=EDGE_LOOP('',(#64827,#64828,#64829,#64830));
#16084=EDGE_LOOP('',(#64831,#64832,#64833,#64834));
#16085=EDGE_LOOP('',(#64835,#64836,#64837,#64838));
#16086=EDGE_LOOP('',(#64839,#64840,#64841,#64842));
#16087=EDGE_LOOP('',(#64843,#64844,#64845,#64846));
#16088=EDGE_LOOP('',(#64847,#64848,#64849,#64850));
#16089=EDGE_LOOP('',(#64851,#64852,#64853,#64854));
#16090=EDGE_LOOP('',(#64855,#64856,#64857,#64858));
#16091=EDGE_LOOP('',(#64859,#64860,#64861,#64862));
#16092=EDGE_LOOP('',(#64863,#64864,#64865,#64866));
#16093=EDGE_LOOP('',(#64867,#64868,#64869,#64870));
#16094=EDGE_LOOP('',(#64871,#64872,#64873,#64874));
#16095=EDGE_LOOP('',(#64875,#64876,#64877,#64878));
#16096=EDGE_LOOP('',(#64879,#64880,#64881,#64882));
#16097=EDGE_LOOP('',(#64883,#64884,#64885,#64886));
#16098=EDGE_LOOP('',(#64887,#64888,#64889,#64890));
#16099=EDGE_LOOP('',(#64891,#64892,#64893,#64894));
#16100=EDGE_LOOP('',(#64895,#64896,#64897,#64898));
#16101=EDGE_LOOP('',(#64899,#64900,#64901,#64902));
#16102=EDGE_LOOP('',(#64903,#64904,#64905,#64906));
#16103=EDGE_LOOP('',(#64907,#64908,#64909,#64910));
#16104=EDGE_LOOP('',(#64911,#64912,#64913,#64914));
#16105=EDGE_LOOP('',(#64915,#64916,#64917,#64918,#64919));
#16106=EDGE_LOOP('',(#64920,#64921,#64922,#64923));
#16107=EDGE_LOOP('',(#64924,#64925,#64926,#64927));
#16108=EDGE_LOOP('',(#64928,#64929,#64930,#64931));
#16109=EDGE_LOOP('',(#64932,#64933,#64934,#64935));
#16110=EDGE_LOOP('',(#64936,#64937,#64938,#64939));
#16111=EDGE_LOOP('',(#64940,#64941,#64942,#64943));
#16112=EDGE_LOOP('',(#64944,#64945,#64946,#64947));
#16113=EDGE_LOOP('',(#64948,#64949,#64950,#64951));
#16114=EDGE_LOOP('',(#64952,#64953,#64954,#64955));
#16115=EDGE_LOOP('',(#64956,#64957,#64958,#64959));
#16116=EDGE_LOOP('',(#64960,#64961,#64962,#64963));
#16117=EDGE_LOOP('',(#64964,#64965,#64966,#64967));
#16118=EDGE_LOOP('',(#64968,#64969,#64970,#64971));
#16119=EDGE_LOOP('',(#64972,#64973,#64974,#64975));
#16120=EDGE_LOOP('',(#64976,#64977,#64978,#64979));
#16121=EDGE_LOOP('',(#64980,#64981,#64982,#64983));
#16122=EDGE_LOOP('',(#64984,#64985,#64986,#64987));
#16123=EDGE_LOOP('',(#64988,#64989,#64990,#64991));
#16124=EDGE_LOOP('',(#64992,#64993,#64994,#64995));
#16125=EDGE_LOOP('',(#64996,#64997,#64998,#64999));
#16126=EDGE_LOOP('',(#65000,#65001,#65002,#65003));
#16127=EDGE_LOOP('',(#65004,#65005,#65006,#65007));
#16128=EDGE_LOOP('',(#65008,#65009,#65010,#65011));
#16129=EDGE_LOOP('',(#65012,#65013,#65014,#65015));
#16130=EDGE_LOOP('',(#65016,#65017,#65018,#65019));
#16131=EDGE_LOOP('',(#65020,#65021,#65022,#65023));
#16132=EDGE_LOOP('',(#65024,#65025,#65026,#65027));
#16133=EDGE_LOOP('',(#65028,#65029,#65030,#65031));
#16134=EDGE_LOOP('',(#65032,#65033,#65034,#65035));
#16135=EDGE_LOOP('',(#65036,#65037,#65038,#65039));
#16136=EDGE_LOOP('',(#65040,#65041,#65042,#65043));
#16137=EDGE_LOOP('',(#65044,#65045,#65046,#65047));
#16138=EDGE_LOOP('',(#65048,#65049,#65050,#65051));
#16139=EDGE_LOOP('',(#65052,#65053,#65054,#65055));
#16140=EDGE_LOOP('',(#65056,#65057,#65058,#65059));
#16141=EDGE_LOOP('',(#65060,#65061,#65062,#65063));
#16142=EDGE_LOOP('',(#65064,#65065,#65066,#65067));
#16143=EDGE_LOOP('',(#65068,#65069,#65070,#65071));
#16144=EDGE_LOOP('',(#65072,#65073,#65074,#65075));
#16145=EDGE_LOOP('',(#65076,#65077,#65078,#65079));
#16146=EDGE_LOOP('',(#65080,#65081,#65082,#65083));
#16147=EDGE_LOOP('',(#65084,#65085,#65086,#65087));
#16148=EDGE_LOOP('',(#65088,#65089,#65090,#65091));
#16149=EDGE_LOOP('',(#65092,#65093,#65094,#65095));
#16150=EDGE_LOOP('',(#65096,#65097,#65098,#65099));
#16151=EDGE_LOOP('',(#65100,#65101,#65102,#65103));
#16152=EDGE_LOOP('',(#65104,#65105,#65106,#65107));
#16153=EDGE_LOOP('',(#65108,#65109,#65110,#65111));
#16154=EDGE_LOOP('',(#65112,#65113,#65114,#65115));
#16155=EDGE_LOOP('',(#65116,#65117,#65118,#65119));
#16156=EDGE_LOOP('',(#65120,#65121,#65122,#65123));
#16157=EDGE_LOOP('',(#65124,#65125,#65126,#65127));
#16158=EDGE_LOOP('',(#65128,#65129,#65130,#65131));
#16159=EDGE_LOOP('',(#65132,#65133,#65134,#65135));
#16160=EDGE_LOOP('',(#65136,#65137,#65138,#65139));
#16161=EDGE_LOOP('',(#65140,#65141,#65142,#65143));
#16162=EDGE_LOOP('',(#65144,#65145,#65146,#65147));
#16163=EDGE_LOOP('',(#65148,#65149,#65150,#65151));
#16164=EDGE_LOOP('',(#65152,#65153,#65154,#65155));
#16165=EDGE_LOOP('',(#65156,#65157,#65158,#65159));
#16166=EDGE_LOOP('',(#65160,#65161,#65162,#65163));
#16167=EDGE_LOOP('',(#65164,#65165,#65166,#65167));
#16168=EDGE_LOOP('',(#65168,#65169,#65170,#65171));
#16169=EDGE_LOOP('',(#65172,#65173,#65174,#65175));
#16170=EDGE_LOOP('',(#65176,#65177,#65178,#65179));
#16171=EDGE_LOOP('',(#65180,#65181,#65182,#65183));
#16172=EDGE_LOOP('',(#65184,#65185,#65186,#65187));
#16173=EDGE_LOOP('',(#65188,#65189,#65190,#65191));
#16174=EDGE_LOOP('',(#65192,#65193,#65194,#65195));
#16175=EDGE_LOOP('',(#65196,#65197,#65198,#65199));
#16176=EDGE_LOOP('',(#65200,#65201,#65202,#65203));
#16177=EDGE_LOOP('',(#65204,#65205,#65206,#65207));
#16178=EDGE_LOOP('',(#65208,#65209,#65210,#65211));
#16179=EDGE_LOOP('',(#65212,#65213,#65214,#65215));
#16180=EDGE_LOOP('',(#65216,#65217,#65218,#65219,#65220));
#16181=EDGE_LOOP('',(#65221,#65222,#65223,#65224));
#16182=EDGE_LOOP('',(#65225,#65226,#65227,#65228));
#16183=EDGE_LOOP('',(#65229,#65230,#65231,#65232));
#16184=EDGE_LOOP('',(#65233,#65234,#65235,#65236));
#16185=EDGE_LOOP('',(#65237,#65238,#65239,#65240));
#16186=EDGE_LOOP('',(#65241,#65242,#65243,#65244));
#16187=EDGE_LOOP('',(#65245,#65246,#65247,#65248));
#16188=EDGE_LOOP('',(#65249,#65250,#65251,#65252));
#16189=EDGE_LOOP('',(#65253,#65254,#65255,#65256));
#16190=EDGE_LOOP('',(#65257,#65258,#65259,#65260));
#16191=EDGE_LOOP('',(#65261,#65262,#65263,#65264));
#16192=EDGE_LOOP('',(#65265,#65266,#65267,#65268));
#16193=EDGE_LOOP('',(#65269,#65270,#65271,#65272));
#16194=EDGE_LOOP('',(#65273,#65274,#65275,#65276));
#16195=EDGE_LOOP('',(#65277,#65278,#65279,#65280));
#16196=EDGE_LOOP('',(#65281,#65282,#65283,#65284));
#16197=EDGE_LOOP('',(#65285,#65286,#65287,#65288));
#16198=EDGE_LOOP('',(#65289,#65290,#65291,#65292));
#16199=EDGE_LOOP('',(#65293,#65294,#65295,#65296));
#16200=EDGE_LOOP('',(#65297,#65298,#65299,#65300));
#16201=EDGE_LOOP('',(#65301,#65302,#65303,#65304));
#16202=EDGE_LOOP('',(#65305,#65306,#65307,#65308));
#16203=EDGE_LOOP('',(#65309,#65310,#65311,#65312));
#16204=EDGE_LOOP('',(#65313,#65314,#65315,#65316));
#16205=EDGE_LOOP('',(#65317,#65318,#65319,#65320));
#16206=EDGE_LOOP('',(#65321,#65322,#65323,#65324));
#16207=EDGE_LOOP('',(#65325,#65326,#65327,#65328));
#16208=EDGE_LOOP('',(#65329,#65330,#65331,#65332));
#16209=EDGE_LOOP('',(#65333,#65334,#65335,#65336));
#16210=EDGE_LOOP('',(#65337,#65338,#65339,#65340));
#16211=EDGE_LOOP('',(#65341,#65342,#65343,#65344));
#16212=EDGE_LOOP('',(#65345,#65346,#65347,#65348));
#16213=EDGE_LOOP('',(#65349,#65350,#65351,#65352));
#16214=EDGE_LOOP('',(#65353,#65354,#65355,#65356));
#16215=EDGE_LOOP('',(#65357,#65358,#65359,#65360));
#16216=EDGE_LOOP('',(#65361,#65362,#65363,#65364));
#16217=EDGE_LOOP('',(#65365,#65366,#65367,#65368));
#16218=EDGE_LOOP('',(#65369,#65370,#65371,#65372));
#16219=EDGE_LOOP('',(#65373,#65374,#65375,#65376));
#16220=EDGE_LOOP('',(#65377,#65378,#65379,#65380));
#16221=EDGE_LOOP('',(#65381,#65382,#65383,#65384));
#16222=EDGE_LOOP('',(#65385,#65386,#65387,#65388));
#16223=EDGE_LOOP('',(#65389,#65390,#65391,#65392));
#16224=EDGE_LOOP('',(#65393,#65394,#65395,#65396));
#16225=EDGE_LOOP('',(#65397,#65398,#65399,#65400));
#16226=EDGE_LOOP('',(#65401,#65402,#65403,#65404));
#16227=EDGE_LOOP('',(#65405,#65406,#65407,#65408));
#16228=EDGE_LOOP('',(#65409,#65410,#65411,#65412));
#16229=EDGE_LOOP('',(#65413,#65414,#65415,#65416));
#16230=EDGE_LOOP('',(#65417,#65418,#65419,#65420));
#16231=EDGE_LOOP('',(#65421,#65422,#65423,#65424));
#16232=EDGE_LOOP('',(#65425,#65426,#65427,#65428));
#16233=EDGE_LOOP('',(#65429,#65430,#65431,#65432));
#16234=EDGE_LOOP('',(#65433,#65434,#65435,#65436));
#16235=EDGE_LOOP('',(#65437,#65438,#65439,#65440));
#16236=EDGE_LOOP('',(#65441,#65442,#65443,#65444));
#16237=EDGE_LOOP('',(#65445,#65446,#65447,#65448));
#16238=EDGE_LOOP('',(#65449,#65450,#65451,#65452));
#16239=EDGE_LOOP('',(#65453,#65454,#65455,#65456));
#16240=EDGE_LOOP('',(#65457,#65458,#65459,#65460));
#16241=EDGE_LOOP('',(#65461,#65462,#65463,#65464));
#16242=EDGE_LOOP('',(#65465,#65466,#65467,#65468));
#16243=EDGE_LOOP('',(#65469,#65470,#65471,#65472));
#16244=EDGE_LOOP('',(#65473,#65474,#65475,#65476));
#16245=EDGE_LOOP('',(#65477,#65478,#65479,#65480));
#16246=EDGE_LOOP('',(#65481,#65482,#65483,#65484));
#16247=EDGE_LOOP('',(#65485,#65486,#65487,#65488));
#16248=EDGE_LOOP('',(#65489,#65490,#65491,#65492));
#16249=EDGE_LOOP('',(#65493,#65494,#65495,#65496));
#16250=EDGE_LOOP('',(#65497,#65498,#65499,#65500));
#16251=EDGE_LOOP('',(#65501,#65502,#65503,#65504));
#16252=EDGE_LOOP('',(#65505,#65506,#65507,#65508));
#16253=EDGE_LOOP('',(#65509,#65510,#65511,#65512));
#16254=EDGE_LOOP('',(#65513,#65514,#65515,#65516));
#16255=EDGE_LOOP('',(#65517,#65518,#65519,#65520));
#16256=EDGE_LOOP('',(#65521,#65522,#65523,#65524));
#16257=EDGE_LOOP('',(#65525,#65526,#65527,#65528));
#16258=EDGE_LOOP('',(#65529,#65530,#65531,#65532));
#16259=EDGE_LOOP('',(#65533,#65534,#65535,#65536));
#16260=EDGE_LOOP('',(#65537,#65538,#65539,#65540));
#16261=EDGE_LOOP('',(#65541,#65542,#65543,#65544));
#16262=EDGE_LOOP('',(#65545,#65546,#65547,#65548));
#16263=EDGE_LOOP('',(#65549,#65550,#65551,#65552));
#16264=EDGE_LOOP('',(#65553,#65554,#65555,#65556));
#16265=EDGE_LOOP('',(#65557,#65558,#65559,#65560));
#16266=EDGE_LOOP('',(#65561,#65562,#65563,#65564));
#16267=EDGE_LOOP('',(#65565,#65566,#65567,#65568));
#16268=EDGE_LOOP('',(#65569,#65570,#65571,#65572));
#16269=EDGE_LOOP('',(#65573,#65574,#65575,#65576));
#16270=EDGE_LOOP('',(#65577,#65578,#65579,#65580));
#16271=EDGE_LOOP('',(#65581,#65582,#65583,#65584));
#16272=EDGE_LOOP('',(#65585,#65586,#65587,#65588));
#16273=EDGE_LOOP('',(#65589,#65590,#65591,#65592));
#16274=EDGE_LOOP('',(#65593,#65594,#65595,#65596));
#16275=EDGE_LOOP('',(#65597,#65598,#65599,#65600));
#16276=EDGE_LOOP('',(#65601,#65602,#65603,#65604,#65605));
#16277=EDGE_LOOP('',(#65606,#65607,#65608,#65609));
#16278=EDGE_LOOP('',(#65610,#65611,#65612,#65613));
#16279=EDGE_LOOP('',(#65614,#65615,#65616,#65617));
#16280=EDGE_LOOP('',(#65618,#65619,#65620,#65621));
#16281=EDGE_LOOP('',(#65622,#65623,#65624,#65625));
#16282=EDGE_LOOP('',(#65626,#65627,#65628,#65629));
#16283=EDGE_LOOP('',(#65630,#65631,#65632,#65633));
#16284=EDGE_LOOP('',(#65634,#65635,#65636,#65637));
#16285=EDGE_LOOP('',(#65638,#65639,#65640,#65641));
#16286=EDGE_LOOP('',(#65642,#65643,#65644,#65645));
#16287=EDGE_LOOP('',(#65646,#65647,#65648,#65649));
#16288=EDGE_LOOP('',(#65650,#65651,#65652,#65653));
#16289=EDGE_LOOP('',(#65654,#65655,#65656,#65657));
#16290=EDGE_LOOP('',(#65658,#65659,#65660,#65661));
#16291=EDGE_LOOP('',(#65662,#65663,#65664,#65665));
#16292=EDGE_LOOP('',(#65666,#65667,#65668,#65669));
#16293=EDGE_LOOP('',(#65670,#65671,#65672,#65673));
#16294=EDGE_LOOP('',(#65674,#65675,#65676,#65677));
#16295=EDGE_LOOP('',(#65678,#65679,#65680,#65681));
#16296=EDGE_LOOP('',(#65682,#65683,#65684));
#16297=EDGE_LOOP('',(#65685,#65686,#65687,#65688,#65689,#65690,#65691,#65692));
#16298=EDGE_LOOP('',(#65693,#65694,#65695,#65696,#65697));
#16299=EDGE_LOOP('',(#65698,#65699,#65700,#65701));
#16300=EDGE_LOOP('',(#65702,#65703,#65704,#65705));
#16301=EDGE_LOOP('',(#65706,#65707,#65708,#65709,#65710,#65711,#65712,#65713,
#65714));
#16302=EDGE_LOOP('',(#65715,#65716,#65717,#65718));
#16303=EDGE_LOOP('',(#65719,#65720,#65721,#65722,#65723,#65724,#65725,#65726,
#65727,#65728,#65729,#65730,#65731,#65732,#65733,#65734,#65735));
#16304=EDGE_LOOP('',(#65736,#65737,#65738,#65739));
#16305=EDGE_LOOP('',(#65740,#65741,#65742,#65743));
#16306=EDGE_LOOP('',(#65744,#65745,#65746,#65747));
#16307=EDGE_LOOP('',(#65748,#65749,#65750,#65751,#65752,#65753,#65754,#65755,
#65756,#65757,#65758,#65759,#65760,#65761,#65762,#65763,#65764));
#16308=EDGE_LOOP('',(#65765,#65766,#65767,#65768,#65769,#65770));
#16309=EDGE_LOOP('',(#65771,#65772,#65773,#65774,#65775,#65776,#65777,#65778,
#65779,#65780,#65781,#65782,#65783,#65784,#65785,#65786,#65787,#65788,#65789,
#65790,#65791,#65792,#65793,#65794,#65795,#65796,#65797,#65798,#65799,#65800,
#65801,#65802,#65803,#65804,#65805,#65806,#65807,#65808,#65809,#65810,#65811,
#65812,#65813,#65814));
#16310=EDGE_LOOP('',(#65815,#65816,#65817,#65818,#65819,#65820));
#16311=EDGE_LOOP('',(#65821,#65822,#65823,#65824,#65825,#65826,#65827,#65828,
#65829,#65830,#65831,#65832,#65833,#65834,#65835,#65836,#65837));
#16312=EDGE_LOOP('',(#65838,#65839,#65840,#65841));
#16313=EDGE_LOOP('',(#65842,#65843,#65844,#65845));
#16314=EDGE_LOOP('',(#65846,#65847,#65848,#65849));
#16315=EDGE_LOOP('',(#65850,#65851,#65852,#65853,#65854,#65855,#65856));
#16316=EDGE_LOOP('',(#65857,#65858,#65859,#65860));
#16317=EDGE_LOOP('',(#65861,#65862,#65863,#65864));
#16318=EDGE_LOOP('',(#65865,#65866,#65867,#65868));
#16319=EDGE_LOOP('',(#65869,#65870,#65871,#65872));
#16320=EDGE_LOOP('',(#65873,#65874,#65875,#65876));
#16321=EDGE_LOOP('',(#65877,#65878,#65879,#65880));
#16322=EDGE_LOOP('',(#65881,#65882,#65883,#65884));
#16323=EDGE_LOOP('',(#65885,#65886,#65887,#65888));
#16324=EDGE_LOOP('',(#65889,#65890,#65891,#65892));
#16325=EDGE_LOOP('',(#65893,#65894,#65895,#65896));
#16326=EDGE_LOOP('',(#65897,#65898,#65899,#65900));
#16327=EDGE_LOOP('',(#65901,#65902,#65903,#65904));
#16328=EDGE_LOOP('',(#65905,#65906,#65907,#65908));
#16329=EDGE_LOOP('',(#65909,#65910,#65911,#65912));
#16330=EDGE_LOOP('',(#65913,#65914,#65915,#65916));
#16331=EDGE_LOOP('',(#65917,#65918,#65919,#65920));
#16332=EDGE_LOOP('',(#65921,#65922,#65923,#65924));
#16333=EDGE_LOOP('',(#65925,#65926,#65927,#65928));
#16334=EDGE_LOOP('',(#65929,#65930,#65931,#65932));
#16335=EDGE_LOOP('',(#65933,#65934,#65935,#65936));
#16336=EDGE_LOOP('',(#65937,#65938,#65939));
#16337=EDGE_LOOP('',(#65940,#65941,#65942,#65943,#65944));
#16338=EDGE_LOOP('',(#65945,#65946,#65947,#65948));
#16339=EDGE_LOOP('',(#65949,#65950,#65951,#65952));
#16340=EDGE_LOOP('',(#65953,#65954,#65955,#65956));
#16341=EDGE_LOOP('',(#65957,#65958,#65959,#65960));
#16342=EDGE_LOOP('',(#65961,#65962,#65963,#65964));
#16343=EDGE_LOOP('',(#65965,#65966,#65967,#65968,#65969));
#16344=EDGE_LOOP('',(#65970,#65971,#65972,#65973,#65974));
#16345=EDGE_LOOP('',(#65975,#65976,#65977,#65978));
#16346=EDGE_LOOP('',(#65979,#65980,#65981,#65982));
#16347=EDGE_LOOP('',(#65983,#65984,#65985,#65986));
#16348=EDGE_LOOP('',(#65987,#65988,#65989,#65990));
#16349=EDGE_LOOP('',(#65991,#65992,#65993,#65994));
#16350=EDGE_LOOP('',(#65995,#65996,#65997,#65998));
#16351=EDGE_LOOP('',(#65999,#66000,#66001,#66002));
#16352=EDGE_LOOP('',(#66003,#66004,#66005,#66006));
#16353=EDGE_LOOP('',(#66007,#66008,#66009,#66010));
#16354=EDGE_LOOP('',(#66011,#66012,#66013,#66014));
#16355=EDGE_LOOP('',(#66015,#66016,#66017,#66018));
#16356=EDGE_LOOP('',(#66019,#66020,#66021,#66022));
#16357=EDGE_LOOP('',(#66023,#66024,#66025,#66026));
#16358=EDGE_LOOP('',(#66027,#66028,#66029,#66030));
#16359=EDGE_LOOP('',(#66031,#66032,#66033,#66034,#66035,#66036,#66037,#66038));
#16360=EDGE_LOOP('',(#66039));
#16361=EDGE_LOOP('',(#66040));
#16362=EDGE_LOOP('',(#66041,#66042,#66043,#66044));
#16363=EDGE_LOOP('',(#66045,#66046,#66047,#66048));
#16364=EDGE_LOOP('',(#66049,#66050,#66051,#66052));
#16365=EDGE_LOOP('',(#66053,#66054,#66055,#66056));
#16366=EDGE_LOOP('',(#66057,#66058,#66059,#66060));
#16367=EDGE_LOOP('',(#66061,#66062,#66063,#66064));
#16368=EDGE_LOOP('',(#66065,#66066,#66067,#66068));
#16369=EDGE_LOOP('',(#66069,#66070,#66071,#66072,#66073,#66074));
#16370=EDGE_LOOP('',(#66075));
#16371=EDGE_LOOP('',(#66076));
#16372=EDGE_LOOP('',(#66077,#66078,#66079,#66080));
#16373=EDGE_LOOP('',(#66081,#66082,#66083,#66084));
#16374=EDGE_LOOP('',(#66085,#66086,#66087));
#16375=EDGE_LOOP('',(#66088,#66089,#66090,#66091,#66092,#66093,#66094,#66095,
#66096,#66097,#66098,#66099,#66100,#66101,#66102,#66103,#66104,#66105));
#16376=EDGE_LOOP('',(#66106,#66107,#66108,#66109,#66110));
#16377=EDGE_LOOP('',(#66111,#66112,#66113,#66114));
#16378=EDGE_LOOP('',(#66115,#66116,#66117,#66118));
#16379=EDGE_LOOP('',(#66119,#66120,#66121,#66122));
#16380=EDGE_LOOP('',(#66123,#66124,#66125,#66126,#66127,#66128,#66129,#66130,
#66131,#66132,#66133,#66134,#66135,#66136,#66137,#66138,#66139,#66140));
#16381=EDGE_LOOP('',(#66141,#66142,#66143,#66144));
#16382=EDGE_LOOP('',(#66145,#66146,#66147,#66148));
#16383=EDGE_LOOP('',(#66149,#66150,#66151,#66152));
#16384=EDGE_LOOP('',(#66153,#66154,#66155,#66156,#66157,#66158,#66159,#66160,
#66161,#66162,#66163,#66164,#66165,#66166,#66167,#66168,#66169,#66170));
#16385=EDGE_LOOP('',(#66171,#66172,#66173,#66174));
#16386=EDGE_LOOP('',(#66175,#66176,#66177,#66178));
#16387=EDGE_LOOP('',(#66179,#66180,#66181,#66182));
#16388=EDGE_LOOP('',(#66183,#66184,#66185,#66186,#66187,#66188,#66189,#66190,
#66191,#66192,#66193,#66194,#66195,#66196,#66197,#66198));
#16389=EDGE_LOOP('',(#66199,#66200,#66201,#66202));
#16390=EDGE_LOOP('',(#66203,#66204,#66205,#66206,#66207,#66208,#66209,#66210,
#66211,#66212,#66213,#66214,#66215,#66216,#66217,#66218));
#16391=EDGE_LOOP('',(#66219,#66220,#66221,#66222));
#16392=EDGE_LOOP('',(#66223,#66224,#66225,#66226,#66227));
#16393=EDGE_LOOP('',(#66228,#66229,#66230,#66231,#66232,#66233,#66234,#66235,
#66236,#66237,#66238,#66239,#66240,#66241,#66242,#66243,#66244,#66245));
#16394=EDGE_LOOP('',(#66246,#66247,#66248,#66249));
#16395=EDGE_LOOP('',(#66250,#66251,#66252,#66253));
#16396=EDGE_LOOP('',(#66254,#66255,#66256,#66257));
#16397=EDGE_LOOP('',(#66258,#66259,#66260,#66261,#66262,#66263,#66264,#66265,
#66266,#66267,#66268,#66269,#66270,#66271,#66272,#66273,#66274,#66275));
#16398=EDGE_LOOP('',(#66276,#66277,#66278,#66279));
#16399=EDGE_LOOP('',(#66280,#66281,#66282));
#16400=EDGE_LOOP('',(#66283,#66284,#66285,#66286,#66287,#66288));
#16401=EDGE_LOOP('',(#66289,#66290,#66291));
#16402=EDGE_LOOP('',(#66292,#66293,#66294,#66295));
#16403=EDGE_LOOP('',(#66296,#66297,#66298,#66299,#66300,#66301,#66302,#66303,
#66304,#66305,#66306,#66307,#66308,#66309,#66310,#66311,#66312));
#16404=EDGE_LOOP('',(#66313,#66314,#66315,#66316,#66317,#66318,#66319,#66320,
#66321,#66322,#66323,#66324,#66325,#66326,#66327,#66328,#66329,#66330));
#16405=EDGE_LOOP('',(#66331,#66332,#66333,#66334));
#16406=EDGE_LOOP('',(#66335,#66336,#66337,#66338));
#16407=EDGE_LOOP('',(#66339,#66340,#66341,#66342));
#16408=EDGE_LOOP('',(#66343,#66344,#66345,#66346));
#16409=EDGE_LOOP('',(#66347,#66348,#66349,#66350,#66351,#66352,#66353,#66354,
#66355,#66356,#66357,#66358,#66359,#66360,#66361,#66362,#66363,#66364));
#16410=EDGE_LOOP('',(#66365,#66366,#66367,#66368));
#16411=EDGE_LOOP('',(#66369,#66370,#66371,#66372));
#16412=EDGE_LOOP('',(#66373,#66374,#66375,#66376));
#16413=EDGE_LOOP('',(#66377,#66378,#66379,#66380,#66381,#66382,#66383,#66384,
#66385,#66386,#66387,#66388));
#16414=EDGE_LOOP('',(#66389,#66390,#66391,#66392));
#16415=EDGE_LOOP('',(#66393,#66394,#66395,#66396));
#16416=EDGE_LOOP('',(#66397,#66398,#66399,#66400));
#16417=EDGE_LOOP('',(#66401,#66402,#66403,#66404,#66405,#66406,#66407,#66408));
#16418=EDGE_LOOP('',(#66409,#66410,#66411,#66412));
#16419=EDGE_LOOP('',(#66413,#66414,#66415,#66416));
#16420=EDGE_LOOP('',(#66417,#66418,#66419,#66420,#66421,#66422,#66423,#66424,
#66425,#66426,#66427));
#16421=EDGE_LOOP('',(#66428,#66429,#66430,#66431));
#16422=EDGE_LOOP('',(#66432,#66433,#66434,#66435));
#16423=EDGE_LOOP('',(#66436,#66437,#66438,#66439));
#16424=EDGE_LOOP('',(#66440,#66441,#66442,#66443,#66444,#66445,#66446,#66447,
#66448,#66449,#66450,#66451));
#16425=EDGE_LOOP('',(#66452,#66453,#66454,#66455));
#16426=EDGE_LOOP('',(#66456,#66457,#66458,#66459));
#16427=EDGE_LOOP('',(#66460,#66461,#66462,#66463));
#16428=EDGE_LOOP('',(#66464,#66465,#66466,#66467,#66468,#66469,#66470,#66471,
#66472,#66473,#66474,#66475,#66476,#66477,#66478,#66479,#66480,#66481));
#16429=EDGE_LOOP('',(#66482,#66483,#66484,#66485));
#16430=EDGE_LOOP('',(#66486,#66487,#66488,#66489));
#16431=EDGE_LOOP('',(#66490,#66491,#66492,#66493));
#16432=EDGE_LOOP('',(#66494,#66495,#66496,#66497,#66498,#66499,#66500,#66501,
#66502,#66503,#66504,#66505,#66506,#66507,#66508,#66509,#66510,#66511));
#16433=EDGE_LOOP('',(#66512,#66513,#66514,#66515));
#16434=EDGE_LOOP('',(#66516,#66517,#66518));
#16435=EDGE_LOOP('',(#66519,#66520,#66521,#66522,#66523));
#16436=EDGE_LOOP('',(#66524,#66525,#66526,#66527,#66528,#66529,#66530,#66531,
#66532,#66533,#66534,#66535,#66536,#66537,#66538,#66539));
#16437=EDGE_LOOP('',(#66540,#66541,#66542,#66543));
#16438=EDGE_LOOP('',(#66544,#66545,#66546,#66547));
#16439=EDGE_LOOP('',(#66548,#66549,#66550,#66551,#66552,#66553,#66554,#66555,
#66556,#66557,#66558,#66559,#66560,#66561,#66562,#66563));
#16440=EDGE_LOOP('',(#66564,#66565,#66566,#66567));
#16441=EDGE_LOOP('',(#66568,#66569,#66570,#66571));
#16442=EDGE_LOOP('',(#66572,#66573,#66574,#66575));
#16443=EDGE_LOOP('',(#66576,#66577,#66578,#66579,#66580,#66581,#66582,#66583,
#66584,#66585,#66586,#66587,#66588,#66589,#66590,#66591,#66592));
#16444=EDGE_LOOP('',(#66593,#66594,#66595,#66596));
#16445=EDGE_LOOP('',(#66597,#66598,#66599,#66600));
#16446=EDGE_LOOP('',(#66601,#66602,#66603,#66604,#66605));
#16447=EDGE_LOOP('',(#66606,#66607,#66608,#66609,#66610,#66611,#66612,#66613,
#66614,#66615,#66616,#66617,#66618,#66619));
#16448=EDGE_LOOP('',(#66620,#66621,#66622,#66623));
#16449=EDGE_LOOP('',(#66624,#66625,#66626,#66627));
#16450=EDGE_LOOP('',(#66628,#66629,#66630,#66631,#66632,#66633,#66634,#66635,
#66636,#66637,#66638,#66639,#66640,#66641));
#16451=EDGE_LOOP('',(#66642,#66643,#66644,#66645));
#16452=EDGE_LOOP('',(#66646,#66647,#66648,#66649));
#16453=EDGE_LOOP('',(#66650,#66651,#66652,#66653));
#16454=EDGE_LOOP('',(#66654,#66655,#66656,#66657));
#16455=EDGE_LOOP('',(#66658,#66659,#66660,#66661,#66662,#66663,#66664,#66665,
#66666,#66667,#66668,#66669,#66670));
#16456=EDGE_LOOP('',(#66671,#66672,#66673,#66674));
#16457=EDGE_LOOP('',(#66675,#66676,#66677,#66678));
#16458=EDGE_LOOP('',(#66679,#66680,#66681,#66682,#66683,#66684,#66685,#66686,
#66687,#66688,#66689,#66690));
#16459=EDGE_LOOP('',(#66691,#66692,#66693,#66694));
#16460=EDGE_LOOP('',(#66695,#66696,#66697,#66698));
#16461=EDGE_LOOP('',(#66699,#66700,#66701,#66702));
#16462=EDGE_LOOP('',(#66703,#66704,#66705,#66706));
#16463=EDGE_LOOP('',(#66707,#66708,#66709,#66710,#66711,#66712,#66713,#66714,
#66715,#66716,#66717,#66718));
#16464=EDGE_LOOP('',(#66719,#66720,#66721,#66722));
#16465=EDGE_LOOP('',(#66723,#66724,#66725,#66726));
#16466=EDGE_LOOP('',(#66727,#66728,#66729,#66730,#66731,#66732,#66733,#66734,
#66735,#66736,#66737,#66738));
#16467=EDGE_LOOP('',(#66739,#66740,#66741,#66742));
#16468=EDGE_LOOP('',(#66743,#66744,#66745,#66746));
#16469=EDGE_LOOP('',(#66747,#66748,#66749,#66750));
#16470=EDGE_LOOP('',(#66751,#66752,#66753,#66754));
#16471=EDGE_LOOP('',(#66755,#66756,#66757,#66758,#66759,#66760,#66761,#66762,
#66763,#66764,#66765,#66766));
#16472=EDGE_LOOP('',(#66767,#66768,#66769,#66770));
#16473=EDGE_LOOP('',(#66771,#66772,#66773,#66774));
#16474=EDGE_LOOP('',(#66775,#66776,#66777,#66778,#66779,#66780,#66781,#66782,
#66783,#66784,#66785,#66786));
#16475=EDGE_LOOP('',(#66787,#66788,#66789,#66790));
#16476=EDGE_LOOP('',(#66791,#66792,#66793,#66794));
#16477=EDGE_LOOP('',(#66795,#66796,#66797,#66798));
#16478=EDGE_LOOP('',(#66799,#66800,#66801,#66802));
#16479=EDGE_LOOP('',(#66803,#66804,#66805,#66806,#66807,#66808,#66809,#66810,
#66811,#66812,#66813,#66814));
#16480=EDGE_LOOP('',(#66815,#66816,#66817,#66818));
#16481=EDGE_LOOP('',(#66819,#66820,#66821,#66822));
#16482=EDGE_LOOP('',(#66823,#66824,#66825,#66826,#66827,#66828,#66829,#66830,
#66831,#66832,#66833,#66834,#66835));
#16483=EDGE_LOOP('',(#66836,#66837,#66838,#66839));
#16484=EDGE_LOOP('',(#66840,#66841,#66842,#66843));
#16485=EDGE_LOOP('',(#66844,#66845,#66846,#66847));
#16486=EDGE_LOOP('',(#66848,#66849,#66850,#66851));
#16487=EDGE_LOOP('',(#66852,#66853,#66854,#66855,#66856,#66857,#66858,#66859,
#66860,#66861,#66862,#66863,#66864,#66865));
#16488=EDGE_LOOP('',(#66866,#66867,#66868,#66869));
#16489=EDGE_LOOP('',(#66870,#66871,#66872,#66873));
#16490=EDGE_LOOP('',(#66874,#66875,#66876,#66877));
#16491=EDGE_LOOP('',(#66878,#66879,#66880,#66881,#66882,#66883,#66884,#66885,
#66886,#66887,#66888,#66889,#66890,#66891));
#16492=EDGE_LOOP('',(#66892,#66893,#66894,#66895,#66896));
#16493=EDGE_LOOP('',(#66897,#66898,#66899,#66900));
#16494=EDGE_LOOP('',(#66901,#66902,#66903,#66904,#66905));
#16495=EDGE_LOOP('',(#66906,#66907,#66908,#66909,#66910));
#16496=EDGE_LOOP('',(#66911,#66912,#66913,#66914));
#16497=EDGE_LOOP('',(#66915,#66916,#66917,#66918,#66919));
#16498=EDGE_LOOP('',(#66920,#66921,#66922,#66923,#66924,#66925,#66926));
#16499=EDGE_LOOP('',(#66927,#66928,#66929,#66930));
#16500=EDGE_LOOP('',(#66931,#66932,#66933,#66934));
#16501=EDGE_LOOP('',(#66935,#66936,#66937,#66938));
#16502=EDGE_LOOP('',(#66939,#66940,#66941,#66942,#66943,#66944,#66945));
#16503=EDGE_LOOP('',(#66946,#66947,#66948,#66949));
#16504=EDGE_LOOP('',(#66950,#66951,#66952,#66953));
#16505=EDGE_LOOP('',(#66954,#66955,#66956,#66957,#66958,#66959,#66960));
#16506=EDGE_LOOP('',(#66961,#66962,#66963,#66964));
#16507=EDGE_LOOP('',(#66965,#66966,#66967,#66968));
#16508=EDGE_LOOP('',(#66969,#66970,#66971,#66972));
#16509=EDGE_LOOP('',(#66973,#66974,#66975,#66976));
#16510=EDGE_LOOP('',(#66977,#66978,#66979,#66980,#66981,#66982,#66983,#66984,
#66985));
#16511=EDGE_LOOP('',(#66986,#66987,#66988,#66989));
#16512=EDGE_LOOP('',(#66990,#66991,#66992,#66993));
#16513=EDGE_LOOP('',(#66994,#66995,#66996,#66997));
#16514=EDGE_LOOP('',(#66998,#66999,#67000,#67001,#67002,#67003,#67004,#67005,
#67006,#67007));
#16515=EDGE_LOOP('',(#67008,#67009,#67010,#67011));
#16516=EDGE_LOOP('',(#67012,#67013,#67014,#67015));
#16517=EDGE_LOOP('',(#67016,#67017,#67018,#67019));
#16518=EDGE_LOOP('',(#67020,#67021,#67022,#67023,#67024,#67025,#67026,#67027,
#67028,#67029,#67030));
#16519=EDGE_LOOP('',(#67031,#67032,#67033,#67034));
#16520=EDGE_LOOP('',(#67035,#67036,#67037,#67038,#67039,#67040));
#16521=EDGE_LOOP('',(#67041,#67042,#67043,#67044));
#16522=EDGE_LOOP('',(#67045,#67046,#67047,#67048,#67049,#67050,#67051,#67052,
#67053,#67054,#67055,#67056,#67057,#67058));
#16523=EDGE_LOOP('',(#67059,#67060,#67061,#67062));
#16524=EDGE_LOOP('',(#67063,#67064,#67065,#67066));
#16525=EDGE_LOOP('',(#67067,#67068,#67069,#67070,#67071,#67072,#67073,#67074,
#67075,#67076,#67077,#67078,#67079,#67080));
#16526=EDGE_LOOP('',(#67081,#67082,#67083,#67084));
#16527=EDGE_LOOP('',(#67085,#67086,#67087,#67088));
#16528=EDGE_LOOP('',(#67089,#67090,#67091,#67092));
#16529=EDGE_LOOP('',(#67093,#67094,#67095,#67096));
#16530=EDGE_LOOP('',(#67097,#67098,#67099,#67100,#67101,#67102,#67103,#67104,
#67105,#67106,#67107,#67108,#67109,#67110));
#16531=EDGE_LOOP('',(#67111,#67112,#67113,#67114,#67115));
#16532=EDGE_LOOP('',(#67116,#67117,#67118,#67119));
#16533=EDGE_LOOP('',(#67120,#67121,#67122,#67123,#67124,#67125,#67126,#67127,
#67128,#67129,#67130,#67131));
#16534=EDGE_LOOP('',(#67132,#67133,#67134,#67135));
#16535=EDGE_LOOP('',(#67136,#67137,#67138,#67139));
#16536=EDGE_LOOP('',(#67140,#67141,#67142,#67143));
#16537=EDGE_LOOP('',(#67144,#67145,#67146,#67147));
#16538=EDGE_LOOP('',(#67148,#67149,#67150,#67151,#67152,#67153,#67154,#67155,
#67156,#67157,#67158,#67159));
#16539=EDGE_LOOP('',(#67160,#67161,#67162,#67163,#67164));
#16540=EDGE_LOOP('',(#67165,#67166,#67167,#67168));
#16541=EDGE_LOOP('',(#67169,#67170,#67171,#67172,#67173,#67174,#67175,#67176,
#67177,#67178,#67179,#67180));
#16542=EDGE_LOOP('',(#67181,#67182,#67183,#67184));
#16543=EDGE_LOOP('',(#67185,#67186,#67187,#67188));
#16544=EDGE_LOOP('',(#67189,#67190,#67191,#67192));
#16545=EDGE_LOOP('',(#67193,#67194,#67195,#67196));
#16546=EDGE_LOOP('',(#67197,#67198,#67199,#67200));
#16547=EDGE_LOOP('',(#67201,#67202,#67203,#67204));
#16548=EDGE_LOOP('',(#67205,#67206,#67207,#67208,#67209,#67210));
#16549=EDGE_LOOP('',(#67211,#67212,#67213,#67214));
#16550=EDGE_LOOP('',(#67215,#67216,#67217,#67218));
#16551=EDGE_LOOP('',(#67219,#67220,#67221,#67222));
#16552=EDGE_LOOP('',(#67223,#67224,#67225,#67226));
#16553=EDGE_LOOP('',(#67227,#67228,#67229,#67230));
#16554=EDGE_LOOP('',(#67231,#67232,#67233,#67234));
#16555=EDGE_LOOP('',(#67235,#67236,#67237,#67238));
#16556=EDGE_LOOP('',(#67239,#67240,#67241,#67242));
#16557=EDGE_LOOP('',(#67243,#67244,#67245,#67246));
#16558=EDGE_LOOP('',(#67247,#67248,#67249,#67250));
#16559=EDGE_LOOP('',(#67251,#67252,#67253,#67254));
#16560=EDGE_LOOP('',(#67255,#67256,#67257,#67258));
#16561=EDGE_LOOP('',(#67259,#67260,#67261,#67262));
#16562=EDGE_LOOP('',(#67263,#67264,#67265,#67266));
#16563=EDGE_LOOP('',(#67267,#67268,#67269,#67270));
#16564=EDGE_LOOP('',(#67271,#67272,#67273,#67274));
#16565=EDGE_LOOP('',(#67275,#67276,#67277,#67278));
#16566=EDGE_LOOP('',(#67279,#67280,#67281,#67282,#67283,#67284,#67285,#67286));
#16567=EDGE_LOOP('',(#67287,#67288,#67289,#67290,#67291,#67292,#67293,#67294));
#16568=EDGE_LOOP('',(#67295,#67296,#67297,#67298));
#16569=EDGE_LOOP('',(#67299,#67300,#67301,#67302));
#16570=EDGE_LOOP('',(#67303,#67304,#67305,#67306));
#16571=EDGE_LOOP('',(#67307,#67308,#67309,#67310));
#16572=EDGE_LOOP('',(#67311,#67312,#67313,#67314));
#16573=EDGE_LOOP('',(#67315,#67316,#67317,#67318));
#16574=EDGE_LOOP('',(#67319,#67320,#67321,#67322));
#16575=EDGE_LOOP('',(#67323,#67324,#67325,#67326));
#16576=EDGE_LOOP('',(#67327,#67328,#67329,#67330));
#16577=EDGE_LOOP('',(#67331,#67332,#67333,#67334));
#16578=EDGE_LOOP('',(#67335,#67336,#67337,#67338));
#16579=EDGE_LOOP('',(#67339,#67340,#67341,#67342));
#16580=EDGE_LOOP('',(#67343,#67344,#67345,#67346));
#16581=EDGE_LOOP('',(#67347,#67348,#67349,#67350));
#16582=EDGE_LOOP('',(#67351,#67352,#67353,#67354));
#16583=EDGE_LOOP('',(#67355,#67356,#67357,#67358));
#16584=EDGE_LOOP('',(#67359,#67360,#67361,#67362));
#16585=EDGE_LOOP('',(#67363,#67364,#67365,#67366));
#16586=EDGE_LOOP('',(#67367,#67368,#67369,#67370));
#16587=EDGE_LOOP('',(#67371,#67372,#67373,#67374,#67375,#67376,#67377,#67378,
#67379));
#16588=EDGE_LOOP('',(#67380,#67381,#67382,#67383));
#16589=EDGE_LOOP('',(#67384,#67385,#67386,#67387));
#16590=EDGE_LOOP('',(#67388,#67389,#67390,#67391));
#16591=EDGE_LOOP('',(#67392,#67393,#67394,#67395));
#16592=EDGE_LOOP('',(#67396,#67397,#67398,#67399));
#16593=EDGE_LOOP('',(#67400,#67401,#67402,#67403));
#16594=EDGE_LOOP('',(#67404,#67405,#67406,#67407));
#16595=EDGE_LOOP('',(#67408,#67409,#67410,#67411));
#16596=EDGE_LOOP('',(#67412,#67413,#67414,#67415));
#16597=EDGE_LOOP('',(#67416,#67417,#67418,#67419));
#16598=EDGE_LOOP('',(#67420,#67421,#67422,#67423));
#16599=EDGE_LOOP('',(#67424,#67425,#67426,#67427));
#16600=EDGE_LOOP('',(#67428,#67429,#67430,#67431));
#16601=EDGE_LOOP('',(#67432,#67433,#67434,#67435));
#16602=EDGE_LOOP('',(#67436,#67437,#67438,#67439,#67440));
#16603=EDGE_LOOP('',(#67441,#67442,#67443));
#16604=EDGE_LOOP('',(#67444,#67445,#67446,#67447));
#16605=EDGE_LOOP('',(#67448,#67449,#67450,#67451));
#16606=EDGE_LOOP('',(#67452,#67453,#67454,#67455));
#16607=EDGE_LOOP('',(#67456,#67457,#67458,#67459));
#16608=EDGE_LOOP('',(#67460,#67461,#67462,#67463));
#16609=EDGE_LOOP('',(#67464,#67465,#67466,#67467,#67468,#67469));
#16610=EDGE_LOOP('',(#67470,#67471,#67472,#67473));
#16611=EDGE_LOOP('',(#67474,#67475,#67476,#67477));
#16612=EDGE_LOOP('',(#67478,#67479,#67480,#67481));
#16613=EDGE_LOOP('',(#67482,#67483,#67484,#67485));
#16614=EDGE_LOOP('',(#67486,#67487,#67488,#67489));
#16615=EDGE_LOOP('',(#67490,#67491,#67492,#67493,#67494,#67495,#67496,#67497,
#67498));
#16616=EDGE_LOOP('',(#67499,#67500,#67501,#67502));
#16617=EDGE_LOOP('',(#67503,#67504,#67505,#67506));
#16618=EDGE_LOOP('',(#67507,#67508,#67509,#67510,#67511));
#16619=EDGE_LOOP('',(#67512,#67513,#67514,#67515));
#16620=EDGE_LOOP('',(#67516,#67517,#67518,#67519));
#16621=EDGE_LOOP('',(#67520,#67521,#67522,#67523,#67524));
#16622=EDGE_LOOP('',(#67525,#67526,#67527,#67528,#67529));
#16623=EDGE_LOOP('',(#67530,#67531,#67532,#67533,#67534,#67535,#67536,#67537,
#67538));
#16624=EDGE_LOOP('',(#67539,#67540,#67541,#67542,#67543,#67544,#67545,#67546,
#67547,#67548,#67549,#67550));
#16625=EDGE_LOOP('',(#67551,#67552,#67553,#67554));
#16626=EDGE_LOOP('',(#67555,#67556,#67557,#67558,#67559,#67560));
#16627=EDGE_LOOP('',(#67561,#67562,#67563,#67564,#67565));
#16628=EDGE_LOOP('',(#67566,#67567,#67568,#67569));
#16629=EDGE_LOOP('',(#67570,#67571,#67572,#67573));
#16630=EDGE_LOOP('',(#67574,#67575,#67576,#67577));
#16631=EDGE_LOOP('',(#67578,#67579,#67580,#67581));
#16632=EDGE_LOOP('',(#67582,#67583,#67584,#67585));
#16633=EDGE_LOOP('',(#67586,#67587,#67588,#67589));
#16634=EDGE_LOOP('',(#67590,#67591,#67592,#67593));
#16635=EDGE_LOOP('',(#67594,#67595,#67596,#67597));
#16636=EDGE_LOOP('',(#67598,#67599,#67600,#67601));
#16637=EDGE_LOOP('',(#67602,#67603,#67604,#67605));
#16638=EDGE_LOOP('',(#67606,#67607,#67608,#67609));
#16639=EDGE_LOOP('',(#67610,#67611,#67612,#67613));
#16640=EDGE_LOOP('',(#67614,#67615,#67616,#67617));
#16641=EDGE_LOOP('',(#67618,#67619,#67620,#67621));
#16642=EDGE_LOOP('',(#67622,#67623,#67624,#67625));
#16643=EDGE_LOOP('',(#67626,#67627,#67628,#67629));
#16644=EDGE_LOOP('',(#67630,#67631,#67632,#67633));
#16645=EDGE_LOOP('',(#67634,#67635,#67636,#67637));
#16646=EDGE_LOOP('',(#67638,#67639,#67640,#67641));
#16647=EDGE_LOOP('',(#67642,#67643,#67644,#67645,#67646));
#16648=EDGE_LOOP('',(#67647,#67648,#67649,#67650));
#16649=EDGE_LOOP('',(#67651,#67652,#67653,#67654));
#16650=EDGE_LOOP('',(#67655,#67656,#67657,#67658));
#16651=EDGE_LOOP('',(#67659,#67660,#67661,#67662));
#16652=EDGE_LOOP('',(#67663,#67664,#67665,#67666));
#16653=EDGE_LOOP('',(#67667,#67668,#67669,#67670));
#16654=EDGE_LOOP('',(#67671,#67672,#67673,#67674));
#16655=EDGE_LOOP('',(#67675,#67676,#67677,#67678));
#16656=EDGE_LOOP('',(#67679,#67680,#67681,#67682));
#16657=EDGE_LOOP('',(#67683,#67684,#67685,#67686));
#16658=EDGE_LOOP('',(#67687,#67688,#67689,#67690));
#16659=EDGE_LOOP('',(#67691,#67692,#67693,#67694));
#16660=EDGE_LOOP('',(#67695,#67696,#67697,#67698));
#16661=EDGE_LOOP('',(#67699,#67700,#67701,#67702));
#16662=EDGE_LOOP('',(#67703,#67704,#67705,#67706));
#16663=EDGE_LOOP('',(#67707,#67708,#67709,#67710));
#16664=EDGE_LOOP('',(#67711,#67712,#67713,#67714));
#16665=EDGE_LOOP('',(#67715,#67716,#67717,#67718));
#16666=EDGE_LOOP('',(#67719,#67720,#67721,#67722));
#16667=EDGE_LOOP('',(#67723,#67724,#67725,#67726));
#16668=EDGE_LOOP('',(#67727,#67728,#67729,#67730));
#16669=EDGE_LOOP('',(#67731,#67732,#67733,#67734));
#16670=EDGE_LOOP('',(#67735,#67736,#67737,#67738));
#16671=EDGE_LOOP('',(#67739,#67740,#67741,#67742));
#16672=EDGE_LOOP('',(#67743,#67744,#67745,#67746));
#16673=EDGE_LOOP('',(#67747,#67748,#67749,#67750));
#16674=EDGE_LOOP('',(#67751,#67752,#67753,#67754));
#16675=EDGE_LOOP('',(#67755,#67756,#67757,#67758));
#16676=EDGE_LOOP('',(#67759,#67760,#67761,#67762));
#16677=EDGE_LOOP('',(#67763,#67764,#67765,#67766));
#16678=EDGE_LOOP('',(#67767,#67768,#67769,#67770));
#16679=EDGE_LOOP('',(#67771,#67772,#67773,#67774));
#16680=EDGE_LOOP('',(#67775,#67776,#67777,#67778));
#16681=EDGE_LOOP('',(#67779,#67780,#67781,#67782));
#16682=EDGE_LOOP('',(#67783,#67784,#67785,#67786));
#16683=EDGE_LOOP('',(#67787,#67788,#67789,#67790));
#16684=EDGE_LOOP('',(#67791,#67792,#67793,#67794));
#16685=EDGE_LOOP('',(#67795,#67796,#67797,#67798));
#16686=EDGE_LOOP('',(#67799,#67800,#67801,#67802));
#16687=EDGE_LOOP('',(#67803,#67804,#67805,#67806));
#16688=EDGE_LOOP('',(#67807,#67808,#67809,#67810));
#16689=EDGE_LOOP('',(#67811,#67812,#67813,#67814));
#16690=EDGE_LOOP('',(#67815,#67816,#67817,#67818));
#16691=EDGE_LOOP('',(#67819,#67820,#67821,#67822));
#16692=EDGE_LOOP('',(#67823,#67824,#67825,#67826));
#16693=EDGE_LOOP('',(#67827,#67828,#67829,#67830));
#16694=EDGE_LOOP('',(#67831,#67832,#67833,#67834));
#16695=EDGE_LOOP('',(#67835,#67836,#67837,#67838));
#16696=EDGE_LOOP('',(#67839,#67840,#67841,#67842));
#16697=EDGE_LOOP('',(#67843,#67844,#67845,#67846));
#16698=EDGE_LOOP('',(#67847,#67848,#67849,#67850));
#16699=EDGE_LOOP('',(#67851,#67852,#67853,#67854));
#16700=EDGE_LOOP('',(#67855,#67856,#67857,#67858));
#16701=EDGE_LOOP('',(#67859,#67860,#67861,#67862));
#16702=EDGE_LOOP('',(#67863,#67864,#67865,#67866));
#16703=EDGE_LOOP('',(#67867,#67868,#67869,#67870));
#16704=EDGE_LOOP('',(#67871,#67872,#67873,#67874));
#16705=EDGE_LOOP('',(#67875,#67876,#67877,#67878));
#16706=EDGE_LOOP('',(#67879,#67880,#67881,#67882));
#16707=EDGE_LOOP('',(#67883,#67884,#67885,#67886));
#16708=EDGE_LOOP('',(#67887,#67888,#67889,#67890));
#16709=EDGE_LOOP('',(#67891,#67892,#67893,#67894));
#16710=EDGE_LOOP('',(#67895,#67896,#67897,#67898));
#16711=EDGE_LOOP('',(#67899,#67900,#67901,#67902));
#16712=EDGE_LOOP('',(#67903,#67904,#67905,#67906));
#16713=EDGE_LOOP('',(#67907,#67908,#67909,#67910));
#16714=EDGE_LOOP('',(#67911,#67912,#67913,#67914));
#16715=EDGE_LOOP('',(#67915,#67916,#67917,#67918));
#16716=EDGE_LOOP('',(#67919,#67920,#67921,#67922));
#16717=EDGE_LOOP('',(#67923,#67924,#67925,#67926));
#16718=EDGE_LOOP('',(#67927,#67928,#67929,#67930));
#16719=EDGE_LOOP('',(#67931,#67932,#67933,#67934));
#16720=EDGE_LOOP('',(#67935,#67936,#67937,#67938));
#16721=EDGE_LOOP('',(#67939,#67940,#67941,#67942));
#16722=EDGE_LOOP('',(#67943,#67944,#67945,#67946));
#16723=EDGE_LOOP('',(#67947,#67948,#67949,#67950));
#16724=EDGE_LOOP('',(#67951,#67952,#67953,#67954,#67955,#67956,#67957,#67958,
#67959,#67960,#67961,#67962,#67963,#67964,#67965,#67966));
#16725=EDGE_LOOP('',(#67967,#67968,#67969,#67970));
#16726=EDGE_LOOP('',(#67971,#67972,#67973,#67974));
#16727=EDGE_LOOP('',(#67975,#67976,#67977,#67978));
#16728=EDGE_LOOP('',(#67979,#67980,#67981,#67982));
#16729=EDGE_LOOP('',(#67983,#67984,#67985,#67986,#67987,#67988,#67989,#67990,
#67991,#67992,#67993,#67994,#67995,#67996,#67997,#67998,#67999,#68000,#68001));
#16730=EDGE_LOOP('',(#68002,#68003,#68004,#68005));
#16731=EDGE_LOOP('',(#68006,#68007,#68008,#68009));
#16732=EDGE_LOOP('',(#68010,#68011,#68012,#68013));
#16733=EDGE_LOOP('',(#68014,#68015,#68016,#68017));
#16734=EDGE_LOOP('',(#68018,#68019,#68020,#68021,#68022,#68023,#68024,#68025,
#68026,#68027,#68028,#68029,#68030,#68031,#68032,#68033,#68034,#68035,#68036,
#68037,#68038,#68039,#68040,#68041,#68042,#68043,#68044,#68045,#68046,#68047,
#68048,#68049,#68050,#68051,#68052,#68053,#68054,#68055));
#16735=EDGE_LOOP('',(#68056,#68057,#68058,#68059,#68060,#68061));
#16736=EDGE_LOOP('',(#68062,#68063,#68064,#68065));
#16737=EDGE_LOOP('',(#68066,#68067,#68068,#68069));
#16738=EDGE_LOOP('',(#68070,#68071,#68072,#68073));
#16739=EDGE_LOOP('',(#68074,#68075,#68076,#68077));
#16740=EDGE_LOOP('',(#68078,#68079,#68080,#68081));
#16741=EDGE_LOOP('',(#68082,#68083,#68084,#68085));
#16742=EDGE_LOOP('',(#68086,#68087,#68088,#68089));
#16743=EDGE_LOOP('',(#68090,#68091,#68092,#68093));
#16744=EDGE_LOOP('',(#68094,#68095,#68096,#68097));
#16745=EDGE_LOOP('',(#68098,#68099,#68100,#68101));
#16746=EDGE_LOOP('',(#68102,#68103,#68104,#68105));
#16747=EDGE_LOOP('',(#68106,#68107,#68108,#68109));
#16748=EDGE_LOOP('',(#68110,#68111,#68112,#68113));
#16749=EDGE_LOOP('',(#68114,#68115,#68116,#68117));
#16750=EDGE_LOOP('',(#68118,#68119,#68120,#68121));
#16751=EDGE_LOOP('',(#68122,#68123,#68124,#68125));
#16752=EDGE_LOOP('',(#68126,#68127,#68128,#68129));
#16753=EDGE_LOOP('',(#68130,#68131,#68132,#68133));
#16754=EDGE_LOOP('',(#68134,#68135,#68136,#68137));
#16755=EDGE_LOOP('',(#68138,#68139,#68140,#68141));
#16756=EDGE_LOOP('',(#68142,#68143,#68144,#68145));
#16757=EDGE_LOOP('',(#68146,#68147,#68148,#68149));
#16758=EDGE_LOOP('',(#68150,#68151,#68152,#68153));
#16759=EDGE_LOOP('',(#68154,#68155,#68156,#68157));
#16760=EDGE_LOOP('',(#68158,#68159,#68160,#68161));
#16761=EDGE_LOOP('',(#68162,#68163,#68164,#68165));
#16762=EDGE_LOOP('',(#68166,#68167,#68168,#68169));
#16763=EDGE_LOOP('',(#68170,#68171,#68172,#68173));
#16764=EDGE_LOOP('',(#68174,#68175,#68176,#68177));
#16765=EDGE_LOOP('',(#68178,#68179,#68180,#68181));
#16766=EDGE_LOOP('',(#68182,#68183,#68184,#68185,#68186));
#16767=EDGE_LOOP('',(#68187,#68188,#68189,#68190));
#16768=EDGE_LOOP('',(#68191,#68192,#68193,#68194));
#16769=EDGE_LOOP('',(#68195,#68196,#68197,#68198));
#16770=EDGE_LOOP('',(#68199,#68200,#68201,#68202));
#16771=EDGE_LOOP('',(#68203,#68204,#68205,#68206,#68207));
#16772=EDGE_LOOP('',(#68208,#68209,#68210,#68211,#68212,#68213));
#16773=EDGE_LOOP('',(#68214,#68215,#68216,#68217));
#16774=EDGE_LOOP('',(#68218,#68219,#68220,#68221));
#16775=EDGE_LOOP('',(#68222,#68223,#68224,#68225));
#16776=EDGE_LOOP('',(#68226,#68227,#68228,#68229,#68230,#68231,#68232,#68233,
#68234,#68235,#68236,#68237,#68238,#68239,#68240,#68241,#68242,#68243,#68244,
#68245,#68246,#68247,#68248,#68249,#68250,#68251,#68252,#68253,#68254,#68255,
#68256,#68257,#68258,#68259,#68260,#68261,#68262,#68263,#68264,#68265));
#16777=EDGE_LOOP('',(#68266,#68267,#68268,#68269,#68270,#68271,#68272,#68273,
#68274,#68275,#68276,#68277,#68278,#68279,#68280,#68281,#68282,#68283,#68284));
#16778=EDGE_LOOP('',(#68285,#68286,#68287,#68288));
#16779=EDGE_LOOP('',(#68289,#68290,#68291,#68292));
#16780=EDGE_LOOP('',(#68293,#68294,#68295,#68296));
#16781=EDGE_LOOP('',(#68297,#68298,#68299,#68300));
#16782=EDGE_LOOP('',(#68301,#68302,#68303,#68304,#68305,#68306,#68307,#68308,
#68309,#68310,#68311,#68312,#68313,#68314,#68315,#68316,#68317,#68318,#68319));
#16783=EDGE_LOOP('',(#68320,#68321,#68322,#68323));
#16784=EDGE_LOOP('',(#68324,#68325,#68326,#68327));
#16785=EDGE_LOOP('',(#68328,#68329,#68330,#68331));
#16786=EDGE_LOOP('',(#68332,#68333,#68334,#68335,#68336));
#16787=EDGE_LOOP('',(#68337,#68338,#68339,#68340));
#16788=EDGE_LOOP('',(#68341,#68342,#68343,#68344));
#16789=EDGE_LOOP('',(#68345,#68346,#68347,#68348));
#16790=EDGE_LOOP('',(#68349,#68350,#68351,#68352));
#16791=EDGE_LOOP('',(#68353,#68354,#68355,#68356));
#16792=EDGE_LOOP('',(#68357,#68358,#68359,#68360,#68361,#68362,#68363,#68364,
#68365,#68366,#68367,#68368,#68369,#68370,#68371,#68372,#68373,#68374,#68375,
#68376,#68377,#68378,#68379,#68380,#68381,#68382,#68383,#68384,#68385,#68386,
#68387,#68388,#68389,#68390,#68391,#68392,#68393,#68394,#68395,#68396,#68397,
#68398));
#16793=EDGE_LOOP('',(#68399,#68400,#68401,#68402));
#16794=EDGE_LOOP('',(#68403,#68404,#68405,#68406,#68407,#68408,#68409,#68410,
#68411,#68412,#68413,#68414,#68415,#68416,#68417,#68418,#68419,#68420,#68421,
#68422,#68423,#68424,#68425,#68426,#68427,#68428,#68429,#68430,#68431,#68432,
#68433,#68434));
#16795=EDGE_LOOP('',(#68435));
#16796=EDGE_LOOP('',(#68436));
#16797=EDGE_LOOP('',(#68437));
#16798=EDGE_LOOP('',(#68438));
#16799=EDGE_LOOP('',(#68439,#68440,#68441,#68442));
#16800=EDGE_LOOP('',(#68443,#68444,#68445,#68446));
#16801=EDGE_LOOP('',(#68447,#68448,#68449,#68450));
#16802=EDGE_LOOP('',(#68451,#68452,#68453,#68454,#68455,#68456,#68457,#68458));
#16803=EDGE_LOOP('',(#68459,#68460,#68461,#68462,#68463,#68464,#68465,#68466));
#16804=EDGE_LOOP('',(#68467,#68468,#68469,#68470,#68471,#68472,#68473,#68474,
#68475,#68476,#68477,#68478,#68479,#68480,#68481,#68482,#68483,#68484,#68485,
#68486,#68487,#68488,#68489,#68490,#68491,#68492,#68493,#68494,#68495,#68496,
#68497,#68498,#68499,#68500,#68501,#68502,#68503,#68504,#68505,#68506,#68507,
#68508,#68509,#68510,#68511,#68512,#68513,#68514,#68515,#68516,#68517,#68518,
#68519,#68520,#68521,#68522,#68523,#68524,#68525,#68526,#68527,#68528));
#16805=EDGE_LOOP('',(#68529,#68530,#68531,#68532,#68533,#68534));
#16806=EDGE_LOOP('',(#68535,#68536,#68537,#68538));
#16807=EDGE_LOOP('',(#68539,#68540,#68541,#68542));
#16808=EDGE_LOOP('',(#68543,#68544,#68545,#68546,#68547,#68548,#68549,#68550,
#68551,#68552,#68553,#68554,#68555,#68556,#68557,#68558,#68559,#68560,#68561,
#68562,#68563,#68564,#68565,#68566,#68567,#68568,#68569,#68570,#68571,#68572,
#68573,#68574,#68575,#68576,#68577,#68578,#68579,#68580,#68581,#68582));
#16809=EDGE_LOOP('',(#68583,#68584,#68585,#68586,#68587,#68588));
#16810=EDGE_LOOP('',(#68589,#68590,#68591,#68592,#68593,#68594,#68595,#68596,
#68597,#68598,#68599,#68600,#68601,#68602,#68603,#68604,#68605,#68606,#68607,
#68608,#68609,#68610,#68611,#68612,#68613,#68614,#68615,#68616,#68617,#68618,
#68619,#68620));
#16811=EDGE_LOOP('',(#68621));
#16812=EDGE_LOOP('',(#68622));
#16813=EDGE_LOOP('',(#68623));
#16814=EDGE_LOOP('',(#68624));
#16815=EDGE_LOOP('',(#68625,#68626,#68627,#68628));
#16816=EDGE_LOOP('',(#68629,#68630,#68631,#68632));
#16817=EDGE_LOOP('',(#68633,#68634,#68635,#68636));
#16818=EDGE_LOOP('',(#68637,#68638,#68639,#68640));
#16819=EDGE_LOOP('',(#68641,#68642,#68643,#68644));
#16820=EDGE_LOOP('',(#68645,#68646,#68647,#68648));
#16821=EDGE_LOOP('',(#68649,#68650,#68651,#68652,#68653,#68654,#68655,#68656));
#16822=EDGE_LOOP('',(#68657,#68658));
#16823=EDGE_LOOP('',(#68659,#68660));
#16824=EDGE_LOOP('',(#68661,#68662));
#16825=EDGE_LOOP('',(#68663,#68664));
#16826=EDGE_LOOP('',(#68665,#68666));
#16827=EDGE_LOOP('',(#68667,#68668));
#16828=EDGE_LOOP('',(#68669,#68670,#68671,#68672,#68673));
#16829=EDGE_LOOP('',(#68674));
#16830=EDGE_LOOP('',(#68675));
#16831=EDGE_LOOP('',(#68676,#68677,#68678,#68679,#68680,#68681));
#16832=EDGE_LOOP('',(#68682,#68683,#68684,#68685,#68686));
#16833=EDGE_LOOP('',(#68687,#68688,#68689,#68690));
#16834=EDGE_LOOP('',(#68691));
#16835=EDGE_LOOP('',(#68692,#68693,#68694,#68695));
#16836=EDGE_LOOP('',(#68696));
#16837=EDGE_LOOP('',(#68697));
#16838=EDGE_LOOP('',(#68698,#68699,#68700,#68701));
#16839=EDGE_LOOP('',(#68702));
#16840=EDGE_LOOP('',(#68703,#68704,#68705,#68706));
#16841=EDGE_LOOP('',(#68707,#68708,#68709,#68710,#68711));
#16842=EDGE_LOOP('',(#68712,#68713,#68714,#68715));
#16843=EDGE_LOOP('',(#68716,#68717,#68718,#68719));
#16844=EDGE_LOOP('',(#68720,#68721,#68722));
#16845=EDGE_LOOP('',(#68723,#68724,#68725,#68726));
#16846=EDGE_LOOP('',(#68727,#68728,#68729,#68730));
#16847=EDGE_LOOP('',(#68731,#68732,#68733,#68734));
#16848=EDGE_LOOP('',(#68735,#68736,#68737,#68738));
#16849=EDGE_LOOP('',(#68739,#68740,#68741,#68742));
#16850=EDGE_LOOP('',(#68743,#68744,#68745,#68746));
#16851=EDGE_LOOP('',(#68747,#68748,#68749,#68750));
#16852=EDGE_LOOP('',(#68751,#68752,#68753,#68754));
#16853=EDGE_LOOP('',(#68755,#68756,#68757,#68758,#68759));
#16854=EDGE_LOOP('',(#68760,#68761,#68762));
#16855=EDGE_LOOP('',(#68763,#68764,#68765,#68766));
#16856=EDGE_LOOP('',(#68767,#68768,#68769,#68770));
#16857=EDGE_LOOP('',(#68771,#68772,#68773,#68774));
#16858=EDGE_LOOP('',(#68775,#68776,#68777,#68778));
#16859=EDGE_LOOP('',(#68779,#68780,#68781,#68782));
#16860=EDGE_LOOP('',(#68783,#68784,#68785));
#16861=EDGE_LOOP('',(#68786,#68787,#68788,#68789));
#16862=EDGE_LOOP('',(#68790,#68791,#68792,#68793));
#16863=EDGE_LOOP('',(#68794,#68795,#68796,#68797));
#16864=EDGE_LOOP('',(#68798,#68799,#68800,#68801));
#16865=EDGE_LOOP('',(#68802,#68803,#68804));
#16866=EDGE_LOOP('',(#68805,#68806,#68807,#68808));
#16867=EDGE_LOOP('',(#68809,#68810,#68811,#68812));
#16868=EDGE_LOOP('',(#68813,#68814,#68815,#68816));
#16869=EDGE_LOOP('',(#68817,#68818,#68819,#68820));
#16870=EDGE_LOOP('',(#68821,#68822,#68823,#68824));
#16871=EDGE_LOOP('',(#68825,#68826,#68827,#68828));
#16872=EDGE_LOOP('',(#68829,#68830,#68831,#68832));
#16873=EDGE_LOOP('',(#68833,#68834,#68835,#68836));
#16874=EDGE_LOOP('',(#68837,#68838,#68839,#68840));
#16875=EDGE_LOOP('',(#68841,#68842,#68843,#68844));
#16876=EDGE_LOOP('',(#68845,#68846,#68847,#68848));
#16877=EDGE_LOOP('',(#68849,#68850,#68851,#68852));
#16878=EDGE_LOOP('',(#68853,#68854,#68855,#68856));
#16879=EDGE_LOOP('',(#68857,#68858,#68859,#68860));
#16880=EDGE_LOOP('',(#68861,#68862,#68863,#68864));
#16881=EDGE_LOOP('',(#68865,#68866,#68867,#68868));
#16882=EDGE_LOOP('',(#68869,#68870,#68871,#68872));
#16883=EDGE_LOOP('',(#68873,#68874,#68875,#68876));
#16884=EDGE_LOOP('',(#68877,#68878,#68879,#68880));
#16885=EDGE_LOOP('',(#68881,#68882,#68883,#68884));
#16886=EDGE_LOOP('',(#68885,#68886,#68887,#68888));
#16887=EDGE_LOOP('',(#68889,#68890,#68891,#68892));
#16888=EDGE_LOOP('',(#68893,#68894,#68895,#68896));
#16889=EDGE_LOOP('',(#68897,#68898,#68899,#68900));
#16890=EDGE_LOOP('',(#68901,#68902,#68903,#68904));
#16891=EDGE_LOOP('',(#68905,#68906,#68907,#68908));
#16892=EDGE_LOOP('',(#68909,#68910,#68911,#68912));
#16893=EDGE_LOOP('',(#68913,#68914,#68915,#68916));
#16894=EDGE_LOOP('',(#68917,#68918,#68919,#68920,#68921));
#16895=EDGE_LOOP('',(#68922,#68923,#68924,#68925));
#16896=EDGE_LOOP('',(#68926,#68927,#68928,#68929));
#16897=EDGE_LOOP('',(#68930,#68931,#68932,#68933));
#16898=EDGE_LOOP('',(#68934,#68935,#68936,#68937));
#16899=EDGE_LOOP('',(#68938,#68939,#68940,#68941));
#16900=EDGE_LOOP('',(#68942,#68943,#68944,#68945));
#16901=EDGE_LOOP('',(#68946,#68947,#68948,#68949));
#16902=EDGE_LOOP('',(#68950,#68951,#68952,#68953,#68954,#68955));
#16903=EDGE_LOOP('',(#68956,#68957,#68958,#68959));
#16904=EDGE_LOOP('',(#68960,#68961,#68962,#68963));
#16905=EDGE_LOOP('',(#68964,#68965,#68966,#68967,#68968));
#16906=EDGE_LOOP('',(#68969,#68970,#68971,#68972));
#16907=EDGE_LOOP('',(#68973,#68974,#68975,#68976));
#16908=EDGE_LOOP('',(#68977,#68978,#68979,#68980));
#16909=EDGE_LOOP('',(#68981,#68982,#68983,#68984,#68985));
#16910=EDGE_LOOP('',(#68986,#68987,#68988,#68989));
#16911=EDGE_LOOP('',(#68990,#68991,#68992,#68993));
#16912=EDGE_LOOP('',(#68994,#68995,#68996,#68997));
#16913=EDGE_LOOP('',(#68998,#68999,#69000,#69001));
#16914=EDGE_LOOP('',(#69002,#69003,#69004,#69005,#69006));
#16915=EDGE_LOOP('',(#69007,#69008,#69009,#69010));
#16916=EDGE_LOOP('',(#69011,#69012,#69013,#69014));
#16917=EDGE_LOOP('',(#69015,#69016,#69017,#69018));
#16918=EDGE_LOOP('',(#69019,#69020,#69021,#69022));
#16919=EDGE_LOOP('',(#69023,#69024,#69025,#69026));
#16920=EDGE_LOOP('',(#69027,#69028,#69029,#69030,#69031));
#16921=EDGE_LOOP('',(#69032,#69033,#69034,#69035,#69036,#69037));
#16922=EDGE_LOOP('',(#69038,#69039,#69040,#69041,#69042,#69043));
#16923=EDGE_LOOP('',(#69044,#69045,#69046,#69047,#69048,#69049));
#16924=EDGE_LOOP('',(#69050,#69051,#69052,#69053,#69054));
#16925=EDGE_LOOP('',(#69055,#69056,#69057,#69058,#69059,#69060,#69061));
#16926=EDGE_LOOP('',(#69062,#69063,#69064,#69065,#69066));
#16927=EDGE_LOOP('',(#69067,#69068,#69069,#69070,#69071));
#16928=EDGE_LOOP('',(#69072,#69073,#69074,#69075));
#16929=EDGE_LOOP('',(#69076,#69077,#69078,#69079));
#16930=EDGE_LOOP('',(#69080,#69081,#69082,#69083));
#16931=EDGE_LOOP('',(#69084,#69085,#69086,#69087));
#16932=EDGE_LOOP('',(#69088,#69089,#69090,#69091));
#16933=EDGE_LOOP('',(#69092,#69093,#69094,#69095));
#16934=EDGE_LOOP('',(#69096,#69097,#69098,#69099));
#16935=EDGE_LOOP('',(#69100,#69101,#69102,#69103));
#16936=EDGE_LOOP('',(#69104,#69105,#69106,#69107));
#16937=EDGE_LOOP('',(#69108,#69109,#69110,#69111));
#16938=EDGE_LOOP('',(#69112,#69113,#69114,#69115));
#16939=EDGE_LOOP('',(#69116,#69117,#69118,#69119));
#16940=EDGE_LOOP('',(#69120,#69121,#69122,#69123));
#16941=EDGE_LOOP('',(#69124,#69125,#69126,#69127));
#16942=EDGE_LOOP('',(#69128,#69129,#69130,#69131));
#16943=EDGE_LOOP('',(#69132,#69133,#69134,#69135));
#16944=EDGE_LOOP('',(#69136,#69137,#69138,#69139));
#16945=EDGE_LOOP('',(#69140,#69141,#69142,#69143));
#16946=EDGE_LOOP('',(#69144,#69145,#69146,#69147));
#16947=EDGE_LOOP('',(#69148,#69149,#69150,#69151));
#16948=EDGE_LOOP('',(#69152,#69153,#69154,#69155));
#16949=EDGE_LOOP('',(#69156,#69157,#69158,#69159));
#16950=EDGE_LOOP('',(#69160,#69161,#69162,#69163));
#16951=EDGE_LOOP('',(#69164,#69165,#69166,#69167));
#16952=EDGE_LOOP('',(#69168,#69169,#69170,#69171));
#16953=EDGE_LOOP('',(#69172,#69173,#69174,#69175));
#16954=EDGE_LOOP('',(#69176,#69177,#69178,#69179));
#16955=EDGE_LOOP('',(#69180,#69181,#69182,#69183));
#16956=EDGE_LOOP('',(#69184,#69185,#69186,#69187));
#16957=EDGE_LOOP('',(#69188,#69189,#69190,#69191));
#16958=EDGE_LOOP('',(#69192,#69193,#69194,#69195));
#16959=EDGE_LOOP('',(#69196,#69197,#69198,#69199));
#16960=EDGE_LOOP('',(#69200,#69201,#69202,#69203));
#16961=EDGE_LOOP('',(#69204,#69205,#69206,#69207));
#16962=EDGE_LOOP('',(#69208,#69209,#69210,#69211));
#16963=EDGE_LOOP('',(#69212,#69213,#69214,#69215));
#16964=EDGE_LOOP('',(#69216,#69217,#69218,#69219));
#16965=EDGE_LOOP('',(#69220,#69221,#69222,#69223));
#16966=EDGE_LOOP('',(#69224,#69225,#69226,#69227));
#16967=EDGE_LOOP('',(#69228,#69229,#69230,#69231));
#16968=EDGE_LOOP('',(#69232,#69233,#69234,#69235));
#16969=EDGE_LOOP('',(#69236,#69237,#69238,#69239));
#16970=EDGE_LOOP('',(#69240,#69241,#69242,#69243));
#16971=EDGE_LOOP('',(#69244,#69245,#69246,#69247));
#16972=EDGE_LOOP('',(#69248,#69249,#69250,#69251));
#16973=EDGE_LOOP('',(#69252,#69253,#69254,#69255));
#16974=EDGE_LOOP('',(#69256,#69257,#69258,#69259));
#16975=EDGE_LOOP('',(#69260,#69261,#69262,#69263));
#16976=EDGE_LOOP('',(#69264,#69265,#69266,#69267));
#16977=EDGE_LOOP('',(#69268,#69269,#69270,#69271));
#16978=EDGE_LOOP('',(#69272,#69273,#69274,#69275));
#16979=EDGE_LOOP('',(#69276,#69277,#69278,#69279));
#16980=EDGE_LOOP('',(#69280,#69281,#69282,#69283));
#16981=EDGE_LOOP('',(#69284,#69285,#69286,#69287));
#16982=EDGE_LOOP('',(#69288,#69289,#69290,#69291));
#16983=EDGE_LOOP('',(#69292,#69293,#69294,#69295));
#16984=EDGE_LOOP('',(#69296,#69297,#69298,#69299));
#16985=EDGE_LOOP('',(#69300,#69301,#69302,#69303));
#16986=EDGE_LOOP('',(#69304,#69305,#69306,#69307));
#16987=EDGE_LOOP('',(#69308,#69309,#69310,#69311));
#16988=EDGE_LOOP('',(#69312,#69313,#69314,#69315));
#16989=EDGE_LOOP('',(#69316,#69317,#69318,#69319));
#16990=EDGE_LOOP('',(#69320,#69321,#69322,#69323));
#16991=EDGE_LOOP('',(#69324,#69325,#69326,#69327));
#16992=EDGE_LOOP('',(#69328,#69329,#69330,#69331));
#16993=EDGE_LOOP('',(#69332,#69333,#69334,#69335));
#16994=EDGE_LOOP('',(#69336,#69337,#69338,#69339));
#16995=EDGE_LOOP('',(#69340,#69341,#69342,#69343));
#16996=EDGE_LOOP('',(#69344,#69345,#69346,#69347));
#16997=EDGE_LOOP('',(#69348,#69349,#69350,#69351));
#16998=EDGE_LOOP('',(#69352,#69353,#69354,#69355));
#16999=EDGE_LOOP('',(#69356,#69357,#69358,#69359));
#17000=EDGE_LOOP('',(#69360,#69361,#69362,#69363));
#17001=EDGE_LOOP('',(#69364,#69365,#69366,#69367));
#17002=EDGE_LOOP('',(#69368,#69369,#69370,#69371));
#17003=EDGE_LOOP('',(#69372,#69373,#69374,#69375));
#17004=EDGE_LOOP('',(#69376,#69377,#69378,#69379));
#17005=EDGE_LOOP('',(#69380,#69381,#69382,#69383));
#17006=EDGE_LOOP('',(#69384,#69385,#69386,#69387));
#17007=EDGE_LOOP('',(#69388,#69389,#69390,#69391));
#17008=EDGE_LOOP('',(#69392,#69393,#69394,#69395));
#17009=EDGE_LOOP('',(#69396,#69397,#69398,#69399));
#17010=EDGE_LOOP('',(#69400,#69401,#69402,#69403));
#17011=EDGE_LOOP('',(#69404,#69405,#69406,#69407));
#17012=EDGE_LOOP('',(#69408,#69409,#69410,#69411));
#17013=EDGE_LOOP('',(#69412,#69413,#69414,#69415));
#17014=EDGE_LOOP('',(#69416,#69417,#69418,#69419));
#17015=EDGE_LOOP('',(#69420,#69421,#69422,#69423));
#17016=EDGE_LOOP('',(#69424,#69425,#69426,#69427));
#17017=EDGE_LOOP('',(#69428,#69429,#69430,#69431));
#17018=EDGE_LOOP('',(#69432,#69433,#69434,#69435));
#17019=EDGE_LOOP('',(#69436,#69437,#69438,#69439));
#17020=EDGE_LOOP('',(#69440,#69441,#69442,#69443));
#17021=EDGE_LOOP('',(#69444,#69445,#69446,#69447));
#17022=EDGE_LOOP('',(#69448,#69449,#69450,#69451));
#17023=EDGE_LOOP('',(#69452,#69453,#69454,#69455));
#17024=EDGE_LOOP('',(#69456,#69457,#69458,#69459));
#17025=EDGE_LOOP('',(#69460,#69461,#69462,#69463));
#17026=EDGE_LOOP('',(#69464,#69465,#69466,#69467));
#17027=EDGE_LOOP('',(#69468,#69469,#69470,#69471));
#17028=EDGE_LOOP('',(#69472,#69473,#69474,#69475));
#17029=EDGE_LOOP('',(#69476,#69477,#69478,#69479));
#17030=EDGE_LOOP('',(#69480,#69481,#69482,#69483));
#17031=EDGE_LOOP('',(#69484,#69485,#69486,#69487));
#17032=EDGE_LOOP('',(#69488,#69489,#69490,#69491));
#17033=EDGE_LOOP('',(#69492,#69493,#69494,#69495));
#17034=EDGE_LOOP('',(#69496,#69497,#69498,#69499));
#17035=EDGE_LOOP('',(#69500,#69501,#69502,#69503));
#17036=EDGE_LOOP('',(#69504,#69505,#69506,#69507));
#17037=EDGE_LOOP('',(#69508,#69509,#69510,#69511));
#17038=EDGE_LOOP('',(#69512,#69513,#69514,#69515));
#17039=EDGE_LOOP('',(#69516,#69517,#69518,#69519));
#17040=EDGE_LOOP('',(#69520,#69521,#69522,#69523));
#17041=EDGE_LOOP('',(#69524,#69525,#69526,#69527));
#17042=EDGE_LOOP('',(#69528,#69529,#69530,#69531));
#17043=EDGE_LOOP('',(#69532,#69533,#69534,#69535));
#17044=EDGE_LOOP('',(#69536,#69537,#69538,#69539));
#17045=EDGE_LOOP('',(#69540,#69541,#69542,#69543));
#17046=EDGE_LOOP('',(#69544,#69545,#69546,#69547));
#17047=EDGE_LOOP('',(#69548,#69549,#69550,#69551));
#17048=EDGE_LOOP('',(#69552,#69553,#69554,#69555));
#17049=EDGE_LOOP('',(#69556,#69557,#69558,#69559));
#17050=EDGE_LOOP('',(#69560,#69561,#69562,#69563));
#17051=EDGE_LOOP('',(#69564,#69565,#69566,#69567));
#17052=EDGE_LOOP('',(#69568,#69569,#69570,#69571));
#17053=EDGE_LOOP('',(#69572,#69573,#69574,#69575));
#17054=EDGE_LOOP('',(#69576,#69577,#69578,#69579));
#17055=EDGE_LOOP('',(#69580,#69581,#69582,#69583));
#17056=EDGE_LOOP('',(#69584,#69585,#69586,#69587));
#17057=EDGE_LOOP('',(#69588,#69589,#69590,#69591));
#17058=EDGE_LOOP('',(#69592,#69593,#69594,#69595));
#17059=EDGE_LOOP('',(#69596,#69597,#69598,#69599));
#17060=EDGE_LOOP('',(#69600,#69601,#69602,#69603));
#17061=EDGE_LOOP('',(#69604,#69605,#69606,#69607));
#17062=EDGE_LOOP('',(#69608,#69609,#69610,#69611));
#17063=EDGE_LOOP('',(#69612,#69613,#69614,#69615));
#17064=EDGE_LOOP('',(#69616,#69617,#69618,#69619));
#17065=EDGE_LOOP('',(#69620,#69621,#69622,#69623));
#17066=EDGE_LOOP('',(#69624,#69625,#69626,#69627));
#17067=EDGE_LOOP('',(#69628,#69629,#69630,#69631));
#17068=EDGE_LOOP('',(#69632,#69633,#69634,#69635));
#17069=EDGE_LOOP('',(#69636,#69637,#69638,#69639));
#17070=EDGE_LOOP('',(#69640,#69641,#69642,#69643));
#17071=EDGE_LOOP('',(#69644,#69645,#69646,#69647));
#17072=EDGE_LOOP('',(#69648,#69649,#69650,#69651));
#17073=EDGE_LOOP('',(#69652,#69653,#69654,#69655));
#17074=EDGE_LOOP('',(#69656,#69657,#69658,#69659));
#17075=EDGE_LOOP('',(#69660,#69661,#69662,#69663));
#17076=EDGE_LOOP('',(#69664,#69665,#69666,#69667));
#17077=EDGE_LOOP('',(#69668,#69669,#69670,#69671));
#17078=EDGE_LOOP('',(#69672,#69673,#69674,#69675));
#17079=EDGE_LOOP('',(#69676,#69677,#69678,#69679));
#17080=EDGE_LOOP('',(#69680,#69681,#69682,#69683));
#17081=EDGE_LOOP('',(#69684,#69685,#69686,#69687));
#17082=EDGE_LOOP('',(#69688,#69689,#69690,#69691));
#17083=EDGE_LOOP('',(#69692,#69693,#69694,#69695));
#17084=EDGE_LOOP('',(#69696,#69697,#69698,#69699));
#17085=EDGE_LOOP('',(#69700,#69701,#69702,#69703));
#17086=EDGE_LOOP('',(#69704,#69705,#69706,#69707));
#17087=EDGE_LOOP('',(#69708,#69709,#69710,#69711));
#17088=EDGE_LOOP('',(#69712,#69713,#69714,#69715));
#17089=EDGE_LOOP('',(#69716,#69717,#69718,#69719));
#17090=EDGE_LOOP('',(#69720,#69721,#69722,#69723));
#17091=EDGE_LOOP('',(#69724,#69725,#69726,#69727));
#17092=EDGE_LOOP('',(#69728,#69729,#69730,#69731));
#17093=EDGE_LOOP('',(#69732,#69733,#69734,#69735));
#17094=EDGE_LOOP('',(#69736,#69737,#69738,#69739));
#17095=EDGE_LOOP('',(#69740,#69741,#69742,#69743));
#17096=EDGE_LOOP('',(#69744,#69745,#69746,#69747));
#17097=EDGE_LOOP('',(#69748,#69749,#69750,#69751));
#17098=EDGE_LOOP('',(#69752,#69753,#69754,#69755));
#17099=EDGE_LOOP('',(#69756,#69757,#69758,#69759));
#17100=EDGE_LOOP('',(#69760,#69761,#69762,#69763));
#17101=EDGE_LOOP('',(#69764,#69765,#69766,#69767));
#17102=EDGE_LOOP('',(#69768,#69769,#69770,#69771));
#17103=EDGE_LOOP('',(#69772,#69773,#69774,#69775));
#17104=EDGE_LOOP('',(#69776,#69777,#69778,#69779));
#17105=EDGE_LOOP('',(#69780,#69781,#69782,#69783));
#17106=EDGE_LOOP('',(#69784,#69785,#69786,#69787));
#17107=EDGE_LOOP('',(#69788,#69789,#69790,#69791));
#17108=EDGE_LOOP('',(#69792,#69793,#69794,#69795));
#17109=EDGE_LOOP('',(#69796,#69797,#69798,#69799));
#17110=EDGE_LOOP('',(#69800,#69801,#69802,#69803));
#17111=EDGE_LOOP('',(#69804,#69805,#69806,#69807));
#17112=EDGE_LOOP('',(#69808,#69809,#69810,#69811));
#17113=EDGE_LOOP('',(#69812,#69813,#69814,#69815));
#17114=EDGE_LOOP('',(#69816,#69817,#69818,#69819));
#17115=EDGE_LOOP('',(#69820,#69821,#69822,#69823));
#17116=EDGE_LOOP('',(#69824,#69825,#69826,#69827));
#17117=EDGE_LOOP('',(#69828,#69829,#69830,#69831));
#17118=EDGE_LOOP('',(#69832,#69833,#69834,#69835));
#17119=EDGE_LOOP('',(#69836,#69837,#69838,#69839));
#17120=EDGE_LOOP('',(#69840,#69841,#69842,#69843));
#17121=EDGE_LOOP('',(#69844,#69845,#69846,#69847));
#17122=EDGE_LOOP('',(#69848,#69849,#69850,#69851));
#17123=EDGE_LOOP('',(#69852,#69853,#69854,#69855));
#17124=EDGE_LOOP('',(#69856,#69857,#69858,#69859));
#17125=EDGE_LOOP('',(#69860,#69861,#69862,#69863));
#17126=EDGE_LOOP('',(#69864,#69865,#69866,#69867));
#17127=EDGE_LOOP('',(#69868,#69869,#69870,#69871));
#17128=EDGE_LOOP('',(#69872,#69873,#69874,#69875));
#17129=EDGE_LOOP('',(#69876,#69877,#69878,#69879));
#17130=EDGE_LOOP('',(#69880,#69881,#69882,#69883));
#17131=EDGE_LOOP('',(#69884,#69885,#69886,#69887));
#17132=EDGE_LOOP('',(#69888,#69889,#69890,#69891));
#17133=EDGE_LOOP('',(#69892,#69893,#69894,#69895));
#17134=EDGE_LOOP('',(#69896,#69897,#69898,#69899));
#17135=EDGE_LOOP('',(#69900,#69901,#69902,#69903));
#17136=EDGE_LOOP('',(#69904,#69905,#69906,#69907));
#17137=EDGE_LOOP('',(#69908,#69909,#69910,#69911));
#17138=EDGE_LOOP('',(#69912,#69913,#69914,#69915));
#17139=EDGE_LOOP('',(#69916,#69917,#69918,#69919));
#17140=EDGE_LOOP('',(#69920,#69921,#69922,#69923));
#17141=EDGE_LOOP('',(#69924,#69925,#69926,#69927));
#17142=EDGE_LOOP('',(#69928,#69929,#69930,#69931));
#17143=EDGE_LOOP('',(#69932,#69933,#69934,#69935));
#17144=EDGE_LOOP('',(#69936,#69937,#69938,#69939));
#17145=EDGE_LOOP('',(#69940,#69941,#69942,#69943));
#17146=EDGE_LOOP('',(#69944,#69945,#69946,#69947));
#17147=EDGE_LOOP('',(#69948,#69949,#69950,#69951));
#17148=EDGE_LOOP('',(#69952,#69953,#69954,#69955));
#17149=EDGE_LOOP('',(#69956,#69957,#69958,#69959));
#17150=EDGE_LOOP('',(#69960,#69961,#69962,#69963));
#17151=EDGE_LOOP('',(#69964,#69965,#69966,#69967));
#17152=EDGE_LOOP('',(#69968,#69969,#69970,#69971));
#17153=EDGE_LOOP('',(#69972,#69973,#69974,#69975));
#17154=EDGE_LOOP('',(#69976,#69977,#69978,#69979));
#17155=EDGE_LOOP('',(#69980,#69981,#69982,#69983));
#17156=EDGE_LOOP('',(#69984,#69985,#69986,#69987));
#17157=EDGE_LOOP('',(#69988,#69989,#69990,#69991));
#17158=EDGE_LOOP('',(#69992,#69993,#69994,#69995));
#17159=EDGE_LOOP('',(#69996,#69997,#69998,#69999));
#17160=EDGE_LOOP('',(#70000,#70001,#70002,#70003));
#17161=EDGE_LOOP('',(#70004,#70005,#70006,#70007));
#17162=EDGE_LOOP('',(#70008,#70009,#70010,#70011));
#17163=EDGE_LOOP('',(#70012,#70013,#70014,#70015));
#17164=EDGE_LOOP('',(#70016,#70017,#70018,#70019));
#17165=EDGE_LOOP('',(#70020,#70021,#70022,#70023));
#17166=EDGE_LOOP('',(#70024,#70025,#70026,#70027));
#17167=EDGE_LOOP('',(#70028,#70029,#70030,#70031));
#17168=EDGE_LOOP('',(#70032,#70033,#70034,#70035));
#17169=EDGE_LOOP('',(#70036,#70037,#70038,#70039));
#17170=EDGE_LOOP('',(#70040,#70041,#70042,#70043));
#17171=EDGE_LOOP('',(#70044,#70045,#70046,#70047));
#17172=EDGE_LOOP('',(#70048,#70049,#70050,#70051));
#17173=EDGE_LOOP('',(#70052,#70053,#70054,#70055));
#17174=EDGE_LOOP('',(#70056,#70057,#70058,#70059));
#17175=EDGE_LOOP('',(#70060,#70061,#70062,#70063));
#17176=EDGE_LOOP('',(#70064,#70065,#70066,#70067));
#17177=EDGE_LOOP('',(#70068,#70069,#70070,#70071));
#17178=EDGE_LOOP('',(#70072,#70073,#70074,#70075));
#17179=EDGE_LOOP('',(#70076,#70077,#70078,#70079));
#17180=EDGE_LOOP('',(#70080,#70081,#70082,#70083));
#17181=EDGE_LOOP('',(#70084,#70085,#70086,#70087));
#17182=EDGE_LOOP('',(#70088,#70089,#70090,#70091));
#17183=EDGE_LOOP('',(#70092,#70093,#70094,#70095));
#17184=EDGE_LOOP('',(#70096,#70097,#70098,#70099));
#17185=EDGE_LOOP('',(#70100,#70101,#70102,#70103));
#17186=EDGE_LOOP('',(#70104,#70105,#70106,#70107));
#17187=EDGE_LOOP('',(#70108,#70109,#70110,#70111));
#17188=EDGE_LOOP('',(#70112,#70113,#70114,#70115));
#17189=EDGE_LOOP('',(#70116,#70117,#70118,#70119));
#17190=EDGE_LOOP('',(#70120,#70121,#70122,#70123));
#17191=EDGE_LOOP('',(#70124,#70125,#70126,#70127));
#17192=EDGE_LOOP('',(#70128,#70129,#70130,#70131));
#17193=EDGE_LOOP('',(#70132,#70133,#70134,#70135));
#17194=EDGE_LOOP('',(#70136,#70137,#70138,#70139));
#17195=EDGE_LOOP('',(#70140,#70141,#70142,#70143));
#17196=EDGE_LOOP('',(#70144,#70145,#70146,#70147));
#17197=EDGE_LOOP('',(#70148,#70149,#70150,#70151));
#17198=EDGE_LOOP('',(#70152,#70153,#70154,#70155));
#17199=EDGE_LOOP('',(#70156,#70157,#70158,#70159));
#17200=EDGE_LOOP('',(#70160,#70161,#70162,#70163));
#17201=EDGE_LOOP('',(#70164,#70165,#70166,#70167));
#17202=EDGE_LOOP('',(#70168,#70169,#70170,#70171));
#17203=EDGE_LOOP('',(#70172,#70173,#70174,#70175));
#17204=EDGE_LOOP('',(#70176,#70177,#70178,#70179));
#17205=EDGE_LOOP('',(#70180,#70181,#70182,#70183));
#17206=EDGE_LOOP('',(#70184,#70185,#70186,#70187));
#17207=EDGE_LOOP('',(#70188,#70189,#70190,#70191));
#17208=EDGE_LOOP('',(#70192,#70193,#70194,#70195));
#17209=EDGE_LOOP('',(#70196,#70197,#70198,#70199));
#17210=EDGE_LOOP('',(#70200,#70201,#70202,#70203));
#17211=EDGE_LOOP('',(#70204,#70205,#70206,#70207));
#17212=EDGE_LOOP('',(#70208,#70209,#70210,#70211));
#17213=EDGE_LOOP('',(#70212,#70213,#70214,#70215));
#17214=EDGE_LOOP('',(#70216,#70217,#70218,#70219));
#17215=EDGE_LOOP('',(#70220,#70221,#70222,#70223));
#17216=EDGE_LOOP('',(#70224,#70225,#70226,#70227));
#17217=EDGE_LOOP('',(#70228,#70229,#70230,#70231));
#17218=EDGE_LOOP('',(#70232,#70233,#70234,#70235));
#17219=EDGE_LOOP('',(#70236,#70237,#70238,#70239));
#17220=EDGE_LOOP('',(#70240,#70241,#70242,#70243));
#17221=EDGE_LOOP('',(#70244,#70245,#70246,#70247));
#17222=EDGE_LOOP('',(#70248,#70249,#70250,#70251));
#17223=EDGE_LOOP('',(#70252,#70253,#70254,#70255));
#17224=EDGE_LOOP('',(#70256,#70257,#70258,#70259));
#17225=EDGE_LOOP('',(#70260,#70261,#70262,#70263));
#17226=EDGE_LOOP('',(#70264,#70265,#70266,#70267));
#17227=EDGE_LOOP('',(#70268,#70269,#70270,#70271,#70272,#70273));
#17228=EDGE_LOOP('',(#70274,#70275,#70276,#70277));
#17229=EDGE_LOOP('',(#70278,#70279,#70280,#70281));
#17230=EDGE_LOOP('',(#70282,#70283,#70284,#70285));
#17231=EDGE_LOOP('',(#70286,#70287,#70288,#70289));
#17232=EDGE_LOOP('',(#70290,#70291,#70292,#70293));
#17233=EDGE_LOOP('',(#70294,#70295,#70296,#70297));
#17234=EDGE_LOOP('',(#70298,#70299,#70300,#70301));
#17235=EDGE_LOOP('',(#70302,#70303,#70304,#70305,#70306,#70307,#70308,#70309,
#70310));
#17236=EDGE_LOOP('',(#70311,#70312,#70313,#70314));
#17237=EDGE_LOOP('',(#70315,#70316,#70317,#70318));
#17238=EDGE_LOOP('',(#70319,#70320,#70321,#70322));
#17239=EDGE_LOOP('',(#70323,#70324,#70325,#70326));
#17240=EDGE_LOOP('',(#70327,#70328,#70329,#70330));
#17241=EDGE_LOOP('',(#70331,#70332,#70333,#70334));
#17242=EDGE_LOOP('',(#70335,#70336,#70337,#70338));
#17243=EDGE_LOOP('',(#70339,#70340,#70341,#70342,#70343));
#17244=EDGE_LOOP('',(#70344,#70345,#70346,#70347));
#17245=EDGE_LOOP('',(#70348,#70349,#70350,#70351));
#17246=EDGE_LOOP('',(#70352,#70353,#70354,#70355));
#17247=EDGE_LOOP('',(#70356,#70357,#70358,#70359,#70360));
#17248=EDGE_LOOP('',(#70361,#70362,#70363,#70364));
#17249=EDGE_LOOP('',(#70365,#70366,#70367));
#17250=EDGE_LOOP('',(#70368,#70369,#70370,#70371,#70372,#70373,#70374,#70375,
#70376,#70377));
#17251=EDGE_LOOP('',(#70378,#70379,#70380));
#17252=EDGE_LOOP('',(#70381,#70382,#70383,#70384));
#17253=EDGE_LOOP('',(#70385,#70386,#70387,#70388,#70389));
#17254=EDGE_LOOP('',(#70390,#70391,#70392,#70393));
#17255=EDGE_LOOP('',(#70394,#70395,#70396,#70397));
#17256=EDGE_LOOP('',(#70398,#70399,#70400,#70401));
#17257=EDGE_LOOP('',(#70402,#70403,#70404,#70405,#70406));
#17258=EDGE_LOOP('',(#70407,#70408,#70409));
#17259=EDGE_LOOP('',(#70410,#70411,#70412,#70413));
#17260=EDGE_LOOP('',(#70414,#70415,#70416,#70417,#70418));
#17261=EDGE_LOOP('',(#70419,#70420,#70421,#70422));
#17262=EDGE_LOOP('',(#70423,#70424,#70425,#70426));
#17263=EDGE_LOOP('',(#70427,#70428,#70429,#70430));
#17264=EDGE_LOOP('',(#70431,#70432,#70433,#70434,#70435));
#17265=EDGE_LOOP('',(#70436,#70437,#70438,#70439));
#17266=EDGE_LOOP('',(#70440,#70441,#70442,#70443,#70444,#70445,#70446));
#17267=EDGE_LOOP('',(#70447,#70448,#70449));
#17268=EDGE_LOOP('',(#70450,#70451,#70452,#70453,#70454));
#17269=EDGE_LOOP('',(#70455,#70456,#70457,#70458));
#17270=EDGE_LOOP('',(#70459,#70460,#70461,#70462));
#17271=EDGE_LOOP('',(#70463,#70464,#70465,#70466));
#17272=EDGE_LOOP('',(#70467,#70468,#70469,#70470));
#17273=EDGE_LOOP('',(#70471,#70472,#70473,#70474,#70475));
#17274=EDGE_LOOP('',(#70476,#70477,#70478,#70479));
#17275=EDGE_LOOP('',(#70480,#70481,#70482,#70483));
#17276=EDGE_LOOP('',(#70484,#70485,#70486,#70487));
#17277=EDGE_LOOP('',(#70488,#70489,#70490,#70491));
#17278=EDGE_LOOP('',(#70492,#70493,#70494,#70495));
#17279=EDGE_LOOP('',(#70496,#70497,#70498,#70499));
#17280=EDGE_LOOP('',(#70500,#70501,#70502,#70503));
#17281=EDGE_LOOP('',(#70504,#70505,#70506,#70507));
#17282=EDGE_LOOP('',(#70508,#70509,#70510,#70511));
#17283=EDGE_LOOP('',(#70512,#70513,#70514,#70515));
#17284=EDGE_LOOP('',(#70516,#70517,#70518,#70519));
#17285=EDGE_LOOP('',(#70520,#70521,#70522,#70523));
#17286=EDGE_LOOP('',(#70524,#70525,#70526,#70527));
#17287=EDGE_LOOP('',(#70528,#70529,#70530,#70531));
#17288=EDGE_LOOP('',(#70532,#70533,#70534,#70535));
#17289=EDGE_LOOP('',(#70536,#70537,#70538,#70539));
#17290=EDGE_LOOP('',(#70540,#70541,#70542,#70543));
#17291=EDGE_LOOP('',(#70544,#70545,#70546,#70547));
#17292=EDGE_LOOP('',(#70548,#70549,#70550,#70551));
#17293=EDGE_LOOP('',(#70552,#70553,#70554,#70555));
#17294=EDGE_LOOP('',(#70556,#70557,#70558,#70559));
#17295=EDGE_LOOP('',(#70560,#70561,#70562,#70563));
#17296=EDGE_LOOP('',(#70564,#70565,#70566,#70567));
#17297=EDGE_LOOP('',(#70568,#70569,#70570,#70571));
#17298=EDGE_LOOP('',(#70572,#70573,#70574,#70575));
#17299=EDGE_LOOP('',(#70576,#70577,#70578,#70579));
#17300=EDGE_LOOP('',(#70580,#70581,#70582,#70583));
#17301=EDGE_LOOP('',(#70584,#70585,#70586,#70587));
#17302=EDGE_LOOP('',(#70588,#70589,#70590,#70591));
#17303=EDGE_LOOP('',(#70592,#70593,#70594,#70595));
#17304=EDGE_LOOP('',(#70596,#70597,#70598,#70599));
#17305=EDGE_LOOP('',(#70600,#70601,#70602,#70603));
#17306=EDGE_LOOP('',(#70604,#70605,#70606,#70607));
#17307=EDGE_LOOP('',(#70608,#70609,#70610,#70611));
#17308=EDGE_LOOP('',(#70612,#70613,#70614,#70615));
#17309=EDGE_LOOP('',(#70616,#70617,#70618,#70619));
#17310=EDGE_LOOP('',(#70620,#70621,#70622,#70623));
#17311=EDGE_LOOP('',(#70624,#70625,#70626,#70627));
#17312=EDGE_LOOP('',(#70628,#70629,#70630,#70631));
#17313=EDGE_LOOP('',(#70632,#70633,#70634,#70635));
#17314=EDGE_LOOP('',(#70636,#70637,#70638,#70639));
#17315=EDGE_LOOP('',(#70640,#70641,#70642,#70643));
#17316=EDGE_LOOP('',(#70644,#70645,#70646,#70647));
#17317=EDGE_LOOP('',(#70648,#70649,#70650,#70651));
#17318=EDGE_LOOP('',(#70652,#70653,#70654,#70655));
#17319=EDGE_LOOP('',(#70656,#70657,#70658,#70659));
#17320=EDGE_LOOP('',(#70660,#70661,#70662,#70663));
#17321=EDGE_LOOP('',(#70664,#70665,#70666,#70667));
#17322=EDGE_LOOP('',(#70668,#70669,#70670,#70671));
#17323=EDGE_LOOP('',(#70672,#70673,#70674,#70675));
#17324=EDGE_LOOP('',(#70676,#70677,#70678,#70679));
#17325=EDGE_LOOP('',(#70680,#70681,#70682,#70683));
#17326=EDGE_LOOP('',(#70684,#70685,#70686,#70687));
#17327=EDGE_LOOP('',(#70688,#70689,#70690,#70691));
#17328=EDGE_LOOP('',(#70692,#70693,#70694,#70695));
#17329=EDGE_LOOP('',(#70696,#70697,#70698,#70699));
#17330=EDGE_LOOP('',(#70700,#70701,#70702,#70703));
#17331=EDGE_LOOP('',(#70704,#70705,#70706,#70707));
#17332=EDGE_LOOP('',(#70708,#70709,#70710,#70711));
#17333=EDGE_LOOP('',(#70712,#70713,#70714,#70715));
#17334=EDGE_LOOP('',(#70716,#70717,#70718,#70719));
#17335=EDGE_LOOP('',(#70720,#70721,#70722,#70723));
#17336=EDGE_LOOP('',(#70724,#70725,#70726,#70727));
#17337=EDGE_LOOP('',(#70728,#70729,#70730,#70731));
#17338=EDGE_LOOP('',(#70732,#70733,#70734,#70735));
#17339=EDGE_LOOP('',(#70736,#70737,#70738,#70739));
#17340=EDGE_LOOP('',(#70740,#70741,#70742,#70743));
#17341=EDGE_LOOP('',(#70744,#70745,#70746,#70747));
#17342=EDGE_LOOP('',(#70748,#70749,#70750,#70751));
#17343=EDGE_LOOP('',(#70752,#70753,#70754,#70755));
#17344=EDGE_LOOP('',(#70756,#70757,#70758,#70759));
#17345=EDGE_LOOP('',(#70760,#70761,#70762,#70763));
#17346=EDGE_LOOP('',(#70764,#70765,#70766,#70767));
#17347=EDGE_LOOP('',(#70768,#70769,#70770,#70771));
#17348=EDGE_LOOP('',(#70772,#70773,#70774,#70775));
#17349=EDGE_LOOP('',(#70776,#70777,#70778,#70779));
#17350=EDGE_LOOP('',(#70780,#70781,#70782,#70783));
#17351=EDGE_LOOP('',(#70784,#70785,#70786,#70787));
#17352=EDGE_LOOP('',(#70788,#70789,#70790,#70791));
#17353=EDGE_LOOP('',(#70792,#70793,#70794,#70795));
#17354=EDGE_LOOP('',(#70796,#70797,#70798,#70799));
#17355=EDGE_LOOP('',(#70800,#70801,#70802,#70803));
#17356=EDGE_LOOP('',(#70804,#70805,#70806,#70807));
#17357=EDGE_LOOP('',(#70808,#70809,#70810,#70811));
#17358=EDGE_LOOP('',(#70812,#70813,#70814,#70815));
#17359=EDGE_LOOP('',(#70816,#70817,#70818,#70819));
#17360=EDGE_LOOP('',(#70820,#70821,#70822,#70823));
#17361=EDGE_LOOP('',(#70824,#70825,#70826,#70827));
#17362=EDGE_LOOP('',(#70828,#70829,#70830,#70831));
#17363=EDGE_LOOP('',(#70832,#70833,#70834,#70835));
#17364=EDGE_LOOP('',(#70836,#70837,#70838,#70839));
#17365=EDGE_LOOP('',(#70840,#70841,#70842,#70843));
#17366=EDGE_LOOP('',(#70844,#70845,#70846,#70847));
#17367=EDGE_LOOP('',(#70848,#70849,#70850,#70851));
#17368=EDGE_LOOP('',(#70852,#70853,#70854,#70855));
#17369=EDGE_LOOP('',(#70856,#70857,#70858,#70859));
#17370=EDGE_LOOP('',(#70860,#70861,#70862,#70863));
#17371=EDGE_LOOP('',(#70864,#70865,#70866,#70867));
#17372=EDGE_LOOP('',(#70868,#70869,#70870,#70871));
#17373=EDGE_LOOP('',(#70872,#70873,#70874,#70875));
#17374=EDGE_LOOP('',(#70876,#70877,#70878,#70879));
#17375=EDGE_LOOP('',(#70880,#70881,#70882,#70883));
#17376=EDGE_LOOP('',(#70884,#70885,#70886,#70887));
#17377=EDGE_LOOP('',(#70888,#70889,#70890,#70891));
#17378=EDGE_LOOP('',(#70892,#70893,#70894,#70895));
#17379=EDGE_LOOP('',(#70896,#70897,#70898,#70899));
#17380=EDGE_LOOP('',(#70900,#70901,#70902,#70903));
#17381=EDGE_LOOP('',(#70904,#70905,#70906,#70907));
#17382=EDGE_LOOP('',(#70908,#70909,#70910,#70911));
#17383=EDGE_LOOP('',(#70912,#70913,#70914,#70915));
#17384=EDGE_LOOP('',(#70916,#70917,#70918,#70919));
#17385=EDGE_LOOP('',(#70920,#70921,#70922,#70923));
#17386=EDGE_LOOP('',(#70924,#70925,#70926,#70927));
#17387=EDGE_LOOP('',(#70928,#70929,#70930,#70931));
#17388=EDGE_LOOP('',(#70932,#70933,#70934,#70935));
#17389=EDGE_LOOP('',(#70936,#70937,#70938,#70939));
#17390=EDGE_LOOP('',(#70940,#70941,#70942,#70943));
#17391=EDGE_LOOP('',(#70944,#70945,#70946,#70947));
#17392=EDGE_LOOP('',(#70948,#70949,#70950,#70951));
#17393=EDGE_LOOP('',(#70952,#70953,#70954,#70955));
#17394=EDGE_LOOP('',(#70956,#70957,#70958,#70959));
#17395=EDGE_LOOP('',(#70960,#70961,#70962,#70963));
#17396=EDGE_LOOP('',(#70964,#70965,#70966,#70967));
#17397=EDGE_LOOP('',(#70968,#70969,#70970,#70971));
#17398=EDGE_LOOP('',(#70972,#70973,#70974,#70975));
#17399=EDGE_LOOP('',(#70976,#70977,#70978,#70979));
#17400=EDGE_LOOP('',(#70980,#70981,#70982,#70983));
#17401=EDGE_LOOP('',(#70984,#70985,#70986,#70987));
#17402=EDGE_LOOP('',(#70988,#70989,#70990,#70991));
#17403=EDGE_LOOP('',(#70992,#70993,#70994,#70995));
#17404=EDGE_LOOP('',(#70996,#70997,#70998,#70999));
#17405=EDGE_LOOP('',(#71000,#71001,#71002,#71003));
#17406=EDGE_LOOP('',(#71004,#71005,#71006,#71007));
#17407=EDGE_LOOP('',(#71008,#71009,#71010,#71011));
#17408=EDGE_LOOP('',(#71012,#71013,#71014,#71015));
#17409=EDGE_LOOP('',(#71016,#71017,#71018,#71019));
#17410=EDGE_LOOP('',(#71020,#71021,#71022,#71023));
#17411=EDGE_LOOP('',(#71024,#71025,#71026,#71027));
#17412=EDGE_LOOP('',(#71028,#71029,#71030,#71031));
#17413=EDGE_LOOP('',(#71032,#71033,#71034,#71035));
#17414=EDGE_LOOP('',(#71036,#71037,#71038,#71039));
#17415=EDGE_LOOP('',(#71040,#71041,#71042,#71043));
#17416=EDGE_LOOP('',(#71044,#71045,#71046,#71047));
#17417=EDGE_LOOP('',(#71048,#71049,#71050,#71051));
#17418=EDGE_LOOP('',(#71052,#71053,#71054,#71055));
#17419=EDGE_LOOP('',(#71056,#71057,#71058,#71059));
#17420=EDGE_LOOP('',(#71060,#71061,#71062,#71063));
#17421=EDGE_LOOP('',(#71064,#71065,#71066,#71067));
#17422=EDGE_LOOP('',(#71068,#71069,#71070,#71071));
#17423=EDGE_LOOP('',(#71072,#71073,#71074,#71075));
#17424=EDGE_LOOP('',(#71076,#71077,#71078,#71079));
#17425=EDGE_LOOP('',(#71080,#71081,#71082,#71083));
#17426=EDGE_LOOP('',(#71084,#71085,#71086,#71087));
#17427=EDGE_LOOP('',(#71088,#71089,#71090,#71091));
#17428=EDGE_LOOP('',(#71092,#71093,#71094,#71095));
#17429=EDGE_LOOP('',(#71096,#71097,#71098,#71099));
#17430=EDGE_LOOP('',(#71100,#71101,#71102,#71103));
#17431=EDGE_LOOP('',(#71104,#71105,#71106,#71107));
#17432=EDGE_LOOP('',(#71108,#71109,#71110,#71111));
#17433=EDGE_LOOP('',(#71112,#71113,#71114,#71115));
#17434=EDGE_LOOP('',(#71116,#71117,#71118,#71119));
#17435=EDGE_LOOP('',(#71120,#71121,#71122,#71123));
#17436=EDGE_LOOP('',(#71124,#71125,#71126,#71127));
#17437=EDGE_LOOP('',(#71128,#71129,#71130,#71131));
#17438=EDGE_LOOP('',(#71132,#71133,#71134,#71135));
#17439=EDGE_LOOP('',(#71136,#71137,#71138,#71139));
#17440=EDGE_LOOP('',(#71140,#71141,#71142,#71143));
#17441=EDGE_LOOP('',(#71144,#71145,#71146,#71147));
#17442=EDGE_LOOP('',(#71148,#71149,#71150,#71151));
#17443=EDGE_LOOP('',(#71152,#71153,#71154,#71155));
#17444=EDGE_LOOP('',(#71156,#71157,#71158,#71159));
#17445=EDGE_LOOP('',(#71160,#71161,#71162,#71163));
#17446=EDGE_LOOP('',(#71164,#71165,#71166,#71167));
#17447=EDGE_LOOP('',(#71168,#71169,#71170,#71171));
#17448=EDGE_LOOP('',(#71172,#71173,#71174,#71175));
#17449=EDGE_LOOP('',(#71176,#71177,#71178,#71179));
#17450=EDGE_LOOP('',(#71180,#71181,#71182,#71183));
#17451=EDGE_LOOP('',(#71184,#71185,#71186,#71187));
#17452=EDGE_LOOP('',(#71188,#71189,#71190,#71191));
#17453=EDGE_LOOP('',(#71192,#71193,#71194,#71195));
#17454=EDGE_LOOP('',(#71196,#71197,#71198,#71199));
#17455=EDGE_LOOP('',(#71200,#71201,#71202,#71203));
#17456=EDGE_LOOP('',(#71204,#71205,#71206,#71207));
#17457=EDGE_LOOP('',(#71208,#71209,#71210,#71211));
#17458=EDGE_LOOP('',(#71212,#71213,#71214,#71215));
#17459=EDGE_LOOP('',(#71216,#71217,#71218,#71219));
#17460=EDGE_LOOP('',(#71220,#71221,#71222,#71223));
#17461=EDGE_LOOP('',(#71224,#71225,#71226,#71227));
#17462=EDGE_LOOP('',(#71228,#71229,#71230,#71231));
#17463=EDGE_LOOP('',(#71232,#71233,#71234,#71235));
#17464=EDGE_LOOP('',(#71236,#71237,#71238,#71239));
#17465=EDGE_LOOP('',(#71240,#71241,#71242,#71243));
#17466=EDGE_LOOP('',(#71244,#71245,#71246,#71247));
#17467=EDGE_LOOP('',(#71248,#71249,#71250,#71251));
#17468=EDGE_LOOP('',(#71252,#71253,#71254,#71255));
#17469=EDGE_LOOP('',(#71256,#71257,#71258,#71259));
#17470=EDGE_LOOP('',(#71260,#71261,#71262,#71263));
#17471=EDGE_LOOP('',(#71264,#71265,#71266,#71267));
#17472=EDGE_LOOP('',(#71268,#71269,#71270,#71271));
#17473=EDGE_LOOP('',(#71272,#71273,#71274,#71275));
#17474=EDGE_LOOP('',(#71276,#71277,#71278,#71279));
#17475=EDGE_LOOP('',(#71280,#71281,#71282,#71283));
#17476=EDGE_LOOP('',(#71284,#71285,#71286,#71287));
#17477=EDGE_LOOP('',(#71288,#71289,#71290,#71291));
#17478=EDGE_LOOP('',(#71292,#71293,#71294,#71295));
#17479=EDGE_LOOP('',(#71296,#71297,#71298,#71299));
#17480=EDGE_LOOP('',(#71300,#71301,#71302,#71303));
#17481=EDGE_LOOP('',(#71304,#71305,#71306,#71307));
#17482=EDGE_LOOP('',(#71308,#71309,#71310,#71311));
#17483=EDGE_LOOP('',(#71312,#71313,#71314,#71315));
#17484=EDGE_LOOP('',(#71316,#71317,#71318,#71319));
#17485=EDGE_LOOP('',(#71320,#71321,#71322,#71323));
#17486=EDGE_LOOP('',(#71324,#71325,#71326,#71327));
#17487=EDGE_LOOP('',(#71328,#71329,#71330,#71331));
#17488=EDGE_LOOP('',(#71332,#71333,#71334,#71335));
#17489=EDGE_LOOP('',(#71336,#71337,#71338,#71339));
#17490=EDGE_LOOP('',(#71340,#71341,#71342,#71343));
#17491=EDGE_LOOP('',(#71344,#71345,#71346,#71347));
#17492=EDGE_LOOP('',(#71348,#71349,#71350,#71351));
#17493=EDGE_LOOP('',(#71352,#71353,#71354));
#17494=EDGE_LOOP('',(#71355,#71356,#71357));
#17495=EDGE_LOOP('',(#71358,#71359,#71360));
#17496=EDGE_LOOP('',(#71361,#71362,#71363,#71364));
#17497=EDGE_LOOP('',(#71365,#71366,#71367,#71368));
#17498=EDGE_LOOP('',(#71369,#71370,#71371,#71372));
#17499=EDGE_LOOP('',(#71373,#71374,#71375,#71376));
#17500=EDGE_LOOP('',(#71377,#71378,#71379,#71380));
#17501=EDGE_LOOP('',(#71381,#71382,#71383,#71384));
#17502=EDGE_LOOP('',(#71385,#71386,#71387,#71388));
#17503=EDGE_LOOP('',(#71389,#71390,#71391,#71392));
#17504=EDGE_LOOP('',(#71393,#71394,#71395,#71396));
#17505=EDGE_LOOP('',(#71397,#71398,#71399,#71400));
#17506=EDGE_LOOP('',(#71401,#71402,#71403,#71404));
#17507=EDGE_LOOP('',(#71405,#71406,#71407,#71408));
#17508=EDGE_LOOP('',(#71409,#71410,#71411,#71412));
#17509=EDGE_LOOP('',(#71413,#71414,#71415,#71416,#71417));
#17510=EDGE_LOOP('',(#71418,#71419,#71420,#71421,#71422));
#17511=EDGE_LOOP('',(#71423,#71424,#71425,#71426,#71427));
#17512=EDGE_LOOP('',(#71428,#71429,#71430,#71431,#71432));
#17513=EDGE_LOOP('',(#71433,#71434,#71435,#71436,#71437));
#17514=EDGE_LOOP('',(#71438,#71439,#71440,#71441,#71442,#71443,#71444,#71445));
#17515=EDGE_LOOP('',(#71446,#71447,#71448,#71449,#71450));
#17516=EDGE_LOOP('',(#71451,#71452,#71453,#71454,#71455));
#17517=EDGE_LOOP('',(#71456,#71457,#71458,#71459,#71460,#71461,#71462,#71463));
#17518=EDGE_LOOP('',(#71464,#71465,#71466,#71467,#71468));
#17519=EDGE_LOOP('',(#71469,#71470,#71471,#71472));
#17520=EDGE_LOOP('',(#71473,#71474,#71475,#71476));
#17521=EDGE_LOOP('',(#71477,#71478,#71479,#71480));
#17522=EDGE_LOOP('',(#71481,#71482,#71483,#71484));
#17523=EDGE_LOOP('',(#71485,#71486,#71487,#71488));
#17524=EDGE_LOOP('',(#71489,#71490,#71491,#71492));
#17525=EDGE_LOOP('',(#71493,#71494,#71495,#71496));
#17526=EDGE_LOOP('',(#71497,#71498,#71499,#71500));
#17527=EDGE_LOOP('',(#71501,#71502,#71503,#71504));
#17528=EDGE_LOOP('',(#71505,#71506,#71507,#71508,#71509,#71510,#71511,#71512));
#17529=EDGE_LOOP('',(#71513,#71514,#71515,#71516));
#17530=EDGE_LOOP('',(#71517,#71518,#71519,#71520,#71521,#71522,#71523,#71524,
#71525,#71526,#71527,#71528));
#17531=EDGE_LOOP('',(#71529,#71530,#71531,#71532));
#17532=EDGE_LOOP('',(#71533,#71534,#71535,#71536,#71537,#71538));
#17533=EDGE_LOOP('',(#71539,#71540,#71541,#71542,#71543,#71544,#71545,#71546,
#71547,#71548,#71549,#71550,#71551,#71552,#71553,#71554,#71555,#71556));
#17534=EDGE_LOOP('',(#71557,#71558,#71559,#71560,#71561,#71562));
#17535=EDGE_LOOP('',(#71563,#71564,#71565,#71566,#71567,#71568,#71569,#71570,
#71571,#71572,#71573,#71574,#71575,#71576,#71577,#71578));
#17536=EDGE_LOOP('',(#71579,#71580));
#17537=EDGE_LOOP('',(#71581,#71582,#71583,#71584,#71585,#71586,#71587,#71588,
#71589,#71590,#71591,#71592));
#17538=EDGE_LOOP('',(#71593,#71594));
#17539=EDGE_LOOP('',(#71595,#71596));
#17540=EDGE_LOOP('',(#71597,#71598));
#17541=EDGE_LOOP('',(#71599,#71600));
#17542=EDGE_LOOP('',(#71601,#71602,#71603));
#17543=EDGE_LOOP('',(#71604,#71605,#71606,#71607));
#17544=EDGE_LOOP('',(#71608,#71609,#71610,#71611));
#17545=EDGE_LOOP('',(#71612,#71613,#71614,#71615));
#17546=EDGE_LOOP('',(#71616,#71617,#71618,#71619));
#17547=EDGE_LOOP('',(#71620,#71621,#71622,#71623,#71624,#71625));
#17548=EDGE_LOOP('',(#71626,#71627,#71628));
#17549=EDGE_LOOP('',(#71629,#71630,#71631,#71632,#71633,#71634,#71635,#71636));
#17550=EDGE_LOOP('',(#71637,#71638,#71639));
#17551=EDGE_LOOP('',(#71640,#71641,#71642,#71643,#71644,#71645,#71646,#71647,
#71648,#71649,#71650,#71651,#71652,#71653,#71654,#71655,#71656,#71657,#71658,
#71659,#71660,#71661));
#17552=EDGE_LOOP('',(#71662,#71663,#71664,#71665,#71666,#71667));
#17553=EDGE_LOOP('',(#71668,#71669,#71670,#71671));
#17554=EDGE_LOOP('',(#71672,#71673,#71674,#71675));
#17555=EDGE_LOOP('',(#71676,#71677,#71678,#71679));
#17556=EDGE_LOOP('',(#71680,#71681,#71682,#71683));
#17557=EDGE_LOOP('',(#71684,#71685,#71686,#71687));
#17558=EDGE_LOOP('',(#71688,#71689,#71690,#71691));
#17559=EDGE_LOOP('',(#71692,#71693,#71694,#71695));
#17560=EDGE_LOOP('',(#71696));
#17561=EDGE_LOOP('',(#71697,#71698,#71699,#71700,#71701,#71702));
#17562=EDGE_LOOP('',(#71703));
#17563=EDGE_LOOP('',(#71704,#71705,#71706,#71707,#71708));
#17564=EDGE_LOOP('',(#71709,#71710,#71711,#71712,#71713,#71714));
#17565=EDGE_LOOP('',(#71715));
#17566=EDGE_LOOP('',(#71716,#71717,#71718));
#17567=EDGE_LOOP('',(#71719,#71720,#71721));
#17568=EDGE_LOOP('',(#71722,#71723,#71724,#71725));
#17569=EDGE_LOOP('',(#71726,#71727,#71728,#71729,#71730,#71731,#71732,#71733));
#17570=EDGE_LOOP('',(#71734,#71735,#71736));
#17571=EDGE_LOOP('',(#71737,#71738,#71739));
#17572=EDGE_LOOP('',(#71740,#71741,#71742,#71743));
#17573=EDGE_LOOP('',(#71744,#71745,#71746,#71747));
#17574=EDGE_LOOP('',(#71748,#71749,#71750,#71751));
#17575=EDGE_LOOP('',(#71752,#71753,#71754,#71755));
#17576=EDGE_LOOP('',(#71756,#71757,#71758,#71759));
#17577=EDGE_LOOP('',(#71760,#71761,#71762,#71763));
#17578=EDGE_LOOP('',(#71764,#71765,#71766,#71767));
#17579=EDGE_LOOP('',(#71768,#71769,#71770,#71771,#71772,#71773,#71774,#71775,
#71776,#71777,#71778,#71779,#71780,#71781,#71782,#71783,#71784));
#17580=EDGE_LOOP('',(#71785,#71786,#71787,#71788));
#17581=EDGE_LOOP('',(#71789,#71790,#71791,#71792));
#17582=EDGE_LOOP('',(#71793,#71794,#71795,#71796));
#17583=EDGE_LOOP('',(#71797,#71798,#71799,#71800));
#17584=EDGE_LOOP('',(#71801,#71802,#71803,#71804));
#17585=EDGE_LOOP('',(#71805,#71806,#71807,#71808));
#17586=EDGE_LOOP('',(#71809,#71810,#71811,#71812));
#17587=EDGE_LOOP('',(#71813,#71814,#71815,#71816));
#17588=EDGE_LOOP('',(#71817,#71818,#71819,#71820));
#17589=EDGE_LOOP('',(#71821,#71822,#71823,#71824));
#17590=EDGE_LOOP('',(#71825,#71826,#71827,#71828));
#17591=EDGE_LOOP('',(#71829,#71830,#71831,#71832));
#17592=EDGE_LOOP('',(#71833,#71834,#71835,#71836));
#17593=EDGE_LOOP('',(#71837,#71838,#71839,#71840));
#17594=EDGE_LOOP('',(#71841,#71842,#71843,#71844,#71845));
#17595=EDGE_LOOP('',(#71846,#71847,#71848,#71849,#71850));
#17596=EDGE_LOOP('',(#71851,#71852,#71853,#71854,#71855));
#17597=EDGE_LOOP('',(#71856,#71857,#71858,#71859,#71860));
#17598=EDGE_LOOP('',(#71861,#71862,#71863,#71864,#71865));
#17599=EDGE_LOOP('',(#71866,#71867,#71868,#71869,#71870,#71871,#71872,#71873));
#17600=EDGE_LOOP('',(#71874,#71875,#71876,#71877,#71878));
#17601=EDGE_LOOP('',(#71879,#71880,#71881,#71882,#71883));
#17602=EDGE_LOOP('',(#71884,#71885,#71886,#71887,#71888,#71889,#71890,#71891));
#17603=EDGE_LOOP('',(#71892,#71893,#71894,#71895,#71896));
#17604=EDGE_LOOP('',(#71897,#71898,#71899,#71900));
#17605=EDGE_LOOP('',(#71901,#71902,#71903,#71904));
#17606=EDGE_LOOP('',(#71905,#71906,#71907,#71908));
#17607=EDGE_LOOP('',(#71909,#71910,#71911,#71912));
#17608=EDGE_LOOP('',(#71913,#71914,#71915,#71916));
#17609=EDGE_LOOP('',(#71917,#71918,#71919,#71920));
#17610=EDGE_LOOP('',(#71921,#71922,#71923,#71924));
#17611=EDGE_LOOP('',(#71925,#71926,#71927,#71928));
#17612=EDGE_LOOP('',(#71929,#71930,#71931,#71932));
#17613=EDGE_LOOP('',(#71933,#71934,#71935,#71936,#71937,#71938,#71939,#71940));
#17614=EDGE_LOOP('',(#71941,#71942,#71943,#71944));
#17615=EDGE_LOOP('',(#71945,#71946,#71947,#71948));
#17616=EDGE_LOOP('',(#71949,#71950,#71951,#71952,#71953,#71954,#71955,#71956));
#17617=EDGE_LOOP('',(#71957,#71958,#71959,#71960,#71961,#71962,#71963,#71964,
#71965,#71966,#71967,#71968,#71969,#71970,#71971,#71972,#71973,#71974));
#17618=EDGE_LOOP('',(#71975,#71976,#71977,#71978,#71979,#71980,#71981,#71982,
#71983,#71984));
#17619=EDGE_LOOP('',(#71985,#71986,#71987,#71988,#71989,#71990,#71991,#71992,
#71993,#71994,#71995,#71996,#71997,#71998,#71999,#72000,#72001,#72002,#72003,
#72004));
#17620=EDGE_LOOP('',(#72005,#72006,#72007,#72008));
#17621=EDGE_LOOP('',(#72009,#72010,#72011,#72012));
#17622=EDGE_LOOP('',(#72013,#72014,#72015,#72016));
#17623=EDGE_LOOP('',(#72017,#72018,#72019,#72020));
#17624=EDGE_LOOP('',(#72021,#72022,#72023,#72024));
#17625=EDGE_LOOP('',(#72025,#72026,#72027,#72028));
#17626=EDGE_LOOP('',(#72029,#72030,#72031,#72032));
#17627=EDGE_LOOP('',(#72033,#72034,#72035,#72036));
#17628=EDGE_LOOP('',(#72037,#72038,#72039,#72040));
#17629=EDGE_LOOP('',(#72041,#72042,#72043,#72044));
#17630=EDGE_LOOP('',(#72045,#72046,#72047,#72048));
#17631=EDGE_LOOP('',(#72049,#72050,#72051,#72052));
#17632=EDGE_LOOP('',(#72053,#72054,#72055,#72056));
#17633=EDGE_LOOP('',(#72057,#72058,#72059,#72060));
#17634=EDGE_LOOP('',(#72061,#72062,#72063,#72064));
#17635=EDGE_LOOP('',(#72065,#72066,#72067,#72068));
#17636=EDGE_LOOP('',(#72069,#72070,#72071,#72072));
#17637=EDGE_LOOP('',(#72073,#72074,#72075,#72076));
#17638=EDGE_LOOP('',(#72077,#72078,#72079,#72080));
#17639=EDGE_LOOP('',(#72081,#72082,#72083,#72084));
#17640=EDGE_LOOP('',(#72085,#72086,#72087,#72088));
#17641=EDGE_LOOP('',(#72089,#72090,#72091,#72092));
#17642=EDGE_LOOP('',(#72093,#72094,#72095,#72096));
#17643=EDGE_LOOP('',(#72097,#72098,#72099,#72100));
#17644=EDGE_LOOP('',(#72101,#72102,#72103,#72104));
#17645=EDGE_LOOP('',(#72105,#72106,#72107,#72108));
#17646=EDGE_LOOP('',(#72109,#72110,#72111,#72112));
#17647=EDGE_LOOP('',(#72113,#72114,#72115,#72116));
#17648=EDGE_LOOP('',(#72117,#72118,#72119,#72120));
#17649=EDGE_LOOP('',(#72121,#72122,#72123,#72124));
#17650=EDGE_LOOP('',(#72125,#72126,#72127,#72128));
#17651=EDGE_LOOP('',(#72129,#72130,#72131,#72132));
#17652=EDGE_LOOP('',(#72133,#72134,#72135,#72136));
#17653=EDGE_LOOP('',(#72137,#72138,#72139,#72140));
#17654=EDGE_LOOP('',(#72141,#72142,#72143,#72144));
#17655=EDGE_LOOP('',(#72145,#72146,#72147,#72148));
#17656=EDGE_LOOP('',(#72149,#72150,#72151,#72152));
#17657=EDGE_LOOP('',(#72153,#72154,#72155,#72156));
#17658=EDGE_LOOP('',(#72157,#72158,#72159,#72160));
#17659=EDGE_LOOP('',(#72161,#72162,#72163,#72164));
#17660=EDGE_LOOP('',(#72165,#72166,#72167,#72168));
#17661=EDGE_LOOP('',(#72169,#72170,#72171,#72172));
#17662=EDGE_LOOP('',(#72173,#72174,#72175,#72176));
#17663=EDGE_LOOP('',(#72177,#72178,#72179,#72180));
#17664=EDGE_LOOP('',(#72181,#72182,#72183,#72184));
#17665=EDGE_LOOP('',(#72185,#72186,#72187,#72188));
#17666=EDGE_LOOP('',(#72189,#72190,#72191,#72192));
#17667=EDGE_LOOP('',(#72193,#72194,#72195,#72196));
#17668=EDGE_LOOP('',(#72197,#72198,#72199,#72200));
#17669=EDGE_LOOP('',(#72201,#72202,#72203,#72204));
#17670=EDGE_LOOP('',(#72205,#72206,#72207,#72208));
#17671=EDGE_LOOP('',(#72209,#72210,#72211,#72212));
#17672=EDGE_LOOP('',(#72213,#72214,#72215,#72216));
#17673=EDGE_LOOP('',(#72217,#72218,#72219,#72220));
#17674=EDGE_LOOP('',(#72221,#72222,#72223,#72224));
#17675=EDGE_LOOP('',(#72225,#72226,#72227,#72228));
#17676=EDGE_LOOP('',(#72229,#72230,#72231,#72232));
#17677=EDGE_LOOP('',(#72233,#72234,#72235,#72236));
#17678=EDGE_LOOP('',(#72237,#72238,#72239,#72240));
#17679=EDGE_LOOP('',(#72241,#72242,#72243,#72244));
#17680=EDGE_LOOP('',(#72245,#72246,#72247,#72248));
#17681=EDGE_LOOP('',(#72249,#72250,#72251,#72252));
#17682=EDGE_LOOP('',(#72253,#72254,#72255,#72256));
#17683=EDGE_LOOP('',(#72257,#72258,#72259,#72260));
#17684=EDGE_LOOP('',(#72261,#72262,#72263,#72264));
#17685=EDGE_LOOP('',(#72265,#72266,#72267,#72268));
#17686=EDGE_LOOP('',(#72269,#72270,#72271,#72272));
#17687=EDGE_LOOP('',(#72273,#72274,#72275,#72276));
#17688=EDGE_LOOP('',(#72277,#72278,#72279,#72280));
#17689=EDGE_LOOP('',(#72281,#72282,#72283,#72284,#72285));
#17690=EDGE_LOOP('',(#72286,#72287,#72288,#72289,#72290));
#17691=EDGE_LOOP('',(#72291,#72292,#72293,#72294));
#17692=EDGE_LOOP('',(#72295,#72296,#72297,#72298));
#17693=EDGE_LOOP('',(#72299,#72300,#72301));
#17694=EDGE_LOOP('',(#72302,#72303,#72304,#72305));
#17695=EDGE_LOOP('',(#72306,#72307,#72308,#72309));
#17696=EDGE_LOOP('',(#72310,#72311,#72312,#72313));
#17697=EDGE_LOOP('',(#72314,#72315,#72316,#72317));
#17698=EDGE_LOOP('',(#72318,#72319,#72320,#72321));
#17699=EDGE_LOOP('',(#72322,#72323,#72324,#72325));
#17700=EDGE_LOOP('',(#72326,#72327,#72328,#72329));
#17701=EDGE_LOOP('',(#72330,#72331,#72332,#72333));
#17702=EDGE_LOOP('',(#72334,#72335,#72336,#72337,#72338));
#17703=EDGE_LOOP('',(#72339,#72340,#72341));
#17704=EDGE_LOOP('',(#72342,#72343,#72344,#72345));
#17705=EDGE_LOOP('',(#72346,#72347,#72348,#72349));
#17706=EDGE_LOOP('',(#72350,#72351,#72352,#72353));
#17707=EDGE_LOOP('',(#72354,#72355,#72356,#72357));
#17708=EDGE_LOOP('',(#72358,#72359,#72360,#72361));
#17709=EDGE_LOOP('',(#72362,#72363,#72364));
#17710=EDGE_LOOP('',(#72365,#72366,#72367,#72368));
#17711=EDGE_LOOP('',(#72369,#72370,#72371,#72372));
#17712=EDGE_LOOP('',(#72373,#72374,#72375,#72376));
#17713=EDGE_LOOP('',(#72377,#72378,#72379,#72380));
#17714=EDGE_LOOP('',(#72381,#72382,#72383));
#17715=EDGE_LOOP('',(#72384,#72385,#72386,#72387));
#17716=EDGE_LOOP('',(#72388,#72389,#72390,#72391));
#17717=EDGE_LOOP('',(#72392,#72393,#72394,#72395));
#17718=EDGE_LOOP('',(#72396,#72397,#72398,#72399));
#17719=EDGE_LOOP('',(#72400,#72401,#72402,#72403));
#17720=EDGE_LOOP('',(#72404,#72405,#72406,#72407));
#17721=EDGE_LOOP('',(#72408,#72409,#72410,#72411));
#17722=EDGE_LOOP('',(#72412,#72413,#72414,#72415));
#17723=EDGE_LOOP('',(#72416,#72417,#72418,#72419));
#17724=EDGE_LOOP('',(#72420,#72421,#72422,#72423));
#17725=EDGE_LOOP('',(#72424,#72425,#72426,#72427));
#17726=EDGE_LOOP('',(#72428,#72429,#72430,#72431));
#17727=EDGE_LOOP('',(#72432,#72433,#72434,#72435));
#17728=EDGE_LOOP('',(#72436,#72437,#72438,#72439));
#17729=EDGE_LOOP('',(#72440,#72441,#72442,#72443));
#17730=EDGE_LOOP('',(#72444,#72445,#72446,#72447));
#17731=EDGE_LOOP('',(#72448,#72449,#72450,#72451));
#17732=EDGE_LOOP('',(#72452,#72453,#72454,#72455));
#17733=EDGE_LOOP('',(#72456,#72457,#72458,#72459));
#17734=EDGE_LOOP('',(#72460,#72461,#72462,#72463));
#17735=EDGE_LOOP('',(#72464,#72465,#72466,#72467));
#17736=EDGE_LOOP('',(#72468,#72469,#72470,#72471));
#17737=EDGE_LOOP('',(#72472,#72473,#72474,#72475));
#17738=EDGE_LOOP('',(#72476,#72477,#72478,#72479));
#17739=EDGE_LOOP('',(#72480,#72481,#72482,#72483));
#17740=EDGE_LOOP('',(#72484,#72485,#72486,#72487));
#17741=EDGE_LOOP('',(#72488,#72489,#72490,#72491));
#17742=EDGE_LOOP('',(#72492,#72493,#72494,#72495));
#17743=EDGE_LOOP('',(#72496,#72497,#72498,#72499));
#17744=EDGE_LOOP('',(#72500,#72501,#72502,#72503));
#17745=EDGE_LOOP('',(#72504,#72505,#72506,#72507,#72508));
#17746=EDGE_LOOP('',(#72509,#72510,#72511,#72512));
#17747=EDGE_LOOP('',(#72513,#72514,#72515,#72516));
#17748=EDGE_LOOP('',(#72517,#72518,#72519,#72520));
#17749=EDGE_LOOP('',(#72521,#72522,#72523,#72524));
#17750=EDGE_LOOP('',(#72525,#72526,#72527,#72528));
#17751=EDGE_LOOP('',(#72529,#72530,#72531,#72532));
#17752=EDGE_LOOP('',(#72533,#72534,#72535,#72536));
#17753=EDGE_LOOP('',(#72537,#72538,#72539,#72540,#72541,#72542));
#17754=EDGE_LOOP('',(#72543,#72544,#72545,#72546));
#17755=EDGE_LOOP('',(#72547,#72548,#72549,#72550));
#17756=EDGE_LOOP('',(#72551,#72552,#72553,#72554,#72555));
#17757=EDGE_LOOP('',(#72556,#72557,#72558,#72559));
#17758=EDGE_LOOP('',(#72560,#72561,#72562,#72563));
#17759=EDGE_LOOP('',(#72564,#72565,#72566,#72567));
#17760=EDGE_LOOP('',(#72568,#72569,#72570,#72571,#72572));
#17761=EDGE_LOOP('',(#72573,#72574,#72575,#72576));
#17762=EDGE_LOOP('',(#72577,#72578,#72579,#72580));
#17763=EDGE_LOOP('',(#72581,#72582,#72583,#72584));
#17764=EDGE_LOOP('',(#72585,#72586,#72587,#72588));
#17765=EDGE_LOOP('',(#72589,#72590,#72591,#72592,#72593));
#17766=EDGE_LOOP('',(#72594,#72595,#72596,#72597));
#17767=EDGE_LOOP('',(#72598,#72599,#72600,#72601));
#17768=EDGE_LOOP('',(#72602,#72603,#72604,#72605));
#17769=EDGE_LOOP('',(#72606,#72607,#72608,#72609));
#17770=EDGE_LOOP('',(#72610,#72611,#72612,#72613));
#17771=EDGE_LOOP('',(#72614,#72615,#72616,#72617,#72618));
#17772=EDGE_LOOP('',(#72619,#72620,#72621,#72622,#72623,#72624));
#17773=EDGE_LOOP('',(#72625,#72626,#72627,#72628,#72629,#72630));
#17774=EDGE_LOOP('',(#72631,#72632,#72633,#72634,#72635,#72636));
#17775=EDGE_LOOP('',(#72637,#72638,#72639,#72640,#72641));
#17776=EDGE_LOOP('',(#72642,#72643,#72644,#72645,#72646,#72647,#72648));
#17777=EDGE_LOOP('',(#72649,#72650,#72651,#72652,#72653));
#17778=EDGE_LOOP('',(#72654,#72655,#72656,#72657,#72658));
#17779=EDGE_LOOP('',(#72659,#72660,#72661,#72662));
#17780=EDGE_LOOP('',(#72663,#72664,#72665,#72666));
#17781=EDGE_LOOP('',(#72667,#72668,#72669,#72670));
#17782=EDGE_LOOP('',(#72671,#72672,#72673,#72674));
#17783=EDGE_LOOP('',(#72675,#72676,#72677,#72678));
#17784=EDGE_LOOP('',(#72679,#72680,#72681,#72682));
#17785=EDGE_LOOP('',(#72683,#72684,#72685,#72686));
#17786=EDGE_LOOP('',(#72687,#72688,#72689,#72690));
#17787=EDGE_LOOP('',(#72691,#72692,#72693,#72694));
#17788=EDGE_LOOP('',(#72695,#72696,#72697,#72698));
#17789=EDGE_LOOP('',(#72699,#72700,#72701,#72702));
#17790=EDGE_LOOP('',(#72703,#72704,#72705,#72706));
#17791=EDGE_LOOP('',(#72707,#72708,#72709,#72710));
#17792=EDGE_LOOP('',(#72711,#72712,#72713,#72714));
#17793=EDGE_LOOP('',(#72715,#72716,#72717,#72718));
#17794=EDGE_LOOP('',(#72719,#72720,#72721,#72722));
#17795=EDGE_LOOP('',(#72723,#72724,#72725,#72726));
#17796=EDGE_LOOP('',(#72727,#72728,#72729,#72730));
#17797=EDGE_LOOP('',(#72731,#72732,#72733,#72734));
#17798=EDGE_LOOP('',(#72735,#72736,#72737,#72738));
#17799=EDGE_LOOP('',(#72739,#72740,#72741,#72742));
#17800=EDGE_LOOP('',(#72743,#72744,#72745,#72746));
#17801=EDGE_LOOP('',(#72747,#72748,#72749,#72750));
#17802=EDGE_LOOP('',(#72751,#72752,#72753,#72754));
#17803=EDGE_LOOP('',(#72755,#72756,#72757,#72758));
#17804=EDGE_LOOP('',(#72759,#72760,#72761,#72762));
#17805=EDGE_LOOP('',(#72763,#72764,#72765,#72766));
#17806=EDGE_LOOP('',(#72767,#72768,#72769,#72770));
#17807=EDGE_LOOP('',(#72771,#72772,#72773,#72774));
#17808=EDGE_LOOP('',(#72775,#72776,#72777,#72778));
#17809=EDGE_LOOP('',(#72779,#72780,#72781,#72782));
#17810=EDGE_LOOP('',(#72783,#72784,#72785,#72786));
#17811=EDGE_LOOP('',(#72787,#72788,#72789,#72790));
#17812=EDGE_LOOP('',(#72791,#72792,#72793,#72794));
#17813=EDGE_LOOP('',(#72795,#72796,#72797,#72798));
#17814=EDGE_LOOP('',(#72799,#72800,#72801,#72802));
#17815=EDGE_LOOP('',(#72803,#72804,#72805,#72806));
#17816=EDGE_LOOP('',(#72807,#72808,#72809,#72810));
#17817=EDGE_LOOP('',(#72811,#72812,#72813,#72814));
#17818=EDGE_LOOP('',(#72815,#72816,#72817,#72818));
#17819=EDGE_LOOP('',(#72819,#72820,#72821,#72822));
#17820=EDGE_LOOP('',(#72823,#72824,#72825,#72826));
#17821=EDGE_LOOP('',(#72827,#72828,#72829,#72830));
#17822=EDGE_LOOP('',(#72831,#72832,#72833,#72834));
#17823=EDGE_LOOP('',(#72835,#72836,#72837,#72838));
#17824=EDGE_LOOP('',(#72839,#72840,#72841,#72842));
#17825=EDGE_LOOP('',(#72843,#72844,#72845,#72846));
#17826=EDGE_LOOP('',(#72847,#72848,#72849,#72850));
#17827=EDGE_LOOP('',(#72851,#72852,#72853,#72854));
#17828=EDGE_LOOP('',(#72855,#72856,#72857,#72858));
#17829=EDGE_LOOP('',(#72859,#72860,#72861,#72862));
#17830=EDGE_LOOP('',(#72863,#72864,#72865,#72866));
#17831=EDGE_LOOP('',(#72867,#72868,#72869,#72870));
#17832=EDGE_LOOP('',(#72871,#72872,#72873,#72874));
#17833=EDGE_LOOP('',(#72875,#72876,#72877,#72878));
#17834=EDGE_LOOP('',(#72879,#72880,#72881,#72882));
#17835=EDGE_LOOP('',(#72883,#72884,#72885,#72886));
#17836=EDGE_LOOP('',(#72887,#72888,#72889,#72890));
#17837=EDGE_LOOP('',(#72891,#72892,#72893,#72894));
#17838=EDGE_LOOP('',(#72895,#72896,#72897,#72898));
#17839=EDGE_LOOP('',(#72899,#72900,#72901,#72902));
#17840=EDGE_LOOP('',(#72903,#72904,#72905,#72906));
#17841=EDGE_LOOP('',(#72907,#72908,#72909,#72910));
#17842=EDGE_LOOP('',(#72911,#72912,#72913,#72914));
#17843=EDGE_LOOP('',(#72915,#72916,#72917,#72918));
#17844=EDGE_LOOP('',(#72919,#72920,#72921,#72922));
#17845=EDGE_LOOP('',(#72923,#72924,#72925,#72926));
#17846=EDGE_LOOP('',(#72927,#72928,#72929,#72930));
#17847=EDGE_LOOP('',(#72931,#72932,#72933,#72934));
#17848=EDGE_LOOP('',(#72935,#72936,#72937,#72938));
#17849=EDGE_LOOP('',(#72939,#72940,#72941,#72942));
#17850=EDGE_LOOP('',(#72943,#72944,#72945,#72946));
#17851=EDGE_LOOP('',(#72947,#72948,#72949,#72950));
#17852=EDGE_LOOP('',(#72951,#72952,#72953,#72954));
#17853=EDGE_LOOP('',(#72955,#72956,#72957,#72958));
#17854=EDGE_LOOP('',(#72959,#72960,#72961,#72962));
#17855=EDGE_LOOP('',(#72963,#72964,#72965,#72966));
#17856=EDGE_LOOP('',(#72967,#72968,#72969,#72970));
#17857=EDGE_LOOP('',(#72971,#72972,#72973,#72974));
#17858=EDGE_LOOP('',(#72975,#72976,#72977,#72978));
#17859=EDGE_LOOP('',(#72979,#72980,#72981,#72982));
#17860=EDGE_LOOP('',(#72983,#72984,#72985,#72986));
#17861=EDGE_LOOP('',(#72987,#72988,#72989,#72990));
#17862=EDGE_LOOP('',(#72991,#72992,#72993,#72994));
#17863=EDGE_LOOP('',(#72995,#72996,#72997,#72998));
#17864=EDGE_LOOP('',(#72999,#73000,#73001,#73002));
#17865=EDGE_LOOP('',(#73003,#73004,#73005,#73006));
#17866=EDGE_LOOP('',(#73007,#73008,#73009,#73010));
#17867=EDGE_LOOP('',(#73011,#73012,#73013,#73014));
#17868=EDGE_LOOP('',(#73015,#73016,#73017,#73018));
#17869=EDGE_LOOP('',(#73019,#73020,#73021,#73022));
#17870=EDGE_LOOP('',(#73023,#73024,#73025,#73026));
#17871=EDGE_LOOP('',(#73027,#73028,#73029,#73030));
#17872=EDGE_LOOP('',(#73031,#73032,#73033,#73034));
#17873=EDGE_LOOP('',(#73035,#73036,#73037,#73038));
#17874=EDGE_LOOP('',(#73039,#73040,#73041,#73042));
#17875=EDGE_LOOP('',(#73043,#73044,#73045,#73046));
#17876=EDGE_LOOP('',(#73047,#73048,#73049,#73050));
#17877=EDGE_LOOP('',(#73051,#73052,#73053,#73054));
#17878=EDGE_LOOP('',(#73055,#73056,#73057,#73058));
#17879=EDGE_LOOP('',(#73059,#73060,#73061,#73062));
#17880=EDGE_LOOP('',(#73063,#73064,#73065,#73066));
#17881=EDGE_LOOP('',(#73067,#73068,#73069,#73070));
#17882=EDGE_LOOP('',(#73071,#73072,#73073,#73074));
#17883=EDGE_LOOP('',(#73075,#73076,#73077,#73078));
#17884=EDGE_LOOP('',(#73079,#73080,#73081,#73082));
#17885=EDGE_LOOP('',(#73083,#73084,#73085,#73086));
#17886=EDGE_LOOP('',(#73087,#73088,#73089,#73090));
#17887=EDGE_LOOP('',(#73091,#73092,#73093,#73094));
#17888=EDGE_LOOP('',(#73095,#73096,#73097,#73098));
#17889=EDGE_LOOP('',(#73099,#73100,#73101,#73102));
#17890=EDGE_LOOP('',(#73103,#73104,#73105,#73106));
#17891=EDGE_LOOP('',(#73107,#73108,#73109,#73110));
#17892=EDGE_LOOP('',(#73111,#73112,#73113,#73114));
#17893=EDGE_LOOP('',(#73115,#73116,#73117,#73118));
#17894=EDGE_LOOP('',(#73119,#73120,#73121,#73122));
#17895=EDGE_LOOP('',(#73123,#73124,#73125,#73126));
#17896=EDGE_LOOP('',(#73127,#73128,#73129,#73130));
#17897=EDGE_LOOP('',(#73131,#73132,#73133,#73134));
#17898=EDGE_LOOP('',(#73135,#73136,#73137,#73138));
#17899=EDGE_LOOP('',(#73139,#73140,#73141,#73142));
#17900=EDGE_LOOP('',(#73143,#73144,#73145,#73146));
#17901=EDGE_LOOP('',(#73147,#73148,#73149,#73150));
#17902=EDGE_LOOP('',(#73151,#73152,#73153,#73154));
#17903=EDGE_LOOP('',(#73155,#73156,#73157,#73158));
#17904=EDGE_LOOP('',(#73159,#73160,#73161,#73162));
#17905=EDGE_LOOP('',(#73163,#73164,#73165,#73166));
#17906=EDGE_LOOP('',(#73167,#73168,#73169,#73170));
#17907=EDGE_LOOP('',(#73171,#73172,#73173,#73174));
#17908=EDGE_LOOP('',(#73175,#73176,#73177,#73178));
#17909=EDGE_LOOP('',(#73179,#73180,#73181,#73182));
#17910=EDGE_LOOP('',(#73183,#73184,#73185,#73186));
#17911=EDGE_LOOP('',(#73187,#73188,#73189,#73190));
#17912=EDGE_LOOP('',(#73191,#73192,#73193,#73194));
#17913=EDGE_LOOP('',(#73195,#73196,#73197,#73198));
#17914=EDGE_LOOP('',(#73199,#73200,#73201,#73202));
#17915=EDGE_LOOP('',(#73203,#73204,#73205,#73206));
#17916=EDGE_LOOP('',(#73207,#73208,#73209,#73210));
#17917=EDGE_LOOP('',(#73211,#73212,#73213,#73214));
#17918=EDGE_LOOP('',(#73215,#73216,#73217,#73218));
#17919=EDGE_LOOP('',(#73219,#73220,#73221,#73222));
#17920=EDGE_LOOP('',(#73223,#73224,#73225,#73226));
#17921=EDGE_LOOP('',(#73227,#73228,#73229,#73230));
#17922=EDGE_LOOP('',(#73231,#73232,#73233,#73234));
#17923=EDGE_LOOP('',(#73235,#73236,#73237,#73238));
#17924=EDGE_LOOP('',(#73239,#73240,#73241,#73242));
#17925=EDGE_LOOP('',(#73243,#73244,#73245,#73246));
#17926=EDGE_LOOP('',(#73247,#73248,#73249,#73250));
#17927=EDGE_LOOP('',(#73251,#73252,#73253,#73254));
#17928=EDGE_LOOP('',(#73255,#73256,#73257,#73258));
#17929=EDGE_LOOP('',(#73259,#73260,#73261,#73262));
#17930=EDGE_LOOP('',(#73263,#73264,#73265,#73266));
#17931=EDGE_LOOP('',(#73267,#73268,#73269,#73270));
#17932=EDGE_LOOP('',(#73271,#73272,#73273,#73274));
#17933=EDGE_LOOP('',(#73275,#73276,#73277,#73278));
#17934=EDGE_LOOP('',(#73279,#73280,#73281,#73282));
#17935=EDGE_LOOP('',(#73283,#73284,#73285,#73286));
#17936=EDGE_LOOP('',(#73287,#73288,#73289,#73290));
#17937=EDGE_LOOP('',(#73291,#73292,#73293,#73294));
#17938=EDGE_LOOP('',(#73295,#73296,#73297,#73298));
#17939=EDGE_LOOP('',(#73299,#73300,#73301,#73302));
#17940=EDGE_LOOP('',(#73303,#73304,#73305,#73306));
#17941=EDGE_LOOP('',(#73307,#73308,#73309,#73310));
#17942=EDGE_LOOP('',(#73311,#73312,#73313,#73314));
#17943=EDGE_LOOP('',(#73315,#73316,#73317,#73318));
#17944=EDGE_LOOP('',(#73319,#73320,#73321,#73322));
#17945=EDGE_LOOP('',(#73323,#73324,#73325,#73326));
#17946=EDGE_LOOP('',(#73327,#73328,#73329,#73330));
#17947=EDGE_LOOP('',(#73331,#73332,#73333,#73334));
#17948=EDGE_LOOP('',(#73335,#73336,#73337,#73338));
#17949=EDGE_LOOP('',(#73339,#73340,#73341,#73342));
#17950=EDGE_LOOP('',(#73343,#73344,#73345,#73346));
#17951=EDGE_LOOP('',(#73347,#73348,#73349,#73350));
#17952=EDGE_LOOP('',(#73351,#73352,#73353,#73354));
#17953=EDGE_LOOP('',(#73355,#73356,#73357,#73358));
#17954=EDGE_LOOP('',(#73359,#73360,#73361,#73362));
#17955=EDGE_LOOP('',(#73363,#73364,#73365,#73366));
#17956=EDGE_LOOP('',(#73367,#73368,#73369,#73370));
#17957=EDGE_LOOP('',(#73371,#73372,#73373,#73374));
#17958=EDGE_LOOP('',(#73375,#73376,#73377,#73378));
#17959=EDGE_LOOP('',(#73379,#73380,#73381,#73382));
#17960=EDGE_LOOP('',(#73383,#73384,#73385,#73386));
#17961=EDGE_LOOP('',(#73387,#73388,#73389,#73390));
#17962=EDGE_LOOP('',(#73391,#73392,#73393,#73394));
#17963=EDGE_LOOP('',(#73395,#73396,#73397,#73398));
#17964=EDGE_LOOP('',(#73399,#73400,#73401,#73402));
#17965=EDGE_LOOP('',(#73403,#73404,#73405,#73406));
#17966=EDGE_LOOP('',(#73407,#73408,#73409,#73410));
#17967=EDGE_LOOP('',(#73411,#73412,#73413,#73414));
#17968=EDGE_LOOP('',(#73415,#73416,#73417,#73418));
#17969=EDGE_LOOP('',(#73419,#73420,#73421,#73422));
#17970=EDGE_LOOP('',(#73423,#73424,#73425,#73426));
#17971=EDGE_LOOP('',(#73427,#73428,#73429,#73430));
#17972=EDGE_LOOP('',(#73431,#73432,#73433,#73434));
#17973=EDGE_LOOP('',(#73435,#73436,#73437,#73438));
#17974=EDGE_LOOP('',(#73439,#73440,#73441,#73442));
#17975=EDGE_LOOP('',(#73443,#73444,#73445,#73446));
#17976=EDGE_LOOP('',(#73447,#73448,#73449,#73450));
#17977=EDGE_LOOP('',(#73451,#73452,#73453,#73454));
#17978=EDGE_LOOP('',(#73455,#73456,#73457,#73458));
#17979=EDGE_LOOP('',(#73459,#73460,#73461,#73462));
#17980=EDGE_LOOP('',(#73463,#73464,#73465,#73466));
#17981=EDGE_LOOP('',(#73467,#73468,#73469,#73470));
#17982=EDGE_LOOP('',(#73471,#73472,#73473,#73474));
#17983=EDGE_LOOP('',(#73475,#73476,#73477,#73478));
#17984=EDGE_LOOP('',(#73479,#73480,#73481,#73482));
#17985=EDGE_LOOP('',(#73483,#73484,#73485,#73486));
#17986=EDGE_LOOP('',(#73487,#73488,#73489,#73490));
#17987=EDGE_LOOP('',(#73491,#73492,#73493,#73494));
#17988=EDGE_LOOP('',(#73495,#73496,#73497,#73498));
#17989=EDGE_LOOP('',(#73499,#73500,#73501,#73502));
#17990=EDGE_LOOP('',(#73503,#73504,#73505,#73506));
#17991=EDGE_LOOP('',(#73507,#73508,#73509,#73510));
#17992=EDGE_LOOP('',(#73511,#73512,#73513,#73514));
#17993=EDGE_LOOP('',(#73515,#73516,#73517,#73518));
#17994=EDGE_LOOP('',(#73519,#73520,#73521,#73522));
#17995=EDGE_LOOP('',(#73523,#73524,#73525,#73526));
#17996=EDGE_LOOP('',(#73527,#73528,#73529,#73530));
#17997=EDGE_LOOP('',(#73531,#73532,#73533,#73534));
#17998=EDGE_LOOP('',(#73535,#73536,#73537,#73538));
#17999=EDGE_LOOP('',(#73539,#73540,#73541,#73542));
#18000=EDGE_LOOP('',(#73543,#73544,#73545,#73546));
#18001=EDGE_LOOP('',(#73547,#73548,#73549,#73550));
#18002=EDGE_LOOP('',(#73551,#73552,#73553,#73554));
#18003=EDGE_LOOP('',(#73555,#73556,#73557,#73558));
#18004=EDGE_LOOP('',(#73559,#73560,#73561,#73562));
#18005=EDGE_LOOP('',(#73563,#73564,#73565,#73566));
#18006=EDGE_LOOP('',(#73567,#73568,#73569,#73570));
#18007=EDGE_LOOP('',(#73571,#73572,#73573,#73574));
#18008=EDGE_LOOP('',(#73575,#73576,#73577,#73578));
#18009=EDGE_LOOP('',(#73579,#73580,#73581,#73582));
#18010=EDGE_LOOP('',(#73583,#73584,#73585,#73586));
#18011=EDGE_LOOP('',(#73587,#73588,#73589,#73590));
#18012=EDGE_LOOP('',(#73591,#73592,#73593,#73594));
#18013=EDGE_LOOP('',(#73595,#73596,#73597,#73598));
#18014=EDGE_LOOP('',(#73599,#73600,#73601,#73602));
#18015=EDGE_LOOP('',(#73603,#73604,#73605,#73606));
#18016=EDGE_LOOP('',(#73607,#73608,#73609,#73610));
#18017=EDGE_LOOP('',(#73611,#73612,#73613,#73614));
#18018=EDGE_LOOP('',(#73615,#73616,#73617,#73618));
#18019=EDGE_LOOP('',(#73619,#73620,#73621,#73622));
#18020=EDGE_LOOP('',(#73623,#73624,#73625,#73626));
#18021=EDGE_LOOP('',(#73627,#73628,#73629,#73630));
#18022=EDGE_LOOP('',(#73631,#73632,#73633,#73634));
#18023=EDGE_LOOP('',(#73635,#73636,#73637,#73638));
#18024=EDGE_LOOP('',(#73639,#73640,#73641,#73642));
#18025=EDGE_LOOP('',(#73643,#73644,#73645,#73646));
#18026=EDGE_LOOP('',(#73647,#73648,#73649,#73650));
#18027=EDGE_LOOP('',(#73651,#73652,#73653,#73654));
#18028=EDGE_LOOP('',(#73655,#73656,#73657,#73658));
#18029=EDGE_LOOP('',(#73659,#73660,#73661,#73662));
#18030=EDGE_LOOP('',(#73663,#73664,#73665,#73666));
#18031=EDGE_LOOP('',(#73667,#73668,#73669,#73670));
#18032=EDGE_LOOP('',(#73671,#73672,#73673,#73674));
#18033=EDGE_LOOP('',(#73675,#73676,#73677,#73678));
#18034=EDGE_LOOP('',(#73679,#73680,#73681,#73682));
#18035=EDGE_LOOP('',(#73683,#73684,#73685,#73686));
#18036=EDGE_LOOP('',(#73687,#73688,#73689,#73690));
#18037=EDGE_LOOP('',(#73691,#73692,#73693,#73694));
#18038=EDGE_LOOP('',(#73695,#73696,#73697,#73698));
#18039=EDGE_LOOP('',(#73699,#73700,#73701,#73702));
#18040=EDGE_LOOP('',(#73703,#73704,#73705,#73706));
#18041=EDGE_LOOP('',(#73707,#73708,#73709,#73710));
#18042=EDGE_LOOP('',(#73711,#73712,#73713,#73714));
#18043=EDGE_LOOP('',(#73715,#73716,#73717,#73718));
#18044=EDGE_LOOP('',(#73719,#73720,#73721,#73722));
#18045=EDGE_LOOP('',(#73723,#73724,#73725,#73726));
#18046=EDGE_LOOP('',(#73727,#73728,#73729,#73730));
#18047=EDGE_LOOP('',(#73731,#73732,#73733,#73734));
#18048=EDGE_LOOP('',(#73735,#73736,#73737,#73738));
#18049=EDGE_LOOP('',(#73739,#73740,#73741,#73742));
#18050=EDGE_LOOP('',(#73743,#73744,#73745,#73746));
#18051=EDGE_LOOP('',(#73747,#73748,#73749,#73750));
#18052=EDGE_LOOP('',(#73751,#73752,#73753,#73754));
#18053=EDGE_LOOP('',(#73755,#73756,#73757,#73758));
#18054=EDGE_LOOP('',(#73759,#73760,#73761,#73762));
#18055=EDGE_LOOP('',(#73763,#73764,#73765,#73766));
#18056=EDGE_LOOP('',(#73767,#73768,#73769,#73770));
#18057=EDGE_LOOP('',(#73771,#73772,#73773,#73774));
#18058=EDGE_LOOP('',(#73775,#73776,#73777,#73778));
#18059=EDGE_LOOP('',(#73779,#73780,#73781,#73782));
#18060=EDGE_LOOP('',(#73783,#73784,#73785,#73786));
#18061=EDGE_LOOP('',(#73787,#73788,#73789,#73790));
#18062=EDGE_LOOP('',(#73791,#73792,#73793,#73794));
#18063=EDGE_LOOP('',(#73795,#73796,#73797,#73798));
#18064=EDGE_LOOP('',(#73799,#73800,#73801,#73802));
#18065=EDGE_LOOP('',(#73803,#73804,#73805,#73806));
#18066=EDGE_LOOP('',(#73807,#73808,#73809,#73810));
#18067=EDGE_LOOP('',(#73811,#73812,#73813,#73814));
#18068=EDGE_LOOP('',(#73815,#73816,#73817,#73818));
#18069=EDGE_LOOP('',(#73819,#73820,#73821,#73822));
#18070=EDGE_LOOP('',(#73823,#73824,#73825,#73826));
#18071=EDGE_LOOP('',(#73827,#73828,#73829,#73830));
#18072=EDGE_LOOP('',(#73831,#73832,#73833,#73834));
#18073=EDGE_LOOP('',(#73835,#73836,#73837,#73838));
#18074=EDGE_LOOP('',(#73839,#73840,#73841,#73842));
#18075=EDGE_LOOP('',(#73843,#73844,#73845,#73846));
#18076=EDGE_LOOP('',(#73847,#73848,#73849,#73850));
#18077=EDGE_LOOP('',(#73851,#73852,#73853,#73854));
#18078=EDGE_LOOP('',(#73855,#73856,#73857,#73858));
#18079=EDGE_LOOP('',(#73859,#73860,#73861,#73862));
#18080=EDGE_LOOP('',(#73863,#73864,#73865,#73866));
#18081=EDGE_LOOP('',(#73867,#73868,#73869,#73870));
#18082=EDGE_LOOP('',(#73871,#73872,#73873,#73874));
#18083=EDGE_LOOP('',(#73875,#73876,#73877,#73878));
#18084=EDGE_LOOP('',(#73879,#73880,#73881,#73882));
#18085=EDGE_LOOP('',(#73883,#73884,#73885,#73886));
#18086=EDGE_LOOP('',(#73887,#73888,#73889,#73890,#73891,#73892));
#18087=EDGE_LOOP('',(#73893,#73894,#73895,#73896));
#18088=EDGE_LOOP('',(#73897,#73898,#73899,#73900));
#18089=EDGE_LOOP('',(#73901,#73902,#73903,#73904));
#18090=EDGE_LOOP('',(#73905,#73906,#73907,#73908));
#18091=EDGE_LOOP('',(#73909,#73910,#73911,#73912));
#18092=EDGE_LOOP('',(#73913,#73914,#73915,#73916));
#18093=EDGE_LOOP('',(#73917,#73918,#73919,#73920));
#18094=EDGE_LOOP('',(#73921,#73922,#73923,#73924,#73925,#73926,#73927,#73928,
#73929));
#18095=EDGE_LOOP('',(#73930,#73931,#73932,#73933));
#18096=EDGE_LOOP('',(#73934,#73935,#73936,#73937));
#18097=EDGE_LOOP('',(#73938,#73939,#73940,#73941));
#18098=EDGE_LOOP('',(#73942,#73943,#73944,#73945));
#18099=EDGE_LOOP('',(#73946,#73947,#73948,#73949));
#18100=EDGE_LOOP('',(#73950,#73951,#73952,#73953));
#18101=EDGE_LOOP('',(#73954,#73955,#73956,#73957));
#18102=EDGE_LOOP('',(#73958,#73959,#73960,#73961,#73962,#73963,#73964,#73965,
#73966));
#18103=EDGE_LOOP('',(#73967,#73968,#73969,#73970,#73971));
#18104=EDGE_LOOP('',(#73972,#73973,#73974,#73975));
#18105=EDGE_LOOP('',(#73976,#73977,#73978,#73979));
#18106=EDGE_LOOP('',(#73980,#73981,#73982,#73983));
#18107=EDGE_LOOP('',(#73984,#73985,#73986,#73987,#73988));
#18108=EDGE_LOOP('',(#73989,#73990,#73991,#73992));
#18109=EDGE_LOOP('',(#73993,#73994,#73995));
#18110=EDGE_LOOP('',(#73996,#73997,#73998,#73999,#74000,#74001,#74002,#74003,
#74004,#74005));
#18111=EDGE_LOOP('',(#74006,#74007,#74008));
#18112=EDGE_LOOP('',(#74009,#74010,#74011,#74012));
#18113=EDGE_LOOP('',(#74013,#74014,#74015,#74016,#74017));
#18114=EDGE_LOOP('',(#74018,#74019,#74020,#74021));
#18115=EDGE_LOOP('',(#74022,#74023,#74024,#74025));
#18116=EDGE_LOOP('',(#74026,#74027,#74028,#74029));
#18117=EDGE_LOOP('',(#74030,#74031,#74032,#74033,#74034));
#18118=EDGE_LOOP('',(#74035,#74036,#74037,#74038,#74039,#74040,#74041,#74042,
#74043,#74044,#74045));
#18119=EDGE_LOOP('',(#74046,#74047,#74048));
#18120=EDGE_LOOP('',(#74049,#74050,#74051,#74052));
#18121=EDGE_LOOP('',(#74053,#74054,#74055,#74056,#74057));
#18122=EDGE_LOOP('',(#74058,#74059,#74060,#74061));
#18123=EDGE_LOOP('',(#74062,#74063,#74064,#74065));
#18124=EDGE_LOOP('',(#74066,#74067,#74068,#74069));
#18125=EDGE_LOOP('',(#74070,#74071,#74072,#74073,#74074));
#18126=EDGE_LOOP('',(#74075,#74076,#74077,#74078));
#18127=EDGE_LOOP('',(#74079,#74080,#74081,#74082,#74083,#74084,#74085));
#18128=EDGE_LOOP('',(#74086,#74087,#74088));
#18129=EDGE_LOOP('',(#74089,#74090,#74091,#74092,#74093));
#18130=EDGE_LOOP('',(#74094,#74095,#74096,#74097));
#18131=EDGE_LOOP('',(#74098,#74099,#74100,#74101));
#18132=EDGE_LOOP('',(#74102,#74103,#74104,#74105));
#18133=EDGE_LOOP('',(#74106,#74107,#74108,#74109));
#18134=EDGE_LOOP('',(#74110,#74111,#74112,#74113,#74114));
#18135=EDGE_LOOP('',(#74115,#74116,#74117,#74118));
#18136=EDGE_LOOP('',(#74119,#74120,#74121,#74122));
#18137=EDGE_LOOP('',(#74123,#74124,#74125,#74126));
#18138=EDGE_LOOP('',(#74127,#74128,#74129,#74130));
#18139=EDGE_LOOP('',(#74131,#74132,#74133,#74134));
#18140=EDGE_LOOP('',(#74135,#74136,#74137,#74138));
#18141=EDGE_LOOP('',(#74139,#74140,#74141,#74142));
#18142=EDGE_LOOP('',(#74143,#74144,#74145,#74146));
#18143=EDGE_LOOP('',(#74147,#74148,#74149,#74150));
#18144=EDGE_LOOP('',(#74151,#74152,#74153,#74154));
#18145=EDGE_LOOP('',(#74155,#74156,#74157,#74158));
#18146=EDGE_LOOP('',(#74159,#74160,#74161,#74162));
#18147=EDGE_LOOP('',(#74163,#74164,#74165,#74166));
#18148=EDGE_LOOP('',(#74167,#74168,#74169,#74170));
#18149=EDGE_LOOP('',(#74171,#74172,#74173,#74174));
#18150=EDGE_LOOP('',(#74175,#74176,#74177,#74178));
#18151=EDGE_LOOP('',(#74179,#74180,#74181,#74182));
#18152=EDGE_LOOP('',(#74183,#74184,#74185,#74186));
#18153=EDGE_LOOP('',(#74187,#74188,#74189,#74190));
#18154=EDGE_LOOP('',(#74191,#74192,#74193,#74194));
#18155=EDGE_LOOP('',(#74195,#74196,#74197,#74198));
#18156=EDGE_LOOP('',(#74199,#74200,#74201,#74202));
#18157=EDGE_LOOP('',(#74203,#74204,#74205,#74206));
#18158=EDGE_LOOP('',(#74207,#74208,#74209,#74210));
#18159=EDGE_LOOP('',(#74211,#74212,#74213,#74214));
#18160=EDGE_LOOP('',(#74215,#74216,#74217,#74218));
#18161=EDGE_LOOP('',(#74219,#74220,#74221,#74222));
#18162=EDGE_LOOP('',(#74223,#74224,#74225,#74226));
#18163=EDGE_LOOP('',(#74227,#74228,#74229,#74230));
#18164=EDGE_LOOP('',(#74231,#74232,#74233,#74234));
#18165=EDGE_LOOP('',(#74235,#74236,#74237,#74238));
#18166=EDGE_LOOP('',(#74239,#74240,#74241,#74242));
#18167=EDGE_LOOP('',(#74243,#74244,#74245,#74246));
#18168=EDGE_LOOP('',(#74247,#74248,#74249,#74250));
#18169=EDGE_LOOP('',(#74251,#74252,#74253,#74254));
#18170=EDGE_LOOP('',(#74255,#74256,#74257,#74258));
#18171=EDGE_LOOP('',(#74259,#74260,#74261,#74262));
#18172=EDGE_LOOP('',(#74263,#74264,#74265,#74266));
#18173=EDGE_LOOP('',(#74267,#74268,#74269,#74270));
#18174=EDGE_LOOP('',(#74271,#74272,#74273,#74274));
#18175=EDGE_LOOP('',(#74275,#74276,#74277,#74278));
#18176=EDGE_LOOP('',(#74279,#74280,#74281,#74282));
#18177=EDGE_LOOP('',(#74283,#74284,#74285,#74286));
#18178=EDGE_LOOP('',(#74287,#74288,#74289,#74290));
#18179=EDGE_LOOP('',(#74291,#74292,#74293,#74294));
#18180=EDGE_LOOP('',(#74295,#74296,#74297,#74298));
#18181=EDGE_LOOP('',(#74299,#74300,#74301,#74302));
#18182=EDGE_LOOP('',(#74303,#74304,#74305,#74306));
#18183=EDGE_LOOP('',(#74307,#74308,#74309,#74310));
#18184=EDGE_LOOP('',(#74311,#74312,#74313,#74314));
#18185=EDGE_LOOP('',(#74315,#74316,#74317,#74318));
#18186=EDGE_LOOP('',(#74319,#74320,#74321,#74322));
#18187=EDGE_LOOP('',(#74323,#74324,#74325,#74326));
#18188=EDGE_LOOP('',(#74327,#74328,#74329,#74330));
#18189=EDGE_LOOP('',(#74331,#74332,#74333,#74334));
#18190=EDGE_LOOP('',(#74335,#74336,#74337,#74338));
#18191=EDGE_LOOP('',(#74339,#74340,#74341,#74342));
#18192=EDGE_LOOP('',(#74343,#74344,#74345,#74346));
#18193=EDGE_LOOP('',(#74347,#74348,#74349,#74350));
#18194=EDGE_LOOP('',(#74351,#74352,#74353,#74354));
#18195=EDGE_LOOP('',(#74355,#74356,#74357,#74358));
#18196=EDGE_LOOP('',(#74359,#74360,#74361,#74362));
#18197=EDGE_LOOP('',(#74363,#74364,#74365,#74366));
#18198=EDGE_LOOP('',(#74367,#74368,#74369,#74370));
#18199=EDGE_LOOP('',(#74371,#74372,#74373,#74374));
#18200=EDGE_LOOP('',(#74375,#74376,#74377,#74378));
#18201=EDGE_LOOP('',(#74379,#74380,#74381,#74382));
#18202=EDGE_LOOP('',(#74383,#74384,#74385,#74386));
#18203=EDGE_LOOP('',(#74387,#74388,#74389,#74390));
#18204=EDGE_LOOP('',(#74391,#74392,#74393,#74394));
#18205=EDGE_LOOP('',(#74395,#74396,#74397,#74398));
#18206=EDGE_LOOP('',(#74399,#74400,#74401,#74402));
#18207=EDGE_LOOP('',(#74403,#74404,#74405,#74406));
#18208=EDGE_LOOP('',(#74407,#74408,#74409,#74410));
#18209=EDGE_LOOP('',(#74411,#74412,#74413,#74414));
#18210=EDGE_LOOP('',(#74415,#74416,#74417,#74418));
#18211=EDGE_LOOP('',(#74419,#74420,#74421,#74422));
#18212=EDGE_LOOP('',(#74423,#74424,#74425,#74426));
#18213=EDGE_LOOP('',(#74427,#74428,#74429,#74430));
#18214=EDGE_LOOP('',(#74431,#74432,#74433,#74434));
#18215=EDGE_LOOP('',(#74435,#74436,#74437,#74438));
#18216=EDGE_LOOP('',(#74439,#74440,#74441,#74442));
#18217=EDGE_LOOP('',(#74443,#74444,#74445,#74446));
#18218=EDGE_LOOP('',(#74447,#74448,#74449,#74450));
#18219=EDGE_LOOP('',(#74451,#74452,#74453,#74454));
#18220=EDGE_LOOP('',(#74455,#74456,#74457,#74458));
#18221=EDGE_LOOP('',(#74459,#74460,#74461,#74462));
#18222=EDGE_LOOP('',(#74463,#74464,#74465,#74466));
#18223=EDGE_LOOP('',(#74467,#74468,#74469,#74470));
#18224=EDGE_LOOP('',(#74471,#74472,#74473,#74474));
#18225=EDGE_LOOP('',(#74475,#74476,#74477,#74478));
#18226=EDGE_LOOP('',(#74479,#74480,#74481,#74482));
#18227=EDGE_LOOP('',(#74483,#74484,#74485,#74486));
#18228=EDGE_LOOP('',(#74487,#74488,#74489,#74490));
#18229=EDGE_LOOP('',(#74491,#74492,#74493,#74494));
#18230=EDGE_LOOP('',(#74495,#74496,#74497,#74498));
#18231=EDGE_LOOP('',(#74499,#74500,#74501,#74502));
#18232=EDGE_LOOP('',(#74503,#74504,#74505,#74506));
#18233=EDGE_LOOP('',(#74507,#74508,#74509,#74510));
#18234=EDGE_LOOP('',(#74511,#74512,#74513,#74514));
#18235=EDGE_LOOP('',(#74515,#74516,#74517,#74518));
#18236=EDGE_LOOP('',(#74519,#74520,#74521,#74522));
#18237=EDGE_LOOP('',(#74523,#74524,#74525,#74526));
#18238=EDGE_LOOP('',(#74527,#74528,#74529,#74530));
#18239=EDGE_LOOP('',(#74531,#74532,#74533,#74534));
#18240=EDGE_LOOP('',(#74535,#74536,#74537,#74538));
#18241=EDGE_LOOP('',(#74539,#74540,#74541,#74542));
#18242=EDGE_LOOP('',(#74543,#74544,#74545,#74546));
#18243=EDGE_LOOP('',(#74547,#74548,#74549,#74550));
#18244=EDGE_LOOP('',(#74551,#74552,#74553,#74554));
#18245=EDGE_LOOP('',(#74555,#74556,#74557,#74558));
#18246=EDGE_LOOP('',(#74559,#74560,#74561,#74562));
#18247=EDGE_LOOP('',(#74563,#74564,#74565,#74566));
#18248=EDGE_LOOP('',(#74567,#74568,#74569,#74570));
#18249=EDGE_LOOP('',(#74571,#74572,#74573,#74574));
#18250=EDGE_LOOP('',(#74575,#74576,#74577,#74578));
#18251=EDGE_LOOP('',(#74579,#74580,#74581,#74582));
#18252=EDGE_LOOP('',(#74583,#74584,#74585,#74586));
#18253=EDGE_LOOP('',(#74587,#74588,#74589,#74590));
#18254=EDGE_LOOP('',(#74591,#74592,#74593,#74594));
#18255=EDGE_LOOP('',(#74595,#74596,#74597,#74598));
#18256=EDGE_LOOP('',(#74599,#74600,#74601,#74602));
#18257=EDGE_LOOP('',(#74603,#74604,#74605,#74606));
#18258=EDGE_LOOP('',(#74607,#74608,#74609,#74610));
#18259=EDGE_LOOP('',(#74611,#74612,#74613,#74614));
#18260=EDGE_LOOP('',(#74615,#74616,#74617,#74618));
#18261=EDGE_LOOP('',(#74619,#74620,#74621,#74622));
#18262=EDGE_LOOP('',(#74623,#74624,#74625,#74626));
#18263=EDGE_LOOP('',(#74627,#74628,#74629,#74630));
#18264=EDGE_LOOP('',(#74631,#74632,#74633,#74634));
#18265=EDGE_LOOP('',(#74635,#74636,#74637,#74638));
#18266=EDGE_LOOP('',(#74639,#74640,#74641,#74642));
#18267=EDGE_LOOP('',(#74643,#74644,#74645,#74646));
#18268=EDGE_LOOP('',(#74647,#74648,#74649,#74650));
#18269=EDGE_LOOP('',(#74651,#74652,#74653,#74654));
#18270=EDGE_LOOP('',(#74655,#74656,#74657,#74658));
#18271=EDGE_LOOP('',(#74659,#74660,#74661,#74662));
#18272=EDGE_LOOP('',(#74663,#74664,#74665,#74666));
#18273=EDGE_LOOP('',(#74667,#74668,#74669,#74670));
#18274=EDGE_LOOP('',(#74671,#74672,#74673,#74674));
#18275=EDGE_LOOP('',(#74675,#74676,#74677,#74678));
#18276=EDGE_LOOP('',(#74679,#74680,#74681,#74682));
#18277=EDGE_LOOP('',(#74683));
#18278=EDGE_LOOP('',(#74684,#74685,#74686,#74687));
#18279=EDGE_LOOP('',(#74688));
#18280=EDGE_LOOP('',(#74689));
#18281=EDGE_LOOP('',(#74690,#74691,#74692,#74693));
#18282=EDGE_LOOP('',(#74694,#74695,#74696,#74697));
#18283=EDGE_LOOP('',(#74698,#74699,#74700,#74701,#74702,#74703,#74704,#74705,
#74706,#74707,#74708,#74709,#74710,#74711,#74712,#74713,#74714,#74715,#74716,
#74717,#74718,#74719,#74720,#74721,#74722,#74723,#74724,#74725,#74726,#74727,
#74728,#74729,#74730,#74731,#74732,#74733,#74734,#74735,#74736,#74737,#74738,
#74739,#74740,#74741,#74742,#74743,#74744,#74745,#74746,#74747,#74748,#74749));
#18284=EDGE_LOOP('',(#74750,#74751,#74752,#74753));
#18285=EDGE_LOOP('',(#74754,#74755,#74756,#74757));
#18286=EDGE_LOOP('',(#74758,#74759,#74760,#74761));
#18287=EDGE_LOOP('',(#74762,#74763,#74764,#74765));
#18288=EDGE_LOOP('',(#74766,#74767,#74768,#74769));
#18289=EDGE_LOOP('',(#74770,#74771,#74772,#74773));
#18290=EDGE_LOOP('',(#74774,#74775,#74776,#74777));
#18291=EDGE_LOOP('',(#74778,#74779,#74780,#74781));
#18292=EDGE_LOOP('',(#74782,#74783,#74784,#74785));
#18293=EDGE_LOOP('',(#74786,#74787,#74788,#74789));
#18294=EDGE_LOOP('',(#74790,#74791,#74792,#74793));
#18295=EDGE_LOOP('',(#74794,#74795,#74796,#74797));
#18296=EDGE_LOOP('',(#74798,#74799,#74800,#74801));
#18297=EDGE_LOOP('',(#74802,#74803,#74804,#74805));
#18298=EDGE_LOOP('',(#74806,#74807,#74808,#74809));
#18299=EDGE_LOOP('',(#74810,#74811,#74812,#74813));
#18300=EDGE_LOOP('',(#74814,#74815,#74816,#74817));
#18301=EDGE_LOOP('',(#74818,#74819,#74820,#74821));
#18302=EDGE_LOOP('',(#74822,#74823,#74824,#74825));
#18303=EDGE_LOOP('',(#74826,#74827,#74828,#74829));
#18304=EDGE_LOOP('',(#74830,#74831,#74832,#74833));
#18305=EDGE_LOOP('',(#74834,#74835,#74836,#74837));
#18306=EDGE_LOOP('',(#74838,#74839,#74840,#74841));
#18307=EDGE_LOOP('',(#74842,#74843,#74844,#74845));
#18308=EDGE_LOOP('',(#74846,#74847,#74848,#74849));
#18309=EDGE_LOOP('',(#74850,#74851,#74852,#74853));
#18310=EDGE_LOOP('',(#74854,#74855,#74856,#74857));
#18311=EDGE_LOOP('',(#74858,#74859,#74860,#74861));
#18312=EDGE_LOOP('',(#74862,#74863,#74864,#74865));
#18313=EDGE_LOOP('',(#74866,#74867,#74868,#74869));
#18314=EDGE_LOOP('',(#74870,#74871,#74872,#74873));
#18315=EDGE_LOOP('',(#74874,#74875,#74876,#74877));
#18316=EDGE_LOOP('',(#74878,#74879,#74880,#74881));
#18317=EDGE_LOOP('',(#74882,#74883,#74884,#74885));
#18318=EDGE_LOOP('',(#74886,#74887,#74888,#74889));
#18319=EDGE_LOOP('',(#74890,#74891,#74892,#74893));
#18320=EDGE_LOOP('',(#74894,#74895,#74896,#74897));
#18321=EDGE_LOOP('',(#74898,#74899,#74900,#74901));
#18322=EDGE_LOOP('',(#74902,#74903,#74904,#74905));
#18323=EDGE_LOOP('',(#74906,#74907,#74908,#74909));
#18324=EDGE_LOOP('',(#74910,#74911,#74912,#74913));
#18325=EDGE_LOOP('',(#74914,#74915,#74916,#74917));
#18326=EDGE_LOOP('',(#74918,#74919,#74920,#74921));
#18327=EDGE_LOOP('',(#74922,#74923,#74924,#74925));
#18328=EDGE_LOOP('',(#74926,#74927,#74928,#74929));
#18329=EDGE_LOOP('',(#74930,#74931,#74932,#74933));
#18330=EDGE_LOOP('',(#74934,#74935,#74936,#74937));
#18331=EDGE_LOOP('',(#74938,#74939,#74940,#74941));
#18332=EDGE_LOOP('',(#74942,#74943,#74944,#74945));
#18333=EDGE_LOOP('',(#74946,#74947,#74948,#74949));
#18334=EDGE_LOOP('',(#74950,#74951,#74952,#74953));
#18335=EDGE_LOOP('',(#74954,#74955,#74956,#74957));
#18336=EDGE_LOOP('',(#74958,#74959,#74960,#74961));
#18337=EDGE_LOOP('',(#74962,#74963,#74964,#74965));
#18338=EDGE_LOOP('',(#74966,#74967,#74968,#74969));
#18339=EDGE_LOOP('',(#74970,#74971,#74972,#74973));
#18340=EDGE_LOOP('',(#74974,#74975,#74976,#74977));
#18341=EDGE_LOOP('',(#74978,#74979,#74980,#74981));
#18342=EDGE_LOOP('',(#74982,#74983,#74984,#74985));
#18343=EDGE_LOOP('',(#74986,#74987,#74988,#74989));
#18344=EDGE_LOOP('',(#74990,#74991,#74992,#74993));
#18345=EDGE_LOOP('',(#74994,#74995,#74996,#74997));
#18346=EDGE_LOOP('',(#74998,#74999,#75000,#75001));
#18347=EDGE_LOOP('',(#75002,#75003,#75004,#75005));
#18348=EDGE_LOOP('',(#75006,#75007,#75008,#75009));
#18349=EDGE_LOOP('',(#75010,#75011,#75012,#75013));
#18350=EDGE_LOOP('',(#75014,#75015,#75016,#75017));
#18351=EDGE_LOOP('',(#75018,#75019,#75020,#75021,#75022,#75023,#75024,#75025,
#75026,#75027,#75028,#75029,#75030,#75031,#75032,#75033,#75034,#75035,#75036,
#75037,#75038,#75039,#75040,#75041));
#18352=EDGE_LOOP('',(#75042,#75043,#75044,#75045,#75046,#75047,#75048,#75049));
#18353=EDGE_LOOP('',(#75050,#75051,#75052,#75053,#75054,#75055,#75056,#75057));
#18354=EDGE_LOOP('',(#75058,#75059,#75060,#75061,#75062,#75063,#75064,#75065));
#18355=EDGE_LOOP('',(#75066,#75067,#75068,#75069,#75070,#75071,#75072,#75073));
#18356=EDGE_LOOP('',(#75074,#75075,#75076,#75077,#75078,#75079,#75080,#75081));
#18357=EDGE_LOOP('',(#75082,#75083,#75084,#75085,#75086,#75087,#75088,#75089));
#18358=EDGE_LOOP('',(#75090,#75091,#75092,#75093,#75094,#75095,#75096,#75097));
#18359=EDGE_LOOP('',(#75098,#75099,#75100,#75101,#75102,#75103,#75104,#75105));
#18360=EDGE_LOOP('',(#75106,#75107,#75108,#75109,#75110,#75111,#75112,#75113));
#18361=EDGE_LOOP('',(#75114,#75115,#75116,#75117,#75118,#75119,#75120,#75121));
#18362=EDGE_LOOP('',(#75122,#75123,#75124,#75125,#75126,#75127,#75128,#75129,
#75130,#75131));
#18363=EDGE_LOOP('',(#75132,#75133,#75134,#75135,#75136,#75137,#75138,#75139,
#75140,#75141));
#18364=EDGE_LOOP('',(#75142,#75143,#75144,#75145,#75146,#75147,#75148,#75149));
#18365=EDGE_LOOP('',(#75150,#75151,#75152,#75153,#75154,#75155,#75156,#75157));
#18366=EDGE_LOOP('',(#75158,#75159,#75160,#75161,#75162,#75163,#75164,#75165));
#18367=EDGE_LOOP('',(#75166,#75167,#75168,#75169,#75170,#75171,#75172,#75173));
#18368=EDGE_LOOP('',(#75174,#75175,#75176,#75177,#75178,#75179,#75180,#75181));
#18369=EDGE_LOOP('',(#75182,#75183,#75184,#75185,#75186,#75187));
#18370=EDGE_LOOP('',(#75188,#75189,#75190,#75191,#75192,#75193,#75194,#75195));
#18371=EDGE_LOOP('',(#75196,#75197,#75198,#75199,#75200,#75201,#75202,#75203));
#18372=EDGE_LOOP('',(#75204,#75205,#75206,#75207,#75208,#75209,#75210,#75211));
#18373=EDGE_LOOP('',(#75212,#75213,#75214,#75215,#75216,#75217,#75218,#75219,
#75220,#75221));
#18374=EDGE_LOOP('',(#75222,#75223,#75224,#75225,#75226,#75227,#75228,#75229,
#75230,#75231));
#18375=EDGE_LOOP('',(#75232,#75233,#75234,#75235,#75236,#75237,#75238,#75239));
#18376=EDGE_LOOP('',(#75240,#75241,#75242,#75243,#75244,#75245,#75246,#75247));
#18377=EDGE_LOOP('',(#75248,#75249,#75250,#75251,#75252,#75253));
#18378=EDGE_LOOP('',(#75254,#75255,#75256,#75257,#75258,#75259,#75260,#75261,
#75262,#75263));
#18379=EDGE_LOOP('',(#75264,#75265,#75266,#75267,#75268,#75269,#75270,#75271));
#18380=EDGE_LOOP('',(#75272,#75273,#75274,#75275,#75276,#75277,#75278,#75279));
#18381=EDGE_LOOP('',(#75280,#75281,#75282,#75283,#75284,#75285,#75286,#75287,
#75288));
#18382=EDGE_LOOP('',(#75289,#75290,#75291,#75292,#75293,#75294,#75295,#75296));
#18383=EDGE_LOOP('',(#75297,#75298,#75299,#75300,#75301,#75302,#75303,#75304,
#75305));
#18384=EDGE_LOOP('',(#75306,#75307,#75308,#75309,#75310,#75311,#75312,#75313));
#18385=EDGE_LOOP('',(#75314,#75315,#75316,#75317,#75318,#75319,#75320,#75321,
#75322,#75323));
#18386=EDGE_LOOP('',(#75324,#75325,#75326,#75327,#75328,#75329,#75330,#75331));
#18387=EDGE_LOOP('',(#75332,#75333,#75334,#75335,#75336,#75337,#75338,#75339));
#18388=EDGE_LOOP('',(#75340,#75341,#75342,#75343,#75344,#75345,#75346,#75347));
#18389=EDGE_LOOP('',(#75348,#75349,#75350,#75351,#75352,#75353,#75354,#75355));
#18390=EDGE_LOOP('',(#75356,#75357,#75358,#75359,#75360,#75361,#75362,#75363));
#18391=EDGE_LOOP('',(#75364,#75365,#75366,#75367,#75368,#75369,#75370,#75371));
#18392=EDGE_LOOP('',(#75372,#75373,#75374,#75375,#75376,#75377,#75378,#75379));
#18393=EDGE_LOOP('',(#75380,#75381,#75382,#75383,#75384,#75385,#75386,#75387));
#18394=EDGE_LOOP('',(#75388,#75389,#75390,#75391,#75392,#75393,#75394,#75395));
#18395=EDGE_LOOP('',(#75396,#75397,#75398,#75399,#75400,#75401,#75402,#75403));
#18396=EDGE_LOOP('',(#75404,#75405,#75406,#75407,#75408,#75409,#75410,#75411,
#75412,#75413));
#18397=EDGE_LOOP('',(#75414,#75415,#75416,#75417,#75418,#75419,#75420,#75421,
#75422,#75423));
#18398=EDGE_LOOP('',(#75424,#75425,#75426,#75427,#75428,#75429,#75430,#75431));
#18399=EDGE_LOOP('',(#75432,#75433,#75434,#75435,#75436,#75437,#75438,#75439));
#18400=EDGE_LOOP('',(#75440,#75441,#75442,#75443,#75444,#75445,#75446,#75447));
#18401=EDGE_LOOP('',(#75448,#75449,#75450,#75451,#75452,#75453,#75454,#75455));
#18402=EDGE_LOOP('',(#75456,#75457,#75458,#75459,#75460,#75461,#75462,#75463));
#18403=EDGE_LOOP('',(#75464,#75465,#75466,#75467,#75468,#75469));
#18404=EDGE_LOOP('',(#75470,#75471,#75472,#75473,#75474,#75475,#75476,#75477));
#18405=EDGE_LOOP('',(#75478,#75479,#75480,#75481,#75482,#75483,#75484,#75485));
#18406=EDGE_LOOP('',(#75486,#75487,#75488,#75489,#75490,#75491,#75492,#75493));
#18407=EDGE_LOOP('',(#75494,#75495,#75496,#75497,#75498,#75499,#75500,#75501,
#75502,#75503));
#18408=EDGE_LOOP('',(#75504,#75505,#75506,#75507,#75508,#75509,#75510,#75511,
#75512,#75513));
#18409=EDGE_LOOP('',(#75514,#75515,#75516,#75517,#75518,#75519,#75520,#75521));
#18410=EDGE_LOOP('',(#75522,#75523,#75524,#75525,#75526,#75527,#75528,#75529));
#18411=EDGE_LOOP('',(#75530,#75531,#75532,#75533,#75534,#75535));
#18412=EDGE_LOOP('',(#75536,#75537,#75538,#75539,#75540,#75541,#75542,#75543,
#75544,#75545));
#18413=EDGE_LOOP('',(#75546,#75547,#75548,#75549,#75550,#75551,#75552,#75553));
#18414=EDGE_LOOP('',(#75554,#75555,#75556,#75557,#75558,#75559,#75560,#75561));
#18415=EDGE_LOOP('',(#75562,#75563,#75564,#75565,#75566,#75567,#75568,#75569,
#75570));
#18416=EDGE_LOOP('',(#75571,#75572,#75573,#75574,#75575,#75576,#75577,#75578));
#18417=EDGE_LOOP('',(#75579,#75580,#75581,#75582,#75583,#75584,#75585,#75586,
#75587));
#18418=EDGE_LOOP('',(#75588,#75589,#75590,#75591,#75592,#75593,#75594,#75595));
#18419=EDGE_LOOP('',(#75596,#75597,#75598,#75599,#75600,#75601,#75602,#75603,
#75604,#75605));
#18420=EDGE_LOOP('',(#75606,#75607,#75608,#75609));
#18421=EDGE_LOOP('',(#75610,#75611,#75612,#75613));
#18422=EDGE_LOOP('',(#75614,#75615,#75616,#75617));
#18423=EDGE_LOOP('',(#75618,#75619,#75620,#75621));
#18424=EDGE_LOOP('',(#75622,#75623,#75624,#75625));
#18425=EDGE_LOOP('',(#75626,#75627,#75628,#75629));
#18426=EDGE_LOOP('',(#75630,#75631,#75632,#75633));
#18427=EDGE_LOOP('',(#75634,#75635,#75636,#75637));
#18428=EDGE_LOOP('',(#75638,#75639,#75640,#75641));
#18429=EDGE_LOOP('',(#75642,#75643,#75644));
#18430=EDGE_LOOP('',(#75645,#75646,#75647));
#18431=EDGE_LOOP('',(#75648,#75649,#75650));
#18432=EDGE_LOOP('',(#75651,#75652,#75653,#75654));
#18433=EDGE_LOOP('',(#75655,#75656,#75657,#75658));
#18434=EDGE_LOOP('',(#75659,#75660,#75661,#75662));
#18435=EDGE_LOOP('',(#75663,#75664,#75665,#75666));
#18436=EDGE_LOOP('',(#75667,#75668,#75669,#75670));
#18437=EDGE_LOOP('',(#75671,#75672,#75673,#75674));
#18438=EDGE_LOOP('',(#75675,#75676,#75677,#75678,#75679,#75680,#75681,#75682,
#75683,#75684,#75685,#75686,#75687,#75688,#75689,#75690));
#18439=EDGE_LOOP('',(#75691,#75692,#75693,#75694,#75695,#75696,#75697,#75698,
#75699,#75700,#75701,#75702));
#18440=EDGE_LOOP('',(#75703,#75704,#75705,#75706));
#18441=EDGE_LOOP('',(#75707,#75708,#75709,#75710));
#18442=EDGE_LOOP('',(#75711,#75712,#75713,#75714,#75715,#75716,#75717,#75718,
#75719,#75720,#75721,#75722));
#18443=EDGE_LOOP('',(#75723,#75724,#75725,#75726));
#18444=EDGE_LOOP('',(#75727,#75728,#75729,#75730));
#18445=EDGE_LOOP('',(#75731,#75732,#75733,#75734));
#18446=EDGE_LOOP('',(#75735,#75736,#75737,#75738));
#18447=EDGE_LOOP('',(#75739,#75740,#75741,#75742));
#18448=EDGE_LOOP('',(#75743,#75744,#75745,#75746));
#18449=EDGE_LOOP('',(#75747,#75748,#75749,#75750,#75751));
#18450=EDGE_LOOP('',(#75752,#75753,#75754,#75755,#75756));
#18451=EDGE_LOOP('',(#75757,#75758,#75759,#75760,#75761));
#18452=EDGE_LOOP('',(#75762,#75763,#75764,#75765,#75766));
#18453=EDGE_LOOP('',(#75767,#75768,#75769,#75770,#75771));
#18454=EDGE_LOOP('',(#75772,#75773,#75774,#75775,#75776,#75777,#75778,#75779));
#18455=EDGE_LOOP('',(#75780,#75781,#75782,#75783,#75784));
#18456=EDGE_LOOP('',(#75785,#75786,#75787,#75788,#75789));
#18457=EDGE_LOOP('',(#75790,#75791,#75792,#75793,#75794,#75795,#75796,#75797));
#18458=EDGE_LOOP('',(#75798,#75799,#75800,#75801,#75802));
#18459=EDGE_LOOP('',(#75803,#75804,#75805,#75806,#75807,#75808,#75809,#75810));
#18460=EDGE_LOOP('',(#75811,#75812,#75813,#75814,#75815,#75816,#75817,#75818,
#75819,#75820,#75821,#75822,#75823,#75824,#75825,#75826));
#18461=EDGE_LOOP('',(#75827,#75828,#75829,#75830,#75831,#75832,#75833,#75834,
#75835,#75836,#75837,#75838,#75839,#75840,#75841,#75842));
#18462=EDGE_LOOP('',(#75843,#75844,#75845,#75846));
#18463=EDGE_LOOP('',(#75847,#75848,#75849,#75850));
#18464=EDGE_LOOP('',(#75851,#75852,#75853,#75854));
#18465=EDGE_LOOP('',(#75855,#75856,#75857,#75858));
#18466=EDGE_LOOP('',(#75859,#75860,#75861,#75862));
#18467=EDGE_LOOP('',(#75863,#75864,#75865,#75866));
#18468=EDGE_LOOP('',(#75867,#75868,#75869,#75870));
#18469=EDGE_LOOP('',(#75871,#75872,#75873,#75874));
#18470=EDGE_LOOP('',(#75875,#75876,#75877,#75878));
#18471=EDGE_LOOP('',(#75879,#75880,#75881,#75882));
#18472=EDGE_LOOP('',(#75883,#75884,#75885,#75886));
#18473=EDGE_LOOP('',(#75887,#75888,#75889,#75890,#75891,#75892,#75893,#75894));
#18474=EDGE_LOOP('',(#75895,#75896,#75897,#75898));
#18475=EDGE_LOOP('',(#75899,#75900,#75901,#75902,#75903,#75904,#75905,#75906));
#18476=EDGE_LOOP('',(#75907,#75908,#75909,#75910,#75911,#75912,#75913,#75914,
#75915,#75916,#75917,#75918));
#18477=EDGE_LOOP('',(#75919,#75920,#75921,#75922));
#18478=EDGE_LOOP('',(#75923,#75924,#75925,#75926,#75927,#75928));
#18479=EDGE_LOOP('',(#75929,#75930,#75931,#75932,#75933,#75934,#75935,#75936,
#75937,#75938,#75939,#75940,#75941,#75942,#75943,#75944,#75945,#75946));
#18480=EDGE_LOOP('',(#75947,#75948,#75949,#75950,#75951,#75952));
#18481=EDGE_LOOP('',(#75953,#75954,#75955,#75956,#75957,#75958,#75959,#75960,
#75961,#75962,#75963,#75964,#75965,#75966,#75967,#75968));
#18482=EDGE_LOOP('',(#75969,#75970));
#18483=EDGE_LOOP('',(#75971,#75972));
#18484=EDGE_LOOP('',(#75973,#75974,#75975,#75976,#75977,#75978,#75979,#75980,
#75981,#75982,#75983,#75984));
#18485=EDGE_LOOP('',(#75985,#75986));
#18486=EDGE_LOOP('',(#75987,#75988));
#18487=EDGE_LOOP('',(#75989,#75990));
#18488=EDGE_LOOP('',(#75991,#75992));
#18489=EDGE_LOOP('',(#75993,#75994));
#18490=EDGE_LOOP('',(#75995,#75996,#75997));
#18491=EDGE_LOOP('',(#75998,#75999,#76000,#76001));
#18492=EDGE_LOOP('',(#76002,#76003,#76004,#76005));
#18493=EDGE_LOOP('',(#76006,#76007,#76008,#76009));
#18494=EDGE_LOOP('',(#76010,#76011,#76012,#76013));
#18495=EDGE_LOOP('',(#76014,#76015,#76016,#76017,#76018,#76019));
#18496=EDGE_LOOP('',(#76020,#76021,#76022));
#18497=EDGE_LOOP('',(#76023,#76024,#76025,#76026,#76027,#76028,#76029,#76030));
#18498=EDGE_LOOP('',(#76031,#76032,#76033));
#18499=EDGE_LOOP('',(#76034,#76035,#76036,#76037,#76038,#76039,#76040,#76041,
#76042,#76043,#76044,#76045,#76046,#76047,#76048,#76049,#76050,#76051,#76052,
#76053,#76054,#76055));
#18500=EDGE_LOOP('',(#76056,#76057,#76058,#76059,#76060,#76061));
#18501=EDGE_LOOP('',(#76062,#76063,#76064,#76065));
#18502=EDGE_LOOP('',(#76066,#76067,#76068,#76069));
#18503=EDGE_LOOP('',(#76070,#76071,#76072,#76073));
#18504=EDGE_LOOP('',(#76074,#76075,#76076,#76077));
#18505=EDGE_LOOP('',(#76078,#76079,#76080,#76081));
#18506=EDGE_LOOP('',(#76082,#76083,#76084,#76085));
#18507=EDGE_LOOP('',(#76086,#76087,#76088,#76089));
#18508=EDGE_LOOP('',(#76090));
#18509=EDGE_LOOP('',(#76091,#76092,#76093,#76094,#76095,#76096));
#18510=EDGE_LOOP('',(#76097));
#18511=EDGE_LOOP('',(#76098,#76099,#76100,#76101,#76102));
#18512=EDGE_LOOP('',(#76103,#76104,#76105,#76106,#76107,#76108));
#18513=EDGE_LOOP('',(#76109));
#18514=EDGE_LOOP('',(#76110,#76111,#76112));
#18515=EDGE_LOOP('',(#76113,#76114,#76115));
#18516=EDGE_LOOP('',(#76116,#76117,#76118,#76119));
#18517=EDGE_LOOP('',(#76120,#76121,#76122,#76123,#76124,#76125,#76126,#76127));
#18518=EDGE_LOOP('',(#76128,#76129,#76130));
#18519=EDGE_LOOP('',(#76131,#76132,#76133));
#18520=EDGE_LOOP('',(#76134,#76135,#76136,#76137));
#18521=EDGE_LOOP('',(#76138,#76139,#76140,#76141));
#18522=EDGE_LOOP('',(#76142,#76143,#76144,#76145));
#18523=EDGE_LOOP('',(#76146,#76147,#76148,#76149));
#18524=EDGE_LOOP('',(#76150,#76151,#76152,#76153));
#18525=EDGE_LOOP('',(#76154,#76155,#76156,#76157));
#18526=EDGE_LOOP('',(#76158,#76159,#76160,#76161));
#18527=EDGE_LOOP('',(#76162,#76163,#76164,#76165,#76166,#76167,#76168,#76169,
#76170,#76171,#76172,#76173,#76174,#76175,#76176,#76177,#76178,#76179));
#18528=EDGE_LOOP('',(#76180,#76181,#76182,#76183,#76184,#76185,#76186,#76187,
#76188,#76189,#76190,#76191,#76192,#76193,#76194,#76195,#76196,#76197,#76198,
#76199));
#18529=EDGE_LOOP('',(#76200,#76201,#76202,#76203,#76204,#76205,#76206,#76207,
#76208,#76209,#76210,#76211,#76212,#76213,#76214,#76215,#76216));
#18530=EDGE_LOOP('',(#76217,#76218,#76219,#76220,#76221,#76222,#76223,#76224,
#76225,#76226,#76227,#76228,#76229,#76230,#76231,#76232));
#18531=EDGE_LOOP('',(#76233,#76234,#76235,#76236,#76237,#76238,#76239,#76240,
#76241,#76242));
#18532=EDGE_LOOP('',(#76243,#76244,#76245,#76246,#76247,#76248,#76249,#76250));
#18533=EDGE_LOOP('',(#76251,#76252,#76253,#76254,#76255,#76256,#76257,#76258));
#18534=EDGE_LOOP('',(#76259,#76260,#76261,#76262,#76263,#76264,#76265,#76266));
#18535=EDGE_LOOP('',(#76267,#76268,#76269,#76270,#76271,#76272,#76273,#76274,
#76275));
#18536=EDGE_LOOP('',(#76276,#76277,#76278,#76279,#76280,#76281,#76282,#76283));
#18537=EDGE_LOOP('',(#76284,#76285,#76286,#76287,#76288,#76289,#76290,#76291));
#18538=EDGE_LOOP('',(#76292,#76293,#76294,#76295,#76296,#76297,#76298,#76299));
#18539=EDGE_LOOP('',(#76300,#76301,#76302,#76303,#76304,#76305,#76306,#76307));
#18540=EDGE_LOOP('',(#76308,#76309,#76310,#76311,#76312,#76313,#76314,#76315));
#18541=EDGE_LOOP('',(#76316,#76317,#76318,#76319,#76320,#76321,#76322,#76323,
#76324,#76325));
#18542=EDGE_LOOP('',(#76326,#76327,#76328,#76329,#76330,#76331,#76332,#76333));
#18543=EDGE_LOOP('',(#76334,#76335,#76336,#76337,#76338,#76339,#76340,#76341));
#18544=EDGE_LOOP('',(#76342,#76343,#76344,#76345,#76346,#76347,#76348,#76349,
#76350,#76351));
#18545=EDGE_LOOP('',(#76352,#76353,#76354,#76355,#76356,#76357,#76358,#76359,
#76360,#76361));
#18546=EDGE_LOOP('',(#76362,#76363,#76364,#76365,#76366,#76367,#76368,#76369));
#18547=EDGE_LOOP('',(#76370,#76371,#76372,#76373,#76374,#76375,#76376,#76377));
#18548=EDGE_LOOP('',(#76378,#76379,#76380,#76381,#76382,#76383,#76384,#76385));
#18549=EDGE_LOOP('',(#76386,#76387,#76388,#76389,#76390,#76391,#76392,#76393));
#18550=EDGE_LOOP('',(#76394,#76395,#76396,#76397,#76398,#76399,#76400,#76401,
#76402));
#18551=EDGE_LOOP('',(#76403,#76404,#76405,#76406,#76407,#76408,#76409,#76410));
#18552=EDGE_LOOP('',(#76411,#76412,#76413,#76414,#76415,#76416,#76417,#76418,
#76419,#76420));
#18553=EDGE_LOOP('',(#76421,#76422,#76423,#76424,#76425,#76426,#76427,#76428));
#18554=EDGE_LOOP('',(#76429,#76430,#76431,#76432,#76433,#76434,#76435,#76436,
#76437,#76438));
#18555=EDGE_LOOP('',(#76439,#76440,#76441,#76442,#76443,#76444,#76445,#76446));
#18556=EDGE_LOOP('',(#76447,#76448,#76449,#76450,#76451,#76452,#76453,#76454));
#18557=EDGE_LOOP('',(#76455,#76456,#76457,#76458,#76459,#76460,#76461,#76462));
#18558=EDGE_LOOP('',(#76463,#76464,#76465,#76466,#76467,#76468,#76469,#76470));
#18559=EDGE_LOOP('',(#76471,#76472,#76473,#76474,#76475,#76476));
#18560=EDGE_LOOP('',(#76477,#76478,#76479,#76480,#76481,#76482));
#18561=EDGE_LOOP('',(#76483,#76484,#76485,#76486,#76487,#76488,#76489,#76490,
#76491,#76492,#76493,#76494,#76495,#76496,#76497,#76498,#76499,#76500,#76501,
#76502,#76503,#76504,#76505,#76506,#76507,#76508,#76509,#76510,#76511,#76512,
#76513,#76514,#76515,#76516,#76517,#76518,#76519,#76520,#76521,#76522,#76523,
#76524,#76525,#76526,#76527,#76528,#76529,#76530,#76531,#76532,#76533,#76534,
#76535,#76536,#76537,#76538,#76539,#76540,#76541,#76542,#76543,#76544,#76545,
#76546,#76547));
#18562=EDGE_LOOP('',(#76548,#76549,#76550,#76551,#76552,#76553,#76554,#76555,
#76556,#76557));
#18563=EDGE_LOOP('',(#76558,#76559,#76560,#76561,#76562,#76563,#76564,#76565));
#18564=EDGE_LOOP('',(#76566,#76567,#76568,#76569,#76570,#76571,#76572,#76573));
#18565=EDGE_LOOP('',(#76574,#76575,#76576,#76577,#76578,#76579,#76580,#76581));
#18566=EDGE_LOOP('',(#76582,#76583,#76584,#76585,#76586,#76587,#76588,#76589,
#76590));
#18567=EDGE_LOOP('',(#76591,#76592,#76593,#76594,#76595,#76596,#76597,#76598));
#18568=EDGE_LOOP('',(#76599,#76600,#76601,#76602,#76603,#76604,#76605,#76606));
#18569=EDGE_LOOP('',(#76607,#76608,#76609,#76610,#76611,#76612,#76613,#76614));
#18570=EDGE_LOOP('',(#76615,#76616,#76617,#76618,#76619,#76620,#76621,#76622));
#18571=EDGE_LOOP('',(#76623,#76624,#76625,#76626,#76627,#76628,#76629,#76630));
#18572=EDGE_LOOP('',(#76631,#76632,#76633,#76634,#76635,#76636,#76637,#76638,
#76639,#76640));
#18573=EDGE_LOOP('',(#76641,#76642,#76643,#76644,#76645,#76646,#76647,#76648));
#18574=EDGE_LOOP('',(#76649,#76650,#76651,#76652,#76653,#76654,#76655,#76656));
#18575=EDGE_LOOP('',(#76657,#76658,#76659,#76660,#76661,#76662,#76663,#76664,
#76665,#76666));
#18576=EDGE_LOOP('',(#76667,#76668,#76669,#76670,#76671,#76672,#76673,#76674,
#76675,#76676));
#18577=EDGE_LOOP('',(#76677,#76678,#76679,#76680,#76681,#76682,#76683,#76684));
#18578=EDGE_LOOP('',(#76685,#76686,#76687,#76688,#76689,#76690,#76691,#76692));
#18579=EDGE_LOOP('',(#76693,#76694,#76695,#76696,#76697,#76698,#76699,#76700));
#18580=EDGE_LOOP('',(#76701,#76702,#76703,#76704,#76705,#76706,#76707,#76708));
#18581=EDGE_LOOP('',(#76709,#76710,#76711,#76712,#76713,#76714,#76715,#76716,
#76717));
#18582=EDGE_LOOP('',(#76718,#76719,#76720,#76721,#76722,#76723,#76724,#76725));
#18583=EDGE_LOOP('',(#76726,#76727,#76728,#76729,#76730,#76731,#76732,#76733,
#76734,#76735));
#18584=EDGE_LOOP('',(#76736,#76737,#76738,#76739,#76740,#76741,#76742,#76743));
#18585=EDGE_LOOP('',(#76744,#76745,#76746,#76747,#76748,#76749,#76750,#76751,
#76752,#76753));
#18586=EDGE_LOOP('',(#76754,#76755,#76756,#76757,#76758,#76759,#76760,#76761));
#18587=EDGE_LOOP('',(#76762,#76763,#76764,#76765,#76766,#76767,#76768,#76769));
#18588=EDGE_LOOP('',(#76770,#76771,#76772,#76773,#76774,#76775,#76776,#76777));
#18589=EDGE_LOOP('',(#76778,#76779,#76780,#76781,#76782,#76783,#76784,#76785));
#18590=EDGE_LOOP('',(#76786,#76787,#76788,#76789,#76790,#76791));
#18591=EDGE_LOOP('',(#76792,#76793,#76794,#76795,#76796,#76797));
#18592=EDGE_LOOP('',(#76798,#76799,#76800,#76801));
#18593=EDGE_LOOP('',(#76802,#76803,#76804,#76805));
#18594=EDGE_LOOP('',(#76806,#76807,#76808,#76809));
#18595=EDGE_LOOP('',(#76810,#76811,#76812,#76813));
#18596=EDGE_LOOP('',(#76814,#76815,#76816,#76817));
#18597=EDGE_LOOP('',(#76818,#76819,#76820,#76821));
#18598=EDGE_LOOP('',(#76822,#76823,#76824,#76825));
#18599=EDGE_LOOP('',(#76826,#76827,#76828,#76829));
#18600=EDGE_LOOP('',(#76830,#76831,#76832,#76833));
#18601=EDGE_LOOP('',(#76834,#76835,#76836,#76837,#76838,#76839,#76840,#76841,
#76842,#76843,#76844,#76845,#76846,#76847,#76848,#76849));
#18602=EDGE_LOOP('',(#76850,#76851,#76852,#76853,#76854,#76855,#76856,#76857,
#76858,#76859,#76860,#76861,#76862,#76863,#76864,#76865));
#18603=EDGE_LOOP('',(#76866,#76867,#76868,#76869));
#18604=EDGE_LOOP('',(#76870,#76871,#76872,#76873));
#18605=EDGE_LOOP('',(#76874,#76875,#76876,#76877));
#18606=EDGE_LOOP('',(#76878,#76879,#76880,#76881));
#18607=EDGE_LOOP('',(#76882,#76883,#76884,#76885));
#18608=EDGE_LOOP('',(#76886,#76887,#76888,#76889));
#18609=EDGE_LOOP('',(#76890,#76891,#76892,#76893));
#18610=EDGE_LOOP('',(#76894,#76895,#76896,#76897));
#18611=EDGE_LOOP('',(#76898,#76899,#76900,#76901));
#18612=EDGE_LOOP('',(#76902,#76903,#76904,#76905,#76906));
#18613=EDGE_LOOP('',(#76907,#76908,#76909,#76910,#76911));
#18614=EDGE_LOOP('',(#76912,#76913,#76914,#76915,#76916));
#18615=EDGE_LOOP('',(#76917,#76918,#76919,#76920,#76921));
#18616=EDGE_LOOP('',(#76922,#76923,#76924,#76925,#76926));
#18617=EDGE_LOOP('',(#76927,#76928,#76929,#76930,#76931,#76932,#76933,#76934));
#18618=EDGE_LOOP('',(#76935,#76936,#76937,#76938,#76939));
#18619=EDGE_LOOP('',(#76940,#76941,#76942,#76943,#76944));
#18620=EDGE_LOOP('',(#76945,#76946,#76947,#76948,#76949,#76950,#76951,#76952));
#18621=EDGE_LOOP('',(#76953,#76954,#76955,#76956,#76957));
#18622=EDGE_LOOP('',(#76958,#76959,#76960,#76961,#76962,#76963,#76964,#76965));
#18623=EDGE_LOOP('',(#76966,#76967,#76968,#76969,#76970,#76971,#76972,#76973,
#76974,#76975,#76976,#76977,#76978,#76979,#76980,#76981));
#18624=EDGE_LOOP('',(#76982,#76983,#76984,#76985,#76986,#76987,#76988,#76989,
#76990,#76991,#76992,#76993,#76994,#76995,#76996,#76997));
#18625=EDGE_LOOP('',(#76998,#76999,#77000,#77001,#77002,#77003,#77004,#77005,
#77006,#77007,#77008,#77009,#77010,#77011,#77012,#77013));
#18626=EDGE_LOOP('',(#77014,#77015,#77016,#77017,#77018,#77019,#77020,#77021,
#77022,#77023,#77024,#77025,#77026,#77027,#77028,#77029));
#18627=EDGE_LOOP('',(#77030,#77031,#77032,#77033));
#18628=EDGE_LOOP('',(#77034,#77035,#77036,#77037));
#18629=EDGE_LOOP('',(#77038,#77039,#77040,#77041));
#18630=EDGE_LOOP('',(#77042,#77043,#77044,#77045));
#18631=EDGE_LOOP('',(#77046,#77047,#77048,#77049));
#18632=EDGE_LOOP('',(#77050,#77051,#77052,#77053));
#18633=EDGE_LOOP('',(#77054,#77055,#77056,#77057));
#18634=EDGE_LOOP('',(#77058,#77059,#77060,#77061));
#18635=EDGE_LOOP('',(#77062,#77063,#77064,#77065));
#18636=EDGE_LOOP('',(#77066,#77067,#77068,#77069));
#18637=EDGE_LOOP('',(#77070,#77071,#77072,#77073));
#18638=EDGE_LOOP('',(#77074,#77075,#77076,#77077,#77078,#77079,#77080,#77081));
#18639=EDGE_LOOP('',(#77082,#77083,#77084,#77085));
#18640=EDGE_LOOP('',(#77086,#77087,#77088,#77089,#77090,#77091,#77092,#77093,
#77094,#77095,#77096));
#18641=EDGE_LOOP('',(#77097,#77098,#77099,#77100,#77101,#77102,#77103,#77104,
#77105,#77106,#77107,#77108,#77109,#77110,#77111,#77112,#77113,#77114,#77115,
#77116,#77117,#77118,#77119,#77120,#77121,#77122,#77123,#77124,#77125,#77126,
#77127,#77128,#77129));
#18642=EDGE_LOOP('',(#77130,#77131,#77132,#77133,#77134,#77135,#77136,#77137,
#77138,#77139,#77140,#77141,#77142,#77143,#77144,#77145));
#18643=EDGE_LOOP('',(#77146,#77147,#77148,#77149));
#18644=EDGE_LOOP('',(#77150,#77151,#77152,#77153,#77154,#77155,#77156,#77157));
#18645=EDGE_LOOP('',(#77158,#77159,#77160,#77161,#77162,#77163,#77164,#77165,
#77166,#77167,#77168,#77169,#77170,#77171,#77172,#77173,#77174,#77175));
#18646=EDGE_LOOP('',(#77176,#77177,#77178,#77179,#77180,#77181,#77182,#77183,
#77184,#77185));
#18647=EDGE_LOOP('',(#77186,#77187,#77188,#77189,#77190,#77191,#77192,#77193,
#77194,#77195,#77196,#77197,#77198,#77199,#77200,#77201,#77202,#77203,#77204,
#77205));
#18648=EDGE_LOOP('',(#77206,#77207,#77208,#77209));
#18649=EDGE_LOOP('',(#77210,#77211,#77212,#77213));
#18650=EDGE_LOOP('',(#77214,#77215,#77216,#77217));
#18651=EDGE_LOOP('',(#77218,#77219,#77220,#77221));
#18652=EDGE_LOOP('',(#77222,#77223,#77224,#77225));
#18653=EDGE_LOOP('',(#77226,#77227,#77228,#77229));
#18654=EDGE_LOOP('',(#77230,#77231,#77232,#77233));
#18655=EDGE_LOOP('',(#77234,#77235,#77236,#77237));
#18656=EDGE_LOOP('',(#77238,#77239,#77240,#77241));
#18657=EDGE_LOOP('',(#77242,#77243,#77244,#77245));
#18658=EDGE_LOOP('',(#77246,#77247,#77248,#77249));
#18659=EDGE_LOOP('',(#77250,#77251,#77252,#77253));
#18660=EDGE_LOOP('',(#77254,#77255,#77256,#77257));
#18661=EDGE_LOOP('',(#77258,#77259,#77260,#77261));
#18662=EDGE_LOOP('',(#77262,#77263,#77264,#77265));
#18663=EDGE_LOOP('',(#77266,#77267,#77268,#77269));
#18664=EDGE_LOOP('',(#77270,#77271,#77272,#77273));
#18665=EDGE_LOOP('',(#77274,#77275,#77276,#77277));
#18666=EDGE_LOOP('',(#77278,#77279,#77280,#77281));
#18667=EDGE_LOOP('',(#77282,#77283,#77284,#77285,#77286,#77287,#77288,#77289,
#77290,#77291,#77292,#77293,#77294,#77295,#77296,#77297,#77298,#77299,#77300,
#77301,#77302,#77303,#77304,#77305,#77306,#77307,#77308,#77309,#77310,#77311,
#77312,#77313,#77314,#77315,#77316,#77317,#77318,#77319,#77320,#77321));
#18668=EDGE_LOOP('',(#77322,#77323,#77324,#77325,#77326,#77327,#77328,#77329,
#77330,#77331,#77332,#77333,#77334,#77335,#77336,#77337,#77338,#77339,#77340,
#77341,#77342,#77343,#77344,#77345));
#18669=EDGE_LOOP('',(#77346,#77347,#77348,#77349));
#18670=EDGE_LOOP('',(#77350,#77351,#77352,#77353));
#18671=EDGE_LOOP('',(#77354,#77355,#77356,#77357));
#18672=EDGE_LOOP('',(#77358,#77359,#77360,#77361));
#18673=EDGE_LOOP('',(#77362,#77363,#77364,#77365));
#18674=EDGE_LOOP('',(#77366,#77367,#77368,#77369));
#18675=EDGE_LOOP('',(#77370,#77371,#77372,#77373));
#18676=EDGE_LOOP('',(#77374,#77375,#77376,#77377));
#18677=EDGE_LOOP('',(#77378,#77379,#77380,#77381));
#18678=EDGE_LOOP('',(#77382,#77383,#77384,#77385));
#18679=EDGE_LOOP('',(#77386,#77387,#77388,#77389));
#18680=EDGE_LOOP('',(#77390,#77391,#77392,#77393));
#18681=EDGE_LOOP('',(#77394,#77395,#77396,#77397));
#18682=EDGE_LOOP('',(#77398,#77399,#77400,#77401));
#18683=EDGE_LOOP('',(#77402,#77403,#77404,#77405));
#18684=EDGE_LOOP('',(#77406,#77407,#77408,#77409));
#18685=EDGE_LOOP('',(#77410,#77411,#77412,#77413));
#18686=EDGE_LOOP('',(#77414,#77415,#77416,#77417));
#18687=EDGE_LOOP('',(#77418,#77419,#77420,#77421));
#18688=EDGE_LOOP('',(#77422,#77423,#77424,#77425));
#18689=EDGE_LOOP('',(#77426,#77427,#77428,#77429));
#18690=EDGE_LOOP('',(#77430,#77431,#77432,#77433));
#18691=EDGE_LOOP('',(#77434,#77435,#77436,#77437));
#18692=EDGE_LOOP('',(#77438,#77439,#77440,#77441));
#18693=EDGE_LOOP('',(#77442,#77443,#77444,#77445));
#18694=EDGE_LOOP('',(#77446,#77447,#77448,#77449));
#18695=EDGE_LOOP('',(#77450,#77451,#77452,#77453));
#18696=EDGE_LOOP('',(#77454,#77455,#77456,#77457));
#18697=EDGE_LOOP('',(#77458,#77459,#77460,#77461));
#18698=EDGE_LOOP('',(#77462,#77463,#77464,#77465));
#18699=EDGE_LOOP('',(#77466,#77467,#77468,#77469));
#18700=EDGE_LOOP('',(#77470,#77471,#77472,#77473));
#18701=EDGE_LOOP('',(#77474,#77475,#77476,#77477));
#18702=EDGE_LOOP('',(#77478,#77479,#77480,#77481));
#18703=EDGE_LOOP('',(#77482,#77483,#77484,#77485));
#18704=EDGE_LOOP('',(#77486,#77487,#77488,#77489));
#18705=EDGE_LOOP('',(#77490,#77491,#77492,#77493));
#18706=EDGE_LOOP('',(#77494,#77495,#77496,#77497));
#18707=EDGE_LOOP('',(#77498,#77499,#77500,#77501));
#18708=EDGE_LOOP('',(#77502,#77503,#77504,#77505));
#18709=EDGE_LOOP('',(#77506,#77507,#77508,#77509));
#18710=EDGE_LOOP('',(#77510,#77511,#77512,#77513));
#18711=EDGE_LOOP('',(#77514,#77515,#77516,#77517));
#18712=EDGE_LOOP('',(#77518,#77519,#77520,#77521));
#18713=EDGE_LOOP('',(#77522,#77523,#77524,#77525));
#18714=EDGE_LOOP('',(#77526,#77527,#77528,#77529));
#18715=EDGE_LOOP('',(#77530,#77531,#77532,#77533));
#18716=EDGE_LOOP('',(#77534,#77535,#77536,#77537));
#18717=EDGE_LOOP('',(#77538,#77539,#77540,#77541));
#18718=EDGE_LOOP('',(#77542,#77543,#77544,#77545));
#18719=EDGE_LOOP('',(#77546,#77547,#77548,#77549,#77550));
#18720=EDGE_LOOP('',(#77551,#77552,#77553,#77554));
#18721=EDGE_LOOP('',(#77555,#77556,#77557,#77558));
#18722=EDGE_LOOP('',(#77559,#77560,#77561,#77562));
#18723=EDGE_LOOP('',(#77563,#77564,#77565,#77566));
#18724=EDGE_LOOP('',(#77567,#77568,#77569,#77570));
#18725=EDGE_LOOP('',(#77571,#77572,#77573,#77574));
#18726=EDGE_LOOP('',(#77575,#77576,#77577,#77578,#77579,#77580,#77581,#77582));
#18727=EDGE_LOOP('',(#77583,#77584));
#18728=EDGE_LOOP('',(#77585,#77586));
#18729=EDGE_LOOP('',(#77587,#77588));
#18730=EDGE_LOOP('',(#77589,#77590));
#18731=EDGE_LOOP('',(#77591,#77592));
#18732=EDGE_LOOP('',(#77593,#77594));
#18733=EDGE_LOOP('',(#77595,#77596,#77597,#77598,#77599));
#18734=EDGE_LOOP('',(#77600));
#18735=EDGE_LOOP('',(#77601));
#18736=EDGE_LOOP('',(#77602,#77603,#77604,#77605,#77606,#77607));
#18737=EDGE_LOOP('',(#77608,#77609,#77610,#77611,#77612));
#18738=EDGE_LOOP('',(#77613,#77614,#77615,#77616,#77617,#77618));
#18739=EDGE_LOOP('',(#77619,#77620,#77621));
#18740=EDGE_LOOP('',(#77622,#77623,#77624));
#18741=EDGE_LOOP('',(#77625,#77626,#77627));
#18742=EDGE_LOOP('',(#77628,#77629,#77630));
#18743=EDGE_LOOP('',(#77631,#77632,#77633));
#18744=EDGE_LOOP('',(#77634,#77635,#77636));
#18745=EDGE_LOOP('',(#77637,#77638,#77639,#77640,#77641,#77642));
#18746=EDGE_LOOP('',(#77643,#77644,#77645));
#18747=EDGE_LOOP('',(#77646,#77647,#77648));
#18748=EDGE_LOOP('',(#77649,#77650,#77651));
#18749=EDGE_LOOP('',(#77652,#77653,#77654));
#18750=EDGE_LOOP('',(#77655,#77656,#77657));
#18751=EDGE_LOOP('',(#77658,#77659,#77660));
#18752=EDGE_LOOP('',(#77661,#77662,#77663,#77664,#77665,#77666));
#18753=EDGE_LOOP('',(#77667,#77668,#77669,#77670,#77671,#77672));
#18754=EDGE_LOOP('',(#77673,#77674,#77675,#77676,#77677,#77678));
#18755=EDGE_LOOP('',(#77679,#77680,#77681,#77682,#77683,#77684));
#18756=EDGE_LOOP('',(#77685,#77686,#77687,#77688,#77689,#77690));
#18757=EDGE_LOOP('',(#77691,#77692,#77693,#77694,#77695,#77696));
#18758=EDGE_LOOP('',(#77697,#77698,#77699,#77700,#77701,#77702));
#18759=EDGE_LOOP('',(#77703,#77704,#77705));
#18760=EDGE_LOOP('',(#77706,#77707,#77708));
#18761=EDGE_LOOP('',(#77709,#77710,#77711));
#18762=EDGE_LOOP('',(#77712,#77713,#77714));
#18763=EDGE_LOOP('',(#77715,#77716,#77717));
#18764=EDGE_LOOP('',(#77718,#77719,#77720));
#18765=EDGE_LOOP('',(#77721,#77722,#77723,#77724,#77725,#77726));
#18766=EDGE_LOOP('',(#77727,#77728,#77729));
#18767=EDGE_LOOP('',(#77730,#77731,#77732));
#18768=EDGE_LOOP('',(#77733,#77734,#77735));
#18769=EDGE_LOOP('',(#77736,#77737,#77738));
#18770=EDGE_LOOP('',(#77739,#77740,#77741));
#18771=EDGE_LOOP('',(#77742,#77743,#77744));
#18772=EDGE_LOOP('',(#77745,#77746,#77747,#77748,#77749,#77750));
#18773=EDGE_LOOP('',(#77751,#77752,#77753,#77754,#77755,#77756));
#18774=EDGE_LOOP('',(#77757,#77758,#77759,#77760,#77761,#77762));
#18775=EDGE_LOOP('',(#77763,#77764,#77765,#77766,#77767,#77768));
#18776=EDGE_LOOP('',(#77769,#77770,#77771,#77772,#77773,#77774));
#18777=EDGE_LOOP('',(#77775,#77776,#77777,#77778,#77779,#77780));
#18778=EDGE_LOOP('',(#77781,#77782,#77783,#77784));
#18779=EDGE_LOOP('',(#77785,#77786,#77787,#77788));
#18780=EDGE_LOOP('',(#77789,#77790,#77791,#77792));
#18781=EDGE_LOOP('',(#77793,#77794,#77795,#77796));
#18782=EDGE_LOOP('',(#77797,#77798,#77799,#77800));
#18783=EDGE_LOOP('',(#77801,#77802,#77803,#77804));
#18784=EDGE_LOOP('',(#77805,#77806,#77807,#77808,#77809,#77810,#77811,#77812));
#18785=EDGE_LOOP('',(#77813,#77814));
#18786=EDGE_LOOP('',(#77815,#77816));
#18787=EDGE_LOOP('',(#77817,#77818));
#18788=EDGE_LOOP('',(#77819,#77820));
#18789=EDGE_LOOP('',(#77821,#77822));
#18790=EDGE_LOOP('',(#77823,#77824));
#18791=EDGE_LOOP('',(#77825,#77826,#77827,#77828,#77829));
#18792=EDGE_LOOP('',(#77830));
#18793=EDGE_LOOP('',(#77831));
#18794=EDGE_LOOP('',(#77832,#77833,#77834,#77835,#77836,#77837));
#18795=EDGE_LOOP('',(#77838,#77839,#77840,#77841,#77842));
#18796=EDGE_LOOP('',(#77843));
#18797=EDGE_LOOP('',(#77844,#77845,#77846,#77847));
#18798=EDGE_LOOP('',(#77848,#77849,#77850,#77851,#77852));
#18799=EDGE_LOOP('',(#77853,#77854,#77855,#77856,#77857));
#18800=EDGE_LOOP('',(#77858,#77859,#77860,#77861));
#18801=EDGE_LOOP('',(#77862,#77863,#77864,#77865));
#18802=EDGE_LOOP('',(#77866,#77867,#77868,#77869));
#18803=EDGE_LOOP('',(#77870,#77871,#77872,#77873));
#18804=EDGE_LOOP('',(#77874,#77875,#77876,#77877));
#18805=EDGE_LOOP('',(#77878));
#18806=EDGE_LOOP('',(#77879,#77880,#77881,#77882));
#18807=EDGE_LOOP('',(#77883,#77884,#77885,#77886,#77887,#77888));
#18808=EDGE_LOOP('',(#77889));
#18809=EDGE_LOOP('',(#77890));
#18810=EDGE_LOOP('',(#77891,#77892,#77893,#77894));
#18811=EDGE_LOOP('',(#77895));
#18812=EDGE_LOOP('',(#77896,#77897,#77898,#77899));
#18813=EDGE_LOOP('',(#77900));
#18814=EDGE_LOOP('',(#77901));
#18815=EDGE_LOOP('',(#77902,#77903,#77904,#77905));
#18816=EDGE_LOOP('',(#77906));
#18817=EDGE_LOOP('',(#77907,#77908,#77909,#77910));
#18818=EDGE_LOOP('',(#77911,#77912,#77913,#77914));
#18819=EDGE_LOOP('',(#77915,#77916,#77917,#77918));
#18820=EDGE_LOOP('',(#77919,#77920,#77921,#77922));
#18821=EDGE_LOOP('',(#77923,#77924,#77925,#77926));
#18822=EDGE_LOOP('',(#77927,#77928,#77929,#77930));
#18823=EDGE_LOOP('',(#77931,#77932,#77933,#77934));
#18824=EDGE_LOOP('',(#77935,#77936,#77937,#77938));
#18825=EDGE_LOOP('',(#77939,#77940,#77941,#77942));
#18826=EDGE_LOOP('',(#77943,#77944,#77945,#77946));
#18827=EDGE_LOOP('',(#77947,#77948,#77949,#77950));
#18828=EDGE_LOOP('',(#77951,#77952,#77953,#77954));
#18829=EDGE_LOOP('',(#77955));
#18830=EDGE_LOOP('',(#77956));
#18831=EDGE_LOOP('',(#77957,#77958,#77959,#77960));
#18832=EDGE_LOOP('',(#77961,#77962,#77963,#77964));
#18833=EDGE_LOOP('',(#77965,#77966,#77967,#77968));
#18834=EDGE_LOOP('',(#77969,#77970,#77971,#77972));
#18835=EDGE_LOOP('',(#77973,#77974,#77975,#77976));
#18836=EDGE_LOOP('',(#77977,#77978,#77979,#77980));
#18837=EDGE_LOOP('',(#77981,#77982,#77983,#77984));
#18838=EDGE_LOOP('',(#77985,#77986,#77987,#77988));
#18839=EDGE_LOOP('',(#77989,#77990,#77991,#77992));
#18840=EDGE_LOOP('',(#77993,#77994,#77995,#77996));
#18841=EDGE_LOOP('',(#77997,#77998,#77999,#78000));
#18842=EDGE_LOOP('',(#78001,#78002,#78003,#78004));
#18843=EDGE_LOOP('',(#78005,#78006,#78007,#78008));
#18844=EDGE_LOOP('',(#78009,#78010,#78011,#78012));
#18845=EDGE_LOOP('',(#78013,#78014,#78015,#78016));
#18846=EDGE_LOOP('',(#78017,#78018,#78019,#78020));
#18847=EDGE_LOOP('',(#78021,#78022,#78023,#78024));
#18848=EDGE_LOOP('',(#78025));
#18849=EDGE_LOOP('',(#78026));
#18850=EDGE_LOOP('',(#78027,#78028,#78029,#78030));
#18851=EDGE_LOOP('',(#78031,#78032,#78033,#78034));
#18852=EDGE_LOOP('',(#78035,#78036,#78037,#78038));
#18853=EDGE_LOOP('',(#78039,#78040,#78041,#78042));
#18854=EDGE_LOOP('',(#78043,#78044,#78045,#78046));
#18855=EDGE_LOOP('',(#78047,#78048,#78049,#78050,#78051,#78052,#78053,#78054));
#18856=EDGE_LOOP('',(#78055,#78056,#78057,#78058));
#18857=EDGE_LOOP('',(#78059,#78060,#78061,#78062));
#18858=EDGE_LOOP('',(#78063,#78064,#78065,#78066));
#18859=EDGE_LOOP('',(#78067,#78068,#78069,#78070,#78071,#78072,#78073,#78074));
#18860=EDGE_LOOP('',(#78075,#78076,#78077,#78078,#78079,#78080,#78081,#78082));
#18861=EDGE_LOOP('',(#78083,#78084,#78085,#78086));
#18862=EDGE_LOOP('',(#78087,#78088,#78089,#78090));
#18863=EDGE_LOOP('',(#78091,#78092,#78093,#78094));
#18864=EDGE_LOOP('',(#78095,#78096,#78097,#78098));
#18865=EDGE_LOOP('',(#78099,#78100,#78101,#78102));
#18866=EDGE_LOOP('',(#78103,#78104,#78105,#78106,#78107,#78108,#78109,#78110));
#18867=EDGE_LOOP('',(#78111));
#18868=EDGE_LOOP('',(#78112,#78113,#78114,#78115));
#18869=EDGE_LOOP('',(#78116,#78117,#78118,#78119,#78120));
#18870=EDGE_LOOP('',(#78121,#78122,#78123,#78124,#78125));
#18871=EDGE_LOOP('',(#78126,#78127,#78128,#78129));
#18872=EDGE_LOOP('',(#78130,#78131,#78132,#78133));
#18873=EDGE_LOOP('',(#78134,#78135,#78136,#78137));
#18874=EDGE_LOOP('',(#78138,#78139,#78140,#78141));
#18875=EDGE_LOOP('',(#78142,#78143,#78144,#78145));
#18876=EDGE_LOOP('',(#78146));
#18877=EDGE_LOOP('',(#78147,#78148,#78149,#78150));
#18878=EDGE_LOOP('',(#78151,#78152,#78153,#78154,#78155,#78156));
#18879=EDGE_LOOP('',(#78157));
#18880=EDGE_LOOP('',(#78158));
#18881=EDGE_LOOP('',(#78159,#78160,#78161,#78162));
#18882=EDGE_LOOP('',(#78163,#78164,#78165,#78166));
#18883=EDGE_LOOP('',(#78167,#78168,#78169,#78170));
#18884=EDGE_LOOP('',(#78171,#78172,#78173,#78174));
#18885=EDGE_LOOP('',(#78175,#78176,#78177,#78178));
#18886=EDGE_LOOP('',(#78179,#78180,#78181,#78182));
#18887=EDGE_LOOP('',(#78183,#78184,#78185,#78186));
#18888=EDGE_LOOP('',(#78187,#78188,#78189,#78190));
#18889=EDGE_LOOP('',(#78191,#78192,#78193,#78194));
#18890=EDGE_LOOP('',(#78195,#78196,#78197,#78198));
#18891=EDGE_LOOP('',(#78199,#78200,#78201,#78202));
#18892=EDGE_LOOP('',(#78203,#78204,#78205,#78206));
#18893=EDGE_LOOP('',(#78207,#78208,#78209,#78210));
#18894=EDGE_LOOP('',(#78211,#78212,#78213,#78214));
#18895=EDGE_LOOP('',(#78215,#78216,#78217,#78218));
#18896=EDGE_LOOP('',(#78219,#78220,#78221,#78222));
#18897=EDGE_LOOP('',(#78223,#78224,#78225,#78226));
#18898=EDGE_LOOP('',(#78227,#78228,#78229,#78230));
#18899=EDGE_LOOP('',(#78231,#78232,#78233,#78234));
#18900=EDGE_LOOP('',(#78235,#78236,#78237,#78238));
#18901=EDGE_LOOP('',(#78239,#78240,#78241,#78242));
#18902=EDGE_LOOP('',(#78243,#78244,#78245,#78246));
#18903=EDGE_LOOP('',(#78247,#78248,#78249,#78250));
#18904=EDGE_LOOP('',(#78251,#78252,#78253,#78254));
#18905=EDGE_LOOP('',(#78255,#78256,#78257,#78258));
#18906=EDGE_LOOP('',(#78259,#78260,#78261,#78262));
#18907=EDGE_LOOP('',(#78263,#78264,#78265,#78266));
#18908=EDGE_LOOP('',(#78267,#78268,#78269,#78270));
#18909=EDGE_LOOP('',(#78271,#78272,#78273,#78274));
#18910=EDGE_LOOP('',(#78275,#78276,#78277,#78278));
#18911=EDGE_LOOP('',(#78279,#78280,#78281,#78282));
#18912=EDGE_LOOP('',(#78283,#78284,#78285,#78286));
#18913=EDGE_LOOP('',(#78287,#78288,#78289,#78290));
#18914=EDGE_LOOP('',(#78291,#78292,#78293,#78294));
#18915=EDGE_LOOP('',(#78295,#78296,#78297,#78298));
#18916=EDGE_LOOP('',(#78299,#78300,#78301,#78302));
#18917=EDGE_LOOP('',(#78303,#78304,#78305,#78306));
#18918=EDGE_LOOP('',(#78307,#78308,#78309,#78310));
#18919=EDGE_LOOP('',(#78311,#78312,#78313,#78314));
#18920=EDGE_LOOP('',(#78315,#78316,#78317,#78318));
#18921=EDGE_LOOP('',(#78319,#78320,#78321,#78322));
#18922=EDGE_LOOP('',(#78323,#78324,#78325,#78326));
#18923=EDGE_LOOP('',(#78327,#78328,#78329,#78330));
#18924=EDGE_LOOP('',(#78331,#78332,#78333,#78334));
#18925=EDGE_LOOP('',(#78335,#78336,#78337,#78338));
#18926=EDGE_LOOP('',(#78339,#78340,#78341,#78342));
#18927=EDGE_LOOP('',(#78343,#78344,#78345,#78346));
#18928=EDGE_LOOP('',(#78347,#78348,#78349,#78350));
#18929=EDGE_LOOP('',(#78351,#78352,#78353,#78354));
#18930=EDGE_LOOP('',(#78355,#78356,#78357,#78358));
#18931=EDGE_LOOP('',(#78359,#78360,#78361,#78362));
#18932=EDGE_LOOP('',(#78363,#78364,#78365,#78366));
#18933=EDGE_LOOP('',(#78367,#78368,#78369,#78370));
#18934=EDGE_LOOP('',(#78371,#78372,#78373,#78374));
#18935=EDGE_LOOP('',(#78375,#78376,#78377,#78378));
#18936=EDGE_LOOP('',(#78379,#78380,#78381,#78382));
#18937=EDGE_LOOP('',(#78383,#78384,#78385,#78386));
#18938=EDGE_LOOP('',(#78387,#78388,#78389,#78390));
#18939=EDGE_LOOP('',(#78391,#78392,#78393,#78394));
#18940=EDGE_LOOP('',(#78395,#78396,#78397,#78398));
#18941=EDGE_LOOP('',(#78399,#78400,#78401,#78402));
#18942=EDGE_LOOP('',(#78403,#78404,#78405,#78406));
#18943=EDGE_LOOP('',(#78407,#78408,#78409,#78410));
#18944=EDGE_LOOP('',(#78411,#78412,#78413,#78414));
#18945=EDGE_LOOP('',(#78415,#78416,#78417,#78418));
#18946=EDGE_LOOP('',(#78419,#78420,#78421,#78422));
#18947=EDGE_LOOP('',(#78423,#78424,#78425,#78426));
#18948=EDGE_LOOP('',(#78427,#78428,#78429,#78430));
#18949=EDGE_LOOP('',(#78431,#78432,#78433,#78434));
#18950=EDGE_LOOP('',(#78435,#78436,#78437,#78438));
#18951=EDGE_LOOP('',(#78439,#78440,#78441,#78442));
#18952=EDGE_LOOP('',(#78443,#78444,#78445,#78446));
#18953=EDGE_LOOP('',(#78447,#78448,#78449,#78450));
#18954=EDGE_LOOP('',(#78451,#78452,#78453,#78454));
#18955=EDGE_LOOP('',(#78455,#78456,#78457,#78458));
#18956=EDGE_LOOP('',(#78459,#78460,#78461,#78462));
#18957=EDGE_LOOP('',(#78463,#78464,#78465,#78466));
#18958=EDGE_LOOP('',(#78467,#78468,#78469,#78470));
#18959=EDGE_LOOP('',(#78471,#78472,#78473,#78474));
#18960=EDGE_LOOP('',(#78475,#78476,#78477,#78478));
#18961=EDGE_LOOP('',(#78479,#78480,#78481,#78482));
#18962=EDGE_LOOP('',(#78483,#78484,#78485,#78486));
#18963=EDGE_LOOP('',(#78487,#78488,#78489,#78490));
#18964=EDGE_LOOP('',(#78491,#78492,#78493,#78494));
#18965=EDGE_LOOP('',(#78495,#78496,#78497,#78498));
#18966=EDGE_LOOP('',(#78499,#78500,#78501,#78502));
#18967=EDGE_LOOP('',(#78503,#78504,#78505,#78506));
#18968=EDGE_LOOP('',(#78507,#78508,#78509,#78510));
#18969=EDGE_LOOP('',(#78511,#78512,#78513,#78514));
#18970=EDGE_LOOP('',(#78515,#78516,#78517,#78518));
#18971=EDGE_LOOP('',(#78519,#78520,#78521,#78522));
#18972=EDGE_LOOP('',(#78523,#78524,#78525,#78526));
#18973=EDGE_LOOP('',(#78527,#78528,#78529,#78530));
#18974=EDGE_LOOP('',(#78531,#78532,#78533,#78534));
#18975=EDGE_LOOP('',(#78535,#78536,#78537,#78538));
#18976=EDGE_LOOP('',(#78539,#78540,#78541,#78542));
#18977=EDGE_LOOP('',(#78543,#78544,#78545,#78546));
#18978=EDGE_LOOP('',(#78547,#78548,#78549,#78550));
#18979=EDGE_LOOP('',(#78551,#78552,#78553,#78554));
#18980=EDGE_LOOP('',(#78555,#78556,#78557,#78558));
#18981=EDGE_LOOP('',(#78559,#78560,#78561,#78562));
#18982=EDGE_LOOP('',(#78563,#78564,#78565,#78566));
#18983=EDGE_LOOP('',(#78567,#78568,#78569,#78570));
#18984=EDGE_LOOP('',(#78571,#78572,#78573,#78574));
#18985=EDGE_LOOP('',(#78575,#78576,#78577,#78578));
#18986=EDGE_LOOP('',(#78579,#78580,#78581,#78582));
#18987=EDGE_LOOP('',(#78583,#78584,#78585,#78586));
#18988=EDGE_LOOP('',(#78587,#78588,#78589,#78590));
#18989=EDGE_LOOP('',(#78591,#78592,#78593,#78594));
#18990=EDGE_LOOP('',(#78595,#78596,#78597,#78598));
#18991=EDGE_LOOP('',(#78599,#78600,#78601,#78602));
#18992=EDGE_LOOP('',(#78603,#78604,#78605,#78606));
#18993=EDGE_LOOP('',(#78607,#78608,#78609,#78610));
#18994=EDGE_LOOP('',(#78611,#78612,#78613,#78614));
#18995=EDGE_LOOP('',(#78615,#78616,#78617,#78618));
#18996=EDGE_LOOP('',(#78619,#78620,#78621,#78622));
#18997=EDGE_LOOP('',(#78623,#78624,#78625,#78626));
#18998=EDGE_LOOP('',(#78627,#78628,#78629,#78630));
#18999=EDGE_LOOP('',(#78631,#78632,#78633,#78634));
#19000=EDGE_LOOP('',(#78635,#78636,#78637,#78638));
#19001=EDGE_LOOP('',(#78639,#78640,#78641,#78642));
#19002=EDGE_LOOP('',(#78643,#78644,#78645,#78646));
#19003=EDGE_LOOP('',(#78647,#78648,#78649,#78650));
#19004=EDGE_LOOP('',(#78651,#78652,#78653,#78654));
#19005=EDGE_LOOP('',(#78655,#78656,#78657,#78658));
#19006=EDGE_LOOP('',(#78659,#78660,#78661,#78662));
#19007=EDGE_LOOP('',(#78663,#78664,#78665,#78666));
#19008=EDGE_LOOP('',(#78667,#78668,#78669,#78670));
#19009=EDGE_LOOP('',(#78671,#78672,#78673,#78674));
#19010=EDGE_LOOP('',(#78675,#78676,#78677,#78678));
#19011=EDGE_LOOP('',(#78679,#78680,#78681,#78682));
#19012=EDGE_LOOP('',(#78683,#78684,#78685,#78686));
#19013=EDGE_LOOP('',(#78687,#78688,#78689,#78690));
#19014=EDGE_LOOP('',(#78691,#78692,#78693,#78694));
#19015=EDGE_LOOP('',(#78695,#78696,#78697,#78698));
#19016=EDGE_LOOP('',(#78699,#78700,#78701,#78702));
#19017=EDGE_LOOP('',(#78703,#78704,#78705,#78706));
#19018=EDGE_LOOP('',(#78707,#78708,#78709,#78710));
#19019=EDGE_LOOP('',(#78711,#78712,#78713,#78714,#78715,#78716,#78717,#78718,
#78719,#78720,#78721,#78722,#78723,#78724,#78725,#78726,#78727,#78728,#78729,
#78730,#78731,#78732,#78733,#78734,#78735,#78736,#78737,#78738,#78739,#78740,
#78741,#78742,#78743,#78744,#78745,#78746,#78747,#78748,#78749,#78750,#78751,
#78752,#78753,#78754,#78755,#78756,#78757,#78758,#78759,#78760,#78761,#78762,
#78763,#78764,#78765,#78766,#78767,#78768,#78769,#78770,#78771,#78772,#78773,
#78774,#78775,#78776,#78777,#78778,#78779,#78780,#78781,#78782,#78783,#78784,
#78785,#78786,#78787,#78788,#78789,#78790,#78791,#78792,#78793,#78794));
#19020=EDGE_LOOP('',(#78795,#78796,#78797,#78798,#78799));
#19021=EDGE_LOOP('',(#78800,#78801,#78802,#78803,#78804));
#19022=EDGE_LOOP('',(#78805,#78806,#78807,#78808));
#19023=EDGE_LOOP('',(#78809,#78810,#78811,#78812));
#19024=EDGE_LOOP('',(#78813,#78814,#78815,#78816));
#19025=EDGE_LOOP('',(#78817,#78818,#78819,#78820,#78821));
#19026=EDGE_LOOP('',(#78822,#78823,#78824,#78825,#78826));
#19027=EDGE_LOOP('',(#78827,#78828,#78829,#78830,#78831));
#19028=EDGE_LOOP('',(#78832,#78833,#78834,#78835,#78836));
#19029=EDGE_LOOP('',(#78837,#78838,#78839,#78840,#78841));
#19030=EDGE_LOOP('',(#78842,#78843,#78844,#78845,#78846));
#19031=EDGE_LOOP('',(#78847,#78848,#78849,#78850,#78851));
#19032=EDGE_LOOP('',(#78852,#78853,#78854,#78855,#78856));
#19033=EDGE_LOOP('',(#78857,#78858,#78859,#78860,#78861));
#19034=EDGE_LOOP('',(#78862,#78863,#78864,#78865,#78866));
#19035=EDGE_LOOP('',(#78867,#78868,#78869,#78870));
#19036=EDGE_LOOP('',(#78871,#78872,#78873,#78874));
#19037=EDGE_LOOP('',(#78875,#78876,#78877,#78878));
#19038=EDGE_LOOP('',(#78879,#78880,#78881,#78882,#78883));
#19039=EDGE_LOOP('',(#78884,#78885,#78886,#78887,#78888));
#19040=EDGE_LOOP('',(#78889,#78890,#78891,#78892));
#19041=EDGE_LOOP('',(#78893,#78894,#78895,#78896));
#19042=EDGE_LOOP('',(#78897,#78898,#78899,#78900));
#19043=EDGE_LOOP('',(#78901,#78902,#78903,#78904,#78905));
#19044=EDGE_LOOP('',(#78906,#78907,#78908,#78909,#78910));
#19045=EDGE_LOOP('',(#78911,#78912,#78913,#78914));
#19046=EDGE_LOOP('',(#78915,#78916,#78917,#78918));
#19047=EDGE_LOOP('',(#78919,#78920,#78921,#78922));
#19048=EDGE_LOOP('',(#78923,#78924,#78925,#78926,#78927));
#19049=EDGE_LOOP('',(#78928,#78929,#78930,#78931,#78932));
#19050=EDGE_LOOP('',(#78933,#78934,#78935,#78936));
#19051=EDGE_LOOP('',(#78937,#78938,#78939,#78940));
#19052=EDGE_LOOP('',(#78941,#78942,#78943,#78944));
#19053=EDGE_LOOP('',(#78945,#78946,#78947,#78948,#78949));
#19054=EDGE_LOOP('',(#78950,#78951,#78952,#78953,#78954));
#19055=EDGE_LOOP('',(#78955,#78956,#78957,#78958));
#19056=EDGE_LOOP('',(#78959,#78960,#78961,#78962));
#19057=EDGE_LOOP('',(#78963,#78964,#78965,#78966));
#19058=EDGE_LOOP('',(#78967,#78968,#78969,#78970));
#19059=EDGE_LOOP('',(#78971,#78972,#78973,#78974));
#19060=EDGE_LOOP('',(#78975,#78976,#78977,#78978));
#19061=EDGE_LOOP('',(#78979,#78980,#78981,#78982,#78983));
#19062=EDGE_LOOP('',(#78984,#78985,#78986,#78987,#78988,#78989,#78990,#78991,
#78992,#78993,#78994,#78995,#78996,#78997,#78998,#78999,#79000,#79001,#79002,
#79003,#79004,#79005,#79006,#79007,#79008,#79009,#79010,#79011,#79012,#79013,
#79014,#79015,#79016,#79017,#79018,#79019,#79020,#79021,#79022,#79023,#79024,
#79025,#79026,#79027,#79028,#79029,#79030,#79031,#79032,#79033,#79034,#79035,
#79036,#79037,#79038,#79039,#79040,#79041,#79042,#79043,#79044,#79045,#79046,
#79047,#79048,#79049,#79050,#79051,#79052,#79053,#79054,#79055,#79056,#79057,
#79058,#79059,#79060,#79061,#79062,#79063,#79064,#79065,#79066,#79067,#79068,
#79069,#79070,#79071,#79072,#79073,#79074,#79075,#79076,#79077,#79078,#79079,
#79080,#79081,#79082,#79083,#79084,#79085,#79086,#79087,#79088,#79089));
#19063=EDGE_LOOP('',(#79090,#79091,#79092,#79093));
#19064=EDGE_LOOP('',(#79094,#79095,#79096,#79097,#79098));
#19065=EDGE_LOOP('',(#79099,#79100,#79101,#79102));
#19066=EDGE_LOOP('',(#79103,#79104,#79105,#79106));
#19067=EDGE_LOOP('',(#79107,#79108,#79109,#79110));
#19068=EDGE_LOOP('',(#79111,#79112,#79113,#79114));
#19069=EDGE_LOOP('',(#79115,#79116,#79117,#79118));
#19070=EDGE_LOOP('',(#79119,#79120,#79121,#79122));
#19071=EDGE_LOOP('',(#79123,#79124,#79125,#79126));
#19072=EDGE_LOOP('',(#79127,#79128,#79129,#79130));
#19073=EDGE_LOOP('',(#79131,#79132,#79133,#79134));
#19074=EDGE_LOOP('',(#79135,#79136,#79137,#79138));
#19075=EDGE_LOOP('',(#79139,#79140,#79141,#79142));
#19076=EDGE_LOOP('',(#79143,#79144,#79145,#79146));
#19077=EDGE_LOOP('',(#79147,#79148,#79149,#79150));
#19078=EDGE_LOOP('',(#79151,#79152,#79153,#79154));
#19079=EDGE_LOOP('',(#79155,#79156,#79157,#79158));
#19080=EDGE_LOOP('',(#79159,#79160,#79161,#79162));
#19081=EDGE_LOOP('',(#79163,#79164,#79165,#79166,#79167));
#19082=EDGE_LOOP('',(#79168,#79169,#79170,#79171));
#19083=EDGE_LOOP('',(#79172,#79173,#79174,#79175));
#19084=EDGE_LOOP('',(#79176,#79177,#79178,#79179));
#19085=EDGE_LOOP('',(#79180,#79181,#79182,#79183,#79184,#79185));
#19086=EDGE_LOOP('',(#79186,#79187,#79188,#79189));
#19087=EDGE_LOOP('',(#79190,#79191,#79192,#79193,#79194));
#19088=EDGE_LOOP('',(#79195,#79196,#79197,#79198));
#19089=EDGE_LOOP('',(#79199,#79200,#79201,#79202,#79203,#79204));
#19090=EDGE_LOOP('',(#79205,#79206,#79207,#79208,#79209,#79210));
#19091=EDGE_LOOP('',(#79211,#79212,#79213));
#19092=EDGE_LOOP('',(#79214,#79215,#79216));
#19093=EDGE_LOOP('',(#79217,#79218,#79219));
#19094=EDGE_LOOP('',(#79220,#79221,#79222));
#19095=EDGE_LOOP('',(#79223,#79224,#79225));
#19096=EDGE_LOOP('',(#79226,#79227,#79228));
#19097=EDGE_LOOP('',(#79229,#79230,#79231,#79232,#79233,#79234));
#19098=EDGE_LOOP('',(#79235,#79236,#79237));
#19099=EDGE_LOOP('',(#79238,#79239,#79240));
#19100=EDGE_LOOP('',(#79241,#79242,#79243));
#19101=EDGE_LOOP('',(#79244,#79245,#79246));
#19102=EDGE_LOOP('',(#79247,#79248,#79249));
#19103=EDGE_LOOP('',(#79250,#79251,#79252));
#19104=EDGE_LOOP('',(#79253,#79254,#79255,#79256,#79257,#79258));
#19105=EDGE_LOOP('',(#79259,#79260,#79261,#79262,#79263,#79264));
#19106=EDGE_LOOP('',(#79265,#79266,#79267,#79268,#79269,#79270));
#19107=EDGE_LOOP('',(#79271,#79272,#79273,#79274,#79275,#79276));
#19108=EDGE_LOOP('',(#79277,#79278,#79279,#79280,#79281,#79282));
#19109=EDGE_LOOP('',(#79283,#79284,#79285,#79286,#79287,#79288));
#19110=EDGE_LOOP('',(#79289,#79290,#79291,#79292,#79293,#79294));
#19111=EDGE_LOOP('',(#79295,#79296,#79297));
#19112=EDGE_LOOP('',(#79298,#79299,#79300));
#19113=EDGE_LOOP('',(#79301,#79302,#79303));
#19114=EDGE_LOOP('',(#79304,#79305,#79306));
#19115=EDGE_LOOP('',(#79307,#79308,#79309));
#19116=EDGE_LOOP('',(#79310,#79311,#79312));
#19117=EDGE_LOOP('',(#79313,#79314,#79315,#79316,#79317,#79318));
#19118=EDGE_LOOP('',(#79319,#79320,#79321));
#19119=EDGE_LOOP('',(#79322,#79323,#79324));
#19120=EDGE_LOOP('',(#79325,#79326,#79327));
#19121=EDGE_LOOP('',(#79328,#79329,#79330));
#19122=EDGE_LOOP('',(#79331,#79332,#79333));
#19123=EDGE_LOOP('',(#79334,#79335,#79336));
#19124=EDGE_LOOP('',(#79337,#79338,#79339,#79340,#79341,#79342));
#19125=EDGE_LOOP('',(#79343,#79344,#79345,#79346,#79347,#79348));
#19126=EDGE_LOOP('',(#79349,#79350,#79351,#79352,#79353,#79354));
#19127=EDGE_LOOP('',(#79355,#79356,#79357,#79358,#79359,#79360));
#19128=EDGE_LOOP('',(#79361,#79362,#79363,#79364,#79365,#79366));
#19129=EDGE_LOOP('',(#79367,#79368,#79369,#79370,#79371,#79372));
#19130=EDGE_LOOP('',(#79373,#79374,#79375,#79376));
#19131=EDGE_LOOP('',(#79377,#79378,#79379,#79380));
#19132=EDGE_LOOP('',(#79381,#79382,#79383,#79384));
#19133=EDGE_LOOP('',(#79385,#79386,#79387,#79388));
#19134=EDGE_LOOP('',(#79389,#79390,#79391,#79392));
#19135=EDGE_LOOP('',(#79393,#79394,#79395,#79396));
#19136=EDGE_LOOP('',(#79397,#79398,#79399,#79400,#79401,#79402,#79403,#79404));
#19137=EDGE_LOOP('',(#79405,#79406));
#19138=EDGE_LOOP('',(#79407,#79408));
#19139=EDGE_LOOP('',(#79409,#79410));
#19140=EDGE_LOOP('',(#79411,#79412));
#19141=EDGE_LOOP('',(#79413,#79414));
#19142=EDGE_LOOP('',(#79415,#79416));
#19143=EDGE_LOOP('',(#79417,#79418,#79419,#79420,#79421));
#19144=EDGE_LOOP('',(#79422));
#19145=EDGE_LOOP('',(#79423));
#19146=EDGE_LOOP('',(#79424,#79425,#79426,#79427,#79428,#79429));
#19147=EDGE_LOOP('',(#79430,#79431,#79432,#79433,#79434));
#19148=EDGE_LOOP('',(#79435,#79436,#79437));
#19149=EDGE_LOOP('',(#79438,#79439,#79440));
#19150=EDGE_LOOP('',(#79441,#79442,#79443,#79444));
#19151=EDGE_LOOP('',(#79445,#79446,#79447,#79448));
#19152=EDGE_LOOP('',(#79449,#79450,#79451));
#19153=EDGE_LOOP('',(#79452,#79453,#79454,#79455));
#19154=EDGE_LOOP('',(#79456,#79457,#79458));
#19155=EDGE_LOOP('',(#79459,#79460,#79461));
#19156=EDGE_LOOP('',(#79462,#79463,#79464));
#19157=EDGE_LOOP('',(#79465,#79466,#79467));
#19158=EDGE_LOOP('',(#79468,#79469,#79470,#79471));
#19159=EDGE_LOOP('',(#79472,#79473,#79474));
#19160=EDGE_LOOP('',(#79475,#79476,#79477,#79478));
#19161=EDGE_LOOP('',(#79479,#79480,#79481,#79482));
#19162=EDGE_LOOP('',(#79483,#79484,#79485,#79486));
#19163=EDGE_LOOP('',(#79487,#79488,#79489,#79490));
#19164=EDGE_LOOP('',(#79491,#79492,#79493,#79494));
#19165=EDGE_LOOP('',(#79495,#79496,#79497,#79498,#79499,#79500,#79501,#79502,
#79503,#79504));
#19166=EDGE_LOOP('',(#79505,#79506,#79507));
#19167=EDGE_LOOP('',(#79508,#79509,#79510));
#19168=EDGE_LOOP('',(#79511,#79512,#79513,#79514));
#19169=EDGE_LOOP('',(#79515,#79516,#79517,#79518));
#19170=EDGE_LOOP('',(#79519,#79520,#79521));
#19171=EDGE_LOOP('',(#79522,#79523,#79524,#79525));
#19172=EDGE_LOOP('',(#79526,#79527,#79528));
#19173=EDGE_LOOP('',(#79529,#79530,#79531));
#19174=EDGE_LOOP('',(#79532,#79533,#79534));
#19175=EDGE_LOOP('',(#79535,#79536,#79537));
#19176=EDGE_LOOP('',(#79538,#79539,#79540,#79541));
#19177=EDGE_LOOP('',(#79542,#79543,#79544));
#19178=EDGE_LOOP('',(#79545,#79546,#79547,#79548));
#19179=EDGE_LOOP('',(#79549,#79550,#79551,#79552));
#19180=EDGE_LOOP('',(#79553,#79554,#79555,#79556));
#19181=EDGE_LOOP('',(#79557,#79558,#79559,#79560));
#19182=EDGE_LOOP('',(#79561,#79562,#79563,#79564));
#19183=EDGE_LOOP('',(#79565,#79566,#79567,#79568));
#19184=EDGE_LOOP('',(#79569,#79570,#79571,#79572));
#19185=EDGE_LOOP('',(#79573,#79574,#79575,#79576,#79577,#79578,#79579,#79580,
#79581,#79582));
#19186=EDGE_LOOP('',(#79583,#79584,#79585,#79586));
#19187=EDGE_LOOP('',(#79587,#79588,#79589,#79590));
#19188=EDGE_LOOP('',(#79591,#79592,#79593,#79594));
#19189=EDGE_LOOP('',(#79595,#79596,#79597,#79598));
#19190=EDGE_LOOP('',(#79599,#79600,#79601,#79602));
#19191=EDGE_LOOP('',(#79603,#79604,#79605,#79606));
#19192=EDGE_LOOP('',(#79607,#79608,#79609,#79610));
#19193=EDGE_LOOP('',(#79611,#79612,#79613,#79614));
#19194=EDGE_LOOP('',(#79615,#79616,#79617,#79618));
#19195=EDGE_LOOP('',(#79619,#79620,#79621,#79622));
#19196=EDGE_LOOP('',(#79623,#79624,#79625,#79626,#79627,#79628,#79629,#79630));
#19197=EDGE_LOOP('',(#79631,#79632,#79633,#79634));
#19198=EDGE_LOOP('',(#79635,#79636,#79637,#79638));
#19199=EDGE_LOOP('',(#79639,#79640,#79641,#79642));
#19200=EDGE_LOOP('',(#79643,#79644,#79645,#79646));
#19201=EDGE_LOOP('',(#79647,#79648,#79649,#79650));
#19202=EDGE_LOOP('',(#79651,#79652,#79653,#79654));
#19203=EDGE_LOOP('',(#79655,#79656,#79657,#79658));
#19204=EDGE_LOOP('',(#79659,#79660,#79661,#79662));
#19205=EDGE_LOOP('',(#79663,#79664,#79665,#79666));
#19206=EDGE_LOOP('',(#79667,#79668,#79669,#79670,#79671,#79672,#79673,#79674,
#79675,#79676,#79677,#79678,#79679,#79680,#79681,#79682,#79683,#79684,#79685,
#79686,#79687,#79688,#79689,#79690,#79691,#79692,#79693,#79694,#79695,#79696,
#79697,#79698,#79699,#79700,#79701,#79702,#79703,#79704,#79705,#79706,#79707,
#79708,#79709,#79710,#79711,#79712,#79713,#79714,#79715,#79716,#79717,#79718));
#19207=EDGE_LOOP('',(#79719,#79720,#79721,#79722,#79723,#79724,#79725,#79726,
#79727,#79728,#79729,#79730,#79731,#79732,#79733,#79734));
#19208=EDGE_LOOP('',(#79735,#79736,#79737,#79738,#79739,#79740,#79741,#79742,
#79743,#79744,#79745,#79746,#79747,#79748));
#19209=EDGE_LOOP('',(#79749,#79750,#79751,#79752));
#19210=EDGE_LOOP('',(#79753,#79754,#79755,#79756));
#19211=EDGE_LOOP('',(#79757,#79758,#79759,#79760));
#19212=EDGE_LOOP('',(#79761,#79762,#79763,#79764));
#19213=EDGE_LOOP('',(#79765,#79766,#79767,#79768));
#19214=EDGE_LOOP('',(#79769,#79770,#79771,#79772));
#19215=EDGE_LOOP('',(#79773,#79774,#79775,#79776));
#19216=EDGE_LOOP('',(#79777,#79778,#79779,#79780));
#19217=EDGE_LOOP('',(#79781,#79782,#79783,#79784));
#19218=EDGE_LOOP('',(#79785,#79786,#79787,#79788));
#19219=EDGE_LOOP('',(#79789,#79790,#79791,#79792));
#19220=EDGE_LOOP('',(#79793,#79794,#79795,#79796));
#19221=EDGE_LOOP('',(#79797,#79798,#79799,#79800));
#19222=EDGE_LOOP('',(#79801,#79802,#79803,#79804));
#19223=EDGE_LOOP('',(#79805,#79806,#79807,#79808));
#19224=EDGE_LOOP('',(#79809,#79810,#79811,#79812));
#19225=EDGE_LOOP('',(#79813,#79814,#79815,#79816));
#19226=EDGE_LOOP('',(#79817,#79818,#79819,#79820));
#19227=EDGE_LOOP('',(#79821,#79822,#79823,#79824));
#19228=EDGE_LOOP('',(#79825,#79826,#79827,#79828));
#19229=EDGE_LOOP('',(#79829,#79830,#79831,#79832));
#19230=EDGE_LOOP('',(#79833,#79834,#79835,#79836));
#19231=EDGE_LOOP('',(#79837,#79838,#79839,#79840));
#19232=EDGE_LOOP('',(#79841,#79842,#79843,#79844));
#19233=EDGE_LOOP('',(#79845,#79846,#79847,#79848));
#19234=EDGE_LOOP('',(#79849,#79850,#79851,#79852));
#19235=EDGE_LOOP('',(#79853,#79854,#79855,#79856));
#19236=EDGE_LOOP('',(#79857,#79858,#79859,#79860));
#19237=EDGE_LOOP('',(#79861,#79862,#79863,#79864));
#19238=EDGE_LOOP('',(#79865,#79866,#79867,#79868));
#19239=EDGE_LOOP('',(#79869,#79870,#79871,#79872));
#19240=EDGE_LOOP('',(#79873,#79874,#79875,#79876));
#19241=EDGE_LOOP('',(#79877,#79878,#79879,#79880));
#19242=EDGE_LOOP('',(#79881,#79882,#79883,#79884));
#19243=EDGE_LOOP('',(#79885,#79886,#79887,#79888));
#19244=EDGE_LOOP('',(#79889,#79890,#79891,#79892));
#19245=EDGE_LOOP('',(#79893,#79894,#79895,#79896));
#19246=EDGE_LOOP('',(#79897,#79898,#79899,#79900));
#19247=EDGE_LOOP('',(#79901,#79902,#79903,#79904));
#19248=EDGE_LOOP('',(#79905,#79906,#79907,#79908));
#19249=EDGE_LOOP('',(#79909,#79910,#79911,#79912));
#19250=EDGE_LOOP('',(#79913,#79914,#79915,#79916,#79917,#79918));
#19251=EDGE_LOOP('',(#79919,#79920,#79921,#79922));
#19252=EDGE_LOOP('',(#79923,#79924,#79925,#79926));
#19253=EDGE_LOOP('',(#79927,#79928,#79929,#79930));
#19254=EDGE_LOOP('',(#79931,#79932,#79933,#79934));
#19255=EDGE_LOOP('',(#79935,#79936,#79937,#79938));
#19256=EDGE_LOOP('',(#79939,#79940,#79941,#79942));
#19257=EDGE_LOOP('',(#79943,#79944,#79945,#79946));
#19258=EDGE_LOOP('',(#79947,#79948,#79949,#79950));
#19259=EDGE_LOOP('',(#79951,#79952,#79953,#79954));
#19260=EDGE_LOOP('',(#79955,#79956,#79957,#79958));
#19261=EDGE_LOOP('',(#79959,#79960,#79961,#79962));
#19262=EDGE_LOOP('',(#79963,#79964,#79965,#79966));
#19263=EDGE_LOOP('',(#79967,#79968,#79969,#79970));
#19264=EDGE_LOOP('',(#79971,#79972,#79973,#79974));
#19265=EDGE_LOOP('',(#79975,#79976,#79977,#79978));
#19266=EDGE_LOOP('',(#79979,#79980,#79981,#79982));
#19267=EDGE_LOOP('',(#79983,#79984,#79985));
#19268=EDGE_LOOP('',(#79986,#79987,#79988,#79989));
#19269=EDGE_LOOP('',(#79990,#79991,#79992,#79993));
#19270=EDGE_LOOP('',(#79994,#79995,#79996,#79997));
#19271=EDGE_LOOP('',(#79998,#79999,#80000,#80001));
#19272=EDGE_LOOP('',(#80002,#80003,#80004,#80005));
#19273=EDGE_LOOP('',(#80006,#80007,#80008,#80009));
#19274=EDGE_LOOP('',(#80010,#80011,#80012,#80013));
#19275=EDGE_LOOP('',(#80014,#80015,#80016,#80017));
#19276=EDGE_LOOP('',(#80018,#80019,#80020,#80021));
#19277=EDGE_LOOP('',(#80022,#80023,#80024,#80025));
#19278=EDGE_LOOP('',(#80026,#80027,#80028,#80029));
#19279=EDGE_LOOP('',(#80030,#80031,#80032,#80033));
#19280=EDGE_LOOP('',(#80034,#80035,#80036,#80037));
#19281=EDGE_LOOP('',(#80038,#80039,#80040,#80041));
#19282=EDGE_LOOP('',(#80042,#80043,#80044,#80045));
#19283=EDGE_LOOP('',(#80046,#80047,#80048,#80049));
#19284=EDGE_LOOP('',(#80050,#80051,#80052,#80053));
#19285=EDGE_LOOP('',(#80054,#80055,#80056,#80057,#80058,#80059));
#19286=EDGE_LOOP('',(#80060,#80061,#80062,#80063));
#19287=EDGE_LOOP('',(#80064,#80065,#80066,#80067,#80068,#80069));
#19288=EDGE_LOOP('',(#80070,#80071,#80072,#80073));
#19289=EDGE_LOOP('',(#80074,#80075,#80076,#80077));
#19290=EDGE_LOOP('',(#80078,#80079,#80080,#80081));
#19291=EDGE_LOOP('',(#80082,#80083,#80084,#80085));
#19292=EDGE_LOOP('',(#80086,#80087,#80088,#80089));
#19293=EDGE_LOOP('',(#80090,#80091,#80092,#80093));
#19294=EDGE_LOOP('',(#80094,#80095,#80096,#80097));
#19295=EDGE_LOOP('',(#80098,#80099,#80100,#80101));
#19296=EDGE_LOOP('',(#80102,#80103,#80104,#80105));
#19297=EDGE_LOOP('',(#80106,#80107,#80108,#80109));
#19298=EDGE_LOOP('',(#80110,#80111,#80112,#80113));
#19299=EDGE_LOOP('',(#80114,#80115,#80116,#80117));
#19300=EDGE_LOOP('',(#80118,#80119,#80120,#80121));
#19301=EDGE_LOOP('',(#80122,#80123,#80124,#80125));
#19302=EDGE_LOOP('',(#80126,#80127,#80128,#80129));
#19303=EDGE_LOOP('',(#80130,#80131,#80132,#80133));
#19304=EDGE_LOOP('',(#80134,#80135,#80136));
#19305=EDGE_LOOP('',(#80137,#80138,#80139));
#19306=EDGE_LOOP('',(#80140,#80141,#80142,#80143));
#19307=EDGE_LOOP('',(#80144,#80145,#80146,#80147));
#19308=EDGE_LOOP('',(#80148,#80149,#80150,#80151));
#19309=EDGE_LOOP('',(#80152,#80153,#80154,#80155));
#19310=EDGE_LOOP('',(#80156,#80157,#80158,#80159));
#19311=EDGE_LOOP('',(#80160,#80161,#80162,#80163));
#19312=EDGE_LOOP('',(#80164,#80165,#80166,#80167));
#19313=EDGE_LOOP('',(#80168,#80169,#80170,#80171));
#19314=EDGE_LOOP('',(#80172,#80173,#80174,#80175));
#19315=EDGE_LOOP('',(#80176,#80177,#80178,#80179));
#19316=EDGE_LOOP('',(#80180,#80181,#80182,#80183));
#19317=EDGE_LOOP('',(#80184,#80185,#80186,#80187));
#19318=EDGE_LOOP('',(#80188,#80189,#80190,#80191));
#19319=EDGE_LOOP('',(#80192,#80193,#80194,#80195));
#19320=EDGE_LOOP('',(#80196,#80197,#80198,#80199));
#19321=EDGE_LOOP('',(#80200,#80201,#80202,#80203));
#19322=EDGE_LOOP('',(#80204,#80205,#80206,#80207));
#19323=EDGE_LOOP('',(#80208,#80209,#80210,#80211));
#19324=EDGE_LOOP('',(#80212,#80213,#80214,#80215));
#19325=EDGE_LOOP('',(#80216,#80217,#80218,#80219,#80220,#80221));
#19326=EDGE_LOOP('',(#80222,#80223,#80224,#80225));
#19327=EDGE_LOOP('',(#80226,#80227,#80228,#80229));
#19328=EDGE_LOOP('',(#80230,#80231,#80232,#80233));
#19329=EDGE_LOOP('',(#80234,#80235,#80236,#80237));
#19330=EDGE_LOOP('',(#80238,#80239,#80240,#80241));
#19331=EDGE_LOOP('',(#80242,#80243,#80244,#80245));
#19332=EDGE_LOOP('',(#80246,#80247,#80248,#80249));
#19333=EDGE_LOOP('',(#80250,#80251,#80252,#80253));
#19334=EDGE_LOOP('',(#80254,#80255,#80256,#80257));
#19335=EDGE_LOOP('',(#80258,#80259,#80260,#80261));
#19336=EDGE_LOOP('',(#80262,#80263,#80264,#80265));
#19337=EDGE_LOOP('',(#80266,#80267,#80268,#80269));
#19338=EDGE_LOOP('',(#80270,#80271,#80272,#80273));
#19339=EDGE_LOOP('',(#80274,#80275,#80276,#80277));
#19340=EDGE_LOOP('',(#80278,#80279,#80280,#80281));
#19341=EDGE_LOOP('',(#80282,#80283,#80284,#80285));
#19342=EDGE_LOOP('',(#80286,#80287,#80288));
#19343=EDGE_LOOP('',(#80289,#80290,#80291,#80292));
#19344=EDGE_LOOP('',(#80293,#80294,#80295,#80296,#80297,#80298));
#19345=EDGE_LOOP('',(#80299,#80300,#80301,#80302));
#19346=EDGE_LOOP('',(#80303,#80304,#80305,#80306));
#19347=EDGE_LOOP('',(#80307,#80308,#80309,#80310));
#19348=EDGE_LOOP('',(#80311,#80312,#80313,#80314));
#19349=EDGE_LOOP('',(#80315,#80316,#80317,#80318));
#19350=EDGE_LOOP('',(#80319,#80320,#80321,#80322));
#19351=EDGE_LOOP('',(#80323,#80324,#80325,#80326));
#19352=EDGE_LOOP('',(#80327,#80328,#80329,#80330));
#19353=EDGE_LOOP('',(#80331,#80332,#80333,#80334));
#19354=EDGE_LOOP('',(#80335,#80336,#80337,#80338));
#19355=EDGE_LOOP('',(#80339,#80340,#80341,#80342));
#19356=EDGE_LOOP('',(#80343,#80344,#80345,#80346));
#19357=EDGE_LOOP('',(#80347,#80348,#80349,#80350));
#19358=EDGE_LOOP('',(#80351,#80352,#80353,#80354));
#19359=EDGE_LOOP('',(#80355,#80356,#80357,#80358));
#19360=EDGE_LOOP('',(#80359,#80360,#80361,#80362));
#19361=EDGE_LOOP('',(#80363,#80364,#80365));
#19362=EDGE_LOOP('',(#80366,#80367,#80368,#80369,#80370,#80371,#80372,#80373));
#19363=EDGE_LOOP('',(#80374,#80375,#80376,#80377,#80378,#80379));
#19364=EDGE_LOOP('',(#80380,#80381,#80382,#80383,#80384,#80385,#80386));
#19365=EDGE_LOOP('',(#80387,#80388,#80389,#80390));
#19366=EDGE_LOOP('',(#80391,#80392,#80393,#80394));
#19367=EDGE_LOOP('',(#80395,#80396,#80397,#80398));
#19368=EDGE_LOOP('',(#80399,#80400,#80401,#80402));
#19369=EDGE_LOOP('',(#80403,#80404,#80405,#80406,#80407,#80408,#80409,#80410));
#19370=EDGE_LOOP('',(#80411));
#19371=EDGE_LOOP('',(#80412));
#19372=EDGE_LOOP('',(#80413,#80414,#80415,#80416,#80417,#80418,#80419,#80420,
#80421,#80422,#80423,#80424,#80425,#80426));
#19373=EDGE_LOOP('',(#80427));
#19374=EDGE_LOOP('',(#80428));
#19375=EDGE_LOOP('',(#80429,#80430,#80431,#80432));
#19376=EDGE_LOOP('',(#80433,#80434,#80435,#80436));
#19377=EDGE_LOOP('',(#80437));
#19378=EDGE_LOOP('',(#80438));
#19379=EDGE_LOOP('',(#80439));
#19380=EDGE_LOOP('',(#80440,#80441,#80442,#80443));
#19381=EDGE_LOOP('',(#80444,#80445,#80446,#80447));
#19382=EDGE_LOOP('',(#80448));
#19383=EDGE_LOOP('',(#80449));
#19384=EDGE_LOOP('',(#80450));
#19385=EDGE_LOOP('',(#80451,#80452,#80453,#80454));
#19386=EDGE_LOOP('',(#80455,#80456,#80457,#80458,#80459,#80460));
#19387=EDGE_LOOP('',(#80461));
#19388=EDGE_LOOP('',(#80462));
#19389=EDGE_LOOP('',(#80463));
#19390=EDGE_LOOP('',(#80464,#80465,#80466,#80467));
#19391=EDGE_LOOP('',(#80468,#80469,#80470,#80471,#80472,#80473));
#19392=EDGE_LOOP('',(#80474));
#19393=EDGE_LOOP('',(#80475,#80476,#80477,#80478,#80479));
#19394=EDGE_LOOP('',(#80480,#80481,#80482,#80483,#80484));
#19395=EDGE_LOOP('',(#80485,#80486,#80487,#80488,#80489,#80490));
#19396=EDGE_LOOP('',(#80491,#80492,#80493,#80494));
#19397=EDGE_LOOP('',(#80495,#80496,#80497,#80498));
#19398=EDGE_LOOP('',(#80499,#80500,#80501,#80502));
#19399=EDGE_LOOP('',(#80503,#80504,#80505,#80506));
#19400=EDGE_LOOP('',(#80507,#80508,#80509,#80510));
#19401=EDGE_LOOP('',(#80511,#80512,#80513,#80514));
#19402=EDGE_LOOP('',(#80515,#80516,#80517,#80518,#80519,#80520,#80521,#80522));
#19403=EDGE_LOOP('',(#80523,#80524));
#19404=EDGE_LOOP('',(#80525,#80526));
#19405=EDGE_LOOP('',(#80527,#80528));
#19406=EDGE_LOOP('',(#80529,#80530));
#19407=EDGE_LOOP('',(#80531,#80532));
#19408=EDGE_LOOP('',(#80533,#80534));
#19409=EDGE_LOOP('',(#80535,#80536,#80537,#80538,#80539,#80540));
#19410=EDGE_LOOP('',(#80541));
#19411=EDGE_LOOP('',(#80542,#80543,#80544,#80545,#80546,#80547));
#19412=EDGE_LOOP('',(#80548,#80549,#80550,#80551,#80552,#80553,#80554));
#19413=EDGE_LOOP('',(#80555,#80556));
#19414=EDGE_LOOP('',(#80557,#80558));
#19415=EDGE_LOOP('',(#80559,#80560));
#19416=EDGE_LOOP('',(#80561,#80562));
#19417=EDGE_LOOP('',(#80563,#80564,#80565));
#19418=EDGE_LOOP('',(#80566,#80567,#80568,#80569,#80570,#80571));
#19419=EDGE_LOOP('',(#80572,#80573,#80574,#80575));
#19420=EDGE_LOOP('',(#80576,#80577,#80578,#80579));
#19421=EDGE_LOOP('',(#80580,#80581,#80582,#80583));
#19422=EDGE_LOOP('',(#80584,#80585,#80586,#80587,#80588));
#19423=EDGE_LOOP('',(#80589,#80590,#80591));
#19424=EDGE_LOOP('',(#80592,#80593,#80594,#80595));
#19425=EDGE_LOOP('',(#80596,#80597,#80598));
#19426=EDGE_LOOP('',(#80599,#80600,#80601));
#19427=EDGE_LOOP('',(#80602,#80603,#80604,#80605));
#19428=EDGE_LOOP('',(#80606,#80607,#80608));
#19429=EDGE_LOOP('',(#80609,#80610,#80611,#80612,#80613));
#19430=EDGE_LOOP('',(#80614,#80615,#80616,#80617,#80618));
#19431=EDGE_LOOP('',(#80619,#80620,#80621,#80622,#80623));
#19432=EDGE_LOOP('',(#80624,#80625,#80626,#80627,#80628,#80629));
#19433=EDGE_LOOP('',(#80630,#80631,#80632,#80633,#80634,#80635));
#19434=EDGE_LOOP('',(#80636,#80637,#80638,#80639));
#19435=EDGE_LOOP('',(#80640,#80641,#80642,#80643,#80644));
#19436=EDGE_LOOP('',(#80645,#80646,#80647,#80648));
#19437=EDGE_LOOP('',(#80649,#80650,#80651,#80652));
#19438=EDGE_LOOP('',(#80653,#80654,#80655));
#19439=EDGE_LOOP('',(#80656,#80657,#80658,#80659));
#19440=EDGE_LOOP('',(#80660,#80661,#80662,#80663));
#19441=EDGE_LOOP('',(#80664,#80665,#80666,#80667));
#19442=EDGE_LOOP('',(#80668,#80669,#80670,#80671));
#19443=EDGE_LOOP('',(#80672,#80673,#80674));
#19444=EDGE_LOOP('',(#80675,#80676,#80677,#80678));
#19445=EDGE_LOOP('',(#80679,#80680,#80681,#80682));
#19446=EDGE_LOOP('',(#80683,#80684,#80685,#80686));
#19447=EDGE_LOOP('',(#80687,#80688,#80689,#80690));
#19448=EDGE_LOOP('',(#80691,#80692,#80693,#80694,#80695,#80696,#80697,#80698));
#19449=EDGE_LOOP('',(#80699,#80700,#80701,#80702,#80703));
#19450=EDGE_LOOP('',(#80704,#80705,#80706,#80707,#80708,#80709));
#19451=EDGE_LOOP('',(#80710,#80711,#80712,#80713,#80714,#80715,#80716,#80717,
#80718,#80719,#80720,#80721,#80722));
#19452=EDGE_LOOP('',(#80723,#80724,#80725,#80726));
#19453=EDGE_LOOP('',(#80727,#80728,#80729,#80730));
#19454=EDGE_LOOP('',(#80731,#80732,#80733,#80734));
#19455=EDGE_LOOP('',(#80735,#80736,#80737,#80738));
#19456=EDGE_LOOP('',(#80739,#80740,#80741,#80742));
#19457=EDGE_LOOP('',(#80743,#80744,#80745,#80746));
#19458=EDGE_LOOP('',(#80747,#80748,#80749,#80750));
#19459=EDGE_LOOP('',(#80751,#80752,#80753,#80754));
#19460=EDGE_LOOP('',(#80755,#80756,#80757,#80758));
#19461=EDGE_LOOP('',(#80759,#80760,#80761,#80762));
#19462=EDGE_LOOP('',(#80763,#80764,#80765,#80766));
#19463=EDGE_LOOP('',(#80767,#80768,#80769,#80770));
#19464=EDGE_LOOP('',(#80771,#80772,#80773,#80774));
#19465=EDGE_LOOP('',(#80775,#80776,#80777,#80778));
#19466=EDGE_LOOP('',(#80779,#80780,#80781,#80782,#80783));
#19467=EDGE_LOOP('',(#80784,#80785,#80786,#80787));
#19468=EDGE_LOOP('',(#80788,#80789,#80790,#80791));
#19469=EDGE_LOOP('',(#80792,#80793,#80794,#80795));
#19470=EDGE_LOOP('',(#80796,#80797,#80798,#80799));
#19471=EDGE_LOOP('',(#80800,#80801,#80802,#80803));
#19472=EDGE_LOOP('',(#80804,#80805,#80806,#80807));
#19473=EDGE_LOOP('',(#80808,#80809,#80810,#80811));
#19474=EDGE_LOOP('',(#80812,#80813,#80814,#80815));
#19475=EDGE_LOOP('',(#80816,#80817,#80818,#80819));
#19476=EDGE_LOOP('',(#80820,#80821,#80822,#80823));
#19477=EDGE_LOOP('',(#80824,#80825,#80826,#80827));
#19478=EDGE_LOOP('',(#80828,#80829,#80830,#80831));
#19479=EDGE_LOOP('',(#80832,#80833,#80834,#80835));
#19480=EDGE_LOOP('',(#80836,#80837,#80838,#80839));
#19481=EDGE_LOOP('',(#80840,#80841,#80842,#80843));
#19482=EDGE_LOOP('',(#80844,#80845,#80846,#80847));
#19483=EDGE_LOOP('',(#80848,#80849,#80850,#80851));
#19484=EDGE_LOOP('',(#80852,#80853,#80854,#80855));
#19485=EDGE_LOOP('',(#80856,#80857,#80858,#80859));
#19486=EDGE_LOOP('',(#80860,#80861,#80862,#80863));
#19487=EDGE_LOOP('',(#80864,#80865,#80866,#80867));
#19488=EDGE_LOOP('',(#80868,#80869,#80870,#80871));
#19489=EDGE_LOOP('',(#80872,#80873,#80874,#80875));
#19490=EDGE_LOOP('',(#80876,#80877,#80878,#80879));
#19491=EDGE_LOOP('',(#80880,#80881,#80882,#80883));
#19492=EDGE_LOOP('',(#80884,#80885,#80886,#80887));
#19493=EDGE_LOOP('',(#80888,#80889,#80890,#80891));
#19494=EDGE_LOOP('',(#80892,#80893,#80894,#80895));
#19495=EDGE_LOOP('',(#80896,#80897,#80898,#80899));
#19496=EDGE_LOOP('',(#80900,#80901,#80902,#80903));
#19497=EDGE_LOOP('',(#80904,#80905,#80906,#80907));
#19498=EDGE_LOOP('',(#80908,#80909,#80910,#80911));
#19499=EDGE_LOOP('',(#80912,#80913,#80914,#80915));
#19500=EDGE_LOOP('',(#80916,#80917,#80918,#80919));
#19501=EDGE_LOOP('',(#80920,#80921,#80922,#80923));
#19502=EDGE_LOOP('',(#80924,#80925,#80926,#80927));
#19503=EDGE_LOOP('',(#80928,#80929,#80930,#80931));
#19504=EDGE_LOOP('',(#80932,#80933,#80934,#80935));
#19505=EDGE_LOOP('',(#80936,#80937,#80938,#80939));
#19506=EDGE_LOOP('',(#80940,#80941,#80942,#80943));
#19507=EDGE_LOOP('',(#80944,#80945,#80946,#80947));
#19508=EDGE_LOOP('',(#80948,#80949,#80950,#80951));
#19509=EDGE_LOOP('',(#80952,#80953,#80954,#80955));
#19510=EDGE_LOOP('',(#80956,#80957,#80958,#80959));
#19511=EDGE_LOOP('',(#80960,#80961,#80962,#80963));
#19512=EDGE_LOOP('',(#80964,#80965,#80966,#80967));
#19513=EDGE_LOOP('',(#80968,#80969,#80970,#80971));
#19514=EDGE_LOOP('',(#80972,#80973,#80974,#80975,#80976));
#19515=EDGE_LOOP('',(#80977,#80978,#80979,#80980,#80981,#80982));
#19516=EDGE_LOOP('',(#80983,#80984,#80985,#80986));
#19517=EDGE_LOOP('',(#80987,#80988));
#19518=EDGE_LOOP('',(#80989,#80990));
#19519=EDGE_LOOP('',(#80991,#80992,#80993,#80994));
#19520=EDGE_LOOP('',(#80995,#80996));
#19521=EDGE_LOOP('',(#80997,#80998,#80999));
#19522=EDGE_LOOP('',(#81000,#81001,#81002,#81003,#81004));
#19523=EDGE_LOOP('',(#81005,#81006,#81007,#81008,#81009,#81010,#81011,#81012,
#81013,#81014));
#19524=EDGE_LOOP('',(#81015,#81016,#81017,#81018));
#19525=EDGE_LOOP('',(#81019,#81020));
#19526=EDGE_LOOP('',(#81021,#81022,#81023,#81024,#81025,#81026,#81027,#81028,
#81029,#81030,#81031,#81032,#81033,#81034,#81035,#81036,#81037,#81038,#81039,
#81040,#81041,#81042,#81043,#81044,#81045,#81046,#81047,#81048,#81049,#81050,
#81051,#81052,#81053,#81054,#81055,#81056,#81057,#81058,#81059,#81060,#81061,
#81062,#81063,#81064));
#19527=EDGE_LOOP('',(#81065,#81066,#81067,#81068));
#19528=EDGE_LOOP('',(#81069,#81070,#81071,#81072,#81073,#81074,#81075,#81076,
#81077,#81078,#81079,#81080,#81081,#81082,#81083,#81084,#81085,#81086,#81087,
#81088,#81089,#81090,#81091,#81092,#81093,#81094,#81095,#81096,#81097,#81098,
#81099,#81100,#81101,#81102,#81103,#81104,#81105,#81106,#81107,#81108,#81109));
#19529=EDGE_LOOP('',(#81110,#81111));
#19530=EDGE_LOOP('',(#81112,#81113));
#19531=EDGE_LOOP('',(#81114,#81115,#81116,#81117));
#19532=EDGE_LOOP('',(#81118,#81119,#81120));
#19533=EDGE_LOOP('',(#81121,#81122,#81123,#81124,#81125,#81126,#81127,#81128));
#19534=EDGE_LOOP('',(#81129,#81130,#81131,#81132));
#19535=EDGE_LOOP('',(#81133,#81134));
#19536=EDGE_LOOP('',(#81135,#81136,#81137,#81138,#81139,#81140,#81141,#81142,
#81143,#81144,#81145,#81146,#81147,#81148,#81149,#81150,#81151,#81152,#81153,
#81154,#81155,#81156,#81157,#81158,#81159,#81160,#81161,#81162,#81163,#81164,
#81165,#81166,#81167,#81168,#81169,#81170,#81171,#81172,#81173,#81174,#81175,
#81176,#81177,#81178));
#19537=EDGE_LOOP('',(#81179,#81180,#81181,#81182,#81183));
#19538=EDGE_LOOP('',(#81184,#81185,#81186,#81187,#81188,#81189,#81190,#81191,
#81192,#81193,#81194,#81195,#81196,#81197,#81198,#81199,#81200,#81201,#81202,
#81203,#81204,#81205,#81206,#81207,#81208,#81209,#81210,#81211,#81212,#81213,
#81214,#81215,#81216,#81217,#81218,#81219,#81220,#81221,#81222,#81223));
#19539=EDGE_LOOP('',(#81224,#81225,#81226,#81227));
#19540=EDGE_LOOP('',(#81228,#81229,#81230,#81231,#81232,#81233));
#19541=EDGE_LOOP('',(#81234,#81235));
#19542=EDGE_LOOP('',(#81236,#81237,#81238,#81239));
#19543=EDGE_LOOP('',(#81240,#81241,#81242));
#19544=EDGE_LOOP('',(#81243,#81244,#81245,#81246,#81247,#81248,#81249,#81250));
#19545=EDGE_LOOP('',(#81251,#81252,#81253,#81254));
#19546=EDGE_LOOP('',(#81255,#81256));
#19547=EDGE_LOOP('',(#81257,#81258,#81259,#81260,#81261,#81262,#81263,#81264,
#81265,#81266,#81267,#81268,#81269,#81270,#81271,#81272,#81273,#81274,#81275,
#81276,#81277,#81278,#81279,#81280,#81281,#81282,#81283,#81284,#81285,#81286,
#81287,#81288,#81289,#81290,#81291,#81292,#81293,#81294,#81295,#81296,#81297,
#81298,#81299));
#19548=EDGE_LOOP('',(#81300,#81301,#81302,#81303,#81304));
#19549=EDGE_LOOP('',(#81305,#81306,#81307,#81308,#81309,#81310,#81311,#81312,
#81313,#81314,#81315,#81316,#81317,#81318,#81319,#81320,#81321,#81322,#81323,
#81324,#81325,#81326,#81327,#81328,#81329,#81330,#81331,#81332,#81333,#81334,
#81335,#81336,#81337,#81338,#81339,#81340,#81341,#81342,#81343,#81344));
#19550=EDGE_LOOP('',(#81345,#81346,#81347,#81348));
#19551=EDGE_LOOP('',(#81349,#81350,#81351,#81352));
#19552=EDGE_LOOP('',(#81353,#81354));
#19553=EDGE_LOOP('',(#81355,#81356,#81357));
#19554=EDGE_LOOP('',(#81358,#81359,#81360,#81361,#81362));
#19555=EDGE_LOOP('',(#81363,#81364,#81365,#81366,#81367,#81368,#81369,#81370,
#81371,#81372));
#19556=EDGE_LOOP('',(#81373,#81374,#81375,#81376,#81377,#81378,#81379,#81380,
#81381,#81382,#81383,#81384,#81385,#81386,#81387,#81388,#81389,#81390,#81391,
#81392,#81393,#81394,#81395,#81396,#81397,#81398,#81399,#81400,#81401,#81402,
#81403,#81404));
#19557=EDGE_LOOP('',(#81405,#81406,#81407,#81408));
#19558=EDGE_LOOP('',(#81409,#81410,#81411,#81412));
#19559=EDGE_LOOP('',(#81413,#81414,#81415,#81416));
#19560=EDGE_LOOP('',(#81417,#81418,#81419,#81420));
#19561=EDGE_LOOP('',(#81421,#81422,#81423,#81424));
#19562=EDGE_LOOP('',(#81425,#81426));
#19563=EDGE_LOOP('',(#81427,#81428,#81429,#81430,#81431,#81432,#81433,#81434,
#81435,#81436,#81437,#81438,#81439,#81440,#81441,#81442,#81443,#81444,#81445,
#81446,#81447,#81448,#81449,#81450,#81451,#81452,#81453,#81454,#81455,#81456,
#81457,#81458,#81459,#81460,#81461,#81462,#81463,#81464,#81465,#81466,#81467,
#81468,#81469));
#19564=EDGE_LOOP('',(#81470,#81471,#81472));
#19565=EDGE_LOOP('',(#81473,#81474,#81475,#81476,#81477,#81478,#81479,#81480,
#81481,#81482,#81483,#81484,#81485,#81486,#81487,#81488,#81489,#81490,#81491,
#81492,#81493,#81494,#81495,#81496,#81497,#81498,#81499,#81500,#81501,#81502,
#81503,#81504,#81505,#81506,#81507,#81508,#81509,#81510,#81511,#81512,#81513));
#19566=EDGE_LOOP('',(#81514,#81515,#81516,#81517,#81518,#81519));
#19567=EDGE_LOOP('',(#81520,#81521,#81522,#81523,#81524,#81525));
#19568=EDGE_LOOP('',(#81526,#81527,#81528,#81529,#81530,#81531,#81532,#81533,
#81534,#81535,#81536,#81537,#81538,#81539,#81540,#81541,#81542,#81543,#81544,
#81545,#81546,#81547,#81548,#81549,#81550,#81551,#81552,#81553,#81554,#81555,
#81556,#81557,#81558,#81559,#81560,#81561,#81562,#81563));
#19569=EDGE_LOOP('',(#81564,#81565));
#19570=EDGE_LOOP('',(#81566,#81567));
#19571=EDGE_LOOP('',(#81568,#81569));
#19572=EDGE_LOOP('',(#81570,#81571));
#19573=EDGE_LOOP('',(#81572,#81573,#81574,#81575));
#19574=EDGE_LOOP('',(#81576,#81577,#81578,#81579,#81580,#81581));
#19575=EDGE_LOOP('',(#81582,#81583,#81584));
#19576=EDGE_LOOP('',(#81585,#81586,#81587,#81588,#81589));
#19577=EDGE_LOOP('',(#81590,#81591,#81592,#81593,#81594,#81595,#81596,#81597));
#19578=EDGE_LOOP('',(#81598,#81599,#81600));
#19579=EDGE_LOOP('',(#81601,#81602,#81603,#81604,#81605,#81606));
#19580=EDGE_LOOP('',(#81607,#81608,#81609,#81610,#81611,#81612));
#19581=EDGE_LOOP('',(#81613,#81614,#81615));
#19582=EDGE_LOOP('',(#81616,#81617,#81618,#81619,#81620,#81621));
#19583=EDGE_LOOP('',(#81622,#81623,#81624,#81625,#81626,#81627));
#19584=EDGE_LOOP('',(#81628,#81629,#81630));
#19585=EDGE_LOOP('',(#81631,#81632,#81633,#81634,#81635));
#19586=EDGE_LOOP('',(#81636,#81637,#81638,#81639));
#19587=EDGE_LOOP('',(#81640,#81641,#81642,#81643,#81644,#81645,#81646,#81647));
#19588=EDGE_LOOP('',(#81648,#81649,#81650,#81651));
#19589=EDGE_LOOP('',(#81652,#81653,#81654,#81655));
#19590=EDGE_LOOP('',(#81656,#81657,#81658,#81659));
#19591=EDGE_LOOP('',(#81660,#81661,#81662,#81663));
#19592=EDGE_LOOP('',(#81664,#81665,#81666,#81667));
#19593=EDGE_LOOP('',(#81668,#81669,#81670,#81671));
#19594=EDGE_LOOP('',(#81672,#81673,#81674));
#19595=EDGE_LOOP('',(#81675,#81676,#81677));
#19596=EDGE_LOOP('',(#81678,#81679,#81680,#81681));
#19597=EDGE_LOOP('',(#81682,#81683,#81684,#81685,#81686,#81687,#81688));
#19598=EDGE_LOOP('',(#81689,#81690,#81691,#81692));
#19599=EDGE_LOOP('',(#81693,#81694,#81695,#81696));
#19600=EDGE_LOOP('',(#81697,#81698,#81699,#81700));
#19601=EDGE_LOOP('',(#81701,#81702,#81703,#81704));
#19602=EDGE_LOOP('',(#81705,#81706,#81707,#81708));
#19603=EDGE_LOOP('',(#81709,#81710,#81711,#81712));
#19604=EDGE_LOOP('',(#81713,#81714,#81715,#81716));
#19605=EDGE_LOOP('',(#81717,#81718,#81719,#81720));
#19606=EDGE_LOOP('',(#81721,#81722,#81723,#81724));
#19607=EDGE_LOOP('',(#81725,#81726,#81727,#81728));
#19608=EDGE_LOOP('',(#81729,#81730,#81731,#81732,#81733,#81734,#81735,#81736));
#19609=EDGE_LOOP('',(#81737,#81738,#81739,#81740,#81741,#81742,#81743,#81744));
#19610=EDGE_LOOP('',(#81745,#81746,#81747,#81748,#81749,#81750,#81751,#81752));
#19611=EDGE_LOOP('',(#81753,#81754,#81755,#81756,#81757,#81758,#81759,#81760));
#19612=EDGE_LOOP('',(#81761,#81762,#81763,#81764,#81765,#81766,#81767,#81768));
#19613=EDGE_LOOP('',(#81769,#81770,#81771,#81772,#81773,#81774,#81775,#81776));
#19614=EDGE_LOOP('',(#81777,#81778,#81779,#81780));
#19615=EDGE_LOOP('',(#81781,#81782,#81783,#81784));
#19616=EDGE_LOOP('',(#81785,#81786,#81787,#81788,#81789,#81790,#81791,#81792,
#81793,#81794,#81795,#81796,#81797,#81798,#81799,#81800,#81801,#81802,#81803,
#81804,#81805,#81806,#81807,#81808,#81809,#81810,#81811,#81812,#81813,#81814));
#19617=EDGE_LOOP('',(#81815,#81816,#81817,#81818));
#19618=EDGE_LOOP('',(#81819));
#19619=EDGE_LOOP('',(#81820,#81821,#81822,#81823));
#19620=EDGE_LOOP('',(#81824,#81825,#81826,#81827,#81828,#81829));
#19621=EDGE_LOOP('',(#81830,#81831,#81832,#81833,#81834,#81835));
#19622=EDGE_LOOP('',(#81836,#81837,#81838,#81839,#81840,#81841));
#19623=EDGE_LOOP('',(#81842,#81843,#81844,#81845,#81846,#81847));
#19624=EDGE_LOOP('',(#81848,#81849,#81850,#81851,#81852,#81853));
#19625=EDGE_LOOP('',(#81854,#81855,#81856,#81857,#81858,#81859));
#19626=EDGE_LOOP('',(#81860,#81861,#81862,#81863,#81864,#81865));
#19627=EDGE_LOOP('',(#81866,#81867,#81868,#81869,#81870,#81871));
#19628=EDGE_LOOP('',(#81872,#81873,#81874,#81875,#81876,#81877));
#19629=EDGE_LOOP('',(#81878,#81879,#81880,#81881,#81882,#81883));
#19630=EDGE_LOOP('',(#81884,#81885,#81886,#81887,#81888,#81889));
#19631=EDGE_LOOP('',(#81890,#81891,#81892,#81893,#81894,#81895));
#19632=EDGE_LOOP('',(#81896,#81897,#81898,#81899,#81900,#81901));
#19633=EDGE_LOOP('',(#81902,#81903,#81904,#81905,#81906,#81907));
#19634=EDGE_LOOP('',(#81908,#81909,#81910,#81911));
#19635=EDGE_LOOP('',(#81912,#81913,#81914,#81915));
#19636=EDGE_LOOP('',(#81916,#81917,#81918,#81919));
#19637=EDGE_LOOP('',(#81920,#81921,#81922,#81923));
#19638=EDGE_LOOP('',(#81924,#81925,#81926,#81927));
#19639=EDGE_LOOP('',(#81928,#81929,#81930,#81931));
#19640=EDGE_LOOP('',(#81932,#81933,#81934,#81935));
#19641=EDGE_LOOP('',(#81936,#81937,#81938,#81939));
#19642=EDGE_LOOP('',(#81940,#81941,#81942,#81943));
#19643=EDGE_LOOP('',(#81944,#81945,#81946,#81947));
#19644=EDGE_LOOP('',(#81948,#81949,#81950,#81951));
#19645=EDGE_LOOP('',(#81952,#81953,#81954,#81955));
#19646=EDGE_LOOP('',(#81956,#81957,#81958,#81959));
#19647=EDGE_LOOP('',(#81960,#81961,#81962,#81963));
#19648=EDGE_LOOP('',(#81964,#81965,#81966,#81967,#81968,#81969));
#19649=EDGE_LOOP('',(#81970,#81971,#81972,#81973,#81974,#81975));
#19650=EDGE_LOOP('',(#81976,#81977,#81978,#81979,#81980,#81981));
#19651=EDGE_LOOP('',(#81982,#81983,#81984,#81985,#81986,#81987));
#19652=EDGE_LOOP('',(#81988,#81989,#81990,#81991,#81992,#81993));
#19653=EDGE_LOOP('',(#81994,#81995,#81996,#81997,#81998,#81999));
#19654=EDGE_LOOP('',(#82000,#82001,#82002,#82003,#82004,#82005));
#19655=EDGE_LOOP('',(#82006,#82007,#82008,#82009,#82010,#82011));
#19656=EDGE_LOOP('',(#82012,#82013,#82014,#82015,#82016,#82017));
#19657=EDGE_LOOP('',(#82018,#82019,#82020,#82021,#82022,#82023));
#19658=EDGE_LOOP('',(#82024,#82025,#82026,#82027,#82028,#82029));
#19659=EDGE_LOOP('',(#82030,#82031,#82032,#82033,#82034,#82035));
#19660=EDGE_LOOP('',(#82036,#82037,#82038,#82039,#82040,#82041));
#19661=EDGE_LOOP('',(#82042,#82043,#82044,#82045,#82046,#82047));
#19662=EDGE_LOOP('',(#82048,#82049,#82050,#82051,#82052,#82053));
#19663=EDGE_LOOP('',(#82054,#82055,#82056,#82057));
#19664=EDGE_LOOP('',(#82058,#82059,#82060,#82061,#82062,#82063));
#19665=EDGE_LOOP('',(#82064,#82065,#82066,#82067,#82068,#82069,#82070,#82071,
#82072,#82073,#82074,#82075,#82076,#82077,#82078,#82079,#82080,#82081,#82082,
#82083,#82084,#82085,#82086,#82087,#82088,#82089,#82090,#82091,#82092,#82093));
#19666=EDGE_LOOP('',(#82094));
#19667=EDGE_LOOP('',(#82095,#82096,#82097,#82098));
#19668=EDGE_LOOP('',(#82099,#82100,#82101,#82102));
#19669=EDGE_LOOP('',(#82103,#82104,#82105,#82106,#82107,#82108,#82109,#82110));
#19670=EDGE_LOOP('',(#82111,#82112,#82113,#82114));
#19671=EDGE_LOOP('',(#82115,#82116,#82117,#82118,#82119,#82120,#82121,#82122));
#19672=EDGE_LOOP('',(#82123,#82124,#82125,#82126));
#19673=EDGE_LOOP('',(#82127,#82128,#82129,#82130));
#19674=EDGE_LOOP('',(#82131,#82132,#82133,#82134));
#19675=EDGE_LOOP('',(#82135,#82136,#82137,#82138));
#19676=EDGE_LOOP('',(#82139,#82140,#82141,#82142));
#19677=EDGE_LOOP('',(#82143,#82144,#82145,#82146));
#19678=EDGE_LOOP('',(#82147,#82148,#82149,#82150));
#19679=EDGE_LOOP('',(#82151,#82152,#82153,#82154));
#19680=EDGE_LOOP('',(#82155,#82156,#82157,#82158));
#19681=EDGE_LOOP('',(#82159,#82160,#82161,#82162));
#19682=EDGE_LOOP('',(#82163,#82164,#82165,#82166,#82167,#82168,#82169,#82170));
#19683=EDGE_LOOP('',(#82171,#82172,#82173,#82174));
#19684=EDGE_LOOP('',(#82175,#82176,#82177,#82178));
#19685=EDGE_LOOP('',(#82179,#82180,#82181,#82182));
#19686=EDGE_LOOP('',(#82183,#82184,#82185,#82186));
#19687=EDGE_LOOP('',(#82187,#82188,#82189,#82190));
#19688=EDGE_LOOP('',(#82191,#82192,#82193,#82194));
#19689=EDGE_LOOP('',(#82195,#82196,#82197,#82198,#82199,#82200,#82201,#82202));
#19690=EDGE_LOOP('',(#82203,#82204,#82205,#82206));
#19691=EDGE_LOOP('',(#82207,#82208,#82209,#82210));
#19692=EDGE_LOOP('',(#82211,#82212,#82213,#82214,#82215,#82216,#82217,#82218));
#19693=EDGE_LOOP('',(#82219,#82220,#82221,#82222));
#19694=EDGE_LOOP('',(#82223,#82224,#82225,#82226,#82227,#82228,#82229,#82230));
#19695=EDGE_LOOP('',(#82231,#82232,#82233,#82234));
#19696=EDGE_LOOP('',(#82235,#82236,#82237,#82238));
#19697=EDGE_LOOP('',(#82239,#82240,#82241,#82242,#82243,#82244,#82245,#82246));
#19698=EDGE_LOOP('',(#82247,#82248,#82249,#82250));
#19699=EDGE_LOOP('',(#82251,#82252,#82253,#82254));
#19700=EDGE_LOOP('',(#82255,#82256,#82257,#82258,#82259,#82260,#82261,#82262));
#19701=EDGE_LOOP('',(#82263,#82264,#82265,#82266));
#19702=EDGE_LOOP('',(#82267,#82268,#82269,#82270));
#19703=EDGE_LOOP('',(#82271,#82272,#82273,#82274,#82275,#82276,#82277,#82278));
#19704=EDGE_LOOP('',(#82279,#82280,#82281,#82282));
#19705=EDGE_LOOP('',(#82283,#82284,#82285,#82286));
#19706=EDGE_LOOP('',(#82287,#82288,#82289,#82290));
#19707=EDGE_LOOP('',(#82291,#82292,#82293,#82294));
#19708=EDGE_LOOP('',(#82295,#82296,#82297,#82298));
#19709=EDGE_LOOP('',(#82299,#82300,#82301,#82302));
#19710=EDGE_LOOP('',(#82303,#82304,#82305,#82306));
#19711=EDGE_LOOP('',(#82307,#82308,#82309,#82310));
#19712=EDGE_LOOP('',(#82311,#82312,#82313,#82314));
#19713=EDGE_LOOP('',(#82315));
#19714=EDGE_LOOP('',(#82316,#82317,#82318,#82319));
#19715=EDGE_LOOP('',(#82320));
#19716=EDGE_LOOP('',(#82321,#82322,#82323,#82324));
#19717=EDGE_LOOP('',(#82325,#82326,#82327,#82328));
#19718=EDGE_LOOP('',(#82329,#82330,#82331,#82332));
#19719=EDGE_LOOP('',(#82333,#82334,#82335,#82336));
#19720=EDGE_LOOP('',(#82337,#82338,#82339,#82340,#82341,#82342,#82343,#82344));
#19721=EDGE_LOOP('',(#82345,#82346,#82347,#82348,#82349,#82350,#82351,#82352));
#19722=EDGE_LOOP('',(#82353,#82354,#82355,#82356,#82357,#82358,#82359,#82360));
#19723=EDGE_LOOP('',(#82361,#82362,#82363,#82364,#82365,#82366,#82367,#82368));
#19724=EDGE_LOOP('',(#82369,#82370,#82371,#82372,#82373,#82374,#82375,#82376));
#19725=EDGE_LOOP('',(#82377,#82378,#82379,#82380,#82381,#82382,#82383,#82384));
#19726=EDGE_LOOP('',(#82385,#82386,#82387,#82388,#82389,#82390,#82391,#82392));
#19727=EDGE_LOOP('',(#82393,#82394,#82395,#82396,#82397,#82398,#82399,#82400));
#19728=EDGE_LOOP('',(#82401,#82402,#82403,#82404,#82405,#82406,#82407,#82408));
#19729=EDGE_LOOP('',(#82409,#82410,#82411,#82412,#82413,#82414,#82415,#82416));
#19730=EDGE_LOOP('',(#82417,#82418,#82419,#82420,#82421,#82422,#82423,#82424));
#19731=EDGE_LOOP('',(#82425,#82426,#82427,#82428,#82429,#82430,#82431,#82432));
#19732=EDGE_LOOP('',(#82433,#82434,#82435,#82436,#82437,#82438));
#19733=EDGE_LOOP('',(#82439,#82440,#82441,#82442));
#19734=EDGE_LOOP('',(#82443,#82444,#82445,#82446,#82447,#82448));
#19735=EDGE_LOOP('',(#82449,#82450,#82451,#82452));
#19736=EDGE_LOOP('',(#82453,#82454,#82455,#82456,#82457,#82458,#82459,#82460,
#82461,#82462,#82463,#82464,#82465,#82466,#82467,#82468,#82469,#82470,#82471,
#82472,#82473,#82474,#82475,#82476,#82477,#82478,#82479,#82480,#82481,#82482,
#82483,#82484,#82485,#82486,#82487,#82488,#82489,#82490,#82491,#82492,#82493,
#82494,#82495,#82496,#82497,#82498,#82499,#82500,#82501,#82502,#82503,#82504,
#82505,#82506,#82507,#82508,#82509,#82510,#82511,#82512));
#19737=EDGE_LOOP('',(#82513,#82514,#82515,#82516));
#19738=EDGE_LOOP('',(#82517));
#19739=EDGE_LOOP('',(#82518,#82519,#82520,#82521));
#19740=EDGE_LOOP('',(#82522,#82523,#82524,#82525,#82526,#82527));
#19741=EDGE_LOOP('',(#82528,#82529,#82530,#82531,#82532,#82533));
#19742=EDGE_LOOP('',(#82534,#82535,#82536,#82537,#82538,#82539));
#19743=EDGE_LOOP('',(#82540,#82541,#82542,#82543,#82544,#82545));
#19744=EDGE_LOOP('',(#82546,#82547,#82548,#82549,#82550,#82551));
#19745=EDGE_LOOP('',(#82552,#82553,#82554,#82555,#82556,#82557));
#19746=EDGE_LOOP('',(#82558,#82559,#82560,#82561,#82562,#82563));
#19747=EDGE_LOOP('',(#82564,#82565,#82566,#82567,#82568,#82569));
#19748=EDGE_LOOP('',(#82570,#82571,#82572,#82573,#82574,#82575));
#19749=EDGE_LOOP('',(#82576,#82577,#82578,#82579,#82580,#82581));
#19750=EDGE_LOOP('',(#82582,#82583,#82584,#82585,#82586,#82587));
#19751=EDGE_LOOP('',(#82588,#82589,#82590,#82591,#82592,#82593));
#19752=EDGE_LOOP('',(#82594,#82595,#82596,#82597,#82598,#82599));
#19753=EDGE_LOOP('',(#82600,#82601,#82602,#82603,#82604,#82605));
#19754=EDGE_LOOP('',(#82606,#82607,#82608,#82609,#82610,#82611));
#19755=EDGE_LOOP('',(#82612,#82613,#82614,#82615,#82616,#82617));
#19756=EDGE_LOOP('',(#82618,#82619,#82620,#82621,#82622,#82623));
#19757=EDGE_LOOP('',(#82624,#82625,#82626,#82627,#82628,#82629));
#19758=EDGE_LOOP('',(#82630,#82631,#82632,#82633,#82634,#82635));
#19759=EDGE_LOOP('',(#82636,#82637,#82638,#82639,#82640,#82641));
#19760=EDGE_LOOP('',(#82642,#82643,#82644,#82645,#82646,#82647));
#19761=EDGE_LOOP('',(#82648,#82649,#82650,#82651,#82652,#82653));
#19762=EDGE_LOOP('',(#82654,#82655,#82656,#82657,#82658,#82659));
#19763=EDGE_LOOP('',(#82660,#82661,#82662,#82663,#82664,#82665));
#19764=EDGE_LOOP('',(#82666,#82667,#82668,#82669,#82670,#82671));
#19765=EDGE_LOOP('',(#82672,#82673,#82674,#82675,#82676,#82677));
#19766=EDGE_LOOP('',(#82678,#82679,#82680,#82681,#82682,#82683));
#19767=EDGE_LOOP('',(#82684,#82685,#82686,#82687,#82688,#82689));
#19768=EDGE_LOOP('',(#82690,#82691,#82692,#82693));
#19769=EDGE_LOOP('',(#82694,#82695,#82696,#82697));
#19770=EDGE_LOOP('',(#82698,#82699,#82700,#82701));
#19771=EDGE_LOOP('',(#82702,#82703,#82704,#82705));
#19772=EDGE_LOOP('',(#82706,#82707,#82708,#82709));
#19773=EDGE_LOOP('',(#82710,#82711,#82712,#82713));
#19774=EDGE_LOOP('',(#82714,#82715,#82716,#82717));
#19775=EDGE_LOOP('',(#82718,#82719,#82720,#82721));
#19776=EDGE_LOOP('',(#82722,#82723,#82724,#82725));
#19777=EDGE_LOOP('',(#82726,#82727,#82728,#82729));
#19778=EDGE_LOOP('',(#82730,#82731,#82732,#82733));
#19779=EDGE_LOOP('',(#82734,#82735,#82736,#82737));
#19780=EDGE_LOOP('',(#82738,#82739,#82740,#82741));
#19781=EDGE_LOOP('',(#82742,#82743,#82744,#82745));
#19782=EDGE_LOOP('',(#82746,#82747,#82748,#82749));
#19783=EDGE_LOOP('',(#82750,#82751,#82752,#82753));
#19784=EDGE_LOOP('',(#82754,#82755,#82756,#82757));
#19785=EDGE_LOOP('',(#82758,#82759,#82760,#82761));
#19786=EDGE_LOOP('',(#82762,#82763,#82764,#82765));
#19787=EDGE_LOOP('',(#82766,#82767,#82768,#82769));
#19788=EDGE_LOOP('',(#82770,#82771,#82772,#82773));
#19789=EDGE_LOOP('',(#82774,#82775,#82776,#82777));
#19790=EDGE_LOOP('',(#82778,#82779,#82780,#82781));
#19791=EDGE_LOOP('',(#82782,#82783,#82784,#82785));
#19792=EDGE_LOOP('',(#82786,#82787,#82788,#82789));
#19793=EDGE_LOOP('',(#82790,#82791,#82792,#82793));
#19794=EDGE_LOOP('',(#82794,#82795,#82796,#82797));
#19795=EDGE_LOOP('',(#82798,#82799,#82800,#82801));
#19796=EDGE_LOOP('',(#82802,#82803,#82804,#82805,#82806,#82807));
#19797=EDGE_LOOP('',(#82808,#82809,#82810,#82811,#82812,#82813));
#19798=EDGE_LOOP('',(#82814,#82815,#82816,#82817,#82818,#82819));
#19799=EDGE_LOOP('',(#82820,#82821,#82822,#82823,#82824,#82825));
#19800=EDGE_LOOP('',(#82826,#82827,#82828,#82829,#82830,#82831));
#19801=EDGE_LOOP('',(#82832,#82833,#82834,#82835,#82836,#82837));
#19802=EDGE_LOOP('',(#82838,#82839,#82840,#82841,#82842,#82843));
#19803=EDGE_LOOP('',(#82844,#82845,#82846,#82847,#82848,#82849));
#19804=EDGE_LOOP('',(#82850,#82851,#82852,#82853,#82854,#82855));
#19805=EDGE_LOOP('',(#82856,#82857,#82858,#82859,#82860,#82861));
#19806=EDGE_LOOP('',(#82862,#82863,#82864,#82865,#82866,#82867));
#19807=EDGE_LOOP('',(#82868,#82869,#82870,#82871,#82872,#82873));
#19808=EDGE_LOOP('',(#82874,#82875,#82876,#82877,#82878,#82879));
#19809=EDGE_LOOP('',(#82880,#82881,#82882,#82883,#82884,#82885));
#19810=EDGE_LOOP('',(#82886,#82887,#82888,#82889,#82890,#82891));
#19811=EDGE_LOOP('',(#82892,#82893,#82894,#82895,#82896,#82897));
#19812=EDGE_LOOP('',(#82898,#82899,#82900,#82901,#82902,#82903));
#19813=EDGE_LOOP('',(#82904,#82905,#82906,#82907,#82908,#82909));
#19814=EDGE_LOOP('',(#82910,#82911,#82912,#82913,#82914,#82915));
#19815=EDGE_LOOP('',(#82916,#82917,#82918,#82919,#82920,#82921));
#19816=EDGE_LOOP('',(#82922,#82923,#82924,#82925,#82926,#82927));
#19817=EDGE_LOOP('',(#82928,#82929,#82930,#82931,#82932,#82933));
#19818=EDGE_LOOP('',(#82934,#82935,#82936,#82937,#82938,#82939));
#19819=EDGE_LOOP('',(#82940,#82941,#82942,#82943,#82944,#82945));
#19820=EDGE_LOOP('',(#82946,#82947,#82948,#82949,#82950,#82951));
#19821=EDGE_LOOP('',(#82952,#82953,#82954,#82955,#82956,#82957));
#19822=EDGE_LOOP('',(#82958,#82959,#82960,#82961,#82962,#82963));
#19823=EDGE_LOOP('',(#82964,#82965,#82966,#82967,#82968,#82969));
#19824=EDGE_LOOP('',(#82970,#82971,#82972,#82973,#82974,#82975));
#19825=EDGE_LOOP('',(#82976,#82977,#82978,#82979));
#19826=EDGE_LOOP('',(#82980,#82981,#82982,#82983,#82984,#82985));
#19827=EDGE_LOOP('',(#82986,#82987,#82988,#82989,#82990,#82991,#82992,#82993,
#82994,#82995,#82996,#82997,#82998,#82999,#83000,#83001,#83002,#83003,#83004,
#83005,#83006,#83007,#83008,#83009,#83010,#83011,#83012,#83013,#83014,#83015,
#83016,#83017,#83018,#83019,#83020,#83021,#83022,#83023,#83024,#83025,#83026,
#83027,#83028,#83029,#83030,#83031,#83032,#83033,#83034,#83035,#83036,#83037,
#83038,#83039,#83040,#83041,#83042,#83043,#83044,#83045));
#19828=EDGE_LOOP('',(#83046));
#19829=EDGE_LOOP('',(#83047,#83048,#83049,#83050));
#19830=EDGE_LOOP('',(#83051,#83052,#83053,#83054));
#19831=EDGE_LOOP('',(#83055,#83056,#83057,#83058,#83059,#83060,#83061,#83062));
#19832=EDGE_LOOP('',(#83063,#83064,#83065,#83066));
#19833=EDGE_LOOP('',(#83067,#83068,#83069,#83070));
#19834=EDGE_LOOP('',(#83071,#83072,#83073,#83074,#83075,#83076,#83077,#83078));
#19835=EDGE_LOOP('',(#83079,#83080,#83081,#83082));
#19836=EDGE_LOOP('',(#83083,#83084,#83085,#83086));
#19837=EDGE_LOOP('',(#83087,#83088,#83089,#83090));
#19838=EDGE_LOOP('',(#83091,#83092,#83093,#83094));
#19839=EDGE_LOOP('',(#83095,#83096,#83097,#83098));
#19840=EDGE_LOOP('',(#83099,#83100,#83101,#83102));
#19841=EDGE_LOOP('',(#83103,#83104,#83105,#83106));
#19842=EDGE_LOOP('',(#83107,#83108,#83109,#83110));
#19843=EDGE_LOOP('',(#83111,#83112,#83113,#83114,#83115,#83116,#83117,#83118));
#19844=EDGE_LOOP('',(#83119,#83120,#83121,#83122));
#19845=EDGE_LOOP('',(#83123,#83124,#83125,#83126));
#19846=EDGE_LOOP('',(#83127,#83128,#83129,#83130));
#19847=EDGE_LOOP('',(#83131,#83132,#83133,#83134));
#19848=EDGE_LOOP('',(#83135,#83136,#83137,#83138));
#19849=EDGE_LOOP('',(#83139,#83140,#83141,#83142));
#19850=EDGE_LOOP('',(#83143,#83144,#83145,#83146));
#19851=EDGE_LOOP('',(#83147,#83148,#83149,#83150));
#19852=EDGE_LOOP('',(#83151,#83152,#83153,#83154,#83155,#83156,#83157,#83158));
#19853=EDGE_LOOP('',(#83159,#83160,#83161,#83162));
#19854=EDGE_LOOP('',(#83163,#83164,#83165,#83166));
#19855=EDGE_LOOP('',(#83167,#83168,#83169,#83170));
#19856=EDGE_LOOP('',(#83171,#83172,#83173,#83174));
#19857=EDGE_LOOP('',(#83175,#83176,#83177,#83178));
#19858=EDGE_LOOP('',(#83179,#83180,#83181,#83182));
#19859=EDGE_LOOP('',(#83183,#83184,#83185,#83186));
#19860=EDGE_LOOP('',(#83187,#83188,#83189,#83190));
#19861=EDGE_LOOP('',(#83191,#83192,#83193,#83194));
#19862=EDGE_LOOP('',(#83195,#83196,#83197,#83198));
#19863=EDGE_LOOP('',(#83199,#83200,#83201,#83202));
#19864=EDGE_LOOP('',(#83203,#83204,#83205,#83206));
#19865=EDGE_LOOP('',(#83207,#83208,#83209,#83210));
#19866=EDGE_LOOP('',(#83211,#83212,#83213,#83214));
#19867=EDGE_LOOP('',(#83215,#83216,#83217,#83218,#83219,#83220,#83221,#83222));
#19868=EDGE_LOOP('',(#83223,#83224,#83225,#83226));
#19869=EDGE_LOOP('',(#83227,#83228,#83229,#83230));
#19870=EDGE_LOOP('',(#83231,#83232,#83233,#83234,#83235,#83236,#83237,#83238));
#19871=EDGE_LOOP('',(#83239,#83240,#83241,#83242));
#19872=EDGE_LOOP('',(#83243,#83244,#83245,#83246));
#19873=EDGE_LOOP('',(#83247,#83248,#83249,#83250,#83251,#83252,#83253,#83254));
#19874=EDGE_LOOP('',(#83255,#83256,#83257,#83258));
#19875=EDGE_LOOP('',(#83259,#83260,#83261,#83262,#83263,#83264,#83265,#83266));
#19876=EDGE_LOOP('',(#83267,#83268,#83269,#83270));
#19877=EDGE_LOOP('',(#83271,#83272,#83273,#83274));
#19878=EDGE_LOOP('',(#83275,#83276,#83277,#83278,#83279,#83280,#83281,#83282));
#19879=EDGE_LOOP('',(#83283,#83284,#83285,#83286));
#19880=EDGE_LOOP('',(#83287,#83288,#83289,#83290));
#19881=EDGE_LOOP('',(#83291,#83292,#83293,#83294,#83295,#83296,#83297,#83298));
#19882=EDGE_LOOP('',(#83299,#83300,#83301,#83302));
#19883=EDGE_LOOP('',(#83303,#83304,#83305,#83306));
#19884=EDGE_LOOP('',(#83307,#83308,#83309,#83310,#83311,#83312,#83313,#83314));
#19885=EDGE_LOOP('',(#83315,#83316,#83317,#83318));
#19886=EDGE_LOOP('',(#83319,#83320,#83321,#83322));
#19887=EDGE_LOOP('',(#83323,#83324,#83325,#83326,#83327,#83328,#83329,#83330));
#19888=EDGE_LOOP('',(#83331,#83332,#83333,#83334));
#19889=EDGE_LOOP('',(#83335,#83336,#83337,#83338));
#19890=EDGE_LOOP('',(#83339,#83340,#83341,#83342,#83343,#83344,#83345,#83346));
#19891=EDGE_LOOP('',(#83347,#83348,#83349,#83350));
#19892=EDGE_LOOP('',(#83351,#83352,#83353,#83354,#83355,#83356,#83357,#83358));
#19893=EDGE_LOOP('',(#83359,#83360,#83361,#83362));
#19894=EDGE_LOOP('',(#83363,#83364,#83365,#83366));
#19895=EDGE_LOOP('',(#83367,#83368,#83369,#83370,#83371,#83372,#83373,#83374));
#19896=EDGE_LOOP('',(#83375,#83376,#83377,#83378));
#19897=EDGE_LOOP('',(#83379,#83380,#83381,#83382));
#19898=EDGE_LOOP('',(#83383,#83384,#83385,#83386,#83387,#83388,#83389,#83390));
#19899=EDGE_LOOP('',(#83391,#83392,#83393,#83394));
#19900=EDGE_LOOP('',(#83395,#83396,#83397,#83398));
#19901=EDGE_LOOP('',(#83399,#83400,#83401,#83402,#83403,#83404,#83405,#83406));
#19902=EDGE_LOOP('',(#83407,#83408,#83409,#83410));
#19903=EDGE_LOOP('',(#83411,#83412,#83413,#83414));
#19904=EDGE_LOOP('',(#83415,#83416,#83417,#83418,#83419,#83420,#83421,#83422));
#19905=EDGE_LOOP('',(#83423,#83424,#83425,#83426));
#19906=EDGE_LOOP('',(#83427,#83428,#83429,#83430));
#19907=EDGE_LOOP('',(#83431,#83432,#83433,#83434));
#19908=EDGE_LOOP('',(#83435,#83436,#83437,#83438));
#19909=EDGE_LOOP('',(#83439,#83440,#83441,#83442));
#19910=EDGE_LOOP('',(#83443,#83444,#83445,#83446));
#19911=EDGE_LOOP('',(#83447,#83448,#83449,#83450));
#19912=EDGE_LOOP('',(#83451,#83452,#83453,#83454));
#19913=EDGE_LOOP('',(#83455,#83456,#83457,#83458));
#19914=EDGE_LOOP('',(#83459,#83460,#83461,#83462));
#19915=EDGE_LOOP('',(#83463));
#19916=EDGE_LOOP('',(#83464));
#19917=EDGE_LOOP('',(#83465,#83466,#83467,#83468));
#19918=EDGE_LOOP('',(#83469));
#19919=EDGE_LOOP('',(#83470));
#19920=EDGE_LOOP('',(#83471,#83472,#83473,#83474));
#19921=EDGE_LOOP('',(#83475,#83476,#83477,#83478));
#19922=EDGE_LOOP('',(#83479,#83480,#83481,#83482));
#19923=EDGE_LOOP('',(#83483,#83484,#83485,#83486));
#19924=EDGE_LOOP('',(#83487));
#19925=EDGE_LOOP('',(#83488));
#19926=EDGE_LOOP('',(#83489,#83490,#83491,#83492));
#19927=EDGE_LOOP('',(#83493));
#19928=EDGE_LOOP('',(#83494));
#19929=EDGE_LOOP('',(#83495,#83496,#83497,#83498));
#19930=EDGE_LOOP('',(#83499,#83500,#83501,#83502));
#19931=EDGE_LOOP('',(#83503,#83504,#83505,#83506));
#19932=EDGE_LOOP('',(#83507,#83508,#83509,#83510));
#19933=EDGE_LOOP('',(#83511));
#19934=EDGE_LOOP('',(#83512));
#19935=EDGE_LOOP('',(#83513,#83514,#83515,#83516));
#19936=EDGE_LOOP('',(#83517));
#19937=EDGE_LOOP('',(#83518));
#19938=EDGE_LOOP('',(#83519,#83520,#83521,#83522));
#19939=EDGE_LOOP('',(#83523,#83524,#83525,#83526));
#19940=EDGE_LOOP('',(#83527,#83528,#83529,#83530));
#19941=EDGE_LOOP('',(#83531,#83532,#83533,#83534));
#19942=EDGE_LOOP('',(#83535));
#19943=EDGE_LOOP('',(#83536));
#19944=EDGE_LOOP('',(#83537));
#19945=EDGE_LOOP('',(#83538));
#19946=EDGE_LOOP('',(#83539));
#19947=EDGE_LOOP('',(#83540));
#19948=EDGE_LOOP('',(#83541));
#19949=EDGE_LOOP('',(#83542));
#19950=EDGE_LOOP('',(#83543,#83544,#83545,#83546));
#19951=EDGE_LOOP('',(#83547,#83548,#83549,#83550));
#19952=EDGE_LOOP('',(#83551,#83552,#83553,#83554));
#19953=EDGE_LOOP('',(#83555,#83556,#83557,#83558));
#19954=EDGE_LOOP('',(#83559,#83560,#83561,#83562));
#19955=EDGE_LOOP('',(#83563,#83564,#83565,#83566));
#19956=EDGE_LOOP('',(#83567,#83568,#83569,#83570));
#19957=EDGE_LOOP('',(#83571,#83572,#83573,#83574));
#19958=EDGE_LOOP('',(#83575,#83576,#83577,#83578));
#19959=EDGE_LOOP('',(#83579,#83580,#83581,#83582));
#19960=EDGE_LOOP('',(#83583));
#19961=EDGE_LOOP('',(#83584));
#19962=EDGE_LOOP('',(#83585));
#19963=EDGE_LOOP('',(#83586));
#19964=EDGE_LOOP('',(#83587,#83588));
#19965=EDGE_LOOP('',(#83589));
#19966=EDGE_LOOP('',(#83590));
#19967=EDGE_LOOP('',(#83591,#83592,#83593,#83594));
#19968=EDGE_LOOP('',(#83595,#83596,#83597,#83598));
#19969=EDGE_LOOP('',(#83599,#83600,#83601,#83602));
#19970=EDGE_LOOP('',(#83603));
#19971=EDGE_LOOP('',(#83604));
#19972=EDGE_LOOP('',(#83605));
#19973=EDGE_LOOP('',(#83606));
#19974=EDGE_LOOP('',(#83607,#83608));
#19975=EDGE_LOOP('',(#83609,#83610));
#19976=EDGE_LOOP('',(#83611,#83612));
#19977=EDGE_LOOP('',(#83613,#83614));
#19978=EDGE_LOOP('',(#83615,#83616));
#19979=EDGE_LOOP('',(#83617,#83618));
#19980=EDGE_LOOP('',(#83619,#83620));
#19981=EDGE_LOOP('',(#83621,#83622));
#19982=EDGE_LOOP('',(#83623,#83624));
#19983=EDGE_LOOP('',(#83625,#83626));
#19984=EDGE_LOOP('',(#83627,#83628));
#19985=EDGE_LOOP('',(#83629,#83630));
#19986=EDGE_LOOP('',(#83631,#83632));
#19987=EDGE_LOOP('',(#83633,#83634));
#19988=EDGE_LOOP('',(#83635,#83636));
#19989=EDGE_LOOP('',(#83637,#83638));
#19990=EDGE_LOOP('',(#83639,#83640));
#19991=EDGE_LOOP('',(#83641,#83642));
#19992=EDGE_LOOP('',(#83643,#83644));
#19993=EDGE_LOOP('',(#83645,#83646));
#19994=EDGE_LOOP('',(#83647,#83648));
#19995=EDGE_LOOP('',(#83649,#83650));
#19996=EDGE_LOOP('',(#83651,#83652));
#19997=EDGE_LOOP('',(#83653,#83654));
#19998=EDGE_LOOP('',(#83655,#83656,#83657,#83658));
#19999=EDGE_LOOP('',(#83659,#83660,#83661,#83662));
#20000=EDGE_LOOP('',(#83663,#83664,#83665,#83666));
#20001=EDGE_LOOP('',(#83667,#83668,#83669,#83670));
#20002=EDGE_LOOP('',(#83671,#83672,#83673,#83674));
#20003=EDGE_LOOP('',(#83675,#83676,#83677,#83678));
#20004=EDGE_LOOP('',(#83679,#83680,#83681,#83682));
#20005=EDGE_LOOP('',(#83683,#83684,#83685,#83686));
#20006=EDGE_LOOP('',(#83687,#83688,#83689,#83690));
#20007=EDGE_LOOP('',(#83691,#83692,#83693,#83694));
#20008=EDGE_LOOP('',(#83695,#83696,#83697,#83698,#83699,#83700));
#20009=EDGE_LOOP('',(#83701));
#20010=EDGE_LOOP('',(#83702,#83703,#83704,#83705,#83706,#83707));
#20011=EDGE_LOOP('',(#83708));
#20012=EDGE_LOOP('',(#83709));
#20013=EDGE_LOOP('',(#83710));
#20014=EDGE_LOOP('',(#83711));
#20015=EDGE_LOOP('',(#83712));
#20016=EDGE_LOOP('',(#83713));
#20017=EDGE_LOOP('',(#83714));
#20018=EDGE_LOOP('',(#83715,#83716,#83717));
#20019=EDGE_LOOP('',(#83718,#83719,#83720,#83721,#83722));
#20020=EDGE_LOOP('',(#83723,#83724,#83725,#83726));
#20021=EDGE_LOOP('',(#83727,#83728,#83729,#83730));
#20022=EDGE_LOOP('',(#83731,#83732,#83733,#83734));
#20023=EDGE_LOOP('',(#83735,#83736,#83737));
#20024=EDGE_LOOP('',(#83738,#83739,#83740,#83741));
#20025=EDGE_LOOP('',(#83742,#83743,#83744));
#20026=EDGE_LOOP('',(#83745,#83746,#83747,#83748,#83749));
#20027=EDGE_LOOP('',(#83750,#83751,#83752,#83753));
#20028=EDGE_LOOP('',(#83754,#83755,#83756,#83757));
#20029=EDGE_LOOP('',(#83758,#83759,#83760,#83761));
#20030=EDGE_LOOP('',(#83762,#83763,#83764,#83765));
#20031=EDGE_LOOP('',(#83766,#83767,#83768,#83769));
#20032=EDGE_LOOP('',(#83770,#83771,#83772,#83773,#83774,#83775,#83776,#83777));
#20033=EDGE_LOOP('',(#83778,#83779,#83780,#83781,#83782,#83783,#83784,#83785,
#83786));
#20034=EDGE_LOOP('',(#83787,#83788,#83789,#83790,#83791,#83792));
#20035=EDGE_LOOP('',(#83793));
#20036=EDGE_LOOP('',(#83794,#83795,#83796,#83797,#83798,#83799));
#20037=EDGE_LOOP('',(#83800,#83801,#83802,#83803,#83804,#83805));
#20038=EDGE_LOOP('',(#83806,#83807,#83808,#83809,#83810,#83811));
#20039=EDGE_LOOP('',(#83812,#83813,#83814,#83815,#83816,#83817));
#20040=EDGE_LOOP('',(#83818,#83819,#83820,#83821,#83822,#83823));
#20041=EDGE_LOOP('',(#83824,#83825,#83826,#83827,#83828,#83829));
#20042=EDGE_LOOP('',(#83830,#83831,#83832,#83833,#83834,#83835));
#20043=EDGE_LOOP('',(#83836));
#20044=EDGE_LOOP('',(#83837,#83838,#83839));
#20045=EDGE_LOOP('',(#83840,#83841,#83842));
#20046=EDGE_LOOP('',(#83843,#83844,#83845));
#20047=EDGE_LOOP('',(#83846,#83847,#83848));
#20048=EDGE_LOOP('',(#83849,#83850,#83851));
#20049=EDGE_LOOP('',(#83852,#83853,#83854));
#20050=EDGE_LOOP('',(#83855,#83856,#83857));
#20051=EDGE_LOOP('',(#83858,#83859,#83860));
#20052=EDGE_LOOP('',(#83861,#83862,#83863));
#20053=EDGE_LOOP('',(#83864,#83865,#83866));
#20054=EDGE_LOOP('',(#83867,#83868,#83869));
#20055=EDGE_LOOP('',(#83870,#83871,#83872));
#20056=EDGE_LOOP('',(#83873,#83874,#83875,#83876,#83877,#83878,#83879,#83880,
#83881,#83882,#83883,#83884,#83885,#83886,#83887));
#20057=EDGE_LOOP('',(#83888,#83889,#83890,#83891,#83892,#83893,#83894,#83895,
#83896,#83897,#83898,#83899,#83900,#83901,#83902,#83903,#83904));
#20058=EDGE_LOOP('',(#83905,#83906,#83907,#83908));
#20059=EDGE_LOOP('',(#83909,#83910,#83911,#83912));
#20060=EDGE_LOOP('',(#83913,#83914,#83915,#83916));
#20061=EDGE_LOOP('',(#83917,#83918,#83919,#83920));
#20062=EDGE_LOOP('',(#83921,#83922,#83923,#83924));
#20063=EDGE_LOOP('',(#83925,#83926,#83927,#83928));
#20064=EDGE_LOOP('',(#83929,#83930,#83931));
#20065=EDGE_LOOP('',(#83932,#83933,#83934));
#20066=EDGE_LOOP('',(#83935,#83936,#83937,#83938));
#20067=EDGE_LOOP('',(#83939,#83940,#83941,#83942));
#20068=EDGE_LOOP('',(#83943,#83944,#83945,#83946));
#20069=EDGE_LOOP('',(#83947,#83948,#83949,#83950));
#20070=EDGE_LOOP('',(#83951,#83952,#83953,#83954));
#20071=EDGE_LOOP('',(#83955,#83956,#83957,#83958));
#20072=EDGE_LOOP('',(#83959,#83960,#83961,#83962));
#20073=EDGE_LOOP('',(#83963));
#20074=EDGE_LOOP('',(#83964));
#20075=EDGE_LOOP('',(#83965,#83966,#83967,#83968,#83969,#83970));
#20076=EDGE_LOOP('',(#83971,#83972,#83973,#83974,#83975,#83976,#83977,#83978,
#83979,#83980));
#20077=EDGE_LOOP('',(#83981,#83982,#83983,#83984,#83985,#83986,#83987,#83988));
#20078=EDGE_LOOP('',(#83989));
#20079=EDGE_LOOP('',(#83990));
#20080=EDGE_LOOP('',(#83991,#83992,#83993,#83994));
#20081=EDGE_LOOP('',(#83995,#83996,#83997,#83998));
#20082=EDGE_LOOP('',(#83999,#84000,#84001,#84002));
#20083=EDGE_LOOP('',(#84003,#84004,#84005,#84006));
#20084=EDGE_LOOP('',(#84007,#84008,#84009,#84010));
#20085=EDGE_LOOP('',(#84011,#84012,#84013,#84014,#84015));
#20086=EDGE_LOOP('',(#84016));
#20087=EDGE_LOOP('',(#84017));
#20088=EDGE_LOOP('',(#84018,#84019,#84020,#84021));
#20089=EDGE_LOOP('',(#84022,#84023,#84024,#84025,#84026,#84027,#84028,#84029,
#84030,#84031,#84032,#84033,#84034,#84035,#84036,#84037));
#20090=EDGE_LOOP('',(#84038,#84039,#84040,#84041,#84042,#84043,#84044,#84045,
#84046,#84047,#84048,#84049,#84050,#84051,#84052,#84053,#84054));
#20091=EDGE_LOOP('',(#84055,#84056,#84057,#84058));
#20092=EDGE_LOOP('',(#84059,#84060,#84061,#84062));
#20093=EDGE_LOOP('',(#84063,#84064,#84065,#84066,#84067,#84068,#84069,#84070));
#20094=EDGE_LOOP('',(#84071,#84072,#84073,#84074));
#20095=EDGE_LOOP('',(#84075,#84076,#84077,#84078,#84079));
#20096=EDGE_LOOP('',(#84080,#84081,#84082,#84083,#84084,#84085));
#20097=EDGE_LOOP('',(#84086,#84087,#84088,#84089));
#20098=EDGE_LOOP('',(#84090));
#20099=EDGE_LOOP('',(#84091,#84092,#84093,#84094));
#20100=EDGE_LOOP('',(#84095,#84096,#84097));
#20101=EDGE_LOOP('',(#84098,#84099,#84100,#84101));
#20102=EDGE_LOOP('',(#84102,#84103,#84104,#84105));
#20103=EDGE_LOOP('',(#84106,#84107,#84108,#84109));
#20104=EDGE_LOOP('',(#84110,#84111,#84112,#84113));
#20105=EDGE_LOOP('',(#84114,#84115,#84116,#84117));
#20106=EDGE_LOOP('',(#84118,#84119,#84120,#84121));
#20107=EDGE_LOOP('',(#84122,#84123,#84124,#84125));
#20108=EDGE_LOOP('',(#84126,#84127,#84128,#84129));
#20109=EDGE_LOOP('',(#84130,#84131,#84132,#84133));
#20110=EDGE_LOOP('',(#84134,#84135,#84136,#84137));
#20111=EDGE_LOOP('',(#84138,#84139,#84140,#84141));
#20112=EDGE_LOOP('',(#84142,#84143,#84144,#84145));
#20113=EDGE_LOOP('',(#84146,#84147,#84148,#84149));
#20114=EDGE_LOOP('',(#84150,#84151,#84152,#84153));
#20115=EDGE_LOOP('',(#84154,#84155,#84156,#84157));
#20116=EDGE_LOOP('',(#84158,#84159,#84160,#84161));
#20117=EDGE_LOOP('',(#84162,#84163,#84164,#84165));
#20118=EDGE_LOOP('',(#84166,#84167,#84168,#84169));
#20119=EDGE_LOOP('',(#84170,#84171,#84172,#84173));
#20120=EDGE_LOOP('',(#84174,#84175,#84176,#84177));
#20121=EDGE_LOOP('',(#84178,#84179,#84180,#84181));
#20122=EDGE_LOOP('',(#84182,#84183,#84184,#84185));
#20123=EDGE_LOOP('',(#84186,#84187,#84188,#84189));
#20124=EDGE_LOOP('',(#84190,#84191,#84192,#84193));
#20125=EDGE_LOOP('',(#84194,#84195,#84196,#84197));
#20126=EDGE_LOOP('',(#84198,#84199,#84200,#84201));
#20127=EDGE_LOOP('',(#84202,#84203,#84204,#84205));
#20128=EDGE_LOOP('',(#84206,#84207,#84208,#84209));
#20129=EDGE_LOOP('',(#84210,#84211,#84212,#84213));
#20130=EDGE_LOOP('',(#84214,#84215,#84216,#84217));
#20131=EDGE_LOOP('',(#84218,#84219,#84220,#84221));
#20132=EDGE_LOOP('',(#84222,#84223,#84224,#84225));
#20133=EDGE_LOOP('',(#84226,#84227,#84228,#84229));
#20134=EDGE_LOOP('',(#84230,#84231,#84232,#84233));
#20135=EDGE_LOOP('',(#84234,#84235,#84236,#84237));
#20136=EDGE_LOOP('',(#84238,#84239,#84240,#84241));
#20137=EDGE_LOOP('',(#84242,#84243,#84244,#84245));
#20138=EDGE_LOOP('',(#84246,#84247,#84248,#84249));
#20139=EDGE_LOOP('',(#84250,#84251,#84252,#84253));
#20140=EDGE_LOOP('',(#84254,#84255,#84256,#84257));
#20141=EDGE_LOOP('',(#84258,#84259,#84260,#84261));
#20142=EDGE_LOOP('',(#84262,#84263,#84264,#84265));
#20143=EDGE_LOOP('',(#84266,#84267,#84268,#84269));
#20144=EDGE_LOOP('',(#84270,#84271,#84272,#84273));
#20145=EDGE_LOOP('',(#84274,#84275,#84276,#84277));
#20146=EDGE_LOOP('',(#84278,#84279,#84280,#84281));
#20147=EDGE_LOOP('',(#84282,#84283,#84284,#84285));
#20148=EDGE_LOOP('',(#84286,#84287,#84288,#84289));
#20149=EDGE_LOOP('',(#84290,#84291,#84292,#84293));
#20150=EDGE_LOOP('',(#84294,#84295,#84296,#84297));
#20151=EDGE_LOOP('',(#84298,#84299,#84300,#84301));
#20152=EDGE_LOOP('',(#84302,#84303,#84304,#84305));
#20153=EDGE_LOOP('',(#84306,#84307,#84308,#84309));
#20154=EDGE_LOOP('',(#84310,#84311,#84312,#84313));
#20155=EDGE_LOOP('',(#84314,#84315,#84316,#84317));
#20156=EDGE_LOOP('',(#84318,#84319,#84320,#84321));
#20157=EDGE_LOOP('',(#84322,#84323,#84324,#84325));
#20158=EDGE_LOOP('',(#84326,#84327,#84328,#84329));
#20159=EDGE_LOOP('',(#84330,#84331,#84332,#84333));
#20160=EDGE_LOOP('',(#84334,#84335,#84336,#84337));
#20161=EDGE_LOOP('',(#84338,#84339,#84340,#84341));
#20162=EDGE_LOOP('',(#84342,#84343,#84344,#84345));
#20163=EDGE_LOOP('',(#84346,#84347,#84348,#84349));
#20164=EDGE_LOOP('',(#84350,#84351,#84352,#84353));
#20165=EDGE_LOOP('',(#84354,#84355,#84356));
#20166=EDGE_LOOP('',(#84357,#84358,#84359,#84360,#84361,#84362,#84363,#84364));
#20167=EDGE_LOOP('',(#84365,#84366,#84367,#84368,#84369,#84370,#84371,#84372));
#20168=EDGE_LOOP('',(#84373,#84374,#84375,#84376));
#20169=EDGE_LOOP('',(#84377,#84378,#84379,#84380,#84381,#84382,#84383,#84384,
#84385,#84386,#84387,#84388,#84389,#84390,#84391,#84392,#84393,#84394,#84395,
#84396,#84397,#84398,#84399,#84400,#84401,#84402,#84403,#84404,#84405,#84406,
#84407));
#20170=EDGE_LOOP('',(#84408,#84409,#84410,#84411,#84412,#84413,#84414,#84415,
#84416,#84417,#84418,#84419,#84420,#84421,#84422,#84423,#84424,#84425,#84426,
#84427,#84428,#84429,#84430,#84431,#84432,#84433,#84434,#84435,#84436,#84437));
#20171=EDGE_LOOP('',(#84438,#84439,#84440,#84441));
#20172=EDGE_LOOP('',(#84442));
#20173=EDGE_LOOP('',(#84443,#84444,#84445,#84446));
#20174=EDGE_LOOP('',(#84447,#84448,#84449,#84450));
#20175=EDGE_LOOP('',(#84451,#84452,#84453,#84454));
#20176=EDGE_LOOP('',(#84455,#84456,#84457,#84458,#84459,#84460));
#20177=EDGE_LOOP('',(#84461,#84462,#84463,#84464));
#20178=EDGE_LOOP('',(#84465,#84466,#84467,#84468));
#20179=EDGE_LOOP('',(#84469,#84470,#84471,#84472));
#20180=EDGE_LOOP('',(#84473,#84474,#84475,#84476));
#20181=EDGE_LOOP('',(#84477,#84478,#84479,#84480,#84481,#84482));
#20182=EDGE_LOOP('',(#84483,#84484,#84485,#84486,#84487,#84488));
#20183=EDGE_LOOP('',(#84489,#84490,#84491,#84492,#84493,#84494));
#20184=EDGE_LOOP('',(#84495,#84496,#84497,#84498,#84499,#84500));
#20185=EDGE_LOOP('',(#84501,#84502,#84503,#84504,#84505,#84506));
#20186=EDGE_LOOP('',(#84507,#84508,#84509,#84510,#84511,#84512));
#20187=EDGE_LOOP('',(#84513,#84514,#84515,#84516,#84517,#84518));
#20188=EDGE_LOOP('',(#84519));
#20189=EDGE_LOOP('',(#84520,#84521,#84522));
#20190=EDGE_LOOP('',(#84523,#84524,#84525));
#20191=EDGE_LOOP('',(#84526,#84527,#84528));
#20192=EDGE_LOOP('',(#84529,#84530,#84531));
#20193=EDGE_LOOP('',(#84532,#84533,#84534));
#20194=EDGE_LOOP('',(#84535,#84536,#84537));
#20195=EDGE_LOOP('',(#84538,#84539,#84540));
#20196=EDGE_LOOP('',(#84541,#84542,#84543));
#20197=EDGE_LOOP('',(#84544,#84545,#84546));
#20198=EDGE_LOOP('',(#84547,#84548,#84549));
#20199=EDGE_LOOP('',(#84550,#84551,#84552));
#20200=EDGE_LOOP('',(#84553,#84554,#84555));
#20201=EDGE_LOOP('',(#84556,#84557,#84558,#84559));
#20202=EDGE_LOOP('',(#84560,#84561,#84562,#84563,#84564,#84565,#84566,#84567,
#84568,#84569,#84570,#84571,#84572,#84573,#84574,#84575,#84576,#84577,#84578,
#84579,#84580,#84581,#84582,#84583,#84584,#84585,#84586,#84587,#84588,#84589,
#84590,#84591,#84592,#84593,#84594,#84595,#84596,#84597,#84598,#84599,#84600,
#84601,#84602));
#20203=EDGE_LOOP('',(#84603,#84604,#84605,#84606,#84607,#84608,#84609,#84610,
#84611,#84612,#84613,#84614,#84615,#84616,#84617,#84618,#84619,#84620,#84621,
#84622,#84623,#84624,#84625,#84626,#84627,#84628,#84629,#84630,#84631,#84632,
#84633,#84634,#84635,#84636,#84637,#84638,#84639,#84640,#84641,#84642,#84643,
#84644));
#20204=EDGE_LOOP('',(#84645,#84646,#84647,#84648));
#20205=EDGE_LOOP('',(#84649,#84650,#84651,#84652));
#20206=EDGE_LOOP('',(#84653,#84654,#84655,#84656));
#20207=EDGE_LOOP('',(#84657,#84658,#84659,#84660));
#20208=EDGE_LOOP('',(#84661,#84662,#84663,#84664));
#20209=EDGE_LOOP('',(#84665,#84666,#84667,#84668));
#20210=EDGE_LOOP('',(#84669,#84670,#84671,#84672));
#20211=EDGE_LOOP('',(#84673,#84674,#84675,#84676));
#20212=EDGE_LOOP('',(#84677,#84678,#84679,#84680));
#20213=EDGE_LOOP('',(#84681,#84682,#84683,#84684));
#20214=EDGE_LOOP('',(#84685,#84686,#84687,#84688));
#20215=EDGE_LOOP('',(#84689,#84690,#84691,#84692));
#20216=EDGE_LOOP('',(#84693));
#20217=EDGE_LOOP('',(#84694));
#20218=EDGE_LOOP('',(#84695,#84696,#84697,#84698));
#20219=EDGE_LOOP('',(#84699,#84700,#84701,#84702,#84703));
#20220=EDGE_LOOP('',(#84704,#84705,#84706,#84707,#84708));
#20221=EDGE_LOOP('',(#84709,#84710,#84711,#84712));
#20222=EDGE_LOOP('',(#84713,#84714,#84715,#84716));
#20223=EDGE_LOOP('',(#84717));
#20224=EDGE_LOOP('',(#84718));
#20225=EDGE_LOOP('',(#84719));
#20226=EDGE_LOOP('',(#84720));
#20227=EDGE_LOOP('',(#84721));
#20228=EDGE_LOOP('',(#84722));
#20229=EDGE_LOOP('',(#84723));
#20230=EDGE_LOOP('',(#84724));
#20231=EDGE_LOOP('',(#84725));
#20232=EDGE_LOOP('',(#84726));
#20233=EDGE_LOOP('',(#84727));
#20234=EDGE_LOOP('',(#84728));
#20235=EDGE_LOOP('',(#84729));
#20236=EDGE_LOOP('',(#84730));
#20237=EDGE_LOOP('',(#84731));
#20238=EDGE_LOOP('',(#84732));
#20239=EDGE_LOOP('',(#84733));
#20240=EDGE_LOOP('',(#84734));
#20241=EDGE_LOOP('',(#84735));
#20242=EDGE_LOOP('',(#84736));
#20243=EDGE_LOOP('',(#84737));
#20244=EDGE_LOOP('',(#84738));
#20245=EDGE_LOOP('',(#84739));
#20246=EDGE_LOOP('',(#84740));
#20247=EDGE_LOOP('',(#84741));
#20248=EDGE_LOOP('',(#84742));
#20249=EDGE_LOOP('',(#84743,#84744,#84745,#84746));
#20250=EDGE_LOOP('',(#84747,#84748,#84749,#84750));
#20251=EDGE_LOOP('',(#84751,#84752,#84753,#84754));
#20252=EDGE_LOOP('',(#84755,#84756,#84757,#84758));
#20253=EDGE_LOOP('',(#84759,#84760,#84761,#84762));
#20254=EDGE_LOOP('',(#84763,#84764,#84765,#84766));
#20255=EDGE_LOOP('',(#84767,#84768,#84769,#84770));
#20256=EDGE_LOOP('',(#84771,#84772,#84773,#84774));
#20257=EDGE_LOOP('',(#84775,#84776,#84777,#84778));
#20258=EDGE_LOOP('',(#84779,#84780,#84781,#84782));
#20259=EDGE_LOOP('',(#84783,#84784,#84785,#84786));
#20260=EDGE_LOOP('',(#84787,#84788,#84789,#84790));
#20261=EDGE_LOOP('',(#84791,#84792,#84793,#84794));
#20262=EDGE_LOOP('',(#84795,#84796,#84797,#84798));
#20263=EDGE_LOOP('',(#84799,#84800,#84801,#84802));
#20264=EDGE_LOOP('',(#84803,#84804,#84805,#84806));
#20265=EDGE_LOOP('',(#84807,#84808,#84809,#84810));
#20266=EDGE_LOOP('',(#84811,#84812,#84813,#84814));
#20267=EDGE_LOOP('',(#84815,#84816,#84817,#84818));
#20268=EDGE_LOOP('',(#84819,#84820,#84821,#84822));
#20269=EDGE_LOOP('',(#84823,#84824,#84825,#84826));
#20270=EDGE_LOOP('',(#84827,#84828,#84829,#84830));
#20271=EDGE_LOOP('',(#84831,#84832,#84833,#84834));
#20272=EDGE_LOOP('',(#84835,#84836,#84837,#84838));
#20273=EDGE_LOOP('',(#84839,#84840,#84841,#84842));
#20274=EDGE_LOOP('',(#84843,#84844,#84845,#84846));
#20275=EDGE_LOOP('',(#84847,#84848,#84849,#84850,#84851,#84852,#84853,#84854));
#20276=EDGE_LOOP('',(#84855,#84856,#84857,#84858,#84859,#84860,#84861,#84862));
#20277=EDGE_LOOP('',(#84863,#84864,#84865,#84866));
#20278=EDGE_LOOP('',(#84867,#84868,#84869,#84870));
#20279=EDGE_LOOP('',(#84871,#84872,#84873,#84874));
#20280=EDGE_LOOP('',(#84875));
#20281=EDGE_LOOP('',(#84876));
#20282=EDGE_LOOP('',(#84877,#84878,#84879,#84880));
#20283=EDGE_LOOP('',(#84881));
#20284=EDGE_LOOP('',(#84882));
#20285=EDGE_LOOP('',(#84883));
#20286=EDGE_LOOP('',(#84884,#84885,#84886,#84887));
#20287=EDGE_LOOP('',(#84888));
#20288=EDGE_LOOP('',(#84889));
#20289=EDGE_LOOP('',(#84890));
#20290=EDGE_LOOP('',(#84891,#84892,#84893,#84894));
#20291=EDGE_LOOP('',(#84895));
#20292=EDGE_LOOP('',(#84896));
#20293=EDGE_LOOP('',(#84897));
#20294=EDGE_LOOP('',(#84898,#84899,#84900,#84901));
#20295=EDGE_LOOP('',(#84902));
#20296=EDGE_LOOP('',(#84903));
#20297=EDGE_LOOP('',(#84904,#84905,#84906,#84907));
#20298=EDGE_LOOP('',(#84908));
#20299=EDGE_LOOP('',(#84909));
#20300=EDGE_LOOP('',(#84910));
#20301=EDGE_LOOP('',(#84911,#84912,#84913,#84914));
#20302=EDGE_LOOP('',(#84915,#84916,#84917,#84918));
#20303=EDGE_LOOP('',(#84919,#84920,#84921,#84922));
#20304=EDGE_LOOP('',(#84923,#84924,#84925,#84926));
#20305=EDGE_LOOP('',(#84927,#84928,#84929,#84930));
#20306=EDGE_LOOP('',(#84931,#84932,#84933,#84934));
#20307=EDGE_LOOP('',(#84935,#84936,#84937,#84938));
#20308=EDGE_LOOP('',(#84939,#84940,#84941,#84942));
#20309=EDGE_LOOP('',(#84943,#84944,#84945,#84946));
#20310=EDGE_LOOP('',(#84947,#84948,#84949,#84950));
#20311=EDGE_LOOP('',(#84951,#84952,#84953,#84954));
#20312=EDGE_LOOP('',(#84955,#84956,#84957,#84958));
#20313=EDGE_LOOP('',(#84959,#84960,#84961,#84962));
#20314=EDGE_LOOP('',(#84963,#84964,#84965,#84966));
#20315=EDGE_LOOP('',(#84967,#84968,#84969,#84970));
#20316=EDGE_LOOP('',(#84971,#84972,#84973,#84974));
#20317=EDGE_LOOP('',(#84975,#84976,#84977,#84978));
#20318=EDGE_LOOP('',(#84979,#84980,#84981,#84982));
#20319=EDGE_LOOP('',(#84983));
#20320=EDGE_LOOP('',(#84984));
#20321=EDGE_LOOP('',(#84985,#84986,#84987,#84988));
#20322=EDGE_LOOP('',(#84989,#84990,#84991,#84992));
#20323=EDGE_LOOP('',(#84993,#84994,#84995,#84996));
#20324=EDGE_LOOP('',(#84997));
#20325=EDGE_LOOP('',(#84998));
#20326=EDGE_LOOP('',(#84999,#85000,#85001,#85002));
#20327=EDGE_LOOP('',(#85003,#85004,#85005,#85006));
#20328=EDGE_LOOP('',(#85007,#85008,#85009,#85010));
#20329=EDGE_LOOP('',(#85011,#85012,#85013,#85014,#85015));
#20330=EDGE_LOOP('',(#85016,#85017,#85018,#85019,#85020));
#20331=EDGE_LOOP('',(#85021,#85022,#85023,#85024));
#20332=EDGE_LOOP('',(#85025,#85026,#85027,#85028));
#20333=EDGE_LOOP('',(#85029,#85030,#85031,#85032));
#20334=EDGE_LOOP('',(#85033,#85034,#85035,#85036));
#20335=EDGE_LOOP('',(#85037,#85038,#85039,#85040));
#20336=EDGE_LOOP('',(#85041,#85042,#85043,#85044));
#20337=EDGE_LOOP('',(#85045,#85046,#85047,#85048));
#20338=EDGE_LOOP('',(#85049,#85050,#85051,#85052));
#20339=EDGE_LOOP('',(#85053,#85054,#85055,#85056));
#20340=EDGE_LOOP('',(#85057,#85058,#85059,#85060));
#20341=EDGE_LOOP('',(#85061,#85062,#85063,#85064));
#20342=EDGE_LOOP('',(#85065,#85066,#85067,#85068));
#20343=EDGE_LOOP('',(#85069,#85070,#85071,#85072));
#20344=EDGE_LOOP('',(#85073,#85074,#85075,#85076));
#20345=EDGE_LOOP('',(#85077,#85078,#85079,#85080));
#20346=EDGE_LOOP('',(#85081,#85082,#85083,#85084));
#20347=EDGE_LOOP('',(#85085,#85086,#85087,#85088,#85089,#85090,#85091,#85092,
#85093));
#20348=EDGE_LOOP('',(#85094,#85095,#85096));
#20349=EDGE_LOOP('',(#85097,#85098,#85099,#85100,#85101));
#20350=EDGE_LOOP('',(#85102,#85103,#85104,#85105));
#20351=EDGE_LOOP('',(#85106,#85107,#85108,#85109));
#20352=EDGE_LOOP('',(#85110,#85111,#85112,#85113));
#20353=EDGE_LOOP('',(#85114,#85115,#85116,#85117));
#20354=EDGE_LOOP('',(#85118,#85119,#85120,#85121));
#20355=EDGE_LOOP('',(#85122,#85123,#85124,#85125));
#20356=EDGE_LOOP('',(#85126,#85127,#85128,#85129));
#20357=EDGE_LOOP('',(#85130,#85131,#85132,#85133));
#20358=EDGE_LOOP('',(#85134,#85135,#85136,#85137));
#20359=EDGE_LOOP('',(#85138,#85139,#85140,#85141));
#20360=EDGE_LOOP('',(#85142,#85143,#85144,#85145));
#20361=EDGE_LOOP('',(#85146,#85147,#85148,#85149));
#20362=EDGE_LOOP('',(#85150,#85151,#85152,#85153));
#20363=EDGE_LOOP('',(#85154,#85155,#85156,#85157));
#20364=EDGE_LOOP('',(#85158,#85159,#85160,#85161,#85162));
#20365=EDGE_LOOP('',(#85163));
#20366=EDGE_LOOP('',(#85164,#85165,#85166,#85167,#85168,#85169,#85170,#85171,
#85172));
#20367=EDGE_LOOP('',(#85173,#85174,#85175,#85176,#85177,#85178,#85179,#85180,
#85181,#85182,#85183,#85184,#85185,#85186,#85187,#85188,#85189,#85190,#85191,
#85192,#85193,#85194,#85195,#85196,#85197,#85198,#85199,#85200,#85201,#85202,
#85203,#85204,#85205,#85206,#85207,#85208,#85209,#85210));
#20368=EDGE_LOOP('',(#85211,#85212,#85213,#85214,#85215,#85216,#85217,#85218,
#85219,#85220,#85221,#85222,#85223,#85224,#85225,#85226,#85227,#85228,#85229,
#85230,#85231,#85232,#85233,#85234,#85235,#85236,#85237,#85238,#85239,#85240,
#85241,#85242,#85243,#85244,#85245,#85246,#85247,#85248,#85249,#85250));
#20369=EDGE_LOOP('',(#85251,#85252,#85253));
#20370=EDGE_LOOP('',(#85254,#85255,#85256,#85257));
#20371=EDGE_LOOP('',(#85258,#85259,#85260,#85261));
#20372=EDGE_LOOP('',(#85262,#85263,#85264,#85265));
#20373=EDGE_LOOP('',(#85266,#85267,#85268,#85269));
#20374=EDGE_LOOP('',(#85270,#85271,#85272,#85273));
#20375=EDGE_LOOP('',(#85274,#85275,#85276,#85277));
#20376=EDGE_LOOP('',(#85278,#85279,#85280,#85281));
#20377=EDGE_LOOP('',(#85282,#85283,#85284,#85285));
#20378=EDGE_LOOP('',(#85286,#85287,#85288,#85289));
#20379=EDGE_LOOP('',(#85290,#85291,#85292,#85293));
#20380=EDGE_LOOP('',(#85294,#85295,#85296,#85297));
#20381=EDGE_LOOP('',(#85298,#85299,#85300,#85301));
#20382=EDGE_LOOP('',(#85302,#85303,#85304,#85305));
#20383=EDGE_LOOP('',(#85306,#85307,#85308,#85309));
#20384=EDGE_LOOP('',(#85310,#85311,#85312,#85313));
#20385=EDGE_LOOP('',(#85314,#85315,#85316,#85317));
#20386=EDGE_LOOP('',(#85318,#85319,#85320,#85321));
#20387=EDGE_LOOP('',(#85322,#85323,#85324,#85325));
#20388=EDGE_LOOP('',(#85326,#85327,#85328,#85329));
#20389=EDGE_LOOP('',(#85330,#85331,#85332,#85333));
#20390=EDGE_LOOP('',(#85334,#85335,#85336,#85337,#85338,#85339,#85340,#85341));
#20391=EDGE_LOOP('',(#85342,#85343,#85344,#85345));
#20392=EDGE_LOOP('',(#85346,#85347,#85348,#85349));
#20393=EDGE_LOOP('',(#85350,#85351,#85352,#85353,#85354,#85355,#85356,#85357));
#20394=EDGE_LOOP('',(#85358,#85359,#85360,#85361));
#20395=EDGE_LOOP('',(#85362,#85363,#85364,#85365));
#20396=EDGE_LOOP('',(#85366,#85367,#85368,#85369));
#20397=EDGE_LOOP('',(#85370,#85371,#85372,#85373));
#20398=EDGE_LOOP('',(#85374,#85375,#85376,#85377));
#20399=EDGE_LOOP('',(#85378,#85379,#85380,#85381));
#20400=EDGE_LOOP('',(#85382,#85383,#85384,#85385));
#20401=EDGE_LOOP('',(#85386,#85387,#85388,#85389));
#20402=EDGE_LOOP('',(#85390,#85391,#85392,#85393));
#20403=EDGE_LOOP('',(#85394,#85395,#85396,#85397));
#20404=EDGE_LOOP('',(#85398,#85399,#85400,#85401));
#20405=EDGE_LOOP('',(#85402,#85403,#85404,#85405));
#20406=EDGE_LOOP('',(#85406,#85407,#85408,#85409));
#20407=EDGE_LOOP('',(#85410,#85411,#85412,#85413));
#20408=EDGE_LOOP('',(#85414,#85415,#85416,#85417));
#20409=EDGE_LOOP('',(#85418,#85419,#85420,#85421));
#20410=EDGE_LOOP('',(#85422,#85423,#85424,#85425));
#20411=EDGE_LOOP('',(#85426,#85427,#85428,#85429));
#20412=EDGE_LOOP('',(#85430,#85431,#85432,#85433));
#20413=EDGE_LOOP('',(#85434,#85435,#85436,#85437));
#20414=EDGE_LOOP('',(#85438,#85439,#85440,#85441));
#20415=EDGE_LOOP('',(#85442,#85443,#85444,#85445));
#20416=EDGE_LOOP('',(#85446,#85447,#85448,#85449));
#20417=EDGE_LOOP('',(#85450,#85451,#85452,#85453,#85454,#85455));
#20418=EDGE_LOOP('',(#85456,#85457,#85458,#85459,#85460,#85461,#85462,#85463));
#20419=EDGE_LOOP('',(#85464,#85465,#85466,#85467,#85468,#85469,#85470,#85471));
#20420=EDGE_LOOP('',(#85472,#85473,#85474,#85475));
#20421=EDGE_LOOP('',(#85476,#85477,#85478));
#20422=EDGE_LOOP('',(#85479,#85480,#85481));
#20423=EDGE_LOOP('',(#85482,#85483,#85484));
#20424=EDGE_LOOP('',(#85485,#85486,#85487));
#20425=EDGE_LOOP('',(#85488,#85489,#85490));
#20426=EDGE_LOOP('',(#85491,#85492,#85493));
#20427=EDGE_LOOP('',(#85494,#85495,#85496,#85497,#85498));
#20428=EDGE_LOOP('',(#85499,#85500,#85501,#85502,#85503));
#20429=EDGE_LOOP('',(#85504,#85505,#85506,#85507,#85508));
#20430=EDGE_LOOP('',(#85509,#85510,#85511,#85512,#85513));
#20431=EDGE_LOOP('',(#85514,#85515,#85516,#85517,#85518));
#20432=EDGE_LOOP('',(#85519,#85520,#85521,#85522,#85523));
#20433=EDGE_LOOP('',(#85524,#85525,#85526,#85527,#85528,#85529));
#20434=EDGE_LOOP('',(#85530));
#20435=EDGE_LOOP('',(#85531,#85532,#85533,#85534));
#20436=EDGE_LOOP('',(#85535,#85536,#85537,#85538));
#20437=EDGE_LOOP('',(#85539,#85540,#85541,#85542));
#20438=EDGE_LOOP('',(#85543,#85544,#85545,#85546));
#20439=EDGE_LOOP('',(#85547,#85548,#85549,#85550));
#20440=EDGE_LOOP('',(#85551,#85552,#85553,#85554));
#20441=EDGE_LOOP('',(#85555,#85556,#85557,#85558));
#20442=EDGE_LOOP('',(#85559,#85560,#85561,#85562,#85563));
#20443=EDGE_LOOP('',(#85564,#85565,#85566,#85567));
#20444=EDGE_LOOP('',(#85568,#85569,#85570,#85571));
#20445=EDGE_LOOP('',(#85572,#85573,#85574,#85575));
#20446=EDGE_LOOP('',(#85576,#85577,#85578));
#20447=EDGE_LOOP('',(#85579,#85580,#85581,#85582,#85583,#85584,#85585,#85586,
#85587,#85588,#85589,#85590,#85591,#85592,#85593));
#20448=EDGE_LOOP('',(#85594,#85595,#85596,#85597,#85598));
#20449=EDGE_LOOP('',(#85599,#85600,#85601,#85602,#85603,#85604,#85605,#85606,
#85607,#85608,#85609,#85610,#85611));
#20450=EDGE_LOOP('',(#85612,#85613,#85614,#85615));
#20451=EDGE_LOOP('',(#85616,#85617,#85618,#85619));
#20452=EDGE_LOOP('',(#85620,#85621,#85622,#85623));
#20453=EDGE_LOOP('',(#85624,#85625,#85626,#85627));
#20454=EDGE_LOOP('',(#85628,#85629,#85630,#85631));
#20455=EDGE_LOOP('',(#85632,#85633,#85634,#85635));
#20456=EDGE_LOOP('',(#85636,#85637,#85638,#85639));
#20457=EDGE_LOOP('',(#85640,#85641,#85642,#85643));
#20458=EDGE_LOOP('',(#85644,#85645,#85646,#85647));
#20459=EDGE_LOOP('',(#85648,#85649,#85650,#85651));
#20460=EDGE_LOOP('',(#85652,#85653,#85654,#85655));
#20461=EDGE_LOOP('',(#85656,#85657,#85658,#85659));
#20462=EDGE_LOOP('',(#85660,#85661,#85662,#85663));
#20463=EDGE_LOOP('',(#85664,#85665,#85666,#85667));
#20464=EDGE_LOOP('',(#85668,#85669,#85670,#85671));
#20465=EDGE_LOOP('',(#85672,#85673,#85674,#85675));
#20466=EDGE_LOOP('',(#85676,#85677,#85678,#85679));
#20467=EDGE_LOOP('',(#85680,#85681,#85682,#85683));
#20468=EDGE_LOOP('',(#85684,#85685,#85686,#85687));
#20469=EDGE_LOOP('',(#85688,#85689,#85690,#85691,#85692,#85693));
#20470=EDGE_LOOP('',(#85694,#85695,#85696,#85697,#85698,#85699));
#20471=EDGE_LOOP('',(#85700,#85701,#85702,#85703,#85704,#85705));
#20472=EDGE_LOOP('',(#85706,#85707,#85708,#85709,#85710,#85711));
#20473=EDGE_LOOP('',(#85712,#85713,#85714,#85715,#85716,#85717));
#20474=EDGE_LOOP('',(#85718,#85719,#85720,#85721,#85722,#85723));
#20475=EDGE_LOOP('',(#85724,#85725,#85726,#85727,#85728,#85729));
#20476=EDGE_LOOP('',(#85730));
#20477=EDGE_LOOP('',(#85731,#85732,#85733,#85734,#85735,#85736));
#20478=EDGE_LOOP('',(#85737));
#20479=EDGE_LOOP('',(#85738,#85739,#85740,#85741,#85742,#85743,#85744,#85745,
#85746));
#20480=EDGE_LOOP('',(#85747,#85748,#85749,#85750,#85751,#85752,#85753,#85754));
#20481=LINE('',#131019,#24828);
#20482=LINE('',#131025,#24829);
#20483=LINE('',#131031,#24830);
#20484=LINE('',#131037,#24831);
#20485=LINE('',#131043,#24832);
#20486=LINE('',#131049,#24833);
#20487=LINE('',#131055,#24834);
#20488=LINE('',#131061,#24835);
#20489=LINE('',#131067,#24836);
#20490=LINE('',#131073,#24837);
#20491=LINE('',#131079,#24838);
#20492=LINE('',#131085,#24839);
#20493=LINE('',#131090,#24840);
#20494=LINE('',#131092,#24841);
#20495=LINE('',#131094,#24842);
#20496=LINE('',#131095,#24843);
#20497=LINE('',#131098,#24844);
#20498=LINE('',#131100,#24845);
#20499=LINE('',#131101,#24846);
#20500=LINE('',#131105,#24847);
#20501=LINE('',#131107,#24848);
#20502=LINE('',#131109,#24849);
#20503=LINE('',#131110,#24850);
#20504=LINE('',#131114,#24851);
#20505=LINE('',#131116,#24852);
#20506=LINE('',#131118,#24853);
#20507=LINE('',#131119,#24854);
#20508=LINE('',#131122,#24855);
#20509=LINE('',#131124,#24856);
#20510=LINE('',#131125,#24857);
#20511=LINE('',#131128,#24858);
#20512=LINE('',#131130,#24859);
#20513=LINE('',#131131,#24860);
#20514=LINE('',#131135,#24861);
#20515=LINE('',#131137,#24862);
#20516=LINE('',#131139,#24863);
#20517=LINE('',#131140,#24864);
#20518=LINE('',#131143,#24865);
#20519=LINE('',#131145,#24866);
#20520=LINE('',#131146,#24867);
#20521=LINE('',#131166,#24868);
#20522=LINE('',#131172,#24869);
#20523=LINE('',#131178,#24870);
#20524=LINE('',#131184,#24871);
#20525=LINE('',#131190,#24872);
#20526=LINE('',#131196,#24873);
#20527=LINE('',#131202,#24874);
#20528=LINE('',#131208,#24875);
#20529=LINE('',#131214,#24876);
#20530=LINE('',#131220,#24877);
#20531=LINE('',#131226,#24878);
#20532=LINE('',#131232,#24879);
#20533=LINE('',#131237,#24880);
#20534=LINE('',#131239,#24881);
#20535=LINE('',#131241,#24882);
#20536=LINE('',#131242,#24883);
#20537=LINE('',#131245,#24884);
#20538=LINE('',#131247,#24885);
#20539=LINE('',#131248,#24886);
#20540=LINE('',#131252,#24887);
#20541=LINE('',#131254,#24888);
#20542=LINE('',#131256,#24889);
#20543=LINE('',#131257,#24890);
#20544=LINE('',#131261,#24891);
#20545=LINE('',#131263,#24892);
#20546=LINE('',#131265,#24893);
#20547=LINE('',#131266,#24894);
#20548=LINE('',#131269,#24895);
#20549=LINE('',#131271,#24896);
#20550=LINE('',#131272,#24897);
#20551=LINE('',#131275,#24898);
#20552=LINE('',#131277,#24899);
#20553=LINE('',#131278,#24900);
#20554=LINE('',#131282,#24901);
#20555=LINE('',#131284,#24902);
#20556=LINE('',#131286,#24903);
#20557=LINE('',#131287,#24904);
#20558=LINE('',#131290,#24905);
#20559=LINE('',#131292,#24906);
#20560=LINE('',#131293,#24907);
#20561=LINE('',#131313,#24908);
#20562=LINE('',#131319,#24909);
#20563=LINE('',#131326,#24910);
#20564=LINE('',#131332,#24911);
#20565=LINE('',#131338,#24912);
#20566=LINE('',#131345,#24913);
#20567=LINE('',#131350,#24914);
#20568=LINE('',#131354,#24915);
#20569=LINE('',#131374,#24916);
#20570=LINE('',#131378,#24917);
#20571=LINE('',#131416,#24918);
#20572=LINE('',#131420,#24919);
#20573=LINE('',#131425,#24920);
#20574=LINE('',#131427,#24921);
#20575=LINE('',#131437,#24922);
#20576=LINE('',#131447,#24923);
#20577=LINE('',#131449,#24924);
#20578=LINE('',#131471,#24925);
#20579=LINE('',#131509,#24926);
#20580=LINE('',#131511,#24927);
#20581=LINE('',#131513,#24928);
#20582=LINE('',#131523,#24929);
#20583=LINE('',#131532,#24930);
#20584=LINE('',#131542,#24931);
#20585=LINE('',#131546,#24932);
#20586=LINE('',#131549,#24933);
#20587=LINE('',#131550,#24934);
#20588=LINE('',#131580,#24935);
#20589=LINE('',#131582,#24936);
#20590=LINE('',#131592,#24937);
#20591=LINE('',#131602,#24938);
#20592=LINE('',#131604,#24939);
#20593=LINE('',#131606,#24940);
#20594=LINE('',#131616,#24941);
#20595=LINE('',#131626,#24942);
#20596=LINE('',#131627,#24943);
#20597=LINE('',#131628,#24944);
#20598=LINE('',#131631,#24945);
#20599=LINE('',#131682,#24946);
#20600=LINE('',#131683,#24947);
#20601=LINE('',#131697,#24948);
#20602=LINE('',#131702,#24949);
#20603=LINE('',#131894,#24950);
#20604=LINE('',#131895,#24951);
#20605=LINE('',#131909,#24952);
#20606=LINE('',#131913,#24953);
#20607=LINE('',#132070,#24954);
#20608=LINE('',#132071,#24955);
#20609=LINE('',#132085,#24956);
#20610=LINE('',#132087,#24957);
#20611=LINE('',#132180,#24958);
#20612=LINE('',#132184,#24959);
#20613=LINE('',#132220,#24960);
#20614=LINE('',#132222,#24961);
#20615=LINE('',#132353,#24962);
#20616=LINE('',#132356,#24963);
#20617=LINE('',#132370,#24964);
#20618=LINE('',#132372,#24965);
#20619=LINE('',#132513,#24966);
#20620=LINE('',#132514,#24967);
#20621=LINE('',#132528,#24968);
#20622=LINE('',#132530,#24969);
#20623=LINE('',#132701,#24970);
#20624=LINE('',#132702,#24971);
#20625=LINE('',#132754,#24972);
#20626=LINE('',#132758,#24973);
#20627=LINE('',#132781,#24974);
#20628=LINE('',#132785,#24975);
#20629=LINE('',#132840,#24976);
#20630=LINE('',#132844,#24977);
#20631=LINE('',#132910,#24978);
#20632=LINE('',#132914,#24979);
#20633=LINE('',#132952,#24980);
#20634=LINE('',#132956,#24981);
#20635=LINE('',#133051,#24982);
#20636=LINE('',#133055,#24983);
#20637=LINE('',#133112,#24984);
#20638=LINE('',#133116,#24985);
#20639=LINE('',#133176,#24986);
#20640=LINE('',#133180,#24987);
#20641=LINE('',#133185,#24988);
#20642=LINE('',#133187,#24989);
#20643=LINE('',#133197,#24990);
#20644=LINE('',#133207,#24991);
#20645=LINE('',#133209,#24992);
#20646=LINE('',#133231,#24993);
#20647=LINE('',#133233,#24994);
#20648=LINE('',#133235,#24995);
#20649=LINE('',#133237,#24996);
#20650=LINE('',#133247,#24997);
#20651=LINE('',#133256,#24998);
#20652=LINE('',#133266,#24999);
#20653=LINE('',#133270,#25000);
#20654=LINE('',#133273,#25001);
#20655=LINE('',#133274,#25002);
#20656=LINE('',#133284,#25003);
#20657=LINE('',#133286,#25004);
#20658=LINE('',#133296,#25005);
#20659=LINE('',#133306,#25006);
#20660=LINE('',#133307,#25007);
#20661=LINE('',#133308,#25008);
#20662=LINE('',#133327,#25009);
#20663=LINE('',#133337,#25010);
#20664=LINE('',#133346,#25011);
#20665=LINE('',#133376,#25012);
#20666=LINE('',#133387,#25013);
#20667=LINE('',#133472,#25014);
#20668=LINE('',#133484,#25015);
#20669=LINE('',#133632,#25016);
#20670=LINE('',#133644,#25017);
#20671=LINE('',#133825,#25018);
#20672=LINE('',#133837,#25019);
#20673=LINE('',#133932,#25020);
#20674=LINE('',#133943,#25021);
#20675=LINE('',#134047,#25022);
#20676=LINE('',#134058,#25023);
#20677=LINE('',#134095,#25024);
#20678=LINE('',#134121,#25025);
#20679=LINE('',#134151,#25026);
#20680=LINE('',#134181,#25027);
#20681=LINE('',#134184,#25028);
#20682=LINE('',#134224,#25029);
#20683=LINE('',#134260,#25030);
#20684=LINE('',#134276,#25031);
#20685=LINE('',#134306,#25032);
#20686=LINE('',#134336,#25033);
#20687=LINE('',#134338,#25034);
#20688=LINE('',#134368,#25035);
#20689=LINE('',#134393,#25036);
#20690=LINE('',#134424,#25037);
#20691=LINE('',#134454,#25038);
#20692=LINE('',#134494,#25039);
#20693=LINE('',#134510,#25040);
#20694=LINE('',#134540,#25041);
#20695=LINE('',#134570,#25042);
#20696=LINE('',#134572,#25043);
#20697=LINE('',#134576,#25044);
#20698=LINE('',#134601,#25045);
#20699=LINE('',#134632,#25046);
#20700=LINE('',#134662,#25047);
#20701=LINE('',#134665,#25048);
#20702=LINE('',#134694,#25049);
#20703=LINE('',#134739,#25050);
#20704=LINE('',#134755,#25051);
#20705=LINE('',#134785,#25052);
#20706=LINE('',#134815,#25053);
#20707=LINE('',#134853,#25054);
#20708=LINE('',#134870,#25055);
#20709=LINE('',#134886,#25056);
#20710=LINE('',#134916,#25057);
#20711=LINE('',#134946,#25058);
#20712=LINE('',#134950,#25059);
#20713=LINE('',#134976,#25060);
#20714=LINE('',#135006,#25061);
#20715=LINE('',#135040,#25062);
#20716=LINE('',#135043,#25063);
#20717=LINE('',#135056,#25064);
#20718=LINE('',#135064,#25065);
#20719=LINE('',#135067,#25066);
#20720=LINE('',#135070,#25067);
#20721=LINE('',#135075,#25068);
#20722=LINE('',#135078,#25069);
#20723=LINE('',#135080,#25070);
#20724=LINE('',#135081,#25071);
#20725=LINE('',#135084,#25072);
#20726=LINE('',#135243,#25073);
#20727=LINE('',#135246,#25074);
#20728=LINE('',#135269,#25075);
#20729=LINE('',#135281,#25076);
#20730=LINE('',#135285,#25077);
#20731=LINE('',#135289,#25078);
#20732=LINE('',#135292,#25079);
#20733=LINE('',#135301,#25080);
#20734=LINE('',#135304,#25081);
#20735=LINE('',#135313,#25082);
#20736=LINE('',#135316,#25083);
#20737=LINE('',#135386,#25084);
#20738=LINE('',#135389,#25085);
#20739=LINE('',#135398,#25086);
#20740=LINE('',#135401,#25087);
#20741=LINE('',#135410,#25088);
#20742=LINE('',#135413,#25089);
#20743=LINE('',#135466,#25090);
#20744=LINE('',#135468,#25091);
#20745=LINE('',#135474,#25092);
#20746=LINE('',#135477,#25093);
#20747=LINE('',#135486,#25094);
#20748=LINE('',#135489,#25095);
#20749=LINE('',#135498,#25096);
#20750=LINE('',#135501,#25097);
#20751=LINE('',#135504,#25098);
#20752=LINE('',#135508,#25099);
#20753=LINE('',#135514,#25100);
#20754=LINE('',#135517,#25101);
#20755=LINE('',#135526,#25102);
#20756=LINE('',#135529,#25103);
#20757=LINE('',#135538,#25104);
#20758=LINE('',#135541,#25105);
#20759=LINE('',#135544,#25106);
#20760=LINE('',#135548,#25107);
#20761=LINE('',#135553,#25108);
#20762=LINE('',#135554,#25109);
#20763=LINE('',#135557,#25110);
#20764=LINE('',#135559,#25111);
#20765=LINE('',#135561,#25112);
#20766=LINE('',#135563,#25113);
#20767=LINE('',#135576,#25114);
#20768=LINE('',#135609,#25115);
#20769=LINE('',#135614,#25116);
#20770=LINE('',#135637,#25117);
#20771=LINE('',#135638,#25118);
#20772=LINE('',#135641,#25119);
#20773=LINE('',#135644,#25120);
#20774=LINE('',#135655,#25121);
#20775=LINE('',#135656,#25122);
#20776=LINE('',#135679,#25123);
#20777=LINE('',#135680,#25124);
#20778=LINE('',#135703,#25125);
#20779=LINE('',#135704,#25126);
#20780=LINE('',#135727,#25127);
#20781=LINE('',#135728,#25128);
#20782=LINE('',#135767,#25129);
#20783=LINE('',#135805,#25130);
#20784=LINE('',#135927,#25131);
#20785=LINE('',#135930,#25132);
#20786=LINE('',#135944,#25133);
#20787=LINE('',#135946,#25134);
#20788=LINE('',#136104,#25135);
#20789=LINE('',#136107,#25136);
#20790=LINE('',#136121,#25137);
#20791=LINE('',#136123,#25138);
#20792=LINE('',#136281,#25139);
#20793=LINE('',#136284,#25140);
#20794=LINE('',#136298,#25141);
#20795=LINE('',#136300,#25142);
#20796=LINE('',#136396,#25143);
#20797=LINE('',#136402,#25144);
#20798=LINE('',#136404,#25145);
#20799=LINE('',#136512,#25146);
#20800=LINE('',#136515,#25147);
#20801=LINE('',#136625,#25148);
#20802=LINE('',#136715,#25149);
#20803=LINE('',#136775,#25150);
#20804=LINE('',#137031,#25151);
#20805=LINE('',#137052,#25152);
#20806=LINE('',#137107,#25153);
#20807=LINE('',#137111,#25154);
#20808=LINE('',#137114,#25155);
#20809=LINE('',#137140,#25156);
#20810=LINE('',#137161,#25157);
#20811=LINE('',#137165,#25158);
#20812=LINE('',#137166,#25159);
#20813=LINE('',#137169,#25160);
#20814=LINE('',#137188,#25161);
#20815=LINE('',#137192,#25162);
#20816=LINE('',#137217,#25163);
#20817=LINE('',#137273,#25164);
#20818=LINE('',#137277,#25165);
#20819=LINE('',#137280,#25166);
#20820=LINE('',#137315,#25167);
#20821=LINE('',#137372,#25168);
#20822=LINE('',#137375,#25169);
#20823=LINE('',#137379,#25170);
#20824=LINE('',#137405,#25171);
#20825=LINE('',#137409,#25172);
#20826=LINE('',#137410,#25173);
#20827=LINE('',#137413,#25174);
#20828=LINE('',#137433,#25175);
#20829=LINE('',#137436,#25176);
#20830=LINE('',#137549,#25177);
#20831=LINE('',#137834,#25178);
#20832=LINE('',#137892,#25179);
#20833=LINE('',#138042,#25180);
#20834=LINE('',#138045,#25181);
#20835=LINE('',#138048,#25182);
#20836=LINE('',#138051,#25183);
#20837=LINE('',#138052,#25184);
#20838=LINE('',#138055,#25185);
#20839=LINE('',#138059,#25186);
#20840=LINE('',#138062,#25187);
#20841=LINE('',#138065,#25188);
#20842=LINE('',#138066,#25189);
#20843=LINE('',#138069,#25190);
#20844=LINE('',#138074,#25191);
#20845=LINE('',#138078,#25192);
#20846=LINE('',#138117,#25193);
#20847=LINE('',#138151,#25194);
#20848=LINE('',#138204,#25195);
#20849=LINE('',#138208,#25196);
#20850=LINE('',#138212,#25197);
#20851=LINE('',#138214,#25198);
#20852=LINE('',#138235,#25199);
#20853=LINE('',#138262,#25200);
#20854=LINE('',#138266,#25201);
#20855=LINE('',#138267,#25202);
#20856=LINE('',#138270,#25203);
#20857=LINE('',#138314,#25204);
#20858=LINE('',#138340,#25205);
#20859=LINE('',#138344,#25206);
#20860=LINE('',#138439,#25207);
#20861=LINE('',#138479,#25208);
#20862=LINE('',#138502,#25209);
#20863=LINE('',#138743,#25210);
#20864=LINE('',#138764,#25211);
#20865=LINE('',#138786,#25212);
#20866=LINE('',#138850,#25213);
#20867=LINE('',#138878,#25214);
#20868=LINE('',#138889,#25215);
#20869=LINE('',#139046,#25216);
#20870=LINE('',#139057,#25217);
#20871=LINE('',#139084,#25218);
#20872=LINE('',#139159,#25219);
#20873=LINE('',#139199,#25220);
#20874=LINE('',#139222,#25221);
#20875=LINE('',#139447,#25222);
#20876=LINE('',#139470,#25223);
#20877=LINE('',#139512,#25224);
#20878=LINE('',#139551,#25225);
#20879=LINE('',#139555,#25226);
#20880=LINE('',#139559,#25227);
#20881=LINE('',#139588,#25228);
#20882=LINE('',#139612,#25229);
#20883=LINE('',#139616,#25230);
#20884=LINE('',#139617,#25231);
#20885=LINE('',#139620,#25232);
#20886=LINE('',#139656,#25233);
#20887=LINE('',#139685,#25234);
#20888=LINE('',#139687,#25235);
#20889=LINE('',#139691,#25236);
#20890=LINE('',#139769,#25237);
#20891=LINE('',#139803,#25238);
#20892=LINE('',#139807,#25239);
#20893=LINE('',#139808,#25240);
#20894=LINE('',#139818,#25241);
#20895=LINE('',#139819,#25242);
#20896=LINE('',#139918,#25243);
#20897=LINE('',#139968,#25244);
#20898=LINE('',#140003,#25245);
#20899=LINE('',#140005,#25246);
#20900=LINE('',#140009,#25247);
#20901=LINE('',#140013,#25248);
#20902=LINE('',#140014,#25249);
#20903=LINE('',#140017,#25250);
#20904=LINE('',#140021,#25251);
#20905=LINE('',#140022,#25252);
#20906=LINE('',#140025,#25253);
#20907=LINE('',#140062,#25254);
#20908=LINE('',#140075,#25255);
#20909=LINE('',#140077,#25256);
#20910=LINE('',#140081,#25257);
#20911=LINE('',#140095,#25258);
#20912=LINE('',#140135,#25259);
#20913=LINE('',#140137,#25260);
#20914=LINE('',#140138,#25261);
#20915=LINE('',#140224,#25262);
#20916=LINE('',#140228,#25263);
#20917=LINE('',#140252,#25264);
#20918=LINE('',#140300,#25265);
#20919=LINE('',#140317,#25266);
#20920=LINE('',#140362,#25267);
#20921=LINE('',#140366,#25268);
#20922=LINE('',#140370,#25269);
#20923=LINE('',#140372,#25270);
#20924=LINE('',#140385,#25271);
#20925=LINE('',#140429,#25272);
#20926=LINE('',#140463,#25273);
#20927=LINE('',#140466,#25274);
#20928=LINE('',#140470,#25275);
#20929=LINE('',#140471,#25276);
#20930=LINE('',#140474,#25277);
#20931=LINE('',#140479,#25278);
#20932=LINE('',#140483,#25279);
#20933=LINE('',#140486,#25280);
#20934=LINE('',#140542,#25281);
#20935=LINE('',#140583,#25282);
#20936=LINE('',#140595,#25283);
#20937=LINE('',#140600,#25284);
#20938=LINE('',#140601,#25285);
#20939=LINE('',#140688,#25286);
#20940=LINE('',#140691,#25287);
#20941=LINE('',#140695,#25288);
#20942=LINE('',#140735,#25289);
#20943=LINE('',#140738,#25290);
#20944=LINE('',#140742,#25291);
#20945=LINE('',#140743,#25292);
#20946=LINE('',#140746,#25293);
#20947=LINE('',#140830,#25294);
#20948=LINE('',#140833,#25295);
#20949=LINE('',#140920,#25296);
#20950=LINE('',#140921,#25297);
#20951=LINE('',#140923,#25298);
#20952=LINE('',#140927,#25299);
#20953=LINE('',#140928,#25300);
#20954=LINE('',#140931,#25301);
#20955=LINE('',#140935,#25302);
#20956=LINE('',#140936,#25303);
#20957=LINE('',#140939,#25304);
#20958=LINE('',#140943,#25305);
#20959=LINE('',#140946,#25306);
#20960=LINE('',#140990,#25307);
#20961=LINE('',#140996,#25308);
#20962=LINE('',#140997,#25309);
#20963=LINE('',#141096,#25310);
#20964=LINE('',#141143,#25311);
#20965=LINE('',#141180,#25312);
#20966=LINE('',#141182,#25313);
#20967=LINE('',#141186,#25314);
#20968=LINE('',#141190,#25315);
#20969=LINE('',#141191,#25316);
#20970=LINE('',#141194,#25317);
#20971=LINE('',#141198,#25318);
#20972=LINE('',#141199,#25319);
#20973=LINE('',#141202,#25320);
#20974=LINE('',#141249,#25321);
#20975=LINE('',#141251,#25322);
#20976=LINE('',#141273,#25323);
#20977=LINE('',#141286,#25324);
#20978=LINE('',#141288,#25325);
#20979=LINE('',#141292,#25326);
#20980=LINE('',#141295,#25327);
#20981=LINE('',#141317,#25328);
#20982=LINE('',#141319,#25329);
#20983=LINE('',#141324,#25330);
#20984=LINE('',#141328,#25331);
#20985=LINE('',#141362,#25332);
#20986=LINE('',#141416,#25333);
#20987=LINE('',#141467,#25334);
#20988=LINE('',#141512,#25335);
#20989=LINE('',#141516,#25336);
#20990=LINE('',#141520,#25337);
#20991=LINE('',#141522,#25338);
#20992=LINE('',#141535,#25339);
#20993=LINE('',#141579,#25340);
#20994=LINE('',#141616,#25341);
#20995=LINE('',#141619,#25342);
#20996=LINE('',#141623,#25343);
#20997=LINE('',#141624,#25344);
#20998=LINE('',#141627,#25345);
#20999=LINE('',#141632,#25346);
#21000=LINE('',#141636,#25347);
#21001=LINE('',#141639,#25348);
#21002=LINE('',#141689,#25349);
#21003=LINE('',#141730,#25350);
#21004=LINE('',#141742,#25351);
#21005=LINE('',#141858,#25352);
#21006=LINE('',#141897,#25353);
#21007=LINE('',#141901,#25354);
#21008=LINE('',#141902,#25355);
#21009=LINE('',#141959,#25356);
#21010=LINE('',#141993,#25357);
#21011=LINE('',#141995,#25358);
#21012=LINE('',#141997,#25359);
#21013=LINE('',#142027,#25360);
#21014=LINE('',#142029,#25361);
#21015=LINE('',#142033,#25362);
#21016=LINE('',#142037,#25363);
#21017=LINE('',#142038,#25364);
#21018=LINE('',#142041,#25365);
#21019=LINE('',#142045,#25366);
#21020=LINE('',#142046,#25367);
#21021=LINE('',#142049,#25368);
#21022=LINE('',#142054,#25369);
#21023=LINE('',#142058,#25370);
#21024=LINE('',#142072,#25371);
#21025=LINE('',#142119,#25372);
#21026=LINE('',#142157,#25373);
#21027=LINE('',#142169,#25374);
#21028=LINE('',#142205,#25375);
#21029=LINE('',#142206,#25376);
#21030=LINE('',#142254,#25377);
#21031=LINE('',#142258,#25378);
#21032=LINE('',#142262,#25379);
#21033=LINE('',#142264,#25380);
#21034=LINE('',#142277,#25381);
#21035=LINE('',#142327,#25382);
#21036=LINE('',#142367,#25383);
#21037=LINE('',#142370,#25384);
#21038=LINE('',#142374,#25385);
#21039=LINE('',#142375,#25386);
#21040=LINE('',#142378,#25387);
#21041=LINE('',#142425,#25388);
#21042=LINE('',#142429,#25389);
#21043=LINE('',#142432,#25390);
#21044=LINE('',#142488,#25391);
#21045=LINE('',#142526,#25392);
#21046=LINE('',#142538,#25393);
#21047=LINE('',#142540,#25394);
#21048=LINE('',#142547,#25395);
#21049=LINE('',#142554,#25396);
#21050=LINE('',#142608,#25397);
#21051=LINE('',#142614,#25398);
#21052=LINE('',#142668,#25399);
#21053=LINE('',#142674,#25400);
#21054=LINE('',#142678,#25401);
#21055=LINE('',#142679,#25402);
#21056=LINE('',#142795,#25403);
#21057=LINE('',#142797,#25404);
#21058=LINE('',#142874,#25405);
#21059=LINE('',#142876,#25406);
#21060=LINE('',#142972,#25407);
#21061=LINE('',#142985,#25408);
#21062=LINE('',#142989,#25409);
#21063=LINE('',#142990,#25410);
#21064=LINE('',#143005,#25411);
#21065=LINE('',#143023,#25412);
#21066=LINE('',#143036,#25413);
#21067=LINE('',#143040,#25414);
#21068=LINE('',#143041,#25415);
#21069=LINE('',#143056,#25416);
#21070=LINE('',#143071,#25417);
#21071=LINE('',#143088,#25418);
#21072=LINE('',#143123,#25419);
#21073=LINE('',#143169,#25420);
#21074=LINE('',#143215,#25421);
#21075=LINE('',#143216,#25422);
#21076=LINE('',#143219,#25423);
#21077=LINE('',#143223,#25424);
#21078=LINE('',#143227,#25425);
#21079=LINE('',#143231,#25426);
#21080=LINE('',#143233,#25427);
#21081=LINE('',#143249,#25428);
#21082=LINE('',#143251,#25429);
#21083=LINE('',#143261,#25430);
#21084=LINE('',#143271,#25431);
#21085=LINE('',#143273,#25432);
#21086=LINE('',#143275,#25433);
#21087=LINE('',#143285,#25434);
#21088=LINE('',#143294,#25435);
#21089=LINE('',#143298,#25436);
#21090=LINE('',#143304,#25437);
#21091=LINE('',#143313,#25438);
#21092=LINE('',#143366,#25439);
#21093=LINE('',#143370,#25440);
#21094=LINE('',#143392,#25441);
#21095=LINE('',#143396,#25442);
#21096=LINE('',#143453,#25443);
#21097=LINE('',#143457,#25444);
#21098=LINE('',#143511,#25445);
#21099=LINE('',#143515,#25446);
#21100=LINE('',#143576,#25447);
#21101=LINE('',#143580,#25448);
#21102=LINE('',#143641,#25449);
#21103=LINE('',#143645,#25450);
#21104=LINE('',#143698,#25451);
#21105=LINE('',#143705,#25452);
#21106=LINE('',#143715,#25453);
#21107=LINE('',#143717,#25454);
#21108=LINE('',#143727,#25455);
#21109=LINE('',#143737,#25456);
#21110=LINE('',#143739,#25457);
#21111=LINE('',#143754,#25458);
#21112=LINE('',#143756,#25459);
#21113=LINE('',#143758,#25460);
#21114=LINE('',#143768,#25461);
#21115=LINE('',#143777,#25462);
#21116=LINE('',#143780,#25463);
#21117=LINE('',#143784,#25464);
#21118=LINE('',#143788,#25465);
#21119=LINE('',#143792,#25466);
#21120=LINE('',#143808,#25467);
#21121=LINE('',#143810,#25468);
#21122=LINE('',#143820,#25469);
#21123=LINE('',#143830,#25470);
#21124=LINE('',#143832,#25471);
#21125=LINE('',#143834,#25472);
#21126=LINE('',#143844,#25473);
#21127=LINE('',#143853,#25474);
#21128=LINE('',#143889,#25475);
#21129=LINE('',#143897,#25476);
#21130=LINE('',#143898,#25477);
#21131=LINE('',#143899,#25478);
#21132=LINE('',#143934,#25479);
#21133=LINE('',#143937,#25480);
#21134=LINE('',#143972,#25481);
#21135=LINE('',#143980,#25482);
#21136=LINE('',#143981,#25483);
#21137=LINE('',#143983,#25484);
#21138=LINE('',#143987,#25485);
#21139=LINE('',#144034,#25486);
#21140=LINE('',#144038,#25487);
#21141=LINE('',#144039,#25488);
#21142=LINE('',#144324,#25489);
#21143=LINE('',#144327,#25490);
#21144=LINE('',#144372,#25491);
#21145=LINE('',#144472,#25492);
#21146=LINE('',#144530,#25493);
#21147=LINE('',#144532,#25494);
#21148=LINE('',#144608,#25495);
#21149=LINE('',#144709,#25496);
#21150=LINE('',#144776,#25497);
#21151=LINE('',#144782,#25498);
#21152=LINE('',#144862,#25499);
#21153=LINE('',#144890,#25500);
#21154=LINE('',#144969,#25501);
#21155=LINE('',#145038,#25502);
#21156=LINE('',#145254,#25503);
#21157=LINE('',#145264,#25504);
#21158=LINE('',#145270,#25505);
#21159=LINE('',#145355,#25506);
#21160=LINE('',#145427,#25507);
#21161=LINE('',#145540,#25508);
#21162=LINE('',#145613,#25509);
#21163=LINE('',#145629,#25510);
#21164=LINE('',#145635,#25511);
#21165=LINE('',#145660,#25512);
#21166=LINE('',#145743,#25513);
#21167=LINE('',#145894,#25514);
#21168=LINE('',#146025,#25515);
#21169=LINE('',#146028,#25516);
#21170=LINE('',#146214,#25517);
#21171=LINE('',#146329,#25518);
#21172=LINE('',#146469,#25519);
#21173=LINE('',#146472,#25520);
#21174=LINE('',#146596,#25521);
#21175=LINE('',#146702,#25522);
#21176=LINE('',#146885,#25523);
#21177=LINE('',#146888,#25524);
#21178=LINE('',#147055,#25525);
#21179=LINE('',#147171,#25526);
#21180=LINE('',#147276,#25527);
#21181=LINE('',#147282,#25528);
#21182=LINE('',#147307,#25529);
#21183=LINE('',#147314,#25530);
#21184=LINE('',#147447,#25531);
#21185=LINE('',#147558,#25532);
#21186=LINE('',#147574,#25533);
#21187=LINE('',#147597,#25534);
#21188=LINE('',#147766,#25535);
#21189=LINE('',#147780,#25536);
#21190=LINE('',#147853,#25537);
#21191=LINE('',#147971,#25538);
#21192=LINE('',#147974,#25539);
#21193=LINE('',#147986,#25540);
#21194=LINE('',#148021,#25541);
#21195=LINE('',#148028,#25542);
#21196=LINE('',#148199,#25543);
#21197=LINE('',#148253,#25544);
#21198=LINE('',#148345,#25545);
#21199=LINE('',#148481,#25546);
#21200=LINE('',#148529,#25547);
#21201=LINE('',#148543,#25548);
#21202=LINE('',#148549,#25549);
#21203=LINE('',#148555,#25550);
#21204=LINE('',#148611,#25551);
#21205=LINE('',#148725,#25552);
#21206=LINE('',#148798,#25553);
#21207=LINE('',#149017,#25554);
#21208=LINE('',#149177,#25555);
#21209=LINE('',#149191,#25556);
#21210=LINE('',#149327,#25557);
#21211=LINE('',#149468,#25558);
#21212=LINE('',#149471,#25559);
#21213=LINE('',#149476,#25560);
#21214=LINE('',#149510,#25561);
#21215=LINE('',#149517,#25562);
#21216=LINE('',#149585,#25563);
#21217=LINE('',#149742,#25564);
#21218=LINE('',#149832,#25565);
#21219=LINE('',#149927,#25566);
#21220=LINE('',#150033,#25567);
#21221=LINE('',#150081,#25568);
#21222=LINE('',#150095,#25569);
#21223=LINE('',#150101,#25570);
#21224=LINE('',#150107,#25571);
#21225=LINE('',#150163,#25572);
#21226=LINE('',#150277,#25573);
#21227=LINE('',#150388,#25574);
#21228=LINE('',#150496,#25575);
#21229=LINE('',#150503,#25576);
#21230=LINE('',#150583,#25577);
#21231=LINE('',#150707,#25578);
#21232=LINE('',#150721,#25579);
#21233=LINE('',#150758,#25580);
#21234=LINE('',#150765,#25581);
#21235=LINE('',#150771,#25582);
#21236=LINE('',#150829,#25583);
#21237=LINE('',#150974,#25584);
#21238=LINE('',#151117,#25585);
#21239=LINE('',#151240,#25586);
#21240=LINE('',#151360,#25587);
#21241=LINE('',#151408,#25588);
#21242=LINE('',#151422,#25589);
#21243=LINE('',#151428,#25590);
#21244=LINE('',#151435,#25591);
#21245=LINE('',#151493,#25592);
#21246=LINE('',#151585,#25593);
#21247=LINE('',#151669,#25594);
#21248=LINE('',#151676,#25595);
#21249=LINE('',#151751,#25596);
#21250=LINE('',#151771,#25597);
#21251=LINE('',#151793,#25598);
#21252=LINE('',#151815,#25599);
#21253=LINE('',#152356,#25600);
#21254=LINE('',#152378,#25601);
#21255=LINE('',#152426,#25602);
#21256=LINE('',#152448,#25603);
#21257=LINE('',#152495,#25604);
#21258=LINE('',#152515,#25605);
#21259=LINE('',#152537,#25606);
#21260=LINE('',#152559,#25607);
#21261=LINE('',#152639,#25608);
#21262=LINE('',#152732,#25609);
#21263=LINE('',#152734,#25610);
#21264=LINE('',#152736,#25611);
#21265=LINE('',#152785,#25612);
#21266=LINE('',#152786,#25613);
#21267=LINE('',#152788,#25614);
#21268=LINE('',#153027,#25615);
#21269=LINE('',#153029,#25616);
#21270=LINE('',#153030,#25617);
#21271=LINE('',#153080,#25618);
#21272=LINE('',#153104,#25619);
#21273=LINE('',#153106,#25620);
#21274=LINE('',#153197,#25621);
#21275=LINE('',#153199,#25622);
#21276=LINE('',#153209,#25623);
#21277=LINE('',#153211,#25624);
#21278=LINE('',#153331,#25625);
#21279=LINE('',#153333,#25626);
#21280=LINE('',#153410,#25627);
#21281=LINE('',#153412,#25628);
#21282=LINE('',#153462,#25629);
#21283=LINE('',#153464,#25630);
#21284=LINE('',#153472,#25631);
#21285=LINE('',#153473,#25632);
#21286=LINE('',#153477,#25633);
#21287=LINE('',#153479,#25634);
#21288=LINE('',#153481,#25635);
#21289=LINE('',#153482,#25636);
#21290=LINE('',#153487,#25637);
#21291=LINE('',#153491,#25638);
#21292=LINE('',#153493,#25639);
#21293=LINE('',#153494,#25640);
#21294=LINE('',#153798,#25641);
#21295=LINE('',#153799,#25642);
#21296=LINE('',#154231,#25643);
#21297=LINE('',#154232,#25644);
#21298=LINE('',#154233,#25645);
#21299=LINE('',#154237,#25646);
#21300=LINE('',#154239,#25647);
#21301=LINE('',#154241,#25648);
#21302=LINE('',#154242,#25649);
#21303=LINE('',#154247,#25650);
#21304=LINE('',#154251,#25651);
#21305=LINE('',#154253,#25652);
#21306=LINE('',#154254,#25653);
#21307=LINE('',#154603,#25654);
#21308=LINE('',#154618,#25655);
#21309=LINE('',#154810,#25656);
#21310=LINE('',#154812,#25657);
#21311=LINE('',#154814,#25658);
#21312=LINE('',#154815,#25659);
#21313=LINE('',#154820,#25660);
#21314=LINE('',#154824,#25661);
#21315=LINE('',#154826,#25662);
#21316=LINE('',#154827,#25663);
#21317=LINE('',#154831,#25664);
#21318=LINE('',#154833,#25665);
#21319=LINE('',#154997,#25666);
#21320=LINE('',#154998,#25667);
#21321=LINE('',#155371,#25668);
#21322=LINE('',#155373,#25669);
#21323=LINE('',#155376,#25670);
#21324=LINE('',#155810,#25671);
#21325=LINE('',#155816,#25672);
#21326=LINE('',#156128,#25673);
#21327=LINE('',#156130,#25674);
#21328=LINE('',#156132,#25675);
#21329=LINE('',#156133,#25676);
#21330=LINE('',#156137,#25677);
#21331=LINE('',#156142,#25678);
#21332=LINE('',#156144,#25679);
#21333=LINE('',#156145,#25680);
#21334=LINE('',#156240,#25681);
#21335=LINE('',#156242,#25682);
#21336=LINE('',#156244,#25683);
#21337=LINE('',#156245,#25684);
#21338=LINE('',#156250,#25685);
#21339=LINE('',#156254,#25686);
#21340=LINE('',#156256,#25687);
#21341=LINE('',#156257,#25688);
#21342=LINE('',#156261,#25689);
#21343=LINE('',#156263,#25690);
#21344=LINE('',#156427,#25691);
#21345=LINE('',#156428,#25692);
#21346=LINE('',#156709,#25693);
#21347=LINE('',#156711,#25694);
#21348=LINE('',#156714,#25695);
#21349=LINE('',#157090,#25696);
#21350=LINE('',#157096,#25697);
#21351=LINE('',#157100,#25698);
#21352=LINE('',#157102,#25699);
#21353=LINE('',#157104,#25700);
#21354=LINE('',#157105,#25701);
#21355=LINE('',#157109,#25702);
#21356=LINE('',#157114,#25703);
#21357=LINE('',#157116,#25704);
#21358=LINE('',#157117,#25705);
#21359=LINE('',#157344,#25706);
#21360=LINE('',#157348,#25707);
#21361=LINE('',#157352,#25708);
#21362=LINE('',#157355,#25709);
#21363=LINE('',#157379,#25710);
#21364=LINE('',#157400,#25711);
#21365=LINE('',#157647,#25712);
#21366=LINE('',#157651,#25713);
#21367=LINE('',#157652,#25714);
#21368=LINE('',#157656,#25715);
#21369=LINE('',#157658,#25716);
#21370=LINE('',#157660,#25717);
#21371=LINE('',#157661,#25718);
#21372=LINE('',#157722,#25719);
#21373=LINE('',#157743,#25720);
#21374=LINE('',#158254,#25721);
#21375=LINE('',#158281,#25722);
#21376=LINE('',#158569,#25723);
#21377=LINE('',#158593,#25724);
#21378=LINE('',#158974,#25725);
#21379=LINE('',#158995,#25726);
#21380=LINE('',#159250,#25727);
#21381=LINE('',#159270,#25728);
#21382=LINE('',#159272,#25729);
#21383=LINE('',#159274,#25730);
#21384=LINE('',#159275,#25731);
#21385=LINE('',#159279,#25732);
#21386=LINE('',#159283,#25733);
#21387=LINE('',#159288,#25734);
#21388=LINE('',#159292,#25735);
#21389=LINE('',#159317,#25736);
#21390=LINE('',#159338,#25737);
#21391=LINE('',#159553,#25738);
#21392=LINE('',#159556,#25739);
#21393=LINE('',#159560,#25740);
#21394=LINE('',#159561,#25741);
#21395=LINE('',#159562,#25742);
#21396=LINE('',#159566,#25743);
#21397=LINE('',#159567,#25744);
#21398=LINE('',#159568,#25745);
#21399=LINE('',#159592,#25746);
#21400=LINE('',#159610,#25747);
#21401=LINE('',#159614,#25748);
#21402=LINE('',#159616,#25749);
#21403=LINE('',#159618,#25750);
#21404=LINE('',#159619,#25751);
#21405=LINE('',#159640,#25752);
#21406=LINE('',#159658,#25753);
#21407=LINE('',#159688,#25754);
#21408=LINE('',#159715,#25755);
#21409=LINE('',#159719,#25756);
#21410=LINE('',#159723,#25757);
#21411=LINE('',#160105,#25758);
#21412=LINE('',#160415,#25759);
#21413=LINE('',#160576,#25760);
#21414=LINE('',#160655,#25761);
#21415=LINE('',#160886,#25762);
#21416=LINE('',#160965,#25763);
#21417=LINE('',#161038,#25764);
#21418=LINE('',#161139,#25765);
#21419=LINE('',#161300,#25766);
#21420=LINE('',#161337,#25767);
#21421=LINE('',#161409,#25768);
#21422=LINE('',#161491,#25769);
#21423=LINE('',#161576,#25770);
#21424=LINE('',#163686,#25771);
#21425=LINE('',#163847,#25772);
#21426=LINE('',#163926,#25773);
#21427=LINE('',#164157,#25774);
#21428=LINE('',#164236,#25775);
#21429=LINE('',#164309,#25776);
#21430=LINE('',#164331,#25777);
#21431=LINE('',#164403,#25778);
#21432=LINE('',#164892,#25779);
#21433=LINE('',#164893,#25780);
#21434=LINE('',#164894,#25781);
#21435=LINE('',#164898,#25782);
#21436=LINE('',#164941,#25783);
#21437=LINE('',#164947,#25784);
#21438=LINE('',#164948,#25785);
#21439=LINE('',#164957,#25786);
#21440=LINE('',#165053,#25787);
#21441=LINE('',#165156,#25788);
#21442=LINE('',#165202,#25789);
#21443=LINE('',#165203,#25790);
#21444=LINE('',#165205,#25791);
#21445=LINE('',#165211,#25792);
#21446=LINE('',#165214,#25793);
#21447=LINE('',#165223,#25794);
#21448=LINE('',#165233,#25795);
#21449=LINE('',#165240,#25796);
#21450=LINE('',#165243,#25797);
#21451=LINE('',#165245,#25798);
#21452=LINE('',#165290,#25799);
#21453=LINE('',#165399,#25800);
#21454=LINE('',#165576,#25801);
#21455=LINE('',#165579,#25802);
#21456=LINE('',#165661,#25803);
#21457=LINE('',#165668,#25804);
#21458=LINE('',#165670,#25805);
#21459=LINE('',#165793,#25806);
#21460=LINE('',#165909,#25807);
#21461=LINE('',#165955,#25808);
#21462=LINE('',#165956,#25809);
#21463=LINE('',#165958,#25810);
#21464=LINE('',#165967,#25811);
#21465=LINE('',#165973,#25812);
#21466=LINE('',#165976,#25813);
#21467=LINE('',#165979,#25814);
#21468=LINE('',#165982,#25815);
#21469=LINE('',#165985,#25816);
#21470=LINE('',#166083,#25817);
#21471=LINE('',#166089,#25818);
#21472=LINE('',#166093,#25819);
#21473=LINE('',#166094,#25820);
#21474=LINE('',#166227,#25821);
#21475=LINE('',#166333,#25822);
#21476=LINE('',#166340,#25823);
#21477=LINE('',#166344,#25824);
#21478=LINE('',#166345,#25825);
#21479=LINE('',#166469,#25826);
#21480=LINE('',#166637,#25827);
#21481=LINE('',#166737,#25828);
#21482=LINE('',#166781,#25829);
#21483=LINE('',#166782,#25830);
#21484=LINE('',#166784,#25831);
#21485=LINE('',#166793,#25832);
#21486=LINE('',#166803,#25833);
#21487=LINE('',#166810,#25834);
#21488=LINE('',#166813,#25835);
#21489=LINE('',#166815,#25836);
#21490=LINE('',#166860,#25837);
#21491=LINE('',#166981,#25838);
#21492=LINE('',#167068,#25839);
#21493=LINE('',#167071,#25840);
#21494=LINE('',#167224,#25841);
#21495=LINE('',#167345,#25842);
#21496=LINE('',#167471,#25843);
#21497=LINE('',#167472,#25844);
#21498=LINE('',#167474,#25845);
#21499=LINE('',#167477,#25846);
#21500=LINE('',#167479,#25847);
#21501=LINE('',#167485,#25848);
#21502=LINE('',#167488,#25849);
#21503=LINE('',#167532,#25850);
#21504=LINE('',#167533,#25851);
#21505=LINE('',#167536,#25852);
#21506=LINE('',#167544,#25853);
#21507=LINE('',#167621,#25854);
#21508=LINE('',#167668,#25855);
#21509=LINE('',#167675,#25856);
#21510=LINE('',#167799,#25857);
#21511=LINE('',#167999,#25858);
#21512=LINE('',#168006,#25859);
#21513=LINE('',#168010,#25860);
#21514=LINE('',#168012,#25861);
#21515=LINE('',#168056,#25862);
#21516=LINE('',#168059,#25863);
#21517=LINE('',#168064,#25864);
#21518=LINE('',#168065,#25865);
#21519=LINE('',#168251,#25866);
#21520=LINE('',#168254,#25867);
#21521=LINE('',#168266,#25868);
#21522=LINE('',#168269,#25869);
#21523=LINE('',#168278,#25870);
#21524=LINE('',#168374,#25871);
#21525=LINE('',#168397,#25872);
#21526=LINE('',#168483,#25873);
#21527=LINE('',#168486,#25874);
#21528=LINE('',#168498,#25875);
#21529=LINE('',#168500,#25876);
#21530=LINE('',#168512,#25877);
#21531=LINE('',#168515,#25878);
#21532=LINE('',#168693,#25879);
#21533=LINE('',#168694,#25880);
#21534=LINE('',#168699,#25881);
#21535=LINE('',#168700,#25882);
#21536=LINE('',#168711,#25883);
#21537=LINE('',#168885,#25884);
#21538=LINE('',#168985,#25885);
#21539=LINE('',#169029,#25886);
#21540=LINE('',#169030,#25887);
#21541=LINE('',#169032,#25888);
#21542=LINE('',#169041,#25889);
#21543=LINE('',#169051,#25890);
#21544=LINE('',#169058,#25891);
#21545=LINE('',#169061,#25892);
#21546=LINE('',#169063,#25893);
#21547=LINE('',#169108,#25894);
#21548=LINE('',#169229,#25895);
#21549=LINE('',#169307,#25896);
#21550=LINE('',#169310,#25897);
#21551=LINE('',#169451,#25898);
#21552=LINE('',#169515,#25899);
#21553=LINE('',#169695,#25900);
#21554=LINE('',#169698,#25901);
#21555=LINE('',#169742,#25902);
#21556=LINE('',#169743,#25903);
#21557=LINE('',#169746,#25904);
#21558=LINE('',#169755,#25905);
#21559=LINE('',#169847,#25906);
#21560=LINE('',#169849,#25907);
#21561=LINE('',#169850,#25908);
#21562=LINE('',#169855,#25909);
#21563=LINE('',#169856,#25910);
#21564=LINE('',#169865,#25911);
#21565=LINE('',#169872,#25912);
#21566=LINE('',#169986,#25913);
#21567=LINE('',#170112,#25914);
#21568=LINE('',#170119,#25915);
#21569=LINE('',#170123,#25916);
#21570=LINE('',#170125,#25917);
#21571=LINE('',#170173,#25918);
#21572=LINE('',#170176,#25919);
#21573=LINE('',#170179,#25920);
#21574=LINE('',#170182,#25921);
#21575=LINE('',#170276,#25922);
#21576=LINE('',#170363,#25923);
#21577=LINE('',#170370,#25924);
#21578=LINE('',#170374,#25925);
#21579=LINE('',#170375,#25926);
#21580=LINE('',#170583,#25927);
#21581=LINE('',#170663,#25928);
#21582=LINE('',#170664,#25929);
#21583=LINE('',#170667,#25930);
#21584=LINE('',#170675,#25931);
#21585=LINE('',#170744,#25932);
#21586=LINE('',#170754,#25933);
#21587=LINE('',#170760,#25934);
#21588=LINE('',#170762,#25935);
#21589=LINE('',#170843,#25936);
#21590=LINE('',#171193,#25937);
#21591=LINE('',#171261,#25938);
#21592=LINE('',#171262,#25939);
#21593=LINE('',#171386,#25940);
#21594=LINE('',#171387,#25941);
#21595=LINE('',#171394,#25942);
#21596=LINE('',#171399,#25943);
#21597=LINE('',#171482,#25944);
#21598=LINE('',#171484,#25945);
#21599=LINE('',#171553,#25946);
#21600=LINE('',#171774,#25947);
#21601=LINE('',#171824,#25948);
#21602=LINE('',#171825,#25949);
#21603=LINE('',#171916,#25950);
#21604=LINE('',#171917,#25951);
#21605=LINE('',#171921,#25952);
#21606=LINE('',#171926,#25953);
#21607=LINE('',#171985,#25954);
#21608=LINE('',#171987,#25955);
#21609=LINE('',#172038,#25956);
#21610=LINE('',#172247,#25957);
#21611=LINE('',#172315,#25958);
#21612=LINE('',#172316,#25959);
#21613=LINE('',#172431,#25960);
#21614=LINE('',#172434,#25961);
#21615=LINE('',#172441,#25962);
#21616=LINE('',#172446,#25963);
#21617=LINE('',#172529,#25964);
#21618=LINE('',#172531,#25965);
#21619=LINE('',#172600,#25966);
#21620=LINE('',#172905,#25967);
#21621=LINE('',#172982,#25968);
#21622=LINE('',#172983,#25969);
#21623=LINE('',#172990,#25970);
#21624=LINE('',#173071,#25971);
#21625=LINE('',#173081,#25972);
#21626=LINE('',#173088,#25973);
#21627=LINE('',#173091,#25974);
#21628=LINE('',#173093,#25975);
#21629=LINE('',#173166,#25976);
#21630=LINE('',#173510,#25977);
#21631=LINE('',#173629,#25978);
#21632=LINE('',#173716,#25979);
#21633=LINE('',#173717,#25980);
#21634=LINE('',#173719,#25981);
#21635=LINE('',#173728,#25982);
#21636=LINE('',#173742,#25983);
#21637=LINE('',#174056,#25984);
#21638=LINE('',#174059,#25985);
#21639=LINE('',#174071,#25986);
#21640=LINE('',#174073,#25987);
#21641=LINE('',#174085,#25988);
#21642=LINE('',#174088,#25989);
#21643=LINE('',#174293,#25990);
#21644=LINE('',#174386,#25991);
#21645=LINE('',#174587,#25992);
#21646=LINE('',#174630,#25993);
#21647=LINE('',#174748,#25994);
#21648=LINE('',#174758,#25995);
#21649=LINE('',#174842,#25996);
#21650=LINE('',#175171,#25997);
#21651=LINE('',#175279,#25998);
#21652=LINE('',#175282,#25999);
#21653=LINE('',#175290,#26000);
#21654=LINE('',#175299,#26001);
#21655=LINE('',#175371,#26002);
#21656=LINE('',#175607,#26003);
#21657=LINE('',#175687,#26004);
#21658=LINE('',#175690,#26005);
#21659=LINE('',#175746,#26006);
#21660=LINE('',#175805,#26007);
#21661=LINE('',#175806,#26008);
#21662=LINE('',#176249,#26009);
#21663=LINE('',#176267,#26010);
#21664=LINE('',#176271,#26011);
#21665=LINE('',#176290,#26012);
#21666=LINE('',#176329,#26013);
#21667=LINE('',#176403,#26014);
#21668=LINE('',#176406,#26015);
#21669=LINE('',#176648,#26016);
#21670=LINE('',#176650,#26017);
#21671=LINE('',#176651,#26018);
#21672=LINE('',#176655,#26019);
#21673=LINE('',#176659,#26020);
#21674=LINE('',#176663,#26021);
#21675=LINE('',#176666,#26022);
#21676=LINE('',#176667,#26023);
#21677=LINE('',#176670,#26024);
#21678=LINE('',#176674,#26025);
#21679=LINE('',#176679,#26026);
#21680=LINE('',#176682,#26027);
#21681=LINE('',#176683,#26028);
#21682=LINE('',#176687,#26029);
#21683=LINE('',#176691,#26030);
#21684=LINE('',#176695,#26031);
#21685=LINE('',#176699,#26032);
#21686=LINE('',#176701,#26033);
#21687=LINE('',#176716,#26034);
#21688=LINE('',#176717,#26035);
#21689=LINE('',#176849,#26036);
#21690=LINE('',#176895,#26037);
#21691=LINE('',#176978,#26038);
#21692=LINE('',#176981,#26039);
#21693=LINE('',#176983,#26040);
#21694=LINE('',#177000,#26041);
#21695=LINE('',#177017,#26042);
#21696=LINE('',#177020,#26043);
#21697=LINE('',#177023,#26044);
#21698=LINE('',#177024,#26045);
#21699=LINE('',#177028,#26046);
#21700=LINE('',#177044,#26047);
#21701=LINE('',#177061,#26048);
#21702=LINE('',#177064,#26049);
#21703=LINE('',#177067,#26050);
#21704=LINE('',#177068,#26051);
#21705=LINE('',#177072,#26052);
#21706=LINE('',#177090,#26053);
#21707=LINE('',#177367,#26054);
#21708=LINE('',#177371,#26055);
#21709=LINE('',#177375,#26056);
#21710=LINE('',#177377,#26057);
#21711=LINE('',#177383,#26058);
#21712=LINE('',#177589,#26059);
#21713=LINE('',#177593,#26060);
#21714=LINE('',#177597,#26061);
#21715=LINE('',#177599,#26062);
#21716=LINE('',#177608,#26063);
#21717=LINE('',#177729,#26064);
#21718=LINE('',#177730,#26065);
#21719=LINE('',#177838,#26066);
#21720=LINE('',#177839,#26067);
#21721=LINE('',#177843,#26068);
#21722=LINE('',#177851,#26069);
#21723=LINE('',#177854,#26070);
#21724=LINE('',#177857,#26071);
#21725=LINE('',#177862,#26072);
#21726=LINE('',#177871,#26073);
#21727=LINE('',#177876,#26074);
#21728=LINE('',#177877,#26075);
#21729=LINE('',#177882,#26076);
#21730=LINE('',#177885,#26077);
#21731=LINE('',#177915,#26078);
#21732=LINE('',#177916,#26079);
#21733=LINE('',#177920,#26080);
#21734=LINE('',#177928,#26081);
#21735=LINE('',#177931,#26082);
#21736=LINE('',#177934,#26083);
#21737=LINE('',#177937,#26084);
#21738=LINE('',#177952,#26085);
#21739=LINE('',#177953,#26086);
#21740=LINE('',#178118,#26087);
#21741=LINE('',#178121,#26088);
#21742=LINE('',#178122,#26089);
#21743=LINE('',#178171,#26090);
#21744=LINE('',#178174,#26091);
#21745=LINE('',#178291,#26092);
#21746=LINE('',#178410,#26093);
#21747=LINE('',#178411,#26094);
#21748=LINE('',#178469,#26095);
#21749=LINE('',#178472,#26096);
#21750=LINE('',#178473,#26097);
#21751=LINE('',#178522,#26098);
#21752=LINE('',#178525,#26099);
#21753=LINE('',#178640,#26100);
#21754=LINE('',#178642,#26101);
#21755=LINE('',#178833,#26102);
#21756=LINE('',#178834,#26103);
#21757=LINE('',#178886,#26104);
#21758=LINE('',#178889,#26105);
#21759=LINE('',#178890,#26106);
#21760=LINE('',#178945,#26107);
#21761=LINE('',#178948,#26108);
#21762=LINE('',#179070,#26109);
#21763=LINE('',#179172,#26110);
#21764=LINE('',#179173,#26111);
#21765=LINE('',#179187,#26112);
#21766=LINE('',#179188,#26113);
#21767=LINE('',#179342,#26114);
#21768=LINE('',#179345,#26115);
#21769=LINE('',#179346,#26116);
#21770=LINE('',#179401,#26117);
#21771=LINE('',#179404,#26118);
#21772=LINE('',#179626,#26119);
#21773=LINE('',#179628,#26120);
#21774=LINE('',#179641,#26121);
#21775=LINE('',#179642,#26122);
#21776=LINE('',#179700,#26123);
#21777=LINE('',#179703,#26124);
#21778=LINE('',#179704,#26125);
#21779=LINE('',#179753,#26126);
#21780=LINE('',#179756,#26127);
#21781=LINE('',#180023,#26128);
#21782=LINE('',#180024,#26129);
#21783=LINE('',#180025,#26130);
#21784=LINE('',#180083,#26131);
#21785=LINE('',#180086,#26132);
#21786=LINE('',#180087,#26133);
#21787=LINE('',#180136,#26134);
#21788=LINE('',#180139,#26135);
#21789=LINE('',#180150,#26136);
#21790=LINE('',#180359,#26137);
#21791=LINE('',#180373,#26138);
#21792=LINE('',#180374,#26139);
#21793=LINE('',#180426,#26140);
#21794=LINE('',#180429,#26141);
#21795=LINE('',#180430,#26142);
#21796=LINE('',#180485,#26143);
#21797=LINE('',#180488,#26144);
#21798=LINE('',#180610,#26145);
#21799=LINE('',#180667,#26146);
#21800=LINE('',#180668,#26147);
#21801=LINE('',#180820,#26148);
#21802=LINE('',#180821,#26149);
#21803=LINE('',#180873,#26150);
#21804=LINE('',#180876,#26151);
#21805=LINE('',#180877,#26152);
#21806=LINE('',#180932,#26153);
#21807=LINE('',#180935,#26154);
#21808=LINE('',#181157,#26155);
#21809=LINE('',#181160,#26156);
#21810=LINE('',#181162,#26157);
#21811=LINE('',#181185,#26158);
#21812=LINE('',#181186,#26159);
#21813=LINE('',#181222,#26160);
#21814=LINE('',#181226,#26161);
#21815=LINE('',#181281,#26162);
#21816=LINE('',#181284,#26163);
#21817=LINE('',#181307,#26164);
#21818=LINE('',#181731,#26165);
#21819=LINE('',#181754,#26166);
#21820=LINE('',#182148,#26167);
#21821=LINE('',#182171,#26168);
#21822=LINE('',#182580,#26169);
#21823=LINE('',#182603,#26170);
#21824=LINE('',#182604,#26171);
#21825=LINE('',#182671,#26172);
#21826=LINE('',#182675,#26173);
#21827=LINE('',#182754,#26174);
#21828=LINE('',#182757,#26175);
#21829=LINE('',#182807,#26176);
#21830=LINE('',#182808,#26177);
#21831=LINE('',#182859,#26178);
#21832=LINE('',#182863,#26179);
#21833=LINE('',#182918,#26180);
#21834=LINE('',#182922,#26181);
#21835=LINE('',#182983,#26182);
#21836=LINE('',#183013,#26183);
#21837=LINE('',#183459,#26184);
#21838=LINE('',#183461,#26185);
#21839=LINE('',#183484,#26186);
#21840=LINE('',#183546,#26187);
#21841=LINE('',#184038,#26188);
#21842=LINE('',#184040,#26189);
#21843=LINE('',#184077,#26190);
#21844=LINE('',#184078,#26191);
#21845=LINE('',#184079,#26192);
#21846=LINE('',#184164,#26193);
#21847=LINE('',#184168,#26194);
#21848=LINE('',#184187,#26195);
#21849=LINE('',#184190,#26196);
#21850=LINE('',#184192,#26197);
#21851=LINE('',#184294,#26198);
#21852=LINE('',#184366,#26199);
#21853=LINE('',#184369,#26200);
#21854=LINE('',#184371,#26201);
#21855=LINE('',#184390,#26202);
#21856=LINE('',#184394,#26203);
#21857=LINE('',#184395,#26204);
#21858=LINE('',#184431,#26205);
#21859=LINE('',#184435,#26206);
#21860=LINE('',#184490,#26207);
#21861=LINE('',#184493,#26208);
#21862=LINE('',#184495,#26209);
#21863=LINE('',#184516,#26210);
#21864=LINE('',#184520,#26211);
#21865=LINE('',#185013,#26212);
#21866=LINE('',#185015,#26213);
#21867=LINE('',#185066,#26214);
#21868=LINE('',#185070,#26215);
#21869=LINE('',#185109,#26216);
#21870=LINE('',#185274,#26217);
#21871=LINE('',#185470,#26218);
#21872=LINE('',#185525,#26219);
#21873=LINE('',#185531,#26220);
#21874=LINE('',#185683,#26221);
#21875=LINE('',#185689,#26222);
#21876=LINE('',#185815,#26223);
#21877=LINE('',#185821,#26224);
#21878=LINE('',#185897,#26225);
#21879=LINE('',#185901,#26226);
#21880=LINE('',#185911,#26227);
#21881=LINE('',#185927,#26228);
#21882=LINE('',#185943,#26229);
#21883=LINE('',#185959,#26230);
#21884=LINE('',#185969,#26231);
#21885=LINE('',#185974,#26232);
#21886=LINE('',#185981,#26233);
#21887=LINE('',#185983,#26234);
#21888=LINE('',#185987,#26235);
#21889=LINE('',#185988,#26236);
#21890=LINE('',#185992,#26237);
#21891=LINE('',#185994,#26238);
#21892=LINE('',#185998,#26239);
#21893=LINE('',#186006,#26240);
#21894=LINE('',#186012,#26241);
#21895=LINE('',#186014,#26242);
#21896=LINE('',#186018,#26243);
#21897=LINE('',#186026,#26244);
#21898=LINE('',#186032,#26245);
#21899=LINE('',#186035,#26246);
#21900=LINE('',#186068,#26247);
#21901=LINE('',#186076,#26248);
#21902=LINE('',#186082,#26249);
#21903=LINE('',#186088,#26250);
#21904=LINE('',#186096,#26251);
#21905=LINE('',#186104,#26252);
#21906=LINE('',#186108,#26253);
#21907=LINE('',#186112,#26254);
#21908=LINE('',#186326,#26255);
#21909=LINE('',#186333,#26256);
#21910=LINE('',#186335,#26257);
#21911=LINE('',#186339,#26258);
#21912=LINE('',#186343,#26259);
#21913=LINE('',#186345,#26260);
#21914=LINE('',#186349,#26261);
#21915=LINE('',#186353,#26262);
#21916=LINE('',#186359,#26263);
#21917=LINE('',#186391,#26264);
#21918=LINE('',#186420,#26265);
#21919=LINE('',#186422,#26266);
#21920=LINE('',#186426,#26267);
#21921=LINE('',#186457,#26268);
#21922=LINE('',#186486,#26269);
#21923=LINE('',#186489,#26270);
#21924=LINE('',#186509,#26271);
#21925=LINE('',#186549,#26272);
#21926=LINE('',#186581,#26273);
#21927=LINE('',#186610,#26274);
#21928=LINE('',#186613,#26275);
#21929=LINE('',#186655,#26276);
#21930=LINE('',#186673,#26277);
#21931=LINE('',#186677,#26278);
#21932=LINE('',#186708,#26279);
#21933=LINE('',#186738,#26280);
#21934=LINE('',#186740,#26281);
#21935=LINE('',#186746,#26282);
#21936=LINE('',#186750,#26283);
#21937=LINE('',#186781,#26284);
#21938=LINE('',#186810,#26285);
#21939=LINE('',#186813,#26286);
#21940=LINE('',#186854,#26287);
#21941=LINE('',#186884,#26288);
#21942=LINE('',#186914,#26289);
#21943=LINE('',#186916,#26290);
#21944=LINE('',#187000,#26291);
#21945=LINE('',#187003,#26292);
#21946=LINE('',#187035,#26293);
#21947=LINE('',#187064,#26294);
#21948=LINE('',#187067,#26295);
#21949=LINE('',#187108,#26296);
#21950=LINE('',#187169,#26297);
#21951=LINE('',#187174,#26298);
#21952=LINE('',#187205,#26299);
#21953=LINE('',#187234,#26300);
#21954=LINE('',#187236,#26301);
#21955=LINE('',#187333,#26302);
#21956=LINE('',#187338,#26303);
#21957=LINE('',#187459,#26304);
#21958=LINE('',#187464,#26305);
#21959=LINE('',#187620,#26306);
#21960=LINE('',#187625,#26307);
#21961=LINE('',#187746,#26308);
#21962=LINE('',#187751,#26309);
#21963=LINE('',#187928,#26310);
#21964=LINE('',#187933,#26311);
#21965=LINE('',#188102,#26312);
#21966=LINE('',#188108,#26313);
#21967=LINE('',#188183,#26314);
#21968=LINE('',#188185,#26315);
#21969=LINE('',#188186,#26316);
#21970=LINE('',#188191,#26317);
#21971=LINE('',#188193,#26318);
#21972=LINE('',#188194,#26319);
#21973=LINE('',#188201,#26320);
#21974=LINE('',#188203,#26321);
#21975=LINE('',#188204,#26322);
#21976=LINE('',#188259,#26323);
#21977=LINE('',#188260,#26324);
#21978=LINE('',#188333,#26325);
#21979=LINE('',#188476,#26326);
#21980=LINE('',#188481,#26327);
#21981=LINE('',#188606,#26328);
#21982=LINE('',#188612,#26329);
#21983=LINE('',#188730,#26330);
#21984=LINE('',#188735,#26331);
#21985=LINE('',#188819,#26332);
#21986=LINE('',#188824,#26333);
#21987=LINE('',#188945,#26334);
#21988=LINE('',#188950,#26335);
#21989=LINE('',#189117,#26336);
#21990=LINE('',#189122,#26337);
#21991=LINE('',#189169,#26338);
#21992=LINE('',#189172,#26339);
#21993=LINE('',#189174,#26340);
#21994=LINE('',#189175,#26341);
#21995=LINE('',#189180,#26342);
#21996=LINE('',#189182,#26343);
#21997=LINE('',#189183,#26344);
#21998=LINE('',#189190,#26345);
#21999=LINE('',#189192,#26346);
#22000=LINE('',#189193,#26347);
#22001=LINE('',#189294,#26348);
#22002=LINE('',#189296,#26349);
#22003=LINE('',#189313,#26350);
#22004=LINE('',#189319,#26351);
#22005=LINE('',#189326,#26352);
#22006=LINE('',#189336,#26353);
#22007=LINE('',#189346,#26354);
#22008=LINE('',#189356,#26355);
#22009=LINE('',#189372,#26356);
#22010=LINE('',#189398,#26357);
#22011=LINE('',#189403,#26358);
#22012=LINE('',#189409,#26359);
#22013=LINE('',#189416,#26360);
#22014=LINE('',#191638,#26361);
#22015=LINE('',#191641,#26362);
#22016=LINE('',#191678,#26363);
#22017=LINE('',#191679,#26364);
#22018=LINE('',#191682,#26365);
#22019=LINE('',#191685,#26366);
#22020=LINE('',#191721,#26367);
#22021=LINE('',#191722,#26368);
#22022=LINE('',#191725,#26369);
#22023=LINE('',#191728,#26370);
#22024=LINE('',#191764,#26371);
#22025=LINE('',#191765,#26372);
#22026=LINE('',#191768,#26373);
#22027=LINE('',#191771,#26374);
#22028=LINE('',#191807,#26375);
#22029=LINE('',#191808,#26376);
#22030=LINE('',#191810,#26377);
#22031=LINE('',#191811,#26378);
#22032=LINE('',#191813,#26379);
#22033=LINE('',#191814,#26380);
#22034=LINE('',#191816,#26381);
#22035=LINE('',#191817,#26382);
#22036=LINE('',#191819,#26383);
#22037=LINE('',#191820,#26384);
#22038=LINE('',#191822,#26385);
#22039=LINE('',#191823,#26386);
#22040=LINE('',#191825,#26387);
#22041=LINE('',#191826,#26388);
#22042=LINE('',#191828,#26389);
#22043=LINE('',#191829,#26390);
#22044=LINE('',#191831,#26391);
#22045=LINE('',#191832,#26392);
#22046=LINE('',#191846,#26393);
#22047=LINE('',#191847,#26394);
#22048=LINE('',#191870,#26395);
#22049=LINE('',#191871,#26396);
#22050=LINE('',#191891,#26397);
#22051=LINE('',#191892,#26398);
#22052=LINE('',#191906,#26399);
#22053=LINE('',#191907,#26400);
#22054=LINE('',#191930,#26401);
#22055=LINE('',#191931,#26402);
#22056=LINE('',#191936,#26403);
#22057=LINE('',#191937,#26404);
#22058=LINE('',#191954,#26405);
#22059=LINE('',#191955,#26406);
#22060=LINE('',#191978,#26407);
#22061=LINE('',#191979,#26408);
#22062=LINE('',#191984,#26409);
#22063=LINE('',#191985,#26410);
#22064=LINE('',#192002,#26411);
#22065=LINE('',#192003,#26412);
#22066=LINE('',#192008,#26413);
#22067=LINE('',#192009,#26414);
#22068=LINE('',#192026,#26415);
#22069=LINE('',#192027,#26416);
#22070=LINE('',#192032,#26417);
#22071=LINE('',#192033,#26418);
#22072=LINE('',#192050,#26419);
#22073=LINE('',#192051,#26420);
#22074=LINE('',#192056,#26421);
#22075=LINE('',#192057,#26422);
#22076=LINE('',#192080,#26423);
#22077=LINE('',#192081,#26424);
#22078=LINE('',#192104,#26425);
#22079=LINE('',#192105,#26426);
#22080=LINE('',#192110,#26427);
#22081=LINE('',#192111,#26428);
#22082=LINE('',#192128,#26429);
#22083=LINE('',#192129,#26430);
#22084=LINE('',#192134,#26431);
#22085=LINE('',#192135,#26432);
#22086=LINE('',#192152,#26433);
#22087=LINE('',#192153,#26434);
#22088=LINE('',#192158,#26435);
#22089=LINE('',#192159,#26436);
#22090=LINE('',#192176,#26437);
#22091=LINE('',#192177,#26438);
#22092=LINE('',#192182,#26439);
#22093=LINE('',#192183,#26440);
#22094=LINE('',#192200,#26441);
#22095=LINE('',#192201,#26442);
#22096=LINE('',#192206,#26443);
#22097=LINE('',#192207,#26444);
#22098=LINE('',#192224,#26445);
#22099=LINE('',#192225,#26446);
#22100=LINE('',#192230,#26447);
#22101=LINE('',#192231,#26448);
#22102=LINE('',#192248,#26449);
#22103=LINE('',#192249,#26450);
#22104=LINE('',#192254,#26451);
#22105=LINE('',#192255,#26452);
#22106=LINE('',#192272,#26453);
#22107=LINE('',#192273,#26454);
#22108=LINE('',#192278,#26455);
#22109=LINE('',#192279,#26456);
#22110=LINE('',#192296,#26457);
#22111=LINE('',#192297,#26458);
#22112=LINE('',#192302,#26459);
#22113=LINE('',#192303,#26460);
#22114=LINE('',#192320,#26461);
#22115=LINE('',#192321,#26462);
#22116=LINE('',#192344,#26463);
#22117=LINE('',#192345,#26464);
#22118=LINE('',#192350,#26465);
#22119=LINE('',#192351,#26466);
#22120=LINE('',#192368,#26467);
#22121=LINE('',#192369,#26468);
#22122=LINE('',#192404,#26469);
#22123=LINE('',#192405,#26470);
#22124=LINE('',#192410,#26471);
#22125=LINE('',#192411,#26472);
#22126=LINE('',#192428,#26473);
#22127=LINE('',#192429,#26474);
#22128=LINE('',#192452,#26475);
#22129=LINE('',#192453,#26476);
#22130=LINE('',#192458,#26477);
#22131=LINE('',#192459,#26478);
#22132=LINE('',#192476,#26479);
#22133=LINE('',#192477,#26480);
#22134=LINE('',#192482,#26481);
#22135=LINE('',#192483,#26482);
#22136=LINE('',#192500,#26483);
#22137=LINE('',#192501,#26484);
#22138=LINE('',#192524,#26485);
#22139=LINE('',#192525,#26486);
#22140=LINE('',#192530,#26487);
#22141=LINE('',#192531,#26488);
#22142=LINE('',#192545,#26489);
#22143=LINE('',#192546,#26490);
#22144=LINE('',#192560,#26491);
#22145=LINE('',#192561,#26492);
#22146=LINE('',#192566,#26493);
#22147=LINE('',#192567,#26494);
#22148=LINE('',#192584,#26495);
#22149=LINE('',#192585,#26496);
#22150=LINE('',#192605,#26497);
#22151=LINE('',#192606,#26498);
#22152=LINE('',#192620,#26499);
#22153=LINE('',#192621,#26500);
#22154=LINE('',#192626,#26501);
#22155=LINE('',#192627,#26502);
#22156=LINE('',#192644,#26503);
#22157=LINE('',#192645,#26504);
#22158=LINE('',#192650,#26505);
#22159=LINE('',#192651,#26506);
#22160=LINE('',#192668,#26507);
#22161=LINE('',#192669,#26508);
#22162=LINE('',#192674,#26509);
#22163=LINE('',#192675,#26510);
#22164=LINE('',#192698,#26511);
#22165=LINE('',#192699,#26512);
#22166=LINE('',#192716,#26513);
#22167=LINE('',#192717,#26514);
#22168=LINE('',#192722,#26515);
#22169=LINE('',#192723,#26516);
#22170=LINE('',#192740,#26517);
#22171=LINE('',#192741,#26518);
#22172=LINE('',#192746,#26519);
#22173=LINE('',#192747,#26520);
#22174=LINE('',#192764,#26521);
#22175=LINE('',#192765,#26522);
#22176=LINE('',#192770,#26523);
#22177=LINE('',#192771,#26524);
#22178=LINE('',#192788,#26525);
#22179=LINE('',#192789,#26526);
#22180=LINE('',#192794,#26527);
#22181=LINE('',#192795,#26528);
#22182=LINE('',#192812,#26529);
#22183=LINE('',#192813,#26530);
#22184=LINE('',#192818,#26531);
#22185=LINE('',#192819,#26532);
#22186=LINE('',#192836,#26533);
#22187=LINE('',#192837,#26534);
#22188=LINE('',#192866,#26535);
#22189=LINE('',#192867,#26536);
#22190=LINE('',#192872,#26537);
#22191=LINE('',#192873,#26538);
#22192=LINE('',#192896,#26539);
#22193=LINE('',#192897,#26540);
#22194=LINE('',#192914,#26541);
#22195=LINE('',#192915,#26542);
#22196=LINE('',#192920,#26543);
#22197=LINE('',#192921,#26544);
#22198=LINE('',#192944,#26545);
#22199=LINE('',#192945,#26546);
#22200=LINE('',#192974,#26547);
#22201=LINE('',#192975,#26548);
#22202=LINE('',#192980,#26549);
#22203=LINE('',#192981,#26550);
#22204=LINE('',#192998,#26551);
#22205=LINE('',#192999,#26552);
#22206=LINE('',#193004,#26553);
#22207=LINE('',#193005,#26554);
#22208=LINE('',#193022,#26555);
#22209=LINE('',#193023,#26556);
#22210=LINE('',#193028,#26557);
#22211=LINE('',#193029,#26558);
#22212=LINE('',#193046,#26559);
#22213=LINE('',#193047,#26560);
#22214=LINE('',#193082,#26561);
#22215=LINE('',#193083,#26562);
#22216=LINE('',#193088,#26563);
#22217=LINE('',#193089,#26564);
#22218=LINE('',#193106,#26565);
#22219=LINE('',#193107,#26566);
#22220=LINE('',#193130,#26567);
#22221=LINE('',#193131,#26568);
#22222=LINE('',#193136,#26569);
#22223=LINE('',#193137,#26570);
#22224=LINE('',#193154,#26571);
#22225=LINE('',#193155,#26572);
#22226=LINE('',#193160,#26573);
#22227=LINE('',#193161,#26574);
#22228=LINE('',#193178,#26575);
#22229=LINE('',#193179,#26576);
#22230=LINE('',#193184,#26577);
#22231=LINE('',#193185,#26578);
#22232=LINE('',#193202,#26579);
#22233=LINE('',#193203,#26580);
#22234=LINE('',#193226,#26581);
#22235=LINE('',#193227,#26582);
#22236=LINE('',#193232,#26583);
#22237=LINE('',#193233,#26584);
#22238=LINE('',#193250,#26585);
#22239=LINE('',#193251,#26586);
#22240=LINE('',#193256,#26587);
#22241=LINE('',#193257,#26588);
#22242=LINE('',#193274,#26589);
#22243=LINE('',#193275,#26590);
#22244=LINE('',#193295,#26591);
#22245=LINE('',#193296,#26592);
#22246=LINE('',#193310,#26593);
#22247=LINE('',#193311,#26594);
#22248=LINE('',#193331,#26595);
#22249=LINE('',#193332,#26596);
#22250=LINE('',#193445,#26597);
#22251=LINE('',#193446,#26598);
#22252=LINE('',#193469,#26599);
#22253=LINE('',#193470,#26600);
#22254=LINE('',#193508,#26601);
#22255=LINE('',#193509,#26602);
#22256=LINE('',#193532,#26603);
#22257=LINE('',#193533,#26604);
#22258=LINE('',#193571,#26605);
#22259=LINE('',#193572,#26606);
#22260=LINE('',#193595,#26607);
#22261=LINE('',#193596,#26608);
#22262=LINE('',#193634,#26609);
#22263=LINE('',#193635,#26610);
#22264=LINE('',#193658,#26611);
#22265=LINE('',#193659,#26612);
#22266=LINE('',#199112,#26613);
#22267=LINE('',#199113,#26614);
#22268=LINE('',#199116,#26615);
#22269=LINE('',#199119,#26616);
#22270=LINE('',#199122,#26617);
#22271=LINE('',#199125,#26618);
#22272=LINE('',#199128,#26619);
#22273=LINE('',#199131,#26620);
#22274=LINE('',#199134,#26621);
#22275=LINE('',#199137,#26622);
#22276=LINE('',#199140,#26623);
#22277=LINE('',#199143,#26624);
#22278=LINE('',#199146,#26625);
#22279=LINE('',#199149,#26626);
#22280=LINE('',#199152,#26627);
#22281=LINE('',#199155,#26628);
#22282=LINE('',#199158,#26629);
#22283=LINE('',#199161,#26630);
#22284=LINE('',#199166,#26631);
#22285=LINE('',#199167,#26632);
#22286=LINE('',#199170,#26633);
#22287=LINE('',#199173,#26634);
#22288=LINE('',#199176,#26635);
#22289=LINE('',#199179,#26636);
#22290=LINE('',#199182,#26637);
#22291=LINE('',#199185,#26638);
#22292=LINE('',#199188,#26639);
#22293=LINE('',#199191,#26640);
#22294=LINE('',#199194,#26641);
#22295=LINE('',#199197,#26642);
#22296=LINE('',#199200,#26643);
#22297=LINE('',#199203,#26644);
#22298=LINE('',#199206,#26645);
#22299=LINE('',#199209,#26646);
#22300=LINE('',#199212,#26647);
#22301=LINE('',#199215,#26648);
#22302=LINE('',#199218,#26649);
#22303=LINE('',#199221,#26650);
#22304=LINE('',#199224,#26651);
#22305=LINE('',#199227,#26652);
#22306=LINE('',#199230,#26653);
#22307=LINE('',#199233,#26654);
#22308=LINE('',#199236,#26655);
#22309=LINE('',#199239,#26656);
#22310=LINE('',#199242,#26657);
#22311=LINE('',#199245,#26658);
#22312=LINE('',#199248,#26659);
#22313=LINE('',#199251,#26660);
#22314=LINE('',#199254,#26661);
#22315=LINE('',#199257,#26662);
#22316=LINE('',#199260,#26663);
#22317=LINE('',#199263,#26664);
#22318=LINE('',#199266,#26665);
#22319=LINE('',#199269,#26666);
#22320=LINE('',#199274,#26667);
#22321=LINE('',#199275,#26668);
#22322=LINE('',#199278,#26669);
#22323=LINE('',#199281,#26670);
#22324=LINE('',#199284,#26671);
#22325=LINE('',#199287,#26672);
#22326=LINE('',#199290,#26673);
#22327=LINE('',#199293,#26674);
#22328=LINE('',#199296,#26675);
#22329=LINE('',#199299,#26676);
#22330=LINE('',#199302,#26677);
#22331=LINE('',#199305,#26678);
#22332=LINE('',#199308,#26679);
#22333=LINE('',#199311,#26680);
#22334=LINE('',#199314,#26681);
#22335=LINE('',#199317,#26682);
#22336=LINE('',#199320,#26683);
#22337=LINE('',#199323,#26684);
#22338=LINE('',#199326,#26685);
#22339=LINE('',#199329,#26686);
#22340=LINE('',#199332,#26687);
#22341=LINE('',#199335,#26688);
#22342=LINE('',#199338,#26689);
#22343=LINE('',#199341,#26690);
#22344=LINE('',#199344,#26691);
#22345=LINE('',#199347,#26692);
#22346=LINE('',#199350,#26693);
#22347=LINE('',#199353,#26694);
#22348=LINE('',#199356,#26695);
#22349=LINE('',#199359,#26696);
#22350=LINE('',#199362,#26697);
#22351=LINE('',#199365,#26698);
#22352=LINE('',#199368,#26699);
#22353=LINE('',#199371,#26700);
#22354=LINE('',#199374,#26701);
#22355=LINE('',#199377,#26702);
#22356=LINE('',#199380,#26703);
#22357=LINE('',#199383,#26704);
#22358=LINE('',#199386,#26705);
#22359=LINE('',#199389,#26706);
#22360=LINE('',#199392,#26707);
#22361=LINE('',#199395,#26708);
#22362=LINE('',#199398,#26709);
#22363=LINE('',#199401,#26710);
#22364=LINE('',#199404,#26711);
#22365=LINE('',#199407,#26712);
#22366=LINE('',#199410,#26713);
#22367=LINE('',#199413,#26714);
#22368=LINE('',#199416,#26715);
#22369=LINE('',#199419,#26716);
#22370=LINE('',#199422,#26717);
#22371=LINE('',#199425,#26718);
#22372=LINE('',#199428,#26719);
#22373=LINE('',#199431,#26720);
#22374=LINE('',#199434,#26721);
#22375=LINE('',#199437,#26722);
#22376=LINE('',#199440,#26723);
#22377=LINE('',#199443,#26724);
#22378=LINE('',#199446,#26725);
#22379=LINE('',#199449,#26726);
#22380=LINE('',#199452,#26727);
#22381=LINE('',#199455,#26728);
#22382=LINE('',#199458,#26729);
#22383=LINE('',#199461,#26730);
#22384=LINE('',#199464,#26731);
#22385=LINE('',#199467,#26732);
#22386=LINE('',#199470,#26733);
#22387=LINE('',#199473,#26734);
#22388=LINE('',#199476,#26735);
#22389=LINE('',#199479,#26736);
#22390=LINE('',#199482,#26737);
#22391=LINE('',#199485,#26738);
#22392=LINE('',#199488,#26739);
#22393=LINE('',#199491,#26740);
#22394=LINE('',#199494,#26741);
#22395=LINE('',#199497,#26742);
#22396=LINE('',#199500,#26743);
#22397=LINE('',#199503,#26744);
#22398=LINE('',#199506,#26745);
#22399=LINE('',#199509,#26746);
#22400=LINE('',#199512,#26747);
#22401=LINE('',#199515,#26748);
#22402=LINE('',#199518,#26749);
#22403=LINE('',#199521,#26750);
#22404=LINE('',#199524,#26751);
#22405=LINE('',#199527,#26752);
#22406=LINE('',#199530,#26753);
#22407=LINE('',#199533,#26754);
#22408=LINE('',#199536,#26755);
#22409=LINE('',#199539,#26756);
#22410=LINE('',#199542,#26757);
#22411=LINE('',#199545,#26758);
#22412=LINE('',#199548,#26759);
#22413=LINE('',#199551,#26760);
#22414=LINE('',#199554,#26761);
#22415=LINE('',#199557,#26762);
#22416=LINE('',#199560,#26763);
#22417=LINE('',#199563,#26764);
#22418=LINE('',#199566,#26765);
#22419=LINE('',#199569,#26766);
#22420=LINE('',#199572,#26767);
#22421=LINE('',#199575,#26768);
#22422=LINE('',#199578,#26769);
#22423=LINE('',#199581,#26770);
#22424=LINE('',#199584,#26771);
#22425=LINE('',#199587,#26772);
#22426=LINE('',#199590,#26773);
#22427=LINE('',#199593,#26774);
#22428=LINE('',#199596,#26775);
#22429=LINE('',#199599,#26776);
#22430=LINE('',#199602,#26777);
#22431=LINE('',#199605,#26778);
#22432=LINE('',#199608,#26779);
#22433=LINE('',#199611,#26780);
#22434=LINE('',#199614,#26781);
#22435=LINE('',#199617,#26782);
#22436=LINE('',#199622,#26783);
#22437=LINE('',#199623,#26784);
#22438=LINE('',#199626,#26785);
#22439=LINE('',#199629,#26786);
#22440=LINE('',#199632,#26787);
#22441=LINE('',#199635,#26788);
#22442=LINE('',#199638,#26789);
#22443=LINE('',#199641,#26790);
#22444=LINE('',#199644,#26791);
#22445=LINE('',#199647,#26792);
#22446=LINE('',#199650,#26793);
#22447=LINE('',#199653,#26794);
#22448=LINE('',#199656,#26795);
#22449=LINE('',#199659,#26796);
#22450=LINE('',#199662,#26797);
#22451=LINE('',#199665,#26798);
#22452=LINE('',#199668,#26799);
#22453=LINE('',#199671,#26800);
#22454=LINE('',#199674,#26801);
#22455=LINE('',#199677,#26802);
#22456=LINE('',#199680,#26803);
#22457=LINE('',#199683,#26804);
#22458=LINE('',#199686,#26805);
#22459=LINE('',#199689,#26806);
#22460=LINE('',#199692,#26807);
#22461=LINE('',#199695,#26808);
#22462=LINE('',#199698,#26809);
#22463=LINE('',#199701,#26810);
#22464=LINE('',#199704,#26811);
#22465=LINE('',#199707,#26812);
#22466=LINE('',#199710,#26813);
#22467=LINE('',#199713,#26814);
#22468=LINE('',#199716,#26815);
#22469=LINE('',#199719,#26816);
#22470=LINE('',#199722,#26817);
#22471=LINE('',#199725,#26818);
#22472=LINE('',#199728,#26819);
#22473=LINE('',#199731,#26820);
#22474=LINE('',#199734,#26821);
#22475=LINE('',#199737,#26822);
#22476=LINE('',#199740,#26823);
#22477=LINE('',#199743,#26824);
#22478=LINE('',#199746,#26825);
#22479=LINE('',#199749,#26826);
#22480=LINE('',#199752,#26827);
#22481=LINE('',#199755,#26828);
#22482=LINE('',#199758,#26829);
#22483=LINE('',#199761,#26830);
#22484=LINE('',#199766,#26831);
#22485=LINE('',#199767,#26832);
#22486=LINE('',#199770,#26833);
#22487=LINE('',#199773,#26834);
#22488=LINE('',#199776,#26835);
#22489=LINE('',#199779,#26836);
#22490=LINE('',#199782,#26837);
#22491=LINE('',#199785,#26838);
#22492=LINE('',#199788,#26839);
#22493=LINE('',#199791,#26840);
#22494=LINE('',#199794,#26841);
#22495=LINE('',#199797,#26842);
#22496=LINE('',#199800,#26843);
#22497=LINE('',#199803,#26844);
#22498=LINE('',#199806,#26845);
#22499=LINE('',#199809,#26846);
#22500=LINE('',#199812,#26847);
#22501=LINE('',#199815,#26848);
#22502=LINE('',#199818,#26849);
#22503=LINE('',#199821,#26850);
#22504=LINE('',#199824,#26851);
#22505=LINE('',#199827,#26852);
#22506=LINE('',#199830,#26853);
#22507=LINE('',#199833,#26854);
#22508=LINE('',#199836,#26855);
#22509=LINE('',#199839,#26856);
#22510=LINE('',#199842,#26857);
#22511=LINE('',#199845,#26858);
#22512=LINE('',#199848,#26859);
#22513=LINE('',#199851,#26860);
#22514=LINE('',#199854,#26861);
#22515=LINE('',#199857,#26862);
#22516=LINE('',#199862,#26863);
#22517=LINE('',#199863,#26864);
#22518=LINE('',#199866,#26865);
#22519=LINE('',#199869,#26866);
#22520=LINE('',#199872,#26867);
#22521=LINE('',#199875,#26868);
#22522=LINE('',#199878,#26869);
#22523=LINE('',#199881,#26870);
#22524=LINE('',#199884,#26871);
#22525=LINE('',#199887,#26872);
#22526=LINE('',#199892,#26873);
#22527=LINE('',#199893,#26874);
#22528=LINE('',#199896,#26875);
#22529=LINE('',#199899,#26876);
#22530=LINE('',#199904,#26877);
#22531=LINE('',#199905,#26878);
#22532=LINE('',#199908,#26879);
#22533=LINE('',#199911,#26880);
#22534=LINE('',#199914,#26881);
#22535=LINE('',#199917,#26882);
#22536=LINE('',#199920,#26883);
#22537=LINE('',#199923,#26884);
#22538=LINE('',#199926,#26885);
#22539=LINE('',#199931,#26886);
#22540=LINE('',#199939,#26887);
#22541=LINE('',#199941,#26888);
#22542=LINE('',#199949,#26889);
#22543=LINE('',#199951,#26890);
#22544=LINE('',#199957,#26891);
#22545=LINE('',#199959,#26892);
#22546=LINE('',#199961,#26893);
#22547=LINE('',#199963,#26894);
#22548=LINE('',#199965,#26895);
#22549=LINE('',#199967,#26896);
#22550=LINE('',#199969,#26897);
#22551=LINE('',#199971,#26898);
#22552=LINE('',#199973,#26899);
#22553=LINE('',#199975,#26900);
#22554=LINE('',#199977,#26901);
#22555=LINE('',#199979,#26902);
#22556=LINE('',#199981,#26903);
#22557=LINE('',#199983,#26904);
#22558=LINE('',#199985,#26905);
#22559=LINE('',#199987,#26906);
#22560=LINE('',#199989,#26907);
#22561=LINE('',#199991,#26908);
#22562=LINE('',#199993,#26909);
#22563=LINE('',#199995,#26910);
#22564=LINE('',#199997,#26911);
#22565=LINE('',#199999,#26912);
#22566=LINE('',#200001,#26913);
#22567=LINE('',#200003,#26914);
#22568=LINE('',#200005,#26915);
#22569=LINE('',#200007,#26916);
#22570=LINE('',#200009,#26917);
#22571=LINE('',#200011,#26918);
#22572=LINE('',#200013,#26919);
#22573=LINE('',#200015,#26920);
#22574=LINE('',#200017,#26921);
#22575=LINE('',#200019,#26922);
#22576=LINE('',#200023,#26923);
#22577=LINE('',#200025,#26924);
#22578=LINE('',#200027,#26925);
#22579=LINE('',#200028,#26926);
#22580=LINE('',#200032,#26927);
#22581=LINE('',#200033,#26928);
#22582=LINE('',#200034,#26929);
#22583=LINE('',#200037,#26930);
#22584=LINE('',#200039,#26931);
#22585=LINE('',#200040,#26932);
#22586=LINE('',#200042,#26933);
#22587=LINE('',#200044,#26934);
#22588=LINE('',#200046,#26935);
#22589=LINE('',#200048,#26936);
#22590=LINE('',#200050,#26937);
#22591=LINE('',#200052,#26938);
#22592=LINE('',#200054,#26939);
#22593=LINE('',#200056,#26940);
#22594=LINE('',#200058,#26941);
#22595=LINE('',#200060,#26942);
#22596=LINE('',#200062,#26943);
#22597=LINE('',#200064,#26944);
#22598=LINE('',#200066,#26945);
#22599=LINE('',#200068,#26946);
#22600=LINE('',#200070,#26947);
#22601=LINE('',#200072,#26948);
#22602=LINE('',#200074,#26949);
#22603=LINE('',#200076,#26950);
#22604=LINE('',#200078,#26951);
#22605=LINE('',#200080,#26952);
#22606=LINE('',#200082,#26953);
#22607=LINE('',#200084,#26954);
#22608=LINE('',#200088,#26955);
#22609=LINE('',#200092,#26956);
#22610=LINE('',#200098,#26957);
#22611=LINE('',#200104,#26958);
#22612=LINE('',#200110,#26959);
#22613=LINE('',#200116,#26960);
#22614=LINE('',#200122,#26961);
#22615=LINE('',#200128,#26962);
#22616=LINE('',#200133,#26963);
#22617=LINE('',#200137,#26964);
#22618=LINE('',#200152,#26965);
#22619=LINE('',#200164,#26966);
#22620=LINE('',#200173,#26967);
#22621=LINE('',#200181,#26968);
#22622=LINE('',#200183,#26969);
#22623=LINE('',#200204,#26970);
#22624=LINE('',#200205,#26971);
#22625=LINE('',#200223,#26972);
#22626=LINE('',#200224,#26973);
#22627=LINE('',#200232,#26974);
#22628=LINE('',#200234,#26975);
#22629=LINE('',#200249,#26976);
#22630=LINE('',#200252,#26977);
#22631=LINE('',#200258,#26978);
#22632=LINE('',#200261,#26979);
#22633=LINE('',#200266,#26980);
#22634=LINE('',#200272,#26981);
#22635=LINE('',#200290,#26982);
#22636=LINE('',#200293,#26983);
#22637=LINE('',#202386,#26984);
#22638=LINE('',#202394,#26985);
#22639=LINE('',#202412,#26986);
#22640=LINE('',#202418,#26987);
#22641=LINE('',#202423,#26988);
#22642=LINE('',#202426,#26989);
#22643=LINE('',#202438,#26990);
#22644=LINE('',#202452,#26991);
#22645=LINE('',#202458,#26992);
#22646=LINE('',#202461,#26993);
#22647=LINE('',#202467,#26994);
#22648=LINE('',#202473,#26995);
#22649=LINE('',#202479,#26996);
#22650=LINE('',#202485,#26997);
#22651=LINE('',#202488,#26998);
#22652=LINE('',#202494,#26999);
#22653=LINE('',#203630,#27000);
#22654=LINE('',#203728,#27001);
#22655=LINE('',#203730,#27002);
#22656=LINE('',#204868,#27003);
#22657=LINE('',#204871,#27004);
#22658=LINE('',#204875,#27005);
#22659=LINE('',#204879,#27006);
#22660=LINE('',#204884,#27007);
#22661=LINE('',#204887,#27008);
#22662=LINE('',#204892,#27009);
#22663=LINE('',#204895,#27010);
#22664=LINE('',#204901,#27011);
#22665=LINE('',#204908,#27012);
#22666=LINE('',#205010,#27013);
#22667=LINE('',#205013,#27014);
#22668=LINE('',#205016,#27015);
#22669=LINE('',#205020,#27016);
#22670=LINE('',#205024,#27017);
#22671=LINE('',#205028,#27018);
#22672=LINE('',#205032,#27019);
#22673=LINE('',#205037,#27020);
#22674=LINE('',#205040,#27021);
#22675=LINE('',#205043,#27022);
#22676=LINE('',#205046,#27023);
#22677=LINE('',#205049,#27024);
#22678=LINE('',#205053,#27025);
#22679=LINE('',#205057,#27026);
#22680=LINE('',#205061,#27027);
#22681=LINE('',#205065,#27028);
#22682=LINE('',#205149,#27029);
#22683=LINE('',#205248,#27030);
#22684=LINE('',#205334,#27031);
#22685=LINE('',#205454,#27032);
#22686=LINE('',#205460,#27033);
#22687=LINE('',#205461,#27034);
#22688=LINE('',#205463,#27035);
#22689=LINE('',#205465,#27036);
#22690=LINE('',#205467,#27037);
#22691=LINE('',#205468,#27038);
#22692=LINE('',#205470,#27039);
#22693=LINE('',#205472,#27040);
#22694=LINE('',#205475,#27041);
#22695=LINE('',#205478,#27042);
#22696=LINE('',#205482,#27043);
#22697=LINE('',#205486,#27044);
#22698=LINE('',#205490,#27045);
#22699=LINE('',#205493,#27046);
#22700=LINE('',#205496,#27047);
#22701=LINE('',#205500,#27048);
#22702=LINE('',#206972,#27049);
#22703=LINE('',#206974,#27050);
#22704=LINE('',#206976,#27051);
#22705=LINE('',#206978,#27052);
#22706=LINE('',#206980,#27053);
#22707=LINE('',#206982,#27054);
#22708=LINE('',#206984,#27055);
#22709=LINE('',#206986,#27056);
#22710=LINE('',#206988,#27057);
#22711=LINE('',#206990,#27058);
#22712=LINE('',#206999,#27059);
#22713=LINE('',#207001,#27060);
#22714=LINE('',#207003,#27061);
#22715=LINE('',#207005,#27062);
#22716=LINE('',#207007,#27063);
#22717=LINE('',#207009,#27064);
#22718=LINE('',#207011,#27065);
#22719=LINE('',#207013,#27066);
#22720=LINE('',#207015,#27067);
#22721=LINE('',#207017,#27068);
#22722=LINE('',#207019,#27069);
#22723=LINE('',#207021,#27070);
#22724=LINE('',#207023,#27071);
#22725=LINE('',#207025,#27072);
#22726=LINE('',#207043,#27073);
#22727=LINE('',#207045,#27074);
#22728=LINE('',#207047,#27075);
#22729=LINE('',#207049,#27076);
#22730=LINE('',#207051,#27077);
#22731=LINE('',#207053,#27078);
#22732=LINE('',#207055,#27079);
#22733=LINE('',#207057,#27080);
#22734=LINE('',#207059,#27081);
#22735=LINE('',#207061,#27082);
#22736=LINE('',#207063,#27083);
#22737=LINE('',#207065,#27084);
#22738=LINE('',#207067,#27085);
#22739=LINE('',#207069,#27086);
#22740=LINE('',#207071,#27087);
#22741=LINE('',#207073,#27088);
#22742=LINE('',#207075,#27089);
#22743=LINE('',#207077,#27090);
#22744=LINE('',#207079,#27091);
#22745=LINE('',#207081,#27092);
#22746=LINE('',#207083,#27093);
#22747=LINE('',#207085,#27094);
#22748=LINE('',#207087,#27095);
#22749=LINE('',#207089,#27096);
#22750=LINE('',#207091,#27097);
#22751=LINE('',#207093,#27098);
#22752=LINE('',#207095,#27099);
#22753=LINE('',#207097,#27100);
#22754=LINE('',#210831,#27101);
#22755=LINE('',#210833,#27102);
#22756=LINE('',#210871,#27103);
#22757=LINE('',#210872,#27104);
#22758=LINE('',#210875,#27105);
#22759=LINE('',#210877,#27106);
#22760=LINE('',#210914,#27107);
#22761=LINE('',#210915,#27108);
#22762=LINE('',#210918,#27109);
#22763=LINE('',#210920,#27110);
#22764=LINE('',#210957,#27111);
#22765=LINE('',#210958,#27112);
#22766=LINE('',#210961,#27113);
#22767=LINE('',#210963,#27114);
#22768=LINE('',#211000,#27115);
#22769=LINE('',#211001,#27116);
#22770=LINE('',#211003,#27117);
#22771=LINE('',#211004,#27118);
#22772=LINE('',#211006,#27119);
#22773=LINE('',#211007,#27120);
#22774=LINE('',#211009,#27121);
#22775=LINE('',#211010,#27122);
#22776=LINE('',#211012,#27123);
#22777=LINE('',#211013,#27124);
#22778=LINE('',#211015,#27125);
#22779=LINE('',#211016,#27126);
#22780=LINE('',#211018,#27127);
#22781=LINE('',#211019,#27128);
#22782=LINE('',#211021,#27129);
#22783=LINE('',#211022,#27130);
#22784=LINE('',#211024,#27131);
#22785=LINE('',#211025,#27132);
#22786=LINE('',#211039,#27133);
#22787=LINE('',#211040,#27134);
#22788=LINE('',#211063,#27135);
#22789=LINE('',#211064,#27136);
#22790=LINE('',#211084,#27137);
#22791=LINE('',#211085,#27138);
#22792=LINE('',#211099,#27139);
#22793=LINE('',#211100,#27140);
#22794=LINE('',#211123,#27141);
#22795=LINE('',#211124,#27142);
#22796=LINE('',#211129,#27143);
#22797=LINE('',#211130,#27144);
#22798=LINE('',#211147,#27145);
#22799=LINE('',#211148,#27146);
#22800=LINE('',#211171,#27147);
#22801=LINE('',#211172,#27148);
#22802=LINE('',#211177,#27149);
#22803=LINE('',#211178,#27150);
#22804=LINE('',#211195,#27151);
#22805=LINE('',#211196,#27152);
#22806=LINE('',#211201,#27153);
#22807=LINE('',#211202,#27154);
#22808=LINE('',#211219,#27155);
#22809=LINE('',#211220,#27156);
#22810=LINE('',#211225,#27157);
#22811=LINE('',#211226,#27158);
#22812=LINE('',#211243,#27159);
#22813=LINE('',#211244,#27160);
#22814=LINE('',#211249,#27161);
#22815=LINE('',#211250,#27162);
#22816=LINE('',#211273,#27163);
#22817=LINE('',#211274,#27164);
#22818=LINE('',#211297,#27165);
#22819=LINE('',#211298,#27166);
#22820=LINE('',#211303,#27167);
#22821=LINE('',#211304,#27168);
#22822=LINE('',#211321,#27169);
#22823=LINE('',#211322,#27170);
#22824=LINE('',#211327,#27171);
#22825=LINE('',#211328,#27172);
#22826=LINE('',#211345,#27173);
#22827=LINE('',#211346,#27174);
#22828=LINE('',#211351,#27175);
#22829=LINE('',#211352,#27176);
#22830=LINE('',#211369,#27177);
#22831=LINE('',#211370,#27178);
#22832=LINE('',#211375,#27179);
#22833=LINE('',#211376,#27180);
#22834=LINE('',#211393,#27181);
#22835=LINE('',#211394,#27182);
#22836=LINE('',#211399,#27183);
#22837=LINE('',#211400,#27184);
#22838=LINE('',#211417,#27185);
#22839=LINE('',#211418,#27186);
#22840=LINE('',#211423,#27187);
#22841=LINE('',#211424,#27188);
#22842=LINE('',#211441,#27189);
#22843=LINE('',#211442,#27190);
#22844=LINE('',#211447,#27191);
#22845=LINE('',#211448,#27192);
#22846=LINE('',#211465,#27193);
#22847=LINE('',#211466,#27194);
#22848=LINE('',#211471,#27195);
#22849=LINE('',#211472,#27196);
#22850=LINE('',#211489,#27197);
#22851=LINE('',#211490,#27198);
#22852=LINE('',#211495,#27199);
#22853=LINE('',#211496,#27200);
#22854=LINE('',#211513,#27201);
#22855=LINE('',#211514,#27202);
#22856=LINE('',#211537,#27203);
#22857=LINE('',#211538,#27204);
#22858=LINE('',#211543,#27205);
#22859=LINE('',#211544,#27206);
#22860=LINE('',#211561,#27207);
#22861=LINE('',#211562,#27208);
#22862=LINE('',#211597,#27209);
#22863=LINE('',#211598,#27210);
#22864=LINE('',#211603,#27211);
#22865=LINE('',#211604,#27212);
#22866=LINE('',#211621,#27213);
#22867=LINE('',#211622,#27214);
#22868=LINE('',#211645,#27215);
#22869=LINE('',#211646,#27216);
#22870=LINE('',#211651,#27217);
#22871=LINE('',#211652,#27218);
#22872=LINE('',#211669,#27219);
#22873=LINE('',#211670,#27220);
#22874=LINE('',#211675,#27221);
#22875=LINE('',#211676,#27222);
#22876=LINE('',#211693,#27223);
#22877=LINE('',#211694,#27224);
#22878=LINE('',#211717,#27225);
#22879=LINE('',#211718,#27226);
#22880=LINE('',#211723,#27227);
#22881=LINE('',#211724,#27228);
#22882=LINE('',#211738,#27229);
#22883=LINE('',#211739,#27230);
#22884=LINE('',#211753,#27231);
#22885=LINE('',#211754,#27232);
#22886=LINE('',#211759,#27233);
#22887=LINE('',#211760,#27234);
#22888=LINE('',#211777,#27235);
#22889=LINE('',#211778,#27236);
#22890=LINE('',#211798,#27237);
#22891=LINE('',#211799,#27238);
#22892=LINE('',#211813,#27239);
#22893=LINE('',#211814,#27240);
#22894=LINE('',#211819,#27241);
#22895=LINE('',#211820,#27242);
#22896=LINE('',#211837,#27243);
#22897=LINE('',#211838,#27244);
#22898=LINE('',#211843,#27245);
#22899=LINE('',#211844,#27246);
#22900=LINE('',#211861,#27247);
#22901=LINE('',#211862,#27248);
#22902=LINE('',#211867,#27249);
#22903=LINE('',#211868,#27250);
#22904=LINE('',#211891,#27251);
#22905=LINE('',#211892,#27252);
#22906=LINE('',#211909,#27253);
#22907=LINE('',#211910,#27254);
#22908=LINE('',#211915,#27255);
#22909=LINE('',#211916,#27256);
#22910=LINE('',#211933,#27257);
#22911=LINE('',#211934,#27258);
#22912=LINE('',#211939,#27259);
#22913=LINE('',#211940,#27260);
#22914=LINE('',#211957,#27261);
#22915=LINE('',#211958,#27262);
#22916=LINE('',#211963,#27263);
#22917=LINE('',#211964,#27264);
#22918=LINE('',#211981,#27265);
#22919=LINE('',#211982,#27266);
#22920=LINE('',#211987,#27267);
#22921=LINE('',#211988,#27268);
#22922=LINE('',#212005,#27269);
#22923=LINE('',#212006,#27270);
#22924=LINE('',#212011,#27271);
#22925=LINE('',#212012,#27272);
#22926=LINE('',#212029,#27273);
#22927=LINE('',#212030,#27274);
#22928=LINE('',#212059,#27275);
#22929=LINE('',#212060,#27276);
#22930=LINE('',#212065,#27277);
#22931=LINE('',#212066,#27278);
#22932=LINE('',#212089,#27279);
#22933=LINE('',#212090,#27280);
#22934=LINE('',#212107,#27281);
#22935=LINE('',#212108,#27282);
#22936=LINE('',#212113,#27283);
#22937=LINE('',#212114,#27284);
#22938=LINE('',#212137,#27285);
#22939=LINE('',#212138,#27286);
#22940=LINE('',#212167,#27287);
#22941=LINE('',#212168,#27288);
#22942=LINE('',#212173,#27289);
#22943=LINE('',#212174,#27290);
#22944=LINE('',#212191,#27291);
#22945=LINE('',#212192,#27292);
#22946=LINE('',#212197,#27293);
#22947=LINE('',#212198,#27294);
#22948=LINE('',#212215,#27295);
#22949=LINE('',#212216,#27296);
#22950=LINE('',#212221,#27297);
#22951=LINE('',#212222,#27298);
#22952=LINE('',#212239,#27299);
#22953=LINE('',#212240,#27300);
#22954=LINE('',#212275,#27301);
#22955=LINE('',#212276,#27302);
#22956=LINE('',#212281,#27303);
#22957=LINE('',#212282,#27304);
#22958=LINE('',#212299,#27305);
#22959=LINE('',#212300,#27306);
#22960=LINE('',#212323,#27307);
#22961=LINE('',#212324,#27308);
#22962=LINE('',#212329,#27309);
#22963=LINE('',#212330,#27310);
#22964=LINE('',#212347,#27311);
#22965=LINE('',#212348,#27312);
#22966=LINE('',#212353,#27313);
#22967=LINE('',#212354,#27314);
#22968=LINE('',#212371,#27315);
#22969=LINE('',#212372,#27316);
#22970=LINE('',#212377,#27317);
#22971=LINE('',#212378,#27318);
#22972=LINE('',#212395,#27319);
#22973=LINE('',#212396,#27320);
#22974=LINE('',#212419,#27321);
#22975=LINE('',#212420,#27322);
#22976=LINE('',#212425,#27323);
#22977=LINE('',#212426,#27324);
#22978=LINE('',#212443,#27325);
#22979=LINE('',#212444,#27326);
#22980=LINE('',#212449,#27327);
#22981=LINE('',#212450,#27328);
#22982=LINE('',#212467,#27329);
#22983=LINE('',#212468,#27330);
#22984=LINE('',#212488,#27331);
#22985=LINE('',#212489,#27332);
#22986=LINE('',#212503,#27333);
#22987=LINE('',#212504,#27334);
#22988=LINE('',#212524,#27335);
#22989=LINE('',#212525,#27336);
#22990=LINE('',#212662,#27337);
#22991=LINE('',#212663,#27338);
#22992=LINE('',#212686,#27339);
#22993=LINE('',#212687,#27340);
#22994=LINE('',#212725,#27341);
#22995=LINE('',#212726,#27342);
#22996=LINE('',#212749,#27343);
#22997=LINE('',#212750,#27344);
#22998=LINE('',#212788,#27345);
#22999=LINE('',#212789,#27346);
#23000=LINE('',#212812,#27347);
#23001=LINE('',#212813,#27348);
#23002=LINE('',#212851,#27349);
#23003=LINE('',#212852,#27350);
#23004=LINE('',#212875,#27351);
#23005=LINE('',#212876,#27352);
#23006=LINE('',#222192,#27353);
#23007=LINE('',#222193,#27354);
#23008=LINE('',#222196,#27355);
#23009=LINE('',#222198,#27356);
#23010=LINE('',#222202,#27357);
#23011=LINE('',#222204,#27358);
#23012=LINE('',#222208,#27359);
#23013=LINE('',#222210,#27360);
#23014=LINE('',#222214,#27361);
#23015=LINE('',#222216,#27362);
#23016=LINE('',#222220,#27363);
#23017=LINE('',#222222,#27364);
#23018=LINE('',#222226,#27365);
#23019=LINE('',#222228,#27366);
#23020=LINE('',#222232,#27367);
#23021=LINE('',#222234,#27368);
#23022=LINE('',#222238,#27369);
#23023=LINE('',#222240,#27370);
#23024=LINE('',#222246,#27371);
#23025=LINE('',#222247,#27372);
#23026=LINE('',#222250,#27373);
#23027=LINE('',#222252,#27374);
#23028=LINE('',#222256,#27375);
#23029=LINE('',#222258,#27376);
#23030=LINE('',#222262,#27377);
#23031=LINE('',#222264,#27378);
#23032=LINE('',#222268,#27379);
#23033=LINE('',#222270,#27380);
#23034=LINE('',#222274,#27381);
#23035=LINE('',#222276,#27382);
#23036=LINE('',#222280,#27383);
#23037=LINE('',#222282,#27384);
#23038=LINE('',#222286,#27385);
#23039=LINE('',#222288,#27386);
#23040=LINE('',#222292,#27387);
#23041=LINE('',#222294,#27388);
#23042=LINE('',#222298,#27389);
#23043=LINE('',#222300,#27390);
#23044=LINE('',#222304,#27391);
#23045=LINE('',#222306,#27392);
#23046=LINE('',#222310,#27393);
#23047=LINE('',#222312,#27394);
#23048=LINE('',#222316,#27395);
#23049=LINE('',#222318,#27396);
#23050=LINE('',#222322,#27397);
#23051=LINE('',#222324,#27398);
#23052=LINE('',#222328,#27399);
#23053=LINE('',#222330,#27400);
#23054=LINE('',#222334,#27401);
#23055=LINE('',#222336,#27402);
#23056=LINE('',#222340,#27403);
#23057=LINE('',#222342,#27404);
#23058=LINE('',#222346,#27405);
#23059=LINE('',#222348,#27406);
#23060=LINE('',#222354,#27407);
#23061=LINE('',#222355,#27408);
#23062=LINE('',#222358,#27409);
#23063=LINE('',#222360,#27410);
#23064=LINE('',#222364,#27411);
#23065=LINE('',#222366,#27412);
#23066=LINE('',#222370,#27413);
#23067=LINE('',#222372,#27414);
#23068=LINE('',#222376,#27415);
#23069=LINE('',#222378,#27416);
#23070=LINE('',#222382,#27417);
#23071=LINE('',#222384,#27418);
#23072=LINE('',#222388,#27419);
#23073=LINE('',#222390,#27420);
#23074=LINE('',#222394,#27421);
#23075=LINE('',#222396,#27422);
#23076=LINE('',#222400,#27423);
#23077=LINE('',#222402,#27424);
#23078=LINE('',#222406,#27425);
#23079=LINE('',#222408,#27426);
#23080=LINE('',#222412,#27427);
#23081=LINE('',#222414,#27428);
#23082=LINE('',#222418,#27429);
#23083=LINE('',#222420,#27430);
#23084=LINE('',#222424,#27431);
#23085=LINE('',#222426,#27432);
#23086=LINE('',#222430,#27433);
#23087=LINE('',#222432,#27434);
#23088=LINE('',#222436,#27435);
#23089=LINE('',#222438,#27436);
#23090=LINE('',#222442,#27437);
#23091=LINE('',#222444,#27438);
#23092=LINE('',#222448,#27439);
#23093=LINE('',#222450,#27440);
#23094=LINE('',#222454,#27441);
#23095=LINE('',#222456,#27442);
#23096=LINE('',#222460,#27443);
#23097=LINE('',#222462,#27444);
#23098=LINE('',#222466,#27445);
#23099=LINE('',#222468,#27446);
#23100=LINE('',#222472,#27447);
#23101=LINE('',#222474,#27448);
#23102=LINE('',#222478,#27449);
#23103=LINE('',#222480,#27450);
#23104=LINE('',#222484,#27451);
#23105=LINE('',#222486,#27452);
#23106=LINE('',#222490,#27453);
#23107=LINE('',#222492,#27454);
#23108=LINE('',#222496,#27455);
#23109=LINE('',#222498,#27456);
#23110=LINE('',#222502,#27457);
#23111=LINE('',#222504,#27458);
#23112=LINE('',#222508,#27459);
#23113=LINE('',#222510,#27460);
#23114=LINE('',#222514,#27461);
#23115=LINE('',#222516,#27462);
#23116=LINE('',#222520,#27463);
#23117=LINE('',#222522,#27464);
#23118=LINE('',#222526,#27465);
#23119=LINE('',#222528,#27466);
#23120=LINE('',#222532,#27467);
#23121=LINE('',#222534,#27468);
#23122=LINE('',#222538,#27469);
#23123=LINE('',#222540,#27470);
#23124=LINE('',#222544,#27471);
#23125=LINE('',#222546,#27472);
#23126=LINE('',#222550,#27473);
#23127=LINE('',#222552,#27474);
#23128=LINE('',#222556,#27475);
#23129=LINE('',#222558,#27476);
#23130=LINE('',#222562,#27477);
#23131=LINE('',#222564,#27478);
#23132=LINE('',#222568,#27479);
#23133=LINE('',#222570,#27480);
#23134=LINE('',#222574,#27481);
#23135=LINE('',#222576,#27482);
#23136=LINE('',#222580,#27483);
#23137=LINE('',#222582,#27484);
#23138=LINE('',#222586,#27485);
#23139=LINE('',#222588,#27486);
#23140=LINE('',#222592,#27487);
#23141=LINE('',#222594,#27488);
#23142=LINE('',#222598,#27489);
#23143=LINE('',#222600,#27490);
#23144=LINE('',#222604,#27491);
#23145=LINE('',#222606,#27492);
#23146=LINE('',#222610,#27493);
#23147=LINE('',#222612,#27494);
#23148=LINE('',#222616,#27495);
#23149=LINE('',#222618,#27496);
#23150=LINE('',#222622,#27497);
#23151=LINE('',#222624,#27498);
#23152=LINE('',#222628,#27499);
#23153=LINE('',#222630,#27500);
#23154=LINE('',#222634,#27501);
#23155=LINE('',#222636,#27502);
#23156=LINE('',#222640,#27503);
#23157=LINE('',#222642,#27504);
#23158=LINE('',#222646,#27505);
#23159=LINE('',#222648,#27506);
#23160=LINE('',#222652,#27507);
#23161=LINE('',#222654,#27508);
#23162=LINE('',#222658,#27509);
#23163=LINE('',#222660,#27510);
#23164=LINE('',#222664,#27511);
#23165=LINE('',#222666,#27512);
#23166=LINE('',#222670,#27513);
#23167=LINE('',#222672,#27514);
#23168=LINE('',#222676,#27515);
#23169=LINE('',#222678,#27516);
#23170=LINE('',#222682,#27517);
#23171=LINE('',#222684,#27518);
#23172=LINE('',#222688,#27519);
#23173=LINE('',#222690,#27520);
#23174=LINE('',#222694,#27521);
#23175=LINE('',#222696,#27522);
#23176=LINE('',#222702,#27523);
#23177=LINE('',#222703,#27524);
#23178=LINE('',#222706,#27525);
#23179=LINE('',#222708,#27526);
#23180=LINE('',#222712,#27527);
#23181=LINE('',#222714,#27528);
#23182=LINE('',#222718,#27529);
#23183=LINE('',#222720,#27530);
#23184=LINE('',#222724,#27531);
#23185=LINE('',#222726,#27532);
#23186=LINE('',#222730,#27533);
#23187=LINE('',#222732,#27534);
#23188=LINE('',#222736,#27535);
#23189=LINE('',#222738,#27536);
#23190=LINE('',#222742,#27537);
#23191=LINE('',#222744,#27538);
#23192=LINE('',#222748,#27539);
#23193=LINE('',#222750,#27540);
#23194=LINE('',#222754,#27541);
#23195=LINE('',#222756,#27542);
#23196=LINE('',#222760,#27543);
#23197=LINE('',#222762,#27544);
#23198=LINE('',#222766,#27545);
#23199=LINE('',#222768,#27546);
#23200=LINE('',#222772,#27547);
#23201=LINE('',#222774,#27548);
#23202=LINE('',#222778,#27549);
#23203=LINE('',#222780,#27550);
#23204=LINE('',#222784,#27551);
#23205=LINE('',#222786,#27552);
#23206=LINE('',#222790,#27553);
#23207=LINE('',#222792,#27554);
#23208=LINE('',#222796,#27555);
#23209=LINE('',#222798,#27556);
#23210=LINE('',#222802,#27557);
#23211=LINE('',#222804,#27558);
#23212=LINE('',#222808,#27559);
#23213=LINE('',#222810,#27560);
#23214=LINE('',#222814,#27561);
#23215=LINE('',#222816,#27562);
#23216=LINE('',#222820,#27563);
#23217=LINE('',#222822,#27564);
#23218=LINE('',#222826,#27565);
#23219=LINE('',#222828,#27566);
#23220=LINE('',#222832,#27567);
#23221=LINE('',#222834,#27568);
#23222=LINE('',#222838,#27569);
#23223=LINE('',#222840,#27570);
#23224=LINE('',#222846,#27571);
#23225=LINE('',#222847,#27572);
#23226=LINE('',#222850,#27573);
#23227=LINE('',#222852,#27574);
#23228=LINE('',#222856,#27575);
#23229=LINE('',#222858,#27576);
#23230=LINE('',#222862,#27577);
#23231=LINE('',#222864,#27578);
#23232=LINE('',#222868,#27579);
#23233=LINE('',#222870,#27580);
#23234=LINE('',#222874,#27581);
#23235=LINE('',#222876,#27582);
#23236=LINE('',#222880,#27583);
#23237=LINE('',#222882,#27584);
#23238=LINE('',#222886,#27585);
#23239=LINE('',#222888,#27586);
#23240=LINE('',#222892,#27587);
#23241=LINE('',#222894,#27588);
#23242=LINE('',#222898,#27589);
#23243=LINE('',#222900,#27590);
#23244=LINE('',#222904,#27591);
#23245=LINE('',#222906,#27592);
#23246=LINE('',#222910,#27593);
#23247=LINE('',#222912,#27594);
#23248=LINE('',#222916,#27595);
#23249=LINE('',#222918,#27596);
#23250=LINE('',#222922,#27597);
#23251=LINE('',#222924,#27598);
#23252=LINE('',#222928,#27599);
#23253=LINE('',#222930,#27600);
#23254=LINE('',#222934,#27601);
#23255=LINE('',#222936,#27602);
#23256=LINE('',#222942,#27603);
#23257=LINE('',#222943,#27604);
#23258=LINE('',#222946,#27605);
#23259=LINE('',#222948,#27606);
#23260=LINE('',#222952,#27607);
#23261=LINE('',#222954,#27608);
#23262=LINE('',#222958,#27609);
#23263=LINE('',#222960,#27610);
#23264=LINE('',#222964,#27611);
#23265=LINE('',#222966,#27612);
#23266=LINE('',#222972,#27613);
#23267=LINE('',#222973,#27614);
#23268=LINE('',#222976,#27615);
#23269=LINE('',#222978,#27616);
#23270=LINE('',#222984,#27617);
#23271=LINE('',#222985,#27618);
#23272=LINE('',#222988,#27619);
#23273=LINE('',#222990,#27620);
#23274=LINE('',#222994,#27621);
#23275=LINE('',#222996,#27622);
#23276=LINE('',#223000,#27623);
#23277=LINE('',#223002,#27624);
#23278=LINE('',#223006,#27625);
#23279=LINE('',#223010,#27626);
#23280=LINE('',#223016,#27627);
#23281=LINE('',#223024,#27628);
#23282=LINE('',#223045,#27629);
#23283=LINE('',#223047,#27630);
#23284=LINE('',#223055,#27631);
#23285=LINE('',#223057,#27632);
#23286=LINE('',#223063,#27633);
#23287=LINE('',#223065,#27634);
#23288=LINE('',#223067,#27635);
#23289=LINE('',#223069,#27636);
#23290=LINE('',#223071,#27637);
#23291=LINE('',#223073,#27638);
#23292=LINE('',#223075,#27639);
#23293=LINE('',#223077,#27640);
#23294=LINE('',#223079,#27641);
#23295=LINE('',#223081,#27642);
#23296=LINE('',#223083,#27643);
#23297=LINE('',#223085,#27644);
#23298=LINE('',#223087,#27645);
#23299=LINE('',#223089,#27646);
#23300=LINE('',#223091,#27647);
#23301=LINE('',#223093,#27648);
#23302=LINE('',#223095,#27649);
#23303=LINE('',#223097,#27650);
#23304=LINE('',#223099,#27651);
#23305=LINE('',#223101,#27652);
#23306=LINE('',#223103,#27653);
#23307=LINE('',#223105,#27654);
#23308=LINE('',#223107,#27655);
#23309=LINE('',#223109,#27656);
#23310=LINE('',#223111,#27657);
#23311=LINE('',#223113,#27658);
#23312=LINE('',#223115,#27659);
#23313=LINE('',#223117,#27660);
#23314=LINE('',#223119,#27661);
#23315=LINE('',#223121,#27662);
#23316=LINE('',#223123,#27663);
#23317=LINE('',#223125,#27664);
#23318=LINE('',#223129,#27665);
#23319=LINE('',#223131,#27666);
#23320=LINE('',#223133,#27667);
#23321=LINE('',#223134,#27668);
#23322=LINE('',#223138,#27669);
#23323=LINE('',#223139,#27670);
#23324=LINE('',#223140,#27671);
#23325=LINE('',#223143,#27672);
#23326=LINE('',#223145,#27673);
#23327=LINE('',#223146,#27674);
#23328=LINE('',#223148,#27675);
#23329=LINE('',#223150,#27676);
#23330=LINE('',#223152,#27677);
#23331=LINE('',#223154,#27678);
#23332=LINE('',#223156,#27679);
#23333=LINE('',#223158,#27680);
#23334=LINE('',#223160,#27681);
#23335=LINE('',#223162,#27682);
#23336=LINE('',#223164,#27683);
#23337=LINE('',#223166,#27684);
#23338=LINE('',#223168,#27685);
#23339=LINE('',#223170,#27686);
#23340=LINE('',#223172,#27687);
#23341=LINE('',#223174,#27688);
#23342=LINE('',#223176,#27689);
#23343=LINE('',#223178,#27690);
#23344=LINE('',#223180,#27691);
#23345=LINE('',#223182,#27692);
#23346=LINE('',#223184,#27693);
#23347=LINE('',#223186,#27694);
#23348=LINE('',#223188,#27695);
#23349=LINE('',#223190,#27696);
#23350=LINE('',#223211,#27697);
#23351=LINE('',#223212,#27698);
#23352=LINE('',#223213,#27699);
#23353=LINE('',#223214,#27700);
#23354=LINE('',#223215,#27701);
#23355=LINE('',#223216,#27702);
#23356=LINE('',#223217,#27703);
#23357=LINE('',#223218,#27704);
#23358=LINE('',#223219,#27705);
#23359=LINE('',#223221,#27706);
#23360=LINE('',#223223,#27707);
#23361=LINE('',#223224,#27708);
#23362=LINE('',#223225,#27709);
#23363=LINE('',#223226,#27710);
#23364=LINE('',#223227,#27711);
#23365=LINE('',#223229,#27712);
#23366=LINE('',#223230,#27713);
#23367=LINE('',#223236,#27714);
#23368=LINE('',#223237,#27715);
#23369=LINE('',#223243,#27716);
#23370=LINE('',#223244,#27717);
#23371=LINE('',#223246,#27718);
#23372=LINE('',#223247,#27719);
#23373=LINE('',#223249,#27720);
#23374=LINE('',#223250,#27721);
#23375=LINE('',#223252,#27722);
#23376=LINE('',#223253,#27723);
#23377=LINE('',#223255,#27724);
#23378=LINE('',#223256,#27725);
#23379=LINE('',#223257,#27726);
#23380=LINE('',#223259,#27727);
#23381=LINE('',#223260,#27728);
#23382=LINE('',#223261,#27729);
#23383=LINE('',#223262,#27730);
#23384=LINE('',#223263,#27731);
#23385=LINE('',#223264,#27732);
#23386=LINE('',#223265,#27733);
#23387=LINE('',#223266,#27734);
#23388=LINE('',#223272,#27735);
#23389=LINE('',#223278,#27736);
#23390=LINE('',#223279,#27737);
#23391=LINE('',#223280,#27738);
#23392=LINE('',#223281,#27739);
#23393=LINE('',#223282,#27740);
#23394=LINE('',#223284,#27741);
#23395=LINE('',#223285,#27742);
#23396=LINE('',#223286,#27743);
#23397=LINE('',#223287,#27744);
#23398=LINE('',#223288,#27745);
#23399=LINE('',#223289,#27746);
#23400=LINE('',#223290,#27747);
#23401=LINE('',#223291,#27748);
#23402=LINE('',#223294,#27749);
#23403=LINE('',#223296,#27750);
#23404=LINE('',#223301,#27751);
#23405=LINE('',#223304,#27752);
#23406=LINE('',#223308,#27753);
#23407=LINE('',#223312,#27754);
#23408=LINE('',#223317,#27755);
#23409=LINE('',#223320,#27756);
#23410=LINE('',#223327,#27757);
#23411=LINE('',#223336,#27758);
#23412=LINE('',#223340,#27759);
#23413=LINE('',#223341,#27760);
#23414=LINE('',#223347,#27761);
#23415=LINE('',#223362,#27762);
#23416=LINE('',#223377,#27763);
#23417=LINE('',#223378,#27764);
#23418=LINE('',#223386,#27765);
#23419=LINE('',#223388,#27766);
#23420=LINE('',#223405,#27767);
#23421=LINE('',#223407,#27768);
#23422=LINE('',#223428,#27769);
#23423=LINE('',#223429,#27770);
#23424=LINE('',#225928,#27771);
#23425=LINE('',#225931,#27772);
#23426=LINE('',#225939,#27773);
#23427=LINE('',#225948,#27774);
#23428=LINE('',#225954,#27775);
#23429=LINE('',#225960,#27776);
#23430=LINE('',#225977,#27777);
#23431=LINE('',#225980,#27778);
#23432=LINE('',#228081,#27779);
#23433=LINE('',#228088,#27780);
#23434=LINE('',#228101,#27781);
#23435=LINE('',#228111,#27782);
#23436=LINE('',#228118,#27783);
#23437=LINE('',#228120,#27784);
#23438=LINE('',#228131,#27785);
#23439=LINE('',#228143,#27786);
#23440=LINE('',#228177,#27787);
#23441=LINE('',#228178,#27788);
#23442=LINE('',#228182,#27789);
#23443=LINE('',#228186,#27790);
#23444=LINE('',#228190,#27791);
#23445=LINE('',#228196,#27792);
#23446=LINE('',#228200,#27793);
#23447=LINE('',#228204,#27794);
#23448=LINE('',#229182,#27795);
#23449=LINE('',#229254,#27796);
#23450=LINE('',#229256,#27797);
#23451=LINE('',#230393,#27798);
#23452=LINE('',#230394,#27799);
#23453=LINE('',#230396,#27800);
#23454=LINE('',#230398,#27801);
#23455=LINE('',#230401,#27802);
#23456=LINE('',#230402,#27803);
#23457=LINE('',#230405,#27804);
#23458=LINE('',#230406,#27805);
#23459=LINE('',#230411,#27806);
#23460=LINE('',#230416,#27807);
#23461=LINE('',#230770,#27808);
#23462=LINE('',#230772,#27809);
#23463=LINE('',#230776,#27810);
#23464=LINE('',#230780,#27811);
#23465=LINE('',#230784,#27812);
#23466=LINE('',#230788,#27813);
#23467=LINE('',#230792,#27814);
#23468=LINE('',#230799,#27815);
#23469=LINE('',#230821,#27816);
#23470=LINE('',#230822,#27817);
#23471=LINE('',#230825,#27818);
#23472=LINE('',#230827,#27819);
#23473=LINE('',#230829,#27820);
#23474=LINE('',#230831,#27821);
#23475=LINE('',#230833,#27822);
#23476=LINE('',#230835,#27823);
#23477=LINE('',#230918,#27824);
#23478=LINE('',#231017,#27825);
#23479=LINE('',#231103,#27826);
#23480=LINE('',#231223,#27827);
#23481=LINE('',#231229,#27828);
#23482=LINE('',#231230,#27829);
#23483=LINE('',#231232,#27830);
#23484=LINE('',#231234,#27831);
#23485=LINE('',#231236,#27832);
#23486=LINE('',#231237,#27833);
#23487=LINE('',#231239,#27834);
#23488=LINE('',#231241,#27835);
#23489=LINE('',#231263,#27836);
#23490=LINE('',#231264,#27837);
#23491=LINE('',#231266,#27838);
#23492=LINE('',#231268,#27839);
#23493=LINE('',#231270,#27840);
#23494=LINE('',#231273,#27841);
#23495=LINE('',#231275,#27842);
#23496=LINE('',#231277,#27843);
#23497=LINE('',#232815,#27844);
#23498=LINE('',#232821,#27845);
#23499=LINE('',#232828,#27846);
#23500=LINE('',#232838,#27847);
#23501=LINE('',#232848,#27848);
#23502=LINE('',#232858,#27849);
#23503=LINE('',#232874,#27850);
#23504=LINE('',#232900,#27851);
#23505=LINE('',#233024,#27852);
#23506=LINE('',#233025,#27853);
#23507=LINE('',#233027,#27854);
#23508=LINE('',#233029,#27855);
#23509=LINE('',#233031,#27856);
#23510=LINE('',#233033,#27857);
#23511=LINE('',#233158,#27858);
#23512=LINE('',#233159,#27859);
#23513=LINE('',#233161,#27860);
#23514=LINE('',#233163,#27861);
#23515=LINE('',#233165,#27862);
#23516=LINE('',#233167,#27863);
#23517=LINE('',#233172,#27864);
#23518=LINE('',#233178,#27865);
#23519=LINE('',#233185,#27866);
#23520=LINE('',#233195,#27867);
#23521=LINE('',#233205,#27868);
#23522=LINE('',#233215,#27869);
#23523=LINE('',#233231,#27870);
#23524=LINE('',#233257,#27871);
#23525=LINE('',#233322,#27872);
#23526=LINE('',#233325,#27873);
#23527=LINE('',#233327,#27874);
#23528=LINE('',#233328,#27875);
#23529=LINE('',#233330,#27876);
#23530=LINE('',#233332,#27877);
#23531=LINE('',#233340,#27878);
#23532=LINE('',#233342,#27879);
#23533=LINE('',#233348,#27880);
#23534=LINE('',#233354,#27881);
#23535=LINE('',#233361,#27882);
#23536=LINE('',#233376,#27883);
#23537=LINE('',#233377,#27884);
#23538=LINE('',#233382,#27885);
#23539=LINE('',#233383,#27886);
#23540=LINE('',#233400,#27887);
#23541=LINE('',#233401,#27888);
#23542=LINE('',#233406,#27889);
#23543=LINE('',#233407,#27890);
#23544=LINE('',#233413,#27891);
#23545=LINE('',#233415,#27892);
#23546=LINE('',#233416,#27893);
#23547=LINE('',#233419,#27894);
#23548=LINE('',#233423,#27895);
#23549=LINE('',#233428,#27896);
#23550=LINE('',#233430,#27897);
#23551=LINE('',#233432,#27898);
#23552=LINE('',#233433,#27899);
#23553=LINE('',#233449,#27900);
#23554=LINE('',#233458,#27901);
#23555=LINE('',#233475,#27902);
#23556=LINE('',#233477,#27903);
#23557=LINE('',#233481,#27904);
#23558=LINE('',#233485,#27905);
#23559=LINE('',#233491,#27906);
#23560=LINE('',#233494,#27907);
#23561=LINE('',#233507,#27908);
#23562=LINE('',#233509,#27909);
#23563=LINE('',#233519,#27910);
#23564=LINE('',#233521,#27911);
#23565=LINE('',#233533,#27912);
#23566=LINE('',#233535,#27913);
#23567=LINE('',#233539,#27914);
#23568=LINE('',#233541,#27915);
#23569=LINE('',#233544,#27916);
#23570=LINE('',#233545,#27917);
#23571=LINE('',#233547,#27918);
#23572=LINE('',#233549,#27919);
#23573=LINE('',#233551,#27920);
#23574=LINE('',#233553,#27921);
#23575=LINE('',#233555,#27922);
#23576=LINE('',#233557,#27923);
#23577=LINE('',#233560,#27924);
#23578=LINE('',#233562,#27925);
#23579=LINE('',#233564,#27926);
#23580=LINE('',#233566,#27927);
#23581=LINE('',#233568,#27928);
#23582=LINE('',#233634,#27929);
#23583=LINE('',#233637,#27930);
#23584=LINE('',#233639,#27931);
#23585=LINE('',#233640,#27932);
#23586=LINE('',#233642,#27933);
#23587=LINE('',#233644,#27934);
#23588=LINE('',#233652,#27935);
#23589=LINE('',#233654,#27936);
#23590=LINE('',#233661,#27937);
#23591=LINE('',#233673,#27938);
#23592=LINE('',#233684,#27939);
#23593=LINE('',#233685,#27940);
#23594=LINE('',#233705,#27941);
#23595=LINE('',#233706,#27942);
#23596=LINE('',#233712,#27943);
#23597=LINE('',#233715,#27944);
#23598=LINE('',#233726,#27945);
#23599=LINE('',#233727,#27946);
#23600=LINE('',#233747,#27947);
#23601=LINE('',#233748,#27948);
#23602=LINE('',#233754,#27949);
#23603=LINE('',#233757,#27950);
#23604=LINE('',#233768,#27951);
#23605=LINE('',#233769,#27952);
#23606=LINE('',#233780,#27953);
#23607=LINE('',#233781,#27954);
#23608=LINE('',#233792,#27955);
#23609=LINE('',#233793,#27956);
#23610=LINE('',#233804,#27957);
#23611=LINE('',#233805,#27958);
#23612=LINE('',#233811,#27959);
#23613=LINE('',#233814,#27960);
#23614=LINE('',#233825,#27961);
#23615=LINE('',#233826,#27962);
#23616=LINE('',#233846,#27963);
#23617=LINE('',#233847,#27964);
#23618=LINE('',#233853,#27965);
#23619=LINE('',#233856,#27966);
#23620=LINE('',#233867,#27967);
#23621=LINE('',#233868,#27968);
#23622=LINE('',#233885,#27969);
#23623=LINE('',#233886,#27970);
#23624=LINE('',#233897,#27971);
#23625=LINE('',#233898,#27972);
#23626=LINE('',#233909,#27973);
#23627=LINE('',#233910,#27974);
#23628=LINE('',#233916,#27975);
#23629=LINE('',#233919,#27976);
#23630=LINE('',#233930,#27977);
#23631=LINE('',#233931,#27978);
#23632=LINE('',#233954,#27979);
#23633=LINE('',#233955,#27980);
#23634=LINE('',#233966,#27981);
#23635=LINE('',#233967,#27982);
#23636=LINE('',#233973,#27983);
#23637=LINE('',#233976,#27984);
#23638=LINE('',#233987,#27985);
#23639=LINE('',#233988,#27986);
#23640=LINE('',#234011,#27987);
#23641=LINE('',#234012,#27988);
#23642=LINE('',#234023,#27989);
#23643=LINE('',#234024,#27990);
#23644=LINE('',#234030,#27991);
#23645=LINE('',#234033,#27992);
#23646=LINE('',#234044,#27993);
#23647=LINE('',#234045,#27994);
#23648=LINE('',#234068,#27995);
#23649=LINE('',#234069,#27996);
#23650=LINE('',#234080,#27997);
#23651=LINE('',#234081,#27998);
#23652=LINE('',#234087,#27999);
#23653=LINE('',#234090,#28000);
#23654=LINE('',#234101,#28001);
#23655=LINE('',#234102,#28002);
#23656=LINE('',#234125,#28003);
#23657=LINE('',#234126,#28004);
#23658=LINE('',#234137,#28005);
#23659=LINE('',#234138,#28006);
#23660=LINE('',#234144,#28007);
#23661=LINE('',#234147,#28008);
#23662=LINE('',#234158,#28009);
#23663=LINE('',#234159,#28010);
#23664=LINE('',#234182,#28011);
#23665=LINE('',#234183,#28012);
#23666=LINE('',#234194,#28013);
#23667=LINE('',#234195,#28014);
#23668=LINE('',#234201,#28015);
#23669=LINE('',#234204,#28016);
#23670=LINE('',#234215,#28017);
#23671=LINE('',#234216,#28018);
#23672=LINE('',#234239,#28019);
#23673=LINE('',#234240,#28020);
#23674=LINE('',#234251,#28021);
#23675=LINE('',#234252,#28022);
#23676=LINE('',#234258,#28023);
#23677=LINE('',#234261,#28024);
#23678=LINE('',#234272,#28025);
#23679=LINE('',#234273,#28026);
#23680=LINE('',#234284,#28027);
#23681=LINE('',#234285,#28028);
#23682=LINE('',#234302,#28029);
#23683=LINE('',#234303,#28030);
#23684=LINE('',#234314,#28031);
#23685=LINE('',#234315,#28032);
#23686=LINE('',#234321,#28033);
#23687=LINE('',#234324,#28034);
#23688=LINE('',#234335,#28035);
#23689=LINE('',#234336,#28036);
#23690=LINE('',#234347,#28037);
#23691=LINE('',#234348,#28038);
#23692=LINE('',#234359,#28039);
#23693=LINE('',#234360,#28040);
#23694=LINE('',#234371,#28041);
#23695=LINE('',#234372,#28042);
#23696=LINE('',#234387,#28043);
#23697=LINE('',#234390,#28044);
#23698=LINE('',#234401,#28045);
#23699=LINE('',#234402,#28046);
#23700=LINE('',#234413,#28047);
#23701=LINE('',#234414,#28048);
#23702=LINE('',#234417,#28049);
#23703=LINE('',#234419,#28050);
#23704=LINE('',#234423,#28051);
#23705=LINE('',#234425,#28052);
#23706=LINE('',#234429,#28053);
#23707=LINE('',#234431,#28054);
#23708=LINE('',#234435,#28055);
#23709=LINE('',#234437,#28056);
#23710=LINE('',#234441,#28057);
#23711=LINE('',#234443,#28058);
#23712=LINE('',#234447,#28059);
#23713=LINE('',#234449,#28060);
#23714=LINE('',#234453,#28061);
#23715=LINE('',#234455,#28062);
#23716=LINE('',#234459,#28063);
#23717=LINE('',#234461,#28064);
#23718=LINE('',#234465,#28065);
#23719=LINE('',#234467,#28066);
#23720=LINE('',#234471,#28067);
#23721=LINE('',#234473,#28068);
#23722=LINE('',#234477,#28069);
#23723=LINE('',#234479,#28070);
#23724=LINE('',#234483,#28071);
#23725=LINE('',#234485,#28072);
#23726=LINE('',#234489,#28073);
#23727=LINE('',#234491,#28074);
#23728=LINE('',#234495,#28075);
#23729=LINE('',#234497,#28076);
#23730=LINE('',#234501,#28077);
#23731=LINE('',#234503,#28078);
#23732=LINE('',#234507,#28079);
#23733=LINE('',#234509,#28080);
#23734=LINE('',#234513,#28081);
#23735=LINE('',#234515,#28082);
#23736=LINE('',#234519,#28083);
#23737=LINE('',#234521,#28084);
#23738=LINE('',#234525,#28085);
#23739=LINE('',#234527,#28086);
#23740=LINE('',#234531,#28087);
#23741=LINE('',#234533,#28088);
#23742=LINE('',#234537,#28089);
#23743=LINE('',#234539,#28090);
#23744=LINE('',#234543,#28091);
#23745=LINE('',#234545,#28092);
#23746=LINE('',#234549,#28093);
#23747=LINE('',#234551,#28094);
#23748=LINE('',#234555,#28095);
#23749=LINE('',#234557,#28096);
#23750=LINE('',#234561,#28097);
#23751=LINE('',#234563,#28098);
#23752=LINE('',#234567,#28099);
#23753=LINE('',#234569,#28100);
#23754=LINE('',#234576,#28101);
#23755=LINE('',#234577,#28102);
#23756=LINE('',#234579,#28103);
#23757=LINE('',#234580,#28104);
#23758=LINE('',#234581,#28105);
#23759=LINE('',#234582,#28106);
#23760=LINE('',#234583,#28107);
#23761=LINE('',#234584,#28108);
#23762=LINE('',#234585,#28109);
#23763=LINE('',#234586,#28110);
#23764=LINE('',#234587,#28111);
#23765=LINE('',#234588,#28112);
#23766=LINE('',#234589,#28113);
#23767=LINE('',#234591,#28114);
#23768=LINE('',#234594,#28115);
#23769=LINE('',#234597,#28116);
#23770=LINE('',#234599,#28117);
#23771=LINE('',#234601,#28118);
#23772=LINE('',#234604,#28119);
#23773=LINE('',#234605,#28120);
#23774=LINE('',#234607,#28121);
#23775=LINE('',#234609,#28122);
#23776=LINE('',#234611,#28123);
#23777=LINE('',#234613,#28124);
#23778=LINE('',#234615,#28125);
#23779=LINE('',#234617,#28126);
#23780=LINE('',#234619,#28127);
#23781=LINE('',#234621,#28128);
#23782=LINE('',#234623,#28129);
#23783=LINE('',#234625,#28130);
#23784=LINE('',#234627,#28131);
#23785=LINE('',#234628,#28132);
#23786=LINE('',#234633,#28133);
#23787=LINE('',#234635,#28134);
#23788=LINE('',#234637,#28135);
#23789=LINE('',#234638,#28136);
#23790=LINE('',#234643,#28137);
#23791=LINE('',#234645,#28138);
#23792=LINE('',#234647,#28139);
#23793=LINE('',#234648,#28140);
#23794=LINE('',#234653,#28141);
#23795=LINE('',#234655,#28142);
#23796=LINE('',#234657,#28143);
#23797=LINE('',#234658,#28144);
#23798=LINE('',#234663,#28145);
#23799=LINE('',#234665,#28146);
#23800=LINE('',#234667,#28147);
#23801=LINE('',#234668,#28148);
#23802=LINE('',#234671,#28149);
#23803=LINE('',#234674,#28150);
#23804=LINE('',#234677,#28151);
#23805=LINE('',#234680,#28152);
#23806=LINE('',#234683,#28153);
#23807=LINE('',#234685,#28154);
#23808=LINE('',#234686,#28155);
#23809=LINE('',#234687,#28156);
#23810=LINE('',#234688,#28157);
#23811=LINE('',#234690,#28158);
#23812=LINE('',#234692,#28159);
#23813=LINE('',#234693,#28160);
#23814=LINE('',#234694,#28161);
#23815=LINE('',#234695,#28162);
#23816=LINE('',#234696,#28163);
#23817=LINE('',#234698,#28164);
#23818=LINE('',#234701,#28165);
#23819=LINE('',#234703,#28166);
#23820=LINE('',#234704,#28167);
#23821=LINE('',#234705,#28168);
#23822=LINE('',#234707,#28169);
#23823=LINE('',#234710,#28170);
#23824=LINE('',#234714,#28171);
#23825=LINE('',#234717,#28172);
#23826=LINE('',#234720,#28173);
#23827=LINE('',#234723,#28174);
#23828=LINE('',#234727,#28175);
#23829=LINE('',#234732,#28176);
#23830=LINE('',#234735,#28177);
#23831=LINE('',#234737,#28178);
#23832=LINE('',#234741,#28179);
#23833=LINE('',#234743,#28180);
#23834=LINE('',#234747,#28181);
#23835=LINE('',#234872,#28182);
#23836=LINE('',#234873,#28183);
#23837=LINE('',#234875,#28184);
#23838=LINE('',#234877,#28185);
#23839=LINE('',#234879,#28186);
#23840=LINE('',#234881,#28187);
#23841=LINE('',#235006,#28188);
#23842=LINE('',#235007,#28189);
#23843=LINE('',#235009,#28190);
#23844=LINE('',#235011,#28191);
#23845=LINE('',#235013,#28192);
#23846=LINE('',#235015,#28193);
#23847=LINE('',#235020,#28194);
#23848=LINE('',#235026,#28195);
#23849=LINE('',#235033,#28196);
#23850=LINE('',#235043,#28197);
#23851=LINE('',#235053,#28198);
#23852=LINE('',#235063,#28199);
#23853=LINE('',#235079,#28200);
#23854=LINE('',#235105,#28201);
#23855=LINE('',#235112,#28202);
#23856=LINE('',#235116,#28203);
#23857=LINE('',#235128,#28204);
#23858=LINE('',#235131,#28205);
#23859=LINE('',#235212,#28206);
#23860=LINE('',#235215,#28207);
#23861=LINE('',#235221,#28208);
#23862=LINE('',#235233,#28209);
#23863=LINE('',#235235,#28210);
#23864=LINE('',#235236,#28211);
#23865=LINE('',#235238,#28212);
#23866=LINE('',#235239,#28213);
#23867=LINE('',#235241,#28214);
#23868=LINE('',#235243,#28215);
#23869=LINE('',#235245,#28216);
#23870=LINE('',#235247,#28217);
#23871=LINE('',#235249,#28218);
#23872=LINE('',#235250,#28219);
#23873=LINE('',#235254,#28220);
#23874=LINE('',#235264,#28221);
#23875=LINE('',#235275,#28222);
#23876=LINE('',#235276,#28223);
#23877=LINE('',#235357,#28224);
#23878=LINE('',#235360,#28225);
#23879=LINE('',#235366,#28226);
#23880=LINE('',#235444,#28227);
#23881=LINE('',#235446,#28228);
#23882=LINE('',#235447,#28229);
#23883=LINE('',#235449,#28230);
#23884=LINE('',#235450,#28231);
#23885=LINE('',#235452,#28232);
#23886=LINE('',#235453,#28233);
#23887=LINE('',#235455,#28234);
#23888=LINE('',#235456,#28235);
#23889=LINE('',#235458,#28236);
#23890=LINE('',#235460,#28237);
#23891=LINE('',#235462,#28238);
#23892=LINE('',#235464,#28239);
#23893=LINE('',#235466,#28240);
#23894=LINE('',#235467,#28241);
#23895=LINE('',#235471,#28242);
#23896=LINE('',#235517,#28243);
#23897=LINE('',#235525,#28244);
#23898=LINE('',#235526,#28245);
#23899=LINE('',#235530,#28246);
#23900=LINE('',#235538,#28247);
#23901=LINE('',#235539,#28248);
#23902=LINE('',#235543,#28249);
#23903=LINE('',#235547,#28250);
#23904=LINE('',#235550,#28251);
#23905=LINE('',#235554,#28252);
#23906=LINE('',#235558,#28253);
#23907=LINE('',#235602,#28254);
#23908=LINE('',#235606,#28255);
#23909=LINE('',#235614,#28256);
#23910=LINE('',#235615,#28257);
#23911=LINE('',#235619,#28258);
#23912=LINE('',#235627,#28259);
#23913=LINE('',#235628,#28260);
#23914=LINE('',#235630,#28261);
#23915=LINE('',#235631,#28262);
#23916=LINE('',#235633,#28263);
#23917=LINE('',#235635,#28264);
#23918=LINE('',#235641,#28265);
#23919=LINE('',#235696,#28266);
#23920=LINE('',#235772,#28267);
#23921=LINE('',#235850,#28268);
#23922=LINE('',#235928,#28269);
#23923=LINE('',#236004,#28270);
#23924=LINE('',#236080,#28271);
#23925=LINE('',#236156,#28272);
#23926=LINE('',#236232,#28273);
#23927=LINE('',#236310,#28274);
#23928=LINE('',#236388,#28275);
#23929=LINE('',#236464,#28276);
#23930=LINE('',#236540,#28277);
#23931=LINE('',#236616,#28278);
#23932=LINE('',#236692,#28279);
#23933=LINE('',#236768,#28280);
#23934=LINE('',#236846,#28281);
#23935=LINE('',#236924,#28282);
#23936=LINE('',#237000,#28283);
#23937=LINE('',#237028,#28284);
#23938=LINE('',#237065,#28285);
#23939=LINE('',#237141,#28286);
#23940=LINE('',#237219,#28287);
#23941=LINE('',#237295,#28288);
#23942=LINE('',#237371,#28289);
#23943=LINE('',#237447,#28290);
#23944=LINE('',#237523,#28291);
#23945=LINE('',#237601,#28292);
#23946=LINE('',#237677,#28293);
#23947=LINE('',#237755,#28294);
#23948=LINE('',#237831,#28295);
#23949=LINE('',#237907,#28296);
#23950=LINE('',#237983,#28297);
#23951=LINE('',#238059,#28298);
#23952=LINE('',#238137,#28299);
#23953=LINE('',#238213,#28300);
#23954=LINE('',#238291,#28301);
#23955=LINE('',#238367,#28302);
#23956=LINE('',#238413,#28303);
#23957=LINE('',#238431,#28304);
#23958=LINE('',#238476,#28305);
#23959=LINE('',#238506,#28306);
#23960=LINE('',#238536,#28307);
#23961=LINE('',#238566,#28308);
#23962=LINE('',#238596,#28309);
#23963=LINE('',#238626,#28310);
#23964=LINE('',#238656,#28311);
#23965=LINE('',#238686,#28312);
#23966=LINE('',#238716,#28313);
#23967=LINE('',#238746,#28314);
#23968=LINE('',#238776,#28315);
#23969=LINE('',#238806,#28316);
#23970=LINE('',#238836,#28317);
#23971=LINE('',#238866,#28318);
#23972=LINE('',#238896,#28319);
#23973=LINE('',#238926,#28320);
#23974=LINE('',#238956,#28321);
#23975=LINE('',#238967,#28322);
#23976=LINE('',#239038,#28323);
#23977=LINE('',#239114,#28324);
#23978=LINE('',#239190,#28325);
#23979=LINE('',#239268,#28326);
#23980=LINE('',#239344,#28327);
#23981=LINE('',#239420,#28328);
#23982=LINE('',#239498,#28329);
#23983=LINE('',#239574,#28330);
#23984=LINE('',#239650,#28331);
#23985=LINE('',#239726,#28332);
#23986=LINE('',#239804,#28333);
#23987=LINE('',#239880,#28334);
#23988=LINE('',#239956,#28335);
#23989=LINE('',#240034,#28336);
#23990=LINE('',#240110,#28337);
#23991=LINE('',#240186,#28338);
#23992=LINE('',#240262,#28339);
#23993=LINE('',#240347,#28340);
#23994=LINE('',#240375,#28341);
#23995=LINE('',#240420,#28342);
#23996=LINE('',#240450,#28343);
#23997=LINE('',#240480,#28344);
#23998=LINE('',#240510,#28345);
#23999=LINE('',#240540,#28346);
#24000=LINE('',#240570,#28347);
#24001=LINE('',#240600,#28348);
#24002=LINE('',#240630,#28349);
#24003=LINE('',#240660,#28350);
#24004=LINE('',#240690,#28351);
#24005=LINE('',#240720,#28352);
#24006=LINE('',#240750,#28353);
#24007=LINE('',#240780,#28354);
#24008=LINE('',#240810,#28355);
#24009=LINE('',#240840,#28356);
#24010=LINE('',#240870,#28357);
#24011=LINE('',#240900,#28358);
#24012=LINE('',#240911,#28359);
#24013=LINE('',#240927,#28360);
#24014=LINE('',#241005,#28361);
#24015=LINE('',#241081,#28362);
#24016=LINE('',#241157,#28363);
#24017=LINE('',#241233,#28364);
#24018=LINE('',#241309,#28365);
#24019=LINE('',#241385,#28366);
#24020=LINE('',#241463,#28367);
#24021=LINE('',#241541,#28368);
#24022=LINE('',#241617,#28369);
#24023=LINE('',#241693,#28370);
#24024=LINE('',#241769,#28371);
#24025=LINE('',#241845,#28372);
#24026=LINE('',#241921,#28373);
#24027=LINE('',#242001,#28374);
#24028=LINE('',#242077,#28375);
#24029=LINE('',#242153,#28376);
#24030=LINE('',#242229,#28377);
#24031=LINE('',#242293,#28378);
#24032=LINE('',#242311,#28379);
#24033=LINE('',#242356,#28380);
#24034=LINE('',#242386,#28381);
#24035=LINE('',#242416,#28382);
#24036=LINE('',#242446,#28383);
#24037=LINE('',#242476,#28384);
#24038=LINE('',#242506,#28385);
#24039=LINE('',#242536,#28386);
#24040=LINE('',#242566,#28387);
#24041=LINE('',#242596,#28388);
#24042=LINE('',#242626,#28389);
#24043=LINE('',#242656,#28390);
#24044=LINE('',#242686,#28391);
#24045=LINE('',#242716,#28392);
#24046=LINE('',#242746,#28393);
#24047=LINE('',#242776,#28394);
#24048=LINE('',#242806,#28395);
#24049=LINE('',#242836,#28396);
#24050=LINE('',#242847,#28397);
#24051=LINE('',#242865,#28398);
#24052=LINE('',#242910,#28399);
#24053=LINE('',#242940,#28400);
#24054=LINE('',#242970,#28401);
#24055=LINE('',#243000,#28402);
#24056=LINE('',#243030,#28403);
#24057=LINE('',#243060,#28404);
#24058=LINE('',#243090,#28405);
#24059=LINE('',#243120,#28406);
#24060=LINE('',#243150,#28407);
#24061=LINE('',#243180,#28408);
#24062=LINE('',#243210,#28409);
#24063=LINE('',#243240,#28410);
#24064=LINE('',#243270,#28411);
#24065=LINE('',#243300,#28412);
#24066=LINE('',#243330,#28413);
#24067=LINE('',#243360,#28414);
#24068=LINE('',#243390,#28415);
#24069=LINE('',#243401,#28416);
#24070=LINE('',#243403,#28417);
#24071=LINE('',#243405,#28418);
#24072=LINE('',#243407,#28419);
#24073=LINE('',#243409,#28420);
#24074=LINE('',#243411,#28421);
#24075=LINE('',#243413,#28422);
#24076=LINE('',#243414,#28423);
#24077=LINE('',#243418,#28424);
#24078=LINE('',#243421,#28425);
#24079=LINE('',#243423,#28426);
#24080=LINE('',#243468,#28427);
#24081=LINE('',#243470,#28428);
#24082=LINE('',#243472,#28429);
#24083=LINE('',#243474,#28430);
#24084=LINE('',#243521,#28431);
#24085=LINE('',#243523,#28432);
#24086=LINE('',#243525,#28433);
#24087=LINE('',#243526,#28434);
#24088=LINE('',#243529,#28435);
#24089=LINE('',#243531,#28436);
#24090=LINE('',#243532,#28437);
#24091=LINE('',#243535,#28438);
#24092=LINE('',#243537,#28439);
#24093=LINE('',#243538,#28440);
#24094=LINE('',#243540,#28441);
#24095=LINE('',#243541,#28442);
#24096=LINE('',#243544,#28443);
#24097=LINE('',#243548,#28444);
#24098=LINE('',#243550,#28445);
#24099=LINE('',#243553,#28446);
#24100=LINE('',#243575,#28447);
#24101=LINE('',#243725,#28448);
#24102=LINE('',#243729,#28449);
#24103=LINE('',#243816,#28450);
#24104=LINE('',#243840,#28451);
#24105=LINE('',#243843,#28452);
#24106=LINE('',#243852,#28453);
#24107=LINE('',#243855,#28454);
#24108=LINE('',#243864,#28455);
#24109=LINE('',#243886,#28456);
#24110=LINE('',#243913,#28457);
#24111=LINE('',#243918,#28458);
#24112=LINE('',#243947,#28459);
#24113=LINE('',#243953,#28460);
#24114=LINE('',#243960,#28461);
#24115=LINE('',#243970,#28462);
#24116=LINE('',#243980,#28463);
#24117=LINE('',#243990,#28464);
#24118=LINE('',#244006,#28465);
#24119=LINE('',#244020,#28466);
#24120=LINE('',#244023,#28467);
#24121=LINE('',#246688,#28468);
#24122=LINE('',#246702,#28469);
#24123=LINE('',#246877,#28470);
#24124=LINE('',#247114,#28471);
#24125=LINE('',#247116,#28472);
#24126=LINE('',#247489,#28473);
#24127=LINE('',#247490,#28474);
#24128=LINE('',#247673,#28475);
#24129=LINE('',#247674,#28476);
#24130=LINE('',#247839,#28477);
#24131=LINE('',#247865,#28478);
#24132=LINE('',#247866,#28479);
#24133=LINE('',#247962,#28480);
#24134=LINE('',#247975,#28481);
#24135=LINE('',#247979,#28482);
#24136=LINE('',#247999,#28483);
#24137=LINE('',#248003,#28484);
#24138=LINE('',#248023,#28485);
#24139=LINE('',#248027,#28486);
#24140=LINE('',#248076,#28487);
#24141=LINE('',#248080,#28488);
#24142=LINE('',#248090,#28489);
#24143=LINE('',#248094,#28490);
#24144=LINE('',#248102,#28491);
#24145=LINE('',#248187,#28492);
#24146=LINE('',#248224,#28493);
#24147=LINE('',#248228,#28494);
#24148=LINE('',#248238,#28495);
#24149=LINE('',#248242,#28496);
#24150=LINE('',#248255,#28497);
#24151=LINE('',#248256,#28498);
#24152=LINE('',#248337,#28499);
#24153=LINE('',#248498,#28500);
#24154=LINE('',#248520,#28501);
#24155=LINE('',#248525,#28502);
#24156=LINE('',#248547,#28503);
#24157=LINE('',#248552,#28504);
#24158=LINE('',#248574,#28505);
#24159=LINE('',#248579,#28506);
#24160=LINE('',#248601,#28507);
#24161=LINE('',#248638,#28508);
#24162=LINE('',#248663,#28509);
#24163=LINE('',#248668,#28510);
#24164=LINE('',#248693,#28511);
#24165=LINE('',#248700,#28512);
#24166=LINE('',#248785,#28513);
#24167=LINE('',#248850,#28514);
#24168=LINE('',#248875,#28515);
#24169=LINE('',#248880,#28516);
#24170=LINE('',#248905,#28517);
#24171=LINE('',#248912,#28518);
#24172=LINE('',#248997,#28519);
#24173=LINE('',#249165,#28520);
#24174=LINE('',#251064,#28521);
#24175=LINE('',#251466,#28522);
#24176=LINE('',#252014,#28523);
#24177=LINE('',#252036,#28524);
#24178=LINE('',#255718,#28525);
#24179=LINE('',#255959,#28526);
#24180=LINE('',#256078,#28527);
#24181=LINE('',#259888,#28528);
#24182=LINE('',#260125,#28529);
#24183=LINE('',#260242,#28530);
#24184=LINE('',#263459,#28531);
#24185=LINE('',#263853,#28532);
#24186=LINE('',#264375,#28533);
#24187=LINE('',#264397,#28534);
#24188=LINE('',#268790,#28535);
#24189=LINE('',#269480,#28536);
#24190=LINE('',#271077,#28537);
#24191=LINE('',#271078,#28538);
#24192=LINE('',#271199,#28539);
#24193=LINE('',#271201,#28540);
#24194=LINE('',#271203,#28541);
#24195=LINE('',#271204,#28542);
#24196=LINE('',#271207,#28543);
#24197=LINE('',#271209,#28544);
#24198=LINE('',#271210,#28545);
#24199=LINE('',#271213,#28546);
#24200=LINE('',#271215,#28547);
#24201=LINE('',#271216,#28548);
#24202=LINE('',#271218,#28549);
#24203=LINE('',#271219,#28550);
#24204=LINE('',#271232,#28551);
#24205=LINE('',#271246,#28552);
#24206=LINE('',#271254,#28553);
#24207=LINE('',#271265,#28554);
#24208=LINE('',#271281,#28555);
#24209=LINE('',#271302,#28556);
#24210=LINE('',#271318,#28557);
#24211=LINE('',#271337,#28558);
#24212=LINE('',#271353,#28559);
#24213=LINE('',#271379,#28560);
#24214=LINE('',#271394,#28561);
#24215=LINE('',#271407,#28562);
#24216=LINE('',#271423,#28563);
#24217=LINE('',#271442,#28564);
#24218=LINE('',#271458,#28565);
#24219=LINE('',#271475,#28566);
#24220=LINE('',#271485,#28567);
#24221=LINE('',#271491,#28568);
#24222=LINE('',#271494,#28569);
#24223=LINE('',#271539,#28570);
#24224=LINE('',#271541,#28571);
#24225=LINE('',#271542,#28572);
#24226=LINE('',#271545,#28573);
#24227=LINE('',#271547,#28574);
#24228=LINE('',#271548,#28575);
#24229=LINE('',#271905,#28576);
#24230=LINE('',#271908,#28577);
#24231=LINE('',#271911,#28578);
#24232=LINE('',#271913,#28579);
#24233=LINE('',#271917,#28580);
#24234=LINE('',#271919,#28581);
#24235=LINE('',#271923,#28582);
#24236=LINE('',#271925,#28583);
#24237=LINE('',#271930,#28584);
#24238=LINE('',#271933,#28585);
#24239=LINE('',#271935,#28586);
#24240=LINE('',#271939,#28587);
#24241=LINE('',#271942,#28588);
#24242=LINE('',#271945,#28589);
#24243=LINE('',#271948,#28590);
#24244=LINE('',#271951,#28591);
#24245=LINE('',#271953,#28592);
#24246=LINE('',#271957,#28593);
#24247=LINE('',#271960,#28594);
#24248=LINE('',#271963,#28595);
#24249=LINE('',#271966,#28596);
#24250=LINE('',#271969,#28597);
#24251=LINE('',#271971,#28598);
#24252=LINE('',#271975,#28599);
#24253=LINE('',#271978,#28600);
#24254=LINE('',#271981,#28601);
#24255=LINE('',#271983,#28602);
#24256=LINE('',#272340,#28603);
#24257=LINE('',#272374,#28604);
#24258=LINE('',#272376,#28605);
#24259=LINE('',#272379,#28606);
#24260=LINE('',#272390,#28607);
#24261=LINE('',#272392,#28608);
#24262=LINE('',#272399,#28609);
#24263=LINE('',#272401,#28610);
#24264=LINE('',#272404,#28611);
#24265=LINE('',#272406,#28612);
#24266=LINE('',#272409,#28613);
#24267=LINE('',#272412,#28614);
#24268=LINE('',#272414,#28615);
#24269=LINE('',#272417,#28616);
#24270=LINE('',#272419,#28617);
#24271=LINE('',#272422,#28618);
#24272=LINE('',#272424,#28619);
#24273=LINE('',#272427,#28620);
#24274=LINE('',#272428,#28621);
#24275=LINE('',#272435,#28622);
#24276=LINE('',#272442,#28623);
#24277=LINE('',#272445,#28624);
#24278=LINE('',#272448,#28625);
#24279=LINE('',#272450,#28626);
#24280=LINE('',#272451,#28627);
#24281=LINE('',#272454,#28628);
#24282=LINE('',#272456,#28629);
#24283=LINE('',#272457,#28630);
#24284=LINE('',#272459,#28631);
#24285=LINE('',#272460,#28632);
#24286=LINE('',#272472,#28633);
#24287=LINE('',#272484,#28634);
#24288=LINE('',#272494,#28635);
#24289=LINE('',#272507,#28636);
#24290=LINE('',#272515,#28637);
#24291=LINE('',#272532,#28638);
#24292=LINE('',#272552,#28639);
#24293=LINE('',#272575,#28640);
#24294=LINE('',#272595,#28641);
#24295=LINE('',#272618,#28642);
#24296=LINE('',#272638,#28643);
#24297=LINE('',#272661,#28644);
#24298=LINE('',#272681,#28645);
#24299=LINE('',#272698,#28646);
#24300=LINE('',#272718,#28647);
#24301=LINE('',#272737,#28648);
#24302=LINE('',#272757,#28649);
#24303=LINE('',#272789,#28650);
#24304=LINE('',#272804,#28651);
#24305=LINE('',#272821,#28652);
#24306=LINE('',#272841,#28653);
#24307=LINE('',#272871,#28654);
#24308=LINE('',#272886,#28655);
#24309=LINE('',#272903,#28656);
#24310=LINE('',#272923,#28657);
#24311=LINE('',#272946,#28658);
#24312=LINE('',#272966,#28659);
#24313=LINE('',#272989,#28660);
#24314=LINE('',#273009,#28661);
#24315=LINE('',#273057,#28662);
#24316=LINE('',#273058,#28663);
#24317=LINE('',#273100,#28664);
#24318=LINE('',#273103,#28665);
#24319=LINE('',#273187,#28666);
#24320=LINE('',#273189,#28667);
#24321=LINE('',#273190,#28668);
#24322=LINE('',#273193,#28669);
#24323=LINE('',#273195,#28670);
#24324=LINE('',#273196,#28671);
#24325=LINE('',#273973,#28672);
#24326=LINE('',#273976,#28673);
#24327=LINE('',#273979,#28674);
#24328=LINE('',#273981,#28675);
#24329=LINE('',#273985,#28676);
#24330=LINE('',#273987,#28677);
#24331=LINE('',#273991,#28678);
#24332=LINE('',#273993,#28679);
#24333=LINE('',#273997,#28680);
#24334=LINE('',#274000,#28681);
#24335=LINE('',#274003,#28682);
#24336=LINE('',#274007,#28683);
#24337=LINE('',#274009,#28684);
#24338=LINE('',#274013,#28685);
#24339=LINE('',#274016,#28686);
#24340=LINE('',#274019,#28687);
#24341=LINE('',#274021,#28688);
#24342=LINE('',#274025,#28689);
#24343=LINE('',#274029,#28690);
#24344=LINE('',#274032,#28691);
#24345=LINE('',#274035,#28692);
#24346=LINE('',#274037,#28693);
#24347=LINE('',#274041,#28694);
#24348=LINE('',#274044,#28695);
#24349=LINE('',#274047,#28696);
#24350=LINE('',#274049,#28697);
#24351=LINE('',#274053,#28698);
#24352=LINE('',#274056,#28699);
#24353=LINE('',#274059,#28700);
#24354=LINE('',#274061,#28701);
#24355=LINE('',#274065,#28702);
#24356=LINE('',#274067,#28703);
#24357=LINE('',#274071,#28704);
#24358=LINE('',#274074,#28705);
#24359=LINE('',#274077,#28706);
#24360=LINE('',#274079,#28707);
#24361=LINE('',#274083,#28708);
#24362=LINE('',#274086,#28709);
#24363=LINE('',#274089,#28710);
#24364=LINE('',#274091,#28711);
#24365=LINE('',#274095,#28712);
#24366=LINE('',#274098,#28713);
#24367=LINE('',#274101,#28714);
#24368=LINE('',#274103,#28715);
#24369=LINE('',#274107,#28716);
#24370=LINE('',#274109,#28717);
#24371=LINE('',#274113,#28718);
#24372=LINE('',#274116,#28719);
#24373=LINE('',#274119,#28720);
#24374=LINE('',#274122,#28721);
#24375=LINE('',#274125,#28722);
#24376=LINE('',#274127,#28723);
#24377=LINE('',#274131,#28724);
#24378=LINE('',#274133,#28725);
#24379=LINE('',#274893,#28726);
#24380=LINE('',#274895,#28727);
#24381=LINE('',#274951,#28728);
#24382=LINE('',#274953,#28729);
#24383=LINE('',#274956,#28730);
#24384=LINE('',#274958,#28731);
#24385=LINE('',#274967,#28732);
#24386=LINE('',#274969,#28733);
#24387=LINE('',#274978,#28734);
#24388=LINE('',#274980,#28735);
#24389=LINE('',#274995,#28736);
#24390=LINE('',#274997,#28737);
#24391=LINE('',#275000,#28738);
#24392=LINE('',#275002,#28739);
#24393=LINE('',#275005,#28740);
#24394=LINE('',#275007,#28741);
#24395=LINE('',#275010,#28742);
#24396=LINE('',#275013,#28743);
#24397=LINE('',#275015,#28744);
#24398=LINE('',#275018,#28745);
#24399=LINE('',#275020,#28746);
#24400=LINE('',#275023,#28747);
#24401=LINE('',#275025,#28748);
#24402=LINE('',#275028,#28749);
#24403=LINE('',#275030,#28750);
#24404=LINE('',#275033,#28751);
#24405=LINE('',#275035,#28752);
#24406=LINE('',#275038,#28753);
#24407=LINE('',#275041,#28754);
#24408=LINE('',#275043,#28755);
#24409=LINE('',#275046,#28756);
#24410=LINE('',#275048,#28757);
#24411=LINE('',#275051,#28758);
#24412=LINE('',#275053,#28759);
#24413=LINE('',#275056,#28760);
#24414=LINE('',#275058,#28761);
#24415=LINE('',#275061,#28762);
#24416=LINE('',#275062,#28763);
#24417=LINE('',#275070,#28764);
#24418=LINE('',#275077,#28765);
#24419=LINE('',#275080,#28766);
#24420=LINE('',#275085,#28767);
#24421=LINE('',#275091,#28768);
#24422=LINE('',#275097,#28769);
#24423=LINE('',#275108,#28770);
#24424=LINE('',#275114,#28771);
#24425=LINE('',#275121,#28772);
#24426=LINE('',#275124,#28773);
#24427=LINE('',#275138,#28774);
#24428=LINE('',#275140,#28775);
#24429=LINE('',#275146,#28776);
#24430=LINE('',#275154,#28777);
#24431=LINE('',#275301,#28778);
#24432=LINE('',#275307,#28779);
#24433=LINE('',#275313,#28780);
#24434=LINE('',#275319,#28781);
#24435=LINE('',#275346,#28782);
#24436=LINE('',#275359,#28783);
#24437=LINE('',#275361,#28784);
#24438=LINE('',#275364,#28785);
#24439=LINE('',#275388,#28786);
#24440=LINE('',#275497,#28787);
#24441=LINE('',#275503,#28788);
#24442=LINE('',#275509,#28789);
#24443=LINE('',#275515,#28790);
#24444=LINE('',#275520,#28791);
#24445=LINE('',#275522,#28792);
#24446=LINE('',#275524,#28793);
#24447=LINE('',#275525,#28794);
#24448=LINE('',#275528,#28795);
#24449=LINE('',#275530,#28796);
#24450=LINE('',#275531,#28797);
#24451=LINE('',#275534,#28798);
#24452=LINE('',#275536,#28799);
#24453=LINE('',#275537,#28800);
#24454=LINE('',#275540,#28801);
#24455=LINE('',#275542,#28802);
#24456=LINE('',#275543,#28803);
#24457=LINE('',#275546,#28804);
#24458=LINE('',#275548,#28805);
#24459=LINE('',#275549,#28806);
#24460=LINE('',#275551,#28807);
#24461=LINE('',#275552,#28808);
#24462=LINE('',#275563,#28809);
#24463=LINE('',#275572,#28810);
#24464=LINE('',#275618,#28811);
#24465=LINE('',#275664,#28812);
#24466=LINE('',#275710,#28813);
#24467=LINE('',#275736,#28814);
#24468=LINE('',#275748,#28815);
#24469=LINE('',#275766,#28816);
#24470=LINE('',#275780,#28817);
#24471=LINE('',#275858,#28818);
#24472=LINE('',#275934,#28819);
#24473=LINE('',#276010,#28820);
#24474=LINE('',#276086,#28821);
#24475=LINE('',#276221,#28822);
#24476=LINE('',#276278,#28823);
#24477=LINE('',#276337,#28824);
#24478=LINE('',#276347,#28825);
#24479=LINE('',#276364,#28826);
#24480=LINE('',#276381,#28827);
#24481=LINE('',#276398,#28828);
#24482=LINE('',#276415,#28829);
#24483=LINE('',#280646,#28830);
#24484=LINE('',#280675,#28831);
#24485=LINE('',#280721,#28832);
#24486=LINE('',#280767,#28833);
#24487=LINE('',#280813,#28834);
#24488=LINE('',#280859,#28835);
#24489=LINE('',#280870,#28836);
#24490=LINE('',#280884,#28837);
#24491=LINE('',#280960,#28838);
#24492=LINE('',#281036,#28839);
#24493=LINE('',#281112,#28840);
#24494=LINE('',#281188,#28841);
#24495=LINE('',#281266,#28842);
#24496=LINE('',#281394,#28843);
#24497=LINE('',#281422,#28844);
#24498=LINE('',#281470,#28845);
#24499=LINE('',#281471,#28846);
#24500=LINE('',#281473,#28847);
#24501=LINE('',#281475,#28848);
#24502=LINE('',#281477,#28849);
#24503=LINE('',#281479,#28850);
#24504=LINE('',#285709,#28851);
#24505=LINE('',#285765,#28852);
#24506=LINE('',#290042,#28853);
#24507=LINE('',#290053,#28854);
#24508=LINE('',#290099,#28855);
#24509=LINE('',#290145,#28856);
#24510=LINE('',#290191,#28857);
#24511=LINE('',#290237,#28858);
#24512=LINE('',#290283,#28859);
#24513=LINE('',#290329,#28860);
#24514=LINE('',#290375,#28861);
#24515=LINE('',#290421,#28862);
#24516=LINE('',#290467,#28863);
#24517=LINE('',#290513,#28864);
#24518=LINE('',#290559,#28865);
#24519=LINE('',#290605,#28866);
#24520=LINE('',#290651,#28867);
#24521=LINE('',#290697,#28868);
#24522=LINE('',#290743,#28869);
#24523=LINE('',#290789,#28870);
#24524=LINE('',#290835,#28871);
#24525=LINE('',#290881,#28872);
#24526=LINE('',#290927,#28873);
#24527=LINE('',#290958,#28874);
#24528=LINE('',#291004,#28875);
#24529=LINE('',#291050,#28876);
#24530=LINE('',#291096,#28877);
#24531=LINE('',#291142,#28878);
#24532=LINE('',#291188,#28879);
#24533=LINE('',#291234,#28880);
#24534=LINE('',#291280,#28881);
#24535=LINE('',#291326,#28882);
#24536=LINE('',#291372,#28883);
#24537=LINE('',#291418,#28884);
#24538=LINE('',#291464,#28885);
#24539=LINE('',#291510,#28886);
#24540=LINE('',#291529,#28887);
#24541=LINE('',#291607,#28888);
#24542=LINE('',#291685,#28889);
#24543=LINE('',#291761,#28890);
#24544=LINE('',#291837,#28891);
#24545=LINE('',#291913,#28892);
#24546=LINE('',#291989,#28893);
#24547=LINE('',#292067,#28894);
#24548=LINE('',#292143,#28895);
#24549=LINE('',#292219,#28896);
#24550=LINE('',#292297,#28897);
#24551=LINE('',#292373,#28898);
#24552=LINE('',#292449,#28899);
#24553=LINE('',#292496,#28900);
#24554=LINE('',#292574,#28901);
#24555=LINE('',#292652,#28902);
#24556=LINE('',#292728,#28903);
#24557=LINE('',#292804,#28904);
#24558=LINE('',#292880,#28905);
#24559=LINE('',#292956,#28906);
#24560=LINE('',#293032,#28907);
#24561=LINE('',#293108,#28908);
#24562=LINE('',#293186,#28909);
#24563=LINE('',#293264,#28910);
#24564=LINE('',#293340,#28911);
#24565=LINE('',#293416,#28912);
#24566=LINE('',#293492,#28913);
#24567=LINE('',#293568,#28914);
#24568=LINE('',#293644,#28915);
#24569=LINE('',#293720,#28916);
#24570=LINE('',#293796,#28917);
#24571=LINE('',#293903,#28918);
#24572=LINE('',#294010,#28919);
#24573=LINE('',#298273,#28920);
#24574=LINE('',#298275,#28921);
#24575=LINE('',#298277,#28922);
#24576=LINE('',#298278,#28923);
#24577=LINE('',#298282,#28924);
#24578=LINE('',#298284,#28925);
#24579=LINE('',#298286,#28926);
#24580=LINE('',#298287,#28927);
#24581=LINE('',#298301,#28928);
#24582=LINE('',#298302,#28929);
#24583=LINE('',#298304,#28930);
#24584=LINE('',#298306,#28931);
#24585=LINE('',#298311,#28932);
#24586=LINE('',#298320,#28933);
#24587=LINE('',#298337,#28934);
#24588=LINE('',#298354,#28935);
#24589=LINE('',#298371,#28936);
#24590=LINE('',#298388,#28937);
#24591=LINE('',#302627,#28938);
#24592=LINE('',#302633,#28939);
#24593=LINE('',#302639,#28940);
#24594=LINE('',#302645,#28941);
#24595=LINE('',#302651,#28942);
#24596=LINE('',#302657,#28943);
#24597=LINE('',#302663,#28944);
#24598=LINE('',#302669,#28945);
#24599=LINE('',#302675,#28946);
#24600=LINE('',#302681,#28947);
#24601=LINE('',#302687,#28948);
#24602=LINE('',#302709,#28949);
#24603=LINE('',#302717,#28950);
#24604=LINE('',#302736,#28951);
#24605=LINE('',#302738,#28952);
#24606=LINE('',#302740,#28953);
#24607=LINE('',#302741,#28954);
#24608=LINE('',#302744,#28955);
#24609=LINE('',#302746,#28956);
#24610=LINE('',#302748,#28957);
#24611=LINE('',#302749,#28958);
#24612=LINE('',#302753,#28959);
#24613=LINE('',#302755,#28960);
#24614=LINE('',#302757,#28961);
#24615=LINE('',#302758,#28962);
#24616=LINE('',#302761,#28963);
#24617=LINE('',#302763,#28964);
#24618=LINE('',#302765,#28965);
#24619=LINE('',#302766,#28966);
#24620=LINE('',#302768,#28967);
#24621=LINE('',#302769,#28968);
#24622=LINE('',#302771,#28969);
#24623=LINE('',#302773,#28970);
#24624=LINE('',#302776,#28971);
#24625=LINE('',#302777,#28972);
#24626=LINE('',#302779,#28973);
#24627=LINE('',#302781,#28974);
#24628=LINE('',#302787,#28975);
#24629=LINE('',#302789,#28976);
#24630=LINE('',#302791,#28977);
#24631=LINE('',#302792,#28978);
#24632=LINE('',#302795,#28979);
#24633=LINE('',#302797,#28980);
#24634=LINE('',#302798,#28981);
#24635=LINE('',#302801,#28982);
#24636=LINE('',#302803,#28983);
#24637=LINE('',#302804,#28984);
#24638=LINE('',#302806,#28985);
#24639=LINE('',#302807,#28986);
#24640=LINE('',#302816,#28987);
#24641=LINE('',#302822,#28988);
#24642=LINE('',#302828,#28989);
#24643=LINE('',#302834,#28990);
#24644=LINE('',#302840,#28991);
#24645=LINE('',#302846,#28992);
#24646=LINE('',#302852,#28993);
#24647=LINE('',#302858,#28994);
#24648=LINE('',#302863,#28995);
#24649=LINE('',#302865,#28996);
#24650=LINE('',#302867,#28997);
#24651=LINE('',#302869,#28998);
#24652=LINE('',#302871,#28999);
#24653=LINE('',#302873,#29000);
#24654=LINE('',#302875,#29001);
#24655=LINE('',#302876,#29002);
#24656=LINE('',#302880,#29003);
#24657=LINE('',#302882,#29004);
#24658=LINE('',#302884,#29005);
#24659=LINE('',#302886,#29006);
#24660=LINE('',#302888,#29007);
#24661=LINE('',#302890,#29008);
#24662=LINE('',#302892,#29009);
#24663=LINE('',#302893,#29010);
#24664=LINE('',#302895,#29011);
#24665=LINE('',#302896,#29012);
#24666=LINE('',#302898,#29013);
#24667=LINE('',#302899,#29014);
#24668=LINE('',#302901,#29015);
#24669=LINE('',#302902,#29016);
#24670=LINE('',#302906,#29017);
#24671=LINE('',#302908,#29018);
#24672=LINE('',#302915,#29019);
#24673=LINE('',#302921,#29020);
#24674=LINE('',#302926,#29021);
#24675=LINE('',#302928,#29022);
#24676=LINE('',#302930,#29023);
#24677=LINE('',#302931,#29024);
#24678=LINE('',#302935,#29025);
#24679=LINE('',#302937,#29026);
#24680=LINE('',#302939,#29027);
#24681=LINE('',#302940,#29028);
#24682=LINE('',#302943,#29029);
#24683=LINE('',#302945,#29030);
#24684=LINE('',#302946,#29031);
#24685=LINE('',#302949,#29032);
#24686=LINE('',#302951,#29033);
#24687=LINE('',#302952,#29034);
#24688=LINE('',#302955,#29035);
#24689=LINE('',#302957,#29036);
#24690=LINE('',#302958,#29037);
#24691=LINE('',#302961,#29038);
#24692=LINE('',#302963,#29039);
#24693=LINE('',#302964,#29040);
#24694=LINE('',#302966,#29041);
#24695=LINE('',#302967,#29042);
#24696=LINE('',#302969,#29043);
#24697=LINE('',#302970,#29044);
#24698=LINE('',#302974,#29045);
#24699=LINE('',#302979,#29046);
#24700=LINE('',#302981,#29047);
#24701=LINE('',#302982,#29048);
#24702=LINE('',#302987,#29049);
#24703=LINE('',#302995,#29050);
#24704=LINE('',#302999,#29051);
#24705=LINE('',#303000,#29052);
#24706=LINE('',#303002,#29053);
#24707=LINE('',#303004,#29054);
#24708=LINE('',#303007,#29055);
#24709=LINE('',#303009,#29056);
#24710=LINE('',#303020,#29057);
#24711=LINE('',#303057,#29058);
#24712=LINE('',#303123,#29059);
#24713=LINE('',#303158,#29060);
#24714=LINE('',#303234,#29061);
#24715=LINE('',#303312,#29062);
#24716=LINE('',#303388,#29063);
#24717=LINE('',#303464,#29064);
#24718=LINE('',#303540,#29065);
#24719=LINE('',#303616,#29066);
#24720=LINE('',#303692,#29067);
#24721=LINE('',#303768,#29068);
#24722=LINE('',#303846,#29069);
#24723=LINE('',#303924,#29070);
#24724=LINE('',#304000,#29071);
#24725=LINE('',#304076,#29072);
#24726=LINE('',#304152,#29073);
#24727=LINE('',#304228,#29074);
#24728=LINE('',#304305,#29075);
#24729=LINE('',#304314,#29076);
#24730=LINE('',#304328,#29077);
#24731=LINE('',#304335,#29078);
#24732=LINE('',#304381,#29079);
#24733=LINE('',#304427,#29080);
#24734=LINE('',#304473,#29081);
#24735=LINE('',#304519,#29082);
#24736=LINE('',#304565,#29083);
#24737=LINE('',#304611,#29084);
#24738=LINE('',#304657,#29085);
#24739=LINE('',#304703,#29086);
#24740=LINE('',#304749,#29087);
#24741=LINE('',#304795,#29088);
#24742=LINE('',#304841,#29089);
#24743=LINE('',#304887,#29090);
#24744=LINE('',#304933,#29091);
#24745=LINE('',#304979,#29092);
#24746=LINE('',#305025,#29093);
#24747=LINE('',#305115,#29094);
#24748=LINE('',#306983,#29095);
#24749=LINE('',#307004,#29096);
#24750=LINE('',#307063,#29097);
#24751=LINE('',#307122,#29098);
#24752=LINE('',#307203,#29099);
#24753=LINE('',#307216,#29100);
#24754=LINE('',#307251,#29101);
#24755=LINE('',#307286,#29102);
#24756=LINE('',#307359,#29103);
#24757=LINE('',#307380,#29104);
#24758=LINE('',#307439,#29105);
#24759=LINE('',#307498,#29106);
#24760=LINE('',#307579,#29107);
#24761=LINE('',#307592,#29108);
#24762=LINE('',#307627,#29109);
#24763=LINE('',#307662,#29110);
#24764=LINE('',#307989,#29111);
#24765=LINE('',#307991,#29112);
#24766=LINE('',#307993,#29113);
#24767=LINE('',#307994,#29114);
#24768=LINE('',#308034,#29115);
#24769=LINE('',#308036,#29116);
#24770=LINE('',#308079,#29117);
#24771=LINE('',#308130,#29118);
#24772=LINE('',#308189,#29119);
#24773=LINE('',#308232,#29120);
#24774=LINE('',#308283,#29121);
#24775=LINE('',#308342,#29122);
#24776=LINE('',#308458,#29123);
#24777=LINE('',#308460,#29124);
#24778=LINE('',#308503,#29125);
#24779=LINE('',#308554,#29126);
#24780=LINE('',#308613,#29127);
#24781=LINE('',#308656,#29128);
#24782=LINE('',#308707,#29129);
#24783=LINE('',#308766,#29130);
#24784=LINE('',#308845,#29131);
#24785=LINE('',#308847,#29132);
#24786=LINE('',#308848,#29133);
#24787=LINE('',#308851,#29134);
#24788=LINE('',#308852,#29135);
#24789=LINE('',#308855,#29136);
#24790=LINE('',#308856,#29137);
#24791=LINE('',#308858,#29138);
#24792=LINE('',#308922,#29139);
#24793=LINE('',#308924,#29140);
#24794=LINE('',#308925,#29141);
#24795=LINE('',#308928,#29142);
#24796=LINE('',#308929,#29143);
#24797=LINE('',#308932,#29144);
#24798=LINE('',#308933,#29145);
#24799=LINE('',#308936,#29146);
#24800=LINE('',#308937,#29147);
#24801=LINE('',#308940,#29148);
#24802=LINE('',#308941,#29149);
#24803=LINE('',#308943,#29150);
#24804=LINE('',#308951,#29151);
#24805=LINE('',#308980,#29152);
#24806=LINE('',#309023,#29153);
#24807=LINE('',#309099,#29154);
#24808=LINE('',#309175,#29155);
#24809=LINE('',#309251,#29156);
#24810=LINE('',#309300,#29157);
#24811=LINE('',#309332,#29158);
#24812=LINE('',#309378,#29159);
#24813=LINE('',#309424,#29160);
#24814=LINE('',#310224,#29161);
#24815=LINE('',#310236,#29162);
#24816=LINE('',#310251,#29163);
#24817=LINE('',#310263,#29164);
#24818=LINE('',#310278,#29165);
#24819=LINE('',#310290,#29166);
#24820=LINE('',#310305,#29167);
#24821=LINE('',#310317,#29168);
#24822=LINE('',#310332,#29169);
#24823=LINE('',#310344,#29170);
#24824=LINE('',#310359,#29171);
#24825=LINE('',#310371,#29172);
#24826=LINE('',#310494,#29173);
#24827=LINE('',#310496,#29174);
#24828=VECTOR('',#104872,7.5);
#24829=VECTOR('',#104879,7.5);
#24830=VECTOR('',#104886,7.50000000000001);
#24831=VECTOR('',#104893,7.5);
#24832=VECTOR('',#104900,7.50000000000001);
#24833=VECTOR('',#104907,7.5);
#24834=VECTOR('',#104914,7.5);
#24835=VECTOR('',#104921,7.5);
#24836=VECTOR('',#104928,7.5);
#24837=VECTOR('',#104935,7.5);
#24838=VECTOR('',#104942,7.5);
#24839=VECTOR('',#104949,7.50000000000001);
#24840=VECTOR('',#104954,1000.);
#24841=VECTOR('',#104955,1000.);
#24842=VECTOR('',#104956,1000.);
#24843=VECTOR('',#104957,1000.);
#24844=VECTOR('',#104960,1000.);
#24845=VECTOR('',#104961,1000.);
#24846=VECTOR('',#104962,1000.);
#24847=VECTOR('',#104965,1000.);
#24848=VECTOR('',#104966,1000.);
#24849=VECTOR('',#104967,1000.);
#24850=VECTOR('',#104968,1000.);
#24851=VECTOR('',#104971,1000.);
#24852=VECTOR('',#104972,1000.);
#24853=VECTOR('',#104973,1000.);
#24854=VECTOR('',#104974,1000.);
#24855=VECTOR('',#104977,1000.);
#24856=VECTOR('',#104978,1000.);
#24857=VECTOR('',#104979,1000.);
#24858=VECTOR('',#104982,1000.);
#24859=VECTOR('',#104983,1000.);
#24860=VECTOR('',#104984,1000.);
#24861=VECTOR('',#104987,1000.);
#24862=VECTOR('',#104988,1000.);
#24863=VECTOR('',#104989,1000.);
#24864=VECTOR('',#104990,1000.);
#24865=VECTOR('',#104993,1000.);
#24866=VECTOR('',#104994,1000.);
#24867=VECTOR('',#104995,1000.);
#24868=VECTOR('',#105030,7.50000000000001);
#24869=VECTOR('',#105037,7.50000000000001);
#24870=VECTOR('',#105044,7.50000000000001);
#24871=VECTOR('',#105051,7.50000000000001);
#24872=VECTOR('',#105058,7.50000000000001);
#24873=VECTOR('',#105065,7.50000000000001);
#24874=VECTOR('',#105072,7.50000000000001);
#24875=VECTOR('',#105079,7.50000000000001);
#24876=VECTOR('',#105086,7.5);
#24877=VECTOR('',#105093,7.50000000000001);
#24878=VECTOR('',#105100,7.50000000000001);
#24879=VECTOR('',#105107,7.50000000000001);
#24880=VECTOR('',#105112,1000.);
#24881=VECTOR('',#105113,1000.);
#24882=VECTOR('',#105114,1000.);
#24883=VECTOR('',#105115,1000.);
#24884=VECTOR('',#105118,1000.);
#24885=VECTOR('',#105119,1000.);
#24886=VECTOR('',#105120,1000.);
#24887=VECTOR('',#105123,1000.);
#24888=VECTOR('',#105124,1000.);
#24889=VECTOR('',#105125,1000.);
#24890=VECTOR('',#105126,1000.);
#24891=VECTOR('',#105129,1000.);
#24892=VECTOR('',#105130,1000.);
#24893=VECTOR('',#105131,1000.);
#24894=VECTOR('',#105132,1000.);
#24895=VECTOR('',#105135,1000.);
#24896=VECTOR('',#105136,1000.);
#24897=VECTOR('',#105137,1000.);
#24898=VECTOR('',#105140,1000.);
#24899=VECTOR('',#105141,1000.);
#24900=VECTOR('',#105142,1000.);
#24901=VECTOR('',#105145,1000.);
#24902=VECTOR('',#105146,1000.);
#24903=VECTOR('',#105147,1000.);
#24904=VECTOR('',#105148,1000.);
#24905=VECTOR('',#105151,1000.);
#24906=VECTOR('',#105152,1000.);
#24907=VECTOR('',#105153,1000.);
#24908=VECTOR('',#105188,1.47499999999998);
#24909=VECTOR('',#105197,2.);
#24910=VECTOR('',#105206,2.5);
#24911=VECTOR('',#105213,1.47499999999998);
#24912=VECTOR('',#105222,2.);
#24913=VECTOR('',#105231,2.5);
#24914=VECTOR('',#105236,1000.);
#24915=VECTOR('',#105239,1000.);
#24916=VECTOR('',#105246,1000.);
#24917=VECTOR('',#105249,1000.);
#24918=VECTOR('',#105262,1000.);
#24919=VECTOR('',#105265,1000.);
#24920=VECTOR('',#105270,1000.);
#24921=VECTOR('',#105271,1000.);
#24922=VECTOR('',#105272,1000.);
#24923=VECTOR('',#105273,1000.);
#24924=VECTOR('',#105274,1000.);
#24925=VECTOR('',#105275,1000.);
#24926=VECTOR('',#105276,1000.);
#24927=VECTOR('',#105277,1000.);
#24928=VECTOR('',#105278,1000.);
#24929=VECTOR('',#105279,1000.);
#24930=VECTOR('',#105280,1000.);
#24931=VECTOR('',#105291,1000.);
#24932=VECTOR('',#105294,1000.);
#24933=VECTOR('',#105299,1000.);
#24934=VECTOR('',#105300,1000.);
#24935=VECTOR('',#105311,1000.);
#24936=VECTOR('',#105312,1000.);
#24937=VECTOR('',#105313,1000.);
#24938=VECTOR('',#105314,1000.);
#24939=VECTOR('',#105315,1000.);
#24940=VECTOR('',#105316,1000.);
#24941=VECTOR('',#105317,1000.);
#24942=VECTOR('',#105318,1000.);
#24943=VECTOR('',#105319,1000.);
#24944=VECTOR('',#105320,1000.);
#24945=VECTOR('',#105323,1000.);
#24946=VECTOR('',#105332,1000.);
#24947=VECTOR('',#105333,1000.);
#24948=VECTOR('',#105348,1000.);
#24949=VECTOR('',#105353,1000.);
#24950=VECTOR('',#105370,1000.);
#24951=VECTOR('',#105371,1000.);
#24952=VECTOR('',#105386,1000.);
#24953=VECTOR('',#105391,1000.);
#24954=VECTOR('',#105408,1000.);
#24955=VECTOR('',#105409,1000.);
#24956=VECTOR('',#105424,1000.);
#24957=VECTOR('',#105427,1000.);
#24958=VECTOR('',#105438,1000.);
#24959=VECTOR('',#105441,1000.);
#24960=VECTOR('',#105454,1000.);
#24961=VECTOR('',#105457,1000.);
#24962=VECTOR('',#105472,1000.);
#24963=VECTOR('',#105475,1000.);
#24964=VECTOR('',#105490,1000.);
#24965=VECTOR('',#105493,1000.);
#24966=VECTOR('',#105508,1000.);
#24967=VECTOR('',#105509,1000.);
#24968=VECTOR('',#105524,1000.);
#24969=VECTOR('',#105527,1000.);
#24970=VECTOR('',#105542,1000.);
#24971=VECTOR('',#105543,1000.);
#24972=VECTOR('',#105558,1000.);
#24973=VECTOR('',#105561,1000.);
#24974=VECTOR('',#105570,1000.);
#24975=VECTOR('',#105573,1000.);
#24976=VECTOR('',#105576,1000.);
#24977=VECTOR('',#105579,1000.);
#24978=VECTOR('',#105582,1000.);
#24979=VECTOR('',#105585,1000.);
#24980=VECTOR('',#105588,1000.);
#24981=VECTOR('',#105591,1000.);
#24982=VECTOR('',#105594,1000.);
#24983=VECTOR('',#105597,1000.);
#24984=VECTOR('',#105600,1000.);
#24985=VECTOR('',#105603,1000.);
#24986=VECTOR('',#105618,1000.);
#24987=VECTOR('',#105621,1000.);
#24988=VECTOR('',#105626,1000.);
#24989=VECTOR('',#105627,1000.);
#24990=VECTOR('',#105628,1000.);
#24991=VECTOR('',#105629,1000.);
#24992=VECTOR('',#105630,1000.);
#24993=VECTOR('',#105631,1000.);
#24994=VECTOR('',#105634,1000.);
#24995=VECTOR('',#105635,1000.);
#24996=VECTOR('',#105636,1000.);
#24997=VECTOR('',#105637,1000.);
#24998=VECTOR('',#105638,1000.);
#24999=VECTOR('',#105649,1000.);
#25000=VECTOR('',#105652,1000.);
#25001=VECTOR('',#105657,1000.);
#25002=VECTOR('',#105658,1000.);
#25003=VECTOR('',#105669,1000.);
#25004=VECTOR('',#105670,1000.);
#25005=VECTOR('',#105671,1000.);
#25006=VECTOR('',#105672,1000.);
#25007=VECTOR('',#105673,1000.);
#25008=VECTOR('',#105674,1000.);
#25009=VECTOR('',#105675,1000.);
#25010=VECTOR('',#105676,1000.);
#25011=VECTOR('',#105677,1000.);
#25012=VECTOR('',#105684,1000.);
#25013=VECTOR('',#105697,1000.);
#25014=VECTOR('',#105714,1000.);
#25015=VECTOR('',#105729,1000.);
#25016=VECTOR('',#105742,1000.);
#25017=VECTOR('',#105757,1000.);
#25018=VECTOR('',#105770,1000.);
#25019=VECTOR('',#105785,1000.);
#25020=VECTOR('',#105798,1000.);
#25021=VECTOR('',#105811,1000.);
#25022=VECTOR('',#105828,1000.);
#25023=VECTOR('',#105841,1000.);
#25024=VECTOR('',#105846,1000.);
#25025=VECTOR('',#105853,1000.);
#25026=VECTOR('',#105860,1000.);
#25027=VECTOR('',#105867,1000.);
#25028=VECTOR('',#105870,1000.);
#25029=VECTOR('',#105877,1000.);
#25030=VECTOR('',#105882,1000.);
#25031=VECTOR('',#105889,1000.);
#25032=VECTOR('',#105896,1000.);
#25033=VECTOR('',#105903,1000.);
#25034=VECTOR('',#105906,1000.);
#25035=VECTOR('',#105911,1000.);
#25036=VECTOR('',#105916,1000.);
#25037=VECTOR('',#105925,1000.);
#25038=VECTOR('',#105932,1000.);
#25039=VECTOR('',#105935,1000.);
#25040=VECTOR('',#105942,1000.);
#25041=VECTOR('',#105949,1000.);
#25042=VECTOR('',#105956,1000.);
#25043=VECTOR('',#105959,1000.);
#25044=VECTOR('',#105962,1000.);
#25045=VECTOR('',#105967,1000.);
#25046=VECTOR('',#105976,1000.);
#25047=VECTOR('',#105983,1000.);
#25048=VECTOR('',#105986,1000.);
#25049=VECTOR('',#105995,1000.);
#25050=VECTOR('',#106002,1000.);
#25051=VECTOR('',#106009,1000.);
#25052=VECTOR('',#106016,1000.);
#25053=VECTOR('',#106023,1000.);
#25054=VECTOR('',#106030,1000.);
#25055=VECTOR('',#106037,1000.);
#25056=VECTOR('',#106044,1000.);
#25057=VECTOR('',#106051,1000.);
#25058=VECTOR('',#106058,1000.);
#25059=VECTOR('',#106061,1000.);
#25060=VECTOR('',#106068,1000.);
#25061=VECTOR('',#106075,1000.);
#25062=VECTOR('',#106086,1000.);
#25063=VECTOR('',#106089,1000.);
#25064=VECTOR('',#106092,1000.);
#25065=VECTOR('',#106099,1000.);
#25066=VECTOR('',#106102,1000.);
#25067=VECTOR('',#106105,1000.);
#25068=VECTOR('',#106110,1000.);
#25069=VECTOR('',#106113,1000.);
#25070=VECTOR('',#106114,1000.);
#25071=VECTOR('',#106115,1000.);
#25072=VECTOR('',#106118,1000.);
#25073=VECTOR('',#106143,1000.);
#25074=VECTOR('',#106146,1000.);
#25075=VECTOR('',#106149,1000.);
#25076=VECTOR('',#106150,1000.);
#25077=VECTOR('',#106153,1000.);
#25078=VECTOR('',#106158,1000.);
#25079=VECTOR('',#106161,1000.);
#25080=VECTOR('',#106172,1000.);
#25081=VECTOR('',#106175,1000.);
#25082=VECTOR('',#106186,1000.);
#25083=VECTOR('',#106189,1000.);
#25084=VECTOR('',#106204,1000.);
#25085=VECTOR('',#106207,1000.);
#25086=VECTOR('',#106218,1000.);
#25087=VECTOR('',#106221,1000.);
#25088=VECTOR('',#106232,1000.);
#25089=VECTOR('',#106235,1000.);
#25090=VECTOR('',#106248,1000.);
#25091=VECTOR('',#106249,1000.);
#25092=VECTOR('',#106256,1000.);
#25093=VECTOR('',#106259,1000.);
#25094=VECTOR('',#106270,1000.);
#25095=VECTOR('',#106273,1000.);
#25096=VECTOR('',#106284,1000.);
#25097=VECTOR('',#106287,1000.);
#25098=VECTOR('',#106290,1000.);
#25099=VECTOR('',#106293,1000.);
#25100=VECTOR('',#106300,1000.);
#25101=VECTOR('',#106303,1000.);
#25102=VECTOR('',#106314,1000.);
#25103=VECTOR('',#106317,1000.);
#25104=VECTOR('',#106328,1000.);
#25105=VECTOR('',#106331,1000.);
#25106=VECTOR('',#106334,1000.);
#25107=VECTOR('',#106337,1000.);
#25108=VECTOR('',#106344,1000.);
#25109=VECTOR('',#106345,1000.);
#25110=VECTOR('',#106348,1000.);
#25111=VECTOR('',#106349,1000.);
#25112=VECTOR('',#106350,1000.);
#25113=VECTOR('',#106351,1000.);
#25114=VECTOR('',#106352,1000.);
#25115=VECTOR('',#106353,1000.);
#25116=VECTOR('',#106358,1000.);
#25117=VECTOR('',#106373,1000.);
#25118=VECTOR('',#106374,1000.);
#25119=VECTOR('',#106377,1000.);
#25120=VECTOR('',#106380,1000.);
#25121=VECTOR('',#106393,1000.);
#25122=VECTOR('',#106394,1000.);
#25123=VECTOR('',#106423,1000.);
#25124=VECTOR('',#106424,1000.);
#25125=VECTOR('',#106453,1000.);
#25126=VECTOR('',#106454,1000.);
#25127=VECTOR('',#106483,1000.);
#25128=VECTOR('',#106484,1000.);
#25129=VECTOR('',#106497,2.75);
#25130=VECTOR('',#106508,2.75);
#25131=VECTOR('',#106519,1000.);
#25132=VECTOR('',#106522,1000.);
#25133=VECTOR('',#106537,1000.);
#25134=VECTOR('',#106540,1000.);
#25135=VECTOR('',#106555,1000.);
#25136=VECTOR('',#106558,1000.);
#25137=VECTOR('',#106573,1000.);
#25138=VECTOR('',#106576,1000.);
#25139=VECTOR('',#106589,1000.);
#25140=VECTOR('',#106592,1000.);
#25141=VECTOR('',#106607,1000.);
#25142=VECTOR('',#106610,1000.);
#25143=VECTOR('',#106615,1000.);
#25144=VECTOR('',#106616,1000.);
#25145=VECTOR('',#106617,1000.);
#25146=VECTOR('',#106632,1000.);
#25147=VECTOR('',#106635,1000.);
#25148=VECTOR('',#106644,1000.);
#25149=VECTOR('',#106657,1000.);
#25150=VECTOR('',#106660,1000.);
#25151=VECTOR('',#106671,1000.);
#25152=VECTOR('',#106672,1000.);
#25153=VECTOR('',#106683,1000.);
#25154=VECTOR('',#106686,1000.);
#25155=VECTOR('',#106689,1000.);
#25156=VECTOR('',#106692,1000.);
#25157=VECTOR('',#106695,1000.);
#25158=VECTOR('',#106700,1000.);
#25159=VECTOR('',#106701,1000.);
#25160=VECTOR('',#106704,1000.);
#25161=VECTOR('',#106713,1000.);
#25162=VECTOR('',#106716,1000.);
#25163=VECTOR('',#106719,1000.);
#25164=VECTOR('',#106730,1000.);
#25165=VECTOR('',#106733,1000.);
#25166=VECTOR('',#106736,1000.);
#25167=VECTOR('',#106739,1000.);
#25168=VECTOR('',#106756,1000.);
#25169=VECTOR('',#106759,1000.);
#25170=VECTOR('',#106762,1000.);
#25171=VECTOR('',#106767,1000.);
#25172=VECTOR('',#106772,1000.);
#25173=VECTOR('',#106773,1000.);
#25174=VECTOR('',#106776,1000.);
#25175=VECTOR('',#106783,1000.);
#25176=VECTOR('',#106786,1000.);
#25177=VECTOR('',#106799,1000.);
#25178=VECTOR('',#106814,1000.);
#25179=VECTOR('',#106823,1000.);
#25180=VECTOR('',#106830,1000.);
#25181=VECTOR('',#106833,1000.);
#25182=VECTOR('',#106836,1000.);
#25183=VECTOR('',#106839,1000.);
#25184=VECTOR('',#106840,1000.);
#25185=VECTOR('',#106843,1000.);
#25186=VECTOR('',#106848,1000.);
#25187=VECTOR('',#106851,1000.);
#25188=VECTOR('',#106854,1000.);
#25189=VECTOR('',#106855,1000.);
#25190=VECTOR('',#106858,1000.);
#25191=VECTOR('',#106863,1000.);
#25192=VECTOR('',#106866,1000.);
#25193=VECTOR('',#106871,1000.);
#25194=VECTOR('',#106874,1000.);
#25195=VECTOR('',#106885,1000.);
#25196=VECTOR('',#106888,1000.);
#25197=VECTOR('',#106891,1000.);
#25198=VECTOR('',#106892,1000.);
#25199=VECTOR('',#106895,1000.);
#25200=VECTOR('',#106898,1000.);
#25201=VECTOR('',#106903,1000.);
#25202=VECTOR('',#106904,1000.);
#25203=VECTOR('',#106907,1000.);
#25204=VECTOR('',#106916,1000.);
#25205=VECTOR('',#106919,1000.);
#25206=VECTOR('',#106922,1000.);
#25207=VECTOR('',#106933,1000.);
#25208=VECTOR('',#106934,1000.);
#25209=VECTOR('',#106937,1000.);
#25210=VECTOR('',#106948,1000.);
#25211=VECTOR('',#106949,1000.);
#25212=VECTOR('',#106952,1000.);
#25213=VECTOR('',#106961,1000.);
#25214=VECTOR('',#106962,1000.);
#25215=VECTOR('',#106967,1000.);
#25216=VECTOR('',#106984,1000.);
#25217=VECTOR('',#106989,1000.);
#25218=VECTOR('',#106990,1000.);
#25219=VECTOR('',#106999,1000.);
#25220=VECTOR('',#107000,1000.);
#25221=VECTOR('',#107003,1000.);
#25222=VECTOR('',#107014,1000.);
#25223=VECTOR('',#107017,1000.);
#25224=VECTOR('',#107018,1000.);
#25225=VECTOR('',#107027,1000.);
#25226=VECTOR('',#107030,1000.);
#25227=VECTOR('',#107033,1000.);
#25228=VECTOR('',#107036,1000.);
#25229=VECTOR('',#107039,1000.);
#25230=VECTOR('',#107044,1000.);
#25231=VECTOR('',#107045,1000.);
#25232=VECTOR('',#107048,1000.);
#25233=VECTOR('',#107057,1000.);
#25234=VECTOR('',#107060,1000.);
#25235=VECTOR('',#107061,1000.);
#25236=VECTOR('',#107064,1000.);
#25237=VECTOR('',#107077,1000.);
#25238=VECTOR('',#107080,1000.);
#25239=VECTOR('',#107083,1000.);
#25240=VECTOR('',#107084,1000.);
#25241=VECTOR('',#107089,1000.);
#25242=VECTOR('',#107090,1000.);
#25243=VECTOR('',#107097,1000.);
#25244=VECTOR('',#107098,1000.);
#25245=VECTOR('',#107099,1000.);
#25246=VECTOR('',#107100,1000.);
#25247=VECTOR('',#107103,1000.);
#25248=VECTOR('',#107106,1000.);
#25249=VECTOR('',#107107,1000.);
#25250=VECTOR('',#107110,1000.);
#25251=VECTOR('',#107115,1000.);
#25252=VECTOR('',#107116,1000.);
#25253=VECTOR('',#107119,1000.);
#25254=VECTOR('',#107124,1000.);
#25255=VECTOR('',#107125,1000.);
#25256=VECTOR('',#107126,1000.);
#25257=VECTOR('',#107129,1000.);
#25258=VECTOR('',#107132,1000.);
#25259=VECTOR('',#107133,1000.);
#25260=VECTOR('',#107134,1000.);
#25261=VECTOR('',#107135,1000.);
#25262=VECTOR('',#107142,1000.);
#25263=VECTOR('',#107145,1000.);
#25264=VECTOR('',#107150,1000.);
#25265=VECTOR('',#107151,1000.);
#25266=VECTOR('',#107162,1000.);
#25267=VECTOR('',#107167,1000.);
#25268=VECTOR('',#107170,1000.);
#25269=VECTOR('',#107173,1000.);
#25270=VECTOR('',#107174,1000.);
#25271=VECTOR('',#107175,1000.);
#25272=VECTOR('',#107176,1000.);
#25273=VECTOR('',#107177,1000.);
#25274=VECTOR('',#107180,1000.);
#25275=VECTOR('',#107185,1000.);
#25276=VECTOR('',#107186,1000.);
#25277=VECTOR('',#107189,1000.);
#25278=VECTOR('',#107194,1000.);
#25279=VECTOR('',#107197,1000.);
#25280=VECTOR('',#107200,1000.);
#25281=VECTOR('',#107201,1000.);
#25282=VECTOR('',#107202,1000.);
#25283=VECTOR('',#107203,1000.);
#25284=VECTOR('',#107208,1000.);
#25285=VECTOR('',#107209,1000.);
#25286=VECTOR('',#107216,1000.);
#25287=VECTOR('',#107219,1000.);
#25288=VECTOR('',#107222,1000.);
#25289=VECTOR('',#107223,1000.);
#25290=VECTOR('',#107226,1000.);
#25291=VECTOR('',#107231,1000.);
#25292=VECTOR('',#107232,1000.);
#25293=VECTOR('',#107235,1000.);
#25294=VECTOR('',#107240,1000.);
#25295=VECTOR('',#107243,1000.);
#25296=VECTOR('',#107252,1000.);
#25297=VECTOR('',#107253,1000.);
#25298=VECTOR('',#107254,1000.);
#25299=VECTOR('',#107257,1000.);
#25300=VECTOR('',#107258,1000.);
#25301=VECTOR('',#107261,1000.);
#25302=VECTOR('',#107266,1000.);
#25303=VECTOR('',#107267,1000.);
#25304=VECTOR('',#107270,1000.);
#25305=VECTOR('',#107275,1000.);
#25306=VECTOR('',#107278,1000.);
#25307=VECTOR('',#107279,1000.);
#25308=VECTOR('',#107286,1000.);
#25309=VECTOR('',#107287,1000.);
#25310=VECTOR('',#107294,1000.);
#25311=VECTOR('',#107295,1000.);
#25312=VECTOR('',#107296,1000.);
#25313=VECTOR('',#107297,1000.);
#25314=VECTOR('',#107300,1000.);
#25315=VECTOR('',#107303,1000.);
#25316=VECTOR('',#107304,1000.);
#25317=VECTOR('',#107307,1000.);
#25318=VECTOR('',#107312,1000.);
#25319=VECTOR('',#107313,1000.);
#25320=VECTOR('',#107316,1000.);
#25321=VECTOR('',#107323,1000.);
#25322=VECTOR('',#107324,1000.);
#25323=VECTOR('',#107325,1000.);
#25324=VECTOR('',#107326,1000.);
#25325=VECTOR('',#107327,1000.);
#25326=VECTOR('',#107330,1000.);
#25327=VECTOR('',#107333,1000.);
#25328=VECTOR('',#107334,1000.);
#25329=VECTOR('',#107335,1000.);
#25330=VECTOR('',#107340,1000.);
#25331=VECTOR('',#107343,1000.);
#25332=VECTOR('',#107352,1000.);
#25333=VECTOR('',#107353,1000.);
#25334=VECTOR('',#107366,1000.);
#25335=VECTOR('',#107371,1000.);
#25336=VECTOR('',#107374,1000.);
#25337=VECTOR('',#107377,1000.);
#25338=VECTOR('',#107378,1000.);
#25339=VECTOR('',#107379,1000.);
#25340=VECTOR('',#107380,1000.);
#25341=VECTOR('',#107381,1000.);
#25342=VECTOR('',#107384,1000.);
#25343=VECTOR('',#107389,1000.);
#25344=VECTOR('',#107390,1000.);
#25345=VECTOR('',#107393,1000.);
#25346=VECTOR('',#107398,1000.);
#25347=VECTOR('',#107401,1000.);
#25348=VECTOR('',#107404,1000.);
#25349=VECTOR('',#107405,1000.);
#25350=VECTOR('',#107406,1000.);
#25351=VECTOR('',#107407,1000.);
#25352=VECTOR('',#107420,1000.);
#25353=VECTOR('',#107425,1000.);
#25354=VECTOR('',#107428,1000.);
#25355=VECTOR('',#107429,1000.);
#25356=VECTOR('',#107434,1000.);
#25357=VECTOR('',#107435,1000.);
#25358=VECTOR('',#107436,1000.);
#25359=VECTOR('',#107437,1000.);
#25360=VECTOR('',#107438,1000.);
#25361=VECTOR('',#107439,1000.);
#25362=VECTOR('',#107442,1000.);
#25363=VECTOR('',#107445,1000.);
#25364=VECTOR('',#107446,1000.);
#25365=VECTOR('',#107449,1000.);
#25366=VECTOR('',#107454,1000.);
#25367=VECTOR('',#107455,1000.);
#25368=VECTOR('',#107458,1000.);
#25369=VECTOR('',#107463,1000.);
#25370=VECTOR('',#107466,1000.);
#25371=VECTOR('',#107469,1000.);
#25372=VECTOR('',#107470,1000.);
#25373=VECTOR('',#107471,1000.);
#25374=VECTOR('',#107472,1000.);
#25375=VECTOR('',#107479,1000.);
#25376=VECTOR('',#107480,1000.);
#25377=VECTOR('',#107485,1000.);
#25378=VECTOR('',#107488,1000.);
#25379=VECTOR('',#107491,1000.);
#25380=VECTOR('',#107492,1000.);
#25381=VECTOR('',#107493,1000.);
#25382=VECTOR('',#107494,1000.);
#25383=VECTOR('',#107495,1000.);
#25384=VECTOR('',#107498,1000.);
#25385=VECTOR('',#107503,1000.);
#25386=VECTOR('',#107504,1000.);
#25387=VECTOR('',#107507,1000.);
#25388=VECTOR('',#107514,1000.);
#25389=VECTOR('',#107517,1000.);
#25390=VECTOR('',#107520,1000.);
#25391=VECTOR('',#107521,1000.);
#25392=VECTOR('',#107522,1000.);
#25393=VECTOR('',#107523,1000.);
#25394=VECTOR('',#107526,1000.);
#25395=VECTOR('',#107535,2.);
#25396=VECTOR('',#107544,2.75);
#25397=VECTOR('',#107575,2.);
#25398=VECTOR('',#107584,2.75);
#25399=VECTOR('',#107595,1000.);
#25400=VECTOR('',#107604,1000.);
#25401=VECTOR('',#107609,1000.);
#25402=VECTOR('',#107610,1000.);
#25403=VECTOR('',#107629,1000.);
#25404=VECTOR('',#107632,1000.);
#25405=VECTOR('',#107641,1000.);
#25406=VECTOR('',#107644,1000.);
#25407=VECTOR('',#107657,1000.);
#25408=VECTOR('',#107662,1000.);
#25409=VECTOR('',#107667,1000.);
#25410=VECTOR('',#107668,1000.);
#25411=VECTOR('',#107677,1000.);
#25412=VECTOR('',#107678,1000.);
#25413=VECTOR('',#107683,1000.);
#25414=VECTOR('',#107688,1000.);
#25415=VECTOR('',#107689,1000.);
#25416=VECTOR('',#107698,1000.);
#25417=VECTOR('',#107699,1000.);
#25418=VECTOR('',#107712,1000.);
#25419=VECTOR('',#107719,1000.);
#25420=VECTOR('',#107726,1000.);
#25421=VECTOR('',#107729,1000.);
#25422=VECTOR('',#107730,1000.);
#25423=VECTOR('',#107733,1000.);
#25424=VECTOR('',#107738,1000.);
#25425=VECTOR('',#107743,1000.);
#25426=VECTOR('',#107748,1000.);
#25427=VECTOR('',#107749,1000.);
#25428=VECTOR('',#107750,1000.);
#25429=VECTOR('',#107751,1000.);
#25430=VECTOR('',#107752,1000.);
#25431=VECTOR('',#107753,1000.);
#25432=VECTOR('',#107754,1000.);
#25433=VECTOR('',#107755,1000.);
#25434=VECTOR('',#107756,1000.);
#25435=VECTOR('',#107757,1000.);
#25436=VECTOR('',#107760,1000.);
#25437=VECTOR('',#107761,1000.);
#25438=VECTOR('',#107764,1000.);
#25439=VECTOR('',#107769,1000.);
#25440=VECTOR('',#107772,1000.);
#25441=VECTOR('',#107777,1000.);
#25442=VECTOR('',#107780,1000.);
#25443=VECTOR('',#107783,1000.);
#25444=VECTOR('',#107786,1000.);
#25445=VECTOR('',#107789,1000.);
#25446=VECTOR('',#107792,1000.);
#25447=VECTOR('',#107795,1000.);
#25448=VECTOR('',#107798,1000.);
#25449=VECTOR('',#107801,1000.);
#25450=VECTOR('',#107804,1000.);
#25451=VECTOR('',#107809,1000.);
#25452=VECTOR('',#107810,1000.);
#25453=VECTOR('',#107813,1000.);
#25454=VECTOR('',#107814,1000.);
#25455=VECTOR('',#107815,1000.);
#25456=VECTOR('',#107816,1000.);
#25457=VECTOR('',#107817,1000.);
#25458=VECTOR('',#107818,1000.);
#25459=VECTOR('',#107819,1000.);
#25460=VECTOR('',#107820,1000.);
#25461=VECTOR('',#107821,1000.);
#25462=VECTOR('',#107822,1000.);
#25463=VECTOR('',#107825,1000.);
#25464=VECTOR('',#107830,1000.);
#25465=VECTOR('',#107835,1000.);
#25466=VECTOR('',#107840,1000.);
#25467=VECTOR('',#107841,1000.);
#25468=VECTOR('',#107842,1000.);
#25469=VECTOR('',#107843,1000.);
#25470=VECTOR('',#107844,1000.);
#25471=VECTOR('',#107845,1000.);
#25472=VECTOR('',#107846,1000.);
#25473=VECTOR('',#107847,1000.);
#25474=VECTOR('',#107848,1000.);
#25475=VECTOR('',#107855,1000.);
#25476=VECTOR('',#107862,1000.);
#25477=VECTOR('',#107863,1000.);
#25478=VECTOR('',#107864,1000.);
#25479=VECTOR('',#107871,1000.);
#25480=VECTOR('',#107874,1000.);
#25481=VECTOR('',#107881,1000.);
#25482=VECTOR('',#107888,1000.);
#25483=VECTOR('',#107889,1000.);
#25484=VECTOR('',#107892,1000.);
#25485=VECTOR('',#107897,1000.);
#25486=VECTOR('',#107906,1000.);
#25487=VECTOR('',#107911,1000.);
#25488=VECTOR('',#107912,1000.);
#25489=VECTOR('',#107943,1000.);
#25490=VECTOR('',#107948,1000.);
#25491=VECTOR('',#107961,1000.);
#25492=VECTOR('',#107972,1000.);
#25493=VECTOR('',#107977,1000.);
#25494=VECTOR('',#107980,1000.);
#25495=VECTOR('',#107993,1000.);
#25496=VECTOR('',#108002,1000.);
#25497=VECTOR('',#108015,1000.);
#25498=VECTOR('',#108024,1000.);
#25499=VECTOR('',#108039,1000.);
#25500=VECTOR('',#108044,1000.);
#25501=VECTOR('',#108057,1000.);
#25502=VECTOR('',#108070,1000.);
#25503=VECTOR('',#108113,1000.);
#25504=VECTOR('',#108128,1000.);
#25505=VECTOR('',#108135,1000.);
#25506=VECTOR('',#108156,1000.);
#25507=VECTOR('',#108163,1000.);
#25508=VECTOR('',#108176,1000.);
#25509=VECTOR('',#108193,1000.);
#25510=VECTOR('',#108204,1000.);
#25511=VECTOR('',#108213,1000.);
#25512=VECTOR('',#108224,1000.);
#25513=VECTOR('',#108249,1000.);
#25514=VECTOR('',#108258,1000.);
#25515=VECTOR('',#108275,1000.);
#25516=VECTOR('',#108278,1000.);
#25517=VECTOR('',#108303,1000.);
#25518=VECTOR('',#108314,1000.);
#25519=VECTOR('',#108333,1000.);
#25520=VECTOR('',#108336,1000.);
#25521=VECTOR('',#108365,1000.);
#25522=VECTOR('',#108376,1000.);
#25523=VECTOR('',#108393,1000.);
#25524=VECTOR('',#108396,1000.);
#25525=VECTOR('',#108421,1000.);
#25526=VECTOR('',#108430,1000.);
#25527=VECTOR('',#108455,1000.);
#25528=VECTOR('',#108464,1000.);
#25529=VECTOR('',#108475,1000.);
#25530=VECTOR('',#108484,1000.);
#25531=VECTOR('',#108503,1000.);
#25532=VECTOR('',#108520,1000.);
#25533=VECTOR('',#108529,1000.);
#25534=VECTOR('',#108536,1000.);
#25535=VECTOR('',#108567,1000.);
#25536=VECTOR('',#108578,1000.);
#25537=VECTOR('',#108591,1000.);
#25538=VECTOR('',#108602,1000.);
#25539=VECTOR('',#108605,1000.);
#25540=VECTOR('',#108626,1000.);
#25541=VECTOR('',#108633,1000.);
#25542=VECTOR('',#108642,1000.);
#25543=VECTOR('',#108669,1000.);
#25544=VECTOR('',#108676,1000.);
#25545=VECTOR('',#108697,1000.);
#25546=VECTOR('',#108708,1000.);
#25547=VECTOR('',#108719,1000.);
#25548=VECTOR('',#108730,1000.);
#25549=VECTOR('',#108739,1000.);
#25550=VECTOR('',#108746,1000.);
#25551=VECTOR('',#108761,1000.);
#25552=VECTOR('',#108772,1000.);
#25553=VECTOR('',#108781,1000.);
#25554=VECTOR('',#108824,1000.);
#25555=VECTOR('',#108873,1000.);
#25556=VECTOR('',#108884,1000.);
#25557=VECTOR('',#108899,1000.);
#25558=VECTOR('',#108908,1000.);
#25559=VECTOR('',#108911,1000.);
#25560=VECTOR('',#108920,1000.);
#25561=VECTOR('',#108925,1000.);
#25562=VECTOR('',#108934,1000.);
#25563=VECTOR('',#108951,1000.);
#25564=VECTOR('',#108974,1000.);
#25565=VECTOR('',#108985,1000.);
#25566=VECTOR('',#109006,1000.);
#25567=VECTOR('',#109017,1000.);
#25568=VECTOR('',#109028,1000.);
#25569=VECTOR('',#109039,1000.);
#25570=VECTOR('',#109048,1000.);
#25571=VECTOR('',#109055,1000.);
#25572=VECTOR('',#109070,1000.);
#25573=VECTOR('',#109081,1000.);
#25574=VECTOR('',#109090,1000.);
#25575=VECTOR('',#109115,1000.);
#25576=VECTOR('',#109126,1000.);
#25577=VECTOR('',#109135,1000.);
#25578=VECTOR('',#109154,1000.);
#25579=VECTOR('',#109165,1000.);
#25580=VECTOR('',#109176,1000.);
#25581=VECTOR('',#109187,1000.);
#25582=VECTOR('',#109194,1000.);
#25583=VECTOR('',#109211,1000.);
#25584=VECTOR('',#109222,1000.);
#25585=VECTOR('',#109235,1000.);
#25586=VECTOR('',#109258,1000.);
#25587=VECTOR('',#109269,1000.);
#25588=VECTOR('',#109280,1000.);
#25589=VECTOR('',#109291,1000.);
#25590=VECTOR('',#109300,1000.);
#25591=VECTOR('',#109309,1000.);
#25592=VECTOR('',#109326,1000.);
#25593=VECTOR('',#109337,1000.);
#25594=VECTOR('',#109344,1000.);
#25595=VECTOR('',#109357,1000.);
#25596=VECTOR('',#109384,1000.);
#25597=VECTOR('',#109387,1000.);
#25598=VECTOR('',#109394,1000.);
#25599=VECTOR('',#109399,1000.);
#25600=VECTOR('',#109488,1000.);
#25601=VECTOR('',#109495,1000.);
#25602=VECTOR('',#109504,1000.);
#25603=VECTOR('',#109511,1000.);
#25604=VECTOR('',#109532,1000.);
#25605=VECTOR('',#109535,1000.);
#25606=VECTOR('',#109542,1000.);
#25607=VECTOR('',#109547,1000.);
#25608=VECTOR('',#109550,1000.);
#25609=VECTOR('',#109569,1000.);
#25610=VECTOR('',#109572,1000.);
#25611=VECTOR('',#109575,1000.);
#25612=VECTOR('',#109584,1000.);
#25613=VECTOR('',#109585,1000.);
#25614=VECTOR('',#109588,1000.);
#25615=VECTOR('',#109611,1000.);
#25616=VECTOR('',#109614,1000.);
#25617=VECTOR('',#109615,1000.);
#25618=VECTOR('',#109626,1000.);
#25619=VECTOR('',#109633,1000.);
#25620=VECTOR('',#109636,1000.);
#25621=VECTOR('',#109661,1000.);
#25622=VECTOR('',#109664,1000.);
#25623=VECTOR('',#109675,1000.);
#25624=VECTOR('',#109678,1000.);
#25625=VECTOR('',#109707,1000.);
#25626=VECTOR('',#109710,1000.);
#25627=VECTOR('',#109725,1000.);
#25628=VECTOR('',#109728,1000.);
#25629=VECTOR('',#109747,1000.);
#25630=VECTOR('',#109750,1000.);
#25631=VECTOR('',#109759,1000.);
#25632=VECTOR('',#109760,1000.);
#25633=VECTOR('',#109763,1000.);
#25634=VECTOR('',#109764,1000.);
#25635=VECTOR('',#109765,1000.);
#25636=VECTOR('',#109766,1000.);
#25637=VECTOR('',#109771,1000.);
#25638=VECTOR('',#109776,1000.);
#25639=VECTOR('',#109777,1000.);
#25640=VECTOR('',#109778,1000.);
#25641=VECTOR('',#109785,1000.);
#25642=VECTOR('',#109786,1000.);
#25643=VECTOR('',#109797,1000.);
#25644=VECTOR('',#109798,1000.);
#25645=VECTOR('',#109799,1000.);
#25646=VECTOR('',#109802,1000.);
#25647=VECTOR('',#109803,1000.);
#25648=VECTOR('',#109804,1000.);
#25649=VECTOR('',#109805,1000.);
#25650=VECTOR('',#109810,1000.);
#25651=VECTOR('',#109815,1000.);
#25652=VECTOR('',#109816,1000.);
#25653=VECTOR('',#109817,1000.);
#25654=VECTOR('',#109828,1000.);
#25655=VECTOR('',#109829,1000.);
#25656=VECTOR('',#109832,1000.);
#25657=VECTOR('',#109833,1000.);
#25658=VECTOR('',#109834,1000.);
#25659=VECTOR('',#109835,1000.);
#25660=VECTOR('',#109840,1000.);
#25661=VECTOR('',#109845,1000.);
#25662=VECTOR('',#109846,1000.);
#25663=VECTOR('',#109847,1000.);
#25664=VECTOR('',#109850,1000.);
#25665=VECTOR('',#109851,1000.);
#25666=VECTOR('',#109856,1000.);
#25667=VECTOR('',#109857,1000.);
#25668=VECTOR('',#109868,1000.);
#25669=VECTOR('',#109869,1000.);
#25670=VECTOR('',#109872,1000.);
#25671=VECTOR('',#109881,1000.);
#25672=VECTOR('',#109882,1000.);
#25673=VECTOR('',#109885,1000.);
#25674=VECTOR('',#109886,1000.);
#25675=VECTOR('',#109887,1000.);
#25676=VECTOR('',#109888,1000.);
#25677=VECTOR('',#109891,1000.);
#25678=VECTOR('',#109898,1000.);
#25679=VECTOR('',#109899,1000.);
#25680=VECTOR('',#109900,1000.);
#25681=VECTOR('',#109915,1000.);
#25682=VECTOR('',#109916,1000.);
#25683=VECTOR('',#109917,1000.);
#25684=VECTOR('',#109918,1000.);
#25685=VECTOR('',#109923,1000.);
#25686=VECTOR('',#109928,1000.);
#25687=VECTOR('',#109929,1000.);
#25688=VECTOR('',#109930,1000.);
#25689=VECTOR('',#109933,1000.);
#25690=VECTOR('',#109934,1000.);
#25691=VECTOR('',#109939,1000.);
#25692=VECTOR('',#109940,1000.);
#25693=VECTOR('',#109955,1000.);
#25694=VECTOR('',#109956,1000.);
#25695=VECTOR('',#109959,1000.);
#25696=VECTOR('',#109970,1000.);
#25697=VECTOR('',#109971,1000.);
#25698=VECTOR('',#109974,1000.);
#25699=VECTOR('',#109975,1000.);
#25700=VECTOR('',#109976,1000.);
#25701=VECTOR('',#109977,1000.);
#25702=VECTOR('',#109980,1000.);
#25703=VECTOR('',#109987,1000.);
#25704=VECTOR('',#109988,1000.);
#25705=VECTOR('',#109989,1000.);
#25706=VECTOR('',#109996,1000.);
#25707=VECTOR('',#109999,1000.);
#25708=VECTOR('',#110004,1000.);
#25709=VECTOR('',#110007,1000.);
#25710=VECTOR('',#110010,1000.);
#25711=VECTOR('',#110011,1000.);
#25712=VECTOR('',#110018,1000.);
#25713=VECTOR('',#110021,1000.);
#25714=VECTOR('',#110022,1000.);
#25715=VECTOR('',#110025,1000.);
#25716=VECTOR('',#110026,1000.);
#25717=VECTOR('',#110027,1000.);
#25718=VECTOR('',#110028,1000.);
#25719=VECTOR('',#110041,1000.);
#25720=VECTOR('',#110042,1000.);
#25721=VECTOR('',#110051,1000.);
#25722=VECTOR('',#110052,1000.);
#25723=VECTOR('',#110065,1000.);
#25724=VECTOR('',#110066,1000.);
#25725=VECTOR('',#110077,1000.);
#25726=VECTOR('',#110078,1000.);
#25727=VECTOR('',#110085,1000.);
#25728=VECTOR('',#110090,1000.);
#25729=VECTOR('',#110091,1000.);
#25730=VECTOR('',#110092,1000.);
#25731=VECTOR('',#110093,1000.);
#25732=VECTOR('',#110098,1000.);
#25733=VECTOR('',#110103,1000.);
#25734=VECTOR('',#110108,1000.);
#25735=VECTOR('',#110111,1000.);
#25736=VECTOR('',#110116,1000.);
#25737=VECTOR('',#110117,1000.);
#25738=VECTOR('',#110124,1000.);
#25739=VECTOR('',#110127,1000.);
#25740=VECTOR('',#110130,1000.);
#25741=VECTOR('',#110131,1000.);
#25742=VECTOR('',#110132,1000.);
#25743=VECTOR('',#110135,1000.);
#25744=VECTOR('',#110136,1000.);
#25745=VECTOR('',#110137,1000.);
#25746=VECTOR('',#110140,1000.);
#25747=VECTOR('',#110141,1000.);
#25748=VECTOR('',#110144,1000.);
#25749=VECTOR('',#110145,1000.);
#25750=VECTOR('',#110146,1000.);
#25751=VECTOR('',#110147,1000.);
#25752=VECTOR('',#110150,1000.);
#25753=VECTOR('',#110151,1000.);
#25754=VECTOR('',#110154,1000.);
#25755=VECTOR('',#110155,1000.);
#25756=VECTOR('',#110158,1000.);
#25757=VECTOR('',#110161,1000.);
#25758=VECTOR('',#110174,1000.);
#25759=VECTOR('',#110191,1000.);
#25760=VECTOR('',#110198,1000.);
#25761=VECTOR('',#110205,1000.);
#25762=VECTOR('',#110212,1000.);
#25763=VECTOR('',#110219,1000.);
#25764=VECTOR('',#110220,1000.);
#25765=VECTOR('',#110253,1000.);
#25766=VECTOR('',#110260,1000.);
#25767=VECTOR('',#110267,1000.);
#25768=VECTOR('',#110268,1000.);
#25769=VECTOR('',#110275,1000.);
#25770=VECTOR('',#110282,1000.);
#25771=VECTOR('',#110429,1000.);
#25772=VECTOR('',#110436,1000.);
#25773=VECTOR('',#110443,1000.);
#25774=VECTOR('',#110450,1000.);
#25775=VECTOR('',#110457,1000.);
#25776=VECTOR('',#110458,1000.);
#25777=VECTOR('',#110487,1000.);
#25778=VECTOR('',#110488,1000.);
#25779=VECTOR('',#110499,1000.);
#25780=VECTOR('',#110500,1000.);
#25781=VECTOR('',#110501,1000.);
#25782=VECTOR('',#110504,1000.);
#25783=VECTOR('',#110505,1000.);
#25784=VECTOR('',#110512,1000.);
#25785=VECTOR('',#110513,1000.);
#25786=VECTOR('',#110524,1000.);
#25787=VECTOR('',#110537,1000.);
#25788=VECTOR('',#110548,1000.);
#25789=VECTOR('',#110555,1000.);
#25790=VECTOR('',#110556,1000.);
#25791=VECTOR('',#110559,1000.);
#25792=VECTOR('',#110564,1000.);
#25793=VECTOR('',#110567,1000.);
#25794=VECTOR('',#110578,1000.);
#25795=VECTOR('',#110591,1000.);
#25796=VECTOR('',#110602,1000.);
#25797=VECTOR('',#110605,1000.);
#25798=VECTOR('',#110608,1000.);
#25799=VECTOR('',#110613,1000.);
#25800=VECTOR('',#110624,1000.);
#25801=VECTOR('',#110635,1000.);
#25802=VECTOR('',#110638,1000.);
#25803=VECTOR('',#110653,1000.);
#25804=VECTOR('',#110660,1000.);
#25805=VECTOR('',#110663,1000.);
#25806=VECTOR('',#110672,1000.);
#25807=VECTOR('',#110685,1000.);
#25808=VECTOR('',#110692,1000.);
#25809=VECTOR('',#110693,1000.);
#25810=VECTOR('',#110696,1000.);
#25811=VECTOR('',#110707,1000.);
#25812=VECTOR('',#110714,1000.);
#25813=VECTOR('',#110717,1000.);
#25814=VECTOR('',#110720,1000.);
#25815=VECTOR('',#110723,1000.);
#25816=VECTOR('',#110726,1000.);
#25817=VECTOR('',#110743,1000.);
#25818=VECTOR('',#110752,1000.);
#25819=VECTOR('',#110757,1000.);
#25820=VECTOR('',#110758,1000.);
#25821=VECTOR('',#110771,1000.);
#25822=VECTOR('',#110780,1000.);
#25823=VECTOR('',#110791,1000.);
#25824=VECTOR('',#110796,1000.);
#25825=VECTOR('',#110797,1000.);
#25826=VECTOR('',#110818,1000.);
#25827=VECTOR('',#110833,1000.);
#25828=VECTOR('',#110844,1000.);
#25829=VECTOR('',#110849,1000.);
#25830=VECTOR('',#110850,1000.);
#25831=VECTOR('',#110853,1000.);
#25832=VECTOR('',#110864,1000.);
#25833=VECTOR('',#110877,1000.);
#25834=VECTOR('',#110888,1000.);
#25835=VECTOR('',#110891,1000.);
#25836=VECTOR('',#110894,1000.);
#25837=VECTOR('',#110899,1000.);
#25838=VECTOR('',#110910,1000.);
#25839=VECTOR('',#110921,1000.);
#25840=VECTOR('',#110924,1000.);
#25841=VECTOR('',#110939,1000.);
#25842=VECTOR('',#110960,1000.);
#25843=VECTOR('',#110973,1000.);
#25844=VECTOR('',#110974,1000.);
#25845=VECTOR('',#110977,1000.);
#25846=VECTOR('',#110980,1000.);
#25847=VECTOR('',#110981,1000.);
#25848=VECTOR('',#110988,1000.);
#25849=VECTOR('',#110991,1000.);
#25850=VECTOR('',#110996,1000.);
#25851=VECTOR('',#110997,1000.);
#25852=VECTOR('',#111000,1000.);
#25853=VECTOR('',#111011,1000.);
#25854=VECTOR('',#111020,1000.);
#25855=VECTOR('',#111033,1000.);
#25856=VECTOR('',#111042,1000.);
#25857=VECTOR('',#111053,1000.);
#25858=VECTOR('',#111070,1000.);
#25859=VECTOR('',#111081,1000.);
#25860=VECTOR('',#111086,1000.);
#25861=VECTOR('',#111087,1000.);
#25862=VECTOR('',#111092,1000.);
#25863=VECTOR('',#111095,1000.);
#25864=VECTOR('',#111100,1000.);
#25865=VECTOR('',#111101,1000.);
#25866=VECTOR('',#111116,1000.);
#25867=VECTOR('',#111119,1000.);
#25868=VECTOR('',#111132,1000.);
#25869=VECTOR('',#111135,1000.);
#25870=VECTOR('',#111146,1000.);
#25871=VECTOR('',#111147,1000.);
#25872=VECTOR('',#111150,1000.);
#25873=VECTOR('',#111161,1000.);
#25874=VECTOR('',#111164,1000.);
#25875=VECTOR('',#111177,1000.);
#25876=VECTOR('',#111178,1000.);
#25877=VECTOR('',#111193,1000.);
#25878=VECTOR('',#111196,1000.);
#25879=VECTOR('',#111207,1000.);
#25880=VECTOR('',#111208,1000.);
#25881=VECTOR('',#111213,1000.);
#25882=VECTOR('',#111214,1000.);
#25883=VECTOR('',#111229,1000.);
#25884=VECTOR('',#111244,1000.);
#25885=VECTOR('',#111255,1000.);
#25886=VECTOR('',#111260,1000.);
#25887=VECTOR('',#111261,1000.);
#25888=VECTOR('',#111264,1000.);
#25889=VECTOR('',#111275,1000.);
#25890=VECTOR('',#111288,1000.);
#25891=VECTOR('',#111299,1000.);
#25892=VECTOR('',#111302,1000.);
#25893=VECTOR('',#111305,1000.);
#25894=VECTOR('',#111310,1000.);
#25895=VECTOR('',#111321,1000.);
#25896=VECTOR('',#111332,1000.);
#25897=VECTOR('',#111335,1000.);
#25898=VECTOR('',#111350,1000.);
#25899=VECTOR('',#111363,1000.);
#25900=VECTOR('',#111380,1000.);
#25901=VECTOR('',#111383,1000.);
#25902=VECTOR('',#111388,1000.);
#25903=VECTOR('',#111389,1000.);
#25904=VECTOR('',#111392,1000.);
#25905=VECTOR('',#111405,1000.);
#25906=VECTOR('',#111412,1000.);
#25907=VECTOR('',#111415,1000.);
#25908=VECTOR('',#111416,1000.);
#25909=VECTOR('',#111421,1000.);
#25910=VECTOR('',#111422,1000.);
#25911=VECTOR('',#111433,1000.);
#25912=VECTOR('',#111442,1000.);
#25913=VECTOR('',#111451,1000.);
#25914=VECTOR('',#111468,1000.);
#25915=VECTOR('',#111479,1000.);
#25916=VECTOR('',#111484,1000.);
#25917=VECTOR('',#111485,1000.);
#25918=VECTOR('',#111496,1000.);
#25919=VECTOR('',#111499,1000.);
#25920=VECTOR('',#111502,1000.);
#25921=VECTOR('',#111505,1000.);
#25922=VECTOR('',#111516,1000.);
#25923=VECTOR('',#111523,1000.);
#25924=VECTOR('',#111534,1000.);
#25925=VECTOR('',#111539,1000.);
#25926=VECTOR('',#111540,1000.);
#25927=VECTOR('',#111553,1000.);
#25928=VECTOR('',#111564,1000.);
#25929=VECTOR('',#111565,1000.);
#25930=VECTOR('',#111568,1000.);
#25931=VECTOR('',#111579,1000.);
#25932=VECTOR('',#111594,1000.);
#25933=VECTOR('',#111607,1000.);
#25934=VECTOR('',#111616,1000.);
#25935=VECTOR('',#111619,1000.);
#25936=VECTOR('',#111630,1000.);
#25937=VECTOR('',#111645,1000.);
#25938=VECTOR('',#111656,1000.);
#25939=VECTOR('',#111657,1000.);
#25940=VECTOR('',#111666,1000.);
#25941=VECTOR('',#111667,1000.);
#25942=VECTOR('',#111670,1000.);
#25943=VECTOR('',#111675,1000.);
#25944=VECTOR('',#111680,1000.);
#25945=VECTOR('',#111683,1000.);
#25946=VECTOR('',#111694,1000.);
#25947=VECTOR('',#111713,1000.);
#25948=VECTOR('',#111726,1000.);
#25949=VECTOR('',#111727,1000.);
#25950=VECTOR('',#111736,1000.);
#25951=VECTOR('',#111737,1000.);
#25952=VECTOR('',#111742,1000.);
#25953=VECTOR('',#111747,1000.);
#25954=VECTOR('',#111752,1000.);
#25955=VECTOR('',#111755,1000.);
#25956=VECTOR('',#111768,1000.);
#25957=VECTOR('',#111787,1000.);
#25958=VECTOR('',#111798,1000.);
#25959=VECTOR('',#111799,1000.);
#25960=VECTOR('',#111806,1000.);
#25961=VECTOR('',#111809,1000.);
#25962=VECTOR('',#111812,1000.);
#25963=VECTOR('',#111817,1000.);
#25964=VECTOR('',#111822,1000.);
#25965=VECTOR('',#111825,1000.);
#25966=VECTOR('',#111836,1000.);
#25967=VECTOR('',#111851,1000.);
#25968=VECTOR('',#111862,1000.);
#25969=VECTOR('',#111863,1000.);
#25970=VECTOR('',#111872,1000.);
#25971=VECTOR('',#111887,1000.);
#25972=VECTOR('',#111900,1000.);
#25973=VECTOR('',#111911,1000.);
#25974=VECTOR('',#111914,1000.);
#25975=VECTOR('',#111917,1000.);
#25976=VECTOR('',#111928,1000.);
#25977=VECTOR('',#111945,1000.);
#25978=VECTOR('',#111956,1000.);
#25979=VECTOR('',#111969,1000.);
#25980=VECTOR('',#111970,1000.);
#25981=VECTOR('',#111973,1000.);
#25982=VECTOR('',#111984,1000.);
#25983=VECTOR('',#112003,1000.);
#25984=VECTOR('',#112036,1000.);
#25985=VECTOR('',#112039,1000.);
#25986=VECTOR('',#112052,1000.);
#25987=VECTOR('',#112053,1000.);
#25988=VECTOR('',#112068,1000.);
#25989=VECTOR('',#112071,1000.);
#25990=VECTOR('',#112100,1000.);
#25991=VECTOR('',#112117,1000.);
#25992=VECTOR('',#112134,1000.);
#25993=VECTOR('',#112145,1000.);
#25994=VECTOR('',#112162,1000.);
#25995=VECTOR('',#112175,1000.);
#25996=VECTOR('',#112192,1000.);
#25997=VECTOR('',#112207,1000.);
#25998=VECTOR('',#112218,1000.);
#25999=VECTOR('',#112221,1000.);
#26000=VECTOR('',#112224,1000.);
#26001=VECTOR('',#112229,1000.);
#26002=VECTOR('',#112240,1000.);
#26003=VECTOR('',#112259,1000.);
#26004=VECTOR('',#112270,1000.);
#26005=VECTOR('',#112273,1000.);
#26006=VECTOR('',#112276,1000.);
#26007=VECTOR('',#112283,1000.);
#26008=VECTOR('',#112284,1000.);
#26009=VECTOR('',#112321,1000.);
#26010=VECTOR('',#112322,1000.);
#26011=VECTOR('',#112327,1000.);
#26012=VECTOR('',#112330,1000.);
#26013=VECTOR('',#112349,1000.);
#26014=VECTOR('',#112354,1000.);
#26015=VECTOR('',#112357,1000.);
#26016=VECTOR('',#112372,1000.);
#26017=VECTOR('',#112373,1000.);
#26018=VECTOR('',#112374,1000.);
#26019=VECTOR('',#112379,1000.);
#26020=VECTOR('',#112384,1000.);
#26021=VECTOR('',#112389,1000.);
#26022=VECTOR('',#112392,1000.);
#26023=VECTOR('',#112393,1000.);
#26024=VECTOR('',#112396,1000.);
#26025=VECTOR('',#112401,1000.);
#26026=VECTOR('',#112408,1000.);
#26027=VECTOR('',#112411,1000.);
#26028=VECTOR('',#112412,1000.);
#26029=VECTOR('',#112417,1000.);
#26030=VECTOR('',#112422,1000.);
#26031=VECTOR('',#112427,1000.);
#26032=VECTOR('',#112430,1000.);
#26033=VECTOR('',#112431,1000.);
#26034=VECTOR('',#112432,1000.);
#26035=VECTOR('',#112433,1000.);
#26036=VECTOR('',#112442,1000.);
#26037=VECTOR('',#112449,1000.);
#26038=VECTOR('',#112454,1000.);
#26039=VECTOR('',#112457,1000.);
#26040=VECTOR('',#112458,1000.);
#26041=VECTOR('',#112469,1000.);
#26042=VECTOR('',#112478,1000.);
#26043=VECTOR('',#112481,1000.);
#26044=VECTOR('',#112484,1000.);
#26045=VECTOR('',#112485,1000.);
#26046=VECTOR('',#112490,1000.);
#26047=VECTOR('',#112499,1000.);
#26048=VECTOR('',#112508,1000.);
#26049=VECTOR('',#112511,1000.);
#26050=VECTOR('',#112514,1000.);
#26051=VECTOR('',#112515,1000.);
#26052=VECTOR('',#112520,1000.);
#26053=VECTOR('',#112531,1000.);
#26054=VECTOR('',#112542,1000.);
#26055=VECTOR('',#112545,1000.);
#26056=VECTOR('',#112550,1000.);
#26057=VECTOR('',#112551,1000.);
#26058=VECTOR('',#112558,1000.);
#26059=VECTOR('',#112571,1000.);
#26060=VECTOR('',#112574,1000.);
#26061=VECTOR('',#112579,1000.);
#26062=VECTOR('',#112580,1000.);
#26063=VECTOR('',#112585,1000.);
#26064=VECTOR('',#112598,1000.);
#26065=VECTOR('',#112599,1000.);
#26066=VECTOR('',#112612,1000.);
#26067=VECTOR('',#112613,1000.);
#26068=VECTOR('',#112618,1000.);
#26069=VECTOR('',#112629,1000.);
#26070=VECTOR('',#112632,1000.);
#26071=VECTOR('',#112635,1000.);
#26072=VECTOR('',#112640,2.75);
#26073=VECTOR('',#112653,2.);
#26074=VECTOR('',#112658,1000.);
#26075=VECTOR('',#112659,1000.);
#26076=VECTOR('',#112664,1000.);
#26077=VECTOR('',#112667,1000.);
#26078=VECTOR('',#112684,1000.);
#26079=VECTOR('',#112685,1000.);
#26080=VECTOR('',#112690,2.75);
#26081=VECTOR('',#112701,2.);
#26082=VECTOR('',#112704,1000.);
#26083=VECTOR('',#112707,1000.);
#26084=VECTOR('',#112710,1000.);
#26085=VECTOR('',#112715,1000.);
#26086=VECTOR('',#112716,1000.);
#26087=VECTOR('',#112723,1000.);
#26088=VECTOR('',#112726,1000.);
#26089=VECTOR('',#112727,1000.);
#26090=VECTOR('',#112730,1000.);
#26091=VECTOR('',#112733,1000.);
#26092=VECTOR('',#112738,1000.);
#26093=VECTOR('',#112743,1000.);
#26094=VECTOR('',#112744,1000.);
#26095=VECTOR('',#112747,1000.);
#26096=VECTOR('',#112750,1000.);
#26097=VECTOR('',#112751,1000.);
#26098=VECTOR('',#112754,1000.);
#26099=VECTOR('',#112757,1000.);
#26100=VECTOR('',#112762,1000.);
#26101=VECTOR('',#112763,1000.);
#26102=VECTOR('',#112770,1000.);
#26103=VECTOR('',#112771,1000.);
#26104=VECTOR('',#112774,1000.);
#26105=VECTOR('',#112777,1000.);
#26106=VECTOR('',#112778,1000.);
#26107=VECTOR('',#112781,1000.);
#26108=VECTOR('',#112784,1000.);
#26109=VECTOR('',#112791,1000.);
#26110=VECTOR('',#112802,1000.);
#26111=VECTOR('',#112803,1000.);
#26112=VECTOR('',#112806,1000.);
#26113=VECTOR('',#112807,1000.);
#26114=VECTOR('',#112812,1000.);
#26115=VECTOR('',#112815,1000.);
#26116=VECTOR('',#112816,1000.);
#26117=VECTOR('',#112819,1000.);
#26118=VECTOR('',#112822,1000.);
#26119=VECTOR('',#112829,1000.);
#26120=VECTOR('',#112832,1000.);
#26121=VECTOR('',#112833,1000.);
#26122=VECTOR('',#112834,1000.);
#26123=VECTOR('',#112837,1000.);
#26124=VECTOR('',#112840,1000.);
#26125=VECTOR('',#112841,1000.);
#26126=VECTOR('',#112844,1000.);
#26127=VECTOR('',#112847,1000.);
#26128=VECTOR('',#112854,1000.);
#26129=VECTOR('',#112855,1000.);
#26130=VECTOR('',#112856,1000.);
#26131=VECTOR('',#112859,1000.);
#26132=VECTOR('',#112862,1000.);
#26133=VECTOR('',#112863,1000.);
#26134=VECTOR('',#112866,1000.);
#26135=VECTOR('',#112869,1000.);
#26136=VECTOR('',#112870,1000.);
#26137=VECTOR('',#112877,1000.);
#26138=VECTOR('',#112880,1000.);
#26139=VECTOR('',#112881,1000.);
#26140=VECTOR('',#112884,1000.);
#26141=VECTOR('',#112887,1000.);
#26142=VECTOR('',#112888,1000.);
#26143=VECTOR('',#112891,1000.);
#26144=VECTOR('',#112894,1000.);
#26145=VECTOR('',#112901,1000.);
#26146=VECTOR('',#112906,1000.);
#26147=VECTOR('',#112907,1000.);
#26148=VECTOR('',#112914,1000.);
#26149=VECTOR('',#112915,1000.);
#26150=VECTOR('',#112918,1000.);
#26151=VECTOR('',#112921,1000.);
#26152=VECTOR('',#112922,1000.);
#26153=VECTOR('',#112925,1000.);
#26154=VECTOR('',#112928,1000.);
#26155=VECTOR('',#112935,1000.);
#26156=VECTOR('',#112938,1000.);
#26157=VECTOR('',#112939,1000.);
#26158=VECTOR('',#112954,1000.);
#26159=VECTOR('',#112955,1000.);
#26160=VECTOR('',#112962,1000.);
#26161=VECTOR('',#112967,1000.);
#26162=VECTOR('',#112970,1000.);
#26163=VECTOR('',#112973,1000.);
#26164=VECTOR('',#112988,1000.);
#26165=VECTOR('',#112997,1000.);
#26166=VECTOR('',#113012,1000.);
#26167=VECTOR('',#113021,1000.);
#26168=VECTOR('',#113036,1000.);
#26169=VECTOR('',#113045,1000.);
#26170=VECTOR('',#113060,1000.);
#26171=VECTOR('',#113061,1000.);
#26172=VECTOR('',#113068,1000.);
#26173=VECTOR('',#113073,1000.);
#26174=VECTOR('',#113076,1000.);
#26175=VECTOR('',#113079,1000.);
#26176=VECTOR('',#113096,1000.);
#26177=VECTOR('',#113097,1000.);
#26178=VECTOR('',#113100,1000.);
#26179=VECTOR('',#113105,1000.);
#26180=VECTOR('',#113114,1000.);
#26181=VECTOR('',#113119,1000.);
#26182=VECTOR('',#113126,1000.);
#26183=VECTOR('',#113127,1000.);
#26184=VECTOR('',#113132,1000.);
#26185=VECTOR('',#113135,1000.);
#26186=VECTOR('',#113150,1000.);
#26187=VECTOR('',#113151,1000.);
#26188=VECTOR('',#113160,1000.);
#26189=VECTOR('',#113163,1000.);
#26190=VECTOR('',#113180,1000.);
#26191=VECTOR('',#113181,1000.);
#26192=VECTOR('',#113182,1000.);
#26193=VECTOR('',#113185,1000.);
#26194=VECTOR('',#113190,1000.);
#26195=VECTOR('',#113193,1000.);
#26196=VECTOR('',#113196,1000.);
#26197=VECTOR('',#113199,1000.);
#26198=VECTOR('',#113208,1000.);
#26199=VECTOR('',#113209,1000.);
#26200=VECTOR('',#113212,1000.);
#26201=VECTOR('',#113215,1000.);
#26202=VECTOR('',#113226,1000.);
#26203=VECTOR('',#113229,1000.);
#26204=VECTOR('',#113230,1000.);
#26205=VECTOR('',#113237,1000.);
#26206=VECTOR('',#113242,1000.);
#26207=VECTOR('',#113245,1000.);
#26208=VECTOR('',#113248,1000.);
#26209=VECTOR('',#113251,1000.);
#26210=VECTOR('',#113264,1000.);
#26211=VECTOR('',#113267,1000.);
#26212=VECTOR('',#113276,1000.);
#26213=VECTOR('',#113279,1000.);
#26214=VECTOR('',#113292,1000.);
#26215=VECTOR('',#113295,1000.);
#26216=VECTOR('',#113296,1000.);
#26217=VECTOR('',#113307,1000.);
#26218=VECTOR('',#113318,1000.);
#26219=VECTOR('',#113327,1000.);
#26220=VECTOR('',#113336,1000.);
#26221=VECTOR('',#113347,1000.);
#26222=VECTOR('',#113356,1000.);
#26223=VECTOR('',#113369,1000.);
#26224=VECTOR('',#113378,1000.);
#26225=VECTOR('',#113381,2.75);
#26226=VECTOR('',#113386,2.75);
#26227=VECTOR('',#113399,1000.);
#26228=VECTOR('',#113422,1000.);
#26229=VECTOR('',#113445,1000.);
#26230=VECTOR('',#113468,1000.);
#26231=VECTOR('',#113481,1000.);
#26232=VECTOR('',#113488,1000.);
#26233=VECTOR('',#113497,1000.);
#26234=VECTOR('',#113498,1000.);
#26235=VECTOR('',#113503,1000.);
#26236=VECTOR('',#113504,1000.);
#26237=VECTOR('',#113509,1000.);
#26238=VECTOR('',#113512,1000.);
#26239=VECTOR('',#113517,1000.);
#26240=VECTOR('',#113528,1000.);
#26241=VECTOR('',#113537,1000.);
#26242=VECTOR('',#113540,1000.);
#26243=VECTOR('',#113545,1000.);
#26244=VECTOR('',#113556,1000.);
#26245=VECTOR('',#113565,1000.);
#26246=VECTOR('',#113568,1000.);
#26247=VECTOR('',#113581,1000.);
#26248=VECTOR('',#113592,1000.);
#26249=VECTOR('',#113601,1000.);
#26250=VECTOR('',#113610,1000.);
#26251=VECTOR('',#113621,1000.);
#26252=VECTOR('',#113632,1000.);
#26253=VECTOR('',#113637,1000.);
#26254=VECTOR('',#113642,1000.);
#26255=VECTOR('',#113659,1000.);
#26256=VECTOR('',#113668,1000.);
#26257=VECTOR('',#113669,1000.);
#26258=VECTOR('',#113672,1000.);
#26259=VECTOR('',#113677,1000.);
#26260=VECTOR('',#113678,1000.);
#26261=VECTOR('',#113681,1000.);
#26262=VECTOR('',#113686,1000.);
#26263=VECTOR('',#113693,1000.);
#26264=VECTOR('',#113702,1000.);
#26265=VECTOR('',#113707,1000.);
#26266=VECTOR('',#113710,1000.);
#26267=VECTOR('',#113715,1000.);
#26268=VECTOR('',#113722,1000.);
#26269=VECTOR('',#113727,1000.);
#26270=VECTOR('',#113730,1000.);
#26271=VECTOR('',#113741,1000.);
#26272=VECTOR('',#113744,1000.);
#26273=VECTOR('',#113753,1000.);
#26274=VECTOR('',#113758,1000.);
#26275=VECTOR('',#113761,1000.);
#26276=VECTOR('',#113768,1000.);
#26277=VECTOR('',#113775,1000.);
#26278=VECTOR('',#113780,1000.);
#26279=VECTOR('',#113787,1000.);
#26280=VECTOR('',#113794,1000.);
#26281=VECTOR('',#113797,1000.);
#26282=VECTOR('',#113804,1000.);
#26283=VECTOR('',#113809,1000.);
#26284=VECTOR('',#113816,1000.);
#26285=VECTOR('',#113821,1000.);
#26286=VECTOR('',#113824,1000.);
#26287=VECTOR('',#113833,1000.);
#26288=VECTOR('',#113838,1000.);
#26289=VECTOR('',#113845,1000.);
#26290=VECTOR('',#113848,1000.);
#26291=VECTOR('',#113857,1000.);
#26292=VECTOR('',#113860,1000.);
#26293=VECTOR('',#113869,1000.);
#26294=VECTOR('',#113874,1000.);
#26295=VECTOR('',#113877,1000.);
#26296=VECTOR('',#113882,1000.);
#26297=VECTOR('',#113889,1000.);
#26298=VECTOR('',#113896,1000.);
#26299=VECTOR('',#113903,1000.);
#26300=VECTOR('',#113908,1000.);
#26301=VECTOR('',#113911,1000.);
#26302=VECTOR('',#113918,1000.);
#26303=VECTOR('',#113925,1000.);
#26304=VECTOR('',#113940,1000.);
#26305=VECTOR('',#113947,1000.);
#26306=VECTOR('',#113960,1000.);
#26307=VECTOR('',#113967,1000.);
#26308=VECTOR('',#113980,1000.);
#26309=VECTOR('',#113987,1000.);
#26310=VECTOR('',#114000,1000.);
#26311=VECTOR('',#114007,1000.);
#26312=VECTOR('',#114022,1000.);
#26313=VECTOR('',#114031,1000.);
#26314=VECTOR('',#114036,1000.);
#26315=VECTOR('',#114037,1000.);
#26316=VECTOR('',#114038,1000.);
#26317=VECTOR('',#114045,1000.);
#26318=VECTOR('',#114046,1000.);
#26319=VECTOR('',#114047,1000.);
#26320=VECTOR('',#114058,1000.);
#26321=VECTOR('',#114059,1000.);
#26322=VECTOR('',#114060,1000.);
#26323=VECTOR('',#114079,1000.);
#26324=VECTOR('',#114080,1000.);
#26325=VECTOR('',#114095,1000.);
#26326=VECTOR('',#114108,1000.);
#26327=VECTOR('',#114115,1000.);
#26328=VECTOR('',#114128,1000.);
#26329=VECTOR('',#114137,1000.);
#26330=VECTOR('',#114150,1000.);
#26331=VECTOR('',#114157,1000.);
#26332=VECTOR('',#114172,1000.);
#26333=VECTOR('',#114179,1000.);
#26334=VECTOR('',#114194,1000.);
#26335=VECTOR('',#114201,1000.);
#26336=VECTOR('',#114216,1000.);
#26337=VECTOR('',#114223,1000.);
#26338=VECTOR('',#114234,1000.);
#26339=VECTOR('',#114237,1000.);
#26340=VECTOR('',#114238,1000.);
#26341=VECTOR('',#114239,1000.);
#26342=VECTOR('',#114246,1000.);
#26343=VECTOR('',#114247,1000.);
#26344=VECTOR('',#114248,1000.);
#26345=VECTOR('',#114259,1000.);
#26346=VECTOR('',#114260,1000.);
#26347=VECTOR('',#114261,1000.);
#26348=VECTOR('',#114314,1000.);
#26349=VECTOR('',#114317,1000.);
#26350=VECTOR('',#114346,1000.);
#26351=VECTOR('',#114347,1000.);
#26352=VECTOR('',#114350,1000.);
#26353=VECTOR('',#114353,1000.);
#26354=VECTOR('',#114356,1000.);
#26355=VECTOR('',#114359,1000.);
#26356=VECTOR('',#114364,2.);
#26357=VECTOR('',#114407,3.25);
#26358=VECTOR('',#114412,1.47499999999998);
#26359=VECTOR('',#114421,2.);
#26360=VECTOR('',#114430,2.5);
#26361=VECTOR('',#114693,1000.);
#26362=VECTOR('',#114696,1000.);
#26363=VECTOR('',#114721,1000.);
#26364=VECTOR('',#114722,1000.);
#26365=VECTOR('',#114725,1000.);
#26366=VECTOR('',#114728,1000.);
#26367=VECTOR('',#114751,1000.);
#26368=VECTOR('',#114752,1000.);
#26369=VECTOR('',#114755,1000.);
#26370=VECTOR('',#114758,1000.);
#26371=VECTOR('',#114781,1000.);
#26372=VECTOR('',#114782,1000.);
#26373=VECTOR('',#114785,1000.);
#26374=VECTOR('',#114788,1000.);
#26375=VECTOR('',#114811,1000.);
#26376=VECTOR('',#114812,1000.);
#26377=VECTOR('',#114815,1000.);
#26378=VECTOR('',#114816,1000.);
#26379=VECTOR('',#114819,1000.);
#26380=VECTOR('',#114820,1000.);
#26381=VECTOR('',#114823,1000.);
#26382=VECTOR('',#114824,1000.);
#26383=VECTOR('',#114827,1000.);
#26384=VECTOR('',#114828,1000.);
#26385=VECTOR('',#114831,1000.);
#26386=VECTOR('',#114832,1000.);
#26387=VECTOR('',#114835,1000.);
#26388=VECTOR('',#114836,1000.);
#26389=VECTOR('',#114839,1000.);
#26390=VECTOR('',#114840,1000.);
#26391=VECTOR('',#114843,1000.);
#26392=VECTOR('',#114844,1000.);
#26393=VECTOR('',#114859,1000.);
#26394=VECTOR('',#114860,1000.);
#26395=VECTOR('',#114889,1000.);
#26396=VECTOR('',#114890,1000.);
#26397=VECTOR('',#114917,1000.);
#26398=VECTOR('',#114918,1000.);
#26399=VECTOR('',#114933,1000.);
#26400=VECTOR('',#114934,1000.);
#26401=VECTOR('',#114963,1000.);
#26402=VECTOR('',#114964,1000.);
#26403=VECTOR('',#114969,1000.);
#26404=VECTOR('',#114970,1000.);
#26405=VECTOR('',#114991,1000.);
#26406=VECTOR('',#114992,1000.);
#26407=VECTOR('',#115021,1000.);
#26408=VECTOR('',#115022,1000.);
#26409=VECTOR('',#115027,1000.);
#26410=VECTOR('',#115028,1000.);
#26411=VECTOR('',#115049,1000.);
#26412=VECTOR('',#115050,1000.);
#26413=VECTOR('',#115055,1000.);
#26414=VECTOR('',#115056,1000.);
#26415=VECTOR('',#115077,1000.);
#26416=VECTOR('',#115078,1000.);
#26417=VECTOR('',#115083,1000.);
#26418=VECTOR('',#115084,1000.);
#26419=VECTOR('',#115105,1000.);
#26420=VECTOR('',#115106,1000.);
#26421=VECTOR('',#115111,1000.);
#26422=VECTOR('',#115112,1000.);
#26423=VECTOR('',#115141,1000.);
#26424=VECTOR('',#115142,1000.);
#26425=VECTOR('',#115171,1000.);
#26426=VECTOR('',#115172,1000.);
#26427=VECTOR('',#115177,1000.);
#26428=VECTOR('',#115178,1000.);
#26429=VECTOR('',#115199,1000.);
#26430=VECTOR('',#115200,1000.);
#26431=VECTOR('',#115205,1000.);
#26432=VECTOR('',#115206,1000.);
#26433=VECTOR('',#115227,1000.);
#26434=VECTOR('',#115228,1000.);
#26435=VECTOR('',#115233,1000.);
#26436=VECTOR('',#115234,1000.);
#26437=VECTOR('',#115255,1000.);
#26438=VECTOR('',#115256,1000.);
#26439=VECTOR('',#115261,1000.);
#26440=VECTOR('',#115262,1000.);
#26441=VECTOR('',#115283,1000.);
#26442=VECTOR('',#115284,1000.);
#26443=VECTOR('',#115289,1000.);
#26444=VECTOR('',#115290,1000.);
#26445=VECTOR('',#115311,1000.);
#26446=VECTOR('',#115312,1000.);
#26447=VECTOR('',#115317,1000.);
#26448=VECTOR('',#115318,1000.);
#26449=VECTOR('',#115339,1000.);
#26450=VECTOR('',#115340,1000.);
#26451=VECTOR('',#115345,1000.);
#26452=VECTOR('',#115346,1000.);
#26453=VECTOR('',#115367,1000.);
#26454=VECTOR('',#115368,1000.);
#26455=VECTOR('',#115373,1000.);
#26456=VECTOR('',#115374,1000.);
#26457=VECTOR('',#115395,1000.);
#26458=VECTOR('',#115396,1000.);
#26459=VECTOR('',#115401,1000.);
#26460=VECTOR('',#115402,1000.);
#26461=VECTOR('',#115423,1000.);
#26462=VECTOR('',#115424,1000.);
#26463=VECTOR('',#115453,1000.);
#26464=VECTOR('',#115454,1000.);
#26465=VECTOR('',#115459,1000.);
#26466=VECTOR('',#115460,1000.);
#26467=VECTOR('',#115481,1000.);
#26468=VECTOR('',#115482,1000.);
#26469=VECTOR('',#115527,1000.);
#26470=VECTOR('',#115528,1000.);
#26471=VECTOR('',#115533,1000.);
#26472=VECTOR('',#115534,1000.);
#26473=VECTOR('',#115555,1000.);
#26474=VECTOR('',#115556,1000.);
#26475=VECTOR('',#115585,1000.);
#26476=VECTOR('',#115586,1000.);
#26477=VECTOR('',#115591,1000.);
#26478=VECTOR('',#115592,1000.);
#26479=VECTOR('',#115613,1000.);
#26480=VECTOR('',#115614,1000.);
#26481=VECTOR('',#115619,1000.);
#26482=VECTOR('',#115620,1000.);
#26483=VECTOR('',#115641,1000.);
#26484=VECTOR('',#115642,1000.);
#26485=VECTOR('',#115671,1000.);
#26486=VECTOR('',#115672,1000.);
#26487=VECTOR('',#115677,1000.);
#26488=VECTOR('',#115678,1000.);
#26489=VECTOR('',#115697,1000.);
#26490=VECTOR('',#115698,1000.);
#26491=VECTOR('',#115713,1000.);
#26492=VECTOR('',#115714,1000.);
#26493=VECTOR('',#115719,1000.);
#26494=VECTOR('',#115720,1000.);
#26495=VECTOR('',#115741,1000.);
#26496=VECTOR('',#115742,1000.);
#26497=VECTOR('',#115769,1000.);
#26498=VECTOR('',#115770,1000.);
#26499=VECTOR('',#115785,1000.);
#26500=VECTOR('',#115786,1000.);
#26501=VECTOR('',#115791,1000.);
#26502=VECTOR('',#115792,1000.);
#26503=VECTOR('',#115813,1000.);
#26504=VECTOR('',#115814,1000.);
#26505=VECTOR('',#115819,1000.);
#26506=VECTOR('',#115820,1000.);
#26507=VECTOR('',#115841,1000.);
#26508=VECTOR('',#115842,1000.);
#26509=VECTOR('',#115847,1000.);
#26510=VECTOR('',#115848,1000.);
#26511=VECTOR('',#115877,1000.);
#26512=VECTOR('',#115878,1000.);
#26513=VECTOR('',#115899,1000.);
#26514=VECTOR('',#115900,1000.);
#26515=VECTOR('',#115905,1000.);
#26516=VECTOR('',#115906,1000.);
#26517=VECTOR('',#115927,1000.);
#26518=VECTOR('',#115928,1000.);
#26519=VECTOR('',#115933,1000.);
#26520=VECTOR('',#115934,1000.);
#26521=VECTOR('',#115955,1000.);
#26522=VECTOR('',#115956,1000.);
#26523=VECTOR('',#115961,1000.);
#26524=VECTOR('',#115962,1000.);
#26525=VECTOR('',#115983,1000.);
#26526=VECTOR('',#115984,1000.);
#26527=VECTOR('',#115989,1000.);
#26528=VECTOR('',#115990,1000.);
#26529=VECTOR('',#116011,1000.);
#26530=VECTOR('',#116012,1000.);
#26531=VECTOR('',#116017,1000.);
#26532=VECTOR('',#116018,1000.);
#26533=VECTOR('',#116039,1000.);
#26534=VECTOR('',#116040,1000.);
#26535=VECTOR('',#116077,1000.);
#26536=VECTOR('',#116078,1000.);
#26537=VECTOR('',#116083,1000.);
#26538=VECTOR('',#116084,1000.);
#26539=VECTOR('',#116113,1000.);
#26540=VECTOR('',#116114,1000.);
#26541=VECTOR('',#116135,1000.);
#26542=VECTOR('',#116136,1000.);
#26543=VECTOR('',#116141,1000.);
#26544=VECTOR('',#116142,1000.);
#26545=VECTOR('',#116171,1000.);
#26546=VECTOR('',#116172,1000.);
#26547=VECTOR('',#116209,1000.);
#26548=VECTOR('',#116210,1000.);
#26549=VECTOR('',#116215,1000.);
#26550=VECTOR('',#116216,1000.);
#26551=VECTOR('',#116237,1000.);
#26552=VECTOR('',#116238,1000.);
#26553=VECTOR('',#116243,1000.);
#26554=VECTOR('',#116244,1000.);
#26555=VECTOR('',#116265,1000.);
#26556=VECTOR('',#116266,1000.);
#26557=VECTOR('',#116271,1000.);
#26558=VECTOR('',#116272,1000.);
#26559=VECTOR('',#116293,1000.);
#26560=VECTOR('',#116294,1000.);
#26561=VECTOR('',#116339,1000.);
#26562=VECTOR('',#116340,1000.);
#26563=VECTOR('',#116345,1000.);
#26564=VECTOR('',#116346,1000.);
#26565=VECTOR('',#116367,1000.);
#26566=VECTOR('',#116368,1000.);
#26567=VECTOR('',#116397,1000.);
#26568=VECTOR('',#116398,1000.);
#26569=VECTOR('',#116403,1000.);
#26570=VECTOR('',#116404,1000.);
#26571=VECTOR('',#116425,1000.);
#26572=VECTOR('',#116426,1000.);
#26573=VECTOR('',#116431,1000.);
#26574=VECTOR('',#116432,1000.);
#26575=VECTOR('',#116453,1000.);
#26576=VECTOR('',#116454,1000.);
#26577=VECTOR('',#116459,1000.);
#26578=VECTOR('',#116460,1000.);
#26579=VECTOR('',#116481,1000.);
#26580=VECTOR('',#116482,1000.);
#26581=VECTOR('',#116511,1000.);
#26582=VECTOR('',#116512,1000.);
#26583=VECTOR('',#116517,1000.);
#26584=VECTOR('',#116518,1000.);
#26585=VECTOR('',#116539,1000.);
#26586=VECTOR('',#116540,1000.);
#26587=VECTOR('',#116545,1000.);
#26588=VECTOR('',#116546,1000.);
#26589=VECTOR('',#116567,1000.);
#26590=VECTOR('',#116568,1000.);
#26591=VECTOR('',#116595,1000.);
#26592=VECTOR('',#116596,1000.);
#26593=VECTOR('',#116611,1000.);
#26594=VECTOR('',#116612,1000.);
#26595=VECTOR('',#116639,1000.);
#26596=VECTOR('',#116640,1000.);
#26597=VECTOR('',#116769,1000.);
#26598=VECTOR('',#116770,1000.);
#26599=VECTOR('',#116799,1000.);
#26600=VECTOR('',#116800,1000.);
#26601=VECTOR('',#116819,1000.);
#26602=VECTOR('',#116820,1000.);
#26603=VECTOR('',#116849,1000.);
#26604=VECTOR('',#116850,1000.);
#26605=VECTOR('',#116869,1000.);
#26606=VECTOR('',#116870,1000.);
#26607=VECTOR('',#116899,1000.);
#26608=VECTOR('',#116900,1000.);
#26609=VECTOR('',#116919,1000.);
#26610=VECTOR('',#116920,1000.);
#26611=VECTOR('',#116949,1000.);
#26612=VECTOR('',#116950,1000.);
#26613=VECTOR('',#117167,1000.);
#26614=VECTOR('',#117168,1000.);
#26615=VECTOR('',#117171,1000.);
#26616=VECTOR('',#117174,1000.);
#26617=VECTOR('',#117177,1000.);
#26618=VECTOR('',#117180,1000.);
#26619=VECTOR('',#117183,1000.);
#26620=VECTOR('',#117186,1000.);
#26621=VECTOR('',#117189,1000.);
#26622=VECTOR('',#117192,1000.);
#26623=VECTOR('',#117195,1000.);
#26624=VECTOR('',#117198,1000.);
#26625=VECTOR('',#117201,1000.);
#26626=VECTOR('',#117204,1000.);
#26627=VECTOR('',#117207,1000.);
#26628=VECTOR('',#117210,1000.);
#26629=VECTOR('',#117213,1000.);
#26630=VECTOR('',#117216,1000.);
#26631=VECTOR('',#117221,1000.);
#26632=VECTOR('',#117222,1000.);
#26633=VECTOR('',#117225,1000.);
#26634=VECTOR('',#117228,1000.);
#26635=VECTOR('',#117231,1000.);
#26636=VECTOR('',#117234,1000.);
#26637=VECTOR('',#117237,1000.);
#26638=VECTOR('',#117240,1000.);
#26639=VECTOR('',#117243,1000.);
#26640=VECTOR('',#117246,1000.);
#26641=VECTOR('',#117249,1000.);
#26642=VECTOR('',#117252,1000.);
#26643=VECTOR('',#117255,1000.);
#26644=VECTOR('',#117258,1000.);
#26645=VECTOR('',#117261,1000.);
#26646=VECTOR('',#117264,1000.);
#26647=VECTOR('',#117267,1000.);
#26648=VECTOR('',#117270,1000.);
#26649=VECTOR('',#117273,1000.);
#26650=VECTOR('',#117276,1000.);
#26651=VECTOR('',#117279,1000.);
#26652=VECTOR('',#117282,1000.);
#26653=VECTOR('',#117285,1000.);
#26654=VECTOR('',#117288,1000.);
#26655=VECTOR('',#117291,1000.);
#26656=VECTOR('',#117294,1000.);
#26657=VECTOR('',#117297,1000.);
#26658=VECTOR('',#117300,1000.);
#26659=VECTOR('',#117303,1000.);
#26660=VECTOR('',#117306,1000.);
#26661=VECTOR('',#117309,1000.);
#26662=VECTOR('',#117312,1000.);
#26663=VECTOR('',#117315,1000.);
#26664=VECTOR('',#117318,1000.);
#26665=VECTOR('',#117321,1000.);
#26666=VECTOR('',#117324,1000.);
#26667=VECTOR('',#117329,1000.);
#26668=VECTOR('',#117330,1000.);
#26669=VECTOR('',#117333,1000.);
#26670=VECTOR('',#117336,1000.);
#26671=VECTOR('',#117339,1000.);
#26672=VECTOR('',#117342,1000.);
#26673=VECTOR('',#117345,1000.);
#26674=VECTOR('',#117348,1000.);
#26675=VECTOR('',#117351,1000.);
#26676=VECTOR('',#117354,1000.);
#26677=VECTOR('',#117357,1000.);
#26678=VECTOR('',#117360,1000.);
#26679=VECTOR('',#117363,1000.);
#26680=VECTOR('',#117366,1000.);
#26681=VECTOR('',#117369,1000.);
#26682=VECTOR('',#117372,1000.);
#26683=VECTOR('',#117375,1000.);
#26684=VECTOR('',#117378,1000.);
#26685=VECTOR('',#117381,1000.);
#26686=VECTOR('',#117384,1000.);
#26687=VECTOR('',#117387,1000.);
#26688=VECTOR('',#117390,1000.);
#26689=VECTOR('',#117393,1000.);
#26690=VECTOR('',#117396,1000.);
#26691=VECTOR('',#117399,1000.);
#26692=VECTOR('',#117402,1000.);
#26693=VECTOR('',#117405,1000.);
#26694=VECTOR('',#117408,1000.);
#26695=VECTOR('',#117411,1000.);
#26696=VECTOR('',#117414,1000.);
#26697=VECTOR('',#117417,1000.);
#26698=VECTOR('',#117420,1000.);
#26699=VECTOR('',#117423,1000.);
#26700=VECTOR('',#117426,1000.);
#26701=VECTOR('',#117429,1000.);
#26702=VECTOR('',#117432,1000.);
#26703=VECTOR('',#117435,1000.);
#26704=VECTOR('',#117438,1000.);
#26705=VECTOR('',#117441,1000.);
#26706=VECTOR('',#117444,1000.);
#26707=VECTOR('',#117447,1000.);
#26708=VECTOR('',#117450,1000.);
#26709=VECTOR('',#117453,1000.);
#26710=VECTOR('',#117456,1000.);
#26711=VECTOR('',#117459,1000.);
#26712=VECTOR('',#117462,1000.);
#26713=VECTOR('',#117465,1000.);
#26714=VECTOR('',#117468,1000.);
#26715=VECTOR('',#117471,1000.);
#26716=VECTOR('',#117474,1000.);
#26717=VECTOR('',#117477,1000.);
#26718=VECTOR('',#117480,1000.);
#26719=VECTOR('',#117483,1000.);
#26720=VECTOR('',#117486,1000.);
#26721=VECTOR('',#117489,1000.);
#26722=VECTOR('',#117492,1000.);
#26723=VECTOR('',#117495,1000.);
#26724=VECTOR('',#117498,1000.);
#26725=VECTOR('',#117501,1000.);
#26726=VECTOR('',#117504,1000.);
#26727=VECTOR('',#117507,1000.);
#26728=VECTOR('',#117510,1000.);
#26729=VECTOR('',#117513,1000.);
#26730=VECTOR('',#117516,1000.);
#26731=VECTOR('',#117519,1000.);
#26732=VECTOR('',#117522,1000.);
#26733=VECTOR('',#117525,1000.);
#26734=VECTOR('',#117528,1000.);
#26735=VECTOR('',#117531,1000.);
#26736=VECTOR('',#117534,1000.);
#26737=VECTOR('',#117537,1000.);
#26738=VECTOR('',#117540,1000.);
#26739=VECTOR('',#117543,1000.);
#26740=VECTOR('',#117546,1000.);
#26741=VECTOR('',#117549,1000.);
#26742=VECTOR('',#117552,1000.);
#26743=VECTOR('',#117555,1000.);
#26744=VECTOR('',#117558,1000.);
#26745=VECTOR('',#117561,1000.);
#26746=VECTOR('',#117564,1000.);
#26747=VECTOR('',#117567,1000.);
#26748=VECTOR('',#117570,1000.);
#26749=VECTOR('',#117573,1000.);
#26750=VECTOR('',#117576,1000.);
#26751=VECTOR('',#117579,1000.);
#26752=VECTOR('',#117582,1000.);
#26753=VECTOR('',#117585,1000.);
#26754=VECTOR('',#117588,1000.);
#26755=VECTOR('',#117591,1000.);
#26756=VECTOR('',#117594,1000.);
#26757=VECTOR('',#117597,1000.);
#26758=VECTOR('',#117600,1000.);
#26759=VECTOR('',#117603,1000.);
#26760=VECTOR('',#117606,1000.);
#26761=VECTOR('',#117609,1000.);
#26762=VECTOR('',#117612,1000.);
#26763=VECTOR('',#117615,1000.);
#26764=VECTOR('',#117618,1000.);
#26765=VECTOR('',#117621,1000.);
#26766=VECTOR('',#117624,1000.);
#26767=VECTOR('',#117627,1000.);
#26768=VECTOR('',#117630,1000.);
#26769=VECTOR('',#117633,1000.);
#26770=VECTOR('',#117636,1000.);
#26771=VECTOR('',#117639,1000.);
#26772=VECTOR('',#117642,1000.);
#26773=VECTOR('',#117645,1000.);
#26774=VECTOR('',#117648,1000.);
#26775=VECTOR('',#117651,1000.);
#26776=VECTOR('',#117654,1000.);
#26777=VECTOR('',#117657,1000.);
#26778=VECTOR('',#117660,1000.);
#26779=VECTOR('',#117663,1000.);
#26780=VECTOR('',#117666,1000.);
#26781=VECTOR('',#117669,1000.);
#26782=VECTOR('',#117672,1000.);
#26783=VECTOR('',#117677,1000.);
#26784=VECTOR('',#117678,1000.);
#26785=VECTOR('',#117681,1000.);
#26786=VECTOR('',#117684,1000.);
#26787=VECTOR('',#117687,1000.);
#26788=VECTOR('',#117690,1000.);
#26789=VECTOR('',#117693,1000.);
#26790=VECTOR('',#117696,1000.);
#26791=VECTOR('',#117699,1000.);
#26792=VECTOR('',#117702,1000.);
#26793=VECTOR('',#117705,1000.);
#26794=VECTOR('',#117708,1000.);
#26795=VECTOR('',#117711,1000.);
#26796=VECTOR('',#117714,1000.);
#26797=VECTOR('',#117717,1000.);
#26798=VECTOR('',#117720,1000.);
#26799=VECTOR('',#117723,1000.);
#26800=VECTOR('',#117726,1000.);
#26801=VECTOR('',#117729,1000.);
#26802=VECTOR('',#117732,1000.);
#26803=VECTOR('',#117735,1000.);
#26804=VECTOR('',#117738,1000.);
#26805=VECTOR('',#117741,1000.);
#26806=VECTOR('',#117744,1000.);
#26807=VECTOR('',#117747,1000.);
#26808=VECTOR('',#117750,1000.);
#26809=VECTOR('',#117753,1000.);
#26810=VECTOR('',#117756,1000.);
#26811=VECTOR('',#117759,1000.);
#26812=VECTOR('',#117762,1000.);
#26813=VECTOR('',#117765,1000.);
#26814=VECTOR('',#117768,1000.);
#26815=VECTOR('',#117771,1000.);
#26816=VECTOR('',#117774,1000.);
#26817=VECTOR('',#117777,1000.);
#26818=VECTOR('',#117780,1000.);
#26819=VECTOR('',#117783,1000.);
#26820=VECTOR('',#117786,1000.);
#26821=VECTOR('',#117789,1000.);
#26822=VECTOR('',#117792,1000.);
#26823=VECTOR('',#117795,1000.);
#26824=VECTOR('',#117798,1000.);
#26825=VECTOR('',#117801,1000.);
#26826=VECTOR('',#117804,1000.);
#26827=VECTOR('',#117807,1000.);
#26828=VECTOR('',#117810,1000.);
#26829=VECTOR('',#117813,1000.);
#26830=VECTOR('',#117816,1000.);
#26831=VECTOR('',#117821,1000.);
#26832=VECTOR('',#117822,1000.);
#26833=VECTOR('',#117825,1000.);
#26834=VECTOR('',#117828,1000.);
#26835=VECTOR('',#117831,1000.);
#26836=VECTOR('',#117834,1000.);
#26837=VECTOR('',#117837,1000.);
#26838=VECTOR('',#117840,1000.);
#26839=VECTOR('',#117843,1000.);
#26840=VECTOR('',#117846,1000.);
#26841=VECTOR('',#117849,1000.);
#26842=VECTOR('',#117852,1000.);
#26843=VECTOR('',#117855,1000.);
#26844=VECTOR('',#117858,1000.);
#26845=VECTOR('',#117861,1000.);
#26846=VECTOR('',#117864,1000.);
#26847=VECTOR('',#117867,1000.);
#26848=VECTOR('',#117870,1000.);
#26849=VECTOR('',#117873,1000.);
#26850=VECTOR('',#117876,1000.);
#26851=VECTOR('',#117879,1000.);
#26852=VECTOR('',#117882,1000.);
#26853=VECTOR('',#117885,1000.);
#26854=VECTOR('',#117888,1000.);
#26855=VECTOR('',#117891,1000.);
#26856=VECTOR('',#117894,1000.);
#26857=VECTOR('',#117897,1000.);
#26858=VECTOR('',#117900,1000.);
#26859=VECTOR('',#117903,1000.);
#26860=VECTOR('',#117906,1000.);
#26861=VECTOR('',#117909,1000.);
#26862=VECTOR('',#117912,1000.);
#26863=VECTOR('',#117917,1000.);
#26864=VECTOR('',#117918,1000.);
#26865=VECTOR('',#117921,1000.);
#26866=VECTOR('',#117924,1000.);
#26867=VECTOR('',#117927,1000.);
#26868=VECTOR('',#117930,1000.);
#26869=VECTOR('',#117933,1000.);
#26870=VECTOR('',#117936,1000.);
#26871=VECTOR('',#117939,1000.);
#26872=VECTOR('',#117942,1000.);
#26873=VECTOR('',#117947,1000.);
#26874=VECTOR('',#117948,1000.);
#26875=VECTOR('',#117951,1000.);
#26876=VECTOR('',#117954,1000.);
#26877=VECTOR('',#117959,1000.);
#26878=VECTOR('',#117960,1000.);
#26879=VECTOR('',#117963,1000.);
#26880=VECTOR('',#117966,1000.);
#26881=VECTOR('',#117969,1000.);
#26882=VECTOR('',#117972,1000.);
#26883=VECTOR('',#117975,1000.);
#26884=VECTOR('',#117978,1000.);
#26885=VECTOR('',#117981,1000.);
#26886=VECTOR('',#117988,1000.);
#26887=VECTOR('',#118003,1000.);
#26888=VECTOR('',#118006,1000.);
#26889=VECTOR('',#118021,1000.);
#26890=VECTOR('',#118024,1000.);
#26891=VECTOR('',#118035,1000.);
#26892=VECTOR('',#118038,1000.);
#26893=VECTOR('',#118041,1000.);
#26894=VECTOR('',#118044,1000.);
#26895=VECTOR('',#118047,1000.);
#26896=VECTOR('',#118050,1000.);
#26897=VECTOR('',#118053,1000.);
#26898=VECTOR('',#118056,1000.);
#26899=VECTOR('',#118059,1000.);
#26900=VECTOR('',#118062,1000.);
#26901=VECTOR('',#118065,1000.);
#26902=VECTOR('',#118068,1000.);
#26903=VECTOR('',#118071,1000.);
#26904=VECTOR('',#118074,1000.);
#26905=VECTOR('',#118077,1000.);
#26906=VECTOR('',#118080,1000.);
#26907=VECTOR('',#118083,1000.);
#26908=VECTOR('',#118086,1000.);
#26909=VECTOR('',#118089,1000.);
#26910=VECTOR('',#118092,1000.);
#26911=VECTOR('',#118095,1000.);
#26912=VECTOR('',#118098,1000.);
#26913=VECTOR('',#118101,1000.);
#26914=VECTOR('',#118104,1000.);
#26915=VECTOR('',#118107,1000.);
#26916=VECTOR('',#118110,1000.);
#26917=VECTOR('',#118113,1000.);
#26918=VECTOR('',#118116,1000.);
#26919=VECTOR('',#118119,1000.);
#26920=VECTOR('',#118122,1000.);
#26921=VECTOR('',#118125,1000.);
#26922=VECTOR('',#118128,1000.);
#26923=VECTOR('',#118131,1000.);
#26924=VECTOR('',#118132,1000.);
#26925=VECTOR('',#118133,1000.);
#26926=VECTOR('',#118134,1000.);
#26927=VECTOR('',#118137,1000.);
#26928=VECTOR('',#118138,1000.);
#26929=VECTOR('',#118139,1000.);
#26930=VECTOR('',#118142,1000.);
#26931=VECTOR('',#118143,1000.);
#26932=VECTOR('',#118144,1000.);
#26933=VECTOR('',#118147,1000.);
#26934=VECTOR('',#118150,1000.);
#26935=VECTOR('',#118153,1000.);
#26936=VECTOR('',#118156,1000.);
#26937=VECTOR('',#118159,1000.);
#26938=VECTOR('',#118162,1000.);
#26939=VECTOR('',#118165,1000.);
#26940=VECTOR('',#118168,1000.);
#26941=VECTOR('',#118171,1000.);
#26942=VECTOR('',#118174,1000.);
#26943=VECTOR('',#118177,1000.);
#26944=VECTOR('',#118180,1000.);
#26945=VECTOR('',#118183,1000.);
#26946=VECTOR('',#118186,1000.);
#26947=VECTOR('',#118189,1000.);
#26948=VECTOR('',#118192,1000.);
#26949=VECTOR('',#118195,1000.);
#26950=VECTOR('',#118198,1000.);
#26951=VECTOR('',#118201,1000.);
#26952=VECTOR('',#118204,1000.);
#26953=VECTOR('',#118207,1000.);
#26954=VECTOR('',#118210,1000.);
#26955=VECTOR('',#118213,1000.);
#26956=VECTOR('',#118216,1000.);
#26957=VECTOR('',#118223,1000.);
#26958=VECTOR('',#118230,1000.);
#26959=VECTOR('',#118237,1000.);
#26960=VECTOR('',#118244,1000.);
#26961=VECTOR('',#118251,1000.);
#26962=VECTOR('',#118258,1000.);
#26963=VECTOR('',#118263,1000.);
#26964=VECTOR('',#118266,1000.);
#26965=VECTOR('',#118269,10.);
#26966=VECTOR('',#118274,1000.);
#26967=VECTOR('',#118277,10.);
#26968=VECTOR('',#118280,1000.);
#26969=VECTOR('',#118281,1000.);
#26970=VECTOR('',#118284,1000.);
#26971=VECTOR('',#118285,1000.);
#26972=VECTOR('',#118294,1000.);
#26973=VECTOR('',#118295,1000.);
#26974=VECTOR('',#118298,1000.);
#26975=VECTOR('',#118299,1000.);
#26976=VECTOR('',#118310,1000.);
#26977=VECTOR('',#118313,1000.);
#26978=VECTOR('',#118318,1000.);
#26979=VECTOR('',#118321,1000.);
#26980=VECTOR('',#118326,1000.);
#26981=VECTOR('',#118333,1000.);
#26982=VECTOR('',#118346,1000.);
#26983=VECTOR('',#118349,1000.);
#26984=VECTOR('',#118360,1000.);
#26985=VECTOR('',#118361,1000.);
#26986=VECTOR('',#118364,1000.);
#26987=VECTOR('',#118373,1000.);
#26988=VECTOR('',#118378,1000.);
#26989=VECTOR('',#118381,1000.);
#26990=VECTOR('',#118384,1000.);
#26991=VECTOR('',#118393,1000.);
#26992=VECTOR('',#118398,1000.);
#26993=VECTOR('',#118401,1000.);
#26994=VECTOR('',#118408,1000.);
#26995=VECTOR('',#118415,1000.);
#26996=VECTOR('',#118422,1000.);
#26997=VECTOR('',#118427,1000.);
#26998=VECTOR('',#118430,1000.);
#26999=VECTOR('',#118437,1000.);
#27000=VECTOR('',#118494,1000.);
#27001=VECTOR('',#118517,10.);
#27002=VECTOR('',#118520,10.);
#27003=VECTOR('',#118527,1000.);
#27004=VECTOR('',#118530,1000.);
#27005=VECTOR('',#118535,1000.);
#27006=VECTOR('',#118540,1000.);
#27007=VECTOR('',#118547,1000.);
#27008=VECTOR('',#118550,1000.);
#27009=VECTOR('',#118557,1000.);
#27010=VECTOR('',#118560,1000.);
#27011=VECTOR('',#118567,3.35);
#27012=VECTOR('',#118578,3.35000000000079);
#27013=VECTOR('',#118611,1000.);
#27014=VECTOR('',#118614,1000.);
#27015=VECTOR('',#118617,1000.);
#27016=VECTOR('',#118622,1000.);
#27017=VECTOR('',#118627,1000.);
#27018=VECTOR('',#118632,1000.);
#27019=VECTOR('',#118637,1000.);
#27020=VECTOR('',#118644,1000.);
#27021=VECTOR('',#118647,1000.);
#27022=VECTOR('',#118650,1000.);
#27023=VECTOR('',#118653,1000.);
#27024=VECTOR('',#118656,1000.);
#27025=VECTOR('',#118661,1000.);
#27026=VECTOR('',#118666,1000.);
#27027=VECTOR('',#118671,1000.);
#27028=VECTOR('',#118676,1000.);
#27029=VECTOR('',#118681,1000.);
#27030=VECTOR('',#118682,1000.);
#27031=VECTOR('',#118683,1000.);
#27032=VECTOR('',#118684,1000.);
#27033=VECTOR('',#118687,1000.);
#27034=VECTOR('',#118688,1000.);
#27035=VECTOR('',#118691,1000.);
#27036=VECTOR('',#118694,1000.);
#27037=VECTOR('',#118697,1000.);
#27038=VECTOR('',#118698,1000.);
#27039=VECTOR('',#118701,1000.);
#27040=VECTOR('',#118704,1000.);
#27041=VECTOR('',#118707,1000.);
#27042=VECTOR('',#118710,1000.);
#27043=VECTOR('',#118715,1000.);
#27044=VECTOR('',#118720,1000.);
#27045=VECTOR('',#118725,1000.);
#27046=VECTOR('',#118728,1000.);
#27047=VECTOR('',#118731,1000.);
#27048=VECTOR('',#118736,1000.);
#27049=VECTOR('',#118769,1000.);
#27050=VECTOR('',#118772,1000.);
#27051=VECTOR('',#118775,1000.);
#27052=VECTOR('',#118778,1000.);
#27053=VECTOR('',#118781,1000.);
#27054=VECTOR('',#118784,1000.);
#27055=VECTOR('',#118787,1000.);
#27056=VECTOR('',#118790,1000.);
#27057=VECTOR('',#118793,1000.);
#27058=VECTOR('',#118796,1000.);
#27059=VECTOR('',#118813,1000.);
#27060=VECTOR('',#118816,1000.);
#27061=VECTOR('',#118819,1000.);
#27062=VECTOR('',#118822,1000.);
#27063=VECTOR('',#118825,1000.);
#27064=VECTOR('',#118828,1000.);
#27065=VECTOR('',#118831,1000.);
#27066=VECTOR('',#118834,1000.);
#27067=VECTOR('',#118837,1000.);
#27068=VECTOR('',#118840,1000.);
#27069=VECTOR('',#118843,1000.);
#27070=VECTOR('',#118846,1000.);
#27071=VECTOR('',#118849,1000.);
#27072=VECTOR('',#118852,1000.);
#27073=VECTOR('',#118887,1000.);
#27074=VECTOR('',#118890,1000.);
#27075=VECTOR('',#118893,1000.);
#27076=VECTOR('',#118896,1000.);
#27077=VECTOR('',#118899,1000.);
#27078=VECTOR('',#118902,1000.);
#27079=VECTOR('',#118905,1000.);
#27080=VECTOR('',#118908,1000.);
#27081=VECTOR('',#118911,1000.);
#27082=VECTOR('',#118914,1000.);
#27083=VECTOR('',#118917,1000.);
#27084=VECTOR('',#118920,1000.);
#27085=VECTOR('',#118923,1000.);
#27086=VECTOR('',#118926,1000.);
#27087=VECTOR('',#118929,1000.);
#27088=VECTOR('',#118932,1000.);
#27089=VECTOR('',#118935,1000.);
#27090=VECTOR('',#118938,1000.);
#27091=VECTOR('',#118941,1000.);
#27092=VECTOR('',#118944,1000.);
#27093=VECTOR('',#118947,1000.);
#27094=VECTOR('',#118950,1000.);
#27095=VECTOR('',#118953,1000.);
#27096=VECTOR('',#118956,1000.);
#27097=VECTOR('',#118959,1000.);
#27098=VECTOR('',#118962,1000.);
#27099=VECTOR('',#118965,1000.);
#27100=VECTOR('',#118968,1000.);
#27101=VECTOR('',#119249,1000.);
#27102=VECTOR('',#119250,1000.);
#27103=VECTOR('',#119277,1000.);
#27104=VECTOR('',#119278,1000.);
#27105=VECTOR('',#119281,1000.);
#27106=VECTOR('',#119282,1000.);
#27107=VECTOR('',#119307,1000.);
#27108=VECTOR('',#119308,1000.);
#27109=VECTOR('',#119311,1000.);
#27110=VECTOR('',#119312,1000.);
#27111=VECTOR('',#119337,1000.);
#27112=VECTOR('',#119338,1000.);
#27113=VECTOR('',#119341,1000.);
#27114=VECTOR('',#119342,1000.);
#27115=VECTOR('',#119367,1000.);
#27116=VECTOR('',#119368,1000.);
#27117=VECTOR('',#119371,1000.);
#27118=VECTOR('',#119372,1000.);
#27119=VECTOR('',#119375,1000.);
#27120=VECTOR('',#119376,1000.);
#27121=VECTOR('',#119379,1000.);
#27122=VECTOR('',#119380,1000.);
#27123=VECTOR('',#119383,1000.);
#27124=VECTOR('',#119384,1000.);
#27125=VECTOR('',#119387,1000.);
#27126=VECTOR('',#119388,1000.);
#27127=VECTOR('',#119391,1000.);
#27128=VECTOR('',#119392,1000.);
#27129=VECTOR('',#119395,1000.);
#27130=VECTOR('',#119396,1000.);
#27131=VECTOR('',#119399,1000.);
#27132=VECTOR('',#119400,1000.);
#27133=VECTOR('',#119415,1000.);
#27134=VECTOR('',#119416,1000.);
#27135=VECTOR('',#119445,1000.);
#27136=VECTOR('',#119446,1000.);
#27137=VECTOR('',#119473,1000.);
#27138=VECTOR('',#119474,1000.);
#27139=VECTOR('',#119489,1000.);
#27140=VECTOR('',#119490,1000.);
#27141=VECTOR('',#119519,1000.);
#27142=VECTOR('',#119520,1000.);
#27143=VECTOR('',#119525,1000.);
#27144=VECTOR('',#119526,1000.);
#27145=VECTOR('',#119547,1000.);
#27146=VECTOR('',#119548,1000.);
#27147=VECTOR('',#119577,1000.);
#27148=VECTOR('',#119578,1000.);
#27149=VECTOR('',#119583,1000.);
#27150=VECTOR('',#119584,1000.);
#27151=VECTOR('',#119605,1000.);
#27152=VECTOR('',#119606,1000.);
#27153=VECTOR('',#119611,1000.);
#27154=VECTOR('',#119612,1000.);
#27155=VECTOR('',#119633,1000.);
#27156=VECTOR('',#119634,1000.);
#27157=VECTOR('',#119639,1000.);
#27158=VECTOR('',#119640,1000.);
#27159=VECTOR('',#119661,1000.);
#27160=VECTOR('',#119662,1000.);
#27161=VECTOR('',#119667,1000.);
#27162=VECTOR('',#119668,1000.);
#27163=VECTOR('',#119697,1000.);
#27164=VECTOR('',#119698,1000.);
#27165=VECTOR('',#119727,1000.);
#27166=VECTOR('',#119728,1000.);
#27167=VECTOR('',#119733,1000.);
#27168=VECTOR('',#119734,1000.);
#27169=VECTOR('',#119755,1000.);
#27170=VECTOR('',#119756,1000.);
#27171=VECTOR('',#119761,1000.);
#27172=VECTOR('',#119762,1000.);
#27173=VECTOR('',#119783,1000.);
#27174=VECTOR('',#119784,1000.);
#27175=VECTOR('',#119789,1000.);
#27176=VECTOR('',#119790,1000.);
#27177=VECTOR('',#119811,1000.);
#27178=VECTOR('',#119812,1000.);
#27179=VECTOR('',#119817,1000.);
#27180=VECTOR('',#119818,1000.);
#27181=VECTOR('',#119839,1000.);
#27182=VECTOR('',#119840,1000.);
#27183=VECTOR('',#119845,1000.);
#27184=VECTOR('',#119846,1000.);
#27185=VECTOR('',#119867,1000.);
#27186=VECTOR('',#119868,1000.);
#27187=VECTOR('',#119873,1000.);
#27188=VECTOR('',#119874,1000.);
#27189=VECTOR('',#119895,1000.);
#27190=VECTOR('',#119896,1000.);
#27191=VECTOR('',#119901,1000.);
#27192=VECTOR('',#119902,1000.);
#27193=VECTOR('',#119923,1000.);
#27194=VECTOR('',#119924,1000.);
#27195=VECTOR('',#119929,1000.);
#27196=VECTOR('',#119930,1000.);
#27197=VECTOR('',#119951,1000.);
#27198=VECTOR('',#119952,1000.);
#27199=VECTOR('',#119957,1000.);
#27200=VECTOR('',#119958,1000.);
#27201=VECTOR('',#119979,1000.);
#27202=VECTOR('',#119980,1000.);
#27203=VECTOR('',#120009,1000.);
#27204=VECTOR('',#120010,1000.);
#27205=VECTOR('',#120015,1000.);
#27206=VECTOR('',#120016,1000.);
#27207=VECTOR('',#120037,1000.);
#27208=VECTOR('',#120038,1000.);
#27209=VECTOR('',#120083,1000.);
#27210=VECTOR('',#120084,1000.);
#27211=VECTOR('',#120089,1000.);
#27212=VECTOR('',#120090,1000.);
#27213=VECTOR('',#120111,1000.);
#27214=VECTOR('',#120112,1000.);
#27215=VECTOR('',#120141,1000.);
#27216=VECTOR('',#120142,1000.);
#27217=VECTOR('',#120147,1000.);
#27218=VECTOR('',#120148,1000.);
#27219=VECTOR('',#120169,1000.);
#27220=VECTOR('',#120170,1000.);
#27221=VECTOR('',#120175,1000.);
#27222=VECTOR('',#120176,1000.);
#27223=VECTOR('',#120197,1000.);
#27224=VECTOR('',#120198,1000.);
#27225=VECTOR('',#120227,1000.);
#27226=VECTOR('',#120228,1000.);
#27227=VECTOR('',#120233,1000.);
#27228=VECTOR('',#120234,1000.);
#27229=VECTOR('',#120253,1000.);
#27230=VECTOR('',#120254,1000.);
#27231=VECTOR('',#120269,1000.);
#27232=VECTOR('',#120270,1000.);
#27233=VECTOR('',#120275,1000.);
#27234=VECTOR('',#120276,1000.);
#27235=VECTOR('',#120297,1000.);
#27236=VECTOR('',#120298,1000.);
#27237=VECTOR('',#120325,1000.);
#27238=VECTOR('',#120326,1000.);
#27239=VECTOR('',#120341,1000.);
#27240=VECTOR('',#120342,1000.);
#27241=VECTOR('',#120347,1000.);
#27242=VECTOR('',#120348,1000.);
#27243=VECTOR('',#120369,1000.);
#27244=VECTOR('',#120370,1000.);
#27245=VECTOR('',#120375,1000.);
#27246=VECTOR('',#120376,1000.);
#27247=VECTOR('',#120397,1000.);
#27248=VECTOR('',#120398,1000.);
#27249=VECTOR('',#120403,1000.);
#27250=VECTOR('',#120404,1000.);
#27251=VECTOR('',#120433,1000.);
#27252=VECTOR('',#120434,1000.);
#27253=VECTOR('',#120455,1000.);
#27254=VECTOR('',#120456,1000.);
#27255=VECTOR('',#120461,1000.);
#27256=VECTOR('',#120462,1000.);
#27257=VECTOR('',#120483,1000.);
#27258=VECTOR('',#120484,1000.);
#27259=VECTOR('',#120489,1000.);
#27260=VECTOR('',#120490,1000.);
#27261=VECTOR('',#120511,1000.);
#27262=VECTOR('',#120512,1000.);
#27263=VECTOR('',#120517,1000.);
#27264=VECTOR('',#120518,1000.);
#27265=VECTOR('',#120539,1000.);
#27266=VECTOR('',#120540,1000.);
#27267=VECTOR('',#120545,1000.);
#27268=VECTOR('',#120546,1000.);
#27269=VECTOR('',#120567,1000.);
#27270=VECTOR('',#120568,1000.);
#27271=VECTOR('',#120573,1000.);
#27272=VECTOR('',#120574,1000.);
#27273=VECTOR('',#120595,1000.);
#27274=VECTOR('',#120596,1000.);
#27275=VECTOR('',#120633,1000.);
#27276=VECTOR('',#120634,1000.);
#27277=VECTOR('',#120639,1000.);
#27278=VECTOR('',#120640,1000.);
#27279=VECTOR('',#120669,1000.);
#27280=VECTOR('',#120670,1000.);
#27281=VECTOR('',#120691,1000.);
#27282=VECTOR('',#120692,1000.);
#27283=VECTOR('',#120697,1000.);
#27284=VECTOR('',#120698,1000.);
#27285=VECTOR('',#120727,1000.);
#27286=VECTOR('',#120728,1000.);
#27287=VECTOR('',#120765,1000.);
#27288=VECTOR('',#120766,1000.);
#27289=VECTOR('',#120771,1000.);
#27290=VECTOR('',#120772,1000.);
#27291=VECTOR('',#120793,1000.);
#27292=VECTOR('',#120794,1000.);
#27293=VECTOR('',#120799,1000.);
#27294=VECTOR('',#120800,1000.);
#27295=VECTOR('',#120821,1000.);
#27296=VECTOR('',#120822,1000.);
#27297=VECTOR('',#120827,1000.);
#27298=VECTOR('',#120828,1000.);
#27299=VECTOR('',#120849,1000.);
#27300=VECTOR('',#120850,1000.);
#27301=VECTOR('',#120895,1000.);
#27302=VECTOR('',#120896,1000.);
#27303=VECTOR('',#120901,1000.);
#27304=VECTOR('',#120902,1000.);
#27305=VECTOR('',#120923,1000.);
#27306=VECTOR('',#120924,1000.);
#27307=VECTOR('',#120953,1000.);
#27308=VECTOR('',#120954,1000.);
#27309=VECTOR('',#120959,1000.);
#27310=VECTOR('',#120960,1000.);
#27311=VECTOR('',#120981,1000.);
#27312=VECTOR('',#120982,1000.);
#27313=VECTOR('',#120987,1000.);
#27314=VECTOR('',#120988,1000.);
#27315=VECTOR('',#121009,1000.);
#27316=VECTOR('',#121010,1000.);
#27317=VECTOR('',#121015,1000.);
#27318=VECTOR('',#121016,1000.);
#27319=VECTOR('',#121037,1000.);
#27320=VECTOR('',#121038,1000.);
#27321=VECTOR('',#121067,1000.);
#27322=VECTOR('',#121068,1000.);
#27323=VECTOR('',#121073,1000.);
#27324=VECTOR('',#121074,1000.);
#27325=VECTOR('',#121095,1000.);
#27326=VECTOR('',#121096,1000.);
#27327=VECTOR('',#121101,1000.);
#27328=VECTOR('',#121102,1000.);
#27329=VECTOR('',#121123,1000.);
#27330=VECTOR('',#121124,1000.);
#27331=VECTOR('',#121151,1000.);
#27332=VECTOR('',#121152,1000.);
#27333=VECTOR('',#121167,1000.);
#27334=VECTOR('',#121168,1000.);
#27335=VECTOR('',#121195,1000.);
#27336=VECTOR('',#121196,1000.);
#27337=VECTOR('',#121365,1000.);
#27338=VECTOR('',#121366,1000.);
#27339=VECTOR('',#121395,1000.);
#27340=VECTOR('',#121396,1000.);
#27341=VECTOR('',#121415,1000.);
#27342=VECTOR('',#121416,1000.);
#27343=VECTOR('',#121445,1000.);
#27344=VECTOR('',#121446,1000.);
#27345=VECTOR('',#121465,1000.);
#27346=VECTOR('',#121466,1000.);
#27347=VECTOR('',#121495,1000.);
#27348=VECTOR('',#121496,1000.);
#27349=VECTOR('',#121515,1000.);
#27350=VECTOR('',#121516,1000.);
#27351=VECTOR('',#121545,1000.);
#27352=VECTOR('',#121546,1000.);
#27353=VECTOR('',#121775,1000.);
#27354=VECTOR('',#121776,1000.);
#27355=VECTOR('',#121779,1000.);
#27356=VECTOR('',#121780,1000.);
#27357=VECTOR('',#121785,1000.);
#27358=VECTOR('',#121786,1000.);
#27359=VECTOR('',#121791,1000.);
#27360=VECTOR('',#121792,1000.);
#27361=VECTOR('',#121797,1000.);
#27362=VECTOR('',#121798,1000.);
#27363=VECTOR('',#121803,1000.);
#27364=VECTOR('',#121804,1000.);
#27365=VECTOR('',#121809,1000.);
#27366=VECTOR('',#121810,1000.);
#27367=VECTOR('',#121815,1000.);
#27368=VECTOR('',#121816,1000.);
#27369=VECTOR('',#121821,1000.);
#27370=VECTOR('',#121822,1000.);
#27371=VECTOR('',#121829,1000.);
#27372=VECTOR('',#121830,1000.);
#27373=VECTOR('',#121833,1000.);
#27374=VECTOR('',#121834,1000.);
#27375=VECTOR('',#121839,1000.);
#27376=VECTOR('',#121840,1000.);
#27377=VECTOR('',#121845,1000.);
#27378=VECTOR('',#121846,1000.);
#27379=VECTOR('',#121851,1000.);
#27380=VECTOR('',#121852,1000.);
#27381=VECTOR('',#121857,1000.);
#27382=VECTOR('',#121858,1000.);
#27383=VECTOR('',#121863,1000.);
#27384=VECTOR('',#121864,1000.);
#27385=VECTOR('',#121869,1000.);
#27386=VECTOR('',#121870,1000.);
#27387=VECTOR('',#121875,1000.);
#27388=VECTOR('',#121876,1000.);
#27389=VECTOR('',#121881,1000.);
#27390=VECTOR('',#121882,1000.);
#27391=VECTOR('',#121887,1000.);
#27392=VECTOR('',#121888,1000.);
#27393=VECTOR('',#121893,1000.);
#27394=VECTOR('',#121894,1000.);
#27395=VECTOR('',#121899,1000.);
#27396=VECTOR('',#121900,1000.);
#27397=VECTOR('',#121905,1000.);
#27398=VECTOR('',#121906,1000.);
#27399=VECTOR('',#121911,1000.);
#27400=VECTOR('',#121912,1000.);
#27401=VECTOR('',#121917,1000.);
#27402=VECTOR('',#121918,1000.);
#27403=VECTOR('',#121923,1000.);
#27404=VECTOR('',#121924,1000.);
#27405=VECTOR('',#121929,1000.);
#27406=VECTOR('',#121930,1000.);
#27407=VECTOR('',#121937,1000.);
#27408=VECTOR('',#121938,1000.);
#27409=VECTOR('',#121941,1000.);
#27410=VECTOR('',#121942,1000.);
#27411=VECTOR('',#121947,1000.);
#27412=VECTOR('',#121948,1000.);
#27413=VECTOR('',#121953,1000.);
#27414=VECTOR('',#121954,1000.);
#27415=VECTOR('',#121959,1000.);
#27416=VECTOR('',#121960,1000.);
#27417=VECTOR('',#121965,1000.);
#27418=VECTOR('',#121966,1000.);
#27419=VECTOR('',#121971,1000.);
#27420=VECTOR('',#121972,1000.);
#27421=VECTOR('',#121977,1000.);
#27422=VECTOR('',#121978,1000.);
#27423=VECTOR('',#121983,1000.);
#27424=VECTOR('',#121984,1000.);
#27425=VECTOR('',#121989,1000.);
#27426=VECTOR('',#121990,1000.);
#27427=VECTOR('',#121995,1000.);
#27428=VECTOR('',#121996,1000.);
#27429=VECTOR('',#122001,1000.);
#27430=VECTOR('',#122002,1000.);
#27431=VECTOR('',#122007,1000.);
#27432=VECTOR('',#122008,1000.);
#27433=VECTOR('',#122013,1000.);
#27434=VECTOR('',#122014,1000.);
#27435=VECTOR('',#122019,1000.);
#27436=VECTOR('',#122020,1000.);
#27437=VECTOR('',#122025,1000.);
#27438=VECTOR('',#122026,1000.);
#27439=VECTOR('',#122031,1000.);
#27440=VECTOR('',#122032,1000.);
#27441=VECTOR('',#122037,1000.);
#27442=VECTOR('',#122038,1000.);
#27443=VECTOR('',#122043,1000.);
#27444=VECTOR('',#122044,1000.);
#27445=VECTOR('',#122049,1000.);
#27446=VECTOR('',#122050,1000.);
#27447=VECTOR('',#122055,1000.);
#27448=VECTOR('',#122056,1000.);
#27449=VECTOR('',#122061,1000.);
#27450=VECTOR('',#122062,1000.);
#27451=VECTOR('',#122067,1000.);
#27452=VECTOR('',#122068,1000.);
#27453=VECTOR('',#122073,1000.);
#27454=VECTOR('',#122074,1000.);
#27455=VECTOR('',#122079,1000.);
#27456=VECTOR('',#122080,1000.);
#27457=VECTOR('',#122085,1000.);
#27458=VECTOR('',#122086,1000.);
#27459=VECTOR('',#122091,1000.);
#27460=VECTOR('',#122092,1000.);
#27461=VECTOR('',#122097,1000.);
#27462=VECTOR('',#122098,1000.);
#27463=VECTOR('',#122103,1000.);
#27464=VECTOR('',#122104,1000.);
#27465=VECTOR('',#122109,1000.);
#27466=VECTOR('',#122110,1000.);
#27467=VECTOR('',#122115,1000.);
#27468=VECTOR('',#122116,1000.);
#27469=VECTOR('',#122121,1000.);
#27470=VECTOR('',#122122,1000.);
#27471=VECTOR('',#122127,1000.);
#27472=VECTOR('',#122128,1000.);
#27473=VECTOR('',#122133,1000.);
#27474=VECTOR('',#122134,1000.);
#27475=VECTOR('',#122139,1000.);
#27476=VECTOR('',#122140,1000.);
#27477=VECTOR('',#122145,1000.);
#27478=VECTOR('',#122146,1000.);
#27479=VECTOR('',#122151,1000.);
#27480=VECTOR('',#122152,1000.);
#27481=VECTOR('',#122157,1000.);
#27482=VECTOR('',#122158,1000.);
#27483=VECTOR('',#122163,1000.);
#27484=VECTOR('',#122164,1000.);
#27485=VECTOR('',#122169,1000.);
#27486=VECTOR('',#122170,1000.);
#27487=VECTOR('',#122175,1000.);
#27488=VECTOR('',#122176,1000.);
#27489=VECTOR('',#122181,1000.);
#27490=VECTOR('',#122182,1000.);
#27491=VECTOR('',#122187,1000.);
#27492=VECTOR('',#122188,1000.);
#27493=VECTOR('',#122193,1000.);
#27494=VECTOR('',#122194,1000.);
#27495=VECTOR('',#122199,1000.);
#27496=VECTOR('',#122200,1000.);
#27497=VECTOR('',#122205,1000.);
#27498=VECTOR('',#122206,1000.);
#27499=VECTOR('',#122211,1000.);
#27500=VECTOR('',#122212,1000.);
#27501=VECTOR('',#122217,1000.);
#27502=VECTOR('',#122218,1000.);
#27503=VECTOR('',#122223,1000.);
#27504=VECTOR('',#122224,1000.);
#27505=VECTOR('',#122229,1000.);
#27506=VECTOR('',#122230,1000.);
#27507=VECTOR('',#122235,1000.);
#27508=VECTOR('',#122236,1000.);
#27509=VECTOR('',#122241,1000.);
#27510=VECTOR('',#122242,1000.);
#27511=VECTOR('',#122247,1000.);
#27512=VECTOR('',#122248,1000.);
#27513=VECTOR('',#122253,1000.);
#27514=VECTOR('',#122254,1000.);
#27515=VECTOR('',#122259,1000.);
#27516=VECTOR('',#122260,1000.);
#27517=VECTOR('',#122265,1000.);
#27518=VECTOR('',#122266,1000.);
#27519=VECTOR('',#122271,1000.);
#27520=VECTOR('',#122272,1000.);
#27521=VECTOR('',#122277,1000.);
#27522=VECTOR('',#122278,1000.);
#27523=VECTOR('',#122285,1000.);
#27524=VECTOR('',#122286,1000.);
#27525=VECTOR('',#122289,1000.);
#27526=VECTOR('',#122290,1000.);
#27527=VECTOR('',#122295,1000.);
#27528=VECTOR('',#122296,1000.);
#27529=VECTOR('',#122301,1000.);
#27530=VECTOR('',#122302,1000.);
#27531=VECTOR('',#122307,1000.);
#27532=VECTOR('',#122308,1000.);
#27533=VECTOR('',#122313,1000.);
#27534=VECTOR('',#122314,1000.);
#27535=VECTOR('',#122319,1000.);
#27536=VECTOR('',#122320,1000.);
#27537=VECTOR('',#122325,1000.);
#27538=VECTOR('',#122326,1000.);
#27539=VECTOR('',#122331,1000.);
#27540=VECTOR('',#122332,1000.);
#27541=VECTOR('',#122337,1000.);
#27542=VECTOR('',#122338,1000.);
#27543=VECTOR('',#122343,1000.);
#27544=VECTOR('',#122344,1000.);
#27545=VECTOR('',#122349,1000.);
#27546=VECTOR('',#122350,1000.);
#27547=VECTOR('',#122355,1000.);
#27548=VECTOR('',#122356,1000.);
#27549=VECTOR('',#122361,1000.);
#27550=VECTOR('',#122362,1000.);
#27551=VECTOR('',#122367,1000.);
#27552=VECTOR('',#122368,1000.);
#27553=VECTOR('',#122373,1000.);
#27554=VECTOR('',#122374,1000.);
#27555=VECTOR('',#122379,1000.);
#27556=VECTOR('',#122380,1000.);
#27557=VECTOR('',#122385,1000.);
#27558=VECTOR('',#122386,1000.);
#27559=VECTOR('',#122391,1000.);
#27560=VECTOR('',#122392,1000.);
#27561=VECTOR('',#122397,1000.);
#27562=VECTOR('',#122398,1000.);
#27563=VECTOR('',#122403,1000.);
#27564=VECTOR('',#122404,1000.);
#27565=VECTOR('',#122409,1000.);
#27566=VECTOR('',#122410,1000.);
#27567=VECTOR('',#122415,1000.);
#27568=VECTOR('',#122416,1000.);
#27569=VECTOR('',#122421,1000.);
#27570=VECTOR('',#122422,1000.);
#27571=VECTOR('',#122429,1000.);
#27572=VECTOR('',#122430,1000.);
#27573=VECTOR('',#122433,1000.);
#27574=VECTOR('',#122434,1000.);
#27575=VECTOR('',#122439,1000.);
#27576=VECTOR('',#122440,1000.);
#27577=VECTOR('',#122445,1000.);
#27578=VECTOR('',#122446,1000.);
#27579=VECTOR('',#122451,1000.);
#27580=VECTOR('',#122452,1000.);
#27581=VECTOR('',#122457,1000.);
#27582=VECTOR('',#122458,1000.);
#27583=VECTOR('',#122463,1000.);
#27584=VECTOR('',#122464,1000.);
#27585=VECTOR('',#122469,1000.);
#27586=VECTOR('',#122470,1000.);
#27587=VECTOR('',#122475,1000.);
#27588=VECTOR('',#122476,1000.);
#27589=VECTOR('',#122481,1000.);
#27590=VECTOR('',#122482,1000.);
#27591=VECTOR('',#122487,1000.);
#27592=VECTOR('',#122488,1000.);
#27593=VECTOR('',#122493,1000.);
#27594=VECTOR('',#122494,1000.);
#27595=VECTOR('',#122499,1000.);
#27596=VECTOR('',#122500,1000.);
#27597=VECTOR('',#122505,1000.);
#27598=VECTOR('',#122506,1000.);
#27599=VECTOR('',#122511,1000.);
#27600=VECTOR('',#122512,1000.);
#27601=VECTOR('',#122517,1000.);
#27602=VECTOR('',#122518,1000.);
#27603=VECTOR('',#122525,1000.);
#27604=VECTOR('',#122526,1000.);
#27605=VECTOR('',#122529,1000.);
#27606=VECTOR('',#122530,1000.);
#27607=VECTOR('',#122535,1000.);
#27608=VECTOR('',#122536,1000.);
#27609=VECTOR('',#122541,1000.);
#27610=VECTOR('',#122542,1000.);
#27611=VECTOR('',#122547,1000.);
#27612=VECTOR('',#122548,1000.);
#27613=VECTOR('',#122555,1000.);
#27614=VECTOR('',#122556,1000.);
#27615=VECTOR('',#122559,1000.);
#27616=VECTOR('',#122560,1000.);
#27617=VECTOR('',#122567,1000.);
#27618=VECTOR('',#122568,1000.);
#27619=VECTOR('',#122571,1000.);
#27620=VECTOR('',#122572,1000.);
#27621=VECTOR('',#122577,1000.);
#27622=VECTOR('',#122578,1000.);
#27623=VECTOR('',#122583,1000.);
#27624=VECTOR('',#122584,1000.);
#27625=VECTOR('',#122589,1000.);
#27626=VECTOR('',#122594,1000.);
#27627=VECTOR('',#122603,4.62535);
#27628=VECTOR('',#122616,8.10553955266686);
#27629=VECTOR('',#122657,1000.);
#27630=VECTOR('',#122660,1000.);
#27631=VECTOR('',#122675,1000.);
#27632=VECTOR('',#122678,1000.);
#27633=VECTOR('',#122689,1000.);
#27634=VECTOR('',#122692,1000.);
#27635=VECTOR('',#122695,1000.);
#27636=VECTOR('',#122698,1000.);
#27637=VECTOR('',#122701,1000.);
#27638=VECTOR('',#122704,1000.);
#27639=VECTOR('',#122707,1000.);
#27640=VECTOR('',#122710,1000.);
#27641=VECTOR('',#122713,1000.);
#27642=VECTOR('',#122716,1000.);
#27643=VECTOR('',#122719,1000.);
#27644=VECTOR('',#122722,1000.);
#27645=VECTOR('',#122725,1000.);
#27646=VECTOR('',#122728,1000.);
#27647=VECTOR('',#122731,1000.);
#27648=VECTOR('',#122734,1000.);
#27649=VECTOR('',#122737,1000.);
#27650=VECTOR('',#122740,1000.);
#27651=VECTOR('',#122743,1000.);
#27652=VECTOR('',#122746,1000.);
#27653=VECTOR('',#122749,1000.);
#27654=VECTOR('',#122752,1000.);
#27655=VECTOR('',#122755,1000.);
#27656=VECTOR('',#122758,1000.);
#27657=VECTOR('',#122761,1000.);
#27658=VECTOR('',#122764,1000.);
#27659=VECTOR('',#122767,1000.);
#27660=VECTOR('',#122770,1000.);
#27661=VECTOR('',#122773,1000.);
#27662=VECTOR('',#122776,1000.);
#27663=VECTOR('',#122779,1000.);
#27664=VECTOR('',#122782,1000.);
#27665=VECTOR('',#122785,1000.);
#27666=VECTOR('',#122786,1000.);
#27667=VECTOR('',#122787,1000.);
#27668=VECTOR('',#122788,1000.);
#27669=VECTOR('',#122791,1000.);
#27670=VECTOR('',#122792,1000.);
#27671=VECTOR('',#122793,1000.);
#27672=VECTOR('',#122796,1000.);
#27673=VECTOR('',#122797,1000.);
#27674=VECTOR('',#122798,1000.);
#27675=VECTOR('',#122801,1000.);
#27676=VECTOR('',#122804,1000.);
#27677=VECTOR('',#122807,1000.);
#27678=VECTOR('',#122810,1000.);
#27679=VECTOR('',#122813,1000.);
#27680=VECTOR('',#122816,1000.);
#27681=VECTOR('',#122819,1000.);
#27682=VECTOR('',#122822,1000.);
#27683=VECTOR('',#122825,1000.);
#27684=VECTOR('',#122828,1000.);
#27685=VECTOR('',#122831,1000.);
#27686=VECTOR('',#122834,1000.);
#27687=VECTOR('',#122837,1000.);
#27688=VECTOR('',#122840,1000.);
#27689=VECTOR('',#122843,1000.);
#27690=VECTOR('',#122846,1000.);
#27691=VECTOR('',#122849,1000.);
#27692=VECTOR('',#122852,1000.);
#27693=VECTOR('',#122855,1000.);
#27694=VECTOR('',#122858,1000.);
#27695=VECTOR('',#122861,1000.);
#27696=VECTOR('',#122864,1000.);
#27697=VECTOR('',#122889,1000.);
#27698=VECTOR('',#122890,1000.);
#27699=VECTOR('',#122891,1000.);
#27700=VECTOR('',#122892,1000.);
#27701=VECTOR('',#122893,1000.);
#27702=VECTOR('',#122894,1000.);
#27703=VECTOR('',#122895,1000.);
#27704=VECTOR('',#122896,1000.);
#27705=VECTOR('',#122897,1000.);
#27706=VECTOR('',#122900,1000.);
#27707=VECTOR('',#122903,1000.);
#27708=VECTOR('',#122904,1000.);
#27709=VECTOR('',#122905,1000.);
#27710=VECTOR('',#122906,1000.);
#27711=VECTOR('',#122907,1000.);
#27712=VECTOR('',#122910,1000.);
#27713=VECTOR('',#122911,1000.);
#27714=VECTOR('',#122918,1000.);
#27715=VECTOR('',#122919,1000.);
#27716=VECTOR('',#122926,1000.);
#27717=VECTOR('',#122927,1000.);
#27718=VECTOR('',#122930,1000.);
#27719=VECTOR('',#122931,1000.);
#27720=VECTOR('',#122934,1000.);
#27721=VECTOR('',#122935,1000.);
#27722=VECTOR('',#122938,1000.);
#27723=VECTOR('',#122939,1000.);
#27724=VECTOR('',#122942,1000.);
#27725=VECTOR('',#122943,1000.);
#27726=VECTOR('',#122944,1000.);
#27727=VECTOR('',#122947,1000.);
#27728=VECTOR('',#122948,1000.);
#27729=VECTOR('',#122949,1000.);
#27730=VECTOR('',#122950,1000.);
#27731=VECTOR('',#122951,1000.);
#27732=VECTOR('',#122952,1000.);
#27733=VECTOR('',#122953,1000.);
#27734=VECTOR('',#122954,1000.);
#27735=VECTOR('',#122961,1000.);
#27736=VECTOR('',#122968,1000.);
#27737=VECTOR('',#122969,1000.);
#27738=VECTOR('',#122970,1000.);
#27739=VECTOR('',#122971,1000.);
#27740=VECTOR('',#122972,1000.);
#27741=VECTOR('',#122975,1000.);
#27742=VECTOR('',#122976,1000.);
#27743=VECTOR('',#122977,1000.);
#27744=VECTOR('',#122978,1000.);
#27745=VECTOR('',#122979,1000.);
#27746=VECTOR('',#122980,1000.);
#27747=VECTOR('',#122981,1000.);
#27748=VECTOR('',#122982,1000.);
#27749=VECTOR('',#122985,1000.);
#27750=VECTOR('',#122986,1000.);
#27751=VECTOR('',#122993,1000.);
#27752=VECTOR('',#122996,1000.);
#27753=VECTOR('',#123001,1000.);
#27754=VECTOR('',#123006,1000.);
#27755=VECTOR('',#123013,1000.);
#27756=VECTOR('',#123016,1000.);
#27757=VECTOR('',#123025,1000.);
#27758=VECTOR('',#123026,1000.);
#27759=VECTOR('',#123031,10.);
#27760=VECTOR('',#123032,10.);
#27761=VECTOR('',#123037,1000.);
#27762=VECTOR('',#123040,10.);
#27763=VECTOR('',#123043,1000.);
#27764=VECTOR('',#123044,1000.);
#27765=VECTOR('',#123047,1000.);
#27766=VECTOR('',#123048,1000.);
#27767=VECTOR('',#123057,1000.);
#27768=VECTOR('',#123058,1000.);
#27769=VECTOR('',#123061,1000.);
#27770=VECTOR('',#123062,1000.);
#27771=VECTOR('',#123073,1000.);
#27772=VECTOR('',#123076,1000.);
#27773=VECTOR('',#123087,1000.);
#27774=VECTOR('',#123100,1000.);
#27775=VECTOR('',#123107,1000.);
#27776=VECTOR('',#123114,1000.);
#27777=VECTOR('',#123125,1000.);
#27778=VECTOR('',#123128,1000.);
#27779=VECTOR('',#123139,1000.);
#27780=VECTOR('',#123140,1000.);
#27781=VECTOR('',#123145,1000.);
#27782=VECTOR('',#123150,1000.);
#27783=VECTOR('',#123157,1000.);
#27784=VECTOR('',#123160,1000.);
#27785=VECTOR('',#123165,1000.);
#27786=VECTOR('',#123170,1000.);
#27787=VECTOR('',#123205,1000.);
#27788=VECTOR('',#123206,1000.);
#27789=VECTOR('',#123211,1000.);
#27790=VECTOR('',#123216,1000.);
#27791=VECTOR('',#123221,1000.);
#27792=VECTOR('',#123230,1000.);
#27793=VECTOR('',#123235,1000.);
#27794=VECTOR('',#123240,1000.);
#27795=VECTOR('',#123293,1000.);
#27796=VECTOR('',#123318,10.);
#27797=VECTOR('',#123321,10.);
#27798=VECTOR('',#123328,1000.);
#27799=VECTOR('',#123329,1000.);
#27800=VECTOR('',#123332,1000.);
#27801=VECTOR('',#123335,1000.);
#27802=VECTOR('',#123340,1000.);
#27803=VECTOR('',#123341,1000.);
#27804=VECTOR('',#123346,1000.);
#27805=VECTOR('',#123347,1000.);
#27806=VECTOR('',#123354,3.35);
#27807=VECTOR('',#123361,3.35000000000079);
#27808=VECTOR('',#123394,1000.);
#27809=VECTOR('',#123395,1000.);
#27810=VECTOR('',#123400,1000.);
#27811=VECTOR('',#123405,1000.);
#27812=VECTOR('',#123410,1000.);
#27813=VECTOR('',#123415,1000.);
#27814=VECTOR('',#123420,1000.);
#27815=VECTOR('',#123431,1000.);
#27816=VECTOR('',#123458,1000.);
#27817=VECTOR('',#123459,1000.);
#27818=VECTOR('',#123464,1000.);
#27819=VECTOR('',#123467,1000.);
#27820=VECTOR('',#123470,1000.);
#27821=VECTOR('',#123473,1000.);
#27822=VECTOR('',#123476,1000.);
#27823=VECTOR('',#123479,1000.);
#27824=VECTOR('',#123482,1000.);
#27825=VECTOR('',#123483,1000.);
#27826=VECTOR('',#123484,1000.);
#27827=VECTOR('',#123485,1000.);
#27828=VECTOR('',#123488,1000.);
#27829=VECTOR('',#123489,1000.);
#27830=VECTOR('',#123492,1000.);
#27831=VECTOR('',#123495,1000.);
#27832=VECTOR('',#123498,1000.);
#27833=VECTOR('',#123499,1000.);
#27834=VECTOR('',#123502,1000.);
#27835=VECTOR('',#123505,1000.);
#27836=VECTOR('',#123532,1000.);
#27837=VECTOR('',#123533,1000.);
#27838=VECTOR('',#123536,1000.);
#27839=VECTOR('',#123539,1000.);
#27840=VECTOR('',#123542,1000.);
#27841=VECTOR('',#123547,1000.);
#27842=VECTOR('',#123550,1000.);
#27843=VECTOR('',#123553,1000.);
#27844=VECTOR('',#123714,1000.);
#27845=VECTOR('',#123715,1000.);
#27846=VECTOR('',#123718,1000.);
#27847=VECTOR('',#123721,1000.);
#27848=VECTOR('',#123724,1000.);
#27849=VECTOR('',#123727,1000.);
#27850=VECTOR('',#123732,2.);
#27851=VECTOR('',#123775,3.25);
#27852=VECTOR('',#123830,1000.);
#27853=VECTOR('',#123831,1000.);
#27854=VECTOR('',#123834,1000.);
#27855=VECTOR('',#123837,1000.);
#27856=VECTOR('',#123840,1000.);
#27857=VECTOR('',#123843,1000.);
#27858=VECTOR('',#123900,1000.);
#27859=VECTOR('',#123901,1000.);
#27860=VECTOR('',#123904,1000.);
#27861=VECTOR('',#123907,1000.);
#27862=VECTOR('',#123910,1000.);
#27863=VECTOR('',#123913,1000.);
#27864=VECTOR('',#123918,1000.);
#27865=VECTOR('',#123919,1000.);
#27866=VECTOR('',#123922,1000.);
#27867=VECTOR('',#123925,1000.);
#27868=VECTOR('',#123928,1000.);
#27869=VECTOR('',#123931,1000.);
#27870=VECTOR('',#123936,2.);
#27871=VECTOR('',#123979,3.25);
#27872=VECTOR('',#124010,1000.);
#27873=VECTOR('',#124013,1000.);
#27874=VECTOR('',#124016,1000.);
#27875=VECTOR('',#124017,1000.);
#27876=VECTOR('',#124020,1000.);
#27877=VECTOR('',#124023,1000.);
#27878=VECTOR('',#124034,7.8);
#27879=VECTOR('',#124037,8.8);
#27880=VECTOR('',#124044,1.47499999999998);
#27881=VECTOR('',#124053,2.);
#27882=VECTOR('',#124062,2.5);
#27883=VECTOR('',#124079,1000.);
#27884=VECTOR('',#124080,1000.);
#27885=VECTOR('',#124085,1000.);
#27886=VECTOR('',#124086,1000.);
#27887=VECTOR('',#124107,1000.);
#27888=VECTOR('',#124108,1000.);
#27889=VECTOR('',#124113,1000.);
#27890=VECTOR('',#124114,1000.);
#27891=VECTOR('',#124123,1000.);
#27892=VECTOR('',#124124,1000.);
#27893=VECTOR('',#124125,1000.);
#27894=VECTOR('',#124128,1000.);
#27895=VECTOR('',#124133,1000.);
#27896=VECTOR('',#124138,1000.);
#27897=VECTOR('',#124139,1000.);
#27898=VECTOR('',#124140,1000.);
#27899=VECTOR('',#124141,1000.);
#27900=VECTOR('',#124160,1000.);
#27901=VECTOR('',#124171,1000.);
#27902=VECTOR('',#124194,1000.);
#27903=VECTOR('',#124197,1000.);
#27904=VECTOR('',#124200,1000.);
#27905=VECTOR('',#124203,1000.);
#27906=VECTOR('',#124210,1000.);
#27907=VECTOR('',#124213,1000.);
#27908=VECTOR('',#124230,1000.);
#27909=VECTOR('',#124231,1000.);
#27910=VECTOR('',#124244,1000.);
#27911=VECTOR('',#124247,1000.);
#27912=VECTOR('',#124262,1000.);
#27913=VECTOR('',#124263,1000.);
#27914=VECTOR('',#124268,1000.);
#27915=VECTOR('',#124269,1000.);
#27916=VECTOR('',#124274,1000.);
#27917=VECTOR('',#124275,1000.);
#27918=VECTOR('',#124278,1000.);
#27919=VECTOR('',#124281,1000.);
#27920=VECTOR('',#124284,1000.);
#27921=VECTOR('',#124287,1000.);
#27922=VECTOR('',#124290,1000.);
#27923=VECTOR('',#124293,1000.);
#27924=VECTOR('',#124298,1000.);
#27925=VECTOR('',#124301,1000.);
#27926=VECTOR('',#124304,7.8);
#27927=VECTOR('',#124307,7.8);
#27928=VECTOR('',#124310,1000.);
#27929=VECTOR('',#124343,1000.);
#27930=VECTOR('',#124346,1000.);
#27931=VECTOR('',#124349,1000.);
#27932=VECTOR('',#124350,1000.);
#27933=VECTOR('',#124353,1000.);
#27934=VECTOR('',#124356,1000.);
#27935=VECTOR('',#124367,7.8);
#27936=VECTOR('',#124370,8.8);
#27937=VECTOR('',#124377,1000.);
#27938=VECTOR('',#124378,1000.);
#27939=VECTOR('',#124391,1000.);
#27940=VECTOR('',#124392,1000.);
#27941=VECTOR('',#124403,1000.);
#27942=VECTOR('',#124404,1000.);
#27943=VECTOR('',#124409,1000.);
#27944=VECTOR('',#124412,1000.);
#27945=VECTOR('',#124425,1000.);
#27946=VECTOR('',#124426,1000.);
#27947=VECTOR('',#124437,1000.);
#27948=VECTOR('',#124438,1000.);
#27949=VECTOR('',#124443,1000.);
#27950=VECTOR('',#124446,1000.);
#27951=VECTOR('',#124459,1000.);
#27952=VECTOR('',#124460,1000.);
#27953=VECTOR('',#124473,1000.);
#27954=VECTOR('',#124474,1000.);
#27955=VECTOR('',#124487,1000.);
#27956=VECTOR('',#124488,1000.);
#27957=VECTOR('',#124501,1000.);
#27958=VECTOR('',#124502,1000.);
#27959=VECTOR('',#124507,1000.);
#27960=VECTOR('',#124510,1000.);
#27961=VECTOR('',#124523,1000.);
#27962=VECTOR('',#124524,1000.);
#27963=VECTOR('',#124535,1000.);
#27964=VECTOR('',#124536,1000.);
#27965=VECTOR('',#124541,1000.);
#27966=VECTOR('',#124544,1000.);
#27967=VECTOR('',#124557,1000.);
#27968=VECTOR('',#124558,1000.);
#27969=VECTOR('',#124579,1000.);
#27970=VECTOR('',#124580,1000.);
#27971=VECTOR('',#124593,1000.);
#27972=VECTOR('',#124594,1000.);
#27973=VECTOR('',#124607,1000.);
#27974=VECTOR('',#124608,1000.);
#27975=VECTOR('',#124613,1000.);
#27976=VECTOR('',#124616,1000.);
#27977=VECTOR('',#124629,1000.);
#27978=VECTOR('',#124630,1000.);
#27979=VECTOR('',#124659,1000.);
#27980=VECTOR('',#124660,1000.);
#27981=VECTOR('',#124673,1000.);
#27982=VECTOR('',#124674,1000.);
#27983=VECTOR('',#124679,1000.);
#27984=VECTOR('',#124682,1000.);
#27985=VECTOR('',#124695,1000.);
#27986=VECTOR('',#124696,1000.);
#27987=VECTOR('',#124725,1000.);
#27988=VECTOR('',#124726,1000.);
#27989=VECTOR('',#124739,1000.);
#27990=VECTOR('',#124740,1000.);
#27991=VECTOR('',#124745,1000.);
#27992=VECTOR('',#124748,1000.);
#27993=VECTOR('',#124761,1000.);
#27994=VECTOR('',#124762,1000.);
#27995=VECTOR('',#124791,1000.);
#27996=VECTOR('',#124792,1000.);
#27997=VECTOR('',#124805,1000.);
#27998=VECTOR('',#124806,1000.);
#27999=VECTOR('',#124811,1000.);
#28000=VECTOR('',#124814,1000.);
#28001=VECTOR('',#124827,1000.);
#28002=VECTOR('',#124828,1000.);
#28003=VECTOR('',#124857,1000.);
#28004=VECTOR('',#124858,1000.);
#28005=VECTOR('',#124871,1000.);
#28006=VECTOR('',#124872,1000.);
#28007=VECTOR('',#124877,1000.);
#28008=VECTOR('',#124880,1000.);
#28009=VECTOR('',#124893,1000.);
#28010=VECTOR('',#124894,1000.);
#28011=VECTOR('',#124923,1000.);
#28012=VECTOR('',#124924,1000.);
#28013=VECTOR('',#124937,1000.);
#28014=VECTOR('',#124938,1000.);
#28015=VECTOR('',#124943,1000.);
#28016=VECTOR('',#124946,1000.);
#28017=VECTOR('',#124959,1000.);
#28018=VECTOR('',#124960,1000.);
#28019=VECTOR('',#124989,1000.);
#28020=VECTOR('',#124990,1000.);
#28021=VECTOR('',#125003,1000.);
#28022=VECTOR('',#125004,1000.);
#28023=VECTOR('',#125009,1000.);
#28024=VECTOR('',#125012,1000.);
#28025=VECTOR('',#125025,1000.);
#28026=VECTOR('',#125026,1000.);
#28027=VECTOR('',#125039,1000.);
#28028=VECTOR('',#125040,1000.);
#28029=VECTOR('',#125061,1000.);
#28030=VECTOR('',#125062,1000.);
#28031=VECTOR('',#125075,1000.);
#28032=VECTOR('',#125076,1000.);
#28033=VECTOR('',#125081,1000.);
#28034=VECTOR('',#125084,1000.);
#28035=VECTOR('',#125097,1000.);
#28036=VECTOR('',#125098,1000.);
#28037=VECTOR('',#125111,1000.);
#28038=VECTOR('',#125112,1000.);
#28039=VECTOR('',#125125,1000.);
#28040=VECTOR('',#125126,1000.);
#28041=VECTOR('',#125139,1000.);
#28042=VECTOR('',#125140,1000.);
#28043=VECTOR('',#125143,1000.);
#28044=VECTOR('',#125146,1000.);
#28045=VECTOR('',#125159,1000.);
#28046=VECTOR('',#125160,1000.);
#28047=VECTOR('',#125173,1000.);
#28048=VECTOR('',#125174,1000.);
#28049=VECTOR('',#125177,1000.);
#28050=VECTOR('',#125178,1000.);
#28051=VECTOR('',#125183,1000.);
#28052=VECTOR('',#125184,1000.);
#28053=VECTOR('',#125189,1000.);
#28054=VECTOR('',#125190,1000.);
#28055=VECTOR('',#125195,1000.);
#28056=VECTOR('',#125196,1000.);
#28057=VECTOR('',#125201,1000.);
#28058=VECTOR('',#125202,1000.);
#28059=VECTOR('',#125207,1000.);
#28060=VECTOR('',#125208,1000.);
#28061=VECTOR('',#125213,1000.);
#28062=VECTOR('',#125214,1000.);
#28063=VECTOR('',#125219,1000.);
#28064=VECTOR('',#125220,1000.);
#28065=VECTOR('',#125225,1000.);
#28066=VECTOR('',#125226,1000.);
#28067=VECTOR('',#125231,1000.);
#28068=VECTOR('',#125232,1000.);
#28069=VECTOR('',#125237,1000.);
#28070=VECTOR('',#125238,1000.);
#28071=VECTOR('',#125243,1000.);
#28072=VECTOR('',#125244,1000.);
#28073=VECTOR('',#125249,1000.);
#28074=VECTOR('',#125250,1000.);
#28075=VECTOR('',#125255,1000.);
#28076=VECTOR('',#125256,1000.);
#28077=VECTOR('',#125261,1000.);
#28078=VECTOR('',#125262,1000.);
#28079=VECTOR('',#125267,1000.);
#28080=VECTOR('',#125268,1000.);
#28081=VECTOR('',#125273,1000.);
#28082=VECTOR('',#125274,1000.);
#28083=VECTOR('',#125279,1000.);
#28084=VECTOR('',#125280,1000.);
#28085=VECTOR('',#125285,1000.);
#28086=VECTOR('',#125286,1000.);
#28087=VECTOR('',#125291,1000.);
#28088=VECTOR('',#125292,1000.);
#28089=VECTOR('',#125297,1000.);
#28090=VECTOR('',#125298,1000.);
#28091=VECTOR('',#125303,1000.);
#28092=VECTOR('',#125304,1000.);
#28093=VECTOR('',#125309,1000.);
#28094=VECTOR('',#125310,1000.);
#28095=VECTOR('',#125315,1000.);
#28096=VECTOR('',#125316,1000.);
#28097=VECTOR('',#125321,1000.);
#28098=VECTOR('',#125322,1000.);
#28099=VECTOR('',#125327,1000.);
#28100=VECTOR('',#125328,1000.);
#28101=VECTOR('',#125337,1000.);
#28102=VECTOR('',#125338,1000.);
#28103=VECTOR('',#125341,1000.);
#28104=VECTOR('',#125342,1000.);
#28105=VECTOR('',#125343,1000.);
#28106=VECTOR('',#125344,1000.);
#28107=VECTOR('',#125345,1000.);
#28108=VECTOR('',#125346,1000.);
#28109=VECTOR('',#125347,1000.);
#28110=VECTOR('',#125348,1000.);
#28111=VECTOR('',#125349,1000.);
#28112=VECTOR('',#125350,1000.);
#28113=VECTOR('',#125351,1000.);
#28114=VECTOR('',#125354,1000.);
#28115=VECTOR('',#125357,1000.);
#28116=VECTOR('',#125360,1000.);
#28117=VECTOR('',#125363,1000.);
#28118=VECTOR('',#125366,1000.);
#28119=VECTOR('',#125369,1000.);
#28120=VECTOR('',#125370,1000.);
#28121=VECTOR('',#125373,1000.);
#28122=VECTOR('',#125376,1000.);
#28123=VECTOR('',#125379,1000.);
#28124=VECTOR('',#125382,1000.);
#28125=VECTOR('',#125385,1000.);
#28126=VECTOR('',#125388,1000.);
#28127=VECTOR('',#125391,1000.);
#28128=VECTOR('',#125394,1000.);
#28129=VECTOR('',#125397,1000.);
#28130=VECTOR('',#125400,1000.);
#28131=VECTOR('',#125403,1000.);
#28132=VECTOR('',#125404,1000.);
#28133=VECTOR('',#125413,1000.);
#28134=VECTOR('',#125416,1000.);
#28135=VECTOR('',#125419,1000.);
#28136=VECTOR('',#125420,1000.);
#28137=VECTOR('',#125429,1000.);
#28138=VECTOR('',#125432,1000.);
#28139=VECTOR('',#125435,1000.);
#28140=VECTOR('',#125436,1000.);
#28141=VECTOR('',#125445,1000.);
#28142=VECTOR('',#125448,1000.);
#28143=VECTOR('',#125451,1000.);
#28144=VECTOR('',#125452,1000.);
#28145=VECTOR('',#125461,1000.);
#28146=VECTOR('',#125464,1000.);
#28147=VECTOR('',#125467,1000.);
#28148=VECTOR('',#125468,1000.);
#28149=VECTOR('',#125473,1000.);
#28150=VECTOR('',#125476,1000.);
#28151=VECTOR('',#125481,1000.);
#28152=VECTOR('',#125484,1000.);
#28153=VECTOR('',#125489,1000.);
#28154=VECTOR('',#125492,1000.);
#28155=VECTOR('',#125493,1000.);
#28156=VECTOR('',#125494,1000.);
#28157=VECTOR('',#125495,1000.);
#28158=VECTOR('',#125498,1000.);
#28159=VECTOR('',#125501,1000.);
#28160=VECTOR('',#125502,1000.);
#28161=VECTOR('',#125503,1000.);
#28162=VECTOR('',#125504,1000.);
#28163=VECTOR('',#125505,1000.);
#28164=VECTOR('',#125506,1000.);
#28165=VECTOR('',#125509,1000.);
#28166=VECTOR('',#125510,1000.);
#28167=VECTOR('',#125511,1000.);
#28168=VECTOR('',#125512,1000.);
#28169=VECTOR('',#125513,1000.);
#28170=VECTOR('',#125516,1000.);
#28171=VECTOR('',#125523,1000.);
#28172=VECTOR('',#125528,1000.);
#28173=VECTOR('',#125533,1000.);
#28174=VECTOR('',#125538,1000.);
#28175=VECTOR('',#125545,1000.);
#28176=VECTOR('',#125554,1000.);
#28177=VECTOR('',#125559,1000.);
#28178=VECTOR('',#125562,1000.);
#28179=VECTOR('',#125569,1000.);
#28180=VECTOR('',#125572,1000.);
#28181=VECTOR('',#125579,1000.);
#28182=VECTOR('',#125636,1000.);
#28183=VECTOR('',#125637,1000.);
#28184=VECTOR('',#125640,1000.);
#28185=VECTOR('',#125643,1000.);
#28186=VECTOR('',#125646,1000.);
#28187=VECTOR('',#125649,1000.);
#28188=VECTOR('',#125706,1000.);
#28189=VECTOR('',#125707,1000.);
#28190=VECTOR('',#125710,1000.);
#28191=VECTOR('',#125713,1000.);
#28192=VECTOR('',#125716,1000.);
#28193=VECTOR('',#125719,1000.);
#28194=VECTOR('',#125724,1000.);
#28195=VECTOR('',#125725,1000.);
#28196=VECTOR('',#125728,1000.);
#28197=VECTOR('',#125731,1000.);
#28198=VECTOR('',#125734,1000.);
#28199=VECTOR('',#125737,1000.);
#28200=VECTOR('',#125742,2.);
#28201=VECTOR('',#125785,3.25);
#28202=VECTOR('',#125792,1000.);
#28203=VECTOR('',#125795,1000.);
#28204=VECTOR('',#125810,1000.);
#28205=VECTOR('',#125813,1000.);
#28206=VECTOR('',#125872,1000.);
#28207=VECTOR('',#125875,1000.);
#28208=VECTOR('',#125880,1000.);
#28209=VECTOR('',#125881,1000.);
#28210=VECTOR('',#125884,1000.);
#28211=VECTOR('',#125885,1000.);
#28212=VECTOR('',#125888,1000.);
#28213=VECTOR('',#125889,1000.);
#28214=VECTOR('',#125892,1000.);
#28215=VECTOR('',#125893,1000.);
#28216=VECTOR('',#125894,1000.);
#28217=VECTOR('',#125895,1000.);
#28218=VECTOR('',#125896,1000.);
#28219=VECTOR('',#125897,1000.);
#28220=VECTOR('',#125900,1000.);
#28221=VECTOR('',#125911,1000.);
#28222=VECTOR('',#125924,1000.);
#28223=VECTOR('',#125925,1000.);
#28224=VECTOR('',#125984,1000.);
#28225=VECTOR('',#125987,1000.);
#28226=VECTOR('',#125992,1000.);
#28227=VECTOR('',#125993,1000.);
#28228=VECTOR('',#125996,1000.);
#28229=VECTOR('',#125997,1000.);
#28230=VECTOR('',#126000,1000.);
#28231=VECTOR('',#126001,1000.);
#28232=VECTOR('',#126004,1000.);
#28233=VECTOR('',#126005,1000.);
#28234=VECTOR('',#126008,1000.);
#28235=VECTOR('',#126009,1000.);
#28236=VECTOR('',#126012,1000.);
#28237=VECTOR('',#126013,1000.);
#28238=VECTOR('',#126014,1000.);
#28239=VECTOR('',#126015,1000.);
#28240=VECTOR('',#126016,1000.);
#28241=VECTOR('',#126017,1000.);
#28242=VECTOR('',#126022,1000.);
#28243=VECTOR('',#126029,1000.);
#28244=VECTOR('',#126040,1000.);
#28245=VECTOR('',#126041,1000.);
#28246=VECTOR('',#126046,1000.);
#28247=VECTOR('',#126057,1000.);
#28248=VECTOR('',#126058,1000.);
#28249=VECTOR('',#126063,1000.);
#28250=VECTOR('',#126068,1000.);
#28251=VECTOR('',#126071,1000.);
#28252=VECTOR('',#126076,1000.);
#28253=VECTOR('',#126081,1000.);
#28254=VECTOR('',#126086,1000.);
#28255=VECTOR('',#126091,1000.);
#28256=VECTOR('',#126102,1000.);
#28257=VECTOR('',#126103,1000.);
#28258=VECTOR('',#126108,1000.);
#28259=VECTOR('',#126119,1000.);
#28260=VECTOR('',#126120,1000.);
#28261=VECTOR('',#126123,1000.);
#28262=VECTOR('',#126124,1000.);
#28263=VECTOR('',#126127,1000.);
#28264=VECTOR('',#126130,1000.);
#28265=VECTOR('',#126137,2.);
#28266=VECTOR('',#126142,2.);
#28267=VECTOR('',#126145,2.);
#28268=VECTOR('',#126148,2.);
#28269=VECTOR('',#126151,2.);
#28270=VECTOR('',#126154,2.);
#28271=VECTOR('',#126157,2.);
#28272=VECTOR('',#126160,2.);
#28273=VECTOR('',#126163,2.);
#28274=VECTOR('',#126166,2.);
#28275=VECTOR('',#126169,2.);
#28276=VECTOR('',#126172,2.);
#28277=VECTOR('',#126175,2.);
#28278=VECTOR('',#126178,2.);
#28279=VECTOR('',#126181,2.);
#28280=VECTOR('',#126184,2.);
#28281=VECTOR('',#126187,2.);
#28282=VECTOR('',#126190,2.);
#28283=VECTOR('',#126193,2.);
#28284=VECTOR('',#126196,2.);
#28285=VECTOR('',#126201,2.);
#28286=VECTOR('',#126204,2.);
#28287=VECTOR('',#126207,2.);
#28288=VECTOR('',#126210,2.);
#28289=VECTOR('',#126213,2.);
#28290=VECTOR('',#126216,2.);
#28291=VECTOR('',#126219,2.);
#28292=VECTOR('',#126222,2.);
#28293=VECTOR('',#126225,2.);
#28294=VECTOR('',#126228,2.);
#28295=VECTOR('',#126231,2.);
#28296=VECTOR('',#126234,2.);
#28297=VECTOR('',#126237,2.);
#28298=VECTOR('',#126240,2.);
#28299=VECTOR('',#126243,2.);
#28300=VECTOR('',#126246,2.);
#28301=VECTOR('',#126249,2.);
#28302=VECTOR('',#126252,2.);
#28303=VECTOR('',#126255,1.66874528305244);
#28304=VECTOR('',#126258,1.66874528305244);
#28305=VECTOR('',#126261,1.66874528305244);
#28306=VECTOR('',#126264,1.66874528305244);
#28307=VECTOR('',#126267,1.66874528305244);
#28308=VECTOR('',#126270,1.66874528305244);
#28309=VECTOR('',#126273,1.66874528305244);
#28310=VECTOR('',#126276,1.66874528305244);
#28311=VECTOR('',#126279,1.66874528305244);
#28312=VECTOR('',#126282,1.66874528305244);
#28313=VECTOR('',#126285,1.66874528305244);
#28314=VECTOR('',#126288,1.66874528305244);
#28315=VECTOR('',#126291,1.66874528305244);
#28316=VECTOR('',#126294,1.66874528305244);
#28317=VECTOR('',#126297,1.66874528305244);
#28318=VECTOR('',#126300,1.66874528305244);
#28319=VECTOR('',#126303,1.66874528305244);
#28320=VECTOR('',#126306,1.66874528305244);
#28321=VECTOR('',#126309,1.66874528305244);
#28322=VECTOR('',#126314,2.);
#28323=VECTOR('',#126319,2.);
#28324=VECTOR('',#126322,2.);
#28325=VECTOR('',#126325,2.);
#28326=VECTOR('',#126328,2.);
#28327=VECTOR('',#126331,2.);
#28328=VECTOR('',#126334,2.);
#28329=VECTOR('',#126337,2.);
#28330=VECTOR('',#126340,2.);
#28331=VECTOR('',#126343,2.);
#28332=VECTOR('',#126346,2.);
#28333=VECTOR('',#126349,2.);
#28334=VECTOR('',#126352,2.);
#28335=VECTOR('',#126355,2.);
#28336=VECTOR('',#126358,2.);
#28337=VECTOR('',#126361,2.);
#28338=VECTOR('',#126364,2.);
#28339=VECTOR('',#126367,2.);
#28340=VECTOR('',#126372,1.66874528305248);
#28341=VECTOR('',#126375,1.66874528305248);
#28342=VECTOR('',#126378,1.66874528305248);
#28343=VECTOR('',#126381,1.66874528305248);
#28344=VECTOR('',#126384,1.66874528305248);
#28345=VECTOR('',#126387,1.66874528305248);
#28346=VECTOR('',#126390,1.66874528305248);
#28347=VECTOR('',#126393,1.66874528305248);
#28348=VECTOR('',#126396,1.66874528305248);
#28349=VECTOR('',#126399,1.66874528305248);
#28350=VECTOR('',#126402,1.66874528305248);
#28351=VECTOR('',#126405,1.66874528305248);
#28352=VECTOR('',#126408,1.66874528305248);
#28353=VECTOR('',#126411,1.66874528305248);
#28354=VECTOR('',#126414,1.66874528305248);
#28355=VECTOR('',#126417,1.66874528305248);
#28356=VECTOR('',#126420,1.66874528305248);
#28357=VECTOR('',#126423,1.66874528305248);
#28358=VECTOR('',#126426,1.66874528305248);
#28359=VECTOR('',#126431,2.);
#28360=VECTOR('',#126436,2.);
#28361=VECTOR('',#126439,2.);
#28362=VECTOR('',#126442,2.);
#28363=VECTOR('',#126445,2.);
#28364=VECTOR('',#126448,2.);
#28365=VECTOR('',#126451,2.);
#28366=VECTOR('',#126454,2.);
#28367=VECTOR('',#126457,2.);
#28368=VECTOR('',#126460,2.);
#28369=VECTOR('',#126463,2.);
#28370=VECTOR('',#126466,2.);
#28371=VECTOR('',#126469,2.);
#28372=VECTOR('',#126472,2.);
#28373=VECTOR('',#126475,2.);
#28374=VECTOR('',#126478,2.);
#28375=VECTOR('',#126481,2.);
#28376=VECTOR('',#126484,2.);
#28377=VECTOR('',#126487,2.);
#28378=VECTOR('',#126490,1.66874528305242);
#28379=VECTOR('',#126493,1.66874528305242);
#28380=VECTOR('',#126496,1.66874528305242);
#28381=VECTOR('',#126499,1.66874528305242);
#28382=VECTOR('',#126502,1.66874528305242);
#28383=VECTOR('',#126505,1.66874528305242);
#28384=VECTOR('',#126508,1.66874528305242);
#28385=VECTOR('',#126511,1.66874528305242);
#28386=VECTOR('',#126514,1.66874528305242);
#28387=VECTOR('',#126517,1.66874528305242);
#28388=VECTOR('',#126520,1.66874528305242);
#28389=VECTOR('',#126523,1.66874528305242);
#28390=VECTOR('',#126526,1.66874528305242);
#28391=VECTOR('',#126529,1.66874528305242);
#28392=VECTOR('',#126532,1.66874528305242);
#28393=VECTOR('',#126535,1.66874528305242);
#28394=VECTOR('',#126538,1.66874528305242);
#28395=VECTOR('',#126541,1.66874528305242);
#28396=VECTOR('',#126544,1.66874528305242);
#28397=VECTOR('',#126549,1.66874528305242);
#28398=VECTOR('',#126552,1.66874528305242);
#28399=VECTOR('',#126555,1.66874528305242);
#28400=VECTOR('',#126558,1.66874528305242);
#28401=VECTOR('',#126561,1.66874528305242);
#28402=VECTOR('',#126564,1.66874528305242);
#28403=VECTOR('',#126567,1.66874528305242);
#28404=VECTOR('',#126570,1.66874528305242);
#28405=VECTOR('',#126573,1.66874528305242);
#28406=VECTOR('',#126576,1.66874528305242);
#28407=VECTOR('',#126579,1.66874528305242);
#28408=VECTOR('',#126582,1.66874528305242);
#28409=VECTOR('',#126585,1.66874528305242);
#28410=VECTOR('',#126588,1.66874528305242);
#28411=VECTOR('',#126591,1.66874528305242);
#28412=VECTOR('',#126594,1.66874528305242);
#28413=VECTOR('',#126597,1.66874528305242);
#28414=VECTOR('',#126600,1.66874528305242);
#28415=VECTOR('',#126603,1.66874528305242);
#28416=VECTOR('',#126608,1000.);
#28417=VECTOR('',#126609,1000.);
#28418=VECTOR('',#126610,1000.);
#28419=VECTOR('',#126611,1000.);
#28420=VECTOR('',#126612,1000.);
#28421=VECTOR('',#126613,1000.);
#28422=VECTOR('',#126614,1000.);
#28423=VECTOR('',#126615,1000.);
#28424=VECTOR('',#126618,1000.);
#28425=VECTOR('',#126621,1000.);
#28426=VECTOR('',#126622,1000.);
#28427=VECTOR('',#126627,1000.);
#28428=VECTOR('',#126628,1000.);
#28429=VECTOR('',#126629,1000.);
#28430=VECTOR('',#126630,1000.);
#28431=VECTOR('',#126633,1000.);
#28432=VECTOR('',#126634,1000.);
#28433=VECTOR('',#126635,1000.);
#28434=VECTOR('',#126636,1000.);
#28435=VECTOR('',#126639,1000.);
#28436=VECTOR('',#126640,1000.);
#28437=VECTOR('',#126641,1000.);
#28438=VECTOR('',#126644,1000.);
#28439=VECTOR('',#126645,1000.);
#28440=VECTOR('',#126646,1000.);
#28441=VECTOR('',#126649,1000.);
#28442=VECTOR('',#126650,1000.);
#28443=VECTOR('',#126653,1000.);
#28444=VECTOR('',#126656,1000.);
#28445=VECTOR('',#126657,1000.);
#28446=VECTOR('',#126660,1000.);
#28447=VECTOR('',#126665,1000.);
#28448=VECTOR('',#126666,1000.);
#28449=VECTOR('',#126669,1000.);
#28450=VECTOR('',#126670,1000.);
#28451=VECTOR('',#126681,3.);
#28452=VECTOR('',#126686,6.);
#28453=VECTOR('',#126697,3.);
#28454=VECTOR('',#126702,6.);
#28455=VECTOR('',#126713,3.);
#28456=VECTOR('',#126718,6.);
#28457=VECTOR('',#126729,3.);
#28458=VECTOR('',#126736,6.00000000000001);
#28459=VECTOR('',#126773,1000.);
#28460=VECTOR('',#126774,1000.);
#28461=VECTOR('',#126777,1000.);
#28462=VECTOR('',#126780,1000.);
#28463=VECTOR('',#126783,1000.);
#28464=VECTOR('',#126786,1000.);
#28465=VECTOR('',#126791,3.);
#28466=VECTOR('',#126818,6.);
#28467=VECTOR('',#126823,7.);
#28468=VECTOR('',#126846,10.);
#28469=VECTOR('',#126847,10.);
#28470=VECTOR('',#126852,10.);
#28471=VECTOR('',#126861,1000.);
#28472=VECTOR('',#126862,1000.);
#28473=VECTOR('',#126873,1000.);
#28474=VECTOR('',#126874,1000.);
#28475=VECTOR('',#126897,1000.);
#28476=VECTOR('',#126898,1000.);
#28477=VECTOR('',#126903,1000.);
#28478=VECTOR('',#126920,1000.);
#28479=VECTOR('',#126921,1000.);
#28480=VECTOR('',#126926,1000.);
#28481=VECTOR('',#126941,1000.);
#28482=VECTOR('',#126944,1000.);
#28483=VECTOR('',#126947,1000.);
#28484=VECTOR('',#126950,1000.);
#28485=VECTOR('',#126953,1000.);
#28486=VECTOR('',#126956,1000.);
#28487=VECTOR('',#126963,1000.);
#28488=VECTOR('',#126966,1000.);
#28489=VECTOR('',#126969,1000.);
#28490=VECTOR('',#126972,1000.);
#28491=VECTOR('',#126975,1000.);
#28492=VECTOR('',#126992,1000.);
#28493=VECTOR('',#126999,1000.);
#28494=VECTOR('',#127002,1000.);
#28495=VECTOR('',#127005,1000.);
#28496=VECTOR('',#127008,1000.);
#28497=VECTOR('',#127011,1000.);
#28498=VECTOR('',#127012,1000.);
#28499=VECTOR('',#127029,1000.);
#28500=VECTOR('',#127044,1000.);
#28501=VECTOR('',#127045,1000.);
#28502=VECTOR('',#127050,1000.);
#28503=VECTOR('',#127051,1000.);
#28504=VECTOR('',#127056,1000.);
#28505=VECTOR('',#127057,1000.);
#28506=VECTOR('',#127062,1000.);
#28507=VECTOR('',#127063,1000.);
#28508=VECTOR('',#127078,1000.);
#28509=VECTOR('',#127079,1000.);
#28510=VECTOR('',#127084,1000.);
#28511=VECTOR('',#127085,1000.);
#28512=VECTOR('',#127090,1000.);
#28513=VECTOR('',#127107,1000.);
#28514=VECTOR('',#127124,1000.);
#28515=VECTOR('',#127125,1000.);
#28516=VECTOR('',#127130,1000.);
#28517=VECTOR('',#127131,1000.);
#28518=VECTOR('',#127136,1000.);
#28519=VECTOR('',#127153,1000.);
#28520=VECTOR('',#127196,1000.);
#28521=VECTOR('',#127211,10.);
#28522=VECTOR('',#127212,10.);
#28523=VECTOR('',#127215,10.);
#28524=VECTOR('',#127216,10.);
#28525=VECTOR('',#127223,10.);
#28526=VECTOR('',#127226,10.);
#28527=VECTOR('',#127227,10.);
#28528=VECTOR('',#127234,10.);
#28529=VECTOR('',#127237,10.);
#28530=VECTOR('',#127238,10.);
#28531=VECTOR('',#127245,10.);
#28532=VECTOR('',#127246,10.);
#28533=VECTOR('',#127249,10.);
#28534=VECTOR('',#127250,10.);
#28535=VECTOR('',#127265,10.);
#28536=VECTOR('',#127266,10.);
#28537=VECTOR('',#127271,1000.);
#28538=VECTOR('',#127272,1000.);
#28539=VECTOR('',#127317,1000.);
#28540=VECTOR('',#127318,1000.);
#28541=VECTOR('',#127319,1000.);
#28542=VECTOR('',#127320,1000.);
#28543=VECTOR('',#127323,1000.);
#28544=VECTOR('',#127324,1000.);
#28545=VECTOR('',#127325,1000.);
#28546=VECTOR('',#127328,1000.);
#28547=VECTOR('',#127329,1000.);
#28548=VECTOR('',#127330,1000.);
#28549=VECTOR('',#127333,1000.);
#28550=VECTOR('',#127334,1000.);
#28551=VECTOR('',#127353,32.4);
#28552=VECTOR('',#127358,1000.);
#28553=VECTOR('',#127359,1000.);
#28554=VECTOR('',#127362,1000.);
#28555=VECTOR('',#127365,1000.);
#28556=VECTOR('',#127372,1000.);
#28557=VECTOR('',#127375,1000.);
#28558=VECTOR('',#127380,1000.);
#28559=VECTOR('',#127383,1000.);
#28560=VECTOR('',#127388,1000.);
#28561=VECTOR('',#127391,1000.);
#28562=VECTOR('',#127396,1000.);
#28563=VECTOR('',#127399,1000.);
#28564=VECTOR('',#127404,1000.);
#28565=VECTOR('',#127407,1000.);
#28566=VECTOR('',#127410,1000.);
#28567=VECTOR('',#127411,1000.);
#28568=VECTOR('',#127416,1000.);
#28569=VECTOR('',#127419,1000.);
#28570=VECTOR('',#127470,1000.);
#28571=VECTOR('',#127471,1000.);
#28572=VECTOR('',#127472,1000.);
#28573=VECTOR('',#127475,1000.);
#28574=VECTOR('',#127476,1000.);
#28575=VECTOR('',#127477,1000.);
#28576=VECTOR('',#127536,1000.);
#28577=VECTOR('',#127539,1000.);
#28578=VECTOR('',#127542,1000.);
#28579=VECTOR('',#127543,1000.);
#28580=VECTOR('',#127548,1000.);
#28581=VECTOR('',#127549,1000.);
#28582=VECTOR('',#127554,1000.);
#28583=VECTOR('',#127555,1000.);
#28584=VECTOR('',#127562,1000.);
#28585=VECTOR('',#127565,1000.);
#28586=VECTOR('',#127566,1000.);
#28587=VECTOR('',#127571,1000.);
#28588=VECTOR('',#127574,1000.);
#28589=VECTOR('',#127577,1000.);
#28590=VECTOR('',#127580,1000.);
#28591=VECTOR('',#127583,1000.);
#28592=VECTOR('',#127584,1000.);
#28593=VECTOR('',#127589,1000.);
#28594=VECTOR('',#127592,1000.);
#28595=VECTOR('',#127595,1000.);
#28596=VECTOR('',#127598,1000.);
#28597=VECTOR('',#127601,1000.);
#28598=VECTOR('',#127602,1000.);
#28599=VECTOR('',#127607,1000.);
#28600=VECTOR('',#127610,1000.);
#28601=VECTOR('',#127613,1000.);
#28602=VECTOR('',#127614,1000.);
#28603=VECTOR('',#127679,1000.);
#28604=VECTOR('',#127708,1000.);
#28605=VECTOR('',#127711,1000.);
#28606=VECTOR('',#127716,1000.);
#28607=VECTOR('',#127737,1000.);
#28608=VECTOR('',#127740,1000.);
#28609=VECTOR('',#127753,1000.);
#28610=VECTOR('',#127756,1000.);
#28611=VECTOR('',#127761,1000.);
#28612=VECTOR('',#127764,1000.);
#28613=VECTOR('',#127769,1000.);
#28614=VECTOR('',#127774,1000.);
#28615=VECTOR('',#127777,1000.);
#28616=VECTOR('',#127782,1000.);
#28617=VECTOR('',#127785,1000.);
#28618=VECTOR('',#127790,1000.);
#28619=VECTOR('',#127793,1000.);
#28620=VECTOR('',#127798,1000.);
#28621=VECTOR('',#127799,1000.);
#28622=VECTOR('',#127808,10.12);
#28623=VECTOR('',#127815,1000.);
#28624=VECTOR('',#127818,1000.);
#28625=VECTOR('',#127821,1000.);
#28626=VECTOR('',#127822,1000.);
#28627=VECTOR('',#127823,1000.);
#28628=VECTOR('',#127826,1000.);
#28629=VECTOR('',#127827,1000.);
#28630=VECTOR('',#127828,1000.);
#28631=VECTOR('',#127831,1000.);
#28632=VECTOR('',#127832,1000.);
#28633=VECTOR('',#127849,25.2);
#28634=VECTOR('',#127854,1000.);
#28635=VECTOR('',#127855,1000.);
#28636=VECTOR('',#127858,1000.);
#28637=VECTOR('',#127859,1000.);
#28638=VECTOR('',#127864,1000.);
#28639=VECTOR('',#127867,1000.);
#28640=VECTOR('',#127872,1000.);
#28641=VECTOR('',#127875,1000.);
#28642=VECTOR('',#127880,1000.);
#28643=VECTOR('',#127883,1000.);
#28644=VECTOR('',#127888,1000.);
#28645=VECTOR('',#127891,1000.);
#28646=VECTOR('',#127894,1000.);
#28647=VECTOR('',#127897,1000.);
#28648=VECTOR('',#127902,1000.);
#28649=VECTOR('',#127905,1000.);
#28650=VECTOR('',#127912,1000.);
#28651=VECTOR('',#127915,1000.);
#28652=VECTOR('',#127920,1000.);
#28653=VECTOR('',#127923,1000.);
#28654=VECTOR('',#127928,1000.);
#28655=VECTOR('',#127931,1000.);
#28656=VECTOR('',#127936,1000.);
#28657=VECTOR('',#127939,1000.);
#28658=VECTOR('',#127944,1000.);
#28659=VECTOR('',#127947,1000.);
#28660=VECTOR('',#127952,1000.);
#28661=VECTOR('',#127955,1000.);
#28662=VECTOR('',#127966,1000.);
#28663=VECTOR('',#127967,1000.);
#28664=VECTOR('',#127976,1000.);
#28665=VECTOR('',#127979,1000.);
#28666=VECTOR('',#128076,1000.);
#28667=VECTOR('',#128077,1000.);
#28668=VECTOR('',#128078,1000.);
#28669=VECTOR('',#128081,1000.);
#28670=VECTOR('',#128082,1000.);
#28671=VECTOR('',#128083,1000.);
#28672=VECTOR('',#128198,1000.);
#28673=VECTOR('',#128201,1000.);
#28674=VECTOR('',#128204,1000.);
#28675=VECTOR('',#128205,1000.);
#28676=VECTOR('',#128210,1000.);
#28677=VECTOR('',#128211,1000.);
#28678=VECTOR('',#128216,1000.);
#28679=VECTOR('',#128217,1000.);
#28680=VECTOR('',#128222,1000.);
#28681=VECTOR('',#128225,1000.);
#28682=VECTOR('',#128228,1000.);
#28683=VECTOR('',#128233,1000.);
#28684=VECTOR('',#128234,1000.);
#28685=VECTOR('',#128239,1000.);
#28686=VECTOR('',#128242,1000.);
#28687=VECTOR('',#128245,1000.);
#28688=VECTOR('',#128246,1000.);
#28689=VECTOR('',#128251,1000.);
#28690=VECTOR('',#128256,1000.);
#28691=VECTOR('',#128259,1000.);
#28692=VECTOR('',#128262,1000.);
#28693=VECTOR('',#128263,1000.);
#28694=VECTOR('',#128268,1000.);
#28695=VECTOR('',#128271,1000.);
#28696=VECTOR('',#128274,1000.);
#28697=VECTOR('',#128275,1000.);
#28698=VECTOR('',#128280,1000.);
#28699=VECTOR('',#128283,1000.);
#28700=VECTOR('',#128286,1000.);
#28701=VECTOR('',#128287,1000.);
#28702=VECTOR('',#128292,1000.);
#28703=VECTOR('',#128293,1000.);
#28704=VECTOR('',#128298,1000.);
#28705=VECTOR('',#128301,1000.);
#28706=VECTOR('',#128304,1000.);
#28707=VECTOR('',#128305,1000.);
#28708=VECTOR('',#128310,1000.);
#28709=VECTOR('',#128313,1000.);
#28710=VECTOR('',#128316,1000.);
#28711=VECTOR('',#128317,1000.);
#28712=VECTOR('',#128322,1000.);
#28713=VECTOR('',#128325,1000.);
#28714=VECTOR('',#128328,1000.);
#28715=VECTOR('',#128329,1000.);
#28716=VECTOR('',#128334,1000.);
#28717=VECTOR('',#128335,1000.);
#28718=VECTOR('',#128340,1000.);
#28719=VECTOR('',#128343,1000.);
#28720=VECTOR('',#128346,1000.);
#28721=VECTOR('',#128349,1000.);
#28722=VECTOR('',#128352,1000.);
#28723=VECTOR('',#128353,1000.);
#28724=VECTOR('',#128358,1000.);
#28725=VECTOR('',#128359,1000.);
#28726=VECTOR('',#128480,1000.);
#28727=VECTOR('',#128481,1000.);
#28728=VECTOR('',#128528,1000.);
#28729=VECTOR('',#128531,1000.);
#28730=VECTOR('',#128536,1000.);
#28731=VECTOR('',#128539,1000.);
#28732=VECTOR('',#128556,1000.);
#28733=VECTOR('',#128559,1000.);
#28734=VECTOR('',#128576,1000.);
#28735=VECTOR('',#128579,1000.);
#28736=VECTOR('',#128608,1000.);
#28737=VECTOR('',#128611,1000.);
#28738=VECTOR('',#128616,1000.);
#28739=VECTOR('',#128619,1000.);
#28740=VECTOR('',#128624,1000.);
#28741=VECTOR('',#128627,1000.);
#28742=VECTOR('',#128632,1000.);
#28743=VECTOR('',#128637,1000.);
#28744=VECTOR('',#128640,1000.);
#28745=VECTOR('',#128645,1000.);
#28746=VECTOR('',#128648,1000.);
#28747=VECTOR('',#128653,1000.);
#28748=VECTOR('',#128656,1000.);
#28749=VECTOR('',#128661,1000.);
#28750=VECTOR('',#128664,1000.);
#28751=VECTOR('',#128669,1000.);
#28752=VECTOR('',#128672,1000.);
#28753=VECTOR('',#128677,1000.);
#28754=VECTOR('',#128682,1000.);
#28755=VECTOR('',#128685,1000.);
#28756=VECTOR('',#128690,1000.);
#28757=VECTOR('',#128693,1000.);
#28758=VECTOR('',#128698,1000.);
#28759=VECTOR('',#128701,1000.);
#28760=VECTOR('',#128706,1000.);
#28761=VECTOR('',#128709,1000.);
#28762=VECTOR('',#128714,1000.);
#28763=VECTOR('',#128715,1000.);
#28764=VECTOR('',#128726,3.95);
#28765=VECTOR('',#128733,1000.);
#28766=VECTOR('',#128736,1000.);
#28767=VECTOR('',#128741,3.95);
#28768=VECTOR('',#128748,1000.);
#28769=VECTOR('',#128755,1000.);
#28770=VECTOR('',#128772,3.95);
#28771=VECTOR('',#128779,3.95);
#28772=VECTOR('',#128786,1000.);
#28773=VECTOR('',#128789,1000.);
#28774=VECTOR('',#128808,1000.);
#28775=VECTOR('',#128811,1000.);
#28776=VECTOR('',#128818,3.95);
#28777=VECTOR('',#128829,3.95);
#28778=VECTOR('',#129118,36.25);
#28779=VECTOR('',#129125,36.25);
#28780=VECTOR('',#129132,45.);
#28781=VECTOR('',#129139,30.);
#28782=VECTOR('',#129178,16.0850661013937);
#28783=VECTOR('',#129197,23.4);
#28784=VECTOR('',#129200,23.4);
#28785=VECTOR('',#129203,23.4);
#28786=VECTOR('',#129234,36.);
#28787=VECTOR('',#129349,7.25);
#28788=VECTOR('',#129356,16.);
#28789=VECTOR('',#129363,7.25);
#28790=VECTOR('',#129370,16.);
#28791=VECTOR('',#129375,1000.);
#28792=VECTOR('',#129376,1000.);
#28793=VECTOR('',#129377,1000.);
#28794=VECTOR('',#129378,1000.);
#28795=VECTOR('',#129381,1000.);
#28796=VECTOR('',#129382,1000.);
#28797=VECTOR('',#129383,1000.);
#28798=VECTOR('',#129386,1000.);
#28799=VECTOR('',#129387,1000.);
#28800=VECTOR('',#129388,1000.);
#28801=VECTOR('',#129391,1000.);
#28802=VECTOR('',#129392,1000.);
#28803=VECTOR('',#129393,1000.);
#28804=VECTOR('',#129396,1000.);
#28805=VECTOR('',#129397,1000.);
#28806=VECTOR('',#129398,1000.);
#28807=VECTOR('',#129401,1000.);
#28808=VECTOR('',#129402,1000.);
#28809=VECTOR('',#129419,10.0514428414941);
#28810=VECTOR('',#129424,10.0514428414941);
#28811=VECTOR('',#129429,10.0514428414941);
#28812=VECTOR('',#129432,10.0514428414941);
#28813=VECTOR('',#129435,10.0514428414941);
#28814=VECTOR('',#129440,12.);
#28815=VECTOR('',#129443,13.05);
#28816=VECTOR('',#129446,12.);
#28817=VECTOR('',#129451,12.);
#28818=VECTOR('',#129456,12.);
#28819=VECTOR('',#129459,12.);
#28820=VECTOR('',#129462,12.);
#28821=VECTOR('',#129465,12.);
#28822=VECTOR('',#129472,13.05);
#28823=VECTOR('',#129477,12.);
#28824=VECTOR('',#129496,1000.);
#28825=VECTOR('',#129497,1000.);
#28826=VECTOR('',#129500,1000.);
#28827=VECTOR('',#129503,1000.);
#28828=VECTOR('',#129506,1000.);
#28829=VECTOR('',#129509,1000.);
#28830=VECTOR('',#129554,10.0514428414941);
#28831=VECTOR('',#129559,10.0514428414941);
#28832=VECTOR('',#129562,10.0514428414941);
#28833=VECTOR('',#129565,10.0514428414941);
#28834=VECTOR('',#129568,10.0514428414941);
#28835=VECTOR('',#129571,10.0514428414941);
#28836=VECTOR('',#129576,12.);
#28837=VECTOR('',#129581,12.);
#28838=VECTOR('',#129584,12.);
#28839=VECTOR('',#129587,12.);
#28840=VECTOR('',#129590,12.);
#28841=VECTOR('',#129593,12.);
#28842=VECTOR('',#129596,12.);
#28843=VECTOR('',#129623,12.9453125);
#28844=VECTOR('',#129628,12.);
#28845=VECTOR('',#129635,1000.);
#28846=VECTOR('',#129636,1000.);
#28847=VECTOR('',#129639,1000.);
#28848=VECTOR('',#129642,1000.);
#28849=VECTOR('',#129645,1000.);
#28850=VECTOR('',#129648,1000.);
#28851=VECTOR('',#129659,10.0514428414941);
#28852=VECTOR('',#129664,12.);
#28853=VECTOR('',#129681,10.0514428414941);
#28854=VECTOR('',#129686,10.0514428414941);
#28855=VECTOR('',#129689,10.0514428414941);
#28856=VECTOR('',#129692,10.0514428414941);
#28857=VECTOR('',#129695,10.0514428414941);
#28858=VECTOR('',#129698,10.0514428414941);
#28859=VECTOR('',#129701,10.0514428414941);
#28860=VECTOR('',#129704,10.0514428414941);
#28861=VECTOR('',#129707,10.0514428414941);
#28862=VECTOR('',#129710,10.0514428414941);
#28863=VECTOR('',#129713,10.0514428414941);
#28864=VECTOR('',#129716,10.0514428414941);
#28865=VECTOR('',#129719,10.0514428414941);
#28866=VECTOR('',#129722,10.0514428414941);
#28867=VECTOR('',#129725,10.0514428414941);
#28868=VECTOR('',#129728,10.0514428414941);
#28869=VECTOR('',#129731,10.0514428414941);
#28870=VECTOR('',#129734,10.0514428414941);
#28871=VECTOR('',#129737,10.0514428414941);
#28872=VECTOR('',#129740,10.0514428414941);
#28873=VECTOR('',#129743,10.0514428414941);
#28874=VECTOR('',#129748,10.0514428414941);
#28875=VECTOR('',#129751,10.0514428414941);
#28876=VECTOR('',#129754,10.0514428414941);
#28877=VECTOR('',#129757,10.0514428414941);
#28878=VECTOR('',#129760,10.0514428414941);
#28879=VECTOR('',#129763,10.0514428414941);
#28880=VECTOR('',#129766,10.0514428414941);
#28881=VECTOR('',#129769,10.0514428414941);
#28882=VECTOR('',#129772,10.0514428414941);
#28883=VECTOR('',#129775,10.0514428414941);
#28884=VECTOR('',#129778,10.0514428414941);
#28885=VECTOR('',#129781,10.0514428414941);
#28886=VECTOR('',#129784,12.);
#28887=VECTOR('',#129789,12.);
#28888=VECTOR('',#129792,12.);
#28889=VECTOR('',#129795,12.);
#28890=VECTOR('',#129798,12.);
#28891=VECTOR('',#129801,12.);
#28892=VECTOR('',#129804,12.);
#28893=VECTOR('',#129807,12.);
#28894=VECTOR('',#129810,12.);
#28895=VECTOR('',#129813,12.);
#28896=VECTOR('',#129816,12.);
#28897=VECTOR('',#129819,12.);
#28898=VECTOR('',#129822,12.);
#28899=VECTOR('',#129825,12.);
#28900=VECTOR('',#129830,12.);
#28901=VECTOR('',#129833,12.);
#28902=VECTOR('',#129836,12.);
#28903=VECTOR('',#129839,12.);
#28904=VECTOR('',#129842,12.);
#28905=VECTOR('',#129845,12.);
#28906=VECTOR('',#129848,12.);
#28907=VECTOR('',#129851,12.);
#28908=VECTOR('',#129854,12.);
#28909=VECTOR('',#129857,12.);
#28910=VECTOR('',#129860,12.);
#28911=VECTOR('',#129863,12.);
#28912=VECTOR('',#129866,12.);
#28913=VECTOR('',#129869,12.);
#28914=VECTOR('',#129872,12.);
#28915=VECTOR('',#129875,12.);
#28916=VECTOR('',#129878,12.);
#28917=VECTOR('',#129881,12.);
#28918=VECTOR('',#129888,13.05);
#28919=VECTOR('',#129897,9.90000000000001);
#28920=VECTOR('',#129910,1000.);
#28921=VECTOR('',#129911,1000.);
#28922=VECTOR('',#129912,1000.);
#28923=VECTOR('',#129913,1000.);
#28924=VECTOR('',#129916,1000.);
#28925=VECTOR('',#129917,1000.);
#28926=VECTOR('',#129918,1000.);
#28927=VECTOR('',#129919,1000.);
#28928=VECTOR('',#129934,1000.);
#28929=VECTOR('',#129935,1000.);
#28930=VECTOR('',#129938,1000.);
#28931=VECTOR('',#129941,1000.);
#28932=VECTOR('',#129946,1000.);
#28933=VECTOR('',#129947,1000.);
#28934=VECTOR('',#129950,1000.);
#28935=VECTOR('',#129953,1000.);
#28936=VECTOR('',#129956,1000.);
#28937=VECTOR('',#129959,1000.);
#28938=VECTOR('',#130008,1.190625);
#28939=VECTOR('',#130015,1.190625);
#28940=VECTOR('',#130022,1.190625);
#28941=VECTOR('',#130029,1.19062499999999);
#28942=VECTOR('',#130036,1.190625);
#28943=VECTOR('',#130043,1.190625);
#28944=VECTOR('',#130050,1.190625);
#28945=VECTOR('',#130057,1.190625);
#28946=VECTOR('',#130064,1.190625);
#28947=VECTOR('',#130071,55.2538194444444);
#28948=VECTOR('',#130078,44.5707880434783);
#28949=VECTOR('',#130107,16.8332621659243);
#28950=VECTOR('',#130118,44.5707880434783);
#28951=VECTOR('',#130151,1000.);
#28952=VECTOR('',#130152,1000.);
#28953=VECTOR('',#130153,1000.);
#28954=VECTOR('',#130154,1000.);
#28955=VECTOR('',#130155,1000.);
#28956=VECTOR('',#130156,1000.);
#28957=VECTOR('',#130157,1000.);
#28958=VECTOR('',#130158,1000.);
#28959=VECTOR('',#130161,1000.);
#28960=VECTOR('',#130162,1000.);
#28961=VECTOR('',#130163,1000.);
#28962=VECTOR('',#130164,1000.);
#28963=VECTOR('',#130165,1000.);
#28964=VECTOR('',#130166,1000.);
#28965=VECTOR('',#130167,1000.);
#28966=VECTOR('',#130168,1000.);
#28967=VECTOR('',#130171,1000.);
#28968=VECTOR('',#130172,1000.);
#28969=VECTOR('',#130175,1000.);
#28970=VECTOR('',#130178,1000.);
#28971=VECTOR('',#130183,1000.);
#28972=VECTOR('',#130184,1000.);
#28973=VECTOR('',#130187,1000.);
#28974=VECTOR('',#130190,1000.);
#28975=VECTOR('',#130197,1000.);
#28976=VECTOR('',#130198,1000.);
#28977=VECTOR('',#130199,1000.);
#28978=VECTOR('',#130200,1000.);
#28979=VECTOR('',#130203,1000.);
#28980=VECTOR('',#130204,1000.);
#28981=VECTOR('',#130205,1000.);
#28982=VECTOR('',#130208,1000.);
#28983=VECTOR('',#130209,1000.);
#28984=VECTOR('',#130210,1000.);
#28985=VECTOR('',#130213,1000.);
#28986=VECTOR('',#130214,1000.);
#28987=VECTOR('',#130227,6.00000000000001);
#28988=VECTOR('',#130234,6.00000000000001);
#28989=VECTOR('',#130241,6.00000000000001);
#28990=VECTOR('',#130248,6.00000000000001);
#28991=VECTOR('',#130255,6.00000000000001);
#28992=VECTOR('',#130262,6.00000000000001);
#28993=VECTOR('',#130269,6.00000000000001);
#28994=VECTOR('',#130276,6.00000000000001);
#28995=VECTOR('',#130281,1000.);
#28996=VECTOR('',#130282,1000.);
#28997=VECTOR('',#130283,1000.);
#28998=VECTOR('',#130284,1000.);
#28999=VECTOR('',#130285,1000.);
#29000=VECTOR('',#130286,1000.);
#29001=VECTOR('',#130287,1000.);
#29002=VECTOR('',#130288,1000.);
#29003=VECTOR('',#130291,1000.);
#29004=VECTOR('',#130292,1000.);
#29005=VECTOR('',#130293,1000.);
#29006=VECTOR('',#130294,1000.);
#29007=VECTOR('',#130295,1000.);
#29008=VECTOR('',#130296,1000.);
#29009=VECTOR('',#130297,1000.);
#29010=VECTOR('',#130298,1000.);
#29011=VECTOR('',#130301,1000.);
#29012=VECTOR('',#130302,1000.);
#29013=VECTOR('',#130305,1000.);
#29014=VECTOR('',#130306,1000.);
#29015=VECTOR('',#130309,1000.);
#29016=VECTOR('',#130310,1000.);
#29017=VECTOR('',#130317,1000.);
#29018=VECTOR('',#130320,1000.);
#29019=VECTOR('',#130329,7.00000000000001);
#29020=VECTOR('',#130336,7.);
#29021=VECTOR('',#130341,1000.);
#29022=VECTOR('',#130342,1000.);
#29023=VECTOR('',#130343,1000.);
#29024=VECTOR('',#130344,1000.);
#29025=VECTOR('',#130347,1000.);
#29026=VECTOR('',#130348,1000.);
#29027=VECTOR('',#130349,1000.);
#29028=VECTOR('',#130350,1000.);
#29029=VECTOR('',#130353,1000.);
#29030=VECTOR('',#130354,1000.);
#29031=VECTOR('',#130355,1000.);
#29032=VECTOR('',#130358,1000.);
#29033=VECTOR('',#130359,1000.);
#29034=VECTOR('',#130360,1000.);
#29035=VECTOR('',#130363,1000.);
#29036=VECTOR('',#130364,1000.);
#29037=VECTOR('',#130365,1000.);
#29038=VECTOR('',#130368,1000.);
#29039=VECTOR('',#130369,1000.);
#29040=VECTOR('',#130370,1000.);
#29041=VECTOR('',#130373,1000.);
#29042=VECTOR('',#130374,1000.);
#29043=VECTOR('',#130377,1000.);
#29044=VECTOR('',#130378,1000.);
#29045=VECTOR('',#130381,1000.);
#29046=VECTOR('',#130388,1000.);
#29047=VECTOR('',#130389,1000.);
#29048=VECTOR('',#130390,1000.);
#29049=VECTOR('',#130395,1000.);
#29050=VECTOR('',#130406,1000.);
#29051=VECTOR('',#130413,1000.);
#29052=VECTOR('',#130414,1000.);
#29053=VECTOR('',#130417,1000.);
#29054=VECTOR('',#130420,1000.);
#29055=VECTOR('',#130425,1000.);
#29056=VECTOR('',#130428,1000.);
#29057=VECTOR('',#130445,6.);
#29058=VECTOR('',#130452,6.);
#29059=VECTOR('',#130457,6.);
#29060=VECTOR('',#130462,6.);
#29061=VECTOR('',#130465,6.);
#29062=VECTOR('',#130468,6.);
#29063=VECTOR('',#130471,6.);
#29064=VECTOR('',#130474,6.);
#29065=VECTOR('',#130477,6.);
#29066=VECTOR('',#130480,6.);
#29067=VECTOR('',#130483,6.);
#29068=VECTOR('',#130486,6.);
#29069=VECTOR('',#130489,6.);
#29070=VECTOR('',#130492,6.);
#29071=VECTOR('',#130495,6.);
#29072=VECTOR('',#130498,6.);
#29073=VECTOR('',#130501,6.);
#29074=VECTOR('',#130504,6.);
#29075=VECTOR('',#130509,6.);
#29076=VECTOR('',#130512,6.);
#29077=VECTOR('',#130517,4.86334165753294);
#29078=VECTOR('',#130520,4.86334165753294);
#29079=VECTOR('',#130523,4.86334165753294);
#29080=VECTOR('',#130526,4.86334165753294);
#29081=VECTOR('',#130529,4.86334165753294);
#29082=VECTOR('',#130532,4.86334165753294);
#29083=VECTOR('',#130535,4.86334165753294);
#29084=VECTOR('',#130538,4.86334165753294);
#29085=VECTOR('',#130541,4.86334165753294);
#29086=VECTOR('',#130544,4.86334165753294);
#29087=VECTOR('',#130547,4.86334165753294);
#29088=VECTOR('',#130550,4.86334165753294);
#29089=VECTOR('',#130553,4.86334165753294);
#29090=VECTOR('',#130556,4.86334165753294);
#29091=VECTOR('',#130559,4.86334165753294);
#29092=VECTOR('',#130562,4.86334165753294);
#29093=VECTOR('',#130565,4.86334165753294);
#29094=VECTOR('',#130576,4.6875);
#29095=VECTOR('',#130587,1000.);
#29096=VECTOR('',#130588,1000.);
#29097=VECTOR('',#130589,1000.);
#29098=VECTOR('',#130590,1000.);
#29099=VECTOR('',#130591,1000.);
#29100=VECTOR('',#130592,1000.);
#29101=VECTOR('',#130593,1000.);
#29102=VECTOR('',#130594,1000.);
#29103=VECTOR('',#130595,1000.);
#29104=VECTOR('',#130596,1000.);
#29105=VECTOR('',#130597,1000.);
#29106=VECTOR('',#130598,1000.);
#29107=VECTOR('',#130599,1000.);
#29108=VECTOR('',#130600,1000.);
#29109=VECTOR('',#130601,1000.);
#29110=VECTOR('',#130602,1000.);
#29111=VECTOR('',#130609,1000.);
#29112=VECTOR('',#130610,1000.);
#29113=VECTOR('',#130611,1000.);
#29114=VECTOR('',#130612,1000.);
#29115=VECTOR('',#130613,1000.);
#29116=VECTOR('',#130614,1000.);
#29117=VECTOR('',#130615,1000.);
#29118=VECTOR('',#130616,1000.);
#29119=VECTOR('',#130617,1000.);
#29120=VECTOR('',#130618,1000.);
#29121=VECTOR('',#130619,1000.);
#29122=VECTOR('',#130620,1000.);
#29123=VECTOR('',#130621,1000.);
#29124=VECTOR('',#130622,1000.);
#29125=VECTOR('',#130623,1000.);
#29126=VECTOR('',#130624,1000.);
#29127=VECTOR('',#130625,1000.);
#29128=VECTOR('',#130626,1000.);
#29129=VECTOR('',#130627,1000.);
#29130=VECTOR('',#130628,1000.);
#29131=VECTOR('',#130631,1000.);
#29132=VECTOR('',#130632,1000.);
#29133=VECTOR('',#130633,1000.);
#29134=VECTOR('',#130636,1000.);
#29135=VECTOR('',#130637,1000.);
#29136=VECTOR('',#130640,1000.);
#29137=VECTOR('',#130641,1000.);
#29138=VECTOR('',#130644,1000.);
#29139=VECTOR('',#130673,1000.);
#29140=VECTOR('',#130674,1000.);
#29141=VECTOR('',#130675,1000.);
#29142=VECTOR('',#130678,1000.);
#29143=VECTOR('',#130679,1000.);
#29144=VECTOR('',#130682,1000.);
#29145=VECTOR('',#130683,1000.);
#29146=VECTOR('',#130686,1000.);
#29147=VECTOR('',#130687,1000.);
#29148=VECTOR('',#130690,1000.);
#29149=VECTOR('',#130691,1000.);
#29150=VECTOR('',#130694,1000.);
#29151=VECTOR('',#130705,6.);
#29152=VECTOR('',#130710,6.);
#29153=VECTOR('',#130715,6.);
#29154=VECTOR('',#130718,6.);
#29155=VECTOR('',#130721,6.);
#29156=VECTOR('',#130724,6.);
#29157=VECTOR('',#130731,4.86334165753295);
#29158=VECTOR('',#130734,4.86334165753295);
#29159=VECTOR('',#130737,4.86334165753295);
#29160=VECTOR('',#130740,4.86334165753295);
#29161=VECTOR('',#130749,1000.);
#29162=VECTOR('',#130750,1000.);
#29163=VECTOR('',#130753,1000.);
#29164=VECTOR('',#130754,1000.);
#29165=VECTOR('',#130757,1000.);
#29166=VECTOR('',#130758,1000.);
#29167=VECTOR('',#130761,1000.);
#29168=VECTOR('',#130762,1000.);
#29169=VECTOR('',#130765,1000.);
#29170=VECTOR('',#130766,1000.);
#29171=VECTOR('',#130769,1000.);
#29172=VECTOR('',#130770,1000.);
#29173=VECTOR('',#130843,6.7);
#29174=VECTOR('',#130846,6.);
#29175=CIRCLE('',#93966,7.5);
#29176=CIRCLE('',#93967,7.5);
#29177=CIRCLE('',#93969,7.5);
#29178=CIRCLE('',#93970,7.5);
#29179=CIRCLE('',#93972,7.50000000000001);
#29180=CIRCLE('',#93973,7.50000000000001);
#29181=CIRCLE('',#93975,7.5);
#29182=CIRCLE('',#93976,7.5);
#29183=CIRCLE('',#93978,7.50000000000001);
#29184=CIRCLE('',#93979,7.50000000000001);
#29185=CIRCLE('',#93981,7.5);
#29186=CIRCLE('',#93982,7.5);
#29187=CIRCLE('',#93984,7.5);
#29188=CIRCLE('',#93985,7.5);
#29189=CIRCLE('',#93987,7.5);
#29190=CIRCLE('',#93988,7.5);
#29191=CIRCLE('',#93990,7.5);
#29192=CIRCLE('',#93991,7.5);
#29193=CIRCLE('',#93993,7.5);
#29194=CIRCLE('',#93994,7.5);
#29195=CIRCLE('',#93996,7.5);
#29196=CIRCLE('',#93997,7.5);
#29197=CIRCLE('',#93999,7.50000000000001);
#29198=CIRCLE('',#94000,7.50000000000001);
#29199=CIRCLE('',#94010,2.);
#29200=CIRCLE('',#94011,2.);
#29201=CIRCLE('',#94012,2.);
#29202=CIRCLE('',#94013,2.);
#29203=CIRCLE('',#94015,2.);
#29204=CIRCLE('',#94016,2.);
#29205=CIRCLE('',#94017,2.);
#29206=CIRCLE('',#94018,2.);
#29207=CIRCLE('',#94025,7.50000000000001);
#29208=CIRCLE('',#94026,7.50000000000001);
#29209=CIRCLE('',#94028,7.50000000000001);
#29210=CIRCLE('',#94029,7.50000000000001);
#29211=CIRCLE('',#94031,7.50000000000001);
#29212=CIRCLE('',#94032,7.50000000000001);
#29213=CIRCLE('',#94034,7.50000000000001);
#29214=CIRCLE('',#94035,7.50000000000001);
#29215=CIRCLE('',#94037,7.50000000000001);
#29216=CIRCLE('',#94038,7.50000000000001);
#29217=CIRCLE('',#94040,7.50000000000001);
#29218=CIRCLE('',#94041,7.50000000000001);
#29219=CIRCLE('',#94043,7.50000000000001);
#29220=CIRCLE('',#94044,7.50000000000001);
#29221=CIRCLE('',#94046,7.50000000000001);
#29222=CIRCLE('',#94047,7.50000000000001);
#29223=CIRCLE('',#94049,7.5);
#29224=CIRCLE('',#94050,7.5);
#29225=CIRCLE('',#94052,7.50000000000001);
#29226=CIRCLE('',#94053,7.50000000000001);
#29227=CIRCLE('',#94055,7.50000000000001);
#29228=CIRCLE('',#94056,7.50000000000001);
#29229=CIRCLE('',#94058,7.50000000000001);
#29230=CIRCLE('',#94059,7.50000000000001);
#29231=CIRCLE('',#94069,2.);
#29232=CIRCLE('',#94070,2.);
#29233=CIRCLE('',#94071,2.);
#29234=CIRCLE('',#94072,2.);
#29235=CIRCLE('',#94074,2.);
#29236=CIRCLE('',#94075,2.);
#29237=CIRCLE('',#94076,2.);
#29238=CIRCLE('',#94077,2.);
#29239=CIRCLE('',#94084,2.);
#29240=CIRCLE('',#94085,1.47499999999998);
#29241=CIRCLE('',#94088,2.);
#29242=CIRCLE('',#94090,2.5);
#29243=CIRCLE('',#94092,2.5);
#29244=CIRCLE('',#94095,2.);
#29245=CIRCLE('',#94096,1.47499999999998);
#29246=CIRCLE('',#94099,2.);
#29247=CIRCLE('',#94101,2.5);
#29248=CIRCLE('',#94103,2.5);
#29249=CIRCLE('',#94106,5.);
#29250=CIRCLE('',#94107,5.);
#29251=CIRCLE('',#94109,3.);
#29252=CIRCLE('',#94110,3.);
#29253=CIRCLE('',#94112,0.499999999999997);
#29254=CIRCLE('',#94113,0.499999999999997);
#29255=CIRCLE('',#94114,2.5);
#29256=CIRCLE('',#94115,0.499999999999999);
#29257=CIRCLE('',#94117,3.);
#29258=CIRCLE('',#94118,3.);
#29259=CIRCLE('',#94121,1.);
#29260=CIRCLE('',#94122,1.);
#29261=CIRCLE('',#94123,2.);
#29262=CIRCLE('',#94125,3.);
#29263=CIRCLE('',#94126,3.);
#29264=CIRCLE('',#94129,0.999999999999996);
#29265=CIRCLE('',#94130,1.);
#29266=CIRCLE('',#94131,2.);
#29267=CIRCLE('',#94134,0.5);
#29268=CIRCLE('',#94135,0.500000000000004);
#29269=CIRCLE('',#94137,0.5);
#29270=CIRCLE('',#94139,58.2938077870648);
#29271=CIRCLE('',#94140,0.999575812491136);
#29272=CIRCLE('',#94141,58.3875000000282);
#29273=CIRCLE('',#94144,0.5);
#29274=CIRCLE('',#94145,0.5);
#29275=CIRCLE('',#94146,0.5);
#29276=CIRCLE('',#94147,0.5);
#29277=CIRCLE('',#94148,0.499999999999999);
#29278=CIRCLE('',#94149,57.7596339908719);
#29279=CIRCLE('',#94150,0.499999999999994);
#29280=CIRCLE('',#94151,67.9400604629212);
#29281=CIRCLE('',#94152,0.5);
#29282=CIRCLE('',#94154,0.5);
#29283=CIRCLE('',#94156,58.2938077870648);
#29284=CIRCLE('',#94158,58.3875000000282);
#29285=CIRCLE('',#94161,0.5);
#29286=CIRCLE('',#94162,0.5);
#29287=CIRCLE('',#94163,0.5);
#29288=CIRCLE('',#94164,0.499999999999998);
#29289=CIRCLE('',#94166,58.3875000000282);
#29290=CIRCLE('',#94167,0.499999999999999);
#29291=CIRCLE('',#94168,58.8875000000282);
#29292=CIRCLE('',#94169,0.5);
#29293=CIRCLE('',#94171,0.5);
#29294=CIRCLE('',#94173,58.2938077870648);
#29295=CIRCLE('',#94175,58.3875000000282);
#29296=CIRCLE('',#94178,0.5);
#29297=CIRCLE('',#94179,0.5);
#29298=CIRCLE('',#94180,0.499999999999997);
#29299=CIRCLE('',#94182,58.3875000000282);
#29300=CIRCLE('',#94183,58.8875000000282);
#29301=CIRCLE('',#94185,5.);
#29302=CIRCLE('',#94187,58.2060351304332);
#29303=CIRCLE('',#94188,0.999999999999997);
#29304=CIRCLE('',#94189,58.3875000000282);
#29305=CIRCLE('',#94191,0.5);
#29306=CIRCLE('',#94192,0.5);
#29307=CIRCLE('',#94193,0.499999999999999);
#29308=CIRCLE('',#94195,0.5);
#29309=CIRCLE('',#94196,58.8875000000282);
#29310=CIRCLE('',#94197,58.3875000000282);
#29311=CIRCLE('',#94198,0.5);
#29312=CIRCLE('',#94200,0.5);
#29313=CIRCLE('',#94202,58.2938077870648);
#29314=CIRCLE('',#94204,58.3875000000282);
#29315=CIRCLE('',#94207,0.5);
#29316=CIRCLE('',#94208,0.5);
#29317=CIRCLE('',#94209,0.499999999999999);
#29318=CIRCLE('',#94210,0.500000000000003);
#29319=CIRCLE('',#94211,64.7291249062775);
#29320=CIRCLE('',#94212,56.5371804123853);
#29321=CIRCLE('',#94213,0.5);
#29322=CIRCLE('',#94215,0.5);
#29323=CIRCLE('',#94217,58.2938077870648);
#29324=CIRCLE('',#94219,58.3875000000282);
#29325=CIRCLE('',#94220,0.991843022345032);
#29326=CIRCLE('',#94222,0.5);
#29327=CIRCLE('',#94223,0.5);
#29328=CIRCLE('',#94224,0.5);
#29329=CIRCLE('',#94225,0.500000000000002);
#29330=CIRCLE('',#94226,68.2241973717388);
#29331=CIRCLE('',#94227,57.986356128794);
#29332=CIRCLE('',#94228,0.5);
#29333=CIRCLE('',#94230,0.5);
#29334=CIRCLE('',#94231,0.500000000000004);
#29335=CIRCLE('',#94232,0.499999999999998);
#29336=CIRCLE('',#94234,0.500000000000002);
#29337=CIRCLE('',#94235,4.5);
#29338=CIRCLE('',#94236,0.5);
#29339=CIRCLE('',#94238,5.);
#29340=CIRCLE('',#94239,5.);
#29341=CIRCLE('',#94240,1.41062672174051);
#29342=CIRCLE('',#94242,58.3875000000282);
#29343=CIRCLE('',#94243,58.3875000000282);
#29344=CIRCLE('',#94244,58.3875000000282);
#29345=CIRCLE('',#94245,58.3875000000282);
#29346=CIRCLE('',#94246,57.8151740222928);
#29347=CIRCLE('',#94247,58.3875000000282);
#29348=CIRCLE('',#94248,57.9944820942039);
#29349=CIRCLE('',#94249,58.3875000000282);
#29350=CIRCLE('',#94250,57.7939200862669);
#29351=CIRCLE('',#94251,58.3875000000282);
#29352=CIRCLE('',#94252,58.3875000000282);
#29353=CIRCLE('',#94253,58.3875000000282);
#29354=CIRCLE('',#94254,0.500000000000002);
#29355=CIRCLE('',#94255,0.499999999999999);
#29356=CIRCLE('',#94257,0.500000000000002);
#29357=CIRCLE('',#94258,4.5);
#29358=CIRCLE('',#94259,0.5);
#29359=CIRCLE('',#94261,3.);
#29360=CIRCLE('',#94262,3.);
#29361=CIRCLE('',#94266,0.999999999999997);
#29362=CIRCLE('',#94267,1.);
#29363=CIRCLE('',#94268,2.);
#29364=CIRCLE('',#94270,3.);
#29365=CIRCLE('',#94271,3.);
#29366=CIRCLE('',#94274,0.999999999999996);
#29367=CIRCLE('',#94275,0.999999999999997);
#29368=CIRCLE('',#94276,2.);
#29369=CIRCLE('',#94278,0.5);
#29370=CIRCLE('',#94280,0.5);
#29371=CIRCLE('',#94282,58.2938077870648);
#29372=CIRCLE('',#94286,0.5);
#29373=CIRCLE('',#94287,0.5);
#29374=CIRCLE('',#94288,0.499999999999999);
#29375=CIRCLE('',#94290,0.500000000000001);
#29376=CIRCLE('',#94291,58.8875000000282);
#29377=CIRCLE('',#94292,0.5);
#29378=CIRCLE('',#94294,0.5);
#29379=CIRCLE('',#94296,58.2938077870648);
#29380=CIRCLE('',#94300,0.5);
#29381=CIRCLE('',#94301,0.5);
#29382=CIRCLE('',#94302,0.500000000000001);
#29383=CIRCLE('',#94303,0.499999999999998);
#29384=CIRCLE('',#94304,67.9880753527063);
#29385=CIRCLE('',#94305,0.5);
#29386=CIRCLE('',#94307,0.5);
#29387=CIRCLE('',#94309,58.2938077870648);
#29388=CIRCLE('',#94311,0.999496026332483);
#29389=CIRCLE('',#94313,0.5);
#29390=CIRCLE('',#94314,0.5);
#29391=CIRCLE('',#94315,0.499999999999998);
#29392=CIRCLE('',#94316,0.499999999999999);
#29393=CIRCLE('',#94317,68.156308837608);
#29394=CIRCLE('',#94318,0.5);
#29395=CIRCLE('',#94320,0.5);
#29396=CIRCLE('',#94322,58.2938077870648);
#29397=CIRCLE('',#94323,0.999648707757584);
#29398=CIRCLE('',#94326,0.5);
#29399=CIRCLE('',#94327,0.5);
#29400=CIRCLE('',#94328,0.499999999999997);
#29401=CIRCLE('',#94329,0.500000000000001);
#29402=CIRCLE('',#94330,68.0319603210185);
#29403=CIRCLE('',#94331,0.5);
#29404=CIRCLE('',#94333,0.5);
#29405=CIRCLE('',#94335,58.2938077870648);
#29406=CIRCLE('',#94339,0.5);
#29407=CIRCLE('',#94340,0.5);
#29408=CIRCLE('',#94341,0.500000000000001);
#29409=CIRCLE('',#94343,0.499999999999998);
#29410=CIRCLE('',#94344,58.8875000000282);
#29411=CIRCLE('',#94345,0.5);
#29412=CIRCLE('',#94347,0.5);
#29413=CIRCLE('',#94349,58.2938077870648);
#29414=CIRCLE('',#94353,0.5);
#29415=CIRCLE('',#94354,0.5);
#29416=CIRCLE('',#94357,0.5);
#29417=CIRCLE('',#94358,0.5);
#29418=CIRCLE('',#94359,0.500000000000005);
#29419=CIRCLE('',#94361,0.500000000000005);
#29420=CIRCLE('',#94362,0.5);
#29421=CIRCLE('',#94364,0.5);
#29422=CIRCLE('',#94366,0.5);
#29423=CIRCLE('',#94368,0.5);
#29424=CIRCLE('',#94369,0.999999999999996);
#29425=CIRCLE('',#94372,0.5);
#29426=CIRCLE('',#94373,0.5);
#29427=CIRCLE('',#94374,0.500000000000005);
#29428=CIRCLE('',#94376,0.500000000000005);
#29429=CIRCLE('',#94377,0.5);
#29430=CIRCLE('',#94379,0.5);
#29431=CIRCLE('',#94381,1.);
#29432=CIRCLE('',#94384,0.5);
#29433=CIRCLE('',#94385,0.5);
#29434=CIRCLE('',#94386,0.499999999999999);
#29435=CIRCLE('',#94388,0.499999999999999);
#29436=CIRCLE('',#94389,0.5);
#29437=CIRCLE('',#94391,0.5);
#29438=CIRCLE('',#94394,0.5);
#29439=CIRCLE('',#94395,0.5);
#29440=CIRCLE('',#94396,0.499999999999999);
#29441=CIRCLE('',#94398,0.499999999999999);
#29442=CIRCLE('',#94399,0.5);
#29443=CIRCLE('',#94401,0.5);
#29444=CIRCLE('',#94405,0.5);
#29445=CIRCLE('',#94406,0.5);
#29446=CIRCLE('',#94407,0.499999999999999);
#29447=CIRCLE('',#94409,0.499999999999999);
#29448=CIRCLE('',#94410,0.5);
#29449=CIRCLE('',#94412,0.5);
#29450=CIRCLE('',#94414,0.5);
#29451=CIRCLE('',#94417,0.5);
#29452=CIRCLE('',#94418,0.999999999999998);
#29453=CIRCLE('',#94419,1.);
#29454=CIRCLE('',#94422,0.5);
#29455=CIRCLE('',#94423,0.5);
#29456=CIRCLE('',#94424,0.499999999999999);
#29457=CIRCLE('',#94426,0.499999999999999);
#29458=CIRCLE('',#94427,0.5);
#29459=CIRCLE('',#94429,0.5);
#29460=CIRCLE('',#94430,1.);
#29461=CIRCLE('',#94432,0.5);
#29462=CIRCLE('',#94433,0.5);
#29463=CIRCLE('',#94437,0.5);
#29464=CIRCLE('',#94438,0.5);
#29465=CIRCLE('',#94439,0.499999999999998);
#29466=CIRCLE('',#94441,0.499999999999998);
#29467=CIRCLE('',#94442,0.5);
#29468=CIRCLE('',#94444,0.5);
#29469=CIRCLE('',#94447,0.5);
#29470=CIRCLE('',#94448,0.5);
#29471=CIRCLE('',#94449,0.499999999999998);
#29472=CIRCLE('',#94451,0.499999999999998);
#29473=CIRCLE('',#94452,0.5);
#29474=CIRCLE('',#94453,0.5);
#29475=CIRCLE('',#94455,0.5);
#29476=CIRCLE('',#94456,0.5);
#29477=CIRCLE('',#94459,0.5);
#29478=CIRCLE('',#94460,59.);
#29479=CIRCLE('',#94461,0.5);
#29480=CIRCLE('',#94462,2.75);
#29481=CIRCLE('',#94464,2.75);
#29482=CIRCLE('',#94465,2.75);
#29483=CIRCLE('',#94468,0.5);
#29484=CIRCLE('',#94469,0.499999999999999);
#29485=CIRCLE('',#94472,0.500000000000001);
#29486=CIRCLE('',#94473,0.5);
#29487=CIRCLE('',#94475,0.5);
#29488=CIRCLE('',#94476,1.);
#29489=CIRCLE('',#94477,0.5);
#29490=CIRCLE('',#94478,0.5);
#29491=CIRCLE('',#94480,0.5);
#29492=CIRCLE('',#94482,3.);
#29493=CIRCLE('',#94483,3.);
#29494=CIRCLE('',#94485,0.5);
#29495=CIRCLE('',#94487,1.);
#29496=CIRCLE('',#94488,0.5);
#29497=CIRCLE('',#94489,0.5);
#29498=CIRCLE('',#94491,0.5);
#29499=CIRCLE('',#94493,1.);
#29500=CIRCLE('',#94494,0.5);
#29501=CIRCLE('',#94495,0.5);
#29502=CIRCLE('',#94497,0.5);
#29503=CIRCLE('',#94500,44.2689250265968);
#29504=CIRCLE('',#94502,45.1752328136335);
#29505=CIRCLE('',#94504,0.5);
#29506=CIRCLE('',#94505,0.5);
#29507=CIRCLE('',#94507,1.);
#29508=CIRCLE('',#94508,0.5);
#29509=CIRCLE('',#94509,0.5);
#29510=CIRCLE('',#94511,0.5);
#29511=CIRCLE('',#94513,0.999999999999999);
#29512=CIRCLE('',#94514,0.5);
#29513=CIRCLE('',#94515,0.5);
#29514=CIRCLE('',#94517,0.5);
#29515=CIRCLE('',#94519,45.1752328136335);
#29516=CIRCLE('',#94520,1.);
#29517=CIRCLE('',#94521,1.02387173403494);
#29518=CIRCLE('',#94522,1.);
#29519=CIRCLE('',#94524,1.);
#29520=CIRCLE('',#94526,0.5);
#29521=CIRCLE('',#94527,0.5);
#29522=CIRCLE('',#94529,1.);
#29523=CIRCLE('',#94530,0.5);
#29524=CIRCLE('',#94531,0.5);
#29525=CIRCLE('',#94533,0.5);
#29526=CIRCLE('',#94535,1.);
#29527=CIRCLE('',#94536,0.5);
#29528=CIRCLE('',#94537,0.5);
#29529=CIRCLE('',#94539,0.5);
#29530=CIRCLE('',#94541,1.);
#29531=CIRCLE('',#94542,1.);
#29532=CIRCLE('',#94544,0.5);
#29533=CIRCLE('',#94545,0.5);
#29534=CIRCLE('',#94547,1.);
#29535=CIRCLE('',#94548,0.5);
#29536=CIRCLE('',#94549,0.5);
#29537=CIRCLE('',#94551,0.5);
#29538=CIRCLE('',#94553,1.);
#29539=CIRCLE('',#94554,0.5);
#29540=CIRCLE('',#94555,0.5);
#29541=CIRCLE('',#94557,0.5);
#29542=CIRCLE('',#94559,1.);
#29543=CIRCLE('',#94560,1.);
#29544=CIRCLE('',#94562,0.5);
#29545=CIRCLE('',#94565,3.);
#29546=CIRCLE('',#94567,0.5);
#29547=CIRCLE('',#94568,4.5);
#29548=CIRCLE('',#94569,0.500000000000003);
#29549=CIRCLE('',#94570,5.);
#29550=CIRCLE('',#94572,0.499999999999999);
#29551=CIRCLE('',#94574,5.);
#29552=CIRCLE('',#94576,0.250000000000003);
#29553=CIRCLE('',#94577,0.249999999999998);
#29554=CIRCLE('',#94578,5.25);
#29555=CIRCLE('',#94580,0.250000000000003);
#29556=CIRCLE('',#94582,0.250000000000003);
#29557=CIRCLE('',#94583,3.);
#29558=CIRCLE('',#94584,2.75);
#29559=CIRCLE('',#94586,0.250000000000003);
#29560=CIRCLE('',#94587,67.5);
#29561=CIRCLE('',#94588,67.25);
#29562=CIRCLE('',#94590,0.249999999999997);
#29563=CIRCLE('',#94591,3.);
#29564=CIRCLE('',#94592,2.75);
#29565=CIRCLE('',#94594,0.249999999999997);
#29566=CIRCLE('',#94596,0.249999999999997);
#29567=CIRCLE('',#94597,5.);
#29568=CIRCLE('',#94598,5.25);
#29569=CIRCLE('',#94600,0.249999999999997);
#29570=CIRCLE('',#94601,58.5);
#29571=CIRCLE('',#94602,58.25);
#29572=CIRCLE('',#94604,0.249999999999997);
#29573=CIRCLE('',#94605,5.);
#29574=CIRCLE('',#94606,5.25);
#29575=CIRCLE('',#94608,0.250000000000003);
#29576=CIRCLE('',#94610,0.250000000000003);
#29577=CIRCLE('',#94611,3.);
#29578=CIRCLE('',#94612,2.75);
#29579=CIRCLE('',#94614,0.250000000000003);
#29580=CIRCLE('',#94615,67.5);
#29581=CIRCLE('',#94616,67.25);
#29582=CIRCLE('',#94618,0.250000000000003);
#29583=CIRCLE('',#94619,3.);
#29584=CIRCLE('',#94620,2.75);
#29585=CIRCLE('',#94622,0.250000000000003);
#29586=CIRCLE('',#94624,0.250000000000002);
#29587=CIRCLE('',#94625,3.);
#29588=CIRCLE('',#94626,3.25);
#29589=CIRCLE('',#94628,2.75);
#29590=CIRCLE('',#94629,2.75);
#29591=CIRCLE('',#94630,2.75);
#29592=CIRCLE('',#94631,2.75);
#29593=CIRCLE('',#94633,2.75);
#29594=CIRCLE('',#94634,2.75);
#29595=CIRCLE('',#94635,2.75);
#29596=CIRCLE('',#94636,0.5);
#29597=CIRCLE('',#94637,0.500000000000001);
#29598=CIRCLE('',#94639,0.5);
#29599=CIRCLE('',#94641,58.5);
#29600=CIRCLE('',#94643,58.4063077870367);
#29601=CIRCLE('',#94646,0.5);
#29602=CIRCLE('',#94647,0.5);
#29603=CIRCLE('',#94648,0.500000000000002);
#29604=CIRCLE('',#94650,0.500000000000005);
#29605=CIRCLE('',#94651,59.);
#29606=CIRCLE('',#94652,58.5);
#29607=CIRCLE('',#94653,0.5);
#29608=CIRCLE('',#94655,0.5);
#29609=CIRCLE('',#94657,58.5);
#29610=CIRCLE('',#94659,58.4063077870367);
#29611=CIRCLE('',#94662,0.5);
#29612=CIRCLE('',#94663,0.5);
#29613=CIRCLE('',#94664,0.499999999999999);
#29614=CIRCLE('',#94665,0.500000000000005);
#29615=CIRCLE('',#94666,68.1417998565621);
#29616=CIRCLE('',#94667,57.9169670944157);
#29617=CIRCLE('',#94668,0.5);
#29618=CIRCLE('',#94670,0.5);
#29619=CIRCLE('',#94672,58.5);
#29620=CIRCLE('',#94673,0.999577393236284);
#29621=CIRCLE('',#94674,58.4063077870366);
#29622=CIRCLE('',#94677,0.5);
#29623=CIRCLE('',#94678,0.5);
#29624=CIRCLE('',#94679,0.500000000000002);
#29625=CIRCLE('',#94681,0.499999999999999);
#29626=CIRCLE('',#94682,0.499999999999998);
#29627=CIRCLE('',#94684,59.);
#29628=CIRCLE('',#94685,58.5);
#29629=CIRCLE('',#94686,0.5);
#29630=CIRCLE('',#94688,0.5);
#29631=CIRCLE('',#94689,0.499999999999994);
#29632=CIRCLE('',#94696,0.499999999999998);
#29633=CIRCLE('',#94700,0.5);
#29634=CIRCLE('',#94701,0.5);
#29635=CIRCLE('',#94702,0.500000000000005);
#29636=CIRCLE('',#94707,0.500000000000001);
#29637=CIRCLE('',#94710,2.5);
#29638=CIRCLE('',#94711,2.5);
#29639=CIRCLE('',#94714,0.5);
#29640=CIRCLE('',#94717,0.5);
#29641=CIRCLE('',#94718,0.499999999999997);
#29642=CIRCLE('',#94721,2.5);
#29643=CIRCLE('',#94722,2.5);
#29644=CIRCLE('',#94725,0.499999999999998);
#29645=CIRCLE('',#94728,2.5);
#29646=CIRCLE('',#94729,2.5);
#29647=CIRCLE('',#94732,0.5);
#29648=CIRCLE('',#94734,58.1182624738004);
#29649=CIRCLE('',#94735,0.99506488582092);
#29650=CIRCLE('',#94737,0.500000000000003);
#29651=CIRCLE('',#94739,2.5);
#29652=CIRCLE('',#94740,0.5);
#29653=CIRCLE('',#94741,0.491297296893067);
#29654=CIRCLE('',#94743,0.5);
#29655=CIRCLE('',#94746,0.5);
#29656=CIRCLE('',#94749,0.5);
#29657=CIRCLE('',#94750,2.5);
#29658=CIRCLE('',#94751,0.500000000000001);
#29659=CIRCLE('',#94754,0.499999999999999);
#29660=CIRCLE('',#94756,0.551233577645565);
#29661=CIRCLE('',#94757,0.5);
#29662=CIRCLE('',#94758,64.5806717409052);
#29663=CIRCLE('',#94759,0.5);
#29664=CIRCLE('',#94760,0.500000000000002);
#29665=CIRCLE('',#94765,0.500000000000001);
#29666=CIRCLE('',#94767,0.5);
#29667=CIRCLE('',#94768,0.5);
#29668=CIRCLE('',#94771,0.5);
#29669=CIRCLE('',#94774,0.5);
#29670=CIRCLE('',#94776,0.5);
#29671=CIRCLE('',#94779,0.5);
#29672=CIRCLE('',#94781,2.5);
#29673=CIRCLE('',#94782,2.5);
#29674=CIRCLE('',#94785,0.499999999999998);
#29675=CIRCLE('',#94788,0.499999999999997);
#29676=CIRCLE('',#94790,2.5);
#29677=CIRCLE('',#94791,2.5);
#29678=CIRCLE('',#94794,0.5);
#29679=CIRCLE('',#94797,0.5);
#29680=CIRCLE('',#94798,0.5);
#29681=CIRCLE('',#94802,2.5);
#29682=CIRCLE('',#94803,2.5);
#29683=CIRCLE('',#94805,0.499999999999998);
#29684=CIRCLE('',#94809,0.5);
#29685=CIRCLE('',#94810,0.5);
#29686=CIRCLE('',#94811,0.499999999999998);
#29687=CIRCLE('',#94816,0.500000000000002);
#29688=CIRCLE('',#94822,0.5);
#29689=CIRCLE('',#94823,109.36143880173);
#29690=CIRCLE('',#94824,0.5);
#29691=CIRCLE('',#94825,0.5);
#29692=CIRCLE('',#94832,0.5);
#29693=CIRCLE('',#94836,0.5);
#29694=CIRCLE('',#94837,0.5);
#29695=CIRCLE('',#94838,0.500000000000001);
#29696=CIRCLE('',#94844,0.500000000000003);
#29697=CIRCLE('',#94846,2.5);
#29698=CIRCLE('',#94847,2.5);
#29699=CIRCLE('',#94850,0.5);
#29700=CIRCLE('',#94853,0.5);
#29701=CIRCLE('',#94854,0.499999999999999);
#29702=CIRCLE('',#94858,2.5);
#29703=CIRCLE('',#94859,2.5);
#29704=CIRCLE('',#94862,0.499999999999999);
#29705=CIRCLE('',#94865,2.5);
#29706=CIRCLE('',#94866,2.5);
#29707=CIRCLE('',#94868,59.024570260837);
#29708=CIRCLE('',#94869,0.5);
#29709=CIRCLE('',#94870,0.5);
#29710=CIRCLE('',#94872,2.5);
#29711=CIRCLE('',#94873,2.5);
#29712=CIRCLE('',#94875,0.5);
#29713=CIRCLE('',#94878,0.5);
#29714=CIRCLE('',#94880,2.5);
#29715=CIRCLE('',#94881,2.5);
#29716=CIRCLE('',#94882,0.5);
#29717=CIRCLE('',#94883,0.5);
#29718=CIRCLE('',#94885,2.5);
#29719=CIRCLE('',#94886,2.5);
#29720=CIRCLE('',#94889,58.1182624738004);
#29721=CIRCLE('',#94891,59.024570260837);
#29722=CIRCLE('',#94893,0.5);
#29723=CIRCLE('',#94895,2.5);
#29724=CIRCLE('',#94896,2.5);
#29725=CIRCLE('',#94898,0.5);
#29726=CIRCLE('',#94901,0.5);
#29727=CIRCLE('',#94903,2.5);
#29728=CIRCLE('',#94904,2.5);
#29729=CIRCLE('',#94906,59.024570260837);
#29730=CIRCLE('',#94907,0.5);
#29731=CIRCLE('',#94908,0.5);
#29732=CIRCLE('',#94910,2.5);
#29733=CIRCLE('',#94911,0.5);
#29734=CIRCLE('',#94913,0.5);
#29735=CIRCLE('',#94916,0.5);
#29736=CIRCLE('',#94918,0.5);
#29737=CIRCLE('',#94919,2.5);
#29738=CIRCLE('',#94920,0.499999999999997);
#29739=CIRCLE('',#94921,0.5);
#29740=CIRCLE('',#94923,2.5);
#29741=CIRCLE('',#94925,0.5);
#29742=CIRCLE('',#94928,0.5);
#29743=CIRCLE('',#94930,2.5);
#29744=CIRCLE('',#94931,0.5);
#29745=CIRCLE('',#94933,59.024570260837);
#29746=CIRCLE('',#94934,0.5);
#29747=CIRCLE('',#94935,0.5);
#29748=CIRCLE('',#94937,2.5);
#29749=CIRCLE('',#94938,2.5);
#29750=CIRCLE('',#94940,0.5);
#29751=CIRCLE('',#94943,0.5);
#29752=CIRCLE('',#94944,0.5);
#29753=CIRCLE('',#94946,2.5);
#29754=CIRCLE('',#94947,2.5);
#29755=CIRCLE('',#94948,3.5);
#29756=CIRCLE('',#94950,2.5);
#29757=CIRCLE('',#94951,2.5);
#29758=CIRCLE('',#94955,0.5);
#29759=CIRCLE('',#94957,58.1182624738004);
#29760=CIRCLE('',#94959,59.024570260837);
#29761=CIRCLE('',#94961,0.5);
#29762=CIRCLE('',#94963,2.5);
#29763=CIRCLE('',#94964,2.5);
#29764=CIRCLE('',#94966,0.5);
#29765=CIRCLE('',#94969,0.5);
#29766=CIRCLE('',#94971,2.5);
#29767=CIRCLE('',#94972,2.5);
#29768=CIRCLE('',#94974,58.1182624738004);
#29769=CIRCLE('',#94975,59.024570260837);
#29770=CIRCLE('',#94977,0.499999999999998);
#29771=CIRCLE('',#94980,2.5);
#29772=CIRCLE('',#94981,2.5);
#29773=CIRCLE('',#94982,0.5);
#29774=CIRCLE('',#94984,2.5);
#29775=CIRCLE('',#94985,2.5);
#29776=CIRCLE('',#94987,0.5);
#29777=CIRCLE('',#94990,0.5);
#29778=CIRCLE('',#94992,2.5);
#29779=CIRCLE('',#94993,2.5);
#29780=CIRCLE('',#94994,0.5);
#29781=CIRCLE('',#94996,59.024570260837);
#29782=CIRCLE('',#94997,0.5);
#29783=CIRCLE('',#94999,2.5);
#29784=CIRCLE('',#95000,2.5);
#29785=CIRCLE('',#95002,0.5);
#29786=CIRCLE('',#95005,0.5);
#29787=CIRCLE('',#95006,0.5);
#29788=CIRCLE('',#95008,2.5);
#29789=CIRCLE('',#95009,2.5);
#29790=CIRCLE('',#95012,0.5);
#29791=CIRCLE('',#95014,2.);
#29792=CIRCLE('',#95015,2.);
#29793=CIRCLE('',#95017,2.75);
#29794=CIRCLE('',#95020,0.5);
#29795=CIRCLE('',#95021,0.5);
#29796=CIRCLE('',#95022,0.5);
#29797=CIRCLE('',#95023,1.);
#29798=CIRCLE('',#95025,0.500000000000002);
#29799=CIRCLE('',#95026,58.5);
#29800=CIRCLE('',#95027,0.5);
#29801=CIRCLE('',#95028,1.);
#29802=CIRCLE('',#95031,0.5);
#29803=CIRCLE('',#95033,2.);
#29804=CIRCLE('',#95034,2.);
#29805=CIRCLE('',#95036,2.75);
#29806=CIRCLE('',#95038,2.75);
#29807=CIRCLE('',#95040,0.5);
#29808=CIRCLE('',#95042,3.);
#29809=CIRCLE('',#95043,3.);
#29810=CIRCLE('',#95045,0.5);
#29811=CIRCLE('',#95047,0.5);
#29812=CIRCLE('',#95049,0.5);
#29813=CIRCLE('',#95050,0.500000000000001);
#29814=CIRCLE('',#95051,0.500000000000002);
#29815=CIRCLE('',#95053,0.5);
#29816=CIRCLE('',#95055,0.5);
#29817=CIRCLE('',#95056,0.5);
#29818=CIRCLE('',#95060,0.500000000000001);
#29819=CIRCLE('',#95061,0.5);
#29820=CIRCLE('',#95065,0.499999999999998);
#29821=CIRCLE('',#95066,0.499999999999999);
#29822=CIRCLE('',#95070,0.5);
#29823=CIRCLE('',#95072,0.5);
#29824=CIRCLE('',#95075,0.5);
#29825=CIRCLE('',#95076,0.5);
#29826=CIRCLE('',#95078,0.5);
#29827=CIRCLE('',#95080,0.5);
#29828=CIRCLE('',#95083,0.5);
#29829=CIRCLE('',#95084,0.5);
#29830=CIRCLE('',#95086,0.5);
#29831=CIRCLE('',#95088,0.5);
#29832=CIRCLE('',#95090,0.5);
#29833=CIRCLE('',#95091,0.5);
#29834=CIRCLE('',#95092,0.5);
#29835=CIRCLE('',#95094,0.5);
#29836=CIRCLE('',#95095,0.5);
#29837=CIRCLE('',#95097,0.5);
#29838=CIRCLE('',#95100,3.);
#29839=CIRCLE('',#95102,67.5);
#29840=CIRCLE('',#95104,3.);
#29841=CIRCLE('',#95109,58.5);
#29842=CIRCLE('',#95110,58.5);
#29843=CIRCLE('',#95111,58.5);
#29844=CIRCLE('',#95113,58.5);
#29845=CIRCLE('',#95114,57.9482170030838);
#29846=CIRCLE('',#95115,58.5);
#29847=CIRCLE('',#95116,58.1064453881508);
#29848=CIRCLE('',#95117,58.5);
#29849=CIRCLE('',#95118,57.9666974474879);
#29850=CIRCLE('',#95119,58.5);
#29851=CIRCLE('',#95120,58.5);
#29852=CIRCLE('',#95121,58.5);
#29853=CIRCLE('',#95122,58.5);
#29854=CIRCLE('',#95126,3.);
#29855=CIRCLE('',#95128,67.5);
#29856=CIRCLE('',#95130,3.);
#29857=CIRCLE('',#95132,0.5);
#29858=CIRCLE('',#95133,0.5);
#29859=CIRCLE('',#95135,2.);
#29860=CIRCLE('',#95136,66.5);
#29861=CIRCLE('',#95137,2.);
#29862=CIRCLE('',#95138,0.5);
#29863=CIRCLE('',#95139,0.5);
#29864=CIRCLE('',#95141,0.5);
#29865=CIRCLE('',#95142,0.5);
#29866=CIRCLE('',#95143,0.5);
#29867=CIRCLE('',#95145,2.);
#29868=CIRCLE('',#95146,66.5);
#29869=CIRCLE('',#95147,2.);
#29870=CIRCLE('',#95150,0.5);
#29871=CIRCLE('',#95151,0.499999999999997);
#29872=CIRCLE('',#95153,0.499999999999998);
#29873=CIRCLE('',#95155,0.5);
#29874=CIRCLE('',#95158,0.5);
#29875=CIRCLE('',#95159,0.499999999999994);
#29876=CIRCLE('',#95161,0.500000000000001);
#29877=CIRCLE('',#95162,0.5);
#29878=CIRCLE('',#95163,0.5);
#29879=CIRCLE('',#95164,0.500000000000002);
#29880=CIRCLE('',#95166,0.500000000000003);
#29881=CIRCLE('',#95168,0.5);
#29882=CIRCLE('',#95169,0.5);
#29883=CIRCLE('',#95170,0.999999999999994);
#29884=CIRCLE('',#95172,0.5);
#29885=CIRCLE('',#95174,0.499999999999999);
#29886=CIRCLE('',#95175,0.499999999999998);
#29887=CIRCLE('',#95176,0.5);
#29888=CIRCLE('',#95179,0.5);
#29889=CIRCLE('',#95181,0.499999999999998);
#29890=CIRCLE('',#95182,0.5);
#29891=CIRCLE('',#95184,0.5);
#29892=CIRCLE('',#95185,0.499999999999998);
#29893=CIRCLE('',#95189,0.500000000000003);
#29894=CIRCLE('',#95190,0.499999999999994);
#29895=CIRCLE('',#95191,0.5);
#29896=CIRCLE('',#95193,0.5);
#29897=CIRCLE('',#95194,0.499999999999999);
#29898=CIRCLE('',#95195,0.5);
#29899=CIRCLE('',#95197,0.5);
#29900=CIRCLE('',#95198,0.499999999999999);
#29901=CIRCLE('',#95200,0.5);
#29902=CIRCLE('',#95201,3.);
#29903=CIRCLE('',#95203,0.5);
#29904=CIRCLE('',#95205,3.);
#29905=CIRCLE('',#95207,3.);
#29906=CIRCLE('',#95209,0.5);
#29907=CIRCLE('',#95210,0.499999999999999);
#29908=CIRCLE('',#95211,0.500000000000003);
#29909=CIRCLE('',#95212,0.5);
#29910=CIRCLE('',#95214,0.5);
#29911=CIRCLE('',#95216,0.5);
#29912=CIRCLE('',#95218,3.);
#29913=CIRCLE('',#95219,0.499999999999997);
#29914=CIRCLE('',#95220,0.5);
#29915=CIRCLE('',#95222,0.5);
#29916=CIRCLE('',#95223,0.500000000000003);
#29917=CIRCLE('',#95225,0.5);
#29918=CIRCLE('',#95226,3.);
#29919=CIRCLE('',#95228,0.5);
#29920=CIRCLE('',#95231,0.500000000000002);
#29921=CIRCLE('',#95232,0.499999999999999);
#29922=CIRCLE('',#95233,0.5);
#29923=CIRCLE('',#95234,0.5);
#29924=CIRCLE('',#95237,3.);
#29925=CIRCLE('',#95239,3.);
#29926=CIRCLE('',#95242,0.5);
#29927=CIRCLE('',#95243,0.500000000000001);
#29928=CIRCLE('',#95244,0.500000000000001);
#29929=CIRCLE('',#95246,3.);
#29930=CIRCLE('',#95247,0.5);
#29931=CIRCLE('',#95249,3.);
#29932=CIRCLE('',#95251,0.5);
#29933=CIRCLE('',#95253,3.);
#29934=CIRCLE('',#95254,0.5);
#29935=CIRCLE('',#95256,3.);
#29936=CIRCLE('',#95258,0.5);
#29937=CIRCLE('',#95260,0.5);
#29938=CIRCLE('',#95262,0.5);
#29939=CIRCLE('',#95263,0.5);
#29940=CIRCLE('',#95264,0.499999999999994);
#29941=CIRCLE('',#95266,0.500000000000001);
#29942=CIRCLE('',#95267,0.5);
#29943=CIRCLE('',#95269,0.5);
#29944=CIRCLE('',#95270,0.500000000000001);
#29945=CIRCLE('',#95272,0.5);
#29946=CIRCLE('',#95274,3.);
#29947=CIRCLE('',#95275,0.500000000000002);
#29948=CIRCLE('',#95276,0.5);
#29949=CIRCLE('',#95278,0.5);
#29950=CIRCLE('',#95279,0.500000000000003);
#29951=CIRCLE('',#95280,0.500000000000001);
#29952=CIRCLE('',#95281,0.5);
#29953=CIRCLE('',#95284,0.5);
#29954=CIRCLE('',#95286,0.5);
#29955=CIRCLE('',#95288,0.5);
#29956=CIRCLE('',#95289,3.);
#29957=CIRCLE('',#95291,0.5);
#29958=CIRCLE('',#95293,3.);
#29959=CIRCLE('',#95295,3.);
#29960=CIRCLE('',#95297,0.5);
#29961=CIRCLE('',#95298,0.500000000000001);
#29962=CIRCLE('',#95300,0.5);
#29963=CIRCLE('',#95302,0.5);
#29964=CIRCLE('',#95303,3.);
#29965=CIRCLE('',#95305,0.5);
#29966=CIRCLE('',#95306,0.5);
#29967=CIRCLE('',#95307,0.500000000000002);
#29968=CIRCLE('',#95309,0.499999999999994);
#29969=CIRCLE('',#95310,0.5);
#29970=CIRCLE('',#95312,0.5);
#29971=CIRCLE('',#95313,0.500000000000001);
#29972=CIRCLE('',#95314,0.5);
#29973=CIRCLE('',#95316,0.5);
#29974=CIRCLE('',#95317,0.500000000000001);
#29975=CIRCLE('',#95318,0.499999999999999);
#29976=CIRCLE('',#95319,0.5);
#29977=CIRCLE('',#95322,0.5);
#29978=CIRCLE('',#95323,0.5);
#29979=CIRCLE('',#95327,0.5);
#29980=CIRCLE('',#95328,0.5);
#29981=CIRCLE('',#95330,0.5);
#29982=CIRCLE('',#95331,0.5);
#29983=CIRCLE('',#95332,0.500000000000003);
#29984=CIRCLE('',#95334,0.500000000000006);
#29985=CIRCLE('',#95335,0.5);
#29986=CIRCLE('',#95337,0.5);
#29987=CIRCLE('',#95339,0.499999999999999);
#29988=CIRCLE('',#95340,0.5);
#29989=CIRCLE('',#95342,0.5);
#29990=CIRCLE('',#95343,0.499999999999999);
#29991=CIRCLE('',#95345,0.500000000000001);
#29992=CIRCLE('',#95346,0.5);
#29993=CIRCLE('',#95347,0.999497967753729);
#29994=CIRCLE('',#95349,0.5);
#29995=CIRCLE('',#95350,0.5);
#29996=CIRCLE('',#95353,98.8061397010869);
#29997=CIRCLE('',#95355,0.5);
#29998=CIRCLE('',#95356,0.5);
#29999=CIRCLE('',#95358,0.5);
#30000=CIRCLE('',#95359,0.5);
#30001=CIRCLE('',#95360,0.499999999999996);
#30002=CIRCLE('',#95361,0.999650016963681);
#30003=CIRCLE('',#95362,0.499999999999999);
#30004=CIRCLE('',#95363,0.5);
#30005=CIRCLE('',#95366,0.5);
#30006=CIRCLE('',#95368,0.500000000000002);
#30007=CIRCLE('',#95369,0.5);
#30008=CIRCLE('',#95371,0.5);
#30009=CIRCLE('',#95372,0.500000000000002);
#30010=CIRCLE('',#95373,0.499999999999998);
#30011=CIRCLE('',#95374,0.5);
#30012=CIRCLE('',#95377,0.5);
#30013=CIRCLE('',#95378,0.5);
#30014=CIRCLE('',#95382,0.5);
#30015=CIRCLE('',#95383,0.499999999999999);
#30016=CIRCLE('',#95385,0.5);
#30017=CIRCLE('',#95386,0.5);
#30018=CIRCLE('',#95387,0.499999999999999);
#30019=CIRCLE('',#95389,0.500000000000002);
#30020=CIRCLE('',#95390,0.5);
#30021=CIRCLE('',#95392,0.5);
#30022=CIRCLE('',#95393,0.499999999999999);
#30023=CIRCLE('',#95394,0.5);
#30024=CIRCLE('',#95396,0.5);
#30025=CIRCLE('',#95397,0.499999999999999);
#30026=CIRCLE('',#95398,0.499999999999998);
#30027=CIRCLE('',#95399,0.5);
#30028=CIRCLE('',#95402,0.5);
#30029=CIRCLE('',#95404,0.5);
#30030=CIRCLE('',#95405,3.);
#30031=CIRCLE('',#95406,0.5);
#30032=CIRCLE('',#95408,0.5);
#30033=CIRCLE('',#95410,3.);
#30034=CIRCLE('',#95412,3.);
#30035=CIRCLE('',#95414,0.5);
#30036=CIRCLE('',#95415,0.500000000000003);
#30037=CIRCLE('',#95417,0.5);
#30038=CIRCLE('',#95419,0.5);
#30039=CIRCLE('',#95420,3.);
#30040=CIRCLE('',#95423,0.5);
#30041=CIRCLE('',#95424,0.5);
#30042=CIRCLE('',#95425,0.499999999999996);
#30043=CIRCLE('',#95427,0.499999999999997);
#30044=CIRCLE('',#95428,0.5);
#30045=CIRCLE('',#95430,0.5);
#30046=CIRCLE('',#95431,0.500000000000002);
#30047=CIRCLE('',#95432,0.499999999999999);
#30048=CIRCLE('',#95433,0.5);
#30049=CIRCLE('',#95436,0.5);
#30050=CIRCLE('',#95438,0.5);
#30051=CIRCLE('',#95440,0.5);
#30052=CIRCLE('',#95441,3.);
#30053=CIRCLE('',#95443,0.5);
#30054=CIRCLE('',#95445,0.5);
#30055=CIRCLE('',#95446,0.499999999999997);
#30056=CIRCLE('',#95447,0.999999999999999);
#30057=CIRCLE('',#95449,0.5);
#30058=CIRCLE('',#95451,0.5);
#30059=CIRCLE('',#95453,58.1182624738004);
#30060=CIRCLE('',#95454,0.5);
#30061=CIRCLE('',#95455,0.5);
#30062=CIRCLE('',#95456,0.5);
#30063=CIRCLE('',#95458,0.5);
#30064=CIRCLE('',#95460,0.5);
#30065=CIRCLE('',#95462,0.5);
#30066=CIRCLE('',#95463,3.);
#30067=CIRCLE('',#95465,0.5);
#30068=CIRCLE('',#95467,3.);
#30069=CIRCLE('',#95468,0.500000000000002);
#30070=CIRCLE('',#95469,0.5);
#30071=CIRCLE('',#95471,0.5);
#30072=CIRCLE('',#95472,0.499999999999999);
#30073=CIRCLE('',#95473,0.499999999999993);
#30074=CIRCLE('',#95474,0.5);
#30075=CIRCLE('',#95478,3.);
#30076=CIRCLE('',#95480,0.5);
#30077=CIRCLE('',#95482,0.5);
#30078=CIRCLE('',#95484,1.);
#30079=CIRCLE('',#95485,1.);
#30080=CIRCLE('',#95487,0.5);
#30081=CIRCLE('',#95488,0.5);
#30082=CIRCLE('',#95490,0.5);
#30083=CIRCLE('',#95492,0.5);
#30084=CIRCLE('',#95493,3.);
#30085=CIRCLE('',#95496,0.5);
#30086=CIRCLE('',#95497,0.5);
#30087=CIRCLE('',#95498,0.5);
#30088=CIRCLE('',#95500,0.499999999999998);
#30089=CIRCLE('',#95501,0.5);
#30090=CIRCLE('',#95502,0.5);
#30091=CIRCLE('',#95503,0.992001837837135);
#30092=CIRCLE('',#95504,0.499999999999998);
#30093=CIRCLE('',#95505,0.5);
#30094=CIRCLE('',#95507,0.5);
#30095=CIRCLE('',#95508,0.499999999999998);
#30096=CIRCLE('',#95510,0.5);
#30097=CIRCLE('',#95512,3.);
#30098=CIRCLE('',#95514,0.500000000000004);
#30099=CIRCLE('',#95515,0.5);
#30100=CIRCLE('',#95517,0.5);
#30101=CIRCLE('',#95518,0.5);
#30102=CIRCLE('',#95520,0.5);
#30103=CIRCLE('',#95521,0.500000000000001);
#30104=CIRCLE('',#95522,0.500000000000001);
#30105=CIRCLE('',#95523,0.5);
#30106=CIRCLE('',#95525,0.5);
#30107=CIRCLE('',#95526,0.5);
#30108=CIRCLE('',#95528,0.5);
#30109=CIRCLE('',#95530,0.5);
#30110=CIRCLE('',#95532,0.5);
#30111=CIRCLE('',#95533,3.);
#30112=CIRCLE('',#95535,0.5);
#30113=CIRCLE('',#95537,3.);
#30114=CIRCLE('',#95539,3.);
#30115=CIRCLE('',#95541,0.5);
#30116=CIRCLE('',#95543,0.5);
#30117=CIRCLE('',#95545,0.5);
#30118=CIRCLE('',#95546,0.5);
#30119=CIRCLE('',#95547,0.5);
#30120=CIRCLE('',#95549,0.5);
#30121=CIRCLE('',#95550,0.500000000000001);
#30122=CIRCLE('',#95551,0.500000000000002);
#30123=CIRCLE('',#95552,0.5);
#30124=CIRCLE('',#95554,0.5);
#30125=CIRCLE('',#95555,0.500000000000001);
#30126=CIRCLE('',#95556,0.500000000000002);
#30127=CIRCLE('',#95558,0.5);
#30128=CIRCLE('',#95560,3.);
#30129=CIRCLE('',#95562,58.1182624738004);
#30130=CIRCLE('',#95564,0.5);
#30131=CIRCLE('',#95566,0.5);
#30132=CIRCLE('',#95567,0.500000000000003);
#30133=CIRCLE('',#95568,0.500000000000001);
#30134=CIRCLE('',#95569,0.5);
#30135=CIRCLE('',#95572,3.);
#30136=CIRCLE('',#95574,3.);
#30137=CIRCLE('',#95577,0.5);
#30138=CIRCLE('',#95578,0.5);
#30139=CIRCLE('',#95581,0.5);
#30140=CIRCLE('',#95583,3.);
#30141=CIRCLE('',#95585,3.);
#30142=CIRCLE('',#95588,0.5);
#30143=CIRCLE('',#95589,0.500000000000002);
#30144=CIRCLE('',#95590,0.500000000000001);
#30145=CIRCLE('',#95592,58.1182624738004);
#30146=CIRCLE('',#95594,0.5);
#30147=CIRCLE('',#95596,0.5);
#30148=CIRCLE('',#95597,0.5);
#30149=CIRCLE('',#95598,0.5);
#30150=CIRCLE('',#95599,0.5);
#30151=CIRCLE('',#95601,0.5);
#30152=CIRCLE('',#95603,0.5);
#30153=CIRCLE('',#95605,0.5);
#30154=CIRCLE('',#95606,3.);
#30155=CIRCLE('',#95608,0.5);
#30156=CIRCLE('',#95610,3.);
#30157=CIRCLE('',#95611,0.499999999999998);
#30158=CIRCLE('',#95612,0.499999999999999);
#30159=CIRCLE('',#95613,0.5);
#30160=CIRCLE('',#95615,0.5);
#30161=CIRCLE('',#95616,0.500000000000001);
#30162=CIRCLE('',#95617,0.5);
#30163=CIRCLE('',#95618,0.5);
#30164=CIRCLE('',#95621,3.);
#30165=CIRCLE('',#95623,0.5);
#30166=CIRCLE('',#95626,0.5);
#30167=CIRCLE('',#95628,0.5);
#30168=CIRCLE('',#95629,3.);
#30169=CIRCLE('',#95632,0.5);
#30170=CIRCLE('',#95633,0.5);
#30171=CIRCLE('',#95634,0.5);
#30172=CIRCLE('',#95637,0.5);
#30173=CIRCLE('',#95639,0.5);
#30174=CIRCLE('',#95641,0.5);
#30175=CIRCLE('',#95642,0.5);
#30176=CIRCLE('',#95643,0.500000000000003);
#30177=CIRCLE('',#95644,0.500000000000004);
#30178=CIRCLE('',#95645,0.992138051716334);
#30179=CIRCLE('',#95646,0.499999999999999);
#30180=CIRCLE('',#95647,0.5);
#30181=CIRCLE('',#95649,0.5);
#30182=CIRCLE('',#95650,0.500000000000001);
#30183=CIRCLE('',#95651,0.499999999999998);
#30184=CIRCLE('',#95652,0.500000000000002);
#30185=CIRCLE('',#95654,0.5);
#30186=CIRCLE('',#95656,3.);
#30187=CIRCLE('',#95658,0.499999999999997);
#30188=CIRCLE('',#95659,0.5);
#30189=CIRCLE('',#95661,0.499999999999998);
#30190=CIRCLE('',#95662,0.5);
#30191=CIRCLE('',#95664,0.5);
#30192=CIRCLE('',#95665,0.499999999999999);
#30193=CIRCLE('',#95666,0.499999999999994);
#30194=CIRCLE('',#95667,0.5);
#30195=CIRCLE('',#95669,0.5);
#30196=CIRCLE('',#95670,0.5);
#30197=CIRCLE('',#95672,0.5);
#30198=CIRCLE('',#95674,0.5);
#30199=CIRCLE('',#95676,0.5);
#30200=CIRCLE('',#95677,3.);
#30201=CIRCLE('',#95679,0.5);
#30202=CIRCLE('',#95681,3.);
#30203=CIRCLE('',#95683,3.);
#30204=CIRCLE('',#95685,0.5);
#30205=CIRCLE('',#95687,0.5);
#30206=CIRCLE('',#95689,0.5);
#30207=CIRCLE('',#95690,0.5);
#30208=CIRCLE('',#95691,0.5);
#30209=CIRCLE('',#95693,0.5);
#30210=CIRCLE('',#95694,0.499999999999994);
#30211=CIRCLE('',#95695,0.500000000000001);
#30212=CIRCLE('',#95696,0.5);
#30213=CIRCLE('',#95698,0.5);
#30214=CIRCLE('',#95699,0.499999999999999);
#30215=CIRCLE('',#95700,0.500000000000003);
#30216=CIRCLE('',#95702,0.5);
#30217=CIRCLE('',#95704,3.);
#30218=CIRCLE('',#95706,0.500000000000002);
#30219=CIRCLE('',#95707,0.499999999999999);
#30220=CIRCLE('',#95708,0.5);
#30221=CIRCLE('',#95709,0.5);
#30222=CIRCLE('',#95710,0.5);
#30223=CIRCLE('',#95712,0.5);
#30224=CIRCLE('',#95714,0.5);
#30225=CIRCLE('',#95717,0.5);
#30226=CIRCLE('',#95718,3.);
#30227=CIRCLE('',#95720,0.500000000000002);
#30228=CIRCLE('',#95721,0.5);
#30229=CIRCLE('',#95723,0.5);
#30230=CIRCLE('',#95724,0.500000000000002);
#30231=CIRCLE('',#95725,0.499999999999998);
#30232=CIRCLE('',#95727,0.5);
#30233=CIRCLE('',#95728,0.5);
#30234=CIRCLE('',#95730,0.5);
#30235=CIRCLE('',#95732,0.5);
#30236=CIRCLE('',#95734,0.5);
#30237=CIRCLE('',#95735,3.);
#30238=CIRCLE('',#95737,0.5);
#30239=CIRCLE('',#95739,3.);
#30240=CIRCLE('',#95740,0.5);
#30241=CIRCLE('',#95742,0.5);
#30242=CIRCLE('',#95744,0.5);
#30243=CIRCLE('',#95747,3.);
#30244=CIRCLE('',#95749,0.5);
#30245=CIRCLE('',#95751,0.5);
#30246=CIRCLE('',#95753,0.5);
#30247=CIRCLE('',#95754,0.5);
#30248=CIRCLE('',#95755,0.5);
#30249=CIRCLE('',#95756,0.5);
#30250=CIRCLE('',#95758,0.5);
#30251=CIRCLE('',#95759,0.499999999999996);
#30252=CIRCLE('',#95760,0.499999999999999);
#30253=CIRCLE('',#95761,0.5);
#30254=CIRCLE('',#95763,0.5);
#30255=CIRCLE('',#95764,0.499999999999999);
#30256=CIRCLE('',#95765,0.500000000000001);
#30257=CIRCLE('',#95766,0.5);
#30258=CIRCLE('',#95769,0.5);
#30259=CIRCLE('',#95771,3.);
#30260=CIRCLE('',#95773,58.1182624738004);
#30261=CIRCLE('',#95775,0.5);
#30262=CIRCLE('',#95776,0.499999999999998);
#30263=CIRCLE('',#95777,0.500000000000003);
#30264=CIRCLE('',#95778,0.5);
#30265=CIRCLE('',#95780,0.5);
#30266=CIRCLE('',#95781,0.499999999999997);
#30267=CIRCLE('',#95782,0.5);
#30268=CIRCLE('',#95783,0.5);
#30269=CIRCLE('',#95785,0.5);
#30270=CIRCLE('',#95786,0.5);
#30271=CIRCLE('',#95788,0.5);
#30272=CIRCLE('',#95790,0.5);
#30273=CIRCLE('',#95792,0.5);
#30274=CIRCLE('',#95793,3.);
#30275=CIRCLE('',#95795,0.5);
#30276=CIRCLE('',#95797,3.);
#30277=CIRCLE('',#95799,3.);
#30278=CIRCLE('',#95801,0.5);
#30279=CIRCLE('',#95804,0.5);
#30280=CIRCLE('',#95806,0.5);
#30281=CIRCLE('',#95807,0.5);
#30282=CIRCLE('',#95808,0.5);
#30283=CIRCLE('',#95809,0.5);
#30284=CIRCLE('',#95811,0.5);
#30285=CIRCLE('',#95812,0.500000000000007);
#30286=CIRCLE('',#95813,0.499999999999999);
#30287=CIRCLE('',#95814,0.5);
#30288=CIRCLE('',#95816,0.5);
#30289=CIRCLE('',#95817,0.499999999999999);
#30290=CIRCLE('',#95819,0.5);
#30291=CIRCLE('',#95821,3.);
#30292=CIRCLE('',#95823,0.5);
#30293=CIRCLE('',#95828,0.999999999999999);
#30294=CIRCLE('',#95830,1.);
#30295=CIRCLE('',#95832,0.999999999999998);
#30296=CIRCLE('',#95834,1.);
#30297=CIRCLE('',#95836,0.5);
#30298=CIRCLE('',#95838,0.5);
#30299=CIRCLE('',#95840,0.5);
#30300=CIRCLE('',#95842,0.5);
#30301=CIRCLE('',#95844,1.);
#30302=CIRCLE('',#95845,0.999999999999997);
#30303=CIRCLE('',#95846,0.499999999999997);
#30304=CIRCLE('',#95847,0.499999999999998);
#30305=CIRCLE('',#95849,0.499999999999999);
#30306=CIRCLE('',#95850,59.);
#30307=CIRCLE('',#95852,58.4063077870367);
#30308=CIRCLE('',#95853,0.499999999999999);
#30309=CIRCLE('',#95855,0.500000000000003);
#30310=CIRCLE('',#95856,59.);
#30311=CIRCLE('',#95857,0.5);
#30312=CIRCLE('',#95859,58.4063077870367);
#30313=CIRCLE('',#95860,0.5);
#30314=CIRCLE('',#95861,0.500000000000004);
#30315=CIRCLE('',#95862,68.2176100637577);
#30316=CIRCLE('',#95864,58.4063077870366);
#30317=CIRCLE('',#95865,0.499999999999997);
#30318=CIRCLE('',#95866,0.500000000000001);
#30319=CIRCLE('',#95867,68.2630953041282);
#30320=CIRCLE('',#95869,58.4063077870367);
#30321=CIRCLE('',#95870,0.500000000000003);
#30322=CIRCLE('',#95871,0.500000000000002);
#30323=CIRCLE('',#95872,68.1807062067102);
#30324=CIRCLE('',#95874,58.4063077870367);
#30325=CIRCLE('',#95875,0.500000000000001);
#30326=CIRCLE('',#95876,0.500000000000002);
#30327=CIRCLE('',#95878,0.500000000000001);
#30328=CIRCLE('',#95879,59.);
#30329=CIRCLE('',#95881,58.4063077870367);
#30330=CIRCLE('',#95882,0.499999999999997);
#30331=CIRCLE('',#95884,0.500000000000002);
#30332=CIRCLE('',#95885,59.);
#30333=CIRCLE('',#95886,0.499999999999997);
#30334=CIRCLE('',#95887,0.999999999999996);
#30335=CIRCLE('',#95889,0.5);
#30336=CIRCLE('',#95891,0.499999999999998);
#30337=CIRCLE('',#95893,1.);
#30338=CIRCLE('',#95894,1.);
#30339=CIRCLE('',#95896,0.5);
#30340=CIRCLE('',#95898,0.5);
#30341=CIRCLE('',#95900,0.999999999999998);
#30342=CIRCLE('',#95902,1.);
#30343=CIRCLE('',#95904,0.999999999999999);
#30344=CIRCLE('',#95906,0.500000000000007);
#30345=CIRCLE('',#95908,0.500000000000006);
#30346=CIRCLE('',#95910,0.500000000000006);
#30347=CIRCLE('',#95912,0.500000000000006);
#30348=CIRCLE('',#95914,0.999999999999999);
#30349=CIRCLE('',#95917,59.1370702608075);
#30350=CIRCLE('',#95918,58.2307624737709);
#30351=CIRCLE('',#95955,5.38573144442823);
#30352=CIRCLE('',#95956,0.999999999999997);
#30353=CIRCLE('',#95958,59.1370702608075);
#30354=CIRCLE('',#95959,58.2307624737709);
#30355=CIRCLE('',#95975,58.2307624737709);
#30356=CIRCLE('',#95977,59.1370702608075);
#30357=CIRCLE('',#95980,59.1370702608075);
#30358=CIRCLE('',#95981,58.2307624737709);
#30359=CIRCLE('',#95990,58.2307624737708);
#30360=CIRCLE('',#95992,59.1370702608075);
#30361=CIRCLE('',#95997,59.1370702608075);
#30362=CIRCLE('',#95999,58.2307624737708);
#30363=CIRCLE('',#96008,59.1370702608075);
#30364=CIRCLE('',#96011,3.);
#30365=CIRCLE('',#96012,3.);
#30366=CIRCLE('',#96015,58.1182624738004);
#30367=CIRCLE('',#96018,58.2307624737708);
#30368=CIRCLE('',#96020,59.1370702608075);
#30369=CIRCLE('',#96024,3.);
#30370=CIRCLE('',#96025,3.);
#30371=CIRCLE('',#96028,0.995738858064582);
#30372=CIRCLE('',#96029,58.2307624737708);
#30373=CIRCLE('',#96034,3.);
#30374=CIRCLE('',#96035,3.);
#30375=CIRCLE('',#96038,59.1370702608075);
#30376=CIRCLE('',#96041,58.2307624737709);
#30377=CIRCLE('',#96043,0.994758623428062);
#30378=CIRCLE('',#96045,59.1370702608075);
#30379=CIRCLE('',#96047,58.2307624737709);
#30380=CIRCLE('',#96052,3.);
#30381=CIRCLE('',#96053,3.);
#30382=CIRCLE('',#96056,58.1182624738004);
#30383=CIRCLE('',#96058,58.1182624738004);
#30384=CIRCLE('',#96060,58.2307624737709);
#30385=CIRCLE('',#96063,3.);
#30386=CIRCLE('',#96064,3.);
#30387=CIRCLE('',#96067,59.1370702608075);
#30388=CIRCLE('',#96070,58.2307624737709);
#30389=CIRCLE('',#96071,0.5);
#30390=CIRCLE('',#96072,1.);
#30391=CIRCLE('',#96073,0.5);
#30392=CIRCLE('',#96074,0.5);
#30393=CIRCLE('',#96076,59.1370702608075);
#30394=CIRCLE('',#96079,0.999999999999997);
#30395=CIRCLE('',#96080,5.38573144425447);
#30396=CIRCLE('',#96084,3.);
#30397=CIRCLE('',#96085,3.);
#30398=CIRCLE('',#96088,58.1182624738004);
#30399=CIRCLE('',#96090,3.);
#30400=CIRCLE('',#96091,3.);
#30401=CIRCLE('',#96093,59.);
#30402=CIRCLE('',#96096,58.4063077870367);
#30403=CIRCLE('',#96098,59.);
#30404=CIRCLE('',#96101,3.);
#30405=CIRCLE('',#96102,3.);
#30406=CIRCLE('',#96104,0.5);
#30407=CIRCLE('',#96107,58.4063077870367);
#30408=CIRCLE('',#96108,68.2195020909334);
#30409=CIRCLE('',#96112,58.4063077870366);
#30410=CIRCLE('',#96113,68.2630953041282);
#30411=CIRCLE('',#96114,98.8061397010869);
#30412=CIRCLE('',#96118,58.4063077870367);
#30413=CIRCLE('',#96119,68.1826171111001);
#30414=CIRCLE('',#96122,58.4063077870367);
#30415=CIRCLE('',#96124,0.5);
#30416=CIRCLE('',#96127,3.);
#30417=CIRCLE('',#96128,3.);
#30418=CIRCLE('',#96130,59.);
#30419=CIRCLE('',#96132,3.);
#30420=CIRCLE('',#96133,3.);
#30421=CIRCLE('',#96136,58.4063077870367);
#30422=CIRCLE('',#96138,59.);
#30423=CIRCLE('',#96146,3.);
#30424=CIRCLE('',#96147,3.);
#30425=CIRCLE('',#96149,0.994491935959051);
#30426=CIRCLE('',#96152,3.);
#30427=CIRCLE('',#96153,3.);
#30428=CIRCLE('',#96154,0.5);
#30429=CIRCLE('',#96155,0.5);
#30430=CIRCLE('',#96156,0.5);
#30431=CIRCLE('',#96157,1.);
#30432=CIRCLE('',#96158,0.999999999999999);
#30433=CIRCLE('',#96159,0.999999999999994);
#30434=CIRCLE('',#96161,0.500000000000006);
#30435=CIRCLE('',#96162,0.5);
#30436=CIRCLE('',#96164,0.500000000000006);
#30437=CIRCLE('',#96165,0.5);
#30438=CIRCLE('',#96167,0.5);
#30439=CIRCLE('',#96168,0.500000000000006);
#30440=CIRCLE('',#96170,0.500000000000007);
#30441=CIRCLE('',#96171,0.5);
#30442=CIRCLE('',#96173,0.999999999999999);
#30443=CIRCLE('',#96175,3.);
#30444=CIRCLE('',#96176,1.);
#30445=CIRCLE('',#96177,2.);
#30446=CIRCLE('',#96179,67.5);
#30447=CIRCLE('',#96180,0.999999999999998);
#30448=CIRCLE('',#96181,66.5);
#30449=CIRCLE('',#96183,3.);
#30450=CIRCLE('',#96184,1.);
#30451=CIRCLE('',#96185,2.);
#30452=CIRCLE('',#96186,0.5);
#30453=CIRCLE('',#96187,0.5);
#30454=CIRCLE('',#96189,0.5);
#30455=CIRCLE('',#96190,0.5);
#30456=CIRCLE('',#96192,1.);
#30457=CIRCLE('',#96193,0.999999999999996);
#30458=CIRCLE('',#96195,0.5);
#30459=CIRCLE('',#96196,0.499999999999998);
#30460=CIRCLE('',#96198,0.5);
#30461=CIRCLE('',#96199,0.5);
#30462=CIRCLE('',#96201,0.5);
#30463=CIRCLE('',#96202,0.499999999999997);
#30464=CIRCLE('',#96204,0.500000000000002);
#30465=CIRCLE('',#96207,58.5);
#30466=CIRCLE('',#96208,0.499999999999997);
#30467=CIRCLE('',#96209,0.5);
#30468=CIRCLE('',#96211,58.5);
#30469=CIRCLE('',#96214,0.500000000000001);
#30470=CIRCLE('',#96215,0.5);
#30471=CIRCLE('',#96217,0.500000000000002);
#30472=CIRCLE('',#96218,58.5);
#30473=CIRCLE('',#96219,0.500000000000001);
#30474=CIRCLE('',#96220,0.5);
#30475=CIRCLE('',#96223,58.5);
#30476=CIRCLE('',#96226,0.500000000000002);
#30477=CIRCLE('',#96227,0.5);
#30478=CIRCLE('',#96228,57.9482170028185);
#30479=CIRCLE('',#96229,0.500000000000003);
#30480=CIRCLE('',#96230,0.5);
#30481=CIRCLE('',#96232,58.5);
#30482=CIRCLE('',#96235,0.500000000000001);
#30483=CIRCLE('',#96236,0.5);
#30484=CIRCLE('',#96237,58.1061766845785);
#30485=CIRCLE('',#96238,0.499999999999997);
#30486=CIRCLE('',#96239,0.5);
#30487=CIRCLE('',#96241,58.5);
#30488=CIRCLE('',#96244,0.500000000000004);
#30489=CIRCLE('',#96245,0.5);
#30490=CIRCLE('',#96246,57.9664310113591);
#30491=CIRCLE('',#96247,0.5);
#30492=CIRCLE('',#96248,0.5);
#30493=CIRCLE('',#96250,58.5);
#30494=CIRCLE('',#96253,0.5);
#30495=CIRCLE('',#96254,0.5);
#30496=CIRCLE('',#96255,0.500000000000003);
#30497=CIRCLE('',#96257,0.499999999999999);
#30498=CIRCLE('',#96258,58.5);
#30499=CIRCLE('',#96259,0.5);
#30500=CIRCLE('',#96261,58.5);
#30501=CIRCLE('',#96264,0.5);
#30502=CIRCLE('',#96265,0.499999999999999);
#30503=CIRCLE('',#96267,58.5);
#30504=CIRCLE('',#96268,0.499999999999998);
#30505=CIRCLE('',#96269,0.499999999999997);
#30506=CIRCLE('',#96270,0.999999999999997);
#30507=CIRCLE('',#96271,0.5);
#30508=CIRCLE('',#96272,1.);
#30509=CIRCLE('',#96274,0.5);
#30510=CIRCLE('',#96275,0.5);
#30511=CIRCLE('',#96277,0.5);
#30512=CIRCLE('',#96278,0.5);
#30513=CIRCLE('',#96280,0.5);
#30514=CIRCLE('',#96281,0.5);
#30515=CIRCLE('',#96283,0.5);
#30516=CIRCLE('',#96284,0.5);
#30517=CIRCLE('',#96286,1.);
#30518=CIRCLE('',#96288,3.);
#30519=CIRCLE('',#96289,0.999999999999998);
#30520=CIRCLE('',#96290,2.);
#30521=CIRCLE('',#96292,67.5);
#30522=CIRCLE('',#96293,1.);
#30523=CIRCLE('',#96294,66.5);
#30524=CIRCLE('',#96296,3.);
#30525=CIRCLE('',#96297,0.999999999999999);
#30526=CIRCLE('',#96298,2.);
#30527=CIRCLE('',#96301,0.5);
#30528=CIRCLE('',#96302,0.5);
#30529=CIRCLE('',#96303,0.5);
#30530=CIRCLE('',#96306,58.5);
#30531=CIRCLE('',#96308,2.75);
#30532=CIRCLE('',#96310,0.5);
#30533=CIRCLE('',#96311,2.5);
#30534=CIRCLE('',#96312,0.5);
#30535=CIRCLE('',#96314,0.5);
#30536=CIRCLE('',#96315,0.499999999999999);
#30537=CIRCLE('',#96316,0.499999999999999);
#30538=CIRCLE('',#96317,0.5);
#30539=CIRCLE('',#96319,0.5);
#30540=CIRCLE('',#96320,0.499999999999999);
#30541=CIRCLE('',#96321,0.500000000000007);
#30542=CIRCLE('',#96322,0.5);
#30543=CIRCLE('',#96324,0.5);
#30544=CIRCLE('',#96325,0.5);
#30545=CIRCLE('',#96326,0.5);
#30546=CIRCLE('',#96330,0.5);
#30547=CIRCLE('',#96331,0.5);
#30548=CIRCLE('',#96333,2.5);
#30549=CIRCLE('',#96334,0.5);
#30550=CIRCLE('',#96335,3.);
#30551=CIRCLE('',#96337,3.);
#30552=CIRCLE('',#96339,0.5);
#30553=CIRCLE('',#96340,2.5);
#30554=CIRCLE('',#96341,0.5);
#30555=CIRCLE('',#96343,0.5);
#30556=CIRCLE('',#96345,2.5);
#30557=CIRCLE('',#96346,0.5);
#30558=CIRCLE('',#96349,0.5);
#30559=CIRCLE('',#96350,0.5);
#30560=CIRCLE('',#96352,0.5);
#30561=CIRCLE('',#96353,0.5);
#30562=CIRCLE('',#96354,0.499999999999997);
#30563=CIRCLE('',#96355,0.5);
#30564=CIRCLE('',#96357,0.5);
#30565=CIRCLE('',#96358,0.500000000000003);
#30566=CIRCLE('',#96359,0.499999999999998);
#30567=CIRCLE('',#96360,0.5);
#30568=CIRCLE('',#96362,0.5);
#30569=CIRCLE('',#96364,59.024570260837);
#30570=CIRCLE('',#96366,0.5);
#30571=CIRCLE('',#96367,2.5);
#30572=CIRCLE('',#96368,0.5);
#30573=CIRCLE('',#96370,0.5);
#30574=CIRCLE('',#96372,0.5);
#30575=CIRCLE('',#96373,0.5);
#30576=CIRCLE('',#96374,0.500000000000001);
#30577=CIRCLE('',#96375,0.499999999999999);
#30578=CIRCLE('',#96376,0.5);
#30579=CIRCLE('',#96378,0.5);
#30580=CIRCLE('',#96379,0.499999999999999);
#30581=CIRCLE('',#96380,0.499999999999996);
#30582=CIRCLE('',#96381,0.5);
#30583=CIRCLE('',#96383,0.5);
#30584=CIRCLE('',#96384,0.5);
#30585=CIRCLE('',#96385,0.5);
#30586=CIRCLE('',#96389,2.5);
#30587=CIRCLE('',#96390,0.5);
#30588=CIRCLE('',#96391,3.);
#30589=CIRCLE('',#96393,3.);
#30590=CIRCLE('',#96395,0.5);
#30591=CIRCLE('',#96396,0.5);
#30592=CIRCLE('',#96398,0.5);
#30593=CIRCLE('',#96400,0.5);
#30594=CIRCLE('',#96401,0.5);
#30595=CIRCLE('',#96403,0.5);
#30596=CIRCLE('',#96404,0.5);
#30597=CIRCLE('',#96405,2.5);
#30598=CIRCLE('',#96407,0.5);
#30599=CIRCLE('',#96409,0.5);
#30600=CIRCLE('',#96410,2.5);
#30601=CIRCLE('',#96413,0.5);
#30602=CIRCLE('',#96414,0.499999999999998);
#30603=CIRCLE('',#96415,0.5);
#30604=CIRCLE('',#96416,0.500000000000002);
#30605=CIRCLE('',#96417,0.5);
#30606=CIRCLE('',#96419,0.5);
#30607=CIRCLE('',#96420,0.500000000000002);
#30608=CIRCLE('',#96421,0.500000000000002);
#30609=CIRCLE('',#96423,0.5);
#30610=CIRCLE('',#96424,0.5);
#30611=CIRCLE('',#96426,2.5);
#30612=CIRCLE('',#96427,0.5);
#30613=CIRCLE('',#96430,0.5);
#30614=CIRCLE('',#96431,0.499999999999998);
#30615=CIRCLE('',#96435,58.1182624738004);
#30616=CIRCLE('',#96437,0.5);
#30617=CIRCLE('',#96438,2.5);
#30618=CIRCLE('',#96439,0.5);
#30619=CIRCLE('',#96441,0.5);
#30620=CIRCLE('',#96442,0.500000000000003);
#30621=CIRCLE('',#96443,0.5);
#30622=CIRCLE('',#96444,0.499999999999999);
#30623=CIRCLE('',#96445,0.5);
#30624=CIRCLE('',#96447,0.5);
#30625=CIRCLE('',#96448,0.500000000000001);
#30626=CIRCLE('',#96449,0.499999999999994);
#30627=CIRCLE('',#96450,0.5);
#30628=CIRCLE('',#96452,0.5);
#30629=CIRCLE('',#96453,0.5);
#30630=CIRCLE('',#96457,2.5);
#30631=CIRCLE('',#96458,0.5);
#30632=CIRCLE('',#96459,3.);
#30633=CIRCLE('',#96461,3.);
#30634=CIRCLE('',#96463,0.5);
#30635=CIRCLE('',#96464,2.5);
#30636=CIRCLE('',#96465,0.5);
#30637=CIRCLE('',#96467,0.5);
#30638=CIRCLE('',#96469,2.5);
#30639=CIRCLE('',#96470,0.5);
#30640=CIRCLE('',#96473,0.5);
#30641=CIRCLE('',#96474,0.5);
#30642=CIRCLE('',#96476,0.5);
#30643=CIRCLE('',#96477,0.499999999999994);
#30644=CIRCLE('',#96478,0.499999999999999);
#30645=CIRCLE('',#96479,0.5);
#30646=CIRCLE('',#96481,0.5);
#30647=CIRCLE('',#96482,0.499999999999998);
#30648=CIRCLE('',#96483,0.499999999999997);
#30649=CIRCLE('',#96485,0.5);
#30650=CIRCLE('',#96486,0.5);
#30651=CIRCLE('',#96488,58.1182624738004);
#30652=CIRCLE('',#96490,0.5);
#30653=CIRCLE('',#96491,2.5);
#30654=CIRCLE('',#96492,0.5);
#30655=CIRCLE('',#96494,0.5);
#30656=CIRCLE('',#96495,0.5);
#30657=CIRCLE('',#96497,0.500000000000002);
#30658=CIRCLE('',#96499,0.499999999999998);
#30659=CIRCLE('',#96501,0.500000000000001);
#30660=CIRCLE('',#96502,0.5);
#30661=CIRCLE('',#96504,0.5);
#30662=CIRCLE('',#96505,0.499999999999999);
#30663=CIRCLE('',#96506,0.500000000000004);
#30664=CIRCLE('',#96507,0.500000000000003);
#30665=CIRCLE('',#96508,0.5);
#30666=CIRCLE('',#96512,0.5);
#30667=CIRCLE('',#96514,0.5);
#30668=CIRCLE('',#96515,0.5);
#30669=CIRCLE('',#96516,0.5);
#30670=CIRCLE('',#96519,0.5);
#30671=CIRCLE('',#96521,2.5);
#30672=CIRCLE('',#96522,0.5);
#30673=CIRCLE('',#96524,0.5);
#30674=CIRCLE('',#96525,0.5);
#30675=CIRCLE('',#96526,0.5);
#30676=CIRCLE('',#96528,1.);
#30677=CIRCLE('',#96530,2.5);
#30678=CIRCLE('',#96531,0.5);
#30679=CIRCLE('',#96532,3.);
#30680=CIRCLE('',#96534,3.);
#30681=CIRCLE('',#96536,0.5);
#30682=CIRCLE('',#96537,0.5);
#30683=CIRCLE('',#96538,0.5);
#30684=CIRCLE('',#96539,0.500000000000001);
#30685=CIRCLE('',#96540,0.5);
#30686=CIRCLE('',#96542,0.5);
#30687=CIRCLE('',#96543,0.499999999999999);
#30688=CIRCLE('',#96544,0.499999999999998);
#30689=CIRCLE('',#96545,0.5);
#30690=CIRCLE('',#96547,0.5);
#30691=CIRCLE('',#96548,2.5);
#30692=CIRCLE('',#96549,0.5);
#30693=CIRCLE('',#96551,0.5);
#30694=CIRCLE('',#96553,2.5);
#30695=CIRCLE('',#96554,0.5);
#30696=CIRCLE('',#96557,0.5);
#30697=CIRCLE('',#96558,0.5);
#30698=CIRCLE('',#96560,0.5);
#30699=CIRCLE('',#96562,0.5);
#30700=CIRCLE('',#96564,59.024570260837);
#30701=CIRCLE('',#96565,0.5);
#30702=CIRCLE('',#96566,0.500000000000001);
#30703=CIRCLE('',#96567,0.500000000000002);
#30704=CIRCLE('',#96568,0.5);
#30705=CIRCLE('',#96570,0.5);
#30706=CIRCLE('',#96572,0.5);
#30707=CIRCLE('',#96573,2.5);
#30708=CIRCLE('',#96574,0.5);
#30709=CIRCLE('',#96575,3.);
#30710=CIRCLE('',#96577,3.);
#30711=CIRCLE('',#96579,0.5);
#30712=CIRCLE('',#96580,2.5);
#30713=CIRCLE('',#96581,0.5);
#30714=CIRCLE('',#96584,1.);
#30715=CIRCLE('',#96585,0.499999999999999);
#30716=CIRCLE('',#96586,0.5);
#30717=CIRCLE('',#96587,0.5);
#30718=CIRCLE('',#96589,0.5);
#30719=CIRCLE('',#96591,0.5);
#30720=CIRCLE('',#96592,2.5);
#30721=CIRCLE('',#96593,0.5);
#30722=CIRCLE('',#96594,3.);
#30723=CIRCLE('',#96596,3.);
#30724=CIRCLE('',#96598,0.5);
#30725=CIRCLE('',#96599,2.5);
#30726=CIRCLE('',#96600,0.5);
#30727=CIRCLE('',#96602,0.5);
#30728=CIRCLE('',#96603,0.5);
#30729=CIRCLE('',#96604,0.500000000000001);
#30730=CIRCLE('',#96605,0.500000000000003);
#30731=CIRCLE('',#96606,0.5);
#30732=CIRCLE('',#96608,0.5);
#30733=CIRCLE('',#96610,0.5);
#30734=CIRCLE('',#96612,59.024570260837);
#30735=CIRCLE('',#96614,0.5);
#30736=CIRCLE('',#96615,2.5);
#30737=CIRCLE('',#96616,0.5);
#30738=CIRCLE('',#96618,0.5);
#30739=CIRCLE('',#96619,0.500000000000002);
#30740=CIRCLE('',#96620,0.5);
#30741=CIRCLE('',#96621,0.500000000000001);
#30742=CIRCLE('',#96622,0.5);
#30743=CIRCLE('',#96624,0.5);
#30744=CIRCLE('',#96625,0.500000000000002);
#30745=CIRCLE('',#96626,0.500000000000001);
#30746=CIRCLE('',#96627,0.5);
#30747=CIRCLE('',#96629,0.5);
#30748=CIRCLE('',#96630,0.5);
#30749=CIRCLE('',#96634,2.5);
#30750=CIRCLE('',#96635,0.5);
#30751=CIRCLE('',#96636,3.);
#30752=CIRCLE('',#96638,3.);
#30753=CIRCLE('',#96640,0.5);
#30754=CIRCLE('',#96641,2.5);
#30755=CIRCLE('',#96642,0.5);
#30756=CIRCLE('',#96644,0.5);
#30757=CIRCLE('',#96646,2.5);
#30758=CIRCLE('',#96647,0.5);
#30759=CIRCLE('',#96650,0.5);
#30760=CIRCLE('',#96651,0.5);
#30761=CIRCLE('',#96653,0.5);
#30762=CIRCLE('',#96654,0.500000000000001);
#30763=CIRCLE('',#96655,0.500000000000001);
#30764=CIRCLE('',#96656,0.5);
#30765=CIRCLE('',#96658,0.5);
#30766=CIRCLE('',#96659,0.5);
#30767=CIRCLE('',#96660,0.500000000000004);
#30768=CIRCLE('',#96662,0.5);
#30769=CIRCLE('',#96663,0.5);
#30770=CIRCLE('',#96665,58.1182624738004);
#30771=CIRCLE('',#96667,0.5);
#30772=CIRCLE('',#96668,2.5);
#30773=CIRCLE('',#96669,0.5);
#30774=CIRCLE('',#96671,0.5);
#30775=CIRCLE('',#96672,0.499999999999998);
#30776=CIRCLE('',#96673,0.499999999999998);
#30777=CIRCLE('',#96674,0.5);
#30778=CIRCLE('',#96676,0.5);
#30779=CIRCLE('',#96677,0.499999999999998);
#30780=CIRCLE('',#96678,0.5);
#30781=CIRCLE('',#96679,0.5);
#30782=CIRCLE('',#96680,0.5);
#30783=CIRCLE('',#96681,0.5);
#30784=CIRCLE('',#96684,0.5);
#30785=CIRCLE('',#96685,0.5);
#30786=CIRCLE('',#96686,0.5);
#30787=CIRCLE('',#96689,0.5);
#30788=CIRCLE('',#96691,0.5);
#30789=CIRCLE('',#96692,2.5);
#30790=CIRCLE('',#96694,0.5);
#30791=CIRCLE('',#96695,0.5);
#30792=CIRCLE('',#96696,0.5);
#30793=CIRCLE('',#96700,0.5);
#30794=CIRCLE('',#96702,0.5);
#30795=CIRCLE('',#96703,3.);
#30796=CIRCLE('',#96704,2.5);
#30797=CIRCLE('',#96706,3.);
#30798=CIRCLE('',#96708,0.5);
#30799=CIRCLE('',#96709,0.5);
#30800=CIRCLE('',#96710,0.499999999999993);
#30801=CIRCLE('',#96711,0.499999999999999);
#30802=CIRCLE('',#96712,0.5);
#30803=CIRCLE('',#96714,0.5);
#30804=CIRCLE('',#96715,0.500000000000002);
#30805=CIRCLE('',#96716,0.5);
#30806=CIRCLE('',#96718,0.5);
#30807=CIRCLE('',#96719,2.5);
#30808=CIRCLE('',#96720,0.5);
#30809=CIRCLE('',#96722,0.5);
#30810=CIRCLE('',#96724,2.5);
#30811=CIRCLE('',#96725,0.5);
#30812=CIRCLE('',#96728,0.5);
#30813=CIRCLE('',#96729,0.5);
#30814=CIRCLE('',#96731,59.024570260837);
#30815=CIRCLE('',#96732,0.999999999999999);
#30816=CIRCLE('',#96734,0.5);
#30817=CIRCLE('',#96736,0.5);
#30818=CIRCLE('',#96737,0.499999999999997);
#30819=CIRCLE('',#96738,0.499999999999999);
#30820=CIRCLE('',#96739,0.5);
#30821=CIRCLE('',#96741,0.5);
#30822=CIRCLE('',#96742,0.500000000000002);
#30823=CIRCLE('',#96744,0.5);
#30824=CIRCLE('',#96745,0.5);
#30825=CIRCLE('',#96747,2.5);
#30826=CIRCLE('',#96748,0.5);
#30827=CIRCLE('',#96751,0.5);
#30828=CIRCLE('',#96753,0.499999999999999);
#30829=CIRCLE('',#96754,0.5);
#30830=CIRCLE('',#96755,0.500000000000003);
#30831=CIRCLE('',#96757,0.5);
#30832=CIRCLE('',#96758,0.499999999999997);
#30833=CIRCLE('',#96759,0.499999999999996);
#30834=CIRCLE('',#96761,0.5);
#30835=CIRCLE('',#96764,0.5);
#30836=CIRCLE('',#96766,2.5);
#30837=CIRCLE('',#96767,0.5);
#30838=CIRCLE('',#96769,0.5);
#30839=CIRCLE('',#96770,0.499999999999999);
#30840=CIRCLE('',#96772,2.5);
#30841=CIRCLE('',#96773,0.5);
#30842=CIRCLE('',#96774,3.);
#30843=CIRCLE('',#96776,3.);
#30844=CIRCLE('',#96778,0.5);
#30845=CIRCLE('',#96779,2.5);
#30846=CIRCLE('',#96780,0.5);
#30847=CIRCLE('',#96782,0.5);
#30848=CIRCLE('',#96784,2.5);
#30849=CIRCLE('',#96786,0.5);
#30850=CIRCLE('',#96788,0.499999999999998);
#30851=CIRCLE('',#96789,0.499999999999999);
#30852=CIRCLE('',#96790,0.5);
#30853=CIRCLE('',#96792,0.5);
#30854=CIRCLE('',#96793,0.499999999999999);
#30855=CIRCLE('',#96794,0.500000000000003);
#30856=CIRCLE('',#96795,0.5);
#30857=CIRCLE('',#96796,0.499999999999999);
#30858=CIRCLE('',#96798,0.5);
#30859=CIRCLE('',#96799,0.500000000000002);
#30860=CIRCLE('',#96800,0.499999999999999);
#30861=CIRCLE('',#96801,0.5);
#30862=CIRCLE('',#96804,0.5);
#30863=CIRCLE('',#96805,0.500000000000001);
#30864=CIRCLE('',#96807,0.5);
#30865=CIRCLE('',#96810,0.5);
#30866=CIRCLE('',#96811,0.5);
#30867=CIRCLE('',#96813,0.5);
#30868=CIRCLE('',#96815,0.499999999999998);
#30869=CIRCLE('',#96816,0.500000000000002);
#30870=CIRCLE('',#96817,0.5);
#30871=CIRCLE('',#96819,0.5);
#30872=CIRCLE('',#96820,0.500000000000002);
#30873=CIRCLE('',#96821,0.5);
#30874=CIRCLE('',#96823,0.5);
#30875=CIRCLE('',#96824,0.5);
#30876=CIRCLE('',#96827,0.5);
#30877=CIRCLE('',#96828,0.499999999999999);
#30878=CIRCLE('',#96830,0.499999999999996);
#30879=CIRCLE('',#96831,0.5);
#30880=CIRCLE('',#96834,0.5);
#30881=CIRCLE('',#96835,0.5);
#30882=CIRCLE('',#96837,0.5);
#30883=CIRCLE('',#96839,109.361438801731);
#30884=CIRCLE('',#96841,0.5);
#30885=CIRCLE('',#96842,0.5);
#30886=CIRCLE('',#96844,0.5);
#30887=CIRCLE('',#96846,0.500000000000001);
#30888=CIRCLE('',#96847,0.499999999999999);
#30889=CIRCLE('',#96849,0.5);
#30890=CIRCLE('',#96851,0.5);
#30891=CIRCLE('',#96853,0.499999999999999);
#30892=CIRCLE('',#96855,0.500000000000002);
#30893=CIRCLE('',#96856,0.5);
#30894=CIRCLE('',#96857,0.5);
#30895=CIRCLE('',#96859,0.5);
#30896=CIRCLE('',#96860,0.500000000000006);
#30897=CIRCLE('',#96861,0.500000000000003);
#30898=CIRCLE('',#96862,0.5);
#30899=CIRCLE('',#96865,0.5);
#30900=CIRCLE('',#96866,0.499999999999998);
#30901=CIRCLE('',#96868,0.5);
#30902=CIRCLE('',#96871,0.5);
#30903=CIRCLE('',#96872,0.5);
#30904=CIRCLE('',#96874,0.5);
#30905=CIRCLE('',#96876,0.499999999999999);
#30906=CIRCLE('',#96877,0.500000000000001);
#30907=CIRCLE('',#96878,0.5);
#30908=CIRCLE('',#96880,0.5);
#30909=CIRCLE('',#96881,0.500000000000001);
#30910=CIRCLE('',#96882,0.499999999999998);
#30911=CIRCLE('',#96883,0.5);
#30912=CIRCLE('',#96884,0.500000000000001);
#30913=CIRCLE('',#96886,0.5);
#30914=CIRCLE('',#96887,0.499999999999994);
#30915=CIRCLE('',#96888,0.500000000000002);
#30916=CIRCLE('',#96890,0.5);
#30917=CIRCLE('',#96893,2.5);
#30918=CIRCLE('',#96894,0.5);
#30919=CIRCLE('',#96896,0.5);
#30920=CIRCLE('',#96897,0.5);
#30921=CIRCLE('',#96899,2.5);
#30922=CIRCLE('',#96900,0.5);
#30923=CIRCLE('',#96901,3.);
#30924=CIRCLE('',#96903,3.);
#30925=CIRCLE('',#96905,0.5);
#30926=CIRCLE('',#96906,2.5);
#30927=CIRCLE('',#96907,0.5);
#30928=CIRCLE('',#96909,0.5);
#30929=CIRCLE('',#96911,2.5);
#30930=CIRCLE('',#96912,0.5);
#30931=CIRCLE('',#96915,0.5);
#30932=CIRCLE('',#96917,0.500000000000001);
#30933=CIRCLE('',#96918,0.500000000000003);
#30934=CIRCLE('',#96919,0.5);
#30935=CIRCLE('',#96921,0.5);
#30936=CIRCLE('',#96922,0.500000000000002);
#30937=CIRCLE('',#96923,0.499999999999997);
#30938=CIRCLE('',#96925,0.5);
#30939=CIRCLE('',#96926,2.5);
#30940=CIRCLE('',#96927,0.5);
#30941=CIRCLE('',#96929,0.5);
#30942=CIRCLE('',#96930,0.499999999999998);
#30943=CIRCLE('',#96931,0.500000000000001);
#30944=CIRCLE('',#96932,0.5);
#30945=CIRCLE('',#96934,0.5);
#30946=CIRCLE('',#96935,0.500000000000001);
#30947=CIRCLE('',#96936,0.499999999999994);
#30948=CIRCLE('',#96938,0.5);
#30949=CIRCLE('',#96942,2.5);
#30950=CIRCLE('',#96943,0.5);
#30951=CIRCLE('',#96944,3.);
#30952=CIRCLE('',#96946,3.);
#30953=CIRCLE('',#96948,0.5);
#30954=CIRCLE('',#96949,2.5);
#30955=CIRCLE('',#96951,2.5);
#30956=CIRCLE('',#96952,0.5);
#30957=CIRCLE('',#96953,3.);
#30958=CIRCLE('',#96955,3.);
#30959=CIRCLE('',#96957,0.5);
#30960=CIRCLE('',#96958,2.5);
#30961=CIRCLE('',#96959,0.500000000000001);
#30962=CIRCLE('',#96960,0.500000000000001);
#30963=CIRCLE('',#96961,0.500000000000002);
#30964=CIRCLE('',#96962,0.5);
#30965=CIRCLE('',#96963,0.500000000000001);
#30966=CIRCLE('',#96965,0.499999999999999);
#30967=CIRCLE('',#96966,0.499999999999999);
#30968=CIRCLE('',#96967,0.500000000000001);
#30969=CIRCLE('',#96968,0.500000000000001);
#30970=CIRCLE('',#96969,0.5);
#30971=CIRCLE('',#96971,0.5);
#30972=CIRCLE('',#96973,0.5);
#30973=CIRCLE('',#96974,2.5);
#30974=CIRCLE('',#96975,0.5);
#30975=CIRCLE('',#96976,3.);
#30976=CIRCLE('',#96978,3.);
#30977=CIRCLE('',#96980,0.5);
#30978=CIRCLE('',#96981,2.5);
#30979=CIRCLE('',#96982,0.5);
#30980=CIRCLE('',#96984,0.5);
#30981=CIRCLE('',#96985,0.5);
#30982=CIRCLE('',#96986,0.5);
#30983=CIRCLE('',#96987,0.500000000000002);
#30984=CIRCLE('',#96988,0.499999999999997);
#30985=CIRCLE('',#96989,0.500000000000003);
#30986=CIRCLE('',#96990,0.993248606213802);
#30987=CIRCLE('',#96991,0.491297296891938);
#30988=CIRCLE('',#96993,58.1182624738004);
#30989=CIRCLE('',#96995,0.5);
#30990=CIRCLE('',#96996,2.5);
#30991=CIRCLE('',#96997,0.5);
#30992=CIRCLE('',#96998,3.);
#30993=CIRCLE('',#97000,0.5);
#30994=CIRCLE('',#97002,2.5);
#30995=CIRCLE('',#97003,0.5);
#30996=CIRCLE('',#97004,0.499999999999997);
#30997=CIRCLE('',#97005,0.500000000000003);
#30998=CIRCLE('',#97006,0.5);
#30999=CIRCLE('',#97008,0.5);
#31000=CIRCLE('',#97009,0.499999999999997);
#31001=CIRCLE('',#97010,0.499999999999998);
#31002=CIRCLE('',#97012,0.5);
#31003=CIRCLE('',#97013,2.5);
#31004=CIRCLE('',#97014,0.5);
#31005=CIRCLE('',#97016,0.5);
#31006=CIRCLE('',#97017,0.5);
#31007=CIRCLE('',#97018,0.499999999999999);
#31008=CIRCLE('',#97020,0.5);
#31009=CIRCLE('',#97021,0.500000000000003);
#31010=CIRCLE('',#97022,0.499999999999998);
#31011=CIRCLE('',#97023,0.499999999999997);
#31012=CIRCLE('',#97025,2.5);
#31013=CIRCLE('',#97026,0.5);
#31014=CIRCLE('',#97027,3.);
#31015=CIRCLE('',#97029,3.);
#31016=CIRCLE('',#97031,0.5);
#31017=CIRCLE('',#97032,2.5);
#31018=CIRCLE('',#97033,0.5);
#31019=CIRCLE('',#97035,0.5);
#31020=CIRCLE('',#97037,2.5);
#31021=CIRCLE('',#97038,0.5);
#31022=CIRCLE('',#97039,0.499999999999994);
#31023=CIRCLE('',#97040,0.499999999999999);
#31024=CIRCLE('',#97041,0.5);
#31025=CIRCLE('',#97043,0.5);
#31026=CIRCLE('',#97044,0.499999999999999);
#31027=CIRCLE('',#97045,0.500000000000001);
#31028=CIRCLE('',#97046,0.5);
#31029=CIRCLE('',#97047,0.500000000000003);
#31030=CIRCLE('',#97049,0.5);
#31031=CIRCLE('',#97050,0.499999999999994);
#31032=CIRCLE('',#97051,0.500000000000001);
#31033=CIRCLE('',#97052,0.500000000000005);
#31034=CIRCLE('',#97054,0.5);
#31035=CIRCLE('',#97055,0.5);
#31036=CIRCLE('',#97058,0.5);
#31037=CIRCLE('',#97059,0.5);
#31038=CIRCLE('',#97060,0.500000000000002);
#31039=CIRCLE('',#97061,0.499999999999998);
#31040=CIRCLE('',#97062,0.5);
#31041=CIRCLE('',#97064,0.5);
#31042=CIRCLE('',#97065,0.499999999999998);
#31043=CIRCLE('',#97066,0.499999999999998);
#31044=CIRCLE('',#97068,0.5);
#31045=CIRCLE('',#97069,0.499999999999999);
#31046=CIRCLE('',#97072,0.5);
#31047=CIRCLE('',#97073,0.499999999999998);
#31048=CIRCLE('',#97075,0.500000000000003);
#31049=CIRCLE('',#97076,0.499999999999994);
#31050=CIRCLE('',#97078,59.);
#31051=CIRCLE('',#97080,0.499999999999998);
#31052=CIRCLE('',#97081,0.5);
#31053=CIRCLE('',#97083,0.5);
#31054=CIRCLE('',#97087,58.4063077870366);
#31055=CIRCLE('',#97088,0.5);
#31056=CIRCLE('',#97091,68.1438279981623);
#31057=CIRCLE('',#97092,0.5);
#31058=CIRCLE('',#97096,58.4063077870367);
#31059=CIRCLE('',#97097,0.5);
#31060=CIRCLE('',#97102,59.);
#31061=CIRCLE('',#97104,0.5);
#31062=CIRCLE('',#97108,58.4063077870367);
#31063=CIRCLE('',#97109,0.5);
#31064=CIRCLE('',#97114,2.75);
#31065=CIRCLE('',#97116,2.75);
#31066=CIRCLE('',#97118,2.75);
#31067=CIRCLE('',#97120,2.75);
#31068=CIRCLE('',#97121,2.75);
#31069=CIRCLE('',#97124,3.);
#31070=CIRCLE('',#97126,67.5);
#31071=CIRCLE('',#97128,3.);
#31072=CIRCLE('',#97131,5.);
#31073=CIRCLE('',#97133,58.5);
#31074=CIRCLE('',#97135,5.);
#31075=CIRCLE('',#97138,3.);
#31076=CIRCLE('',#97140,67.5);
#31077=CIRCLE('',#97142,3.);
#31078=CIRCLE('',#97144,0.5);
#31079=CIRCLE('',#97145,0.499999999999999);
#31080=CIRCLE('',#97147,0.5);
#31081=CIRCLE('',#97148,0.5);
#31082=CIRCLE('',#97150,0.5);
#31083=CIRCLE('',#97151,0.5);
#31084=CIRCLE('',#97154,0.5);
#31085=CIRCLE('',#97155,0.5);
#31086=CIRCLE('',#97156,0.5);
#31087=CIRCLE('',#97157,1.);
#31088=CIRCLE('',#97159,1.);
#31089=CIRCLE('',#97160,0.5);
#31090=CIRCLE('',#97161,0.5);
#31091=CIRCLE('',#97163,0.5);
#31092=CIRCLE('',#97166,0.5);
#31093=CIRCLE('',#97167,0.5);
#31094=CIRCLE('',#97168,0.5);
#31095=CIRCLE('',#97169,1.);
#31096=CIRCLE('',#97171,1.);
#31097=CIRCLE('',#97172,0.5);
#31098=CIRCLE('',#97173,0.5);
#31099=CIRCLE('',#97175,0.5);
#31100=CIRCLE('',#97178,0.5);
#31101=CIRCLE('',#97179,0.5);
#31102=CIRCLE('',#97180,0.5);
#31103=CIRCLE('',#97181,1.);
#31104=CIRCLE('',#97184,0.499999999999998);
#31105=CIRCLE('',#97185,0.5);
#31106=CIRCLE('',#97186,0.551233577645565);
#31107=CIRCLE('',#97187,1.02402724953616);
#31108=CIRCLE('',#97189,0.5);
#31109=CIRCLE('',#97190,0.5);
#31110=CIRCLE('',#97192,64.5806717409052);
#31111=CIRCLE('',#97194,0.5);
#31112=CIRCLE('',#97195,0.5);
#31113=CIRCLE('',#97196,0.5);
#31114=CIRCLE('',#97199,0.5);
#31115=CIRCLE('',#97201,0.5);
#31116=CIRCLE('',#97202,0.5);
#31117=CIRCLE('',#97205,0.5);
#31118=CIRCLE('',#97206,0.5);
#31119=CIRCLE('',#97207,0.5);
#31120=CIRCLE('',#97208,0.500000000000001);
#31121=CIRCLE('',#97209,0.5);
#31122=CIRCLE('',#97211,0.5);
#31123=CIRCLE('',#97213,0.500000000000002);
#31124=CIRCLE('',#97214,3.5);
#31125=CIRCLE('',#97215,3.);
#31126=CIRCLE('',#97216,0.5);
#31127=CIRCLE('',#97219,0.5);
#31128=CIRCLE('',#97221,2.5);
#31129=CIRCLE('',#97222,0.5);
#31130=CIRCLE('',#97223,3.);
#31131=CIRCLE('',#97226,0.5);
#31132=CIRCLE('',#97228,2.75);
#31133=CIRCLE('',#97229,2.75);
#31134=CIRCLE('',#97230,2.75);
#31135=CIRCLE('',#97232,2.);
#31136=CIRCLE('',#97234,2.);
#31137=CIRCLE('',#97236,0.5);
#31138=CIRCLE('',#97238,0.5);
#31139=CIRCLE('',#97239,0.5);
#31140=CIRCLE('',#97240,0.500000000000002);
#31141=CIRCLE('',#97241,0.5);
#31142=CIRCLE('',#97243,0.5);
#31143=CIRCLE('',#97244,59.);
#31144=CIRCLE('',#97245,0.5);
#31145=CIRCLE('',#97246,0.5);
#31146=CIRCLE('',#97249,2.75);
#31147=CIRCLE('',#97250,2.75);
#31148=CIRCLE('',#97252,2.);
#31149=CIRCLE('',#97254,2.);
#31150=CIRCLE('',#97256,0.5);
#31151=CIRCLE('',#97258,59.024570260837);
#31152=CIRCLE('',#97260,0.5);
#31153=CIRCLE('',#97261,0.5);
#31154=CIRCLE('',#97266,0.5);
#31155=CIRCLE('',#97268,0.5);
#31156=CIRCLE('',#97274,0.5);
#31157=CIRCLE('',#97276,0.5);
#31158=CIRCLE('',#97283,0.5);
#31159=CIRCLE('',#97285,59.024570260837);
#31160=CIRCLE('',#97287,1.);
#31161=CIRCLE('',#97288,0.5);
#31162=CIRCLE('',#97292,0.5);
#31163=CIRCLE('',#97297,0.5);
#31164=CIRCLE('',#97298,0.5);
#31165=CIRCLE('',#97305,0.5);
#31166=CIRCLE('',#97306,0.5);
#31167=CIRCLE('',#97312,0.5);
#31168=CIRCLE('',#97313,0.5);
#31169=CIRCLE('',#97320,0.5);
#31170=CIRCLE('',#97322,59.024570260837);
#31171=CIRCLE('',#97325,0.5);
#31172=CIRCLE('',#97326,0.5);
#31173=CIRCLE('',#97332,0.5);
#31174=CIRCLE('',#97333,0.5);
#31175=CIRCLE('',#97337,0.5);
#31176=CIRCLE('',#97340,58.2938077870648);
#31177=CIRCLE('',#97344,0.5);
#31178=CIRCLE('',#97347,58.8875000000282);
#31179=CIRCLE('',#97351,0.5);
#31180=CIRCLE('',#97354,58.2938077870648);
#31181=CIRCLE('',#97358,0.5);
#31182=CIRCLE('',#97359,68.0339423779013);
#31183=CIRCLE('',#97362,0.5);
#31184=CIRCLE('',#97365,58.2938077870648);
#31185=CIRCLE('',#97369,0.5);
#31186=CIRCLE('',#97370,68.156308837608);
#31187=CIRCLE('',#97373,0.5);
#31188=CIRCLE('',#97376,58.2938077870648);
#31189=CIRCLE('',#97380,0.5);
#31190=CIRCLE('',#97381,67.990141838142);
#31191=CIRCLE('',#97384,0.5);
#31192=CIRCLE('',#97387,58.2938077870648);
#31193=CIRCLE('',#97391,0.5);
#31194=CIRCLE('',#97394,58.8875000000282);
#31195=CIRCLE('',#97398,0.5);
#31196=CIRCLE('',#97401,58.2938077870648);
#31197=CIRCLE('',#97402,0.5);
#31198=CIRCLE('',#97407,4.5);
#31199=CIRCLE('',#97413,4.5);
#31200=CIRCLE('',#97417,68.2241973717388);
#31201=CIRCLE('',#97420,0.5);
#31202=CIRCLE('',#97423,44.2689250265968);
#31203=CIRCLE('',#97424,58.2938077870648);
#31204=CIRCLE('',#97428,0.5);
#31205=CIRCLE('',#97429,64.7291249062775);
#31206=CIRCLE('',#97432,0.5);
#31207=CIRCLE('',#97435,58.2938077870648);
#31208=CIRCLE('',#97436,0.5);
#31209=CIRCLE('',#97442,58.8875000000282);
#31210=CIRCLE('',#97446,0.5);
#31211=CIRCLE('',#97448,58.2060351304332);
#31212=CIRCLE('',#97452,0.5);
#31213=CIRCLE('',#97455,58.2938077870648);
#31214=CIRCLE('',#97459,0.5);
#31215=CIRCLE('',#97462,58.8875000000282);
#31216=CIRCLE('',#97466,0.5);
#31217=CIRCLE('',#97467,0.5);
#31218=CIRCLE('',#97470,58.2938077870648);
#31219=CIRCLE('',#97474,0.5);
#31220=CIRCLE('',#97475,67.9422846909627);
#31221=CIRCLE('',#97478,0.5);
#31222=CIRCLE('',#97479,0.5);
#31223=CIRCLE('',#97482,58.2938077870648);
#31224=CIRCLE('',#97486,0.5);
#31225=CIRCLE('',#97487,0.5);
#31226=CIRCLE('',#97489,0.5);
#31227=CIRCLE('',#97491,0.500000000000001);
#31228=CIRCLE('',#97492,58.5);
#31229=CIRCLE('',#97493,0.499999999999999);
#31230=CIRCLE('',#97495,3.);
#31231=CIRCLE('',#97496,0.500000000000002);
#31232=CIRCLE('',#97497,0.5);
#31233=CIRCLE('',#97500,58.5);
#31234=CIRCLE('',#97502,0.5);
#31235=CIRCLE('',#97503,0.500000000000005);
#31236=CIRCLE('',#97504,57.916967095156);
#31237=CIRCLE('',#97505,0.499999999999999);
#31238=CIRCLE('',#97506,0.5);
#31239=CIRCLE('',#97509,58.5);
#31240=CIRCLE('',#97511,0.5);
#31241=CIRCLE('',#97512,0.500000000000005);
#31242=CIRCLE('',#97514,58.5);
#31243=CIRCLE('',#97515,0.500000000000002);
#31244=CIRCLE('',#97516,0.5);
#31245=CIRCLE('',#97519,58.5);
#31246=CIRCLE('',#97521,0.5);
#31247=CIRCLE('',#97523,2.75);
#31248=CIRCLE('',#97525,2.75);
#31249=CIRCLE('',#97527,0.250000000000002);
#31250=CIRCLE('',#97528,3.25);
#31251=CIRCLE('',#97529,0.250000000000003);
#31252=CIRCLE('',#97531,0.250000000000003);
#31253=CIRCLE('',#97533,2.75);
#31254=CIRCLE('',#97534,0.250000000000003);
#31255=CIRCLE('',#97536,67.25);
#31256=CIRCLE('',#97537,0.250000000000003);
#31257=CIRCLE('',#97539,2.75);
#31258=CIRCLE('',#97540,0.250000000000003);
#31259=CIRCLE('',#97542,0.249999999999997);
#31260=CIRCLE('',#97544,5.25);
#31261=CIRCLE('',#97545,0.249999999999997);
#31262=CIRCLE('',#97547,58.25);
#31263=CIRCLE('',#97548,0.249999999999997);
#31264=CIRCLE('',#97550,5.25);
#31265=CIRCLE('',#97551,0.249999999999997);
#31266=CIRCLE('',#97553,0.249999999999997);
#31267=CIRCLE('',#97555,2.75);
#31268=CIRCLE('',#97556,0.250000000000003);
#31269=CIRCLE('',#97558,67.25);
#31270=CIRCLE('',#97559,0.250000000000003);
#31271=CIRCLE('',#97561,2.75);
#31272=CIRCLE('',#97562,0.250000000000003);
#31273=CIRCLE('',#97564,0.250000000000003);
#31274=CIRCLE('',#97566,5.25);
#31275=CIRCLE('',#97567,0.249999999999998);
#31276=CIRCLE('',#97568,5.);
#31277=CIRCLE('',#97570,5.);
#31278=CIRCLE('',#97572,0.5);
#31279=CIRCLE('',#97574,0.500000000000003);
#31280=CIRCLE('',#97575,4.5);
#31281=CIRCLE('',#97577,3.);
#31282=CIRCLE('',#97580,0.5);
#31283=CIRCLE('',#97583,0.5);
#31284=CIRCLE('',#97585,0.5);
#31285=CIRCLE('',#97586,1.);
#31286=CIRCLE('',#97588,0.5);
#31287=CIRCLE('',#97590,0.5);
#31288=CIRCLE('',#97591,1.);
#31289=CIRCLE('',#97595,0.5);
#31290=CIRCLE('',#97597,0.5);
#31291=CIRCLE('',#97598,1.);
#31292=CIRCLE('',#97600,0.5);
#31293=CIRCLE('',#97602,0.5);
#31294=CIRCLE('',#97603,1.);
#31295=CIRCLE('',#97606,1.);
#31296=CIRCLE('',#97607,1.);
#31297=CIRCLE('',#97609,45.1752328136335);
#31298=CIRCLE('',#97611,0.5);
#31299=CIRCLE('',#97613,0.5);
#31300=CIRCLE('',#97614,0.999999999999999);
#31301=CIRCLE('',#97616,0.5);
#31302=CIRCLE('',#97618,0.5);
#31303=CIRCLE('',#97619,1.);
#31304=CIRCLE('',#97622,45.1752328136335);
#31305=CIRCLE('',#97624,0.5);
#31306=CIRCLE('',#97626,0.5);
#31307=CIRCLE('',#97627,1.);
#31308=CIRCLE('',#97629,0.5);
#31309=CIRCLE('',#97631,0.5);
#31310=CIRCLE('',#97632,1.);
#31311=CIRCLE('',#97634,0.5);
#31312=CIRCLE('',#97636,3.);
#31313=CIRCLE('',#97638,0.5);
#31314=CIRCLE('',#97640,1.);
#31315=CIRCLE('',#97641,0.500000000000001);
#31316=CIRCLE('',#97643,0.499999999999999);
#31317=CIRCLE('',#97645,0.5);
#31318=CIRCLE('',#97648,2.5);
#31319=CIRCLE('',#97649,58.8875000000282);
#31320=CIRCLE('',#97651,2.);
#31321=CIRCLE('',#97652,2.);
#31322=CIRCLE('',#97654,2.);
#31323=CIRCLE('',#97655,2.);
#31324=CIRCLE('',#97657,1.);
#31325=CIRCLE('',#97659,0.5);
#31326=CIRCLE('',#97660,0.5);
#31327=CIRCLE('',#97661,0.499999999999998);
#31328=CIRCLE('',#97663,0.499999999999998);
#31329=CIRCLE('',#97664,0.5);
#31330=CIRCLE('',#97668,0.5);
#31331=CIRCLE('',#97669,0.499999999999998);
#31332=CIRCLE('',#97671,0.499999999999998);
#31333=CIRCLE('',#97672,0.5);
#31334=CIRCLE('',#97675,1.);
#31335=CIRCLE('',#97676,0.500000000000004);
#31336=CIRCLE('',#97678,0.5);
#31337=CIRCLE('',#97681,0.5);
#31338=CIRCLE('',#97682,0.499999999999999);
#31339=CIRCLE('',#97684,0.499999999999999);
#31340=CIRCLE('',#97685,0.5);
#31341=CIRCLE('',#97688,0.999999999999998);
#31342=CIRCLE('',#97690,0.5);
#31343=CIRCLE('',#97691,0.5);
#31344=CIRCLE('',#97694,0.999999999999997);
#31345=CIRCLE('',#97696,0.5);
#31346=CIRCLE('',#97697,0.499999999999999);
#31347=CIRCLE('',#97699,0.499999999999999);
#31348=CIRCLE('',#97700,0.5);
#31349=CIRCLE('',#97704,1.);
#31350=CIRCLE('',#97705,0.999999999999996);
#31351=CIRCLE('',#97707,0.5);
#31352=CIRCLE('',#97708,0.499999999999999);
#31353=CIRCLE('',#97710,0.499999999999999);
#31354=CIRCLE('',#97711,0.5);
#31355=CIRCLE('',#97714,0.999999999999997);
#31356=CIRCLE('',#97715,1.);
#31357=CIRCLE('',#97717,0.5);
#31358=CIRCLE('',#97718,0.499999999999999);
#31359=CIRCLE('',#97720,0.499999999999999);
#31360=CIRCLE('',#97721,0.5);
#31361=CIRCLE('',#97724,0.999999999999997);
#31362=CIRCLE('',#97726,1.);
#31363=CIRCLE('',#97727,0.999999999999996);
#31364=CIRCLE('',#97729,0.5);
#31365=CIRCLE('',#97730,0.500000000000005);
#31366=CIRCLE('',#97732,0.500000000000005);
#31367=CIRCLE('',#97733,0.5);
#31368=CIRCLE('',#97736,0.999999999999996);
#31369=CIRCLE('',#97738,0.5);
#31370=CIRCLE('',#97739,0.499999999999999);
#31371=CIRCLE('',#97741,1.);
#31372=CIRCLE('',#97743,0.5);
#31373=CIRCLE('',#97744,0.500000000000005);
#31374=CIRCLE('',#97746,0.500000000000005);
#31375=CIRCLE('',#97747,0.5);
#31376=CIRCLE('',#97750,0.499999999999999);
#31377=CIRCLE('',#97751,0.5);
#31378=CIRCLE('',#97754,58.3875000000282);
#31379=CIRCLE('',#97756,0.5);
#31380=CIRCLE('',#97757,0.499999999999998);
#31381=CIRCLE('',#97759,58.3875000000282);
#31382=CIRCLE('',#97760,0.500000000000001);
#31383=CIRCLE('',#97761,0.5);
#31384=CIRCLE('',#97764,58.3875000000282);
#31385=CIRCLE('',#97766,0.5);
#31386=CIRCLE('',#97767,0.500000000000001);
#31387=CIRCLE('',#97768,0.499999999999997);
#31388=CIRCLE('',#97769,57.8151740222928);
#31389=CIRCLE('',#97770,0.5);
#31390=CIRCLE('',#97773,58.3875000000282);
#31391=CIRCLE('',#97775,0.5);
#31392=CIRCLE('',#97776,0.499999999999999);
#31393=CIRCLE('',#97777,0.499999999999998);
#31394=CIRCLE('',#97778,57.9942131824662);
#31395=CIRCLE('',#97779,0.5);
#31396=CIRCLE('',#97782,58.3875000000282);
#31397=CIRCLE('',#97784,0.5);
#31398=CIRCLE('',#97785,0.499999999999998);
#31399=CIRCLE('',#97786,0.500000000000001);
#31400=CIRCLE('',#97787,57.7939200874014);
#31401=CIRCLE('',#97788,0.5);
#31402=CIRCLE('',#97791,58.3875000000282);
#31403=CIRCLE('',#97793,0.5);
#31404=CIRCLE('',#97794,0.500000000000001);
#31405=CIRCLE('',#97796,58.3875000000282);
#31406=CIRCLE('',#97797,0.499999999999999);
#31407=CIRCLE('',#97798,0.5);
#31408=CIRCLE('',#97801,58.3875000000282);
#31409=CIRCLE('',#97803,0.5);
#31410=CIRCLE('',#97804,0.5);
#31411=CIRCLE('',#97807,3.);
#31412=CIRCLE('',#97810,3.);
#31413=CIRCLE('',#97812,3.);
#31414=CIRCLE('',#97815,3.);
#31415=CIRCLE('',#97816,0.500000000000002);
#31416=CIRCLE('',#97818,0.500000000000002);
#31417=CIRCLE('',#97819,5.);
#31418=CIRCLE('',#97820,1.40932613287356);
#31419=CIRCLE('',#97822,58.3875000000282);
#31420=CIRCLE('',#97824,5.);
#31421=CIRCLE('',#97825,0.500000000000002);
#31422=CIRCLE('',#97827,0.499999999999998);
#31423=CIRCLE('',#97828,5.);
#31424=CIRCLE('',#97830,0.5);
#31425=CIRCLE('',#97831,0.500000000000002);
#31426=CIRCLE('',#97832,57.9863561268404);
#31427=CIRCLE('',#97833,0.5);
#31428=CIRCLE('',#97834,0.5);
#31429=CIRCLE('',#97837,58.3875000000282);
#31430=CIRCLE('',#97839,0.5);
#31431=CIRCLE('',#97840,0.500000000000003);
#31432=CIRCLE('',#97841,56.5371804123359);
#31433=CIRCLE('',#97842,0.499999999999999);
#31434=CIRCLE('',#97843,0.5);
#31435=CIRCLE('',#97846,58.3875000000282);
#31436=CIRCLE('',#97848,0.5);
#31437=CIRCLE('',#97849,0.5);
#31438=CIRCLE('',#97851,58.3875000000282);
#31439=CIRCLE('',#97852,0.499999999999999);
#31440=CIRCLE('',#97853,0.5);
#31441=CIRCLE('',#97856,58.3875000000282);
#31442=CIRCLE('',#97858,5.);
#31443=CIRCLE('',#97860,0.499999999999997);
#31444=CIRCLE('',#97861,0.499999999999997);
#31445=CIRCLE('',#97862,58.3875000000282);
#31446=CIRCLE('',#97863,0.5);
#31447=CIRCLE('',#97866,58.3875000000282);
#31448=CIRCLE('',#97868,0.5);
#31449=CIRCLE('',#97869,0.499999999999999);
#31450=CIRCLE('',#97871,0.499999999999998);
#31451=CIRCLE('',#97872,58.3875000000282);
#31452=CIRCLE('',#97873,0.5);
#31453=CIRCLE('',#97876,58.3875000000282);
#31454=CIRCLE('',#97878,0.5);
#31455=CIRCLE('',#97879,0.499999999999994);
#31456=CIRCLE('',#97880,0.499999999999999);
#31457=CIRCLE('',#97881,57.7596339908634);
#31458=CIRCLE('',#97882,0.5);
#31459=CIRCLE('',#97883,0.5);
#31460=CIRCLE('',#97886,58.3875000000282);
#31461=CIRCLE('',#97888,0.5);
#31462=CIRCLE('',#97889,0.500000000000004);
#31463=CIRCLE('',#97891,58.3875000000282);
#31464=CIRCLE('',#97892,57.9914298998865);
#31465=CIRCLE('',#97895,3.);
#31466=CIRCLE('',#97898,3.);
#31467=CIRCLE('',#97900,3.);
#31468=CIRCLE('',#97903,3.);
#31469=CIRCLE('',#97904,0.499999999999997);
#31470=CIRCLE('',#97906,3.);
#31471=CIRCLE('',#97908,3.);
#31472=CIRCLE('',#97909,68.1760805737352);
#31473=CIRCLE('',#97910,121.707040772094);
#31474=CIRCLE('',#97912,109.54163477943);
#31475=CIRCLE('',#97913,68.2880455456965);
#31476=CIRCLE('',#97914,58.1059293197714);
#31477=CIRCLE('',#97916,58.5);
#31478=CIRCLE('',#97918,58.25);
#31479=CIRCLE('',#97920,58.25);
#31480=CIRCLE('',#97922,58.5);
#31481=CIRCLE('',#97924,58.5);
#31482=CIRCLE('',#97926,59.);
#31483=CIRCLE('',#97930,45.1752328136335);
#31484=CIRCLE('',#97932,44.2689250265968);
#31485=CIRCLE('',#97934,58.2938077870648);
#31486=CIRCLE('',#97936,58.3875000000282);
#31487=CIRCLE('',#97938,58.3875000000282);
#31488=CIRCLE('',#97940,5.);
#31489=CIRCLE('',#97950,1.73205080756888);
#31490=CIRCLE('',#97952,1.73205080756888);
#31491=CIRCLE('',#97954,1.73205080756888);
#31492=CIRCLE('',#97956,1.73205080756888);
#31493=CIRCLE('',#97958,1.73205080756888);
#31494=CIRCLE('',#97960,1.73205080756888);
#31495=CIRCLE('',#97962,3.);
#31496=CIRCLE('',#97963,0.25);
#31497=CIRCLE('',#97964,3.25);
#31498=CIRCLE('',#97965,3.25);
#31499=CIRCLE('',#97967,3.25);
#31500=CIRCLE('',#97971,2.);
#31501=CIRCLE('',#97972,1.47499999999998);
#31502=CIRCLE('',#97975,2.);
#31503=CIRCLE('',#97977,2.5);
#31504=CIRCLE('',#97979,2.5);
#31505=CIRCLE('',#97981,0.500000000000001);
#31506=CIRCLE('',#97982,0.499999999999997);
#31507=CIRCLE('',#97984,4.01589928084082);
#31508=CIRCLE('',#97985,0.5);
#31509=CIRCLE('',#97986,3.51597543326262);
#31510=CIRCLE('',#97987,3.51597543326262);
#31511=CIRCLE('',#97988,0.499999999999999);
#31512=CIRCLE('',#97989,0.500000000000002);
#31513=CIRCLE('',#97990,0.50000000000001);
#31514=CIRCLE('',#97992,0.500000000000004);
#31515=CIRCLE('',#97993,0.500000000000002);
#31516=CIRCLE('',#97994,0.499999999999999);
#31517=CIRCLE('',#97996,0.499999999999997);
#31518=CIRCLE('',#97997,2.);
#31519=CIRCLE('',#97998,1.49999999999999);
#31520=CIRCLE('',#97999,0.500000000000002);
#31521=CIRCLE('',#98001,0.5);
#31522=CIRCLE('',#98002,74.3);
#31523=CIRCLE('',#98003,73.8);
#31524=CIRCLE('',#98004,0.500000000000002);
#31525=CIRCLE('',#98006,0.499999999999999);
#31526=CIRCLE('',#98007,2.);
#31527=CIRCLE('',#98008,1.5);
#31528=CIRCLE('',#98009,0.499999999999993);
#31529=CIRCLE('',#98010,0.500000000000006);
#31530=CIRCLE('',#98011,0.500000000000012);
#31531=CIRCLE('',#98014,0.499999999999999);
#31532=CIRCLE('',#98015,0.500000000000001);
#31533=CIRCLE('',#98016,0.499999999999998);
#31534=CIRCLE('',#98017,0.5);
#31535=CIRCLE('',#98018,0.5);
#31536=CIRCLE('',#98019,0.500000000000006);
#31537=CIRCLE('',#98020,0.500000000000001);
#31538=CIRCLE('',#98022,0.500000000000003);
#31539=CIRCLE('',#98023,0.499999999999998);
#31540=CIRCLE('',#98024,0.50000000000001);
#31541=CIRCLE('',#98025,0.499999999999999);
#31542=CIRCLE('',#98026,0.499999999999999);
#31543=CIRCLE('',#98028,0.499999999999998);
#31544=CIRCLE('',#98029,1.5);
#31545=CIRCLE('',#98030,2.);
#31546=CIRCLE('',#98032,0.499999999999997);
#31547=CIRCLE('',#98033,0.499999999999998);
#31548=CIRCLE('',#98035,0.5);
#31549=CIRCLE('',#98036,73.8);
#31550=CIRCLE('',#98037,74.3);
#31551=CIRCLE('',#98038,0.499999999999997);
#31552=CIRCLE('',#98040,2.);
#31553=CIRCLE('',#98041,1.5);
#31554=CIRCLE('',#98043,0.500000000000001);
#31555=CIRCLE('',#98044,12.0057534629026);
#31556=CIRCLE('',#98045,0.500000000000002);
#31557=CIRCLE('',#98046,11.5058296153244);
#31558=CIRCLE('',#98048,0.500000000000001);
#31559=CIRCLE('',#98049,77.6552534828746);
#31560=CIRCLE('',#98050,77.1553296352964);
#31561=CIRCLE('',#98052,0.499999999999998);
#31562=CIRCLE('',#98053,12.0057534629026);
#31563=CIRCLE('',#98054,11.5058296153244);
#31564=CIRCLE('',#98056,0.499999999999998);
#31565=CIRCLE('',#98057,1067.5427534629);
#31566=CIRCLE('',#98058,1067.04282961532);
#31567=CIRCLE('',#98060,0.499999999999999);
#31568=CIRCLE('',#98061,12.0057534629025);
#31569=CIRCLE('',#98062,11.5058296153244);
#31570=CIRCLE('',#98064,0.500000000000001);
#31571=CIRCLE('',#98065,77.6552534828746);
#31572=CIRCLE('',#98066,77.1553296352964);
#31573=CIRCLE('',#98068,0.500000000000002);
#31574=CIRCLE('',#98069,12.0057534629026);
#31575=CIRCLE('',#98070,11.5058296153244);
#31576=CIRCLE('',#98071,64.9438263390348);
#31577=CIRCLE('',#98072,0.500000000000001);
#31578=CIRCLE('',#98073,64.8942562468481);
#31579=CIRCLE('',#98074,0.499999999999998);
#31580=CIRCLE('',#98076,0.499999999999996);
#31581=CIRCLE('',#98077,0.500000000000001);
#31582=CIRCLE('',#98078,0.50000000000001);
#31583=CIRCLE('',#98079,368.00584558015);
#31584=CIRCLE('',#98080,365.618325533514);
#31585=CIRCLE('',#98081,0.499999999999998);
#31586=CIRCLE('',#98082,431.08166328569);
#31587=CIRCLE('',#98083,429.776000990187);
#31588=CIRCLE('',#98084,0.5);
#31589=CIRCLE('',#98085,0.499999999999998);
#31590=CIRCLE('',#98086,0.5);
#31591=CIRCLE('',#98087,0.499999999999998);
#31592=CIRCLE('',#98088,0.499999999999998);
#31593=CIRCLE('',#98089,0.499999999999997);
#31594=CIRCLE('',#98091,77.1139810037387);
#31595=CIRCLE('',#98092,77.1139048513169);
#31596=CIRCLE('',#98093,0.500000000000002);
#31597=CIRCLE('',#98094,0.500000000000003);
#31598=CIRCLE('',#98096,0.499999999999998);
#31599=CIRCLE('',#98097,77.1139048513167);
#31600=CIRCLE('',#98098,77.1139810037385);
#31601=CIRCLE('',#98099,0.500000000000003);
#31602=CIRCLE('',#98100,0.5);
#31603=CIRCLE('',#98101,0.499999999999995);
#31604=CIRCLE('',#98102,0.500000000000002);
#31605=CIRCLE('',#98103,0.500000000000004);
#31606=CIRCLE('',#98104,329.616230392321);
#31607=CIRCLE('',#98105,329.186676134887);
#31608=CIRCLE('',#98106,0.499999999999997);
#31609=CIRCLE('',#98107,0.499999999999999);
#31610=CIRCLE('',#98108,462.991628528349);
#31611=CIRCLE('',#98109,463.797803513665);
#31612=CIRCLE('',#98111,0.750000000000001);
#31613=CIRCLE('',#98112,1.5);
#31614=CIRCLE('',#98113,0.750000000000001);
#31615=CIRCLE('',#98114,0.75);
#31616=CIRCLE('',#98116,73.05);
#31617=CIRCLE('',#98117,0.750000000000002);
#31618=CIRCLE('',#98118,73.8);
#31619=CIRCLE('',#98119,73.05);
#31620=CIRCLE('',#98120,0.749999999999996);
#31621=CIRCLE('',#98121,1.5);
#31622=CIRCLE('',#98122,0.750000000000001);
#31623=CIRCLE('',#98125,0.750000000000003);
#31624=CIRCLE('',#98126,1.5);
#31625=CIRCLE('',#98127,0.750000000000001);
#31626=CIRCLE('',#98128,0.750000000000004);
#31627=CIRCLE('',#98130,0.749999999999998);
#31628=CIRCLE('',#98131,77.1139048513167);
#31629=CIRCLE('',#98132,76.3639048513167);
#31630=CIRCLE('',#98133,0.75);
#31631=CIRCLE('',#98134,1.5);
#31632=CIRCLE('',#98135,0.750000000000001);
#31633=CIRCLE('',#98138,0.749999999999999);
#31634=CIRCLE('',#98139,0.749999999999999);
#31635=CIRCLE('',#98140,1.5);
#31636=CIRCLE('',#98141,0.750000000000001);
#31637=CIRCLE('',#98143,0.75);
#31638=CIRCLE('',#98144,77.1139048513169);
#31639=CIRCLE('',#98145,76.3639048513169);
#31640=CIRCLE('',#98146,0.750000000000001);
#31641=CIRCLE('',#98147,0.750000000000005);
#31642=CIRCLE('',#98148,1.5);
#31643=CIRCLE('',#98151,0.75);
#31644=CIRCLE('',#98152,0.750000000000003);
#31645=CIRCLE('',#98153,1.49999999999999);
#31646=CIRCLE('',#98154,0.749999999999994);
#31647=CIRCLE('',#98156,0.750000000000004);
#31648=CIRCLE('',#98157,73.8);
#31649=CIRCLE('',#98158,73.05);
#31650=CIRCLE('',#98159,0.750000000000001);
#31651=CIRCLE('',#98160,0.75);
#31652=CIRCLE('',#98161,1.5);
#31653=CIRCLE('',#98172,1.2);
#31654=CIRCLE('',#98173,0.450000000000006);
#31655=CIRCLE('',#98174,0.750000000000001);
#31656=CIRCLE('',#98175,0.450000000000001);
#31657=CIRCLE('',#98177,0.450000000000006);
#31658=CIRCLE('',#98179,0.45);
#31659=CIRCLE('',#98180,204.945690815561);
#31660=CIRCLE('',#98181,204.49569081556);
#31661=CIRCLE('',#98183,0.450000000000006);
#31662=CIRCLE('',#98184,0.750000000000001);
#31663=CIRCLE('',#98185,1.2);
#31664=CIRCLE('',#98187,0.450000000000001);
#31665=CIRCLE('',#98188,1.45);
#31666=CIRCLE('',#98189,1.);
#31667=CIRCLE('',#98191,0.450000000000006);
#31668=CIRCLE('',#98193,0.450000000000001);
#31669=CIRCLE('',#98194,48.45);
#31670=CIRCLE('',#98195,48.);
#31671=CIRCLE('',#98197,0.450000000000006);
#31672=CIRCLE('',#98198,0.750000000000001);
#31673=CIRCLE('',#98199,1.2);
#31674=CIRCLE('',#98201,0.450000000000006);
#31675=CIRCLE('',#98202,1.2);
#31676=CIRCLE('',#98203,0.750000000000001);
#31677=CIRCLE('',#98206,1.2);
#31678=CIRCLE('',#98207,0.450000000000006);
#31679=CIRCLE('',#98208,0.750000000000001);
#31680=CIRCLE('',#98209,0.450000000000001);
#31681=CIRCLE('',#98211,0.450000000000006);
#31682=CIRCLE('',#98213,0.449999999999999);
#31683=CIRCLE('',#98214,204.945690815561);
#31684=CIRCLE('',#98215,204.49569081556);
#31685=CIRCLE('',#98217,0.450000000000006);
#31686=CIRCLE('',#98218,0.750000000000001);
#31687=CIRCLE('',#98219,1.2);
#31688=CIRCLE('',#98221,0.450000000000006);
#31689=CIRCLE('',#98222,1.2);
#31690=CIRCLE('',#98223,0.750000000000001);
#31691=CIRCLE('',#98225,0.450000000000006);
#31692=CIRCLE('',#98227,0.450000000000006);
#31693=CIRCLE('',#98229,1.2);
#31694=CIRCLE('',#98230,0.750000000000001);
#31695=CIRCLE('',#98232,1.2);
#31696=CIRCLE('',#98233,0.450000000000006);
#31697=CIRCLE('',#98234,0.750000000000001);
#31698=CIRCLE('',#98235,0.449999999999999);
#31699=CIRCLE('',#98237,0.450000000000006);
#31700=CIRCLE('',#98239,0.450000000000001);
#31701=CIRCLE('',#98240,204.945690815561);
#31702=CIRCLE('',#98241,204.49569081556);
#31703=CIRCLE('',#98243,0.450000000000006);
#31704=CIRCLE('',#98244,0.750000000000001);
#31705=CIRCLE('',#98245,1.2);
#31706=CIRCLE('',#98247,0.450000000000006);
#31707=CIRCLE('',#98248,1.2);
#31708=CIRCLE('',#98249,0.750000000000001);
#31709=CIRCLE('',#98251,0.450000000000006);
#31710=CIRCLE('',#98253,0.450000000000006);
#31711=CIRCLE('',#98255,1.2);
#31712=CIRCLE('',#98256,0.750000000000001);
#31713=CIRCLE('',#98258,0.449999999999999);
#31714=CIRCLE('',#98259,1.2);
#31715=CIRCLE('',#98260,0.450000000000006);
#31716=CIRCLE('',#98261,0.750000000000001);
#31717=CIRCLE('',#98263,0.450000000000006);
#31718=CIRCLE('',#98265,0.450000000000006);
#31719=CIRCLE('',#98267,0.450000000000006);
#31720=CIRCLE('',#98268,0.750000000000001);
#31721=CIRCLE('',#98269,1.2);
#31722=CIRCLE('',#98271,0.450000000000006);
#31723=CIRCLE('',#98272,1.2);
#31724=CIRCLE('',#98273,0.750000000000001);
#31725=CIRCLE('',#98275,0.450000000000006);
#31726=CIRCLE('',#98277,0.450000000000006);
#31727=CIRCLE('',#98279,1.2);
#31728=CIRCLE('',#98280,0.750000000000001);
#31729=CIRCLE('',#98282,0.450000000000006);
#31730=CIRCLE('',#98283,1.2);
#31731=CIRCLE('',#98284,0.450000000000006);
#31732=CIRCLE('',#98285,0.750000000000001);
#31733=CIRCLE('',#98287,0.450000000000006);
#31734=CIRCLE('',#98289,0.450000000000006);
#31735=CIRCLE('',#98291,0.45);
#31736=CIRCLE('',#98292,0.75);
#31737=CIRCLE('',#98293,1.2);
#31738=CIRCLE('',#98295,0.450000000000006);
#31739=CIRCLE('',#98296,1.2);
#31740=CIRCLE('',#98297,0.750000000000001);
#31741=CIRCLE('',#98299,0.45);
#31742=CIRCLE('',#98300,13.1055395526668);
#31743=CIRCLE('',#98301,12.6555395526668);
#31744=CIRCLE('',#98303,0.450000000000001);
#31745=CIRCLE('',#98305,0.45);
#31746=CIRCLE('',#98306,10.);
#31747=CIRCLE('',#98307,10.45);
#31748=CIRCLE('',#98309,0.75);
#31749=CIRCLE('',#98310,1.2);
#31750=CIRCLE('',#98312,0.450000000000006);
#31751=CIRCLE('',#98313,1.2);
#31752=CIRCLE('',#98314,0.450000000000006);
#31753=CIRCLE('',#98315,0.750000000000001);
#31754=CIRCLE('',#98317,0.450000000000001);
#31755=CIRCLE('',#98319,0.450000000000006);
#31756=CIRCLE('',#98321,0.450000000000006);
#31757=CIRCLE('',#98322,0.75);
#31758=CIRCLE('',#98323,1.2);
#31759=CIRCLE('',#98325,0.450000000000006);
#31760=CIRCLE('',#98326,1.2);
#31761=CIRCLE('',#98327,0.750000000000001);
#31762=CIRCLE('',#98329,0.450000000000006);
#31763=CIRCLE('',#98331,0.449999999999999);
#31764=CIRCLE('',#98333,1.2);
#31765=CIRCLE('',#98334,0.75);
#31766=CIRCLE('',#98336,0.450000000000006);
#31767=CIRCLE('',#98337,1.2);
#31768=CIRCLE('',#98338,0.450000000000006);
#31769=CIRCLE('',#98339,0.750000000000001);
#31770=CIRCLE('',#98341,0.450000000000006);
#31771=CIRCLE('',#98343,0.450000000000006);
#31772=CIRCLE('',#98345,0.450000000000006);
#31773=CIRCLE('',#98346,0.750000000000001);
#31774=CIRCLE('',#98347,1.2);
#31775=CIRCLE('',#98349,0.450000000000006);
#31776=CIRCLE('',#98350,1.2);
#31777=CIRCLE('',#98351,0.750000000000001);
#31778=CIRCLE('',#98353,0.450000000000006);
#31779=CIRCLE('',#98355,0.450000000000006);
#31780=CIRCLE('',#98357,1.2);
#31781=CIRCLE('',#98358,0.750000000000001);
#31782=CIRCLE('',#98360,0.450000000000006);
#31783=CIRCLE('',#98361,1.2);
#31784=CIRCLE('',#98362,0.450000000000006);
#31785=CIRCLE('',#98363,0.750000000000001);
#31786=CIRCLE('',#98365,0.450000000000006);
#31787=CIRCLE('',#98367,0.450000000000006);
#31788=CIRCLE('',#98369,0.450000000000006);
#31789=CIRCLE('',#98370,0.750000000000001);
#31790=CIRCLE('',#98371,1.2);
#31791=CIRCLE('',#98373,0.450000000000006);
#31792=CIRCLE('',#98374,1.2);
#31793=CIRCLE('',#98375,0.750000000000001);
#31794=CIRCLE('',#98377,0.450000000000006);
#31795=CIRCLE('',#98379,0.450000000000006);
#31796=CIRCLE('',#98381,1.2);
#31797=CIRCLE('',#98382,0.750000000000001);
#31798=CIRCLE('',#98384,0.450000000000006);
#31799=CIRCLE('',#98385,1.2);
#31800=CIRCLE('',#98386,0.450000000000006);
#31801=CIRCLE('',#98387,0.750000000000001);
#31802=CIRCLE('',#98389,0.449999999999999);
#31803=CIRCLE('',#98391,0.450000000000006);
#31804=CIRCLE('',#98393,0.450000000000006);
#31805=CIRCLE('',#98394,0.75);
#31806=CIRCLE('',#98395,1.2);
#31807=CIRCLE('',#98397,0.450000000000006);
#31808=CIRCLE('',#98398,1.2);
#31809=CIRCLE('',#98399,0.750000000000001);
#31810=CIRCLE('',#98401,0.450000000000006);
#31811=CIRCLE('',#98403,0.450000000000006);
#31812=CIRCLE('',#98405,1.2);
#31813=CIRCLE('',#98406,0.75);
#31814=CIRCLE('',#98408,0.450000000000006);
#31815=CIRCLE('',#98409,1.2);
#31816=CIRCLE('',#98410,0.450000000000006);
#31817=CIRCLE('',#98411,0.750000000000001);
#31818=CIRCLE('',#98413,0.449999999999999);
#31819=CIRCLE('',#98415,0.450000000000006);
#31820=CIRCLE('',#98417,0.450000000000006);
#31821=CIRCLE('',#98418,0.75);
#31822=CIRCLE('',#98419,1.2);
#31823=CIRCLE('',#98421,0.449999999999997);
#31824=CIRCLE('',#98422,1.2);
#31825=CIRCLE('',#98423,0.750000000000001);
#31826=CIRCLE('',#98425,0.450000000000006);
#31827=CIRCLE('',#98427,0.449999999999998);
#31828=CIRCLE('',#98428,677.884816028482);
#31829=CIRCLE('',#98429,677.434816028482);
#31830=CIRCLE('',#98431,1.2);
#31831=CIRCLE('',#98432,0.75);
#31832=CIRCLE('',#98434,0.450000000000006);
#31833=CIRCLE('',#98435,1.2);
#31834=CIRCLE('',#98436,0.450000000000006);
#31835=CIRCLE('',#98437,0.750000000000001);
#31836=CIRCLE('',#98439,0.450000000000006);
#31837=CIRCLE('',#98441,0.450000000000006);
#31838=CIRCLE('',#98443,0.450000000000006);
#31839=CIRCLE('',#98444,0.750000000000001);
#31840=CIRCLE('',#98445,1.2);
#31841=CIRCLE('',#98447,0.449999999999998);
#31842=CIRCLE('',#98448,1.2);
#31843=CIRCLE('',#98449,0.750000000000001);
#31844=CIRCLE('',#98451,0.450000000000006);
#31845=CIRCLE('',#98453,0.45);
#31846=CIRCLE('',#98454,48.45);
#31847=CIRCLE('',#98455,48.);
#31848=CIRCLE('',#98457,0.449999999999997);
#31849=CIRCLE('',#98458,0.750000000000001);
#31850=CIRCLE('',#98459,1.2);
#31851=CIRCLE('',#98461,0.449999999999997);
#31852=CIRCLE('',#98462,1.45);
#31853=CIRCLE('',#98463,0.999999999999999);
#31854=CIRCLE('',#98465,677.884816028482);
#31855=CIRCLE('',#98466,677.434816028482);
#31856=CIRCLE('',#98468,0.450000000000006);
#31857=CIRCLE('',#98469,1.2);
#31858=CIRCLE('',#98470,0.450000000000006);
#31859=CIRCLE('',#98471,0.75);
#31860=CIRCLE('',#98473,0.449999999999999);
#31861=CIRCLE('',#98475,0.450000000000006);
#31862=CIRCLE('',#98477,0.450000000000006);
#31863=CIRCLE('',#98478,0.750000000000001);
#31864=CIRCLE('',#98479,1.2);
#31865=CIRCLE('',#98481,0.45);
#31866=CIRCLE('',#98482,1.2);
#31867=CIRCLE('',#98483,0.75);
#31868=CIRCLE('',#98485,0.450000000000006);
#31869=CIRCLE('',#98487,0.449999999999999);
#31870=CIRCLE('',#98488,677.884816028482);
#31871=CIRCLE('',#98489,677.434816028482);
#31872=CIRCLE('',#98491,1.2);
#31873=CIRCLE('',#98492,0.750000000000001);
#31874=CIRCLE('',#98494,0.450000000000006);
#31875=CIRCLE('',#98495,1.2);
#31876=CIRCLE('',#98496,0.450000000000006);
#31877=CIRCLE('',#98497,0.75);
#31878=CIRCLE('',#98499,0.449999999999999);
#31879=CIRCLE('',#98501,0.450000000000006);
#31880=CIRCLE('',#98503,0.450000000000006);
#31881=CIRCLE('',#98504,0.750000000000001);
#31882=CIRCLE('',#98505,1.2);
#31883=CIRCLE('',#98507,0.450000000000006);
#31884=CIRCLE('',#98508,1.2);
#31885=CIRCLE('',#98509,0.75);
#31886=CIRCLE('',#98511,0.450000000000006);
#31887=CIRCLE('',#98513,0.450000000000006);
#31888=CIRCLE('',#98515,1.2);
#31889=CIRCLE('',#98516,0.750000000000001);
#31890=CIRCLE('',#98518,0.45);
#31891=CIRCLE('',#98519,1.2);
#31892=CIRCLE('',#98520,0.450000000000006);
#31893=CIRCLE('',#98521,0.750000000000001);
#31894=CIRCLE('',#98523,0.450000000000006);
#31895=CIRCLE('',#98525,0.45);
#31896=CIRCLE('',#98526,11.6555395526668);
#31897=CIRCLE('',#98527,12.1055395526668);
#31898=CIRCLE('',#98529,0.450000000000006);
#31899=CIRCLE('',#98530,0.750000000000001);
#31900=CIRCLE('',#98531,1.2);
#31901=CIRCLE('',#98533,0.450000000000006);
#31902=CIRCLE('',#98534,10.45);
#31903=CIRCLE('',#98535,10.);
#31904=CIRCLE('',#98537,0.450000000000006);
#31905=CIRCLE('',#98539,0.450000000000006);
#31906=CIRCLE('',#98541,0.450000000000006);
#31907=CIRCLE('',#98542,0.75);
#31908=CIRCLE('',#98543,1.2);
#31909=CIRCLE('',#98545,0.450000000000006);
#31910=CIRCLE('',#98546,1.2);
#31911=CIRCLE('',#98547,0.75);
#31912=CIRCLE('',#98550,0.450000000000001);
#31913=CIRCLE('',#98551,1.2);
#31914=CIRCLE('',#98552,0.450000000000006);
#31915=CIRCLE('',#98553,0.750000000000001);
#31916=CIRCLE('',#98555,0.450000000000006);
#31917=CIRCLE('',#98557,0.450000000000006);
#31918=CIRCLE('',#98559,0.450000000000006);
#31919=CIRCLE('',#98560,0.750000000000001);
#31920=CIRCLE('',#98561,1.2);
#31921=CIRCLE('',#98563,0.450000000000001);
#31922=CIRCLE('',#98564,10.45);
#31923=CIRCLE('',#98565,10.);
#31924=CIRCLE('',#98567,0.449999999999999);
#31925=CIRCLE('',#98569,0.45);
#31926=CIRCLE('',#98570,11.6555395526668);
#31927=CIRCLE('',#98571,12.1055395526668);
#31928=CIRCLE('',#98573,0.450000000000006);
#31929=CIRCLE('',#98574,0.750000000000001);
#31930=CIRCLE('',#98575,1.2);
#31931=CIRCLE('',#98577,0.450000000000006);
#31932=CIRCLE('',#98578,1.2);
#31933=CIRCLE('',#98579,0.750000000000001);
#31934=CIRCLE('',#98582,0.450000000000006);
#31935=CIRCLE('',#98583,1.2);
#31936=CIRCLE('',#98584,0.450000000000006);
#31937=CIRCLE('',#98585,0.750000000000001);
#31938=CIRCLE('',#98587,0.450000000000006);
#31939=CIRCLE('',#98589,0.450000000000006);
#31940=CIRCLE('',#98591,0.450000000000006);
#31941=CIRCLE('',#98592,0.750000000000001);
#31942=CIRCLE('',#98593,1.2);
#31943=CIRCLE('',#98595,0.450000000000006);
#31944=CIRCLE('',#98596,1.2);
#31945=CIRCLE('',#98597,0.750000000000001);
#31946=CIRCLE('',#98599,0.449999999999999);
#31947=CIRCLE('',#98601,0.450000000000006);
#31948=CIRCLE('',#98603,1.2);
#31949=CIRCLE('',#98604,0.750000000000001);
#31950=CIRCLE('',#98606,0.450000000000006);
#31951=CIRCLE('',#98607,1.2);
#31952=CIRCLE('',#98608,0.450000000000006);
#31953=CIRCLE('',#98609,0.750000000000001);
#31954=CIRCLE('',#98611,0.450000000000006);
#31955=CIRCLE('',#98613,0.450000000000006);
#31956=CIRCLE('',#98615,0.45);
#31957=CIRCLE('',#98616,0.750000000000001);
#31958=CIRCLE('',#98617,1.2);
#31959=CIRCLE('',#98619,0.450000000000006);
#31960=CIRCLE('',#98620,1.2);
#31961=CIRCLE('',#98621,0.750000000000001);
#31962=CIRCLE('',#98623,0.449999999999999);
#31963=CIRCLE('',#98624,677.434816028482);
#31964=CIRCLE('',#98625,677.884816028482);
#31965=CIRCLE('',#98627,0.450000000000006);
#31966=CIRCLE('',#98629,1.2);
#31967=CIRCLE('',#98630,0.750000000000001);
#31968=CIRCLE('',#98632,0.450000000000006);
#31969=CIRCLE('',#98633,1.2);
#31970=CIRCLE('',#98634,0.450000000000006);
#31971=CIRCLE('',#98635,0.750000000000001);
#31972=CIRCLE('',#98637,0.450000000000006);
#31973=CIRCLE('',#98639,0.450000000000006);
#31974=CIRCLE('',#98641,0.450000000000006);
#31975=CIRCLE('',#98642,0.750000000000001);
#31976=CIRCLE('',#98643,1.2);
#31977=CIRCLE('',#98645,0.450000000000006);
#31978=CIRCLE('',#98646,1.2);
#31979=CIRCLE('',#98647,0.750000000000001);
#31980=CIRCLE('',#98649,0.449999999999999);
#31981=CIRCLE('',#98651,0.450000000000006);
#31982=CIRCLE('',#98653,1.2);
#31983=CIRCLE('',#98654,0.750000000000001);
#31984=CIRCLE('',#98656,0.450000000000006);
#31985=CIRCLE('',#98657,1.2);
#31986=CIRCLE('',#98658,0.450000000000006);
#31987=CIRCLE('',#98659,0.750000000000001);
#31988=CIRCLE('',#98661,0.450000000000006);
#31989=CIRCLE('',#98663,0.450000000000006);
#31990=CIRCLE('',#98665,0.450000000000006);
#31991=CIRCLE('',#98666,0.750000000000001);
#31992=CIRCLE('',#98667,1.2);
#31993=CIRCLE('',#98669,0.450000000000006);
#31994=CIRCLE('',#98670,1.2);
#31995=CIRCLE('',#98671,0.750000000000001);
#31996=CIRCLE('',#98673,0.450000000000001);
#31997=CIRCLE('',#98675,0.450000000000006);
#31998=CIRCLE('',#98677,1.2);
#31999=CIRCLE('',#98678,0.750000000000001);
#32000=CIRCLE('',#98680,0.450000000000006);
#32001=CIRCLE('',#98681,1.2);
#32002=CIRCLE('',#98682,0.449999999999999);
#32003=CIRCLE('',#98683,0.750000000000001);
#32004=CIRCLE('',#98685,0.450000000000006);
#32005=CIRCLE('',#98687,0.450000000000006);
#32006=CIRCLE('',#98689,0.450000000000006);
#32007=CIRCLE('',#98690,0.750000000000001);
#32008=CIRCLE('',#98691,1.2);
#32009=CIRCLE('',#98693,0.45);
#32010=CIRCLE('',#98694,1.2);
#32011=CIRCLE('',#98695,0.750000000000001);
#32012=CIRCLE('',#98697,0.450000000000006);
#32013=CIRCLE('',#98699,0.45);
#32014=CIRCLE('',#98700,12.6555395526668);
#32015=CIRCLE('',#98701,13.1055395526668);
#32016=CIRCLE('',#98703,1.2);
#32017=CIRCLE('',#98704,0.450000000000001);
#32018=CIRCLE('',#98705,0.750000000000001);
#32019=CIRCLE('',#98707,10.);
#32020=CIRCLE('',#98708,10.45);
#32021=CIRCLE('',#98710,0.450000000000006);
#32022=CIRCLE('',#98711,1.2);
#32023=CIRCLE('',#98712,0.450000000000006);
#32024=CIRCLE('',#98713,0.750000000000001);
#32025=CIRCLE('',#98715,0.450000000000006);
#32026=CIRCLE('',#98717,0.450000000000006);
#32027=CIRCLE('',#98719,0.449999999999997);
#32028=CIRCLE('',#98720,0.750000000000001);
#32029=CIRCLE('',#98721,1.2);
#32030=CIRCLE('',#98723,0.450000000000006);
#32031=CIRCLE('',#98724,1.2);
#32032=CIRCLE('',#98725,0.750000000000001);
#32033=CIRCLE('',#98727,0.449999999999998);
#32034=CIRCLE('',#98728,677.434816028482);
#32035=CIRCLE('',#98729,677.884816028482);
#32036=CIRCLE('',#98731,0.450000000000006);
#32037=CIRCLE('',#98733,1.2);
#32038=CIRCLE('',#98734,0.750000000000001);
#32039=CIRCLE('',#98736,0.449999999999999);
#32040=CIRCLE('',#98737,1.2);
#32041=CIRCLE('',#98738,0.450000000000006);
#32042=CIRCLE('',#98739,0.750000000000001);
#32043=CIRCLE('',#98741,0.450000000000006);
#32044=CIRCLE('',#98743,0.450000000000006);
#32045=CIRCLE('',#98745,0.45);
#32046=CIRCLE('',#98746,0.750000000000001);
#32047=CIRCLE('',#98747,1.2);
#32048=CIRCLE('',#98749,0.450000000000006);
#32049=CIRCLE('',#98750,1.2);
#32050=CIRCLE('',#98751,0.750000000000001);
#32051=CIRCLE('',#98753,0.45);
#32052=CIRCLE('',#98754,48.);
#32053=CIRCLE('',#98755,48.45);
#32054=CIRCLE('',#98757,0.450000000000006);
#32055=CIRCLE('',#98759,0.449999999999997);
#32056=CIRCLE('',#98760,1.);
#32057=CIRCLE('',#98761,1.45);
#32058=CIRCLE('',#98763,0.449999999999997);
#32059=CIRCLE('',#98764,1.2);
#32060=CIRCLE('',#98765,0.750000000000001);
#32061=CIRCLE('',#98767,677.884816028482);
#32062=CIRCLE('',#98768,677.434816028482);
#32063=CIRCLE('',#98770,0.450000000000006);
#32064=CIRCLE('',#98771,1.2);
#32065=CIRCLE('',#98772,0.450000000000006);
#32066=CIRCLE('',#98773,0.750000000000001);
#32067=CIRCLE('',#98775,0.450000000000006);
#32068=CIRCLE('',#98777,0.450000000000006);
#32069=CIRCLE('',#98779,0.450000000000006);
#32070=CIRCLE('',#98780,0.750000000000001);
#32071=CIRCLE('',#98781,1.2);
#32072=CIRCLE('',#98783,0.450000000000006);
#32073=CIRCLE('',#98784,1.2);
#32074=CIRCLE('',#98785,0.750000000000001);
#32075=CIRCLE('',#98787,0.449999999999999);
#32076=CIRCLE('',#98789,0.450000000000006);
#32077=CIRCLE('',#98791,1.2);
#32078=CIRCLE('',#98792,0.750000000000001);
#32079=CIRCLE('',#98794,0.449999999999999);
#32080=CIRCLE('',#98795,1.2);
#32081=CIRCLE('',#98796,0.450000000000006);
#32082=CIRCLE('',#98797,0.750000000000001);
#32083=CIRCLE('',#98799,0.450000000000006);
#32084=CIRCLE('',#98801,0.450000000000006);
#32085=CIRCLE('',#98803,0.450000000000006);
#32086=CIRCLE('',#98804,0.750000000000001);
#32087=CIRCLE('',#98805,1.2);
#32088=CIRCLE('',#98807,0.45);
#32089=CIRCLE('',#98808,1.2);
#32090=CIRCLE('',#98809,0.750000000000001);
#32091=CIRCLE('',#98811,0.450000000000006);
#32092=CIRCLE('',#98813,0.45);
#32093=CIRCLE('',#98814,48.45);
#32094=CIRCLE('',#98815,48.);
#32095=CIRCLE('',#98817,0.450000000000003);
#32096=CIRCLE('',#98818,0.750000000000001);
#32097=CIRCLE('',#98819,1.2);
#32098=CIRCLE('',#98821,0.450000000000001);
#32099=CIRCLE('',#98822,1.44999999999997);
#32100=CIRCLE('',#98823,0.999999999999959);
#32101=CIRCLE('',#98825,677.884816028482);
#32102=CIRCLE('',#98826,677.434816028482);
#32103=CIRCLE('',#98828,0.449999999999999);
#32104=CIRCLE('',#98829,1.2);
#32105=CIRCLE('',#98830,0.450000000000006);
#32106=CIRCLE('',#98831,0.750000000000001);
#32107=CIRCLE('',#98833,0.450000000000006);
#32108=CIRCLE('',#98835,0.450000000000006);
#32109=CIRCLE('',#98837,0.450000000000006);
#32110=CIRCLE('',#98838,0.750000000000001);
#32111=CIRCLE('',#98839,1.2);
#32112=CIRCLE('',#98841,0.450000000000003);
#32113=CIRCLE('',#98842,1.2);
#32114=CIRCLE('',#98843,0.750000000000001);
#32115=CIRCLE('',#98845,0.450000000000006);
#32116=CIRCLE('',#98847,0.449999999999998);
#32117=CIRCLE('',#98848,677.884816028482);
#32118=CIRCLE('',#98849,677.434816028482);
#32119=CIRCLE('',#98851,1.2);
#32120=CIRCLE('',#98852,0.750000000000001);
#32121=CIRCLE('',#98854,0.450000000000001);
#32122=CIRCLE('',#98855,1.2);
#32123=CIRCLE('',#98856,0.450000000000006);
#32124=CIRCLE('',#98857,0.750000000000001);
#32125=CIRCLE('',#98859,0.450000000000006);
#32126=CIRCLE('',#98861,0.450000000000006);
#32127=CIRCLE('',#98863,0.450000000000006);
#32128=CIRCLE('',#98864,0.750000000000001);
#32129=CIRCLE('',#98865,1.2);
#32130=CIRCLE('',#98867,0.450000000000006);
#32131=CIRCLE('',#98868,1.2);
#32132=CIRCLE('',#98869,0.750000000000001);
#32133=CIRCLE('',#98871,0.449999999999999);
#32134=CIRCLE('',#98873,0.450000000000006);
#32135=CIRCLE('',#98875,1.2);
#32136=CIRCLE('',#98876,0.750000000000001);
#32137=CIRCLE('',#98878,0.450000000000006);
#32138=CIRCLE('',#98879,1.2);
#32139=CIRCLE('',#98880,0.450000000000006);
#32140=CIRCLE('',#98881,0.750000000000001);
#32141=CIRCLE('',#98883,0.449999999999999);
#32142=CIRCLE('',#98885,0.450000000000006);
#32143=CIRCLE('',#98887,0.450000000000006);
#32144=CIRCLE('',#98888,0.750000000000001);
#32145=CIRCLE('',#98889,1.2);
#32146=CIRCLE('',#98891,0.449999999999999);
#32147=CIRCLE('',#98892,1.2);
#32148=CIRCLE('',#98893,0.750000000000001);
#32149=CIRCLE('',#98895,0.450000000000006);
#32150=CIRCLE('',#98897,0.449999999999999);
#32151=CIRCLE('',#98898,677.884816028482);
#32152=CIRCLE('',#98899,677.434816028482);
#32153=CIRCLE('',#98901,1.2);
#32154=CIRCLE('',#98902,0.750000000000001);
#32155=CIRCLE('',#98904,0.450000000000006);
#32156=CIRCLE('',#98905,1.2);
#32157=CIRCLE('',#98906,0.449999999999999);
#32158=CIRCLE('',#98907,0.750000000000001);
#32159=CIRCLE('',#98909,0.450000000000006);
#32160=CIRCLE('',#98911,0.450000000000006);
#32161=CIRCLE('',#98913,0.450000000000006);
#32162=CIRCLE('',#98914,0.750000000000001);
#32163=CIRCLE('',#98915,1.2);
#32164=CIRCLE('',#98917,0.449999999999999);
#32165=CIRCLE('',#98918,1.2);
#32166=CIRCLE('',#98919,0.750000000000001);
#32167=CIRCLE('',#98921,0.450000000000006);
#32168=CIRCLE('',#98923,0.450000000000006);
#32169=CIRCLE('',#98925,1.2);
#32170=CIRCLE('',#98926,0.750000000000001);
#32171=CIRCLE('',#98928,0.449999999999999);
#32172=CIRCLE('',#98929,1.2);
#32173=CIRCLE('',#98930,0.450000000000006);
#32174=CIRCLE('',#98931,0.750000000000001);
#32175=CIRCLE('',#98933,0.450000000000006);
#32176=CIRCLE('',#98935,0.45);
#32177=CIRCLE('',#98936,48.45);
#32178=CIRCLE('',#98937,48.);
#32179=CIRCLE('',#98939,0.450000000000006);
#32180=CIRCLE('',#98940,0.750000000000001);
#32181=CIRCLE('',#98941,1.2);
#32182=CIRCLE('',#98943,0.450000000000006);
#32183=CIRCLE('',#98944,1.2);
#32184=CIRCLE('',#98945,0.750000000000001);
#32185=CIRCLE('',#98948,1.2);
#32186=CIRCLE('',#98949,0.450000000000006);
#32187=CIRCLE('',#98950,0.750000000000001);
#32188=CIRCLE('',#98951,0.450000000000002);
#32189=CIRCLE('',#98953,0.450000000000006);
#32190=CIRCLE('',#98955,0.449999999999999);
#32191=CIRCLE('',#98956,48.45);
#32192=CIRCLE('',#98957,48.);
#32193=CIRCLE('',#98959,0.450000000000006);
#32194=CIRCLE('',#98960,0.750000000000001);
#32195=CIRCLE('',#98961,1.2);
#32196=CIRCLE('',#98963,0.450000000000006);
#32197=CIRCLE('',#98964,1.2);
#32198=CIRCLE('',#98965,0.750000000000001);
#32199=CIRCLE('',#98968,0.450000000000002);
#32200=CIRCLE('',#98969,5.99999999999992);
#32201=CIRCLE('',#98970,0.45);
#32202=CIRCLE('',#98971,6.44999999999991);
#32203=CIRCLE('',#98973,0.45);
#32204=CIRCLE('',#98974,53.);
#32205=CIRCLE('',#98975,53.45);
#32206=CIRCLE('',#98977,0.449999999999997);
#32207=CIRCLE('',#98978,6.);
#32208=CIRCLE('',#98979,6.45);
#32209=CIRCLE('',#98981,0.449999999999997);
#32210=CIRCLE('',#98982,682.434816028482);
#32211=CIRCLE('',#98983,682.884816028482);
#32212=CIRCLE('',#98985,0.45);
#32213=CIRCLE('',#98986,6.);
#32214=CIRCLE('',#98987,6.45);
#32215=CIRCLE('',#98989,0.449999999999998);
#32216=CIRCLE('',#98990,53.);
#32217=CIRCLE('',#98991,53.45);
#32218=CIRCLE('',#98993,0.45);
#32219=CIRCLE('',#98994,6.);
#32220=CIRCLE('',#98995,6.45);
#32221=CIRCLE('',#98997,0.450000000000002);
#32222=CIRCLE('',#98998,4.34999999999995);
#32223=CIRCLE('',#98999,0.45);
#32224=CIRCLE('',#99000,4.8);
#32225=CIRCLE('',#99002,0.45);
#32226=CIRCLE('',#99003,51.35);
#32227=CIRCLE('',#99004,51.8);
#32228=CIRCLE('',#99006,0.449999999999997);
#32229=CIRCLE('',#99007,4.35);
#32230=CIRCLE('',#99008,4.8);
#32231=CIRCLE('',#99010,0.449999999999997);
#32232=CIRCLE('',#99011,680.784816028482);
#32233=CIRCLE('',#99012,681.234816028482);
#32234=CIRCLE('',#99014,0.45);
#32235=CIRCLE('',#99015,4.35);
#32236=CIRCLE('',#99016,4.8);
#32237=CIRCLE('',#99018,0.450000000000002);
#32238=CIRCLE('',#99019,51.35);
#32239=CIRCLE('',#99020,51.8);
#32240=CIRCLE('',#99022,0.45);
#32241=CIRCLE('',#99023,4.35);
#32242=CIRCLE('',#99024,4.8);
#32243=CIRCLE('',#99026,0.45);
#32244=CIRCLE('',#99027,1.2);
#32245=CIRCLE('',#99028,0.75);
#32246=CIRCLE('',#99030,0.45);
#32247=CIRCLE('',#99032,1.2);
#32248=CIRCLE('',#99033,0.75);
#32249=CIRCLE('',#99034,0.45);
#32250=CIRCLE('',#99036,0.450000000000001);
#32251=CIRCLE('',#99037,11.5555395526669);
#32252=CIRCLE('',#99038,11.1055395526669);
#32253=CIRCLE('',#99040,0.450000000000006);
#32254=CIRCLE('',#99041,1.2);
#32255=CIRCLE('',#99042,0.750000000000001);
#32256=CIRCLE('',#99044,0.450000000000006);
#32257=CIRCLE('',#99046,1.2);
#32258=CIRCLE('',#99047,0.750000000000001);
#32259=CIRCLE('',#99049,0.450000000000006);
#32260=CIRCLE('',#99050,1.2);
#32261=CIRCLE('',#99051,0.750000000000001);
#32262=CIRCLE('',#99053,0.450000000000006);
#32263=CIRCLE('',#99055,0.450000000000001);
#32264=CIRCLE('',#99056,1.2);
#32265=CIRCLE('',#99057,0.750000000000001);
#32266=CIRCLE('',#99059,0.449999999999999);
#32267=CIRCLE('',#99060,11.5555395526669);
#32268=CIRCLE('',#99061,11.1055395526669);
#32269=CIRCLE('',#99063,0.45);
#32270=CIRCLE('',#99064,1.2);
#32271=CIRCLE('',#99065,0.750000000000001);
#32272=CIRCLE('',#99067,0.45);
#32273=CIRCLE('',#99069,1.2);
#32274=CIRCLE('',#99070,0.750000000000001);
#32275=CIRCLE('',#99072,0.45);
#32276=CIRCLE('',#99073,1.2);
#32277=CIRCLE('',#99074,0.75);
#32278=CIRCLE('',#99076,0.450000000000006);
#32279=CIRCLE('',#99078,1.2);
#32280=CIRCLE('',#99079,0.75);
#32281=CIRCLE('',#99080,0.45);
#32282=CIRCLE('',#99082,0.45);
#32283=CIRCLE('',#99083,11.5555395526669);
#32284=CIRCLE('',#99084,11.1055395526669);
#32285=CIRCLE('',#99086,0.45);
#32286=CIRCLE('',#99087,1.2);
#32287=CIRCLE('',#99088,0.75);
#32288=CIRCLE('',#99090,0.45);
#32289=CIRCLE('',#99092,1.2);
#32290=CIRCLE('',#99093,0.75);
#32291=CIRCLE('',#99095,0.750000000000001);
#32292=CIRCLE('',#99096,0.45);
#32293=CIRCLE('',#99097,1.2);
#32294=CIRCLE('',#99099,0.45);
#32295=CIRCLE('',#99101,0.450000000000001);
#32296=CIRCLE('',#99102,1.2);
#32297=CIRCLE('',#99103,0.750000000000001);
#32298=CIRCLE('',#99105,0.450000000000001);
#32299=CIRCLE('',#99106,11.5555395526669);
#32300=CIRCLE('',#99107,11.1055395526669);
#32301=CIRCLE('',#99109,0.450000000000006);
#32302=CIRCLE('',#99110,1.2);
#32303=CIRCLE('',#99111,0.750000000000001);
#32304=CIRCLE('',#99113,0.450000000000006);
#32305=CIRCLE('',#99115,1.2);
#32306=CIRCLE('',#99116,0.750000000000001);
#32307=CIRCLE('',#99118,1.5);
#32308=CIRCLE('',#99119,14.0401304794059);
#32309=CIRCLE('',#99120,1.5);
#32310=CIRCLE('',#99121,12.5403589366713);
#32311=CIRCLE('',#99123,1.5);
#32312=CIRCLE('',#99124,79.6896304993778);
#32313=CIRCLE('',#99125,78.1898589566432);
#32314=CIRCLE('',#99127,1.5);
#32315=CIRCLE('',#99128,14.0401304794058);
#32316=CIRCLE('',#99129,12.5403589366712);
#32317=CIRCLE('',#99131,1.5);
#32318=CIRCLE('',#99132,1069.5771304794);
#32319=CIRCLE('',#99133,1068.07735893667);
#32320=CIRCLE('',#99135,1.5);
#32321=CIRCLE('',#99136,14.0401304794058);
#32322=CIRCLE('',#99137,12.5403589366712);
#32323=CIRCLE('',#99139,1.5);
#32324=CIRCLE('',#99140,79.6896304993778);
#32325=CIRCLE('',#99141,78.1898589566432);
#32326=CIRCLE('',#99143,1.50000000000001);
#32327=CIRCLE('',#99144,14.0401304794059);
#32328=CIRCLE('',#99145,12.5403589366713);
#32329=CIRCLE('',#99146,1.5);
#32330=CIRCLE('',#99147,1.5);
#32331=CIRCLE('',#99148,1.5);
#32332=CIRCLE('',#99149,1.5);
#32333=CIRCLE('',#99150,213.52922045504);
#32334=CIRCLE('',#99151,211.963156195019);
#32335=CIRCLE('',#99152,1.5);
#32336=CIRCLE('',#99153,1.5);
#32337=CIRCLE('',#99154,1.5);
#32338=CIRCLE('',#99155,1.5);
#32339=CIRCLE('',#99156,687.655553461799);
#32340=CIRCLE('',#99157,696.813945754993);
#32341=CIRCLE('',#99158,1.5);
#32342=CIRCLE('',#99159,1.5);
#32343=CIRCLE('',#99160,1.5);
#32344=CIRCLE('',#99161,1.5);
#32345=CIRCLE('',#99162,687.392615253502);
#32346=CIRCLE('',#99163,696.57627117557);
#32347=CIRCLE('',#99164,1.5);
#32348=CIRCLE('',#99165,1.5);
#32349=CIRCLE('',#99166,1.5);
#32350=CIRCLE('',#99167,1.5);
#32351=CIRCLE('',#99168,687.588787872307);
#32352=CIRCLE('',#99169,697.569175020784);
#32353=CIRCLE('',#99170,1.5);
#32354=CIRCLE('',#99171,5.);
#32355=CIRCLE('',#99172,72.6244975536409);
#32356=CIRCLE('',#99173,5.);
#32357=CIRCLE('',#99174,5.16933481208913);
#32358=CIRCLE('',#99175,10.1322440903793);
#32359=CIRCLE('',#99176,4.99999999999999);
#32360=CIRCLE('',#99177,5.);
#32361=CIRCLE('',#99178,1029.30060997527);
#32362=CIRCLE('',#99179,1066.87927691535);
#32363=CIRCLE('',#99180,3.);
#32364=CIRCLE('',#99181,3.);
#32365=CIRCLE('',#99182,3.);
#32366=CIRCLE('',#99183,3.);
#32367=CIRCLE('',#99184,1066.87014162396);
#32368=CIRCLE('',#99185,5.);
#32369=CIRCLE('',#99186,1029.24694971421);
#32370=CIRCLE('',#99187,4.99999999999999);
#32371=CIRCLE('',#99188,5.00000000000001);
#32372=CIRCLE('',#99189,5.);
#32373=CIRCLE('',#99190,4.98383829446029);
#32374=CIRCLE('',#99191,9.93127307062933);
#32375=CIRCLE('',#99193,3.);
#32376=CIRCLE('',#99194,3.);
#32377=CIRCLE('',#99197,1067.00041769809);
#32378=CIRCLE('',#99198,5.);
#32379=CIRCLE('',#99199,1032.95041731725);
#32380=CIRCLE('',#99200,5.00000000000001);
#32381=CIRCLE('',#99201,5.);
#32382=CIRCLE('',#99202,5.);
#32383=CIRCLE('',#99203,10.1961875685922);
#32384=CIRCLE('',#99206,5.);
#32385=CIRCLE('',#99208,5.00000000000001);
#32386=CIRCLE('',#99210,3.);
#32387=CIRCLE('',#99211,5.);
#32388=CIRCLE('',#99213,2.28316188307923);
#32389=CIRCLE('',#99214,3.);
#32390=CIRCLE('',#99215,5.);
#32391=CIRCLE('',#99216,5.);
#32392=CIRCLE('',#99217,5.);
#32393=CIRCLE('',#99218,9.92561537912225);
#32394=CIRCLE('',#99219,5.01368139939068);
#32395=CIRCLE('',#99221,0.75);
#32396=CIRCLE('',#99223,0.750000000000001);
#32397=CIRCLE('',#99225,0.750000000000001);
#32398=CIRCLE('',#99227,0.750000000000001);
#32399=CIRCLE('',#99229,0.750000000000001);
#32400=CIRCLE('',#99231,0.750000000000001);
#32401=CIRCLE('',#99233,0.75);
#32402=CIRCLE('',#99235,0.75);
#32403=CIRCLE('',#99237,0.75);
#32404=CIRCLE('',#99239,0.750000000000001);
#32405=CIRCLE('',#99241,0.750000000000001);
#32406=CIRCLE('',#99243,0.750000000000001);
#32407=CIRCLE('',#99245,0.750000000000001);
#32408=CIRCLE('',#99247,0.750000000000001);
#32409=CIRCLE('',#99249,0.750000000000001);
#32410=CIRCLE('',#99251,0.750000000000001);
#32411=CIRCLE('',#99253,0.75);
#32412=CIRCLE('',#99255,0.75);
#32413=CIRCLE('',#99257,0.75);
#32414=CIRCLE('',#99259,0.750000000000001);
#32415=CIRCLE('',#99261,0.750000000000001);
#32416=CIRCLE('',#99263,0.75);
#32417=CIRCLE('',#99265,0.750000000000001);
#32418=CIRCLE('',#99267,0.750000000000001);
#32419=CIRCLE('',#99269,0.750000000000001);
#32420=CIRCLE('',#99271,0.750000000000001);
#32421=CIRCLE('',#99273,0.750000000000001);
#32422=CIRCLE('',#99275,0.750000000000001);
#32423=CIRCLE('',#99277,0.750000000000001);
#32424=CIRCLE('',#99279,0.750000000000001);
#32425=CIRCLE('',#99281,0.750000000000001);
#32426=CIRCLE('',#99283,0.750000000000001);
#32427=CIRCLE('',#99285,0.750000000000001);
#32428=CIRCLE('',#99287,0.750000000000001);
#32429=CIRCLE('',#99289,0.75);
#32430=CIRCLE('',#99291,0.75);
#32431=CIRCLE('',#99293,0.750000000000001);
#32432=CIRCLE('',#99295,0.750000000000001);
#32433=CIRCLE('',#99297,0.750000000000001);
#32434=CIRCLE('',#99299,0.750000000000001);
#32435=CIRCLE('',#99301,0.750000000000001);
#32436=CIRCLE('',#99303,0.750000000000001);
#32437=CIRCLE('',#99305,0.750000000000001);
#32438=CIRCLE('',#99307,0.750000000000001);
#32439=CIRCLE('',#99309,0.75);
#32440=CIRCLE('',#99311,0.75);
#32441=CIRCLE('',#99313,0.750000000000001);
#32442=CIRCLE('',#99315,0.750000000000001);
#32443=CIRCLE('',#99317,0.750000000000001);
#32444=CIRCLE('',#99319,0.750000000000001);
#32445=CIRCLE('',#99321,0.750000000000001);
#32446=CIRCLE('',#99323,0.750000000000001);
#32447=CIRCLE('',#99325,0.750000000000001);
#32448=CIRCLE('',#99327,0.750000000000001);
#32449=CIRCLE('',#99329,0.750000000000001);
#32450=CIRCLE('',#99331,0.750000000000001);
#32451=CIRCLE('',#99333,0.750000000000001);
#32452=CIRCLE('',#99335,0.750000000000001);
#32453=CIRCLE('',#99337,0.750000000000001);
#32454=CIRCLE('',#99339,0.750000000000001);
#32455=CIRCLE('',#99341,0.750000000000001);
#32456=CIRCLE('',#99343,0.750000000000001);
#32457=CIRCLE('',#99345,0.750000000000001);
#32458=CIRCLE('',#99347,0.750000000000001);
#32459=CIRCLE('',#99349,0.750000000000001);
#32460=CIRCLE('',#99351,0.750000000000001);
#32461=CIRCLE('',#99353,0.750000000000001);
#32462=CIRCLE('',#99355,0.750000000000001);
#32463=CIRCLE('',#99357,0.750000000000001);
#32464=CIRCLE('',#99359,0.750000000000001);
#32465=CIRCLE('',#99361,0.750000000000001);
#32466=CIRCLE('',#99363,0.75);
#32467=CIRCLE('',#99365,0.750000000000001);
#32468=CIRCLE('',#99367,0.750000000000001);
#32469=CIRCLE('',#99369,0.75);
#32470=CIRCLE('',#99371,0.750000000000001);
#32471=CIRCLE('',#99373,0.75);
#32472=CIRCLE('',#99375,0.75);
#32473=CIRCLE('',#99377,0.750000000000001);
#32474=CIRCLE('',#99379,0.750000000000001);
#32475=CIRCLE('',#99381,0.750000000000001);
#32476=CIRCLE('',#99383,0.750000000000001);
#32477=CIRCLE('',#99385,0.750000000000001);
#32478=CIRCLE('',#99387,0.750000000000001);
#32479=CIRCLE('',#99389,0.750000000000001);
#32480=CIRCLE('',#99391,0.750000000000001);
#32481=CIRCLE('',#99393,0.750000000000001);
#32482=CIRCLE('',#99395,0.750000000000001);
#32483=CIRCLE('',#99397,0.750000000000001);
#32484=CIRCLE('',#99399,0.750000000000001);
#32485=CIRCLE('',#99401,0.750000000000001);
#32486=CIRCLE('',#99403,0.750000000000001);
#32487=CIRCLE('',#99405,0.750000000000001);
#32488=CIRCLE('',#99407,0.750000000000001);
#32489=CIRCLE('',#99409,0.750000000000001);
#32490=CIRCLE('',#99411,0.750000000000001);
#32491=CIRCLE('',#99413,0.750000000000001);
#32492=CIRCLE('',#99415,0.75);
#32493=CIRCLE('',#99417,0.75);
#32494=CIRCLE('',#99419,0.750000000000001);
#32495=CIRCLE('',#99421,0.750000000000001);
#32496=CIRCLE('',#99423,0.750000000000001);
#32497=CIRCLE('',#99425,0.750000000000001);
#32498=CIRCLE('',#99427,0.750000000000001);
#32499=CIRCLE('',#99429,0.750000000000001);
#32500=CIRCLE('',#99431,0.750000000000001);
#32501=CIRCLE('',#99433,0.750000000000001);
#32502=CIRCLE('',#99435,0.750000000000001);
#32503=CIRCLE('',#99437,0.750000000000001);
#32504=CIRCLE('',#99439,0.750000000000001);
#32505=CIRCLE('',#99441,0.750000000000001);
#32506=CIRCLE('',#99443,0.750000000000001);
#32507=CIRCLE('',#99445,0.750000000000001);
#32508=CIRCLE('',#99447,0.750000000000001);
#32509=CIRCLE('',#99449,0.750000000000001);
#32510=CIRCLE('',#99451,0.750000000000001);
#32511=CIRCLE('',#99453,0.750000000000001);
#32512=CIRCLE('',#99455,0.750000000000001);
#32513=CIRCLE('',#99457,0.750000000000001);
#32514=CIRCLE('',#99459,0.750000000000001);
#32515=CIRCLE('',#99461,0.750000000000001);
#32516=CIRCLE('',#99463,0.750000000000001);
#32517=CIRCLE('',#99465,0.750000000000001);
#32518=CIRCLE('',#99467,0.750000000000001);
#32519=CIRCLE('',#99469,0.750000000000001);
#32520=CIRCLE('',#99471,0.750000000000001);
#32521=CIRCLE('',#99473,0.750000000000001);
#32522=CIRCLE('',#99475,0.750000000000001);
#32523=CIRCLE('',#99477,0.750000000000001);
#32524=CIRCLE('',#99479,0.75);
#32525=CIRCLE('',#99481,0.75);
#32526=CIRCLE('',#99483,0.750000000000001);
#32527=CIRCLE('',#99485,0.750000000000001);
#32528=CIRCLE('',#99487,0.750000000000001);
#32529=CIRCLE('',#99489,10.);
#32530=CIRCLE('',#99491,10.);
#32531=CIRCLE('',#99493,10.);
#32532=CIRCLE('',#99495,10.);
#32533=CIRCLE('',#99497,13.1055395526668);
#32534=CIRCLE('',#99499,13.1055395526668);
#32535=CIRCLE('',#99501,11.1055395526669);
#32536=CIRCLE('',#99505,11.1055395526669);
#32537=CIRCLE('',#99507,12.1055395526668);
#32538=CIRCLE('',#99509,11.1055395526669);
#32539=CIRCLE('',#99513,11.1055395526669);
#32540=CIRCLE('',#99515,12.1055395526668);
#32541=CIRCLE('',#99574,3.5);
#32542=CIRCLE('',#99575,3.5);
#32543=CIRCLE('',#99577,50.5);
#32544=CIRCLE('',#99578,50.5);
#32545=CIRCLE('',#99580,3.5);
#32546=CIRCLE('',#99581,3.5);
#32547=CIRCLE('',#99583,679.934816028482);
#32548=CIRCLE('',#99584,679.934816028482);
#32549=CIRCLE('',#99586,3.5);
#32550=CIRCLE('',#99587,3.5);
#32551=CIRCLE('',#99589,50.5);
#32552=CIRCLE('',#99590,50.5);
#32553=CIRCLE('',#99592,3.49999999999996);
#32554=CIRCLE('',#99593,3.49999999999996);
#32555=CIRCLE('',#99595,5.98129380707219);
#32556=CIRCLE('',#99598,5.9812938070714);
#32557=CIRCLE('',#99603,74.6139048513169);
#32558=CIRCLE('',#99604,74.6139048513169);
#32559=CIRCLE('',#99608,74.6139048513167);
#32560=CIRCLE('',#99609,74.6139048513167);
#32561=CIRCLE('',#99611,8.5);
#32562=CIRCLE('',#99612,8.5);
#32563=CIRCLE('',#99614,8.5);
#32564=CIRCLE('',#99615,8.5);
#32565=CIRCLE('',#99617,55.5);
#32566=CIRCLE('',#99618,55.5);
#32567=CIRCLE('',#99620,8.5);
#32568=CIRCLE('',#99621,8.5);
#32569=CIRCLE('',#99623,684.934816028482);
#32570=CIRCLE('',#99624,684.934816028482);
#32571=CIRCLE('',#99626,8.5);
#32572=CIRCLE('',#99627,8.5);
#32573=CIRCLE('',#99629,55.5);
#32574=CIRCLE('',#99630,55.5);
#32575=CIRCLE('',#99632,9.05766167355557);
#32576=CIRCLE('',#99634,74.7071616935275);
#32577=CIRCLE('',#99636,9.05766167355546);
#32578=CIRCLE('',#99637,6.68387219307026);
#32579=CIRCLE('',#99639,9.05766167355555);
#32580=CIRCLE('',#99640,6.41600556626386);
#32581=CIRCLE('',#99642,74.7071616935275);
#32582=CIRCLE('',#99644,9.05766167355558);
#32583=CIRCLE('',#99645,6.41130036340322);
#32584=CIRCLE('',#99647,1067.49961917989);
#32585=CIRCLE('',#99648,1067.09466167355);
#32586=CIRCLE('',#99650,11.9626191798902);
#32587=CIRCLE('',#99651,11.5576616735555);
#32588=CIRCLE('',#99653,77.6121191998622);
#32589=CIRCLE('',#99654,77.2071616935275);
#32590=CIRCLE('',#99656,11.9626191798902);
#32591=CIRCLE('',#99657,11.5576616735556);
#32592=CIRCLE('',#99659,11.9626191798902);
#32593=CIRCLE('',#99660,11.5576616735556);
#32594=CIRCLE('',#99662,77.6121191998622);
#32595=CIRCLE('',#99663,77.2071616935275);
#32596=CIRCLE('',#99665,11.9626191798902);
#32597=CIRCLE('',#99666,11.5576616735555);
#32598=CIRCLE('',#99668,1064.59466167355);
#32599=CIRCLE('',#99669,211.167112167648);
#32600=CIRCLE('',#99671,684.934816028482);
#32601=CIRCLE('',#99672,705.368683747858);
#32602=CIRCLE('',#99673,684.934816028482);
#32603=CIRCLE('',#99675,5.80674315778922);
#32604=CIRCLE('',#99677,5.80674315779001);
#32605=CIRCLE('',#99679,211.99569081556);
#32606=CIRCLE('',#99681,211.99569081556);
#32607=CIRCLE('',#99683,684.934816028482);
#32608=CIRCLE('',#99685,684.934816028482);
#32609=CIRCLE('',#99687,684.934816028482);
#32610=CIRCLE('',#99689,684.934816028482);
#32611=CIRCLE('',#99691,5.9812938070714);
#32612=CIRCLE('',#99693,684.934816028482);
#32613=CIRCLE('',#99695,684.934816028482);
#32614=CIRCLE('',#99697,684.934816028482);
#32615=CIRCLE('',#99699,684.934816028482);
#32616=CIRCLE('',#99701,684.934816028482);
#32617=CIRCLE('',#99707,1.);
#32618=CIRCLE('',#99709,48.);
#32619=CIRCLE('',#99711,0.999999999999999);
#32620=CIRCLE('',#99713,677.434816028482);
#32621=CIRCLE('',#99715,1.);
#32622=CIRCLE('',#99717,48.);
#32623=CIRCLE('',#99719,0.999999999999959);
#32624=CIRCLE('',#99721,3.35);
#32625=CIRCLE('',#99723,3.51597543326183);
#32626=CIRCLE('',#99724,3.51597543326183);
#32627=CIRCLE('',#99726,3.35000000000079);
#32628=CIRCLE('',#99733,4.01589928084002);
#32629=CIRCLE('',#99744,51.8);
#32630=CIRCLE('',#99746,4.8);
#32631=CIRCLE('',#99748,681.234816028482);
#32632=CIRCLE('',#99750,4.8);
#32633=CIRCLE('',#99752,51.8);
#32634=CIRCLE('',#99754,4.8);
#32635=CIRCLE('',#99756,4.8);
#32636=CIRCLE('',#99758,5.99999999999992);
#32637=CIRCLE('',#99760,6.);
#32638=CIRCLE('',#99762,53.);
#32639=CIRCLE('',#99764,6.);
#32640=CIRCLE('',#99766,682.434816028482);
#32641=CIRCLE('',#99768,6.);
#32642=CIRCLE('',#99770,53.);
#32643=CIRCLE('',#99778,1070.);
#32644=CIRCLE('',#99780,14.463);
#32645=CIRCLE('',#99782,80.1125000199719);
#32646=CIRCLE('',#99784,14.463);
#32647=CIRCLE('',#99786,14.463);
#32648=CIRCLE('',#99788,80.1125000199719);
#32649=CIRCLE('',#99790,14.463);
#32650=CIRCLE('',#99795,677.434816028482);
#32651=CIRCLE('',#99797,677.434816028482);
#32652=CIRCLE('',#99799,677.434816028482);
#32653=CIRCLE('',#99801,677.434816028482);
#32654=CIRCLE('',#99803,677.434816028482);
#32655=CIRCLE('',#99815,204.49569081556);
#32656=CIRCLE('',#99817,677.434816028482);
#32657=CIRCLE('',#99819,206.99569081556);
#32658=CIRCLE('',#99820,206.99569081556);
#32659=CIRCLE('',#99836,204.49569081556);
#32660=CIRCLE('',#99838,204.49569081556);
#32661=CIRCLE('',#99840,677.434816028482);
#32662=CIRCLE('',#99842,677.434816028482);
#32663=CIRCLE('',#99844,48.);
#32664=CIRCLE('',#99846,48.);
#32665=CIRCLE('',#99848,48.);
#32666=CIRCLE('',#99850,48.);
#32667=CIRCLE('',#99879,0.500000000000001);
#32668=CIRCLE('',#99880,0.499999999999997);
#32669=CIRCLE('',#99882,4.01589928084002);
#32670=CIRCLE('',#99883,3.51597543326183);
#32671=CIRCLE('',#99884,3.51597543326183);
#32672=CIRCLE('',#99886,4.01589928084082);
#32673=CIRCLE('',#99887,0.5);
#32674=CIRCLE('',#99888,3.51597543326262);
#32675=CIRCLE('',#99889,3.51597543326262);
#32676=CIRCLE('',#99890,0.499999999999999);
#32677=CIRCLE('',#99891,0.500000000000002);
#32678=CIRCLE('',#99892,0.50000000000001);
#32679=CIRCLE('',#99894,0.500000000000004);
#32680=CIRCLE('',#99895,0.500000000000002);
#32681=CIRCLE('',#99896,0.499999999999999);
#32682=CIRCLE('',#99898,0.499999999999997);
#32683=CIRCLE('',#99899,1.49999999999999);
#32684=CIRCLE('',#99900,2.);
#32685=CIRCLE('',#99901,0.500000000000002);
#32686=CIRCLE('',#99903,0.5);
#32687=CIRCLE('',#99904,73.8);
#32688=CIRCLE('',#99905,74.3);
#32689=CIRCLE('',#99906,0.500000000000002);
#32690=CIRCLE('',#99908,0.499999999999999);
#32691=CIRCLE('',#99909,1.5);
#32692=CIRCLE('',#99910,2.);
#32693=CIRCLE('',#99911,0.499999999999993);
#32694=CIRCLE('',#99912,0.500000000000006);
#32695=CIRCLE('',#99913,0.500000000000012);
#32696=CIRCLE('',#99916,0.499999999999999);
#32697=CIRCLE('',#99917,0.500000000000001);
#32698=CIRCLE('',#99918,0.499999999999998);
#32699=CIRCLE('',#99919,0.5);
#32700=CIRCLE('',#99920,0.5);
#32701=CIRCLE('',#99921,0.500000000000006);
#32702=CIRCLE('',#99922,0.500000000000001);
#32703=CIRCLE('',#99924,0.500000000000003);
#32704=CIRCLE('',#99925,0.499999999999998);
#32705=CIRCLE('',#99926,0.50000000000001);
#32706=CIRCLE('',#99927,0.499999999999999);
#32707=CIRCLE('',#99928,0.499999999999999);
#32708=CIRCLE('',#99930,0.499999999999998);
#32709=CIRCLE('',#99931,2.);
#32710=CIRCLE('',#99932,1.5);
#32711=CIRCLE('',#99934,0.499999999999997);
#32712=CIRCLE('',#99935,0.499999999999998);
#32713=CIRCLE('',#99937,0.5);
#32714=CIRCLE('',#99938,74.3);
#32715=CIRCLE('',#99939,73.8);
#32716=CIRCLE('',#99940,0.499999999999997);
#32717=CIRCLE('',#99942,1.5);
#32718=CIRCLE('',#99943,2.);
#32719=CIRCLE('',#99945,232.042829615324);
#32720=CIRCLE('',#99946,232.542753462903);
#32721=CIRCLE('',#99947,0.500000000000002);
#32722=CIRCLE('',#99949,0.500000000000001);
#32723=CIRCLE('',#99950,11.5058296153244);
#32724=CIRCLE('',#99951,12.0057534629026);
#32725=CIRCLE('',#99953,0.500000000000001);
#32726=CIRCLE('',#99954,77.1553296352964);
#32727=CIRCLE('',#99955,77.6552534828746);
#32728=CIRCLE('',#99957,0.499999999999998);
#32729=CIRCLE('',#99958,11.5058296153244);
#32730=CIRCLE('',#99959,12.0057534629026);
#32731=CIRCLE('',#99961,0.499999999999998);
#32732=CIRCLE('',#99962,1067.04282961532);
#32733=CIRCLE('',#99963,1067.5427534629);
#32734=CIRCLE('',#99965,0.499999999999999);
#32735=CIRCLE('',#99966,11.5058296153244);
#32736=CIRCLE('',#99967,12.0057534629025);
#32737=CIRCLE('',#99969,0.500000000000001);
#32738=CIRCLE('',#99970,77.1553296352964);
#32739=CIRCLE('',#99971,77.6552534828746);
#32740=CIRCLE('',#99973,0.500000000000002);
#32741=CIRCLE('',#99974,11.5058296153244);
#32742=CIRCLE('',#99975,12.0057534629026);
#32743=CIRCLE('',#99977,1067.5427534629);
#32744=CIRCLE('',#99978,1067.04282961532);
#32745=CIRCLE('',#99979,64.9438262487296);
#32746=CIRCLE('',#99980,64.8942573619905);
#32747=CIRCLE('',#99981,0.500000000000001);
#32748=CIRCLE('',#99982,0.499999999999998);
#32749=CIRCLE('',#99984,0.499999999999996);
#32750=CIRCLE('',#99985,0.500000000000001);
#32751=CIRCLE('',#99986,0.50000000000001);
#32752=CIRCLE('',#99987,365.618325533514);
#32753=CIRCLE('',#99988,368.00584558015);
#32754=CIRCLE('',#99989,0.499999999999998);
#32755=CIRCLE('',#99990,429.776000990187);
#32756=CIRCLE('',#99991,431.08166328569);
#32757=CIRCLE('',#99992,0.5);
#32758=CIRCLE('',#99993,0.499999999999998);
#32759=CIRCLE('',#99994,0.5);
#32760=CIRCLE('',#99995,0.499999999999998);
#32761=CIRCLE('',#99996,0.499999999999998);
#32762=CIRCLE('',#99997,0.499999999999997);
#32763=CIRCLE('',#99999,77.1139048513169);
#32764=CIRCLE('',#100000,77.1139810037387);
#32765=CIRCLE('',#100001,0.500000000000002);
#32766=CIRCLE('',#100002,0.500000000000003);
#32767=CIRCLE('',#100004,0.499999999999998);
#32768=CIRCLE('',#100005,77.1139810037385);
#32769=CIRCLE('',#100006,77.1139048513167);
#32770=CIRCLE('',#100007,0.500000000000003);
#32771=CIRCLE('',#100008,0.5);
#32772=CIRCLE('',#100009,0.499999999999995);
#32773=CIRCLE('',#100010,0.500000000000002);
#32774=CIRCLE('',#100011,0.500000000000004);
#32775=CIRCLE('',#100012,329.186676141438);
#32776=CIRCLE('',#100013,329.616230392321);
#32777=CIRCLE('',#100014,0.499999999999997);
#32778=CIRCLE('',#100015,0.499999999999999);
#32779=CIRCLE('',#100016,463.797803513665);
#32780=CIRCLE('',#100017,462.991628528349);
#32781=CIRCLE('',#100019,0.750000000000001);
#32782=CIRCLE('',#100020,1.5);
#32783=CIRCLE('',#100021,0.75);
#32784=CIRCLE('',#100022,0.750000000000001);
#32785=CIRCLE('',#100024,73.05);
#32786=CIRCLE('',#100025,73.05);
#32787=CIRCLE('',#100026,73.8);
#32788=CIRCLE('',#100027,0.750000000000002);
#32789=CIRCLE('',#100028,0.749999999999996);
#32790=CIRCLE('',#100029,0.750000000000001);
#32791=CIRCLE('',#100030,1.5);
#32792=CIRCLE('',#100033,0.750000000000003);
#32793=CIRCLE('',#100034,1.5);
#32794=CIRCLE('',#100035,0.750000000000004);
#32795=CIRCLE('',#100036,0.750000000000001);
#32796=CIRCLE('',#100038,0.749999999999998);
#32797=CIRCLE('',#100039,76.3639048513167);
#32798=CIRCLE('',#100040,77.1139048513167);
#32799=CIRCLE('',#100041,0.75);
#32800=CIRCLE('',#100042,0.750000000000001);
#32801=CIRCLE('',#100043,1.5);
#32802=CIRCLE('',#100046,0.749999999999999);
#32803=CIRCLE('',#100047,0.749999999999999);
#32804=CIRCLE('',#100048,0.750000000000001);
#32805=CIRCLE('',#100049,1.5);
#32806=CIRCLE('',#100051,0.75);
#32807=CIRCLE('',#100052,76.3639048513169);
#32808=CIRCLE('',#100053,77.1139048513169);
#32809=CIRCLE('',#100054,0.750000000000001);
#32810=CIRCLE('',#100055,1.5);
#32811=CIRCLE('',#100056,0.750000000000005);
#32812=CIRCLE('',#100059,0.75);
#32813=CIRCLE('',#100060,0.750000000000003);
#32814=CIRCLE('',#100061,0.749999999999994);
#32815=CIRCLE('',#100062,1.49999999999999);
#32816=CIRCLE('',#100064,0.750000000000004);
#32817=CIRCLE('',#100065,73.05);
#32818=CIRCLE('',#100066,73.8);
#32819=CIRCLE('',#100067,0.750000000000001);
#32820=CIRCLE('',#100068,1.5);
#32821=CIRCLE('',#100069,0.75);
#32822=CIRCLE('',#100080,1.2);
#32823=CIRCLE('',#100081,0.450000000000001);
#32824=CIRCLE('',#100082,0.750000000000001);
#32825=CIRCLE('',#100083,0.450000000000006);
#32826=CIRCLE('',#100085,0.450000000000006);
#32827=CIRCLE('',#100087,0.45);
#32828=CIRCLE('',#100088,204.49569081556);
#32829=CIRCLE('',#100089,204.945690815561);
#32830=CIRCLE('',#100091,0.450000000000006);
#32831=CIRCLE('',#100092,1.2);
#32832=CIRCLE('',#100093,0.750000000000001);
#32833=CIRCLE('',#100095,0.450000000000001);
#32834=CIRCLE('',#100096,1.);
#32835=CIRCLE('',#100097,1.45);
#32836=CIRCLE('',#100099,0.450000000000006);
#32837=CIRCLE('',#100101,0.450000000000001);
#32838=CIRCLE('',#100102,48.);
#32839=CIRCLE('',#100103,48.45);
#32840=CIRCLE('',#100105,0.450000000000006);
#32841=CIRCLE('',#100106,1.2);
#32842=CIRCLE('',#100107,0.750000000000001);
#32843=CIRCLE('',#100109,0.450000000000006);
#32844=CIRCLE('',#100110,0.750000000000001);
#32845=CIRCLE('',#100111,1.2);
#32846=CIRCLE('',#100114,1.2);
#32847=CIRCLE('',#100115,0.450000000000001);
#32848=CIRCLE('',#100116,0.750000000000001);
#32849=CIRCLE('',#100117,0.450000000000006);
#32850=CIRCLE('',#100119,0.450000000000006);
#32851=CIRCLE('',#100121,0.449999999999999);
#32852=CIRCLE('',#100122,204.49569081556);
#32853=CIRCLE('',#100123,204.945690815561);
#32854=CIRCLE('',#100125,0.450000000000006);
#32855=CIRCLE('',#100126,1.2);
#32856=CIRCLE('',#100127,0.750000000000001);
#32857=CIRCLE('',#100129,0.450000000000006);
#32858=CIRCLE('',#100130,0.750000000000001);
#32859=CIRCLE('',#100131,1.2);
#32860=CIRCLE('',#100133,0.450000000000006);
#32861=CIRCLE('',#100135,0.450000000000006);
#32862=CIRCLE('',#100137,0.750000000000001);
#32863=CIRCLE('',#100138,1.2);
#32864=CIRCLE('',#100140,1.2);
#32865=CIRCLE('',#100141,0.449999999999999);
#32866=CIRCLE('',#100142,0.750000000000001);
#32867=CIRCLE('',#100143,0.450000000000006);
#32868=CIRCLE('',#100145,0.450000000000006);
#32869=CIRCLE('',#100147,0.450000000000001);
#32870=CIRCLE('',#100148,204.49569081556);
#32871=CIRCLE('',#100149,204.945690815561);
#32872=CIRCLE('',#100151,0.450000000000006);
#32873=CIRCLE('',#100152,1.2);
#32874=CIRCLE('',#100153,0.750000000000001);
#32875=CIRCLE('',#100155,0.450000000000006);
#32876=CIRCLE('',#100156,0.750000000000001);
#32877=CIRCLE('',#100157,1.2);
#32878=CIRCLE('',#100159,0.450000000000006);
#32879=CIRCLE('',#100161,0.450000000000006);
#32880=CIRCLE('',#100163,0.750000000000001);
#32881=CIRCLE('',#100164,1.2);
#32882=CIRCLE('',#100166,0.449999999999999);
#32883=CIRCLE('',#100167,0.750000000000001);
#32884=CIRCLE('',#100168,0.450000000000006);
#32885=CIRCLE('',#100169,1.2);
#32886=CIRCLE('',#100171,0.450000000000006);
#32887=CIRCLE('',#100173,0.450000000000006);
#32888=CIRCLE('',#100175,0.450000000000006);
#32889=CIRCLE('',#100176,1.2);
#32890=CIRCLE('',#100177,0.750000000000001);
#32891=CIRCLE('',#100179,0.450000000000006);
#32892=CIRCLE('',#100180,0.750000000000001);
#32893=CIRCLE('',#100181,1.2);
#32894=CIRCLE('',#100183,0.450000000000006);
#32895=CIRCLE('',#100185,0.450000000000006);
#32896=CIRCLE('',#100187,0.750000000000001);
#32897=CIRCLE('',#100188,1.2);
#32898=CIRCLE('',#100190,0.450000000000006);
#32899=CIRCLE('',#100191,0.750000000000001);
#32900=CIRCLE('',#100192,0.450000000000006);
#32901=CIRCLE('',#100193,1.2);
#32902=CIRCLE('',#100195,0.450000000000006);
#32903=CIRCLE('',#100197,0.450000000000006);
#32904=CIRCLE('',#100199,0.45);
#32905=CIRCLE('',#100200,1.2);
#32906=CIRCLE('',#100201,0.75);
#32907=CIRCLE('',#100203,0.450000000000006);
#32908=CIRCLE('',#100204,0.750000000000001);
#32909=CIRCLE('',#100205,1.2);
#32910=CIRCLE('',#100207,0.45);
#32911=CIRCLE('',#100208,12.6555395526668);
#32912=CIRCLE('',#100209,13.1055395526668);
#32913=CIRCLE('',#100211,0.450000000000001);
#32914=CIRCLE('',#100213,0.45);
#32915=CIRCLE('',#100214,10.45);
#32916=CIRCLE('',#100215,10.);
#32917=CIRCLE('',#100217,1.2);
#32918=CIRCLE('',#100218,0.75);
#32919=CIRCLE('',#100220,0.450000000000006);
#32920=CIRCLE('',#100221,0.750000000000001);
#32921=CIRCLE('',#100222,0.450000000000006);
#32922=CIRCLE('',#100223,1.2);
#32923=CIRCLE('',#100225,0.450000000000001);
#32924=CIRCLE('',#100227,0.450000000000006);
#32925=CIRCLE('',#100229,0.450000000000006);
#32926=CIRCLE('',#100230,1.2);
#32927=CIRCLE('',#100231,0.75);
#32928=CIRCLE('',#100233,0.450000000000006);
#32929=CIRCLE('',#100234,0.750000000000001);
#32930=CIRCLE('',#100235,1.2);
#32931=CIRCLE('',#100237,0.450000000000006);
#32932=CIRCLE('',#100239,0.449999999999999);
#32933=CIRCLE('',#100241,0.75);
#32934=CIRCLE('',#100242,1.2);
#32935=CIRCLE('',#100244,0.450000000000006);
#32936=CIRCLE('',#100245,0.750000000000001);
#32937=CIRCLE('',#100246,0.450000000000006);
#32938=CIRCLE('',#100247,1.2);
#32939=CIRCLE('',#100249,0.450000000000006);
#32940=CIRCLE('',#100251,0.450000000000006);
#32941=CIRCLE('',#100253,0.450000000000006);
#32942=CIRCLE('',#100254,1.2);
#32943=CIRCLE('',#100255,0.750000000000001);
#32944=CIRCLE('',#100257,0.450000000000006);
#32945=CIRCLE('',#100258,0.750000000000001);
#32946=CIRCLE('',#100259,1.2);
#32947=CIRCLE('',#100261,0.450000000000006);
#32948=CIRCLE('',#100263,0.450000000000006);
#32949=CIRCLE('',#100265,0.750000000000001);
#32950=CIRCLE('',#100266,1.2);
#32951=CIRCLE('',#100268,0.450000000000006);
#32952=CIRCLE('',#100269,0.750000000000001);
#32953=CIRCLE('',#100270,0.450000000000006);
#32954=CIRCLE('',#100271,1.2);
#32955=CIRCLE('',#100273,0.450000000000006);
#32956=CIRCLE('',#100275,0.450000000000006);
#32957=CIRCLE('',#100277,0.450000000000006);
#32958=CIRCLE('',#100278,1.2);
#32959=CIRCLE('',#100279,0.750000000000001);
#32960=CIRCLE('',#100281,0.450000000000006);
#32961=CIRCLE('',#100282,0.750000000000001);
#32962=CIRCLE('',#100283,1.2);
#32963=CIRCLE('',#100285,0.450000000000006);
#32964=CIRCLE('',#100287,0.450000000000006);
#32965=CIRCLE('',#100289,0.750000000000001);
#32966=CIRCLE('',#100290,1.2);
#32967=CIRCLE('',#100292,0.450000000000006);
#32968=CIRCLE('',#100293,0.750000000000001);
#32969=CIRCLE('',#100294,0.450000000000006);
#32970=CIRCLE('',#100295,1.2);
#32971=CIRCLE('',#100297,0.449999999999999);
#32972=CIRCLE('',#100299,0.450000000000006);
#32973=CIRCLE('',#100301,0.450000000000006);
#32974=CIRCLE('',#100302,1.2);
#32975=CIRCLE('',#100303,0.75);
#32976=CIRCLE('',#100305,0.450000000000006);
#32977=CIRCLE('',#100306,0.750000000000001);
#32978=CIRCLE('',#100307,1.2);
#32979=CIRCLE('',#100309,0.450000000000006);
#32980=CIRCLE('',#100311,0.450000000000006);
#32981=CIRCLE('',#100313,0.75);
#32982=CIRCLE('',#100314,1.2);
#32983=CIRCLE('',#100316,0.450000000000006);
#32984=CIRCLE('',#100317,0.750000000000001);
#32985=CIRCLE('',#100318,0.450000000000006);
#32986=CIRCLE('',#100319,1.2);
#32987=CIRCLE('',#100321,0.449999999999999);
#32988=CIRCLE('',#100323,0.450000000000006);
#32989=CIRCLE('',#100325,0.450000000000006);
#32990=CIRCLE('',#100326,1.2);
#32991=CIRCLE('',#100327,0.75);
#32992=CIRCLE('',#100329,0.449999999999997);
#32993=CIRCLE('',#100330,0.750000000000001);
#32994=CIRCLE('',#100331,1.2);
#32995=CIRCLE('',#100333,0.450000000000006);
#32996=CIRCLE('',#100335,0.449999999999998);
#32997=CIRCLE('',#100336,677.434816028482);
#32998=CIRCLE('',#100337,677.884816028482);
#32999=CIRCLE('',#100339,0.75);
#33000=CIRCLE('',#100340,1.2);
#33001=CIRCLE('',#100342,0.450000000000006);
#33002=CIRCLE('',#100343,0.750000000000001);
#33003=CIRCLE('',#100344,0.450000000000006);
#33004=CIRCLE('',#100345,1.2);
#33005=CIRCLE('',#100347,0.450000000000006);
#33006=CIRCLE('',#100349,0.450000000000006);
#33007=CIRCLE('',#100351,0.450000000000006);
#33008=CIRCLE('',#100352,1.2);
#33009=CIRCLE('',#100353,0.750000000000001);
#33010=CIRCLE('',#100355,0.449999999999998);
#33011=CIRCLE('',#100356,0.750000000000001);
#33012=CIRCLE('',#100357,1.2);
#33013=CIRCLE('',#100359,0.450000000000006);
#33014=CIRCLE('',#100361,0.45);
#33015=CIRCLE('',#100362,48.);
#33016=CIRCLE('',#100363,48.45);
#33017=CIRCLE('',#100365,0.449999999999997);
#33018=CIRCLE('',#100366,1.2);
#33019=CIRCLE('',#100367,0.750000000000001);
#33020=CIRCLE('',#100369,0.449999999999997);
#33021=CIRCLE('',#100370,0.999999999999999);
#33022=CIRCLE('',#100371,1.45);
#33023=CIRCLE('',#100373,677.434816028482);
#33024=CIRCLE('',#100374,677.884816028482);
#33025=CIRCLE('',#100376,0.450000000000006);
#33026=CIRCLE('',#100377,0.75);
#33027=CIRCLE('',#100378,0.450000000000006);
#33028=CIRCLE('',#100379,1.2);
#33029=CIRCLE('',#100381,0.449999999999999);
#33030=CIRCLE('',#100383,0.450000000000006);
#33031=CIRCLE('',#100385,0.450000000000006);
#33032=CIRCLE('',#100386,1.2);
#33033=CIRCLE('',#100387,0.750000000000001);
#33034=CIRCLE('',#100389,0.45);
#33035=CIRCLE('',#100390,0.75);
#33036=CIRCLE('',#100391,1.2);
#33037=CIRCLE('',#100393,0.450000000000006);
#33038=CIRCLE('',#100395,0.449999999999999);
#33039=CIRCLE('',#100396,677.434816028482);
#33040=CIRCLE('',#100397,677.884816028482);
#33041=CIRCLE('',#100399,0.750000000000001);
#33042=CIRCLE('',#100400,1.2);
#33043=CIRCLE('',#100402,0.450000000000006);
#33044=CIRCLE('',#100403,0.75);
#33045=CIRCLE('',#100404,0.450000000000006);
#33046=CIRCLE('',#100405,1.2);
#33047=CIRCLE('',#100407,0.449999999999999);
#33048=CIRCLE('',#100409,0.450000000000006);
#33049=CIRCLE('',#100411,0.450000000000006);
#33050=CIRCLE('',#100412,1.2);
#33051=CIRCLE('',#100413,0.750000000000001);
#33052=CIRCLE('',#100415,0.450000000000006);
#33053=CIRCLE('',#100416,0.75);
#33054=CIRCLE('',#100417,1.2);
#33055=CIRCLE('',#100419,0.450000000000006);
#33056=CIRCLE('',#100421,0.450000000000006);
#33057=CIRCLE('',#100423,0.750000000000001);
#33058=CIRCLE('',#100424,1.2);
#33059=CIRCLE('',#100426,0.45);
#33060=CIRCLE('',#100427,0.750000000000001);
#33061=CIRCLE('',#100428,0.450000000000006);
#33062=CIRCLE('',#100429,1.2);
#33063=CIRCLE('',#100431,0.450000000000006);
#33064=CIRCLE('',#100433,0.45);
#33065=CIRCLE('',#100434,12.1055395526668);
#33066=CIRCLE('',#100435,11.6555395526668);
#33067=CIRCLE('',#100437,0.450000000000006);
#33068=CIRCLE('',#100438,1.2);
#33069=CIRCLE('',#100439,0.750000000000001);
#33070=CIRCLE('',#100441,0.450000000000006);
#33071=CIRCLE('',#100442,10.);
#33072=CIRCLE('',#100443,10.45);
#33073=CIRCLE('',#100445,0.450000000000006);
#33074=CIRCLE('',#100447,0.450000000000006);
#33075=CIRCLE('',#100449,0.450000000000006);
#33076=CIRCLE('',#100450,1.2);
#33077=CIRCLE('',#100451,0.75);
#33078=CIRCLE('',#100453,0.450000000000006);
#33079=CIRCLE('',#100454,0.75);
#33080=CIRCLE('',#100455,1.2);
#33081=CIRCLE('',#100458,0.450000000000001);
#33082=CIRCLE('',#100459,0.750000000000001);
#33083=CIRCLE('',#100460,0.450000000000006);
#33084=CIRCLE('',#100461,1.2);
#33085=CIRCLE('',#100463,0.450000000000006);
#33086=CIRCLE('',#100465,0.450000000000006);
#33087=CIRCLE('',#100467,0.450000000000006);
#33088=CIRCLE('',#100468,1.2);
#33089=CIRCLE('',#100469,0.750000000000001);
#33090=CIRCLE('',#100471,0.450000000000001);
#33091=CIRCLE('',#100472,10.);
#33092=CIRCLE('',#100473,10.45);
#33093=CIRCLE('',#100475,0.449999999999999);
#33094=CIRCLE('',#100477,0.45);
#33095=CIRCLE('',#100478,12.1055395526668);
#33096=CIRCLE('',#100479,11.6555395526668);
#33097=CIRCLE('',#100481,0.450000000000006);
#33098=CIRCLE('',#100482,1.2);
#33099=CIRCLE('',#100483,0.750000000000001);
#33100=CIRCLE('',#100485,0.450000000000006);
#33101=CIRCLE('',#100486,0.750000000000001);
#33102=CIRCLE('',#100487,1.2);
#33103=CIRCLE('',#100490,0.450000000000006);
#33104=CIRCLE('',#100491,0.750000000000001);
#33105=CIRCLE('',#100492,0.450000000000006);
#33106=CIRCLE('',#100493,1.2);
#33107=CIRCLE('',#100495,0.450000000000006);
#33108=CIRCLE('',#100497,0.450000000000006);
#33109=CIRCLE('',#100499,0.450000000000006);
#33110=CIRCLE('',#100500,1.2);
#33111=CIRCLE('',#100501,0.750000000000001);
#33112=CIRCLE('',#100503,0.450000000000006);
#33113=CIRCLE('',#100504,0.750000000000001);
#33114=CIRCLE('',#100505,1.2);
#33115=CIRCLE('',#100507,0.449999999999999);
#33116=CIRCLE('',#100509,0.450000000000006);
#33117=CIRCLE('',#100511,0.750000000000001);
#33118=CIRCLE('',#100512,1.2);
#33119=CIRCLE('',#100514,0.450000000000006);
#33120=CIRCLE('',#100515,0.750000000000001);
#33121=CIRCLE('',#100516,0.450000000000006);
#33122=CIRCLE('',#100517,1.2);
#33123=CIRCLE('',#100519,0.450000000000006);
#33124=CIRCLE('',#100521,0.450000000000006);
#33125=CIRCLE('',#100523,0.45);
#33126=CIRCLE('',#100524,1.2);
#33127=CIRCLE('',#100525,0.750000000000001);
#33128=CIRCLE('',#100527,0.450000000000006);
#33129=CIRCLE('',#100528,0.750000000000001);
#33130=CIRCLE('',#100529,1.2);
#33131=CIRCLE('',#100531,0.449999999999999);
#33132=CIRCLE('',#100532,677.884816028482);
#33133=CIRCLE('',#100533,677.434816028482);
#33134=CIRCLE('',#100535,0.450000000000006);
#33135=CIRCLE('',#100537,0.750000000000001);
#33136=CIRCLE('',#100538,1.2);
#33137=CIRCLE('',#100540,0.450000000000006);
#33138=CIRCLE('',#100541,0.750000000000001);
#33139=CIRCLE('',#100542,0.450000000000006);
#33140=CIRCLE('',#100543,1.2);
#33141=CIRCLE('',#100545,0.450000000000006);
#33142=CIRCLE('',#100547,0.450000000000006);
#33143=CIRCLE('',#100549,0.450000000000006);
#33144=CIRCLE('',#100550,1.2);
#33145=CIRCLE('',#100551,0.750000000000001);
#33146=CIRCLE('',#100553,0.450000000000006);
#33147=CIRCLE('',#100554,0.750000000000001);
#33148=CIRCLE('',#100555,1.2);
#33149=CIRCLE('',#100557,0.449999999999999);
#33150=CIRCLE('',#100559,0.450000000000006);
#33151=CIRCLE('',#100561,0.750000000000001);
#33152=CIRCLE('',#100562,1.2);
#33153=CIRCLE('',#100564,0.450000000000006);
#33154=CIRCLE('',#100565,0.750000000000001);
#33155=CIRCLE('',#100566,0.450000000000006);
#33156=CIRCLE('',#100567,1.2);
#33157=CIRCLE('',#100569,0.450000000000006);
#33158=CIRCLE('',#100571,0.450000000000006);
#33159=CIRCLE('',#100573,0.450000000000006);
#33160=CIRCLE('',#100574,1.2);
#33161=CIRCLE('',#100575,0.750000000000001);
#33162=CIRCLE('',#100577,0.450000000000006);
#33163=CIRCLE('',#100578,0.750000000000001);
#33164=CIRCLE('',#100579,1.2);
#33165=CIRCLE('',#100581,0.450000000000001);
#33166=CIRCLE('',#100583,0.450000000000006);
#33167=CIRCLE('',#100585,0.750000000000001);
#33168=CIRCLE('',#100586,1.2);
#33169=CIRCLE('',#100588,0.450000000000006);
#33170=CIRCLE('',#100589,0.750000000000001);
#33171=CIRCLE('',#100590,0.449999999999999);
#33172=CIRCLE('',#100591,1.2);
#33173=CIRCLE('',#100593,0.450000000000006);
#33174=CIRCLE('',#100595,0.450000000000006);
#33175=CIRCLE('',#100597,0.450000000000006);
#33176=CIRCLE('',#100598,1.2);
#33177=CIRCLE('',#100599,0.750000000000001);
#33178=CIRCLE('',#100601,0.45);
#33179=CIRCLE('',#100602,0.750000000000001);
#33180=CIRCLE('',#100603,1.2);
#33181=CIRCLE('',#100605,0.450000000000006);
#33182=CIRCLE('',#100607,0.45);
#33183=CIRCLE('',#100608,13.1055395526668);
#33184=CIRCLE('',#100609,12.6555395526668);
#33185=CIRCLE('',#100611,1.2);
#33186=CIRCLE('',#100612,0.750000000000001);
#33187=CIRCLE('',#100613,0.450000000000001);
#33188=CIRCLE('',#100615,10.45);
#33189=CIRCLE('',#100616,10.);
#33190=CIRCLE('',#100618,0.450000000000006);
#33191=CIRCLE('',#100619,0.750000000000001);
#33192=CIRCLE('',#100620,0.450000000000006);
#33193=CIRCLE('',#100621,1.2);
#33194=CIRCLE('',#100623,0.450000000000006);
#33195=CIRCLE('',#100625,0.450000000000006);
#33196=CIRCLE('',#100627,0.449999999999997);
#33197=CIRCLE('',#100628,1.2);
#33198=CIRCLE('',#100629,0.750000000000001);
#33199=CIRCLE('',#100631,0.450000000000006);
#33200=CIRCLE('',#100632,0.750000000000001);
#33201=CIRCLE('',#100633,1.2);
#33202=CIRCLE('',#100635,0.449999999999998);
#33203=CIRCLE('',#100636,677.884816028482);
#33204=CIRCLE('',#100637,677.434816028482);
#33205=CIRCLE('',#100639,0.450000000000006);
#33206=CIRCLE('',#100641,0.750000000000001);
#33207=CIRCLE('',#100642,1.2);
#33208=CIRCLE('',#100644,0.449999999999999);
#33209=CIRCLE('',#100645,0.750000000000001);
#33210=CIRCLE('',#100646,0.450000000000006);
#33211=CIRCLE('',#100647,1.2);
#33212=CIRCLE('',#100649,0.450000000000006);
#33213=CIRCLE('',#100651,0.450000000000006);
#33214=CIRCLE('',#100653,0.45);
#33215=CIRCLE('',#100654,1.2);
#33216=CIRCLE('',#100655,0.750000000000001);
#33217=CIRCLE('',#100657,0.450000000000006);
#33218=CIRCLE('',#100658,0.750000000000001);
#33219=CIRCLE('',#100659,1.2);
#33220=CIRCLE('',#100661,0.45);
#33221=CIRCLE('',#100662,48.45);
#33222=CIRCLE('',#100663,48.);
#33223=CIRCLE('',#100665,0.450000000000006);
#33224=CIRCLE('',#100667,0.449999999999997);
#33225=CIRCLE('',#100668,1.45);
#33226=CIRCLE('',#100669,1.);
#33227=CIRCLE('',#100671,0.449999999999997);
#33228=CIRCLE('',#100672,0.750000000000001);
#33229=CIRCLE('',#100673,1.2);
#33230=CIRCLE('',#100675,677.434816028482);
#33231=CIRCLE('',#100676,677.884816028482);
#33232=CIRCLE('',#100678,0.450000000000006);
#33233=CIRCLE('',#100679,0.750000000000001);
#33234=CIRCLE('',#100680,0.450000000000006);
#33235=CIRCLE('',#100681,1.2);
#33236=CIRCLE('',#100683,0.450000000000006);
#33237=CIRCLE('',#100685,0.450000000000006);
#33238=CIRCLE('',#100687,0.450000000000006);
#33239=CIRCLE('',#100688,1.2);
#33240=CIRCLE('',#100689,0.750000000000001);
#33241=CIRCLE('',#100691,0.450000000000006);
#33242=CIRCLE('',#100692,0.750000000000001);
#33243=CIRCLE('',#100693,1.2);
#33244=CIRCLE('',#100695,0.449999999999999);
#33245=CIRCLE('',#100697,0.450000000000006);
#33246=CIRCLE('',#100699,0.750000000000001);
#33247=CIRCLE('',#100700,1.2);
#33248=CIRCLE('',#100702,0.449999999999999);
#33249=CIRCLE('',#100703,0.750000000000001);
#33250=CIRCLE('',#100704,0.450000000000006);
#33251=CIRCLE('',#100705,1.2);
#33252=CIRCLE('',#100707,0.450000000000006);
#33253=CIRCLE('',#100709,0.450000000000006);
#33254=CIRCLE('',#100711,0.450000000000006);
#33255=CIRCLE('',#100712,1.2);
#33256=CIRCLE('',#100713,0.750000000000001);
#33257=CIRCLE('',#100715,0.45);
#33258=CIRCLE('',#100716,0.750000000000001);
#33259=CIRCLE('',#100717,1.2);
#33260=CIRCLE('',#100719,0.450000000000006);
#33261=CIRCLE('',#100721,0.45);
#33262=CIRCLE('',#100722,48.);
#33263=CIRCLE('',#100723,48.45);
#33264=CIRCLE('',#100725,0.450000000000003);
#33265=CIRCLE('',#100726,1.2);
#33266=CIRCLE('',#100727,0.750000000000001);
#33267=CIRCLE('',#100729,0.450000000000001);
#33268=CIRCLE('',#100730,0.999999999999959);
#33269=CIRCLE('',#100731,1.44999999999997);
#33270=CIRCLE('',#100733,677.434816028482);
#33271=CIRCLE('',#100734,677.884816028482);
#33272=CIRCLE('',#100736,0.449999999999999);
#33273=CIRCLE('',#100737,0.750000000000001);
#33274=CIRCLE('',#100738,0.450000000000006);
#33275=CIRCLE('',#100739,1.2);
#33276=CIRCLE('',#100741,0.450000000000006);
#33277=CIRCLE('',#100743,0.450000000000006);
#33278=CIRCLE('',#100745,0.450000000000006);
#33279=CIRCLE('',#100746,1.2);
#33280=CIRCLE('',#100747,0.750000000000001);
#33281=CIRCLE('',#100749,0.450000000000003);
#33282=CIRCLE('',#100750,0.750000000000001);
#33283=CIRCLE('',#100751,1.2);
#33284=CIRCLE('',#100753,0.450000000000006);
#33285=CIRCLE('',#100755,0.449999999999998);
#33286=CIRCLE('',#100756,677.434816028482);
#33287=CIRCLE('',#100757,677.884816028482);
#33288=CIRCLE('',#100759,0.750000000000001);
#33289=CIRCLE('',#100760,1.2);
#33290=CIRCLE('',#100762,0.450000000000001);
#33291=CIRCLE('',#100763,0.750000000000001);
#33292=CIRCLE('',#100764,0.450000000000006);
#33293=CIRCLE('',#100765,1.2);
#33294=CIRCLE('',#100767,0.450000000000006);
#33295=CIRCLE('',#100769,0.450000000000006);
#33296=CIRCLE('',#100771,0.450000000000006);
#33297=CIRCLE('',#100772,1.2);
#33298=CIRCLE('',#100773,0.750000000000001);
#33299=CIRCLE('',#100775,0.450000000000006);
#33300=CIRCLE('',#100776,0.750000000000001);
#33301=CIRCLE('',#100777,1.2);
#33302=CIRCLE('',#100779,0.449999999999999);
#33303=CIRCLE('',#100781,0.450000000000006);
#33304=CIRCLE('',#100783,0.750000000000001);
#33305=CIRCLE('',#100784,1.2);
#33306=CIRCLE('',#100786,0.450000000000006);
#33307=CIRCLE('',#100787,0.750000000000001);
#33308=CIRCLE('',#100788,0.450000000000006);
#33309=CIRCLE('',#100789,1.2);
#33310=CIRCLE('',#100791,0.449999999999999);
#33311=CIRCLE('',#100793,0.450000000000006);
#33312=CIRCLE('',#100795,0.450000000000006);
#33313=CIRCLE('',#100796,1.2);
#33314=CIRCLE('',#100797,0.750000000000001);
#33315=CIRCLE('',#100799,0.449999999999999);
#33316=CIRCLE('',#100800,0.750000000000001);
#33317=CIRCLE('',#100801,1.2);
#33318=CIRCLE('',#100803,0.450000000000006);
#33319=CIRCLE('',#100805,0.449999999999999);
#33320=CIRCLE('',#100806,677.434816028482);
#33321=CIRCLE('',#100807,677.884816028482);
#33322=CIRCLE('',#100809,0.750000000000001);
#33323=CIRCLE('',#100810,1.2);
#33324=CIRCLE('',#100812,0.450000000000006);
#33325=CIRCLE('',#100813,0.750000000000001);
#33326=CIRCLE('',#100814,0.449999999999999);
#33327=CIRCLE('',#100815,1.2);
#33328=CIRCLE('',#100817,0.450000000000006);
#33329=CIRCLE('',#100819,0.450000000000006);
#33330=CIRCLE('',#100821,0.450000000000006);
#33331=CIRCLE('',#100822,1.2);
#33332=CIRCLE('',#100823,0.750000000000001);
#33333=CIRCLE('',#100825,0.449999999999999);
#33334=CIRCLE('',#100826,0.750000000000001);
#33335=CIRCLE('',#100827,1.2);
#33336=CIRCLE('',#100829,0.450000000000006);
#33337=CIRCLE('',#100831,0.450000000000006);
#33338=CIRCLE('',#100833,0.750000000000001);
#33339=CIRCLE('',#100834,1.2);
#33340=CIRCLE('',#100836,0.449999999999999);
#33341=CIRCLE('',#100837,0.750000000000001);
#33342=CIRCLE('',#100838,0.450000000000006);
#33343=CIRCLE('',#100839,1.2);
#33344=CIRCLE('',#100841,0.450000000000006);
#33345=CIRCLE('',#100843,0.45);
#33346=CIRCLE('',#100844,48.);
#33347=CIRCLE('',#100845,48.45);
#33348=CIRCLE('',#100847,0.450000000000006);
#33349=CIRCLE('',#100848,1.2);
#33350=CIRCLE('',#100849,0.750000000000001);
#33351=CIRCLE('',#100851,0.450000000000006);
#33352=CIRCLE('',#100852,0.750000000000001);
#33353=CIRCLE('',#100853,1.2);
#33354=CIRCLE('',#100856,1.2);
#33355=CIRCLE('',#100857,0.450000000000002);
#33356=CIRCLE('',#100858,0.750000000000001);
#33357=CIRCLE('',#100859,0.450000000000006);
#33358=CIRCLE('',#100861,0.450000000000006);
#33359=CIRCLE('',#100863,0.449999999999999);
#33360=CIRCLE('',#100864,48.);
#33361=CIRCLE('',#100865,48.45);
#33362=CIRCLE('',#100867,0.450000000000006);
#33363=CIRCLE('',#100868,1.2);
#33364=CIRCLE('',#100869,0.750000000000001);
#33365=CIRCLE('',#100871,0.450000000000006);
#33366=CIRCLE('',#100872,0.750000000000001);
#33367=CIRCLE('',#100873,1.2);
#33368=CIRCLE('',#100876,7.65553955266686);
#33369=CIRCLE('',#100877,0.45);
#33370=CIRCLE('',#100878,8.10553955266686);
#33371=CIRCLE('',#100880,4.62535);
#33372=CIRCLE('',#100881,0.45);
#33373=CIRCLE('',#100882,5.07535);
#33374=CIRCLE('',#100884,0.45);
#33375=CIRCLE('',#100885,682.884816028482);
#33376=CIRCLE('',#100886,682.434816028482);
#33377=CIRCLE('',#100888,0.450000000000002);
#33378=CIRCLE('',#100889,6.44999999999991);
#33379=CIRCLE('',#100890,5.99999999999992);
#33380=CIRCLE('',#100892,0.45);
#33381=CIRCLE('',#100893,53.45);
#33382=CIRCLE('',#100894,53.);
#33383=CIRCLE('',#100896,0.449999999999997);
#33384=CIRCLE('',#100897,6.45);
#33385=CIRCLE('',#100898,6.);
#33386=CIRCLE('',#100900,0.449999999999997);
#33387=CIRCLE('',#100901,682.884816028482);
#33388=CIRCLE('',#100902,682.434816028482);
#33389=CIRCLE('',#100904,0.45);
#33390=CIRCLE('',#100905,6.45);
#33391=CIRCLE('',#100906,6.);
#33392=CIRCLE('',#100908,0.449999999999998);
#33393=CIRCLE('',#100909,53.45);
#33394=CIRCLE('',#100910,53.);
#33395=CIRCLE('',#100912,0.45);
#33396=CIRCLE('',#100913,6.45);
#33397=CIRCLE('',#100914,6.);
#33398=CIRCLE('',#100916,209.945690815561);
#33399=CIRCLE('',#100917,209.495690815561);
#33400=CIRCLE('',#100919,0.45);
#33401=CIRCLE('',#100920,681.234816028482);
#33402=CIRCLE('',#100921,680.784816028482);
#33403=CIRCLE('',#100923,0.450000000000002);
#33404=CIRCLE('',#100924,4.8);
#33405=CIRCLE('',#100925,4.34999999999995);
#33406=CIRCLE('',#100927,0.45);
#33407=CIRCLE('',#100928,51.8);
#33408=CIRCLE('',#100929,51.35);
#33409=CIRCLE('',#100931,0.449999999999997);
#33410=CIRCLE('',#100932,4.8);
#33411=CIRCLE('',#100933,4.35);
#33412=CIRCLE('',#100935,0.449999999999997);
#33413=CIRCLE('',#100936,681.234816028482);
#33414=CIRCLE('',#100937,680.784816028482);
#33415=CIRCLE('',#100939,0.45);
#33416=CIRCLE('',#100940,4.8);
#33417=CIRCLE('',#100941,4.35);
#33418=CIRCLE('',#100943,0.450000000000002);
#33419=CIRCLE('',#100944,51.8);
#33420=CIRCLE('',#100945,51.35);
#33421=CIRCLE('',#100947,0.45);
#33422=CIRCLE('',#100948,4.8);
#33423=CIRCLE('',#100949,4.35);
#33424=CIRCLE('',#100951,208.29569081556);
#33425=CIRCLE('',#100952,207.845690815561);
#33426=CIRCLE('',#100954,0.45);
#33427=CIRCLE('',#100955,0.75);
#33428=CIRCLE('',#100956,1.2);
#33429=CIRCLE('',#100958,0.45);
#33430=CIRCLE('',#100960,1.2);
#33431=CIRCLE('',#100961,0.45);
#33432=CIRCLE('',#100962,0.75);
#33433=CIRCLE('',#100964,0.450000000000001);
#33434=CIRCLE('',#100965,11.1055395526669);
#33435=CIRCLE('',#100966,11.5555395526669);
#33436=CIRCLE('',#100968,0.450000000000006);
#33437=CIRCLE('',#100969,0.750000000000001);
#33438=CIRCLE('',#100970,1.2);
#33439=CIRCLE('',#100972,0.450000000000006);
#33440=CIRCLE('',#100974,0.750000000000001);
#33441=CIRCLE('',#100975,1.2);
#33442=CIRCLE('',#100977,0.450000000000006);
#33443=CIRCLE('',#100978,0.750000000000001);
#33444=CIRCLE('',#100979,1.2);
#33445=CIRCLE('',#100981,0.450000000000006);
#33446=CIRCLE('',#100983,0.450000000000001);
#33447=CIRCLE('',#100984,0.750000000000001);
#33448=CIRCLE('',#100985,1.2);
#33449=CIRCLE('',#100987,0.449999999999999);
#33450=CIRCLE('',#100988,11.1055395526669);
#33451=CIRCLE('',#100989,11.5555395526669);
#33452=CIRCLE('',#100991,0.45);
#33453=CIRCLE('',#100992,0.750000000000001);
#33454=CIRCLE('',#100993,1.2);
#33455=CIRCLE('',#100995,0.45);
#33456=CIRCLE('',#100997,0.750000000000001);
#33457=CIRCLE('',#100998,1.2);
#33458=CIRCLE('',#101000,0.45);
#33459=CIRCLE('',#101001,0.75);
#33460=CIRCLE('',#101002,1.2);
#33461=CIRCLE('',#101004,0.450000000000006);
#33462=CIRCLE('',#101006,1.2);
#33463=CIRCLE('',#101007,0.45);
#33464=CIRCLE('',#101008,0.75);
#33465=CIRCLE('',#101010,0.45);
#33466=CIRCLE('',#101011,11.1055395526669);
#33467=CIRCLE('',#101012,11.5555395526669);
#33468=CIRCLE('',#101014,0.45);
#33469=CIRCLE('',#101015,0.75);
#33470=CIRCLE('',#101016,1.2);
#33471=CIRCLE('',#101018,0.45);
#33472=CIRCLE('',#101020,0.75);
#33473=CIRCLE('',#101021,1.2);
#33474=CIRCLE('',#101023,1.2);
#33475=CIRCLE('',#101024,0.45);
#33476=CIRCLE('',#101025,0.750000000000001);
#33477=CIRCLE('',#101027,0.45);
#33478=CIRCLE('',#101029,0.450000000000001);
#33479=CIRCLE('',#101030,0.750000000000001);
#33480=CIRCLE('',#101031,1.2);
#33481=CIRCLE('',#101033,0.450000000000001);
#33482=CIRCLE('',#101034,11.1055395526669);
#33483=CIRCLE('',#101035,11.5555395526669);
#33484=CIRCLE('',#101037,0.450000000000006);
#33485=CIRCLE('',#101038,0.750000000000001);
#33486=CIRCLE('',#101039,1.2);
#33487=CIRCLE('',#101041,0.450000000000006);
#33488=CIRCLE('',#101043,0.750000000000001);
#33489=CIRCLE('',#101044,1.2);
#33490=CIRCLE('',#101046,233.077358936672);
#33491=CIRCLE('',#101047,234.577130479406);
#33492=CIRCLE('',#101048,1.5);
#33493=CIRCLE('',#101050,1.5);
#33494=CIRCLE('',#101051,12.5403589366713);
#33495=CIRCLE('',#101052,14.0401304794059);
#33496=CIRCLE('',#101054,1.5);
#33497=CIRCLE('',#101055,78.1898589566432);
#33498=CIRCLE('',#101056,79.6896304993778);
#33499=CIRCLE('',#101058,1.5);
#33500=CIRCLE('',#101059,12.5403589366712);
#33501=CIRCLE('',#101060,14.0401304794058);
#33502=CIRCLE('',#101062,1.5);
#33503=CIRCLE('',#101063,1068.07735893667);
#33504=CIRCLE('',#101064,1069.5771304794);
#33505=CIRCLE('',#101066,1.5);
#33506=CIRCLE('',#101067,12.5403589366712);
#33507=CIRCLE('',#101068,14.0401304794058);
#33508=CIRCLE('',#101070,1.5);
#33509=CIRCLE('',#101071,78.1898589566432);
#33510=CIRCLE('',#101072,79.6896304993778);
#33511=CIRCLE('',#101074,1.50000000000001);
#33512=CIRCLE('',#101075,12.5403589366713);
#33513=CIRCLE('',#101076,14.0401304794059);
#33514=CIRCLE('',#101078,1068.07735893667);
#33515=CIRCLE('',#101079,1069.5771304794);
#33516=CIRCLE('',#101080,1.5);
#33517=CIRCLE('',#101081,1.5);
#33518=CIRCLE('',#101083,1.5);
#33519=CIRCLE('',#101084,211.96315619496);
#33520=CIRCLE('',#101085,213.52922045504);
#33521=CIRCLE('',#101086,1.5);
#33522=CIRCLE('',#101087,1.5);
#33523=CIRCLE('',#101088,1.5);
#33524=CIRCLE('',#101089,1.5);
#33525=CIRCLE('',#101090,696.813945754987);
#33526=CIRCLE('',#101091,687.655553461799);
#33527=CIRCLE('',#101092,1.5);
#33528=CIRCLE('',#101093,1.5);
#33529=CIRCLE('',#101094,1.5);
#33530=CIRCLE('',#101095,1.5);
#33531=CIRCLE('',#101096,696.576271176166);
#33532=CIRCLE('',#101097,687.392615253502);
#33533=CIRCLE('',#101098,1.5);
#33534=CIRCLE('',#101099,1.5);
#33535=CIRCLE('',#101100,1.5);
#33536=CIRCLE('',#101101,1.5);
#33537=CIRCLE('',#101102,697.569175023773);
#33538=CIRCLE('',#101103,687.588787872307);
#33539=CIRCLE('',#101104,1.5);
#33540=CIRCLE('',#101105,72.6268730892939);
#33541=CIRCLE('',#101106,5.);
#33542=CIRCLE('',#101107,5.);
#33543=CIRCLE('',#101108,10.1322440903793);
#33544=CIRCLE('',#101110,4.99999999999999);
#33545=CIRCLE('',#101111,5.);
#33546=CIRCLE('',#101112,1066.87927691535);
#33547=CIRCLE('',#101113,1029.30060997527);
#33548=CIRCLE('',#101115,3.);
#33549=CIRCLE('',#101116,3.);
#33550=CIRCLE('',#101117,3.);
#33551=CIRCLE('',#101118,3.);
#33552=CIRCLE('',#101119,1029.24694971421);
#33553=CIRCLE('',#101120,5.);
#33554=CIRCLE('',#101121,1066.87014162396);
#33555=CIRCLE('',#101122,4.99999999999999);
#33556=CIRCLE('',#101123,5.00000000000001);
#33557=CIRCLE('',#101124,5.);
#33558=CIRCLE('',#101125,9.93127307062933);
#33559=CIRCLE('',#101126,4.98383829944567);
#33560=CIRCLE('',#101128,3.);
#33561=CIRCLE('',#101130,3.);
#33562=CIRCLE('',#101133,1032.95041731725);
#33563=CIRCLE('',#101134,5.);
#33564=CIRCLE('',#101135,1067.00041835739);
#33565=CIRCLE('',#101136,5.00000000000001);
#33566=CIRCLE('',#101137,5.);
#33567=CIRCLE('',#101138,5.);
#33568=CIRCLE('',#101139,10.1960538523774);
#33569=CIRCLE('',#101143,5.00000000000001);
#33570=CIRCLE('',#101145,3.);
#33571=CIRCLE('',#101146,2.28316188307923);
#33572=CIRCLE('',#101148,5.);
#33573=CIRCLE('',#101149,3.);
#33574=CIRCLE('',#101150,5.);
#33575=CIRCLE('',#101151,5.);
#33576=CIRCLE('',#101152,5.);
#33577=CIRCLE('',#101153,9.92561537912225);
#33578=CIRCLE('',#101155,0.75);
#33579=CIRCLE('',#101157,0.750000000000001);
#33580=CIRCLE('',#101159,0.750000000000001);
#33581=CIRCLE('',#101161,0.750000000000001);
#33582=CIRCLE('',#101163,0.750000000000001);
#33583=CIRCLE('',#101165,0.750000000000001);
#33584=CIRCLE('',#101167,0.75);
#33585=CIRCLE('',#101169,0.75);
#33586=CIRCLE('',#101171,0.75);
#33587=CIRCLE('',#101173,0.750000000000001);
#33588=CIRCLE('',#101175,0.750000000000001);
#33589=CIRCLE('',#101177,0.750000000000001);
#33590=CIRCLE('',#101179,0.750000000000001);
#33591=CIRCLE('',#101181,0.750000000000001);
#33592=CIRCLE('',#101183,0.750000000000001);
#33593=CIRCLE('',#101185,0.750000000000001);
#33594=CIRCLE('',#101187,0.75);
#33595=CIRCLE('',#101189,0.75);
#33596=CIRCLE('',#101191,0.75);
#33597=CIRCLE('',#101193,0.750000000000001);
#33598=CIRCLE('',#101195,0.750000000000001);
#33599=CIRCLE('',#101197,0.75);
#33600=CIRCLE('',#101199,0.750000000000001);
#33601=CIRCLE('',#101201,0.750000000000001);
#33602=CIRCLE('',#101203,0.750000000000001);
#33603=CIRCLE('',#101205,0.750000000000001);
#33604=CIRCLE('',#101207,0.750000000000001);
#33605=CIRCLE('',#101209,0.750000000000001);
#33606=CIRCLE('',#101211,0.750000000000001);
#33607=CIRCLE('',#101213,0.750000000000001);
#33608=CIRCLE('',#101215,0.750000000000001);
#33609=CIRCLE('',#101217,0.750000000000001);
#33610=CIRCLE('',#101219,0.750000000000001);
#33611=CIRCLE('',#101221,0.750000000000001);
#33612=CIRCLE('',#101223,0.75);
#33613=CIRCLE('',#101225,0.75);
#33614=CIRCLE('',#101227,0.750000000000001);
#33615=CIRCLE('',#101229,0.750000000000001);
#33616=CIRCLE('',#101231,0.750000000000001);
#33617=CIRCLE('',#101233,0.750000000000001);
#33618=CIRCLE('',#101235,0.750000000000001);
#33619=CIRCLE('',#101237,0.750000000000001);
#33620=CIRCLE('',#101239,0.750000000000001);
#33621=CIRCLE('',#101241,0.750000000000001);
#33622=CIRCLE('',#101243,0.75);
#33623=CIRCLE('',#101245,0.75);
#33624=CIRCLE('',#101247,0.750000000000001);
#33625=CIRCLE('',#101249,0.750000000000001);
#33626=CIRCLE('',#101251,0.750000000000001);
#33627=CIRCLE('',#101253,0.750000000000001);
#33628=CIRCLE('',#101255,0.750000000000001);
#33629=CIRCLE('',#101257,0.750000000000001);
#33630=CIRCLE('',#101259,0.750000000000001);
#33631=CIRCLE('',#101261,0.750000000000001);
#33632=CIRCLE('',#101263,0.750000000000001);
#33633=CIRCLE('',#101265,0.750000000000001);
#33634=CIRCLE('',#101267,0.750000000000001);
#33635=CIRCLE('',#101269,0.750000000000001);
#33636=CIRCLE('',#101271,0.750000000000001);
#33637=CIRCLE('',#101273,0.750000000000001);
#33638=CIRCLE('',#101275,0.750000000000001);
#33639=CIRCLE('',#101277,0.750000000000001);
#33640=CIRCLE('',#101279,0.750000000000001);
#33641=CIRCLE('',#101281,0.750000000000001);
#33642=CIRCLE('',#101283,0.750000000000001);
#33643=CIRCLE('',#101285,0.750000000000001);
#33644=CIRCLE('',#101287,0.750000000000001);
#33645=CIRCLE('',#101289,0.750000000000001);
#33646=CIRCLE('',#101291,0.750000000000001);
#33647=CIRCLE('',#101293,0.750000000000001);
#33648=CIRCLE('',#101295,0.750000000000001);
#33649=CIRCLE('',#101297,0.75);
#33650=CIRCLE('',#101299,0.750000000000001);
#33651=CIRCLE('',#101301,0.750000000000001);
#33652=CIRCLE('',#101303,0.75);
#33653=CIRCLE('',#101305,0.750000000000001);
#33654=CIRCLE('',#101307,0.75);
#33655=CIRCLE('',#101309,0.75);
#33656=CIRCLE('',#101311,0.750000000000001);
#33657=CIRCLE('',#101313,0.750000000000001);
#33658=CIRCLE('',#101315,0.750000000000001);
#33659=CIRCLE('',#101317,0.750000000000001);
#33660=CIRCLE('',#101319,0.750000000000001);
#33661=CIRCLE('',#101321,0.750000000000001);
#33662=CIRCLE('',#101323,0.750000000000001);
#33663=CIRCLE('',#101325,0.750000000000001);
#33664=CIRCLE('',#101327,0.750000000000001);
#33665=CIRCLE('',#101329,0.750000000000001);
#33666=CIRCLE('',#101331,0.750000000000001);
#33667=CIRCLE('',#101333,0.750000000000001);
#33668=CIRCLE('',#101335,0.750000000000001);
#33669=CIRCLE('',#101337,0.750000000000001);
#33670=CIRCLE('',#101339,0.750000000000001);
#33671=CIRCLE('',#101341,0.750000000000001);
#33672=CIRCLE('',#101343,0.750000000000001);
#33673=CIRCLE('',#101345,0.750000000000001);
#33674=CIRCLE('',#101347,0.750000000000001);
#33675=CIRCLE('',#101349,0.75);
#33676=CIRCLE('',#101351,0.75);
#33677=CIRCLE('',#101353,0.750000000000001);
#33678=CIRCLE('',#101355,0.750000000000001);
#33679=CIRCLE('',#101357,0.750000000000001);
#33680=CIRCLE('',#101359,0.750000000000001);
#33681=CIRCLE('',#101361,0.750000000000001);
#33682=CIRCLE('',#101363,0.750000000000001);
#33683=CIRCLE('',#101365,0.750000000000001);
#33684=CIRCLE('',#101367,0.750000000000001);
#33685=CIRCLE('',#101369,0.750000000000001);
#33686=CIRCLE('',#101371,0.750000000000001);
#33687=CIRCLE('',#101373,0.750000000000001);
#33688=CIRCLE('',#101375,0.750000000000001);
#33689=CIRCLE('',#101377,0.750000000000001);
#33690=CIRCLE('',#101379,0.750000000000001);
#33691=CIRCLE('',#101381,0.750000000000001);
#33692=CIRCLE('',#101383,0.750000000000001);
#33693=CIRCLE('',#101385,0.750000000000001);
#33694=CIRCLE('',#101387,0.750000000000001);
#33695=CIRCLE('',#101389,0.750000000000001);
#33696=CIRCLE('',#101391,0.750000000000001);
#33697=CIRCLE('',#101393,0.750000000000001);
#33698=CIRCLE('',#101395,0.750000000000001);
#33699=CIRCLE('',#101397,0.750000000000001);
#33700=CIRCLE('',#101399,0.750000000000001);
#33701=CIRCLE('',#101401,0.750000000000001);
#33702=CIRCLE('',#101403,0.750000000000001);
#33703=CIRCLE('',#101405,0.750000000000001);
#33704=CIRCLE('',#101407,0.750000000000001);
#33705=CIRCLE('',#101409,0.750000000000001);
#33706=CIRCLE('',#101411,0.750000000000001);
#33707=CIRCLE('',#101413,0.75);
#33708=CIRCLE('',#101415,0.75);
#33709=CIRCLE('',#101417,0.750000000000001);
#33710=CIRCLE('',#101419,0.750000000000001);
#33711=CIRCLE('',#101421,0.750000000000001);
#33712=CIRCLE('',#101423,10.);
#33713=CIRCLE('',#101425,10.);
#33714=CIRCLE('',#101427,10.);
#33715=CIRCLE('',#101429,10.);
#33716=CIRCLE('',#101431,4.62535);
#33717=CIRCLE('',#101435,13.1055395526668);
#33718=CIRCLE('',#101437,13.1055395526668);
#33719=CIRCLE('',#101439,8.10553955266685);
#33720=CIRCLE('',#101440,8.10553955266686);
#33721=CIRCLE('',#101441,8.10553955266685);
#33722=CIRCLE('',#101442,8.10553955266686);
#33723=CIRCLE('',#101443,8.10553955266685);
#33724=CIRCLE('',#101444,8.10553955266686);
#33725=CIRCLE('',#101445,8.10553955266685);
#33726=CIRCLE('',#101446,8.10553955266686);
#33727=CIRCLE('',#101447,8.10553955266685);
#33728=CIRCLE('',#101448,8.10553955266686);
#33729=CIRCLE('',#101449,8.10553955266685);
#33730=CIRCLE('',#101450,8.10553955266686);
#33731=CIRCLE('',#101451,8.10553955266685);
#33732=CIRCLE('',#101452,8.10553955266686);
#33733=CIRCLE('',#101453,8.10553955266685);
#33734=CIRCLE('',#101454,8.10553955266686);
#33735=CIRCLE('',#101455,8.10553955266685);
#33736=CIRCLE('',#101457,11.1055395526669);
#33737=CIRCLE('',#101461,11.1055395526669);
#33738=CIRCLE('',#101463,12.1055395526668);
#33739=CIRCLE('',#101465,11.1055395526669);
#33740=CIRCLE('',#101469,11.1055395526669);
#33741=CIRCLE('',#101471,12.1055395526668);
#33742=CIRCLE('',#101530,206.99569081556);
#33743=CIRCLE('',#101531,679.934816028482);
#33744=CIRCLE('',#101532,3.49999999999996);
#33745=CIRCLE('',#101533,50.5);
#33746=CIRCLE('',#101534,3.5);
#33747=CIRCLE('',#101535,679.934816028482);
#33748=CIRCLE('',#101536,3.5);
#33749=CIRCLE('',#101537,50.5);
#33750=CIRCLE('',#101538,3.5);
#33751=CIRCLE('',#101539,206.99569081556);
#33752=CIRCLE('',#101540,677.434816028482);
#33753=CIRCLE('',#101541,204.49569081556);
#33754=CIRCLE('',#101542,204.49569081556);
#33755=CIRCLE('',#101543,677.434816028482);
#33756=CIRCLE('',#101544,204.49569081556);
#33757=CIRCLE('',#101545,1.);
#33758=CIRCLE('',#101546,48.);
#33759=CIRCLE('',#101547,48.);
#33760=CIRCLE('',#101548,0.999999999999999);
#33761=CIRCLE('',#101549,677.434816028482);
#33762=CIRCLE('',#101550,677.434816028482);
#33763=CIRCLE('',#101551,677.434816028482);
#33764=CIRCLE('',#101552,677.434816028482);
#33765=CIRCLE('',#101553,677.434816028482);
#33766=CIRCLE('',#101554,48.);
#33767=CIRCLE('',#101555,677.434816028482);
#33768=CIRCLE('',#101556,1.);
#33769=CIRCLE('',#101557,48.);
#33770=CIRCLE('',#101558,48.);
#33771=CIRCLE('',#101559,0.999999999999959);
#33772=CIRCLE('',#101560,677.434816028482);
#33773=CIRCLE('',#101561,48.);
#33774=CIRCLE('',#101563,3.5);
#33775=CIRCLE('',#101565,50.5);
#33776=CIRCLE('',#101567,3.5);
#33777=CIRCLE('',#101569,679.934816028482);
#33778=CIRCLE('',#101571,3.5);
#33779=CIRCLE('',#101573,50.5);
#33780=CIRCLE('',#101575,3.49999999999996);
#33781=CIRCLE('',#101577,679.934816028482);
#33782=CIRCLE('',#101579,5.98129380707219);
#33783=CIRCLE('',#101582,5.9812938070714);
#33784=CIRCLE('',#101587,74.6139048513169);
#33785=CIRCLE('',#101588,74.6139048513169);
#33786=CIRCLE('',#101592,74.6139048513167);
#33787=CIRCLE('',#101593,74.6139048513167);
#33788=CIRCLE('',#101595,8.5);
#33789=CIRCLE('',#101596,8.5);
#33790=CIRCLE('',#101598,684.934816028482);
#33791=CIRCLE('',#101599,684.934816028482);
#33792=CIRCLE('',#101601,211.99569081556);
#33793=CIRCLE('',#101602,211.99569081556);
#33794=CIRCLE('',#101603,211.99569081556);
#33795=CIRCLE('',#101604,211.99569081556);
#33796=CIRCLE('',#101606,8.5);
#33797=CIRCLE('',#101607,8.5);
#33798=CIRCLE('',#101609,55.5);
#33799=CIRCLE('',#101610,55.5);
#33800=CIRCLE('',#101612,8.5);
#33801=CIRCLE('',#101613,8.5);
#33802=CIRCLE('',#101615,684.934816028482);
#33803=CIRCLE('',#101616,684.934816028482);
#33804=CIRCLE('',#101618,8.5);
#33805=CIRCLE('',#101619,8.5);
#33806=CIRCLE('',#101621,55.5);
#33807=CIRCLE('',#101622,55.5);
#33808=CIRCLE('',#101624,9.05766167355557);
#33809=CIRCLE('',#101626,74.7071616935275);
#33810=CIRCLE('',#101628,9.05766167355546);
#33811=CIRCLE('',#101629,6.68387219307026);
#33812=CIRCLE('',#101631,9.05766167355555);
#33813=CIRCLE('',#101632,6.41600556624483);
#33814=CIRCLE('',#101634,74.7071616935275);
#33815=CIRCLE('',#101636,9.05766167355558);
#33816=CIRCLE('',#101637,6.41130036340322);
#33817=CIRCLE('',#101639,1064.59466167355);
#33818=CIRCLE('',#101641,232.094661673555);
#33819=CIRCLE('',#101642,1067.09466167355);
#33820=CIRCLE('',#101643,11.5576616735556);
#33821=CIRCLE('',#101644,77.2071616935275);
#33822=CIRCLE('',#101645,11.5576616735555);
#33823=CIRCLE('',#101646,1067.09466167355);
#33824=CIRCLE('',#101647,11.5576616735555);
#33825=CIRCLE('',#101648,77.2071616935275);
#33826=CIRCLE('',#101649,11.5576616735556);
#33827=CIRCLE('',#101650,229.594661673555);
#33828=CIRCLE('',#101651,1064.59466167355);
#33829=CIRCLE('',#101653,1067.49961917989);
#33830=CIRCLE('',#101655,11.9626191798902);
#33831=CIRCLE('',#101657,77.6121191998622);
#33832=CIRCLE('',#101659,11.9626191798902);
#33833=CIRCLE('',#101661,232.49961917989);
#33834=CIRCLE('',#101663,1067.49961917989);
#33835=CIRCLE('',#101665,11.9626191798902);
#33836=CIRCLE('',#101667,77.6121191998622);
#33837=CIRCLE('',#101669,11.9626191798902);
#33838=CIRCLE('',#101671,211.167112167697);
#33839=CIRCLE('',#101674,684.934816028482);
#33840=CIRCLE('',#101675,684.934816028482);
#33841=CIRCLE('',#101676,705.368683747911);
#33842=CIRCLE('',#101678,5.80674315778922);
#33843=CIRCLE('',#101680,5.80674315779001);
#33844=CIRCLE('',#101685,684.934816028482);
#33845=CIRCLE('',#101687,684.934816028482);
#33846=CIRCLE('',#101689,684.934816028482);
#33847=CIRCLE('',#101692,684.934816028482);
#33848=CIRCLE('',#101694,5.9812938070714);
#33849=CIRCLE('',#101696,684.934816028482);
#33850=CIRCLE('',#101698,684.934816028482);
#33851=CIRCLE('',#101700,684.934816028482);
#33852=CIRCLE('',#101702,684.934816028482);
#33853=CIRCLE('',#101704,684.934816028482);
#33854=CIRCLE('',#101717,3.35);
#33855=CIRCLE('',#101720,3.35000000000079);
#33856=CIRCLE('',#101738,51.8);
#33857=CIRCLE('',#101740,4.8);
#33858=CIRCLE('',#101742,681.234816028482);
#33859=CIRCLE('',#101744,4.8);
#33860=CIRCLE('',#101746,51.8);
#33861=CIRCLE('',#101748,4.8);
#33862=CIRCLE('',#101750,681.234816028482);
#33863=CIRCLE('',#101752,208.295690815561);
#33864=CIRCLE('',#101754,4.8);
#33865=CIRCLE('',#101756,682.434816028482);
#33866=CIRCLE('',#101757,209.495690815561);
#33867=CIRCLE('',#101758,6.);
#33868=CIRCLE('',#101759,53.);
#33869=CIRCLE('',#101760,6.);
#33870=CIRCLE('',#101761,682.434816028482);
#33871=CIRCLE('',#101762,6.);
#33872=CIRCLE('',#101763,53.);
#33873=CIRCLE('',#101764,5.99999999999992);
#33874=CIRCLE('',#101782,235.);
#33875=CIRCLE('',#101783,1070.);
#33876=CIRCLE('',#101784,14.463);
#33877=CIRCLE('',#101785,80.1125000199719);
#33878=CIRCLE('',#101786,14.463);
#33879=CIRCLE('',#101787,1070.);
#33880=CIRCLE('',#101788,14.463);
#33881=CIRCLE('',#101789,80.1125000199719);
#33882=CIRCLE('',#101790,14.463);
#33883=CIRCLE('',#101824,206.99569081556);
#33884=CIRCLE('',#101826,206.99569081556);
#33885=CIRCLE('',#101887,1.73205080756888);
#33886=CIRCLE('',#101889,1.73205080756888);
#33887=CIRCLE('',#101891,1.73205080756888);
#33888=CIRCLE('',#101893,1.73205080756888);
#33889=CIRCLE('',#101895,1.73205080756888);
#33890=CIRCLE('',#101897,1.73205080756888);
#33891=CIRCLE('',#101899,3.);
#33892=CIRCLE('',#101900,0.25);
#33893=CIRCLE('',#101901,3.25);
#33894=CIRCLE('',#101902,3.25);
#33895=CIRCLE('',#101904,3.25);
#33896=CIRCLE('',#101908,5.);
#33897=CIRCLE('',#101909,5.);
#33898=CIRCLE('',#101910,5.);
#33899=CIRCLE('',#101911,5.);
#33900=CIRCLE('',#101912,5.);
#33901=CIRCLE('',#101913,5.);
#33902=CIRCLE('',#101921,5.);
#33903=CIRCLE('',#101922,5.);
#33904=CIRCLE('',#101923,5.);
#33905=CIRCLE('',#101924,5.);
#33906=CIRCLE('',#101925,5.);
#33907=CIRCLE('',#101926,5.);
#33908=CIRCLE('',#101940,5.);
#33909=CIRCLE('',#101941,5.);
#33910=CIRCLE('',#101942,5.);
#33911=CIRCLE('',#101943,5.);
#33912=CIRCLE('',#101944,5.);
#33913=CIRCLE('',#101945,5.);
#33914=CIRCLE('',#101953,5.);
#33915=CIRCLE('',#101954,5.);
#33916=CIRCLE('',#101955,5.);
#33917=CIRCLE('',#101956,5.);
#33918=CIRCLE('',#101957,5.);
#33919=CIRCLE('',#101958,5.);
#33920=CIRCLE('',#101979,1.73205080756888);
#33921=CIRCLE('',#101981,1.73205080756888);
#33922=CIRCLE('',#101983,1.73205080756888);
#33923=CIRCLE('',#101985,1.73205080756888);
#33924=CIRCLE('',#101987,1.73205080756888);
#33925=CIRCLE('',#101989,1.73205080756888);
#33926=CIRCLE('',#101991,3.);
#33927=CIRCLE('',#101992,0.25);
#33928=CIRCLE('',#101993,3.25);
#33929=CIRCLE('',#101994,3.25);
#33930=CIRCLE('',#101996,3.25);
#33931=CIRCLE('',#102000,8.65629040278471);
#33932=CIRCLE('',#102001,20.3599346995449);
#33933=CIRCLE('',#102002,20.3599346995449);
#33934=CIRCLE('',#102004,8.8);
#33935=CIRCLE('',#102005,8.8);
#33936=CIRCLE('',#102006,0.25);
#33937=CIRCLE('',#102008,8.55);
#33938=CIRCLE('',#102009,0.25);
#33939=CIRCLE('',#102010,8.8);
#33940=CIRCLE('',#102011,8.8);
#33941=CIRCLE('',#102013,0.750000000000001);
#33942=CIRCLE('',#102014,0.750000000000001);
#33943=CIRCLE('',#102020,7.8);
#33944=CIRCLE('',#102022,7.8);
#33945=CIRCLE('',#102026,2.);
#33946=CIRCLE('',#102027,1.47499999999998);
#33947=CIRCLE('',#102030,2.);
#33948=CIRCLE('',#102032,2.5);
#33949=CIRCLE('',#102034,2.5);
#33950=CIRCLE('',#102037,0.5);
#33951=CIRCLE('',#102038,6.50000000000001);
#33952=CIRCLE('',#102039,0.5);
#33953=CIRCLE('',#102040,7.00000000000001);
#33954=CIRCLE('',#102042,0.5);
#33955=CIRCLE('',#102044,0.5);
#33956=CIRCLE('',#102046,0.5);
#33957=CIRCLE('',#102047,7.00000000000001);
#33958=CIRCLE('',#102048,6.50000000000001);
#33959=CIRCLE('',#102050,0.5);
#33960=CIRCLE('',#102051,6.50000000000001);
#33961=CIRCLE('',#102052,7.00000000000001);
#33962=CIRCLE('',#102054,0.5);
#33963=CIRCLE('',#102056,0.5);
#33964=CIRCLE('',#102058,6.50000000000001);
#33965=CIRCLE('',#102059,7.00000000000001);
#33966=CIRCLE('',#102062,7.00000000000001);
#33967=CIRCLE('',#102064,7.00000000000001);
#33968=CIRCLE('',#102066,7.8);
#33969=CIRCLE('',#102067,7.8);
#33970=CIRCLE('',#102069,1.);
#33971=CIRCLE('',#102070,4.);
#33972=CIRCLE('',#102071,1.);
#33973=CIRCLE('',#102072,5.);
#33974=CIRCLE('',#102074,1.);
#33975=CIRCLE('',#102076,1.);
#33976=CIRCLE('',#102077,4.);
#33977=CIRCLE('',#102078,5.);
#33978=CIRCLE('',#102080,4.);
#33979=CIRCLE('',#102082,1.);
#33980=CIRCLE('',#102083,3.);
#33981=CIRCLE('',#102084,1.);
#33982=CIRCLE('',#102086,1.);
#33983=CIRCLE('',#102087,3.);
#33984=CIRCLE('',#102088,1.);
#33985=CIRCLE('',#102089,4.);
#33986=CIRCLE('',#102093,4.);
#33987=CIRCLE('',#102094,4.);
#33988=CIRCLE('',#102096,1.);
#33989=CIRCLE('',#102097,1.);
#33990=CIRCLE('',#102099,1.);
#33991=CIRCLE('',#102100,3.);
#33992=CIRCLE('',#102102,1.);
#33993=CIRCLE('',#102103,4.);
#33994=CIRCLE('',#102104,3.);
#33995=CIRCLE('',#102106,4.);
#33996=CIRCLE('',#102108,1.);
#33997=CIRCLE('',#102109,5.);
#33998=CIRCLE('',#102110,1.);
#33999=CIRCLE('',#102112,1.);
#34000=CIRCLE('',#102114,5.);
#34001=CIRCLE('',#102115,1.);
#34002=CIRCLE('',#102117,7.8);
#34003=CIRCLE('',#102118,7.8);
#34004=CIRCLE('',#102120,7.00000000000001);
#34005=CIRCLE('',#102122,7.00000000000001);
#34006=CIRCLE('',#102138,8.65629040278469);
#34007=CIRCLE('',#102139,20.3599346995449);
#34008=CIRCLE('',#102140,20.3599346995449);
#34009=CIRCLE('',#102142,8.8);
#34010=CIRCLE('',#102143,8.8);
#34011=CIRCLE('',#102144,0.25);
#34012=CIRCLE('',#102146,8.55);
#34013=CIRCLE('',#102147,0.25);
#34014=CIRCLE('',#102148,8.8);
#34015=CIRCLE('',#102149,8.8);
#34016=CIRCLE('',#102151,0.750000000000001);
#34017=CIRCLE('',#102152,0.750000000000001);
#34018=CIRCLE('',#102158,7.8);
#34019=CIRCLE('',#102160,7.8);
#34020=CIRCLE('',#102164,0.499999999999998);
#34021=CIRCLE('',#102166,0.5);
#34022=CIRCLE('',#102167,1.);
#34023=CIRCLE('',#102168,0.5);
#34024=CIRCLE('',#102170,0.5);
#34025=CIRCLE('',#102172,0.5);
#34026=CIRCLE('',#102173,1.);
#34027=CIRCLE('',#102174,0.5);
#34028=CIRCLE('',#102177,0.5);
#34029=CIRCLE('',#102178,0.5);
#34030=CIRCLE('',#102180,0.5);
#34031=CIRCLE('',#102181,1.);
#34032=CIRCLE('',#102182,0.5);
#34033=CIRCLE('',#102184,0.5);
#34034=CIRCLE('',#102186,0.499999999999998);
#34035=CIRCLE('',#102187,1.);
#34036=CIRCLE('',#102188,0.5);
#34037=CIRCLE('',#102191,0.5);
#34038=CIRCLE('',#102192,0.5);
#34039=CIRCLE('',#102194,0.5);
#34040=CIRCLE('',#102195,2.5);
#34041=CIRCLE('',#102196,3.);
#34042=CIRCLE('',#102198,0.5);
#34043=CIRCLE('',#102200,0.5);
#34044=CIRCLE('',#102201,0.5);
#34045=CIRCLE('',#102202,1.);
#34046=CIRCLE('',#102204,0.5);
#34047=CIRCLE('',#102206,0.5);
#34048=CIRCLE('',#102207,0.5);
#34049=CIRCLE('',#102208,1.);
#34050=CIRCLE('',#102210,0.5);
#34051=CIRCLE('',#102212,0.5);
#34052=CIRCLE('',#102213,2.5);
#34053=CIRCLE('',#102214,3.);
#34054=CIRCLE('',#102216,0.5);
#34055=CIRCLE('',#102218,0.5);
#34056=CIRCLE('',#102219,0.5);
#34057=CIRCLE('',#102221,0.5);
#34058=CIRCLE('',#102222,2.5);
#34059=CIRCLE('',#102223,3.);
#34060=CIRCLE('',#102225,0.5);
#34061=CIRCLE('',#102227,0.499999999999998);
#34062=CIRCLE('',#102228,0.5);
#34063=CIRCLE('',#102229,1.);
#34064=CIRCLE('',#102232,0.5);
#34065=CIRCLE('',#102233,0.5);
#34066=CIRCLE('',#102235,0.5);
#34067=CIRCLE('',#102236,2.5);
#34068=CIRCLE('',#102237,3.);
#34069=CIRCLE('',#102239,0.5);
#34070=CIRCLE('',#102241,0.500000000000003);
#34071=CIRCLE('',#102242,0.5);
#34072=CIRCLE('',#102243,1.);
#34073=CIRCLE('',#102245,0.5);
#34074=CIRCLE('',#102246,5.);
#34075=CIRCLE('',#102247,5.5);
#34076=CIRCLE('',#102249,0.5);
#34077=CIRCLE('',#102251,0.5);
#34078=CIRCLE('',#102252,0.5);
#34079=CIRCLE('',#102253,1.);
#34080=CIRCLE('',#102255,0.5);
#34081=CIRCLE('',#102257,0.5);
#34082=CIRCLE('',#102258,2.5);
#34083=CIRCLE('',#102259,3.);
#34084=CIRCLE('',#102261,0.5);
#34085=CIRCLE('',#102263,0.5);
#34086=CIRCLE('',#102264,0.5);
#34087=CIRCLE('',#102266,0.5);
#34088=CIRCLE('',#102267,2.5);
#34089=CIRCLE('',#102268,3.);
#34090=CIRCLE('',#102270,0.5);
#34091=CIRCLE('',#102272,0.499999999999998);
#34092=CIRCLE('',#102273,0.5);
#34093=CIRCLE('',#102274,0.999999999999998);
#34094=CIRCLE('',#102276,0.499999999999999);
#34095=CIRCLE('',#102277,58.5);
#34096=CIRCLE('',#102278,58.);
#34097=CIRCLE('',#102280,0.5);
#34098=CIRCLE('',#102281,0.5);
#34099=CIRCLE('',#102282,1.);
#34100=CIRCLE('',#102284,0.5);
#34101=CIRCLE('',#102286,0.5);
#34102=CIRCLE('',#102287,2.5);
#34103=CIRCLE('',#102288,3.);
#34104=CIRCLE('',#102290,0.5);
#34105=CIRCLE('',#102292,0.5);
#34106=CIRCLE('',#102293,0.5);
#34107=CIRCLE('',#102295,0.5);
#34108=CIRCLE('',#102296,2.5);
#34109=CIRCLE('',#102297,3.);
#34110=CIRCLE('',#102299,0.5);
#34111=CIRCLE('',#102301,0.500000000000002);
#34112=CIRCLE('',#102302,0.5);
#34113=CIRCLE('',#102303,1.);
#34114=CIRCLE('',#102305,0.500000000000001);
#34115=CIRCLE('',#102306,58.5);
#34116=CIRCLE('',#102307,58.);
#34117=CIRCLE('',#102309,0.5);
#34118=CIRCLE('',#102310,0.5);
#34119=CIRCLE('',#102311,1.);
#34120=CIRCLE('',#102313,0.5);
#34121=CIRCLE('',#102315,0.5);
#34122=CIRCLE('',#102316,2.5);
#34123=CIRCLE('',#102317,3.);
#34124=CIRCLE('',#102319,0.5);
#34125=CIRCLE('',#102321,0.5);
#34126=CIRCLE('',#102322,0.5);
#34127=CIRCLE('',#102324,0.5);
#34128=CIRCLE('',#102325,2.5);
#34129=CIRCLE('',#102326,3.);
#34130=CIRCLE('',#102328,0.5);
#34131=CIRCLE('',#102330,0.499999999999999);
#34132=CIRCLE('',#102331,0.5);
#34133=CIRCLE('',#102332,1.);
#34134=CIRCLE('',#102334,0.499999999999998);
#34135=CIRCLE('',#102335,58.5);
#34136=CIRCLE('',#102336,58.);
#34137=CIRCLE('',#102338,0.5);
#34138=CIRCLE('',#102339,0.5);
#34139=CIRCLE('',#102340,1.);
#34140=CIRCLE('',#102342,0.5);
#34141=CIRCLE('',#102344,0.5);
#34142=CIRCLE('',#102345,2.5);
#34143=CIRCLE('',#102346,3.);
#34144=CIRCLE('',#102348,0.5);
#34145=CIRCLE('',#102350,0.5);
#34146=CIRCLE('',#102351,0.5);
#34147=CIRCLE('',#102353,0.5);
#34148=CIRCLE('',#102354,2.5);
#34149=CIRCLE('',#102355,3.);
#34150=CIRCLE('',#102357,0.5);
#34151=CIRCLE('',#102359,0.499999999999997);
#34152=CIRCLE('',#102360,0.5);
#34153=CIRCLE('',#102361,1.);
#34154=CIRCLE('',#102363,0.500000000000002);
#34155=CIRCLE('',#102364,58.5);
#34156=CIRCLE('',#102365,58.);
#34157=CIRCLE('',#102367,0.5);
#34158=CIRCLE('',#102368,0.5);
#34159=CIRCLE('',#102369,0.999999999999999);
#34160=CIRCLE('',#102371,0.5);
#34161=CIRCLE('',#102373,0.5);
#34162=CIRCLE('',#102374,2.5);
#34163=CIRCLE('',#102375,3.);
#34164=CIRCLE('',#102377,0.5);
#34165=CIRCLE('',#102379,0.5);
#34166=CIRCLE('',#102380,0.5);
#34167=CIRCLE('',#102382,0.5);
#34168=CIRCLE('',#102383,2.5);
#34169=CIRCLE('',#102384,3.);
#34170=CIRCLE('',#102386,0.5);
#34171=CIRCLE('',#102388,0.500000000000002);
#34172=CIRCLE('',#102389,0.5);
#34173=CIRCLE('',#102390,1.);
#34174=CIRCLE('',#102392,0.499999999999997);
#34175=CIRCLE('',#102393,58.5);
#34176=CIRCLE('',#102394,58.);
#34177=CIRCLE('',#102396,0.5);
#34178=CIRCLE('',#102397,0.5);
#34179=CIRCLE('',#102398,1.);
#34180=CIRCLE('',#102400,0.5);
#34181=CIRCLE('',#102402,0.5);
#34182=CIRCLE('',#102403,2.5);
#34183=CIRCLE('',#102404,3.);
#34184=CIRCLE('',#102406,0.5);
#34185=CIRCLE('',#102408,0.5);
#34186=CIRCLE('',#102409,0.5);
#34187=CIRCLE('',#102411,0.5);
#34188=CIRCLE('',#102412,2.5);
#34189=CIRCLE('',#102413,3.);
#34190=CIRCLE('',#102415,0.5);
#34191=CIRCLE('',#102417,0.499999999999999);
#34192=CIRCLE('',#102418,0.5);
#34193=CIRCLE('',#102419,0.999999999999999);
#34194=CIRCLE('',#102421,0.499999999999999);
#34195=CIRCLE('',#102422,58.5);
#34196=CIRCLE('',#102423,58.);
#34197=CIRCLE('',#102425,0.5);
#34198=CIRCLE('',#102426,0.5);
#34199=CIRCLE('',#102427,1.);
#34200=CIRCLE('',#102429,0.5);
#34201=CIRCLE('',#102431,0.5);
#34202=CIRCLE('',#102432,2.5);
#34203=CIRCLE('',#102433,3.);
#34204=CIRCLE('',#102435,0.5);
#34205=CIRCLE('',#102437,0.5);
#34206=CIRCLE('',#102438,0.5);
#34207=CIRCLE('',#102440,0.5);
#34208=CIRCLE('',#102441,2.5);
#34209=CIRCLE('',#102442,3.);
#34210=CIRCLE('',#102444,0.5);
#34211=CIRCLE('',#102446,0.5);
#34212=CIRCLE('',#102447,0.5);
#34213=CIRCLE('',#102448,1.);
#34214=CIRCLE('',#102450,0.5);
#34215=CIRCLE('',#102452,0.500000000000003);
#34216=CIRCLE('',#102453,5.);
#34217=CIRCLE('',#102454,5.5);
#34218=CIRCLE('',#102456,0.5);
#34219=CIRCLE('',#102457,0.5);
#34220=CIRCLE('',#102458,0.999999999999999);
#34221=CIRCLE('',#102460,0.5);
#34222=CIRCLE('',#102462,0.5);
#34223=CIRCLE('',#102463,2.5);
#34224=CIRCLE('',#102464,3.);
#34225=CIRCLE('',#102466,0.5);
#34226=CIRCLE('',#102468,0.5);
#34227=CIRCLE('',#102469,0.5);
#34228=CIRCLE('',#102471,0.5);
#34229=CIRCLE('',#102472,2.5);
#34230=CIRCLE('',#102473,3.);
#34231=CIRCLE('',#102475,0.5);
#34232=CIRCLE('',#102477,0.5);
#34233=CIRCLE('',#102478,0.5);
#34234=CIRCLE('',#102479,1.);
#34235=CIRCLE('',#102481,0.5);
#34236=CIRCLE('',#102483,0.5);
#34237=CIRCLE('',#102484,0.5);
#34238=CIRCLE('',#102485,1.);
#34239=CIRCLE('',#102487,0.5);
#34240=CIRCLE('',#102489,0.5);
#34241=CIRCLE('',#102490,2.5);
#34242=CIRCLE('',#102491,3.);
#34243=CIRCLE('',#102493,0.5);
#34244=CIRCLE('',#102495,0.500000000000001);
#34245=CIRCLE('',#102497,0.5);
#34246=CIRCLE('',#102498,0.5);
#34247=CIRCLE('',#102499,1.);
#34248=CIRCLE('',#102501,0.5);
#34249=CIRCLE('',#102503,0.5);
#34250=CIRCLE('',#102504,2.5);
#34251=CIRCLE('',#102505,3.);
#34252=CIRCLE('',#102507,0.5);
#34253=CIRCLE('',#102509,0.5);
#34254=CIRCLE('',#102511,0.5);
#34255=CIRCLE('',#102513,0.5);
#34256=CIRCLE('',#102515,0.5);
#34257=CIRCLE('',#102517,0.5);
#34258=CIRCLE('',#102519,0.5);
#34259=CIRCLE('',#102521,0.5);
#34260=CIRCLE('',#102523,0.5);
#34261=CIRCLE('',#102525,0.5);
#34262=CIRCLE('',#102527,0.5);
#34263=CIRCLE('',#102529,0.5);
#34264=CIRCLE('',#102531,0.5);
#34265=CIRCLE('',#102533,0.5);
#34266=CIRCLE('',#102535,0.5);
#34267=CIRCLE('',#102537,0.5);
#34268=CIRCLE('',#102539,0.5);
#34269=CIRCLE('',#102541,0.5);
#34270=CIRCLE('',#102543,0.5);
#34271=CIRCLE('',#102545,0.5);
#34272=CIRCLE('',#102547,0.5);
#34273=CIRCLE('',#102549,0.5);
#34274=CIRCLE('',#102551,0.5);
#34275=CIRCLE('',#102553,0.5);
#34276=CIRCLE('',#102555,0.5);
#34277=CIRCLE('',#102557,0.5);
#34278=CIRCLE('',#102559,0.5);
#34279=CIRCLE('',#102561,77.1121191998622);
#34280=CIRCLE('',#102562,231.99961917989);
#34281=CIRCLE('',#102563,77.1121191998622);
#34282=CIRCLE('',#102566,231.99961917989);
#34283=CIRCLE('',#102583,58.5);
#34284=CIRCLE('',#102589,58.5);
#34285=CIRCLE('',#102595,58.5);
#34286=CIRCLE('',#102601,58.5);
#34287=CIRCLE('',#102608,5.);
#34288=CIRCLE('',#102611,5.);
#34289=CIRCLE('',#102614,58.5);
#34290=CIRCLE('',#102615,58.5);
#34291=CIRCLE('',#102616,77.1121191998622);
#34292=CIRCLE('',#102617,77.1121191998622);
#34293=CIRCLE('',#102646,5.);
#34294=CIRCLE('',#102647,5.);
#34295=CIRCLE('',#102648,5.);
#34296=CIRCLE('',#102649,5.);
#34297=CIRCLE('',#102650,5.);
#34298=CIRCLE('',#102651,5.);
#34299=CIRCLE('',#102659,5.);
#34300=CIRCLE('',#102660,5.);
#34301=CIRCLE('',#102661,5.);
#34302=CIRCLE('',#102662,5.);
#34303=CIRCLE('',#102663,5.);
#34304=CIRCLE('',#102664,5.);
#34305=CIRCLE('',#102678,5.);
#34306=CIRCLE('',#102679,5.);
#34307=CIRCLE('',#102680,5.);
#34308=CIRCLE('',#102681,5.);
#34309=CIRCLE('',#102682,5.);
#34310=CIRCLE('',#102683,5.);
#34311=CIRCLE('',#102691,5.);
#34312=CIRCLE('',#102692,5.);
#34313=CIRCLE('',#102693,5.);
#34314=CIRCLE('',#102694,5.);
#34315=CIRCLE('',#102695,5.);
#34316=CIRCLE('',#102696,5.);
#34317=CIRCLE('',#102717,1.73205080756888);
#34318=CIRCLE('',#102719,1.73205080756888);
#34319=CIRCLE('',#102721,1.73205080756888);
#34320=CIRCLE('',#102723,1.73205080756888);
#34321=CIRCLE('',#102725,1.73205080756888);
#34322=CIRCLE('',#102727,1.73205080756888);
#34323=CIRCLE('',#102729,3.);
#34324=CIRCLE('',#102730,0.25);
#34325=CIRCLE('',#102731,3.25);
#34326=CIRCLE('',#102732,3.25);
#34327=CIRCLE('',#102734,3.25);
#34328=CIRCLE('',#102742,0.75);
#34329=CIRCLE('',#102744,0.643324430555217);
#34330=CIRCLE('',#102745,0.750000000000001);
#34331=CIRCLE('',#102746,0.750000000000001);
#34332=CIRCLE('',#102748,0.750000000000001);
#34333=CIRCLE('',#102750,0.643324430555217);
#34334=CIRCLE('',#102751,0.749999999999999);
#34335=CIRCLE('',#102753,0.750000000000005);
#34336=CIRCLE('',#102754,0.750000000000001);
#34337=CIRCLE('',#102755,1.75);
#34338=CIRCLE('',#102757,0.750000000000001);
#34339=CIRCLE('',#102758,0.633028767237975);
#34340=CIRCLE('',#102760,493.060657452016);
#34341=CIRCLE('',#102762,0.750000000000007);
#34342=CIRCLE('',#102763,493.060657452016);
#34343=CIRCLE('',#102765,0.749999999999994);
#34344=CIRCLE('',#102766,0.633028767237989);
#34345=CIRCLE('',#102768,0.750000000000001);
#34346=CIRCLE('',#102769,1.75);
#34347=CIRCLE('',#102771,0.750000000000001);
#34348=CIRCLE('',#102772,1.75);
#34349=CIRCLE('',#102774,0.750000000000001);
#34350=CIRCLE('',#102775,1.75);
#34351=CIRCLE('',#102788,0.75);
#34352=CIRCLE('',#102791,0.750000000000001);
#34353=CIRCLE('',#102792,0.643324430555217);
#34354=CIRCLE('',#102793,0.750000000000001);
#34355=CIRCLE('',#102795,0.750000000000001);
#34356=CIRCLE('',#102797,0.749999999999999);
#34357=CIRCLE('',#102798,0.643324430555217);
#34358=CIRCLE('',#102800,0.750000000000001);
#34359=CIRCLE('',#102801,0.750000000000005);
#34360=CIRCLE('',#102802,1.75);
#34361=CIRCLE('',#102804,0.633028767237975);
#34362=CIRCLE('',#102805,0.750000000000001);
#34363=CIRCLE('',#102807,493.060657452016);
#34364=CIRCLE('',#102809,493.060657452016);
#34365=CIRCLE('',#102810,0.750000000000007);
#34366=CIRCLE('',#102812,0.633028767237989);
#34367=CIRCLE('',#102813,0.749999999999994);
#34368=CIRCLE('',#102815,0.750000000000001);
#34369=CIRCLE('',#102816,1.75);
#34370=CIRCLE('',#102818,1.75);
#34371=CIRCLE('',#102819,0.750000000000001);
#34372=CIRCLE('',#102821,0.750000000000001);
#34373=CIRCLE('',#102822,1.75);
#34374=CIRCLE('',#102834,0.750000000000001);
#34375=CIRCLE('',#102835,0.750000000000001);
#34376=CIRCLE('',#102837,0.750000000000001);
#34377=CIRCLE('',#102839,0.750000000000001);
#34378=CIRCLE('',#102840,7.00000000000001);
#34379=CIRCLE('',#102841,6.25000000000001);
#34380=CIRCLE('',#102844,0.750000000000001);
#34381=CIRCLE('',#102846,0.750000000000001);
#34382=CIRCLE('',#102847,6.25000000000001);
#34383=CIRCLE('',#102848,7.00000000000001);
#34384=CIRCLE('',#102851,7.00000000000001);
#34385=CIRCLE('',#102853,7.00000000000001);
#34386=CIRCLE('',#102855,7.00000000000001);
#34387=CIRCLE('',#102856,7.00000000000001);
#34388=CIRCLE('',#102858,0.750000000000001);
#34389=CIRCLE('',#102859,0.750000000000001);
#34390=CIRCLE('',#102862,0.750000000000001);
#34391=CIRCLE('',#102864,0.750000000000001);
#34392=CIRCLE('',#102865,6.25000000000001);
#34393=CIRCLE('',#102866,7.00000000000001);
#34394=CIRCLE('',#102869,0.750000000000001);
#34395=CIRCLE('',#102871,0.750000000000001);
#34396=CIRCLE('',#102872,7.00000000000001);
#34397=CIRCLE('',#102873,6.25000000000001);
#34398=CIRCLE('',#102881,2.);
#34399=CIRCLE('',#102901,2.);
#34400=CIRCLE('',#102939,1.66874528305244);
#34401=CIRCLE('',#102941,2.);
#34402=CIRCLE('',#102959,2.16001782903144);
#34403=CIRCLE('',#102979,1.66874528305248);
#34404=CIRCLE('',#102981,2.);
#34405=CIRCLE('',#103019,1.66874528305242);
#34406=CIRCLE('',#103039,1.66874528305242);
#34407=CIRCLE('',#103042,10.);
#34408=CIRCLE('',#103043,10.);
#34409=CIRCLE('',#103050,6.00000000000001);
#34410=CIRCLE('',#103051,6.00000000000001);
#34411=CIRCLE('',#103052,6.00000000000001);
#34412=CIRCLE('',#103053,6.);
#34413=CIRCLE('',#103054,55.3875000000282);
#34414=CIRCLE('',#103057,6.);
#34415=CIRCLE('',#103058,3.);
#34416=CIRCLE('',#103060,3.);
#34417=CIRCLE('',#103064,6.);
#34418=CIRCLE('',#103065,3.);
#34419=CIRCLE('',#103067,3.);
#34420=CIRCLE('',#103071,6.);
#34421=CIRCLE('',#103072,3.);
#34422=CIRCLE('',#103074,3.);
#34423=CIRCLE('',#103078,6.);
#34424=CIRCLE('',#103079,3.);
#34425=CIRCLE('',#103081,3.);
#34426=CIRCLE('',#103083,6.00000000000001);
#34427=CIRCLE('',#103084,6.00000000000001);
#34428=CIRCLE('',#103087,7.00000000000001);
#34429=CIRCLE('',#103088,7.00000000000001);
#34430=CIRCLE('',#103089,6.75);
#34431=CIRCLE('',#103091,5.89644660940673);
#34432=CIRCLE('',#103092,0.25);
#34433=CIRCLE('',#103093,6.07322330470337);
#34434=CIRCLE('',#103094,6.07322330470337);
#34435=CIRCLE('',#103096,6.92677669529664);
#34436=CIRCLE('',#103097,6.92677669529664);
#34437=CIRCLE('',#103098,0.25);
#34438=CIRCLE('',#103099,7.);
#34439=CIRCLE('',#103100,7.);
#34440=CIRCLE('',#103109,2.88675134594813);
#34441=CIRCLE('',#103111,2.88675134594813);
#34442=CIRCLE('',#103113,2.88675134594813);
#34443=CIRCLE('',#103115,2.88675134594813);
#34444=CIRCLE('',#103117,2.88675134594813);
#34445=CIRCLE('',#103119,2.88675134594813);
#34446=CIRCLE('',#103123,202.199982478859);
#34447=CIRCLE('',#103125,0.500000000000001);
#34448=CIRCLE('',#103126,0.499999999999999);
#34449=CIRCLE('',#103127,0.500000000000002);
#34450=CIRCLE('',#103130,0.499999999999998);
#34451=CIRCLE('',#103131,0.499999999999997);
#34452=CIRCLE('',#103132,0.999999999999999);
#34453=CIRCLE('',#103133,0.999999999999998);
#34454=CIRCLE('',#103134,0.999999999999999);
#34455=CIRCLE('',#103135,0.999999999999997);
#34456=CIRCLE('',#103136,1.);
#34457=CIRCLE('',#103139,0.999999999999997);
#34458=CIRCLE('',#103140,0.999999999999997);
#34459=CIRCLE('',#103141,0.999999999999997);
#34460=CIRCLE('',#103144,1.);
#34461=CIRCLE('',#103146,2.5626088159608);
#34462=CIRCLE('',#103147,1.);
#34463=CIRCLE('',#103148,1.);
#34464=CIRCLE('',#103149,7716.37708104352);
#34465=CIRCLE('',#103150,7759.01836682707);
#34466=CIRCLE('',#103152,1.);
#34467=CIRCLE('',#103153,0.999999999999999);
#34468=CIRCLE('',#103155,1.);
#34469=CIRCLE('',#103156,1.);
#34470=CIRCLE('',#103158,7824.7826781668);
#34471=CIRCLE('',#103159,7740.55951768335);
#34472=CIRCLE('',#103160,0.999999999999997);
#34473=CIRCLE('',#103162,0.999999999999999);
#34474=CIRCLE('',#103163,1.);
#34475=CIRCLE('',#103165,1.);
#34476=CIRCLE('',#103166,1.);
#34477=CIRCLE('',#103170,20.);
#34478=CIRCLE('',#103175,3.);
#34479=CIRCLE('',#103177,3.);
#34480=CIRCLE('',#103179,3.);
#34481=CIRCLE('',#103180,1.5);
#34482=CIRCLE('',#103181,1.5);
#34483=CIRCLE('',#103183,3.);
#34484=CIRCLE('',#103185,3.);
#34485=CIRCLE('',#103187,1.5);
#34486=CIRCLE('',#103188,1.5);
#34487=CIRCLE('',#103190,67.5);
#34488=CIRCLE('',#103191,67.5);
#34489=CIRCLE('',#103192,1.5);
#34490=CIRCLE('',#103193,1.5);
#34491=CIRCLE('',#103195,1.5);
#34492=CIRCLE('',#103196,1.5);
#34493=CIRCLE('',#103198,3.);
#34494=CIRCLE('',#103200,3.);
#34495=CIRCLE('',#103202,1.5);
#34496=CIRCLE('',#103203,1.5);
#34497=CIRCLE('',#103205,67.5);
#34498=CIRCLE('',#103206,67.5);
#34499=CIRCLE('',#103207,1.5);
#34500=CIRCLE('',#103208,1.5);
#34501=CIRCLE('',#103210,1.5);
#34502=CIRCLE('',#103211,1.5);
#34503=CIRCLE('',#103213,66.3628828433995);
#34504=CIRCLE('',#103215,66.3628828433995);
#34505=CIRCLE('',#103217,3.);
#34506=CIRCLE('',#103219,3.);
#34507=CIRCLE('',#103221,3.);
#34508=CIRCLE('',#103223,3.);
#34509=CIRCLE('',#103225,58.3875000000282);
#34510=CIRCLE('',#103226,58.3875000000282);
#34511=CIRCLE('',#103227,1.5);
#34512=CIRCLE('',#103228,1.5);
#34513=CIRCLE('',#103230,3.);
#34514=CIRCLE('',#103232,3.);
#34515=CIRCLE('',#103234,1.5);
#34516=CIRCLE('',#103235,1.5);
#34517=CIRCLE('',#103237,67.5);
#34518=CIRCLE('',#103238,67.5);
#34519=CIRCLE('',#103239,1.5);
#34520=CIRCLE('',#103240,1.5);
#34521=CIRCLE('',#103242,1.5);
#34522=CIRCLE('',#103243,1.5);
#34523=CIRCLE('',#103245,58.3875000000282);
#34524=CIRCLE('',#103246,58.3875000000282);
#34525=CIRCLE('',#103247,1.5);
#34526=CIRCLE('',#103248,1.5);
#34527=CIRCLE('',#103250,3.);
#34528=CIRCLE('',#103252,3.);
#34529=CIRCLE('',#103254,1.5);
#34530=CIRCLE('',#103255,1.5);
#34531=CIRCLE('',#103257,67.5);
#34532=CIRCLE('',#103258,67.5);
#34533=CIRCLE('',#103259,1.5);
#34534=CIRCLE('',#103260,1.5);
#34535=CIRCLE('',#103262,1.5);
#34536=CIRCLE('',#103263,1.5);
#34537=CIRCLE('',#103265,58.3875000000282);
#34538=CIRCLE('',#103266,58.3875000000282);
#34539=CIRCLE('',#103268,57.2503828434276);
#34540=CIRCLE('',#103270,54.6455781044285);
#34541=CIRCLE('',#103271,53.8875000000282);
#34542=CIRCLE('',#103273,53.8875000000282);
#34543=CIRCLE('',#103275,57.2503828434277);
#34544=CIRCLE('',#103277,57.2503828434277);
#34545=CIRCLE('',#103279,66.3628828433995);
#34546=CIRCLE('',#103281,66.3628828433995);
#34547=CIRCLE('',#103283,3.);
#34548=CIRCLE('',#103285,58.3875000000282);
#34549=CIRCLE('',#103286,58.3875000000282);
#34550=CIRCLE('',#103288,57.2503828434277);
#34551=CIRCLE('',#103290,2.12684354297908);
#34552=CIRCLE('',#103291,2.13919470072314);
#34553=CIRCLE('',#103298,2.16007343674245);
#34554=CIRCLE('',#103302,2.13474728493424);
#34555=CIRCLE('',#103303,2.14445192257171);
#34556=CIRCLE('',#103313,10.);
#34557=CIRCLE('',#103314,10.);
#34558=CIRCLE('',#103315,10.);
#34559=CIRCLE('',#103317,10.);
#34560=CIRCLE('',#103319,10.);
#34561=CIRCLE('',#103320,10.);
#34562=CIRCLE('',#103322,10.);
#34563=CIRCLE('',#103324,10.);
#34564=CIRCLE('',#103326,10.);
#34565=CIRCLE('',#103342,32.976);
#34566=CIRCLE('',#103343,0.576);
#34567=CIRCLE('',#103344,32.4);
#34568=CIRCLE('',#103346,32.4);
#34569=CIRCLE('',#103349,5.77396800000001);
#34570=CIRCLE('',#103350,5.77396800000001);
#34571=CIRCLE('',#103352,5.773968);
#34572=CIRCLE('',#103353,5.77396800000001);
#34573=CIRCLE('',#103355,5.773968);
#34574=CIRCLE('',#103356,5.773968);
#34575=CIRCLE('',#103358,5.773968);
#34576=CIRCLE('',#103359,5.77396800000001);
#34577=CIRCLE('',#103361,5.773968);
#34578=CIRCLE('',#103362,5.77396800000001);
#34579=CIRCLE('',#103364,5.77396800000001);
#34580=CIRCLE('',#103365,5.77396800000001);
#34581=CIRCLE('',#103368,15.12);
#34582=CIRCLE('',#103369,15.12);
#34583=CIRCLE('',#103371,5.77396800000001);
#34584=CIRCLE('',#103372,40.6764810164406);
#34585=CIRCLE('',#103373,5.773968);
#34586=CIRCLE('',#103374,40.6764810164406);
#34587=CIRCLE('',#103375,5.773968);
#34588=CIRCLE('',#103376,40.6764810164406);
#34589=CIRCLE('',#103377,5.773968);
#34590=CIRCLE('',#103378,40.6764810164406);
#34591=CIRCLE('',#103379,5.77396800000001);
#34592=CIRCLE('',#103380,40.6764810164406);
#34593=CIRCLE('',#103381,40.6764810164406);
#34594=CIRCLE('',#103382,40.6764810164406);
#34595=CIRCLE('',#103383,40.6764810164406);
#34596=CIRCLE('',#103384,40.6764810164406);
#34597=CIRCLE('',#103385,40.6764810164406);
#34598=CIRCLE('',#103386,40.6764810164406);
#34599=CIRCLE('',#103387,5.77396800000001);
#34600=CIRCLE('',#103388,40.6764810164406);
#34601=CIRCLE('',#103389,5.773968);
#34602=CIRCLE('',#103390,40.6764810164406);
#34603=CIRCLE('',#103391,5.77396800000001);
#34604=CIRCLE('',#103392,40.6764810164406);
#34605=CIRCLE('',#103393,5.773968);
#34606=CIRCLE('',#103394,40.6764810164406);
#34607=CIRCLE('',#103397,49.6934108978581);
#34608=CIRCLE('',#103399,49.6934108978581);
#34609=CIRCLE('',#103401,49.6934108978581);
#34610=CIRCLE('',#103403,49.6934108978581);
#34611=CIRCLE('',#103405,49.6934108978581);
#34612=CIRCLE('',#103407,49.6934108978581);
#34613=CIRCLE('',#103409,49.6934108978581);
#34614=CIRCLE('',#103411,49.6934108978581);
#34615=CIRCLE('',#103413,49.6934108978581);
#34616=CIRCLE('',#103415,49.6934108978581);
#34617=CIRCLE('',#103417,49.6934108978581);
#34618=CIRCLE('',#103419,49.6934108978581);
#34619=CIRCLE('',#103421,49.6934108978581);
#34620=CIRCLE('',#103423,49.6934108978581);
#34621=CIRCLE('',#103425,49.6934108978581);
#34622=CIRCLE('',#103427,49.6934108978581);
#34623=CIRCLE('',#103429,49.6934108978581);
#34624=CIRCLE('',#103431,49.6934108978581);
#34625=CIRCLE('',#103433,49.6934108978581);
#34626=CIRCLE('',#103435,49.6934108978581);
#34627=CIRCLE('',#103437,49.6934108978581);
#34628=CIRCLE('',#103439,49.6934108978581);
#34629=CIRCLE('',#103441,49.6934108978581);
#34630=CIRCLE('',#103443,49.6934108978581);
#34631=CIRCLE('',#103445,49.6934108978581);
#34632=CIRCLE('',#103447,49.6934108978581);
#34633=CIRCLE('',#103449,49.6934108978581);
#34634=CIRCLE('',#103451,49.6934108978581);
#34635=CIRCLE('',#103453,40.6764810164406);
#34636=CIRCLE('',#103455,40.6764810164406);
#34637=CIRCLE('',#103457,40.6764810164406);
#34638=CIRCLE('',#103459,40.6764810164406);
#34639=CIRCLE('',#103461,40.6764810164406);
#34640=CIRCLE('',#103463,40.6764810164406);
#34641=CIRCLE('',#103465,40.6764810164406);
#34642=CIRCLE('',#103467,40.6764810164406);
#34643=CIRCLE('',#103469,40.6764810164406);
#34644=CIRCLE('',#103471,40.6764810164406);
#34645=CIRCLE('',#103473,40.6764810164406);
#34646=CIRCLE('',#103475,40.6764810164406);
#34647=CIRCLE('',#103477,40.6764810164406);
#34648=CIRCLE('',#103479,40.6764810164406);
#34649=CIRCLE('',#103481,49.6934108978581);
#34650=CIRCLE('',#103483,49.6934108978581);
#34651=CIRCLE('',#103485,40.6764810164406);
#34652=CIRCLE('',#103487,5.77396800000001);
#34653=CIRCLE('',#103488,5.77396800000001);
#34654=CIRCLE('',#103489,5.77396800000001);
#34655=CIRCLE('',#103490,5.77396800000001);
#34656=CIRCLE('',#103491,5.773968);
#34657=CIRCLE('',#103492,5.77396800000001);
#34658=CIRCLE('',#103493,5.773968);
#34659=CIRCLE('',#103494,5.77396800000001);
#34660=CIRCLE('',#103495,5.77396800000001);
#34661=CIRCLE('',#103537,10.12);
#34662=CIRCLE('',#103538,10.12);
#34663=CIRCLE('',#103540,15.12);
#34664=CIRCLE('',#103541,15.12);
#34665=CIRCLE('',#103549,25.536);
#34666=CIRCLE('',#103550,0.336);
#34667=CIRCLE('',#103551,25.2);
#34668=CIRCLE('',#103553,25.2);
#34669=CIRCLE('',#103557,3.36814799999999);
#34670=CIRCLE('',#103558,3.36814799999999);
#34671=CIRCLE('',#103560,3.368148);
#34672=CIRCLE('',#103561,3.36814799999999);
#34673=CIRCLE('',#103563,3.36814799999999);
#34674=CIRCLE('',#103564,3.36814799999999);
#34675=CIRCLE('',#103566,3.36814799999999);
#34676=CIRCLE('',#103567,3.36814799999999);
#34677=CIRCLE('',#103569,3.36814799999999);
#34678=CIRCLE('',#103570,3.36814799999999);
#34679=CIRCLE('',#103572,3.36814799999999);
#34680=CIRCLE('',#103573,3.368148);
#34681=CIRCLE('',#103575,3.36814799999999);
#34682=CIRCLE('',#103576,3.36814799999999);
#34683=CIRCLE('',#103578,3.36814799999999);
#34684=CIRCLE('',#103579,3.36814799999999);
#34685=CIRCLE('',#103581,3.368148);
#34686=CIRCLE('',#103582,3.36814799999999);
#34687=CIRCLE('',#103584,3.36814799999999);
#34688=CIRCLE('',#103585,3.36814799999999);
#34689=CIRCLE('',#103587,3.36814799999999);
#34690=CIRCLE('',#103588,3.36814799999999);
#34691=CIRCLE('',#103590,3.368148);
#34692=CIRCLE('',#103591,3.36814799999999);
#34693=CIRCLE('',#103593,54.361863151615);
#34694=CIRCLE('',#103594,49.1019873874548);
#34695=CIRCLE('',#103596,54.361863151615);
#34696=CIRCLE('',#103598,49.1019873874548);
#34697=CIRCLE('',#103600,8.82);
#34698=CIRCLE('',#103601,8.82);
#34699=CIRCLE('',#103603,3.368148);
#34700=CIRCLE('',#103604,49.1019873874548);
#34701=CIRCLE('',#103605,3.368148);
#34702=CIRCLE('',#103606,49.1019873874548);
#34703=CIRCLE('',#103607,3.36814799999999);
#34704=CIRCLE('',#103608,49.1019873874548);
#34705=CIRCLE('',#103609,3.368148);
#34706=CIRCLE('',#103610,49.1019873874548);
#34707=CIRCLE('',#103611,3.368148);
#34708=CIRCLE('',#103612,49.1019873874548);
#34709=CIRCLE('',#103613,3.36814799999999);
#34710=CIRCLE('',#103614,49.1019873874548);
#34711=CIRCLE('',#103615,3.36814799999999);
#34712=CIRCLE('',#103616,49.1019873874548);
#34713=CIRCLE('',#103617,3.36814799999999);
#34714=CIRCLE('',#103618,49.1019873874548);
#34715=CIRCLE('',#103619,3.36814799999999);
#34716=CIRCLE('',#103620,49.1019873874548);
#34717=CIRCLE('',#103621,49.1019873874548);
#34718=CIRCLE('',#103622,49.1019873874548);
#34719=CIRCLE('',#103623,49.1019873874548);
#34720=CIRCLE('',#103624,49.1019873874548);
#34721=CIRCLE('',#103625,49.1019873874548);
#34722=CIRCLE('',#103626,49.1019873874548);
#34723=CIRCLE('',#103627,49.1019873874548);
#34724=CIRCLE('',#103628,49.1019873874548);
#34725=CIRCLE('',#103629,49.1019873874548);
#34726=CIRCLE('',#103630,49.1019873874548);
#34727=CIRCLE('',#103631,49.1019873874548);
#34728=CIRCLE('',#103632,49.1019873874548);
#34729=CIRCLE('',#103633,3.36814799999999);
#34730=CIRCLE('',#103634,49.1019873874548);
#34731=CIRCLE('',#103635,3.36814799999999);
#34732=CIRCLE('',#103636,49.1019873874548);
#34733=CIRCLE('',#103637,3.36814799999999);
#34734=CIRCLE('',#103638,49.1019873874548);
#34735=CIRCLE('',#103639,3.36814799999999);
#34736=CIRCLE('',#103640,49.1019873874548);
#34737=CIRCLE('',#103641,3.36814799999999);
#34738=CIRCLE('',#103642,49.1019873874548);
#34739=CIRCLE('',#103643,3.36814799999999);
#34740=CIRCLE('',#103644,49.1019873874548);
#34741=CIRCLE('',#103645,3.368148);
#34742=CIRCLE('',#103646,49.1019873874548);
#34743=CIRCLE('',#103647,3.36814799999999);
#34744=CIRCLE('',#103648,49.1019873874548);
#34745=CIRCLE('',#103649,3.368148);
#34746=CIRCLE('',#103652,54.361863151615);
#34747=CIRCLE('',#103654,54.361863151615);
#34748=CIRCLE('',#103656,54.361863151615);
#34749=CIRCLE('',#103658,54.361863151615);
#34750=CIRCLE('',#103660,54.361863151615);
#34751=CIRCLE('',#103662,54.361863151615);
#34752=CIRCLE('',#103664,54.361863151615);
#34753=CIRCLE('',#103666,54.361863151615);
#34754=CIRCLE('',#103668,54.361863151615);
#34755=CIRCLE('',#103670,54.361863151615);
#34756=CIRCLE('',#103672,54.361863151615);
#34757=CIRCLE('',#103674,54.361863151615);
#34758=CIRCLE('',#103676,54.361863151615);
#34759=CIRCLE('',#103678,54.361863151615);
#34760=CIRCLE('',#103680,54.361863151615);
#34761=CIRCLE('',#103682,54.361863151615);
#34762=CIRCLE('',#103684,54.361863151615);
#34763=CIRCLE('',#103686,54.361863151615);
#34764=CIRCLE('',#103688,54.361863151615);
#34765=CIRCLE('',#103690,54.361863151615);
#34766=CIRCLE('',#103692,54.361863151615);
#34767=CIRCLE('',#103694,54.361863151615);
#34768=CIRCLE('',#103696,54.361863151615);
#34769=CIRCLE('',#103698,54.361863151615);
#34770=CIRCLE('',#103700,54.361863151615);
#34771=CIRCLE('',#103702,54.361863151615);
#34772=CIRCLE('',#103704,54.361863151615);
#34773=CIRCLE('',#103706,54.361863151615);
#34774=CIRCLE('',#103708,54.361863151615);
#34775=CIRCLE('',#103710,54.361863151615);
#34776=CIRCLE('',#103712,54.361863151615);
#34777=CIRCLE('',#103714,54.361863151615);
#34778=CIRCLE('',#103716,54.361863151615);
#34779=CIRCLE('',#103718,54.361863151615);
#34780=CIRCLE('',#103720,54.361863151615);
#34781=CIRCLE('',#103722,54.361863151615);
#34782=CIRCLE('',#103724,54.361863151615);
#34783=CIRCLE('',#103726,54.361863151615);
#34784=CIRCLE('',#103728,54.361863151615);
#34785=CIRCLE('',#103730,54.361863151615);
#34786=CIRCLE('',#103732,54.361863151615);
#34787=CIRCLE('',#103734,54.361863151615);
#34788=CIRCLE('',#103736,54.361863151615);
#34789=CIRCLE('',#103738,54.361863151615);
#34790=CIRCLE('',#103740,54.361863151615);
#34791=CIRCLE('',#103742,54.361863151615);
#34792=CIRCLE('',#103744,54.361863151615);
#34793=CIRCLE('',#103746,54.361863151615);
#34794=CIRCLE('',#103748,54.361863151615);
#34795=CIRCLE('',#103750,54.361863151615);
#34796=CIRCLE('',#103752,54.361863151615);
#34797=CIRCLE('',#103754,54.361863151615);
#34798=CIRCLE('',#103756,54.361863151615);
#34799=CIRCLE('',#103758,54.361863151615);
#34800=CIRCLE('',#103760,54.361863151615);
#34801=CIRCLE('',#103762,54.361863151615);
#34802=CIRCLE('',#103764,49.1019873874548);
#34803=CIRCLE('',#103766,49.1019873874548);
#34804=CIRCLE('',#103768,49.1019873874548);
#34805=CIRCLE('',#103770,49.1019873874548);
#34806=CIRCLE('',#103772,49.1019873874548);
#34807=CIRCLE('',#103774,49.1019873874548);
#34808=CIRCLE('',#103776,49.1019873874548);
#34809=CIRCLE('',#103778,49.1019873874548);
#34810=CIRCLE('',#103780,49.1019873874548);
#34811=CIRCLE('',#103782,49.1019873874548);
#34812=CIRCLE('',#103784,49.1019873874548);
#34813=CIRCLE('',#103786,49.1019873874548);
#34814=CIRCLE('',#103788,49.1019873874548);
#34815=CIRCLE('',#103790,49.1019873874548);
#34816=CIRCLE('',#103792,49.1019873874548);
#34817=CIRCLE('',#103794,49.1019873874548);
#34818=CIRCLE('',#103796,49.1019873874548);
#34819=CIRCLE('',#103798,49.1019873874548);
#34820=CIRCLE('',#103800,49.1019873874548);
#34821=CIRCLE('',#103802,49.1019873874548);
#34822=CIRCLE('',#103804,49.1019873874548);
#34823=CIRCLE('',#103806,49.1019873874548);
#34824=CIRCLE('',#103808,49.1019873874548);
#34825=CIRCLE('',#103810,49.1019873874548);
#34826=CIRCLE('',#103812,49.1019873874548);
#34827=CIRCLE('',#103814,49.1019873874548);
#34828=CIRCLE('',#103816,49.1019873874548);
#34829=CIRCLE('',#103818,49.1019873874548);
#34830=CIRCLE('',#103820,54.361863151615);
#34831=CIRCLE('',#103822,54.361863151615);
#34832=CIRCLE('',#103824,49.1019873874548);
#34833=CIRCLE('',#103826,3.36814799999999);
#34834=CIRCLE('',#103827,3.36814799999999);
#34835=CIRCLE('',#103828,3.36814799999999);
#34836=CIRCLE('',#103829,3.36814799999999);
#34837=CIRCLE('',#103830,3.36814799999999);
#34838=CIRCLE('',#103831,3.36814799999999);
#34839=CIRCLE('',#103832,3.36814799999999);
#34840=CIRCLE('',#103833,3.36814799999999);
#34841=CIRCLE('',#103834,3.36814799999999);
#34842=CIRCLE('',#103835,3.36814799999999);
#34843=CIRCLE('',#103836,3.36814799999999);
#34844=CIRCLE('',#103837,3.36814799999999);
#34845=CIRCLE('',#103838,3.36814799999999);
#34846=CIRCLE('',#103839,3.36814799999999);
#34847=CIRCLE('',#103840,3.36814799999999);
#34848=CIRCLE('',#103841,3.36814799999999);
#34849=CIRCLE('',#103842,3.36814799999999);
#34850=CIRCLE('',#103843,3.36814799999999);
#34851=CIRCLE('',#103925,3.95);
#34852=CIRCLE('',#103926,3.95);
#34853=CIRCLE('',#103928,10.5);
#34854=CIRCLE('',#103929,10.5);
#34855=CIRCLE('',#103931,3.95);
#34856=CIRCLE('',#103932,3.95);
#34857=CIRCLE('',#103934,10.5);
#34858=CIRCLE('',#103935,10.5);
#34859=CIRCLE('',#103937,10.5);
#34860=CIRCLE('',#103938,10.5);
#34861=CIRCLE('',#103940,10.5);
#34862=CIRCLE('',#103941,10.5);
#34863=CIRCLE('',#103945,3.95);
#34864=CIRCLE('',#103946,3.95);
#34865=CIRCLE('',#103948,3.95);
#34866=CIRCLE('',#103949,3.95);
#34867=CIRCLE('',#103951,10.5);
#34868=CIRCLE('',#103952,10.5);
#34869=CIRCLE('',#103954,10.5);
#34870=CIRCLE('',#103955,10.5);
#34871=CIRCLE('',#103956,10.5);
#34872=CIRCLE('',#103958,10.5);
#34873=CIRCLE('',#103959,10.5);
#34874=CIRCLE('',#103960,10.5);
#34875=CIRCLE('',#103965,3.95);
#34876=CIRCLE('',#103966,3.95);
#34877=CIRCLE('',#103970,3.95);
#34878=CIRCLE('',#103971,3.95);
#34879=CIRCLE('',#104114,36.25);
#34880=CIRCLE('',#104115,36.25);
#34881=CIRCLE('',#104117,36.25);
#34882=CIRCLE('',#104118,36.25);
#34883=CIRCLE('',#104120,45.);
#34884=CIRCLE('',#104121,45.);
#34885=CIRCLE('',#104123,30.);
#34886=CIRCLE('',#104124,30.);
#34887=CIRCLE('',#104131,16.0425342723895);
#34888=CIRCLE('',#104132,1.);
#34889=CIRCLE('',#104133,15.0434011963687);
#34890=CIRCLE('',#104135,23.4);
#34891=CIRCLE('',#104136,5.238);
#34892=CIRCLE('',#104137,23.4);
#34893=CIRCLE('',#104139,23.4);
#34894=CIRCLE('',#104140,5.238);
#34895=CIRCLE('',#104141,23.4);
#34896=CIRCLE('',#104143,16.0850661013937);
#34897=CIRCLE('',#104145,1.);
#34898=CIRCLE('',#104146,17.0841991774145);
#34899=CIRCLE('',#104148,22.4);
#34900=CIRCLE('',#104149,1.);
#34901=CIRCLE('',#104150,23.4);
#34902=CIRCLE('',#104154,23.4);
#34903=CIRCLE('',#104156,1.);
#34904=CIRCLE('',#104157,22.4);
#34905=CIRCLE('',#104161,32.6421664440783);
#34906=CIRCLE('',#104162,29.7197077738478);
#34907=CIRCLE('',#104163,29.7197077738479);
#34908=CIRCLE('',#104165,35.);
#34909=CIRCLE('',#104166,1.);
#34910=CIRCLE('',#104167,36.);
#34911=CIRCLE('',#104169,36.);
#34912=CIRCLE('',#104171,1.);
#34913=CIRCLE('',#104172,35.);
#34914=CIRCLE('',#104176,5.238);
#34915=CIRCLE('',#104178,5.238);
#34916=CIRCLE('',#104180,5.238);
#34917=CIRCLE('',#104182,5.238);
#34918=CIRCLE('',#104184,5.238);
#34919=CIRCLE('',#104186,5.238);
#34920=CIRCLE('',#104188,5.238);
#34921=CIRCLE('',#104190,5.238);
#34922=CIRCLE('',#104192,5.238);
#34923=CIRCLE('',#104194,5.238);
#34924=CIRCLE('',#104196,5.238);
#34925=CIRCLE('',#104198,5.238);
#34926=CIRCLE('',#104200,5.238);
#34927=CIRCLE('',#104202,5.238);
#34928=CIRCLE('',#104204,5.238);
#34929=CIRCLE('',#104206,5.238);
#34930=CIRCLE('',#104208,5.238);
#34931=CIRCLE('',#104210,5.238);
#34932=CIRCLE('',#104212,5.238);
#34933=CIRCLE('',#104214,5.238);
#34934=CIRCLE('',#104216,5.238);
#34935=CIRCLE('',#104218,5.238);
#34936=CIRCLE('',#104220,5.238);
#34937=CIRCLE('',#104222,5.238);
#34938=CIRCLE('',#104225,7.25);
#34939=CIRCLE('',#104226,7.25);
#34940=CIRCLE('',#104228,16.);
#34941=CIRCLE('',#104229,16.);
#34942=CIRCLE('',#104231,7.25);
#34943=CIRCLE('',#104232,7.25);
#34944=CIRCLE('',#104234,16.);
#34945=CIRCLE('',#104235,16.);
#34946=CIRCLE('',#104250,10.0514428414941);
#34947=CIRCLE('',#104252,10.0514428414941);
#34948=CIRCLE('',#104256,10.0514428414944);
#34949=CIRCLE('',#104260,12.);
#34950=CIRCLE('',#104262,12.);
#34951=CIRCLE('',#104267,12.);
#34952=CIRCLE('',#104270,13.05);
#34953=CIRCLE('',#104272,13.05);
#34954=CIRCLE('',#104274,18.);
#34955=CIRCLE('',#104275,18.);
#34956=CIRCLE('',#104276,18.);
#34957=CIRCLE('',#104277,18.);
#34958=CIRCLE('',#104278,18.);
#34959=CIRCLE('',#104279,18.);
#34960=CIRCLE('',#104287,18.);
#34961=CIRCLE('',#104288,18.);
#34962=CIRCLE('',#104289,18.);
#34963=CIRCLE('',#104290,18.);
#34964=CIRCLE('',#104291,18.);
#34965=CIRCLE('',#104292,18.);
#34966=CIRCLE('',#104307,10.0514428414941);
#34967=CIRCLE('',#104313,10.0514428414941);
#34968=CIRCLE('',#104315,12.);
#34969=CIRCLE('',#104322,12.);
#34970=CIRCLE('',#104325,44.1739130434783);
#34971=CIRCLE('',#104327,22.0315642065426);
#34972=CIRCLE('',#104328,20.8911550302128);
#34973=CIRCLE('',#104329,20.8911550302128);
#34974=CIRCLE('',#104330,20.8911550302128);
#34975=CIRCLE('',#104331,20.8911550302128);
#34976=CIRCLE('',#104332,20.8911550302128);
#34977=CIRCLE('',#104333,20.8911550302128);
#34978=CIRCLE('',#104335,12.9453125);
#34979=CIRCLE('',#104337,12.525);
#34980=CIRCLE('',#104349,10.0514428414939);
#34981=CIRCLE('',#104351,13.05);
#34982=CIRCLE('',#104352,12.);
#34983=CIRCLE('',#104354,12.);
#34984=CIRCLE('',#104356,10.0514428414941);
#34985=CIRCLE('',#104359,10.0514428414941);
#34986=CIRCLE('',#104380,10.0514428414941);
#34987=CIRCLE('',#104394,12.);
#34988=CIRCLE('',#104408,12.);
#34989=CIRCLE('',#104428,12.);
#34990=CIRCLE('',#104430,13.05);
#34991=CIRCLE('',#104431,10.0514428414942);
#34992=CIRCLE('',#104433,10.0514428414949);
#34993=CIRCLE('',#104434,9.90000000000002);
#34994=CIRCLE('',#104436,12.);
#34995=CIRCLE('',#104441,18.);
#34996=CIRCLE('',#104442,18.);
#34997=CIRCLE('',#104443,18.);
#34998=CIRCLE('',#104444,18.);
#34999=CIRCLE('',#104445,18.);
#35000=CIRCLE('',#104446,18.);
#35001=CIRCLE('',#104458,18.);
#35002=CIRCLE('',#104459,18.);
#35003=CIRCLE('',#104460,18.);
#35004=CIRCLE('',#104461,18.);
#35005=CIRCLE('',#104462,18.);
#35006=CIRCLE('',#104463,18.);
#35007=CIRCLE('',#104479,1.190625);
#35008=CIRCLE('',#104480,1.190625);
#35009=CIRCLE('',#104482,1.190625);
#35010=CIRCLE('',#104483,1.190625);
#35011=CIRCLE('',#104485,1.190625);
#35012=CIRCLE('',#104486,1.190625);
#35013=CIRCLE('',#104488,1.19062499999999);
#35014=CIRCLE('',#104489,1.19062499999999);
#35015=CIRCLE('',#104491,1.190625);
#35016=CIRCLE('',#104492,1.190625);
#35017=CIRCLE('',#104494,1.190625);
#35018=CIRCLE('',#104495,1.190625);
#35019=CIRCLE('',#104497,1.190625);
#35020=CIRCLE('',#104498,1.190625);
#35021=CIRCLE('',#104500,1.190625);
#35022=CIRCLE('',#104501,1.190625);
#35023=CIRCLE('',#104503,1.190625);
#35024=CIRCLE('',#104504,1.190625);
#35025=CIRCLE('',#104506,55.2538194444444);
#35026=CIRCLE('',#104507,55.2538194444444);
#35027=CIRCLE('',#104509,44.5707880434783);
#35028=CIRCLE('',#104510,44.5707880434783);
#35029=CIRCLE('',#104512,22.4667164334275);
#35030=CIRCLE('',#104513,16.8332621659243);
#35031=CIRCLE('',#104515,44.5707880434783);
#35032=CIRCLE('',#104516,0.396875);
#35033=CIRCLE('',#104517,44.9676630434783);
#35034=CIRCLE('',#104519,17.2301371659243);
#35035=CIRCLE('',#104520,0.396875);
#35036=CIRCLE('',#104521,16.8332621659243);
#35037=CIRCLE('',#104522,16.8332621659243);
#35038=CIRCLE('',#104525,43.9357880434783);
#35039=CIRCLE('',#104526,0.635000000000001);
#35040=CIRCLE('',#104527,44.5707880434783);
#35041=CIRCLE('',#104564,6.00000000000001);
#35042=CIRCLE('',#104565,6.00000000000001);
#35043=CIRCLE('',#104567,6.00000000000001);
#35044=CIRCLE('',#104568,6.00000000000001);
#35045=CIRCLE('',#104570,5.99999999999999);
#35046=CIRCLE('',#104571,6.00000000000001);
#35047=CIRCLE('',#104573,5.99999999999999);
#35048=CIRCLE('',#104574,6.00000000000001);
#35049=CIRCLE('',#104576,5.99999999999999);
#35050=CIRCLE('',#104577,6.00000000000001);
#35051=CIRCLE('',#104579,6.00000000000001);
#35052=CIRCLE('',#104580,6.00000000000001);
#35053=CIRCLE('',#104582,6.00000000000001);
#35054=CIRCLE('',#104583,6.00000000000001);
#35055=CIRCLE('',#104585,6.00000000000001);
#35056=CIRCLE('',#104586,6.00000000000001);
#35057=CIRCLE('',#104599,7.00000000000001);
#35058=CIRCLE('',#104600,7.00000000000001);
#35059=CIRCLE('',#104602,7.);
#35060=CIRCLE('',#104603,7.);
#35061=CIRCLE('',#104613,6.4732);
#35062=CIRCLE('',#104614,0.736599999999997);
#35063=CIRCLE('',#104617,6.4732);
#35064=CIRCLE('',#104618,0.736599999999997);
#35065=CIRCLE('',#104620,6.4732);
#35066=CIRCLE('',#104621,0.736599999999997);
#35067=CIRCLE('',#104623,6.4732);
#35068=CIRCLE('',#104624,0.736599999999997);
#35069=CIRCLE('',#104639,4.86334165753398);
#35070=CIRCLE('',#104640,4.86334165753398);
#35071=CIRCLE('',#104642,6.);
#35072=CIRCLE('',#104644,6.);
#35073=CIRCLE('',#104661,6.);
#35074=CIRCLE('',#104662,6.);
#35075=CIRCLE('',#104663,6.);
#35076=CIRCLE('',#104681,4.86334165753294);
#35077=CIRCLE('',#104683,4.6875);
#35078=CIRCLE('',#104685,4.86334165753294);
#35079=CIRCLE('',#104699,9.5);
#35080=CIRCLE('',#104700,9.5);
#35081=CIRCLE('',#104701,9.5);
#35082=CIRCLE('',#104702,9.5);
#35083=CIRCLE('',#104703,9.5);
#35084=CIRCLE('',#104704,9.5);
#35085=CIRCLE('',#104722,4.86334165753295);
#35086=CIRCLE('',#104724,6.);
#35087=CIRCLE('',#104729,6.);
#35088=CIRCLE('',#104730,6.);
#35089=CIRCLE('',#104735,4.86334165753295);
#35090=CIRCLE('',#104737,4.86334165753295);
#35091=CIRCLE('',#104745,9.5);
#35092=CIRCLE('',#104747,9.5);
#35093=CIRCLE('',#104749,9.5);
#35094=CIRCLE('',#104751,9.5);
#35095=CIRCLE('',#104753,9.5);
#35096=CIRCLE('',#104755,9.5);
#35097=CIRCLE('',#104757,9.5);
#35098=CIRCLE('',#104759,9.5);
#35099=CIRCLE('',#104761,9.5);
#35100=CIRCLE('',#104763,9.5);
#35101=CIRCLE('',#104765,9.5);
#35102=CIRCLE('',#104767,9.5);
#35103=CIRCLE('',#104776,6.7);
#35104=CIRCLE('',#104778,6.7);
#35105=VERTEX_POINT('',#131016);
#35106=VERTEX_POINT('',#131018);
#35107=VERTEX_POINT('',#131022);
#35108=VERTEX_POINT('',#131024);
#35109=VERTEX_POINT('',#131028);
#35110=VERTEX_POINT('',#131030);
#35111=VERTEX_POINT('',#131034);
#35112=VERTEX_POINT('',#131036);
#35113=VERTEX_POINT('',#131040);
#35114=VERTEX_POINT('',#131042);
#35115=VERTEX_POINT('',#131046);
#35116=VERTEX_POINT('',#131048);
#35117=VERTEX_POINT('',#131052);
#35118=VERTEX_POINT('',#131054);
#35119=VERTEX_POINT('',#131058);
#35120=VERTEX_POINT('',#131060);
#35121=VERTEX_POINT('',#131064);
#35122=VERTEX_POINT('',#131066);
#35123=VERTEX_POINT('',#131070);
#35124=VERTEX_POINT('',#131072);
#35125=VERTEX_POINT('',#131076);
#35126=VERTEX_POINT('',#131078);
#35127=VERTEX_POINT('',#131082);
#35128=VERTEX_POINT('',#131084);
#35129=VERTEX_POINT('',#131088);
#35130=VERTEX_POINT('',#131089);
#35131=VERTEX_POINT('',#131091);
#35132=VERTEX_POINT('',#131093);
#35133=VERTEX_POINT('',#131097);
#35134=VERTEX_POINT('',#131099);
#35135=VERTEX_POINT('',#131103);
#35136=VERTEX_POINT('',#131104);
#35137=VERTEX_POINT('',#131106);
#35138=VERTEX_POINT('',#131108);
#35139=VERTEX_POINT('',#131112);
#35140=VERTEX_POINT('',#131113);
#35141=VERTEX_POINT('',#131115);
#35142=VERTEX_POINT('',#131117);
#35143=VERTEX_POINT('',#131121);
#35144=VERTEX_POINT('',#131123);
#35145=VERTEX_POINT('',#131127);
#35146=VERTEX_POINT('',#131129);
#35147=VERTEX_POINT('',#131133);
#35148=VERTEX_POINT('',#131134);
#35149=VERTEX_POINT('',#131136);
#35150=VERTEX_POINT('',#131138);
#35151=VERTEX_POINT('',#131142);
#35152=VERTEX_POINT('',#131144);
#35153=VERTEX_POINT('',#131163);
#35154=VERTEX_POINT('',#131165);
#35155=VERTEX_POINT('',#131169);
#35156=VERTEX_POINT('',#131171);
#35157=VERTEX_POINT('',#131175);
#35158=VERTEX_POINT('',#131177);
#35159=VERTEX_POINT('',#131181);
#35160=VERTEX_POINT('',#131183);
#35161=VERTEX_POINT('',#131187);
#35162=VERTEX_POINT('',#131189);
#35163=VERTEX_POINT('',#131193);
#35164=VERTEX_POINT('',#131195);
#35165=VERTEX_POINT('',#131199);
#35166=VERTEX_POINT('',#131201);
#35167=VERTEX_POINT('',#131205);
#35168=VERTEX_POINT('',#131207);
#35169=VERTEX_POINT('',#131211);
#35170=VERTEX_POINT('',#131213);
#35171=VERTEX_POINT('',#131217);
#35172=VERTEX_POINT('',#131219);
#35173=VERTEX_POINT('',#131223);
#35174=VERTEX_POINT('',#131225);
#35175=VERTEX_POINT('',#131229);
#35176=VERTEX_POINT('',#131231);
#35177=VERTEX_POINT('',#131235);
#35178=VERTEX_POINT('',#131236);
#35179=VERTEX_POINT('',#131238);
#35180=VERTEX_POINT('',#131240);
#35181=VERTEX_POINT('',#131244);
#35182=VERTEX_POINT('',#131246);
#35183=VERTEX_POINT('',#131250);
#35184=VERTEX_POINT('',#131251);
#35185=VERTEX_POINT('',#131253);
#35186=VERTEX_POINT('',#131255);
#35187=VERTEX_POINT('',#131259);
#35188=VERTEX_POINT('',#131260);
#35189=VERTEX_POINT('',#131262);
#35190=VERTEX_POINT('',#131264);
#35191=VERTEX_POINT('',#131268);
#35192=VERTEX_POINT('',#131270);
#35193=VERTEX_POINT('',#131274);
#35194=VERTEX_POINT('',#131276);
#35195=VERTEX_POINT('',#131280);
#35196=VERTEX_POINT('',#131281);
#35197=VERTEX_POINT('',#131283);
#35198=VERTEX_POINT('',#131285);
#35199=VERTEX_POINT('',#131289);
#35200=VERTEX_POINT('',#131291);
#35201=VERTEX_POINT('',#131310);
#35202=VERTEX_POINT('',#131312);
#35203=VERTEX_POINT('',#131317);
#35204=VERTEX_POINT('',#131321);
#35205=VERTEX_POINT('',#131324);
#35206=VERTEX_POINT('',#131329);
#35207=VERTEX_POINT('',#131331);
#35208=VERTEX_POINT('',#131336);
#35209=VERTEX_POINT('',#131340);
#35210=VERTEX_POINT('',#131343);
#35211=VERTEX_POINT('',#131348);
#35212=VERTEX_POINT('',#131349);
#35213=VERTEX_POINT('',#131351);
#35214=VERTEX_POINT('',#131353);
#35215=VERTEX_POINT('',#131355);
#35216=VERTEX_POINT('',#131363);
#35217=VERTEX_POINT('',#131370);
#35218=VERTEX_POINT('',#131371);
#35219=VERTEX_POINT('',#131373);
#35220=VERTEX_POINT('',#131375);
#35221=VERTEX_POINT('',#131377);
#35222=VERTEX_POINT('',#131384);
#35223=VERTEX_POINT('',#131386);
#35224=VERTEX_POINT('',#131401);
#35225=VERTEX_POINT('',#131414);
#35226=VERTEX_POINT('',#131415);
#35227=VERTEX_POINT('',#131417);
#35228=VERTEX_POINT('',#131419);
#35229=VERTEX_POINT('',#131423);
#35230=VERTEX_POINT('',#131424);
#35231=VERTEX_POINT('',#131426);
#35232=VERTEX_POINT('',#131428);
#35233=VERTEX_POINT('',#131436);
#35234=VERTEX_POINT('',#131438);
#35235=VERTEX_POINT('',#131446);
#35236=VERTEX_POINT('',#131448);
#35237=VERTEX_POINT('',#131450);
#35238=VERTEX_POINT('',#131470);
#35239=VERTEX_POINT('',#131510);
#35240=VERTEX_POINT('',#131512);
#35241=VERTEX_POINT('',#131514);
#35242=VERTEX_POINT('',#131522);
#35243=VERTEX_POINT('',#131524);
#35244=VERTEX_POINT('',#131534);
#35245=VERTEX_POINT('',#131536);
#35246=VERTEX_POINT('',#131540);
#35247=VERTEX_POINT('',#131541);
#35248=VERTEX_POINT('',#131543);
#35249=VERTEX_POINT('',#131545);
#35250=VERTEX_POINT('',#131552);
#35251=VERTEX_POINT('',#131554);
#35252=VERTEX_POINT('',#131558);
#35253=VERTEX_POINT('',#131559);
#35254=VERTEX_POINT('',#131579);
#35255=VERTEX_POINT('',#131581);
#35256=VERTEX_POINT('',#131583);
#35257=VERTEX_POINT('',#131591);
#35258=VERTEX_POINT('',#131593);
#35259=VERTEX_POINT('',#131601);
#35260=VERTEX_POINT('',#131603);
#35261=VERTEX_POINT('',#131605);
#35262=VERTEX_POINT('',#131607);
#35263=VERTEX_POINT('',#131615);
#35264=VERTEX_POINT('',#131617);
#35265=VERTEX_POINT('',#131625);
#35266=VERTEX_POINT('',#131629);
#35267=VERTEX_POINT('',#131656);
#35268=VERTEX_POINT('',#131657);
#35269=VERTEX_POINT('',#131659);
#35270=VERTEX_POINT('',#131668);
#35271=VERTEX_POINT('',#131679);
#35272=VERTEX_POINT('',#131680);
#35273=VERTEX_POINT('',#131685);
#35274=VERTEX_POINT('',#131686);
#35275=VERTEX_POINT('',#131689);
#35276=VERTEX_POINT('',#131693);
#35277=VERTEX_POINT('',#131694);
#35278=VERTEX_POINT('',#131696);
#35279=VERTEX_POINT('',#131698);
#35280=VERTEX_POINT('',#131701);
#35281=VERTEX_POINT('',#131734);
#35282=VERTEX_POINT('',#131781);
#35283=VERTEX_POINT('',#131805);
#35284=VERTEX_POINT('',#131807);
#35285=VERTEX_POINT('',#131840);
#35286=VERTEX_POINT('',#131878);
#35287=VERTEX_POINT('',#131891);
#35288=VERTEX_POINT('',#131892);
#35289=VERTEX_POINT('',#131897);
#35290=VERTEX_POINT('',#131898);
#35291=VERTEX_POINT('',#131901);
#35292=VERTEX_POINT('',#131905);
#35293=VERTEX_POINT('',#131906);
#35294=VERTEX_POINT('',#131908);
#35295=VERTEX_POINT('',#131910);
#35296=VERTEX_POINT('',#131932);
#35297=VERTEX_POINT('',#131939);
#35298=VERTEX_POINT('',#131948);
#35299=VERTEX_POINT('',#131950);
#35300=VERTEX_POINT('',#131983);
#35301=VERTEX_POINT('',#132027);
#35302=VERTEX_POINT('',#132067);
#35303=VERTEX_POINT('',#132068);
#35304=VERTEX_POINT('',#132073);
#35305=VERTEX_POINT('',#132074);
#35306=VERTEX_POINT('',#132077);
#35307=VERTEX_POINT('',#132081);
#35308=VERTEX_POINT('',#132082);
#35309=VERTEX_POINT('',#132084);
#35310=VERTEX_POINT('',#132118);
#35311=VERTEX_POINT('',#132162);
#35312=VERTEX_POINT('',#132178);
#35313=VERTEX_POINT('',#132179);
#35314=VERTEX_POINT('',#132181);
#35315=VERTEX_POINT('',#132183);
#35316=VERTEX_POINT('',#132205);
#35317=VERTEX_POINT('',#132206);
#35318=VERTEX_POINT('',#132209);
#35319=VERTEX_POINT('',#132216);
#35320=VERTEX_POINT('',#132217);
#35321=VERTEX_POINT('',#132219);
#35322=VERTEX_POINT('',#132241);
#35323=VERTEX_POINT('',#132242);
#35324=VERTEX_POINT('',#132257);
#35325=VERTEX_POINT('',#132258);
#35326=VERTEX_POINT('',#132292);
#35327=VERTEX_POINT('',#132293);
#35328=VERTEX_POINT('',#132352);
#35329=VERTEX_POINT('',#132354);
#35330=VERTEX_POINT('',#132358);
#35331=VERTEX_POINT('',#132359);
#35332=VERTEX_POINT('',#132362);
#35333=VERTEX_POINT('',#132366);
#35334=VERTEX_POINT('',#132367);
#35335=VERTEX_POINT('',#132369);
#35336=VERTEX_POINT('',#132403);
#35337=VERTEX_POINT('',#132404);
#35338=VERTEX_POINT('',#132471);
#35339=VERTEX_POINT('',#132472);
#35340=VERTEX_POINT('',#132494);
#35341=VERTEX_POINT('',#132495);
#35342=VERTEX_POINT('',#132510);
#35343=VERTEX_POINT('',#132511);
#35344=VERTEX_POINT('',#132516);
#35345=VERTEX_POINT('',#132517);
#35346=VERTEX_POINT('',#132520);
#35347=VERTEX_POINT('',#132524);
#35348=VERTEX_POINT('',#132525);
#35349=VERTEX_POINT('',#132527);
#35350=VERTEX_POINT('',#132561);
#35351=VERTEX_POINT('',#132562);
#35352=VERTEX_POINT('',#132598);
#35353=VERTEX_POINT('',#132599);
#35354=VERTEX_POINT('',#132639);
#35355=VERTEX_POINT('',#132640);
#35356=VERTEX_POINT('',#132698);
#35357=VERTEX_POINT('',#132699);
#35358=VERTEX_POINT('',#132715);
#35359=VERTEX_POINT('',#132717);
#35360=VERTEX_POINT('',#132724);
#35361=VERTEX_POINT('',#132739);
#35362=VERTEX_POINT('',#132752);
#35363=VERTEX_POINT('',#132753);
#35364=VERTEX_POINT('',#132755);
#35365=VERTEX_POINT('',#132757);
#35366=VERTEX_POINT('',#132759);
#35367=VERTEX_POINT('',#132766);
#35368=VERTEX_POINT('',#132771);
#35369=VERTEX_POINT('',#132780);
#35370=VERTEX_POINT('',#132782);
#35371=VERTEX_POINT('',#132784);
#35372=VERTEX_POINT('',#132786);
#35373=VERTEX_POINT('',#132830);
#35374=VERTEX_POINT('',#132832);
#35375=VERTEX_POINT('',#132839);
#35376=VERTEX_POINT('',#132841);
#35377=VERTEX_POINT('',#132843);
#35378=VERTEX_POINT('',#132845);
#35379=VERTEX_POINT('',#132854);
#35380=VERTEX_POINT('',#132856);
#35381=VERTEX_POINT('',#132909);
#35382=VERTEX_POINT('',#132911);
#35383=VERTEX_POINT('',#132913);
#35384=VERTEX_POINT('',#132915);
#35385=VERTEX_POINT('',#132926);
#35386=VERTEX_POINT('',#132928);
#35387=VERTEX_POINT('',#132951);
#35388=VERTEX_POINT('',#132953);
#35389=VERTEX_POINT('',#132955);
#35390=VERTEX_POINT('',#132957);
#35391=VERTEX_POINT('',#133001);
#35392=VERTEX_POINT('',#133003);
#35393=VERTEX_POINT('',#133050);
#35394=VERTEX_POINT('',#133052);
#35395=VERTEX_POINT('',#133054);
#35396=VERTEX_POINT('',#133056);
#35397=VERTEX_POINT('',#133100);
#35398=VERTEX_POINT('',#133102);
#35399=VERTEX_POINT('',#133111);
#35400=VERTEX_POINT('',#133113);
#35401=VERTEX_POINT('',#133115);
#35402=VERTEX_POINT('',#133135);
#35403=VERTEX_POINT('',#133137);
#35404=VERTEX_POINT('',#133144);
#35405=VERTEX_POINT('',#133165);
#35406=VERTEX_POINT('',#133174);
#35407=VERTEX_POINT('',#133175);
#35408=VERTEX_POINT('',#133177);
#35409=VERTEX_POINT('',#133179);
#35410=VERTEX_POINT('',#133183);
#35411=VERTEX_POINT('',#133184);
#35412=VERTEX_POINT('',#133186);
#35413=VERTEX_POINT('',#133188);
#35414=VERTEX_POINT('',#133196);
#35415=VERTEX_POINT('',#133198);
#35416=VERTEX_POINT('',#133206);
#35417=VERTEX_POINT('',#133208);
#35418=VERTEX_POINT('',#133210);
#35419=VERTEX_POINT('',#133230);
#35420=VERTEX_POINT('',#133234);
#35421=VERTEX_POINT('',#133236);
#35422=VERTEX_POINT('',#133238);
#35423=VERTEX_POINT('',#133246);
#35424=VERTEX_POINT('',#133248);
#35425=VERTEX_POINT('',#133258);
#35426=VERTEX_POINT('',#133260);
#35427=VERTEX_POINT('',#133264);
#35428=VERTEX_POINT('',#133265);
#35429=VERTEX_POINT('',#133267);
#35430=VERTEX_POINT('',#133269);
#35431=VERTEX_POINT('',#133276);
#35432=VERTEX_POINT('',#133278);
#35433=VERTEX_POINT('',#133282);
#35434=VERTEX_POINT('',#133283);
#35435=VERTEX_POINT('',#133285);
#35436=VERTEX_POINT('',#133287);
#35437=VERTEX_POINT('',#133295);
#35438=VERTEX_POINT('',#133297);
#35439=VERTEX_POINT('',#133305);
#35440=VERTEX_POINT('',#133309);
#35441=VERTEX_POINT('',#133326);
#35442=VERTEX_POINT('',#133328);
#35443=VERTEX_POINT('',#133336);
#35444=VERTEX_POINT('',#133338);
#35445=VERTEX_POINT('',#133365);
#35446=VERTEX_POINT('',#133374);
#35447=VERTEX_POINT('',#133378);
#35448=VERTEX_POINT('',#133379);
#35449=VERTEX_POINT('',#133384);
#35450=VERTEX_POINT('',#133386);
#35451=VERTEX_POINT('',#133413);
#35452=VERTEX_POINT('',#133424);
#35453=VERTEX_POINT('',#133457);
#35454=VERTEX_POINT('',#133470);
#35455=VERTEX_POINT('',#133474);
#35456=VERTEX_POINT('',#133475);
#35457=VERTEX_POINT('',#133480);
#35458=VERTEX_POINT('',#133482);
#35459=VERTEX_POINT('',#133515);
#35460=VERTEX_POINT('',#133539);
#35461=VERTEX_POINT('',#133578);
#35462=VERTEX_POINT('',#133630);
#35463=VERTEX_POINT('',#133634);
#35464=VERTEX_POINT('',#133635);
#35465=VERTEX_POINT('',#133640);
#35466=VERTEX_POINT('',#133642);
#35467=VERTEX_POINT('',#133675);
#35468=VERTEX_POINT('',#133738);
#35469=VERTEX_POINT('',#133771);
#35470=VERTEX_POINT('',#133823);
#35471=VERTEX_POINT('',#133827);
#35472=VERTEX_POINT('',#133828);
#35473=VERTEX_POINT('',#133833);
#35474=VERTEX_POINT('',#133835);
#35475=VERTEX_POINT('',#133868);
#35476=VERTEX_POINT('',#133892);
#35477=VERTEX_POINT('',#133919);
#35478=VERTEX_POINT('',#133930);
#35479=VERTEX_POINT('',#133934);
#35480=VERTEX_POINT('',#133935);
#35481=VERTEX_POINT('',#133940);
#35482=VERTEX_POINT('',#133942);
#35483=VERTEX_POINT('',#133963);
#35484=VERTEX_POINT('',#133972);
#35485=VERTEX_POINT('',#134005);
#35486=VERTEX_POINT('',#134045);
#35487=VERTEX_POINT('',#134049);
#35488=VERTEX_POINT('',#134050);
#35489=VERTEX_POINT('',#134055);
#35490=VERTEX_POINT('',#134057);
#35491=VERTEX_POINT('',#134093);
#35492=VERTEX_POINT('',#134094);
#35493=VERTEX_POINT('',#134117);
#35494=VERTEX_POINT('',#134119);
#35495=VERTEX_POINT('',#134140);
#35496=VERTEX_POINT('',#134149);
#35497=VERTEX_POINT('',#134170);
#35498=VERTEX_POINT('',#134179);
#35499=VERTEX_POINT('',#134183);
#35500=VERTEX_POINT('',#134213);
#35501=VERTEX_POINT('',#134222);
#35502=VERTEX_POINT('',#134243);
#35503=VERTEX_POINT('',#134245);
#35504=VERTEX_POINT('',#134259);
#35505=VERTEX_POINT('',#134272);
#35506=VERTEX_POINT('',#134274);
#35507=VERTEX_POINT('',#134295);
#35508=VERTEX_POINT('',#134304);
#35509=VERTEX_POINT('',#134325);
#35510=VERTEX_POINT('',#134334);
#35511=VERTEX_POINT('',#134357);
#35512=VERTEX_POINT('',#134366);
#35513=VERTEX_POINT('',#134367);
#35514=VERTEX_POINT('',#134390);
#35515=VERTEX_POINT('',#134392);
#35516=VERTEX_POINT('',#134413);
#35517=VERTEX_POINT('',#134422);
#35518=VERTEX_POINT('',#134443);
#35519=VERTEX_POINT('',#134452);
#35520=VERTEX_POINT('',#134473);
#35521=VERTEX_POINT('',#134493);
#35522=VERTEX_POINT('',#134506);
#35523=VERTEX_POINT('',#134508);
#35524=VERTEX_POINT('',#134529);
#35525=VERTEX_POINT('',#134538);
#35526=VERTEX_POINT('',#134559);
#35527=VERTEX_POINT('',#134568);
#35528=VERTEX_POINT('',#134574);
#35529=VERTEX_POINT('',#134575);
#35530=VERTEX_POINT('',#134598);
#35531=VERTEX_POINT('',#134600);
#35532=VERTEX_POINT('',#134621);
#35533=VERTEX_POINT('',#134630);
#35534=VERTEX_POINT('',#134651);
#35535=VERTEX_POINT('',#134660);
#35536=VERTEX_POINT('',#134664);
#35537=VERTEX_POINT('',#134688);
#35538=VERTEX_POINT('',#134692);
#35539=VERTEX_POINT('',#134713);
#35540=VERTEX_POINT('',#134715);
#35541=VERTEX_POINT('',#134722);
#35542=VERTEX_POINT('',#134738);
#35543=VERTEX_POINT('',#134751);
#35544=VERTEX_POINT('',#134753);
#35545=VERTEX_POINT('',#134774);
#35546=VERTEX_POINT('',#134783);
#35547=VERTEX_POINT('',#134804);
#35548=VERTEX_POINT('',#134813);
#35549=VERTEX_POINT('',#134834);
#35550=VERTEX_POINT('',#134835);
#35551=VERTEX_POINT('',#134850);
#35552=VERTEX_POINT('',#134852);
#35553=VERTEX_POINT('',#134869);
#35554=VERTEX_POINT('',#134882);
#35555=VERTEX_POINT('',#134884);
#35556=VERTEX_POINT('',#134905);
#35557=VERTEX_POINT('',#134914);
#35558=VERTEX_POINT('',#134935);
#35559=VERTEX_POINT('',#134944);
#35560=VERTEX_POINT('',#134948);
#35561=VERTEX_POINT('',#134949);
#35562=VERTEX_POINT('',#134972);
#35563=VERTEX_POINT('',#134974);
#35564=VERTEX_POINT('',#134995);
#35565=VERTEX_POINT('',#135004);
#35566=VERTEX_POINT('',#135025);
#35567=VERTEX_POINT('',#135027);
#35568=VERTEX_POINT('',#135036);
#35569=VERTEX_POINT('',#135038);
#35570=VERTEX_POINT('',#135042);
#35571=VERTEX_POINT('',#135055);
#35572=VERTEX_POINT('',#135057);
#35573=VERTEX_POINT('',#135059);
#35574=VERTEX_POINT('',#135061);
#35575=VERTEX_POINT('',#135063);
#35576=VERTEX_POINT('',#135065);
#35577=VERTEX_POINT('',#135069);
#35578=VERTEX_POINT('',#135071);
#35579=VERTEX_POINT('',#135073);
#35580=VERTEX_POINT('',#135077);
#35581=VERTEX_POINT('',#135079);
#35582=VERTEX_POINT('',#135083);
#35583=VERTEX_POINT('',#135098);
#35584=VERTEX_POINT('',#135099);
#35585=VERTEX_POINT('',#135115);
#35586=VERTEX_POINT('',#135120);
#35587=VERTEX_POINT('',#135168);
#35588=VERTEX_POINT('',#135209);
#35589=VERTEX_POINT('',#135224);
#35590=VERTEX_POINT('',#135233);
#35591=VERTEX_POINT('',#135234);
#35592=VERTEX_POINT('',#135236);
#35593=VERTEX_POINT('',#135238);
#35594=VERTEX_POINT('',#135242);
#35595=VERTEX_POINT('',#135244);
#35596=VERTEX_POINT('',#135248);
#35597=VERTEX_POINT('',#135249);
#35598=VERTEX_POINT('',#135256);
#35599=VERTEX_POINT('',#135263);
#35600=VERTEX_POINT('',#135268);
#35601=VERTEX_POINT('',#135280);
#35602=VERTEX_POINT('',#135282);
#35603=VERTEX_POINT('',#135284);
#35604=VERTEX_POINT('',#135288);
#35605=VERTEX_POINT('',#135290);
#35606=VERTEX_POINT('',#135294);
#35607=VERTEX_POINT('',#135296);
#35608=VERTEX_POINT('',#135300);
#35609=VERTEX_POINT('',#135302);
#35610=VERTEX_POINT('',#135306);
#35611=VERTEX_POINT('',#135308);
#35612=VERTEX_POINT('',#135312);
#35613=VERTEX_POINT('',#135314);
#35614=VERTEX_POINT('',#135318);
#35615=VERTEX_POINT('',#135319);
#35616=VERTEX_POINT('',#135321);
#35617=VERTEX_POINT('',#135323);
#35618=VERTEX_POINT('',#135337);
#35619=VERTEX_POINT('',#135383);
#35620=VERTEX_POINT('',#135385);
#35621=VERTEX_POINT('',#135387);
#35622=VERTEX_POINT('',#135391);
#35623=VERTEX_POINT('',#135393);
#35624=VERTEX_POINT('',#135397);
#35625=VERTEX_POINT('',#135399);
#35626=VERTEX_POINT('',#135403);
#35627=VERTEX_POINT('',#135405);
#35628=VERTEX_POINT('',#135409);
#35629=VERTEX_POINT('',#135411);
#35630=VERTEX_POINT('',#135415);
#35631=VERTEX_POINT('',#135417);
#35632=VERTEX_POINT('',#135438);
#35633=VERTEX_POINT('',#135445);
#35634=VERTEX_POINT('',#135447);
#35635=VERTEX_POINT('',#135465);
#35636=VERTEX_POINT('',#135467);
#35637=VERTEX_POINT('',#135471);
#35638=VERTEX_POINT('',#135473);
#35639=VERTEX_POINT('',#135475);
#35640=VERTEX_POINT('',#135479);
#35641=VERTEX_POINT('',#135481);
#35642=VERTEX_POINT('',#135485);
#35643=VERTEX_POINT('',#135487);
#35644=VERTEX_POINT('',#135491);
#35645=VERTEX_POINT('',#135493);
#35646=VERTEX_POINT('',#135497);
#35647=VERTEX_POINT('',#135499);
#35648=VERTEX_POINT('',#135503);
#35649=VERTEX_POINT('',#135505);
#35650=VERTEX_POINT('',#135507);
#35651=VERTEX_POINT('',#135511);
#35652=VERTEX_POINT('',#135513);
#35653=VERTEX_POINT('',#135515);
#35654=VERTEX_POINT('',#135519);
#35655=VERTEX_POINT('',#135521);
#35656=VERTEX_POINT('',#135525);
#35657=VERTEX_POINT('',#135527);
#35658=VERTEX_POINT('',#135531);
#35659=VERTEX_POINT('',#135533);
#35660=VERTEX_POINT('',#135537);
#35661=VERTEX_POINT('',#135539);
#35662=VERTEX_POINT('',#135543);
#35663=VERTEX_POINT('',#135545);
#35664=VERTEX_POINT('',#135547);
#35665=VERTEX_POINT('',#135551);
#35666=VERTEX_POINT('',#135556);
#35667=VERTEX_POINT('',#135558);
#35668=VERTEX_POINT('',#135560);
#35669=VERTEX_POINT('',#135562);
#35670=VERTEX_POINT('',#135564);
#35671=VERTEX_POINT('',#135575);
#35672=VERTEX_POINT('',#135577);
#35673=VERTEX_POINT('',#135611);
#35674=VERTEX_POINT('',#135613);
#35675=VERTEX_POINT('',#135626);
#35676=VERTEX_POINT('',#135627);
#35677=VERTEX_POINT('',#135629);
#35678=VERTEX_POINT('',#135631);
#35679=VERTEX_POINT('',#135635);
#35680=VERTEX_POINT('',#135640);
#35681=VERTEX_POINT('',#135642);
#35682=VERTEX_POINT('',#135646);
#35683=VERTEX_POINT('',#135648);
#35684=VERTEX_POINT('',#135652);
#35685=VERTEX_POINT('',#135653);
#35686=VERTEX_POINT('',#135658);
#35687=VERTEX_POINT('',#135659);
#35688=VERTEX_POINT('',#135664);
#35689=VERTEX_POINT('',#135665);
#35690=VERTEX_POINT('',#135670);
#35691=VERTEX_POINT('',#135671);
#35692=VERTEX_POINT('',#135676);
#35693=VERTEX_POINT('',#135677);
#35694=VERTEX_POINT('',#135682);
#35695=VERTEX_POINT('',#135683);
#35696=VERTEX_POINT('',#135688);
#35697=VERTEX_POINT('',#135689);
#35698=VERTEX_POINT('',#135694);
#35699=VERTEX_POINT('',#135695);
#35700=VERTEX_POINT('',#135700);
#35701=VERTEX_POINT('',#135701);
#35702=VERTEX_POINT('',#135706);
#35703=VERTEX_POINT('',#135707);
#35704=VERTEX_POINT('',#135712);
#35705=VERTEX_POINT('',#135713);
#35706=VERTEX_POINT('',#135718);
#35707=VERTEX_POINT('',#135719);
#35708=VERTEX_POINT('',#135724);
#35709=VERTEX_POINT('',#135725);
#35710=VERTEX_POINT('',#135730);
#35711=VERTEX_POINT('',#135731);
#35712=VERTEX_POINT('',#135736);
#35713=VERTEX_POINT('',#135737);
#35714=VERTEX_POINT('',#135764);
#35715=VERTEX_POINT('',#135766);
#35716=VERTEX_POINT('',#135769);
#35717=VERTEX_POINT('',#135771);
#35718=VERTEX_POINT('',#135792);
#35719=VERTEX_POINT('',#135793);
#35720=VERTEX_POINT('',#135795);
#35721=VERTEX_POINT('',#135804);
#35722=VERTEX_POINT('',#135807);
#35723=VERTEX_POINT('',#135816);
#35724=VERTEX_POINT('',#135866);
#35725=VERTEX_POINT('',#135867);
#35726=VERTEX_POINT('',#135869);
#35727=VERTEX_POINT('',#135880);
#35728=VERTEX_POINT('',#135926);
#35729=VERTEX_POINT('',#135928);
#35730=VERTEX_POINT('',#135932);
#35731=VERTEX_POINT('',#135934);
#35732=VERTEX_POINT('',#135936);
#35733=VERTEX_POINT('',#135940);
#35734=VERTEX_POINT('',#135941);
#35735=VERTEX_POINT('',#135943);
#35736=VERTEX_POINT('',#135977);
#35737=VERTEX_POINT('',#135978);
#35738=VERTEX_POINT('',#136064);
#35739=VERTEX_POINT('',#136065);
#35740=VERTEX_POINT('',#136087);
#35741=VERTEX_POINT('',#136094);
#35742=VERTEX_POINT('',#136103);
#35743=VERTEX_POINT('',#136105);
#35744=VERTEX_POINT('',#136109);
#35745=VERTEX_POINT('',#136111);
#35746=VERTEX_POINT('',#136113);
#35747=VERTEX_POINT('',#136117);
#35748=VERTEX_POINT('',#136118);
#35749=VERTEX_POINT('',#136120);
#35750=VERTEX_POINT('',#136148);
#35751=VERTEX_POINT('',#136149);
#35752=VERTEX_POINT('',#136179);
#35753=VERTEX_POINT('',#136180);
#35754=VERTEX_POINT('',#136214);
#35755=VERTEX_POINT('',#136267);
#35756=VERTEX_POINT('',#136280);
#35757=VERTEX_POINT('',#136282);
#35758=VERTEX_POINT('',#136286);
#35759=VERTEX_POINT('',#136288);
#35760=VERTEX_POINT('',#136290);
#35761=VERTEX_POINT('',#136294);
#35762=VERTEX_POINT('',#136295);
#35763=VERTEX_POINT('',#136297);
#35764=VERTEX_POINT('',#136331);
#35765=VERTEX_POINT('',#136332);
#35766=VERTEX_POINT('',#136394);
#35767=VERTEX_POINT('',#136395);
#35768=VERTEX_POINT('',#136397);
#35769=VERTEX_POINT('',#136403);
#35770=VERTEX_POINT('',#136423);
#35771=VERTEX_POINT('',#136424);
#35772=VERTEX_POINT('',#136426);
#35773=VERTEX_POINT('',#136469);
#35774=VERTEX_POINT('',#136480);
#35775=VERTEX_POINT('',#136511);
#35776=VERTEX_POINT('',#136513);
#35777=VERTEX_POINT('',#136613);
#35778=VERTEX_POINT('',#136617);
#35779=VERTEX_POINT('',#136622);
#35780=VERTEX_POINT('',#136624);
#35781=VERTEX_POINT('',#136626);
#35782=VERTEX_POINT('',#136628);
#35783=VERTEX_POINT('',#136635);
#35784=VERTEX_POINT('',#136636);
#35785=VERTEX_POINT('',#136672);
#35786=VERTEX_POINT('',#136676);
#35787=VERTEX_POINT('',#136714);
#35788=VERTEX_POINT('',#136753);
#35789=VERTEX_POINT('',#136755);
#35790=VERTEX_POINT('',#136760);
#35791=VERTEX_POINT('',#136774);
#35792=VERTEX_POINT('',#136776);
#35793=VERTEX_POINT('',#136836);
#35794=VERTEX_POINT('',#136864);
#35795=VERTEX_POINT('',#136917);
#35796=VERTEX_POINT('',#136977);
#35797=VERTEX_POINT('',#136981);
#35798=VERTEX_POINT('',#137032);
#35799=VERTEX_POINT('',#137037);
#35800=VERTEX_POINT('',#137051);
#35801=VERTEX_POINT('',#137053);
#35802=VERTEX_POINT('',#137067);
#35803=VERTEX_POINT('',#137074);
#35804=VERTEX_POINT('',#137075);
#35805=VERTEX_POINT('',#137102);
#35806=VERTEX_POINT('',#137106);
#35807=VERTEX_POINT('',#137108);
#35808=VERTEX_POINT('',#137110);
#35809=VERTEX_POINT('',#137112);
#35810=VERTEX_POINT('',#137115);
#35811=VERTEX_POINT('',#137117);
#35812=VERTEX_POINT('',#137122);
#35813=VERTEX_POINT('',#137139);
#35814=VERTEX_POINT('',#137141);
#35815=VERTEX_POINT('',#137160);
#35816=VERTEX_POINT('',#137164);
#35817=VERTEX_POINT('',#137168);
#35818=VERTEX_POINT('',#137183);
#35819=VERTEX_POINT('',#137187);
#35820=VERTEX_POINT('',#137189);
#35821=VERTEX_POINT('',#137191);
#35822=VERTEX_POINT('',#137194);
#35823=VERTEX_POINT('',#137199);
#35824=VERTEX_POINT('',#137216);
#35825=VERTEX_POINT('',#137218);
#35826=VERTEX_POINT('',#137232);
#35827=VERTEX_POINT('',#137239);
#35828=VERTEX_POINT('',#137240);
#35829=VERTEX_POINT('',#137268);
#35830=VERTEX_POINT('',#137272);
#35831=VERTEX_POINT('',#137274);
#35832=VERTEX_POINT('',#137276);
#35833=VERTEX_POINT('',#137278);
#35834=VERTEX_POINT('',#137281);
#35835=VERTEX_POINT('',#137283);
#35836=VERTEX_POINT('',#137288);
#35837=VERTEX_POINT('',#137314);
#35838=VERTEX_POINT('',#137316);
#35839=VERTEX_POINT('',#137343);
#35840=VERTEX_POINT('',#137344);
#35841=VERTEX_POINT('',#137367);
#35842=VERTEX_POINT('',#137371);
#35843=VERTEX_POINT('',#137373);
#35844=VERTEX_POINT('',#137376);
#35845=VERTEX_POINT('',#137378);
#35846=VERTEX_POINT('',#137380);
#35847=VERTEX_POINT('',#137397);
#35848=VERTEX_POINT('',#137404);
#35849=VERTEX_POINT('',#137408);
#35850=VERTEX_POINT('',#137412);
#35851=VERTEX_POINT('',#137416);
#35852=VERTEX_POINT('',#137418);
#35853=VERTEX_POINT('',#137423);
#35854=VERTEX_POINT('',#137432);
#35855=VERTEX_POINT('',#137435);
#35856=VERTEX_POINT('',#137452);
#35857=VERTEX_POINT('',#137453);
#35858=VERTEX_POINT('',#137480);
#35859=VERTEX_POINT('',#137484);
#35860=VERTEX_POINT('',#137550);
#35861=VERTEX_POINT('',#137552);
#35862=VERTEX_POINT('',#137587);
#35863=VERTEX_POINT('',#137638);
#35864=VERTEX_POINT('',#137666);
#35865=VERTEX_POINT('',#137716);
#35866=VERTEX_POINT('',#137791);
#35867=VERTEX_POINT('',#137795);
#35868=VERTEX_POINT('',#137856);
#35869=VERTEX_POINT('',#137860);
#35870=VERTEX_POINT('',#137893);
#35871=VERTEX_POINT('',#137940);
#35872=VERTEX_POINT('',#137966);
#35873=VERTEX_POINT('',#138011);
#35874=VERTEX_POINT('',#138044);
#35875=VERTEX_POINT('',#138046);
#35876=VERTEX_POINT('',#138050);
#35877=VERTEX_POINT('',#138054);
#35878=VERTEX_POINT('',#138058);
#35879=VERTEX_POINT('',#138060);
#35880=VERTEX_POINT('',#138064);
#35881=VERTEX_POINT('',#138068);
#35882=VERTEX_POINT('',#138072);
#35883=VERTEX_POINT('',#138073);
#35884=VERTEX_POINT('',#138075);
#35885=VERTEX_POINT('',#138077);
#35886=VERTEX_POINT('',#138080);
#35887=VERTEX_POINT('',#138082);
#35888=VERTEX_POINT('',#138090);
#35889=VERTEX_POINT('',#138116);
#35890=VERTEX_POINT('',#138118);
#35891=VERTEX_POINT('',#138141);
#35892=VERTEX_POINT('',#138149);
#35893=VERTEX_POINT('',#138166);
#35894=VERTEX_POINT('',#138167);
#35895=VERTEX_POINT('',#138199);
#35896=VERTEX_POINT('',#138203);
#35897=VERTEX_POINT('',#138205);
#35898=VERTEX_POINT('',#138207);
#35899=VERTEX_POINT('',#138209);
#35900=VERTEX_POINT('',#138211);
#35901=VERTEX_POINT('',#138213);
#35902=VERTEX_POINT('',#138215);
#35903=VERTEX_POINT('',#138217);
#35904=VERTEX_POINT('',#138225);
#35905=VERTEX_POINT('',#138234);
#35906=VERTEX_POINT('',#138236);
#35907=VERTEX_POINT('',#138261);
#35908=VERTEX_POINT('',#138265);
#35909=VERTEX_POINT('',#138269);
#35910=VERTEX_POINT('',#138284);
#35911=VERTEX_POINT('',#138288);
#35912=VERTEX_POINT('',#138296);
#35913=VERTEX_POINT('',#138313);
#35914=VERTEX_POINT('',#138315);
#35915=VERTEX_POINT('',#138329);
#35916=VERTEX_POINT('',#138337);
#35917=VERTEX_POINT('',#138339);
#35918=VERTEX_POINT('',#138341);
#35919=VERTEX_POINT('',#138343);
#35920=VERTEX_POINT('',#138347);
#35921=VERTEX_POINT('',#138348);
#35922=VERTEX_POINT('',#138381);
#35923=VERTEX_POINT('',#138385);
#35924=VERTEX_POINT('',#138438);
#35925=VERTEX_POINT('',#138440);
#35926=VERTEX_POINT('',#138478);
#35927=VERTEX_POINT('',#138480);
#35928=VERTEX_POINT('',#138482);
#35929=VERTEX_POINT('',#138487);
#35930=VERTEX_POINT('',#138501);
#35931=VERTEX_POINT('',#138503);
#35932=VERTEX_POINT('',#138563);
#35933=VERTEX_POINT('',#138591);
#35934=VERTEX_POINT('',#138652);
#35935=VERTEX_POINT('',#138703);
#35936=VERTEX_POINT('',#138707);
#35937=VERTEX_POINT('',#138708);
#35938=VERTEX_POINT('',#138744);
#35939=VERTEX_POINT('',#138749);
#35940=VERTEX_POINT('',#138763);
#35941=VERTEX_POINT('',#138765);
#35942=VERTEX_POINT('',#138779);
#35943=VERTEX_POINT('',#138784);
#35944=VERTEX_POINT('',#138788);
#35945=VERTEX_POINT('',#138789);
#35946=VERTEX_POINT('',#138816);
#35947=VERTEX_POINT('',#138820);
#35948=VERTEX_POINT('',#138849);
#35949=VERTEX_POINT('',#138851);
#35950=VERTEX_POINT('',#138877);
#35951=VERTEX_POINT('',#138879);
#35952=VERTEX_POINT('',#138881);
#35953=VERTEX_POINT('',#138886);
#35954=VERTEX_POINT('',#138888);
#35955=VERTEX_POINT('',#138890);
#35956=VERTEX_POINT('',#138926);
#35957=VERTEX_POINT('',#138950);
#35958=VERTEX_POINT('',#138992);
#35959=VERTEX_POINT('',#139034);
#35960=VERTEX_POINT('',#139038);
#35961=VERTEX_POINT('',#139043);
#35962=VERTEX_POINT('',#139045);
#35963=VERTEX_POINT('',#139047);
#35964=VERTEX_POINT('',#139049);
#35965=VERTEX_POINT('',#139054);
#35966=VERTEX_POINT('',#139056);
#35967=VERTEX_POINT('',#139058);
#35968=VERTEX_POINT('',#139086);
#35969=VERTEX_POINT('',#139087);
#35970=VERTEX_POINT('',#139116);
#35971=VERTEX_POINT('',#139120);
#35972=VERTEX_POINT('',#139158);
#35973=VERTEX_POINT('',#139160);
#35974=VERTEX_POINT('',#139198);
#35975=VERTEX_POINT('',#139200);
#35976=VERTEX_POINT('',#139202);
#35977=VERTEX_POINT('',#139207);
#35978=VERTEX_POINT('',#139221);
#35979=VERTEX_POINT('',#139223);
#35980=VERTEX_POINT('',#139283);
#35981=VERTEX_POINT('',#139311);
#35982=VERTEX_POINT('',#139372);
#35983=VERTEX_POINT('',#139423);
#35984=VERTEX_POINT('',#139427);
#35985=VERTEX_POINT('',#139432);
#35986=VERTEX_POINT('',#139446);
#35987=VERTEX_POINT('',#139448);
#35988=VERTEX_POINT('',#139462);
#35989=VERTEX_POINT('',#139467);
#35990=VERTEX_POINT('',#139469);
#35991=VERTEX_POINT('',#139471);
#35992=VERTEX_POINT('',#139514);
#35993=VERTEX_POINT('',#139515);
#35994=VERTEX_POINT('',#139546);
#35995=VERTEX_POINT('',#139550);
#35996=VERTEX_POINT('',#139552);
#35997=VERTEX_POINT('',#139554);
#35998=VERTEX_POINT('',#139556);
#35999=VERTEX_POINT('',#139558);
#36000=VERTEX_POINT('',#139560);
#36001=VERTEX_POINT('',#139562);
#36002=VERTEX_POINT('',#139570);
#36003=VERTEX_POINT('',#139587);
#36004=VERTEX_POINT('',#139589);
#36005=VERTEX_POINT('',#139611);
#36006=VERTEX_POINT('',#139615);
#36007=VERTEX_POINT('',#139619);
#36008=VERTEX_POINT('',#139634);
#36009=VERTEX_POINT('',#139638);
#36010=VERTEX_POINT('',#139646);
#36011=VERTEX_POINT('',#139655);
#36012=VERTEX_POINT('',#139657);
#36013=VERTEX_POINT('',#139674);
#36014=VERTEX_POINT('',#139682);
#36015=VERTEX_POINT('',#139684);
#36016=VERTEX_POINT('',#139686);
#36017=VERTEX_POINT('',#139688);
#36018=VERTEX_POINT('',#139690);
#36019=VERTEX_POINT('',#139694);
#36020=VERTEX_POINT('',#139695);
#36021=VERTEX_POINT('',#139727);
#36022=VERTEX_POINT('',#139731);
#36023=VERTEX_POINT('',#139732);
#36024=VERTEX_POINT('',#139734);
#36025=VERTEX_POINT('',#139742);
#36026=VERTEX_POINT('',#139768);
#36027=VERTEX_POINT('',#139770);
#36028=VERTEX_POINT('',#139800);
#36029=VERTEX_POINT('',#139802);
#36030=VERTEX_POINT('',#139804);
#36031=VERTEX_POINT('',#139806);
#36032=VERTEX_POINT('',#139810);
#36033=VERTEX_POINT('',#139811);
#36034=VERTEX_POINT('',#139816);
#36035=VERTEX_POINT('',#139850);
#36036=VERTEX_POINT('',#139892);
#36037=VERTEX_POINT('',#139905);
#36038=VERTEX_POINT('',#139906);
#36039=VERTEX_POINT('',#139917);
#36040=VERTEX_POINT('',#139919);
#36041=VERTEX_POINT('',#139924);
#36042=VERTEX_POINT('',#139950);
#36043=VERTEX_POINT('',#139967);
#36044=VERTEX_POINT('',#139969);
#36045=VERTEX_POINT('',#139983);
#36046=VERTEX_POINT('',#140004);
#36047=VERTEX_POINT('',#140006);
#36048=VERTEX_POINT('',#140008);
#36049=VERTEX_POINT('',#140010);
#36050=VERTEX_POINT('',#140012);
#36051=VERTEX_POINT('',#140016);
#36052=VERTEX_POINT('',#140020);
#36053=VERTEX_POINT('',#140024);
#36054=VERTEX_POINT('',#140028);
#36055=VERTEX_POINT('',#140029);
#36056=VERTEX_POINT('',#140061);
#36057=VERTEX_POINT('',#140063);
#36058=VERTEX_POINT('',#140074);
#36059=VERTEX_POINT('',#140076);
#36060=VERTEX_POINT('',#140078);
#36061=VERTEX_POINT('',#140080);
#36062=VERTEX_POINT('',#140083);
#36063=VERTEX_POINT('',#140094);
#36064=VERTEX_POINT('',#140096);
#36065=VERTEX_POINT('',#140134);
#36066=VERTEX_POINT('',#140136);
#36067=VERTEX_POINT('',#140188);
#36068=VERTEX_POINT('',#140222);
#36069=VERTEX_POINT('',#140223);
#36070=VERTEX_POINT('',#140225);
#36071=VERTEX_POINT('',#140227);
#36072=VERTEX_POINT('',#140230);
#36073=VERTEX_POINT('',#140232);
#36074=VERTEX_POINT('',#140237);
#36075=VERTEX_POINT('',#140251);
#36076=VERTEX_POINT('',#140253);
#36077=VERTEX_POINT('',#140276);
#36078=VERTEX_POINT('',#140281);
#36079=VERTEX_POINT('',#140286);
#36080=VERTEX_POINT('',#140302);
#36081=VERTEX_POINT('',#140303);
#36082=VERTEX_POINT('',#140306);
#36083=VERTEX_POINT('',#140348);
#36084=VERTEX_POINT('',#140361);
#36085=VERTEX_POINT('',#140363);
#36086=VERTEX_POINT('',#140365);
#36087=VERTEX_POINT('',#140367);
#36088=VERTEX_POINT('',#140369);
#36089=VERTEX_POINT('',#140371);
#36090=VERTEX_POINT('',#140373);
#36091=VERTEX_POINT('',#140384);
#36092=VERTEX_POINT('',#140386);
#36093=VERTEX_POINT('',#140406);
#36094=VERTEX_POINT('',#140411);
#36095=VERTEX_POINT('',#140428);
#36096=VERTEX_POINT('',#140430);
#36097=VERTEX_POINT('',#140444);
#36098=VERTEX_POINT('',#140449);
#36099=VERTEX_POINT('',#140465);
#36100=VERTEX_POINT('',#140469);
#36101=VERTEX_POINT('',#140473);
#36102=VERTEX_POINT('',#140477);
#36103=VERTEX_POINT('',#140478);
#36104=VERTEX_POINT('',#140480);
#36105=VERTEX_POINT('',#140482);
#36106=VERTEX_POINT('',#140485);
#36107=VERTEX_POINT('',#140487);
#36108=VERTEX_POINT('',#140510);
#36109=VERTEX_POINT('',#140515);
#36110=VERTEX_POINT('',#140541);
#36111=VERTEX_POINT('',#140543);
#36112=VERTEX_POINT('',#140560);
#36113=VERTEX_POINT('',#140565);
#36114=VERTEX_POINT('',#140582);
#36115=VERTEX_POINT('',#140584);
#36116=VERTEX_POINT('',#140597);
#36117=VERTEX_POINT('',#140598);
#36118=VERTEX_POINT('',#140632);
#36119=VERTEX_POINT('',#140674);
#36120=VERTEX_POINT('',#140687);
#36121=VERTEX_POINT('',#140689);
#36122=VERTEX_POINT('',#140692);
#36123=VERTEX_POINT('',#140694);
#36124=VERTEX_POINT('',#140696);
#36125=VERTEX_POINT('',#140710);
#36126=VERTEX_POINT('',#140715);
#36127=VERTEX_POINT('',#140737);
#36128=VERTEX_POINT('',#140741);
#36129=VERTEX_POINT('',#140745);
#36130=VERTEX_POINT('',#140749);
#36131=VERTEX_POINT('',#140790);
#36132=VERTEX_POINT('',#140810);
#36133=VERTEX_POINT('',#140815);
#36134=VERTEX_POINT('',#140829);
#36135=VERTEX_POINT('',#140832);
#36136=VERTEX_POINT('',#140902);
#36137=VERTEX_POINT('',#140918);
#36138=VERTEX_POINT('',#140919);
#36139=VERTEX_POINT('',#140922);
#36140=VERTEX_POINT('',#140924);
#36141=VERTEX_POINT('',#140926);
#36142=VERTEX_POINT('',#140930);
#36143=VERTEX_POINT('',#140934);
#36144=VERTEX_POINT('',#140938);
#36145=VERTEX_POINT('',#140942);
#36146=VERTEX_POINT('',#140945);
#36147=VERTEX_POINT('',#140947);
#36148=VERTEX_POINT('',#140967);
#36149=VERTEX_POINT('',#140972);
#36150=VERTEX_POINT('',#140989);
#36151=VERTEX_POINT('',#140993);
#36152=VERTEX_POINT('',#140994);
#36153=VERTEX_POINT('',#141028);
#36154=VERTEX_POINT('',#141070);
#36155=VERTEX_POINT('',#141083);
#36156=VERTEX_POINT('',#141084);
#36157=VERTEX_POINT('',#141095);
#36158=VERTEX_POINT('',#141097);
#36159=VERTEX_POINT('',#141117);
#36160=VERTEX_POINT('',#141122);
#36161=VERTEX_POINT('',#141142);
#36162=VERTEX_POINT('',#141144);
#36163=VERTEX_POINT('',#141161);
#36164=VERTEX_POINT('',#141166);
#36165=VERTEX_POINT('',#141181);
#36166=VERTEX_POINT('',#141183);
#36167=VERTEX_POINT('',#141185);
#36168=VERTEX_POINT('',#141187);
#36169=VERTEX_POINT('',#141189);
#36170=VERTEX_POINT('',#141193);
#36171=VERTEX_POINT('',#141197);
#36172=VERTEX_POINT('',#141201);
#36173=VERTEX_POINT('',#141234);
#36174=VERTEX_POINT('',#141247);
#36175=VERTEX_POINT('',#141248);
#36176=VERTEX_POINT('',#141250);
#36177=VERTEX_POINT('',#141252);
#36178=VERTEX_POINT('',#141272);
#36179=VERTEX_POINT('',#141274);
#36180=VERTEX_POINT('',#141285);
#36181=VERTEX_POINT('',#141287);
#36182=VERTEX_POINT('',#141289);
#36183=VERTEX_POINT('',#141291);
#36184=VERTEX_POINT('',#141294);
#36185=VERTEX_POINT('',#141296);
#36186=VERTEX_POINT('',#141316);
#36187=VERTEX_POINT('',#141318);
#36188=VERTEX_POINT('',#141322);
#36189=VERTEX_POINT('',#141323);
#36190=VERTEX_POINT('',#141325);
#36191=VERTEX_POINT('',#141327);
#36192=VERTEX_POINT('',#141330);
#36193=VERTEX_POINT('',#141332);
#36194=VERTEX_POINT('',#141334);
#36195=VERTEX_POINT('',#141336);
#36196=VERTEX_POINT('',#141344);
#36197=VERTEX_POINT('',#141361);
#36198=VERTEX_POINT('',#141363);
#36199=VERTEX_POINT('',#141389);
#36200=VERTEX_POINT('',#141397);
#36201=VERTEX_POINT('',#141402);
#36202=VERTEX_POINT('',#141442);
#36203=VERTEX_POINT('',#141452);
#36204=VERTEX_POINT('',#141453);
#36205=VERTEX_POINT('',#141456);
#36206=VERTEX_POINT('',#141498);
#36207=VERTEX_POINT('',#141511);
#36208=VERTEX_POINT('',#141513);
#36209=VERTEX_POINT('',#141515);
#36210=VERTEX_POINT('',#141517);
#36211=VERTEX_POINT('',#141519);
#36212=VERTEX_POINT('',#141521);
#36213=VERTEX_POINT('',#141523);
#36214=VERTEX_POINT('',#141534);
#36215=VERTEX_POINT('',#141536);
#36216=VERTEX_POINT('',#141556);
#36217=VERTEX_POINT('',#141561);
#36218=VERTEX_POINT('',#141578);
#36219=VERTEX_POINT('',#141580);
#36220=VERTEX_POINT('',#141597);
#36221=VERTEX_POINT('',#141602);
#36222=VERTEX_POINT('',#141618);
#36223=VERTEX_POINT('',#141622);
#36224=VERTEX_POINT('',#141626);
#36225=VERTEX_POINT('',#141630);
#36226=VERTEX_POINT('',#141631);
#36227=VERTEX_POINT('',#141633);
#36228=VERTEX_POINT('',#141635);
#36229=VERTEX_POINT('',#141638);
#36230=VERTEX_POINT('',#141640);
#36231=VERTEX_POINT('',#141663);
#36232=VERTEX_POINT('',#141668);
#36233=VERTEX_POINT('',#141688);
#36234=VERTEX_POINT('',#141690);
#36235=VERTEX_POINT('',#141707);
#36236=VERTEX_POINT('',#141712);
#36237=VERTEX_POINT('',#141729);
#36238=VERTEX_POINT('',#141731);
#36239=VERTEX_POINT('',#141744);
#36240=VERTEX_POINT('',#141745);
#36241=VERTEX_POINT('',#141747);
#36242=VERTEX_POINT('',#141778);
#36243=VERTEX_POINT('',#141812);
#36244=VERTEX_POINT('',#141813);
#36245=VERTEX_POINT('',#141827);
#36246=VERTEX_POINT('',#141832);
#36247=VERTEX_POINT('',#141840);
#36248=VERTEX_POINT('',#141857);
#36249=VERTEX_POINT('',#141859);
#36250=VERTEX_POINT('',#141885);
#36251=VERTEX_POINT('',#141894);
#36252=VERTEX_POINT('',#141896);
#36253=VERTEX_POINT('',#141898);
#36254=VERTEX_POINT('',#141900);
#36255=VERTEX_POINT('',#141933);
#36256=VERTEX_POINT('',#141946);
#36257=VERTEX_POINT('',#141947);
#36258=VERTEX_POINT('',#141958);
#36259=VERTEX_POINT('',#141960);
#36260=VERTEX_POINT('',#141992);
#36261=VERTEX_POINT('',#141994);
#36262=VERTEX_POINT('',#141996);
#36263=VERTEX_POINT('',#141998);
#36264=VERTEX_POINT('',#142028);
#36265=VERTEX_POINT('',#142030);
#36266=VERTEX_POINT('',#142032);
#36267=VERTEX_POINT('',#142034);
#36268=VERTEX_POINT('',#142036);
#36269=VERTEX_POINT('',#142040);
#36270=VERTEX_POINT('',#142044);
#36271=VERTEX_POINT('',#142048);
#36272=VERTEX_POINT('',#142052);
#36273=VERTEX_POINT('',#142053);
#36274=VERTEX_POINT('',#142055);
#36275=VERTEX_POINT('',#142057);
#36276=VERTEX_POINT('',#142060);
#36277=VERTEX_POINT('',#142071);
#36278=VERTEX_POINT('',#142073);
#36279=VERTEX_POINT('',#142093);
#36280=VERTEX_POINT('',#142098);
#36281=VERTEX_POINT('',#142118);
#36282=VERTEX_POINT('',#142120);
#36283=VERTEX_POINT('',#142137);
#36284=VERTEX_POINT('',#142142);
#36285=VERTEX_POINT('',#142156);
#36286=VERTEX_POINT('',#142158);
#36287=VERTEX_POINT('',#142202);
#36288=VERTEX_POINT('',#142203);
#36289=VERTEX_POINT('',#142237);
#36290=VERTEX_POINT('',#142253);
#36291=VERTEX_POINT('',#142255);
#36292=VERTEX_POINT('',#142257);
#36293=VERTEX_POINT('',#142259);
#36294=VERTEX_POINT('',#142261);
#36295=VERTEX_POINT('',#142263);
#36296=VERTEX_POINT('',#142265);
#36297=VERTEX_POINT('',#142276);
#36298=VERTEX_POINT('',#142278);
#36299=VERTEX_POINT('',#142301);
#36300=VERTEX_POINT('',#142306);
#36301=VERTEX_POINT('',#142326);
#36302=VERTEX_POINT('',#142328);
#36303=VERTEX_POINT('',#142345);
#36304=VERTEX_POINT('',#142350);
#36305=VERTEX_POINT('',#142369);
#36306=VERTEX_POINT('',#142373);
#36307=VERTEX_POINT('',#142377);
#36308=VERTEX_POINT('',#142410);
#36309=VERTEX_POINT('',#142423);
#36310=VERTEX_POINT('',#142424);
#36311=VERTEX_POINT('',#142426);
#36312=VERTEX_POINT('',#142428);
#36313=VERTEX_POINT('',#142431);
#36314=VERTEX_POINT('',#142433);
#36315=VERTEX_POINT('',#142453);
#36316=VERTEX_POINT('',#142458);
#36317=VERTEX_POINT('',#142487);
#36318=VERTEX_POINT('',#142489);
#36319=VERTEX_POINT('',#142506);
#36320=VERTEX_POINT('',#142511);
#36321=VERTEX_POINT('',#142525);
#36322=VERTEX_POINT('',#142527);
#36323=VERTEX_POINT('',#142544);
#36324=VERTEX_POINT('',#142546);
#36325=VERTEX_POINT('',#142550);
#36326=VERTEX_POINT('',#142553);
#36327=VERTEX_POINT('',#142583);
#36328=VERTEX_POINT('',#142587);
#36329=VERTEX_POINT('',#142605);
#36330=VERTEX_POINT('',#142607);
#36331=VERTEX_POINT('',#142611);
#36332=VERTEX_POINT('',#142615);
#36333=VERTEX_POINT('',#142642);
#36334=VERTEX_POINT('',#142665);
#36335=VERTEX_POINT('',#142667);
#36336=VERTEX_POINT('',#142673);
#36337=VERTEX_POINT('',#142677);
#36338=VERTEX_POINT('',#142739);
#36339=VERTEX_POINT('',#142764);
#36340=VERTEX_POINT('',#142940);
#36341=VERTEX_POINT('',#142984);
#36342=VERTEX_POINT('',#142988);
#36343=VERTEX_POINT('',#143004);
#36344=VERTEX_POINT('',#143006);
#36345=VERTEX_POINT('',#143035);
#36346=VERTEX_POINT('',#143039);
#36347=VERTEX_POINT('',#143055);
#36348=VERTEX_POINT('',#143057);
#36349=VERTEX_POINT('',#143085);
#36350=VERTEX_POINT('',#143121);
#36351=VERTEX_POINT('',#143154);
#36352=VERTEX_POINT('',#143167);
#36353=VERTEX_POINT('',#143214);
#36354=VERTEX_POINT('',#143218);
#36355=VERTEX_POINT('',#143222);
#36356=VERTEX_POINT('',#143226);
#36357=VERTEX_POINT('',#143230);
#36358=VERTEX_POINT('',#143232);
#36359=VERTEX_POINT('',#143234);
#36360=VERTEX_POINT('',#143248);
#36361=VERTEX_POINT('',#143250);
#36362=VERTEX_POINT('',#143252);
#36363=VERTEX_POINT('',#143260);
#36364=VERTEX_POINT('',#143262);
#36365=VERTEX_POINT('',#143270);
#36366=VERTEX_POINT('',#143272);
#36367=VERTEX_POINT('',#143274);
#36368=VERTEX_POINT('',#143276);
#36369=VERTEX_POINT('',#143284);
#36370=VERTEX_POINT('',#143286);
#36371=VERTEX_POINT('',#143296);
#36372=VERTEX_POINT('',#143297);
#36373=VERTEX_POINT('',#143303);
#36374=VERTEX_POINT('',#143312);
#36375=VERTEX_POINT('',#143314);
#36376=VERTEX_POINT('',#143316);
#36377=VERTEX_POINT('',#143318);
#36378=VERTEX_POINT('',#143365);
#36379=VERTEX_POINT('',#143367);
#36380=VERTEX_POINT('',#143369);
#36381=VERTEX_POINT('',#143371);
#36382=VERTEX_POINT('',#143380);
#36383=VERTEX_POINT('',#143382);
#36384=VERTEX_POINT('',#143389);
#36385=VERTEX_POINT('',#143391);
#36386=VERTEX_POINT('',#143393);
#36387=VERTEX_POINT('',#143395);
#36388=VERTEX_POINT('',#143397);
#36389=VERTEX_POINT('',#143441);
#36390=VERTEX_POINT('',#143443);
#36391=VERTEX_POINT('',#143452);
#36392=VERTEX_POINT('',#143454);
#36393=VERTEX_POINT('',#143456);
#36394=VERTEX_POINT('',#143458);
#36395=VERTEX_POINT('',#143467);
#36396=VERTEX_POINT('',#143469);
#36397=VERTEX_POINT('',#143510);
#36398=VERTEX_POINT('',#143512);
#36399=VERTEX_POINT('',#143514);
#36400=VERTEX_POINT('',#143516);
#36401=VERTEX_POINT('',#143566);
#36402=VERTEX_POINT('',#143568);
#36403=VERTEX_POINT('',#143575);
#36404=VERTEX_POINT('',#143577);
#36405=VERTEX_POINT('',#143579);
#36406=VERTEX_POINT('',#143581);
#36407=VERTEX_POINT('',#143586);
#36408=VERTEX_POINT('',#143591);
#36409=VERTEX_POINT('',#143593);
#36410=VERTEX_POINT('',#143640);
#36411=VERTEX_POINT('',#143642);
#36412=VERTEX_POINT('',#143644);
#36413=VERTEX_POINT('',#143646);
#36414=VERTEX_POINT('',#143690);
#36415=VERTEX_POINT('',#143697);
#36416=VERTEX_POINT('',#143699);
#36417=VERTEX_POINT('',#143704);
#36418=VERTEX_POINT('',#143713);
#36419=VERTEX_POINT('',#143714);
#36420=VERTEX_POINT('',#143716);
#36421=VERTEX_POINT('',#143718);
#36422=VERTEX_POINT('',#143726);
#36423=VERTEX_POINT('',#143728);
#36424=VERTEX_POINT('',#143736);
#36425=VERTEX_POINT('',#143738);
#36426=VERTEX_POINT('',#143753);
#36427=VERTEX_POINT('',#143755);
#36428=VERTEX_POINT('',#143757);
#36429=VERTEX_POINT('',#143759);
#36430=VERTEX_POINT('',#143767);
#36431=VERTEX_POINT('',#143769);
#36432=VERTEX_POINT('',#143779);
#36433=VERTEX_POINT('',#143783);
#36434=VERTEX_POINT('',#143787);
#36435=VERTEX_POINT('',#143791);
#36436=VERTEX_POINT('',#143793);
#36437=VERTEX_POINT('',#143807);
#36438=VERTEX_POINT('',#143809);
#36439=VERTEX_POINT('',#143811);
#36440=VERTEX_POINT('',#143819);
#36441=VERTEX_POINT('',#143821);
#36442=VERTEX_POINT('',#143829);
#36443=VERTEX_POINT('',#143831);
#36444=VERTEX_POINT('',#143833);
#36445=VERTEX_POINT('',#143835);
#36446=VERTEX_POINT('',#143843);
#36447=VERTEX_POINT('',#143845);
#36448=VERTEX_POINT('',#143887);
#36449=VERTEX_POINT('',#143888);
#36450=VERTEX_POINT('',#143890);
#36451=VERTEX_POINT('',#143892);
#36452=VERTEX_POINT('',#143894);
#36453=VERTEX_POINT('',#143896);
#36454=VERTEX_POINT('',#143933);
#36455=VERTEX_POINT('',#143935);
#36456=VERTEX_POINT('',#143971);
#36457=VERTEX_POINT('',#143973);
#36458=VERTEX_POINT('',#143975);
#36459=VERTEX_POINT('',#143977);
#36460=VERTEX_POINT('',#143979);
#36461=VERTEX_POINT('',#143985);
#36462=VERTEX_POINT('',#144002);
#36463=VERTEX_POINT('',#144007);
#36464=VERTEX_POINT('',#144033);
#36465=VERTEX_POINT('',#144037);
#36466=VERTEX_POINT('',#144056);
#36467=VERTEX_POINT('',#144061);
#36468=VERTEX_POINT('',#144127);
#36469=VERTEX_POINT('',#144155);
#36470=VERTEX_POINT('',#144231);
#36471=VERTEX_POINT('',#144244);
#36472=VERTEX_POINT('',#144309);
#36473=VERTEX_POINT('',#144310);
#36474=VERTEX_POINT('',#144323);
#36475=VERTEX_POINT('',#144366);
#36476=VERTEX_POINT('',#144370);
#36477=VERTEX_POINT('',#144404);
#36478=VERTEX_POINT('',#144470);
#36479=VERTEX_POINT('',#144578);
#36480=VERTEX_POINT('',#144606);
#36481=VERTEX_POINT('',#144651);
#36482=VERTEX_POINT('',#144707);
#36483=VERTEX_POINT('',#144770);
#36484=VERTEX_POINT('',#144774);
#36485=VERTEX_POINT('',#144780);
#36486=VERTEX_POINT('',#144829);
#36487=VERTEX_POINT('',#144860);
#36488=VERTEX_POINT('',#144888);
#36489=VERTEX_POINT('',#144911);
#36490=VERTEX_POINT('',#144967);
#36491=VERTEX_POINT('',#145033);
#36492=VERTEX_POINT('',#145041);
#36493=VERTEX_POINT('',#145042);
#36494=VERTEX_POINT('',#145248);
#36495=VERTEX_POINT('',#145252);
#36496=VERTEX_POINT('',#145258);
#36497=VERTEX_POINT('',#145262);
#36498=VERTEX_POINT('',#145268);
#36499=VERTEX_POINT('',#145269);
#36500=VERTEX_POINT('',#145297);
#36501=VERTEX_POINT('',#145318);
#36502=VERTEX_POINT('',#145344);
#36503=VERTEX_POINT('',#145353);
#36504=VERTEX_POINT('',#145425);
#36505=VERTEX_POINT('',#145448);
#36506=VERTEX_POINT('',#145538);
#36507=VERTEX_POINT('',#145559);
#36508=VERTEX_POINT('',#145585);
#36509=VERTEX_POINT('',#145610);
#36510=VERTEX_POINT('',#145612);
#36511=VERTEX_POINT('',#145623);
#36512=VERTEX_POINT('',#145627);
#36513=VERTEX_POINT('',#145633);
#36514=VERTEX_POINT('',#145658);
#36515=VERTEX_POINT('',#145662);
#36516=VERTEX_POINT('',#145663);
#36517=VERTEX_POINT('',#145685);
#36518=VERTEX_POINT('',#145706);
#36519=VERTEX_POINT('',#145732);
#36520=VERTEX_POINT('',#145741);
#36521=VERTEX_POINT('',#145814);
#36522=VERTEX_POINT('',#145892);
#36523=VERTEX_POINT('',#145913);
#36524=VERTEX_POINT('',#145933);
#36525=VERTEX_POINT('',#145997);
#36526=VERTEX_POINT('',#145999);
#36527=VERTEX_POINT('',#146027);
#36528=VERTEX_POINT('',#146090);
#36529=VERTEX_POINT('',#146163);
#36530=VERTEX_POINT('',#146178);
#36531=VERTEX_POINT('',#146202);
#36532=VERTEX_POINT('',#146212);
#36533=VERTEX_POINT('',#146276);
#36534=VERTEX_POINT('',#146327);
#36535=VERTEX_POINT('',#146342);
#36536=VERTEX_POINT('',#146357);
#36537=VERTEX_POINT('',#146409);
#36538=VERTEX_POINT('',#146411);
#36539=VERTEX_POINT('',#146471);
#36540=VERTEX_POINT('',#146519);
#36541=VERTEX_POINT('',#146557);
#36542=VERTEX_POINT('',#146572);
#36543=VERTEX_POINT('',#146590);
#36544=VERTEX_POINT('',#146594);
#36545=VERTEX_POINT('',#146634);
#36546=VERTEX_POINT('',#146700);
#36547=VERTEX_POINT('',#146721);
#36548=VERTEX_POINT('',#146760);
#36549=VERTEX_POINT('',#146824);
#36550=VERTEX_POINT('',#146826);
#36551=VERTEX_POINT('',#146887);
#36552=VERTEX_POINT('',#146950);
#36553=VERTEX_POINT('',#146986);
#36554=VERTEX_POINT('',#147001);
#36555=VERTEX_POINT('',#147025);
#36556=VERTEX_POINT('',#147053);
#36557=VERTEX_POINT('',#147104);
#36558=VERTEX_POINT('',#147169);
#36559=VERTEX_POINT('',#147190);
#36560=VERTEX_POINT('',#147238);
#36561=VERTEX_POINT('',#147263);
#36562=VERTEX_POINT('',#147265);
#36563=VERTEX_POINT('',#147267);
#36564=VERTEX_POINT('',#147274);
#36565=VERTEX_POINT('',#147280);
#36566=VERTEX_POINT('',#147305);
#36567=VERTEX_POINT('',#147309);
#36568=VERTEX_POINT('',#147313);
#36569=VERTEX_POINT('',#147367);
#36570=VERTEX_POINT('',#147388);
#36571=VERTEX_POINT('',#147414);
#36572=VERTEX_POINT('',#147445);
#36573=VERTEX_POINT('',#147491);
#36574=VERTEX_POINT('',#147548);
#36575=VERTEX_POINT('',#147555);
#36576=VERTEX_POINT('',#147557);
#36577=VERTEX_POINT('',#147570);
#36578=VERTEX_POINT('',#147595);
#36579=VERTEX_POINT('',#147616);
#36580=VERTEX_POINT('',#147685);
#36581=VERTEX_POINT('',#147686);
#36582=VERTEX_POINT('',#147707);
#36583=VERTEX_POINT('',#147745);
#36584=VERTEX_POINT('',#147747);
#36585=VERTEX_POINT('',#147763);
#36586=VERTEX_POINT('',#147765);
#36587=VERTEX_POINT('',#147774);
#36588=VERTEX_POINT('',#147778);
#36589=VERTEX_POINT('',#147838);
#36590=VERTEX_POINT('',#147851);
#36591=VERTEX_POINT('',#147884);
#36592=VERTEX_POINT('',#147947);
#36593=VERTEX_POINT('',#147967);
#36594=VERTEX_POINT('',#147973);
#36595=VERTEX_POINT('',#147985);
#36596=VERTEX_POINT('',#148019);
#36597=VERTEX_POINT('',#148023);
#36598=VERTEX_POINT('',#148027);
#36599=VERTEX_POINT('',#148124);
#36600=VERTEX_POINT('',#148139);
#36601=VERTEX_POINT('',#148163);
#36602=VERTEX_POINT('',#148197);
#36603=VERTEX_POINT('',#148224);
#36604=VERTEX_POINT('',#148251);
#36605=VERTEX_POINT('',#148257);
#36606=VERTEX_POINT('',#148330);
#36607=VERTEX_POINT('',#148343);
#36608=VERTEX_POINT('',#148376);
#36609=VERTEX_POINT('',#148430);
#36610=VERTEX_POINT('',#148466);
#36611=VERTEX_POINT('',#148479);
#36612=VERTEX_POINT('',#148526);
#36613=VERTEX_POINT('',#148528);
#36614=VERTEX_POINT('',#148537);
#36615=VERTEX_POINT('',#148541);
#36616=VERTEX_POINT('',#148547);
#36617=VERTEX_POINT('',#148553);
#36618=VERTEX_POINT('',#148554);
#36619=VERTEX_POINT('',#148596);
#36620=VERTEX_POINT('',#148609);
#36621=VERTEX_POINT('',#148630);
#36622=VERTEX_POINT('',#148650);
#36623=VERTEX_POINT('',#148680);
#36624=VERTEX_POINT('',#148723);
#36625=VERTEX_POINT('',#148750);
#36626=VERTEX_POINT('',#148796);
#36627=VERTEX_POINT('',#148802);
#36628=VERTEX_POINT('',#148803);
#36629=VERTEX_POINT('',#148854);
#36630=VERTEX_POINT('',#149051);
#36631=VERTEX_POINT('',#149103);
#36632=VERTEX_POINT('',#149104);
#36633=VERTEX_POINT('',#149156);
#36634=VERTEX_POINT('',#149158);
#36635=VERTEX_POINT('',#149174);
#36636=VERTEX_POINT('',#149176);
#36637=VERTEX_POINT('',#149185);
#36638=VERTEX_POINT('',#149189);
#36639=VERTEX_POINT('',#149237);
#36640=VERTEX_POINT('',#149273);
#36641=VERTEX_POINT('',#149325);
#36642=VERTEX_POINT('',#149364);
#36643=VERTEX_POINT('',#149427);
#36644=VERTEX_POINT('',#149457);
#36645=VERTEX_POINT('',#149470);
#36646=VERTEX_POINT('',#149508);
#36647=VERTEX_POINT('',#149512);
#36648=VERTEX_POINT('',#149516);
#36649=VERTEX_POINT('',#149572);
#36650=VERTEX_POINT('',#149573);
#36651=VERTEX_POINT('',#149584);
#36652=VERTEX_POINT('',#149614);
#36653=VERTEX_POINT('',#149653);
#36654=VERTEX_POINT('',#149674);
#36655=VERTEX_POINT('',#149700);
#36656=VERTEX_POINT('',#149740);
#36657=VERTEX_POINT('',#149767);
#36658=VERTEX_POINT('',#149830);
#36659=VERTEX_POINT('',#149836);
#36660=VERTEX_POINT('',#149912);
#36661=VERTEX_POINT('',#149925);
#36662=VERTEX_POINT('',#149958);
#36663=VERTEX_POINT('',#149982);
#36664=VERTEX_POINT('',#150018);
#36665=VERTEX_POINT('',#150031);
#36666=VERTEX_POINT('',#150078);
#36667=VERTEX_POINT('',#150080);
#36668=VERTEX_POINT('',#150089);
#36669=VERTEX_POINT('',#150093);
#36670=VERTEX_POINT('',#150099);
#36671=VERTEX_POINT('',#150105);
#36672=VERTEX_POINT('',#150106);
#36673=VERTEX_POINT('',#150148);
#36674=VERTEX_POINT('',#150161);
#36675=VERTEX_POINT('',#150182);
#36676=VERTEX_POINT('',#150202);
#36677=VERTEX_POINT('',#150232);
#36678=VERTEX_POINT('',#150275);
#36679=VERTEX_POINT('',#150302);
#36680=VERTEX_POINT('',#150386);
#36681=VERTEX_POINT('',#150392);
#36682=VERTEX_POINT('',#150393);
#36683=VERTEX_POINT('',#150474);
#36684=VERTEX_POINT('',#150486);
#36685=VERTEX_POINT('',#150493);
#36686=VERTEX_POINT('',#150495);
#36687=VERTEX_POINT('',#150499);
#36688=VERTEX_POINT('',#150541);
#36689=VERTEX_POINT('',#150581);
#36690=VERTEX_POINT('',#150608);
#36691=VERTEX_POINT('',#150638);
#36692=VERTEX_POINT('',#150704);
#36693=VERTEX_POINT('',#150706);
#36694=VERTEX_POINT('',#150715);
#36695=VERTEX_POINT('',#150719);
#36696=VERTEX_POINT('',#150756);
#36697=VERTEX_POINT('',#150763);
#36698=VERTEX_POINT('',#150769);
#36699=VERTEX_POINT('',#150770);
#36700=VERTEX_POINT('',#150780);
#36701=VERTEX_POINT('',#150814);
#36702=VERTEX_POINT('',#150827);
#36703=VERTEX_POINT('',#150860);
#36704=VERTEX_POINT('',#150884);
#36705=VERTEX_POINT('',#150920);
#36706=VERTEX_POINT('',#150972);
#36707=VERTEX_POINT('',#151011);
#36708=VERTEX_POINT('',#151074);
#36709=VERTEX_POINT('',#151115);
#36710=VERTEX_POINT('',#151121);
#36711=VERTEX_POINT('',#151162);
#36712=VERTEX_POINT('',#151192);
#36713=VERTEX_POINT('',#151238);
#36714=VERTEX_POINT('',#151265);
#36715=VERTEX_POINT('',#151325);
#36716=VERTEX_POINT('',#151349);
#36717=VERTEX_POINT('',#151358);
#36718=VERTEX_POINT('',#151405);
#36719=VERTEX_POINT('',#151407);
#36720=VERTEX_POINT('',#151416);
#36721=VERTEX_POINT('',#151420);
#36722=VERTEX_POINT('',#151426);
#36723=VERTEX_POINT('',#151433);
#36724=VERTEX_POINT('',#151434);
#36725=VERTEX_POINT('',#151444);
#36726=VERTEX_POINT('',#151478);
#36727=VERTEX_POINT('',#151491);
#36728=VERTEX_POINT('',#151518);
#36729=VERTEX_POINT('',#151540);
#36730=VERTEX_POINT('',#151570);
#36731=VERTEX_POINT('',#151583);
#36732=VERTEX_POINT('',#151667);
#36733=VERTEX_POINT('',#151813);
#36734=VERTEX_POINT('',#151834);
#36735=VERTEX_POINT('',#151957);
#36736=VERTEX_POINT('',#152235);
#36737=VERTEX_POINT('',#152349);
#36738=VERTEX_POINT('',#152417);
#36739=VERTEX_POINT('',#152557);
#36740=VERTEX_POINT('',#153125);
#36741=VERTEX_POINT('',#153468);
#36742=VERTEX_POINT('',#153469);
#36743=VERTEX_POINT('',#153471);
#36744=VERTEX_POINT('',#153475);
#36745=VERTEX_POINT('',#153476);
#36746=VERTEX_POINT('',#153478);
#36747=VERTEX_POINT('',#153480);
#36748=VERTEX_POINT('',#153484);
#36749=VERTEX_POINT('',#153486);
#36750=VERTEX_POINT('',#153490);
#36751=VERTEX_POINT('',#153492);
#36752=VERTEX_POINT('',#153496);
#36753=VERTEX_POINT('',#153497);
#36754=VERTEX_POINT('',#153514);
#36755=VERTEX_POINT('',#153531);
#36756=VERTEX_POINT('',#153549);
#36757=VERTEX_POINT('',#153550);
#36758=VERTEX_POINT('',#153792);
#36759=VERTEX_POINT('',#153793);
#36760=VERTEX_POINT('',#153812);
#36761=VERTEX_POINT('',#153813);
#36762=VERTEX_POINT('',#154067);
#36763=VERTEX_POINT('',#154068);
#36764=VERTEX_POINT('',#154091);
#36765=VERTEX_POINT('',#154092);
#36766=VERTEX_POINT('',#154229);
#36767=VERTEX_POINT('',#154230);
#36768=VERTEX_POINT('',#154235);
#36769=VERTEX_POINT('',#154236);
#36770=VERTEX_POINT('',#154238);
#36771=VERTEX_POINT('',#154240);
#36772=VERTEX_POINT('',#154244);
#36773=VERTEX_POINT('',#154246);
#36774=VERTEX_POINT('',#154250);
#36775=VERTEX_POINT('',#154252);
#36776=VERTEX_POINT('',#154256);
#36777=VERTEX_POINT('',#154257);
#36778=VERTEX_POINT('',#154271);
#36779=VERTEX_POINT('',#154273);
#36780=VERTEX_POINT('',#154369);
#36781=VERTEX_POINT('',#154398);
#36782=VERTEX_POINT('',#154452);
#36783=VERTEX_POINT('',#154508);
#36784=VERTEX_POINT('',#154602);
#36785=VERTEX_POINT('',#154604);
#36786=VERTEX_POINT('',#154637);
#36787=VERTEX_POINT('',#154723);
#36788=VERTEX_POINT('',#154808);
#36789=VERTEX_POINT('',#154809);
#36790=VERTEX_POINT('',#154811);
#36791=VERTEX_POINT('',#154813);
#36792=VERTEX_POINT('',#154817);
#36793=VERTEX_POINT('',#154819);
#36794=VERTEX_POINT('',#154823);
#36795=VERTEX_POINT('',#154825);
#36796=VERTEX_POINT('',#154829);
#36797=VERTEX_POINT('',#154830);
#36798=VERTEX_POINT('',#154832);
#36799=VERTEX_POINT('',#154853);
#36800=VERTEX_POINT('',#154854);
#36801=VERTEX_POINT('',#154868);
#36802=VERTEX_POINT('',#154945);
#36803=VERTEX_POINT('',#154982);
#36804=VERTEX_POINT('',#154983);
#36805=VERTEX_POINT('',#155017);
#36806=VERTEX_POINT('',#155018);
#36807=VERTEX_POINT('',#155239);
#36808=VERTEX_POINT('',#155240);
#36809=VERTEX_POINT('',#155306);
#36810=VERTEX_POINT('',#155308);
#36811=VERTEX_POINT('',#155369);
#36812=VERTEX_POINT('',#155370);
#36813=VERTEX_POINT('',#155372);
#36814=VERTEX_POINT('',#155374);
#36815=VERTEX_POINT('',#155378);
#36816=VERTEX_POINT('',#155449);
#36817=VERTEX_POINT('',#155519);
#36818=VERTEX_POINT('',#155524);
#36819=VERTEX_POINT('',#155569);
#36820=VERTEX_POINT('',#155673);
#36821=VERTEX_POINT('',#155809);
#36822=VERTEX_POINT('',#155811);
#36823=VERTEX_POINT('',#155829);
#36824=VERTEX_POINT('',#155951);
#36825=VERTEX_POINT('',#156126);
#36826=VERTEX_POINT('',#156127);
#36827=VERTEX_POINT('',#156129);
#36828=VERTEX_POINT('',#156131);
#36829=VERTEX_POINT('',#156135);
#36830=VERTEX_POINT('',#156136);
#36831=VERTEX_POINT('',#156141);
#36832=VERTEX_POINT('',#156143);
#36833=VERTEX_POINT('',#156147);
#36834=VERTEX_POINT('',#156152);
#36835=VERTEX_POINT('',#156171);
#36836=VERTEX_POINT('',#156172);
#36837=VERTEX_POINT('',#156189);
#36838=VERTEX_POINT('',#156203);
#36839=VERTEX_POINT('',#156210);
#36840=VERTEX_POINT('',#156211);
#36841=VERTEX_POINT('',#156225);
#36842=VERTEX_POINT('',#156238);
#36843=VERTEX_POINT('',#156239);
#36844=VERTEX_POINT('',#156241);
#36845=VERTEX_POINT('',#156243);
#36846=VERTEX_POINT('',#156247);
#36847=VERTEX_POINT('',#156249);
#36848=VERTEX_POINT('',#156253);
#36849=VERTEX_POINT('',#156255);
#36850=VERTEX_POINT('',#156259);
#36851=VERTEX_POINT('',#156260);
#36852=VERTEX_POINT('',#156262);
#36853=VERTEX_POINT('',#156277);
#36854=VERTEX_POINT('',#156278);
#36855=VERTEX_POINT('',#156283);
#36856=VERTEX_POINT('',#156357);
#36857=VERTEX_POINT('',#156421);
#36858=VERTEX_POINT('',#156422);
#36859=VERTEX_POINT('',#156441);
#36860=VERTEX_POINT('',#156442);
#36861=VERTEX_POINT('',#156657);
#36862=VERTEX_POINT('',#156658);
#36863=VERTEX_POINT('',#156698);
#36864=VERTEX_POINT('',#156699);
#36865=VERTEX_POINT('',#156701);
#36866=VERTEX_POINT('',#156703);
#36867=VERTEX_POINT('',#156707);
#36868=VERTEX_POINT('',#156708);
#36869=VERTEX_POINT('',#156710);
#36870=VERTEX_POINT('',#156712);
#36871=VERTEX_POINT('',#156716);
#36872=VERTEX_POINT('',#156798);
#36873=VERTEX_POINT('',#156864);
#36874=VERTEX_POINT('',#156956);
#36875=VERTEX_POINT('',#157089);
#36876=VERTEX_POINT('',#157091);
#36877=VERTEX_POINT('',#157098);
#36878=VERTEX_POINT('',#157099);
#36879=VERTEX_POINT('',#157101);
#36880=VERTEX_POINT('',#157103);
#36881=VERTEX_POINT('',#157107);
#36882=VERTEX_POINT('',#157108);
#36883=VERTEX_POINT('',#157113);
#36884=VERTEX_POINT('',#157115);
#36885=VERTEX_POINT('',#157119);
#36886=VERTEX_POINT('',#157120);
#36887=VERTEX_POINT('',#157122);
#36888=VERTEX_POINT('',#157158);
#36889=VERTEX_POINT('',#157342);
#36890=VERTEX_POINT('',#157343);
#36891=VERTEX_POINT('',#157345);
#36892=VERTEX_POINT('',#157347);
#36893=VERTEX_POINT('',#157351);
#36894=VERTEX_POINT('',#157353);
#36895=VERTEX_POINT('',#157357);
#36896=VERTEX_POINT('',#157358);
#36897=VERTEX_POINT('',#157378);
#36898=VERTEX_POINT('',#157380);
#36899=VERTEX_POINT('',#157419);
#36900=VERTEX_POINT('',#157420);
#36901=VERTEX_POINT('',#157570);
#36902=VERTEX_POINT('',#157571);
#36903=VERTEX_POINT('',#157645);
#36904=VERTEX_POINT('',#157646);
#36905=VERTEX_POINT('',#157648);
#36906=VERTEX_POINT('',#157650);
#36907=VERTEX_POINT('',#157654);
#36908=VERTEX_POINT('',#157655);
#36909=VERTEX_POINT('',#157657);
#36910=VERTEX_POINT('',#157659);
#36911=VERTEX_POINT('',#157666);
#36912=VERTEX_POINT('',#157700);
#36913=VERTEX_POINT('',#157701);
#36914=VERTEX_POINT('',#157721);
#36915=VERTEX_POINT('',#157723);
#36916=VERTEX_POINT('',#157768);
#36917=VERTEX_POINT('',#157769);
#36918=VERTEX_POINT('',#157936);
#36919=VERTEX_POINT('',#157937);
#36920=VERTEX_POINT('',#158010);
#36921=VERTEX_POINT('',#158011);
#36922=VERTEX_POINT('',#158124);
#36923=VERTEX_POINT('',#158126);
#36924=VERTEX_POINT('',#158232);
#36925=VERTEX_POINT('',#158233);
#36926=VERTEX_POINT('',#158253);
#36927=VERTEX_POINT('',#158255);
#36928=VERTEX_POINT('',#158300);
#36929=VERTEX_POINT('',#158301);
#36930=VERTEX_POINT('',#158393);
#36931=VERTEX_POINT('',#158394);
#36932=VERTEX_POINT('',#158433);
#36933=VERTEX_POINT('',#158434);
#36934=VERTEX_POINT('',#158496);
#36935=VERTEX_POINT('',#158498);
#36936=VERTEX_POINT('',#158541);
#36937=VERTEX_POINT('',#158542);
#36938=VERTEX_POINT('',#158568);
#36939=VERTEX_POINT('',#158570);
#36940=VERTEX_POINT('',#158618);
#36941=VERTEX_POINT('',#158619);
#36942=VERTEX_POINT('',#158726);
#36943=VERTEX_POINT('',#158727);
#36944=VERTEX_POINT('',#158785);
#36945=VERTEX_POINT('',#158786);
#36946=VERTEX_POINT('',#158817);
#36947=VERTEX_POINT('',#158819);
#36948=VERTEX_POINT('',#158955);
#36949=VERTEX_POINT('',#158956);
#36950=VERTEX_POINT('',#158973);
#36951=VERTEX_POINT('',#158975);
#36952=VERTEX_POINT('',#159014);
#36953=VERTEX_POINT('',#159015);
#36954=VERTEX_POINT('',#159212);
#36955=VERTEX_POINT('',#159213);
#36956=VERTEX_POINT('',#159248);
#36957=VERTEX_POINT('',#159249);
#36958=VERTEX_POINT('',#159251);
#36959=VERTEX_POINT('',#159268);
#36960=VERTEX_POINT('',#159269);
#36961=VERTEX_POINT('',#159271);
#36962=VERTEX_POINT('',#159273);
#36963=VERTEX_POINT('',#159277);
#36964=VERTEX_POINT('',#159282);
#36965=VERTEX_POINT('',#159286);
#36966=VERTEX_POINT('',#159287);
#36967=VERTEX_POINT('',#159289);
#36968=VERTEX_POINT('',#159291);
#36969=VERTEX_POINT('',#159295);
#36970=VERTEX_POINT('',#159296);
#36971=VERTEX_POINT('',#159316);
#36972=VERTEX_POINT('',#159318);
#36973=VERTEX_POINT('',#159357);
#36974=VERTEX_POINT('',#159358);
#36975=VERTEX_POINT('',#159501);
#36976=VERTEX_POINT('',#159502);
#36977=VERTEX_POINT('',#159552);
#36978=VERTEX_POINT('',#159554);
#36979=VERTEX_POINT('',#159558);
#36980=VERTEX_POINT('',#159559);
#36981=VERTEX_POINT('',#159564);
#36982=VERTEX_POINT('',#159565);
#36983=VERTEX_POINT('',#159570);
#36984=VERTEX_POINT('',#159571);
#36985=VERTEX_POINT('',#159591);
#36986=VERTEX_POINT('',#159593);
#36987=VERTEX_POINT('',#159612);
#36988=VERTEX_POINT('',#159613);
#36989=VERTEX_POINT('',#159615);
#36990=VERTEX_POINT('',#159617);
#36991=VERTEX_POINT('',#159621);
#36992=VERTEX_POINT('',#159622);
#36993=VERTEX_POINT('',#159639);
#36994=VERTEX_POINT('',#159641);
#36995=VERTEX_POINT('',#159660);
#36996=VERTEX_POINT('',#159661);
#36997=VERTEX_POINT('',#159687);
#36998=VERTEX_POINT('',#159689);
#36999=VERTEX_POINT('',#159717);
#37000=VERTEX_POINT('',#159718);
#37001=VERTEX_POINT('',#159720);
#37002=VERTEX_POINT('',#159722);
#37003=VERTEX_POINT('',#159742);
#37004=VERTEX_POINT('',#159744);
#37005=VERTEX_POINT('',#159831);
#37006=VERTEX_POINT('',#159832);
#37007=VERTEX_POINT('',#159928);
#37008=VERTEX_POINT('',#159929);
#37009=VERTEX_POINT('',#160102);
#37010=VERTEX_POINT('',#160104);
#37011=VERTEX_POINT('',#160125);
#37012=VERTEX_POINT('',#160126);
#37013=VERTEX_POINT('',#160364);
#37014=VERTEX_POINT('',#160365);
#37015=VERTEX_POINT('',#160367);
#37016=VERTEX_POINT('',#160369);
#37017=VERTEX_POINT('',#160396);
#37018=VERTEX_POINT('',#160398);
#37019=VERTEX_POINT('',#160414);
#37020=VERTEX_POINT('',#160507);
#37021=VERTEX_POINT('',#160509);
#37022=VERTEX_POINT('',#160565);
#37023=VERTEX_POINT('',#160575);
#37024=VERTEX_POINT('',#160596);
#37025=VERTEX_POINT('',#160604);
#37026=VERTEX_POINT('',#160653);
#37027=VERTEX_POINT('',#160654);
#37028=VERTEX_POINT('',#160817);
#37029=VERTEX_POINT('',#160818);
#37030=VERTEX_POINT('',#160820);
#37031=VERTEX_POINT('',#160885);
#37032=VERTEX_POINT('',#160906);
#37033=VERTEX_POINT('',#160914);
#37034=VERTEX_POINT('',#160963);
#37035=VERTEX_POINT('',#160964);
#37036=VERTEX_POINT('',#160966);
#37037=VERTEX_POINT('',#161037);
#37038=VERTEX_POINT('',#161041);
#37039=VERTEX_POINT('',#161043);
#37040=VERTEX_POINT('',#161047);
#37041=VERTEX_POINT('',#161049);
#37042=VERTEX_POINT('',#161053);
#37043=VERTEX_POINT('',#161055);
#37044=VERTEX_POINT('',#161076);
#37045=VERTEX_POINT('',#161078);
#37046=VERTEX_POINT('',#161128);
#37047=VERTEX_POINT('',#161138);
#37048=VERTEX_POINT('',#161159);
#37049=VERTEX_POINT('',#161167);
#37050=VERTEX_POINT('',#161222);
#37051=VERTEX_POINT('',#161299);
#37052=VERTEX_POINT('',#161320);
#37053=VERTEX_POINT('',#161336);
#37054=VERTEX_POINT('',#161338);
#37055=VERTEX_POINT('',#161428);
#37056=VERTEX_POINT('',#161429);
#37057=VERTEX_POINT('',#161431);
#37058=VERTEX_POINT('',#161490);
#37059=VERTEX_POINT('',#161511);
#37060=VERTEX_POINT('',#161519);
#37061=VERTEX_POINT('',#161574);
#37062=VERTEX_POINT('',#161575);
#37063=VERTEX_POINT('',#161735);
#37064=VERTEX_POINT('',#161825);
#37065=VERTEX_POINT('',#161826);
#37066=VERTEX_POINT('',#161828);
#37067=VERTEX_POINT('',#161843);
#37068=VERTEX_POINT('',#161885);
#37069=VERTEX_POINT('',#161890);
#37070=VERTEX_POINT('',#161923);
#37071=VERTEX_POINT('',#161924);
#37072=VERTEX_POINT('',#162034);
#37073=VERTEX_POINT('',#162035);
#37074=VERTEX_POINT('',#162063);
#37075=VERTEX_POINT('',#162065);
#37076=VERTEX_POINT('',#162139);
#37077=VERTEX_POINT('',#162152);
#37078=VERTEX_POINT('',#162173);
#37079=VERTEX_POINT('',#162218);
#37080=VERTEX_POINT('',#162219);
#37081=VERTEX_POINT('',#162233);
#37082=VERTEX_POINT('',#162234);
#37083=VERTEX_POINT('',#162268);
#37084=VERTEX_POINT('',#162270);
#37085=VERTEX_POINT('',#162335);
#37086=VERTEX_POINT('',#162392);
#37087=VERTEX_POINT('',#162419);
#37088=VERTEX_POINT('',#162502);
#37089=VERTEX_POINT('',#162520);
#37090=VERTEX_POINT('',#162521);
#37091=VERTEX_POINT('',#162549);
#37092=VERTEX_POINT('',#162551);
#37093=VERTEX_POINT('',#162628);
#37094=VERTEX_POINT('',#162659);
#37095=VERTEX_POINT('',#162698);
#37096=VERTEX_POINT('',#162739);
#37097=VERTEX_POINT('',#162830);
#37098=VERTEX_POINT('',#162831);
#37099=VERTEX_POINT('',#162865);
#37100=VERTEX_POINT('',#162867);
#37101=VERTEX_POINT('',#162938);
#37102=VERTEX_POINT('',#163001);
#37103=VERTEX_POINT('',#163022);
#37104=VERTEX_POINT('',#163051);
#37105=VERTEX_POINT('',#163103);
#37106=VERTEX_POINT('',#163104);
#37107=VERTEX_POINT('',#163120);
#37108=VERTEX_POINT('',#163122);
#37109=VERTEX_POINT('',#163129);
#37110=VERTEX_POINT('',#163180);
#37111=VERTEX_POINT('',#163211);
#37112=VERTEX_POINT('',#163244);
#37113=VERTEX_POINT('',#163245);
#37114=VERTEX_POINT('',#163310);
#37115=VERTEX_POINT('',#163311);
#37116=VERTEX_POINT('',#163345);
#37117=VERTEX_POINT('',#163346);
#37118=VERTEX_POINT('',#163348);
#37119=VERTEX_POINT('',#163464);
#37120=VERTEX_POINT('',#163479);
#37121=VERTEX_POINT('',#163487);
#37122=VERTEX_POINT('',#163538);
#37123=VERTEX_POINT('',#163573);
#37124=VERTEX_POINT('',#163630);
#37125=VERTEX_POINT('',#163631);
#37126=VERTEX_POINT('',#163669);
#37127=VERTEX_POINT('',#163685);
#37128=VERTEX_POINT('',#163778);
#37129=VERTEX_POINT('',#163780);
#37130=VERTEX_POINT('',#163836);
#37131=VERTEX_POINT('',#163846);
#37132=VERTEX_POINT('',#163867);
#37133=VERTEX_POINT('',#163875);
#37134=VERTEX_POINT('',#163924);
#37135=VERTEX_POINT('',#163925);
#37136=VERTEX_POINT('',#164088);
#37137=VERTEX_POINT('',#164089);
#37138=VERTEX_POINT('',#164091);
#37139=VERTEX_POINT('',#164156);
#37140=VERTEX_POINT('',#164177);
#37141=VERTEX_POINT('',#164185);
#37142=VERTEX_POINT('',#164234);
#37143=VERTEX_POINT('',#164235);
#37144=VERTEX_POINT('',#164237);
#37145=VERTEX_POINT('',#164308);
#37146=VERTEX_POINT('',#164312);
#37147=VERTEX_POINT('',#164314);
#37148=VERTEX_POINT('',#164318);
#37149=VERTEX_POINT('',#164320);
#37150=VERTEX_POINT('',#164324);
#37151=VERTEX_POINT('',#164326);
#37152=VERTEX_POINT('',#164330);
#37153=VERTEX_POINT('',#164332);
#37154=VERTEX_POINT('',#164405);
#37155=VERTEX_POINT('',#164406);
#37156=VERTEX_POINT('',#164408);
#37157=VERTEX_POINT('',#164429);
#37158=VERTEX_POINT('',#164430);
#37159=VERTEX_POINT('',#164659);
#37160=VERTEX_POINT('',#164660);
#37161=VERTEX_POINT('',#164677);
#37162=VERTEX_POINT('',#164784);
#37163=VERTEX_POINT('',#164890);
#37164=VERTEX_POINT('',#164891);
#37165=VERTEX_POINT('',#164896);
#37166=VERTEX_POINT('',#164897);
#37167=VERTEX_POINT('',#164899);
#37168=VERTEX_POINT('',#164940);
#37169=VERTEX_POINT('',#164944);
#37170=VERTEX_POINT('',#164945);
#37171=VERTEX_POINT('',#164950);
#37172=VERTEX_POINT('',#164952);
#37173=VERTEX_POINT('',#164956);
#37174=VERTEX_POINT('',#164971);
#37175=VERTEX_POINT('',#164973);
#37176=VERTEX_POINT('',#164990);
#37177=VERTEX_POINT('',#165020);
#37178=VERTEX_POINT('',#165051);
#37179=VERTEX_POINT('',#165078);
#37180=VERTEX_POINT('',#165108);
#37181=VERTEX_POINT('',#165138);
#37182=VERTEX_POINT('',#165154);
#37183=VERTEX_POINT('',#165187);
#37184=VERTEX_POINT('',#165188);
#37185=VERTEX_POINT('',#165207);
#37186=VERTEX_POINT('',#165208);
#37187=VERTEX_POINT('',#165210);
#37188=VERTEX_POINT('',#165212);
#37189=VERTEX_POINT('',#165216);
#37190=VERTEX_POINT('',#165218);
#37191=VERTEX_POINT('',#165222);
#37192=VERTEX_POINT('',#165226);
#37193=VERTEX_POINT('',#165228);
#37194=VERTEX_POINT('',#165232);
#37195=VERTEX_POINT('',#165236);
#37196=VERTEX_POINT('',#165242);
#37197=VERTEX_POINT('',#165276);
#37198=VERTEX_POINT('',#165289);
#37199=VERTEX_POINT('',#165310);
#37200=VERTEX_POINT('',#165346);
#37201=VERTEX_POINT('',#165376);
#37202=VERTEX_POINT('',#165398);
#37203=VERTEX_POINT('',#165425);
#37204=VERTEX_POINT('',#165455);
#37205=VERTEX_POINT('',#165479);
#37206=VERTEX_POINT('',#165496);
#37207=VERTEX_POINT('',#165575);
#37208=VERTEX_POINT('',#165577);
#37209=VERTEX_POINT('',#165581);
#37210=VERTEX_POINT('',#165654);
#37211=VERTEX_POINT('',#165656);
#37212=VERTEX_POINT('',#165660);
#37213=VERTEX_POINT('',#165664);
#37214=VERTEX_POINT('',#165665);
#37215=VERTEX_POINT('',#165667);
#37216=VERTEX_POINT('',#165695);
#37217=VERTEX_POINT('',#165728);
#37218=VERTEX_POINT('',#165770);
#37219=VERTEX_POINT('',#165792);
#37220=VERTEX_POINT('',#165825);
#37221=VERTEX_POINT('',#165855);
#37222=VERTEX_POINT('',#165891);
#37223=VERTEX_POINT('',#165907);
#37224=VERTEX_POINT('',#165940);
#37225=VERTEX_POINT('',#165941);
#37226=VERTEX_POINT('',#165960);
#37227=VERTEX_POINT('',#165962);
#37228=VERTEX_POINT('',#165966);
#37229=VERTEX_POINT('',#165970);
#37230=VERTEX_POINT('',#165971);
#37231=VERTEX_POINT('',#165974);
#37232=VERTEX_POINT('',#165978);
#37233=VERTEX_POINT('',#165980);
#37234=VERTEX_POINT('',#165984);
#37235=VERTEX_POINT('',#166017);
#37236=VERTEX_POINT('',#166046);
#37237=VERTEX_POINT('',#166075);
#37238=VERTEX_POINT('',#166077);
#37239=VERTEX_POINT('',#166081);
#37240=VERTEX_POINT('',#166085);
#37241=VERTEX_POINT('',#166091);
#37242=VERTEX_POINT('',#166147);
#37243=VERTEX_POINT('',#166149);
#37244=VERTEX_POINT('',#166173);
#37245=VERTEX_POINT('',#166206);
#37246=VERTEX_POINT('',#166225);
#37247=VERTEX_POINT('',#166246);
#37248=VERTEX_POINT('',#166291);
#37249=VERTEX_POINT('',#166292);
#37250=VERTEX_POINT('',#166330);
#37251=VERTEX_POINT('',#166332);
#37252=VERTEX_POINT('',#166336);
#37253=VERTEX_POINT('',#166342);
#37254=VERTEX_POINT('',#166454);
#37255=VERTEX_POINT('',#166455);
#37256=VERTEX_POINT('',#166462);
#37257=VERTEX_POINT('',#166464);
#37258=VERTEX_POINT('',#166468);
#37259=VERTEX_POINT('',#166489);
#37260=VERTEX_POINT('',#166491);
#37261=VERTEX_POINT('',#166547);
#37262=VERTEX_POINT('',#166583);
#37263=VERTEX_POINT('',#166613);
#37264=VERTEX_POINT('',#166635);
#37265=VERTEX_POINT('',#166662);
#37266=VERTEX_POINT('',#166692);
#37267=VERTEX_POINT('',#166716);
#37268=VERTEX_POINT('',#166735);
#37269=VERTEX_POINT('',#166768);
#37270=VERTEX_POINT('',#166786);
#37271=VERTEX_POINT('',#166788);
#37272=VERTEX_POINT('',#166792);
#37273=VERTEX_POINT('',#166796);
#37274=VERTEX_POINT('',#166798);
#37275=VERTEX_POINT('',#166802);
#37276=VERTEX_POINT('',#166806);
#37277=VERTEX_POINT('',#166812);
#37278=VERTEX_POINT('',#166846);
#37279=VERTEX_POINT('',#166859);
#37280=VERTEX_POINT('',#166892);
#37281=VERTEX_POINT('',#166925);
#37282=VERTEX_POINT('',#166961);
#37283=VERTEX_POINT('',#166980);
#37284=VERTEX_POINT('',#167007);
#37285=VERTEX_POINT('',#167037);
#37286=VERTEX_POINT('',#167042);
#37287=VERTEX_POINT('',#167064);
#37288=VERTEX_POINT('',#167065);
#37289=VERTEX_POINT('',#167067);
#37290=VERTEX_POINT('',#167069);
#37291=VERTEX_POINT('',#167186);
#37292=VERTEX_POINT('',#167217);
#37293=VERTEX_POINT('',#167219);
#37294=VERTEX_POINT('',#167223);
#37295=VERTEX_POINT('',#167238);
#37296=VERTEX_POINT('',#167239);
#37297=VERTEX_POINT('',#167241);
#37298=VERTEX_POINT('',#167243);
#37299=VERTEX_POINT('',#167270);
#37300=VERTEX_POINT('',#167292);
#37301=VERTEX_POINT('',#167325);
#37302=VERTEX_POINT('',#167344);
#37303=VERTEX_POINT('',#167365);
#37304=VERTEX_POINT('',#167410);
#37305=VERTEX_POINT('',#167431);
#37306=VERTEX_POINT('',#167455);
#37307=VERTEX_POINT('',#167476);
#37308=VERTEX_POINT('',#167478);
#37309=VERTEX_POINT('',#167482);
#37310=VERTEX_POINT('',#167484);
#37311=VERTEX_POINT('',#167486);
#37312=VERTEX_POINT('',#167519);
#37313=VERTEX_POINT('',#167535);
#37314=VERTEX_POINT('',#167539);
#37315=VERTEX_POINT('',#167543);
#37316=VERTEX_POINT('',#167576);
#37317=VERTEX_POINT('',#167577);
#37318=VERTEX_POINT('',#167579);
#37319=VERTEX_POINT('',#167599);
#37320=VERTEX_POINT('',#167601);
#37321=VERTEX_POINT('',#167619);
#37322=VERTEX_POINT('',#167620);
#37323=VERTEX_POINT('',#167661);
#37324=VERTEX_POINT('',#167663);
#37325=VERTEX_POINT('',#167667);
#37326=VERTEX_POINT('',#167671);
#37327=VERTEX_POINT('',#167673);
#37328=VERTEX_POINT('',#167700);
#37329=VERTEX_POINT('',#167733);
#37330=VERTEX_POINT('',#167775);
#37331=VERTEX_POINT('',#167797);
#37332=VERTEX_POINT('',#167830);
#37333=VERTEX_POINT('',#167860);
#37334=VERTEX_POINT('',#167896);
#37335=VERTEX_POINT('',#167897);
#37336=VERTEX_POINT('',#167992);
#37337=VERTEX_POINT('',#167994);
#37338=VERTEX_POINT('',#167998);
#37339=VERTEX_POINT('',#168002);
#37340=VERTEX_POINT('',#168008);
#37341=VERTEX_POINT('',#168011);
#37342=VERTEX_POINT('',#168055);
#37343=VERTEX_POINT('',#168057);
#37344=VERTEX_POINT('',#168061);
#37345=VERTEX_POINT('',#168062);
#37346=VERTEX_POINT('',#168092);
#37347=VERTEX_POINT('',#168093);
#37348=VERTEX_POINT('',#168095);
#37349=VERTEX_POINT('',#168201);
#37350=VERTEX_POINT('',#168231);
#37351=VERTEX_POINT('',#168250);
#37352=VERTEX_POINT('',#168252);
#37353=VERTEX_POINT('',#168256);
#37354=VERTEX_POINT('',#168257);
#37355=VERTEX_POINT('',#168259);
#37356=VERTEX_POINT('',#168261);
#37357=VERTEX_POINT('',#168265);
#37358=VERTEX_POINT('',#168267);
#37359=VERTEX_POINT('',#168271);
#37360=VERTEX_POINT('',#168273);
#37361=VERTEX_POINT('',#168277);
#37362=VERTEX_POINT('',#168279);
#37363=VERTEX_POINT('',#168376);
#37364=VERTEX_POINT('',#168396);
#37365=VERTEX_POINT('',#168411);
#37366=VERTEX_POINT('',#168412);
#37367=VERTEX_POINT('',#168414);
#37368=VERTEX_POINT('',#168466);
#37369=VERTEX_POINT('',#168482);
#37370=VERTEX_POINT('',#168484);
#37371=VERTEX_POINT('',#168488);
#37372=VERTEX_POINT('',#168489);
#37373=VERTEX_POINT('',#168491);
#37374=VERTEX_POINT('',#168493);
#37375=VERTEX_POINT('',#168497);
#37376=VERTEX_POINT('',#168499);
#37377=VERTEX_POINT('',#168503);
#37378=VERTEX_POINT('',#168505);
#37379=VERTEX_POINT('',#168509);
#37380=VERTEX_POINT('',#168511);
#37381=VERTEX_POINT('',#168513);
#37382=VERTEX_POINT('',#168540);
#37383=VERTEX_POINT('',#168567);
#37384=VERTEX_POINT('',#168591);
#37385=VERTEX_POINT('',#168592);
#37386=VERTEX_POINT('',#168690);
#37387=VERTEX_POINT('',#168691);
#37388=VERTEX_POINT('',#168696);
#37389=VERTEX_POINT('',#168697);
#37390=VERTEX_POINT('',#168704);
#37391=VERTEX_POINT('',#168706);
#37392=VERTEX_POINT('',#168710);
#37393=VERTEX_POINT('',#168731);
#37394=VERTEX_POINT('',#168733);
#37395=VERTEX_POINT('',#168789);
#37396=VERTEX_POINT('',#168825);
#37397=VERTEX_POINT('',#168855);
#37398=VERTEX_POINT('',#168883);
#37399=VERTEX_POINT('',#168910);
#37400=VERTEX_POINT('',#168940);
#37401=VERTEX_POINT('',#168964);
#37402=VERTEX_POINT('',#168983);
#37403=VERTEX_POINT('',#169016);
#37404=VERTEX_POINT('',#169034);
#37405=VERTEX_POINT('',#169036);
#37406=VERTEX_POINT('',#169040);
#37407=VERTEX_POINT('',#169044);
#37408=VERTEX_POINT('',#169046);
#37409=VERTEX_POINT('',#169050);
#37410=VERTEX_POINT('',#169054);
#37411=VERTEX_POINT('',#169060);
#37412=VERTEX_POINT('',#169094);
#37413=VERTEX_POINT('',#169107);
#37414=VERTEX_POINT('',#169140);
#37415=VERTEX_POINT('',#169173);
#37416=VERTEX_POINT('',#169209);
#37417=VERTEX_POINT('',#169228);
#37418=VERTEX_POINT('',#169255);
#37419=VERTEX_POINT('',#169282);
#37420=VERTEX_POINT('',#169287);
#37421=VERTEX_POINT('',#169303);
#37422=VERTEX_POINT('',#169304);
#37423=VERTEX_POINT('',#169306);
#37424=VERTEX_POINT('',#169308);
#37425=VERTEX_POINT('',#169425);
#37426=VERTEX_POINT('',#169444);
#37427=VERTEX_POINT('',#169446);
#37428=VERTEX_POINT('',#169450);
#37429=VERTEX_POINT('',#169465);
#37430=VERTEX_POINT('',#169467);
#37431=VERTEX_POINT('',#169497);
#37432=VERTEX_POINT('',#169513);
#37433=VERTEX_POINT('',#169534);
#37434=VERTEX_POINT('',#169570);
#37435=VERTEX_POINT('',#169588);
#37436=VERTEX_POINT('',#169612);
#37437=VERTEX_POINT('',#169613);
#37438=VERTEX_POINT('',#169674);
#37439=VERTEX_POINT('',#169688);
#37440=VERTEX_POINT('',#169692);
#37441=VERTEX_POINT('',#169694);
#37442=VERTEX_POINT('',#169696);
#37443=VERTEX_POINT('',#169729);
#37444=VERTEX_POINT('',#169745);
#37445=VERTEX_POINT('',#169749);
#37446=VERTEX_POINT('',#169753);
#37447=VERTEX_POINT('',#169786);
#37448=VERTEX_POINT('',#169787);
#37449=VERTEX_POINT('',#169789);
#37450=VERTEX_POINT('',#169852);
#37451=VERTEX_POINT('',#169853);
#37452=VERTEX_POINT('',#169858);
#37453=VERTEX_POINT('',#169859);
#37454=VERTEX_POINT('',#169864);
#37455=VERTEX_POINT('',#169868);
#37456=VERTEX_POINT('',#169870);
#37457=VERTEX_POINT('',#169885);
#37458=VERTEX_POINT('',#169909);
#37459=VERTEX_POINT('',#169966);
#37460=VERTEX_POINT('',#169985);
#37461=VERTEX_POINT('',#170012);
#37462=VERTEX_POINT('',#170057);
#37463=VERTEX_POINT('',#170077);
#37464=VERTEX_POINT('',#170105);
#37465=VERTEX_POINT('',#170107);
#37466=VERTEX_POINT('',#170111);
#37467=VERTEX_POINT('',#170115);
#37468=VERTEX_POINT('',#170121);
#37469=VERTEX_POINT('',#170124);
#37470=VERTEX_POINT('',#170168);
#37471=VERTEX_POINT('',#170172);
#37472=VERTEX_POINT('',#170174);
#37473=VERTEX_POINT('',#170178);
#37474=VERTEX_POINT('',#170180);
#37475=VERTEX_POINT('',#170217);
#37476=VERTEX_POINT('',#170219);
#37477=VERTEX_POINT('',#170246);
#37478=VERTEX_POINT('',#170274);
#37479=VERTEX_POINT('',#170295);
#37480=VERTEX_POINT('',#170296);
#37481=VERTEX_POINT('',#170360);
#37482=VERTEX_POINT('',#170362);
#37483=VERTEX_POINT('',#170366);
#37484=VERTEX_POINT('',#170372);
#37485=VERTEX_POINT('',#170407);
#37486=VERTEX_POINT('',#170408);
#37487=VERTEX_POINT('',#170451);
#37488=VERTEX_POINT('',#170568);
#37489=VERTEX_POINT('',#170570);
#37490=VERTEX_POINT('',#170581);
#37491=VERTEX_POINT('',#170602);
#37492=VERTEX_POINT('',#170638);
#37493=VERTEX_POINT('',#170659);
#37494=VERTEX_POINT('',#170666);
#37495=VERTEX_POINT('',#170670);
#37496=VERTEX_POINT('',#170674);
#37497=VERTEX_POINT('',#170695);
#37498=VERTEX_POINT('',#170727);
#37499=VERTEX_POINT('',#170737);
#37500=VERTEX_POINT('',#170739);
#37501=VERTEX_POINT('',#170743);
#37502=VERTEX_POINT('',#170747);
#37503=VERTEX_POINT('',#170749);
#37504=VERTEX_POINT('',#170753);
#37505=VERTEX_POINT('',#170759);
#37506=VERTEX_POINT('',#170775);
#37507=VERTEX_POINT('',#170796);
#37508=VERTEX_POINT('',#170823);
#37509=VERTEX_POINT('',#170842);
#37510=VERTEX_POINT('',#170863);
#37511=VERTEX_POINT('',#170864);
#37512=VERTEX_POINT('',#171000);
#37513=VERTEX_POINT('',#171001);
#37514=VERTEX_POINT('',#171050);
#37515=VERTEX_POINT('',#171173);
#37516=VERTEX_POINT('',#171175);
#37517=VERTEX_POINT('',#171191);
#37518=VERTEX_POINT('',#171212);
#37519=VERTEX_POINT('',#171239);
#37520=VERTEX_POINT('',#171257);
#37521=VERTEX_POINT('',#171305);
#37522=VERTEX_POINT('',#171359);
#37523=VERTEX_POINT('',#171376);
#37524=VERTEX_POINT('',#171383);
#37525=VERTEX_POINT('',#171384);
#37526=VERTEX_POINT('',#171389);
#37527=VERTEX_POINT('',#171396);
#37528=VERTEX_POINT('',#171398);
#37529=VERTEX_POINT('',#171481);
#37530=VERTEX_POINT('',#171497);
#37531=VERTEX_POINT('',#171512);
#37532=VERTEX_POINT('',#171536);
#37533=VERTEX_POINT('',#171552);
#37534=VERTEX_POINT('',#171573);
#37535=VERTEX_POINT('',#171587);
#37536=VERTEX_POINT('',#171665);
#37537=VERTEX_POINT('',#171670);
#37538=VERTEX_POINT('',#171712);
#37539=VERTEX_POINT('',#171766);
#37540=VERTEX_POINT('',#171768);
#37541=VERTEX_POINT('',#171772);
#37542=VERTEX_POINT('',#171787);
#37543=VERTEX_POINT('',#171802);
#37544=VERTEX_POINT('',#171820);
#37545=VERTEX_POINT('',#171856);
#37546=VERTEX_POINT('',#171895);
#37547=VERTEX_POINT('',#171906);
#37548=VERTEX_POINT('',#171913);
#37549=VERTEX_POINT('',#171914);
#37550=VERTEX_POINT('',#171919);
#37551=VERTEX_POINT('',#171923);
#37552=VERTEX_POINT('',#171925);
#37553=VERTEX_POINT('',#171984);
#37554=VERTEX_POINT('',#172000);
#37555=VERTEX_POINT('',#172015);
#37556=VERTEX_POINT('',#172033);
#37557=VERTEX_POINT('',#172037);
#37558=VERTEX_POINT('',#172052);
#37559=VERTEX_POINT('',#172054);
#37560=VERTEX_POINT('',#172069);
#37561=VERTEX_POINT('',#172074);
#37562=VERTEX_POINT('',#172119);
#37563=VERTEX_POINT('',#172227);
#37564=VERTEX_POINT('',#172229);
#37565=VERTEX_POINT('',#172245);
#37566=VERTEX_POINT('',#172266);
#37567=VERTEX_POINT('',#172293);
#37568=VERTEX_POINT('',#172311);
#37569=VERTEX_POINT('',#172359);
#37570=VERTEX_POINT('',#172407);
#37571=VERTEX_POINT('',#172423);
#37572=VERTEX_POINT('',#172430);
#37573=VERTEX_POINT('',#172432);
#37574=VERTEX_POINT('',#172436);
#37575=VERTEX_POINT('',#172443);
#37576=VERTEX_POINT('',#172445);
#37577=VERTEX_POINT('',#172528);
#37578=VERTEX_POINT('',#172544);
#37579=VERTEX_POINT('',#172559);
#37580=VERTEX_POINT('',#172583);
#37581=VERTEX_POINT('',#172599);
#37582=VERTEX_POINT('',#172620);
#37583=VERTEX_POINT('',#172634);
#37584=VERTEX_POINT('',#172712);
#37585=VERTEX_POINT('',#172717);
#37586=VERTEX_POINT('',#172759);
#37587=VERTEX_POINT('',#172882);
#37588=VERTEX_POINT('',#172884);
#37589=VERTEX_POINT('',#172903);
#37590=VERTEX_POINT('',#172924);
#37591=VERTEX_POINT('',#172957);
#37592=VERTEX_POINT('',#172978);
#37593=VERTEX_POINT('',#172985);
#37594=VERTEX_POINT('',#172989);
#37595=VERTEX_POINT('',#173010);
#37596=VERTEX_POINT('',#173054);
#37597=VERTEX_POINT('',#173064);
#37598=VERTEX_POINT('',#173066);
#37599=VERTEX_POINT('',#173070);
#37600=VERTEX_POINT('',#173074);
#37601=VERTEX_POINT('',#173076);
#37602=VERTEX_POINT('',#173080);
#37603=VERTEX_POINT('',#173084);
#37604=VERTEX_POINT('',#173090);
#37605=VERTEX_POINT('',#173106);
#37606=VERTEX_POINT('',#173127);
#37607=VERTEX_POINT('',#173154);
#37608=VERTEX_POINT('',#173165);
#37609=VERTEX_POINT('',#173186);
#37610=VERTEX_POINT('',#173187);
#37611=VERTEX_POINT('',#173320);
#37612=VERTEX_POINT('',#173321);
#37613=VERTEX_POINT('',#173379);
#37614=VERTEX_POINT('',#173503);
#37615=VERTEX_POINT('',#173505);
#37616=VERTEX_POINT('',#173509);
#37617=VERTEX_POINT('',#173530);
#37618=VERTEX_POINT('',#173531);
#37619=VERTEX_POINT('',#173533);
#37620=VERTEX_POINT('',#173600);
#37621=VERTEX_POINT('',#173628);
#37622=VERTEX_POINT('',#173649);
#37623=VERTEX_POINT('',#173691);
#37624=VERTEX_POINT('',#173712);
#37625=VERTEX_POINT('',#173721);
#37626=VERTEX_POINT('',#173723);
#37627=VERTEX_POINT('',#173727);
#37628=VERTEX_POINT('',#173731);
#37629=VERTEX_POINT('',#173735);
#37630=VERTEX_POINT('',#173737);
#37631=VERTEX_POINT('',#173741);
#37632=VERTEX_POINT('',#173745);
#37633=VERTEX_POINT('',#173760);
#37634=VERTEX_POINT('',#173761);
#37635=VERTEX_POINT('',#173763);
#37636=VERTEX_POINT('',#173778);
#37637=VERTEX_POINT('',#173796);
#37638=VERTEX_POINT('',#173797);
#37639=VERTEX_POINT('',#173799);
#37640=VERTEX_POINT('',#173804);
#37641=VERTEX_POINT('',#173832);
#37642=VERTEX_POINT('',#173833);
#37643=VERTEX_POINT('',#173835);
#37644=VERTEX_POINT('',#173837);
#37645=VERTEX_POINT('',#173855);
#37646=VERTEX_POINT('',#173856);
#37647=VERTEX_POINT('',#173893);
#37648=VERTEX_POINT('',#173894);
#37649=VERTEX_POINT('',#173896);
#37650=VERTEX_POINT('',#173901);
#37651=VERTEX_POINT('',#173940);
#37652=VERTEX_POINT('',#173949);
#37653=VERTEX_POINT('',#174055);
#37654=VERTEX_POINT('',#174057);
#37655=VERTEX_POINT('',#174061);
#37656=VERTEX_POINT('',#174062);
#37657=VERTEX_POINT('',#174064);
#37658=VERTEX_POINT('',#174066);
#37659=VERTEX_POINT('',#174070);
#37660=VERTEX_POINT('',#174072);
#37661=VERTEX_POINT('',#174076);
#37662=VERTEX_POINT('',#174078);
#37663=VERTEX_POINT('',#174082);
#37664=VERTEX_POINT('',#174084);
#37665=VERTEX_POINT('',#174086);
#37666=VERTEX_POINT('',#174107);
#37667=VERTEX_POINT('',#174137);
#37668=VERTEX_POINT('',#174138);
#37669=VERTEX_POINT('',#174187);
#37670=VERTEX_POINT('',#174188);
#37671=VERTEX_POINT('',#174276);
#37672=VERTEX_POINT('',#174277);
#37673=VERTEX_POINT('',#174284);
#37674=VERTEX_POINT('',#174285);
#37675=VERTEX_POINT('',#174287);
#37676=VERTEX_POINT('',#174292);
#37677=VERTEX_POINT('',#174296);
#37678=VERTEX_POINT('',#174311);
#37679=VERTEX_POINT('',#174312);
#37680=VERTEX_POINT('',#174314);
#37681=VERTEX_POINT('',#174357);
#37682=VERTEX_POINT('',#174385);
#37683=VERTEX_POINT('',#174406);
#37684=VERTEX_POINT('',#174426);
#37685=VERTEX_POINT('',#174479);
#37686=VERTEX_POINT('',#174484);
#37687=VERTEX_POINT('',#174523);
#37688=VERTEX_POINT('',#174580);
#37689=VERTEX_POINT('',#174582);
#37690=VERTEX_POINT('',#174586);
#37691=VERTEX_POINT('',#174607);
#37692=VERTEX_POINT('',#174609);
#37693=VERTEX_POINT('',#174628);
#37694=VERTEX_POINT('',#174649);
#37695=VERTEX_POINT('',#174676);
#37696=VERTEX_POINT('',#174677);
#37697=VERTEX_POINT('',#174714);
#37698=VERTEX_POINT('',#174734);
#37699=VERTEX_POINT('',#174741);
#37700=VERTEX_POINT('',#174743);
#37701=VERTEX_POINT('',#174747);
#37702=VERTEX_POINT('',#174751);
#37703=VERTEX_POINT('',#174753);
#37704=VERTEX_POINT('',#174757);
#37705=VERTEX_POINT('',#174761);
#37706=VERTEX_POINT('',#174776);
#37707=VERTEX_POINT('',#174777);
#37708=VERTEX_POINT('',#174779);
#37709=VERTEX_POINT('',#174822);
#37710=VERTEX_POINT('',#174841);
#37711=VERTEX_POINT('',#174862);
#37712=VERTEX_POINT('',#174876);
#37713=VERTEX_POINT('',#174987);
#37714=VERTEX_POINT('',#174992);
#37715=VERTEX_POINT('',#175031);
#37716=VERTEX_POINT('',#175151);
#37717=VERTEX_POINT('',#175153);
#37718=VERTEX_POINT('',#175169);
#37719=VERTEX_POINT('',#175190);
#37720=VERTEX_POINT('',#175217);
#37721=VERTEX_POINT('',#175218);
#37722=VERTEX_POINT('',#175252);
#37723=VERTEX_POINT('',#175268);
#37724=VERTEX_POINT('',#175275);
#37725=VERTEX_POINT('',#175276);
#37726=VERTEX_POINT('',#175278);
#37727=VERTEX_POINT('',#175280);
#37728=VERTEX_POINT('',#175284);
#37729=VERTEX_POINT('',#175289);
#37730=VERTEX_POINT('',#175296);
#37731=VERTEX_POINT('',#175298);
#37732=VERTEX_POINT('',#175313);
#37733=VERTEX_POINT('',#175314);
#37734=VERTEX_POINT('',#175316);
#37735=VERTEX_POINT('',#175354);
#37736=VERTEX_POINT('',#175370);
#37737=VERTEX_POINT('',#175391);
#37738=VERTEX_POINT('',#175405);
#37739=VERTEX_POINT('',#175489);
#37740=VERTEX_POINT('',#175494);
#37741=VERTEX_POINT('',#175572);
#37742=VERTEX_POINT('',#175599);
#37743=VERTEX_POINT('',#175601);
#37744=VERTEX_POINT('',#175605);
#37745=VERTEX_POINT('',#175620);
#37746=VERTEX_POINT('',#175635);
#37747=VERTEX_POINT('',#175636);
#37748=VERTEX_POINT('',#175666);
#37749=VERTEX_POINT('',#175679);
#37750=VERTEX_POINT('',#175686);
#37751=VERTEX_POINT('',#175688);
#37752=VERTEX_POINT('',#175692);
#37753=VERTEX_POINT('',#175739);
#37754=VERTEX_POINT('',#175788);
#37755=VERTEX_POINT('',#175790);
#37756=VERTEX_POINT('',#175819);
#37757=VERTEX_POINT('',#175820);
#37758=VERTEX_POINT('',#175838);
#37759=VERTEX_POINT('',#175839);
#37760=VERTEX_POINT('',#175885);
#37761=VERTEX_POINT('',#175923);
#37762=VERTEX_POINT('',#176036);
#37763=VERTEX_POINT('',#176112);
#37764=VERTEX_POINT('',#176223);
#37765=VERTEX_POINT('',#176224);
#37766=VERTEX_POINT('',#176242);
#37767=VERTEX_POINT('',#176243);
#37768=VERTEX_POINT('',#176248);
#37769=VERTEX_POINT('',#176250);
#37770=VERTEX_POINT('',#176269);
#37771=VERTEX_POINT('',#176273);
#37772=VERTEX_POINT('',#176303);
#37773=VERTEX_POINT('',#176304);
#37774=VERTEX_POINT('',#176322);
#37775=VERTEX_POINT('',#176323);
#37776=VERTEX_POINT('',#176328);
#37777=VERTEX_POINT('',#176401);
#37778=VERTEX_POINT('',#176405);
#37779=VERTEX_POINT('',#176438);
#37780=VERTEX_POINT('',#176564);
#37781=VERTEX_POINT('',#176647);
#37782=VERTEX_POINT('',#176649);
#37783=VERTEX_POINT('',#176653);
#37784=VERTEX_POINT('',#176657);
#37785=VERTEX_POINT('',#176661);
#37786=VERTEX_POINT('',#176665);
#37787=VERTEX_POINT('',#176669);
#37788=VERTEX_POINT('',#176673);
#37789=VERTEX_POINT('',#176677);
#37790=VERTEX_POINT('',#176681);
#37791=VERTEX_POINT('',#176685);
#37792=VERTEX_POINT('',#176689);
#37793=VERTEX_POINT('',#176693);
#37794=VERTEX_POINT('',#176697);
#37795=VERTEX_POINT('',#176698);
#37796=VERTEX_POINT('',#176700);
#37797=VERTEX_POINT('',#176702);
#37798=VERTEX_POINT('',#176748);
#37799=VERTEX_POINT('',#176750);
#37800=VERTEX_POINT('',#176847);
#37801=VERTEX_POINT('',#176880);
#37802=VERTEX_POINT('',#176893);
#37803=VERTEX_POINT('',#176926);
#37804=VERTEX_POINT('',#176980);
#37805=VERTEX_POINT('',#176982);
#37806=VERTEX_POINT('',#176994);
#37807=VERTEX_POINT('',#176996);
#37808=VERTEX_POINT('',#177010);
#37809=VERTEX_POINT('',#177012);
#37810=VERTEX_POINT('',#177016);
#37811=VERTEX_POINT('',#177018);
#37812=VERTEX_POINT('',#177022);
#37813=VERTEX_POINT('',#177026);
#37814=VERTEX_POINT('',#177038);
#37815=VERTEX_POINT('',#177040);
#37816=VERTEX_POINT('',#177054);
#37817=VERTEX_POINT('',#177056);
#37818=VERTEX_POINT('',#177060);
#37819=VERTEX_POINT('',#177062);
#37820=VERTEX_POINT('',#177066);
#37821=VERTEX_POINT('',#177070);
#37822=VERTEX_POINT('',#177082);
#37823=VERTEX_POINT('',#177084);
#37824=VERTEX_POINT('',#177088);
#37825=VERTEX_POINT('',#177210);
#37826=VERTEX_POINT('',#177311);
#37827=VERTEX_POINT('',#177359);
#37828=VERTEX_POINT('',#177360);
#37829=VERTEX_POINT('',#177365);
#37830=VERTEX_POINT('',#177366);
#37831=VERTEX_POINT('',#177368);
#37832=VERTEX_POINT('',#177370);
#37833=VERTEX_POINT('',#177374);
#37834=VERTEX_POINT('',#177376);
#37835=VERTEX_POINT('',#177380);
#37836=VERTEX_POINT('',#177382);
#37837=VERTEX_POINT('',#177421);
#37838=VERTEX_POINT('',#177456);
#37839=VERTEX_POINT('',#177458);
#37840=VERTEX_POINT('',#177514);
#37841=VERTEX_POINT('',#177516);
#37842=VERTEX_POINT('',#177578);
#37843=VERTEX_POINT('',#177587);
#37844=VERTEX_POINT('',#177588);
#37845=VERTEX_POINT('',#177590);
#37846=VERTEX_POINT('',#177592);
#37847=VERTEX_POINT('',#177596);
#37848=VERTEX_POINT('',#177598);
#37849=VERTEX_POINT('',#177605);
#37850=VERTEX_POINT('',#177607);
#37851=VERTEX_POINT('',#177628);
#37852=VERTEX_POINT('',#177630);
#37853=VERTEX_POINT('',#177690);
#37854=VERTEX_POINT('',#177727);
#37855=VERTEX_POINT('',#177732);
#37856=VERTEX_POINT('',#177818);
#37857=VERTEX_POINT('',#177837);
#37858=VERTEX_POINT('',#177841);
#37859=VERTEX_POINT('',#177845);
#37860=VERTEX_POINT('',#177847);
#37861=VERTEX_POINT('',#177853);
#37862=VERTEX_POINT('',#177855);
#37863=VERTEX_POINT('',#177859);
#37864=VERTEX_POINT('',#177861);
#37865=VERTEX_POINT('',#177866);
#37866=VERTEX_POINT('',#177869);
#37867=VERTEX_POINT('',#177873);
#37868=VERTEX_POINT('',#177874);
#37869=VERTEX_POINT('',#177879);
#37870=VERTEX_POINT('',#177881);
#37871=VERTEX_POINT('',#177883);
#37872=VERTEX_POINT('',#177895);
#37873=VERTEX_POINT('',#177899);
#37874=VERTEX_POINT('',#177911);
#37875=VERTEX_POINT('',#177918);
#37876=VERTEX_POINT('',#177923);
#37877=VERTEX_POINT('',#177926);
#37878=VERTEX_POINT('',#177930);
#37879=VERTEX_POINT('',#177932);
#37880=VERTEX_POINT('',#177936);
#37881=VERTEX_POINT('',#177940);
#37882=VERTEX_POINT('',#177951);
#37883=VERTEX_POINT('',#177984);
#37884=VERTEX_POINT('',#178058);
#37885=VERTEX_POINT('',#178062);
#37886=VERTEX_POINT('',#178120);
#37887=VERTEX_POINT('',#178124);
#37888=VERTEX_POINT('',#178173);
#37889=VERTEX_POINT('',#178218);
#37890=VERTEX_POINT('',#178322);
#37891=VERTEX_POINT('',#178323);
#37892=VERTEX_POINT('',#178409);
#37893=VERTEX_POINT('',#178413);
#37894=VERTEX_POINT('',#178471);
#37895=VERTEX_POINT('',#178475);
#37896=VERTEX_POINT('',#178524);
#37897=VERTEX_POINT('',#178566);
#37898=VERTEX_POINT('',#178639);
#37899=VERTEX_POINT('',#178641);
#37900=VERTEX_POINT('',#178692);
#37901=VERTEX_POINT('',#178821);
#37902=VERTEX_POINT('',#178832);
#37903=VERTEX_POINT('',#178836);
#37904=VERTEX_POINT('',#178888);
#37905=VERTEX_POINT('',#178892);
#37906=VERTEX_POINT('',#178947);
#37907=VERTEX_POINT('',#178989);
#37908=VERTEX_POINT('',#179068);
#37909=VERTEX_POINT('',#179072);
#37910=VERTEX_POINT('',#179123);
#37911=VERTEX_POINT('',#179124);
#37912=VERTEX_POINT('',#179171);
#37913=VERTEX_POINT('',#179175);
#37914=VERTEX_POINT('',#179186);
#37915=VERTEX_POINT('',#179219);
#37916=VERTEX_POINT('',#179292);
#37917=VERTEX_POINT('',#179344);
#37918=VERTEX_POINT('',#179348);
#37919=VERTEX_POINT('',#179403);
#37920=VERTEX_POINT('',#179445);
#37921=VERTEX_POINT('',#179547);
#37922=VERTEX_POINT('',#179629);
#37923=VERTEX_POINT('',#179640);
#37924=VERTEX_POINT('',#179644);
#37925=VERTEX_POINT('',#179702);
#37926=VERTEX_POINT('',#179706);
#37927=VERTEX_POINT('',#179755);
#37928=VERTEX_POINT('',#179800);
#37929=VERTEX_POINT('',#179908);
#37930=VERTEX_POINT('',#179909);
#37931=VERTEX_POINT('',#180022);
#37932=VERTEX_POINT('',#180027);
#37933=VERTEX_POINT('',#180085);
#37934=VERTEX_POINT('',#180089);
#37935=VERTEX_POINT('',#180138);
#37936=VERTEX_POINT('',#180181);
#37937=VERTEX_POINT('',#180286);
#37938=VERTEX_POINT('',#180361);
#37939=VERTEX_POINT('',#180372);
#37940=VERTEX_POINT('',#180376);
#37941=VERTEX_POINT('',#180428);
#37942=VERTEX_POINT('',#180432);
#37943=VERTEX_POINT('',#180487);
#37944=VERTEX_POINT('',#180529);
#37945=VERTEX_POINT('',#180608);
#37946=VERTEX_POINT('',#180634);
#37947=VERTEX_POINT('',#180666);
#37948=VERTEX_POINT('',#180687);
#37949=VERTEX_POINT('',#180735);
#37950=VERTEX_POINT('',#180736);
#37951=VERTEX_POINT('',#180819);
#37952=VERTEX_POINT('',#180823);
#37953=VERTEX_POINT('',#180875);
#37954=VERTEX_POINT('',#180879);
#37955=VERTEX_POINT('',#180934);
#37956=VERTEX_POINT('',#180976);
#37957=VERTEX_POINT('',#181078);
#37958=VERTEX_POINT('',#181159);
#37959=VERTEX_POINT('',#181161);
#37960=VERTEX_POINT('',#181176);
#37961=VERTEX_POINT('',#181182);
#37962=VERTEX_POINT('',#181184);
#37963=VERTEX_POINT('',#181199);
#37964=VERTEX_POINT('',#181203);
#37965=VERTEX_POINT('',#181224);
#37966=VERTEX_POINT('',#181228);
#37967=VERTEX_POINT('',#181283);
#37968=VERTEX_POINT('',#181298);
#37969=VERTEX_POINT('',#181304);
#37970=VERTEX_POINT('',#181306);
#37971=VERTEX_POINT('',#181357);
#37972=VERTEX_POINT('',#181402);
#37973=VERTEX_POINT('',#181459);
#37974=VERTEX_POINT('',#181633);
#37975=VERTEX_POINT('',#181730);
#37976=VERTEX_POINT('',#181745);
#37977=VERTEX_POINT('',#181751);
#37978=VERTEX_POINT('',#181753);
#37979=VERTEX_POINT('',#181795);
#37980=VERTEX_POINT('',#181828);
#37981=VERTEX_POINT('',#181954);
#37982=VERTEX_POINT('',#182047);
#37983=VERTEX_POINT('',#182147);
#37984=VERTEX_POINT('',#182162);
#37985=VERTEX_POINT('',#182168);
#37986=VERTEX_POINT('',#182170);
#37987=VERTEX_POINT('',#182221);
#37988=VERTEX_POINT('',#182266);
#37989=VERTEX_POINT('',#182385);
#37990=VERTEX_POINT('',#182461);
#37991=VERTEX_POINT('',#182579);
#37992=VERTEX_POINT('',#182594);
#37993=VERTEX_POINT('',#182600);
#37994=VERTEX_POINT('',#182602);
#37995=VERTEX_POINT('',#182617);
#37996=VERTEX_POINT('',#182621);
#37997=VERTEX_POINT('',#182673);
#37998=VERTEX_POINT('',#182677);
#37999=VERTEX_POINT('',#182756);
#38000=VERTEX_POINT('',#182771);
#38001=VERTEX_POINT('',#182788);
#38002=VERTEX_POINT('',#182789);
#38003=VERTEX_POINT('',#182806);
#38004=VERTEX_POINT('',#182810);
#38005=VERTEX_POINT('',#182854);
#38006=VERTEX_POINT('',#182861);
#38007=VERTEX_POINT('',#182865);
#38008=VERTEX_POINT('',#182881);
#38009=VERTEX_POINT('',#182883);
#38010=VERTEX_POINT('',#182920);
#38011=VERTEX_POINT('',#182924);
#38012=VERTEX_POINT('',#182979);
#38013=VERTEX_POINT('',#182980);
#38014=VERTEX_POINT('',#182982);
#38015=VERTEX_POINT('',#183012);
#38016=VERTEX_POINT('',#183014);
#38017=VERTEX_POINT('',#183055);
#38018=VERTEX_POINT('',#183223);
#38019=VERTEX_POINT('',#183355);
#38020=VERTEX_POINT('',#183458);
#38021=VERTEX_POINT('',#183474);
#38022=VERTEX_POINT('',#183481);
#38023=VERTEX_POINT('',#183483);
#38024=VERTEX_POINT('',#183559);
#38025=VERTEX_POINT('',#183598);
#38026=VERTEX_POINT('',#183781);
#38027=VERTEX_POINT('',#183907);
#38028=VERTEX_POINT('',#184037);
#38029=VERTEX_POINT('',#184053);
#38030=VERTEX_POINT('',#184070);
#38031=VERTEX_POINT('',#184071);
#38032=VERTEX_POINT('',#184076);
#38033=VERTEX_POINT('',#184081);
#38034=VERTEX_POINT('',#184166);
#38035=VERTEX_POINT('',#184170);
#38036=VERTEX_POINT('',#184189);
#38037=VERTEX_POINT('',#184205);
#38038=VERTEX_POINT('',#184224);
#38039=VERTEX_POINT('',#184226);
#38040=VERTEX_POINT('',#184293);
#38041=VERTEX_POINT('',#184295);
#38042=VERTEX_POINT('',#184368);
#38043=VERTEX_POINT('',#184384);
#38044=VERTEX_POINT('',#184391);
#38045=VERTEX_POINT('',#184393);
#38046=VERTEX_POINT('',#184408);
#38047=VERTEX_POINT('',#184412);
#38048=VERTEX_POINT('',#184433);
#38049=VERTEX_POINT('',#184437);
#38050=VERTEX_POINT('',#184492);
#38051=VERTEX_POINT('',#184508);
#38052=VERTEX_POINT('',#184510);
#38053=VERTEX_POINT('',#184517);
#38054=VERTEX_POINT('',#184519);
#38055=VERTEX_POINT('',#184579);
#38056=VERTEX_POINT('',#184618);
#38057=VERTEX_POINT('',#184777);
#38058=VERTEX_POINT('',#184909);
#38059=VERTEX_POINT('',#185012);
#38060=VERTEX_POINT('',#185028);
#38061=VERTEX_POINT('',#185030);
#38062=VERTEX_POINT('',#185036);
#38063=VERTEX_POINT('',#185037);
#38064=VERTEX_POINT('',#185067);
#38065=VERTEX_POINT('',#185069);
#38066=VERTEX_POINT('',#185071);
#38067=VERTEX_POINT('',#185122);
#38068=VERTEX_POINT('',#185161);
#38069=VERTEX_POINT('',#185226);
#38070=VERTEX_POINT('',#185272);
#38071=VERTEX_POINT('',#185305);
#38072=VERTEX_POINT('',#185420);
#38073=VERTEX_POINT('',#185422);
#38074=VERTEX_POINT('',#185469);
#38075=VERTEX_POINT('',#185502);
#38076=VERTEX_POINT('',#185504);
#38077=VERTEX_POINT('',#185529);
#38078=VERTEX_POINT('',#185562);
#38079=VERTEX_POINT('',#185628);
#38080=VERTEX_POINT('',#185655);
#38081=VERTEX_POINT('',#185687);
#38082=VERTEX_POINT('',#185708);
#38083=VERTEX_POINT('',#185733);
#38084=VERTEX_POINT('',#185766);
#38085=VERTEX_POINT('',#185819);
#38086=VERTEX_POINT('',#185896);
#38087=VERTEX_POINT('',#185900);
#38088=VERTEX_POINT('',#185904);
#38089=VERTEX_POINT('',#185906);
#38090=VERTEX_POINT('',#185910);
#38091=VERTEX_POINT('',#185914);
#38092=VERTEX_POINT('',#185918);
#38093=VERTEX_POINT('',#185922);
#38094=VERTEX_POINT('',#185926);
#38095=VERTEX_POINT('',#185930);
#38096=VERTEX_POINT('',#185934);
#38097=VERTEX_POINT('',#185938);
#38098=VERTEX_POINT('',#185942);
#38099=VERTEX_POINT('',#185946);
#38100=VERTEX_POINT('',#185950);
#38101=VERTEX_POINT('',#185954);
#38102=VERTEX_POINT('',#185958);
#38103=VERTEX_POINT('',#185962);
#38104=VERTEX_POINT('',#185964);
#38105=VERTEX_POINT('',#185968);
#38106=VERTEX_POINT('',#185972);
#38107=VERTEX_POINT('',#185976);
#38108=VERTEX_POINT('',#185980);
#38109=VERTEX_POINT('',#185982);
#38110=VERTEX_POINT('',#185986);
#38111=VERTEX_POINT('',#185990);
#38112=VERTEX_POINT('',#185996);
#38113=VERTEX_POINT('',#186000);
#38114=VERTEX_POINT('',#186004);
#38115=VERTEX_POINT('',#186008);
#38116=VERTEX_POINT('',#186016);
#38117=VERTEX_POINT('',#186020);
#38118=VERTEX_POINT('',#186024);
#38119=VERTEX_POINT('',#186028);
#38120=VERTEX_POINT('',#186034);
#38121=VERTEX_POINT('',#186055);
#38122=VERTEX_POINT('',#186066);
#38123=VERTEX_POINT('',#186070);
#38124=VERTEX_POINT('',#186074);
#38125=VERTEX_POINT('',#186078);
#38126=VERTEX_POINT('',#186086);
#38127=VERTEX_POINT('',#186090);
#38128=VERTEX_POINT('',#186094);
#38129=VERTEX_POINT('',#186098);
#38130=VERTEX_POINT('',#186102);
#38131=VERTEX_POINT('',#186106);
#38132=VERTEX_POINT('',#186110);
#38133=VERTEX_POINT('',#186157);
#38134=VERTEX_POINT('',#186159);
#38135=VERTEX_POINT('',#186246);
#38136=VERTEX_POINT('',#186270);
#38137=VERTEX_POINT('',#186274);
#38138=VERTEX_POINT('',#186312);
#38139=VERTEX_POINT('',#186328);
#38140=VERTEX_POINT('',#186332);
#38141=VERTEX_POINT('',#186334);
#38142=VERTEX_POINT('',#186336);
#38143=VERTEX_POINT('',#186338);
#38144=VERTEX_POINT('',#186342);
#38145=VERTEX_POINT('',#186344);
#38146=VERTEX_POINT('',#186346);
#38147=VERTEX_POINT('',#186348);
#38148=VERTEX_POINT('',#186352);
#38149=VERTEX_POINT('',#186356);
#38150=VERTEX_POINT('',#186358);
#38151=VERTEX_POINT('',#186379);
#38152=VERTEX_POINT('',#186389);
#38153=VERTEX_POINT('',#186410);
#38154=VERTEX_POINT('',#186424);
#38155=VERTEX_POINT('',#186445);
#38156=VERTEX_POINT('',#186455);
#38157=VERTEX_POINT('',#186476);
#38158=VERTEX_POINT('',#186488);
#38159=VERTEX_POINT('',#186503);
#38160=VERTEX_POINT('',#186505);
#38161=VERTEX_POINT('',#186548);
#38162=VERTEX_POINT('',#186569);
#38163=VERTEX_POINT('',#186579);
#38164=VERTEX_POINT('',#186600);
#38165=VERTEX_POINT('',#186612);
#38166=VERTEX_POINT('',#186653);
#38167=VERTEX_POINT('',#186668);
#38168=VERTEX_POINT('',#186672);
#38169=VERTEX_POINT('',#186676);
#38170=VERTEX_POINT('',#186697);
#38171=VERTEX_POINT('',#186707);
#38172=VERTEX_POINT('',#186728);
#38173=VERTEX_POINT('',#186742);
#38174=VERTEX_POINT('',#186744);
#38175=VERTEX_POINT('',#186748);
#38176=VERTEX_POINT('',#186769);
#38177=VERTEX_POINT('',#186779);
#38178=VERTEX_POINT('',#186800);
#38179=VERTEX_POINT('',#186812);
#38180=VERTEX_POINT('',#186833);
#38181=VERTEX_POINT('',#186852);
#38182=VERTEX_POINT('',#186873);
#38183=VERTEX_POINT('',#186883);
#38184=VERTEX_POINT('',#186904);
#38185=VERTEX_POINT('',#186935);
#38186=VERTEX_POINT('',#186996);
#38187=VERTEX_POINT('',#186998);
#38188=VERTEX_POINT('',#187002);
#38189=VERTEX_POINT('',#187023);
#38190=VERTEX_POINT('',#187033);
#38191=VERTEX_POINT('',#187054);
#38192=VERTEX_POINT('',#187066);
#38193=VERTEX_POINT('',#187107);
#38194=VERTEX_POINT('',#187128);
#38195=VERTEX_POINT('',#187168);
#38196=VERTEX_POINT('',#187172);
#38197=VERTEX_POINT('',#187193);
#38198=VERTEX_POINT('',#187203);
#38199=VERTEX_POINT('',#187224);
#38200=VERTEX_POINT('',#187261);
#38201=VERTEX_POINT('',#187263);
#38202=VERTEX_POINT('',#187337);
#38203=VERTEX_POINT('',#187370);
#38204=VERTEX_POINT('',#187416);
#38205=VERTEX_POINT('',#187437);
#38206=VERTEX_POINT('',#187463);
#38207=VERTEX_POINT('',#187490);
#38208=VERTEX_POINT('',#187532);
#38209=VERTEX_POINT('',#187565);
#38210=VERTEX_POINT('',#187624);
#38211=VERTEX_POINT('',#187657);
#38212=VERTEX_POINT('',#187688);
#38213=VERTEX_POINT('',#187721);
#38214=VERTEX_POINT('',#187750);
#38215=VERTEX_POINT('',#187789);
#38216=VERTEX_POINT('',#187846);
#38217=VERTEX_POINT('',#187879);
#38218=VERTEX_POINT('',#187932);
#38219=VERTEX_POINT('',#187965);
#38220=VERTEX_POINT('',#188011);
#38221=VERTEX_POINT('',#188038);
#38222=VERTEX_POINT('',#188106);
#38223=VERTEX_POINT('',#188127);
#38224=VERTEX_POINT('',#188182);
#38225=VERTEX_POINT('',#188184);
#38226=VERTEX_POINT('',#188190);
#38227=VERTEX_POINT('',#188192);
#38228=VERTEX_POINT('',#188200);
#38229=VERTEX_POINT('',#188202);
#38230=VERTEX_POINT('',#188225);
#38231=VERTEX_POINT('',#188239);
#38232=VERTEX_POINT('',#188256);
#38233=VERTEX_POINT('',#188257);
#38234=VERTEX_POINT('',#188275);
#38235=VERTEX_POINT('',#188285);
#38236=VERTEX_POINT('',#188332);
#38237=VERTEX_POINT('',#188371);
#38238=VERTEX_POINT('',#188428);
#38239=VERTEX_POINT('',#188461);
#38240=VERTEX_POINT('',#188480);
#38241=VERTEX_POINT('',#188501);
#38242=VERTEX_POINT('',#188527);
#38243=VERTEX_POINT('',#188560);
#38244=VERTEX_POINT('',#188610);
#38245=VERTEX_POINT('',#188643);
#38246=VERTEX_POINT('',#188692);
#38247=VERTEX_POINT('',#188713);
#38248=VERTEX_POINT('',#188734);
#38249=VERTEX_POINT('',#188738);
#38250=VERTEX_POINT('',#188740);
#38251=VERTEX_POINT('',#188773);
#38252=VERTEX_POINT('',#188823);
#38253=VERTEX_POINT('',#188856);
#38254=VERTEX_POINT('',#188902);
#38255=VERTEX_POINT('',#188923);
#38256=VERTEX_POINT('',#188949);
#38257=VERTEX_POINT('',#188982);
#38258=VERTEX_POINT('',#189033);
#38259=VERTEX_POINT('',#189066);
#38260=VERTEX_POINT('',#189067);
#38261=VERTEX_POINT('',#189121);
#38262=VERTEX_POINT('',#189148);
#38263=VERTEX_POINT('',#189166);
#38264=VERTEX_POINT('',#189171);
#38265=VERTEX_POINT('',#189173);
#38266=VERTEX_POINT('',#189179);
#38267=VERTEX_POINT('',#189181);
#38268=VERTEX_POINT('',#189189);
#38269=VERTEX_POINT('',#189191);
#38270=VERTEX_POINT('',#189208);
#38271=VERTEX_POINT('',#189311);
#38272=VERTEX_POINT('',#189312);
#38273=VERTEX_POINT('',#189314);
#38274=VERTEX_POINT('',#189318);
#38275=VERTEX_POINT('',#189324);
#38276=VERTEX_POINT('',#189325);
#38277=VERTEX_POINT('',#189334);
#38278=VERTEX_POINT('',#189335);
#38279=VERTEX_POINT('',#189344);
#38280=VERTEX_POINT('',#189345);
#38281=VERTEX_POINT('',#189354);
#38282=VERTEX_POINT('',#189355);
#38283=VERTEX_POINT('',#189371);
#38284=VERTEX_POINT('',#189386);
#38285=VERTEX_POINT('',#189388);
#38286=VERTEX_POINT('',#189390);
#38287=VERTEX_POINT('',#189394);
#38288=VERTEX_POINT('',#189400);
#38289=VERTEX_POINT('',#189402);
#38290=VERTEX_POINT('',#189407);
#38291=VERTEX_POINT('',#189411);
#38292=VERTEX_POINT('',#189414);
#38293=VERTEX_POINT('',#189436);
#38294=VERTEX_POINT('',#189437);
#38295=VERTEX_POINT('',#189439);
#38296=VERTEX_POINT('',#189446);
#38297=VERTEX_POINT('',#189455);
#38298=VERTEX_POINT('',#189457);
#38299=VERTEX_POINT('',#189459);
#38300=VERTEX_POINT('',#189492);
#38301=VERTEX_POINT('',#189493);
#38302=VERTEX_POINT('',#189495);
#38303=VERTEX_POINT('',#189527);
#38304=VERTEX_POINT('',#189551);
#38305=VERTEX_POINT('',#189552);
#38306=VERTEX_POINT('',#189578);
#38307=VERTEX_POINT('',#189611);
#38308=VERTEX_POINT('',#189612);
#38309=VERTEX_POINT('',#189677);
#38310=VERTEX_POINT('',#189678);
#38311=VERTEX_POINT('',#189700);
#38312=VERTEX_POINT('',#189701);
#38313=VERTEX_POINT('',#189717);
#38314=VERTEX_POINT('',#189718);
#38315=VERTEX_POINT('',#189752);
#38316=VERTEX_POINT('',#189753);
#38317=VERTEX_POINT('',#189815);
#38318=VERTEX_POINT('',#189816);
#38319=VERTEX_POINT('',#189832);
#38320=VERTEX_POINT('',#189833);
#38321=VERTEX_POINT('',#189855);
#38322=VERTEX_POINT('',#189856);
#38323=VERTEX_POINT('',#189884);
#38324=VERTEX_POINT('',#189886);
#38325=VERTEX_POINT('',#189957);
#38326=VERTEX_POINT('',#189958);
#38327=VERTEX_POINT('',#189960);
#38328=VERTEX_POINT('',#189973);
#38329=VERTEX_POINT('',#190042);
#38330=VERTEX_POINT('',#190043);
#38331=VERTEX_POINT('',#190080);
#38332=VERTEX_POINT('',#190081);
#38333=VERTEX_POINT('',#190133);
#38334=VERTEX_POINT('',#190134);
#38335=VERTEX_POINT('',#190178);
#38336=VERTEX_POINT('',#190179);
#38337=VERTEX_POINT('',#190244);
#38338=VERTEX_POINT('',#190259);
#38339=VERTEX_POINT('',#190260);
#38340=VERTEX_POINT('',#190297);
#38341=VERTEX_POINT('',#190298);
#38342=VERTEX_POINT('',#190332);
#38343=VERTEX_POINT('',#190333);
#38344=VERTEX_POINT('',#190352);
#38345=VERTEX_POINT('',#190353);
#38346=VERTEX_POINT('',#190358);
#38347=VERTEX_POINT('',#190362);
#38348=VERTEX_POINT('',#190363);
#38349=VERTEX_POINT('',#190379);
#38350=VERTEX_POINT('',#190380);
#38351=VERTEX_POINT('',#190394);
#38352=VERTEX_POINT('',#190395);
#38353=VERTEX_POINT('',#190397);
#38354=VERTEX_POINT('',#190399);
#38355=VERTEX_POINT('',#190403);
#38356=VERTEX_POINT('',#190404);
#38357=VERTEX_POINT('',#190409);
#38358=VERTEX_POINT('',#190410);
#38359=VERTEX_POINT('',#190415);
#38360=VERTEX_POINT('',#190416);
#38361=VERTEX_POINT('',#190421);
#38362=VERTEX_POINT('',#190422);
#38363=VERTEX_POINT('',#190427);
#38364=VERTEX_POINT('',#190428);
#38365=VERTEX_POINT('',#190433);
#38366=VERTEX_POINT('',#190434);
#38367=VERTEX_POINT('',#190450);
#38368=VERTEX_POINT('',#190452);
#38369=VERTEX_POINT('',#190467);
#38370=VERTEX_POINT('',#190468);
#38371=VERTEX_POINT('',#190511);
#38372=VERTEX_POINT('',#190524);
#38373=VERTEX_POINT('',#190574);
#38374=VERTEX_POINT('',#190575);
#38375=VERTEX_POINT('',#190635);
#38376=VERTEX_POINT('',#190636);
#38377=VERTEX_POINT('',#190652);
#38378=VERTEX_POINT('',#190653);
#38379=VERTEX_POINT('',#190669);
#38380=VERTEX_POINT('',#190670);
#38381=VERTEX_POINT('',#190707);
#38382=VERTEX_POINT('',#190708);
#38383=VERTEX_POINT('',#190757);
#38384=VERTEX_POINT('',#190758);
#38385=VERTEX_POINT('',#190800);
#38386=VERTEX_POINT('',#190801);
#38387=VERTEX_POINT('',#190873);
#38388=VERTEX_POINT('',#190874);
#38389=VERTEX_POINT('',#190966);
#38390=VERTEX_POINT('',#190967);
#38391=VERTEX_POINT('',#191069);
#38392=VERTEX_POINT('',#191070);
#38393=VERTEX_POINT('',#191072);
#38394=VERTEX_POINT('',#191091);
#38395=VERTEX_POINT('',#191112);
#38396=VERTEX_POINT('',#191113);
#38397=VERTEX_POINT('',#191141);
#38398=VERTEX_POINT('',#191142);
#38399=VERTEX_POINT('',#191214);
#38400=VERTEX_POINT('',#191215);
#38401=VERTEX_POINT('',#191272);
#38402=VERTEX_POINT('',#191273);
#38403=VERTEX_POINT('',#191319);
#38404=VERTEX_POINT('',#191320);
#38405=VERTEX_POINT('',#191322);
#38406=VERTEX_POINT('',#191360);
#38407=VERTEX_POINT('',#191361);
#38408=VERTEX_POINT('',#191377);
#38409=VERTEX_POINT('',#191378);
#38410=VERTEX_POINT('',#191549);
#38411=VERTEX_POINT('',#191550);
#38412=VERTEX_POINT('',#191637);
#38413=VERTEX_POINT('',#191639);
#38414=VERTEX_POINT('',#191651);
#38415=VERTEX_POINT('',#191653);
#38416=VERTEX_POINT('',#191657);
#38417=VERTEX_POINT('',#191659);
#38418=VERTEX_POINT('',#191672);
#38419=VERTEX_POINT('',#191673);
#38420=VERTEX_POINT('',#191681);
#38421=VERTEX_POINT('',#191683);
#38422=VERTEX_POINT('',#191695);
#38423=VERTEX_POINT('',#191697);
#38424=VERTEX_POINT('',#191701);
#38425=VERTEX_POINT('',#191702);
#38426=VERTEX_POINT('',#191715);
#38427=VERTEX_POINT('',#191716);
#38428=VERTEX_POINT('',#191724);
#38429=VERTEX_POINT('',#191726);
#38430=VERTEX_POINT('',#191738);
#38431=VERTEX_POINT('',#191739);
#38432=VERTEX_POINT('',#191744);
#38433=VERTEX_POINT('',#191745);
#38434=VERTEX_POINT('',#191758);
#38435=VERTEX_POINT('',#191760);
#38436=VERTEX_POINT('',#191767);
#38437=VERTEX_POINT('',#191769);
#38438=VERTEX_POINT('',#191781);
#38439=VERTEX_POINT('',#191782);
#38440=VERTEX_POINT('',#191787);
#38441=VERTEX_POINT('',#191788);
#38442=VERTEX_POINT('',#191801);
#38443=VERTEX_POINT('',#191803);
#38444=VERTEX_POINT('',#191834);
#38445=VERTEX_POINT('',#191835);
#38446=VERTEX_POINT('',#191837);
#38447=VERTEX_POINT('',#191839);
#38448=VERTEX_POINT('',#191843);
#38449=VERTEX_POINT('',#191844);
#38450=VERTEX_POINT('',#191849);
#38451=VERTEX_POINT('',#191850);
#38452=VERTEX_POINT('',#191855);
#38453=VERTEX_POINT('',#191856);
#38454=VERTEX_POINT('',#191861);
#38455=VERTEX_POINT('',#191862);
#38456=VERTEX_POINT('',#191867);
#38457=VERTEX_POINT('',#191868);
#38458=VERTEX_POINT('',#191873);
#38459=VERTEX_POINT('',#191874);
#38460=VERTEX_POINT('',#191879);
#38461=VERTEX_POINT('',#191880);
#38462=VERTEX_POINT('',#191885);
#38463=VERTEX_POINT('',#191886);
#38464=VERTEX_POINT('',#191894);
#38465=VERTEX_POINT('',#191895);
#38466=VERTEX_POINT('',#191897);
#38467=VERTEX_POINT('',#191899);
#38468=VERTEX_POINT('',#191903);
#38469=VERTEX_POINT('',#191904);
#38470=VERTEX_POINT('',#191909);
#38471=VERTEX_POINT('',#191910);
#38472=VERTEX_POINT('',#191915);
#38473=VERTEX_POINT('',#191916);
#38474=VERTEX_POINT('',#191921);
#38475=VERTEX_POINT('',#191922);
#38476=VERTEX_POINT('',#191927);
#38477=VERTEX_POINT('',#191928);
#38478=VERTEX_POINT('',#191933);
#38479=VERTEX_POINT('',#191934);
#38480=VERTEX_POINT('',#191942);
#38481=VERTEX_POINT('',#191943);
#38482=VERTEX_POINT('',#191945);
#38483=VERTEX_POINT('',#191947);
#38484=VERTEX_POINT('',#191951);
#38485=VERTEX_POINT('',#191952);
#38486=VERTEX_POINT('',#191957);
#38487=VERTEX_POINT('',#191958);
#38488=VERTEX_POINT('',#191963);
#38489=VERTEX_POINT('',#191964);
#38490=VERTEX_POINT('',#191969);
#38491=VERTEX_POINT('',#191970);
#38492=VERTEX_POINT('',#191975);
#38493=VERTEX_POINT('',#191976);
#38494=VERTEX_POINT('',#191981);
#38495=VERTEX_POINT('',#191982);
#38496=VERTEX_POINT('',#191990);
#38497=VERTEX_POINT('',#191991);
#38498=VERTEX_POINT('',#191993);
#38499=VERTEX_POINT('',#191995);
#38500=VERTEX_POINT('',#191999);
#38501=VERTEX_POINT('',#192000);
#38502=VERTEX_POINT('',#192005);
#38503=VERTEX_POINT('',#192006);
#38504=VERTEX_POINT('',#192011);
#38505=VERTEX_POINT('',#192012);
#38506=VERTEX_POINT('',#192017);
#38507=VERTEX_POINT('',#192018);
#38508=VERTEX_POINT('',#192023);
#38509=VERTEX_POINT('',#192024);
#38510=VERTEX_POINT('',#192029);
#38511=VERTEX_POINT('',#192030);
#38512=VERTEX_POINT('',#192038);
#38513=VERTEX_POINT('',#192039);
#38514=VERTEX_POINT('',#192041);
#38515=VERTEX_POINT('',#192043);
#38516=VERTEX_POINT('',#192047);
#38517=VERTEX_POINT('',#192048);
#38518=VERTEX_POINT('',#192053);
#38519=VERTEX_POINT('',#192054);
#38520=VERTEX_POINT('',#192059);
#38521=VERTEX_POINT('',#192060);
#38522=VERTEX_POINT('',#192065);
#38523=VERTEX_POINT('',#192066);
#38524=VERTEX_POINT('',#192071);
#38525=VERTEX_POINT('',#192072);
#38526=VERTEX_POINT('',#192077);
#38527=VERTEX_POINT('',#192078);
#38528=VERTEX_POINT('',#192083);
#38529=VERTEX_POINT('',#192084);
#38530=VERTEX_POINT('',#192092);
#38531=VERTEX_POINT('',#192093);
#38532=VERTEX_POINT('',#192095);
#38533=VERTEX_POINT('',#192097);
#38534=VERTEX_POINT('',#192101);
#38535=VERTEX_POINT('',#192102);
#38536=VERTEX_POINT('',#192107);
#38537=VERTEX_POINT('',#192108);
#38538=VERTEX_POINT('',#192113);
#38539=VERTEX_POINT('',#192114);
#38540=VERTEX_POINT('',#192119);
#38541=VERTEX_POINT('',#192120);
#38542=VERTEX_POINT('',#192125);
#38543=VERTEX_POINT('',#192126);
#38544=VERTEX_POINT('',#192131);
#38545=VERTEX_POINT('',#192132);
#38546=VERTEX_POINT('',#192140);
#38547=VERTEX_POINT('',#192141);
#38548=VERTEX_POINT('',#192143);
#38549=VERTEX_POINT('',#192145);
#38550=VERTEX_POINT('',#192149);
#38551=VERTEX_POINT('',#192150);
#38552=VERTEX_POINT('',#192155);
#38553=VERTEX_POINT('',#192156);
#38554=VERTEX_POINT('',#192161);
#38555=VERTEX_POINT('',#192162);
#38556=VERTEX_POINT('',#192167);
#38557=VERTEX_POINT('',#192168);
#38558=VERTEX_POINT('',#192173);
#38559=VERTEX_POINT('',#192174);
#38560=VERTEX_POINT('',#192179);
#38561=VERTEX_POINT('',#192180);
#38562=VERTEX_POINT('',#192188);
#38563=VERTEX_POINT('',#192189);
#38564=VERTEX_POINT('',#192191);
#38565=VERTEX_POINT('',#192193);
#38566=VERTEX_POINT('',#192197);
#38567=VERTEX_POINT('',#192198);
#38568=VERTEX_POINT('',#192203);
#38569=VERTEX_POINT('',#192204);
#38570=VERTEX_POINT('',#192209);
#38571=VERTEX_POINT('',#192210);
#38572=VERTEX_POINT('',#192215);
#38573=VERTEX_POINT('',#192216);
#38574=VERTEX_POINT('',#192221);
#38575=VERTEX_POINT('',#192222);
#38576=VERTEX_POINT('',#192227);
#38577=VERTEX_POINT('',#192228);
#38578=VERTEX_POINT('',#192236);
#38579=VERTEX_POINT('',#192237);
#38580=VERTEX_POINT('',#192239);
#38581=VERTEX_POINT('',#192241);
#38582=VERTEX_POINT('',#192245);
#38583=VERTEX_POINT('',#192246);
#38584=VERTEX_POINT('',#192251);
#38585=VERTEX_POINT('',#192252);
#38586=VERTEX_POINT('',#192257);
#38587=VERTEX_POINT('',#192258);
#38588=VERTEX_POINT('',#192263);
#38589=VERTEX_POINT('',#192264);
#38590=VERTEX_POINT('',#192269);
#38591=VERTEX_POINT('',#192270);
#38592=VERTEX_POINT('',#192275);
#38593=VERTEX_POINT('',#192276);
#38594=VERTEX_POINT('',#192284);
#38595=VERTEX_POINT('',#192285);
#38596=VERTEX_POINT('',#192287);
#38597=VERTEX_POINT('',#192289);
#38598=VERTEX_POINT('',#192293);
#38599=VERTEX_POINT('',#192294);
#38600=VERTEX_POINT('',#192299);
#38601=VERTEX_POINT('',#192300);
#38602=VERTEX_POINT('',#192305);
#38603=VERTEX_POINT('',#192306);
#38604=VERTEX_POINT('',#192311);
#38605=VERTEX_POINT('',#192312);
#38606=VERTEX_POINT('',#192317);
#38607=VERTEX_POINT('',#192318);
#38608=VERTEX_POINT('',#192323);
#38609=VERTEX_POINT('',#192324);
#38610=VERTEX_POINT('',#192332);
#38611=VERTEX_POINT('',#192333);
#38612=VERTEX_POINT('',#192335);
#38613=VERTEX_POINT('',#192337);
#38614=VERTEX_POINT('',#192341);
#38615=VERTEX_POINT('',#192342);
#38616=VERTEX_POINT('',#192347);
#38617=VERTEX_POINT('',#192348);
#38618=VERTEX_POINT('',#192353);
#38619=VERTEX_POINT('',#192354);
#38620=VERTEX_POINT('',#192359);
#38621=VERTEX_POINT('',#192360);
#38622=VERTEX_POINT('',#192365);
#38623=VERTEX_POINT('',#192366);
#38624=VERTEX_POINT('',#192371);
#38625=VERTEX_POINT('',#192372);
#38626=VERTEX_POINT('',#192377);
#38627=VERTEX_POINT('',#192378);
#38628=VERTEX_POINT('',#192383);
#38629=VERTEX_POINT('',#192384);
#38630=VERTEX_POINT('',#192392);
#38631=VERTEX_POINT('',#192393);
#38632=VERTEX_POINT('',#192395);
#38633=VERTEX_POINT('',#192397);
#38634=VERTEX_POINT('',#192401);
#38635=VERTEX_POINT('',#192402);
#38636=VERTEX_POINT('',#192407);
#38637=VERTEX_POINT('',#192408);
#38638=VERTEX_POINT('',#192413);
#38639=VERTEX_POINT('',#192414);
#38640=VERTEX_POINT('',#192419);
#38641=VERTEX_POINT('',#192420);
#38642=VERTEX_POINT('',#192425);
#38643=VERTEX_POINT('',#192426);
#38644=VERTEX_POINT('',#192431);
#38645=VERTEX_POINT('',#192432);
#38646=VERTEX_POINT('',#192440);
#38647=VERTEX_POINT('',#192441);
#38648=VERTEX_POINT('',#192443);
#38649=VERTEX_POINT('',#192445);
#38650=VERTEX_POINT('',#192449);
#38651=VERTEX_POINT('',#192450);
#38652=VERTEX_POINT('',#192455);
#38653=VERTEX_POINT('',#192456);
#38654=VERTEX_POINT('',#192461);
#38655=VERTEX_POINT('',#192462);
#38656=VERTEX_POINT('',#192467);
#38657=VERTEX_POINT('',#192468);
#38658=VERTEX_POINT('',#192473);
#38659=VERTEX_POINT('',#192474);
#38660=VERTEX_POINT('',#192479);
#38661=VERTEX_POINT('',#192480);
#38662=VERTEX_POINT('',#192488);
#38663=VERTEX_POINT('',#192489);
#38664=VERTEX_POINT('',#192491);
#38665=VERTEX_POINT('',#192493);
#38666=VERTEX_POINT('',#192497);
#38667=VERTEX_POINT('',#192498);
#38668=VERTEX_POINT('',#192503);
#38669=VERTEX_POINT('',#192504);
#38670=VERTEX_POINT('',#192509);
#38671=VERTEX_POINT('',#192510);
#38672=VERTEX_POINT('',#192515);
#38673=VERTEX_POINT('',#192516);
#38674=VERTEX_POINT('',#192521);
#38675=VERTEX_POINT('',#192522);
#38676=VERTEX_POINT('',#192527);
#38677=VERTEX_POINT('',#192528);
#38678=VERTEX_POINT('',#192533);
#38679=VERTEX_POINT('',#192534);
#38680=VERTEX_POINT('',#192539);
#38681=VERTEX_POINT('',#192540);
#38682=VERTEX_POINT('',#192548);
#38683=VERTEX_POINT('',#192549);
#38684=VERTEX_POINT('',#192551);
#38685=VERTEX_POINT('',#192553);
#38686=VERTEX_POINT('',#192557);
#38687=VERTEX_POINT('',#192558);
#38688=VERTEX_POINT('',#192563);
#38689=VERTEX_POINT('',#192564);
#38690=VERTEX_POINT('',#192569);
#38691=VERTEX_POINT('',#192570);
#38692=VERTEX_POINT('',#192575);
#38693=VERTEX_POINT('',#192576);
#38694=VERTEX_POINT('',#192581);
#38695=VERTEX_POINT('',#192582);
#38696=VERTEX_POINT('',#192587);
#38697=VERTEX_POINT('',#192588);
#38698=VERTEX_POINT('',#192593);
#38699=VERTEX_POINT('',#192594);
#38700=VERTEX_POINT('',#192599);
#38701=VERTEX_POINT('',#192600);
#38702=VERTEX_POINT('',#192608);
#38703=VERTEX_POINT('',#192609);
#38704=VERTEX_POINT('',#192611);
#38705=VERTEX_POINT('',#192613);
#38706=VERTEX_POINT('',#192617);
#38707=VERTEX_POINT('',#192618);
#38708=VERTEX_POINT('',#192623);
#38709=VERTEX_POINT('',#192624);
#38710=VERTEX_POINT('',#192629);
#38711=VERTEX_POINT('',#192630);
#38712=VERTEX_POINT('',#192635);
#38713=VERTEX_POINT('',#192636);
#38714=VERTEX_POINT('',#192641);
#38715=VERTEX_POINT('',#192642);
#38716=VERTEX_POINT('',#192647);
#38717=VERTEX_POINT('',#192648);
#38718=VERTEX_POINT('',#192656);
#38719=VERTEX_POINT('',#192657);
#38720=VERTEX_POINT('',#192659);
#38721=VERTEX_POINT('',#192661);
#38722=VERTEX_POINT('',#192665);
#38723=VERTEX_POINT('',#192666);
#38724=VERTEX_POINT('',#192671);
#38725=VERTEX_POINT('',#192672);
#38726=VERTEX_POINT('',#192677);
#38727=VERTEX_POINT('',#192678);
#38728=VERTEX_POINT('',#192683);
#38729=VERTEX_POINT('',#192684);
#38730=VERTEX_POINT('',#192689);
#38731=VERTEX_POINT('',#192690);
#38732=VERTEX_POINT('',#192695);
#38733=VERTEX_POINT('',#192696);
#38734=VERTEX_POINT('',#192704);
#38735=VERTEX_POINT('',#192705);
#38736=VERTEX_POINT('',#192707);
#38737=VERTEX_POINT('',#192709);
#38738=VERTEX_POINT('',#192713);
#38739=VERTEX_POINT('',#192714);
#38740=VERTEX_POINT('',#192719);
#38741=VERTEX_POINT('',#192720);
#38742=VERTEX_POINT('',#192725);
#38743=VERTEX_POINT('',#192726);
#38744=VERTEX_POINT('',#192731);
#38745=VERTEX_POINT('',#192732);
#38746=VERTEX_POINT('',#192737);
#38747=VERTEX_POINT('',#192738);
#38748=VERTEX_POINT('',#192743);
#38749=VERTEX_POINT('',#192744);
#38750=VERTEX_POINT('',#192752);
#38751=VERTEX_POINT('',#192753);
#38752=VERTEX_POINT('',#192755);
#38753=VERTEX_POINT('',#192757);
#38754=VERTEX_POINT('',#192761);
#38755=VERTEX_POINT('',#192762);
#38756=VERTEX_POINT('',#192767);
#38757=VERTEX_POINT('',#192768);
#38758=VERTEX_POINT('',#192773);
#38759=VERTEX_POINT('',#192774);
#38760=VERTEX_POINT('',#192779);
#38761=VERTEX_POINT('',#192780);
#38762=VERTEX_POINT('',#192785);
#38763=VERTEX_POINT('',#192786);
#38764=VERTEX_POINT('',#192791);
#38765=VERTEX_POINT('',#192792);
#38766=VERTEX_POINT('',#192800);
#38767=VERTEX_POINT('',#192801);
#38768=VERTEX_POINT('',#192803);
#38769=VERTEX_POINT('',#192805);
#38770=VERTEX_POINT('',#192809);
#38771=VERTEX_POINT('',#192810);
#38772=VERTEX_POINT('',#192815);
#38773=VERTEX_POINT('',#192816);
#38774=VERTEX_POINT('',#192821);
#38775=VERTEX_POINT('',#192822);
#38776=VERTEX_POINT('',#192827);
#38777=VERTEX_POINT('',#192828);
#38778=VERTEX_POINT('',#192833);
#38779=VERTEX_POINT('',#192834);
#38780=VERTEX_POINT('',#192839);
#38781=VERTEX_POINT('',#192840);
#38782=VERTEX_POINT('',#192845);
#38783=VERTEX_POINT('',#192847);
#38784=VERTEX_POINT('',#192854);
#38785=VERTEX_POINT('',#192855);
#38786=VERTEX_POINT('',#192857);
#38787=VERTEX_POINT('',#192859);
#38788=VERTEX_POINT('',#192863);
#38789=VERTEX_POINT('',#192864);
#38790=VERTEX_POINT('',#192869);
#38791=VERTEX_POINT('',#192870);
#38792=VERTEX_POINT('',#192875);
#38793=VERTEX_POINT('',#192876);
#38794=VERTEX_POINT('',#192881);
#38795=VERTEX_POINT('',#192882);
#38796=VERTEX_POINT('',#192887);
#38797=VERTEX_POINT('',#192888);
#38798=VERTEX_POINT('',#192893);
#38799=VERTEX_POINT('',#192894);
#38800=VERTEX_POINT('',#192902);
#38801=VERTEX_POINT('',#192903);
#38802=VERTEX_POINT('',#192905);
#38803=VERTEX_POINT('',#192907);
#38804=VERTEX_POINT('',#192911);
#38805=VERTEX_POINT('',#192912);
#38806=VERTEX_POINT('',#192917);
#38807=VERTEX_POINT('',#192918);
#38808=VERTEX_POINT('',#192923);
#38809=VERTEX_POINT('',#192924);
#38810=VERTEX_POINT('',#192929);
#38811=VERTEX_POINT('',#192930);
#38812=VERTEX_POINT('',#192935);
#38813=VERTEX_POINT('',#192936);
#38814=VERTEX_POINT('',#192941);
#38815=VERTEX_POINT('',#192942);
#38816=VERTEX_POINT('',#192947);
#38817=VERTEX_POINT('',#192948);
#38818=VERTEX_POINT('',#192953);
#38819=VERTEX_POINT('',#192954);
#38820=VERTEX_POINT('',#192962);
#38821=VERTEX_POINT('',#192963);
#38822=VERTEX_POINT('',#192965);
#38823=VERTEX_POINT('',#192967);
#38824=VERTEX_POINT('',#192971);
#38825=VERTEX_POINT('',#192972);
#38826=VERTEX_POINT('',#192977);
#38827=VERTEX_POINT('',#192978);
#38828=VERTEX_POINT('',#192983);
#38829=VERTEX_POINT('',#192984);
#38830=VERTEX_POINT('',#192989);
#38831=VERTEX_POINT('',#192990);
#38832=VERTEX_POINT('',#192995);
#38833=VERTEX_POINT('',#192996);
#38834=VERTEX_POINT('',#193001);
#38835=VERTEX_POINT('',#193002);
#38836=VERTEX_POINT('',#193010);
#38837=VERTEX_POINT('',#193011);
#38838=VERTEX_POINT('',#193013);
#38839=VERTEX_POINT('',#193015);
#38840=VERTEX_POINT('',#193019);
#38841=VERTEX_POINT('',#193020);
#38842=VERTEX_POINT('',#193025);
#38843=VERTEX_POINT('',#193026);
#38844=VERTEX_POINT('',#193031);
#38845=VERTEX_POINT('',#193032);
#38846=VERTEX_POINT('',#193037);
#38847=VERTEX_POINT('',#193038);
#38848=VERTEX_POINT('',#193043);
#38849=VERTEX_POINT('',#193044);
#38850=VERTEX_POINT('',#193049);
#38851=VERTEX_POINT('',#193050);
#38852=VERTEX_POINT('',#193055);
#38853=VERTEX_POINT('',#193056);
#38854=VERTEX_POINT('',#193061);
#38855=VERTEX_POINT('',#193062);
#38856=VERTEX_POINT('',#193070);
#38857=VERTEX_POINT('',#193071);
#38858=VERTEX_POINT('',#193073);
#38859=VERTEX_POINT('',#193075);
#38860=VERTEX_POINT('',#193079);
#38861=VERTEX_POINT('',#193080);
#38862=VERTEX_POINT('',#193085);
#38863=VERTEX_POINT('',#193086);
#38864=VERTEX_POINT('',#193091);
#38865=VERTEX_POINT('',#193092);
#38866=VERTEX_POINT('',#193097);
#38867=VERTEX_POINT('',#193098);
#38868=VERTEX_POINT('',#193103);
#38869=VERTEX_POINT('',#193104);
#38870=VERTEX_POINT('',#193109);
#38871=VERTEX_POINT('',#193110);
#38872=VERTEX_POINT('',#193118);
#38873=VERTEX_POINT('',#193119);
#38874=VERTEX_POINT('',#193121);
#38875=VERTEX_POINT('',#193123);
#38876=VERTEX_POINT('',#193127);
#38877=VERTEX_POINT('',#193128);
#38878=VERTEX_POINT('',#193133);
#38879=VERTEX_POINT('',#193134);
#38880=VERTEX_POINT('',#193139);
#38881=VERTEX_POINT('',#193140);
#38882=VERTEX_POINT('',#193145);
#38883=VERTEX_POINT('',#193146);
#38884=VERTEX_POINT('',#193151);
#38885=VERTEX_POINT('',#193152);
#38886=VERTEX_POINT('',#193157);
#38887=VERTEX_POINT('',#193158);
#38888=VERTEX_POINT('',#193166);
#38889=VERTEX_POINT('',#193167);
#38890=VERTEX_POINT('',#193169);
#38891=VERTEX_POINT('',#193171);
#38892=VERTEX_POINT('',#193175);
#38893=VERTEX_POINT('',#193176);
#38894=VERTEX_POINT('',#193181);
#38895=VERTEX_POINT('',#193182);
#38896=VERTEX_POINT('',#193187);
#38897=VERTEX_POINT('',#193188);
#38898=VERTEX_POINT('',#193193);
#38899=VERTEX_POINT('',#193194);
#38900=VERTEX_POINT('',#193199);
#38901=VERTEX_POINT('',#193200);
#38902=VERTEX_POINT('',#193205);
#38903=VERTEX_POINT('',#193206);
#38904=VERTEX_POINT('',#193214);
#38905=VERTEX_POINT('',#193215);
#38906=VERTEX_POINT('',#193217);
#38907=VERTEX_POINT('',#193219);
#38908=VERTEX_POINT('',#193223);
#38909=VERTEX_POINT('',#193224);
#38910=VERTEX_POINT('',#193229);
#38911=VERTEX_POINT('',#193230);
#38912=VERTEX_POINT('',#193235);
#38913=VERTEX_POINT('',#193236);
#38914=VERTEX_POINT('',#193241);
#38915=VERTEX_POINT('',#193242);
#38916=VERTEX_POINT('',#193247);
#38917=VERTEX_POINT('',#193248);
#38918=VERTEX_POINT('',#193253);
#38919=VERTEX_POINT('',#193254);
#38920=VERTEX_POINT('',#193262);
#38921=VERTEX_POINT('',#193263);
#38922=VERTEX_POINT('',#193265);
#38923=VERTEX_POINT('',#193267);
#38924=VERTEX_POINT('',#193271);
#38925=VERTEX_POINT('',#193272);
#38926=VERTEX_POINT('',#193277);
#38927=VERTEX_POINT('',#193278);
#38928=VERTEX_POINT('',#193283);
#38929=VERTEX_POINT('',#193284);
#38930=VERTEX_POINT('',#193289);
#38931=VERTEX_POINT('',#193290);
#38932=VERTEX_POINT('',#193298);
#38933=VERTEX_POINT('',#193299);
#38934=VERTEX_POINT('',#193301);
#38935=VERTEX_POINT('',#193303);
#38936=VERTEX_POINT('',#193307);
#38937=VERTEX_POINT('',#193308);
#38938=VERTEX_POINT('',#193313);
#38939=VERTEX_POINT('',#193314);
#38940=VERTEX_POINT('',#193319);
#38941=VERTEX_POINT('',#193320);
#38942=VERTEX_POINT('',#193325);
#38943=VERTEX_POINT('',#193326);
#38944=VERTEX_POINT('',#193334);
#38945=VERTEX_POINT('',#193335);
#38946=VERTEX_POINT('',#193337);
#38947=VERTEX_POINT('',#193339);
#38948=VERTEX_POINT('',#193343);
#38949=VERTEX_POINT('',#193344);
#38950=VERTEX_POINT('',#193349);
#38951=VERTEX_POINT('',#193350);
#38952=VERTEX_POINT('',#193355);
#38953=VERTEX_POINT('',#193356);
#38954=VERTEX_POINT('',#193361);
#38955=VERTEX_POINT('',#193362);
#38956=VERTEX_POINT('',#193367);
#38957=VERTEX_POINT('',#193368);
#38958=VERTEX_POINT('',#193373);
#38959=VERTEX_POINT('',#193374);
#38960=VERTEX_POINT('',#193379);
#38961=VERTEX_POINT('',#193380);
#38962=VERTEX_POINT('',#193382);
#38963=VERTEX_POINT('',#193384);
#38964=VERTEX_POINT('',#193388);
#38965=VERTEX_POINT('',#193389);
#38966=VERTEX_POINT('',#193394);
#38967=VERTEX_POINT('',#193395);
#38968=VERTEX_POINT('',#193400);
#38969=VERTEX_POINT('',#193401);
#38970=VERTEX_POINT('',#193406);
#38971=VERTEX_POINT('',#193407);
#38972=VERTEX_POINT('',#193412);
#38973=VERTEX_POINT('',#193413);
#38974=VERTEX_POINT('',#193418);
#38975=VERTEX_POINT('',#193419);
#38976=VERTEX_POINT('',#193424);
#38977=VERTEX_POINT('',#193425);
#38978=VERTEX_POINT('',#193427);
#38979=VERTEX_POINT('',#193429);
#38980=VERTEX_POINT('',#193442);
#38981=VERTEX_POINT('',#193443);
#38982=VERTEX_POINT('',#193448);
#38983=VERTEX_POINT('',#193450);
#38984=VERTEX_POINT('',#193454);
#38985=VERTEX_POINT('',#193455);
#38986=VERTEX_POINT('',#193460);
#38987=VERTEX_POINT('',#193461);
#38988=VERTEX_POINT('',#193466);
#38989=VERTEX_POINT('',#193467);
#38990=VERTEX_POINT('',#193472);
#38991=VERTEX_POINT('',#193473);
#38992=VERTEX_POINT('',#193487);
#38993=VERTEX_POINT('',#193488);
#38994=VERTEX_POINT('',#193490);
#38995=VERTEX_POINT('',#193492);
#38996=VERTEX_POINT('',#193505);
#38997=VERTEX_POINT('',#193506);
#38998=VERTEX_POINT('',#193511);
#38999=VERTEX_POINT('',#193512);
#39000=VERTEX_POINT('',#193517);
#39001=VERTEX_POINT('',#193518);
#39002=VERTEX_POINT('',#193523);
#39003=VERTEX_POINT('',#193524);
#39004=VERTEX_POINT('',#193529);
#39005=VERTEX_POINT('',#193530);
#39006=VERTEX_POINT('',#193535);
#39007=VERTEX_POINT('',#193536);
#39008=VERTEX_POINT('',#193550);
#39009=VERTEX_POINT('',#193551);
#39010=VERTEX_POINT('',#193553);
#39011=VERTEX_POINT('',#193555);
#39012=VERTEX_POINT('',#193568);
#39013=VERTEX_POINT('',#193569);
#39014=VERTEX_POINT('',#193574);
#39015=VERTEX_POINT('',#193576);
#39016=VERTEX_POINT('',#193580);
#39017=VERTEX_POINT('',#193581);
#39018=VERTEX_POINT('',#193586);
#39019=VERTEX_POINT('',#193587);
#39020=VERTEX_POINT('',#193592);
#39021=VERTEX_POINT('',#193593);
#39022=VERTEX_POINT('',#193598);
#39023=VERTEX_POINT('',#193599);
#39024=VERTEX_POINT('',#193613);
#39025=VERTEX_POINT('',#193614);
#39026=VERTEX_POINT('',#193625);
#39027=VERTEX_POINT('',#193627);
#39028=VERTEX_POINT('',#193631);
#39029=VERTEX_POINT('',#193632);
#39030=VERTEX_POINT('',#193637);
#39031=VERTEX_POINT('',#193638);
#39032=VERTEX_POINT('',#193643);
#39033=VERTEX_POINT('',#193644);
#39034=VERTEX_POINT('',#193649);
#39035=VERTEX_POINT('',#193650);
#39036=VERTEX_POINT('',#193655);
#39037=VERTEX_POINT('',#193656);
#39038=VERTEX_POINT('',#193661);
#39039=VERTEX_POINT('',#193662);
#39040=VERTEX_POINT('',#193676);
#39041=VERTEX_POINT('',#193677);
#39042=VERTEX_POINT('',#193679);
#39043=VERTEX_POINT('',#193681);
#39044=VERTEX_POINT('',#193685);
#39045=VERTEX_POINT('',#193686);
#39046=VERTEX_POINT('',#193691);
#39047=VERTEX_POINT('',#193692);
#39048=VERTEX_POINT('',#193697);
#39049=VERTEX_POINT('',#193698);
#39050=VERTEX_POINT('',#193703);
#39051=VERTEX_POINT('',#193704);
#39052=VERTEX_POINT('',#193709);
#39053=VERTEX_POINT('',#193710);
#39054=VERTEX_POINT('',#193715);
#39055=VERTEX_POINT('',#193716);
#39056=VERTEX_POINT('',#193864);
#39057=VERTEX_POINT('',#193865);
#39058=VERTEX_POINT('',#193888);
#39059=VERTEX_POINT('',#193915);
#39060=VERTEX_POINT('',#193917);
#39061=VERTEX_POINT('',#194030);
#39062=VERTEX_POINT('',#194055);
#39063=VERTEX_POINT('',#194056);
#39064=VERTEX_POINT('',#194078);
#39065=VERTEX_POINT('',#194079);
#39066=VERTEX_POINT('',#194161);
#39067=VERTEX_POINT('',#194162);
#39068=VERTEX_POINT('',#194263);
#39069=VERTEX_POINT('',#194264);
#39070=VERTEX_POINT('',#194469);
#39071=VERTEX_POINT('',#194470);
#39072=VERTEX_POINT('',#194567);
#39073=VERTEX_POINT('',#194568);
#39074=VERTEX_POINT('',#194584);
#39075=VERTEX_POINT('',#194585);
#39076=VERTEX_POINT('',#194907);
#39077=VERTEX_POINT('',#194908);
#39078=VERTEX_POINT('',#194910);
#39079=VERTEX_POINT('',#194963);
#39080=VERTEX_POINT('',#195004);
#39081=VERTEX_POINT('',#195049);
#39082=VERTEX_POINT('',#195066);
#39083=VERTEX_POINT('',#195310);
#39084=VERTEX_POINT('',#195311);
#39085=VERTEX_POINT('',#195333);
#39086=VERTEX_POINT('',#195334);
#39087=VERTEX_POINT('',#195434);
#39088=VERTEX_POINT('',#195435);
#39089=VERTEX_POINT('',#195551);
#39090=VERTEX_POINT('',#195552);
#39091=VERTEX_POINT('',#195766);
#39092=VERTEX_POINT('',#195767);
#39093=VERTEX_POINT('',#195864);
#39094=VERTEX_POINT('',#195865);
#39095=VERTEX_POINT('',#195881);
#39096=VERTEX_POINT('',#195882);
#39097=VERTEX_POINT('',#195904);
#39098=VERTEX_POINT('',#195909);
#39099=VERTEX_POINT('',#195924);
#39100=VERTEX_POINT('',#195925);
#39101=VERTEX_POINT('',#196007);
#39102=VERTEX_POINT('',#196008);
#39103=VERTEX_POINT('',#196086);
#39104=VERTEX_POINT('',#196087);
#39105=VERTEX_POINT('',#196147);
#39106=VERTEX_POINT('',#196148);
#39107=VERTEX_POINT('',#196155);
#39108=VERTEX_POINT('',#196174);
#39109=VERTEX_POINT('',#196175);
#39110=VERTEX_POINT('',#196666);
#39111=VERTEX_POINT('',#196667);
#39112=VERTEX_POINT('',#196693);
#39113=VERTEX_POINT('',#196737);
#39114=VERTEX_POINT('',#196766);
#39115=VERTEX_POINT('',#196787);
#39116=VERTEX_POINT('',#196817);
#39117=VERTEX_POINT('',#196843);
#39118=VERTEX_POINT('',#197287);
#39119=VERTEX_POINT('',#197315);
#39120=VERTEX_POINT('',#197316);
#39121=VERTEX_POINT('',#197341);
#39122=VERTEX_POINT('',#197343);
#39123=VERTEX_POINT('',#197364);
#39124=VERTEX_POINT('',#197365);
#39125=VERTEX_POINT('',#197458);
#39126=VERTEX_POINT('',#197459);
#39127=VERTEX_POINT('',#197632);
#39128=VERTEX_POINT('',#197633);
#39129=VERTEX_POINT('',#197666);
#39130=VERTEX_POINT('',#197667);
#39131=VERTEX_POINT('',#197669);
#39132=VERTEX_POINT('',#197747);
#39133=VERTEX_POINT('',#197748);
#39134=VERTEX_POINT('',#197764);
#39135=VERTEX_POINT('',#197766);
#39136=VERTEX_POINT('',#197799);
#39137=VERTEX_POINT('',#197800);
#39138=VERTEX_POINT('',#197903);
#39139=VERTEX_POINT('',#197904);
#39140=VERTEX_POINT('',#197970);
#39141=VERTEX_POINT('',#197971);
#39142=VERTEX_POINT('',#198002);
#39143=VERTEX_POINT('',#198003);
#39144=VERTEX_POINT('',#198005);
#39145=VERTEX_POINT('',#198007);
#39146=VERTEX_POINT('',#198196);
#39147=VERTEX_POINT('',#198197);
#39148=VERTEX_POINT('',#198221);
#39149=VERTEX_POINT('',#198256);
#39150=VERTEX_POINT('',#198275);
#39151=VERTEX_POINT('',#198498);
#39152=VERTEX_POINT('',#198543);
#39153=VERTEX_POINT('',#198544);
#39154=VERTEX_POINT('',#198549);
#39155=VERTEX_POINT('',#198565);
#39156=VERTEX_POINT('',#198604);
#39157=VERTEX_POINT('',#198605);
#39158=VERTEX_POINT('',#198762);
#39159=VERTEX_POINT('',#198763);
#39160=VERTEX_POINT('',#198924);
#39161=VERTEX_POINT('',#198925);
#39162=VERTEX_POINT('',#199109);
#39163=VERTEX_POINT('',#199110);
#39164=VERTEX_POINT('',#199115);
#39165=VERTEX_POINT('',#199117);
#39166=VERTEX_POINT('',#199121);
#39167=VERTEX_POINT('',#199123);
#39168=VERTEX_POINT('',#199127);
#39169=VERTEX_POINT('',#199129);
#39170=VERTEX_POINT('',#199133);
#39171=VERTEX_POINT('',#199135);
#39172=VERTEX_POINT('',#199139);
#39173=VERTEX_POINT('',#199141);
#39174=VERTEX_POINT('',#199145);
#39175=VERTEX_POINT('',#199147);
#39176=VERTEX_POINT('',#199151);
#39177=VERTEX_POINT('',#199153);
#39178=VERTEX_POINT('',#199157);
#39179=VERTEX_POINT('',#199159);
#39180=VERTEX_POINT('',#199163);
#39181=VERTEX_POINT('',#199164);
#39182=VERTEX_POINT('',#199169);
#39183=VERTEX_POINT('',#199171);
#39184=VERTEX_POINT('',#199175);
#39185=VERTEX_POINT('',#199177);
#39186=VERTEX_POINT('',#199181);
#39187=VERTEX_POINT('',#199183);
#39188=VERTEX_POINT('',#199187);
#39189=VERTEX_POINT('',#199189);
#39190=VERTEX_POINT('',#199193);
#39191=VERTEX_POINT('',#199195);
#39192=VERTEX_POINT('',#199199);
#39193=VERTEX_POINT('',#199201);
#39194=VERTEX_POINT('',#199205);
#39195=VERTEX_POINT('',#199207);
#39196=VERTEX_POINT('',#199211);
#39197=VERTEX_POINT('',#199213);
#39198=VERTEX_POINT('',#199217);
#39199=VERTEX_POINT('',#199219);
#39200=VERTEX_POINT('',#199223);
#39201=VERTEX_POINT('',#199225);
#39202=VERTEX_POINT('',#199229);
#39203=VERTEX_POINT('',#199231);
#39204=VERTEX_POINT('',#199235);
#39205=VERTEX_POINT('',#199237);
#39206=VERTEX_POINT('',#199241);
#39207=VERTEX_POINT('',#199243);
#39208=VERTEX_POINT('',#199247);
#39209=VERTEX_POINT('',#199249);
#39210=VERTEX_POINT('',#199253);
#39211=VERTEX_POINT('',#199255);
#39212=VERTEX_POINT('',#199259);
#39213=VERTEX_POINT('',#199261);
#39214=VERTEX_POINT('',#199265);
#39215=VERTEX_POINT('',#199267);
#39216=VERTEX_POINT('',#199271);
#39217=VERTEX_POINT('',#199272);
#39218=VERTEX_POINT('',#199277);
#39219=VERTEX_POINT('',#199279);
#39220=VERTEX_POINT('',#199283);
#39221=VERTEX_POINT('',#199285);
#39222=VERTEX_POINT('',#199289);
#39223=VERTEX_POINT('',#199291);
#39224=VERTEX_POINT('',#199295);
#39225=VERTEX_POINT('',#199297);
#39226=VERTEX_POINT('',#199301);
#39227=VERTEX_POINT('',#199303);
#39228=VERTEX_POINT('',#199307);
#39229=VERTEX_POINT('',#199309);
#39230=VERTEX_POINT('',#199313);
#39231=VERTEX_POINT('',#199315);
#39232=VERTEX_POINT('',#199319);
#39233=VERTEX_POINT('',#199321);
#39234=VERTEX_POINT('',#199325);
#39235=VERTEX_POINT('',#199327);
#39236=VERTEX_POINT('',#199331);
#39237=VERTEX_POINT('',#199333);
#39238=VERTEX_POINT('',#199337);
#39239=VERTEX_POINT('',#199339);
#39240=VERTEX_POINT('',#199343);
#39241=VERTEX_POINT('',#199345);
#39242=VERTEX_POINT('',#199349);
#39243=VERTEX_POINT('',#199351);
#39244=VERTEX_POINT('',#199355);
#39245=VERTEX_POINT('',#199357);
#39246=VERTEX_POINT('',#199361);
#39247=VERTEX_POINT('',#199363);
#39248=VERTEX_POINT('',#199367);
#39249=VERTEX_POINT('',#199369);
#39250=VERTEX_POINT('',#199373);
#39251=VERTEX_POINT('',#199375);
#39252=VERTEX_POINT('',#199379);
#39253=VERTEX_POINT('',#199381);
#39254=VERTEX_POINT('',#199385);
#39255=VERTEX_POINT('',#199387);
#39256=VERTEX_POINT('',#199391);
#39257=VERTEX_POINT('',#199393);
#39258=VERTEX_POINT('',#199397);
#39259=VERTEX_POINT('',#199399);
#39260=VERTEX_POINT('',#199403);
#39261=VERTEX_POINT('',#199405);
#39262=VERTEX_POINT('',#199409);
#39263=VERTEX_POINT('',#199411);
#39264=VERTEX_POINT('',#199415);
#39265=VERTEX_POINT('',#199417);
#39266=VERTEX_POINT('',#199421);
#39267=VERTEX_POINT('',#199423);
#39268=VERTEX_POINT('',#199427);
#39269=VERTEX_POINT('',#199429);
#39270=VERTEX_POINT('',#199433);
#39271=VERTEX_POINT('',#199435);
#39272=VERTEX_POINT('',#199439);
#39273=VERTEX_POINT('',#199441);
#39274=VERTEX_POINT('',#199445);
#39275=VERTEX_POINT('',#199447);
#39276=VERTEX_POINT('',#199451);
#39277=VERTEX_POINT('',#199453);
#39278=VERTEX_POINT('',#199457);
#39279=VERTEX_POINT('',#199459);
#39280=VERTEX_POINT('',#199463);
#39281=VERTEX_POINT('',#199465);
#39282=VERTEX_POINT('',#199469);
#39283=VERTEX_POINT('',#199471);
#39284=VERTEX_POINT('',#199475);
#39285=VERTEX_POINT('',#199477);
#39286=VERTEX_POINT('',#199481);
#39287=VERTEX_POINT('',#199483);
#39288=VERTEX_POINT('',#199487);
#39289=VERTEX_POINT('',#199489);
#39290=VERTEX_POINT('',#199493);
#39291=VERTEX_POINT('',#199495);
#39292=VERTEX_POINT('',#199499);
#39293=VERTEX_POINT('',#199501);
#39294=VERTEX_POINT('',#199505);
#39295=VERTEX_POINT('',#199507);
#39296=VERTEX_POINT('',#199511);
#39297=VERTEX_POINT('',#199513);
#39298=VERTEX_POINT('',#199517);
#39299=VERTEX_POINT('',#199519);
#39300=VERTEX_POINT('',#199523);
#39301=VERTEX_POINT('',#199525);
#39302=VERTEX_POINT('',#199529);
#39303=VERTEX_POINT('',#199531);
#39304=VERTEX_POINT('',#199535);
#39305=VERTEX_POINT('',#199537);
#39306=VERTEX_POINT('',#199541);
#39307=VERTEX_POINT('',#199543);
#39308=VERTEX_POINT('',#199547);
#39309=VERTEX_POINT('',#199549);
#39310=VERTEX_POINT('',#199553);
#39311=VERTEX_POINT('',#199555);
#39312=VERTEX_POINT('',#199559);
#39313=VERTEX_POINT('',#199561);
#39314=VERTEX_POINT('',#199565);
#39315=VERTEX_POINT('',#199567);
#39316=VERTEX_POINT('',#199571);
#39317=VERTEX_POINT('',#199573);
#39318=VERTEX_POINT('',#199577);
#39319=VERTEX_POINT('',#199579);
#39320=VERTEX_POINT('',#199583);
#39321=VERTEX_POINT('',#199585);
#39322=VERTEX_POINT('',#199589);
#39323=VERTEX_POINT('',#199591);
#39324=VERTEX_POINT('',#199595);
#39325=VERTEX_POINT('',#199597);
#39326=VERTEX_POINT('',#199601);
#39327=VERTEX_POINT('',#199603);
#39328=VERTEX_POINT('',#199607);
#39329=VERTEX_POINT('',#199609);
#39330=VERTEX_POINT('',#199613);
#39331=VERTEX_POINT('',#199615);
#39332=VERTEX_POINT('',#199619);
#39333=VERTEX_POINT('',#199620);
#39334=VERTEX_POINT('',#199625);
#39335=VERTEX_POINT('',#199627);
#39336=VERTEX_POINT('',#199631);
#39337=VERTEX_POINT('',#199633);
#39338=VERTEX_POINT('',#199637);
#39339=VERTEX_POINT('',#199639);
#39340=VERTEX_POINT('',#199643);
#39341=VERTEX_POINT('',#199645);
#39342=VERTEX_POINT('',#199649);
#39343=VERTEX_POINT('',#199651);
#39344=VERTEX_POINT('',#199655);
#39345=VERTEX_POINT('',#199657);
#39346=VERTEX_POINT('',#199661);
#39347=VERTEX_POINT('',#199663);
#39348=VERTEX_POINT('',#199667);
#39349=VERTEX_POINT('',#199669);
#39350=VERTEX_POINT('',#199673);
#39351=VERTEX_POINT('',#199675);
#39352=VERTEX_POINT('',#199679);
#39353=VERTEX_POINT('',#199681);
#39354=VERTEX_POINT('',#199685);
#39355=VERTEX_POINT('',#199687);
#39356=VERTEX_POINT('',#199691);
#39357=VERTEX_POINT('',#199693);
#39358=VERTEX_POINT('',#199697);
#39359=VERTEX_POINT('',#199699);
#39360=VERTEX_POINT('',#199703);
#39361=VERTEX_POINT('',#199705);
#39362=VERTEX_POINT('',#199709);
#39363=VERTEX_POINT('',#199711);
#39364=VERTEX_POINT('',#199715);
#39365=VERTEX_POINT('',#199717);
#39366=VERTEX_POINT('',#199721);
#39367=VERTEX_POINT('',#199723);
#39368=VERTEX_POINT('',#199727);
#39369=VERTEX_POINT('',#199729);
#39370=VERTEX_POINT('',#199733);
#39371=VERTEX_POINT('',#199735);
#39372=VERTEX_POINT('',#199739);
#39373=VERTEX_POINT('',#199741);
#39374=VERTEX_POINT('',#199745);
#39375=VERTEX_POINT('',#199747);
#39376=VERTEX_POINT('',#199751);
#39377=VERTEX_POINT('',#199753);
#39378=VERTEX_POINT('',#199757);
#39379=VERTEX_POINT('',#199759);
#39380=VERTEX_POINT('',#199763);
#39381=VERTEX_POINT('',#199764);
#39382=VERTEX_POINT('',#199769);
#39383=VERTEX_POINT('',#199771);
#39384=VERTEX_POINT('',#199775);
#39385=VERTEX_POINT('',#199777);
#39386=VERTEX_POINT('',#199781);
#39387=VERTEX_POINT('',#199783);
#39388=VERTEX_POINT('',#199787);
#39389=VERTEX_POINT('',#199789);
#39390=VERTEX_POINT('',#199793);
#39391=VERTEX_POINT('',#199795);
#39392=VERTEX_POINT('',#199799);
#39393=VERTEX_POINT('',#199801);
#39394=VERTEX_POINT('',#199805);
#39395=VERTEX_POINT('',#199807);
#39396=VERTEX_POINT('',#199811);
#39397=VERTEX_POINT('',#199813);
#39398=VERTEX_POINT('',#199817);
#39399=VERTEX_POINT('',#199819);
#39400=VERTEX_POINT('',#199823);
#39401=VERTEX_POINT('',#199825);
#39402=VERTEX_POINT('',#199829);
#39403=VERTEX_POINT('',#199831);
#39404=VERTEX_POINT('',#199835);
#39405=VERTEX_POINT('',#199837);
#39406=VERTEX_POINT('',#199841);
#39407=VERTEX_POINT('',#199843);
#39408=VERTEX_POINT('',#199847);
#39409=VERTEX_POINT('',#199849);
#39410=VERTEX_POINT('',#199853);
#39411=VERTEX_POINT('',#199855);
#39412=VERTEX_POINT('',#199859);
#39413=VERTEX_POINT('',#199860);
#39414=VERTEX_POINT('',#199865);
#39415=VERTEX_POINT('',#199867);
#39416=VERTEX_POINT('',#199871);
#39417=VERTEX_POINT('',#199873);
#39418=VERTEX_POINT('',#199877);
#39419=VERTEX_POINT('',#199879);
#39420=VERTEX_POINT('',#199883);
#39421=VERTEX_POINT('',#199885);
#39422=VERTEX_POINT('',#199889);
#39423=VERTEX_POINT('',#199890);
#39424=VERTEX_POINT('',#199895);
#39425=VERTEX_POINT('',#199897);
#39426=VERTEX_POINT('',#199901);
#39427=VERTEX_POINT('',#199902);
#39428=VERTEX_POINT('',#199907);
#39429=VERTEX_POINT('',#199909);
#39430=VERTEX_POINT('',#199913);
#39431=VERTEX_POINT('',#199915);
#39432=VERTEX_POINT('',#199919);
#39433=VERTEX_POINT('',#199921);
#39434=VERTEX_POINT('',#199925);
#39435=VERTEX_POINT('',#199929);
#39436=VERTEX_POINT('',#200021);
#39437=VERTEX_POINT('',#200022);
#39438=VERTEX_POINT('',#200024);
#39439=VERTEX_POINT('',#200026);
#39440=VERTEX_POINT('',#200030);
#39441=VERTEX_POINT('',#200031);
#39442=VERTEX_POINT('',#200036);
#39443=VERTEX_POINT('',#200038);
#39444=VERTEX_POINT('',#200086);
#39445=VERTEX_POINT('',#200087);
#39446=VERTEX_POINT('',#200089);
#39447=VERTEX_POINT('',#200091);
#39448=VERTEX_POINT('',#200095);
#39449=VERTEX_POINT('',#200097);
#39450=VERTEX_POINT('',#200101);
#39451=VERTEX_POINT('',#200103);
#39452=VERTEX_POINT('',#200107);
#39453=VERTEX_POINT('',#200109);
#39454=VERTEX_POINT('',#200113);
#39455=VERTEX_POINT('',#200115);
#39456=VERTEX_POINT('',#200119);
#39457=VERTEX_POINT('',#200121);
#39458=VERTEX_POINT('',#200125);
#39459=VERTEX_POINT('',#200127);
#39460=VERTEX_POINT('',#200131);
#39461=VERTEX_POINT('',#200132);
#39462=VERTEX_POINT('',#200134);
#39463=VERTEX_POINT('',#200136);
#39464=VERTEX_POINT('',#200145);
#39465=VERTEX_POINT('',#200154);
#39466=VERTEX_POINT('',#200155);
#39467=VERTEX_POINT('',#200157);
#39468=VERTEX_POINT('',#200166);
#39469=VERTEX_POINT('',#200175);
#39470=VERTEX_POINT('',#200176);
#39471=VERTEX_POINT('',#200180);
#39472=VERTEX_POINT('',#200182);
#39473=VERTEX_POINT('',#200191);
#39474=VERTEX_POINT('',#200192);
#39475=VERTEX_POINT('',#200196);
#39476=VERTEX_POINT('',#200203);
#39477=VERTEX_POINT('',#200210);
#39478=VERTEX_POINT('',#200211);
#39479=VERTEX_POINT('',#200215);
#39480=VERTEX_POINT('',#200222);
#39481=VERTEX_POINT('',#200226);
#39482=VERTEX_POINT('',#200227);
#39483=VERTEX_POINT('',#200231);
#39484=VERTEX_POINT('',#200233);
#39485=VERTEX_POINT('',#200245);
#39486=VERTEX_POINT('',#200246);
#39487=VERTEX_POINT('',#200248);
#39488=VERTEX_POINT('',#200250);
#39489=VERTEX_POINT('',#200254);
#39490=VERTEX_POINT('',#200255);
#39491=VERTEX_POINT('',#200257);
#39492=VERTEX_POINT('',#200259);
#39493=VERTEX_POINT('',#200263);
#39494=VERTEX_POINT('',#200265);
#39495=VERTEX_POINT('',#200269);
#39496=VERTEX_POINT('',#200271);
#39497=VERTEX_POINT('',#200275);
#39498=VERTEX_POINT('',#200276);
#39499=VERTEX_POINT('',#200286);
#39500=VERTEX_POINT('',#200287);
#39501=VERTEX_POINT('',#200289);
#39502=VERTEX_POINT('',#200291);
#39503=VERTEX_POINT('',#200661);
#39504=VERTEX_POINT('',#200662);
#39505=VERTEX_POINT('',#200683);
#39506=VERTEX_POINT('',#200688);
#39507=VERTEX_POINT('',#200695);
#39508=VERTEX_POINT('',#201283);
#39509=VERTEX_POINT('',#201284);
#39510=VERTEX_POINT('',#201309);
#39511=VERTEX_POINT('',#201320);
#39512=VERTEX_POINT('',#201345);
#39513=VERTEX_POINT('',#201724);
#39514=VERTEX_POINT('',#201725);
#39515=VERTEX_POINT('',#201744);
#39516=VERTEX_POINT('',#201758);
#39517=VERTEX_POINT('',#201765);
#39518=VERTEX_POINT('',#202316);
#39519=VERTEX_POINT('',#202317);
#39520=VERTEX_POINT('',#202334);
#39521=VERTEX_POINT('',#202342);
#39522=VERTEX_POINT('',#202369);
#39523=VERTEX_POINT('',#202383);
#39524=VERTEX_POINT('',#202384);
#39525=VERTEX_POINT('',#202387);
#39526=VERTEX_POINT('',#202404);
#39527=VERTEX_POINT('',#202411);
#39528=VERTEX_POINT('',#202415);
#39529=VERTEX_POINT('',#202420);
#39530=VERTEX_POINT('',#202421);
#39531=VERTEX_POINT('',#202424);
#39532=VERTEX_POINT('',#202428);
#39533=VERTEX_POINT('',#202437);
#39534=VERTEX_POINT('',#202449);
#39535=VERTEX_POINT('',#202454);
#39536=VERTEX_POINT('',#202455);
#39537=VERTEX_POINT('',#202457);
#39538=VERTEX_POINT('',#202459);
#39539=VERTEX_POINT('',#202463);
#39540=VERTEX_POINT('',#202465);
#39541=VERTEX_POINT('',#202469);
#39542=VERTEX_POINT('',#202471);
#39543=VERTEX_POINT('',#202475);
#39544=VERTEX_POINT('',#202477);
#39545=VERTEX_POINT('',#202481);
#39546=VERTEX_POINT('',#202482);
#39547=VERTEX_POINT('',#202484);
#39548=VERTEX_POINT('',#202486);
#39549=VERTEX_POINT('',#202490);
#39550=VERTEX_POINT('',#202492);
#39551=VERTEX_POINT('',#202514);
#39552=VERTEX_POINT('',#202521);
#39553=VERTEX_POINT('',#202550);
#39554=VERTEX_POINT('',#202557);
#39555=VERTEX_POINT('',#202769);
#39556=VERTEX_POINT('',#202771);
#39557=VERTEX_POINT('',#202855);
#39558=VERTEX_POINT('',#202879);
#39559=VERTEX_POINT('',#202881);
#39560=VERTEX_POINT('',#202905);
#39561=VERTEX_POINT('',#202953);
#39562=VERTEX_POINT('',#202960);
#39563=VERTEX_POINT('',#203164);
#39564=VERTEX_POINT('',#203209);
#39565=VERTEX_POINT('',#203216);
#39566=VERTEX_POINT('',#203230);
#39567=VERTEX_POINT('',#203237);
#39568=VERTEX_POINT('',#203525);
#39569=VERTEX_POINT('',#203563);
#39570=VERTEX_POINT('',#203564);
#39571=VERTEX_POINT('',#203579);
#39572=VERTEX_POINT('',#203588);
#39573=VERTEX_POINT('',#203589);
#39574=VERTEX_POINT('',#203598);
#39575=VERTEX_POINT('',#203599);
#39576=VERTEX_POINT('',#203608);
#39577=VERTEX_POINT('',#203609);
#39578=VERTEX_POINT('',#203618);
#39579=VERTEX_POINT('',#203619);
#39580=VERTEX_POINT('',#203628);
#39581=VERTEX_POINT('',#203632);
#39582=VERTEX_POINT('',#203641);
#39583=VERTEX_POINT('',#203652);
#39584=VERTEX_POINT('',#203653);
#39585=VERTEX_POINT('',#203670);
#39586=VERTEX_POINT('',#203679);
#39587=VERTEX_POINT('',#203680);
#39588=VERTEX_POINT('',#203719);
#39589=VERTEX_POINT('',#204831);
#39590=VERTEX_POINT('',#204842);
#39591=VERTEX_POINT('',#204867);
#39592=VERTEX_POINT('',#204869);
#39593=VERTEX_POINT('',#204873);
#39594=VERTEX_POINT('',#204877);
#39595=VERTEX_POINT('',#204883);
#39596=VERTEX_POINT('',#204885);
#39597=VERTEX_POINT('',#204891);
#39598=VERTEX_POINT('',#204893);
#39599=VERTEX_POINT('',#204897);
#39600=VERTEX_POINT('',#204900);
#39601=VERTEX_POINT('',#204905);
#39602=VERTEX_POINT('',#205009);
#39603=VERTEX_POINT('',#205011);
#39604=VERTEX_POINT('',#205015);
#39605=VERTEX_POINT('',#205019);
#39606=VERTEX_POINT('',#205023);
#39607=VERTEX_POINT('',#205027);
#39608=VERTEX_POINT('',#205031);
#39609=VERTEX_POINT('',#205035);
#39610=VERTEX_POINT('',#205039);
#39611=VERTEX_POINT('',#205041);
#39612=VERTEX_POINT('',#205045);
#39613=VERTEX_POINT('',#205047);
#39614=VERTEX_POINT('',#205051);
#39615=VERTEX_POINT('',#205055);
#39616=VERTEX_POINT('',#205059);
#39617=VERTEX_POINT('',#205063);
#39618=VERTEX_POINT('',#205474);
#39619=VERTEX_POINT('',#205476);
#39620=VERTEX_POINT('',#205480);
#39621=VERTEX_POINT('',#205484);
#39622=VERTEX_POINT('',#205488);
#39623=VERTEX_POINT('',#205492);
#39624=VERTEX_POINT('',#205494);
#39625=VERTEX_POINT('',#205498);
#39626=VERTEX_POINT('',#207116);
#39627=VERTEX_POINT('',#207117);
#39628=VERTEX_POINT('',#207119);
#39629=VERTEX_POINT('',#207172);
#39630=VERTEX_POINT('',#207201);
#39631=VERTEX_POINT('',#207205);
#39632=VERTEX_POINT('',#207207);
#39633=VERTEX_POINT('',#207209);
#39634=VERTEX_POINT('',#207242);
#39635=VERTEX_POINT('',#207243);
#39636=VERTEX_POINT('',#207245);
#39637=VERTEX_POINT('',#207325);
#39638=VERTEX_POINT('',#207370);
#39639=VERTEX_POINT('',#207371);
#39640=VERTEX_POINT('',#207424);
#39641=VERTEX_POINT('',#207457);
#39642=VERTEX_POINT('',#207458);
#39643=VERTEX_POINT('',#207524);
#39644=VERTEX_POINT('',#207525);
#39645=VERTEX_POINT('',#207547);
#39646=VERTEX_POINT('',#207548);
#39647=VERTEX_POINT('',#207583);
#39648=VERTEX_POINT('',#207584);
#39649=VERTEX_POINT('',#207618);
#39650=VERTEX_POINT('',#207619);
#39651=VERTEX_POINT('',#207744);
#39652=VERTEX_POINT('',#207745);
#39653=VERTEX_POINT('',#207761);
#39654=VERTEX_POINT('',#207762);
#39655=VERTEX_POINT('',#207795);
#39656=VERTEX_POINT('',#207796);
#39657=VERTEX_POINT('',#207854);
#39658=VERTEX_POINT('',#207905);
#39659=VERTEX_POINT('',#208000);
#39660=VERTEX_POINT('',#208001);
#39661=VERTEX_POINT('',#208003);
#39662=VERTEX_POINT('',#208038);
#39663=VERTEX_POINT('',#208079);
#39664=VERTEX_POINT('',#208080);
#39665=VERTEX_POINT('',#208108);
#39666=VERTEX_POINT('',#208109);
#39667=VERTEX_POINT('',#208158);
#39668=VERTEX_POINT('',#208159);
#39669=VERTEX_POINT('',#208331);
#39670=VERTEX_POINT('',#208332);
#39671=VERTEX_POINT('',#208398);
#39672=VERTEX_POINT('',#208413);
#39673=VERTEX_POINT('',#208414);
#39674=VERTEX_POINT('',#208447);
#39675=VERTEX_POINT('',#208448);
#39676=VERTEX_POINT('',#208482);
#39677=VERTEX_POINT('',#208483);
#39678=VERTEX_POINT('',#208590);
#39679=VERTEX_POINT('',#208591);
#39680=VERTEX_POINT('',#208596);
#39681=VERTEX_POINT('',#208600);
#39682=VERTEX_POINT('',#208601);
#39683=VERTEX_POINT('',#208617);
#39684=VERTEX_POINT('',#208618);
#39685=VERTEX_POINT('',#208632);
#39686=VERTEX_POINT('',#208634);
#39687=VERTEX_POINT('',#208638);
#39688=VERTEX_POINT('',#208639);
#39689=VERTEX_POINT('',#208644);
#39690=VERTEX_POINT('',#208645);
#39691=VERTEX_POINT('',#208650);
#39692=VERTEX_POINT('',#208651);
#39693=VERTEX_POINT('',#208656);
#39694=VERTEX_POINT('',#208657);
#39695=VERTEX_POINT('',#208662);
#39696=VERTEX_POINT('',#208663);
#39697=VERTEX_POINT('',#208668);
#39698=VERTEX_POINT('',#208669);
#39699=VERTEX_POINT('',#208674);
#39700=VERTEX_POINT('',#208675);
#39701=VERTEX_POINT('',#208694);
#39702=VERTEX_POINT('',#208696);
#39703=VERTEX_POINT('',#208711);
#39704=VERTEX_POINT('',#208712);
#39705=VERTEX_POINT('',#208755);
#39706=VERTEX_POINT('',#208788);
#39707=VERTEX_POINT('',#208849);
#39708=VERTEX_POINT('',#208850);
#39709=VERTEX_POINT('',#209011);
#39710=VERTEX_POINT('',#209012);
#39711=VERTEX_POINT('',#209028);
#39712=VERTEX_POINT('',#209029);
#39713=VERTEX_POINT('',#209045);
#39714=VERTEX_POINT('',#209046);
#39715=VERTEX_POINT('',#209119);
#39716=VERTEX_POINT('',#209120);
#39717=VERTEX_POINT('',#209208);
#39718=VERTEX_POINT('',#209209);
#39719=VERTEX_POINT('',#209377);
#39720=VERTEX_POINT('',#209378);
#39721=VERTEX_POINT('',#209563);
#39722=VERTEX_POINT('',#209564);
#39723=VERTEX_POINT('',#209735);
#39724=VERTEX_POINT('',#209736);
#39725=VERTEX_POINT('',#209914);
#39726=VERTEX_POINT('',#209915);
#39727=VERTEX_POINT('',#209917);
#39728=VERTEX_POINT('',#210015);
#39729=VERTEX_POINT('',#210036);
#39730=VERTEX_POINT('',#210037);
#39731=VERTEX_POINT('',#210065);
#39732=VERTEX_POINT('',#210066);
#39733=VERTEX_POINT('',#210257);
#39734=VERTEX_POINT('',#210258);
#39735=VERTEX_POINT('',#210391);
#39736=VERTEX_POINT('',#210392);
#39737=VERTEX_POINT('',#210471);
#39738=VERTEX_POINT('',#210472);
#39739=VERTEX_POINT('',#210509);
#39740=VERTEX_POINT('',#210554);
#39741=VERTEX_POINT('',#210555);
#39742=VERTEX_POINT('',#210571);
#39743=VERTEX_POINT('',#210572);
#39744=VERTEX_POINT('',#210732);
#39745=VERTEX_POINT('',#210733);
#39746=VERTEX_POINT('',#210830);
#39747=VERTEX_POINT('',#210832);
#39748=VERTEX_POINT('',#210844);
#39749=VERTEX_POINT('',#210846);
#39750=VERTEX_POINT('',#210850);
#39751=VERTEX_POINT('',#210853);
#39752=VERTEX_POINT('',#210865);
#39753=VERTEX_POINT('',#210866);
#39754=VERTEX_POINT('',#210874);
#39755=VERTEX_POINT('',#210876);
#39756=VERTEX_POINT('',#210888);
#39757=VERTEX_POINT('',#210890);
#39758=VERTEX_POINT('',#210894);
#39759=VERTEX_POINT('',#210895);
#39760=VERTEX_POINT('',#210908);
#39761=VERTEX_POINT('',#210909);
#39762=VERTEX_POINT('',#210917);
#39763=VERTEX_POINT('',#210919);
#39764=VERTEX_POINT('',#210931);
#39765=VERTEX_POINT('',#210932);
#39766=VERTEX_POINT('',#210937);
#39767=VERTEX_POINT('',#210938);
#39768=VERTEX_POINT('',#210951);
#39769=VERTEX_POINT('',#210953);
#39770=VERTEX_POINT('',#210960);
#39771=VERTEX_POINT('',#210962);
#39772=VERTEX_POINT('',#210974);
#39773=VERTEX_POINT('',#210975);
#39774=VERTEX_POINT('',#210980);
#39775=VERTEX_POINT('',#210981);
#39776=VERTEX_POINT('',#210994);
#39777=VERTEX_POINT('',#210996);
#39778=VERTEX_POINT('',#211027);
#39779=VERTEX_POINT('',#211028);
#39780=VERTEX_POINT('',#211030);
#39781=VERTEX_POINT('',#211032);
#39782=VERTEX_POINT('',#211036);
#39783=VERTEX_POINT('',#211037);
#39784=VERTEX_POINT('',#211042);
#39785=VERTEX_POINT('',#211043);
#39786=VERTEX_POINT('',#211048);
#39787=VERTEX_POINT('',#211049);
#39788=VERTEX_POINT('',#211054);
#39789=VERTEX_POINT('',#211055);
#39790=VERTEX_POINT('',#211060);
#39791=VERTEX_POINT('',#211061);
#39792=VERTEX_POINT('',#211066);
#39793=VERTEX_POINT('',#211067);
#39794=VERTEX_POINT('',#211072);
#39795=VERTEX_POINT('',#211073);
#39796=VERTEX_POINT('',#211078);
#39797=VERTEX_POINT('',#211079);
#39798=VERTEX_POINT('',#211087);
#39799=VERTEX_POINT('',#211088);
#39800=VERTEX_POINT('',#211090);
#39801=VERTEX_POINT('',#211092);
#39802=VERTEX_POINT('',#211096);
#39803=VERTEX_POINT('',#211097);
#39804=VERTEX_POINT('',#211102);
#39805=VERTEX_POINT('',#211103);
#39806=VERTEX_POINT('',#211108);
#39807=VERTEX_POINT('',#211109);
#39808=VERTEX_POINT('',#211114);
#39809=VERTEX_POINT('',#211115);
#39810=VERTEX_POINT('',#211120);
#39811=VERTEX_POINT('',#211121);
#39812=VERTEX_POINT('',#211126);
#39813=VERTEX_POINT('',#211127);
#39814=VERTEX_POINT('',#211135);
#39815=VERTEX_POINT('',#211136);
#39816=VERTEX_POINT('',#211138);
#39817=VERTEX_POINT('',#211140);
#39818=VERTEX_POINT('',#211144);
#39819=VERTEX_POINT('',#211145);
#39820=VERTEX_POINT('',#211150);
#39821=VERTEX_POINT('',#211151);
#39822=VERTEX_POINT('',#211156);
#39823=VERTEX_POINT('',#211157);
#39824=VERTEX_POINT('',#211162);
#39825=VERTEX_POINT('',#211163);
#39826=VERTEX_POINT('',#211168);
#39827=VERTEX_POINT('',#211169);
#39828=VERTEX_POINT('',#211174);
#39829=VERTEX_POINT('',#211175);
#39830=VERTEX_POINT('',#211183);
#39831=VERTEX_POINT('',#211184);
#39832=VERTEX_POINT('',#211186);
#39833=VERTEX_POINT('',#211188);
#39834=VERTEX_POINT('',#211192);
#39835=VERTEX_POINT('',#211193);
#39836=VERTEX_POINT('',#211198);
#39837=VERTEX_POINT('',#211199);
#39838=VERTEX_POINT('',#211204);
#39839=VERTEX_POINT('',#211205);
#39840=VERTEX_POINT('',#211210);
#39841=VERTEX_POINT('',#211211);
#39842=VERTEX_POINT('',#211216);
#39843=VERTEX_POINT('',#211217);
#39844=VERTEX_POINT('',#211222);
#39845=VERTEX_POINT('',#211223);
#39846=VERTEX_POINT('',#211231);
#39847=VERTEX_POINT('',#211232);
#39848=VERTEX_POINT('',#211234);
#39849=VERTEX_POINT('',#211236);
#39850=VERTEX_POINT('',#211240);
#39851=VERTEX_POINT('',#211241);
#39852=VERTEX_POINT('',#211246);
#39853=VERTEX_POINT('',#211247);
#39854=VERTEX_POINT('',#211252);
#39855=VERTEX_POINT('',#211253);
#39856=VERTEX_POINT('',#211258);
#39857=VERTEX_POINT('',#211259);
#39858=VERTEX_POINT('',#211264);
#39859=VERTEX_POINT('',#211265);
#39860=VERTEX_POINT('',#211270);
#39861=VERTEX_POINT('',#211271);
#39862=VERTEX_POINT('',#211276);
#39863=VERTEX_POINT('',#211277);
#39864=VERTEX_POINT('',#211285);
#39865=VERTEX_POINT('',#211286);
#39866=VERTEX_POINT('',#211288);
#39867=VERTEX_POINT('',#211290);
#39868=VERTEX_POINT('',#211294);
#39869=VERTEX_POINT('',#211295);
#39870=VERTEX_POINT('',#211300);
#39871=VERTEX_POINT('',#211301);
#39872=VERTEX_POINT('',#211306);
#39873=VERTEX_POINT('',#211307);
#39874=VERTEX_POINT('',#211312);
#39875=VERTEX_POINT('',#211313);
#39876=VERTEX_POINT('',#211318);
#39877=VERTEX_POINT('',#211319);
#39878=VERTEX_POINT('',#211324);
#39879=VERTEX_POINT('',#211325);
#39880=VERTEX_POINT('',#211333);
#39881=VERTEX_POINT('',#211334);
#39882=VERTEX_POINT('',#211336);
#39883=VERTEX_POINT('',#211338);
#39884=VERTEX_POINT('',#211342);
#39885=VERTEX_POINT('',#211343);
#39886=VERTEX_POINT('',#211348);
#39887=VERTEX_POINT('',#211349);
#39888=VERTEX_POINT('',#211354);
#39889=VERTEX_POINT('',#211355);
#39890=VERTEX_POINT('',#211360);
#39891=VERTEX_POINT('',#211361);
#39892=VERTEX_POINT('',#211366);
#39893=VERTEX_POINT('',#211367);
#39894=VERTEX_POINT('',#211372);
#39895=VERTEX_POINT('',#211373);
#39896=VERTEX_POINT('',#211381);
#39897=VERTEX_POINT('',#211382);
#39898=VERTEX_POINT('',#211384);
#39899=VERTEX_POINT('',#211386);
#39900=VERTEX_POINT('',#211390);
#39901=VERTEX_POINT('',#211391);
#39902=VERTEX_POINT('',#211396);
#39903=VERTEX_POINT('',#211397);
#39904=VERTEX_POINT('',#211402);
#39905=VERTEX_POINT('',#211403);
#39906=VERTEX_POINT('',#211408);
#39907=VERTEX_POINT('',#211409);
#39908=VERTEX_POINT('',#211414);
#39909=VERTEX_POINT('',#211415);
#39910=VERTEX_POINT('',#211420);
#39911=VERTEX_POINT('',#211421);
#39912=VERTEX_POINT('',#211429);
#39913=VERTEX_POINT('',#211430);
#39914=VERTEX_POINT('',#211432);
#39915=VERTEX_POINT('',#211434);
#39916=VERTEX_POINT('',#211438);
#39917=VERTEX_POINT('',#211439);
#39918=VERTEX_POINT('',#211444);
#39919=VERTEX_POINT('',#211445);
#39920=VERTEX_POINT('',#211450);
#39921=VERTEX_POINT('',#211451);
#39922=VERTEX_POINT('',#211456);
#39923=VERTEX_POINT('',#211457);
#39924=VERTEX_POINT('',#211462);
#39925=VERTEX_POINT('',#211463);
#39926=VERTEX_POINT('',#211468);
#39927=VERTEX_POINT('',#211469);
#39928=VERTEX_POINT('',#211477);
#39929=VERTEX_POINT('',#211478);
#39930=VERTEX_POINT('',#211480);
#39931=VERTEX_POINT('',#211482);
#39932=VERTEX_POINT('',#211486);
#39933=VERTEX_POINT('',#211487);
#39934=VERTEX_POINT('',#211492);
#39935=VERTEX_POINT('',#211493);
#39936=VERTEX_POINT('',#211498);
#39937=VERTEX_POINT('',#211499);
#39938=VERTEX_POINT('',#211504);
#39939=VERTEX_POINT('',#211505);
#39940=VERTEX_POINT('',#211510);
#39941=VERTEX_POINT('',#211511);
#39942=VERTEX_POINT('',#211516);
#39943=VERTEX_POINT('',#211517);
#39944=VERTEX_POINT('',#211525);
#39945=VERTEX_POINT('',#211526);
#39946=VERTEX_POINT('',#211528);
#39947=VERTEX_POINT('',#211530);
#39948=VERTEX_POINT('',#211534);
#39949=VERTEX_POINT('',#211535);
#39950=VERTEX_POINT('',#211540);
#39951=VERTEX_POINT('',#211541);
#39952=VERTEX_POINT('',#211546);
#39953=VERTEX_POINT('',#211547);
#39954=VERTEX_POINT('',#211552);
#39955=VERTEX_POINT('',#211553);
#39956=VERTEX_POINT('',#211558);
#39957=VERTEX_POINT('',#211559);
#39958=VERTEX_POINT('',#211564);
#39959=VERTEX_POINT('',#211565);
#39960=VERTEX_POINT('',#211570);
#39961=VERTEX_POINT('',#211571);
#39962=VERTEX_POINT('',#211576);
#39963=VERTEX_POINT('',#211577);
#39964=VERTEX_POINT('',#211585);
#39965=VERTEX_POINT('',#211586);
#39966=VERTEX_POINT('',#211588);
#39967=VERTEX_POINT('',#211590);
#39968=VERTEX_POINT('',#211594);
#39969=VERTEX_POINT('',#211595);
#39970=VERTEX_POINT('',#211600);
#39971=VERTEX_POINT('',#211601);
#39972=VERTEX_POINT('',#211606);
#39973=VERTEX_POINT('',#211607);
#39974=VERTEX_POINT('',#211612);
#39975=VERTEX_POINT('',#211613);
#39976=VERTEX_POINT('',#211618);
#39977=VERTEX_POINT('',#211619);
#39978=VERTEX_POINT('',#211624);
#39979=VERTEX_POINT('',#211625);
#39980=VERTEX_POINT('',#211633);
#39981=VERTEX_POINT('',#211634);
#39982=VERTEX_POINT('',#211636);
#39983=VERTEX_POINT('',#211638);
#39984=VERTEX_POINT('',#211642);
#39985=VERTEX_POINT('',#211643);
#39986=VERTEX_POINT('',#211648);
#39987=VERTEX_POINT('',#211649);
#39988=VERTEX_POINT('',#211654);
#39989=VERTEX_POINT('',#211655);
#39990=VERTEX_POINT('',#211660);
#39991=VERTEX_POINT('',#211661);
#39992=VERTEX_POINT('',#211666);
#39993=VERTEX_POINT('',#211667);
#39994=VERTEX_POINT('',#211672);
#39995=VERTEX_POINT('',#211673);
#39996=VERTEX_POINT('',#211681);
#39997=VERTEX_POINT('',#211682);
#39998=VERTEX_POINT('',#211684);
#39999=VERTEX_POINT('',#211686);
#40000=VERTEX_POINT('',#211690);
#40001=VERTEX_POINT('',#211691);
#40002=VERTEX_POINT('',#211696);
#40003=VERTEX_POINT('',#211697);
#40004=VERTEX_POINT('',#211702);
#40005=VERTEX_POINT('',#211703);
#40006=VERTEX_POINT('',#211708);
#40007=VERTEX_POINT('',#211709);
#40008=VERTEX_POINT('',#211714);
#40009=VERTEX_POINT('',#211715);
#40010=VERTEX_POINT('',#211720);
#40011=VERTEX_POINT('',#211721);
#40012=VERTEX_POINT('',#211726);
#40013=VERTEX_POINT('',#211727);
#40014=VERTEX_POINT('',#211732);
#40015=VERTEX_POINT('',#211733);
#40016=VERTEX_POINT('',#211741);
#40017=VERTEX_POINT('',#211742);
#40018=VERTEX_POINT('',#211744);
#40019=VERTEX_POINT('',#211746);
#40020=VERTEX_POINT('',#211750);
#40021=VERTEX_POINT('',#211751);
#40022=VERTEX_POINT('',#211756);
#40023=VERTEX_POINT('',#211757);
#40024=VERTEX_POINT('',#211762);
#40025=VERTEX_POINT('',#211763);
#40026=VERTEX_POINT('',#211768);
#40027=VERTEX_POINT('',#211769);
#40028=VERTEX_POINT('',#211774);
#40029=VERTEX_POINT('',#211775);
#40030=VERTEX_POINT('',#211780);
#40031=VERTEX_POINT('',#211781);
#40032=VERTEX_POINT('',#211786);
#40033=VERTEX_POINT('',#211787);
#40034=VERTEX_POINT('',#211792);
#40035=VERTEX_POINT('',#211793);
#40036=VERTEX_POINT('',#211801);
#40037=VERTEX_POINT('',#211802);
#40038=VERTEX_POINT('',#211804);
#40039=VERTEX_POINT('',#211806);
#40040=VERTEX_POINT('',#211810);
#40041=VERTEX_POINT('',#211811);
#40042=VERTEX_POINT('',#211816);
#40043=VERTEX_POINT('',#211817);
#40044=VERTEX_POINT('',#211822);
#40045=VERTEX_POINT('',#211823);
#40046=VERTEX_POINT('',#211828);
#40047=VERTEX_POINT('',#211829);
#40048=VERTEX_POINT('',#211834);
#40049=VERTEX_POINT('',#211835);
#40050=VERTEX_POINT('',#211840);
#40051=VERTEX_POINT('',#211841);
#40052=VERTEX_POINT('',#211849);
#40053=VERTEX_POINT('',#211850);
#40054=VERTEX_POINT('',#211852);
#40055=VERTEX_POINT('',#211854);
#40056=VERTEX_POINT('',#211858);
#40057=VERTEX_POINT('',#211859);
#40058=VERTEX_POINT('',#211864);
#40059=VERTEX_POINT('',#211865);
#40060=VERTEX_POINT('',#211870);
#40061=VERTEX_POINT('',#211871);
#40062=VERTEX_POINT('',#211876);
#40063=VERTEX_POINT('',#211877);
#40064=VERTEX_POINT('',#211882);
#40065=VERTEX_POINT('',#211883);
#40066=VERTEX_POINT('',#211888);
#40067=VERTEX_POINT('',#211889);
#40068=VERTEX_POINT('',#211897);
#40069=VERTEX_POINT('',#211898);
#40070=VERTEX_POINT('',#211900);
#40071=VERTEX_POINT('',#211902);
#40072=VERTEX_POINT('',#211906);
#40073=VERTEX_POINT('',#211907);
#40074=VERTEX_POINT('',#211912);
#40075=VERTEX_POINT('',#211913);
#40076=VERTEX_POINT('',#211918);
#40077=VERTEX_POINT('',#211919);
#40078=VERTEX_POINT('',#211924);
#40079=VERTEX_POINT('',#211925);
#40080=VERTEX_POINT('',#211930);
#40081=VERTEX_POINT('',#211931);
#40082=VERTEX_POINT('',#211936);
#40083=VERTEX_POINT('',#211937);
#40084=VERTEX_POINT('',#211945);
#40085=VERTEX_POINT('',#211946);
#40086=VERTEX_POINT('',#211948);
#40087=VERTEX_POINT('',#211950);
#40088=VERTEX_POINT('',#211954);
#40089=VERTEX_POINT('',#211955);
#40090=VERTEX_POINT('',#211960);
#40091=VERTEX_POINT('',#211961);
#40092=VERTEX_POINT('',#211966);
#40093=VERTEX_POINT('',#211967);
#40094=VERTEX_POINT('',#211972);
#40095=VERTEX_POINT('',#211973);
#40096=VERTEX_POINT('',#211978);
#40097=VERTEX_POINT('',#211979);
#40098=VERTEX_POINT('',#211984);
#40099=VERTEX_POINT('',#211985);
#40100=VERTEX_POINT('',#211993);
#40101=VERTEX_POINT('',#211994);
#40102=VERTEX_POINT('',#211996);
#40103=VERTEX_POINT('',#211998);
#40104=VERTEX_POINT('',#212002);
#40105=VERTEX_POINT('',#212003);
#40106=VERTEX_POINT('',#212008);
#40107=VERTEX_POINT('',#212009);
#40108=VERTEX_POINT('',#212014);
#40109=VERTEX_POINT('',#212015);
#40110=VERTEX_POINT('',#212020);
#40111=VERTEX_POINT('',#212021);
#40112=VERTEX_POINT('',#212026);
#40113=VERTEX_POINT('',#212027);
#40114=VERTEX_POINT('',#212032);
#40115=VERTEX_POINT('',#212033);
#40116=VERTEX_POINT('',#212038);
#40117=VERTEX_POINT('',#212040);
#40118=VERTEX_POINT('',#212047);
#40119=VERTEX_POINT('',#212048);
#40120=VERTEX_POINT('',#212050);
#40121=VERTEX_POINT('',#212052);
#40122=VERTEX_POINT('',#212056);
#40123=VERTEX_POINT('',#212057);
#40124=VERTEX_POINT('',#212062);
#40125=VERTEX_POINT('',#212063);
#40126=VERTEX_POINT('',#212068);
#40127=VERTEX_POINT('',#212069);
#40128=VERTEX_POINT('',#212074);
#40129=VERTEX_POINT('',#212075);
#40130=VERTEX_POINT('',#212080);
#40131=VERTEX_POINT('',#212081);
#40132=VERTEX_POINT('',#212086);
#40133=VERTEX_POINT('',#212087);
#40134=VERTEX_POINT('',#212095);
#40135=VERTEX_POINT('',#212096);
#40136=VERTEX_POINT('',#212098);
#40137=VERTEX_POINT('',#212100);
#40138=VERTEX_POINT('',#212104);
#40139=VERTEX_POINT('',#212105);
#40140=VERTEX_POINT('',#212110);
#40141=VERTEX_POINT('',#212111);
#40142=VERTEX_POINT('',#212116);
#40143=VERTEX_POINT('',#212117);
#40144=VERTEX_POINT('',#212122);
#40145=VERTEX_POINT('',#212123);
#40146=VERTEX_POINT('',#212128);
#40147=VERTEX_POINT('',#212129);
#40148=VERTEX_POINT('',#212134);
#40149=VERTEX_POINT('',#212135);
#40150=VERTEX_POINT('',#212140);
#40151=VERTEX_POINT('',#212141);
#40152=VERTEX_POINT('',#212146);
#40153=VERTEX_POINT('',#212147);
#40154=VERTEX_POINT('',#212155);
#40155=VERTEX_POINT('',#212156);
#40156=VERTEX_POINT('',#212158);
#40157=VERTEX_POINT('',#212160);
#40158=VERTEX_POINT('',#212164);
#40159=VERTEX_POINT('',#212165);
#40160=VERTEX_POINT('',#212170);
#40161=VERTEX_POINT('',#212171);
#40162=VERTEX_POINT('',#212176);
#40163=VERTEX_POINT('',#212177);
#40164=VERTEX_POINT('',#212182);
#40165=VERTEX_POINT('',#212183);
#40166=VERTEX_POINT('',#212188);
#40167=VERTEX_POINT('',#212189);
#40168=VERTEX_POINT('',#212194);
#40169=VERTEX_POINT('',#212195);
#40170=VERTEX_POINT('',#212203);
#40171=VERTEX_POINT('',#212204);
#40172=VERTEX_POINT('',#212206);
#40173=VERTEX_POINT('',#212208);
#40174=VERTEX_POINT('',#212212);
#40175=VERTEX_POINT('',#212213);
#40176=VERTEX_POINT('',#212218);
#40177=VERTEX_POINT('',#212219);
#40178=VERTEX_POINT('',#212224);
#40179=VERTEX_POINT('',#212225);
#40180=VERTEX_POINT('',#212230);
#40181=VERTEX_POINT('',#212231);
#40182=VERTEX_POINT('',#212236);
#40183=VERTEX_POINT('',#212237);
#40184=VERTEX_POINT('',#212242);
#40185=VERTEX_POINT('',#212243);
#40186=VERTEX_POINT('',#212248);
#40187=VERTEX_POINT('',#212249);
#40188=VERTEX_POINT('',#212254);
#40189=VERTEX_POINT('',#212255);
#40190=VERTEX_POINT('',#212263);
#40191=VERTEX_POINT('',#212264);
#40192=VERTEX_POINT('',#212266);
#40193=VERTEX_POINT('',#212268);
#40194=VERTEX_POINT('',#212272);
#40195=VERTEX_POINT('',#212273);
#40196=VERTEX_POINT('',#212278);
#40197=VERTEX_POINT('',#212279);
#40198=VERTEX_POINT('',#212284);
#40199=VERTEX_POINT('',#212285);
#40200=VERTEX_POINT('',#212290);
#40201=VERTEX_POINT('',#212291);
#40202=VERTEX_POINT('',#212296);
#40203=VERTEX_POINT('',#212297);
#40204=VERTEX_POINT('',#212302);
#40205=VERTEX_POINT('',#212303);
#40206=VERTEX_POINT('',#212311);
#40207=VERTEX_POINT('',#212312);
#40208=VERTEX_POINT('',#212314);
#40209=VERTEX_POINT('',#212316);
#40210=VERTEX_POINT('',#212320);
#40211=VERTEX_POINT('',#212321);
#40212=VERTEX_POINT('',#212326);
#40213=VERTEX_POINT('',#212327);
#40214=VERTEX_POINT('',#212332);
#40215=VERTEX_POINT('',#212333);
#40216=VERTEX_POINT('',#212338);
#40217=VERTEX_POINT('',#212339);
#40218=VERTEX_POINT('',#212344);
#40219=VERTEX_POINT('',#212345);
#40220=VERTEX_POINT('',#212350);
#40221=VERTEX_POINT('',#212351);
#40222=VERTEX_POINT('',#212359);
#40223=VERTEX_POINT('',#212360);
#40224=VERTEX_POINT('',#212362);
#40225=VERTEX_POINT('',#212364);
#40226=VERTEX_POINT('',#212368);
#40227=VERTEX_POINT('',#212369);
#40228=VERTEX_POINT('',#212374);
#40229=VERTEX_POINT('',#212375);
#40230=VERTEX_POINT('',#212380);
#40231=VERTEX_POINT('',#212381);
#40232=VERTEX_POINT('',#212386);
#40233=VERTEX_POINT('',#212387);
#40234=VERTEX_POINT('',#212392);
#40235=VERTEX_POINT('',#212393);
#40236=VERTEX_POINT('',#212398);
#40237=VERTEX_POINT('',#212399);
#40238=VERTEX_POINT('',#212407);
#40239=VERTEX_POINT('',#212408);
#40240=VERTEX_POINT('',#212410);
#40241=VERTEX_POINT('',#212412);
#40242=VERTEX_POINT('',#212416);
#40243=VERTEX_POINT('',#212417);
#40244=VERTEX_POINT('',#212422);
#40245=VERTEX_POINT('',#212423);
#40246=VERTEX_POINT('',#212428);
#40247=VERTEX_POINT('',#212429);
#40248=VERTEX_POINT('',#212434);
#40249=VERTEX_POINT('',#212435);
#40250=VERTEX_POINT('',#212440);
#40251=VERTEX_POINT('',#212441);
#40252=VERTEX_POINT('',#212446);
#40253=VERTEX_POINT('',#212447);
#40254=VERTEX_POINT('',#212455);
#40255=VERTEX_POINT('',#212456);
#40256=VERTEX_POINT('',#212458);
#40257=VERTEX_POINT('',#212460);
#40258=VERTEX_POINT('',#212464);
#40259=VERTEX_POINT('',#212465);
#40260=VERTEX_POINT('',#212470);
#40261=VERTEX_POINT('',#212471);
#40262=VERTEX_POINT('',#212476);
#40263=VERTEX_POINT('',#212477);
#40264=VERTEX_POINT('',#212482);
#40265=VERTEX_POINT('',#212483);
#40266=VERTEX_POINT('',#212491);
#40267=VERTEX_POINT('',#212492);
#40268=VERTEX_POINT('',#212494);
#40269=VERTEX_POINT('',#212496);
#40270=VERTEX_POINT('',#212500);
#40271=VERTEX_POINT('',#212501);
#40272=VERTEX_POINT('',#212506);
#40273=VERTEX_POINT('',#212507);
#40274=VERTEX_POINT('',#212512);
#40275=VERTEX_POINT('',#212513);
#40276=VERTEX_POINT('',#212518);
#40277=VERTEX_POINT('',#212519);
#40278=VERTEX_POINT('',#212527);
#40279=VERTEX_POINT('',#212529);
#40280=VERTEX_POINT('',#212533);
#40281=VERTEX_POINT('',#212535);
#40282=VERTEX_POINT('',#212539);
#40283=VERTEX_POINT('',#212540);
#40284=VERTEX_POINT('',#212545);
#40285=VERTEX_POINT('',#212546);
#40286=VERTEX_POINT('',#212551);
#40287=VERTEX_POINT('',#212552);
#40288=VERTEX_POINT('',#212557);
#40289=VERTEX_POINT('',#212558);
#40290=VERTEX_POINT('',#212563);
#40291=VERTEX_POINT('',#212564);
#40292=VERTEX_POINT('',#212569);
#40293=VERTEX_POINT('',#212570);
#40294=VERTEX_POINT('',#212575);
#40295=VERTEX_POINT('',#212576);
#40296=VERTEX_POINT('',#212581);
#40297=VERTEX_POINT('',#212582);
#40298=VERTEX_POINT('',#212590);
#40299=VERTEX_POINT('',#212591);
#40300=VERTEX_POINT('',#212596);
#40301=VERTEX_POINT('',#212597);
#40302=VERTEX_POINT('',#212602);
#40303=VERTEX_POINT('',#212603);
#40304=VERTEX_POINT('',#212608);
#40305=VERTEX_POINT('',#212609);
#40306=VERTEX_POINT('',#212614);
#40307=VERTEX_POINT('',#212615);
#40308=VERTEX_POINT('',#212620);
#40309=VERTEX_POINT('',#212621);
#40310=VERTEX_POINT('',#212626);
#40311=VERTEX_POINT('',#212627);
#40312=VERTEX_POINT('',#212632);
#40313=VERTEX_POINT('',#212633);
#40314=VERTEX_POINT('',#212641);
#40315=VERTEX_POINT('',#212642);
#40316=VERTEX_POINT('',#212644);
#40317=VERTEX_POINT('',#212646);
#40318=VERTEX_POINT('',#212659);
#40319=VERTEX_POINT('',#212660);
#40320=VERTEX_POINT('',#212665);
#40321=VERTEX_POINT('',#212667);
#40322=VERTEX_POINT('',#212671);
#40323=VERTEX_POINT('',#212672);
#40324=VERTEX_POINT('',#212677);
#40325=VERTEX_POINT('',#212678);
#40326=VERTEX_POINT('',#212683);
#40327=VERTEX_POINT('',#212684);
#40328=VERTEX_POINT('',#212689);
#40329=VERTEX_POINT('',#212690);
#40330=VERTEX_POINT('',#212704);
#40331=VERTEX_POINT('',#212705);
#40332=VERTEX_POINT('',#212707);
#40333=VERTEX_POINT('',#212709);
#40334=VERTEX_POINT('',#212722);
#40335=VERTEX_POINT('',#212723);
#40336=VERTEX_POINT('',#212728);
#40337=VERTEX_POINT('',#212729);
#40338=VERTEX_POINT('',#212734);
#40339=VERTEX_POINT('',#212735);
#40340=VERTEX_POINT('',#212740);
#40341=VERTEX_POINT('',#212741);
#40342=VERTEX_POINT('',#212746);
#40343=VERTEX_POINT('',#212747);
#40344=VERTEX_POINT('',#212752);
#40345=VERTEX_POINT('',#212753);
#40346=VERTEX_POINT('',#212767);
#40347=VERTEX_POINT('',#212768);
#40348=VERTEX_POINT('',#212770);
#40349=VERTEX_POINT('',#212772);
#40350=VERTEX_POINT('',#212785);
#40351=VERTEX_POINT('',#212786);
#40352=VERTEX_POINT('',#212791);
#40353=VERTEX_POINT('',#212793);
#40354=VERTEX_POINT('',#212797);
#40355=VERTEX_POINT('',#212798);
#40356=VERTEX_POINT('',#212803);
#40357=VERTEX_POINT('',#212804);
#40358=VERTEX_POINT('',#212809);
#40359=VERTEX_POINT('',#212810);
#40360=VERTEX_POINT('',#212815);
#40361=VERTEX_POINT('',#212816);
#40362=VERTEX_POINT('',#212830);
#40363=VERTEX_POINT('',#212831);
#40364=VERTEX_POINT('',#212842);
#40365=VERTEX_POINT('',#212844);
#40366=VERTEX_POINT('',#212848);
#40367=VERTEX_POINT('',#212849);
#40368=VERTEX_POINT('',#212854);
#40369=VERTEX_POINT('',#212855);
#40370=VERTEX_POINT('',#212860);
#40371=VERTEX_POINT('',#212861);
#40372=VERTEX_POINT('',#212866);
#40373=VERTEX_POINT('',#212867);
#40374=VERTEX_POINT('',#212872);
#40375=VERTEX_POINT('',#212873);
#40376=VERTEX_POINT('',#212878);
#40377=VERTEX_POINT('',#212879);
#40378=VERTEX_POINT('',#212893);
#40379=VERTEX_POINT('',#212895);
#40380=VERTEX_POINT('',#212899);
#40381=VERTEX_POINT('',#212900);
#40382=VERTEX_POINT('',#212905);
#40383=VERTEX_POINT('',#212906);
#40384=VERTEX_POINT('',#212911);
#40385=VERTEX_POINT('',#212912);
#40386=VERTEX_POINT('',#212917);
#40387=VERTEX_POINT('',#212918);
#40388=VERTEX_POINT('',#212923);
#40389=VERTEX_POINT('',#212924);
#40390=VERTEX_POINT('',#212929);
#40391=VERTEX_POINT('',#212930);
#40392=VERTEX_POINT('',#212935);
#40393=VERTEX_POINT('',#212936);
#40394=VERTEX_POINT('',#213087);
#40395=VERTEX_POINT('',#213088);
#40396=VERTEX_POINT('',#213141);
#40397=VERTEX_POINT('',#213176);
#40398=VERTEX_POINT('',#213408);
#40399=VERTEX_POINT('',#213409);
#40400=VERTEX_POINT('',#213428);
#40401=VERTEX_POINT('',#213429);
#40402=VERTEX_POINT('',#213511);
#40403=VERTEX_POINT('',#213512);
#40404=VERTEX_POINT('',#213662);
#40405=VERTEX_POINT('',#213663);
#40406=VERTEX_POINT('',#213895);
#40407=VERTEX_POINT('',#213896);
#40408=VERTEX_POINT('',#214052);
#40409=VERTEX_POINT('',#214053);
#40410=VERTEX_POINT('',#214069);
#40411=VERTEX_POINT('',#214070);
#40412=VERTEX_POINT('',#214401);
#40413=VERTEX_POINT('',#214402);
#40414=VERTEX_POINT('',#214558);
#40415=VERTEX_POINT('',#214593);
#40416=VERTEX_POINT('',#214600);
#40417=VERTEX_POINT('',#214626);
#40418=VERTEX_POINT('',#214802);
#40419=VERTEX_POINT('',#214925);
#40420=VERTEX_POINT('',#214926);
#40421=VERTEX_POINT('',#214960);
#40422=VERTEX_POINT('',#214961);
#40423=VERTEX_POINT('',#215061);
#40424=VERTEX_POINT('',#215062);
#40425=VERTEX_POINT('',#215390);
#40426=VERTEX_POINT('',#215391);
#40427=VERTEX_POINT('',#215635);
#40428=VERTEX_POINT('',#215636);
#40429=VERTEX_POINT('',#215773);
#40430=VERTEX_POINT('',#215774);
#40431=VERTEX_POINT('',#215790);
#40432=VERTEX_POINT('',#215791);
#40433=VERTEX_POINT('',#216122);
#40434=VERTEX_POINT('',#216123);
#40435=VERTEX_POINT('',#216224);
#40436=VERTEX_POINT('',#216271);
#40437=VERTEX_POINT('',#216604);
#40438=VERTEX_POINT('',#216739);
#40439=VERTEX_POINT('',#216762);
#40440=VERTEX_POINT('',#216777);
#40441=VERTEX_POINT('',#216778);
#40442=VERTEX_POINT('',#216860);
#40443=VERTEX_POINT('',#216861);
#40444=VERTEX_POINT('',#217213);
#40445=VERTEX_POINT('',#217214);
#40446=VERTEX_POINT('',#217260);
#40447=VERTEX_POINT('',#217261);
#40448=VERTEX_POINT('',#217278);
#40449=VERTEX_POINT('',#217293);
#40450=VERTEX_POINT('',#217294);
#40451=VERTEX_POINT('',#217752);
#40452=VERTEX_POINT('',#217753);
#40453=VERTEX_POINT('',#218158);
#40454=VERTEX_POINT('',#218238);
#40455=VERTEX_POINT('',#218306);
#40456=VERTEX_POINT('',#218345);
#40457=VERTEX_POINT('',#218378);
#40458=VERTEX_POINT('',#218503);
#40459=VERTEX_POINT('',#218571);
#40460=VERTEX_POINT('',#218591);
#40461=VERTEX_POINT('',#218592);
#40462=VERTEX_POINT('',#218617);
#40463=VERTEX_POINT('',#218619);
#40464=VERTEX_POINT('',#218640);
#40465=VERTEX_POINT('',#218641);
#40466=VERTEX_POINT('',#218741);
#40467=VERTEX_POINT('',#218742);
#40468=VERTEX_POINT('',#219016);
#40469=VERTEX_POINT('',#219017);
#40470=VERTEX_POINT('',#219446);
#40471=VERTEX_POINT('',#219447);
#40472=VERTEX_POINT('',#219462);
#40473=VERTEX_POINT('',#219479);
#40474=VERTEX_POINT('',#219826);
#40475=VERTEX_POINT('',#219841);
#40476=VERTEX_POINT('',#219867);
#40477=VERTEX_POINT('',#219932);
#40478=VERTEX_POINT('',#219967);
#40479=VERTEX_POINT('',#220114);
#40480=VERTEX_POINT('',#220129);
#40481=VERTEX_POINT('',#220130);
#40482=VERTEX_POINT('',#220146);
#40483=VERTEX_POINT('',#220148);
#40484=VERTEX_POINT('',#220181);
#40485=VERTEX_POINT('',#220182);
#40486=VERTEX_POINT('',#220396);
#40487=VERTEX_POINT('',#220397);
#40488=VERTEX_POINT('',#220606);
#40489=VERTEX_POINT('',#220607);
#40490=VERTEX_POINT('',#220644);
#40491=VERTEX_POINT('',#220646);
#40492=VERTEX_POINT('',#220835);
#40493=VERTEX_POINT('',#220836);
#40494=VERTEX_POINT('',#220881);
#40495=VERTEX_POINT('',#221048);
#40496=VERTEX_POINT('',#221113);
#40497=VERTEX_POINT('',#221287);
#40498=VERTEX_POINT('',#221329);
#40499=VERTEX_POINT('',#221330);
#40500=VERTEX_POINT('',#221342);
#40501=VERTEX_POINT('',#221357);
#40502=VERTEX_POINT('',#221396);
#40503=VERTEX_POINT('',#221397);
#40504=VERTEX_POINT('',#221499);
#40505=VERTEX_POINT('',#221500);
#40506=VERTEX_POINT('',#221825);
#40507=VERTEX_POINT('',#221826);
#40508=VERTEX_POINT('',#222189);
#40509=VERTEX_POINT('',#222190);
#40510=VERTEX_POINT('',#222195);
#40511=VERTEX_POINT('',#222197);
#40512=VERTEX_POINT('',#222201);
#40513=VERTEX_POINT('',#222203);
#40514=VERTEX_POINT('',#222207);
#40515=VERTEX_POINT('',#222209);
#40516=VERTEX_POINT('',#222213);
#40517=VERTEX_POINT('',#222215);
#40518=VERTEX_POINT('',#222219);
#40519=VERTEX_POINT('',#222221);
#40520=VERTEX_POINT('',#222225);
#40521=VERTEX_POINT('',#222227);
#40522=VERTEX_POINT('',#222231);
#40523=VERTEX_POINT('',#222233);
#40524=VERTEX_POINT('',#222237);
#40525=VERTEX_POINT('',#222239);
#40526=VERTEX_POINT('',#222243);
#40527=VERTEX_POINT('',#222244);
#40528=VERTEX_POINT('',#222249);
#40529=VERTEX_POINT('',#222251);
#40530=VERTEX_POINT('',#222255);
#40531=VERTEX_POINT('',#222257);
#40532=VERTEX_POINT('',#222261);
#40533=VERTEX_POINT('',#222263);
#40534=VERTEX_POINT('',#222267);
#40535=VERTEX_POINT('',#222269);
#40536=VERTEX_POINT('',#222273);
#40537=VERTEX_POINT('',#222275);
#40538=VERTEX_POINT('',#222279);
#40539=VERTEX_POINT('',#222281);
#40540=VERTEX_POINT('',#222285);
#40541=VERTEX_POINT('',#222287);
#40542=VERTEX_POINT('',#222291);
#40543=VERTEX_POINT('',#222293);
#40544=VERTEX_POINT('',#222297);
#40545=VERTEX_POINT('',#222299);
#40546=VERTEX_POINT('',#222303);
#40547=VERTEX_POINT('',#222305);
#40548=VERTEX_POINT('',#222309);
#40549=VERTEX_POINT('',#222311);
#40550=VERTEX_POINT('',#222315);
#40551=VERTEX_POINT('',#222317);
#40552=VERTEX_POINT('',#222321);
#40553=VERTEX_POINT('',#222323);
#40554=VERTEX_POINT('',#222327);
#40555=VERTEX_POINT('',#222329);
#40556=VERTEX_POINT('',#222333);
#40557=VERTEX_POINT('',#222335);
#40558=VERTEX_POINT('',#222339);
#40559=VERTEX_POINT('',#222341);
#40560=VERTEX_POINT('',#222345);
#40561=VERTEX_POINT('',#222347);
#40562=VERTEX_POINT('',#222351);
#40563=VERTEX_POINT('',#222352);
#40564=VERTEX_POINT('',#222357);
#40565=VERTEX_POINT('',#222359);
#40566=VERTEX_POINT('',#222363);
#40567=VERTEX_POINT('',#222365);
#40568=VERTEX_POINT('',#222369);
#40569=VERTEX_POINT('',#222371);
#40570=VERTEX_POINT('',#222375);
#40571=VERTEX_POINT('',#222377);
#40572=VERTEX_POINT('',#222381);
#40573=VERTEX_POINT('',#222383);
#40574=VERTEX_POINT('',#222387);
#40575=VERTEX_POINT('',#222389);
#40576=VERTEX_POINT('',#222393);
#40577=VERTEX_POINT('',#222395);
#40578=VERTEX_POINT('',#222399);
#40579=VERTEX_POINT('',#222401);
#40580=VERTEX_POINT('',#222405);
#40581=VERTEX_POINT('',#222407);
#40582=VERTEX_POINT('',#222411);
#40583=VERTEX_POINT('',#222413);
#40584=VERTEX_POINT('',#222417);
#40585=VERTEX_POINT('',#222419);
#40586=VERTEX_POINT('',#222423);
#40587=VERTEX_POINT('',#222425);
#40588=VERTEX_POINT('',#222429);
#40589=VERTEX_POINT('',#222431);
#40590=VERTEX_POINT('',#222435);
#40591=VERTEX_POINT('',#222437);
#40592=VERTEX_POINT('',#222441);
#40593=VERTEX_POINT('',#222443);
#40594=VERTEX_POINT('',#222447);
#40595=VERTEX_POINT('',#222449);
#40596=VERTEX_POINT('',#222453);
#40597=VERTEX_POINT('',#222455);
#40598=VERTEX_POINT('',#222459);
#40599=VERTEX_POINT('',#222461);
#40600=VERTEX_POINT('',#222465);
#40601=VERTEX_POINT('',#222467);
#40602=VERTEX_POINT('',#222471);
#40603=VERTEX_POINT('',#222473);
#40604=VERTEX_POINT('',#222477);
#40605=VERTEX_POINT('',#222479);
#40606=VERTEX_POINT('',#222483);
#40607=VERTEX_POINT('',#222485);
#40608=VERTEX_POINT('',#222489);
#40609=VERTEX_POINT('',#222491);
#40610=VERTEX_POINT('',#222495);
#40611=VERTEX_POINT('',#222497);
#40612=VERTEX_POINT('',#222501);
#40613=VERTEX_POINT('',#222503);
#40614=VERTEX_POINT('',#222507);
#40615=VERTEX_POINT('',#222509);
#40616=VERTEX_POINT('',#222513);
#40617=VERTEX_POINT('',#222515);
#40618=VERTEX_POINT('',#222519);
#40619=VERTEX_POINT('',#222521);
#40620=VERTEX_POINT('',#222525);
#40621=VERTEX_POINT('',#222527);
#40622=VERTEX_POINT('',#222531);
#40623=VERTEX_POINT('',#222533);
#40624=VERTEX_POINT('',#222537);
#40625=VERTEX_POINT('',#222539);
#40626=VERTEX_POINT('',#222543);
#40627=VERTEX_POINT('',#222545);
#40628=VERTEX_POINT('',#222549);
#40629=VERTEX_POINT('',#222551);
#40630=VERTEX_POINT('',#222555);
#40631=VERTEX_POINT('',#222557);
#40632=VERTEX_POINT('',#222561);
#40633=VERTEX_POINT('',#222563);
#40634=VERTEX_POINT('',#222567);
#40635=VERTEX_POINT('',#222569);
#40636=VERTEX_POINT('',#222573);
#40637=VERTEX_POINT('',#222575);
#40638=VERTEX_POINT('',#222579);
#40639=VERTEX_POINT('',#222581);
#40640=VERTEX_POINT('',#222585);
#40641=VERTEX_POINT('',#222587);
#40642=VERTEX_POINT('',#222591);
#40643=VERTEX_POINT('',#222593);
#40644=VERTEX_POINT('',#222597);
#40645=VERTEX_POINT('',#222599);
#40646=VERTEX_POINT('',#222603);
#40647=VERTEX_POINT('',#222605);
#40648=VERTEX_POINT('',#222609);
#40649=VERTEX_POINT('',#222611);
#40650=VERTEX_POINT('',#222615);
#40651=VERTEX_POINT('',#222617);
#40652=VERTEX_POINT('',#222621);
#40653=VERTEX_POINT('',#222623);
#40654=VERTEX_POINT('',#222627);
#40655=VERTEX_POINT('',#222629);
#40656=VERTEX_POINT('',#222633);
#40657=VERTEX_POINT('',#222635);
#40658=VERTEX_POINT('',#222639);
#40659=VERTEX_POINT('',#222641);
#40660=VERTEX_POINT('',#222645);
#40661=VERTEX_POINT('',#222647);
#40662=VERTEX_POINT('',#222651);
#40663=VERTEX_POINT('',#222653);
#40664=VERTEX_POINT('',#222657);
#40665=VERTEX_POINT('',#222659);
#40666=VERTEX_POINT('',#222663);
#40667=VERTEX_POINT('',#222665);
#40668=VERTEX_POINT('',#222669);
#40669=VERTEX_POINT('',#222671);
#40670=VERTEX_POINT('',#222675);
#40671=VERTEX_POINT('',#222677);
#40672=VERTEX_POINT('',#222681);
#40673=VERTEX_POINT('',#222683);
#40674=VERTEX_POINT('',#222687);
#40675=VERTEX_POINT('',#222689);
#40676=VERTEX_POINT('',#222693);
#40677=VERTEX_POINT('',#222695);
#40678=VERTEX_POINT('',#222699);
#40679=VERTEX_POINT('',#222700);
#40680=VERTEX_POINT('',#222705);
#40681=VERTEX_POINT('',#222707);
#40682=VERTEX_POINT('',#222711);
#40683=VERTEX_POINT('',#222713);
#40684=VERTEX_POINT('',#222717);
#40685=VERTEX_POINT('',#222719);
#40686=VERTEX_POINT('',#222723);
#40687=VERTEX_POINT('',#222725);
#40688=VERTEX_POINT('',#222729);
#40689=VERTEX_POINT('',#222731);
#40690=VERTEX_POINT('',#222735);
#40691=VERTEX_POINT('',#222737);
#40692=VERTEX_POINT('',#222741);
#40693=VERTEX_POINT('',#222743);
#40694=VERTEX_POINT('',#222747);
#40695=VERTEX_POINT('',#222749);
#40696=VERTEX_POINT('',#222753);
#40697=VERTEX_POINT('',#222755);
#40698=VERTEX_POINT('',#222759);
#40699=VERTEX_POINT('',#222761);
#40700=VERTEX_POINT('',#222765);
#40701=VERTEX_POINT('',#222767);
#40702=VERTEX_POINT('',#222771);
#40703=VERTEX_POINT('',#222773);
#40704=VERTEX_POINT('',#222777);
#40705=VERTEX_POINT('',#222779);
#40706=VERTEX_POINT('',#222783);
#40707=VERTEX_POINT('',#222785);
#40708=VERTEX_POINT('',#222789);
#40709=VERTEX_POINT('',#222791);
#40710=VERTEX_POINT('',#222795);
#40711=VERTEX_POINT('',#222797);
#40712=VERTEX_POINT('',#222801);
#40713=VERTEX_POINT('',#222803);
#40714=VERTEX_POINT('',#222807);
#40715=VERTEX_POINT('',#222809);
#40716=VERTEX_POINT('',#222813);
#40717=VERTEX_POINT('',#222815);
#40718=VERTEX_POINT('',#222819);
#40719=VERTEX_POINT('',#222821);
#40720=VERTEX_POINT('',#222825);
#40721=VERTEX_POINT('',#222827);
#40722=VERTEX_POINT('',#222831);
#40723=VERTEX_POINT('',#222833);
#40724=VERTEX_POINT('',#222837);
#40725=VERTEX_POINT('',#222839);
#40726=VERTEX_POINT('',#222843);
#40727=VERTEX_POINT('',#222844);
#40728=VERTEX_POINT('',#222849);
#40729=VERTEX_POINT('',#222851);
#40730=VERTEX_POINT('',#222855);
#40731=VERTEX_POINT('',#222857);
#40732=VERTEX_POINT('',#222861);
#40733=VERTEX_POINT('',#222863);
#40734=VERTEX_POINT('',#222867);
#40735=VERTEX_POINT('',#222869);
#40736=VERTEX_POINT('',#222873);
#40737=VERTEX_POINT('',#222875);
#40738=VERTEX_POINT('',#222879);
#40739=VERTEX_POINT('',#222881);
#40740=VERTEX_POINT('',#222885);
#40741=VERTEX_POINT('',#222887);
#40742=VERTEX_POINT('',#222891);
#40743=VERTEX_POINT('',#222893);
#40744=VERTEX_POINT('',#222897);
#40745=VERTEX_POINT('',#222899);
#40746=VERTEX_POINT('',#222903);
#40747=VERTEX_POINT('',#222905);
#40748=VERTEX_POINT('',#222909);
#40749=VERTEX_POINT('',#222911);
#40750=VERTEX_POINT('',#222915);
#40751=VERTEX_POINT('',#222917);
#40752=VERTEX_POINT('',#222921);
#40753=VERTEX_POINT('',#222923);
#40754=VERTEX_POINT('',#222927);
#40755=VERTEX_POINT('',#222929);
#40756=VERTEX_POINT('',#222933);
#40757=VERTEX_POINT('',#222935);
#40758=VERTEX_POINT('',#222939);
#40759=VERTEX_POINT('',#222940);
#40760=VERTEX_POINT('',#222945);
#40761=VERTEX_POINT('',#222947);
#40762=VERTEX_POINT('',#222951);
#40763=VERTEX_POINT('',#222953);
#40764=VERTEX_POINT('',#222957);
#40765=VERTEX_POINT('',#222959);
#40766=VERTEX_POINT('',#222963);
#40767=VERTEX_POINT('',#222965);
#40768=VERTEX_POINT('',#222969);
#40769=VERTEX_POINT('',#222970);
#40770=VERTEX_POINT('',#222975);
#40771=VERTEX_POINT('',#222977);
#40772=VERTEX_POINT('',#222981);
#40773=VERTEX_POINT('',#222982);
#40774=VERTEX_POINT('',#222987);
#40775=VERTEX_POINT('',#222989);
#40776=VERTEX_POINT('',#222993);
#40777=VERTEX_POINT('',#222995);
#40778=VERTEX_POINT('',#222999);
#40779=VERTEX_POINT('',#223001);
#40780=VERTEX_POINT('',#223005);
#40781=VERTEX_POINT('',#223009);
#40782=VERTEX_POINT('',#223013);
#40783=VERTEX_POINT('',#223023);
#40784=VERTEX_POINT('',#223127);
#40785=VERTEX_POINT('',#223128);
#40786=VERTEX_POINT('',#223130);
#40787=VERTEX_POINT('',#223132);
#40788=VERTEX_POINT('',#223136);
#40789=VERTEX_POINT('',#223137);
#40790=VERTEX_POINT('',#223142);
#40791=VERTEX_POINT('',#223144);
#40792=VERTEX_POINT('',#223193);
#40793=VERTEX_POINT('',#223195);
#40794=VERTEX_POINT('',#223197);
#40795=VERTEX_POINT('',#223199);
#40796=VERTEX_POINT('',#223201);
#40797=VERTEX_POINT('',#223203);
#40798=VERTEX_POINT('',#223205);
#40799=VERTEX_POINT('',#223207);
#40800=VERTEX_POINT('',#223231);
#40801=VERTEX_POINT('',#223233);
#40802=VERTEX_POINT('',#223238);
#40803=VERTEX_POINT('',#223240);
#40804=VERTEX_POINT('',#223267);
#40805=VERTEX_POINT('',#223269);
#40806=VERTEX_POINT('',#223273);
#40807=VERTEX_POINT('',#223275);
#40808=VERTEX_POINT('',#223293);
#40809=VERTEX_POINT('',#223295);
#40810=VERTEX_POINT('',#223299);
#40811=VERTEX_POINT('',#223303);
#40812=VERTEX_POINT('',#223307);
#40813=VERTEX_POINT('',#223311);
#40814=VERTEX_POINT('',#223315);
#40815=VERTEX_POINT('',#223319);
#40816=VERTEX_POINT('',#223325);
#40817=VERTEX_POINT('',#223326);
#40818=VERTEX_POINT('',#223328);
#40819=VERTEX_POINT('',#223335);
#40820=VERTEX_POINT('',#223339);
#40821=VERTEX_POINT('',#223343);
#40822=VERTEX_POINT('',#223344);
#40823=VERTEX_POINT('',#223346);
#40824=VERTEX_POINT('',#223355);
#40825=VERTEX_POINT('',#223364);
#40826=VERTEX_POINT('',#223365);
#40827=VERTEX_POINT('',#223369);
#40828=VERTEX_POINT('',#223376);
#40829=VERTEX_POINT('',#223380);
#40830=VERTEX_POINT('',#223381);
#40831=VERTEX_POINT('',#223385);
#40832=VERTEX_POINT('',#223387);
#40833=VERTEX_POINT('',#223399);
#40834=VERTEX_POINT('',#223400);
#40835=VERTEX_POINT('',#223404);
#40836=VERTEX_POINT('',#223406);
#40837=VERTEX_POINT('',#223415);
#40838=VERTEX_POINT('',#223416);
#40839=VERTEX_POINT('',#223420);
#40840=VERTEX_POINT('',#223427);
#40841=VERTEX_POINT('',#224658);
#40842=VERTEX_POINT('',#224659);
#40843=VERTEX_POINT('',#224674);
#40844=VERTEX_POINT('',#224681);
#40845=VERTEX_POINT('',#224702);
#40846=VERTEX_POINT('',#224899);
#40847=VERTEX_POINT('',#224940);
#40848=VERTEX_POINT('',#224947);
#40849=VERTEX_POINT('',#224968);
#40850=VERTEX_POINT('',#224975);
#40851=VERTEX_POINT('',#225592);
#40852=VERTEX_POINT('',#225593);
#40853=VERTEX_POINT('',#225600);
#40854=VERTEX_POINT('',#225862);
#40855=VERTEX_POINT('',#225873);
#40856=VERTEX_POINT('',#225880);
#40857=VERTEX_POINT('',#225891);
#40858=VERTEX_POINT('',#225924);
#40859=VERTEX_POINT('',#225925);
#40860=VERTEX_POINT('',#225927);
#40861=VERTEX_POINT('',#225929);
#40862=VERTEX_POINT('',#225936);
#40863=VERTEX_POINT('',#225938);
#40864=VERTEX_POINT('',#225944);
#40865=VERTEX_POINT('',#225946);
#40866=VERTEX_POINT('',#225950);
#40867=VERTEX_POINT('',#225952);
#40868=VERTEX_POINT('',#225956);
#40869=VERTEX_POINT('',#225958);
#40870=VERTEX_POINT('',#225962);
#40871=VERTEX_POINT('',#225964);
#40872=VERTEX_POINT('',#225973);
#40873=VERTEX_POINT('',#225974);
#40874=VERTEX_POINT('',#225976);
#40875=VERTEX_POINT('',#225978);
#40876=VERTEX_POINT('',#226348);
#40877=VERTEX_POINT('',#226349);
#40878=VERTEX_POINT('',#226370);
#40879=VERTEX_POINT('',#226384);
#40880=VERTEX_POINT('',#226407);
#40881=VERTEX_POINT('',#226977);
#40882=VERTEX_POINT('',#226978);
#40883=VERTEX_POINT('',#227001);
#40884=VERTEX_POINT('',#227006);
#40885=VERTEX_POINT('',#227017);
#40886=VERTEX_POINT('',#227419);
#40887=VERTEX_POINT('',#227420);
#40888=VERTEX_POINT('',#227441);
#40889=VERTEX_POINT('',#227455);
#40890=VERTEX_POINT('',#227480);
#40891=VERTEX_POINT('',#228011);
#40892=VERTEX_POINT('',#228012);
#40893=VERTEX_POINT('',#228029);
#40894=VERTEX_POINT('',#228034);
#40895=VERTEX_POINT('',#228043);
#40896=VERTEX_POINT('',#228077);
#40897=VERTEX_POINT('',#228078);
#40898=VERTEX_POINT('',#228080);
#40899=VERTEX_POINT('',#228098);
#40900=VERTEX_POINT('',#228100);
#40901=VERTEX_POINT('',#228109);
#40902=VERTEX_POINT('',#228114);
#40903=VERTEX_POINT('',#228115);
#40904=VERTEX_POINT('',#228117);
#40905=VERTEX_POINT('',#228128);
#40906=VERTEX_POINT('',#228130);
#40907=VERTEX_POINT('',#228141);
#40908=VERTEX_POINT('',#228154);
#40909=VERTEX_POINT('',#228156);
#40910=VERTEX_POINT('',#228158);
#40911=VERTEX_POINT('',#228160);
#40912=VERTEX_POINT('',#228162);
#40913=VERTEX_POINT('',#228164);
#40914=VERTEX_POINT('',#228166);
#40915=VERTEX_POINT('',#228168);
#40916=VERTEX_POINT('',#228174);
#40917=VERTEX_POINT('',#228175);
#40918=VERTEX_POINT('',#228180);
#40919=VERTEX_POINT('',#228184);
#40920=VERTEX_POINT('',#228188);
#40921=VERTEX_POINT('',#228194);
#40922=VERTEX_POINT('',#228198);
#40923=VERTEX_POINT('',#228202);
#40924=VERTEX_POINT('',#228223);
#40925=VERTEX_POINT('',#228230);
#40926=VERTEX_POINT('',#228259);
#40927=VERTEX_POINT('',#228266);
#40928=VERTEX_POINT('',#228486);
#40929=VERTEX_POINT('',#228529);
#40930=VERTEX_POINT('',#228536);
#40931=VERTEX_POINT('',#228740);
#40932=VERTEX_POINT('',#228755);
#40933=VERTEX_POINT('',#228762);
#40934=VERTEX_POINT('',#228806);
#40935=VERTEX_POINT('',#228813);
#40936=VERTEX_POINT('',#229101);
#40937=VERTEX_POINT('',#229148);
#40938=VERTEX_POINT('',#229149);
#40939=VERTEX_POINT('',#229158);
#40940=VERTEX_POINT('',#229159);
#40941=VERTEX_POINT('',#229168);
#40942=VERTEX_POINT('',#229169);
#40943=VERTEX_POINT('',#229181);
#40944=VERTEX_POINT('',#229185);
#40945=VERTEX_POINT('',#229194);
#40946=VERTEX_POINT('',#229205);
#40947=VERTEX_POINT('',#229206);
#40948=VERTEX_POINT('',#229223);
#40949=VERTEX_POINT('',#229232);
#40950=VERTEX_POINT('',#229233);
#40951=VERTEX_POINT('',#230357);
#40952=VERTEX_POINT('',#230376);
#40953=VERTEX_POINT('',#230408);
#40954=VERTEX_POINT('',#230413);
#40955=VERTEX_POINT('',#230769);
#40956=VERTEX_POINT('',#230771);
#40957=VERTEX_POINT('',#230775);
#40958=VERTEX_POINT('',#230779);
#40959=VERTEX_POINT('',#230783);
#40960=VERTEX_POINT('',#230787);
#40961=VERTEX_POINT('',#230791);
#40962=VERTEX_POINT('',#230797);
#40963=VERTEX_POINT('',#230803);
#40964=VERTEX_POINT('',#230805);
#40965=VERTEX_POINT('',#230807);
#40966=VERTEX_POINT('',#230809);
#40967=VERTEX_POINT('',#230811);
#40968=VERTEX_POINT('',#230813);
#40969=VERTEX_POINT('',#230815);
#40970=VERTEX_POINT('',#230817);
#40971=VERTEX_POINT('',#231244);
#40972=VERTEX_POINT('',#231246);
#40973=VERTEX_POINT('',#231248);
#40974=VERTEX_POINT('',#231250);
#40975=VERTEX_POINT('',#231252);
#40976=VERTEX_POINT('',#231254);
#40977=VERTEX_POINT('',#231256);
#40978=VERTEX_POINT('',#231258);
#40979=VERTEX_POINT('',#232813);
#40980=VERTEX_POINT('',#232814);
#40981=VERTEX_POINT('',#232816);
#40982=VERTEX_POINT('',#232820);
#40983=VERTEX_POINT('',#232826);
#40984=VERTEX_POINT('',#232827);
#40985=VERTEX_POINT('',#232836);
#40986=VERTEX_POINT('',#232837);
#40987=VERTEX_POINT('',#232846);
#40988=VERTEX_POINT('',#232847);
#40989=VERTEX_POINT('',#232856);
#40990=VERTEX_POINT('',#232857);
#40991=VERTEX_POINT('',#232873);
#40992=VERTEX_POINT('',#232888);
#40993=VERTEX_POINT('',#232890);
#40994=VERTEX_POINT('',#232892);
#40995=VERTEX_POINT('',#232896);
#40996=VERTEX_POINT('',#232902);
#40997=VERTEX_POINT('',#232903);
#40998=VERTEX_POINT('',#232905);
#40999=VERTEX_POINT('',#232907);
#41000=VERTEX_POINT('',#232909);
#41001=VERTEX_POINT('',#232911);
#41002=VERTEX_POINT('',#232915);
#41003=VERTEX_POINT('',#232923);
#41004=VERTEX_POINT('',#232931);
#41005=VERTEX_POINT('',#232939);
#41006=VERTEX_POINT('',#232947);
#41007=VERTEX_POINT('',#232955);
#41008=VERTEX_POINT('',#232963);
#41009=VERTEX_POINT('',#232964);
#41010=VERTEX_POINT('',#232966);
#41011=VERTEX_POINT('',#232968);
#41012=VERTEX_POINT('',#232970);
#41013=VERTEX_POINT('',#232972);
#41014=VERTEX_POINT('',#232976);
#41015=VERTEX_POINT('',#232984);
#41016=VERTEX_POINT('',#232992);
#41017=VERTEX_POINT('',#233000);
#41018=VERTEX_POINT('',#233008);
#41019=VERTEX_POINT('',#233016);
#41020=VERTEX_POINT('',#233036);
#41021=VERTEX_POINT('',#233037);
#41022=VERTEX_POINT('',#233039);
#41023=VERTEX_POINT('',#233041);
#41024=VERTEX_POINT('',#233043);
#41025=VERTEX_POINT('',#233045);
#41026=VERTEX_POINT('',#233049);
#41027=VERTEX_POINT('',#233057);
#41028=VERTEX_POINT('',#233065);
#41029=VERTEX_POINT('',#233073);
#41030=VERTEX_POINT('',#233081);
#41031=VERTEX_POINT('',#233089);
#41032=VERTEX_POINT('',#233097);
#41033=VERTEX_POINT('',#233098);
#41034=VERTEX_POINT('',#233100);
#41035=VERTEX_POINT('',#233102);
#41036=VERTEX_POINT('',#233104);
#41037=VERTEX_POINT('',#233106);
#41038=VERTEX_POINT('',#233110);
#41039=VERTEX_POINT('',#233118);
#41040=VERTEX_POINT('',#233126);
#41041=VERTEX_POINT('',#233134);
#41042=VERTEX_POINT('',#233142);
#41043=VERTEX_POINT('',#233150);
#41044=VERTEX_POINT('',#233170);
#41045=VERTEX_POINT('',#233171);
#41046=VERTEX_POINT('',#233173);
#41047=VERTEX_POINT('',#233177);
#41048=VERTEX_POINT('',#233183);
#41049=VERTEX_POINT('',#233184);
#41050=VERTEX_POINT('',#233193);
#41051=VERTEX_POINT('',#233194);
#41052=VERTEX_POINT('',#233203);
#41053=VERTEX_POINT('',#233204);
#41054=VERTEX_POINT('',#233213);
#41055=VERTEX_POINT('',#233214);
#41056=VERTEX_POINT('',#233230);
#41057=VERTEX_POINT('',#233245);
#41058=VERTEX_POINT('',#233247);
#41059=VERTEX_POINT('',#233249);
#41060=VERTEX_POINT('',#233253);
#41061=VERTEX_POINT('',#233259);
#41062=VERTEX_POINT('',#233261);
#41063=VERTEX_POINT('',#233262);
#41064=VERTEX_POINT('',#233264);
#41065=VERTEX_POINT('',#233283);
#41066=VERTEX_POINT('',#233304);
#41067=VERTEX_POINT('',#233305);
#41068=VERTEX_POINT('',#233310);
#41069=VERTEX_POINT('',#233312);
#41070=VERTEX_POINT('',#233314);
#41071=VERTEX_POINT('',#233318);
#41072=VERTEX_POINT('',#233319);
#41073=VERTEX_POINT('',#233321);
#41074=VERTEX_POINT('',#233323);
#41075=VERTEX_POINT('',#233335);
#41076=VERTEX_POINT('',#233338);
#41077=VERTEX_POINT('',#233345);
#41078=VERTEX_POINT('',#233347);
#41079=VERTEX_POINT('',#233352);
#41080=VERTEX_POINT('',#233356);
#41081=VERTEX_POINT('',#233359);
#41082=VERTEX_POINT('',#233364);
#41083=VERTEX_POINT('',#233365);
#41084=VERTEX_POINT('',#233367);
#41085=VERTEX_POINT('',#233369);
#41086=VERTEX_POINT('',#233373);
#41087=VERTEX_POINT('',#233374);
#41088=VERTEX_POINT('',#233379);
#41089=VERTEX_POINT('',#233380);
#41090=VERTEX_POINT('',#233385);
#41091=VERTEX_POINT('',#233386);
#41092=VERTEX_POINT('',#233391);
#41093=VERTEX_POINT('',#233392);
#41094=VERTEX_POINT('',#233397);
#41095=VERTEX_POINT('',#233398);
#41096=VERTEX_POINT('',#233403);
#41097=VERTEX_POINT('',#233404);
#41098=VERTEX_POINT('',#233412);
#41099=VERTEX_POINT('',#233414);
#41100=VERTEX_POINT('',#233418);
#41101=VERTEX_POINT('',#233422);
#41102=VERTEX_POINT('',#233426);
#41103=VERTEX_POINT('',#233427);
#41104=VERTEX_POINT('',#233429);
#41105=VERTEX_POINT('',#233431);
#41106=VERTEX_POINT('',#233434);
#41107=VERTEX_POINT('',#233436);
#41108=VERTEX_POINT('',#233439);
#41109=VERTEX_POINT('',#233441);
#41110=VERTEX_POINT('',#233443);
#41111=VERTEX_POINT('',#233447);
#41112=VERTEX_POINT('',#233451);
#41113=VERTEX_POINT('',#233452);
#41114=VERTEX_POINT('',#233457);
#41115=VERTEX_POINT('',#233461);
#41116=VERTEX_POINT('',#233463);
#41117=VERTEX_POINT('',#233467);
#41118=VERTEX_POINT('',#233469);
#41119=VERTEX_POINT('',#233471);
#41120=VERTEX_POINT('',#233479);
#41121=VERTEX_POINT('',#233480);
#41122=VERTEX_POINT('',#233482);
#41123=VERTEX_POINT('',#233484);
#41124=VERTEX_POINT('',#233488);
#41125=VERTEX_POINT('',#233489);
#41126=VERTEX_POINT('',#233492);
#41127=VERTEX_POINT('',#233496);
#41128=VERTEX_POINT('',#233500);
#41129=VERTEX_POINT('',#233501);
#41130=VERTEX_POINT('',#233506);
#41131=VERTEX_POINT('',#233508);
#41132=VERTEX_POINT('',#233512);
#41133=VERTEX_POINT('',#233514);
#41134=VERTEX_POINT('',#233518);
#41135=VERTEX_POINT('',#233523);
#41136=VERTEX_POINT('',#233527);
#41137=VERTEX_POINT('',#233529);
#41138=VERTEX_POINT('',#233532);
#41139=VERTEX_POINT('',#233534);
#41140=VERTEX_POINT('',#233538);
#41141=VERTEX_POINT('',#233540);
#41142=VERTEX_POINT('',#233571);
#41143=VERTEX_POINT('',#233573);
#41144=VERTEX_POINT('',#233574);
#41145=VERTEX_POINT('',#233576);
#41146=VERTEX_POINT('',#233595);
#41147=VERTEX_POINT('',#233616);
#41148=VERTEX_POINT('',#233617);
#41149=VERTEX_POINT('',#233622);
#41150=VERTEX_POINT('',#233624);
#41151=VERTEX_POINT('',#233626);
#41152=VERTEX_POINT('',#233630);
#41153=VERTEX_POINT('',#233631);
#41154=VERTEX_POINT('',#233633);
#41155=VERTEX_POINT('',#233635);
#41156=VERTEX_POINT('',#233647);
#41157=VERTEX_POINT('',#233650);
#41158=VERTEX_POINT('',#233657);
#41159=VERTEX_POINT('',#233658);
#41160=VERTEX_POINT('',#233660);
#41161=VERTEX_POINT('',#233662);
#41162=VERTEX_POINT('',#233675);
#41163=VERTEX_POINT('',#233676);
#41164=VERTEX_POINT('',#233681);
#41165=VERTEX_POINT('',#233682);
#41166=VERTEX_POINT('',#233687);
#41167=VERTEX_POINT('',#233688);
#41168=VERTEX_POINT('',#233693);
#41169=VERTEX_POINT('',#233694);
#41170=VERTEX_POINT('',#233708);
#41171=VERTEX_POINT('',#233709);
#41172=VERTEX_POINT('',#233711);
#41173=VERTEX_POINT('',#233713);
#41174=VERTEX_POINT('',#233717);
#41175=VERTEX_POINT('',#233718);
#41176=VERTEX_POINT('',#233723);
#41177=VERTEX_POINT('',#233724);
#41178=VERTEX_POINT('',#233729);
#41179=VERTEX_POINT('',#233730);
#41180=VERTEX_POINT('',#233735);
#41181=VERTEX_POINT('',#233736);
#41182=VERTEX_POINT('',#233750);
#41183=VERTEX_POINT('',#233751);
#41184=VERTEX_POINT('',#233753);
#41185=VERTEX_POINT('',#233755);
#41186=VERTEX_POINT('',#233759);
#41187=VERTEX_POINT('',#233760);
#41188=VERTEX_POINT('',#233765);
#41189=VERTEX_POINT('',#233766);
#41190=VERTEX_POINT('',#233771);
#41191=VERTEX_POINT('',#233772);
#41192=VERTEX_POINT('',#233777);
#41193=VERTEX_POINT('',#233778);
#41194=VERTEX_POINT('',#233783);
#41195=VERTEX_POINT('',#233784);
#41196=VERTEX_POINT('',#233789);
#41197=VERTEX_POINT('',#233790);
#41198=VERTEX_POINT('',#233795);
#41199=VERTEX_POINT('',#233796);
#41200=VERTEX_POINT('',#233801);
#41201=VERTEX_POINT('',#233802);
#41202=VERTEX_POINT('',#233807);
#41203=VERTEX_POINT('',#233808);
#41204=VERTEX_POINT('',#233810);
#41205=VERTEX_POINT('',#233812);
#41206=VERTEX_POINT('',#233816);
#41207=VERTEX_POINT('',#233817);
#41208=VERTEX_POINT('',#233822);
#41209=VERTEX_POINT('',#233823);
#41210=VERTEX_POINT('',#233828);
#41211=VERTEX_POINT('',#233829);
#41212=VERTEX_POINT('',#233834);
#41213=VERTEX_POINT('',#233835);
#41214=VERTEX_POINT('',#233849);
#41215=VERTEX_POINT('',#233850);
#41216=VERTEX_POINT('',#233852);
#41217=VERTEX_POINT('',#233854);
#41218=VERTEX_POINT('',#233858);
#41219=VERTEX_POINT('',#233859);
#41220=VERTEX_POINT('',#233864);
#41221=VERTEX_POINT('',#233865);
#41222=VERTEX_POINT('',#233870);
#41223=VERTEX_POINT('',#233871);
#41224=VERTEX_POINT('',#233876);
#41225=VERTEX_POINT('',#233877);
#41226=VERTEX_POINT('',#233882);
#41227=VERTEX_POINT('',#233883);
#41228=VERTEX_POINT('',#233888);
#41229=VERTEX_POINT('',#233889);
#41230=VERTEX_POINT('',#233894);
#41231=VERTEX_POINT('',#233895);
#41232=VERTEX_POINT('',#233900);
#41233=VERTEX_POINT('',#233901);
#41234=VERTEX_POINT('',#233906);
#41235=VERTEX_POINT('',#233907);
#41236=VERTEX_POINT('',#233912);
#41237=VERTEX_POINT('',#233913);
#41238=VERTEX_POINT('',#233915);
#41239=VERTEX_POINT('',#233917);
#41240=VERTEX_POINT('',#233921);
#41241=VERTEX_POINT('',#233922);
#41242=VERTEX_POINT('',#233927);
#41243=VERTEX_POINT('',#233928);
#41244=VERTEX_POINT('',#233933);
#41245=VERTEX_POINT('',#233934);
#41246=VERTEX_POINT('',#233939);
#41247=VERTEX_POINT('',#233940);
#41248=VERTEX_POINT('',#233945);
#41249=VERTEX_POINT('',#233946);
#41250=VERTEX_POINT('',#233951);
#41251=VERTEX_POINT('',#233952);
#41252=VERTEX_POINT('',#233957);
#41253=VERTEX_POINT('',#233958);
#41254=VERTEX_POINT('',#233963);
#41255=VERTEX_POINT('',#233964);
#41256=VERTEX_POINT('',#233969);
#41257=VERTEX_POINT('',#233970);
#41258=VERTEX_POINT('',#233972);
#41259=VERTEX_POINT('',#233974);
#41260=VERTEX_POINT('',#233978);
#41261=VERTEX_POINT('',#233979);
#41262=VERTEX_POINT('',#233984);
#41263=VERTEX_POINT('',#233985);
#41264=VERTEX_POINT('',#233990);
#41265=VERTEX_POINT('',#233991);
#41266=VERTEX_POINT('',#233996);
#41267=VERTEX_POINT('',#233997);
#41268=VERTEX_POINT('',#234002);
#41269=VERTEX_POINT('',#234003);
#41270=VERTEX_POINT('',#234008);
#41271=VERTEX_POINT('',#234009);
#41272=VERTEX_POINT('',#234014);
#41273=VERTEX_POINT('',#234015);
#41274=VERTEX_POINT('',#234020);
#41275=VERTEX_POINT('',#234021);
#41276=VERTEX_POINT('',#234026);
#41277=VERTEX_POINT('',#234027);
#41278=VERTEX_POINT('',#234029);
#41279=VERTEX_POINT('',#234031);
#41280=VERTEX_POINT('',#234035);
#41281=VERTEX_POINT('',#234036);
#41282=VERTEX_POINT('',#234041);
#41283=VERTEX_POINT('',#234042);
#41284=VERTEX_POINT('',#234047);
#41285=VERTEX_POINT('',#234048);
#41286=VERTEX_POINT('',#234053);
#41287=VERTEX_POINT('',#234054);
#41288=VERTEX_POINT('',#234059);
#41289=VERTEX_POINT('',#234060);
#41290=VERTEX_POINT('',#234065);
#41291=VERTEX_POINT('',#234066);
#41292=VERTEX_POINT('',#234071);
#41293=VERTEX_POINT('',#234072);
#41294=VERTEX_POINT('',#234077);
#41295=VERTEX_POINT('',#234078);
#41296=VERTEX_POINT('',#234083);
#41297=VERTEX_POINT('',#234084);
#41298=VERTEX_POINT('',#234086);
#41299=VERTEX_POINT('',#234088);
#41300=VERTEX_POINT('',#234092);
#41301=VERTEX_POINT('',#234093);
#41302=VERTEX_POINT('',#234098);
#41303=VERTEX_POINT('',#234099);
#41304=VERTEX_POINT('',#234104);
#41305=VERTEX_POINT('',#234105);
#41306=VERTEX_POINT('',#234110);
#41307=VERTEX_POINT('',#234111);
#41308=VERTEX_POINT('',#234116);
#41309=VERTEX_POINT('',#234117);
#41310=VERTEX_POINT('',#234122);
#41311=VERTEX_POINT('',#234123);
#41312=VERTEX_POINT('',#234128);
#41313=VERTEX_POINT('',#234129);
#41314=VERTEX_POINT('',#234134);
#41315=VERTEX_POINT('',#234135);
#41316=VERTEX_POINT('',#234140);
#41317=VERTEX_POINT('',#234141);
#41318=VERTEX_POINT('',#234143);
#41319=VERTEX_POINT('',#234145);
#41320=VERTEX_POINT('',#234149);
#41321=VERTEX_POINT('',#234150);
#41322=VERTEX_POINT('',#234155);
#41323=VERTEX_POINT('',#234156);
#41324=VERTEX_POINT('',#234161);
#41325=VERTEX_POINT('',#234162);
#41326=VERTEX_POINT('',#234167);
#41327=VERTEX_POINT('',#234168);
#41328=VERTEX_POINT('',#234173);
#41329=VERTEX_POINT('',#234174);
#41330=VERTEX_POINT('',#234179);
#41331=VERTEX_POINT('',#234180);
#41332=VERTEX_POINT('',#234185);
#41333=VERTEX_POINT('',#234186);
#41334=VERTEX_POINT('',#234191);
#41335=VERTEX_POINT('',#234192);
#41336=VERTEX_POINT('',#234197);
#41337=VERTEX_POINT('',#234198);
#41338=VERTEX_POINT('',#234200);
#41339=VERTEX_POINT('',#234202);
#41340=VERTEX_POINT('',#234206);
#41341=VERTEX_POINT('',#234207);
#41342=VERTEX_POINT('',#234212);
#41343=VERTEX_POINT('',#234213);
#41344=VERTEX_POINT('',#234218);
#41345=VERTEX_POINT('',#234219);
#41346=VERTEX_POINT('',#234224);
#41347=VERTEX_POINT('',#234225);
#41348=VERTEX_POINT('',#234230);
#41349=VERTEX_POINT('',#234231);
#41350=VERTEX_POINT('',#234236);
#41351=VERTEX_POINT('',#234237);
#41352=VERTEX_POINT('',#234242);
#41353=VERTEX_POINT('',#234243);
#41354=VERTEX_POINT('',#234248);
#41355=VERTEX_POINT('',#234249);
#41356=VERTEX_POINT('',#234254);
#41357=VERTEX_POINT('',#234255);
#41358=VERTEX_POINT('',#234257);
#41359=VERTEX_POINT('',#234259);
#41360=VERTEX_POINT('',#234263);
#41361=VERTEX_POINT('',#234264);
#41362=VERTEX_POINT('',#234269);
#41363=VERTEX_POINT('',#234270);
#41364=VERTEX_POINT('',#234275);
#41365=VERTEX_POINT('',#234276);
#41366=VERTEX_POINT('',#234281);
#41367=VERTEX_POINT('',#234282);
#41368=VERTEX_POINT('',#234287);
#41369=VERTEX_POINT('',#234288);
#41370=VERTEX_POINT('',#234293);
#41371=VERTEX_POINT('',#234294);
#41372=VERTEX_POINT('',#234299);
#41373=VERTEX_POINT('',#234300);
#41374=VERTEX_POINT('',#234305);
#41375=VERTEX_POINT('',#234306);
#41376=VERTEX_POINT('',#234311);
#41377=VERTEX_POINT('',#234312);
#41378=VERTEX_POINT('',#234317);
#41379=VERTEX_POINT('',#234318);
#41380=VERTEX_POINT('',#234320);
#41381=VERTEX_POINT('',#234322);
#41382=VERTEX_POINT('',#234326);
#41383=VERTEX_POINT('',#234327);
#41384=VERTEX_POINT('',#234332);
#41385=VERTEX_POINT('',#234333);
#41386=VERTEX_POINT('',#234338);
#41387=VERTEX_POINT('',#234339);
#41388=VERTEX_POINT('',#234344);
#41389=VERTEX_POINT('',#234345);
#41390=VERTEX_POINT('',#234350);
#41391=VERTEX_POINT('',#234351);
#41392=VERTEX_POINT('',#234356);
#41393=VERTEX_POINT('',#234357);
#41394=VERTEX_POINT('',#234362);
#41395=VERTEX_POINT('',#234363);
#41396=VERTEX_POINT('',#234368);
#41397=VERTEX_POINT('',#234369);
#41398=VERTEX_POINT('',#234374);
#41399=VERTEX_POINT('',#234375);
#41400=VERTEX_POINT('',#234386);
#41401=VERTEX_POINT('',#234388);
#41402=VERTEX_POINT('',#234392);
#41403=VERTEX_POINT('',#234393);
#41404=VERTEX_POINT('',#234398);
#41405=VERTEX_POINT('',#234399);
#41406=VERTEX_POINT('',#234404);
#41407=VERTEX_POINT('',#234405);
#41408=VERTEX_POINT('',#234410);
#41409=VERTEX_POINT('',#234411);
#41410=VERTEX_POINT('',#234416);
#41411=VERTEX_POINT('',#234418);
#41412=VERTEX_POINT('',#234422);
#41413=VERTEX_POINT('',#234424);
#41414=VERTEX_POINT('',#234428);
#41415=VERTEX_POINT('',#234430);
#41416=VERTEX_POINT('',#234434);
#41417=VERTEX_POINT('',#234436);
#41418=VERTEX_POINT('',#234440);
#41419=VERTEX_POINT('',#234442);
#41420=VERTEX_POINT('',#234446);
#41421=VERTEX_POINT('',#234448);
#41422=VERTEX_POINT('',#234452);
#41423=VERTEX_POINT('',#234454);
#41424=VERTEX_POINT('',#234458);
#41425=VERTEX_POINT('',#234460);
#41426=VERTEX_POINT('',#234464);
#41427=VERTEX_POINT('',#234466);
#41428=VERTEX_POINT('',#234470);
#41429=VERTEX_POINT('',#234472);
#41430=VERTEX_POINT('',#234476);
#41431=VERTEX_POINT('',#234478);
#41432=VERTEX_POINT('',#234482);
#41433=VERTEX_POINT('',#234484);
#41434=VERTEX_POINT('',#234488);
#41435=VERTEX_POINT('',#234490);
#41436=VERTEX_POINT('',#234494);
#41437=VERTEX_POINT('',#234496);
#41438=VERTEX_POINT('',#234500);
#41439=VERTEX_POINT('',#234502);
#41440=VERTEX_POINT('',#234506);
#41441=VERTEX_POINT('',#234508);
#41442=VERTEX_POINT('',#234512);
#41443=VERTEX_POINT('',#234514);
#41444=VERTEX_POINT('',#234518);
#41445=VERTEX_POINT('',#234520);
#41446=VERTEX_POINT('',#234524);
#41447=VERTEX_POINT('',#234526);
#41448=VERTEX_POINT('',#234530);
#41449=VERTEX_POINT('',#234532);
#41450=VERTEX_POINT('',#234536);
#41451=VERTEX_POINT('',#234538);
#41452=VERTEX_POINT('',#234542);
#41453=VERTEX_POINT('',#234544);
#41454=VERTEX_POINT('',#234548);
#41455=VERTEX_POINT('',#234550);
#41456=VERTEX_POINT('',#234554);
#41457=VERTEX_POINT('',#234556);
#41458=VERTEX_POINT('',#234560);
#41459=VERTEX_POINT('',#234562);
#41460=VERTEX_POINT('',#234566);
#41461=VERTEX_POINT('',#234568);
#41462=VERTEX_POINT('',#234573);
#41463=VERTEX_POINT('',#234575);
#41464=VERTEX_POINT('',#234593);
#41465=VERTEX_POINT('',#234595);
#41466=VERTEX_POINT('',#234603);
#41467=VERTEX_POINT('',#234673);
#41468=VERTEX_POINT('',#234679);
#41469=VERTEX_POINT('',#234697);
#41470=VERTEX_POINT('',#234699);
#41471=VERTEX_POINT('',#234702);
#41472=VERTEX_POINT('',#234706);
#41473=VERTEX_POINT('',#234708);
#41474=VERTEX_POINT('',#234750);
#41475=VERTEX_POINT('',#234751);
#41476=VERTEX_POINT('',#234753);
#41477=VERTEX_POINT('',#234755);
#41478=VERTEX_POINT('',#234757);
#41479=VERTEX_POINT('',#234759);
#41480=VERTEX_POINT('',#234763);
#41481=VERTEX_POINT('',#234771);
#41482=VERTEX_POINT('',#234779);
#41483=VERTEX_POINT('',#234787);
#41484=VERTEX_POINT('',#234795);
#41485=VERTEX_POINT('',#234803);
#41486=VERTEX_POINT('',#234811);
#41487=VERTEX_POINT('',#234812);
#41488=VERTEX_POINT('',#234814);
#41489=VERTEX_POINT('',#234816);
#41490=VERTEX_POINT('',#234818);
#41491=VERTEX_POINT('',#234820);
#41492=VERTEX_POINT('',#234824);
#41493=VERTEX_POINT('',#234832);
#41494=VERTEX_POINT('',#234840);
#41495=VERTEX_POINT('',#234848);
#41496=VERTEX_POINT('',#234856);
#41497=VERTEX_POINT('',#234864);
#41498=VERTEX_POINT('',#234884);
#41499=VERTEX_POINT('',#234885);
#41500=VERTEX_POINT('',#234887);
#41501=VERTEX_POINT('',#234889);
#41502=VERTEX_POINT('',#234891);
#41503=VERTEX_POINT('',#234893);
#41504=VERTEX_POINT('',#234897);
#41505=VERTEX_POINT('',#234905);
#41506=VERTEX_POINT('',#234913);
#41507=VERTEX_POINT('',#234921);
#41508=VERTEX_POINT('',#234929);
#41509=VERTEX_POINT('',#234937);
#41510=VERTEX_POINT('',#234945);
#41511=VERTEX_POINT('',#234946);
#41512=VERTEX_POINT('',#234948);
#41513=VERTEX_POINT('',#234950);
#41514=VERTEX_POINT('',#234952);
#41515=VERTEX_POINT('',#234954);
#41516=VERTEX_POINT('',#234958);
#41517=VERTEX_POINT('',#234966);
#41518=VERTEX_POINT('',#234974);
#41519=VERTEX_POINT('',#234982);
#41520=VERTEX_POINT('',#234990);
#41521=VERTEX_POINT('',#234998);
#41522=VERTEX_POINT('',#235018);
#41523=VERTEX_POINT('',#235019);
#41524=VERTEX_POINT('',#235021);
#41525=VERTEX_POINT('',#235025);
#41526=VERTEX_POINT('',#235031);
#41527=VERTEX_POINT('',#235032);
#41528=VERTEX_POINT('',#235041);
#41529=VERTEX_POINT('',#235042);
#41530=VERTEX_POINT('',#235051);
#41531=VERTEX_POINT('',#235052);
#41532=VERTEX_POINT('',#235061);
#41533=VERTEX_POINT('',#235062);
#41534=VERTEX_POINT('',#235078);
#41535=VERTEX_POINT('',#235093);
#41536=VERTEX_POINT('',#235095);
#41537=VERTEX_POINT('',#235097);
#41538=VERTEX_POINT('',#235101);
#41539=VERTEX_POINT('',#235107);
#41540=VERTEX_POINT('',#235108);
#41541=VERTEX_POINT('',#235110);
#41542=VERTEX_POINT('',#235114);
#41543=VERTEX_POINT('',#235115);
#41544=VERTEX_POINT('',#235117);
#41545=VERTEX_POINT('',#235121);
#41546=VERTEX_POINT('',#235123);
#41547=VERTEX_POINT('',#235127);
#41548=VERTEX_POINT('',#235129);
#41549=VERTEX_POINT('',#235133);
#41550=VERTEX_POINT('',#235137);
#41551=VERTEX_POINT('',#235138);
#41552=VERTEX_POINT('',#235140);
#41553=VERTEX_POINT('',#235145);
#41554=VERTEX_POINT('',#235149);
#41555=VERTEX_POINT('',#235153);
#41556=VERTEX_POINT('',#235162);
#41557=VERTEX_POINT('',#235163);
#41558=VERTEX_POINT('',#235165);
#41559=VERTEX_POINT('',#235174);
#41560=VERTEX_POINT('',#235178);
#41561=VERTEX_POINT('',#235179);
#41562=VERTEX_POINT('',#235187);
#41563=VERTEX_POINT('',#235188);
#41564=VERTEX_POINT('',#235190);
#41565=VERTEX_POINT('',#235199);
#41566=VERTEX_POINT('',#235204);
#41567=VERTEX_POINT('',#235208);
#41568=VERTEX_POINT('',#235209);
#41569=VERTEX_POINT('',#235211);
#41570=VERTEX_POINT('',#235213);
#41571=VERTEX_POINT('',#235217);
#41572=VERTEX_POINT('',#235218);
#41573=VERTEX_POINT('',#235220);
#41574=VERTEX_POINT('',#235222);
#41575=VERTEX_POINT('',#235242);
#41576=VERTEX_POINT('',#235244);
#41577=VERTEX_POINT('',#235246);
#41578=VERTEX_POINT('',#235248);
#41579=VERTEX_POINT('',#235252);
#41580=VERTEX_POINT('',#235253);
#41581=VERTEX_POINT('',#235255);
#41582=VERTEX_POINT('',#235259);
#41583=VERTEX_POINT('',#235260);
#41584=VERTEX_POINT('',#235262);
#41585=VERTEX_POINT('',#235266);
#41586=VERTEX_POINT('',#235267);
#41587=VERTEX_POINT('',#235272);
#41588=VERTEX_POINT('',#235273);
#41589=VERTEX_POINT('',#235278);
#41590=VERTEX_POINT('',#235282);
#41591=VERTEX_POINT('',#235283);
#41592=VERTEX_POINT('',#235285);
#41593=VERTEX_POINT('',#235290);
#41594=VERTEX_POINT('',#235294);
#41595=VERTEX_POINT('',#235298);
#41596=VERTEX_POINT('',#235307);
#41597=VERTEX_POINT('',#235308);
#41598=VERTEX_POINT('',#235310);
#41599=VERTEX_POINT('',#235319);
#41600=VERTEX_POINT('',#235323);
#41601=VERTEX_POINT('',#235328);
#41602=VERTEX_POINT('',#235332);
#41603=VERTEX_POINT('',#235333);
#41604=VERTEX_POINT('',#235335);
#41605=VERTEX_POINT('',#235344);
#41606=VERTEX_POINT('',#235345);
#41607=VERTEX_POINT('',#235353);
#41608=VERTEX_POINT('',#235354);
#41609=VERTEX_POINT('',#235356);
#41610=VERTEX_POINT('',#235358);
#41611=VERTEX_POINT('',#235362);
#41612=VERTEX_POINT('',#235363);
#41613=VERTEX_POINT('',#235365);
#41614=VERTEX_POINT('',#235367);
#41615=VERTEX_POINT('',#235459);
#41616=VERTEX_POINT('',#235461);
#41617=VERTEX_POINT('',#235463);
#41618=VERTEX_POINT('',#235465);
#41619=VERTEX_POINT('',#235469);
#41620=VERTEX_POINT('',#235502);
#41621=VERTEX_POINT('',#235515);
#41622=VERTEX_POINT('',#235519);
#41623=VERTEX_POINT('',#235520);
#41624=VERTEX_POINT('',#235528);
#41625=VERTEX_POINT('',#235532);
#41626=VERTEX_POINT('',#235533);
#41627=VERTEX_POINT('',#235541);
#41628=VERTEX_POINT('',#235545);
#41629=VERTEX_POINT('',#235549);
#41630=VERTEX_POINT('',#235552);
#41631=VERTEX_POINT('',#235556);
#41632=VERTEX_POINT('',#235589);
#41633=VERTEX_POINT('',#235604);
#41634=VERTEX_POINT('',#235608);
#41635=VERTEX_POINT('',#235609);
#41636=VERTEX_POINT('',#235617);
#41637=VERTEX_POINT('',#235621);
#41638=VERTEX_POINT('',#235622);
#41639=VERTEX_POINT('',#235639);
#41640=VERTEX_POINT('',#235640);
#41641=VERTEX_POINT('',#235642);
#41642=VERTEX_POINT('',#235663);
#41643=VERTEX_POINT('',#235694);
#41644=VERTEX_POINT('',#235695);
#41645=VERTEX_POINT('',#235770);
#41646=VERTEX_POINT('',#235771);
#41647=VERTEX_POINT('',#235848);
#41648=VERTEX_POINT('',#235849);
#41649=VERTEX_POINT('',#235926);
#41650=VERTEX_POINT('',#235927);
#41651=VERTEX_POINT('',#236002);
#41652=VERTEX_POINT('',#236003);
#41653=VERTEX_POINT('',#236078);
#41654=VERTEX_POINT('',#236079);
#41655=VERTEX_POINT('',#236154);
#41656=VERTEX_POINT('',#236155);
#41657=VERTEX_POINT('',#236230);
#41658=VERTEX_POINT('',#236231);
#41659=VERTEX_POINT('',#236308);
#41660=VERTEX_POINT('',#236309);
#41661=VERTEX_POINT('',#236386);
#41662=VERTEX_POINT('',#236387);
#41663=VERTEX_POINT('',#236462);
#41664=VERTEX_POINT('',#236463);
#41665=VERTEX_POINT('',#236538);
#41666=VERTEX_POINT('',#236539);
#41667=VERTEX_POINT('',#236614);
#41668=VERTEX_POINT('',#236615);
#41669=VERTEX_POINT('',#236690);
#41670=VERTEX_POINT('',#236691);
#41671=VERTEX_POINT('',#236766);
#41672=VERTEX_POINT('',#236767);
#41673=VERTEX_POINT('',#236844);
#41674=VERTEX_POINT('',#236845);
#41675=VERTEX_POINT('',#236922);
#41676=VERTEX_POINT('',#236923);
#41677=VERTEX_POINT('',#236998);
#41678=VERTEX_POINT('',#236999);
#41679=VERTEX_POINT('',#237001);
#41680=VERTEX_POINT('',#237010);
#41681=VERTEX_POINT('',#237026);
#41682=VERTEX_POINT('',#237027);
#41683=VERTEX_POINT('',#237029);
#41684=VERTEX_POINT('',#237042);
#41685=VERTEX_POINT('',#237063);
#41686=VERTEX_POINT('',#237064);
#41687=VERTEX_POINT('',#237139);
#41688=VERTEX_POINT('',#237140);
#41689=VERTEX_POINT('',#237217);
#41690=VERTEX_POINT('',#237218);
#41691=VERTEX_POINT('',#237293);
#41692=VERTEX_POINT('',#237294);
#41693=VERTEX_POINT('',#237369);
#41694=VERTEX_POINT('',#237370);
#41695=VERTEX_POINT('',#237445);
#41696=VERTEX_POINT('',#237446);
#41697=VERTEX_POINT('',#237521);
#41698=VERTEX_POINT('',#237522);
#41699=VERTEX_POINT('',#237599);
#41700=VERTEX_POINT('',#237600);
#41701=VERTEX_POINT('',#237675);
#41702=VERTEX_POINT('',#237676);
#41703=VERTEX_POINT('',#237753);
#41704=VERTEX_POINT('',#237754);
#41705=VERTEX_POINT('',#237829);
#41706=VERTEX_POINT('',#237830);
#41707=VERTEX_POINT('',#237905);
#41708=VERTEX_POINT('',#237906);
#41709=VERTEX_POINT('',#237981);
#41710=VERTEX_POINT('',#237982);
#41711=VERTEX_POINT('',#238057);
#41712=VERTEX_POINT('',#238058);
#41713=VERTEX_POINT('',#238135);
#41714=VERTEX_POINT('',#238136);
#41715=VERTEX_POINT('',#238211);
#41716=VERTEX_POINT('',#238212);
#41717=VERTEX_POINT('',#238289);
#41718=VERTEX_POINT('',#238290);
#41719=VERTEX_POINT('',#238365);
#41720=VERTEX_POINT('',#238366);
#41721=VERTEX_POINT('',#238368);
#41722=VERTEX_POINT('',#238385);
#41723=VERTEX_POINT('',#238411);
#41724=VERTEX_POINT('',#238412);
#41725=VERTEX_POINT('',#238414);
#41726=VERTEX_POINT('',#238418);
#41727=VERTEX_POINT('',#238429);
#41728=VERTEX_POINT('',#238430);
#41729=VERTEX_POINT('',#238432);
#41730=VERTEX_POINT('',#238440);
#41731=VERTEX_POINT('',#238474);
#41732=VERTEX_POINT('',#238475);
#41733=VERTEX_POINT('',#238504);
#41734=VERTEX_POINT('',#238505);
#41735=VERTEX_POINT('',#238534);
#41736=VERTEX_POINT('',#238535);
#41737=VERTEX_POINT('',#238564);
#41738=VERTEX_POINT('',#238565);
#41739=VERTEX_POINT('',#238594);
#41740=VERTEX_POINT('',#238595);
#41741=VERTEX_POINT('',#238624);
#41742=VERTEX_POINT('',#238625);
#41743=VERTEX_POINT('',#238654);
#41744=VERTEX_POINT('',#238655);
#41745=VERTEX_POINT('',#238684);
#41746=VERTEX_POINT('',#238685);
#41747=VERTEX_POINT('',#238714);
#41748=VERTEX_POINT('',#238715);
#41749=VERTEX_POINT('',#238744);
#41750=VERTEX_POINT('',#238745);
#41751=VERTEX_POINT('',#238774);
#41752=VERTEX_POINT('',#238775);
#41753=VERTEX_POINT('',#238804);
#41754=VERTEX_POINT('',#238805);
#41755=VERTEX_POINT('',#238834);
#41756=VERTEX_POINT('',#238835);
#41757=VERTEX_POINT('',#238864);
#41758=VERTEX_POINT('',#238865);
#41759=VERTEX_POINT('',#238894);
#41760=VERTEX_POINT('',#238895);
#41761=VERTEX_POINT('',#238924);
#41762=VERTEX_POINT('',#238925);
#41763=VERTEX_POINT('',#238954);
#41764=VERTEX_POINT('',#238955);
#41765=VERTEX_POINT('',#238957);
#41766=VERTEX_POINT('',#238965);
#41767=VERTEX_POINT('',#238966);
#41768=VERTEX_POINT('',#238968);
#41769=VERTEX_POINT('',#238997);
#41770=VERTEX_POINT('',#239036);
#41771=VERTEX_POINT('',#239037);
#41772=VERTEX_POINT('',#239112);
#41773=VERTEX_POINT('',#239113);
#41774=VERTEX_POINT('',#239188);
#41775=VERTEX_POINT('',#239189);
#41776=VERTEX_POINT('',#239266);
#41777=VERTEX_POINT('',#239267);
#41778=VERTEX_POINT('',#239342);
#41779=VERTEX_POINT('',#239343);
#41780=VERTEX_POINT('',#239418);
#41781=VERTEX_POINT('',#239419);
#41782=VERTEX_POINT('',#239496);
#41783=VERTEX_POINT('',#239497);
#41784=VERTEX_POINT('',#239572);
#41785=VERTEX_POINT('',#239573);
#41786=VERTEX_POINT('',#239648);
#41787=VERTEX_POINT('',#239649);
#41788=VERTEX_POINT('',#239724);
#41789=VERTEX_POINT('',#239725);
#41790=VERTEX_POINT('',#239802);
#41791=VERTEX_POINT('',#239803);
#41792=VERTEX_POINT('',#239878);
#41793=VERTEX_POINT('',#239879);
#41794=VERTEX_POINT('',#239954);
#41795=VERTEX_POINT('',#239955);
#41796=VERTEX_POINT('',#240032);
#41797=VERTEX_POINT('',#240033);
#41798=VERTEX_POINT('',#240108);
#41799=VERTEX_POINT('',#240109);
#41800=VERTEX_POINT('',#240184);
#41801=VERTEX_POINT('',#240185);
#41802=VERTEX_POINT('',#240260);
#41803=VERTEX_POINT('',#240261);
#41804=VERTEX_POINT('',#240263);
#41805=VERTEX_POINT('',#240270);
#41806=VERTEX_POINT('',#240281);
#41807=VERTEX_POINT('',#240308);
#41808=VERTEX_POINT('',#240345);
#41809=VERTEX_POINT('',#240346);
#41810=VERTEX_POINT('',#240348);
#41811=VERTEX_POINT('',#240352);
#41812=VERTEX_POINT('',#240373);
#41813=VERTEX_POINT('',#240374);
#41814=VERTEX_POINT('',#240376);
#41815=VERTEX_POINT('',#240384);
#41816=VERTEX_POINT('',#240418);
#41817=VERTEX_POINT('',#240419);
#41818=VERTEX_POINT('',#240448);
#41819=VERTEX_POINT('',#240449);
#41820=VERTEX_POINT('',#240478);
#41821=VERTEX_POINT('',#240479);
#41822=VERTEX_POINT('',#240508);
#41823=VERTEX_POINT('',#240509);
#41824=VERTEX_POINT('',#240538);
#41825=VERTEX_POINT('',#240539);
#41826=VERTEX_POINT('',#240568);
#41827=VERTEX_POINT('',#240569);
#41828=VERTEX_POINT('',#240598);
#41829=VERTEX_POINT('',#240599);
#41830=VERTEX_POINT('',#240628);
#41831=VERTEX_POINT('',#240629);
#41832=VERTEX_POINT('',#240658);
#41833=VERTEX_POINT('',#240659);
#41834=VERTEX_POINT('',#240688);
#41835=VERTEX_POINT('',#240689);
#41836=VERTEX_POINT('',#240718);
#41837=VERTEX_POINT('',#240719);
#41838=VERTEX_POINT('',#240748);
#41839=VERTEX_POINT('',#240749);
#41840=VERTEX_POINT('',#240778);
#41841=VERTEX_POINT('',#240779);
#41842=VERTEX_POINT('',#240808);
#41843=VERTEX_POINT('',#240809);
#41844=VERTEX_POINT('',#240838);
#41845=VERTEX_POINT('',#240839);
#41846=VERTEX_POINT('',#240868);
#41847=VERTEX_POINT('',#240869);
#41848=VERTEX_POINT('',#240898);
#41849=VERTEX_POINT('',#240899);
#41850=VERTEX_POINT('',#240901);
#41851=VERTEX_POINT('',#240909);
#41852=VERTEX_POINT('',#240910);
#41853=VERTEX_POINT('',#240912);
#41854=VERTEX_POINT('',#240925);
#41855=VERTEX_POINT('',#240926);
#41856=VERTEX_POINT('',#241003);
#41857=VERTEX_POINT('',#241004);
#41858=VERTEX_POINT('',#241079);
#41859=VERTEX_POINT('',#241080);
#41860=VERTEX_POINT('',#241155);
#41861=VERTEX_POINT('',#241156);
#41862=VERTEX_POINT('',#241231);
#41863=VERTEX_POINT('',#241232);
#41864=VERTEX_POINT('',#241307);
#41865=VERTEX_POINT('',#241308);
#41866=VERTEX_POINT('',#241383);
#41867=VERTEX_POINT('',#241384);
#41868=VERTEX_POINT('',#241461);
#41869=VERTEX_POINT('',#241462);
#41870=VERTEX_POINT('',#241539);
#41871=VERTEX_POINT('',#241540);
#41872=VERTEX_POINT('',#241615);
#41873=VERTEX_POINT('',#241616);
#41874=VERTEX_POINT('',#241691);
#41875=VERTEX_POINT('',#241692);
#41876=VERTEX_POINT('',#241767);
#41877=VERTEX_POINT('',#241768);
#41878=VERTEX_POINT('',#241843);
#41879=VERTEX_POINT('',#241844);
#41880=VERTEX_POINT('',#241919);
#41881=VERTEX_POINT('',#241920);
#41882=VERTEX_POINT('',#241999);
#41883=VERTEX_POINT('',#242000);
#41884=VERTEX_POINT('',#242075);
#41885=VERTEX_POINT('',#242076);
#41886=VERTEX_POINT('',#242151);
#41887=VERTEX_POINT('',#242152);
#41888=VERTEX_POINT('',#242227);
#41889=VERTEX_POINT('',#242228);
#41890=VERTEX_POINT('',#242230);
#41891=VERTEX_POINT('',#242257);
#41892=VERTEX_POINT('',#242291);
#41893=VERTEX_POINT('',#242292);
#41894=VERTEX_POINT('',#242294);
#41895=VERTEX_POINT('',#242298);
#41896=VERTEX_POINT('',#242309);
#41897=VERTEX_POINT('',#242310);
#41898=VERTEX_POINT('',#242312);
#41899=VERTEX_POINT('',#242320);
#41900=VERTEX_POINT('',#242354);
#41901=VERTEX_POINT('',#242355);
#41902=VERTEX_POINT('',#242384);
#41903=VERTEX_POINT('',#242385);
#41904=VERTEX_POINT('',#242414);
#41905=VERTEX_POINT('',#242415);
#41906=VERTEX_POINT('',#242444);
#41907=VERTEX_POINT('',#242445);
#41908=VERTEX_POINT('',#242474);
#41909=VERTEX_POINT('',#242475);
#41910=VERTEX_POINT('',#242504);
#41911=VERTEX_POINT('',#242505);
#41912=VERTEX_POINT('',#242534);
#41913=VERTEX_POINT('',#242535);
#41914=VERTEX_POINT('',#242564);
#41915=VERTEX_POINT('',#242565);
#41916=VERTEX_POINT('',#242594);
#41917=VERTEX_POINT('',#242595);
#41918=VERTEX_POINT('',#242624);
#41919=VERTEX_POINT('',#242625);
#41920=VERTEX_POINT('',#242654);
#41921=VERTEX_POINT('',#242655);
#41922=VERTEX_POINT('',#242684);
#41923=VERTEX_POINT('',#242685);
#41924=VERTEX_POINT('',#242714);
#41925=VERTEX_POINT('',#242715);
#41926=VERTEX_POINT('',#242744);
#41927=VERTEX_POINT('',#242745);
#41928=VERTEX_POINT('',#242774);
#41929=VERTEX_POINT('',#242775);
#41930=VERTEX_POINT('',#242804);
#41931=VERTEX_POINT('',#242805);
#41932=VERTEX_POINT('',#242834);
#41933=VERTEX_POINT('',#242835);
#41934=VERTEX_POINT('',#242837);
#41935=VERTEX_POINT('',#242845);
#41936=VERTEX_POINT('',#242846);
#41937=VERTEX_POINT('',#242848);
#41938=VERTEX_POINT('',#242852);
#41939=VERTEX_POINT('',#242863);
#41940=VERTEX_POINT('',#242864);
#41941=VERTEX_POINT('',#242866);
#41942=VERTEX_POINT('',#242874);
#41943=VERTEX_POINT('',#242908);
#41944=VERTEX_POINT('',#242909);
#41945=VERTEX_POINT('',#242938);
#41946=VERTEX_POINT('',#242939);
#41947=VERTEX_POINT('',#242968);
#41948=VERTEX_POINT('',#242969);
#41949=VERTEX_POINT('',#242998);
#41950=VERTEX_POINT('',#242999);
#41951=VERTEX_POINT('',#243028);
#41952=VERTEX_POINT('',#243029);
#41953=VERTEX_POINT('',#243058);
#41954=VERTEX_POINT('',#243059);
#41955=VERTEX_POINT('',#243088);
#41956=VERTEX_POINT('',#243089);
#41957=VERTEX_POINT('',#243118);
#41958=VERTEX_POINT('',#243119);
#41959=VERTEX_POINT('',#243148);
#41960=VERTEX_POINT('',#243149);
#41961=VERTEX_POINT('',#243178);
#41962=VERTEX_POINT('',#243179);
#41963=VERTEX_POINT('',#243208);
#41964=VERTEX_POINT('',#243209);
#41965=VERTEX_POINT('',#243238);
#41966=VERTEX_POINT('',#243239);
#41967=VERTEX_POINT('',#243268);
#41968=VERTEX_POINT('',#243269);
#41969=VERTEX_POINT('',#243298);
#41970=VERTEX_POINT('',#243299);
#41971=VERTEX_POINT('',#243328);
#41972=VERTEX_POINT('',#243329);
#41973=VERTEX_POINT('',#243358);
#41974=VERTEX_POINT('',#243359);
#41975=VERTEX_POINT('',#243388);
#41976=VERTEX_POINT('',#243389);
#41977=VERTEX_POINT('',#243391);
#41978=VERTEX_POINT('',#243399);
#41979=VERTEX_POINT('',#243400);
#41980=VERTEX_POINT('',#243402);
#41981=VERTEX_POINT('',#243404);
#41982=VERTEX_POINT('',#243406);
#41983=VERTEX_POINT('',#243408);
#41984=VERTEX_POINT('',#243410);
#41985=VERTEX_POINT('',#243412);
#41986=VERTEX_POINT('',#243416);
#41987=VERTEX_POINT('',#243417);
#41988=VERTEX_POINT('',#243419);
#41989=VERTEX_POINT('',#243422);
#41990=VERTEX_POINT('',#243426);
#41991=VERTEX_POINT('',#243427);
#41992=VERTEX_POINT('',#243469);
#41993=VERTEX_POINT('',#243471);
#41994=VERTEX_POINT('',#243473);
#41995=VERTEX_POINT('',#243519);
#41996=VERTEX_POINT('',#243520);
#41997=VERTEX_POINT('',#243522);
#41998=VERTEX_POINT('',#243524);
#41999=VERTEX_POINT('',#243528);
#42000=VERTEX_POINT('',#243530);
#42001=VERTEX_POINT('',#243534);
#42002=VERTEX_POINT('',#243536);
#42003=VERTEX_POINT('',#243543);
#42004=VERTEX_POINT('',#243545);
#42005=VERTEX_POINT('',#243547);
#42006=VERTEX_POINT('',#243549);
#42007=VERTEX_POINT('',#243551);
#42008=VERTEX_POINT('',#243554);
#42009=VERTEX_POINT('',#243556);
#42010=VERTEX_POINT('',#243558);
#42011=VERTEX_POINT('',#243559);
#42012=VERTEX_POINT('',#243574);
#42013=VERTEX_POINT('',#243576);
#42014=VERTEX_POINT('',#243583);
#42015=VERTEX_POINT('',#243590);
#42016=VERTEX_POINT('',#243724);
#42017=VERTEX_POINT('',#243726);
#42018=VERTEX_POINT('',#243728);
#42019=VERTEX_POINT('',#243730);
#42020=VERTEX_POINT('',#243801);
#42021=VERTEX_POINT('',#243808);
#42022=VERTEX_POINT('',#243815);
#42023=VERTEX_POINT('',#243817);
#42024=VERTEX_POINT('',#243834);
#42025=VERTEX_POINT('',#243836);
#42026=VERTEX_POINT('',#243839);
#42027=VERTEX_POINT('',#243846);
#42028=VERTEX_POINT('',#243848);
#42029=VERTEX_POINT('',#243851);
#42030=VERTEX_POINT('',#243858);
#42031=VERTEX_POINT('',#243860);
#42032=VERTEX_POINT('',#243863);
#42033=VERTEX_POINT('',#243867);
#42034=VERTEX_POINT('',#243907);
#42035=VERTEX_POINT('',#243909);
#42036=VERTEX_POINT('',#243912);
#42037=VERTEX_POINT('',#243916);
#42038=VERTEX_POINT('',#243922);
#42039=VERTEX_POINT('',#243927);
#42040=VERTEX_POINT('',#243929);
#42041=VERTEX_POINT('',#243931);
#42042=VERTEX_POINT('',#243935);
#42043=VERTEX_POINT('',#243936);
#42044=VERTEX_POINT('',#243939);
#42045=VERTEX_POINT('',#243941);
#42046=VERTEX_POINT('',#243945);
#42047=VERTEX_POINT('',#243946);
#42048=VERTEX_POINT('',#243948);
#42049=VERTEX_POINT('',#243952);
#42050=VERTEX_POINT('',#243958);
#42051=VERTEX_POINT('',#243959);
#42052=VERTEX_POINT('',#243968);
#42053=VERTEX_POINT('',#243969);
#42054=VERTEX_POINT('',#243978);
#42055=VERTEX_POINT('',#243979);
#42056=VERTEX_POINT('',#243988);
#42057=VERTEX_POINT('',#243989);
#42058=VERTEX_POINT('',#244005);
#42059=VERTEX_POINT('',#244374);
#42060=VERTEX_POINT('',#244375);
#42061=VERTEX_POINT('',#245374);
#42062=VERTEX_POINT('',#245375);
#42063=VERTEX_POINT('',#246033);
#42064=VERTEX_POINT('',#246034);
#42065=VERTEX_POINT('',#246036);
#42066=VERTEX_POINT('',#246081);
#42067=VERTEX_POINT('',#246082);
#42068=VERTEX_POINT('',#246175);
#42069=VERTEX_POINT('',#246202);
#42070=VERTEX_POINT('',#246248);
#42071=VERTEX_POINT('',#246249);
#42072=VERTEX_POINT('',#246265);
#42073=VERTEX_POINT('',#246266);
#42074=VERTEX_POINT('',#246327);
#42075=VERTEX_POINT('',#246328);
#42076=VERTEX_POINT('',#246461);
#42077=VERTEX_POINT('',#246462);
#42078=VERTEX_POINT('',#246500);
#42079=VERTEX_POINT('',#246583);
#42080=VERTEX_POINT('',#246619);
#42081=VERTEX_POINT('',#246701);
#42082=VERTEX_POINT('',#246722);
#42083=VERTEX_POINT('',#246864);
#42084=VERTEX_POINT('',#246869);
#42085=VERTEX_POINT('',#246876);
#42086=VERTEX_POINT('',#246926);
#42087=VERTEX_POINT('',#246927);
#42088=VERTEX_POINT('',#246929);
#42089=VERTEX_POINT('',#247111);
#42090=VERTEX_POINT('',#247112);
#42091=VERTEX_POINT('',#247115);
#42092=VERTEX_POINT('',#247291);
#42093=VERTEX_POINT('',#247368);
#42094=VERTEX_POINT('',#247475);
#42095=VERTEX_POINT('',#247477);
#42096=VERTEX_POINT('',#247486);
#42097=VERTEX_POINT('',#247487);
#42098=VERTEX_POINT('',#247643);
#42099=VERTEX_POINT('',#247645);
#42100=VERTEX_POINT('',#247660);
#42101=VERTEX_POINT('',#247661);
#42102=VERTEX_POINT('',#247666);
#42103=VERTEX_POINT('',#247670);
#42104=VERTEX_POINT('',#247671);
#42105=VERTEX_POINT('',#247711);
#42106=VERTEX_POINT('',#247852);
#42107=VERTEX_POINT('',#247854);
#42108=VERTEX_POINT('',#247858);
#42109=VERTEX_POINT('',#247862);
#42110=VERTEX_POINT('',#247863);
#42111=VERTEX_POINT('',#247903);
#42112=VERTEX_POINT('',#247973);
#42113=VERTEX_POINT('',#247974);
#42114=VERTEX_POINT('',#247976);
#42115=VERTEX_POINT('',#247978);
#42116=VERTEX_POINT('',#247997);
#42117=VERTEX_POINT('',#247998);
#42118=VERTEX_POINT('',#248000);
#42119=VERTEX_POINT('',#248002);
#42120=VERTEX_POINT('',#248021);
#42121=VERTEX_POINT('',#248022);
#42122=VERTEX_POINT('',#248024);
#42123=VERTEX_POINT('',#248026);
#42124=VERTEX_POINT('',#248056);
#42125=VERTEX_POINT('',#248058);
#42126=VERTEX_POINT('',#248074);
#42127=VERTEX_POINT('',#248075);
#42128=VERTEX_POINT('',#248077);
#42129=VERTEX_POINT('',#248079);
#42130=VERTEX_POINT('',#248088);
#42131=VERTEX_POINT('',#248089);
#42132=VERTEX_POINT('',#248091);
#42133=VERTEX_POINT('',#248093);
#42134=VERTEX_POINT('',#248125);
#42135=VERTEX_POINT('',#248127);
#42136=VERTEX_POINT('',#248166);
#42137=VERTEX_POINT('',#248168);
#42138=VERTEX_POINT('',#248204);
#42139=VERTEX_POINT('',#248206);
#42140=VERTEX_POINT('',#248222);
#42141=VERTEX_POINT('',#248223);
#42142=VERTEX_POINT('',#248225);
#42143=VERTEX_POINT('',#248227);
#42144=VERTEX_POINT('',#248236);
#42145=VERTEX_POINT('',#248237);
#42146=VERTEX_POINT('',#248239);
#42147=VERTEX_POINT('',#248241);
#42148=VERTEX_POINT('',#248254);
#42149=VERTEX_POINT('',#248275);
#42150=VERTEX_POINT('',#248277);
#42151=VERTEX_POINT('',#248316);
#42152=VERTEX_POINT('',#248318);
#42153=VERTEX_POINT('',#248354);
#42154=VERTEX_POINT('',#248356);
#42155=VERTEX_POINT('',#248496);
#42156=VERTEX_POINT('',#248497);
#42157=VERTEX_POINT('',#248499);
#42158=VERTEX_POINT('',#248519);
#42159=VERTEX_POINT('',#248523);
#42160=VERTEX_POINT('',#248524);
#42161=VERTEX_POINT('',#248526);
#42162=VERTEX_POINT('',#248546);
#42163=VERTEX_POINT('',#248550);
#42164=VERTEX_POINT('',#248551);
#42165=VERTEX_POINT('',#248553);
#42166=VERTEX_POINT('',#248573);
#42167=VERTEX_POINT('',#248577);
#42168=VERTEX_POINT('',#248578);
#42169=VERTEX_POINT('',#248580);
#42170=VERTEX_POINT('',#248600);
#42171=VERTEX_POINT('',#248618);
#42172=VERTEX_POINT('',#248620);
#42173=VERTEX_POINT('',#248636);
#42174=VERTEX_POINT('',#248637);
#42175=VERTEX_POINT('',#248639);
#42176=VERTEX_POINT('',#248662);
#42177=VERTEX_POINT('',#248666);
#42178=VERTEX_POINT('',#248667);
#42179=VERTEX_POINT('',#248669);
#42180=VERTEX_POINT('',#248692);
#42181=VERTEX_POINT('',#248719);
#42182=VERTEX_POINT('',#248721);
#42183=VERTEX_POINT('',#248760);
#42184=VERTEX_POINT('',#248762);
#42185=VERTEX_POINT('',#248798);
#42186=VERTEX_POINT('',#248800);
#42187=VERTEX_POINT('',#248830);
#42188=VERTEX_POINT('',#248832);
#42189=VERTEX_POINT('',#248848);
#42190=VERTEX_POINT('',#248849);
#42191=VERTEX_POINT('',#248851);
#42192=VERTEX_POINT('',#248874);
#42193=VERTEX_POINT('',#248878);
#42194=VERTEX_POINT('',#248879);
#42195=VERTEX_POINT('',#248881);
#42196=VERTEX_POINT('',#248904);
#42197=VERTEX_POINT('',#248931);
#42198=VERTEX_POINT('',#248933);
#42199=VERTEX_POINT('',#248972);
#42200=VERTEX_POINT('',#248974);
#42201=VERTEX_POINT('',#249010);
#42202=VERTEX_POINT('',#249012);
#42203=VERTEX_POINT('',#249164);
#42204=VERTEX_POINT('',#249546);
#42205=VERTEX_POINT('',#249547);
#42206=VERTEX_POINT('',#250188);
#42207=VERTEX_POINT('',#250220);
#42208=VERTEX_POINT('',#251062);
#42209=VERTEX_POINT('',#251063);
#42210=VERTEX_POINT('',#251065);
#42211=VERTEX_POINT('',#251464);
#42212=VERTEX_POINT('',#251465);
#42213=VERTEX_POINT('',#252013);
#42214=VERTEX_POINT('',#252015);
#42215=VERTEX_POINT('',#253783);
#42216=VERTEX_POINT('',#254405);
#42217=VERTEX_POINT('',#254406);
#42218=VERTEX_POINT('',#255306);
#42219=VERTEX_POINT('',#255716);
#42220=VERTEX_POINT('',#255717);
#42221=VERTEX_POINT('',#255958);
#42222=VERTEX_POINT('',#255960);
#42223=VERTEX_POINT('',#256077);
#42224=VERTEX_POINT('',#256079);
#42225=VERTEX_POINT('',#257914);
#42226=VERTEX_POINT('',#258538);
#42227=VERTEX_POINT('',#258559);
#42228=VERTEX_POINT('',#258689);
#42229=VERTEX_POINT('',#258720);
#42230=VERTEX_POINT('',#259886);
#42231=VERTEX_POINT('',#259887);
#42232=VERTEX_POINT('',#260124);
#42233=VERTEX_POINT('',#260126);
#42234=VERTEX_POINT('',#260241);
#42235=VERTEX_POINT('',#262002);
#42236=VERTEX_POINT('',#262606);
#42237=VERTEX_POINT('',#262615);
#42238=VERTEX_POINT('',#263457);
#42239=VERTEX_POINT('',#263458);
#42240=VERTEX_POINT('',#263851);
#42241=VERTEX_POINT('',#263852);
#42242=VERTEX_POINT('',#264374);
#42243=VERTEX_POINT('',#264376);
#42244=VERTEX_POINT('',#271076);
#42245=VERTEX_POINT('',#271197);
#42246=VERTEX_POINT('',#271198);
#42247=VERTEX_POINT('',#271200);
#42248=VERTEX_POINT('',#271202);
#42249=VERTEX_POINT('',#271206);
#42250=VERTEX_POINT('',#271208);
#42251=VERTEX_POINT('',#271212);
#42252=VERTEX_POINT('',#271214);
#42253=VERTEX_POINT('',#271225);
#42254=VERTEX_POINT('',#271227);
#42255=VERTEX_POINT('',#271231);
#42256=VERTEX_POINT('',#271235);
#42257=VERTEX_POINT('',#271236);
#42258=VERTEX_POINT('',#271245);
#42259=VERTEX_POINT('',#271247);
#42260=VERTEX_POINT('',#271256);
#42261=VERTEX_POINT('',#271257);
#42262=VERTEX_POINT('',#271264);
#42263=VERTEX_POINT('',#271266);
#42264=VERTEX_POINT('',#271271);
#42265=VERTEX_POINT('',#271273);
#42266=VERTEX_POINT('',#271280);
#42267=VERTEX_POINT('',#271282);
#42268=VERTEX_POINT('',#271291);
#42269=VERTEX_POINT('',#271292);
#42270=VERTEX_POINT('',#271294);
#42271=VERTEX_POINT('',#271301);
#42272=VERTEX_POINT('',#271303);
#42273=VERTEX_POINT('',#271308);
#42274=VERTEX_POINT('',#271310);
#42275=VERTEX_POINT('',#271317);
#42276=VERTEX_POINT('',#271326);
#42277=VERTEX_POINT('',#271327);
#42278=VERTEX_POINT('',#271329);
#42279=VERTEX_POINT('',#271336);
#42280=VERTEX_POINT('',#271338);
#42281=VERTEX_POINT('',#271343);
#42282=VERTEX_POINT('',#271345);
#42283=VERTEX_POINT('',#271352);
#42284=VERTEX_POINT('',#271361);
#42285=VERTEX_POINT('',#271362);
#42286=VERTEX_POINT('',#271369);
#42287=VERTEX_POINT('',#271371);
#42288=VERTEX_POINT('',#271378);
#42289=VERTEX_POINT('',#271380);
#42290=VERTEX_POINT('',#271385);
#42291=VERTEX_POINT('',#271387);
#42292=VERTEX_POINT('',#271396);
#42293=VERTEX_POINT('',#271397);
#42294=VERTEX_POINT('',#271399);
#42295=VERTEX_POINT('',#271406);
#42296=VERTEX_POINT('',#271408);
#42297=VERTEX_POINT('',#271413);
#42298=VERTEX_POINT('',#271415);
#42299=VERTEX_POINT('',#271422);
#42300=VERTEX_POINT('',#271431);
#42301=VERTEX_POINT('',#271432);
#42302=VERTEX_POINT('',#271434);
#42303=VERTEX_POINT('',#271441);
#42304=VERTEX_POINT('',#271443);
#42305=VERTEX_POINT('',#271448);
#42306=VERTEX_POINT('',#271450);
#42307=VERTEX_POINT('',#271457);
#42308=VERTEX_POINT('',#271466);
#42309=VERTEX_POINT('',#271467);
#42310=VERTEX_POINT('',#271474);
#42311=VERTEX_POINT('',#271476);
#42312=VERTEX_POINT('',#271487);
#42313=VERTEX_POINT('',#271488);
#42314=VERTEX_POINT('',#271490);
#42315=VERTEX_POINT('',#271492);
#42316=VERTEX_POINT('',#271496);
#42317=VERTEX_POINT('',#271497);
#42318=VERTEX_POINT('',#271499);
#42319=VERTEX_POINT('',#271501);
#42320=VERTEX_POINT('',#271503);
#42321=VERTEX_POINT('',#271505);
#42322=VERTEX_POINT('',#271507);
#42323=VERTEX_POINT('',#271509);
#42324=VERTEX_POINT('',#271511);
#42325=VERTEX_POINT('',#271513);
#42326=VERTEX_POINT('',#271521);
#42327=VERTEX_POINT('',#271523);
#42328=VERTEX_POINT('',#271525);
#42329=VERTEX_POINT('',#271527);
#42330=VERTEX_POINT('',#271529);
#42331=VERTEX_POINT('',#271531);
#42332=VERTEX_POINT('',#271533);
#42333=VERTEX_POINT('',#271535);
#42334=VERTEX_POINT('',#271538);
#42335=VERTEX_POINT('',#271540);
#42336=VERTEX_POINT('',#271544);
#42337=VERTEX_POINT('',#271546);
#42338=VERTEX_POINT('',#271550);
#42339=VERTEX_POINT('',#271551);
#42340=VERTEX_POINT('',#271560);
#42341=VERTEX_POINT('',#271562);
#42342=VERTEX_POINT('',#271582);
#42343=VERTEX_POINT('',#271589);
#42344=VERTEX_POINT('',#271596);
#42345=VERTEX_POINT('',#271605);
#42346=VERTEX_POINT('',#271614);
#42347=VERTEX_POINT('',#271621);
#42348=VERTEX_POINT('',#271628);
#42349=VERTEX_POINT('',#271637);
#42350=VERTEX_POINT('',#271646);
#42351=VERTEX_POINT('',#271653);
#42352=VERTEX_POINT('',#271660);
#42353=VERTEX_POINT('',#271669);
#42354=VERTEX_POINT('',#271678);
#42355=VERTEX_POINT('',#271680);
#42356=VERTEX_POINT('',#271700);
#42357=VERTEX_POINT('',#271707);
#42358=VERTEX_POINT('',#271714);
#42359=VERTEX_POINT('',#271723);
#42360=VERTEX_POINT('',#271732);
#42361=VERTEX_POINT('',#271733);
#42362=VERTEX_POINT('',#271742);
#42363=VERTEX_POINT('',#271744);
#42364=VERTEX_POINT('',#271764);
#42365=VERTEX_POINT('',#271773);
#42366=VERTEX_POINT('',#271782);
#42367=VERTEX_POINT('',#271789);
#42368=VERTEX_POINT('',#271798);
#42369=VERTEX_POINT('',#271807);
#42370=VERTEX_POINT('',#271816);
#42371=VERTEX_POINT('',#271825);
#42372=VERTEX_POINT('',#271834);
#42373=VERTEX_POINT('',#271843);
#42374=VERTEX_POINT('',#271852);
#42375=VERTEX_POINT('',#271861);
#42376=VERTEX_POINT('',#271870);
#42377=VERTEX_POINT('',#271872);
#42378=VERTEX_POINT('',#271886);
#42379=VERTEX_POINT('',#271895);
#42380=VERTEX_POINT('',#271904);
#42381=VERTEX_POINT('',#271906);
#42382=VERTEX_POINT('',#271910);
#42383=VERTEX_POINT('',#271912);
#42384=VERTEX_POINT('',#271916);
#42385=VERTEX_POINT('',#271918);
#42386=VERTEX_POINT('',#271922);
#42387=VERTEX_POINT('',#271924);
#42388=VERTEX_POINT('',#271928);
#42389=VERTEX_POINT('',#271932);
#42390=VERTEX_POINT('',#271934);
#42391=VERTEX_POINT('',#271938);
#42392=VERTEX_POINT('',#271940);
#42393=VERTEX_POINT('',#271944);
#42394=VERTEX_POINT('',#271946);
#42395=VERTEX_POINT('',#271950);
#42396=VERTEX_POINT('',#271952);
#42397=VERTEX_POINT('',#271956);
#42398=VERTEX_POINT('',#271958);
#42399=VERTEX_POINT('',#271962);
#42400=VERTEX_POINT('',#271964);
#42401=VERTEX_POINT('',#271968);
#42402=VERTEX_POINT('',#271970);
#42403=VERTEX_POINT('',#271974);
#42404=VERTEX_POINT('',#271976);
#42405=VERTEX_POINT('',#271980);
#42406=VERTEX_POINT('',#271982);
#42407=VERTEX_POINT('',#271986);
#42408=VERTEX_POINT('',#271993);
#42409=VERTEX_POINT('',#272000);
#42410=VERTEX_POINT('',#272002);
#42411=VERTEX_POINT('',#272016);
#42412=VERTEX_POINT('',#272017);
#42413=VERTEX_POINT('',#272030);
#42414=VERTEX_POINT('',#272037);
#42415=VERTEX_POINT('',#272046);
#42416=VERTEX_POINT('',#272047);
#42417=VERTEX_POINT('',#272060);
#42418=VERTEX_POINT('',#272067);
#42419=VERTEX_POINT('',#272076);
#42420=VERTEX_POINT('',#272077);
#42421=VERTEX_POINT('',#272090);
#42422=VERTEX_POINT('',#272097);
#42423=VERTEX_POINT('',#272106);
#42424=VERTEX_POINT('',#272113);
#42425=VERTEX_POINT('',#272115);
#42426=VERTEX_POINT('',#272129);
#42427=VERTEX_POINT('',#272130);
#42428=VERTEX_POINT('',#272143);
#42429=VERTEX_POINT('',#272150);
#42430=VERTEX_POINT('',#272159);
#42431=VERTEX_POINT('',#272166);
#42432=VERTEX_POINT('',#272173);
#42433=VERTEX_POINT('',#272175);
#42434=VERTEX_POINT('',#272213);
#42435=VERTEX_POINT('',#272220);
#42436=VERTEX_POINT('',#272283);
#42437=VERTEX_POINT('',#272285);
#42438=VERTEX_POINT('',#272321);
#42439=VERTEX_POINT('',#272328);
#42440=VERTEX_POINT('',#272339);
#42441=VERTEX_POINT('',#272343);
#42442=VERTEX_POINT('',#272348);
#42443=VERTEX_POINT('',#272355);
#42444=VERTEX_POINT('',#272432);
#42445=VERTEX_POINT('',#272434);
#42446=VERTEX_POINT('',#272438);
#42447=VERTEX_POINT('',#272439);
#42448=VERTEX_POINT('',#272441);
#42449=VERTEX_POINT('',#272443);
#42450=VERTEX_POINT('',#272447);
#42451=VERTEX_POINT('',#272449);
#42452=VERTEX_POINT('',#272453);
#42453=VERTEX_POINT('',#272455);
#42454=VERTEX_POINT('',#272465);
#42455=VERTEX_POINT('',#272467);
#42456=VERTEX_POINT('',#272471);
#42457=VERTEX_POINT('',#272475);
#42458=VERTEX_POINT('',#272476);
#42459=VERTEX_POINT('',#272483);
#42460=VERTEX_POINT('',#272485);
#42461=VERTEX_POINT('',#272496);
#42462=VERTEX_POINT('',#272497);
#42463=VERTEX_POINT('',#272506);
#42464=VERTEX_POINT('',#272508);
#42465=VERTEX_POINT('',#272517);
#42466=VERTEX_POINT('',#272518);
#42467=VERTEX_POINT('',#272520);
#42468=VERTEX_POINT('',#272531);
#42469=VERTEX_POINT('',#272533);
#42470=VERTEX_POINT('',#272538);
#42471=VERTEX_POINT('',#272540);
#42472=VERTEX_POINT('',#272551);
#42473=VERTEX_POINT('',#272560);
#42474=VERTEX_POINT('',#272561);
#42475=VERTEX_POINT('',#272563);
#42476=VERTEX_POINT('',#272574);
#42477=VERTEX_POINT('',#272576);
#42478=VERTEX_POINT('',#272581);
#42479=VERTEX_POINT('',#272583);
#42480=VERTEX_POINT('',#272594);
#42481=VERTEX_POINT('',#272603);
#42482=VERTEX_POINT('',#272604);
#42483=VERTEX_POINT('',#272606);
#42484=VERTEX_POINT('',#272617);
#42485=VERTEX_POINT('',#272619);
#42486=VERTEX_POINT('',#272624);
#42487=VERTEX_POINT('',#272626);
#42488=VERTEX_POINT('',#272637);
#42489=VERTEX_POINT('',#272646);
#42490=VERTEX_POINT('',#272647);
#42491=VERTEX_POINT('',#272649);
#42492=VERTEX_POINT('',#272660);
#42493=VERTEX_POINT('',#272662);
#42494=VERTEX_POINT('',#272667);
#42495=VERTEX_POINT('',#272669);
#42496=VERTEX_POINT('',#272680);
#42497=VERTEX_POINT('',#272689);
#42498=VERTEX_POINT('',#272690);
#42499=VERTEX_POINT('',#272697);
#42500=VERTEX_POINT('',#272699);
#42501=VERTEX_POINT('',#272704);
#42502=VERTEX_POINT('',#272706);
#42503=VERTEX_POINT('',#272717);
#42504=VERTEX_POINT('',#272719);
#42505=VERTEX_POINT('',#272728);
#42506=VERTEX_POINT('',#272729);
#42507=VERTEX_POINT('',#272736);
#42508=VERTEX_POINT('',#272738);
#42509=VERTEX_POINT('',#272743);
#42510=VERTEX_POINT('',#272745);
#42511=VERTEX_POINT('',#272756);
#42512=VERTEX_POINT('',#272758);
#42513=VERTEX_POINT('',#272767);
#42514=VERTEX_POINT('',#272768);
#42515=VERTEX_POINT('',#272775);
#42516=VERTEX_POINT('',#272777);
#42517=VERTEX_POINT('',#272788);
#42518=VERTEX_POINT('',#272790);
#42519=VERTEX_POINT('',#272795);
#42520=VERTEX_POINT('',#272797);
#42521=VERTEX_POINT('',#272806);
#42522=VERTEX_POINT('',#272807);
#42523=VERTEX_POINT('',#272809);
#42524=VERTEX_POINT('',#272820);
#42525=VERTEX_POINT('',#272822);
#42526=VERTEX_POINT('',#272827);
#42527=VERTEX_POINT('',#272829);
#42528=VERTEX_POINT('',#272840);
#42529=VERTEX_POINT('',#272849);
#42530=VERTEX_POINT('',#272850);
#42531=VERTEX_POINT('',#272857);
#42532=VERTEX_POINT('',#272859);
#42533=VERTEX_POINT('',#272870);
#42534=VERTEX_POINT('',#272872);
#42535=VERTEX_POINT('',#272877);
#42536=VERTEX_POINT('',#272879);
#42537=VERTEX_POINT('',#272888);
#42538=VERTEX_POINT('',#272889);
#42539=VERTEX_POINT('',#272891);
#42540=VERTEX_POINT('',#272902);
#42541=VERTEX_POINT('',#272904);
#42542=VERTEX_POINT('',#272909);
#42543=VERTEX_POINT('',#272911);
#42544=VERTEX_POINT('',#272922);
#42545=VERTEX_POINT('',#272931);
#42546=VERTEX_POINT('',#272932);
#42547=VERTEX_POINT('',#272934);
#42548=VERTEX_POINT('',#272945);
#42549=VERTEX_POINT('',#272947);
#42550=VERTEX_POINT('',#272952);
#42551=VERTEX_POINT('',#272954);
#42552=VERTEX_POINT('',#272965);
#42553=VERTEX_POINT('',#272974);
#42554=VERTEX_POINT('',#272975);
#42555=VERTEX_POINT('',#272977);
#42556=VERTEX_POINT('',#272988);
#42557=VERTEX_POINT('',#272990);
#42558=VERTEX_POINT('',#272995);
#42559=VERTEX_POINT('',#272997);
#42560=VERTEX_POINT('',#273008);
#42561=VERTEX_POINT('',#273017);
#42562=VERTEX_POINT('',#273018);
#42563=VERTEX_POINT('',#273020);
#42564=VERTEX_POINT('',#273027);
#42565=VERTEX_POINT('',#273038);
#42566=VERTEX_POINT('',#273040);
#42567=VERTEX_POINT('',#273054);
#42568=VERTEX_POINT('',#273055);
#42569=VERTEX_POINT('',#273060);
#42570=VERTEX_POINT('',#273061);
#42571=VERTEX_POINT('',#273063);
#42572=VERTEX_POINT('',#273078);
#42573=VERTEX_POINT('',#273096);
#42574=VERTEX_POINT('',#273097);
#42575=VERTEX_POINT('',#273099);
#42576=VERTEX_POINT('',#273101);
#42577=VERTEX_POINT('',#273105);
#42578=VERTEX_POINT('',#273107);
#42579=VERTEX_POINT('',#273109);
#42580=VERTEX_POINT('',#273111);
#42581=VERTEX_POINT('',#273113);
#42582=VERTEX_POINT('',#273115);
#42583=VERTEX_POINT('',#273117);
#42584=VERTEX_POINT('',#273119);
#42585=VERTEX_POINT('',#273121);
#42586=VERTEX_POINT('',#273123);
#42587=VERTEX_POINT('',#273125);
#42588=VERTEX_POINT('',#273127);
#42589=VERTEX_POINT('',#273129);
#42590=VERTEX_POINT('',#273131);
#42591=VERTEX_POINT('',#273133);
#42592=VERTEX_POINT('',#273135);
#42593=VERTEX_POINT('',#273137);
#42594=VERTEX_POINT('',#273151);
#42595=VERTEX_POINT('',#273153);
#42596=VERTEX_POINT('',#273155);
#42597=VERTEX_POINT('',#273157);
#42598=VERTEX_POINT('',#273159);
#42599=VERTEX_POINT('',#273161);
#42600=VERTEX_POINT('',#273163);
#42601=VERTEX_POINT('',#273165);
#42602=VERTEX_POINT('',#273167);
#42603=VERTEX_POINT('',#273169);
#42604=VERTEX_POINT('',#273171);
#42605=VERTEX_POINT('',#273173);
#42606=VERTEX_POINT('',#273175);
#42607=VERTEX_POINT('',#273177);
#42608=VERTEX_POINT('',#273179);
#42609=VERTEX_POINT('',#273181);
#42610=VERTEX_POINT('',#273183);
#42611=VERTEX_POINT('',#273186);
#42612=VERTEX_POINT('',#273188);
#42613=VERTEX_POINT('',#273192);
#42614=VERTEX_POINT('',#273194);
#42615=VERTEX_POINT('',#273198);
#42616=VERTEX_POINT('',#273199);
#42617=VERTEX_POINT('',#273208);
#42618=VERTEX_POINT('',#273210);
#42619=VERTEX_POINT('',#273234);
#42620=VERTEX_POINT('',#273245);
#42621=VERTEX_POINT('',#273252);
#42622=VERTEX_POINT('',#273261);
#42623=VERTEX_POINT('',#273270);
#42624=VERTEX_POINT('',#273281);
#42625=VERTEX_POINT('',#273288);
#42626=VERTEX_POINT('',#273297);
#42627=VERTEX_POINT('',#273306);
#42628=VERTEX_POINT('',#273317);
#42629=VERTEX_POINT('',#273324);
#42630=VERTEX_POINT('',#273333);
#42631=VERTEX_POINT('',#273342);
#42632=VERTEX_POINT('',#273343);
#42633=VERTEX_POINT('',#273352);
#42634=VERTEX_POINT('',#273354);
#42635=VERTEX_POINT('',#273388);
#42636=VERTEX_POINT('',#273395);
#42637=VERTEX_POINT('',#273406);
#42638=VERTEX_POINT('',#273417);
#42639=VERTEX_POINT('',#273424);
#42640=VERTEX_POINT('',#273433);
#42641=VERTEX_POINT('',#273442);
#42642=VERTEX_POINT('',#273443);
#42643=VERTEX_POINT('',#273452);
#42644=VERTEX_POINT('',#273454);
#42645=VERTEX_POINT('',#273478);
#42646=VERTEX_POINT('',#273489);
#42647=VERTEX_POINT('',#273496);
#42648=VERTEX_POINT('',#273505);
#42649=VERTEX_POINT('',#273514);
#42650=VERTEX_POINT('',#273531);
#42651=VERTEX_POINT('',#273540);
#42652=VERTEX_POINT('',#273541);
#42653=VERTEX_POINT('',#273550);
#42654=VERTEX_POINT('',#273552);
#42655=VERTEX_POINT('',#273576);
#42656=VERTEX_POINT('',#273587);
#42657=VERTEX_POINT('',#273594);
#42658=VERTEX_POINT('',#273603);
#42659=VERTEX_POINT('',#273612);
#42660=VERTEX_POINT('',#273613);
#42661=VERTEX_POINT('',#273622);
#42662=VERTEX_POINT('',#273624);
#42663=VERTEX_POINT('',#273648);
#42664=VERTEX_POINT('',#273659);
#42665=VERTEX_POINT('',#273666);
#42666=VERTEX_POINT('',#273675);
#42667=VERTEX_POINT('',#273684);
#42668=VERTEX_POINT('',#273693);
#42669=VERTEX_POINT('',#273702);
#42670=VERTEX_POINT('',#273711);
#42671=VERTEX_POINT('',#273720);
#42672=VERTEX_POINT('',#273729);
#42673=VERTEX_POINT('',#273738);
#42674=VERTEX_POINT('',#273747);
#42675=VERTEX_POINT('',#273756);
#42676=VERTEX_POINT('',#273765);
#42677=VERTEX_POINT('',#273774);
#42678=VERTEX_POINT('',#273783);
#42679=VERTEX_POINT('',#273792);
#42680=VERTEX_POINT('',#273799);
#42681=VERTEX_POINT('',#273808);
#42682=VERTEX_POINT('',#273817);
#42683=VERTEX_POINT('',#273826);
#42684=VERTEX_POINT('',#273835);
#42685=VERTEX_POINT('',#273844);
#42686=VERTEX_POINT('',#273853);
#42687=VERTEX_POINT('',#273862);
#42688=VERTEX_POINT('',#273871);
#42689=VERTEX_POINT('',#273880);
#42690=VERTEX_POINT('',#273882);
#42691=VERTEX_POINT('',#273900);
#42692=VERTEX_POINT('',#273901);
#42693=VERTEX_POINT('',#273910);
#42694=VERTEX_POINT('',#273912);
#42695=VERTEX_POINT('',#273936);
#42696=VERTEX_POINT('',#273945);
#42697=VERTEX_POINT('',#273954);
#42698=VERTEX_POINT('',#273963);
#42699=VERTEX_POINT('',#273972);
#42700=VERTEX_POINT('',#273974);
#42701=VERTEX_POINT('',#273978);
#42702=VERTEX_POINT('',#273980);
#42703=VERTEX_POINT('',#273984);
#42704=VERTEX_POINT('',#273986);
#42705=VERTEX_POINT('',#273990);
#42706=VERTEX_POINT('',#273992);
#42707=VERTEX_POINT('',#273996);
#42708=VERTEX_POINT('',#273998);
#42709=VERTEX_POINT('',#274002);
#42710=VERTEX_POINT('',#274006);
#42711=VERTEX_POINT('',#274008);
#42712=VERTEX_POINT('',#274012);
#42713=VERTEX_POINT('',#274014);
#42714=VERTEX_POINT('',#274018);
#42715=VERTEX_POINT('',#274020);
#42716=VERTEX_POINT('',#274024);
#42717=VERTEX_POINT('',#274028);
#42718=VERTEX_POINT('',#274030);
#42719=VERTEX_POINT('',#274034);
#42720=VERTEX_POINT('',#274036);
#42721=VERTEX_POINT('',#274040);
#42722=VERTEX_POINT('',#274042);
#42723=VERTEX_POINT('',#274046);
#42724=VERTEX_POINT('',#274048);
#42725=VERTEX_POINT('',#274052);
#42726=VERTEX_POINT('',#274054);
#42727=VERTEX_POINT('',#274058);
#42728=VERTEX_POINT('',#274060);
#42729=VERTEX_POINT('',#274064);
#42730=VERTEX_POINT('',#274066);
#42731=VERTEX_POINT('',#274070);
#42732=VERTEX_POINT('',#274072);
#42733=VERTEX_POINT('',#274076);
#42734=VERTEX_POINT('',#274078);
#42735=VERTEX_POINT('',#274082);
#42736=VERTEX_POINT('',#274084);
#42737=VERTEX_POINT('',#274088);
#42738=VERTEX_POINT('',#274090);
#42739=VERTEX_POINT('',#274094);
#42740=VERTEX_POINT('',#274096);
#42741=VERTEX_POINT('',#274100);
#42742=VERTEX_POINT('',#274102);
#42743=VERTEX_POINT('',#274106);
#42744=VERTEX_POINT('',#274108);
#42745=VERTEX_POINT('',#274112);
#42746=VERTEX_POINT('',#274114);
#42747=VERTEX_POINT('',#274118);
#42748=VERTEX_POINT('',#274120);
#42749=VERTEX_POINT('',#274124);
#42750=VERTEX_POINT('',#274126);
#42751=VERTEX_POINT('',#274130);
#42752=VERTEX_POINT('',#274132);
#42753=VERTEX_POINT('',#274136);
#42754=VERTEX_POINT('',#274143);
#42755=VERTEX_POINT('',#274154);
#42756=VERTEX_POINT('',#274156);
#42757=VERTEX_POINT('',#274170);
#42758=VERTEX_POINT('',#274171);
#42759=VERTEX_POINT('',#274184);
#42760=VERTEX_POINT('',#274191);
#42761=VERTEX_POINT('',#274204);
#42762=VERTEX_POINT('',#274205);
#42763=VERTEX_POINT('',#274218);
#42764=VERTEX_POINT('',#274225);
#42765=VERTEX_POINT('',#274238);
#42766=VERTEX_POINT('',#274239);
#42767=VERTEX_POINT('',#274252);
#42768=VERTEX_POINT('',#274259);
#42769=VERTEX_POINT('',#274272);
#42770=VERTEX_POINT('',#274279);
#42771=VERTEX_POINT('',#274290);
#42772=VERTEX_POINT('',#274292);
#42773=VERTEX_POINT('',#274306);
#42774=VERTEX_POINT('',#274311);
#42775=VERTEX_POINT('',#274318);
#42776=VERTEX_POINT('',#274331);
#42777=VERTEX_POINT('',#274332);
#42778=VERTEX_POINT('',#274345);
#42779=VERTEX_POINT('',#274352);
#42780=VERTEX_POINT('',#274365);
#42781=VERTEX_POINT('',#274372);
#42782=VERTEX_POINT('',#274383);
#42783=VERTEX_POINT('',#274385);
#42784=VERTEX_POINT('',#274399);
#42785=VERTEX_POINT('',#274400);
#42786=VERTEX_POINT('',#274413);
#42787=VERTEX_POINT('',#274420);
#42788=VERTEX_POINT('',#274433);
#42789=VERTEX_POINT('',#274434);
#42790=VERTEX_POINT('',#274447);
#42791=VERTEX_POINT('',#274460);
#42792=VERTEX_POINT('',#274467);
#42793=VERTEX_POINT('',#274478);
#42794=VERTEX_POINT('',#274480);
#42795=VERTEX_POINT('',#274494);
#42796=VERTEX_POINT('',#274495);
#42797=VERTEX_POINT('',#274508);
#42798=VERTEX_POINT('',#274515);
#42799=VERTEX_POINT('',#274528);
#42800=VERTEX_POINT('',#274535);
#42801=VERTEX_POINT('',#274546);
#42802=VERTEX_POINT('',#274548);
#42803=VERTEX_POINT('',#274562);
#42804=VERTEX_POINT('',#274563);
#42805=VERTEX_POINT('',#274576);
#42806=VERTEX_POINT('',#274583);
#42807=VERTEX_POINT('',#274700);
#42808=VERTEX_POINT('',#274707);
#42809=VERTEX_POINT('',#274774);
#42810=VERTEX_POINT('',#274776);
#42811=VERTEX_POINT('',#274790);
#42812=VERTEX_POINT('',#274797);
#42813=VERTEX_POINT('',#274808);
#42814=VERTEX_POINT('',#274810);
#42815=VERTEX_POINT('',#274856);
#42816=VERTEX_POINT('',#274867);
#42817=VERTEX_POINT('',#274874);
#42818=VERTEX_POINT('',#274883);
#42819=VERTEX_POINT('',#274892);
#42820=VERTEX_POINT('',#274894);
#42821=VERTEX_POINT('',#274898);
#42822=VERTEX_POINT('',#274899);
#42823=VERTEX_POINT('',#274912);
#42824=VERTEX_POINT('',#274919);
#42825=VERTEX_POINT('',#275067);
#42826=VERTEX_POINT('',#275069);
#42827=VERTEX_POINT('',#275073);
#42828=VERTEX_POINT('',#275074);
#42829=VERTEX_POINT('',#275076);
#42830=VERTEX_POINT('',#275078);
#42831=VERTEX_POINT('',#275082);
#42832=VERTEX_POINT('',#275084);
#42833=VERTEX_POINT('',#275088);
#42834=VERTEX_POINT('',#275090);
#42835=VERTEX_POINT('',#275094);
#42836=VERTEX_POINT('',#275096);
#42837=VERTEX_POINT('',#275105);
#42838=VERTEX_POINT('',#275107);
#42839=VERTEX_POINT('',#275111);
#42840=VERTEX_POINT('',#275113);
#42841=VERTEX_POINT('',#275117);
#42842=VERTEX_POINT('',#275118);
#42843=VERTEX_POINT('',#275120);
#42844=VERTEX_POINT('',#275122);
#42845=VERTEX_POINT('',#275126);
#42846=VERTEX_POINT('',#275128);
#42847=VERTEX_POINT('',#275132);
#42848=VERTEX_POINT('',#275134);
#42849=VERTEX_POINT('',#275143);
#42850=VERTEX_POINT('',#275145);
#42851=VERTEX_POINT('',#275151);
#42852=VERTEX_POINT('',#275153);
#42853=VERTEX_POINT('',#275298);
#42854=VERTEX_POINT('',#275300);
#42855=VERTEX_POINT('',#275304);
#42856=VERTEX_POINT('',#275306);
#42857=VERTEX_POINT('',#275310);
#42858=VERTEX_POINT('',#275312);
#42859=VERTEX_POINT('',#275316);
#42860=VERTEX_POINT('',#275318);
#42861=VERTEX_POINT('',#275327);
#42862=VERTEX_POINT('',#275329);
#42863=VERTEX_POINT('',#275333);
#42864=VERTEX_POINT('',#275335);
#42865=VERTEX_POINT('',#275339);
#42866=VERTEX_POINT('',#275341);
#42867=VERTEX_POINT('',#275345);
#42868=VERTEX_POINT('',#275349);
#42869=VERTEX_POINT('',#275353);
#42870=VERTEX_POINT('',#275355);
#42871=VERTEX_POINT('',#275363);
#42872=VERTEX_POINT('',#275367);
#42873=VERTEX_POINT('',#275373);
#42874=VERTEX_POINT('',#275374);
#42875=VERTEX_POINT('',#275376);
#42876=VERTEX_POINT('',#275378);
#42877=VERTEX_POINT('',#275381);
#42878=VERTEX_POINT('',#275383);
#42879=VERTEX_POINT('',#275387);
#42880=VERTEX_POINT('',#275391);
#42881=VERTEX_POINT('',#275397);
#42882=VERTEX_POINT('',#275398);
#42883=VERTEX_POINT('',#275401);
#42884=VERTEX_POINT('',#275402);
#42885=VERTEX_POINT('',#275405);
#42886=VERTEX_POINT('',#275406);
#42887=VERTEX_POINT('',#275409);
#42888=VERTEX_POINT('',#275410);
#42889=VERTEX_POINT('',#275413);
#42890=VERTEX_POINT('',#275414);
#42891=VERTEX_POINT('',#275417);
#42892=VERTEX_POINT('',#275418);
#42893=VERTEX_POINT('',#275421);
#42894=VERTEX_POINT('',#275422);
#42895=VERTEX_POINT('',#275425);
#42896=VERTEX_POINT('',#275426);
#42897=VERTEX_POINT('',#275429);
#42898=VERTEX_POINT('',#275430);
#42899=VERTEX_POINT('',#275433);
#42900=VERTEX_POINT('',#275434);
#42901=VERTEX_POINT('',#275437);
#42902=VERTEX_POINT('',#275438);
#42903=VERTEX_POINT('',#275441);
#42904=VERTEX_POINT('',#275442);
#42905=VERTEX_POINT('',#275445);
#42906=VERTEX_POINT('',#275446);
#42907=VERTEX_POINT('',#275449);
#42908=VERTEX_POINT('',#275450);
#42909=VERTEX_POINT('',#275453);
#42910=VERTEX_POINT('',#275454);
#42911=VERTEX_POINT('',#275457);
#42912=VERTEX_POINT('',#275458);
#42913=VERTEX_POINT('',#275461);
#42914=VERTEX_POINT('',#275462);
#42915=VERTEX_POINT('',#275465);
#42916=VERTEX_POINT('',#275466);
#42917=VERTEX_POINT('',#275469);
#42918=VERTEX_POINT('',#275470);
#42919=VERTEX_POINT('',#275473);
#42920=VERTEX_POINT('',#275474);
#42921=VERTEX_POINT('',#275477);
#42922=VERTEX_POINT('',#275478);
#42923=VERTEX_POINT('',#275481);
#42924=VERTEX_POINT('',#275482);
#42925=VERTEX_POINT('',#275485);
#42926=VERTEX_POINT('',#275486);
#42927=VERTEX_POINT('',#275489);
#42928=VERTEX_POINT('',#275490);
#42929=VERTEX_POINT('',#275494);
#42930=VERTEX_POINT('',#275496);
#42931=VERTEX_POINT('',#275500);
#42932=VERTEX_POINT('',#275502);
#42933=VERTEX_POINT('',#275506);
#42934=VERTEX_POINT('',#275508);
#42935=VERTEX_POINT('',#275512);
#42936=VERTEX_POINT('',#275514);
#42937=VERTEX_POINT('',#275518);
#42938=VERTEX_POINT('',#275519);
#42939=VERTEX_POINT('',#275521);
#42940=VERTEX_POINT('',#275523);
#42941=VERTEX_POINT('',#275527);
#42942=VERTEX_POINT('',#275529);
#42943=VERTEX_POINT('',#275533);
#42944=VERTEX_POINT('',#275535);
#42945=VERTEX_POINT('',#275539);
#42946=VERTEX_POINT('',#275541);
#42947=VERTEX_POINT('',#275545);
#42948=VERTEX_POINT('',#275547);
#42949=VERTEX_POINT('',#275561);
#42950=VERTEX_POINT('',#275562);
#42951=VERTEX_POINT('',#275564);
#42952=VERTEX_POINT('',#275570);
#42953=VERTEX_POINT('',#275571);
#42954=VERTEX_POINT('',#275573);
#42955=VERTEX_POINT('',#275616);
#42956=VERTEX_POINT('',#275617);
#42957=VERTEX_POINT('',#275662);
#42958=VERTEX_POINT('',#275663);
#42959=VERTEX_POINT('',#275708);
#42960=VERTEX_POINT('',#275709);
#42961=VERTEX_POINT('',#275711);
#42962=VERTEX_POINT('',#275721);
#42963=VERTEX_POINT('',#275735);
#42964=VERTEX_POINT('',#275746);
#42965=VERTEX_POINT('',#275747);
#42966=VERTEX_POINT('',#275764);
#42967=VERTEX_POINT('',#275765);
#42968=VERTEX_POINT('',#275767);
#42969=VERTEX_POINT('',#275778);
#42970=VERTEX_POINT('',#275779);
#42971=VERTEX_POINT('',#275781);
#42972=VERTEX_POINT('',#275856);
#42973=VERTEX_POINT('',#275857);
#42974=VERTEX_POINT('',#275932);
#42975=VERTEX_POINT('',#275933);
#42976=VERTEX_POINT('',#276008);
#42977=VERTEX_POINT('',#276009);
#42978=VERTEX_POINT('',#276084);
#42979=VERTEX_POINT('',#276085);
#42980=VERTEX_POINT('',#276087);
#42981=VERTEX_POINT('',#276108);
#42982=VERTEX_POINT('',#276220);
#42983=VERTEX_POINT('',#276272);
#42984=VERTEX_POINT('',#276277);
#42985=VERTEX_POINT('',#276319);
#42986=VERTEX_POINT('',#276320);
#42987=VERTEX_POINT('',#276322);
#42988=VERTEX_POINT('',#276324);
#42989=VERTEX_POINT('',#276326);
#42990=VERTEX_POINT('',#276328);
#42991=VERTEX_POINT('',#276332);
#42992=VERTEX_POINT('',#276336);
#42993=VERTEX_POINT('',#276338);
#42994=VERTEX_POINT('',#276342);
#42995=VERTEX_POINT('',#276346);
#42996=VERTEX_POINT('',#276355);
#42997=VERTEX_POINT('',#276359);
#42998=VERTEX_POINT('',#276363);
#42999=VERTEX_POINT('',#276372);
#43000=VERTEX_POINT('',#276376);
#43001=VERTEX_POINT('',#276380);
#43002=VERTEX_POINT('',#276389);
#43003=VERTEX_POINT('',#276393);
#43004=VERTEX_POINT('',#276397);
#43005=VERTEX_POINT('',#276406);
#43006=VERTEX_POINT('',#276410);
#43007=VERTEX_POINT('',#276414);
#43008=VERTEX_POINT('',#276423);
#43009=VERTEX_POINT('',#280644);
#43010=VERTEX_POINT('',#280645);
#43011=VERTEX_POINT('',#280647);
#43012=VERTEX_POINT('',#280657);
#43013=VERTEX_POINT('',#280673);
#43014=VERTEX_POINT('',#280674);
#43015=VERTEX_POINT('',#280719);
#43016=VERTEX_POINT('',#280720);
#43017=VERTEX_POINT('',#280765);
#43018=VERTEX_POINT('',#280766);
#43019=VERTEX_POINT('',#280811);
#43020=VERTEX_POINT('',#280812);
#43021=VERTEX_POINT('',#280857);
#43022=VERTEX_POINT('',#280858);
#43023=VERTEX_POINT('',#280860);
#43024=VERTEX_POINT('',#280868);
#43025=VERTEX_POINT('',#280869);
#43026=VERTEX_POINT('',#280871);
#43027=VERTEX_POINT('',#280882);
#43028=VERTEX_POINT('',#280883);
#43029=VERTEX_POINT('',#280958);
#43030=VERTEX_POINT('',#280959);
#43031=VERTEX_POINT('',#281034);
#43032=VERTEX_POINT('',#281035);
#43033=VERTEX_POINT('',#281110);
#43034=VERTEX_POINT('',#281111);
#43035=VERTEX_POINT('',#281186);
#43036=VERTEX_POINT('',#281187);
#43037=VERTEX_POINT('',#281264);
#43038=VERTEX_POINT('',#281265);
#43039=VERTEX_POINT('',#281267);
#43040=VERTEX_POINT('',#281272);
#43041=VERTEX_POINT('',#281358);
#43042=VERTEX_POINT('',#281361);
#43043=VERTEX_POINT('',#281363);
#43044=VERTEX_POINT('',#281364);
#43045=VERTEX_POINT('',#281366);
#43046=VERTEX_POINT('',#281368);
#43047=VERTEX_POINT('',#281370);
#43048=VERTEX_POINT('',#281372);
#43049=VERTEX_POINT('',#281376);
#43050=VERTEX_POINT('',#281377);
#43051=VERTEX_POINT('',#281381);
#43052=VERTEX_POINT('',#281385);
#43053=VERTEX_POINT('',#281389);
#43054=VERTEX_POINT('',#281393);
#43055=VERTEX_POINT('',#281396);
#43056=VERTEX_POINT('',#281400);
#43057=VERTEX_POINT('',#281408);
#43058=VERTEX_POINT('',#281421);
#43059=VERTEX_POINT('',#285707);
#43060=VERTEX_POINT('',#285708);
#43061=VERTEX_POINT('',#285710);
#43062=VERTEX_POINT('',#285724);
#43063=VERTEX_POINT('',#285738);
#43064=VERTEX_POINT('',#285739);
#43065=VERTEX_POINT('',#285764);
#43066=VERTEX_POINT('',#285787);
#43067=VERTEX_POINT('',#285802);
#43068=VERTEX_POINT('',#285803);
#43069=VERTEX_POINT('',#287902);
#43070=VERTEX_POINT('',#290006);
#43071=VERTEX_POINT('',#290040);
#43072=VERTEX_POINT('',#290041);
#43073=VERTEX_POINT('',#290043);
#43074=VERTEX_POINT('',#290051);
#43075=VERTEX_POINT('',#290052);
#43076=VERTEX_POINT('',#290097);
#43077=VERTEX_POINT('',#290098);
#43078=VERTEX_POINT('',#290143);
#43079=VERTEX_POINT('',#290144);
#43080=VERTEX_POINT('',#290189);
#43081=VERTEX_POINT('',#290190);
#43082=VERTEX_POINT('',#290235);
#43083=VERTEX_POINT('',#290236);
#43084=VERTEX_POINT('',#290281);
#43085=VERTEX_POINT('',#290282);
#43086=VERTEX_POINT('',#290327);
#43087=VERTEX_POINT('',#290328);
#43088=VERTEX_POINT('',#290373);
#43089=VERTEX_POINT('',#290374);
#43090=VERTEX_POINT('',#290419);
#43091=VERTEX_POINT('',#290420);
#43092=VERTEX_POINT('',#290465);
#43093=VERTEX_POINT('',#290466);
#43094=VERTEX_POINT('',#290511);
#43095=VERTEX_POINT('',#290512);
#43096=VERTEX_POINT('',#290557);
#43097=VERTEX_POINT('',#290558);
#43098=VERTEX_POINT('',#290603);
#43099=VERTEX_POINT('',#290604);
#43100=VERTEX_POINT('',#290649);
#43101=VERTEX_POINT('',#290650);
#43102=VERTEX_POINT('',#290695);
#43103=VERTEX_POINT('',#290696);
#43104=VERTEX_POINT('',#290741);
#43105=VERTEX_POINT('',#290742);
#43106=VERTEX_POINT('',#290787);
#43107=VERTEX_POINT('',#290788);
#43108=VERTEX_POINT('',#290833);
#43109=VERTEX_POINT('',#290834);
#43110=VERTEX_POINT('',#290879);
#43111=VERTEX_POINT('',#290880);
#43112=VERTEX_POINT('',#290925);
#43113=VERTEX_POINT('',#290926);
#43114=VERTEX_POINT('',#290928);
#43115=VERTEX_POINT('',#290942);
#43116=VERTEX_POINT('',#290956);
#43117=VERTEX_POINT('',#290957);
#43118=VERTEX_POINT('',#291002);
#43119=VERTEX_POINT('',#291003);
#43120=VERTEX_POINT('',#291048);
#43121=VERTEX_POINT('',#291049);
#43122=VERTEX_POINT('',#291094);
#43123=VERTEX_POINT('',#291095);
#43124=VERTEX_POINT('',#291140);
#43125=VERTEX_POINT('',#291141);
#43126=VERTEX_POINT('',#291186);
#43127=VERTEX_POINT('',#291187);
#43128=VERTEX_POINT('',#291232);
#43129=VERTEX_POINT('',#291233);
#43130=VERTEX_POINT('',#291278);
#43131=VERTEX_POINT('',#291279);
#43132=VERTEX_POINT('',#291324);
#43133=VERTEX_POINT('',#291325);
#43134=VERTEX_POINT('',#291370);
#43135=VERTEX_POINT('',#291371);
#43136=VERTEX_POINT('',#291416);
#43137=VERTEX_POINT('',#291417);
#43138=VERTEX_POINT('',#291462);
#43139=VERTEX_POINT('',#291463);
#43140=VERTEX_POINT('',#291508);
#43141=VERTEX_POINT('',#291509);
#43142=VERTEX_POINT('',#291511);
#43143=VERTEX_POINT('',#291520);
#43144=VERTEX_POINT('',#291527);
#43145=VERTEX_POINT('',#291528);
#43146=VERTEX_POINT('',#291605);
#43147=VERTEX_POINT('',#291606);
#43148=VERTEX_POINT('',#291683);
#43149=VERTEX_POINT('',#291684);
#43150=VERTEX_POINT('',#291759);
#43151=VERTEX_POINT('',#291760);
#43152=VERTEX_POINT('',#291835);
#43153=VERTEX_POINT('',#291836);
#43154=VERTEX_POINT('',#291911);
#43155=VERTEX_POINT('',#291912);
#43156=VERTEX_POINT('',#291987);
#43157=VERTEX_POINT('',#291988);
#43158=VERTEX_POINT('',#292065);
#43159=VERTEX_POINT('',#292066);
#43160=VERTEX_POINT('',#292141);
#43161=VERTEX_POINT('',#292142);
#43162=VERTEX_POINT('',#292217);
#43163=VERTEX_POINT('',#292218);
#43164=VERTEX_POINT('',#292295);
#43165=VERTEX_POINT('',#292296);
#43166=VERTEX_POINT('',#292371);
#43167=VERTEX_POINT('',#292372);
#43168=VERTEX_POINT('',#292447);
#43169=VERTEX_POINT('',#292448);
#43170=VERTEX_POINT('',#292450);
#43171=VERTEX_POINT('',#292473);
#43172=VERTEX_POINT('',#292494);
#43173=VERTEX_POINT('',#292495);
#43174=VERTEX_POINT('',#292572);
#43175=VERTEX_POINT('',#292573);
#43176=VERTEX_POINT('',#292650);
#43177=VERTEX_POINT('',#292651);
#43178=VERTEX_POINT('',#292726);
#43179=VERTEX_POINT('',#292727);
#43180=VERTEX_POINT('',#292802);
#43181=VERTEX_POINT('',#292803);
#43182=VERTEX_POINT('',#292878);
#43183=VERTEX_POINT('',#292879);
#43184=VERTEX_POINT('',#292954);
#43185=VERTEX_POINT('',#292955);
#43186=VERTEX_POINT('',#293030);
#43187=VERTEX_POINT('',#293031);
#43188=VERTEX_POINT('',#293106);
#43189=VERTEX_POINT('',#293107);
#43190=VERTEX_POINT('',#293184);
#43191=VERTEX_POINT('',#293185);
#43192=VERTEX_POINT('',#293262);
#43193=VERTEX_POINT('',#293263);
#43194=VERTEX_POINT('',#293338);
#43195=VERTEX_POINT('',#293339);
#43196=VERTEX_POINT('',#293414);
#43197=VERTEX_POINT('',#293415);
#43198=VERTEX_POINT('',#293490);
#43199=VERTEX_POINT('',#293491);
#43200=VERTEX_POINT('',#293566);
#43201=VERTEX_POINT('',#293567);
#43202=VERTEX_POINT('',#293642);
#43203=VERTEX_POINT('',#293643);
#43204=VERTEX_POINT('',#293718);
#43205=VERTEX_POINT('',#293719);
#43206=VERTEX_POINT('',#293794);
#43207=VERTEX_POINT('',#293795);
#43208=VERTEX_POINT('',#293872);
#43209=VERTEX_POINT('',#293883);
#43210=VERTEX_POINT('',#293902);
#43211=VERTEX_POINT('',#293905);
#43212=VERTEX_POINT('',#293932);
#43213=VERTEX_POINT('',#293947);
#43214=VERTEX_POINT('',#293948);
#43215=VERTEX_POINT('',#293959);
#43216=VERTEX_POINT('',#294009);
#43217=VERTEX_POINT('',#294013);
#43218=VERTEX_POINT('',#294036);
#43219=VERTEX_POINT('',#298271);
#43220=VERTEX_POINT('',#298272);
#43221=VERTEX_POINT('',#298274);
#43222=VERTEX_POINT('',#298276);
#43223=VERTEX_POINT('',#298280);
#43224=VERTEX_POINT('',#298281);
#43225=VERTEX_POINT('',#298283);
#43226=VERTEX_POINT('',#298285);
#43227=VERTEX_POINT('',#298288);
#43228=VERTEX_POINT('',#298289);
#43229=VERTEX_POINT('',#298291);
#43230=VERTEX_POINT('',#298293);
#43231=VERTEX_POINT('',#298295);
#43232=VERTEX_POINT('',#298297);
#43233=VERTEX_POINT('',#298309);
#43234=VERTEX_POINT('',#298310);
#43235=VERTEX_POINT('',#298315);
#43236=VERTEX_POINT('',#298319);
#43237=VERTEX_POINT('',#298321);
#43238=VERTEX_POINT('',#298332);
#43239=VERTEX_POINT('',#298336);
#43240=VERTEX_POINT('',#298338);
#43241=VERTEX_POINT('',#298349);
#43242=VERTEX_POINT('',#298353);
#43243=VERTEX_POINT('',#298355);
#43244=VERTEX_POINT('',#298366);
#43245=VERTEX_POINT('',#298370);
#43246=VERTEX_POINT('',#298372);
#43247=VERTEX_POINT('',#298383);
#43248=VERTEX_POINT('',#298387);
#43249=VERTEX_POINT('',#298389);
#43250=VERTEX_POINT('',#298403);
#43251=VERTEX_POINT('',#302624);
#43252=VERTEX_POINT('',#302626);
#43253=VERTEX_POINT('',#302630);
#43254=VERTEX_POINT('',#302632);
#43255=VERTEX_POINT('',#302636);
#43256=VERTEX_POINT('',#302638);
#43257=VERTEX_POINT('',#302642);
#43258=VERTEX_POINT('',#302644);
#43259=VERTEX_POINT('',#302648);
#43260=VERTEX_POINT('',#302650);
#43261=VERTEX_POINT('',#302654);
#43262=VERTEX_POINT('',#302656);
#43263=VERTEX_POINT('',#302660);
#43264=VERTEX_POINT('',#302662);
#43265=VERTEX_POINT('',#302666);
#43266=VERTEX_POINT('',#302668);
#43267=VERTEX_POINT('',#302672);
#43268=VERTEX_POINT('',#302674);
#43269=VERTEX_POINT('',#302678);
#43270=VERTEX_POINT('',#302680);
#43271=VERTEX_POINT('',#302684);
#43272=VERTEX_POINT('',#302686);
#43273=VERTEX_POINT('',#302690);
#43274=VERTEX_POINT('',#302692);
#43275=VERTEX_POINT('',#302695);
#43276=VERTEX_POINT('',#302697);
#43277=VERTEX_POINT('',#302701);
#43278=VERTEX_POINT('',#302703);
#43279=VERTEX_POINT('',#302705);
#43280=VERTEX_POINT('',#302711);
#43281=VERTEX_POINT('',#302713);
#43282=VERTEX_POINT('',#302734);
#43283=VERTEX_POINT('',#302735);
#43284=VERTEX_POINT('',#302737);
#43285=VERTEX_POINT('',#302739);
#43286=VERTEX_POINT('',#302742);
#43287=VERTEX_POINT('',#302743);
#43288=VERTEX_POINT('',#302745);
#43289=VERTEX_POINT('',#302747);
#43290=VERTEX_POINT('',#302751);
#43291=VERTEX_POINT('',#302752);
#43292=VERTEX_POINT('',#302754);
#43293=VERTEX_POINT('',#302756);
#43294=VERTEX_POINT('',#302759);
#43295=VERTEX_POINT('',#302760);
#43296=VERTEX_POINT('',#302762);
#43297=VERTEX_POINT('',#302764);
#43298=VERTEX_POINT('',#302785);
#43299=VERTEX_POINT('',#302786);
#43300=VERTEX_POINT('',#302788);
#43301=VERTEX_POINT('',#302790);
#43302=VERTEX_POINT('',#302794);
#43303=VERTEX_POINT('',#302796);
#43304=VERTEX_POINT('',#302800);
#43305=VERTEX_POINT('',#302802);
#43306=VERTEX_POINT('',#302813);
#43307=VERTEX_POINT('',#302815);
#43308=VERTEX_POINT('',#302819);
#43309=VERTEX_POINT('',#302821);
#43310=VERTEX_POINT('',#302825);
#43311=VERTEX_POINT('',#302827);
#43312=VERTEX_POINT('',#302831);
#43313=VERTEX_POINT('',#302833);
#43314=VERTEX_POINT('',#302837);
#43315=VERTEX_POINT('',#302839);
#43316=VERTEX_POINT('',#302843);
#43317=VERTEX_POINT('',#302845);
#43318=VERTEX_POINT('',#302849);
#43319=VERTEX_POINT('',#302851);
#43320=VERTEX_POINT('',#302855);
#43321=VERTEX_POINT('',#302857);
#43322=VERTEX_POINT('',#302861);
#43323=VERTEX_POINT('',#302862);
#43324=VERTEX_POINT('',#302864);
#43325=VERTEX_POINT('',#302866);
#43326=VERTEX_POINT('',#302868);
#43327=VERTEX_POINT('',#302870);
#43328=VERTEX_POINT('',#302872);
#43329=VERTEX_POINT('',#302874);
#43330=VERTEX_POINT('',#302878);
#43331=VERTEX_POINT('',#302879);
#43332=VERTEX_POINT('',#302881);
#43333=VERTEX_POINT('',#302883);
#43334=VERTEX_POINT('',#302885);
#43335=VERTEX_POINT('',#302887);
#43336=VERTEX_POINT('',#302889);
#43337=VERTEX_POINT('',#302891);
#43338=VERTEX_POINT('',#302912);
#43339=VERTEX_POINT('',#302914);
#43340=VERTEX_POINT('',#302918);
#43341=VERTEX_POINT('',#302920);
#43342=VERTEX_POINT('',#302924);
#43343=VERTEX_POINT('',#302925);
#43344=VERTEX_POINT('',#302927);
#43345=VERTEX_POINT('',#302929);
#43346=VERTEX_POINT('',#302933);
#43347=VERTEX_POINT('',#302934);
#43348=VERTEX_POINT('',#302936);
#43349=VERTEX_POINT('',#302938);
#43350=VERTEX_POINT('',#302942);
#43351=VERTEX_POINT('',#302944);
#43352=VERTEX_POINT('',#302948);
#43353=VERTEX_POINT('',#302950);
#43354=VERTEX_POINT('',#302954);
#43355=VERTEX_POINT('',#302956);
#43356=VERTEX_POINT('',#302960);
#43357=VERTEX_POINT('',#302962);
#43358=VERTEX_POINT('',#302972);
#43359=VERTEX_POINT('',#302973);
#43360=VERTEX_POINT('',#302978);
#43361=VERTEX_POINT('',#302980);
#43362=VERTEX_POINT('',#302984);
#43363=VERTEX_POINT('',#302986);
#43364=VERTEX_POINT('',#302993);
#43365=VERTEX_POINT('',#302994);
#43366=VERTEX_POINT('',#303018);
#43367=VERTEX_POINT('',#303019);
#43368=VERTEX_POINT('',#303021);
#43369=VERTEX_POINT('',#303038);
#43370=VERTEX_POINT('',#303040);
#43371=VERTEX_POINT('',#303055);
#43372=VERTEX_POINT('',#303056);
#43373=VERTEX_POINT('',#303058);
#43374=VERTEX_POINT('',#303121);
#43375=VERTEX_POINT('',#303122);
#43376=VERTEX_POINT('',#303124);
#43377=VERTEX_POINT('',#303141);
#43378=VERTEX_POINT('',#303156);
#43379=VERTEX_POINT('',#303157);
#43380=VERTEX_POINT('',#303232);
#43381=VERTEX_POINT('',#303233);
#43382=VERTEX_POINT('',#303310);
#43383=VERTEX_POINT('',#303311);
#43384=VERTEX_POINT('',#303386);
#43385=VERTEX_POINT('',#303387);
#43386=VERTEX_POINT('',#303462);
#43387=VERTEX_POINT('',#303463);
#43388=VERTEX_POINT('',#303538);
#43389=VERTEX_POINT('',#303539);
#43390=VERTEX_POINT('',#303614);
#43391=VERTEX_POINT('',#303615);
#43392=VERTEX_POINT('',#303690);
#43393=VERTEX_POINT('',#303691);
#43394=VERTEX_POINT('',#303766);
#43395=VERTEX_POINT('',#303767);
#43396=VERTEX_POINT('',#303844);
#43397=VERTEX_POINT('',#303845);
#43398=VERTEX_POINT('',#303922);
#43399=VERTEX_POINT('',#303923);
#43400=VERTEX_POINT('',#303998);
#43401=VERTEX_POINT('',#303999);
#43402=VERTEX_POINT('',#304074);
#43403=VERTEX_POINT('',#304075);
#43404=VERTEX_POINT('',#304150);
#43405=VERTEX_POINT('',#304151);
#43406=VERTEX_POINT('',#304226);
#43407=VERTEX_POINT('',#304227);
#43408=VERTEX_POINT('',#304302);
#43409=VERTEX_POINT('',#304304);
#43410=VERTEX_POINT('',#304306);
#43411=VERTEX_POINT('',#304308);
#43412=VERTEX_POINT('',#304313);
#43413=VERTEX_POINT('',#304327);
#43414=VERTEX_POINT('',#304333);
#43415=VERTEX_POINT('',#304334);
#43416=VERTEX_POINT('',#304379);
#43417=VERTEX_POINT('',#304380);
#43418=VERTEX_POINT('',#304425);
#43419=VERTEX_POINT('',#304426);
#43420=VERTEX_POINT('',#304471);
#43421=VERTEX_POINT('',#304472);
#43422=VERTEX_POINT('',#304517);
#43423=VERTEX_POINT('',#304518);
#43424=VERTEX_POINT('',#304563);
#43425=VERTEX_POINT('',#304564);
#43426=VERTEX_POINT('',#304609);
#43427=VERTEX_POINT('',#304610);
#43428=VERTEX_POINT('',#304655);
#43429=VERTEX_POINT('',#304656);
#43430=VERTEX_POINT('',#304701);
#43431=VERTEX_POINT('',#304702);
#43432=VERTEX_POINT('',#304747);
#43433=VERTEX_POINT('',#304748);
#43434=VERTEX_POINT('',#304793);
#43435=VERTEX_POINT('',#304794);
#43436=VERTEX_POINT('',#304839);
#43437=VERTEX_POINT('',#304840);
#43438=VERTEX_POINT('',#304885);
#43439=VERTEX_POINT('',#304886);
#43440=VERTEX_POINT('',#304931);
#43441=VERTEX_POINT('',#304932);
#43442=VERTEX_POINT('',#304977);
#43443=VERTEX_POINT('',#304978);
#43444=VERTEX_POINT('',#305023);
#43445=VERTEX_POINT('',#305024);
#43446=VERTEX_POINT('',#305026);
#43447=VERTEX_POINT('',#305069);
#43448=VERTEX_POINT('',#305072);
#43449=VERTEX_POINT('',#305088);
#43450=VERTEX_POINT('',#306685);
#43451=VERTEX_POINT('',#306686);
#43452=VERTEX_POINT('',#306706);
#43453=VERTEX_POINT('',#306726);
#43454=VERTEX_POINT('',#306766);
#43455=VERTEX_POINT('',#306767);
#43456=VERTEX_POINT('',#306779);
#43457=VERTEX_POINT('',#306791);
#43458=VERTEX_POINT('',#306815);
#43459=VERTEX_POINT('',#306816);
#43460=VERTEX_POINT('',#306836);
#43461=VERTEX_POINT('',#306856);
#43462=VERTEX_POINT('',#306896);
#43463=VERTEX_POINT('',#306897);
#43464=VERTEX_POINT('',#306909);
#43465=VERTEX_POINT('',#306921);
#43466=VERTEX_POINT('',#306982);
#43467=VERTEX_POINT('',#306984);
#43468=VERTEX_POINT('',#307043);
#43469=VERTEX_POINT('',#307102);
#43470=VERTEX_POINT('',#307202);
#43471=VERTEX_POINT('',#307204);
#43472=VERTEX_POINT('',#307239);
#43473=VERTEX_POINT('',#307274);
#43474=VERTEX_POINT('',#307358);
#43475=VERTEX_POINT('',#307360);
#43476=VERTEX_POINT('',#307419);
#43477=VERTEX_POINT('',#307478);
#43478=VERTEX_POINT('',#307578);
#43479=VERTEX_POINT('',#307580);
#43480=VERTEX_POINT('',#307615);
#43481=VERTEX_POINT('',#307650);
#43482=VERTEX_POINT('',#307697);
#43483=VERTEX_POINT('',#307698);
#43484=VERTEX_POINT('',#307710);
#43485=VERTEX_POINT('',#307730);
#43486=VERTEX_POINT('',#307750);
#43487=VERTEX_POINT('',#307770);
#43488=VERTEX_POINT('',#307790);
#43489=VERTEX_POINT('',#307802);
#43490=VERTEX_POINT('',#307842);
#43491=VERTEX_POINT('',#307843);
#43492=VERTEX_POINT('',#307855);
#43493=VERTEX_POINT('',#307875);
#43494=VERTEX_POINT('',#307895);
#43495=VERTEX_POINT('',#307915);
#43496=VERTEX_POINT('',#307935);
#43497=VERTEX_POINT('',#307947);
#43498=VERTEX_POINT('',#307987);
#43499=VERTEX_POINT('',#307988);
#43500=VERTEX_POINT('',#307990);
#43501=VERTEX_POINT('',#307992);
#43502=VERTEX_POINT('',#308033);
#43503=VERTEX_POINT('',#308035);
#43504=VERTEX_POINT('',#308078);
#43505=VERTEX_POINT('',#308129);
#43506=VERTEX_POINT('',#308188);
#43507=VERTEX_POINT('',#308231);
#43508=VERTEX_POINT('',#308282);
#43509=VERTEX_POINT('',#308341);
#43510=VERTEX_POINT('',#308457);
#43511=VERTEX_POINT('',#308459);
#43512=VERTEX_POINT('',#308502);
#43513=VERTEX_POINT('',#308553);
#43514=VERTEX_POINT('',#308612);
#43515=VERTEX_POINT('',#308655);
#43516=VERTEX_POINT('',#308706);
#43517=VERTEX_POINT('',#308765);
#43518=VERTEX_POINT('',#308844);
#43519=VERTEX_POINT('',#308846);
#43520=VERTEX_POINT('',#308850);
#43521=VERTEX_POINT('',#308854);
#43522=VERTEX_POINT('',#308860);
#43523=VERTEX_POINT('',#308861);
#43524=VERTEX_POINT('',#308863);
#43525=VERTEX_POINT('',#308865);
#43526=VERTEX_POINT('',#308867);
#43527=VERTEX_POINT('',#308869);
#43528=VERTEX_POINT('',#308873);
#43529=VERTEX_POINT('',#308881);
#43530=VERTEX_POINT('',#308889);
#43531=VERTEX_POINT('',#308897);
#43532=VERTEX_POINT('',#308905);
#43533=VERTEX_POINT('',#308913);
#43534=VERTEX_POINT('',#308921);
#43535=VERTEX_POINT('',#308923);
#43536=VERTEX_POINT('',#308927);
#43537=VERTEX_POINT('',#308931);
#43538=VERTEX_POINT('',#308935);
#43539=VERTEX_POINT('',#308939);
#43540=VERTEX_POINT('',#308949);
#43541=VERTEX_POINT('',#308950);
#43542=VERTEX_POINT('',#308952);
#43543=VERTEX_POINT('',#308961);
#43544=VERTEX_POINT('',#308978);
#43545=VERTEX_POINT('',#308979);
#43546=VERTEX_POINT('',#308981);
#43547=VERTEX_POINT('',#308998);
#43548=VERTEX_POINT('',#309021);
#43549=VERTEX_POINT('',#309022);
#43550=VERTEX_POINT('',#309097);
#43551=VERTEX_POINT('',#309098);
#43552=VERTEX_POINT('',#309173);
#43553=VERTEX_POINT('',#309174);
#43554=VERTEX_POINT('',#309249);
#43555=VERTEX_POINT('',#309250);
#43556=VERTEX_POINT('',#309252);
#43557=VERTEX_POINT('',#309271);
#43558=VERTEX_POINT('',#309273);
#43559=VERTEX_POINT('',#309298);
#43560=VERTEX_POINT('',#309299);
#43561=VERTEX_POINT('',#309330);
#43562=VERTEX_POINT('',#309331);
#43563=VERTEX_POINT('',#309376);
#43564=VERTEX_POINT('',#309377);
#43565=VERTEX_POINT('',#309422);
#43566=VERTEX_POINT('',#309423);
#43567=VERTEX_POINT('',#309425);
#43568=VERTEX_POINT('',#309767);
#43569=VERTEX_POINT('',#309819);
#43570=VERTEX_POINT('',#310211);
#43571=VERTEX_POINT('',#310212);
#43572=VERTEX_POINT('',#310223);
#43573=VERTEX_POINT('',#310225);
#43574=VERTEX_POINT('',#310238);
#43575=VERTEX_POINT('',#310239);
#43576=VERTEX_POINT('',#310250);
#43577=VERTEX_POINT('',#310252);
#43578=VERTEX_POINT('',#310265);
#43579=VERTEX_POINT('',#310266);
#43580=VERTEX_POINT('',#310277);
#43581=VERTEX_POINT('',#310279);
#43582=VERTEX_POINT('',#310292);
#43583=VERTEX_POINT('',#310293);
#43584=VERTEX_POINT('',#310304);
#43585=VERTEX_POINT('',#310306);
#43586=VERTEX_POINT('',#310319);
#43587=VERTEX_POINT('',#310320);
#43588=VERTEX_POINT('',#310331);
#43589=VERTEX_POINT('',#310333);
#43590=VERTEX_POINT('',#310346);
#43591=VERTEX_POINT('',#310347);
#43592=VERTEX_POINT('',#310358);
#43593=VERTEX_POINT('',#310360);
#43594=VERTEX_POINT('',#310373);
#43595=VERTEX_POINT('',#310377);
#43596=VERTEX_POINT('',#310386);
#43597=VERTEX_POINT('',#310395);
#43598=VERTEX_POINT('',#310404);
#43599=VERTEX_POINT('',#310413);
#43600=VERTEX_POINT('',#310427);
#43601=VERTEX_POINT('',#310431);
#43602=VERTEX_POINT('',#310440);
#43603=VERTEX_POINT('',#310449);
#43604=VERTEX_POINT('',#310458);
#43605=VERTEX_POINT('',#310467);
#43606=VERTEX_POINT('',#310488);
#43607=VERTEX_POINT('',#310491);
#43608=EDGE_CURVE('',#35105,#35105,#29175,.T.);
#43609=EDGE_CURVE('',#35105,#35106,#20481,.T.);
#43610=EDGE_CURVE('',#35106,#35106,#29176,.T.);
#43611=EDGE_CURVE('',#35107,#35107,#29177,.T.);
#43612=EDGE_CURVE('',#35107,#35108,#20482,.T.);
#43613=EDGE_CURVE('',#35108,#35108,#29178,.T.);
#43614=EDGE_CURVE('',#35109,#35109,#29179,.T.);
#43615=EDGE_CURVE('',#35109,#35110,#20483,.T.);
#43616=EDGE_CURVE('',#35110,#35110,#29180,.T.);
#43617=EDGE_CURVE('',#35111,#35111,#29181,.T.);
#43618=EDGE_CURVE('',#35111,#35112,#20484,.T.);
#43619=EDGE_CURVE('',#35112,#35112,#29182,.T.);
#43620=EDGE_CURVE('',#35113,#35113,#29183,.T.);
#43621=EDGE_CURVE('',#35113,#35114,#20485,.T.);
#43622=EDGE_CURVE('',#35114,#35114,#29184,.T.);
#43623=EDGE_CURVE('',#35115,#35115,#29185,.T.);
#43624=EDGE_CURVE('',#35115,#35116,#20486,.T.);
#43625=EDGE_CURVE('',#35116,#35116,#29186,.T.);
#43626=EDGE_CURVE('',#35117,#35117,#29187,.T.);
#43627=EDGE_CURVE('',#35117,#35118,#20487,.T.);
#43628=EDGE_CURVE('',#35118,#35118,#29188,.T.);
#43629=EDGE_CURVE('',#35119,#35119,#29189,.T.);
#43630=EDGE_CURVE('',#35119,#35120,#20488,.T.);
#43631=EDGE_CURVE('',#35120,#35120,#29190,.T.);
#43632=EDGE_CURVE('',#35121,#35121,#29191,.T.);
#43633=EDGE_CURVE('',#35121,#35122,#20489,.T.);
#43634=EDGE_CURVE('',#35122,#35122,#29192,.T.);
#43635=EDGE_CURVE('',#35123,#35123,#29193,.T.);
#43636=EDGE_CURVE('',#35123,#35124,#20490,.T.);
#43637=EDGE_CURVE('',#35124,#35124,#29194,.T.);
#43638=EDGE_CURVE('',#35125,#35125,#29195,.T.);
#43639=EDGE_CURVE('',#35125,#35126,#20491,.T.);
#43640=EDGE_CURVE('',#35126,#35126,#29196,.T.);
#43641=EDGE_CURVE('',#35127,#35127,#29197,.T.);
#43642=EDGE_CURVE('',#35127,#35128,#20492,.T.);
#43643=EDGE_CURVE('',#35128,#35128,#29198,.T.);
#43644=EDGE_CURVE('',#35129,#35130,#20493,.T.);
#43645=EDGE_CURVE('',#35131,#35130,#20494,.T.);
#43646=EDGE_CURVE('',#35132,#35131,#20495,.T.);
#43647=EDGE_CURVE('',#35132,#35129,#20496,.T.);
#43648=EDGE_CURVE('',#35130,#35133,#20497,.T.);
#43649=EDGE_CURVE('',#35133,#35134,#20498,.T.);
#43650=EDGE_CURVE('',#35131,#35134,#20499,.T.);
#43651=EDGE_CURVE('',#35135,#35136,#20500,.T.);
#43652=EDGE_CURVE('',#35136,#35137,#20501,.T.);
#43653=EDGE_CURVE('',#35138,#35137,#20502,.T.);
#43654=EDGE_CURVE('',#35138,#35135,#20503,.T.);
#43655=EDGE_CURVE('',#35139,#35140,#20504,.T.);
#43656=EDGE_CURVE('',#35139,#35141,#20505,.T.);
#43657=EDGE_CURVE('',#35141,#35142,#20506,.T.);
#43658=EDGE_CURVE('',#35140,#35142,#20507,.T.);
#43659=EDGE_CURVE('',#35142,#35143,#20508,.T.);
#43660=EDGE_CURVE('',#35144,#35143,#20509,.T.);
#43661=EDGE_CURVE('',#35140,#35144,#20510,.T.);
#43662=EDGE_CURVE('',#35143,#35145,#20511,.T.);
#43663=EDGE_CURVE('',#35145,#35146,#20512,.T.);
#43664=EDGE_CURVE('',#35144,#35146,#20513,.T.);
#43665=EDGE_CURVE('',#35147,#35148,#20514,.T.);
#43666=EDGE_CURVE('',#35148,#35149,#20515,.T.);
#43667=EDGE_CURVE('',#35150,#35149,#20516,.T.);
#43668=EDGE_CURVE('',#35150,#35147,#20517,.T.);
#43669=EDGE_CURVE('',#35151,#35132,#20518,.T.);
#43670=EDGE_CURVE('',#35151,#35152,#20519,.T.);
#43671=EDGE_CURVE('',#35152,#35129,#20520,.T.);
#43672=EDGE_CURVE('',#35137,#35139,#29199,.T.);
#43673=EDGE_CURVE('',#35146,#35150,#29200,.T.);
#43674=EDGE_CURVE('',#35149,#35151,#29201,.T.);
#43675=EDGE_CURVE('',#35134,#35138,#29202,.T.);
#43676=EDGE_CURVE('',#35141,#35136,#29203,.T.);
#43677=EDGE_CURVE('',#35135,#35133,#29204,.T.);
#43678=EDGE_CURVE('',#35152,#35148,#29205,.T.);
#43679=EDGE_CURVE('',#35147,#35145,#29206,.T.);
#43680=EDGE_CURVE('',#35153,#35153,#29207,.T.);
#43681=EDGE_CURVE('',#35153,#35154,#20521,.T.);
#43682=EDGE_CURVE('',#35154,#35154,#29208,.T.);
#43683=EDGE_CURVE('',#35155,#35155,#29209,.T.);
#43684=EDGE_CURVE('',#35155,#35156,#20522,.T.);
#43685=EDGE_CURVE('',#35156,#35156,#29210,.T.);
#43686=EDGE_CURVE('',#35157,#35157,#29211,.T.);
#43687=EDGE_CURVE('',#35157,#35158,#20523,.T.);
#43688=EDGE_CURVE('',#35158,#35158,#29212,.T.);
#43689=EDGE_CURVE('',#35159,#35159,#29213,.T.);
#43690=EDGE_CURVE('',#35159,#35160,#20524,.T.);
#43691=EDGE_CURVE('',#35160,#35160,#29214,.T.);
#43692=EDGE_CURVE('',#35161,#35161,#29215,.T.);
#43693=EDGE_CURVE('',#35161,#35162,#20525,.T.);
#43694=EDGE_CURVE('',#35162,#35162,#29216,.T.);
#43695=EDGE_CURVE('',#35163,#35163,#29217,.T.);
#43696=EDGE_CURVE('',#35163,#35164,#20526,.T.);
#43697=EDGE_CURVE('',#35164,#35164,#29218,.T.);
#43698=EDGE_CURVE('',#35165,#35165,#29219,.T.);
#43699=EDGE_CURVE('',#35165,#35166,#20527,.T.);
#43700=EDGE_CURVE('',#35166,#35166,#29220,.T.);
#43701=EDGE_CURVE('',#35167,#35167,#29221,.T.);
#43702=EDGE_CURVE('',#35167,#35168,#20528,.T.);
#43703=EDGE_CURVE('',#35168,#35168,#29222,.T.);
#43704=EDGE_CURVE('',#35169,#35169,#29223,.T.);
#43705=EDGE_CURVE('',#35169,#35170,#20529,.T.);
#43706=EDGE_CURVE('',#35170,#35170,#29224,.T.);
#43707=EDGE_CURVE('',#35171,#35171,#29225,.T.);
#43708=EDGE_CURVE('',#35171,#35172,#20530,.T.);
#43709=EDGE_CURVE('',#35172,#35172,#29226,.T.);
#43710=EDGE_CURVE('',#35173,#35173,#29227,.T.);
#43711=EDGE_CURVE('',#35173,#35174,#20531,.T.);
#43712=EDGE_CURVE('',#35174,#35174,#29228,.T.);
#43713=EDGE_CURVE('',#35175,#35175,#29229,.T.);
#43714=EDGE_CURVE('',#35175,#35176,#20532,.T.);
#43715=EDGE_CURVE('',#35176,#35176,#29230,.T.);
#43716=EDGE_CURVE('',#35177,#35178,#20533,.T.);
#43717=EDGE_CURVE('',#35179,#35178,#20534,.T.);
#43718=EDGE_CURVE('',#35180,#35179,#20535,.T.);
#43719=EDGE_CURVE('',#35180,#35177,#20536,.T.);
#43720=EDGE_CURVE('',#35178,#35181,#20537,.T.);
#43721=EDGE_CURVE('',#35181,#35182,#20538,.T.);
#43722=EDGE_CURVE('',#35179,#35182,#20539,.T.);
#43723=EDGE_CURVE('',#35183,#35184,#20540,.T.);
#43724=EDGE_CURVE('',#35184,#35185,#20541,.T.);
#43725=EDGE_CURVE('',#35186,#35185,#20542,.T.);
#43726=EDGE_CURVE('',#35186,#35183,#20543,.T.);
#43727=EDGE_CURVE('',#35187,#35188,#20544,.T.);
#43728=EDGE_CURVE('',#35187,#35189,#20545,.T.);
#43729=EDGE_CURVE('',#35189,#35190,#20546,.T.);
#43730=EDGE_CURVE('',#35188,#35190,#20547,.T.);
#43731=EDGE_CURVE('',#35190,#35191,#20548,.T.);
#43732=EDGE_CURVE('',#35192,#35191,#20549,.T.);
#43733=EDGE_CURVE('',#35188,#35192,#20550,.T.);
#43734=EDGE_CURVE('',#35191,#35193,#20551,.T.);
#43735=EDGE_CURVE('',#35193,#35194,#20552,.T.);
#43736=EDGE_CURVE('',#35192,#35194,#20553,.T.);
#43737=EDGE_CURVE('',#35195,#35196,#20554,.T.);
#43738=EDGE_CURVE('',#35196,#35197,#20555,.T.);
#43739=EDGE_CURVE('',#35198,#35197,#20556,.T.);
#43740=EDGE_CURVE('',#35198,#35195,#20557,.T.);
#43741=EDGE_CURVE('',#35199,#35180,#20558,.T.);
#43742=EDGE_CURVE('',#35199,#35200,#20559,.T.);
#43743=EDGE_CURVE('',#35200,#35177,#20560,.T.);
#43744=EDGE_CURVE('',#35185,#35187,#29231,.T.);
#43745=EDGE_CURVE('',#35194,#35198,#29232,.T.);
#43746=EDGE_CURVE('',#35197,#35199,#29233,.T.);
#43747=EDGE_CURVE('',#35182,#35186,#29234,.T.);
#43748=EDGE_CURVE('',#35189,#35184,#29235,.T.);
#43749=EDGE_CURVE('',#35183,#35181,#29236,.T.);
#43750=EDGE_CURVE('',#35200,#35196,#29237,.T.);
#43751=EDGE_CURVE('',#35195,#35193,#29238,.T.);
#43752=EDGE_CURVE('',#35201,#35201,#29239,.T.);
#43753=EDGE_CURVE('',#35201,#35202,#20561,.T.);
#43754=EDGE_CURVE('',#35202,#35202,#29240,.T.);
#43755=EDGE_CURVE('',#35203,#35203,#29241,.T.);
#43756=EDGE_CURVE('',#35203,#35201,#20562,.T.);
#43757=EDGE_CURVE('',#35204,#35204,#29242,.T.);
#43758=EDGE_CURVE('',#35205,#35205,#29243,.T.);
#43759=EDGE_CURVE('',#35205,#35204,#20563,.T.);
#43760=EDGE_CURVE('',#35206,#35206,#29244,.T.);
#43761=EDGE_CURVE('',#35206,#35207,#20564,.T.);
#43762=EDGE_CURVE('',#35207,#35207,#29245,.T.);
#43763=EDGE_CURVE('',#35208,#35208,#29246,.T.);
#43764=EDGE_CURVE('',#35208,#35206,#20565,.T.);
#43765=EDGE_CURVE('',#35209,#35209,#29247,.T.);
#43766=EDGE_CURVE('',#35210,#35210,#29248,.T.);
#43767=EDGE_CURVE('',#35210,#35209,#20566,.T.);
#43768=EDGE_CURVE('',#35211,#35212,#20567,.T.);
#43769=EDGE_CURVE('',#35212,#35213,#29249,.T.);
#43770=EDGE_CURVE('',#35213,#35214,#20568,.T.);
#43771=EDGE_CURVE('',#35215,#35214,#4127,.T.);
#43772=EDGE_CURVE('',#35216,#35215,#29250,.T.);
#43773=EDGE_CURVE('',#35211,#35216,#4128,.T.);
#43774=EDGE_CURVE('',#35217,#35218,#29251,.T.);
#43775=EDGE_CURVE('',#35217,#35219,#20569,.T.);
#43776=EDGE_CURVE('',#35219,#35220,#29252,.T.);
#43777=EDGE_CURVE('',#35220,#35221,#20570,.T.);
#43778=EDGE_CURVE('',#35218,#35221,#4129,.T.);
#43779=EDGE_CURVE('',#35217,#35222,#29253,.T.);
#43780=EDGE_CURVE('',#35218,#35223,#29254,.T.);
#43781=EDGE_CURVE('',#35223,#35222,#29255,.T.);
#43782=EDGE_CURVE('',#35221,#35224,#29256,.T.);
#43783=EDGE_CURVE('',#35224,#35223,#4130,.T.);
#43784=EDGE_CURVE('',#35225,#35226,#20571,.T.);
#43785=EDGE_CURVE('',#35226,#35227,#29257,.T.);
#43786=EDGE_CURVE('',#35227,#35228,#20572,.T.);
#43787=EDGE_CURVE('',#35225,#35228,#29258,.T.);
#43788=EDGE_CURVE('',#35229,#35230,#20573,.T.);
#43789=EDGE_CURVE('',#35231,#35229,#20574,.T.);
#43790=EDGE_CURVE('',#35232,#35231,#4131,.T.);
#43791=EDGE_CURVE('',#35233,#35232,#20575,.T.);
#43792=EDGE_CURVE('',#35234,#35233,#4132,.T.);
#43793=EDGE_CURVE('',#35235,#35234,#20576,.T.);
#43794=EDGE_CURVE('',#35236,#35235,#20577,.T.);
#43795=EDGE_CURVE('',#35237,#35236,#4133,.T.);
#43796=EDGE_CURVE('',#35238,#35237,#20578,.T.);
#43797=EDGE_CURVE('',#35221,#35238,#4134,.T.);
#43798=EDGE_CURVE('',#35226,#35220,#20579,.T.);
#43799=EDGE_CURVE('',#35239,#35225,#20580,.T.);
#43800=EDGE_CURVE('',#35240,#35239,#20581,.T.);
#43801=EDGE_CURVE('',#35241,#35240,#4135,.T.);
#43802=EDGE_CURVE('',#35242,#35241,#20582,.T.);
#43803=EDGE_CURVE('',#35243,#35242,#4136,.T.);
#43804=EDGE_CURVE('',#35230,#35243,#20583,.T.);
#43805=EDGE_CURVE('',#35225,#35244,#29259,.T.);
#43806=EDGE_CURVE('',#35228,#35245,#29260,.T.);
#43807=EDGE_CURVE('',#35245,#35244,#29261,.T.);
#43808=EDGE_CURVE('',#35246,#35247,#20584,.T.);
#43809=EDGE_CURVE('',#35247,#35248,#29262,.T.);
#43810=EDGE_CURVE('',#35248,#35249,#20585,.T.);
#43811=EDGE_CURVE('',#35246,#35249,#29263,.T.);
#43812=EDGE_CURVE('',#35247,#35227,#20586,.T.);
#43813=EDGE_CURVE('',#35228,#35246,#20587,.T.);
#43814=EDGE_CURVE('',#35246,#35250,#29264,.T.);
#43815=EDGE_CURVE('',#35249,#35251,#29265,.T.);
#43816=EDGE_CURVE('',#35251,#35250,#29266,.T.);
#43817=EDGE_CURVE('',#35252,#35253,#4137,.T.);
#43818=EDGE_CURVE('',#35254,#35252,#20588,.T.);
#43819=EDGE_CURVE('',#35255,#35254,#20589,.T.);
#43820=EDGE_CURVE('',#35256,#35255,#4138,.T.);
#43821=EDGE_CURVE('',#35257,#35256,#20590,.T.);
#43822=EDGE_CURVE('',#35258,#35257,#4139,.T.);
#43823=EDGE_CURVE('',#35259,#35258,#20591,.T.);
#43824=EDGE_CURVE('',#35260,#35259,#20592,.T.);
#43825=EDGE_CURVE('',#35261,#35260,#20593,.T.);
#43826=EDGE_CURVE('',#35262,#35261,#4140,.T.);
#43827=EDGE_CURVE('',#35263,#35262,#20594,.T.);
#43828=EDGE_CURVE('',#35264,#35263,#4141,.T.);
#43829=EDGE_CURVE('',#35265,#35264,#20595,.T.);
#43830=EDGE_CURVE('',#35249,#35265,#20596,.T.);
#43831=EDGE_CURVE('',#35212,#35248,#20597,.T.);
#43832=EDGE_CURVE('',#35266,#35211,#1771,.T.);
#43833=EDGE_CURVE('',#35253,#35266,#20598,.T.);
#43834=EDGE_CURVE('',#35267,#35268,#29267,.T.);
#43835=EDGE_CURVE('',#35267,#35269,#4142,.T.);
#43836=EDGE_CURVE('',#35269,#35270,#29268,.T.);
#43837=EDGE_CURVE('',#35270,#35268,#4143,.T.);
#43838=EDGE_CURVE('',#35271,#35272,#29269,.T.);
#43839=EDGE_CURVE('',#35271,#35267,#20599,.T.);
#43840=EDGE_CURVE('',#35268,#35272,#20600,.T.);
#43841=EDGE_CURVE('',#35273,#35274,#29270,.T.);
#43842=EDGE_CURVE('',#35272,#35274,#29271,.T.);
#43843=EDGE_CURVE('',#35272,#35275,#29272,.T.);
#43844=EDGE_CURVE('',#35273,#35275,#1772,.T.);
#43845=EDGE_CURVE('',#35276,#35277,#29273,.T.);
#43846=EDGE_CURVE('',#35277,#35278,#20601,.T.);
#43847=EDGE_CURVE('',#35279,#35278,#29274,.T.);
#43848=EDGE_CURVE('',#35275,#35279,#29275,.T.);
#43849=EDGE_CURVE('',#35275,#35280,#20602,.T.);
#43850=EDGE_CURVE('',#35280,#35276,#29276,.T.);
#43851=EDGE_CURVE('',#35280,#35281,#4144,.T.);
#43852=EDGE_CURVE('',#35281,#35282,#29277,.T.);
#43853=EDGE_CURVE('',#35282,#35277,#4145,.T.);
#43854=EDGE_CURVE('',#35281,#35283,#29278,.T.);
#43855=EDGE_CURVE('',#35283,#35284,#29279,.T.);
#43856=EDGE_CURVE('',#35284,#35282,#29280,.T.);
#43857=EDGE_CURVE('',#35283,#35285,#4146,.T.);
#43858=EDGE_CURVE('',#35286,#35285,#29281,.T.);
#43859=EDGE_CURVE('',#35286,#35284,#4147,.T.);
#43860=EDGE_CURVE('',#35287,#35288,#29282,.T.);
#43861=EDGE_CURVE('',#35287,#35286,#20603,.T.);
#43862=EDGE_CURVE('',#35285,#35288,#20604,.T.);
#43863=EDGE_CURVE('',#35289,#35290,#29283,.T.);
#43864=EDGE_CURVE('',#35288,#35290,#1773,.T.);
#43865=EDGE_CURVE('',#35288,#35291,#29284,.T.);
#43866=EDGE_CURVE('',#35289,#35291,#1774,.T.);
#43867=EDGE_CURVE('',#35292,#35293,#29285,.T.);
#43868=EDGE_CURVE('',#35293,#35294,#20605,.T.);
#43869=EDGE_CURVE('',#35295,#35294,#29286,.T.);
#43870=EDGE_CURVE('',#35291,#35295,#29287,.T.);
#43871=EDGE_CURVE('',#35291,#35292,#20606,.T.);
#43872=EDGE_CURVE('',#35292,#35296,#4148,.T.);
#43873=EDGE_CURVE('',#35296,#35297,#29288,.T.);
#43874=EDGE_CURVE('',#35297,#35293,#4149,.T.);
#43875=EDGE_CURVE('',#35296,#35298,#29289,.T.);
#43876=EDGE_CURVE('',#35298,#35299,#29290,.T.);
#43877=EDGE_CURVE('',#35299,#35297,#29291,.T.);
#43878=EDGE_CURVE('',#35298,#35300,#4150,.T.);
#43879=EDGE_CURVE('',#35301,#35300,#29292,.T.);
#43880=EDGE_CURVE('',#35301,#35299,#4151,.T.);
#43881=EDGE_CURVE('',#35302,#35303,#29293,.T.);
#43882=EDGE_CURVE('',#35302,#35301,#20607,.T.);
#43883=EDGE_CURVE('',#35300,#35303,#20608,.T.);
#43884=EDGE_CURVE('',#35304,#35305,#29294,.T.);
#43885=EDGE_CURVE('',#35303,#35305,#1775,.T.);
#43886=EDGE_CURVE('',#35303,#35306,#29295,.T.);
#43887=EDGE_CURVE('',#35304,#35306,#1776,.T.);
#43888=EDGE_CURVE('',#35307,#35308,#29296,.T.);
#43889=EDGE_CURVE('',#35308,#35309,#20609,.T.);
#43890=EDGE_CURVE('',#35306,#35309,#29297,.T.);
#43891=EDGE_CURVE('',#35306,#35307,#20610,.T.);
#43892=EDGE_CURVE('',#35307,#35310,#4152,.T.);
#43893=EDGE_CURVE('',#35310,#35311,#29298,.T.);
#43894=EDGE_CURVE('',#35311,#35308,#4153,.T.);
#43895=EDGE_CURVE('',#35310,#35217,#29299,.T.);
#43896=EDGE_CURVE('',#35222,#35311,#29300,.T.);
#43897=EDGE_CURVE('',#35312,#35313,#20611,.T.);
#43898=EDGE_CURVE('',#35313,#35314,#29301,.T.);
#43899=EDGE_CURVE('',#35314,#35315,#20612,.T.);
#43900=EDGE_CURVE('',#35312,#35315,#4154,.T.);
#43901=EDGE_CURVE('',#35316,#35317,#29302,.T.);
#43902=EDGE_CURVE('',#35315,#35317,#29303,.T.);
#43903=EDGE_CURVE('',#35315,#35318,#29304,.T.);
#43904=EDGE_CURVE('',#35316,#35318,#4155,.T.);
#43905=EDGE_CURVE('',#35319,#35320,#29305,.T.);
#43906=EDGE_CURVE('',#35319,#35321,#20613,.T.);
#43907=EDGE_CURVE('',#35321,#35318,#29306,.T.);
#43908=EDGE_CURVE('',#35318,#35320,#20614,.T.);
#43909=EDGE_CURVE('',#35322,#35323,#29307,.T.);
#43910=EDGE_CURVE('',#35322,#35319,#4156,.T.);
#43911=EDGE_CURVE('',#35320,#35323,#4157,.T.);
#43912=EDGE_CURVE('',#35324,#35325,#29308,.T.);
#43913=EDGE_CURVE('',#35324,#35322,#29309,.T.);
#43914=EDGE_CURVE('',#35323,#35325,#29310,.T.);
#43915=EDGE_CURVE('',#35326,#35327,#29311,.T.);
#43916=EDGE_CURVE('',#35326,#35324,#4158,.T.);
#43917=EDGE_CURVE('',#35325,#35327,#4159,.T.);
#43918=EDGE_CURVE('',#35327,#35328,#20615,.T.);
#43919=EDGE_CURVE('',#35328,#35329,#29312,.T.);
#43920=EDGE_CURVE('',#35329,#35326,#20616,.T.);
#43921=EDGE_CURVE('',#35330,#35331,#29313,.T.);
#43922=EDGE_CURVE('',#35328,#35331,#1777,.T.);
#43923=EDGE_CURVE('',#35328,#35332,#29314,.T.);
#43924=EDGE_CURVE('',#35330,#35332,#1778,.T.);
#43925=EDGE_CURVE('',#35333,#35334,#29315,.T.);
#43926=EDGE_CURVE('',#35333,#35335,#20617,.T.);
#43927=EDGE_CURVE('',#35335,#35332,#29316,.T.);
#43928=EDGE_CURVE('',#35332,#35334,#20618,.T.);
#43929=EDGE_CURVE('',#35336,#35337,#29317,.T.);
#43930=EDGE_CURVE('',#35336,#35333,#4160,.T.);
#43931=EDGE_CURVE('',#35334,#35337,#4161,.T.);
#43932=EDGE_CURVE('',#35338,#35339,#29318,.T.);
#43933=EDGE_CURVE('',#35338,#35336,#29319,.T.);
#43934=EDGE_CURVE('',#35337,#35339,#29320,.T.);
#43935=EDGE_CURVE('',#35340,#35341,#29321,.T.);
#43936=EDGE_CURVE('',#35340,#35338,#4162,.T.);
#43937=EDGE_CURVE('',#35339,#35341,#4163,.T.);
#43938=EDGE_CURVE('',#35342,#35343,#29322,.T.);
#43939=EDGE_CURVE('',#35342,#35340,#20619,.T.);
#43940=EDGE_CURVE('',#35341,#35343,#20620,.T.);
#43941=EDGE_CURVE('',#35344,#35345,#29323,.T.);
#43942=EDGE_CURVE('',#35343,#35345,#1779,.T.);
#43943=EDGE_CURVE('',#35343,#35346,#29324,.T.);
#43944=EDGE_CURVE('',#35344,#35346,#29325,.T.);
#43945=EDGE_CURVE('',#35347,#35348,#29326,.T.);
#43946=EDGE_CURVE('',#35347,#35349,#20621,.T.);
#43947=EDGE_CURVE('',#35349,#35346,#29327,.T.);
#43948=EDGE_CURVE('',#35346,#35348,#20622,.T.);
#43949=EDGE_CURVE('',#35350,#35351,#29328,.T.);
#43950=EDGE_CURVE('',#35350,#35347,#4164,.T.);
#43951=EDGE_CURVE('',#35348,#35351,#4165,.T.);
#43952=EDGE_CURVE('',#35352,#35353,#29329,.T.);
#43953=EDGE_CURVE('',#35352,#35350,#29330,.T.);
#43954=EDGE_CURVE('',#35351,#35353,#29331,.T.);
#43955=EDGE_CURVE('',#35354,#35355,#29332,.T.);
#43956=EDGE_CURVE('',#35354,#35352,#4166,.T.);
#43957=EDGE_CURVE('',#35353,#35355,#4167,.T.);
#43958=EDGE_CURVE('',#35356,#35357,#29333,.T.);
#43959=EDGE_CURVE('',#35356,#35354,#20623,.T.);
#43960=EDGE_CURVE('',#35355,#35357,#20624,.T.);
#43961=EDGE_CURVE('',#35211,#35358,#29334,.T.);
#43962=EDGE_CURVE('',#35216,#35359,#29335,.T.);
#43963=EDGE_CURVE('',#35359,#35358,#4168,.T.);
#43964=EDGE_CURVE('',#35215,#35360,#29336,.T.);
#43965=EDGE_CURVE('',#35360,#35359,#29337,.T.);
#43966=EDGE_CURVE('',#35214,#35361,#29338,.T.);
#43967=EDGE_CURVE('',#35361,#35360,#4169,.T.);
#43968=EDGE_CURVE('',#35362,#35363,#20625,.T.);
#43969=EDGE_CURVE('',#35363,#35364,#29339,.T.);
#43970=EDGE_CURVE('',#35364,#35365,#20626,.T.);
#43971=EDGE_CURVE('',#35366,#35365,#4170,.T.);
#43972=EDGE_CURVE('',#35367,#35366,#29340,.T.);
#43973=EDGE_CURVE('',#35362,#35367,#29341,.T.);
#43974=EDGE_CURVE('',#35213,#35363,#29342,.T.);
#43975=EDGE_CURVE('',#35368,#35362,#4171,.T.);
#43976=EDGE_CURVE('',#35369,#35368,#20627,.T.);
#43977=EDGE_CURVE('',#35370,#35369,#29343,.T.);
#43978=EDGE_CURVE('',#35371,#35370,#20628,.T.);
#43979=EDGE_CURVE('',#35372,#35371,#4172,.T.);
#43980=EDGE_CURVE('',#35373,#35372,#29344,.T.);
#43981=EDGE_CURVE('',#35374,#35373,#4173,.T.);
#43982=EDGE_CURVE('',#35375,#35374,#20629,.T.);
#43983=EDGE_CURVE('',#35376,#35375,#29345,.T.);
#43984=EDGE_CURVE('',#35377,#35376,#20630,.T.);
#43985=EDGE_CURVE('',#35378,#35377,#4174,.T.);
#43986=EDGE_CURVE('',#35379,#35378,#29346,.T.);
#43987=EDGE_CURVE('',#35380,#35379,#4175,.T.);
#43988=EDGE_CURVE('',#35381,#35380,#20631,.T.);
#43989=EDGE_CURVE('',#35382,#35381,#29347,.T.);
#43990=EDGE_CURVE('',#35383,#35382,#20632,.T.);
#43991=EDGE_CURVE('',#35384,#35383,#4176,.T.);
#43992=EDGE_CURVE('',#35385,#35384,#29348,.T.);
#43993=EDGE_CURVE('',#35386,#35385,#4177,.T.);
#43994=EDGE_CURVE('',#35387,#35386,#20633,.T.);
#43995=EDGE_CURVE('',#35388,#35387,#29349,.T.);
#43996=EDGE_CURVE('',#35389,#35388,#20634,.T.);
#43997=EDGE_CURVE('',#35390,#35389,#4178,.T.);
#43998=EDGE_CURVE('',#35391,#35390,#29350,.T.);
#43999=EDGE_CURVE('',#35392,#35391,#4179,.T.);
#44000=EDGE_CURVE('',#35393,#35392,#20635,.T.);
#44001=EDGE_CURVE('',#35394,#35393,#29351,.T.);
#44002=EDGE_CURVE('',#35395,#35394,#20636,.T.);
#44003=EDGE_CURVE('',#35396,#35395,#4180,.T.);
#44004=EDGE_CURVE('',#35397,#35396,#29352,.T.);
#44005=EDGE_CURVE('',#35398,#35397,#4181,.T.);
#44006=EDGE_CURVE('',#35399,#35398,#20637,.T.);
#44007=EDGE_CURVE('',#35400,#35399,#29353,.T.);
#44008=EDGE_CURVE('',#35401,#35400,#20638,.T.);
#44009=EDGE_CURVE('',#35214,#35401,#4182,.T.);
#44010=EDGE_CURVE('',#35402,#35367,#29354,.T.);
#44011=EDGE_CURVE('',#35402,#35403,#4183,.T.);
#44012=EDGE_CURVE('',#35403,#35362,#29355,.T.);
#44013=EDGE_CURVE('',#35366,#35404,#29356,.T.);
#44014=EDGE_CURVE('',#35404,#35402,#29357,.T.);
#44015=EDGE_CURVE('',#35365,#35405,#29358,.T.);
#44016=EDGE_CURVE('',#35405,#35404,#4184,.T.);
#44017=EDGE_CURVE('',#35406,#35407,#20639,.T.);
#44018=EDGE_CURVE('',#35407,#35408,#29359,.T.);
#44019=EDGE_CURVE('',#35408,#35409,#20640,.T.);
#44020=EDGE_CURVE('',#35406,#35409,#29360,.T.);
#44021=EDGE_CURVE('',#35410,#35411,#20641,.T.);
#44022=EDGE_CURVE('',#35412,#35410,#20642,.T.);
#44023=EDGE_CURVE('',#35413,#35412,#4185,.T.);
#44024=EDGE_CURVE('',#35414,#35413,#20643,.T.);
#44025=EDGE_CURVE('',#35415,#35414,#4186,.T.);
#44026=EDGE_CURVE('',#35416,#35415,#20644,.T.);
#44027=EDGE_CURVE('',#35417,#35416,#20645,.T.);
#44028=EDGE_CURVE('',#35418,#35417,#4187,.T.);
#44029=EDGE_CURVE('',#35419,#35418,#20646,.T.);
#44030=EDGE_CURVE('',#35365,#35419,#1780,.T.);
#44031=EDGE_CURVE('',#35407,#35364,#20647,.T.);
#44032=EDGE_CURVE('',#35420,#35406,#20648,.T.);
#44033=EDGE_CURVE('',#35421,#35420,#20649,.T.);
#44034=EDGE_CURVE('',#35422,#35421,#4188,.T.);
#44035=EDGE_CURVE('',#35423,#35422,#20650,.T.);
#44036=EDGE_CURVE('',#35424,#35423,#4189,.T.);
#44037=EDGE_CURVE('',#35411,#35424,#20651,.T.);
#44038=EDGE_CURVE('',#35406,#35425,#29361,.T.);
#44039=EDGE_CURVE('',#35409,#35426,#29362,.T.);
#44040=EDGE_CURVE('',#35426,#35425,#29363,.T.);
#44041=EDGE_CURVE('',#35427,#35428,#20652,.T.);
#44042=EDGE_CURVE('',#35428,#35429,#29364,.T.);
#44043=EDGE_CURVE('',#35429,#35430,#20653,.T.);
#44044=EDGE_CURVE('',#35427,#35430,#29365,.T.);
#44045=EDGE_CURVE('',#35428,#35408,#20654,.T.);
#44046=EDGE_CURVE('',#35409,#35427,#20655,.T.);
#44047=EDGE_CURVE('',#35427,#35431,#29366,.T.);
#44048=EDGE_CURVE('',#35430,#35432,#29367,.T.);
#44049=EDGE_CURVE('',#35432,#35431,#29368,.T.);
#44050=EDGE_CURVE('',#35433,#35434,#20656,.T.);
#44051=EDGE_CURVE('',#35435,#35433,#20657,.T.);
#44052=EDGE_CURVE('',#35436,#35435,#4190,.T.);
#44053=EDGE_CURVE('',#35437,#35436,#20658,.T.);
#44054=EDGE_CURVE('',#35438,#35437,#4191,.T.);
#44055=EDGE_CURVE('',#35439,#35438,#20659,.T.);
#44056=EDGE_CURVE('',#35430,#35439,#20660,.T.);
#44057=EDGE_CURVE('',#35313,#35429,#20661,.T.);
#44058=EDGE_CURVE('',#35440,#35312,#4192,.T.);
#44059=EDGE_CURVE('',#35441,#35440,#20662,.T.);
#44060=EDGE_CURVE('',#35442,#35441,#4193,.T.);
#44061=EDGE_CURVE('',#35443,#35442,#20663,.T.);
#44062=EDGE_CURVE('',#35444,#35443,#4194,.T.);
#44063=EDGE_CURVE('',#35434,#35444,#20664,.T.);
#44064=EDGE_CURVE('',#35401,#35445,#29369,.T.);
#44065=EDGE_CURVE('',#35445,#35361,#4195,.T.);
#44066=EDGE_CURVE('',#35400,#35446,#29370,.T.);
#44067=EDGE_CURVE('',#35446,#35445,#20665,.T.);
#44068=EDGE_CURVE('',#35447,#35448,#29371,.T.);
#44069=EDGE_CURVE('',#35400,#35448,#1781,.T.);
#44070=EDGE_CURVE('',#35447,#35399,#1782,.T.);
#44071=EDGE_CURVE('',#35449,#35398,#29372,.T.);
#44072=EDGE_CURVE('',#35449,#35450,#20666,.T.);
#44073=EDGE_CURVE('',#35450,#35399,#29373,.T.);
#44074=EDGE_CURVE('',#35451,#35397,#29374,.T.);
#44075=EDGE_CURVE('',#35451,#35449,#4196,.T.);
#44076=EDGE_CURVE('',#35452,#35396,#29375,.T.);
#44077=EDGE_CURVE('',#35452,#35451,#29376,.T.);
#44078=EDGE_CURVE('',#35453,#35395,#29377,.T.);
#44079=EDGE_CURVE('',#35453,#35452,#4197,.T.);
#44080=EDGE_CURVE('',#35454,#35394,#29378,.T.);
#44081=EDGE_CURVE('',#35454,#35453,#20667,.T.);
#44082=EDGE_CURVE('',#35455,#35456,#29379,.T.);
#44083=EDGE_CURVE('',#35394,#35456,#1783,.T.);
#44084=EDGE_CURVE('',#35455,#35393,#1784,.T.);
#44085=EDGE_CURVE('',#35393,#35457,#29380,.T.);
#44086=EDGE_CURVE('',#35392,#35458,#29381,.T.);
#44087=EDGE_CURVE('',#35458,#35457,#20668,.T.);
#44088=EDGE_CURVE('',#35391,#35459,#29382,.T.);
#44089=EDGE_CURVE('',#35459,#35458,#4198,.T.);
#44090=EDGE_CURVE('',#35390,#35460,#29383,.T.);
#44091=EDGE_CURVE('',#35460,#35459,#29384,.T.);
#44092=EDGE_CURVE('',#35461,#35389,#29385,.T.);
#44093=EDGE_CURVE('',#35461,#35460,#4199,.T.);
#44094=EDGE_CURVE('',#35462,#35388,#29386,.T.);
#44095=EDGE_CURVE('',#35462,#35461,#20669,.T.);
#44096=EDGE_CURVE('',#35463,#35464,#29387,.T.);
#44097=EDGE_CURVE('',#35388,#35464,#1785,.T.);
#44098=EDGE_CURVE('',#35463,#35387,#29388,.T.);
#44099=EDGE_CURVE('',#35387,#35465,#29389,.T.);
#44100=EDGE_CURVE('',#35386,#35466,#29390,.T.);
#44101=EDGE_CURVE('',#35466,#35465,#20670,.T.);
#44102=EDGE_CURVE('',#35385,#35467,#29391,.T.);
#44103=EDGE_CURVE('',#35467,#35466,#4200,.T.);
#44104=EDGE_CURVE('',#35384,#35468,#29392,.T.);
#44105=EDGE_CURVE('',#35468,#35467,#29393,.T.);
#44106=EDGE_CURVE('',#35469,#35383,#29394,.T.);
#44107=EDGE_CURVE('',#35469,#35468,#4201,.T.);
#44108=EDGE_CURVE('',#35470,#35382,#29395,.T.);
#44109=EDGE_CURVE('',#35470,#35469,#20671,.T.);
#44110=EDGE_CURVE('',#35471,#35472,#29396,.T.);
#44111=EDGE_CURVE('',#35382,#35472,#29397,.T.);
#44112=EDGE_CURVE('',#35471,#35381,#1786,.T.);
#44113=EDGE_CURVE('',#35381,#35473,#29398,.T.);
#44114=EDGE_CURVE('',#35380,#35474,#29399,.T.);
#44115=EDGE_CURVE('',#35474,#35473,#20672,.T.);
#44116=EDGE_CURVE('',#35379,#35475,#29400,.T.);
#44117=EDGE_CURVE('',#35475,#35474,#4202,.T.);
#44118=EDGE_CURVE('',#35378,#35476,#29401,.T.);
#44119=EDGE_CURVE('',#35476,#35475,#29402,.T.);
#44120=EDGE_CURVE('',#35477,#35377,#29403,.T.);
#44121=EDGE_CURVE('',#35477,#35476,#4203,.T.);
#44122=EDGE_CURVE('',#35478,#35376,#29404,.T.);
#44123=EDGE_CURVE('',#35478,#35477,#20673,.T.);
#44124=EDGE_CURVE('',#35479,#35480,#29405,.T.);
#44125=EDGE_CURVE('',#35376,#35480,#1787,.T.);
#44126=EDGE_CURVE('',#35479,#35375,#1788,.T.);
#44127=EDGE_CURVE('',#35481,#35374,#29406,.T.);
#44128=EDGE_CURVE('',#35481,#35482,#20674,.T.);
#44129=EDGE_CURVE('',#35482,#35375,#29407,.T.);
#44130=EDGE_CURVE('',#35483,#35373,#29408,.T.);
#44131=EDGE_CURVE('',#35483,#35481,#4204,.T.);
#44132=EDGE_CURVE('',#35484,#35372,#29409,.T.);
#44133=EDGE_CURVE('',#35484,#35483,#29410,.T.);
#44134=EDGE_CURVE('',#35485,#35371,#29411,.T.);
#44135=EDGE_CURVE('',#35485,#35484,#4205,.T.);
#44136=EDGE_CURVE('',#35486,#35370,#29412,.T.);
#44137=EDGE_CURVE('',#35486,#35485,#20675,.T.);
#44138=EDGE_CURVE('',#35487,#35488,#29413,.T.);
#44139=EDGE_CURVE('',#35370,#35488,#1789,.T.);
#44140=EDGE_CURVE('',#35487,#35369,#1790,.T.);
#44141=EDGE_CURVE('',#35489,#35368,#29414,.T.);
#44142=EDGE_CURVE('',#35489,#35490,#20676,.T.);
#44143=EDGE_CURVE('',#35490,#35369,#29415,.T.);
#44144=EDGE_CURVE('',#35403,#35489,#4206,.T.);
#44145=EDGE_CURVE('',#35491,#35492,#20677,.T.);
#44146=EDGE_CURVE('',#35229,#35492,#4207,.T.);
#44147=EDGE_CURVE('',#35491,#35230,#4208,.T.);
#44148=EDGE_CURVE('',#35230,#35493,#29416,.T.);
#44149=EDGE_CURVE('',#35243,#35494,#29417,.T.);
#44150=EDGE_CURVE('',#35494,#35493,#20678,.T.);
#44151=EDGE_CURVE('',#35242,#35495,#29418,.T.);
#44152=EDGE_CURVE('',#35495,#35494,#4209,.T.);
#44153=EDGE_CURVE('',#35241,#35496,#29419,.T.);
#44154=EDGE_CURVE('',#35496,#35495,#20679,.T.);
#44155=EDGE_CURVE('',#35240,#35497,#29420,.T.);
#44156=EDGE_CURVE('',#35497,#35496,#4210,.T.);
#44157=EDGE_CURVE('',#35239,#35498,#29421,.T.);
#44158=EDGE_CURVE('',#35498,#35497,#20680,.T.);
#44159=EDGE_CURVE('',#35244,#35499,#20681,.T.);
#44160=EDGE_CURVE('',#35239,#35499,#4211,.T.);
#44161=EDGE_CURVE('',#35500,#35238,#29422,.T.);
#44162=EDGE_CURVE('',#35500,#35224,#4212,.T.);
#44163=EDGE_CURVE('',#35501,#35237,#29423,.T.);
#44164=EDGE_CURVE('',#35501,#35500,#20682,.T.);
#44165=EDGE_CURVE('',#35502,#35236,#29424,.T.);
#44166=EDGE_CURVE('',#35502,#35503,#4213,.T.);
#44167=EDGE_CURVE('',#35237,#35503,#4214,.T.);
#44168=EDGE_CURVE('',#35504,#35502,#20683,.T.);
#44169=EDGE_CURVE('',#35504,#35235,#4215,.T.);
#44170=EDGE_CURVE('',#35235,#35505,#29425,.T.);
#44171=EDGE_CURVE('',#35234,#35506,#29426,.T.);
#44172=EDGE_CURVE('',#35506,#35505,#20684,.T.);
#44173=EDGE_CURVE('',#35233,#35507,#29427,.T.);
#44174=EDGE_CURVE('',#35507,#35506,#4216,.T.);
#44175=EDGE_CURVE('',#35232,#35508,#29428,.T.);
#44176=EDGE_CURVE('',#35508,#35507,#20685,.T.);
#44177=EDGE_CURVE('',#35509,#35231,#29429,.T.);
#44178=EDGE_CURVE('',#35509,#35508,#4217,.T.);
#44179=EDGE_CURVE('',#35510,#35229,#29430,.T.);
#44180=EDGE_CURVE('',#35510,#35509,#20686,.T.);
#44181=EDGE_CURVE('',#35250,#35245,#20687,.T.);
#44182=EDGE_CURVE('',#35312,#35511,#29431,.T.);
#44183=EDGE_CURVE('',#35317,#35511,#4218,.T.);
#44184=EDGE_CURVE('',#35512,#35513,#20688,.T.);
#44185=EDGE_CURVE('',#35433,#35513,#4219,.T.);
#44186=EDGE_CURVE('',#35512,#35434,#4220,.T.);
#44187=EDGE_CURVE('',#35514,#35444,#29432,.T.);
#44188=EDGE_CURVE('',#35514,#35515,#20689,.T.);
#44189=EDGE_CURVE('',#35515,#35434,#29433,.T.);
#44190=EDGE_CURVE('',#35516,#35443,#29434,.T.);
#44191=EDGE_CURVE('',#35516,#35514,#4221,.T.);
#44192=EDGE_CURVE('',#35517,#35442,#29435,.T.);
#44193=EDGE_CURVE('',#35517,#35516,#20690,.T.);
#44194=EDGE_CURVE('',#35518,#35441,#29436,.T.);
#44195=EDGE_CURVE('',#35518,#35517,#4222,.T.);
#44196=EDGE_CURVE('',#35440,#35519,#29437,.T.);
#44197=EDGE_CURVE('',#35519,#35518,#20691,.T.);
#44198=EDGE_CURVE('',#35511,#35520,#4223,.T.);
#44199=EDGE_CURVE('',#35440,#35520,#4224,.T.);
#44200=EDGE_CURVE('',#35521,#35432,#20692,.T.);
#44201=EDGE_CURVE('',#35521,#35439,#4225,.T.);
#44202=EDGE_CURVE('',#35439,#35522,#29438,.T.);
#44203=EDGE_CURVE('',#35438,#35523,#29439,.T.);
#44204=EDGE_CURVE('',#35523,#35522,#20693,.T.);
#44205=EDGE_CURVE('',#35437,#35524,#29440,.T.);
#44206=EDGE_CURVE('',#35524,#35523,#4226,.T.);
#44207=EDGE_CURVE('',#35436,#35525,#29441,.T.);
#44208=EDGE_CURVE('',#35525,#35524,#20694,.T.);
#44209=EDGE_CURVE('',#35435,#35526,#29442,.T.);
#44210=EDGE_CURVE('',#35526,#35525,#4227,.T.);
#44211=EDGE_CURVE('',#35433,#35527,#29443,.T.);
#44212=EDGE_CURVE('',#35527,#35526,#20695,.T.);
#44213=EDGE_CURVE('',#35431,#35426,#20696,.T.);
#44214=EDGE_CURVE('',#35528,#35529,#20697,.T.);
#44215=EDGE_CURVE('',#35410,#35529,#4228,.T.);
#44216=EDGE_CURVE('',#35528,#35411,#4229,.T.);
#44217=EDGE_CURVE('',#35530,#35424,#29444,.T.);
#44218=EDGE_CURVE('',#35530,#35531,#20698,.T.);
#44219=EDGE_CURVE('',#35531,#35411,#29445,.T.);
#44220=EDGE_CURVE('',#35532,#35423,#29446,.T.);
#44221=EDGE_CURVE('',#35532,#35530,#4230,.T.);
#44222=EDGE_CURVE('',#35533,#35422,#29447,.T.);
#44223=EDGE_CURVE('',#35533,#35532,#20699,.T.);
#44224=EDGE_CURVE('',#35534,#35421,#29448,.T.);
#44225=EDGE_CURVE('',#35534,#35533,#4231,.T.);
#44226=EDGE_CURVE('',#35535,#35420,#29449,.T.);
#44227=EDGE_CURVE('',#35535,#35534,#20700,.T.);
#44228=EDGE_CURVE('',#35425,#35536,#20701,.T.);
#44229=EDGE_CURVE('',#35420,#35536,#4232,.T.);
#44230=EDGE_CURVE('',#35419,#35537,#29450,.T.);
#44231=EDGE_CURVE('',#35537,#35405,#1791,.T.);
#44232=EDGE_CURVE('',#35418,#35538,#29451,.T.);
#44233=EDGE_CURVE('',#35538,#35537,#20702,.T.);
#44234=EDGE_CURVE('',#35539,#35417,#29452,.T.);
#44235=EDGE_CURVE('',#35539,#35540,#1068,.T.);
#44236=EDGE_CURVE('',#35540,#35541,#29453,.T.);
#44237=EDGE_CURVE('',#35418,#35541,#4233,.T.);
#44238=EDGE_CURVE('',#35542,#35539,#20703,.T.);
#44239=EDGE_CURVE('',#35542,#35416,#4234,.T.);
#44240=EDGE_CURVE('',#35416,#35543,#29454,.T.);
#44241=EDGE_CURVE('',#35415,#35544,#29455,.T.);
#44242=EDGE_CURVE('',#35544,#35543,#20704,.T.);
#44243=EDGE_CURVE('',#35414,#35545,#29456,.T.);
#44244=EDGE_CURVE('',#35545,#35544,#4235,.T.);
#44245=EDGE_CURVE('',#35413,#35546,#29457,.T.);
#44246=EDGE_CURVE('',#35546,#35545,#20705,.T.);
#44247=EDGE_CURVE('',#35547,#35412,#29458,.T.);
#44248=EDGE_CURVE('',#35547,#35546,#4236,.T.);
#44249=EDGE_CURVE('',#35548,#35410,#29459,.T.);
#44250=EDGE_CURVE('',#35548,#35547,#20706,.T.);
#44251=EDGE_CURVE('',#35549,#35550,#4237,.T.);
#44252=EDGE_CURVE('',#35252,#35550,#29460,.T.);
#44253=EDGE_CURVE('',#35549,#35253,#4238,.T.);
#44254=EDGE_CURVE('',#35551,#35266,#29461,.T.);
#44255=EDGE_CURVE('',#35551,#35552,#20707,.T.);
#44256=EDGE_CURVE('',#35552,#35253,#29462,.T.);
#44257=EDGE_CURVE('',#35358,#35551,#1792,.T.);
#44258=EDGE_CURVE('',#35553,#35251,#20708,.T.);
#44259=EDGE_CURVE('',#35553,#35265,#4239,.T.);
#44260=EDGE_CURVE('',#35265,#35554,#29463,.T.);
#44261=EDGE_CURVE('',#35264,#35555,#29464,.T.);
#44262=EDGE_CURVE('',#35555,#35554,#20709,.T.);
#44263=EDGE_CURVE('',#35263,#35556,#29465,.T.);
#44264=EDGE_CURVE('',#35556,#35555,#4240,.T.);
#44265=EDGE_CURVE('',#35262,#35557,#29466,.T.);
#44266=EDGE_CURVE('',#35557,#35556,#20710,.T.);
#44267=EDGE_CURVE('',#35261,#35558,#29467,.T.);
#44268=EDGE_CURVE('',#35558,#35557,#4241,.T.);
#44269=EDGE_CURVE('',#35260,#35559,#29468,.T.);
#44270=EDGE_CURVE('',#35559,#35558,#20711,.T.);
#44271=EDGE_CURVE('',#35560,#35561,#20712,.T.);
#44272=EDGE_CURVE('',#35260,#35561,#4242,.T.);
#44273=EDGE_CURVE('',#35560,#35259,#4243,.T.);
#44274=EDGE_CURVE('',#35259,#35562,#29469,.T.);
#44275=EDGE_CURVE('',#35258,#35563,#29470,.T.);
#44276=EDGE_CURVE('',#35563,#35562,#20713,.T.);
#44277=EDGE_CURVE('',#35257,#35564,#29471,.T.);
#44278=EDGE_CURVE('',#35564,#35563,#4244,.T.);
#44279=EDGE_CURVE('',#35256,#35565,#29472,.T.);
#44280=EDGE_CURVE('',#35565,#35564,#20714,.T.);
#44281=EDGE_CURVE('',#35566,#35255,#29473,.T.);
#44282=EDGE_CURVE('',#35567,#35566,#29474,.T.);
#44283=EDGE_CURVE('',#35567,#35565,#4245,.T.);
#44284=EDGE_CURVE('',#35568,#35254,#29475,.T.);
#44285=EDGE_CURVE('',#35569,#35568,#29476,.T.);
#44286=EDGE_CURVE('',#35569,#35567,#20715,.T.);
#44287=EDGE_CURVE('',#35550,#35570,#20716,.T.);
#44288=EDGE_CURVE('',#35254,#35570,#4246,.T.);
#44289=EDGE_CURVE('',#35571,#35521,#20717,.T.);
#44290=EDGE_CURVE('',#35572,#35571,#29477,.T.);
#44291=EDGE_CURVE('',#35573,#35572,#29478,.T.);
#44292=EDGE_CURVE('',#35574,#35573,#29479,.T.);
#44293=EDGE_CURVE('',#35575,#35574,#20718,.T.);
#44294=EDGE_CURVE('',#35575,#35576,#29480,.T.);
#44295=EDGE_CURVE('',#35536,#35576,#20719,.T.);
#44296=EDGE_CURVE('',#35577,#35553,#20720,.T.);
#44297=EDGE_CURVE('',#35577,#35578,#29481,.T.);
#44298=EDGE_CURVE('',#35578,#35579,#29482,.T.);
#44299=EDGE_CURVE('',#35499,#35579,#20721,.T.);
#44300=EDGE_CURVE('',#35580,#35223,#20722,.T.);
#44301=EDGE_CURVE('',#35581,#35580,#20723,.T.);
#44302=EDGE_CURVE('',#35311,#35581,#20724,.T.);
#44303=EDGE_CURVE('',#35500,#35582,#20725,.T.);
#44304=EDGE_CURVE('',#35580,#35582,#29483,.T.);
#44305=EDGE_CURVE('',#35583,#35584,#29484,.T.);
#44306=EDGE_CURVE('',#35584,#35356,#1793,.T.);
#44307=EDGE_CURVE('',#35357,#35583,#1794,.T.);
#44308=EDGE_CURVE('',#35583,#35585,#4247,.T.);
#44309=EDGE_CURVE('',#35585,#35586,#29485,.T.);
#44310=EDGE_CURVE('',#35586,#35584,#4248,.T.);
#44311=EDGE_CURVE('',#35585,#35587,#4249,.T.);
#44312=EDGE_CURVE('',#35587,#35588,#1069,.T.);
#44313=EDGE_CURVE('',#35588,#35589,#29486,.T.);
#44314=EDGE_CURVE('',#35589,#35586,#4250,.T.);
#44315=EDGE_CURVE('',#35590,#35591,#29487,.T.);
#44316=EDGE_CURVE('',#35590,#35592,#29488,.T.);
#44317=EDGE_CURVE('',#35592,#35593,#29489,.T.);
#44318=EDGE_CURVE('',#35593,#35591,#29490,.T.);
#44319=EDGE_CURVE('',#35592,#35594,#20726,.T.);
#44320=EDGE_CURVE('',#35594,#35595,#29491,.T.);
#44321=EDGE_CURVE('',#35595,#35593,#20727,.T.);
#44322=EDGE_CURVE('',#35596,#35597,#4251,.T.);
#44323=EDGE_CURVE('',#35598,#35596,#4252,.T.);
#44324=EDGE_CURVE('',#35599,#35598,#4253,.T.);
#44325=EDGE_CURVE('',#35600,#35599,#20728,.T.);
#44326=EDGE_CURVE('',#35594,#35600,#4254,.T.);
#44327=EDGE_CURVE('',#35594,#35601,#20729,.T.);
#44328=EDGE_CURVE('',#35601,#35602,#29492,.T.);
#44329=EDGE_CURVE('',#35602,#35603,#20730,.T.);
#44330=EDGE_CURVE('',#35597,#35603,#29493,.T.);
#44331=EDGE_CURVE('',#35588,#35604,#20731,.T.);
#44332=EDGE_CURVE('',#35604,#35605,#29494,.T.);
#44333=EDGE_CURVE('',#35605,#35589,#20732,.T.);
#44334=EDGE_CURVE('',#35604,#35606,#29495,.T.);
#44335=EDGE_CURVE('',#35606,#35607,#29496,.T.);
#44336=EDGE_CURVE('',#35607,#35605,#29497,.T.);
#44337=EDGE_CURVE('',#35606,#35608,#20733,.T.);
#44338=EDGE_CURVE('',#35608,#35609,#29498,.T.);
#44339=EDGE_CURVE('',#35609,#35607,#20734,.T.);
#44340=EDGE_CURVE('',#35608,#35610,#29499,.T.);
#44341=EDGE_CURVE('',#35610,#35611,#29500,.T.);
#44342=EDGE_CURVE('',#35611,#35609,#29501,.T.);
#44343=EDGE_CURVE('',#35610,#35612,#20735,.T.);
#44344=EDGE_CURVE('',#35612,#35613,#29502,.T.);
#44345=EDGE_CURVE('',#35613,#35611,#20736,.T.);
#44346=EDGE_CURVE('',#35614,#35615,#1795,.T.);
#44347=EDGE_CURVE('',#35614,#35616,#29503,.T.);
#44348=EDGE_CURVE('',#35617,#35616,#1796,.T.);
#44349=EDGE_CURVE('',#35612,#35617,#4255,.T.);
#44350=EDGE_CURVE('',#35612,#35618,#29504,.T.);
#44351=EDGE_CURVE('',#35615,#35618,#4256,.T.);
#44352=EDGE_CURVE('',#35618,#35619,#29505,.T.);
#44353=EDGE_CURVE('',#35618,#35620,#20737,.T.);
#44354=EDGE_CURVE('',#35620,#35621,#29506,.T.);
#44355=EDGE_CURVE('',#35621,#35619,#20738,.T.);
#44356=EDGE_CURVE('',#35620,#35622,#29507,.T.);
#44357=EDGE_CURVE('',#35622,#35623,#29508,.T.);
#44358=EDGE_CURVE('',#35623,#35621,#29509,.T.);
#44359=EDGE_CURVE('',#35622,#35624,#20739,.T.);
#44360=EDGE_CURVE('',#35624,#35625,#29510,.T.);
#44361=EDGE_CURVE('',#35625,#35623,#20740,.T.);
#44362=EDGE_CURVE('',#35624,#35626,#29511,.T.);
#44363=EDGE_CURVE('',#35626,#35627,#29512,.T.);
#44364=EDGE_CURVE('',#35627,#35625,#29513,.T.);
#44365=EDGE_CURVE('',#35626,#35628,#20741,.T.);
#44366=EDGE_CURVE('',#35628,#35629,#29514,.T.);
#44367=EDGE_CURVE('',#35629,#35627,#20742,.T.);
#44368=EDGE_CURVE('',#35628,#35630,#29515,.T.);
#44369=EDGE_CURVE('',#35631,#35630,#29516,.T.);
#44370=EDGE_CURVE('',#35628,#35631,#29517,.T.);
#44371=EDGE_CURVE('',#35630,#35632,#4257,.T.);
#44372=EDGE_CURVE('',#35633,#35632,#29518,.T.);
#44373=EDGE_CURVE('',#35633,#35634,#4258,.T.);
#44374=EDGE_CURVE('',#35631,#35634,#4259,.T.);
#44375=EDGE_CURVE('',#35635,#35633,#20743,.T.);
#44376=EDGE_CURVE('',#35632,#35636,#20744,.T.);
#44377=EDGE_CURVE('',#35635,#35636,#29519,.T.);
#44378=EDGE_CURVE('',#35636,#35637,#29520,.T.);
#44379=EDGE_CURVE('',#35636,#35638,#20745,.T.);
#44380=EDGE_CURVE('',#35638,#35639,#29521,.T.);
#44381=EDGE_CURVE('',#35639,#35637,#20746,.T.);
#44382=EDGE_CURVE('',#35638,#35640,#29522,.T.);
#44383=EDGE_CURVE('',#35640,#35641,#29523,.T.);
#44384=EDGE_CURVE('',#35641,#35639,#29524,.T.);
#44385=EDGE_CURVE('',#35640,#35642,#20747,.T.);
#44386=EDGE_CURVE('',#35642,#35643,#29525,.T.);
#44387=EDGE_CURVE('',#35643,#35641,#20748,.T.);
#44388=EDGE_CURVE('',#35642,#35644,#29526,.T.);
#44389=EDGE_CURVE('',#35644,#35645,#29527,.T.);
#44390=EDGE_CURVE('',#35645,#35643,#29528,.T.);
#44391=EDGE_CURVE('',#35644,#35646,#20749,.T.);
#44392=EDGE_CURVE('',#35646,#35647,#29529,.T.);
#44393=EDGE_CURVE('',#35647,#35645,#20750,.T.);
#44394=EDGE_CURVE('',#35646,#35648,#20751,.T.);
#44395=EDGE_CURVE('',#35649,#35648,#29530,.T.);
#44396=EDGE_CURVE('',#35649,#35650,#20752,.T.);
#44397=EDGE_CURVE('',#35646,#35650,#29531,.T.);
#44398=EDGE_CURVE('',#35648,#35651,#29532,.T.);
#44399=EDGE_CURVE('',#35648,#35652,#20753,.T.);
#44400=EDGE_CURVE('',#35652,#35653,#29533,.T.);
#44401=EDGE_CURVE('',#35653,#35651,#20754,.T.);
#44402=EDGE_CURVE('',#35652,#35654,#29534,.T.);
#44403=EDGE_CURVE('',#35654,#35655,#29535,.T.);
#44404=EDGE_CURVE('',#35655,#35653,#29536,.T.);
#44405=EDGE_CURVE('',#35654,#35656,#20755,.T.);
#44406=EDGE_CURVE('',#35656,#35657,#29537,.T.);
#44407=EDGE_CURVE('',#35657,#35655,#20756,.T.);
#44408=EDGE_CURVE('',#35656,#35658,#29538,.T.);
#44409=EDGE_CURVE('',#35658,#35659,#29539,.T.);
#44410=EDGE_CURVE('',#35659,#35657,#29540,.T.);
#44411=EDGE_CURVE('',#35658,#35660,#20757,.T.);
#44412=EDGE_CURVE('',#35660,#35661,#29541,.T.);
#44413=EDGE_CURVE('',#35661,#35659,#20758,.T.);
#44414=EDGE_CURVE('',#35660,#35662,#20759,.T.);
#44415=EDGE_CURVE('',#35663,#35662,#29542,.T.);
#44416=EDGE_CURVE('',#35663,#35664,#20760,.T.);
#44417=EDGE_CURVE('',#35660,#35664,#29543,.T.);
#44418=EDGE_CURVE('',#35662,#35665,#29544,.T.);
#44419=EDGE_CURVE('',#35662,#35590,#20761,.T.);
#44420=EDGE_CURVE('',#35591,#35665,#20762,.T.);
#44421=EDGE_CURVE('',#35603,#35666,#20763,.T.);
#44422=EDGE_CURVE('',#35602,#35667,#20764,.T.);
#44423=EDGE_CURVE('',#35668,#35667,#20765,.T.);
#44424=EDGE_CURVE('',#35669,#35668,#20766,.T.);
#44425=EDGE_CURVE('',#35670,#35669,#1070,.T.);
#44426=EDGE_CURVE('',#35671,#35670,#20767,.T.);
#44427=EDGE_CURVE('',#35672,#35671,#4260,.T.);
#44428=EDGE_CURVE('',#35666,#35672,#20768,.T.);
#44429=EDGE_CURVE('',#35667,#35673,#29545,.T.);
#44430=EDGE_CURVE('',#35673,#35674,#20769,.T.);
#44431=EDGE_CURVE('',#35668,#35674,#4261,.T.);
#44432=EDGE_CURVE('',#35675,#35676,#29546,.T.);
#44433=EDGE_CURVE('',#35675,#35677,#29547,.T.);
#44434=EDGE_CURVE('',#35677,#35678,#29548,.T.);
#44435=EDGE_CURVE('',#35678,#35676,#29549,.T.);
#44436=EDGE_CURVE('',#35674,#35679,#29550,.T.);
#44437=EDGE_CURVE('',#35674,#35675,#20770,.T.);
#44438=EDGE_CURVE('',#35676,#35679,#20771,.T.);
#44439=EDGE_CURVE('',#35678,#35680,#20772,.T.);
#44440=EDGE_CURVE('',#35681,#35680,#29551,.T.);
#44441=EDGE_CURVE('',#35681,#35676,#20773,.T.);
#44442=EDGE_CURVE('',#35681,#35682,#29552,.T.);
#44443=EDGE_CURVE('',#35680,#35683,#29553,.T.);
#44444=EDGE_CURVE('',#35683,#35682,#29554,.T.);
#44445=EDGE_CURVE('',#35684,#35685,#29555,.T.);
#44446=EDGE_CURVE('',#35684,#35681,#20774,.T.);
#44447=EDGE_CURVE('',#35682,#35685,#20775,.T.);
#44448=EDGE_CURVE('',#35686,#35687,#29556,.T.);
#44449=EDGE_CURVE('',#35686,#35684,#29557,.T.);
#44450=EDGE_CURVE('',#35685,#35687,#29558,.T.);
#44451=EDGE_CURVE('',#35688,#35689,#29559,.T.);
#44452=EDGE_CURVE('',#35688,#35686,#29560,.T.);
#44453=EDGE_CURVE('',#35687,#35689,#29561,.T.);
#44454=EDGE_CURVE('',#35690,#35691,#29562,.T.);
#44455=EDGE_CURVE('',#35690,#35688,#29563,.T.);
#44456=EDGE_CURVE('',#35689,#35691,#29564,.T.);
#44457=EDGE_CURVE('',#35692,#35693,#29565,.T.);
#44458=EDGE_CURVE('',#35692,#35690,#20776,.T.);
#44459=EDGE_CURVE('',#35691,#35693,#20777,.T.);
#44460=EDGE_CURVE('',#35694,#35695,#29566,.T.);
#44461=EDGE_CURVE('',#35694,#35692,#29567,.T.);
#44462=EDGE_CURVE('',#35693,#35695,#29568,.T.);
#44463=EDGE_CURVE('',#35696,#35697,#29569,.T.);
#44464=EDGE_CURVE('',#35696,#35694,#29570,.T.);
#44465=EDGE_CURVE('',#35695,#35697,#29571,.T.);
#44466=EDGE_CURVE('',#35698,#35699,#29572,.T.);
#44467=EDGE_CURVE('',#35698,#35696,#29573,.T.);
#44468=EDGE_CURVE('',#35697,#35699,#29574,.T.);
#44469=EDGE_CURVE('',#35700,#35701,#29575,.T.);
#44470=EDGE_CURVE('',#35700,#35698,#20778,.T.);
#44471=EDGE_CURVE('',#35699,#35701,#20779,.T.);
#44472=EDGE_CURVE('',#35702,#35703,#29576,.T.);
#44473=EDGE_CURVE('',#35702,#35700,#29577,.T.);
#44474=EDGE_CURVE('',#35701,#35703,#29578,.T.);
#44475=EDGE_CURVE('',#35704,#35705,#29579,.T.);
#44476=EDGE_CURVE('',#35704,#35702,#29580,.T.);
#44477=EDGE_CURVE('',#35703,#35705,#29581,.T.);
#44478=EDGE_CURVE('',#35706,#35707,#29582,.T.);
#44479=EDGE_CURVE('',#35706,#35704,#29583,.T.);
#44480=EDGE_CURVE('',#35705,#35707,#29584,.T.);
#44481=EDGE_CURVE('',#35708,#35709,#29585,.T.);
#44482=EDGE_CURVE('',#35708,#35706,#20780,.T.);
#44483=EDGE_CURVE('',#35707,#35709,#20781,.T.);
#44484=EDGE_CURVE('',#35710,#35711,#29586,.T.);
#44485=EDGE_CURVE('',#35710,#35708,#29587,.T.);
#44486=EDGE_CURVE('',#35709,#35711,#29588,.T.);
#44487=EDGE_CURVE('',#35712,#35713,#4262,.F.);
#44488=EDGE_CURVE('',#35713,#35714,#29589,.T.);
#44489=EDGE_CURVE('',#35714,#35715,#20782,.T.);
#44490=EDGE_CURVE('',#35715,#35715,#29590,.T.);
#44491=EDGE_CURVE('',#35714,#35716,#29591,.T.);
#44492=EDGE_CURVE('',#35716,#35717,#4263,.T.);
#44493=EDGE_CURVE('',#35717,#35712,#29592,.T.);
#44494=EDGE_CURVE('',#35718,#35719,#29593,.T.);
#44495=EDGE_CURVE('',#35719,#35720,#4264,.T.);
#44496=EDGE_CURVE('',#35720,#35721,#20783,.T.);
#44497=EDGE_CURVE('',#35721,#35721,#29594,.T.);
#44498=EDGE_CURVE('',#35720,#35722,#4265,.T.);
#44499=EDGE_CURVE('',#35722,#35723,#29595,.T.);
#44500=EDGE_CURVE('',#35723,#35718,#4266,.T.);
#44501=EDGE_CURVE('',#35724,#35725,#29596,.T.);
#44502=EDGE_CURVE('',#35725,#35726,#4267,.T.);
#44503=EDGE_CURVE('',#35726,#35727,#29597,.T.);
#44504=EDGE_CURVE('',#35727,#35724,#4268,.T.);
#44505=EDGE_CURVE('',#35724,#35728,#20784,.T.);
#44506=EDGE_CURVE('',#35728,#35729,#29598,.T.);
#44507=EDGE_CURVE('',#35729,#35725,#20785,.T.);
#44508=EDGE_CURVE('',#35728,#35730,#29599,.T.);
#44509=EDGE_CURVE('',#35731,#35730,#1797,.T.);
#44510=EDGE_CURVE('',#35731,#35732,#29600,.T.);
#44511=EDGE_CURVE('',#35728,#35732,#1798,.T.);
#44512=EDGE_CURVE('',#35733,#35734,#29601,.T.);
#44513=EDGE_CURVE('',#35733,#35735,#20786,.T.);
#44514=EDGE_CURVE('',#35735,#35730,#29602,.T.);
#44515=EDGE_CURVE('',#35730,#35734,#20787,.T.);
#44516=EDGE_CURVE('',#35736,#35737,#29603,.T.);
#44517=EDGE_CURVE('',#35736,#35733,#4269,.T.);
#44518=EDGE_CURVE('',#35734,#35737,#4270,.T.);
#44519=EDGE_CURVE('',#35738,#35739,#29604,.T.);
#44520=EDGE_CURVE('',#35738,#35736,#29605,.T.);
#44521=EDGE_CURVE('',#35737,#35739,#29606,.T.);
#44522=EDGE_CURVE('',#35739,#35740,#4271,.T.);
#44523=EDGE_CURVE('',#35740,#35741,#29607,.T.);
#44524=EDGE_CURVE('',#35741,#35738,#4272,.T.);
#44525=EDGE_CURVE('',#35740,#35742,#20788,.T.);
#44526=EDGE_CURVE('',#35742,#35743,#29608,.T.);
#44527=EDGE_CURVE('',#35743,#35741,#20789,.T.);
#44528=EDGE_CURVE('',#35742,#35744,#29609,.T.);
#44529=EDGE_CURVE('',#35745,#35744,#1799,.T.);
#44530=EDGE_CURVE('',#35745,#35746,#29610,.T.);
#44531=EDGE_CURVE('',#35742,#35746,#1800,.T.);
#44532=EDGE_CURVE('',#35747,#35748,#29611,.T.);
#44533=EDGE_CURVE('',#35747,#35749,#20790,.T.);
#44534=EDGE_CURVE('',#35749,#35744,#29612,.T.);
#44535=EDGE_CURVE('',#35744,#35748,#20791,.T.);
#44536=EDGE_CURVE('',#35750,#35751,#29613,.T.);
#44537=EDGE_CURVE('',#35750,#35747,#4273,.T.);
#44538=EDGE_CURVE('',#35748,#35751,#4274,.T.);
#44539=EDGE_CURVE('',#35752,#35753,#29614,.T.);
#44540=EDGE_CURVE('',#35752,#35750,#29615,.T.);
#44541=EDGE_CURVE('',#35751,#35753,#29616,.T.);
#44542=EDGE_CURVE('',#35753,#35754,#4275,.T.);
#44543=EDGE_CURVE('',#35754,#35755,#29617,.T.);
#44544=EDGE_CURVE('',#35755,#35752,#4276,.T.);
#44545=EDGE_CURVE('',#35754,#35756,#20792,.T.);
#44546=EDGE_CURVE('',#35756,#35757,#29618,.T.);
#44547=EDGE_CURVE('',#35757,#35755,#20793,.T.);
#44548=EDGE_CURVE('',#35756,#35758,#29619,.T.);
#44549=EDGE_CURVE('',#35759,#35758,#29620,.T.);
#44550=EDGE_CURVE('',#35759,#35760,#29621,.T.);
#44551=EDGE_CURVE('',#35756,#35760,#1801,.T.);
#44552=EDGE_CURVE('',#35761,#35762,#29622,.T.);
#44553=EDGE_CURVE('',#35761,#35763,#20794,.T.);
#44554=EDGE_CURVE('',#35763,#35758,#29623,.T.);
#44555=EDGE_CURVE('',#35758,#35762,#20795,.T.);
#44556=EDGE_CURVE('',#35764,#35765,#29624,.T.);
#44557=EDGE_CURVE('',#35764,#35761,#4277,.T.);
#44558=EDGE_CURVE('',#35762,#35765,#4278,.T.);
#44559=EDGE_CURVE('',#35766,#35767,#20796,.T.);
#44560=EDGE_CURVE('',#35768,#35766,#4279,.T.);
#44561=EDGE_CURVE('',#35768,#35708,#20797,.T.);
#44562=EDGE_CURVE('',#35710,#35769,#20798,.T.);
#44563=EDGE_CURVE('',#35767,#35769,#4280,.T.);
#44564=EDGE_CURVE('',#35770,#35771,#29625,.T.);
#44565=EDGE_CURVE('',#35770,#35772,#4281,.T.);
#44566=EDGE_CURVE('',#35772,#35769,#29626,.T.);
#44567=EDGE_CURVE('',#35769,#35771,#4282,.T.);
#44568=EDGE_CURVE('',#35726,#35770,#29627,.T.);
#44569=EDGE_CURVE('',#35771,#35727,#29628,.T.);
#44570=EDGE_CURVE('',#35764,#35773,#1071,.T.);
#44571=EDGE_CURVE('',#35773,#35774,#29629,.T.);
#44572=EDGE_CURVE('',#35774,#35761,#4283,.T.);
#44573=EDGE_CURVE('',#35773,#35775,#20799,.T.);
#44574=EDGE_CURVE('',#35775,#35776,#29630,.T.);
#44575=EDGE_CURVE('',#35776,#35774,#20800,.T.);
#44576=EDGE_CURVE('',#35267,#35776,#4284,.T.);
#44577=EDGE_CURVE('',#35775,#35269,#4285,.T.);
#44578=EDGE_CURVE('',#35777,#35274,#29631,.T.);
#44579=EDGE_CURVE('',#35777,#35271,#1802,.T.);
#44580=EDGE_CURVE('',#35778,#35777,#1072,.T.);
#44581=EDGE_CURVE('',#35779,#35778,#1803,.T.);
#44582=EDGE_CURVE('',#35780,#35779,#20801,.T.);
#44583=EDGE_CURVE('',#35781,#35780,#1804,.T.);
#44584=EDGE_CURVE('',#35782,#35781,#1073,.T.);
#44585=EDGE_CURVE('',#35763,#35782,#1805,.T.);
#44586=EDGE_CURVE('',#35783,#35784,#4286,.T.);
#44587=EDGE_CURVE('',#35274,#35783,#4287,.T.);
#44588=EDGE_CURVE('',#35784,#35273,#4288,.T.);
#44589=EDGE_CURVE('',#35273,#35785,#29632,.T.);
#44590=EDGE_CURVE('',#35278,#35785,#1806,.T.);
#44591=EDGE_CURVE('',#35786,#35277,#4289,.T.);
#44592=EDGE_CURVE('',#35787,#35786,#20802,.T.);
#44593=EDGE_CURVE('',#35755,#35787,#4290,.T.);
#44594=EDGE_CURVE('',#35788,#35757,#1807,.T.);
#44595=EDGE_CURVE('',#35789,#35788,#1074,.T.);
#44596=EDGE_CURVE('',#35790,#35789,#4291,.T.);
#44597=EDGE_CURVE('',#35791,#35790,#20803,.T.);
#44598=EDGE_CURVE('',#35792,#35791,#4292,.T.);
#44599=EDGE_CURVE('',#35785,#35792,#1075,.T.);
#44600=EDGE_CURVE('',#35282,#35793,#1076,.T.);
#44601=EDGE_CURVE('',#35793,#35786,#29633,.T.);
#44602=EDGE_CURVE('',#35794,#35284,#4293,.T.);
#44603=EDGE_CURVE('',#35794,#35793,#4294,.T.);
#44604=EDGE_CURVE('',#35286,#35795,#4295,.T.);
#44605=EDGE_CURVE('',#35794,#35795,#29634,.T.);
#44606=EDGE_CURVE('',#35796,#35290,#29635,.T.);
#44607=EDGE_CURVE('',#35796,#35287,#1808,.T.);
#44608=EDGE_CURVE('',#35797,#35747,#4296,.T.);
#44609=EDGE_CURVE('',#35795,#35797,#20804,.T.);
#44610=EDGE_CURVE('',#35798,#35796,#1077,.T.);
#44611=EDGE_CURVE('',#35799,#35798,#4297,.T.);
#44612=EDGE_CURVE('',#35800,#35799,#20805,.T.);
#44613=EDGE_CURVE('',#35801,#35800,#4298,.T.);
#44614=EDGE_CURVE('',#35802,#35801,#1078,.T.);
#44615=EDGE_CURVE('',#35749,#35802,#1809,.T.);
#44616=EDGE_CURVE('',#35803,#35804,#4299,.T.);
#44617=EDGE_CURVE('',#35290,#35803,#1079,.T.);
#44618=EDGE_CURVE('',#35804,#35289,#4300,.T.);
#44619=EDGE_CURVE('',#35289,#35805,#29636,.T.);
#44620=EDGE_CURVE('',#35294,#35805,#1810,.T.);
#44621=EDGE_CURVE('',#35806,#35293,#20806,.T.);
#44622=EDGE_CURVE('',#35807,#35806,#29637,.T.);
#44623=EDGE_CURVE('',#35808,#35807,#20807,.T.);
#44624=EDGE_CURVE('',#35809,#35808,#29638,.T.);
#44625=EDGE_CURVE('',#35741,#35809,#20808,.T.);
#44626=EDGE_CURVE('',#35810,#35743,#1811,.T.);
#44627=EDGE_CURVE('',#35811,#35810,#4301,.T.);
#44628=EDGE_CURVE('',#35812,#35811,#4302,.T.);
#44629=EDGE_CURVE('',#35813,#35812,#20809,.T.);
#44630=EDGE_CURVE('',#35814,#35813,#4303,.T.);
#44631=EDGE_CURVE('',#35805,#35814,#4304,.T.);
#44632=EDGE_CURVE('',#35297,#35815,#20810,.T.);
#44633=EDGE_CURVE('',#35815,#35806,#29639,.T.);
#44634=EDGE_CURVE('',#35816,#35299,#20811,.T.);
#44635=EDGE_CURVE('',#35815,#35816,#20812,.T.);
#44636=EDGE_CURVE('',#35301,#35817,#20813,.T.);
#44637=EDGE_CURVE('',#35816,#35817,#29640,.T.);
#44638=EDGE_CURVE('',#35818,#35305,#29641,.T.);
#44639=EDGE_CURVE('',#35818,#35302,#1812,.T.);
#44640=EDGE_CURVE('',#35819,#35733,#20814,.T.);
#44641=EDGE_CURVE('',#35820,#35819,#29642,.T.);
#44642=EDGE_CURVE('',#35821,#35820,#20815,.T.);
#44643=EDGE_CURVE('',#35817,#35821,#29643,.T.);
#44644=EDGE_CURVE('',#35822,#35818,#4305,.T.);
#44645=EDGE_CURVE('',#35823,#35822,#4306,.T.);
#44646=EDGE_CURVE('',#35824,#35823,#20816,.T.);
#44647=EDGE_CURVE('',#35825,#35824,#4307,.T.);
#44648=EDGE_CURVE('',#35826,#35825,#4308,.T.);
#44649=EDGE_CURVE('',#35735,#35826,#1813,.T.);
#44650=EDGE_CURVE('',#35827,#35828,#4309,.T.);
#44651=EDGE_CURVE('',#35305,#35827,#1080,.T.);
#44652=EDGE_CURVE('',#35828,#35304,#4310,.T.);
#44653=EDGE_CURVE('',#35304,#35829,#29644,.T.);
#44654=EDGE_CURVE('',#35309,#35829,#1814,.T.);
#44655=EDGE_CURVE('',#35830,#35308,#20817,.T.);
#44656=EDGE_CURVE('',#35831,#35830,#29645,.T.);
#44657=EDGE_CURVE('',#35832,#35831,#20818,.T.);
#44658=EDGE_CURVE('',#35833,#35832,#29646,.T.);
#44659=EDGE_CURVE('',#35725,#35833,#20819,.T.);
#44660=EDGE_CURVE('',#35834,#35729,#1815,.T.);
#44661=EDGE_CURVE('',#35835,#35834,#4311,.T.);
#44662=EDGE_CURVE('',#35836,#35835,#4312,.T.);
#44663=EDGE_CURVE('',#35837,#35836,#20820,.T.);
#44664=EDGE_CURVE('',#35838,#35837,#4313,.T.);
#44665=EDGE_CURVE('',#35829,#35838,#4314,.T.);
#44666=EDGE_CURVE('',#35581,#35830,#29647,.T.);
#44667=EDGE_CURVE('',#35839,#35840,#29648,.T.);
#44668=EDGE_CURVE('',#35520,#35840,#4315,.T.);
#44669=EDGE_CURVE('',#35839,#35316,#29649,.T.);
#44670=EDGE_CURVE('',#35321,#35841,#1816,.T.);
#44671=EDGE_CURVE('',#35841,#35316,#29650,.T.);
#44672=EDGE_CURVE('',#35842,#35319,#20821,.T.);
#44673=EDGE_CURVE('',#35843,#35842,#29651,.T.);
#44674=EDGE_CURVE('',#35645,#35843,#20822,.T.);
#44675=EDGE_CURVE('',#35844,#35647,#29652,.T.);
#44676=EDGE_CURVE('',#35845,#35844,#20823,.T.);
#44677=EDGE_CURVE('',#35846,#35845,#4316,.T.);
#44678=EDGE_CURVE('',#35847,#35846,#4317,.T.);
#44679=EDGE_CURVE('',#35841,#35847,#29653,.T.);
#44680=EDGE_CURVE('',#35322,#35848,#20824,.T.);
#44681=EDGE_CURVE('',#35848,#35842,#29654,.T.);
#44682=EDGE_CURVE('',#35849,#35324,#20825,.T.);
#44683=EDGE_CURVE('',#35848,#35849,#20826,.T.);
#44684=EDGE_CURVE('',#35326,#35850,#20827,.T.);
#44685=EDGE_CURVE('',#35849,#35850,#29655,.T.);
#44686=EDGE_CURVE('',#35851,#35329,#1817,.T.);
#44687=EDGE_CURVE('',#35852,#35851,#4318,.T.);
#44688=EDGE_CURVE('',#35853,#35852,#4319,.T.);
#44689=EDGE_CURVE('',#35854,#35853,#20828,.T.);
#44690=EDGE_CURVE('',#35637,#35854,#29656,.T.);
#44691=EDGE_CURVE('',#35855,#35639,#20829,.T.);
#44692=EDGE_CURVE('',#35850,#35855,#29657,.T.);
#44693=EDGE_CURVE('',#35331,#35851,#29658,.T.);
#44694=EDGE_CURVE('',#35856,#35857,#4320,.T.);
#44695=EDGE_CURVE('',#35331,#35856,#4321,.T.);
#44696=EDGE_CURVE('',#35857,#35330,#1081,.T.);
#44697=EDGE_CURVE('',#35335,#35858,#1818,.T.);
#44698=EDGE_CURVE('',#35858,#35330,#29659,.T.);
#44699=EDGE_CURVE('',#35859,#35333,#4322,.T.);
#44700=EDGE_CURVE('',#35627,#35859,#20830,.T.);
#44701=EDGE_CURVE('',#35860,#35629,#29660,.T.);
#44702=EDGE_CURVE('',#35861,#35860,#4323,.T.);
#44703=EDGE_CURVE('',#35862,#35861,#4324,.T.);
#44704=EDGE_CURVE('',#35858,#35862,#4325,.T.);
#44705=EDGE_CURVE('',#35336,#35863,#4326,.T.);
#44706=EDGE_CURVE('',#35863,#35859,#29661,.T.);
#44707=EDGE_CURVE('',#35864,#35338,#4327,.T.);
#44708=EDGE_CURVE('',#35864,#35863,#29662,.T.);
#44709=EDGE_CURVE('',#35340,#35865,#4328,.T.);
#44710=EDGE_CURVE('',#35865,#35864,#29663,.T.);
#44711=EDGE_CURVE('',#35345,#35866,#29664,.T.);
#44712=EDGE_CURVE('',#35866,#35342,#1819,.T.);
#44713=EDGE_CURVE('',#35867,#35866,#4329,.T.);
#44714=EDGE_CURVE('',#35619,#35867,#4330,.T.);
#44715=EDGE_CURVE('',#35865,#35621,#20831,.T.);
#44716=EDGE_CURVE('',#35345,#35614,#4331,.T.);
#44717=EDGE_CURVE('',#35616,#35344,#4332,.T.);
#44718=EDGE_CURVE('',#35349,#35868,#1820,.T.);
#44719=EDGE_CURVE('',#35868,#35344,#29665,.T.);
#44720=EDGE_CURVE('',#35869,#35347,#4333,.T.);
#44721=EDGE_CURVE('',#35611,#35869,#20832,.T.);
#44722=EDGE_CURVE('',#35870,#35613,#4334,.T.);
#44723=EDGE_CURVE('',#35868,#35870,#1082,.T.);
#44724=EDGE_CURVE('',#35350,#35871,#1083,.T.);
#44725=EDGE_CURVE('',#35871,#35869,#29666,.T.);
#44726=EDGE_CURVE('',#35872,#35352,#4335,.T.);
#44727=EDGE_CURVE('',#35872,#35871,#4336,.T.);
#44728=EDGE_CURVE('',#35354,#35873,#4337,.T.);
#44729=EDGE_CURVE('',#35873,#35872,#29667,.T.);
#44730=EDGE_CURVE('',#35873,#35605,#20833,.T.);
#44731=EDGE_CURVE('',#35402,#35874,#20834,.T.);
#44732=EDGE_CURVE('',#35874,#35875,#29668,.T.);
#44733=EDGE_CURVE('',#35875,#35489,#20835,.T.);
#44734=EDGE_CURVE('',#35876,#35404,#20836,.T.);
#44735=EDGE_CURVE('',#35874,#35876,#20837,.T.);
#44736=EDGE_CURVE('',#35537,#35877,#20838,.T.);
#44737=EDGE_CURVE('',#35876,#35877,#29669,.T.);
#44738=EDGE_CURVE('',#35359,#35878,#20839,.T.);
#44739=EDGE_CURVE('',#35878,#35879,#29670,.T.);
#44740=EDGE_CURVE('',#35879,#35551,#20840,.T.);
#44741=EDGE_CURVE('',#35880,#35360,#20841,.T.);
#44742=EDGE_CURVE('',#35878,#35880,#20842,.T.);
#44743=EDGE_CURVE('',#35445,#35881,#20843,.T.);
#44744=EDGE_CURVE('',#35880,#35881,#29671,.T.);
#44745=EDGE_CURVE('',#35882,#35883,#20844,.T.);
#44746=EDGE_CURVE('',#35884,#35882,#29672,.T.);
#44747=EDGE_CURVE('',#35885,#35884,#20845,.T.);
#44748=EDGE_CURVE('',#35881,#35885,#29673,.T.);
#44749=EDGE_CURVE('',#35886,#35446,#1821,.T.);
#44750=EDGE_CURVE('',#35887,#35886,#4338,.T.);
#44751=EDGE_CURVE('',#35888,#35887,#4339,.T.);
#44752=EDGE_CURVE('',#35889,#35888,#20846,.T.);
#44753=EDGE_CURVE('',#35890,#35889,#4340,.T.);
#44754=EDGE_CURVE('',#35891,#35890,#4341,.T.);
#44755=EDGE_CURVE('',#35892,#35891,#1822,.T.);
#44756=EDGE_CURVE('',#35883,#35892,#20847,.T.);
#44757=EDGE_CURVE('',#35448,#35886,#29674,.T.);
#44758=EDGE_CURVE('',#35893,#35894,#4342,.T.);
#44759=EDGE_CURVE('',#35448,#35893,#1084,.T.);
#44760=EDGE_CURVE('',#35894,#35447,#4343,.T.);
#44761=EDGE_CURVE('',#35450,#35895,#1823,.T.);
#44762=EDGE_CURVE('',#35895,#35447,#29675,.T.);
#44763=EDGE_CURVE('',#35896,#35449,#20848,.T.);
#44764=EDGE_CURVE('',#35897,#35896,#29676,.T.);
#44765=EDGE_CURVE('',#35898,#35897,#20849,.T.);
#44766=EDGE_CURVE('',#35899,#35898,#29677,.T.);
#44767=EDGE_CURVE('',#35900,#35899,#20850,.T.);
#44768=EDGE_CURVE('',#35901,#35900,#20851,.T.);
#44769=EDGE_CURVE('',#35902,#35901,#1824,.T.);
#44770=EDGE_CURVE('',#35903,#35902,#4344,.T.);
#44771=EDGE_CURVE('',#35904,#35903,#4345,.T.);
#44772=EDGE_CURVE('',#35905,#35904,#20852,.T.);
#44773=EDGE_CURVE('',#35906,#35905,#4346,.T.);
#44774=EDGE_CURVE('',#35895,#35906,#4347,.T.);
#44775=EDGE_CURVE('',#35451,#35907,#20853,.T.);
#44776=EDGE_CURVE('',#35907,#35896,#29678,.T.);
#44777=EDGE_CURVE('',#35908,#35452,#20854,.T.);
#44778=EDGE_CURVE('',#35907,#35908,#20855,.T.);
#44779=EDGE_CURVE('',#35453,#35909,#20856,.T.);
#44780=EDGE_CURVE('',#35908,#35909,#29679,.T.);
#44781=EDGE_CURVE('',#35910,#35456,#29680,.T.);
#44782=EDGE_CURVE('',#35910,#35454,#1825,.T.);
#44783=EDGE_CURVE('',#35911,#35910,#4348,.T.);
#44784=EDGE_CURVE('',#35912,#35911,#4349,.T.);
#44785=EDGE_CURVE('',#35913,#35912,#20857,.T.);
#44786=EDGE_CURVE('',#35914,#35913,#4350,.T.);
#44787=EDGE_CURVE('',#35915,#35914,#4351,.T.);
#44788=EDGE_CURVE('',#35916,#35915,#1826,.T.);
#44789=EDGE_CURVE('',#35917,#35916,#20858,.T.);
#44790=EDGE_CURVE('',#35918,#35917,#29681,.T.);
#44791=EDGE_CURVE('',#35919,#35918,#20859,.T.);
#44792=EDGE_CURVE('',#35909,#35919,#29682,.T.);
#44793=EDGE_CURVE('',#35920,#35921,#4352,.T.);
#44794=EDGE_CURVE('',#35456,#35920,#4353,.T.);
#44795=EDGE_CURVE('',#35921,#35455,#1085,.T.);
#44796=EDGE_CURVE('',#35455,#35922,#29683,.T.);
#44797=EDGE_CURVE('',#35457,#35922,#1827,.T.);
#44798=EDGE_CURVE('',#35923,#35458,#4354,.T.);
#44799=EDGE_CURVE('',#35924,#35923,#20860,.T.);
#44800=EDGE_CURVE('',#35925,#35924,#4355,.T.);
#44801=EDGE_CURVE('',#35926,#35925,#20861,.T.);
#44802=EDGE_CURVE('',#35927,#35926,#1828,.T.);
#44803=EDGE_CURVE('',#35928,#35927,#4356,.T.);
#44804=EDGE_CURVE('',#35929,#35928,#4357,.T.);
#44805=EDGE_CURVE('',#35930,#35929,#20862,.T.);
#44806=EDGE_CURVE('',#35931,#35930,#4358,.T.);
#44807=EDGE_CURVE('',#35922,#35931,#4359,.T.);
#44808=EDGE_CURVE('',#35459,#35932,#4360,.T.);
#44809=EDGE_CURVE('',#35932,#35923,#29684,.T.);
#44810=EDGE_CURVE('',#35933,#35460,#4361,.T.);
#44811=EDGE_CURVE('',#35933,#35932,#4362,.T.);
#44812=EDGE_CURVE('',#35461,#35934,#4363,.T.);
#44813=EDGE_CURVE('',#35933,#35934,#29685,.T.);
#44814=EDGE_CURVE('',#35935,#35464,#29686,.T.);
#44815=EDGE_CURVE('',#35935,#35462,#1829,.T.);
#44816=EDGE_CURVE('',#35936,#35937,#4364,.T.);
#44817=EDGE_CURVE('',#35934,#35936,#20863,.T.);
#44818=EDGE_CURVE('',#35938,#35935,#1086,.T.);
#44819=EDGE_CURVE('',#35939,#35938,#4365,.T.);
#44820=EDGE_CURVE('',#35940,#35939,#20864,.T.);
#44821=EDGE_CURVE('',#35941,#35940,#4366,.T.);
#44822=EDGE_CURVE('',#35942,#35941,#1087,.T.);
#44823=EDGE_CURVE('',#35943,#35942,#1830,.T.);
#44824=EDGE_CURVE('',#35937,#35943,#20865,.T.);
#44825=EDGE_CURVE('',#35944,#35945,#4367,.T.);
#44826=EDGE_CURVE('',#35464,#35944,#1088,.T.);
#44827=EDGE_CURVE('',#35945,#35463,#4368,.T.);
#44828=EDGE_CURVE('',#35463,#35946,#29687,.T.);
#44829=EDGE_CURVE('',#35465,#35946,#1831,.T.);
#44830=EDGE_CURVE('',#35947,#35466,#4369,.T.);
#44831=EDGE_CURVE('',#35948,#35947,#20866,.T.);
#44832=EDGE_CURVE('',#35949,#35948,#4370,.T.);
#44833=EDGE_CURVE('',#35950,#35949,#20867,.T.);
#44834=EDGE_CURVE('',#35951,#35950,#1832,.T.);
#44835=EDGE_CURVE('',#35952,#35951,#1089,.T.);
#44836=EDGE_CURVE('',#35953,#35952,#1833,.T.);
#44837=EDGE_CURVE('',#35954,#35953,#20868,.T.);
#44838=EDGE_CURVE('',#35955,#35954,#1834,.T.);
#44839=EDGE_CURVE('',#35946,#35955,#1090,.T.);
#44840=EDGE_CURVE('',#35467,#35956,#1091,.T.);
#44841=EDGE_CURVE('',#35956,#35947,#29688,.T.);
#44842=EDGE_CURVE('',#35957,#35468,#1092,.T.);
#44843=EDGE_CURVE('',#35957,#35956,#29689,.T.);
#44844=EDGE_CURVE('',#35469,#35958,#4371,.T.);
#44845=EDGE_CURVE('',#35958,#35957,#29690,.T.);
#44846=EDGE_CURVE('',#35959,#35472,#29691,.T.);
#44847=EDGE_CURVE('',#35959,#35470,#1835,.T.);
#44848=EDGE_CURVE('',#35960,#35959,#1093,.T.);
#44849=EDGE_CURVE('',#35961,#35960,#1836,.T.);
#44850=EDGE_CURVE('',#35962,#35961,#20869,.T.);
#44851=EDGE_CURVE('',#35963,#35962,#1837,.T.);
#44852=EDGE_CURVE('',#35964,#35963,#4372,.T.);
#44853=EDGE_CURVE('',#35965,#35964,#1838,.T.);
#44854=EDGE_CURVE('',#35966,#35965,#20870,.T.);
#44855=EDGE_CURVE('',#35967,#35966,#4373,.T.);
#44856=EDGE_CURVE('',#35958,#35967,#20871,.T.);
#44857=EDGE_CURVE('',#35968,#35969,#1094,.T.);
#44858=EDGE_CURVE('',#35472,#35968,#4374,.T.);
#44859=EDGE_CURVE('',#35969,#35471,#1095,.T.);
#44860=EDGE_CURVE('',#35471,#35970,#29692,.T.);
#44861=EDGE_CURVE('',#35473,#35970,#1839,.T.);
#44862=EDGE_CURVE('',#35971,#35474,#4375,.T.);
#44863=EDGE_CURVE('',#35972,#35971,#20872,.T.);
#44864=EDGE_CURVE('',#35973,#35972,#4376,.T.);
#44865=EDGE_CURVE('',#35974,#35973,#20873,.T.);
#44866=EDGE_CURVE('',#35975,#35974,#1840,.T.);
#44867=EDGE_CURVE('',#35976,#35975,#1096,.T.);
#44868=EDGE_CURVE('',#35977,#35976,#4377,.T.);
#44869=EDGE_CURVE('',#35978,#35977,#20874,.T.);
#44870=EDGE_CURVE('',#35979,#35978,#4378,.T.);
#44871=EDGE_CURVE('',#35970,#35979,#1097,.T.);
#44872=EDGE_CURVE('',#35475,#35980,#1098,.T.);
#44873=EDGE_CURVE('',#35980,#35971,#29693,.T.);
#44874=EDGE_CURVE('',#35981,#35476,#4379,.T.);
#44875=EDGE_CURVE('',#35981,#35980,#4380,.T.);
#44876=EDGE_CURVE('',#35477,#35982,#4381,.T.);
#44877=EDGE_CURVE('',#35982,#35981,#29694,.T.);
#44878=EDGE_CURVE('',#35983,#35480,#29695,.T.);
#44879=EDGE_CURVE('',#35983,#35478,#1841,.T.);
#44880=EDGE_CURVE('',#35984,#35983,#4382,.T.);
#44881=EDGE_CURVE('',#35985,#35984,#4383,.T.);
#44882=EDGE_CURVE('',#35986,#35985,#20875,.T.);
#44883=EDGE_CURVE('',#35987,#35986,#4384,.T.);
#44884=EDGE_CURVE('',#35988,#35987,#4385,.T.);
#44885=EDGE_CURVE('',#35989,#35988,#1842,.T.);
#44886=EDGE_CURVE('',#35990,#35989,#20876,.T.);
#44887=EDGE_CURVE('',#35991,#35990,#4386,.T.);
#44888=EDGE_CURVE('',#35982,#35991,#20877,.T.);
#44889=EDGE_CURVE('',#35992,#35993,#4387,.T.);
#44890=EDGE_CURVE('',#35480,#35992,#1099,.T.);
#44891=EDGE_CURVE('',#35993,#35479,#4388,.T.);
#44892=EDGE_CURVE('',#35482,#35994,#1843,.T.);
#44893=EDGE_CURVE('',#35994,#35479,#29696,.T.);
#44894=EDGE_CURVE('',#35995,#35481,#20878,.T.);
#44895=EDGE_CURVE('',#35996,#35995,#29697,.T.);
#44896=EDGE_CURVE('',#35997,#35996,#20879,.T.);
#44897=EDGE_CURVE('',#35998,#35997,#29698,.T.);
#44898=EDGE_CURVE('',#35999,#35998,#20880,.T.);
#44899=EDGE_CURVE('',#36000,#35999,#1844,.T.);
#44900=EDGE_CURVE('',#36001,#36000,#4389,.T.);
#44901=EDGE_CURVE('',#36002,#36001,#4390,.T.);
#44902=EDGE_CURVE('',#36003,#36002,#20881,.T.);
#44903=EDGE_CURVE('',#36004,#36003,#4391,.T.);
#44904=EDGE_CURVE('',#35994,#36004,#4392,.T.);
#44905=EDGE_CURVE('',#35483,#36005,#20882,.T.);
#44906=EDGE_CURVE('',#36005,#35995,#29699,.T.);
#44907=EDGE_CURVE('',#36006,#35484,#20883,.T.);
#44908=EDGE_CURVE('',#36005,#36006,#20884,.T.);
#44909=EDGE_CURVE('',#35485,#36007,#20885,.T.);
#44910=EDGE_CURVE('',#36006,#36007,#29700,.T.);
#44911=EDGE_CURVE('',#36008,#35488,#29701,.T.);
#44912=EDGE_CURVE('',#36008,#35486,#1845,.T.);
#44913=EDGE_CURVE('',#36009,#36008,#4393,.T.);
#44914=EDGE_CURVE('',#36010,#36009,#4394,.T.);
#44915=EDGE_CURVE('',#36011,#36010,#20886,.T.);
#44916=EDGE_CURVE('',#36012,#36011,#4395,.T.);
#44917=EDGE_CURVE('',#36013,#36012,#4396,.T.);
#44918=EDGE_CURVE('',#36014,#36013,#1846,.T.);
#44919=EDGE_CURVE('',#36015,#36014,#20887,.T.);
#44920=EDGE_CURVE('',#36016,#36015,#20888,.T.);
#44921=EDGE_CURVE('',#36017,#36016,#29702,.T.);
#44922=EDGE_CURVE('',#36018,#36017,#20889,.T.);
#44923=EDGE_CURVE('',#36007,#36018,#29703,.T.);
#44924=EDGE_CURVE('',#36019,#36020,#4397,.T.);
#44925=EDGE_CURVE('',#35488,#36019,#1100,.T.);
#44926=EDGE_CURVE('',#36020,#35487,#1101,.T.);
#44927=EDGE_CURVE('',#35490,#36021,#1847,.T.);
#44928=EDGE_CURVE('',#36021,#35487,#29704,.T.);
#44929=EDGE_CURVE('',#36022,#36023,#1848,.T.);
#44930=EDGE_CURVE('',#36024,#36022,#4398,.T.);
#44931=EDGE_CURVE('',#36025,#36024,#4399,.T.);
#44932=EDGE_CURVE('',#36026,#36025,#20890,.T.);
#44933=EDGE_CURVE('',#36027,#36026,#4400,.T.);
#44934=EDGE_CURVE('',#36021,#36027,#4401,.T.);
#44935=EDGE_CURVE('',#36028,#35875,#29705,.T.);
#44936=EDGE_CURVE('',#36029,#36028,#20891,.T.);
#44937=EDGE_CURVE('',#36030,#36029,#29706,.T.);
#44938=EDGE_CURVE('',#36031,#36030,#20892,.T.);
#44939=EDGE_CURVE('',#36023,#36031,#20893,.T.);
#44940=EDGE_CURVE('',#36032,#36033,#4402,.T.);
#44941=EDGE_CURVE('',#36034,#36032,#29707,.T.);
#44942=EDGE_CURVE('',#35492,#36034,#20894,.T.);
#44943=EDGE_CURVE('',#36033,#35491,#20895,.T.);
#44944=EDGE_CURVE('',#35491,#36035,#29708,.T.);
#44945=EDGE_CURVE('',#35493,#36035,#1102,.T.);
#44946=EDGE_CURVE('',#36036,#35492,#29709,.T.);
#44947=EDGE_CURVE('',#36036,#35510,#1103,.T.);
#44948=EDGE_CURVE('',#36037,#36038,#1104,.T.);
#44949=EDGE_CURVE('',#36039,#36037,#20896,.T.);
#44950=EDGE_CURVE('',#36040,#36039,#4403,.T.);
#44951=EDGE_CURVE('',#36041,#36040,#4404,.T.);
#44952=EDGE_CURVE('',#36042,#36041,#4405,.T.);
#44953=EDGE_CURVE('',#36043,#36042,#20897,.T.);
#44954=EDGE_CURVE('',#36044,#36043,#4406,.T.);
#44955=EDGE_CURVE('',#36045,#36044,#4407,.T.);
#44956=EDGE_CURVE('',#36035,#36045,#20898,.T.);
#44957=EDGE_CURVE('',#36046,#35494,#20899,.T.);
#44958=EDGE_CURVE('',#36047,#36046,#29710,.T.);
#44959=EDGE_CURVE('',#36048,#36047,#20900,.T.);
#44960=EDGE_CURVE('',#36049,#36048,#29711,.T.);
#44961=EDGE_CURVE('',#36050,#36049,#20901,.T.);
#44962=EDGE_CURVE('',#36038,#36050,#20902,.T.);
#44963=EDGE_CURVE('',#35495,#36051,#20903,.T.);
#44964=EDGE_CURVE('',#36051,#36046,#29712,.T.);
#44965=EDGE_CURVE('',#36052,#35496,#20904,.T.);
#44966=EDGE_CURVE('',#36051,#36052,#20905,.T.);
#44967=EDGE_CURVE('',#35497,#36053,#20906,.T.);
#44968=EDGE_CURVE('',#36053,#36052,#29713,.T.);
#44969=EDGE_CURVE('',#36054,#36055,#4408,.T.);
#44970=EDGE_CURVE('',#36056,#36054,#20907,.T.);
#44971=EDGE_CURVE('',#36057,#36056,#1105,.T.);
#44972=EDGE_CURVE('',#36058,#36057,#20908,.T.);
#44973=EDGE_CURVE('',#36059,#36058,#20909,.T.);
#44974=EDGE_CURVE('',#36060,#36059,#29714,.T.);
#44975=EDGE_CURVE('',#36061,#36060,#20910,.T.);
#44976=EDGE_CURVE('',#36053,#36061,#29715,.T.);
#44977=EDGE_CURVE('',#36062,#35498,#1106,.T.);
#44978=EDGE_CURVE('',#36063,#36062,#20911,.T.);
#44979=EDGE_CURVE('',#36064,#36063,#4409,.T.);
#44980=EDGE_CURVE('',#36065,#36064,#20912,.T.);
#44981=EDGE_CURVE('',#36066,#36065,#20913,.T.);
#44982=EDGE_CURVE('',#36055,#36066,#20914,.T.);
#44983=EDGE_CURVE('',#35499,#36062,#29716,.T.);
#44984=EDGE_CURVE('',#36067,#35503,#29717,.T.);
#44985=EDGE_CURVE('',#36067,#35501,#4410,.T.);
#44986=EDGE_CURVE('',#36068,#36069,#20915,.T.);
#44987=EDGE_CURVE('',#36070,#36068,#29718,.T.);
#44988=EDGE_CURVE('',#36071,#36070,#20916,.T.);
#44989=EDGE_CURVE('',#35582,#36071,#29719,.T.);
#44990=EDGE_CURVE('',#36072,#36067,#1849,.T.);
#44991=EDGE_CURVE('',#36073,#36072,#4411,.T.);
#44992=EDGE_CURVE('',#36074,#36073,#4412,.T.);
#44993=EDGE_CURVE('',#36075,#36074,#20917,.T.);
#44994=EDGE_CURVE('',#36076,#36075,#4413,.T.);
#44995=EDGE_CURVE('',#36077,#36076,#4414,.T.);
#44996=EDGE_CURVE('',#36078,#36077,#4415,.T.);
#44997=EDGE_CURVE('',#36079,#36078,#4416,.T.);
#44998=EDGE_CURVE('',#36069,#36079,#20918,.T.);
#44999=EDGE_CURVE('',#36080,#36081,#29720,.T.);
#45000=EDGE_CURVE('',#35503,#36081,#1850,.T.);
#45001=EDGE_CURVE('',#35502,#36082,#29721,.T.);
#45002=EDGE_CURVE('',#36080,#36082,#4417,.T.);
#45003=EDGE_CURVE('',#36082,#35504,#20919,.T.);
#45004=EDGE_CURVE('',#35504,#36083,#29722,.T.);
#45005=EDGE_CURVE('',#35505,#36083,#1107,.T.);
#45006=EDGE_CURVE('',#36084,#35506,#20920,.T.);
#45007=EDGE_CURVE('',#36085,#36084,#29723,.T.);
#45008=EDGE_CURVE('',#36086,#36085,#20921,.T.);
#45009=EDGE_CURVE('',#36087,#36086,#29724,.T.);
#45010=EDGE_CURVE('',#36088,#36087,#20922,.T.);
#45011=EDGE_CURVE('',#36089,#36088,#20923,.T.);
#45012=EDGE_CURVE('',#36090,#36089,#1108,.T.);
#45013=EDGE_CURVE('',#36091,#36090,#20924,.T.);
#45014=EDGE_CURVE('',#36092,#36091,#4418,.T.);
#45015=EDGE_CURVE('',#36093,#36092,#4419,.T.);
#45016=EDGE_CURVE('',#36094,#36093,#4420,.T.);
#45017=EDGE_CURVE('',#36095,#36094,#20925,.T.);
#45018=EDGE_CURVE('',#36096,#36095,#4421,.T.);
#45019=EDGE_CURVE('',#36097,#36096,#4422,.T.);
#45020=EDGE_CURVE('',#36098,#36097,#4423,.T.);
#45021=EDGE_CURVE('',#36083,#36098,#20926,.T.);
#45022=EDGE_CURVE('',#35507,#36099,#20927,.T.);
#45023=EDGE_CURVE('',#36099,#36084,#29725,.T.);
#45024=EDGE_CURVE('',#36100,#35508,#20928,.T.);
#45025=EDGE_CURVE('',#36099,#36100,#20929,.T.);
#45026=EDGE_CURVE('',#35509,#36101,#20930,.T.);
#45027=EDGE_CURVE('',#36100,#36101,#29726,.T.);
#45028=EDGE_CURVE('',#36102,#36103,#20931,.T.);
#45029=EDGE_CURVE('',#36104,#36102,#29727,.T.);
#45030=EDGE_CURVE('',#36105,#36104,#20932,.T.);
#45031=EDGE_CURVE('',#36101,#36105,#29728,.T.);
#45032=EDGE_CURVE('',#36106,#36036,#20933,.T.);
#45033=EDGE_CURVE('',#36107,#36106,#4424,.T.);
#45034=EDGE_CURVE('',#36108,#36107,#4425,.T.);
#45035=EDGE_CURVE('',#36109,#36108,#4426,.T.);
#45036=EDGE_CURVE('',#36110,#36109,#20934,.T.);
#45037=EDGE_CURVE('',#36111,#36110,#4427,.T.);
#45038=EDGE_CURVE('',#36112,#36111,#4428,.T.);
#45039=EDGE_CURVE('',#36113,#36112,#4429,.T.);
#45040=EDGE_CURVE('',#36114,#36113,#20935,.T.);
#45041=EDGE_CURVE('',#36115,#36114,#1109,.T.);
#45042=EDGE_CURVE('',#36103,#36115,#20936,.T.);
#45043=EDGE_CURVE('',#36116,#36117,#29729,.T.);
#45044=EDGE_CURVE('',#35513,#36116,#20937,.T.);
#45045=EDGE_CURVE('',#36117,#35512,#20938,.T.);
#45046=EDGE_CURVE('',#35515,#36118,#1110,.T.);
#45047=EDGE_CURVE('',#36118,#35512,#29730,.T.);
#45048=EDGE_CURVE('',#35513,#36119,#29731,.T.);
#45049=EDGE_CURVE('',#36119,#35527,#1111,.T.);
#45050=EDGE_CURVE('',#36120,#35514,#20939,.T.);
#45051=EDGE_CURVE('',#36121,#36120,#29732,.T.);
#45052=EDGE_CURVE('',#35659,#36121,#20940,.T.);
#45053=EDGE_CURVE('',#36122,#35661,#29733,.T.);
#45054=EDGE_CURVE('',#36123,#36122,#20941,.T.);
#45055=EDGE_CURVE('',#36124,#36123,#4430,.T.);
#45056=EDGE_CURVE('',#36125,#36124,#4431,.T.);
#45057=EDGE_CURVE('',#36126,#36125,#4432,.T.);
#45058=EDGE_CURVE('',#36118,#36126,#20942,.T.);
#45059=EDGE_CURVE('',#35516,#36127,#20943,.T.);
#45060=EDGE_CURVE('',#36127,#36120,#29734,.T.);
#45061=EDGE_CURVE('',#36128,#35517,#20944,.T.);
#45062=EDGE_CURVE('',#36127,#36128,#20945,.T.);
#45063=EDGE_CURVE('',#35518,#36129,#20946,.T.);
#45064=EDGE_CURVE('',#36128,#36129,#29735,.T.);
#45065=EDGE_CURVE('',#36130,#35519,#4433,.T.);
#45066=EDGE_CURVE('',#36131,#36130,#4434,.T.);
#45067=EDGE_CURVE('',#36132,#36131,#4435,.T.);
#45068=EDGE_CURVE('',#36133,#36132,#4436,.T.);
#45069=EDGE_CURVE('',#36134,#36133,#20947,.T.);
#45070=EDGE_CURVE('',#35651,#36134,#29736,.T.);
#45071=EDGE_CURVE('',#36135,#35653,#20948,.T.);
#45072=EDGE_CURVE('',#36129,#36135,#29737,.T.);
#45073=EDGE_CURVE('',#35520,#36130,#29738,.T.);
#45074=EDGE_CURVE('',#35521,#36136,#29739,.T.);
#45075=EDGE_CURVE('',#35522,#36136,#4437,.T.);
#45076=EDGE_CURVE('',#36137,#36138,#20949,.T.);
#45077=EDGE_CURVE('',#36136,#36137,#20950,.T.);
#45078=EDGE_CURVE('',#36139,#35523,#20951,.T.);
#45079=EDGE_CURVE('',#36140,#36139,#29740,.T.);
#45080=EDGE_CURVE('',#36141,#36140,#20952,.T.);
#45081=EDGE_CURVE('',#36138,#36141,#20953,.T.);
#45082=EDGE_CURVE('',#35524,#36142,#20954,.T.);
#45083=EDGE_CURVE('',#36142,#36139,#29741,.T.);
#45084=EDGE_CURVE('',#36143,#35525,#20955,.T.);
#45085=EDGE_CURVE('',#36142,#36143,#20956,.T.);
#45086=EDGE_CURVE('',#35526,#36144,#20957,.T.);
#45087=EDGE_CURVE('',#36143,#36144,#29742,.T.);
#45088=EDGE_CURVE('',#36145,#35591,#20958,.T.);
#45089=EDGE_CURVE('',#36144,#36145,#29743,.T.);
#45090=EDGE_CURVE('',#36146,#36119,#20959,.T.);
#45091=EDGE_CURVE('',#36147,#36146,#4438,.T.);
#45092=EDGE_CURVE('',#36148,#36147,#1112,.T.);
#45093=EDGE_CURVE('',#36149,#36148,#4439,.T.);
#45094=EDGE_CURVE('',#36150,#36149,#20960,.T.);
#45095=EDGE_CURVE('',#35665,#36150,#29744,.T.);
#45096=EDGE_CURVE('',#36151,#36152,#29745,.T.);
#45097=EDGE_CURVE('',#35529,#36151,#20961,.T.);
#45098=EDGE_CURVE('',#36152,#35528,#20962,.T.);
#45099=EDGE_CURVE('',#35531,#36153,#1113,.T.);
#45100=EDGE_CURVE('',#36153,#35528,#29746,.T.);
#45101=EDGE_CURVE('',#36154,#35529,#29747,.T.);
#45102=EDGE_CURVE('',#36154,#35548,#1114,.T.);
#45103=EDGE_CURVE('',#36155,#36156,#1115,.T.);
#45104=EDGE_CURVE('',#36157,#36155,#20963,.T.);
#45105=EDGE_CURVE('',#36158,#36157,#4440,.T.);
#45106=EDGE_CURVE('',#36159,#36158,#1116,.T.);
#45107=EDGE_CURVE('',#36160,#36159,#4441,.T.);
#45108=EDGE_CURVE('',#36161,#36160,#20964,.T.);
#45109=EDGE_CURVE('',#36162,#36161,#4442,.T.);
#45110=EDGE_CURVE('',#36163,#36162,#1117,.T.);
#45111=EDGE_CURVE('',#36164,#36163,#4443,.T.);
#45112=EDGE_CURVE('',#36153,#36164,#20965,.T.);
#45113=EDGE_CURVE('',#36165,#35530,#20966,.T.);
#45114=EDGE_CURVE('',#36166,#36165,#29748,.T.);
#45115=EDGE_CURVE('',#36167,#36166,#20967,.T.);
#45116=EDGE_CURVE('',#36168,#36167,#29749,.T.);
#45117=EDGE_CURVE('',#36169,#36168,#20968,.T.);
#45118=EDGE_CURVE('',#36156,#36169,#20969,.T.);
#45119=EDGE_CURVE('',#35532,#36170,#20970,.T.);
#45120=EDGE_CURVE('',#36170,#36165,#29750,.T.);
#45121=EDGE_CURVE('',#36171,#35533,#20971,.T.);
#45122=EDGE_CURVE('',#36170,#36171,#20972,.T.);
#45123=EDGE_CURVE('',#35534,#36172,#20973,.T.);
#45124=EDGE_CURVE('',#36171,#36172,#29751,.T.);
#45125=EDGE_CURVE('',#36173,#35536,#29752,.T.);
#45126=EDGE_CURVE('',#36173,#35535,#1118,.T.);
#45127=EDGE_CURVE('',#36174,#36175,#20974,.T.);
#45128=EDGE_CURVE('',#36176,#36174,#20975,.T.);
#45129=EDGE_CURVE('',#36177,#36176,#4444,.T.);
#45130=EDGE_CURVE('',#36178,#36177,#20976,.T.);
#45131=EDGE_CURVE('',#36179,#36178,#1119,.T.);
#45132=EDGE_CURVE('',#36180,#36179,#20977,.T.);
#45133=EDGE_CURVE('',#36181,#36180,#20978,.T.);
#45134=EDGE_CURVE('',#36182,#36181,#29753,.T.);
#45135=EDGE_CURVE('',#36183,#36182,#20979,.T.);
#45136=EDGE_CURVE('',#36172,#36183,#29754,.T.);
#45137=EDGE_CURVE('',#36184,#36173,#20980,.T.);
#45138=EDGE_CURVE('',#36185,#36184,#4445,.T.);
#45139=EDGE_CURVE('',#36186,#36185,#20981,.T.);
#45140=EDGE_CURVE('',#36187,#36186,#20982,.T.);
#45141=EDGE_CURVE('',#36175,#36187,#29755,.T.);
#45142=EDGE_CURVE('',#36188,#36189,#20983,.T.);
#45143=EDGE_CURVE('',#36190,#36188,#29756,.T.);
#45144=EDGE_CURVE('',#36191,#36190,#20984,.T.);
#45145=EDGE_CURVE('',#35877,#36191,#29757,.T.);
#45146=EDGE_CURVE('',#36192,#35538,#1851,.T.);
#45147=EDGE_CURVE('',#36193,#36192,#1852,.T.);
#45148=EDGE_CURVE('',#36194,#36193,#1853,.T.);
#45149=EDGE_CURVE('',#36195,#36194,#4446,.T.);
#45150=EDGE_CURVE('',#36196,#36195,#4447,.T.);
#45151=EDGE_CURVE('',#36197,#36196,#20985,.T.);
#45152=EDGE_CURVE('',#36198,#36197,#4448,.T.);
#45153=EDGE_CURVE('',#36199,#36198,#4449,.T.);
#45154=EDGE_CURVE('',#36200,#36199,#4450,.T.);
#45155=EDGE_CURVE('',#36201,#36200,#4451,.T.);
#45156=EDGE_CURVE('',#36189,#36201,#20986,.T.);
#45157=EDGE_CURVE('',#35541,#36192,#29758,.T.);
#45158=EDGE_CURVE('',#35540,#36202,#4452,.T.);
#45159=EDGE_CURVE('',#35541,#36202,#4453,.T.);
#45160=EDGE_CURVE('',#36203,#36204,#29759,.T.);
#45161=EDGE_CURVE('',#36202,#36204,#1854,.T.);
#45162=EDGE_CURVE('',#35539,#36205,#29760,.T.);
#45163=EDGE_CURVE('',#36203,#36205,#4454,.T.);
#45164=EDGE_CURVE('',#36205,#35542,#20987,.T.);
#45165=EDGE_CURVE('',#35542,#36206,#29761,.T.);
#45166=EDGE_CURVE('',#35543,#36206,#1120,.T.);
#45167=EDGE_CURVE('',#36207,#35544,#20988,.T.);
#45168=EDGE_CURVE('',#36208,#36207,#29762,.T.);
#45169=EDGE_CURVE('',#36209,#36208,#20989,.T.);
#45170=EDGE_CURVE('',#36210,#36209,#29763,.T.);
#45171=EDGE_CURVE('',#36211,#36210,#20990,.T.);
#45172=EDGE_CURVE('',#36212,#36211,#20991,.T.);
#45173=EDGE_CURVE('',#36213,#36212,#1121,.T.);
#45174=EDGE_CURVE('',#36214,#36213,#20992,.T.);
#45175=EDGE_CURVE('',#36215,#36214,#4455,.T.);
#45176=EDGE_CURVE('',#36216,#36215,#4456,.T.);
#45177=EDGE_CURVE('',#36217,#36216,#4457,.T.);
#45178=EDGE_CURVE('',#36218,#36217,#20993,.T.);
#45179=EDGE_CURVE('',#36219,#36218,#4458,.T.);
#45180=EDGE_CURVE('',#36220,#36219,#4459,.T.);
#45181=EDGE_CURVE('',#36221,#36220,#4460,.T.);
#45182=EDGE_CURVE('',#36206,#36221,#20994,.T.);
#45183=EDGE_CURVE('',#35545,#36222,#20995,.T.);
#45184=EDGE_CURVE('',#36222,#36207,#29764,.T.);
#45185=EDGE_CURVE('',#36223,#35546,#20996,.T.);
#45186=EDGE_CURVE('',#36222,#36223,#20997,.T.);
#45187=EDGE_CURVE('',#35547,#36224,#20998,.T.);
#45188=EDGE_CURVE('',#36223,#36224,#29765,.T.);
#45189=EDGE_CURVE('',#36225,#36226,#20999,.T.);
#45190=EDGE_CURVE('',#36227,#36225,#29766,.T.);
#45191=EDGE_CURVE('',#36228,#36227,#21000,.T.);
#45192=EDGE_CURVE('',#36224,#36228,#29767,.T.);
#45193=EDGE_CURVE('',#36229,#36154,#21001,.T.);
#45194=EDGE_CURVE('',#36230,#36229,#4461,.T.);
#45195=EDGE_CURVE('',#36231,#36230,#4462,.T.);
#45196=EDGE_CURVE('',#36232,#36231,#4463,.T.);
#45197=EDGE_CURVE('',#36233,#36232,#21002,.T.);
#45198=EDGE_CURVE('',#36234,#36233,#4464,.T.);
#45199=EDGE_CURVE('',#36235,#36234,#4465,.T.);
#45200=EDGE_CURVE('',#36236,#36235,#4466,.T.);
#45201=EDGE_CURVE('',#36237,#36236,#21003,.T.);
#45202=EDGE_CURVE('',#36238,#36237,#1122,.T.);
#45203=EDGE_CURVE('',#36226,#36238,#21004,.T.);
#45204=EDGE_CURVE('',#36239,#36240,#29768,.T.);
#45205=EDGE_CURVE('',#36241,#36240,#4467,.T.);
#45206=EDGE_CURVE('',#36241,#35550,#29769,.T.);
#45207=EDGE_CURVE('',#36239,#35549,#1855,.T.);
#45208=EDGE_CURVE('',#35552,#36242,#4468,.T.);
#45209=EDGE_CURVE('',#36242,#35549,#29770,.T.);
#45210=EDGE_CURVE('',#36243,#36244,#4469,.T.);
#45211=EDGE_CURVE('',#36245,#36243,#4470,.T.);
#45212=EDGE_CURVE('',#36246,#36245,#4471,.T.);
#45213=EDGE_CURVE('',#36247,#36246,#4472,.T.);
#45214=EDGE_CURVE('',#36248,#36247,#21005,.T.);
#45215=EDGE_CURVE('',#36249,#36248,#4473,.T.);
#45216=EDGE_CURVE('',#36250,#36249,#4474,.T.);
#45217=EDGE_CURVE('',#36242,#36250,#1856,.T.);
#45218=EDGE_CURVE('',#36251,#35879,#29771,.T.);
#45219=EDGE_CURVE('',#36252,#36251,#21006,.T.);
#45220=EDGE_CURVE('',#36253,#36252,#29772,.T.);
#45221=EDGE_CURVE('',#36254,#36253,#21007,.T.);
#45222=EDGE_CURVE('',#36244,#36254,#21008,.T.);
#45223=EDGE_CURVE('',#35553,#36255,#29773,.T.);
#45224=EDGE_CURVE('',#35554,#36255,#1123,.T.);
#45225=EDGE_CURVE('',#36256,#36257,#1124,.T.);
#45226=EDGE_CURVE('',#36258,#36256,#21009,.T.);
#45227=EDGE_CURVE('',#36259,#36258,#4475,.T.);
#45228=EDGE_CURVE('',#36260,#36259,#21010,.T.);
#45229=EDGE_CURVE('',#36261,#36260,#21011,.T.);
#45230=EDGE_CURVE('',#36262,#36261,#21012,.T.);
#45231=EDGE_CURVE('',#36263,#36262,#4476,.T.);
#45232=EDGE_CURVE('',#36255,#36263,#21013,.T.);
#45233=EDGE_CURVE('',#36264,#35555,#21014,.T.);
#45234=EDGE_CURVE('',#36265,#36264,#29774,.T.);
#45235=EDGE_CURVE('',#36266,#36265,#21015,.T.);
#45236=EDGE_CURVE('',#36267,#36266,#29775,.T.);
#45237=EDGE_CURVE('',#36268,#36267,#21016,.T.);
#45238=EDGE_CURVE('',#36257,#36268,#21017,.T.);
#45239=EDGE_CURVE('',#35556,#36269,#21018,.T.);
#45240=EDGE_CURVE('',#36264,#36269,#29776,.T.);
#45241=EDGE_CURVE('',#36270,#35557,#21019,.T.);
#45242=EDGE_CURVE('',#36269,#36270,#21020,.T.);
#45243=EDGE_CURVE('',#35558,#36271,#21021,.T.);
#45244=EDGE_CURVE('',#36270,#36271,#29777,.T.);
#45245=EDGE_CURVE('',#36272,#36273,#21022,.T.);
#45246=EDGE_CURVE('',#36274,#36272,#29778,.T.);
#45247=EDGE_CURVE('',#36275,#36274,#21023,.T.);
#45248=EDGE_CURVE('',#36271,#36275,#29779,.T.);
#45249=EDGE_CURVE('',#36276,#35559,#1125,.T.);
#45250=EDGE_CURVE('',#36277,#36276,#21024,.T.);
#45251=EDGE_CURVE('',#36278,#36277,#4477,.T.);
#45252=EDGE_CURVE('',#36279,#36278,#1126,.T.);
#45253=EDGE_CURVE('',#36280,#36279,#4478,.T.);
#45254=EDGE_CURVE('',#36281,#36280,#21025,.T.);
#45255=EDGE_CURVE('',#36282,#36281,#4479,.T.);
#45256=EDGE_CURVE('',#36283,#36282,#1127,.T.);
#45257=EDGE_CURVE('',#36284,#36283,#4480,.T.);
#45258=EDGE_CURVE('',#36285,#36284,#21026,.T.);
#45259=EDGE_CURVE('',#36286,#36285,#1128,.T.);
#45260=EDGE_CURVE('',#36273,#36286,#21027,.T.);
#45261=EDGE_CURVE('',#35561,#36276,#29780,.T.);
#45262=EDGE_CURVE('',#36287,#36288,#29781,.T.);
#45263=EDGE_CURVE('',#35561,#36287,#21028,.T.);
#45264=EDGE_CURVE('',#36288,#35560,#21029,.T.);
#45265=EDGE_CURVE('',#35560,#36289,#29782,.T.);
#45266=EDGE_CURVE('',#35562,#36289,#4481,.T.);
#45267=EDGE_CURVE('',#36290,#35563,#21030,.T.);
#45268=EDGE_CURVE('',#36291,#36290,#29783,.T.);
#45269=EDGE_CURVE('',#36292,#36291,#21031,.T.);
#45270=EDGE_CURVE('',#36293,#36292,#29784,.T.);
#45271=EDGE_CURVE('',#36294,#36293,#21032,.T.);
#45272=EDGE_CURVE('',#36295,#36294,#21033,.T.);
#45273=EDGE_CURVE('',#36296,#36295,#1129,.T.);
#45274=EDGE_CURVE('',#36297,#36296,#21034,.T.);
#45275=EDGE_CURVE('',#36298,#36297,#4482,.T.);
#45276=EDGE_CURVE('',#36299,#36298,#4483,.T.);
#45277=EDGE_CURVE('',#36300,#36299,#4484,.T.);
#45278=EDGE_CURVE('',#36301,#36300,#21035,.T.);
#45279=EDGE_CURVE('',#36302,#36301,#4485,.T.);
#45280=EDGE_CURVE('',#36303,#36302,#4486,.T.);
#45281=EDGE_CURVE('',#36304,#36303,#4487,.T.);
#45282=EDGE_CURVE('',#36289,#36304,#21036,.T.);
#45283=EDGE_CURVE('',#35564,#36305,#21037,.T.);
#45284=EDGE_CURVE('',#36305,#36290,#29785,.T.);
#45285=EDGE_CURVE('',#36306,#35565,#21038,.T.);
#45286=EDGE_CURVE('',#36305,#36306,#21039,.T.);
#45287=EDGE_CURVE('',#35567,#36307,#21040,.T.);
#45288=EDGE_CURVE('',#36306,#36307,#29786,.T.);
#45289=EDGE_CURVE('',#36308,#35570,#29787,.T.);
#45290=EDGE_CURVE('',#36308,#35569,#1130,.T.);
#45291=EDGE_CURVE('',#36309,#36310,#21041,.T.);
#45292=EDGE_CURVE('',#36311,#36309,#29788,.T.);
#45293=EDGE_CURVE('',#36312,#36311,#21042,.T.);
#45294=EDGE_CURVE('',#36307,#36312,#29789,.T.);
#45295=EDGE_CURVE('',#36313,#36308,#21043,.T.);
#45296=EDGE_CURVE('',#36314,#36313,#4488,.T.);
#45297=EDGE_CURVE('',#36315,#36314,#4489,.T.);
#45298=EDGE_CURVE('',#36316,#36315,#4490,.T.);
#45299=EDGE_CURVE('',#36317,#36316,#21044,.T.);
#45300=EDGE_CURVE('',#36318,#36317,#4491,.T.);
#45301=EDGE_CURVE('',#36319,#36318,#4492,.T.);
#45302=EDGE_CURVE('',#36320,#36319,#4493,.T.);
#45303=EDGE_CURVE('',#36321,#36320,#21045,.T.);
#45304=EDGE_CURVE('',#36322,#36321,#1131,.T.);
#45305=EDGE_CURVE('',#36310,#36322,#21046,.T.);
#45306=EDGE_CURVE('',#35570,#36241,#21047,.T.);
#45307=EDGE_CURVE('',#36184,#35576,#29790,.T.);
#45308=EDGE_CURVE('',#36323,#36323,#29791,.T.);
#45309=EDGE_CURVE('',#36323,#36324,#21048,.T.);
#45310=EDGE_CURVE('',#36324,#36324,#29792,.T.);
#45311=EDGE_CURVE('',#36325,#36325,#29793,.T.);
#45312=EDGE_CURVE('',#36325,#36326,#21049,.T.);
#45313=EDGE_CURVE('',#35576,#36326,#4494,.F.);
#45314=EDGE_CURVE('',#36326,#35575,#4495,.F.);
#45315=EDGE_CURVE('',#35575,#36185,#29794,.T.);
#45316=EDGE_CURVE('',#35574,#36186,#29795,.T.);
#45317=EDGE_CURVE('',#35573,#36327,#29796,.T.);
#45318=EDGE_CURVE('',#36327,#36186,#29797,.T.);
#45319=EDGE_CURVE('',#35572,#36328,#29798,.T.);
#45320=EDGE_CURVE('',#36328,#36327,#29799,.T.);
#45321=EDGE_CURVE('',#35571,#36137,#29800,.T.);
#45322=EDGE_CURVE('',#36137,#36328,#29801,.T.);
#45323=EDGE_CURVE('',#35579,#36063,#29802,.T.);
#45324=EDGE_CURVE('',#36329,#36329,#29803,.T.);
#45325=EDGE_CURVE('',#36329,#36330,#21050,.T.);
#45326=EDGE_CURVE('',#36330,#36330,#29804,.T.);
#45327=EDGE_CURVE('',#36331,#36331,#29805,.T.);
#45328=EDGE_CURVE('',#36331,#35578,#21051,.T.);
#45329=EDGE_CURVE('',#36332,#35577,#4496,.T.);
#45330=EDGE_CURVE('',#36333,#36332,#29806,.T.);
#45331=EDGE_CURVE('',#35579,#36333,#4497,.T.);
#45332=EDGE_CURVE('',#35577,#36263,#29807,.T.);
#45333=EDGE_CURVE('',#36334,#35580,#29808,.T.);
#45334=EDGE_CURVE('',#36334,#36335,#21052,.T.);
#45335=EDGE_CURVE('',#35581,#36335,#29809,.T.);
#45336=EDGE_CURVE('',#36334,#36071,#29810,.T.);
#45337=EDGE_CURVE('',#35593,#36336,#21053,.T.);
#45338=EDGE_CURVE('',#36336,#36145,#29811,.T.);
#45339=EDGE_CURVE('',#36337,#35595,#21054,.T.);
#45340=EDGE_CURVE('',#36336,#36337,#21055,.T.);
#45341=EDGE_CURVE('',#35600,#36141,#29812,.T.);
#45342=EDGE_CURVE('',#36141,#35595,#4498,.T.);
#45343=EDGE_CURVE('',#35596,#36338,#29813,.T.);
#45344=EDGE_CURVE('',#35597,#36187,#29814,.T.);
#45345=EDGE_CURVE('',#36187,#36338,#4499,.T.);
#45346=EDGE_CURVE('',#35603,#36175,#29815,.T.);
#45347=EDGE_CURVE('',#35599,#36138,#29816,.T.);
#45348=EDGE_CURVE('',#35598,#36339,#29817,.T.);
#45349=EDGE_CURVE('',#36339,#36138,#4500,.T.);
#45350=EDGE_CURVE('',#36338,#36339,#4501,.T.);
#45351=EDGE_CURVE('',#35607,#35872,#21056,.T.);
#45352=EDGE_CURVE('',#35871,#35609,#21057,.T.);
#45353=EDGE_CURVE('',#35870,#35616,#29818,.T.);
#45354=EDGE_CURVE('',#35614,#35867,#29819,.T.);
#45355=EDGE_CURVE('',#35623,#35864,#21058,.T.);
#45356=EDGE_CURVE('',#35863,#35625,#21059,.T.);
#45357=EDGE_CURVE('',#35631,#35860,#29820,.T.);
#45358=EDGE_CURVE('',#35861,#35634,#29821,.T.);
#45359=EDGE_CURVE('',#35633,#36340,#1857,.T.);
#45360=EDGE_CURVE('',#35856,#36340,#4502,.T.);
#45361=EDGE_CURVE('',#35634,#35857,#1858,.T.);
#45362=EDGE_CURVE('',#36340,#35635,#21060,.T.);
#45363=EDGE_CURVE('',#35635,#35854,#29822,.T.);
#45364=EDGE_CURVE('',#35641,#36341,#21061,.T.);
#45365=EDGE_CURVE('',#36341,#35855,#29823,.T.);
#45366=EDGE_CURVE('',#36342,#35643,#21062,.T.);
#45367=EDGE_CURVE('',#36341,#36342,#21063,.T.);
#45368=EDGE_CURVE('',#36342,#35843,#29824,.T.);
#45369=EDGE_CURVE('',#35844,#35650,#29825,.T.);
#45370=EDGE_CURVE('',#36343,#35649,#21064,.T.);
#45371=EDGE_CURVE('',#36344,#36343,#4503,.T.);
#45372=EDGE_CURVE('',#35650,#36344,#21065,.T.);
#45373=EDGE_CURVE('',#35649,#36134,#29826,.T.);
#45374=EDGE_CURVE('',#35655,#36345,#21066,.T.);
#45375=EDGE_CURVE('',#36345,#36135,#29827,.T.);
#45376=EDGE_CURVE('',#36346,#35657,#21067,.T.);
#45377=EDGE_CURVE('',#36345,#36346,#21068,.T.);
#45378=EDGE_CURVE('',#36346,#36121,#29828,.T.);
#45379=EDGE_CURVE('',#36122,#35664,#29829,.T.);
#45380=EDGE_CURVE('',#36347,#35663,#21069,.T.);
#45381=EDGE_CURVE('',#36348,#36347,#4504,.T.);
#45382=EDGE_CURVE('',#35664,#36348,#21070,.T.);
#45383=EDGE_CURVE('',#35663,#36150,#29830,.T.);
#45384=EDGE_CURVE('',#36174,#35666,#29831,.T.);
#45385=EDGE_CURVE('',#35666,#36349,#29832,.T.);
#45386=EDGE_CURVE('',#35672,#35723,#29833,.T.);
#45387=EDGE_CURVE('',#35723,#36349,#21071,.T.);
#45388=EDGE_CURVE('',#35671,#35718,#29834,.T.);
#45389=EDGE_CURVE('',#35670,#36350,#29835,.T.);
#45390=EDGE_CURVE('',#36350,#35718,#21072,.T.);
#45391=EDGE_CURVE('',#35669,#36351,#29836,.T.);
#45392=EDGE_CURVE('',#36351,#36350,#4505,.T.);
#45393=EDGE_CURVE('',#35668,#36352,#29837,.T.);
#45394=EDGE_CURVE('',#36352,#36351,#21073,.T.);
#45395=EDGE_CURVE('',#35679,#36352,#4506,.T.);
#45396=EDGE_CURVE('',#36353,#35684,#21074,.T.);
#45397=EDGE_CURVE('',#36351,#36353,#21075,.T.);
#45398=EDGE_CURVE('',#35686,#36354,#21076,.T.);
#45399=EDGE_CURVE('',#36353,#36354,#29838,.T.);
#45400=EDGE_CURVE('',#36355,#35688,#21077,.T.);
#45401=EDGE_CURVE('',#36354,#36355,#29839,.T.);
#45402=EDGE_CURVE('',#35690,#36356,#21078,.T.);
#45403=EDGE_CURVE('',#36355,#36356,#29840,.T.);
#45404=EDGE_CURVE('',#36356,#36357,#21079,.T.);
#45405=EDGE_CURVE('',#36358,#35692,#21080,.T.);
#45406=EDGE_CURVE('',#36359,#36358,#4507,.T.);
#45407=EDGE_CURVE('',#36360,#36359,#21081,.T.);
#45408=EDGE_CURVE('',#36361,#36360,#21082,.T.);
#45409=EDGE_CURVE('',#36362,#36361,#4508,.T.);
#45410=EDGE_CURVE('',#36363,#36362,#21083,.T.);
#45411=EDGE_CURVE('',#36364,#36363,#4509,.T.);
#45412=EDGE_CURVE('',#36365,#36364,#21084,.T.);
#45413=EDGE_CURVE('',#36366,#36365,#21085,.T.);
#45414=EDGE_CURVE('',#36367,#36366,#21086,.T.);
#45415=EDGE_CURVE('',#36368,#36367,#4510,.T.);
#45416=EDGE_CURVE('',#36369,#36368,#21087,.T.);
#45417=EDGE_CURVE('',#36370,#36369,#4511,.T.);
#45418=EDGE_CURVE('',#36357,#36370,#21088,.T.);
#45419=EDGE_CURVE('',#36371,#36372,#21089,.T.);
#45420=EDGE_CURVE('',#36358,#36371,#4512,.T.);
#45421=EDGE_CURVE('',#35694,#36373,#21090,.T.);
#45422=EDGE_CURVE('',#36372,#36373,#4513,.T.);
#45423=EDGE_CURVE('',#36374,#35696,#21091,.T.);
#45424=EDGE_CURVE('',#36375,#36374,#1859,.T.);
#45425=EDGE_CURVE('',#36376,#36375,#29841,.T.);
#45426=EDGE_CURVE('',#36377,#36376,#4514,.T.);
#45427=EDGE_CURVE('',#36378,#36377,#21092,.T.);
#45428=EDGE_CURVE('',#36379,#36378,#29842,.T.);
#45429=EDGE_CURVE('',#36380,#36379,#21093,.T.);
#45430=EDGE_CURVE('',#36381,#36380,#4515,.T.);
#45431=EDGE_CURVE('',#36382,#36381,#29843,.T.);
#45432=EDGE_CURVE('',#36383,#36382,#4516,.T.);
#45433=EDGE_CURVE('',#36384,#36383,#1860,.T.);
#45434=EDGE_CURVE('',#36385,#36384,#21094,.T.);
#45435=EDGE_CURVE('',#36386,#36385,#29844,.T.);
#45436=EDGE_CURVE('',#36387,#36386,#21095,.T.);
#45437=EDGE_CURVE('',#36388,#36387,#4517,.T.);
#45438=EDGE_CURVE('',#36389,#36388,#29845,.T.);
#45439=EDGE_CURVE('',#36390,#36389,#4518,.T.);
#45440=EDGE_CURVE('',#36391,#36390,#21096,.T.);
#45441=EDGE_CURVE('',#36392,#36391,#29846,.T.);
#45442=EDGE_CURVE('',#36393,#36392,#21097,.T.);
#45443=EDGE_CURVE('',#36394,#36393,#4519,.T.);
#45444=EDGE_CURVE('',#36395,#36394,#29847,.T.);
#45445=EDGE_CURVE('',#36396,#36395,#4520,.T.);
#45446=EDGE_CURVE('',#36397,#36396,#21098,.T.);
#45447=EDGE_CURVE('',#36398,#36397,#29848,.T.);
#45448=EDGE_CURVE('',#36399,#36398,#21099,.T.);
#45449=EDGE_CURVE('',#36400,#36399,#4521,.T.);
#45450=EDGE_CURVE('',#36401,#36400,#29849,.T.);
#45451=EDGE_CURVE('',#36402,#36401,#4522,.T.);
#45452=EDGE_CURVE('',#36403,#36402,#21100,.T.);
#45453=EDGE_CURVE('',#36404,#36403,#29850,.T.);
#45454=EDGE_CURVE('',#36405,#36404,#21101,.T.);
#45455=EDGE_CURVE('',#36406,#36405,#4523,.T.);
#45456=EDGE_CURVE('',#36407,#36406,#4524,.T.);
#45457=EDGE_CURVE('',#36408,#36407,#29851,.T.);
#45458=EDGE_CURVE('',#36409,#36408,#4525,.T.);
#45459=EDGE_CURVE('',#36410,#36409,#21102,.T.);
#45460=EDGE_CURVE('',#36411,#36410,#29852,.T.);
#45461=EDGE_CURVE('',#36412,#36411,#21103,.T.);
#45462=EDGE_CURVE('',#36413,#36412,#4526,.T.);
#45463=EDGE_CURVE('',#36414,#36413,#29853,.T.);
#45464=EDGE_CURVE('',#36373,#36414,#4527,.T.);
#45465=EDGE_CURVE('',#35698,#36415,#21104,.T.);
#45466=EDGE_CURVE('',#36416,#36415,#4528,.T.);
#45467=EDGE_CURVE('',#36417,#36416,#21105,.T.);
#45468=EDGE_CURVE('',#36374,#36417,#4529,.T.);
#45469=EDGE_CURVE('',#36418,#36419,#21106,.T.);
#45470=EDGE_CURVE('',#36420,#36418,#21107,.T.);
#45471=EDGE_CURVE('',#36421,#36420,#4530,.T.);
#45472=EDGE_CURVE('',#36422,#36421,#21108,.T.);
#45473=EDGE_CURVE('',#36423,#36422,#4531,.T.);
#45474=EDGE_CURVE('',#36424,#36423,#21109,.T.);
#45475=EDGE_CURVE('',#36425,#36424,#21110,.T.);
#45476=EDGE_CURVE('',#36415,#36425,#4532,.T.);
#45477=EDGE_CURVE('',#36426,#35700,#21111,.T.);
#45478=EDGE_CURVE('',#36427,#36426,#21112,.T.);
#45479=EDGE_CURVE('',#36428,#36427,#21113,.T.);
#45480=EDGE_CURVE('',#36429,#36428,#4533,.T.);
#45481=EDGE_CURVE('',#36430,#36429,#21114,.T.);
#45482=EDGE_CURVE('',#36431,#36430,#4534,.T.);
#45483=EDGE_CURVE('',#36419,#36431,#21115,.T.);
#45484=EDGE_CURVE('',#35702,#36432,#21116,.T.);
#45485=EDGE_CURVE('',#36426,#36432,#29854,.T.);
#45486=EDGE_CURVE('',#36433,#35704,#21117,.T.);
#45487=EDGE_CURVE('',#36432,#36433,#29855,.T.);
#45488=EDGE_CURVE('',#35706,#36434,#21118,.T.);
#45489=EDGE_CURVE('',#36433,#36434,#29856,.T.);
#45490=EDGE_CURVE('',#36434,#36435,#21119,.T.);
#45491=EDGE_CURVE('',#36436,#35768,#4535,.T.);
#45492=EDGE_CURVE('',#36437,#36436,#21120,.T.);
#45493=EDGE_CURVE('',#36438,#36437,#21121,.T.);
#45494=EDGE_CURVE('',#36439,#36438,#4536,.T.);
#45495=EDGE_CURVE('',#36440,#36439,#21122,.T.);
#45496=EDGE_CURVE('',#36441,#36440,#4537,.T.);
#45497=EDGE_CURVE('',#36442,#36441,#21123,.T.);
#45498=EDGE_CURVE('',#36443,#36442,#21124,.T.);
#45499=EDGE_CURVE('',#36444,#36443,#21125,.T.);
#45500=EDGE_CURVE('',#36445,#36444,#4538,.T.);
#45501=EDGE_CURVE('',#36446,#36445,#21126,.T.);
#45502=EDGE_CURVE('',#36447,#36446,#4539,.T.);
#45503=EDGE_CURVE('',#36435,#36447,#21127,.T.);
#45504=EDGE_CURVE('',#36054,#35716,#29857,.T.);
#45505=EDGE_CURVE('',#36055,#35717,#29858,.T.);
#45506=EDGE_CURVE('',#36448,#36449,#21128,.T.);
#45507=EDGE_CURVE('',#36450,#36448,#29859,.T.);
#45508=EDGE_CURVE('',#36451,#36450,#29860,.T.);
#45509=EDGE_CURVE('',#36452,#36451,#29861,.T.);
#45510=EDGE_CURVE('',#36453,#36452,#21129,.T.);
#45511=EDGE_CURVE('',#35716,#36453,#21130,.T.);
#45512=EDGE_CURVE('',#36449,#35713,#21131,.T.);
#45513=EDGE_CURVE('',#36259,#35712,#29862,.T.);
#45514=EDGE_CURVE('',#36258,#35713,#29863,.T.);
#45515=EDGE_CURVE('',#36454,#35717,#21132,.T.);
#45516=EDGE_CURVE('',#36455,#36454,#29864,.T.);
#45517=EDGE_CURVE('',#35712,#36455,#21133,.T.);
#45518=EDGE_CURVE('',#36177,#35719,#29865,.T.);
#45519=EDGE_CURVE('',#36176,#35722,#29866,.T.);
#45520=EDGE_CURVE('',#36456,#36350,#21134,.T.);
#45521=EDGE_CURVE('',#36457,#36456,#29867,.T.);
#45522=EDGE_CURVE('',#36458,#36457,#29868,.T.);
#45523=EDGE_CURVE('',#36459,#36458,#29869,.T.);
#45524=EDGE_CURVE('',#36460,#36459,#21135,.T.);
#45525=EDGE_CURVE('',#35719,#36460,#21136,.T.);
#45526=EDGE_CURVE('',#36349,#35722,#21137,.T.);
#45527=EDGE_CURVE('',#36461,#35833,#29870,.T.);
#45528=EDGE_CURVE('',#36461,#35726,#21138,.T.);
#45529=EDGE_CURVE('',#35732,#35834,#29871,.T.);
#45530=EDGE_CURVE('',#36462,#35731,#1132,.T.);
#45531=EDGE_CURVE('',#36463,#36462,#4540,.T.);
#45532=EDGE_CURVE('',#35732,#36463,#4541,.T.);
#45533=EDGE_CURVE('',#35826,#35731,#29872,.T.);
#45534=EDGE_CURVE('',#35736,#36464,#21139,.T.);
#45535=EDGE_CURVE('',#36464,#35819,#29873,.T.);
#45536=EDGE_CURVE('',#36465,#35738,#21140,.T.);
#45537=EDGE_CURVE('',#36464,#36465,#21141,.T.);
#45538=EDGE_CURVE('',#36465,#35809,#29874,.T.);
#45539=EDGE_CURVE('',#35746,#35810,#29875,.T.);
#45540=EDGE_CURVE('',#36466,#35745,#1133,.T.);
#45541=EDGE_CURVE('',#36467,#36466,#4542,.T.);
#45542=EDGE_CURVE('',#35746,#36467,#4543,.T.);
#45543=EDGE_CURVE('',#35802,#35745,#29876,.T.);
#45544=EDGE_CURVE('',#35750,#36468,#4544,.T.);
#45545=EDGE_CURVE('',#36468,#35797,#29877,.T.);
#45546=EDGE_CURVE('',#36469,#35752,#4545,.T.);
#45547=EDGE_CURVE('',#36469,#36468,#4546,.T.);
#45548=EDGE_CURVE('',#36469,#35787,#29878,.T.);
#45549=EDGE_CURVE('',#35760,#35788,#29879,.T.);
#45550=EDGE_CURVE('',#36470,#35759,#4547,.T.);
#45551=EDGE_CURVE('',#36471,#36470,#4548,.T.);
#45552=EDGE_CURVE('',#35760,#36471,#1134,.T.);
#45553=EDGE_CURVE('',#35782,#35759,#29880,.T.);
#45554=EDGE_CURVE('',#36069,#35767,#29881,.T.);
#45555=EDGE_CURVE('',#36079,#35766,#29882,.T.);
#45556=EDGE_CURVE('',#35772,#36069,#4549,.T.);
#45557=EDGE_CURVE('',#36472,#36473,#1135,.T.);
#45558=EDGE_CURVE('',#35768,#36473,#29883,.T.);
#45559=EDGE_CURVE('',#36472,#35766,#4550,.T.);
#45560=EDGE_CURVE('',#35770,#36474,#21142,.T.);
#45561=EDGE_CURVE('',#36474,#36068,#29884,.T.);
#45562=EDGE_CURVE('',#36474,#36461,#21143,.T.);
#45563=EDGE_CURVE('',#35778,#35783,#29885,.T.);
#45564=EDGE_CURVE('',#35781,#36470,#29886,.T.);
#45565=EDGE_CURVE('',#35780,#36475,#29887,.T.);
#45566=EDGE_CURVE('',#36475,#36470,#1861,.T.);
#45567=EDGE_CURVE('',#35779,#36476,#29888,.T.);
#45568=EDGE_CURVE('',#36476,#36475,#21144,.T.);
#45569=EDGE_CURVE('',#35783,#36476,#1862,.T.);
#45570=EDGE_CURVE('',#36477,#36476,#4551,.T.);
#45571=EDGE_CURVE('',#36477,#35784,#4552,.T.);
#45572=EDGE_CURVE('',#35784,#35792,#29889,.T.);
#45573=EDGE_CURVE('',#36477,#35791,#29890,.T.);
#45574=EDGE_CURVE('',#36478,#35790,#29891,.T.);
#45575=EDGE_CURVE('',#36478,#36477,#21145,.T.);
#45576=EDGE_CURVE('',#36471,#35789,#29892,.T.);
#45577=EDGE_CURVE('',#36471,#36478,#4553,.T.);
#45578=EDGE_CURVE('',#35793,#36469,#21146,.T.);
#45579=EDGE_CURVE('',#36468,#35794,#21147,.T.);
#45580=EDGE_CURVE('',#35798,#35803,#29893,.T.);
#45581=EDGE_CURVE('',#35801,#36466,#29894,.T.);
#45582=EDGE_CURVE('',#35800,#36479,#29895,.T.);
#45583=EDGE_CURVE('',#36479,#36466,#4554,.T.);
#45584=EDGE_CURVE('',#35799,#36480,#29896,.T.);
#45585=EDGE_CURVE('',#36480,#36479,#21148,.T.);
#45586=EDGE_CURVE('',#35803,#36480,#4555,.T.);
#45587=EDGE_CURVE('',#36481,#36480,#4556,.T.);
#45588=EDGE_CURVE('',#36481,#35804,#1136,.T.);
#45589=EDGE_CURVE('',#35804,#35814,#29897,.T.);
#45590=EDGE_CURVE('',#36481,#35813,#29898,.T.);
#45591=EDGE_CURVE('',#36482,#35812,#29899,.T.);
#45592=EDGE_CURVE('',#36482,#36481,#21149,.T.);
#45593=EDGE_CURVE('',#36467,#35811,#29900,.T.);
#45594=EDGE_CURVE('',#36467,#36482,#4557,.T.);
#45595=EDGE_CURVE('',#36483,#35808,#29901,.T.);
#45596=EDGE_CURVE('',#36483,#36465,#29902,.T.);
#45597=EDGE_CURVE('',#36484,#35807,#29903,.T.);
#45598=EDGE_CURVE('',#36484,#36483,#21150,.T.);
#45599=EDGE_CURVE('',#35815,#36484,#29904,.T.);
#45600=EDGE_CURVE('',#36485,#35816,#29905,.T.);
#45601=EDGE_CURVE('',#36485,#36484,#21151,.T.);
#45602=EDGE_CURVE('',#36485,#35821,#29906,.T.);
#45603=EDGE_CURVE('',#35822,#35827,#29907,.T.);
#45604=EDGE_CURVE('',#35825,#36462,#29908,.T.);
#45605=EDGE_CURVE('',#35824,#36486,#29909,.T.);
#45606=EDGE_CURVE('',#36486,#36462,#4558,.T.);
#45607=EDGE_CURVE('',#35823,#36487,#29910,.T.);
#45608=EDGE_CURVE('',#36487,#36486,#21152,.T.);
#45609=EDGE_CURVE('',#35827,#36487,#4559,.T.);
#45610=EDGE_CURVE('',#36488,#35820,#29911,.T.);
#45611=EDGE_CURVE('',#36488,#36485,#21153,.T.);
#45612=EDGE_CURVE('',#36464,#36488,#29912,.T.);
#45613=EDGE_CURVE('',#36489,#36487,#4560,.T.);
#45614=EDGE_CURVE('',#36489,#35828,#1137,.T.);
#45615=EDGE_CURVE('',#35828,#35838,#29913,.T.);
#45616=EDGE_CURVE('',#36489,#35837,#29914,.T.);
#45617=EDGE_CURVE('',#36490,#35836,#29915,.T.);
#45618=EDGE_CURVE('',#36490,#36489,#21154,.T.);
#45619=EDGE_CURVE('',#36463,#35835,#29916,.T.);
#45620=EDGE_CURVE('',#36463,#36490,#4561,.T.);
#45621=EDGE_CURVE('',#36491,#35832,#29917,.T.);
#45622=EDGE_CURVE('',#36491,#36461,#29918,.T.);
#45623=EDGE_CURVE('',#36335,#35831,#29919,.T.);
#45624=EDGE_CURVE('',#36335,#36491,#21155,.T.);
#45625=EDGE_CURVE('',#36492,#36493,#4562,.T.);
#45626=EDGE_CURVE('',#35840,#36492,#4563,.T.);
#45627=EDGE_CURVE('',#36493,#35839,#1138,.T.);
#45628=EDGE_CURVE('',#35847,#35839,#29920,.T.);
#45629=EDGE_CURVE('',#35840,#36131,#29921,.T.);
#45630=EDGE_CURVE('',#35846,#36493,#29922,.T.);
#45631=EDGE_CURVE('',#35845,#36344,#29923,.T.);
#45632=EDGE_CURVE('',#36344,#36493,#4564,.T.);
#45633=EDGE_CURVE('',#35848,#36342,#29924,.T.);
#45634=EDGE_CURVE('',#36341,#35849,#29925,.T.);
#45635=EDGE_CURVE('',#36340,#35853,#29926,.T.);
#45636=EDGE_CURVE('',#35856,#35852,#29927,.T.);
#45637=EDGE_CURVE('',#35862,#35857,#29928,.T.);
#45638=EDGE_CURVE('',#35874,#36494,#29929,.T.);
#45639=EDGE_CURVE('',#36494,#36028,#29930,.T.);
#45640=EDGE_CURVE('',#36495,#35876,#29931,.T.);
#45641=EDGE_CURVE('',#36495,#36494,#21156,.T.);
#45642=EDGE_CURVE('',#36495,#36191,#29932,.T.);
#45643=EDGE_CURVE('',#35878,#36496,#29933,.T.);
#45644=EDGE_CURVE('',#36496,#36251,#29934,.T.);
#45645=EDGE_CURVE('',#36497,#35880,#29935,.T.);
#45646=EDGE_CURVE('',#36497,#36496,#21157,.T.);
#45647=EDGE_CURVE('',#36497,#35885,#29936,.T.);
#45648=EDGE_CURVE('',#36498,#36499,#21158,.T.);
#45649=EDGE_CURVE('',#36499,#35882,#29937,.T.);
#45650=EDGE_CURVE('',#36498,#35883,#4565,.T.);
#45651=EDGE_CURVE('',#36378,#35892,#29938,.T.);
#45652=EDGE_CURVE('',#36377,#35883,#29939,.T.);
#45653=EDGE_CURVE('',#36500,#35891,#29940,.T.);
#45654=EDGE_CURVE('',#36500,#36378,#1863,.T.);
#45655=EDGE_CURVE('',#36501,#35890,#29941,.T.);
#45656=EDGE_CURVE('',#36501,#36500,#4566,.T.);
#45657=EDGE_CURVE('',#36502,#35889,#29942,.T.);
#45658=EDGE_CURVE('',#36502,#36501,#4567,.T.);
#45659=EDGE_CURVE('',#36503,#35888,#29943,.T.);
#45660=EDGE_CURVE('',#36503,#36502,#21159,.T.);
#45661=EDGE_CURVE('',#35893,#35887,#29944,.T.);
#45662=EDGE_CURVE('',#35893,#36503,#4568,.T.);
#45663=EDGE_CURVE('',#36504,#35884,#29945,.T.);
#45664=EDGE_CURVE('',#36504,#36497,#21160,.T.);
#45665=EDGE_CURVE('',#36499,#36504,#29946,.T.);
#45666=EDGE_CURVE('',#36505,#36503,#4569,.T.);
#45667=EDGE_CURVE('',#36505,#35894,#4570,.T.);
#45668=EDGE_CURVE('',#35906,#35894,#29947,.T.);
#45669=EDGE_CURVE('',#36505,#35905,#29948,.T.);
#45670=EDGE_CURVE('',#36506,#35904,#29949,.T.);
#45671=EDGE_CURVE('',#36506,#36505,#21161,.T.);
#45672=EDGE_CURVE('',#36507,#35903,#29950,.T.);
#45673=EDGE_CURVE('',#36507,#36506,#4571,.T.);
#45674=EDGE_CURVE('',#36508,#35902,#29951,.T.);
#45675=EDGE_CURVE('',#36508,#36507,#4572,.T.);
#45676=EDGE_CURVE('',#36379,#35901,#29952,.T.);
#45677=EDGE_CURVE('',#36379,#36508,#1864,.T.);
#45678=EDGE_CURVE('',#36380,#35900,#29953,.T.);
#45679=EDGE_CURVE('',#36509,#35899,#29954,.T.);
#45680=EDGE_CURVE('',#36509,#36510,#21162,.T.);
#45681=EDGE_CURVE('',#35900,#36510,#4573,.T.);
#45682=EDGE_CURVE('',#36511,#35898,#29955,.T.);
#45683=EDGE_CURVE('',#36511,#36509,#29956,.T.);
#45684=EDGE_CURVE('',#36512,#35897,#29957,.T.);
#45685=EDGE_CURVE('',#36512,#36511,#21163,.T.);
#45686=EDGE_CURVE('',#35907,#36512,#29958,.T.);
#45687=EDGE_CURVE('',#36513,#35908,#29959,.T.);
#45688=EDGE_CURVE('',#36513,#36512,#21164,.T.);
#45689=EDGE_CURVE('',#36513,#35919,#29960,.T.);
#45690=EDGE_CURVE('',#35911,#35920,#29961,.T.);
#45691=EDGE_CURVE('',#36514,#35918,#29962,.T.);
#45692=EDGE_CURVE('',#36514,#36513,#21165,.T.);
#45693=EDGE_CURVE('',#36515,#36516,#29963,.T.);
#45694=EDGE_CURVE('',#36515,#36514,#29964,.T.);
#45695=EDGE_CURVE('',#36516,#35917,#4574,.T.);
#45696=EDGE_CURVE('',#36385,#35916,#29965,.T.);
#45697=EDGE_CURVE('',#36384,#35917,#29966,.T.);
#45698=EDGE_CURVE('',#36517,#35915,#29967,.T.);
#45699=EDGE_CURVE('',#36517,#36385,#1865,.T.);
#45700=EDGE_CURVE('',#36518,#35914,#29968,.T.);
#45701=EDGE_CURVE('',#36518,#36517,#1139,.T.);
#45702=EDGE_CURVE('',#35913,#36519,#29969,.T.);
#45703=EDGE_CURVE('',#36519,#36518,#1140,.T.);
#45704=EDGE_CURVE('',#35912,#36520,#29970,.T.);
#45705=EDGE_CURVE('',#36520,#36519,#21166,.T.);
#45706=EDGE_CURVE('',#35920,#36520,#4575,.T.);
#45707=EDGE_CURVE('',#36521,#36520,#4576,.T.);
#45708=EDGE_CURVE('',#36521,#35921,#4577,.T.);
#45709=EDGE_CURVE('',#35921,#35931,#29971,.T.);
#45710=EDGE_CURVE('',#36521,#35930,#29972,.T.);
#45711=EDGE_CURVE('',#36522,#35929,#29973,.T.);
#45712=EDGE_CURVE('',#36522,#36521,#21167,.T.);
#45713=EDGE_CURVE('',#36523,#35928,#29974,.T.);
#45714=EDGE_CURVE('',#36523,#36522,#4578,.T.);
#45715=EDGE_CURVE('',#36524,#35927,#29975,.T.);
#45716=EDGE_CURVE('',#36524,#36523,#1141,.T.);
#45717=EDGE_CURVE('',#36386,#35926,#29976,.T.);
#45718=EDGE_CURVE('',#36386,#36524,#1866,.T.);
#45719=EDGE_CURVE('',#36387,#35925,#29977,.T.);
#45720=EDGE_CURVE('',#36525,#35924,#29978,.T.);
#45721=EDGE_CURVE('',#36525,#36526,#4579,.T.);
#45722=EDGE_CURVE('',#35925,#36526,#4580,.T.);
#45723=EDGE_CURVE('',#35932,#36525,#21168,.T.);
#45724=EDGE_CURVE('',#36527,#35933,#21169,.T.);
#45725=EDGE_CURVE('',#36525,#36527,#4581,.T.);
#45726=EDGE_CURVE('',#36527,#35936,#29979,.T.);
#45727=EDGE_CURVE('',#35938,#35944,#29980,.T.);
#45728=EDGE_CURVE('',#36528,#36527,#1142,.T.);
#45729=EDGE_CURVE('',#36528,#35937,#4582,.T.);
#45730=EDGE_CURVE('',#35937,#36390,#29981,.T.);
#45731=EDGE_CURVE('',#35943,#36391,#29982,.T.);
#45732=EDGE_CURVE('',#35942,#36529,#29983,.T.);
#45733=EDGE_CURVE('',#36529,#36391,#1867,.T.);
#45734=EDGE_CURVE('',#35941,#36530,#29984,.T.);
#45735=EDGE_CURVE('',#36530,#36529,#1143,.T.);
#45736=EDGE_CURVE('',#35940,#36531,#29985,.T.);
#45737=EDGE_CURVE('',#36531,#36530,#4583,.T.);
#45738=EDGE_CURVE('',#35939,#36532,#29986,.T.);
#45739=EDGE_CURVE('',#36532,#36531,#21170,.T.);
#45740=EDGE_CURVE('',#35944,#36532,#4584,.T.);
#45741=EDGE_CURVE('',#36533,#36532,#4585,.T.);
#45742=EDGE_CURVE('',#36533,#35945,#1868,.T.);
#45743=EDGE_CURVE('',#35945,#35955,#29987,.T.);
#45744=EDGE_CURVE('',#36533,#35954,#29988,.T.);
#45745=EDGE_CURVE('',#36534,#35953,#29989,.T.);
#45746=EDGE_CURVE('',#36534,#36533,#21171,.T.);
#45747=EDGE_CURVE('',#36535,#35952,#29990,.T.);
#45748=EDGE_CURVE('',#36535,#36534,#1869,.T.);
#45749=EDGE_CURVE('',#36536,#35951,#29991,.T.);
#45750=EDGE_CURVE('',#36536,#36535,#4586,.T.);
#45751=EDGE_CURVE('',#36392,#35950,#29992,.T.);
#45752=EDGE_CURVE('',#36392,#36536,#29993,.T.);
#45753=EDGE_CURVE('',#36393,#35949,#29994,.T.);
#45754=EDGE_CURVE('',#36537,#35948,#29995,.T.);
#45755=EDGE_CURVE('',#36537,#36538,#1144,.T.);
#45756=EDGE_CURVE('',#35949,#36538,#4587,.T.);
#45757=EDGE_CURVE('',#35956,#36537,#21172,.T.);
#45758=EDGE_CURVE('',#36539,#35957,#21173,.T.);
#45759=EDGE_CURVE('',#36537,#36539,#29996,.T.);
#45760=EDGE_CURVE('',#35967,#36539,#29997,.T.);
#45761=EDGE_CURVE('',#35960,#35968,#29998,.T.);
#45762=EDGE_CURVE('',#36540,#36539,#1145,.T.);
#45763=EDGE_CURVE('',#36540,#35966,#4588,.T.);
#45764=EDGE_CURVE('',#35966,#36396,#29999,.T.);
#45765=EDGE_CURVE('',#35965,#36397,#30000,.T.);
#45766=EDGE_CURVE('',#35964,#36541,#30001,.T.);
#45767=EDGE_CURVE('',#36541,#36397,#30002,.T.);
#45768=EDGE_CURVE('',#35963,#36542,#30003,.T.);
#45769=EDGE_CURVE('',#36542,#36541,#4589,.T.);
#45770=EDGE_CURVE('',#35962,#36543,#30004,.T.);
#45771=EDGE_CURVE('',#36543,#36542,#1870,.T.);
#45772=EDGE_CURVE('',#35961,#36544,#30005,.T.);
#45773=EDGE_CURVE('',#36544,#36543,#21174,.T.);
#45774=EDGE_CURVE('',#35968,#36544,#1871,.T.);
#45775=EDGE_CURVE('',#36545,#36544,#4590,.T.);
#45776=EDGE_CURVE('',#36545,#35969,#4591,.T.);
#45777=EDGE_CURVE('',#35969,#35979,#30006,.T.);
#45778=EDGE_CURVE('',#36545,#35978,#30007,.T.);
#45779=EDGE_CURVE('',#36546,#35977,#30008,.T.);
#45780=EDGE_CURVE('',#36546,#36545,#21175,.T.);
#45781=EDGE_CURVE('',#36547,#35976,#30009,.T.);
#45782=EDGE_CURVE('',#36547,#36546,#4592,.T.);
#45783=EDGE_CURVE('',#36548,#35975,#30010,.T.);
#45784=EDGE_CURVE('',#36548,#36547,#1146,.T.);
#45785=EDGE_CURVE('',#36398,#35974,#30011,.T.);
#45786=EDGE_CURVE('',#36398,#36548,#1872,.T.);
#45787=EDGE_CURVE('',#36399,#35973,#30012,.T.);
#45788=EDGE_CURVE('',#36549,#35972,#30013,.T.);
#45789=EDGE_CURVE('',#36549,#36550,#4593,.T.);
#45790=EDGE_CURVE('',#35973,#36550,#4594,.T.);
#45791=EDGE_CURVE('',#35980,#36549,#21176,.T.);
#45792=EDGE_CURVE('',#36551,#35981,#21177,.T.);
#45793=EDGE_CURVE('',#36549,#36551,#4595,.T.);
#45794=EDGE_CURVE('',#35991,#36551,#30014,.T.);
#45795=EDGE_CURVE('',#35984,#35992,#30015,.T.);
#45796=EDGE_CURVE('',#36552,#36551,#4596,.T.);
#45797=EDGE_CURVE('',#36552,#35990,#4597,.T.);
#45798=EDGE_CURVE('',#35990,#36402,#30016,.T.);
#45799=EDGE_CURVE('',#35989,#36403,#30017,.T.);
#45800=EDGE_CURVE('',#35988,#36553,#30018,.T.);
#45801=EDGE_CURVE('',#36553,#36403,#1873,.T.);
#45802=EDGE_CURVE('',#35987,#36554,#30019,.T.);
#45803=EDGE_CURVE('',#36554,#36553,#1147,.T.);
#45804=EDGE_CURVE('',#35986,#36555,#30020,.T.);
#45805=EDGE_CURVE('',#36555,#36554,#4598,.T.);
#45806=EDGE_CURVE('',#35985,#36556,#30021,.T.);
#45807=EDGE_CURVE('',#36556,#36555,#21178,.T.);
#45808=EDGE_CURVE('',#35992,#36556,#4599,.T.);
#45809=EDGE_CURVE('',#36557,#36556,#4600,.T.);
#45810=EDGE_CURVE('',#36557,#35993,#1148,.T.);
#45811=EDGE_CURVE('',#36004,#35993,#30022,.T.);
#45812=EDGE_CURVE('',#36557,#36003,#30023,.T.);
#45813=EDGE_CURVE('',#36558,#36002,#30024,.T.);
#45814=EDGE_CURVE('',#36558,#36557,#21179,.T.);
#45815=EDGE_CURVE('',#36559,#36001,#30025,.T.);
#45816=EDGE_CURVE('',#36559,#36558,#4601,.T.);
#45817=EDGE_CURVE('',#36560,#36000,#30026,.T.);
#45818=EDGE_CURVE('',#36560,#36559,#4602,.T.);
#45819=EDGE_CURVE('',#36404,#35999,#30027,.T.);
#45820=EDGE_CURVE('',#36404,#36560,#1874,.T.);
#45821=EDGE_CURVE('',#36405,#35998,#30028,.T.);
#45822=EDGE_CURVE('',#36561,#35997,#30029,.T.);
#45823=EDGE_CURVE('',#36561,#36562,#30030,.T.);
#45824=EDGE_CURVE('',#36562,#36563,#30031,.T.);
#45825=EDGE_CURVE('',#35998,#36563,#4603,.T.);
#45826=EDGE_CURVE('',#36564,#35996,#30032,.T.);
#45827=EDGE_CURVE('',#36564,#36561,#21180,.T.);
#45828=EDGE_CURVE('',#36005,#36564,#30033,.T.);
#45829=EDGE_CURVE('',#36565,#36006,#30034,.T.);
#45830=EDGE_CURVE('',#36565,#36564,#21181,.T.);
#45831=EDGE_CURVE('',#36565,#36018,#30035,.T.);
#45832=EDGE_CURVE('',#36009,#36019,#30036,.T.);
#45833=EDGE_CURVE('',#36566,#36017,#30037,.T.);
#45834=EDGE_CURVE('',#36566,#36565,#21182,.T.);
#45835=EDGE_CURVE('',#36567,#36016,#30038,.T.);
#45836=EDGE_CURVE('',#36567,#36566,#30039,.T.);
#45837=EDGE_CURVE('',#36568,#36567,#21183,.T.);
#45838=EDGE_CURVE('',#36568,#36015,#4604,.T.);
#45839=EDGE_CURVE('',#36410,#36014,#30040,.T.);
#45840=EDGE_CURVE('',#36409,#36015,#30041,.T.);
#45841=EDGE_CURVE('',#36569,#36013,#30042,.T.);
#45842=EDGE_CURVE('',#36569,#36410,#1875,.T.);
#45843=EDGE_CURVE('',#36570,#36012,#30043,.T.);
#45844=EDGE_CURVE('',#36570,#36569,#4605,.T.);
#45845=EDGE_CURVE('',#36011,#36571,#30044,.T.);
#45846=EDGE_CURVE('',#36571,#36570,#4606,.T.);
#45847=EDGE_CURVE('',#36010,#36572,#30045,.T.);
#45848=EDGE_CURVE('',#36572,#36571,#21184,.T.);
#45849=EDGE_CURVE('',#36019,#36572,#4607,.T.);
#45850=EDGE_CURVE('',#36573,#36572,#4608,.T.);
#45851=EDGE_CURVE('',#36573,#36020,#4609,.T.);
#45852=EDGE_CURVE('',#36027,#36020,#30046,.T.);
#45853=EDGE_CURVE('',#36022,#36574,#30047,.T.);
#45854=EDGE_CURVE('',#36023,#36411,#30048,.T.);
#45855=EDGE_CURVE('',#36411,#36574,#1876,.T.);
#45856=EDGE_CURVE('',#36031,#36412,#30049,.T.);
#45857=EDGE_CURVE('',#36575,#36030,#30050,.T.);
#45858=EDGE_CURVE('',#36575,#36576,#21185,.T.);
#45859=EDGE_CURVE('',#36031,#36576,#4610,.T.);
#45860=EDGE_CURVE('',#36577,#36029,#30051,.T.);
#45861=EDGE_CURVE('',#36577,#36575,#30052,.T.);
#45862=EDGE_CURVE('',#36494,#36577,#21186,.T.);
#45863=EDGE_CURVE('',#36026,#36573,#30053,.T.);
#45864=EDGE_CURVE('',#36025,#36578,#30054,.T.);
#45865=EDGE_CURVE('',#36578,#36573,#21187,.T.);
#45866=EDGE_CURVE('',#36024,#36579,#30055,.T.);
#45867=EDGE_CURVE('',#36579,#36578,#4611,.T.);
#45868=EDGE_CURVE('',#36574,#36579,#4612,.T.);
#45869=EDGE_CURVE('',#36580,#36581,#4613,.T.);
#45870=EDGE_CURVE('',#36032,#36581,#30056,.T.);
#45871=EDGE_CURVE('',#36580,#36033,#4614,.T.);
#45872=EDGE_CURVE('',#36033,#36045,#30057,.T.);
#45873=EDGE_CURVE('',#36106,#36034,#30058,.T.);
#45874=EDGE_CURVE('',#36581,#36582,#30059,.T.);
#45875=EDGE_CURVE('',#36034,#36582,#4615,.T.);
#45876=EDGE_CURVE('',#36037,#36583,#30060,.T.);
#45877=EDGE_CURVE('',#36038,#36584,#30061,.T.);
#45878=EDGE_CURVE('',#36584,#36443,#30062,.T.);
#45879=EDGE_CURVE('',#36443,#36583,#4616,.T.);
#45880=EDGE_CURVE('',#36050,#36444,#30063,.T.);
#45881=EDGE_CURVE('',#36585,#36049,#30064,.T.);
#45882=EDGE_CURVE('',#36585,#36586,#21188,.T.);
#45883=EDGE_CURVE('',#36050,#36586,#4617,.T.);
#45884=EDGE_CURVE('',#36587,#36048,#30065,.T.);
#45885=EDGE_CURVE('',#36587,#36585,#30066,.T.);
#45886=EDGE_CURVE('',#36588,#36047,#30067,.T.);
#45887=EDGE_CURVE('',#36588,#36587,#21189,.T.);
#45888=EDGE_CURVE('',#36051,#36588,#30068,.T.);
#45889=EDGE_CURVE('',#36580,#36044,#30069,.T.);
#45890=EDGE_CURVE('',#36589,#36043,#30070,.T.);
#45891=EDGE_CURVE('',#36589,#36580,#4618,.T.);
#45892=EDGE_CURVE('',#36042,#36590,#30071,.T.);
#45893=EDGE_CURVE('',#36590,#36589,#21190,.T.);
#45894=EDGE_CURVE('',#36041,#36591,#30072,.T.);
#45895=EDGE_CURVE('',#36591,#36590,#4619,.T.);
#45896=EDGE_CURVE('',#36040,#36592,#30073,.T.);
#45897=EDGE_CURVE('',#36592,#36591,#4620,.T.);
#45898=EDGE_CURVE('',#36039,#36593,#30074,.T.);
#45899=EDGE_CURVE('',#36593,#36592,#1877,.T.);
#45900=EDGE_CURVE('',#36583,#36593,#21191,.T.);
#45901=EDGE_CURVE('',#36594,#36588,#21192,.T.);
#45902=EDGE_CURVE('',#36594,#36052,#30075,.T.);
#45903=EDGE_CURVE('',#36061,#36594,#30076,.T.);
#45904=EDGE_CURVE('',#36066,#36454,#30077,.T.);
#45905=EDGE_CURVE('',#36261,#36065,#30078,.T.);
#45906=EDGE_CURVE('',#36066,#36260,#30079,.T.);
#45907=EDGE_CURVE('',#36333,#36064,#30080,.T.);
#45908=EDGE_CURVE('',#36333,#36595,#21193,.T.);
#45909=EDGE_CURVE('',#36595,#36065,#30081,.T.);
#45910=EDGE_CURVE('',#36060,#36596,#30082,.T.);
#45911=EDGE_CURVE('',#36596,#36594,#21194,.T.);
#45912=EDGE_CURVE('',#36059,#36597,#30083,.T.);
#45913=EDGE_CURVE('',#36597,#36596,#30084,.T.);
#45914=EDGE_CURVE('',#36598,#36597,#21195,.T.);
#45915=EDGE_CURVE('',#36598,#36058,#4621,.T.);
#45916=EDGE_CURVE('',#36058,#36447,#30085,.T.);
#45917=EDGE_CURVE('',#36057,#36435,#30086,.T.);
#45918=EDGE_CURVE('',#36056,#36453,#30087,.T.);
#45919=EDGE_CURVE('',#36453,#36435,#4622,.T.);
#45920=EDGE_CURVE('',#36072,#36081,#30088,.T.);
#45921=EDGE_CURVE('',#36078,#36472,#30089,.T.);
#45922=EDGE_CURVE('',#36077,#36599,#30090,.T.);
#45923=EDGE_CURVE('',#36599,#36472,#30091,.T.);
#45924=EDGE_CURVE('',#36076,#36600,#30092,.T.);
#45925=EDGE_CURVE('',#36600,#36599,#1149,.T.);
#45926=EDGE_CURVE('',#36075,#36601,#30093,.T.);
#45927=EDGE_CURVE('',#36601,#36600,#4623,.T.);
#45928=EDGE_CURVE('',#36074,#36602,#30094,.T.);
#45929=EDGE_CURVE('',#36602,#36601,#21196,.T.);
#45930=EDGE_CURVE('',#36073,#36603,#30095,.T.);
#45931=EDGE_CURVE('',#36603,#36602,#4624,.T.);
#45932=EDGE_CURVE('',#36081,#36603,#1150,.T.);
#45933=EDGE_CURVE('',#36604,#36070,#30096,.T.);
#45934=EDGE_CURVE('',#36604,#36334,#21197,.T.);
#45935=EDGE_CURVE('',#36474,#36604,#30097,.T.);
#45936=EDGE_CURVE('',#36603,#36605,#4625,.T.);
#45937=EDGE_CURVE('',#36605,#36080,#1151,.T.);
#45938=EDGE_CURVE('',#36080,#36097,#30098,.T.);
#45939=EDGE_CURVE('',#36082,#36098,#30099,.T.);
#45940=EDGE_CURVE('',#36605,#36096,#30100,.T.);
#45941=EDGE_CURVE('',#36606,#36095,#30101,.T.);
#45942=EDGE_CURVE('',#36606,#36605,#4626,.T.);
#45943=EDGE_CURVE('',#36607,#36094,#30102,.T.);
#45944=EDGE_CURVE('',#36607,#36606,#21198,.T.);
#45945=EDGE_CURVE('',#36608,#36093,#30103,.T.);
#45946=EDGE_CURVE('',#36608,#36607,#4627,.T.);
#45947=EDGE_CURVE('',#36609,#36092,#30104,.T.);
#45948=EDGE_CURVE('',#36609,#36608,#1152,.T.);
#45949=EDGE_CURVE('',#36610,#36091,#30105,.T.);
#45950=EDGE_CURVE('',#36610,#36609,#4628,.T.);
#45951=EDGE_CURVE('',#36611,#36090,#30106,.T.);
#45952=EDGE_CURVE('',#36611,#36610,#21199,.T.);
#45953=EDGE_CURVE('',#36437,#36089,#30107,.T.);
#45954=EDGE_CURVE('',#36437,#36611,#4629,.T.);
#45955=EDGE_CURVE('',#36438,#36088,#30108,.T.);
#45956=EDGE_CURVE('',#36612,#36087,#30109,.T.);
#45957=EDGE_CURVE('',#36612,#36613,#21200,.T.);
#45958=EDGE_CURVE('',#36088,#36613,#4630,.T.);
#45959=EDGE_CURVE('',#36614,#36086,#30110,.T.);
#45960=EDGE_CURVE('',#36614,#36612,#30111,.T.);
#45961=EDGE_CURVE('',#36615,#36085,#30112,.T.);
#45962=EDGE_CURVE('',#36615,#36614,#21201,.T.);
#45963=EDGE_CURVE('',#36099,#36615,#30113,.T.);
#45964=EDGE_CURVE('',#36616,#36100,#30114,.T.);
#45965=EDGE_CURVE('',#36616,#36615,#21202,.T.);
#45966=EDGE_CURVE('',#36616,#36105,#30115,.T.);
#45967=EDGE_CURVE('',#36617,#36618,#21203,.T.);
#45968=EDGE_CURVE('',#36618,#36102,#30116,.T.);
#45969=EDGE_CURVE('',#36617,#36103,#4631,.T.);
#45970=EDGE_CURVE('',#36103,#36441,#30117,.T.);
#45971=EDGE_CURVE('',#36115,#36442,#30118,.T.);
#45972=EDGE_CURVE('',#36114,#36619,#30119,.T.);
#45973=EDGE_CURVE('',#36619,#36442,#4632,.T.);
#45974=EDGE_CURVE('',#36113,#36620,#30120,.T.);
#45975=EDGE_CURVE('',#36620,#36619,#21204,.T.);
#45976=EDGE_CURVE('',#36112,#36621,#30121,.T.);
#45977=EDGE_CURVE('',#36621,#36620,#4633,.T.);
#45978=EDGE_CURVE('',#36111,#36622,#30122,.T.);
#45979=EDGE_CURVE('',#36622,#36621,#4634,.T.);
#45980=EDGE_CURVE('',#36110,#36623,#30123,.T.);
#45981=EDGE_CURVE('',#36623,#36622,#4635,.T.);
#45982=EDGE_CURVE('',#36109,#36624,#30124,.T.);
#45983=EDGE_CURVE('',#36624,#36623,#21205,.T.);
#45984=EDGE_CURVE('',#36108,#36625,#30125,.T.);
#45985=EDGE_CURVE('',#36625,#36624,#4636,.T.);
#45986=EDGE_CURVE('',#36107,#36582,#30126,.T.);
#45987=EDGE_CURVE('',#36582,#36625,#4637,.T.);
#45988=EDGE_CURVE('',#36626,#36104,#30127,.T.);
#45989=EDGE_CURVE('',#36626,#36616,#21206,.T.);
#45990=EDGE_CURVE('',#36618,#36626,#30128,.T.);
#45991=EDGE_CURVE('',#36627,#36628,#30129,.T.);
#45992=EDGE_CURVE('',#36116,#36628,#4638,.T.);
#45993=EDGE_CURVE('',#36627,#36117,#4639,.T.);
#45994=EDGE_CURVE('',#36126,#36117,#30130,.T.);
#45995=EDGE_CURVE('',#36116,#36146,#30131,.T.);
#45996=EDGE_CURVE('',#36125,#36627,#30132,.T.);
#45997=EDGE_CURVE('',#36124,#36629,#30133,.T.);
#45998=EDGE_CURVE('',#36629,#36627,#4640,.T.);
#45999=EDGE_CURVE('',#36123,#36348,#30134,.T.);
#46000=EDGE_CURVE('',#36348,#36629,#4641,.T.);
#46001=EDGE_CURVE('',#36127,#36346,#30135,.T.);
#46002=EDGE_CURVE('',#36345,#36128,#30136,.T.);
#46003=EDGE_CURVE('',#36343,#36133,#30137,.T.);
#46004=EDGE_CURVE('',#36492,#36132,#30138,.T.);
#46005=EDGE_CURVE('',#36492,#36343,#4642,.T.);
#46006=EDGE_CURVE('',#36339,#36328,#21207,.T.);
#46007=EDGE_CURVE('',#36337,#36140,#30139,.T.);
#46008=EDGE_CURVE('',#36142,#36337,#30140,.T.);
#46009=EDGE_CURVE('',#36336,#36143,#30141,.T.);
#46010=EDGE_CURVE('',#36347,#36149,#30142,.T.);
#46011=EDGE_CURVE('',#36630,#36148,#30143,.T.);
#46012=EDGE_CURVE('',#36630,#36347,#4643,.T.);
#46013=EDGE_CURVE('',#36628,#36147,#30144,.T.);
#46014=EDGE_CURVE('',#36628,#36630,#4644,.T.);
#46015=EDGE_CURVE('',#36631,#36632,#30145,.T.);
#46016=EDGE_CURVE('',#36151,#36632,#4645,.T.);
#46017=EDGE_CURVE('',#36631,#36152,#4646,.T.);
#46018=EDGE_CURVE('',#36164,#36152,#30146,.T.);
#46019=EDGE_CURVE('',#36229,#36151,#30147,.T.);
#46020=EDGE_CURVE('',#36155,#36633,#30148,.T.);
#46021=EDGE_CURVE('',#36156,#36634,#30149,.T.);
#46022=EDGE_CURVE('',#36634,#36366,#30150,.T.);
#46023=EDGE_CURVE('',#36366,#36633,#4647,.T.);
#46024=EDGE_CURVE('',#36169,#36367,#30151,.T.);
#46025=EDGE_CURVE('',#36635,#36168,#30152,.T.);
#46026=EDGE_CURVE('',#36635,#36636,#21208,.T.);
#46027=EDGE_CURVE('',#36169,#36636,#4648,.T.);
#46028=EDGE_CURVE('',#36637,#36167,#30153,.T.);
#46029=EDGE_CURVE('',#36637,#36635,#30154,.T.);
#46030=EDGE_CURVE('',#36638,#36166,#30155,.T.);
#46031=EDGE_CURVE('',#36638,#36637,#21209,.T.);
#46032=EDGE_CURVE('',#36170,#36638,#30156,.T.);
#46033=EDGE_CURVE('',#36163,#36631,#30157,.T.);
#46034=EDGE_CURVE('',#36162,#36639,#30158,.T.);
#46035=EDGE_CURVE('',#36639,#36631,#4649,.T.);
#46036=EDGE_CURVE('',#36161,#36640,#30159,.T.);
#46037=EDGE_CURVE('',#36640,#36639,#4650,.T.);
#46038=EDGE_CURVE('',#36160,#36641,#30160,.T.);
#46039=EDGE_CURVE('',#36641,#36640,#21210,.T.);
#46040=EDGE_CURVE('',#36159,#36642,#30161,.T.);
#46041=EDGE_CURVE('',#36642,#36641,#4651,.T.);
#46042=EDGE_CURVE('',#36158,#36643,#30162,.T.);
#46043=EDGE_CURVE('',#36643,#36642,#4652,.T.);
#46044=EDGE_CURVE('',#36157,#36644,#30163,.T.);
#46045=EDGE_CURVE('',#36644,#36643,#4653,.T.);
#46046=EDGE_CURVE('',#36633,#36644,#21211,.T.);
#46047=EDGE_CURVE('',#36645,#36638,#21212,.T.);
#46048=EDGE_CURVE('',#36645,#36171,#30164,.T.);
#46049=EDGE_CURVE('',#36645,#36183,#30165,.T.);
#46050=EDGE_CURVE('',#36327,#36338,#21213,.T.);
#46051=EDGE_CURVE('',#36646,#36182,#30166,.T.);
#46052=EDGE_CURVE('',#36646,#36645,#21214,.T.);
#46053=EDGE_CURVE('',#36647,#36181,#30167,.T.);
#46054=EDGE_CURVE('',#36647,#36646,#30168,.T.);
#46055=EDGE_CURVE('',#36648,#36647,#21215,.T.);
#46056=EDGE_CURVE('',#36648,#36180,#4654,.T.);
#46057=EDGE_CURVE('',#36180,#36370,#30169,.T.);
#46058=EDGE_CURVE('',#36179,#36357,#30170,.T.);
#46059=EDGE_CURVE('',#36178,#36460,#30171,.T.);
#46060=EDGE_CURVE('',#36460,#36357,#4655,.T.);
#46061=EDGE_CURVE('',#36349,#36174,#30172,.T.);
#46062=EDGE_CURVE('',#36649,#36650,#4656,.T.);
#46063=EDGE_CURVE('',#36649,#36651,#21216,.T.);
#46064=EDGE_CURVE('',#36651,#36188,#30173,.T.);
#46065=EDGE_CURVE('',#36650,#36189,#4657,.T.);
#46066=EDGE_CURVE('',#36371,#36201,#30174,.T.);
#46067=EDGE_CURVE('',#36372,#36189,#30175,.T.);
#46068=EDGE_CURVE('',#36652,#36200,#30176,.T.);
#46069=EDGE_CURVE('',#36652,#36371,#4658,.T.);
#46070=EDGE_CURVE('',#36653,#36199,#30177,.T.);
#46071=EDGE_CURVE('',#36653,#36652,#30178,.T.);
#46072=EDGE_CURVE('',#36654,#36198,#30179,.T.);
#46073=EDGE_CURVE('',#36654,#36653,#4659,.T.);
#46074=EDGE_CURVE('',#36655,#36197,#30180,.T.);
#46075=EDGE_CURVE('',#36655,#36654,#4660,.T.);
#46076=EDGE_CURVE('',#36656,#36196,#30181,.T.);
#46077=EDGE_CURVE('',#36656,#36655,#21217,.T.);
#46078=EDGE_CURVE('',#36657,#36195,#30182,.T.);
#46079=EDGE_CURVE('',#36657,#36656,#4661,.T.);
#46080=EDGE_CURVE('',#36204,#36194,#30183,.T.);
#46081=EDGE_CURVE('',#36204,#36657,#1153,.T.);
#46082=EDGE_CURVE('',#36202,#36193,#30184,.T.);
#46083=EDGE_CURVE('',#36658,#36190,#30185,.T.);
#46084=EDGE_CURVE('',#36658,#36495,#21218,.T.);
#46085=EDGE_CURVE('',#36651,#36658,#30186,.T.);
#46086=EDGE_CURVE('',#36657,#36659,#4662,.T.);
#46087=EDGE_CURVE('',#36659,#36203,#4663,.T.);
#46088=EDGE_CURVE('',#36203,#36220,#30187,.T.);
#46089=EDGE_CURVE('',#36205,#36221,#30188,.T.);
#46090=EDGE_CURVE('',#36659,#36219,#30189,.T.);
#46091=EDGE_CURVE('',#36660,#36218,#30190,.T.);
#46092=EDGE_CURVE('',#36660,#36659,#4664,.T.);
#46093=EDGE_CURVE('',#36661,#36217,#30191,.T.);
#46094=EDGE_CURVE('',#36661,#36660,#21219,.T.);
#46095=EDGE_CURVE('',#36662,#36216,#30192,.T.);
#46096=EDGE_CURVE('',#36662,#36661,#4665,.T.);
#46097=EDGE_CURVE('',#36663,#36215,#30193,.T.);
#46098=EDGE_CURVE('',#36663,#36662,#4666,.T.);
#46099=EDGE_CURVE('',#36664,#36214,#30194,.T.);
#46100=EDGE_CURVE('',#36664,#36663,#4667,.T.);
#46101=EDGE_CURVE('',#36665,#36213,#30195,.T.);
#46102=EDGE_CURVE('',#36665,#36664,#21220,.T.);
#46103=EDGE_CURVE('',#36360,#36212,#30196,.T.);
#46104=EDGE_CURVE('',#36360,#36665,#4668,.T.);
#46105=EDGE_CURVE('',#36361,#36211,#30197,.T.);
#46106=EDGE_CURVE('',#36666,#36210,#30198,.T.);
#46107=EDGE_CURVE('',#36666,#36667,#21221,.T.);
#46108=EDGE_CURVE('',#36211,#36667,#4669,.T.);
#46109=EDGE_CURVE('',#36668,#36209,#30199,.T.);
#46110=EDGE_CURVE('',#36668,#36666,#30200,.T.);
#46111=EDGE_CURVE('',#36669,#36208,#30201,.T.);
#46112=EDGE_CURVE('',#36669,#36668,#21222,.T.);
#46113=EDGE_CURVE('',#36222,#36669,#30202,.T.);
#46114=EDGE_CURVE('',#36670,#36223,#30203,.T.);
#46115=EDGE_CURVE('',#36670,#36669,#21223,.T.);
#46116=EDGE_CURVE('',#36670,#36228,#30204,.T.);
#46117=EDGE_CURVE('',#36671,#36672,#21224,.T.);
#46118=EDGE_CURVE('',#36672,#36225,#30205,.T.);
#46119=EDGE_CURVE('',#36671,#36226,#4670,.T.);
#46120=EDGE_CURVE('',#36226,#36364,#30206,.T.);
#46121=EDGE_CURVE('',#36238,#36365,#30207,.T.);
#46122=EDGE_CURVE('',#36237,#36673,#30208,.T.);
#46123=EDGE_CURVE('',#36673,#36365,#4671,.T.);
#46124=EDGE_CURVE('',#36236,#36674,#30209,.T.);
#46125=EDGE_CURVE('',#36674,#36673,#21225,.T.);
#46126=EDGE_CURVE('',#36235,#36675,#30210,.T.);
#46127=EDGE_CURVE('',#36675,#36674,#4672,.T.);
#46128=EDGE_CURVE('',#36234,#36676,#30211,.T.);
#46129=EDGE_CURVE('',#36676,#36675,#4673,.T.);
#46130=EDGE_CURVE('',#36233,#36677,#30212,.T.);
#46131=EDGE_CURVE('',#36677,#36676,#4674,.T.);
#46132=EDGE_CURVE('',#36232,#36678,#30213,.T.);
#46133=EDGE_CURVE('',#36678,#36677,#21226,.T.);
#46134=EDGE_CURVE('',#36231,#36679,#30214,.T.);
#46135=EDGE_CURVE('',#36679,#36678,#4675,.T.);
#46136=EDGE_CURVE('',#36230,#36632,#30215,.T.);
#46137=EDGE_CURVE('',#36632,#36679,#4676,.T.);
#46138=EDGE_CURVE('',#36680,#36227,#30216,.T.);
#46139=EDGE_CURVE('',#36680,#36670,#21227,.T.);
#46140=EDGE_CURVE('',#36672,#36680,#30217,.T.);
#46141=EDGE_CURVE('',#36681,#36682,#4677,.T.);
#46142=EDGE_CURVE('',#36240,#36681,#4678,.T.);
#46143=EDGE_CURVE('',#36682,#36239,#4679,.T.);
#46144=EDGE_CURVE('',#36250,#36239,#30218,.T.);
#46145=EDGE_CURVE('',#36314,#36240,#30219,.T.);
#46146=EDGE_CURVE('',#36313,#36241,#30220,.T.);
#46147=EDGE_CURVE('',#36243,#36683,#30221,.T.);
#46148=EDGE_CURVE('',#36244,#36416,#30222,.T.);
#46149=EDGE_CURVE('',#36416,#36683,#4680,.T.);
#46150=EDGE_CURVE('',#36254,#36417,#30223,.T.);
#46151=EDGE_CURVE('',#36254,#36684,#4681,.T.);
#46152=EDGE_CURVE('',#36685,#36253,#30224,.T.);
#46153=EDGE_CURVE('',#36685,#36686,#21228,.T.);
#46154=EDGE_CURVE('',#36684,#36686,#1878,.T.);
#46155=EDGE_CURVE('',#36687,#36252,#30225,.T.);
#46156=EDGE_CURVE('',#36687,#36685,#30226,.T.);
#46157=EDGE_CURVE('',#36496,#36687,#21229,.T.);
#46158=EDGE_CURVE('',#36249,#36682,#30227,.T.);
#46159=EDGE_CURVE('',#36248,#36688,#30228,.T.);
#46160=EDGE_CURVE('',#36688,#36682,#4682,.T.);
#46161=EDGE_CURVE('',#36247,#36689,#30229,.T.);
#46162=EDGE_CURVE('',#36689,#36688,#21230,.T.);
#46163=EDGE_CURVE('',#36246,#36690,#30230,.T.);
#46164=EDGE_CURVE('',#36690,#36689,#4683,.T.);
#46165=EDGE_CURVE('',#36245,#36691,#30231,.T.);
#46166=EDGE_CURVE('',#36691,#36690,#1154,.T.);
#46167=EDGE_CURVE('',#36683,#36691,#1879,.T.);
#46168=EDGE_CURVE('',#36256,#36449,#30232,.T.);
#46169=EDGE_CURVE('',#36257,#36427,#30233,.T.);
#46170=EDGE_CURVE('',#36427,#36449,#4684,.T.);
#46171=EDGE_CURVE('',#36268,#36428,#30234,.T.);
#46172=EDGE_CURVE('',#36267,#36692,#30235,.T.);
#46173=EDGE_CURVE('',#36692,#36693,#21231,.T.);
#46174=EDGE_CURVE('',#36268,#36693,#4685,.T.);
#46175=EDGE_CURVE('',#36266,#36694,#30236,.T.);
#46176=EDGE_CURVE('',#36694,#36692,#30237,.T.);
#46177=EDGE_CURVE('',#36265,#36695,#30238,.T.);
#46178=EDGE_CURVE('',#36695,#36694,#21232,.T.);
#46179=EDGE_CURVE('',#36269,#36695,#30239,.T.);
#46180=EDGE_CURVE('',#36332,#36262,#30240,.T.);
#46181=EDGE_CURVE('',#36696,#36261,#30241,.T.);
#46182=EDGE_CURVE('',#36696,#36332,#21233,.T.);
#46183=EDGE_CURVE('',#36260,#36455,#30242,.T.);
#46184=EDGE_CURVE('',#36697,#36270,#30243,.T.);
#46185=EDGE_CURVE('',#36697,#36695,#21234,.T.);
#46186=EDGE_CURVE('',#36697,#36275,#30244,.T.);
#46187=EDGE_CURVE('',#36698,#36699,#21235,.T.);
#46188=EDGE_CURVE('',#36699,#36272,#30245,.T.);
#46189=EDGE_CURVE('',#36698,#36273,#4686,.T.);
#46190=EDGE_CURVE('',#36700,#36419,#30246,.T.);
#46191=EDGE_CURVE('',#36273,#36431,#30247,.T.);
#46192=EDGE_CURVE('',#36286,#36700,#30248,.T.);
#46193=EDGE_CURVE('',#36285,#36701,#30249,.T.);
#46194=EDGE_CURVE('',#36701,#36419,#4687,.T.);
#46195=EDGE_CURVE('',#36284,#36702,#30250,.T.);
#46196=EDGE_CURVE('',#36702,#36701,#21236,.T.);
#46197=EDGE_CURVE('',#36283,#36703,#30251,.T.);
#46198=EDGE_CURVE('',#36703,#36702,#4688,.T.);
#46199=EDGE_CURVE('',#36282,#36704,#30252,.T.);
#46200=EDGE_CURVE('',#36704,#36703,#4689,.T.);
#46201=EDGE_CURVE('',#36705,#36281,#30253,.T.);
#46202=EDGE_CURVE('',#36705,#36704,#4690,.T.);
#46203=EDGE_CURVE('',#36706,#36280,#30254,.T.);
#46204=EDGE_CURVE('',#36706,#36705,#21237,.T.);
#46205=EDGE_CURVE('',#36707,#36279,#30255,.T.);
#46206=EDGE_CURVE('',#36707,#36706,#4691,.T.);
#46207=EDGE_CURVE('',#36708,#36278,#30256,.T.);
#46208=EDGE_CURVE('',#36708,#36707,#4692,.T.);
#46209=EDGE_CURVE('',#36287,#36277,#30257,.T.);
#46210=EDGE_CURVE('',#36287,#36708,#4693,.T.);
#46211=EDGE_CURVE('',#36709,#36274,#30258,.T.);
#46212=EDGE_CURVE('',#36709,#36697,#21238,.T.);
#46213=EDGE_CURVE('',#36699,#36709,#30259,.T.);
#46214=EDGE_CURVE('',#36710,#36708,#30260,.T.);
#46215=EDGE_CURVE('',#36710,#36288,#4694,.T.);
#46216=EDGE_CURVE('',#36288,#36304,#30261,.T.);
#46217=EDGE_CURVE('',#36710,#36303,#30262,.T.);
#46218=EDGE_CURVE('',#36711,#36302,#30263,.T.);
#46219=EDGE_CURVE('',#36711,#36710,#4695,.T.);
#46220=EDGE_CURVE('',#36712,#36301,#30264,.T.);
#46221=EDGE_CURVE('',#36712,#36711,#4696,.T.);
#46222=EDGE_CURVE('',#36713,#36300,#30265,.T.);
#46223=EDGE_CURVE('',#36713,#36712,#21239,.T.);
#46224=EDGE_CURVE('',#36714,#36299,#30266,.T.);
#46225=EDGE_CURVE('',#36714,#36713,#4697,.T.);
#46226=EDGE_CURVE('',#36715,#36298,#30267,.T.);
#46227=EDGE_CURVE('',#36715,#36714,#4698,.T.);
#46228=EDGE_CURVE('',#36716,#36297,#30268,.T.);
#46229=EDGE_CURVE('',#36716,#36715,#4699,.T.);
#46230=EDGE_CURVE('',#36717,#36296,#30269,.T.);
#46231=EDGE_CURVE('',#36717,#36716,#21240,.T.);
#46232=EDGE_CURVE('',#36418,#36295,#30270,.T.);
#46233=EDGE_CURVE('',#36418,#36717,#4700,.T.);
#46234=EDGE_CURVE('',#36420,#36294,#30271,.T.);
#46235=EDGE_CURVE('',#36718,#36293,#30272,.T.);
#46236=EDGE_CURVE('',#36718,#36719,#21241,.T.);
#46237=EDGE_CURVE('',#36294,#36719,#4701,.T.);
#46238=EDGE_CURVE('',#36720,#36292,#30273,.T.);
#46239=EDGE_CURVE('',#36720,#36718,#30274,.T.);
#46240=EDGE_CURVE('',#36721,#36291,#30275,.T.);
#46241=EDGE_CURVE('',#36721,#36720,#21242,.T.);
#46242=EDGE_CURVE('',#36305,#36721,#30276,.T.);
#46243=EDGE_CURVE('',#36722,#36306,#30277,.T.);
#46244=EDGE_CURVE('',#36722,#36721,#21243,.T.);
#46245=EDGE_CURVE('',#36722,#36312,#30278,.T.);
#46246=EDGE_CURVE('',#36723,#36724,#21244,.T.);
#46247=EDGE_CURVE('',#36724,#36309,#30279,.T.);
#46248=EDGE_CURVE('',#36723,#36310,#4702,.T.);
#46249=EDGE_CURVE('',#36725,#36424,#30280,.T.);
#46250=EDGE_CURVE('',#36310,#36423,#30281,.T.);
#46251=EDGE_CURVE('',#36322,#36725,#30282,.T.);
#46252=EDGE_CURVE('',#36321,#36726,#30283,.T.);
#46253=EDGE_CURVE('',#36726,#36424,#4703,.T.);
#46254=EDGE_CURVE('',#36320,#36727,#30284,.T.);
#46255=EDGE_CURVE('',#36727,#36726,#21245,.T.);
#46256=EDGE_CURVE('',#36319,#36728,#30285,.T.);
#46257=EDGE_CURVE('',#36728,#36727,#4704,.T.);
#46258=EDGE_CURVE('',#36318,#36729,#30286,.T.);
#46259=EDGE_CURVE('',#36729,#36728,#4705,.T.);
#46260=EDGE_CURVE('',#36317,#36730,#30287,.T.);
#46261=EDGE_CURVE('',#36730,#36729,#4706,.T.);
#46262=EDGE_CURVE('',#36316,#36731,#30288,.T.);
#46263=EDGE_CURVE('',#36731,#36730,#21246,.T.);
#46264=EDGE_CURVE('',#36315,#36681,#30289,.T.);
#46265=EDGE_CURVE('',#36681,#36731,#4707,.T.);
#46266=EDGE_CURVE('',#36732,#36311,#30290,.T.);
#46267=EDGE_CURVE('',#36732,#36722,#21247,.T.);
#46268=EDGE_CURVE('',#36724,#36732,#30291,.T.);
#46269=EDGE_CURVE('',#36595,#36696,#30292,.T.);
#46270=EDGE_CURVE('',#36491,#36604,#21248,.T.);
#46271=EDGE_CURVE('',#36630,#36629,#4708,.T.);
#46272=EDGE_CURVE('',#36456,#36353,#30293,.T.);
#46273=EDGE_CURVE('',#36457,#36354,#30294,.T.);
#46274=EDGE_CURVE('',#36458,#36355,#30295,.T.);
#46275=EDGE_CURVE('',#36459,#36356,#30296,.T.);
#46276=EDGE_CURVE('',#36648,#36369,#30297,.T.);
#46277=EDGE_CURVE('',#36636,#36368,#30298,.T.);
#46278=EDGE_CURVE('',#36636,#36648,#21249,.T.);
#46279=EDGE_CURVE('',#36673,#36633,#21250,.T.);
#46280=EDGE_CURVE('',#36671,#36363,#30299,.T.);
#46281=EDGE_CURVE('',#36667,#36362,#30300,.T.);
#46282=EDGE_CURVE('',#36667,#36671,#21251,.T.);
#46283=EDGE_CURVE('',#36359,#36733,#30301,.T.);
#46284=EDGE_CURVE('',#36733,#36665,#21252,.T.);
#46285=EDGE_CURVE('',#36358,#36734,#30302,.T.);
#46286=EDGE_CURVE('',#36734,#36733,#1155,.T.);
#46287=EDGE_CURVE('',#36650,#36373,#30303,.T.);
#46288=EDGE_CURVE('',#36652,#36734,#1156,.T.);
#46289=EDGE_CURVE('',#36649,#36414,#30304,.T.);
#46290=EDGE_CURVE('',#36576,#36413,#30305,.T.);
#46291=EDGE_CURVE('',#36576,#36649,#30306,.T.);
#46292=EDGE_CURVE('',#36569,#36574,#30307,.T.);
#46293=EDGE_CURVE('',#36408,#36568,#30308,.T.);
#46294=EDGE_CURVE('',#36407,#36735,#30309,.T.);
#46295=EDGE_CURVE('',#36735,#36568,#30310,.T.);
#46296=EDGE_CURVE('',#36406,#36563,#30311,.T.);
#46297=EDGE_CURVE('',#36563,#36735,#4709,.T.);
#46298=EDGE_CURVE('',#36553,#36560,#30312,.T.);
#46299=EDGE_CURVE('',#36552,#36401,#30313,.T.);
#46300=EDGE_CURVE('',#36550,#36400,#30314,.T.);
#46301=EDGE_CURVE('',#36550,#36552,#30315,.T.);
#46302=EDGE_CURVE('',#36541,#36548,#30316,.T.);
#46303=EDGE_CURVE('',#36540,#36395,#30317,.T.);
#46304=EDGE_CURVE('',#36538,#36394,#30318,.T.);
#46305=EDGE_CURVE('',#36538,#36540,#30319,.T.);
#46306=EDGE_CURVE('',#36529,#36536,#30320,.T.);
#46307=EDGE_CURVE('',#36528,#36389,#30321,.T.);
#46308=EDGE_CURVE('',#36526,#36388,#30322,.T.);
#46309=EDGE_CURVE('',#36526,#36528,#30323,.T.);
#46310=EDGE_CURVE('',#36517,#36524,#30324,.T.);
#46311=EDGE_CURVE('',#36383,#36516,#30325,.T.);
#46312=EDGE_CURVE('',#36382,#36736,#30326,.T.);
#46313=EDGE_CURVE('',#36736,#36516,#4710,.T.);
#46314=EDGE_CURVE('',#36381,#36510,#30327,.T.);
#46315=EDGE_CURVE('',#36510,#36736,#30328,.T.);
#46316=EDGE_CURVE('',#36500,#36508,#30329,.T.);
#46317=EDGE_CURVE('',#36498,#36376,#30330,.T.);
#46318=EDGE_CURVE('',#36686,#36375,#30331,.T.);
#46319=EDGE_CURVE('',#36686,#36498,#30332,.T.);
#46320=EDGE_CURVE('',#36684,#36374,#30333,.T.);
#46321=EDGE_CURVE('',#36737,#36415,#30334,.T.);
#46322=EDGE_CURVE('',#36737,#36683,#4711,.T.);
#46323=EDGE_CURVE('',#36701,#36717,#21253,.T.);
#46324=EDGE_CURVE('',#36698,#36430,#30335,.T.);
#46325=EDGE_CURVE('',#36693,#36429,#30336,.T.);
#46326=EDGE_CURVE('',#36693,#36698,#21254,.T.);
#46327=EDGE_CURVE('',#36448,#36426,#30337,.T.);
#46328=EDGE_CURVE('',#36738,#36425,#30338,.T.);
#46329=EDGE_CURVE('',#36738,#36737,#1157,.T.);
#46330=EDGE_CURVE('',#36726,#36738,#21255,.T.);
#46331=EDGE_CURVE('',#36723,#36422,#30339,.T.);
#46332=EDGE_CURVE('',#36719,#36421,#30340,.T.);
#46333=EDGE_CURVE('',#36719,#36723,#21256,.T.);
#46334=EDGE_CURVE('',#36450,#36432,#30341,.T.);
#46335=EDGE_CURVE('',#36451,#36433,#30342,.T.);
#46336=EDGE_CURVE('',#36452,#36434,#30343,.T.);
#46337=EDGE_CURVE('',#36598,#36446,#30344,.T.);
#46338=EDGE_CURVE('',#36586,#36445,#30345,.T.);
#46339=EDGE_CURVE('',#36586,#36598,#21257,.T.);
#46340=EDGE_CURVE('',#36619,#36583,#21258,.T.);
#46341=EDGE_CURVE('',#36617,#36440,#30346,.T.);
#46342=EDGE_CURVE('',#36613,#36439,#30347,.T.);
#46343=EDGE_CURVE('',#36613,#36617,#21259,.T.);
#46344=EDGE_CURVE('',#36436,#36739,#30348,.T.);
#46345=EDGE_CURVE('',#36739,#36611,#21260,.T.);
#46346=EDGE_CURVE('',#36473,#36739,#4712,.T.);
#46347=EDGE_CURVE('',#36486,#36490,#4713,.T.);
#46348=EDGE_CURVE('',#36483,#36488,#21261,.T.);
#46349=EDGE_CURVE('',#36479,#36482,#4714,.T.);
#46350=EDGE_CURVE('',#36475,#36478,#4715,.T.);
#46351=EDGE_CURVE('',#36610,#36739,#30349,.T.);
#46352=EDGE_CURVE('',#36599,#36609,#30350,.T.);
#46353=EDGE_CURVE('',#36577,#36658,#21262,.T.);
#46354=EDGE_CURVE('',#36687,#36504,#21263,.T.);
#46355=EDGE_CURVE('',#36499,#36685,#21264,.T.);
#46356=EDGE_CURVE('',#36507,#36501,#4716,.T.);
#46357=EDGE_CURVE('',#36502,#36506,#4717,.T.);
#46358=EDGE_CURVE('',#36515,#36509,#21265,.T.);
#46359=EDGE_CURVE('',#36736,#36515,#21266,.T.);
#46360=EDGE_CURVE('',#36511,#36514,#21267,.T.);
#46361=EDGE_CURVE('',#36523,#36518,#4718,.T.);
#46362=EDGE_CURVE('',#36519,#36522,#4719,.T.);
#46363=EDGE_CURVE('',#36535,#36530,#1158,.T.);
#46364=EDGE_CURVE('',#36531,#36534,#4720,.T.);
#46365=EDGE_CURVE('',#36547,#36542,#4721,.T.);
#46366=EDGE_CURVE('',#36543,#36546,#4722,.T.);
#46367=EDGE_CURVE('',#36559,#36554,#4723,.T.);
#46368=EDGE_CURVE('',#36555,#36558,#4724,.T.);
#46369=EDGE_CURVE('',#36562,#36735,#21268,.T.);
#46370=EDGE_CURVE('',#36561,#36566,#21269,.T.);
#46371=EDGE_CURVE('',#36567,#36562,#21270,.T.);
#46372=EDGE_CURVE('',#36579,#36570,#4725,.T.);
#46373=EDGE_CURVE('',#36571,#36578,#4726,.T.);
#46374=EDGE_CURVE('',#36651,#36575,#21271,.T.);
#46375=EDGE_CURVE('',#36589,#36624,#4727,.T.);
#46376=EDGE_CURVE('',#36625,#36581,#4728,.T.);
#46377=EDGE_CURVE('',#36597,#36585,#21272,.T.);
#46378=EDGE_CURVE('',#36587,#36596,#21273,.T.);
#46379=EDGE_CURVE('',#36623,#36590,#4729,.T.);
#46380=EDGE_CURVE('',#36740,#36591,#30351,.T.);
#46381=EDGE_CURVE('',#36740,#36622,#4730,.T.);
#46382=EDGE_CURVE('',#36740,#36592,#30352,.T.);
#46383=EDGE_CURVE('',#36593,#36620,#30353,.T.);
#46384=EDGE_CURVE('',#36621,#36740,#30354,.T.);
#46385=EDGE_CURVE('',#36608,#36600,#4731,.T.);
#46386=EDGE_CURVE('',#36601,#36607,#4732,.T.);
#46387=EDGE_CURVE('',#36606,#36602,#4733,.T.);
#46388=EDGE_CURVE('',#36618,#36612,#21274,.T.);
#46389=EDGE_CURVE('',#36614,#36626,#21275,.T.);
#46390=EDGE_CURVE('',#36679,#36639,#4734,.T.);
#46391=EDGE_CURVE('',#36647,#36635,#21276,.T.);
#46392=EDGE_CURVE('',#36637,#36646,#21277,.T.);
#46393=EDGE_CURVE('',#36640,#36678,#4735,.T.);
#46394=EDGE_CURVE('',#36677,#36641,#4736,.T.);
#46395=EDGE_CURVE('',#36642,#36676,#4737,.T.);
#46396=EDGE_CURVE('',#36675,#36643,#30355,.T.);
#46397=EDGE_CURVE('',#36644,#36674,#30356,.T.);
#46398=EDGE_CURVE('',#36664,#36733,#30357,.T.);
#46399=EDGE_CURVE('',#36653,#36663,#30358,.T.);
#46400=EDGE_CURVE('',#36662,#36654,#4738,.T.);
#46401=EDGE_CURVE('',#36655,#36661,#4739,.T.);
#46402=EDGE_CURVE('',#36660,#36656,#4740,.T.);
#46403=EDGE_CURVE('',#36672,#36666,#21278,.T.);
#46404=EDGE_CURVE('',#36668,#36680,#21279,.T.);
#46405=EDGE_CURVE('',#36688,#36731,#4741,.T.);
#46406=EDGE_CURVE('',#36730,#36689,#4742,.T.);
#46407=EDGE_CURVE('',#36690,#36729,#4743,.T.);
#46408=EDGE_CURVE('',#36728,#36691,#30359,.T.);
#46409=EDGE_CURVE('',#36738,#36727,#30360,.T.);
#46410=EDGE_CURVE('',#36699,#36692,#21280,.T.);
#46411=EDGE_CURVE('',#36694,#36709,#21281,.T.);
#46412=EDGE_CURVE('',#36716,#36702,#30361,.T.);
#46413=EDGE_CURVE('',#36703,#36715,#30362,.T.);
#46414=EDGE_CURVE('',#36714,#36704,#4744,.T.);
#46415=EDGE_CURVE('',#36705,#36713,#4745,.T.);
#46416=EDGE_CURVE('',#36712,#36706,#4746,.T.);
#46417=EDGE_CURVE('',#36707,#36711,#4747,.T.);
#46418=EDGE_CURVE('',#36724,#36718,#21282,.T.);
#46419=EDGE_CURVE('',#36720,#36732,#21283,.T.);
#46420=EDGE_CURVE('',#36741,#36742,#30363,.T.);
#46421=EDGE_CURVE('',#36742,#36743,#21284,.T.);
#46422=EDGE_CURVE('',#36743,#36741,#21285,.T.);
#46423=EDGE_CURVE('',#36744,#36745,#21286,.T.);
#46424=EDGE_CURVE('',#36745,#36746,#21287,.T.);
#46425=EDGE_CURVE('',#36746,#36747,#21288,.T.);
#46426=EDGE_CURVE('',#36747,#36744,#21289,.T.);
#46427=EDGE_CURVE('',#36746,#36748,#30364,.T.);
#46428=EDGE_CURVE('',#36749,#36748,#21290,.T.);
#46429=EDGE_CURVE('',#36749,#36747,#30365,.T.);
#46430=EDGE_CURVE('',#36748,#36750,#21291,.T.);
#46431=EDGE_CURVE('',#36750,#36751,#21292,.T.);
#46432=EDGE_CURVE('',#36751,#36749,#21293,.T.);
#46433=EDGE_CURVE('',#36752,#36753,#4748,.T.);
#46434=EDGE_CURVE('',#36753,#36754,#4749,.T.);
#46435=EDGE_CURVE('',#36754,#36755,#30366,.T.);
#46436=EDGE_CURVE('',#36755,#36752,#4750,.T.);
#46437=EDGE_CURVE('',#36756,#36757,#4751,.T.);
#46438=EDGE_CURVE('',#36756,#36753,#4752,.T.);
#46439=EDGE_CURVE('',#36752,#36757,#4753,.T.);
#46440=EDGE_CURVE('',#36758,#36759,#4754,.T.);
#46441=EDGE_CURVE('',#36759,#36756,#21294,.T.);
#46442=EDGE_CURVE('',#36757,#36758,#21295,.T.);
#46443=EDGE_CURVE('',#36760,#36761,#4755,.T.);
#46444=EDGE_CURVE('',#36760,#36759,#4756,.T.);
#46445=EDGE_CURVE('',#36758,#36761,#4757,.T.);
#46446=EDGE_CURVE('',#36762,#36763,#30367,.T.);
#46447=EDGE_CURVE('',#36763,#36760,#4758,.T.);
#46448=EDGE_CURVE('',#36761,#36762,#4759,.T.);
#46449=EDGE_CURVE('',#36764,#36765,#30368,.T.);
#46450=EDGE_CURVE('',#36764,#36763,#4760,.T.);
#46451=EDGE_CURVE('',#36762,#36765,#4761,.T.);
#46452=EDGE_CURVE('',#36766,#36767,#21296,.T.);
#46453=EDGE_CURVE('',#36767,#36764,#21297,.T.);
#46454=EDGE_CURVE('',#36765,#36766,#21298,.T.);
#46455=EDGE_CURVE('',#36768,#36769,#21299,.T.);
#46456=EDGE_CURVE('',#36769,#36770,#21300,.T.);
#46457=EDGE_CURVE('',#36770,#36771,#21301,.T.);
#46458=EDGE_CURVE('',#36771,#36768,#21302,.T.);
#46459=EDGE_CURVE('',#36770,#36772,#30369,.T.);
#46460=EDGE_CURVE('',#36773,#36772,#21303,.T.);
#46461=EDGE_CURVE('',#36773,#36771,#30370,.T.);
#46462=EDGE_CURVE('',#36772,#36774,#21304,.T.);
#46463=EDGE_CURVE('',#36774,#36775,#21305,.T.);
#46464=EDGE_CURVE('',#36775,#36773,#21306,.T.);
#46465=EDGE_CURVE('',#36776,#36777,#4762,.T.);
#46466=EDGE_CURVE('',#36777,#36778,#30371,.T.);
#46467=EDGE_CURVE('',#36779,#36778,#30372,.T.);
#46468=EDGE_CURVE('',#36779,#36742,#4763,.T.);
#46469=EDGE_CURVE('',#36741,#36776,#4764,.T.);
#46470=EDGE_CURVE('',#36778,#36780,#4765,.T.);
#46471=EDGE_CURVE('',#36780,#36781,#4766,.T.);
#46472=EDGE_CURVE('',#36781,#36779,#4767,.T.);
#46473=EDGE_CURVE('',#36780,#36782,#4768,.T.);
#46474=EDGE_CURVE('',#36783,#36782,#4769,.T.);
#46475=EDGE_CURVE('',#36783,#36781,#4770,.T.);
#46476=EDGE_CURVE('',#36782,#36784,#21307,.T.);
#46477=EDGE_CURVE('',#36784,#36785,#4771,.T.);
#46478=EDGE_CURVE('',#36785,#36783,#21308,.T.);
#46479=EDGE_CURVE('',#36784,#36786,#4772,.T.);
#46480=EDGE_CURVE('',#36787,#36786,#4773,.T.);
#46481=EDGE_CURVE('',#36787,#36785,#4774,.T.);
#46482=EDGE_CURVE('',#36788,#36789,#21309,.T.);
#46483=EDGE_CURVE('',#36789,#36790,#21310,.T.);
#46484=EDGE_CURVE('',#36790,#36791,#21311,.T.);
#46485=EDGE_CURVE('',#36791,#36788,#21312,.T.);
#46486=EDGE_CURVE('',#36790,#36792,#30373,.T.);
#46487=EDGE_CURVE('',#36793,#36792,#21313,.T.);
#46488=EDGE_CURVE('',#36793,#36791,#30374,.T.);
#46489=EDGE_CURVE('',#36792,#36794,#21314,.T.);
#46490=EDGE_CURVE('',#36794,#36795,#21315,.T.);
#46491=EDGE_CURVE('',#36795,#36793,#21316,.T.);
#46492=EDGE_CURVE('',#36796,#36797,#21317,.T.);
#46493=EDGE_CURVE('',#36797,#36798,#21318,.T.);
#46494=EDGE_CURVE('',#36798,#36796,#30375,.T.);
#46495=EDGE_CURVE('',#36799,#36800,#4775,.T.);
#46496=EDGE_CURVE('',#36799,#36801,#4776,.T.);
#46497=EDGE_CURVE('',#36802,#36801,#4777,.T.);
#46498=EDGE_CURVE('',#36802,#36800,#4778,.T.);
#46499=EDGE_CURVE('',#36803,#36804,#4779,.T.);
#46500=EDGE_CURVE('',#36804,#36799,#21319,.T.);
#46501=EDGE_CURVE('',#36800,#36803,#21320,.T.);
#46502=EDGE_CURVE('',#36805,#36806,#4780,.T.);
#46503=EDGE_CURVE('',#36805,#36804,#4781,.T.);
#46504=EDGE_CURVE('',#36803,#36806,#4782,.T.);
#46505=EDGE_CURVE('',#36807,#36808,#30376,.T.);
#46506=EDGE_CURVE('',#36808,#36805,#4783,.T.);
#46507=EDGE_CURVE('',#36806,#36807,#4784,.T.);
#46508=EDGE_CURVE('',#36798,#36808,#4785,.T.);
#46509=EDGE_CURVE('',#36807,#36809,#30377,.T.);
#46510=EDGE_CURVE('',#36809,#36810,#4786,.T.);
#46511=EDGE_CURVE('',#36810,#36796,#4787,.T.);
#46512=EDGE_CURVE('',#36811,#36812,#21321,.T.);
#46513=EDGE_CURVE('',#36812,#36813,#21322,.T.);
#46514=EDGE_CURVE('',#36813,#36814,#30378,.T.);
#46515=EDGE_CURVE('',#36814,#36811,#21323,.T.);
#46516=EDGE_CURVE('',#36813,#36815,#4788,.T.);
#46517=EDGE_CURVE('',#36816,#36815,#30379,.T.);
#46518=EDGE_CURVE('',#36816,#36814,#4789,.T.);
#46519=EDGE_CURVE('',#36815,#36817,#4790,.T.);
#46520=EDGE_CURVE('',#36817,#36818,#4791,.T.);
#46521=EDGE_CURVE('',#36818,#36816,#4792,.T.);
#46522=EDGE_CURVE('',#36817,#36819,#4793,.T.);
#46523=EDGE_CURVE('',#36820,#36819,#4794,.T.);
#46524=EDGE_CURVE('',#36820,#36818,#4795,.T.);
#46525=EDGE_CURVE('',#36819,#36821,#21324,.T.);
#46526=EDGE_CURVE('',#36821,#36822,#4796,.T.);
#46527=EDGE_CURVE('',#36822,#36820,#21325,.T.);
#46528=EDGE_CURVE('',#36821,#36823,#4797,.T.);
#46529=EDGE_CURVE('',#36824,#36823,#4798,.T.);
#46530=EDGE_CURVE('',#36824,#36822,#4799,.T.);
#46531=EDGE_CURVE('',#36825,#36826,#21326,.T.);
#46532=EDGE_CURVE('',#36826,#36827,#21327,.T.);
#46533=EDGE_CURVE('',#36827,#36828,#21328,.T.);
#46534=EDGE_CURVE('',#36828,#36825,#21329,.T.);
#46535=EDGE_CURVE('',#36829,#36830,#21330,.T.);
#46536=EDGE_CURVE('',#36829,#36826,#30380,.T.);
#46537=EDGE_CURVE('',#36825,#36830,#30381,.T.);
#46538=EDGE_CURVE('',#36830,#36831,#21331,.T.);
#46539=EDGE_CURVE('',#36831,#36832,#21332,.T.);
#46540=EDGE_CURVE('',#36832,#36829,#21333,.T.);
#46541=EDGE_CURVE('',#36823,#36833,#4800,.T.);
#46542=EDGE_CURVE('',#36833,#36834,#30382,.T.);
#46543=EDGE_CURVE('',#36834,#36824,#4801,.T.);
#46544=EDGE_CURVE('',#36835,#36836,#4802,.T.);
#46545=EDGE_CURVE('',#36836,#36837,#4803,.T.);
#46546=EDGE_CURVE('',#36837,#36838,#30383,.T.);
#46547=EDGE_CURVE('',#36838,#36835,#4804,.T.);
#46548=EDGE_CURVE('',#36839,#36840,#4805,.T.);
#46549=EDGE_CURVE('',#36840,#36841,#4806,.T.);
#46550=EDGE_CURVE('',#36841,#36839,#30384,.T.);
#46551=EDGE_CURVE('',#36842,#36843,#21334,.T.);
#46552=EDGE_CURVE('',#36843,#36844,#21335,.T.);
#46553=EDGE_CURVE('',#36844,#36845,#21336,.T.);
#46554=EDGE_CURVE('',#36845,#36842,#21337,.T.);
#46555=EDGE_CURVE('',#36844,#36846,#30385,.T.);
#46556=EDGE_CURVE('',#36847,#36846,#21338,.T.);
#46557=EDGE_CURVE('',#36847,#36845,#30386,.T.);
#46558=EDGE_CURVE('',#36846,#36848,#21339,.T.);
#46559=EDGE_CURVE('',#36848,#36849,#21340,.T.);
#46560=EDGE_CURVE('',#36849,#36847,#21341,.T.);
#46561=EDGE_CURVE('',#36850,#36851,#21342,.T.);
#46562=EDGE_CURVE('',#36851,#36852,#21343,.T.);
#46563=EDGE_CURVE('',#36852,#36850,#30387,.T.);
#46564=EDGE_CURVE('',#36853,#36854,#4807,.T.);
#46565=EDGE_CURVE('',#36853,#36855,#4808,.T.);
#46566=EDGE_CURVE('',#36856,#36855,#4809,.T.);
#46567=EDGE_CURVE('',#36856,#36854,#4810,.T.);
#46568=EDGE_CURVE('',#36857,#36858,#4811,.T.);
#46569=EDGE_CURVE('',#36858,#36853,#21344,.T.);
#46570=EDGE_CURVE('',#36854,#36857,#21345,.T.);
#46571=EDGE_CURVE('',#36859,#36860,#4812,.T.);
#46572=EDGE_CURVE('',#36859,#36858,#4813,.T.);
#46573=EDGE_CURVE('',#36857,#36860,#4814,.T.);
#46574=EDGE_CURVE('',#36861,#36862,#30388,.T.);
#46575=EDGE_CURVE('',#36862,#36859,#4815,.T.);
#46576=EDGE_CURVE('',#36860,#36861,#4816,.T.);
#46577=EDGE_CURVE('',#36863,#36864,#30389,.T.);
#46578=EDGE_CURVE('',#36865,#36864,#30390,.T.);
#46579=EDGE_CURVE('',#36866,#36865,#30391,.T.);
#46580=EDGE_CURVE('',#36863,#36866,#30392,.T.);
#46581=EDGE_CURVE('',#36867,#36868,#21346,.T.);
#46582=EDGE_CURVE('',#36868,#36869,#21347,.T.);
#46583=EDGE_CURVE('',#36869,#36870,#30393,.T.);
#46584=EDGE_CURVE('',#36870,#36867,#21348,.T.);
#46585=EDGE_CURVE('',#36869,#36871,#1880,.T.);
#46586=EDGE_CURVE('',#36839,#36871,#30394,.T.);
#46587=EDGE_CURVE('',#36841,#36870,#4817,.T.);
#46588=EDGE_CURVE('',#36871,#36872,#4818,.T.);
#46589=EDGE_CURVE('',#36839,#36872,#30395,.T.);
#46590=EDGE_CURVE('',#36872,#36873,#4819,.T.);
#46591=EDGE_CURVE('',#36874,#36873,#4820,.T.);
#46592=EDGE_CURVE('',#36874,#36840,#4821,.T.);
#46593=EDGE_CURVE('',#36873,#36875,#21349,.T.);
#46594=EDGE_CURVE('',#36875,#36876,#4822,.T.);
#46595=EDGE_CURVE('',#36876,#36874,#21350,.T.);
#46596=EDGE_CURVE('',#36877,#36878,#21351,.T.);
#46597=EDGE_CURVE('',#36878,#36879,#21352,.T.);
#46598=EDGE_CURVE('',#36879,#36880,#21353,.T.);
#46599=EDGE_CURVE('',#36880,#36877,#21354,.T.);
#46600=EDGE_CURVE('',#36881,#36882,#21355,.T.);
#46601=EDGE_CURVE('',#36881,#36878,#30396,.T.);
#46602=EDGE_CURVE('',#36877,#36882,#30397,.T.);
#46603=EDGE_CURVE('',#36882,#36883,#21356,.T.);
#46604=EDGE_CURVE('',#36883,#36884,#21357,.T.);
#46605=EDGE_CURVE('',#36884,#36881,#21358,.T.);
#46606=EDGE_CURVE('',#36885,#36886,#30398,.T.);
#46607=EDGE_CURVE('',#36886,#36887,#4823,.T.);
#46608=EDGE_CURVE('',#36887,#36885,#4824,.T.);
#46609=EDGE_CURVE('',#36875,#36888,#4825,.T.);
#46610=EDGE_CURVE('',#36888,#36885,#4826,.T.);
#46611=EDGE_CURVE('',#36887,#36876,#4827,.T.);
#46612=EDGE_CURVE('',#36889,#36890,#21359,.T.);
#46613=EDGE_CURVE('',#36889,#36891,#30399,.T.);
#46614=EDGE_CURVE('',#36892,#36891,#21360,.T.);
#46615=EDGE_CURVE('',#36892,#36890,#30400,.T.);
#46616=EDGE_CURVE('',#36891,#36893,#21361,.T.);
#46617=EDGE_CURVE('',#36893,#36894,#30401,.T.);
#46618=EDGE_CURVE('',#36894,#36892,#21362,.T.);
#46619=EDGE_CURVE('',#36895,#36896,#4828,.T.);
#46620=EDGE_CURVE('',#36896,#36897,#21363,.T.);
#46621=EDGE_CURVE('',#36897,#36898,#4829,.T.);
#46622=EDGE_CURVE('',#36898,#36895,#21364,.T.);
#46623=EDGE_CURVE('',#36899,#36900,#4830,.T.);
#46624=EDGE_CURVE('',#36899,#36896,#4831,.T.);
#46625=EDGE_CURVE('',#36895,#36900,#4832,.T.);
#46626=EDGE_CURVE('',#36901,#36902,#30402,.T.);
#46627=EDGE_CURVE('',#36902,#36899,#4833,.T.);
#46628=EDGE_CURVE('',#36900,#36901,#4834,.T.);
#46629=EDGE_CURVE('',#36903,#36904,#21365,.T.);
#46630=EDGE_CURVE('',#36904,#36905,#30403,.T.);
#46631=EDGE_CURVE('',#36905,#36906,#21366,.T.);
#46632=EDGE_CURVE('',#36906,#36903,#21367,.T.);
#46633=EDGE_CURVE('',#36907,#36908,#21368,.T.);
#46634=EDGE_CURVE('',#36908,#36909,#21369,.T.);
#46635=EDGE_CURVE('',#36909,#36910,#21370,.T.);
#46636=EDGE_CURVE('',#36910,#36907,#21371,.T.);
#46637=EDGE_CURVE('',#36909,#36903,#30404,.T.);
#46638=EDGE_CURVE('',#36906,#36910,#30405,.T.);
#46639=EDGE_CURVE('',#36903,#36911,#30406,.T.);
#46640=EDGE_CURVE('',#36911,#36904,#4835,.T.);
#46641=EDGE_CURVE('',#36912,#36913,#4836,.T.);
#46642=EDGE_CURVE('',#36913,#36914,#21372,.T.);
#46643=EDGE_CURVE('',#36914,#36915,#4837,.T.);
#46644=EDGE_CURVE('',#36915,#36912,#21373,.T.);
#46645=EDGE_CURVE('',#36916,#36917,#4838,.T.);
#46646=EDGE_CURVE('',#36916,#36915,#4839,.T.);
#46647=EDGE_CURVE('',#36914,#36917,#4840,.T.);
#46648=EDGE_CURVE('',#36918,#36919,#30407,.T.);
#46649=EDGE_CURVE('',#36919,#36916,#4841,.T.);
#46650=EDGE_CURVE('',#36917,#36918,#4842,.T.);
#46651=EDGE_CURVE('',#36920,#36921,#4843,.T.);
#46652=EDGE_CURVE('',#36921,#36922,#30408,.T.);
#46653=EDGE_CURVE('',#36922,#36923,#4844,.T.);
#46654=EDGE_CURVE('',#36920,#36923,#4845,.T.);
#46655=EDGE_CURVE('',#36924,#36925,#4846,.T.);
#46656=EDGE_CURVE('',#36925,#36926,#21374,.T.);
#46657=EDGE_CURVE('',#36926,#36927,#4847,.T.);
#46658=EDGE_CURVE('',#36927,#36924,#21375,.T.);
#46659=EDGE_CURVE('',#36928,#36929,#4848,.T.);
#46660=EDGE_CURVE('',#36928,#36925,#4849,.T.);
#46661=EDGE_CURVE('',#36924,#36929,#1881,.T.);
#46662=EDGE_CURVE('',#36930,#36931,#30409,.T.);
#46663=EDGE_CURVE('',#36931,#36928,#4850,.T.);
#46664=EDGE_CURVE('',#36929,#36930,#4851,.T.);
#46665=EDGE_CURVE('',#36932,#36933,#4852,.T.);
#46666=EDGE_CURVE('',#36933,#36934,#30410,.T.);
#46667=EDGE_CURVE('',#36934,#36935,#4853,.T.);
#46668=EDGE_CURVE('',#36932,#36935,#30411,.T.);
#46669=EDGE_CURVE('',#36936,#36937,#4854,.T.);
#46670=EDGE_CURVE('',#36937,#36938,#21376,.T.);
#46671=EDGE_CURVE('',#36938,#36939,#4855,.T.);
#46672=EDGE_CURVE('',#36939,#36936,#21377,.T.);
#46673=EDGE_CURVE('',#36940,#36941,#4856,.T.);
#46674=EDGE_CURVE('',#36940,#36937,#1882,.T.);
#46675=EDGE_CURVE('',#36936,#36941,#4857,.T.);
#46676=EDGE_CURVE('',#36942,#36943,#30412,.T.);
#46677=EDGE_CURVE('',#36943,#36940,#4858,.T.);
#46678=EDGE_CURVE('',#36941,#36942,#4859,.T.);
#46679=EDGE_CURVE('',#36944,#36945,#4860,.T.);
#46680=EDGE_CURVE('',#36945,#36946,#30413,.T.);
#46681=EDGE_CURVE('',#36946,#36947,#4861,.T.);
#46682=EDGE_CURVE('',#36944,#36947,#4862,.T.);
#46683=EDGE_CURVE('',#36948,#36949,#4863,.T.);
#46684=EDGE_CURVE('',#36949,#36950,#21378,.T.);
#46685=EDGE_CURVE('',#36950,#36951,#4864,.T.);
#46686=EDGE_CURVE('',#36951,#36948,#21379,.T.);
#46687=EDGE_CURVE('',#36952,#36953,#4865,.T.);
#46688=EDGE_CURVE('',#36952,#36949,#4866,.T.);
#46689=EDGE_CURVE('',#36948,#36953,#4867,.T.);
#46690=EDGE_CURVE('',#36954,#36955,#30414,.T.);
#46691=EDGE_CURVE('',#36955,#36952,#4868,.T.);
#46692=EDGE_CURVE('',#36953,#36954,#4869,.T.);
#46693=EDGE_CURVE('',#36956,#36957,#21380,.T.);
#46694=EDGE_CURVE('',#36956,#36958,#4870,.T.);
#46695=EDGE_CURVE('',#36957,#36958,#30415,.T.);
#46696=EDGE_CURVE('',#36959,#36960,#21381,.T.);
#46697=EDGE_CURVE('',#36960,#36961,#21382,.T.);
#46698=EDGE_CURVE('',#36961,#36962,#21383,.T.);
#46699=EDGE_CURVE('',#36962,#36959,#21384,.T.);
#46700=EDGE_CURVE('',#36961,#36963,#30416,.T.);
#46701=EDGE_CURVE('',#36957,#36963,#21385,.T.);
#46702=EDGE_CURVE('',#36957,#36962,#30417,.T.);
#46703=EDGE_CURVE('',#36963,#36964,#21386,.T.);
#46704=EDGE_CURVE('',#36964,#36956,#30418,.T.);
#46705=EDGE_CURVE('',#36965,#36966,#21387,.T.);
#46706=EDGE_CURVE('',#36965,#36967,#30419,.T.);
#46707=EDGE_CURVE('',#36968,#36967,#21388,.T.);
#46708=EDGE_CURVE('',#36968,#36966,#30420,.T.);
#46709=EDGE_CURVE('',#36969,#36970,#4871,.T.);
#46710=EDGE_CURVE('',#36970,#36971,#21389,.T.);
#46711=EDGE_CURVE('',#36971,#36972,#4872,.T.);
#46712=EDGE_CURVE('',#36972,#36969,#21390,.T.);
#46713=EDGE_CURVE('',#36973,#36974,#4873,.T.);
#46714=EDGE_CURVE('',#36973,#36972,#4874,.T.);
#46715=EDGE_CURVE('',#36971,#36974,#4875,.T.);
#46716=EDGE_CURVE('',#36975,#36976,#30421,.T.);
#46717=EDGE_CURVE('',#36976,#36973,#4876,.T.);
#46718=EDGE_CURVE('',#36974,#36975,#4877,.T.);
#46719=EDGE_CURVE('',#36967,#36977,#21391,.T.);
#46720=EDGE_CURVE('',#36977,#36978,#30422,.T.);
#46721=EDGE_CURVE('',#36978,#36968,#21392,.T.);
#46722=EDGE_CURVE('',#36979,#36980,#21393,.T.);
#46723=EDGE_CURVE('',#36980,#36965,#21394,.T.);
#46724=EDGE_CURVE('',#36966,#36979,#21395,.T.);
#46725=EDGE_CURVE('',#36981,#36982,#21396,.T.);
#46726=EDGE_CURVE('',#36982,#36889,#21397,.T.);
#46727=EDGE_CURVE('',#36890,#36981,#21398,.T.);
#46728=EDGE_CURVE('',#36983,#36984,#4878,.T.);
#46729=EDGE_CURVE('',#36984,#36985,#21399,.T.);
#46730=EDGE_CURVE('',#36985,#36986,#4879,.T.);
#46731=EDGE_CURVE('',#36986,#36983,#21400,.T.);
#46732=EDGE_CURVE('',#36987,#36988,#21401,.T.);
#46733=EDGE_CURVE('',#36988,#36989,#21402,.T.);
#46734=EDGE_CURVE('',#36989,#36990,#21403,.T.);
#46735=EDGE_CURVE('',#36990,#36987,#21404,.T.);
#46736=EDGE_CURVE('',#36991,#36992,#4880,.T.);
#46737=EDGE_CURVE('',#36992,#36993,#21405,.T.);
#46738=EDGE_CURVE('',#36993,#36994,#4881,.T.);
#46739=EDGE_CURVE('',#36994,#36991,#21406,.T.);
#46740=EDGE_CURVE('',#36995,#36996,#4882,.T.);
#46741=EDGE_CURVE('',#36996,#36997,#21407,.T.);
#46742=EDGE_CURVE('',#36997,#36998,#4883,.T.);
#46743=EDGE_CURVE('',#36998,#36995,#21408,.T.);
#46744=EDGE_CURVE('',#36999,#37000,#21409,.T.);
#46745=EDGE_CURVE('',#36999,#37001,#30423,.T.);
#46746=EDGE_CURVE('',#37002,#37001,#21410,.T.);
#46747=EDGE_CURVE('',#37002,#37000,#30424,.T.);
#46748=EDGE_CURVE('',#36852,#36862,#4884,.T.);
#46749=EDGE_CURVE('',#36861,#37003,#30425,.T.);
#46750=EDGE_CURVE('',#37003,#37004,#4885,.T.);
#46751=EDGE_CURVE('',#37004,#36850,#4886,.T.);
#46752=EDGE_CURVE('',#37005,#37006,#4887,.T.);
#46753=EDGE_CURVE('',#37005,#36996,#4888,.T.);
#46754=EDGE_CURVE('',#36995,#37006,#1883,.T.);
#46755=EDGE_CURVE('',#37007,#37008,#4889,.T.);
#46756=EDGE_CURVE('',#37007,#36992,#4890,.T.);
#46757=EDGE_CURVE('',#36991,#37008,#4891,.T.);
#46758=EDGE_CURVE('',#36989,#37009,#30426,.T.);
#46759=EDGE_CURVE('',#37010,#37009,#21411,.T.);
#46760=EDGE_CURVE('',#37010,#36990,#30427,.T.);
#46761=EDGE_CURVE('',#37011,#37012,#4892,.T.);
#46762=EDGE_CURVE('',#37011,#36984,#4893,.T.);
#46763=EDGE_CURVE('',#36983,#37012,#4894,.T.);
#46764=EDGE_CURVE('',#37013,#37014,#30428,.T.);
#46765=EDGE_CURVE('',#37015,#37014,#30429,.T.);
#46766=EDGE_CURVE('',#37016,#37015,#30430,.T.);
#46767=EDGE_CURVE('',#37013,#37016,#30431,.T.);
#46768=EDGE_CURVE('',#37017,#36850,#30432,.T.);
#46769=EDGE_CURVE('',#37018,#37004,#30433,.T.);
#46770=EDGE_CURVE('',#37017,#37018,#4895,.T.);
#46771=EDGE_CURVE('',#37019,#37017,#21412,.T.);
#46772=EDGE_CURVE('',#37019,#36851,#4896,.T.);
#46773=EDGE_CURVE('',#36848,#37020,#30434,.T.);
#46774=EDGE_CURVE('',#37021,#36848,#4897,.T.);
#46775=EDGE_CURVE('',#37022,#37021,#30435,.T.);
#46776=EDGE_CURVE('',#37020,#37022,#4898,.T.);
#46777=EDGE_CURVE('',#37023,#37020,#21413,.T.);
#46778=EDGE_CURVE('',#36849,#37023,#30436,.T.);
#46779=EDGE_CURVE('',#37024,#37023,#4899,.T.);
#46780=EDGE_CURVE('',#37025,#37024,#30437,.T.);
#46781=EDGE_CURVE('',#36849,#37025,#4900,.T.);
#46782=EDGE_CURVE('',#37026,#37027,#21414,.T.);
#46783=EDGE_CURVE('',#37026,#36868,#4901,.T.);
#46784=EDGE_CURVE('',#36867,#37027,#4902,.T.);
#46785=EDGE_CURVE('',#37028,#37029,#30438,.T.);
#46786=EDGE_CURVE('',#37030,#37029,#4903,.T.);
#46787=EDGE_CURVE('',#36883,#37030,#30439,.T.);
#46788=EDGE_CURVE('',#37028,#36883,#4904,.T.);
#46789=EDGE_CURVE('',#37031,#37030,#21415,.T.);
#46790=EDGE_CURVE('',#36884,#37031,#30440,.T.);
#46791=EDGE_CURVE('',#37032,#37031,#4905,.T.);
#46792=EDGE_CURVE('',#37033,#37032,#30441,.T.);
#46793=EDGE_CURVE('',#36884,#37033,#4906,.T.);
#46794=EDGE_CURVE('',#37034,#37035,#21416,.T.);
#46795=EDGE_CURVE('',#37034,#37036,#4907,.T.);
#46796=EDGE_CURVE('',#37037,#37036,#21417,.T.);
#46797=EDGE_CURVE('',#37035,#37037,#30442,.T.);
#46798=EDGE_CURVE('',#37038,#37037,#30443,.T.);
#46799=EDGE_CURVE('',#37039,#37038,#30444,.T.);
#46800=EDGE_CURVE('',#37035,#37039,#30445,.T.);
#46801=EDGE_CURVE('',#37040,#37038,#30446,.T.);
#46802=EDGE_CURVE('',#37041,#37040,#30447,.T.);
#46803=EDGE_CURVE('',#37039,#37041,#30448,.T.);
#46804=EDGE_CURVE('',#37042,#37040,#30449,.T.);
#46805=EDGE_CURVE('',#37043,#37042,#30450,.T.);
#46806=EDGE_CURVE('',#37041,#37043,#30451,.T.);
#46807=EDGE_CURVE('',#36750,#37044,#30452,.T.);
#46808=EDGE_CURVE('',#37045,#36750,#4908,.T.);
#46809=EDGE_CURVE('',#37046,#37045,#30453,.T.);
#46810=EDGE_CURVE('',#37044,#37046,#4909,.T.);
#46811=EDGE_CURVE('',#37047,#37044,#21418,.T.);
#46812=EDGE_CURVE('',#36751,#37047,#30454,.T.);
#46813=EDGE_CURVE('',#37048,#37047,#4910,.T.);
#46814=EDGE_CURVE('',#37049,#37048,#30455,.T.);
#46815=EDGE_CURVE('',#36751,#37049,#4911,.T.);
#46816=EDGE_CURVE('',#36743,#37050,#4912,.T.);
#46817=EDGE_CURVE('',#37051,#37050,#21419,.T.);
#46818=EDGE_CURVE('',#36741,#37051,#30456,.T.);
#46819=EDGE_CURVE('',#37052,#37051,#4913,.T.);
#46820=EDGE_CURVE('',#36776,#37052,#30457,.T.);
#46821=EDGE_CURVE('',#37053,#37042,#21420,.T.);
#46822=EDGE_CURVE('',#37053,#37054,#4914,.T.);
#46823=EDGE_CURVE('',#37043,#37054,#21421,.T.);
#46824=EDGE_CURVE('',#37055,#37056,#30458,.T.);
#46825=EDGE_CURVE('',#37057,#37056,#4915,.T.);
#46826=EDGE_CURVE('',#36774,#37057,#30459,.T.);
#46827=EDGE_CURVE('',#37055,#36774,#4916,.T.);
#46828=EDGE_CURVE('',#37058,#37057,#21422,.T.);
#46829=EDGE_CURVE('',#36775,#37058,#30460,.T.);
#46830=EDGE_CURVE('',#37059,#37058,#4917,.T.);
#46831=EDGE_CURVE('',#37060,#37059,#30461,.T.);
#46832=EDGE_CURVE('',#36775,#37060,#4918,.T.);
#46833=EDGE_CURVE('',#37061,#37062,#21423,.T.);
#46834=EDGE_CURVE('',#37061,#36767,#4919,.T.);
#46835=EDGE_CURVE('',#36766,#37062,#4920,.T.);
#46836=EDGE_CURVE('',#37063,#37052,#4921,.T.);
#46837=EDGE_CURVE('',#37063,#36777,#4922,.T.);
#46838=EDGE_CURVE('',#37064,#37065,#30462,.T.);
#46839=EDGE_CURVE('',#37066,#37065,#4923,.T.);
#46840=EDGE_CURVE('',#37067,#37066,#30463,.T.);
#46841=EDGE_CURVE('',#37064,#37067,#4924,.T.);
#46842=EDGE_CURVE('',#37068,#37066,#1884,.T.);
#46843=EDGE_CURVE('',#36977,#37068,#30464,.T.);
#46844=EDGE_CURVE('',#37067,#36977,#1885,.T.);
#46845=EDGE_CURVE('',#37069,#37068,#30465,.T.);
#46846=EDGE_CURVE('',#36978,#37069,#30466,.T.);
#46847=EDGE_CURVE('',#37070,#37071,#30467,.T.);
#46848=EDGE_CURVE('',#36978,#37071,#4925,.T.);
#46849=EDGE_CURVE('',#37070,#37069,#4926,.T.);
#46850=EDGE_CURVE('',#37072,#37073,#30468,.T.);
#46851=EDGE_CURVE('',#37072,#36976,#1886,.T.);
#46852=EDGE_CURVE('',#36975,#37073,#1887,.T.);
#46853=EDGE_CURVE('',#37074,#36964,#30469,.T.);
#46854=EDGE_CURVE('',#37075,#36964,#4927,.T.);
#46855=EDGE_CURVE('',#37076,#37075,#30470,.T.);
#46856=EDGE_CURVE('',#37074,#37076,#4928,.T.);
#46857=EDGE_CURVE('',#37077,#36956,#30471,.T.);
#46858=EDGE_CURVE('',#37077,#37074,#30472,.T.);
#46859=EDGE_CURVE('',#37078,#36958,#30473,.T.);
#46860=EDGE_CURVE('',#37078,#37077,#4929,.T.);
#46861=EDGE_CURVE('',#37079,#37080,#30474,.T.);
#46862=EDGE_CURVE('',#36958,#37080,#4930,.T.);
#46863=EDGE_CURVE('',#37079,#37078,#1888,.T.);
#46864=EDGE_CURVE('',#37081,#37082,#30475,.T.);
#46865=EDGE_CURVE('',#37081,#36955,#1889,.T.);
#46866=EDGE_CURVE('',#36954,#37082,#1890,.T.);
#46867=EDGE_CURVE('',#36945,#37083,#30476,.T.);
#46868=EDGE_CURVE('',#37084,#36945,#4931,.T.);
#46869=EDGE_CURVE('',#37085,#37084,#30477,.T.);
#46870=EDGE_CURVE('',#37083,#37085,#4932,.T.);
#46871=EDGE_CURVE('',#37086,#37083,#30478,.T.);
#46872=EDGE_CURVE('',#36946,#37086,#30479,.T.);
#46873=EDGE_CURVE('',#37087,#37086,#4933,.T.);
#46874=EDGE_CURVE('',#37088,#37087,#30480,.T.);
#46875=EDGE_CURVE('',#36946,#37088,#4934,.T.);
#46876=EDGE_CURVE('',#37089,#37090,#30481,.T.);
#46877=EDGE_CURVE('',#37089,#36943,#1891,.T.);
#46878=EDGE_CURVE('',#36942,#37090,#1892,.T.);
#46879=EDGE_CURVE('',#36933,#37091,#30482,.T.);
#46880=EDGE_CURVE('',#37092,#36933,#4935,.T.);
#46881=EDGE_CURVE('',#37093,#37092,#30483,.T.);
#46882=EDGE_CURVE('',#37091,#37093,#4936,.T.);
#46883=EDGE_CURVE('',#37094,#37091,#30484,.T.);
#46884=EDGE_CURVE('',#36934,#37094,#30485,.T.);
#46885=EDGE_CURVE('',#37095,#37094,#4937,.T.);
#46886=EDGE_CURVE('',#37096,#37095,#30486,.T.);
#46887=EDGE_CURVE('',#36934,#37096,#4938,.T.);
#46888=EDGE_CURVE('',#37097,#37098,#30487,.T.);
#46889=EDGE_CURVE('',#37097,#36931,#1893,.T.);
#46890=EDGE_CURVE('',#36930,#37098,#1894,.T.);
#46891=EDGE_CURVE('',#36921,#37099,#30488,.T.);
#46892=EDGE_CURVE('',#37100,#36921,#4939,.T.);
#46893=EDGE_CURVE('',#37101,#37100,#30489,.T.);
#46894=EDGE_CURVE('',#37099,#37101,#4940,.T.);
#46895=EDGE_CURVE('',#37102,#37099,#30490,.T.);
#46896=EDGE_CURVE('',#36922,#37102,#30491,.T.);
#46897=EDGE_CURVE('',#37103,#37102,#4941,.T.);
#46898=EDGE_CURVE('',#37104,#37103,#30492,.T.);
#46899=EDGE_CURVE('',#36922,#37104,#4942,.T.);
#46900=EDGE_CURVE('',#37105,#37106,#30493,.T.);
#46901=EDGE_CURVE('',#37105,#36919,#1895,.T.);
#46902=EDGE_CURVE('',#36918,#37106,#1896,.T.);
#46903=EDGE_CURVE('',#37107,#36911,#30494,.T.);
#46904=EDGE_CURVE('',#37108,#36911,#4943,.T.);
#46905=EDGE_CURVE('',#37109,#37108,#30495,.T.);
#46906=EDGE_CURVE('',#37107,#37109,#4944,.T.);
#46907=EDGE_CURVE('',#37110,#36904,#30496,.T.);
#46908=EDGE_CURVE('',#37110,#37107,#4945,.T.);
#46909=EDGE_CURVE('',#37111,#36905,#30497,.T.);
#46910=EDGE_CURVE('',#37111,#37110,#30498,.T.);
#46911=EDGE_CURVE('',#37112,#37113,#30499,.T.);
#46912=EDGE_CURVE('',#36905,#37113,#4946,.T.);
#46913=EDGE_CURVE('',#37112,#37111,#4947,.T.);
#46914=EDGE_CURVE('',#37114,#37115,#30500,.T.);
#46915=EDGE_CURVE('',#37114,#36902,#1897,.T.);
#46916=EDGE_CURVE('',#36901,#37115,#1898,.T.);
#46917=EDGE_CURVE('',#37116,#37117,#30501,.T.);
#46918=EDGE_CURVE('',#37118,#37117,#4948,.T.);
#46919=EDGE_CURVE('',#36893,#37118,#30502,.T.);
#46920=EDGE_CURVE('',#37116,#36893,#4949,.T.);
#46921=EDGE_CURVE('',#37119,#37118,#30503,.T.);
#46922=EDGE_CURVE('',#36894,#37119,#30504,.T.);
#46923=EDGE_CURVE('',#37120,#37119,#4950,.T.);
#46924=EDGE_CURVE('',#37121,#37120,#30505,.T.);
#46925=EDGE_CURVE('',#36894,#37121,#4951,.T.);
#46926=EDGE_CURVE('',#36809,#37122,#4952,.T.);
#46927=EDGE_CURVE('',#37123,#37122,#4953,.T.);
#46928=EDGE_CURVE('',#37123,#36810,#30506,.T.);
#46929=EDGE_CURVE('',#37124,#37125,#30507,.T.);
#46930=EDGE_CURVE('',#37121,#37125,#4954,.T.);
#46931=EDGE_CURVE('',#37124,#37120,#4955,.T.);
#46932=EDGE_CURVE('',#37126,#36796,#30508,.T.);
#46933=EDGE_CURVE('',#37126,#37123,#4956,.T.);
#46934=EDGE_CURVE('',#37127,#37126,#21424,.T.);
#46935=EDGE_CURVE('',#37127,#36797,#4957,.T.);
#46936=EDGE_CURVE('',#36794,#37128,#30509,.T.);
#46937=EDGE_CURVE('',#37129,#36794,#4958,.T.);
#46938=EDGE_CURVE('',#37130,#37129,#30510,.T.);
#46939=EDGE_CURVE('',#37128,#37130,#4959,.T.);
#46940=EDGE_CURVE('',#37131,#37128,#21425,.T.);
#46941=EDGE_CURVE('',#36795,#37131,#30511,.T.);
#46942=EDGE_CURVE('',#37132,#37131,#4960,.T.);
#46943=EDGE_CURVE('',#37133,#37132,#30512,.T.);
#46944=EDGE_CURVE('',#36795,#37133,#4961,.T.);
#46945=EDGE_CURVE('',#37134,#37135,#21426,.T.);
#46946=EDGE_CURVE('',#37134,#36812,#4962,.T.);
#46947=EDGE_CURVE('',#36811,#37135,#4963,.T.);
#46948=EDGE_CURVE('',#37136,#37137,#30513,.T.);
#46949=EDGE_CURVE('',#37138,#37137,#4964,.T.);
#46950=EDGE_CURVE('',#36831,#37138,#30514,.T.);
#46951=EDGE_CURVE('',#37136,#36831,#4965,.T.);
#46952=EDGE_CURVE('',#37139,#37138,#21427,.T.);
#46953=EDGE_CURVE('',#36832,#37139,#30515,.T.);
#46954=EDGE_CURVE('',#37140,#37139,#4966,.T.);
#46955=EDGE_CURVE('',#37141,#37140,#30516,.T.);
#46956=EDGE_CURVE('',#36832,#37141,#4967,.T.);
#46957=EDGE_CURVE('',#37142,#37143,#21428,.T.);
#46958=EDGE_CURVE('',#37142,#37144,#4968,.T.);
#46959=EDGE_CURVE('',#37145,#37144,#21429,.T.);
#46960=EDGE_CURVE('',#37143,#37145,#30517,.T.);
#46961=EDGE_CURVE('',#37146,#37145,#30518,.T.);
#46962=EDGE_CURVE('',#37147,#37146,#30519,.T.);
#46963=EDGE_CURVE('',#37143,#37147,#30520,.T.);
#46964=EDGE_CURVE('',#37148,#37146,#30521,.T.);
#46965=EDGE_CURVE('',#37149,#37148,#30522,.T.);
#46966=EDGE_CURVE('',#37147,#37149,#30523,.T.);
#46967=EDGE_CURVE('',#37150,#37148,#30524,.T.);
#46968=EDGE_CURVE('',#37151,#37150,#30525,.T.);
#46969=EDGE_CURVE('',#37149,#37151,#30526,.T.);
#46970=EDGE_CURVE('',#37152,#37150,#21430,.T.);
#46971=EDGE_CURVE('',#37152,#37153,#4969,.T.);
#46972=EDGE_CURVE('',#37151,#37153,#21431,.T.);
#46973=EDGE_CURVE('',#37154,#37155,#30527,.T.);
#46974=EDGE_CURVE('',#37156,#37154,#30528,.T.);
#46975=EDGE_CURVE('',#37155,#37156,#30529,.T.);
#46976=EDGE_CURVE('',#37157,#37158,#4970,.T.);
#46977=EDGE_CURVE('',#37157,#36836,#4971,.T.);
#46978=EDGE_CURVE('',#36835,#37158,#4972,.T.);
#46979=EDGE_CURVE('',#37159,#37160,#4973,.T.);
#46980=EDGE_CURVE('',#37159,#37161,#4974,.T.);
#46981=EDGE_CURVE('',#37162,#37161,#4975,.T.);
#46982=EDGE_CURVE('',#37162,#37160,#4976,.T.);
#46983=EDGE_CURVE('',#37163,#37164,#21432,.T.);
#46984=EDGE_CURVE('',#37164,#36999,#21433,.T.);
#46985=EDGE_CURVE('',#37000,#37163,#21434,.T.);
#46986=EDGE_CURVE('',#37165,#37166,#21435,.T.);
#46987=EDGE_CURVE('',#37166,#37167,#4977,.T.);
#46988=EDGE_CURVE('',#37167,#37168,#21436,.T.);
#46989=EDGE_CURVE('',#37168,#37165,#30530,.T.);
#46990=EDGE_CURVE('',#37169,#37170,#30531,.T.);
#46991=EDGE_CURVE('',#37169,#36863,#21437,.T.);
#46992=EDGE_CURVE('',#36866,#37170,#21438,.T.);
#46993=EDGE_CURVE('',#36749,#37171,#30532,.T.);
#46994=EDGE_CURVE('',#37172,#37171,#30533,.T.);
#46995=EDGE_CURVE('',#36747,#37172,#30534,.T.);
#46996=EDGE_CURVE('',#37173,#37172,#21439,.T.);
#46997=EDGE_CURVE('',#36744,#37173,#30535,.T.);
#46998=EDGE_CURVE('',#37174,#36787,#30536,.T.);
#46999=EDGE_CURVE('',#37175,#36787,#4978,.T.);
#47000=EDGE_CURVE('',#37176,#37175,#30537,.T.);
#47001=EDGE_CURVE('',#37174,#37176,#4979,.T.);
#47002=EDGE_CURVE('',#37177,#36785,#30538,.T.);
#47003=EDGE_CURVE('',#37177,#37174,#4980,.T.);
#47004=EDGE_CURVE('',#37178,#36783,#30539,.T.);
#47005=EDGE_CURVE('',#37178,#37177,#21440,.T.);
#47006=EDGE_CURVE('',#37179,#36781,#30540,.T.);
#47007=EDGE_CURVE('',#37179,#37178,#4981,.T.);
#47008=EDGE_CURVE('',#37180,#36779,#30541,.T.);
#47009=EDGE_CURVE('',#37180,#37179,#4982,.T.);
#47010=EDGE_CURVE('',#37181,#36742,#30542,.T.);
#47011=EDGE_CURVE('',#37181,#37180,#4983,.T.);
#47012=EDGE_CURVE('',#37182,#36743,#30543,.T.);
#47013=EDGE_CURVE('',#37182,#37181,#21441,.T.);
#47014=EDGE_CURVE('',#37183,#37184,#30544,.T.);
#47015=EDGE_CURVE('',#37184,#37050,#30545,.T.);
#47016=EDGE_CURVE('',#37183,#37182,#1159,.T.);
#47017=EDGE_CURVE('',#37049,#37183,#21442,.T.);
#47018=EDGE_CURVE('',#37050,#37048,#21443,.T.);
#47019=EDGE_CURVE('',#37171,#37049,#21444,.T.);
#47020=EDGE_CURVE('',#37185,#37186,#30546,.T.);
#47021=EDGE_CURVE('',#37187,#37186,#21445,.T.);
#47022=EDGE_CURVE('',#37188,#37187,#30547,.T.);
#47023=EDGE_CURVE('',#37185,#37188,#21446,.T.);
#47024=EDGE_CURVE('',#37189,#37173,#30548,.T.);
#47025=EDGE_CURVE('',#37190,#37189,#30549,.T.);
#47026=EDGE_CURVE('',#36744,#37190,#30550,.T.);
#47027=EDGE_CURVE('',#37191,#37190,#21447,.T.);
#47028=EDGE_CURVE('',#37191,#36745,#30551,.T.);
#47029=EDGE_CURVE('',#37191,#37192,#30552,.T.);
#47030=EDGE_CURVE('',#37193,#37192,#30553,.T.);
#47031=EDGE_CURVE('',#36745,#37193,#30554,.T.);
#47032=EDGE_CURVE('',#37194,#37193,#21448,.T.);
#47033=EDGE_CURVE('',#36746,#37194,#30555,.T.);
#47034=EDGE_CURVE('',#37195,#37194,#30556,.T.);
#47035=EDGE_CURVE('',#36748,#37195,#30557,.T.);
#47036=EDGE_CURVE('',#37045,#37195,#21449,.T.);
#47037=EDGE_CURVE('',#37196,#37045,#21450,.T.);
#47038=EDGE_CURVE('',#37061,#37196,#30558,.T.);
#47039=EDGE_CURVE('',#37046,#37061,#21451,.T.);
#47040=EDGE_CURVE('',#37197,#37196,#1160,.T.);
#47041=EDGE_CURVE('',#36767,#37197,#30559,.T.);
#47042=EDGE_CURVE('',#37198,#37197,#21452,.T.);
#47043=EDGE_CURVE('',#36764,#37198,#30560,.T.);
#47044=EDGE_CURVE('',#37199,#37198,#4984,.T.);
#47045=EDGE_CURVE('',#36763,#37199,#30561,.T.);
#47046=EDGE_CURVE('',#37200,#37199,#4985,.T.);
#47047=EDGE_CURVE('',#36760,#37200,#30562,.T.);
#47048=EDGE_CURVE('',#37201,#37200,#4986,.T.);
#47049=EDGE_CURVE('',#36759,#37201,#30563,.T.);
#47050=EDGE_CURVE('',#37202,#37201,#21453,.T.);
#47051=EDGE_CURVE('',#36756,#37202,#30564,.T.);
#47052=EDGE_CURVE('',#37203,#37202,#4987,.T.);
#47053=EDGE_CURVE('',#36753,#37203,#30565,.T.);
#47054=EDGE_CURVE('',#37204,#37203,#4988,.T.);
#47055=EDGE_CURVE('',#36754,#37204,#30566,.T.);
#47056=EDGE_CURVE('',#37205,#37204,#4989,.T.);
#47057=EDGE_CURVE('',#37206,#37205,#30567,.T.);
#47058=EDGE_CURVE('',#36754,#37206,#4990,.T.);
#47059=EDGE_CURVE('',#37207,#37205,#21454,.T.);
#47060=EDGE_CURVE('',#37208,#37207,#30568,.T.);
#47061=EDGE_CURVE('',#37206,#37208,#21455,.T.);
#47062=EDGE_CURVE('',#37209,#37206,#30569,.T.);
#47063=EDGE_CURVE('',#37209,#36755,#4991,.T.);
#47064=EDGE_CURVE('',#36773,#37210,#30570,.T.);
#47065=EDGE_CURVE('',#37211,#37210,#30571,.T.);
#47066=EDGE_CURVE('',#36771,#37211,#30572,.T.);
#47067=EDGE_CURVE('',#37212,#37211,#21456,.T.);
#47068=EDGE_CURVE('',#36768,#37212,#30573,.T.);
#47069=EDGE_CURVE('',#37213,#37214,#30574,.T.);
#47070=EDGE_CURVE('',#37215,#37214,#21457,.T.);
#47071=EDGE_CURVE('',#37209,#37215,#30575,.T.);
#47072=EDGE_CURVE('',#37213,#37209,#21458,.T.);
#47073=EDGE_CURVE('',#37216,#37215,#4992,.T.);
#47074=EDGE_CURVE('',#36755,#37216,#30576,.T.);
#47075=EDGE_CURVE('',#37217,#37216,#1161,.T.);
#47076=EDGE_CURVE('',#36752,#37217,#30577,.T.);
#47077=EDGE_CURVE('',#37218,#37217,#4993,.T.);
#47078=EDGE_CURVE('',#36757,#37218,#30578,.T.);
#47079=EDGE_CURVE('',#37219,#37218,#21459,.T.);
#47080=EDGE_CURVE('',#36758,#37219,#30579,.T.);
#47081=EDGE_CURVE('',#37220,#36761,#30580,.T.);
#47082=EDGE_CURVE('',#37220,#37219,#4994,.T.);
#47083=EDGE_CURVE('',#37221,#36762,#30581,.T.);
#47084=EDGE_CURVE('',#37221,#37220,#1162,.T.);
#47085=EDGE_CURVE('',#37222,#36765,#30582,.T.);
#47086=EDGE_CURVE('',#37222,#37221,#4995,.T.);
#47087=EDGE_CURVE('',#37223,#36766,#30583,.T.);
#47088=EDGE_CURVE('',#37223,#37222,#21460,.T.);
#47089=EDGE_CURVE('',#37224,#37225,#30584,.T.);
#47090=EDGE_CURVE('',#37225,#37062,#30585,.T.);
#47091=EDGE_CURVE('',#37224,#37223,#1163,.T.);
#47092=EDGE_CURVE('',#37060,#37224,#21461,.T.);
#47093=EDGE_CURVE('',#37062,#37059,#21462,.T.);
#47094=EDGE_CURVE('',#37210,#37060,#21463,.T.);
#47095=EDGE_CURVE('',#37226,#37212,#30586,.T.);
#47096=EDGE_CURVE('',#37227,#37226,#30587,.T.);
#47097=EDGE_CURVE('',#36768,#37227,#30588,.T.);
#47098=EDGE_CURVE('',#37228,#37227,#21464,.T.);
#47099=EDGE_CURVE('',#37228,#36769,#30589,.T.);
#47100=EDGE_CURVE('',#37229,#37230,#30590,.T.);
#47101=EDGE_CURVE('',#37054,#37230,#21465,.T.);
#47102=EDGE_CURVE('',#37231,#37054,#30591,.T.);
#47103=EDGE_CURVE('',#37229,#37231,#21466,.T.);
#47104=EDGE_CURVE('',#37232,#37015,#21467,.T.);
#47105=EDGE_CURVE('',#37233,#37232,#30592,.T.);
#47106=EDGE_CURVE('',#37016,#37233,#21468,.T.);
#47107=EDGE_CURVE('',#37234,#36865,#21469,.T.);
#47108=EDGE_CURVE('',#37170,#37234,#30593,.T.);
#47109=EDGE_CURVE('',#37235,#37234,#4996,.T.);
#47110=EDGE_CURVE('',#37236,#37235,#30594,.T.);
#47111=EDGE_CURVE('',#37170,#37236,#4997,.F.);
#47112=EDGE_CURVE('',#37237,#36769,#30595,.T.);
#47113=EDGE_CURVE('',#37238,#37228,#30596,.T.);
#47114=EDGE_CURVE('',#37237,#37238,#30597,.T.);
#47115=EDGE_CURVE('',#37239,#36770,#30598,.T.);
#47116=EDGE_CURVE('',#37239,#37237,#21470,.T.);
#47117=EDGE_CURVE('',#37240,#36772,#30599,.T.);
#47118=EDGE_CURVE('',#37240,#37239,#30600,.T.);
#47119=EDGE_CURVE('',#37055,#37240,#21471,.T.);
#47120=EDGE_CURVE('',#37241,#37053,#30601,.T.);
#47121=EDGE_CURVE('',#37056,#37053,#21472,.T.);
#47122=EDGE_CURVE('',#37241,#37055,#21473,.T.);
#47123=EDGE_CURVE('',#37231,#37241,#1164,.T.);
#47124=EDGE_CURVE('',#37242,#36778,#30602,.T.);
#47125=EDGE_CURVE('',#37243,#36777,#30603,.T.);
#47126=EDGE_CURVE('',#37242,#37243,#4998,.T.);
#47127=EDGE_CURVE('',#37244,#36780,#30604,.T.);
#47128=EDGE_CURVE('',#37244,#37242,#4999,.T.);
#47129=EDGE_CURVE('',#37245,#36782,#30605,.T.);
#47130=EDGE_CURVE('',#37245,#37244,#5000,.T.);
#47131=EDGE_CURVE('',#37246,#36784,#30606,.T.);
#47132=EDGE_CURVE('',#37246,#37245,#21474,.T.);
#47133=EDGE_CURVE('',#37247,#36786,#30607,.T.);
#47134=EDGE_CURVE('',#37247,#37246,#5001,.T.);
#47135=EDGE_CURVE('',#37248,#37249,#30608,.T.);
#47136=EDGE_CURVE('',#36786,#37249,#5002,.T.);
#47137=EDGE_CURVE('',#37248,#37247,#5003,.T.);
#47138=EDGE_CURVE('',#36980,#37250,#30609,.T.);
#47139=EDGE_CURVE('',#37251,#37250,#21475,.T.);
#47140=EDGE_CURVE('',#36965,#37251,#30610,.T.);
#47141=EDGE_CURVE('',#37252,#37251,#30611,.T.);
#47142=EDGE_CURVE('',#36967,#37252,#30612,.T.);
#47143=EDGE_CURVE('',#37064,#37252,#21476,.T.);
#47144=EDGE_CURVE('',#37253,#37063,#30613,.T.);
#47145=EDGE_CURVE('',#37065,#37063,#21477,.T.);
#47146=EDGE_CURVE('',#37253,#37064,#21478,.T.);
#47147=EDGE_CURVE('',#37243,#37253,#5004,.T.);
#47148=EDGE_CURVE('',#37186,#37175,#5005,.T.);
#47149=EDGE_CURVE('',#37176,#37185,#5006,.T.);
#47150=EDGE_CURVE('',#37254,#37255,#30614,.T.);
#47151=EDGE_CURVE('',#37249,#37255,#1899,.T.);
#47152=EDGE_CURVE('',#37254,#37248,#1900,.T.);
#47153=EDGE_CURVE('',#37249,#37175,#30615,.T.);
#47154=EDGE_CURVE('',#36793,#37256,#30616,.T.);
#47155=EDGE_CURVE('',#37257,#37256,#30617,.T.);
#47156=EDGE_CURVE('',#36791,#37257,#30618,.T.);
#47157=EDGE_CURVE('',#37258,#37257,#21479,.T.);
#47158=EDGE_CURVE('',#36788,#37258,#30619,.T.);
#47159=EDGE_CURVE('',#37259,#36834,#30620,.T.);
#47160=EDGE_CURVE('',#37260,#36834,#5007,.T.);
#47161=EDGE_CURVE('',#37261,#37260,#30621,.T.);
#47162=EDGE_CURVE('',#37259,#37261,#5008,.T.);
#47163=EDGE_CURVE('',#37262,#36824,#30622,.T.);
#47164=EDGE_CURVE('',#37262,#37259,#5009,.T.);
#47165=EDGE_CURVE('',#37263,#36822,#30623,.T.);
#47166=EDGE_CURVE('',#37263,#37262,#5010,.T.);
#47167=EDGE_CURVE('',#37264,#36820,#30624,.T.);
#47168=EDGE_CURVE('',#37264,#37263,#21480,.T.);
#47169=EDGE_CURVE('',#37265,#36818,#30625,.T.);
#47170=EDGE_CURVE('',#37265,#37264,#5011,.T.);
#47171=EDGE_CURVE('',#37266,#36816,#30626,.T.);
#47172=EDGE_CURVE('',#37266,#37265,#5012,.T.);
#47173=EDGE_CURVE('',#37267,#36814,#30627,.T.);
#47174=EDGE_CURVE('',#37267,#37266,#5013,.T.);
#47175=EDGE_CURVE('',#37268,#36811,#30628,.T.);
#47176=EDGE_CURVE('',#37268,#37267,#21481,.T.);
#47177=EDGE_CURVE('',#37269,#37135,#30629,.T.);
#47178=EDGE_CURVE('',#37269,#37268,#1165,.T.);
#47179=EDGE_CURVE('',#37135,#37132,#21482,.T.);
#47180=EDGE_CURVE('',#37133,#37269,#21483,.T.);
#47181=EDGE_CURVE('',#37256,#37133,#21484,.T.);
#47182=EDGE_CURVE('',#37270,#37258,#30630,.T.);
#47183=EDGE_CURVE('',#37271,#37270,#30631,.T.);
#47184=EDGE_CURVE('',#36788,#37271,#30632,.T.);
#47185=EDGE_CURVE('',#37272,#37271,#21485,.T.);
#47186=EDGE_CURVE('',#37272,#36789,#30633,.T.);
#47187=EDGE_CURVE('',#37272,#37273,#30634,.T.);
#47188=EDGE_CURVE('',#37274,#37273,#30635,.T.);
#47189=EDGE_CURVE('',#36789,#37274,#30636,.T.);
#47190=EDGE_CURVE('',#37275,#37274,#21486,.T.);
#47191=EDGE_CURVE('',#36790,#37275,#30637,.T.);
#47192=EDGE_CURVE('',#37276,#37275,#30638,.T.);
#47193=EDGE_CURVE('',#36792,#37276,#30639,.T.);
#47194=EDGE_CURVE('',#37129,#37276,#21487,.T.);
#47195=EDGE_CURVE('',#37277,#37129,#21488,.T.);
#47196=EDGE_CURVE('',#37127,#37277,#30640,.T.);
#47197=EDGE_CURVE('',#37130,#37127,#21489,.T.);
#47198=EDGE_CURVE('',#37278,#37277,#1166,.T.);
#47199=EDGE_CURVE('',#36797,#37278,#30641,.T.);
#47200=EDGE_CURVE('',#37279,#37278,#21490,.T.);
#47201=EDGE_CURVE('',#36798,#37279,#30642,.T.);
#47202=EDGE_CURVE('',#37280,#37279,#5014,.T.);
#47203=EDGE_CURVE('',#36808,#37280,#30643,.T.);
#47204=EDGE_CURVE('',#37281,#37280,#5015,.T.);
#47205=EDGE_CURVE('',#36805,#37281,#30644,.T.);
#47206=EDGE_CURVE('',#37282,#37281,#5016,.T.);
#47207=EDGE_CURVE('',#36804,#37282,#30645,.T.);
#47208=EDGE_CURVE('',#37283,#37282,#21491,.T.);
#47209=EDGE_CURVE('',#36799,#37283,#30646,.T.);
#47210=EDGE_CURVE('',#37284,#37283,#5017,.T.);
#47211=EDGE_CURVE('',#36801,#37284,#30647,.T.);
#47212=EDGE_CURVE('',#37285,#37284,#5018,.T.);
#47213=EDGE_CURVE('',#37286,#37285,#30648,.T.);
#47214=EDGE_CURVE('',#36801,#37286,#5019,.T.);
#47215=EDGE_CURVE('',#37287,#37288,#30649,.T.);
#47216=EDGE_CURVE('',#37289,#37288,#21492,.T.);
#47217=EDGE_CURVE('',#37290,#37289,#30650,.T.);
#47218=EDGE_CURVE('',#37287,#37290,#21493,.T.);
#47219=EDGE_CURVE('',#37288,#37285,#5020,.T.);
#47220=EDGE_CURVE('',#37286,#37287,#5021,.T.);
#47221=EDGE_CURVE('',#37286,#37291,#30651,.T.);
#47222=EDGE_CURVE('',#37291,#36802,#5022,.T.);
#47223=EDGE_CURVE('',#36892,#37292,#30652,.T.);
#47224=EDGE_CURVE('',#37293,#37292,#30653,.T.);
#47225=EDGE_CURVE('',#36890,#37293,#30654,.T.);
#47226=EDGE_CURVE('',#37294,#37293,#21494,.T.);
#47227=EDGE_CURVE('',#36981,#37294,#30655,.T.);
#47228=EDGE_CURVE('',#37295,#37296,#30656,.T.);
#47229=EDGE_CURVE('',#37297,#37296,#1901,.T.);
#47230=EDGE_CURVE('',#37298,#37297,#30657,.T.);
#47231=EDGE_CURVE('',#37295,#37298,#5023,.T.);
#47232=EDGE_CURVE('',#37299,#37297,#1902,.T.);
#47233=EDGE_CURVE('',#37291,#37299,#30658,.T.);
#47234=EDGE_CURVE('',#37298,#37291,#1903,.T.);
#47235=EDGE_CURVE('',#37300,#37299,#5024,.T.);
#47236=EDGE_CURVE('',#36802,#37300,#30659,.T.);
#47237=EDGE_CURVE('',#37301,#37300,#5025,.T.);
#47238=EDGE_CURVE('',#36800,#37301,#30660,.T.);
#47239=EDGE_CURVE('',#37302,#37301,#21495,.T.);
#47240=EDGE_CURVE('',#36803,#37302,#30661,.T.);
#47241=EDGE_CURVE('',#37303,#37302,#5026,.T.);
#47242=EDGE_CURVE('',#36806,#37303,#30662,.T.);
#47243=EDGE_CURVE('',#37304,#37303,#5027,.T.);
#47244=EDGE_CURVE('',#36807,#37304,#30663,.T.);
#47245=EDGE_CURVE('',#37305,#37304,#5028,.T.);
#47246=EDGE_CURVE('',#36809,#37305,#30664,.T.);
#47247=EDGE_CURVE('',#37306,#37305,#5029,.T.);
#47248=EDGE_CURVE('',#37122,#37306,#30665,.T.);
#47249=EDGE_CURVE('',#37125,#37306,#21496,.T.);
#47250=EDGE_CURVE('',#37122,#37124,#21497,.T.);
#47251=EDGE_CURVE('',#37292,#37125,#21498,.T.);
#47252=EDGE_CURVE('',#37156,#37307,#21499,.T.);
#47253=EDGE_CURVE('',#37308,#37154,#21500,.T.);
#47254=EDGE_CURVE('',#37308,#37307,#30666,.T.);
#47255=EDGE_CURVE('',#37309,#37142,#30667,.T.);
#47256=EDGE_CURVE('',#37310,#37142,#21501,.T.);
#47257=EDGE_CURVE('',#37311,#37310,#30668,.T.);
#47258=EDGE_CURVE('',#37309,#37311,#21502,.T.);
#47259=EDGE_CURVE('',#37312,#37144,#30669,.T.);
#47260=EDGE_CURVE('',#37312,#37309,#1167,.T.);
#47261=EDGE_CURVE('',#37144,#37140,#21503,.T.);
#47262=EDGE_CURVE('',#37141,#37312,#21504,.T.);
#47263=EDGE_CURVE('',#37313,#37141,#21505,.T.);
#47264=EDGE_CURVE('',#36829,#37313,#30670,.T.);
#47265=EDGE_CURVE('',#37314,#37313,#30671,.T.);
#47266=EDGE_CURVE('',#36826,#37314,#30672,.T.);
#47267=EDGE_CURVE('',#37315,#37314,#21506,.T.);
#47268=EDGE_CURVE('',#36827,#37315,#30673,.T.);
#47269=EDGE_CURVE('',#37316,#37317,#30674,.T.);
#47270=EDGE_CURVE('',#37318,#37316,#5030,.T.);
#47271=EDGE_CURVE('',#37319,#37318,#30675,.T.);
#47272=EDGE_CURVE('',#37320,#37319,#5031,.F.);
#47273=EDGE_CURVE('',#37317,#37320,#5032,.F.);
#47274=EDGE_CURVE('',#37321,#37322,#21507,.T.);
#47275=EDGE_CURVE('',#37321,#37166,#5033,.T.);
#47276=EDGE_CURVE('',#37165,#37322,#30676,.T.);
#47277=EDGE_CURVE('',#37323,#37315,#30677,.T.);
#47278=EDGE_CURVE('',#37324,#37323,#30678,.T.);
#47279=EDGE_CURVE('',#36827,#37324,#30679,.T.);
#47280=EDGE_CURVE('',#37325,#37324,#21508,.T.);
#47281=EDGE_CURVE('',#37325,#36828,#30680,.T.);
#47282=EDGE_CURVE('',#37326,#36813,#30681,.T.);
#47283=EDGE_CURVE('',#37327,#36812,#30682,.T.);
#47284=EDGE_CURVE('',#37326,#37327,#21509,.T.);
#47285=EDGE_CURVE('',#37328,#36815,#30683,.T.);
#47286=EDGE_CURVE('',#37328,#37326,#5034,.T.);
#47287=EDGE_CURVE('',#37329,#36817,#30684,.T.);
#47288=EDGE_CURVE('',#37329,#37328,#1168,.T.);
#47289=EDGE_CURVE('',#37330,#36819,#30685,.T.);
#47290=EDGE_CURVE('',#37330,#37329,#5035,.T.);
#47291=EDGE_CURVE('',#37331,#36821,#30686,.T.);
#47292=EDGE_CURVE('',#37331,#37330,#21510,.T.);
#47293=EDGE_CURVE('',#37332,#36823,#30687,.T.);
#47294=EDGE_CURVE('',#37332,#37331,#5036,.T.);
#47295=EDGE_CURVE('',#37333,#36833,#30688,.T.);
#47296=EDGE_CURVE('',#37333,#37332,#1169,.T.);
#47297=EDGE_CURVE('',#37334,#37335,#30689,.T.);
#47298=EDGE_CURVE('',#36833,#37335,#5037,.T.);
#47299=EDGE_CURVE('',#37334,#37333,#5038,.T.);
#47300=EDGE_CURVE('',#37325,#37336,#30690,.T.);
#47301=EDGE_CURVE('',#37337,#37336,#30691,.T.);
#47302=EDGE_CURVE('',#36828,#37337,#30692,.T.);
#47303=EDGE_CURVE('',#37338,#37337,#21511,.T.);
#47304=EDGE_CURVE('',#36825,#37338,#30693,.T.);
#47305=EDGE_CURVE('',#37339,#37338,#30694,.T.);
#47306=EDGE_CURVE('',#36830,#37339,#30695,.T.);
#47307=EDGE_CURVE('',#37136,#37339,#21512,.T.);
#47308=EDGE_CURVE('',#37340,#37134,#30696,.T.);
#47309=EDGE_CURVE('',#37137,#37134,#21513,.T.);
#47310=EDGE_CURVE('',#37341,#37136,#21514,.T.);
#47311=EDGE_CURVE('',#37341,#37340,#30697,.T.);
#47312=EDGE_CURVE('',#37327,#37341,#1170,.T.);
#47313=EDGE_CURVE('',#37342,#37260,#21515,.T.);
#47314=EDGE_CURVE('',#37343,#37342,#30698,.T.);
#47315=EDGE_CURVE('',#37261,#37343,#21516,.T.);
#47316=EDGE_CURVE('',#37344,#37345,#30699,.T.);
#47317=EDGE_CURVE('',#37335,#37345,#21517,.T.);
#47318=EDGE_CURVE('',#37344,#37334,#21518,.T.);
#47319=EDGE_CURVE('',#37260,#37335,#30700,.T.);
#47320=EDGE_CURVE('',#37346,#37347,#30701,.T.);
#47321=EDGE_CURVE('',#37348,#37347,#5039,.T.);
#47322=EDGE_CURVE('',#36838,#37348,#30702,.T.);
#47323=EDGE_CURVE('',#37346,#36838,#5040,.T.);
#47324=EDGE_CURVE('',#37349,#37348,#1171,.T.);
#47325=EDGE_CURVE('',#36835,#37349,#30703,.T.);
#47326=EDGE_CURVE('',#37350,#37349,#5041,.T.);
#47327=EDGE_CURVE('',#37158,#37350,#30704,.T.);
#47328=EDGE_CURVE('',#37351,#37350,#21519,.T.);
#47329=EDGE_CURVE('',#37352,#37351,#30705,.T.);
#47330=EDGE_CURVE('',#37158,#37352,#21520,.T.);
#47331=EDGE_CURVE('',#37353,#37354,#30706,.T.);
#47332=EDGE_CURVE('',#37355,#37354,#30707,.T.);
#47333=EDGE_CURVE('',#37356,#37355,#30708,.T.);
#47334=EDGE_CURVE('',#37353,#37356,#30709,.T.);
#47335=EDGE_CURVE('',#37357,#37356,#21521,.T.);
#47336=EDGE_CURVE('',#37357,#37358,#30710,.T.);
#47337=EDGE_CURVE('',#37353,#37358,#21522,.T.);
#47338=EDGE_CURVE('',#37357,#37359,#30711,.T.);
#47339=EDGE_CURVE('',#37360,#37359,#30712,.T.);
#47340=EDGE_CURVE('',#37358,#37360,#30713,.T.);
#47341=EDGE_CURVE('',#37361,#37360,#21523,.T.);
#47342=EDGE_CURVE('',#37361,#37362,#5042,.T.);
#47343=EDGE_CURVE('',#37358,#37362,#21524,.T.);
#47344=EDGE_CURVE('',#37167,#37363,#5043,.T.);
#47345=EDGE_CURVE('',#37364,#37363,#21525,.T.);
#47346=EDGE_CURVE('',#37364,#37168,#30714,.T.);
#47347=EDGE_CURVE('',#37365,#37366,#30715,.T.);
#47348=EDGE_CURVE('',#37367,#37366,#5044,.T.);
#47349=EDGE_CURVE('',#37162,#37367,#30716,.T.);
#47350=EDGE_CURVE('',#37365,#37162,#5045,.T.);
#47351=EDGE_CURVE('',#37368,#37367,#5046,.T.);
#47352=EDGE_CURVE('',#37160,#37368,#30717,.T.);
#47353=EDGE_CURVE('',#37369,#37368,#21526,.T.);
#47354=EDGE_CURVE('',#37370,#37369,#30718,.T.);
#47355=EDGE_CURVE('',#37160,#37370,#21527,.T.);
#47356=EDGE_CURVE('',#37371,#37372,#30719,.T.);
#47357=EDGE_CURVE('',#37373,#37372,#30720,.T.);
#47358=EDGE_CURVE('',#37374,#37373,#30721,.T.);
#47359=EDGE_CURVE('',#37371,#37374,#30722,.T.);
#47360=EDGE_CURVE('',#37371,#37375,#21528,.T.);
#47361=EDGE_CURVE('',#37376,#37374,#21529,.T.);
#47362=EDGE_CURVE('',#37376,#37375,#30723,.T.);
#47363=EDGE_CURVE('',#37376,#37377,#30724,.T.);
#47364=EDGE_CURVE('',#37378,#37377,#30725,.T.);
#47365=EDGE_CURVE('',#37375,#37378,#30726,.T.);
#47366=EDGE_CURVE('',#37379,#37157,#30727,.T.);
#47367=EDGE_CURVE('',#37380,#37157,#21530,.T.);
#47368=EDGE_CURVE('',#37381,#37380,#30728,.T.);
#47369=EDGE_CURVE('',#37379,#37381,#21531,.T.);
#47370=EDGE_CURVE('',#37382,#36836,#30729,.T.);
#47371=EDGE_CURVE('',#37382,#37379,#5047,.T.);
#47372=EDGE_CURVE('',#37383,#36837,#30730,.T.);
#47373=EDGE_CURVE('',#37383,#37382,#5048,.T.);
#47374=EDGE_CURVE('',#37384,#37385,#30731,.T.);
#47375=EDGE_CURVE('',#36837,#37385,#5049,.T.);
#47376=EDGE_CURVE('',#37384,#37383,#5050,.T.);
#47377=EDGE_CURVE('',#37386,#37387,#30732,.T.);
#47378=EDGE_CURVE('',#37347,#37387,#21532,.T.);
#47379=EDGE_CURVE('',#37386,#37346,#21533,.T.);
#47380=EDGE_CURVE('',#37388,#37389,#30733,.T.);
#47381=EDGE_CURVE('',#37385,#37389,#21534,.T.);
#47382=EDGE_CURVE('',#37388,#37384,#21535,.T.);
#47383=EDGE_CURVE('',#37346,#37385,#30734,.T.);
#47384=EDGE_CURVE('',#36847,#37390,#30735,.T.);
#47385=EDGE_CURVE('',#37391,#37390,#30736,.T.);
#47386=EDGE_CURVE('',#36845,#37391,#30737,.T.);
#47387=EDGE_CURVE('',#37392,#37391,#21536,.T.);
#47388=EDGE_CURVE('',#36842,#37392,#30738,.T.);
#47389=EDGE_CURVE('',#37393,#36886,#30739,.T.);
#47390=EDGE_CURVE('',#37394,#36886,#5051,.T.);
#47391=EDGE_CURVE('',#37395,#37394,#30740,.T.);
#47392=EDGE_CURVE('',#37393,#37395,#5052,.T.);
#47393=EDGE_CURVE('',#37396,#36887,#30741,.T.);
#47394=EDGE_CURVE('',#37396,#37393,#5053,.T.);
#47395=EDGE_CURVE('',#37397,#36876,#30742,.T.);
#47396=EDGE_CURVE('',#37397,#37396,#5054,.T.);
#47397=EDGE_CURVE('',#37398,#36874,#30743,.T.);
#47398=EDGE_CURVE('',#37398,#37397,#21537,.T.);
#47399=EDGE_CURVE('',#37399,#36840,#30744,.T.);
#47400=EDGE_CURVE('',#37399,#37398,#5055,.T.);
#47401=EDGE_CURVE('',#37400,#36841,#30745,.T.);
#47402=EDGE_CURVE('',#37400,#37399,#5056,.T.);
#47403=EDGE_CURVE('',#37401,#36870,#30746,.T.);
#47404=EDGE_CURVE('',#37401,#37400,#5057,.T.);
#47405=EDGE_CURVE('',#37402,#36867,#30747,.T.);
#47406=EDGE_CURVE('',#37402,#37401,#21538,.T.);
#47407=EDGE_CURVE('',#37403,#37027,#30748,.T.);
#47408=EDGE_CURVE('',#37403,#37402,#1172,.T.);
#47409=EDGE_CURVE('',#37027,#37024,#21539,.T.);
#47410=EDGE_CURVE('',#37025,#37403,#21540,.T.);
#47411=EDGE_CURVE('',#37390,#37025,#21541,.T.);
#47412=EDGE_CURVE('',#37404,#37392,#30749,.T.);
#47413=EDGE_CURVE('',#37405,#37404,#30750,.T.);
#47414=EDGE_CURVE('',#36842,#37405,#30751,.T.);
#47415=EDGE_CURVE('',#37406,#37405,#21542,.T.);
#47416=EDGE_CURVE('',#37406,#36843,#30752,.T.);
#47417=EDGE_CURVE('',#37406,#37407,#30753,.T.);
#47418=EDGE_CURVE('',#37408,#37407,#30754,.T.);
#47419=EDGE_CURVE('',#36843,#37408,#30755,.T.);
#47420=EDGE_CURVE('',#37409,#37408,#21543,.T.);
#47421=EDGE_CURVE('',#36844,#37409,#30756,.T.);
#47422=EDGE_CURVE('',#37410,#37409,#30757,.T.);
#47423=EDGE_CURVE('',#36846,#37410,#30758,.T.);
#47424=EDGE_CURVE('',#37021,#37410,#21544,.T.);
#47425=EDGE_CURVE('',#37411,#37021,#21545,.T.);
#47426=EDGE_CURVE('',#37019,#37411,#30759,.T.);
#47427=EDGE_CURVE('',#37022,#37019,#21546,.T.);
#47428=EDGE_CURVE('',#37412,#37411,#1173,.T.);
#47429=EDGE_CURVE('',#36851,#37412,#30760,.T.);
#47430=EDGE_CURVE('',#37413,#37412,#21547,.T.);
#47431=EDGE_CURVE('',#36852,#37413,#30761,.T.);
#47432=EDGE_CURVE('',#37414,#37413,#5058,.T.);
#47433=EDGE_CURVE('',#36862,#37414,#30762,.T.);
#47434=EDGE_CURVE('',#37415,#37414,#5059,.T.);
#47435=EDGE_CURVE('',#36859,#37415,#30763,.T.);
#47436=EDGE_CURVE('',#37416,#37415,#5060,.T.);
#47437=EDGE_CURVE('',#36858,#37416,#30764,.T.);
#47438=EDGE_CURVE('',#37417,#37416,#21548,.T.);
#47439=EDGE_CURVE('',#36853,#37417,#30765,.T.);
#47440=EDGE_CURVE('',#37418,#37417,#5061,.T.);
#47441=EDGE_CURVE('',#36855,#37418,#30766,.T.);
#47442=EDGE_CURVE('',#37419,#37418,#5062,.T.);
#47443=EDGE_CURVE('',#37420,#37419,#30767,.T.);
#47444=EDGE_CURVE('',#36855,#37420,#5063,.T.);
#47445=EDGE_CURVE('',#37421,#37422,#30768,.T.);
#47446=EDGE_CURVE('',#37423,#37422,#21549,.T.);
#47447=EDGE_CURVE('',#37424,#37423,#30769,.T.);
#47448=EDGE_CURVE('',#37421,#37424,#21550,.T.);
#47449=EDGE_CURVE('',#37422,#37419,#5064,.T.);
#47450=EDGE_CURVE('',#37420,#37421,#5065,.T.);
#47451=EDGE_CURVE('',#37420,#37425,#30770,.T.);
#47452=EDGE_CURVE('',#37425,#36856,#5066,.T.);
#47453=EDGE_CURVE('',#37002,#37426,#30771,.T.);
#47454=EDGE_CURVE('',#37427,#37426,#30772,.T.);
#47455=EDGE_CURVE('',#37000,#37427,#30773,.T.);
#47456=EDGE_CURVE('',#37428,#37427,#21551,.T.);
#47457=EDGE_CURVE('',#37163,#37428,#30774,.T.);
#47458=EDGE_CURVE('',#37429,#36856,#30775,.T.);
#47459=EDGE_CURVE('',#37430,#37425,#30776,.T.);
#47460=EDGE_CURVE('',#37429,#37430,#5067,.T.);
#47461=EDGE_CURVE('',#37431,#36854,#30777,.T.);
#47462=EDGE_CURVE('',#37431,#37429,#5068,.T.);
#47463=EDGE_CURVE('',#37432,#36857,#30778,.T.);
#47464=EDGE_CURVE('',#37432,#37431,#21552,.T.);
#47465=EDGE_CURVE('',#37433,#36860,#30779,.T.);
#47466=EDGE_CURVE('',#37433,#37432,#5069,.T.);
#47467=EDGE_CURVE('',#37434,#36861,#30780,.T.);
#47468=EDGE_CURVE('',#37434,#37433,#5070,.T.);
#47469=EDGE_CURVE('',#37435,#37003,#30781,.T.);
#47470=EDGE_CURVE('',#37435,#37434,#5071,.T.);
#47471=EDGE_CURVE('',#37436,#37437,#30782,.T.);
#47472=EDGE_CURVE('',#37003,#37437,#5072,.T.);
#47473=EDGE_CURVE('',#37436,#37435,#5073,.T.);
#47474=EDGE_CURVE('',#37438,#37425,#5074,.T.);
#47475=EDGE_CURVE('',#37439,#37438,#30783,.T.);
#47476=EDGE_CURVE('',#37430,#37439,#1904,.T.);
#47477=EDGE_CURVE('',#37440,#37034,#30784,.T.);
#47478=EDGE_CURVE('',#37441,#37034,#21553,.T.);
#47479=EDGE_CURVE('',#37442,#37441,#30785,.T.);
#47480=EDGE_CURVE('',#37440,#37442,#21554,.T.);
#47481=EDGE_CURVE('',#37443,#37036,#30786,.T.);
#47482=EDGE_CURVE('',#37443,#37440,#1174,.T.);
#47483=EDGE_CURVE('',#37036,#37032,#21555,.T.);
#47484=EDGE_CURVE('',#37033,#37443,#21556,.T.);
#47485=EDGE_CURVE('',#37444,#37033,#21557,.T.);
#47486=EDGE_CURVE('',#37444,#36881,#30787,.T.);
#47487=EDGE_CURVE('',#37445,#36878,#30788,.T.);
#47488=EDGE_CURVE('',#37445,#37444,#30789,.T.);
#47489=EDGE_CURVE('',#37446,#36879,#30790,.T.);
#47490=EDGE_CURVE('',#37446,#37445,#21558,.T.);
#47491=EDGE_CURVE('',#37447,#37448,#30791,.T.);
#47492=EDGE_CURVE('',#37449,#37448,#5075,.T.);
#47493=EDGE_CURVE('',#37169,#37449,#30792,.T.);
#47494=EDGE_CURVE('',#37447,#37169,#5076,.T.);
#47495=EDGE_CURVE('',#36864,#37449,#21559,.T.);
#47496=EDGE_CURVE('',#37013,#36864,#21560,.T.);
#47497=EDGE_CURVE('',#36865,#37016,#21561,.T.);
#47498=EDGE_CURVE('',#37450,#37451,#30793,.T.);
#47499=EDGE_CURVE('',#37014,#37451,#21562,.T.);
#47500=EDGE_CURVE('',#37450,#37013,#21563,.T.);
#47501=EDGE_CURVE('',#37452,#37453,#30794,.T.);
#47502=EDGE_CURVE('',#36879,#37453,#30795,.T.);
#47503=EDGE_CURVE('',#37452,#37446,#30796,.T.);
#47504=EDGE_CURVE('',#37454,#37453,#21564,.T.);
#47505=EDGE_CURVE('',#37454,#36880,#30797,.T.);
#47506=EDGE_CURVE('',#37455,#36869,#30798,.T.);
#47507=EDGE_CURVE('',#37456,#36868,#30799,.T.);
#47508=EDGE_CURVE('',#37455,#37456,#21565,.T.);
#47509=EDGE_CURVE('',#37457,#36871,#30800,.T.);
#47510=EDGE_CURVE('',#37457,#37455,#5077,.T.);
#47511=EDGE_CURVE('',#37458,#36872,#30801,.T.);
#47512=EDGE_CURVE('',#37458,#37457,#5078,.T.);
#47513=EDGE_CURVE('',#37459,#36873,#30802,.T.);
#47514=EDGE_CURVE('',#37459,#37458,#5079,.T.);
#47515=EDGE_CURVE('',#37460,#37459,#21566,.T.);
#47516=EDGE_CURVE('',#36875,#37460,#30803,.T.);
#47517=EDGE_CURVE('',#37461,#37460,#5080,.T.);
#47518=EDGE_CURVE('',#36888,#37461,#30804,.T.);
#47519=EDGE_CURVE('',#37462,#37461,#5081,.T.);
#47520=EDGE_CURVE('',#37463,#37462,#30805,.T.);
#47521=EDGE_CURVE('',#36888,#37463,#5082,.T.);
#47522=EDGE_CURVE('',#37454,#37464,#30806,.T.);
#47523=EDGE_CURVE('',#37465,#37464,#30807,.T.);
#47524=EDGE_CURVE('',#36880,#37465,#30808,.T.);
#47525=EDGE_CURVE('',#37466,#37465,#21567,.T.);
#47526=EDGE_CURVE('',#36877,#37466,#30809,.T.);
#47527=EDGE_CURVE('',#37467,#37466,#30810,.T.);
#47528=EDGE_CURVE('',#36882,#37467,#30811,.T.);
#47529=EDGE_CURVE('',#37028,#37467,#21568,.T.);
#47530=EDGE_CURVE('',#37468,#37026,#30812,.T.);
#47531=EDGE_CURVE('',#37029,#37026,#21569,.T.);
#47532=EDGE_CURVE('',#37469,#37028,#21570,.T.);
#47533=EDGE_CURVE('',#37469,#37468,#30813,.T.);
#47534=EDGE_CURVE('',#37456,#37469,#1175,.T.);
#47535=EDGE_CURVE('',#37394,#37470,#30814,.T.);
#47536=EDGE_CURVE('',#37470,#36885,#30815,.T.);
#47537=EDGE_CURVE('',#37471,#37394,#21571,.T.);
#47538=EDGE_CURVE('',#37472,#37471,#30816,.T.);
#47539=EDGE_CURVE('',#37395,#37472,#21572,.T.);
#47540=EDGE_CURVE('',#37473,#37462,#21573,.T.);
#47541=EDGE_CURVE('',#37474,#37473,#30817,.T.);
#47542=EDGE_CURVE('',#37463,#37474,#21574,.T.);
#47543=EDGE_CURVE('',#37470,#37463,#5083,.T.);
#47544=EDGE_CURVE('',#37475,#36899,#30818,.T.);
#47545=EDGE_CURVE('',#37476,#36902,#30819,.T.);
#47546=EDGE_CURVE('',#37475,#37476,#5084,.T.);
#47547=EDGE_CURVE('',#37477,#36896,#30820,.T.);
#47548=EDGE_CURVE('',#37477,#37475,#5085,.T.);
#47549=EDGE_CURVE('',#37478,#36897,#30821,.T.);
#47550=EDGE_CURVE('',#37478,#37477,#21575,.T.);
#47551=EDGE_CURVE('',#37479,#37480,#30822,.T.);
#47552=EDGE_CURVE('',#36897,#37480,#5086,.T.);
#47553=EDGE_CURVE('',#37479,#37478,#5087,.T.);
#47554=EDGE_CURVE('',#36982,#37481,#30823,.T.);
#47555=EDGE_CURVE('',#37482,#37481,#21576,.T.);
#47556=EDGE_CURVE('',#36889,#37482,#30824,.T.);
#47557=EDGE_CURVE('',#37483,#37482,#30825,.T.);
#47558=EDGE_CURVE('',#36891,#37483,#30826,.T.);
#47559=EDGE_CURVE('',#37116,#37483,#21577,.T.);
#47560=EDGE_CURVE('',#37484,#37114,#30827,.T.);
#47561=EDGE_CURVE('',#37117,#37114,#21578,.T.);
#47562=EDGE_CURVE('',#37484,#37116,#21579,.T.);
#47563=EDGE_CURVE('',#37476,#37484,#1905,.T.);
#47564=EDGE_CURVE('',#37485,#37486,#30828,.T.);
#47565=EDGE_CURVE('',#37480,#37486,#5088,.T.);
#47566=EDGE_CURVE('',#37485,#37479,#5089,.T.);
#47567=EDGE_CURVE('',#37487,#37480,#5090,.T.);
#47568=EDGE_CURVE('',#37487,#36898,#5091,.T.);
#47569=EDGE_CURVE('',#37488,#36898,#30829,.T.);
#47570=EDGE_CURVE('',#37489,#37487,#30830,.T.);
#47571=EDGE_CURVE('',#37488,#37489,#5092,.T.);
#47572=EDGE_CURVE('',#37490,#36895,#30831,.T.);
#47573=EDGE_CURVE('',#37490,#37488,#21580,.T.);
#47574=EDGE_CURVE('',#37491,#37490,#5093,.T.);
#47575=EDGE_CURVE('',#36900,#37491,#30832,.T.);
#47576=EDGE_CURVE('',#37492,#37491,#5094,.T.);
#47577=EDGE_CURVE('',#36901,#37492,#30833,.T.);
#47578=EDGE_CURVE('',#37493,#37492,#1906,.T.);
#47579=EDGE_CURVE('',#37115,#37493,#30834,.T.);
#47580=EDGE_CURVE('',#37113,#37493,#21581,.T.);
#47581=EDGE_CURVE('',#37115,#37112,#21582,.T.);
#47582=EDGE_CURVE('',#37494,#37113,#21583,.T.);
#47583=EDGE_CURVE('',#36906,#37494,#30835,.T.);
#47584=EDGE_CURVE('',#37495,#37494,#30836,.T.);
#47585=EDGE_CURVE('',#36910,#37495,#30837,.T.);
#47586=EDGE_CURVE('',#37496,#37495,#21584,.T.);
#47587=EDGE_CURVE('',#36907,#37496,#30838,.T.);
#47588=EDGE_CURVE('',#37497,#37487,#5095,.T.);
#47589=EDGE_CURVE('',#37498,#37497,#30839,.T.);
#47590=EDGE_CURVE('',#37489,#37498,#5096,.T.);
#47591=EDGE_CURVE('',#37499,#37496,#30840,.T.);
#47592=EDGE_CURVE('',#37500,#37499,#30841,.T.);
#47593=EDGE_CURVE('',#36907,#37500,#30842,.T.);
#47594=EDGE_CURVE('',#37501,#37500,#21585,.T.);
#47595=EDGE_CURVE('',#37501,#36908,#30843,.T.);
#47596=EDGE_CURVE('',#37501,#37502,#30844,.T.);
#47597=EDGE_CURVE('',#37503,#37502,#30845,.T.);
#47598=EDGE_CURVE('',#36908,#37503,#30846,.T.);
#47599=EDGE_CURVE('',#37504,#37503,#21586,.T.);
#47600=EDGE_CURVE('',#36909,#37504,#30847,.T.);
#47601=EDGE_CURVE('',#37108,#37504,#30848,.T.);
#47602=EDGE_CURVE('',#37505,#37108,#21587,.T.);
#47603=EDGE_CURVE('',#37105,#37505,#30849,.T.);
#47604=EDGE_CURVE('',#37109,#37105,#21588,.T.);
#47605=EDGE_CURVE('',#37506,#37505,#1907,.T.);
#47606=EDGE_CURVE('',#36919,#37506,#30850,.T.);
#47607=EDGE_CURVE('',#37507,#37506,#5097,.T.);
#47608=EDGE_CURVE('',#36916,#37507,#30851,.T.);
#47609=EDGE_CURVE('',#37508,#37507,#5098,.T.);
#47610=EDGE_CURVE('',#36915,#37508,#30852,.T.);
#47611=EDGE_CURVE('',#37509,#37508,#21589,.T.);
#47612=EDGE_CURVE('',#36912,#37509,#30853,.T.);
#47613=EDGE_CURVE('',#37510,#37511,#30854,.T.);
#47614=EDGE_CURVE('',#36912,#37511,#5099,.T.);
#47615=EDGE_CURVE('',#37510,#37509,#5100,.T.);
#47616=EDGE_CURVE('',#37512,#37513,#30855,.T.);
#47617=EDGE_CURVE('',#37511,#37513,#5101,.T.);
#47618=EDGE_CURVE('',#37512,#37510,#5102,.T.);
#47619=EDGE_CURVE('',#37514,#37511,#5103,.T.);
#47620=EDGE_CURVE('',#37514,#36913,#5104,.T.);
#47621=EDGE_CURVE('',#37515,#36913,#30856,.T.);
#47622=EDGE_CURVE('',#37516,#37514,#30857,.T.);
#47623=EDGE_CURVE('',#37515,#37516,#5105,.T.);
#47624=EDGE_CURVE('',#37517,#36914,#30858,.T.);
#47625=EDGE_CURVE('',#37517,#37515,#21590,.T.);
#47626=EDGE_CURVE('',#37518,#36917,#30859,.T.);
#47627=EDGE_CURVE('',#37518,#37517,#5106,.T.);
#47628=EDGE_CURVE('',#37519,#36918,#30860,.T.);
#47629=EDGE_CURVE('',#37519,#37518,#5107,.T.);
#47630=EDGE_CURVE('',#37520,#37106,#30861,.T.);
#47631=EDGE_CURVE('',#37520,#37519,#1908,.T.);
#47632=EDGE_CURVE('',#37106,#37103,#21591,.T.);
#47633=EDGE_CURVE('',#37104,#37520,#21592,.T.);
#47634=EDGE_CURVE('',#37521,#37104,#5108,.T.);
#47635=EDGE_CURVE('',#37521,#36923,#30862,.T.);
#47636=EDGE_CURVE('',#37522,#37514,#5109,.T.);
#47637=EDGE_CURVE('',#37523,#37522,#30863,.T.);
#47638=EDGE_CURVE('',#37516,#37523,#5110,.T.);
#47639=EDGE_CURVE('',#37524,#37525,#30864,.T.);
#47640=EDGE_CURVE('',#36923,#37525,#21593,.T.);
#47641=EDGE_CURVE('',#37524,#37521,#21594,.T.);
#47642=EDGE_CURVE('',#37525,#37526,#5111,.T.);
#47643=EDGE_CURVE('',#37526,#36920,#21595,.T.);
#47644=EDGE_CURVE('',#37526,#37527,#30865,.T.);
#47645=EDGE_CURVE('',#37528,#37527,#21596,.T.);
#47646=EDGE_CURVE('',#36920,#37528,#30866,.T.);
#47647=EDGE_CURVE('',#37100,#37528,#5112,.T.);
#47648=EDGE_CURVE('',#37529,#37100,#21597,.T.);
#47649=EDGE_CURVE('',#37097,#37529,#30867,.T.);
#47650=EDGE_CURVE('',#37101,#37097,#21598,.T.);
#47651=EDGE_CURVE('',#37530,#37529,#1909,.T.);
#47652=EDGE_CURVE('',#36931,#37530,#30868,.T.);
#47653=EDGE_CURVE('',#37531,#37530,#1176,.T.);
#47654=EDGE_CURVE('',#36928,#37531,#30869,.T.);
#47655=EDGE_CURVE('',#37532,#37531,#5113,.T.);
#47656=EDGE_CURVE('',#36925,#37532,#30870,.T.);
#47657=EDGE_CURVE('',#37533,#37532,#21599,.T.);
#47658=EDGE_CURVE('',#36926,#37533,#30871,.T.);
#47659=EDGE_CURVE('',#37534,#37533,#5114,.T.);
#47660=EDGE_CURVE('',#37535,#37534,#30872,.T.);
#47661=EDGE_CURVE('',#36926,#37535,#5115,.T.);
#47662=EDGE_CURVE('',#37536,#37534,#1177,.T.);
#47663=EDGE_CURVE('',#37537,#37536,#30873,.T.);
#47664=EDGE_CURVE('',#37535,#37537,#5116,.T.);
#47665=EDGE_CURVE('',#37538,#37535,#5117,.T.);
#47666=EDGE_CURVE('',#37538,#36927,#1910,.T.);
#47667=EDGE_CURVE('',#37539,#36927,#30874,.T.);
#47668=EDGE_CURVE('',#37540,#37538,#30875,.T.);
#47669=EDGE_CURVE('',#37539,#37540,#1911,.T.);
#47670=EDGE_CURVE('',#37541,#36924,#30876,.T.);
#47671=EDGE_CURVE('',#37541,#37539,#21600,.T.);
#47672=EDGE_CURVE('',#37542,#36929,#30877,.T.);
#47673=EDGE_CURVE('',#37542,#37541,#1912,.T.);
#47674=EDGE_CURVE('',#37543,#36930,#30878,.T.);
#47675=EDGE_CURVE('',#37543,#37542,#5118,.T.);
#47676=EDGE_CURVE('',#37544,#37098,#30879,.T.);
#47677=EDGE_CURVE('',#37544,#37543,#1913,.T.);
#47678=EDGE_CURVE('',#37098,#37095,#21601,.T.);
#47679=EDGE_CURVE('',#37096,#37544,#21602,.T.);
#47680=EDGE_CURVE('',#37545,#37096,#5119,.T.);
#47681=EDGE_CURVE('',#37545,#36935,#30880,.T.);
#47682=EDGE_CURVE('',#37546,#37538,#5120,.T.);
#47683=EDGE_CURVE('',#37547,#37546,#30881,.T.);
#47684=EDGE_CURVE('',#37540,#37547,#1178,.T.);
#47685=EDGE_CURVE('',#37548,#37549,#30882,.T.);
#47686=EDGE_CURVE('',#36935,#37549,#21603,.T.);
#47687=EDGE_CURVE('',#37548,#37545,#21604,.T.);
#47688=EDGE_CURVE('',#37549,#37550,#30883,.T.);
#47689=EDGE_CURVE('',#37550,#36932,#21605,.T.);
#47690=EDGE_CURVE('',#37550,#37551,#30884,.T.);
#47691=EDGE_CURVE('',#37552,#37551,#21606,.T.);
#47692=EDGE_CURVE('',#36932,#37552,#30885,.T.);
#47693=EDGE_CURVE('',#37092,#37552,#5121,.T.);
#47694=EDGE_CURVE('',#37553,#37092,#21607,.T.);
#47695=EDGE_CURVE('',#37089,#37553,#30886,.T.);
#47696=EDGE_CURVE('',#37093,#37089,#21608,.T.);
#47697=EDGE_CURVE('',#37554,#37553,#1914,.T.);
#47698=EDGE_CURVE('',#36943,#37554,#30887,.T.);
#47699=EDGE_CURVE('',#37555,#37554,#1179,.T.);
#47700=EDGE_CURVE('',#36940,#37555,#30888,.T.);
#47701=EDGE_CURVE('',#37556,#37555,#1915,.T.);
#47702=EDGE_CURVE('',#36937,#37556,#30889,.T.);
#47703=EDGE_CURVE('',#37557,#37556,#21609,.T.);
#47704=EDGE_CURVE('',#36938,#37557,#30890,.T.);
#47705=EDGE_CURVE('',#37558,#37557,#1916,.T.);
#47706=EDGE_CURVE('',#37559,#37558,#30891,.T.);
#47707=EDGE_CURVE('',#36938,#37559,#1917,.T.);
#47708=EDGE_CURVE('',#37560,#37558,#1180,.T.);
#47709=EDGE_CURVE('',#37561,#37560,#30892,.T.);
#47710=EDGE_CURVE('',#37559,#37561,#5122,.T.);
#47711=EDGE_CURVE('',#37562,#37559,#5123,.T.);
#47712=EDGE_CURVE('',#37562,#36939,#5124,.T.);
#47713=EDGE_CURVE('',#37563,#36939,#30893,.T.);
#47714=EDGE_CURVE('',#37564,#37562,#30894,.T.);
#47715=EDGE_CURVE('',#37563,#37564,#5125,.T.);
#47716=EDGE_CURVE('',#37565,#36936,#30895,.T.);
#47717=EDGE_CURVE('',#37565,#37563,#21610,.T.);
#47718=EDGE_CURVE('',#37566,#36941,#30896,.T.);
#47719=EDGE_CURVE('',#37566,#37565,#5126,.T.);
#47720=EDGE_CURVE('',#37567,#36942,#30897,.T.);
#47721=EDGE_CURVE('',#37567,#37566,#1181,.T.);
#47722=EDGE_CURVE('',#37568,#37090,#30898,.T.);
#47723=EDGE_CURVE('',#37568,#37567,#1918,.T.);
#47724=EDGE_CURVE('',#37090,#37087,#21611,.T.);
#47725=EDGE_CURVE('',#37088,#37568,#21612,.T.);
#47726=EDGE_CURVE('',#37569,#37088,#5127,.T.);
#47727=EDGE_CURVE('',#36947,#37569,#30899,.T.);
#47728=EDGE_CURVE('',#37570,#37562,#5128,.T.);
#47729=EDGE_CURVE('',#37571,#37570,#30900,.T.);
#47730=EDGE_CURVE('',#37564,#37571,#1182,.T.);
#47731=EDGE_CURVE('',#37572,#37569,#21613,.T.);
#47732=EDGE_CURVE('',#37573,#37572,#30901,.T.);
#47733=EDGE_CURVE('',#36947,#37573,#21614,.T.);
#47734=EDGE_CURVE('',#37573,#37574,#5129,.T.);
#47735=EDGE_CURVE('',#37574,#36944,#21615,.T.);
#47736=EDGE_CURVE('',#37574,#37575,#30902,.T.);
#47737=EDGE_CURVE('',#37576,#37575,#21616,.T.);
#47738=EDGE_CURVE('',#36944,#37576,#30903,.T.);
#47739=EDGE_CURVE('',#37084,#37576,#5130,.T.);
#47740=EDGE_CURVE('',#37577,#37084,#21617,.T.);
#47741=EDGE_CURVE('',#37081,#37577,#30904,.T.);
#47742=EDGE_CURVE('',#37085,#37081,#21618,.T.);
#47743=EDGE_CURVE('',#37578,#37577,#1919,.T.);
#47744=EDGE_CURVE('',#36955,#37578,#30905,.T.);
#47745=EDGE_CURVE('',#37579,#37578,#5131,.T.);
#47746=EDGE_CURVE('',#36952,#37579,#30906,.T.);
#47747=EDGE_CURVE('',#37580,#37579,#5132,.T.);
#47748=EDGE_CURVE('',#36949,#37580,#30907,.T.);
#47749=EDGE_CURVE('',#37581,#37580,#21619,.T.);
#47750=EDGE_CURVE('',#36950,#37581,#30908,.T.);
#47751=EDGE_CURVE('',#37582,#37581,#5133,.T.);
#47752=EDGE_CURVE('',#37583,#37582,#30909,.T.);
#47753=EDGE_CURVE('',#36950,#37583,#5134,.T.);
#47754=EDGE_CURVE('',#37584,#37582,#5135,.T.);
#47755=EDGE_CURVE('',#37585,#37584,#30910,.T.);
#47756=EDGE_CURVE('',#37583,#37585,#5136,.T.);
#47757=EDGE_CURVE('',#37586,#37583,#5137,.T.);
#47758=EDGE_CURVE('',#37586,#36951,#5138,.T.);
#47759=EDGE_CURVE('',#37587,#36951,#30911,.T.);
#47760=EDGE_CURVE('',#37588,#37586,#30912,.T.);
#47761=EDGE_CURVE('',#37587,#37588,#5139,.T.);
#47762=EDGE_CURVE('',#37589,#36948,#30913,.T.);
#47763=EDGE_CURVE('',#37589,#37587,#21620,.T.);
#47764=EDGE_CURVE('',#37590,#37589,#5140,.T.);
#47765=EDGE_CURVE('',#36953,#37590,#30914,.T.);
#47766=EDGE_CURVE('',#37591,#37590,#5141,.T.);
#47767=EDGE_CURVE('',#36954,#37591,#30915,.T.);
#47768=EDGE_CURVE('',#37592,#37591,#1920,.T.);
#47769=EDGE_CURVE('',#37082,#37592,#30916,.T.);
#47770=EDGE_CURVE('',#37080,#37592,#21621,.T.);
#47771=EDGE_CURVE('',#37082,#37079,#21622,.T.);
#47772=EDGE_CURVE('',#37593,#37080,#30917,.T.);
#47773=EDGE_CURVE('',#36962,#37593,#30918,.T.);
#47774=EDGE_CURVE('',#37594,#37593,#21623,.T.);
#47775=EDGE_CURVE('',#36959,#37594,#30919,.T.);
#47776=EDGE_CURVE('',#37595,#37586,#5142,.T.);
#47777=EDGE_CURVE('',#37596,#37595,#30920,.T.);
#47778=EDGE_CURVE('',#37588,#37596,#5143,.T.);
#47779=EDGE_CURVE('',#37597,#37594,#30921,.T.);
#47780=EDGE_CURVE('',#37598,#37597,#30922,.T.);
#47781=EDGE_CURVE('',#36959,#37598,#30923,.T.);
#47782=EDGE_CURVE('',#37599,#37598,#21624,.T.);
#47783=EDGE_CURVE('',#37599,#36960,#30924,.T.);
#47784=EDGE_CURVE('',#37599,#37600,#30925,.T.);
#47785=EDGE_CURVE('',#37601,#37600,#30926,.T.);
#47786=EDGE_CURVE('',#36960,#37601,#30927,.T.);
#47787=EDGE_CURVE('',#37602,#37601,#21625,.T.);
#47788=EDGE_CURVE('',#36961,#37602,#30928,.T.);
#47789=EDGE_CURVE('',#37603,#37602,#30929,.T.);
#47790=EDGE_CURVE('',#36963,#37603,#30930,.T.);
#47791=EDGE_CURVE('',#37075,#37603,#21626,.T.);
#47792=EDGE_CURVE('',#37604,#37075,#21627,.T.);
#47793=EDGE_CURVE('',#37072,#37604,#30931,.T.);
#47794=EDGE_CURVE('',#37076,#37072,#21628,.T.);
#47795=EDGE_CURVE('',#37605,#37604,#1921,.T.);
#47796=EDGE_CURVE('',#36976,#37605,#30932,.T.);
#47797=EDGE_CURVE('',#37606,#37605,#5144,.T.);
#47798=EDGE_CURVE('',#36973,#37606,#30933,.T.);
#47799=EDGE_CURVE('',#37607,#37606,#5145,.T.);
#47800=EDGE_CURVE('',#36972,#37607,#30934,.T.);
#47801=EDGE_CURVE('',#37608,#37607,#21629,.T.);
#47802=EDGE_CURVE('',#36969,#37608,#30935,.T.);
#47803=EDGE_CURVE('',#37609,#37610,#30936,.T.);
#47804=EDGE_CURVE('',#36969,#37610,#5146,.T.);
#47805=EDGE_CURVE('',#37609,#37608,#5147,.T.);
#47806=EDGE_CURVE('',#37611,#37612,#30937,.T.);
#47807=EDGE_CURVE('',#37610,#37612,#5148,.T.);
#47808=EDGE_CURVE('',#37611,#37609,#5149,.T.);
#47809=EDGE_CURVE('',#37613,#37610,#5150,.T.);
#47810=EDGE_CURVE('',#37613,#36970,#5151,.T.);
#47811=EDGE_CURVE('',#36968,#37614,#30938,.T.);
#47812=EDGE_CURVE('',#37615,#37614,#30939,.T.);
#47813=EDGE_CURVE('',#36966,#37615,#30940,.T.);
#47814=EDGE_CURVE('',#37616,#37615,#21630,.T.);
#47815=EDGE_CURVE('',#36979,#37616,#30941,.T.);
#47816=EDGE_CURVE('',#37617,#37618,#30942,.T.);
#47817=EDGE_CURVE('',#37619,#37618,#5152,.T.);
#47818=EDGE_CURVE('',#37613,#37619,#30943,.T.);
#47819=EDGE_CURVE('',#37617,#37613,#5153,.T.);
#47820=EDGE_CURVE('',#37620,#37619,#5154,.T.);
#47821=EDGE_CURVE('',#36970,#37620,#30944,.T.);
#47822=EDGE_CURVE('',#37621,#37620,#21631,.T.);
#47823=EDGE_CURVE('',#36971,#37621,#30945,.T.);
#47824=EDGE_CURVE('',#37622,#37621,#5155,.T.);
#47825=EDGE_CURVE('',#36974,#37622,#30946,.T.);
#47826=EDGE_CURVE('',#37623,#37622,#5156,.T.);
#47827=EDGE_CURVE('',#36975,#37623,#30947,.T.);
#47828=EDGE_CURVE('',#37624,#37623,#1922,.T.);
#47829=EDGE_CURVE('',#37073,#37624,#30948,.T.);
#47830=EDGE_CURVE('',#37071,#37624,#21632,.T.);
#47831=EDGE_CURVE('',#37073,#37070,#21633,.T.);
#47832=EDGE_CURVE('',#37614,#37071,#21634,.T.);
#47833=EDGE_CURVE('',#37625,#37616,#30949,.T.);
#47834=EDGE_CURVE('',#37626,#37625,#30950,.T.);
#47835=EDGE_CURVE('',#36979,#37626,#30951,.T.);
#47836=EDGE_CURVE('',#37627,#37626,#21635,.T.);
#47837=EDGE_CURVE('',#37627,#36980,#30952,.T.);
#47838=EDGE_CURVE('',#37627,#37628,#30953,.T.);
#47839=EDGE_CURVE('',#37250,#37628,#30954,.T.);
#47840=EDGE_CURVE('',#37629,#37294,#30955,.T.);
#47841=EDGE_CURVE('',#37630,#37629,#30956,.T.);
#47842=EDGE_CURVE('',#36981,#37630,#30957,.T.);
#47843=EDGE_CURVE('',#37631,#37630,#21636,.T.);
#47844=EDGE_CURVE('',#37631,#36982,#30958,.T.);
#47845=EDGE_CURVE('',#37631,#37632,#30959,.T.);
#47846=EDGE_CURVE('',#37481,#37632,#30960,.T.);
#47847=EDGE_CURVE('',#37633,#37634,#30961,.T.);
#47848=EDGE_CURVE('',#37635,#37634,#5157,.T.);
#47849=EDGE_CURVE('',#37636,#37635,#30962,.T.);
#47850=EDGE_CURVE('',#37633,#37636,#1183,.T.);
#47851=EDGE_CURVE('',#37637,#37638,#30963,.T.);
#47852=EDGE_CURVE('',#37639,#37638,#5158,.T.);
#47853=EDGE_CURVE('',#37640,#37639,#30964,.T.);
#47854=EDGE_CURVE('',#37637,#37640,#5159,.T.);
#47855=EDGE_CURVE('',#37641,#37642,#30965,.T.);
#47856=EDGE_CURVE('',#37643,#37642,#1923,.T.);
#47857=EDGE_CURVE('',#37644,#37643,#30966,.T.);
#47858=EDGE_CURVE('',#37641,#37644,#5160,.T.);
#47859=EDGE_CURVE('',#37645,#37646,#30967,.T.);
#47860=EDGE_CURVE('',#37642,#37646,#5161,.T.);
#47861=EDGE_CURVE('',#37645,#37641,#5162,.T.);
#47862=EDGE_CURVE('',#37647,#37648,#30968,.T.);
#47863=EDGE_CURVE('',#37649,#37648,#5163,.T.);
#47864=EDGE_CURVE('',#37650,#37649,#30969,.T.);
#47865=EDGE_CURVE('',#37647,#37650,#5164,.T.);
#47866=EDGE_CURVE('',#37651,#37649,#5165,.T.);
#47867=EDGE_CURVE('',#37652,#37651,#30970,.T.);
#47868=EDGE_CURVE('',#37650,#37652,#5166,.T.);
#47869=EDGE_CURVE('',#37653,#37651,#21637,.T.);
#47870=EDGE_CURVE('',#37654,#37653,#30971,.T.);
#47871=EDGE_CURVE('',#37652,#37654,#21638,.T.);
#47872=EDGE_CURVE('',#37655,#37656,#30972,.T.);
#47873=EDGE_CURVE('',#37657,#37656,#30973,.T.);
#47874=EDGE_CURVE('',#37658,#37657,#30974,.T.);
#47875=EDGE_CURVE('',#37655,#37658,#30975,.T.);
#47876=EDGE_CURVE('',#37655,#37659,#21639,.T.);
#47877=EDGE_CURVE('',#37660,#37658,#21640,.T.);
#47878=EDGE_CURVE('',#37660,#37659,#30976,.T.);
#47879=EDGE_CURVE('',#37660,#37661,#30977,.T.);
#47880=EDGE_CURVE('',#37662,#37661,#30978,.T.);
#47881=EDGE_CURVE('',#37659,#37662,#30979,.T.);
#47882=EDGE_CURVE('',#37663,#37159,#30980,.T.);
#47883=EDGE_CURVE('',#37664,#37159,#21641,.T.);
#47884=EDGE_CURVE('',#37665,#37664,#30981,.T.);
#47885=EDGE_CURVE('',#37663,#37665,#21642,.T.);
#47886=EDGE_CURVE('',#37666,#37161,#30982,.T.);
#47887=EDGE_CURVE('',#37666,#37663,#5167,.T.);
#47888=EDGE_CURVE('',#37667,#37668,#30983,.T.);
#47889=EDGE_CURVE('',#37161,#37668,#5168,.T.);
#47890=EDGE_CURVE('',#37667,#37666,#5169,.T.);
#47891=EDGE_CURVE('',#37669,#37670,#30984,.T.);
#47892=EDGE_CURVE('',#37366,#37670,#5170,.T.);
#47893=EDGE_CURVE('',#37669,#37365,#5171,.T.);
#47894=EDGE_CURVE('',#37671,#37672,#30985,.T.);
#47895=EDGE_CURVE('',#37668,#37672,#30986,.T.);
#47896=EDGE_CURVE('',#37671,#37667,#30987,.T.);
#47897=EDGE_CURVE('',#37668,#37365,#30988,.T.);
#47898=EDGE_CURVE('',#37673,#37674,#30989,.T.);
#47899=EDGE_CURVE('',#37675,#37674,#30990,.T.);
#47900=EDGE_CURVE('',#37164,#37675,#30991,.T.);
#47901=EDGE_CURVE('',#37673,#37164,#30992,.T.);
#47902=EDGE_CURVE('',#37676,#37675,#21643,.T.);
#47903=EDGE_CURVE('',#36999,#37676,#30993,.T.);
#47904=EDGE_CURVE('',#37677,#37676,#30994,.T.);
#47905=EDGE_CURVE('',#37001,#37677,#30995,.T.);
#47906=EDGE_CURVE('',#37678,#37679,#30996,.T.);
#47907=EDGE_CURVE('',#37680,#37679,#5172,.T.);
#47908=EDGE_CURVE('',#37011,#37680,#30997,.T.);
#47909=EDGE_CURVE('',#37678,#37011,#5173,.T.);
#47910=EDGE_CURVE('',#37681,#37680,#5174,.T.);
#47911=EDGE_CURVE('',#36984,#37681,#30998,.T.);
#47912=EDGE_CURVE('',#37682,#37681,#21644,.T.);
#47913=EDGE_CURVE('',#36985,#37682,#30999,.T.);
#47914=EDGE_CURVE('',#37683,#37682,#5175,.T.);
#47915=EDGE_CURVE('',#37684,#37683,#31000,.T.);
#47916=EDGE_CURVE('',#36985,#37684,#5176,.T.);
#47917=EDGE_CURVE('',#37685,#37683,#5177,.T.);
#47918=EDGE_CURVE('',#37686,#37685,#31001,.T.);
#47919=EDGE_CURVE('',#37684,#37686,#5178,.T.);
#47920=EDGE_CURVE('',#37687,#37684,#5179,.T.);
#47921=EDGE_CURVE('',#37687,#36986,#5180,.T.);
#47922=EDGE_CURVE('',#37010,#37688,#31002,.T.);
#47923=EDGE_CURVE('',#37689,#37688,#31003,.T.);
#47924=EDGE_CURVE('',#36990,#37689,#31004,.T.);
#47925=EDGE_CURVE('',#37690,#37689,#21645,.T.);
#47926=EDGE_CURVE('',#36987,#37690,#31005,.T.);
#47927=EDGE_CURVE('',#37691,#36986,#31006,.T.);
#47928=EDGE_CURVE('',#37692,#37687,#31007,.T.);
#47929=EDGE_CURVE('',#37691,#37692,#5181,.T.);
#47930=EDGE_CURVE('',#37693,#36983,#31008,.T.);
#47931=EDGE_CURVE('',#37693,#37691,#21646,.T.);
#47932=EDGE_CURVE('',#37694,#37012,#31009,.T.);
#47933=EDGE_CURVE('',#37694,#37693,#5182,.T.);
#47934=EDGE_CURVE('',#37695,#37696,#31010,.T.);
#47935=EDGE_CURVE('',#37012,#37696,#5183,.T.);
#47936=EDGE_CURVE('',#37695,#37694,#5184,.T.);
#47937=EDGE_CURVE('',#37697,#37687,#5185,.T.);
#47938=EDGE_CURVE('',#37698,#37697,#31011,.T.);
#47939=EDGE_CURVE('',#37692,#37698,#5186,.T.);
#47940=EDGE_CURVE('',#37699,#37690,#31012,.T.);
#47941=EDGE_CURVE('',#37700,#37699,#31013,.T.);
#47942=EDGE_CURVE('',#36987,#37700,#31014,.T.);
#47943=EDGE_CURVE('',#37701,#37700,#21647,.T.);
#47944=EDGE_CURVE('',#37701,#36988,#31015,.T.);
#47945=EDGE_CURVE('',#37701,#37702,#31016,.T.);
#47946=EDGE_CURVE('',#37703,#37702,#31017,.T.);
#47947=EDGE_CURVE('',#36988,#37703,#31018,.T.);
#47948=EDGE_CURVE('',#37704,#37703,#21648,.T.);
#47949=EDGE_CURVE('',#36989,#37704,#31019,.T.);
#47950=EDGE_CURVE('',#37705,#37704,#31020,.T.);
#47951=EDGE_CURVE('',#37009,#37705,#31021,.T.);
#47952=EDGE_CURVE('',#37706,#37707,#31022,.T.);
#47953=EDGE_CURVE('',#37708,#37707,#5187,.T.);
#47954=EDGE_CURVE('',#37007,#37708,#31023,.T.);
#47955=EDGE_CURVE('',#37706,#37007,#5188,.T.);
#47956=EDGE_CURVE('',#37709,#37708,#5189,.T.);
#47957=EDGE_CURVE('',#36992,#37709,#31024,.T.);
#47958=EDGE_CURVE('',#37710,#37709,#21649,.T.);
#47959=EDGE_CURVE('',#36993,#37710,#31025,.T.);
#47960=EDGE_CURVE('',#37711,#37710,#5190,.T.);
#47961=EDGE_CURVE('',#37712,#37711,#31026,.T.);
#47962=EDGE_CURVE('',#36993,#37712,#5191,.T.);
#47963=EDGE_CURVE('',#37713,#37711,#5192,.T.);
#47964=EDGE_CURVE('',#37714,#37713,#31027,.T.);
#47965=EDGE_CURVE('',#37712,#37714,#5193,.T.);
#47966=EDGE_CURVE('',#37715,#37712,#5194,.T.);
#47967=EDGE_CURVE('',#37715,#36994,#5195,.T.);
#47968=EDGE_CURVE('',#37716,#36994,#31028,.T.);
#47969=EDGE_CURVE('',#37717,#37715,#31029,.T.);
#47970=EDGE_CURVE('',#37716,#37717,#5196,.T.);
#47971=EDGE_CURVE('',#37718,#36991,#31030,.T.);
#47972=EDGE_CURVE('',#37718,#37716,#21650,.T.);
#47973=EDGE_CURVE('',#37719,#37008,#31031,.T.);
#47974=EDGE_CURVE('',#37719,#37718,#5197,.T.);
#47975=EDGE_CURVE('',#37720,#37721,#31032,.T.);
#47976=EDGE_CURVE('',#37008,#37721,#5198,.T.);
#47977=EDGE_CURVE('',#37720,#37719,#1184,.T.);
#47978=EDGE_CURVE('',#37722,#37715,#5199,.T.);
#47979=EDGE_CURVE('',#37723,#37722,#31033,.T.);
#47980=EDGE_CURVE('',#37717,#37723,#1185,.T.);
#47981=EDGE_CURVE('',#37724,#37725,#31034,.T.);
#47982=EDGE_CURVE('',#37726,#37725,#21651,.T.);
#47983=EDGE_CURVE('',#37727,#37726,#31035,.T.);
#47984=EDGE_CURVE('',#37724,#37727,#21652,.T.);
#47985=EDGE_CURVE('',#37727,#37728,#5200,.T.);
#47986=EDGE_CURVE('',#37728,#37729,#21653,.T.);
#47987=EDGE_CURVE('',#37729,#37724,#5201,.T.);
#47988=EDGE_CURVE('',#37728,#37730,#31036,.T.);
#47989=EDGE_CURVE('',#37731,#37730,#21654,.T.);
#47990=EDGE_CURVE('',#37729,#37731,#31037,.T.);
#47991=EDGE_CURVE('',#37732,#37733,#31038,.T.);
#47992=EDGE_CURVE('',#37734,#37733,#1186,.T.);
#47993=EDGE_CURVE('',#37005,#37734,#31039,.T.);
#47994=EDGE_CURVE('',#37732,#37005,#5202,.T.);
#47995=EDGE_CURVE('',#37735,#37734,#5203,.T.);
#47996=EDGE_CURVE('',#36996,#37735,#31040,.T.);
#47997=EDGE_CURVE('',#37736,#37735,#21655,.T.);
#47998=EDGE_CURVE('',#36997,#37736,#31041,.T.);
#47999=EDGE_CURVE('',#37737,#37736,#5204,.T.);
#48000=EDGE_CURVE('',#37738,#37737,#31042,.T.);
#48001=EDGE_CURVE('',#36997,#37738,#5205,.T.);
#48002=EDGE_CURVE('',#37739,#37737,#1187,.T.);
#48003=EDGE_CURVE('',#37740,#37739,#31043,.T.);
#48004=EDGE_CURVE('',#37738,#37740,#5206,.T.);
#48005=EDGE_CURVE('',#37741,#37738,#5207,.T.);
#48006=EDGE_CURVE('',#37741,#36998,#1924,.T.);
#48007=EDGE_CURVE('',#37742,#36998,#31044,.T.);
#48008=EDGE_CURVE('',#37743,#37741,#31045,.T.);
#48009=EDGE_CURVE('',#37742,#37743,#1925,.T.);
#48010=EDGE_CURVE('',#37744,#36995,#31046,.T.);
#48011=EDGE_CURVE('',#37744,#37742,#21656,.T.);
#48012=EDGE_CURVE('',#37745,#37006,#31047,.T.);
#48013=EDGE_CURVE('',#37745,#37744,#1926,.T.);
#48014=EDGE_CURVE('',#37746,#37747,#31048,.T.);
#48015=EDGE_CURVE('',#37006,#37747,#5208,.T.);
#48016=EDGE_CURVE('',#37746,#37745,#1188,.T.);
#48017=EDGE_CURVE('',#37748,#37741,#5209,.T.);
#48018=EDGE_CURVE('',#37749,#37748,#31049,.T.);
#48019=EDGE_CURVE('',#37743,#37749,#1189,.T.);
#48020=EDGE_CURVE('',#37001,#37750,#21657,.T.);
#48021=EDGE_CURVE('',#37750,#37751,#31050,.T.);
#48022=EDGE_CURVE('',#37751,#37002,#21658,.T.);
#48023=EDGE_CURVE('',#37751,#37752,#5210,.T.);
#48024=EDGE_CURVE('',#37752,#37753,#5211,.T.);
#48025=EDGE_CURVE('',#37426,#37753,#21659,.T.);
#48026=EDGE_CURVE('',#37018,#37437,#5212,.T.);
#48027=EDGE_CURVE('',#37752,#37754,#31051,.T.);
#48028=EDGE_CURVE('',#37755,#37754,#5213,.T.);
#48029=EDGE_CURVE('',#37753,#37755,#31052,.T.);
#48030=EDGE_CURVE('',#37437,#37755,#21660,.T.);
#48031=EDGE_CURVE('',#37753,#37436,#21661,.T.);
#48032=EDGE_CURVE('',#37756,#37757,#31053,.T.);
#48033=EDGE_CURVE('',#37747,#37757,#1927,.T.);
#48034=EDGE_CURVE('',#37756,#37746,#1928,.T.);
#48035=EDGE_CURVE('',#37747,#37732,#31054,.T.);
#48036=EDGE_CURVE('',#37758,#37759,#31055,.T.);
#48037=EDGE_CURVE('',#37733,#37759,#1929,.T.);
#48038=EDGE_CURVE('',#37758,#37732,#1930,.T.);
#48039=EDGE_CURVE('',#37760,#37731,#5214,.T.);
#48040=EDGE_CURVE('',#37760,#37761,#5215,.T.);
#48041=EDGE_CURVE('',#37729,#37761,#5216,.T.);
#48042=EDGE_CURVE('',#37761,#37762,#31056,.T.);
#48043=EDGE_CURVE('',#37762,#37724,#5217,.T.);
#48044=EDGE_CURVE('',#37762,#37763,#5218,.T.);
#48045=EDGE_CURVE('',#37725,#37763,#5219,.T.);
#48046=EDGE_CURVE('',#37764,#37765,#31057,.T.);
#48047=EDGE_CURVE('',#37721,#37765,#1931,.T.);
#48048=EDGE_CURVE('',#37764,#37720,#1932,.T.);
#48049=EDGE_CURVE('',#37721,#37706,#31058,.T.);
#48050=EDGE_CURVE('',#37766,#37767,#31059,.T.);
#48051=EDGE_CURVE('',#37707,#37767,#1933,.T.);
#48052=EDGE_CURVE('',#37766,#37706,#1934,.T.);
#48053=EDGE_CURVE('',#37768,#37705,#21662,.T.);
#48054=EDGE_CURVE('',#37768,#37769,#5220,.T.);
#48055=EDGE_CURVE('',#37009,#37769,#21663,.T.);
#48056=EDGE_CURVE('',#37769,#37770,#31060,.T.);
#48057=EDGE_CURVE('',#37770,#37010,#21664,.T.);
#48058=EDGE_CURVE('',#37770,#37771,#5221,.T.);
#48059=EDGE_CURVE('',#37688,#37771,#21665,.T.);
#48060=EDGE_CURVE('',#37772,#37773,#31061,.T.);
#48061=EDGE_CURVE('',#37696,#37773,#1935,.T.);
#48062=EDGE_CURVE('',#37772,#37695,#1936,.T.);
#48063=EDGE_CURVE('',#37696,#37678,#31062,.T.);
#48064=EDGE_CURVE('',#37774,#37775,#31063,.T.);
#48065=EDGE_CURVE('',#37679,#37775,#1937,.T.);
#48066=EDGE_CURVE('',#37774,#37678,#1938,.T.);
#48067=EDGE_CURVE('',#37776,#37677,#21666,.T.);
#48068=EDGE_CURVE('',#37776,#37750,#5222,.T.);
#48069=EDGE_CURVE('',#37307,#37777,#31064,.T.);
#48070=EDGE_CURVE('',#37777,#37156,#21667,.T.);
#48071=EDGE_CURVE('',#37153,#37778,#21668,.T.);
#48072=EDGE_CURVE('',#37778,#37310,#31065,.T.);
#48073=EDGE_CURVE('',#37310,#37779,#5223,.T.);
#48074=EDGE_CURVE('',#37779,#37307,#5224,.T.);
#48075=EDGE_CURVE('',#37311,#37308,#5225,.T.);
#48076=EDGE_CURVE('',#37451,#37232,#31066,.T.);
#48077=EDGE_CURVE('',#37232,#37230,#5226,.T.);
#48078=EDGE_CURVE('',#37233,#37229,#5227,.T.);
#48079=EDGE_CURVE('',#37230,#37780,#31067,.T.);
#48080=EDGE_CURVE('',#37780,#37441,#31068,.T.);
#48081=EDGE_CURVE('',#37441,#37451,#5228,.T.);
#48082=EDGE_CURVE('',#37442,#37450,#5229,.T.);
#48083=EDGE_CURVE('',#37018,#37781,#21669,.T.);
#48084=EDGE_CURVE('',#37781,#37782,#21670,.T.);
#48085=EDGE_CURVE('',#37782,#37037,#21671,.T.);
#48086=EDGE_CURVE('',#37782,#37783,#31069,.T.);
#48087=EDGE_CURVE('',#37038,#37783,#21672,.T.);
#48088=EDGE_CURVE('',#37783,#37784,#31070,.T.);
#48089=EDGE_CURVE('',#37784,#37040,#21673,.T.);
#48090=EDGE_CURVE('',#37784,#37785,#31071,.T.);
#48091=EDGE_CURVE('',#37042,#37785,#21674,.T.);
#48092=EDGE_CURVE('',#37785,#37786,#21675,.T.);
#48093=EDGE_CURVE('',#37786,#37052,#21676,.T.);
#48094=EDGE_CURVE('',#37066,#37787,#21677,.T.);
#48095=EDGE_CURVE('',#37786,#37787,#31072,.T.);
#48096=EDGE_CURVE('',#37788,#37120,#21678,.T.);
#48097=EDGE_CURVE('',#37787,#37788,#31073,.T.);
#48098=EDGE_CURVE('',#37788,#37789,#31074,.T.);
#48099=EDGE_CURVE('',#37123,#37789,#21679,.T.);
#48100=EDGE_CURVE('',#37789,#37790,#21680,.T.);
#48101=EDGE_CURVE('',#37790,#37145,#21681,.T.);
#48102=EDGE_CURVE('',#37790,#37791,#31075,.T.);
#48103=EDGE_CURVE('',#37146,#37791,#21682,.T.);
#48104=EDGE_CURVE('',#37791,#37792,#31076,.T.);
#48105=EDGE_CURVE('',#37792,#37148,#21683,.T.);
#48106=EDGE_CURVE('',#37792,#37793,#31077,.T.);
#48107=EDGE_CURVE('',#37150,#37793,#21684,.T.);
#48108=EDGE_CURVE('',#37794,#37795,#21685,.T.);
#48109=EDGE_CURVE('',#37795,#37796,#21686,.T.);
#48110=EDGE_CURVE('',#37796,#37797,#5230,.T.);
#48111=EDGE_CURVE('',#37797,#37152,#21687,.T.);
#48112=EDGE_CURVE('',#37793,#37794,#21688,.T.);
#48113=EDGE_CURVE('',#37798,#37797,#31078,.T.);
#48114=EDGE_CURVE('',#37799,#37796,#31079,.T.);
#48115=EDGE_CURVE('',#37798,#37799,#5231,.T.);
#48116=EDGE_CURVE('',#37800,#37152,#31080,.T.);
#48117=EDGE_CURVE('',#37800,#37798,#21689,.T.);
#48118=EDGE_CURVE('',#37801,#37153,#31081,.T.);
#48119=EDGE_CURVE('',#37801,#37800,#1190,.T.);
#48120=EDGE_CURVE('',#37802,#37778,#31082,.T.);
#48121=EDGE_CURVE('',#37802,#37801,#21690,.T.);
#48122=EDGE_CURVE('',#37803,#37777,#31083,.T.);
#48123=EDGE_CURVE('',#37777,#37778,#5232,.T.);
#48124=EDGE_CURVE('',#37803,#37802,#5233,.T.);
#48125=EDGE_CURVE('',#37155,#37803,#21691,.T.);
#48126=EDGE_CURVE('',#37154,#37804,#21692,.T.);
#48127=EDGE_CURVE('',#37805,#37155,#21693,.T.);
#48128=EDGE_CURVE('',#37805,#37804,#31084,.T.);
#48129=EDGE_CURVE('',#37806,#37351,#31085,.T.);
#48130=EDGE_CURVE('',#37807,#37806,#31086,.T.);
#48131=EDGE_CURVE('',#37352,#37807,#31087,.T.);
#48132=EDGE_CURVE('',#37352,#37380,#21694,.T.);
#48133=EDGE_CURVE('',#37808,#37380,#31088,.T.);
#48134=EDGE_CURVE('',#37808,#37809,#31089,.T.);
#48135=EDGE_CURVE('',#37381,#37809,#31090,.T.);
#48136=EDGE_CURVE('',#37810,#37378,#21695,.T.);
#48137=EDGE_CURVE('',#37810,#37811,#31091,.T.);
#48138=EDGE_CURVE('',#37375,#37811,#21696,.T.);
#48139=EDGE_CURVE('',#37811,#37812,#21697,.T.);
#48140=EDGE_CURVE('',#37812,#37371,#21698,.T.);
#48141=EDGE_CURVE('',#37812,#37813,#31092,.T.);
#48142=EDGE_CURVE('',#37372,#37813,#21699,.T.);
#48143=EDGE_CURVE('',#37814,#37369,#31093,.T.);
#48144=EDGE_CURVE('',#37815,#37814,#31094,.T.);
#48145=EDGE_CURVE('',#37370,#37815,#31095,.T.);
#48146=EDGE_CURVE('',#37370,#37664,#21700,.T.);
#48147=EDGE_CURVE('',#37816,#37664,#31096,.T.);
#48148=EDGE_CURVE('',#37816,#37817,#31097,.T.);
#48149=EDGE_CURVE('',#37665,#37817,#31098,.T.);
#48150=EDGE_CURVE('',#37818,#37662,#21701,.T.);
#48151=EDGE_CURVE('',#37818,#37819,#31099,.T.);
#48152=EDGE_CURVE('',#37659,#37819,#21702,.T.);
#48153=EDGE_CURVE('',#37819,#37820,#21703,.T.);
#48154=EDGE_CURVE('',#37820,#37655,#21704,.T.);
#48155=EDGE_CURVE('',#37820,#37821,#31100,.T.);
#48156=EDGE_CURVE('',#37656,#37821,#21705,.T.);
#48157=EDGE_CURVE('',#37822,#37653,#31101,.T.);
#48158=EDGE_CURVE('',#37823,#37822,#31102,.T.);
#48159=EDGE_CURVE('',#37654,#37823,#31103,.T.);
#48160=EDGE_CURVE('',#37824,#37652,#1939,.T.);
#48161=EDGE_CURVE('',#37654,#37824,#21706,.T.);
#48162=EDGE_CURVE('',#37824,#37643,#5234,.T.);
#48163=EDGE_CURVE('',#37650,#37642,#5235,.T.);
#48164=EDGE_CURVE('',#37825,#37643,#5236,.T.);
#48165=EDGE_CURVE('',#37825,#37826,#31104,.T.);
#48166=EDGE_CURVE('',#37644,#37826,#5237,.T.);
#48167=EDGE_CURVE('',#37827,#37828,#31105,.T.);
#48168=EDGE_CURVE('',#37826,#37828,#31106,.T.);
#48169=EDGE_CURVE('',#37827,#37825,#31107,.T.);
#48170=EDGE_CURVE('',#37829,#37830,#21707,.T.);
#48171=EDGE_CURVE('',#37829,#37831,#31108,.T.);
#48172=EDGE_CURVE('',#37832,#37831,#21708,.T.);
#48173=EDGE_CURVE('',#37832,#37830,#31109,.T.);
#48174=EDGE_CURVE('',#37831,#37833,#21709,.T.);
#48175=EDGE_CURVE('',#37833,#37834,#21710,.T.);
#48176=EDGE_CURVE('',#37834,#37832,#31110,.T.);
#48177=EDGE_CURVE('',#37833,#37835,#31111,.T.);
#48178=EDGE_CURVE('',#37836,#37835,#21711,.T.);
#48179=EDGE_CURVE('',#37836,#37834,#31112,.T.);
#48180=EDGE_CURVE('',#37837,#37639,#5238,.T.);
#48181=EDGE_CURVE('',#37838,#37837,#31113,.T.);
#48182=EDGE_CURVE('',#37839,#37838,#5239,.T.);
#48183=EDGE_CURVE('',#37640,#37839,#1940,.T.);
#48184=EDGE_CURVE('',#37840,#37635,#1941,.T.);
#48185=EDGE_CURVE('',#37841,#37840,#5240,.T.);
#48186=EDGE_CURVE('',#37841,#37842,#31114,.T.);
#48187=EDGE_CURVE('',#37636,#37842,#5241,.T.);
#48188=EDGE_CURVE('',#37843,#37844,#21712,.T.);
#48189=EDGE_CURVE('',#37843,#37845,#31115,.T.);
#48190=EDGE_CURVE('',#37846,#37845,#21713,.T.);
#48191=EDGE_CURVE('',#37846,#37844,#31116,.T.);
#48192=EDGE_CURVE('',#37845,#37847,#21714,.T.);
#48193=EDGE_CURVE('',#37847,#37848,#21715,.T.);
#48194=EDGE_CURVE('',#37848,#37846,#5242,.T.);
#48195=EDGE_CURVE('',#37847,#37849,#31117,.T.);
#48196=EDGE_CURVE('',#37850,#37849,#21716,.T.);
#48197=EDGE_CURVE('',#37850,#37848,#31118,.T.);
#48198=EDGE_CURVE('',#37851,#37167,#31119,.T.);
#48199=EDGE_CURVE('',#37852,#37166,#31120,.T.);
#48200=EDGE_CURVE('',#37851,#37852,#5243,.T.);
#48201=EDGE_CURVE('',#37853,#37363,#31121,.T.);
#48202=EDGE_CURVE('',#37853,#37851,#5244,.T.);
#48203=EDGE_CURVE('',#37854,#37361,#31122,.T.);
#48204=EDGE_CURVE('',#37363,#37361,#21717,.T.);
#48205=EDGE_CURVE('',#37854,#37853,#21718,.T.);
#48206=EDGE_CURVE('',#37855,#37321,#31123,.T.);
#48207=EDGE_CURVE('',#37804,#37321,#31124,.T.);
#48208=EDGE_CURVE('',#37855,#37805,#31125,.T.);
#48209=EDGE_CURVE('',#37852,#37855,#5245,.T.);
#48210=EDGE_CURVE('',#37856,#37362,#31126,.T.);
#48211=EDGE_CURVE('',#37856,#37854,#5246,.T.);
#48212=EDGE_CURVE('',#37362,#37857,#21719,.T.);
#48213=EDGE_CURVE('',#37857,#37353,#21720,.T.);
#48214=EDGE_CURVE('',#37857,#37858,#31127,.T.);
#48215=EDGE_CURVE('',#37354,#37858,#21721,.T.);
#48216=EDGE_CURVE('',#37859,#37428,#31128,.T.);
#48217=EDGE_CURVE('',#37860,#37859,#31129,.T.);
#48218=EDGE_CURVE('',#37163,#37860,#31130,.T.);
#48219=EDGE_CURVE('',#37673,#37860,#21722,.T.);
#48220=EDGE_CURVE('',#37861,#37235,#21723,.T.);
#48221=EDGE_CURVE('',#37862,#37861,#31131,.T.);
#48222=EDGE_CURVE('',#37236,#37862,#21724,.T.);
#48223=EDGE_CURVE('',#37863,#37863,#31132,.T.);
#48224=EDGE_CURVE('',#37863,#37864,#21725,.T.);
#48225=EDGE_CURVE('',#37864,#37447,#31133,.T.);
#48226=EDGE_CURVE('',#37236,#37864,#31134,.T.);
#48227=EDGE_CURVE('',#37865,#37865,#31135,.T.);
#48228=EDGE_CURVE('',#37866,#37866,#31136,.T.);
#48229=EDGE_CURVE('',#37866,#37865,#21726,.T.);
#48230=EDGE_CURVE('',#37867,#37868,#31137,.T.);
#48231=EDGE_CURVE('',#37448,#37868,#21727,.T.);
#48232=EDGE_CURVE('',#37867,#37447,#21728,.T.);
#48233=EDGE_CURVE('',#37869,#37364,#31138,.T.);
#48234=EDGE_CURVE('',#37870,#37364,#21729,.T.);
#48235=EDGE_CURVE('',#37871,#37870,#31139,.T.);
#48236=EDGE_CURVE('',#37869,#37871,#21730,.T.);
#48237=EDGE_CURVE('',#37872,#37168,#31140,.T.);
#48238=EDGE_CURVE('',#37872,#37869,#31141,.T.);
#48239=EDGE_CURVE('',#37873,#37165,#31142,.T.);
#48240=EDGE_CURVE('',#37873,#37872,#31143,.T.);
#48241=EDGE_CURVE('',#37874,#37322,#31144,.T.);
#48242=EDGE_CURVE('',#37874,#37873,#31145,.T.);
#48243=EDGE_CURVE('',#37322,#37318,#21731,.T.);
#48244=EDGE_CURVE('',#37319,#37874,#21732,.T.);
#48245=EDGE_CURVE('',#37875,#37875,#31146,.T.);
#48246=EDGE_CURVE('',#37875,#37320,#21733,.T.);
#48247=EDGE_CURVE('',#37319,#37317,#31147,.T.);
#48248=EDGE_CURVE('',#37876,#37876,#31148,.T.);
#48249=EDGE_CURVE('',#37877,#37877,#31149,.T.);
#48250=EDGE_CURVE('',#37877,#37876,#21734,.T.);
#48251=EDGE_CURVE('',#37878,#37317,#21735,.T.);
#48252=EDGE_CURVE('',#37879,#37878,#31150,.T.);
#48253=EDGE_CURVE('',#37316,#37879,#21736,.T.);
#48254=EDGE_CURVE('',#37880,#37187,#21737,.T.);
#48255=EDGE_CURVE('',#37186,#37880,#31151,.T.);
#48256=EDGE_CURVE('',#37188,#37881,#1191,.T.);
#48257=EDGE_CURVE('',#37881,#37882,#21738,.T.);
#48258=EDGE_CURVE('',#37882,#37189,#21739,.T.);
#48259=EDGE_CURVE('',#37883,#37187,#5247,.T.);
#48260=EDGE_CURVE('',#37884,#37883,#31152,.T.);
#48261=EDGE_CURVE('',#37881,#37884,#31153,.T.);
#48262=EDGE_CURVE('',#37882,#37885,#5248,.T.);
#48263=EDGE_CURVE('',#37190,#37885,#21740,.T.);
#48264=EDGE_CURVE('',#37885,#37886,#21741,.T.);
#48265=EDGE_CURVE('',#37886,#37191,#21742,.T.);
#48266=EDGE_CURVE('',#37886,#37887,#5249,.T.);
#48267=EDGE_CURVE('',#37192,#37887,#21743,.T.);
#48268=EDGE_CURVE('',#37887,#37888,#21744,.T.);
#48269=EDGE_CURVE('',#37888,#37207,#5250,.T.);
#48270=EDGE_CURVE('',#37889,#37888,#31154,.T.);
#48271=EDGE_CURVE('',#37208,#37889,#5251,.T.);
#48272=EDGE_CURVE('',#37208,#37213,#21745,.T.);
#48273=EDGE_CURVE('',#37890,#37891,#31155,.T.);
#48274=EDGE_CURVE('',#37214,#37891,#1192,.T.);
#48275=EDGE_CURVE('',#37890,#37213,#5252,.T.);
#48276=EDGE_CURVE('',#37891,#37892,#21746,.T.);
#48277=EDGE_CURVE('',#37892,#37226,#21747,.T.);
#48278=EDGE_CURVE('',#37892,#37893,#5253,.T.);
#48279=EDGE_CURVE('',#37227,#37893,#21748,.T.);
#48280=EDGE_CURVE('',#37893,#37894,#21749,.T.);
#48281=EDGE_CURVE('',#37894,#37228,#21750,.T.);
#48282=EDGE_CURVE('',#37894,#37895,#5254,.T.);
#48283=EDGE_CURVE('',#37238,#37895,#21751,.T.);
#48284=EDGE_CURVE('',#37895,#37896,#21752,.T.);
#48285=EDGE_CURVE('',#37896,#37861,#1193,.T.);
#48286=EDGE_CURVE('',#37897,#37896,#31156,.T.);
#48287=EDGE_CURVE('',#37862,#37897,#5255,.T.);
#48288=EDGE_CURVE('',#37628,#37898,#21753,.T.);
#48289=EDGE_CURVE('',#37898,#37899,#21754,.T.);
#48290=EDGE_CURVE('',#37899,#37254,#5256,.T.);
#48291=EDGE_CURVE('',#37899,#37900,#31157,.T.);
#48292=EDGE_CURVE('',#37255,#37900,#5257,.T.);
#48293=EDGE_CURVE('',#37255,#37880,#5258,.T.);
#48294=EDGE_CURVE('',#37343,#37901,#1194,.T.);
#48295=EDGE_CURVE('',#37901,#37902,#21755,.T.);
#48296=EDGE_CURVE('',#37902,#37270,#21756,.T.);
#48297=EDGE_CURVE('',#37902,#37903,#5259,.T.);
#48298=EDGE_CURVE('',#37271,#37903,#21757,.T.);
#48299=EDGE_CURVE('',#37903,#37904,#21758,.T.);
#48300=EDGE_CURVE('',#37904,#37272,#21759,.T.);
#48301=EDGE_CURVE('',#37904,#37905,#5260,.T.);
#48302=EDGE_CURVE('',#37273,#37905,#21760,.T.);
#48303=EDGE_CURVE('',#37905,#37906,#21761,.T.);
#48304=EDGE_CURVE('',#37906,#37289,#1195,.T.);
#48305=EDGE_CURVE('',#37907,#37906,#31158,.T.);
#48306=EDGE_CURVE('',#37290,#37907,#5261,.T.);
#48307=EDGE_CURVE('',#37908,#37287,#31159,.T.);
#48308=EDGE_CURVE('',#37290,#37908,#21762,.T.);
#48309=EDGE_CURVE('',#37908,#37909,#5262,.T.);
#48310=EDGE_CURVE('',#37909,#37298,#5263,.T.);
#48311=EDGE_CURVE('',#37909,#37295,#31160,.T.);
#48312=EDGE_CURVE('',#37910,#37911,#31161,.T.);
#48313=EDGE_CURVE('',#37296,#37911,#1942,.T.);
#48314=EDGE_CURVE('',#37910,#37295,#5264,.T.);
#48315=EDGE_CURVE('',#37911,#37912,#21763,.T.);
#48316=EDGE_CURVE('',#37912,#37629,#21764,.T.);
#48317=EDGE_CURVE('',#37879,#37913,#1196,.T.);
#48318=EDGE_CURVE('',#37913,#37914,#21765,.T.);
#48319=EDGE_CURVE('',#37914,#37323,#21766,.T.);
#48320=EDGE_CURVE('',#37915,#37878,#5265,.T.);
#48321=EDGE_CURVE('',#37913,#37915,#31162,.T.);
#48322=EDGE_CURVE('',#37914,#37916,#5266,.T.);
#48323=EDGE_CURVE('',#37324,#37916,#21767,.T.);
#48324=EDGE_CURVE('',#37916,#37917,#21768,.T.);
#48325=EDGE_CURVE('',#37917,#37325,#21769,.T.);
#48326=EDGE_CURVE('',#37917,#37918,#5267,.T.);
#48327=EDGE_CURVE('',#37336,#37918,#21770,.T.);
#48328=EDGE_CURVE('',#37918,#37919,#21771,.T.);
#48329=EDGE_CURVE('',#37919,#37344,#1197,.T.);
#48330=EDGE_CURVE('',#37920,#37342,#5268,.T.);
#48331=EDGE_CURVE('',#37901,#37920,#31163,.T.);
#48332=EDGE_CURVE('',#37919,#37921,#31164,.T.);
#48333=EDGE_CURVE('',#37345,#37921,#5269,.T.);
#48334=EDGE_CURVE('',#37345,#37342,#21772,.T.);
#48335=EDGE_CURVE('',#37858,#37806,#21773,.T.);
#48336=EDGE_CURVE('',#37387,#37922,#1198,.T.);
#48337=EDGE_CURVE('',#37922,#37923,#21774,.T.);
#48338=EDGE_CURVE('',#37923,#37355,#21775,.T.);
#48339=EDGE_CURVE('',#37923,#37924,#5270,.T.);
#48340=EDGE_CURVE('',#37356,#37924,#21776,.T.);
#48341=EDGE_CURVE('',#37924,#37925,#21777,.T.);
#48342=EDGE_CURVE('',#37925,#37357,#21778,.T.);
#48343=EDGE_CURVE('',#37925,#37926,#5271,.T.);
#48344=EDGE_CURVE('',#37359,#37926,#21779,.T.);
#48345=EDGE_CURVE('',#37926,#37927,#21780,.T.);
#48346=EDGE_CURVE('',#37927,#37870,#5272,.T.);
#48347=EDGE_CURVE('',#37928,#37927,#31165,.T.);
#48348=EDGE_CURVE('',#37871,#37928,#5273,.T.);
#48349=EDGE_CURVE('',#37929,#37930,#31166,.T.);
#48350=EDGE_CURVE('',#37670,#37930,#5274,.T.);
#48351=EDGE_CURVE('',#37929,#37669,#5275,.T.);
#48352=EDGE_CURVE('',#37930,#37931,#21781,.T.);
#48353=EDGE_CURVE('',#37931,#37373,#21782,.T.);
#48354=EDGE_CURVE('',#37813,#37814,#21783,.T.);
#48355=EDGE_CURVE('',#37931,#37932,#5276,.T.);
#48356=EDGE_CURVE('',#37374,#37932,#21784,.T.);
#48357=EDGE_CURVE('',#37932,#37933,#21785,.T.);
#48358=EDGE_CURVE('',#37933,#37376,#21786,.T.);
#48359=EDGE_CURVE('',#37933,#37934,#5277,.T.);
#48360=EDGE_CURVE('',#37377,#37934,#21787,.T.);
#48361=EDGE_CURVE('',#37934,#37935,#21788,.T.);
#48362=EDGE_CURVE('',#37935,#37388,#1199,.T.);
#48363=EDGE_CURVE('',#37809,#37810,#21789,.T.);
#48364=EDGE_CURVE('',#37936,#37922,#31167,.T.);
#48365=EDGE_CURVE('',#37936,#37386,#5278,.T.);
#48366=EDGE_CURVE('',#37935,#37937,#31168,.T.);
#48367=EDGE_CURVE('',#37389,#37937,#5279,.T.);
#48368=EDGE_CURVE('',#37389,#37386,#21790,.T.);
#48369=EDGE_CURVE('',#37472,#37938,#1200,.T.);
#48370=EDGE_CURVE('',#37938,#37939,#21791,.T.);
#48371=EDGE_CURVE('',#37939,#37404,#21792,.T.);
#48372=EDGE_CURVE('',#37939,#37940,#5280,.T.);
#48373=EDGE_CURVE('',#37405,#37940,#21793,.T.);
#48374=EDGE_CURVE('',#37940,#37941,#21794,.T.);
#48375=EDGE_CURVE('',#37941,#37406,#21795,.T.);
#48376=EDGE_CURVE('',#37941,#37942,#5281,.T.);
#48377=EDGE_CURVE('',#37407,#37942,#21796,.T.);
#48378=EDGE_CURVE('',#37942,#37943,#21797,.T.);
#48379=EDGE_CURVE('',#37943,#37423,#1201,.T.);
#48380=EDGE_CURVE('',#37944,#37943,#31169,.T.);
#48381=EDGE_CURVE('',#37424,#37944,#5282,.T.);
#48382=EDGE_CURVE('',#37945,#37421,#31170,.T.);
#48383=EDGE_CURVE('',#37424,#37945,#21798,.T.);
#48384=EDGE_CURVE('',#37945,#37438,#5283,.T.);
#48385=EDGE_CURVE('',#37439,#37946,#5284,.T.);
#48386=EDGE_CURVE('',#37946,#37947,#21799,.T.);
#48387=EDGE_CURVE('',#37947,#37859,#21800,.T.);
#48388=EDGE_CURVE('',#37948,#37438,#5285,.T.);
#48389=EDGE_CURVE('',#37946,#37948,#31171,.T.);
#48390=EDGE_CURVE('',#37949,#37950,#31172,.T.);
#48391=EDGE_CURVE('',#37868,#37950,#1202,.T.);
#48392=EDGE_CURVE('',#37949,#37867,#5286,.T.);
#48393=EDGE_CURVE('',#37950,#37951,#21801,.T.);
#48394=EDGE_CURVE('',#37951,#37452,#21802,.T.);
#48395=EDGE_CURVE('',#37951,#37952,#5287,.T.);
#48396=EDGE_CURVE('',#37453,#37952,#21803,.T.);
#48397=EDGE_CURVE('',#37952,#37953,#21804,.T.);
#48398=EDGE_CURVE('',#37953,#37454,#21805,.T.);
#48399=EDGE_CURVE('',#37953,#37954,#5288,.T.);
#48400=EDGE_CURVE('',#37464,#37954,#21806,.T.);
#48401=EDGE_CURVE('',#37954,#37955,#21807,.T.);
#48402=EDGE_CURVE('',#37955,#37473,#1203,.T.);
#48403=EDGE_CURVE('',#37956,#37471,#5289,.T.);
#48404=EDGE_CURVE('',#37938,#37956,#31173,.T.);
#48405=EDGE_CURVE('',#37957,#37955,#31174,.T.);
#48406=EDGE_CURVE('',#37474,#37957,#5290,.T.);
#48407=EDGE_CURVE('',#37474,#37471,#21808,.T.);
#48408=EDGE_CURVE('',#37632,#37958,#21809,.T.);
#48409=EDGE_CURVE('',#37958,#37959,#21810,.T.);
#48410=EDGE_CURVE('',#37959,#37485,#1943,.T.);
#48411=EDGE_CURVE('',#37959,#37960,#31175,.T.);
#48412=EDGE_CURVE('',#37486,#37960,#1944,.T.);
#48413=EDGE_CURVE('',#37486,#37497,#31176,.T.);
#48414=EDGE_CURVE('',#37498,#37961,#1945,.T.);
#48415=EDGE_CURVE('',#37961,#37962,#21811,.T.);
#48416=EDGE_CURVE('',#37962,#37499,#21812,.T.);
#48417=EDGE_CURVE('',#37963,#37497,#1946,.T.);
#48418=EDGE_CURVE('',#37961,#37963,#31177,.T.);
#48419=EDGE_CURVE('',#37962,#37964,#5291,.T.);
#48420=EDGE_CURVE('',#37500,#37964,#21813,.T.);
#48421=EDGE_CURVE('',#37964,#37965,#31178,.T.);
#48422=EDGE_CURVE('',#37965,#37501,#21814,.T.);
#48423=EDGE_CURVE('',#37965,#37966,#5292,.T.);
#48424=EDGE_CURVE('',#37502,#37966,#21815,.T.);
#48425=EDGE_CURVE('',#37966,#37967,#21816,.T.);
#48426=EDGE_CURVE('',#37967,#37512,#1947,.T.);
#48427=EDGE_CURVE('',#37967,#37968,#31179,.T.);
#48428=EDGE_CURVE('',#37513,#37968,#1948,.T.);
#48429=EDGE_CURVE('',#37513,#37522,#31180,.T.);
#48430=EDGE_CURVE('',#37523,#37969,#1949,.T.);
#48431=EDGE_CURVE('',#37969,#37970,#21817,.T.);
#48432=EDGE_CURVE('',#37970,#37524,#5293,.T.);
#48433=EDGE_CURVE('',#37971,#37522,#1950,.T.);
#48434=EDGE_CURVE('',#37969,#37971,#31181,.T.);
#48435=EDGE_CURVE('',#37970,#37972,#5294,.T.);
#48436=EDGE_CURVE('',#37525,#37972,#5295,.T.);
#48437=EDGE_CURVE('',#37972,#37973,#31182,.T.);
#48438=EDGE_CURVE('',#37973,#37526,#5296,.T.);
#48439=EDGE_CURVE('',#37973,#37974,#5297,.T.);
#48440=EDGE_CURVE('',#37527,#37974,#5298,.T.);
#48441=EDGE_CURVE('',#37974,#37975,#21818,.T.);
#48442=EDGE_CURVE('',#37975,#37536,#1951,.T.);
#48443=EDGE_CURVE('',#37976,#37975,#31183,.T.);
#48444=EDGE_CURVE('',#37537,#37976,#1952,.T.);
#48445=EDGE_CURVE('',#37537,#37546,#31184,.T.);
#48446=EDGE_CURVE('',#37547,#37977,#1953,.T.);
#48447=EDGE_CURVE('',#37977,#37978,#21819,.T.);
#48448=EDGE_CURVE('',#37978,#37548,#5299,.T.);
#48449=EDGE_CURVE('',#37979,#37546,#1954,.T.);
#48450=EDGE_CURVE('',#37977,#37979,#31185,.T.);
#48451=EDGE_CURVE('',#37978,#37980,#5300,.T.);
#48452=EDGE_CURVE('',#37549,#37980,#5301,.T.);
#48453=EDGE_CURVE('',#37980,#37981,#31186,.T.);
#48454=EDGE_CURVE('',#37981,#37550,#5302,.T.);
#48455=EDGE_CURVE('',#37981,#37982,#5303,.T.);
#48456=EDGE_CURVE('',#37551,#37982,#5304,.T.);
#48457=EDGE_CURVE('',#37982,#37983,#21820,.T.);
#48458=EDGE_CURVE('',#37983,#37560,#1955,.T.);
#48459=EDGE_CURVE('',#37984,#37983,#31187,.T.);
#48460=EDGE_CURVE('',#37561,#37984,#1956,.T.);
#48461=EDGE_CURVE('',#37561,#37570,#31188,.T.);
#48462=EDGE_CURVE('',#37571,#37985,#1957,.T.);
#48463=EDGE_CURVE('',#37985,#37986,#21821,.T.);
#48464=EDGE_CURVE('',#37986,#37572,#5305,.T.);
#48465=EDGE_CURVE('',#37987,#37570,#1958,.T.);
#48466=EDGE_CURVE('',#37985,#37987,#31189,.T.);
#48467=EDGE_CURVE('',#37986,#37988,#5306,.T.);
#48468=EDGE_CURVE('',#37573,#37988,#5307,.T.);
#48469=EDGE_CURVE('',#37988,#37989,#31190,.T.);
#48470=EDGE_CURVE('',#37989,#37574,#5308,.T.);
#48471=EDGE_CURVE('',#37989,#37990,#5309,.T.);
#48472=EDGE_CURVE('',#37575,#37990,#5310,.T.);
#48473=EDGE_CURVE('',#37990,#37991,#21822,.T.);
#48474=EDGE_CURVE('',#37991,#37584,#1959,.T.);
#48475=EDGE_CURVE('',#37992,#37991,#31191,.T.);
#48476=EDGE_CURVE('',#37585,#37992,#1960,.T.);
#48477=EDGE_CURVE('',#37585,#37595,#31192,.T.);
#48478=EDGE_CURVE('',#37596,#37993,#1961,.T.);
#48479=EDGE_CURVE('',#37993,#37994,#21823,.T.);
#48480=EDGE_CURVE('',#37994,#37597,#21824,.T.);
#48481=EDGE_CURVE('',#37995,#37595,#1962,.T.);
#48482=EDGE_CURVE('',#37993,#37995,#31193,.T.);
#48483=EDGE_CURVE('',#37994,#37996,#5311,.T.);
#48484=EDGE_CURVE('',#37598,#37996,#21825,.T.);
#48485=EDGE_CURVE('',#37996,#37997,#31194,.T.);
#48486=EDGE_CURVE('',#37997,#37599,#21826,.T.);
#48487=EDGE_CURVE('',#37997,#37998,#5312,.T.);
#48488=EDGE_CURVE('',#37600,#37998,#21827,.T.);
#48489=EDGE_CURVE('',#37998,#37999,#21828,.T.);
#48490=EDGE_CURVE('',#37999,#37611,#1963,.T.);
#48491=EDGE_CURVE('',#37999,#38000,#31195,.T.);
#48492=EDGE_CURVE('',#37612,#38000,#1964,.T.);
#48493=EDGE_CURVE('',#37612,#37617,#31196,.T.);
#48494=EDGE_CURVE('',#38001,#38002,#31197,.T.);
#48495=EDGE_CURVE('',#37618,#38002,#1965,.T.);
#48496=EDGE_CURVE('',#38001,#37617,#5313,.T.);
#48497=EDGE_CURVE('',#38002,#38003,#21829,.T.);
#48498=EDGE_CURVE('',#38003,#37625,#21830,.T.);
#48499=EDGE_CURVE('',#38003,#38004,#5314,.T.);
#48500=EDGE_CURVE('',#38004,#38005,#5315,.T.);
#48501=EDGE_CURVE('',#37626,#38005,#21831,.T.);
#48502=EDGE_CURVE('',#38005,#38006,#31198,.T.);
#48503=EDGE_CURVE('',#38006,#37627,#21832,.T.);
#48504=EDGE_CURVE('',#38006,#38007,#5316,.T.);
#48505=EDGE_CURVE('',#38007,#37898,#1966,.T.);
#48506=EDGE_CURVE('',#37912,#38008,#1967,.T.);
#48507=EDGE_CURVE('',#38008,#38009,#5317,.T.);
#48508=EDGE_CURVE('',#37630,#38009,#21833,.T.);
#48509=EDGE_CURVE('',#38009,#38010,#31199,.T.);
#48510=EDGE_CURVE('',#38010,#37631,#21834,.T.);
#48511=EDGE_CURVE('',#38010,#38011,#5318,.T.);
#48512=EDGE_CURVE('',#38011,#37958,#5319,.T.);
#48513=EDGE_CURVE('',#38012,#38013,#1968,.T.);
#48514=EDGE_CURVE('',#38013,#38014,#21835,.T.);
#48515=EDGE_CURVE('',#38014,#37850,#5320,.T.);
#48516=EDGE_CURVE('',#37849,#38015,#21836,.T.);
#48517=EDGE_CURVE('',#38015,#38016,#5321,.T.);
#48518=EDGE_CURVE('',#38016,#38012,#5322,.T.);
#48519=EDGE_CURVE('',#38014,#38017,#5323,.T.);
#48520=EDGE_CURVE('',#37848,#38017,#5324,.T.);
#48521=EDGE_CURVE('',#38017,#38018,#31200,.T.);
#48522=EDGE_CURVE('',#38018,#37846,#5325,.T.);
#48523=EDGE_CURVE('',#38018,#38019,#5326,.T.);
#48524=EDGE_CURVE('',#37844,#38019,#5327,.T.);
#48525=EDGE_CURVE('',#38019,#38020,#21837,.T.);
#48526=EDGE_CURVE('',#38020,#37633,#1969,.T.);
#48527=EDGE_CURVE('',#37842,#37843,#21838,.T.);
#48528=EDGE_CURVE('',#38020,#38021,#31201,.T.);
#48529=EDGE_CURVE('',#37634,#38021,#1970,.T.);
#48530=EDGE_CURVE('',#37640,#37635,#31202,.T.);
#48531=EDGE_CURVE('',#37634,#37637,#31203,.T.);
#48532=EDGE_CURVE('',#37638,#38022,#1971,.T.);
#48533=EDGE_CURVE('',#38022,#38023,#21839,.T.);
#48534=EDGE_CURVE('',#38023,#37836,#5328,.T.);
#48535=EDGE_CURVE('',#37835,#37837,#21840,.T.);
#48536=EDGE_CURVE('',#38024,#37637,#1972,.T.);
#48537=EDGE_CURVE('',#38022,#38024,#31204,.T.);
#48538=EDGE_CURVE('',#38023,#38025,#5329,.T.);
#48539=EDGE_CURVE('',#37834,#38025,#5330,.T.);
#48540=EDGE_CURVE('',#38025,#38026,#31205,.T.);
#48541=EDGE_CURVE('',#38026,#37832,#5331,.T.);
#48542=EDGE_CURVE('',#38026,#38027,#5332,.T.);
#48543=EDGE_CURVE('',#37830,#38027,#5333,.T.);
#48544=EDGE_CURVE('',#38027,#38028,#21841,.T.);
#48545=EDGE_CURVE('',#38028,#37645,#1973,.T.);
#48546=EDGE_CURVE('',#37828,#37829,#21842,.T.);
#48547=EDGE_CURVE('',#38028,#38029,#31206,.T.);
#48548=EDGE_CURVE('',#37646,#38029,#1974,.T.);
#48549=EDGE_CURVE('',#37646,#37647,#31207,.T.);
#48550=EDGE_CURVE('',#38030,#38031,#31208,.T.);
#48551=EDGE_CURVE('',#37648,#38031,#1975,.T.);
#48552=EDGE_CURVE('',#38030,#37647,#1976,.T.);
#48553=EDGE_CURVE('',#38031,#38032,#21843,.T.);
#48554=EDGE_CURVE('',#38032,#37657,#21844,.T.);
#48555=EDGE_CURVE('',#37821,#37822,#21845,.T.);
#48556=EDGE_CURVE('',#38032,#38033,#5334,.T.);
#48557=EDGE_CURVE('',#37658,#38033,#21846,.T.);
#48558=EDGE_CURVE('',#38033,#38034,#31209,.T.);
#48559=EDGE_CURVE('',#38034,#37660,#21847,.T.);
#48560=EDGE_CURVE('',#38034,#38035,#5335,.T.);
#48561=EDGE_CURVE('',#37661,#38035,#21848,.T.);
#48562=EDGE_CURVE('',#38035,#38036,#21849,.T.);
#48563=EDGE_CURVE('',#38036,#37671,#1977,.T.);
#48564=EDGE_CURVE('',#37817,#37818,#21850,.T.);
#48565=EDGE_CURVE('',#38036,#38037,#31210,.T.);
#48566=EDGE_CURVE('',#37672,#38037,#5336,.T.);
#48567=EDGE_CURVE('',#37672,#38038,#31211,.T.);
#48568=EDGE_CURVE('',#38038,#38039,#5337,.T.);
#48569=EDGE_CURVE('',#38039,#37669,#5338,.T.);
#48570=EDGE_CURVE('',#38040,#37673,#21851,.T.);
#48571=EDGE_CURVE('',#38040,#38041,#5339,.T.);
#48572=EDGE_CURVE('',#37674,#38041,#21852,.T.);
#48573=EDGE_CURVE('',#38041,#38042,#21853,.T.);
#48574=EDGE_CURVE('',#38042,#37685,#1978,.T.);
#48575=EDGE_CURVE('',#37775,#37776,#21854,.T.);
#48576=EDGE_CURVE('',#38043,#38042,#31212,.T.);
#48577=EDGE_CURVE('',#37686,#38043,#1979,.T.);
#48578=EDGE_CURVE('',#37686,#37697,#31213,.T.);
#48579=EDGE_CURVE('',#37771,#37772,#21855,.T.);
#48580=EDGE_CURVE('',#37698,#38044,#1980,.T.);
#48581=EDGE_CURVE('',#38044,#38045,#21856,.T.);
#48582=EDGE_CURVE('',#38045,#37699,#21857,.T.);
#48583=EDGE_CURVE('',#38046,#37697,#1981,.T.);
#48584=EDGE_CURVE('',#38044,#38046,#31214,.T.);
#48585=EDGE_CURVE('',#38045,#38047,#5340,.T.);
#48586=EDGE_CURVE('',#37700,#38047,#21858,.T.);
#48587=EDGE_CURVE('',#38047,#38048,#31215,.T.);
#48588=EDGE_CURVE('',#38048,#37701,#21859,.T.);
#48589=EDGE_CURVE('',#38048,#38049,#5341,.T.);
#48590=EDGE_CURVE('',#37702,#38049,#21860,.T.);
#48591=EDGE_CURVE('',#38049,#38050,#21861,.T.);
#48592=EDGE_CURVE('',#38050,#37713,#1982,.T.);
#48593=EDGE_CURVE('',#37767,#37768,#21862,.T.);
#48594=EDGE_CURVE('',#38051,#38050,#31216,.T.);
#48595=EDGE_CURVE('',#38052,#38051,#31217,.T.);
#48596=EDGE_CURVE('',#37714,#38052,#1983,.T.);
#48597=EDGE_CURVE('',#37714,#37722,#31218,.T.);
#48598=EDGE_CURVE('',#37763,#37764,#21863,.T.);
#48599=EDGE_CURVE('',#37723,#38053,#1984,.T.);
#48600=EDGE_CURVE('',#38053,#38054,#21864,.T.);
#48601=EDGE_CURVE('',#38054,#37726,#5342,.T.);
#48602=EDGE_CURVE('',#38055,#37722,#1985,.T.);
#48603=EDGE_CURVE('',#38053,#38055,#31219,.T.);
#48604=EDGE_CURVE('',#38054,#38056,#5343,.T.);
#48605=EDGE_CURVE('',#37727,#38056,#5344,.T.);
#48606=EDGE_CURVE('',#38056,#38057,#31220,.T.);
#48607=EDGE_CURVE('',#38057,#37728,#5345,.T.);
#48608=EDGE_CURVE('',#38057,#38058,#5346,.T.);
#48609=EDGE_CURVE('',#37730,#38058,#5347,.T.);
#48610=EDGE_CURVE('',#38058,#38059,#21865,.T.);
#48611=EDGE_CURVE('',#38059,#37739,#1986,.T.);
#48612=EDGE_CURVE('',#37759,#37760,#21866,.T.);
#48613=EDGE_CURVE('',#38060,#38059,#31221,.T.);
#48614=EDGE_CURVE('',#38061,#38060,#31222,.T.);
#48615=EDGE_CURVE('',#37740,#38061,#1987,.T.);
#48616=EDGE_CURVE('',#37740,#37748,#31223,.T.);
#48617=EDGE_CURVE('',#38062,#38063,#5348,.T.);
#48618=EDGE_CURVE('',#38063,#37756,#21867,.T.);
#48619=EDGE_CURVE('',#37749,#38064,#1988,.T.);
#48620=EDGE_CURVE('',#38064,#38065,#21868,.T.);
#48621=EDGE_CURVE('',#38065,#38066,#5349,.T.);
#48622=EDGE_CURVE('',#38066,#38062,#21869,.T.);
#48623=EDGE_CURVE('',#38067,#37748,#1989,.T.);
#48624=EDGE_CURVE('',#38064,#38067,#31224,.T.);
#48625=EDGE_CURVE('',#38065,#38068,#5350,.T.);
#48626=EDGE_CURVE('',#38069,#38068,#5351,.T.);
#48627=EDGE_CURVE('',#38069,#38066,#31225,.T.);
#48628=EDGE_CURVE('',#38070,#38062,#31226,.T.);
#48629=EDGE_CURVE('',#38070,#38069,#21870,.T.);
#48630=EDGE_CURVE('',#38071,#38070,#5352,.T.);
#48631=EDGE_CURVE('',#38071,#38063,#5353,.T.);
#48632=EDGE_CURVE('',#37750,#38072,#31227,.T.);
#48633=EDGE_CURVE('',#38073,#38072,#31228,.T.);
#48634=EDGE_CURVE('',#37751,#38073,#31229,.T.);
#48635=EDGE_CURVE('',#37754,#38073,#5354,.T.);
#48636=EDGE_CURVE('',#38074,#37754,#21871,.T.);
#48637=EDGE_CURVE('',#38074,#37781,#31230,.T.);
#48638=EDGE_CURVE('',#38071,#38075,#31231,.T.);
#48639=EDGE_CURVE('',#38076,#38075,#5355,.T.);
#48640=EDGE_CURVE('',#38063,#38076,#31232,.T.);
#48641=EDGE_CURVE('',#37757,#38076,#21872,.T.);
#48642=EDGE_CURVE('',#37758,#37757,#31233,.T.);
#48643=EDGE_CURVE('',#38077,#37760,#31234,.T.);
#48644=EDGE_CURVE('',#38077,#37758,#21873,.T.);
#48645=EDGE_CURVE('',#37761,#38078,#31235,.T.);
#48646=EDGE_CURVE('',#38078,#38077,#5356,.T.);
#48647=EDGE_CURVE('',#38079,#38078,#31236,.T.);
#48648=EDGE_CURVE('',#37762,#38079,#31237,.T.);
#48649=EDGE_CURVE('',#38080,#38079,#5357,.T.);
#48650=EDGE_CURVE('',#37763,#38080,#31238,.T.);
#48651=EDGE_CURVE('',#37765,#38080,#21874,.T.);
#48652=EDGE_CURVE('',#37766,#37765,#31239,.T.);
#48653=EDGE_CURVE('',#38081,#37768,#31240,.T.);
#48654=EDGE_CURVE('',#38081,#37766,#21875,.T.);
#48655=EDGE_CURVE('',#37769,#38082,#31241,.T.);
#48656=EDGE_CURVE('',#38082,#38081,#5358,.T.);
#48657=EDGE_CURVE('',#38083,#38082,#31242,.T.);
#48658=EDGE_CURVE('',#37770,#38083,#31243,.T.);
#48659=EDGE_CURVE('',#38084,#38083,#5359,.T.);
#48660=EDGE_CURVE('',#37771,#38084,#31244,.T.);
#48661=EDGE_CURVE('',#37773,#38084,#21876,.T.);
#48662=EDGE_CURVE('',#37774,#37773,#31245,.T.);
#48663=EDGE_CURVE('',#38085,#37776,#31246,.T.);
#48664=EDGE_CURVE('',#38085,#37774,#21877,.T.);
#48665=EDGE_CURVE('',#38072,#38085,#5360,.T.);
#48666=EDGE_CURVE('',#37779,#38086,#21878,.T.);
#48667=EDGE_CURVE('',#38086,#38086,#31247,.T.);
#48668=EDGE_CURVE('',#37780,#38087,#21879,.T.);
#48669=EDGE_CURVE('',#38087,#38087,#31248,.T.);
#48670=EDGE_CURVE('',#38074,#38088,#31249,.T.);
#48671=EDGE_CURVE('',#38089,#38088,#31250,.T.);
#48672=EDGE_CURVE('',#37781,#38089,#31251,.T.);
#48673=EDGE_CURVE('',#38090,#38089,#21880,.T.);
#48674=EDGE_CURVE('',#37782,#38090,#31252,.T.);
#48675=EDGE_CURVE('',#38091,#38090,#31253,.T.);
#48676=EDGE_CURVE('',#37783,#38091,#31254,.T.);
#48677=EDGE_CURVE('',#38092,#38091,#31255,.T.);
#48678=EDGE_CURVE('',#37784,#38092,#31256,.T.);
#48679=EDGE_CURVE('',#38093,#38092,#31257,.T.);
#48680=EDGE_CURVE('',#37785,#38093,#31258,.T.);
#48681=EDGE_CURVE('',#38094,#38093,#21881,.T.);
#48682=EDGE_CURVE('',#37786,#38094,#31259,.T.);
#48683=EDGE_CURVE('',#38095,#38094,#31260,.T.);
#48684=EDGE_CURVE('',#37787,#38095,#31261,.T.);
#48685=EDGE_CURVE('',#38096,#38095,#31262,.T.);
#48686=EDGE_CURVE('',#37788,#38096,#31263,.T.);
#48687=EDGE_CURVE('',#38097,#38096,#31264,.T.);
#48688=EDGE_CURVE('',#37789,#38097,#31265,.T.);
#48689=EDGE_CURVE('',#38098,#38097,#21882,.T.);
#48690=EDGE_CURVE('',#37790,#38098,#31266,.T.);
#48691=EDGE_CURVE('',#38099,#38098,#31267,.T.);
#48692=EDGE_CURVE('',#37791,#38099,#31268,.T.);
#48693=EDGE_CURVE('',#38100,#38099,#31269,.T.);
#48694=EDGE_CURVE('',#37792,#38100,#31270,.T.);
#48695=EDGE_CURVE('',#38101,#38100,#31271,.T.);
#48696=EDGE_CURVE('',#37793,#38101,#31272,.T.);
#48697=EDGE_CURVE('',#38102,#38101,#21883,.T.);
#48698=EDGE_CURVE('',#37794,#38102,#31273,.T.);
#48699=EDGE_CURVE('',#38103,#38102,#31274,.T.);
#48700=EDGE_CURVE('',#38104,#38103,#31275,.T.);
#48701=EDGE_CURVE('',#37794,#38104,#31276,.T.);
#48702=EDGE_CURVE('',#38105,#38104,#21884,.T.);
#48703=EDGE_CURVE('',#38105,#37795,#31277,.T.);
#48704=EDGE_CURVE('',#38106,#37795,#31278,.T.);
#48705=EDGE_CURVE('',#37799,#38106,#21885,.T.);
#48706=EDGE_CURVE('',#38107,#38105,#31279,.T.);
#48707=EDGE_CURVE('',#38106,#38107,#31280,.T.);
#48708=EDGE_CURVE('',#37798,#38108,#21886,.T.);
#48709=EDGE_CURVE('',#38109,#37799,#21887,.T.);
#48710=EDGE_CURVE('',#38108,#38109,#31281,.T.);
#48711=EDGE_CURVE('',#38110,#38108,#21888,.T.);
#48712=EDGE_CURVE('',#38110,#37805,#21889,.T.);
#48713=EDGE_CURVE('',#38111,#37858,#31282,.T.);
#48714=EDGE_CURVE('',#37807,#38111,#21890,.T.);
#48715=EDGE_CURVE('',#37808,#37807,#21891,.T.);
#48716=EDGE_CURVE('',#38112,#37810,#31283,.T.);
#48717=EDGE_CURVE('',#38112,#37808,#21892,.T.);
#48718=EDGE_CURVE('',#38113,#37811,#31284,.T.);
#48719=EDGE_CURVE('',#38113,#38112,#31285,.T.);
#48720=EDGE_CURVE('',#38114,#37812,#31286,.T.);
#48721=EDGE_CURVE('',#38114,#38113,#21893,.T.);
#48722=EDGE_CURVE('',#38115,#37813,#31287,.T.);
#48723=EDGE_CURVE('',#38115,#38114,#31288,.T.);
#48724=EDGE_CURVE('',#37815,#38115,#21894,.T.);
#48725=EDGE_CURVE('',#37816,#37815,#21895,.T.);
#48726=EDGE_CURVE('',#38116,#37818,#31289,.T.);
#48727=EDGE_CURVE('',#38116,#37816,#21896,.T.);
#48728=EDGE_CURVE('',#38117,#37819,#31290,.T.);
#48729=EDGE_CURVE('',#38117,#38116,#31291,.T.);
#48730=EDGE_CURVE('',#38118,#37820,#31292,.T.);
#48731=EDGE_CURVE('',#38118,#38117,#21897,.T.);
#48732=EDGE_CURVE('',#38119,#37821,#31293,.T.);
#48733=EDGE_CURVE('',#38119,#38118,#31294,.T.);
#48734=EDGE_CURVE('',#37823,#38119,#21898,.T.);
#48735=EDGE_CURVE('',#38120,#37823,#21899,.T.);
#48736=EDGE_CURVE('',#37824,#38120,#31295,.T.);
#48737=EDGE_CURVE('',#37825,#38121,#31296,.T.);
#48738=EDGE_CURVE('',#38121,#38120,#5361,.T.);
#48739=EDGE_CURVE('',#37827,#38121,#31297,.T.);
#48740=EDGE_CURVE('',#38122,#37829,#31298,.T.);
#48741=EDGE_CURVE('',#38122,#37827,#21900,.T.);
#48742=EDGE_CURVE('',#38123,#37831,#31299,.T.);
#48743=EDGE_CURVE('',#38123,#38122,#31300,.T.);
#48744=EDGE_CURVE('',#38124,#37833,#31301,.T.);
#48745=EDGE_CURVE('',#38124,#38123,#21901,.T.);
#48746=EDGE_CURVE('',#38125,#37835,#31302,.T.);
#48747=EDGE_CURVE('',#38125,#38124,#31303,.T.);
#48748=EDGE_CURVE('',#37838,#38125,#21902,.T.);
#48749=EDGE_CURVE('',#37841,#37838,#31304,.T.);
#48750=EDGE_CURVE('',#38126,#37843,#31305,.T.);
#48751=EDGE_CURVE('',#38126,#37841,#21903,.T.);
#48752=EDGE_CURVE('',#38127,#37845,#31306,.T.);
#48753=EDGE_CURVE('',#38127,#38126,#31307,.T.);
#48754=EDGE_CURVE('',#38128,#37847,#31308,.T.);
#48755=EDGE_CURVE('',#38128,#38127,#21904,.T.);
#48756=EDGE_CURVE('',#38129,#37849,#31309,.T.);
#48757=EDGE_CURVE('',#38129,#38128,#31310,.T.);
#48758=EDGE_CURVE('',#38130,#38015,#31311,.T.);
#48759=EDGE_CURVE('',#38130,#38129,#21905,.T.);
#48760=EDGE_CURVE('',#38131,#38110,#31312,.T.);
#48761=EDGE_CURVE('',#37856,#38131,#21906,.T.);
#48762=EDGE_CURVE('',#38132,#37857,#31313,.T.);
#48763=EDGE_CURVE('',#38132,#37856,#21907,.T.);
#48764=EDGE_CURVE('',#38111,#38132,#31314,.T.);
#48765=EDGE_CURVE('',#38133,#38016,#31315,.T.);
#48766=EDGE_CURVE('',#38134,#38130,#5362,.T.);
#48767=EDGE_CURVE('',#38133,#38134,#1990,.T.);
#48768=EDGE_CURVE('',#38135,#38012,#31316,.T.);
#48769=EDGE_CURVE('',#38135,#38133,#5363,.T.);
#48770=EDGE_CURVE('',#38136,#38135,#1991,.T.);
#48771=EDGE_CURVE('',#38013,#38136,#31317,.T.);
#48772=EDGE_CURVE('',#37947,#38137,#5364,.T.);
#48773=EDGE_CURVE('',#38137,#38138,#5365,.T.);
#48774=EDGE_CURVE('',#37860,#38138,#21908,.T.);
#48775=EDGE_CURVE('',#38138,#38139,#31318,.T.);
#48776=EDGE_CURVE('',#38139,#38040,#31319,.T.);
#48777=EDGE_CURVE('',#38140,#37867,#21909,.T.);
#48778=EDGE_CURVE('',#37862,#38141,#21910,.T.);
#48779=EDGE_CURVE('',#38141,#38142,#31320,.T.);
#48780=EDGE_CURVE('',#38142,#38143,#21911,.T.);
#48781=EDGE_CURVE('',#38143,#38140,#31321,.T.);
#48782=EDGE_CURVE('',#38144,#37878,#21912,.T.);
#48783=EDGE_CURVE('',#37871,#38145,#21913,.T.);
#48784=EDGE_CURVE('',#38145,#38146,#31322,.T.);
#48785=EDGE_CURVE('',#38146,#38147,#21914,.T.);
#48786=EDGE_CURVE('',#38147,#38144,#31323,.T.);
#48787=EDGE_CURVE('',#37883,#38148,#21915,.T.);
#48788=EDGE_CURVE('',#38148,#37880,#31324,.T.);
#48789=EDGE_CURVE('',#37882,#38149,#31325,.T.);
#48790=EDGE_CURVE('',#38150,#37883,#21916,.T.);
#48791=EDGE_CURVE('',#38149,#38150,#31326,.T.);
#48792=EDGE_CURVE('',#38151,#37885,#31327,.T.);
#48793=EDGE_CURVE('',#38151,#38150,#5366,.T.);
#48794=EDGE_CURVE('',#38152,#37886,#31328,.T.);
#48795=EDGE_CURVE('',#38152,#38151,#21917,.T.);
#48796=EDGE_CURVE('',#38153,#37887,#31329,.T.);
#48797=EDGE_CURVE('',#38153,#38152,#5367,.T.);
#48798=EDGE_CURVE('',#37889,#38153,#21918,.T.);
#48799=EDGE_CURVE('',#37890,#37889,#21919,.T.);
#48800=EDGE_CURVE('',#38154,#37892,#31330,.T.);
#48801=EDGE_CURVE('',#38154,#37890,#21920,.T.);
#48802=EDGE_CURVE('',#38155,#37893,#31331,.T.);
#48803=EDGE_CURVE('',#38155,#38154,#5368,.T.);
#48804=EDGE_CURVE('',#38156,#37894,#31332,.T.);
#48805=EDGE_CURVE('',#38156,#38155,#21921,.T.);
#48806=EDGE_CURVE('',#38157,#37895,#31333,.T.);
#48807=EDGE_CURVE('',#38157,#38156,#5369,.T.);
#48808=EDGE_CURVE('',#37897,#38157,#21922,.T.);
#48809=EDGE_CURVE('',#38158,#37897,#21923,.T.);
#48810=EDGE_CURVE('',#38158,#38141,#31334,.T.);
#48811=EDGE_CURVE('',#38159,#38007,#31335,.T.);
#48812=EDGE_CURVE('',#38160,#38159,#1992,.T.);
#48813=EDGE_CURVE('',#37898,#38160,#31336,.T.);
#48814=EDGE_CURVE('',#37900,#38160,#21924,.T.);
#48815=EDGE_CURVE('',#38148,#37900,#5370,.T.);
#48816=EDGE_CURVE('',#38161,#37920,#21925,.T.);
#48817=EDGE_CURVE('',#37902,#38161,#31337,.T.);
#48818=EDGE_CURVE('',#38162,#37903,#31338,.T.);
#48819=EDGE_CURVE('',#38162,#38161,#5371,.T.);
#48820=EDGE_CURVE('',#38163,#37904,#31339,.T.);
#48821=EDGE_CURVE('',#38163,#38162,#21926,.T.);
#48822=EDGE_CURVE('',#38164,#37905,#31340,.T.);
#48823=EDGE_CURVE('',#38164,#38163,#5372,.T.);
#48824=EDGE_CURVE('',#37907,#38164,#21927,.T.);
#48825=EDGE_CURVE('',#38165,#37907,#21928,.T.);
#48826=EDGE_CURVE('',#37908,#38165,#31341,.T.);
#48827=EDGE_CURVE('',#37910,#38165,#5373,.T.);
#48828=EDGE_CURVE('',#38166,#37912,#31342,.T.);
#48829=EDGE_CURVE('',#38166,#37910,#21929,.T.);
#48830=EDGE_CURVE('',#38167,#38008,#31343,.T.);
#48831=EDGE_CURVE('',#38167,#38166,#1993,.T.);
#48832=EDGE_CURVE('',#37915,#38168,#21930,.T.);
#48833=EDGE_CURVE('',#38168,#38144,#31344,.T.);
#48834=EDGE_CURVE('',#38169,#37915,#21931,.T.);
#48835=EDGE_CURVE('',#37914,#38169,#31345,.T.);
#48836=EDGE_CURVE('',#38170,#38169,#5374,.T.);
#48837=EDGE_CURVE('',#37916,#38170,#31346,.T.);
#48838=EDGE_CURVE('',#38171,#38170,#21932,.T.);
#48839=EDGE_CURVE('',#37917,#38171,#31347,.T.);
#48840=EDGE_CURVE('',#38172,#38171,#5375,.T.);
#48841=EDGE_CURVE('',#37918,#38172,#31348,.T.);
#48842=EDGE_CURVE('',#37921,#38172,#21933,.T.);
#48843=EDGE_CURVE('',#37920,#37921,#21934,.T.);
#48844=EDGE_CURVE('',#38173,#38147,#31349,.T.);
#48845=EDGE_CURVE('',#38174,#38146,#31350,.T.);
#48846=EDGE_CURVE('',#38173,#38174,#21935,.T.);
#48847=EDGE_CURVE('',#38175,#37923,#31351,.T.);
#48848=EDGE_CURVE('',#38175,#37936,#21936,.T.);
#48849=EDGE_CURVE('',#38176,#37924,#31352,.T.);
#48850=EDGE_CURVE('',#38176,#38175,#5376,.T.);
#48851=EDGE_CURVE('',#38177,#37925,#31353,.T.);
#48852=EDGE_CURVE('',#38177,#38176,#21937,.T.);
#48853=EDGE_CURVE('',#38178,#37926,#31354,.T.);
#48854=EDGE_CURVE('',#38178,#38177,#5377,.T.);
#48855=EDGE_CURVE('',#37928,#38178,#21938,.T.);
#48856=EDGE_CURVE('',#38179,#37928,#21939,.T.);
#48857=EDGE_CURVE('',#38179,#38145,#31355,.T.);
#48858=EDGE_CURVE('',#37929,#38180,#5378,.T.);
#48859=EDGE_CURVE('',#38180,#38039,#31356,.T.);
#48860=EDGE_CURVE('',#37931,#38181,#31357,.T.);
#48861=EDGE_CURVE('',#38181,#37929,#21940,.T.);
#48862=EDGE_CURVE('',#38182,#38181,#5379,.T.);
#48863=EDGE_CURVE('',#37932,#38182,#31358,.T.);
#48864=EDGE_CURVE('',#38183,#38182,#21941,.T.);
#48865=EDGE_CURVE('',#37933,#38183,#31359,.T.);
#48866=EDGE_CURVE('',#38184,#38183,#5380,.T.);
#48867=EDGE_CURVE('',#37934,#38184,#31360,.T.);
#48868=EDGE_CURVE('',#37937,#38184,#21942,.T.);
#48869=EDGE_CURVE('',#37936,#37937,#21943,.T.);
#48870=EDGE_CURVE('',#38185,#38038,#31361,.T.);
#48871=EDGE_CURVE('',#38180,#38185,#5381,.T.);
#48872=EDGE_CURVE('',#38186,#38143,#31362,.T.);
#48873=EDGE_CURVE('',#38187,#38142,#31363,.T.);
#48874=EDGE_CURVE('',#38186,#38187,#21944,.T.);
#48875=EDGE_CURVE('',#38188,#37956,#21945,.T.);
#48876=EDGE_CURVE('',#37939,#38188,#31364,.T.);
#48877=EDGE_CURVE('',#38189,#37940,#31365,.T.);
#48878=EDGE_CURVE('',#38189,#38188,#5382,.T.);
#48879=EDGE_CURVE('',#38190,#37941,#31366,.T.);
#48880=EDGE_CURVE('',#38190,#38189,#21946,.T.);
#48881=EDGE_CURVE('',#38191,#37942,#31367,.T.);
#48882=EDGE_CURVE('',#38191,#38190,#5383,.T.);
#48883=EDGE_CURVE('',#37944,#38191,#21947,.T.);
#48884=EDGE_CURVE('',#38192,#37944,#21948,.T.);
#48885=EDGE_CURVE('',#37945,#38192,#31368,.T.);
#48886=EDGE_CURVE('',#37948,#38192,#5384,.T.);
#48887=EDGE_CURVE('',#38193,#37948,#21949,.T.);
#48888=EDGE_CURVE('',#37947,#38193,#31369,.T.);
#48889=EDGE_CURVE('',#38194,#38137,#31370,.T.);
#48890=EDGE_CURVE('',#38194,#38193,#5385,.T.);
#48891=EDGE_CURVE('',#37949,#38195,#21950,.T.);
#48892=EDGE_CURVE('',#38195,#38140,#31371,.T.);
#48893=EDGE_CURVE('',#38196,#37951,#31372,.T.);
#48894=EDGE_CURVE('',#38196,#37949,#21951,.T.);
#48895=EDGE_CURVE('',#38197,#37952,#31373,.T.);
#48896=EDGE_CURVE('',#38197,#38196,#5386,.T.);
#48897=EDGE_CURVE('',#38198,#37953,#31374,.T.);
#48898=EDGE_CURVE('',#38198,#38197,#21952,.T.);
#48899=EDGE_CURVE('',#38199,#37954,#31375,.T.);
#48900=EDGE_CURVE('',#38199,#38198,#5387,.T.);
#48901=EDGE_CURVE('',#37957,#38199,#21953,.T.);
#48902=EDGE_CURVE('',#37956,#37957,#21954,.T.);
#48903=EDGE_CURVE('',#38011,#38200,#31376,.T.);
#48904=EDGE_CURVE('',#38201,#38200,#5388,.T.);
#48905=EDGE_CURVE('',#37958,#38201,#31377,.T.);
#48906=EDGE_CURVE('',#37960,#38201,#21955,.T.);
#48907=EDGE_CURVE('',#37963,#37960,#31378,.T.);
#48908=EDGE_CURVE('',#38202,#37963,#21956,.T.);
#48909=EDGE_CURVE('',#37962,#38202,#31379,.T.);
#48910=EDGE_CURVE('',#38203,#38202,#5389,.T.);
#48911=EDGE_CURVE('',#37964,#38203,#31380,.T.);
#48912=EDGE_CURVE('',#38204,#38203,#31381,.T.);
#48913=EDGE_CURVE('',#37965,#38204,#31382,.T.);
#48914=EDGE_CURVE('',#38205,#38204,#5390,.T.);
#48915=EDGE_CURVE('',#37966,#38205,#31383,.T.);
#48916=EDGE_CURVE('',#37968,#38205,#21957,.T.);
#48917=EDGE_CURVE('',#37971,#37968,#31384,.T.);
#48918=EDGE_CURVE('',#38206,#37971,#21958,.T.);
#48919=EDGE_CURVE('',#37970,#38206,#31385,.T.);
#48920=EDGE_CURVE('',#38207,#37972,#31386,.T.);
#48921=EDGE_CURVE('',#38207,#38206,#5391,.T.);
#48922=EDGE_CURVE('',#38208,#37973,#31387,.T.);
#48923=EDGE_CURVE('',#38208,#38207,#31388,.T.);
#48924=EDGE_CURVE('',#38209,#37974,#31389,.T.);
#48925=EDGE_CURVE('',#38209,#38208,#5392,.T.);
#48926=EDGE_CURVE('',#37976,#38209,#21959,.T.);
#48927=EDGE_CURVE('',#37979,#37976,#31390,.T.);
#48928=EDGE_CURVE('',#38210,#37979,#21960,.T.);
#48929=EDGE_CURVE('',#37978,#38210,#31391,.T.);
#48930=EDGE_CURVE('',#38211,#37980,#31392,.T.);
#48931=EDGE_CURVE('',#38211,#38210,#5393,.T.);
#48932=EDGE_CURVE('',#38212,#37981,#31393,.T.);
#48933=EDGE_CURVE('',#38212,#38211,#31394,.T.);
#48934=EDGE_CURVE('',#38213,#37982,#31395,.T.);
#48935=EDGE_CURVE('',#38213,#38212,#5394,.T.);
#48936=EDGE_CURVE('',#37984,#38213,#21961,.T.);
#48937=EDGE_CURVE('',#37987,#37984,#31396,.T.);
#48938=EDGE_CURVE('',#38214,#37987,#21962,.T.);
#48939=EDGE_CURVE('',#37986,#38214,#31397,.T.);
#48940=EDGE_CURVE('',#38215,#37988,#31398,.T.);
#48941=EDGE_CURVE('',#38215,#38214,#5395,.T.);
#48942=EDGE_CURVE('',#38216,#37989,#31399,.T.);
#48943=EDGE_CURVE('',#38216,#38215,#31400,.T.);
#48944=EDGE_CURVE('',#38217,#37990,#31401,.T.);
#48945=EDGE_CURVE('',#38217,#38216,#5396,.T.);
#48946=EDGE_CURVE('',#37992,#38217,#21963,.T.);
#48947=EDGE_CURVE('',#37995,#37992,#31402,.T.);
#48948=EDGE_CURVE('',#38218,#37995,#21964,.T.);
#48949=EDGE_CURVE('',#37994,#38218,#31403,.T.);
#48950=EDGE_CURVE('',#38219,#38218,#5397,.T.);
#48951=EDGE_CURVE('',#37996,#38219,#31404,.T.);
#48952=EDGE_CURVE('',#38220,#38219,#31405,.T.);
#48953=EDGE_CURVE('',#37997,#38220,#31406,.T.);
#48954=EDGE_CURVE('',#38221,#38220,#5398,.T.);
#48955=EDGE_CURVE('',#37998,#38221,#31407,.T.);
#48956=EDGE_CURVE('',#38000,#38221,#21965,.T.);
#48957=EDGE_CURVE('',#38001,#38000,#31408,.T.);
#48958=EDGE_CURVE('',#38222,#38003,#31409,.T.);
#48959=EDGE_CURVE('',#38222,#38001,#21966,.T.);
#48960=EDGE_CURVE('',#38223,#38004,#31410,.T.);
#48961=EDGE_CURVE('',#38223,#38222,#5399,.T.);
#48962=EDGE_CURVE('',#38180,#38224,#21967,.T.);
#48963=EDGE_CURVE('',#38224,#38225,#21968,.T.);
#48964=EDGE_CURVE('',#38225,#38179,#21969,.T.);
#48965=EDGE_CURVE('',#38174,#38179,#31411,.T.);
#48966=EDGE_CURVE('',#38226,#38173,#21970,.T.);
#48967=EDGE_CURVE('',#38174,#38227,#21971,.T.);
#48968=EDGE_CURVE('',#38227,#38226,#21972,.T.);
#48969=EDGE_CURVE('',#38227,#38225,#31412,.T.);
#48970=EDGE_CURVE('',#38168,#38173,#31413,.T.);
#48971=EDGE_CURVE('',#38168,#38228,#21973,.T.);
#48972=EDGE_CURVE('',#38228,#38229,#21974,.T.);
#48973=EDGE_CURVE('',#38229,#38167,#21975,.T.);
#48974=EDGE_CURVE('',#38228,#38226,#31414,.T.);
#48975=EDGE_CURVE('',#38230,#38009,#31415,.T.);
#48976=EDGE_CURVE('',#38230,#38167,#5400,.T.);
#48977=EDGE_CURVE('',#38010,#38231,#31416,.T.);
#48978=EDGE_CURVE('',#38231,#38230,#31417,.T.);
#48979=EDGE_CURVE('',#38200,#38231,#31418,.T.);
#48980=EDGE_CURVE('',#38232,#38233,#31419,.T.);
#48981=EDGE_CURVE('',#38232,#38223,#21976,.T.);
#48982=EDGE_CURVE('',#38200,#38233,#21977,.T.);
#48983=EDGE_CURVE('',#38233,#38229,#31420,.T.);
#48984=EDGE_CURVE('',#38234,#38005,#31421,.T.);
#48985=EDGE_CURVE('',#38234,#38223,#5401,.T.);
#48986=EDGE_CURVE('',#38235,#38006,#31422,.T.);
#48987=EDGE_CURVE('',#38235,#38234,#31423,.T.);
#48988=EDGE_CURVE('',#38159,#38235,#5402,.T.);
#48989=EDGE_CURVE('',#38236,#38136,#21978,.T.);
#48990=EDGE_CURVE('',#38014,#38236,#31424,.T.);
#48991=EDGE_CURVE('',#38237,#38236,#5403,.T.);
#48992=EDGE_CURVE('',#38017,#38237,#31425,.T.);
#48993=EDGE_CURVE('',#38238,#38237,#31426,.T.);
#48994=EDGE_CURVE('',#38018,#38238,#31427,.T.);
#48995=EDGE_CURVE('',#38239,#38238,#5404,.T.);
#48996=EDGE_CURVE('',#38019,#38239,#31428,.T.);
#48997=EDGE_CURVE('',#38021,#38239,#21979,.T.);
#48998=EDGE_CURVE('',#38024,#38021,#31429,.T.);
#48999=EDGE_CURVE('',#38240,#38024,#21980,.T.);
#49000=EDGE_CURVE('',#38023,#38240,#31430,.T.);
#49001=EDGE_CURVE('',#38241,#38240,#5405,.T.);
#49002=EDGE_CURVE('',#38025,#38241,#31431,.T.);
#49003=EDGE_CURVE('',#38242,#38241,#31432,.T.);
#49004=EDGE_CURVE('',#38026,#38242,#31433,.T.);
#49005=EDGE_CURVE('',#38243,#38242,#5406,.T.);
#49006=EDGE_CURVE('',#38027,#38243,#31434,.T.);
#49007=EDGE_CURVE('',#38029,#38243,#21981,.T.);
#49008=EDGE_CURVE('',#38030,#38029,#31435,.T.);
#49009=EDGE_CURVE('',#38032,#38244,#31436,.T.);
#49010=EDGE_CURVE('',#38244,#38030,#21982,.T.);
#49011=EDGE_CURVE('',#38245,#38244,#5407,.T.);
#49012=EDGE_CURVE('',#38033,#38245,#31437,.T.);
#49013=EDGE_CURVE('',#38246,#38245,#31438,.T.);
#49014=EDGE_CURVE('',#38034,#38246,#31439,.T.);
#49015=EDGE_CURVE('',#38247,#38246,#5408,.T.);
#49016=EDGE_CURVE('',#38035,#38247,#31440,.T.);
#49017=EDGE_CURVE('',#38037,#38247,#21983,.T.);
#49018=EDGE_CURVE('',#38185,#38037,#31441,.T.);
#49019=EDGE_CURVE('',#38248,#38185,#21984,.T.);
#49020=EDGE_CURVE('',#38224,#38248,#31442,.T.);
#49021=EDGE_CURVE('',#38249,#38040,#31443,.T.);
#49022=EDGE_CURVE('',#38250,#38139,#31444,.T.);
#49023=EDGE_CURVE('',#38249,#38250,#31445,.T.);
#49024=EDGE_CURVE('',#38251,#38041,#31446,.T.);
#49025=EDGE_CURVE('',#38251,#38249,#5409,.T.);
#49026=EDGE_CURVE('',#38043,#38251,#21985,.T.);
#49027=EDGE_CURVE('',#38046,#38043,#31447,.T.);
#49028=EDGE_CURVE('',#38252,#38046,#21986,.T.);
#49029=EDGE_CURVE('',#38045,#38252,#31448,.T.);
#49030=EDGE_CURVE('',#38253,#38047,#31449,.T.);
#49031=EDGE_CURVE('',#38253,#38252,#5410,.T.);
#49032=EDGE_CURVE('',#38254,#38048,#31450,.T.);
#49033=EDGE_CURVE('',#38254,#38253,#31451,.T.);
#49034=EDGE_CURVE('',#38255,#38049,#31452,.T.);
#49035=EDGE_CURVE('',#38255,#38254,#5411,.T.);
#49036=EDGE_CURVE('',#38052,#38255,#21987,.T.);
#49037=EDGE_CURVE('',#38055,#38052,#31453,.T.);
#49038=EDGE_CURVE('',#38256,#38055,#21988,.T.);
#49039=EDGE_CURVE('',#38054,#38256,#31454,.T.);
#49040=EDGE_CURVE('',#38257,#38056,#31455,.T.);
#49041=EDGE_CURVE('',#38257,#38256,#5412,.T.);
#49042=EDGE_CURVE('',#38258,#38057,#31456,.T.);
#49043=EDGE_CURVE('',#38258,#38257,#31457,.T.);
#49044=EDGE_CURVE('',#38259,#38260,#31458,.T.);
#49045=EDGE_CURVE('',#38260,#38058,#31459,.T.);
#49046=EDGE_CURVE('',#38259,#38258,#5413,.T.);
#49047=EDGE_CURVE('',#38061,#38259,#21989,.T.);
#49048=EDGE_CURVE('',#38067,#38061,#31460,.T.);
#49049=EDGE_CURVE('',#38261,#38067,#21990,.T.);
#49050=EDGE_CURVE('',#38065,#38261,#31461,.T.);
#49051=EDGE_CURVE('',#38262,#38261,#5414,.T.);
#49052=EDGE_CURVE('',#38068,#38262,#31462,.T.);
#49053=EDGE_CURVE('',#35219,#38263,#31463,.T.);
#49054=EDGE_CURVE('',#35270,#38262,#31464,.T.);
#49055=EDGE_CURVE('',#38250,#38263,#21991,.T.);
#49056=EDGE_CURVE('',#38159,#38264,#21992,.T.);
#49057=EDGE_CURVE('',#38264,#38265,#21993,.T.);
#49058=EDGE_CURVE('',#38265,#38158,#21994,.T.);
#49059=EDGE_CURVE('',#38187,#38158,#31465,.T.);
#49060=EDGE_CURVE('',#38266,#38186,#21995,.T.);
#49061=EDGE_CURVE('',#38187,#38267,#21996,.T.);
#49062=EDGE_CURVE('',#38267,#38266,#21997,.T.);
#49063=EDGE_CURVE('',#38267,#38265,#31466,.T.);
#49064=EDGE_CURVE('',#38195,#38186,#31467,.T.);
#49065=EDGE_CURVE('',#38195,#38268,#21998,.T.);
#49066=EDGE_CURVE('',#38268,#38269,#21999,.T.);
#49067=EDGE_CURVE('',#38269,#38194,#22000,.T.);
#49068=EDGE_CURVE('',#38268,#38266,#31468,.T.);
#49069=EDGE_CURVE('',#38270,#38138,#31469,.T.);
#49070=EDGE_CURVE('',#38270,#38194,#5415,.T.);
#49071=EDGE_CURVE('',#38250,#38270,#31470,.T.);
#49072=EDGE_CURVE('',#38263,#38269,#31471,.T.);
#49073=EDGE_CURVE('',#38068,#35269,#31472,.T.);
#49074=EDGE_CURVE('',#38069,#35775,#31473,.T.);
#49075=EDGE_CURVE('',#35773,#38070,#31474,.T.);
#49076=EDGE_CURVE('',#35764,#38071,#31475,.T.);
#49077=EDGE_CURVE('',#38075,#35765,#31476,.F.);
#49078=EDGE_CURVE('',#35710,#38074,#31477,.T.);
#49079=EDGE_CURVE('',#38088,#35711,#31478,.T.);
#49080=EDGE_CURVE('',#35683,#38103,#31479,.T.);
#49081=EDGE_CURVE('',#38104,#35680,#31480,.T.);
#49082=EDGE_CURVE('',#35678,#38105,#31481,.T.);
#49083=EDGE_CURVE('',#38107,#35677,#31482,.T.);
#49084=EDGE_CURVE('',#38109,#35673,#22001,.T.);
#49085=EDGE_CURVE('',#35601,#38131,#22002,.T.);
#49086=EDGE_CURVE('',#35588,#38130,#31483,.T.);
#49087=EDGE_CURVE('',#38133,#35585,#31484,.T.);
#49088=EDGE_CURVE('',#35583,#38135,#31485,.T.);
#49089=EDGE_CURVE('',#38136,#35357,#31486,.T.);
#49090=EDGE_CURVE('',#38248,#35314,#31487,.T.);
#49091=EDGE_CURVE('',#38264,#38232,#31488,.T.);
#49092=EDGE_CURVE('',#38271,#38272,#22003,.T.);
#49093=EDGE_CURVE('',#38272,#38273,#1204,.T.);
#49094=EDGE_CURVE('',#38274,#38273,#22004,.T.);
#49095=EDGE_CURVE('',#38274,#38271,#1205,.T.);
#49096=EDGE_CURVE('',#38275,#38276,#22005,.T.);
#49097=EDGE_CURVE('',#38276,#38272,#1206,.T.);
#49098=EDGE_CURVE('',#38271,#38275,#1207,.T.);
#49099=EDGE_CURVE('',#38277,#38278,#22006,.T.);
#49100=EDGE_CURVE('',#38278,#38276,#1208,.T.);
#49101=EDGE_CURVE('',#38275,#38277,#1209,.T.);
#49102=EDGE_CURVE('',#38279,#38280,#22007,.T.);
#49103=EDGE_CURVE('',#38280,#38278,#1210,.T.);
#49104=EDGE_CURVE('',#38277,#38279,#1211,.T.);
#49105=EDGE_CURVE('',#38281,#38282,#22008,.T.);
#49106=EDGE_CURVE('',#38282,#38280,#1212,.T.);
#49107=EDGE_CURVE('',#38279,#38281,#1213,.T.);
#49108=EDGE_CURVE('',#38273,#38282,#1214,.T.);
#49109=EDGE_CURVE('',#38281,#38274,#1215,.T.);
#49110=EDGE_CURVE('',#38283,#38277,#22009,.T.);
#49111=EDGE_CURVE('',#38272,#38273,#31489,.T.);
#49112=EDGE_CURVE('',#38276,#38272,#31490,.T.);
#49113=EDGE_CURVE('',#38278,#38276,#31491,.T.);
#49114=EDGE_CURVE('',#38280,#38278,#31492,.T.);
#49115=EDGE_CURVE('',#38282,#38280,#31493,.T.);
#49116=EDGE_CURVE('',#38273,#38282,#31494,.T.);
#49117=EDGE_CURVE('',#38284,#38284,#31495,.T.);
#49118=EDGE_CURVE('',#38284,#38285,#31496,.T.);
#49119=EDGE_CURVE('',#38286,#38285,#31497,.T.);
#49120=EDGE_CURVE('',#38285,#38286,#31498,.T.);
#49121=EDGE_CURVE('',#38287,#38287,#31499,.T.);
#49122=EDGE_CURVE('',#38287,#38286,#22010,.T.);
#49123=EDGE_CURVE('',#38288,#38288,#31500,.T.);
#49124=EDGE_CURVE('',#38288,#38289,#22011,.T.);
#49125=EDGE_CURVE('',#38289,#38289,#31501,.T.);
#49126=EDGE_CURVE('',#38290,#38290,#31502,.T.);
#49127=EDGE_CURVE('',#38290,#38288,#22012,.T.);
#49128=EDGE_CURVE('',#38291,#38291,#31503,.T.);
#49129=EDGE_CURVE('',#38292,#38292,#31504,.T.);
#49130=EDGE_CURVE('',#38292,#38291,#22013,.T.);
#49131=EDGE_CURVE('',#38293,#38294,#31505,.T.);
#49132=EDGE_CURVE('',#38293,#38295,#5416,.T.);
#49133=EDGE_CURVE('',#38296,#38295,#31506,.T.);
#49134=EDGE_CURVE('',#38296,#38294,#1216,.T.);
#49135=EDGE_CURVE('',#38297,#38297,#31507,.T.);
#49136=EDGE_CURVE('',#38297,#38298,#31508,.T.);
#49137=EDGE_CURVE('',#38298,#38299,#31509,.T.);
#49138=EDGE_CURVE('',#38299,#38298,#31510,.T.);
#49139=EDGE_CURVE('',#38300,#38301,#31511,.T.);
#49140=EDGE_CURVE('',#38300,#38302,#5417,.T.);
#49141=EDGE_CURVE('',#38303,#38302,#31512,.T.);
#49142=EDGE_CURVE('',#38303,#38301,#5418,.T.);
#49143=EDGE_CURVE('',#38304,#38305,#31513,.T.);
#49144=EDGE_CURVE('',#38304,#38303,#5419,.T.);
#49145=EDGE_CURVE('',#38302,#38305,#5420,.T.);
#49146=EDGE_CURVE('',#38306,#38300,#31514,.T.);
#49147=EDGE_CURVE('',#38306,#38301,#31515,.T.);
#49148=EDGE_CURVE('',#38307,#38308,#31516,.T.);
#49149=EDGE_CURVE('',#38307,#38304,#5421,.T.);
#49150=EDGE_CURVE('',#38305,#38308,#5422,.T.);
#49151=EDGE_CURVE('',#38309,#38310,#31517,.T.);
#49152=EDGE_CURVE('',#38309,#38306,#31518,.T.);
#49153=EDGE_CURVE('',#38301,#38310,#31519,.T.);
#49154=EDGE_CURVE('',#38311,#38312,#31520,.T.);
#49155=EDGE_CURVE('',#38311,#38307,#5423,.T.);
#49156=EDGE_CURVE('',#38308,#38312,#5424,.T.);
#49157=EDGE_CURVE('',#38313,#38314,#31521,.T.);
#49158=EDGE_CURVE('',#38313,#38309,#31522,.T.);
#49159=EDGE_CURVE('',#38310,#38314,#31523,.T.);
#49160=EDGE_CURVE('',#38315,#38316,#31524,.T.);
#49161=EDGE_CURVE('',#38315,#38311,#5425,.T.);
#49162=EDGE_CURVE('',#38312,#38316,#5426,.T.);
#49163=EDGE_CURVE('',#38317,#38318,#31525,.T.);
#49164=EDGE_CURVE('',#38317,#38313,#31526,.T.);
#49165=EDGE_CURVE('',#38314,#38318,#31527,.T.);
#49166=EDGE_CURVE('',#38319,#38320,#31528,.T.);
#49167=EDGE_CURVE('',#38319,#38315,#5427,.T.);
#49168=EDGE_CURVE('',#38316,#38320,#5428,.T.);
#49169=EDGE_CURVE('',#38321,#38322,#31529,.T.);
#49170=EDGE_CURVE('',#38321,#38317,#5429,.T.);
#49171=EDGE_CURVE('',#38318,#38322,#5430,.T.);
#49172=EDGE_CURVE('',#38322,#38323,#31530,.T.);
#49173=EDGE_CURVE('',#38322,#38324,#1994,.T.);
#49174=EDGE_CURVE('',#38324,#38319,#5431,.T.);
#49175=EDGE_CURVE('',#38320,#38323,#5432,.T.);
#49176=EDGE_CURVE('',#38323,#38321,#31531,.T.);
#49177=EDGE_CURVE('',#38325,#38326,#31532,.T.);
#49178=EDGE_CURVE('',#38325,#38327,#5433,.T.);
#49179=EDGE_CURVE('',#38328,#38327,#31533,.T.);
#49180=EDGE_CURVE('',#38328,#38326,#5434,.T.);
#49181=EDGE_CURVE('',#38329,#38330,#31534,.T.);
#49182=EDGE_CURVE('',#38329,#38328,#5435,.T.);
#49183=EDGE_CURVE('',#38327,#38330,#5436,.T.);
#49184=EDGE_CURVE('',#38331,#38332,#31535,.T.);
#49185=EDGE_CURVE('',#38331,#38325,#5437,.T.);
#49186=EDGE_CURVE('',#38326,#38332,#5438,.T.);
#49187=EDGE_CURVE('',#38333,#38334,#31536,.T.);
#49188=EDGE_CURVE('',#38333,#38329,#5439,.T.);
#49189=EDGE_CURVE('',#38330,#38334,#5440,.T.);
#49190=EDGE_CURVE('',#38335,#38336,#31537,.T.);
#49191=EDGE_CURVE('',#38335,#38331,#5441,.T.);
#49192=EDGE_CURVE('',#38332,#38336,#5442,.T.);
#49193=EDGE_CURVE('',#38333,#38337,#31538,.T.);
#49194=EDGE_CURVE('',#38334,#38337,#31539,.T.);
#49195=EDGE_CURVE('',#38338,#38339,#31540,.T.);
#49196=EDGE_CURVE('',#38338,#38335,#5443,.T.);
#49197=EDGE_CURVE('',#38336,#38339,#5444,.T.);
#49198=EDGE_CURVE('',#38340,#38341,#31541,.T.);
#49199=EDGE_CURVE('',#38340,#38333,#5445,.T.);
#49200=EDGE_CURVE('',#38337,#38341,#5446,.T.);
#49201=EDGE_CURVE('',#38342,#38343,#31542,.T.);
#49202=EDGE_CURVE('',#38342,#38338,#5447,.T.);
#49203=EDGE_CURVE('',#38339,#38343,#5448,.T.);
#49204=EDGE_CURVE('',#38344,#38345,#31543,.T.);
#49205=EDGE_CURVE('',#38344,#38340,#31544,.T.);
#49206=EDGE_CURVE('',#38341,#38345,#31545,.T.);
#49207=EDGE_CURVE('',#38346,#38342,#31546,.T.);
#49208=EDGE_CURVE('',#38346,#38343,#31547,.T.);
#49209=EDGE_CURVE('',#38347,#38348,#31548,.T.);
#49210=EDGE_CURVE('',#38347,#38344,#31549,.T.);
#49211=EDGE_CURVE('',#38345,#38348,#31550,.T.);
#49212=EDGE_CURVE('',#38349,#38350,#31551,.T.);
#49213=EDGE_CURVE('',#38349,#38346,#5449,.T.);
#49214=EDGE_CURVE('',#38343,#38350,#5450,.T.);
#49215=EDGE_CURVE('',#38348,#38349,#31552,.T.);
#49216=EDGE_CURVE('',#38350,#38347,#31553,.T.);
#49217=EDGE_CURVE('',#38351,#38352,#31554,.T.);
#49218=EDGE_CURVE('',#38351,#38353,#31555,.T.);
#49219=EDGE_CURVE('',#38353,#38354,#31556,.T.);
#49220=EDGE_CURVE('',#38354,#38352,#31557,.T.);
#49221=EDGE_CURVE('',#38355,#38356,#31558,.T.);
#49222=EDGE_CURVE('',#38355,#38351,#31559,.T.);
#49223=EDGE_CURVE('',#38352,#38356,#31560,.T.);
#49224=EDGE_CURVE('',#38357,#38358,#31561,.T.);
#49225=EDGE_CURVE('',#38357,#38355,#31562,.T.);
#49226=EDGE_CURVE('',#38356,#38358,#31563,.T.);
#49227=EDGE_CURVE('',#38359,#38360,#31564,.T.);
#49228=EDGE_CURVE('',#38359,#38357,#31565,.T.);
#49229=EDGE_CURVE('',#38358,#38360,#31566,.T.);
#49230=EDGE_CURVE('',#38361,#38362,#31567,.T.);
#49231=EDGE_CURVE('',#38361,#38359,#31568,.T.);
#49232=EDGE_CURVE('',#38360,#38362,#31569,.T.);
#49233=EDGE_CURVE('',#38363,#38364,#31570,.T.);
#49234=EDGE_CURVE('',#38363,#38361,#31571,.T.);
#49235=EDGE_CURVE('',#38362,#38364,#31572,.T.);
#49236=EDGE_CURVE('',#38365,#38366,#31573,.T.);
#49237=EDGE_CURVE('',#38365,#38363,#31574,.T.);
#49238=EDGE_CURVE('',#38364,#38366,#31575,.T.);
#49239=EDGE_CURVE('',#38306,#38367,#31576,.T.);
#49240=EDGE_CURVE('',#38368,#38367,#31577,.T.);
#49241=EDGE_CURVE('',#38368,#38300,#31578,.T.);
#49242=EDGE_CURVE('',#38369,#38370,#31579,.T.);
#49243=EDGE_CURVE('',#38369,#38368,#1995,.T.);
#49244=EDGE_CURVE('',#38367,#38370,#5451,.T.);
#49245=EDGE_CURVE('',#38323,#38371,#5452,.T.);
#49246=EDGE_CURVE('',#38372,#38371,#31580,.T.);
#49247=EDGE_CURVE('',#38372,#38321,#5453,.T.);
#49248=EDGE_CURVE('',#38373,#38374,#31581,.T.);
#49249=EDGE_CURVE('',#38373,#38369,#5454,.T.);
#49250=EDGE_CURVE('',#38370,#38374,#5455,.T.);
#49251=EDGE_CURVE('',#38375,#38376,#31582,.T.);
#49252=EDGE_CURVE('',#38375,#38372,#31583,.T.);
#49253=EDGE_CURVE('',#38371,#38376,#31584,.T.);
#49254=EDGE_CURVE('',#38377,#38378,#31585,.T.);
#49255=EDGE_CURVE('',#38377,#38373,#31586,.T.);
#49256=EDGE_CURVE('',#38374,#38378,#31587,.T.);
#49257=EDGE_CURVE('',#38379,#38380,#31588,.T.);
#49258=EDGE_CURVE('',#38379,#38375,#5456,.T.);
#49259=EDGE_CURVE('',#38376,#38380,#5457,.T.);
#49260=EDGE_CURVE('',#38381,#38382,#31589,.T.);
#49261=EDGE_CURVE('',#38381,#38377,#5458,.T.);
#49262=EDGE_CURVE('',#38378,#38382,#5459,.T.);
#49263=EDGE_CURVE('',#38383,#38384,#31590,.T.);
#49264=EDGE_CURVE('',#38383,#38379,#5460,.T.);
#49265=EDGE_CURVE('',#38380,#38384,#5461,.T.);
#49266=EDGE_CURVE('',#38385,#38386,#31591,.T.);
#49267=EDGE_CURVE('',#38385,#38381,#5462,.T.);
#49268=EDGE_CURVE('',#38382,#38386,#5463,.T.);
#49269=EDGE_CURVE('',#38387,#38388,#31592,.T.);
#49270=EDGE_CURVE('',#38387,#38383,#5464,.T.);
#49271=EDGE_CURVE('',#38384,#38388,#5465,.T.);
#49272=EDGE_CURVE('',#38389,#38390,#31593,.T.);
#49273=EDGE_CURVE('',#38389,#38385,#5466,.T.);
#49274=EDGE_CURVE('',#38386,#38390,#5467,.T.);
#49275=EDGE_CURVE('',#38388,#38389,#31594,.T.);
#49276=EDGE_CURVE('',#38390,#38387,#31595,.T.);
#49277=EDGE_CURVE('',#38391,#38392,#31596,.T.);
#49278=EDGE_CURVE('',#38391,#38393,#5468,.T.);
#49279=EDGE_CURVE('',#38394,#38393,#31597,.T.);
#49280=EDGE_CURVE('',#38394,#38392,#5469,.T.);
#49281=EDGE_CURVE('',#38395,#38396,#31598,.T.);
#49282=EDGE_CURVE('',#38395,#38394,#31599,.T.);
#49283=EDGE_CURVE('',#38393,#38396,#31600,.T.);
#49284=EDGE_CURVE('',#38397,#38398,#31601,.T.);
#49285=EDGE_CURVE('',#38397,#38391,#5470,.T.);
#49286=EDGE_CURVE('',#38392,#38398,#5471,.T.);
#49287=EDGE_CURVE('',#38399,#38400,#31602,.T.);
#49288=EDGE_CURVE('',#38399,#38395,#5472,.T.);
#49289=EDGE_CURVE('',#38396,#38400,#5473,.T.);
#49290=EDGE_CURVE('',#38401,#38402,#31603,.T.);
#49291=EDGE_CURVE('',#38401,#38397,#5474,.T.);
#49292=EDGE_CURVE('',#38398,#38402,#5475,.T.);
#49293=EDGE_CURVE('',#38403,#38404,#31604,.T.);
#49294=EDGE_CURVE('',#38403,#38405,#5476,.T.);
#49295=EDGE_CURVE('',#38405,#38399,#5477,.T.);
#49296=EDGE_CURVE('',#38400,#38404,#5478,.T.);
#49297=EDGE_CURVE('',#38406,#38407,#31605,.T.);
#49298=EDGE_CURVE('',#38406,#38401,#31606,.T.);
#49299=EDGE_CURVE('',#38402,#38407,#31607,.T.);
#49300=EDGE_CURVE('',#38408,#38409,#31608,.T.);
#49301=EDGE_CURVE('',#38408,#38403,#5479,.T.);
#49302=EDGE_CURVE('',#38404,#38409,#5480,.T.);
#49303=EDGE_CURVE('',#38334,#38406,#5481,.T.);
#49304=EDGE_CURVE('',#38407,#38337,#5482,.T.);
#49305=EDGE_CURVE('',#38410,#38411,#31609,.T.);
#49306=EDGE_CURVE('',#38410,#38408,#31610,.T.);
#49307=EDGE_CURVE('',#38409,#38411,#31611,.T.);
#49308=EDGE_CURVE('',#38346,#38410,#5483,.T.);
#49309=EDGE_CURVE('',#38411,#38342,#5484,.T.);
#49310=EDGE_CURVE('',#38332,#38412,#22014,.T.);
#49311=EDGE_CURVE('',#38413,#38412,#31612,.T.);
#49312=EDGE_CURVE('',#38413,#38336,#22015,.T.);
#49313=EDGE_CURVE('',#38414,#38413,#31613,.T.);
#49314=EDGE_CURVE('',#38412,#38415,#31614,.T.);
#49315=EDGE_CURVE('',#38414,#38415,#31615,.T.);
#49316=EDGE_CURVE('',#38293,#38416,#31616,.T.);
#49317=EDGE_CURVE('',#38417,#38416,#31617,.T.);
#49318=EDGE_CURVE('',#38417,#38414,#31618,.T.);
#49319=EDGE_CURVE('',#38415,#38295,#31619,.T.);
#49320=EDGE_CURVE('',#38418,#38419,#31620,.T.);
#49321=EDGE_CURVE('',#38418,#38417,#31621,.T.);
#49322=EDGE_CURVE('',#38416,#38419,#31622,.T.);
#49323=EDGE_CURVE('',#38328,#38418,#22016,.T.);
#49324=EDGE_CURVE('',#38419,#38326,#22017,.T.);
#49325=EDGE_CURVE('',#38349,#38420,#22018,.T.);
#49326=EDGE_CURVE('',#38421,#38420,#31623,.T.);
#49327=EDGE_CURVE('',#38421,#38410,#22019,.T.);
#49328=EDGE_CURVE('',#38422,#38421,#31624,.T.);
#49329=EDGE_CURVE('',#38420,#38423,#31625,.T.);
#49330=EDGE_CURVE('',#38422,#38423,#31626,.T.);
#49331=EDGE_CURVE('',#38424,#38425,#31627,.T.);
#49332=EDGE_CURVE('',#38424,#38422,#31628,.T.);
#49333=EDGE_CURVE('',#38423,#38425,#31629,.T.);
#49334=EDGE_CURVE('',#38426,#38427,#31630,.T.);
#49335=EDGE_CURVE('',#38426,#38424,#31631,.T.);
#49336=EDGE_CURVE('',#38425,#38427,#31632,.T.);
#49337=EDGE_CURVE('',#38407,#38426,#22020,.T.);
#49338=EDGE_CURVE('',#38427,#38341,#22021,.T.);
#49339=EDGE_CURVE('',#38370,#38428,#22022,.T.);
#49340=EDGE_CURVE('',#38429,#38428,#31633,.T.);
#49341=EDGE_CURVE('',#38429,#38374,#22023,.T.);
#49342=EDGE_CURVE('',#38430,#38431,#31634,.T.);
#49343=EDGE_CURVE('',#38430,#38429,#31635,.T.);
#49344=EDGE_CURVE('',#38428,#38431,#31636,.T.);
#49345=EDGE_CURVE('',#38432,#38433,#31637,.T.);
#49346=EDGE_CURVE('',#38432,#38430,#31638,.T.);
#49347=EDGE_CURVE('',#38431,#38433,#31639,.T.);
#49348=EDGE_CURVE('',#38433,#38434,#31640,.T.);
#49349=EDGE_CURVE('',#38435,#38434,#31641,.T.);
#49350=EDGE_CURVE('',#38435,#38432,#31642,.T.);
#49351=EDGE_CURVE('',#38372,#38435,#22024,.T.);
#49352=EDGE_CURVE('',#38434,#38317,#22025,.T.);
#49353=EDGE_CURVE('',#38307,#38436,#22026,.T.);
#49354=EDGE_CURVE('',#38437,#38436,#31643,.T.);
#49355=EDGE_CURVE('',#38437,#38304,#22027,.T.);
#49356=EDGE_CURVE('',#38438,#38439,#31644,.T.);
#49357=EDGE_CURVE('',#38438,#38437,#31645,.T.);
#49358=EDGE_CURVE('',#38436,#38439,#31646,.T.);
#49359=EDGE_CURVE('',#38440,#38441,#31647,.T.);
#49360=EDGE_CURVE('',#38440,#38438,#31648,.T.);
#49361=EDGE_CURVE('',#38439,#38441,#31649,.T.);
#49362=EDGE_CURVE('',#38441,#38442,#31650,.T.);
#49363=EDGE_CURVE('',#38443,#38442,#31651,.T.);
#49364=EDGE_CURVE('',#38443,#38440,#31652,.T.);
#49365=EDGE_CURVE('',#38315,#38443,#22028,.T.);
#49366=EDGE_CURVE('',#38442,#38311,#22029,.T.);
#49367=EDGE_CURVE('',#38394,#38424,#22030,.T.);
#49368=EDGE_CURVE('',#38426,#38398,#22031,.T.);
#49369=EDGE_CURVE('',#38403,#38421,#22032,.T.);
#49370=EDGE_CURVE('',#38422,#38395,#22033,.T.);
#49371=EDGE_CURVE('',#38344,#38417,#22034,.T.);
#49372=EDGE_CURVE('',#38418,#38329,#22035,.T.);
#49373=EDGE_CURVE('',#38339,#38413,#22036,.T.);
#49374=EDGE_CURVE('',#38414,#38347,#22037,.T.);
#49375=EDGE_CURVE('',#38303,#38437,#22038,.T.);
#49376=EDGE_CURVE('',#38438,#38310,#22039,.T.);
#49377=EDGE_CURVE('',#38443,#38319,#22040,.T.);
#49378=EDGE_CURVE('',#38314,#38440,#22041,.T.);
#49379=EDGE_CURVE('',#38387,#38432,#22042,.T.);
#49380=EDGE_CURVE('',#38435,#38379,#22043,.T.);
#49381=EDGE_CURVE('',#38382,#38429,#22044,.T.);
#49382=EDGE_CURVE('',#38430,#38390,#22045,.T.);
#49383=EDGE_CURVE('',#38444,#38445,#31653,.T.);
#49384=EDGE_CURVE('',#38446,#38445,#31654,.T.);
#49385=EDGE_CURVE('',#38446,#38447,#31655,.T.);
#49386=EDGE_CURVE('',#38444,#38447,#31656,.T.);
#49387=EDGE_CURVE('',#38448,#38449,#31657,.T.);
#49388=EDGE_CURVE('',#38448,#38446,#22046,.T.);
#49389=EDGE_CURVE('',#38445,#38449,#22047,.T.);
#49390=EDGE_CURVE('',#38450,#38451,#31658,.T.);
#49391=EDGE_CURVE('',#38450,#38444,#31659,.T.);
#49392=EDGE_CURVE('',#38447,#38451,#31660,.T.);
#49393=EDGE_CURVE('',#38452,#38453,#31661,.T.);
#49394=EDGE_CURVE('',#38452,#38448,#31662,.T.);
#49395=EDGE_CURVE('',#38449,#38453,#31663,.T.);
#49396=EDGE_CURVE('',#38454,#38455,#31664,.T.);
#49397=EDGE_CURVE('',#38454,#38450,#31665,.T.);
#49398=EDGE_CURVE('',#38451,#38455,#31666,.T.);
#49399=EDGE_CURVE('',#38456,#38457,#31667,.T.);
#49400=EDGE_CURVE('',#38456,#38452,#22048,.T.);
#49401=EDGE_CURVE('',#38453,#38457,#22049,.T.);
#49402=EDGE_CURVE('',#38458,#38459,#31668,.T.);
#49403=EDGE_CURVE('',#38458,#38454,#31669,.T.);
#49404=EDGE_CURVE('',#38455,#38459,#31670,.T.);
#49405=EDGE_CURVE('',#38460,#38461,#31671,.T.);
#49406=EDGE_CURVE('',#38460,#38456,#31672,.T.);
#49407=EDGE_CURVE('',#38457,#38461,#31673,.T.);
#49408=EDGE_CURVE('',#38462,#38463,#31674,.T.);
#49409=EDGE_CURVE('',#38462,#38458,#31675,.T.);
#49410=EDGE_CURVE('',#38459,#38463,#31676,.T.);
#49411=EDGE_CURVE('',#38461,#38462,#22050,.T.);
#49412=EDGE_CURVE('',#38463,#38460,#22051,.T.);
#49413=EDGE_CURVE('',#38464,#38465,#31677,.T.);
#49414=EDGE_CURVE('',#38466,#38465,#31678,.T.);
#49415=EDGE_CURVE('',#38466,#38467,#31679,.T.);
#49416=EDGE_CURVE('',#38464,#38467,#31680,.T.);
#49417=EDGE_CURVE('',#38468,#38469,#31681,.T.);
#49418=EDGE_CURVE('',#38468,#38466,#22052,.T.);
#49419=EDGE_CURVE('',#38465,#38469,#22053,.T.);
#49420=EDGE_CURVE('',#38470,#38471,#31682,.T.);
#49421=EDGE_CURVE('',#38470,#38464,#31683,.T.);
#49422=EDGE_CURVE('',#38467,#38471,#31684,.T.);
#49423=EDGE_CURVE('',#38472,#38473,#31685,.T.);
#49424=EDGE_CURVE('',#38472,#38468,#31686,.T.);
#49425=EDGE_CURVE('',#38469,#38473,#31687,.T.);
#49426=EDGE_CURVE('',#38474,#38475,#31688,.T.);
#49427=EDGE_CURVE('',#38474,#38470,#31689,.T.);
#49428=EDGE_CURVE('',#38471,#38475,#31690,.T.);
#49429=EDGE_CURVE('',#38476,#38477,#31691,.T.);
#49430=EDGE_CURVE('',#38476,#38472,#22054,.T.);
#49431=EDGE_CURVE('',#38473,#38477,#22055,.T.);
#49432=EDGE_CURVE('',#38478,#38479,#31692,.T.);
#49433=EDGE_CURVE('',#38478,#38474,#22056,.T.);
#49434=EDGE_CURVE('',#38475,#38479,#22057,.T.);
#49435=EDGE_CURVE('',#38477,#38478,#31693,.T.);
#49436=EDGE_CURVE('',#38479,#38476,#31694,.T.);
#49437=EDGE_CURVE('',#38480,#38481,#31695,.T.);
#49438=EDGE_CURVE('',#38482,#38481,#31696,.T.);
#49439=EDGE_CURVE('',#38482,#38483,#31697,.T.);
#49440=EDGE_CURVE('',#38480,#38483,#31698,.T.);
#49441=EDGE_CURVE('',#38484,#38485,#31699,.T.);
#49442=EDGE_CURVE('',#38484,#38482,#22058,.T.);
#49443=EDGE_CURVE('',#38481,#38485,#22059,.T.);
#49444=EDGE_CURVE('',#38486,#38487,#31700,.T.);
#49445=EDGE_CURVE('',#38486,#38480,#31701,.T.);
#49446=EDGE_CURVE('',#38483,#38487,#31702,.T.);
#49447=EDGE_CURVE('',#38488,#38489,#31703,.T.);
#49448=EDGE_CURVE('',#38488,#38484,#31704,.T.);
#49449=EDGE_CURVE('',#38485,#38489,#31705,.T.);
#49450=EDGE_CURVE('',#38490,#38491,#31706,.T.);
#49451=EDGE_CURVE('',#38490,#38486,#31707,.T.);
#49452=EDGE_CURVE('',#38487,#38491,#31708,.T.);
#49453=EDGE_CURVE('',#38492,#38493,#31709,.T.);
#49454=EDGE_CURVE('',#38492,#38488,#22060,.T.);
#49455=EDGE_CURVE('',#38489,#38493,#22061,.T.);
#49456=EDGE_CURVE('',#38494,#38495,#31710,.T.);
#49457=EDGE_CURVE('',#38494,#38490,#22062,.T.);
#49458=EDGE_CURVE('',#38491,#38495,#22063,.T.);
#49459=EDGE_CURVE('',#38493,#38494,#31711,.T.);
#49460=EDGE_CURVE('',#38495,#38492,#31712,.T.);
#49461=EDGE_CURVE('',#38496,#38497,#31713,.T.);
#49462=EDGE_CURVE('',#38496,#38498,#31714,.T.);
#49463=EDGE_CURVE('',#38499,#38498,#31715,.T.);
#49464=EDGE_CURVE('',#38499,#38497,#31716,.T.);
#49465=EDGE_CURVE('',#38500,#38501,#31717,.T.);
#49466=EDGE_CURVE('',#38500,#38499,#22064,.T.);
#49467=EDGE_CURVE('',#38498,#38501,#22065,.T.);
#49468=EDGE_CURVE('',#38502,#38503,#31718,.T.);
#49469=EDGE_CURVE('',#38502,#38496,#22066,.T.);
#49470=EDGE_CURVE('',#38497,#38503,#22067,.T.);
#49471=EDGE_CURVE('',#38504,#38505,#31719,.T.);
#49472=EDGE_CURVE('',#38504,#38500,#31720,.T.);
#49473=EDGE_CURVE('',#38501,#38505,#31721,.T.);
#49474=EDGE_CURVE('',#38506,#38507,#31722,.T.);
#49475=EDGE_CURVE('',#38506,#38502,#31723,.T.);
#49476=EDGE_CURVE('',#38503,#38507,#31724,.T.);
#49477=EDGE_CURVE('',#38508,#38509,#31725,.T.);
#49478=EDGE_CURVE('',#38508,#38504,#22068,.T.);
#49479=EDGE_CURVE('',#38505,#38509,#22069,.T.);
#49480=EDGE_CURVE('',#38510,#38511,#31726,.T.);
#49481=EDGE_CURVE('',#38510,#38506,#22070,.T.);
#49482=EDGE_CURVE('',#38507,#38511,#22071,.T.);
#49483=EDGE_CURVE('',#38509,#38510,#31727,.T.);
#49484=EDGE_CURVE('',#38511,#38508,#31728,.T.);
#49485=EDGE_CURVE('',#38512,#38513,#31729,.T.);
#49486=EDGE_CURVE('',#38512,#38514,#31730,.T.);
#49487=EDGE_CURVE('',#38515,#38514,#31731,.T.);
#49488=EDGE_CURVE('',#38515,#38513,#31732,.T.);
#49489=EDGE_CURVE('',#38516,#38517,#31733,.T.);
#49490=EDGE_CURVE('',#38516,#38515,#22072,.T.);
#49491=EDGE_CURVE('',#38514,#38517,#22073,.T.);
#49492=EDGE_CURVE('',#38518,#38519,#31734,.T.);
#49493=EDGE_CURVE('',#38518,#38512,#22074,.T.);
#49494=EDGE_CURVE('',#38513,#38519,#22075,.T.);
#49495=EDGE_CURVE('',#38520,#38521,#31735,.T.);
#49496=EDGE_CURVE('',#38520,#38516,#31736,.T.);
#49497=EDGE_CURVE('',#38517,#38521,#31737,.T.);
#49498=EDGE_CURVE('',#38522,#38523,#31738,.T.);
#49499=EDGE_CURVE('',#38522,#38518,#31739,.T.);
#49500=EDGE_CURVE('',#38519,#38523,#31740,.T.);
#49501=EDGE_CURVE('',#38524,#38525,#31741,.T.);
#49502=EDGE_CURVE('',#38524,#38520,#31742,.T.);
#49503=EDGE_CURVE('',#38521,#38525,#31743,.T.);
#49504=EDGE_CURVE('',#38526,#38527,#31744,.T.);
#49505=EDGE_CURVE('',#38526,#38522,#22076,.T.);
#49506=EDGE_CURVE('',#38523,#38527,#22077,.T.);
#49507=EDGE_CURVE('',#38528,#38529,#31745,.T.);
#49508=EDGE_CURVE('',#38528,#38524,#31746,.T.);
#49509=EDGE_CURVE('',#38525,#38529,#31747,.T.);
#49510=EDGE_CURVE('',#38527,#38528,#31748,.T.);
#49511=EDGE_CURVE('',#38529,#38526,#31749,.T.);
#49512=EDGE_CURVE('',#38530,#38531,#31750,.T.);
#49513=EDGE_CURVE('',#38530,#38532,#31751,.T.);
#49514=EDGE_CURVE('',#38533,#38532,#31752,.T.);
#49515=EDGE_CURVE('',#38533,#38531,#31753,.T.);
#49516=EDGE_CURVE('',#38534,#38535,#31754,.T.);
#49517=EDGE_CURVE('',#38534,#38533,#22078,.T.);
#49518=EDGE_CURVE('',#38532,#38535,#22079,.T.);
#49519=EDGE_CURVE('',#38536,#38537,#31755,.T.);
#49520=EDGE_CURVE('',#38536,#38530,#22080,.T.);
#49521=EDGE_CURVE('',#38531,#38537,#22081,.T.);
#49522=EDGE_CURVE('',#38538,#38539,#31756,.T.);
#49523=EDGE_CURVE('',#38538,#38534,#31757,.T.);
#49524=EDGE_CURVE('',#38535,#38539,#31758,.T.);
#49525=EDGE_CURVE('',#38540,#38541,#31759,.T.);
#49526=EDGE_CURVE('',#38540,#38536,#31760,.T.);
#49527=EDGE_CURVE('',#38537,#38541,#31761,.T.);
#49528=EDGE_CURVE('',#38542,#38543,#31762,.T.);
#49529=EDGE_CURVE('',#38542,#38538,#22082,.T.);
#49530=EDGE_CURVE('',#38539,#38543,#22083,.T.);
#49531=EDGE_CURVE('',#38544,#38545,#31763,.T.);
#49532=EDGE_CURVE('',#38544,#38540,#22084,.T.);
#49533=EDGE_CURVE('',#38541,#38545,#22085,.T.);
#49534=EDGE_CURVE('',#38543,#38544,#31764,.T.);
#49535=EDGE_CURVE('',#38545,#38542,#31765,.T.);
#49536=EDGE_CURVE('',#38546,#38547,#31766,.T.);
#49537=EDGE_CURVE('',#38546,#38548,#31767,.T.);
#49538=EDGE_CURVE('',#38549,#38548,#31768,.T.);
#49539=EDGE_CURVE('',#38549,#38547,#31769,.T.);
#49540=EDGE_CURVE('',#38550,#38551,#31770,.T.);
#49541=EDGE_CURVE('',#38550,#38549,#22086,.T.);
#49542=EDGE_CURVE('',#38548,#38551,#22087,.T.);
#49543=EDGE_CURVE('',#38552,#38553,#31771,.T.);
#49544=EDGE_CURVE('',#38552,#38546,#22088,.T.);
#49545=EDGE_CURVE('',#38547,#38553,#22089,.T.);
#49546=EDGE_CURVE('',#38554,#38555,#31772,.T.);
#49547=EDGE_CURVE('',#38554,#38550,#31773,.T.);
#49548=EDGE_CURVE('',#38551,#38555,#31774,.T.);
#49549=EDGE_CURVE('',#38556,#38557,#31775,.T.);
#49550=EDGE_CURVE('',#38556,#38552,#31776,.T.);
#49551=EDGE_CURVE('',#38553,#38557,#31777,.T.);
#49552=EDGE_CURVE('',#38558,#38559,#31778,.T.);
#49553=EDGE_CURVE('',#38558,#38554,#22090,.T.);
#49554=EDGE_CURVE('',#38555,#38559,#22091,.T.);
#49555=EDGE_CURVE('',#38560,#38561,#31779,.T.);
#49556=EDGE_CURVE('',#38560,#38556,#22092,.T.);
#49557=EDGE_CURVE('',#38557,#38561,#22093,.T.);
#49558=EDGE_CURVE('',#38559,#38560,#31780,.T.);
#49559=EDGE_CURVE('',#38561,#38558,#31781,.T.);
#49560=EDGE_CURVE('',#38562,#38563,#31782,.T.);
#49561=EDGE_CURVE('',#38562,#38564,#31783,.T.);
#49562=EDGE_CURVE('',#38565,#38564,#31784,.T.);
#49563=EDGE_CURVE('',#38565,#38563,#31785,.T.);
#49564=EDGE_CURVE('',#38566,#38567,#31786,.T.);
#49565=EDGE_CURVE('',#38566,#38565,#22094,.T.);
#49566=EDGE_CURVE('',#38564,#38567,#22095,.T.);
#49567=EDGE_CURVE('',#38568,#38569,#31787,.T.);
#49568=EDGE_CURVE('',#38568,#38562,#22096,.T.);
#49569=EDGE_CURVE('',#38563,#38569,#22097,.T.);
#49570=EDGE_CURVE('',#38570,#38571,#31788,.T.);
#49571=EDGE_CURVE('',#38570,#38566,#31789,.T.);
#49572=EDGE_CURVE('',#38567,#38571,#31790,.T.);
#49573=EDGE_CURVE('',#38572,#38573,#31791,.T.);
#49574=EDGE_CURVE('',#38572,#38568,#31792,.T.);
#49575=EDGE_CURVE('',#38569,#38573,#31793,.T.);
#49576=EDGE_CURVE('',#38574,#38575,#31794,.T.);
#49577=EDGE_CURVE('',#38574,#38570,#22098,.T.);
#49578=EDGE_CURVE('',#38571,#38575,#22099,.T.);
#49579=EDGE_CURVE('',#38576,#38577,#31795,.T.);
#49580=EDGE_CURVE('',#38576,#38572,#22100,.T.);
#49581=EDGE_CURVE('',#38573,#38577,#22101,.T.);
#49582=EDGE_CURVE('',#38575,#38576,#31796,.T.);
#49583=EDGE_CURVE('',#38577,#38574,#31797,.T.);
#49584=EDGE_CURVE('',#38578,#38579,#31798,.T.);
#49585=EDGE_CURVE('',#38578,#38580,#31799,.T.);
#49586=EDGE_CURVE('',#38581,#38580,#31800,.T.);
#49587=EDGE_CURVE('',#38581,#38579,#31801,.T.);
#49588=EDGE_CURVE('',#38582,#38583,#31802,.T.);
#49589=EDGE_CURVE('',#38582,#38581,#22102,.T.);
#49590=EDGE_CURVE('',#38580,#38583,#22103,.T.);
#49591=EDGE_CURVE('',#38584,#38585,#31803,.T.);
#49592=EDGE_CURVE('',#38584,#38578,#22104,.T.);
#49593=EDGE_CURVE('',#38579,#38585,#22105,.T.);
#49594=EDGE_CURVE('',#38586,#38587,#31804,.T.);
#49595=EDGE_CURVE('',#38586,#38582,#31805,.T.);
#49596=EDGE_CURVE('',#38583,#38587,#31806,.T.);
#49597=EDGE_CURVE('',#38588,#38589,#31807,.T.);
#49598=EDGE_CURVE('',#38588,#38584,#31808,.T.);
#49599=EDGE_CURVE('',#38585,#38589,#31809,.T.);
#49600=EDGE_CURVE('',#38590,#38591,#31810,.T.);
#49601=EDGE_CURVE('',#38590,#38586,#22106,.T.);
#49602=EDGE_CURVE('',#38587,#38591,#22107,.T.);
#49603=EDGE_CURVE('',#38592,#38593,#31811,.T.);
#49604=EDGE_CURVE('',#38592,#38588,#22108,.T.);
#49605=EDGE_CURVE('',#38589,#38593,#22109,.T.);
#49606=EDGE_CURVE('',#38591,#38592,#31812,.T.);
#49607=EDGE_CURVE('',#38593,#38590,#31813,.T.);
#49608=EDGE_CURVE('',#38594,#38595,#31814,.T.);
#49609=EDGE_CURVE('',#38594,#38596,#31815,.T.);
#49610=EDGE_CURVE('',#38597,#38596,#31816,.T.);
#49611=EDGE_CURVE('',#38597,#38595,#31817,.T.);
#49612=EDGE_CURVE('',#38598,#38599,#31818,.T.);
#49613=EDGE_CURVE('',#38598,#38597,#22110,.T.);
#49614=EDGE_CURVE('',#38596,#38599,#22111,.T.);
#49615=EDGE_CURVE('',#38600,#38601,#31819,.T.);
#49616=EDGE_CURVE('',#38600,#38594,#22112,.T.);
#49617=EDGE_CURVE('',#38595,#38601,#22113,.T.);
#49618=EDGE_CURVE('',#38602,#38603,#31820,.T.);
#49619=EDGE_CURVE('',#38602,#38598,#31821,.T.);
#49620=EDGE_CURVE('',#38599,#38603,#31822,.T.);
#49621=EDGE_CURVE('',#38604,#38605,#31823,.T.);
#49622=EDGE_CURVE('',#38604,#38600,#31824,.T.);
#49623=EDGE_CURVE('',#38601,#38605,#31825,.T.);
#49624=EDGE_CURVE('',#38606,#38607,#31826,.T.);
#49625=EDGE_CURVE('',#38606,#38602,#22114,.T.);
#49626=EDGE_CURVE('',#38603,#38607,#22115,.T.);
#49627=EDGE_CURVE('',#38608,#38609,#31827,.T.);
#49628=EDGE_CURVE('',#38608,#38604,#31828,.T.);
#49629=EDGE_CURVE('',#38605,#38609,#31829,.T.);
#49630=EDGE_CURVE('',#38607,#38608,#31830,.T.);
#49631=EDGE_CURVE('',#38609,#38606,#31831,.T.);
#49632=EDGE_CURVE('',#38610,#38611,#31832,.T.);
#49633=EDGE_CURVE('',#38610,#38612,#31833,.T.);
#49634=EDGE_CURVE('',#38613,#38612,#31834,.T.);
#49635=EDGE_CURVE('',#38613,#38611,#31835,.T.);
#49636=EDGE_CURVE('',#38614,#38615,#31836,.T.);
#49637=EDGE_CURVE('',#38614,#38613,#22116,.T.);
#49638=EDGE_CURVE('',#38612,#38615,#22117,.T.);
#49639=EDGE_CURVE('',#38616,#38617,#31837,.T.);
#49640=EDGE_CURVE('',#38616,#38610,#22118,.T.);
#49641=EDGE_CURVE('',#38611,#38617,#22119,.T.);
#49642=EDGE_CURVE('',#38618,#38619,#31838,.T.);
#49643=EDGE_CURVE('',#38618,#38614,#31839,.T.);
#49644=EDGE_CURVE('',#38615,#38619,#31840,.T.);
#49645=EDGE_CURVE('',#38620,#38621,#31841,.T.);
#49646=EDGE_CURVE('',#38620,#38616,#31842,.T.);
#49647=EDGE_CURVE('',#38617,#38621,#31843,.T.);
#49648=EDGE_CURVE('',#38622,#38623,#31844,.T.);
#49649=EDGE_CURVE('',#38622,#38618,#22120,.T.);
#49650=EDGE_CURVE('',#38619,#38623,#22121,.T.);
#49651=EDGE_CURVE('',#38624,#38625,#31845,.T.);
#49652=EDGE_CURVE('',#38624,#38620,#31846,.T.);
#49653=EDGE_CURVE('',#38621,#38625,#31847,.T.);
#49654=EDGE_CURVE('',#38626,#38627,#31848,.T.);
#49655=EDGE_CURVE('',#38626,#38622,#31849,.T.);
#49656=EDGE_CURVE('',#38623,#38627,#31850,.T.);
#49657=EDGE_CURVE('',#38628,#38629,#31851,.T.);
#49658=EDGE_CURVE('',#38628,#38624,#31852,.T.);
#49659=EDGE_CURVE('',#38625,#38629,#31853,.T.);
#49660=EDGE_CURVE('',#38627,#38628,#31854,.T.);
#49661=EDGE_CURVE('',#38629,#38626,#31855,.T.);
#49662=EDGE_CURVE('',#38630,#38631,#31856,.T.);
#49663=EDGE_CURVE('',#38630,#38632,#31857,.T.);
#49664=EDGE_CURVE('',#38633,#38632,#31858,.T.);
#49665=EDGE_CURVE('',#38633,#38631,#31859,.T.);
#49666=EDGE_CURVE('',#38634,#38635,#31860,.T.);
#49667=EDGE_CURVE('',#38634,#38633,#22122,.T.);
#49668=EDGE_CURVE('',#38632,#38635,#22123,.T.);
#49669=EDGE_CURVE('',#38636,#38637,#31861,.T.);
#49670=EDGE_CURVE('',#38636,#38630,#22124,.T.);
#49671=EDGE_CURVE('',#38631,#38637,#22125,.T.);
#49672=EDGE_CURVE('',#38638,#38639,#31862,.T.);
#49673=EDGE_CURVE('',#38638,#38634,#31863,.T.);
#49674=EDGE_CURVE('',#38635,#38639,#31864,.T.);
#49675=EDGE_CURVE('',#38640,#38641,#31865,.T.);
#49676=EDGE_CURVE('',#38640,#38636,#31866,.T.);
#49677=EDGE_CURVE('',#38637,#38641,#31867,.T.);
#49678=EDGE_CURVE('',#38642,#38643,#31868,.T.);
#49679=EDGE_CURVE('',#38642,#38638,#22126,.T.);
#49680=EDGE_CURVE('',#38639,#38643,#22127,.T.);
#49681=EDGE_CURVE('',#38644,#38645,#31869,.T.);
#49682=EDGE_CURVE('',#38644,#38640,#31870,.T.);
#49683=EDGE_CURVE('',#38641,#38645,#31871,.T.);
#49684=EDGE_CURVE('',#38643,#38644,#31872,.T.);
#49685=EDGE_CURVE('',#38645,#38642,#31873,.T.);
#49686=EDGE_CURVE('',#38646,#38647,#31874,.T.);
#49687=EDGE_CURVE('',#38646,#38648,#31875,.T.);
#49688=EDGE_CURVE('',#38649,#38648,#31876,.T.);
#49689=EDGE_CURVE('',#38649,#38647,#31877,.T.);
#49690=EDGE_CURVE('',#38650,#38651,#31878,.T.);
#49691=EDGE_CURVE('',#38650,#38649,#22128,.T.);
#49692=EDGE_CURVE('',#38648,#38651,#22129,.T.);
#49693=EDGE_CURVE('',#38652,#38653,#31879,.T.);
#49694=EDGE_CURVE('',#38652,#38646,#22130,.T.);
#49695=EDGE_CURVE('',#38647,#38653,#22131,.T.);
#49696=EDGE_CURVE('',#38654,#38655,#31880,.T.);
#49697=EDGE_CURVE('',#38654,#38650,#31881,.T.);
#49698=EDGE_CURVE('',#38651,#38655,#31882,.T.);
#49699=EDGE_CURVE('',#38656,#38657,#31883,.T.);
#49700=EDGE_CURVE('',#38656,#38652,#31884,.T.);
#49701=EDGE_CURVE('',#38653,#38657,#31885,.T.);
#49702=EDGE_CURVE('',#38658,#38659,#31886,.T.);
#49703=EDGE_CURVE('',#38658,#38654,#22132,.T.);
#49704=EDGE_CURVE('',#38655,#38659,#22133,.T.);
#49705=EDGE_CURVE('',#38660,#38661,#31887,.T.);
#49706=EDGE_CURVE('',#38660,#38656,#22134,.T.);
#49707=EDGE_CURVE('',#38657,#38661,#22135,.T.);
#49708=EDGE_CURVE('',#38659,#38660,#31888,.T.);
#49709=EDGE_CURVE('',#38661,#38658,#31889,.T.);
#49710=EDGE_CURVE('',#38662,#38663,#31890,.T.);
#49711=EDGE_CURVE('',#38662,#38664,#31891,.T.);
#49712=EDGE_CURVE('',#38665,#38664,#31892,.T.);
#49713=EDGE_CURVE('',#38665,#38663,#31893,.T.);
#49714=EDGE_CURVE('',#38666,#38667,#31894,.T.);
#49715=EDGE_CURVE('',#38666,#38665,#22136,.T.);
#49716=EDGE_CURVE('',#38664,#38667,#22137,.T.);
#49717=EDGE_CURVE('',#38668,#38669,#31895,.T.);
#49718=EDGE_CURVE('',#38668,#38662,#31896,.T.);
#49719=EDGE_CURVE('',#38663,#38669,#31897,.T.);
#49720=EDGE_CURVE('',#38670,#38671,#31898,.T.);
#49721=EDGE_CURVE('',#38670,#38666,#31899,.T.);
#49722=EDGE_CURVE('',#38667,#38671,#31900,.T.);
#49723=EDGE_CURVE('',#38672,#38673,#31901,.T.);
#49724=EDGE_CURVE('',#38672,#38668,#31902,.T.);
#49725=EDGE_CURVE('',#38669,#38673,#31903,.T.);
#49726=EDGE_CURVE('',#38674,#38675,#31904,.T.);
#49727=EDGE_CURVE('',#38674,#38670,#22138,.T.);
#49728=EDGE_CURVE('',#38671,#38675,#22139,.T.);
#49729=EDGE_CURVE('',#38676,#38677,#31905,.T.);
#49730=EDGE_CURVE('',#38676,#38672,#22140,.T.);
#49731=EDGE_CURVE('',#38673,#38677,#22141,.T.);
#49732=EDGE_CURVE('',#38678,#38679,#31906,.T.);
#49733=EDGE_CURVE('',#38678,#38674,#31907,.T.);
#49734=EDGE_CURVE('',#38675,#38679,#31908,.T.);
#49735=EDGE_CURVE('',#38680,#38681,#31909,.T.);
#49736=EDGE_CURVE('',#38680,#38676,#31910,.T.);
#49737=EDGE_CURVE('',#38677,#38681,#31911,.T.);
#49738=EDGE_CURVE('',#38679,#38680,#22142,.T.);
#49739=EDGE_CURVE('',#38681,#38678,#22143,.T.);
#49740=EDGE_CURVE('',#38682,#38683,#31912,.T.);
#49741=EDGE_CURVE('',#38682,#38684,#31913,.T.);
#49742=EDGE_CURVE('',#38685,#38684,#31914,.T.);
#49743=EDGE_CURVE('',#38685,#38683,#31915,.T.);
#49744=EDGE_CURVE('',#38686,#38687,#31916,.T.);
#49745=EDGE_CURVE('',#38686,#38685,#22144,.T.);
#49746=EDGE_CURVE('',#38684,#38687,#22145,.T.);
#49747=EDGE_CURVE('',#38688,#38689,#31917,.T.);
#49748=EDGE_CURVE('',#38688,#38682,#22146,.T.);
#49749=EDGE_CURVE('',#38683,#38689,#22147,.T.);
#49750=EDGE_CURVE('',#38690,#38691,#31918,.T.);
#49751=EDGE_CURVE('',#38690,#38686,#31919,.T.);
#49752=EDGE_CURVE('',#38687,#38691,#31920,.T.);
#49753=EDGE_CURVE('',#38692,#38693,#31921,.T.);
#49754=EDGE_CURVE('',#38692,#38688,#31922,.T.);
#49755=EDGE_CURVE('',#38689,#38693,#31923,.T.);
#49756=EDGE_CURVE('',#38694,#38695,#31924,.T.);
#49757=EDGE_CURVE('',#38694,#38690,#22148,.T.);
#49758=EDGE_CURVE('',#38691,#38695,#22149,.T.);
#49759=EDGE_CURVE('',#38696,#38697,#31925,.T.);
#49760=EDGE_CURVE('',#38696,#38692,#31926,.T.);
#49761=EDGE_CURVE('',#38693,#38697,#31927,.T.);
#49762=EDGE_CURVE('',#38698,#38699,#31928,.T.);
#49763=EDGE_CURVE('',#38698,#38694,#31929,.T.);
#49764=EDGE_CURVE('',#38695,#38699,#31930,.T.);
#49765=EDGE_CURVE('',#38700,#38701,#31931,.T.);
#49766=EDGE_CURVE('',#38700,#38696,#31932,.T.);
#49767=EDGE_CURVE('',#38697,#38701,#31933,.T.);
#49768=EDGE_CURVE('',#38699,#38700,#22150,.T.);
#49769=EDGE_CURVE('',#38701,#38698,#22151,.T.);
#49770=EDGE_CURVE('',#38702,#38703,#31934,.T.);
#49771=EDGE_CURVE('',#38702,#38704,#31935,.T.);
#49772=EDGE_CURVE('',#38705,#38704,#31936,.T.);
#49773=EDGE_CURVE('',#38705,#38703,#31937,.T.);
#49774=EDGE_CURVE('',#38706,#38707,#31938,.T.);
#49775=EDGE_CURVE('',#38706,#38705,#22152,.T.);
#49776=EDGE_CURVE('',#38704,#38707,#22153,.T.);
#49777=EDGE_CURVE('',#38708,#38709,#31939,.T.);
#49778=EDGE_CURVE('',#38708,#38702,#22154,.T.);
#49779=EDGE_CURVE('',#38703,#38709,#22155,.T.);
#49780=EDGE_CURVE('',#38710,#38711,#31940,.T.);
#49781=EDGE_CURVE('',#38710,#38706,#31941,.T.);
#49782=EDGE_CURVE('',#38707,#38711,#31942,.T.);
#49783=EDGE_CURVE('',#38712,#38713,#31943,.T.);
#49784=EDGE_CURVE('',#38712,#38708,#31944,.T.);
#49785=EDGE_CURVE('',#38709,#38713,#31945,.T.);
#49786=EDGE_CURVE('',#38714,#38715,#31946,.T.);
#49787=EDGE_CURVE('',#38714,#38710,#22156,.T.);
#49788=EDGE_CURVE('',#38711,#38715,#22157,.T.);
#49789=EDGE_CURVE('',#38716,#38717,#31947,.T.);
#49790=EDGE_CURVE('',#38716,#38712,#22158,.T.);
#49791=EDGE_CURVE('',#38713,#38717,#22159,.T.);
#49792=EDGE_CURVE('',#38715,#38716,#31948,.T.);
#49793=EDGE_CURVE('',#38717,#38714,#31949,.T.);
#49794=EDGE_CURVE('',#38718,#38719,#31950,.T.);
#49795=EDGE_CURVE('',#38718,#38720,#31951,.T.);
#49796=EDGE_CURVE('',#38721,#38720,#31952,.T.);
#49797=EDGE_CURVE('',#38721,#38719,#31953,.T.);
#49798=EDGE_CURVE('',#38722,#38723,#31954,.T.);
#49799=EDGE_CURVE('',#38722,#38721,#22160,.T.);
#49800=EDGE_CURVE('',#38720,#38723,#22161,.T.);
#49801=EDGE_CURVE('',#38724,#38725,#31955,.T.);
#49802=EDGE_CURVE('',#38724,#38718,#22162,.T.);
#49803=EDGE_CURVE('',#38719,#38725,#22163,.T.);
#49804=EDGE_CURVE('',#38726,#38727,#31956,.T.);
#49805=EDGE_CURVE('',#38726,#38722,#31957,.T.);
#49806=EDGE_CURVE('',#38723,#38727,#31958,.T.);
#49807=EDGE_CURVE('',#38728,#38729,#31959,.T.);
#49808=EDGE_CURVE('',#38728,#38724,#31960,.T.);
#49809=EDGE_CURVE('',#38725,#38729,#31961,.T.);
#49810=EDGE_CURVE('',#38730,#38731,#31962,.T.);
#49811=EDGE_CURVE('',#38730,#38726,#31963,.T.);
#49812=EDGE_CURVE('',#38727,#38731,#31964,.T.);
#49813=EDGE_CURVE('',#38732,#38733,#31965,.T.);
#49814=EDGE_CURVE('',#38732,#38728,#22164,.T.);
#49815=EDGE_CURVE('',#38729,#38733,#22165,.T.);
#49816=EDGE_CURVE('',#38731,#38732,#31966,.T.);
#49817=EDGE_CURVE('',#38733,#38730,#31967,.T.);
#49818=EDGE_CURVE('',#38734,#38735,#31968,.T.);
#49819=EDGE_CURVE('',#38734,#38736,#31969,.T.);
#49820=EDGE_CURVE('',#38737,#38736,#31970,.T.);
#49821=EDGE_CURVE('',#38737,#38735,#31971,.T.);
#49822=EDGE_CURVE('',#38738,#38739,#31972,.T.);
#49823=EDGE_CURVE('',#38738,#38737,#22166,.T.);
#49824=EDGE_CURVE('',#38736,#38739,#22167,.T.);
#49825=EDGE_CURVE('',#38740,#38741,#31973,.T.);
#49826=EDGE_CURVE('',#38740,#38734,#22168,.T.);
#49827=EDGE_CURVE('',#38735,#38741,#22169,.T.);
#49828=EDGE_CURVE('',#38742,#38743,#31974,.T.);
#49829=EDGE_CURVE('',#38742,#38738,#31975,.T.);
#49830=EDGE_CURVE('',#38739,#38743,#31976,.T.);
#49831=EDGE_CURVE('',#38744,#38745,#31977,.T.);
#49832=EDGE_CURVE('',#38744,#38740,#31978,.T.);
#49833=EDGE_CURVE('',#38741,#38745,#31979,.T.);
#49834=EDGE_CURVE('',#38746,#38747,#31980,.T.);
#49835=EDGE_CURVE('',#38746,#38742,#22170,.T.);
#49836=EDGE_CURVE('',#38743,#38747,#22171,.T.);
#49837=EDGE_CURVE('',#38748,#38749,#31981,.T.);
#49838=EDGE_CURVE('',#38748,#38744,#22172,.T.);
#49839=EDGE_CURVE('',#38745,#38749,#22173,.T.);
#49840=EDGE_CURVE('',#38747,#38748,#31982,.T.);
#49841=EDGE_CURVE('',#38749,#38746,#31983,.T.);
#49842=EDGE_CURVE('',#38750,#38751,#31984,.T.);
#49843=EDGE_CURVE('',#38750,#38752,#31985,.T.);
#49844=EDGE_CURVE('',#38753,#38752,#31986,.T.);
#49845=EDGE_CURVE('',#38753,#38751,#31987,.T.);
#49846=EDGE_CURVE('',#38754,#38755,#31988,.T.);
#49847=EDGE_CURVE('',#38754,#38753,#22174,.T.);
#49848=EDGE_CURVE('',#38752,#38755,#22175,.T.);
#49849=EDGE_CURVE('',#38756,#38757,#31989,.T.);
#49850=EDGE_CURVE('',#38756,#38750,#22176,.T.);
#49851=EDGE_CURVE('',#38751,#38757,#22177,.T.);
#49852=EDGE_CURVE('',#38758,#38759,#31990,.T.);
#49853=EDGE_CURVE('',#38758,#38754,#31991,.T.);
#49854=EDGE_CURVE('',#38755,#38759,#31992,.T.);
#49855=EDGE_CURVE('',#38760,#38761,#31993,.T.);
#49856=EDGE_CURVE('',#38760,#38756,#31994,.T.);
#49857=EDGE_CURVE('',#38757,#38761,#31995,.T.);
#49858=EDGE_CURVE('',#38762,#38763,#31996,.T.);
#49859=EDGE_CURVE('',#38762,#38758,#22178,.T.);
#49860=EDGE_CURVE('',#38759,#38763,#22179,.T.);
#49861=EDGE_CURVE('',#38764,#38765,#31997,.T.);
#49862=EDGE_CURVE('',#38764,#38760,#22180,.T.);
#49863=EDGE_CURVE('',#38761,#38765,#22181,.T.);
#49864=EDGE_CURVE('',#38763,#38764,#31998,.T.);
#49865=EDGE_CURVE('',#38765,#38762,#31999,.T.);
#49866=EDGE_CURVE('',#38766,#38767,#32000,.T.);
#49867=EDGE_CURVE('',#38766,#38768,#32001,.T.);
#49868=EDGE_CURVE('',#38769,#38768,#32002,.T.);
#49869=EDGE_CURVE('',#38769,#38767,#32003,.T.);
#49870=EDGE_CURVE('',#38770,#38771,#32004,.T.);
#49871=EDGE_CURVE('',#38770,#38769,#22182,.T.);
#49872=EDGE_CURVE('',#38768,#38771,#22183,.T.);
#49873=EDGE_CURVE('',#38772,#38773,#32005,.T.);
#49874=EDGE_CURVE('',#38772,#38766,#22184,.T.);
#49875=EDGE_CURVE('',#38767,#38773,#22185,.T.);
#49876=EDGE_CURVE('',#38774,#38775,#32006,.T.);
#49877=EDGE_CURVE('',#38774,#38770,#32007,.T.);
#49878=EDGE_CURVE('',#38771,#38775,#32008,.T.);
#49879=EDGE_CURVE('',#38776,#38777,#32009,.T.);
#49880=EDGE_CURVE('',#38776,#38772,#32010,.T.);
#49881=EDGE_CURVE('',#38773,#38777,#32011,.T.);
#49882=EDGE_CURVE('',#38778,#38779,#32012,.T.);
#49883=EDGE_CURVE('',#38778,#38774,#22186,.T.);
#49884=EDGE_CURVE('',#38775,#38779,#22187,.T.);
#49885=EDGE_CURVE('',#38780,#38781,#32013,.T.);
#49886=EDGE_CURVE('',#38780,#38776,#32014,.T.);
#49887=EDGE_CURVE('',#38777,#38781,#32015,.T.);
#49888=EDGE_CURVE('',#38779,#38782,#32016,.T.);
#49889=EDGE_CURVE('',#38783,#38782,#32017,.T.);
#49890=EDGE_CURVE('',#38783,#38778,#32018,.T.);
#49891=EDGE_CURVE('',#38781,#38783,#32019,.T.);
#49892=EDGE_CURVE('',#38782,#38780,#32020,.T.);
#49893=EDGE_CURVE('',#38784,#38785,#32021,.T.);
#49894=EDGE_CURVE('',#38784,#38786,#32022,.T.);
#49895=EDGE_CURVE('',#38787,#38786,#32023,.T.);
#49896=EDGE_CURVE('',#38787,#38785,#32024,.T.);
#49897=EDGE_CURVE('',#38788,#38789,#32025,.T.);
#49898=EDGE_CURVE('',#38788,#38787,#22188,.T.);
#49899=EDGE_CURVE('',#38786,#38789,#22189,.T.);
#49900=EDGE_CURVE('',#38790,#38791,#32026,.T.);
#49901=EDGE_CURVE('',#38790,#38784,#22190,.T.);
#49902=EDGE_CURVE('',#38785,#38791,#22191,.T.);
#49903=EDGE_CURVE('',#38792,#38793,#32027,.T.);
#49904=EDGE_CURVE('',#38792,#38788,#32028,.T.);
#49905=EDGE_CURVE('',#38789,#38793,#32029,.T.);
#49906=EDGE_CURVE('',#38794,#38795,#32030,.T.);
#49907=EDGE_CURVE('',#38794,#38790,#32031,.T.);
#49908=EDGE_CURVE('',#38791,#38795,#32032,.T.);
#49909=EDGE_CURVE('',#38796,#38797,#32033,.T.);
#49910=EDGE_CURVE('',#38796,#38792,#32034,.T.);
#49911=EDGE_CURVE('',#38793,#38797,#32035,.T.);
#49912=EDGE_CURVE('',#38798,#38799,#32036,.T.);
#49913=EDGE_CURVE('',#38798,#38794,#22192,.T.);
#49914=EDGE_CURVE('',#38795,#38799,#22193,.T.);
#49915=EDGE_CURVE('',#38797,#38798,#32037,.T.);
#49916=EDGE_CURVE('',#38799,#38796,#32038,.T.);
#49917=EDGE_CURVE('',#38800,#38801,#32039,.T.);
#49918=EDGE_CURVE('',#38800,#38802,#32040,.T.);
#49919=EDGE_CURVE('',#38803,#38802,#32041,.T.);
#49920=EDGE_CURVE('',#38803,#38801,#32042,.T.);
#49921=EDGE_CURVE('',#38804,#38805,#32043,.T.);
#49922=EDGE_CURVE('',#38804,#38803,#22194,.T.);
#49923=EDGE_CURVE('',#38802,#38805,#22195,.T.);
#49924=EDGE_CURVE('',#38806,#38807,#32044,.T.);
#49925=EDGE_CURVE('',#38806,#38800,#22196,.T.);
#49926=EDGE_CURVE('',#38801,#38807,#22197,.T.);
#49927=EDGE_CURVE('',#38808,#38809,#32045,.T.);
#49928=EDGE_CURVE('',#38808,#38804,#32046,.T.);
#49929=EDGE_CURVE('',#38805,#38809,#32047,.T.);
#49930=EDGE_CURVE('',#38810,#38811,#32048,.T.);
#49931=EDGE_CURVE('',#38810,#38806,#32049,.T.);
#49932=EDGE_CURVE('',#38807,#38811,#32050,.T.);
#49933=EDGE_CURVE('',#38812,#38813,#32051,.T.);
#49934=EDGE_CURVE('',#38812,#38808,#32052,.T.);
#49935=EDGE_CURVE('',#38809,#38813,#32053,.T.);
#49936=EDGE_CURVE('',#38814,#38815,#32054,.T.);
#49937=EDGE_CURVE('',#38814,#38810,#22198,.T.);
#49938=EDGE_CURVE('',#38811,#38815,#22199,.T.);
#49939=EDGE_CURVE('',#38816,#38817,#32055,.T.);
#49940=EDGE_CURVE('',#38816,#38812,#32056,.T.);
#49941=EDGE_CURVE('',#38813,#38817,#32057,.T.);
#49942=EDGE_CURVE('',#38818,#38819,#32058,.T.);
#49943=EDGE_CURVE('',#38818,#38814,#32059,.T.);
#49944=EDGE_CURVE('',#38815,#38819,#32060,.T.);
#49945=EDGE_CURVE('',#38817,#38818,#32061,.T.);
#49946=EDGE_CURVE('',#38819,#38816,#32062,.T.);
#49947=EDGE_CURVE('',#38820,#38821,#32063,.T.);
#49948=EDGE_CURVE('',#38820,#38822,#32064,.T.);
#49949=EDGE_CURVE('',#38823,#38822,#32065,.T.);
#49950=EDGE_CURVE('',#38823,#38821,#32066,.T.);
#49951=EDGE_CURVE('',#38824,#38825,#32067,.T.);
#49952=EDGE_CURVE('',#38824,#38823,#22200,.T.);
#49953=EDGE_CURVE('',#38822,#38825,#22201,.T.);
#49954=EDGE_CURVE('',#38826,#38827,#32068,.T.);
#49955=EDGE_CURVE('',#38826,#38820,#22202,.T.);
#49956=EDGE_CURVE('',#38821,#38827,#22203,.T.);
#49957=EDGE_CURVE('',#38828,#38829,#32069,.T.);
#49958=EDGE_CURVE('',#38828,#38824,#32070,.T.);
#49959=EDGE_CURVE('',#38825,#38829,#32071,.T.);
#49960=EDGE_CURVE('',#38830,#38831,#32072,.T.);
#49961=EDGE_CURVE('',#38830,#38826,#32073,.T.);
#49962=EDGE_CURVE('',#38827,#38831,#32074,.T.);
#49963=EDGE_CURVE('',#38832,#38833,#32075,.T.);
#49964=EDGE_CURVE('',#38832,#38828,#22204,.T.);
#49965=EDGE_CURVE('',#38829,#38833,#22205,.T.);
#49966=EDGE_CURVE('',#38834,#38835,#32076,.T.);
#49967=EDGE_CURVE('',#38834,#38830,#22206,.T.);
#49968=EDGE_CURVE('',#38831,#38835,#22207,.T.);
#49969=EDGE_CURVE('',#38833,#38834,#32077,.T.);
#49970=EDGE_CURVE('',#38835,#38832,#32078,.T.);
#49971=EDGE_CURVE('',#38836,#38837,#32079,.T.);
#49972=EDGE_CURVE('',#38836,#38838,#32080,.T.);
#49973=EDGE_CURVE('',#38839,#38838,#32081,.T.);
#49974=EDGE_CURVE('',#38839,#38837,#32082,.T.);
#49975=EDGE_CURVE('',#38840,#38841,#32083,.T.);
#49976=EDGE_CURVE('',#38840,#38839,#22208,.T.);
#49977=EDGE_CURVE('',#38838,#38841,#22209,.T.);
#49978=EDGE_CURVE('',#38842,#38843,#32084,.T.);
#49979=EDGE_CURVE('',#38842,#38836,#22210,.T.);
#49980=EDGE_CURVE('',#38837,#38843,#22211,.T.);
#49981=EDGE_CURVE('',#38844,#38845,#32085,.T.);
#49982=EDGE_CURVE('',#38844,#38840,#32086,.T.);
#49983=EDGE_CURVE('',#38841,#38845,#32087,.T.);
#49984=EDGE_CURVE('',#38846,#38847,#32088,.T.);
#49985=EDGE_CURVE('',#38846,#38842,#32089,.T.);
#49986=EDGE_CURVE('',#38843,#38847,#32090,.T.);
#49987=EDGE_CURVE('',#38848,#38849,#32091,.T.);
#49988=EDGE_CURVE('',#38848,#38844,#22212,.T.);
#49989=EDGE_CURVE('',#38845,#38849,#22213,.T.);
#49990=EDGE_CURVE('',#38850,#38851,#32092,.T.);
#49991=EDGE_CURVE('',#38850,#38846,#32093,.T.);
#49992=EDGE_CURVE('',#38847,#38851,#32094,.T.);
#49993=EDGE_CURVE('',#38852,#38853,#32095,.T.);
#49994=EDGE_CURVE('',#38852,#38848,#32096,.T.);
#49995=EDGE_CURVE('',#38849,#38853,#32097,.T.);
#49996=EDGE_CURVE('',#38854,#38855,#32098,.T.);
#49997=EDGE_CURVE('',#38854,#38850,#32099,.T.);
#49998=EDGE_CURVE('',#38851,#38855,#32100,.T.);
#49999=EDGE_CURVE('',#38853,#38854,#32101,.T.);
#50000=EDGE_CURVE('',#38855,#38852,#32102,.T.);
#50001=EDGE_CURVE('',#38856,#38857,#32103,.T.);
#50002=EDGE_CURVE('',#38856,#38858,#32104,.T.);
#50003=EDGE_CURVE('',#38859,#38858,#32105,.T.);
#50004=EDGE_CURVE('',#38859,#38857,#32106,.T.);
#50005=EDGE_CURVE('',#38860,#38861,#32107,.T.);
#50006=EDGE_CURVE('',#38860,#38859,#22214,.T.);
#50007=EDGE_CURVE('',#38858,#38861,#22215,.T.);
#50008=EDGE_CURVE('',#38862,#38863,#32108,.T.);
#50009=EDGE_CURVE('',#38862,#38856,#22216,.T.);
#50010=EDGE_CURVE('',#38857,#38863,#22217,.T.);
#50011=EDGE_CURVE('',#38864,#38865,#32109,.T.);
#50012=EDGE_CURVE('',#38864,#38860,#32110,.T.);
#50013=EDGE_CURVE('',#38861,#38865,#32111,.T.);
#50014=EDGE_CURVE('',#38866,#38867,#32112,.T.);
#50015=EDGE_CURVE('',#38866,#38862,#32113,.T.);
#50016=EDGE_CURVE('',#38863,#38867,#32114,.T.);
#50017=EDGE_CURVE('',#38868,#38869,#32115,.T.);
#50018=EDGE_CURVE('',#38868,#38864,#22218,.T.);
#50019=EDGE_CURVE('',#38865,#38869,#22219,.T.);
#50020=EDGE_CURVE('',#38870,#38871,#32116,.T.);
#50021=EDGE_CURVE('',#38870,#38866,#32117,.T.);
#50022=EDGE_CURVE('',#38867,#38871,#32118,.T.);
#50023=EDGE_CURVE('',#38869,#38870,#32119,.T.);
#50024=EDGE_CURVE('',#38871,#38868,#32120,.T.);
#50025=EDGE_CURVE('',#38872,#38873,#32121,.T.);
#50026=EDGE_CURVE('',#38872,#38874,#32122,.T.);
#50027=EDGE_CURVE('',#38875,#38874,#32123,.T.);
#50028=EDGE_CURVE('',#38875,#38873,#32124,.T.);
#50029=EDGE_CURVE('',#38876,#38877,#32125,.T.);
#50030=EDGE_CURVE('',#38876,#38875,#22220,.T.);
#50031=EDGE_CURVE('',#38874,#38877,#22221,.T.);
#50032=EDGE_CURVE('',#38878,#38879,#32126,.T.);
#50033=EDGE_CURVE('',#38878,#38872,#22222,.T.);
#50034=EDGE_CURVE('',#38873,#38879,#22223,.T.);
#50035=EDGE_CURVE('',#38880,#38881,#32127,.T.);
#50036=EDGE_CURVE('',#38880,#38876,#32128,.T.);
#50037=EDGE_CURVE('',#38877,#38881,#32129,.T.);
#50038=EDGE_CURVE('',#38882,#38883,#32130,.T.);
#50039=EDGE_CURVE('',#38882,#38878,#32131,.T.);
#50040=EDGE_CURVE('',#38879,#38883,#32132,.T.);
#50041=EDGE_CURVE('',#38884,#38885,#32133,.T.);
#50042=EDGE_CURVE('',#38884,#38880,#22224,.T.);
#50043=EDGE_CURVE('',#38881,#38885,#22225,.T.);
#50044=EDGE_CURVE('',#38886,#38887,#32134,.T.);
#50045=EDGE_CURVE('',#38886,#38882,#22226,.T.);
#50046=EDGE_CURVE('',#38883,#38887,#22227,.T.);
#50047=EDGE_CURVE('',#38885,#38886,#32135,.T.);
#50048=EDGE_CURVE('',#38887,#38884,#32136,.T.);
#50049=EDGE_CURVE('',#38888,#38889,#32137,.T.);
#50050=EDGE_CURVE('',#38888,#38890,#32138,.T.);
#50051=EDGE_CURVE('',#38891,#38890,#32139,.T.);
#50052=EDGE_CURVE('',#38891,#38889,#32140,.T.);
#50053=EDGE_CURVE('',#38892,#38893,#32141,.T.);
#50054=EDGE_CURVE('',#38892,#38891,#22228,.T.);
#50055=EDGE_CURVE('',#38890,#38893,#22229,.T.);
#50056=EDGE_CURVE('',#38894,#38895,#32142,.T.);
#50057=EDGE_CURVE('',#38894,#38888,#22230,.T.);
#50058=EDGE_CURVE('',#38889,#38895,#22231,.T.);
#50059=EDGE_CURVE('',#38896,#38897,#32143,.T.);
#50060=EDGE_CURVE('',#38896,#38892,#32144,.T.);
#50061=EDGE_CURVE('',#38893,#38897,#32145,.T.);
#50062=EDGE_CURVE('',#38898,#38899,#32146,.T.);
#50063=EDGE_CURVE('',#38898,#38894,#32147,.T.);
#50064=EDGE_CURVE('',#38895,#38899,#32148,.T.);
#50065=EDGE_CURVE('',#38900,#38901,#32149,.T.);
#50066=EDGE_CURVE('',#38900,#38896,#22232,.T.);
#50067=EDGE_CURVE('',#38897,#38901,#22233,.T.);
#50068=EDGE_CURVE('',#38902,#38903,#32150,.T.);
#50069=EDGE_CURVE('',#38902,#38898,#32151,.T.);
#50070=EDGE_CURVE('',#38899,#38903,#32152,.T.);
#50071=EDGE_CURVE('',#38901,#38902,#32153,.T.);
#50072=EDGE_CURVE('',#38903,#38900,#32154,.T.);
#50073=EDGE_CURVE('',#38904,#38905,#32155,.T.);
#50074=EDGE_CURVE('',#38904,#38906,#32156,.T.);
#50075=EDGE_CURVE('',#38907,#38906,#32157,.T.);
#50076=EDGE_CURVE('',#38907,#38905,#32158,.T.);
#50077=EDGE_CURVE('',#38908,#38909,#32159,.T.);
#50078=EDGE_CURVE('',#38908,#38907,#22234,.T.);
#50079=EDGE_CURVE('',#38906,#38909,#22235,.T.);
#50080=EDGE_CURVE('',#38910,#38911,#32160,.T.);
#50081=EDGE_CURVE('',#38910,#38904,#22236,.T.);
#50082=EDGE_CURVE('',#38905,#38911,#22237,.T.);
#50083=EDGE_CURVE('',#38912,#38913,#32161,.T.);
#50084=EDGE_CURVE('',#38912,#38908,#32162,.T.);
#50085=EDGE_CURVE('',#38909,#38913,#32163,.T.);
#50086=EDGE_CURVE('',#38914,#38915,#32164,.T.);
#50087=EDGE_CURVE('',#38914,#38910,#32165,.T.);
#50088=EDGE_CURVE('',#38911,#38915,#32166,.T.);
#50089=EDGE_CURVE('',#38916,#38917,#32167,.T.);
#50090=EDGE_CURVE('',#38916,#38912,#22238,.T.);
#50091=EDGE_CURVE('',#38913,#38917,#22239,.T.);
#50092=EDGE_CURVE('',#38918,#38919,#32168,.T.);
#50093=EDGE_CURVE('',#38918,#38914,#22240,.T.);
#50094=EDGE_CURVE('',#38915,#38919,#22241,.T.);
#50095=EDGE_CURVE('',#38917,#38918,#32169,.T.);
#50096=EDGE_CURVE('',#38919,#38916,#32170,.T.);
#50097=EDGE_CURVE('',#38920,#38921,#32171,.T.);
#50098=EDGE_CURVE('',#38920,#38922,#32172,.T.);
#50099=EDGE_CURVE('',#38923,#38922,#32173,.T.);
#50100=EDGE_CURVE('',#38923,#38921,#32174,.T.);
#50101=EDGE_CURVE('',#38924,#38925,#32175,.T.);
#50102=EDGE_CURVE('',#38924,#38923,#22242,.T.);
#50103=EDGE_CURVE('',#38922,#38925,#22243,.T.);
#50104=EDGE_CURVE('',#38926,#38927,#32176,.T.);
#50105=EDGE_CURVE('',#38926,#38920,#32177,.T.);
#50106=EDGE_CURVE('',#38921,#38927,#32178,.T.);
#50107=EDGE_CURVE('',#38928,#38929,#32179,.T.);
#50108=EDGE_CURVE('',#38928,#38924,#32180,.T.);
#50109=EDGE_CURVE('',#38925,#38929,#32181,.T.);
#50110=EDGE_CURVE('',#38930,#38931,#32182,.T.);
#50111=EDGE_CURVE('',#38930,#38926,#32183,.T.);
#50112=EDGE_CURVE('',#38927,#38931,#32184,.T.);
#50113=EDGE_CURVE('',#38929,#38930,#22244,.T.);
#50114=EDGE_CURVE('',#38931,#38928,#22245,.T.);
#50115=EDGE_CURVE('',#38932,#38933,#32185,.T.);
#50116=EDGE_CURVE('',#38934,#38933,#32186,.T.);
#50117=EDGE_CURVE('',#38934,#38935,#32187,.T.);
#50118=EDGE_CURVE('',#38932,#38935,#32188,.T.);
#50119=EDGE_CURVE('',#38936,#38937,#32189,.T.);
#50120=EDGE_CURVE('',#38936,#38934,#22246,.T.);
#50121=EDGE_CURVE('',#38933,#38937,#22247,.T.);
#50122=EDGE_CURVE('',#38938,#38939,#32190,.T.);
#50123=EDGE_CURVE('',#38938,#38932,#32191,.T.);
#50124=EDGE_CURVE('',#38935,#38939,#32192,.T.);
#50125=EDGE_CURVE('',#38940,#38941,#32193,.T.);
#50126=EDGE_CURVE('',#38940,#38936,#32194,.T.);
#50127=EDGE_CURVE('',#38937,#38941,#32195,.T.);
#50128=EDGE_CURVE('',#38942,#38943,#32196,.T.);
#50129=EDGE_CURVE('',#38942,#38938,#32197,.T.);
#50130=EDGE_CURVE('',#38939,#38943,#32198,.T.);
#50131=EDGE_CURVE('',#38941,#38942,#22248,.T.);
#50132=EDGE_CURVE('',#38943,#38940,#22249,.T.);
#50133=EDGE_CURVE('',#38944,#38945,#32199,.T.);
#50134=EDGE_CURVE('',#38944,#38946,#32200,.T.);
#50135=EDGE_CURVE('',#38946,#38947,#32201,.T.);
#50136=EDGE_CURVE('',#38947,#38945,#32202,.T.);
#50137=EDGE_CURVE('',#38948,#38949,#32203,.T.);
#50138=EDGE_CURVE('',#38948,#38944,#32204,.T.);
#50139=EDGE_CURVE('',#38945,#38949,#32205,.T.);
#50140=EDGE_CURVE('',#38950,#38951,#32206,.T.);
#50141=EDGE_CURVE('',#38950,#38948,#32207,.T.);
#50142=EDGE_CURVE('',#38949,#38951,#32208,.T.);
#50143=EDGE_CURVE('',#38952,#38953,#32209,.T.);
#50144=EDGE_CURVE('',#38952,#38950,#32210,.T.);
#50145=EDGE_CURVE('',#38951,#38953,#32211,.T.);
#50146=EDGE_CURVE('',#38954,#38955,#32212,.T.);
#50147=EDGE_CURVE('',#38954,#38952,#32213,.T.);
#50148=EDGE_CURVE('',#38953,#38955,#32214,.T.);
#50149=EDGE_CURVE('',#38956,#38957,#32215,.T.);
#50150=EDGE_CURVE('',#38956,#38954,#32216,.T.);
#50151=EDGE_CURVE('',#38955,#38957,#32217,.T.);
#50152=EDGE_CURVE('',#38958,#38959,#32218,.T.);
#50153=EDGE_CURVE('',#38958,#38956,#32219,.T.);
#50154=EDGE_CURVE('',#38957,#38959,#32220,.T.);
#50155=EDGE_CURVE('',#38960,#38961,#32221,.T.);
#50156=EDGE_CURVE('',#38960,#38962,#32222,.T.);
#50157=EDGE_CURVE('',#38962,#38963,#32223,.T.);
#50158=EDGE_CURVE('',#38963,#38961,#32224,.T.);
#50159=EDGE_CURVE('',#38964,#38965,#32225,.T.);
#50160=EDGE_CURVE('',#38964,#38960,#32226,.T.);
#50161=EDGE_CURVE('',#38961,#38965,#32227,.T.);
#50162=EDGE_CURVE('',#38966,#38967,#32228,.T.);
#50163=EDGE_CURVE('',#38966,#38964,#32229,.T.);
#50164=EDGE_CURVE('',#38965,#38967,#32230,.T.);
#50165=EDGE_CURVE('',#38968,#38969,#32231,.T.);
#50166=EDGE_CURVE('',#38968,#38966,#32232,.T.);
#50167=EDGE_CURVE('',#38967,#38969,#32233,.T.);
#50168=EDGE_CURVE('',#38970,#38971,#32234,.T.);
#50169=EDGE_CURVE('',#38970,#38968,#32235,.T.);
#50170=EDGE_CURVE('',#38969,#38971,#32236,.T.);
#50171=EDGE_CURVE('',#38972,#38973,#32237,.T.);
#50172=EDGE_CURVE('',#38972,#38970,#32238,.T.);
#50173=EDGE_CURVE('',#38971,#38973,#32239,.T.);
#50174=EDGE_CURVE('',#38974,#38975,#32240,.T.);
#50175=EDGE_CURVE('',#38974,#38972,#32241,.T.);
#50176=EDGE_CURVE('',#38973,#38975,#32242,.T.);
#50177=EDGE_CURVE('',#38976,#38977,#32243,.T.);
#50178=EDGE_CURVE('',#38976,#38978,#32244,.T.);
#50179=EDGE_CURVE('',#38978,#38979,#5485,.T.);
#50180=EDGE_CURVE('',#38979,#38977,#32245,.T.);
#50181=EDGE_CURVE('',#38980,#38981,#32246,.T.);
#50182=EDGE_CURVE('',#38980,#38976,#22250,.T.);
#50183=EDGE_CURVE('',#38977,#38981,#22251,.T.);
#50184=EDGE_CURVE('',#38982,#38980,#32247,.T.);
#50185=EDGE_CURVE('',#38981,#38983,#32248,.T.);
#50186=EDGE_CURVE('',#38982,#38983,#32249,.T.);
#50187=EDGE_CURVE('',#38984,#38985,#32250,.T.);
#50188=EDGE_CURVE('',#38984,#38982,#32251,.T.);
#50189=EDGE_CURVE('',#38983,#38985,#32252,.T.);
#50190=EDGE_CURVE('',#38986,#38987,#32253,.T.);
#50191=EDGE_CURVE('',#38986,#38984,#32254,.T.);
#50192=EDGE_CURVE('',#38985,#38987,#32255,.T.);
#50193=EDGE_CURVE('',#38988,#38989,#32256,.T.);
#50194=EDGE_CURVE('',#38988,#38986,#22252,.T.);
#50195=EDGE_CURVE('',#38987,#38989,#22253,.T.);
#50196=EDGE_CURVE('',#38990,#38991,#5486,.T.);
#50197=EDGE_CURVE('',#38991,#38988,#32257,.T.);
#50198=EDGE_CURVE('',#38989,#38990,#32258,.T.);
#50199=EDGE_CURVE('',#38992,#38993,#32259,.T.);
#50200=EDGE_CURVE('',#38992,#38994,#32260,.T.);
#50201=EDGE_CURVE('',#38994,#38995,#5487,.T.);
#50202=EDGE_CURVE('',#38995,#38993,#32261,.T.);
#50203=EDGE_CURVE('',#38996,#38997,#32262,.T.);
#50204=EDGE_CURVE('',#38996,#38992,#22254,.T.);
#50205=EDGE_CURVE('',#38993,#38997,#22255,.T.);
#50206=EDGE_CURVE('',#38998,#38999,#32263,.T.);
#50207=EDGE_CURVE('',#38998,#38996,#32264,.T.);
#50208=EDGE_CURVE('',#38997,#38999,#32265,.T.);
#50209=EDGE_CURVE('',#39000,#39001,#32266,.T.);
#50210=EDGE_CURVE('',#39000,#38998,#32267,.T.);
#50211=EDGE_CURVE('',#38999,#39001,#32268,.T.);
#50212=EDGE_CURVE('',#39002,#39003,#32269,.T.);
#50213=EDGE_CURVE('',#39002,#39000,#32270,.T.);
#50214=EDGE_CURVE('',#39001,#39003,#32271,.T.);
#50215=EDGE_CURVE('',#39004,#39005,#32272,.T.);
#50216=EDGE_CURVE('',#39004,#39002,#22256,.T.);
#50217=EDGE_CURVE('',#39003,#39005,#22257,.T.);
#50218=EDGE_CURVE('',#39006,#39007,#5488,.T.);
#50219=EDGE_CURVE('',#39007,#39004,#32273,.T.);
#50220=EDGE_CURVE('',#39005,#39006,#32274,.T.);
#50221=EDGE_CURVE('',#39008,#39009,#32275,.T.);
#50222=EDGE_CURVE('',#39008,#39010,#32276,.T.);
#50223=EDGE_CURVE('',#39010,#39011,#5489,.T.);
#50224=EDGE_CURVE('',#39011,#39009,#32277,.T.);
#50225=EDGE_CURVE('',#39012,#39013,#32278,.T.);
#50226=EDGE_CURVE('',#39012,#39008,#22258,.T.);
#50227=EDGE_CURVE('',#39009,#39013,#22259,.T.);
#50228=EDGE_CURVE('',#39014,#39012,#32279,.T.);
#50229=EDGE_CURVE('',#39013,#39015,#32280,.T.);
#50230=EDGE_CURVE('',#39014,#39015,#32281,.T.);
#50231=EDGE_CURVE('',#39016,#39017,#32282,.T.);
#50232=EDGE_CURVE('',#39016,#39014,#32283,.T.);
#50233=EDGE_CURVE('',#39015,#39017,#32284,.T.);
#50234=EDGE_CURVE('',#39018,#39019,#32285,.T.);
#50235=EDGE_CURVE('',#39018,#39016,#32286,.T.);
#50236=EDGE_CURVE('',#39017,#39019,#32287,.T.);
#50237=EDGE_CURVE('',#39020,#39021,#32288,.T.);
#50238=EDGE_CURVE('',#39020,#39018,#22260,.T.);
#50239=EDGE_CURVE('',#39019,#39021,#22261,.T.);
#50240=EDGE_CURVE('',#39022,#39023,#5490,.T.);
#50241=EDGE_CURVE('',#39023,#39020,#32289,.T.);
#50242=EDGE_CURVE('',#39021,#39022,#32290,.T.);
#50243=EDGE_CURVE('',#39024,#39025,#5491,.F.);
#50244=EDGE_CURVE('',#39025,#39026,#32291,.T.);
#50245=EDGE_CURVE('',#39027,#39026,#32292,.T.);
#50246=EDGE_CURVE('',#39027,#39024,#32293,.T.);
#50247=EDGE_CURVE('',#39028,#39029,#32294,.T.);
#50248=EDGE_CURVE('',#39028,#39027,#22262,.T.);
#50249=EDGE_CURVE('',#39026,#39029,#22263,.T.);
#50250=EDGE_CURVE('',#39030,#39031,#32295,.T.);
#50251=EDGE_CURVE('',#39030,#39028,#32296,.T.);
#50252=EDGE_CURVE('',#39029,#39031,#32297,.T.);
#50253=EDGE_CURVE('',#39032,#39033,#32298,.T.);
#50254=EDGE_CURVE('',#39032,#39030,#32299,.T.);
#50255=EDGE_CURVE('',#39031,#39033,#32300,.T.);
#50256=EDGE_CURVE('',#39034,#39035,#32301,.T.);
#50257=EDGE_CURVE('',#39034,#39032,#32302,.T.);
#50258=EDGE_CURVE('',#39033,#39035,#32303,.T.);
#50259=EDGE_CURVE('',#39036,#39037,#32304,.T.);
#50260=EDGE_CURVE('',#39036,#39034,#22264,.T.);
#50261=EDGE_CURVE('',#39035,#39037,#22265,.T.);
#50262=EDGE_CURVE('',#39038,#39039,#5492,.T.);
#50263=EDGE_CURVE('',#39039,#39036,#32305,.T.);
#50264=EDGE_CURVE('',#39037,#39038,#32306,.T.);
#50265=EDGE_CURVE('',#39040,#39041,#32307,.T.);
#50266=EDGE_CURVE('',#39040,#39042,#32308,.T.);
#50267=EDGE_CURVE('',#39042,#39043,#32309,.T.);
#50268=EDGE_CURVE('',#39043,#39041,#32310,.T.);
#50269=EDGE_CURVE('',#39044,#39045,#32311,.T.);
#50270=EDGE_CURVE('',#39044,#39040,#32312,.T.);
#50271=EDGE_CURVE('',#39041,#39045,#32313,.T.);
#50272=EDGE_CURVE('',#39046,#39047,#32314,.T.);
#50273=EDGE_CURVE('',#39046,#39044,#32315,.T.);
#50274=EDGE_CURVE('',#39045,#39047,#32316,.T.);
#50275=EDGE_CURVE('',#39048,#39049,#32317,.T.);
#50276=EDGE_CURVE('',#39048,#39046,#32318,.T.);
#50277=EDGE_CURVE('',#39047,#39049,#32319,.T.);
#50278=EDGE_CURVE('',#39050,#39051,#32320,.T.);
#50279=EDGE_CURVE('',#39050,#39048,#32321,.T.);
#50280=EDGE_CURVE('',#39049,#39051,#32322,.T.);
#50281=EDGE_CURVE('',#39052,#39053,#32323,.T.);
#50282=EDGE_CURVE('',#39052,#39050,#32324,.T.);
#50283=EDGE_CURVE('',#39051,#39053,#32325,.T.);
#50284=EDGE_CURVE('',#39054,#39055,#32326,.T.);
#50285=EDGE_CURVE('',#39054,#39052,#32327,.T.);
#50286=EDGE_CURVE('',#39053,#39055,#32328,.T.);
#50287=EDGE_CURVE('',#39056,#39057,#5493,.T.);
#50288=EDGE_CURVE('',#39057,#39058,#5494,.T.);
#50289=EDGE_CURVE('',#39058,#39059,#32329,.T.);
#50290=EDGE_CURVE('',#39059,#39060,#5495,.T.);
#50291=EDGE_CURVE('',#39061,#39060,#32330,.T.);
#50292=EDGE_CURVE('',#39061,#39056,#5496,.T.);
#50293=EDGE_CURVE('',#39062,#39063,#32331,.T.);
#50294=EDGE_CURVE('',#39062,#39061,#5497,.T.);
#50295=EDGE_CURVE('',#39060,#39063,#5498,.T.);
#50296=EDGE_CURVE('',#39064,#39065,#32332,.T.);
#50297=EDGE_CURVE('',#39064,#39062,#32333,.T.);
#50298=EDGE_CURVE('',#39063,#39065,#32334,.T.);
#50299=EDGE_CURVE('',#39066,#39067,#32335,.T.);
#50300=EDGE_CURVE('',#39066,#39064,#5499,.T.);
#50301=EDGE_CURVE('',#39065,#39067,#5500,.T.);
#50302=EDGE_CURVE('',#39068,#39069,#32336,.T.);
#50303=EDGE_CURVE('',#39068,#39066,#5501,.T.);
#50304=EDGE_CURVE('',#39067,#39069,#5502,.T.);
#50305=EDGE_CURVE('',#39070,#39071,#32337,.T.);
#50306=EDGE_CURVE('',#39070,#39068,#5503,.T.);
#50307=EDGE_CURVE('',#39069,#39071,#5504,.T.);
#50308=EDGE_CURVE('',#39072,#39073,#32338,.T.);
#50309=EDGE_CURVE('',#39072,#39070,#32339,.T.);
#50310=EDGE_CURVE('',#39071,#39073,#32340,.T.);
#50311=EDGE_CURVE('',#39074,#39075,#32341,.T.);
#50312=EDGE_CURVE('',#39074,#39072,#5505,.T.);
#50313=EDGE_CURVE('',#39073,#39075,#5506,.T.);
#50314=EDGE_CURVE('',#39076,#39077,#32342,.T.);
#50315=EDGE_CURVE('',#39076,#39078,#5507,.T.);
#50316=EDGE_CURVE('',#39078,#39079,#5508,.T.);
#50317=EDGE_CURVE('',#39079,#39080,#5509,.T.);
#50318=EDGE_CURVE('',#39080,#39081,#5510,.T.);
#50319=EDGE_CURVE('',#39081,#39082,#5511,.T.);
#50320=EDGE_CURVE('',#39082,#39074,#5512,.T.);
#50321=EDGE_CURVE('',#39075,#39077,#5513,.T.);
#50322=EDGE_CURVE('',#39083,#39084,#32343,.T.);
#50323=EDGE_CURVE('',#39083,#39076,#5514,.T.);
#50324=EDGE_CURVE('',#39077,#39084,#5515,.T.);
#50325=EDGE_CURVE('',#39085,#39086,#32344,.T.);
#50326=EDGE_CURVE('',#39085,#39083,#32345,.T.);
#50327=EDGE_CURVE('',#39084,#39086,#32346,.T.);
#50328=EDGE_CURVE('',#39087,#39088,#32347,.T.);
#50329=EDGE_CURVE('',#39087,#39085,#5516,.T.);
#50330=EDGE_CURVE('',#39086,#39088,#5517,.T.);
#50331=EDGE_CURVE('',#39089,#39090,#32348,.T.);
#50332=EDGE_CURVE('',#39089,#39087,#5518,.T.);
#50333=EDGE_CURVE('',#39088,#39090,#5519,.T.);
#50334=EDGE_CURVE('',#39091,#39092,#32349,.T.);
#50335=EDGE_CURVE('',#39091,#39089,#5520,.T.);
#50336=EDGE_CURVE('',#39090,#39092,#5521,.T.);
#50337=EDGE_CURVE('',#39093,#39094,#32350,.T.);
#50338=EDGE_CURVE('',#39093,#39091,#32351,.T.);
#50339=EDGE_CURVE('',#39092,#39094,#32352,.T.);
#50340=EDGE_CURVE('',#39095,#39096,#32353,.T.);
#50341=EDGE_CURVE('',#39095,#39093,#5522,.T.);
#50342=EDGE_CURVE('',#39094,#39096,#5523,.T.);
#50343=EDGE_CURVE('',#38385,#39097,#1217,.T.);
#50344=EDGE_CURVE('',#39098,#39097,#32354,.T.);
#50345=EDGE_CURVE('',#39098,#38377,#32355,.T.);
#50346=EDGE_CURVE('',#39099,#39100,#32356,.T.);
#50347=EDGE_CURVE('',#39099,#39098,#32357,.T.);
#50348=EDGE_CURVE('',#39097,#39100,#32358,.T.);
#50349=EDGE_CURVE('',#39101,#39102,#32359,.T.);
#50350=EDGE_CURVE('',#39101,#39099,#5524,.T.);
#50351=EDGE_CURVE('',#39100,#39102,#5525,.T.);
#50352=EDGE_CURVE('',#39103,#39104,#32360,.T.);
#50353=EDGE_CURVE('',#39103,#39101,#5526,.T.);
#50354=EDGE_CURVE('',#39102,#39104,#5527,.T.);
#50355=EDGE_CURVE('',#39105,#39106,#5528,.T.);
#50356=EDGE_CURVE('',#39107,#39105,#5529,.T.);
#50357=EDGE_CURVE('',#39107,#39103,#32361,.T.);
#50358=EDGE_CURVE('',#39104,#39106,#32362,.T.);
#50359=EDGE_CURVE('',#39108,#39109,#5530,.T.);
#50360=EDGE_CURVE('',#39109,#39107,#32363,.T.);
#50361=EDGE_CURVE('',#39108,#39105,#32364,.T.);
#50362=EDGE_CURVE('',#39108,#39106,#5531,.T.);
#50363=EDGE_CURVE('',#39110,#39111,#5532,.T.);
#50364=EDGE_CURVE('',#39110,#39112,#5533,.T.);
#50365=EDGE_CURVE('',#39112,#39113,#5534,.T.);
#50366=EDGE_CURVE('',#39113,#39114,#5535,.T.);
#50367=EDGE_CURVE('',#39114,#39115,#5536,.T.);
#50368=EDGE_CURVE('',#39115,#39116,#5537,.T.);
#50369=EDGE_CURVE('',#39116,#39117,#5538,.T.);
#50370=EDGE_CURVE('',#39117,#39108,#5539,.T.);
#50371=EDGE_CURVE('',#39106,#39111,#5540,.T.);
#50372=EDGE_CURVE('',#39110,#39118,#32365,.T.);
#50373=EDGE_CURVE('',#39118,#39111,#5541,.T.);
#50374=EDGE_CURVE('',#39119,#39120,#32366,.T.);
#50375=EDGE_CURVE('',#39120,#39110,#5542,.T.);
#50376=EDGE_CURVE('',#39119,#39118,#5543,.T.);
#50377=EDGE_CURVE('',#39111,#39121,#32367,.T.);
#50378=EDGE_CURVE('',#39122,#39121,#32368,.T.);
#50379=EDGE_CURVE('',#39122,#39119,#32369,.T.);
#50380=EDGE_CURVE('',#39123,#39124,#32370,.T.);
#50381=EDGE_CURVE('',#39123,#39122,#5544,.T.);
#50382=EDGE_CURVE('',#39121,#39124,#5545,.T.);
#50383=EDGE_CURVE('',#39125,#39126,#32371,.T.);
#50384=EDGE_CURVE('',#39125,#39123,#5546,.T.);
#50385=EDGE_CURVE('',#39124,#39126,#5547,.T.);
#50386=EDGE_CURVE('',#39127,#39128,#32372,.T.);
#50387=EDGE_CURVE('',#39127,#39125,#32373,.T.);
#50388=EDGE_CURVE('',#39126,#39128,#32374,.T.);
#50389=EDGE_CURVE('',#38401,#39127,#1996,.T.);
#50390=EDGE_CURVE('',#39128,#38391,#5548,.T.);
#50391=EDGE_CURVE('',#39129,#39130,#32375,.T.);
#50392=EDGE_CURVE('',#39129,#39131,#5549,.T.);
#50393=EDGE_CURVE('',#39130,#39131,#5550,.T.);
#50394=EDGE_CURVE('',#39132,#39133,#32376,.T.);
#50395=EDGE_CURVE('',#39133,#39129,#1997,.T.);
#50396=EDGE_CURVE('',#39132,#39130,#1998,.T.);
#50397=EDGE_CURVE('',#39131,#39134,#32377,.T.);
#50398=EDGE_CURVE('',#39135,#39134,#32378,.T.);
#50399=EDGE_CURVE('',#39135,#39132,#32379,.T.);
#50400=EDGE_CURVE('',#39136,#39137,#32380,.T.);
#50401=EDGE_CURVE('',#39136,#39135,#5551,.T.);
#50402=EDGE_CURVE('',#39134,#39137,#5552,.T.);
#50403=EDGE_CURVE('',#39138,#39139,#32381,.T.);
#50404=EDGE_CURVE('',#39138,#39136,#5553,.T.);
#50405=EDGE_CURVE('',#39137,#39139,#5554,.T.);
#50406=EDGE_CURVE('',#39140,#39141,#32382,.T.);
#50407=EDGE_CURVE('',#39140,#39138,#5555,.T.);
#50408=EDGE_CURVE('',#39139,#39141,#32383,.T.);
#50409=EDGE_CURVE('',#38376,#39140,#1999,.T.);
#50410=EDGE_CURVE('',#39141,#38384,#5556,.T.);
#50411=EDGE_CURVE('',#39142,#39143,#32384,.T.);
#50412=EDGE_CURVE('',#39143,#39144,#2000,.T.);
#50413=EDGE_CURVE('',#39145,#39144,#32385,.T.);
#50414=EDGE_CURVE('',#39145,#39142,#2001,.T.);
#50415=EDGE_CURVE('',#39146,#39147,#5557,.T.);
#50416=EDGE_CURVE('',#39147,#39148,#5558,.T.);
#50417=EDGE_CURVE('',#39148,#39149,#5559,.T.);
#50418=EDGE_CURVE('',#39150,#39149,#5560,.T.);
#50419=EDGE_CURVE('',#39150,#39145,#5561,.T.);
#50420=EDGE_CURVE('',#39144,#39146,#5562,.T.);
#50421=EDGE_CURVE('',#39150,#39151,#5563,.T.);
#50422=EDGE_CURVE('',#39151,#39149,#32386,.T.);
#50423=EDGE_CURVE('',#39152,#39153,#1218,.T.);
#50424=EDGE_CURVE('',#39154,#39153,#32387,.T.);
#50425=EDGE_CURVE('',#39154,#39150,#2002,.T.);
#50426=EDGE_CURVE('',#39152,#39151,#32388,.T.);
#50427=EDGE_CURVE('',#39149,#39155,#5564,.T.);
#50428=EDGE_CURVE('',#39155,#39152,#32389,.T.);
#50429=EDGE_CURVE('',#39156,#39157,#32390,.T.);
#50430=EDGE_CURVE('',#39156,#39154,#5565,.T.);
#50431=EDGE_CURVE('',#39153,#39157,#5566,.T.);
#50432=EDGE_CURVE('',#39158,#39159,#32391,.T.);
#50433=EDGE_CURVE('',#39158,#39156,#1219,.T.);
#50434=EDGE_CURVE('',#39157,#39159,#5567,.T.);
#50435=EDGE_CURVE('',#39160,#39161,#32392,.T.);
#50436=EDGE_CURVE('',#39160,#39158,#32393,.T.);
#50437=EDGE_CURVE('',#39159,#39161,#32394,.T.);
#50438=EDGE_CURVE('',#38400,#39160,#1220,.T.);
#50439=EDGE_CURVE('',#39161,#38409,#5568,.T.);
#50440=EDGE_CURVE('',#39095,#39133,#5569,.T.);
#50441=EDGE_CURVE('',#39132,#39093,#5570,.T.);
#50442=EDGE_CURVE('',#39083,#39107,#5571,.T.);
#50443=EDGE_CURVE('',#39109,#39076,#5572,.T.);
#50444=EDGE_CURVE('',#39074,#39120,#5573,.T.);
#50445=EDGE_CURVE('',#39119,#39072,#5574,.T.);
#50446=EDGE_CURVE('',#39062,#39152,#1221,.T.);
#50447=EDGE_CURVE('',#39155,#39061,#5575,.T.);
#50448=EDGE_CURVE('',#39162,#39163,#32395,.T.);
#50449=EDGE_CURVE('',#39163,#38983,#22266,.T.);
#50450=EDGE_CURVE('',#38981,#39162,#22267,.T.);
#50451=EDGE_CURVE('',#39037,#39164,#22268,.T.);
#50452=EDGE_CURVE('',#39164,#39165,#32396,.T.);
#50453=EDGE_CURVE('',#39165,#39038,#22269,.T.);
#50454=EDGE_CURVE('',#38997,#39166,#22270,.T.);
#50455=EDGE_CURVE('',#39166,#39167,#32397,.T.);
#50456=EDGE_CURVE('',#39167,#38999,#22271,.T.);
#50457=EDGE_CURVE('',#38995,#39168,#22272,.T.);
#50458=EDGE_CURVE('',#39168,#39169,#32398,.T.);
#50459=EDGE_CURVE('',#39169,#38993,#22273,.T.);
#50460=EDGE_CURVE('',#38989,#39170,#22274,.T.);
#50461=EDGE_CURVE('',#39170,#39171,#32399,.T.);
#50462=EDGE_CURVE('',#39171,#38990,#22275,.T.);
#50463=EDGE_CURVE('',#38985,#39172,#22276,.T.);
#50464=EDGE_CURVE('',#39172,#39173,#32400,.T.);
#50465=EDGE_CURVE('',#39173,#38987,#22277,.T.);
#50466=EDGE_CURVE('',#38979,#39174,#22278,.T.);
#50467=EDGE_CURVE('',#39174,#39175,#32401,.T.);
#50468=EDGE_CURVE('',#39175,#38977,#22279,.T.);
#50469=EDGE_CURVE('',#39021,#39176,#22280,.T.);
#50470=EDGE_CURVE('',#39176,#39177,#32402,.T.);
#50471=EDGE_CURVE('',#39177,#39022,#22281,.T.);
#50472=EDGE_CURVE('',#39011,#39178,#22282,.T.);
#50473=EDGE_CURVE('',#39178,#39179,#32403,.T.);
#50474=EDGE_CURVE('',#39179,#39009,#22283,.T.);
#50475=EDGE_CURVE('',#39180,#39181,#32404,.T.);
#50476=EDGE_CURVE('',#39181,#38778,#22284,.T.);
#50477=EDGE_CURVE('',#38783,#39180,#22285,.T.);
#50478=EDGE_CURVE('',#38697,#39182,#22286,.T.);
#50479=EDGE_CURVE('',#39182,#39183,#32405,.T.);
#50480=EDGE_CURVE('',#39183,#38701,#22287,.T.);
#50481=EDGE_CURVE('',#38685,#39184,#22288,.T.);
#50482=EDGE_CURVE('',#39184,#39185,#32406,.T.);
#50483=EDGE_CURVE('',#39185,#38683,#22289,.T.);
#50484=EDGE_CURVE('',#38690,#39186,#22290,.T.);
#50485=EDGE_CURVE('',#39186,#39187,#32407,.T.);
#50486=EDGE_CURVE('',#39187,#38686,#22291,.T.);
#50487=EDGE_CURVE('',#38698,#39188,#22292,.T.);
#50488=EDGE_CURVE('',#39188,#39189,#32408,.T.);
#50489=EDGE_CURVE('',#39189,#38694,#22293,.T.);
#50490=EDGE_CURVE('',#38665,#39190,#22294,.T.);
#50491=EDGE_CURVE('',#39190,#39191,#32409,.T.);
#50492=EDGE_CURVE('',#39191,#38663,#22295,.T.);
#50493=EDGE_CURVE('',#38670,#39192,#22296,.T.);
#50494=EDGE_CURVE('',#39192,#39193,#32410,.T.);
#50495=EDGE_CURVE('',#39193,#38666,#22297,.T.);
#50496=EDGE_CURVE('',#38678,#39194,#22298,.T.);
#50497=EDGE_CURVE('',#39194,#39195,#32411,.T.);
#50498=EDGE_CURVE('',#39195,#38674,#22299,.T.);
#50499=EDGE_CURVE('',#38677,#39196,#22300,.T.);
#50500=EDGE_CURVE('',#39196,#39197,#32412,.T.);
#50501=EDGE_CURVE('',#39197,#38681,#22301,.T.);
#50502=EDGE_CURVE('',#38527,#39198,#22302,.T.);
#50503=EDGE_CURVE('',#39198,#39199,#32413,.T.);
#50504=EDGE_CURVE('',#39199,#38528,#22303,.T.);
#50505=EDGE_CURVE('',#38519,#39200,#22304,.T.);
#50506=EDGE_CURVE('',#39200,#39201,#32414,.T.);
#50507=EDGE_CURVE('',#39201,#38523,#22305,.T.);
#50508=EDGE_CURVE('',#38515,#39202,#22306,.T.);
#50509=EDGE_CURVE('',#39202,#39203,#32415,.T.);
#50510=EDGE_CURVE('',#39203,#38513,#22307,.T.);
#50511=EDGE_CURVE('',#38520,#39204,#22308,.T.);
#50512=EDGE_CURVE('',#39204,#39205,#32416,.T.);
#50513=EDGE_CURVE('',#39205,#38516,#22309,.T.);
#50514=EDGE_CURVE('',#38773,#39206,#22310,.T.);
#50515=EDGE_CURVE('',#39206,#39207,#32417,.T.);
#50516=EDGE_CURVE('',#39207,#38777,#22311,.T.);
#50517=EDGE_CURVE('',#38769,#39208,#22312,.T.);
#50518=EDGE_CURVE('',#39208,#39209,#32418,.T.);
#50519=EDGE_CURVE('',#39209,#38767,#22313,.T.);
#50520=EDGE_CURVE('',#38774,#39210,#22314,.T.);
#50521=EDGE_CURVE('',#39210,#39211,#32419,.T.);
#50522=EDGE_CURVE('',#39211,#38770,#22315,.T.);
#50523=EDGE_CURVE('',#38940,#39212,#22316,.T.);
#50524=EDGE_CURVE('',#39212,#39213,#32420,.T.);
#50525=EDGE_CURVE('',#39213,#38936,#22317,.T.);
#50526=EDGE_CURVE('',#38939,#39214,#22318,.T.);
#50527=EDGE_CURVE('',#39214,#39215,#32421,.T.);
#50528=EDGE_CURVE('',#39215,#38943,#22319,.T.);
#50529=EDGE_CURVE('',#39216,#39217,#32422,.T.);
#50530=EDGE_CURVE('',#39217,#38935,#22320,.T.);
#50531=EDGE_CURVE('',#38934,#39216,#22321,.T.);
#50532=EDGE_CURVE('',#38569,#39218,#22322,.T.);
#50533=EDGE_CURVE('',#39218,#39219,#32423,.T.);
#50534=EDGE_CURVE('',#39219,#38573,#22323,.T.);
#50535=EDGE_CURVE('',#38565,#39220,#22324,.T.);
#50536=EDGE_CURVE('',#39220,#39221,#32424,.T.);
#50537=EDGE_CURVE('',#39221,#38563,#22325,.T.);
#50538=EDGE_CURVE('',#38570,#39222,#22326,.T.);
#50539=EDGE_CURVE('',#39222,#39223,#32425,.T.);
#50540=EDGE_CURVE('',#39223,#38566,#22327,.T.);
#50541=EDGE_CURVE('',#38577,#39224,#22328,.T.);
#50542=EDGE_CURVE('',#39224,#39225,#32426,.T.);
#50543=EDGE_CURVE('',#39225,#38574,#22329,.T.);
#50544=EDGE_CURVE('',#38585,#39226,#22330,.T.);
#50545=EDGE_CURVE('',#39226,#39227,#32427,.T.);
#50546=EDGE_CURVE('',#39227,#38589,#22331,.T.);
#50547=EDGE_CURVE('',#38581,#39228,#22332,.T.);
#50548=EDGE_CURVE('',#39228,#39229,#32428,.T.);
#50549=EDGE_CURVE('',#39229,#38579,#22333,.T.);
#50550=EDGE_CURVE('',#38586,#39230,#22334,.T.);
#50551=EDGE_CURVE('',#39230,#39231,#32429,.T.);
#50552=EDGE_CURVE('',#39231,#38582,#22335,.T.);
#50553=EDGE_CURVE('',#38593,#39232,#22336,.T.);
#50554=EDGE_CURVE('',#39232,#39233,#32430,.T.);
#50555=EDGE_CURVE('',#39233,#38590,#22337,.T.);
#50556=EDGE_CURVE('',#38839,#39234,#22338,.T.);
#50557=EDGE_CURVE('',#39234,#39235,#32431,.T.);
#50558=EDGE_CURVE('',#39235,#38837,#22339,.T.);
#50559=EDGE_CURVE('',#38844,#39236,#22340,.T.);
#50560=EDGE_CURVE('',#39236,#39237,#32432,.T.);
#50561=EDGE_CURVE('',#39237,#38840,#22341,.T.);
#50562=EDGE_CURVE('',#38852,#39238,#22342,.T.);
#50563=EDGE_CURVE('',#39238,#39239,#32433,.T.);
#50564=EDGE_CURVE('',#39239,#38848,#22343,.T.);
#50565=EDGE_CURVE('',#38843,#39240,#22344,.T.);
#50566=EDGE_CURVE('',#39240,#39241,#32434,.T.);
#50567=EDGE_CURVE('',#39241,#38847,#22345,.T.);
#50568=EDGE_CURVE('',#38803,#39242,#22346,.T.);
#50569=EDGE_CURVE('',#39242,#39243,#32435,.T.);
#50570=EDGE_CURVE('',#39243,#38801,#22347,.T.);
#50571=EDGE_CURVE('',#38808,#39244,#22348,.T.);
#50572=EDGE_CURVE('',#39244,#39245,#32436,.T.);
#50573=EDGE_CURVE('',#39245,#38804,#22349,.T.);
#50574=EDGE_CURVE('',#38815,#39246,#22350,.T.);
#50575=EDGE_CURVE('',#39246,#39247,#32437,.T.);
#50576=EDGE_CURVE('',#39247,#38819,#22351,.T.);
#50577=EDGE_CURVE('',#38807,#39248,#22352,.T.);
#50578=EDGE_CURVE('',#39248,#39249,#32438,.T.);
#50579=EDGE_CURVE('',#39249,#38811,#22353,.T.);
#50580=EDGE_CURVE('',#38653,#39250,#22354,.T.);
#50581=EDGE_CURVE('',#39250,#39251,#32439,.T.);
#50582=EDGE_CURVE('',#39251,#38657,#22355,.T.);
#50583=EDGE_CURVE('',#38649,#39252,#22356,.T.);
#50584=EDGE_CURVE('',#39252,#39253,#32440,.T.);
#50585=EDGE_CURVE('',#39253,#38647,#22357,.T.);
#50586=EDGE_CURVE('',#38654,#39254,#22358,.T.);
#50587=EDGE_CURVE('',#39254,#39255,#32441,.T.);
#50588=EDGE_CURVE('',#39255,#38650,#22359,.T.);
#50589=EDGE_CURVE('',#38661,#39256,#22360,.T.);
#50590=EDGE_CURVE('',#39256,#39257,#32442,.T.);
#50591=EDGE_CURVE('',#39257,#38658,#22361,.T.);
#50592=EDGE_CURVE('',#38717,#39258,#22362,.T.);
#50593=EDGE_CURVE('',#39258,#39259,#32443,.T.);
#50594=EDGE_CURVE('',#39259,#38714,#22363,.T.);
#50595=EDGE_CURVE('',#38709,#39260,#22364,.T.);
#50596=EDGE_CURVE('',#39260,#39261,#32444,.T.);
#50597=EDGE_CURVE('',#39261,#38713,#22365,.T.);
#50598=EDGE_CURVE('',#38705,#39262,#22366,.T.);
#50599=EDGE_CURVE('',#39262,#39263,#32445,.T.);
#50600=EDGE_CURVE('',#39263,#38703,#22367,.T.);
#50601=EDGE_CURVE('',#38710,#39264,#22368,.T.);
#50602=EDGE_CURVE('',#39264,#39265,#32446,.T.);
#50603=EDGE_CURVE('',#39265,#38706,#22369,.T.);
#50604=EDGE_CURVE('',#38737,#39266,#22370,.T.);
#50605=EDGE_CURVE('',#39266,#39267,#32447,.T.);
#50606=EDGE_CURVE('',#39267,#38735,#22371,.T.);
#50607=EDGE_CURVE('',#38742,#39268,#22372,.T.);
#50608=EDGE_CURVE('',#39268,#39269,#32448,.T.);
#50609=EDGE_CURVE('',#39269,#38738,#22373,.T.);
#50610=EDGE_CURVE('',#38749,#39270,#22374,.T.);
#50611=EDGE_CURVE('',#39270,#39271,#32449,.T.);
#50612=EDGE_CURVE('',#39271,#38746,#22375,.T.);
#50613=EDGE_CURVE('',#38741,#39272,#22376,.T.);
#50614=EDGE_CURVE('',#39272,#39273,#32450,.T.);
#50615=EDGE_CURVE('',#39273,#38745,#22377,.T.);
#50616=EDGE_CURVE('',#38928,#39274,#22378,.T.);
#50617=EDGE_CURVE('',#39274,#39275,#32451,.T.);
#50618=EDGE_CURVE('',#39275,#38924,#22379,.T.);
#50619=EDGE_CURVE('',#38927,#39276,#22380,.T.);
#50620=EDGE_CURVE('',#39276,#39277,#32452,.T.);
#50621=EDGE_CURVE('',#39277,#38931,#22381,.T.);
#50622=EDGE_CURVE('',#38923,#39278,#22382,.T.);
#50623=EDGE_CURVE('',#39278,#39279,#32453,.T.);
#50624=EDGE_CURVE('',#39279,#38921,#22383,.T.);
#50625=EDGE_CURVE('',#38828,#39280,#22384,.T.);
#50626=EDGE_CURVE('',#39280,#39281,#32454,.T.);
#50627=EDGE_CURVE('',#39281,#38824,#22385,.T.);
#50628=EDGE_CURVE('',#38835,#39282,#22386,.T.);
#50629=EDGE_CURVE('',#39282,#39283,#32455,.T.);
#50630=EDGE_CURVE('',#39283,#38832,#22387,.T.);
#50631=EDGE_CURVE('',#38827,#39284,#22388,.T.);
#50632=EDGE_CURVE('',#39284,#39285,#32456,.T.);
#50633=EDGE_CURVE('',#39285,#38831,#22389,.T.);
#50634=EDGE_CURVE('',#38823,#39286,#22390,.T.);
#50635=EDGE_CURVE('',#39286,#39287,#32457,.T.);
#50636=EDGE_CURVE('',#39287,#38821,#22391,.T.);
#50637=EDGE_CURVE('',#38791,#39288,#22392,.T.);
#50638=EDGE_CURVE('',#39288,#39289,#32458,.T.);
#50639=EDGE_CURVE('',#39289,#38795,#22393,.T.);
#50640=EDGE_CURVE('',#38787,#39290,#22394,.T.);
#50641=EDGE_CURVE('',#39290,#39291,#32459,.T.);
#50642=EDGE_CURVE('',#39291,#38785,#22395,.T.);
#50643=EDGE_CURVE('',#38792,#39292,#22396,.T.);
#50644=EDGE_CURVE('',#39292,#39293,#32460,.T.);
#50645=EDGE_CURVE('',#39293,#38788,#22397,.T.);
#50646=EDGE_CURVE('',#38799,#39294,#22398,.T.);
#50647=EDGE_CURVE('',#39294,#39295,#32461,.T.);
#50648=EDGE_CURVE('',#39295,#38796,#22399,.T.);
#50649=EDGE_CURVE('',#38725,#39296,#22400,.T.);
#50650=EDGE_CURVE('',#39296,#39297,#32462,.T.);
#50651=EDGE_CURVE('',#39297,#38729,#22401,.T.);
#50652=EDGE_CURVE('',#38721,#39298,#22402,.T.);
#50653=EDGE_CURVE('',#39298,#39299,#32463,.T.);
#50654=EDGE_CURVE('',#39299,#38719,#22403,.T.);
#50655=EDGE_CURVE('',#38726,#39300,#22404,.T.);
#50656=EDGE_CURVE('',#39300,#39301,#32464,.T.);
#50657=EDGE_CURVE('',#39301,#38722,#22405,.T.);
#50658=EDGE_CURVE('',#38733,#39302,#22406,.T.);
#50659=EDGE_CURVE('',#39302,#39303,#32465,.T.);
#50660=EDGE_CURVE('',#39303,#38730,#22407,.T.);
#50661=EDGE_CURVE('',#38633,#39304,#22408,.T.);
#50662=EDGE_CURVE('',#39304,#39305,#32466,.T.);
#50663=EDGE_CURVE('',#39305,#38631,#22409,.T.);
#50664=EDGE_CURVE('',#38638,#39306,#22410,.T.);
#50665=EDGE_CURVE('',#39306,#39307,#32467,.T.);
#50666=EDGE_CURVE('',#39307,#38634,#22411,.T.);
#50667=EDGE_CURVE('',#38645,#39308,#22412,.T.);
#50668=EDGE_CURVE('',#39308,#39309,#32468,.T.);
#50669=EDGE_CURVE('',#39309,#38642,#22413,.T.);
#50670=EDGE_CURVE('',#38637,#39310,#22414,.T.);
#50671=EDGE_CURVE('',#39310,#39311,#32469,.T.);
#50672=EDGE_CURVE('',#39311,#38641,#22415,.T.);
#50673=EDGE_CURVE('',#38597,#39312,#22416,.T.);
#50674=EDGE_CURVE('',#39312,#39313,#32470,.T.);
#50675=EDGE_CURVE('',#39313,#38595,#22417,.T.);
#50676=EDGE_CURVE('',#38602,#39314,#22418,.T.);
#50677=EDGE_CURVE('',#39314,#39315,#32471,.T.);
#50678=EDGE_CURVE('',#39315,#38598,#22419,.T.);
#50679=EDGE_CURVE('',#38609,#39316,#22420,.T.);
#50680=EDGE_CURVE('',#39316,#39317,#32472,.T.);
#50681=EDGE_CURVE('',#39317,#38606,#22421,.T.);
#50682=EDGE_CURVE('',#38601,#39318,#22422,.T.);
#50683=EDGE_CURVE('',#39318,#39319,#32473,.T.);
#50684=EDGE_CURVE('',#39319,#38605,#22423,.T.);
#50685=EDGE_CURVE('',#38613,#39320,#22424,.T.);
#50686=EDGE_CURVE('',#39320,#39321,#32474,.T.);
#50687=EDGE_CURVE('',#39321,#38611,#22425,.T.);
#50688=EDGE_CURVE('',#38618,#39322,#22426,.T.);
#50689=EDGE_CURVE('',#39322,#39323,#32475,.T.);
#50690=EDGE_CURVE('',#39323,#38614,#22427,.T.);
#50691=EDGE_CURVE('',#38626,#39324,#22428,.T.);
#50692=EDGE_CURVE('',#39324,#39325,#32476,.T.);
#50693=EDGE_CURVE('',#39325,#38622,#22429,.T.);
#50694=EDGE_CURVE('',#38617,#39326,#22430,.T.);
#50695=EDGE_CURVE('',#39326,#39327,#32477,.T.);
#50696=EDGE_CURVE('',#39327,#38621,#22431,.T.);
#50697=EDGE_CURVE('',#38460,#39328,#22432,.T.);
#50698=EDGE_CURVE('',#39328,#39329,#32478,.T.);
#50699=EDGE_CURVE('',#39329,#38456,#22433,.T.);
#50700=EDGE_CURVE('',#38459,#39330,#22434,.T.);
#50701=EDGE_CURVE('',#39330,#39331,#32479,.T.);
#50702=EDGE_CURVE('',#39331,#38463,#22435,.T.);
#50703=EDGE_CURVE('',#39332,#39333,#32480,.T.);
#50704=EDGE_CURVE('',#39333,#38447,#22436,.T.);
#50705=EDGE_CURVE('',#38446,#39332,#22437,.T.);
#50706=EDGE_CURVE('',#38452,#39334,#22438,.T.);
#50707=EDGE_CURVE('',#39334,#39335,#32481,.T.);
#50708=EDGE_CURVE('',#39335,#38448,#22439,.T.);
#50709=EDGE_CURVE('',#38863,#39336,#22440,.T.);
#50710=EDGE_CURVE('',#39336,#39337,#32482,.T.);
#50711=EDGE_CURVE('',#39337,#38867,#22441,.T.);
#50712=EDGE_CURVE('',#38859,#39338,#22442,.T.);
#50713=EDGE_CURVE('',#39338,#39339,#32483,.T.);
#50714=EDGE_CURVE('',#39339,#38857,#22443,.T.);
#50715=EDGE_CURVE('',#38864,#39340,#22444,.T.);
#50716=EDGE_CURVE('',#39340,#39341,#32484,.T.);
#50717=EDGE_CURVE('',#39341,#38860,#22445,.T.);
#50718=EDGE_CURVE('',#38871,#39342,#22446,.T.);
#50719=EDGE_CURVE('',#39342,#39343,#32485,.T.);
#50720=EDGE_CURVE('',#39343,#38868,#22447,.T.);
#50721=EDGE_CURVE('',#38553,#39344,#22448,.T.);
#50722=EDGE_CURVE('',#39344,#39345,#32486,.T.);
#50723=EDGE_CURVE('',#39345,#38557,#22449,.T.);
#50724=EDGE_CURVE('',#38549,#39346,#22450,.T.);
#50725=EDGE_CURVE('',#39346,#39347,#32487,.T.);
#50726=EDGE_CURVE('',#39347,#38547,#22451,.T.);
#50727=EDGE_CURVE('',#38554,#39348,#22452,.T.);
#50728=EDGE_CURVE('',#39348,#39349,#32488,.T.);
#50729=EDGE_CURVE('',#39349,#38550,#22453,.T.);
#50730=EDGE_CURVE('',#38561,#39350,#22454,.T.);
#50731=EDGE_CURVE('',#39350,#39351,#32489,.T.);
#50732=EDGE_CURVE('',#39351,#38558,#22455,.T.);
#50733=EDGE_CURVE('',#38537,#39352,#22456,.T.);
#50734=EDGE_CURVE('',#39352,#39353,#32490,.T.);
#50735=EDGE_CURVE('',#39353,#38541,#22457,.T.);
#50736=EDGE_CURVE('',#38533,#39354,#22458,.T.);
#50737=EDGE_CURVE('',#39354,#39355,#32491,.T.);
#50738=EDGE_CURVE('',#39355,#38531,#22459,.T.);
#50739=EDGE_CURVE('',#38538,#39356,#22460,.T.);
#50740=EDGE_CURVE('',#39356,#39357,#32492,.T.);
#50741=EDGE_CURVE('',#39357,#38534,#22461,.T.);
#50742=EDGE_CURVE('',#38545,#39358,#22462,.T.);
#50743=EDGE_CURVE('',#39358,#39359,#32493,.T.);
#50744=EDGE_CURVE('',#39359,#38542,#22463,.T.);
#50745=EDGE_CURVE('',#38753,#39360,#22464,.T.);
#50746=EDGE_CURVE('',#39360,#39361,#32494,.T.);
#50747=EDGE_CURVE('',#39361,#38751,#22465,.T.);
#50748=EDGE_CURVE('',#38758,#39362,#22466,.T.);
#50749=EDGE_CURVE('',#39362,#39363,#32495,.T.);
#50750=EDGE_CURVE('',#39363,#38754,#22467,.T.);
#50751=EDGE_CURVE('',#38765,#39364,#22468,.T.);
#50752=EDGE_CURVE('',#39364,#39365,#32496,.T.);
#50753=EDGE_CURVE('',#39365,#38762,#22469,.T.);
#50754=EDGE_CURVE('',#38757,#39366,#22470,.T.);
#50755=EDGE_CURVE('',#39366,#39367,#32497,.T.);
#50756=EDGE_CURVE('',#39367,#38761,#22471,.T.);
#50757=EDGE_CURVE('',#38880,#39368,#22472,.T.);
#50758=EDGE_CURVE('',#39368,#39369,#32498,.T.);
#50759=EDGE_CURVE('',#39369,#38876,#22473,.T.);
#50760=EDGE_CURVE('',#38887,#39370,#22474,.T.);
#50761=EDGE_CURVE('',#39370,#39371,#32499,.T.);
#50762=EDGE_CURVE('',#39371,#38884,#22475,.T.);
#50763=EDGE_CURVE('',#38879,#39372,#22476,.T.);
#50764=EDGE_CURVE('',#39372,#39373,#32500,.T.);
#50765=EDGE_CURVE('',#39373,#38883,#22477,.T.);
#50766=EDGE_CURVE('',#38875,#39374,#22478,.T.);
#50767=EDGE_CURVE('',#39374,#39375,#32501,.T.);
#50768=EDGE_CURVE('',#39375,#38873,#22479,.T.);
#50769=EDGE_CURVE('',#38479,#39376,#22480,.T.);
#50770=EDGE_CURVE('',#39376,#39377,#32502,.T.);
#50771=EDGE_CURVE('',#39377,#38476,#22481,.T.);
#50772=EDGE_CURVE('',#38471,#39378,#22482,.T.);
#50773=EDGE_CURVE('',#39378,#39379,#32503,.T.);
#50774=EDGE_CURVE('',#39379,#38475,#22483,.T.);
#50775=EDGE_CURVE('',#39380,#39381,#32504,.T.);
#50776=EDGE_CURVE('',#39381,#38467,#22484,.T.);
#50777=EDGE_CURVE('',#38466,#39380,#22485,.T.);
#50778=EDGE_CURVE('',#38472,#39382,#22486,.T.);
#50779=EDGE_CURVE('',#39382,#39383,#32505,.T.);
#50780=EDGE_CURVE('',#39383,#38468,#22487,.T.);
#50781=EDGE_CURVE('',#38895,#39384,#22488,.T.);
#50782=EDGE_CURVE('',#39384,#39385,#32506,.T.);
#50783=EDGE_CURVE('',#39385,#38899,#22489,.T.);
#50784=EDGE_CURVE('',#38891,#39386,#22490,.T.);
#50785=EDGE_CURVE('',#39386,#39387,#32507,.T.);
#50786=EDGE_CURVE('',#39387,#38889,#22491,.T.);
#50787=EDGE_CURVE('',#38896,#39388,#22492,.T.);
#50788=EDGE_CURVE('',#39388,#39389,#32508,.T.);
#50789=EDGE_CURVE('',#39389,#38892,#22493,.T.);
#50790=EDGE_CURVE('',#38903,#39390,#22494,.T.);
#50791=EDGE_CURVE('',#39390,#39391,#32509,.T.);
#50792=EDGE_CURVE('',#39391,#38900,#22495,.T.);
#50793=EDGE_CURVE('',#38503,#39392,#22496,.T.);
#50794=EDGE_CURVE('',#39392,#39393,#32510,.T.);
#50795=EDGE_CURVE('',#39393,#38507,#22497,.T.);
#50796=EDGE_CURVE('',#38499,#39394,#22498,.T.);
#50797=EDGE_CURVE('',#39394,#39395,#32511,.T.);
#50798=EDGE_CURVE('',#39395,#38497,#22499,.T.);
#50799=EDGE_CURVE('',#38504,#39396,#22500,.T.);
#50800=EDGE_CURVE('',#39396,#39397,#32512,.T.);
#50801=EDGE_CURVE('',#39397,#38500,#22501,.T.);
#50802=EDGE_CURVE('',#38511,#39398,#22502,.T.);
#50803=EDGE_CURVE('',#39398,#39399,#32513,.T.);
#50804=EDGE_CURVE('',#39399,#38508,#22503,.T.);
#50805=EDGE_CURVE('',#38912,#39400,#22504,.T.);
#50806=EDGE_CURVE('',#39400,#39401,#32514,.T.);
#50807=EDGE_CURVE('',#39401,#38908,#22505,.T.);
#50808=EDGE_CURVE('',#38919,#39402,#22506,.T.);
#50809=EDGE_CURVE('',#39402,#39403,#32515,.T.);
#50810=EDGE_CURVE('',#39403,#38916,#22507,.T.);
#50811=EDGE_CURVE('',#38911,#39404,#22508,.T.);
#50812=EDGE_CURVE('',#39404,#39405,#32516,.T.);
#50813=EDGE_CURVE('',#39405,#38915,#22509,.T.);
#50814=EDGE_CURVE('',#38907,#39406,#22510,.T.);
#50815=EDGE_CURVE('',#39406,#39407,#32517,.T.);
#50816=EDGE_CURVE('',#39407,#38905,#22511,.T.);
#50817=EDGE_CURVE('',#38495,#39408,#22512,.T.);
#50818=EDGE_CURVE('',#39408,#39409,#32518,.T.);
#50819=EDGE_CURVE('',#39409,#38492,#22513,.T.);
#50820=EDGE_CURVE('',#38487,#39410,#22514,.T.);
#50821=EDGE_CURVE('',#39410,#39411,#32519,.T.);
#50822=EDGE_CURVE('',#39411,#38491,#22515,.T.);
#50823=EDGE_CURVE('',#39412,#39413,#32520,.T.);
#50824=EDGE_CURVE('',#39413,#38483,#22516,.T.);
#50825=EDGE_CURVE('',#38482,#39412,#22517,.T.);
#50826=EDGE_CURVE('',#38488,#39414,#22518,.T.);
#50827=EDGE_CURVE('',#39414,#39415,#32521,.T.);
#50828=EDGE_CURVE('',#39415,#38484,#22519,.T.);
#50829=EDGE_CURVE('',#39001,#39416,#22520,.T.);
#50830=EDGE_CURVE('',#39416,#39417,#32522,.T.);
#50831=EDGE_CURVE('',#39417,#39003,#22521,.T.);
#50832=EDGE_CURVE('',#39029,#39418,#22522,.T.);
#50833=EDGE_CURVE('',#39418,#39419,#32523,.T.);
#50834=EDGE_CURVE('',#39419,#39031,#22523,.T.);
#50835=EDGE_CURVE('',#39017,#39420,#22524,.T.);
#50836=EDGE_CURVE('',#39420,#39421,#32524,.T.);
#50837=EDGE_CURVE('',#39421,#39019,#22525,.T.);
#50838=EDGE_CURVE('',#39422,#39423,#32525,.T.);
#50839=EDGE_CURVE('',#39423,#39015,#22526,.T.);
#50840=EDGE_CURVE('',#39013,#39422,#22527,.T.);
#50841=EDGE_CURVE('',#39033,#39424,#22528,.T.);
#50842=EDGE_CURVE('',#39424,#39425,#32526,.T.);
#50843=EDGE_CURVE('',#39425,#39035,#22529,.T.);
#50844=EDGE_CURVE('',#39426,#39427,#32527,.T.);
#50845=EDGE_CURVE('',#39427,#39026,#22530,.T.);
#50846=EDGE_CURVE('',#39025,#39426,#22531,.T.);
#50847=EDGE_CURVE('',#39005,#39428,#22532,.T.);
#50848=EDGE_CURVE('',#39428,#39429,#32528,.T.);
#50849=EDGE_CURVE('',#39429,#39006,#22533,.T.);
#50850=EDGE_CURVE('',#38669,#39430,#22534,.T.);
#50851=EDGE_CURVE('',#39430,#39431,#32529,.T.);
#50852=EDGE_CURVE('',#39431,#38673,#22535,.T.);
#50853=EDGE_CURVE('',#38689,#39432,#22536,.T.);
#50854=EDGE_CURVE('',#39432,#39433,#32530,.T.);
#50855=EDGE_CURVE('',#39433,#38693,#22537,.T.);
#50856=EDGE_CURVE('',#38781,#39434,#22538,.T.);
#50857=EDGE_CURVE('',#39434,#39180,#32531,.T.);
#50858=EDGE_CURVE('',#39199,#39435,#32532,.T.);
#50859=EDGE_CURVE('',#39435,#38524,#22539,.T.);
#50860=EDGE_CURVE('',#39207,#39434,#32533,.T.);
#50861=EDGE_CURVE('',#39435,#39204,#32534,.T.);
#50862=EDGE_CURVE('',#39424,#39419,#32535,.T.);
#50863=EDGE_CURVE('',#39418,#39427,#22540,.T.);
#50864=EDGE_CURVE('',#39428,#39417,#22541,.T.);
#50865=EDGE_CURVE('',#39416,#39167,#32536,.T.);
#50866=EDGE_CURVE('',#39433,#39182,#32537,.T.);
#50867=EDGE_CURVE('',#39420,#39423,#32538,.T.);
#50868=EDGE_CURVE('',#39421,#39176,#22542,.T.);
#50869=EDGE_CURVE('',#39175,#39162,#22543,.T.);
#50870=EDGE_CURVE('',#39172,#39163,#32539,.T.);
#50871=EDGE_CURVE('',#39191,#39430,#32540,.T.);
#50872=EDGE_CURVE('',#39224,#39219,#22544,.T.);
#50873=EDGE_CURVE('',#39320,#39323,#22545,.T.);
#50874=EDGE_CURVE('',#39312,#39315,#22546,.T.);
#50875=EDGE_CURVE('',#39232,#39227,#22547,.T.);
#50876=EDGE_CURVE('',#39304,#39307,#22548,.T.);
#50877=EDGE_CURVE('',#39256,#39251,#22549,.T.);
#50878=EDGE_CURVE('',#39296,#39299,#22550,.T.);
#50879=EDGE_CURVE('',#39264,#39259,#22551,.T.);
#50880=EDGE_CURVE('',#39248,#39243,#22552,.T.);
#50881=EDGE_CURVE('',#39280,#39283,#22553,.T.);
#50882=EDGE_CURVE('',#39288,#39291,#22554,.T.);
#50883=EDGE_CURVE('',#39272,#39267,#22555,.T.);
#50884=EDGE_CURVE('',#39274,#39277,#22556,.T.);
#50885=EDGE_CURVE('',#39240,#39235,#22557,.T.);
#50886=EDGE_CURVE('',#39216,#39213,#22558,.T.);
#50887=EDGE_CURVE('',#39328,#39331,#22559,.T.);
#50888=EDGE_CURVE('',#39376,#39379,#22560,.T.);
#50889=EDGE_CURVE('',#39332,#39335,#22561,.T.);
#50890=EDGE_CURVE('',#39220,#39223,#22562,.T.);
#50891=EDGE_CURVE('',#39350,#39345,#22563,.T.);
#50892=EDGE_CURVE('',#39236,#39239,#22564,.T.);
#50893=EDGE_CURVE('',#39336,#39339,#22565,.T.);
#50894=EDGE_CURVE('',#39228,#39231,#22566,.T.);
#50895=EDGE_CURVE('',#39358,#39353,#22567,.T.);
#50896=EDGE_CURVE('',#39252,#39255,#22568,.T.);
#50897=EDGE_CURVE('',#39192,#39195,#22569,.T.);
#50898=EDGE_CURVE('',#39260,#39263,#22570,.T.);
#50899=EDGE_CURVE('',#39186,#39189,#22571,.T.);
#50900=EDGE_CURVE('',#39284,#39287,#22572,.T.);
#50901=EDGE_CURVE('',#39368,#39371,#22573,.T.);
#50902=EDGE_CURVE('',#39268,#39271,#22574,.T.);
#50903=EDGE_CURVE('',#39366,#39361,#22575,.T.);
#50904=EDGE_CURVE('',#39436,#39437,#22576,.T.);
#50905=EDGE_CURVE('',#39438,#39437,#22577,.T.);
#50906=EDGE_CURVE('',#39439,#39438,#22578,.T.);
#50907=EDGE_CURVE('',#39436,#39439,#22579,.T.);
#50908=EDGE_CURVE('',#39440,#39441,#22580,.T.);
#50909=EDGE_CURVE('',#39437,#39441,#22581,.T.);
#50910=EDGE_CURVE('',#39440,#39436,#22582,.T.);
#50911=EDGE_CURVE('',#39442,#39438,#22583,.T.);
#50912=EDGE_CURVE('',#39442,#39443,#22584,.T.);
#50913=EDGE_CURVE('',#39439,#39443,#22585,.T.);
#50914=EDGE_CURVE('',#39408,#39411,#22586,.T.);
#50915=EDGE_CURVE('',#39380,#39383,#22587,.T.);
#50916=EDGE_CURVE('',#39346,#39349,#22588,.T.);
#50917=EDGE_CURVE('',#39398,#39393,#22589,.T.);
#50918=EDGE_CURVE('',#39340,#39343,#22590,.T.);
#50919=EDGE_CURVE('',#39384,#39387,#22591,.T.);
#50920=EDGE_CURVE('',#39354,#39357,#22592,.T.);
#50921=EDGE_CURVE('',#39198,#39201,#22593,.T.);
#50922=EDGE_CURVE('',#39196,#39431,#22594,.T.);
#50923=EDGE_CURVE('',#39432,#39185,#22595,.T.);
#50924=EDGE_CURVE('',#39372,#39375,#22596,.T.);
#50925=EDGE_CURVE('',#39400,#39403,#22597,.T.);
#50926=EDGE_CURVE('',#39362,#39365,#22598,.T.);
#50927=EDGE_CURVE('',#39210,#39181,#22599,.T.);
#50928=EDGE_CURVE('',#39202,#39205,#22600,.T.);
#50929=EDGE_CURVE('',#39404,#39407,#22601,.T.);
#50930=EDGE_CURVE('',#39206,#39209,#22602,.T.);
#50931=EDGE_CURVE('',#39164,#39425,#22603,.T.);
#50932=EDGE_CURVE('',#39422,#39179,#22604,.T.);
#50933=EDGE_CURVE('',#39394,#39397,#22605,.T.);
#50934=EDGE_CURVE('',#39412,#39415,#22606,.T.);
#50935=EDGE_CURVE('',#39388,#39391,#22607,.T.);
#50936=EDGE_CURVE('',#39444,#39445,#22608,.T.);
#50937=EDGE_CURVE('',#39445,#39446,#32541,.T.);
#50938=EDGE_CURVE('',#39447,#39446,#22609,.T.);
#50939=EDGE_CURVE('',#39444,#39447,#32542,.T.);
#50940=EDGE_CURVE('',#39448,#39446,#32543,.T.);
#50941=EDGE_CURVE('',#39449,#39448,#22610,.T.);
#50942=EDGE_CURVE('',#39447,#39449,#32544,.T.);
#50943=EDGE_CURVE('',#39448,#39450,#32545,.T.);
#50944=EDGE_CURVE('',#39451,#39450,#22611,.T.);
#50945=EDGE_CURVE('',#39449,#39451,#32546,.T.);
#50946=EDGE_CURVE('',#39450,#39452,#32547,.T.);
#50947=EDGE_CURVE('',#39453,#39452,#22612,.T.);
#50948=EDGE_CURVE('',#39451,#39453,#32548,.T.);
#50949=EDGE_CURVE('',#39452,#39454,#32549,.T.);
#50950=EDGE_CURVE('',#39455,#39454,#22613,.T.);
#50951=EDGE_CURVE('',#39453,#39455,#32550,.T.);
#50952=EDGE_CURVE('',#39456,#39454,#32551,.T.);
#50953=EDGE_CURVE('',#39457,#39456,#22614,.T.);
#50954=EDGE_CURVE('',#39455,#39457,#32552,.T.);
#50955=EDGE_CURVE('',#39456,#39458,#32553,.T.);
#50956=EDGE_CURVE('',#39459,#39458,#22615,.T.);
#50957=EDGE_CURVE('',#39457,#39459,#32554,.T.);
#50958=EDGE_CURVE('',#39460,#39461,#22616,.T.);
#50959=EDGE_CURVE('',#39462,#39461,#32555,.T.);
#50960=EDGE_CURVE('',#39462,#39463,#22617,.T.);
#50961=EDGE_CURVE('',#39460,#39463,#5576,.T.);
#50962=EDGE_CURVE('',#39464,#39460,#5577,.T.);
#50963=EDGE_CURVE('',#39464,#39461,#22618,.T.);
#50964=EDGE_CURVE('',#39465,#39466,#32556,.T.);
#50965=EDGE_CURVE('',#39466,#39467,#5578,.T.);
#50966=EDGE_CURVE('',#39467,#39465,#22619,.T.);
#50967=EDGE_CURVE('',#39468,#39467,#5579,.T.);
#50968=EDGE_CURVE('',#39468,#39465,#22620,.T.);
#50969=EDGE_CURVE('',#39469,#39470,#1222,.T.);
#50970=EDGE_CURVE('',#39469,#39471,#22621,.T.);
#50971=EDGE_CURVE('',#39472,#39471,#22622,.T.);
#50972=EDGE_CURVE('',#39472,#39470,#5580,.T.);
#50973=EDGE_CURVE('',#39473,#39474,#1223,.T.);
#50974=EDGE_CURVE('',#39473,#39475,#5581,.T.);
#50975=EDGE_CURVE('',#39476,#39475,#22623,.T.);
#50976=EDGE_CURVE('',#39474,#39476,#22624,.T.);
#50977=EDGE_CURVE('',#39474,#39469,#32557,.T.);
#50978=EDGE_CURVE('',#39471,#39476,#32558,.T.);
#50979=EDGE_CURVE('',#39477,#39478,#1224,.T.);
#50980=EDGE_CURVE('',#39477,#39479,#5582,.T.);
#50981=EDGE_CURVE('',#39480,#39479,#22625,.T.);
#50982=EDGE_CURVE('',#39478,#39480,#22626,.T.);
#50983=EDGE_CURVE('',#39481,#39482,#1225,.T.);
#50984=EDGE_CURVE('',#39481,#39483,#22627,.T.);
#50985=EDGE_CURVE('',#39484,#39483,#22628,.T.);
#50986=EDGE_CURVE('',#39484,#39482,#5583,.T.);
#50987=EDGE_CURVE('',#39478,#39481,#32559,.T.);
#50988=EDGE_CURVE('',#39483,#39480,#32560,.T.);
#50989=EDGE_CURVE('',#39485,#39486,#32561,.T.);
#50990=EDGE_CURVE('',#39487,#39486,#22629,.T.);
#50991=EDGE_CURVE('',#39488,#39487,#32562,.T.);
#50992=EDGE_CURVE('',#39488,#39485,#22630,.T.);
#50993=EDGE_CURVE('',#39489,#39490,#32563,.T.);
#50994=EDGE_CURVE('',#39491,#39490,#22631,.T.);
#50995=EDGE_CURVE('',#39492,#39491,#32564,.T.);
#50996=EDGE_CURVE('',#39492,#39489,#22632,.T.);
#50997=EDGE_CURVE('',#39490,#39493,#32565,.T.);
#50998=EDGE_CURVE('',#39494,#39493,#22633,.T.);
#50999=EDGE_CURVE('',#39491,#39494,#32566,.T.);
#51000=EDGE_CURVE('',#39493,#39495,#32567,.T.);
#51001=EDGE_CURVE('',#39496,#39495,#22634,.T.);
#51002=EDGE_CURVE('',#39494,#39496,#32568,.T.);
#51003=EDGE_CURVE('',#39497,#39498,#5584,.T.);
#51004=EDGE_CURVE('',#39496,#39497,#32569,.T.);
#51005=EDGE_CURVE('',#39495,#39498,#32570,.T.);
#51006=EDGE_CURVE('',#39499,#39500,#32571,.T.);
#51007=EDGE_CURVE('',#39501,#39500,#22635,.T.);
#51008=EDGE_CURVE('',#39502,#39501,#32572,.T.);
#51009=EDGE_CURVE('',#39502,#39499,#22636,.T.);
#51010=EDGE_CURVE('',#39500,#39485,#32573,.T.);
#51011=EDGE_CURVE('',#39501,#39488,#32574,.T.);
#51012=EDGE_CURVE('',#39503,#39504,#5585,.T.);
#51013=EDGE_CURVE('',#39503,#39505,#5586,.T.);
#51014=EDGE_CURVE('',#39506,#39505,#5587,.T.);
#51015=EDGE_CURVE('',#39506,#39507,#5588,.T.);
#51016=EDGE_CURVE('',#39504,#39507,#5589,.T.);
#51017=EDGE_CURVE('',#39508,#39509,#5590,.T.);
#51018=EDGE_CURVE('',#39508,#39510,#5591,.T.);
#51019=EDGE_CURVE('',#39510,#39511,#5592,.T.);
#51020=EDGE_CURVE('',#39511,#39512,#5593,.T.);
#51021=EDGE_CURVE('',#39509,#39512,#5594,.T.);
#51022=EDGE_CURVE('',#39513,#39514,#5595,.T.);
#51023=EDGE_CURVE('',#39513,#39515,#5596,.T.);
#51024=EDGE_CURVE('',#39516,#39515,#5597,.T.);
#51025=EDGE_CURVE('',#39516,#39517,#5598,.T.);
#51026=EDGE_CURVE('',#39514,#39517,#5599,.T.);
#51027=EDGE_CURVE('',#39518,#39519,#5600,.T.);
#51028=EDGE_CURVE('',#39518,#39520,#5601,.T.);
#51029=EDGE_CURVE('',#39520,#39521,#5602,.T.);
#51030=EDGE_CURVE('',#39521,#39522,#5603,.T.);
#51031=EDGE_CURVE('',#39522,#39519,#5604,.T.);
#51032=EDGE_CURVE('',#39523,#39524,#32575,.T.);
#51033=EDGE_CURVE('',#39511,#39524,#22637,.T.);
#51034=EDGE_CURVE('',#39525,#39510,#5605,.T.);
#51035=EDGE_CURVE('',#39525,#39523,#22638,.T.);
#51036=EDGE_CURVE('',#39473,#39525,#5606,.T.);
#51037=EDGE_CURVE('',#39526,#39470,#5607,.T.);
#51038=EDGE_CURVE('',#39526,#39527,#22639,.T.);
#51039=EDGE_CURVE('',#39527,#39523,#32576,.T.);
#51040=EDGE_CURVE('',#39528,#39527,#32577,.T.);
#51041=EDGE_CURVE('',#39526,#39507,#32578,.T.);
#51042=EDGE_CURVE('',#39506,#39528,#22640,.T.);
#51043=EDGE_CURVE('',#39529,#39530,#32579,.T.);
#51044=EDGE_CURVE('',#39521,#39530,#22641,.T.);
#51045=EDGE_CURVE('',#39531,#39520,#32580,.T.);
#51046=EDGE_CURVE('',#39531,#39529,#22642,.T.);
#51047=EDGE_CURVE('',#39532,#39482,#5608,.T.);
#51048=EDGE_CURVE('',#39532,#39533,#22643,.T.);
#51049=EDGE_CURVE('',#39533,#39529,#32581,.T.);
#51050=EDGE_CURVE('',#39477,#39531,#5609,.T.);
#51051=EDGE_CURVE('',#39534,#39533,#32582,.T.);
#51052=EDGE_CURVE('',#39532,#39517,#32583,.T.);
#51053=EDGE_CURVE('',#39516,#39534,#22644,.T.);
#51054=EDGE_CURVE('',#39535,#39536,#32584,.T.);
#51055=EDGE_CURVE('',#39537,#39536,#22645,.T.);
#51056=EDGE_CURVE('',#39538,#39537,#32585,.T.);
#51057=EDGE_CURVE('',#39538,#39535,#22646,.T.);
#51058=EDGE_CURVE('',#39539,#39535,#32586,.T.);
#51059=EDGE_CURVE('',#39540,#39538,#32587,.T.);
#51060=EDGE_CURVE('',#39540,#39539,#22647,.T.);
#51061=EDGE_CURVE('',#39541,#39539,#32588,.T.);
#51062=EDGE_CURVE('',#39542,#39540,#32589,.T.);
#51063=EDGE_CURVE('',#39542,#39541,#22648,.T.);
#51064=EDGE_CURVE('',#39543,#39541,#32590,.T.);
#51065=EDGE_CURVE('',#39544,#39542,#32591,.T.);
#51066=EDGE_CURVE('',#39544,#39543,#22649,.T.);
#51067=EDGE_CURVE('',#39545,#39546,#32592,.T.);
#51068=EDGE_CURVE('',#39547,#39546,#22650,.T.);
#51069=EDGE_CURVE('',#39548,#39547,#32593,.T.);
#51070=EDGE_CURVE('',#39548,#39545,#22651,.T.);
#51071=EDGE_CURVE('',#39549,#39545,#32594,.T.);
#51072=EDGE_CURVE('',#39550,#39548,#32595,.T.);
#51073=EDGE_CURVE('',#39550,#39549,#22652,.T.);
#51074=EDGE_CURVE('',#39536,#39549,#32596,.T.);
#51075=EDGE_CURVE('',#39537,#39550,#32597,.T.);
#51076=EDGE_CURVE('',#39551,#39503,#5610,.T.);
#51077=EDGE_CURVE('',#39551,#39552,#5611,.T.);
#51078=EDGE_CURVE('',#39552,#39505,#5612,.T.);
#51079=EDGE_CURVE('',#39522,#39553,#5613,.T.);
#51080=EDGE_CURVE('',#39553,#39554,#5614,.T.);
#51081=EDGE_CURVE('',#39519,#39554,#5615,.T.);
#51082=EDGE_CURVE('',#39553,#39552,#5616,.T.);
#51083=EDGE_CURVE('',#39530,#39528,#32598,.T.);
#51084=EDGE_CURVE('',#39555,#39513,#32599,.T.);
#51085=EDGE_CURVE('',#39555,#39556,#5617,.T.);
#51086=EDGE_CURVE('',#39556,#39515,#5618,.T.);
#51087=EDGE_CURVE('',#39557,#39499,#32600,.T.);
#51088=EDGE_CURVE('',#39557,#39551,#5619,.T.);
#51089=EDGE_CURVE('',#39504,#39508,#5620,.T.);
#51090=EDGE_CURVE('',#39509,#39558,#32601,.T.);
#51091=EDGE_CURVE('',#39559,#39558,#5621,.T.);
#51092=EDGE_CURVE('',#39486,#39559,#32602,.T.);
#51093=EDGE_CURVE('',#39558,#39560,#5622,.T.);
#51094=EDGE_CURVE('',#39512,#39560,#5623,.T.);
#51095=EDGE_CURVE('',#39484,#39561,#5624,.T.);
#51096=EDGE_CURVE('',#39562,#39479,#5625,.T.);
#51097=EDGE_CURVE('',#39562,#39561,#32603,.T.);
#51098=EDGE_CURVE('',#39562,#39563,#5626,.T.);
#51099=EDGE_CURVE('',#39514,#39518,#5627,.T.);
#51100=EDGE_CURVE('',#39561,#39468,#5628,.T.);
#51101=EDGE_CURVE('',#39564,#39466,#5629,.T.);
#51102=EDGE_CURVE('',#39565,#39564,#5630,.T.);
#51103=EDGE_CURVE('',#39565,#39563,#5631,.T.);
#51104=EDGE_CURVE('',#39566,#39475,#5632,.T.);
#51105=EDGE_CURVE('',#39566,#39567,#32604,.T.);
#51106=EDGE_CURVE('',#39472,#39567,#5633,.T.);
#51107=EDGE_CURVE('',#39566,#39568,#5634,.T.);
#51108=EDGE_CURVE('',#39464,#39567,#5635,.F.);
#51109=EDGE_CURVE('',#39463,#39568,#5636,.T.);
#51110=EDGE_CURVE('',#39569,#39570,#32605,.T.);
#51111=EDGE_CURVE('',#39569,#39570,#5637,.T.);
#51112=EDGE_CURVE('',#39554,#39498,#5638,.T.);
#51113=EDGE_CURVE('',#39571,#39489,#32606,.T.);
#51114=EDGE_CURVE('',#39571,#39555,#5639,.T.);
#51115=EDGE_CURVE('',#39572,#39573,#32607,.T.);
#51116=EDGE_CURVE('',#39572,#39573,#5640,.T.);
#51117=EDGE_CURVE('',#39574,#39575,#32608,.T.);
#51118=EDGE_CURVE('',#39574,#39575,#5641,.T.);
#51119=EDGE_CURVE('',#39576,#39577,#32609,.T.);
#51120=EDGE_CURVE('',#39576,#39577,#5642,.T.);
#51121=EDGE_CURVE('',#39578,#39579,#5643,.T.);
#51122=EDGE_CURVE('',#39579,#39578,#32610,.T.);
#51123=EDGE_CURVE('',#39564,#39580,#32611,.T.);
#51124=EDGE_CURVE('',#39580,#39565,#22653,.T.);
#51125=EDGE_CURVE('',#39581,#39575,#5644,.T.);
#51126=EDGE_CURVE('',#39582,#39581,#32612,.T.);
#51127=EDGE_CURVE('',#39582,#39574,#5645,.T.);
#51128=EDGE_CURVE('',#39583,#39584,#32613,.T.);
#51129=EDGE_CURVE('',#39583,#39572,#5646,.T.);
#51130=EDGE_CURVE('',#39573,#39584,#5647,.T.);
#51131=EDGE_CURVE('',#39585,#39502,#32614,.T.);
#51132=EDGE_CURVE('',#39585,#39557,#5648,.T.);
#51133=EDGE_CURVE('',#39586,#39587,#32615,.T.);
#51134=EDGE_CURVE('',#39586,#39576,#5649,.T.);
#51135=EDGE_CURVE('',#39577,#39587,#5650,.T.);
#51136=EDGE_CURVE('',#39579,#39559,#5651,.T.);
#51137=EDGE_CURVE('',#39578,#39588,#5652,.T.);
#51138=EDGE_CURVE('',#39487,#39588,#32616,.T.);
#51139=EDGE_CURVE('',#39462,#39568,#22654,.T.);
#51140=EDGE_CURVE('',#39580,#39563,#22655,.T.);
#51141=EDGE_CURVE('',#39589,#39583,#5653,.T.);
#51142=EDGE_CURVE('',#39589,#39497,#5654,.T.);
#51143=EDGE_CURVE('',#39590,#39585,#5655,.T.);
#51144=EDGE_CURVE('',#39587,#39590,#5656,.T.);
#51145=EDGE_CURVE('',#39581,#39586,#5657,.T.);
#51146=EDGE_CURVE('',#39584,#39582,#5658,.T.);
#51147=EDGE_CURVE('',#39591,#38451,#22656,.T.);
#51148=EDGE_CURVE('',#39591,#39592,#32617,.T.);
#51149=EDGE_CURVE('',#39592,#38455,#22657,.T.);
#51150=EDGE_CURVE('',#39327,#39593,#32618,.T.);
#51151=EDGE_CURVE('',#39593,#38625,#22658,.T.);
#51152=EDGE_CURVE('',#39593,#39594,#32619,.T.);
#51153=EDGE_CURVE('',#39594,#38629,#22659,.T.);
#51154=EDGE_CURVE('',#39319,#39316,#32620,.T.);
#51155=EDGE_CURVE('',#39595,#38816,#22660,.T.);
#51156=EDGE_CURVE('',#39595,#39596,#32621,.T.);
#51157=EDGE_CURVE('',#39596,#38812,#22661,.T.);
#51158=EDGE_CURVE('',#39596,#39244,#32622,.T.);
#51159=EDGE_CURVE('',#39597,#38851,#22662,.T.);
#51160=EDGE_CURVE('',#39597,#39598,#32623,.T.);
#51161=EDGE_CURVE('',#39598,#38855,#22663,.T.);
#51162=EDGE_CURVE('',#39599,#39599,#32624,.T.);
#51163=EDGE_CURVE('',#39599,#39600,#22664,.T.);
#51164=EDGE_CURVE('',#38294,#39600,#32625,.T.);
#51165=EDGE_CURVE('',#39600,#38296,#32626,.T.);
#51166=EDGE_CURVE('',#39601,#39601,#32627,.T.);
#51167=EDGE_CURVE('',#39601,#38299,#22665,.T.);
#51168=EDGE_CURVE('',#38295,#38293,#32628,.T.);
#51169=EDGE_CURVE('',#39602,#38971,#22666,.T.);
#51170=EDGE_CURVE('',#39603,#39602,#32629,.T.);
#51171=EDGE_CURVE('',#39603,#38973,#22667,.T.);
#51172=EDGE_CURVE('',#39604,#38969,#22668,.T.);
#51173=EDGE_CURVE('',#39602,#39604,#32630,.T.);
#51174=EDGE_CURVE('',#39605,#38967,#22669,.T.);
#51175=EDGE_CURVE('',#39604,#39605,#32631,.T.);
#51176=EDGE_CURVE('',#39606,#38965,#22670,.T.);
#51177=EDGE_CURVE('',#39605,#39606,#32632,.T.);
#51178=EDGE_CURVE('',#39607,#38961,#22671,.T.);
#51179=EDGE_CURVE('',#39606,#39607,#32633,.T.);
#51180=EDGE_CURVE('',#39608,#38963,#22672,.T.);
#51181=EDGE_CURVE('',#39607,#39608,#32634,.T.);
#51182=EDGE_CURVE('',#39609,#39603,#32635,.T.);
#51183=EDGE_CURVE('',#39609,#38975,#22673,.T.);
#51184=EDGE_CURVE('',#39610,#38944,#22674,.T.);
#51185=EDGE_CURVE('',#39610,#39611,#32636,.T.);
#51186=EDGE_CURVE('',#39611,#38946,#22675,.T.);
#51187=EDGE_CURVE('',#39612,#38958,#22676,.T.);
#51188=EDGE_CURVE('',#39612,#39613,#32637,.T.);
#51189=EDGE_CURVE('',#39613,#38956,#22677,.T.);
#51190=EDGE_CURVE('',#39613,#39614,#32638,.T.);
#51191=EDGE_CURVE('',#39614,#38954,#22678,.T.);
#51192=EDGE_CURVE('',#39614,#39615,#32639,.T.);
#51193=EDGE_CURVE('',#39615,#38952,#22679,.T.);
#51194=EDGE_CURVE('',#39615,#39616,#32640,.T.);
#51195=EDGE_CURVE('',#39616,#38950,#22680,.T.);
#51196=EDGE_CURVE('',#39616,#39617,#32641,.T.);
#51197=EDGE_CURVE('',#39617,#38948,#22681,.T.);
#51198=EDGE_CURVE('',#39617,#39610,#32642,.T.);
#51199=EDGE_CURVE('',#39087,#39099,#5659,.T.);
#51200=EDGE_CURVE('',#39085,#39103,#22682,.T.);
#51201=EDGE_CURVE('',#39091,#39135,#22683,.T.);
#51202=EDGE_CURVE('',#39089,#39138,#5660,.T.);
#51203=EDGE_CURVE('',#39066,#39159,#5661,.T.);
#51204=EDGE_CURVE('',#39064,#39153,#22684,.T.);
#51205=EDGE_CURVE('',#39122,#39070,#22685,.T.);
#51206=EDGE_CURVE('',#39068,#39125,#5662,.T.);
#51207=EDGE_CURVE('',#39141,#38364,#22686,.T.);
#51208=EDGE_CURVE('',#39137,#38366,#22687,.T.);
#51209=EDGE_CURVE('',#39097,#38362,#22688,.T.);
#51210=EDGE_CURVE('',#39102,#38360,#22689,.T.);
#51211=EDGE_CURVE('',#39128,#38356,#22690,.T.);
#51212=EDGE_CURVE('',#39124,#38358,#22691,.T.);
#51213=EDGE_CURVE('',#39160,#38352,#22692,.T.);
#51214=EDGE_CURVE('',#39156,#38354,#22693,.T.);
#51215=EDGE_CURVE('',#39048,#39618,#22694,.T.);
#51216=EDGE_CURVE('',#39619,#39618,#32643,.T.);
#51217=EDGE_CURVE('',#39046,#39619,#22695,.T.);
#51218=EDGE_CURVE('',#39620,#39619,#32644,.T.);
#51219=EDGE_CURVE('',#39044,#39620,#22696,.T.);
#51220=EDGE_CURVE('',#39621,#39620,#32645,.T.);
#51221=EDGE_CURVE('',#39040,#39621,#22697,.T.);
#51222=EDGE_CURVE('',#39622,#39621,#32646,.T.);
#51223=EDGE_CURVE('',#39042,#39622,#22698,.T.);
#51224=EDGE_CURVE('',#39054,#39623,#22699,.T.);
#51225=EDGE_CURVE('',#39624,#39623,#32647,.T.);
#51226=EDGE_CURVE('',#39052,#39624,#22700,.T.);
#51227=EDGE_CURVE('',#39625,#39624,#32648,.T.);
#51228=EDGE_CURVE('',#39050,#39625,#22701,.T.);
#51229=EDGE_CURVE('',#39618,#39625,#32649,.T.);
#51230=EDGE_CURVE('',#39594,#39324,#32650,.T.);
#51231=EDGE_CURVE('',#39311,#39308,#32651,.T.);
#51232=EDGE_CURVE('',#39303,#39300,#32652,.T.);
#51233=EDGE_CURVE('',#39295,#39292,#32653,.T.);
#51234=EDGE_CURVE('',#39247,#39595,#32654,.T.);
#51235=EDGE_CURVE('',#39208,#39211,#22702,.T.);
#51236=EDGE_CURVE('',#39402,#39405,#22703,.T.);
#51237=EDGE_CURVE('',#39170,#39173,#22704,.T.);
#51238=EDGE_CURVE('',#39166,#39169,#22705,.T.);
#51239=EDGE_CURVE('',#39406,#39401,#22706,.T.);
#51240=EDGE_CURVE('',#39386,#39389,#22707,.T.);
#51241=EDGE_CURVE('',#39200,#39203,#22708,.T.);
#51242=EDGE_CURVE('',#39396,#39399,#22709,.T.);
#51243=EDGE_CURVE('',#39392,#39395,#22710,.T.);
#51244=EDGE_CURVE('',#39414,#39409,#22711,.T.);
#51245=EDGE_CURVE('',#39413,#39410,#32655,.T.);
#51246=EDGE_CURVE('',#39385,#39390,#32656,.T.);
#51247=EDGE_CURVE('',#39445,#39440,#32657,.T.);
#51248=EDGE_CURVE('',#39441,#39444,#32658,.T.);
#51249=EDGE_CURVE('',#39364,#39367,#22712,.T.);
#51250=EDGE_CURVE('',#39370,#39373,#22713,.T.);
#51251=EDGE_CURVE('',#39184,#39187,#22714,.T.);
#51252=EDGE_CURVE('',#39360,#39363,#22715,.T.);
#51253=EDGE_CURVE('',#39190,#39193,#22716,.T.);
#51254=EDGE_CURVE('',#39188,#39183,#22717,.T.);
#51255=EDGE_CURVE('',#39356,#39359,#22718,.T.);
#51256=EDGE_CURVE('',#39194,#39197,#22719,.T.);
#51257=EDGE_CURVE('',#39374,#39369,#22720,.T.);
#51258=EDGE_CURVE('',#39338,#39341,#22721,.T.);
#51259=EDGE_CURVE('',#39352,#39355,#22722,.T.);
#51260=EDGE_CURVE('',#39348,#39351,#22723,.T.);
#51261=EDGE_CURVE('',#39344,#39347,#22724,.T.);
#51262=EDGE_CURVE('',#39382,#39377,#22725,.T.);
#51263=EDGE_CURVE('',#39381,#39378,#32659,.T.);
#51264=EDGE_CURVE('',#39333,#39591,#32660,.T.);
#51265=EDGE_CURVE('',#39337,#39342,#32661,.T.);
#51266=EDGE_CURVE('',#39598,#39238,#32662,.T.);
#51267=EDGE_CURVE('',#39592,#39330,#32663,.T.);
#51268=EDGE_CURVE('',#39217,#39214,#32664,.T.);
#51269=EDGE_CURVE('',#39241,#39597,#32665,.T.);
#51270=EDGE_CURVE('',#39279,#39276,#32666,.T.);
#51271=EDGE_CURVE('',#39270,#39273,#22726,.T.);
#51272=EDGE_CURVE('',#39290,#39293,#22727,.T.);
#51273=EDGE_CURVE('',#39282,#39285,#22728,.T.);
#51274=EDGE_CURVE('',#39246,#39249,#22729,.T.);
#51275=EDGE_CURVE('',#39262,#39265,#22730,.T.);
#51276=EDGE_CURVE('',#39298,#39301,#22731,.T.);
#51277=EDGE_CURVE('',#39266,#39269,#22732,.T.);
#51278=EDGE_CURVE('',#39294,#39289,#22733,.T.);
#51279=EDGE_CURVE('',#39254,#39257,#22734,.T.);
#51280=EDGE_CURVE('',#39306,#39309,#22735,.T.);
#51281=EDGE_CURVE('',#39258,#39261,#22736,.T.);
#51282=EDGE_CURVE('',#39302,#39297,#22737,.T.);
#51283=EDGE_CURVE('',#39230,#39233,#22738,.T.);
#51284=EDGE_CURVE('',#39314,#39317,#22739,.T.);
#51285=EDGE_CURVE('',#39250,#39253,#22740,.T.);
#51286=EDGE_CURVE('',#39310,#39305,#22741,.T.);
#51287=EDGE_CURVE('',#39286,#39281,#22742,.T.);
#51288=EDGE_CURVE('',#39242,#39245,#22743,.T.);
#51289=EDGE_CURVE('',#39234,#39237,#22744,.T.);
#51290=EDGE_CURVE('',#39278,#39275,#22745,.T.);
#51291=EDGE_CURVE('',#39226,#39229,#22746,.T.);
#51292=EDGE_CURVE('',#39318,#39313,#22747,.T.);
#51293=EDGE_CURVE('',#39222,#39225,#22748,.T.);
#51294=EDGE_CURVE('',#39322,#39325,#22749,.T.);
#51295=EDGE_CURVE('',#39218,#39221,#22750,.T.);
#51296=EDGE_CURVE('',#39326,#39321,#22751,.T.);
#51297=EDGE_CURVE('',#39334,#39329,#22752,.T.);
#51298=EDGE_CURVE('',#39212,#39215,#22753,.T.);
#51299=EDGE_CURVE('',#39626,#39627,#32667,.T.);
#51300=EDGE_CURVE('',#39628,#39627,#5663,.T.);
#51301=EDGE_CURVE('',#39628,#39629,#32668,.T.);
#51302=EDGE_CURVE('',#39626,#39629,#5664,.T.);
#51303=EDGE_CURVE('',#39629,#39626,#32669,.T.);
#51304=EDGE_CURVE('',#39630,#39628,#32670,.T.);
#51305=EDGE_CURVE('',#39627,#39630,#32671,.T.);
#51306=EDGE_CURVE('',#39631,#39631,#32672,.T.);
#51307=EDGE_CURVE('',#39631,#39632,#32673,.T.);
#51308=EDGE_CURVE('',#39633,#39632,#32674,.T.);
#51309=EDGE_CURVE('',#39632,#39633,#32675,.T.);
#51310=EDGE_CURVE('',#39634,#39635,#32676,.T.);
#51311=EDGE_CURVE('',#39636,#39635,#5665,.T.);
#51312=EDGE_CURVE('',#39636,#39637,#32677,.T.);
#51313=EDGE_CURVE('',#39634,#39637,#5666,.T.);
#51314=EDGE_CURVE('',#39638,#39639,#32678,.T.);
#51315=EDGE_CURVE('',#39637,#39639,#5667,.T.);
#51316=EDGE_CURVE('',#39638,#39636,#5668,.T.);
#51317=EDGE_CURVE('',#39640,#39634,#32679,.T.);
#51318=EDGE_CURVE('',#39640,#39635,#32680,.T.);
#51319=EDGE_CURVE('',#39641,#39642,#32681,.T.);
#51320=EDGE_CURVE('',#39639,#39642,#5669,.T.);
#51321=EDGE_CURVE('',#39641,#39638,#5670,.T.);
#51322=EDGE_CURVE('',#39643,#39644,#32682,.T.);
#51323=EDGE_CURVE('',#39635,#39644,#32683,.T.);
#51324=EDGE_CURVE('',#39643,#39640,#32684,.T.);
#51325=EDGE_CURVE('',#39645,#39646,#32685,.T.);
#51326=EDGE_CURVE('',#39642,#39646,#5671,.T.);
#51327=EDGE_CURVE('',#39645,#39641,#5672,.T.);
#51328=EDGE_CURVE('',#39647,#39648,#32686,.T.);
#51329=EDGE_CURVE('',#39644,#39648,#32687,.T.);
#51330=EDGE_CURVE('',#39647,#39643,#32688,.T.);
#51331=EDGE_CURVE('',#39649,#39650,#32689,.T.);
#51332=EDGE_CURVE('',#39646,#39650,#5673,.T.);
#51333=EDGE_CURVE('',#39649,#39645,#5674,.T.);
#51334=EDGE_CURVE('',#39651,#39652,#32690,.T.);
#51335=EDGE_CURVE('',#39648,#39652,#32691,.T.);
#51336=EDGE_CURVE('',#39651,#39647,#32692,.T.);
#51337=EDGE_CURVE('',#39653,#39654,#32693,.T.);
#51338=EDGE_CURVE('',#39650,#39654,#5675,.T.);
#51339=EDGE_CURVE('',#39653,#39649,#5676,.T.);
#51340=EDGE_CURVE('',#39655,#39656,#32694,.T.);
#51341=EDGE_CURVE('',#39652,#39656,#5677,.T.);
#51342=EDGE_CURVE('',#39655,#39651,#5678,.T.);
#51343=EDGE_CURVE('',#39656,#39657,#32695,.T.);
#51344=EDGE_CURVE('',#39654,#39657,#5679,.T.);
#51345=EDGE_CURVE('',#39658,#39653,#5680,.T.);
#51346=EDGE_CURVE('',#39656,#39658,#2003,.T.);
#51347=EDGE_CURVE('',#39657,#39655,#32696,.T.);
#51348=EDGE_CURVE('',#39659,#39660,#32697,.T.);
#51349=EDGE_CURVE('',#39661,#39660,#5681,.T.);
#51350=EDGE_CURVE('',#39661,#39662,#32698,.T.);
#51351=EDGE_CURVE('',#39659,#39662,#5682,.T.);
#51352=EDGE_CURVE('',#39663,#39664,#32699,.T.);
#51353=EDGE_CURVE('',#39662,#39664,#5683,.T.);
#51354=EDGE_CURVE('',#39663,#39661,#5684,.T.);
#51355=EDGE_CURVE('',#39665,#39666,#32700,.T.);
#51356=EDGE_CURVE('',#39660,#39666,#5685,.T.);
#51357=EDGE_CURVE('',#39665,#39659,#5686,.T.);
#51358=EDGE_CURVE('',#39667,#39668,#32701,.T.);
#51359=EDGE_CURVE('',#39664,#39668,#5687,.T.);
#51360=EDGE_CURVE('',#39667,#39663,#5688,.T.);
#51361=EDGE_CURVE('',#39669,#39670,#32702,.T.);
#51362=EDGE_CURVE('',#39666,#39670,#5689,.T.);
#51363=EDGE_CURVE('',#39669,#39665,#5690,.T.);
#51364=EDGE_CURVE('',#39667,#39671,#32703,.T.);
#51365=EDGE_CURVE('',#39668,#39671,#32704,.T.);
#51366=EDGE_CURVE('',#39672,#39673,#32705,.T.);
#51367=EDGE_CURVE('',#39670,#39673,#5691,.T.);
#51368=EDGE_CURVE('',#39672,#39669,#5692,.T.);
#51369=EDGE_CURVE('',#39674,#39675,#32706,.T.);
#51370=EDGE_CURVE('',#39671,#39675,#5693,.T.);
#51371=EDGE_CURVE('',#39674,#39667,#5694,.T.);
#51372=EDGE_CURVE('',#39676,#39677,#32707,.T.);
#51373=EDGE_CURVE('',#39673,#39677,#5695,.T.);
#51374=EDGE_CURVE('',#39676,#39672,#5696,.T.);
#51375=EDGE_CURVE('',#39678,#39679,#32708,.T.);
#51376=EDGE_CURVE('',#39675,#39679,#32709,.T.);
#51377=EDGE_CURVE('',#39678,#39674,#32710,.T.);
#51378=EDGE_CURVE('',#39680,#39676,#32711,.T.);
#51379=EDGE_CURVE('',#39680,#39677,#32712,.T.);
#51380=EDGE_CURVE('',#39681,#39682,#32713,.T.);
#51381=EDGE_CURVE('',#39679,#39682,#32714,.T.);
#51382=EDGE_CURVE('',#39681,#39678,#32715,.T.);
#51383=EDGE_CURVE('',#39683,#39684,#32716,.T.);
#51384=EDGE_CURVE('',#39677,#39684,#5697,.T.);
#51385=EDGE_CURVE('',#39683,#39680,#5698,.T.);
#51386=EDGE_CURVE('',#39684,#39681,#32717,.T.);
#51387=EDGE_CURVE('',#39682,#39683,#32718,.T.);
#51388=EDGE_CURVE('',#38354,#39685,#32719,.T.);
#51389=EDGE_CURVE('',#39686,#38353,#32720,.T.);
#51390=EDGE_CURVE('',#39686,#39685,#32721,.T.);
#51391=EDGE_CURVE('',#39687,#39688,#32722,.T.);
#51392=EDGE_CURVE('',#39685,#39688,#32723,.T.);
#51393=EDGE_CURVE('',#39687,#39686,#32724,.T.);
#51394=EDGE_CURVE('',#39689,#39690,#32725,.T.);
#51395=EDGE_CURVE('',#39688,#39690,#32726,.T.);
#51396=EDGE_CURVE('',#39689,#39687,#32727,.T.);
#51397=EDGE_CURVE('',#39691,#39692,#32728,.T.);
#51398=EDGE_CURVE('',#39690,#39692,#32729,.T.);
#51399=EDGE_CURVE('',#39691,#39689,#32730,.T.);
#51400=EDGE_CURVE('',#39693,#39694,#32731,.T.);
#51401=EDGE_CURVE('',#39692,#39694,#32732,.T.);
#51402=EDGE_CURVE('',#39693,#39691,#32733,.T.);
#51403=EDGE_CURVE('',#39695,#39696,#32734,.T.);
#51404=EDGE_CURVE('',#39694,#39696,#32735,.T.);
#51405=EDGE_CURVE('',#39695,#39693,#32736,.T.);
#51406=EDGE_CURVE('',#39697,#39698,#32737,.T.);
#51407=EDGE_CURVE('',#39696,#39698,#32738,.T.);
#51408=EDGE_CURVE('',#39697,#39695,#32739,.T.);
#51409=EDGE_CURVE('',#39699,#39700,#32740,.T.);
#51410=EDGE_CURVE('',#39698,#39700,#32741,.T.);
#51411=EDGE_CURVE('',#39699,#39697,#32742,.T.);
#51412=EDGE_CURVE('',#38365,#39699,#32743,.T.);
#51413=EDGE_CURVE('',#39700,#38366,#32744,.T.);
#51414=EDGE_CURVE('',#39640,#39701,#32745,.T.);
#51415=EDGE_CURVE('',#39702,#39634,#32746,.T.);
#51416=EDGE_CURVE('',#39702,#39701,#32747,.T.);
#51417=EDGE_CURVE('',#39703,#39704,#32748,.T.);
#51418=EDGE_CURVE('',#39701,#39704,#5699,.T.);
#51419=EDGE_CURVE('',#39703,#39702,#2004,.T.);
#51420=EDGE_CURVE('',#39657,#39705,#5700,.T.);
#51421=EDGE_CURVE('',#39706,#39655,#5701,.T.);
#51422=EDGE_CURVE('',#39706,#39705,#32749,.T.);
#51423=EDGE_CURVE('',#39707,#39708,#32750,.T.);
#51424=EDGE_CURVE('',#39704,#39708,#5702,.T.);
#51425=EDGE_CURVE('',#39707,#39703,#5703,.T.);
#51426=EDGE_CURVE('',#39709,#39710,#32751,.T.);
#51427=EDGE_CURVE('',#39705,#39710,#32752,.T.);
#51428=EDGE_CURVE('',#39709,#39706,#32753,.T.);
#51429=EDGE_CURVE('',#39711,#39712,#32754,.T.);
#51430=EDGE_CURVE('',#39708,#39712,#32755,.T.);
#51431=EDGE_CURVE('',#39711,#39707,#32756,.T.);
#51432=EDGE_CURVE('',#39713,#39714,#32757,.T.);
#51433=EDGE_CURVE('',#39710,#39714,#5704,.T.);
#51434=EDGE_CURVE('',#39713,#39709,#5705,.T.);
#51435=EDGE_CURVE('',#39715,#39716,#32758,.T.);
#51436=EDGE_CURVE('',#39712,#39716,#5706,.T.);
#51437=EDGE_CURVE('',#39715,#39711,#5707,.T.);
#51438=EDGE_CURVE('',#39717,#39718,#32759,.T.);
#51439=EDGE_CURVE('',#39714,#39718,#5708,.T.);
#51440=EDGE_CURVE('',#39717,#39713,#5709,.T.);
#51441=EDGE_CURVE('',#39719,#39720,#32760,.T.);
#51442=EDGE_CURVE('',#39716,#39720,#5710,.T.);
#51443=EDGE_CURVE('',#39719,#39715,#5711,.T.);
#51444=EDGE_CURVE('',#39721,#39722,#32761,.T.);
#51445=EDGE_CURVE('',#39718,#39722,#5712,.T.);
#51446=EDGE_CURVE('',#39721,#39717,#5713,.T.);
#51447=EDGE_CURVE('',#39723,#39724,#32762,.T.);
#51448=EDGE_CURVE('',#39720,#39724,#5714,.T.);
#51449=EDGE_CURVE('',#39723,#39719,#5715,.T.);
#51450=EDGE_CURVE('',#39724,#39721,#32763,.T.);
#51451=EDGE_CURVE('',#39722,#39723,#32764,.T.);
#51452=EDGE_CURVE('',#39725,#39726,#32765,.T.);
#51453=EDGE_CURVE('',#39727,#39726,#5716,.T.);
#51454=EDGE_CURVE('',#39727,#39728,#32766,.T.);
#51455=EDGE_CURVE('',#39725,#39728,#5717,.T.);
#51456=EDGE_CURVE('',#39729,#39730,#32767,.T.);
#51457=EDGE_CURVE('',#39728,#39730,#32768,.T.);
#51458=EDGE_CURVE('',#39729,#39727,#32769,.T.);
#51459=EDGE_CURVE('',#39731,#39732,#32770,.T.);
#51460=EDGE_CURVE('',#39726,#39732,#5718,.T.);
#51461=EDGE_CURVE('',#39731,#39725,#5719,.T.);
#51462=EDGE_CURVE('',#39733,#39734,#32771,.T.);
#51463=EDGE_CURVE('',#39730,#39734,#5720,.T.);
#51464=EDGE_CURVE('',#39733,#39729,#5721,.T.);
#51465=EDGE_CURVE('',#39735,#39736,#32772,.T.);
#51466=EDGE_CURVE('',#39732,#39736,#5722,.T.);
#51467=EDGE_CURVE('',#39735,#39731,#5723,.T.);
#51468=EDGE_CURVE('',#39737,#39738,#32773,.T.);
#51469=EDGE_CURVE('',#39734,#39738,#5724,.T.);
#51470=EDGE_CURVE('',#39739,#39733,#5725,.T.);
#51471=EDGE_CURVE('',#39737,#39739,#5726,.T.);
#51472=EDGE_CURVE('',#39740,#39741,#32774,.T.);
#51473=EDGE_CURVE('',#39736,#39741,#32775,.T.);
#51474=EDGE_CURVE('',#39740,#39735,#32776,.T.);
#51475=EDGE_CURVE('',#39742,#39743,#32777,.T.);
#51476=EDGE_CURVE('',#39738,#39743,#5727,.T.);
#51477=EDGE_CURVE('',#39742,#39737,#5728,.T.);
#51478=EDGE_CURVE('',#39668,#39740,#5729,.T.);
#51479=EDGE_CURVE('',#39741,#39671,#5730,.T.);
#51480=EDGE_CURVE('',#39744,#39745,#32778,.T.);
#51481=EDGE_CURVE('',#39743,#39745,#32779,.T.);
#51482=EDGE_CURVE('',#39744,#39742,#32780,.T.);
#51483=EDGE_CURVE('',#39680,#39744,#5731,.T.);
#51484=EDGE_CURVE('',#39745,#39676,#5732,.T.);
#51485=EDGE_CURVE('',#39666,#39746,#22754,.T.);
#51486=EDGE_CURVE('',#39747,#39670,#22755,.T.);
#51487=EDGE_CURVE('',#39747,#39746,#32781,.T.);
#51488=EDGE_CURVE('',#39748,#39747,#32782,.T.);
#51489=EDGE_CURVE('',#39748,#39749,#32783,.T.);
#51490=EDGE_CURVE('',#39746,#39749,#32784,.T.);
#51491=EDGE_CURVE('',#39626,#39750,#32785,.T.);
#51492=EDGE_CURVE('',#39749,#39629,#32786,.T.);
#51493=EDGE_CURVE('',#39751,#39748,#32787,.T.);
#51494=EDGE_CURVE('',#39751,#39750,#32788,.T.);
#51495=EDGE_CURVE('',#39752,#39753,#32789,.T.);
#51496=EDGE_CURVE('',#39750,#39753,#32790,.T.);
#51497=EDGE_CURVE('',#39752,#39751,#32791,.T.);
#51498=EDGE_CURVE('',#39661,#39752,#22756,.T.);
#51499=EDGE_CURVE('',#39753,#39660,#22757,.T.);
#51500=EDGE_CURVE('',#39683,#39754,#22758,.T.);
#51501=EDGE_CURVE('',#39755,#39744,#22759,.T.);
#51502=EDGE_CURVE('',#39755,#39754,#32792,.T.);
#51503=EDGE_CURVE('',#39756,#39755,#32793,.T.);
#51504=EDGE_CURVE('',#39756,#39757,#32794,.T.);
#51505=EDGE_CURVE('',#39754,#39757,#32795,.T.);
#51506=EDGE_CURVE('',#39758,#39759,#32796,.T.);
#51507=EDGE_CURVE('',#39757,#39759,#32797,.T.);
#51508=EDGE_CURVE('',#39758,#39756,#32798,.T.);
#51509=EDGE_CURVE('',#39760,#39761,#32799,.T.);
#51510=EDGE_CURVE('',#39759,#39761,#32800,.T.);
#51511=EDGE_CURVE('',#39760,#39758,#32801,.T.);
#51512=EDGE_CURVE('',#39761,#39675,#22760,.T.);
#51513=EDGE_CURVE('',#39741,#39760,#22761,.T.);
#51514=EDGE_CURVE('',#39704,#39762,#22762,.T.);
#51515=EDGE_CURVE('',#39763,#39708,#22763,.T.);
#51516=EDGE_CURVE('',#39763,#39762,#32802,.T.);
#51517=EDGE_CURVE('',#39764,#39765,#32803,.T.);
#51518=EDGE_CURVE('',#39762,#39765,#32804,.T.);
#51519=EDGE_CURVE('',#39764,#39763,#32805,.T.);
#51520=EDGE_CURVE('',#39766,#39767,#32806,.T.);
#51521=EDGE_CURVE('',#39765,#39767,#32807,.T.);
#51522=EDGE_CURVE('',#39766,#39764,#32808,.T.);
#51523=EDGE_CURVE('',#39767,#39768,#32809,.T.);
#51524=EDGE_CURVE('',#39769,#39766,#32810,.T.);
#51525=EDGE_CURVE('',#39769,#39768,#32811,.T.);
#51526=EDGE_CURVE('',#39768,#39651,#22764,.T.);
#51527=EDGE_CURVE('',#39706,#39769,#22765,.T.);
#51528=EDGE_CURVE('',#39641,#39770,#22766,.T.);
#51529=EDGE_CURVE('',#39771,#39638,#22767,.T.);
#51530=EDGE_CURVE('',#39771,#39770,#32812,.T.);
#51531=EDGE_CURVE('',#39772,#39773,#32813,.T.);
#51532=EDGE_CURVE('',#39770,#39773,#32814,.T.);
#51533=EDGE_CURVE('',#39772,#39771,#32815,.T.);
#51534=EDGE_CURVE('',#39774,#39775,#32816,.T.);
#51535=EDGE_CURVE('',#39773,#39775,#32817,.T.);
#51536=EDGE_CURVE('',#39774,#39772,#32818,.T.);
#51537=EDGE_CURVE('',#39775,#39776,#32819,.T.);
#51538=EDGE_CURVE('',#39777,#39774,#32820,.T.);
#51539=EDGE_CURVE('',#39777,#39776,#32821,.T.);
#51540=EDGE_CURVE('',#39649,#39777,#22768,.T.);
#51541=EDGE_CURVE('',#39776,#39645,#22769,.T.);
#51542=EDGE_CURVE('',#39727,#39758,#22770,.T.);
#51543=EDGE_CURVE('',#39760,#39732,#22771,.T.);
#51544=EDGE_CURVE('',#39756,#39729,#22772,.T.);
#51545=EDGE_CURVE('',#39737,#39755,#22773,.T.);
#51546=EDGE_CURVE('',#39678,#39751,#22774,.T.);
#51547=EDGE_CURVE('',#39752,#39663,#22775,.T.);
#51548=EDGE_CURVE('',#39673,#39747,#22776,.T.);
#51549=EDGE_CURVE('',#39748,#39681,#22777,.T.);
#51550=EDGE_CURVE('',#39636,#39771,#22778,.T.);
#51551=EDGE_CURVE('',#39772,#39644,#22779,.T.);
#51552=EDGE_CURVE('',#39648,#39774,#22780,.T.);
#51553=EDGE_CURVE('',#39777,#39653,#22781,.T.);
#51554=EDGE_CURVE('',#39769,#39713,#22782,.T.);
#51555=EDGE_CURVE('',#39721,#39766,#22783,.T.);
#51556=EDGE_CURVE('',#39764,#39724,#22784,.T.);
#51557=EDGE_CURVE('',#39716,#39763,#22785,.T.);
#51558=EDGE_CURVE('',#39778,#39779,#32822,.T.);
#51559=EDGE_CURVE('',#39778,#39780,#32823,.T.);
#51560=EDGE_CURVE('',#39781,#39780,#32824,.T.);
#51561=EDGE_CURVE('',#39781,#39779,#32825,.T.);
#51562=EDGE_CURVE('',#39782,#39783,#32826,.T.);
#51563=EDGE_CURVE('',#39779,#39783,#22786,.T.);
#51564=EDGE_CURVE('',#39782,#39781,#22787,.T.);
#51565=EDGE_CURVE('',#39784,#39785,#32827,.T.);
#51566=EDGE_CURVE('',#39780,#39785,#32828,.T.);
#51567=EDGE_CURVE('',#39784,#39778,#32829,.T.);
#51568=EDGE_CURVE('',#39786,#39787,#32830,.T.);
#51569=EDGE_CURVE('',#39783,#39787,#32831,.T.);
#51570=EDGE_CURVE('',#39786,#39782,#32832,.T.);
#51571=EDGE_CURVE('',#39788,#39789,#32833,.T.);
#51572=EDGE_CURVE('',#39785,#39789,#32834,.T.);
#51573=EDGE_CURVE('',#39788,#39784,#32835,.T.);
#51574=EDGE_CURVE('',#39790,#39791,#32836,.T.);
#51575=EDGE_CURVE('',#39787,#39791,#22788,.T.);
#51576=EDGE_CURVE('',#39790,#39786,#22789,.T.);
#51577=EDGE_CURVE('',#39792,#39793,#32837,.T.);
#51578=EDGE_CURVE('',#39789,#39793,#32838,.T.);
#51579=EDGE_CURVE('',#39792,#39788,#32839,.T.);
#51580=EDGE_CURVE('',#39794,#39795,#32840,.T.);
#51581=EDGE_CURVE('',#39791,#39795,#32841,.T.);
#51582=EDGE_CURVE('',#39794,#39790,#32842,.T.);
#51583=EDGE_CURVE('',#39796,#39797,#32843,.T.);
#51584=EDGE_CURVE('',#39793,#39797,#32844,.T.);
#51585=EDGE_CURVE('',#39796,#39792,#32845,.T.);
#51586=EDGE_CURVE('',#39797,#39794,#22790,.T.);
#51587=EDGE_CURVE('',#39795,#39796,#22791,.T.);
#51588=EDGE_CURVE('',#39798,#39799,#32846,.T.);
#51589=EDGE_CURVE('',#39798,#39800,#32847,.T.);
#51590=EDGE_CURVE('',#39801,#39800,#32848,.T.);
#51591=EDGE_CURVE('',#39801,#39799,#32849,.T.);
#51592=EDGE_CURVE('',#39802,#39803,#32850,.T.);
#51593=EDGE_CURVE('',#39799,#39803,#22792,.T.);
#51594=EDGE_CURVE('',#39802,#39801,#22793,.T.);
#51595=EDGE_CURVE('',#39804,#39805,#32851,.T.);
#51596=EDGE_CURVE('',#39800,#39805,#32852,.T.);
#51597=EDGE_CURVE('',#39804,#39798,#32853,.T.);
#51598=EDGE_CURVE('',#39806,#39807,#32854,.T.);
#51599=EDGE_CURVE('',#39803,#39807,#32855,.T.);
#51600=EDGE_CURVE('',#39806,#39802,#32856,.T.);
#51601=EDGE_CURVE('',#39808,#39809,#32857,.T.);
#51602=EDGE_CURVE('',#39805,#39809,#32858,.T.);
#51603=EDGE_CURVE('',#39808,#39804,#32859,.T.);
#51604=EDGE_CURVE('',#39810,#39811,#32860,.T.);
#51605=EDGE_CURVE('',#39807,#39811,#22794,.T.);
#51606=EDGE_CURVE('',#39810,#39806,#22795,.T.);
#51607=EDGE_CURVE('',#39812,#39813,#32861,.T.);
#51608=EDGE_CURVE('',#39809,#39813,#22796,.T.);
#51609=EDGE_CURVE('',#39812,#39808,#22797,.T.);
#51610=EDGE_CURVE('',#39813,#39810,#32862,.T.);
#51611=EDGE_CURVE('',#39811,#39812,#32863,.T.);
#51612=EDGE_CURVE('',#39814,#39815,#32864,.T.);
#51613=EDGE_CURVE('',#39814,#39816,#32865,.T.);
#51614=EDGE_CURVE('',#39817,#39816,#32866,.T.);
#51615=EDGE_CURVE('',#39817,#39815,#32867,.T.);
#51616=EDGE_CURVE('',#39818,#39819,#32868,.T.);
#51617=EDGE_CURVE('',#39815,#39819,#22798,.T.);
#51618=EDGE_CURVE('',#39818,#39817,#22799,.T.);
#51619=EDGE_CURVE('',#39820,#39821,#32869,.T.);
#51620=EDGE_CURVE('',#39816,#39821,#32870,.T.);
#51621=EDGE_CURVE('',#39820,#39814,#32871,.T.);
#51622=EDGE_CURVE('',#39822,#39823,#32872,.T.);
#51623=EDGE_CURVE('',#39819,#39823,#32873,.T.);
#51624=EDGE_CURVE('',#39822,#39818,#32874,.T.);
#51625=EDGE_CURVE('',#39824,#39825,#32875,.T.);
#51626=EDGE_CURVE('',#39821,#39825,#32876,.T.);
#51627=EDGE_CURVE('',#39824,#39820,#32877,.T.);
#51628=EDGE_CURVE('',#39826,#39827,#32878,.T.);
#51629=EDGE_CURVE('',#39823,#39827,#22800,.T.);
#51630=EDGE_CURVE('',#39826,#39822,#22801,.T.);
#51631=EDGE_CURVE('',#39828,#39829,#32879,.T.);
#51632=EDGE_CURVE('',#39825,#39829,#22802,.T.);
#51633=EDGE_CURVE('',#39828,#39824,#22803,.T.);
#51634=EDGE_CURVE('',#39829,#39826,#32880,.T.);
#51635=EDGE_CURVE('',#39827,#39828,#32881,.T.);
#51636=EDGE_CURVE('',#39830,#39831,#32882,.T.);
#51637=EDGE_CURVE('',#39832,#39831,#32883,.T.);
#51638=EDGE_CURVE('',#39832,#39833,#32884,.T.);
#51639=EDGE_CURVE('',#39830,#39833,#32885,.T.);
#51640=EDGE_CURVE('',#39834,#39835,#32886,.T.);
#51641=EDGE_CURVE('',#39833,#39835,#22804,.T.);
#51642=EDGE_CURVE('',#39834,#39832,#22805,.T.);
#51643=EDGE_CURVE('',#39836,#39837,#32887,.T.);
#51644=EDGE_CURVE('',#39831,#39837,#22806,.T.);
#51645=EDGE_CURVE('',#39836,#39830,#22807,.T.);
#51646=EDGE_CURVE('',#39838,#39839,#32888,.T.);
#51647=EDGE_CURVE('',#39835,#39839,#32889,.T.);
#51648=EDGE_CURVE('',#39838,#39834,#32890,.T.);
#51649=EDGE_CURVE('',#39840,#39841,#32891,.T.);
#51650=EDGE_CURVE('',#39837,#39841,#32892,.T.);
#51651=EDGE_CURVE('',#39840,#39836,#32893,.T.);
#51652=EDGE_CURVE('',#39842,#39843,#32894,.T.);
#51653=EDGE_CURVE('',#39839,#39843,#22808,.T.);
#51654=EDGE_CURVE('',#39842,#39838,#22809,.T.);
#51655=EDGE_CURVE('',#39844,#39845,#32895,.T.);
#51656=EDGE_CURVE('',#39841,#39845,#22810,.T.);
#51657=EDGE_CURVE('',#39844,#39840,#22811,.T.);
#51658=EDGE_CURVE('',#39845,#39842,#32896,.T.);
#51659=EDGE_CURVE('',#39843,#39844,#32897,.T.);
#51660=EDGE_CURVE('',#39846,#39847,#32898,.T.);
#51661=EDGE_CURVE('',#39848,#39847,#32899,.T.);
#51662=EDGE_CURVE('',#39848,#39849,#32900,.T.);
#51663=EDGE_CURVE('',#39846,#39849,#32901,.T.);
#51664=EDGE_CURVE('',#39850,#39851,#32902,.T.);
#51665=EDGE_CURVE('',#39849,#39851,#22812,.T.);
#51666=EDGE_CURVE('',#39850,#39848,#22813,.T.);
#51667=EDGE_CURVE('',#39852,#39853,#32903,.T.);
#51668=EDGE_CURVE('',#39847,#39853,#22814,.T.);
#51669=EDGE_CURVE('',#39852,#39846,#22815,.T.);
#51670=EDGE_CURVE('',#39854,#39855,#32904,.T.);
#51671=EDGE_CURVE('',#39851,#39855,#32905,.T.);
#51672=EDGE_CURVE('',#39854,#39850,#32906,.T.);
#51673=EDGE_CURVE('',#39856,#39857,#32907,.T.);
#51674=EDGE_CURVE('',#39853,#39857,#32908,.T.);
#51675=EDGE_CURVE('',#39856,#39852,#32909,.T.);
#51676=EDGE_CURVE('',#39858,#39859,#32910,.T.);
#51677=EDGE_CURVE('',#39855,#39859,#32911,.T.);
#51678=EDGE_CURVE('',#39858,#39854,#32912,.T.);
#51679=EDGE_CURVE('',#39860,#39861,#32913,.T.);
#51680=EDGE_CURVE('',#39857,#39861,#22816,.T.);
#51681=EDGE_CURVE('',#39860,#39856,#22817,.T.);
#51682=EDGE_CURVE('',#39862,#39863,#32914,.T.);
#51683=EDGE_CURVE('',#39859,#39863,#32915,.T.);
#51684=EDGE_CURVE('',#39862,#39858,#32916,.T.);
#51685=EDGE_CURVE('',#39863,#39860,#32917,.T.);
#51686=EDGE_CURVE('',#39861,#39862,#32918,.T.);
#51687=EDGE_CURVE('',#39864,#39865,#32919,.T.);
#51688=EDGE_CURVE('',#39866,#39865,#32920,.T.);
#51689=EDGE_CURVE('',#39866,#39867,#32921,.T.);
#51690=EDGE_CURVE('',#39864,#39867,#32922,.T.);
#51691=EDGE_CURVE('',#39868,#39869,#32923,.T.);
#51692=EDGE_CURVE('',#39867,#39869,#22818,.T.);
#51693=EDGE_CURVE('',#39868,#39866,#22819,.T.);
#51694=EDGE_CURVE('',#39870,#39871,#32924,.T.);
#51695=EDGE_CURVE('',#39865,#39871,#22820,.T.);
#51696=EDGE_CURVE('',#39870,#39864,#22821,.T.);
#51697=EDGE_CURVE('',#39872,#39873,#32925,.T.);
#51698=EDGE_CURVE('',#39869,#39873,#32926,.T.);
#51699=EDGE_CURVE('',#39872,#39868,#32927,.T.);
#51700=EDGE_CURVE('',#39874,#39875,#32928,.T.);
#51701=EDGE_CURVE('',#39871,#39875,#32929,.T.);
#51702=EDGE_CURVE('',#39874,#39870,#32930,.T.);
#51703=EDGE_CURVE('',#39876,#39877,#32931,.T.);
#51704=EDGE_CURVE('',#39873,#39877,#22822,.T.);
#51705=EDGE_CURVE('',#39876,#39872,#22823,.T.);
#51706=EDGE_CURVE('',#39878,#39879,#32932,.T.);
#51707=EDGE_CURVE('',#39875,#39879,#22824,.T.);
#51708=EDGE_CURVE('',#39878,#39874,#22825,.T.);
#51709=EDGE_CURVE('',#39879,#39876,#32933,.T.);
#51710=EDGE_CURVE('',#39877,#39878,#32934,.T.);
#51711=EDGE_CURVE('',#39880,#39881,#32935,.T.);
#51712=EDGE_CURVE('',#39882,#39881,#32936,.T.);
#51713=EDGE_CURVE('',#39882,#39883,#32937,.T.);
#51714=EDGE_CURVE('',#39880,#39883,#32938,.T.);
#51715=EDGE_CURVE('',#39884,#39885,#32939,.T.);
#51716=EDGE_CURVE('',#39883,#39885,#22826,.T.);
#51717=EDGE_CURVE('',#39884,#39882,#22827,.T.);
#51718=EDGE_CURVE('',#39886,#39887,#32940,.T.);
#51719=EDGE_CURVE('',#39881,#39887,#22828,.T.);
#51720=EDGE_CURVE('',#39886,#39880,#22829,.T.);
#51721=EDGE_CURVE('',#39888,#39889,#32941,.T.);
#51722=EDGE_CURVE('',#39885,#39889,#32942,.T.);
#51723=EDGE_CURVE('',#39888,#39884,#32943,.T.);
#51724=EDGE_CURVE('',#39890,#39891,#32944,.T.);
#51725=EDGE_CURVE('',#39887,#39891,#32945,.T.);
#51726=EDGE_CURVE('',#39890,#39886,#32946,.T.);
#51727=EDGE_CURVE('',#39892,#39893,#32947,.T.);
#51728=EDGE_CURVE('',#39889,#39893,#22830,.T.);
#51729=EDGE_CURVE('',#39892,#39888,#22831,.T.);
#51730=EDGE_CURVE('',#39894,#39895,#32948,.T.);
#51731=EDGE_CURVE('',#39891,#39895,#22832,.T.);
#51732=EDGE_CURVE('',#39894,#39890,#22833,.T.);
#51733=EDGE_CURVE('',#39895,#39892,#32949,.T.);
#51734=EDGE_CURVE('',#39893,#39894,#32950,.T.);
#51735=EDGE_CURVE('',#39896,#39897,#32951,.T.);
#51736=EDGE_CURVE('',#39898,#39897,#32952,.T.);
#51737=EDGE_CURVE('',#39898,#39899,#32953,.T.);
#51738=EDGE_CURVE('',#39896,#39899,#32954,.T.);
#51739=EDGE_CURVE('',#39900,#39901,#32955,.T.);
#51740=EDGE_CURVE('',#39899,#39901,#22834,.T.);
#51741=EDGE_CURVE('',#39900,#39898,#22835,.T.);
#51742=EDGE_CURVE('',#39902,#39903,#32956,.T.);
#51743=EDGE_CURVE('',#39897,#39903,#22836,.T.);
#51744=EDGE_CURVE('',#39902,#39896,#22837,.T.);
#51745=EDGE_CURVE('',#39904,#39905,#32957,.T.);
#51746=EDGE_CURVE('',#39901,#39905,#32958,.T.);
#51747=EDGE_CURVE('',#39904,#39900,#32959,.T.);
#51748=EDGE_CURVE('',#39906,#39907,#32960,.T.);
#51749=EDGE_CURVE('',#39903,#39907,#32961,.T.);
#51750=EDGE_CURVE('',#39906,#39902,#32962,.T.);
#51751=EDGE_CURVE('',#39908,#39909,#32963,.T.);
#51752=EDGE_CURVE('',#39905,#39909,#22838,.T.);
#51753=EDGE_CURVE('',#39908,#39904,#22839,.T.);
#51754=EDGE_CURVE('',#39910,#39911,#32964,.T.);
#51755=EDGE_CURVE('',#39907,#39911,#22840,.T.);
#51756=EDGE_CURVE('',#39910,#39906,#22841,.T.);
#51757=EDGE_CURVE('',#39911,#39908,#32965,.T.);
#51758=EDGE_CURVE('',#39909,#39910,#32966,.T.);
#51759=EDGE_CURVE('',#39912,#39913,#32967,.T.);
#51760=EDGE_CURVE('',#39914,#39913,#32968,.T.);
#51761=EDGE_CURVE('',#39914,#39915,#32969,.T.);
#51762=EDGE_CURVE('',#39912,#39915,#32970,.T.);
#51763=EDGE_CURVE('',#39916,#39917,#32971,.T.);
#51764=EDGE_CURVE('',#39915,#39917,#22842,.T.);
#51765=EDGE_CURVE('',#39916,#39914,#22843,.T.);
#51766=EDGE_CURVE('',#39918,#39919,#32972,.T.);
#51767=EDGE_CURVE('',#39913,#39919,#22844,.T.);
#51768=EDGE_CURVE('',#39918,#39912,#22845,.T.);
#51769=EDGE_CURVE('',#39920,#39921,#32973,.T.);
#51770=EDGE_CURVE('',#39917,#39921,#32974,.T.);
#51771=EDGE_CURVE('',#39920,#39916,#32975,.T.);
#51772=EDGE_CURVE('',#39922,#39923,#32976,.T.);
#51773=EDGE_CURVE('',#39919,#39923,#32977,.T.);
#51774=EDGE_CURVE('',#39922,#39918,#32978,.T.);
#51775=EDGE_CURVE('',#39924,#39925,#32979,.T.);
#51776=EDGE_CURVE('',#39921,#39925,#22846,.T.);
#51777=EDGE_CURVE('',#39924,#39920,#22847,.T.);
#51778=EDGE_CURVE('',#39926,#39927,#32980,.T.);
#51779=EDGE_CURVE('',#39923,#39927,#22848,.T.);
#51780=EDGE_CURVE('',#39926,#39922,#22849,.T.);
#51781=EDGE_CURVE('',#39927,#39924,#32981,.T.);
#51782=EDGE_CURVE('',#39925,#39926,#32982,.T.);
#51783=EDGE_CURVE('',#39928,#39929,#32983,.T.);
#51784=EDGE_CURVE('',#39930,#39929,#32984,.T.);
#51785=EDGE_CURVE('',#39930,#39931,#32985,.T.);
#51786=EDGE_CURVE('',#39928,#39931,#32986,.T.);
#51787=EDGE_CURVE('',#39932,#39933,#32987,.T.);
#51788=EDGE_CURVE('',#39931,#39933,#22850,.T.);
#51789=EDGE_CURVE('',#39932,#39930,#22851,.T.);
#51790=EDGE_CURVE('',#39934,#39935,#32988,.T.);
#51791=EDGE_CURVE('',#39929,#39935,#22852,.T.);
#51792=EDGE_CURVE('',#39934,#39928,#22853,.T.);
#51793=EDGE_CURVE('',#39936,#39937,#32989,.T.);
#51794=EDGE_CURVE('',#39933,#39937,#32990,.T.);
#51795=EDGE_CURVE('',#39936,#39932,#32991,.T.);
#51796=EDGE_CURVE('',#39938,#39939,#32992,.T.);
#51797=EDGE_CURVE('',#39935,#39939,#32993,.T.);
#51798=EDGE_CURVE('',#39938,#39934,#32994,.T.);
#51799=EDGE_CURVE('',#39940,#39941,#32995,.T.);
#51800=EDGE_CURVE('',#39937,#39941,#22854,.T.);
#51801=EDGE_CURVE('',#39940,#39936,#22855,.T.);
#51802=EDGE_CURVE('',#39942,#39943,#32996,.T.);
#51803=EDGE_CURVE('',#39939,#39943,#32997,.T.);
#51804=EDGE_CURVE('',#39942,#39938,#32998,.T.);
#51805=EDGE_CURVE('',#39943,#39940,#32999,.T.);
#51806=EDGE_CURVE('',#39941,#39942,#33000,.T.);
#51807=EDGE_CURVE('',#39944,#39945,#33001,.T.);
#51808=EDGE_CURVE('',#39946,#39945,#33002,.T.);
#51809=EDGE_CURVE('',#39946,#39947,#33003,.T.);
#51810=EDGE_CURVE('',#39944,#39947,#33004,.T.);
#51811=EDGE_CURVE('',#39948,#39949,#33005,.T.);
#51812=EDGE_CURVE('',#39947,#39949,#22856,.T.);
#51813=EDGE_CURVE('',#39948,#39946,#22857,.T.);
#51814=EDGE_CURVE('',#39950,#39951,#33006,.T.);
#51815=EDGE_CURVE('',#39945,#39951,#22858,.T.);
#51816=EDGE_CURVE('',#39950,#39944,#22859,.T.);
#51817=EDGE_CURVE('',#39952,#39953,#33007,.T.);
#51818=EDGE_CURVE('',#39949,#39953,#33008,.T.);
#51819=EDGE_CURVE('',#39952,#39948,#33009,.T.);
#51820=EDGE_CURVE('',#39954,#39955,#33010,.T.);
#51821=EDGE_CURVE('',#39951,#39955,#33011,.T.);
#51822=EDGE_CURVE('',#39954,#39950,#33012,.T.);
#51823=EDGE_CURVE('',#39956,#39957,#33013,.T.);
#51824=EDGE_CURVE('',#39953,#39957,#22860,.T.);
#51825=EDGE_CURVE('',#39956,#39952,#22861,.T.);
#51826=EDGE_CURVE('',#39958,#39959,#33014,.T.);
#51827=EDGE_CURVE('',#39955,#39959,#33015,.T.);
#51828=EDGE_CURVE('',#39958,#39954,#33016,.T.);
#51829=EDGE_CURVE('',#39960,#39961,#33017,.T.);
#51830=EDGE_CURVE('',#39957,#39961,#33018,.T.);
#51831=EDGE_CURVE('',#39960,#39956,#33019,.T.);
#51832=EDGE_CURVE('',#39962,#39963,#33020,.T.);
#51833=EDGE_CURVE('',#39959,#39963,#33021,.T.);
#51834=EDGE_CURVE('',#39962,#39958,#33022,.T.);
#51835=EDGE_CURVE('',#39963,#39960,#33023,.T.);
#51836=EDGE_CURVE('',#39961,#39962,#33024,.T.);
#51837=EDGE_CURVE('',#39964,#39965,#33025,.T.);
#51838=EDGE_CURVE('',#39966,#39965,#33026,.T.);
#51839=EDGE_CURVE('',#39966,#39967,#33027,.T.);
#51840=EDGE_CURVE('',#39964,#39967,#33028,.T.);
#51841=EDGE_CURVE('',#39968,#39969,#33029,.T.);
#51842=EDGE_CURVE('',#39967,#39969,#22862,.T.);
#51843=EDGE_CURVE('',#39968,#39966,#22863,.T.);
#51844=EDGE_CURVE('',#39970,#39971,#33030,.T.);
#51845=EDGE_CURVE('',#39965,#39971,#22864,.T.);
#51846=EDGE_CURVE('',#39970,#39964,#22865,.T.);
#51847=EDGE_CURVE('',#39972,#39973,#33031,.T.);
#51848=EDGE_CURVE('',#39969,#39973,#33032,.T.);
#51849=EDGE_CURVE('',#39972,#39968,#33033,.T.);
#51850=EDGE_CURVE('',#39974,#39975,#33034,.T.);
#51851=EDGE_CURVE('',#39971,#39975,#33035,.T.);
#51852=EDGE_CURVE('',#39974,#39970,#33036,.T.);
#51853=EDGE_CURVE('',#39976,#39977,#33037,.T.);
#51854=EDGE_CURVE('',#39973,#39977,#22866,.T.);
#51855=EDGE_CURVE('',#39976,#39972,#22867,.T.);
#51856=EDGE_CURVE('',#39978,#39979,#33038,.T.);
#51857=EDGE_CURVE('',#39975,#39979,#33039,.T.);
#51858=EDGE_CURVE('',#39978,#39974,#33040,.T.);
#51859=EDGE_CURVE('',#39979,#39976,#33041,.T.);
#51860=EDGE_CURVE('',#39977,#39978,#33042,.T.);
#51861=EDGE_CURVE('',#39980,#39981,#33043,.T.);
#51862=EDGE_CURVE('',#39982,#39981,#33044,.T.);
#51863=EDGE_CURVE('',#39982,#39983,#33045,.T.);
#51864=EDGE_CURVE('',#39980,#39983,#33046,.T.);
#51865=EDGE_CURVE('',#39984,#39985,#33047,.T.);
#51866=EDGE_CURVE('',#39983,#39985,#22868,.T.);
#51867=EDGE_CURVE('',#39984,#39982,#22869,.T.);
#51868=EDGE_CURVE('',#39986,#39987,#33048,.T.);
#51869=EDGE_CURVE('',#39981,#39987,#22870,.T.);
#51870=EDGE_CURVE('',#39986,#39980,#22871,.T.);
#51871=EDGE_CURVE('',#39988,#39989,#33049,.T.);
#51872=EDGE_CURVE('',#39985,#39989,#33050,.T.);
#51873=EDGE_CURVE('',#39988,#39984,#33051,.T.);
#51874=EDGE_CURVE('',#39990,#39991,#33052,.T.);
#51875=EDGE_CURVE('',#39987,#39991,#33053,.T.);
#51876=EDGE_CURVE('',#39990,#39986,#33054,.T.);
#51877=EDGE_CURVE('',#39992,#39993,#33055,.T.);
#51878=EDGE_CURVE('',#39989,#39993,#22872,.T.);
#51879=EDGE_CURVE('',#39992,#39988,#22873,.T.);
#51880=EDGE_CURVE('',#39994,#39995,#33056,.T.);
#51881=EDGE_CURVE('',#39991,#39995,#22874,.T.);
#51882=EDGE_CURVE('',#39994,#39990,#22875,.T.);
#51883=EDGE_CURVE('',#39995,#39992,#33057,.T.);
#51884=EDGE_CURVE('',#39993,#39994,#33058,.T.);
#51885=EDGE_CURVE('',#39996,#39997,#33059,.T.);
#51886=EDGE_CURVE('',#39998,#39997,#33060,.T.);
#51887=EDGE_CURVE('',#39998,#39999,#33061,.T.);
#51888=EDGE_CURVE('',#39996,#39999,#33062,.T.);
#51889=EDGE_CURVE('',#40000,#40001,#33063,.T.);
#51890=EDGE_CURVE('',#39999,#40001,#22876,.T.);
#51891=EDGE_CURVE('',#40000,#39998,#22877,.T.);
#51892=EDGE_CURVE('',#40002,#40003,#33064,.T.);
#51893=EDGE_CURVE('',#39997,#40003,#33065,.T.);
#51894=EDGE_CURVE('',#40002,#39996,#33066,.T.);
#51895=EDGE_CURVE('',#40004,#40005,#33067,.T.);
#51896=EDGE_CURVE('',#40001,#40005,#33068,.T.);
#51897=EDGE_CURVE('',#40004,#40000,#33069,.T.);
#51898=EDGE_CURVE('',#40006,#40007,#33070,.T.);
#51899=EDGE_CURVE('',#40003,#40007,#33071,.T.);
#51900=EDGE_CURVE('',#40006,#40002,#33072,.T.);
#51901=EDGE_CURVE('',#40008,#40009,#33073,.T.);
#51902=EDGE_CURVE('',#40005,#40009,#22878,.T.);
#51903=EDGE_CURVE('',#40008,#40004,#22879,.T.);
#51904=EDGE_CURVE('',#40010,#40011,#33074,.T.);
#51905=EDGE_CURVE('',#40007,#40011,#22880,.T.);
#51906=EDGE_CURVE('',#40010,#40006,#22881,.T.);
#51907=EDGE_CURVE('',#40012,#40013,#33075,.T.);
#51908=EDGE_CURVE('',#40009,#40013,#33076,.T.);
#51909=EDGE_CURVE('',#40012,#40008,#33077,.T.);
#51910=EDGE_CURVE('',#40014,#40015,#33078,.T.);
#51911=EDGE_CURVE('',#40011,#40015,#33079,.T.);
#51912=EDGE_CURVE('',#40014,#40010,#33080,.T.);
#51913=EDGE_CURVE('',#40015,#40012,#22882,.T.);
#51914=EDGE_CURVE('',#40013,#40014,#22883,.T.);
#51915=EDGE_CURVE('',#40016,#40017,#33081,.T.);
#51916=EDGE_CURVE('',#40018,#40017,#33082,.T.);
#51917=EDGE_CURVE('',#40018,#40019,#33083,.T.);
#51918=EDGE_CURVE('',#40016,#40019,#33084,.T.);
#51919=EDGE_CURVE('',#40020,#40021,#33085,.T.);
#51920=EDGE_CURVE('',#40019,#40021,#22884,.T.);
#51921=EDGE_CURVE('',#40020,#40018,#22885,.T.);
#51922=EDGE_CURVE('',#40022,#40023,#33086,.T.);
#51923=EDGE_CURVE('',#40017,#40023,#22886,.T.);
#51924=EDGE_CURVE('',#40022,#40016,#22887,.T.);
#51925=EDGE_CURVE('',#40024,#40025,#33087,.T.);
#51926=EDGE_CURVE('',#40021,#40025,#33088,.T.);
#51927=EDGE_CURVE('',#40024,#40020,#33089,.T.);
#51928=EDGE_CURVE('',#40026,#40027,#33090,.T.);
#51929=EDGE_CURVE('',#40023,#40027,#33091,.T.);
#51930=EDGE_CURVE('',#40026,#40022,#33092,.T.);
#51931=EDGE_CURVE('',#40028,#40029,#33093,.T.);
#51932=EDGE_CURVE('',#40025,#40029,#22888,.T.);
#51933=EDGE_CURVE('',#40028,#40024,#22889,.T.);
#51934=EDGE_CURVE('',#40030,#40031,#33094,.T.);
#51935=EDGE_CURVE('',#40027,#40031,#33095,.T.);
#51936=EDGE_CURVE('',#40030,#40026,#33096,.T.);
#51937=EDGE_CURVE('',#40032,#40033,#33097,.T.);
#51938=EDGE_CURVE('',#40029,#40033,#33098,.T.);
#51939=EDGE_CURVE('',#40032,#40028,#33099,.T.);
#51940=EDGE_CURVE('',#40034,#40035,#33100,.T.);
#51941=EDGE_CURVE('',#40031,#40035,#33101,.T.);
#51942=EDGE_CURVE('',#40034,#40030,#33102,.T.);
#51943=EDGE_CURVE('',#40035,#40032,#22890,.T.);
#51944=EDGE_CURVE('',#40033,#40034,#22891,.T.);
#51945=EDGE_CURVE('',#40036,#40037,#33103,.T.);
#51946=EDGE_CURVE('',#40038,#40037,#33104,.T.);
#51947=EDGE_CURVE('',#40038,#40039,#33105,.T.);
#51948=EDGE_CURVE('',#40036,#40039,#33106,.T.);
#51949=EDGE_CURVE('',#40040,#40041,#33107,.T.);
#51950=EDGE_CURVE('',#40039,#40041,#22892,.T.);
#51951=EDGE_CURVE('',#40040,#40038,#22893,.T.);
#51952=EDGE_CURVE('',#40042,#40043,#33108,.T.);
#51953=EDGE_CURVE('',#40037,#40043,#22894,.T.);
#51954=EDGE_CURVE('',#40042,#40036,#22895,.T.);
#51955=EDGE_CURVE('',#40044,#40045,#33109,.T.);
#51956=EDGE_CURVE('',#40041,#40045,#33110,.T.);
#51957=EDGE_CURVE('',#40044,#40040,#33111,.T.);
#51958=EDGE_CURVE('',#40046,#40047,#33112,.T.);
#51959=EDGE_CURVE('',#40043,#40047,#33113,.T.);
#51960=EDGE_CURVE('',#40046,#40042,#33114,.T.);
#51961=EDGE_CURVE('',#40048,#40049,#33115,.T.);
#51962=EDGE_CURVE('',#40045,#40049,#22896,.T.);
#51963=EDGE_CURVE('',#40048,#40044,#22897,.T.);
#51964=EDGE_CURVE('',#40050,#40051,#33116,.T.);
#51965=EDGE_CURVE('',#40047,#40051,#22898,.T.);
#51966=EDGE_CURVE('',#40050,#40046,#22899,.T.);
#51967=EDGE_CURVE('',#40051,#40048,#33117,.T.);
#51968=EDGE_CURVE('',#40049,#40050,#33118,.T.);
#51969=EDGE_CURVE('',#40052,#40053,#33119,.T.);
#51970=EDGE_CURVE('',#40054,#40053,#33120,.T.);
#51971=EDGE_CURVE('',#40054,#40055,#33121,.T.);
#51972=EDGE_CURVE('',#40052,#40055,#33122,.T.);
#51973=EDGE_CURVE('',#40056,#40057,#33123,.T.);
#51974=EDGE_CURVE('',#40055,#40057,#22900,.T.);
#51975=EDGE_CURVE('',#40056,#40054,#22901,.T.);
#51976=EDGE_CURVE('',#40058,#40059,#33124,.T.);
#51977=EDGE_CURVE('',#40053,#40059,#22902,.T.);
#51978=EDGE_CURVE('',#40058,#40052,#22903,.T.);
#51979=EDGE_CURVE('',#40060,#40061,#33125,.T.);
#51980=EDGE_CURVE('',#40057,#40061,#33126,.T.);
#51981=EDGE_CURVE('',#40060,#40056,#33127,.T.);
#51982=EDGE_CURVE('',#40062,#40063,#33128,.T.);
#51983=EDGE_CURVE('',#40059,#40063,#33129,.T.);
#51984=EDGE_CURVE('',#40062,#40058,#33130,.T.);
#51985=EDGE_CURVE('',#40064,#40065,#33131,.T.);
#51986=EDGE_CURVE('',#40061,#40065,#33132,.T.);
#51987=EDGE_CURVE('',#40064,#40060,#33133,.T.);
#51988=EDGE_CURVE('',#40066,#40067,#33134,.T.);
#51989=EDGE_CURVE('',#40063,#40067,#22904,.T.);
#51990=EDGE_CURVE('',#40066,#40062,#22905,.T.);
#51991=EDGE_CURVE('',#40067,#40064,#33135,.T.);
#51992=EDGE_CURVE('',#40065,#40066,#33136,.T.);
#51993=EDGE_CURVE('',#40068,#40069,#33137,.T.);
#51994=EDGE_CURVE('',#40070,#40069,#33138,.T.);
#51995=EDGE_CURVE('',#40070,#40071,#33139,.T.);
#51996=EDGE_CURVE('',#40068,#40071,#33140,.T.);
#51997=EDGE_CURVE('',#40072,#40073,#33141,.T.);
#51998=EDGE_CURVE('',#40071,#40073,#22906,.T.);
#51999=EDGE_CURVE('',#40072,#40070,#22907,.T.);
#52000=EDGE_CURVE('',#40074,#40075,#33142,.T.);
#52001=EDGE_CURVE('',#40069,#40075,#22908,.T.);
#52002=EDGE_CURVE('',#40074,#40068,#22909,.T.);
#52003=EDGE_CURVE('',#40076,#40077,#33143,.T.);
#52004=EDGE_CURVE('',#40073,#40077,#33144,.T.);
#52005=EDGE_CURVE('',#40076,#40072,#33145,.T.);
#52006=EDGE_CURVE('',#40078,#40079,#33146,.T.);
#52007=EDGE_CURVE('',#40075,#40079,#33147,.T.);
#52008=EDGE_CURVE('',#40078,#40074,#33148,.T.);
#52009=EDGE_CURVE('',#40080,#40081,#33149,.T.);
#52010=EDGE_CURVE('',#40077,#40081,#22910,.T.);
#52011=EDGE_CURVE('',#40080,#40076,#22911,.T.);
#52012=EDGE_CURVE('',#40082,#40083,#33150,.T.);
#52013=EDGE_CURVE('',#40079,#40083,#22912,.T.);
#52014=EDGE_CURVE('',#40082,#40078,#22913,.T.);
#52015=EDGE_CURVE('',#40083,#40080,#33151,.T.);
#52016=EDGE_CURVE('',#40081,#40082,#33152,.T.);
#52017=EDGE_CURVE('',#40084,#40085,#33153,.T.);
#52018=EDGE_CURVE('',#40086,#40085,#33154,.T.);
#52019=EDGE_CURVE('',#40086,#40087,#33155,.T.);
#52020=EDGE_CURVE('',#40084,#40087,#33156,.T.);
#52021=EDGE_CURVE('',#40088,#40089,#33157,.T.);
#52022=EDGE_CURVE('',#40087,#40089,#22914,.T.);
#52023=EDGE_CURVE('',#40088,#40086,#22915,.T.);
#52024=EDGE_CURVE('',#40090,#40091,#33158,.T.);
#52025=EDGE_CURVE('',#40085,#40091,#22916,.T.);
#52026=EDGE_CURVE('',#40090,#40084,#22917,.T.);
#52027=EDGE_CURVE('',#40092,#40093,#33159,.T.);
#52028=EDGE_CURVE('',#40089,#40093,#33160,.T.);
#52029=EDGE_CURVE('',#40092,#40088,#33161,.T.);
#52030=EDGE_CURVE('',#40094,#40095,#33162,.T.);
#52031=EDGE_CURVE('',#40091,#40095,#33163,.T.);
#52032=EDGE_CURVE('',#40094,#40090,#33164,.T.);
#52033=EDGE_CURVE('',#40096,#40097,#33165,.T.);
#52034=EDGE_CURVE('',#40093,#40097,#22918,.T.);
#52035=EDGE_CURVE('',#40096,#40092,#22919,.T.);
#52036=EDGE_CURVE('',#40098,#40099,#33166,.T.);
#52037=EDGE_CURVE('',#40095,#40099,#22920,.T.);
#52038=EDGE_CURVE('',#40098,#40094,#22921,.T.);
#52039=EDGE_CURVE('',#40099,#40096,#33167,.T.);
#52040=EDGE_CURVE('',#40097,#40098,#33168,.T.);
#52041=EDGE_CURVE('',#40100,#40101,#33169,.T.);
#52042=EDGE_CURVE('',#40102,#40101,#33170,.T.);
#52043=EDGE_CURVE('',#40102,#40103,#33171,.T.);
#52044=EDGE_CURVE('',#40100,#40103,#33172,.T.);
#52045=EDGE_CURVE('',#40104,#40105,#33173,.T.);
#52046=EDGE_CURVE('',#40103,#40105,#22922,.T.);
#52047=EDGE_CURVE('',#40104,#40102,#22923,.T.);
#52048=EDGE_CURVE('',#40106,#40107,#33174,.T.);
#52049=EDGE_CURVE('',#40101,#40107,#22924,.T.);
#52050=EDGE_CURVE('',#40106,#40100,#22925,.T.);
#52051=EDGE_CURVE('',#40108,#40109,#33175,.T.);
#52052=EDGE_CURVE('',#40105,#40109,#33176,.T.);
#52053=EDGE_CURVE('',#40108,#40104,#33177,.T.);
#52054=EDGE_CURVE('',#40110,#40111,#33178,.T.);
#52055=EDGE_CURVE('',#40107,#40111,#33179,.T.);
#52056=EDGE_CURVE('',#40110,#40106,#33180,.T.);
#52057=EDGE_CURVE('',#40112,#40113,#33181,.T.);
#52058=EDGE_CURVE('',#40109,#40113,#22926,.T.);
#52059=EDGE_CURVE('',#40112,#40108,#22927,.T.);
#52060=EDGE_CURVE('',#40114,#40115,#33182,.T.);
#52061=EDGE_CURVE('',#40111,#40115,#33183,.T.);
#52062=EDGE_CURVE('',#40114,#40110,#33184,.T.);
#52063=EDGE_CURVE('',#40113,#40116,#33185,.T.);
#52064=EDGE_CURVE('',#40117,#40112,#33186,.T.);
#52065=EDGE_CURVE('',#40117,#40116,#33187,.T.);
#52066=EDGE_CURVE('',#40116,#40114,#33188,.T.);
#52067=EDGE_CURVE('',#40115,#40117,#33189,.T.);
#52068=EDGE_CURVE('',#40118,#40119,#33190,.T.);
#52069=EDGE_CURVE('',#40120,#40119,#33191,.T.);
#52070=EDGE_CURVE('',#40120,#40121,#33192,.T.);
#52071=EDGE_CURVE('',#40118,#40121,#33193,.T.);
#52072=EDGE_CURVE('',#40122,#40123,#33194,.T.);
#52073=EDGE_CURVE('',#40121,#40123,#22928,.T.);
#52074=EDGE_CURVE('',#40122,#40120,#22929,.T.);
#52075=EDGE_CURVE('',#40124,#40125,#33195,.T.);
#52076=EDGE_CURVE('',#40119,#40125,#22930,.T.);
#52077=EDGE_CURVE('',#40124,#40118,#22931,.T.);
#52078=EDGE_CURVE('',#40126,#40127,#33196,.T.);
#52079=EDGE_CURVE('',#40123,#40127,#33197,.T.);
#52080=EDGE_CURVE('',#40126,#40122,#33198,.T.);
#52081=EDGE_CURVE('',#40128,#40129,#33199,.T.);
#52082=EDGE_CURVE('',#40125,#40129,#33200,.T.);
#52083=EDGE_CURVE('',#40128,#40124,#33201,.T.);
#52084=EDGE_CURVE('',#40130,#40131,#33202,.T.);
#52085=EDGE_CURVE('',#40127,#40131,#33203,.T.);
#52086=EDGE_CURVE('',#40130,#40126,#33204,.T.);
#52087=EDGE_CURVE('',#40132,#40133,#33205,.T.);
#52088=EDGE_CURVE('',#40129,#40133,#22932,.T.);
#52089=EDGE_CURVE('',#40132,#40128,#22933,.T.);
#52090=EDGE_CURVE('',#40133,#40130,#33206,.T.);
#52091=EDGE_CURVE('',#40131,#40132,#33207,.T.);
#52092=EDGE_CURVE('',#40134,#40135,#33208,.T.);
#52093=EDGE_CURVE('',#40136,#40135,#33209,.T.);
#52094=EDGE_CURVE('',#40136,#40137,#33210,.T.);
#52095=EDGE_CURVE('',#40134,#40137,#33211,.T.);
#52096=EDGE_CURVE('',#40138,#40139,#33212,.T.);
#52097=EDGE_CURVE('',#40137,#40139,#22934,.T.);
#52098=EDGE_CURVE('',#40138,#40136,#22935,.T.);
#52099=EDGE_CURVE('',#40140,#40141,#33213,.T.);
#52100=EDGE_CURVE('',#40135,#40141,#22936,.T.);
#52101=EDGE_CURVE('',#40140,#40134,#22937,.T.);
#52102=EDGE_CURVE('',#40142,#40143,#33214,.T.);
#52103=EDGE_CURVE('',#40139,#40143,#33215,.T.);
#52104=EDGE_CURVE('',#40142,#40138,#33216,.T.);
#52105=EDGE_CURVE('',#40144,#40145,#33217,.T.);
#52106=EDGE_CURVE('',#40141,#40145,#33218,.T.);
#52107=EDGE_CURVE('',#40144,#40140,#33219,.T.);
#52108=EDGE_CURVE('',#40146,#40147,#33220,.T.);
#52109=EDGE_CURVE('',#40143,#40147,#33221,.T.);
#52110=EDGE_CURVE('',#40146,#40142,#33222,.T.);
#52111=EDGE_CURVE('',#40148,#40149,#33223,.T.);
#52112=EDGE_CURVE('',#40145,#40149,#22938,.T.);
#52113=EDGE_CURVE('',#40148,#40144,#22939,.T.);
#52114=EDGE_CURVE('',#40150,#40151,#33224,.T.);
#52115=EDGE_CURVE('',#40147,#40151,#33225,.T.);
#52116=EDGE_CURVE('',#40150,#40146,#33226,.T.);
#52117=EDGE_CURVE('',#40152,#40153,#33227,.T.);
#52118=EDGE_CURVE('',#40149,#40153,#33228,.T.);
#52119=EDGE_CURVE('',#40152,#40148,#33229,.T.);
#52120=EDGE_CURVE('',#40153,#40150,#33230,.T.);
#52121=EDGE_CURVE('',#40151,#40152,#33231,.T.);
#52122=EDGE_CURVE('',#40154,#40155,#33232,.T.);
#52123=EDGE_CURVE('',#40156,#40155,#33233,.T.);
#52124=EDGE_CURVE('',#40156,#40157,#33234,.T.);
#52125=EDGE_CURVE('',#40154,#40157,#33235,.T.);
#52126=EDGE_CURVE('',#40158,#40159,#33236,.T.);
#52127=EDGE_CURVE('',#40157,#40159,#22940,.T.);
#52128=EDGE_CURVE('',#40158,#40156,#22941,.T.);
#52129=EDGE_CURVE('',#40160,#40161,#33237,.T.);
#52130=EDGE_CURVE('',#40155,#40161,#22942,.T.);
#52131=EDGE_CURVE('',#40160,#40154,#22943,.T.);
#52132=EDGE_CURVE('',#40162,#40163,#33238,.T.);
#52133=EDGE_CURVE('',#40159,#40163,#33239,.T.);
#52134=EDGE_CURVE('',#40162,#40158,#33240,.T.);
#52135=EDGE_CURVE('',#40164,#40165,#33241,.T.);
#52136=EDGE_CURVE('',#40161,#40165,#33242,.T.);
#52137=EDGE_CURVE('',#40164,#40160,#33243,.T.);
#52138=EDGE_CURVE('',#40166,#40167,#33244,.T.);
#52139=EDGE_CURVE('',#40163,#40167,#22944,.T.);
#52140=EDGE_CURVE('',#40166,#40162,#22945,.T.);
#52141=EDGE_CURVE('',#40168,#40169,#33245,.T.);
#52142=EDGE_CURVE('',#40165,#40169,#22946,.T.);
#52143=EDGE_CURVE('',#40168,#40164,#22947,.T.);
#52144=EDGE_CURVE('',#40169,#40166,#33246,.T.);
#52145=EDGE_CURVE('',#40167,#40168,#33247,.T.);
#52146=EDGE_CURVE('',#40170,#40171,#33248,.T.);
#52147=EDGE_CURVE('',#40172,#40171,#33249,.T.);
#52148=EDGE_CURVE('',#40172,#40173,#33250,.T.);
#52149=EDGE_CURVE('',#40170,#40173,#33251,.T.);
#52150=EDGE_CURVE('',#40174,#40175,#33252,.T.);
#52151=EDGE_CURVE('',#40173,#40175,#22948,.T.);
#52152=EDGE_CURVE('',#40174,#40172,#22949,.T.);
#52153=EDGE_CURVE('',#40176,#40177,#33253,.T.);
#52154=EDGE_CURVE('',#40171,#40177,#22950,.T.);
#52155=EDGE_CURVE('',#40176,#40170,#22951,.T.);
#52156=EDGE_CURVE('',#40178,#40179,#33254,.T.);
#52157=EDGE_CURVE('',#40175,#40179,#33255,.T.);
#52158=EDGE_CURVE('',#40178,#40174,#33256,.T.);
#52159=EDGE_CURVE('',#40180,#40181,#33257,.T.);
#52160=EDGE_CURVE('',#40177,#40181,#33258,.T.);
#52161=EDGE_CURVE('',#40180,#40176,#33259,.T.);
#52162=EDGE_CURVE('',#40182,#40183,#33260,.T.);
#52163=EDGE_CURVE('',#40179,#40183,#22952,.T.);
#52164=EDGE_CURVE('',#40182,#40178,#22953,.T.);
#52165=EDGE_CURVE('',#40184,#40185,#33261,.T.);
#52166=EDGE_CURVE('',#40181,#40185,#33262,.T.);
#52167=EDGE_CURVE('',#40184,#40180,#33263,.T.);
#52168=EDGE_CURVE('',#40186,#40187,#33264,.T.);
#52169=EDGE_CURVE('',#40183,#40187,#33265,.T.);
#52170=EDGE_CURVE('',#40186,#40182,#33266,.T.);
#52171=EDGE_CURVE('',#40188,#40189,#33267,.T.);
#52172=EDGE_CURVE('',#40185,#40189,#33268,.T.);
#52173=EDGE_CURVE('',#40188,#40184,#33269,.T.);
#52174=EDGE_CURVE('',#40189,#40186,#33270,.T.);
#52175=EDGE_CURVE('',#40187,#40188,#33271,.T.);
#52176=EDGE_CURVE('',#40190,#40191,#33272,.T.);
#52177=EDGE_CURVE('',#40192,#40191,#33273,.T.);
#52178=EDGE_CURVE('',#40192,#40193,#33274,.T.);
#52179=EDGE_CURVE('',#40190,#40193,#33275,.T.);
#52180=EDGE_CURVE('',#40194,#40195,#33276,.T.);
#52181=EDGE_CURVE('',#40193,#40195,#22954,.T.);
#52182=EDGE_CURVE('',#40194,#40192,#22955,.T.);
#52183=EDGE_CURVE('',#40196,#40197,#33277,.T.);
#52184=EDGE_CURVE('',#40191,#40197,#22956,.T.);
#52185=EDGE_CURVE('',#40196,#40190,#22957,.T.);
#52186=EDGE_CURVE('',#40198,#40199,#33278,.T.);
#52187=EDGE_CURVE('',#40195,#40199,#33279,.T.);
#52188=EDGE_CURVE('',#40198,#40194,#33280,.T.);
#52189=EDGE_CURVE('',#40200,#40201,#33281,.T.);
#52190=EDGE_CURVE('',#40197,#40201,#33282,.T.);
#52191=EDGE_CURVE('',#40200,#40196,#33283,.T.);
#52192=EDGE_CURVE('',#40202,#40203,#33284,.T.);
#52193=EDGE_CURVE('',#40199,#40203,#22958,.T.);
#52194=EDGE_CURVE('',#40202,#40198,#22959,.T.);
#52195=EDGE_CURVE('',#40204,#40205,#33285,.T.);
#52196=EDGE_CURVE('',#40201,#40205,#33286,.T.);
#52197=EDGE_CURVE('',#40204,#40200,#33287,.T.);
#52198=EDGE_CURVE('',#40205,#40202,#33288,.T.);
#52199=EDGE_CURVE('',#40203,#40204,#33289,.T.);
#52200=EDGE_CURVE('',#40206,#40207,#33290,.T.);
#52201=EDGE_CURVE('',#40208,#40207,#33291,.T.);
#52202=EDGE_CURVE('',#40208,#40209,#33292,.T.);
#52203=EDGE_CURVE('',#40206,#40209,#33293,.T.);
#52204=EDGE_CURVE('',#40210,#40211,#33294,.T.);
#52205=EDGE_CURVE('',#40209,#40211,#22960,.T.);
#52206=EDGE_CURVE('',#40210,#40208,#22961,.T.);
#52207=EDGE_CURVE('',#40212,#40213,#33295,.T.);
#52208=EDGE_CURVE('',#40207,#40213,#22962,.T.);
#52209=EDGE_CURVE('',#40212,#40206,#22963,.T.);
#52210=EDGE_CURVE('',#40214,#40215,#33296,.T.);
#52211=EDGE_CURVE('',#40211,#40215,#33297,.T.);
#52212=EDGE_CURVE('',#40214,#40210,#33298,.T.);
#52213=EDGE_CURVE('',#40216,#40217,#33299,.T.);
#52214=EDGE_CURVE('',#40213,#40217,#33300,.T.);
#52215=EDGE_CURVE('',#40216,#40212,#33301,.T.);
#52216=EDGE_CURVE('',#40218,#40219,#33302,.T.);
#52217=EDGE_CURVE('',#40215,#40219,#22964,.T.);
#52218=EDGE_CURVE('',#40218,#40214,#22965,.T.);
#52219=EDGE_CURVE('',#40220,#40221,#33303,.T.);
#52220=EDGE_CURVE('',#40217,#40221,#22966,.T.);
#52221=EDGE_CURVE('',#40220,#40216,#22967,.T.);
#52222=EDGE_CURVE('',#40221,#40218,#33304,.T.);
#52223=EDGE_CURVE('',#40219,#40220,#33305,.T.);
#52224=EDGE_CURVE('',#40222,#40223,#33306,.T.);
#52225=EDGE_CURVE('',#40224,#40223,#33307,.T.);
#52226=EDGE_CURVE('',#40224,#40225,#33308,.T.);
#52227=EDGE_CURVE('',#40222,#40225,#33309,.T.);
#52228=EDGE_CURVE('',#40226,#40227,#33310,.T.);
#52229=EDGE_CURVE('',#40225,#40227,#22968,.T.);
#52230=EDGE_CURVE('',#40226,#40224,#22969,.T.);
#52231=EDGE_CURVE('',#40228,#40229,#33311,.T.);
#52232=EDGE_CURVE('',#40223,#40229,#22970,.T.);
#52233=EDGE_CURVE('',#40228,#40222,#22971,.T.);
#52234=EDGE_CURVE('',#40230,#40231,#33312,.T.);
#52235=EDGE_CURVE('',#40227,#40231,#33313,.T.);
#52236=EDGE_CURVE('',#40230,#40226,#33314,.T.);
#52237=EDGE_CURVE('',#40232,#40233,#33315,.T.);
#52238=EDGE_CURVE('',#40229,#40233,#33316,.T.);
#52239=EDGE_CURVE('',#40232,#40228,#33317,.T.);
#52240=EDGE_CURVE('',#40234,#40235,#33318,.T.);
#52241=EDGE_CURVE('',#40231,#40235,#22972,.T.);
#52242=EDGE_CURVE('',#40234,#40230,#22973,.T.);
#52243=EDGE_CURVE('',#40236,#40237,#33319,.T.);
#52244=EDGE_CURVE('',#40233,#40237,#33320,.T.);
#52245=EDGE_CURVE('',#40236,#40232,#33321,.T.);
#52246=EDGE_CURVE('',#40237,#40234,#33322,.T.);
#52247=EDGE_CURVE('',#40235,#40236,#33323,.T.);
#52248=EDGE_CURVE('',#40238,#40239,#33324,.T.);
#52249=EDGE_CURVE('',#40240,#40239,#33325,.T.);
#52250=EDGE_CURVE('',#40240,#40241,#33326,.T.);
#52251=EDGE_CURVE('',#40238,#40241,#33327,.T.);
#52252=EDGE_CURVE('',#40242,#40243,#33328,.T.);
#52253=EDGE_CURVE('',#40241,#40243,#22974,.T.);
#52254=EDGE_CURVE('',#40242,#40240,#22975,.T.);
#52255=EDGE_CURVE('',#40244,#40245,#33329,.T.);
#52256=EDGE_CURVE('',#40239,#40245,#22976,.T.);
#52257=EDGE_CURVE('',#40244,#40238,#22977,.T.);
#52258=EDGE_CURVE('',#40246,#40247,#33330,.T.);
#52259=EDGE_CURVE('',#40243,#40247,#33331,.T.);
#52260=EDGE_CURVE('',#40246,#40242,#33332,.T.);
#52261=EDGE_CURVE('',#40248,#40249,#33333,.T.);
#52262=EDGE_CURVE('',#40245,#40249,#33334,.T.);
#52263=EDGE_CURVE('',#40248,#40244,#33335,.T.);
#52264=EDGE_CURVE('',#40250,#40251,#33336,.T.);
#52265=EDGE_CURVE('',#40247,#40251,#22978,.T.);
#52266=EDGE_CURVE('',#40250,#40246,#22979,.T.);
#52267=EDGE_CURVE('',#40252,#40253,#33337,.T.);
#52268=EDGE_CURVE('',#40249,#40253,#22980,.T.);
#52269=EDGE_CURVE('',#40252,#40248,#22981,.T.);
#52270=EDGE_CURVE('',#40253,#40250,#33338,.T.);
#52271=EDGE_CURVE('',#40251,#40252,#33339,.T.);
#52272=EDGE_CURVE('',#40254,#40255,#33340,.T.);
#52273=EDGE_CURVE('',#40256,#40255,#33341,.T.);
#52274=EDGE_CURVE('',#40256,#40257,#33342,.T.);
#52275=EDGE_CURVE('',#40254,#40257,#33343,.T.);
#52276=EDGE_CURVE('',#40258,#40259,#33344,.T.);
#52277=EDGE_CURVE('',#40257,#40259,#22982,.T.);
#52278=EDGE_CURVE('',#40258,#40256,#22983,.T.);
#52279=EDGE_CURVE('',#40260,#40261,#33345,.T.);
#52280=EDGE_CURVE('',#40255,#40261,#33346,.T.);
#52281=EDGE_CURVE('',#40260,#40254,#33347,.T.);
#52282=EDGE_CURVE('',#40262,#40263,#33348,.T.);
#52283=EDGE_CURVE('',#40259,#40263,#33349,.T.);
#52284=EDGE_CURVE('',#40262,#40258,#33350,.T.);
#52285=EDGE_CURVE('',#40264,#40265,#33351,.T.);
#52286=EDGE_CURVE('',#40261,#40265,#33352,.T.);
#52287=EDGE_CURVE('',#40264,#40260,#33353,.T.);
#52288=EDGE_CURVE('',#40265,#40262,#22984,.T.);
#52289=EDGE_CURVE('',#40263,#40264,#22985,.T.);
#52290=EDGE_CURVE('',#40266,#40267,#33354,.T.);
#52291=EDGE_CURVE('',#40266,#40268,#33355,.T.);
#52292=EDGE_CURVE('',#40269,#40268,#33356,.T.);
#52293=EDGE_CURVE('',#40269,#40267,#33357,.T.);
#52294=EDGE_CURVE('',#40270,#40271,#33358,.T.);
#52295=EDGE_CURVE('',#40267,#40271,#22986,.T.);
#52296=EDGE_CURVE('',#40270,#40269,#22987,.T.);
#52297=EDGE_CURVE('',#40272,#40273,#33359,.T.);
#52298=EDGE_CURVE('',#40268,#40273,#33360,.T.);
#52299=EDGE_CURVE('',#40272,#40266,#33361,.T.);
#52300=EDGE_CURVE('',#40274,#40275,#33362,.T.);
#52301=EDGE_CURVE('',#40271,#40275,#33363,.T.);
#52302=EDGE_CURVE('',#40274,#40270,#33364,.T.);
#52303=EDGE_CURVE('',#40276,#40277,#33365,.T.);
#52304=EDGE_CURVE('',#40273,#40277,#33366,.T.);
#52305=EDGE_CURVE('',#40276,#40272,#33367,.T.);
#52306=EDGE_CURVE('',#40277,#40274,#22988,.T.);
#52307=EDGE_CURVE('',#40275,#40276,#22989,.T.);
#52308=EDGE_CURVE('',#40278,#40278,#33368,.T.);
#52309=EDGE_CURVE('',#40278,#40279,#33369,.T.);
#52310=EDGE_CURVE('',#40279,#40279,#33370,.T.);
#52311=EDGE_CURVE('',#40280,#40280,#33371,.T.);
#52312=EDGE_CURVE('',#40280,#40281,#33372,.T.);
#52313=EDGE_CURVE('',#40281,#40281,#33373,.T.);
#52314=EDGE_CURVE('',#40282,#40283,#33374,.T.);
#52315=EDGE_CURVE('',#38947,#40283,#33375,.T.);
#52316=EDGE_CURVE('',#40282,#38946,#33376,.T.);
#52317=EDGE_CURVE('',#40284,#40285,#33377,.T.);
#52318=EDGE_CURVE('',#40283,#40285,#33378,.T.);
#52319=EDGE_CURVE('',#40284,#40282,#33379,.T.);
#52320=EDGE_CURVE('',#40286,#40287,#33380,.T.);
#52321=EDGE_CURVE('',#40285,#40287,#33381,.T.);
#52322=EDGE_CURVE('',#40286,#40284,#33382,.T.);
#52323=EDGE_CURVE('',#40288,#40289,#33383,.T.);
#52324=EDGE_CURVE('',#40287,#40289,#33384,.T.);
#52325=EDGE_CURVE('',#40288,#40286,#33385,.T.);
#52326=EDGE_CURVE('',#40290,#40291,#33386,.T.);
#52327=EDGE_CURVE('',#40289,#40291,#33387,.T.);
#52328=EDGE_CURVE('',#40290,#40288,#33388,.T.);
#52329=EDGE_CURVE('',#40292,#40293,#33389,.T.);
#52330=EDGE_CURVE('',#40291,#40293,#33390,.T.);
#52331=EDGE_CURVE('',#40292,#40290,#33391,.T.);
#52332=EDGE_CURVE('',#40294,#40295,#33392,.T.);
#52333=EDGE_CURVE('',#40293,#40295,#33393,.T.);
#52334=EDGE_CURVE('',#40294,#40292,#33394,.T.);
#52335=EDGE_CURVE('',#40296,#40297,#33395,.T.);
#52336=EDGE_CURVE('',#40295,#40297,#33396,.T.);
#52337=EDGE_CURVE('',#40296,#40294,#33397,.T.);
#52338=EDGE_CURVE('',#40297,#38959,#33398,.T.);
#52339=EDGE_CURVE('',#38958,#40296,#33399,.T.);
#52340=EDGE_CURVE('',#40298,#40299,#33400,.T.);
#52341=EDGE_CURVE('',#38963,#40299,#33401,.T.);
#52342=EDGE_CURVE('',#40298,#38962,#33402,.T.);
#52343=EDGE_CURVE('',#40300,#40301,#33403,.T.);
#52344=EDGE_CURVE('',#40299,#40301,#33404,.T.);
#52345=EDGE_CURVE('',#40300,#40298,#33405,.T.);
#52346=EDGE_CURVE('',#40302,#40303,#33406,.T.);
#52347=EDGE_CURVE('',#40301,#40303,#33407,.T.);
#52348=EDGE_CURVE('',#40302,#40300,#33408,.T.);
#52349=EDGE_CURVE('',#40304,#40305,#33409,.T.);
#52350=EDGE_CURVE('',#40303,#40305,#33410,.T.);
#52351=EDGE_CURVE('',#40304,#40302,#33411,.T.);
#52352=EDGE_CURVE('',#40306,#40307,#33412,.T.);
#52353=EDGE_CURVE('',#40305,#40307,#33413,.T.);
#52354=EDGE_CURVE('',#40306,#40304,#33414,.T.);
#52355=EDGE_CURVE('',#40308,#40309,#33415,.T.);
#52356=EDGE_CURVE('',#40307,#40309,#33416,.T.);
#52357=EDGE_CURVE('',#40308,#40306,#33417,.T.);
#52358=EDGE_CURVE('',#40310,#40311,#33418,.T.);
#52359=EDGE_CURVE('',#40309,#40311,#33419,.T.);
#52360=EDGE_CURVE('',#40310,#40308,#33420,.T.);
#52361=EDGE_CURVE('',#40312,#40313,#33421,.T.);
#52362=EDGE_CURVE('',#40311,#40313,#33422,.T.);
#52363=EDGE_CURVE('',#40312,#40310,#33423,.T.);
#52364=EDGE_CURVE('',#40313,#38975,#33424,.T.);
#52365=EDGE_CURVE('',#38974,#40312,#33425,.T.);
#52366=EDGE_CURVE('',#40314,#40315,#33426,.T.);
#52367=EDGE_CURVE('',#40316,#40315,#33427,.T.);
#52368=EDGE_CURVE('',#40317,#40316,#5733,.T.);
#52369=EDGE_CURVE('',#40314,#40317,#33428,.T.);
#52370=EDGE_CURVE('',#40318,#40319,#33429,.T.);
#52371=EDGE_CURVE('',#40315,#40319,#22990,.T.);
#52372=EDGE_CURVE('',#40318,#40314,#22991,.T.);
#52373=EDGE_CURVE('',#40320,#40318,#33430,.T.);
#52374=EDGE_CURVE('',#40320,#40321,#33431,.T.);
#52375=EDGE_CURVE('',#40319,#40321,#33432,.T.);
#52376=EDGE_CURVE('',#40322,#40323,#33433,.T.);
#52377=EDGE_CURVE('',#40321,#40323,#33434,.T.);
#52378=EDGE_CURVE('',#40322,#40320,#33435,.T.);
#52379=EDGE_CURVE('',#40324,#40325,#33436,.T.);
#52380=EDGE_CURVE('',#40323,#40325,#33437,.T.);
#52381=EDGE_CURVE('',#40324,#40322,#33438,.T.);
#52382=EDGE_CURVE('',#40326,#40327,#33439,.T.);
#52383=EDGE_CURVE('',#40325,#40327,#22992,.T.);
#52384=EDGE_CURVE('',#40326,#40324,#22993,.T.);
#52385=EDGE_CURVE('',#40328,#40329,#5734,.T.);
#52386=EDGE_CURVE('',#40327,#40328,#33440,.T.);
#52387=EDGE_CURVE('',#40329,#40326,#33441,.T.);
#52388=EDGE_CURVE('',#40330,#40331,#33442,.T.);
#52389=EDGE_CURVE('',#40332,#40331,#33443,.T.);
#52390=EDGE_CURVE('',#40333,#40332,#5735,.T.);
#52391=EDGE_CURVE('',#40330,#40333,#33444,.T.);
#52392=EDGE_CURVE('',#40334,#40335,#33445,.T.);
#52393=EDGE_CURVE('',#40331,#40335,#22994,.T.);
#52394=EDGE_CURVE('',#40334,#40330,#22995,.T.);
#52395=EDGE_CURVE('',#40336,#40337,#33446,.T.);
#52396=EDGE_CURVE('',#40335,#40337,#33447,.T.);
#52397=EDGE_CURVE('',#40336,#40334,#33448,.T.);
#52398=EDGE_CURVE('',#40338,#40339,#33449,.T.);
#52399=EDGE_CURVE('',#40337,#40339,#33450,.T.);
#52400=EDGE_CURVE('',#40338,#40336,#33451,.T.);
#52401=EDGE_CURVE('',#40340,#40341,#33452,.T.);
#52402=EDGE_CURVE('',#40339,#40341,#33453,.T.);
#52403=EDGE_CURVE('',#40340,#40338,#33454,.T.);
#52404=EDGE_CURVE('',#40342,#40343,#33455,.T.);
#52405=EDGE_CURVE('',#40341,#40343,#22996,.T.);
#52406=EDGE_CURVE('',#40342,#40340,#22997,.T.);
#52407=EDGE_CURVE('',#40344,#40345,#5736,.T.);
#52408=EDGE_CURVE('',#40343,#40344,#33456,.T.);
#52409=EDGE_CURVE('',#40345,#40342,#33457,.T.);
#52410=EDGE_CURVE('',#40346,#40347,#33458,.T.);
#52411=EDGE_CURVE('',#40348,#40347,#33459,.T.);
#52412=EDGE_CURVE('',#40349,#40348,#5737,.T.);
#52413=EDGE_CURVE('',#40346,#40349,#33460,.T.);
#52414=EDGE_CURVE('',#40350,#40351,#33461,.T.);
#52415=EDGE_CURVE('',#40347,#40351,#22998,.T.);
#52416=EDGE_CURVE('',#40350,#40346,#22999,.T.);
#52417=EDGE_CURVE('',#40352,#40350,#33462,.T.);
#52418=EDGE_CURVE('',#40352,#40353,#33463,.T.);
#52419=EDGE_CURVE('',#40351,#40353,#33464,.T.);
#52420=EDGE_CURVE('',#40354,#40355,#33465,.T.);
#52421=EDGE_CURVE('',#40353,#40355,#33466,.T.);
#52422=EDGE_CURVE('',#40354,#40352,#33467,.T.);
#52423=EDGE_CURVE('',#40356,#40357,#33468,.T.);
#52424=EDGE_CURVE('',#40355,#40357,#33469,.T.);
#52425=EDGE_CURVE('',#40356,#40354,#33470,.T.);
#52426=EDGE_CURVE('',#40358,#40359,#33471,.T.);
#52427=EDGE_CURVE('',#40357,#40359,#23000,.T.);
#52428=EDGE_CURVE('',#40358,#40356,#23001,.T.);
#52429=EDGE_CURVE('',#40360,#40361,#5738,.T.);
#52430=EDGE_CURVE('',#40359,#40360,#33472,.T.);
#52431=EDGE_CURVE('',#40361,#40358,#33473,.T.);
#52432=EDGE_CURVE('',#40362,#40363,#5739,.T.);
#52433=EDGE_CURVE('',#40364,#40362,#33474,.T.);
#52434=EDGE_CURVE('',#40364,#40365,#33475,.T.);
#52435=EDGE_CURVE('',#40363,#40365,#33476,.T.);
#52436=EDGE_CURVE('',#40366,#40367,#33477,.T.);
#52437=EDGE_CURVE('',#40365,#40367,#23002,.T.);
#52438=EDGE_CURVE('',#40366,#40364,#23003,.T.);
#52439=EDGE_CURVE('',#40368,#40369,#33478,.T.);
#52440=EDGE_CURVE('',#40367,#40369,#33479,.T.);
#52441=EDGE_CURVE('',#40368,#40366,#33480,.T.);
#52442=EDGE_CURVE('',#40370,#40371,#33481,.T.);
#52443=EDGE_CURVE('',#40369,#40371,#33482,.T.);
#52444=EDGE_CURVE('',#40370,#40368,#33483,.T.);
#52445=EDGE_CURVE('',#40372,#40373,#33484,.T.);
#52446=EDGE_CURVE('',#40371,#40373,#33485,.T.);
#52447=EDGE_CURVE('',#40372,#40370,#33486,.T.);
#52448=EDGE_CURVE('',#40374,#40375,#33487,.T.);
#52449=EDGE_CURVE('',#40373,#40375,#23004,.T.);
#52450=EDGE_CURVE('',#40374,#40372,#23005,.T.);
#52451=EDGE_CURVE('',#40376,#40377,#5740,.T.);
#52452=EDGE_CURVE('',#40375,#40376,#33488,.T.);
#52453=EDGE_CURVE('',#40377,#40374,#33489,.T.);
#52454=EDGE_CURVE('',#39043,#40378,#33490,.T.);
#52455=EDGE_CURVE('',#40379,#39042,#33491,.T.);
#52456=EDGE_CURVE('',#40379,#40378,#33492,.T.);
#52457=EDGE_CURVE('',#40380,#40381,#33493,.T.);
#52458=EDGE_CURVE('',#40378,#40381,#33494,.T.);
#52459=EDGE_CURVE('',#40380,#40379,#33495,.T.);
#52460=EDGE_CURVE('',#40382,#40383,#33496,.T.);
#52461=EDGE_CURVE('',#40381,#40383,#33497,.T.);
#52462=EDGE_CURVE('',#40382,#40380,#33498,.T.);
#52463=EDGE_CURVE('',#40384,#40385,#33499,.T.);
#52464=EDGE_CURVE('',#40383,#40385,#33500,.T.);
#52465=EDGE_CURVE('',#40384,#40382,#33501,.T.);
#52466=EDGE_CURVE('',#40386,#40387,#33502,.T.);
#52467=EDGE_CURVE('',#40385,#40387,#33503,.T.);
#52468=EDGE_CURVE('',#40386,#40384,#33504,.T.);
#52469=EDGE_CURVE('',#40388,#40389,#33505,.T.);
#52470=EDGE_CURVE('',#40387,#40389,#33506,.T.);
#52471=EDGE_CURVE('',#40388,#40386,#33507,.T.);
#52472=EDGE_CURVE('',#40390,#40391,#33508,.T.);
#52473=EDGE_CURVE('',#40389,#40391,#33509,.T.);
#52474=EDGE_CURVE('',#40390,#40388,#33510,.T.);
#52475=EDGE_CURVE('',#40392,#40393,#33511,.T.);
#52476=EDGE_CURVE('',#40391,#40393,#33512,.T.);
#52477=EDGE_CURVE('',#40392,#40390,#33513,.T.);
#52478=EDGE_CURVE('',#40393,#39055,#33514,.T.);
#52479=EDGE_CURVE('',#39054,#40392,#33515,.T.);
#52480=EDGE_CURVE('',#40394,#40395,#5741,.T.);
#52481=EDGE_CURVE('',#40396,#40394,#5742,.T.);
#52482=EDGE_CURVE('',#40396,#40397,#33516,.T.);
#52483=EDGE_CURVE('',#39059,#40397,#5743,.T.);
#52484=EDGE_CURVE('',#40395,#39058,#5744,.T.);
#52485=EDGE_CURVE('',#40398,#40399,#33517,.T.);
#52486=EDGE_CURVE('',#40397,#40399,#5745,.T.);
#52487=EDGE_CURVE('',#40398,#40396,#2005,.T.);
#52488=EDGE_CURVE('',#40400,#40401,#33518,.T.);
#52489=EDGE_CURVE('',#40399,#40401,#33519,.T.);
#52490=EDGE_CURVE('',#40400,#40398,#33520,.T.);
#52491=EDGE_CURVE('',#40402,#40403,#33521,.T.);
#52492=EDGE_CURVE('',#40401,#40403,#5746,.T.);
#52493=EDGE_CURVE('',#40402,#40400,#5747,.T.);
#52494=EDGE_CURVE('',#40404,#40405,#33522,.T.);
#52495=EDGE_CURVE('',#40403,#40405,#5748,.T.);
#52496=EDGE_CURVE('',#40404,#40402,#5749,.T.);
#52497=EDGE_CURVE('',#40406,#40407,#33523,.T.);
#52498=EDGE_CURVE('',#40405,#40407,#5750,.T.);
#52499=EDGE_CURVE('',#40406,#40404,#5751,.T.);
#52500=EDGE_CURVE('',#40408,#40409,#33524,.T.);
#52501=EDGE_CURVE('',#40407,#40409,#33525,.T.);
#52502=EDGE_CURVE('',#40408,#40406,#33526,.T.);
#52503=EDGE_CURVE('',#40410,#40411,#33527,.T.);
#52504=EDGE_CURVE('',#40409,#40411,#5752,.T.);
#52505=EDGE_CURVE('',#40410,#40408,#5753,.T.);
#52506=EDGE_CURVE('',#40412,#40413,#33528,.T.);
#52507=EDGE_CURVE('',#40411,#40413,#5754,.T.);
#52508=EDGE_CURVE('',#40414,#40410,#5755,.T.);
#52509=EDGE_CURVE('',#40415,#40414,#5756,.T.);
#52510=EDGE_CURVE('',#40416,#40415,#5757,.T.);
#52511=EDGE_CURVE('',#40417,#40416,#5758,.T.);
#52512=EDGE_CURVE('',#40418,#40417,#5759,.T.);
#52513=EDGE_CURVE('',#40412,#40418,#5760,.T.);
#52514=EDGE_CURVE('',#40419,#40420,#33529,.T.);
#52515=EDGE_CURVE('',#40413,#40420,#5761,.T.);
#52516=EDGE_CURVE('',#40419,#40412,#5762,.T.);
#52517=EDGE_CURVE('',#40421,#40422,#33530,.T.);
#52518=EDGE_CURVE('',#40420,#40422,#33531,.T.);
#52519=EDGE_CURVE('',#40421,#40419,#33532,.T.);
#52520=EDGE_CURVE('',#40423,#40424,#33533,.T.);
#52521=EDGE_CURVE('',#40422,#40424,#5763,.T.);
#52522=EDGE_CURVE('',#40423,#40421,#5764,.T.);
#52523=EDGE_CURVE('',#40425,#40426,#33534,.T.);
#52524=EDGE_CURVE('',#40424,#40426,#5765,.T.);
#52525=EDGE_CURVE('',#40425,#40423,#5766,.T.);
#52526=EDGE_CURVE('',#40427,#40428,#33535,.T.);
#52527=EDGE_CURVE('',#40426,#40428,#5767,.T.);
#52528=EDGE_CURVE('',#40427,#40425,#5768,.T.);
#52529=EDGE_CURVE('',#40429,#40430,#33536,.T.);
#52530=EDGE_CURVE('',#40428,#40430,#33537,.T.);
#52531=EDGE_CURVE('',#40429,#40427,#33538,.T.);
#52532=EDGE_CURVE('',#40431,#40432,#33539,.T.);
#52533=EDGE_CURVE('',#40430,#40432,#5769,.T.);
#52534=EDGE_CURVE('',#40431,#40429,#5770,.T.);
#52535=EDGE_CURVE('',#40433,#40434,#5771,.T.);
#52536=EDGE_CURVE('',#40433,#40435,#5772,.T.);
#52537=EDGE_CURVE('',#40435,#40436,#5773,.T.);
#52538=EDGE_CURVE('',#40436,#39095,#5774,.T.);
#52539=EDGE_CURVE('',#40432,#39096,#5775,.T.);
#52540=EDGE_CURVE('',#40437,#40431,#5776,.T.);
#52541=EDGE_CURVE('',#40434,#40437,#5777,.T.);
#52542=EDGE_CURVE('',#39719,#40438,#5778,.T.);
#52543=EDGE_CURVE('',#40439,#39711,#33540,.T.);
#52544=EDGE_CURVE('',#40439,#40438,#33541,.T.);
#52545=EDGE_CURVE('',#40440,#40441,#33542,.T.);
#52546=EDGE_CURVE('',#40438,#40441,#33543,.T.);
#52547=EDGE_CURVE('',#40440,#40439,#2006,.T.);
#52548=EDGE_CURVE('',#40442,#40443,#33544,.T.);
#52549=EDGE_CURVE('',#40441,#40443,#5779,.T.);
#52550=EDGE_CURVE('',#40442,#40440,#5780,.T.);
#52551=EDGE_CURVE('',#40444,#40445,#33545,.T.);
#52552=EDGE_CURVE('',#40443,#40445,#5781,.T.);
#52553=EDGE_CURVE('',#40444,#40442,#5782,.T.);
#52554=EDGE_CURVE('',#40446,#40447,#5783,.T.);
#52555=EDGE_CURVE('',#40445,#40447,#33546,.T.);
#52556=EDGE_CURVE('',#40448,#40444,#33547,.T.);
#52557=EDGE_CURVE('',#40448,#40446,#2007,.T.);
#52558=EDGE_CURVE('',#40449,#40450,#5784,.T.);
#52559=EDGE_CURVE('',#40449,#40446,#33548,.T.);
#52560=EDGE_CURVE('',#40450,#40448,#33549,.T.);
#52561=EDGE_CURVE('',#40449,#40447,#5785,.T.);
#52562=EDGE_CURVE('',#40451,#40452,#5786,.T.);
#52563=EDGE_CURVE('',#40447,#40452,#5787,.T.);
#52564=EDGE_CURVE('',#40453,#40449,#5788,.T.);
#52565=EDGE_CURVE('',#40454,#40453,#5789,.T.);
#52566=EDGE_CURVE('',#40455,#40454,#5790,.T.);
#52567=EDGE_CURVE('',#40456,#40455,#5791,.T.);
#52568=EDGE_CURVE('',#40457,#40456,#5792,.T.);
#52569=EDGE_CURVE('',#40458,#40457,#5793,.T.);
#52570=EDGE_CURVE('',#40451,#40458,#5794,.T.);
#52571=EDGE_CURVE('',#40451,#40459,#33550,.T.);
#52572=EDGE_CURVE('',#40459,#40452,#5795,.T.);
#52573=EDGE_CURVE('',#40460,#40461,#33551,.T.);
#52574=EDGE_CURVE('',#40460,#40459,#5796,.T.);
#52575=EDGE_CURVE('',#40461,#40451,#5797,.T.);
#52576=EDGE_CURVE('',#40462,#40460,#33552,.T.);
#52577=EDGE_CURVE('',#40462,#40463,#33553,.T.);
#52578=EDGE_CURVE('',#40452,#40463,#33554,.T.);
#52579=EDGE_CURVE('',#40464,#40465,#33555,.T.);
#52580=EDGE_CURVE('',#40463,#40465,#5798,.T.);
#52581=EDGE_CURVE('',#40464,#40462,#5799,.T.);
#52582=EDGE_CURVE('',#40466,#40467,#33556,.T.);
#52583=EDGE_CURVE('',#40465,#40467,#5800,.T.);
#52584=EDGE_CURVE('',#40466,#40464,#5801,.T.);
#52585=EDGE_CURVE('',#40468,#40469,#33557,.T.);
#52586=EDGE_CURVE('',#40467,#40469,#33558,.T.);
#52587=EDGE_CURVE('',#40468,#40466,#33559,.T.);
#52588=EDGE_CURVE('',#40469,#39725,#5802,.T.);
#52589=EDGE_CURVE('',#39735,#40468,#2008,.T.);
#52590=EDGE_CURVE('',#40470,#40471,#5803,.T.);
#52591=EDGE_CURVE('',#40472,#40470,#5804,.T.);
#52592=EDGE_CURVE('',#40472,#40473,#5805,.T.);
#52593=EDGE_CURVE('',#39131,#40473,#5806,.T.);
#52594=EDGE_CURVE('',#39129,#40474,#5807,.T.);
#52595=EDGE_CURVE('',#40474,#40475,#5808,.T.);
#52596=EDGE_CURVE('',#40475,#40476,#5809,.T.);
#52597=EDGE_CURVE('',#40476,#40477,#5810,.T.);
#52598=EDGE_CURVE('',#40478,#40477,#5811,.T.);
#52599=EDGE_CURVE('',#40471,#40478,#5812,.T.);
#52600=EDGE_CURVE('',#40472,#40479,#33560,.T.);
#52601=EDGE_CURVE('',#40479,#40473,#2009,.T.);
#52602=EDGE_CURVE('',#40480,#40481,#33561,.T.);
#52603=EDGE_CURVE('',#40480,#40479,#2010,.T.);
#52604=EDGE_CURVE('',#40481,#40472,#2011,.T.);
#52605=EDGE_CURVE('',#40482,#40480,#33562,.T.);
#52606=EDGE_CURVE('',#40482,#40483,#33563,.T.);
#52607=EDGE_CURVE('',#40473,#40483,#33564,.T.);
#52608=EDGE_CURVE('',#40484,#40485,#33565,.T.);
#52609=EDGE_CURVE('',#40483,#40485,#5813,.T.);
#52610=EDGE_CURVE('',#40484,#40482,#5814,.T.);
#52611=EDGE_CURVE('',#40486,#40487,#33566,.T.);
#52612=EDGE_CURVE('',#40485,#40487,#5815,.T.);
#52613=EDGE_CURVE('',#40486,#40484,#5816,.T.);
#52614=EDGE_CURVE('',#40488,#40489,#33567,.T.);
#52615=EDGE_CURVE('',#40487,#40489,#33568,.T.);
#52616=EDGE_CURVE('',#40488,#40486,#5817,.T.);
#52617=EDGE_CURVE('',#39710,#40488,#2012,.T.);
#52618=EDGE_CURVE('',#40489,#39718,#5818,.T.);
#52619=EDGE_CURVE('',#40490,#39142,#2013,.T.);
#52620=EDGE_CURVE('',#40490,#40491,#33569,.T.);
#52621=EDGE_CURVE('',#39143,#40491,#2014,.T.);
#52622=EDGE_CURVE('',#40492,#40493,#5819,.T.);
#52623=EDGE_CURVE('',#40491,#40492,#5820,.T.);
#52624=EDGE_CURVE('',#40494,#40490,#5821,.T.);
#52625=EDGE_CURVE('',#40494,#40495,#5822,.T.);
#52626=EDGE_CURVE('',#40496,#40495,#5823,.T.);
#52627=EDGE_CURVE('',#40493,#40496,#5824,.T.);
#52628=EDGE_CURVE('',#40494,#40497,#5825,.T.);
#52629=EDGE_CURVE('',#40497,#40495,#33570,.T.);
#52630=EDGE_CURVE('',#40498,#40499,#5826,.T.);
#52631=EDGE_CURVE('',#40498,#40497,#33571,.T.);
#52632=EDGE_CURVE('',#40500,#40494,#2015,.T.);
#52633=EDGE_CURVE('',#40500,#40499,#33572,.T.);
#52634=EDGE_CURVE('',#40501,#40498,#33573,.T.);
#52635=EDGE_CURVE('',#40495,#40501,#5827,.T.);
#52636=EDGE_CURVE('',#40502,#40503,#33574,.T.);
#52637=EDGE_CURVE('',#40499,#40503,#5828,.T.);
#52638=EDGE_CURVE('',#40502,#40500,#5829,.T.);
#52639=EDGE_CURVE('',#40504,#40505,#33575,.T.);
#52640=EDGE_CURVE('',#40503,#40505,#5830,.T.);
#52641=EDGE_CURVE('',#40504,#40502,#5831,.T.);
#52642=EDGE_CURVE('',#40506,#40507,#33576,.T.);
#52643=EDGE_CURVE('',#40505,#40507,#5832,.T.);
#52644=EDGE_CURVE('',#40506,#40504,#33577,.T.);
#52645=EDGE_CURVE('',#40507,#39743,#5833,.T.);
#52646=EDGE_CURVE('',#39734,#40506,#5834,.T.);
#52647=EDGE_CURVE('',#40431,#40481,#5835,.T.);
#52648=EDGE_CURVE('',#40480,#40429,#5836,.T.);
#52649=EDGE_CURVE('',#40419,#40448,#5837,.T.);
#52650=EDGE_CURVE('',#40450,#40412,#5838,.T.);
#52651=EDGE_CURVE('',#40410,#40461,#5839,.T.);
#52652=EDGE_CURVE('',#40460,#40408,#5840,.T.);
#52653=EDGE_CURVE('',#40398,#40498,#5841,.T.);
#52654=EDGE_CURVE('',#40501,#40396,#5842,.T.);
#52655=EDGE_CURVE('',#40508,#40509,#33578,.T.);
#52656=EDGE_CURVE('',#40319,#40508,#23006,.T.);
#52657=EDGE_CURVE('',#40509,#40321,#23007,.T.);
#52658=EDGE_CURVE('',#40375,#40510,#23008,.T.);
#52659=EDGE_CURVE('',#40511,#40376,#23009,.T.);
#52660=EDGE_CURVE('',#40510,#40511,#33579,.T.);
#52661=EDGE_CURVE('',#40335,#40512,#23010,.T.);
#52662=EDGE_CURVE('',#40513,#40337,#23011,.T.);
#52663=EDGE_CURVE('',#40512,#40513,#33580,.T.);
#52664=EDGE_CURVE('',#40332,#40514,#23012,.T.);
#52665=EDGE_CURVE('',#40515,#40331,#23013,.T.);
#52666=EDGE_CURVE('',#40514,#40515,#33581,.T.);
#52667=EDGE_CURVE('',#40327,#40516,#23014,.T.);
#52668=EDGE_CURVE('',#40517,#40328,#23015,.T.);
#52669=EDGE_CURVE('',#40516,#40517,#33582,.T.);
#52670=EDGE_CURVE('',#40323,#40518,#23016,.T.);
#52671=EDGE_CURVE('',#40519,#40325,#23017,.T.);
#52672=EDGE_CURVE('',#40518,#40519,#33583,.T.);
#52673=EDGE_CURVE('',#40316,#40520,#23018,.T.);
#52674=EDGE_CURVE('',#40521,#40315,#23019,.T.);
#52675=EDGE_CURVE('',#40520,#40521,#33584,.T.);
#52676=EDGE_CURVE('',#40359,#40522,#23020,.T.);
#52677=EDGE_CURVE('',#40523,#40360,#23021,.T.);
#52678=EDGE_CURVE('',#40522,#40523,#33585,.T.);
#52679=EDGE_CURVE('',#40348,#40524,#23022,.T.);
#52680=EDGE_CURVE('',#40525,#40347,#23023,.T.);
#52681=EDGE_CURVE('',#40524,#40525,#33586,.T.);
#52682=EDGE_CURVE('',#40526,#40527,#33587,.T.);
#52683=EDGE_CURVE('',#40117,#40526,#23024,.T.);
#52684=EDGE_CURVE('',#40527,#40112,#23025,.T.);
#52685=EDGE_CURVE('',#40031,#40528,#23026,.T.);
#52686=EDGE_CURVE('',#40529,#40035,#23027,.T.);
#52687=EDGE_CURVE('',#40528,#40529,#33588,.T.);
#52688=EDGE_CURVE('',#40018,#40530,#23028,.T.);
#52689=EDGE_CURVE('',#40531,#40017,#23029,.T.);
#52690=EDGE_CURVE('',#40530,#40531,#33589,.T.);
#52691=EDGE_CURVE('',#40024,#40532,#23030,.T.);
#52692=EDGE_CURVE('',#40533,#40020,#23031,.T.);
#52693=EDGE_CURVE('',#40532,#40533,#33590,.T.);
#52694=EDGE_CURVE('',#40032,#40534,#23032,.T.);
#52695=EDGE_CURVE('',#40535,#40028,#23033,.T.);
#52696=EDGE_CURVE('',#40534,#40535,#33591,.T.);
#52697=EDGE_CURVE('',#39998,#40536,#23034,.T.);
#52698=EDGE_CURVE('',#40537,#39997,#23035,.T.);
#52699=EDGE_CURVE('',#40536,#40537,#33592,.T.);
#52700=EDGE_CURVE('',#40004,#40538,#23036,.T.);
#52701=EDGE_CURVE('',#40539,#40000,#23037,.T.);
#52702=EDGE_CURVE('',#40538,#40539,#33593,.T.);
#52703=EDGE_CURVE('',#40012,#40540,#23038,.T.);
#52704=EDGE_CURVE('',#40541,#40008,#23039,.T.);
#52705=EDGE_CURVE('',#40540,#40541,#33594,.T.);
#52706=EDGE_CURVE('',#40011,#40542,#23040,.T.);
#52707=EDGE_CURVE('',#40543,#40015,#23041,.T.);
#52708=EDGE_CURVE('',#40542,#40543,#33595,.T.);
#52709=EDGE_CURVE('',#39861,#40544,#23042,.T.);
#52710=EDGE_CURVE('',#40545,#39862,#23043,.T.);
#52711=EDGE_CURVE('',#40544,#40545,#33596,.T.);
#52712=EDGE_CURVE('',#39853,#40546,#23044,.T.);
#52713=EDGE_CURVE('',#40547,#39857,#23045,.T.);
#52714=EDGE_CURVE('',#40546,#40547,#33597,.T.);
#52715=EDGE_CURVE('',#39848,#40548,#23046,.T.);
#52716=EDGE_CURVE('',#40549,#39847,#23047,.T.);
#52717=EDGE_CURVE('',#40548,#40549,#33598,.T.);
#52718=EDGE_CURVE('',#39854,#40550,#23048,.T.);
#52719=EDGE_CURVE('',#40551,#39850,#23049,.T.);
#52720=EDGE_CURVE('',#40550,#40551,#33599,.T.);
#52721=EDGE_CURVE('',#40107,#40552,#23050,.T.);
#52722=EDGE_CURVE('',#40553,#40111,#23051,.T.);
#52723=EDGE_CURVE('',#40552,#40553,#33600,.T.);
#52724=EDGE_CURVE('',#40102,#40554,#23052,.T.);
#52725=EDGE_CURVE('',#40555,#40101,#23053,.T.);
#52726=EDGE_CURVE('',#40554,#40555,#33601,.T.);
#52727=EDGE_CURVE('',#40108,#40556,#23054,.T.);
#52728=EDGE_CURVE('',#40557,#40104,#23055,.T.);
#52729=EDGE_CURVE('',#40556,#40557,#33602,.T.);
#52730=EDGE_CURVE('',#40274,#40558,#23056,.T.);
#52731=EDGE_CURVE('',#40559,#40270,#23057,.T.);
#52732=EDGE_CURVE('',#40558,#40559,#33603,.T.);
#52733=EDGE_CURVE('',#40273,#40560,#23058,.T.);
#52734=EDGE_CURVE('',#40561,#40277,#23059,.T.);
#52735=EDGE_CURVE('',#40560,#40561,#33604,.T.);
#52736=EDGE_CURVE('',#40562,#40563,#33605,.T.);
#52737=EDGE_CURVE('',#40269,#40562,#23060,.T.);
#52738=EDGE_CURVE('',#40563,#40268,#23061,.T.);
#52739=EDGE_CURVE('',#39903,#40564,#23062,.T.);
#52740=EDGE_CURVE('',#40565,#39907,#23063,.T.);
#52741=EDGE_CURVE('',#40564,#40565,#33606,.T.);
#52742=EDGE_CURVE('',#39898,#40566,#23064,.T.);
#52743=EDGE_CURVE('',#40567,#39897,#23065,.T.);
#52744=EDGE_CURVE('',#40566,#40567,#33607,.T.);
#52745=EDGE_CURVE('',#39904,#40568,#23066,.T.);
#52746=EDGE_CURVE('',#40569,#39900,#23067,.T.);
#52747=EDGE_CURVE('',#40568,#40569,#33608,.T.);
#52748=EDGE_CURVE('',#39911,#40570,#23068,.T.);
#52749=EDGE_CURVE('',#40571,#39908,#23069,.T.);
#52750=EDGE_CURVE('',#40570,#40571,#33609,.T.);
#52751=EDGE_CURVE('',#39919,#40572,#23070,.T.);
#52752=EDGE_CURVE('',#40573,#39923,#23071,.T.);
#52753=EDGE_CURVE('',#40572,#40573,#33610,.T.);
#52754=EDGE_CURVE('',#39914,#40574,#23072,.T.);
#52755=EDGE_CURVE('',#40575,#39913,#23073,.T.);
#52756=EDGE_CURVE('',#40574,#40575,#33611,.T.);
#52757=EDGE_CURVE('',#39920,#40576,#23074,.T.);
#52758=EDGE_CURVE('',#40577,#39916,#23075,.T.);
#52759=EDGE_CURVE('',#40576,#40577,#33612,.T.);
#52760=EDGE_CURVE('',#39927,#40578,#23076,.T.);
#52761=EDGE_CURVE('',#40579,#39924,#23077,.T.);
#52762=EDGE_CURVE('',#40578,#40579,#33613,.T.);
#52763=EDGE_CURVE('',#40172,#40580,#23078,.T.);
#52764=EDGE_CURVE('',#40581,#40171,#23079,.T.);
#52765=EDGE_CURVE('',#40580,#40581,#33614,.T.);
#52766=EDGE_CURVE('',#40178,#40582,#23080,.T.);
#52767=EDGE_CURVE('',#40583,#40174,#23081,.T.);
#52768=EDGE_CURVE('',#40582,#40583,#33615,.T.);
#52769=EDGE_CURVE('',#40186,#40584,#23082,.T.);
#52770=EDGE_CURVE('',#40585,#40182,#23083,.T.);
#52771=EDGE_CURVE('',#40584,#40585,#33616,.T.);
#52772=EDGE_CURVE('',#40177,#40586,#23084,.T.);
#52773=EDGE_CURVE('',#40587,#40181,#23085,.T.);
#52774=EDGE_CURVE('',#40586,#40587,#33617,.T.);
#52775=EDGE_CURVE('',#40136,#40588,#23086,.T.);
#52776=EDGE_CURVE('',#40589,#40135,#23087,.T.);
#52777=EDGE_CURVE('',#40588,#40589,#33618,.T.);
#52778=EDGE_CURVE('',#40142,#40590,#23088,.T.);
#52779=EDGE_CURVE('',#40591,#40138,#23089,.T.);
#52780=EDGE_CURVE('',#40590,#40591,#33619,.T.);
#52781=EDGE_CURVE('',#40149,#40592,#23090,.T.);
#52782=EDGE_CURVE('',#40593,#40153,#23091,.T.);
#52783=EDGE_CURVE('',#40592,#40593,#33620,.T.);
#52784=EDGE_CURVE('',#40141,#40594,#23092,.T.);
#52785=EDGE_CURVE('',#40595,#40145,#23093,.T.);
#52786=EDGE_CURVE('',#40594,#40595,#33621,.T.);
#52787=EDGE_CURVE('',#39987,#40596,#23094,.T.);
#52788=EDGE_CURVE('',#40597,#39991,#23095,.T.);
#52789=EDGE_CURVE('',#40596,#40597,#33622,.T.);
#52790=EDGE_CURVE('',#39982,#40598,#23096,.T.);
#52791=EDGE_CURVE('',#40599,#39981,#23097,.T.);
#52792=EDGE_CURVE('',#40598,#40599,#33623,.T.);
#52793=EDGE_CURVE('',#39988,#40600,#23098,.T.);
#52794=EDGE_CURVE('',#40601,#39984,#23099,.T.);
#52795=EDGE_CURVE('',#40600,#40601,#33624,.T.);
#52796=EDGE_CURVE('',#39995,#40602,#23100,.T.);
#52797=EDGE_CURVE('',#40603,#39992,#23101,.T.);
#52798=EDGE_CURVE('',#40602,#40603,#33625,.T.);
#52799=EDGE_CURVE('',#40051,#40604,#23102,.T.);
#52800=EDGE_CURVE('',#40605,#40048,#23103,.T.);
#52801=EDGE_CURVE('',#40604,#40605,#33626,.T.);
#52802=EDGE_CURVE('',#40043,#40606,#23104,.T.);
#52803=EDGE_CURVE('',#40607,#40047,#23105,.T.);
#52804=EDGE_CURVE('',#40606,#40607,#33627,.T.);
#52805=EDGE_CURVE('',#40038,#40608,#23106,.T.);
#52806=EDGE_CURVE('',#40609,#40037,#23107,.T.);
#52807=EDGE_CURVE('',#40608,#40609,#33628,.T.);
#52808=EDGE_CURVE('',#40044,#40610,#23108,.T.);
#52809=EDGE_CURVE('',#40611,#40040,#23109,.T.);
#52810=EDGE_CURVE('',#40610,#40611,#33629,.T.);
#52811=EDGE_CURVE('',#40070,#40612,#23110,.T.);
#52812=EDGE_CURVE('',#40613,#40069,#23111,.T.);
#52813=EDGE_CURVE('',#40612,#40613,#33630,.T.);
#52814=EDGE_CURVE('',#40076,#40614,#23112,.T.);
#52815=EDGE_CURVE('',#40615,#40072,#23113,.T.);
#52816=EDGE_CURVE('',#40614,#40615,#33631,.T.);
#52817=EDGE_CURVE('',#40083,#40616,#23114,.T.);
#52818=EDGE_CURVE('',#40617,#40080,#23115,.T.);
#52819=EDGE_CURVE('',#40616,#40617,#33632,.T.);
#52820=EDGE_CURVE('',#40075,#40618,#23116,.T.);
#52821=EDGE_CURVE('',#40619,#40079,#23117,.T.);
#52822=EDGE_CURVE('',#40618,#40619,#33633,.T.);
#52823=EDGE_CURVE('',#40262,#40620,#23118,.T.);
#52824=EDGE_CURVE('',#40621,#40258,#23119,.T.);
#52825=EDGE_CURVE('',#40620,#40621,#33634,.T.);
#52826=EDGE_CURVE('',#40261,#40622,#23120,.T.);
#52827=EDGE_CURVE('',#40623,#40265,#23121,.T.);
#52828=EDGE_CURVE('',#40622,#40623,#33635,.T.);
#52829=EDGE_CURVE('',#40256,#40624,#23122,.T.);
#52830=EDGE_CURVE('',#40625,#40255,#23123,.T.);
#52831=EDGE_CURVE('',#40624,#40625,#33636,.T.);
#52832=EDGE_CURVE('',#40162,#40626,#23124,.T.);
#52833=EDGE_CURVE('',#40627,#40158,#23125,.T.);
#52834=EDGE_CURVE('',#40626,#40627,#33637,.T.);
#52835=EDGE_CURVE('',#40169,#40628,#23126,.T.);
#52836=EDGE_CURVE('',#40629,#40166,#23127,.T.);
#52837=EDGE_CURVE('',#40628,#40629,#33638,.T.);
#52838=EDGE_CURVE('',#40161,#40630,#23128,.T.);
#52839=EDGE_CURVE('',#40631,#40165,#23129,.T.);
#52840=EDGE_CURVE('',#40630,#40631,#33639,.T.);
#52841=EDGE_CURVE('',#40156,#40632,#23130,.T.);
#52842=EDGE_CURVE('',#40633,#40155,#23131,.T.);
#52843=EDGE_CURVE('',#40632,#40633,#33640,.T.);
#52844=EDGE_CURVE('',#40125,#40634,#23132,.T.);
#52845=EDGE_CURVE('',#40635,#40129,#23133,.T.);
#52846=EDGE_CURVE('',#40634,#40635,#33641,.T.);
#52847=EDGE_CURVE('',#40120,#40636,#23134,.T.);
#52848=EDGE_CURVE('',#40637,#40119,#23135,.T.);
#52849=EDGE_CURVE('',#40636,#40637,#33642,.T.);
#52850=EDGE_CURVE('',#40126,#40638,#23136,.T.);
#52851=EDGE_CURVE('',#40639,#40122,#23137,.T.);
#52852=EDGE_CURVE('',#40638,#40639,#33643,.T.);
#52853=EDGE_CURVE('',#40133,#40640,#23138,.T.);
#52854=EDGE_CURVE('',#40641,#40130,#23139,.T.);
#52855=EDGE_CURVE('',#40640,#40641,#33644,.T.);
#52856=EDGE_CURVE('',#40059,#40642,#23140,.T.);
#52857=EDGE_CURVE('',#40643,#40063,#23141,.T.);
#52858=EDGE_CURVE('',#40642,#40643,#33645,.T.);
#52859=EDGE_CURVE('',#40054,#40644,#23142,.T.);
#52860=EDGE_CURVE('',#40645,#40053,#23143,.T.);
#52861=EDGE_CURVE('',#40644,#40645,#33646,.T.);
#52862=EDGE_CURVE('',#40060,#40646,#23144,.T.);
#52863=EDGE_CURVE('',#40647,#40056,#23145,.T.);
#52864=EDGE_CURVE('',#40646,#40647,#33647,.T.);
#52865=EDGE_CURVE('',#40067,#40648,#23146,.T.);
#52866=EDGE_CURVE('',#40649,#40064,#23147,.T.);
#52867=EDGE_CURVE('',#40648,#40649,#33648,.T.);
#52868=EDGE_CURVE('',#39966,#40650,#23148,.T.);
#52869=EDGE_CURVE('',#40651,#39965,#23149,.T.);
#52870=EDGE_CURVE('',#40650,#40651,#33649,.T.);
#52871=EDGE_CURVE('',#39972,#40652,#23150,.T.);
#52872=EDGE_CURVE('',#40653,#39968,#23151,.T.);
#52873=EDGE_CURVE('',#40652,#40653,#33650,.T.);
#52874=EDGE_CURVE('',#39979,#40654,#23152,.T.);
#52875=EDGE_CURVE('',#40655,#39976,#23153,.T.);
#52876=EDGE_CURVE('',#40654,#40655,#33651,.T.);
#52877=EDGE_CURVE('',#39971,#40656,#23154,.T.);
#52878=EDGE_CURVE('',#40657,#39975,#23155,.T.);
#52879=EDGE_CURVE('',#40656,#40657,#33652,.T.);
#52880=EDGE_CURVE('',#39930,#40658,#23156,.T.);
#52881=EDGE_CURVE('',#40659,#39929,#23157,.T.);
#52882=EDGE_CURVE('',#40658,#40659,#33653,.T.);
#52883=EDGE_CURVE('',#39936,#40660,#23158,.T.);
#52884=EDGE_CURVE('',#40661,#39932,#23159,.T.);
#52885=EDGE_CURVE('',#40660,#40661,#33654,.T.);
#52886=EDGE_CURVE('',#39943,#40662,#23160,.T.);
#52887=EDGE_CURVE('',#40663,#39940,#23161,.T.);
#52888=EDGE_CURVE('',#40662,#40663,#33655,.T.);
#52889=EDGE_CURVE('',#39935,#40664,#23162,.T.);
#52890=EDGE_CURVE('',#40665,#39939,#23163,.T.);
#52891=EDGE_CURVE('',#40664,#40665,#33656,.T.);
#52892=EDGE_CURVE('',#39946,#40666,#23164,.T.);
#52893=EDGE_CURVE('',#40667,#39945,#23165,.T.);
#52894=EDGE_CURVE('',#40666,#40667,#33657,.T.);
#52895=EDGE_CURVE('',#39952,#40668,#23166,.T.);
#52896=EDGE_CURVE('',#40669,#39948,#23167,.T.);
#52897=EDGE_CURVE('',#40668,#40669,#33658,.T.);
#52898=EDGE_CURVE('',#39960,#40670,#23168,.T.);
#52899=EDGE_CURVE('',#40671,#39956,#23169,.T.);
#52900=EDGE_CURVE('',#40670,#40671,#33659,.T.);
#52901=EDGE_CURVE('',#39951,#40672,#23170,.T.);
#52902=EDGE_CURVE('',#40673,#39955,#23171,.T.);
#52903=EDGE_CURVE('',#40672,#40673,#33660,.T.);
#52904=EDGE_CURVE('',#39794,#40674,#23172,.T.);
#52905=EDGE_CURVE('',#40675,#39790,#23173,.T.);
#52906=EDGE_CURVE('',#40674,#40675,#33661,.T.);
#52907=EDGE_CURVE('',#39793,#40676,#23174,.T.);
#52908=EDGE_CURVE('',#40677,#39797,#23175,.T.);
#52909=EDGE_CURVE('',#40676,#40677,#33662,.T.);
#52910=EDGE_CURVE('',#40678,#40679,#33663,.T.);
#52911=EDGE_CURVE('',#39781,#40678,#23176,.T.);
#52912=EDGE_CURVE('',#40679,#39780,#23177,.T.);
#52913=EDGE_CURVE('',#39786,#40680,#23178,.T.);
#52914=EDGE_CURVE('',#40681,#39782,#23179,.T.);
#52915=EDGE_CURVE('',#40680,#40681,#33664,.T.);
#52916=EDGE_CURVE('',#40197,#40682,#23180,.T.);
#52917=EDGE_CURVE('',#40683,#40201,#23181,.T.);
#52918=EDGE_CURVE('',#40682,#40683,#33665,.T.);
#52919=EDGE_CURVE('',#40192,#40684,#23182,.T.);
#52920=EDGE_CURVE('',#40685,#40191,#23183,.T.);
#52921=EDGE_CURVE('',#40684,#40685,#33666,.T.);
#52922=EDGE_CURVE('',#40198,#40686,#23184,.T.);
#52923=EDGE_CURVE('',#40687,#40194,#23185,.T.);
#52924=EDGE_CURVE('',#40686,#40687,#33667,.T.);
#52925=EDGE_CURVE('',#40205,#40688,#23186,.T.);
#52926=EDGE_CURVE('',#40689,#40202,#23187,.T.);
#52927=EDGE_CURVE('',#40688,#40689,#33668,.T.);
#52928=EDGE_CURVE('',#39887,#40690,#23188,.T.);
#52929=EDGE_CURVE('',#40691,#39891,#23189,.T.);
#52930=EDGE_CURVE('',#40690,#40691,#33669,.T.);
#52931=EDGE_CURVE('',#39882,#40692,#23190,.T.);
#52932=EDGE_CURVE('',#40693,#39881,#23191,.T.);
#52933=EDGE_CURVE('',#40692,#40693,#33670,.T.);
#52934=EDGE_CURVE('',#39888,#40694,#23192,.T.);
#52935=EDGE_CURVE('',#40695,#39884,#23193,.T.);
#52936=EDGE_CURVE('',#40694,#40695,#33671,.T.);
#52937=EDGE_CURVE('',#39895,#40696,#23194,.T.);
#52938=EDGE_CURVE('',#40697,#39892,#23195,.T.);
#52939=EDGE_CURVE('',#40696,#40697,#33672,.T.);
#52940=EDGE_CURVE('',#39871,#40698,#23196,.T.);
#52941=EDGE_CURVE('',#40699,#39875,#23197,.T.);
#52942=EDGE_CURVE('',#40698,#40699,#33673,.T.);
#52943=EDGE_CURVE('',#39866,#40700,#23198,.T.);
#52944=EDGE_CURVE('',#40701,#39865,#23199,.T.);
#52945=EDGE_CURVE('',#40700,#40701,#33674,.T.);
#52946=EDGE_CURVE('',#39872,#40702,#23200,.T.);
#52947=EDGE_CURVE('',#40703,#39868,#23201,.T.);
#52948=EDGE_CURVE('',#40702,#40703,#33675,.T.);
#52949=EDGE_CURVE('',#39879,#40704,#23202,.T.);
#52950=EDGE_CURVE('',#40705,#39876,#23203,.T.);
#52951=EDGE_CURVE('',#40704,#40705,#33676,.T.);
#52952=EDGE_CURVE('',#40086,#40706,#23204,.T.);
#52953=EDGE_CURVE('',#40707,#40085,#23205,.T.);
#52954=EDGE_CURVE('',#40706,#40707,#33677,.T.);
#52955=EDGE_CURVE('',#40092,#40708,#23206,.T.);
#52956=EDGE_CURVE('',#40709,#40088,#23207,.T.);
#52957=EDGE_CURVE('',#40708,#40709,#33678,.T.);
#52958=EDGE_CURVE('',#40099,#40710,#23208,.T.);
#52959=EDGE_CURVE('',#40711,#40096,#23209,.T.);
#52960=EDGE_CURVE('',#40710,#40711,#33679,.T.);
#52961=EDGE_CURVE('',#40091,#40712,#23210,.T.);
#52962=EDGE_CURVE('',#40713,#40095,#23211,.T.);
#52963=EDGE_CURVE('',#40712,#40713,#33680,.T.);
#52964=EDGE_CURVE('',#40214,#40714,#23212,.T.);
#52965=EDGE_CURVE('',#40715,#40210,#23213,.T.);
#52966=EDGE_CURVE('',#40714,#40715,#33681,.T.);
#52967=EDGE_CURVE('',#40221,#40716,#23214,.T.);
#52968=EDGE_CURVE('',#40717,#40218,#23215,.T.);
#52969=EDGE_CURVE('',#40716,#40717,#33682,.T.);
#52970=EDGE_CURVE('',#40213,#40718,#23216,.T.);
#52971=EDGE_CURVE('',#40719,#40217,#23217,.T.);
#52972=EDGE_CURVE('',#40718,#40719,#33683,.T.);
#52973=EDGE_CURVE('',#40208,#40720,#23218,.T.);
#52974=EDGE_CURVE('',#40721,#40207,#23219,.T.);
#52975=EDGE_CURVE('',#40720,#40721,#33684,.T.);
#52976=EDGE_CURVE('',#39813,#40722,#23220,.T.);
#52977=EDGE_CURVE('',#40723,#39810,#23221,.T.);
#52978=EDGE_CURVE('',#40722,#40723,#33685,.T.);
#52979=EDGE_CURVE('',#39805,#40724,#23222,.T.);
#52980=EDGE_CURVE('',#40725,#39809,#23223,.T.);
#52981=EDGE_CURVE('',#40724,#40725,#33686,.T.);
#52982=EDGE_CURVE('',#40726,#40727,#33687,.T.);
#52983=EDGE_CURVE('',#39801,#40726,#23224,.T.);
#52984=EDGE_CURVE('',#40727,#39800,#23225,.T.);
#52985=EDGE_CURVE('',#39806,#40728,#23226,.T.);
#52986=EDGE_CURVE('',#40729,#39802,#23227,.T.);
#52987=EDGE_CURVE('',#40728,#40729,#33688,.T.);
#52988=EDGE_CURVE('',#40229,#40730,#23228,.T.);
#52989=EDGE_CURVE('',#40731,#40233,#23229,.T.);
#52990=EDGE_CURVE('',#40730,#40731,#33689,.T.);
#52991=EDGE_CURVE('',#40224,#40732,#23230,.T.);
#52992=EDGE_CURVE('',#40733,#40223,#23231,.T.);
#52993=EDGE_CURVE('',#40732,#40733,#33690,.T.);
#52994=EDGE_CURVE('',#40230,#40734,#23232,.T.);
#52995=EDGE_CURVE('',#40735,#40226,#23233,.T.);
#52996=EDGE_CURVE('',#40734,#40735,#33691,.T.);
#52997=EDGE_CURVE('',#40237,#40736,#23234,.T.);
#52998=EDGE_CURVE('',#40737,#40234,#23235,.T.);
#52999=EDGE_CURVE('',#40736,#40737,#33692,.T.);
#53000=EDGE_CURVE('',#39837,#40738,#23236,.T.);
#53001=EDGE_CURVE('',#40739,#39841,#23237,.T.);
#53002=EDGE_CURVE('',#40738,#40739,#33693,.T.);
#53003=EDGE_CURVE('',#39832,#40740,#23238,.T.);
#53004=EDGE_CURVE('',#40741,#39831,#23239,.T.);
#53005=EDGE_CURVE('',#40740,#40741,#33694,.T.);
#53006=EDGE_CURVE('',#39838,#40742,#23240,.T.);
#53007=EDGE_CURVE('',#40743,#39834,#23241,.T.);
#53008=EDGE_CURVE('',#40742,#40743,#33695,.T.);
#53009=EDGE_CURVE('',#39845,#40744,#23242,.T.);
#53010=EDGE_CURVE('',#40745,#39842,#23243,.T.);
#53011=EDGE_CURVE('',#40744,#40745,#33696,.T.);
#53012=EDGE_CURVE('',#40246,#40746,#23244,.T.);
#53013=EDGE_CURVE('',#40747,#40242,#23245,.T.);
#53014=EDGE_CURVE('',#40746,#40747,#33697,.T.);
#53015=EDGE_CURVE('',#40253,#40748,#23246,.T.);
#53016=EDGE_CURVE('',#40749,#40250,#23247,.T.);
#53017=EDGE_CURVE('',#40748,#40749,#33698,.T.);
#53018=EDGE_CURVE('',#40245,#40750,#23248,.T.);
#53019=EDGE_CURVE('',#40751,#40249,#23249,.T.);
#53020=EDGE_CURVE('',#40750,#40751,#33699,.T.);
#53021=EDGE_CURVE('',#40240,#40752,#23250,.T.);
#53022=EDGE_CURVE('',#40753,#40239,#23251,.T.);
#53023=EDGE_CURVE('',#40752,#40753,#33700,.T.);
#53024=EDGE_CURVE('',#39829,#40754,#23252,.T.);
#53025=EDGE_CURVE('',#40755,#39826,#23253,.T.);
#53026=EDGE_CURVE('',#40754,#40755,#33701,.T.);
#53027=EDGE_CURVE('',#39821,#40756,#23254,.T.);
#53028=EDGE_CURVE('',#40757,#39825,#23255,.T.);
#53029=EDGE_CURVE('',#40756,#40757,#33702,.T.);
#53030=EDGE_CURVE('',#40758,#40759,#33703,.T.);
#53031=EDGE_CURVE('',#39817,#40758,#23256,.T.);
#53032=EDGE_CURVE('',#40759,#39816,#23257,.T.);
#53033=EDGE_CURVE('',#39822,#40760,#23258,.T.);
#53034=EDGE_CURVE('',#40761,#39818,#23259,.T.);
#53035=EDGE_CURVE('',#40760,#40761,#33704,.T.);
#53036=EDGE_CURVE('',#40339,#40762,#23260,.T.);
#53037=EDGE_CURVE('',#40763,#40341,#23261,.T.);
#53038=EDGE_CURVE('',#40762,#40763,#33705,.T.);
#53039=EDGE_CURVE('',#40367,#40764,#23262,.T.);
#53040=EDGE_CURVE('',#40765,#40369,#23263,.T.);
#53041=EDGE_CURVE('',#40764,#40765,#33706,.T.);
#53042=EDGE_CURVE('',#40355,#40766,#23264,.T.);
#53043=EDGE_CURVE('',#40767,#40357,#23265,.T.);
#53044=EDGE_CURVE('',#40766,#40767,#33707,.T.);
#53045=EDGE_CURVE('',#40768,#40769,#33708,.T.);
#53046=EDGE_CURVE('',#40351,#40768,#23266,.T.);
#53047=EDGE_CURVE('',#40769,#40353,#23267,.T.);
#53048=EDGE_CURVE('',#40371,#40770,#23268,.T.);
#53049=EDGE_CURVE('',#40771,#40373,#23269,.T.);
#53050=EDGE_CURVE('',#40770,#40771,#33709,.T.);
#53051=EDGE_CURVE('',#40772,#40773,#33710,.T.);
#53052=EDGE_CURVE('',#40363,#40772,#23270,.T.);
#53053=EDGE_CURVE('',#40773,#40365,#23271,.T.);
#53054=EDGE_CURVE('',#40343,#40774,#23272,.T.);
#53055=EDGE_CURVE('',#40775,#40344,#23273,.T.);
#53056=EDGE_CURVE('',#40774,#40775,#33711,.T.);
#53057=EDGE_CURVE('',#40003,#40776,#23274,.T.);
#53058=EDGE_CURVE('',#40777,#40007,#23275,.T.);
#53059=EDGE_CURVE('',#40776,#40777,#33712,.T.);
#53060=EDGE_CURVE('',#40023,#40778,#23276,.T.);
#53061=EDGE_CURVE('',#40779,#40027,#23277,.T.);
#53062=EDGE_CURVE('',#40778,#40779,#33713,.T.);
#53063=EDGE_CURVE('',#40115,#40780,#23278,.T.);
#53064=EDGE_CURVE('',#40780,#40526,#33714,.T.);
#53065=EDGE_CURVE('',#40781,#39858,#23279,.T.);
#53066=EDGE_CURVE('',#40545,#40781,#33715,.T.);
#53067=EDGE_CURVE('',#40782,#40782,#33716,.T.);
#53068=EDGE_CURVE('',#40782,#40280,#23280,.T.);
#53069=EDGE_CURVE('',#40553,#40780,#33717,.T.);
#53070=EDGE_CURVE('',#40781,#40550,#33718,.T.);
#53071=EDGE_CURVE('',#40279,#40783,#23281,.T.);
#53072=EDGE_CURVE('',#40783,#39039,#33719,.T.);
#53073=EDGE_CURVE('',#39165,#39426,#33720,.T.);
#53074=EDGE_CURVE('',#39007,#39024,#33721,.T.);
#53075=EDGE_CURVE('',#39429,#39168,#33722,.T.);
#53076=EDGE_CURVE('',#38991,#38994,#33723,.T.);
#53077=EDGE_CURVE('',#39171,#39174,#33724,.T.);
#53078=EDGE_CURVE('',#39023,#38978,#33725,.T.);
#53079=EDGE_CURVE('',#39177,#39178,#33726,.T.);
#53080=EDGE_CURVE('',#39010,#40349,#33727,.T.);
#53081=EDGE_CURVE('',#40523,#40524,#33728,.T.);
#53082=EDGE_CURVE('',#40361,#40317,#33729,.T.);
#53083=EDGE_CURVE('',#40517,#40520,#33730,.T.);
#53084=EDGE_CURVE('',#40329,#40333,#33731,.T.);
#53085=EDGE_CURVE('',#40775,#40514,#33732,.T.);
#53086=EDGE_CURVE('',#40345,#40362,#33733,.T.);
#53087=EDGE_CURVE('',#40511,#40772,#33734,.T.);
#53088=EDGE_CURVE('',#40377,#40783,#33735,.T.);
#53089=EDGE_CURVE('',#40770,#40765,#33736,.T.);
#53090=EDGE_CURVE('',#40764,#40773,#23282,.T.);
#53091=EDGE_CURVE('',#40774,#40763,#23283,.T.);
#53092=EDGE_CURVE('',#40762,#40513,#33737,.T.);
#53093=EDGE_CURVE('',#40779,#40528,#33738,.T.);
#53094=EDGE_CURVE('',#40766,#40769,#33739,.T.);
#53095=EDGE_CURVE('',#40767,#40522,#23284,.T.);
#53096=EDGE_CURVE('',#40521,#40508,#23285,.T.);
#53097=EDGE_CURVE('',#40518,#40509,#33740,.T.);
#53098=EDGE_CURVE('',#40537,#40776,#33741,.T.);
#53099=EDGE_CURVE('',#40570,#40565,#23286,.T.);
#53100=EDGE_CURVE('',#40666,#40669,#23287,.T.);
#53101=EDGE_CURVE('',#40658,#40661,#23288,.T.);
#53102=EDGE_CURVE('',#40578,#40573,#23289,.T.);
#53103=EDGE_CURVE('',#40650,#40653,#23290,.T.);
#53104=EDGE_CURVE('',#40602,#40597,#23291,.T.);
#53105=EDGE_CURVE('',#40642,#40645,#23292,.T.);
#53106=EDGE_CURVE('',#40610,#40605,#23293,.T.);
#53107=EDGE_CURVE('',#40594,#40589,#23294,.T.);
#53108=EDGE_CURVE('',#40626,#40629,#23295,.T.);
#53109=EDGE_CURVE('',#40634,#40637,#23296,.T.);
#53110=EDGE_CURVE('',#40618,#40613,#23297,.T.);
#53111=EDGE_CURVE('',#40620,#40623,#23298,.T.);
#53112=EDGE_CURVE('',#40586,#40581,#23299,.T.);
#53113=EDGE_CURVE('',#40562,#40559,#23300,.T.);
#53114=EDGE_CURVE('',#40674,#40677,#23301,.T.);
#53115=EDGE_CURVE('',#40722,#40725,#23302,.T.);
#53116=EDGE_CURVE('',#40678,#40681,#23303,.T.);
#53117=EDGE_CURVE('',#40566,#40569,#23304,.T.);
#53118=EDGE_CURVE('',#40696,#40691,#23305,.T.);
#53119=EDGE_CURVE('',#40582,#40585,#23306,.T.);
#53120=EDGE_CURVE('',#40682,#40685,#23307,.T.);
#53121=EDGE_CURVE('',#40574,#40577,#23308,.T.);
#53122=EDGE_CURVE('',#40704,#40699,#23309,.T.);
#53123=EDGE_CURVE('',#40598,#40601,#23310,.T.);
#53124=EDGE_CURVE('',#40538,#40541,#23311,.T.);
#53125=EDGE_CURVE('',#40606,#40609,#23312,.T.);
#53126=EDGE_CURVE('',#40532,#40535,#23313,.T.);
#53127=EDGE_CURVE('',#40630,#40633,#23314,.T.);
#53128=EDGE_CURVE('',#40714,#40717,#23315,.T.);
#53129=EDGE_CURVE('',#40614,#40617,#23316,.T.);
#53130=EDGE_CURVE('',#40712,#40707,#23317,.T.);
#53131=EDGE_CURVE('',#40784,#40785,#23318,.T.);
#53132=EDGE_CURVE('',#40784,#40786,#23319,.T.);
#53133=EDGE_CURVE('',#40786,#40787,#23320,.T.);
#53134=EDGE_CURVE('',#40787,#40785,#23321,.T.);
#53135=EDGE_CURVE('',#40788,#40789,#23322,.T.);
#53136=EDGE_CURVE('',#40788,#40784,#23323,.T.);
#53137=EDGE_CURVE('',#40785,#40789,#23324,.T.);
#53138=EDGE_CURVE('',#40786,#40790,#23325,.T.);
#53139=EDGE_CURVE('',#40791,#40790,#23326,.T.);
#53140=EDGE_CURVE('',#40791,#40787,#23327,.T.);
#53141=EDGE_CURVE('',#40754,#40757,#23328,.T.);
#53142=EDGE_CURVE('',#40726,#40729,#23329,.T.);
#53143=EDGE_CURVE('',#40692,#40695,#23330,.T.);
#53144=EDGE_CURVE('',#40744,#40739,#23331,.T.);
#53145=EDGE_CURVE('',#40686,#40689,#23332,.T.);
#53146=EDGE_CURVE('',#40730,#40733,#23333,.T.);
#53147=EDGE_CURVE('',#40700,#40703,#23334,.T.);
#53148=EDGE_CURVE('',#40544,#40547,#23335,.T.);
#53149=EDGE_CURVE('',#40542,#40777,#23336,.T.);
#53150=EDGE_CURVE('',#40778,#40531,#23337,.T.);
#53151=EDGE_CURVE('',#40718,#40721,#23338,.T.);
#53152=EDGE_CURVE('',#40746,#40749,#23339,.T.);
#53153=EDGE_CURVE('',#40708,#40711,#23340,.T.);
#53154=EDGE_CURVE('',#40556,#40527,#23341,.T.);
#53155=EDGE_CURVE('',#40548,#40551,#23342,.T.);
#53156=EDGE_CURVE('',#40750,#40753,#23343,.T.);
#53157=EDGE_CURVE('',#40552,#40555,#23344,.T.);
#53158=EDGE_CURVE('',#40510,#40771,#23345,.T.);
#53159=EDGE_CURVE('',#40768,#40525,#23346,.T.);
#53160=EDGE_CURVE('',#40740,#40743,#23347,.T.);
#53161=EDGE_CURVE('',#40758,#40761,#23348,.T.);
#53162=EDGE_CURVE('',#40734,#40737,#23349,.T.);
#53163=EDGE_CURVE('',#39442,#40791,#33742,.T.);
#53164=EDGE_CURVE('',#40792,#39459,#33743,.T.);
#53165=EDGE_CURVE('',#40793,#40792,#33744,.T.);
#53166=EDGE_CURVE('',#40794,#40793,#33745,.T.);
#53167=EDGE_CURVE('',#40795,#40794,#33746,.T.);
#53168=EDGE_CURVE('',#40796,#40795,#33747,.T.);
#53169=EDGE_CURVE('',#40797,#40796,#33748,.T.);
#53170=EDGE_CURVE('',#40798,#40797,#33749,.T.);
#53171=EDGE_CURVE('',#40799,#40798,#33750,.T.);
#53172=EDGE_CURVE('',#40789,#40799,#33751,.T.);
#53173=EDGE_CURVE('',#40683,#40688,#33752,.T.);
#53174=EDGE_CURVE('',#40684,#40687,#23350,.T.);
#53175=EDGE_CURVE('',#40690,#40693,#23351,.T.);
#53176=EDGE_CURVE('',#40694,#40697,#23352,.T.);
#53177=EDGE_CURVE('',#40698,#40701,#23353,.T.);
#53178=EDGE_CURVE('',#40702,#40705,#23354,.T.);
#53179=EDGE_CURVE('',#40706,#40709,#23355,.T.);
#53180=EDGE_CURVE('',#40710,#40713,#23356,.T.);
#53181=EDGE_CURVE('',#40720,#40715,#23357,.T.);
#53182=EDGE_CURVE('',#40716,#40719,#23358,.T.);
#53183=EDGE_CURVE('',#40727,#40724,#33753,.T.);
#53184=EDGE_CURVE('',#40728,#40723,#23359,.T.);
#53185=EDGE_CURVE('',#40759,#40756,#33754,.T.);
#53186=EDGE_CURVE('',#40760,#40755,#23360,.T.);
#53187=EDGE_CURVE('',#40752,#40747,#23361,.T.);
#53188=EDGE_CURVE('',#40748,#40751,#23362,.T.);
#53189=EDGE_CURVE('',#40738,#40741,#23363,.T.);
#53190=EDGE_CURVE('',#40742,#40745,#23364,.T.);
#53191=EDGE_CURVE('',#40731,#40736,#33755,.T.);
#53192=EDGE_CURVE('',#40732,#40735,#23365,.T.);
#53193=EDGE_CURVE('',#40680,#40675,#23366,.T.);
#53194=EDGE_CURVE('',#40679,#40800,#33756,.T.);
#53195=EDGE_CURVE('',#40800,#40801,#33757,.T.);
#53196=EDGE_CURVE('',#40801,#40676,#33758,.T.);
#53197=EDGE_CURVE('',#40668,#40671,#23367,.T.);
#53198=EDGE_CURVE('',#40672,#40667,#23368,.T.);
#53199=EDGE_CURVE('',#40673,#40802,#33759,.T.);
#53200=EDGE_CURVE('',#40802,#40803,#33760,.T.);
#53201=EDGE_CURVE('',#40803,#40670,#33761,.T.);
#53202=EDGE_CURVE('',#40660,#40663,#23369,.T.);
#53203=EDGE_CURVE('',#40664,#40659,#23370,.T.);
#53204=EDGE_CURVE('',#40665,#40662,#33762,.T.);
#53205=EDGE_CURVE('',#40652,#40655,#23371,.T.);
#53206=EDGE_CURVE('',#40656,#40651,#23372,.T.);
#53207=EDGE_CURVE('',#40657,#40654,#33763,.T.);
#53208=EDGE_CURVE('',#40644,#40647,#23373,.T.);
#53209=EDGE_CURVE('',#40648,#40643,#23374,.T.);
#53210=EDGE_CURVE('',#40649,#40646,#33764,.T.);
#53211=EDGE_CURVE('',#40636,#40639,#23375,.T.);
#53212=EDGE_CURVE('',#40640,#40635,#23376,.T.);
#53213=EDGE_CURVE('',#40641,#40638,#33765,.T.);
#53214=EDGE_CURVE('',#40632,#40627,#23377,.T.);
#53215=EDGE_CURVE('',#40628,#40631,#23378,.T.);
#53216=EDGE_CURVE('',#40624,#40621,#23379,.T.);
#53217=EDGE_CURVE('',#40625,#40622,#33766,.T.);
#53218=EDGE_CURVE('',#40612,#40615,#23380,.T.);
#53219=EDGE_CURVE('',#40616,#40619,#23381,.T.);
#53220=EDGE_CURVE('',#40604,#40607,#23382,.T.);
#53221=EDGE_CURVE('',#40608,#40611,#23383,.T.);
#53222=EDGE_CURVE('',#40596,#40599,#23384,.T.);
#53223=EDGE_CURVE('',#40600,#40603,#23385,.T.);
#53224=EDGE_CURVE('',#40588,#40591,#23386,.T.);
#53225=EDGE_CURVE('',#40592,#40595,#23387,.T.);
#53226=EDGE_CURVE('',#40593,#40804,#33767,.T.);
#53227=EDGE_CURVE('',#40804,#40805,#33768,.T.);
#53228=EDGE_CURVE('',#40805,#40590,#33769,.T.);
#53229=EDGE_CURVE('',#40580,#40583,#23388,.T.);
#53230=EDGE_CURVE('',#40587,#40806,#33770,.T.);
#53231=EDGE_CURVE('',#40806,#40807,#33771,.T.);
#53232=EDGE_CURVE('',#40807,#40584,#33772,.T.);
#53233=EDGE_CURVE('',#40572,#40575,#23389,.T.);
#53234=EDGE_CURVE('',#40576,#40579,#23390,.T.);
#53235=EDGE_CURVE('',#40564,#40567,#23391,.T.);
#53236=EDGE_CURVE('',#40568,#40571,#23392,.T.);
#53237=EDGE_CURVE('',#40558,#40561,#23393,.T.);
#53238=EDGE_CURVE('',#40563,#40560,#33773,.T.);
#53239=EDGE_CURVE('',#40536,#40539,#23394,.T.);
#53240=EDGE_CURVE('',#40540,#40543,#23395,.T.);
#53241=EDGE_CURVE('',#40554,#40557,#23396,.T.);
#53242=EDGE_CURVE('',#40512,#40515,#23397,.T.);
#53243=EDGE_CURVE('',#40546,#40549,#23398,.T.);
#53244=EDGE_CURVE('',#40516,#40519,#23399,.T.);
#53245=EDGE_CURVE('',#40534,#40529,#23400,.T.);
#53246=EDGE_CURVE('',#40530,#40533,#23401,.T.);
#53247=EDGE_CURVE('',#40799,#40808,#23402,.T.);
#53248=EDGE_CURVE('',#40798,#40809,#23403,.T.);
#53249=EDGE_CURVE('',#40808,#40809,#33774,.T.);
#53250=EDGE_CURVE('',#40810,#40809,#33775,.T.);
#53251=EDGE_CURVE('',#40797,#40810,#23404,.T.);
#53252=EDGE_CURVE('',#40796,#40811,#23405,.T.);
#53253=EDGE_CURVE('',#40810,#40811,#33776,.T.);
#53254=EDGE_CURVE('',#40795,#40812,#23406,.T.);
#53255=EDGE_CURVE('',#40811,#40812,#33777,.T.);
#53256=EDGE_CURVE('',#40794,#40813,#23407,.T.);
#53257=EDGE_CURVE('',#40812,#40813,#33778,.T.);
#53258=EDGE_CURVE('',#40814,#40813,#33779,.T.);
#53259=EDGE_CURVE('',#40793,#40814,#23408,.T.);
#53260=EDGE_CURVE('',#40792,#40815,#23409,.T.);
#53261=EDGE_CURVE('',#40814,#40815,#33780,.T.);
#53262=EDGE_CURVE('',#40815,#39458,#33781,.T.);
#53263=EDGE_CURVE('',#40816,#40817,#23410,.T.);
#53264=EDGE_CURVE('',#40816,#40818,#5843,.T.);
#53265=EDGE_CURVE('',#40819,#40818,#23411,.T.);
#53266=EDGE_CURVE('',#40819,#40817,#33782,.T.);
#53267=EDGE_CURVE('',#40820,#40816,#23412,.T.);
#53268=EDGE_CURVE('',#40820,#40817,#23413,.T.);
#53269=EDGE_CURVE('',#40821,#40822,#33783,.T.);
#53270=EDGE_CURVE('',#40823,#40821,#23414,.T.);
#53271=EDGE_CURVE('',#40822,#40823,#5844,.T.);
#53272=EDGE_CURVE('',#40824,#40823,#5845,.T.);
#53273=EDGE_CURVE('',#40824,#40821,#23415,.T.);
#53274=EDGE_CURVE('',#40825,#40826,#1226,.T.);
#53275=EDGE_CURVE('',#40827,#40826,#5846,.T.);
#53276=EDGE_CURVE('',#40827,#40828,#23416,.T.);
#53277=EDGE_CURVE('',#40825,#40828,#23417,.T.);
#53278=EDGE_CURVE('',#40829,#40830,#1227,.T.);
#53279=EDGE_CURVE('',#40830,#40831,#23418,.T.);
#53280=EDGE_CURVE('',#40831,#40832,#23419,.T.);
#53281=EDGE_CURVE('',#40829,#40832,#5847,.T.);
#53282=EDGE_CURVE('',#40830,#40825,#33784,.T.);
#53283=EDGE_CURVE('',#40828,#40831,#33785,.T.);
#53284=EDGE_CURVE('',#40833,#40834,#1228,.T.);
#53285=EDGE_CURVE('',#40834,#40835,#23420,.T.);
#53286=EDGE_CURVE('',#40835,#40836,#23421,.T.);
#53287=EDGE_CURVE('',#40833,#40836,#5848,.T.);
#53288=EDGE_CURVE('',#40837,#40838,#1229,.T.);
#53289=EDGE_CURVE('',#40839,#40838,#5849,.T.);
#53290=EDGE_CURVE('',#40839,#40840,#23422,.T.);
#53291=EDGE_CURVE('',#40837,#40840,#23423,.T.);
#53292=EDGE_CURVE('',#40834,#40837,#33786,.T.);
#53293=EDGE_CURVE('',#40840,#40835,#33787,.T.);
#53294=EDGE_CURVE('',#40841,#40842,#5850,.T.);
#53295=EDGE_CURVE('',#40843,#40841,#5851,.T.);
#53296=EDGE_CURVE('',#40843,#40844,#5852,.T.);
#53297=EDGE_CURVE('',#40844,#39588,#5853,.T.);
#53298=EDGE_CURVE('',#39560,#40845,#5854,.T.);
#53299=EDGE_CURVE('',#40846,#40845,#5855,.T.);
#53300=EDGE_CURVE('',#40847,#40846,#5856,.T.);
#53301=EDGE_CURVE('',#40848,#40847,#5857,.T.);
#53302=EDGE_CURVE('',#40849,#40848,#5858,.T.);
#53303=EDGE_CURVE('',#40849,#40850,#5859,.T.);
#53304=EDGE_CURVE('',#40842,#40850,#5860,.T.);
#53305=EDGE_CURVE('',#40851,#40852,#5861,.T.);
#53306=EDGE_CURVE('',#40852,#40853,#5862,.T.);
#53307=EDGE_CURVE('',#39556,#40853,#5863,.F.);
#53308=EDGE_CURVE('',#39571,#39570,#5864,.T.);
#53309=EDGE_CURVE('',#39569,#40854,#5865,.T.);
#53310=EDGE_CURVE('',#40855,#40854,#5866,.F.);
#53311=EDGE_CURVE('',#40856,#40855,#5867,.T.);
#53312=EDGE_CURVE('',#40856,#40857,#5868,.T.);
#53313=EDGE_CURVE('',#40851,#40857,#5869,.T.);
#53314=EDGE_CURVE('',#40858,#40859,#33788,.T.);
#53315=EDGE_CURVE('',#40860,#40858,#23424,.T.);
#53316=EDGE_CURVE('',#40860,#40861,#33789,.T.);
#53317=EDGE_CURVE('',#40861,#40859,#23425,.T.);
#53318=EDGE_CURVE('',#40842,#40844,#33790,.T.);
#53319=EDGE_CURVE('',#40841,#40843,#33791,.T.);
#53320=EDGE_CURVE('',#39492,#40862,#33792,.T.);
#53321=EDGE_CURVE('',#40862,#40863,#23426,.T.);
#53322=EDGE_CURVE('',#40851,#40863,#33793,.T.);
#53323=EDGE_CURVE('',#40856,#40857,#33794,.T.);
#53324=EDGE_CURVE('',#40854,#40855,#33795,.T.);
#53325=EDGE_CURVE('',#40863,#40864,#33796,.T.);
#53326=EDGE_CURVE('',#40862,#40865,#33797,.T.);
#53327=EDGE_CURVE('',#40865,#40864,#23427,.T.);
#53328=EDGE_CURVE('',#40864,#40866,#33798,.T.);
#53329=EDGE_CURVE('',#40865,#40867,#33799,.T.);
#53330=EDGE_CURVE('',#40867,#40866,#23428,.T.);
#53331=EDGE_CURVE('',#40866,#40868,#33800,.T.);
#53332=EDGE_CURVE('',#40867,#40869,#33801,.T.);
#53333=EDGE_CURVE('',#40869,#40868,#23429,.T.);
#53334=EDGE_CURVE('',#40869,#40870,#33802,.T.);
#53335=EDGE_CURVE('',#40870,#40871,#5870,.T.);
#53336=EDGE_CURVE('',#40868,#40871,#33803,.T.);
#53337=EDGE_CURVE('',#40872,#40873,#33804,.T.);
#53338=EDGE_CURVE('',#40874,#40872,#23430,.T.);
#53339=EDGE_CURVE('',#40874,#40875,#33805,.T.);
#53340=EDGE_CURVE('',#40875,#40873,#23431,.T.);
#53341=EDGE_CURVE('',#40873,#40858,#33806,.T.);
#53342=EDGE_CURVE('',#40875,#40860,#33807,.T.);
#53343=EDGE_CURVE('',#40876,#40877,#5871,.T.);
#53344=EDGE_CURVE('',#40877,#40878,#5872,.T.);
#53345=EDGE_CURVE('',#40879,#40878,#5873,.T.);
#53346=EDGE_CURVE('',#40879,#40880,#5874,.T.);
#53347=EDGE_CURVE('',#40876,#40880,#5875,.T.);
#53348=EDGE_CURVE('',#40881,#40882,#5876,.T.);
#53349=EDGE_CURVE('',#40882,#40883,#5877,.T.);
#53350=EDGE_CURVE('',#40884,#40883,#5878,.T.);
#53351=EDGE_CURVE('',#40885,#40884,#5879,.T.);
#53352=EDGE_CURVE('',#40881,#40885,#5880,.T.);
#53353=EDGE_CURVE('',#40886,#40887,#5881,.T.);
#53354=EDGE_CURVE('',#40887,#40888,#5882,.T.);
#53355=EDGE_CURVE('',#40889,#40888,#5883,.T.);
#53356=EDGE_CURVE('',#40889,#40890,#5884,.T.);
#53357=EDGE_CURVE('',#40886,#40890,#5885,.T.);
#53358=EDGE_CURVE('',#40891,#40892,#5886,.T.);
#53359=EDGE_CURVE('',#40893,#40892,#5887,.T.);
#53360=EDGE_CURVE('',#40894,#40893,#5888,.T.);
#53361=EDGE_CURVE('',#40895,#40894,#5889,.T.);
#53362=EDGE_CURVE('',#40891,#40895,#5890,.T.);
#53363=EDGE_CURVE('',#40896,#40897,#33808,.T.);
#53364=EDGE_CURVE('',#40898,#40896,#23432,.T.);
#53365=EDGE_CURVE('',#40898,#40885,#5891,.T.);
#53366=EDGE_CURVE('',#40884,#40897,#23433,.T.);
#53367=EDGE_CURVE('',#40829,#40898,#5892,.T.);
#53368=EDGE_CURVE('',#40899,#40896,#33809,.T.);
#53369=EDGE_CURVE('',#40900,#40899,#23434,.T.);
#53370=EDGE_CURVE('',#40900,#40826,#5893,.T.);
#53371=EDGE_CURVE('',#40901,#40899,#33810,.T.);
#53372=EDGE_CURVE('',#40879,#40901,#23435,.T.);
#53373=EDGE_CURVE('',#40900,#40878,#33811,.T.);
#53374=EDGE_CURVE('',#40902,#40903,#33812,.T.);
#53375=EDGE_CURVE('',#40904,#40902,#23436,.T.);
#53376=EDGE_CURVE('',#40904,#40895,#33813,.T.);
#53377=EDGE_CURVE('',#40894,#40903,#23437,.T.);
#53378=EDGE_CURVE('',#40833,#40904,#5894,.T.);
#53379=EDGE_CURVE('',#40905,#40902,#33814,.T.);
#53380=EDGE_CURVE('',#40906,#40905,#23438,.T.);
#53381=EDGE_CURVE('',#40906,#40838,#5895,.T.);
#53382=EDGE_CURVE('',#40907,#40905,#33815,.T.);
#53383=EDGE_CURVE('',#40889,#40907,#23439,.T.);
#53384=EDGE_CURVE('',#40906,#40888,#33816,.T.);
#53385=EDGE_CURVE('',#40897,#39524,#33817,.T.);
#53386=EDGE_CURVE('',#40883,#40845,#5896,.T.);
#53387=EDGE_CURVE('',#39544,#40908,#33818,.T.);
#53388=EDGE_CURVE('',#40909,#39547,#33819,.T.);
#53389=EDGE_CURVE('',#40910,#40909,#33820,.T.);
#53390=EDGE_CURVE('',#40911,#40910,#33821,.T.);
#53391=EDGE_CURVE('',#40912,#40911,#33822,.T.);
#53392=EDGE_CURVE('',#40913,#40912,#33823,.T.);
#53393=EDGE_CURVE('',#40914,#40913,#33824,.T.);
#53394=EDGE_CURVE('',#40915,#40914,#33825,.T.);
#53395=EDGE_CURVE('',#40908,#40915,#33826,.T.);
#53396=EDGE_CURVE('',#39534,#40907,#33827,.T.);
#53397=EDGE_CURVE('',#40903,#40901,#33828,.T.);
#53398=EDGE_CURVE('',#40916,#40917,#33829,.T.);
#53399=EDGE_CURVE('',#40913,#40916,#23440,.T.);
#53400=EDGE_CURVE('',#40912,#40917,#23441,.T.);
#53401=EDGE_CURVE('',#40918,#40916,#33830,.T.);
#53402=EDGE_CURVE('',#40914,#40918,#23442,.T.);
#53403=EDGE_CURVE('',#40919,#40918,#33831,.T.);
#53404=EDGE_CURVE('',#40915,#40919,#23443,.T.);
#53405=EDGE_CURVE('',#40920,#40919,#33832,.T.);
#53406=EDGE_CURVE('',#40908,#40920,#23444,.T.);
#53407=EDGE_CURVE('',#39543,#40920,#33833,.T.);
#53408=EDGE_CURVE('',#40921,#39546,#33834,.T.);
#53409=EDGE_CURVE('',#40909,#40921,#23445,.T.);
#53410=EDGE_CURVE('',#40922,#40921,#33835,.T.);
#53411=EDGE_CURVE('',#40910,#40922,#23446,.T.);
#53412=EDGE_CURVE('',#40923,#40922,#33836,.T.);
#53413=EDGE_CURVE('',#40911,#40923,#23447,.T.);
#53414=EDGE_CURVE('',#40917,#40923,#33837,.T.);
#53415=EDGE_CURVE('',#40924,#40876,#5897,.T.);
#53416=EDGE_CURVE('',#40925,#40880,#5898,.T.);
#53417=EDGE_CURVE('',#40924,#40925,#5899,.T.);
#53418=EDGE_CURVE('',#40893,#40926,#5900,.T.);
#53419=EDGE_CURVE('',#40892,#40927,#5901,.T.);
#53420=EDGE_CURVE('',#40926,#40927,#5902,.T.);
#53421=EDGE_CURVE('',#40926,#40925,#5903,.T.);
#53422=EDGE_CURVE('',#40852,#40886,#33838,.T.);
#53423=EDGE_CURVE('',#40853,#40890,#5904,.T.);
#53424=EDGE_CURVE('',#40928,#40872,#33839,.T.);
#53425=EDGE_CURVE('',#40859,#40847,#33840,.T.);
#53426=EDGE_CURVE('',#40882,#40846,#33841,.T.);
#53427=EDGE_CURVE('',#40877,#40881,#5905,.T.);
#53428=EDGE_CURVE('',#40928,#40924,#5906,.T.);
#53429=EDGE_CURVE('',#40839,#40929,#5907,.T.);
#53430=EDGE_CURVE('',#40930,#40929,#33842,.T.);
#53431=EDGE_CURVE('',#40930,#40836,#5908,.T.);
#53432=EDGE_CURVE('',#40930,#40931,#5909,.T.);
#53433=EDGE_CURVE('',#40932,#40931,#5910,.T.);
#53434=EDGE_CURVE('',#40932,#40933,#5911,.T.);
#53435=EDGE_CURVE('',#40933,#40822,#5912,.T.);
#53436=EDGE_CURVE('',#40929,#40824,#5913,.T.);
#53437=EDGE_CURVE('',#40887,#40891,#5914,.T.);
#53438=EDGE_CURVE('',#40827,#40934,#5915,.T.);
#53439=EDGE_CURVE('',#40935,#40934,#33843,.T.);
#53440=EDGE_CURVE('',#40935,#40832,#5916,.T.);
#53441=EDGE_CURVE('',#40935,#40936,#5917,.T.);
#53442=EDGE_CURVE('',#40818,#40936,#5918,.T.);
#53443=EDGE_CURVE('',#40820,#40934,#5919,.T.);
#53444=EDGE_CURVE('',#40927,#40871,#5920,.T.);
#53445=EDGE_CURVE('',#40937,#40938,#33844,.T.);
#53446=EDGE_CURVE('',#40937,#40938,#5921,.T.);
#53447=EDGE_CURVE('',#40939,#40940,#33845,.T.);
#53448=EDGE_CURVE('',#40939,#40940,#5922,.T.);
#53449=EDGE_CURVE('',#40941,#40942,#33846,.T.);
#53450=EDGE_CURVE('',#40941,#40942,#5923,.T.);
#53451=EDGE_CURVE('',#40848,#40849,#33847,.T.);
#53452=EDGE_CURVE('',#40943,#40932,#23448,.T.);
#53453=EDGE_CURVE('',#40933,#40943,#33848,.T.);
#53454=EDGE_CURVE('',#40944,#40940,#5924,.T.);
#53455=EDGE_CURVE('',#40945,#40939,#5925,.T.);
#53456=EDGE_CURVE('',#40945,#40944,#33849,.T.);
#53457=EDGE_CURVE('',#40946,#40947,#33850,.T.);
#53458=EDGE_CURVE('',#40938,#40947,#5926,.T.);
#53459=EDGE_CURVE('',#40946,#40937,#5927,.T.);
#53460=EDGE_CURVE('',#40948,#40928,#5928,.T.);
#53461=EDGE_CURVE('',#40948,#40874,#33851,.T.);
#53462=EDGE_CURVE('',#40949,#40950,#33852,.T.);
#53463=EDGE_CURVE('',#40942,#40950,#5929,.T.);
#53464=EDGE_CURVE('',#40949,#40941,#5930,.T.);
#53465=EDGE_CURVE('',#40861,#40850,#33853,.T.);
#53466=EDGE_CURVE('',#40819,#40936,#23449,.T.);
#53467=EDGE_CURVE('',#40943,#40931,#23450,.T.);
#53468=EDGE_CURVE('',#40951,#40946,#5931,.T.);
#53469=EDGE_CURVE('',#40947,#40945,#5932,.T.);
#53470=EDGE_CURVE('',#40944,#40949,#5933,.T.);
#53471=EDGE_CURVE('',#40950,#40952,#5934,.T.);
#53472=EDGE_CURVE('',#40952,#40948,#5935,.T.);
#53473=EDGE_CURVE('',#40870,#40951,#5936,.T.);
#53474=EDGE_CURVE('',#40800,#39785,#23451,.T.);
#53475=EDGE_CURVE('',#40801,#39789,#23452,.T.);
#53476=EDGE_CURVE('',#40802,#39959,#23453,.T.);
#53477=EDGE_CURVE('',#40803,#39963,#23454,.T.);
#53478=EDGE_CURVE('',#40804,#40150,#23455,.T.);
#53479=EDGE_CURVE('',#40805,#40146,#23456,.T.);
#53480=EDGE_CURVE('',#40806,#40185,#23457,.T.);
#53481=EDGE_CURVE('',#40807,#40189,#23458,.T.);
#53482=EDGE_CURVE('',#40953,#40953,#33854,.T.);
#53483=EDGE_CURVE('',#40953,#39630,#23459,.T.);
#53484=EDGE_CURVE('',#40954,#40954,#33855,.T.);
#53485=EDGE_CURVE('',#40954,#39633,#23460,.T.);
#53486=EDGE_CURVE('',#40955,#40309,#23461,.T.);
#53487=EDGE_CURVE('',#40956,#40311,#23462,.T.);
#53488=EDGE_CURVE('',#40956,#40955,#33856,.T.);
#53489=EDGE_CURVE('',#40957,#40307,#23463,.T.);
#53490=EDGE_CURVE('',#40955,#40957,#33857,.T.);
#53491=EDGE_CURVE('',#40958,#40305,#23464,.T.);
#53492=EDGE_CURVE('',#40957,#40958,#33858,.T.);
#53493=EDGE_CURVE('',#40959,#40303,#23465,.T.);
#53494=EDGE_CURVE('',#40958,#40959,#33859,.T.);
#53495=EDGE_CURVE('',#40960,#40301,#23466,.T.);
#53496=EDGE_CURVE('',#40959,#40960,#33860,.T.);
#53497=EDGE_CURVE('',#40961,#40299,#23467,.T.);
#53498=EDGE_CURVE('',#40960,#40961,#33861,.T.);
#53499=EDGE_CURVE('',#40961,#39608,#33862,.T.);
#53500=EDGE_CURVE('',#39609,#40962,#33863,.T.);
#53501=EDGE_CURVE('',#40962,#40313,#23468,.T.);
#53502=EDGE_CURVE('',#40962,#40956,#33864,.T.);
#53503=EDGE_CURVE('',#40963,#39611,#33865,.T.);
#53504=EDGE_CURVE('',#39612,#40964,#33866,.T.);
#53505=EDGE_CURVE('',#40964,#40965,#33867,.T.);
#53506=EDGE_CURVE('',#40965,#40966,#33868,.T.);
#53507=EDGE_CURVE('',#40966,#40967,#33869,.T.);
#53508=EDGE_CURVE('',#40967,#40968,#33870,.T.);
#53509=EDGE_CURVE('',#40968,#40969,#33871,.T.);
#53510=EDGE_CURVE('',#40969,#40970,#33872,.T.);
#53511=EDGE_CURVE('',#40970,#40963,#33873,.T.);
#53512=EDGE_CURVE('',#40970,#40284,#23469,.T.);
#53513=EDGE_CURVE('',#40963,#40282,#23470,.T.);
#53514=EDGE_CURVE('',#40964,#40296,#23471,.T.);
#53515=EDGE_CURVE('',#40965,#40294,#23472,.T.);
#53516=EDGE_CURVE('',#40966,#40292,#23473,.T.);
#53517=EDGE_CURVE('',#40967,#40290,#23474,.T.);
#53518=EDGE_CURVE('',#40968,#40288,#23475,.T.);
#53519=EDGE_CURVE('',#40969,#40286,#23476,.T.);
#53520=EDGE_CURVE('',#40423,#40440,#5937,.T.);
#53521=EDGE_CURVE('',#40421,#40444,#23477,.T.);
#53522=EDGE_CURVE('',#40427,#40482,#23478,.T.);
#53523=EDGE_CURVE('',#40425,#40486,#5938,.T.);
#53524=EDGE_CURVE('',#40402,#40505,#5939,.T.);
#53525=EDGE_CURVE('',#40400,#40499,#23479,.T.);
#53526=EDGE_CURVE('',#40462,#40406,#23480,.T.);
#53527=EDGE_CURVE('',#40404,#40466,#5940,.T.);
#53528=EDGE_CURVE('',#40489,#39698,#23481,.T.);
#53529=EDGE_CURVE('',#40485,#39700,#23482,.T.);
#53530=EDGE_CURVE('',#40438,#39696,#23483,.T.);
#53531=EDGE_CURVE('',#40443,#39694,#23484,.T.);
#53532=EDGE_CURVE('',#40469,#39690,#23485,.T.);
#53533=EDGE_CURVE('',#40465,#39692,#23486,.T.);
#53534=EDGE_CURVE('',#40506,#39688,#23487,.T.);
#53535=EDGE_CURVE('',#40502,#39685,#23488,.T.);
#53536=EDGE_CURVE('',#39622,#40971,#33874,.T.);
#53537=EDGE_CURVE('',#40972,#39623,#33875,.T.);
#53538=EDGE_CURVE('',#40973,#40972,#33876,.T.);
#53539=EDGE_CURVE('',#40974,#40973,#33877,.T.);
#53540=EDGE_CURVE('',#40975,#40974,#33878,.T.);
#53541=EDGE_CURVE('',#40976,#40975,#33879,.T.);
#53542=EDGE_CURVE('',#40977,#40976,#33880,.T.);
#53543=EDGE_CURVE('',#40978,#40977,#33881,.T.);
#53544=EDGE_CURVE('',#40971,#40978,#33882,.T.);
#53545=EDGE_CURVE('',#40386,#40975,#23489,.T.);
#53546=EDGE_CURVE('',#40384,#40976,#23490,.T.);
#53547=EDGE_CURVE('',#40382,#40977,#23491,.T.);
#53548=EDGE_CURVE('',#40380,#40978,#23492,.T.);
#53549=EDGE_CURVE('',#40379,#40971,#23493,.T.);
#53550=EDGE_CURVE('',#40392,#40972,#23494,.T.);
#53551=EDGE_CURVE('',#40390,#40973,#23495,.T.);
#53552=EDGE_CURVE('',#40388,#40974,#23496,.T.);
#53553=EDGE_CURVE('',#40790,#39443,#33883,.T.);
#53554=EDGE_CURVE('',#40808,#40788,#33884,.T.);
#53555=EDGE_CURVE('',#40979,#40980,#23497,.T.);
#53556=EDGE_CURVE('',#40981,#40979,#1230,.T.);
#53557=EDGE_CURVE('',#40981,#40982,#23498,.T.);
#53558=EDGE_CURVE('',#40980,#40982,#1231,.T.);
#53559=EDGE_CURVE('',#40983,#40984,#23499,.T.);
#53560=EDGE_CURVE('',#40979,#40983,#1232,.T.);
#53561=EDGE_CURVE('',#40984,#40980,#1233,.T.);
#53562=EDGE_CURVE('',#40985,#40986,#23500,.T.);
#53563=EDGE_CURVE('',#40983,#40985,#1234,.T.);
#53564=EDGE_CURVE('',#40986,#40984,#1235,.T.);
#53565=EDGE_CURVE('',#40987,#40988,#23501,.T.);
#53566=EDGE_CURVE('',#40985,#40987,#1236,.T.);
#53567=EDGE_CURVE('',#40988,#40986,#1237,.T.);
#53568=EDGE_CURVE('',#40989,#40990,#23502,.T.);
#53569=EDGE_CURVE('',#40987,#40989,#1238,.T.);
#53570=EDGE_CURVE('',#40990,#40988,#1239,.T.);
#53571=EDGE_CURVE('',#40989,#40981,#1240,.T.);
#53572=EDGE_CURVE('',#40982,#40990,#1241,.T.);
#53573=EDGE_CURVE('',#40991,#40985,#23503,.T.);
#53574=EDGE_CURVE('',#40980,#40982,#33885,.T.);
#53575=EDGE_CURVE('',#40984,#40980,#33886,.T.);
#53576=EDGE_CURVE('',#40986,#40984,#33887,.T.);
#53577=EDGE_CURVE('',#40988,#40986,#33888,.T.);
#53578=EDGE_CURVE('',#40990,#40988,#33889,.T.);
#53579=EDGE_CURVE('',#40982,#40990,#33890,.T.);
#53580=EDGE_CURVE('',#40992,#40992,#33891,.T.);
#53581=EDGE_CURVE('',#40992,#40993,#33892,.T.);
#53582=EDGE_CURVE('',#40993,#40994,#33893,.T.);
#53583=EDGE_CURVE('',#40994,#40993,#33894,.T.);
#53584=EDGE_CURVE('',#40995,#40995,#33895,.T.);
#53585=EDGE_CURVE('',#40995,#40994,#23504,.T.);
#53586=EDGE_CURVE('',#40996,#40997,#33896,.T.);
#53587=EDGE_CURVE('',#40997,#40998,#33897,.T.);
#53588=EDGE_CURVE('',#40998,#40999,#33898,.T.);
#53589=EDGE_CURVE('',#40999,#41000,#33899,.T.);
#53590=EDGE_CURVE('',#41000,#41001,#33900,.T.);
#53591=EDGE_CURVE('',#41001,#40996,#33901,.T.);
#53592=EDGE_CURVE('',#41002,#40998,#1242,.T.);
#53593=EDGE_CURVE('',#40997,#41002,#1243,.T.);
#53594=EDGE_CURVE('',#40998,#41003,#1244,.T.);
#53595=EDGE_CURVE('',#41003,#40999,#1245,.T.);
#53596=EDGE_CURVE('',#40999,#41004,#1246,.T.);
#53597=EDGE_CURVE('',#41004,#41000,#1247,.T.);
#53598=EDGE_CURVE('',#41000,#41005,#1248,.T.);
#53599=EDGE_CURVE('',#41005,#41001,#1249,.T.);
#53600=EDGE_CURVE('',#41001,#41006,#1250,.T.);
#53601=EDGE_CURVE('',#41006,#40996,#1251,.T.);
#53602=EDGE_CURVE('',#40996,#41007,#1252,.T.);
#53603=EDGE_CURVE('',#41007,#40997,#1253,.T.);
#53604=EDGE_CURVE('',#41008,#41009,#33902,.T.);
#53605=EDGE_CURVE('',#41008,#41010,#33903,.T.);
#53606=EDGE_CURVE('',#41010,#41011,#33904,.T.);
#53607=EDGE_CURVE('',#41011,#41012,#33905,.T.);
#53608=EDGE_CURVE('',#41012,#41013,#33906,.T.);
#53609=EDGE_CURVE('',#41013,#41009,#33907,.T.);
#53610=EDGE_CURVE('',#41014,#41008,#1254,.T.);
#53611=EDGE_CURVE('',#41010,#41014,#1255,.T.);
#53612=EDGE_CURVE('',#41015,#41010,#1256,.T.);
#53613=EDGE_CURVE('',#41011,#41015,#1257,.T.);
#53614=EDGE_CURVE('',#41016,#41011,#1258,.T.);
#53615=EDGE_CURVE('',#41012,#41016,#1259,.T.);
#53616=EDGE_CURVE('',#41017,#41012,#1260,.T.);
#53617=EDGE_CURVE('',#41013,#41017,#1261,.T.);
#53618=EDGE_CURVE('',#41018,#41013,#1262,.T.);
#53619=EDGE_CURVE('',#41009,#41018,#1263,.T.);
#53620=EDGE_CURVE('',#41008,#41019,#1264,.T.);
#53621=EDGE_CURVE('',#41019,#41009,#1265,.T.);
#53622=EDGE_CURVE('',#41007,#41014,#23505,.T.);
#53623=EDGE_CURVE('',#41002,#41019,#23506,.T.);
#53624=EDGE_CURVE('',#41006,#41015,#23507,.T.);
#53625=EDGE_CURVE('',#41005,#41016,#23508,.T.);
#53626=EDGE_CURVE('',#41004,#41017,#23509,.T.);
#53627=EDGE_CURVE('',#41003,#41018,#23510,.T.);
#53628=EDGE_CURVE('',#41020,#41021,#33908,.T.);
#53629=EDGE_CURVE('',#41021,#41022,#33909,.T.);
#53630=EDGE_CURVE('',#41022,#41023,#33910,.T.);
#53631=EDGE_CURVE('',#41023,#41024,#33911,.T.);
#53632=EDGE_CURVE('',#41024,#41025,#33912,.T.);
#53633=EDGE_CURVE('',#41025,#41020,#33913,.T.);
#53634=EDGE_CURVE('',#41026,#41022,#1266,.T.);
#53635=EDGE_CURVE('',#41021,#41026,#1267,.T.);
#53636=EDGE_CURVE('',#41022,#41027,#1268,.T.);
#53637=EDGE_CURVE('',#41027,#41023,#1269,.T.);
#53638=EDGE_CURVE('',#41023,#41028,#1270,.T.);
#53639=EDGE_CURVE('',#41028,#41024,#1271,.T.);
#53640=EDGE_CURVE('',#41024,#41029,#1272,.T.);
#53641=EDGE_CURVE('',#41029,#41025,#1273,.T.);
#53642=EDGE_CURVE('',#41025,#41030,#1274,.T.);
#53643=EDGE_CURVE('',#41030,#41020,#1275,.T.);
#53644=EDGE_CURVE('',#41020,#41031,#1276,.T.);
#53645=EDGE_CURVE('',#41031,#41021,#1277,.T.);
#53646=EDGE_CURVE('',#41032,#41033,#33914,.T.);
#53647=EDGE_CURVE('',#41032,#41034,#33915,.T.);
#53648=EDGE_CURVE('',#41034,#41035,#33916,.T.);
#53649=EDGE_CURVE('',#41035,#41036,#33917,.T.);
#53650=EDGE_CURVE('',#41036,#41037,#33918,.T.);
#53651=EDGE_CURVE('',#41037,#41033,#33919,.T.);
#53652=EDGE_CURVE('',#41038,#41032,#1278,.T.);
#53653=EDGE_CURVE('',#41034,#41038,#1279,.T.);
#53654=EDGE_CURVE('',#41039,#41034,#1280,.T.);
#53655=EDGE_CURVE('',#41035,#41039,#1281,.T.);
#53656=EDGE_CURVE('',#41040,#41035,#1282,.T.);
#53657=EDGE_CURVE('',#41036,#41040,#1283,.T.);
#53658=EDGE_CURVE('',#41041,#41036,#1284,.T.);
#53659=EDGE_CURVE('',#41037,#41041,#1285,.T.);
#53660=EDGE_CURVE('',#41042,#41037,#1286,.T.);
#53661=EDGE_CURVE('',#41033,#41042,#1287,.T.);
#53662=EDGE_CURVE('',#41032,#41043,#1288,.T.);
#53663=EDGE_CURVE('',#41043,#41033,#1289,.T.);
#53664=EDGE_CURVE('',#41031,#41038,#23511,.T.);
#53665=EDGE_CURVE('',#41026,#41043,#23512,.T.);
#53666=EDGE_CURVE('',#41030,#41039,#23513,.T.);
#53667=EDGE_CURVE('',#41029,#41040,#23514,.T.);
#53668=EDGE_CURVE('',#41028,#41041,#23515,.T.);
#53669=EDGE_CURVE('',#41027,#41042,#23516,.T.);
#53670=EDGE_CURVE('',#41044,#41045,#23517,.T.);
#53671=EDGE_CURVE('',#41045,#41046,#1290,.T.);
#53672=EDGE_CURVE('',#41047,#41046,#23518,.T.);
#53673=EDGE_CURVE('',#41047,#41044,#1291,.T.);
#53674=EDGE_CURVE('',#41048,#41049,#23519,.T.);
#53675=EDGE_CURVE('',#41049,#41045,#1292,.T.);
#53676=EDGE_CURVE('',#41044,#41048,#1293,.T.);
#53677=EDGE_CURVE('',#41050,#41051,#23520,.T.);
#53678=EDGE_CURVE('',#41051,#41049,#1294,.T.);
#53679=EDGE_CURVE('',#41048,#41050,#1295,.T.);
#53680=EDGE_CURVE('',#41052,#41053,#23521,.T.);
#53681=EDGE_CURVE('',#41053,#41051,#1296,.T.);
#53682=EDGE_CURVE('',#41050,#41052,#1297,.T.);
#53683=EDGE_CURVE('',#41054,#41055,#23522,.T.);
#53684=EDGE_CURVE('',#41055,#41053,#1298,.T.);
#53685=EDGE_CURVE('',#41052,#41054,#1299,.T.);
#53686=EDGE_CURVE('',#41046,#41055,#1300,.T.);
#53687=EDGE_CURVE('',#41054,#41047,#1301,.T.);
#53688=EDGE_CURVE('',#41056,#41050,#23523,.T.);
#53689=EDGE_CURVE('',#41045,#41046,#33920,.T.);
#53690=EDGE_CURVE('',#41049,#41045,#33921,.T.);
#53691=EDGE_CURVE('',#41051,#41049,#33922,.T.);
#53692=EDGE_CURVE('',#41053,#41051,#33923,.T.);
#53693=EDGE_CURVE('',#41055,#41053,#33924,.T.);
#53694=EDGE_CURVE('',#41046,#41055,#33925,.T.);
#53695=EDGE_CURVE('',#41057,#41057,#33926,.T.);
#53696=EDGE_CURVE('',#41057,#41058,#33927,.T.);
#53697=EDGE_CURVE('',#41059,#41058,#33928,.T.);
#53698=EDGE_CURVE('',#41058,#41059,#33929,.T.);
#53699=EDGE_CURVE('',#41060,#41060,#33930,.T.);
#53700=EDGE_CURVE('',#41060,#41059,#23524,.T.);
#53701=EDGE_CURVE('',#41061,#41061,#33931,.T.);
#53702=EDGE_CURVE('',#41062,#41063,#33932,.T.);
#53703=EDGE_CURVE('',#41064,#41062,#5941,.F.);
#53704=EDGE_CURVE('',#41065,#41064,#33933,.T.);
#53705=EDGE_CURVE('',#41063,#41065,#5942,.F.);
#53706=EDGE_CURVE('',#41066,#41067,#33934,.T.);
#53707=EDGE_CURVE('',#41067,#41066,#33935,.T.);
#53708=EDGE_CURVE('',#41067,#41061,#33936,.T.);
#53709=EDGE_CURVE('',#41068,#41068,#33937,.T.);
#53710=EDGE_CURVE('',#41068,#41069,#33938,.T.);
#53711=EDGE_CURVE('',#41070,#41069,#33939,.T.);
#53712=EDGE_CURVE('',#41069,#41070,#33940,.T.);
#53713=EDGE_CURVE('',#41071,#41072,#33941,.T.);
#53714=EDGE_CURVE('',#41073,#41071,#23525,.T.);
#53715=EDGE_CURVE('',#41074,#41073,#33942,.T.);
#53716=EDGE_CURVE('',#41072,#41074,#23526,.T.);
#53717=EDGE_CURVE('',#41063,#41072,#23527,.T.);
#53718=EDGE_CURVE('',#41062,#41074,#23528,.T.);
#53719=EDGE_CURVE('',#41064,#41073,#23529,.T.);
#53720=EDGE_CURVE('',#41065,#41071,#23530,.T.);
#53721=EDGE_CURVE('',#41075,#41075,#33943,.T.);
#53722=EDGE_CURVE('',#41076,#41076,#33944,.T.);
#53723=EDGE_CURVE('',#41076,#41075,#23531,.T.);
#53724=EDGE_CURVE('',#41066,#41070,#23532,.T.);
#53725=EDGE_CURVE('',#41077,#41077,#33945,.T.);
#53726=EDGE_CURVE('',#41077,#41078,#23533,.T.);
#53727=EDGE_CURVE('',#41078,#41078,#33946,.T.);
#53728=EDGE_CURVE('',#41079,#41079,#33947,.T.);
#53729=EDGE_CURVE('',#41079,#41077,#23534,.T.);
#53730=EDGE_CURVE('',#41080,#41080,#33948,.T.);
#53731=EDGE_CURVE('',#41081,#41081,#33949,.T.);
#53732=EDGE_CURVE('',#41081,#41080,#23535,.T.);
#53733=EDGE_CURVE('',#41082,#41083,#33950,.T.);
#53734=EDGE_CURVE('',#41084,#41083,#33951,.T.);
#53735=EDGE_CURVE('',#41084,#41085,#33952,.T.);
#53736=EDGE_CURVE('',#41082,#41085,#33953,.T.);
#53737=EDGE_CURVE('',#41086,#41087,#33954,.T.);
#53738=EDGE_CURVE('',#41085,#41087,#23536,.T.);
#53739=EDGE_CURVE('',#41086,#41084,#23537,.T.);
#53740=EDGE_CURVE('',#41088,#41089,#33955,.T.);
#53741=EDGE_CURVE('',#41083,#41089,#23538,.T.);
#53742=EDGE_CURVE('',#41088,#41082,#23539,.T.);
#53743=EDGE_CURVE('',#41090,#41091,#33956,.T.);
#53744=EDGE_CURVE('',#41087,#41091,#33957,.T.);
#53745=EDGE_CURVE('',#41090,#41086,#33958,.T.);
#53746=EDGE_CURVE('',#41092,#41093,#33959,.T.);
#53747=EDGE_CURVE('',#41089,#41093,#33960,.T.);
#53748=EDGE_CURVE('',#41092,#41088,#33961,.T.);
#53749=EDGE_CURVE('',#41094,#41095,#33962,.T.);
#53750=EDGE_CURVE('',#41091,#41095,#23540,.T.);
#53751=EDGE_CURVE('',#41094,#41090,#23541,.T.);
#53752=EDGE_CURVE('',#41096,#41097,#33963,.T.);
#53753=EDGE_CURVE('',#41093,#41097,#23542,.T.);
#53754=EDGE_CURVE('',#41096,#41092,#23543,.T.);
#53755=EDGE_CURVE('',#41097,#41094,#33964,.T.);
#53756=EDGE_CURVE('',#41095,#41096,#33965,.T.);
#53757=EDGE_CURVE('',#41098,#41096,#23544,.T.);
#53758=EDGE_CURVE('',#41099,#41092,#23545,.T.);
#53759=EDGE_CURVE('',#41098,#41099,#23546,.T.);
#53760=EDGE_CURVE('',#41100,#41095,#23547,.T.);
#53761=EDGE_CURVE('',#41100,#41098,#33966,.T.);
#53762=EDGE_CURVE('',#41101,#41088,#23548,.T.);
#53763=EDGE_CURVE('',#41099,#41101,#33967,.T.);
#53764=EDGE_CURVE('',#41102,#41103,#23549,.T.);
#53765=EDGE_CURVE('',#41104,#41102,#23550,.T.);
#53766=EDGE_CURVE('',#41105,#41104,#23551,.T.);
#53767=EDGE_CURVE('',#41103,#41105,#23552,.T.);
#53768=EDGE_CURVE('',#41106,#41106,#33968,.T.);
#53769=EDGE_CURVE('',#41107,#41107,#33969,.T.);
#53770=EDGE_CURVE('',#41102,#41108,#33970,.T.);
#53771=EDGE_CURVE('',#41102,#41109,#33971,.T.);
#53772=EDGE_CURVE('',#41109,#41110,#33972,.T.);
#53773=EDGE_CURVE('',#41110,#41108,#33973,.T.);
#53774=EDGE_CURVE('',#41104,#41111,#33974,.T.);
#53775=EDGE_CURVE('',#41108,#41111,#23553,.T.);
#53776=EDGE_CURVE('',#41112,#41113,#33975,.T.);
#53777=EDGE_CURVE('',#41112,#41104,#33976,.T.);
#53778=EDGE_CURVE('',#41111,#41113,#33977,.T.);
#53779=EDGE_CURVE('',#41112,#41114,#23554,.T.);
#53780=EDGE_CURVE('',#41105,#41114,#33978,.T.);
#53781=EDGE_CURVE('',#41115,#41114,#33979,.T.);
#53782=EDGE_CURVE('',#41115,#41116,#33980,.T.);
#53783=EDGE_CURVE('',#41116,#41105,#33981,.T.);
#53784=EDGE_CURVE('',#41117,#41103,#33982,.T.);
#53785=EDGE_CURVE('',#41117,#41118,#33983,.T.);
#53786=EDGE_CURVE('',#41118,#41119,#33984,.T.);
#53787=EDGE_CURVE('',#41119,#41103,#33985,.T.);
#53788=EDGE_CURVE('',#41116,#41117,#23555,.T.);
#53789=EDGE_CURVE('',#41119,#41109,#23556,.T.);
#53790=EDGE_CURVE('',#41120,#41121,#23557,.T.);
#53791=EDGE_CURVE('',#41120,#41122,#33986,.T.);
#53792=EDGE_CURVE('',#41123,#41122,#23558,.T.);
#53793=EDGE_CURVE('',#41123,#41121,#33987,.T.);
#53794=EDGE_CURVE('',#41124,#41125,#33988,.T.);
#53795=EDGE_CURVE('',#41122,#41125,#23559,.T.);
#53796=EDGE_CURVE('',#41126,#41122,#33989,.T.);
#53797=EDGE_CURVE('',#41124,#41126,#23560,.T.);
#53798=EDGE_CURVE('',#41127,#41120,#33990,.T.);
#53799=EDGE_CURVE('',#41126,#41127,#33991,.T.);
#53800=EDGE_CURVE('',#41128,#41129,#33992,.T.);
#53801=EDGE_CURVE('',#41125,#41129,#33993,.T.);
#53802=EDGE_CURVE('',#41128,#41124,#33994,.T.);
#53803=EDGE_CURVE('',#41125,#41130,#23561,.T.);
#53804=EDGE_CURVE('',#41131,#41129,#23562,.T.);
#53805=EDGE_CURVE('',#41131,#41130,#33995,.T.);
#53806=EDGE_CURVE('',#41131,#41132,#33996,.T.);
#53807=EDGE_CURVE('',#41133,#41132,#33997,.T.);
#53808=EDGE_CURVE('',#41130,#41133,#33998,.T.);
#53809=EDGE_CURVE('',#41134,#41133,#23563,.T.);
#53810=EDGE_CURVE('',#41123,#41134,#33999,.T.);
#53811=EDGE_CURVE('',#41130,#41123,#23564,.T.);
#53812=EDGE_CURVE('',#41135,#41134,#34000,.T.);
#53813=EDGE_CURVE('',#41121,#41135,#34001,.T.);
#53814=EDGE_CURVE('',#41136,#41136,#34002,.T.);
#53815=EDGE_CURVE('',#41137,#41137,#34003,.T.);
#53816=EDGE_CURVE('',#41138,#41082,#23565,.T.);
#53817=EDGE_CURVE('',#41139,#41085,#23566,.T.);
#53818=EDGE_CURVE('',#41139,#41138,#34004,.T.);
#53819=EDGE_CURVE('',#41140,#41087,#23567,.T.);
#53820=EDGE_CURVE('',#41141,#41091,#23568,.T.);
#53821=EDGE_CURVE('',#41141,#41140,#34005,.T.);
#53822=EDGE_CURVE('',#41110,#41135,#23569,.T.);
#53823=EDGE_CURVE('',#41121,#41109,#23570,.T.);
#53824=EDGE_CURVE('',#41119,#41120,#23571,.T.);
#53825=EDGE_CURVE('',#41127,#41118,#23572,.T.);
#53826=EDGE_CURVE('',#41115,#41128,#23573,.T.);
#53827=EDGE_CURVE('',#41129,#41114,#23574,.T.);
#53828=EDGE_CURVE('',#41112,#41131,#23575,.T.);
#53829=EDGE_CURVE('',#41132,#41113,#23576,.T.);
#53830=EDGE_CURVE('',#41100,#41141,#23577,.T.);
#53831=EDGE_CURVE('',#41138,#41101,#23578,.T.);
#53832=EDGE_CURVE('',#41136,#41106,#23579,.T.);
#53833=EDGE_CURVE('',#41137,#41107,#23580,.T.);
#53834=EDGE_CURVE('',#41140,#41139,#23581,.T.);
#53835=EDGE_CURVE('',#41142,#41142,#34006,.T.);
#53836=EDGE_CURVE('',#41143,#41144,#34007,.T.);
#53837=EDGE_CURVE('',#41145,#41143,#5943,.F.);
#53838=EDGE_CURVE('',#41146,#41145,#34008,.T.);
#53839=EDGE_CURVE('',#41144,#41146,#5944,.F.);
#53840=EDGE_CURVE('',#41147,#41148,#34009,.T.);
#53841=EDGE_CURVE('',#41148,#41147,#34010,.T.);
#53842=EDGE_CURVE('',#41148,#41142,#34011,.T.);
#53843=EDGE_CURVE('',#41149,#41149,#34012,.T.);
#53844=EDGE_CURVE('',#41149,#41150,#34013,.T.);
#53845=EDGE_CURVE('',#41151,#41150,#34014,.T.);
#53846=EDGE_CURVE('',#41150,#41151,#34015,.T.);
#53847=EDGE_CURVE('',#41152,#41153,#34016,.T.);
#53848=EDGE_CURVE('',#41154,#41152,#23582,.T.);
#53849=EDGE_CURVE('',#41155,#41154,#34017,.T.);
#53850=EDGE_CURVE('',#41153,#41155,#23583,.T.);
#53851=EDGE_CURVE('',#41144,#41153,#23584,.T.);
#53852=EDGE_CURVE('',#41143,#41155,#23585,.T.);
#53853=EDGE_CURVE('',#41145,#41154,#23586,.T.);
#53854=EDGE_CURVE('',#41146,#41152,#23587,.T.);
#53855=EDGE_CURVE('',#41156,#41156,#34018,.T.);
#53856=EDGE_CURVE('',#41157,#41157,#34019,.T.);
#53857=EDGE_CURVE('',#41157,#41156,#23588,.T.);
#53858=EDGE_CURVE('',#41147,#41151,#23589,.T.);
#53859=EDGE_CURVE('',#41158,#41159,#34020,.T.);
#53860=EDGE_CURVE('',#41160,#41159,#23590,.T.);
#53861=EDGE_CURVE('',#41161,#41160,#5945,.T.);
#53862=EDGE_CURVE('',#41158,#41161,#23591,.T.);
#53863=EDGE_CURVE('',#41162,#41163,#34021,.T.);
#53864=EDGE_CURVE('',#41159,#41163,#34022,.T.);
#53865=EDGE_CURVE('',#41162,#41158,#34023,.T.);
#53866=EDGE_CURVE('',#41164,#41165,#34024,.T.);
#53867=EDGE_CURVE('',#41163,#41165,#23592,.T.);
#53868=EDGE_CURVE('',#41164,#41162,#23593,.T.);
#53869=EDGE_CURVE('',#41166,#41167,#34025,.T.);
#53870=EDGE_CURVE('',#41165,#41167,#34026,.T.);
#53871=EDGE_CURVE('',#41166,#41164,#34027,.T.);
#53872=EDGE_CURVE('',#41168,#41169,#5946,.T.);
#53873=EDGE_CURVE('',#41167,#41168,#23594,.T.);
#53874=EDGE_CURVE('',#41169,#41166,#23595,.T.);
#53875=EDGE_CURVE('',#41170,#41171,#34028,.T.);
#53876=EDGE_CURVE('',#41172,#41171,#23596,.T.);
#53877=EDGE_CURVE('',#41173,#41172,#34029,.T.);
#53878=EDGE_CURVE('',#41170,#41173,#23597,.T.);
#53879=EDGE_CURVE('',#41174,#41175,#34030,.T.);
#53880=EDGE_CURVE('',#41171,#41175,#34031,.T.);
#53881=EDGE_CURVE('',#41174,#41170,#34032,.T.);
#53882=EDGE_CURVE('',#41176,#41177,#34033,.T.);
#53883=EDGE_CURVE('',#41175,#41177,#23598,.T.);
#53884=EDGE_CURVE('',#41176,#41174,#23599,.T.);
#53885=EDGE_CURVE('',#41178,#41179,#34034,.T.);
#53886=EDGE_CURVE('',#41177,#41179,#34035,.T.);
#53887=EDGE_CURVE('',#41178,#41176,#34036,.T.);
#53888=EDGE_CURVE('',#41180,#41181,#5947,.T.);
#53889=EDGE_CURVE('',#41179,#41180,#23600,.T.);
#53890=EDGE_CURVE('',#41181,#41178,#23601,.T.);
#53891=EDGE_CURVE('',#41182,#41183,#34037,.T.);
#53892=EDGE_CURVE('',#41184,#41183,#23602,.T.);
#53893=EDGE_CURVE('',#41185,#41184,#34038,.T.);
#53894=EDGE_CURVE('',#41182,#41185,#23603,.T.);
#53895=EDGE_CURVE('',#41186,#41187,#34039,.T.);
#53896=EDGE_CURVE('',#41183,#41187,#34040,.T.);
#53897=EDGE_CURVE('',#41186,#41182,#34041,.T.);
#53898=EDGE_CURVE('',#41188,#41189,#34042,.T.);
#53899=EDGE_CURVE('',#41187,#41189,#23604,.T.);
#53900=EDGE_CURVE('',#41188,#41186,#23605,.T.);
#53901=EDGE_CURVE('',#41190,#41191,#34043,.T.);
#53902=EDGE_CURVE('',#41189,#41191,#34044,.T.);
#53903=EDGE_CURVE('',#41190,#41188,#34045,.T.);
#53904=EDGE_CURVE('',#41192,#41193,#34046,.T.);
#53905=EDGE_CURVE('',#41191,#41193,#23606,.T.);
#53906=EDGE_CURVE('',#41192,#41190,#23607,.T.);
#53907=EDGE_CURVE('',#41194,#41195,#34047,.T.);
#53908=EDGE_CURVE('',#41193,#41195,#34048,.T.);
#53909=EDGE_CURVE('',#41194,#41192,#34049,.T.);
#53910=EDGE_CURVE('',#41196,#41197,#34050,.T.);
#53911=EDGE_CURVE('',#41195,#41197,#23608,.T.);
#53912=EDGE_CURVE('',#41196,#41194,#23609,.T.);
#53913=EDGE_CURVE('',#41198,#41199,#34051,.T.);
#53914=EDGE_CURVE('',#41197,#41199,#34052,.T.);
#53915=EDGE_CURVE('',#41198,#41196,#34053,.T.);
#53916=EDGE_CURVE('',#41200,#41201,#34054,.T.);
#53917=EDGE_CURVE('',#41199,#41200,#23610,.T.);
#53918=EDGE_CURVE('',#41201,#41198,#23611,.T.);
#53919=EDGE_CURVE('',#41202,#41203,#34055,.T.);
#53920=EDGE_CURVE('',#41204,#41202,#23612,.T.);
#53921=EDGE_CURVE('',#41204,#41205,#34056,.T.);
#53922=EDGE_CURVE('',#41203,#41205,#23613,.T.);
#53923=EDGE_CURVE('',#41206,#41207,#34057,.T.);
#53924=EDGE_CURVE('',#41205,#41207,#34058,.T.);
#53925=EDGE_CURVE('',#41206,#41204,#34059,.T.);
#53926=EDGE_CURVE('',#41208,#41209,#34060,.T.);
#53927=EDGE_CURVE('',#41207,#41209,#23614,.T.);
#53928=EDGE_CURVE('',#41208,#41206,#23615,.T.);
#53929=EDGE_CURVE('',#41210,#41211,#34061,.T.);
#53930=EDGE_CURVE('',#41209,#41211,#34062,.T.);
#53931=EDGE_CURVE('',#41210,#41208,#34063,.T.);
#53932=EDGE_CURVE('',#41212,#41213,#5948,.T.);
#53933=EDGE_CURVE('',#41211,#41212,#23616,.T.);
#53934=EDGE_CURVE('',#41213,#41210,#23617,.T.);
#53935=EDGE_CURVE('',#41214,#41215,#34064,.T.);
#53936=EDGE_CURVE('',#41216,#41215,#23618,.T.);
#53937=EDGE_CURVE('',#41217,#41216,#34065,.T.);
#53938=EDGE_CURVE('',#41214,#41217,#23619,.T.);
#53939=EDGE_CURVE('',#41218,#41219,#34066,.T.);
#53940=EDGE_CURVE('',#41215,#41219,#34067,.T.);
#53941=EDGE_CURVE('',#41218,#41214,#34068,.T.);
#53942=EDGE_CURVE('',#41220,#41221,#34069,.T.);
#53943=EDGE_CURVE('',#41219,#41221,#23620,.T.);
#53944=EDGE_CURVE('',#41220,#41218,#23621,.T.);
#53945=EDGE_CURVE('',#41222,#41223,#34070,.T.);
#53946=EDGE_CURVE('',#41221,#41223,#34071,.T.);
#53947=EDGE_CURVE('',#41222,#41220,#34072,.T.);
#53948=EDGE_CURVE('',#41224,#41225,#34073,.T.);
#53949=EDGE_CURVE('',#41223,#41225,#34074,.T.);
#53950=EDGE_CURVE('',#41224,#41222,#34075,.T.);
#53951=EDGE_CURVE('',#41226,#41227,#34076,.T.);
#53952=EDGE_CURVE('',#41225,#41227,#23622,.T.);
#53953=EDGE_CURVE('',#41226,#41224,#23623,.T.);
#53954=EDGE_CURVE('',#41228,#41229,#34077,.T.);
#53955=EDGE_CURVE('',#41227,#41229,#34078,.T.);
#53956=EDGE_CURVE('',#41228,#41226,#34079,.T.);
#53957=EDGE_CURVE('',#41230,#41231,#34080,.T.);
#53958=EDGE_CURVE('',#41229,#41231,#23624,.T.);
#53959=EDGE_CURVE('',#41230,#41228,#23625,.T.);
#53960=EDGE_CURVE('',#41232,#41233,#34081,.T.);
#53961=EDGE_CURVE('',#41231,#41233,#34082,.T.);
#53962=EDGE_CURVE('',#41232,#41230,#34083,.T.);
#53963=EDGE_CURVE('',#41234,#41235,#34084,.T.);
#53964=EDGE_CURVE('',#41233,#41234,#23626,.T.);
#53965=EDGE_CURVE('',#41235,#41232,#23627,.T.);
#53966=EDGE_CURVE('',#41236,#41237,#34085,.T.);
#53967=EDGE_CURVE('',#41238,#41237,#23628,.T.);
#53968=EDGE_CURVE('',#41239,#41238,#34086,.T.);
#53969=EDGE_CURVE('',#41236,#41239,#23629,.T.);
#53970=EDGE_CURVE('',#41240,#41241,#34087,.T.);
#53971=EDGE_CURVE('',#41237,#41241,#34088,.T.);
#53972=EDGE_CURVE('',#41240,#41236,#34089,.T.);
#53973=EDGE_CURVE('',#41242,#41243,#34090,.T.);
#53974=EDGE_CURVE('',#41241,#41243,#23630,.T.);
#53975=EDGE_CURVE('',#41242,#41240,#23631,.T.);
#53976=EDGE_CURVE('',#41244,#41245,#34091,.T.);
#53977=EDGE_CURVE('',#41243,#41245,#34092,.T.);
#53978=EDGE_CURVE('',#41244,#41242,#34093,.T.);
#53979=EDGE_CURVE('',#41246,#41247,#34094,.T.);
#53980=EDGE_CURVE('',#41245,#41247,#34095,.T.);
#53981=EDGE_CURVE('',#41246,#41244,#34096,.T.);
#53982=EDGE_CURVE('',#41248,#41249,#34097,.T.);
#53983=EDGE_CURVE('',#41247,#41249,#34098,.T.);
#53984=EDGE_CURVE('',#41248,#41246,#34099,.T.);
#53985=EDGE_CURVE('',#41250,#41251,#34100,.T.);
#53986=EDGE_CURVE('',#41249,#41251,#23632,.T.);
#53987=EDGE_CURVE('',#41250,#41248,#23633,.T.);
#53988=EDGE_CURVE('',#41252,#41253,#34101,.T.);
#53989=EDGE_CURVE('',#41251,#41253,#34102,.T.);
#53990=EDGE_CURVE('',#41252,#41250,#34103,.T.);
#53991=EDGE_CURVE('',#41254,#41255,#34104,.T.);
#53992=EDGE_CURVE('',#41253,#41254,#23634,.T.);
#53993=EDGE_CURVE('',#41255,#41252,#23635,.T.);
#53994=EDGE_CURVE('',#41256,#41257,#34105,.T.);
#53995=EDGE_CURVE('',#41258,#41257,#23636,.T.);
#53996=EDGE_CURVE('',#41259,#41258,#34106,.T.);
#53997=EDGE_CURVE('',#41256,#41259,#23637,.T.);
#53998=EDGE_CURVE('',#41260,#41261,#34107,.T.);
#53999=EDGE_CURVE('',#41257,#41261,#34108,.T.);
#54000=EDGE_CURVE('',#41260,#41256,#34109,.T.);
#54001=EDGE_CURVE('',#41262,#41263,#34110,.T.);
#54002=EDGE_CURVE('',#41261,#41263,#23638,.T.);
#54003=EDGE_CURVE('',#41262,#41260,#23639,.T.);
#54004=EDGE_CURVE('',#41264,#41265,#34111,.T.);
#54005=EDGE_CURVE('',#41263,#41265,#34112,.T.);
#54006=EDGE_CURVE('',#41264,#41262,#34113,.T.);
#54007=EDGE_CURVE('',#41266,#41267,#34114,.T.);
#54008=EDGE_CURVE('',#41265,#41267,#34115,.T.);
#54009=EDGE_CURVE('',#41266,#41264,#34116,.T.);
#54010=EDGE_CURVE('',#41268,#41269,#34117,.T.);
#54011=EDGE_CURVE('',#41267,#41269,#34118,.T.);
#54012=EDGE_CURVE('',#41268,#41266,#34119,.T.);
#54013=EDGE_CURVE('',#41270,#41271,#34120,.T.);
#54014=EDGE_CURVE('',#41269,#41271,#23640,.T.);
#54015=EDGE_CURVE('',#41270,#41268,#23641,.T.);
#54016=EDGE_CURVE('',#41272,#41273,#34121,.T.);
#54017=EDGE_CURVE('',#41271,#41273,#34122,.T.);
#54018=EDGE_CURVE('',#41272,#41270,#34123,.T.);
#54019=EDGE_CURVE('',#41274,#41275,#34124,.T.);
#54020=EDGE_CURVE('',#41273,#41274,#23642,.T.);
#54021=EDGE_CURVE('',#41275,#41272,#23643,.T.);
#54022=EDGE_CURVE('',#41276,#41277,#34125,.T.);
#54023=EDGE_CURVE('',#41278,#41277,#23644,.T.);
#54024=EDGE_CURVE('',#41279,#41278,#34126,.T.);
#54025=EDGE_CURVE('',#41276,#41279,#23645,.T.);
#54026=EDGE_CURVE('',#41280,#41281,#34127,.T.);
#54027=EDGE_CURVE('',#41277,#41281,#34128,.T.);
#54028=EDGE_CURVE('',#41280,#41276,#34129,.T.);
#54029=EDGE_CURVE('',#41282,#41283,#34130,.T.);
#54030=EDGE_CURVE('',#41281,#41283,#23646,.T.);
#54031=EDGE_CURVE('',#41282,#41280,#23647,.T.);
#54032=EDGE_CURVE('',#41284,#41285,#34131,.T.);
#54033=EDGE_CURVE('',#41283,#41285,#34132,.T.);
#54034=EDGE_CURVE('',#41284,#41282,#34133,.T.);
#54035=EDGE_CURVE('',#41286,#41287,#34134,.T.);
#54036=EDGE_CURVE('',#41285,#41287,#34135,.T.);
#54037=EDGE_CURVE('',#41286,#41284,#34136,.T.);
#54038=EDGE_CURVE('',#41288,#41289,#34137,.T.);
#54039=EDGE_CURVE('',#41287,#41289,#34138,.T.);
#54040=EDGE_CURVE('',#41288,#41286,#34139,.T.);
#54041=EDGE_CURVE('',#41290,#41291,#34140,.T.);
#54042=EDGE_CURVE('',#41289,#41291,#23648,.T.);
#54043=EDGE_CURVE('',#41290,#41288,#23649,.T.);
#54044=EDGE_CURVE('',#41292,#41293,#34141,.T.);
#54045=EDGE_CURVE('',#41291,#41293,#34142,.T.);
#54046=EDGE_CURVE('',#41292,#41290,#34143,.T.);
#54047=EDGE_CURVE('',#41294,#41295,#34144,.T.);
#54048=EDGE_CURVE('',#41293,#41294,#23650,.T.);
#54049=EDGE_CURVE('',#41295,#41292,#23651,.T.);
#54050=EDGE_CURVE('',#41296,#41297,#34145,.T.);
#54051=EDGE_CURVE('',#41298,#41297,#23652,.T.);
#54052=EDGE_CURVE('',#41299,#41298,#34146,.T.);
#54053=EDGE_CURVE('',#41296,#41299,#23653,.T.);
#54054=EDGE_CURVE('',#41300,#41301,#34147,.T.);
#54055=EDGE_CURVE('',#41297,#41301,#34148,.T.);
#54056=EDGE_CURVE('',#41300,#41296,#34149,.T.);
#54057=EDGE_CURVE('',#41302,#41303,#34150,.T.);
#54058=EDGE_CURVE('',#41301,#41303,#23654,.T.);
#54059=EDGE_CURVE('',#41302,#41300,#23655,.T.);
#54060=EDGE_CURVE('',#41304,#41305,#34151,.T.);
#54061=EDGE_CURVE('',#41303,#41305,#34152,.T.);
#54062=EDGE_CURVE('',#41304,#41302,#34153,.T.);
#54063=EDGE_CURVE('',#41306,#41307,#34154,.T.);
#54064=EDGE_CURVE('',#41305,#41307,#34155,.T.);
#54065=EDGE_CURVE('',#41306,#41304,#34156,.T.);
#54066=EDGE_CURVE('',#41308,#41309,#34157,.T.);
#54067=EDGE_CURVE('',#41307,#41309,#34158,.T.);
#54068=EDGE_CURVE('',#41308,#41306,#34159,.T.);
#54069=EDGE_CURVE('',#41310,#41311,#34160,.T.);
#54070=EDGE_CURVE('',#41309,#41311,#23656,.T.);
#54071=EDGE_CURVE('',#41310,#41308,#23657,.T.);
#54072=EDGE_CURVE('',#41312,#41313,#34161,.T.);
#54073=EDGE_CURVE('',#41311,#41313,#34162,.T.);
#54074=EDGE_CURVE('',#41312,#41310,#34163,.T.);
#54075=EDGE_CURVE('',#41314,#41315,#34164,.T.);
#54076=EDGE_CURVE('',#41313,#41314,#23658,.T.);
#54077=EDGE_CURVE('',#41315,#41312,#23659,.T.);
#54078=EDGE_CURVE('',#41316,#41317,#34165,.T.);
#54079=EDGE_CURVE('',#41318,#41317,#23660,.T.);
#54080=EDGE_CURVE('',#41319,#41318,#34166,.T.);
#54081=EDGE_CURVE('',#41316,#41319,#23661,.T.);
#54082=EDGE_CURVE('',#41320,#41321,#34167,.T.);
#54083=EDGE_CURVE('',#41317,#41321,#34168,.T.);
#54084=EDGE_CURVE('',#41320,#41316,#34169,.T.);
#54085=EDGE_CURVE('',#41322,#41323,#34170,.T.);
#54086=EDGE_CURVE('',#41321,#41323,#23662,.T.);
#54087=EDGE_CURVE('',#41322,#41320,#23663,.T.);
#54088=EDGE_CURVE('',#41324,#41325,#34171,.T.);
#54089=EDGE_CURVE('',#41323,#41325,#34172,.T.);
#54090=EDGE_CURVE('',#41324,#41322,#34173,.T.);
#54091=EDGE_CURVE('',#41326,#41327,#34174,.T.);
#54092=EDGE_CURVE('',#41325,#41327,#34175,.T.);
#54093=EDGE_CURVE('',#41326,#41324,#34176,.T.);
#54094=EDGE_CURVE('',#41328,#41329,#34177,.T.);
#54095=EDGE_CURVE('',#41327,#41329,#34178,.T.);
#54096=EDGE_CURVE('',#41328,#41326,#34179,.T.);
#54097=EDGE_CURVE('',#41330,#41331,#34180,.T.);
#54098=EDGE_CURVE('',#41329,#41331,#23664,.T.);
#54099=EDGE_CURVE('',#41330,#41328,#23665,.T.);
#54100=EDGE_CURVE('',#41332,#41333,#34181,.T.);
#54101=EDGE_CURVE('',#41331,#41333,#34182,.T.);
#54102=EDGE_CURVE('',#41332,#41330,#34183,.T.);
#54103=EDGE_CURVE('',#41334,#41335,#34184,.T.);
#54104=EDGE_CURVE('',#41333,#41334,#23666,.T.);
#54105=EDGE_CURVE('',#41335,#41332,#23667,.T.);
#54106=EDGE_CURVE('',#41336,#41337,#34185,.T.);
#54107=EDGE_CURVE('',#41338,#41337,#23668,.T.);
#54108=EDGE_CURVE('',#41339,#41338,#34186,.T.);
#54109=EDGE_CURVE('',#41336,#41339,#23669,.T.);
#54110=EDGE_CURVE('',#41340,#41341,#34187,.T.);
#54111=EDGE_CURVE('',#41337,#41341,#34188,.T.);
#54112=EDGE_CURVE('',#41340,#41336,#34189,.T.);
#54113=EDGE_CURVE('',#41342,#41343,#34190,.T.);
#54114=EDGE_CURVE('',#41341,#41343,#23670,.T.);
#54115=EDGE_CURVE('',#41342,#41340,#23671,.T.);
#54116=EDGE_CURVE('',#41344,#41345,#34191,.T.);
#54117=EDGE_CURVE('',#41343,#41345,#34192,.T.);
#54118=EDGE_CURVE('',#41344,#41342,#34193,.T.);
#54119=EDGE_CURVE('',#41346,#41347,#34194,.T.);
#54120=EDGE_CURVE('',#41345,#41347,#34195,.T.);
#54121=EDGE_CURVE('',#41346,#41344,#34196,.T.);
#54122=EDGE_CURVE('',#41348,#41349,#34197,.T.);
#54123=EDGE_CURVE('',#41347,#41349,#34198,.T.);
#54124=EDGE_CURVE('',#41348,#41346,#34199,.T.);
#54125=EDGE_CURVE('',#41350,#41351,#34200,.T.);
#54126=EDGE_CURVE('',#41349,#41351,#23672,.T.);
#54127=EDGE_CURVE('',#41350,#41348,#23673,.T.);
#54128=EDGE_CURVE('',#41352,#41353,#34201,.T.);
#54129=EDGE_CURVE('',#41351,#41353,#34202,.T.);
#54130=EDGE_CURVE('',#41352,#41350,#34203,.T.);
#54131=EDGE_CURVE('',#41354,#41355,#34204,.T.);
#54132=EDGE_CURVE('',#41353,#41354,#23674,.T.);
#54133=EDGE_CURVE('',#41355,#41352,#23675,.T.);
#54134=EDGE_CURVE('',#41356,#41357,#34205,.T.);
#54135=EDGE_CURVE('',#41358,#41357,#23676,.T.);
#54136=EDGE_CURVE('',#41359,#41358,#34206,.T.);
#54137=EDGE_CURVE('',#41356,#41359,#23677,.T.);
#54138=EDGE_CURVE('',#41360,#41361,#34207,.T.);
#54139=EDGE_CURVE('',#41357,#41361,#34208,.T.);
#54140=EDGE_CURVE('',#41360,#41356,#34209,.T.);
#54141=EDGE_CURVE('',#41362,#41363,#34210,.T.);
#54142=EDGE_CURVE('',#41361,#41363,#23678,.T.);
#54143=EDGE_CURVE('',#41362,#41360,#23679,.T.);
#54144=EDGE_CURVE('',#41364,#41365,#34211,.T.);
#54145=EDGE_CURVE('',#41363,#41365,#34212,.T.);
#54146=EDGE_CURVE('',#41364,#41362,#34213,.T.);
#54147=EDGE_CURVE('',#41366,#41367,#34214,.T.);
#54148=EDGE_CURVE('',#41365,#41367,#23680,.T.);
#54149=EDGE_CURVE('',#41366,#41364,#23681,.T.);
#54150=EDGE_CURVE('',#41368,#41369,#34215,.T.);
#54151=EDGE_CURVE('',#41367,#41369,#34216,.T.);
#54152=EDGE_CURVE('',#41368,#41366,#34217,.T.);
#54153=EDGE_CURVE('',#41370,#41371,#34218,.T.);
#54154=EDGE_CURVE('',#41369,#41371,#34219,.T.);
#54155=EDGE_CURVE('',#41370,#41368,#34220,.T.);
#54156=EDGE_CURVE('',#41372,#41373,#34221,.T.);
#54157=EDGE_CURVE('',#41371,#41373,#23682,.T.);
#54158=EDGE_CURVE('',#41372,#41370,#23683,.T.);
#54159=EDGE_CURVE('',#41374,#41375,#34222,.T.);
#54160=EDGE_CURVE('',#41373,#41375,#34223,.T.);
#54161=EDGE_CURVE('',#41374,#41372,#34224,.T.);
#54162=EDGE_CURVE('',#41376,#41377,#34225,.T.);
#54163=EDGE_CURVE('',#41375,#41376,#23684,.T.);
#54164=EDGE_CURVE('',#41377,#41374,#23685,.T.);
#54165=EDGE_CURVE('',#41378,#41379,#34226,.T.);
#54166=EDGE_CURVE('',#41380,#41379,#23686,.T.);
#54167=EDGE_CURVE('',#41381,#41380,#34227,.T.);
#54168=EDGE_CURVE('',#41378,#41381,#23687,.T.);
#54169=EDGE_CURVE('',#41382,#41383,#34228,.T.);
#54170=EDGE_CURVE('',#41379,#41383,#34229,.T.);
#54171=EDGE_CURVE('',#41382,#41378,#34230,.T.);
#54172=EDGE_CURVE('',#41384,#41385,#34231,.T.);
#54173=EDGE_CURVE('',#41383,#41385,#23688,.T.);
#54174=EDGE_CURVE('',#41384,#41382,#23689,.T.);
#54175=EDGE_CURVE('',#41386,#41387,#34232,.T.);
#54176=EDGE_CURVE('',#41385,#41387,#34233,.T.);
#54177=EDGE_CURVE('',#41386,#41384,#34234,.T.);
#54178=EDGE_CURVE('',#41388,#41389,#34235,.T.);
#54179=EDGE_CURVE('',#41387,#41389,#23690,.T.);
#54180=EDGE_CURVE('',#41388,#41386,#23691,.T.);
#54181=EDGE_CURVE('',#41390,#41391,#34236,.T.);
#54182=EDGE_CURVE('',#41389,#41391,#34237,.T.);
#54183=EDGE_CURVE('',#41390,#41388,#34238,.T.);
#54184=EDGE_CURVE('',#41392,#41393,#34239,.T.);
#54185=EDGE_CURVE('',#41391,#41393,#23692,.T.);
#54186=EDGE_CURVE('',#41392,#41390,#23693,.T.);
#54187=EDGE_CURVE('',#41394,#41395,#34240,.T.);
#54188=EDGE_CURVE('',#41393,#41395,#34241,.T.);
#54189=EDGE_CURVE('',#41394,#41392,#34242,.T.);
#54190=EDGE_CURVE('',#41396,#41397,#34243,.T.);
#54191=EDGE_CURVE('',#41395,#41396,#23694,.T.);
#54192=EDGE_CURVE('',#41397,#41394,#23695,.T.);
#54193=EDGE_CURVE('',#41398,#41399,#5949,.T.);
#54194=EDGE_CURVE('',#41400,#41398,#23696,.T.);
#54195=EDGE_CURVE('',#41400,#41401,#34244,.T.);
#54196=EDGE_CURVE('',#41399,#41401,#23697,.T.);
#54197=EDGE_CURVE('',#41402,#41403,#34245,.T.);
#54198=EDGE_CURVE('',#41401,#41403,#34246,.T.);
#54199=EDGE_CURVE('',#41402,#41400,#34247,.T.);
#54200=EDGE_CURVE('',#41404,#41405,#34248,.T.);
#54201=EDGE_CURVE('',#41403,#41405,#23698,.T.);
#54202=EDGE_CURVE('',#41404,#41402,#23699,.T.);
#54203=EDGE_CURVE('',#41406,#41407,#34249,.T.);
#54204=EDGE_CURVE('',#41405,#41407,#34250,.T.);
#54205=EDGE_CURVE('',#41406,#41404,#34251,.T.);
#54206=EDGE_CURVE('',#41408,#41409,#34252,.T.);
#54207=EDGE_CURVE('',#41407,#41408,#23700,.T.);
#54208=EDGE_CURVE('',#41409,#41406,#23701,.T.);
#54209=EDGE_CURVE('',#41209,#41410,#23702,.T.);
#54210=EDGE_CURVE('',#41411,#41211,#23703,.T.);
#54211=EDGE_CURVE('',#41410,#41411,#34253,.T.);
#54212=EDGE_CURVE('',#41178,#41412,#23704,.T.);
#54213=EDGE_CURVE('',#41413,#41176,#23705,.T.);
#54214=EDGE_CURVE('',#41412,#41413,#34254,.T.);
#54215=EDGE_CURVE('',#41401,#41414,#23706,.T.);
#54216=EDGE_CURVE('',#41415,#41403,#23707,.T.);
#54217=EDGE_CURVE('',#41414,#41415,#34255,.T.);
#54218=EDGE_CURVE('',#41162,#41416,#23708,.T.);
#54219=EDGE_CURVE('',#41417,#41158,#23709,.T.);
#54220=EDGE_CURVE('',#41416,#41417,#34256,.T.);
#54221=EDGE_CURVE('',#41166,#41418,#23710,.T.);
#54222=EDGE_CURVE('',#41419,#41164,#23711,.T.);
#54223=EDGE_CURVE('',#41418,#41419,#34257,.T.);
#54224=EDGE_CURVE('',#41385,#41420,#23712,.T.);
#54225=EDGE_CURVE('',#41421,#41387,#23713,.T.);
#54226=EDGE_CURVE('',#41420,#41421,#34258,.T.);
#54227=EDGE_CURVE('',#41363,#41422,#23714,.T.);
#54228=EDGE_CURVE('',#41423,#41365,#23715,.T.);
#54229=EDGE_CURVE('',#41422,#41423,#34259,.T.);
#54230=EDGE_CURVE('',#41343,#41424,#23716,.T.);
#54231=EDGE_CURVE('',#41425,#41345,#23717,.T.);
#54232=EDGE_CURVE('',#41424,#41425,#34260,.T.);
#54233=EDGE_CURVE('',#41323,#41426,#23718,.T.);
#54234=EDGE_CURVE('',#41427,#41325,#23719,.T.);
#54235=EDGE_CURVE('',#41426,#41427,#34261,.T.);
#54236=EDGE_CURVE('',#41303,#41428,#23720,.T.);
#54237=EDGE_CURVE('',#41429,#41305,#23721,.T.);
#54238=EDGE_CURVE('',#41428,#41429,#34262,.T.);
#54239=EDGE_CURVE('',#41283,#41430,#23722,.T.);
#54240=EDGE_CURVE('',#41431,#41285,#23723,.T.);
#54241=EDGE_CURVE('',#41430,#41431,#34263,.T.);
#54242=EDGE_CURVE('',#41307,#41432,#23724,.T.);
#54243=EDGE_CURVE('',#41433,#41309,#23725,.T.);
#54244=EDGE_CURVE('',#41432,#41433,#34264,.T.);
#54245=EDGE_CURVE('',#41327,#41434,#23726,.T.);
#54246=EDGE_CURVE('',#41435,#41329,#23727,.T.);
#54247=EDGE_CURVE('',#41434,#41435,#34265,.T.);
#54248=EDGE_CURVE('',#41347,#41436,#23728,.T.);
#54249=EDGE_CURVE('',#41437,#41349,#23729,.T.);
#54250=EDGE_CURVE('',#41436,#41437,#34266,.T.);
#54251=EDGE_CURVE('',#41369,#41438,#23730,.T.);
#54252=EDGE_CURVE('',#41439,#41371,#23731,.T.);
#54253=EDGE_CURVE('',#41438,#41439,#34267,.T.);
#54254=EDGE_CURVE('',#41389,#41440,#23732,.T.);
#54255=EDGE_CURVE('',#41441,#41391,#23733,.T.);
#54256=EDGE_CURVE('',#41440,#41441,#34268,.T.);
#54257=EDGE_CURVE('',#41287,#41442,#23734,.T.);
#54258=EDGE_CURVE('',#41443,#41289,#23735,.T.);
#54259=EDGE_CURVE('',#41442,#41443,#34269,.T.);
#54260=EDGE_CURVE('',#41263,#41444,#23736,.T.);
#54261=EDGE_CURVE('',#41445,#41265,#23737,.T.);
#54262=EDGE_CURVE('',#41444,#41445,#34270,.T.);
#54263=EDGE_CURVE('',#41267,#41446,#23738,.T.);
#54264=EDGE_CURVE('',#41447,#41269,#23739,.T.);
#54265=EDGE_CURVE('',#41446,#41447,#34271,.T.);
#54266=EDGE_CURVE('',#41243,#41448,#23740,.T.);
#54267=EDGE_CURVE('',#41449,#41245,#23741,.T.);
#54268=EDGE_CURVE('',#41448,#41449,#34272,.T.);
#54269=EDGE_CURVE('',#41221,#41450,#23742,.T.);
#54270=EDGE_CURVE('',#41451,#41223,#23743,.T.);
#54271=EDGE_CURVE('',#41450,#41451,#34273,.T.);
#54272=EDGE_CURVE('',#41247,#41452,#23744,.T.);
#54273=EDGE_CURVE('',#41453,#41249,#23745,.T.);
#54274=EDGE_CURVE('',#41452,#41453,#34274,.T.);
#54275=EDGE_CURVE('',#41227,#41454,#23746,.T.);
#54276=EDGE_CURVE('',#41455,#41229,#23747,.T.);
#54277=EDGE_CURVE('',#41454,#41455,#34275,.T.);
#54278=EDGE_CURVE('',#41189,#41456,#23748,.T.);
#54279=EDGE_CURVE('',#41457,#41191,#23749,.T.);
#54280=EDGE_CURVE('',#41456,#41457,#34276,.T.);
#54281=EDGE_CURVE('',#41193,#41458,#23750,.T.);
#54282=EDGE_CURVE('',#41459,#41195,#23751,.T.);
#54283=EDGE_CURVE('',#41458,#41459,#34277,.T.);
#54284=EDGE_CURVE('',#41174,#41460,#23752,.T.);
#54285=EDGE_CURVE('',#41461,#41170,#23753,.T.);
#54286=EDGE_CURVE('',#41460,#41461,#34278,.T.);
#54287=EDGE_CURVE('',#41160,#41398,#34279,.T.);
#54288=EDGE_CURVE('',#41462,#41168,#34280,.T.);
#54289=EDGE_CURVE('',#41463,#41462,#23754,.T.);
#54290=EDGE_CURVE('',#41172,#41463,#23755,.T.);
#54291=EDGE_CURVE('',#41213,#41180,#34281,.T.);
#54292=EDGE_CURVE('',#41206,#41196,#23756,.T.);
#54293=EDGE_CURVE('',#41186,#41230,#23757,.T.);
#54294=EDGE_CURVE('',#41218,#41250,#23758,.T.);
#54295=EDGE_CURVE('',#41240,#41270,#23759,.T.);
#54296=EDGE_CURVE('',#41260,#41290,#23760,.T.);
#54297=EDGE_CURVE('',#41280,#41310,#23761,.T.);
#54298=EDGE_CURVE('',#41300,#41330,#23762,.T.);
#54299=EDGE_CURVE('',#41320,#41350,#23763,.T.);
#54300=EDGE_CURVE('',#41340,#41372,#23764,.T.);
#54301=EDGE_CURVE('',#41360,#41392,#23765,.T.);
#54302=EDGE_CURVE('',#41382,#41404,#23766,.T.);
#54303=EDGE_CURVE('',#41203,#41410,#23767,.T.);
#54304=EDGE_CURVE('',#41464,#41169,#23768,.T.);
#54305=EDGE_CURVE('',#41465,#41464,#34282,.T.);
#54306=EDGE_CURVE('',#41465,#41462,#23769,.T.);
#54307=EDGE_CURVE('',#41464,#41418,#23770,.T.);
#54308=EDGE_CURVE('',#41413,#41460,#23771,.T.);
#54309=EDGE_CURVE('',#41466,#41173,#23772,.T.);
#54310=EDGE_CURVE('',#41461,#41466,#23773,.T.);
#54311=EDGE_CURVE('',#41459,#41200,#23774,.T.);
#54312=EDGE_CURVE('',#41184,#41456,#23775,.T.);
#54313=EDGE_CURVE('',#41435,#41334,#23776,.T.);
#54314=EDGE_CURVE('',#41318,#41426,#23777,.T.);
#54315=EDGE_CURVE('',#41437,#41354,#23778,.T.);
#54316=EDGE_CURVE('',#41338,#41424,#23779,.T.);
#54317=EDGE_CURVE('',#41358,#41422,#23780,.T.);
#54318=EDGE_CURVE('',#41455,#41234,#23781,.T.);
#54319=EDGE_CURVE('',#41433,#41314,#23782,.T.);
#54320=EDGE_CURVE('',#41298,#41428,#23783,.T.);
#54321=EDGE_CURVE('',#41335,#41299,#23784,.T.);
#54322=EDGE_CURVE('',#41332,#41296,#23785,.T.);
#54323=EDGE_CURVE('',#41429,#41432,#34283,.T.);
#54324=EDGE_CURVE('',#41443,#41294,#23786,.T.);
#54325=EDGE_CURVE('',#41278,#41430,#23787,.T.);
#54326=EDGE_CURVE('',#41315,#41279,#23788,.T.);
#54327=EDGE_CURVE('',#41312,#41276,#23789,.T.);
#54328=EDGE_CURVE('',#41431,#41442,#34284,.T.);
#54329=EDGE_CURVE('',#41447,#41274,#23790,.T.);
#54330=EDGE_CURVE('',#41258,#41444,#23791,.T.);
#54331=EDGE_CURVE('',#41295,#41259,#23792,.T.);
#54332=EDGE_CURVE('',#41292,#41256,#23793,.T.);
#54333=EDGE_CURVE('',#41445,#41446,#34285,.T.);
#54334=EDGE_CURVE('',#41453,#41254,#23794,.T.);
#54335=EDGE_CURVE('',#41238,#41448,#23795,.T.);
#54336=EDGE_CURVE('',#41275,#41239,#23796,.T.);
#54337=EDGE_CURVE('',#41272,#41236,#23797,.T.);
#54338=EDGE_CURVE('',#41449,#41452,#34286,.T.);
#54339=EDGE_CURVE('',#41441,#41396,#23798,.T.);
#54340=EDGE_CURVE('',#41380,#41420,#23799,.T.);
#54341=EDGE_CURVE('',#41409,#41381,#23800,.T.);
#54342=EDGE_CURVE('',#41406,#41378,#23801,.T.);
#54343=EDGE_CURVE('',#41421,#41440,#23802,.T.);
#54344=EDGE_CURVE('',#41467,#41225,#23803,.T.);
#54345=EDGE_CURVE('',#41451,#41467,#34287,.T.);
#54346=EDGE_CURVE('',#41467,#41454,#23804,.T.);
#54347=EDGE_CURVE('',#41367,#41468,#23805,.T.);
#54348=EDGE_CURVE('',#41468,#41438,#34288,.T.);
#54349=EDGE_CURVE('',#41439,#41376,#23806,.T.);
#54350=EDGE_CURVE('',#41415,#41408,#23807,.T.);
#54351=EDGE_CURVE('',#41397,#41359,#23808,.T.);
#54352=EDGE_CURVE('',#41423,#41468,#23809,.T.);
#54353=EDGE_CURVE('',#41377,#41339,#23810,.T.);
#54354=EDGE_CURVE('',#41425,#41436,#34289,.T.);
#54355=EDGE_CURVE('',#41355,#41319,#23811,.T.);
#54356=EDGE_CURVE('',#41427,#41434,#34290,.T.);
#54357=EDGE_CURVE('',#41255,#41217,#23812,.T.);
#54358=EDGE_CURVE('',#41216,#41450,#23813,.T.);
#54359=EDGE_CURVE('',#41235,#41185,#23814,.T.);
#54360=EDGE_CURVE('',#41457,#41458,#23815,.T.);
#54361=EDGE_CURVE('',#41201,#41202,#23816,.T.);
#54362=EDGE_CURVE('',#41411,#41469,#23817,.T.);
#54363=EDGE_CURVE('',#41469,#41470,#34291,.T.);
#54364=EDGE_CURVE('',#41470,#41412,#23818,.T.);
#54365=EDGE_CURVE('',#41466,#41471,#23819,.T.);
#54366=EDGE_CURVE('',#41471,#41465,#23820,.T.);
#54367=EDGE_CURVE('',#41419,#41416,#23821,.T.);
#54368=EDGE_CURVE('',#41417,#41472,#23822,.T.);
#54369=EDGE_CURVE('',#41472,#41473,#34292,.T.);
#54370=EDGE_CURVE('',#41473,#41414,#23823,.T.);
#54371=EDGE_CURVE('',#41394,#41356,#23824,.T.);
#54372=EDGE_CURVE('',#41252,#41214,#23825,.T.);
#54373=EDGE_CURVE('',#41232,#41182,#23826,.T.);
#54374=EDGE_CURVE('',#41374,#41336,#23827,.T.);
#54375=EDGE_CURVE('',#41352,#41316,#23828,.T.);
#54376=EDGE_CURVE('',#41198,#41204,#23829,.T.);
#54377=EDGE_CURVE('',#41470,#41181,#23830,.T.);
#54378=EDGE_CURVE('',#41471,#41463,#23831,.T.);
#54379=EDGE_CURVE('',#41472,#41161,#23832,.T.);
#54380=EDGE_CURVE('',#41473,#41399,#23833,.T.);
#54381=EDGE_CURVE('',#41469,#41212,#23834,.T.);
#54382=EDGE_CURVE('',#41474,#41475,#34293,.T.);
#54383=EDGE_CURVE('',#41475,#41476,#34294,.T.);
#54384=EDGE_CURVE('',#41476,#41477,#34295,.T.);
#54385=EDGE_CURVE('',#41477,#41478,#34296,.T.);
#54386=EDGE_CURVE('',#41478,#41479,#34297,.T.);
#54387=EDGE_CURVE('',#41479,#41474,#34298,.T.);
#54388=EDGE_CURVE('',#41480,#41476,#1302,.T.);
#54389=EDGE_CURVE('',#41475,#41480,#1303,.T.);
#54390=EDGE_CURVE('',#41476,#41481,#1304,.T.);
#54391=EDGE_CURVE('',#41481,#41477,#1305,.T.);
#54392=EDGE_CURVE('',#41477,#41482,#1306,.T.);
#54393=EDGE_CURVE('',#41482,#41478,#1307,.T.);
#54394=EDGE_CURVE('',#41478,#41483,#1308,.T.);
#54395=EDGE_CURVE('',#41483,#41479,#1309,.T.);
#54396=EDGE_CURVE('',#41479,#41484,#1310,.T.);
#54397=EDGE_CURVE('',#41484,#41474,#1311,.T.);
#54398=EDGE_CURVE('',#41474,#41485,#1312,.T.);
#54399=EDGE_CURVE('',#41485,#41475,#1313,.T.);
#54400=EDGE_CURVE('',#41486,#41487,#34299,.T.);
#54401=EDGE_CURVE('',#41486,#41488,#34300,.T.);
#54402=EDGE_CURVE('',#41488,#41489,#34301,.T.);
#54403=EDGE_CURVE('',#41489,#41490,#34302,.T.);
#54404=EDGE_CURVE('',#41490,#41491,#34303,.T.);
#54405=EDGE_CURVE('',#41491,#41487,#34304,.T.);
#54406=EDGE_CURVE('',#41492,#41486,#1314,.T.);
#54407=EDGE_CURVE('',#41488,#41492,#1315,.T.);
#54408=EDGE_CURVE('',#41493,#41488,#1316,.T.);
#54409=EDGE_CURVE('',#41489,#41493,#1317,.T.);
#54410=EDGE_CURVE('',#41494,#41489,#1318,.T.);
#54411=EDGE_CURVE('',#41490,#41494,#1319,.T.);
#54412=EDGE_CURVE('',#41495,#41490,#1320,.T.);
#54413=EDGE_CURVE('',#41491,#41495,#1321,.T.);
#54414=EDGE_CURVE('',#41496,#41491,#1322,.T.);
#54415=EDGE_CURVE('',#41487,#41496,#1323,.T.);
#54416=EDGE_CURVE('',#41486,#41497,#1324,.T.);
#54417=EDGE_CURVE('',#41497,#41487,#1325,.T.);
#54418=EDGE_CURVE('',#41485,#41492,#23835,.T.);
#54419=EDGE_CURVE('',#41480,#41497,#23836,.T.);
#54420=EDGE_CURVE('',#41484,#41493,#23837,.T.);
#54421=EDGE_CURVE('',#41483,#41494,#23838,.T.);
#54422=EDGE_CURVE('',#41482,#41495,#23839,.T.);
#54423=EDGE_CURVE('',#41481,#41496,#23840,.T.);
#54424=EDGE_CURVE('',#41498,#41499,#34305,.T.);
#54425=EDGE_CURVE('',#41499,#41500,#34306,.T.);
#54426=EDGE_CURVE('',#41500,#41501,#34307,.T.);
#54427=EDGE_CURVE('',#41501,#41502,#34308,.T.);
#54428=EDGE_CURVE('',#41502,#41503,#34309,.T.);
#54429=EDGE_CURVE('',#41503,#41498,#34310,.T.);
#54430=EDGE_CURVE('',#41504,#41500,#1326,.T.);
#54431=EDGE_CURVE('',#41499,#41504,#1327,.T.);
#54432=EDGE_CURVE('',#41500,#41505,#1328,.T.);
#54433=EDGE_CURVE('',#41505,#41501,#1329,.T.);
#54434=EDGE_CURVE('',#41501,#41506,#1330,.T.);
#54435=EDGE_CURVE('',#41506,#41502,#1331,.T.);
#54436=EDGE_CURVE('',#41502,#41507,#1332,.T.);
#54437=EDGE_CURVE('',#41507,#41503,#1333,.T.);
#54438=EDGE_CURVE('',#41503,#41508,#1334,.T.);
#54439=EDGE_CURVE('',#41508,#41498,#1335,.T.);
#54440=EDGE_CURVE('',#41498,#41509,#1336,.T.);
#54441=EDGE_CURVE('',#41509,#41499,#1337,.T.);
#54442=EDGE_CURVE('',#41510,#41511,#34311,.T.);
#54443=EDGE_CURVE('',#41510,#41512,#34312,.T.);
#54444=EDGE_CURVE('',#41512,#41513,#34313,.T.);
#54445=EDGE_CURVE('',#41513,#41514,#34314,.T.);
#54446=EDGE_CURVE('',#41514,#41515,#34315,.T.);
#54447=EDGE_CURVE('',#41515,#41511,#34316,.T.);
#54448=EDGE_CURVE('',#41516,#41510,#1338,.T.);
#54449=EDGE_CURVE('',#41512,#41516,#1339,.T.);
#54450=EDGE_CURVE('',#41517,#41512,#1340,.T.);
#54451=EDGE_CURVE('',#41513,#41517,#1341,.T.);
#54452=EDGE_CURVE('',#41518,#41513,#1342,.T.);
#54453=EDGE_CURVE('',#41514,#41518,#1343,.T.);
#54454=EDGE_CURVE('',#41519,#41514,#1344,.T.);
#54455=EDGE_CURVE('',#41515,#41519,#1345,.T.);
#54456=EDGE_CURVE('',#41520,#41515,#1346,.T.);
#54457=EDGE_CURVE('',#41511,#41520,#1347,.T.);
#54458=EDGE_CURVE('',#41510,#41521,#1348,.T.);
#54459=EDGE_CURVE('',#41521,#41511,#1349,.T.);
#54460=EDGE_CURVE('',#41509,#41516,#23841,.T.);
#54461=EDGE_CURVE('',#41504,#41521,#23842,.T.);
#54462=EDGE_CURVE('',#41508,#41517,#23843,.T.);
#54463=EDGE_CURVE('',#41507,#41518,#23844,.T.);
#54464=EDGE_CURVE('',#41506,#41519,#23845,.T.);
#54465=EDGE_CURVE('',#41505,#41520,#23846,.T.);
#54466=EDGE_CURVE('',#41522,#41523,#23847,.T.);
#54467=EDGE_CURVE('',#41524,#41522,#1350,.T.);
#54468=EDGE_CURVE('',#41524,#41525,#23848,.T.);
#54469=EDGE_CURVE('',#41523,#41525,#1351,.T.);
#54470=EDGE_CURVE('',#41526,#41527,#23849,.T.);
#54471=EDGE_CURVE('',#41522,#41526,#1352,.T.);
#54472=EDGE_CURVE('',#41527,#41523,#1353,.T.);
#54473=EDGE_CURVE('',#41528,#41529,#23850,.T.);
#54474=EDGE_CURVE('',#41526,#41528,#1354,.T.);
#54475=EDGE_CURVE('',#41529,#41527,#1355,.T.);
#54476=EDGE_CURVE('',#41530,#41531,#23851,.T.);
#54477=EDGE_CURVE('',#41528,#41530,#1356,.T.);
#54478=EDGE_CURVE('',#41531,#41529,#1357,.T.);
#54479=EDGE_CURVE('',#41532,#41533,#23852,.T.);
#54480=EDGE_CURVE('',#41530,#41532,#1358,.T.);
#54481=EDGE_CURVE('',#41533,#41531,#1359,.T.);
#54482=EDGE_CURVE('',#41532,#41524,#1360,.T.);
#54483=EDGE_CURVE('',#41525,#41533,#1361,.T.);
#54484=EDGE_CURVE('',#41534,#41528,#23853,.T.);
#54485=EDGE_CURVE('',#41523,#41525,#34317,.T.);
#54486=EDGE_CURVE('',#41527,#41523,#34318,.T.);
#54487=EDGE_CURVE('',#41529,#41527,#34319,.T.);
#54488=EDGE_CURVE('',#41531,#41529,#34320,.T.);
#54489=EDGE_CURVE('',#41533,#41531,#34321,.T.);
#54490=EDGE_CURVE('',#41525,#41533,#34322,.T.);
#54491=EDGE_CURVE('',#41535,#41535,#34323,.T.);
#54492=EDGE_CURVE('',#41535,#41536,#34324,.T.);
#54493=EDGE_CURVE('',#41536,#41537,#34325,.T.);
#54494=EDGE_CURVE('',#41537,#41536,#34326,.T.);
#54495=EDGE_CURVE('',#41538,#41538,#34327,.T.);
#54496=EDGE_CURVE('',#41538,#41537,#23854,.T.);
#54497=EDGE_CURVE('',#41539,#41540,#2016,.T.);
#54498=EDGE_CURVE('',#41540,#41541,#2017,.T.);
#54499=EDGE_CURVE('',#41541,#41539,#23855,.T.);
#54500=EDGE_CURVE('',#41542,#41543,#23856,.T.);
#54501=EDGE_CURVE('',#41543,#41544,#2018,.T.);
#54502=EDGE_CURVE('',#41542,#41544,#34328,.T.);
#54503=EDGE_CURVE('',#41544,#41545,#34329,.T.);
#54504=EDGE_CURVE('',#41546,#41545,#34330,.T.);
#54505=EDGE_CURVE('',#41542,#41546,#34331,.T.);
#54506=EDGE_CURVE('',#41545,#41547,#23857,.T.);
#54507=EDGE_CURVE('',#41548,#41547,#34332,.T.);
#54508=EDGE_CURVE('',#41548,#41546,#23858,.T.);
#54509=EDGE_CURVE('',#41547,#41549,#34333,.T.);
#54510=EDGE_CURVE('',#41549,#41548,#34334,.T.);
#54511=EDGE_CURVE('',#41550,#41551,#34335,.T.);
#54512=EDGE_CURVE('',#41550,#41552,#5950,.T.);
#54513=EDGE_CURVE('',#41553,#41552,#34336,.T.);
#54514=EDGE_CURVE('',#41553,#41551,#34337,.T.);
#54515=EDGE_CURVE('',#41554,#41551,#34338,.T.);
#54516=EDGE_CURVE('',#41554,#41550,#34339,.T.);
#54517=EDGE_CURVE('',#41551,#41555,#34340,.T.);
#54518=EDGE_CURVE('',#41555,#41554,#5951,.T.);
#54519=EDGE_CURVE('',#41556,#41557,#34341,.T.);
#54520=EDGE_CURVE('',#41556,#41558,#5952,.T.);
#54521=EDGE_CURVE('',#41558,#41557,#34342,.T.);
#54522=EDGE_CURVE('',#41559,#41557,#34343,.T.);
#54523=EDGE_CURVE('',#41559,#41556,#34344,.T.);
#54524=EDGE_CURVE('',#41560,#41561,#34345,.T.);
#54525=EDGE_CURVE('',#41560,#41559,#5953,.T.);
#54526=EDGE_CURVE('',#41557,#41561,#34346,.T.);
#54527=EDGE_CURVE('',#41562,#41563,#34347,.T.);
#54528=EDGE_CURVE('',#41563,#41564,#5954,.T.);
#54529=EDGE_CURVE('',#41564,#41562,#34348,.T.);
#54530=EDGE_CURVE('',#41549,#41565,#5955,.T.);
#54531=EDGE_CURVE('',#41565,#41566,#34349,.T.);
#54532=EDGE_CURVE('',#41566,#41548,#34350,.T.);
#54533=EDGE_CURVE('',#41567,#41568,#2019,.T.);
#54534=EDGE_CURVE('',#41567,#41569,#23859,.T.);
#54535=EDGE_CURVE('',#41569,#41570,#2020,.T.);
#54536=EDGE_CURVE('',#41570,#41568,#23860,.T.);
#54537=EDGE_CURVE('',#41571,#41572,#2021,.T.);
#54538=EDGE_CURVE('',#41571,#41573,#23861,.T.);
#54539=EDGE_CURVE('',#41574,#41573,#5956,.T.);
#54540=EDGE_CURVE('',#41574,#41572,#23862,.T.);
#54541=EDGE_CURVE('',#41543,#41571,#23863,.T.);
#54542=EDGE_CURVE('',#41573,#41542,#23864,.T.);
#54543=EDGE_CURVE('',#41568,#41541,#23865,.T.);
#54544=EDGE_CURVE('',#41570,#41539,#23866,.T.);
#54545=EDGE_CURVE('',#41555,#41558,#23867,.T.);
#54546=EDGE_CURVE('',#41575,#41553,#23868,.T.);
#54547=EDGE_CURVE('',#41575,#41576,#23869,.T.);
#54548=EDGE_CURVE('',#41576,#41577,#23870,.T.);
#54549=EDGE_CURVE('',#41578,#41577,#23871,.T.);
#54550=EDGE_CURVE('',#41561,#41578,#23872,.T.);
#54551=EDGE_CURVE('',#41579,#41580,#23873,.T.);
#54552=EDGE_CURVE('',#41579,#41581,#2022,.T.);
#54553=EDGE_CURVE('',#41580,#41581,#2023,.T.);
#54554=EDGE_CURVE('',#41582,#41583,#34351,.T.);
#54555=EDGE_CURVE('',#41583,#41584,#2024,.T.);
#54556=EDGE_CURVE('',#41582,#41584,#23874,.T.);
#54557=EDGE_CURVE('',#41585,#41586,#34352,.T.);
#54558=EDGE_CURVE('',#41586,#41583,#34353,.T.);
#54559=EDGE_CURVE('',#41582,#41585,#34354,.T.);
#54560=EDGE_CURVE('',#41587,#41588,#34355,.T.);
#54561=EDGE_CURVE('',#41588,#41586,#23875,.T.);
#54562=EDGE_CURVE('',#41587,#41585,#23876,.T.);
#54563=EDGE_CURVE('',#41589,#41587,#34356,.T.);
#54564=EDGE_CURVE('',#41589,#41588,#34357,.T.);
#54565=EDGE_CURVE('',#41590,#41591,#34358,.T.);
#54566=EDGE_CURVE('',#41591,#41592,#5957,.T.);
#54567=EDGE_CURVE('',#41592,#41593,#34359,.T.);
#54568=EDGE_CURVE('',#41590,#41593,#34360,.T.);
#54569=EDGE_CURVE('',#41592,#41594,#34361,.T.);
#54570=EDGE_CURVE('',#41594,#41593,#34362,.T.);
#54571=EDGE_CURVE('',#41594,#41595,#5958,.T.);
#54572=EDGE_CURVE('',#41593,#41595,#34363,.T.);
#54573=EDGE_CURVE('',#41596,#41597,#34364,.T.);
#54574=EDGE_CURVE('',#41596,#41598,#5959,.T.);
#54575=EDGE_CURVE('',#41598,#41597,#34365,.T.);
#54576=EDGE_CURVE('',#41598,#41599,#34366,.T.);
#54577=EDGE_CURVE('',#41599,#41597,#34367,.T.);
#54578=EDGE_CURVE('',#41599,#41600,#5960,.T.);
#54579=EDGE_CURVE('',#41600,#41601,#34368,.T.);
#54580=EDGE_CURVE('',#41597,#41601,#34369,.T.);
#54581=EDGE_CURVE('',#41602,#41603,#34370,.T.);
#54582=EDGE_CURVE('',#41602,#41604,#5961,.T.);
#54583=EDGE_CURVE('',#41603,#41604,#34371,.T.);
#54584=EDGE_CURVE('',#41605,#41606,#34372,.T.);
#54585=EDGE_CURVE('',#41605,#41589,#5962,.T.);
#54586=EDGE_CURVE('',#41606,#41587,#34373,.T.);
#54587=EDGE_CURVE('',#41607,#41608,#2025,.T.);
#54588=EDGE_CURVE('',#41609,#41607,#23877,.T.);
#54589=EDGE_CURVE('',#41610,#41609,#2026,.T.);
#54590=EDGE_CURVE('',#41608,#41610,#23878,.T.);
#54591=EDGE_CURVE('',#41611,#41612,#2027,.T.);
#54592=EDGE_CURVE('',#41613,#41611,#23879,.T.);
#54593=EDGE_CURVE('',#41613,#41614,#5963,.T.);
#54594=EDGE_CURVE('',#41612,#41614,#23880,.T.);
#54595=EDGE_CURVE('',#41579,#41607,#23881,.T.);
#54596=EDGE_CURVE('',#41609,#41580,#23882,.T.);
#54597=EDGE_CURVE('',#41612,#41584,#23883,.T.);
#54598=EDGE_CURVE('',#41614,#41582,#23884,.T.);
#54599=EDGE_CURVE('',#41567,#41608,#23885,.T.);
#54600=EDGE_CURVE('',#41610,#41569,#23886,.T.);
#54601=EDGE_CURVE('',#41611,#41572,#23887,.T.);
#54602=EDGE_CURVE('',#41574,#41613,#23888,.T.);
#54603=EDGE_CURVE('',#41596,#41595,#23889,.T.);
#54604=EDGE_CURVE('',#41601,#41615,#23890,.T.);
#54605=EDGE_CURVE('',#41615,#41616,#23891,.T.);
#54606=EDGE_CURVE('',#41617,#41616,#23892,.T.);
#54607=EDGE_CURVE('',#41618,#41617,#23893,.T.);
#54608=EDGE_CURVE('',#41618,#41590,#23894,.T.);
#54609=EDGE_CURVE('',#41573,#41619,#34374,.T.);
#54610=EDGE_CURVE('',#41546,#41619,#23895,.T.);
#54611=EDGE_CURVE('',#41574,#41620,#34375,.T.);
#54612=EDGE_CURVE('',#41619,#41620,#1362,.T.);
#54613=EDGE_CURVE('',#41575,#41621,#34376,.T.);
#54614=EDGE_CURVE('',#41552,#41621,#23896,.T.);
#54615=EDGE_CURVE('',#41622,#41623,#34377,.T.);
#54616=EDGE_CURVE('',#41622,#41575,#34378,.T.);
#54617=EDGE_CURVE('',#41621,#41623,#34379,.T.);
#54618=EDGE_CURVE('',#41562,#41622,#23897,.T.);
#54619=EDGE_CURVE('',#41623,#41563,#23898,.T.);
#54620=EDGE_CURVE('',#41624,#41578,#34380,.T.);
#54621=EDGE_CURVE('',#41624,#41560,#23899,.T.);
#54622=EDGE_CURVE('',#41625,#41626,#34381,.T.);
#54623=EDGE_CURVE('',#41625,#41624,#34382,.T.);
#54624=EDGE_CURVE('',#41578,#41626,#34383,.T.);
#54625=EDGE_CURVE('',#41565,#41625,#23900,.T.);
#54626=EDGE_CURVE('',#41626,#41566,#23901,.T.);
#54627=EDGE_CURVE('',#41577,#41627,#34384,.T.);
#54628=EDGE_CURVE('',#41626,#41627,#23902,.T.);
#54629=EDGE_CURVE('',#41628,#41576,#34385,.T.);
#54630=EDGE_CURVE('',#41622,#41628,#23903,.T.);
#54631=EDGE_CURVE('',#41628,#41629,#23904,.T.);
#54632=EDGE_CURVE('',#41629,#41617,#34386,.T.);
#54633=EDGE_CURVE('',#41616,#41630,#34387,.T.);
#54634=EDGE_CURVE('',#41630,#41627,#23905,.T.);
#54635=EDGE_CURVE('',#41614,#41631,#34388,.T.);
#54636=EDGE_CURVE('',#41585,#41631,#23906,.T.);
#54637=EDGE_CURVE('',#41613,#41632,#34389,.T.);
#54638=EDGE_CURVE('',#41631,#41632,#1363,.T.);
#54639=EDGE_CURVE('',#41632,#41620,#23907,.T.);
#54640=EDGE_CURVE('',#41618,#41633,#34390,.T.);
#54641=EDGE_CURVE('',#41591,#41633,#23908,.T.);
#54642=EDGE_CURVE('',#41634,#41635,#34391,.T.);
#54643=EDGE_CURVE('',#41633,#41635,#34392,.T.);
#54644=EDGE_CURVE('',#41634,#41618,#34393,.T.);
#54645=EDGE_CURVE('',#41635,#41604,#23909,.T.);
#54646=EDGE_CURVE('',#41603,#41634,#23910,.T.);
#54647=EDGE_CURVE('',#41636,#41615,#34394,.T.);
#54648=EDGE_CURVE('',#41636,#41600,#23911,.T.);
#54649=EDGE_CURVE('',#41637,#41638,#34395,.T.);
#54650=EDGE_CURVE('',#41615,#41638,#34396,.T.);
#54651=EDGE_CURVE('',#41637,#41636,#34397,.T.);
#54652=EDGE_CURVE('',#41638,#41606,#23912,.T.);
#54653=EDGE_CURVE('',#41605,#41637,#23913,.T.);
#54654=EDGE_CURVE('',#41581,#41602,#23914,.T.);
#54655=EDGE_CURVE('',#41540,#41564,#23915,.T.);
#54656=EDGE_CURVE('',#41634,#41629,#23916,.T.);
#54657=EDGE_CURVE('',#41638,#41630,#23917,.T.);
#54658=EDGE_CURVE('',#41639,#41640,#23918,.T.);
#54659=EDGE_CURVE('',#41640,#41641,#5964,.F.);
#54660=EDGE_CURVE('',#41642,#41641,#34398,.T.);
#54661=EDGE_CURVE('',#41642,#41639,#5965,.F.);
#54662=EDGE_CURVE('',#41643,#41644,#23919,.T.);
#54663=EDGE_CURVE('',#41644,#41640,#5966,.F.);
#54664=EDGE_CURVE('',#41639,#41643,#5967,.F.);
#54665=EDGE_CURVE('',#41645,#41646,#23920,.T.);
#54666=EDGE_CURVE('',#41646,#41644,#5968,.F.);
#54667=EDGE_CURVE('',#41643,#41645,#5969,.F.);
#54668=EDGE_CURVE('',#41647,#41648,#23921,.T.);
#54669=EDGE_CURVE('',#41648,#41646,#5970,.F.);
#54670=EDGE_CURVE('',#41645,#41647,#5971,.F.);
#54671=EDGE_CURVE('',#41649,#41650,#23922,.T.);
#54672=EDGE_CURVE('',#41650,#41648,#5972,.F.);
#54673=EDGE_CURVE('',#41647,#41649,#5973,.F.);
#54674=EDGE_CURVE('',#41651,#41652,#23923,.T.);
#54675=EDGE_CURVE('',#41652,#41650,#5974,.F.);
#54676=EDGE_CURVE('',#41649,#41651,#5975,.F.);
#54677=EDGE_CURVE('',#41653,#41654,#23924,.T.);
#54678=EDGE_CURVE('',#41654,#41652,#5976,.F.);
#54679=EDGE_CURVE('',#41651,#41653,#5977,.F.);
#54680=EDGE_CURVE('',#41655,#41656,#23925,.T.);
#54681=EDGE_CURVE('',#41656,#41654,#5978,.F.);
#54682=EDGE_CURVE('',#41653,#41655,#5979,.F.);
#54683=EDGE_CURVE('',#41657,#41658,#23926,.T.);
#54684=EDGE_CURVE('',#41658,#41656,#5980,.F.);
#54685=EDGE_CURVE('',#41655,#41657,#5981,.F.);
#54686=EDGE_CURVE('',#41659,#41660,#23927,.T.);
#54687=EDGE_CURVE('',#41660,#41658,#5982,.F.);
#54688=EDGE_CURVE('',#41657,#41659,#5983,.F.);
#54689=EDGE_CURVE('',#41661,#41662,#23928,.T.);
#54690=EDGE_CURVE('',#41662,#41660,#5984,.F.);
#54691=EDGE_CURVE('',#41659,#41661,#5985,.F.);
#54692=EDGE_CURVE('',#41663,#41664,#23929,.T.);
#54693=EDGE_CURVE('',#41664,#41662,#5986,.F.);
#54694=EDGE_CURVE('',#41661,#41663,#5987,.F.);
#54695=EDGE_CURVE('',#41665,#41666,#23930,.T.);
#54696=EDGE_CURVE('',#41666,#41664,#5988,.F.);
#54697=EDGE_CURVE('',#41663,#41665,#5989,.F.);
#54698=EDGE_CURVE('',#41667,#41668,#23931,.T.);
#54699=EDGE_CURVE('',#41668,#41666,#5990,.F.);
#54700=EDGE_CURVE('',#41665,#41667,#5991,.F.);
#54701=EDGE_CURVE('',#41669,#41670,#23932,.T.);
#54702=EDGE_CURVE('',#41670,#41668,#5992,.F.);
#54703=EDGE_CURVE('',#41667,#41669,#5993,.F.);
#54704=EDGE_CURVE('',#41671,#41672,#23933,.T.);
#54705=EDGE_CURVE('',#41672,#41670,#5994,.F.);
#54706=EDGE_CURVE('',#41669,#41671,#5995,.F.);
#54707=EDGE_CURVE('',#41673,#41674,#23934,.T.);
#54708=EDGE_CURVE('',#41674,#41672,#5996,.F.);
#54709=EDGE_CURVE('',#41671,#41673,#5997,.F.);
#54710=EDGE_CURVE('',#41675,#41676,#23935,.T.);
#54711=EDGE_CURVE('',#41676,#41674,#5998,.F.);
#54712=EDGE_CURVE('',#41673,#41675,#5999,.F.);
#54713=EDGE_CURVE('',#41677,#41678,#23936,.T.);
#54714=EDGE_CURVE('',#41677,#41679,#6000,.F.);
#54715=EDGE_CURVE('',#41679,#41680,#6001,.T.);
#54716=EDGE_CURVE('',#41680,#41678,#6002,.F.);
#54717=EDGE_CURVE('',#41681,#41682,#23937,.T.);
#54718=EDGE_CURVE('',#41682,#41683,#6003,.F.);
#54719=EDGE_CURVE('',#41683,#41684,#34399,.T.);
#54720=EDGE_CURVE('',#41684,#41681,#6004,.F.);
#54721=EDGE_CURVE('',#41685,#41686,#23938,.T.);
#54722=EDGE_CURVE('',#41686,#41682,#6005,.F.);
#54723=EDGE_CURVE('',#41681,#41685,#6006,.F.);
#54724=EDGE_CURVE('',#41687,#41688,#23939,.T.);
#54725=EDGE_CURVE('',#41688,#41686,#6007,.F.);
#54726=EDGE_CURVE('',#41685,#41687,#6008,.F.);
#54727=EDGE_CURVE('',#41689,#41690,#23940,.T.);
#54728=EDGE_CURVE('',#41690,#41688,#6009,.F.);
#54729=EDGE_CURVE('',#41687,#41689,#6010,.F.);
#54730=EDGE_CURVE('',#41691,#41692,#23941,.T.);
#54731=EDGE_CURVE('',#41692,#41690,#6011,.F.);
#54732=EDGE_CURVE('',#41689,#41691,#6012,.F.);
#54733=EDGE_CURVE('',#41693,#41694,#23942,.T.);
#54734=EDGE_CURVE('',#41694,#41692,#6013,.F.);
#54735=EDGE_CURVE('',#41691,#41693,#6014,.F.);
#54736=EDGE_CURVE('',#41695,#41696,#23943,.T.);
#54737=EDGE_CURVE('',#41696,#41694,#6015,.F.);
#54738=EDGE_CURVE('',#41693,#41695,#6016,.F.);
#54739=EDGE_CURVE('',#41697,#41698,#23944,.T.);
#54740=EDGE_CURVE('',#41698,#41696,#6017,.F.);
#54741=EDGE_CURVE('',#41695,#41697,#6018,.F.);
#54742=EDGE_CURVE('',#41699,#41700,#23945,.T.);
#54743=EDGE_CURVE('',#41700,#41698,#6019,.F.);
#54744=EDGE_CURVE('',#41697,#41699,#6020,.F.);
#54745=EDGE_CURVE('',#41701,#41702,#23946,.T.);
#54746=EDGE_CURVE('',#41702,#41700,#6021,.F.);
#54747=EDGE_CURVE('',#41699,#41701,#6022,.F.);
#54748=EDGE_CURVE('',#41703,#41704,#23947,.T.);
#54749=EDGE_CURVE('',#41704,#41702,#6023,.F.);
#54750=EDGE_CURVE('',#41701,#41703,#6024,.F.);
#54751=EDGE_CURVE('',#41705,#41706,#23948,.T.);
#54752=EDGE_CURVE('',#41706,#41704,#6025,.F.);
#54753=EDGE_CURVE('',#41703,#41705,#6026,.F.);
#54754=EDGE_CURVE('',#41707,#41708,#23949,.T.);
#54755=EDGE_CURVE('',#41708,#41706,#6027,.F.);
#54756=EDGE_CURVE('',#41705,#41707,#6028,.F.);
#54757=EDGE_CURVE('',#41709,#41710,#23950,.T.);
#54758=EDGE_CURVE('',#41710,#41708,#6029,.F.);
#54759=EDGE_CURVE('',#41707,#41709,#6030,.F.);
#54760=EDGE_CURVE('',#41711,#41712,#23951,.T.);
#54761=EDGE_CURVE('',#41712,#41710,#6031,.F.);
#54762=EDGE_CURVE('',#41709,#41711,#6032,.F.);
#54763=EDGE_CURVE('',#41713,#41714,#23952,.T.);
#54764=EDGE_CURVE('',#41714,#41712,#6033,.F.);
#54765=EDGE_CURVE('',#41711,#41713,#6034,.F.);
#54766=EDGE_CURVE('',#41715,#41716,#23953,.T.);
#54767=EDGE_CURVE('',#41716,#41714,#6035,.F.);
#54768=EDGE_CURVE('',#41713,#41715,#6036,.F.);
#54769=EDGE_CURVE('',#41717,#41718,#23954,.T.);
#54770=EDGE_CURVE('',#41718,#41716,#6037,.F.);
#54771=EDGE_CURVE('',#41715,#41717,#6038,.F.);
#54772=EDGE_CURVE('',#41719,#41720,#23955,.T.);
#54773=EDGE_CURVE('',#41719,#41721,#6039,.T.);
#54774=EDGE_CURVE('',#41722,#41721,#6040,.T.);
#54775=EDGE_CURVE('',#41722,#41720,#6041,.F.);
#54776=EDGE_CURVE('',#41723,#41724,#23956,.T.);
#54777=EDGE_CURVE('',#41724,#41725,#1364,.T.);
#54778=EDGE_CURVE('',#41726,#41725,#6042,.T.);
#54779=EDGE_CURVE('',#41723,#41726,#1365,.T.);
#54780=EDGE_CURVE('',#41727,#41728,#23957,.T.);
#54781=EDGE_CURVE('',#41728,#41729,#1366,.T.);
#54782=EDGE_CURVE('',#41730,#41729,#6043,.T.);
#54783=EDGE_CURVE('',#41730,#41724,#1367,.T.);
#54784=EDGE_CURVE('',#41727,#41723,#1368,.T.);
#54785=EDGE_CURVE('',#41731,#41732,#23958,.T.);
#54786=EDGE_CURVE('',#41732,#41728,#1369,.T.);
#54787=EDGE_CURVE('',#41731,#41727,#1370,.T.);
#54788=EDGE_CURVE('',#41733,#41734,#23959,.T.);
#54789=EDGE_CURVE('',#41734,#41732,#1371,.T.);
#54790=EDGE_CURVE('',#41733,#41731,#1372,.T.);
#54791=EDGE_CURVE('',#41735,#41736,#23960,.T.);
#54792=EDGE_CURVE('',#41736,#41734,#1373,.T.);
#54793=EDGE_CURVE('',#41735,#41733,#1374,.T.);
#54794=EDGE_CURVE('',#41737,#41738,#23961,.T.);
#54795=EDGE_CURVE('',#41738,#41736,#1375,.T.);
#54796=EDGE_CURVE('',#41737,#41735,#1376,.T.);
#54797=EDGE_CURVE('',#41739,#41740,#23962,.T.);
#54798=EDGE_CURVE('',#41740,#41738,#1377,.T.);
#54799=EDGE_CURVE('',#41739,#41737,#1378,.T.);
#54800=EDGE_CURVE('',#41741,#41742,#23963,.T.);
#54801=EDGE_CURVE('',#41742,#41740,#1379,.T.);
#54802=EDGE_CURVE('',#41741,#41739,#1380,.T.);
#54803=EDGE_CURVE('',#41743,#41744,#23964,.T.);
#54804=EDGE_CURVE('',#41744,#41742,#1381,.T.);
#54805=EDGE_CURVE('',#41743,#41741,#1382,.T.);
#54806=EDGE_CURVE('',#41745,#41746,#23965,.T.);
#54807=EDGE_CURVE('',#41746,#41744,#1383,.T.);
#54808=EDGE_CURVE('',#41745,#41743,#1384,.T.);
#54809=EDGE_CURVE('',#41747,#41748,#23966,.T.);
#54810=EDGE_CURVE('',#41748,#41746,#1385,.T.);
#54811=EDGE_CURVE('',#41747,#41745,#1386,.T.);
#54812=EDGE_CURVE('',#41749,#41750,#23967,.T.);
#54813=EDGE_CURVE('',#41750,#41748,#1387,.T.);
#54814=EDGE_CURVE('',#41749,#41747,#1388,.T.);
#54815=EDGE_CURVE('',#41751,#41752,#23968,.T.);
#54816=EDGE_CURVE('',#41752,#41750,#1389,.T.);
#54817=EDGE_CURVE('',#41751,#41749,#1390,.T.);
#54818=EDGE_CURVE('',#41753,#41754,#23969,.T.);
#54819=EDGE_CURVE('',#41754,#41752,#1391,.T.);
#54820=EDGE_CURVE('',#41753,#41751,#1392,.T.);
#54821=EDGE_CURVE('',#41755,#41756,#23970,.T.);
#54822=EDGE_CURVE('',#41756,#41754,#1393,.T.);
#54823=EDGE_CURVE('',#41755,#41753,#1394,.T.);
#54824=EDGE_CURVE('',#41757,#41758,#23971,.T.);
#54825=EDGE_CURVE('',#41758,#41756,#1395,.T.);
#54826=EDGE_CURVE('',#41757,#41755,#1396,.T.);
#54827=EDGE_CURVE('',#41759,#41760,#23972,.T.);
#54828=EDGE_CURVE('',#41760,#41758,#1397,.T.);
#54829=EDGE_CURVE('',#41759,#41757,#1398,.T.);
#54830=EDGE_CURVE('',#41761,#41762,#23973,.T.);
#54831=EDGE_CURVE('',#41762,#41760,#1399,.T.);
#54832=EDGE_CURVE('',#41761,#41759,#1400,.T.);
#54833=EDGE_CURVE('',#41763,#41764,#23974,.T.);
#54834=EDGE_CURVE('',#41765,#41763,#34400,.T.);
#54835=EDGE_CURVE('',#41765,#41764,#1401,.T.);
#54836=EDGE_CURVE('',#41766,#41767,#23975,.T.);
#54837=EDGE_CURVE('',#41767,#41768,#6044,.T.);
#54838=EDGE_CURVE('',#41769,#41768,#34401,.T.);
#54839=EDGE_CURVE('',#41769,#41766,#6045,.T.);
#54840=EDGE_CURVE('',#41770,#41771,#23976,.T.);
#54841=EDGE_CURVE('',#41771,#41767,#6046,.T.);
#54842=EDGE_CURVE('',#41766,#41770,#6047,.T.);
#54843=EDGE_CURVE('',#41772,#41773,#23977,.T.);
#54844=EDGE_CURVE('',#41773,#41771,#6048,.T.);
#54845=EDGE_CURVE('',#41770,#41772,#6049,.T.);
#54846=EDGE_CURVE('',#41774,#41775,#23978,.T.);
#54847=EDGE_CURVE('',#41775,#41773,#6050,.T.);
#54848=EDGE_CURVE('',#41772,#41774,#6051,.T.);
#54849=EDGE_CURVE('',#41776,#41777,#23979,.T.);
#54850=EDGE_CURVE('',#41777,#41775,#6052,.T.);
#54851=EDGE_CURVE('',#41774,#41776,#6053,.T.);
#54852=EDGE_CURVE('',#41778,#41779,#23980,.T.);
#54853=EDGE_CURVE('',#41779,#41777,#6054,.T.);
#54854=EDGE_CURVE('',#41776,#41778,#6055,.T.);
#54855=EDGE_CURVE('',#41780,#41781,#23981,.T.);
#54856=EDGE_CURVE('',#41781,#41779,#6056,.T.);
#54857=EDGE_CURVE('',#41778,#41780,#6057,.T.);
#54858=EDGE_CURVE('',#41782,#41783,#23982,.T.);
#54859=EDGE_CURVE('',#41783,#41781,#6058,.T.);
#54860=EDGE_CURVE('',#41780,#41782,#6059,.T.);
#54861=EDGE_CURVE('',#41784,#41785,#23983,.T.);
#54862=EDGE_CURVE('',#41785,#41783,#6060,.T.);
#54863=EDGE_CURVE('',#41782,#41784,#6061,.T.);
#54864=EDGE_CURVE('',#41786,#41787,#23984,.T.);
#54865=EDGE_CURVE('',#41787,#41785,#6062,.T.);
#54866=EDGE_CURVE('',#41784,#41786,#6063,.T.);
#54867=EDGE_CURVE('',#41788,#41789,#23985,.T.);
#54868=EDGE_CURVE('',#41789,#41787,#6064,.T.);
#54869=EDGE_CURVE('',#41786,#41788,#6065,.T.);
#54870=EDGE_CURVE('',#41790,#41791,#23986,.T.);
#54871=EDGE_CURVE('',#41791,#41789,#6066,.T.);
#54872=EDGE_CURVE('',#41788,#41790,#6067,.T.);
#54873=EDGE_CURVE('',#41792,#41793,#23987,.T.);
#54874=EDGE_CURVE('',#41793,#41791,#6068,.T.);
#54875=EDGE_CURVE('',#41790,#41792,#6069,.T.);
#54876=EDGE_CURVE('',#41794,#41795,#23988,.T.);
#54877=EDGE_CURVE('',#41795,#41793,#6070,.T.);
#54878=EDGE_CURVE('',#41792,#41794,#6071,.T.);
#54879=EDGE_CURVE('',#41796,#41797,#23989,.T.);
#54880=EDGE_CURVE('',#41797,#41795,#6072,.T.);
#54881=EDGE_CURVE('',#41794,#41796,#6073,.T.);
#54882=EDGE_CURVE('',#41798,#41799,#23990,.T.);
#54883=EDGE_CURVE('',#41799,#41797,#6074,.T.);
#54884=EDGE_CURVE('',#41796,#41798,#6075,.T.);
#54885=EDGE_CURVE('',#41800,#41801,#23991,.T.);
#54886=EDGE_CURVE('',#41801,#41799,#6076,.T.);
#54887=EDGE_CURVE('',#41798,#41800,#6077,.T.);
#54888=EDGE_CURVE('',#41802,#41803,#23992,.T.);
#54889=EDGE_CURVE('',#41802,#41804,#6078,.T.);
#54890=EDGE_CURVE('',#41804,#41805,#6079,.T.);
#54891=EDGE_CURVE('',#41805,#41806,#6080,.F.);
#54892=EDGE_CURVE('',#41806,#41807,#34402,.T.);
#54893=EDGE_CURVE('',#41807,#41803,#6081,.T.);
#54894=EDGE_CURVE('',#41808,#41809,#23993,.T.);
#54895=EDGE_CURVE('',#41809,#41810,#1402,.T.);
#54896=EDGE_CURVE('',#41811,#41810,#6082,.T.);
#54897=EDGE_CURVE('',#41808,#41811,#1403,.T.);
#54898=EDGE_CURVE('',#41812,#41813,#23994,.T.);
#54899=EDGE_CURVE('',#41813,#41814,#1404,.T.);
#54900=EDGE_CURVE('',#41815,#41814,#6083,.T.);
#54901=EDGE_CURVE('',#41815,#41809,#1405,.T.);
#54902=EDGE_CURVE('',#41812,#41808,#1406,.T.);
#54903=EDGE_CURVE('',#41816,#41817,#23995,.T.);
#54904=EDGE_CURVE('',#41817,#41813,#1407,.T.);
#54905=EDGE_CURVE('',#41816,#41812,#1408,.T.);
#54906=EDGE_CURVE('',#41818,#41819,#23996,.T.);
#54907=EDGE_CURVE('',#41819,#41817,#1409,.T.);
#54908=EDGE_CURVE('',#41818,#41816,#1410,.T.);
#54909=EDGE_CURVE('',#41820,#41821,#23997,.T.);
#54910=EDGE_CURVE('',#41821,#41819,#1411,.T.);
#54911=EDGE_CURVE('',#41820,#41818,#1412,.T.);
#54912=EDGE_CURVE('',#41822,#41823,#23998,.T.);
#54913=EDGE_CURVE('',#41823,#41821,#1413,.T.);
#54914=EDGE_CURVE('',#41822,#41820,#1414,.T.);
#54915=EDGE_CURVE('',#41824,#41825,#23999,.T.);
#54916=EDGE_CURVE('',#41825,#41823,#1415,.T.);
#54917=EDGE_CURVE('',#41824,#41822,#1416,.T.);
#54918=EDGE_CURVE('',#41826,#41827,#24000,.T.);
#54919=EDGE_CURVE('',#41827,#41825,#1417,.T.);
#54920=EDGE_CURVE('',#41826,#41824,#1418,.T.);
#54921=EDGE_CURVE('',#41828,#41829,#24001,.T.);
#54922=EDGE_CURVE('',#41829,#41827,#1419,.T.);
#54923=EDGE_CURVE('',#41828,#41826,#1420,.T.);
#54924=EDGE_CURVE('',#41830,#41831,#24002,.T.);
#54925=EDGE_CURVE('',#41831,#41829,#1421,.T.);
#54926=EDGE_CURVE('',#41830,#41828,#1422,.T.);
#54927=EDGE_CURVE('',#41832,#41833,#24003,.T.);
#54928=EDGE_CURVE('',#41833,#41831,#1423,.T.);
#54929=EDGE_CURVE('',#41832,#41830,#1424,.T.);
#54930=EDGE_CURVE('',#41834,#41835,#24004,.T.);
#54931=EDGE_CURVE('',#41835,#41833,#1425,.T.);
#54932=EDGE_CURVE('',#41834,#41832,#1426,.T.);
#54933=EDGE_CURVE('',#41836,#41837,#24005,.T.);
#54934=EDGE_CURVE('',#41837,#41835,#1427,.T.);
#54935=EDGE_CURVE('',#41836,#41834,#1428,.T.);
#54936=EDGE_CURVE('',#41838,#41839,#24006,.T.);
#54937=EDGE_CURVE('',#41839,#41837,#1429,.T.);
#54938=EDGE_CURVE('',#41838,#41836,#1430,.T.);
#54939=EDGE_CURVE('',#41840,#41841,#24007,.T.);
#54940=EDGE_CURVE('',#41841,#41839,#1431,.T.);
#54941=EDGE_CURVE('',#41840,#41838,#1432,.T.);
#54942=EDGE_CURVE('',#41842,#41843,#24008,.T.);
#54943=EDGE_CURVE('',#41843,#41841,#1433,.T.);
#54944=EDGE_CURVE('',#41842,#41840,#1434,.T.);
#54945=EDGE_CURVE('',#41844,#41845,#24009,.T.);
#54946=EDGE_CURVE('',#41845,#41843,#1435,.T.);
#54947=EDGE_CURVE('',#41844,#41842,#1436,.T.);
#54948=EDGE_CURVE('',#41846,#41847,#24010,.T.);
#54949=EDGE_CURVE('',#41847,#41845,#1437,.T.);
#54950=EDGE_CURVE('',#41846,#41844,#1438,.T.);
#54951=EDGE_CURVE('',#41848,#41849,#24011,.T.);
#54952=EDGE_CURVE('',#41850,#41848,#34403,.T.);
#54953=EDGE_CURVE('',#41850,#41849,#1439,.T.);
#54954=EDGE_CURVE('',#41851,#41852,#24012,.T.);
#54955=EDGE_CURVE('',#41852,#41853,#34404,.T.);
#54956=EDGE_CURVE('',#41853,#41851,#6084,.T.);
#54957=EDGE_CURVE('',#41854,#41855,#24013,.T.);
#54958=EDGE_CURVE('',#41855,#41852,#6085,.T.);
#54959=EDGE_CURVE('',#41851,#41854,#6086,.T.);
#54960=EDGE_CURVE('',#41856,#41857,#24014,.T.);
#54961=EDGE_CURVE('',#41857,#41855,#6087,.T.);
#54962=EDGE_CURVE('',#41854,#41856,#6088,.T.);
#54963=EDGE_CURVE('',#41858,#41859,#24015,.T.);
#54964=EDGE_CURVE('',#41859,#41857,#6089,.T.);
#54965=EDGE_CURVE('',#41856,#41858,#6090,.T.);
#54966=EDGE_CURVE('',#41860,#41861,#24016,.T.);
#54967=EDGE_CURVE('',#41861,#41859,#6091,.T.);
#54968=EDGE_CURVE('',#41858,#41860,#6092,.T.);
#54969=EDGE_CURVE('',#41862,#41863,#24017,.T.);
#54970=EDGE_CURVE('',#41863,#41861,#6093,.T.);
#54971=EDGE_CURVE('',#41860,#41862,#6094,.T.);
#54972=EDGE_CURVE('',#41864,#41865,#24018,.T.);
#54973=EDGE_CURVE('',#41865,#41863,#6095,.T.);
#54974=EDGE_CURVE('',#41862,#41864,#6096,.T.);
#54975=EDGE_CURVE('',#41866,#41867,#24019,.T.);
#54976=EDGE_CURVE('',#41867,#41865,#6097,.T.);
#54977=EDGE_CURVE('',#41864,#41866,#6098,.T.);
#54978=EDGE_CURVE('',#41868,#41869,#24020,.T.);
#54979=EDGE_CURVE('',#41869,#41867,#6099,.T.);
#54980=EDGE_CURVE('',#41866,#41868,#6100,.T.);
#54981=EDGE_CURVE('',#41870,#41871,#24021,.T.);
#54982=EDGE_CURVE('',#41871,#41869,#6101,.T.);
#54983=EDGE_CURVE('',#41868,#41870,#6102,.T.);
#54984=EDGE_CURVE('',#41872,#41873,#24022,.T.);
#54985=EDGE_CURVE('',#41873,#41871,#6103,.T.);
#54986=EDGE_CURVE('',#41870,#41872,#6104,.T.);
#54987=EDGE_CURVE('',#41874,#41875,#24023,.T.);
#54988=EDGE_CURVE('',#41875,#41873,#6105,.T.);
#54989=EDGE_CURVE('',#41872,#41874,#6106,.T.);
#54990=EDGE_CURVE('',#41876,#41877,#24024,.T.);
#54991=EDGE_CURVE('',#41877,#41875,#6107,.T.);
#54992=EDGE_CURVE('',#41874,#41876,#6108,.T.);
#54993=EDGE_CURVE('',#41878,#41879,#24025,.T.);
#54994=EDGE_CURVE('',#41879,#41877,#6109,.T.);
#54995=EDGE_CURVE('',#41876,#41878,#6110,.T.);
#54996=EDGE_CURVE('',#41880,#41881,#24026,.T.);
#54997=EDGE_CURVE('',#41881,#41879,#6111,.T.);
#54998=EDGE_CURVE('',#41878,#41880,#6112,.T.);
#54999=EDGE_CURVE('',#41882,#41883,#24027,.T.);
#55000=EDGE_CURVE('',#41883,#41881,#6113,.T.);
#55001=EDGE_CURVE('',#41880,#41882,#6114,.T.);
#55002=EDGE_CURVE('',#41884,#41885,#24028,.T.);
#55003=EDGE_CURVE('',#41885,#41883,#6115,.T.);
#55004=EDGE_CURVE('',#41882,#41884,#6116,.T.);
#55005=EDGE_CURVE('',#41886,#41887,#24029,.T.);
#55006=EDGE_CURVE('',#41887,#41885,#6117,.T.);
#55007=EDGE_CURVE('',#41884,#41886,#6118,.T.);
#55008=EDGE_CURVE('',#41888,#41889,#24030,.T.);
#55009=EDGE_CURVE('',#41888,#41890,#6119,.T.);
#55010=EDGE_CURVE('',#41891,#41890,#6120,.T.);
#55011=EDGE_CURVE('',#41891,#41889,#6121,.T.);
#55012=EDGE_CURVE('',#41892,#41893,#24031,.T.);
#55013=EDGE_CURVE('',#41893,#41894,#1440,.T.);
#55014=EDGE_CURVE('',#41895,#41894,#6122,.T.);
#55015=EDGE_CURVE('',#41892,#41895,#1441,.T.);
#55016=EDGE_CURVE('',#41896,#41897,#24032,.T.);
#55017=EDGE_CURVE('',#41897,#41898,#1442,.T.);
#55018=EDGE_CURVE('',#41899,#41898,#6123,.T.);
#55019=EDGE_CURVE('',#41899,#41893,#1443,.T.);
#55020=EDGE_CURVE('',#41896,#41892,#1444,.T.);
#55021=EDGE_CURVE('',#41900,#41901,#24033,.T.);
#55022=EDGE_CURVE('',#41901,#41897,#1445,.T.);
#55023=EDGE_CURVE('',#41900,#41896,#1446,.T.);
#55024=EDGE_CURVE('',#41902,#41903,#24034,.T.);
#55025=EDGE_CURVE('',#41903,#41901,#1447,.T.);
#55026=EDGE_CURVE('',#41902,#41900,#1448,.T.);
#55027=EDGE_CURVE('',#41904,#41905,#24035,.T.);
#55028=EDGE_CURVE('',#41905,#41903,#1449,.T.);
#55029=EDGE_CURVE('',#41904,#41902,#1450,.T.);
#55030=EDGE_CURVE('',#41906,#41907,#24036,.T.);
#55031=EDGE_CURVE('',#41907,#41905,#1451,.T.);
#55032=EDGE_CURVE('',#41906,#41904,#1452,.T.);
#55033=EDGE_CURVE('',#41908,#41909,#24037,.T.);
#55034=EDGE_CURVE('',#41909,#41907,#1453,.T.);
#55035=EDGE_CURVE('',#41908,#41906,#1454,.T.);
#55036=EDGE_CURVE('',#41910,#41911,#24038,.T.);
#55037=EDGE_CURVE('',#41911,#41909,#1455,.T.);
#55038=EDGE_CURVE('',#41910,#41908,#1456,.T.);
#55039=EDGE_CURVE('',#41912,#41913,#24039,.T.);
#55040=EDGE_CURVE('',#41913,#41911,#1457,.T.);
#55041=EDGE_CURVE('',#41912,#41910,#1458,.T.);
#55042=EDGE_CURVE('',#41914,#41915,#24040,.T.);
#55043=EDGE_CURVE('',#41915,#41913,#1459,.T.);
#55044=EDGE_CURVE('',#41914,#41912,#1460,.T.);
#55045=EDGE_CURVE('',#41916,#41917,#24041,.T.);
#55046=EDGE_CURVE('',#41917,#41915,#1461,.T.);
#55047=EDGE_CURVE('',#41916,#41914,#1462,.T.);
#55048=EDGE_CURVE('',#41918,#41919,#24042,.T.);
#55049=EDGE_CURVE('',#41919,#41917,#1463,.T.);
#55050=EDGE_CURVE('',#41918,#41916,#1464,.T.);
#55051=EDGE_CURVE('',#41920,#41921,#24043,.T.);
#55052=EDGE_CURVE('',#41921,#41919,#1465,.T.);
#55053=EDGE_CURVE('',#41920,#41918,#1466,.T.);
#55054=EDGE_CURVE('',#41922,#41923,#24044,.T.);
#55055=EDGE_CURVE('',#41923,#41921,#1467,.T.);
#55056=EDGE_CURVE('',#41922,#41920,#1468,.T.);
#55057=EDGE_CURVE('',#41924,#41925,#24045,.T.);
#55058=EDGE_CURVE('',#41925,#41923,#1469,.T.);
#55059=EDGE_CURVE('',#41924,#41922,#1470,.T.);
#55060=EDGE_CURVE('',#41926,#41927,#24046,.T.);
#55061=EDGE_CURVE('',#41927,#41925,#1471,.T.);
#55062=EDGE_CURVE('',#41926,#41924,#1472,.T.);
#55063=EDGE_CURVE('',#41928,#41929,#24047,.T.);
#55064=EDGE_CURVE('',#41929,#41927,#1473,.T.);
#55065=EDGE_CURVE('',#41928,#41926,#1474,.T.);
#55066=EDGE_CURVE('',#41930,#41931,#24048,.T.);
#55067=EDGE_CURVE('',#41931,#41929,#1475,.T.);
#55068=EDGE_CURVE('',#41930,#41928,#1476,.T.);
#55069=EDGE_CURVE('',#41932,#41933,#24049,.T.);
#55070=EDGE_CURVE('',#41934,#41932,#34405,.T.);
#55071=EDGE_CURVE('',#41934,#41933,#1477,.T.);
#55072=EDGE_CURVE('',#41935,#41936,#24050,.T.);
#55073=EDGE_CURVE('',#41936,#41937,#1478,.T.);
#55074=EDGE_CURVE('',#41938,#41937,#6124,.T.);
#55075=EDGE_CURVE('',#41935,#41938,#1479,.T.);
#55076=EDGE_CURVE('',#41939,#41940,#24051,.T.);
#55077=EDGE_CURVE('',#41940,#41941,#1480,.T.);
#55078=EDGE_CURVE('',#41942,#41941,#6125,.T.);
#55079=EDGE_CURVE('',#41942,#41936,#1481,.T.);
#55080=EDGE_CURVE('',#41939,#41935,#1482,.T.);
#55081=EDGE_CURVE('',#41943,#41944,#24052,.T.);
#55082=EDGE_CURVE('',#41944,#41940,#1483,.T.);
#55083=EDGE_CURVE('',#41943,#41939,#1484,.T.);
#55084=EDGE_CURVE('',#41945,#41946,#24053,.T.);
#55085=EDGE_CURVE('',#41946,#41944,#1485,.T.);
#55086=EDGE_CURVE('',#41945,#41943,#1486,.T.);
#55087=EDGE_CURVE('',#41947,#41948,#24054,.T.);
#55088=EDGE_CURVE('',#41948,#41946,#1487,.T.);
#55089=EDGE_CURVE('',#41947,#41945,#1488,.T.);
#55090=EDGE_CURVE('',#41949,#41950,#24055,.T.);
#55091=EDGE_CURVE('',#41950,#41948,#1489,.T.);
#55092=EDGE_CURVE('',#41949,#41947,#1490,.T.);
#55093=EDGE_CURVE('',#41951,#41952,#24056,.T.);
#55094=EDGE_CURVE('',#41952,#41950,#1491,.T.);
#55095=EDGE_CURVE('',#41951,#41949,#1492,.T.);
#55096=EDGE_CURVE('',#41953,#41954,#24057,.T.);
#55097=EDGE_CURVE('',#41954,#41952,#1493,.T.);
#55098=EDGE_CURVE('',#41953,#41951,#1494,.T.);
#55099=EDGE_CURVE('',#41955,#41956,#24058,.T.);
#55100=EDGE_CURVE('',#41956,#41954,#1495,.T.);
#55101=EDGE_CURVE('',#41955,#41953,#1496,.T.);
#55102=EDGE_CURVE('',#41957,#41958,#24059,.T.);
#55103=EDGE_CURVE('',#41958,#41956,#1497,.T.);
#55104=EDGE_CURVE('',#41957,#41955,#1498,.T.);
#55105=EDGE_CURVE('',#41959,#41960,#24060,.T.);
#55106=EDGE_CURVE('',#41960,#41958,#1499,.T.);
#55107=EDGE_CURVE('',#41959,#41957,#1500,.T.);
#55108=EDGE_CURVE('',#41961,#41962,#24061,.T.);
#55109=EDGE_CURVE('',#41962,#41960,#1501,.T.);
#55110=EDGE_CURVE('',#41961,#41959,#1502,.T.);
#55111=EDGE_CURVE('',#41963,#41964,#24062,.T.);
#55112=EDGE_CURVE('',#41964,#41962,#1503,.T.);
#55113=EDGE_CURVE('',#41963,#41961,#1504,.T.);
#55114=EDGE_CURVE('',#41965,#41966,#24063,.T.);
#55115=EDGE_CURVE('',#41966,#41964,#1505,.T.);
#55116=EDGE_CURVE('',#41965,#41963,#1506,.T.);
#55117=EDGE_CURVE('',#41967,#41968,#24064,.T.);
#55118=EDGE_CURVE('',#41968,#41966,#1507,.T.);
#55119=EDGE_CURVE('',#41967,#41965,#1508,.T.);
#55120=EDGE_CURVE('',#41969,#41970,#24065,.T.);
#55121=EDGE_CURVE('',#41970,#41968,#1509,.T.);
#55122=EDGE_CURVE('',#41969,#41967,#1510,.T.);
#55123=EDGE_CURVE('',#41971,#41972,#24066,.T.);
#55124=EDGE_CURVE('',#41972,#41970,#1511,.T.);
#55125=EDGE_CURVE('',#41971,#41969,#1512,.T.);
#55126=EDGE_CURVE('',#41973,#41974,#24067,.T.);
#55127=EDGE_CURVE('',#41974,#41972,#1513,.T.);
#55128=EDGE_CURVE('',#41973,#41971,#1514,.T.);
#55129=EDGE_CURVE('',#41975,#41976,#24068,.T.);
#55130=EDGE_CURVE('',#41977,#41975,#34406,.T.);
#55131=EDGE_CURVE('',#41977,#41976,#1515,.T.);
#55132=EDGE_CURVE('',#41978,#41979,#24069,.T.);
#55133=EDGE_CURVE('',#41979,#41980,#24070,.T.);
#55134=EDGE_CURVE('',#41981,#41980,#24071,.T.);
#55135=EDGE_CURVE('',#41982,#41981,#24072,.T.);
#55136=EDGE_CURVE('',#41983,#41982,#24073,.T.);
#55137=EDGE_CURVE('',#41984,#41983,#24074,.T.);
#55138=EDGE_CURVE('',#41985,#41984,#24075,.T.);
#55139=EDGE_CURVE('',#41985,#41978,#24076,.T.);
#55140=EDGE_CURVE('',#41986,#41987,#24077,.T.);
#55141=EDGE_CURVE('',#41987,#41988,#34407,.T.);
#55142=EDGE_CURVE('',#41988,#41978,#24078,.T.);
#55143=EDGE_CURVE('',#41989,#41985,#24079,.T.);
#55144=EDGE_CURVE('',#41989,#41986,#34408,.T.);
#55145=EDGE_CURVE('',#41990,#41991,#6126,.T.);
#55146=EDGE_CURVE('',#41991,#41987,#24080,.T.);
#55147=EDGE_CURVE('',#41986,#41992,#24081,.T.);
#55148=EDGE_CURVE('',#41992,#41993,#24082,.T.);
#55149=EDGE_CURVE('',#41993,#41994,#24083,.T.);
#55150=EDGE_CURVE('',#41994,#41990,#6127,.T.);
#55151=EDGE_CURVE('',#41995,#41996,#24084,.T.);
#55152=EDGE_CURVE('',#41996,#41997,#24085,.T.);
#55153=EDGE_CURVE('',#41997,#41998,#24086,.T.);
#55154=EDGE_CURVE('',#41998,#41995,#24087,.T.);
#55155=EDGE_CURVE('',#41999,#41981,#24088,.T.);
#55156=EDGE_CURVE('',#42000,#41999,#24089,.T.);
#55157=EDGE_CURVE('',#42000,#41982,#24090,.T.);
#55158=EDGE_CURVE('',#41984,#42001,#24091,.T.);
#55159=EDGE_CURVE('',#42002,#41983,#24092,.T.);
#55160=EDGE_CURVE('',#42001,#42002,#24093,.T.);
#55161=EDGE_CURVE('',#42001,#41999,#24094,.T.);
#55162=EDGE_CURVE('',#42002,#42000,#24095,.T.);
#55163=EDGE_CURVE('',#41988,#42003,#24096,.T.);
#55164=EDGE_CURVE('',#42004,#42003,#34409,.T.);
#55165=EDGE_CURVE('',#42004,#42005,#24097,.T.);
#55166=EDGE_CURVE('',#42005,#42006,#24098,.T.);
#55167=EDGE_CURVE('',#42007,#42006,#34410,.T.);
#55168=EDGE_CURVE('',#42007,#41979,#24099,.T.);
#55169=EDGE_CURVE('',#42008,#42008,#34411,.T.);
#55170=EDGE_CURVE('',#42009,#42009,#34412,.T.);
#55171=EDGE_CURVE('',#42010,#42011,#6128,.T.);
#55172=EDGE_CURVE('',#42012,#42011,#24100,.T.);
#55173=EDGE_CURVE('',#42013,#42012,#6129,.T.);
#55174=EDGE_CURVE('',#42014,#42013,#6130,.T.);
#55175=EDGE_CURVE('',#42015,#42014,#6131,.T.);
#55176=EDGE_CURVE('',#42015,#42016,#24101,.T.);
#55177=EDGE_CURVE('',#42016,#42017,#34413,.T.);
#55178=EDGE_CURVE('',#42017,#42018,#24102,.T.);
#55179=EDGE_CURVE('',#42019,#42018,#6132,.T.);
#55180=EDGE_CURVE('',#42020,#42019,#6133,.T.);
#55181=EDGE_CURVE('',#42021,#42020,#6134,.T.);
#55182=EDGE_CURVE('',#42022,#42021,#24103,.T.);
#55183=EDGE_CURVE('',#42022,#42023,#6135,.T.);
#55184=EDGE_CURVE('',#42023,#42010,#2028,.T.);
#55185=EDGE_CURVE('',#42024,#42024,#34414,.T.);
#55186=EDGE_CURVE('',#42025,#42025,#34415,.T.);
#55187=EDGE_CURVE('',#42025,#42026,#24104,.T.);
#55188=EDGE_CURVE('',#42026,#42026,#34416,.T.);
#55189=EDGE_CURVE('',#42009,#42024,#24105,.T.);
#55190=EDGE_CURVE('',#42027,#42027,#34417,.T.);
#55191=EDGE_CURVE('',#42028,#42028,#34418,.T.);
#55192=EDGE_CURVE('',#42028,#42029,#24106,.T.);
#55193=EDGE_CURVE('',#42029,#42029,#34419,.T.);
#55194=EDGE_CURVE('',#42008,#42027,#24107,.T.);
#55195=EDGE_CURVE('',#42030,#42030,#34420,.T.);
#55196=EDGE_CURVE('',#42031,#42031,#34421,.T.);
#55197=EDGE_CURVE('',#42031,#42032,#24108,.T.);
#55198=EDGE_CURVE('',#42032,#42032,#34422,.T.);
#55199=EDGE_CURVE('',#42006,#42033,#6136,.T.);
#55200=EDGE_CURVE('',#42033,#42030,#24109,.T.);
#55201=EDGE_CURVE('',#42033,#42007,#6137,.T.);
#55202=EDGE_CURVE('',#42034,#42034,#34423,.T.);
#55203=EDGE_CURVE('',#42035,#42035,#34424,.T.);
#55204=EDGE_CURVE('',#42035,#42036,#24110,.T.);
#55205=EDGE_CURVE('',#42036,#42036,#34425,.T.);
#55206=EDGE_CURVE('',#42003,#42037,#34426,.T.);
#55207=EDGE_CURVE('',#42037,#42034,#24111,.T.);
#55208=EDGE_CURVE('',#42037,#42004,#34427,.T.);
#55209=EDGE_CURVE('',#42038,#42010,#34428,.T.);
#55210=EDGE_CURVE('',#42023,#42038,#34429,.T.);
#55211=EDGE_CURVE('',#42011,#42022,#34430,.T.);
#55212=EDGE_CURVE('',#42039,#42039,#34431,.T.);
#55213=EDGE_CURVE('',#42039,#42040,#34432,.T.);
#55214=EDGE_CURVE('',#42041,#42040,#34433,.T.);
#55215=EDGE_CURVE('',#42040,#42041,#34434,.T.);
#55216=EDGE_CURVE('',#42042,#42043,#34435,.T.);
#55217=EDGE_CURVE('',#42043,#42042,#34436,.T.);
#55218=EDGE_CURVE('',#42043,#42044,#34437,.T.);
#55219=EDGE_CURVE('',#42045,#42044,#34438,.T.);
#55220=EDGE_CURVE('',#42044,#42045,#34439,.T.);
#55221=EDGE_CURVE('',#42046,#42047,#24112,.T.);
#55222=EDGE_CURVE('',#42047,#42048,#1516,.T.);
#55223=EDGE_CURVE('',#42049,#42048,#24113,.T.);
#55224=EDGE_CURVE('',#42049,#42046,#1517,.T.);
#55225=EDGE_CURVE('',#42050,#42051,#24114,.T.);
#55226=EDGE_CURVE('',#42051,#42047,#1518,.T.);
#55227=EDGE_CURVE('',#42046,#42050,#1519,.T.);
#55228=EDGE_CURVE('',#42052,#42053,#24115,.T.);
#55229=EDGE_CURVE('',#42053,#42051,#1520,.T.);
#55230=EDGE_CURVE('',#42050,#42052,#1521,.T.);
#55231=EDGE_CURVE('',#42054,#42055,#24116,.T.);
#55232=EDGE_CURVE('',#42055,#42053,#1522,.T.);
#55233=EDGE_CURVE('',#42052,#42054,#1523,.T.);
#55234=EDGE_CURVE('',#42056,#42057,#24117,.T.);
#55235=EDGE_CURVE('',#42057,#42055,#1524,.T.);
#55236=EDGE_CURVE('',#42054,#42056,#1525,.T.);
#55237=EDGE_CURVE('',#42048,#42057,#1526,.T.);
#55238=EDGE_CURVE('',#42056,#42049,#1527,.T.);
#55239=EDGE_CURVE('',#42058,#42049,#24118,.T.);
#55240=EDGE_CURVE('',#42047,#42048,#34440,.T.);
#55241=EDGE_CURVE('',#42051,#42047,#34441,.T.);
#55242=EDGE_CURVE('',#42053,#42051,#34442,.T.);
#55243=EDGE_CURVE('',#42055,#42053,#34443,.T.);
#55244=EDGE_CURVE('',#42057,#42055,#34444,.T.);
#55245=EDGE_CURVE('',#42048,#42057,#34445,.T.);
#55246=EDGE_CURVE('',#42042,#42041,#24119,.T.);
#55247=EDGE_CURVE('',#42038,#42045,#24120,.T.);
#55248=EDGE_CURVE('',#42059,#42060,#6138,.T.);
#55249=EDGE_CURVE('',#42059,#42060,#6139,.T.);
#55250=EDGE_CURVE('',#42059,#42060,#6140,.T.);
#55251=EDGE_CURVE('',#42061,#42062,#6141,.T.);
#55252=EDGE_CURVE('',#42062,#42061,#6142,.T.);
#55253=EDGE_CURVE('',#42062,#42061,#6143,.T.);
#55254=EDGE_CURVE('',#42063,#42064,#34446,.T.);
#55255=EDGE_CURVE('',#42065,#42063,#2029,.T.);
#55256=EDGE_CURVE('',#42065,#42064,#34447,.T.);
#55257=EDGE_CURVE('',#42066,#42067,#34448,.T.);
#55258=EDGE_CURVE('',#42064,#42067,#6144,.T.);
#55259=EDGE_CURVE('',#42068,#42065,#6145,.T.);
#55260=EDGE_CURVE('',#42069,#42068,#6146,.T.);
#55261=EDGE_CURVE('',#42066,#42069,#6147,.T.);
#55262=EDGE_CURVE('',#42070,#42071,#34449,.T.);
#55263=EDGE_CURVE('',#42067,#42071,#2030,.T.);
#55264=EDGE_CURVE('',#42070,#42066,#2031,.T.);
#55265=EDGE_CURVE('',#42072,#42073,#34450,.T.);
#55266=EDGE_CURVE('',#42071,#42073,#6148,.T.);
#55267=EDGE_CURVE('',#42072,#42070,#6149,.T.);
#55268=EDGE_CURVE('',#42074,#42075,#34451,.T.);
#55269=EDGE_CURVE('',#42073,#42075,#6150,.T.);
#55270=EDGE_CURVE('',#42074,#42072,#6151,.T.);
#55271=EDGE_CURVE('',#42076,#42077,#6152,.T.);
#55272=EDGE_CURVE('',#42075,#42076,#6153,.T.);
#55273=EDGE_CURVE('',#42078,#42074,#6154,.T.);
#55274=EDGE_CURVE('',#42077,#42078,#6155,.T.);
#55275=EDGE_CURVE('',#42015,#42079,#6156,.T.);
#55276=EDGE_CURVE('',#42014,#42079,#34452,.T.);
#55277=EDGE_CURVE('',#42013,#42080,#34453,.T.);
#55278=EDGE_CURVE('',#42079,#42080,#6157,.T.);
#55279=EDGE_CURVE('',#42080,#42012,#24121,.T.);
#55280=EDGE_CURVE('',#42021,#42081,#24122,.T.);
#55281=EDGE_CURVE('',#42020,#42081,#34454,.T.);
#55282=EDGE_CURVE('',#42019,#42082,#34455,.T.);
#55283=EDGE_CURVE('',#42081,#42082,#6158,.T.);
#55284=EDGE_CURVE('',#42082,#42018,#6159,.T.);
#55285=EDGE_CURVE('',#42069,#42083,#6160,.T.);
#55286=EDGE_CURVE('',#42084,#42068,#6161,.T.);
#55287=EDGE_CURVE('',#42085,#42084,#24123,.T.);
#55288=EDGE_CURVE('',#42083,#42085,#6162,.T.);
#55289=EDGE_CURVE('',#42086,#42087,#34456,.T.);
#55290=EDGE_CURVE('',#42088,#42087,#6163,.T.);
#55291=EDGE_CURVE('',#42076,#42088,#6164,.T.);
#55292=EDGE_CURVE('',#42086,#42077,#2032,.T.);
#55293=EDGE_CURVE('',#42089,#42090,#34457,.T.);
#55294=EDGE_CURVE('',#42087,#42090,#24124,.T.);
#55295=EDGE_CURVE('',#42091,#42086,#24125,.T.);
#55296=EDGE_CURVE('',#42091,#42089,#34458,.T.);
#55297=EDGE_CURVE('',#42081,#42091,#6165,.T.);
#55298=EDGE_CURVE('',#42090,#42018,#6166,.T.);
#55299=EDGE_CURVE('',#42092,#42085,#6167,.T.);
#55300=EDGE_CURVE('',#42093,#42092,#6168,.T.);
#55301=EDGE_CURVE('',#42093,#42094,#34459,.T.);
#55302=EDGE_CURVE('',#42095,#42094,#2033,.T.);
#55303=EDGE_CURVE('',#42083,#42095,#6169,.T.);
#55304=EDGE_CURVE('',#42096,#42097,#34460,.T.);
#55305=EDGE_CURVE('',#42094,#42097,#24126,.T.);
#55306=EDGE_CURVE('',#42096,#42093,#24127,.T.);
#55307=EDGE_CURVE('',#42015,#42096,#6170,.T.);
#55308=EDGE_CURVE('',#42097,#42080,#6171,.T.);
#55309=EDGE_CURVE('',#42088,#42098,#2034,.T.);
#55310=EDGE_CURVE('',#42099,#42087,#34461,.T.);
#55311=EDGE_CURVE('',#42099,#42098,#34462,.T.);
#55312=EDGE_CURVE('',#42100,#42101,#34463,.T.);
#55313=EDGE_CURVE('',#42098,#42101,#34464,.T.);
#55314=EDGE_CURVE('',#42100,#42099,#34465,.T.);
#55315=EDGE_CURVE('',#42100,#42102,#34466,.T.);
#55316=EDGE_CURVE('',#42101,#42102,#34467,.T.);
#55317=EDGE_CURVE('',#42103,#42104,#34468,.T.);
#55318=EDGE_CURVE('',#42102,#42104,#24128,.T.);
#55319=EDGE_CURVE('',#42103,#42100,#24129,.T.);
#55320=EDGE_CURVE('',#42105,#42017,#34469,.T.);
#55321=EDGE_CURVE('',#42104,#42017,#6172,.T.);
#55322=EDGE_CURVE('',#42105,#42103,#6173,.T.);
#55323=EDGE_CURVE('',#42090,#42105,#24130,.T.);
#55324=EDGE_CURVE('',#42093,#42106,#34470,.T.);
#55325=EDGE_CURVE('',#42107,#42092,#34471,.T.);
#55326=EDGE_CURVE('',#42107,#42106,#34472,.T.);
#55327=EDGE_CURVE('',#42108,#42107,#34473,.T.);
#55328=EDGE_CURVE('',#42108,#42106,#34474,.T.);
#55329=EDGE_CURVE('',#42109,#42110,#34475,.T.);
#55330=EDGE_CURVE('',#42106,#42110,#24131,.T.);
#55331=EDGE_CURVE('',#42109,#42108,#24132,.T.);
#55332=EDGE_CURVE('',#42016,#42111,#34476,.T.);
#55333=EDGE_CURVE('',#42110,#42111,#6174,.T.);
#55334=EDGE_CURVE('',#42016,#42109,#6175,.T.);
#55335=EDGE_CURVE('',#42111,#42096,#24133,.T.);
#55336=EDGE_CURVE('',#42084,#42063,#1528,.T.);
#55337=EDGE_CURVE('',#42078,#42095,#34477,.T.);
#55338=EDGE_CURVE('',#42112,#42113,#24134,.T.);
#55339=EDGE_CURVE('',#42113,#42114,#34478,.T.);
#55340=EDGE_CURVE('',#42114,#42115,#24135,.T.);
#55341=EDGE_CURVE('',#42112,#42115,#6176,.T.);
#55342=EDGE_CURVE('',#42116,#42117,#24136,.T.);
#55343=EDGE_CURVE('',#42117,#42118,#34479,.T.);
#55344=EDGE_CURVE('',#42118,#42119,#24137,.T.);
#55345=EDGE_CURVE('',#42116,#42119,#6177,.T.);
#55346=EDGE_CURVE('',#42120,#42121,#24138,.T.);
#55347=EDGE_CURVE('',#42121,#42122,#34480,.T.);
#55348=EDGE_CURVE('',#42122,#42123,#24139,.T.);
#55349=EDGE_CURVE('',#42120,#42123,#6178,.T.);
#55350=EDGE_CURVE('',#42120,#42124,#34481,.T.);
#55351=EDGE_CURVE('',#42123,#42125,#34482,.T.);
#55352=EDGE_CURVE('',#42125,#42124,#6179,.T.);
#55353=EDGE_CURVE('',#42126,#42127,#24140,.T.);
#55354=EDGE_CURVE('',#42127,#42128,#34483,.T.);
#55355=EDGE_CURVE('',#42128,#42129,#24141,.T.);
#55356=EDGE_CURVE('',#42126,#42129,#6180,.T.);
#55357=EDGE_CURVE('',#42130,#42131,#24142,.T.);
#55358=EDGE_CURVE('',#42131,#42132,#34484,.T.);
#55359=EDGE_CURVE('',#42132,#42133,#24143,.T.);
#55360=EDGE_CURVE('',#42130,#42133,#1529,.T.);
#55361=EDGE_CURVE('',#42131,#42122,#24144,.T.);
#55362=EDGE_CURVE('',#42123,#42130,#6181,.T.);
#55363=EDGE_CURVE('',#42130,#42134,#34485,.T.);
#55364=EDGE_CURVE('',#42133,#42135,#34486,.T.);
#55365=EDGE_CURVE('',#42135,#42134,#6182,.T.);
#55366=EDGE_CURVE('',#42127,#42132,#34487,.T.);
#55367=EDGE_CURVE('',#42133,#42126,#34488,.T.);
#55368=EDGE_CURVE('',#42126,#42136,#34489,.T.);
#55369=EDGE_CURVE('',#42129,#42137,#34490,.T.);
#55370=EDGE_CURVE('',#42137,#42136,#6183,.T.);
#55371=EDGE_CURVE('',#42117,#42128,#24145,.T.);
#55372=EDGE_CURVE('',#42129,#42116,#6184,.T.);
#55373=EDGE_CURVE('',#42116,#42138,#34491,.T.);
#55374=EDGE_CURVE('',#42119,#42139,#34492,.T.);
#55375=EDGE_CURVE('',#42139,#42138,#6185,.T.);
#55376=EDGE_CURVE('',#42140,#42141,#24146,.T.);
#55377=EDGE_CURVE('',#42141,#42142,#34493,.T.);
#55378=EDGE_CURVE('',#42142,#42143,#24147,.T.);
#55379=EDGE_CURVE('',#42140,#42143,#6186,.T.);
#55380=EDGE_CURVE('',#42144,#42145,#24148,.T.);
#55381=EDGE_CURVE('',#42145,#42146,#34494,.T.);
#55382=EDGE_CURVE('',#42146,#42147,#24149,.T.);
#55383=EDGE_CURVE('',#42144,#42147,#1530,.T.);
#55384=EDGE_CURVE('',#42067,#42144,#6187,.T.);
#55385=EDGE_CURVE('',#42148,#42071,#24150,.T.);
#55386=EDGE_CURVE('',#42145,#42148,#24151,.T.);
#55387=EDGE_CURVE('',#42144,#42149,#34495,.T.);
#55388=EDGE_CURVE('',#42147,#42150,#34496,.T.);
#55389=EDGE_CURVE('',#42150,#42149,#6188,.T.);
#55390=EDGE_CURVE('',#42141,#42146,#34497,.T.);
#55391=EDGE_CURVE('',#42147,#42140,#34498,.T.);
#55392=EDGE_CURVE('',#42140,#42151,#34499,.T.);
#55393=EDGE_CURVE('',#42143,#42152,#34500,.T.);
#55394=EDGE_CURVE('',#42152,#42151,#6189,.T.);
#55395=EDGE_CURVE('',#42113,#42142,#24152,.T.);
#55396=EDGE_CURVE('',#42143,#42112,#6190,.T.);
#55397=EDGE_CURVE('',#42112,#42153,#34501,.T.);
#55398=EDGE_CURVE('',#42115,#42154,#34502,.T.);
#55399=EDGE_CURVE('',#42154,#42153,#6191,.T.);
#55400=EDGE_CURVE('',#42153,#42152,#6192,.T.);
#55401=EDGE_CURVE('',#42151,#42150,#34503,.T.);
#55402=EDGE_CURVE('',#42138,#42137,#6193,.T.);
#55403=EDGE_CURVE('',#42136,#42135,#34504,.T.);
#55404=EDGE_CURVE('',#42134,#42125,#6194,.T.);
#55405=EDGE_CURVE('',#42155,#42156,#24153,.T.);
#55406=EDGE_CURVE('',#42155,#42157,#6195,.T.);
#55407=EDGE_CURVE('',#42158,#42157,#24154,.T.);
#55408=EDGE_CURVE('',#42156,#42158,#34505,.T.);
#55409=EDGE_CURVE('',#42159,#42160,#24155,.T.);
#55410=EDGE_CURVE('',#42159,#42161,#6196,.T.);
#55411=EDGE_CURVE('',#42162,#42161,#24156,.T.);
#55412=EDGE_CURVE('',#42160,#42162,#34506,.T.);
#55413=EDGE_CURVE('',#42163,#42164,#24157,.T.);
#55414=EDGE_CURVE('',#42163,#42165,#6197,.T.);
#55415=EDGE_CURVE('',#42166,#42165,#24158,.T.);
#55416=EDGE_CURVE('',#42164,#42166,#34507,.T.);
#55417=EDGE_CURVE('',#42167,#42168,#24159,.T.);
#55418=EDGE_CURVE('',#42167,#42169,#6198,.T.);
#55419=EDGE_CURVE('',#42170,#42169,#24160,.T.);
#55420=EDGE_CURVE('',#42168,#42170,#34508,.T.);
#55421=EDGE_CURVE('',#42120,#42167,#34509,.T.);
#55422=EDGE_CURVE('',#42168,#42121,#34510,.T.);
#55423=EDGE_CURVE('',#42167,#42171,#34511,.T.);
#55424=EDGE_CURVE('',#42172,#42171,#6199,.T.);
#55425=EDGE_CURVE('',#42169,#42172,#34512,.T.);
#55426=EDGE_CURVE('',#42173,#42174,#24161,.T.);
#55427=EDGE_CURVE('',#42173,#42175,#6200,.T.);
#55428=EDGE_CURVE('',#42176,#42175,#24162,.T.);
#55429=EDGE_CURVE('',#42174,#42176,#34513,.T.);
#55430=EDGE_CURVE('',#42177,#42178,#24163,.T.);
#55431=EDGE_CURVE('',#42177,#42179,#6201,.T.);
#55432=EDGE_CURVE('',#42180,#42179,#24164,.T.);
#55433=EDGE_CURVE('',#42178,#42180,#34514,.T.);
#55434=EDGE_CURVE('',#42169,#42177,#6202,.T.);
#55435=EDGE_CURVE('',#42178,#42170,#24165,.T.);
#55436=EDGE_CURVE('',#42177,#42181,#34515,.T.);
#55437=EDGE_CURVE('',#42182,#42181,#6203,.T.);
#55438=EDGE_CURVE('',#42179,#42182,#34516,.T.);
#55439=EDGE_CURVE('',#42179,#42173,#34517,.T.);
#55440=EDGE_CURVE('',#42174,#42180,#34518,.T.);
#55441=EDGE_CURVE('',#42173,#42183,#34519,.T.);
#55442=EDGE_CURVE('',#42184,#42183,#6204,.T.);
#55443=EDGE_CURVE('',#42175,#42184,#34520,.T.);
#55444=EDGE_CURVE('',#42175,#42163,#6205,.T.);
#55445=EDGE_CURVE('',#42164,#42176,#24166,.T.);
#55446=EDGE_CURVE('',#42163,#42185,#34521,.T.);
#55447=EDGE_CURVE('',#42186,#42185,#6206,.T.);
#55448=EDGE_CURVE('',#42165,#42186,#34522,.T.);
#55449=EDGE_CURVE('',#42160,#42166,#34523,.T.);
#55450=EDGE_CURVE('',#42165,#42159,#34524,.T.);
#55451=EDGE_CURVE('',#42159,#42187,#34525,.T.);
#55452=EDGE_CURVE('',#42188,#42187,#6207,.T.);
#55453=EDGE_CURVE('',#42161,#42188,#34526,.T.);
#55454=EDGE_CURVE('',#42189,#42190,#24167,.T.);
#55455=EDGE_CURVE('',#42189,#42191,#6208,.T.);
#55456=EDGE_CURVE('',#42192,#42191,#24168,.T.);
#55457=EDGE_CURVE('',#42190,#42192,#34527,.T.);
#55458=EDGE_CURVE('',#42193,#42194,#24169,.T.);
#55459=EDGE_CURVE('',#42193,#42195,#6209,.T.);
#55460=EDGE_CURVE('',#42196,#42195,#24170,.T.);
#55461=EDGE_CURVE('',#42194,#42196,#34528,.T.);
#55462=EDGE_CURVE('',#42161,#42193,#6210,.T.);
#55463=EDGE_CURVE('',#42194,#42162,#24171,.T.);
#55464=EDGE_CURVE('',#42193,#42197,#34529,.T.);
#55465=EDGE_CURVE('',#42198,#42197,#6211,.T.);
#55466=EDGE_CURVE('',#42195,#42198,#34530,.T.);
#55467=EDGE_CURVE('',#42195,#42189,#34531,.T.);
#55468=EDGE_CURVE('',#42190,#42196,#34532,.T.);
#55469=EDGE_CURVE('',#42189,#42199,#34533,.T.);
#55470=EDGE_CURVE('',#42200,#42199,#6212,.T.);
#55471=EDGE_CURVE('',#42191,#42200,#34534,.T.);
#55472=EDGE_CURVE('',#42191,#42155,#6213,.T.);
#55473=EDGE_CURVE('',#42156,#42192,#24172,.T.);
#55474=EDGE_CURVE('',#42155,#42201,#34535,.T.);
#55475=EDGE_CURVE('',#42202,#42201,#6214,.T.);
#55476=EDGE_CURVE('',#42157,#42202,#34536,.T.);
#55477=EDGE_CURVE('',#42157,#42115,#34537,.T.);
#55478=EDGE_CURVE('',#42114,#42158,#34538,.T.);
#55479=EDGE_CURVE('',#42154,#42202,#34539,.T.);
#55480=EDGE_CURVE('',#42101,#42107,#34540,.T.);
#55481=EDGE_CURVE('',#42108,#42102,#34541,.T.);
#55482=EDGE_CURVE('',#42104,#42109,#34542,.T.);
#55483=EDGE_CURVE('',#42171,#42124,#34543,.T.);
#55484=EDGE_CURVE('',#42187,#42186,#34544,.T.);
#55485=EDGE_CURVE('',#42201,#42200,#6215,.T.);
#55486=EDGE_CURVE('',#42199,#42198,#34545,.T.);
#55487=EDGE_CURVE('',#42197,#42188,#6216,.T.);
#55488=EDGE_CURVE('',#42185,#42184,#6217,.T.);
#55489=EDGE_CURVE('',#42183,#42182,#34546,.T.);
#55490=EDGE_CURVE('',#42181,#42172,#6218,.T.);
#55491=EDGE_CURVE('',#42073,#42203,#24173,.T.);
#55492=EDGE_CURVE('',#42203,#42148,#34547,.T.);
#55493=EDGE_CURVE('',#42119,#42075,#34548,.T.);
#55494=EDGE_CURVE('',#42203,#42118,#34549,.T.);
#55495=EDGE_CURVE('',#42098,#42139,#34550,.T.);
#55496=EDGE_CURVE('',#42149,#42064,#6219,.T.);
#55497=EDGE_CURVE('',#42204,#42205,#6220,.T.);
#55498=EDGE_CURVE('',#42205,#42204,#6221,.T.);
#55499=EDGE_CURVE('',#42204,#42205,#6222,.T.);
#55500=EDGE_CURVE('',#42205,#42206,#6223,.T.);
#55501=EDGE_CURVE('',#42206,#42207,#6224,.T.);
#55502=EDGE_CURVE('',#42207,#42204,#6225,.T.);
#55503=EDGE_CURVE('',#41941,#41942,#6226,.T.);
#55504=EDGE_CURVE('',#42208,#42209,#24174,.T.);
#55505=EDGE_CURVE('',#42208,#42210,#6227,.T.);
#55506=EDGE_CURVE('',#42210,#42209,#6228,.T.);
#55507=EDGE_CURVE('',#42211,#42212,#24175,.T.);
#55508=EDGE_CURVE('',#42211,#42207,#34551,.T.);
#55509=EDGE_CURVE('',#42207,#42206,#6229,.T.);
#55510=EDGE_CURVE('',#42206,#41679,#6230,.T.);
#55511=EDGE_CURVE('',#41679,#42212,#6231,.T.);
#55512=EDGE_CURVE('',#42213,#42211,#24176,.T.);
#55513=EDGE_CURVE('',#42214,#42213,#6232,.T.);
#55514=EDGE_CURVE('',#42214,#42208,#24177,.T.);
#55515=EDGE_CURVE('',#41680,#42208,#34552,.T.);
#55516=EDGE_CURVE('',#41976,#41974,#1531,.T.);
#55517=EDGE_CURVE('',#41975,#41973,#1532,.T.);
#55518=EDGE_CURVE('',#41937,#41680,#6233,.T.);
#55519=EDGE_CURVE('',#41641,#41977,#6234,.T.);
#55520=EDGE_CURVE('',#41678,#41676,#6235,.F.);
#55521=EDGE_CURVE('',#42215,#41677,#6236,.F.);
#55522=EDGE_CURVE('',#42212,#42215,#6237,.T.);
#55523=EDGE_CURVE('',#41975,#41642,#6238,.T.);
#55524=EDGE_CURVE('',#42209,#41938,#6239,.T.);
#55525=EDGE_CURVE('',#41675,#42210,#6240,.F.);
#55526=EDGE_CURVE('',#42216,#42217,#6241,.T.);
#55527=EDGE_CURVE('',#42216,#42217,#6242,.T.);
#55528=EDGE_CURVE('',#41898,#41899,#6243,.T.);
#55529=EDGE_CURVE('',#41722,#42218,#6244,.T.);
#55530=EDGE_CURVE('',#42218,#41895,#6245,.T.);
#55531=EDGE_CURVE('',#41894,#41722,#6246,.T.);
#55532=EDGE_CURVE('',#42219,#42220,#24178,.T.);
#55533=EDGE_CURVE('',#42219,#41721,#2035,.T.);
#55534=EDGE_CURVE('',#41721,#42220,#6247,.T.);
#55535=EDGE_CURVE('',#42221,#42219,#24179,.T.);
#55536=EDGE_CURVE('',#42221,#42222,#6248,.T.);
#55537=EDGE_CURVE('',#42222,#42223,#24180,.T.);
#55538=EDGE_CURVE('',#42224,#42223,#6249,.T.);
#55539=EDGE_CURVE('',#42224,#42218,#6250,.T.);
#55540=EDGE_CURVE('',#41933,#41931,#1533,.T.);
#55541=EDGE_CURVE('',#41932,#41930,#1534,.T.);
#55542=EDGE_CURVE('',#42217,#42216,#6251,.T.);
#55543=EDGE_CURVE('',#41683,#41934,#6252,.T.);
#55544=EDGE_CURVE('',#41720,#41718,#6253,.F.);
#55545=EDGE_CURVE('',#42224,#41719,#6254,.T.);
#55546=EDGE_CURVE('',#42225,#42224,#6255,.T.);
#55547=EDGE_CURVE('',#42220,#42225,#6256,.T.);
#55548=EDGE_CURVE('',#41932,#41684,#6257,.T.);
#55549=EDGE_CURVE('',#41717,#42218,#6258,.F.);
#55550=EDGE_CURVE('',#42226,#42059,#6259,.T.);
#55551=EDGE_CURVE('',#42226,#42227,#6260,.T.);
#55552=EDGE_CURVE('',#42060,#42227,#6261,.T.);
#55553=EDGE_CURVE('',#41889,#41887,#6262,.T.);
#55554=EDGE_CURVE('',#41886,#42228,#6263,.T.);
#55555=EDGE_CURVE('',#42229,#42228,#6264,.T.);
#55556=EDGE_CURVE('',#42229,#41888,#6265,.T.);
#55557=EDGE_CURVE('',#41814,#41815,#6266,.T.);
#55558=EDGE_CURVE('',#41891,#42228,#6267,.T.);
#55559=EDGE_CURVE('',#42228,#41811,#6268,.T.);
#55560=EDGE_CURVE('',#41810,#41891,#6269,.T.);
#55561=EDGE_CURVE('',#42230,#42231,#24181,.T.);
#55562=EDGE_CURVE('',#42230,#41890,#34553,.T.);
#55563=EDGE_CURVE('',#41890,#42231,#6270,.T.);
#55564=EDGE_CURVE('',#42232,#42230,#24182,.T.);
#55565=EDGE_CURVE('',#42232,#42233,#6271,.T.);
#55566=EDGE_CURVE('',#42233,#42234,#24183,.T.);
#55567=EDGE_CURVE('',#42229,#42234,#6272,.T.);
#55568=EDGE_CURVE('',#41849,#41847,#1535,.T.);
#55569=EDGE_CURVE('',#41848,#41846,#1536,.T.);
#55570=EDGE_CURVE('',#42227,#42226,#6273,.T.);
#55571=EDGE_CURVE('',#41852,#41850,#6274,.T.);
#55572=EDGE_CURVE('',#42235,#42229,#6275,.T.);
#55573=EDGE_CURVE('',#42231,#42235,#6276,.T.);
#55574=EDGE_CURVE('',#41848,#41853,#6277,.T.);
#55575=EDGE_CURVE('',#42236,#42061,#6278,.F.);
#55576=EDGE_CURVE('',#42062,#42237,#6279,.T.);
#55577=EDGE_CURVE('',#42237,#42236,#6280,.T.);
#55578=EDGE_CURVE('',#41803,#41801,#6281,.T.);
#55579=EDGE_CURVE('',#41800,#41802,#6282,.T.);
#55580=EDGE_CURVE('',#41729,#41730,#6283,.T.);
#55581=EDGE_CURVE('',#42238,#42239,#24184,.T.);
#55582=EDGE_CURVE('',#42238,#41804,#6284,.T.);
#55583=EDGE_CURVE('',#41804,#42239,#6285,.T.);
#55584=EDGE_CURVE('',#42240,#42241,#24185,.T.);
#55585=EDGE_CURVE('',#42240,#42236,#34554,.T.);
#55586=EDGE_CURVE('',#42236,#42237,#6286,.T.);
#55587=EDGE_CURVE('',#42237,#41806,#6287,.T.);
#55588=EDGE_CURVE('',#41806,#42241,#6288,.T.);
#55589=EDGE_CURVE('',#42242,#42240,#24186,.T.);
#55590=EDGE_CURVE('',#42243,#42242,#6289,.T.);
#55591=EDGE_CURVE('',#42243,#42238,#24187,.T.);
#55592=EDGE_CURVE('',#41807,#42238,#34555,.T.);
#55593=EDGE_CURVE('',#41763,#41769,#6290,.T.);
#55594=EDGE_CURVE('',#41768,#41765,#6291,.T.);
#55595=EDGE_CURVE('',#41764,#41762,#1537,.T.);
#55596=EDGE_CURVE('',#41763,#41761,#1538,.T.);
#55597=EDGE_CURVE('',#41725,#41807,#6292,.T.);
#55598=EDGE_CURVE('',#42241,#41805,#6293,.T.);
#55599=EDGE_CURVE('',#42239,#41726,#6294,.T.);
#55600=EDGE_CURVE('',#42210,#42215,#6295,.T.);
#55601=EDGE_CURVE('',#42233,#42232,#6296,.T.);
#55602=EDGE_CURVE('',#42242,#42243,#6297,.T.);
#55603=EDGE_CURVE('',#42213,#42214,#6298,.T.);
#55604=EDGE_CURVE('',#42222,#42221,#6299,.T.);
#55605=EDGE_CURVE('',#41805,#42240,#6300,.T.);
#55606=EDGE_CURVE('',#42226,#42230,#6301,.T.);
#55607=EDGE_CURVE('',#42234,#42227,#6302,.T.);
#55608=EDGE_CURVE('',#42234,#42235,#24188,.T.);
#55609=EDGE_CURVE('',#42216,#42219,#6303,.T.);
#55610=EDGE_CURVE('',#42223,#42217,#6304,.T.);
#55611=EDGE_CURVE('',#42223,#42225,#24189,.T.);
#55612=EDGE_CURVE('',#42215,#42211,#6305,.T.);
#55613=EDGE_CURVE('',#41980,#42244,#24190,.T.);
#55614=EDGE_CURVE('',#42244,#41989,#24191,.T.);
#55615=EDGE_CURVE('',#42003,#41991,#34556,.T.);
#55616=EDGE_CURVE('',#42037,#41990,#34557,.T.);
#55617=EDGE_CURVE('',#42004,#41994,#34558,.T.);
#55618=EDGE_CURVE('',#41992,#42244,#34559,.T.);
#55619=EDGE_CURVE('',#41993,#41998,#34560,.T.);
#55620=EDGE_CURVE('',#41995,#41992,#34561,.T.);
#55621=EDGE_CURVE('',#42005,#41993,#34562,.T.);
#55622=EDGE_CURVE('',#41995,#42244,#34563,.T.);
#55623=EDGE_CURVE('',#42005,#41998,#34564,.T.);
#55624=EDGE_CURVE('',#41996,#41980,#2036,.T.);
#55625=EDGE_CURVE('',#41979,#41997,#2037,.T.);
#55626=EDGE_CURVE('',#42245,#42246,#24192,.T.);
#55627=EDGE_CURVE('',#42247,#42246,#24193,.T.);
#55628=EDGE_CURVE('',#42248,#42247,#24194,.T.);
#55629=EDGE_CURVE('',#42248,#42245,#24195,.T.);
#55630=EDGE_CURVE('',#42246,#42249,#24196,.T.);
#55631=EDGE_CURVE('',#42250,#42249,#24197,.T.);
#55632=EDGE_CURVE('',#42247,#42250,#24198,.T.);
#55633=EDGE_CURVE('',#42249,#42251,#24199,.T.);
#55634=EDGE_CURVE('',#42252,#42251,#24200,.T.);
#55635=EDGE_CURVE('',#42250,#42252,#24201,.T.);
#55636=EDGE_CURVE('',#42251,#42245,#24202,.T.);
#55637=EDGE_CURVE('',#42252,#42248,#24203,.T.);
#55638=EDGE_CURVE('',#42253,#42253,#34565,.T.);
#55639=EDGE_CURVE('',#42253,#42254,#34566,.T.);
#55640=EDGE_CURVE('',#42254,#42254,#34567,.T.);
#55641=EDGE_CURVE('',#42254,#42255,#24204,.T.);
#55642=EDGE_CURVE('',#42255,#42255,#34568,.T.);
#55643=EDGE_CURVE('',#42256,#42257,#6306,.T.);
#55644=EDGE_CURVE('',#42257,#42258,#24205,.T.);
#55645=EDGE_CURVE('',#42258,#42259,#6307,.T.);
#55646=EDGE_CURVE('',#42259,#42256,#24206,.T.);
#55647=EDGE_CURVE('',#42260,#42261,#6308,.T.);
#55648=EDGE_CURVE('',#42261,#42262,#24207,.T.);
#55649=EDGE_CURVE('',#42262,#42263,#6309,.T.);
#55650=EDGE_CURVE('',#42263,#42264,#34569,.T.);
#55651=EDGE_CURVE('',#42264,#42265,#6310,.T.);
#55652=EDGE_CURVE('',#42266,#42265,#24208,.T.);
#55653=EDGE_CURVE('',#42266,#42267,#6311,.T.);
#55654=EDGE_CURVE('',#42267,#42260,#34570,.T.);
#55655=EDGE_CURVE('',#42268,#42269,#34571,.T.);
#55656=EDGE_CURVE('',#42269,#42270,#6312,.T.);
#55657=EDGE_CURVE('',#42270,#42271,#24209,.T.);
#55658=EDGE_CURVE('',#42271,#42272,#6313,.T.);
#55659=EDGE_CURVE('',#42272,#42273,#34572,.T.);
#55660=EDGE_CURVE('',#42273,#42274,#6314,.T.);
#55661=EDGE_CURVE('',#42275,#42274,#24210,.T.);
#55662=EDGE_CURVE('',#42275,#42268,#6315,.T.);
#55663=EDGE_CURVE('',#42276,#42277,#34573,.T.);
#55664=EDGE_CURVE('',#42277,#42278,#6316,.T.);
#55665=EDGE_CURVE('',#42278,#42279,#24211,.T.);
#55666=EDGE_CURVE('',#42279,#42280,#6317,.T.);
#55667=EDGE_CURVE('',#42280,#42281,#34574,.T.);
#55668=EDGE_CURVE('',#42281,#42282,#6318,.T.);
#55669=EDGE_CURVE('',#42283,#42282,#24212,.T.);
#55670=EDGE_CURVE('',#42283,#42276,#6319,.T.);
#55671=EDGE_CURVE('',#42284,#42285,#6320,.T.);
#55672=EDGE_CURVE('',#42285,#42286,#34575,.T.);
#55673=EDGE_CURVE('',#42286,#42287,#6321,.T.);
#55674=EDGE_CURVE('',#42287,#42288,#24213,.T.);
#55675=EDGE_CURVE('',#42288,#42289,#6322,.T.);
#55676=EDGE_CURVE('',#42289,#42290,#34576,.T.);
#55677=EDGE_CURVE('',#42290,#42291,#6323,.T.);
#55678=EDGE_CURVE('',#42284,#42291,#24214,.T.);
#55679=EDGE_CURVE('',#42292,#42293,#34577,.T.);
#55680=EDGE_CURVE('',#42293,#42294,#6324,.T.);
#55681=EDGE_CURVE('',#42294,#42295,#24215,.T.);
#55682=EDGE_CURVE('',#42295,#42296,#6325,.T.);
#55683=EDGE_CURVE('',#42296,#42297,#34578,.T.);
#55684=EDGE_CURVE('',#42297,#42298,#6326,.T.);
#55685=EDGE_CURVE('',#42299,#42298,#24216,.T.);
#55686=EDGE_CURVE('',#42299,#42292,#6327,.T.);
#55687=EDGE_CURVE('',#42300,#42301,#34579,.T.);
#55688=EDGE_CURVE('',#42301,#42302,#6328,.T.);
#55689=EDGE_CURVE('',#42302,#42303,#24217,.T.);
#55690=EDGE_CURVE('',#42303,#42304,#6329,.T.);
#55691=EDGE_CURVE('',#42304,#42305,#34580,.T.);
#55692=EDGE_CURVE('',#42305,#42306,#6330,.T.);
#55693=EDGE_CURVE('',#42307,#42306,#24218,.T.);
#55694=EDGE_CURVE('',#42307,#42300,#6331,.T.);
#55695=EDGE_CURVE('',#42308,#42309,#6332,.T.);
#55696=EDGE_CURVE('',#42309,#42310,#24219,.T.);
#55697=EDGE_CURVE('',#42310,#42311,#6333,.T.);
#55698=EDGE_CURVE('',#42308,#42311,#24220,.T.);
#55699=EDGE_CURVE('',#42312,#42313,#34581,.T.);
#55700=EDGE_CURVE('',#42313,#42314,#24221,.T.);
#55701=EDGE_CURVE('',#42315,#42314,#34582,.T.);
#55702=EDGE_CURVE('',#42315,#42312,#24222,.T.);
#55703=EDGE_CURVE('',#42316,#42317,#34583,.T.);
#55704=EDGE_CURVE('',#42318,#42316,#34584,.T.);
#55705=EDGE_CURVE('',#42319,#42318,#34585,.T.);
#55706=EDGE_CURVE('',#42320,#42319,#34586,.T.);
#55707=EDGE_CURVE('',#42321,#42320,#34587,.T.);
#55708=EDGE_CURVE('',#42322,#42321,#34588,.T.);
#55709=EDGE_CURVE('',#42323,#42322,#34589,.T.);
#55710=EDGE_CURVE('',#42324,#42323,#34590,.T.);
#55711=EDGE_CURVE('',#42325,#42324,#34591,.T.);
#55712=EDGE_CURVE('',#42260,#42325,#34592,.T.);
#55713=EDGE_CURVE('',#42269,#42267,#34593,.T.);
#55714=EDGE_CURVE('',#42301,#42268,#34594,.T.);
#55715=EDGE_CURVE('',#42293,#42300,#34595,.T.);
#55716=EDGE_CURVE('',#42277,#42292,#34596,.T.);
#55717=EDGE_CURVE('',#42286,#42276,#34597,.T.);
#55718=EDGE_CURVE('',#42326,#42285,#34598,.T.);
#55719=EDGE_CURVE('',#42327,#42326,#34599,.T.);
#55720=EDGE_CURVE('',#42328,#42327,#34600,.T.);
#55721=EDGE_CURVE('',#42329,#42328,#34601,.T.);
#55722=EDGE_CURVE('',#42330,#42329,#34602,.T.);
#55723=EDGE_CURVE('',#42331,#42330,#34603,.T.);
#55724=EDGE_CURVE('',#42332,#42331,#34604,.T.);
#55725=EDGE_CURVE('',#42333,#42332,#34605,.T.);
#55726=EDGE_CURVE('',#42317,#42333,#34606,.T.);
#55727=EDGE_CURVE('',#42313,#42334,#24223,.T.);
#55728=EDGE_CURVE('',#42335,#42312,#24224,.T.);
#55729=EDGE_CURVE('',#42334,#42335,#24225,.T.);
#55730=EDGE_CURVE('',#42314,#42336,#24226,.T.);
#55731=EDGE_CURVE('',#42336,#42337,#24227,.T.);
#55732=EDGE_CURVE('',#42337,#42315,#24228,.T.);
#55733=EDGE_CURVE('',#42338,#42339,#6334,.T.);
#55734=EDGE_CURVE('',#42340,#42338,#34607,.T.);
#55735=EDGE_CURVE('',#42341,#42340,#6335,.T.);
#55736=EDGE_CURVE('',#42318,#42341,#6336,.T.);
#55737=EDGE_CURVE('',#42339,#42316,#6337,.T.);
#55738=EDGE_CURVE('',#42317,#42342,#6338,.T.);
#55739=EDGE_CURVE('',#42343,#42333,#6339,.T.);
#55740=EDGE_CURVE('',#42344,#42343,#6340,.T.);
#55741=EDGE_CURVE('',#42345,#42344,#34608,.T.);
#55742=EDGE_CURVE('',#42342,#42345,#6341,.T.);
#55743=EDGE_CURVE('',#42332,#42346,#6342,.T.);
#55744=EDGE_CURVE('',#42347,#42331,#6343,.T.);
#55745=EDGE_CURVE('',#42348,#42347,#6344,.T.);
#55746=EDGE_CURVE('',#42349,#42348,#34609,.T.);
#55747=EDGE_CURVE('',#42346,#42349,#6345,.T.);
#55748=EDGE_CURVE('',#42330,#42350,#6346,.T.);
#55749=EDGE_CURVE('',#42351,#42329,#6347,.T.);
#55750=EDGE_CURVE('',#42352,#42351,#6348,.T.);
#55751=EDGE_CURVE('',#42353,#42352,#34610,.T.);
#55752=EDGE_CURVE('',#42350,#42353,#6349,.T.);
#55753=EDGE_CURVE('',#42354,#42256,#34611,.T.);
#55754=EDGE_CURVE('',#42355,#42354,#6350,.T.);
#55755=EDGE_CURVE('',#42322,#42355,#6351,.T.);
#55756=EDGE_CURVE('',#42257,#42321,#6352,.T.);
#55757=EDGE_CURVE('',#42320,#42356,#6353,.T.);
#55758=EDGE_CURVE('',#42357,#42319,#6354,.T.);
#55759=EDGE_CURVE('',#42358,#42357,#6355,.T.);
#55760=EDGE_CURVE('',#42359,#42358,#34612,.T.);
#55761=EDGE_CURVE('',#42356,#42359,#6356,.T.);
#55762=EDGE_CURVE('',#42360,#42361,#6357,.T.);
#55763=EDGE_CURVE('',#42362,#42360,#34613,.T.);
#55764=EDGE_CURVE('',#42363,#42362,#6358,.T.);
#55765=EDGE_CURVE('',#42324,#42363,#6359,.T.);
#55766=EDGE_CURVE('',#42361,#42323,#6360,.T.);
#55767=EDGE_CURVE('',#42364,#42266,#6361,.T.);
#55768=EDGE_CURVE('',#42365,#42364,#34614,.T.);
#55769=EDGE_CURVE('',#42270,#42365,#6362,.T.);
#55770=EDGE_CURVE('',#42366,#42325,#6363,.T.);
#55771=EDGE_CURVE('',#42367,#42366,#6364,.T.);
#55772=EDGE_CURVE('',#42368,#42367,#34615,.T.);
#55773=EDGE_CURVE('',#42261,#42368,#6365,.T.);
#55774=EDGE_CURVE('',#42369,#42275,#6366,.T.);
#55775=EDGE_CURVE('',#42370,#42369,#34616,.T.);
#55776=EDGE_CURVE('',#42302,#42370,#6367,.T.);
#55777=EDGE_CURVE('',#42371,#42283,#6368,.T.);
#55778=EDGE_CURVE('',#42372,#42371,#34617,.T.);
#55779=EDGE_CURVE('',#42287,#42372,#6369,.T.);
#55780=EDGE_CURVE('',#42373,#42299,#6370,.T.);
#55781=EDGE_CURVE('',#42374,#42373,#34618,.T.);
#55782=EDGE_CURVE('',#42278,#42374,#6371,.T.);
#55783=EDGE_CURVE('',#42375,#42284,#6372,.T.);
#55784=EDGE_CURVE('',#42376,#42375,#34619,.T.);
#55785=EDGE_CURVE('',#42377,#42376,#6373,.T.);
#55786=EDGE_CURVE('',#42326,#42377,#6374,.T.);
#55787=EDGE_CURVE('',#42378,#42307,#6375,.T.);
#55788=EDGE_CURVE('',#42379,#42378,#34620,.T.);
#55789=EDGE_CURVE('',#42294,#42379,#6376,.T.);
#55790=EDGE_CURVE('',#42380,#42338,#24229,.T.);
#55791=EDGE_CURVE('',#42381,#42380,#34621,.T.);
#55792=EDGE_CURVE('',#42340,#42381,#24230,.T.);
#55793=EDGE_CURVE('',#42345,#42382,#24231,.T.);
#55794=EDGE_CURVE('',#42383,#42344,#24232,.T.);
#55795=EDGE_CURVE('',#42382,#42383,#34622,.T.);
#55796=EDGE_CURVE('',#42349,#42384,#24233,.T.);
#55797=EDGE_CURVE('',#42385,#42348,#24234,.T.);
#55798=EDGE_CURVE('',#42384,#42385,#34623,.T.);
#55799=EDGE_CURVE('',#42353,#42386,#24235,.T.);
#55800=EDGE_CURVE('',#42387,#42352,#24236,.T.);
#55801=EDGE_CURVE('',#42386,#42387,#34624,.T.);
#55802=EDGE_CURVE('',#42388,#42259,#34625,.T.);
#55803=EDGE_CURVE('',#42354,#42388,#24237,.T.);
#55804=EDGE_CURVE('',#42359,#42389,#24238,.T.);
#55805=EDGE_CURVE('',#42390,#42358,#24239,.T.);
#55806=EDGE_CURVE('',#42389,#42390,#34626,.T.);
#55807=EDGE_CURVE('',#42391,#42360,#24240,.T.);
#55808=EDGE_CURVE('',#42392,#42391,#34627,.T.);
#55809=EDGE_CURVE('',#42362,#42392,#24241,.T.);
#55810=EDGE_CURVE('',#42393,#42364,#24242,.T.);
#55811=EDGE_CURVE('',#42394,#42393,#34628,.T.);
#55812=EDGE_CURVE('',#42365,#42394,#24243,.T.);
#55813=EDGE_CURVE('',#42368,#42395,#24244,.T.);
#55814=EDGE_CURVE('',#42396,#42367,#24245,.T.);
#55815=EDGE_CURVE('',#42395,#42396,#34629,.T.);
#55816=EDGE_CURVE('',#42397,#42369,#24246,.T.);
#55817=EDGE_CURVE('',#42398,#42397,#34630,.T.);
#55818=EDGE_CURVE('',#42370,#42398,#24247,.T.);
#55819=EDGE_CURVE('',#42399,#42371,#24248,.T.);
#55820=EDGE_CURVE('',#42400,#42399,#34631,.T.);
#55821=EDGE_CURVE('',#42372,#42400,#24249,.T.);
#55822=EDGE_CURVE('',#42374,#42401,#24250,.T.);
#55823=EDGE_CURVE('',#42402,#42373,#24251,.T.);
#55824=EDGE_CURVE('',#42401,#42402,#34632,.T.);
#55825=EDGE_CURVE('',#42403,#42375,#24252,.T.);
#55826=EDGE_CURVE('',#42404,#42403,#34633,.T.);
#55827=EDGE_CURVE('',#42376,#42404,#24253,.T.);
#55828=EDGE_CURVE('',#42379,#42405,#24254,.T.);
#55829=EDGE_CURVE('',#42406,#42378,#24255,.T.);
#55830=EDGE_CURVE('',#42405,#42406,#34634,.T.);
#55831=EDGE_CURVE('',#42407,#42380,#6377,.T.);
#55832=EDGE_CURVE('',#42408,#42407,#6378,.T.);
#55833=EDGE_CURVE('',#42409,#42408,#34635,.T.);
#55834=EDGE_CURVE('',#42410,#42409,#6379,.T.);
#55835=EDGE_CURVE('',#42381,#42410,#6380,.T.);
#55836=EDGE_CURVE('',#42411,#42412,#6381,.T.);
#55837=EDGE_CURVE('',#42382,#42411,#6382,.T.);
#55838=EDGE_CURVE('',#42413,#42383,#6383,.T.);
#55839=EDGE_CURVE('',#42414,#42413,#6384,.T.);
#55840=EDGE_CURVE('',#42412,#42414,#34636,.T.);
#55841=EDGE_CURVE('',#42415,#42416,#6385,.T.);
#55842=EDGE_CURVE('',#42384,#42415,#6386,.T.);
#55843=EDGE_CURVE('',#42417,#42385,#6387,.T.);
#55844=EDGE_CURVE('',#42418,#42417,#6388,.T.);
#55845=EDGE_CURVE('',#42416,#42418,#34637,.T.);
#55846=EDGE_CURVE('',#42419,#42420,#6389,.T.);
#55847=EDGE_CURVE('',#42386,#42419,#6390,.T.);
#55848=EDGE_CURVE('',#42421,#42387,#6391,.T.);
#55849=EDGE_CURVE('',#42422,#42421,#6392,.T.);
#55850=EDGE_CURVE('',#42420,#42422,#34638,.T.);
#55851=EDGE_CURVE('',#42423,#42258,#6393,.T.);
#55852=EDGE_CURVE('',#42424,#42423,#34639,.T.);
#55853=EDGE_CURVE('',#42425,#42424,#6394,.T.);
#55854=EDGE_CURVE('',#42388,#42425,#6395,.T.);
#55855=EDGE_CURVE('',#42426,#42427,#6396,.T.);
#55856=EDGE_CURVE('',#42389,#42426,#6397,.T.);
#55857=EDGE_CURVE('',#42428,#42390,#6398,.T.);
#55858=EDGE_CURVE('',#42429,#42428,#6399,.T.);
#55859=EDGE_CURVE('',#42427,#42429,#34640,.T.);
#55860=EDGE_CURVE('',#42430,#42391,#6400,.T.);
#55861=EDGE_CURVE('',#42431,#42430,#6401,.T.);
#55862=EDGE_CURVE('',#42432,#42431,#34641,.T.);
#55863=EDGE_CURVE('',#42433,#42432,#6402,.T.);
#55864=EDGE_CURVE('',#42392,#42433,#6403,.T.);
#55865=EDGE_CURVE('',#42265,#42393,#6404,.T.);
#55866=EDGE_CURVE('',#42272,#42264,#34642,.T.);
#55867=EDGE_CURVE('',#42394,#42271,#6405,.T.);
#55868=EDGE_CURVE('',#42395,#42262,#6406,.T.);
#55869=EDGE_CURVE('',#42434,#42396,#6407,.T.);
#55870=EDGE_CURVE('',#42435,#42434,#6408,.T.);
#55871=EDGE_CURVE('',#42263,#42435,#34643,.T.);
#55872=EDGE_CURVE('',#42274,#42397,#6409,.T.);
#55873=EDGE_CURVE('',#42304,#42273,#34644,.T.);
#55874=EDGE_CURVE('',#42398,#42303,#6410,.T.);
#55875=EDGE_CURVE('',#42282,#42399,#6411,.T.);
#55876=EDGE_CURVE('',#42289,#42281,#34645,.T.);
#55877=EDGE_CURVE('',#42400,#42288,#6412,.T.);
#55878=EDGE_CURVE('',#42401,#42279,#6413,.T.);
#55879=EDGE_CURVE('',#42298,#42402,#6414,.T.);
#55880=EDGE_CURVE('',#42280,#42297,#34646,.T.);
#55881=EDGE_CURVE('',#42291,#42403,#6415,.T.);
#55882=EDGE_CURVE('',#42436,#42290,#34647,.T.);
#55883=EDGE_CURVE('',#42437,#42436,#6416,.T.);
#55884=EDGE_CURVE('',#42404,#42437,#6417,.T.);
#55885=EDGE_CURVE('',#42405,#42295,#6418,.T.);
#55886=EDGE_CURVE('',#42306,#42406,#6419,.T.);
#55887=EDGE_CURVE('',#42296,#42305,#34648,.T.);
#55888=EDGE_CURVE('',#42328,#42308,#6420,.T.);
#55889=EDGE_CURVE('',#42438,#42327,#6421,.T.);
#55890=EDGE_CURVE('',#42439,#42438,#6422,.T.);
#55891=EDGE_CURVE('',#42309,#42439,#34649,.T.);
#55892=EDGE_CURVE('',#42440,#42439,#24256,.T.);
#55893=EDGE_CURVE('',#42310,#42440,#34650,.T.);
#55894=EDGE_CURVE('',#42311,#42441,#6423,.T.);
#55895=EDGE_CURVE('',#42442,#42440,#6424,.T.);
#55896=EDGE_CURVE('',#42443,#42442,#6425,.T.);
#55897=EDGE_CURVE('',#42441,#42443,#34651,.T.);
#55898=EDGE_CURVE('',#42412,#42408,#34652,.T.);
#55899=EDGE_CURVE('',#42416,#42414,#34653,.T.);
#55900=EDGE_CURVE('',#42420,#42418,#34654,.T.);
#55901=EDGE_CURVE('',#42441,#42422,#34655,.T.);
#55902=EDGE_CURVE('',#42436,#42443,#34656,.T.);
#55903=EDGE_CURVE('',#42432,#42435,#34657,.T.);
#55904=EDGE_CURVE('',#42424,#42431,#34658,.T.);
#55905=EDGE_CURVE('',#42427,#42423,#34659,.T.);
#55906=EDGE_CURVE('',#42409,#42429,#34660,.T.);
#55907=EDGE_CURVE('',#42438,#42442,#24257,.T.);
#55908=EDGE_CURVE('',#42377,#42437,#24258,.T.);
#55909=EDGE_CURVE('',#42351,#42421,#24259,.T.);
#55910=EDGE_CURVE('',#42366,#42434,#24260,.T.);
#55911=EDGE_CURVE('',#42363,#42433,#24261,.T.);
#55912=EDGE_CURVE('',#42357,#42428,#24262,.T.);
#55913=EDGE_CURVE('',#42341,#42410,#24263,.T.);
#55914=EDGE_CURVE('',#42361,#42430,#24264,.T.);
#55915=EDGE_CURVE('',#42355,#42425,#24265,.T.);
#55916=EDGE_CURVE('',#42356,#42426,#24266,.T.);
#55917=EDGE_CURVE('',#42347,#42417,#24267,.T.);
#55918=EDGE_CURVE('',#42350,#42419,#24268,.T.);
#55919=EDGE_CURVE('',#42343,#42413,#24269,.T.);
#55920=EDGE_CURVE('',#42346,#42415,#24270,.T.);
#55921=EDGE_CURVE('',#42339,#42407,#24271,.T.);
#55922=EDGE_CURVE('',#42342,#42411,#24272,.T.);
#55923=EDGE_CURVE('',#42335,#42337,#24273,.T.);
#55924=EDGE_CURVE('',#42334,#42336,#24274,.T.);
#55925=EDGE_CURVE('',#42444,#42444,#34661,.T.);
#55926=EDGE_CURVE('',#42444,#42445,#24275,.T.);
#55927=EDGE_CURVE('',#42445,#42445,#34662,.T.);
#55928=EDGE_CURVE('',#42446,#42447,#34663,.T.);
#55929=EDGE_CURVE('',#42446,#42448,#24276,.T.);
#55930=EDGE_CURVE('',#42449,#42448,#34664,.T.);
#55931=EDGE_CURVE('',#42447,#42449,#24277,.T.);
#55932=EDGE_CURVE('',#42450,#42446,#24278,.T.);
#55933=EDGE_CURVE('',#42450,#42451,#24279,.T.);
#55934=EDGE_CURVE('',#42448,#42451,#24280,.T.);
#55935=EDGE_CURVE('',#42452,#42450,#24281,.T.);
#55936=EDGE_CURVE('',#42452,#42453,#24282,.T.);
#55937=EDGE_CURVE('',#42451,#42453,#24283,.T.);
#55938=EDGE_CURVE('',#42447,#42452,#24284,.T.);
#55939=EDGE_CURVE('',#42453,#42449,#24285,.T.);
#55940=EDGE_CURVE('',#42454,#42454,#34665,.T.);
#55941=EDGE_CURVE('',#42454,#42455,#34666,.T.);
#55942=EDGE_CURVE('',#42455,#42455,#34667,.T.);
#55943=EDGE_CURVE('',#42455,#42456,#24286,.T.);
#55944=EDGE_CURVE('',#42456,#42456,#34668,.T.);
#55945=EDGE_CURVE('',#42457,#42458,#6426,.T.);
#55946=EDGE_CURVE('',#42458,#42459,#24287,.T.);
#55947=EDGE_CURVE('',#42459,#42460,#6427,.T.);
#55948=EDGE_CURVE('',#42457,#42460,#24288,.T.);
#55949=EDGE_CURVE('',#42461,#42462,#6428,.T.);
#55950=EDGE_CURVE('',#42462,#42463,#24289,.T.);
#55951=EDGE_CURVE('',#42463,#42464,#6429,.T.);
#55952=EDGE_CURVE('',#42464,#42461,#24290,.T.);
#55953=EDGE_CURVE('',#42465,#42466,#34669,.T.);
#55954=EDGE_CURVE('',#42466,#42467,#6430,.T.);
#55955=EDGE_CURVE('',#42467,#42468,#24291,.T.);
#55956=EDGE_CURVE('',#42468,#42469,#6431,.T.);
#55957=EDGE_CURVE('',#42469,#42470,#34670,.T.);
#55958=EDGE_CURVE('',#42470,#42471,#6432,.T.);
#55959=EDGE_CURVE('',#42472,#42471,#24292,.T.);
#55960=EDGE_CURVE('',#42472,#42465,#6433,.T.);
#55961=EDGE_CURVE('',#42473,#42474,#34671,.T.);
#55962=EDGE_CURVE('',#42474,#42475,#6434,.T.);
#55963=EDGE_CURVE('',#42475,#42476,#24293,.T.);
#55964=EDGE_CURVE('',#42476,#42477,#6435,.T.);
#55965=EDGE_CURVE('',#42477,#42478,#34672,.T.);
#55966=EDGE_CURVE('',#42478,#42479,#6436,.T.);
#55967=EDGE_CURVE('',#42480,#42479,#24294,.T.);
#55968=EDGE_CURVE('',#42480,#42473,#6437,.T.);
#55969=EDGE_CURVE('',#42481,#42482,#34673,.T.);
#55970=EDGE_CURVE('',#42482,#42483,#6438,.T.);
#55971=EDGE_CURVE('',#42483,#42484,#24295,.T.);
#55972=EDGE_CURVE('',#42484,#42485,#6439,.T.);
#55973=EDGE_CURVE('',#42485,#42486,#34674,.T.);
#55974=EDGE_CURVE('',#42486,#42487,#6440,.T.);
#55975=EDGE_CURVE('',#42488,#42487,#24296,.T.);
#55976=EDGE_CURVE('',#42488,#42481,#6441,.T.);
#55977=EDGE_CURVE('',#42489,#42490,#34675,.T.);
#55978=EDGE_CURVE('',#42490,#42491,#6442,.T.);
#55979=EDGE_CURVE('',#42491,#42492,#24297,.T.);
#55980=EDGE_CURVE('',#42492,#42493,#6443,.T.);
#55981=EDGE_CURVE('',#42493,#42494,#34676,.T.);
#55982=EDGE_CURVE('',#42494,#42495,#6444,.T.);
#55983=EDGE_CURVE('',#42496,#42495,#24298,.T.);
#55984=EDGE_CURVE('',#42496,#42489,#6445,.T.);
#55985=EDGE_CURVE('',#42497,#42498,#6446,.T.);
#55986=EDGE_CURVE('',#42498,#42499,#24299,.T.);
#55987=EDGE_CURVE('',#42499,#42500,#6447,.T.);
#55988=EDGE_CURVE('',#42500,#42501,#34677,.T.);
#55989=EDGE_CURVE('',#42501,#42502,#6448,.T.);
#55990=EDGE_CURVE('',#42503,#42502,#24300,.T.);
#55991=EDGE_CURVE('',#42503,#42504,#6449,.T.);
#55992=EDGE_CURVE('',#42504,#42497,#34678,.T.);
#55993=EDGE_CURVE('',#42505,#42506,#6450,.T.);
#55994=EDGE_CURVE('',#42506,#42507,#24301,.T.);
#55995=EDGE_CURVE('',#42507,#42508,#6451,.T.);
#55996=EDGE_CURVE('',#42508,#42509,#34679,.T.);
#55997=EDGE_CURVE('',#42509,#42510,#6452,.T.);
#55998=EDGE_CURVE('',#42511,#42510,#24302,.T.);
#55999=EDGE_CURVE('',#42511,#42512,#6453,.T.);
#56000=EDGE_CURVE('',#42512,#42505,#34680,.T.);
#56001=EDGE_CURVE('',#42513,#42514,#6454,.T.);
#56002=EDGE_CURVE('',#42514,#42515,#34681,.T.);
#56003=EDGE_CURVE('',#42515,#42516,#6455,.T.);
#56004=EDGE_CURVE('',#42516,#42517,#24303,.T.);
#56005=EDGE_CURVE('',#42517,#42518,#6456,.T.);
#56006=EDGE_CURVE('',#42518,#42519,#34682,.T.);
#56007=EDGE_CURVE('',#42519,#42520,#6457,.T.);
#56008=EDGE_CURVE('',#42513,#42520,#24304,.T.);
#56009=EDGE_CURVE('',#42521,#42522,#34683,.T.);
#56010=EDGE_CURVE('',#42522,#42523,#6458,.T.);
#56011=EDGE_CURVE('',#42523,#42524,#24305,.T.);
#56012=EDGE_CURVE('',#42524,#42525,#6459,.T.);
#56013=EDGE_CURVE('',#42525,#42526,#34684,.T.);
#56014=EDGE_CURVE('',#42526,#42527,#6460,.T.);
#56015=EDGE_CURVE('',#42528,#42527,#24306,.T.);
#56016=EDGE_CURVE('',#42528,#42521,#6461,.T.);
#56017=EDGE_CURVE('',#42529,#42530,#6462,.T.);
#56018=EDGE_CURVE('',#42530,#42531,#34685,.T.);
#56019=EDGE_CURVE('',#42531,#42532,#6463,.T.);
#56020=EDGE_CURVE('',#42532,#42533,#24307,.T.);
#56021=EDGE_CURVE('',#42533,#42534,#6464,.T.);
#56022=EDGE_CURVE('',#42534,#42535,#34686,.T.);
#56023=EDGE_CURVE('',#42535,#42536,#6465,.T.);
#56024=EDGE_CURVE('',#42529,#42536,#24308,.T.);
#56025=EDGE_CURVE('',#42537,#42538,#34687,.T.);
#56026=EDGE_CURVE('',#42538,#42539,#6466,.T.);
#56027=EDGE_CURVE('',#42539,#42540,#24309,.T.);
#56028=EDGE_CURVE('',#42540,#42541,#6467,.T.);
#56029=EDGE_CURVE('',#42541,#42542,#34688,.T.);
#56030=EDGE_CURVE('',#42542,#42543,#6468,.T.);
#56031=EDGE_CURVE('',#42544,#42543,#24310,.T.);
#56032=EDGE_CURVE('',#42544,#42537,#6469,.T.);
#56033=EDGE_CURVE('',#42545,#42546,#34689,.T.);
#56034=EDGE_CURVE('',#42546,#42547,#6470,.T.);
#56035=EDGE_CURVE('',#42547,#42548,#24311,.T.);
#56036=EDGE_CURVE('',#42548,#42549,#6471,.T.);
#56037=EDGE_CURVE('',#42549,#42550,#34690,.T.);
#56038=EDGE_CURVE('',#42550,#42551,#6472,.T.);
#56039=EDGE_CURVE('',#42552,#42551,#24312,.T.);
#56040=EDGE_CURVE('',#42552,#42545,#6473,.T.);
#56041=EDGE_CURVE('',#42553,#42554,#34691,.T.);
#56042=EDGE_CURVE('',#42554,#42555,#6474,.T.);
#56043=EDGE_CURVE('',#42555,#42556,#24313,.T.);
#56044=EDGE_CURVE('',#42556,#42557,#6475,.T.);
#56045=EDGE_CURVE('',#42557,#42558,#34692,.T.);
#56046=EDGE_CURVE('',#42558,#42559,#6476,.T.);
#56047=EDGE_CURVE('',#42560,#42559,#24314,.T.);
#56048=EDGE_CURVE('',#42560,#42553,#6477,.T.);
#56049=EDGE_CURVE('',#42561,#42562,#34693,.T.);
#56050=EDGE_CURVE('',#42563,#42562,#6478,.T.);
#56051=EDGE_CURVE('',#42564,#42563,#6479,.T.);
#56052=EDGE_CURVE('',#42565,#42564,#34694,.T.);
#56053=EDGE_CURVE('',#42566,#42565,#6480,.T.);
#56054=EDGE_CURVE('',#42561,#42566,#6481,.T.);
#56055=EDGE_CURVE('',#42567,#42568,#34695,.T.);
#56056=EDGE_CURVE('',#42562,#42568,#24315,.T.);
#56057=EDGE_CURVE('',#42567,#42561,#24316,.T.);
#56058=EDGE_CURVE('',#42569,#42570,#34696,.T.);
#56059=EDGE_CURVE('',#42571,#42570,#6482,.T.);
#56060=EDGE_CURVE('',#42568,#42571,#6483,.T.);
#56061=EDGE_CURVE('',#42572,#42567,#6484,.T.);
#56062=EDGE_CURVE('',#42569,#42572,#6485,.T.);
#56063=EDGE_CURVE('',#42573,#42574,#34697,.T.);
#56064=EDGE_CURVE('',#42574,#42575,#24317,.T.);
#56065=EDGE_CURVE('',#42576,#42575,#34698,.T.);
#56066=EDGE_CURVE('',#42576,#42573,#24318,.T.);
#56067=EDGE_CURVE('',#42577,#42569,#34699,.T.);
#56068=EDGE_CURVE('',#42578,#42577,#34700,.T.);
#56069=EDGE_CURVE('',#42579,#42578,#34701,.T.);
#56070=EDGE_CURVE('',#42580,#42579,#34702,.T.);
#56071=EDGE_CURVE('',#42581,#42580,#34703,.T.);
#56072=EDGE_CURVE('',#42582,#42581,#34704,.T.);
#56073=EDGE_CURVE('',#42583,#42582,#34705,.T.);
#56074=EDGE_CURVE('',#42584,#42583,#34706,.T.);
#56075=EDGE_CURVE('',#42585,#42584,#34707,.T.);
#56076=EDGE_CURVE('',#42586,#42585,#34708,.T.);
#56077=EDGE_CURVE('',#42587,#42586,#34709,.T.);
#56078=EDGE_CURVE('',#42588,#42587,#34710,.T.);
#56079=EDGE_CURVE('',#42589,#42588,#34711,.T.);
#56080=EDGE_CURVE('',#42590,#42589,#34712,.T.);
#56081=EDGE_CURVE('',#42591,#42590,#34713,.T.);
#56082=EDGE_CURVE('',#42592,#42591,#34714,.T.);
#56083=EDGE_CURVE('',#42593,#42592,#34715,.T.);
#56084=EDGE_CURVE('',#42497,#42593,#34716,.T.);
#56085=EDGE_CURVE('',#42505,#42504,#34717,.T.);
#56086=EDGE_CURVE('',#42482,#42512,#34718,.T.);
#56087=EDGE_CURVE('',#42490,#42481,#34719,.T.);
#56088=EDGE_CURVE('',#42474,#42489,#34720,.T.);
#56089=EDGE_CURVE('',#42466,#42473,#34721,.T.);
#56090=EDGE_CURVE('',#42554,#42465,#34722,.T.);
#56091=EDGE_CURVE('',#42546,#42553,#34723,.T.);
#56092=EDGE_CURVE('',#42538,#42545,#34724,.T.);
#56093=EDGE_CURVE('',#42522,#42537,#34725,.T.);
#56094=EDGE_CURVE('',#42515,#42521,#34726,.T.);
#56095=EDGE_CURVE('',#42531,#42514,#34727,.T.);
#56096=EDGE_CURVE('',#42594,#42530,#34728,.T.);
#56097=EDGE_CURVE('',#42595,#42594,#34729,.T.);
#56098=EDGE_CURVE('',#42596,#42595,#34730,.T.);
#56099=EDGE_CURVE('',#42597,#42596,#34731,.T.);
#56100=EDGE_CURVE('',#42598,#42597,#34732,.T.);
#56101=EDGE_CURVE('',#42599,#42598,#34733,.T.);
#56102=EDGE_CURVE('',#42600,#42599,#34734,.T.);
#56103=EDGE_CURVE('',#42601,#42600,#34735,.T.);
#56104=EDGE_CURVE('',#42602,#42601,#34736,.T.);
#56105=EDGE_CURVE('',#42603,#42602,#34737,.T.);
#56106=EDGE_CURVE('',#42604,#42603,#34738,.T.);
#56107=EDGE_CURVE('',#42605,#42604,#34739,.T.);
#56108=EDGE_CURVE('',#42606,#42605,#34740,.T.);
#56109=EDGE_CURVE('',#42607,#42606,#34741,.T.);
#56110=EDGE_CURVE('',#42608,#42607,#34742,.T.);
#56111=EDGE_CURVE('',#42609,#42608,#34743,.T.);
#56112=EDGE_CURVE('',#42610,#42609,#34744,.T.);
#56113=EDGE_CURVE('',#42570,#42610,#34745,.T.);
#56114=EDGE_CURVE('',#42574,#42611,#24319,.T.);
#56115=EDGE_CURVE('',#42612,#42573,#24320,.T.);
#56116=EDGE_CURVE('',#42611,#42612,#24321,.T.);
#56117=EDGE_CURVE('',#42575,#42613,#24322,.T.);
#56118=EDGE_CURVE('',#42613,#42614,#24323,.T.);
#56119=EDGE_CURVE('',#42614,#42576,#24324,.T.);
#56120=EDGE_CURVE('',#42615,#42616,#6486,.T.);
#56121=EDGE_CURVE('',#42617,#42615,#34746,.T.);
#56122=EDGE_CURVE('',#42618,#42617,#6487,.T.);
#56123=EDGE_CURVE('',#42578,#42618,#6488,.T.);
#56124=EDGE_CURVE('',#42616,#42577,#6489,.T.);
#56125=EDGE_CURVE('',#42610,#42619,#6490,.T.);
#56126=EDGE_CURVE('',#42620,#42609,#6491,.T.);
#56127=EDGE_CURVE('',#42621,#42620,#6492,.T.);
#56128=EDGE_CURVE('',#42622,#42621,#34747,.T.);
#56129=EDGE_CURVE('',#42619,#42622,#6493,.T.);
#56130=EDGE_CURVE('',#42608,#42623,#6494,.T.);
#56131=EDGE_CURVE('',#42624,#42607,#6495,.T.);
#56132=EDGE_CURVE('',#42625,#42624,#6496,.T.);
#56133=EDGE_CURVE('',#42626,#42625,#34748,.T.);
#56134=EDGE_CURVE('',#42623,#42626,#6497,.T.);
#56135=EDGE_CURVE('',#42606,#42627,#6498,.T.);
#56136=EDGE_CURVE('',#42628,#42605,#6499,.T.);
#56137=EDGE_CURVE('',#42629,#42628,#6500,.T.);
#56138=EDGE_CURVE('',#42630,#42629,#34749,.T.);
#56139=EDGE_CURVE('',#42627,#42630,#6501,.T.);
#56140=EDGE_CURVE('',#42631,#42632,#6502,.T.);
#56141=EDGE_CURVE('',#42633,#42631,#34750,.T.);
#56142=EDGE_CURVE('',#42634,#42633,#6503,.T.);
#56143=EDGE_CURVE('',#42602,#42634,#6504,.T.);
#56144=EDGE_CURVE('',#42632,#42601,#6505,.T.);
#56145=EDGE_CURVE('',#42600,#42457,#6506,.T.);
#56146=EDGE_CURVE('',#42635,#42599,#6507,.T.);
#56147=EDGE_CURVE('',#42636,#42635,#6508,.T.);
#56148=EDGE_CURVE('',#42458,#42636,#34751,.T.);
#56149=EDGE_CURVE('',#42604,#42637,#6509,.T.);
#56150=EDGE_CURVE('',#42638,#42603,#6510,.T.);
#56151=EDGE_CURVE('',#42639,#42638,#6511,.T.);
#56152=EDGE_CURVE('',#42640,#42639,#34752,.T.);
#56153=EDGE_CURVE('',#42637,#42640,#6512,.T.);
#56154=EDGE_CURVE('',#42641,#42642,#6513,.T.);
#56155=EDGE_CURVE('',#42643,#42641,#34753,.T.);
#56156=EDGE_CURVE('',#42644,#42643,#6514,.T.);
#56157=EDGE_CURVE('',#42592,#42644,#6515,.T.);
#56158=EDGE_CURVE('',#42642,#42591,#6516,.T.);
#56159=EDGE_CURVE('',#42590,#42645,#6517,.T.);
#56160=EDGE_CURVE('',#42646,#42589,#6518,.T.);
#56161=EDGE_CURVE('',#42647,#42646,#6519,.T.);
#56162=EDGE_CURVE('',#42648,#42647,#34754,.T.);
#56163=EDGE_CURVE('',#42645,#42648,#6520,.T.);
#56164=EDGE_CURVE('',#42588,#42649,#6521,.T.);
#56165=EDGE_CURVE('',#42462,#42587,#6522,.T.);
#56166=EDGE_CURVE('',#42650,#42461,#34755,.T.);
#56167=EDGE_CURVE('',#42649,#42650,#6523,.T.);
#56168=EDGE_CURVE('',#42651,#42652,#6524,.T.);
#56169=EDGE_CURVE('',#42653,#42651,#34756,.T.);
#56170=EDGE_CURVE('',#42654,#42653,#6525,.T.);
#56171=EDGE_CURVE('',#42586,#42654,#6526,.T.);
#56172=EDGE_CURVE('',#42652,#42585,#6527,.T.);
#56173=EDGE_CURVE('',#42584,#42655,#6528,.T.);
#56174=EDGE_CURVE('',#42656,#42583,#6529,.T.);
#56175=EDGE_CURVE('',#42657,#42656,#6530,.T.);
#56176=EDGE_CURVE('',#42658,#42657,#34757,.T.);
#56177=EDGE_CURVE('',#42655,#42658,#6531,.T.);
#56178=EDGE_CURVE('',#42659,#42660,#6532,.T.);
#56179=EDGE_CURVE('',#42661,#42659,#34758,.T.);
#56180=EDGE_CURVE('',#42662,#42661,#6533,.T.);
#56181=EDGE_CURVE('',#42582,#42662,#6534,.T.);
#56182=EDGE_CURVE('',#42660,#42581,#6535,.T.);
#56183=EDGE_CURVE('',#42580,#42663,#6536,.T.);
#56184=EDGE_CURVE('',#42664,#42579,#6537,.T.);
#56185=EDGE_CURVE('',#42665,#42664,#6538,.T.);
#56186=EDGE_CURVE('',#42666,#42665,#34759,.T.);
#56187=EDGE_CURVE('',#42663,#42666,#6539,.T.);
#56188=EDGE_CURVE('',#42667,#42472,#6540,.T.);
#56189=EDGE_CURVE('',#42668,#42667,#34760,.T.);
#56190=EDGE_CURVE('',#42555,#42668,#6541,.T.);
#56191=EDGE_CURVE('',#42669,#42480,#6542,.T.);
#56192=EDGE_CURVE('',#42670,#42669,#34761,.T.);
#56193=EDGE_CURVE('',#42467,#42670,#6543,.T.);
#56194=EDGE_CURVE('',#42671,#42496,#6544,.T.);
#56195=EDGE_CURVE('',#42672,#42671,#34762,.T.);
#56196=EDGE_CURVE('',#42475,#42672,#6545,.T.);
#56197=EDGE_CURVE('',#42673,#42488,#6546,.T.);
#56198=EDGE_CURVE('',#42674,#42673,#34763,.T.);
#56199=EDGE_CURVE('',#42491,#42674,#6547,.T.);
#56200=EDGE_CURVE('',#42675,#42511,#6548,.T.);
#56201=EDGE_CURVE('',#42676,#42675,#34764,.T.);
#56202=EDGE_CURVE('',#42483,#42676,#6549,.T.);
#56203=EDGE_CURVE('',#42677,#42503,#6550,.T.);
#56204=EDGE_CURVE('',#42678,#42677,#34765,.T.);
#56205=EDGE_CURVE('',#42506,#42678,#6551,.T.);
#56206=EDGE_CURVE('',#42679,#42593,#6552,.T.);
#56207=EDGE_CURVE('',#42680,#42679,#6553,.T.);
#56208=EDGE_CURVE('',#42681,#42680,#34766,.T.);
#56209=EDGE_CURVE('',#42498,#42681,#6554,.T.);
#56210=EDGE_CURVE('',#42682,#42513,#6555,.T.);
#56211=EDGE_CURVE('',#42683,#42682,#34767,.T.);
#56212=EDGE_CURVE('',#42532,#42683,#6556,.T.);
#56213=EDGE_CURVE('',#42684,#42528,#6557,.T.);
#56214=EDGE_CURVE('',#42685,#42684,#34768,.T.);
#56215=EDGE_CURVE('',#42516,#42685,#6558,.T.);
#56216=EDGE_CURVE('',#42686,#42544,#6559,.T.);
#56217=EDGE_CURVE('',#42687,#42686,#34769,.T.);
#56218=EDGE_CURVE('',#42523,#42687,#6560,.T.);
#56219=EDGE_CURVE('',#42688,#42529,#6561,.T.);
#56220=EDGE_CURVE('',#42689,#42688,#34770,.T.);
#56221=EDGE_CURVE('',#42690,#42689,#6562,.T.);
#56222=EDGE_CURVE('',#42594,#42690,#6563,.T.);
#56223=EDGE_CURVE('',#42691,#42692,#6564,.T.);
#56224=EDGE_CURVE('',#42693,#42691,#34771,.T.);
#56225=EDGE_CURVE('',#42694,#42693,#6565,.T.);
#56226=EDGE_CURVE('',#42596,#42694,#6566,.T.);
#56227=EDGE_CURVE('',#42692,#42595,#6567,.T.);
#56228=EDGE_CURVE('',#42695,#42552,#6568,.T.);
#56229=EDGE_CURVE('',#42696,#42695,#34772,.T.);
#56230=EDGE_CURVE('',#42539,#42696,#6569,.T.);
#56231=EDGE_CURVE('',#42697,#42560,#6570,.T.);
#56232=EDGE_CURVE('',#42698,#42697,#34773,.T.);
#56233=EDGE_CURVE('',#42547,#42698,#6571,.T.);
#56234=EDGE_CURVE('',#42699,#42615,#24325,.T.);
#56235=EDGE_CURVE('',#42700,#42699,#34774,.T.);
#56236=EDGE_CURVE('',#42617,#42700,#24326,.T.);
#56237=EDGE_CURVE('',#42622,#42701,#24327,.T.);
#56238=EDGE_CURVE('',#42702,#42621,#24328,.T.);
#56239=EDGE_CURVE('',#42701,#42702,#34775,.T.);
#56240=EDGE_CURVE('',#42626,#42703,#24329,.T.);
#56241=EDGE_CURVE('',#42704,#42625,#24330,.T.);
#56242=EDGE_CURVE('',#42703,#42704,#34776,.T.);
#56243=EDGE_CURVE('',#42630,#42705,#24331,.T.);
#56244=EDGE_CURVE('',#42706,#42629,#24332,.T.);
#56245=EDGE_CURVE('',#42705,#42706,#34777,.T.);
#56246=EDGE_CURVE('',#42707,#42631,#24333,.T.);
#56247=EDGE_CURVE('',#42708,#42707,#34778,.T.);
#56248=EDGE_CURVE('',#42633,#42708,#24334,.T.);
#56249=EDGE_CURVE('',#42709,#42636,#24335,.T.);
#56250=EDGE_CURVE('',#42459,#42709,#34779,.T.);
#56251=EDGE_CURVE('',#42640,#42710,#24336,.T.);
#56252=EDGE_CURVE('',#42711,#42639,#24337,.T.);
#56253=EDGE_CURVE('',#42710,#42711,#34780,.T.);
#56254=EDGE_CURVE('',#42712,#42641,#24338,.T.);
#56255=EDGE_CURVE('',#42713,#42712,#34781,.T.);
#56256=EDGE_CURVE('',#42643,#42713,#24339,.T.);
#56257=EDGE_CURVE('',#42648,#42714,#24340,.T.);
#56258=EDGE_CURVE('',#42715,#42647,#24341,.T.);
#56259=EDGE_CURVE('',#42714,#42715,#34782,.T.);
#56260=EDGE_CURVE('',#42650,#42716,#24342,.T.);
#56261=EDGE_CURVE('',#42716,#42464,#34783,.T.);
#56262=EDGE_CURVE('',#42717,#42651,#24343,.T.);
#56263=EDGE_CURVE('',#42718,#42717,#34784,.T.);
#56264=EDGE_CURVE('',#42653,#42718,#24344,.T.);
#56265=EDGE_CURVE('',#42658,#42719,#24345,.T.);
#56266=EDGE_CURVE('',#42720,#42657,#24346,.T.);
#56267=EDGE_CURVE('',#42719,#42720,#34785,.T.);
#56268=EDGE_CURVE('',#42721,#42659,#24347,.T.);
#56269=EDGE_CURVE('',#42722,#42721,#34786,.T.);
#56270=EDGE_CURVE('',#42661,#42722,#24348,.T.);
#56271=EDGE_CURVE('',#42666,#42723,#24349,.T.);
#56272=EDGE_CURVE('',#42724,#42665,#24350,.T.);
#56273=EDGE_CURVE('',#42723,#42724,#34787,.T.);
#56274=EDGE_CURVE('',#42725,#42667,#24351,.T.);
#56275=EDGE_CURVE('',#42726,#42725,#34788,.T.);
#56276=EDGE_CURVE('',#42668,#42726,#24352,.T.);
#56277=EDGE_CURVE('',#42670,#42727,#24353,.T.);
#56278=EDGE_CURVE('',#42728,#42669,#24354,.T.);
#56279=EDGE_CURVE('',#42727,#42728,#34789,.T.);
#56280=EDGE_CURVE('',#42672,#42729,#24355,.T.);
#56281=EDGE_CURVE('',#42730,#42671,#24356,.T.);
#56282=EDGE_CURVE('',#42729,#42730,#34790,.T.);
#56283=EDGE_CURVE('',#42731,#42673,#24357,.T.);
#56284=EDGE_CURVE('',#42732,#42731,#34791,.T.);
#56285=EDGE_CURVE('',#42674,#42732,#24358,.T.);
#56286=EDGE_CURVE('',#42676,#42733,#24359,.T.);
#56287=EDGE_CURVE('',#42734,#42675,#24360,.T.);
#56288=EDGE_CURVE('',#42733,#42734,#34792,.T.);
#56289=EDGE_CURVE('',#42735,#42677,#24361,.T.);
#56290=EDGE_CURVE('',#42736,#42735,#34793,.T.);
#56291=EDGE_CURVE('',#42678,#42736,#24362,.T.);
#56292=EDGE_CURVE('',#42681,#42737,#24363,.T.);
#56293=EDGE_CURVE('',#42738,#42680,#24364,.T.);
#56294=EDGE_CURVE('',#42737,#42738,#34794,.T.);
#56295=EDGE_CURVE('',#42739,#42682,#24365,.T.);
#56296=EDGE_CURVE('',#42740,#42739,#34795,.T.);
#56297=EDGE_CURVE('',#42683,#42740,#24366,.T.);
#56298=EDGE_CURVE('',#42685,#42741,#24367,.T.);
#56299=EDGE_CURVE('',#42742,#42684,#24368,.T.);
#56300=EDGE_CURVE('',#42741,#42742,#34796,.T.);
#56301=EDGE_CURVE('',#42687,#42743,#24369,.T.);
#56302=EDGE_CURVE('',#42744,#42686,#24370,.T.);
#56303=EDGE_CURVE('',#42743,#42744,#34797,.T.);
#56304=EDGE_CURVE('',#42745,#42688,#24371,.T.);
#56305=EDGE_CURVE('',#42746,#42745,#34798,.T.);
#56306=EDGE_CURVE('',#42689,#42746,#24372,.T.);
#56307=EDGE_CURVE('',#42747,#42691,#24373,.T.);
#56308=EDGE_CURVE('',#42748,#42747,#34799,.T.);
#56309=EDGE_CURVE('',#42693,#42748,#24374,.T.);
#56310=EDGE_CURVE('',#42696,#42749,#24375,.T.);
#56311=EDGE_CURVE('',#42750,#42695,#24376,.T.);
#56312=EDGE_CURVE('',#42749,#42750,#34800,.T.);
#56313=EDGE_CURVE('',#42698,#42751,#24377,.T.);
#56314=EDGE_CURVE('',#42752,#42697,#24378,.T.);
#56315=EDGE_CURVE('',#42751,#42752,#34801,.T.);
#56316=EDGE_CURVE('',#42753,#42699,#6572,.T.);
#56317=EDGE_CURVE('',#42754,#42753,#6573,.T.);
#56318=EDGE_CURVE('',#42755,#42754,#34802,.T.);
#56319=EDGE_CURVE('',#42756,#42755,#6574,.T.);
#56320=EDGE_CURVE('',#42700,#42756,#6575,.T.);
#56321=EDGE_CURVE('',#42757,#42758,#6576,.T.);
#56322=EDGE_CURVE('',#42701,#42757,#6577,.T.);
#56323=EDGE_CURVE('',#42759,#42702,#6578,.T.);
#56324=EDGE_CURVE('',#42760,#42759,#6579,.T.);
#56325=EDGE_CURVE('',#42758,#42760,#34803,.T.);
#56326=EDGE_CURVE('',#42761,#42762,#6580,.T.);
#56327=EDGE_CURVE('',#42703,#42761,#6581,.T.);
#56328=EDGE_CURVE('',#42763,#42704,#6582,.T.);
#56329=EDGE_CURVE('',#42764,#42763,#6583,.T.);
#56330=EDGE_CURVE('',#42762,#42764,#34804,.T.);
#56331=EDGE_CURVE('',#42765,#42766,#6584,.T.);
#56332=EDGE_CURVE('',#42705,#42765,#6585,.T.);
#56333=EDGE_CURVE('',#42767,#42706,#6586,.T.);
#56334=EDGE_CURVE('',#42768,#42767,#6587,.T.);
#56335=EDGE_CURVE('',#42766,#42768,#34805,.T.);
#56336=EDGE_CURVE('',#42769,#42707,#6588,.T.);
#56337=EDGE_CURVE('',#42770,#42769,#6589,.T.);
#56338=EDGE_CURVE('',#42771,#42770,#34806,.T.);
#56339=EDGE_CURVE('',#42772,#42771,#6590,.T.);
#56340=EDGE_CURVE('',#42708,#42772,#6591,.T.);
#56341=EDGE_CURVE('',#42460,#42773,#6592,.T.);
#56342=EDGE_CURVE('',#42774,#42709,#6593,.T.);
#56343=EDGE_CURVE('',#42775,#42774,#6594,.T.);
#56344=EDGE_CURVE('',#42773,#42775,#34807,.T.);
#56345=EDGE_CURVE('',#42776,#42777,#6595,.T.);
#56346=EDGE_CURVE('',#42710,#42776,#6596,.T.);
#56347=EDGE_CURVE('',#42778,#42711,#6597,.T.);
#56348=EDGE_CURVE('',#42779,#42778,#6598,.T.);
#56349=EDGE_CURVE('',#42777,#42779,#34808,.T.);
#56350=EDGE_CURVE('',#42780,#42712,#6599,.T.);
#56351=EDGE_CURVE('',#42781,#42780,#6600,.T.);
#56352=EDGE_CURVE('',#42782,#42781,#34809,.T.);
#56353=EDGE_CURVE('',#42783,#42782,#6601,.T.);
#56354=EDGE_CURVE('',#42713,#42783,#6602,.T.);
#56355=EDGE_CURVE('',#42784,#42785,#6603,.T.);
#56356=EDGE_CURVE('',#42714,#42784,#6604,.T.);
#56357=EDGE_CURVE('',#42786,#42715,#6605,.T.);
#56358=EDGE_CURVE('',#42787,#42786,#6606,.T.);
#56359=EDGE_CURVE('',#42785,#42787,#34810,.T.);
#56360=EDGE_CURVE('',#42788,#42789,#6607,.T.);
#56361=EDGE_CURVE('',#42716,#42788,#6608,.T.);
#56362=EDGE_CURVE('',#42790,#42463,#6609,.T.);
#56363=EDGE_CURVE('',#42789,#42790,#34811,.T.);
#56364=EDGE_CURVE('',#42791,#42717,#6610,.T.);
#56365=EDGE_CURVE('',#42792,#42791,#6611,.T.);
#56366=EDGE_CURVE('',#42793,#42792,#34812,.T.);
#56367=EDGE_CURVE('',#42794,#42793,#6612,.T.);
#56368=EDGE_CURVE('',#42718,#42794,#6613,.T.);
#56369=EDGE_CURVE('',#42795,#42796,#6614,.T.);
#56370=EDGE_CURVE('',#42719,#42795,#6615,.T.);
#56371=EDGE_CURVE('',#42797,#42720,#6616,.T.);
#56372=EDGE_CURVE('',#42798,#42797,#6617,.T.);
#56373=EDGE_CURVE('',#42796,#42798,#34813,.T.);
#56374=EDGE_CURVE('',#42799,#42721,#6618,.T.);
#56375=EDGE_CURVE('',#42800,#42799,#6619,.T.);
#56376=EDGE_CURVE('',#42801,#42800,#34814,.T.);
#56377=EDGE_CURVE('',#42802,#42801,#6620,.T.);
#56378=EDGE_CURVE('',#42722,#42802,#6621,.T.);
#56379=EDGE_CURVE('',#42803,#42804,#6622,.T.);
#56380=EDGE_CURVE('',#42723,#42803,#6623,.T.);
#56381=EDGE_CURVE('',#42805,#42724,#6624,.T.);
#56382=EDGE_CURVE('',#42806,#42805,#6625,.T.);
#56383=EDGE_CURVE('',#42804,#42806,#34815,.T.);
#56384=EDGE_CURVE('',#42471,#42725,#6626,.T.);
#56385=EDGE_CURVE('',#42557,#42470,#34816,.T.);
#56386=EDGE_CURVE('',#42726,#42556,#6627,.T.);
#56387=EDGE_CURVE('',#42727,#42468,#6628,.T.);
#56388=EDGE_CURVE('',#42479,#42728,#6629,.T.);
#56389=EDGE_CURVE('',#42469,#42478,#34817,.T.);
#56390=EDGE_CURVE('',#42729,#42476,#6630,.T.);
#56391=EDGE_CURVE('',#42495,#42730,#6631,.T.);
#56392=EDGE_CURVE('',#42477,#42494,#34818,.T.);
#56393=EDGE_CURVE('',#42487,#42731,#6632,.T.);
#56394=EDGE_CURVE('',#42493,#42486,#34819,.T.);
#56395=EDGE_CURVE('',#42732,#42492,#6633,.T.);
#56396=EDGE_CURVE('',#42733,#42484,#6634,.T.);
#56397=EDGE_CURVE('',#42510,#42734,#6635,.T.);
#56398=EDGE_CURVE('',#42485,#42509,#34820,.T.);
#56399=EDGE_CURVE('',#42502,#42735,#6636,.T.);
#56400=EDGE_CURVE('',#42508,#42501,#34821,.T.);
#56401=EDGE_CURVE('',#42736,#42507,#6637,.T.);
#56402=EDGE_CURVE('',#42737,#42499,#6638,.T.);
#56403=EDGE_CURVE('',#42807,#42738,#6639,.T.);
#56404=EDGE_CURVE('',#42808,#42807,#6640,.T.);
#56405=EDGE_CURVE('',#42500,#42808,#34822,.T.);
#56406=EDGE_CURVE('',#42520,#42739,#6641,.T.);
#56407=EDGE_CURVE('',#42534,#42519,#34823,.T.);
#56408=EDGE_CURVE('',#42740,#42533,#6642,.T.);
#56409=EDGE_CURVE('',#42741,#42517,#6643,.T.);
#56410=EDGE_CURVE('',#42527,#42742,#6644,.T.);
#56411=EDGE_CURVE('',#42518,#42526,#34824,.T.);
#56412=EDGE_CURVE('',#42743,#42524,#6645,.T.);
#56413=EDGE_CURVE('',#42543,#42744,#6646,.T.);
#56414=EDGE_CURVE('',#42525,#42542,#34825,.T.);
#56415=EDGE_CURVE('',#42536,#42745,#6647,.T.);
#56416=EDGE_CURVE('',#42809,#42535,#34826,.T.);
#56417=EDGE_CURVE('',#42810,#42809,#6648,.T.);
#56418=EDGE_CURVE('',#42746,#42810,#6649,.T.);
#56419=EDGE_CURVE('',#42811,#42747,#6650,.T.);
#56420=EDGE_CURVE('',#42812,#42811,#6651,.T.);
#56421=EDGE_CURVE('',#42813,#42812,#34827,.T.);
#56422=EDGE_CURVE('',#42814,#42813,#6652,.T.);
#56423=EDGE_CURVE('',#42748,#42814,#6653,.T.);
#56424=EDGE_CURVE('',#42749,#42540,#6654,.T.);
#56425=EDGE_CURVE('',#42551,#42750,#6655,.T.);
#56426=EDGE_CURVE('',#42541,#42550,#34828,.T.);
#56427=EDGE_CURVE('',#42751,#42548,#6656,.T.);
#56428=EDGE_CURVE('',#42559,#42752,#6657,.T.);
#56429=EDGE_CURVE('',#42549,#42558,#34829,.T.);
#56430=EDGE_CURVE('',#42598,#42815,#6658,.T.);
#56431=EDGE_CURVE('',#42816,#42597,#6659,.T.);
#56432=EDGE_CURVE('',#42817,#42816,#6660,.T.);
#56433=EDGE_CURVE('',#42818,#42817,#34830,.T.);
#56434=EDGE_CURVE('',#42815,#42818,#6661,.T.);
#56435=EDGE_CURVE('',#42818,#42819,#24379,.T.);
#56436=EDGE_CURVE('',#42820,#42817,#24380,.T.);
#56437=EDGE_CURVE('',#42819,#42820,#34831,.T.);
#56438=EDGE_CURVE('',#42821,#42822,#6662,.T.);
#56439=EDGE_CURVE('',#42819,#42821,#6663,.T.);
#56440=EDGE_CURVE('',#42823,#42820,#6664,.T.);
#56441=EDGE_CURVE('',#42824,#42823,#6665,.T.);
#56442=EDGE_CURVE('',#42822,#42824,#34832,.T.);
#56443=EDGE_CURVE('',#42565,#42754,#34833,.T.);
#56444=EDGE_CURVE('',#42758,#42564,#34834,.T.);
#56445=EDGE_CURVE('',#42762,#42760,#34835,.T.);
#56446=EDGE_CURVE('',#42766,#42764,#34836,.T.);
#56447=EDGE_CURVE('',#42777,#42768,#34837,.T.);
#56448=EDGE_CURVE('',#42771,#42779,#34838,.T.);
#56449=EDGE_CURVE('',#42773,#42770,#34839,.T.);
#56450=EDGE_CURVE('',#42822,#42775,#34840,.T.);
#56451=EDGE_CURVE('',#42813,#42824,#34841,.T.);
#56452=EDGE_CURVE('',#42809,#42812,#34842,.T.);
#56453=EDGE_CURVE('',#42782,#42808,#34843,.T.);
#56454=EDGE_CURVE('',#42785,#42781,#34844,.T.);
#56455=EDGE_CURVE('',#42789,#42787,#34845,.T.);
#56456=EDGE_CURVE('',#42793,#42790,#34846,.T.);
#56457=EDGE_CURVE('',#42796,#42792,#34847,.T.);
#56458=EDGE_CURVE('',#42801,#42798,#34848,.T.);
#56459=EDGE_CURVE('',#42804,#42800,#34849,.T.);
#56460=EDGE_CURVE('',#42755,#42806,#34850,.T.);
#56461=EDGE_CURVE('',#42816,#42823,#24381,.T.);
#56462=EDGE_CURVE('',#42694,#42814,#24382,.T.);
#56463=EDGE_CURVE('',#42635,#42774,#24383,.T.);
#56464=EDGE_CURVE('',#42815,#42821,#24384,.T.);
#56465=EDGE_CURVE('',#42692,#42811,#24385,.T.);
#56466=EDGE_CURVE('',#42690,#42810,#24386,.T.);
#56467=EDGE_CURVE('',#42679,#42807,#24387,.T.);
#56468=EDGE_CURVE('',#42644,#42783,#24388,.T.);
#56469=EDGE_CURVE('',#42664,#42805,#24389,.T.);
#56470=EDGE_CURVE('',#42618,#42756,#24390,.T.);
#56471=EDGE_CURVE('',#42656,#42797,#24391,.T.);
#56472=EDGE_CURVE('',#42662,#42802,#24392,.T.);
#56473=EDGE_CURVE('',#42660,#42799,#24393,.T.);
#56474=EDGE_CURVE('',#42663,#42803,#24394,.T.);
#56475=EDGE_CURVE('',#42654,#42794,#24395,.T.);
#56476=EDGE_CURVE('',#42652,#42791,#24396,.T.);
#56477=EDGE_CURVE('',#42655,#42795,#24397,.T.);
#56478=EDGE_CURVE('',#42646,#42786,#24398,.T.);
#56479=EDGE_CURVE('',#42649,#42788,#24399,.T.);
#56480=EDGE_CURVE('',#42642,#42780,#24400,.T.);
#56481=EDGE_CURVE('',#42645,#42784,#24401,.T.);
#56482=EDGE_CURVE('',#42638,#42778,#24402,.T.);
#56483=EDGE_CURVE('',#42634,#42772,#24403,.T.);
#56484=EDGE_CURVE('',#42628,#42767,#24404,.T.);
#56485=EDGE_CURVE('',#42637,#42776,#24405,.T.);
#56486=EDGE_CURVE('',#42632,#42769,#24406,.T.);
#56487=EDGE_CURVE('',#42624,#42763,#24407,.T.);
#56488=EDGE_CURVE('',#42627,#42765,#24408,.T.);
#56489=EDGE_CURVE('',#42620,#42759,#24409,.T.);
#56490=EDGE_CURVE('',#42623,#42761,#24410,.T.);
#56491=EDGE_CURVE('',#42571,#42563,#24411,.T.);
#56492=EDGE_CURVE('',#42619,#42757,#24412,.T.);
#56493=EDGE_CURVE('',#42616,#42753,#24413,.T.);
#56494=EDGE_CURVE('',#42572,#42566,#24414,.T.);
#56495=EDGE_CURVE('',#42612,#42614,#24415,.T.);
#56496=EDGE_CURVE('',#42611,#42613,#24416,.T.);
#56497=EDGE_CURVE('',#42825,#42825,#34851,.T.);
#56498=EDGE_CURVE('',#42825,#42826,#24417,.T.);
#56499=EDGE_CURVE('',#42826,#42826,#34852,.T.);
#56500=EDGE_CURVE('',#42827,#42828,#34853,.T.);
#56501=EDGE_CURVE('',#42827,#42829,#24418,.T.);
#56502=EDGE_CURVE('',#42829,#42830,#34854,.T.);
#56503=EDGE_CURVE('',#42828,#42830,#24419,.T.);
#56504=EDGE_CURVE('',#42831,#42831,#34855,.T.);
#56505=EDGE_CURVE('',#42831,#42832,#24420,.T.);
#56506=EDGE_CURVE('',#42832,#42832,#34856,.T.);
#56507=EDGE_CURVE('',#42830,#42833,#34857,.T.);
#56508=EDGE_CURVE('',#42834,#42833,#24421,.T.);
#56509=EDGE_CURVE('',#42828,#42834,#34858,.T.);
#56510=EDGE_CURVE('',#42833,#42835,#34859,.T.);
#56511=EDGE_CURVE('',#42836,#42835,#24422,.T.);
#56512=EDGE_CURVE('',#42834,#42836,#34860,.T.);
#56513=EDGE_CURVE('',#42829,#42835,#34861,.T.);
#56514=EDGE_CURVE('',#42827,#42836,#34862,.T.);
#56515=EDGE_CURVE('',#42837,#42837,#34863,.T.);
#56516=EDGE_CURVE('',#42837,#42838,#24423,.T.);
#56517=EDGE_CURVE('',#42838,#42838,#34864,.T.);
#56518=EDGE_CURVE('',#42839,#42839,#34865,.T.);
#56519=EDGE_CURVE('',#42839,#42840,#24424,.T.);
#56520=EDGE_CURVE('',#42840,#42840,#34866,.T.);
#56521=EDGE_CURVE('',#42841,#42842,#34867,.T.);
#56522=EDGE_CURVE('',#42841,#42843,#24425,.T.);
#56523=EDGE_CURVE('',#42843,#42844,#34868,.T.);
#56524=EDGE_CURVE('',#42842,#42844,#24426,.T.);
#56525=EDGE_CURVE('',#42842,#42845,#34869,.T.);
#56526=EDGE_CURVE('',#42845,#42846,#34870,.T.);
#56527=EDGE_CURVE('',#42846,#42841,#34871,.T.);
#56528=EDGE_CURVE('',#42844,#42847,#34872,.T.);
#56529=EDGE_CURVE('',#42848,#42843,#34873,.T.);
#56530=EDGE_CURVE('',#42847,#42848,#34874,.T.);
#56531=EDGE_CURVE('',#42845,#42847,#24427,.T.);
#56532=EDGE_CURVE('',#42846,#42848,#24428,.T.);
#56533=EDGE_CURVE('',#42849,#42849,#34875,.T.);
#56534=EDGE_CURVE('',#42849,#42850,#24429,.T.);
#56535=EDGE_CURVE('',#42850,#42850,#34876,.T.);
#56536=EDGE_CURVE('',#42851,#42851,#34877,.T.);
#56537=EDGE_CURVE('',#42851,#42852,#24430,.T.);
#56538=EDGE_CURVE('',#42852,#42852,#34878,.T.);
#56539=EDGE_CURVE('',#42853,#42853,#34879,.T.);
#56540=EDGE_CURVE('',#42853,#42854,#24431,.T.);
#56541=EDGE_CURVE('',#42854,#42854,#34880,.T.);
#56542=EDGE_CURVE('',#42855,#42855,#34881,.T.);
#56543=EDGE_CURVE('',#42855,#42856,#24432,.T.);
#56544=EDGE_CURVE('',#42856,#42856,#34882,.T.);
#56545=EDGE_CURVE('',#42857,#42857,#34883,.T.);
#56546=EDGE_CURVE('',#42857,#42858,#24433,.T.);
#56547=EDGE_CURVE('',#42858,#42858,#34884,.T.);
#56548=EDGE_CURVE('',#42859,#42859,#34885,.T.);
#56549=EDGE_CURVE('',#42859,#42860,#24434,.T.);
#56550=EDGE_CURVE('',#42860,#42860,#34886,.T.);
#56551=EDGE_CURVE('',#42861,#42861,#34887,.T.);
#56552=EDGE_CURVE('',#42861,#42862,#34888,.T.);
#56553=EDGE_CURVE('',#42862,#42862,#34889,.T.);
#56554=EDGE_CURVE('',#42863,#42863,#34890,.T.);
#56555=EDGE_CURVE('',#42863,#42864,#34891,.T.);
#56556=EDGE_CURVE('',#42864,#42864,#34892,.T.);
#56557=EDGE_CURVE('',#42865,#42865,#34893,.T.);
#56558=EDGE_CURVE('',#42865,#42866,#34894,.T.);
#56559=EDGE_CURVE('',#42866,#42866,#34895,.T.);
#56560=EDGE_CURVE('',#42862,#42867,#24435,.T.);
#56561=EDGE_CURVE('',#42867,#42867,#34896,.T.);
#56562=EDGE_CURVE('',#42867,#42868,#34897,.T.);
#56563=EDGE_CURVE('',#42868,#42868,#34898,.T.);
#56564=EDGE_CURVE('',#42869,#42869,#34899,.T.);
#56565=EDGE_CURVE('',#42869,#42870,#34900,.T.);
#56566=EDGE_CURVE('',#42870,#42870,#34901,.T.);
#56567=EDGE_CURVE('',#42870,#42863,#24436,.T.);
#56568=EDGE_CURVE('',#42864,#42865,#24437,.T.);
#56569=EDGE_CURVE('',#42866,#42871,#24438,.T.);
#56570=EDGE_CURVE('',#42871,#42871,#34902,.T.);
#56571=EDGE_CURVE('',#42871,#42872,#34903,.T.);
#56572=EDGE_CURVE('',#42872,#42872,#34904,.T.);
#56573=EDGE_CURVE('',#42873,#42874,#34905,.T.);
#56574=EDGE_CURVE('',#42875,#42875,#34906,.T.);
#56575=EDGE_CURVE('',#42876,#42876,#34907,.T.);
#56576=EDGE_CURVE('',#42877,#42877,#34908,.T.);
#56577=EDGE_CURVE('',#42877,#42878,#34909,.T.);
#56578=EDGE_CURVE('',#42878,#42878,#34910,.T.);
#56579=EDGE_CURVE('',#42878,#42879,#24439,.T.);
#56580=EDGE_CURVE('',#42879,#42879,#34911,.T.);
#56581=EDGE_CURVE('',#42879,#42880,#34912,.T.);
#56582=EDGE_CURVE('',#42880,#42880,#34913,.T.);
#56583=EDGE_CURVE('',#42881,#42882,#34914,.T.);
#56584=EDGE_CURVE('',#42883,#42884,#34915,.T.);
#56585=EDGE_CURVE('',#42885,#42886,#34916,.T.);
#56586=EDGE_CURVE('',#42887,#42888,#34917,.T.);
#56587=EDGE_CURVE('',#42889,#42890,#34918,.T.);
#56588=EDGE_CURVE('',#42891,#42892,#34919,.T.);
#56589=EDGE_CURVE('',#42893,#42894,#34920,.T.);
#56590=EDGE_CURVE('',#42895,#42896,#34921,.T.);
#56591=EDGE_CURVE('',#42897,#42898,#34922,.T.);
#56592=EDGE_CURVE('',#42899,#42900,#34923,.T.);
#56593=EDGE_CURVE('',#42901,#42902,#34924,.T.);
#56594=EDGE_CURVE('',#42903,#42904,#34925,.T.);
#56595=EDGE_CURVE('',#42905,#42906,#34926,.T.);
#56596=EDGE_CURVE('',#42907,#42908,#34927,.T.);
#56597=EDGE_CURVE('',#42909,#42910,#34928,.T.);
#56598=EDGE_CURVE('',#42911,#42912,#34929,.T.);
#56599=EDGE_CURVE('',#42913,#42914,#34930,.T.);
#56600=EDGE_CURVE('',#42915,#42916,#34931,.T.);
#56601=EDGE_CURVE('',#42917,#42918,#34932,.T.);
#56602=EDGE_CURVE('',#42919,#42920,#34933,.T.);
#56603=EDGE_CURVE('',#42921,#42922,#34934,.T.);
#56604=EDGE_CURVE('',#42923,#42924,#34935,.T.);
#56605=EDGE_CURVE('',#42925,#42926,#34936,.T.);
#56606=EDGE_CURVE('',#42927,#42928,#34937,.T.);
#56607=EDGE_CURVE('',#42929,#42929,#34938,.T.);
#56608=EDGE_CURVE('',#42929,#42930,#24440,.T.);
#56609=EDGE_CURVE('',#42930,#42930,#34939,.T.);
#56610=EDGE_CURVE('',#42931,#42931,#34940,.T.);
#56611=EDGE_CURVE('',#42931,#42932,#24441,.T.);
#56612=EDGE_CURVE('',#42932,#42932,#34941,.T.);
#56613=EDGE_CURVE('',#42933,#42933,#34942,.T.);
#56614=EDGE_CURVE('',#42933,#42934,#24442,.T.);
#56615=EDGE_CURVE('',#42934,#42934,#34943,.T.);
#56616=EDGE_CURVE('',#42935,#42935,#34944,.T.);
#56617=EDGE_CURVE('',#42935,#42936,#24443,.T.);
#56618=EDGE_CURVE('',#42936,#42936,#34945,.T.);
#56619=EDGE_CURVE('',#42937,#42938,#24444,.T.);
#56620=EDGE_CURVE('',#42939,#42938,#24445,.T.);
#56621=EDGE_CURVE('',#42940,#42939,#24446,.T.);
#56622=EDGE_CURVE('',#42940,#42937,#24447,.T.);
#56623=EDGE_CURVE('',#42938,#42941,#24448,.T.);
#56624=EDGE_CURVE('',#42942,#42941,#24449,.T.);
#56625=EDGE_CURVE('',#42939,#42942,#24450,.T.);
#56626=EDGE_CURVE('',#42941,#42943,#24451,.T.);
#56627=EDGE_CURVE('',#42944,#42943,#24452,.T.);
#56628=EDGE_CURVE('',#42942,#42944,#24453,.T.);
#56629=EDGE_CURVE('',#42943,#42945,#24454,.T.);
#56630=EDGE_CURVE('',#42946,#42945,#24455,.T.);
#56631=EDGE_CURVE('',#42944,#42946,#24456,.T.);
#56632=EDGE_CURVE('',#42945,#42947,#24457,.T.);
#56633=EDGE_CURVE('',#42948,#42947,#24458,.T.);
#56634=EDGE_CURVE('',#42946,#42948,#24459,.T.);
#56635=EDGE_CURVE('',#42947,#42937,#24460,.T.);
#56636=EDGE_CURVE('',#42948,#42940,#24461,.T.);
#56637=EDGE_CURVE('',#42949,#42950,#24462,.T.);
#56638=EDGE_CURVE('',#42951,#42950,#34946,.T.);
#56639=EDGE_CURVE('',#42949,#42951,#1539,.T.);
#56640=EDGE_CURVE('',#42952,#42953,#24463,.T.);
#56641=EDGE_CURVE('',#42953,#42954,#1540,.T.);
#56642=EDGE_CURVE('',#42950,#42954,#34947,.T.);
#56643=EDGE_CURVE('',#42952,#42949,#1541,.T.);
#56644=EDGE_CURVE('',#42955,#42956,#24464,.T.);
#56645=EDGE_CURVE('',#42956,#42953,#1542,.T.);
#56646=EDGE_CURVE('',#42955,#42952,#1543,.T.);
#56647=EDGE_CURVE('',#42957,#42958,#24465,.T.);
#56648=EDGE_CURVE('',#42958,#42956,#1544,.T.);
#56649=EDGE_CURVE('',#42957,#42955,#1545,.T.);
#56650=EDGE_CURVE('',#42959,#42960,#24466,.T.);
#56651=EDGE_CURVE('',#42961,#42959,#1546,.T.);
#56652=EDGE_CURVE('',#42962,#42961,#34948,.T.);
#56653=EDGE_CURVE('',#42962,#42960,#1547,.T.);
#56654=EDGE_CURVE('',#42950,#42963,#24467,.T.);
#56655=EDGE_CURVE('',#42954,#42963,#6666,.T.);
#56656=EDGE_CURVE('',#42964,#42965,#24468,.T.);
#56657=EDGE_CURVE('',#42964,#42962,#6667,.T.);
#56658=EDGE_CURVE('',#42961,#42965,#6668,.T.);
#56659=EDGE_CURVE('',#42966,#42967,#24469,.T.);
#56660=EDGE_CURVE('',#42968,#42967,#34949,.T.);
#56661=EDGE_CURVE('',#42966,#42968,#6669,.F.);
#56662=EDGE_CURVE('',#42969,#42970,#24470,.T.);
#56663=EDGE_CURVE('',#42971,#42970,#6670,.F.);
#56664=EDGE_CURVE('',#42967,#42971,#34950,.T.);
#56665=EDGE_CURVE('',#42969,#42966,#6671,.F.);
#56666=EDGE_CURVE('',#42972,#42973,#24471,.T.);
#56667=EDGE_CURVE('',#42970,#42973,#6672,.F.);
#56668=EDGE_CURVE('',#42972,#42969,#6673,.F.);
#56669=EDGE_CURVE('',#42974,#42975,#24472,.T.);
#56670=EDGE_CURVE('',#42973,#42975,#6674,.F.);
#56671=EDGE_CURVE('',#42974,#42972,#6675,.F.);
#56672=EDGE_CURVE('',#42976,#42977,#24473,.T.);
#56673=EDGE_CURVE('',#42975,#42977,#6676,.F.);
#56674=EDGE_CURVE('',#42976,#42974,#6677,.F.);
#56675=EDGE_CURVE('',#42978,#42979,#24474,.T.);
#56676=EDGE_CURVE('',#42980,#42978,#6678,.F.);
#56677=EDGE_CURVE('',#42981,#42980,#34951,.T.);
#56678=EDGE_CURVE('',#42979,#42981,#6679,.F.);
#56679=EDGE_CURVE('',#42977,#42979,#6680,.F.);
#56680=EDGE_CURVE('',#42978,#42976,#6681,.F.);
#56681=EDGE_CURVE('',#42965,#42968,#6682,.T.);
#56682=EDGE_CURVE('',#42967,#42982,#24475,.T.);
#56683=EDGE_CURVE('',#42982,#42982,#34952,.T.);
#56684=EDGE_CURVE('',#42971,#42964,#6683,.T.);
#56685=EDGE_CURVE('',#42963,#42981,#6684,.T.);
#56686=EDGE_CURVE('',#42980,#42983,#6685,.T.);
#56687=EDGE_CURVE('',#42983,#42984,#24476,.T.);
#56688=EDGE_CURVE('',#42984,#42984,#34953,.T.);
#56689=EDGE_CURVE('',#42983,#42951,#6686,.T.);
#56690=EDGE_CURVE('',#42985,#42986,#34954,.T.);
#56691=EDGE_CURVE('',#42985,#42987,#34955,.T.);
#56692=EDGE_CURVE('',#42987,#42988,#34956,.T.);
#56693=EDGE_CURVE('',#42988,#42989,#34957,.T.);
#56694=EDGE_CURVE('',#42989,#42990,#34958,.T.);
#56695=EDGE_CURVE('',#42990,#42986,#34959,.T.);
#56696=EDGE_CURVE('',#42991,#42987,#1548,.T.);
#56697=EDGE_CURVE('',#42991,#42992,#24477,.T.);
#56698=EDGE_CURVE('',#42992,#42993,#1549,.T.);
#56699=EDGE_CURVE('',#42993,#42994,#1550,.T.);
#56700=EDGE_CURVE('',#42995,#42994,#24478,.T.);
#56701=EDGE_CURVE('',#42987,#42995,#1551,.T.);
#56702=EDGE_CURVE('',#42995,#42988,#1552,.T.);
#56703=EDGE_CURVE('',#42994,#42996,#1553,.T.);
#56704=EDGE_CURVE('',#42996,#42997,#1554,.T.);
#56705=EDGE_CURVE('',#42998,#42997,#24479,.T.);
#56706=EDGE_CURVE('',#42988,#42998,#1555,.T.);
#56707=EDGE_CURVE('',#42998,#42989,#1556,.T.);
#56708=EDGE_CURVE('',#42997,#42999,#1557,.T.);
#56709=EDGE_CURVE('',#42999,#43000,#1558,.T.);
#56710=EDGE_CURVE('',#43001,#43000,#24480,.T.);
#56711=EDGE_CURVE('',#42989,#43001,#1559,.T.);
#56712=EDGE_CURVE('',#43001,#42990,#1560,.T.);
#56713=EDGE_CURVE('',#43000,#43002,#1561,.T.);
#56714=EDGE_CURVE('',#43002,#43003,#1562,.T.);
#56715=EDGE_CURVE('',#43004,#43003,#24481,.T.);
#56716=EDGE_CURVE('',#42990,#43004,#1563,.T.);
#56717=EDGE_CURVE('',#43004,#42986,#1564,.T.);
#56718=EDGE_CURVE('',#43003,#43005,#1565,.T.);
#56719=EDGE_CURVE('',#43005,#43006,#1566,.T.);
#56720=EDGE_CURVE('',#43007,#43006,#24482,.T.);
#56721=EDGE_CURVE('',#42986,#43007,#1567,.T.);
#56722=EDGE_CURVE('',#43007,#42985,#1568,.T.);
#56723=EDGE_CURVE('',#43006,#43008,#1569,.T.);
#56724=EDGE_CURVE('',#43008,#42992,#1570,.T.);
#56725=EDGE_CURVE('',#42985,#42991,#1571,.T.);
#56726=EDGE_CURVE('',#42993,#43008,#34960,.T.);
#56727=EDGE_CURVE('',#43008,#43005,#34961,.T.);
#56728=EDGE_CURVE('',#43005,#43002,#34962,.T.);
#56729=EDGE_CURVE('',#43002,#42999,#34963,.T.);
#56730=EDGE_CURVE('',#42999,#42996,#34964,.T.);
#56731=EDGE_CURVE('',#42996,#42993,#34965,.T.);
#56732=EDGE_CURVE('',#42960,#42958,#1572,.T.);
#56733=EDGE_CURVE('',#42959,#42957,#1573,.T.);
#56734=EDGE_CURVE('',#43009,#43010,#24483,.T.);
#56735=EDGE_CURVE('',#43010,#43011,#1574,.T.);
#56736=EDGE_CURVE('',#43012,#43011,#34966,.T.);
#56737=EDGE_CURVE('',#43009,#43012,#1575,.T.);
#56738=EDGE_CURVE('',#43013,#43014,#24484,.T.);
#56739=EDGE_CURVE('',#43014,#43010,#1576,.T.);
#56740=EDGE_CURVE('',#43013,#43009,#1577,.T.);
#56741=EDGE_CURVE('',#43015,#43016,#24485,.T.);
#56742=EDGE_CURVE('',#43016,#43014,#1578,.T.);
#56743=EDGE_CURVE('',#43015,#43013,#1579,.T.);
#56744=EDGE_CURVE('',#43017,#43018,#24486,.T.);
#56745=EDGE_CURVE('',#43018,#43016,#1580,.T.);
#56746=EDGE_CURVE('',#43017,#43015,#1581,.T.);
#56747=EDGE_CURVE('',#43019,#43020,#24487,.T.);
#56748=EDGE_CURVE('',#43020,#43018,#1582,.T.);
#56749=EDGE_CURVE('',#43019,#43017,#1583,.T.);
#56750=EDGE_CURVE('',#43021,#43022,#24488,.T.);
#56751=EDGE_CURVE('',#43023,#43021,#34967,.T.);
#56752=EDGE_CURVE('',#43023,#43022,#1584,.T.);
#56753=EDGE_CURVE('',#43024,#43025,#24489,.T.);
#56754=EDGE_CURVE('',#43026,#43025,#34968,.T.);
#56755=EDGE_CURVE('',#43024,#43026,#6687,.F.);
#56756=EDGE_CURVE('',#43027,#43028,#24490,.T.);
#56757=EDGE_CURVE('',#43025,#43028,#6688,.F.);
#56758=EDGE_CURVE('',#43027,#43024,#6689,.F.);
#56759=EDGE_CURVE('',#43029,#43030,#24491,.T.);
#56760=EDGE_CURVE('',#43028,#43030,#6690,.F.);
#56761=EDGE_CURVE('',#43029,#43027,#6691,.F.);
#56762=EDGE_CURVE('',#43031,#43032,#24492,.T.);
#56763=EDGE_CURVE('',#43030,#43032,#6692,.F.);
#56764=EDGE_CURVE('',#43031,#43029,#6693,.F.);
#56765=EDGE_CURVE('',#43033,#43034,#24493,.T.);
#56766=EDGE_CURVE('',#43032,#43034,#6694,.F.);
#56767=EDGE_CURVE('',#43033,#43031,#6695,.F.);
#56768=EDGE_CURVE('',#43035,#43036,#24494,.T.);
#56769=EDGE_CURVE('',#43034,#43036,#6696,.F.);
#56770=EDGE_CURVE('',#43035,#43033,#6697,.F.);
#56771=EDGE_CURVE('',#43037,#43038,#24495,.T.);
#56772=EDGE_CURVE('',#43039,#43037,#6698,.F.);
#56773=EDGE_CURVE('',#43040,#43039,#34969,.T.);
#56774=EDGE_CURVE('',#43038,#43040,#6699,.F.);
#56775=EDGE_CURVE('',#43036,#43038,#6700,.F.);
#56776=EDGE_CURVE('',#43037,#43035,#6701,.F.);
#56777=EDGE_CURVE('',#43041,#43041,#34970,.T.);
#56778=EDGE_CURVE('',#43042,#43042,#34971,.T.);
#56779=EDGE_CURVE('',#43043,#43044,#34972,.T.);
#56780=EDGE_CURVE('',#43045,#43043,#34973,.T.);
#56781=EDGE_CURVE('',#43046,#43045,#34974,.T.);
#56782=EDGE_CURVE('',#43047,#43046,#34975,.T.);
#56783=EDGE_CURVE('',#43048,#43047,#34976,.T.);
#56784=EDGE_CURVE('',#43044,#43048,#34977,.T.);
#56785=EDGE_CURVE('',#43049,#43050,#1585,.F.);
#56786=EDGE_CURVE('',#43050,#43051,#1586,.T.);
#56787=EDGE_CURVE('',#43051,#43052,#1587,.T.);
#56788=EDGE_CURVE('',#43052,#43053,#1588,.T.);
#56789=EDGE_CURVE('',#43053,#43054,#24496,.T.);
#56790=EDGE_CURVE('',#43054,#43054,#34978,.T.);
#56791=EDGE_CURVE('',#43053,#43055,#1589,.T.);
#56792=EDGE_CURVE('',#43055,#43056,#1590,.T.);
#56793=EDGE_CURVE('',#43056,#43049,#1591,.T.);
#56794=EDGE_CURVE('',#43039,#43057,#6702,.T.);
#56795=EDGE_CURVE('',#43057,#43058,#24497,.T.);
#56796=EDGE_CURVE('',#43058,#43058,#34979,.T.);
#56797=EDGE_CURVE('',#43057,#43012,#6703,.T.);
#56798=EDGE_CURVE('',#43011,#43040,#6704,.T.);
#56799=EDGE_CURVE('',#43055,#43043,#24498,.T.);
#56800=EDGE_CURVE('',#43056,#43044,#24499,.T.);
#56801=EDGE_CURVE('',#43049,#43048,#24500,.T.);
#56802=EDGE_CURVE('',#43050,#43047,#24501,.T.);
#56803=EDGE_CURVE('',#43051,#43046,#24502,.T.);
#56804=EDGE_CURVE('',#43052,#43045,#24503,.T.);
#56805=EDGE_CURVE('',#43021,#43026,#6705,.T.);
#56806=EDGE_CURVE('',#43025,#43023,#6706,.T.);
#56807=EDGE_CURVE('',#43022,#43020,#1592,.T.);
#56808=EDGE_CURVE('',#43021,#43019,#1593,.T.);
#56809=EDGE_CURVE('',#43059,#43060,#24504,.T.);
#56810=EDGE_CURVE('',#43061,#43059,#1594,.T.);
#56811=EDGE_CURVE('',#43062,#43061,#34980,.T.);
#56812=EDGE_CURVE('',#43062,#43060,#1595,.T.);
#56813=EDGE_CURVE('',#43063,#43064,#6707,.T.);
#56814=EDGE_CURVE('',#43064,#43065,#24505,.T.);
#56815=EDGE_CURVE('',#43065,#43065,#34981,.T.);
#56816=EDGE_CURVE('',#43064,#43062,#6708,.T.);
#56817=EDGE_CURVE('',#43061,#43066,#6709,.F.);
#56818=EDGE_CURVE('',#43066,#43063,#34982,.T.);
#56819=EDGE_CURVE('',#43067,#43068,#34983,.T.);
#56820=EDGE_CURVE('',#43068,#43063,#1596,.T.);
#56821=EDGE_CURVE('',#43066,#43067,#6710,.F.);
#56822=EDGE_CURVE('',#43059,#43069,#1597,.T.);
#56823=EDGE_CURVE('',#43069,#43067,#6711,.T.);
#56824=EDGE_CURVE('',#43068,#43070,#6712,.T.);
#56825=EDGE_CURVE('',#43060,#43070,#1598,.T.);
#56826=EDGE_CURVE('',#43070,#43069,#34984,.T.);
#56827=EDGE_CURVE('',#43071,#43072,#24506,.T.);
#56828=EDGE_CURVE('',#43073,#43071,#1599,.T.);
#56829=EDGE_CURVE('',#43073,#43072,#34985,.T.);
#56830=EDGE_CURVE('',#43074,#43075,#24507,.T.);
#56831=EDGE_CURVE('',#43071,#43074,#1600,.T.);
#56832=EDGE_CURVE('',#43072,#43075,#1601,.T.);
#56833=EDGE_CURVE('',#43076,#43077,#24508,.T.);
#56834=EDGE_CURVE('',#43074,#43076,#1602,.T.);
#56835=EDGE_CURVE('',#43075,#43077,#1603,.T.);
#56836=EDGE_CURVE('',#43078,#43079,#24509,.T.);
#56837=EDGE_CURVE('',#43076,#43078,#1604,.T.);
#56838=EDGE_CURVE('',#43077,#43079,#1605,.T.);
#56839=EDGE_CURVE('',#43080,#43081,#24510,.T.);
#56840=EDGE_CURVE('',#43078,#43080,#1606,.T.);
#56841=EDGE_CURVE('',#43079,#43081,#1607,.T.);
#56842=EDGE_CURVE('',#43082,#43083,#24511,.T.);
#56843=EDGE_CURVE('',#43080,#43082,#1608,.T.);
#56844=EDGE_CURVE('',#43081,#43083,#1609,.T.);
#56845=EDGE_CURVE('',#43084,#43085,#24512,.T.);
#56846=EDGE_CURVE('',#43082,#43084,#1610,.T.);
#56847=EDGE_CURVE('',#43083,#43085,#1611,.T.);
#56848=EDGE_CURVE('',#43086,#43087,#24513,.T.);
#56849=EDGE_CURVE('',#43084,#43086,#1612,.T.);
#56850=EDGE_CURVE('',#43085,#43087,#1613,.T.);
#56851=EDGE_CURVE('',#43088,#43089,#24514,.T.);
#56852=EDGE_CURVE('',#43086,#43088,#1614,.T.);
#56853=EDGE_CURVE('',#43087,#43089,#1615,.T.);
#56854=EDGE_CURVE('',#43090,#43091,#24515,.T.);
#56855=EDGE_CURVE('',#43088,#43090,#1616,.T.);
#56856=EDGE_CURVE('',#43089,#43091,#1617,.T.);
#56857=EDGE_CURVE('',#43092,#43093,#24516,.T.);
#56858=EDGE_CURVE('',#43090,#43092,#1618,.T.);
#56859=EDGE_CURVE('',#43091,#43093,#1619,.T.);
#56860=EDGE_CURVE('',#43094,#43095,#24517,.T.);
#56861=EDGE_CURVE('',#43092,#43094,#1620,.T.);
#56862=EDGE_CURVE('',#43093,#43095,#1621,.T.);
#56863=EDGE_CURVE('',#43096,#43097,#24518,.T.);
#56864=EDGE_CURVE('',#43094,#43096,#1622,.T.);
#56865=EDGE_CURVE('',#43095,#43097,#1623,.T.);
#56866=EDGE_CURVE('',#43098,#43099,#24519,.T.);
#56867=EDGE_CURVE('',#43096,#43098,#1624,.T.);
#56868=EDGE_CURVE('',#43097,#43099,#1625,.T.);
#56869=EDGE_CURVE('',#43100,#43101,#24520,.T.);
#56870=EDGE_CURVE('',#43098,#43100,#1626,.T.);
#56871=EDGE_CURVE('',#43099,#43101,#1627,.T.);
#56872=EDGE_CURVE('',#43102,#43103,#24521,.T.);
#56873=EDGE_CURVE('',#43100,#43102,#1628,.T.);
#56874=EDGE_CURVE('',#43101,#43103,#1629,.T.);
#56875=EDGE_CURVE('',#43104,#43105,#24522,.T.);
#56876=EDGE_CURVE('',#43102,#43104,#1630,.T.);
#56877=EDGE_CURVE('',#43103,#43105,#1631,.T.);
#56878=EDGE_CURVE('',#43106,#43107,#24523,.T.);
#56879=EDGE_CURVE('',#43104,#43106,#1632,.T.);
#56880=EDGE_CURVE('',#43105,#43107,#1633,.T.);
#56881=EDGE_CURVE('',#43108,#43109,#24524,.T.);
#56882=EDGE_CURVE('',#43106,#43108,#1634,.T.);
#56883=EDGE_CURVE('',#43107,#43109,#1635,.T.);
#56884=EDGE_CURVE('',#43110,#43111,#24525,.T.);
#56885=EDGE_CURVE('',#43108,#43110,#1636,.T.);
#56886=EDGE_CURVE('',#43109,#43111,#1637,.T.);
#56887=EDGE_CURVE('',#43112,#43113,#24526,.T.);
#56888=EDGE_CURVE('',#43114,#43112,#1638,.T.);
#56889=EDGE_CURVE('',#43115,#43114,#34986,.T.);
#56890=EDGE_CURVE('',#43115,#43113,#1639,.T.);
#56891=EDGE_CURVE('',#43116,#43117,#24527,.T.);
#56892=EDGE_CURVE('',#43112,#43116,#1640,.T.);
#56893=EDGE_CURVE('',#43113,#43117,#1641,.T.);
#56894=EDGE_CURVE('',#43118,#43119,#24528,.T.);
#56895=EDGE_CURVE('',#43116,#43118,#1642,.T.);
#56896=EDGE_CURVE('',#43117,#43119,#1643,.T.);
#56897=EDGE_CURVE('',#43120,#43121,#24529,.T.);
#56898=EDGE_CURVE('',#43118,#43120,#1644,.T.);
#56899=EDGE_CURVE('',#43119,#43121,#1645,.T.);
#56900=EDGE_CURVE('',#43122,#43123,#24530,.T.);
#56901=EDGE_CURVE('',#43120,#43122,#1646,.T.);
#56902=EDGE_CURVE('',#43121,#43123,#1647,.T.);
#56903=EDGE_CURVE('',#43124,#43125,#24531,.T.);
#56904=EDGE_CURVE('',#43122,#43124,#1648,.T.);
#56905=EDGE_CURVE('',#43123,#43125,#1649,.T.);
#56906=EDGE_CURVE('',#43126,#43127,#24532,.T.);
#56907=EDGE_CURVE('',#43124,#43126,#1650,.T.);
#56908=EDGE_CURVE('',#43125,#43127,#1651,.T.);
#56909=EDGE_CURVE('',#43128,#43129,#24533,.T.);
#56910=EDGE_CURVE('',#43126,#43128,#1652,.T.);
#56911=EDGE_CURVE('',#43127,#43129,#1653,.T.);
#56912=EDGE_CURVE('',#43130,#43131,#24534,.T.);
#56913=EDGE_CURVE('',#43128,#43130,#1654,.T.);
#56914=EDGE_CURVE('',#43129,#43131,#1655,.T.);
#56915=EDGE_CURVE('',#43132,#43133,#24535,.T.);
#56916=EDGE_CURVE('',#43130,#43132,#1656,.T.);
#56917=EDGE_CURVE('',#43131,#43133,#1657,.T.);
#56918=EDGE_CURVE('',#43134,#43135,#24536,.T.);
#56919=EDGE_CURVE('',#43132,#43134,#1658,.T.);
#56920=EDGE_CURVE('',#43133,#43135,#1659,.T.);
#56921=EDGE_CURVE('',#43136,#43137,#24537,.T.);
#56922=EDGE_CURVE('',#43134,#43136,#1660,.T.);
#56923=EDGE_CURVE('',#43135,#43137,#1661,.T.);
#56924=EDGE_CURVE('',#43138,#43139,#24538,.T.);
#56925=EDGE_CURVE('',#43136,#43138,#1662,.T.);
#56926=EDGE_CURVE('',#43137,#43139,#1663,.T.);
#56927=EDGE_CURVE('',#43140,#43141,#24539,.T.);
#56928=EDGE_CURVE('',#43140,#43142,#6713,.T.);
#56929=EDGE_CURVE('',#43142,#43143,#34987,.T.);
#56930=EDGE_CURVE('',#43143,#43141,#6714,.T.);
#56931=EDGE_CURVE('',#43144,#43145,#24540,.T.);
#56932=EDGE_CURVE('',#43144,#43140,#6715,.T.);
#56933=EDGE_CURVE('',#43141,#43145,#6716,.T.);
#56934=EDGE_CURVE('',#43146,#43147,#24541,.T.);
#56935=EDGE_CURVE('',#43146,#43144,#6717,.T.);
#56936=EDGE_CURVE('',#43145,#43147,#6718,.T.);
#56937=EDGE_CURVE('',#43148,#43149,#24542,.T.);
#56938=EDGE_CURVE('',#43148,#43146,#6719,.T.);
#56939=EDGE_CURVE('',#43147,#43149,#6720,.T.);
#56940=EDGE_CURVE('',#43150,#43151,#24543,.T.);
#56941=EDGE_CURVE('',#43150,#43148,#6721,.T.);
#56942=EDGE_CURVE('',#43149,#43151,#6722,.T.);
#56943=EDGE_CURVE('',#43152,#43153,#24544,.T.);
#56944=EDGE_CURVE('',#43152,#43150,#6723,.T.);
#56945=EDGE_CURVE('',#43151,#43153,#6724,.T.);
#56946=EDGE_CURVE('',#43154,#43155,#24545,.T.);
#56947=EDGE_CURVE('',#43154,#43152,#6725,.T.);
#56948=EDGE_CURVE('',#43153,#43155,#6726,.T.);
#56949=EDGE_CURVE('',#43156,#43157,#24546,.T.);
#56950=EDGE_CURVE('',#43156,#43154,#6727,.T.);
#56951=EDGE_CURVE('',#43155,#43157,#6728,.T.);
#56952=EDGE_CURVE('',#43158,#43159,#24547,.T.);
#56953=EDGE_CURVE('',#43158,#43156,#6729,.T.);
#56954=EDGE_CURVE('',#43157,#43159,#6730,.T.);
#56955=EDGE_CURVE('',#43160,#43161,#24548,.T.);
#56956=EDGE_CURVE('',#43160,#43158,#6731,.T.);
#56957=EDGE_CURVE('',#43159,#43161,#6732,.T.);
#56958=EDGE_CURVE('',#43162,#43163,#24549,.T.);
#56959=EDGE_CURVE('',#43162,#43160,#6733,.T.);
#56960=EDGE_CURVE('',#43161,#43163,#6734,.T.);
#56961=EDGE_CURVE('',#43164,#43165,#24550,.T.);
#56962=EDGE_CURVE('',#43164,#43162,#6735,.T.);
#56963=EDGE_CURVE('',#43163,#43165,#6736,.T.);
#56964=EDGE_CURVE('',#43166,#43167,#24551,.T.);
#56965=EDGE_CURVE('',#43166,#43164,#6737,.T.);
#56966=EDGE_CURVE('',#43165,#43167,#6738,.T.);
#56967=EDGE_CURVE('',#43168,#43169,#24552,.T.);
#56968=EDGE_CURVE('',#43168,#43170,#6739,.T.);
#56969=EDGE_CURVE('',#43171,#43170,#34988,.T.);
#56970=EDGE_CURVE('',#43171,#43169,#6740,.T.);
#56971=EDGE_CURVE('',#43172,#43173,#24553,.T.);
#56972=EDGE_CURVE('',#43172,#43168,#6741,.T.);
#56973=EDGE_CURVE('',#43169,#43173,#6742,.T.);
#56974=EDGE_CURVE('',#43174,#43175,#24554,.T.);
#56975=EDGE_CURVE('',#43174,#43172,#6743,.T.);
#56976=EDGE_CURVE('',#43173,#43175,#6744,.T.);
#56977=EDGE_CURVE('',#43176,#43177,#24555,.T.);
#56978=EDGE_CURVE('',#43176,#43174,#6745,.T.);
#56979=EDGE_CURVE('',#43175,#43177,#6746,.T.);
#56980=EDGE_CURVE('',#43178,#43179,#24556,.T.);
#56981=EDGE_CURVE('',#43178,#43176,#6747,.T.);
#56982=EDGE_CURVE('',#43177,#43179,#6748,.T.);
#56983=EDGE_CURVE('',#43180,#43181,#24557,.T.);
#56984=EDGE_CURVE('',#43180,#43178,#6749,.T.);
#56985=EDGE_CURVE('',#43179,#43181,#6750,.T.);
#56986=EDGE_CURVE('',#43182,#43183,#24558,.T.);
#56987=EDGE_CURVE('',#43182,#43180,#6751,.T.);
#56988=EDGE_CURVE('',#43181,#43183,#6752,.T.);
#56989=EDGE_CURVE('',#43184,#43185,#24559,.T.);
#56990=EDGE_CURVE('',#43184,#43182,#6753,.T.);
#56991=EDGE_CURVE('',#43183,#43185,#6754,.T.);
#56992=EDGE_CURVE('',#43186,#43187,#24560,.T.);
#56993=EDGE_CURVE('',#43186,#43184,#6755,.T.);
#56994=EDGE_CURVE('',#43185,#43187,#6756,.T.);
#56995=EDGE_CURVE('',#43188,#43189,#24561,.T.);
#56996=EDGE_CURVE('',#43188,#43186,#6757,.T.);
#56997=EDGE_CURVE('',#43187,#43189,#6758,.T.);
#56998=EDGE_CURVE('',#43190,#43191,#24562,.T.);
#56999=EDGE_CURVE('',#43190,#43188,#6759,.T.);
#57000=EDGE_CURVE('',#43189,#43191,#6760,.T.);
#57001=EDGE_CURVE('',#43192,#43193,#24563,.T.);
#57002=EDGE_CURVE('',#43192,#43190,#6761,.T.);
#57003=EDGE_CURVE('',#43191,#43193,#6762,.T.);
#57004=EDGE_CURVE('',#43194,#43195,#24564,.T.);
#57005=EDGE_CURVE('',#43194,#43192,#6763,.T.);
#57006=EDGE_CURVE('',#43193,#43195,#6764,.T.);
#57007=EDGE_CURVE('',#43196,#43197,#24565,.T.);
#57008=EDGE_CURVE('',#43196,#43194,#6765,.T.);
#57009=EDGE_CURVE('',#43195,#43197,#6766,.T.);
#57010=EDGE_CURVE('',#43198,#43199,#24566,.T.);
#57011=EDGE_CURVE('',#43198,#43196,#6767,.T.);
#57012=EDGE_CURVE('',#43197,#43199,#6768,.T.);
#57013=EDGE_CURVE('',#43200,#43201,#24567,.T.);
#57014=EDGE_CURVE('',#43200,#43198,#6769,.T.);
#57015=EDGE_CURVE('',#43199,#43201,#6770,.T.);
#57016=EDGE_CURVE('',#43202,#43203,#24568,.T.);
#57017=EDGE_CURVE('',#43202,#43200,#6771,.T.);
#57018=EDGE_CURVE('',#43201,#43203,#6772,.T.);
#57019=EDGE_CURVE('',#43204,#43205,#24569,.T.);
#57020=EDGE_CURVE('',#43204,#43202,#6773,.T.);
#57021=EDGE_CURVE('',#43203,#43205,#6774,.T.);
#57022=EDGE_CURVE('',#43206,#43207,#24570,.T.);
#57023=EDGE_CURVE('',#43206,#43204,#6775,.T.);
#57024=EDGE_CURVE('',#43205,#43207,#6776,.T.);
#57025=EDGE_CURVE('',#43207,#43208,#6777,.T.);
#57026=EDGE_CURVE('',#43208,#43206,#34989,.T.);
#57027=EDGE_CURVE('',#43170,#43209,#6778,.T.);
#57028=EDGE_CURVE('',#43209,#43210,#24571,.T.);
#57029=EDGE_CURVE('',#43210,#43210,#34990,.T.);
#57030=EDGE_CURVE('',#43209,#43211,#6779,.T.);
#57031=EDGE_CURVE('',#43211,#43212,#34991,.T.);
#57032=EDGE_CURVE('',#43212,#43171,#6780,.T.);
#57033=EDGE_CURVE('',#43213,#43214,#6781,.F.);
#57034=EDGE_CURVE('',#43215,#43213,#34992,.T.);
#57035=EDGE_CURVE('',#43143,#43215,#6782,.T.);
#57036=EDGE_CURVE('',#43214,#43142,#6783,.F.);
#57037=EDGE_CURVE('',#43214,#43216,#24572,.T.);
#57038=EDGE_CURVE('',#43216,#43216,#34993,.T.);
#57039=EDGE_CURVE('',#43167,#43217,#6784,.T.);
#57040=EDGE_CURVE('',#43218,#43217,#34994,.T.);
#57041=EDGE_CURVE('',#43218,#43166,#6785,.T.);
#57042=EDGE_CURVE('',#43114,#43218,#6786,.T.);
#57043=EDGE_CURVE('',#43138,#43213,#1664,.T.);
#57044=EDGE_CURVE('',#43217,#43115,#6787,.T.);
#57045=EDGE_CURVE('',#43139,#43215,#1665,.T.);
#57046=EDGE_CURVE('',#43219,#43220,#24573,.T.);
#57047=EDGE_CURVE('',#43220,#43221,#24574,.T.);
#57048=EDGE_CURVE('',#43221,#43222,#24575,.T.);
#57049=EDGE_CURVE('',#43222,#43219,#24576,.T.);
#57050=EDGE_CURVE('',#43223,#43224,#24577,.T.);
#57051=EDGE_CURVE('',#43225,#43223,#24578,.T.);
#57052=EDGE_CURVE('',#43226,#43225,#24579,.T.);
#57053=EDGE_CURVE('',#43224,#43226,#24580,.T.);
#57054=EDGE_CURVE('',#43227,#43228,#34995,.T.);
#57055=EDGE_CURVE('',#43228,#43229,#34996,.T.);
#57056=EDGE_CURVE('',#43229,#43230,#34997,.T.);
#57057=EDGE_CURVE('',#43230,#43231,#34998,.T.);
#57058=EDGE_CURVE('',#43231,#43232,#34999,.T.);
#57059=EDGE_CURVE('',#43232,#43227,#35000,.T.);
#57060=EDGE_CURVE('',#43220,#43224,#24581,.T.);
#57061=EDGE_CURVE('',#43219,#43223,#24582,.T.);
#57062=EDGE_CURVE('',#43221,#43226,#24583,.T.);
#57063=EDGE_CURVE('',#43222,#43225,#24584,.T.);
#57064=EDGE_CURVE('',#43233,#43234,#24585,.T.);
#57065=EDGE_CURVE('',#43234,#43229,#1666,.T.);
#57066=EDGE_CURVE('',#43229,#43235,#1667,.T.);
#57067=EDGE_CURVE('',#43236,#43235,#24586,.T.);
#57068=EDGE_CURVE('',#43237,#43236,#1668,.T.);
#57069=EDGE_CURVE('',#43233,#43237,#1669,.T.);
#57070=EDGE_CURVE('',#43235,#43228,#1670,.T.);
#57071=EDGE_CURVE('',#43228,#43238,#1671,.T.);
#57072=EDGE_CURVE('',#43239,#43238,#24587,.T.);
#57073=EDGE_CURVE('',#43240,#43239,#1672,.T.);
#57074=EDGE_CURVE('',#43236,#43240,#1673,.T.);
#57075=EDGE_CURVE('',#43238,#43227,#1674,.T.);
#57076=EDGE_CURVE('',#43227,#43241,#1675,.T.);
#57077=EDGE_CURVE('',#43242,#43241,#24588,.T.);
#57078=EDGE_CURVE('',#43243,#43242,#1676,.T.);
#57079=EDGE_CURVE('',#43239,#43243,#1677,.T.);
#57080=EDGE_CURVE('',#43241,#43232,#1678,.T.);
#57081=EDGE_CURVE('',#43232,#43244,#1679,.T.);
#57082=EDGE_CURVE('',#43245,#43244,#24589,.T.);
#57083=EDGE_CURVE('',#43246,#43245,#1680,.T.);
#57084=EDGE_CURVE('',#43242,#43246,#1681,.T.);
#57085=EDGE_CURVE('',#43244,#43231,#1682,.T.);
#57086=EDGE_CURVE('',#43231,#43247,#1683,.T.);
#57087=EDGE_CURVE('',#43248,#43247,#24590,.T.);
#57088=EDGE_CURVE('',#43249,#43248,#1684,.T.);
#57089=EDGE_CURVE('',#43245,#43249,#1685,.T.);
#57090=EDGE_CURVE('',#43247,#43230,#1686,.T.);
#57091=EDGE_CURVE('',#43230,#43234,#1687,.T.);
#57092=EDGE_CURVE('',#43250,#43233,#1688,.T.);
#57093=EDGE_CURVE('',#43248,#43250,#1689,.T.);
#57094=EDGE_CURVE('',#43240,#43237,#35001,.T.);
#57095=EDGE_CURVE('',#43240,#43243,#35002,.T.);
#57096=EDGE_CURVE('',#43243,#43246,#35003,.T.);
#57097=EDGE_CURVE('',#43246,#43249,#35004,.T.);
#57098=EDGE_CURVE('',#43249,#43250,#35005,.T.);
#57099=EDGE_CURVE('',#43250,#43237,#35006,.T.);
#57100=EDGE_CURVE('',#43206,#43073,#6788,.T.);
#57101=EDGE_CURVE('',#43072,#43208,#6789,.T.);
#57102=EDGE_CURVE('',#43110,#43211,#1690,.T.);
#57103=EDGE_CURVE('',#43111,#43212,#1691,.T.);
#57104=EDGE_CURVE('',#43251,#43251,#35007,.T.);
#57105=EDGE_CURVE('',#43251,#43252,#24591,.T.);
#57106=EDGE_CURVE('',#43252,#43252,#35008,.T.);
#57107=EDGE_CURVE('',#43253,#43253,#35009,.T.);
#57108=EDGE_CURVE('',#43253,#43254,#24592,.T.);
#57109=EDGE_CURVE('',#43254,#43254,#35010,.T.);
#57110=EDGE_CURVE('',#43255,#43255,#35011,.T.);
#57111=EDGE_CURVE('',#43255,#43256,#24593,.T.);
#57112=EDGE_CURVE('',#43256,#43256,#35012,.T.);
#57113=EDGE_CURVE('',#43257,#43257,#35013,.T.);
#57114=EDGE_CURVE('',#43257,#43258,#24594,.T.);
#57115=EDGE_CURVE('',#43258,#43258,#35014,.T.);
#57116=EDGE_CURVE('',#43259,#43259,#35015,.T.);
#57117=EDGE_CURVE('',#43259,#43260,#24595,.T.);
#57118=EDGE_CURVE('',#43260,#43260,#35016,.T.);
#57119=EDGE_CURVE('',#43261,#43261,#35017,.T.);
#57120=EDGE_CURVE('',#43261,#43262,#24596,.T.);
#57121=EDGE_CURVE('',#43262,#43262,#35018,.T.);
#57122=EDGE_CURVE('',#43263,#43263,#35019,.T.);
#57123=EDGE_CURVE('',#43263,#43264,#24597,.T.);
#57124=EDGE_CURVE('',#43264,#43264,#35020,.T.);
#57125=EDGE_CURVE('',#43265,#43265,#35021,.T.);
#57126=EDGE_CURVE('',#43265,#43266,#24598,.T.);
#57127=EDGE_CURVE('',#43266,#43266,#35022,.T.);
#57128=EDGE_CURVE('',#43267,#43267,#35023,.T.);
#57129=EDGE_CURVE('',#43267,#43268,#24599,.T.);
#57130=EDGE_CURVE('',#43268,#43268,#35024,.T.);
#57131=EDGE_CURVE('',#43269,#43269,#35025,.T.);
#57132=EDGE_CURVE('',#43269,#43270,#24600,.T.);
#57133=EDGE_CURVE('',#43270,#43270,#35026,.T.);
#57134=EDGE_CURVE('',#43271,#43271,#35027,.T.);
#57135=EDGE_CURVE('',#43271,#43272,#24601,.T.);
#57136=EDGE_CURVE('',#43272,#43272,#35028,.T.);
#57137=EDGE_CURVE('',#43273,#43273,#35029,.T.);
#57138=EDGE_CURVE('',#43274,#43274,#35030,.T.);
#57139=EDGE_CURVE('',#43275,#43275,#35031,.T.);
#57140=EDGE_CURVE('',#43275,#43276,#35032,.T.);
#57141=EDGE_CURVE('',#43276,#43276,#35033,.T.);
#57142=EDGE_CURVE('',#43277,#43277,#35034,.T.);
#57143=EDGE_CURVE('',#43277,#43278,#35035,.T.);
#57144=EDGE_CURVE('',#43279,#43278,#35036,.T.);
#57145=EDGE_CURVE('',#43278,#43279,#35037,.T.);
#57146=EDGE_CURVE('',#43274,#43279,#24602,.T.);
#57147=EDGE_CURVE('',#43280,#43280,#35038,.T.);
#57148=EDGE_CURVE('',#43280,#43281,#35039,.T.);
#57149=EDGE_CURVE('',#43281,#43281,#35040,.T.);
#57150=EDGE_CURVE('',#43281,#43275,#24603,.T.);
#57151=EDGE_CURVE('',#43282,#43283,#24604,.T.);
#57152=EDGE_CURVE('',#43283,#43284,#24605,.T.);
#57153=EDGE_CURVE('',#43284,#43285,#24606,.T.);
#57154=EDGE_CURVE('',#43285,#43282,#24607,.T.);
#57155=EDGE_CURVE('',#43286,#43287,#24608,.T.);
#57156=EDGE_CURVE('',#43288,#43286,#24609,.T.);
#57157=EDGE_CURVE('',#43289,#43288,#24610,.T.);
#57158=EDGE_CURVE('',#43287,#43289,#24611,.T.);
#57159=EDGE_CURVE('',#43290,#43291,#24612,.T.);
#57160=EDGE_CURVE('',#43292,#43290,#24613,.T.);
#57161=EDGE_CURVE('',#43293,#43292,#24614,.T.);
#57162=EDGE_CURVE('',#43291,#43293,#24615,.T.);
#57163=EDGE_CURVE('',#43294,#43295,#24616,.T.);
#57164=EDGE_CURVE('',#43295,#43296,#24617,.T.);
#57165=EDGE_CURVE('',#43296,#43297,#24618,.T.);
#57166=EDGE_CURVE('',#43297,#43294,#24619,.T.);
#57167=EDGE_CURVE('',#43283,#43291,#24620,.T.);
#57168=EDGE_CURVE('',#43282,#43290,#24621,.T.);
#57169=EDGE_CURVE('',#43284,#43293,#24622,.T.);
#57170=EDGE_CURVE('',#43285,#43292,#24623,.T.);
#57171=EDGE_CURVE('',#43286,#43295,#24624,.T.);
#57172=EDGE_CURVE('',#43287,#43296,#24625,.T.);
#57173=EDGE_CURVE('',#43289,#43297,#24626,.T.);
#57174=EDGE_CURVE('',#43288,#43294,#24627,.T.);
#57175=EDGE_CURVE('',#43298,#43299,#24628,.T.);
#57176=EDGE_CURVE('',#43300,#43299,#24629,.T.);
#57177=EDGE_CURVE('',#43301,#43300,#24630,.T.);
#57178=EDGE_CURVE('',#43301,#43298,#24631,.T.);
#57179=EDGE_CURVE('',#43299,#43302,#24632,.T.);
#57180=EDGE_CURVE('',#43303,#43302,#24633,.T.);
#57181=EDGE_CURVE('',#43300,#43303,#24634,.T.);
#57182=EDGE_CURVE('',#43302,#43304,#24635,.T.);
#57183=EDGE_CURVE('',#43305,#43304,#24636,.T.);
#57184=EDGE_CURVE('',#43303,#43305,#24637,.T.);
#57185=EDGE_CURVE('',#43304,#43298,#24638,.T.);
#57186=EDGE_CURVE('',#43305,#43301,#24639,.T.);
#57187=EDGE_CURVE('',#43306,#43306,#35041,.T.);
#57188=EDGE_CURVE('',#43306,#43307,#24640,.T.);
#57189=EDGE_CURVE('',#43307,#43307,#35042,.T.);
#57190=EDGE_CURVE('',#43308,#43308,#35043,.T.);
#57191=EDGE_CURVE('',#43308,#43309,#24641,.T.);
#57192=EDGE_CURVE('',#43309,#43309,#35044,.T.);
#57193=EDGE_CURVE('',#43310,#43310,#35045,.T.);
#57194=EDGE_CURVE('',#43310,#43311,#24642,.T.);
#57195=EDGE_CURVE('',#43311,#43311,#35046,.T.);
#57196=EDGE_CURVE('',#43312,#43312,#35047,.T.);
#57197=EDGE_CURVE('',#43312,#43313,#24643,.T.);
#57198=EDGE_CURVE('',#43313,#43313,#35048,.T.);
#57199=EDGE_CURVE('',#43314,#43314,#35049,.T.);
#57200=EDGE_CURVE('',#43314,#43315,#24644,.T.);
#57201=EDGE_CURVE('',#43315,#43315,#35050,.T.);
#57202=EDGE_CURVE('',#43316,#43316,#35051,.T.);
#57203=EDGE_CURVE('',#43316,#43317,#24645,.T.);
#57204=EDGE_CURVE('',#43317,#43317,#35052,.T.);
#57205=EDGE_CURVE('',#43318,#43318,#35053,.T.);
#57206=EDGE_CURVE('',#43318,#43319,#24646,.T.);
#57207=EDGE_CURVE('',#43319,#43319,#35054,.T.);
#57208=EDGE_CURVE('',#43320,#43320,#35055,.T.);
#57209=EDGE_CURVE('',#43320,#43321,#24647,.T.);
#57210=EDGE_CURVE('',#43321,#43321,#35056,.T.);
#57211=EDGE_CURVE('',#43322,#43323,#24648,.T.);
#57212=EDGE_CURVE('',#43323,#43324,#24649,.T.);
#57213=EDGE_CURVE('',#43324,#43325,#24650,.T.);
#57214=EDGE_CURVE('',#43326,#43325,#24651,.T.);
#57215=EDGE_CURVE('',#43327,#43326,#24652,.T.);
#57216=EDGE_CURVE('',#43327,#43328,#24653,.T.);
#57217=EDGE_CURVE('',#43328,#43329,#24654,.T.);
#57218=EDGE_CURVE('',#43329,#43322,#24655,.T.);
#57219=EDGE_CURVE('',#43330,#43331,#24656,.T.);
#57220=EDGE_CURVE('',#43330,#43332,#24657,.T.);
#57221=EDGE_CURVE('',#43332,#43333,#24658,.T.);
#57222=EDGE_CURVE('',#43333,#43334,#24659,.T.);
#57223=EDGE_CURVE('',#43335,#43334,#24660,.T.);
#57224=EDGE_CURVE('',#43335,#43336,#24661,.T.);
#57225=EDGE_CURVE('',#43336,#43337,#24662,.T.);
#57226=EDGE_CURVE('',#43331,#43337,#24663,.T.);
#57227=EDGE_CURVE('',#43324,#43330,#24664,.T.);
#57228=EDGE_CURVE('',#43325,#43331,#24665,.T.);
#57229=EDGE_CURVE('',#43334,#43329,#24666,.T.);
#57230=EDGE_CURVE('',#43328,#43335,#24667,.T.);
#57231=EDGE_CURVE('',#43337,#43326,#24668,.T.);
#57232=EDGE_CURVE('',#43336,#43327,#24669,.T.);
#57233=EDGE_CURVE('',#43323,#43332,#24670,.T.);
#57234=EDGE_CURVE('',#43322,#43333,#24671,.T.);
#57235=EDGE_CURVE('',#43338,#43338,#35057,.T.);
#57236=EDGE_CURVE('',#43338,#43339,#24672,.T.);
#57237=EDGE_CURVE('',#43339,#43339,#35058,.T.);
#57238=EDGE_CURVE('',#43340,#43340,#35059,.T.);
#57239=EDGE_CURVE('',#43340,#43341,#24673,.T.);
#57240=EDGE_CURVE('',#43341,#43341,#35060,.T.);
#57241=EDGE_CURVE('',#43342,#43343,#24674,.T.);
#57242=EDGE_CURVE('',#43342,#43344,#24675,.T.);
#57243=EDGE_CURVE('',#43344,#43345,#24676,.T.);
#57244=EDGE_CURVE('',#43345,#43343,#24677,.T.);
#57245=EDGE_CURVE('',#43346,#43347,#24678,.T.);
#57246=EDGE_CURVE('',#43347,#43348,#24679,.T.);
#57247=EDGE_CURVE('',#43349,#43348,#24680,.T.);
#57248=EDGE_CURVE('',#43349,#43346,#24681,.T.);
#57249=EDGE_CURVE('',#43347,#43350,#24682,.T.);
#57250=EDGE_CURVE('',#43346,#43351,#24683,.T.);
#57251=EDGE_CURVE('',#43351,#43350,#24684,.T.);
#57252=EDGE_CURVE('',#43348,#43352,#24685,.T.);
#57253=EDGE_CURVE('',#43353,#43352,#24686,.T.);
#57254=EDGE_CURVE('',#43349,#43353,#24687,.T.);
#57255=EDGE_CURVE('',#43344,#43354,#24688,.T.);
#57256=EDGE_CURVE('',#43354,#43355,#24689,.T.);
#57257=EDGE_CURVE('',#43355,#43345,#24690,.T.);
#57258=EDGE_CURVE('',#43342,#43356,#24691,.T.);
#57259=EDGE_CURVE('',#43357,#43343,#24692,.T.);
#57260=EDGE_CURVE('',#43356,#43357,#24693,.T.);
#57261=EDGE_CURVE('',#43354,#43356,#24694,.T.);
#57262=EDGE_CURVE('',#43357,#43355,#24695,.T.);
#57263=EDGE_CURVE('',#43350,#43352,#24696,.T.);
#57264=EDGE_CURVE('',#43351,#43353,#24697,.T.);
#57265=EDGE_CURVE('',#43358,#43359,#24698,.T.);
#57266=EDGE_CURVE('',#43355,#43358,#35061,.T.);
#57267=EDGE_CURVE('',#43357,#43359,#35062,.T.);
#57268=EDGE_CURVE('',#43358,#43360,#24699,.T.);
#57269=EDGE_CURVE('',#43359,#43361,#24700,.T.);
#57270=EDGE_CURVE('',#43361,#43360,#24701,.T.);
#57271=EDGE_CURVE('',#43345,#43362,#35063,.T.);
#57272=EDGE_CURVE('',#43363,#43362,#24702,.T.);
#57273=EDGE_CURVE('',#43343,#43363,#35064,.T.);
#57274=EDGE_CURVE('',#43360,#43349,#35065,.T.);
#57275=EDGE_CURVE('',#43361,#43346,#35066,.T.);
#57276=EDGE_CURVE('',#43364,#43365,#24703,.T.);
#57277=EDGE_CURVE('',#43364,#43353,#35067,.T.);
#57278=EDGE_CURVE('',#43365,#43351,#35068,.T.);
#57279=EDGE_CURVE('',#43362,#43364,#24704,.T.);
#57280=EDGE_CURVE('',#43363,#43365,#24705,.T.);
#57281=EDGE_CURVE('',#43360,#43364,#24706,.T.);
#57282=EDGE_CURVE('',#43358,#43362,#24707,.T.);
#57283=EDGE_CURVE('',#43359,#43363,#24708,.T.);
#57284=EDGE_CURVE('',#43361,#43365,#24709,.T.);
#57285=EDGE_CURVE('',#43366,#43367,#24710,.T.);
#57286=EDGE_CURVE('',#43366,#43368,#6790,.T.);
#57287=EDGE_CURVE('',#43368,#43369,#35069,.T.);
#57288=EDGE_CURVE('',#43369,#43370,#35070,.T.);
#57289=EDGE_CURVE('',#43370,#43367,#6791,.F.);
#57290=EDGE_CURVE('',#43371,#43372,#24711,.T.);
#57291=EDGE_CURVE('',#43371,#43373,#35071,.T.);
#57292=EDGE_CURVE('',#43373,#43366,#6792,.T.);
#57293=EDGE_CURVE('',#43367,#43372,#6793,.F.);
#57294=EDGE_CURVE('',#43374,#43375,#24712,.T.);
#57295=EDGE_CURVE('',#43374,#43376,#6794,.F.);
#57296=EDGE_CURVE('',#43376,#43377,#35072,.T.);
#57297=EDGE_CURVE('',#43377,#43375,#6795,.F.);
#57298=EDGE_CURVE('',#43378,#43379,#24713,.T.);
#57299=EDGE_CURVE('',#43378,#43374,#6796,.F.);
#57300=EDGE_CURVE('',#43375,#43379,#6797,.F.);
#57301=EDGE_CURVE('',#43380,#43381,#24714,.T.);
#57302=EDGE_CURVE('',#43380,#43378,#6798,.F.);
#57303=EDGE_CURVE('',#43379,#43381,#6799,.F.);
#57304=EDGE_CURVE('',#43382,#43383,#24715,.T.);
#57305=EDGE_CURVE('',#43382,#43380,#6800,.F.);
#57306=EDGE_CURVE('',#43381,#43383,#6801,.F.);
#57307=EDGE_CURVE('',#43384,#43385,#24716,.T.);
#57308=EDGE_CURVE('',#43384,#43382,#6802,.F.);
#57309=EDGE_CURVE('',#43383,#43385,#6803,.F.);
#57310=EDGE_CURVE('',#43386,#43387,#24717,.T.);
#57311=EDGE_CURVE('',#43386,#43384,#6804,.F.);
#57312=EDGE_CURVE('',#43385,#43387,#6805,.F.);
#57313=EDGE_CURVE('',#43388,#43389,#24718,.T.);
#57314=EDGE_CURVE('',#43388,#43386,#6806,.F.);
#57315=EDGE_CURVE('',#43387,#43389,#6807,.F.);
#57316=EDGE_CURVE('',#43390,#43391,#24719,.T.);
#57317=EDGE_CURVE('',#43390,#43388,#6808,.F.);
#57318=EDGE_CURVE('',#43389,#43391,#6809,.F.);
#57319=EDGE_CURVE('',#43392,#43393,#24720,.T.);
#57320=EDGE_CURVE('',#43392,#43390,#6810,.F.);
#57321=EDGE_CURVE('',#43391,#43393,#6811,.F.);
#57322=EDGE_CURVE('',#43394,#43395,#24721,.T.);
#57323=EDGE_CURVE('',#43394,#43392,#6812,.F.);
#57324=EDGE_CURVE('',#43393,#43395,#6813,.F.);
#57325=EDGE_CURVE('',#43396,#43397,#24722,.T.);
#57326=EDGE_CURVE('',#43396,#43394,#6814,.F.);
#57327=EDGE_CURVE('',#43395,#43397,#6815,.F.);
#57328=EDGE_CURVE('',#43398,#43399,#24723,.T.);
#57329=EDGE_CURVE('',#43398,#43396,#6816,.F.);
#57330=EDGE_CURVE('',#43397,#43399,#6817,.F.);
#57331=EDGE_CURVE('',#43400,#43401,#24724,.T.);
#57332=EDGE_CURVE('',#43400,#43398,#6818,.F.);
#57333=EDGE_CURVE('',#43399,#43401,#6819,.F.);
#57334=EDGE_CURVE('',#43402,#43403,#24725,.T.);
#57335=EDGE_CURVE('',#43402,#43400,#6820,.F.);
#57336=EDGE_CURVE('',#43401,#43403,#6821,.F.);
#57337=EDGE_CURVE('',#43404,#43405,#24726,.T.);
#57338=EDGE_CURVE('',#43404,#43402,#6822,.F.);
#57339=EDGE_CURVE('',#43403,#43405,#6823,.F.);
#57340=EDGE_CURVE('',#43406,#43407,#24727,.T.);
#57341=EDGE_CURVE('',#43406,#43404,#6824,.F.);
#57342=EDGE_CURVE('',#43405,#43407,#6825,.F.);
#57343=EDGE_CURVE('',#43408,#43408,#35073,.T.);
#57344=EDGE_CURVE('',#43408,#43409,#24728,.T.);
#57345=EDGE_CURVE('',#43410,#43409,#35074,.T.);
#57346=EDGE_CURVE('',#43410,#43411,#6826,.F.);
#57347=EDGE_CURVE('',#43411,#43412,#24729,.T.);
#57348=EDGE_CURVE('',#43412,#43373,#6827,.F.);
#57349=EDGE_CURVE('',#43409,#43371,#35075,.T.);
#57350=EDGE_CURVE('',#43413,#43369,#24730,.T.);
#57351=EDGE_CURVE('',#43413,#43370,#1692,.T.);
#57352=EDGE_CURVE('',#43414,#43415,#24731,.T.);
#57353=EDGE_CURVE('',#43414,#43413,#1693,.T.);
#57354=EDGE_CURVE('',#43415,#43368,#1694,.T.);
#57355=EDGE_CURVE('',#43416,#43417,#24732,.T.);
#57356=EDGE_CURVE('',#43416,#43414,#1695,.T.);
#57357=EDGE_CURVE('',#43417,#43415,#1696,.T.);
#57358=EDGE_CURVE('',#43418,#43419,#24733,.T.);
#57359=EDGE_CURVE('',#43418,#43416,#1697,.T.);
#57360=EDGE_CURVE('',#43419,#43417,#1698,.T.);
#57361=EDGE_CURVE('',#43420,#43421,#24734,.T.);
#57362=EDGE_CURVE('',#43420,#43418,#1699,.T.);
#57363=EDGE_CURVE('',#43421,#43419,#1700,.T.);
#57364=EDGE_CURVE('',#43422,#43423,#24735,.T.);
#57365=EDGE_CURVE('',#43422,#43420,#1701,.T.);
#57366=EDGE_CURVE('',#43423,#43421,#1702,.T.);
#57367=EDGE_CURVE('',#43424,#43425,#24736,.T.);
#57368=EDGE_CURVE('',#43424,#43422,#1703,.T.);
#57369=EDGE_CURVE('',#43425,#43423,#1704,.T.);
#57370=EDGE_CURVE('',#43426,#43427,#24737,.T.);
#57371=EDGE_CURVE('',#43426,#43424,#1705,.T.);
#57372=EDGE_CURVE('',#43427,#43425,#1706,.T.);
#57373=EDGE_CURVE('',#43428,#43429,#24738,.T.);
#57374=EDGE_CURVE('',#43428,#43426,#1707,.T.);
#57375=EDGE_CURVE('',#43429,#43427,#1708,.T.);
#57376=EDGE_CURVE('',#43430,#43431,#24739,.T.);
#57377=EDGE_CURVE('',#43430,#43428,#1709,.T.);
#57378=EDGE_CURVE('',#43431,#43429,#1710,.T.);
#57379=EDGE_CURVE('',#43432,#43433,#24740,.T.);
#57380=EDGE_CURVE('',#43432,#43430,#1711,.T.);
#57381=EDGE_CURVE('',#43433,#43431,#1712,.T.);
#57382=EDGE_CURVE('',#43434,#43435,#24741,.T.);
#57383=EDGE_CURVE('',#43434,#43432,#1713,.T.);
#57384=EDGE_CURVE('',#43435,#43433,#1714,.T.);
#57385=EDGE_CURVE('',#43436,#43437,#24742,.T.);
#57386=EDGE_CURVE('',#43436,#43434,#1715,.T.);
#57387=EDGE_CURVE('',#43437,#43435,#1716,.T.);
#57388=EDGE_CURVE('',#43438,#43439,#24743,.T.);
#57389=EDGE_CURVE('',#43438,#43436,#1717,.T.);
#57390=EDGE_CURVE('',#43439,#43437,#1718,.T.);
#57391=EDGE_CURVE('',#43440,#43441,#24744,.T.);
#57392=EDGE_CURVE('',#43440,#43438,#1719,.T.);
#57393=EDGE_CURVE('',#43441,#43439,#1720,.T.);
#57394=EDGE_CURVE('',#43442,#43443,#24745,.T.);
#57395=EDGE_CURVE('',#43442,#43440,#1721,.T.);
#57396=EDGE_CURVE('',#43443,#43441,#1722,.T.);
#57397=EDGE_CURVE('',#43444,#43445,#24746,.T.);
#57398=EDGE_CURVE('',#43444,#43446,#35076,.T.);
#57399=EDGE_CURVE('',#43446,#43442,#1723,.T.);
#57400=EDGE_CURVE('',#43445,#43443,#1724,.T.);
#57401=EDGE_CURVE('',#43447,#43447,#35077,.T.);
#57402=EDGE_CURVE('',#43448,#43444,#35078,.T.);
#57403=EDGE_CURVE('',#43377,#43448,#6828,.F.);
#57404=EDGE_CURVE('',#43449,#43376,#6829,.F.);
#57405=EDGE_CURVE('',#43449,#43447,#24747,.T.);
#57406=EDGE_CURVE('',#43446,#43449,#6830,.F.);
#57407=EDGE_CURVE('',#43407,#43412,#6831,.F.);
#57408=EDGE_CURVE('',#43448,#43445,#1725,.T.);
#57409=EDGE_CURVE('',#43411,#43406,#6832,.F.);
#57410=EDGE_CURVE('',#43372,#43410,#6833,.F.);
#57411=EDGE_CURVE('',#43450,#43451,#6834,.T.);
#57412=EDGE_CURVE('',#43451,#43452,#6835,.T.);
#57413=EDGE_CURVE('',#43452,#43453,#6836,.T.);
#57414=EDGE_CURVE('',#43453,#43450,#6837,.T.);
#57415=EDGE_CURVE('',#43454,#43455,#6838,.T.);
#57416=EDGE_CURVE('',#43455,#43456,#6839,.T.);
#57417=EDGE_CURVE('',#43456,#43457,#6840,.T.);
#57418=EDGE_CURVE('',#43457,#43454,#6841,.T.);
#57419=EDGE_CURVE('',#43458,#43459,#6842,.T.);
#57420=EDGE_CURVE('',#43459,#43460,#6843,.T.);
#57421=EDGE_CURVE('',#43460,#43461,#6844,.T.);
#57422=EDGE_CURVE('',#43461,#43458,#6845,.T.);
#57423=EDGE_CURVE('',#43462,#43463,#6846,.T.);
#57424=EDGE_CURVE('',#43463,#43464,#6847,.T.);
#57425=EDGE_CURVE('',#43464,#43465,#6848,.T.);
#57426=EDGE_CURVE('',#43465,#43462,#6849,.T.);
#57427=EDGE_CURVE('',#43466,#43452,#24748,.T.);
#57428=EDGE_CURVE('',#43467,#43466,#6850,.T.);
#57429=EDGE_CURVE('',#43467,#43453,#24749,.T.);
#57430=EDGE_CURVE('',#43468,#43467,#6851,.T.);
#57431=EDGE_CURVE('',#43468,#43450,#24750,.T.);
#57432=EDGE_CURVE('',#43469,#43468,#6852,.T.);
#57433=EDGE_CURVE('',#43469,#43451,#24751,.T.);
#57434=EDGE_CURVE('',#43466,#43469,#6853,.T.);
#57435=EDGE_CURVE('',#43470,#43456,#24752,.T.);
#57436=EDGE_CURVE('',#43471,#43470,#6854,.T.);
#57437=EDGE_CURVE('',#43471,#43457,#24753,.T.);
#57438=EDGE_CURVE('',#43472,#43471,#6855,.T.);
#57439=EDGE_CURVE('',#43472,#43454,#24754,.T.);
#57440=EDGE_CURVE('',#43473,#43472,#6856,.T.);
#57441=EDGE_CURVE('',#43473,#43455,#24755,.T.);
#57442=EDGE_CURVE('',#43470,#43473,#6857,.T.);
#57443=EDGE_CURVE('',#43474,#43460,#24756,.T.);
#57444=EDGE_CURVE('',#43475,#43474,#6858,.T.);
#57445=EDGE_CURVE('',#43475,#43461,#24757,.T.);
#57446=EDGE_CURVE('',#43476,#43475,#6859,.T.);
#57447=EDGE_CURVE('',#43476,#43458,#24758,.T.);
#57448=EDGE_CURVE('',#43477,#43476,#6860,.T.);
#57449=EDGE_CURVE('',#43477,#43459,#24759,.T.);
#57450=EDGE_CURVE('',#43474,#43477,#6861,.T.);
#57451=EDGE_CURVE('',#43478,#43464,#24760,.T.);
#57452=EDGE_CURVE('',#43479,#43478,#6862,.T.);
#57453=EDGE_CURVE('',#43479,#43465,#24761,.T.);
#57454=EDGE_CURVE('',#43480,#43479,#6863,.T.);
#57455=EDGE_CURVE('',#43480,#43462,#24762,.T.);
#57456=EDGE_CURVE('',#43481,#43480,#6864,.T.);
#57457=EDGE_CURVE('',#43481,#43463,#24763,.T.);
#57458=EDGE_CURVE('',#43478,#43481,#6865,.T.);
#57459=EDGE_CURVE('',#43482,#43483,#6866,.T.);
#57460=EDGE_CURVE('',#43483,#43484,#6867,.T.);
#57461=EDGE_CURVE('',#43484,#43485,#6868,.T.);
#57462=EDGE_CURVE('',#43485,#43486,#6869,.T.);
#57463=EDGE_CURVE('',#43486,#43487,#6870,.T.);
#57464=EDGE_CURVE('',#43487,#43488,#6871,.T.);
#57465=EDGE_CURVE('',#43488,#43489,#6872,.T.);
#57466=EDGE_CURVE('',#43489,#43482,#6873,.T.);
#57467=EDGE_CURVE('',#43490,#43491,#6874,.T.);
#57468=EDGE_CURVE('',#43491,#43492,#6875,.T.);
#57469=EDGE_CURVE('',#43492,#43493,#6876,.T.);
#57470=EDGE_CURVE('',#43493,#43494,#6877,.T.);
#57471=EDGE_CURVE('',#43494,#43495,#6878,.T.);
#57472=EDGE_CURVE('',#43495,#43496,#6879,.T.);
#57473=EDGE_CURVE('',#43496,#43497,#6880,.T.);
#57474=EDGE_CURVE('',#43497,#43490,#6881,.T.);
#57475=EDGE_CURVE('',#43498,#43499,#24764,.T.);
#57476=EDGE_CURVE('',#43499,#43500,#24765,.T.);
#57477=EDGE_CURVE('',#43500,#43501,#24766,.T.);
#57478=EDGE_CURVE('',#43501,#43498,#24767,.T.);
#57479=EDGE_CURVE('',#43487,#43502,#24768,.T.);
#57480=EDGE_CURVE('',#43486,#43503,#24769,.T.);
#57481=EDGE_CURVE('',#43502,#43503,#6882,.T.);
#57482=EDGE_CURVE('',#43488,#43504,#24770,.T.);
#57483=EDGE_CURVE('',#43504,#43502,#6883,.T.);
#57484=EDGE_CURVE('',#43489,#43505,#24771,.T.);
#57485=EDGE_CURVE('',#43505,#43504,#6884,.T.);
#57486=EDGE_CURVE('',#43482,#43506,#24772,.T.);
#57487=EDGE_CURVE('',#43506,#43505,#6885,.T.);
#57488=EDGE_CURVE('',#43483,#43507,#24773,.T.);
#57489=EDGE_CURVE('',#43507,#43506,#6886,.T.);
#57490=EDGE_CURVE('',#43484,#43508,#24774,.T.);
#57491=EDGE_CURVE('',#43508,#43507,#6887,.T.);
#57492=EDGE_CURVE('',#43485,#43509,#24775,.T.);
#57493=EDGE_CURVE('',#43509,#43508,#6888,.T.);
#57494=EDGE_CURVE('',#43503,#43509,#6889,.T.);
#57495=EDGE_CURVE('',#43495,#43510,#24776,.T.);
#57496=EDGE_CURVE('',#43494,#43511,#24777,.T.);
#57497=EDGE_CURVE('',#43510,#43511,#6890,.T.);
#57498=EDGE_CURVE('',#43496,#43512,#24778,.T.);
#57499=EDGE_CURVE('',#43512,#43510,#6891,.T.);
#57500=EDGE_CURVE('',#43497,#43513,#24779,.T.);
#57501=EDGE_CURVE('',#43513,#43512,#6892,.T.);
#57502=EDGE_CURVE('',#43490,#43514,#24780,.T.);
#57503=EDGE_CURVE('',#43514,#43513,#6893,.T.);
#57504=EDGE_CURVE('',#43491,#43515,#24781,.T.);
#57505=EDGE_CURVE('',#43515,#43514,#6894,.T.);
#57506=EDGE_CURVE('',#43492,#43516,#24782,.T.);
#57507=EDGE_CURVE('',#43516,#43515,#6895,.T.);
#57508=EDGE_CURVE('',#43493,#43517,#24783,.T.);
#57509=EDGE_CURVE('',#43517,#43516,#6896,.T.);
#57510=EDGE_CURVE('',#43511,#43517,#6897,.T.);
#57511=EDGE_CURVE('',#43499,#43518,#24784,.T.);
#57512=EDGE_CURVE('',#43498,#43519,#24785,.T.);
#57513=EDGE_CURVE('',#43518,#43519,#24786,.T.);
#57514=EDGE_CURVE('',#43500,#43520,#24787,.T.);
#57515=EDGE_CURVE('',#43520,#43518,#24788,.T.);
#57516=EDGE_CURVE('',#43501,#43521,#24789,.T.);
#57517=EDGE_CURVE('',#43521,#43520,#24790,.T.);
#57518=EDGE_CURVE('',#43519,#43521,#24791,.T.);
#57519=EDGE_CURVE('',#43522,#43523,#35079,.T.);
#57520=EDGE_CURVE('',#43523,#43524,#35080,.T.);
#57521=EDGE_CURVE('',#43524,#43525,#35081,.T.);
#57522=EDGE_CURVE('',#43525,#43526,#35082,.T.);
#57523=EDGE_CURVE('',#43526,#43527,#35083,.T.);
#57524=EDGE_CURVE('',#43527,#43522,#35084,.T.);
#57525=EDGE_CURVE('',#43527,#43528,#1726,.T.);
#57526=EDGE_CURVE('',#43528,#43522,#1727,.T.);
#57527=EDGE_CURVE('',#43522,#43529,#1728,.T.);
#57528=EDGE_CURVE('',#43529,#43523,#1729,.T.);
#57529=EDGE_CURVE('',#43523,#43530,#1730,.T.);
#57530=EDGE_CURVE('',#43530,#43524,#1731,.T.);
#57531=EDGE_CURVE('',#43524,#43531,#1732,.T.);
#57532=EDGE_CURVE('',#43531,#43525,#1733,.T.);
#57533=EDGE_CURVE('',#43526,#43532,#1734,.T.);
#57534=EDGE_CURVE('',#43532,#43527,#1735,.T.);
#57535=EDGE_CURVE('',#43533,#43526,#1736,.T.);
#57536=EDGE_CURVE('',#43525,#43533,#1737,.T.);
#57537=EDGE_CURVE('',#43532,#43534,#24792,.T.);
#57538=EDGE_CURVE('',#43534,#43535,#24793,.T.);
#57539=EDGE_CURVE('',#43528,#43535,#24794,.T.);
#57540=EDGE_CURVE('',#43535,#43536,#24795,.T.);
#57541=EDGE_CURVE('',#43529,#43536,#24796,.T.);
#57542=EDGE_CURVE('',#43536,#43537,#24797,.T.);
#57543=EDGE_CURVE('',#43530,#43537,#24798,.T.);
#57544=EDGE_CURVE('',#43537,#43538,#24799,.T.);
#57545=EDGE_CURVE('',#43531,#43538,#24800,.T.);
#57546=EDGE_CURVE('',#43538,#43539,#24801,.T.);
#57547=EDGE_CURVE('',#43533,#43539,#24802,.T.);
#57548=EDGE_CURVE('',#43539,#43534,#24803,.T.);
#57549=EDGE_CURVE('',#43540,#43541,#24804,.T.);
#57550=EDGE_CURVE('',#43542,#43540,#6898,.T.);
#57551=EDGE_CURVE('',#43543,#43542,#35085,.T.);
#57552=EDGE_CURVE('',#43541,#43543,#6899,.T.);
#57553=EDGE_CURVE('',#43544,#43545,#24805,.T.);
#57554=EDGE_CURVE('',#43546,#43545,#6900,.T.);
#57555=EDGE_CURVE('',#43546,#43547,#35086,.T.);
#57556=EDGE_CURVE('',#43544,#43547,#6901,.T.);
#57557=EDGE_CURVE('',#43548,#43549,#24806,.T.);
#57558=EDGE_CURVE('',#43545,#43549,#6902,.T.);
#57559=EDGE_CURVE('',#43548,#43544,#6903,.T.);
#57560=EDGE_CURVE('',#43550,#43551,#24807,.T.);
#57561=EDGE_CURVE('',#43549,#43551,#6904,.T.);
#57562=EDGE_CURVE('',#43550,#43548,#6905,.T.);
#57563=EDGE_CURVE('',#43552,#43553,#24808,.T.);
#57564=EDGE_CURVE('',#43551,#43553,#6906,.T.);
#57565=EDGE_CURVE('',#43552,#43550,#6907,.T.);
#57566=EDGE_CURVE('',#43554,#43555,#24809,.T.);
#57567=EDGE_CURVE('',#43556,#43554,#6908,.T.);
#57568=EDGE_CURVE('',#43556,#43557,#35087,.T.);
#57569=EDGE_CURVE('',#43557,#43558,#35088,.T.);
#57570=EDGE_CURVE('',#43555,#43558,#6909,.T.);
#57571=EDGE_CURVE('',#43559,#43560,#24810,.T.);
#57572=EDGE_CURVE('',#43560,#43543,#1738,.T.);
#57573=EDGE_CURVE('',#43559,#43542,#1739,.T.);
#57574=EDGE_CURVE('',#43561,#43562,#24811,.T.);
#57575=EDGE_CURVE('',#43562,#43560,#1740,.T.);
#57576=EDGE_CURVE('',#43561,#43559,#1741,.T.);
#57577=EDGE_CURVE('',#43563,#43564,#24812,.T.);
#57578=EDGE_CURVE('',#43564,#43562,#1742,.T.);
#57579=EDGE_CURVE('',#43563,#43561,#1743,.T.);
#57580=EDGE_CURVE('',#43565,#43566,#24813,.T.);
#57581=EDGE_CURVE('',#43565,#43567,#35089,.T.);
#57582=EDGE_CURVE('',#43567,#43566,#1744,.T.);
#57583=EDGE_CURVE('',#43553,#43555,#6910,.T.);
#57584=EDGE_CURVE('',#43558,#43541,#6911,.T.);
#57585=EDGE_CURVE('',#43566,#43564,#1745,.T.);
#57586=EDGE_CURVE('',#43567,#43568,#6912,.T.);
#57587=EDGE_CURVE('',#43568,#43546,#6913,.T.);
#57588=EDGE_CURVE('',#43569,#43563,#1746,.T.);
#57589=EDGE_CURVE('',#43569,#43565,#35090,.T.);
#57590=EDGE_CURVE('',#43540,#43556,#6914,.T.);
#57591=EDGE_CURVE('',#43554,#43552,#6915,.T.);
#57592=EDGE_CURVE('',#43547,#43569,#6916,.T.);
#57593=EDGE_CURVE('',#43570,#43571,#6917,.T.);
#57594=EDGE_CURVE('',#43572,#43570,#24814,.T.);
#57595=EDGE_CURVE('',#43573,#43572,#6918,.T.);
#57596=EDGE_CURVE('',#43571,#43573,#24815,.T.);
#57597=EDGE_CURVE('',#43574,#43575,#6919,.T.);
#57598=EDGE_CURVE('',#43576,#43574,#24816,.T.);
#57599=EDGE_CURVE('',#43577,#43576,#6920,.T.);
#57600=EDGE_CURVE('',#43575,#43577,#24817,.T.);
#57601=EDGE_CURVE('',#43578,#43579,#6921,.T.);
#57602=EDGE_CURVE('',#43580,#43578,#24818,.T.);
#57603=EDGE_CURVE('',#43581,#43580,#6922,.T.);
#57604=EDGE_CURVE('',#43579,#43581,#24819,.T.);
#57605=EDGE_CURVE('',#43582,#43583,#6923,.T.);
#57606=EDGE_CURVE('',#43584,#43582,#24820,.T.);
#57607=EDGE_CURVE('',#43585,#43584,#6924,.T.);
#57608=EDGE_CURVE('',#43583,#43585,#24821,.T.);
#57609=EDGE_CURVE('',#43586,#43587,#6925,.T.);
#57610=EDGE_CURVE('',#43588,#43586,#24822,.T.);
#57611=EDGE_CURVE('',#43589,#43588,#6926,.T.);
#57612=EDGE_CURVE('',#43587,#43589,#24823,.T.);
#57613=EDGE_CURVE('',#43590,#43591,#6927,.T.);
#57614=EDGE_CURVE('',#43592,#43590,#24824,.T.);
#57615=EDGE_CURVE('',#43593,#43592,#6928,.T.);
#57616=EDGE_CURVE('',#43591,#43593,#24825,.T.);
#57617=EDGE_CURVE('',#43593,#43594,#1747,.T.);
#57618=EDGE_CURVE('',#43595,#43592,#1748,.T.);
#57619=EDGE_CURVE('',#43594,#43595,#35091,.T.);
#57620=EDGE_CURVE('',#43589,#43595,#1749,.T.);
#57621=EDGE_CURVE('',#43596,#43588,#1750,.T.);
#57622=EDGE_CURVE('',#43595,#43596,#35092,.T.);
#57623=EDGE_CURVE('',#43585,#43596,#1751,.T.);
#57624=EDGE_CURVE('',#43597,#43584,#1752,.T.);
#57625=EDGE_CURVE('',#43596,#43597,#35093,.T.);
#57626=EDGE_CURVE('',#43581,#43597,#1753,.T.);
#57627=EDGE_CURVE('',#43598,#43580,#1754,.T.);
#57628=EDGE_CURVE('',#43597,#43598,#35094,.T.);
#57629=EDGE_CURVE('',#43577,#43598,#1755,.T.);
#57630=EDGE_CURVE('',#43599,#43576,#1756,.T.);
#57631=EDGE_CURVE('',#43598,#43599,#35095,.T.);
#57632=EDGE_CURVE('',#43573,#43599,#1757,.T.);
#57633=EDGE_CURVE('',#43594,#43572,#1758,.T.);
#57634=EDGE_CURVE('',#43594,#43599,#35096,.T.);
#57635=EDGE_CURVE('',#43600,#43574,#1759,.T.);
#57636=EDGE_CURVE('',#43575,#43601,#1760,.T.);
#57637=EDGE_CURVE('',#43600,#43601,#35097,.T.);
#57638=EDGE_CURVE('',#43601,#43578,#1761,.T.);
#57639=EDGE_CURVE('',#43579,#43602,#1762,.T.);
#57640=EDGE_CURVE('',#43601,#43602,#35098,.T.);
#57641=EDGE_CURVE('',#43602,#43582,#1763,.T.);
#57642=EDGE_CURVE('',#43583,#43603,#1764,.T.);
#57643=EDGE_CURVE('',#43602,#43603,#35099,.T.);
#57644=EDGE_CURVE('',#43603,#43586,#1765,.T.);
#57645=EDGE_CURVE('',#43587,#43604,#1766,.T.);
#57646=EDGE_CURVE('',#43603,#43604,#35100,.T.);
#57647=EDGE_CURVE('',#43604,#43590,#1767,.T.);
#57648=EDGE_CURVE('',#43591,#43605,#1768,.T.);
#57649=EDGE_CURVE('',#43604,#43605,#35101,.T.);
#57650=EDGE_CURVE('',#43605,#43570,#1769,.T.);
#57651=EDGE_CURVE('',#43571,#43600,#1770,.T.);
#57652=EDGE_CURVE('',#43605,#43600,#35102,.T.);
#57653=EDGE_CURVE('',#43606,#43606,#35103,.T.);
#57654=EDGE_CURVE('',#43607,#43607,#35104,.T.);
#57655=EDGE_CURVE('',#43568,#43607,#24826,.T.);
#57656=EDGE_CURVE('',#43557,#43606,#24827,.T.);
#57657=ORIENTED_EDGE('',*,*,#43608,.F.);
#57658=ORIENTED_EDGE('',*,*,#43609,.T.);
#57659=ORIENTED_EDGE('',*,*,#43610,.T.);
#57660=ORIENTED_EDGE('',*,*,#43609,.F.);
#57661=ORIENTED_EDGE('',*,*,#43611,.F.);
#57662=ORIENTED_EDGE('',*,*,#43612,.T.);
#57663=ORIENTED_EDGE('',*,*,#43613,.T.);
#57664=ORIENTED_EDGE('',*,*,#43612,.F.);
#57665=ORIENTED_EDGE('',*,*,#43614,.F.);
#57666=ORIENTED_EDGE('',*,*,#43615,.T.);
#57667=ORIENTED_EDGE('',*,*,#43616,.T.);
#57668=ORIENTED_EDGE('',*,*,#43615,.F.);
#57669=ORIENTED_EDGE('',*,*,#43617,.F.);
#57670=ORIENTED_EDGE('',*,*,#43618,.T.);
#57671=ORIENTED_EDGE('',*,*,#43619,.T.);
#57672=ORIENTED_EDGE('',*,*,#43618,.F.);
#57673=ORIENTED_EDGE('',*,*,#43620,.F.);
#57674=ORIENTED_EDGE('',*,*,#43621,.T.);
#57675=ORIENTED_EDGE('',*,*,#43622,.T.);
#57676=ORIENTED_EDGE('',*,*,#43621,.F.);
#57677=ORIENTED_EDGE('',*,*,#43623,.F.);
#57678=ORIENTED_EDGE('',*,*,#43624,.T.);
#57679=ORIENTED_EDGE('',*,*,#43625,.T.);
#57680=ORIENTED_EDGE('',*,*,#43624,.F.);
#57681=ORIENTED_EDGE('',*,*,#43626,.F.);
#57682=ORIENTED_EDGE('',*,*,#43627,.T.);
#57683=ORIENTED_EDGE('',*,*,#43628,.T.);
#57684=ORIENTED_EDGE('',*,*,#43627,.F.);
#57685=ORIENTED_EDGE('',*,*,#43629,.F.);
#57686=ORIENTED_EDGE('',*,*,#43630,.T.);
#57687=ORIENTED_EDGE('',*,*,#43631,.T.);
#57688=ORIENTED_EDGE('',*,*,#43630,.F.);
#57689=ORIENTED_EDGE('',*,*,#43632,.F.);
#57690=ORIENTED_EDGE('',*,*,#43633,.T.);
#57691=ORIENTED_EDGE('',*,*,#43634,.T.);
#57692=ORIENTED_EDGE('',*,*,#43633,.F.);
#57693=ORIENTED_EDGE('',*,*,#43635,.F.);
#57694=ORIENTED_EDGE('',*,*,#43636,.T.);
#57695=ORIENTED_EDGE('',*,*,#43637,.T.);
#57696=ORIENTED_EDGE('',*,*,#43636,.F.);
#57697=ORIENTED_EDGE('',*,*,#43638,.F.);
#57698=ORIENTED_EDGE('',*,*,#43639,.T.);
#57699=ORIENTED_EDGE('',*,*,#43640,.T.);
#57700=ORIENTED_EDGE('',*,*,#43639,.F.);
#57701=ORIENTED_EDGE('',*,*,#43641,.F.);
#57702=ORIENTED_EDGE('',*,*,#43642,.T.);
#57703=ORIENTED_EDGE('',*,*,#43643,.T.);
#57704=ORIENTED_EDGE('',*,*,#43642,.F.);
#57705=ORIENTED_EDGE('',*,*,#43644,.T.);
#57706=ORIENTED_EDGE('',*,*,#43645,.F.);
#57707=ORIENTED_EDGE('',*,*,#43646,.F.);
#57708=ORIENTED_EDGE('',*,*,#43647,.T.);
#57709=ORIENTED_EDGE('',*,*,#43648,.T.);
#57710=ORIENTED_EDGE('',*,*,#43649,.T.);
#57711=ORIENTED_EDGE('',*,*,#43650,.F.);
#57712=ORIENTED_EDGE('',*,*,#43645,.T.);
#57713=ORIENTED_EDGE('',*,*,#43651,.T.);
#57714=ORIENTED_EDGE('',*,*,#43652,.T.);
#57715=ORIENTED_EDGE('',*,*,#43653,.F.);
#57716=ORIENTED_EDGE('',*,*,#43654,.T.);
#57717=ORIENTED_EDGE('',*,*,#43608,.T.);
#57718=ORIENTED_EDGE('',*,*,#43611,.T.);
#57719=ORIENTED_EDGE('',*,*,#43614,.T.);
#57720=ORIENTED_EDGE('',*,*,#43617,.T.);
#57721=ORIENTED_EDGE('',*,*,#43620,.T.);
#57722=ORIENTED_EDGE('',*,*,#43623,.T.);
#57723=ORIENTED_EDGE('',*,*,#43626,.T.);
#57724=ORIENTED_EDGE('',*,*,#43629,.T.);
#57725=ORIENTED_EDGE('',*,*,#43632,.T.);
#57726=ORIENTED_EDGE('',*,*,#43635,.T.);
#57727=ORIENTED_EDGE('',*,*,#43638,.T.);
#57728=ORIENTED_EDGE('',*,*,#43641,.T.);
#57729=ORIENTED_EDGE('',*,*,#43655,.F.);
#57730=ORIENTED_EDGE('',*,*,#43656,.T.);
#57731=ORIENTED_EDGE('',*,*,#43657,.T.);
#57732=ORIENTED_EDGE('',*,*,#43658,.F.);
#57733=ORIENTED_EDGE('',*,*,#43659,.T.);
#57734=ORIENTED_EDGE('',*,*,#43660,.F.);
#57735=ORIENTED_EDGE('',*,*,#43661,.F.);
#57736=ORIENTED_EDGE('',*,*,#43658,.T.);
#57737=ORIENTED_EDGE('',*,*,#43662,.T.);
#57738=ORIENTED_EDGE('',*,*,#43663,.T.);
#57739=ORIENTED_EDGE('',*,*,#43664,.F.);
#57740=ORIENTED_EDGE('',*,*,#43660,.T.);
#57741=ORIENTED_EDGE('',*,*,#43665,.T.);
#57742=ORIENTED_EDGE('',*,*,#43666,.T.);
#57743=ORIENTED_EDGE('',*,*,#43667,.F.);
#57744=ORIENTED_EDGE('',*,*,#43668,.T.);
#57745=ORIENTED_EDGE('',*,*,#43610,.F.);
#57746=ORIENTED_EDGE('',*,*,#43613,.F.);
#57747=ORIENTED_EDGE('',*,*,#43616,.F.);
#57748=ORIENTED_EDGE('',*,*,#43619,.F.);
#57749=ORIENTED_EDGE('',*,*,#43622,.F.);
#57750=ORIENTED_EDGE('',*,*,#43625,.F.);
#57751=ORIENTED_EDGE('',*,*,#43628,.F.);
#57752=ORIENTED_EDGE('',*,*,#43631,.F.);
#57753=ORIENTED_EDGE('',*,*,#43634,.F.);
#57754=ORIENTED_EDGE('',*,*,#43637,.F.);
#57755=ORIENTED_EDGE('',*,*,#43640,.F.);
#57756=ORIENTED_EDGE('',*,*,#43643,.F.);
#57757=ORIENTED_EDGE('',*,*,#43669,.F.);
#57758=ORIENTED_EDGE('',*,*,#43670,.T.);
#57759=ORIENTED_EDGE('',*,*,#43671,.T.);
#57760=ORIENTED_EDGE('',*,*,#43647,.F.);
#57761=ORIENTED_EDGE('',*,*,#43653,.T.);
#57762=ORIENTED_EDGE('',*,*,#43672,.T.);
#57763=ORIENTED_EDGE('',*,*,#43655,.T.);
#57764=ORIENTED_EDGE('',*,*,#43661,.T.);
#57765=ORIENTED_EDGE('',*,*,#43664,.T.);
#57766=ORIENTED_EDGE('',*,*,#43673,.T.);
#57767=ORIENTED_EDGE('',*,*,#43667,.T.);
#57768=ORIENTED_EDGE('',*,*,#43674,.T.);
#57769=ORIENTED_EDGE('',*,*,#43669,.T.);
#57770=ORIENTED_EDGE('',*,*,#43646,.T.);
#57771=ORIENTED_EDGE('',*,*,#43650,.T.);
#57772=ORIENTED_EDGE('',*,*,#43675,.T.);
#57773=ORIENTED_EDGE('',*,*,#43657,.F.);
#57774=ORIENTED_EDGE('',*,*,#43676,.T.);
#57775=ORIENTED_EDGE('',*,*,#43651,.F.);
#57776=ORIENTED_EDGE('',*,*,#43677,.T.);
#57777=ORIENTED_EDGE('',*,*,#43648,.F.);
#57778=ORIENTED_EDGE('',*,*,#43644,.F.);
#57779=ORIENTED_EDGE('',*,*,#43671,.F.);
#57780=ORIENTED_EDGE('',*,*,#43678,.T.);
#57781=ORIENTED_EDGE('',*,*,#43665,.F.);
#57782=ORIENTED_EDGE('',*,*,#43679,.T.);
#57783=ORIENTED_EDGE('',*,*,#43662,.F.);
#57784=ORIENTED_EDGE('',*,*,#43659,.F.);
#57785=ORIENTED_EDGE('',*,*,#43672,.F.);
#57786=ORIENTED_EDGE('',*,*,#43652,.F.);
#57787=ORIENTED_EDGE('',*,*,#43676,.F.);
#57788=ORIENTED_EDGE('',*,*,#43656,.F.);
#57789=ORIENTED_EDGE('',*,*,#43675,.F.);
#57790=ORIENTED_EDGE('',*,*,#43649,.F.);
#57791=ORIENTED_EDGE('',*,*,#43677,.F.);
#57792=ORIENTED_EDGE('',*,*,#43654,.F.);
#57793=ORIENTED_EDGE('',*,*,#43674,.F.);
#57794=ORIENTED_EDGE('',*,*,#43666,.F.);
#57795=ORIENTED_EDGE('',*,*,#43678,.F.);
#57796=ORIENTED_EDGE('',*,*,#43670,.F.);
#57797=ORIENTED_EDGE('',*,*,#43673,.F.);
#57798=ORIENTED_EDGE('',*,*,#43663,.F.);
#57799=ORIENTED_EDGE('',*,*,#43679,.F.);
#57800=ORIENTED_EDGE('',*,*,#43668,.F.);
#57801=ORIENTED_EDGE('',*,*,#43680,.F.);
#57802=ORIENTED_EDGE('',*,*,#43681,.T.);
#57803=ORIENTED_EDGE('',*,*,#43682,.T.);
#57804=ORIENTED_EDGE('',*,*,#43681,.F.);
#57805=ORIENTED_EDGE('',*,*,#43683,.F.);
#57806=ORIENTED_EDGE('',*,*,#43684,.T.);
#57807=ORIENTED_EDGE('',*,*,#43685,.T.);
#57808=ORIENTED_EDGE('',*,*,#43684,.F.);
#57809=ORIENTED_EDGE('',*,*,#43686,.F.);
#57810=ORIENTED_EDGE('',*,*,#43687,.T.);
#57811=ORIENTED_EDGE('',*,*,#43688,.T.);
#57812=ORIENTED_EDGE('',*,*,#43687,.F.);
#57813=ORIENTED_EDGE('',*,*,#43689,.F.);
#57814=ORIENTED_EDGE('',*,*,#43690,.T.);
#57815=ORIENTED_EDGE('',*,*,#43691,.T.);
#57816=ORIENTED_EDGE('',*,*,#43690,.F.);
#57817=ORIENTED_EDGE('',*,*,#43692,.F.);
#57818=ORIENTED_EDGE('',*,*,#43693,.T.);
#57819=ORIENTED_EDGE('',*,*,#43694,.T.);
#57820=ORIENTED_EDGE('',*,*,#43693,.F.);
#57821=ORIENTED_EDGE('',*,*,#43695,.F.);
#57822=ORIENTED_EDGE('',*,*,#43696,.T.);
#57823=ORIENTED_EDGE('',*,*,#43697,.T.);
#57824=ORIENTED_EDGE('',*,*,#43696,.F.);
#57825=ORIENTED_EDGE('',*,*,#43698,.F.);
#57826=ORIENTED_EDGE('',*,*,#43699,.T.);
#57827=ORIENTED_EDGE('',*,*,#43700,.T.);
#57828=ORIENTED_EDGE('',*,*,#43699,.F.);
#57829=ORIENTED_EDGE('',*,*,#43701,.F.);
#57830=ORIENTED_EDGE('',*,*,#43702,.T.);
#57831=ORIENTED_EDGE('',*,*,#43703,.T.);
#57832=ORIENTED_EDGE('',*,*,#43702,.F.);
#57833=ORIENTED_EDGE('',*,*,#43704,.F.);
#57834=ORIENTED_EDGE('',*,*,#43705,.T.);
#57835=ORIENTED_EDGE('',*,*,#43706,.T.);
#57836=ORIENTED_EDGE('',*,*,#43705,.F.);
#57837=ORIENTED_EDGE('',*,*,#43707,.F.);
#57838=ORIENTED_EDGE('',*,*,#43708,.T.);
#57839=ORIENTED_EDGE('',*,*,#43709,.T.);
#57840=ORIENTED_EDGE('',*,*,#43708,.F.);
#57841=ORIENTED_EDGE('',*,*,#43710,.F.);
#57842=ORIENTED_EDGE('',*,*,#43711,.T.);
#57843=ORIENTED_EDGE('',*,*,#43712,.T.);
#57844=ORIENTED_EDGE('',*,*,#43711,.F.);
#57845=ORIENTED_EDGE('',*,*,#43713,.F.);
#57846=ORIENTED_EDGE('',*,*,#43714,.T.);
#57847=ORIENTED_EDGE('',*,*,#43715,.T.);
#57848=ORIENTED_EDGE('',*,*,#43714,.F.);
#57849=ORIENTED_EDGE('',*,*,#43716,.T.);
#57850=ORIENTED_EDGE('',*,*,#43717,.F.);
#57851=ORIENTED_EDGE('',*,*,#43718,.F.);
#57852=ORIENTED_EDGE('',*,*,#43719,.T.);
#57853=ORIENTED_EDGE('',*,*,#43720,.T.);
#57854=ORIENTED_EDGE('',*,*,#43721,.T.);
#57855=ORIENTED_EDGE('',*,*,#43722,.F.);
#57856=ORIENTED_EDGE('',*,*,#43717,.T.);
#57857=ORIENTED_EDGE('',*,*,#43723,.T.);
#57858=ORIENTED_EDGE('',*,*,#43724,.T.);
#57859=ORIENTED_EDGE('',*,*,#43725,.F.);
#57860=ORIENTED_EDGE('',*,*,#43726,.T.);
#57861=ORIENTED_EDGE('',*,*,#43680,.T.);
#57862=ORIENTED_EDGE('',*,*,#43683,.T.);
#57863=ORIENTED_EDGE('',*,*,#43686,.T.);
#57864=ORIENTED_EDGE('',*,*,#43689,.T.);
#57865=ORIENTED_EDGE('',*,*,#43692,.T.);
#57866=ORIENTED_EDGE('',*,*,#43695,.T.);
#57867=ORIENTED_EDGE('',*,*,#43698,.T.);
#57868=ORIENTED_EDGE('',*,*,#43701,.T.);
#57869=ORIENTED_EDGE('',*,*,#43704,.T.);
#57870=ORIENTED_EDGE('',*,*,#43707,.T.);
#57871=ORIENTED_EDGE('',*,*,#43710,.T.);
#57872=ORIENTED_EDGE('',*,*,#43713,.T.);
#57873=ORIENTED_EDGE('',*,*,#43727,.F.);
#57874=ORIENTED_EDGE('',*,*,#43728,.T.);
#57875=ORIENTED_EDGE('',*,*,#43729,.T.);
#57876=ORIENTED_EDGE('',*,*,#43730,.F.);
#57877=ORIENTED_EDGE('',*,*,#43731,.T.);
#57878=ORIENTED_EDGE('',*,*,#43732,.F.);
#57879=ORIENTED_EDGE('',*,*,#43733,.F.);
#57880=ORIENTED_EDGE('',*,*,#43730,.T.);
#57881=ORIENTED_EDGE('',*,*,#43734,.T.);
#57882=ORIENTED_EDGE('',*,*,#43735,.T.);
#57883=ORIENTED_EDGE('',*,*,#43736,.F.);
#57884=ORIENTED_EDGE('',*,*,#43732,.T.);
#57885=ORIENTED_EDGE('',*,*,#43737,.T.);
#57886=ORIENTED_EDGE('',*,*,#43738,.T.);
#57887=ORIENTED_EDGE('',*,*,#43739,.F.);
#57888=ORIENTED_EDGE('',*,*,#43740,.T.);
#57889=ORIENTED_EDGE('',*,*,#43682,.F.);
#57890=ORIENTED_EDGE('',*,*,#43685,.F.);
#57891=ORIENTED_EDGE('',*,*,#43688,.F.);
#57892=ORIENTED_EDGE('',*,*,#43691,.F.);
#57893=ORIENTED_EDGE('',*,*,#43694,.F.);
#57894=ORIENTED_EDGE('',*,*,#43697,.F.);
#57895=ORIENTED_EDGE('',*,*,#43700,.F.);
#57896=ORIENTED_EDGE('',*,*,#43703,.F.);
#57897=ORIENTED_EDGE('',*,*,#43706,.F.);
#57898=ORIENTED_EDGE('',*,*,#43709,.F.);
#57899=ORIENTED_EDGE('',*,*,#43712,.F.);
#57900=ORIENTED_EDGE('',*,*,#43715,.F.);
#57901=ORIENTED_EDGE('',*,*,#43741,.F.);
#57902=ORIENTED_EDGE('',*,*,#43742,.T.);
#57903=ORIENTED_EDGE('',*,*,#43743,.T.);
#57904=ORIENTED_EDGE('',*,*,#43719,.F.);
#57905=ORIENTED_EDGE('',*,*,#43725,.T.);
#57906=ORIENTED_EDGE('',*,*,#43744,.T.);
#57907=ORIENTED_EDGE('',*,*,#43727,.T.);
#57908=ORIENTED_EDGE('',*,*,#43733,.T.);
#57909=ORIENTED_EDGE('',*,*,#43736,.T.);
#57910=ORIENTED_EDGE('',*,*,#43745,.T.);
#57911=ORIENTED_EDGE('',*,*,#43739,.T.);
#57912=ORIENTED_EDGE('',*,*,#43746,.T.);
#57913=ORIENTED_EDGE('',*,*,#43741,.T.);
#57914=ORIENTED_EDGE('',*,*,#43718,.T.);
#57915=ORIENTED_EDGE('',*,*,#43722,.T.);
#57916=ORIENTED_EDGE('',*,*,#43747,.T.);
#57917=ORIENTED_EDGE('',*,*,#43729,.F.);
#57918=ORIENTED_EDGE('',*,*,#43748,.T.);
#57919=ORIENTED_EDGE('',*,*,#43723,.F.);
#57920=ORIENTED_EDGE('',*,*,#43749,.T.);
#57921=ORIENTED_EDGE('',*,*,#43720,.F.);
#57922=ORIENTED_EDGE('',*,*,#43716,.F.);
#57923=ORIENTED_EDGE('',*,*,#43743,.F.);
#57924=ORIENTED_EDGE('',*,*,#43750,.T.);
#57925=ORIENTED_EDGE('',*,*,#43737,.F.);
#57926=ORIENTED_EDGE('',*,*,#43751,.T.);
#57927=ORIENTED_EDGE('',*,*,#43734,.F.);
#57928=ORIENTED_EDGE('',*,*,#43731,.F.);
#57929=ORIENTED_EDGE('',*,*,#43744,.F.);
#57930=ORIENTED_EDGE('',*,*,#43724,.F.);
#57931=ORIENTED_EDGE('',*,*,#43748,.F.);
#57932=ORIENTED_EDGE('',*,*,#43728,.F.);
#57933=ORIENTED_EDGE('',*,*,#43747,.F.);
#57934=ORIENTED_EDGE('',*,*,#43721,.F.);
#57935=ORIENTED_EDGE('',*,*,#43749,.F.);
#57936=ORIENTED_EDGE('',*,*,#43726,.F.);
#57937=ORIENTED_EDGE('',*,*,#43746,.F.);
#57938=ORIENTED_EDGE('',*,*,#43738,.F.);
#57939=ORIENTED_EDGE('',*,*,#43750,.F.);
#57940=ORIENTED_EDGE('',*,*,#43742,.F.);
#57941=ORIENTED_EDGE('',*,*,#43745,.F.);
#57942=ORIENTED_EDGE('',*,*,#43735,.F.);
#57943=ORIENTED_EDGE('',*,*,#43751,.F.);
#57944=ORIENTED_EDGE('',*,*,#43740,.F.);
#57945=ORIENTED_EDGE('',*,*,#43752,.T.);
#57946=ORIENTED_EDGE('',*,*,#43753,.T.);
#57947=ORIENTED_EDGE('',*,*,#43754,.T.);
#57948=ORIENTED_EDGE('',*,*,#43753,.F.);
#57949=ORIENTED_EDGE('',*,*,#43754,.F.);
#57950=ORIENTED_EDGE('',*,*,#43755,.F.);
#57951=ORIENTED_EDGE('',*,*,#43756,.T.);
#57952=ORIENTED_EDGE('',*,*,#43752,.F.);
#57953=ORIENTED_EDGE('',*,*,#43756,.F.);
#57954=ORIENTED_EDGE('',*,*,#43757,.T.);
#57955=ORIENTED_EDGE('',*,*,#43755,.T.);
#57956=ORIENTED_EDGE('',*,*,#43758,.F.);
#57957=ORIENTED_EDGE('',*,*,#43759,.T.);
#57958=ORIENTED_EDGE('',*,*,#43757,.F.);
#57959=ORIENTED_EDGE('',*,*,#43759,.F.);
#57960=ORIENTED_EDGE('',*,*,#43758,.T.);
#57961=ORIENTED_EDGE('',*,*,#43760,.F.);
#57962=ORIENTED_EDGE('',*,*,#43761,.T.);
#57963=ORIENTED_EDGE('',*,*,#43762,.F.);
#57964=ORIENTED_EDGE('',*,*,#43761,.F.);
#57965=ORIENTED_EDGE('',*,*,#43762,.T.);
#57966=ORIENTED_EDGE('',*,*,#43763,.T.);
#57967=ORIENTED_EDGE('',*,*,#43764,.T.);
#57968=ORIENTED_EDGE('',*,*,#43760,.T.);
#57969=ORIENTED_EDGE('',*,*,#43764,.F.);
#57970=ORIENTED_EDGE('',*,*,#43765,.F.);
#57971=ORIENTED_EDGE('',*,*,#43763,.F.);
#57972=ORIENTED_EDGE('',*,*,#43766,.T.);
#57973=ORIENTED_EDGE('',*,*,#43767,.T.);
#57974=ORIENTED_EDGE('',*,*,#43765,.T.);
#57975=ORIENTED_EDGE('',*,*,#43767,.F.);
#57976=ORIENTED_EDGE('',*,*,#43766,.F.);
#57977=ORIENTED_EDGE('',*,*,#43768,.T.);
#57978=ORIENTED_EDGE('',*,*,#43769,.T.);
#57979=ORIENTED_EDGE('',*,*,#43770,.T.);
#57980=ORIENTED_EDGE('',*,*,#43771,.F.);
#57981=ORIENTED_EDGE('',*,*,#43772,.F.);
#57982=ORIENTED_EDGE('',*,*,#43773,.F.);
#57983=ORIENTED_EDGE('',*,*,#43774,.F.);
#57984=ORIENTED_EDGE('',*,*,#43775,.T.);
#57985=ORIENTED_EDGE('',*,*,#43776,.T.);
#57986=ORIENTED_EDGE('',*,*,#43777,.T.);
#57987=ORIENTED_EDGE('',*,*,#43778,.F.);
#57988=ORIENTED_EDGE('',*,*,#43779,.F.);
#57989=ORIENTED_EDGE('',*,*,#43774,.T.);
#57990=ORIENTED_EDGE('',*,*,#43780,.T.);
#57991=ORIENTED_EDGE('',*,*,#43781,.T.);
#57992=ORIENTED_EDGE('',*,*,#43780,.F.);
#57993=ORIENTED_EDGE('',*,*,#43778,.T.);
#57994=ORIENTED_EDGE('',*,*,#43782,.T.);
#57995=ORIENTED_EDGE('',*,*,#43783,.T.);
#57996=ORIENTED_EDGE('',*,*,#43784,.T.);
#57997=ORIENTED_EDGE('',*,*,#43785,.T.);
#57998=ORIENTED_EDGE('',*,*,#43786,.T.);
#57999=ORIENTED_EDGE('',*,*,#43787,.F.);
#58000=ORIENTED_EDGE('',*,*,#43788,.F.);
#58001=ORIENTED_EDGE('',*,*,#43789,.F.);
#58002=ORIENTED_EDGE('',*,*,#43790,.F.);
#58003=ORIENTED_EDGE('',*,*,#43791,.F.);
#58004=ORIENTED_EDGE('',*,*,#43792,.F.);
#58005=ORIENTED_EDGE('',*,*,#43793,.F.);
#58006=ORIENTED_EDGE('',*,*,#43794,.F.);
#58007=ORIENTED_EDGE('',*,*,#43795,.F.);
#58008=ORIENTED_EDGE('',*,*,#43796,.F.);
#58009=ORIENTED_EDGE('',*,*,#43797,.F.);
#58010=ORIENTED_EDGE('',*,*,#43777,.F.);
#58011=ORIENTED_EDGE('',*,*,#43798,.F.);
#58012=ORIENTED_EDGE('',*,*,#43784,.F.);
#58013=ORIENTED_EDGE('',*,*,#43799,.F.);
#58014=ORIENTED_EDGE('',*,*,#43800,.F.);
#58015=ORIENTED_EDGE('',*,*,#43801,.F.);
#58016=ORIENTED_EDGE('',*,*,#43802,.F.);
#58017=ORIENTED_EDGE('',*,*,#43803,.F.);
#58018=ORIENTED_EDGE('',*,*,#43804,.F.);
#58019=ORIENTED_EDGE('',*,*,#43805,.F.);
#58020=ORIENTED_EDGE('',*,*,#43787,.T.);
#58021=ORIENTED_EDGE('',*,*,#43806,.T.);
#58022=ORIENTED_EDGE('',*,*,#43807,.T.);
#58023=ORIENTED_EDGE('',*,*,#43808,.T.);
#58024=ORIENTED_EDGE('',*,*,#43809,.T.);
#58025=ORIENTED_EDGE('',*,*,#43810,.T.);
#58026=ORIENTED_EDGE('',*,*,#43811,.F.);
#58027=ORIENTED_EDGE('',*,*,#43786,.F.);
#58028=ORIENTED_EDGE('',*,*,#43812,.F.);
#58029=ORIENTED_EDGE('',*,*,#43808,.F.);
#58030=ORIENTED_EDGE('',*,*,#43813,.F.);
#58031=ORIENTED_EDGE('',*,*,#43814,.F.);
#58032=ORIENTED_EDGE('',*,*,#43811,.T.);
#58033=ORIENTED_EDGE('',*,*,#43815,.T.);
#58034=ORIENTED_EDGE('',*,*,#43816,.T.);
#58035=ORIENTED_EDGE('',*,*,#43817,.F.);
#58036=ORIENTED_EDGE('',*,*,#43818,.F.);
#58037=ORIENTED_EDGE('',*,*,#43819,.F.);
#58038=ORIENTED_EDGE('',*,*,#43820,.F.);
#58039=ORIENTED_EDGE('',*,*,#43821,.F.);
#58040=ORIENTED_EDGE('',*,*,#43822,.F.);
#58041=ORIENTED_EDGE('',*,*,#43823,.F.);
#58042=ORIENTED_EDGE('',*,*,#43824,.F.);
#58043=ORIENTED_EDGE('',*,*,#43825,.F.);
#58044=ORIENTED_EDGE('',*,*,#43826,.F.);
#58045=ORIENTED_EDGE('',*,*,#43827,.F.);
#58046=ORIENTED_EDGE('',*,*,#43828,.F.);
#58047=ORIENTED_EDGE('',*,*,#43829,.F.);
#58048=ORIENTED_EDGE('',*,*,#43830,.F.);
#58049=ORIENTED_EDGE('',*,*,#43810,.F.);
#58050=ORIENTED_EDGE('',*,*,#43831,.F.);
#58051=ORIENTED_EDGE('',*,*,#43768,.F.);
#58052=ORIENTED_EDGE('',*,*,#43832,.F.);
#58053=ORIENTED_EDGE('',*,*,#43833,.F.);
#58054=ORIENTED_EDGE('',*,*,#43834,.F.);
#58055=ORIENTED_EDGE('',*,*,#43835,.T.);
#58056=ORIENTED_EDGE('',*,*,#43836,.T.);
#58057=ORIENTED_EDGE('',*,*,#43837,.T.);
#58058=ORIENTED_EDGE('',*,*,#43838,.F.);
#58059=ORIENTED_EDGE('',*,*,#43839,.T.);
#58060=ORIENTED_EDGE('',*,*,#43834,.T.);
#58061=ORIENTED_EDGE('',*,*,#43840,.T.);
#58062=ORIENTED_EDGE('',*,*,#43841,.T.);
#58063=ORIENTED_EDGE('',*,*,#43842,.F.);
#58064=ORIENTED_EDGE('',*,*,#43843,.T.);
#58065=ORIENTED_EDGE('',*,*,#43844,.F.);
#58066=ORIENTED_EDGE('',*,*,#43845,.T.);
#58067=ORIENTED_EDGE('',*,*,#43846,.T.);
#58068=ORIENTED_EDGE('',*,*,#43847,.F.);
#58069=ORIENTED_EDGE('',*,*,#43848,.F.);
#58070=ORIENTED_EDGE('',*,*,#43849,.T.);
#58071=ORIENTED_EDGE('',*,*,#43850,.T.);
#58072=ORIENTED_EDGE('',*,*,#43850,.F.);
#58073=ORIENTED_EDGE('',*,*,#43851,.T.);
#58074=ORIENTED_EDGE('',*,*,#43852,.T.);
#58075=ORIENTED_EDGE('',*,*,#43853,.T.);
#58076=ORIENTED_EDGE('',*,*,#43845,.F.);
#58077=ORIENTED_EDGE('',*,*,#43852,.F.);
#58078=ORIENTED_EDGE('',*,*,#43854,.T.);
#58079=ORIENTED_EDGE('',*,*,#43855,.T.);
#58080=ORIENTED_EDGE('',*,*,#43856,.T.);
#58081=ORIENTED_EDGE('',*,*,#43855,.F.);
#58082=ORIENTED_EDGE('',*,*,#43857,.T.);
#58083=ORIENTED_EDGE('',*,*,#43858,.F.);
#58084=ORIENTED_EDGE('',*,*,#43859,.T.);
#58085=ORIENTED_EDGE('',*,*,#43860,.F.);
#58086=ORIENTED_EDGE('',*,*,#43861,.T.);
#58087=ORIENTED_EDGE('',*,*,#43858,.T.);
#58088=ORIENTED_EDGE('',*,*,#43862,.T.);
#58089=ORIENTED_EDGE('',*,*,#43863,.T.);
#58090=ORIENTED_EDGE('',*,*,#43864,.F.);
#58091=ORIENTED_EDGE('',*,*,#43865,.T.);
#58092=ORIENTED_EDGE('',*,*,#43866,.F.);
#58093=ORIENTED_EDGE('',*,*,#43867,.T.);
#58094=ORIENTED_EDGE('',*,*,#43868,.T.);
#58095=ORIENTED_EDGE('',*,*,#43869,.F.);
#58096=ORIENTED_EDGE('',*,*,#43870,.F.);
#58097=ORIENTED_EDGE('',*,*,#43871,.T.);
#58098=ORIENTED_EDGE('',*,*,#43867,.F.);
#58099=ORIENTED_EDGE('',*,*,#43872,.T.);
#58100=ORIENTED_EDGE('',*,*,#43873,.T.);
#58101=ORIENTED_EDGE('',*,*,#43874,.T.);
#58102=ORIENTED_EDGE('',*,*,#43873,.F.);
#58103=ORIENTED_EDGE('',*,*,#43875,.T.);
#58104=ORIENTED_EDGE('',*,*,#43876,.T.);
#58105=ORIENTED_EDGE('',*,*,#43877,.T.);
#58106=ORIENTED_EDGE('',*,*,#43876,.F.);
#58107=ORIENTED_EDGE('',*,*,#43878,.T.);
#58108=ORIENTED_EDGE('',*,*,#43879,.F.);
#58109=ORIENTED_EDGE('',*,*,#43880,.T.);
#58110=ORIENTED_EDGE('',*,*,#43881,.F.);
#58111=ORIENTED_EDGE('',*,*,#43882,.T.);
#58112=ORIENTED_EDGE('',*,*,#43879,.T.);
#58113=ORIENTED_EDGE('',*,*,#43883,.T.);
#58114=ORIENTED_EDGE('',*,*,#43884,.T.);
#58115=ORIENTED_EDGE('',*,*,#43885,.F.);
#58116=ORIENTED_EDGE('',*,*,#43886,.T.);
#58117=ORIENTED_EDGE('',*,*,#43887,.F.);
#58118=ORIENTED_EDGE('',*,*,#43888,.T.);
#58119=ORIENTED_EDGE('',*,*,#43889,.T.);
#58120=ORIENTED_EDGE('',*,*,#43890,.F.);
#58121=ORIENTED_EDGE('',*,*,#43891,.T.);
#58122=ORIENTED_EDGE('',*,*,#43888,.F.);
#58123=ORIENTED_EDGE('',*,*,#43892,.T.);
#58124=ORIENTED_EDGE('',*,*,#43893,.T.);
#58125=ORIENTED_EDGE('',*,*,#43894,.T.);
#58126=ORIENTED_EDGE('',*,*,#43893,.F.);
#58127=ORIENTED_EDGE('',*,*,#43895,.T.);
#58128=ORIENTED_EDGE('',*,*,#43779,.T.);
#58129=ORIENTED_EDGE('',*,*,#43896,.T.);
#58130=ORIENTED_EDGE('',*,*,#43897,.T.);
#58131=ORIENTED_EDGE('',*,*,#43898,.T.);
#58132=ORIENTED_EDGE('',*,*,#43899,.T.);
#58133=ORIENTED_EDGE('',*,*,#43900,.F.);
#58134=ORIENTED_EDGE('',*,*,#43901,.T.);
#58135=ORIENTED_EDGE('',*,*,#43902,.F.);
#58136=ORIENTED_EDGE('',*,*,#43903,.T.);
#58137=ORIENTED_EDGE('',*,*,#43904,.F.);
#58138=ORIENTED_EDGE('',*,*,#43905,.F.);
#58139=ORIENTED_EDGE('',*,*,#43906,.T.);
#58140=ORIENTED_EDGE('',*,*,#43907,.T.);
#58141=ORIENTED_EDGE('',*,*,#43908,.T.);
#58142=ORIENTED_EDGE('',*,*,#43909,.F.);
#58143=ORIENTED_EDGE('',*,*,#43910,.T.);
#58144=ORIENTED_EDGE('',*,*,#43905,.T.);
#58145=ORIENTED_EDGE('',*,*,#43911,.T.);
#58146=ORIENTED_EDGE('',*,*,#43912,.F.);
#58147=ORIENTED_EDGE('',*,*,#43913,.T.);
#58148=ORIENTED_EDGE('',*,*,#43909,.T.);
#58149=ORIENTED_EDGE('',*,*,#43914,.T.);
#58150=ORIENTED_EDGE('',*,*,#43915,.F.);
#58151=ORIENTED_EDGE('',*,*,#43916,.T.);
#58152=ORIENTED_EDGE('',*,*,#43912,.T.);
#58153=ORIENTED_EDGE('',*,*,#43917,.T.);
#58154=ORIENTED_EDGE('',*,*,#43915,.T.);
#58155=ORIENTED_EDGE('',*,*,#43918,.T.);
#58156=ORIENTED_EDGE('',*,*,#43919,.T.);
#58157=ORIENTED_EDGE('',*,*,#43920,.T.);
#58158=ORIENTED_EDGE('',*,*,#43921,.T.);
#58159=ORIENTED_EDGE('',*,*,#43922,.F.);
#58160=ORIENTED_EDGE('',*,*,#43923,.T.);
#58161=ORIENTED_EDGE('',*,*,#43924,.F.);
#58162=ORIENTED_EDGE('',*,*,#43925,.F.);
#58163=ORIENTED_EDGE('',*,*,#43926,.T.);
#58164=ORIENTED_EDGE('',*,*,#43927,.T.);
#58165=ORIENTED_EDGE('',*,*,#43928,.T.);
#58166=ORIENTED_EDGE('',*,*,#43929,.F.);
#58167=ORIENTED_EDGE('',*,*,#43930,.T.);
#58168=ORIENTED_EDGE('',*,*,#43925,.T.);
#58169=ORIENTED_EDGE('',*,*,#43931,.T.);
#58170=ORIENTED_EDGE('',*,*,#43932,.F.);
#58171=ORIENTED_EDGE('',*,*,#43933,.T.);
#58172=ORIENTED_EDGE('',*,*,#43929,.T.);
#58173=ORIENTED_EDGE('',*,*,#43934,.T.);
#58174=ORIENTED_EDGE('',*,*,#43935,.F.);
#58175=ORIENTED_EDGE('',*,*,#43936,.T.);
#58176=ORIENTED_EDGE('',*,*,#43932,.T.);
#58177=ORIENTED_EDGE('',*,*,#43937,.T.);
#58178=ORIENTED_EDGE('',*,*,#43938,.F.);
#58179=ORIENTED_EDGE('',*,*,#43939,.T.);
#58180=ORIENTED_EDGE('',*,*,#43935,.T.);
#58181=ORIENTED_EDGE('',*,*,#43940,.T.);
#58182=ORIENTED_EDGE('',*,*,#43941,.T.);
#58183=ORIENTED_EDGE('',*,*,#43942,.F.);
#58184=ORIENTED_EDGE('',*,*,#43943,.T.);
#58185=ORIENTED_EDGE('',*,*,#43944,.F.);
#58186=ORIENTED_EDGE('',*,*,#43945,.F.);
#58187=ORIENTED_EDGE('',*,*,#43946,.T.);
#58188=ORIENTED_EDGE('',*,*,#43947,.T.);
#58189=ORIENTED_EDGE('',*,*,#43948,.T.);
#58190=ORIENTED_EDGE('',*,*,#43949,.F.);
#58191=ORIENTED_EDGE('',*,*,#43950,.T.);
#58192=ORIENTED_EDGE('',*,*,#43945,.T.);
#58193=ORIENTED_EDGE('',*,*,#43951,.T.);
#58194=ORIENTED_EDGE('',*,*,#43952,.F.);
#58195=ORIENTED_EDGE('',*,*,#43953,.T.);
#58196=ORIENTED_EDGE('',*,*,#43949,.T.);
#58197=ORIENTED_EDGE('',*,*,#43954,.T.);
#58198=ORIENTED_EDGE('',*,*,#43955,.F.);
#58199=ORIENTED_EDGE('',*,*,#43956,.T.);
#58200=ORIENTED_EDGE('',*,*,#43952,.T.);
#58201=ORIENTED_EDGE('',*,*,#43957,.T.);
#58202=ORIENTED_EDGE('',*,*,#43958,.F.);
#58203=ORIENTED_EDGE('',*,*,#43959,.T.);
#58204=ORIENTED_EDGE('',*,*,#43955,.T.);
#58205=ORIENTED_EDGE('',*,*,#43960,.T.);
#58206=ORIENTED_EDGE('',*,*,#43961,.F.);
#58207=ORIENTED_EDGE('',*,*,#43773,.T.);
#58208=ORIENTED_EDGE('',*,*,#43962,.T.);
#58209=ORIENTED_EDGE('',*,*,#43963,.T.);
#58210=ORIENTED_EDGE('',*,*,#43962,.F.);
#58211=ORIENTED_EDGE('',*,*,#43772,.T.);
#58212=ORIENTED_EDGE('',*,*,#43964,.T.);
#58213=ORIENTED_EDGE('',*,*,#43965,.T.);
#58214=ORIENTED_EDGE('',*,*,#43964,.F.);
#58215=ORIENTED_EDGE('',*,*,#43771,.T.);
#58216=ORIENTED_EDGE('',*,*,#43966,.T.);
#58217=ORIENTED_EDGE('',*,*,#43967,.T.);
#58218=ORIENTED_EDGE('',*,*,#43968,.T.);
#58219=ORIENTED_EDGE('',*,*,#43969,.T.);
#58220=ORIENTED_EDGE('',*,*,#43970,.T.);
#58221=ORIENTED_EDGE('',*,*,#43971,.F.);
#58222=ORIENTED_EDGE('',*,*,#43972,.F.);
#58223=ORIENTED_EDGE('',*,*,#43973,.F.);
#58224=ORIENTED_EDGE('',*,*,#43974,.T.);
#58225=ORIENTED_EDGE('',*,*,#43968,.F.);
#58226=ORIENTED_EDGE('',*,*,#43975,.F.);
#58227=ORIENTED_EDGE('',*,*,#43976,.F.);
#58228=ORIENTED_EDGE('',*,*,#43977,.F.);
#58229=ORIENTED_EDGE('',*,*,#43978,.F.);
#58230=ORIENTED_EDGE('',*,*,#43979,.F.);
#58231=ORIENTED_EDGE('',*,*,#43980,.F.);
#58232=ORIENTED_EDGE('',*,*,#43981,.F.);
#58233=ORIENTED_EDGE('',*,*,#43982,.F.);
#58234=ORIENTED_EDGE('',*,*,#43983,.F.);
#58235=ORIENTED_EDGE('',*,*,#43984,.F.);
#58236=ORIENTED_EDGE('',*,*,#43985,.F.);
#58237=ORIENTED_EDGE('',*,*,#43986,.F.);
#58238=ORIENTED_EDGE('',*,*,#43987,.F.);
#58239=ORIENTED_EDGE('',*,*,#43988,.F.);
#58240=ORIENTED_EDGE('',*,*,#43989,.F.);
#58241=ORIENTED_EDGE('',*,*,#43990,.F.);
#58242=ORIENTED_EDGE('',*,*,#43991,.F.);
#58243=ORIENTED_EDGE('',*,*,#43992,.F.);
#58244=ORIENTED_EDGE('',*,*,#43993,.F.);
#58245=ORIENTED_EDGE('',*,*,#43994,.F.);
#58246=ORIENTED_EDGE('',*,*,#43995,.F.);
#58247=ORIENTED_EDGE('',*,*,#43996,.F.);
#58248=ORIENTED_EDGE('',*,*,#43997,.F.);
#58249=ORIENTED_EDGE('',*,*,#43998,.F.);
#58250=ORIENTED_EDGE('',*,*,#43999,.F.);
#58251=ORIENTED_EDGE('',*,*,#44000,.F.);
#58252=ORIENTED_EDGE('',*,*,#44001,.F.);
#58253=ORIENTED_EDGE('',*,*,#44002,.F.);
#58254=ORIENTED_EDGE('',*,*,#44003,.F.);
#58255=ORIENTED_EDGE('',*,*,#44004,.F.);
#58256=ORIENTED_EDGE('',*,*,#44005,.F.);
#58257=ORIENTED_EDGE('',*,*,#44006,.F.);
#58258=ORIENTED_EDGE('',*,*,#44007,.F.);
#58259=ORIENTED_EDGE('',*,*,#44008,.F.);
#58260=ORIENTED_EDGE('',*,*,#44009,.F.);
#58261=ORIENTED_EDGE('',*,*,#43770,.F.);
#58262=ORIENTED_EDGE('',*,*,#44010,.F.);
#58263=ORIENTED_EDGE('',*,*,#44011,.T.);
#58264=ORIENTED_EDGE('',*,*,#44012,.T.);
#58265=ORIENTED_EDGE('',*,*,#43973,.T.);
#58266=ORIENTED_EDGE('',*,*,#44010,.T.);
#58267=ORIENTED_EDGE('',*,*,#43972,.T.);
#58268=ORIENTED_EDGE('',*,*,#44013,.T.);
#58269=ORIENTED_EDGE('',*,*,#44014,.T.);
#58270=ORIENTED_EDGE('',*,*,#44013,.F.);
#58271=ORIENTED_EDGE('',*,*,#43971,.T.);
#58272=ORIENTED_EDGE('',*,*,#44015,.T.);
#58273=ORIENTED_EDGE('',*,*,#44016,.T.);
#58274=ORIENTED_EDGE('',*,*,#44017,.T.);
#58275=ORIENTED_EDGE('',*,*,#44018,.T.);
#58276=ORIENTED_EDGE('',*,*,#44019,.T.);
#58277=ORIENTED_EDGE('',*,*,#44020,.F.);
#58278=ORIENTED_EDGE('',*,*,#44021,.F.);
#58279=ORIENTED_EDGE('',*,*,#44022,.F.);
#58280=ORIENTED_EDGE('',*,*,#44023,.F.);
#58281=ORIENTED_EDGE('',*,*,#44024,.F.);
#58282=ORIENTED_EDGE('',*,*,#44025,.F.);
#58283=ORIENTED_EDGE('',*,*,#44026,.F.);
#58284=ORIENTED_EDGE('',*,*,#44027,.F.);
#58285=ORIENTED_EDGE('',*,*,#44028,.F.);
#58286=ORIENTED_EDGE('',*,*,#44029,.F.);
#58287=ORIENTED_EDGE('',*,*,#44030,.F.);
#58288=ORIENTED_EDGE('',*,*,#43970,.F.);
#58289=ORIENTED_EDGE('',*,*,#44031,.F.);
#58290=ORIENTED_EDGE('',*,*,#44017,.F.);
#58291=ORIENTED_EDGE('',*,*,#44032,.F.);
#58292=ORIENTED_EDGE('',*,*,#44033,.F.);
#58293=ORIENTED_EDGE('',*,*,#44034,.F.);
#58294=ORIENTED_EDGE('',*,*,#44035,.F.);
#58295=ORIENTED_EDGE('',*,*,#44036,.F.);
#58296=ORIENTED_EDGE('',*,*,#44037,.F.);
#58297=ORIENTED_EDGE('',*,*,#44038,.F.);
#58298=ORIENTED_EDGE('',*,*,#44020,.T.);
#58299=ORIENTED_EDGE('',*,*,#44039,.T.);
#58300=ORIENTED_EDGE('',*,*,#44040,.T.);
#58301=ORIENTED_EDGE('',*,*,#44041,.T.);
#58302=ORIENTED_EDGE('',*,*,#44042,.T.);
#58303=ORIENTED_EDGE('',*,*,#44043,.T.);
#58304=ORIENTED_EDGE('',*,*,#44044,.F.);
#58305=ORIENTED_EDGE('',*,*,#44019,.F.);
#58306=ORIENTED_EDGE('',*,*,#44045,.F.);
#58307=ORIENTED_EDGE('',*,*,#44041,.F.);
#58308=ORIENTED_EDGE('',*,*,#44046,.F.);
#58309=ORIENTED_EDGE('',*,*,#44047,.F.);
#58310=ORIENTED_EDGE('',*,*,#44044,.T.);
#58311=ORIENTED_EDGE('',*,*,#44048,.T.);
#58312=ORIENTED_EDGE('',*,*,#44049,.T.);
#58313=ORIENTED_EDGE('',*,*,#44050,.F.);
#58314=ORIENTED_EDGE('',*,*,#44051,.F.);
#58315=ORIENTED_EDGE('',*,*,#44052,.F.);
#58316=ORIENTED_EDGE('',*,*,#44053,.F.);
#58317=ORIENTED_EDGE('',*,*,#44054,.F.);
#58318=ORIENTED_EDGE('',*,*,#44055,.F.);
#58319=ORIENTED_EDGE('',*,*,#44056,.F.);
#58320=ORIENTED_EDGE('',*,*,#44043,.F.);
#58321=ORIENTED_EDGE('',*,*,#44057,.F.);
#58322=ORIENTED_EDGE('',*,*,#43897,.F.);
#58323=ORIENTED_EDGE('',*,*,#44058,.F.);
#58324=ORIENTED_EDGE('',*,*,#44059,.F.);
#58325=ORIENTED_EDGE('',*,*,#44060,.F.);
#58326=ORIENTED_EDGE('',*,*,#44061,.F.);
#58327=ORIENTED_EDGE('',*,*,#44062,.F.);
#58328=ORIENTED_EDGE('',*,*,#44063,.F.);
#58329=ORIENTED_EDGE('',*,*,#43966,.F.);
#58330=ORIENTED_EDGE('',*,*,#44009,.T.);
#58331=ORIENTED_EDGE('',*,*,#44064,.T.);
#58332=ORIENTED_EDGE('',*,*,#44065,.T.);
#58333=ORIENTED_EDGE('',*,*,#44064,.F.);
#58334=ORIENTED_EDGE('',*,*,#44008,.T.);
#58335=ORIENTED_EDGE('',*,*,#44066,.T.);
#58336=ORIENTED_EDGE('',*,*,#44067,.T.);
#58337=ORIENTED_EDGE('',*,*,#44068,.T.);
#58338=ORIENTED_EDGE('',*,*,#44069,.F.);
#58339=ORIENTED_EDGE('',*,*,#44007,.T.);
#58340=ORIENTED_EDGE('',*,*,#44070,.F.);
#58341=ORIENTED_EDGE('',*,*,#44071,.F.);
#58342=ORIENTED_EDGE('',*,*,#44072,.T.);
#58343=ORIENTED_EDGE('',*,*,#44073,.T.);
#58344=ORIENTED_EDGE('',*,*,#44006,.T.);
#58345=ORIENTED_EDGE('',*,*,#44074,.F.);
#58346=ORIENTED_EDGE('',*,*,#44075,.T.);
#58347=ORIENTED_EDGE('',*,*,#44071,.T.);
#58348=ORIENTED_EDGE('',*,*,#44005,.T.);
#58349=ORIENTED_EDGE('',*,*,#44076,.F.);
#58350=ORIENTED_EDGE('',*,*,#44077,.T.);
#58351=ORIENTED_EDGE('',*,*,#44074,.T.);
#58352=ORIENTED_EDGE('',*,*,#44004,.T.);
#58353=ORIENTED_EDGE('',*,*,#44078,.F.);
#58354=ORIENTED_EDGE('',*,*,#44079,.T.);
#58355=ORIENTED_EDGE('',*,*,#44076,.T.);
#58356=ORIENTED_EDGE('',*,*,#44003,.T.);
#58357=ORIENTED_EDGE('',*,*,#44080,.F.);
#58358=ORIENTED_EDGE('',*,*,#44081,.T.);
#58359=ORIENTED_EDGE('',*,*,#44078,.T.);
#58360=ORIENTED_EDGE('',*,*,#44002,.T.);
#58361=ORIENTED_EDGE('',*,*,#44082,.T.);
#58362=ORIENTED_EDGE('',*,*,#44083,.F.);
#58363=ORIENTED_EDGE('',*,*,#44001,.T.);
#58364=ORIENTED_EDGE('',*,*,#44084,.F.);
#58365=ORIENTED_EDGE('',*,*,#44085,.F.);
#58366=ORIENTED_EDGE('',*,*,#44000,.T.);
#58367=ORIENTED_EDGE('',*,*,#44086,.T.);
#58368=ORIENTED_EDGE('',*,*,#44087,.T.);
#58369=ORIENTED_EDGE('',*,*,#44086,.F.);
#58370=ORIENTED_EDGE('',*,*,#43999,.T.);
#58371=ORIENTED_EDGE('',*,*,#44088,.T.);
#58372=ORIENTED_EDGE('',*,*,#44089,.T.);
#58373=ORIENTED_EDGE('',*,*,#44088,.F.);
#58374=ORIENTED_EDGE('',*,*,#43998,.T.);
#58375=ORIENTED_EDGE('',*,*,#44090,.T.);
#58376=ORIENTED_EDGE('',*,*,#44091,.T.);
#58377=ORIENTED_EDGE('',*,*,#44090,.F.);
#58378=ORIENTED_EDGE('',*,*,#43997,.T.);
#58379=ORIENTED_EDGE('',*,*,#44092,.F.);
#58380=ORIENTED_EDGE('',*,*,#44093,.T.);
#58381=ORIENTED_EDGE('',*,*,#44094,.F.);
#58382=ORIENTED_EDGE('',*,*,#44095,.T.);
#58383=ORIENTED_EDGE('',*,*,#44092,.T.);
#58384=ORIENTED_EDGE('',*,*,#43996,.T.);
#58385=ORIENTED_EDGE('',*,*,#44096,.T.);
#58386=ORIENTED_EDGE('',*,*,#44097,.F.);
#58387=ORIENTED_EDGE('',*,*,#43995,.T.);
#58388=ORIENTED_EDGE('',*,*,#44098,.F.);
#58389=ORIENTED_EDGE('',*,*,#44099,.F.);
#58390=ORIENTED_EDGE('',*,*,#43994,.T.);
#58391=ORIENTED_EDGE('',*,*,#44100,.T.);
#58392=ORIENTED_EDGE('',*,*,#44101,.T.);
#58393=ORIENTED_EDGE('',*,*,#44100,.F.);
#58394=ORIENTED_EDGE('',*,*,#43993,.T.);
#58395=ORIENTED_EDGE('',*,*,#44102,.T.);
#58396=ORIENTED_EDGE('',*,*,#44103,.T.);
#58397=ORIENTED_EDGE('',*,*,#44102,.F.);
#58398=ORIENTED_EDGE('',*,*,#43992,.T.);
#58399=ORIENTED_EDGE('',*,*,#44104,.T.);
#58400=ORIENTED_EDGE('',*,*,#44105,.T.);
#58401=ORIENTED_EDGE('',*,*,#44104,.F.);
#58402=ORIENTED_EDGE('',*,*,#43991,.T.);
#58403=ORIENTED_EDGE('',*,*,#44106,.F.);
#58404=ORIENTED_EDGE('',*,*,#44107,.T.);
#58405=ORIENTED_EDGE('',*,*,#44108,.F.);
#58406=ORIENTED_EDGE('',*,*,#44109,.T.);
#58407=ORIENTED_EDGE('',*,*,#44106,.T.);
#58408=ORIENTED_EDGE('',*,*,#43990,.T.);
#58409=ORIENTED_EDGE('',*,*,#44110,.T.);
#58410=ORIENTED_EDGE('',*,*,#44111,.F.);
#58411=ORIENTED_EDGE('',*,*,#43989,.T.);
#58412=ORIENTED_EDGE('',*,*,#44112,.F.);
#58413=ORIENTED_EDGE('',*,*,#44113,.F.);
#58414=ORIENTED_EDGE('',*,*,#43988,.T.);
#58415=ORIENTED_EDGE('',*,*,#44114,.T.);
#58416=ORIENTED_EDGE('',*,*,#44115,.T.);
#58417=ORIENTED_EDGE('',*,*,#44114,.F.);
#58418=ORIENTED_EDGE('',*,*,#43987,.T.);
#58419=ORIENTED_EDGE('',*,*,#44116,.T.);
#58420=ORIENTED_EDGE('',*,*,#44117,.T.);
#58421=ORIENTED_EDGE('',*,*,#44116,.F.);
#58422=ORIENTED_EDGE('',*,*,#43986,.T.);
#58423=ORIENTED_EDGE('',*,*,#44118,.T.);
#58424=ORIENTED_EDGE('',*,*,#44119,.T.);
#58425=ORIENTED_EDGE('',*,*,#44118,.F.);
#58426=ORIENTED_EDGE('',*,*,#43985,.T.);
#58427=ORIENTED_EDGE('',*,*,#44120,.F.);
#58428=ORIENTED_EDGE('',*,*,#44121,.T.);
#58429=ORIENTED_EDGE('',*,*,#44122,.F.);
#58430=ORIENTED_EDGE('',*,*,#44123,.T.);
#58431=ORIENTED_EDGE('',*,*,#44120,.T.);
#58432=ORIENTED_EDGE('',*,*,#43984,.T.);
#58433=ORIENTED_EDGE('',*,*,#44124,.T.);
#58434=ORIENTED_EDGE('',*,*,#44125,.F.);
#58435=ORIENTED_EDGE('',*,*,#43983,.T.);
#58436=ORIENTED_EDGE('',*,*,#44126,.F.);
#58437=ORIENTED_EDGE('',*,*,#44127,.F.);
#58438=ORIENTED_EDGE('',*,*,#44128,.T.);
#58439=ORIENTED_EDGE('',*,*,#44129,.T.);
#58440=ORIENTED_EDGE('',*,*,#43982,.T.);
#58441=ORIENTED_EDGE('',*,*,#44130,.F.);
#58442=ORIENTED_EDGE('',*,*,#44131,.T.);
#58443=ORIENTED_EDGE('',*,*,#44127,.T.);
#58444=ORIENTED_EDGE('',*,*,#43981,.T.);
#58445=ORIENTED_EDGE('',*,*,#44132,.F.);
#58446=ORIENTED_EDGE('',*,*,#44133,.T.);
#58447=ORIENTED_EDGE('',*,*,#44130,.T.);
#58448=ORIENTED_EDGE('',*,*,#43980,.T.);
#58449=ORIENTED_EDGE('',*,*,#44134,.F.);
#58450=ORIENTED_EDGE('',*,*,#44135,.T.);
#58451=ORIENTED_EDGE('',*,*,#44132,.T.);
#58452=ORIENTED_EDGE('',*,*,#43979,.T.);
#58453=ORIENTED_EDGE('',*,*,#44136,.F.);
#58454=ORIENTED_EDGE('',*,*,#44137,.T.);
#58455=ORIENTED_EDGE('',*,*,#44134,.T.);
#58456=ORIENTED_EDGE('',*,*,#43978,.T.);
#58457=ORIENTED_EDGE('',*,*,#44138,.T.);
#58458=ORIENTED_EDGE('',*,*,#44139,.F.);
#58459=ORIENTED_EDGE('',*,*,#43977,.T.);
#58460=ORIENTED_EDGE('',*,*,#44140,.F.);
#58461=ORIENTED_EDGE('',*,*,#44141,.F.);
#58462=ORIENTED_EDGE('',*,*,#44142,.T.);
#58463=ORIENTED_EDGE('',*,*,#44143,.T.);
#58464=ORIENTED_EDGE('',*,*,#43976,.T.);
#58465=ORIENTED_EDGE('',*,*,#44012,.F.);
#58466=ORIENTED_EDGE('',*,*,#44144,.T.);
#58467=ORIENTED_EDGE('',*,*,#44141,.T.);
#58468=ORIENTED_EDGE('',*,*,#43975,.T.);
#58469=ORIENTED_EDGE('',*,*,#44145,.T.);
#58470=ORIENTED_EDGE('',*,*,#44146,.F.);
#58471=ORIENTED_EDGE('',*,*,#43788,.T.);
#58472=ORIENTED_EDGE('',*,*,#44147,.F.);
#58473=ORIENTED_EDGE('',*,*,#44148,.F.);
#58474=ORIENTED_EDGE('',*,*,#43804,.T.);
#58475=ORIENTED_EDGE('',*,*,#44149,.T.);
#58476=ORIENTED_EDGE('',*,*,#44150,.T.);
#58477=ORIENTED_EDGE('',*,*,#44149,.F.);
#58478=ORIENTED_EDGE('',*,*,#43803,.T.);
#58479=ORIENTED_EDGE('',*,*,#44151,.T.);
#58480=ORIENTED_EDGE('',*,*,#44152,.T.);
#58481=ORIENTED_EDGE('',*,*,#44151,.F.);
#58482=ORIENTED_EDGE('',*,*,#43802,.T.);
#58483=ORIENTED_EDGE('',*,*,#44153,.T.);
#58484=ORIENTED_EDGE('',*,*,#44154,.T.);
#58485=ORIENTED_EDGE('',*,*,#44153,.F.);
#58486=ORIENTED_EDGE('',*,*,#43801,.T.);
#58487=ORIENTED_EDGE('',*,*,#44155,.T.);
#58488=ORIENTED_EDGE('',*,*,#44156,.T.);
#58489=ORIENTED_EDGE('',*,*,#44155,.F.);
#58490=ORIENTED_EDGE('',*,*,#43800,.T.);
#58491=ORIENTED_EDGE('',*,*,#44157,.T.);
#58492=ORIENTED_EDGE('',*,*,#44158,.T.);
#58493=ORIENTED_EDGE('',*,*,#43799,.T.);
#58494=ORIENTED_EDGE('',*,*,#43805,.T.);
#58495=ORIENTED_EDGE('',*,*,#44159,.T.);
#58496=ORIENTED_EDGE('',*,*,#44160,.F.);
#58497=ORIENTED_EDGE('',*,*,#43782,.F.);
#58498=ORIENTED_EDGE('',*,*,#43797,.T.);
#58499=ORIENTED_EDGE('',*,*,#44161,.F.);
#58500=ORIENTED_EDGE('',*,*,#44162,.T.);
#58501=ORIENTED_EDGE('',*,*,#44163,.F.);
#58502=ORIENTED_EDGE('',*,*,#44164,.T.);
#58503=ORIENTED_EDGE('',*,*,#44161,.T.);
#58504=ORIENTED_EDGE('',*,*,#43796,.T.);
#58505=ORIENTED_EDGE('',*,*,#43795,.T.);
#58506=ORIENTED_EDGE('',*,*,#44165,.F.);
#58507=ORIENTED_EDGE('',*,*,#44166,.T.);
#58508=ORIENTED_EDGE('',*,*,#44167,.F.);
#58509=ORIENTED_EDGE('',*,*,#44168,.T.);
#58510=ORIENTED_EDGE('',*,*,#44165,.T.);
#58511=ORIENTED_EDGE('',*,*,#43794,.T.);
#58512=ORIENTED_EDGE('',*,*,#44169,.F.);
#58513=ORIENTED_EDGE('',*,*,#44170,.F.);
#58514=ORIENTED_EDGE('',*,*,#43793,.T.);
#58515=ORIENTED_EDGE('',*,*,#44171,.T.);
#58516=ORIENTED_EDGE('',*,*,#44172,.T.);
#58517=ORIENTED_EDGE('',*,*,#44171,.F.);
#58518=ORIENTED_EDGE('',*,*,#43792,.T.);
#58519=ORIENTED_EDGE('',*,*,#44173,.T.);
#58520=ORIENTED_EDGE('',*,*,#44174,.T.);
#58521=ORIENTED_EDGE('',*,*,#44173,.F.);
#58522=ORIENTED_EDGE('',*,*,#43791,.T.);
#58523=ORIENTED_EDGE('',*,*,#44175,.T.);
#58524=ORIENTED_EDGE('',*,*,#44176,.T.);
#58525=ORIENTED_EDGE('',*,*,#44175,.F.);
#58526=ORIENTED_EDGE('',*,*,#43790,.T.);
#58527=ORIENTED_EDGE('',*,*,#44177,.F.);
#58528=ORIENTED_EDGE('',*,*,#44178,.T.);
#58529=ORIENTED_EDGE('',*,*,#44179,.F.);
#58530=ORIENTED_EDGE('',*,*,#44180,.T.);
#58531=ORIENTED_EDGE('',*,*,#44177,.T.);
#58532=ORIENTED_EDGE('',*,*,#43789,.T.);
#58533=ORIENTED_EDGE('',*,*,#43806,.F.);
#58534=ORIENTED_EDGE('',*,*,#43813,.T.);
#58535=ORIENTED_EDGE('',*,*,#43814,.T.);
#58536=ORIENTED_EDGE('',*,*,#44181,.T.);
#58537=ORIENTED_EDGE('',*,*,#44182,.F.);
#58538=ORIENTED_EDGE('',*,*,#43900,.T.);
#58539=ORIENTED_EDGE('',*,*,#43902,.T.);
#58540=ORIENTED_EDGE('',*,*,#44183,.T.);
#58541=ORIENTED_EDGE('',*,*,#44184,.T.);
#58542=ORIENTED_EDGE('',*,*,#44185,.F.);
#58543=ORIENTED_EDGE('',*,*,#44050,.T.);
#58544=ORIENTED_EDGE('',*,*,#44186,.F.);
#58545=ORIENTED_EDGE('',*,*,#44187,.F.);
#58546=ORIENTED_EDGE('',*,*,#44188,.T.);
#58547=ORIENTED_EDGE('',*,*,#44189,.T.);
#58548=ORIENTED_EDGE('',*,*,#44063,.T.);
#58549=ORIENTED_EDGE('',*,*,#44190,.F.);
#58550=ORIENTED_EDGE('',*,*,#44191,.T.);
#58551=ORIENTED_EDGE('',*,*,#44187,.T.);
#58552=ORIENTED_EDGE('',*,*,#44062,.T.);
#58553=ORIENTED_EDGE('',*,*,#44192,.F.);
#58554=ORIENTED_EDGE('',*,*,#44193,.T.);
#58555=ORIENTED_EDGE('',*,*,#44190,.T.);
#58556=ORIENTED_EDGE('',*,*,#44061,.T.);
#58557=ORIENTED_EDGE('',*,*,#44194,.F.);
#58558=ORIENTED_EDGE('',*,*,#44195,.T.);
#58559=ORIENTED_EDGE('',*,*,#44192,.T.);
#58560=ORIENTED_EDGE('',*,*,#44060,.T.);
#58561=ORIENTED_EDGE('',*,*,#44194,.T.);
#58562=ORIENTED_EDGE('',*,*,#44059,.T.);
#58563=ORIENTED_EDGE('',*,*,#44196,.T.);
#58564=ORIENTED_EDGE('',*,*,#44197,.T.);
#58565=ORIENTED_EDGE('',*,*,#44058,.T.);
#58566=ORIENTED_EDGE('',*,*,#44182,.T.);
#58567=ORIENTED_EDGE('',*,*,#44198,.T.);
#58568=ORIENTED_EDGE('',*,*,#44199,.F.);
#58569=ORIENTED_EDGE('',*,*,#44200,.T.);
#58570=ORIENTED_EDGE('',*,*,#44048,.F.);
#58571=ORIENTED_EDGE('',*,*,#44056,.T.);
#58572=ORIENTED_EDGE('',*,*,#44201,.F.);
#58573=ORIENTED_EDGE('',*,*,#44202,.F.);
#58574=ORIENTED_EDGE('',*,*,#44055,.T.);
#58575=ORIENTED_EDGE('',*,*,#44203,.T.);
#58576=ORIENTED_EDGE('',*,*,#44204,.T.);
#58577=ORIENTED_EDGE('',*,*,#44203,.F.);
#58578=ORIENTED_EDGE('',*,*,#44054,.T.);
#58579=ORIENTED_EDGE('',*,*,#44205,.T.);
#58580=ORIENTED_EDGE('',*,*,#44206,.T.);
#58581=ORIENTED_EDGE('',*,*,#44205,.F.);
#58582=ORIENTED_EDGE('',*,*,#44053,.T.);
#58583=ORIENTED_EDGE('',*,*,#44207,.T.);
#58584=ORIENTED_EDGE('',*,*,#44208,.T.);
#58585=ORIENTED_EDGE('',*,*,#44207,.F.);
#58586=ORIENTED_EDGE('',*,*,#44052,.T.);
#58587=ORIENTED_EDGE('',*,*,#44209,.T.);
#58588=ORIENTED_EDGE('',*,*,#44210,.T.);
#58589=ORIENTED_EDGE('',*,*,#44209,.F.);
#58590=ORIENTED_EDGE('',*,*,#44051,.T.);
#58591=ORIENTED_EDGE('',*,*,#44211,.T.);
#58592=ORIENTED_EDGE('',*,*,#44212,.T.);
#58593=ORIENTED_EDGE('',*,*,#44039,.F.);
#58594=ORIENTED_EDGE('',*,*,#44046,.T.);
#58595=ORIENTED_EDGE('',*,*,#44047,.T.);
#58596=ORIENTED_EDGE('',*,*,#44213,.T.);
#58597=ORIENTED_EDGE('',*,*,#44214,.T.);
#58598=ORIENTED_EDGE('',*,*,#44215,.F.);
#58599=ORIENTED_EDGE('',*,*,#44021,.T.);
#58600=ORIENTED_EDGE('',*,*,#44216,.F.);
#58601=ORIENTED_EDGE('',*,*,#44217,.F.);
#58602=ORIENTED_EDGE('',*,*,#44218,.T.);
#58603=ORIENTED_EDGE('',*,*,#44219,.T.);
#58604=ORIENTED_EDGE('',*,*,#44037,.T.);
#58605=ORIENTED_EDGE('',*,*,#44220,.F.);
#58606=ORIENTED_EDGE('',*,*,#44221,.T.);
#58607=ORIENTED_EDGE('',*,*,#44217,.T.);
#58608=ORIENTED_EDGE('',*,*,#44036,.T.);
#58609=ORIENTED_EDGE('',*,*,#44222,.F.);
#58610=ORIENTED_EDGE('',*,*,#44223,.T.);
#58611=ORIENTED_EDGE('',*,*,#44220,.T.);
#58612=ORIENTED_EDGE('',*,*,#44035,.T.);
#58613=ORIENTED_EDGE('',*,*,#44224,.F.);
#58614=ORIENTED_EDGE('',*,*,#44225,.T.);
#58615=ORIENTED_EDGE('',*,*,#44222,.T.);
#58616=ORIENTED_EDGE('',*,*,#44034,.T.);
#58617=ORIENTED_EDGE('',*,*,#44226,.F.);
#58618=ORIENTED_EDGE('',*,*,#44227,.T.);
#58619=ORIENTED_EDGE('',*,*,#44224,.T.);
#58620=ORIENTED_EDGE('',*,*,#44033,.T.);
#58621=ORIENTED_EDGE('',*,*,#44032,.T.);
#58622=ORIENTED_EDGE('',*,*,#44038,.T.);
#58623=ORIENTED_EDGE('',*,*,#44228,.T.);
#58624=ORIENTED_EDGE('',*,*,#44229,.F.);
#58625=ORIENTED_EDGE('',*,*,#44015,.F.);
#58626=ORIENTED_EDGE('',*,*,#44030,.T.);
#58627=ORIENTED_EDGE('',*,*,#44230,.T.);
#58628=ORIENTED_EDGE('',*,*,#44231,.T.);
#58629=ORIENTED_EDGE('',*,*,#44230,.F.);
#58630=ORIENTED_EDGE('',*,*,#44029,.T.);
#58631=ORIENTED_EDGE('',*,*,#44232,.T.);
#58632=ORIENTED_EDGE('',*,*,#44233,.T.);
#58633=ORIENTED_EDGE('',*,*,#44028,.T.);
#58634=ORIENTED_EDGE('',*,*,#44234,.F.);
#58635=ORIENTED_EDGE('',*,*,#44235,.T.);
#58636=ORIENTED_EDGE('',*,*,#44236,.T.);
#58637=ORIENTED_EDGE('',*,*,#44237,.F.);
#58638=ORIENTED_EDGE('',*,*,#44238,.T.);
#58639=ORIENTED_EDGE('',*,*,#44234,.T.);
#58640=ORIENTED_EDGE('',*,*,#44027,.T.);
#58641=ORIENTED_EDGE('',*,*,#44239,.F.);
#58642=ORIENTED_EDGE('',*,*,#44240,.F.);
#58643=ORIENTED_EDGE('',*,*,#44026,.T.);
#58644=ORIENTED_EDGE('',*,*,#44241,.T.);
#58645=ORIENTED_EDGE('',*,*,#44242,.T.);
#58646=ORIENTED_EDGE('',*,*,#44241,.F.);
#58647=ORIENTED_EDGE('',*,*,#44025,.T.);
#58648=ORIENTED_EDGE('',*,*,#44243,.T.);
#58649=ORIENTED_EDGE('',*,*,#44244,.T.);
#58650=ORIENTED_EDGE('',*,*,#44243,.F.);
#58651=ORIENTED_EDGE('',*,*,#44024,.T.);
#58652=ORIENTED_EDGE('',*,*,#44245,.T.);
#58653=ORIENTED_EDGE('',*,*,#44246,.T.);
#58654=ORIENTED_EDGE('',*,*,#44245,.F.);
#58655=ORIENTED_EDGE('',*,*,#44023,.T.);
#58656=ORIENTED_EDGE('',*,*,#44247,.F.);
#58657=ORIENTED_EDGE('',*,*,#44248,.T.);
#58658=ORIENTED_EDGE('',*,*,#44249,.F.);
#58659=ORIENTED_EDGE('',*,*,#44250,.T.);
#58660=ORIENTED_EDGE('',*,*,#44247,.T.);
#58661=ORIENTED_EDGE('',*,*,#44022,.T.);
#58662=ORIENTED_EDGE('',*,*,#44251,.T.);
#58663=ORIENTED_EDGE('',*,*,#44252,.F.);
#58664=ORIENTED_EDGE('',*,*,#43817,.T.);
#58665=ORIENTED_EDGE('',*,*,#44253,.F.);
#58666=ORIENTED_EDGE('',*,*,#44254,.F.);
#58667=ORIENTED_EDGE('',*,*,#44255,.T.);
#58668=ORIENTED_EDGE('',*,*,#44256,.T.);
#58669=ORIENTED_EDGE('',*,*,#43833,.T.);
#58670=ORIENTED_EDGE('',*,*,#43961,.T.);
#58671=ORIENTED_EDGE('',*,*,#44257,.T.);
#58672=ORIENTED_EDGE('',*,*,#44254,.T.);
#58673=ORIENTED_EDGE('',*,*,#43832,.T.);
#58674=ORIENTED_EDGE('',*,*,#44258,.T.);
#58675=ORIENTED_EDGE('',*,*,#43815,.F.);
#58676=ORIENTED_EDGE('',*,*,#43830,.T.);
#58677=ORIENTED_EDGE('',*,*,#44259,.F.);
#58678=ORIENTED_EDGE('',*,*,#44260,.F.);
#58679=ORIENTED_EDGE('',*,*,#43829,.T.);
#58680=ORIENTED_EDGE('',*,*,#44261,.T.);
#58681=ORIENTED_EDGE('',*,*,#44262,.T.);
#58682=ORIENTED_EDGE('',*,*,#44261,.F.);
#58683=ORIENTED_EDGE('',*,*,#43828,.T.);
#58684=ORIENTED_EDGE('',*,*,#44263,.T.);
#58685=ORIENTED_EDGE('',*,*,#44264,.T.);
#58686=ORIENTED_EDGE('',*,*,#44263,.F.);
#58687=ORIENTED_EDGE('',*,*,#43827,.T.);
#58688=ORIENTED_EDGE('',*,*,#44265,.T.);
#58689=ORIENTED_EDGE('',*,*,#44266,.T.);
#58690=ORIENTED_EDGE('',*,*,#44265,.F.);
#58691=ORIENTED_EDGE('',*,*,#43826,.T.);
#58692=ORIENTED_EDGE('',*,*,#44267,.T.);
#58693=ORIENTED_EDGE('',*,*,#44268,.T.);
#58694=ORIENTED_EDGE('',*,*,#44267,.F.);
#58695=ORIENTED_EDGE('',*,*,#43825,.T.);
#58696=ORIENTED_EDGE('',*,*,#44269,.T.);
#58697=ORIENTED_EDGE('',*,*,#44270,.T.);
#58698=ORIENTED_EDGE('',*,*,#44271,.T.);
#58699=ORIENTED_EDGE('',*,*,#44272,.F.);
#58700=ORIENTED_EDGE('',*,*,#43824,.T.);
#58701=ORIENTED_EDGE('',*,*,#44273,.F.);
#58702=ORIENTED_EDGE('',*,*,#44274,.F.);
#58703=ORIENTED_EDGE('',*,*,#43823,.T.);
#58704=ORIENTED_EDGE('',*,*,#44275,.T.);
#58705=ORIENTED_EDGE('',*,*,#44276,.T.);
#58706=ORIENTED_EDGE('',*,*,#44275,.F.);
#58707=ORIENTED_EDGE('',*,*,#43822,.T.);
#58708=ORIENTED_EDGE('',*,*,#44277,.T.);
#58709=ORIENTED_EDGE('',*,*,#44278,.T.);
#58710=ORIENTED_EDGE('',*,*,#44277,.F.);
#58711=ORIENTED_EDGE('',*,*,#43821,.T.);
#58712=ORIENTED_EDGE('',*,*,#44279,.T.);
#58713=ORIENTED_EDGE('',*,*,#44280,.T.);
#58714=ORIENTED_EDGE('',*,*,#44279,.F.);
#58715=ORIENTED_EDGE('',*,*,#43820,.T.);
#58716=ORIENTED_EDGE('',*,*,#44281,.F.);
#58717=ORIENTED_EDGE('',*,*,#44282,.F.);
#58718=ORIENTED_EDGE('',*,*,#44283,.T.);
#58719=ORIENTED_EDGE('',*,*,#44281,.T.);
#58720=ORIENTED_EDGE('',*,*,#43819,.T.);
#58721=ORIENTED_EDGE('',*,*,#44284,.F.);
#58722=ORIENTED_EDGE('',*,*,#44285,.F.);
#58723=ORIENTED_EDGE('',*,*,#44286,.T.);
#58724=ORIENTED_EDGE('',*,*,#44282,.T.);
#58725=ORIENTED_EDGE('',*,*,#43818,.T.);
#58726=ORIENTED_EDGE('',*,*,#44252,.T.);
#58727=ORIENTED_EDGE('',*,*,#44287,.T.);
#58728=ORIENTED_EDGE('',*,*,#44288,.F.);
#58729=ORIENTED_EDGE('',*,*,#44228,.F.);
#58730=ORIENTED_EDGE('',*,*,#44040,.F.);
#58731=ORIENTED_EDGE('',*,*,#44213,.F.);
#58732=ORIENTED_EDGE('',*,*,#44049,.F.);
#58733=ORIENTED_EDGE('',*,*,#44200,.F.);
#58734=ORIENTED_EDGE('',*,*,#44289,.F.);
#58735=ORIENTED_EDGE('',*,*,#44290,.F.);
#58736=ORIENTED_EDGE('',*,*,#44291,.F.);
#58737=ORIENTED_EDGE('',*,*,#44292,.F.);
#58738=ORIENTED_EDGE('',*,*,#44293,.F.);
#58739=ORIENTED_EDGE('',*,*,#44294,.T.);
#58740=ORIENTED_EDGE('',*,*,#44295,.F.);
#58741=ORIENTED_EDGE('',*,*,#44159,.F.);
#58742=ORIENTED_EDGE('',*,*,#43807,.F.);
#58743=ORIENTED_EDGE('',*,*,#44181,.F.);
#58744=ORIENTED_EDGE('',*,*,#43816,.F.);
#58745=ORIENTED_EDGE('',*,*,#44258,.F.);
#58746=ORIENTED_EDGE('',*,*,#44296,.F.);
#58747=ORIENTED_EDGE('',*,*,#44297,.T.);
#58748=ORIENTED_EDGE('',*,*,#44298,.T.);
#58749=ORIENTED_EDGE('',*,*,#44299,.F.);
#58750=ORIENTED_EDGE('',*,*,#44300,.F.);
#58751=ORIENTED_EDGE('',*,*,#44301,.F.);
#58752=ORIENTED_EDGE('',*,*,#44302,.F.);
#58753=ORIENTED_EDGE('',*,*,#43896,.F.);
#58754=ORIENTED_EDGE('',*,*,#43781,.F.);
#58755=ORIENTED_EDGE('',*,*,#44303,.T.);
#58756=ORIENTED_EDGE('',*,*,#44304,.F.);
#58757=ORIENTED_EDGE('',*,*,#44300,.T.);
#58758=ORIENTED_EDGE('',*,*,#43783,.F.);
#58759=ORIENTED_EDGE('',*,*,#44162,.F.);
#58760=ORIENTED_EDGE('',*,*,#44305,.T.);
#58761=ORIENTED_EDGE('',*,*,#44306,.T.);
#58762=ORIENTED_EDGE('',*,*,#43958,.T.);
#58763=ORIENTED_EDGE('',*,*,#44307,.T.);
#58764=ORIENTED_EDGE('',*,*,#44305,.F.);
#58765=ORIENTED_EDGE('',*,*,#44308,.T.);
#58766=ORIENTED_EDGE('',*,*,#44309,.T.);
#58767=ORIENTED_EDGE('',*,*,#44310,.T.);
#58768=ORIENTED_EDGE('',*,*,#44309,.F.);
#58769=ORIENTED_EDGE('',*,*,#44311,.T.);
#58770=ORIENTED_EDGE('',*,*,#44312,.T.);
#58771=ORIENTED_EDGE('',*,*,#44313,.T.);
#58772=ORIENTED_EDGE('',*,*,#44314,.T.);
#58773=ORIENTED_EDGE('',*,*,#44315,.F.);
#58774=ORIENTED_EDGE('',*,*,#44316,.T.);
#58775=ORIENTED_EDGE('',*,*,#44317,.T.);
#58776=ORIENTED_EDGE('',*,*,#44318,.T.);
#58777=ORIENTED_EDGE('',*,*,#44317,.F.);
#58778=ORIENTED_EDGE('',*,*,#44319,.T.);
#58779=ORIENTED_EDGE('',*,*,#44320,.T.);
#58780=ORIENTED_EDGE('',*,*,#44321,.T.);
#58781=ORIENTED_EDGE('',*,*,#44322,.F.);
#58782=ORIENTED_EDGE('',*,*,#44323,.F.);
#58783=ORIENTED_EDGE('',*,*,#44324,.F.);
#58784=ORIENTED_EDGE('',*,*,#44325,.F.);
#58785=ORIENTED_EDGE('',*,*,#44326,.F.);
#58786=ORIENTED_EDGE('',*,*,#44327,.T.);
#58787=ORIENTED_EDGE('',*,*,#44328,.T.);
#58788=ORIENTED_EDGE('',*,*,#44329,.T.);
#58789=ORIENTED_EDGE('',*,*,#44330,.F.);
#58790=ORIENTED_EDGE('',*,*,#44313,.F.);
#58791=ORIENTED_EDGE('',*,*,#44331,.T.);
#58792=ORIENTED_EDGE('',*,*,#44332,.T.);
#58793=ORIENTED_EDGE('',*,*,#44333,.T.);
#58794=ORIENTED_EDGE('',*,*,#44332,.F.);
#58795=ORIENTED_EDGE('',*,*,#44334,.T.);
#58796=ORIENTED_EDGE('',*,*,#44335,.T.);
#58797=ORIENTED_EDGE('',*,*,#44336,.T.);
#58798=ORIENTED_EDGE('',*,*,#44335,.F.);
#58799=ORIENTED_EDGE('',*,*,#44337,.T.);
#58800=ORIENTED_EDGE('',*,*,#44338,.T.);
#58801=ORIENTED_EDGE('',*,*,#44339,.T.);
#58802=ORIENTED_EDGE('',*,*,#44338,.F.);
#58803=ORIENTED_EDGE('',*,*,#44340,.T.);
#58804=ORIENTED_EDGE('',*,*,#44341,.T.);
#58805=ORIENTED_EDGE('',*,*,#44342,.T.);
#58806=ORIENTED_EDGE('',*,*,#44341,.F.);
#58807=ORIENTED_EDGE('',*,*,#44343,.T.);
#58808=ORIENTED_EDGE('',*,*,#44344,.T.);
#58809=ORIENTED_EDGE('',*,*,#44345,.T.);
#58810=ORIENTED_EDGE('',*,*,#44346,.F.);
#58811=ORIENTED_EDGE('',*,*,#44347,.T.);
#58812=ORIENTED_EDGE('',*,*,#44348,.F.);
#58813=ORIENTED_EDGE('',*,*,#44349,.F.);
#58814=ORIENTED_EDGE('',*,*,#44350,.T.);
#58815=ORIENTED_EDGE('',*,*,#44351,.F.);
#58816=ORIENTED_EDGE('',*,*,#44352,.F.);
#58817=ORIENTED_EDGE('',*,*,#44353,.T.);
#58818=ORIENTED_EDGE('',*,*,#44354,.T.);
#58819=ORIENTED_EDGE('',*,*,#44355,.T.);
#58820=ORIENTED_EDGE('',*,*,#44354,.F.);
#58821=ORIENTED_EDGE('',*,*,#44356,.T.);
#58822=ORIENTED_EDGE('',*,*,#44357,.T.);
#58823=ORIENTED_EDGE('',*,*,#44358,.T.);
#58824=ORIENTED_EDGE('',*,*,#44357,.F.);
#58825=ORIENTED_EDGE('',*,*,#44359,.T.);
#58826=ORIENTED_EDGE('',*,*,#44360,.T.);
#58827=ORIENTED_EDGE('',*,*,#44361,.T.);
#58828=ORIENTED_EDGE('',*,*,#44360,.F.);
#58829=ORIENTED_EDGE('',*,*,#44362,.T.);
#58830=ORIENTED_EDGE('',*,*,#44363,.T.);
#58831=ORIENTED_EDGE('',*,*,#44364,.T.);
#58832=ORIENTED_EDGE('',*,*,#44363,.F.);
#58833=ORIENTED_EDGE('',*,*,#44365,.T.);
#58834=ORIENTED_EDGE('',*,*,#44366,.T.);
#58835=ORIENTED_EDGE('',*,*,#44367,.T.);
#58836=ORIENTED_EDGE('',*,*,#44368,.T.);
#58837=ORIENTED_EDGE('',*,*,#44369,.F.);
#58838=ORIENTED_EDGE('',*,*,#44370,.F.);
#58839=ORIENTED_EDGE('',*,*,#44369,.T.);
#58840=ORIENTED_EDGE('',*,*,#44371,.T.);
#58841=ORIENTED_EDGE('',*,*,#44372,.F.);
#58842=ORIENTED_EDGE('',*,*,#44373,.T.);
#58843=ORIENTED_EDGE('',*,*,#44374,.F.);
#58844=ORIENTED_EDGE('',*,*,#44375,.T.);
#58845=ORIENTED_EDGE('',*,*,#44372,.T.);
#58846=ORIENTED_EDGE('',*,*,#44376,.T.);
#58847=ORIENTED_EDGE('',*,*,#44377,.F.);
#58848=ORIENTED_EDGE('',*,*,#44378,.F.);
#58849=ORIENTED_EDGE('',*,*,#44379,.T.);
#58850=ORIENTED_EDGE('',*,*,#44380,.T.);
#58851=ORIENTED_EDGE('',*,*,#44381,.T.);
#58852=ORIENTED_EDGE('',*,*,#44380,.F.);
#58853=ORIENTED_EDGE('',*,*,#44382,.T.);
#58854=ORIENTED_EDGE('',*,*,#44383,.T.);
#58855=ORIENTED_EDGE('',*,*,#44384,.T.);
#58856=ORIENTED_EDGE('',*,*,#44383,.F.);
#58857=ORIENTED_EDGE('',*,*,#44385,.T.);
#58858=ORIENTED_EDGE('',*,*,#44386,.T.);
#58859=ORIENTED_EDGE('',*,*,#44387,.T.);
#58860=ORIENTED_EDGE('',*,*,#44386,.F.);
#58861=ORIENTED_EDGE('',*,*,#44388,.T.);
#58862=ORIENTED_EDGE('',*,*,#44389,.T.);
#58863=ORIENTED_EDGE('',*,*,#44390,.T.);
#58864=ORIENTED_EDGE('',*,*,#44389,.F.);
#58865=ORIENTED_EDGE('',*,*,#44391,.T.);
#58866=ORIENTED_EDGE('',*,*,#44392,.T.);
#58867=ORIENTED_EDGE('',*,*,#44393,.T.);
#58868=ORIENTED_EDGE('',*,*,#44394,.T.);
#58869=ORIENTED_EDGE('',*,*,#44395,.F.);
#58870=ORIENTED_EDGE('',*,*,#44396,.T.);
#58871=ORIENTED_EDGE('',*,*,#44397,.F.);
#58872=ORIENTED_EDGE('',*,*,#44398,.F.);
#58873=ORIENTED_EDGE('',*,*,#44399,.T.);
#58874=ORIENTED_EDGE('',*,*,#44400,.T.);
#58875=ORIENTED_EDGE('',*,*,#44401,.T.);
#58876=ORIENTED_EDGE('',*,*,#44400,.F.);
#58877=ORIENTED_EDGE('',*,*,#44402,.T.);
#58878=ORIENTED_EDGE('',*,*,#44403,.T.);
#58879=ORIENTED_EDGE('',*,*,#44404,.T.);
#58880=ORIENTED_EDGE('',*,*,#44403,.F.);
#58881=ORIENTED_EDGE('',*,*,#44405,.T.);
#58882=ORIENTED_EDGE('',*,*,#44406,.T.);
#58883=ORIENTED_EDGE('',*,*,#44407,.T.);
#58884=ORIENTED_EDGE('',*,*,#44406,.F.);
#58885=ORIENTED_EDGE('',*,*,#44408,.T.);
#58886=ORIENTED_EDGE('',*,*,#44409,.T.);
#58887=ORIENTED_EDGE('',*,*,#44410,.T.);
#58888=ORIENTED_EDGE('',*,*,#44409,.F.);
#58889=ORIENTED_EDGE('',*,*,#44411,.T.);
#58890=ORIENTED_EDGE('',*,*,#44412,.T.);
#58891=ORIENTED_EDGE('',*,*,#44413,.T.);
#58892=ORIENTED_EDGE('',*,*,#44414,.T.);
#58893=ORIENTED_EDGE('',*,*,#44415,.F.);
#58894=ORIENTED_EDGE('',*,*,#44416,.T.);
#58895=ORIENTED_EDGE('',*,*,#44417,.F.);
#58896=ORIENTED_EDGE('',*,*,#44418,.F.);
#58897=ORIENTED_EDGE('',*,*,#44419,.T.);
#58898=ORIENTED_EDGE('',*,*,#44315,.T.);
#58899=ORIENTED_EDGE('',*,*,#44420,.T.);
#58900=ORIENTED_EDGE('',*,*,#44421,.F.);
#58901=ORIENTED_EDGE('',*,*,#44329,.F.);
#58902=ORIENTED_EDGE('',*,*,#44422,.T.);
#58903=ORIENTED_EDGE('',*,*,#44423,.F.);
#58904=ORIENTED_EDGE('',*,*,#44424,.F.);
#58905=ORIENTED_EDGE('',*,*,#44425,.F.);
#58906=ORIENTED_EDGE('',*,*,#44426,.F.);
#58907=ORIENTED_EDGE('',*,*,#44427,.F.);
#58908=ORIENTED_EDGE('',*,*,#44428,.F.);
#58909=ORIENTED_EDGE('',*,*,#44423,.T.);
#58910=ORIENTED_EDGE('',*,*,#44429,.T.);
#58911=ORIENTED_EDGE('',*,*,#44430,.T.);
#58912=ORIENTED_EDGE('',*,*,#44431,.F.);
#58913=ORIENTED_EDGE('',*,*,#44432,.F.);
#58914=ORIENTED_EDGE('',*,*,#44433,.T.);
#58915=ORIENTED_EDGE('',*,*,#44434,.T.);
#58916=ORIENTED_EDGE('',*,*,#44435,.T.);
#58917=ORIENTED_EDGE('',*,*,#44436,.F.);
#58918=ORIENTED_EDGE('',*,*,#44437,.T.);
#58919=ORIENTED_EDGE('',*,*,#44432,.T.);
#58920=ORIENTED_EDGE('',*,*,#44438,.T.);
#58921=ORIENTED_EDGE('',*,*,#44439,.T.);
#58922=ORIENTED_EDGE('',*,*,#44440,.F.);
#58923=ORIENTED_EDGE('',*,*,#44441,.T.);
#58924=ORIENTED_EDGE('',*,*,#44435,.F.);
#58925=ORIENTED_EDGE('',*,*,#44442,.F.);
#58926=ORIENTED_EDGE('',*,*,#44440,.T.);
#58927=ORIENTED_EDGE('',*,*,#44443,.T.);
#58928=ORIENTED_EDGE('',*,*,#44444,.T.);
#58929=ORIENTED_EDGE('',*,*,#44445,.F.);
#58930=ORIENTED_EDGE('',*,*,#44446,.T.);
#58931=ORIENTED_EDGE('',*,*,#44442,.T.);
#58932=ORIENTED_EDGE('',*,*,#44447,.T.);
#58933=ORIENTED_EDGE('',*,*,#44448,.F.);
#58934=ORIENTED_EDGE('',*,*,#44449,.T.);
#58935=ORIENTED_EDGE('',*,*,#44445,.T.);
#58936=ORIENTED_EDGE('',*,*,#44450,.T.);
#58937=ORIENTED_EDGE('',*,*,#44451,.F.);
#58938=ORIENTED_EDGE('',*,*,#44452,.T.);
#58939=ORIENTED_EDGE('',*,*,#44448,.T.);
#58940=ORIENTED_EDGE('',*,*,#44453,.T.);
#58941=ORIENTED_EDGE('',*,*,#44454,.F.);
#58942=ORIENTED_EDGE('',*,*,#44455,.T.);
#58943=ORIENTED_EDGE('',*,*,#44451,.T.);
#58944=ORIENTED_EDGE('',*,*,#44456,.T.);
#58945=ORIENTED_EDGE('',*,*,#44457,.F.);
#58946=ORIENTED_EDGE('',*,*,#44458,.T.);
#58947=ORIENTED_EDGE('',*,*,#44454,.T.);
#58948=ORIENTED_EDGE('',*,*,#44459,.T.);
#58949=ORIENTED_EDGE('',*,*,#44460,.F.);
#58950=ORIENTED_EDGE('',*,*,#44461,.T.);
#58951=ORIENTED_EDGE('',*,*,#44457,.T.);
#58952=ORIENTED_EDGE('',*,*,#44462,.T.);
#58953=ORIENTED_EDGE('',*,*,#44463,.F.);
#58954=ORIENTED_EDGE('',*,*,#44464,.T.);
#58955=ORIENTED_EDGE('',*,*,#44460,.T.);
#58956=ORIENTED_EDGE('',*,*,#44465,.T.);
#58957=ORIENTED_EDGE('',*,*,#44466,.F.);
#58958=ORIENTED_EDGE('',*,*,#44467,.T.);
#58959=ORIENTED_EDGE('',*,*,#44463,.T.);
#58960=ORIENTED_EDGE('',*,*,#44468,.T.);
#58961=ORIENTED_EDGE('',*,*,#44469,.F.);
#58962=ORIENTED_EDGE('',*,*,#44470,.T.);
#58963=ORIENTED_EDGE('',*,*,#44466,.T.);
#58964=ORIENTED_EDGE('',*,*,#44471,.T.);
#58965=ORIENTED_EDGE('',*,*,#44472,.F.);
#58966=ORIENTED_EDGE('',*,*,#44473,.T.);
#58967=ORIENTED_EDGE('',*,*,#44469,.T.);
#58968=ORIENTED_EDGE('',*,*,#44474,.T.);
#58969=ORIENTED_EDGE('',*,*,#44475,.F.);
#58970=ORIENTED_EDGE('',*,*,#44476,.T.);
#58971=ORIENTED_EDGE('',*,*,#44472,.T.);
#58972=ORIENTED_EDGE('',*,*,#44477,.T.);
#58973=ORIENTED_EDGE('',*,*,#44478,.F.);
#58974=ORIENTED_EDGE('',*,*,#44479,.T.);
#58975=ORIENTED_EDGE('',*,*,#44475,.T.);
#58976=ORIENTED_EDGE('',*,*,#44480,.T.);
#58977=ORIENTED_EDGE('',*,*,#44481,.F.);
#58978=ORIENTED_EDGE('',*,*,#44482,.T.);
#58979=ORIENTED_EDGE('',*,*,#44478,.T.);
#58980=ORIENTED_EDGE('',*,*,#44483,.T.);
#58981=ORIENTED_EDGE('',*,*,#44484,.F.);
#58982=ORIENTED_EDGE('',*,*,#44485,.T.);
#58983=ORIENTED_EDGE('',*,*,#44481,.T.);
#58984=ORIENTED_EDGE('',*,*,#44486,.T.);
#58985=ORIENTED_EDGE('',*,*,#44487,.T.);
#58986=ORIENTED_EDGE('',*,*,#44488,.T.);
#58987=ORIENTED_EDGE('',*,*,#44489,.T.);
#58988=ORIENTED_EDGE('',*,*,#44490,.F.);
#58989=ORIENTED_EDGE('',*,*,#44489,.F.);
#58990=ORIENTED_EDGE('',*,*,#44491,.T.);
#58991=ORIENTED_EDGE('',*,*,#44492,.T.);
#58992=ORIENTED_EDGE('',*,*,#44493,.T.);
#58993=ORIENTED_EDGE('',*,*,#44494,.T.);
#58994=ORIENTED_EDGE('',*,*,#44495,.T.);
#58995=ORIENTED_EDGE('',*,*,#44496,.T.);
#58996=ORIENTED_EDGE('',*,*,#44497,.F.);
#58997=ORIENTED_EDGE('',*,*,#44496,.F.);
#58998=ORIENTED_EDGE('',*,*,#44498,.T.);
#58999=ORIENTED_EDGE('',*,*,#44499,.T.);
#59000=ORIENTED_EDGE('',*,*,#44500,.T.);
#59001=ORIENTED_EDGE('',*,*,#44501,.T.);
#59002=ORIENTED_EDGE('',*,*,#44502,.T.);
#59003=ORIENTED_EDGE('',*,*,#44503,.T.);
#59004=ORIENTED_EDGE('',*,*,#44504,.T.);
#59005=ORIENTED_EDGE('',*,*,#44501,.F.);
#59006=ORIENTED_EDGE('',*,*,#44505,.T.);
#59007=ORIENTED_EDGE('',*,*,#44506,.T.);
#59008=ORIENTED_EDGE('',*,*,#44507,.T.);
#59009=ORIENTED_EDGE('',*,*,#44508,.T.);
#59010=ORIENTED_EDGE('',*,*,#44509,.F.);
#59011=ORIENTED_EDGE('',*,*,#44510,.T.);
#59012=ORIENTED_EDGE('',*,*,#44511,.F.);
#59013=ORIENTED_EDGE('',*,*,#44512,.F.);
#59014=ORIENTED_EDGE('',*,*,#44513,.T.);
#59015=ORIENTED_EDGE('',*,*,#44514,.T.);
#59016=ORIENTED_EDGE('',*,*,#44515,.T.);
#59017=ORIENTED_EDGE('',*,*,#44516,.F.);
#59018=ORIENTED_EDGE('',*,*,#44517,.T.);
#59019=ORIENTED_EDGE('',*,*,#44512,.T.);
#59020=ORIENTED_EDGE('',*,*,#44518,.T.);
#59021=ORIENTED_EDGE('',*,*,#44519,.F.);
#59022=ORIENTED_EDGE('',*,*,#44520,.T.);
#59023=ORIENTED_EDGE('',*,*,#44516,.T.);
#59024=ORIENTED_EDGE('',*,*,#44521,.T.);
#59025=ORIENTED_EDGE('',*,*,#44519,.T.);
#59026=ORIENTED_EDGE('',*,*,#44522,.T.);
#59027=ORIENTED_EDGE('',*,*,#44523,.T.);
#59028=ORIENTED_EDGE('',*,*,#44524,.T.);
#59029=ORIENTED_EDGE('',*,*,#44523,.F.);
#59030=ORIENTED_EDGE('',*,*,#44525,.T.);
#59031=ORIENTED_EDGE('',*,*,#44526,.T.);
#59032=ORIENTED_EDGE('',*,*,#44527,.T.);
#59033=ORIENTED_EDGE('',*,*,#44528,.T.);
#59034=ORIENTED_EDGE('',*,*,#44529,.F.);
#59035=ORIENTED_EDGE('',*,*,#44530,.T.);
#59036=ORIENTED_EDGE('',*,*,#44531,.F.);
#59037=ORIENTED_EDGE('',*,*,#44532,.F.);
#59038=ORIENTED_EDGE('',*,*,#44533,.T.);
#59039=ORIENTED_EDGE('',*,*,#44534,.T.);
#59040=ORIENTED_EDGE('',*,*,#44535,.T.);
#59041=ORIENTED_EDGE('',*,*,#44536,.F.);
#59042=ORIENTED_EDGE('',*,*,#44537,.T.);
#59043=ORIENTED_EDGE('',*,*,#44532,.T.);
#59044=ORIENTED_EDGE('',*,*,#44538,.T.);
#59045=ORIENTED_EDGE('',*,*,#44539,.F.);
#59046=ORIENTED_EDGE('',*,*,#44540,.T.);
#59047=ORIENTED_EDGE('',*,*,#44536,.T.);
#59048=ORIENTED_EDGE('',*,*,#44541,.T.);
#59049=ORIENTED_EDGE('',*,*,#44539,.T.);
#59050=ORIENTED_EDGE('',*,*,#44542,.T.);
#59051=ORIENTED_EDGE('',*,*,#44543,.T.);
#59052=ORIENTED_EDGE('',*,*,#44544,.T.);
#59053=ORIENTED_EDGE('',*,*,#44543,.F.);
#59054=ORIENTED_EDGE('',*,*,#44545,.T.);
#59055=ORIENTED_EDGE('',*,*,#44546,.T.);
#59056=ORIENTED_EDGE('',*,*,#44547,.T.);
#59057=ORIENTED_EDGE('',*,*,#44548,.T.);
#59058=ORIENTED_EDGE('',*,*,#44549,.F.);
#59059=ORIENTED_EDGE('',*,*,#44550,.T.);
#59060=ORIENTED_EDGE('',*,*,#44551,.F.);
#59061=ORIENTED_EDGE('',*,*,#44552,.F.);
#59062=ORIENTED_EDGE('',*,*,#44553,.T.);
#59063=ORIENTED_EDGE('',*,*,#44554,.T.);
#59064=ORIENTED_EDGE('',*,*,#44555,.T.);
#59065=ORIENTED_EDGE('',*,*,#44556,.F.);
#59066=ORIENTED_EDGE('',*,*,#44557,.T.);
#59067=ORIENTED_EDGE('',*,*,#44552,.T.);
#59068=ORIENTED_EDGE('',*,*,#44558,.T.);
#59069=ORIENTED_EDGE('',*,*,#44559,.F.);
#59070=ORIENTED_EDGE('',*,*,#44560,.F.);
#59071=ORIENTED_EDGE('',*,*,#44561,.T.);
#59072=ORIENTED_EDGE('',*,*,#44485,.F.);
#59073=ORIENTED_EDGE('',*,*,#44562,.T.);
#59074=ORIENTED_EDGE('',*,*,#44563,.F.);
#59075=ORIENTED_EDGE('',*,*,#44564,.F.);
#59076=ORIENTED_EDGE('',*,*,#44565,.T.);
#59077=ORIENTED_EDGE('',*,*,#44566,.T.);
#59078=ORIENTED_EDGE('',*,*,#44567,.T.);
#59079=ORIENTED_EDGE('',*,*,#44503,.F.);
#59080=ORIENTED_EDGE('',*,*,#44568,.T.);
#59081=ORIENTED_EDGE('',*,*,#44564,.T.);
#59082=ORIENTED_EDGE('',*,*,#44569,.T.);
#59083=ORIENTED_EDGE('',*,*,#44570,.T.);
#59084=ORIENTED_EDGE('',*,*,#44571,.T.);
#59085=ORIENTED_EDGE('',*,*,#44572,.T.);
#59086=ORIENTED_EDGE('',*,*,#44557,.F.);
#59087=ORIENTED_EDGE('',*,*,#44571,.F.);
#59088=ORIENTED_EDGE('',*,*,#44573,.T.);
#59089=ORIENTED_EDGE('',*,*,#44574,.T.);
#59090=ORIENTED_EDGE('',*,*,#44575,.T.);
#59091=ORIENTED_EDGE('',*,*,#44576,.T.);
#59092=ORIENTED_EDGE('',*,*,#44574,.F.);
#59093=ORIENTED_EDGE('',*,*,#44577,.T.);
#59094=ORIENTED_EDGE('',*,*,#43835,.F.);
#59095=ORIENTED_EDGE('',*,*,#44578,.F.);
#59096=ORIENTED_EDGE('',*,*,#44579,.T.);
#59097=ORIENTED_EDGE('',*,*,#43838,.T.);
#59098=ORIENTED_EDGE('',*,*,#43842,.T.);
#59099=ORIENTED_EDGE('',*,*,#44572,.F.);
#59100=ORIENTED_EDGE('',*,*,#44575,.F.);
#59101=ORIENTED_EDGE('',*,*,#44576,.F.);
#59102=ORIENTED_EDGE('',*,*,#43839,.F.);
#59103=ORIENTED_EDGE('',*,*,#44579,.F.);
#59104=ORIENTED_EDGE('',*,*,#44580,.F.);
#59105=ORIENTED_EDGE('',*,*,#44581,.F.);
#59106=ORIENTED_EDGE('',*,*,#44582,.F.);
#59107=ORIENTED_EDGE('',*,*,#44583,.F.);
#59108=ORIENTED_EDGE('',*,*,#44584,.F.);
#59109=ORIENTED_EDGE('',*,*,#44585,.F.);
#59110=ORIENTED_EDGE('',*,*,#44553,.F.);
#59111=ORIENTED_EDGE('',*,*,#44586,.F.);
#59112=ORIENTED_EDGE('',*,*,#44587,.F.);
#59113=ORIENTED_EDGE('',*,*,#43841,.F.);
#59114=ORIENTED_EDGE('',*,*,#44588,.F.);
#59115=ORIENTED_EDGE('',*,*,#44589,.F.);
#59116=ORIENTED_EDGE('',*,*,#43844,.T.);
#59117=ORIENTED_EDGE('',*,*,#43848,.T.);
#59118=ORIENTED_EDGE('',*,*,#43847,.T.);
#59119=ORIENTED_EDGE('',*,*,#44590,.T.);
#59120=ORIENTED_EDGE('',*,*,#44591,.F.);
#59121=ORIENTED_EDGE('',*,*,#44592,.F.);
#59122=ORIENTED_EDGE('',*,*,#44593,.F.);
#59123=ORIENTED_EDGE('',*,*,#44547,.F.);
#59124=ORIENTED_EDGE('',*,*,#44594,.F.);
#59125=ORIENTED_EDGE('',*,*,#44595,.F.);
#59126=ORIENTED_EDGE('',*,*,#44596,.F.);
#59127=ORIENTED_EDGE('',*,*,#44597,.F.);
#59128=ORIENTED_EDGE('',*,*,#44598,.F.);
#59129=ORIENTED_EDGE('',*,*,#44599,.F.);
#59130=ORIENTED_EDGE('',*,*,#44590,.F.);
#59131=ORIENTED_EDGE('',*,*,#43846,.F.);
#59132=ORIENTED_EDGE('',*,*,#44600,.T.);
#59133=ORIENTED_EDGE('',*,*,#44601,.T.);
#59134=ORIENTED_EDGE('',*,*,#44591,.T.);
#59135=ORIENTED_EDGE('',*,*,#43853,.F.);
#59136=ORIENTED_EDGE('',*,*,#44602,.F.);
#59137=ORIENTED_EDGE('',*,*,#44603,.T.);
#59138=ORIENTED_EDGE('',*,*,#44600,.F.);
#59139=ORIENTED_EDGE('',*,*,#43856,.F.);
#59140=ORIENTED_EDGE('',*,*,#44604,.T.);
#59141=ORIENTED_EDGE('',*,*,#44605,.F.);
#59142=ORIENTED_EDGE('',*,*,#44602,.T.);
#59143=ORIENTED_EDGE('',*,*,#43859,.F.);
#59144=ORIENTED_EDGE('',*,*,#44606,.F.);
#59145=ORIENTED_EDGE('',*,*,#44607,.T.);
#59146=ORIENTED_EDGE('',*,*,#43860,.T.);
#59147=ORIENTED_EDGE('',*,*,#43864,.T.);
#59148=ORIENTED_EDGE('',*,*,#44608,.F.);
#59149=ORIENTED_EDGE('',*,*,#44609,.F.);
#59150=ORIENTED_EDGE('',*,*,#44604,.F.);
#59151=ORIENTED_EDGE('',*,*,#43861,.F.);
#59152=ORIENTED_EDGE('',*,*,#44607,.F.);
#59153=ORIENTED_EDGE('',*,*,#44610,.F.);
#59154=ORIENTED_EDGE('',*,*,#44611,.F.);
#59155=ORIENTED_EDGE('',*,*,#44612,.F.);
#59156=ORIENTED_EDGE('',*,*,#44613,.F.);
#59157=ORIENTED_EDGE('',*,*,#44614,.F.);
#59158=ORIENTED_EDGE('',*,*,#44615,.F.);
#59159=ORIENTED_EDGE('',*,*,#44533,.F.);
#59160=ORIENTED_EDGE('',*,*,#44616,.F.);
#59161=ORIENTED_EDGE('',*,*,#44617,.F.);
#59162=ORIENTED_EDGE('',*,*,#43863,.F.);
#59163=ORIENTED_EDGE('',*,*,#44618,.F.);
#59164=ORIENTED_EDGE('',*,*,#44619,.F.);
#59165=ORIENTED_EDGE('',*,*,#43866,.T.);
#59166=ORIENTED_EDGE('',*,*,#43870,.T.);
#59167=ORIENTED_EDGE('',*,*,#43869,.T.);
#59168=ORIENTED_EDGE('',*,*,#44620,.T.);
#59169=ORIENTED_EDGE('',*,*,#44621,.F.);
#59170=ORIENTED_EDGE('',*,*,#44622,.F.);
#59171=ORIENTED_EDGE('',*,*,#44623,.F.);
#59172=ORIENTED_EDGE('',*,*,#44624,.F.);
#59173=ORIENTED_EDGE('',*,*,#44625,.F.);
#59174=ORIENTED_EDGE('',*,*,#44527,.F.);
#59175=ORIENTED_EDGE('',*,*,#44626,.F.);
#59176=ORIENTED_EDGE('',*,*,#44627,.F.);
#59177=ORIENTED_EDGE('',*,*,#44628,.F.);
#59178=ORIENTED_EDGE('',*,*,#44629,.F.);
#59179=ORIENTED_EDGE('',*,*,#44630,.F.);
#59180=ORIENTED_EDGE('',*,*,#44631,.F.);
#59181=ORIENTED_EDGE('',*,*,#44620,.F.);
#59182=ORIENTED_EDGE('',*,*,#43868,.F.);
#59183=ORIENTED_EDGE('',*,*,#44632,.T.);
#59184=ORIENTED_EDGE('',*,*,#44633,.T.);
#59185=ORIENTED_EDGE('',*,*,#44621,.T.);
#59186=ORIENTED_EDGE('',*,*,#43874,.F.);
#59187=ORIENTED_EDGE('',*,*,#44634,.F.);
#59188=ORIENTED_EDGE('',*,*,#44635,.F.);
#59189=ORIENTED_EDGE('',*,*,#44632,.F.);
#59190=ORIENTED_EDGE('',*,*,#43877,.F.);
#59191=ORIENTED_EDGE('',*,*,#44636,.T.);
#59192=ORIENTED_EDGE('',*,*,#44637,.F.);
#59193=ORIENTED_EDGE('',*,*,#44634,.T.);
#59194=ORIENTED_EDGE('',*,*,#43880,.F.);
#59195=ORIENTED_EDGE('',*,*,#44638,.F.);
#59196=ORIENTED_EDGE('',*,*,#44639,.T.);
#59197=ORIENTED_EDGE('',*,*,#43881,.T.);
#59198=ORIENTED_EDGE('',*,*,#43885,.T.);
#59199=ORIENTED_EDGE('',*,*,#44640,.F.);
#59200=ORIENTED_EDGE('',*,*,#44641,.F.);
#59201=ORIENTED_EDGE('',*,*,#44642,.F.);
#59202=ORIENTED_EDGE('',*,*,#44643,.F.);
#59203=ORIENTED_EDGE('',*,*,#44636,.F.);
#59204=ORIENTED_EDGE('',*,*,#43882,.F.);
#59205=ORIENTED_EDGE('',*,*,#44639,.F.);
#59206=ORIENTED_EDGE('',*,*,#44644,.F.);
#59207=ORIENTED_EDGE('',*,*,#44645,.F.);
#59208=ORIENTED_EDGE('',*,*,#44646,.F.);
#59209=ORIENTED_EDGE('',*,*,#44647,.F.);
#59210=ORIENTED_EDGE('',*,*,#44648,.F.);
#59211=ORIENTED_EDGE('',*,*,#44649,.F.);
#59212=ORIENTED_EDGE('',*,*,#44513,.F.);
#59213=ORIENTED_EDGE('',*,*,#44650,.F.);
#59214=ORIENTED_EDGE('',*,*,#44651,.F.);
#59215=ORIENTED_EDGE('',*,*,#43884,.F.);
#59216=ORIENTED_EDGE('',*,*,#44652,.F.);
#59217=ORIENTED_EDGE('',*,*,#44653,.F.);
#59218=ORIENTED_EDGE('',*,*,#43887,.T.);
#59219=ORIENTED_EDGE('',*,*,#43890,.T.);
#59220=ORIENTED_EDGE('',*,*,#44654,.T.);
#59221=ORIENTED_EDGE('',*,*,#44655,.F.);
#59222=ORIENTED_EDGE('',*,*,#44656,.F.);
#59223=ORIENTED_EDGE('',*,*,#44657,.F.);
#59224=ORIENTED_EDGE('',*,*,#44658,.F.);
#59225=ORIENTED_EDGE('',*,*,#44659,.F.);
#59226=ORIENTED_EDGE('',*,*,#44507,.F.);
#59227=ORIENTED_EDGE('',*,*,#44660,.F.);
#59228=ORIENTED_EDGE('',*,*,#44661,.F.);
#59229=ORIENTED_EDGE('',*,*,#44662,.F.);
#59230=ORIENTED_EDGE('',*,*,#44663,.F.);
#59231=ORIENTED_EDGE('',*,*,#44664,.F.);
#59232=ORIENTED_EDGE('',*,*,#44665,.F.);
#59233=ORIENTED_EDGE('',*,*,#44654,.F.);
#59234=ORIENTED_EDGE('',*,*,#43889,.F.);
#59235=ORIENTED_EDGE('',*,*,#44302,.T.);
#59236=ORIENTED_EDGE('',*,*,#44666,.T.);
#59237=ORIENTED_EDGE('',*,*,#44655,.T.);
#59238=ORIENTED_EDGE('',*,*,#43894,.F.);
#59239=ORIENTED_EDGE('',*,*,#44667,.T.);
#59240=ORIENTED_EDGE('',*,*,#44668,.F.);
#59241=ORIENTED_EDGE('',*,*,#44198,.F.);
#59242=ORIENTED_EDGE('',*,*,#44183,.F.);
#59243=ORIENTED_EDGE('',*,*,#43901,.F.);
#59244=ORIENTED_EDGE('',*,*,#44669,.F.);
#59245=ORIENTED_EDGE('',*,*,#43907,.F.);
#59246=ORIENTED_EDGE('',*,*,#44670,.T.);
#59247=ORIENTED_EDGE('',*,*,#44671,.T.);
#59248=ORIENTED_EDGE('',*,*,#43904,.T.);
#59249=ORIENTED_EDGE('',*,*,#44672,.F.);
#59250=ORIENTED_EDGE('',*,*,#44673,.F.);
#59251=ORIENTED_EDGE('',*,*,#44674,.F.);
#59252=ORIENTED_EDGE('',*,*,#44393,.F.);
#59253=ORIENTED_EDGE('',*,*,#44675,.F.);
#59254=ORIENTED_EDGE('',*,*,#44676,.F.);
#59255=ORIENTED_EDGE('',*,*,#44677,.F.);
#59256=ORIENTED_EDGE('',*,*,#44678,.F.);
#59257=ORIENTED_EDGE('',*,*,#44679,.F.);
#59258=ORIENTED_EDGE('',*,*,#44670,.F.);
#59259=ORIENTED_EDGE('',*,*,#43906,.F.);
#59260=ORIENTED_EDGE('',*,*,#44680,.T.);
#59261=ORIENTED_EDGE('',*,*,#44681,.T.);
#59262=ORIENTED_EDGE('',*,*,#44672,.T.);
#59263=ORIENTED_EDGE('',*,*,#43910,.F.);
#59264=ORIENTED_EDGE('',*,*,#44682,.F.);
#59265=ORIENTED_EDGE('',*,*,#44683,.F.);
#59266=ORIENTED_EDGE('',*,*,#44680,.F.);
#59267=ORIENTED_EDGE('',*,*,#43913,.F.);
#59268=ORIENTED_EDGE('',*,*,#44684,.T.);
#59269=ORIENTED_EDGE('',*,*,#44685,.F.);
#59270=ORIENTED_EDGE('',*,*,#44682,.T.);
#59271=ORIENTED_EDGE('',*,*,#43916,.F.);
#59272=ORIENTED_EDGE('',*,*,#44686,.F.);
#59273=ORIENTED_EDGE('',*,*,#44687,.F.);
#59274=ORIENTED_EDGE('',*,*,#44688,.F.);
#59275=ORIENTED_EDGE('',*,*,#44689,.F.);
#59276=ORIENTED_EDGE('',*,*,#44690,.F.);
#59277=ORIENTED_EDGE('',*,*,#44381,.F.);
#59278=ORIENTED_EDGE('',*,*,#44691,.F.);
#59279=ORIENTED_EDGE('',*,*,#44692,.F.);
#59280=ORIENTED_EDGE('',*,*,#44684,.F.);
#59281=ORIENTED_EDGE('',*,*,#43920,.F.);
#59282=ORIENTED_EDGE('',*,*,#43919,.F.);
#59283=ORIENTED_EDGE('',*,*,#43922,.T.);
#59284=ORIENTED_EDGE('',*,*,#44693,.T.);
#59285=ORIENTED_EDGE('',*,*,#44686,.T.);
#59286=ORIENTED_EDGE('',*,*,#44694,.F.);
#59287=ORIENTED_EDGE('',*,*,#44695,.F.);
#59288=ORIENTED_EDGE('',*,*,#43921,.F.);
#59289=ORIENTED_EDGE('',*,*,#44696,.F.);
#59290=ORIENTED_EDGE('',*,*,#43927,.F.);
#59291=ORIENTED_EDGE('',*,*,#44697,.T.);
#59292=ORIENTED_EDGE('',*,*,#44698,.T.);
#59293=ORIENTED_EDGE('',*,*,#43924,.T.);
#59294=ORIENTED_EDGE('',*,*,#44699,.F.);
#59295=ORIENTED_EDGE('',*,*,#44700,.F.);
#59296=ORIENTED_EDGE('',*,*,#44367,.F.);
#59297=ORIENTED_EDGE('',*,*,#44701,.F.);
#59298=ORIENTED_EDGE('',*,*,#44702,.F.);
#59299=ORIENTED_EDGE('',*,*,#44703,.F.);
#59300=ORIENTED_EDGE('',*,*,#44704,.F.);
#59301=ORIENTED_EDGE('',*,*,#44697,.F.);
#59302=ORIENTED_EDGE('',*,*,#43926,.F.);
#59303=ORIENTED_EDGE('',*,*,#44705,.T.);
#59304=ORIENTED_EDGE('',*,*,#44706,.T.);
#59305=ORIENTED_EDGE('',*,*,#44699,.T.);
#59306=ORIENTED_EDGE('',*,*,#43930,.F.);
#59307=ORIENTED_EDGE('',*,*,#44707,.F.);
#59308=ORIENTED_EDGE('',*,*,#44708,.T.);
#59309=ORIENTED_EDGE('',*,*,#44705,.F.);
#59310=ORIENTED_EDGE('',*,*,#43933,.F.);
#59311=ORIENTED_EDGE('',*,*,#44709,.T.);
#59312=ORIENTED_EDGE('',*,*,#44710,.T.);
#59313=ORIENTED_EDGE('',*,*,#44707,.T.);
#59314=ORIENTED_EDGE('',*,*,#43936,.F.);
#59315=ORIENTED_EDGE('',*,*,#44711,.T.);
#59316=ORIENTED_EDGE('',*,*,#44712,.T.);
#59317=ORIENTED_EDGE('',*,*,#43938,.T.);
#59318=ORIENTED_EDGE('',*,*,#43942,.T.);
#59319=ORIENTED_EDGE('',*,*,#44712,.F.);
#59320=ORIENTED_EDGE('',*,*,#44713,.F.);
#59321=ORIENTED_EDGE('',*,*,#44714,.F.);
#59322=ORIENTED_EDGE('',*,*,#44355,.F.);
#59323=ORIENTED_EDGE('',*,*,#44715,.F.);
#59324=ORIENTED_EDGE('',*,*,#44709,.F.);
#59325=ORIENTED_EDGE('',*,*,#43939,.F.);
#59326=ORIENTED_EDGE('',*,*,#44347,.F.);
#59327=ORIENTED_EDGE('',*,*,#44716,.F.);
#59328=ORIENTED_EDGE('',*,*,#43941,.F.);
#59329=ORIENTED_EDGE('',*,*,#44717,.F.);
#59330=ORIENTED_EDGE('',*,*,#43947,.F.);
#59331=ORIENTED_EDGE('',*,*,#44718,.T.);
#59332=ORIENTED_EDGE('',*,*,#44719,.T.);
#59333=ORIENTED_EDGE('',*,*,#43944,.T.);
#59334=ORIENTED_EDGE('',*,*,#44720,.F.);
#59335=ORIENTED_EDGE('',*,*,#44721,.F.);
#59336=ORIENTED_EDGE('',*,*,#44345,.F.);
#59337=ORIENTED_EDGE('',*,*,#44722,.F.);
#59338=ORIENTED_EDGE('',*,*,#44723,.F.);
#59339=ORIENTED_EDGE('',*,*,#44718,.F.);
#59340=ORIENTED_EDGE('',*,*,#43946,.F.);
#59341=ORIENTED_EDGE('',*,*,#44724,.T.);
#59342=ORIENTED_EDGE('',*,*,#44725,.T.);
#59343=ORIENTED_EDGE('',*,*,#44720,.T.);
#59344=ORIENTED_EDGE('',*,*,#43950,.F.);
#59345=ORIENTED_EDGE('',*,*,#44726,.F.);
#59346=ORIENTED_EDGE('',*,*,#44727,.T.);
#59347=ORIENTED_EDGE('',*,*,#44724,.F.);
#59348=ORIENTED_EDGE('',*,*,#43953,.F.);
#59349=ORIENTED_EDGE('',*,*,#44728,.T.);
#59350=ORIENTED_EDGE('',*,*,#44729,.T.);
#59351=ORIENTED_EDGE('',*,*,#44726,.T.);
#59352=ORIENTED_EDGE('',*,*,#43956,.F.);
#59353=ORIENTED_EDGE('',*,*,#44306,.F.);
#59354=ORIENTED_EDGE('',*,*,#44310,.F.);
#59355=ORIENTED_EDGE('',*,*,#44314,.F.);
#59356=ORIENTED_EDGE('',*,*,#44333,.F.);
#59357=ORIENTED_EDGE('',*,*,#44730,.F.);
#59358=ORIENTED_EDGE('',*,*,#44728,.F.);
#59359=ORIENTED_EDGE('',*,*,#43959,.F.);
#59360=ORIENTED_EDGE('',*,*,#44011,.F.);
#59361=ORIENTED_EDGE('',*,*,#44731,.T.);
#59362=ORIENTED_EDGE('',*,*,#44732,.T.);
#59363=ORIENTED_EDGE('',*,*,#44733,.T.);
#59364=ORIENTED_EDGE('',*,*,#44144,.F.);
#59365=ORIENTED_EDGE('',*,*,#44734,.F.);
#59366=ORIENTED_EDGE('',*,*,#44735,.F.);
#59367=ORIENTED_EDGE('',*,*,#44731,.F.);
#59368=ORIENTED_EDGE('',*,*,#44014,.F.);
#59369=ORIENTED_EDGE('',*,*,#44736,.T.);
#59370=ORIENTED_EDGE('',*,*,#44737,.F.);
#59371=ORIENTED_EDGE('',*,*,#44734,.T.);
#59372=ORIENTED_EDGE('',*,*,#44016,.F.);
#59373=ORIENTED_EDGE('',*,*,#44231,.F.);
#59374=ORIENTED_EDGE('',*,*,#44738,.T.);
#59375=ORIENTED_EDGE('',*,*,#44739,.T.);
#59376=ORIENTED_EDGE('',*,*,#44740,.T.);
#59377=ORIENTED_EDGE('',*,*,#44257,.F.);
#59378=ORIENTED_EDGE('',*,*,#43963,.F.);
#59379=ORIENTED_EDGE('',*,*,#44741,.F.);
#59380=ORIENTED_EDGE('',*,*,#44742,.F.);
#59381=ORIENTED_EDGE('',*,*,#44738,.F.);
#59382=ORIENTED_EDGE('',*,*,#43965,.F.);
#59383=ORIENTED_EDGE('',*,*,#44743,.T.);
#59384=ORIENTED_EDGE('',*,*,#44744,.F.);
#59385=ORIENTED_EDGE('',*,*,#44741,.T.);
#59386=ORIENTED_EDGE('',*,*,#43967,.F.);
#59387=ORIENTED_EDGE('',*,*,#44065,.F.);
#59388=ORIENTED_EDGE('',*,*,#44745,.F.);
#59389=ORIENTED_EDGE('',*,*,#44746,.F.);
#59390=ORIENTED_EDGE('',*,*,#44747,.F.);
#59391=ORIENTED_EDGE('',*,*,#44748,.F.);
#59392=ORIENTED_EDGE('',*,*,#44743,.F.);
#59393=ORIENTED_EDGE('',*,*,#44067,.F.);
#59394=ORIENTED_EDGE('',*,*,#44749,.F.);
#59395=ORIENTED_EDGE('',*,*,#44750,.F.);
#59396=ORIENTED_EDGE('',*,*,#44751,.F.);
#59397=ORIENTED_EDGE('',*,*,#44752,.F.);
#59398=ORIENTED_EDGE('',*,*,#44753,.F.);
#59399=ORIENTED_EDGE('',*,*,#44754,.F.);
#59400=ORIENTED_EDGE('',*,*,#44755,.F.);
#59401=ORIENTED_EDGE('',*,*,#44756,.F.);
#59402=ORIENTED_EDGE('',*,*,#44066,.F.);
#59403=ORIENTED_EDGE('',*,*,#44069,.T.);
#59404=ORIENTED_EDGE('',*,*,#44757,.T.);
#59405=ORIENTED_EDGE('',*,*,#44749,.T.);
#59406=ORIENTED_EDGE('',*,*,#44758,.F.);
#59407=ORIENTED_EDGE('',*,*,#44759,.F.);
#59408=ORIENTED_EDGE('',*,*,#44068,.F.);
#59409=ORIENTED_EDGE('',*,*,#44760,.F.);
#59410=ORIENTED_EDGE('',*,*,#44073,.F.);
#59411=ORIENTED_EDGE('',*,*,#44761,.T.);
#59412=ORIENTED_EDGE('',*,*,#44762,.T.);
#59413=ORIENTED_EDGE('',*,*,#44070,.T.);
#59414=ORIENTED_EDGE('',*,*,#44763,.F.);
#59415=ORIENTED_EDGE('',*,*,#44764,.F.);
#59416=ORIENTED_EDGE('',*,*,#44765,.F.);
#59417=ORIENTED_EDGE('',*,*,#44766,.F.);
#59418=ORIENTED_EDGE('',*,*,#44767,.F.);
#59419=ORIENTED_EDGE('',*,*,#44768,.F.);
#59420=ORIENTED_EDGE('',*,*,#44769,.F.);
#59421=ORIENTED_EDGE('',*,*,#44770,.F.);
#59422=ORIENTED_EDGE('',*,*,#44771,.F.);
#59423=ORIENTED_EDGE('',*,*,#44772,.F.);
#59424=ORIENTED_EDGE('',*,*,#44773,.F.);
#59425=ORIENTED_EDGE('',*,*,#44774,.F.);
#59426=ORIENTED_EDGE('',*,*,#44761,.F.);
#59427=ORIENTED_EDGE('',*,*,#44072,.F.);
#59428=ORIENTED_EDGE('',*,*,#44775,.T.);
#59429=ORIENTED_EDGE('',*,*,#44776,.T.);
#59430=ORIENTED_EDGE('',*,*,#44763,.T.);
#59431=ORIENTED_EDGE('',*,*,#44075,.F.);
#59432=ORIENTED_EDGE('',*,*,#44777,.F.);
#59433=ORIENTED_EDGE('',*,*,#44778,.F.);
#59434=ORIENTED_EDGE('',*,*,#44775,.F.);
#59435=ORIENTED_EDGE('',*,*,#44077,.F.);
#59436=ORIENTED_EDGE('',*,*,#44779,.T.);
#59437=ORIENTED_EDGE('',*,*,#44780,.F.);
#59438=ORIENTED_EDGE('',*,*,#44777,.T.);
#59439=ORIENTED_EDGE('',*,*,#44079,.F.);
#59440=ORIENTED_EDGE('',*,*,#44781,.F.);
#59441=ORIENTED_EDGE('',*,*,#44782,.T.);
#59442=ORIENTED_EDGE('',*,*,#44080,.T.);
#59443=ORIENTED_EDGE('',*,*,#44083,.T.);
#59444=ORIENTED_EDGE('',*,*,#44782,.F.);
#59445=ORIENTED_EDGE('',*,*,#44783,.F.);
#59446=ORIENTED_EDGE('',*,*,#44784,.F.);
#59447=ORIENTED_EDGE('',*,*,#44785,.F.);
#59448=ORIENTED_EDGE('',*,*,#44786,.F.);
#59449=ORIENTED_EDGE('',*,*,#44787,.F.);
#59450=ORIENTED_EDGE('',*,*,#44788,.F.);
#59451=ORIENTED_EDGE('',*,*,#44789,.F.);
#59452=ORIENTED_EDGE('',*,*,#44790,.F.);
#59453=ORIENTED_EDGE('',*,*,#44791,.F.);
#59454=ORIENTED_EDGE('',*,*,#44792,.F.);
#59455=ORIENTED_EDGE('',*,*,#44779,.F.);
#59456=ORIENTED_EDGE('',*,*,#44081,.F.);
#59457=ORIENTED_EDGE('',*,*,#44793,.F.);
#59458=ORIENTED_EDGE('',*,*,#44794,.F.);
#59459=ORIENTED_EDGE('',*,*,#44082,.F.);
#59460=ORIENTED_EDGE('',*,*,#44795,.F.);
#59461=ORIENTED_EDGE('',*,*,#44796,.F.);
#59462=ORIENTED_EDGE('',*,*,#44084,.T.);
#59463=ORIENTED_EDGE('',*,*,#44085,.T.);
#59464=ORIENTED_EDGE('',*,*,#44797,.T.);
#59465=ORIENTED_EDGE('',*,*,#44798,.F.);
#59466=ORIENTED_EDGE('',*,*,#44799,.F.);
#59467=ORIENTED_EDGE('',*,*,#44800,.F.);
#59468=ORIENTED_EDGE('',*,*,#44801,.F.);
#59469=ORIENTED_EDGE('',*,*,#44802,.F.);
#59470=ORIENTED_EDGE('',*,*,#44803,.F.);
#59471=ORIENTED_EDGE('',*,*,#44804,.F.);
#59472=ORIENTED_EDGE('',*,*,#44805,.F.);
#59473=ORIENTED_EDGE('',*,*,#44806,.F.);
#59474=ORIENTED_EDGE('',*,*,#44807,.F.);
#59475=ORIENTED_EDGE('',*,*,#44797,.F.);
#59476=ORIENTED_EDGE('',*,*,#44087,.F.);
#59477=ORIENTED_EDGE('',*,*,#44808,.T.);
#59478=ORIENTED_EDGE('',*,*,#44809,.T.);
#59479=ORIENTED_EDGE('',*,*,#44798,.T.);
#59480=ORIENTED_EDGE('',*,*,#44089,.F.);
#59481=ORIENTED_EDGE('',*,*,#44810,.F.);
#59482=ORIENTED_EDGE('',*,*,#44811,.T.);
#59483=ORIENTED_EDGE('',*,*,#44808,.F.);
#59484=ORIENTED_EDGE('',*,*,#44091,.F.);
#59485=ORIENTED_EDGE('',*,*,#44812,.T.);
#59486=ORIENTED_EDGE('',*,*,#44813,.F.);
#59487=ORIENTED_EDGE('',*,*,#44810,.T.);
#59488=ORIENTED_EDGE('',*,*,#44093,.F.);
#59489=ORIENTED_EDGE('',*,*,#44814,.F.);
#59490=ORIENTED_EDGE('',*,*,#44815,.T.);
#59491=ORIENTED_EDGE('',*,*,#44094,.T.);
#59492=ORIENTED_EDGE('',*,*,#44097,.T.);
#59493=ORIENTED_EDGE('',*,*,#44816,.F.);
#59494=ORIENTED_EDGE('',*,*,#44817,.F.);
#59495=ORIENTED_EDGE('',*,*,#44812,.F.);
#59496=ORIENTED_EDGE('',*,*,#44095,.F.);
#59497=ORIENTED_EDGE('',*,*,#44815,.F.);
#59498=ORIENTED_EDGE('',*,*,#44818,.F.);
#59499=ORIENTED_EDGE('',*,*,#44819,.F.);
#59500=ORIENTED_EDGE('',*,*,#44820,.F.);
#59501=ORIENTED_EDGE('',*,*,#44821,.F.);
#59502=ORIENTED_EDGE('',*,*,#44822,.F.);
#59503=ORIENTED_EDGE('',*,*,#44823,.F.);
#59504=ORIENTED_EDGE('',*,*,#44824,.F.);
#59505=ORIENTED_EDGE('',*,*,#44825,.F.);
#59506=ORIENTED_EDGE('',*,*,#44826,.F.);
#59507=ORIENTED_EDGE('',*,*,#44096,.F.);
#59508=ORIENTED_EDGE('',*,*,#44827,.F.);
#59509=ORIENTED_EDGE('',*,*,#44828,.F.);
#59510=ORIENTED_EDGE('',*,*,#44098,.T.);
#59511=ORIENTED_EDGE('',*,*,#44099,.T.);
#59512=ORIENTED_EDGE('',*,*,#44829,.T.);
#59513=ORIENTED_EDGE('',*,*,#44830,.F.);
#59514=ORIENTED_EDGE('',*,*,#44831,.F.);
#59515=ORIENTED_EDGE('',*,*,#44832,.F.);
#59516=ORIENTED_EDGE('',*,*,#44833,.F.);
#59517=ORIENTED_EDGE('',*,*,#44834,.F.);
#59518=ORIENTED_EDGE('',*,*,#44835,.F.);
#59519=ORIENTED_EDGE('',*,*,#44836,.F.);
#59520=ORIENTED_EDGE('',*,*,#44837,.F.);
#59521=ORIENTED_EDGE('',*,*,#44838,.F.);
#59522=ORIENTED_EDGE('',*,*,#44839,.F.);
#59523=ORIENTED_EDGE('',*,*,#44829,.F.);
#59524=ORIENTED_EDGE('',*,*,#44101,.F.);
#59525=ORIENTED_EDGE('',*,*,#44840,.T.);
#59526=ORIENTED_EDGE('',*,*,#44841,.T.);
#59527=ORIENTED_EDGE('',*,*,#44830,.T.);
#59528=ORIENTED_EDGE('',*,*,#44103,.F.);
#59529=ORIENTED_EDGE('',*,*,#44842,.F.);
#59530=ORIENTED_EDGE('',*,*,#44843,.T.);
#59531=ORIENTED_EDGE('',*,*,#44840,.F.);
#59532=ORIENTED_EDGE('',*,*,#44105,.F.);
#59533=ORIENTED_EDGE('',*,*,#44844,.T.);
#59534=ORIENTED_EDGE('',*,*,#44845,.T.);
#59535=ORIENTED_EDGE('',*,*,#44842,.T.);
#59536=ORIENTED_EDGE('',*,*,#44107,.F.);
#59537=ORIENTED_EDGE('',*,*,#44846,.F.);
#59538=ORIENTED_EDGE('',*,*,#44847,.T.);
#59539=ORIENTED_EDGE('',*,*,#44108,.T.);
#59540=ORIENTED_EDGE('',*,*,#44111,.T.);
#59541=ORIENTED_EDGE('',*,*,#44847,.F.);
#59542=ORIENTED_EDGE('',*,*,#44848,.F.);
#59543=ORIENTED_EDGE('',*,*,#44849,.F.);
#59544=ORIENTED_EDGE('',*,*,#44850,.F.);
#59545=ORIENTED_EDGE('',*,*,#44851,.F.);
#59546=ORIENTED_EDGE('',*,*,#44852,.F.);
#59547=ORIENTED_EDGE('',*,*,#44853,.F.);
#59548=ORIENTED_EDGE('',*,*,#44854,.F.);
#59549=ORIENTED_EDGE('',*,*,#44855,.F.);
#59550=ORIENTED_EDGE('',*,*,#44856,.F.);
#59551=ORIENTED_EDGE('',*,*,#44844,.F.);
#59552=ORIENTED_EDGE('',*,*,#44109,.F.);
#59553=ORIENTED_EDGE('',*,*,#44857,.F.);
#59554=ORIENTED_EDGE('',*,*,#44858,.F.);
#59555=ORIENTED_EDGE('',*,*,#44110,.F.);
#59556=ORIENTED_EDGE('',*,*,#44859,.F.);
#59557=ORIENTED_EDGE('',*,*,#44860,.F.);
#59558=ORIENTED_EDGE('',*,*,#44112,.T.);
#59559=ORIENTED_EDGE('',*,*,#44113,.T.);
#59560=ORIENTED_EDGE('',*,*,#44861,.T.);
#59561=ORIENTED_EDGE('',*,*,#44862,.F.);
#59562=ORIENTED_EDGE('',*,*,#44863,.F.);
#59563=ORIENTED_EDGE('',*,*,#44864,.F.);
#59564=ORIENTED_EDGE('',*,*,#44865,.F.);
#59565=ORIENTED_EDGE('',*,*,#44866,.F.);
#59566=ORIENTED_EDGE('',*,*,#44867,.F.);
#59567=ORIENTED_EDGE('',*,*,#44868,.F.);
#59568=ORIENTED_EDGE('',*,*,#44869,.F.);
#59569=ORIENTED_EDGE('',*,*,#44870,.F.);
#59570=ORIENTED_EDGE('',*,*,#44871,.F.);
#59571=ORIENTED_EDGE('',*,*,#44861,.F.);
#59572=ORIENTED_EDGE('',*,*,#44115,.F.);
#59573=ORIENTED_EDGE('',*,*,#44872,.T.);
#59574=ORIENTED_EDGE('',*,*,#44873,.T.);
#59575=ORIENTED_EDGE('',*,*,#44862,.T.);
#59576=ORIENTED_EDGE('',*,*,#44117,.F.);
#59577=ORIENTED_EDGE('',*,*,#44874,.F.);
#59578=ORIENTED_EDGE('',*,*,#44875,.T.);
#59579=ORIENTED_EDGE('',*,*,#44872,.F.);
#59580=ORIENTED_EDGE('',*,*,#44119,.F.);
#59581=ORIENTED_EDGE('',*,*,#44876,.T.);
#59582=ORIENTED_EDGE('',*,*,#44877,.T.);
#59583=ORIENTED_EDGE('',*,*,#44874,.T.);
#59584=ORIENTED_EDGE('',*,*,#44121,.F.);
#59585=ORIENTED_EDGE('',*,*,#44878,.F.);
#59586=ORIENTED_EDGE('',*,*,#44879,.T.);
#59587=ORIENTED_EDGE('',*,*,#44122,.T.);
#59588=ORIENTED_EDGE('',*,*,#44125,.T.);
#59589=ORIENTED_EDGE('',*,*,#44879,.F.);
#59590=ORIENTED_EDGE('',*,*,#44880,.F.);
#59591=ORIENTED_EDGE('',*,*,#44881,.F.);
#59592=ORIENTED_EDGE('',*,*,#44882,.F.);
#59593=ORIENTED_EDGE('',*,*,#44883,.F.);
#59594=ORIENTED_EDGE('',*,*,#44884,.F.);
#59595=ORIENTED_EDGE('',*,*,#44885,.F.);
#59596=ORIENTED_EDGE('',*,*,#44886,.F.);
#59597=ORIENTED_EDGE('',*,*,#44887,.F.);
#59598=ORIENTED_EDGE('',*,*,#44888,.F.);
#59599=ORIENTED_EDGE('',*,*,#44876,.F.);
#59600=ORIENTED_EDGE('',*,*,#44123,.F.);
#59601=ORIENTED_EDGE('',*,*,#44889,.F.);
#59602=ORIENTED_EDGE('',*,*,#44890,.F.);
#59603=ORIENTED_EDGE('',*,*,#44124,.F.);
#59604=ORIENTED_EDGE('',*,*,#44891,.F.);
#59605=ORIENTED_EDGE('',*,*,#44129,.F.);
#59606=ORIENTED_EDGE('',*,*,#44892,.T.);
#59607=ORIENTED_EDGE('',*,*,#44893,.T.);
#59608=ORIENTED_EDGE('',*,*,#44126,.T.);
#59609=ORIENTED_EDGE('',*,*,#44894,.F.);
#59610=ORIENTED_EDGE('',*,*,#44895,.F.);
#59611=ORIENTED_EDGE('',*,*,#44896,.F.);
#59612=ORIENTED_EDGE('',*,*,#44897,.F.);
#59613=ORIENTED_EDGE('',*,*,#44898,.F.);
#59614=ORIENTED_EDGE('',*,*,#44899,.F.);
#59615=ORIENTED_EDGE('',*,*,#44900,.F.);
#59616=ORIENTED_EDGE('',*,*,#44901,.F.);
#59617=ORIENTED_EDGE('',*,*,#44902,.F.);
#59618=ORIENTED_EDGE('',*,*,#44903,.F.);
#59619=ORIENTED_EDGE('',*,*,#44904,.F.);
#59620=ORIENTED_EDGE('',*,*,#44892,.F.);
#59621=ORIENTED_EDGE('',*,*,#44128,.F.);
#59622=ORIENTED_EDGE('',*,*,#44905,.T.);
#59623=ORIENTED_EDGE('',*,*,#44906,.T.);
#59624=ORIENTED_EDGE('',*,*,#44894,.T.);
#59625=ORIENTED_EDGE('',*,*,#44131,.F.);
#59626=ORIENTED_EDGE('',*,*,#44907,.F.);
#59627=ORIENTED_EDGE('',*,*,#44908,.F.);
#59628=ORIENTED_EDGE('',*,*,#44905,.F.);
#59629=ORIENTED_EDGE('',*,*,#44133,.F.);
#59630=ORIENTED_EDGE('',*,*,#44909,.T.);
#59631=ORIENTED_EDGE('',*,*,#44910,.F.);
#59632=ORIENTED_EDGE('',*,*,#44907,.T.);
#59633=ORIENTED_EDGE('',*,*,#44135,.F.);
#59634=ORIENTED_EDGE('',*,*,#44911,.F.);
#59635=ORIENTED_EDGE('',*,*,#44912,.T.);
#59636=ORIENTED_EDGE('',*,*,#44136,.T.);
#59637=ORIENTED_EDGE('',*,*,#44139,.T.);
#59638=ORIENTED_EDGE('',*,*,#44912,.F.);
#59639=ORIENTED_EDGE('',*,*,#44913,.F.);
#59640=ORIENTED_EDGE('',*,*,#44914,.F.);
#59641=ORIENTED_EDGE('',*,*,#44915,.F.);
#59642=ORIENTED_EDGE('',*,*,#44916,.F.);
#59643=ORIENTED_EDGE('',*,*,#44917,.F.);
#59644=ORIENTED_EDGE('',*,*,#44918,.F.);
#59645=ORIENTED_EDGE('',*,*,#44919,.F.);
#59646=ORIENTED_EDGE('',*,*,#44920,.F.);
#59647=ORIENTED_EDGE('',*,*,#44921,.F.);
#59648=ORIENTED_EDGE('',*,*,#44922,.F.);
#59649=ORIENTED_EDGE('',*,*,#44923,.F.);
#59650=ORIENTED_EDGE('',*,*,#44909,.F.);
#59651=ORIENTED_EDGE('',*,*,#44137,.F.);
#59652=ORIENTED_EDGE('',*,*,#44924,.F.);
#59653=ORIENTED_EDGE('',*,*,#44925,.F.);
#59654=ORIENTED_EDGE('',*,*,#44138,.F.);
#59655=ORIENTED_EDGE('',*,*,#44926,.F.);
#59656=ORIENTED_EDGE('',*,*,#44143,.F.);
#59657=ORIENTED_EDGE('',*,*,#44927,.T.);
#59658=ORIENTED_EDGE('',*,*,#44928,.T.);
#59659=ORIENTED_EDGE('',*,*,#44140,.T.);
#59660=ORIENTED_EDGE('',*,*,#44929,.F.);
#59661=ORIENTED_EDGE('',*,*,#44930,.F.);
#59662=ORIENTED_EDGE('',*,*,#44931,.F.);
#59663=ORIENTED_EDGE('',*,*,#44932,.F.);
#59664=ORIENTED_EDGE('',*,*,#44933,.F.);
#59665=ORIENTED_EDGE('',*,*,#44934,.F.);
#59666=ORIENTED_EDGE('',*,*,#44927,.F.);
#59667=ORIENTED_EDGE('',*,*,#44142,.F.);
#59668=ORIENTED_EDGE('',*,*,#44733,.F.);
#59669=ORIENTED_EDGE('',*,*,#44935,.F.);
#59670=ORIENTED_EDGE('',*,*,#44936,.F.);
#59671=ORIENTED_EDGE('',*,*,#44937,.F.);
#59672=ORIENTED_EDGE('',*,*,#44938,.F.);
#59673=ORIENTED_EDGE('',*,*,#44939,.F.);
#59674=ORIENTED_EDGE('',*,*,#44940,.F.);
#59675=ORIENTED_EDGE('',*,*,#44941,.F.);
#59676=ORIENTED_EDGE('',*,*,#44942,.F.);
#59677=ORIENTED_EDGE('',*,*,#44145,.F.);
#59678=ORIENTED_EDGE('',*,*,#44943,.F.);
#59679=ORIENTED_EDGE('',*,*,#44944,.F.);
#59680=ORIENTED_EDGE('',*,*,#44147,.T.);
#59681=ORIENTED_EDGE('',*,*,#44148,.T.);
#59682=ORIENTED_EDGE('',*,*,#44945,.T.);
#59683=ORIENTED_EDGE('',*,*,#44946,.F.);
#59684=ORIENTED_EDGE('',*,*,#44947,.T.);
#59685=ORIENTED_EDGE('',*,*,#44179,.T.);
#59686=ORIENTED_EDGE('',*,*,#44146,.T.);
#59687=ORIENTED_EDGE('',*,*,#44948,.F.);
#59688=ORIENTED_EDGE('',*,*,#44949,.F.);
#59689=ORIENTED_EDGE('',*,*,#44950,.F.);
#59690=ORIENTED_EDGE('',*,*,#44951,.F.);
#59691=ORIENTED_EDGE('',*,*,#44952,.F.);
#59692=ORIENTED_EDGE('',*,*,#44953,.F.);
#59693=ORIENTED_EDGE('',*,*,#44954,.F.);
#59694=ORIENTED_EDGE('',*,*,#44955,.F.);
#59695=ORIENTED_EDGE('',*,*,#44956,.F.);
#59696=ORIENTED_EDGE('',*,*,#44945,.F.);
#59697=ORIENTED_EDGE('',*,*,#44150,.F.);
#59698=ORIENTED_EDGE('',*,*,#44957,.F.);
#59699=ORIENTED_EDGE('',*,*,#44958,.F.);
#59700=ORIENTED_EDGE('',*,*,#44959,.F.);
#59701=ORIENTED_EDGE('',*,*,#44960,.F.);
#59702=ORIENTED_EDGE('',*,*,#44961,.F.);
#59703=ORIENTED_EDGE('',*,*,#44962,.F.);
#59704=ORIENTED_EDGE('',*,*,#44963,.T.);
#59705=ORIENTED_EDGE('',*,*,#44964,.T.);
#59706=ORIENTED_EDGE('',*,*,#44957,.T.);
#59707=ORIENTED_EDGE('',*,*,#44152,.F.);
#59708=ORIENTED_EDGE('',*,*,#44965,.F.);
#59709=ORIENTED_EDGE('',*,*,#44966,.F.);
#59710=ORIENTED_EDGE('',*,*,#44963,.F.);
#59711=ORIENTED_EDGE('',*,*,#44154,.F.);
#59712=ORIENTED_EDGE('',*,*,#44967,.T.);
#59713=ORIENTED_EDGE('',*,*,#44968,.T.);
#59714=ORIENTED_EDGE('',*,*,#44965,.T.);
#59715=ORIENTED_EDGE('',*,*,#44156,.F.);
#59716=ORIENTED_EDGE('',*,*,#44969,.F.);
#59717=ORIENTED_EDGE('',*,*,#44970,.F.);
#59718=ORIENTED_EDGE('',*,*,#44971,.F.);
#59719=ORIENTED_EDGE('',*,*,#44972,.F.);
#59720=ORIENTED_EDGE('',*,*,#44973,.F.);
#59721=ORIENTED_EDGE('',*,*,#44974,.F.);
#59722=ORIENTED_EDGE('',*,*,#44975,.F.);
#59723=ORIENTED_EDGE('',*,*,#44976,.F.);
#59724=ORIENTED_EDGE('',*,*,#44967,.F.);
#59725=ORIENTED_EDGE('',*,*,#44158,.F.);
#59726=ORIENTED_EDGE('',*,*,#44977,.F.);
#59727=ORIENTED_EDGE('',*,*,#44978,.F.);
#59728=ORIENTED_EDGE('',*,*,#44979,.F.);
#59729=ORIENTED_EDGE('',*,*,#44980,.F.);
#59730=ORIENTED_EDGE('',*,*,#44981,.F.);
#59731=ORIENTED_EDGE('',*,*,#44982,.F.);
#59732=ORIENTED_EDGE('',*,*,#44157,.F.);
#59733=ORIENTED_EDGE('',*,*,#44160,.T.);
#59734=ORIENTED_EDGE('',*,*,#44983,.T.);
#59735=ORIENTED_EDGE('',*,*,#44977,.T.);
#59736=ORIENTED_EDGE('',*,*,#44984,.F.);
#59737=ORIENTED_EDGE('',*,*,#44985,.T.);
#59738=ORIENTED_EDGE('',*,*,#44163,.T.);
#59739=ORIENTED_EDGE('',*,*,#44167,.T.);
#59740=ORIENTED_EDGE('',*,*,#44986,.F.);
#59741=ORIENTED_EDGE('',*,*,#44987,.F.);
#59742=ORIENTED_EDGE('',*,*,#44988,.F.);
#59743=ORIENTED_EDGE('',*,*,#44989,.F.);
#59744=ORIENTED_EDGE('',*,*,#44303,.F.);
#59745=ORIENTED_EDGE('',*,*,#44164,.F.);
#59746=ORIENTED_EDGE('',*,*,#44985,.F.);
#59747=ORIENTED_EDGE('',*,*,#44990,.F.);
#59748=ORIENTED_EDGE('',*,*,#44991,.F.);
#59749=ORIENTED_EDGE('',*,*,#44992,.F.);
#59750=ORIENTED_EDGE('',*,*,#44993,.F.);
#59751=ORIENTED_EDGE('',*,*,#44994,.F.);
#59752=ORIENTED_EDGE('',*,*,#44995,.F.);
#59753=ORIENTED_EDGE('',*,*,#44996,.F.);
#59754=ORIENTED_EDGE('',*,*,#44997,.F.);
#59755=ORIENTED_EDGE('',*,*,#44998,.F.);
#59756=ORIENTED_EDGE('',*,*,#44999,.T.);
#59757=ORIENTED_EDGE('',*,*,#45000,.F.);
#59758=ORIENTED_EDGE('',*,*,#44166,.F.);
#59759=ORIENTED_EDGE('',*,*,#45001,.T.);
#59760=ORIENTED_EDGE('',*,*,#45002,.F.);
#59761=ORIENTED_EDGE('',*,*,#45001,.F.);
#59762=ORIENTED_EDGE('',*,*,#44168,.F.);
#59763=ORIENTED_EDGE('',*,*,#45003,.F.);
#59764=ORIENTED_EDGE('',*,*,#45004,.F.);
#59765=ORIENTED_EDGE('',*,*,#44169,.T.);
#59766=ORIENTED_EDGE('',*,*,#44170,.T.);
#59767=ORIENTED_EDGE('',*,*,#45005,.T.);
#59768=ORIENTED_EDGE('',*,*,#45006,.F.);
#59769=ORIENTED_EDGE('',*,*,#45007,.F.);
#59770=ORIENTED_EDGE('',*,*,#45008,.F.);
#59771=ORIENTED_EDGE('',*,*,#45009,.F.);
#59772=ORIENTED_EDGE('',*,*,#45010,.F.);
#59773=ORIENTED_EDGE('',*,*,#45011,.F.);
#59774=ORIENTED_EDGE('',*,*,#45012,.F.);
#59775=ORIENTED_EDGE('',*,*,#45013,.F.);
#59776=ORIENTED_EDGE('',*,*,#45014,.F.);
#59777=ORIENTED_EDGE('',*,*,#45015,.F.);
#59778=ORIENTED_EDGE('',*,*,#45016,.F.);
#59779=ORIENTED_EDGE('',*,*,#45017,.F.);
#59780=ORIENTED_EDGE('',*,*,#45018,.F.);
#59781=ORIENTED_EDGE('',*,*,#45019,.F.);
#59782=ORIENTED_EDGE('',*,*,#45020,.F.);
#59783=ORIENTED_EDGE('',*,*,#45021,.F.);
#59784=ORIENTED_EDGE('',*,*,#45005,.F.);
#59785=ORIENTED_EDGE('',*,*,#44172,.F.);
#59786=ORIENTED_EDGE('',*,*,#45022,.T.);
#59787=ORIENTED_EDGE('',*,*,#45023,.T.);
#59788=ORIENTED_EDGE('',*,*,#45006,.T.);
#59789=ORIENTED_EDGE('',*,*,#44174,.F.);
#59790=ORIENTED_EDGE('',*,*,#45024,.F.);
#59791=ORIENTED_EDGE('',*,*,#45025,.F.);
#59792=ORIENTED_EDGE('',*,*,#45022,.F.);
#59793=ORIENTED_EDGE('',*,*,#44176,.F.);
#59794=ORIENTED_EDGE('',*,*,#45026,.T.);
#59795=ORIENTED_EDGE('',*,*,#45027,.F.);
#59796=ORIENTED_EDGE('',*,*,#45024,.T.);
#59797=ORIENTED_EDGE('',*,*,#44178,.F.);
#59798=ORIENTED_EDGE('',*,*,#45028,.F.);
#59799=ORIENTED_EDGE('',*,*,#45029,.F.);
#59800=ORIENTED_EDGE('',*,*,#45030,.F.);
#59801=ORIENTED_EDGE('',*,*,#45031,.F.);
#59802=ORIENTED_EDGE('',*,*,#45026,.F.);
#59803=ORIENTED_EDGE('',*,*,#44180,.F.);
#59804=ORIENTED_EDGE('',*,*,#44947,.F.);
#59805=ORIENTED_EDGE('',*,*,#45032,.F.);
#59806=ORIENTED_EDGE('',*,*,#45033,.F.);
#59807=ORIENTED_EDGE('',*,*,#45034,.F.);
#59808=ORIENTED_EDGE('',*,*,#45035,.F.);
#59809=ORIENTED_EDGE('',*,*,#45036,.F.);
#59810=ORIENTED_EDGE('',*,*,#45037,.F.);
#59811=ORIENTED_EDGE('',*,*,#45038,.F.);
#59812=ORIENTED_EDGE('',*,*,#45039,.F.);
#59813=ORIENTED_EDGE('',*,*,#45040,.F.);
#59814=ORIENTED_EDGE('',*,*,#45041,.F.);
#59815=ORIENTED_EDGE('',*,*,#45042,.F.);
#59816=ORIENTED_EDGE('',*,*,#45043,.F.);
#59817=ORIENTED_EDGE('',*,*,#45044,.F.);
#59818=ORIENTED_EDGE('',*,*,#44184,.F.);
#59819=ORIENTED_EDGE('',*,*,#45045,.F.);
#59820=ORIENTED_EDGE('',*,*,#44189,.F.);
#59821=ORIENTED_EDGE('',*,*,#45046,.T.);
#59822=ORIENTED_EDGE('',*,*,#45047,.T.);
#59823=ORIENTED_EDGE('',*,*,#44186,.T.);
#59824=ORIENTED_EDGE('',*,*,#44211,.F.);
#59825=ORIENTED_EDGE('',*,*,#44185,.T.);
#59826=ORIENTED_EDGE('',*,*,#45048,.T.);
#59827=ORIENTED_EDGE('',*,*,#45049,.T.);
#59828=ORIENTED_EDGE('',*,*,#45050,.F.);
#59829=ORIENTED_EDGE('',*,*,#45051,.F.);
#59830=ORIENTED_EDGE('',*,*,#45052,.F.);
#59831=ORIENTED_EDGE('',*,*,#44413,.F.);
#59832=ORIENTED_EDGE('',*,*,#45053,.F.);
#59833=ORIENTED_EDGE('',*,*,#45054,.F.);
#59834=ORIENTED_EDGE('',*,*,#45055,.F.);
#59835=ORIENTED_EDGE('',*,*,#45056,.F.);
#59836=ORIENTED_EDGE('',*,*,#45057,.F.);
#59837=ORIENTED_EDGE('',*,*,#45058,.F.);
#59838=ORIENTED_EDGE('',*,*,#45046,.F.);
#59839=ORIENTED_EDGE('',*,*,#44188,.F.);
#59840=ORIENTED_EDGE('',*,*,#45059,.T.);
#59841=ORIENTED_EDGE('',*,*,#45060,.T.);
#59842=ORIENTED_EDGE('',*,*,#45050,.T.);
#59843=ORIENTED_EDGE('',*,*,#44191,.F.);
#59844=ORIENTED_EDGE('',*,*,#45061,.F.);
#59845=ORIENTED_EDGE('',*,*,#45062,.F.);
#59846=ORIENTED_EDGE('',*,*,#45059,.F.);
#59847=ORIENTED_EDGE('',*,*,#44193,.F.);
#59848=ORIENTED_EDGE('',*,*,#45063,.T.);
#59849=ORIENTED_EDGE('',*,*,#45064,.F.);
#59850=ORIENTED_EDGE('',*,*,#45061,.T.);
#59851=ORIENTED_EDGE('',*,*,#44195,.F.);
#59852=ORIENTED_EDGE('',*,*,#45065,.F.);
#59853=ORIENTED_EDGE('',*,*,#45066,.F.);
#59854=ORIENTED_EDGE('',*,*,#45067,.F.);
#59855=ORIENTED_EDGE('',*,*,#45068,.F.);
#59856=ORIENTED_EDGE('',*,*,#45069,.F.);
#59857=ORIENTED_EDGE('',*,*,#45070,.F.);
#59858=ORIENTED_EDGE('',*,*,#44401,.F.);
#59859=ORIENTED_EDGE('',*,*,#45071,.F.);
#59860=ORIENTED_EDGE('',*,*,#45072,.F.);
#59861=ORIENTED_EDGE('',*,*,#45063,.F.);
#59862=ORIENTED_EDGE('',*,*,#44197,.F.);
#59863=ORIENTED_EDGE('',*,*,#44196,.F.);
#59864=ORIENTED_EDGE('',*,*,#44199,.T.);
#59865=ORIENTED_EDGE('',*,*,#45073,.T.);
#59866=ORIENTED_EDGE('',*,*,#45065,.T.);
#59867=ORIENTED_EDGE('',*,*,#45074,.F.);
#59868=ORIENTED_EDGE('',*,*,#44201,.T.);
#59869=ORIENTED_EDGE('',*,*,#44202,.T.);
#59870=ORIENTED_EDGE('',*,*,#45075,.T.);
#59871=ORIENTED_EDGE('',*,*,#45076,.F.);
#59872=ORIENTED_EDGE('',*,*,#45077,.F.);
#59873=ORIENTED_EDGE('',*,*,#45075,.F.);
#59874=ORIENTED_EDGE('',*,*,#44204,.F.);
#59875=ORIENTED_EDGE('',*,*,#45078,.F.);
#59876=ORIENTED_EDGE('',*,*,#45079,.F.);
#59877=ORIENTED_EDGE('',*,*,#45080,.F.);
#59878=ORIENTED_EDGE('',*,*,#45081,.F.);
#59879=ORIENTED_EDGE('',*,*,#45082,.T.);
#59880=ORIENTED_EDGE('',*,*,#45083,.T.);
#59881=ORIENTED_EDGE('',*,*,#45078,.T.);
#59882=ORIENTED_EDGE('',*,*,#44206,.F.);
#59883=ORIENTED_EDGE('',*,*,#45084,.F.);
#59884=ORIENTED_EDGE('',*,*,#45085,.F.);
#59885=ORIENTED_EDGE('',*,*,#45082,.F.);
#59886=ORIENTED_EDGE('',*,*,#44208,.F.);
#59887=ORIENTED_EDGE('',*,*,#45086,.T.);
#59888=ORIENTED_EDGE('',*,*,#45087,.F.);
#59889=ORIENTED_EDGE('',*,*,#45084,.T.);
#59890=ORIENTED_EDGE('',*,*,#44210,.F.);
#59891=ORIENTED_EDGE('',*,*,#45088,.F.);
#59892=ORIENTED_EDGE('',*,*,#45089,.F.);
#59893=ORIENTED_EDGE('',*,*,#45086,.F.);
#59894=ORIENTED_EDGE('',*,*,#44212,.F.);
#59895=ORIENTED_EDGE('',*,*,#45049,.F.);
#59896=ORIENTED_EDGE('',*,*,#45090,.F.);
#59897=ORIENTED_EDGE('',*,*,#45091,.F.);
#59898=ORIENTED_EDGE('',*,*,#45092,.F.);
#59899=ORIENTED_EDGE('',*,*,#45093,.F.);
#59900=ORIENTED_EDGE('',*,*,#45094,.F.);
#59901=ORIENTED_EDGE('',*,*,#45095,.F.);
#59902=ORIENTED_EDGE('',*,*,#44420,.F.);
#59903=ORIENTED_EDGE('',*,*,#45096,.F.);
#59904=ORIENTED_EDGE('',*,*,#45097,.F.);
#59905=ORIENTED_EDGE('',*,*,#44214,.F.);
#59906=ORIENTED_EDGE('',*,*,#45098,.F.);
#59907=ORIENTED_EDGE('',*,*,#44219,.F.);
#59908=ORIENTED_EDGE('',*,*,#45099,.T.);
#59909=ORIENTED_EDGE('',*,*,#45100,.T.);
#59910=ORIENTED_EDGE('',*,*,#44216,.T.);
#59911=ORIENTED_EDGE('',*,*,#45101,.F.);
#59912=ORIENTED_EDGE('',*,*,#45102,.T.);
#59913=ORIENTED_EDGE('',*,*,#44249,.T.);
#59914=ORIENTED_EDGE('',*,*,#44215,.T.);
#59915=ORIENTED_EDGE('',*,*,#45103,.F.);
#59916=ORIENTED_EDGE('',*,*,#45104,.F.);
#59917=ORIENTED_EDGE('',*,*,#45105,.F.);
#59918=ORIENTED_EDGE('',*,*,#45106,.F.);
#59919=ORIENTED_EDGE('',*,*,#45107,.F.);
#59920=ORIENTED_EDGE('',*,*,#45108,.F.);
#59921=ORIENTED_EDGE('',*,*,#45109,.F.);
#59922=ORIENTED_EDGE('',*,*,#45110,.F.);
#59923=ORIENTED_EDGE('',*,*,#45111,.F.);
#59924=ORIENTED_EDGE('',*,*,#45112,.F.);
#59925=ORIENTED_EDGE('',*,*,#45099,.F.);
#59926=ORIENTED_EDGE('',*,*,#44218,.F.);
#59927=ORIENTED_EDGE('',*,*,#45113,.F.);
#59928=ORIENTED_EDGE('',*,*,#45114,.F.);
#59929=ORIENTED_EDGE('',*,*,#45115,.F.);
#59930=ORIENTED_EDGE('',*,*,#45116,.F.);
#59931=ORIENTED_EDGE('',*,*,#45117,.F.);
#59932=ORIENTED_EDGE('',*,*,#45118,.F.);
#59933=ORIENTED_EDGE('',*,*,#45119,.T.);
#59934=ORIENTED_EDGE('',*,*,#45120,.T.);
#59935=ORIENTED_EDGE('',*,*,#45113,.T.);
#59936=ORIENTED_EDGE('',*,*,#44221,.F.);
#59937=ORIENTED_EDGE('',*,*,#45121,.F.);
#59938=ORIENTED_EDGE('',*,*,#45122,.F.);
#59939=ORIENTED_EDGE('',*,*,#45119,.F.);
#59940=ORIENTED_EDGE('',*,*,#44223,.F.);
#59941=ORIENTED_EDGE('',*,*,#45123,.T.);
#59942=ORIENTED_EDGE('',*,*,#45124,.F.);
#59943=ORIENTED_EDGE('',*,*,#45121,.T.);
#59944=ORIENTED_EDGE('',*,*,#44225,.F.);
#59945=ORIENTED_EDGE('',*,*,#45125,.F.);
#59946=ORIENTED_EDGE('',*,*,#45126,.T.);
#59947=ORIENTED_EDGE('',*,*,#44226,.T.);
#59948=ORIENTED_EDGE('',*,*,#44229,.T.);
#59949=ORIENTED_EDGE('',*,*,#45127,.F.);
#59950=ORIENTED_EDGE('',*,*,#45128,.F.);
#59951=ORIENTED_EDGE('',*,*,#45129,.F.);
#59952=ORIENTED_EDGE('',*,*,#45130,.F.);
#59953=ORIENTED_EDGE('',*,*,#45131,.F.);
#59954=ORIENTED_EDGE('',*,*,#45132,.F.);
#59955=ORIENTED_EDGE('',*,*,#45133,.F.);
#59956=ORIENTED_EDGE('',*,*,#45134,.F.);
#59957=ORIENTED_EDGE('',*,*,#45135,.F.);
#59958=ORIENTED_EDGE('',*,*,#45136,.F.);
#59959=ORIENTED_EDGE('',*,*,#45123,.F.);
#59960=ORIENTED_EDGE('',*,*,#44227,.F.);
#59961=ORIENTED_EDGE('',*,*,#45126,.F.);
#59962=ORIENTED_EDGE('',*,*,#45137,.F.);
#59963=ORIENTED_EDGE('',*,*,#45138,.F.);
#59964=ORIENTED_EDGE('',*,*,#45139,.F.);
#59965=ORIENTED_EDGE('',*,*,#45140,.F.);
#59966=ORIENTED_EDGE('',*,*,#45141,.F.);
#59967=ORIENTED_EDGE('',*,*,#45142,.F.);
#59968=ORIENTED_EDGE('',*,*,#45143,.F.);
#59969=ORIENTED_EDGE('',*,*,#45144,.F.);
#59970=ORIENTED_EDGE('',*,*,#45145,.F.);
#59971=ORIENTED_EDGE('',*,*,#44736,.F.);
#59972=ORIENTED_EDGE('',*,*,#44233,.F.);
#59973=ORIENTED_EDGE('',*,*,#45146,.F.);
#59974=ORIENTED_EDGE('',*,*,#45147,.F.);
#59975=ORIENTED_EDGE('',*,*,#45148,.F.);
#59976=ORIENTED_EDGE('',*,*,#45149,.F.);
#59977=ORIENTED_EDGE('',*,*,#45150,.F.);
#59978=ORIENTED_EDGE('',*,*,#45151,.F.);
#59979=ORIENTED_EDGE('',*,*,#45152,.F.);
#59980=ORIENTED_EDGE('',*,*,#45153,.F.);
#59981=ORIENTED_EDGE('',*,*,#45154,.F.);
#59982=ORIENTED_EDGE('',*,*,#45155,.F.);
#59983=ORIENTED_EDGE('',*,*,#45156,.F.);
#59984=ORIENTED_EDGE('',*,*,#44232,.F.);
#59985=ORIENTED_EDGE('',*,*,#44237,.T.);
#59986=ORIENTED_EDGE('',*,*,#45157,.T.);
#59987=ORIENTED_EDGE('',*,*,#45146,.T.);
#59988=ORIENTED_EDGE('',*,*,#44236,.F.);
#59989=ORIENTED_EDGE('',*,*,#45158,.T.);
#59990=ORIENTED_EDGE('',*,*,#45159,.F.);
#59991=ORIENTED_EDGE('',*,*,#45160,.T.);
#59992=ORIENTED_EDGE('',*,*,#45161,.F.);
#59993=ORIENTED_EDGE('',*,*,#45158,.F.);
#59994=ORIENTED_EDGE('',*,*,#44235,.F.);
#59995=ORIENTED_EDGE('',*,*,#45162,.T.);
#59996=ORIENTED_EDGE('',*,*,#45163,.F.);
#59997=ORIENTED_EDGE('',*,*,#45162,.F.);
#59998=ORIENTED_EDGE('',*,*,#44238,.F.);
#59999=ORIENTED_EDGE('',*,*,#45164,.F.);
#60000=ORIENTED_EDGE('',*,*,#45165,.F.);
#60001=ORIENTED_EDGE('',*,*,#44239,.T.);
#60002=ORIENTED_EDGE('',*,*,#44240,.T.);
#60003=ORIENTED_EDGE('',*,*,#45166,.T.);
#60004=ORIENTED_EDGE('',*,*,#45167,.F.);
#60005=ORIENTED_EDGE('',*,*,#45168,.F.);
#60006=ORIENTED_EDGE('',*,*,#45169,.F.);
#60007=ORIENTED_EDGE('',*,*,#45170,.F.);
#60008=ORIENTED_EDGE('',*,*,#45171,.F.);
#60009=ORIENTED_EDGE('',*,*,#45172,.F.);
#60010=ORIENTED_EDGE('',*,*,#45173,.F.);
#60011=ORIENTED_EDGE('',*,*,#45174,.F.);
#60012=ORIENTED_EDGE('',*,*,#45175,.F.);
#60013=ORIENTED_EDGE('',*,*,#45176,.F.);
#60014=ORIENTED_EDGE('',*,*,#45177,.F.);
#60015=ORIENTED_EDGE('',*,*,#45178,.F.);
#60016=ORIENTED_EDGE('',*,*,#45179,.F.);
#60017=ORIENTED_EDGE('',*,*,#45180,.F.);
#60018=ORIENTED_EDGE('',*,*,#45181,.F.);
#60019=ORIENTED_EDGE('',*,*,#45182,.F.);
#60020=ORIENTED_EDGE('',*,*,#45166,.F.);
#60021=ORIENTED_EDGE('',*,*,#44242,.F.);
#60022=ORIENTED_EDGE('',*,*,#45183,.T.);
#60023=ORIENTED_EDGE('',*,*,#45184,.T.);
#60024=ORIENTED_EDGE('',*,*,#45167,.T.);
#60025=ORIENTED_EDGE('',*,*,#44244,.F.);
#60026=ORIENTED_EDGE('',*,*,#45185,.F.);
#60027=ORIENTED_EDGE('',*,*,#45186,.F.);
#60028=ORIENTED_EDGE('',*,*,#45183,.F.);
#60029=ORIENTED_EDGE('',*,*,#44246,.F.);
#60030=ORIENTED_EDGE('',*,*,#45187,.T.);
#60031=ORIENTED_EDGE('',*,*,#45188,.F.);
#60032=ORIENTED_EDGE('',*,*,#45185,.T.);
#60033=ORIENTED_EDGE('',*,*,#44248,.F.);
#60034=ORIENTED_EDGE('',*,*,#45189,.F.);
#60035=ORIENTED_EDGE('',*,*,#45190,.F.);
#60036=ORIENTED_EDGE('',*,*,#45191,.F.);
#60037=ORIENTED_EDGE('',*,*,#45192,.F.);
#60038=ORIENTED_EDGE('',*,*,#45187,.F.);
#60039=ORIENTED_EDGE('',*,*,#44250,.F.);
#60040=ORIENTED_EDGE('',*,*,#45102,.F.);
#60041=ORIENTED_EDGE('',*,*,#45193,.F.);
#60042=ORIENTED_EDGE('',*,*,#45194,.F.);
#60043=ORIENTED_EDGE('',*,*,#45195,.F.);
#60044=ORIENTED_EDGE('',*,*,#45196,.F.);
#60045=ORIENTED_EDGE('',*,*,#45197,.F.);
#60046=ORIENTED_EDGE('',*,*,#45198,.F.);
#60047=ORIENTED_EDGE('',*,*,#45199,.F.);
#60048=ORIENTED_EDGE('',*,*,#45200,.F.);
#60049=ORIENTED_EDGE('',*,*,#45201,.F.);
#60050=ORIENTED_EDGE('',*,*,#45202,.F.);
#60051=ORIENTED_EDGE('',*,*,#45203,.F.);
#60052=ORIENTED_EDGE('',*,*,#45204,.T.);
#60053=ORIENTED_EDGE('',*,*,#45205,.F.);
#60054=ORIENTED_EDGE('',*,*,#45206,.T.);
#60055=ORIENTED_EDGE('',*,*,#44251,.F.);
#60056=ORIENTED_EDGE('',*,*,#45207,.F.);
#60057=ORIENTED_EDGE('',*,*,#44256,.F.);
#60058=ORIENTED_EDGE('',*,*,#45208,.T.);
#60059=ORIENTED_EDGE('',*,*,#45209,.T.);
#60060=ORIENTED_EDGE('',*,*,#44253,.T.);
#60061=ORIENTED_EDGE('',*,*,#45210,.F.);
#60062=ORIENTED_EDGE('',*,*,#45211,.F.);
#60063=ORIENTED_EDGE('',*,*,#45212,.F.);
#60064=ORIENTED_EDGE('',*,*,#45213,.F.);
#60065=ORIENTED_EDGE('',*,*,#45214,.F.);
#60066=ORIENTED_EDGE('',*,*,#45215,.F.);
#60067=ORIENTED_EDGE('',*,*,#45216,.F.);
#60068=ORIENTED_EDGE('',*,*,#45217,.F.);
#60069=ORIENTED_EDGE('',*,*,#45208,.F.);
#60070=ORIENTED_EDGE('',*,*,#44255,.F.);
#60071=ORIENTED_EDGE('',*,*,#44740,.F.);
#60072=ORIENTED_EDGE('',*,*,#45218,.F.);
#60073=ORIENTED_EDGE('',*,*,#45219,.F.);
#60074=ORIENTED_EDGE('',*,*,#45220,.F.);
#60075=ORIENTED_EDGE('',*,*,#45221,.F.);
#60076=ORIENTED_EDGE('',*,*,#45222,.F.);
#60077=ORIENTED_EDGE('',*,*,#45223,.F.);
#60078=ORIENTED_EDGE('',*,*,#44259,.T.);
#60079=ORIENTED_EDGE('',*,*,#44260,.T.);
#60080=ORIENTED_EDGE('',*,*,#45224,.T.);
#60081=ORIENTED_EDGE('',*,*,#45225,.F.);
#60082=ORIENTED_EDGE('',*,*,#45226,.F.);
#60083=ORIENTED_EDGE('',*,*,#45227,.F.);
#60084=ORIENTED_EDGE('',*,*,#45228,.F.);
#60085=ORIENTED_EDGE('',*,*,#45229,.F.);
#60086=ORIENTED_EDGE('',*,*,#45230,.F.);
#60087=ORIENTED_EDGE('',*,*,#45231,.F.);
#60088=ORIENTED_EDGE('',*,*,#45232,.F.);
#60089=ORIENTED_EDGE('',*,*,#45224,.F.);
#60090=ORIENTED_EDGE('',*,*,#44262,.F.);
#60091=ORIENTED_EDGE('',*,*,#45233,.F.);
#60092=ORIENTED_EDGE('',*,*,#45234,.F.);
#60093=ORIENTED_EDGE('',*,*,#45235,.F.);
#60094=ORIENTED_EDGE('',*,*,#45236,.F.);
#60095=ORIENTED_EDGE('',*,*,#45237,.F.);
#60096=ORIENTED_EDGE('',*,*,#45238,.F.);
#60097=ORIENTED_EDGE('',*,*,#45239,.T.);
#60098=ORIENTED_EDGE('',*,*,#45240,.F.);
#60099=ORIENTED_EDGE('',*,*,#45233,.T.);
#60100=ORIENTED_EDGE('',*,*,#44264,.F.);
#60101=ORIENTED_EDGE('',*,*,#45241,.F.);
#60102=ORIENTED_EDGE('',*,*,#45242,.F.);
#60103=ORIENTED_EDGE('',*,*,#45239,.F.);
#60104=ORIENTED_EDGE('',*,*,#44266,.F.);
#60105=ORIENTED_EDGE('',*,*,#45243,.T.);
#60106=ORIENTED_EDGE('',*,*,#45244,.F.);
#60107=ORIENTED_EDGE('',*,*,#45241,.T.);
#60108=ORIENTED_EDGE('',*,*,#44268,.F.);
#60109=ORIENTED_EDGE('',*,*,#45245,.F.);
#60110=ORIENTED_EDGE('',*,*,#45246,.F.);
#60111=ORIENTED_EDGE('',*,*,#45247,.F.);
#60112=ORIENTED_EDGE('',*,*,#45248,.F.);
#60113=ORIENTED_EDGE('',*,*,#45243,.F.);
#60114=ORIENTED_EDGE('',*,*,#44270,.F.);
#60115=ORIENTED_EDGE('',*,*,#45249,.F.);
#60116=ORIENTED_EDGE('',*,*,#45250,.F.);
#60117=ORIENTED_EDGE('',*,*,#45251,.F.);
#60118=ORIENTED_EDGE('',*,*,#45252,.F.);
#60119=ORIENTED_EDGE('',*,*,#45253,.F.);
#60120=ORIENTED_EDGE('',*,*,#45254,.F.);
#60121=ORIENTED_EDGE('',*,*,#45255,.F.);
#60122=ORIENTED_EDGE('',*,*,#45256,.F.);
#60123=ORIENTED_EDGE('',*,*,#45257,.F.);
#60124=ORIENTED_EDGE('',*,*,#45258,.F.);
#60125=ORIENTED_EDGE('',*,*,#45259,.F.);
#60126=ORIENTED_EDGE('',*,*,#45260,.F.);
#60127=ORIENTED_EDGE('',*,*,#44269,.F.);
#60128=ORIENTED_EDGE('',*,*,#44272,.T.);
#60129=ORIENTED_EDGE('',*,*,#45261,.T.);
#60130=ORIENTED_EDGE('',*,*,#45249,.T.);
#60131=ORIENTED_EDGE('',*,*,#45262,.F.);
#60132=ORIENTED_EDGE('',*,*,#45263,.F.);
#60133=ORIENTED_EDGE('',*,*,#44271,.F.);
#60134=ORIENTED_EDGE('',*,*,#45264,.F.);
#60135=ORIENTED_EDGE('',*,*,#45265,.F.);
#60136=ORIENTED_EDGE('',*,*,#44273,.T.);
#60137=ORIENTED_EDGE('',*,*,#44274,.T.);
#60138=ORIENTED_EDGE('',*,*,#45266,.T.);
#60139=ORIENTED_EDGE('',*,*,#45267,.F.);
#60140=ORIENTED_EDGE('',*,*,#45268,.F.);
#60141=ORIENTED_EDGE('',*,*,#45269,.F.);
#60142=ORIENTED_EDGE('',*,*,#45270,.F.);
#60143=ORIENTED_EDGE('',*,*,#45271,.F.);
#60144=ORIENTED_EDGE('',*,*,#45272,.F.);
#60145=ORIENTED_EDGE('',*,*,#45273,.F.);
#60146=ORIENTED_EDGE('',*,*,#45274,.F.);
#60147=ORIENTED_EDGE('',*,*,#45275,.F.);
#60148=ORIENTED_EDGE('',*,*,#45276,.F.);
#60149=ORIENTED_EDGE('',*,*,#45277,.F.);
#60150=ORIENTED_EDGE('',*,*,#45278,.F.);
#60151=ORIENTED_EDGE('',*,*,#45279,.F.);
#60152=ORIENTED_EDGE('',*,*,#45280,.F.);
#60153=ORIENTED_EDGE('',*,*,#45281,.F.);
#60154=ORIENTED_EDGE('',*,*,#45282,.F.);
#60155=ORIENTED_EDGE('',*,*,#45266,.F.);
#60156=ORIENTED_EDGE('',*,*,#44276,.F.);
#60157=ORIENTED_EDGE('',*,*,#45283,.T.);
#60158=ORIENTED_EDGE('',*,*,#45284,.T.);
#60159=ORIENTED_EDGE('',*,*,#45267,.T.);
#60160=ORIENTED_EDGE('',*,*,#44278,.F.);
#60161=ORIENTED_EDGE('',*,*,#45285,.F.);
#60162=ORIENTED_EDGE('',*,*,#45286,.F.);
#60163=ORIENTED_EDGE('',*,*,#45283,.F.);
#60164=ORIENTED_EDGE('',*,*,#44280,.F.);
#60165=ORIENTED_EDGE('',*,*,#45287,.T.);
#60166=ORIENTED_EDGE('',*,*,#45288,.F.);
#60167=ORIENTED_EDGE('',*,*,#45285,.T.);
#60168=ORIENTED_EDGE('',*,*,#44283,.F.);
#60169=ORIENTED_EDGE('',*,*,#45289,.F.);
#60170=ORIENTED_EDGE('',*,*,#45290,.T.);
#60171=ORIENTED_EDGE('',*,*,#44285,.T.);
#60172=ORIENTED_EDGE('',*,*,#44284,.T.);
#60173=ORIENTED_EDGE('',*,*,#44288,.T.);
#60174=ORIENTED_EDGE('',*,*,#45291,.F.);
#60175=ORIENTED_EDGE('',*,*,#45292,.F.);
#60176=ORIENTED_EDGE('',*,*,#45293,.F.);
#60177=ORIENTED_EDGE('',*,*,#45294,.F.);
#60178=ORIENTED_EDGE('',*,*,#45287,.F.);
#60179=ORIENTED_EDGE('',*,*,#44286,.F.);
#60180=ORIENTED_EDGE('',*,*,#45290,.F.);
#60181=ORIENTED_EDGE('',*,*,#45295,.F.);
#60182=ORIENTED_EDGE('',*,*,#45296,.F.);
#60183=ORIENTED_EDGE('',*,*,#45297,.F.);
#60184=ORIENTED_EDGE('',*,*,#45298,.F.);
#60185=ORIENTED_EDGE('',*,*,#45299,.F.);
#60186=ORIENTED_EDGE('',*,*,#45300,.F.);
#60187=ORIENTED_EDGE('',*,*,#45301,.F.);
#60188=ORIENTED_EDGE('',*,*,#45302,.F.);
#60189=ORIENTED_EDGE('',*,*,#45303,.F.);
#60190=ORIENTED_EDGE('',*,*,#45304,.F.);
#60191=ORIENTED_EDGE('',*,*,#45305,.F.);
#60192=ORIENTED_EDGE('',*,*,#44287,.F.);
#60193=ORIENTED_EDGE('',*,*,#45206,.F.);
#60194=ORIENTED_EDGE('',*,*,#45306,.F.);
#60195=ORIENTED_EDGE('',*,*,#45307,.F.);
#60196=ORIENTED_EDGE('',*,*,#45137,.T.);
#60197=ORIENTED_EDGE('',*,*,#45125,.T.);
#60198=ORIENTED_EDGE('',*,*,#44295,.T.);
#60199=ORIENTED_EDGE('',*,*,#45308,.F.);
#60200=ORIENTED_EDGE('',*,*,#45309,.T.);
#60201=ORIENTED_EDGE('',*,*,#45310,.F.);
#60202=ORIENTED_EDGE('',*,*,#45309,.F.);
#60203=ORIENTED_EDGE('',*,*,#45311,.F.);
#60204=ORIENTED_EDGE('',*,*,#45310,.T.);
#60205=ORIENTED_EDGE('',*,*,#45311,.T.);
#60206=ORIENTED_EDGE('',*,*,#45312,.T.);
#60207=ORIENTED_EDGE('',*,*,#45313,.F.);
#60208=ORIENTED_EDGE('',*,*,#44294,.F.);
#60209=ORIENTED_EDGE('',*,*,#45314,.F.);
#60210=ORIENTED_EDGE('',*,*,#45312,.F.);
#60211=ORIENTED_EDGE('',*,*,#45315,.F.);
#60212=ORIENTED_EDGE('',*,*,#44293,.T.);
#60213=ORIENTED_EDGE('',*,*,#45316,.T.);
#60214=ORIENTED_EDGE('',*,*,#45139,.T.);
#60215=ORIENTED_EDGE('',*,*,#45316,.F.);
#60216=ORIENTED_EDGE('',*,*,#44292,.T.);
#60217=ORIENTED_EDGE('',*,*,#45317,.T.);
#60218=ORIENTED_EDGE('',*,*,#45318,.T.);
#60219=ORIENTED_EDGE('',*,*,#45317,.F.);
#60220=ORIENTED_EDGE('',*,*,#44291,.T.);
#60221=ORIENTED_EDGE('',*,*,#45319,.T.);
#60222=ORIENTED_EDGE('',*,*,#45320,.T.);
#60223=ORIENTED_EDGE('',*,*,#45319,.F.);
#60224=ORIENTED_EDGE('',*,*,#44290,.T.);
#60225=ORIENTED_EDGE('',*,*,#45321,.T.);
#60226=ORIENTED_EDGE('',*,*,#45322,.T.);
#60227=ORIENTED_EDGE('',*,*,#45321,.F.);
#60228=ORIENTED_EDGE('',*,*,#44289,.T.);
#60229=ORIENTED_EDGE('',*,*,#45074,.T.);
#60230=ORIENTED_EDGE('',*,*,#45077,.T.);
#60231=ORIENTED_EDGE('',*,*,#44983,.F.);
#60232=ORIENTED_EDGE('',*,*,#44299,.T.);
#60233=ORIENTED_EDGE('',*,*,#45323,.T.);
#60234=ORIENTED_EDGE('',*,*,#44978,.T.);
#60235=ORIENTED_EDGE('',*,*,#45324,.F.);
#60236=ORIENTED_EDGE('',*,*,#45325,.T.);
#60237=ORIENTED_EDGE('',*,*,#45326,.F.);
#60238=ORIENTED_EDGE('',*,*,#45325,.F.);
#60239=ORIENTED_EDGE('',*,*,#45327,.F.);
#60240=ORIENTED_EDGE('',*,*,#45326,.T.);
#60241=ORIENTED_EDGE('',*,*,#45327,.T.);
#60242=ORIENTED_EDGE('',*,*,#45328,.T.);
#60243=ORIENTED_EDGE('',*,*,#44297,.F.);
#60244=ORIENTED_EDGE('',*,*,#45329,.F.);
#60245=ORIENTED_EDGE('',*,*,#45330,.F.);
#60246=ORIENTED_EDGE('',*,*,#45331,.F.);
#60247=ORIENTED_EDGE('',*,*,#44298,.F.);
#60248=ORIENTED_EDGE('',*,*,#45328,.F.);
#60249=ORIENTED_EDGE('',*,*,#45332,.F.);
#60250=ORIENTED_EDGE('',*,*,#44296,.T.);
#60251=ORIENTED_EDGE('',*,*,#45223,.T.);
#60252=ORIENTED_EDGE('',*,*,#45232,.T.);
#60253=ORIENTED_EDGE('',*,*,#44301,.T.);
#60254=ORIENTED_EDGE('',*,*,#45333,.F.);
#60255=ORIENTED_EDGE('',*,*,#45334,.T.);
#60256=ORIENTED_EDGE('',*,*,#45335,.F.);
#60257=ORIENTED_EDGE('',*,*,#45336,.F.);
#60258=ORIENTED_EDGE('',*,*,#45333,.T.);
#60259=ORIENTED_EDGE('',*,*,#44304,.T.);
#60260=ORIENTED_EDGE('',*,*,#44989,.T.);
#60261=ORIENTED_EDGE('',*,*,#45337,.T.);
#60262=ORIENTED_EDGE('',*,*,#45338,.T.);
#60263=ORIENTED_EDGE('',*,*,#45088,.T.);
#60264=ORIENTED_EDGE('',*,*,#44318,.F.);
#60265=ORIENTED_EDGE('',*,*,#45339,.F.);
#60266=ORIENTED_EDGE('',*,*,#45340,.F.);
#60267=ORIENTED_EDGE('',*,*,#45337,.F.);
#60268=ORIENTED_EDGE('',*,*,#44321,.F.);
#60269=ORIENTED_EDGE('',*,*,#44320,.F.);
#60270=ORIENTED_EDGE('',*,*,#44326,.T.);
#60271=ORIENTED_EDGE('',*,*,#45341,.T.);
#60272=ORIENTED_EDGE('',*,*,#45342,.T.);
#60273=ORIENTED_EDGE('',*,*,#45343,.F.);
#60274=ORIENTED_EDGE('',*,*,#44322,.T.);
#60275=ORIENTED_EDGE('',*,*,#45344,.T.);
#60276=ORIENTED_EDGE('',*,*,#45345,.T.);
#60277=ORIENTED_EDGE('',*,*,#45344,.F.);
#60278=ORIENTED_EDGE('',*,*,#44330,.T.);
#60279=ORIENTED_EDGE('',*,*,#45346,.T.);
#60280=ORIENTED_EDGE('',*,*,#45141,.T.);
#60281=ORIENTED_EDGE('',*,*,#45341,.F.);
#60282=ORIENTED_EDGE('',*,*,#44325,.T.);
#60283=ORIENTED_EDGE('',*,*,#45347,.T.);
#60284=ORIENTED_EDGE('',*,*,#45081,.T.);
#60285=ORIENTED_EDGE('',*,*,#45347,.F.);
#60286=ORIENTED_EDGE('',*,*,#44324,.T.);
#60287=ORIENTED_EDGE('',*,*,#45348,.T.);
#60288=ORIENTED_EDGE('',*,*,#45349,.T.);
#60289=ORIENTED_EDGE('',*,*,#45348,.F.);
#60290=ORIENTED_EDGE('',*,*,#44323,.T.);
#60291=ORIENTED_EDGE('',*,*,#45343,.T.);
#60292=ORIENTED_EDGE('',*,*,#45350,.T.);
#60293=ORIENTED_EDGE('',*,*,#45351,.T.);
#60294=ORIENTED_EDGE('',*,*,#44729,.F.);
#60295=ORIENTED_EDGE('',*,*,#44730,.T.);
#60296=ORIENTED_EDGE('',*,*,#44336,.F.);
#60297=ORIENTED_EDGE('',*,*,#45352,.F.);
#60298=ORIENTED_EDGE('',*,*,#44727,.F.);
#60299=ORIENTED_EDGE('',*,*,#45351,.F.);
#60300=ORIENTED_EDGE('',*,*,#44339,.F.);
#60301=ORIENTED_EDGE('',*,*,#44721,.T.);
#60302=ORIENTED_EDGE('',*,*,#44725,.F.);
#60303=ORIENTED_EDGE('',*,*,#45352,.T.);
#60304=ORIENTED_EDGE('',*,*,#44342,.F.);
#60305=ORIENTED_EDGE('',*,*,#45353,.F.);
#60306=ORIENTED_EDGE('',*,*,#44722,.T.);
#60307=ORIENTED_EDGE('',*,*,#44344,.F.);
#60308=ORIENTED_EDGE('',*,*,#44349,.T.);
#60309=ORIENTED_EDGE('',*,*,#44348,.T.);
#60310=ORIENTED_EDGE('',*,*,#45354,.F.);
#60311=ORIENTED_EDGE('',*,*,#44346,.T.);
#60312=ORIENTED_EDGE('',*,*,#44351,.T.);
#60313=ORIENTED_EDGE('',*,*,#44352,.T.);
#60314=ORIENTED_EDGE('',*,*,#44714,.T.);
#60315=ORIENTED_EDGE('',*,*,#45355,.T.);
#60316=ORIENTED_EDGE('',*,*,#44710,.F.);
#60317=ORIENTED_EDGE('',*,*,#44715,.T.);
#60318=ORIENTED_EDGE('',*,*,#44358,.F.);
#60319=ORIENTED_EDGE('',*,*,#45356,.F.);
#60320=ORIENTED_EDGE('',*,*,#44708,.F.);
#60321=ORIENTED_EDGE('',*,*,#45355,.F.);
#60322=ORIENTED_EDGE('',*,*,#44361,.F.);
#60323=ORIENTED_EDGE('',*,*,#44700,.T.);
#60324=ORIENTED_EDGE('',*,*,#44706,.F.);
#60325=ORIENTED_EDGE('',*,*,#45356,.T.);
#60326=ORIENTED_EDGE('',*,*,#44364,.F.);
#60327=ORIENTED_EDGE('',*,*,#44366,.F.);
#60328=ORIENTED_EDGE('',*,*,#44370,.T.);
#60329=ORIENTED_EDGE('',*,*,#45357,.T.);
#60330=ORIENTED_EDGE('',*,*,#44701,.T.);
#60331=ORIENTED_EDGE('',*,*,#45358,.F.);
#60332=ORIENTED_EDGE('',*,*,#44702,.T.);
#60333=ORIENTED_EDGE('',*,*,#45357,.F.);
#60334=ORIENTED_EDGE('',*,*,#44374,.T.);
#60335=ORIENTED_EDGE('',*,*,#44373,.F.);
#60336=ORIENTED_EDGE('',*,*,#45359,.T.);
#60337=ORIENTED_EDGE('',*,*,#45360,.F.);
#60338=ORIENTED_EDGE('',*,*,#44694,.T.);
#60339=ORIENTED_EDGE('',*,*,#45361,.F.);
#60340=ORIENTED_EDGE('',*,*,#45359,.F.);
#60341=ORIENTED_EDGE('',*,*,#44375,.F.);
#60342=ORIENTED_EDGE('',*,*,#45362,.F.);
#60343=ORIENTED_EDGE('',*,*,#45363,.F.);
#60344=ORIENTED_EDGE('',*,*,#44377,.T.);
#60345=ORIENTED_EDGE('',*,*,#44378,.T.);
#60346=ORIENTED_EDGE('',*,*,#44690,.T.);
#60347=ORIENTED_EDGE('',*,*,#45364,.T.);
#60348=ORIENTED_EDGE('',*,*,#45365,.T.);
#60349=ORIENTED_EDGE('',*,*,#44691,.T.);
#60350=ORIENTED_EDGE('',*,*,#44384,.F.);
#60351=ORIENTED_EDGE('',*,*,#45366,.F.);
#60352=ORIENTED_EDGE('',*,*,#45367,.F.);
#60353=ORIENTED_EDGE('',*,*,#45364,.F.);
#60354=ORIENTED_EDGE('',*,*,#44387,.F.);
#60355=ORIENTED_EDGE('',*,*,#44674,.T.);
#60356=ORIENTED_EDGE('',*,*,#45368,.F.);
#60357=ORIENTED_EDGE('',*,*,#45366,.T.);
#60358=ORIENTED_EDGE('',*,*,#44390,.F.);
#60359=ORIENTED_EDGE('',*,*,#45369,.F.);
#60360=ORIENTED_EDGE('',*,*,#44675,.T.);
#60361=ORIENTED_EDGE('',*,*,#44392,.F.);
#60362=ORIENTED_EDGE('',*,*,#44397,.T.);
#60363=ORIENTED_EDGE('',*,*,#44396,.F.);
#60364=ORIENTED_EDGE('',*,*,#45370,.F.);
#60365=ORIENTED_EDGE('',*,*,#45371,.F.);
#60366=ORIENTED_EDGE('',*,*,#45372,.F.);
#60367=ORIENTED_EDGE('',*,*,#45373,.F.);
#60368=ORIENTED_EDGE('',*,*,#44395,.T.);
#60369=ORIENTED_EDGE('',*,*,#44398,.T.);
#60370=ORIENTED_EDGE('',*,*,#45070,.T.);
#60371=ORIENTED_EDGE('',*,*,#45374,.T.);
#60372=ORIENTED_EDGE('',*,*,#45375,.T.);
#60373=ORIENTED_EDGE('',*,*,#45071,.T.);
#60374=ORIENTED_EDGE('',*,*,#44404,.F.);
#60375=ORIENTED_EDGE('',*,*,#45376,.F.);
#60376=ORIENTED_EDGE('',*,*,#45377,.F.);
#60377=ORIENTED_EDGE('',*,*,#45374,.F.);
#60378=ORIENTED_EDGE('',*,*,#44407,.F.);
#60379=ORIENTED_EDGE('',*,*,#45052,.T.);
#60380=ORIENTED_EDGE('',*,*,#45378,.F.);
#60381=ORIENTED_EDGE('',*,*,#45376,.T.);
#60382=ORIENTED_EDGE('',*,*,#44410,.F.);
#60383=ORIENTED_EDGE('',*,*,#45379,.F.);
#60384=ORIENTED_EDGE('',*,*,#45053,.T.);
#60385=ORIENTED_EDGE('',*,*,#44412,.F.);
#60386=ORIENTED_EDGE('',*,*,#44417,.T.);
#60387=ORIENTED_EDGE('',*,*,#44416,.F.);
#60388=ORIENTED_EDGE('',*,*,#45380,.F.);
#60389=ORIENTED_EDGE('',*,*,#45381,.F.);
#60390=ORIENTED_EDGE('',*,*,#45382,.F.);
#60391=ORIENTED_EDGE('',*,*,#45383,.F.);
#60392=ORIENTED_EDGE('',*,*,#44415,.T.);
#60393=ORIENTED_EDGE('',*,*,#44418,.T.);
#60394=ORIENTED_EDGE('',*,*,#45095,.T.);
#60395=ORIENTED_EDGE('',*,*,#45127,.T.);
#60396=ORIENTED_EDGE('',*,*,#45346,.F.);
#60397=ORIENTED_EDGE('',*,*,#44421,.T.);
#60398=ORIENTED_EDGE('',*,*,#45384,.F.);
#60399=ORIENTED_EDGE('',*,*,#45385,.F.);
#60400=ORIENTED_EDGE('',*,*,#44428,.T.);
#60401=ORIENTED_EDGE('',*,*,#45386,.T.);
#60402=ORIENTED_EDGE('',*,*,#45387,.T.);
#60403=ORIENTED_EDGE('',*,*,#45386,.F.);
#60404=ORIENTED_EDGE('',*,*,#44427,.T.);
#60405=ORIENTED_EDGE('',*,*,#45388,.T.);
#60406=ORIENTED_EDGE('',*,*,#44500,.F.);
#60407=ORIENTED_EDGE('',*,*,#45388,.F.);
#60408=ORIENTED_EDGE('',*,*,#44426,.T.);
#60409=ORIENTED_EDGE('',*,*,#45389,.T.);
#60410=ORIENTED_EDGE('',*,*,#45390,.T.);
#60411=ORIENTED_EDGE('',*,*,#45389,.F.);
#60412=ORIENTED_EDGE('',*,*,#44425,.T.);
#60413=ORIENTED_EDGE('',*,*,#45391,.T.);
#60414=ORIENTED_EDGE('',*,*,#45392,.T.);
#60415=ORIENTED_EDGE('',*,*,#45391,.F.);
#60416=ORIENTED_EDGE('',*,*,#44424,.T.);
#60417=ORIENTED_EDGE('',*,*,#45393,.T.);
#60418=ORIENTED_EDGE('',*,*,#45394,.T.);
#60419=ORIENTED_EDGE('',*,*,#45393,.F.);
#60420=ORIENTED_EDGE('',*,*,#44431,.T.);
#60421=ORIENTED_EDGE('',*,*,#44436,.T.);
#60422=ORIENTED_EDGE('',*,*,#45395,.T.);
#60423=ORIENTED_EDGE('',*,*,#44441,.F.);
#60424=ORIENTED_EDGE('',*,*,#44446,.F.);
#60425=ORIENTED_EDGE('',*,*,#45396,.F.);
#60426=ORIENTED_EDGE('',*,*,#45397,.F.);
#60427=ORIENTED_EDGE('',*,*,#45394,.F.);
#60428=ORIENTED_EDGE('',*,*,#45395,.F.);
#60429=ORIENTED_EDGE('',*,*,#44438,.F.);
#60430=ORIENTED_EDGE('',*,*,#45398,.T.);
#60431=ORIENTED_EDGE('',*,*,#45399,.F.);
#60432=ORIENTED_EDGE('',*,*,#45396,.T.);
#60433=ORIENTED_EDGE('',*,*,#44449,.F.);
#60434=ORIENTED_EDGE('',*,*,#45400,.F.);
#60435=ORIENTED_EDGE('',*,*,#45401,.F.);
#60436=ORIENTED_EDGE('',*,*,#45398,.F.);
#60437=ORIENTED_EDGE('',*,*,#44452,.F.);
#60438=ORIENTED_EDGE('',*,*,#45402,.T.);
#60439=ORIENTED_EDGE('',*,*,#45403,.F.);
#60440=ORIENTED_EDGE('',*,*,#45400,.T.);
#60441=ORIENTED_EDGE('',*,*,#44455,.F.);
#60442=ORIENTED_EDGE('',*,*,#45404,.F.);
#60443=ORIENTED_EDGE('',*,*,#45402,.F.);
#60444=ORIENTED_EDGE('',*,*,#44458,.F.);
#60445=ORIENTED_EDGE('',*,*,#45405,.F.);
#60446=ORIENTED_EDGE('',*,*,#45406,.F.);
#60447=ORIENTED_EDGE('',*,*,#45407,.F.);
#60448=ORIENTED_EDGE('',*,*,#45408,.F.);
#60449=ORIENTED_EDGE('',*,*,#45409,.F.);
#60450=ORIENTED_EDGE('',*,*,#45410,.F.);
#60451=ORIENTED_EDGE('',*,*,#45411,.F.);
#60452=ORIENTED_EDGE('',*,*,#45412,.F.);
#60453=ORIENTED_EDGE('',*,*,#45413,.F.);
#60454=ORIENTED_EDGE('',*,*,#45414,.F.);
#60455=ORIENTED_EDGE('',*,*,#45415,.F.);
#60456=ORIENTED_EDGE('',*,*,#45416,.F.);
#60457=ORIENTED_EDGE('',*,*,#45417,.F.);
#60458=ORIENTED_EDGE('',*,*,#45418,.F.);
#60459=ORIENTED_EDGE('',*,*,#45419,.F.);
#60460=ORIENTED_EDGE('',*,*,#45420,.F.);
#60461=ORIENTED_EDGE('',*,*,#45405,.T.);
#60462=ORIENTED_EDGE('',*,*,#44461,.F.);
#60463=ORIENTED_EDGE('',*,*,#45421,.T.);
#60464=ORIENTED_EDGE('',*,*,#45422,.F.);
#60465=ORIENTED_EDGE('',*,*,#45421,.F.);
#60466=ORIENTED_EDGE('',*,*,#44464,.F.);
#60467=ORIENTED_EDGE('',*,*,#45423,.F.);
#60468=ORIENTED_EDGE('',*,*,#45424,.F.);
#60469=ORIENTED_EDGE('',*,*,#45425,.F.);
#60470=ORIENTED_EDGE('',*,*,#45426,.F.);
#60471=ORIENTED_EDGE('',*,*,#45427,.F.);
#60472=ORIENTED_EDGE('',*,*,#45428,.F.);
#60473=ORIENTED_EDGE('',*,*,#45429,.F.);
#60474=ORIENTED_EDGE('',*,*,#45430,.F.);
#60475=ORIENTED_EDGE('',*,*,#45431,.F.);
#60476=ORIENTED_EDGE('',*,*,#45432,.F.);
#60477=ORIENTED_EDGE('',*,*,#45433,.F.);
#60478=ORIENTED_EDGE('',*,*,#45434,.F.);
#60479=ORIENTED_EDGE('',*,*,#45435,.F.);
#60480=ORIENTED_EDGE('',*,*,#45436,.F.);
#60481=ORIENTED_EDGE('',*,*,#45437,.F.);
#60482=ORIENTED_EDGE('',*,*,#45438,.F.);
#60483=ORIENTED_EDGE('',*,*,#45439,.F.);
#60484=ORIENTED_EDGE('',*,*,#45440,.F.);
#60485=ORIENTED_EDGE('',*,*,#45441,.F.);
#60486=ORIENTED_EDGE('',*,*,#45442,.F.);
#60487=ORIENTED_EDGE('',*,*,#45443,.F.);
#60488=ORIENTED_EDGE('',*,*,#45444,.F.);
#60489=ORIENTED_EDGE('',*,*,#45445,.F.);
#60490=ORIENTED_EDGE('',*,*,#45446,.F.);
#60491=ORIENTED_EDGE('',*,*,#45447,.F.);
#60492=ORIENTED_EDGE('',*,*,#45448,.F.);
#60493=ORIENTED_EDGE('',*,*,#45449,.F.);
#60494=ORIENTED_EDGE('',*,*,#45450,.F.);
#60495=ORIENTED_EDGE('',*,*,#45451,.F.);
#60496=ORIENTED_EDGE('',*,*,#45452,.F.);
#60497=ORIENTED_EDGE('',*,*,#45453,.F.);
#60498=ORIENTED_EDGE('',*,*,#45454,.F.);
#60499=ORIENTED_EDGE('',*,*,#45455,.F.);
#60500=ORIENTED_EDGE('',*,*,#45456,.F.);
#60501=ORIENTED_EDGE('',*,*,#45457,.F.);
#60502=ORIENTED_EDGE('',*,*,#45458,.F.);
#60503=ORIENTED_EDGE('',*,*,#45459,.F.);
#60504=ORIENTED_EDGE('',*,*,#45460,.F.);
#60505=ORIENTED_EDGE('',*,*,#45461,.F.);
#60506=ORIENTED_EDGE('',*,*,#45462,.F.);
#60507=ORIENTED_EDGE('',*,*,#45463,.F.);
#60508=ORIENTED_EDGE('',*,*,#45464,.F.);
#60509=ORIENTED_EDGE('',*,*,#45423,.T.);
#60510=ORIENTED_EDGE('',*,*,#44467,.F.);
#60511=ORIENTED_EDGE('',*,*,#45465,.T.);
#60512=ORIENTED_EDGE('',*,*,#45466,.F.);
#60513=ORIENTED_EDGE('',*,*,#45467,.F.);
#60514=ORIENTED_EDGE('',*,*,#45468,.F.);
#60515=ORIENTED_EDGE('',*,*,#45469,.F.);
#60516=ORIENTED_EDGE('',*,*,#45470,.F.);
#60517=ORIENTED_EDGE('',*,*,#45471,.F.);
#60518=ORIENTED_EDGE('',*,*,#45472,.F.);
#60519=ORIENTED_EDGE('',*,*,#45473,.F.);
#60520=ORIENTED_EDGE('',*,*,#45474,.F.);
#60521=ORIENTED_EDGE('',*,*,#45475,.F.);
#60522=ORIENTED_EDGE('',*,*,#45476,.F.);
#60523=ORIENTED_EDGE('',*,*,#45465,.F.);
#60524=ORIENTED_EDGE('',*,*,#44470,.F.);
#60525=ORIENTED_EDGE('',*,*,#45477,.F.);
#60526=ORIENTED_EDGE('',*,*,#45478,.F.);
#60527=ORIENTED_EDGE('',*,*,#45479,.F.);
#60528=ORIENTED_EDGE('',*,*,#45480,.F.);
#60529=ORIENTED_EDGE('',*,*,#45481,.F.);
#60530=ORIENTED_EDGE('',*,*,#45482,.F.);
#60531=ORIENTED_EDGE('',*,*,#45483,.F.);
#60532=ORIENTED_EDGE('',*,*,#45484,.T.);
#60533=ORIENTED_EDGE('',*,*,#45485,.F.);
#60534=ORIENTED_EDGE('',*,*,#45477,.T.);
#60535=ORIENTED_EDGE('',*,*,#44473,.F.);
#60536=ORIENTED_EDGE('',*,*,#45486,.F.);
#60537=ORIENTED_EDGE('',*,*,#45487,.F.);
#60538=ORIENTED_EDGE('',*,*,#45484,.F.);
#60539=ORIENTED_EDGE('',*,*,#44476,.F.);
#60540=ORIENTED_EDGE('',*,*,#45488,.T.);
#60541=ORIENTED_EDGE('',*,*,#45489,.F.);
#60542=ORIENTED_EDGE('',*,*,#45486,.T.);
#60543=ORIENTED_EDGE('',*,*,#44479,.F.);
#60544=ORIENTED_EDGE('',*,*,#45490,.F.);
#60545=ORIENTED_EDGE('',*,*,#45488,.F.);
#60546=ORIENTED_EDGE('',*,*,#44482,.F.);
#60547=ORIENTED_EDGE('',*,*,#44561,.F.);
#60548=ORIENTED_EDGE('',*,*,#45491,.F.);
#60549=ORIENTED_EDGE('',*,*,#45492,.F.);
#60550=ORIENTED_EDGE('',*,*,#45493,.F.);
#60551=ORIENTED_EDGE('',*,*,#45494,.F.);
#60552=ORIENTED_EDGE('',*,*,#45495,.F.);
#60553=ORIENTED_EDGE('',*,*,#45496,.F.);
#60554=ORIENTED_EDGE('',*,*,#45497,.F.);
#60555=ORIENTED_EDGE('',*,*,#45498,.F.);
#60556=ORIENTED_EDGE('',*,*,#45499,.F.);
#60557=ORIENTED_EDGE('',*,*,#45500,.F.);
#60558=ORIENTED_EDGE('',*,*,#45501,.F.);
#60559=ORIENTED_EDGE('',*,*,#45502,.F.);
#60560=ORIENTED_EDGE('',*,*,#45503,.F.);
#60561=ORIENTED_EDGE('',*,*,#45504,.F.);
#60562=ORIENTED_EDGE('',*,*,#44969,.T.);
#60563=ORIENTED_EDGE('',*,*,#45505,.T.);
#60564=ORIENTED_EDGE('',*,*,#44492,.F.);
#60565=ORIENTED_EDGE('',*,*,#45506,.F.);
#60566=ORIENTED_EDGE('',*,*,#45507,.F.);
#60567=ORIENTED_EDGE('',*,*,#45508,.F.);
#60568=ORIENTED_EDGE('',*,*,#45509,.F.);
#60569=ORIENTED_EDGE('',*,*,#45510,.F.);
#60570=ORIENTED_EDGE('',*,*,#45511,.F.);
#60571=ORIENTED_EDGE('',*,*,#44491,.F.);
#60572=ORIENTED_EDGE('',*,*,#44488,.F.);
#60573=ORIENTED_EDGE('',*,*,#45512,.F.);
#60574=ORIENTED_EDGE('',*,*,#45513,.F.);
#60575=ORIENTED_EDGE('',*,*,#45227,.T.);
#60576=ORIENTED_EDGE('',*,*,#45514,.T.);
#60577=ORIENTED_EDGE('',*,*,#44487,.F.);
#60578=ORIENTED_EDGE('',*,*,#44493,.F.);
#60579=ORIENTED_EDGE('',*,*,#45515,.F.);
#60580=ORIENTED_EDGE('',*,*,#45516,.F.);
#60581=ORIENTED_EDGE('',*,*,#45517,.F.);
#60582=ORIENTED_EDGE('',*,*,#45518,.F.);
#60583=ORIENTED_EDGE('',*,*,#45129,.T.);
#60584=ORIENTED_EDGE('',*,*,#45519,.T.);
#60585=ORIENTED_EDGE('',*,*,#44498,.F.);
#60586=ORIENTED_EDGE('',*,*,#44495,.F.);
#60587=ORIENTED_EDGE('',*,*,#45520,.F.);
#60588=ORIENTED_EDGE('',*,*,#45521,.F.);
#60589=ORIENTED_EDGE('',*,*,#45522,.F.);
#60590=ORIENTED_EDGE('',*,*,#45523,.F.);
#60591=ORIENTED_EDGE('',*,*,#45524,.F.);
#60592=ORIENTED_EDGE('',*,*,#45525,.F.);
#60593=ORIENTED_EDGE('',*,*,#44494,.F.);
#60594=ORIENTED_EDGE('',*,*,#45390,.F.);
#60595=ORIENTED_EDGE('',*,*,#44499,.F.);
#60596=ORIENTED_EDGE('',*,*,#45526,.F.);
#60597=ORIENTED_EDGE('',*,*,#45387,.F.);
#60598=ORIENTED_EDGE('',*,*,#44659,.T.);
#60599=ORIENTED_EDGE('',*,*,#45527,.F.);
#60600=ORIENTED_EDGE('',*,*,#45528,.T.);
#60601=ORIENTED_EDGE('',*,*,#44502,.F.);
#60602=ORIENTED_EDGE('',*,*,#44506,.F.);
#60603=ORIENTED_EDGE('',*,*,#44511,.T.);
#60604=ORIENTED_EDGE('',*,*,#45529,.T.);
#60605=ORIENTED_EDGE('',*,*,#44660,.T.);
#60606=ORIENTED_EDGE('',*,*,#44510,.F.);
#60607=ORIENTED_EDGE('',*,*,#45530,.F.);
#60608=ORIENTED_EDGE('',*,*,#45531,.F.);
#60609=ORIENTED_EDGE('',*,*,#45532,.F.);
#60610=ORIENTED_EDGE('',*,*,#44514,.F.);
#60611=ORIENTED_EDGE('',*,*,#44649,.T.);
#60612=ORIENTED_EDGE('',*,*,#45533,.T.);
#60613=ORIENTED_EDGE('',*,*,#44509,.T.);
#60614=ORIENTED_EDGE('',*,*,#45534,.T.);
#60615=ORIENTED_EDGE('',*,*,#45535,.T.);
#60616=ORIENTED_EDGE('',*,*,#44640,.T.);
#60617=ORIENTED_EDGE('',*,*,#44517,.F.);
#60618=ORIENTED_EDGE('',*,*,#45536,.F.);
#60619=ORIENTED_EDGE('',*,*,#45537,.F.);
#60620=ORIENTED_EDGE('',*,*,#45534,.F.);
#60621=ORIENTED_EDGE('',*,*,#44520,.F.);
#60622=ORIENTED_EDGE('',*,*,#44625,.T.);
#60623=ORIENTED_EDGE('',*,*,#45538,.F.);
#60624=ORIENTED_EDGE('',*,*,#45536,.T.);
#60625=ORIENTED_EDGE('',*,*,#44524,.F.);
#60626=ORIENTED_EDGE('',*,*,#44526,.F.);
#60627=ORIENTED_EDGE('',*,*,#44531,.T.);
#60628=ORIENTED_EDGE('',*,*,#45539,.T.);
#60629=ORIENTED_EDGE('',*,*,#44626,.T.);
#60630=ORIENTED_EDGE('',*,*,#44530,.F.);
#60631=ORIENTED_EDGE('',*,*,#45540,.F.);
#60632=ORIENTED_EDGE('',*,*,#45541,.F.);
#60633=ORIENTED_EDGE('',*,*,#45542,.F.);
#60634=ORIENTED_EDGE('',*,*,#44534,.F.);
#60635=ORIENTED_EDGE('',*,*,#44615,.T.);
#60636=ORIENTED_EDGE('',*,*,#45543,.T.);
#60637=ORIENTED_EDGE('',*,*,#44529,.T.);
#60638=ORIENTED_EDGE('',*,*,#45544,.T.);
#60639=ORIENTED_EDGE('',*,*,#45545,.T.);
#60640=ORIENTED_EDGE('',*,*,#44608,.T.);
#60641=ORIENTED_EDGE('',*,*,#44537,.F.);
#60642=ORIENTED_EDGE('',*,*,#45546,.F.);
#60643=ORIENTED_EDGE('',*,*,#45547,.T.);
#60644=ORIENTED_EDGE('',*,*,#45544,.F.);
#60645=ORIENTED_EDGE('',*,*,#44540,.F.);
#60646=ORIENTED_EDGE('',*,*,#44593,.T.);
#60647=ORIENTED_EDGE('',*,*,#45548,.F.);
#60648=ORIENTED_EDGE('',*,*,#45546,.T.);
#60649=ORIENTED_EDGE('',*,*,#44544,.F.);
#60650=ORIENTED_EDGE('',*,*,#44546,.F.);
#60651=ORIENTED_EDGE('',*,*,#44551,.T.);
#60652=ORIENTED_EDGE('',*,*,#45549,.T.);
#60653=ORIENTED_EDGE('',*,*,#44594,.T.);
#60654=ORIENTED_EDGE('',*,*,#44550,.F.);
#60655=ORIENTED_EDGE('',*,*,#45550,.F.);
#60656=ORIENTED_EDGE('',*,*,#45551,.F.);
#60657=ORIENTED_EDGE('',*,*,#45552,.F.);
#60658=ORIENTED_EDGE('',*,*,#44554,.F.);
#60659=ORIENTED_EDGE('',*,*,#44585,.T.);
#60660=ORIENTED_EDGE('',*,*,#45553,.T.);
#60661=ORIENTED_EDGE('',*,*,#44549,.T.);
#60662=ORIENTED_EDGE('',*,*,#45554,.F.);
#60663=ORIENTED_EDGE('',*,*,#44998,.T.);
#60664=ORIENTED_EDGE('',*,*,#45555,.T.);
#60665=ORIENTED_EDGE('',*,*,#44559,.T.);
#60666=ORIENTED_EDGE('',*,*,#44566,.F.);
#60667=ORIENTED_EDGE('',*,*,#45556,.T.);
#60668=ORIENTED_EDGE('',*,*,#45554,.T.);
#60669=ORIENTED_EDGE('',*,*,#44563,.T.);
#60670=ORIENTED_EDGE('',*,*,#45557,.T.);
#60671=ORIENTED_EDGE('',*,*,#45558,.F.);
#60672=ORIENTED_EDGE('',*,*,#44560,.T.);
#60673=ORIENTED_EDGE('',*,*,#45559,.F.);
#60674=ORIENTED_EDGE('',*,*,#45560,.T.);
#60675=ORIENTED_EDGE('',*,*,#45561,.T.);
#60676=ORIENTED_EDGE('',*,*,#44986,.T.);
#60677=ORIENTED_EDGE('',*,*,#45556,.F.);
#60678=ORIENTED_EDGE('',*,*,#44565,.F.);
#60679=ORIENTED_EDGE('',*,*,#45528,.F.);
#60680=ORIENTED_EDGE('',*,*,#45562,.F.);
#60681=ORIENTED_EDGE('',*,*,#45560,.F.);
#60682=ORIENTED_EDGE('',*,*,#44568,.F.);
#60683=ORIENTED_EDGE('',*,*,#45563,.F.);
#60684=ORIENTED_EDGE('',*,*,#44580,.T.);
#60685=ORIENTED_EDGE('',*,*,#44578,.T.);
#60686=ORIENTED_EDGE('',*,*,#44587,.T.);
#60687=ORIENTED_EDGE('',*,*,#45553,.F.);
#60688=ORIENTED_EDGE('',*,*,#44584,.T.);
#60689=ORIENTED_EDGE('',*,*,#45564,.T.);
#60690=ORIENTED_EDGE('',*,*,#45550,.T.);
#60691=ORIENTED_EDGE('',*,*,#45564,.F.);
#60692=ORIENTED_EDGE('',*,*,#44583,.T.);
#60693=ORIENTED_EDGE('',*,*,#45565,.T.);
#60694=ORIENTED_EDGE('',*,*,#45566,.T.);
#60695=ORIENTED_EDGE('',*,*,#45565,.F.);
#60696=ORIENTED_EDGE('',*,*,#44582,.T.);
#60697=ORIENTED_EDGE('',*,*,#45567,.T.);
#60698=ORIENTED_EDGE('',*,*,#45568,.T.);
#60699=ORIENTED_EDGE('',*,*,#45567,.F.);
#60700=ORIENTED_EDGE('',*,*,#44581,.T.);
#60701=ORIENTED_EDGE('',*,*,#45563,.T.);
#60702=ORIENTED_EDGE('',*,*,#45569,.T.);
#60703=ORIENTED_EDGE('',*,*,#45570,.T.);
#60704=ORIENTED_EDGE('',*,*,#45569,.F.);
#60705=ORIENTED_EDGE('',*,*,#44586,.T.);
#60706=ORIENTED_EDGE('',*,*,#45571,.F.);
#60707=ORIENTED_EDGE('',*,*,#45572,.F.);
#60708=ORIENTED_EDGE('',*,*,#44588,.T.);
#60709=ORIENTED_EDGE('',*,*,#44589,.T.);
#60710=ORIENTED_EDGE('',*,*,#44599,.T.);
#60711=ORIENTED_EDGE('',*,*,#45573,.F.);
#60712=ORIENTED_EDGE('',*,*,#45571,.T.);
#60713=ORIENTED_EDGE('',*,*,#45572,.T.);
#60714=ORIENTED_EDGE('',*,*,#44598,.T.);
#60715=ORIENTED_EDGE('',*,*,#45574,.F.);
#60716=ORIENTED_EDGE('',*,*,#45575,.T.);
#60717=ORIENTED_EDGE('',*,*,#45573,.T.);
#60718=ORIENTED_EDGE('',*,*,#44597,.T.);
#60719=ORIENTED_EDGE('',*,*,#45576,.F.);
#60720=ORIENTED_EDGE('',*,*,#45577,.T.);
#60721=ORIENTED_EDGE('',*,*,#45574,.T.);
#60722=ORIENTED_EDGE('',*,*,#44596,.T.);
#60723=ORIENTED_EDGE('',*,*,#45549,.F.);
#60724=ORIENTED_EDGE('',*,*,#45552,.T.);
#60725=ORIENTED_EDGE('',*,*,#45576,.T.);
#60726=ORIENTED_EDGE('',*,*,#44595,.T.);
#60727=ORIENTED_EDGE('',*,*,#44601,.F.);
#60728=ORIENTED_EDGE('',*,*,#45578,.T.);
#60729=ORIENTED_EDGE('',*,*,#45548,.T.);
#60730=ORIENTED_EDGE('',*,*,#44592,.T.);
#60731=ORIENTED_EDGE('',*,*,#44603,.F.);
#60732=ORIENTED_EDGE('',*,*,#45579,.F.);
#60733=ORIENTED_EDGE('',*,*,#45547,.F.);
#60734=ORIENTED_EDGE('',*,*,#45578,.F.);
#60735=ORIENTED_EDGE('',*,*,#45545,.F.);
#60736=ORIENTED_EDGE('',*,*,#45579,.T.);
#60737=ORIENTED_EDGE('',*,*,#44605,.T.);
#60738=ORIENTED_EDGE('',*,*,#44609,.T.);
#60739=ORIENTED_EDGE('',*,*,#45580,.F.);
#60740=ORIENTED_EDGE('',*,*,#44610,.T.);
#60741=ORIENTED_EDGE('',*,*,#44606,.T.);
#60742=ORIENTED_EDGE('',*,*,#44617,.T.);
#60743=ORIENTED_EDGE('',*,*,#45543,.F.);
#60744=ORIENTED_EDGE('',*,*,#44614,.T.);
#60745=ORIENTED_EDGE('',*,*,#45581,.T.);
#60746=ORIENTED_EDGE('',*,*,#45540,.T.);
#60747=ORIENTED_EDGE('',*,*,#45581,.F.);
#60748=ORIENTED_EDGE('',*,*,#44613,.T.);
#60749=ORIENTED_EDGE('',*,*,#45582,.T.);
#60750=ORIENTED_EDGE('',*,*,#45583,.T.);
#60751=ORIENTED_EDGE('',*,*,#45582,.F.);
#60752=ORIENTED_EDGE('',*,*,#44612,.T.);
#60753=ORIENTED_EDGE('',*,*,#45584,.T.);
#60754=ORIENTED_EDGE('',*,*,#45585,.T.);
#60755=ORIENTED_EDGE('',*,*,#45584,.F.);
#60756=ORIENTED_EDGE('',*,*,#44611,.T.);
#60757=ORIENTED_EDGE('',*,*,#45580,.T.);
#60758=ORIENTED_EDGE('',*,*,#45586,.T.);
#60759=ORIENTED_EDGE('',*,*,#45587,.T.);
#60760=ORIENTED_EDGE('',*,*,#45586,.F.);
#60761=ORIENTED_EDGE('',*,*,#44616,.T.);
#60762=ORIENTED_EDGE('',*,*,#45588,.F.);
#60763=ORIENTED_EDGE('',*,*,#45589,.F.);
#60764=ORIENTED_EDGE('',*,*,#44618,.T.);
#60765=ORIENTED_EDGE('',*,*,#44619,.T.);
#60766=ORIENTED_EDGE('',*,*,#44631,.T.);
#60767=ORIENTED_EDGE('',*,*,#45590,.F.);
#60768=ORIENTED_EDGE('',*,*,#45588,.T.);
#60769=ORIENTED_EDGE('',*,*,#45589,.T.);
#60770=ORIENTED_EDGE('',*,*,#44630,.T.);
#60771=ORIENTED_EDGE('',*,*,#45591,.F.);
#60772=ORIENTED_EDGE('',*,*,#45592,.T.);
#60773=ORIENTED_EDGE('',*,*,#45590,.T.);
#60774=ORIENTED_EDGE('',*,*,#44629,.T.);
#60775=ORIENTED_EDGE('',*,*,#45593,.F.);
#60776=ORIENTED_EDGE('',*,*,#45594,.T.);
#60777=ORIENTED_EDGE('',*,*,#45591,.T.);
#60778=ORIENTED_EDGE('',*,*,#44628,.T.);
#60779=ORIENTED_EDGE('',*,*,#45539,.F.);
#60780=ORIENTED_EDGE('',*,*,#45542,.T.);
#60781=ORIENTED_EDGE('',*,*,#45593,.T.);
#60782=ORIENTED_EDGE('',*,*,#44627,.T.);
#60783=ORIENTED_EDGE('',*,*,#45595,.F.);
#60784=ORIENTED_EDGE('',*,*,#45596,.T.);
#60785=ORIENTED_EDGE('',*,*,#45538,.T.);
#60786=ORIENTED_EDGE('',*,*,#44624,.T.);
#60787=ORIENTED_EDGE('',*,*,#45597,.F.);
#60788=ORIENTED_EDGE('',*,*,#45598,.T.);
#60789=ORIENTED_EDGE('',*,*,#45595,.T.);
#60790=ORIENTED_EDGE('',*,*,#44623,.T.);
#60791=ORIENTED_EDGE('',*,*,#44633,.F.);
#60792=ORIENTED_EDGE('',*,*,#45599,.T.);
#60793=ORIENTED_EDGE('',*,*,#45597,.T.);
#60794=ORIENTED_EDGE('',*,*,#44622,.T.);
#60795=ORIENTED_EDGE('',*,*,#44635,.T.);
#60796=ORIENTED_EDGE('',*,*,#45600,.F.);
#60797=ORIENTED_EDGE('',*,*,#45601,.T.);
#60798=ORIENTED_EDGE('',*,*,#45599,.F.);
#60799=ORIENTED_EDGE('',*,*,#45602,.F.);
#60800=ORIENTED_EDGE('',*,*,#45600,.T.);
#60801=ORIENTED_EDGE('',*,*,#44637,.T.);
#60802=ORIENTED_EDGE('',*,*,#44643,.T.);
#60803=ORIENTED_EDGE('',*,*,#45603,.F.);
#60804=ORIENTED_EDGE('',*,*,#44644,.T.);
#60805=ORIENTED_EDGE('',*,*,#44638,.T.);
#60806=ORIENTED_EDGE('',*,*,#44651,.T.);
#60807=ORIENTED_EDGE('',*,*,#45533,.F.);
#60808=ORIENTED_EDGE('',*,*,#44648,.T.);
#60809=ORIENTED_EDGE('',*,*,#45604,.T.);
#60810=ORIENTED_EDGE('',*,*,#45530,.T.);
#60811=ORIENTED_EDGE('',*,*,#45604,.F.);
#60812=ORIENTED_EDGE('',*,*,#44647,.T.);
#60813=ORIENTED_EDGE('',*,*,#45605,.T.);
#60814=ORIENTED_EDGE('',*,*,#45606,.T.);
#60815=ORIENTED_EDGE('',*,*,#45605,.F.);
#60816=ORIENTED_EDGE('',*,*,#44646,.T.);
#60817=ORIENTED_EDGE('',*,*,#45607,.T.);
#60818=ORIENTED_EDGE('',*,*,#45608,.T.);
#60819=ORIENTED_EDGE('',*,*,#45607,.F.);
#60820=ORIENTED_EDGE('',*,*,#44645,.T.);
#60821=ORIENTED_EDGE('',*,*,#45603,.T.);
#60822=ORIENTED_EDGE('',*,*,#45609,.T.);
#60823=ORIENTED_EDGE('',*,*,#45610,.F.);
#60824=ORIENTED_EDGE('',*,*,#45611,.T.);
#60825=ORIENTED_EDGE('',*,*,#45602,.T.);
#60826=ORIENTED_EDGE('',*,*,#44642,.T.);
#60827=ORIENTED_EDGE('',*,*,#45535,.F.);
#60828=ORIENTED_EDGE('',*,*,#45612,.T.);
#60829=ORIENTED_EDGE('',*,*,#45610,.T.);
#60830=ORIENTED_EDGE('',*,*,#44641,.T.);
#60831=ORIENTED_EDGE('',*,*,#45613,.T.);
#60832=ORIENTED_EDGE('',*,*,#45609,.F.);
#60833=ORIENTED_EDGE('',*,*,#44650,.T.);
#60834=ORIENTED_EDGE('',*,*,#45614,.F.);
#60835=ORIENTED_EDGE('',*,*,#45615,.F.);
#60836=ORIENTED_EDGE('',*,*,#44652,.T.);
#60837=ORIENTED_EDGE('',*,*,#44653,.T.);
#60838=ORIENTED_EDGE('',*,*,#44665,.T.);
#60839=ORIENTED_EDGE('',*,*,#45616,.F.);
#60840=ORIENTED_EDGE('',*,*,#45614,.T.);
#60841=ORIENTED_EDGE('',*,*,#45615,.T.);
#60842=ORIENTED_EDGE('',*,*,#44664,.T.);
#60843=ORIENTED_EDGE('',*,*,#45617,.F.);
#60844=ORIENTED_EDGE('',*,*,#45618,.T.);
#60845=ORIENTED_EDGE('',*,*,#45616,.T.);
#60846=ORIENTED_EDGE('',*,*,#44663,.T.);
#60847=ORIENTED_EDGE('',*,*,#45619,.F.);
#60848=ORIENTED_EDGE('',*,*,#45620,.T.);
#60849=ORIENTED_EDGE('',*,*,#45617,.T.);
#60850=ORIENTED_EDGE('',*,*,#44662,.T.);
#60851=ORIENTED_EDGE('',*,*,#45529,.F.);
#60852=ORIENTED_EDGE('',*,*,#45532,.T.);
#60853=ORIENTED_EDGE('',*,*,#45619,.T.);
#60854=ORIENTED_EDGE('',*,*,#44661,.T.);
#60855=ORIENTED_EDGE('',*,*,#45621,.F.);
#60856=ORIENTED_EDGE('',*,*,#45622,.T.);
#60857=ORIENTED_EDGE('',*,*,#45527,.T.);
#60858=ORIENTED_EDGE('',*,*,#44658,.T.);
#60859=ORIENTED_EDGE('',*,*,#45623,.F.);
#60860=ORIENTED_EDGE('',*,*,#45624,.T.);
#60861=ORIENTED_EDGE('',*,*,#45621,.T.);
#60862=ORIENTED_EDGE('',*,*,#44657,.T.);
#60863=ORIENTED_EDGE('',*,*,#44666,.F.);
#60864=ORIENTED_EDGE('',*,*,#45335,.T.);
#60865=ORIENTED_EDGE('',*,*,#45623,.T.);
#60866=ORIENTED_EDGE('',*,*,#44656,.T.);
#60867=ORIENTED_EDGE('',*,*,#45625,.F.);
#60868=ORIENTED_EDGE('',*,*,#45626,.F.);
#60869=ORIENTED_EDGE('',*,*,#44667,.F.);
#60870=ORIENTED_EDGE('',*,*,#45627,.F.);
#60871=ORIENTED_EDGE('',*,*,#44671,.F.);
#60872=ORIENTED_EDGE('',*,*,#44679,.T.);
#60873=ORIENTED_EDGE('',*,*,#45628,.T.);
#60874=ORIENTED_EDGE('',*,*,#44669,.T.);
#60875=ORIENTED_EDGE('',*,*,#45073,.F.);
#60876=ORIENTED_EDGE('',*,*,#44668,.T.);
#60877=ORIENTED_EDGE('',*,*,#45629,.T.);
#60878=ORIENTED_EDGE('',*,*,#45066,.T.);
#60879=ORIENTED_EDGE('',*,*,#45628,.F.);
#60880=ORIENTED_EDGE('',*,*,#44678,.T.);
#60881=ORIENTED_EDGE('',*,*,#45630,.T.);
#60882=ORIENTED_EDGE('',*,*,#45627,.T.);
#60883=ORIENTED_EDGE('',*,*,#45630,.F.);
#60884=ORIENTED_EDGE('',*,*,#44677,.T.);
#60885=ORIENTED_EDGE('',*,*,#45631,.T.);
#60886=ORIENTED_EDGE('',*,*,#45632,.T.);
#60887=ORIENTED_EDGE('',*,*,#45631,.F.);
#60888=ORIENTED_EDGE('',*,*,#44676,.T.);
#60889=ORIENTED_EDGE('',*,*,#45369,.T.);
#60890=ORIENTED_EDGE('',*,*,#45372,.T.);
#60891=ORIENTED_EDGE('',*,*,#44681,.F.);
#60892=ORIENTED_EDGE('',*,*,#45633,.T.);
#60893=ORIENTED_EDGE('',*,*,#45368,.T.);
#60894=ORIENTED_EDGE('',*,*,#44673,.T.);
#60895=ORIENTED_EDGE('',*,*,#45367,.T.);
#60896=ORIENTED_EDGE('',*,*,#45633,.F.);
#60897=ORIENTED_EDGE('',*,*,#44683,.T.);
#60898=ORIENTED_EDGE('',*,*,#45634,.F.);
#60899=ORIENTED_EDGE('',*,*,#45365,.F.);
#60900=ORIENTED_EDGE('',*,*,#45634,.T.);
#60901=ORIENTED_EDGE('',*,*,#44685,.T.);
#60902=ORIENTED_EDGE('',*,*,#44692,.T.);
#60903=ORIENTED_EDGE('',*,*,#45635,.F.);
#60904=ORIENTED_EDGE('',*,*,#45362,.T.);
#60905=ORIENTED_EDGE('',*,*,#45363,.T.);
#60906=ORIENTED_EDGE('',*,*,#44689,.T.);
#60907=ORIENTED_EDGE('',*,*,#45636,.F.);
#60908=ORIENTED_EDGE('',*,*,#45360,.T.);
#60909=ORIENTED_EDGE('',*,*,#45635,.T.);
#60910=ORIENTED_EDGE('',*,*,#44688,.T.);
#60911=ORIENTED_EDGE('',*,*,#44693,.F.);
#60912=ORIENTED_EDGE('',*,*,#44695,.T.);
#60913=ORIENTED_EDGE('',*,*,#45636,.T.);
#60914=ORIENTED_EDGE('',*,*,#44687,.T.);
#60915=ORIENTED_EDGE('',*,*,#44698,.F.);
#60916=ORIENTED_EDGE('',*,*,#44704,.T.);
#60917=ORIENTED_EDGE('',*,*,#45637,.T.);
#60918=ORIENTED_EDGE('',*,*,#44696,.T.);
#60919=ORIENTED_EDGE('',*,*,#45637,.F.);
#60920=ORIENTED_EDGE('',*,*,#44703,.T.);
#60921=ORIENTED_EDGE('',*,*,#45358,.T.);
#60922=ORIENTED_EDGE('',*,*,#45361,.T.);
#60923=ORIENTED_EDGE('',*,*,#44711,.F.);
#60924=ORIENTED_EDGE('',*,*,#44716,.T.);
#60925=ORIENTED_EDGE('',*,*,#45354,.T.);
#60926=ORIENTED_EDGE('',*,*,#44713,.T.);
#60927=ORIENTED_EDGE('',*,*,#44719,.F.);
#60928=ORIENTED_EDGE('',*,*,#44723,.T.);
#60929=ORIENTED_EDGE('',*,*,#45353,.T.);
#60930=ORIENTED_EDGE('',*,*,#44717,.T.);
#60931=ORIENTED_EDGE('',*,*,#44732,.F.);
#60932=ORIENTED_EDGE('',*,*,#45638,.T.);
#60933=ORIENTED_EDGE('',*,*,#45639,.T.);
#60934=ORIENTED_EDGE('',*,*,#44935,.T.);
#60935=ORIENTED_EDGE('',*,*,#44735,.T.);
#60936=ORIENTED_EDGE('',*,*,#45640,.F.);
#60937=ORIENTED_EDGE('',*,*,#45641,.T.);
#60938=ORIENTED_EDGE('',*,*,#45638,.F.);
#60939=ORIENTED_EDGE('',*,*,#45642,.F.);
#60940=ORIENTED_EDGE('',*,*,#45640,.T.);
#60941=ORIENTED_EDGE('',*,*,#44737,.T.);
#60942=ORIENTED_EDGE('',*,*,#45145,.T.);
#60943=ORIENTED_EDGE('',*,*,#44739,.F.);
#60944=ORIENTED_EDGE('',*,*,#45643,.T.);
#60945=ORIENTED_EDGE('',*,*,#45644,.T.);
#60946=ORIENTED_EDGE('',*,*,#45218,.T.);
#60947=ORIENTED_EDGE('',*,*,#44742,.T.);
#60948=ORIENTED_EDGE('',*,*,#45645,.F.);
#60949=ORIENTED_EDGE('',*,*,#45646,.T.);
#60950=ORIENTED_EDGE('',*,*,#45643,.F.);
#60951=ORIENTED_EDGE('',*,*,#45647,.F.);
#60952=ORIENTED_EDGE('',*,*,#45645,.T.);
#60953=ORIENTED_EDGE('',*,*,#44744,.T.);
#60954=ORIENTED_EDGE('',*,*,#44748,.T.);
#60955=ORIENTED_EDGE('',*,*,#45648,.T.);
#60956=ORIENTED_EDGE('',*,*,#45649,.T.);
#60957=ORIENTED_EDGE('',*,*,#44745,.T.);
#60958=ORIENTED_EDGE('',*,*,#45650,.F.);
#60959=ORIENTED_EDGE('',*,*,#45651,.F.);
#60960=ORIENTED_EDGE('',*,*,#45427,.T.);
#60961=ORIENTED_EDGE('',*,*,#45652,.T.);
#60962=ORIENTED_EDGE('',*,*,#44756,.T.);
#60963=ORIENTED_EDGE('',*,*,#45653,.F.);
#60964=ORIENTED_EDGE('',*,*,#45654,.T.);
#60965=ORIENTED_EDGE('',*,*,#45651,.T.);
#60966=ORIENTED_EDGE('',*,*,#44755,.T.);
#60967=ORIENTED_EDGE('',*,*,#45655,.F.);
#60968=ORIENTED_EDGE('',*,*,#45656,.T.);
#60969=ORIENTED_EDGE('',*,*,#45653,.T.);
#60970=ORIENTED_EDGE('',*,*,#44754,.T.);
#60971=ORIENTED_EDGE('',*,*,#45657,.F.);
#60972=ORIENTED_EDGE('',*,*,#45658,.T.);
#60973=ORIENTED_EDGE('',*,*,#45655,.T.);
#60974=ORIENTED_EDGE('',*,*,#44753,.T.);
#60975=ORIENTED_EDGE('',*,*,#45659,.F.);
#60976=ORIENTED_EDGE('',*,*,#45660,.T.);
#60977=ORIENTED_EDGE('',*,*,#45657,.T.);
#60978=ORIENTED_EDGE('',*,*,#44752,.T.);
#60979=ORIENTED_EDGE('',*,*,#45661,.F.);
#60980=ORIENTED_EDGE('',*,*,#45662,.T.);
#60981=ORIENTED_EDGE('',*,*,#45659,.T.);
#60982=ORIENTED_EDGE('',*,*,#44751,.T.);
#60983=ORIENTED_EDGE('',*,*,#44757,.F.);
#60984=ORIENTED_EDGE('',*,*,#44759,.T.);
#60985=ORIENTED_EDGE('',*,*,#45661,.T.);
#60986=ORIENTED_EDGE('',*,*,#44750,.T.);
#60987=ORIENTED_EDGE('',*,*,#45663,.F.);
#60988=ORIENTED_EDGE('',*,*,#45664,.T.);
#60989=ORIENTED_EDGE('',*,*,#45647,.T.);
#60990=ORIENTED_EDGE('',*,*,#44747,.T.);
#60991=ORIENTED_EDGE('',*,*,#45649,.F.);
#60992=ORIENTED_EDGE('',*,*,#45665,.T.);
#60993=ORIENTED_EDGE('',*,*,#45663,.T.);
#60994=ORIENTED_EDGE('',*,*,#44746,.T.);
#60995=ORIENTED_EDGE('',*,*,#45666,.T.);
#60996=ORIENTED_EDGE('',*,*,#45662,.F.);
#60997=ORIENTED_EDGE('',*,*,#44758,.T.);
#60998=ORIENTED_EDGE('',*,*,#45667,.F.);
#60999=ORIENTED_EDGE('',*,*,#44762,.F.);
#61000=ORIENTED_EDGE('',*,*,#44774,.T.);
#61001=ORIENTED_EDGE('',*,*,#45668,.T.);
#61002=ORIENTED_EDGE('',*,*,#44760,.T.);
#61003=ORIENTED_EDGE('',*,*,#45668,.F.);
#61004=ORIENTED_EDGE('',*,*,#44773,.T.);
#61005=ORIENTED_EDGE('',*,*,#45669,.F.);
#61006=ORIENTED_EDGE('',*,*,#45667,.T.);
#61007=ORIENTED_EDGE('',*,*,#45670,.F.);
#61008=ORIENTED_EDGE('',*,*,#45671,.T.);
#61009=ORIENTED_EDGE('',*,*,#45669,.T.);
#61010=ORIENTED_EDGE('',*,*,#44772,.T.);
#61011=ORIENTED_EDGE('',*,*,#45672,.F.);
#61012=ORIENTED_EDGE('',*,*,#45673,.T.);
#61013=ORIENTED_EDGE('',*,*,#45670,.T.);
#61014=ORIENTED_EDGE('',*,*,#44771,.T.);
#61015=ORIENTED_EDGE('',*,*,#45674,.F.);
#61016=ORIENTED_EDGE('',*,*,#45675,.T.);
#61017=ORIENTED_EDGE('',*,*,#45672,.T.);
#61018=ORIENTED_EDGE('',*,*,#44770,.T.);
#61019=ORIENTED_EDGE('',*,*,#45676,.F.);
#61020=ORIENTED_EDGE('',*,*,#45677,.T.);
#61021=ORIENTED_EDGE('',*,*,#45674,.T.);
#61022=ORIENTED_EDGE('',*,*,#44769,.T.);
#61023=ORIENTED_EDGE('',*,*,#45678,.F.);
#61024=ORIENTED_EDGE('',*,*,#45429,.T.);
#61025=ORIENTED_EDGE('',*,*,#45676,.T.);
#61026=ORIENTED_EDGE('',*,*,#44768,.T.);
#61027=ORIENTED_EDGE('',*,*,#44767,.T.);
#61028=ORIENTED_EDGE('',*,*,#45679,.F.);
#61029=ORIENTED_EDGE('',*,*,#45680,.T.);
#61030=ORIENTED_EDGE('',*,*,#45681,.F.);
#61031=ORIENTED_EDGE('',*,*,#45682,.F.);
#61032=ORIENTED_EDGE('',*,*,#45683,.T.);
#61033=ORIENTED_EDGE('',*,*,#45679,.T.);
#61034=ORIENTED_EDGE('',*,*,#44766,.T.);
#61035=ORIENTED_EDGE('',*,*,#45684,.F.);
#61036=ORIENTED_EDGE('',*,*,#45685,.T.);
#61037=ORIENTED_EDGE('',*,*,#45682,.T.);
#61038=ORIENTED_EDGE('',*,*,#44765,.T.);
#61039=ORIENTED_EDGE('',*,*,#44776,.F.);
#61040=ORIENTED_EDGE('',*,*,#45686,.T.);
#61041=ORIENTED_EDGE('',*,*,#45684,.T.);
#61042=ORIENTED_EDGE('',*,*,#44764,.T.);
#61043=ORIENTED_EDGE('',*,*,#44778,.T.);
#61044=ORIENTED_EDGE('',*,*,#45687,.F.);
#61045=ORIENTED_EDGE('',*,*,#45688,.T.);
#61046=ORIENTED_EDGE('',*,*,#45686,.F.);
#61047=ORIENTED_EDGE('',*,*,#45689,.F.);
#61048=ORIENTED_EDGE('',*,*,#45687,.T.);
#61049=ORIENTED_EDGE('',*,*,#44780,.T.);
#61050=ORIENTED_EDGE('',*,*,#44792,.T.);
#61051=ORIENTED_EDGE('',*,*,#45690,.F.);
#61052=ORIENTED_EDGE('',*,*,#44783,.T.);
#61053=ORIENTED_EDGE('',*,*,#44781,.T.);
#61054=ORIENTED_EDGE('',*,*,#44794,.T.);
#61055=ORIENTED_EDGE('',*,*,#45691,.F.);
#61056=ORIENTED_EDGE('',*,*,#45692,.T.);
#61057=ORIENTED_EDGE('',*,*,#45689,.T.);
#61058=ORIENTED_EDGE('',*,*,#44791,.T.);
#61059=ORIENTED_EDGE('',*,*,#45693,.F.);
#61060=ORIENTED_EDGE('',*,*,#45694,.T.);
#61061=ORIENTED_EDGE('',*,*,#45691,.T.);
#61062=ORIENTED_EDGE('',*,*,#44790,.T.);
#61063=ORIENTED_EDGE('',*,*,#45695,.F.);
#61064=ORIENTED_EDGE('',*,*,#45696,.F.);
#61065=ORIENTED_EDGE('',*,*,#45434,.T.);
#61066=ORIENTED_EDGE('',*,*,#45697,.T.);
#61067=ORIENTED_EDGE('',*,*,#44789,.T.);
#61068=ORIENTED_EDGE('',*,*,#45698,.F.);
#61069=ORIENTED_EDGE('',*,*,#45699,.T.);
#61070=ORIENTED_EDGE('',*,*,#45696,.T.);
#61071=ORIENTED_EDGE('',*,*,#44788,.T.);
#61072=ORIENTED_EDGE('',*,*,#45700,.F.);
#61073=ORIENTED_EDGE('',*,*,#45701,.T.);
#61074=ORIENTED_EDGE('',*,*,#45698,.T.);
#61075=ORIENTED_EDGE('',*,*,#44787,.T.);
#61076=ORIENTED_EDGE('',*,*,#45702,.T.);
#61077=ORIENTED_EDGE('',*,*,#45703,.T.);
#61078=ORIENTED_EDGE('',*,*,#45700,.T.);
#61079=ORIENTED_EDGE('',*,*,#44786,.T.);
#61080=ORIENTED_EDGE('',*,*,#45702,.F.);
#61081=ORIENTED_EDGE('',*,*,#44785,.T.);
#61082=ORIENTED_EDGE('',*,*,#45704,.T.);
#61083=ORIENTED_EDGE('',*,*,#45705,.T.);
#61084=ORIENTED_EDGE('',*,*,#45704,.F.);
#61085=ORIENTED_EDGE('',*,*,#44784,.T.);
#61086=ORIENTED_EDGE('',*,*,#45690,.T.);
#61087=ORIENTED_EDGE('',*,*,#45706,.T.);
#61088=ORIENTED_EDGE('',*,*,#45707,.T.);
#61089=ORIENTED_EDGE('',*,*,#45706,.F.);
#61090=ORIENTED_EDGE('',*,*,#44793,.T.);
#61091=ORIENTED_EDGE('',*,*,#45708,.F.);
#61092=ORIENTED_EDGE('',*,*,#45709,.F.);
#61093=ORIENTED_EDGE('',*,*,#44795,.T.);
#61094=ORIENTED_EDGE('',*,*,#44796,.T.);
#61095=ORIENTED_EDGE('',*,*,#44807,.T.);
#61096=ORIENTED_EDGE('',*,*,#45710,.F.);
#61097=ORIENTED_EDGE('',*,*,#45708,.T.);
#61098=ORIENTED_EDGE('',*,*,#45709,.T.);
#61099=ORIENTED_EDGE('',*,*,#44806,.T.);
#61100=ORIENTED_EDGE('',*,*,#45711,.F.);
#61101=ORIENTED_EDGE('',*,*,#45712,.T.);
#61102=ORIENTED_EDGE('',*,*,#45710,.T.);
#61103=ORIENTED_EDGE('',*,*,#44805,.T.);
#61104=ORIENTED_EDGE('',*,*,#45713,.F.);
#61105=ORIENTED_EDGE('',*,*,#45714,.T.);
#61106=ORIENTED_EDGE('',*,*,#45711,.T.);
#61107=ORIENTED_EDGE('',*,*,#44804,.T.);
#61108=ORIENTED_EDGE('',*,*,#45715,.F.);
#61109=ORIENTED_EDGE('',*,*,#45716,.T.);
#61110=ORIENTED_EDGE('',*,*,#45713,.T.);
#61111=ORIENTED_EDGE('',*,*,#44803,.T.);
#61112=ORIENTED_EDGE('',*,*,#45717,.F.);
#61113=ORIENTED_EDGE('',*,*,#45718,.T.);
#61114=ORIENTED_EDGE('',*,*,#45715,.T.);
#61115=ORIENTED_EDGE('',*,*,#44802,.T.);
#61116=ORIENTED_EDGE('',*,*,#45719,.F.);
#61117=ORIENTED_EDGE('',*,*,#45436,.T.);
#61118=ORIENTED_EDGE('',*,*,#45717,.T.);
#61119=ORIENTED_EDGE('',*,*,#44801,.T.);
#61120=ORIENTED_EDGE('',*,*,#44800,.T.);
#61121=ORIENTED_EDGE('',*,*,#45720,.F.);
#61122=ORIENTED_EDGE('',*,*,#45721,.T.);
#61123=ORIENTED_EDGE('',*,*,#45722,.F.);
#61124=ORIENTED_EDGE('',*,*,#44809,.F.);
#61125=ORIENTED_EDGE('',*,*,#45723,.T.);
#61126=ORIENTED_EDGE('',*,*,#45720,.T.);
#61127=ORIENTED_EDGE('',*,*,#44799,.T.);
#61128=ORIENTED_EDGE('',*,*,#44811,.F.);
#61129=ORIENTED_EDGE('',*,*,#45724,.F.);
#61130=ORIENTED_EDGE('',*,*,#45725,.F.);
#61131=ORIENTED_EDGE('',*,*,#45723,.F.);
#61132=ORIENTED_EDGE('',*,*,#45726,.F.);
#61133=ORIENTED_EDGE('',*,*,#45724,.T.);
#61134=ORIENTED_EDGE('',*,*,#44813,.T.);
#61135=ORIENTED_EDGE('',*,*,#44817,.T.);
#61136=ORIENTED_EDGE('',*,*,#45727,.F.);
#61137=ORIENTED_EDGE('',*,*,#44818,.T.);
#61138=ORIENTED_EDGE('',*,*,#44814,.T.);
#61139=ORIENTED_EDGE('',*,*,#44826,.T.);
#61140=ORIENTED_EDGE('',*,*,#45728,.T.);
#61141=ORIENTED_EDGE('',*,*,#45726,.T.);
#61142=ORIENTED_EDGE('',*,*,#44816,.T.);
#61143=ORIENTED_EDGE('',*,*,#45729,.F.);
#61144=ORIENTED_EDGE('',*,*,#45730,.F.);
#61145=ORIENTED_EDGE('',*,*,#44824,.T.);
#61146=ORIENTED_EDGE('',*,*,#45731,.T.);
#61147=ORIENTED_EDGE('',*,*,#45440,.T.);
#61148=ORIENTED_EDGE('',*,*,#45731,.F.);
#61149=ORIENTED_EDGE('',*,*,#44823,.T.);
#61150=ORIENTED_EDGE('',*,*,#45732,.T.);
#61151=ORIENTED_EDGE('',*,*,#45733,.T.);
#61152=ORIENTED_EDGE('',*,*,#45732,.F.);
#61153=ORIENTED_EDGE('',*,*,#44822,.T.);
#61154=ORIENTED_EDGE('',*,*,#45734,.T.);
#61155=ORIENTED_EDGE('',*,*,#45735,.T.);
#61156=ORIENTED_EDGE('',*,*,#45734,.F.);
#61157=ORIENTED_EDGE('',*,*,#44821,.T.);
#61158=ORIENTED_EDGE('',*,*,#45736,.T.);
#61159=ORIENTED_EDGE('',*,*,#45737,.T.);
#61160=ORIENTED_EDGE('',*,*,#45736,.F.);
#61161=ORIENTED_EDGE('',*,*,#44820,.T.);
#61162=ORIENTED_EDGE('',*,*,#45738,.T.);
#61163=ORIENTED_EDGE('',*,*,#45739,.T.);
#61164=ORIENTED_EDGE('',*,*,#45738,.F.);
#61165=ORIENTED_EDGE('',*,*,#44819,.T.);
#61166=ORIENTED_EDGE('',*,*,#45727,.T.);
#61167=ORIENTED_EDGE('',*,*,#45740,.T.);
#61168=ORIENTED_EDGE('',*,*,#45741,.T.);
#61169=ORIENTED_EDGE('',*,*,#45740,.F.);
#61170=ORIENTED_EDGE('',*,*,#44825,.T.);
#61171=ORIENTED_EDGE('',*,*,#45742,.F.);
#61172=ORIENTED_EDGE('',*,*,#45743,.F.);
#61173=ORIENTED_EDGE('',*,*,#44827,.T.);
#61174=ORIENTED_EDGE('',*,*,#44828,.T.);
#61175=ORIENTED_EDGE('',*,*,#44839,.T.);
#61176=ORIENTED_EDGE('',*,*,#45744,.F.);
#61177=ORIENTED_EDGE('',*,*,#45742,.T.);
#61178=ORIENTED_EDGE('',*,*,#45743,.T.);
#61179=ORIENTED_EDGE('',*,*,#44838,.T.);
#61180=ORIENTED_EDGE('',*,*,#45745,.F.);
#61181=ORIENTED_EDGE('',*,*,#45746,.T.);
#61182=ORIENTED_EDGE('',*,*,#45744,.T.);
#61183=ORIENTED_EDGE('',*,*,#44837,.T.);
#61184=ORIENTED_EDGE('',*,*,#45747,.F.);
#61185=ORIENTED_EDGE('',*,*,#45748,.T.);
#61186=ORIENTED_EDGE('',*,*,#45745,.T.);
#61187=ORIENTED_EDGE('',*,*,#44836,.T.);
#61188=ORIENTED_EDGE('',*,*,#45749,.F.);
#61189=ORIENTED_EDGE('',*,*,#45750,.T.);
#61190=ORIENTED_EDGE('',*,*,#45747,.T.);
#61191=ORIENTED_EDGE('',*,*,#44835,.T.);
#61192=ORIENTED_EDGE('',*,*,#45751,.F.);
#61193=ORIENTED_EDGE('',*,*,#45752,.T.);
#61194=ORIENTED_EDGE('',*,*,#45749,.T.);
#61195=ORIENTED_EDGE('',*,*,#44834,.T.);
#61196=ORIENTED_EDGE('',*,*,#45753,.F.);
#61197=ORIENTED_EDGE('',*,*,#45442,.T.);
#61198=ORIENTED_EDGE('',*,*,#45751,.T.);
#61199=ORIENTED_EDGE('',*,*,#44833,.T.);
#61200=ORIENTED_EDGE('',*,*,#44832,.T.);
#61201=ORIENTED_EDGE('',*,*,#45754,.F.);
#61202=ORIENTED_EDGE('',*,*,#45755,.T.);
#61203=ORIENTED_EDGE('',*,*,#45756,.F.);
#61204=ORIENTED_EDGE('',*,*,#44841,.F.);
#61205=ORIENTED_EDGE('',*,*,#45757,.T.);
#61206=ORIENTED_EDGE('',*,*,#45754,.T.);
#61207=ORIENTED_EDGE('',*,*,#44831,.T.);
#61208=ORIENTED_EDGE('',*,*,#44843,.F.);
#61209=ORIENTED_EDGE('',*,*,#45758,.F.);
#61210=ORIENTED_EDGE('',*,*,#45759,.F.);
#61211=ORIENTED_EDGE('',*,*,#45757,.F.);
#61212=ORIENTED_EDGE('',*,*,#44845,.F.);
#61213=ORIENTED_EDGE('',*,*,#44856,.T.);
#61214=ORIENTED_EDGE('',*,*,#45760,.T.);
#61215=ORIENTED_EDGE('',*,*,#45758,.T.);
#61216=ORIENTED_EDGE('',*,*,#45761,.F.);
#61217=ORIENTED_EDGE('',*,*,#44848,.T.);
#61218=ORIENTED_EDGE('',*,*,#44846,.T.);
#61219=ORIENTED_EDGE('',*,*,#44858,.T.);
#61220=ORIENTED_EDGE('',*,*,#45762,.T.);
#61221=ORIENTED_EDGE('',*,*,#45760,.F.);
#61222=ORIENTED_EDGE('',*,*,#44855,.T.);
#61223=ORIENTED_EDGE('',*,*,#45763,.F.);
#61224=ORIENTED_EDGE('',*,*,#45764,.F.);
#61225=ORIENTED_EDGE('',*,*,#44854,.T.);
#61226=ORIENTED_EDGE('',*,*,#45765,.T.);
#61227=ORIENTED_EDGE('',*,*,#45446,.T.);
#61228=ORIENTED_EDGE('',*,*,#45765,.F.);
#61229=ORIENTED_EDGE('',*,*,#44853,.T.);
#61230=ORIENTED_EDGE('',*,*,#45766,.T.);
#61231=ORIENTED_EDGE('',*,*,#45767,.T.);
#61232=ORIENTED_EDGE('',*,*,#45766,.F.);
#61233=ORIENTED_EDGE('',*,*,#44852,.T.);
#61234=ORIENTED_EDGE('',*,*,#45768,.T.);
#61235=ORIENTED_EDGE('',*,*,#45769,.T.);
#61236=ORIENTED_EDGE('',*,*,#45768,.F.);
#61237=ORIENTED_EDGE('',*,*,#44851,.T.);
#61238=ORIENTED_EDGE('',*,*,#45770,.T.);
#61239=ORIENTED_EDGE('',*,*,#45771,.T.);
#61240=ORIENTED_EDGE('',*,*,#45770,.F.);
#61241=ORIENTED_EDGE('',*,*,#44850,.T.);
#61242=ORIENTED_EDGE('',*,*,#45772,.T.);
#61243=ORIENTED_EDGE('',*,*,#45773,.T.);
#61244=ORIENTED_EDGE('',*,*,#45772,.F.);
#61245=ORIENTED_EDGE('',*,*,#44849,.T.);
#61246=ORIENTED_EDGE('',*,*,#45761,.T.);
#61247=ORIENTED_EDGE('',*,*,#45774,.T.);
#61248=ORIENTED_EDGE('',*,*,#45775,.T.);
#61249=ORIENTED_EDGE('',*,*,#45774,.F.);
#61250=ORIENTED_EDGE('',*,*,#44857,.T.);
#61251=ORIENTED_EDGE('',*,*,#45776,.F.);
#61252=ORIENTED_EDGE('',*,*,#45777,.F.);
#61253=ORIENTED_EDGE('',*,*,#44859,.T.);
#61254=ORIENTED_EDGE('',*,*,#44860,.T.);
#61255=ORIENTED_EDGE('',*,*,#44871,.T.);
#61256=ORIENTED_EDGE('',*,*,#45778,.F.);
#61257=ORIENTED_EDGE('',*,*,#45776,.T.);
#61258=ORIENTED_EDGE('',*,*,#45777,.T.);
#61259=ORIENTED_EDGE('',*,*,#44870,.T.);
#61260=ORIENTED_EDGE('',*,*,#45779,.F.);
#61261=ORIENTED_EDGE('',*,*,#45780,.T.);
#61262=ORIENTED_EDGE('',*,*,#45778,.T.);
#61263=ORIENTED_EDGE('',*,*,#44869,.T.);
#61264=ORIENTED_EDGE('',*,*,#45781,.F.);
#61265=ORIENTED_EDGE('',*,*,#45782,.T.);
#61266=ORIENTED_EDGE('',*,*,#45779,.T.);
#61267=ORIENTED_EDGE('',*,*,#44868,.T.);
#61268=ORIENTED_EDGE('',*,*,#45783,.F.);
#61269=ORIENTED_EDGE('',*,*,#45784,.T.);
#61270=ORIENTED_EDGE('',*,*,#45781,.T.);
#61271=ORIENTED_EDGE('',*,*,#44867,.T.);
#61272=ORIENTED_EDGE('',*,*,#45785,.F.);
#61273=ORIENTED_EDGE('',*,*,#45786,.T.);
#61274=ORIENTED_EDGE('',*,*,#45783,.T.);
#61275=ORIENTED_EDGE('',*,*,#44866,.T.);
#61276=ORIENTED_EDGE('',*,*,#45787,.F.);
#61277=ORIENTED_EDGE('',*,*,#45448,.T.);
#61278=ORIENTED_EDGE('',*,*,#45785,.T.);
#61279=ORIENTED_EDGE('',*,*,#44865,.T.);
#61280=ORIENTED_EDGE('',*,*,#44864,.T.);
#61281=ORIENTED_EDGE('',*,*,#45788,.F.);
#61282=ORIENTED_EDGE('',*,*,#45789,.T.);
#61283=ORIENTED_EDGE('',*,*,#45790,.F.);
#61284=ORIENTED_EDGE('',*,*,#44873,.F.);
#61285=ORIENTED_EDGE('',*,*,#45791,.T.);
#61286=ORIENTED_EDGE('',*,*,#45788,.T.);
#61287=ORIENTED_EDGE('',*,*,#44863,.T.);
#61288=ORIENTED_EDGE('',*,*,#44875,.F.);
#61289=ORIENTED_EDGE('',*,*,#45792,.F.);
#61290=ORIENTED_EDGE('',*,*,#45793,.F.);
#61291=ORIENTED_EDGE('',*,*,#45791,.F.);
#61292=ORIENTED_EDGE('',*,*,#44877,.F.);
#61293=ORIENTED_EDGE('',*,*,#44888,.T.);
#61294=ORIENTED_EDGE('',*,*,#45794,.T.);
#61295=ORIENTED_EDGE('',*,*,#45792,.T.);
#61296=ORIENTED_EDGE('',*,*,#45795,.F.);
#61297=ORIENTED_EDGE('',*,*,#44880,.T.);
#61298=ORIENTED_EDGE('',*,*,#44878,.T.);
#61299=ORIENTED_EDGE('',*,*,#44890,.T.);
#61300=ORIENTED_EDGE('',*,*,#45796,.T.);
#61301=ORIENTED_EDGE('',*,*,#45794,.F.);
#61302=ORIENTED_EDGE('',*,*,#44887,.T.);
#61303=ORIENTED_EDGE('',*,*,#45797,.F.);
#61304=ORIENTED_EDGE('',*,*,#45798,.F.);
#61305=ORIENTED_EDGE('',*,*,#44886,.T.);
#61306=ORIENTED_EDGE('',*,*,#45799,.T.);
#61307=ORIENTED_EDGE('',*,*,#45452,.T.);
#61308=ORIENTED_EDGE('',*,*,#45799,.F.);
#61309=ORIENTED_EDGE('',*,*,#44885,.T.);
#61310=ORIENTED_EDGE('',*,*,#45800,.T.);
#61311=ORIENTED_EDGE('',*,*,#45801,.T.);
#61312=ORIENTED_EDGE('',*,*,#45800,.F.);
#61313=ORIENTED_EDGE('',*,*,#44884,.T.);
#61314=ORIENTED_EDGE('',*,*,#45802,.T.);
#61315=ORIENTED_EDGE('',*,*,#45803,.T.);
#61316=ORIENTED_EDGE('',*,*,#45802,.F.);
#61317=ORIENTED_EDGE('',*,*,#44883,.T.);
#61318=ORIENTED_EDGE('',*,*,#45804,.T.);
#61319=ORIENTED_EDGE('',*,*,#45805,.T.);
#61320=ORIENTED_EDGE('',*,*,#45804,.F.);
#61321=ORIENTED_EDGE('',*,*,#44882,.T.);
#61322=ORIENTED_EDGE('',*,*,#45806,.T.);
#61323=ORIENTED_EDGE('',*,*,#45807,.T.);
#61324=ORIENTED_EDGE('',*,*,#45806,.F.);
#61325=ORIENTED_EDGE('',*,*,#44881,.T.);
#61326=ORIENTED_EDGE('',*,*,#45795,.T.);
#61327=ORIENTED_EDGE('',*,*,#45808,.T.);
#61328=ORIENTED_EDGE('',*,*,#45809,.T.);
#61329=ORIENTED_EDGE('',*,*,#45808,.F.);
#61330=ORIENTED_EDGE('',*,*,#44889,.T.);
#61331=ORIENTED_EDGE('',*,*,#45810,.F.);
#61332=ORIENTED_EDGE('',*,*,#44893,.F.);
#61333=ORIENTED_EDGE('',*,*,#44904,.T.);
#61334=ORIENTED_EDGE('',*,*,#45811,.T.);
#61335=ORIENTED_EDGE('',*,*,#44891,.T.);
#61336=ORIENTED_EDGE('',*,*,#45811,.F.);
#61337=ORIENTED_EDGE('',*,*,#44903,.T.);
#61338=ORIENTED_EDGE('',*,*,#45812,.F.);
#61339=ORIENTED_EDGE('',*,*,#45810,.T.);
#61340=ORIENTED_EDGE('',*,*,#45813,.F.);
#61341=ORIENTED_EDGE('',*,*,#45814,.T.);
#61342=ORIENTED_EDGE('',*,*,#45812,.T.);
#61343=ORIENTED_EDGE('',*,*,#44902,.T.);
#61344=ORIENTED_EDGE('',*,*,#45815,.F.);
#61345=ORIENTED_EDGE('',*,*,#45816,.T.);
#61346=ORIENTED_EDGE('',*,*,#45813,.T.);
#61347=ORIENTED_EDGE('',*,*,#44901,.T.);
#61348=ORIENTED_EDGE('',*,*,#45817,.F.);
#61349=ORIENTED_EDGE('',*,*,#45818,.T.);
#61350=ORIENTED_EDGE('',*,*,#45815,.T.);
#61351=ORIENTED_EDGE('',*,*,#44900,.T.);
#61352=ORIENTED_EDGE('',*,*,#45819,.F.);
#61353=ORIENTED_EDGE('',*,*,#45820,.T.);
#61354=ORIENTED_EDGE('',*,*,#45817,.T.);
#61355=ORIENTED_EDGE('',*,*,#44899,.T.);
#61356=ORIENTED_EDGE('',*,*,#45821,.F.);
#61357=ORIENTED_EDGE('',*,*,#45454,.T.);
#61358=ORIENTED_EDGE('',*,*,#45819,.T.);
#61359=ORIENTED_EDGE('',*,*,#44898,.T.);
#61360=ORIENTED_EDGE('',*,*,#44897,.T.);
#61361=ORIENTED_EDGE('',*,*,#45822,.F.);
#61362=ORIENTED_EDGE('',*,*,#45823,.T.);
#61363=ORIENTED_EDGE('',*,*,#45824,.T.);
#61364=ORIENTED_EDGE('',*,*,#45825,.F.);
#61365=ORIENTED_EDGE('',*,*,#45826,.F.);
#61366=ORIENTED_EDGE('',*,*,#45827,.T.);
#61367=ORIENTED_EDGE('',*,*,#45822,.T.);
#61368=ORIENTED_EDGE('',*,*,#44896,.T.);
#61369=ORIENTED_EDGE('',*,*,#44906,.F.);
#61370=ORIENTED_EDGE('',*,*,#45828,.T.);
#61371=ORIENTED_EDGE('',*,*,#45826,.T.);
#61372=ORIENTED_EDGE('',*,*,#44895,.T.);
#61373=ORIENTED_EDGE('',*,*,#44908,.T.);
#61374=ORIENTED_EDGE('',*,*,#45829,.F.);
#61375=ORIENTED_EDGE('',*,*,#45830,.T.);
#61376=ORIENTED_EDGE('',*,*,#45828,.F.);
#61377=ORIENTED_EDGE('',*,*,#45831,.F.);
#61378=ORIENTED_EDGE('',*,*,#45829,.T.);
#61379=ORIENTED_EDGE('',*,*,#44910,.T.);
#61380=ORIENTED_EDGE('',*,*,#44923,.T.);
#61381=ORIENTED_EDGE('',*,*,#45832,.F.);
#61382=ORIENTED_EDGE('',*,*,#44913,.T.);
#61383=ORIENTED_EDGE('',*,*,#44911,.T.);
#61384=ORIENTED_EDGE('',*,*,#44925,.T.);
#61385=ORIENTED_EDGE('',*,*,#45833,.F.);
#61386=ORIENTED_EDGE('',*,*,#45834,.T.);
#61387=ORIENTED_EDGE('',*,*,#45831,.T.);
#61388=ORIENTED_EDGE('',*,*,#44922,.T.);
#61389=ORIENTED_EDGE('',*,*,#45835,.F.);
#61390=ORIENTED_EDGE('',*,*,#45836,.T.);
#61391=ORIENTED_EDGE('',*,*,#45833,.T.);
#61392=ORIENTED_EDGE('',*,*,#44921,.T.);
#61393=ORIENTED_EDGE('',*,*,#45837,.T.);
#61394=ORIENTED_EDGE('',*,*,#45835,.T.);
#61395=ORIENTED_EDGE('',*,*,#44920,.T.);
#61396=ORIENTED_EDGE('',*,*,#45838,.F.);
#61397=ORIENTED_EDGE('',*,*,#45839,.F.);
#61398=ORIENTED_EDGE('',*,*,#45459,.T.);
#61399=ORIENTED_EDGE('',*,*,#45840,.T.);
#61400=ORIENTED_EDGE('',*,*,#44919,.T.);
#61401=ORIENTED_EDGE('',*,*,#45841,.F.);
#61402=ORIENTED_EDGE('',*,*,#45842,.T.);
#61403=ORIENTED_EDGE('',*,*,#45839,.T.);
#61404=ORIENTED_EDGE('',*,*,#44918,.T.);
#61405=ORIENTED_EDGE('',*,*,#45843,.F.);
#61406=ORIENTED_EDGE('',*,*,#45844,.T.);
#61407=ORIENTED_EDGE('',*,*,#45841,.T.);
#61408=ORIENTED_EDGE('',*,*,#44917,.T.);
#61409=ORIENTED_EDGE('',*,*,#45845,.T.);
#61410=ORIENTED_EDGE('',*,*,#45846,.T.);
#61411=ORIENTED_EDGE('',*,*,#45843,.T.);
#61412=ORIENTED_EDGE('',*,*,#44916,.T.);
#61413=ORIENTED_EDGE('',*,*,#45845,.F.);
#61414=ORIENTED_EDGE('',*,*,#44915,.T.);
#61415=ORIENTED_EDGE('',*,*,#45847,.T.);
#61416=ORIENTED_EDGE('',*,*,#45848,.T.);
#61417=ORIENTED_EDGE('',*,*,#45847,.F.);
#61418=ORIENTED_EDGE('',*,*,#44914,.T.);
#61419=ORIENTED_EDGE('',*,*,#45832,.T.);
#61420=ORIENTED_EDGE('',*,*,#45849,.T.);
#61421=ORIENTED_EDGE('',*,*,#45850,.T.);
#61422=ORIENTED_EDGE('',*,*,#45849,.F.);
#61423=ORIENTED_EDGE('',*,*,#44924,.T.);
#61424=ORIENTED_EDGE('',*,*,#45851,.F.);
#61425=ORIENTED_EDGE('',*,*,#44928,.F.);
#61426=ORIENTED_EDGE('',*,*,#44934,.T.);
#61427=ORIENTED_EDGE('',*,*,#45852,.T.);
#61428=ORIENTED_EDGE('',*,*,#44926,.T.);
#61429=ORIENTED_EDGE('',*,*,#45853,.F.);
#61430=ORIENTED_EDGE('',*,*,#44929,.T.);
#61431=ORIENTED_EDGE('',*,*,#45854,.T.);
#61432=ORIENTED_EDGE('',*,*,#45855,.T.);
#61433=ORIENTED_EDGE('',*,*,#45854,.F.);
#61434=ORIENTED_EDGE('',*,*,#44939,.T.);
#61435=ORIENTED_EDGE('',*,*,#45856,.T.);
#61436=ORIENTED_EDGE('',*,*,#45461,.T.);
#61437=ORIENTED_EDGE('',*,*,#44938,.T.);
#61438=ORIENTED_EDGE('',*,*,#45857,.F.);
#61439=ORIENTED_EDGE('',*,*,#45858,.T.);
#61440=ORIENTED_EDGE('',*,*,#45859,.F.);
#61441=ORIENTED_EDGE('',*,*,#45860,.F.);
#61442=ORIENTED_EDGE('',*,*,#45861,.T.);
#61443=ORIENTED_EDGE('',*,*,#45857,.T.);
#61444=ORIENTED_EDGE('',*,*,#44937,.T.);
#61445=ORIENTED_EDGE('',*,*,#45639,.F.);
#61446=ORIENTED_EDGE('',*,*,#45862,.T.);
#61447=ORIENTED_EDGE('',*,*,#45860,.T.);
#61448=ORIENTED_EDGE('',*,*,#44936,.T.);
#61449=ORIENTED_EDGE('',*,*,#45852,.F.);
#61450=ORIENTED_EDGE('',*,*,#44933,.T.);
#61451=ORIENTED_EDGE('',*,*,#45863,.T.);
#61452=ORIENTED_EDGE('',*,*,#45851,.T.);
#61453=ORIENTED_EDGE('',*,*,#45863,.F.);
#61454=ORIENTED_EDGE('',*,*,#44932,.T.);
#61455=ORIENTED_EDGE('',*,*,#45864,.T.);
#61456=ORIENTED_EDGE('',*,*,#45865,.T.);
#61457=ORIENTED_EDGE('',*,*,#45864,.F.);
#61458=ORIENTED_EDGE('',*,*,#44931,.T.);
#61459=ORIENTED_EDGE('',*,*,#45866,.T.);
#61460=ORIENTED_EDGE('',*,*,#45867,.T.);
#61461=ORIENTED_EDGE('',*,*,#45866,.F.);
#61462=ORIENTED_EDGE('',*,*,#44930,.T.);
#61463=ORIENTED_EDGE('',*,*,#45853,.T.);
#61464=ORIENTED_EDGE('',*,*,#45868,.T.);
#61465=ORIENTED_EDGE('',*,*,#45869,.T.);
#61466=ORIENTED_EDGE('',*,*,#45870,.F.);
#61467=ORIENTED_EDGE('',*,*,#44940,.T.);
#61468=ORIENTED_EDGE('',*,*,#45871,.F.);
#61469=ORIENTED_EDGE('',*,*,#45872,.F.);
#61470=ORIENTED_EDGE('',*,*,#44943,.T.);
#61471=ORIENTED_EDGE('',*,*,#44944,.T.);
#61472=ORIENTED_EDGE('',*,*,#44956,.T.);
#61473=ORIENTED_EDGE('',*,*,#45873,.F.);
#61474=ORIENTED_EDGE('',*,*,#45032,.T.);
#61475=ORIENTED_EDGE('',*,*,#44946,.T.);
#61476=ORIENTED_EDGE('',*,*,#44942,.T.);
#61477=ORIENTED_EDGE('',*,*,#44941,.T.);
#61478=ORIENTED_EDGE('',*,*,#45870,.T.);
#61479=ORIENTED_EDGE('',*,*,#45874,.T.);
#61480=ORIENTED_EDGE('',*,*,#45875,.F.);
#61481=ORIENTED_EDGE('',*,*,#45876,.F.);
#61482=ORIENTED_EDGE('',*,*,#44948,.T.);
#61483=ORIENTED_EDGE('',*,*,#45877,.T.);
#61484=ORIENTED_EDGE('',*,*,#45878,.T.);
#61485=ORIENTED_EDGE('',*,*,#45879,.T.);
#61486=ORIENTED_EDGE('',*,*,#45877,.F.);
#61487=ORIENTED_EDGE('',*,*,#44962,.T.);
#61488=ORIENTED_EDGE('',*,*,#45880,.T.);
#61489=ORIENTED_EDGE('',*,*,#45499,.T.);
#61490=ORIENTED_EDGE('',*,*,#45878,.F.);
#61491=ORIENTED_EDGE('',*,*,#44961,.T.);
#61492=ORIENTED_EDGE('',*,*,#45881,.F.);
#61493=ORIENTED_EDGE('',*,*,#45882,.T.);
#61494=ORIENTED_EDGE('',*,*,#45883,.F.);
#61495=ORIENTED_EDGE('',*,*,#45884,.F.);
#61496=ORIENTED_EDGE('',*,*,#45885,.T.);
#61497=ORIENTED_EDGE('',*,*,#45881,.T.);
#61498=ORIENTED_EDGE('',*,*,#44960,.T.);
#61499=ORIENTED_EDGE('',*,*,#45886,.F.);
#61500=ORIENTED_EDGE('',*,*,#45887,.T.);
#61501=ORIENTED_EDGE('',*,*,#45884,.T.);
#61502=ORIENTED_EDGE('',*,*,#44959,.T.);
#61503=ORIENTED_EDGE('',*,*,#44964,.F.);
#61504=ORIENTED_EDGE('',*,*,#45888,.T.);
#61505=ORIENTED_EDGE('',*,*,#45886,.T.);
#61506=ORIENTED_EDGE('',*,*,#44958,.T.);
#61507=ORIENTED_EDGE('',*,*,#45889,.F.);
#61508=ORIENTED_EDGE('',*,*,#45871,.T.);
#61509=ORIENTED_EDGE('',*,*,#45872,.T.);
#61510=ORIENTED_EDGE('',*,*,#44955,.T.);
#61511=ORIENTED_EDGE('',*,*,#45890,.F.);
#61512=ORIENTED_EDGE('',*,*,#45891,.T.);
#61513=ORIENTED_EDGE('',*,*,#45889,.T.);
#61514=ORIENTED_EDGE('',*,*,#44954,.T.);
#61515=ORIENTED_EDGE('',*,*,#45892,.T.);
#61516=ORIENTED_EDGE('',*,*,#45893,.T.);
#61517=ORIENTED_EDGE('',*,*,#45890,.T.);
#61518=ORIENTED_EDGE('',*,*,#44953,.T.);
#61519=ORIENTED_EDGE('',*,*,#45892,.F.);
#61520=ORIENTED_EDGE('',*,*,#44952,.T.);
#61521=ORIENTED_EDGE('',*,*,#45894,.T.);
#61522=ORIENTED_EDGE('',*,*,#45895,.T.);
#61523=ORIENTED_EDGE('',*,*,#45894,.F.);
#61524=ORIENTED_EDGE('',*,*,#44951,.T.);
#61525=ORIENTED_EDGE('',*,*,#45896,.T.);
#61526=ORIENTED_EDGE('',*,*,#45897,.T.);
#61527=ORIENTED_EDGE('',*,*,#45896,.F.);
#61528=ORIENTED_EDGE('',*,*,#44950,.T.);
#61529=ORIENTED_EDGE('',*,*,#45898,.T.);
#61530=ORIENTED_EDGE('',*,*,#45899,.T.);
#61531=ORIENTED_EDGE('',*,*,#45898,.F.);
#61532=ORIENTED_EDGE('',*,*,#44949,.T.);
#61533=ORIENTED_EDGE('',*,*,#45876,.T.);
#61534=ORIENTED_EDGE('',*,*,#45900,.T.);
#61535=ORIENTED_EDGE('',*,*,#45901,.T.);
#61536=ORIENTED_EDGE('',*,*,#45888,.F.);
#61537=ORIENTED_EDGE('',*,*,#44966,.T.);
#61538=ORIENTED_EDGE('',*,*,#45902,.F.);
#61539=ORIENTED_EDGE('',*,*,#44968,.F.);
#61540=ORIENTED_EDGE('',*,*,#44976,.T.);
#61541=ORIENTED_EDGE('',*,*,#45903,.T.);
#61542=ORIENTED_EDGE('',*,*,#45902,.T.);
#61543=ORIENTED_EDGE('',*,*,#45505,.F.);
#61544=ORIENTED_EDGE('',*,*,#44982,.T.);
#61545=ORIENTED_EDGE('',*,*,#45904,.T.);
#61546=ORIENTED_EDGE('',*,*,#45515,.T.);
#61547=ORIENTED_EDGE('',*,*,#44981,.T.);
#61548=ORIENTED_EDGE('',*,*,#45905,.F.);
#61549=ORIENTED_EDGE('',*,*,#45229,.T.);
#61550=ORIENTED_EDGE('',*,*,#45906,.F.);
#61551=ORIENTED_EDGE('',*,*,#45907,.F.);
#61552=ORIENTED_EDGE('',*,*,#45908,.T.);
#61553=ORIENTED_EDGE('',*,*,#45909,.T.);
#61554=ORIENTED_EDGE('',*,*,#44980,.T.);
#61555=ORIENTED_EDGE('',*,*,#45323,.F.);
#61556=ORIENTED_EDGE('',*,*,#45331,.T.);
#61557=ORIENTED_EDGE('',*,*,#45907,.T.);
#61558=ORIENTED_EDGE('',*,*,#44979,.T.);
#61559=ORIENTED_EDGE('',*,*,#45903,.F.);
#61560=ORIENTED_EDGE('',*,*,#44975,.T.);
#61561=ORIENTED_EDGE('',*,*,#45910,.T.);
#61562=ORIENTED_EDGE('',*,*,#45911,.T.);
#61563=ORIENTED_EDGE('',*,*,#45910,.F.);
#61564=ORIENTED_EDGE('',*,*,#44974,.T.);
#61565=ORIENTED_EDGE('',*,*,#45912,.T.);
#61566=ORIENTED_EDGE('',*,*,#45913,.T.);
#61567=ORIENTED_EDGE('',*,*,#45914,.T.);
#61568=ORIENTED_EDGE('',*,*,#45912,.F.);
#61569=ORIENTED_EDGE('',*,*,#44973,.T.);
#61570=ORIENTED_EDGE('',*,*,#45915,.F.);
#61571=ORIENTED_EDGE('',*,*,#45916,.F.);
#61572=ORIENTED_EDGE('',*,*,#44972,.T.);
#61573=ORIENTED_EDGE('',*,*,#45917,.T.);
#61574=ORIENTED_EDGE('',*,*,#45503,.T.);
#61575=ORIENTED_EDGE('',*,*,#45917,.F.);
#61576=ORIENTED_EDGE('',*,*,#44971,.T.);
#61577=ORIENTED_EDGE('',*,*,#45918,.T.);
#61578=ORIENTED_EDGE('',*,*,#45919,.T.);
#61579=ORIENTED_EDGE('',*,*,#45918,.F.);
#61580=ORIENTED_EDGE('',*,*,#44970,.T.);
#61581=ORIENTED_EDGE('',*,*,#45504,.T.);
#61582=ORIENTED_EDGE('',*,*,#45511,.T.);
#61583=ORIENTED_EDGE('',*,*,#45920,.F.);
#61584=ORIENTED_EDGE('',*,*,#44990,.T.);
#61585=ORIENTED_EDGE('',*,*,#44984,.T.);
#61586=ORIENTED_EDGE('',*,*,#45000,.T.);
#61587=ORIENTED_EDGE('',*,*,#45555,.F.);
#61588=ORIENTED_EDGE('',*,*,#44997,.T.);
#61589=ORIENTED_EDGE('',*,*,#45921,.T.);
#61590=ORIENTED_EDGE('',*,*,#45559,.T.);
#61591=ORIENTED_EDGE('',*,*,#45921,.F.);
#61592=ORIENTED_EDGE('',*,*,#44996,.T.);
#61593=ORIENTED_EDGE('',*,*,#45922,.T.);
#61594=ORIENTED_EDGE('',*,*,#45923,.T.);
#61595=ORIENTED_EDGE('',*,*,#45922,.F.);
#61596=ORIENTED_EDGE('',*,*,#44995,.T.);
#61597=ORIENTED_EDGE('',*,*,#45924,.T.);
#61598=ORIENTED_EDGE('',*,*,#45925,.T.);
#61599=ORIENTED_EDGE('',*,*,#45924,.F.);
#61600=ORIENTED_EDGE('',*,*,#44994,.T.);
#61601=ORIENTED_EDGE('',*,*,#45926,.T.);
#61602=ORIENTED_EDGE('',*,*,#45927,.T.);
#61603=ORIENTED_EDGE('',*,*,#45926,.F.);
#61604=ORIENTED_EDGE('',*,*,#44993,.T.);
#61605=ORIENTED_EDGE('',*,*,#45928,.T.);
#61606=ORIENTED_EDGE('',*,*,#45929,.T.);
#61607=ORIENTED_EDGE('',*,*,#45928,.F.);
#61608=ORIENTED_EDGE('',*,*,#44992,.T.);
#61609=ORIENTED_EDGE('',*,*,#45930,.T.);
#61610=ORIENTED_EDGE('',*,*,#45931,.T.);
#61611=ORIENTED_EDGE('',*,*,#45930,.F.);
#61612=ORIENTED_EDGE('',*,*,#44991,.T.);
#61613=ORIENTED_EDGE('',*,*,#45920,.T.);
#61614=ORIENTED_EDGE('',*,*,#45932,.T.);
#61615=ORIENTED_EDGE('',*,*,#45933,.F.);
#61616=ORIENTED_EDGE('',*,*,#45934,.T.);
#61617=ORIENTED_EDGE('',*,*,#45336,.T.);
#61618=ORIENTED_EDGE('',*,*,#44988,.T.);
#61619=ORIENTED_EDGE('',*,*,#45561,.F.);
#61620=ORIENTED_EDGE('',*,*,#45935,.T.);
#61621=ORIENTED_EDGE('',*,*,#45933,.T.);
#61622=ORIENTED_EDGE('',*,*,#44987,.T.);
#61623=ORIENTED_EDGE('',*,*,#45936,.F.);
#61624=ORIENTED_EDGE('',*,*,#45932,.F.);
#61625=ORIENTED_EDGE('',*,*,#44999,.F.);
#61626=ORIENTED_EDGE('',*,*,#45937,.F.);
#61627=ORIENTED_EDGE('',*,*,#45938,.F.);
#61628=ORIENTED_EDGE('',*,*,#45002,.T.);
#61629=ORIENTED_EDGE('',*,*,#45939,.T.);
#61630=ORIENTED_EDGE('',*,*,#45020,.T.);
#61631=ORIENTED_EDGE('',*,*,#45939,.F.);
#61632=ORIENTED_EDGE('',*,*,#45003,.T.);
#61633=ORIENTED_EDGE('',*,*,#45004,.T.);
#61634=ORIENTED_EDGE('',*,*,#45021,.T.);
#61635=ORIENTED_EDGE('',*,*,#45940,.F.);
#61636=ORIENTED_EDGE('',*,*,#45937,.T.);
#61637=ORIENTED_EDGE('',*,*,#45938,.T.);
#61638=ORIENTED_EDGE('',*,*,#45019,.T.);
#61639=ORIENTED_EDGE('',*,*,#45941,.F.);
#61640=ORIENTED_EDGE('',*,*,#45942,.T.);
#61641=ORIENTED_EDGE('',*,*,#45940,.T.);
#61642=ORIENTED_EDGE('',*,*,#45018,.T.);
#61643=ORIENTED_EDGE('',*,*,#45943,.F.);
#61644=ORIENTED_EDGE('',*,*,#45944,.T.);
#61645=ORIENTED_EDGE('',*,*,#45941,.T.);
#61646=ORIENTED_EDGE('',*,*,#45017,.T.);
#61647=ORIENTED_EDGE('',*,*,#45945,.F.);
#61648=ORIENTED_EDGE('',*,*,#45946,.T.);
#61649=ORIENTED_EDGE('',*,*,#45943,.T.);
#61650=ORIENTED_EDGE('',*,*,#45016,.T.);
#61651=ORIENTED_EDGE('',*,*,#45947,.F.);
#61652=ORIENTED_EDGE('',*,*,#45948,.T.);
#61653=ORIENTED_EDGE('',*,*,#45945,.T.);
#61654=ORIENTED_EDGE('',*,*,#45015,.T.);
#61655=ORIENTED_EDGE('',*,*,#45949,.F.);
#61656=ORIENTED_EDGE('',*,*,#45950,.T.);
#61657=ORIENTED_EDGE('',*,*,#45947,.T.);
#61658=ORIENTED_EDGE('',*,*,#45014,.T.);
#61659=ORIENTED_EDGE('',*,*,#45951,.F.);
#61660=ORIENTED_EDGE('',*,*,#45952,.T.);
#61661=ORIENTED_EDGE('',*,*,#45949,.T.);
#61662=ORIENTED_EDGE('',*,*,#45013,.T.);
#61663=ORIENTED_EDGE('',*,*,#45953,.F.);
#61664=ORIENTED_EDGE('',*,*,#45954,.T.);
#61665=ORIENTED_EDGE('',*,*,#45951,.T.);
#61666=ORIENTED_EDGE('',*,*,#45012,.T.);
#61667=ORIENTED_EDGE('',*,*,#45955,.F.);
#61668=ORIENTED_EDGE('',*,*,#45493,.T.);
#61669=ORIENTED_EDGE('',*,*,#45953,.T.);
#61670=ORIENTED_EDGE('',*,*,#45011,.T.);
#61671=ORIENTED_EDGE('',*,*,#45010,.T.);
#61672=ORIENTED_EDGE('',*,*,#45956,.F.);
#61673=ORIENTED_EDGE('',*,*,#45957,.T.);
#61674=ORIENTED_EDGE('',*,*,#45958,.F.);
#61675=ORIENTED_EDGE('',*,*,#45959,.F.);
#61676=ORIENTED_EDGE('',*,*,#45960,.T.);
#61677=ORIENTED_EDGE('',*,*,#45956,.T.);
#61678=ORIENTED_EDGE('',*,*,#45009,.T.);
#61679=ORIENTED_EDGE('',*,*,#45961,.F.);
#61680=ORIENTED_EDGE('',*,*,#45962,.T.);
#61681=ORIENTED_EDGE('',*,*,#45959,.T.);
#61682=ORIENTED_EDGE('',*,*,#45008,.T.);
#61683=ORIENTED_EDGE('',*,*,#45023,.F.);
#61684=ORIENTED_EDGE('',*,*,#45963,.T.);
#61685=ORIENTED_EDGE('',*,*,#45961,.T.);
#61686=ORIENTED_EDGE('',*,*,#45007,.T.);
#61687=ORIENTED_EDGE('',*,*,#45025,.T.);
#61688=ORIENTED_EDGE('',*,*,#45964,.F.);
#61689=ORIENTED_EDGE('',*,*,#45965,.T.);
#61690=ORIENTED_EDGE('',*,*,#45963,.F.);
#61691=ORIENTED_EDGE('',*,*,#45966,.F.);
#61692=ORIENTED_EDGE('',*,*,#45964,.T.);
#61693=ORIENTED_EDGE('',*,*,#45027,.T.);
#61694=ORIENTED_EDGE('',*,*,#45031,.T.);
#61695=ORIENTED_EDGE('',*,*,#45967,.T.);
#61696=ORIENTED_EDGE('',*,*,#45968,.T.);
#61697=ORIENTED_EDGE('',*,*,#45028,.T.);
#61698=ORIENTED_EDGE('',*,*,#45969,.F.);
#61699=ORIENTED_EDGE('',*,*,#45970,.F.);
#61700=ORIENTED_EDGE('',*,*,#45042,.T.);
#61701=ORIENTED_EDGE('',*,*,#45971,.T.);
#61702=ORIENTED_EDGE('',*,*,#45497,.T.);
#61703=ORIENTED_EDGE('',*,*,#45971,.F.);
#61704=ORIENTED_EDGE('',*,*,#45041,.T.);
#61705=ORIENTED_EDGE('',*,*,#45972,.T.);
#61706=ORIENTED_EDGE('',*,*,#45973,.T.);
#61707=ORIENTED_EDGE('',*,*,#45972,.F.);
#61708=ORIENTED_EDGE('',*,*,#45040,.T.);
#61709=ORIENTED_EDGE('',*,*,#45974,.T.);
#61710=ORIENTED_EDGE('',*,*,#45975,.T.);
#61711=ORIENTED_EDGE('',*,*,#45974,.F.);
#61712=ORIENTED_EDGE('',*,*,#45039,.T.);
#61713=ORIENTED_EDGE('',*,*,#45976,.T.);
#61714=ORIENTED_EDGE('',*,*,#45977,.T.);
#61715=ORIENTED_EDGE('',*,*,#45976,.F.);
#61716=ORIENTED_EDGE('',*,*,#45038,.T.);
#61717=ORIENTED_EDGE('',*,*,#45978,.T.);
#61718=ORIENTED_EDGE('',*,*,#45979,.T.);
#61719=ORIENTED_EDGE('',*,*,#45978,.F.);
#61720=ORIENTED_EDGE('',*,*,#45037,.T.);
#61721=ORIENTED_EDGE('',*,*,#45980,.T.);
#61722=ORIENTED_EDGE('',*,*,#45981,.T.);
#61723=ORIENTED_EDGE('',*,*,#45980,.F.);
#61724=ORIENTED_EDGE('',*,*,#45036,.T.);
#61725=ORIENTED_EDGE('',*,*,#45982,.T.);
#61726=ORIENTED_EDGE('',*,*,#45983,.T.);
#61727=ORIENTED_EDGE('',*,*,#45982,.F.);
#61728=ORIENTED_EDGE('',*,*,#45035,.T.);
#61729=ORIENTED_EDGE('',*,*,#45984,.T.);
#61730=ORIENTED_EDGE('',*,*,#45985,.T.);
#61731=ORIENTED_EDGE('',*,*,#45984,.F.);
#61732=ORIENTED_EDGE('',*,*,#45034,.T.);
#61733=ORIENTED_EDGE('',*,*,#45986,.T.);
#61734=ORIENTED_EDGE('',*,*,#45987,.T.);
#61735=ORIENTED_EDGE('',*,*,#45986,.F.);
#61736=ORIENTED_EDGE('',*,*,#45033,.T.);
#61737=ORIENTED_EDGE('',*,*,#45873,.T.);
#61738=ORIENTED_EDGE('',*,*,#45875,.T.);
#61739=ORIENTED_EDGE('',*,*,#45988,.F.);
#61740=ORIENTED_EDGE('',*,*,#45989,.T.);
#61741=ORIENTED_EDGE('',*,*,#45966,.T.);
#61742=ORIENTED_EDGE('',*,*,#45030,.T.);
#61743=ORIENTED_EDGE('',*,*,#45968,.F.);
#61744=ORIENTED_EDGE('',*,*,#45990,.T.);
#61745=ORIENTED_EDGE('',*,*,#45988,.T.);
#61746=ORIENTED_EDGE('',*,*,#45029,.T.);
#61747=ORIENTED_EDGE('',*,*,#45991,.T.);
#61748=ORIENTED_EDGE('',*,*,#45992,.F.);
#61749=ORIENTED_EDGE('',*,*,#45043,.T.);
#61750=ORIENTED_EDGE('',*,*,#45993,.F.);
#61751=ORIENTED_EDGE('',*,*,#45047,.F.);
#61752=ORIENTED_EDGE('',*,*,#45058,.T.);
#61753=ORIENTED_EDGE('',*,*,#45994,.T.);
#61754=ORIENTED_EDGE('',*,*,#45045,.T.);
#61755=ORIENTED_EDGE('',*,*,#45048,.F.);
#61756=ORIENTED_EDGE('',*,*,#45044,.T.);
#61757=ORIENTED_EDGE('',*,*,#45995,.T.);
#61758=ORIENTED_EDGE('',*,*,#45090,.T.);
#61759=ORIENTED_EDGE('',*,*,#45994,.F.);
#61760=ORIENTED_EDGE('',*,*,#45057,.T.);
#61761=ORIENTED_EDGE('',*,*,#45996,.T.);
#61762=ORIENTED_EDGE('',*,*,#45993,.T.);
#61763=ORIENTED_EDGE('',*,*,#45996,.F.);
#61764=ORIENTED_EDGE('',*,*,#45056,.T.);
#61765=ORIENTED_EDGE('',*,*,#45997,.T.);
#61766=ORIENTED_EDGE('',*,*,#45998,.T.);
#61767=ORIENTED_EDGE('',*,*,#45997,.F.);
#61768=ORIENTED_EDGE('',*,*,#45055,.T.);
#61769=ORIENTED_EDGE('',*,*,#45999,.T.);
#61770=ORIENTED_EDGE('',*,*,#46000,.T.);
#61771=ORIENTED_EDGE('',*,*,#45999,.F.);
#61772=ORIENTED_EDGE('',*,*,#45054,.T.);
#61773=ORIENTED_EDGE('',*,*,#45379,.T.);
#61774=ORIENTED_EDGE('',*,*,#45382,.T.);
#61775=ORIENTED_EDGE('',*,*,#45060,.F.);
#61776=ORIENTED_EDGE('',*,*,#46001,.T.);
#61777=ORIENTED_EDGE('',*,*,#45378,.T.);
#61778=ORIENTED_EDGE('',*,*,#45051,.T.);
#61779=ORIENTED_EDGE('',*,*,#45377,.T.);
#61780=ORIENTED_EDGE('',*,*,#46001,.F.);
#61781=ORIENTED_EDGE('',*,*,#45062,.T.);
#61782=ORIENTED_EDGE('',*,*,#46002,.F.);
#61783=ORIENTED_EDGE('',*,*,#45375,.F.);
#61784=ORIENTED_EDGE('',*,*,#46002,.T.);
#61785=ORIENTED_EDGE('',*,*,#45064,.T.);
#61786=ORIENTED_EDGE('',*,*,#45072,.T.);
#61787=ORIENTED_EDGE('',*,*,#46003,.F.);
#61788=ORIENTED_EDGE('',*,*,#45370,.T.);
#61789=ORIENTED_EDGE('',*,*,#45373,.T.);
#61790=ORIENTED_EDGE('',*,*,#45069,.T.);
#61791=ORIENTED_EDGE('',*,*,#46004,.F.);
#61792=ORIENTED_EDGE('',*,*,#46005,.T.);
#61793=ORIENTED_EDGE('',*,*,#46003,.T.);
#61794=ORIENTED_EDGE('',*,*,#45068,.T.);
#61795=ORIENTED_EDGE('',*,*,#45629,.F.);
#61796=ORIENTED_EDGE('',*,*,#45626,.T.);
#61797=ORIENTED_EDGE('',*,*,#46004,.T.);
#61798=ORIENTED_EDGE('',*,*,#45067,.T.);
#61799=ORIENTED_EDGE('',*,*,#46006,.T.);
#61800=ORIENTED_EDGE('',*,*,#45322,.F.);
#61801=ORIENTED_EDGE('',*,*,#45076,.T.);
#61802=ORIENTED_EDGE('',*,*,#45349,.F.);
#61803=ORIENTED_EDGE('',*,*,#45080,.T.);
#61804=ORIENTED_EDGE('',*,*,#46007,.F.);
#61805=ORIENTED_EDGE('',*,*,#45339,.T.);
#61806=ORIENTED_EDGE('',*,*,#45342,.F.);
#61807=ORIENTED_EDGE('',*,*,#45083,.F.);
#61808=ORIENTED_EDGE('',*,*,#46008,.T.);
#61809=ORIENTED_EDGE('',*,*,#46007,.T.);
#61810=ORIENTED_EDGE('',*,*,#45079,.T.);
#61811=ORIENTED_EDGE('',*,*,#45085,.T.);
#61812=ORIENTED_EDGE('',*,*,#46009,.F.);
#61813=ORIENTED_EDGE('',*,*,#45340,.T.);
#61814=ORIENTED_EDGE('',*,*,#46008,.F.);
#61815=ORIENTED_EDGE('',*,*,#45338,.F.);
#61816=ORIENTED_EDGE('',*,*,#46009,.T.);
#61817=ORIENTED_EDGE('',*,*,#45087,.T.);
#61818=ORIENTED_EDGE('',*,*,#45089,.T.);
#61819=ORIENTED_EDGE('',*,*,#46010,.F.);
#61820=ORIENTED_EDGE('',*,*,#45380,.T.);
#61821=ORIENTED_EDGE('',*,*,#45383,.T.);
#61822=ORIENTED_EDGE('',*,*,#45094,.T.);
#61823=ORIENTED_EDGE('',*,*,#46011,.F.);
#61824=ORIENTED_EDGE('',*,*,#46012,.T.);
#61825=ORIENTED_EDGE('',*,*,#46010,.T.);
#61826=ORIENTED_EDGE('',*,*,#45093,.T.);
#61827=ORIENTED_EDGE('',*,*,#46013,.F.);
#61828=ORIENTED_EDGE('',*,*,#46014,.T.);
#61829=ORIENTED_EDGE('',*,*,#46011,.T.);
#61830=ORIENTED_EDGE('',*,*,#45092,.T.);
#61831=ORIENTED_EDGE('',*,*,#45995,.F.);
#61832=ORIENTED_EDGE('',*,*,#45992,.T.);
#61833=ORIENTED_EDGE('',*,*,#46013,.T.);
#61834=ORIENTED_EDGE('',*,*,#45091,.T.);
#61835=ORIENTED_EDGE('',*,*,#46015,.T.);
#61836=ORIENTED_EDGE('',*,*,#46016,.F.);
#61837=ORIENTED_EDGE('',*,*,#45096,.T.);
#61838=ORIENTED_EDGE('',*,*,#46017,.F.);
#61839=ORIENTED_EDGE('',*,*,#45100,.F.);
#61840=ORIENTED_EDGE('',*,*,#45112,.T.);
#61841=ORIENTED_EDGE('',*,*,#46018,.T.);
#61842=ORIENTED_EDGE('',*,*,#45098,.T.);
#61843=ORIENTED_EDGE('',*,*,#46019,.F.);
#61844=ORIENTED_EDGE('',*,*,#45193,.T.);
#61845=ORIENTED_EDGE('',*,*,#45101,.T.);
#61846=ORIENTED_EDGE('',*,*,#45097,.T.);
#61847=ORIENTED_EDGE('',*,*,#46020,.F.);
#61848=ORIENTED_EDGE('',*,*,#45103,.T.);
#61849=ORIENTED_EDGE('',*,*,#46021,.T.);
#61850=ORIENTED_EDGE('',*,*,#46022,.T.);
#61851=ORIENTED_EDGE('',*,*,#46023,.T.);
#61852=ORIENTED_EDGE('',*,*,#46021,.F.);
#61853=ORIENTED_EDGE('',*,*,#45118,.T.);
#61854=ORIENTED_EDGE('',*,*,#46024,.T.);
#61855=ORIENTED_EDGE('',*,*,#45414,.T.);
#61856=ORIENTED_EDGE('',*,*,#46022,.F.);
#61857=ORIENTED_EDGE('',*,*,#45117,.T.);
#61858=ORIENTED_EDGE('',*,*,#46025,.F.);
#61859=ORIENTED_EDGE('',*,*,#46026,.T.);
#61860=ORIENTED_EDGE('',*,*,#46027,.F.);
#61861=ORIENTED_EDGE('',*,*,#46028,.F.);
#61862=ORIENTED_EDGE('',*,*,#46029,.T.);
#61863=ORIENTED_EDGE('',*,*,#46025,.T.);
#61864=ORIENTED_EDGE('',*,*,#45116,.T.);
#61865=ORIENTED_EDGE('',*,*,#46030,.F.);
#61866=ORIENTED_EDGE('',*,*,#46031,.T.);
#61867=ORIENTED_EDGE('',*,*,#46028,.T.);
#61868=ORIENTED_EDGE('',*,*,#45115,.T.);
#61869=ORIENTED_EDGE('',*,*,#45120,.F.);
#61870=ORIENTED_EDGE('',*,*,#46032,.T.);
#61871=ORIENTED_EDGE('',*,*,#46030,.T.);
#61872=ORIENTED_EDGE('',*,*,#45114,.T.);
#61873=ORIENTED_EDGE('',*,*,#46018,.F.);
#61874=ORIENTED_EDGE('',*,*,#45111,.T.);
#61875=ORIENTED_EDGE('',*,*,#46033,.T.);
#61876=ORIENTED_EDGE('',*,*,#46017,.T.);
#61877=ORIENTED_EDGE('',*,*,#46033,.F.);
#61878=ORIENTED_EDGE('',*,*,#45110,.T.);
#61879=ORIENTED_EDGE('',*,*,#46034,.T.);
#61880=ORIENTED_EDGE('',*,*,#46035,.T.);
#61881=ORIENTED_EDGE('',*,*,#46034,.F.);
#61882=ORIENTED_EDGE('',*,*,#45109,.T.);
#61883=ORIENTED_EDGE('',*,*,#46036,.T.);
#61884=ORIENTED_EDGE('',*,*,#46037,.T.);
#61885=ORIENTED_EDGE('',*,*,#46036,.F.);
#61886=ORIENTED_EDGE('',*,*,#45108,.T.);
#61887=ORIENTED_EDGE('',*,*,#46038,.T.);
#61888=ORIENTED_EDGE('',*,*,#46039,.T.);
#61889=ORIENTED_EDGE('',*,*,#46038,.F.);
#61890=ORIENTED_EDGE('',*,*,#45107,.T.);
#61891=ORIENTED_EDGE('',*,*,#46040,.T.);
#61892=ORIENTED_EDGE('',*,*,#46041,.T.);
#61893=ORIENTED_EDGE('',*,*,#46040,.F.);
#61894=ORIENTED_EDGE('',*,*,#45106,.T.);
#61895=ORIENTED_EDGE('',*,*,#46042,.T.);
#61896=ORIENTED_EDGE('',*,*,#46043,.T.);
#61897=ORIENTED_EDGE('',*,*,#46042,.F.);
#61898=ORIENTED_EDGE('',*,*,#45105,.T.);
#61899=ORIENTED_EDGE('',*,*,#46044,.T.);
#61900=ORIENTED_EDGE('',*,*,#46045,.T.);
#61901=ORIENTED_EDGE('',*,*,#46044,.F.);
#61902=ORIENTED_EDGE('',*,*,#45104,.T.);
#61903=ORIENTED_EDGE('',*,*,#46020,.T.);
#61904=ORIENTED_EDGE('',*,*,#46046,.T.);
#61905=ORIENTED_EDGE('',*,*,#46047,.T.);
#61906=ORIENTED_EDGE('',*,*,#46032,.F.);
#61907=ORIENTED_EDGE('',*,*,#45122,.T.);
#61908=ORIENTED_EDGE('',*,*,#46048,.F.);
#61909=ORIENTED_EDGE('',*,*,#46049,.F.);
#61910=ORIENTED_EDGE('',*,*,#46048,.T.);
#61911=ORIENTED_EDGE('',*,*,#45124,.T.);
#61912=ORIENTED_EDGE('',*,*,#45136,.T.);
#61913=ORIENTED_EDGE('',*,*,#45140,.T.);
#61914=ORIENTED_EDGE('',*,*,#45318,.F.);
#61915=ORIENTED_EDGE('',*,*,#46050,.T.);
#61916=ORIENTED_EDGE('',*,*,#45345,.F.);
#61917=ORIENTED_EDGE('',*,*,#45307,.T.);
#61918=ORIENTED_EDGE('',*,*,#45313,.T.);
#61919=ORIENTED_EDGE('',*,*,#45314,.T.);
#61920=ORIENTED_EDGE('',*,*,#45315,.T.);
#61921=ORIENTED_EDGE('',*,*,#45138,.T.);
#61922=ORIENTED_EDGE('',*,*,#46051,.F.);
#61923=ORIENTED_EDGE('',*,*,#46052,.T.);
#61924=ORIENTED_EDGE('',*,*,#46049,.T.);
#61925=ORIENTED_EDGE('',*,*,#45135,.T.);
#61926=ORIENTED_EDGE('',*,*,#46053,.F.);
#61927=ORIENTED_EDGE('',*,*,#46054,.T.);
#61928=ORIENTED_EDGE('',*,*,#46051,.T.);
#61929=ORIENTED_EDGE('',*,*,#45134,.T.);
#61930=ORIENTED_EDGE('',*,*,#46055,.T.);
#61931=ORIENTED_EDGE('',*,*,#46053,.T.);
#61932=ORIENTED_EDGE('',*,*,#45133,.T.);
#61933=ORIENTED_EDGE('',*,*,#46056,.F.);
#61934=ORIENTED_EDGE('',*,*,#46057,.F.);
#61935=ORIENTED_EDGE('',*,*,#45132,.T.);
#61936=ORIENTED_EDGE('',*,*,#46058,.T.);
#61937=ORIENTED_EDGE('',*,*,#45418,.T.);
#61938=ORIENTED_EDGE('',*,*,#46058,.F.);
#61939=ORIENTED_EDGE('',*,*,#45131,.T.);
#61940=ORIENTED_EDGE('',*,*,#46059,.T.);
#61941=ORIENTED_EDGE('',*,*,#46060,.T.);
#61942=ORIENTED_EDGE('',*,*,#46059,.F.);
#61943=ORIENTED_EDGE('',*,*,#45130,.T.);
#61944=ORIENTED_EDGE('',*,*,#45518,.T.);
#61945=ORIENTED_EDGE('',*,*,#45525,.T.);
#61946=ORIENTED_EDGE('',*,*,#45526,.T.);
#61947=ORIENTED_EDGE('',*,*,#45519,.F.);
#61948=ORIENTED_EDGE('',*,*,#45128,.T.);
#61949=ORIENTED_EDGE('',*,*,#46061,.F.);
#61950=ORIENTED_EDGE('',*,*,#46062,.F.);
#61951=ORIENTED_EDGE('',*,*,#46063,.T.);
#61952=ORIENTED_EDGE('',*,*,#46064,.T.);
#61953=ORIENTED_EDGE('',*,*,#45142,.T.);
#61954=ORIENTED_EDGE('',*,*,#46065,.F.);
#61955=ORIENTED_EDGE('',*,*,#46066,.F.);
#61956=ORIENTED_EDGE('',*,*,#45419,.T.);
#61957=ORIENTED_EDGE('',*,*,#46067,.T.);
#61958=ORIENTED_EDGE('',*,*,#45156,.T.);
#61959=ORIENTED_EDGE('',*,*,#46068,.F.);
#61960=ORIENTED_EDGE('',*,*,#46069,.T.);
#61961=ORIENTED_EDGE('',*,*,#46066,.T.);
#61962=ORIENTED_EDGE('',*,*,#45155,.T.);
#61963=ORIENTED_EDGE('',*,*,#46070,.F.);
#61964=ORIENTED_EDGE('',*,*,#46071,.T.);
#61965=ORIENTED_EDGE('',*,*,#46068,.T.);
#61966=ORIENTED_EDGE('',*,*,#45154,.T.);
#61967=ORIENTED_EDGE('',*,*,#46072,.F.);
#61968=ORIENTED_EDGE('',*,*,#46073,.T.);
#61969=ORIENTED_EDGE('',*,*,#46070,.T.);
#61970=ORIENTED_EDGE('',*,*,#45153,.T.);
#61971=ORIENTED_EDGE('',*,*,#46074,.F.);
#61972=ORIENTED_EDGE('',*,*,#46075,.T.);
#61973=ORIENTED_EDGE('',*,*,#46072,.T.);
#61974=ORIENTED_EDGE('',*,*,#45152,.T.);
#61975=ORIENTED_EDGE('',*,*,#46076,.F.);
#61976=ORIENTED_EDGE('',*,*,#46077,.T.);
#61977=ORIENTED_EDGE('',*,*,#46074,.T.);
#61978=ORIENTED_EDGE('',*,*,#45151,.T.);
#61979=ORIENTED_EDGE('',*,*,#46078,.F.);
#61980=ORIENTED_EDGE('',*,*,#46079,.T.);
#61981=ORIENTED_EDGE('',*,*,#46076,.T.);
#61982=ORIENTED_EDGE('',*,*,#45150,.T.);
#61983=ORIENTED_EDGE('',*,*,#46080,.F.);
#61984=ORIENTED_EDGE('',*,*,#46081,.T.);
#61985=ORIENTED_EDGE('',*,*,#46078,.T.);
#61986=ORIENTED_EDGE('',*,*,#45149,.T.);
#61987=ORIENTED_EDGE('',*,*,#46082,.F.);
#61988=ORIENTED_EDGE('',*,*,#45161,.T.);
#61989=ORIENTED_EDGE('',*,*,#46080,.T.);
#61990=ORIENTED_EDGE('',*,*,#45148,.T.);
#61991=ORIENTED_EDGE('',*,*,#45157,.F.);
#61992=ORIENTED_EDGE('',*,*,#45159,.T.);
#61993=ORIENTED_EDGE('',*,*,#46082,.T.);
#61994=ORIENTED_EDGE('',*,*,#45147,.T.);
#61995=ORIENTED_EDGE('',*,*,#46083,.F.);
#61996=ORIENTED_EDGE('',*,*,#46084,.T.);
#61997=ORIENTED_EDGE('',*,*,#45642,.T.);
#61998=ORIENTED_EDGE('',*,*,#45144,.T.);
#61999=ORIENTED_EDGE('',*,*,#46064,.F.);
#62000=ORIENTED_EDGE('',*,*,#46085,.T.);
#62001=ORIENTED_EDGE('',*,*,#46083,.T.);
#62002=ORIENTED_EDGE('',*,*,#45143,.T.);
#62003=ORIENTED_EDGE('',*,*,#46086,.F.);
#62004=ORIENTED_EDGE('',*,*,#46081,.F.);
#62005=ORIENTED_EDGE('',*,*,#45160,.F.);
#62006=ORIENTED_EDGE('',*,*,#46087,.F.);
#62007=ORIENTED_EDGE('',*,*,#46088,.F.);
#62008=ORIENTED_EDGE('',*,*,#45163,.T.);
#62009=ORIENTED_EDGE('',*,*,#46089,.T.);
#62010=ORIENTED_EDGE('',*,*,#45181,.T.);
#62011=ORIENTED_EDGE('',*,*,#46089,.F.);
#62012=ORIENTED_EDGE('',*,*,#45164,.T.);
#62013=ORIENTED_EDGE('',*,*,#45165,.T.);
#62014=ORIENTED_EDGE('',*,*,#45182,.T.);
#62015=ORIENTED_EDGE('',*,*,#46090,.F.);
#62016=ORIENTED_EDGE('',*,*,#46087,.T.);
#62017=ORIENTED_EDGE('',*,*,#46088,.T.);
#62018=ORIENTED_EDGE('',*,*,#45180,.T.);
#62019=ORIENTED_EDGE('',*,*,#46091,.F.);
#62020=ORIENTED_EDGE('',*,*,#46092,.T.);
#62021=ORIENTED_EDGE('',*,*,#46090,.T.);
#62022=ORIENTED_EDGE('',*,*,#45179,.T.);
#62023=ORIENTED_EDGE('',*,*,#46093,.F.);
#62024=ORIENTED_EDGE('',*,*,#46094,.T.);
#62025=ORIENTED_EDGE('',*,*,#46091,.T.);
#62026=ORIENTED_EDGE('',*,*,#45178,.T.);
#62027=ORIENTED_EDGE('',*,*,#46095,.F.);
#62028=ORIENTED_EDGE('',*,*,#46096,.T.);
#62029=ORIENTED_EDGE('',*,*,#46093,.T.);
#62030=ORIENTED_EDGE('',*,*,#45177,.T.);
#62031=ORIENTED_EDGE('',*,*,#46097,.F.);
#62032=ORIENTED_EDGE('',*,*,#46098,.T.);
#62033=ORIENTED_EDGE('',*,*,#46095,.T.);
#62034=ORIENTED_EDGE('',*,*,#45176,.T.);
#62035=ORIENTED_EDGE('',*,*,#46099,.F.);
#62036=ORIENTED_EDGE('',*,*,#46100,.T.);
#62037=ORIENTED_EDGE('',*,*,#46097,.T.);
#62038=ORIENTED_EDGE('',*,*,#45175,.T.);
#62039=ORIENTED_EDGE('',*,*,#46101,.F.);
#62040=ORIENTED_EDGE('',*,*,#46102,.T.);
#62041=ORIENTED_EDGE('',*,*,#46099,.T.);
#62042=ORIENTED_EDGE('',*,*,#45174,.T.);
#62043=ORIENTED_EDGE('',*,*,#46103,.F.);
#62044=ORIENTED_EDGE('',*,*,#46104,.T.);
#62045=ORIENTED_EDGE('',*,*,#46101,.T.);
#62046=ORIENTED_EDGE('',*,*,#45173,.T.);
#62047=ORIENTED_EDGE('',*,*,#46105,.F.);
#62048=ORIENTED_EDGE('',*,*,#45408,.T.);
#62049=ORIENTED_EDGE('',*,*,#46103,.T.);
#62050=ORIENTED_EDGE('',*,*,#45172,.T.);
#62051=ORIENTED_EDGE('',*,*,#45171,.T.);
#62052=ORIENTED_EDGE('',*,*,#46106,.F.);
#62053=ORIENTED_EDGE('',*,*,#46107,.T.);
#62054=ORIENTED_EDGE('',*,*,#46108,.F.);
#62055=ORIENTED_EDGE('',*,*,#46109,.F.);
#62056=ORIENTED_EDGE('',*,*,#46110,.T.);
#62057=ORIENTED_EDGE('',*,*,#46106,.T.);
#62058=ORIENTED_EDGE('',*,*,#45170,.T.);
#62059=ORIENTED_EDGE('',*,*,#46111,.F.);
#62060=ORIENTED_EDGE('',*,*,#46112,.T.);
#62061=ORIENTED_EDGE('',*,*,#46109,.T.);
#62062=ORIENTED_EDGE('',*,*,#45169,.T.);
#62063=ORIENTED_EDGE('',*,*,#45184,.F.);
#62064=ORIENTED_EDGE('',*,*,#46113,.T.);
#62065=ORIENTED_EDGE('',*,*,#46111,.T.);
#62066=ORIENTED_EDGE('',*,*,#45168,.T.);
#62067=ORIENTED_EDGE('',*,*,#45186,.T.);
#62068=ORIENTED_EDGE('',*,*,#46114,.F.);
#62069=ORIENTED_EDGE('',*,*,#46115,.T.);
#62070=ORIENTED_EDGE('',*,*,#46113,.F.);
#62071=ORIENTED_EDGE('',*,*,#46116,.F.);
#62072=ORIENTED_EDGE('',*,*,#46114,.T.);
#62073=ORIENTED_EDGE('',*,*,#45188,.T.);
#62074=ORIENTED_EDGE('',*,*,#45192,.T.);
#62075=ORIENTED_EDGE('',*,*,#46117,.T.);
#62076=ORIENTED_EDGE('',*,*,#46118,.T.);
#62077=ORIENTED_EDGE('',*,*,#45189,.T.);
#62078=ORIENTED_EDGE('',*,*,#46119,.F.);
#62079=ORIENTED_EDGE('',*,*,#46120,.F.);
#62080=ORIENTED_EDGE('',*,*,#45203,.T.);
#62081=ORIENTED_EDGE('',*,*,#46121,.T.);
#62082=ORIENTED_EDGE('',*,*,#45412,.T.);
#62083=ORIENTED_EDGE('',*,*,#46121,.F.);
#62084=ORIENTED_EDGE('',*,*,#45202,.T.);
#62085=ORIENTED_EDGE('',*,*,#46122,.T.);
#62086=ORIENTED_EDGE('',*,*,#46123,.T.);
#62087=ORIENTED_EDGE('',*,*,#46122,.F.);
#62088=ORIENTED_EDGE('',*,*,#45201,.T.);
#62089=ORIENTED_EDGE('',*,*,#46124,.T.);
#62090=ORIENTED_EDGE('',*,*,#46125,.T.);
#62091=ORIENTED_EDGE('',*,*,#46124,.F.);
#62092=ORIENTED_EDGE('',*,*,#45200,.T.);
#62093=ORIENTED_EDGE('',*,*,#46126,.T.);
#62094=ORIENTED_EDGE('',*,*,#46127,.T.);
#62095=ORIENTED_EDGE('',*,*,#46126,.F.);
#62096=ORIENTED_EDGE('',*,*,#45199,.T.);
#62097=ORIENTED_EDGE('',*,*,#46128,.T.);
#62098=ORIENTED_EDGE('',*,*,#46129,.T.);
#62099=ORIENTED_EDGE('',*,*,#46128,.F.);
#62100=ORIENTED_EDGE('',*,*,#45198,.T.);
#62101=ORIENTED_EDGE('',*,*,#46130,.T.);
#62102=ORIENTED_EDGE('',*,*,#46131,.T.);
#62103=ORIENTED_EDGE('',*,*,#46130,.F.);
#62104=ORIENTED_EDGE('',*,*,#45197,.T.);
#62105=ORIENTED_EDGE('',*,*,#46132,.T.);
#62106=ORIENTED_EDGE('',*,*,#46133,.T.);
#62107=ORIENTED_EDGE('',*,*,#46132,.F.);
#62108=ORIENTED_EDGE('',*,*,#45196,.T.);
#62109=ORIENTED_EDGE('',*,*,#46134,.T.);
#62110=ORIENTED_EDGE('',*,*,#46135,.T.);
#62111=ORIENTED_EDGE('',*,*,#46134,.F.);
#62112=ORIENTED_EDGE('',*,*,#45195,.T.);
#62113=ORIENTED_EDGE('',*,*,#46136,.T.);
#62114=ORIENTED_EDGE('',*,*,#46137,.T.);
#62115=ORIENTED_EDGE('',*,*,#46136,.F.);
#62116=ORIENTED_EDGE('',*,*,#45194,.T.);
#62117=ORIENTED_EDGE('',*,*,#46019,.T.);
#62118=ORIENTED_EDGE('',*,*,#46016,.T.);
#62119=ORIENTED_EDGE('',*,*,#46138,.F.);
#62120=ORIENTED_EDGE('',*,*,#46139,.T.);
#62121=ORIENTED_EDGE('',*,*,#46116,.T.);
#62122=ORIENTED_EDGE('',*,*,#45191,.T.);
#62123=ORIENTED_EDGE('',*,*,#46118,.F.);
#62124=ORIENTED_EDGE('',*,*,#46140,.T.);
#62125=ORIENTED_EDGE('',*,*,#46138,.T.);
#62126=ORIENTED_EDGE('',*,*,#45190,.T.);
#62127=ORIENTED_EDGE('',*,*,#46141,.F.);
#62128=ORIENTED_EDGE('',*,*,#46142,.F.);
#62129=ORIENTED_EDGE('',*,*,#45204,.F.);
#62130=ORIENTED_EDGE('',*,*,#46143,.F.);
#62131=ORIENTED_EDGE('',*,*,#45209,.F.);
#62132=ORIENTED_EDGE('',*,*,#45217,.T.);
#62133=ORIENTED_EDGE('',*,*,#46144,.T.);
#62134=ORIENTED_EDGE('',*,*,#45207,.T.);
#62135=ORIENTED_EDGE('',*,*,#46145,.F.);
#62136=ORIENTED_EDGE('',*,*,#45296,.T.);
#62137=ORIENTED_EDGE('',*,*,#46146,.T.);
#62138=ORIENTED_EDGE('',*,*,#45205,.T.);
#62139=ORIENTED_EDGE('',*,*,#46147,.F.);
#62140=ORIENTED_EDGE('',*,*,#45210,.T.);
#62141=ORIENTED_EDGE('',*,*,#46148,.T.);
#62142=ORIENTED_EDGE('',*,*,#46149,.T.);
#62143=ORIENTED_EDGE('',*,*,#46148,.F.);
#62144=ORIENTED_EDGE('',*,*,#45222,.T.);
#62145=ORIENTED_EDGE('',*,*,#46150,.T.);
#62146=ORIENTED_EDGE('',*,*,#45467,.T.);
#62147=ORIENTED_EDGE('',*,*,#46151,.F.);
#62148=ORIENTED_EDGE('',*,*,#45221,.T.);
#62149=ORIENTED_EDGE('',*,*,#46152,.F.);
#62150=ORIENTED_EDGE('',*,*,#46153,.T.);
#62151=ORIENTED_EDGE('',*,*,#46154,.F.);
#62152=ORIENTED_EDGE('',*,*,#46155,.F.);
#62153=ORIENTED_EDGE('',*,*,#46156,.T.);
#62154=ORIENTED_EDGE('',*,*,#46152,.T.);
#62155=ORIENTED_EDGE('',*,*,#45220,.T.);
#62156=ORIENTED_EDGE('',*,*,#45644,.F.);
#62157=ORIENTED_EDGE('',*,*,#46157,.T.);
#62158=ORIENTED_EDGE('',*,*,#46155,.T.);
#62159=ORIENTED_EDGE('',*,*,#45219,.T.);
#62160=ORIENTED_EDGE('',*,*,#46144,.F.);
#62161=ORIENTED_EDGE('',*,*,#45216,.T.);
#62162=ORIENTED_EDGE('',*,*,#46158,.T.);
#62163=ORIENTED_EDGE('',*,*,#46143,.T.);
#62164=ORIENTED_EDGE('',*,*,#46158,.F.);
#62165=ORIENTED_EDGE('',*,*,#45215,.T.);
#62166=ORIENTED_EDGE('',*,*,#46159,.T.);
#62167=ORIENTED_EDGE('',*,*,#46160,.T.);
#62168=ORIENTED_EDGE('',*,*,#46159,.F.);
#62169=ORIENTED_EDGE('',*,*,#45214,.T.);
#62170=ORIENTED_EDGE('',*,*,#46161,.T.);
#62171=ORIENTED_EDGE('',*,*,#46162,.T.);
#62172=ORIENTED_EDGE('',*,*,#46161,.F.);
#62173=ORIENTED_EDGE('',*,*,#45213,.T.);
#62174=ORIENTED_EDGE('',*,*,#46163,.T.);
#62175=ORIENTED_EDGE('',*,*,#46164,.T.);
#62176=ORIENTED_EDGE('',*,*,#46163,.F.);
#62177=ORIENTED_EDGE('',*,*,#45212,.T.);
#62178=ORIENTED_EDGE('',*,*,#46165,.T.);
#62179=ORIENTED_EDGE('',*,*,#46166,.T.);
#62180=ORIENTED_EDGE('',*,*,#46165,.F.);
#62181=ORIENTED_EDGE('',*,*,#45211,.T.);
#62182=ORIENTED_EDGE('',*,*,#46147,.T.);
#62183=ORIENTED_EDGE('',*,*,#46167,.T.);
#62184=ORIENTED_EDGE('',*,*,#46168,.F.);
#62185=ORIENTED_EDGE('',*,*,#45225,.T.);
#62186=ORIENTED_EDGE('',*,*,#46169,.T.);
#62187=ORIENTED_EDGE('',*,*,#46170,.T.);
#62188=ORIENTED_EDGE('',*,*,#46169,.F.);
#62189=ORIENTED_EDGE('',*,*,#45238,.T.);
#62190=ORIENTED_EDGE('',*,*,#46171,.T.);
#62191=ORIENTED_EDGE('',*,*,#45479,.T.);
#62192=ORIENTED_EDGE('',*,*,#45237,.T.);
#62193=ORIENTED_EDGE('',*,*,#46172,.T.);
#62194=ORIENTED_EDGE('',*,*,#46173,.T.);
#62195=ORIENTED_EDGE('',*,*,#46174,.F.);
#62196=ORIENTED_EDGE('',*,*,#46172,.F.);
#62197=ORIENTED_EDGE('',*,*,#45236,.T.);
#62198=ORIENTED_EDGE('',*,*,#46175,.T.);
#62199=ORIENTED_EDGE('',*,*,#46176,.T.);
#62200=ORIENTED_EDGE('',*,*,#46175,.F.);
#62201=ORIENTED_EDGE('',*,*,#45235,.T.);
#62202=ORIENTED_EDGE('',*,*,#46177,.T.);
#62203=ORIENTED_EDGE('',*,*,#46178,.T.);
#62204=ORIENTED_EDGE('',*,*,#46177,.F.);
#62205=ORIENTED_EDGE('',*,*,#45234,.T.);
#62206=ORIENTED_EDGE('',*,*,#45240,.T.);
#62207=ORIENTED_EDGE('',*,*,#46179,.T.);
#62208=ORIENTED_EDGE('',*,*,#46180,.F.);
#62209=ORIENTED_EDGE('',*,*,#45329,.T.);
#62210=ORIENTED_EDGE('',*,*,#45332,.T.);
#62211=ORIENTED_EDGE('',*,*,#45231,.T.);
#62212=ORIENTED_EDGE('',*,*,#46181,.F.);
#62213=ORIENTED_EDGE('',*,*,#46182,.T.);
#62214=ORIENTED_EDGE('',*,*,#46180,.T.);
#62215=ORIENTED_EDGE('',*,*,#45230,.T.);
#62216=ORIENTED_EDGE('',*,*,#46183,.F.);
#62217=ORIENTED_EDGE('',*,*,#45228,.T.);
#62218=ORIENTED_EDGE('',*,*,#45513,.T.);
#62219=ORIENTED_EDGE('',*,*,#45517,.T.);
#62220=ORIENTED_EDGE('',*,*,#45514,.F.);
#62221=ORIENTED_EDGE('',*,*,#45226,.T.);
#62222=ORIENTED_EDGE('',*,*,#46168,.T.);
#62223=ORIENTED_EDGE('',*,*,#45512,.T.);
#62224=ORIENTED_EDGE('',*,*,#45242,.T.);
#62225=ORIENTED_EDGE('',*,*,#46184,.F.);
#62226=ORIENTED_EDGE('',*,*,#46185,.T.);
#62227=ORIENTED_EDGE('',*,*,#46179,.F.);
#62228=ORIENTED_EDGE('',*,*,#46186,.F.);
#62229=ORIENTED_EDGE('',*,*,#46184,.T.);
#62230=ORIENTED_EDGE('',*,*,#45244,.T.);
#62231=ORIENTED_EDGE('',*,*,#45248,.T.);
#62232=ORIENTED_EDGE('',*,*,#46187,.T.);
#62233=ORIENTED_EDGE('',*,*,#46188,.T.);
#62234=ORIENTED_EDGE('',*,*,#45245,.T.);
#62235=ORIENTED_EDGE('',*,*,#46189,.F.);
#62236=ORIENTED_EDGE('',*,*,#46190,.T.);
#62237=ORIENTED_EDGE('',*,*,#45483,.T.);
#62238=ORIENTED_EDGE('',*,*,#46191,.F.);
#62239=ORIENTED_EDGE('',*,*,#45260,.T.);
#62240=ORIENTED_EDGE('',*,*,#46192,.T.);
#62241=ORIENTED_EDGE('',*,*,#46192,.F.);
#62242=ORIENTED_EDGE('',*,*,#45259,.T.);
#62243=ORIENTED_EDGE('',*,*,#46193,.T.);
#62244=ORIENTED_EDGE('',*,*,#46194,.T.);
#62245=ORIENTED_EDGE('',*,*,#46190,.F.);
#62246=ORIENTED_EDGE('',*,*,#46193,.F.);
#62247=ORIENTED_EDGE('',*,*,#45258,.T.);
#62248=ORIENTED_EDGE('',*,*,#46195,.T.);
#62249=ORIENTED_EDGE('',*,*,#46196,.T.);
#62250=ORIENTED_EDGE('',*,*,#46195,.F.);
#62251=ORIENTED_EDGE('',*,*,#45257,.T.);
#62252=ORIENTED_EDGE('',*,*,#46197,.T.);
#62253=ORIENTED_EDGE('',*,*,#46198,.T.);
#62254=ORIENTED_EDGE('',*,*,#46197,.F.);
#62255=ORIENTED_EDGE('',*,*,#45256,.T.);
#62256=ORIENTED_EDGE('',*,*,#46199,.T.);
#62257=ORIENTED_EDGE('',*,*,#46200,.T.);
#62258=ORIENTED_EDGE('',*,*,#46199,.F.);
#62259=ORIENTED_EDGE('',*,*,#45255,.T.);
#62260=ORIENTED_EDGE('',*,*,#46201,.F.);
#62261=ORIENTED_EDGE('',*,*,#46202,.T.);
#62262=ORIENTED_EDGE('',*,*,#46203,.F.);
#62263=ORIENTED_EDGE('',*,*,#46204,.T.);
#62264=ORIENTED_EDGE('',*,*,#46201,.T.);
#62265=ORIENTED_EDGE('',*,*,#45254,.T.);
#62266=ORIENTED_EDGE('',*,*,#46205,.F.);
#62267=ORIENTED_EDGE('',*,*,#46206,.T.);
#62268=ORIENTED_EDGE('',*,*,#46203,.T.);
#62269=ORIENTED_EDGE('',*,*,#45253,.T.);
#62270=ORIENTED_EDGE('',*,*,#46207,.F.);
#62271=ORIENTED_EDGE('',*,*,#46208,.T.);
#62272=ORIENTED_EDGE('',*,*,#46205,.T.);
#62273=ORIENTED_EDGE('',*,*,#45252,.T.);
#62274=ORIENTED_EDGE('',*,*,#46209,.F.);
#62275=ORIENTED_EDGE('',*,*,#46210,.T.);
#62276=ORIENTED_EDGE('',*,*,#46207,.T.);
#62277=ORIENTED_EDGE('',*,*,#45251,.T.);
#62278=ORIENTED_EDGE('',*,*,#45261,.F.);
#62279=ORIENTED_EDGE('',*,*,#45263,.T.);
#62280=ORIENTED_EDGE('',*,*,#46209,.T.);
#62281=ORIENTED_EDGE('',*,*,#45250,.T.);
#62282=ORIENTED_EDGE('',*,*,#46211,.F.);
#62283=ORIENTED_EDGE('',*,*,#46212,.T.);
#62284=ORIENTED_EDGE('',*,*,#46186,.T.);
#62285=ORIENTED_EDGE('',*,*,#45247,.T.);
#62286=ORIENTED_EDGE('',*,*,#46188,.F.);
#62287=ORIENTED_EDGE('',*,*,#46213,.T.);
#62288=ORIENTED_EDGE('',*,*,#46211,.T.);
#62289=ORIENTED_EDGE('',*,*,#45246,.T.);
#62290=ORIENTED_EDGE('',*,*,#46214,.T.);
#62291=ORIENTED_EDGE('',*,*,#46210,.F.);
#62292=ORIENTED_EDGE('',*,*,#45262,.T.);
#62293=ORIENTED_EDGE('',*,*,#46215,.F.);
#62294=ORIENTED_EDGE('',*,*,#46216,.F.);
#62295=ORIENTED_EDGE('',*,*,#45264,.T.);
#62296=ORIENTED_EDGE('',*,*,#45265,.T.);
#62297=ORIENTED_EDGE('',*,*,#45282,.T.);
#62298=ORIENTED_EDGE('',*,*,#46217,.F.);
#62299=ORIENTED_EDGE('',*,*,#46215,.T.);
#62300=ORIENTED_EDGE('',*,*,#46216,.T.);
#62301=ORIENTED_EDGE('',*,*,#45281,.T.);
#62302=ORIENTED_EDGE('',*,*,#46218,.F.);
#62303=ORIENTED_EDGE('',*,*,#46219,.T.);
#62304=ORIENTED_EDGE('',*,*,#46217,.T.);
#62305=ORIENTED_EDGE('',*,*,#45280,.T.);
#62306=ORIENTED_EDGE('',*,*,#46220,.F.);
#62307=ORIENTED_EDGE('',*,*,#46221,.T.);
#62308=ORIENTED_EDGE('',*,*,#46218,.T.);
#62309=ORIENTED_EDGE('',*,*,#45279,.T.);
#62310=ORIENTED_EDGE('',*,*,#46222,.F.);
#62311=ORIENTED_EDGE('',*,*,#46223,.T.);
#62312=ORIENTED_EDGE('',*,*,#46220,.T.);
#62313=ORIENTED_EDGE('',*,*,#45278,.T.);
#62314=ORIENTED_EDGE('',*,*,#46224,.F.);
#62315=ORIENTED_EDGE('',*,*,#46225,.T.);
#62316=ORIENTED_EDGE('',*,*,#46222,.T.);
#62317=ORIENTED_EDGE('',*,*,#45277,.T.);
#62318=ORIENTED_EDGE('',*,*,#46226,.F.);
#62319=ORIENTED_EDGE('',*,*,#46227,.T.);
#62320=ORIENTED_EDGE('',*,*,#46224,.T.);
#62321=ORIENTED_EDGE('',*,*,#45276,.T.);
#62322=ORIENTED_EDGE('',*,*,#46228,.F.);
#62323=ORIENTED_EDGE('',*,*,#46229,.T.);
#62324=ORIENTED_EDGE('',*,*,#46226,.T.);
#62325=ORIENTED_EDGE('',*,*,#45275,.T.);
#62326=ORIENTED_EDGE('',*,*,#46230,.F.);
#62327=ORIENTED_EDGE('',*,*,#46231,.T.);
#62328=ORIENTED_EDGE('',*,*,#46228,.T.);
#62329=ORIENTED_EDGE('',*,*,#45274,.T.);
#62330=ORIENTED_EDGE('',*,*,#46232,.F.);
#62331=ORIENTED_EDGE('',*,*,#46233,.T.);
#62332=ORIENTED_EDGE('',*,*,#46230,.T.);
#62333=ORIENTED_EDGE('',*,*,#45273,.T.);
#62334=ORIENTED_EDGE('',*,*,#46234,.F.);
#62335=ORIENTED_EDGE('',*,*,#45470,.T.);
#62336=ORIENTED_EDGE('',*,*,#46232,.T.);
#62337=ORIENTED_EDGE('',*,*,#45272,.T.);
#62338=ORIENTED_EDGE('',*,*,#45271,.T.);
#62339=ORIENTED_EDGE('',*,*,#46235,.F.);
#62340=ORIENTED_EDGE('',*,*,#46236,.T.);
#62341=ORIENTED_EDGE('',*,*,#46237,.F.);
#62342=ORIENTED_EDGE('',*,*,#46238,.F.);
#62343=ORIENTED_EDGE('',*,*,#46239,.T.);
#62344=ORIENTED_EDGE('',*,*,#46235,.T.);
#62345=ORIENTED_EDGE('',*,*,#45270,.T.);
#62346=ORIENTED_EDGE('',*,*,#46240,.F.);
#62347=ORIENTED_EDGE('',*,*,#46241,.T.);
#62348=ORIENTED_EDGE('',*,*,#46238,.T.);
#62349=ORIENTED_EDGE('',*,*,#45269,.T.);
#62350=ORIENTED_EDGE('',*,*,#45284,.F.);
#62351=ORIENTED_EDGE('',*,*,#46242,.T.);
#62352=ORIENTED_EDGE('',*,*,#46240,.T.);
#62353=ORIENTED_EDGE('',*,*,#45268,.T.);
#62354=ORIENTED_EDGE('',*,*,#45286,.T.);
#62355=ORIENTED_EDGE('',*,*,#46243,.F.);
#62356=ORIENTED_EDGE('',*,*,#46244,.T.);
#62357=ORIENTED_EDGE('',*,*,#46242,.F.);
#62358=ORIENTED_EDGE('',*,*,#46245,.F.);
#62359=ORIENTED_EDGE('',*,*,#46243,.T.);
#62360=ORIENTED_EDGE('',*,*,#45288,.T.);
#62361=ORIENTED_EDGE('',*,*,#45294,.T.);
#62362=ORIENTED_EDGE('',*,*,#46146,.F.);
#62363=ORIENTED_EDGE('',*,*,#45295,.T.);
#62364=ORIENTED_EDGE('',*,*,#45289,.T.);
#62365=ORIENTED_EDGE('',*,*,#45306,.T.);
#62366=ORIENTED_EDGE('',*,*,#46246,.T.);
#62367=ORIENTED_EDGE('',*,*,#46247,.T.);
#62368=ORIENTED_EDGE('',*,*,#45291,.T.);
#62369=ORIENTED_EDGE('',*,*,#46248,.F.);
#62370=ORIENTED_EDGE('',*,*,#46249,.T.);
#62371=ORIENTED_EDGE('',*,*,#45474,.T.);
#62372=ORIENTED_EDGE('',*,*,#46250,.F.);
#62373=ORIENTED_EDGE('',*,*,#45305,.T.);
#62374=ORIENTED_EDGE('',*,*,#46251,.T.);
#62375=ORIENTED_EDGE('',*,*,#46251,.F.);
#62376=ORIENTED_EDGE('',*,*,#45304,.T.);
#62377=ORIENTED_EDGE('',*,*,#46252,.T.);
#62378=ORIENTED_EDGE('',*,*,#46253,.T.);
#62379=ORIENTED_EDGE('',*,*,#46249,.F.);
#62380=ORIENTED_EDGE('',*,*,#46252,.F.);
#62381=ORIENTED_EDGE('',*,*,#45303,.T.);
#62382=ORIENTED_EDGE('',*,*,#46254,.T.);
#62383=ORIENTED_EDGE('',*,*,#46255,.T.);
#62384=ORIENTED_EDGE('',*,*,#46254,.F.);
#62385=ORIENTED_EDGE('',*,*,#45302,.T.);
#62386=ORIENTED_EDGE('',*,*,#46256,.T.);
#62387=ORIENTED_EDGE('',*,*,#46257,.T.);
#62388=ORIENTED_EDGE('',*,*,#46256,.F.);
#62389=ORIENTED_EDGE('',*,*,#45301,.T.);
#62390=ORIENTED_EDGE('',*,*,#46258,.T.);
#62391=ORIENTED_EDGE('',*,*,#46259,.T.);
#62392=ORIENTED_EDGE('',*,*,#46258,.F.);
#62393=ORIENTED_EDGE('',*,*,#45300,.T.);
#62394=ORIENTED_EDGE('',*,*,#46260,.T.);
#62395=ORIENTED_EDGE('',*,*,#46261,.T.);
#62396=ORIENTED_EDGE('',*,*,#46260,.F.);
#62397=ORIENTED_EDGE('',*,*,#45299,.T.);
#62398=ORIENTED_EDGE('',*,*,#46262,.T.);
#62399=ORIENTED_EDGE('',*,*,#46263,.T.);
#62400=ORIENTED_EDGE('',*,*,#46262,.F.);
#62401=ORIENTED_EDGE('',*,*,#45298,.T.);
#62402=ORIENTED_EDGE('',*,*,#46264,.T.);
#62403=ORIENTED_EDGE('',*,*,#46265,.T.);
#62404=ORIENTED_EDGE('',*,*,#46264,.F.);
#62405=ORIENTED_EDGE('',*,*,#45297,.T.);
#62406=ORIENTED_EDGE('',*,*,#46145,.T.);
#62407=ORIENTED_EDGE('',*,*,#46142,.T.);
#62408=ORIENTED_EDGE('',*,*,#46266,.F.);
#62409=ORIENTED_EDGE('',*,*,#46267,.T.);
#62410=ORIENTED_EDGE('',*,*,#46245,.T.);
#62411=ORIENTED_EDGE('',*,*,#45293,.T.);
#62412=ORIENTED_EDGE('',*,*,#46247,.F.);
#62413=ORIENTED_EDGE('',*,*,#46268,.T.);
#62414=ORIENTED_EDGE('',*,*,#46266,.T.);
#62415=ORIENTED_EDGE('',*,*,#45292,.T.);
#62416=ORIENTED_EDGE('',*,*,#45330,.T.);
#62417=ORIENTED_EDGE('',*,*,#46182,.F.);
#62418=ORIENTED_EDGE('',*,*,#46269,.F.);
#62419=ORIENTED_EDGE('',*,*,#45908,.F.);
#62420=ORIENTED_EDGE('',*,*,#46050,.F.);
#62421=ORIENTED_EDGE('',*,*,#45320,.F.);
#62422=ORIENTED_EDGE('',*,*,#46006,.F.);
#62423=ORIENTED_EDGE('',*,*,#45350,.F.);
#62424=ORIENTED_EDGE('',*,*,#45334,.F.);
#62425=ORIENTED_EDGE('',*,*,#45934,.F.);
#62426=ORIENTED_EDGE('',*,*,#46270,.F.);
#62427=ORIENTED_EDGE('',*,*,#45624,.F.);
#62428=ORIENTED_EDGE('',*,*,#45371,.T.);
#62429=ORIENTED_EDGE('',*,*,#46005,.F.);
#62430=ORIENTED_EDGE('',*,*,#45625,.T.);
#62431=ORIENTED_EDGE('',*,*,#45632,.F.);
#62432=ORIENTED_EDGE('',*,*,#45381,.T.);
#62433=ORIENTED_EDGE('',*,*,#46012,.F.);
#62434=ORIENTED_EDGE('',*,*,#46271,.T.);
#62435=ORIENTED_EDGE('',*,*,#46000,.F.);
#62436=ORIENTED_EDGE('',*,*,#45384,.T.);
#62437=ORIENTED_EDGE('',*,*,#45385,.T.);
#62438=ORIENTED_EDGE('',*,*,#46061,.T.);
#62439=ORIENTED_EDGE('',*,*,#45397,.T.);
#62440=ORIENTED_EDGE('',*,*,#46272,.F.);
#62441=ORIENTED_EDGE('',*,*,#45520,.T.);
#62442=ORIENTED_EDGE('',*,*,#45392,.F.);
#62443=ORIENTED_EDGE('',*,*,#46273,.F.);
#62444=ORIENTED_EDGE('',*,*,#45521,.T.);
#62445=ORIENTED_EDGE('',*,*,#46272,.T.);
#62446=ORIENTED_EDGE('',*,*,#45399,.T.);
#62447=ORIENTED_EDGE('',*,*,#46274,.F.);
#62448=ORIENTED_EDGE('',*,*,#45522,.T.);
#62449=ORIENTED_EDGE('',*,*,#46273,.T.);
#62450=ORIENTED_EDGE('',*,*,#45401,.T.);
#62451=ORIENTED_EDGE('',*,*,#46275,.F.);
#62452=ORIENTED_EDGE('',*,*,#45523,.T.);
#62453=ORIENTED_EDGE('',*,*,#46274,.T.);
#62454=ORIENTED_EDGE('',*,*,#45403,.T.);
#62455=ORIENTED_EDGE('',*,*,#45524,.T.);
#62456=ORIENTED_EDGE('',*,*,#46275,.T.);
#62457=ORIENTED_EDGE('',*,*,#45404,.T.);
#62458=ORIENTED_EDGE('',*,*,#46060,.F.);
#62459=ORIENTED_EDGE('',*,*,#46276,.F.);
#62460=ORIENTED_EDGE('',*,*,#46056,.T.);
#62461=ORIENTED_EDGE('',*,*,#46057,.T.);
#62462=ORIENTED_EDGE('',*,*,#45417,.T.);
#62463=ORIENTED_EDGE('',*,*,#46277,.F.);
#62464=ORIENTED_EDGE('',*,*,#46278,.T.);
#62465=ORIENTED_EDGE('',*,*,#46276,.T.);
#62466=ORIENTED_EDGE('',*,*,#45416,.T.);
#62467=ORIENTED_EDGE('',*,*,#46024,.F.);
#62468=ORIENTED_EDGE('',*,*,#46027,.T.);
#62469=ORIENTED_EDGE('',*,*,#46277,.T.);
#62470=ORIENTED_EDGE('',*,*,#45415,.T.);
#62471=ORIENTED_EDGE('',*,*,#45413,.T.);
#62472=ORIENTED_EDGE('',*,*,#46123,.F.);
#62473=ORIENTED_EDGE('',*,*,#46279,.T.);
#62474=ORIENTED_EDGE('',*,*,#46023,.F.);
#62475=ORIENTED_EDGE('',*,*,#46280,.F.);
#62476=ORIENTED_EDGE('',*,*,#46119,.T.);
#62477=ORIENTED_EDGE('',*,*,#46120,.T.);
#62478=ORIENTED_EDGE('',*,*,#45411,.T.);
#62479=ORIENTED_EDGE('',*,*,#46281,.F.);
#62480=ORIENTED_EDGE('',*,*,#46282,.T.);
#62481=ORIENTED_EDGE('',*,*,#46280,.T.);
#62482=ORIENTED_EDGE('',*,*,#45410,.T.);
#62483=ORIENTED_EDGE('',*,*,#46281,.T.);
#62484=ORIENTED_EDGE('',*,*,#45409,.T.);
#62485=ORIENTED_EDGE('',*,*,#46105,.T.);
#62486=ORIENTED_EDGE('',*,*,#46108,.T.);
#62487=ORIENTED_EDGE('',*,*,#45407,.T.);
#62488=ORIENTED_EDGE('',*,*,#46283,.T.);
#62489=ORIENTED_EDGE('',*,*,#46284,.T.);
#62490=ORIENTED_EDGE('',*,*,#46104,.F.);
#62491=ORIENTED_EDGE('',*,*,#46283,.F.);
#62492=ORIENTED_EDGE('',*,*,#45406,.T.);
#62493=ORIENTED_EDGE('',*,*,#46285,.T.);
#62494=ORIENTED_EDGE('',*,*,#46286,.T.);
#62495=ORIENTED_EDGE('',*,*,#46067,.F.);
#62496=ORIENTED_EDGE('',*,*,#45422,.T.);
#62497=ORIENTED_EDGE('',*,*,#46287,.F.);
#62498=ORIENTED_EDGE('',*,*,#46065,.T.);
#62499=ORIENTED_EDGE('',*,*,#46288,.T.);
#62500=ORIENTED_EDGE('',*,*,#46285,.F.);
#62501=ORIENTED_EDGE('',*,*,#45420,.T.);
#62502=ORIENTED_EDGE('',*,*,#46069,.F.);
#62503=ORIENTED_EDGE('',*,*,#46289,.F.);
#62504=ORIENTED_EDGE('',*,*,#46062,.T.);
#62505=ORIENTED_EDGE('',*,*,#46287,.T.);
#62506=ORIENTED_EDGE('',*,*,#45464,.T.);
#62507=ORIENTED_EDGE('',*,*,#46290,.F.);
#62508=ORIENTED_EDGE('',*,*,#46291,.T.);
#62509=ORIENTED_EDGE('',*,*,#46289,.T.);
#62510=ORIENTED_EDGE('',*,*,#45463,.T.);
#62511=ORIENTED_EDGE('',*,*,#45856,.F.);
#62512=ORIENTED_EDGE('',*,*,#45859,.T.);
#62513=ORIENTED_EDGE('',*,*,#46290,.T.);
#62514=ORIENTED_EDGE('',*,*,#45462,.T.);
#62515=ORIENTED_EDGE('',*,*,#45460,.T.);
#62516=ORIENTED_EDGE('',*,*,#45842,.F.);
#62517=ORIENTED_EDGE('',*,*,#46292,.T.);
#62518=ORIENTED_EDGE('',*,*,#45855,.F.);
#62519=ORIENTED_EDGE('',*,*,#45840,.F.);
#62520=ORIENTED_EDGE('',*,*,#45458,.T.);
#62521=ORIENTED_EDGE('',*,*,#46293,.T.);
#62522=ORIENTED_EDGE('',*,*,#45838,.T.);
#62523=ORIENTED_EDGE('',*,*,#46293,.F.);
#62524=ORIENTED_EDGE('',*,*,#45457,.T.);
#62525=ORIENTED_EDGE('',*,*,#46294,.T.);
#62526=ORIENTED_EDGE('',*,*,#46295,.T.);
#62527=ORIENTED_EDGE('',*,*,#46294,.F.);
#62528=ORIENTED_EDGE('',*,*,#45456,.T.);
#62529=ORIENTED_EDGE('',*,*,#46296,.T.);
#62530=ORIENTED_EDGE('',*,*,#46297,.T.);
#62531=ORIENTED_EDGE('',*,*,#46296,.F.);
#62532=ORIENTED_EDGE('',*,*,#45455,.T.);
#62533=ORIENTED_EDGE('',*,*,#45821,.T.);
#62534=ORIENTED_EDGE('',*,*,#45825,.T.);
#62535=ORIENTED_EDGE('',*,*,#45453,.T.);
#62536=ORIENTED_EDGE('',*,*,#45801,.F.);
#62537=ORIENTED_EDGE('',*,*,#46298,.T.);
#62538=ORIENTED_EDGE('',*,*,#45820,.F.);
#62539=ORIENTED_EDGE('',*,*,#46299,.F.);
#62540=ORIENTED_EDGE('',*,*,#45797,.T.);
#62541=ORIENTED_EDGE('',*,*,#45798,.T.);
#62542=ORIENTED_EDGE('',*,*,#45451,.T.);
#62543=ORIENTED_EDGE('',*,*,#46300,.F.);
#62544=ORIENTED_EDGE('',*,*,#46301,.T.);
#62545=ORIENTED_EDGE('',*,*,#46299,.T.);
#62546=ORIENTED_EDGE('',*,*,#45450,.T.);
#62547=ORIENTED_EDGE('',*,*,#46300,.T.);
#62548=ORIENTED_EDGE('',*,*,#45449,.T.);
#62549=ORIENTED_EDGE('',*,*,#45787,.T.);
#62550=ORIENTED_EDGE('',*,*,#45790,.T.);
#62551=ORIENTED_EDGE('',*,*,#45447,.T.);
#62552=ORIENTED_EDGE('',*,*,#45767,.F.);
#62553=ORIENTED_EDGE('',*,*,#46302,.T.);
#62554=ORIENTED_EDGE('',*,*,#45786,.F.);
#62555=ORIENTED_EDGE('',*,*,#46303,.F.);
#62556=ORIENTED_EDGE('',*,*,#45763,.T.);
#62557=ORIENTED_EDGE('',*,*,#45764,.T.);
#62558=ORIENTED_EDGE('',*,*,#45445,.T.);
#62559=ORIENTED_EDGE('',*,*,#46304,.F.);
#62560=ORIENTED_EDGE('',*,*,#46305,.T.);
#62561=ORIENTED_EDGE('',*,*,#46303,.T.);
#62562=ORIENTED_EDGE('',*,*,#45444,.T.);
#62563=ORIENTED_EDGE('',*,*,#46304,.T.);
#62564=ORIENTED_EDGE('',*,*,#45443,.T.);
#62565=ORIENTED_EDGE('',*,*,#45753,.T.);
#62566=ORIENTED_EDGE('',*,*,#45756,.T.);
#62567=ORIENTED_EDGE('',*,*,#45441,.T.);
#62568=ORIENTED_EDGE('',*,*,#45733,.F.);
#62569=ORIENTED_EDGE('',*,*,#46306,.T.);
#62570=ORIENTED_EDGE('',*,*,#45752,.F.);
#62571=ORIENTED_EDGE('',*,*,#46307,.F.);
#62572=ORIENTED_EDGE('',*,*,#45729,.T.);
#62573=ORIENTED_EDGE('',*,*,#45730,.T.);
#62574=ORIENTED_EDGE('',*,*,#45439,.T.);
#62575=ORIENTED_EDGE('',*,*,#46308,.F.);
#62576=ORIENTED_EDGE('',*,*,#46309,.T.);
#62577=ORIENTED_EDGE('',*,*,#46307,.T.);
#62578=ORIENTED_EDGE('',*,*,#45438,.T.);
#62579=ORIENTED_EDGE('',*,*,#46308,.T.);
#62580=ORIENTED_EDGE('',*,*,#45437,.T.);
#62581=ORIENTED_EDGE('',*,*,#45719,.T.);
#62582=ORIENTED_EDGE('',*,*,#45722,.T.);
#62583=ORIENTED_EDGE('',*,*,#45435,.T.);
#62584=ORIENTED_EDGE('',*,*,#45699,.F.);
#62585=ORIENTED_EDGE('',*,*,#46310,.T.);
#62586=ORIENTED_EDGE('',*,*,#45718,.F.);
#62587=ORIENTED_EDGE('',*,*,#45697,.F.);
#62588=ORIENTED_EDGE('',*,*,#45433,.T.);
#62589=ORIENTED_EDGE('',*,*,#46311,.T.);
#62590=ORIENTED_EDGE('',*,*,#45695,.T.);
#62591=ORIENTED_EDGE('',*,*,#46311,.F.);
#62592=ORIENTED_EDGE('',*,*,#45432,.T.);
#62593=ORIENTED_EDGE('',*,*,#46312,.T.);
#62594=ORIENTED_EDGE('',*,*,#46313,.T.);
#62595=ORIENTED_EDGE('',*,*,#46312,.F.);
#62596=ORIENTED_EDGE('',*,*,#45431,.T.);
#62597=ORIENTED_EDGE('',*,*,#46314,.T.);
#62598=ORIENTED_EDGE('',*,*,#46315,.T.);
#62599=ORIENTED_EDGE('',*,*,#46314,.F.);
#62600=ORIENTED_EDGE('',*,*,#45430,.T.);
#62601=ORIENTED_EDGE('',*,*,#45678,.T.);
#62602=ORIENTED_EDGE('',*,*,#45681,.T.);
#62603=ORIENTED_EDGE('',*,*,#45428,.T.);
#62604=ORIENTED_EDGE('',*,*,#45654,.F.);
#62605=ORIENTED_EDGE('',*,*,#46316,.T.);
#62606=ORIENTED_EDGE('',*,*,#45677,.F.);
#62607=ORIENTED_EDGE('',*,*,#45652,.F.);
#62608=ORIENTED_EDGE('',*,*,#45426,.T.);
#62609=ORIENTED_EDGE('',*,*,#46317,.F.);
#62610=ORIENTED_EDGE('',*,*,#45650,.T.);
#62611=ORIENTED_EDGE('',*,*,#46318,.F.);
#62612=ORIENTED_EDGE('',*,*,#46319,.T.);
#62613=ORIENTED_EDGE('',*,*,#46317,.T.);
#62614=ORIENTED_EDGE('',*,*,#45425,.T.);
#62615=ORIENTED_EDGE('',*,*,#46320,.F.);
#62616=ORIENTED_EDGE('',*,*,#46154,.T.);
#62617=ORIENTED_EDGE('',*,*,#46318,.T.);
#62618=ORIENTED_EDGE('',*,*,#45424,.T.);
#62619=ORIENTED_EDGE('',*,*,#46150,.F.);
#62620=ORIENTED_EDGE('',*,*,#46151,.T.);
#62621=ORIENTED_EDGE('',*,*,#46320,.T.);
#62622=ORIENTED_EDGE('',*,*,#45468,.T.);
#62623=ORIENTED_EDGE('',*,*,#45466,.T.);
#62624=ORIENTED_EDGE('',*,*,#46321,.F.);
#62625=ORIENTED_EDGE('',*,*,#46322,.T.);
#62626=ORIENTED_EDGE('',*,*,#46149,.F.);
#62627=ORIENTED_EDGE('',*,*,#45469,.T.);
#62628=ORIENTED_EDGE('',*,*,#46194,.F.);
#62629=ORIENTED_EDGE('',*,*,#46323,.T.);
#62630=ORIENTED_EDGE('',*,*,#46233,.F.);
#62631=ORIENTED_EDGE('',*,*,#46324,.F.);
#62632=ORIENTED_EDGE('',*,*,#46189,.T.);
#62633=ORIENTED_EDGE('',*,*,#46191,.T.);
#62634=ORIENTED_EDGE('',*,*,#45482,.T.);
#62635=ORIENTED_EDGE('',*,*,#46325,.F.);
#62636=ORIENTED_EDGE('',*,*,#46326,.T.);
#62637=ORIENTED_EDGE('',*,*,#46324,.T.);
#62638=ORIENTED_EDGE('',*,*,#45481,.T.);
#62639=ORIENTED_EDGE('',*,*,#46171,.F.);
#62640=ORIENTED_EDGE('',*,*,#46174,.T.);
#62641=ORIENTED_EDGE('',*,*,#46325,.T.);
#62642=ORIENTED_EDGE('',*,*,#45480,.T.);
#62643=ORIENTED_EDGE('',*,*,#45478,.T.);
#62644=ORIENTED_EDGE('',*,*,#46327,.F.);
#62645=ORIENTED_EDGE('',*,*,#45506,.T.);
#62646=ORIENTED_EDGE('',*,*,#46170,.F.);
#62647=ORIENTED_EDGE('',*,*,#46328,.F.);
#62648=ORIENTED_EDGE('',*,*,#46329,.T.);
#62649=ORIENTED_EDGE('',*,*,#46321,.T.);
#62650=ORIENTED_EDGE('',*,*,#45476,.T.);
#62651=ORIENTED_EDGE('',*,*,#46330,.T.);
#62652=ORIENTED_EDGE('',*,*,#46328,.T.);
#62653=ORIENTED_EDGE('',*,*,#45475,.T.);
#62654=ORIENTED_EDGE('',*,*,#46253,.F.);
#62655=ORIENTED_EDGE('',*,*,#46331,.F.);
#62656=ORIENTED_EDGE('',*,*,#46248,.T.);
#62657=ORIENTED_EDGE('',*,*,#46250,.T.);
#62658=ORIENTED_EDGE('',*,*,#45473,.T.);
#62659=ORIENTED_EDGE('',*,*,#46332,.F.);
#62660=ORIENTED_EDGE('',*,*,#46333,.T.);
#62661=ORIENTED_EDGE('',*,*,#46331,.T.);
#62662=ORIENTED_EDGE('',*,*,#45472,.T.);
#62663=ORIENTED_EDGE('',*,*,#46332,.T.);
#62664=ORIENTED_EDGE('',*,*,#45471,.T.);
#62665=ORIENTED_EDGE('',*,*,#46234,.T.);
#62666=ORIENTED_EDGE('',*,*,#46237,.T.);
#62667=ORIENTED_EDGE('',*,*,#46334,.F.);
#62668=ORIENTED_EDGE('',*,*,#45507,.T.);
#62669=ORIENTED_EDGE('',*,*,#46327,.T.);
#62670=ORIENTED_EDGE('',*,*,#45485,.T.);
#62671=ORIENTED_EDGE('',*,*,#46335,.F.);
#62672=ORIENTED_EDGE('',*,*,#45508,.T.);
#62673=ORIENTED_EDGE('',*,*,#46334,.T.);
#62674=ORIENTED_EDGE('',*,*,#45487,.T.);
#62675=ORIENTED_EDGE('',*,*,#46336,.F.);
#62676=ORIENTED_EDGE('',*,*,#45509,.T.);
#62677=ORIENTED_EDGE('',*,*,#46335,.T.);
#62678=ORIENTED_EDGE('',*,*,#45489,.T.);
#62679=ORIENTED_EDGE('',*,*,#45510,.T.);
#62680=ORIENTED_EDGE('',*,*,#46336,.T.);
#62681=ORIENTED_EDGE('',*,*,#45490,.T.);
#62682=ORIENTED_EDGE('',*,*,#45919,.F.);
#62683=ORIENTED_EDGE('',*,*,#46337,.F.);
#62684=ORIENTED_EDGE('',*,*,#45915,.T.);
#62685=ORIENTED_EDGE('',*,*,#45916,.T.);
#62686=ORIENTED_EDGE('',*,*,#45502,.T.);
#62687=ORIENTED_EDGE('',*,*,#46338,.F.);
#62688=ORIENTED_EDGE('',*,*,#46339,.T.);
#62689=ORIENTED_EDGE('',*,*,#46337,.T.);
#62690=ORIENTED_EDGE('',*,*,#45501,.T.);
#62691=ORIENTED_EDGE('',*,*,#45880,.F.);
#62692=ORIENTED_EDGE('',*,*,#45883,.T.);
#62693=ORIENTED_EDGE('',*,*,#46338,.T.);
#62694=ORIENTED_EDGE('',*,*,#45500,.T.);
#62695=ORIENTED_EDGE('',*,*,#45498,.T.);
#62696=ORIENTED_EDGE('',*,*,#45973,.F.);
#62697=ORIENTED_EDGE('',*,*,#46340,.T.);
#62698=ORIENTED_EDGE('',*,*,#45879,.F.);
#62699=ORIENTED_EDGE('',*,*,#46341,.F.);
#62700=ORIENTED_EDGE('',*,*,#45969,.T.);
#62701=ORIENTED_EDGE('',*,*,#45970,.T.);
#62702=ORIENTED_EDGE('',*,*,#45496,.T.);
#62703=ORIENTED_EDGE('',*,*,#46342,.F.);
#62704=ORIENTED_EDGE('',*,*,#46343,.T.);
#62705=ORIENTED_EDGE('',*,*,#46341,.T.);
#62706=ORIENTED_EDGE('',*,*,#45495,.T.);
#62707=ORIENTED_EDGE('',*,*,#46342,.T.);
#62708=ORIENTED_EDGE('',*,*,#45494,.T.);
#62709=ORIENTED_EDGE('',*,*,#45955,.T.);
#62710=ORIENTED_EDGE('',*,*,#45958,.T.);
#62711=ORIENTED_EDGE('',*,*,#45492,.T.);
#62712=ORIENTED_EDGE('',*,*,#46344,.T.);
#62713=ORIENTED_EDGE('',*,*,#46345,.T.);
#62714=ORIENTED_EDGE('',*,*,#45954,.F.);
#62715=ORIENTED_EDGE('',*,*,#46344,.F.);
#62716=ORIENTED_EDGE('',*,*,#45491,.T.);
#62717=ORIENTED_EDGE('',*,*,#45558,.T.);
#62718=ORIENTED_EDGE('',*,*,#46346,.T.);
#62719=ORIENTED_EDGE('',*,*,#45904,.F.);
#62720=ORIENTED_EDGE('',*,*,#45906,.T.);
#62721=ORIENTED_EDGE('',*,*,#46183,.T.);
#62722=ORIENTED_EDGE('',*,*,#45516,.T.);
#62723=ORIENTED_EDGE('',*,*,#45531,.T.);
#62724=ORIENTED_EDGE('',*,*,#45606,.F.);
#62725=ORIENTED_EDGE('',*,*,#46347,.T.);
#62726=ORIENTED_EDGE('',*,*,#45620,.F.);
#62727=ORIENTED_EDGE('',*,*,#46348,.T.);
#62728=ORIENTED_EDGE('',*,*,#45612,.F.);
#62729=ORIENTED_EDGE('',*,*,#45537,.T.);
#62730=ORIENTED_EDGE('',*,*,#45596,.F.);
#62731=ORIENTED_EDGE('',*,*,#45541,.T.);
#62732=ORIENTED_EDGE('',*,*,#45583,.F.);
#62733=ORIENTED_EDGE('',*,*,#46349,.T.);
#62734=ORIENTED_EDGE('',*,*,#45594,.F.);
#62735=ORIENTED_EDGE('',*,*,#45551,.T.);
#62736=ORIENTED_EDGE('',*,*,#45566,.F.);
#62737=ORIENTED_EDGE('',*,*,#46350,.T.);
#62738=ORIENTED_EDGE('',*,*,#45577,.F.);
#62739=ORIENTED_EDGE('',*,*,#46351,.T.);
#62740=ORIENTED_EDGE('',*,*,#46346,.F.);
#62741=ORIENTED_EDGE('',*,*,#45557,.F.);
#62742=ORIENTED_EDGE('',*,*,#45923,.F.);
#62743=ORIENTED_EDGE('',*,*,#46352,.T.);
#62744=ORIENTED_EDGE('',*,*,#45950,.F.);
#62745=ORIENTED_EDGE('',*,*,#46270,.T.);
#62746=ORIENTED_EDGE('',*,*,#45935,.F.);
#62747=ORIENTED_EDGE('',*,*,#45562,.T.);
#62748=ORIENTED_EDGE('',*,*,#45622,.F.);
#62749=ORIENTED_EDGE('',*,*,#46350,.F.);
#62750=ORIENTED_EDGE('',*,*,#45568,.F.);
#62751=ORIENTED_EDGE('',*,*,#45570,.F.);
#62752=ORIENTED_EDGE('',*,*,#45575,.F.);
#62753=ORIENTED_EDGE('',*,*,#46349,.F.);
#62754=ORIENTED_EDGE('',*,*,#45585,.F.);
#62755=ORIENTED_EDGE('',*,*,#45587,.F.);
#62756=ORIENTED_EDGE('',*,*,#45592,.F.);
#62757=ORIENTED_EDGE('',*,*,#45601,.F.);
#62758=ORIENTED_EDGE('',*,*,#45611,.F.);
#62759=ORIENTED_EDGE('',*,*,#46348,.F.);
#62760=ORIENTED_EDGE('',*,*,#45598,.F.);
#62761=ORIENTED_EDGE('',*,*,#46347,.F.);
#62762=ORIENTED_EDGE('',*,*,#45608,.F.);
#62763=ORIENTED_EDGE('',*,*,#45613,.F.);
#62764=ORIENTED_EDGE('',*,*,#45618,.F.);
#62765=ORIENTED_EDGE('',*,*,#45641,.F.);
#62766=ORIENTED_EDGE('',*,*,#46084,.F.);
#62767=ORIENTED_EDGE('',*,*,#46353,.F.);
#62768=ORIENTED_EDGE('',*,*,#45862,.F.);
#62769=ORIENTED_EDGE('',*,*,#45646,.F.);
#62770=ORIENTED_EDGE('',*,*,#45664,.F.);
#62771=ORIENTED_EDGE('',*,*,#46354,.F.);
#62772=ORIENTED_EDGE('',*,*,#46157,.F.);
#62773=ORIENTED_EDGE('',*,*,#46153,.F.);
#62774=ORIENTED_EDGE('',*,*,#46355,.F.);
#62775=ORIENTED_EDGE('',*,*,#45648,.F.);
#62776=ORIENTED_EDGE('',*,*,#46319,.F.);
#62777=ORIENTED_EDGE('',*,*,#46316,.F.);
#62778=ORIENTED_EDGE('',*,*,#45656,.F.);
#62779=ORIENTED_EDGE('',*,*,#46356,.F.);
#62780=ORIENTED_EDGE('',*,*,#45675,.F.);
#62781=ORIENTED_EDGE('',*,*,#46356,.T.);
#62782=ORIENTED_EDGE('',*,*,#45658,.F.);
#62783=ORIENTED_EDGE('',*,*,#46357,.T.);
#62784=ORIENTED_EDGE('',*,*,#45673,.F.);
#62785=ORIENTED_EDGE('',*,*,#45666,.F.);
#62786=ORIENTED_EDGE('',*,*,#45671,.F.);
#62787=ORIENTED_EDGE('',*,*,#46357,.F.);
#62788=ORIENTED_EDGE('',*,*,#45660,.F.);
#62789=ORIENTED_EDGE('',*,*,#46354,.T.);
#62790=ORIENTED_EDGE('',*,*,#45665,.F.);
#62791=ORIENTED_EDGE('',*,*,#46355,.T.);
#62792=ORIENTED_EDGE('',*,*,#46156,.F.);
#62793=ORIENTED_EDGE('',*,*,#45680,.F.);
#62794=ORIENTED_EDGE('',*,*,#46358,.F.);
#62795=ORIENTED_EDGE('',*,*,#46359,.F.);
#62796=ORIENTED_EDGE('',*,*,#46315,.F.);
#62797=ORIENTED_EDGE('',*,*,#46360,.T.);
#62798=ORIENTED_EDGE('',*,*,#45694,.F.);
#62799=ORIENTED_EDGE('',*,*,#46358,.T.);
#62800=ORIENTED_EDGE('',*,*,#45683,.F.);
#62801=ORIENTED_EDGE('',*,*,#45688,.F.);
#62802=ORIENTED_EDGE('',*,*,#45692,.F.);
#62803=ORIENTED_EDGE('',*,*,#46360,.F.);
#62804=ORIENTED_EDGE('',*,*,#45685,.F.);
#62805=ORIENTED_EDGE('',*,*,#46359,.T.);
#62806=ORIENTED_EDGE('',*,*,#45693,.T.);
#62807=ORIENTED_EDGE('',*,*,#46313,.F.);
#62808=ORIENTED_EDGE('',*,*,#46310,.F.);
#62809=ORIENTED_EDGE('',*,*,#45701,.F.);
#62810=ORIENTED_EDGE('',*,*,#46361,.F.);
#62811=ORIENTED_EDGE('',*,*,#45716,.F.);
#62812=ORIENTED_EDGE('',*,*,#46361,.T.);
#62813=ORIENTED_EDGE('',*,*,#45703,.F.);
#62814=ORIENTED_EDGE('',*,*,#46362,.T.);
#62815=ORIENTED_EDGE('',*,*,#45714,.F.);
#62816=ORIENTED_EDGE('',*,*,#46362,.F.);
#62817=ORIENTED_EDGE('',*,*,#45705,.F.);
#62818=ORIENTED_EDGE('',*,*,#45707,.F.);
#62819=ORIENTED_EDGE('',*,*,#45712,.F.);
#62820=ORIENTED_EDGE('',*,*,#45721,.F.);
#62821=ORIENTED_EDGE('',*,*,#45725,.T.);
#62822=ORIENTED_EDGE('',*,*,#45728,.F.);
#62823=ORIENTED_EDGE('',*,*,#46309,.F.);
#62824=ORIENTED_EDGE('',*,*,#46306,.F.);
#62825=ORIENTED_EDGE('',*,*,#45735,.F.);
#62826=ORIENTED_EDGE('',*,*,#46363,.F.);
#62827=ORIENTED_EDGE('',*,*,#45750,.F.);
#62828=ORIENTED_EDGE('',*,*,#46363,.T.);
#62829=ORIENTED_EDGE('',*,*,#45737,.F.);
#62830=ORIENTED_EDGE('',*,*,#46364,.T.);
#62831=ORIENTED_EDGE('',*,*,#45748,.F.);
#62832=ORIENTED_EDGE('',*,*,#46364,.F.);
#62833=ORIENTED_EDGE('',*,*,#45739,.F.);
#62834=ORIENTED_EDGE('',*,*,#45741,.F.);
#62835=ORIENTED_EDGE('',*,*,#45746,.F.);
#62836=ORIENTED_EDGE('',*,*,#45755,.F.);
#62837=ORIENTED_EDGE('',*,*,#45759,.T.);
#62838=ORIENTED_EDGE('',*,*,#45762,.F.);
#62839=ORIENTED_EDGE('',*,*,#46305,.F.);
#62840=ORIENTED_EDGE('',*,*,#46302,.F.);
#62841=ORIENTED_EDGE('',*,*,#45769,.F.);
#62842=ORIENTED_EDGE('',*,*,#46365,.F.);
#62843=ORIENTED_EDGE('',*,*,#45784,.F.);
#62844=ORIENTED_EDGE('',*,*,#46365,.T.);
#62845=ORIENTED_EDGE('',*,*,#45771,.F.);
#62846=ORIENTED_EDGE('',*,*,#46366,.T.);
#62847=ORIENTED_EDGE('',*,*,#45782,.F.);
#62848=ORIENTED_EDGE('',*,*,#46366,.F.);
#62849=ORIENTED_EDGE('',*,*,#45773,.F.);
#62850=ORIENTED_EDGE('',*,*,#45775,.F.);
#62851=ORIENTED_EDGE('',*,*,#45780,.F.);
#62852=ORIENTED_EDGE('',*,*,#45789,.F.);
#62853=ORIENTED_EDGE('',*,*,#45793,.T.);
#62854=ORIENTED_EDGE('',*,*,#45796,.F.);
#62855=ORIENTED_EDGE('',*,*,#46301,.F.);
#62856=ORIENTED_EDGE('',*,*,#46298,.F.);
#62857=ORIENTED_EDGE('',*,*,#45803,.F.);
#62858=ORIENTED_EDGE('',*,*,#46367,.F.);
#62859=ORIENTED_EDGE('',*,*,#45818,.F.);
#62860=ORIENTED_EDGE('',*,*,#46367,.T.);
#62861=ORIENTED_EDGE('',*,*,#45805,.F.);
#62862=ORIENTED_EDGE('',*,*,#46368,.T.);
#62863=ORIENTED_EDGE('',*,*,#45816,.F.);
#62864=ORIENTED_EDGE('',*,*,#45809,.F.);
#62865=ORIENTED_EDGE('',*,*,#45814,.F.);
#62866=ORIENTED_EDGE('',*,*,#46368,.F.);
#62867=ORIENTED_EDGE('',*,*,#45807,.F.);
#62868=ORIENTED_EDGE('',*,*,#45824,.F.);
#62869=ORIENTED_EDGE('',*,*,#46369,.T.);
#62870=ORIENTED_EDGE('',*,*,#46297,.F.);
#62871=ORIENTED_EDGE('',*,*,#46370,.T.);
#62872=ORIENTED_EDGE('',*,*,#45836,.F.);
#62873=ORIENTED_EDGE('',*,*,#46371,.T.);
#62874=ORIENTED_EDGE('',*,*,#45823,.F.);
#62875=ORIENTED_EDGE('',*,*,#45830,.F.);
#62876=ORIENTED_EDGE('',*,*,#45834,.F.);
#62877=ORIENTED_EDGE('',*,*,#46370,.F.);
#62878=ORIENTED_EDGE('',*,*,#45827,.F.);
#62879=ORIENTED_EDGE('',*,*,#46369,.F.);
#62880=ORIENTED_EDGE('',*,*,#46371,.F.);
#62881=ORIENTED_EDGE('',*,*,#45837,.F.);
#62882=ORIENTED_EDGE('',*,*,#46295,.F.);
#62883=ORIENTED_EDGE('',*,*,#46292,.F.);
#62884=ORIENTED_EDGE('',*,*,#45844,.F.);
#62885=ORIENTED_EDGE('',*,*,#46372,.F.);
#62886=ORIENTED_EDGE('',*,*,#45868,.F.);
#62887=ORIENTED_EDGE('',*,*,#46372,.T.);
#62888=ORIENTED_EDGE('',*,*,#45846,.F.);
#62889=ORIENTED_EDGE('',*,*,#46373,.T.);
#62890=ORIENTED_EDGE('',*,*,#45867,.F.);
#62891=ORIENTED_EDGE('',*,*,#46373,.F.);
#62892=ORIENTED_EDGE('',*,*,#45848,.F.);
#62893=ORIENTED_EDGE('',*,*,#45850,.F.);
#62894=ORIENTED_EDGE('',*,*,#45865,.F.);
#62895=ORIENTED_EDGE('',*,*,#45858,.F.);
#62896=ORIENTED_EDGE('',*,*,#46374,.F.);
#62897=ORIENTED_EDGE('',*,*,#46063,.F.);
#62898=ORIENTED_EDGE('',*,*,#46291,.F.);
#62899=ORIENTED_EDGE('',*,*,#46353,.T.);
#62900=ORIENTED_EDGE('',*,*,#46085,.F.);
#62901=ORIENTED_EDGE('',*,*,#46374,.T.);
#62902=ORIENTED_EDGE('',*,*,#45861,.F.);
#62903=ORIENTED_EDGE('',*,*,#46375,.T.);
#62904=ORIENTED_EDGE('',*,*,#45985,.F.);
#62905=ORIENTED_EDGE('',*,*,#46376,.T.);
#62906=ORIENTED_EDGE('',*,*,#45869,.F.);
#62907=ORIENTED_EDGE('',*,*,#45891,.F.);
#62908=ORIENTED_EDGE('',*,*,#45874,.F.);
#62909=ORIENTED_EDGE('',*,*,#46376,.F.);
#62910=ORIENTED_EDGE('',*,*,#45987,.F.);
#62911=ORIENTED_EDGE('',*,*,#45882,.F.);
#62912=ORIENTED_EDGE('',*,*,#46377,.F.);
#62913=ORIENTED_EDGE('',*,*,#45914,.F.);
#62914=ORIENTED_EDGE('',*,*,#46339,.F.);
#62915=ORIENTED_EDGE('',*,*,#46377,.T.);
#62916=ORIENTED_EDGE('',*,*,#45885,.F.);
#62917=ORIENTED_EDGE('',*,*,#46378,.T.);
#62918=ORIENTED_EDGE('',*,*,#45913,.F.);
#62919=ORIENTED_EDGE('',*,*,#46378,.F.);
#62920=ORIENTED_EDGE('',*,*,#45887,.F.);
#62921=ORIENTED_EDGE('',*,*,#45901,.F.);
#62922=ORIENTED_EDGE('',*,*,#45911,.F.);
#62923=ORIENTED_EDGE('',*,*,#46379,.F.);
#62924=ORIENTED_EDGE('',*,*,#45983,.F.);
#62925=ORIENTED_EDGE('',*,*,#46375,.F.);
#62926=ORIENTED_EDGE('',*,*,#45893,.F.);
#62927=ORIENTED_EDGE('',*,*,#46380,.F.);
#62928=ORIENTED_EDGE('',*,*,#46381,.T.);
#62929=ORIENTED_EDGE('',*,*,#45981,.F.);
#62930=ORIENTED_EDGE('',*,*,#46379,.T.);
#62931=ORIENTED_EDGE('',*,*,#45895,.F.);
#62932=ORIENTED_EDGE('',*,*,#46382,.F.);
#62933=ORIENTED_EDGE('',*,*,#46380,.T.);
#62934=ORIENTED_EDGE('',*,*,#45897,.F.);
#62935=ORIENTED_EDGE('',*,*,#46383,.T.);
#62936=ORIENTED_EDGE('',*,*,#45977,.F.);
#62937=ORIENTED_EDGE('',*,*,#46384,.T.);
#62938=ORIENTED_EDGE('',*,*,#46382,.T.);
#62939=ORIENTED_EDGE('',*,*,#45899,.F.);
#62940=ORIENTED_EDGE('',*,*,#46340,.F.);
#62941=ORIENTED_EDGE('',*,*,#45975,.F.);
#62942=ORIENTED_EDGE('',*,*,#46383,.F.);
#62943=ORIENTED_EDGE('',*,*,#45900,.F.);
#62944=ORIENTED_EDGE('',*,*,#45909,.F.);
#62945=ORIENTED_EDGE('',*,*,#46269,.T.);
#62946=ORIENTED_EDGE('',*,*,#46181,.T.);
#62947=ORIENTED_EDGE('',*,*,#45905,.T.);
#62948=ORIENTED_EDGE('',*,*,#46352,.F.);
#62949=ORIENTED_EDGE('',*,*,#45925,.F.);
#62950=ORIENTED_EDGE('',*,*,#46385,.F.);
#62951=ORIENTED_EDGE('',*,*,#45948,.F.);
#62952=ORIENTED_EDGE('',*,*,#46385,.T.);
#62953=ORIENTED_EDGE('',*,*,#45927,.F.);
#62954=ORIENTED_EDGE('',*,*,#46386,.T.);
#62955=ORIENTED_EDGE('',*,*,#45946,.F.);
#62956=ORIENTED_EDGE('',*,*,#46386,.F.);
#62957=ORIENTED_EDGE('',*,*,#45929,.F.);
#62958=ORIENTED_EDGE('',*,*,#46387,.F.);
#62959=ORIENTED_EDGE('',*,*,#45944,.F.);
#62960=ORIENTED_EDGE('',*,*,#46387,.T.);
#62961=ORIENTED_EDGE('',*,*,#45931,.F.);
#62962=ORIENTED_EDGE('',*,*,#45936,.T.);
#62963=ORIENTED_EDGE('',*,*,#45942,.F.);
#62964=ORIENTED_EDGE('',*,*,#46345,.F.);
#62965=ORIENTED_EDGE('',*,*,#46351,.F.);
#62966=ORIENTED_EDGE('',*,*,#45952,.F.);
#62967=ORIENTED_EDGE('',*,*,#45957,.F.);
#62968=ORIENTED_EDGE('',*,*,#46388,.F.);
#62969=ORIENTED_EDGE('',*,*,#45967,.F.);
#62970=ORIENTED_EDGE('',*,*,#46343,.F.);
#62971=ORIENTED_EDGE('',*,*,#46389,.T.);
#62972=ORIENTED_EDGE('',*,*,#45990,.F.);
#62973=ORIENTED_EDGE('',*,*,#46388,.T.);
#62974=ORIENTED_EDGE('',*,*,#45960,.F.);
#62975=ORIENTED_EDGE('',*,*,#45965,.F.);
#62976=ORIENTED_EDGE('',*,*,#45989,.F.);
#62977=ORIENTED_EDGE('',*,*,#46389,.F.);
#62978=ORIENTED_EDGE('',*,*,#45962,.F.);
#62979=ORIENTED_EDGE('',*,*,#46381,.F.);
#62980=ORIENTED_EDGE('',*,*,#46384,.F.);
#62981=ORIENTED_EDGE('',*,*,#45979,.F.);
#62982=ORIENTED_EDGE('',*,*,#46271,.F.);
#62983=ORIENTED_EDGE('',*,*,#46014,.F.);
#62984=ORIENTED_EDGE('',*,*,#45991,.F.);
#62985=ORIENTED_EDGE('',*,*,#45998,.F.);
#62986=ORIENTED_EDGE('',*,*,#46390,.F.);
#62987=ORIENTED_EDGE('',*,*,#46137,.F.);
#62988=ORIENTED_EDGE('',*,*,#46015,.F.);
#62989=ORIENTED_EDGE('',*,*,#46035,.F.);
#62990=ORIENTED_EDGE('',*,*,#46026,.F.);
#62991=ORIENTED_EDGE('',*,*,#46391,.F.);
#62992=ORIENTED_EDGE('',*,*,#46055,.F.);
#62993=ORIENTED_EDGE('',*,*,#46278,.F.);
#62994=ORIENTED_EDGE('',*,*,#46391,.T.);
#62995=ORIENTED_EDGE('',*,*,#46029,.F.);
#62996=ORIENTED_EDGE('',*,*,#46392,.T.);
#62997=ORIENTED_EDGE('',*,*,#46054,.F.);
#62998=ORIENTED_EDGE('',*,*,#46392,.F.);
#62999=ORIENTED_EDGE('',*,*,#46031,.F.);
#63000=ORIENTED_EDGE('',*,*,#46047,.F.);
#63001=ORIENTED_EDGE('',*,*,#46052,.F.);
#63002=ORIENTED_EDGE('',*,*,#46393,.T.);
#63003=ORIENTED_EDGE('',*,*,#46135,.F.);
#63004=ORIENTED_EDGE('',*,*,#46390,.T.);
#63005=ORIENTED_EDGE('',*,*,#46037,.F.);
#63006=ORIENTED_EDGE('',*,*,#46394,.F.);
#63007=ORIENTED_EDGE('',*,*,#46133,.F.);
#63008=ORIENTED_EDGE('',*,*,#46393,.F.);
#63009=ORIENTED_EDGE('',*,*,#46039,.F.);
#63010=ORIENTED_EDGE('',*,*,#46395,.T.);
#63011=ORIENTED_EDGE('',*,*,#46131,.F.);
#63012=ORIENTED_EDGE('',*,*,#46394,.T.);
#63013=ORIENTED_EDGE('',*,*,#46041,.F.);
#63014=ORIENTED_EDGE('',*,*,#46396,.F.);
#63015=ORIENTED_EDGE('',*,*,#46129,.F.);
#63016=ORIENTED_EDGE('',*,*,#46395,.F.);
#63017=ORIENTED_EDGE('',*,*,#46043,.F.);
#63018=ORIENTED_EDGE('',*,*,#46397,.T.);
#63019=ORIENTED_EDGE('',*,*,#46127,.F.);
#63020=ORIENTED_EDGE('',*,*,#46396,.T.);
#63021=ORIENTED_EDGE('',*,*,#46045,.F.);
#63022=ORIENTED_EDGE('',*,*,#46279,.F.);
#63023=ORIENTED_EDGE('',*,*,#46125,.F.);
#63024=ORIENTED_EDGE('',*,*,#46397,.F.);
#63025=ORIENTED_EDGE('',*,*,#46046,.F.);
#63026=ORIENTED_EDGE('',*,*,#46398,.T.);
#63027=ORIENTED_EDGE('',*,*,#46286,.F.);
#63028=ORIENTED_EDGE('',*,*,#46288,.F.);
#63029=ORIENTED_EDGE('',*,*,#46071,.F.);
#63030=ORIENTED_EDGE('',*,*,#46399,.T.);
#63031=ORIENTED_EDGE('',*,*,#46100,.F.);
#63032=ORIENTED_EDGE('',*,*,#46399,.F.);
#63033=ORIENTED_EDGE('',*,*,#46073,.F.);
#63034=ORIENTED_EDGE('',*,*,#46400,.F.);
#63035=ORIENTED_EDGE('',*,*,#46098,.F.);
#63036=ORIENTED_EDGE('',*,*,#46400,.T.);
#63037=ORIENTED_EDGE('',*,*,#46075,.F.);
#63038=ORIENTED_EDGE('',*,*,#46401,.T.);
#63039=ORIENTED_EDGE('',*,*,#46096,.F.);
#63040=ORIENTED_EDGE('',*,*,#46401,.F.);
#63041=ORIENTED_EDGE('',*,*,#46077,.F.);
#63042=ORIENTED_EDGE('',*,*,#46402,.F.);
#63043=ORIENTED_EDGE('',*,*,#46094,.F.);
#63044=ORIENTED_EDGE('',*,*,#46402,.T.);
#63045=ORIENTED_EDGE('',*,*,#46079,.F.);
#63046=ORIENTED_EDGE('',*,*,#46086,.T.);
#63047=ORIENTED_EDGE('',*,*,#46092,.F.);
#63048=ORIENTED_EDGE('',*,*,#46284,.F.);
#63049=ORIENTED_EDGE('',*,*,#46398,.F.);
#63050=ORIENTED_EDGE('',*,*,#46102,.F.);
#63051=ORIENTED_EDGE('',*,*,#46107,.F.);
#63052=ORIENTED_EDGE('',*,*,#46403,.F.);
#63053=ORIENTED_EDGE('',*,*,#46117,.F.);
#63054=ORIENTED_EDGE('',*,*,#46282,.F.);
#63055=ORIENTED_EDGE('',*,*,#46404,.T.);
#63056=ORIENTED_EDGE('',*,*,#46140,.F.);
#63057=ORIENTED_EDGE('',*,*,#46403,.T.);
#63058=ORIENTED_EDGE('',*,*,#46110,.F.);
#63059=ORIENTED_EDGE('',*,*,#46115,.F.);
#63060=ORIENTED_EDGE('',*,*,#46139,.F.);
#63061=ORIENTED_EDGE('',*,*,#46404,.F.);
#63062=ORIENTED_EDGE('',*,*,#46112,.F.);
#63063=ORIENTED_EDGE('',*,*,#46405,.T.);
#63064=ORIENTED_EDGE('',*,*,#46265,.F.);
#63065=ORIENTED_EDGE('',*,*,#46141,.T.);
#63066=ORIENTED_EDGE('',*,*,#46160,.F.);
#63067=ORIENTED_EDGE('',*,*,#46406,.F.);
#63068=ORIENTED_EDGE('',*,*,#46263,.F.);
#63069=ORIENTED_EDGE('',*,*,#46405,.F.);
#63070=ORIENTED_EDGE('',*,*,#46162,.F.);
#63071=ORIENTED_EDGE('',*,*,#46407,.T.);
#63072=ORIENTED_EDGE('',*,*,#46261,.F.);
#63073=ORIENTED_EDGE('',*,*,#46406,.T.);
#63074=ORIENTED_EDGE('',*,*,#46164,.F.);
#63075=ORIENTED_EDGE('',*,*,#46408,.F.);
#63076=ORIENTED_EDGE('',*,*,#46259,.F.);
#63077=ORIENTED_EDGE('',*,*,#46407,.F.);
#63078=ORIENTED_EDGE('',*,*,#46166,.F.);
#63079=ORIENTED_EDGE('',*,*,#46322,.F.);
#63080=ORIENTED_EDGE('',*,*,#46329,.F.);
#63081=ORIENTED_EDGE('',*,*,#46409,.T.);
#63082=ORIENTED_EDGE('',*,*,#46257,.F.);
#63083=ORIENTED_EDGE('',*,*,#46408,.T.);
#63084=ORIENTED_EDGE('',*,*,#46167,.F.);
#63085=ORIENTED_EDGE('',*,*,#46173,.F.);
#63086=ORIENTED_EDGE('',*,*,#46410,.F.);
#63087=ORIENTED_EDGE('',*,*,#46187,.F.);
#63088=ORIENTED_EDGE('',*,*,#46326,.F.);
#63089=ORIENTED_EDGE('',*,*,#46411,.T.);
#63090=ORIENTED_EDGE('',*,*,#46213,.F.);
#63091=ORIENTED_EDGE('',*,*,#46410,.T.);
#63092=ORIENTED_EDGE('',*,*,#46176,.F.);
#63093=ORIENTED_EDGE('',*,*,#46185,.F.);
#63094=ORIENTED_EDGE('',*,*,#46212,.F.);
#63095=ORIENTED_EDGE('',*,*,#46411,.F.);
#63096=ORIENTED_EDGE('',*,*,#46178,.F.);
#63097=ORIENTED_EDGE('',*,*,#46323,.F.);
#63098=ORIENTED_EDGE('',*,*,#46196,.F.);
#63099=ORIENTED_EDGE('',*,*,#46412,.F.);
#63100=ORIENTED_EDGE('',*,*,#46231,.F.);
#63101=ORIENTED_EDGE('',*,*,#46412,.T.);
#63102=ORIENTED_EDGE('',*,*,#46198,.F.);
#63103=ORIENTED_EDGE('',*,*,#46413,.T.);
#63104=ORIENTED_EDGE('',*,*,#46229,.F.);
#63105=ORIENTED_EDGE('',*,*,#46413,.F.);
#63106=ORIENTED_EDGE('',*,*,#46200,.F.);
#63107=ORIENTED_EDGE('',*,*,#46414,.F.);
#63108=ORIENTED_EDGE('',*,*,#46227,.F.);
#63109=ORIENTED_EDGE('',*,*,#46414,.T.);
#63110=ORIENTED_EDGE('',*,*,#46202,.F.);
#63111=ORIENTED_EDGE('',*,*,#46415,.T.);
#63112=ORIENTED_EDGE('',*,*,#46225,.F.);
#63113=ORIENTED_EDGE('',*,*,#46415,.F.);
#63114=ORIENTED_EDGE('',*,*,#46204,.F.);
#63115=ORIENTED_EDGE('',*,*,#46416,.F.);
#63116=ORIENTED_EDGE('',*,*,#46223,.F.);
#63117=ORIENTED_EDGE('',*,*,#46416,.T.);
#63118=ORIENTED_EDGE('',*,*,#46206,.F.);
#63119=ORIENTED_EDGE('',*,*,#46417,.T.);
#63120=ORIENTED_EDGE('',*,*,#46221,.F.);
#63121=ORIENTED_EDGE('',*,*,#46417,.F.);
#63122=ORIENTED_EDGE('',*,*,#46208,.F.);
#63123=ORIENTED_EDGE('',*,*,#46214,.F.);
#63124=ORIENTED_EDGE('',*,*,#46219,.F.);
#63125=ORIENTED_EDGE('',*,*,#46236,.F.);
#63126=ORIENTED_EDGE('',*,*,#46418,.F.);
#63127=ORIENTED_EDGE('',*,*,#46246,.F.);
#63128=ORIENTED_EDGE('',*,*,#46333,.F.);
#63129=ORIENTED_EDGE('',*,*,#46419,.T.);
#63130=ORIENTED_EDGE('',*,*,#46268,.F.);
#63131=ORIENTED_EDGE('',*,*,#46418,.T.);
#63132=ORIENTED_EDGE('',*,*,#46239,.F.);
#63133=ORIENTED_EDGE('',*,*,#46244,.F.);
#63134=ORIENTED_EDGE('',*,*,#46267,.F.);
#63135=ORIENTED_EDGE('',*,*,#46419,.F.);
#63136=ORIENTED_EDGE('',*,*,#46241,.F.);
#63137=ORIENTED_EDGE('',*,*,#46409,.F.);
#63138=ORIENTED_EDGE('',*,*,#46330,.F.);
#63139=ORIENTED_EDGE('',*,*,#46255,.F.);
#63140=ORIENTED_EDGE('',*,*,#46420,.T.);
#63141=ORIENTED_EDGE('',*,*,#46421,.T.);
#63142=ORIENTED_EDGE('',*,*,#46422,.T.);
#63143=ORIENTED_EDGE('',*,*,#46423,.T.);
#63144=ORIENTED_EDGE('',*,*,#46424,.T.);
#63145=ORIENTED_EDGE('',*,*,#46425,.T.);
#63146=ORIENTED_EDGE('',*,*,#46426,.T.);
#63147=ORIENTED_EDGE('',*,*,#46425,.F.);
#63148=ORIENTED_EDGE('',*,*,#46427,.T.);
#63149=ORIENTED_EDGE('',*,*,#46428,.F.);
#63150=ORIENTED_EDGE('',*,*,#46429,.T.);
#63151=ORIENTED_EDGE('',*,*,#46430,.T.);
#63152=ORIENTED_EDGE('',*,*,#46431,.T.);
#63153=ORIENTED_EDGE('',*,*,#46432,.T.);
#63154=ORIENTED_EDGE('',*,*,#46428,.T.);
#63155=ORIENTED_EDGE('',*,*,#46433,.T.);
#63156=ORIENTED_EDGE('',*,*,#46434,.T.);
#63157=ORIENTED_EDGE('',*,*,#46435,.T.);
#63158=ORIENTED_EDGE('',*,*,#46436,.T.);
#63159=ORIENTED_EDGE('',*,*,#46437,.F.);
#63160=ORIENTED_EDGE('',*,*,#46438,.T.);
#63161=ORIENTED_EDGE('',*,*,#46433,.F.);
#63162=ORIENTED_EDGE('',*,*,#46439,.T.);
#63163=ORIENTED_EDGE('',*,*,#46440,.T.);
#63164=ORIENTED_EDGE('',*,*,#46441,.T.);
#63165=ORIENTED_EDGE('',*,*,#46437,.T.);
#63166=ORIENTED_EDGE('',*,*,#46442,.T.);
#63167=ORIENTED_EDGE('',*,*,#46443,.F.);
#63168=ORIENTED_EDGE('',*,*,#46444,.T.);
#63169=ORIENTED_EDGE('',*,*,#46440,.F.);
#63170=ORIENTED_EDGE('',*,*,#46445,.T.);
#63171=ORIENTED_EDGE('',*,*,#46446,.T.);
#63172=ORIENTED_EDGE('',*,*,#46447,.T.);
#63173=ORIENTED_EDGE('',*,*,#46443,.T.);
#63174=ORIENTED_EDGE('',*,*,#46448,.T.);
#63175=ORIENTED_EDGE('',*,*,#46449,.F.);
#63176=ORIENTED_EDGE('',*,*,#46450,.T.);
#63177=ORIENTED_EDGE('',*,*,#46446,.F.);
#63178=ORIENTED_EDGE('',*,*,#46451,.T.);
#63179=ORIENTED_EDGE('',*,*,#46452,.T.);
#63180=ORIENTED_EDGE('',*,*,#46453,.T.);
#63181=ORIENTED_EDGE('',*,*,#46449,.T.);
#63182=ORIENTED_EDGE('',*,*,#46454,.T.);
#63183=ORIENTED_EDGE('',*,*,#46455,.T.);
#63184=ORIENTED_EDGE('',*,*,#46456,.T.);
#63185=ORIENTED_EDGE('',*,*,#46457,.T.);
#63186=ORIENTED_EDGE('',*,*,#46458,.T.);
#63187=ORIENTED_EDGE('',*,*,#46457,.F.);
#63188=ORIENTED_EDGE('',*,*,#46459,.T.);
#63189=ORIENTED_EDGE('',*,*,#46460,.F.);
#63190=ORIENTED_EDGE('',*,*,#46461,.T.);
#63191=ORIENTED_EDGE('',*,*,#46462,.T.);
#63192=ORIENTED_EDGE('',*,*,#46463,.T.);
#63193=ORIENTED_EDGE('',*,*,#46464,.T.);
#63194=ORIENTED_EDGE('',*,*,#46460,.T.);
#63195=ORIENTED_EDGE('',*,*,#46465,.T.);
#63196=ORIENTED_EDGE('',*,*,#46466,.T.);
#63197=ORIENTED_EDGE('',*,*,#46467,.F.);
#63198=ORIENTED_EDGE('',*,*,#46468,.T.);
#63199=ORIENTED_EDGE('',*,*,#46420,.F.);
#63200=ORIENTED_EDGE('',*,*,#46469,.T.);
#63201=ORIENTED_EDGE('',*,*,#46467,.T.);
#63202=ORIENTED_EDGE('',*,*,#46470,.T.);
#63203=ORIENTED_EDGE('',*,*,#46471,.T.);
#63204=ORIENTED_EDGE('',*,*,#46472,.T.);
#63205=ORIENTED_EDGE('',*,*,#46471,.F.);
#63206=ORIENTED_EDGE('',*,*,#46473,.T.);
#63207=ORIENTED_EDGE('',*,*,#46474,.F.);
#63208=ORIENTED_EDGE('',*,*,#46475,.T.);
#63209=ORIENTED_EDGE('',*,*,#46474,.T.);
#63210=ORIENTED_EDGE('',*,*,#46476,.T.);
#63211=ORIENTED_EDGE('',*,*,#46477,.T.);
#63212=ORIENTED_EDGE('',*,*,#46478,.T.);
#63213=ORIENTED_EDGE('',*,*,#46477,.F.);
#63214=ORIENTED_EDGE('',*,*,#46479,.T.);
#63215=ORIENTED_EDGE('',*,*,#46480,.F.);
#63216=ORIENTED_EDGE('',*,*,#46481,.T.);
#63217=ORIENTED_EDGE('',*,*,#46482,.T.);
#63218=ORIENTED_EDGE('',*,*,#46483,.T.);
#63219=ORIENTED_EDGE('',*,*,#46484,.T.);
#63220=ORIENTED_EDGE('',*,*,#46485,.T.);
#63221=ORIENTED_EDGE('',*,*,#46484,.F.);
#63222=ORIENTED_EDGE('',*,*,#46486,.T.);
#63223=ORIENTED_EDGE('',*,*,#46487,.F.);
#63224=ORIENTED_EDGE('',*,*,#46488,.T.);
#63225=ORIENTED_EDGE('',*,*,#46489,.T.);
#63226=ORIENTED_EDGE('',*,*,#46490,.T.);
#63227=ORIENTED_EDGE('',*,*,#46491,.T.);
#63228=ORIENTED_EDGE('',*,*,#46487,.T.);
#63229=ORIENTED_EDGE('',*,*,#46492,.T.);
#63230=ORIENTED_EDGE('',*,*,#46493,.T.);
#63231=ORIENTED_EDGE('',*,*,#46494,.T.);
#63232=ORIENTED_EDGE('',*,*,#46495,.F.);
#63233=ORIENTED_EDGE('',*,*,#46496,.T.);
#63234=ORIENTED_EDGE('',*,*,#46497,.F.);
#63235=ORIENTED_EDGE('',*,*,#46498,.T.);
#63236=ORIENTED_EDGE('',*,*,#46499,.T.);
#63237=ORIENTED_EDGE('',*,*,#46500,.T.);
#63238=ORIENTED_EDGE('',*,*,#46495,.T.);
#63239=ORIENTED_EDGE('',*,*,#46501,.T.);
#63240=ORIENTED_EDGE('',*,*,#46502,.F.);
#63241=ORIENTED_EDGE('',*,*,#46503,.T.);
#63242=ORIENTED_EDGE('',*,*,#46499,.F.);
#63243=ORIENTED_EDGE('',*,*,#46504,.T.);
#63244=ORIENTED_EDGE('',*,*,#46505,.T.);
#63245=ORIENTED_EDGE('',*,*,#46506,.T.);
#63246=ORIENTED_EDGE('',*,*,#46502,.T.);
#63247=ORIENTED_EDGE('',*,*,#46507,.T.);
#63248=ORIENTED_EDGE('',*,*,#46494,.F.);
#63249=ORIENTED_EDGE('',*,*,#46508,.T.);
#63250=ORIENTED_EDGE('',*,*,#46505,.F.);
#63251=ORIENTED_EDGE('',*,*,#46509,.T.);
#63252=ORIENTED_EDGE('',*,*,#46510,.T.);
#63253=ORIENTED_EDGE('',*,*,#46511,.T.);
#63254=ORIENTED_EDGE('',*,*,#46512,.T.);
#63255=ORIENTED_EDGE('',*,*,#46513,.T.);
#63256=ORIENTED_EDGE('',*,*,#46514,.T.);
#63257=ORIENTED_EDGE('',*,*,#46515,.T.);
#63258=ORIENTED_EDGE('',*,*,#46514,.F.);
#63259=ORIENTED_EDGE('',*,*,#46516,.T.);
#63260=ORIENTED_EDGE('',*,*,#46517,.F.);
#63261=ORIENTED_EDGE('',*,*,#46518,.T.);
#63262=ORIENTED_EDGE('',*,*,#46517,.T.);
#63263=ORIENTED_EDGE('',*,*,#46519,.T.);
#63264=ORIENTED_EDGE('',*,*,#46520,.T.);
#63265=ORIENTED_EDGE('',*,*,#46521,.T.);
#63266=ORIENTED_EDGE('',*,*,#46520,.F.);
#63267=ORIENTED_EDGE('',*,*,#46522,.T.);
#63268=ORIENTED_EDGE('',*,*,#46523,.F.);
#63269=ORIENTED_EDGE('',*,*,#46524,.T.);
#63270=ORIENTED_EDGE('',*,*,#46523,.T.);
#63271=ORIENTED_EDGE('',*,*,#46525,.T.);
#63272=ORIENTED_EDGE('',*,*,#46526,.T.);
#63273=ORIENTED_EDGE('',*,*,#46527,.T.);
#63274=ORIENTED_EDGE('',*,*,#46526,.F.);
#63275=ORIENTED_EDGE('',*,*,#46528,.T.);
#63276=ORIENTED_EDGE('',*,*,#46529,.F.);
#63277=ORIENTED_EDGE('',*,*,#46530,.T.);
#63278=ORIENTED_EDGE('',*,*,#46531,.T.);
#63279=ORIENTED_EDGE('',*,*,#46532,.T.);
#63280=ORIENTED_EDGE('',*,*,#46533,.T.);
#63281=ORIENTED_EDGE('',*,*,#46534,.T.);
#63282=ORIENTED_EDGE('',*,*,#46535,.F.);
#63283=ORIENTED_EDGE('',*,*,#46536,.T.);
#63284=ORIENTED_EDGE('',*,*,#46531,.F.);
#63285=ORIENTED_EDGE('',*,*,#46537,.T.);
#63286=ORIENTED_EDGE('',*,*,#46538,.T.);
#63287=ORIENTED_EDGE('',*,*,#46539,.T.);
#63288=ORIENTED_EDGE('',*,*,#46540,.T.);
#63289=ORIENTED_EDGE('',*,*,#46535,.T.);
#63290=ORIENTED_EDGE('',*,*,#46529,.T.);
#63291=ORIENTED_EDGE('',*,*,#46541,.T.);
#63292=ORIENTED_EDGE('',*,*,#46542,.T.);
#63293=ORIENTED_EDGE('',*,*,#46543,.T.);
#63294=ORIENTED_EDGE('',*,*,#46544,.T.);
#63295=ORIENTED_EDGE('',*,*,#46545,.T.);
#63296=ORIENTED_EDGE('',*,*,#46546,.T.);
#63297=ORIENTED_EDGE('',*,*,#46547,.T.);
#63298=ORIENTED_EDGE('',*,*,#46548,.T.);
#63299=ORIENTED_EDGE('',*,*,#46549,.T.);
#63300=ORIENTED_EDGE('',*,*,#46550,.T.);
#63301=ORIENTED_EDGE('',*,*,#46551,.T.);
#63302=ORIENTED_EDGE('',*,*,#46552,.T.);
#63303=ORIENTED_EDGE('',*,*,#46553,.T.);
#63304=ORIENTED_EDGE('',*,*,#46554,.T.);
#63305=ORIENTED_EDGE('',*,*,#46553,.F.);
#63306=ORIENTED_EDGE('',*,*,#46555,.T.);
#63307=ORIENTED_EDGE('',*,*,#46556,.F.);
#63308=ORIENTED_EDGE('',*,*,#46557,.T.);
#63309=ORIENTED_EDGE('',*,*,#46558,.T.);
#63310=ORIENTED_EDGE('',*,*,#46559,.T.);
#63311=ORIENTED_EDGE('',*,*,#46560,.T.);
#63312=ORIENTED_EDGE('',*,*,#46556,.T.);
#63313=ORIENTED_EDGE('',*,*,#46561,.T.);
#63314=ORIENTED_EDGE('',*,*,#46562,.T.);
#63315=ORIENTED_EDGE('',*,*,#46563,.T.);
#63316=ORIENTED_EDGE('',*,*,#46564,.F.);
#63317=ORIENTED_EDGE('',*,*,#46565,.T.);
#63318=ORIENTED_EDGE('',*,*,#46566,.F.);
#63319=ORIENTED_EDGE('',*,*,#46567,.T.);
#63320=ORIENTED_EDGE('',*,*,#46568,.T.);
#63321=ORIENTED_EDGE('',*,*,#46569,.T.);
#63322=ORIENTED_EDGE('',*,*,#46564,.T.);
#63323=ORIENTED_EDGE('',*,*,#46570,.T.);
#63324=ORIENTED_EDGE('',*,*,#46571,.F.);
#63325=ORIENTED_EDGE('',*,*,#46572,.T.);
#63326=ORIENTED_EDGE('',*,*,#46568,.F.);
#63327=ORIENTED_EDGE('',*,*,#46573,.T.);
#63328=ORIENTED_EDGE('',*,*,#46574,.T.);
#63329=ORIENTED_EDGE('',*,*,#46575,.T.);
#63330=ORIENTED_EDGE('',*,*,#46571,.T.);
#63331=ORIENTED_EDGE('',*,*,#46576,.T.);
#63332=ORIENTED_EDGE('',*,*,#46577,.T.);
#63333=ORIENTED_EDGE('',*,*,#46578,.F.);
#63334=ORIENTED_EDGE('',*,*,#46579,.F.);
#63335=ORIENTED_EDGE('',*,*,#46580,.F.);
#63336=ORIENTED_EDGE('',*,*,#46581,.T.);
#63337=ORIENTED_EDGE('',*,*,#46582,.T.);
#63338=ORIENTED_EDGE('',*,*,#46583,.T.);
#63339=ORIENTED_EDGE('',*,*,#46584,.T.);
#63340=ORIENTED_EDGE('',*,*,#46583,.F.);
#63341=ORIENTED_EDGE('',*,*,#46585,.T.);
#63342=ORIENTED_EDGE('',*,*,#46586,.F.);
#63343=ORIENTED_EDGE('',*,*,#46550,.F.);
#63344=ORIENTED_EDGE('',*,*,#46587,.T.);
#63345=ORIENTED_EDGE('',*,*,#46586,.T.);
#63346=ORIENTED_EDGE('',*,*,#46588,.T.);
#63347=ORIENTED_EDGE('',*,*,#46589,.F.);
#63348=ORIENTED_EDGE('',*,*,#46589,.T.);
#63349=ORIENTED_EDGE('',*,*,#46590,.T.);
#63350=ORIENTED_EDGE('',*,*,#46591,.F.);
#63351=ORIENTED_EDGE('',*,*,#46592,.T.);
#63352=ORIENTED_EDGE('',*,*,#46548,.F.);
#63353=ORIENTED_EDGE('',*,*,#46591,.T.);
#63354=ORIENTED_EDGE('',*,*,#46593,.T.);
#63355=ORIENTED_EDGE('',*,*,#46594,.T.);
#63356=ORIENTED_EDGE('',*,*,#46595,.T.);
#63357=ORIENTED_EDGE('',*,*,#46596,.T.);
#63358=ORIENTED_EDGE('',*,*,#46597,.T.);
#63359=ORIENTED_EDGE('',*,*,#46598,.T.);
#63360=ORIENTED_EDGE('',*,*,#46599,.T.);
#63361=ORIENTED_EDGE('',*,*,#46600,.F.);
#63362=ORIENTED_EDGE('',*,*,#46601,.T.);
#63363=ORIENTED_EDGE('',*,*,#46596,.F.);
#63364=ORIENTED_EDGE('',*,*,#46602,.T.);
#63365=ORIENTED_EDGE('',*,*,#46603,.T.);
#63366=ORIENTED_EDGE('',*,*,#46604,.T.);
#63367=ORIENTED_EDGE('',*,*,#46605,.T.);
#63368=ORIENTED_EDGE('',*,*,#46600,.T.);
#63369=ORIENTED_EDGE('',*,*,#46606,.T.);
#63370=ORIENTED_EDGE('',*,*,#46607,.T.);
#63371=ORIENTED_EDGE('',*,*,#46608,.T.);
#63372=ORIENTED_EDGE('',*,*,#46594,.F.);
#63373=ORIENTED_EDGE('',*,*,#46609,.T.);
#63374=ORIENTED_EDGE('',*,*,#46610,.T.);
#63375=ORIENTED_EDGE('',*,*,#46608,.F.);
#63376=ORIENTED_EDGE('',*,*,#46611,.T.);
#63377=ORIENTED_EDGE('',*,*,#46612,.F.);
#63378=ORIENTED_EDGE('',*,*,#46613,.T.);
#63379=ORIENTED_EDGE('',*,*,#46614,.F.);
#63380=ORIENTED_EDGE('',*,*,#46615,.T.);
#63381=ORIENTED_EDGE('',*,*,#46616,.T.);
#63382=ORIENTED_EDGE('',*,*,#46617,.T.);
#63383=ORIENTED_EDGE('',*,*,#46618,.T.);
#63384=ORIENTED_EDGE('',*,*,#46614,.T.);
#63385=ORIENTED_EDGE('',*,*,#46619,.T.);
#63386=ORIENTED_EDGE('',*,*,#46620,.T.);
#63387=ORIENTED_EDGE('',*,*,#46621,.T.);
#63388=ORIENTED_EDGE('',*,*,#46622,.T.);
#63389=ORIENTED_EDGE('',*,*,#46623,.F.);
#63390=ORIENTED_EDGE('',*,*,#46624,.T.);
#63391=ORIENTED_EDGE('',*,*,#46619,.F.);
#63392=ORIENTED_EDGE('',*,*,#46625,.T.);
#63393=ORIENTED_EDGE('',*,*,#46626,.T.);
#63394=ORIENTED_EDGE('',*,*,#46627,.T.);
#63395=ORIENTED_EDGE('',*,*,#46623,.T.);
#63396=ORIENTED_EDGE('',*,*,#46628,.T.);
#63397=ORIENTED_EDGE('',*,*,#46629,.T.);
#63398=ORIENTED_EDGE('',*,*,#46630,.T.);
#63399=ORIENTED_EDGE('',*,*,#46631,.T.);
#63400=ORIENTED_EDGE('',*,*,#46632,.T.);
#63401=ORIENTED_EDGE('',*,*,#46633,.T.);
#63402=ORIENTED_EDGE('',*,*,#46634,.T.);
#63403=ORIENTED_EDGE('',*,*,#46635,.T.);
#63404=ORIENTED_EDGE('',*,*,#46636,.T.);
#63405=ORIENTED_EDGE('',*,*,#46635,.F.);
#63406=ORIENTED_EDGE('',*,*,#46637,.T.);
#63407=ORIENTED_EDGE('',*,*,#46632,.F.);
#63408=ORIENTED_EDGE('',*,*,#46638,.T.);
#63409=ORIENTED_EDGE('',*,*,#46639,.T.);
#63410=ORIENTED_EDGE('',*,*,#46640,.T.);
#63411=ORIENTED_EDGE('',*,*,#46629,.F.);
#63412=ORIENTED_EDGE('',*,*,#46641,.T.);
#63413=ORIENTED_EDGE('',*,*,#46642,.T.);
#63414=ORIENTED_EDGE('',*,*,#46643,.T.);
#63415=ORIENTED_EDGE('',*,*,#46644,.T.);
#63416=ORIENTED_EDGE('',*,*,#46645,.F.);
#63417=ORIENTED_EDGE('',*,*,#46646,.T.);
#63418=ORIENTED_EDGE('',*,*,#46643,.F.);
#63419=ORIENTED_EDGE('',*,*,#46647,.T.);
#63420=ORIENTED_EDGE('',*,*,#46648,.T.);
#63421=ORIENTED_EDGE('',*,*,#46649,.T.);
#63422=ORIENTED_EDGE('',*,*,#46645,.T.);
#63423=ORIENTED_EDGE('',*,*,#46650,.T.);
#63424=ORIENTED_EDGE('',*,*,#46651,.T.);
#63425=ORIENTED_EDGE('',*,*,#46652,.T.);
#63426=ORIENTED_EDGE('',*,*,#46653,.T.);
#63427=ORIENTED_EDGE('',*,*,#46654,.F.);
#63428=ORIENTED_EDGE('',*,*,#46655,.T.);
#63429=ORIENTED_EDGE('',*,*,#46656,.T.);
#63430=ORIENTED_EDGE('',*,*,#46657,.T.);
#63431=ORIENTED_EDGE('',*,*,#46658,.T.);
#63432=ORIENTED_EDGE('',*,*,#46659,.F.);
#63433=ORIENTED_EDGE('',*,*,#46660,.T.);
#63434=ORIENTED_EDGE('',*,*,#46655,.F.);
#63435=ORIENTED_EDGE('',*,*,#46661,.T.);
#63436=ORIENTED_EDGE('',*,*,#46662,.T.);
#63437=ORIENTED_EDGE('',*,*,#46663,.T.);
#63438=ORIENTED_EDGE('',*,*,#46659,.T.);
#63439=ORIENTED_EDGE('',*,*,#46664,.T.);
#63440=ORIENTED_EDGE('',*,*,#46665,.T.);
#63441=ORIENTED_EDGE('',*,*,#46666,.T.);
#63442=ORIENTED_EDGE('',*,*,#46667,.T.);
#63443=ORIENTED_EDGE('',*,*,#46668,.F.);
#63444=ORIENTED_EDGE('',*,*,#46669,.T.);
#63445=ORIENTED_EDGE('',*,*,#46670,.T.);
#63446=ORIENTED_EDGE('',*,*,#46671,.T.);
#63447=ORIENTED_EDGE('',*,*,#46672,.T.);
#63448=ORIENTED_EDGE('',*,*,#46673,.F.);
#63449=ORIENTED_EDGE('',*,*,#46674,.T.);
#63450=ORIENTED_EDGE('',*,*,#46669,.F.);
#63451=ORIENTED_EDGE('',*,*,#46675,.T.);
#63452=ORIENTED_EDGE('',*,*,#46676,.T.);
#63453=ORIENTED_EDGE('',*,*,#46677,.T.);
#63454=ORIENTED_EDGE('',*,*,#46673,.T.);
#63455=ORIENTED_EDGE('',*,*,#46678,.T.);
#63456=ORIENTED_EDGE('',*,*,#46679,.T.);
#63457=ORIENTED_EDGE('',*,*,#46680,.T.);
#63458=ORIENTED_EDGE('',*,*,#46681,.T.);
#63459=ORIENTED_EDGE('',*,*,#46682,.F.);
#63460=ORIENTED_EDGE('',*,*,#46683,.T.);
#63461=ORIENTED_EDGE('',*,*,#46684,.T.);
#63462=ORIENTED_EDGE('',*,*,#46685,.T.);
#63463=ORIENTED_EDGE('',*,*,#46686,.T.);
#63464=ORIENTED_EDGE('',*,*,#46687,.F.);
#63465=ORIENTED_EDGE('',*,*,#46688,.T.);
#63466=ORIENTED_EDGE('',*,*,#46683,.F.);
#63467=ORIENTED_EDGE('',*,*,#46689,.T.);
#63468=ORIENTED_EDGE('',*,*,#46690,.T.);
#63469=ORIENTED_EDGE('',*,*,#46691,.T.);
#63470=ORIENTED_EDGE('',*,*,#46687,.T.);
#63471=ORIENTED_EDGE('',*,*,#46692,.T.);
#63472=ORIENTED_EDGE('',*,*,#46693,.F.);
#63473=ORIENTED_EDGE('',*,*,#46694,.T.);
#63474=ORIENTED_EDGE('',*,*,#46695,.F.);
#63475=ORIENTED_EDGE('',*,*,#46696,.T.);
#63476=ORIENTED_EDGE('',*,*,#46697,.T.);
#63477=ORIENTED_EDGE('',*,*,#46698,.T.);
#63478=ORIENTED_EDGE('',*,*,#46699,.T.);
#63479=ORIENTED_EDGE('',*,*,#46698,.F.);
#63480=ORIENTED_EDGE('',*,*,#46700,.T.);
#63481=ORIENTED_EDGE('',*,*,#46701,.F.);
#63482=ORIENTED_EDGE('',*,*,#46702,.T.);
#63483=ORIENTED_EDGE('',*,*,#46703,.T.);
#63484=ORIENTED_EDGE('',*,*,#46704,.T.);
#63485=ORIENTED_EDGE('',*,*,#46693,.T.);
#63486=ORIENTED_EDGE('',*,*,#46701,.T.);
#63487=ORIENTED_EDGE('',*,*,#46705,.F.);
#63488=ORIENTED_EDGE('',*,*,#46706,.T.);
#63489=ORIENTED_EDGE('',*,*,#46707,.F.);
#63490=ORIENTED_EDGE('',*,*,#46708,.T.);
#63491=ORIENTED_EDGE('',*,*,#46709,.T.);
#63492=ORIENTED_EDGE('',*,*,#46710,.T.);
#63493=ORIENTED_EDGE('',*,*,#46711,.T.);
#63494=ORIENTED_EDGE('',*,*,#46712,.T.);
#63495=ORIENTED_EDGE('',*,*,#46713,.F.);
#63496=ORIENTED_EDGE('',*,*,#46714,.T.);
#63497=ORIENTED_EDGE('',*,*,#46711,.F.);
#63498=ORIENTED_EDGE('',*,*,#46715,.T.);
#63499=ORIENTED_EDGE('',*,*,#46716,.T.);
#63500=ORIENTED_EDGE('',*,*,#46717,.T.);
#63501=ORIENTED_EDGE('',*,*,#46713,.T.);
#63502=ORIENTED_EDGE('',*,*,#46718,.T.);
#63503=ORIENTED_EDGE('',*,*,#46719,.T.);
#63504=ORIENTED_EDGE('',*,*,#46720,.T.);
#63505=ORIENTED_EDGE('',*,*,#46721,.T.);
#63506=ORIENTED_EDGE('',*,*,#46707,.T.);
#63507=ORIENTED_EDGE('',*,*,#46722,.T.);
#63508=ORIENTED_EDGE('',*,*,#46723,.T.);
#63509=ORIENTED_EDGE('',*,*,#46705,.T.);
#63510=ORIENTED_EDGE('',*,*,#46724,.T.);
#63511=ORIENTED_EDGE('',*,*,#46725,.T.);
#63512=ORIENTED_EDGE('',*,*,#46726,.T.);
#63513=ORIENTED_EDGE('',*,*,#46612,.T.);
#63514=ORIENTED_EDGE('',*,*,#46727,.T.);
#63515=ORIENTED_EDGE('',*,*,#46728,.T.);
#63516=ORIENTED_EDGE('',*,*,#46729,.T.);
#63517=ORIENTED_EDGE('',*,*,#46730,.T.);
#63518=ORIENTED_EDGE('',*,*,#46731,.T.);
#63519=ORIENTED_EDGE('',*,*,#46732,.T.);
#63520=ORIENTED_EDGE('',*,*,#46733,.T.);
#63521=ORIENTED_EDGE('',*,*,#46734,.T.);
#63522=ORIENTED_EDGE('',*,*,#46735,.T.);
#63523=ORIENTED_EDGE('',*,*,#46736,.T.);
#63524=ORIENTED_EDGE('',*,*,#46737,.T.);
#63525=ORIENTED_EDGE('',*,*,#46738,.T.);
#63526=ORIENTED_EDGE('',*,*,#46739,.T.);
#63527=ORIENTED_EDGE('',*,*,#46740,.T.);
#63528=ORIENTED_EDGE('',*,*,#46741,.T.);
#63529=ORIENTED_EDGE('',*,*,#46742,.T.);
#63530=ORIENTED_EDGE('',*,*,#46743,.T.);
#63531=ORIENTED_EDGE('',*,*,#46744,.F.);
#63532=ORIENTED_EDGE('',*,*,#46745,.T.);
#63533=ORIENTED_EDGE('',*,*,#46746,.F.);
#63534=ORIENTED_EDGE('',*,*,#46747,.T.);
#63535=ORIENTED_EDGE('',*,*,#46563,.F.);
#63536=ORIENTED_EDGE('',*,*,#46748,.T.);
#63537=ORIENTED_EDGE('',*,*,#46574,.F.);
#63538=ORIENTED_EDGE('',*,*,#46749,.T.);
#63539=ORIENTED_EDGE('',*,*,#46750,.T.);
#63540=ORIENTED_EDGE('',*,*,#46751,.T.);
#63541=ORIENTED_EDGE('',*,*,#46752,.F.);
#63542=ORIENTED_EDGE('',*,*,#46753,.T.);
#63543=ORIENTED_EDGE('',*,*,#46740,.F.);
#63544=ORIENTED_EDGE('',*,*,#46754,.T.);
#63545=ORIENTED_EDGE('',*,*,#46755,.F.);
#63546=ORIENTED_EDGE('',*,*,#46756,.T.);
#63547=ORIENTED_EDGE('',*,*,#46736,.F.);
#63548=ORIENTED_EDGE('',*,*,#46757,.T.);
#63549=ORIENTED_EDGE('',*,*,#46734,.F.);
#63550=ORIENTED_EDGE('',*,*,#46758,.T.);
#63551=ORIENTED_EDGE('',*,*,#46759,.F.);
#63552=ORIENTED_EDGE('',*,*,#46760,.T.);
#63553=ORIENTED_EDGE('',*,*,#46761,.F.);
#63554=ORIENTED_EDGE('',*,*,#46762,.T.);
#63555=ORIENTED_EDGE('',*,*,#46728,.F.);
#63556=ORIENTED_EDGE('',*,*,#46763,.T.);
#63557=ORIENTED_EDGE('',*,*,#46764,.T.);
#63558=ORIENTED_EDGE('',*,*,#46765,.F.);
#63559=ORIENTED_EDGE('',*,*,#46766,.F.);
#63560=ORIENTED_EDGE('',*,*,#46767,.F.);
#63561=ORIENTED_EDGE('',*,*,#46768,.T.);
#63562=ORIENTED_EDGE('',*,*,#46751,.F.);
#63563=ORIENTED_EDGE('',*,*,#46769,.F.);
#63564=ORIENTED_EDGE('',*,*,#46770,.F.);
#63565=ORIENTED_EDGE('',*,*,#46771,.F.);
#63566=ORIENTED_EDGE('',*,*,#46772,.T.);
#63567=ORIENTED_EDGE('',*,*,#46561,.F.);
#63568=ORIENTED_EDGE('',*,*,#46768,.F.);
#63569=ORIENTED_EDGE('',*,*,#46773,.F.);
#63570=ORIENTED_EDGE('',*,*,#46774,.F.);
#63571=ORIENTED_EDGE('',*,*,#46775,.F.);
#63572=ORIENTED_EDGE('',*,*,#46776,.F.);
#63573=ORIENTED_EDGE('',*,*,#46773,.T.);
#63574=ORIENTED_EDGE('',*,*,#46777,.F.);
#63575=ORIENTED_EDGE('',*,*,#46778,.F.);
#63576=ORIENTED_EDGE('',*,*,#46559,.F.);
#63577=ORIENTED_EDGE('',*,*,#46778,.T.);
#63578=ORIENTED_EDGE('',*,*,#46779,.F.);
#63579=ORIENTED_EDGE('',*,*,#46780,.F.);
#63580=ORIENTED_EDGE('',*,*,#46781,.F.);
#63581=ORIENTED_EDGE('',*,*,#46782,.F.);
#63582=ORIENTED_EDGE('',*,*,#46783,.T.);
#63583=ORIENTED_EDGE('',*,*,#46581,.F.);
#63584=ORIENTED_EDGE('',*,*,#46784,.T.);
#63585=ORIENTED_EDGE('',*,*,#46785,.T.);
#63586=ORIENTED_EDGE('',*,*,#46786,.F.);
#63587=ORIENTED_EDGE('',*,*,#46787,.F.);
#63588=ORIENTED_EDGE('',*,*,#46788,.F.);
#63589=ORIENTED_EDGE('',*,*,#46787,.T.);
#63590=ORIENTED_EDGE('',*,*,#46789,.F.);
#63591=ORIENTED_EDGE('',*,*,#46790,.F.);
#63592=ORIENTED_EDGE('',*,*,#46604,.F.);
#63593=ORIENTED_EDGE('',*,*,#46790,.T.);
#63594=ORIENTED_EDGE('',*,*,#46791,.F.);
#63595=ORIENTED_EDGE('',*,*,#46792,.F.);
#63596=ORIENTED_EDGE('',*,*,#46793,.F.);
#63597=ORIENTED_EDGE('',*,*,#46794,.F.);
#63598=ORIENTED_EDGE('',*,*,#46795,.T.);
#63599=ORIENTED_EDGE('',*,*,#46796,.F.);
#63600=ORIENTED_EDGE('',*,*,#46797,.F.);
#63601=ORIENTED_EDGE('',*,*,#46797,.T.);
#63602=ORIENTED_EDGE('',*,*,#46798,.F.);
#63603=ORIENTED_EDGE('',*,*,#46799,.F.);
#63604=ORIENTED_EDGE('',*,*,#46800,.F.);
#63605=ORIENTED_EDGE('',*,*,#46799,.T.);
#63606=ORIENTED_EDGE('',*,*,#46801,.F.);
#63607=ORIENTED_EDGE('',*,*,#46802,.F.);
#63608=ORIENTED_EDGE('',*,*,#46803,.F.);
#63609=ORIENTED_EDGE('',*,*,#46802,.T.);
#63610=ORIENTED_EDGE('',*,*,#46804,.F.);
#63611=ORIENTED_EDGE('',*,*,#46805,.F.);
#63612=ORIENTED_EDGE('',*,*,#46806,.F.);
#63613=ORIENTED_EDGE('',*,*,#46807,.F.);
#63614=ORIENTED_EDGE('',*,*,#46808,.F.);
#63615=ORIENTED_EDGE('',*,*,#46809,.F.);
#63616=ORIENTED_EDGE('',*,*,#46810,.F.);
#63617=ORIENTED_EDGE('',*,*,#46807,.T.);
#63618=ORIENTED_EDGE('',*,*,#46811,.F.);
#63619=ORIENTED_EDGE('',*,*,#46812,.F.);
#63620=ORIENTED_EDGE('',*,*,#46431,.F.);
#63621=ORIENTED_EDGE('',*,*,#46812,.T.);
#63622=ORIENTED_EDGE('',*,*,#46813,.F.);
#63623=ORIENTED_EDGE('',*,*,#46814,.F.);
#63624=ORIENTED_EDGE('',*,*,#46815,.F.);
#63625=ORIENTED_EDGE('',*,*,#46422,.F.);
#63626=ORIENTED_EDGE('',*,*,#46816,.T.);
#63627=ORIENTED_EDGE('',*,*,#46817,.F.);
#63628=ORIENTED_EDGE('',*,*,#46818,.F.);
#63629=ORIENTED_EDGE('',*,*,#46818,.T.);
#63630=ORIENTED_EDGE('',*,*,#46819,.F.);
#63631=ORIENTED_EDGE('',*,*,#46820,.F.);
#63632=ORIENTED_EDGE('',*,*,#46469,.F.);
#63633=ORIENTED_EDGE('',*,*,#46821,.F.);
#63634=ORIENTED_EDGE('',*,*,#46822,.T.);
#63635=ORIENTED_EDGE('',*,*,#46823,.F.);
#63636=ORIENTED_EDGE('',*,*,#46805,.T.);
#63637=ORIENTED_EDGE('',*,*,#46824,.T.);
#63638=ORIENTED_EDGE('',*,*,#46825,.F.);
#63639=ORIENTED_EDGE('',*,*,#46826,.F.);
#63640=ORIENTED_EDGE('',*,*,#46827,.F.);
#63641=ORIENTED_EDGE('',*,*,#46826,.T.);
#63642=ORIENTED_EDGE('',*,*,#46828,.F.);
#63643=ORIENTED_EDGE('',*,*,#46829,.F.);
#63644=ORIENTED_EDGE('',*,*,#46463,.F.);
#63645=ORIENTED_EDGE('',*,*,#46829,.T.);
#63646=ORIENTED_EDGE('',*,*,#46830,.F.);
#63647=ORIENTED_EDGE('',*,*,#46831,.F.);
#63648=ORIENTED_EDGE('',*,*,#46832,.F.);
#63649=ORIENTED_EDGE('',*,*,#46833,.F.);
#63650=ORIENTED_EDGE('',*,*,#46834,.T.);
#63651=ORIENTED_EDGE('',*,*,#46452,.F.);
#63652=ORIENTED_EDGE('',*,*,#46835,.T.);
#63653=ORIENTED_EDGE('',*,*,#46836,.F.);
#63654=ORIENTED_EDGE('',*,*,#46837,.T.);
#63655=ORIENTED_EDGE('',*,*,#46465,.F.);
#63656=ORIENTED_EDGE('',*,*,#46820,.T.);
#63657=ORIENTED_EDGE('',*,*,#46838,.T.);
#63658=ORIENTED_EDGE('',*,*,#46839,.F.);
#63659=ORIENTED_EDGE('',*,*,#46840,.F.);
#63660=ORIENTED_EDGE('',*,*,#46841,.F.);
#63661=ORIENTED_EDGE('',*,*,#46840,.T.);
#63662=ORIENTED_EDGE('',*,*,#46842,.F.);
#63663=ORIENTED_EDGE('',*,*,#46843,.F.);
#63664=ORIENTED_EDGE('',*,*,#46844,.F.);
#63665=ORIENTED_EDGE('',*,*,#46843,.T.);
#63666=ORIENTED_EDGE('',*,*,#46845,.F.);
#63667=ORIENTED_EDGE('',*,*,#46846,.F.);
#63668=ORIENTED_EDGE('',*,*,#46720,.F.);
#63669=ORIENTED_EDGE('',*,*,#46847,.T.);
#63670=ORIENTED_EDGE('',*,*,#46848,.F.);
#63671=ORIENTED_EDGE('',*,*,#46846,.T.);
#63672=ORIENTED_EDGE('',*,*,#46849,.F.);
#63673=ORIENTED_EDGE('',*,*,#46850,.F.);
#63674=ORIENTED_EDGE('',*,*,#46851,.T.);
#63675=ORIENTED_EDGE('',*,*,#46716,.F.);
#63676=ORIENTED_EDGE('',*,*,#46852,.T.);
#63677=ORIENTED_EDGE('',*,*,#46853,.T.);
#63678=ORIENTED_EDGE('',*,*,#46854,.F.);
#63679=ORIENTED_EDGE('',*,*,#46855,.F.);
#63680=ORIENTED_EDGE('',*,*,#46856,.F.);
#63681=ORIENTED_EDGE('',*,*,#46857,.T.);
#63682=ORIENTED_EDGE('',*,*,#46704,.F.);
#63683=ORIENTED_EDGE('',*,*,#46853,.F.);
#63684=ORIENTED_EDGE('',*,*,#46858,.F.);
#63685=ORIENTED_EDGE('',*,*,#46859,.T.);
#63686=ORIENTED_EDGE('',*,*,#46694,.F.);
#63687=ORIENTED_EDGE('',*,*,#46857,.F.);
#63688=ORIENTED_EDGE('',*,*,#46860,.F.);
#63689=ORIENTED_EDGE('',*,*,#46861,.T.);
#63690=ORIENTED_EDGE('',*,*,#46862,.F.);
#63691=ORIENTED_EDGE('',*,*,#46859,.F.);
#63692=ORIENTED_EDGE('',*,*,#46863,.F.);
#63693=ORIENTED_EDGE('',*,*,#46864,.F.);
#63694=ORIENTED_EDGE('',*,*,#46865,.T.);
#63695=ORIENTED_EDGE('',*,*,#46690,.F.);
#63696=ORIENTED_EDGE('',*,*,#46866,.T.);
#63697=ORIENTED_EDGE('',*,*,#46867,.F.);
#63698=ORIENTED_EDGE('',*,*,#46868,.F.);
#63699=ORIENTED_EDGE('',*,*,#46869,.F.);
#63700=ORIENTED_EDGE('',*,*,#46870,.F.);
#63701=ORIENTED_EDGE('',*,*,#46867,.T.);
#63702=ORIENTED_EDGE('',*,*,#46871,.F.);
#63703=ORIENTED_EDGE('',*,*,#46872,.F.);
#63704=ORIENTED_EDGE('',*,*,#46680,.F.);
#63705=ORIENTED_EDGE('',*,*,#46872,.T.);
#63706=ORIENTED_EDGE('',*,*,#46873,.F.);
#63707=ORIENTED_EDGE('',*,*,#46874,.F.);
#63708=ORIENTED_EDGE('',*,*,#46875,.F.);
#63709=ORIENTED_EDGE('',*,*,#46876,.F.);
#63710=ORIENTED_EDGE('',*,*,#46877,.T.);
#63711=ORIENTED_EDGE('',*,*,#46676,.F.);
#63712=ORIENTED_EDGE('',*,*,#46878,.T.);
#63713=ORIENTED_EDGE('',*,*,#46879,.F.);
#63714=ORIENTED_EDGE('',*,*,#46880,.F.);
#63715=ORIENTED_EDGE('',*,*,#46881,.F.);
#63716=ORIENTED_EDGE('',*,*,#46882,.F.);
#63717=ORIENTED_EDGE('',*,*,#46879,.T.);
#63718=ORIENTED_EDGE('',*,*,#46883,.F.);
#63719=ORIENTED_EDGE('',*,*,#46884,.F.);
#63720=ORIENTED_EDGE('',*,*,#46666,.F.);
#63721=ORIENTED_EDGE('',*,*,#46884,.T.);
#63722=ORIENTED_EDGE('',*,*,#46885,.F.);
#63723=ORIENTED_EDGE('',*,*,#46886,.F.);
#63724=ORIENTED_EDGE('',*,*,#46887,.F.);
#63725=ORIENTED_EDGE('',*,*,#46888,.F.);
#63726=ORIENTED_EDGE('',*,*,#46889,.T.);
#63727=ORIENTED_EDGE('',*,*,#46662,.F.);
#63728=ORIENTED_EDGE('',*,*,#46890,.T.);
#63729=ORIENTED_EDGE('',*,*,#46891,.F.);
#63730=ORIENTED_EDGE('',*,*,#46892,.F.);
#63731=ORIENTED_EDGE('',*,*,#46893,.F.);
#63732=ORIENTED_EDGE('',*,*,#46894,.F.);
#63733=ORIENTED_EDGE('',*,*,#46891,.T.);
#63734=ORIENTED_EDGE('',*,*,#46895,.F.);
#63735=ORIENTED_EDGE('',*,*,#46896,.F.);
#63736=ORIENTED_EDGE('',*,*,#46652,.F.);
#63737=ORIENTED_EDGE('',*,*,#46896,.T.);
#63738=ORIENTED_EDGE('',*,*,#46897,.F.);
#63739=ORIENTED_EDGE('',*,*,#46898,.F.);
#63740=ORIENTED_EDGE('',*,*,#46899,.F.);
#63741=ORIENTED_EDGE('',*,*,#46900,.F.);
#63742=ORIENTED_EDGE('',*,*,#46901,.T.);
#63743=ORIENTED_EDGE('',*,*,#46648,.F.);
#63744=ORIENTED_EDGE('',*,*,#46902,.T.);
#63745=ORIENTED_EDGE('',*,*,#46903,.T.);
#63746=ORIENTED_EDGE('',*,*,#46904,.F.);
#63747=ORIENTED_EDGE('',*,*,#46905,.F.);
#63748=ORIENTED_EDGE('',*,*,#46906,.F.);
#63749=ORIENTED_EDGE('',*,*,#46907,.T.);
#63750=ORIENTED_EDGE('',*,*,#46640,.F.);
#63751=ORIENTED_EDGE('',*,*,#46903,.F.);
#63752=ORIENTED_EDGE('',*,*,#46908,.F.);
#63753=ORIENTED_EDGE('',*,*,#46909,.T.);
#63754=ORIENTED_EDGE('',*,*,#46630,.F.);
#63755=ORIENTED_EDGE('',*,*,#46907,.F.);
#63756=ORIENTED_EDGE('',*,*,#46910,.F.);
#63757=ORIENTED_EDGE('',*,*,#46911,.T.);
#63758=ORIENTED_EDGE('',*,*,#46912,.F.);
#63759=ORIENTED_EDGE('',*,*,#46909,.F.);
#63760=ORIENTED_EDGE('',*,*,#46913,.F.);
#63761=ORIENTED_EDGE('',*,*,#46914,.F.);
#63762=ORIENTED_EDGE('',*,*,#46915,.T.);
#63763=ORIENTED_EDGE('',*,*,#46626,.F.);
#63764=ORIENTED_EDGE('',*,*,#46916,.T.);
#63765=ORIENTED_EDGE('',*,*,#46917,.T.);
#63766=ORIENTED_EDGE('',*,*,#46918,.F.);
#63767=ORIENTED_EDGE('',*,*,#46919,.F.);
#63768=ORIENTED_EDGE('',*,*,#46920,.F.);
#63769=ORIENTED_EDGE('',*,*,#46919,.T.);
#63770=ORIENTED_EDGE('',*,*,#46921,.F.);
#63771=ORIENTED_EDGE('',*,*,#46922,.F.);
#63772=ORIENTED_EDGE('',*,*,#46617,.F.);
#63773=ORIENTED_EDGE('',*,*,#46922,.T.);
#63774=ORIENTED_EDGE('',*,*,#46923,.F.);
#63775=ORIENTED_EDGE('',*,*,#46924,.F.);
#63776=ORIENTED_EDGE('',*,*,#46925,.F.);
#63777=ORIENTED_EDGE('',*,*,#46510,.F.);
#63778=ORIENTED_EDGE('',*,*,#46926,.T.);
#63779=ORIENTED_EDGE('',*,*,#46927,.F.);
#63780=ORIENTED_EDGE('',*,*,#46928,.T.);
#63781=ORIENTED_EDGE('',*,*,#46929,.T.);
#63782=ORIENTED_EDGE('',*,*,#46930,.F.);
#63783=ORIENTED_EDGE('',*,*,#46924,.T.);
#63784=ORIENTED_EDGE('',*,*,#46931,.F.);
#63785=ORIENTED_EDGE('',*,*,#46932,.T.);
#63786=ORIENTED_EDGE('',*,*,#46511,.F.);
#63787=ORIENTED_EDGE('',*,*,#46928,.F.);
#63788=ORIENTED_EDGE('',*,*,#46933,.F.);
#63789=ORIENTED_EDGE('',*,*,#46934,.F.);
#63790=ORIENTED_EDGE('',*,*,#46935,.T.);
#63791=ORIENTED_EDGE('',*,*,#46492,.F.);
#63792=ORIENTED_EDGE('',*,*,#46932,.F.);
#63793=ORIENTED_EDGE('',*,*,#46936,.F.);
#63794=ORIENTED_EDGE('',*,*,#46937,.F.);
#63795=ORIENTED_EDGE('',*,*,#46938,.F.);
#63796=ORIENTED_EDGE('',*,*,#46939,.F.);
#63797=ORIENTED_EDGE('',*,*,#46936,.T.);
#63798=ORIENTED_EDGE('',*,*,#46940,.F.);
#63799=ORIENTED_EDGE('',*,*,#46941,.F.);
#63800=ORIENTED_EDGE('',*,*,#46490,.F.);
#63801=ORIENTED_EDGE('',*,*,#46941,.T.);
#63802=ORIENTED_EDGE('',*,*,#46942,.F.);
#63803=ORIENTED_EDGE('',*,*,#46943,.F.);
#63804=ORIENTED_EDGE('',*,*,#46944,.F.);
#63805=ORIENTED_EDGE('',*,*,#46945,.F.);
#63806=ORIENTED_EDGE('',*,*,#46946,.T.);
#63807=ORIENTED_EDGE('',*,*,#46512,.F.);
#63808=ORIENTED_EDGE('',*,*,#46947,.T.);
#63809=ORIENTED_EDGE('',*,*,#46948,.T.);
#63810=ORIENTED_EDGE('',*,*,#46949,.F.);
#63811=ORIENTED_EDGE('',*,*,#46950,.F.);
#63812=ORIENTED_EDGE('',*,*,#46951,.F.);
#63813=ORIENTED_EDGE('',*,*,#46950,.T.);
#63814=ORIENTED_EDGE('',*,*,#46952,.F.);
#63815=ORIENTED_EDGE('',*,*,#46953,.F.);
#63816=ORIENTED_EDGE('',*,*,#46539,.F.);
#63817=ORIENTED_EDGE('',*,*,#46953,.T.);
#63818=ORIENTED_EDGE('',*,*,#46954,.F.);
#63819=ORIENTED_EDGE('',*,*,#46955,.F.);
#63820=ORIENTED_EDGE('',*,*,#46956,.F.);
#63821=ORIENTED_EDGE('',*,*,#46957,.F.);
#63822=ORIENTED_EDGE('',*,*,#46958,.T.);
#63823=ORIENTED_EDGE('',*,*,#46959,.F.);
#63824=ORIENTED_EDGE('',*,*,#46960,.F.);
#63825=ORIENTED_EDGE('',*,*,#46960,.T.);
#63826=ORIENTED_EDGE('',*,*,#46961,.F.);
#63827=ORIENTED_EDGE('',*,*,#46962,.F.);
#63828=ORIENTED_EDGE('',*,*,#46963,.F.);
#63829=ORIENTED_EDGE('',*,*,#46962,.T.);
#63830=ORIENTED_EDGE('',*,*,#46964,.F.);
#63831=ORIENTED_EDGE('',*,*,#46965,.F.);
#63832=ORIENTED_EDGE('',*,*,#46966,.F.);
#63833=ORIENTED_EDGE('',*,*,#46965,.T.);
#63834=ORIENTED_EDGE('',*,*,#46967,.F.);
#63835=ORIENTED_EDGE('',*,*,#46968,.F.);
#63836=ORIENTED_EDGE('',*,*,#46969,.F.);
#63837=ORIENTED_EDGE('',*,*,#46970,.F.);
#63838=ORIENTED_EDGE('',*,*,#46971,.T.);
#63839=ORIENTED_EDGE('',*,*,#46972,.F.);
#63840=ORIENTED_EDGE('',*,*,#46968,.T.);
#63841=ORIENTED_EDGE('',*,*,#46973,.F.);
#63842=ORIENTED_EDGE('',*,*,#46974,.F.);
#63843=ORIENTED_EDGE('',*,*,#46975,.F.);
#63844=ORIENTED_EDGE('',*,*,#46976,.F.);
#63845=ORIENTED_EDGE('',*,*,#46977,.T.);
#63846=ORIENTED_EDGE('',*,*,#46544,.F.);
#63847=ORIENTED_EDGE('',*,*,#46978,.T.);
#63848=ORIENTED_EDGE('',*,*,#46979,.F.);
#63849=ORIENTED_EDGE('',*,*,#46980,.T.);
#63850=ORIENTED_EDGE('',*,*,#46981,.F.);
#63851=ORIENTED_EDGE('',*,*,#46982,.T.);
#63852=ORIENTED_EDGE('',*,*,#46983,.T.);
#63853=ORIENTED_EDGE('',*,*,#46984,.T.);
#63854=ORIENTED_EDGE('',*,*,#46744,.T.);
#63855=ORIENTED_EDGE('',*,*,#46985,.T.);
#63856=ORIENTED_EDGE('',*,*,#46986,.T.);
#63857=ORIENTED_EDGE('',*,*,#46987,.T.);
#63858=ORIENTED_EDGE('',*,*,#46988,.T.);
#63859=ORIENTED_EDGE('',*,*,#46989,.T.);
#63860=ORIENTED_EDGE('',*,*,#46990,.F.);
#63861=ORIENTED_EDGE('',*,*,#46991,.T.);
#63862=ORIENTED_EDGE('',*,*,#46580,.T.);
#63863=ORIENTED_EDGE('',*,*,#46992,.T.);
#63864=ORIENTED_EDGE('',*,*,#46993,.T.);
#63865=ORIENTED_EDGE('',*,*,#46994,.F.);
#63866=ORIENTED_EDGE('',*,*,#46995,.F.);
#63867=ORIENTED_EDGE('',*,*,#46429,.F.);
#63868=ORIENTED_EDGE('',*,*,#46995,.T.);
#63869=ORIENTED_EDGE('',*,*,#46996,.F.);
#63870=ORIENTED_EDGE('',*,*,#46997,.F.);
#63871=ORIENTED_EDGE('',*,*,#46426,.F.);
#63872=ORIENTED_EDGE('',*,*,#46998,.T.);
#63873=ORIENTED_EDGE('',*,*,#46999,.F.);
#63874=ORIENTED_EDGE('',*,*,#47000,.F.);
#63875=ORIENTED_EDGE('',*,*,#47001,.F.);
#63876=ORIENTED_EDGE('',*,*,#47002,.T.);
#63877=ORIENTED_EDGE('',*,*,#46481,.F.);
#63878=ORIENTED_EDGE('',*,*,#46998,.F.);
#63879=ORIENTED_EDGE('',*,*,#47003,.F.);
#63880=ORIENTED_EDGE('',*,*,#47004,.T.);
#63881=ORIENTED_EDGE('',*,*,#46478,.F.);
#63882=ORIENTED_EDGE('',*,*,#47002,.F.);
#63883=ORIENTED_EDGE('',*,*,#47005,.F.);
#63884=ORIENTED_EDGE('',*,*,#47006,.T.);
#63885=ORIENTED_EDGE('',*,*,#46475,.F.);
#63886=ORIENTED_EDGE('',*,*,#47004,.F.);
#63887=ORIENTED_EDGE('',*,*,#47007,.F.);
#63888=ORIENTED_EDGE('',*,*,#47008,.T.);
#63889=ORIENTED_EDGE('',*,*,#46472,.F.);
#63890=ORIENTED_EDGE('',*,*,#47006,.F.);
#63891=ORIENTED_EDGE('',*,*,#47009,.F.);
#63892=ORIENTED_EDGE('',*,*,#47010,.T.);
#63893=ORIENTED_EDGE('',*,*,#46468,.F.);
#63894=ORIENTED_EDGE('',*,*,#47008,.F.);
#63895=ORIENTED_EDGE('',*,*,#47011,.F.);
#63896=ORIENTED_EDGE('',*,*,#47012,.T.);
#63897=ORIENTED_EDGE('',*,*,#46421,.F.);
#63898=ORIENTED_EDGE('',*,*,#47010,.F.);
#63899=ORIENTED_EDGE('',*,*,#47013,.F.);
#63900=ORIENTED_EDGE('',*,*,#47014,.T.);
#63901=ORIENTED_EDGE('',*,*,#47015,.T.);
#63902=ORIENTED_EDGE('',*,*,#46816,.F.);
#63903=ORIENTED_EDGE('',*,*,#47012,.F.);
#63904=ORIENTED_EDGE('',*,*,#47016,.F.);
#63905=ORIENTED_EDGE('',*,*,#47014,.F.);
#63906=ORIENTED_EDGE('',*,*,#47017,.F.);
#63907=ORIENTED_EDGE('',*,*,#46814,.T.);
#63908=ORIENTED_EDGE('',*,*,#47018,.F.);
#63909=ORIENTED_EDGE('',*,*,#47015,.F.);
#63910=ORIENTED_EDGE('',*,*,#46432,.F.);
#63911=ORIENTED_EDGE('',*,*,#46815,.T.);
#63912=ORIENTED_EDGE('',*,*,#47019,.F.);
#63913=ORIENTED_EDGE('',*,*,#46993,.F.);
#63914=ORIENTED_EDGE('',*,*,#47020,.T.);
#63915=ORIENTED_EDGE('',*,*,#47021,.F.);
#63916=ORIENTED_EDGE('',*,*,#47022,.F.);
#63917=ORIENTED_EDGE('',*,*,#47023,.F.);
#63918=ORIENTED_EDGE('',*,*,#46997,.T.);
#63919=ORIENTED_EDGE('',*,*,#47024,.F.);
#63920=ORIENTED_EDGE('',*,*,#47025,.F.);
#63921=ORIENTED_EDGE('',*,*,#47026,.F.);
#63922=ORIENTED_EDGE('',*,*,#47027,.F.);
#63923=ORIENTED_EDGE('',*,*,#47028,.T.);
#63924=ORIENTED_EDGE('',*,*,#46423,.F.);
#63925=ORIENTED_EDGE('',*,*,#47026,.T.);
#63926=ORIENTED_EDGE('',*,*,#47029,.T.);
#63927=ORIENTED_EDGE('',*,*,#47030,.F.);
#63928=ORIENTED_EDGE('',*,*,#47031,.F.);
#63929=ORIENTED_EDGE('',*,*,#47028,.F.);
#63930=ORIENTED_EDGE('',*,*,#47031,.T.);
#63931=ORIENTED_EDGE('',*,*,#47032,.F.);
#63932=ORIENTED_EDGE('',*,*,#47033,.F.);
#63933=ORIENTED_EDGE('',*,*,#46424,.F.);
#63934=ORIENTED_EDGE('',*,*,#47033,.T.);
#63935=ORIENTED_EDGE('',*,*,#47034,.F.);
#63936=ORIENTED_EDGE('',*,*,#47035,.F.);
#63937=ORIENTED_EDGE('',*,*,#46427,.F.);
#63938=ORIENTED_EDGE('',*,*,#47036,.F.);
#63939=ORIENTED_EDGE('',*,*,#46808,.T.);
#63940=ORIENTED_EDGE('',*,*,#46430,.F.);
#63941=ORIENTED_EDGE('',*,*,#47035,.T.);
#63942=ORIENTED_EDGE('',*,*,#46809,.T.);
#63943=ORIENTED_EDGE('',*,*,#47037,.F.);
#63944=ORIENTED_EDGE('',*,*,#47038,.F.);
#63945=ORIENTED_EDGE('',*,*,#47039,.F.);
#63946=ORIENTED_EDGE('',*,*,#47038,.T.);
#63947=ORIENTED_EDGE('',*,*,#47040,.F.);
#63948=ORIENTED_EDGE('',*,*,#47041,.F.);
#63949=ORIENTED_EDGE('',*,*,#46834,.F.);
#63950=ORIENTED_EDGE('',*,*,#47041,.T.);
#63951=ORIENTED_EDGE('',*,*,#47042,.F.);
#63952=ORIENTED_EDGE('',*,*,#47043,.F.);
#63953=ORIENTED_EDGE('',*,*,#46453,.F.);
#63954=ORIENTED_EDGE('',*,*,#47043,.T.);
#63955=ORIENTED_EDGE('',*,*,#47044,.F.);
#63956=ORIENTED_EDGE('',*,*,#47045,.F.);
#63957=ORIENTED_EDGE('',*,*,#46450,.F.);
#63958=ORIENTED_EDGE('',*,*,#47045,.T.);
#63959=ORIENTED_EDGE('',*,*,#47046,.F.);
#63960=ORIENTED_EDGE('',*,*,#47047,.F.);
#63961=ORIENTED_EDGE('',*,*,#46447,.F.);
#63962=ORIENTED_EDGE('',*,*,#47047,.T.);
#63963=ORIENTED_EDGE('',*,*,#47048,.F.);
#63964=ORIENTED_EDGE('',*,*,#47049,.F.);
#63965=ORIENTED_EDGE('',*,*,#46444,.F.);
#63966=ORIENTED_EDGE('',*,*,#47049,.T.);
#63967=ORIENTED_EDGE('',*,*,#47050,.F.);
#63968=ORIENTED_EDGE('',*,*,#47051,.F.);
#63969=ORIENTED_EDGE('',*,*,#46441,.F.);
#63970=ORIENTED_EDGE('',*,*,#47051,.T.);
#63971=ORIENTED_EDGE('',*,*,#47052,.F.);
#63972=ORIENTED_EDGE('',*,*,#47053,.F.);
#63973=ORIENTED_EDGE('',*,*,#46438,.F.);
#63974=ORIENTED_EDGE('',*,*,#47053,.T.);
#63975=ORIENTED_EDGE('',*,*,#47054,.F.);
#63976=ORIENTED_EDGE('',*,*,#47055,.F.);
#63977=ORIENTED_EDGE('',*,*,#46434,.F.);
#63978=ORIENTED_EDGE('',*,*,#47055,.T.);
#63979=ORIENTED_EDGE('',*,*,#47056,.F.);
#63980=ORIENTED_EDGE('',*,*,#47057,.F.);
#63981=ORIENTED_EDGE('',*,*,#47058,.F.);
#63982=ORIENTED_EDGE('',*,*,#47057,.T.);
#63983=ORIENTED_EDGE('',*,*,#47059,.F.);
#63984=ORIENTED_EDGE('',*,*,#47060,.F.);
#63985=ORIENTED_EDGE('',*,*,#47061,.F.);
#63986=ORIENTED_EDGE('',*,*,#46435,.F.);
#63987=ORIENTED_EDGE('',*,*,#47058,.T.);
#63988=ORIENTED_EDGE('',*,*,#47062,.F.);
#63989=ORIENTED_EDGE('',*,*,#47063,.T.);
#63990=ORIENTED_EDGE('',*,*,#47064,.T.);
#63991=ORIENTED_EDGE('',*,*,#47065,.F.);
#63992=ORIENTED_EDGE('',*,*,#47066,.F.);
#63993=ORIENTED_EDGE('',*,*,#46461,.F.);
#63994=ORIENTED_EDGE('',*,*,#47066,.T.);
#63995=ORIENTED_EDGE('',*,*,#47067,.F.);
#63996=ORIENTED_EDGE('',*,*,#47068,.F.);
#63997=ORIENTED_EDGE('',*,*,#46458,.F.);
#63998=ORIENTED_EDGE('',*,*,#47069,.T.);
#63999=ORIENTED_EDGE('',*,*,#47070,.F.);
#64000=ORIENTED_EDGE('',*,*,#47071,.F.);
#64001=ORIENTED_EDGE('',*,*,#47072,.F.);
#64002=ORIENTED_EDGE('',*,*,#47071,.T.);
#64003=ORIENTED_EDGE('',*,*,#47073,.F.);
#64004=ORIENTED_EDGE('',*,*,#47074,.F.);
#64005=ORIENTED_EDGE('',*,*,#47063,.F.);
#64006=ORIENTED_EDGE('',*,*,#47074,.T.);
#64007=ORIENTED_EDGE('',*,*,#47075,.F.);
#64008=ORIENTED_EDGE('',*,*,#47076,.F.);
#64009=ORIENTED_EDGE('',*,*,#46436,.F.);
#64010=ORIENTED_EDGE('',*,*,#47076,.T.);
#64011=ORIENTED_EDGE('',*,*,#47077,.F.);
#64012=ORIENTED_EDGE('',*,*,#47078,.F.);
#64013=ORIENTED_EDGE('',*,*,#46439,.F.);
#64014=ORIENTED_EDGE('',*,*,#47078,.T.);
#64015=ORIENTED_EDGE('',*,*,#47079,.F.);
#64016=ORIENTED_EDGE('',*,*,#47080,.F.);
#64017=ORIENTED_EDGE('',*,*,#46442,.F.);
#64018=ORIENTED_EDGE('',*,*,#47081,.T.);
#64019=ORIENTED_EDGE('',*,*,#46445,.F.);
#64020=ORIENTED_EDGE('',*,*,#47080,.T.);
#64021=ORIENTED_EDGE('',*,*,#47082,.F.);
#64022=ORIENTED_EDGE('',*,*,#47083,.T.);
#64023=ORIENTED_EDGE('',*,*,#46448,.F.);
#64024=ORIENTED_EDGE('',*,*,#47081,.F.);
#64025=ORIENTED_EDGE('',*,*,#47084,.F.);
#64026=ORIENTED_EDGE('',*,*,#47085,.T.);
#64027=ORIENTED_EDGE('',*,*,#46451,.F.);
#64028=ORIENTED_EDGE('',*,*,#47083,.F.);
#64029=ORIENTED_EDGE('',*,*,#47086,.F.);
#64030=ORIENTED_EDGE('',*,*,#47087,.T.);
#64031=ORIENTED_EDGE('',*,*,#46454,.F.);
#64032=ORIENTED_EDGE('',*,*,#47085,.F.);
#64033=ORIENTED_EDGE('',*,*,#47088,.F.);
#64034=ORIENTED_EDGE('',*,*,#47089,.T.);
#64035=ORIENTED_EDGE('',*,*,#47090,.T.);
#64036=ORIENTED_EDGE('',*,*,#46835,.F.);
#64037=ORIENTED_EDGE('',*,*,#47087,.F.);
#64038=ORIENTED_EDGE('',*,*,#47091,.F.);
#64039=ORIENTED_EDGE('',*,*,#47089,.F.);
#64040=ORIENTED_EDGE('',*,*,#47092,.F.);
#64041=ORIENTED_EDGE('',*,*,#46831,.T.);
#64042=ORIENTED_EDGE('',*,*,#47093,.F.);
#64043=ORIENTED_EDGE('',*,*,#47090,.F.);
#64044=ORIENTED_EDGE('',*,*,#46464,.F.);
#64045=ORIENTED_EDGE('',*,*,#46832,.T.);
#64046=ORIENTED_EDGE('',*,*,#47094,.F.);
#64047=ORIENTED_EDGE('',*,*,#47064,.F.);
#64048=ORIENTED_EDGE('',*,*,#47068,.T.);
#64049=ORIENTED_EDGE('',*,*,#47095,.F.);
#64050=ORIENTED_EDGE('',*,*,#47096,.F.);
#64051=ORIENTED_EDGE('',*,*,#47097,.F.);
#64052=ORIENTED_EDGE('',*,*,#47098,.F.);
#64053=ORIENTED_EDGE('',*,*,#47099,.T.);
#64054=ORIENTED_EDGE('',*,*,#46455,.F.);
#64055=ORIENTED_EDGE('',*,*,#47097,.T.);
#64056=ORIENTED_EDGE('',*,*,#47100,.T.);
#64057=ORIENTED_EDGE('',*,*,#47101,.F.);
#64058=ORIENTED_EDGE('',*,*,#47102,.F.);
#64059=ORIENTED_EDGE('',*,*,#47103,.F.);
#64060=ORIENTED_EDGE('',*,*,#46766,.T.);
#64061=ORIENTED_EDGE('',*,*,#47104,.F.);
#64062=ORIENTED_EDGE('',*,*,#47105,.F.);
#64063=ORIENTED_EDGE('',*,*,#47106,.F.);
#64064=ORIENTED_EDGE('',*,*,#46579,.T.);
#64065=ORIENTED_EDGE('',*,*,#47107,.F.);
#64066=ORIENTED_EDGE('',*,*,#47108,.F.);
#64067=ORIENTED_EDGE('',*,*,#46992,.F.);
#64068=ORIENTED_EDGE('',*,*,#47108,.T.);
#64069=ORIENTED_EDGE('',*,*,#47109,.F.);
#64070=ORIENTED_EDGE('',*,*,#47110,.F.);
#64071=ORIENTED_EDGE('',*,*,#47111,.F.);
#64072=ORIENTED_EDGE('',*,*,#47112,.T.);
#64073=ORIENTED_EDGE('',*,*,#47099,.F.);
#64074=ORIENTED_EDGE('',*,*,#47113,.F.);
#64075=ORIENTED_EDGE('',*,*,#47114,.F.);
#64076=ORIENTED_EDGE('',*,*,#47115,.T.);
#64077=ORIENTED_EDGE('',*,*,#46456,.F.);
#64078=ORIENTED_EDGE('',*,*,#47112,.F.);
#64079=ORIENTED_EDGE('',*,*,#47116,.F.);
#64080=ORIENTED_EDGE('',*,*,#47117,.T.);
#64081=ORIENTED_EDGE('',*,*,#46459,.F.);
#64082=ORIENTED_EDGE('',*,*,#47115,.F.);
#64083=ORIENTED_EDGE('',*,*,#47118,.F.);
#64084=ORIENTED_EDGE('',*,*,#47119,.F.);
#64085=ORIENTED_EDGE('',*,*,#46827,.T.);
#64086=ORIENTED_EDGE('',*,*,#46462,.F.);
#64087=ORIENTED_EDGE('',*,*,#47117,.F.);
#64088=ORIENTED_EDGE('',*,*,#47120,.T.);
#64089=ORIENTED_EDGE('',*,*,#47121,.F.);
#64090=ORIENTED_EDGE('',*,*,#46824,.F.);
#64091=ORIENTED_EDGE('',*,*,#47122,.F.);
#64092=ORIENTED_EDGE('',*,*,#47102,.T.);
#64093=ORIENTED_EDGE('',*,*,#46822,.F.);
#64094=ORIENTED_EDGE('',*,*,#47120,.F.);
#64095=ORIENTED_EDGE('',*,*,#47123,.F.);
#64096=ORIENTED_EDGE('',*,*,#47124,.T.);
#64097=ORIENTED_EDGE('',*,*,#46466,.F.);
#64098=ORIENTED_EDGE('',*,*,#47125,.F.);
#64099=ORIENTED_EDGE('',*,*,#47126,.F.);
#64100=ORIENTED_EDGE('',*,*,#47127,.T.);
#64101=ORIENTED_EDGE('',*,*,#46470,.F.);
#64102=ORIENTED_EDGE('',*,*,#47124,.F.);
#64103=ORIENTED_EDGE('',*,*,#47128,.F.);
#64104=ORIENTED_EDGE('',*,*,#47129,.T.);
#64105=ORIENTED_EDGE('',*,*,#46473,.F.);
#64106=ORIENTED_EDGE('',*,*,#47127,.F.);
#64107=ORIENTED_EDGE('',*,*,#47130,.F.);
#64108=ORIENTED_EDGE('',*,*,#47131,.T.);
#64109=ORIENTED_EDGE('',*,*,#46476,.F.);
#64110=ORIENTED_EDGE('',*,*,#47129,.F.);
#64111=ORIENTED_EDGE('',*,*,#47132,.F.);
#64112=ORIENTED_EDGE('',*,*,#47133,.T.);
#64113=ORIENTED_EDGE('',*,*,#46479,.F.);
#64114=ORIENTED_EDGE('',*,*,#47131,.F.);
#64115=ORIENTED_EDGE('',*,*,#47134,.F.);
#64116=ORIENTED_EDGE('',*,*,#47135,.T.);
#64117=ORIENTED_EDGE('',*,*,#47136,.F.);
#64118=ORIENTED_EDGE('',*,*,#47133,.F.);
#64119=ORIENTED_EDGE('',*,*,#47137,.F.);
#64120=ORIENTED_EDGE('',*,*,#47138,.T.);
#64121=ORIENTED_EDGE('',*,*,#47139,.F.);
#64122=ORIENTED_EDGE('',*,*,#47140,.F.);
#64123=ORIENTED_EDGE('',*,*,#46723,.F.);
#64124=ORIENTED_EDGE('',*,*,#47140,.T.);
#64125=ORIENTED_EDGE('',*,*,#47141,.F.);
#64126=ORIENTED_EDGE('',*,*,#47142,.F.);
#64127=ORIENTED_EDGE('',*,*,#46706,.F.);
#64128=ORIENTED_EDGE('',*,*,#46841,.T.);
#64129=ORIENTED_EDGE('',*,*,#46844,.T.);
#64130=ORIENTED_EDGE('',*,*,#46719,.F.);
#64131=ORIENTED_EDGE('',*,*,#47142,.T.);
#64132=ORIENTED_EDGE('',*,*,#47143,.F.);
#64133=ORIENTED_EDGE('',*,*,#47144,.T.);
#64134=ORIENTED_EDGE('',*,*,#47145,.F.);
#64135=ORIENTED_EDGE('',*,*,#46838,.F.);
#64136=ORIENTED_EDGE('',*,*,#47146,.F.);
#64137=ORIENTED_EDGE('',*,*,#47125,.T.);
#64138=ORIENTED_EDGE('',*,*,#46837,.F.);
#64139=ORIENTED_EDGE('',*,*,#47144,.F.);
#64140=ORIENTED_EDGE('',*,*,#47147,.F.);
#64141=ORIENTED_EDGE('',*,*,#47000,.T.);
#64142=ORIENTED_EDGE('',*,*,#47148,.F.);
#64143=ORIENTED_EDGE('',*,*,#47020,.F.);
#64144=ORIENTED_EDGE('',*,*,#47149,.F.);
#64145=ORIENTED_EDGE('',*,*,#47150,.T.);
#64146=ORIENTED_EDGE('',*,*,#47151,.F.);
#64147=ORIENTED_EDGE('',*,*,#47135,.F.);
#64148=ORIENTED_EDGE('',*,*,#47152,.F.);
#64149=ORIENTED_EDGE('',*,*,#46480,.T.);
#64150=ORIENTED_EDGE('',*,*,#47136,.T.);
#64151=ORIENTED_EDGE('',*,*,#47153,.T.);
#64152=ORIENTED_EDGE('',*,*,#46999,.T.);
#64153=ORIENTED_EDGE('',*,*,#47154,.T.);
#64154=ORIENTED_EDGE('',*,*,#47155,.F.);
#64155=ORIENTED_EDGE('',*,*,#47156,.F.);
#64156=ORIENTED_EDGE('',*,*,#46488,.F.);
#64157=ORIENTED_EDGE('',*,*,#47156,.T.);
#64158=ORIENTED_EDGE('',*,*,#47157,.F.);
#64159=ORIENTED_EDGE('',*,*,#47158,.F.);
#64160=ORIENTED_EDGE('',*,*,#46485,.F.);
#64161=ORIENTED_EDGE('',*,*,#47159,.T.);
#64162=ORIENTED_EDGE('',*,*,#47160,.F.);
#64163=ORIENTED_EDGE('',*,*,#47161,.F.);
#64164=ORIENTED_EDGE('',*,*,#47162,.F.);
#64165=ORIENTED_EDGE('',*,*,#47163,.T.);
#64166=ORIENTED_EDGE('',*,*,#46543,.F.);
#64167=ORIENTED_EDGE('',*,*,#47159,.F.);
#64168=ORIENTED_EDGE('',*,*,#47164,.F.);
#64169=ORIENTED_EDGE('',*,*,#47165,.T.);
#64170=ORIENTED_EDGE('',*,*,#46530,.F.);
#64171=ORIENTED_EDGE('',*,*,#47163,.F.);
#64172=ORIENTED_EDGE('',*,*,#47166,.F.);
#64173=ORIENTED_EDGE('',*,*,#47167,.T.);
#64174=ORIENTED_EDGE('',*,*,#46527,.F.);
#64175=ORIENTED_EDGE('',*,*,#47165,.F.);
#64176=ORIENTED_EDGE('',*,*,#47168,.F.);
#64177=ORIENTED_EDGE('',*,*,#47169,.T.);
#64178=ORIENTED_EDGE('',*,*,#46524,.F.);
#64179=ORIENTED_EDGE('',*,*,#47167,.F.);
#64180=ORIENTED_EDGE('',*,*,#47170,.F.);
#64181=ORIENTED_EDGE('',*,*,#47171,.T.);
#64182=ORIENTED_EDGE('',*,*,#46521,.F.);
#64183=ORIENTED_EDGE('',*,*,#47169,.F.);
#64184=ORIENTED_EDGE('',*,*,#47172,.F.);
#64185=ORIENTED_EDGE('',*,*,#47173,.T.);
#64186=ORIENTED_EDGE('',*,*,#46518,.F.);
#64187=ORIENTED_EDGE('',*,*,#47171,.F.);
#64188=ORIENTED_EDGE('',*,*,#47174,.F.);
#64189=ORIENTED_EDGE('',*,*,#47175,.T.);
#64190=ORIENTED_EDGE('',*,*,#46515,.F.);
#64191=ORIENTED_EDGE('',*,*,#47173,.F.);
#64192=ORIENTED_EDGE('',*,*,#47176,.F.);
#64193=ORIENTED_EDGE('',*,*,#47177,.T.);
#64194=ORIENTED_EDGE('',*,*,#46947,.F.);
#64195=ORIENTED_EDGE('',*,*,#47175,.F.);
#64196=ORIENTED_EDGE('',*,*,#47178,.F.);
#64197=ORIENTED_EDGE('',*,*,#46943,.T.);
#64198=ORIENTED_EDGE('',*,*,#47179,.F.);
#64199=ORIENTED_EDGE('',*,*,#47177,.F.);
#64200=ORIENTED_EDGE('',*,*,#47180,.F.);
#64201=ORIENTED_EDGE('',*,*,#46491,.F.);
#64202=ORIENTED_EDGE('',*,*,#46944,.T.);
#64203=ORIENTED_EDGE('',*,*,#47181,.F.);
#64204=ORIENTED_EDGE('',*,*,#47154,.F.);
#64205=ORIENTED_EDGE('',*,*,#47158,.T.);
#64206=ORIENTED_EDGE('',*,*,#47182,.F.);
#64207=ORIENTED_EDGE('',*,*,#47183,.F.);
#64208=ORIENTED_EDGE('',*,*,#47184,.F.);
#64209=ORIENTED_EDGE('',*,*,#47185,.F.);
#64210=ORIENTED_EDGE('',*,*,#47186,.T.);
#64211=ORIENTED_EDGE('',*,*,#46482,.F.);
#64212=ORIENTED_EDGE('',*,*,#47184,.T.);
#64213=ORIENTED_EDGE('',*,*,#47187,.T.);
#64214=ORIENTED_EDGE('',*,*,#47188,.F.);
#64215=ORIENTED_EDGE('',*,*,#47189,.F.);
#64216=ORIENTED_EDGE('',*,*,#47186,.F.);
#64217=ORIENTED_EDGE('',*,*,#47189,.T.);
#64218=ORIENTED_EDGE('',*,*,#47190,.F.);
#64219=ORIENTED_EDGE('',*,*,#47191,.F.);
#64220=ORIENTED_EDGE('',*,*,#46483,.F.);
#64221=ORIENTED_EDGE('',*,*,#47191,.T.);
#64222=ORIENTED_EDGE('',*,*,#47192,.F.);
#64223=ORIENTED_EDGE('',*,*,#47193,.F.);
#64224=ORIENTED_EDGE('',*,*,#46486,.F.);
#64225=ORIENTED_EDGE('',*,*,#47194,.F.);
#64226=ORIENTED_EDGE('',*,*,#46937,.T.);
#64227=ORIENTED_EDGE('',*,*,#46489,.F.);
#64228=ORIENTED_EDGE('',*,*,#47193,.T.);
#64229=ORIENTED_EDGE('',*,*,#46938,.T.);
#64230=ORIENTED_EDGE('',*,*,#47195,.F.);
#64231=ORIENTED_EDGE('',*,*,#47196,.F.);
#64232=ORIENTED_EDGE('',*,*,#47197,.F.);
#64233=ORIENTED_EDGE('',*,*,#47196,.T.);
#64234=ORIENTED_EDGE('',*,*,#47198,.F.);
#64235=ORIENTED_EDGE('',*,*,#47199,.F.);
#64236=ORIENTED_EDGE('',*,*,#46935,.F.);
#64237=ORIENTED_EDGE('',*,*,#47199,.T.);
#64238=ORIENTED_EDGE('',*,*,#47200,.F.);
#64239=ORIENTED_EDGE('',*,*,#47201,.F.);
#64240=ORIENTED_EDGE('',*,*,#46493,.F.);
#64241=ORIENTED_EDGE('',*,*,#47201,.T.);
#64242=ORIENTED_EDGE('',*,*,#47202,.F.);
#64243=ORIENTED_EDGE('',*,*,#47203,.F.);
#64244=ORIENTED_EDGE('',*,*,#46508,.F.);
#64245=ORIENTED_EDGE('',*,*,#47203,.T.);
#64246=ORIENTED_EDGE('',*,*,#47204,.F.);
#64247=ORIENTED_EDGE('',*,*,#47205,.F.);
#64248=ORIENTED_EDGE('',*,*,#46506,.F.);
#64249=ORIENTED_EDGE('',*,*,#47205,.T.);
#64250=ORIENTED_EDGE('',*,*,#47206,.F.);
#64251=ORIENTED_EDGE('',*,*,#47207,.F.);
#64252=ORIENTED_EDGE('',*,*,#46503,.F.);
#64253=ORIENTED_EDGE('',*,*,#47207,.T.);
#64254=ORIENTED_EDGE('',*,*,#47208,.F.);
#64255=ORIENTED_EDGE('',*,*,#47209,.F.);
#64256=ORIENTED_EDGE('',*,*,#46500,.F.);
#64257=ORIENTED_EDGE('',*,*,#47209,.T.);
#64258=ORIENTED_EDGE('',*,*,#47210,.F.);
#64259=ORIENTED_EDGE('',*,*,#47211,.F.);
#64260=ORIENTED_EDGE('',*,*,#46496,.F.);
#64261=ORIENTED_EDGE('',*,*,#47211,.T.);
#64262=ORIENTED_EDGE('',*,*,#47212,.F.);
#64263=ORIENTED_EDGE('',*,*,#47213,.F.);
#64264=ORIENTED_EDGE('',*,*,#47214,.F.);
#64265=ORIENTED_EDGE('',*,*,#47215,.T.);
#64266=ORIENTED_EDGE('',*,*,#47216,.F.);
#64267=ORIENTED_EDGE('',*,*,#47217,.F.);
#64268=ORIENTED_EDGE('',*,*,#47218,.F.);
#64269=ORIENTED_EDGE('',*,*,#47213,.T.);
#64270=ORIENTED_EDGE('',*,*,#47219,.F.);
#64271=ORIENTED_EDGE('',*,*,#47215,.F.);
#64272=ORIENTED_EDGE('',*,*,#47220,.F.);
#64273=ORIENTED_EDGE('',*,*,#46497,.T.);
#64274=ORIENTED_EDGE('',*,*,#47214,.T.);
#64275=ORIENTED_EDGE('',*,*,#47221,.T.);
#64276=ORIENTED_EDGE('',*,*,#47222,.T.);
#64277=ORIENTED_EDGE('',*,*,#47223,.T.);
#64278=ORIENTED_EDGE('',*,*,#47224,.F.);
#64279=ORIENTED_EDGE('',*,*,#47225,.F.);
#64280=ORIENTED_EDGE('',*,*,#46615,.F.);
#64281=ORIENTED_EDGE('',*,*,#47225,.T.);
#64282=ORIENTED_EDGE('',*,*,#47226,.F.);
#64283=ORIENTED_EDGE('',*,*,#47227,.F.);
#64284=ORIENTED_EDGE('',*,*,#46727,.F.);
#64285=ORIENTED_EDGE('',*,*,#47228,.T.);
#64286=ORIENTED_EDGE('',*,*,#47229,.F.);
#64287=ORIENTED_EDGE('',*,*,#47230,.F.);
#64288=ORIENTED_EDGE('',*,*,#47231,.F.);
#64289=ORIENTED_EDGE('',*,*,#47230,.T.);
#64290=ORIENTED_EDGE('',*,*,#47232,.F.);
#64291=ORIENTED_EDGE('',*,*,#47233,.F.);
#64292=ORIENTED_EDGE('',*,*,#47234,.F.);
#64293=ORIENTED_EDGE('',*,*,#47233,.T.);
#64294=ORIENTED_EDGE('',*,*,#47235,.F.);
#64295=ORIENTED_EDGE('',*,*,#47236,.F.);
#64296=ORIENTED_EDGE('',*,*,#47222,.F.);
#64297=ORIENTED_EDGE('',*,*,#47236,.T.);
#64298=ORIENTED_EDGE('',*,*,#47237,.F.);
#64299=ORIENTED_EDGE('',*,*,#47238,.F.);
#64300=ORIENTED_EDGE('',*,*,#46498,.F.);
#64301=ORIENTED_EDGE('',*,*,#47238,.T.);
#64302=ORIENTED_EDGE('',*,*,#47239,.F.);
#64303=ORIENTED_EDGE('',*,*,#47240,.F.);
#64304=ORIENTED_EDGE('',*,*,#46501,.F.);
#64305=ORIENTED_EDGE('',*,*,#47240,.T.);
#64306=ORIENTED_EDGE('',*,*,#47241,.F.);
#64307=ORIENTED_EDGE('',*,*,#47242,.F.);
#64308=ORIENTED_EDGE('',*,*,#46504,.F.);
#64309=ORIENTED_EDGE('',*,*,#47242,.T.);
#64310=ORIENTED_EDGE('',*,*,#47243,.F.);
#64311=ORIENTED_EDGE('',*,*,#47244,.F.);
#64312=ORIENTED_EDGE('',*,*,#46507,.F.);
#64313=ORIENTED_EDGE('',*,*,#47244,.T.);
#64314=ORIENTED_EDGE('',*,*,#47245,.F.);
#64315=ORIENTED_EDGE('',*,*,#47246,.F.);
#64316=ORIENTED_EDGE('',*,*,#46509,.F.);
#64317=ORIENTED_EDGE('',*,*,#47246,.T.);
#64318=ORIENTED_EDGE('',*,*,#47247,.F.);
#64319=ORIENTED_EDGE('',*,*,#47248,.F.);
#64320=ORIENTED_EDGE('',*,*,#46926,.F.);
#64321=ORIENTED_EDGE('',*,*,#47248,.T.);
#64322=ORIENTED_EDGE('',*,*,#47249,.F.);
#64323=ORIENTED_EDGE('',*,*,#46929,.F.);
#64324=ORIENTED_EDGE('',*,*,#47250,.F.);
#64325=ORIENTED_EDGE('',*,*,#46925,.T.);
#64326=ORIENTED_EDGE('',*,*,#46930,.T.);
#64327=ORIENTED_EDGE('',*,*,#47251,.F.);
#64328=ORIENTED_EDGE('',*,*,#47223,.F.);
#64329=ORIENTED_EDGE('',*,*,#46618,.F.);
#64330=ORIENTED_EDGE('',*,*,#47252,.F.);
#64331=ORIENTED_EDGE('',*,*,#46974,.T.);
#64332=ORIENTED_EDGE('',*,*,#47253,.F.);
#64333=ORIENTED_EDGE('',*,*,#47254,.T.);
#64334=ORIENTED_EDGE('',*,*,#47255,.T.);
#64335=ORIENTED_EDGE('',*,*,#47256,.F.);
#64336=ORIENTED_EDGE('',*,*,#47257,.F.);
#64337=ORIENTED_EDGE('',*,*,#47258,.F.);
#64338=ORIENTED_EDGE('',*,*,#47259,.T.);
#64339=ORIENTED_EDGE('',*,*,#46958,.F.);
#64340=ORIENTED_EDGE('',*,*,#47255,.F.);
#64341=ORIENTED_EDGE('',*,*,#47260,.F.);
#64342=ORIENTED_EDGE('',*,*,#46955,.T.);
#64343=ORIENTED_EDGE('',*,*,#47261,.F.);
#64344=ORIENTED_EDGE('',*,*,#47259,.F.);
#64345=ORIENTED_EDGE('',*,*,#47262,.F.);
#64346=ORIENTED_EDGE('',*,*,#46540,.F.);
#64347=ORIENTED_EDGE('',*,*,#46956,.T.);
#64348=ORIENTED_EDGE('',*,*,#47263,.F.);
#64349=ORIENTED_EDGE('',*,*,#47264,.F.);
#64350=ORIENTED_EDGE('',*,*,#47264,.T.);
#64351=ORIENTED_EDGE('',*,*,#47265,.F.);
#64352=ORIENTED_EDGE('',*,*,#47266,.F.);
#64353=ORIENTED_EDGE('',*,*,#46536,.F.);
#64354=ORIENTED_EDGE('',*,*,#47266,.T.);
#64355=ORIENTED_EDGE('',*,*,#47267,.F.);
#64356=ORIENTED_EDGE('',*,*,#47268,.F.);
#64357=ORIENTED_EDGE('',*,*,#46532,.F.);
#64358=ORIENTED_EDGE('',*,*,#47269,.F.);
#64359=ORIENTED_EDGE('',*,*,#47270,.F.);
#64360=ORIENTED_EDGE('',*,*,#47271,.F.);
#64361=ORIENTED_EDGE('',*,*,#47272,.F.);
#64362=ORIENTED_EDGE('',*,*,#47273,.F.);
#64363=ORIENTED_EDGE('',*,*,#47274,.F.);
#64364=ORIENTED_EDGE('',*,*,#47275,.T.);
#64365=ORIENTED_EDGE('',*,*,#46986,.F.);
#64366=ORIENTED_EDGE('',*,*,#47276,.T.);
#64367=ORIENTED_EDGE('',*,*,#47268,.T.);
#64368=ORIENTED_EDGE('',*,*,#47277,.F.);
#64369=ORIENTED_EDGE('',*,*,#47278,.F.);
#64370=ORIENTED_EDGE('',*,*,#47279,.F.);
#64371=ORIENTED_EDGE('',*,*,#46533,.F.);
#64372=ORIENTED_EDGE('',*,*,#47279,.T.);
#64373=ORIENTED_EDGE('',*,*,#47280,.F.);
#64374=ORIENTED_EDGE('',*,*,#47281,.T.);
#64375=ORIENTED_EDGE('',*,*,#47282,.T.);
#64376=ORIENTED_EDGE('',*,*,#46513,.F.);
#64377=ORIENTED_EDGE('',*,*,#47283,.F.);
#64378=ORIENTED_EDGE('',*,*,#47284,.F.);
#64379=ORIENTED_EDGE('',*,*,#47285,.T.);
#64380=ORIENTED_EDGE('',*,*,#46516,.F.);
#64381=ORIENTED_EDGE('',*,*,#47282,.F.);
#64382=ORIENTED_EDGE('',*,*,#47286,.F.);
#64383=ORIENTED_EDGE('',*,*,#47287,.T.);
#64384=ORIENTED_EDGE('',*,*,#46519,.F.);
#64385=ORIENTED_EDGE('',*,*,#47285,.F.);
#64386=ORIENTED_EDGE('',*,*,#47288,.F.);
#64387=ORIENTED_EDGE('',*,*,#47289,.T.);
#64388=ORIENTED_EDGE('',*,*,#46522,.F.);
#64389=ORIENTED_EDGE('',*,*,#47287,.F.);
#64390=ORIENTED_EDGE('',*,*,#47290,.F.);
#64391=ORIENTED_EDGE('',*,*,#47291,.T.);
#64392=ORIENTED_EDGE('',*,*,#46525,.F.);
#64393=ORIENTED_EDGE('',*,*,#47289,.F.);
#64394=ORIENTED_EDGE('',*,*,#47292,.F.);
#64395=ORIENTED_EDGE('',*,*,#47293,.T.);
#64396=ORIENTED_EDGE('',*,*,#46528,.F.);
#64397=ORIENTED_EDGE('',*,*,#47291,.F.);
#64398=ORIENTED_EDGE('',*,*,#47294,.F.);
#64399=ORIENTED_EDGE('',*,*,#47295,.T.);
#64400=ORIENTED_EDGE('',*,*,#46541,.F.);
#64401=ORIENTED_EDGE('',*,*,#47293,.F.);
#64402=ORIENTED_EDGE('',*,*,#47296,.F.);
#64403=ORIENTED_EDGE('',*,*,#47297,.T.);
#64404=ORIENTED_EDGE('',*,*,#47298,.F.);
#64405=ORIENTED_EDGE('',*,*,#47295,.F.);
#64406=ORIENTED_EDGE('',*,*,#47299,.F.);
#64407=ORIENTED_EDGE('',*,*,#47300,.T.);
#64408=ORIENTED_EDGE('',*,*,#47301,.F.);
#64409=ORIENTED_EDGE('',*,*,#47302,.F.);
#64410=ORIENTED_EDGE('',*,*,#47281,.F.);
#64411=ORIENTED_EDGE('',*,*,#47302,.T.);
#64412=ORIENTED_EDGE('',*,*,#47303,.F.);
#64413=ORIENTED_EDGE('',*,*,#47304,.F.);
#64414=ORIENTED_EDGE('',*,*,#46534,.F.);
#64415=ORIENTED_EDGE('',*,*,#47304,.T.);
#64416=ORIENTED_EDGE('',*,*,#47305,.F.);
#64417=ORIENTED_EDGE('',*,*,#47306,.F.);
#64418=ORIENTED_EDGE('',*,*,#46537,.F.);
#64419=ORIENTED_EDGE('',*,*,#47307,.F.);
#64420=ORIENTED_EDGE('',*,*,#46951,.T.);
#64421=ORIENTED_EDGE('',*,*,#46538,.F.);
#64422=ORIENTED_EDGE('',*,*,#47306,.T.);
#64423=ORIENTED_EDGE('',*,*,#47308,.T.);
#64424=ORIENTED_EDGE('',*,*,#47309,.F.);
#64425=ORIENTED_EDGE('',*,*,#46948,.F.);
#64426=ORIENTED_EDGE('',*,*,#47310,.F.);
#64427=ORIENTED_EDGE('',*,*,#47311,.T.);
#64428=ORIENTED_EDGE('',*,*,#47283,.T.);
#64429=ORIENTED_EDGE('',*,*,#46946,.F.);
#64430=ORIENTED_EDGE('',*,*,#47308,.F.);
#64431=ORIENTED_EDGE('',*,*,#47311,.F.);
#64432=ORIENTED_EDGE('',*,*,#47312,.F.);
#64433=ORIENTED_EDGE('',*,*,#47161,.T.);
#64434=ORIENTED_EDGE('',*,*,#47313,.F.);
#64435=ORIENTED_EDGE('',*,*,#47314,.F.);
#64436=ORIENTED_EDGE('',*,*,#47315,.F.);
#64437=ORIENTED_EDGE('',*,*,#47316,.T.);
#64438=ORIENTED_EDGE('',*,*,#47317,.F.);
#64439=ORIENTED_EDGE('',*,*,#47297,.F.);
#64440=ORIENTED_EDGE('',*,*,#47318,.F.);
#64441=ORIENTED_EDGE('',*,*,#46542,.F.);
#64442=ORIENTED_EDGE('',*,*,#47298,.T.);
#64443=ORIENTED_EDGE('',*,*,#47319,.F.);
#64444=ORIENTED_EDGE('',*,*,#47160,.T.);
#64445=ORIENTED_EDGE('',*,*,#47320,.T.);
#64446=ORIENTED_EDGE('',*,*,#47321,.F.);
#64447=ORIENTED_EDGE('',*,*,#47322,.F.);
#64448=ORIENTED_EDGE('',*,*,#47323,.F.);
#64449=ORIENTED_EDGE('',*,*,#47322,.T.);
#64450=ORIENTED_EDGE('',*,*,#47324,.F.);
#64451=ORIENTED_EDGE('',*,*,#47325,.F.);
#64452=ORIENTED_EDGE('',*,*,#46547,.F.);
#64453=ORIENTED_EDGE('',*,*,#47325,.T.);
#64454=ORIENTED_EDGE('',*,*,#47326,.F.);
#64455=ORIENTED_EDGE('',*,*,#47327,.F.);
#64456=ORIENTED_EDGE('',*,*,#46978,.F.);
#64457=ORIENTED_EDGE('',*,*,#47327,.T.);
#64458=ORIENTED_EDGE('',*,*,#47328,.F.);
#64459=ORIENTED_EDGE('',*,*,#47329,.F.);
#64460=ORIENTED_EDGE('',*,*,#47330,.F.);
#64461=ORIENTED_EDGE('',*,*,#47331,.T.);
#64462=ORIENTED_EDGE('',*,*,#47332,.F.);
#64463=ORIENTED_EDGE('',*,*,#47333,.F.);
#64464=ORIENTED_EDGE('',*,*,#47334,.F.);
#64465=ORIENTED_EDGE('',*,*,#47335,.F.);
#64466=ORIENTED_EDGE('',*,*,#47336,.T.);
#64467=ORIENTED_EDGE('',*,*,#47337,.F.);
#64468=ORIENTED_EDGE('',*,*,#47334,.T.);
#64469=ORIENTED_EDGE('',*,*,#47338,.T.);
#64470=ORIENTED_EDGE('',*,*,#47339,.F.);
#64471=ORIENTED_EDGE('',*,*,#47340,.F.);
#64472=ORIENTED_EDGE('',*,*,#47336,.F.);
#64473=ORIENTED_EDGE('',*,*,#47341,.F.);
#64474=ORIENTED_EDGE('',*,*,#47342,.T.);
#64475=ORIENTED_EDGE('',*,*,#47343,.F.);
#64476=ORIENTED_EDGE('',*,*,#47340,.T.);
#64477=ORIENTED_EDGE('',*,*,#46988,.F.);
#64478=ORIENTED_EDGE('',*,*,#47344,.T.);
#64479=ORIENTED_EDGE('',*,*,#47345,.F.);
#64480=ORIENTED_EDGE('',*,*,#47346,.T.);
#64481=ORIENTED_EDGE('',*,*,#47347,.T.);
#64482=ORIENTED_EDGE('',*,*,#47348,.F.);
#64483=ORIENTED_EDGE('',*,*,#47349,.F.);
#64484=ORIENTED_EDGE('',*,*,#47350,.F.);
#64485=ORIENTED_EDGE('',*,*,#47349,.T.);
#64486=ORIENTED_EDGE('',*,*,#47351,.F.);
#64487=ORIENTED_EDGE('',*,*,#47352,.F.);
#64488=ORIENTED_EDGE('',*,*,#46982,.F.);
#64489=ORIENTED_EDGE('',*,*,#47352,.T.);
#64490=ORIENTED_EDGE('',*,*,#47353,.F.);
#64491=ORIENTED_EDGE('',*,*,#47354,.F.);
#64492=ORIENTED_EDGE('',*,*,#47355,.F.);
#64493=ORIENTED_EDGE('',*,*,#47356,.T.);
#64494=ORIENTED_EDGE('',*,*,#47357,.F.);
#64495=ORIENTED_EDGE('',*,*,#47358,.F.);
#64496=ORIENTED_EDGE('',*,*,#47359,.F.);
#64497=ORIENTED_EDGE('',*,*,#47360,.F.);
#64498=ORIENTED_EDGE('',*,*,#47359,.T.);
#64499=ORIENTED_EDGE('',*,*,#47361,.F.);
#64500=ORIENTED_EDGE('',*,*,#47362,.T.);
#64501=ORIENTED_EDGE('',*,*,#47363,.T.);
#64502=ORIENTED_EDGE('',*,*,#47364,.F.);
#64503=ORIENTED_EDGE('',*,*,#47365,.F.);
#64504=ORIENTED_EDGE('',*,*,#47362,.F.);
#64505=ORIENTED_EDGE('',*,*,#47366,.T.);
#64506=ORIENTED_EDGE('',*,*,#47367,.F.);
#64507=ORIENTED_EDGE('',*,*,#47368,.F.);
#64508=ORIENTED_EDGE('',*,*,#47369,.F.);
#64509=ORIENTED_EDGE('',*,*,#47370,.T.);
#64510=ORIENTED_EDGE('',*,*,#46977,.F.);
#64511=ORIENTED_EDGE('',*,*,#47366,.F.);
#64512=ORIENTED_EDGE('',*,*,#47371,.F.);
#64513=ORIENTED_EDGE('',*,*,#47372,.T.);
#64514=ORIENTED_EDGE('',*,*,#46545,.F.);
#64515=ORIENTED_EDGE('',*,*,#47370,.F.);
#64516=ORIENTED_EDGE('',*,*,#47373,.F.);
#64517=ORIENTED_EDGE('',*,*,#47374,.T.);
#64518=ORIENTED_EDGE('',*,*,#47375,.F.);
#64519=ORIENTED_EDGE('',*,*,#47372,.F.);
#64520=ORIENTED_EDGE('',*,*,#47376,.F.);
#64521=ORIENTED_EDGE('',*,*,#47377,.T.);
#64522=ORIENTED_EDGE('',*,*,#47378,.F.);
#64523=ORIENTED_EDGE('',*,*,#47320,.F.);
#64524=ORIENTED_EDGE('',*,*,#47379,.F.);
#64525=ORIENTED_EDGE('',*,*,#47380,.T.);
#64526=ORIENTED_EDGE('',*,*,#47381,.F.);
#64527=ORIENTED_EDGE('',*,*,#47374,.F.);
#64528=ORIENTED_EDGE('',*,*,#47382,.F.);
#64529=ORIENTED_EDGE('',*,*,#46546,.F.);
#64530=ORIENTED_EDGE('',*,*,#47375,.T.);
#64531=ORIENTED_EDGE('',*,*,#47383,.F.);
#64532=ORIENTED_EDGE('',*,*,#47323,.T.);
#64533=ORIENTED_EDGE('',*,*,#47384,.T.);
#64534=ORIENTED_EDGE('',*,*,#47385,.F.);
#64535=ORIENTED_EDGE('',*,*,#47386,.F.);
#64536=ORIENTED_EDGE('',*,*,#46557,.F.);
#64537=ORIENTED_EDGE('',*,*,#47386,.T.);
#64538=ORIENTED_EDGE('',*,*,#47387,.F.);
#64539=ORIENTED_EDGE('',*,*,#47388,.F.);
#64540=ORIENTED_EDGE('',*,*,#46554,.F.);
#64541=ORIENTED_EDGE('',*,*,#47389,.T.);
#64542=ORIENTED_EDGE('',*,*,#47390,.F.);
#64543=ORIENTED_EDGE('',*,*,#47391,.F.);
#64544=ORIENTED_EDGE('',*,*,#47392,.F.);
#64545=ORIENTED_EDGE('',*,*,#47393,.T.);
#64546=ORIENTED_EDGE('',*,*,#46607,.F.);
#64547=ORIENTED_EDGE('',*,*,#47389,.F.);
#64548=ORIENTED_EDGE('',*,*,#47394,.F.);
#64549=ORIENTED_EDGE('',*,*,#47395,.T.);
#64550=ORIENTED_EDGE('',*,*,#46611,.F.);
#64551=ORIENTED_EDGE('',*,*,#47393,.F.);
#64552=ORIENTED_EDGE('',*,*,#47396,.F.);
#64553=ORIENTED_EDGE('',*,*,#47397,.T.);
#64554=ORIENTED_EDGE('',*,*,#46595,.F.);
#64555=ORIENTED_EDGE('',*,*,#47395,.F.);
#64556=ORIENTED_EDGE('',*,*,#47398,.F.);
#64557=ORIENTED_EDGE('',*,*,#47399,.T.);
#64558=ORIENTED_EDGE('',*,*,#46592,.F.);
#64559=ORIENTED_EDGE('',*,*,#47397,.F.);
#64560=ORIENTED_EDGE('',*,*,#47400,.F.);
#64561=ORIENTED_EDGE('',*,*,#47401,.T.);
#64562=ORIENTED_EDGE('',*,*,#46549,.F.);
#64563=ORIENTED_EDGE('',*,*,#47399,.F.);
#64564=ORIENTED_EDGE('',*,*,#47402,.F.);
#64565=ORIENTED_EDGE('',*,*,#47403,.T.);
#64566=ORIENTED_EDGE('',*,*,#46587,.F.);
#64567=ORIENTED_EDGE('',*,*,#47401,.F.);
#64568=ORIENTED_EDGE('',*,*,#47404,.F.);
#64569=ORIENTED_EDGE('',*,*,#47405,.T.);
#64570=ORIENTED_EDGE('',*,*,#46584,.F.);
#64571=ORIENTED_EDGE('',*,*,#47403,.F.);
#64572=ORIENTED_EDGE('',*,*,#47406,.F.);
#64573=ORIENTED_EDGE('',*,*,#47407,.T.);
#64574=ORIENTED_EDGE('',*,*,#46784,.F.);
#64575=ORIENTED_EDGE('',*,*,#47405,.F.);
#64576=ORIENTED_EDGE('',*,*,#47408,.F.);
#64577=ORIENTED_EDGE('',*,*,#46780,.T.);
#64578=ORIENTED_EDGE('',*,*,#47409,.F.);
#64579=ORIENTED_EDGE('',*,*,#47407,.F.);
#64580=ORIENTED_EDGE('',*,*,#47410,.F.);
#64581=ORIENTED_EDGE('',*,*,#46560,.F.);
#64582=ORIENTED_EDGE('',*,*,#46781,.T.);
#64583=ORIENTED_EDGE('',*,*,#47411,.F.);
#64584=ORIENTED_EDGE('',*,*,#47384,.F.);
#64585=ORIENTED_EDGE('',*,*,#47388,.T.);
#64586=ORIENTED_EDGE('',*,*,#47412,.F.);
#64587=ORIENTED_EDGE('',*,*,#47413,.F.);
#64588=ORIENTED_EDGE('',*,*,#47414,.F.);
#64589=ORIENTED_EDGE('',*,*,#47415,.F.);
#64590=ORIENTED_EDGE('',*,*,#47416,.T.);
#64591=ORIENTED_EDGE('',*,*,#46551,.F.);
#64592=ORIENTED_EDGE('',*,*,#47414,.T.);
#64593=ORIENTED_EDGE('',*,*,#47417,.T.);
#64594=ORIENTED_EDGE('',*,*,#47418,.F.);
#64595=ORIENTED_EDGE('',*,*,#47419,.F.);
#64596=ORIENTED_EDGE('',*,*,#47416,.F.);
#64597=ORIENTED_EDGE('',*,*,#47419,.T.);
#64598=ORIENTED_EDGE('',*,*,#47420,.F.);
#64599=ORIENTED_EDGE('',*,*,#47421,.F.);
#64600=ORIENTED_EDGE('',*,*,#46552,.F.);
#64601=ORIENTED_EDGE('',*,*,#47421,.T.);
#64602=ORIENTED_EDGE('',*,*,#47422,.F.);
#64603=ORIENTED_EDGE('',*,*,#47423,.F.);
#64604=ORIENTED_EDGE('',*,*,#46555,.F.);
#64605=ORIENTED_EDGE('',*,*,#47424,.F.);
#64606=ORIENTED_EDGE('',*,*,#46774,.T.);
#64607=ORIENTED_EDGE('',*,*,#46558,.F.);
#64608=ORIENTED_EDGE('',*,*,#47423,.T.);
#64609=ORIENTED_EDGE('',*,*,#46775,.T.);
#64610=ORIENTED_EDGE('',*,*,#47425,.F.);
#64611=ORIENTED_EDGE('',*,*,#47426,.F.);
#64612=ORIENTED_EDGE('',*,*,#47427,.F.);
#64613=ORIENTED_EDGE('',*,*,#47426,.T.);
#64614=ORIENTED_EDGE('',*,*,#47428,.F.);
#64615=ORIENTED_EDGE('',*,*,#47429,.F.);
#64616=ORIENTED_EDGE('',*,*,#46772,.F.);
#64617=ORIENTED_EDGE('',*,*,#47429,.T.);
#64618=ORIENTED_EDGE('',*,*,#47430,.F.);
#64619=ORIENTED_EDGE('',*,*,#47431,.F.);
#64620=ORIENTED_EDGE('',*,*,#46562,.F.);
#64621=ORIENTED_EDGE('',*,*,#47431,.T.);
#64622=ORIENTED_EDGE('',*,*,#47432,.F.);
#64623=ORIENTED_EDGE('',*,*,#47433,.F.);
#64624=ORIENTED_EDGE('',*,*,#46748,.F.);
#64625=ORIENTED_EDGE('',*,*,#47433,.T.);
#64626=ORIENTED_EDGE('',*,*,#47434,.F.);
#64627=ORIENTED_EDGE('',*,*,#47435,.F.);
#64628=ORIENTED_EDGE('',*,*,#46575,.F.);
#64629=ORIENTED_EDGE('',*,*,#47435,.T.);
#64630=ORIENTED_EDGE('',*,*,#47436,.F.);
#64631=ORIENTED_EDGE('',*,*,#47437,.F.);
#64632=ORIENTED_EDGE('',*,*,#46572,.F.);
#64633=ORIENTED_EDGE('',*,*,#47437,.T.);
#64634=ORIENTED_EDGE('',*,*,#47438,.F.);
#64635=ORIENTED_EDGE('',*,*,#47439,.F.);
#64636=ORIENTED_EDGE('',*,*,#46569,.F.);
#64637=ORIENTED_EDGE('',*,*,#47439,.T.);
#64638=ORIENTED_EDGE('',*,*,#47440,.F.);
#64639=ORIENTED_EDGE('',*,*,#47441,.F.);
#64640=ORIENTED_EDGE('',*,*,#46565,.F.);
#64641=ORIENTED_EDGE('',*,*,#47441,.T.);
#64642=ORIENTED_EDGE('',*,*,#47442,.F.);
#64643=ORIENTED_EDGE('',*,*,#47443,.F.);
#64644=ORIENTED_EDGE('',*,*,#47444,.F.);
#64645=ORIENTED_EDGE('',*,*,#47445,.T.);
#64646=ORIENTED_EDGE('',*,*,#47446,.F.);
#64647=ORIENTED_EDGE('',*,*,#47447,.F.);
#64648=ORIENTED_EDGE('',*,*,#47448,.F.);
#64649=ORIENTED_EDGE('',*,*,#47443,.T.);
#64650=ORIENTED_EDGE('',*,*,#47449,.F.);
#64651=ORIENTED_EDGE('',*,*,#47445,.F.);
#64652=ORIENTED_EDGE('',*,*,#47450,.F.);
#64653=ORIENTED_EDGE('',*,*,#46566,.T.);
#64654=ORIENTED_EDGE('',*,*,#47444,.T.);
#64655=ORIENTED_EDGE('',*,*,#47451,.T.);
#64656=ORIENTED_EDGE('',*,*,#47452,.T.);
#64657=ORIENTED_EDGE('',*,*,#47453,.T.);
#64658=ORIENTED_EDGE('',*,*,#47454,.F.);
#64659=ORIENTED_EDGE('',*,*,#47455,.F.);
#64660=ORIENTED_EDGE('',*,*,#46747,.F.);
#64661=ORIENTED_EDGE('',*,*,#47455,.T.);
#64662=ORIENTED_EDGE('',*,*,#47456,.F.);
#64663=ORIENTED_EDGE('',*,*,#47457,.F.);
#64664=ORIENTED_EDGE('',*,*,#46985,.F.);
#64665=ORIENTED_EDGE('',*,*,#47458,.T.);
#64666=ORIENTED_EDGE('',*,*,#47452,.F.);
#64667=ORIENTED_EDGE('',*,*,#47459,.F.);
#64668=ORIENTED_EDGE('',*,*,#47460,.F.);
#64669=ORIENTED_EDGE('',*,*,#47461,.T.);
#64670=ORIENTED_EDGE('',*,*,#46567,.F.);
#64671=ORIENTED_EDGE('',*,*,#47458,.F.);
#64672=ORIENTED_EDGE('',*,*,#47462,.F.);
#64673=ORIENTED_EDGE('',*,*,#47463,.T.);
#64674=ORIENTED_EDGE('',*,*,#46570,.F.);
#64675=ORIENTED_EDGE('',*,*,#47461,.F.);
#64676=ORIENTED_EDGE('',*,*,#47464,.F.);
#64677=ORIENTED_EDGE('',*,*,#47465,.T.);
#64678=ORIENTED_EDGE('',*,*,#46573,.F.);
#64679=ORIENTED_EDGE('',*,*,#47463,.F.);
#64680=ORIENTED_EDGE('',*,*,#47466,.F.);
#64681=ORIENTED_EDGE('',*,*,#47467,.T.);
#64682=ORIENTED_EDGE('',*,*,#46576,.F.);
#64683=ORIENTED_EDGE('',*,*,#47465,.F.);
#64684=ORIENTED_EDGE('',*,*,#47468,.F.);
#64685=ORIENTED_EDGE('',*,*,#47469,.T.);
#64686=ORIENTED_EDGE('',*,*,#46749,.F.);
#64687=ORIENTED_EDGE('',*,*,#47467,.F.);
#64688=ORIENTED_EDGE('',*,*,#47470,.F.);
#64689=ORIENTED_EDGE('',*,*,#47471,.T.);
#64690=ORIENTED_EDGE('',*,*,#47472,.F.);
#64691=ORIENTED_EDGE('',*,*,#47469,.F.);
#64692=ORIENTED_EDGE('',*,*,#47473,.F.);
#64693=ORIENTED_EDGE('',*,*,#47459,.T.);
#64694=ORIENTED_EDGE('',*,*,#47474,.F.);
#64695=ORIENTED_EDGE('',*,*,#47475,.F.);
#64696=ORIENTED_EDGE('',*,*,#47476,.F.);
#64697=ORIENTED_EDGE('',*,*,#47477,.T.);
#64698=ORIENTED_EDGE('',*,*,#47478,.F.);
#64699=ORIENTED_EDGE('',*,*,#47479,.F.);
#64700=ORIENTED_EDGE('',*,*,#47480,.F.);
#64701=ORIENTED_EDGE('',*,*,#47481,.T.);
#64702=ORIENTED_EDGE('',*,*,#46795,.F.);
#64703=ORIENTED_EDGE('',*,*,#47477,.F.);
#64704=ORIENTED_EDGE('',*,*,#47482,.F.);
#64705=ORIENTED_EDGE('',*,*,#46792,.T.);
#64706=ORIENTED_EDGE('',*,*,#47483,.F.);
#64707=ORIENTED_EDGE('',*,*,#47481,.F.);
#64708=ORIENTED_EDGE('',*,*,#47484,.F.);
#64709=ORIENTED_EDGE('',*,*,#46605,.F.);
#64710=ORIENTED_EDGE('',*,*,#46793,.T.);
#64711=ORIENTED_EDGE('',*,*,#47485,.F.);
#64712=ORIENTED_EDGE('',*,*,#47486,.T.);
#64713=ORIENTED_EDGE('',*,*,#47487,.T.);
#64714=ORIENTED_EDGE('',*,*,#46601,.F.);
#64715=ORIENTED_EDGE('',*,*,#47486,.F.);
#64716=ORIENTED_EDGE('',*,*,#47488,.F.);
#64717=ORIENTED_EDGE('',*,*,#47489,.T.);
#64718=ORIENTED_EDGE('',*,*,#46597,.F.);
#64719=ORIENTED_EDGE('',*,*,#47487,.F.);
#64720=ORIENTED_EDGE('',*,*,#47490,.F.);
#64721=ORIENTED_EDGE('',*,*,#47491,.T.);
#64722=ORIENTED_EDGE('',*,*,#47492,.F.);
#64723=ORIENTED_EDGE('',*,*,#47493,.F.);
#64724=ORIENTED_EDGE('',*,*,#47494,.F.);
#64725=ORIENTED_EDGE('',*,*,#47493,.T.);
#64726=ORIENTED_EDGE('',*,*,#47495,.F.);
#64727=ORIENTED_EDGE('',*,*,#46577,.F.);
#64728=ORIENTED_EDGE('',*,*,#46991,.F.);
#64729=ORIENTED_EDGE('',*,*,#47496,.F.);
#64730=ORIENTED_EDGE('',*,*,#46767,.T.);
#64731=ORIENTED_EDGE('',*,*,#47497,.F.);
#64732=ORIENTED_EDGE('',*,*,#46578,.T.);
#64733=ORIENTED_EDGE('',*,*,#47498,.T.);
#64734=ORIENTED_EDGE('',*,*,#47499,.F.);
#64735=ORIENTED_EDGE('',*,*,#46764,.F.);
#64736=ORIENTED_EDGE('',*,*,#47500,.F.);
#64737=ORIENTED_EDGE('',*,*,#47501,.T.);
#64738=ORIENTED_EDGE('',*,*,#47502,.F.);
#64739=ORIENTED_EDGE('',*,*,#47489,.F.);
#64740=ORIENTED_EDGE('',*,*,#47503,.F.);
#64741=ORIENTED_EDGE('',*,*,#46598,.F.);
#64742=ORIENTED_EDGE('',*,*,#47502,.T.);
#64743=ORIENTED_EDGE('',*,*,#47504,.F.);
#64744=ORIENTED_EDGE('',*,*,#47505,.T.);
#64745=ORIENTED_EDGE('',*,*,#47506,.T.);
#64746=ORIENTED_EDGE('',*,*,#46582,.F.);
#64747=ORIENTED_EDGE('',*,*,#47507,.F.);
#64748=ORIENTED_EDGE('',*,*,#47508,.F.);
#64749=ORIENTED_EDGE('',*,*,#47509,.T.);
#64750=ORIENTED_EDGE('',*,*,#46585,.F.);
#64751=ORIENTED_EDGE('',*,*,#47506,.F.);
#64752=ORIENTED_EDGE('',*,*,#47510,.F.);
#64753=ORIENTED_EDGE('',*,*,#47511,.T.);
#64754=ORIENTED_EDGE('',*,*,#46588,.F.);
#64755=ORIENTED_EDGE('',*,*,#47509,.F.);
#64756=ORIENTED_EDGE('',*,*,#47512,.F.);
#64757=ORIENTED_EDGE('',*,*,#47513,.T.);
#64758=ORIENTED_EDGE('',*,*,#46590,.F.);
#64759=ORIENTED_EDGE('',*,*,#47511,.F.);
#64760=ORIENTED_EDGE('',*,*,#47514,.F.);
#64761=ORIENTED_EDGE('',*,*,#47513,.F.);
#64762=ORIENTED_EDGE('',*,*,#47515,.F.);
#64763=ORIENTED_EDGE('',*,*,#47516,.F.);
#64764=ORIENTED_EDGE('',*,*,#46593,.F.);
#64765=ORIENTED_EDGE('',*,*,#47516,.T.);
#64766=ORIENTED_EDGE('',*,*,#47517,.F.);
#64767=ORIENTED_EDGE('',*,*,#47518,.F.);
#64768=ORIENTED_EDGE('',*,*,#46609,.F.);
#64769=ORIENTED_EDGE('',*,*,#47518,.T.);
#64770=ORIENTED_EDGE('',*,*,#47519,.F.);
#64771=ORIENTED_EDGE('',*,*,#47520,.F.);
#64772=ORIENTED_EDGE('',*,*,#47521,.F.);
#64773=ORIENTED_EDGE('',*,*,#47522,.T.);
#64774=ORIENTED_EDGE('',*,*,#47523,.F.);
#64775=ORIENTED_EDGE('',*,*,#47524,.F.);
#64776=ORIENTED_EDGE('',*,*,#47505,.F.);
#64777=ORIENTED_EDGE('',*,*,#47524,.T.);
#64778=ORIENTED_EDGE('',*,*,#47525,.F.);
#64779=ORIENTED_EDGE('',*,*,#47526,.F.);
#64780=ORIENTED_EDGE('',*,*,#46599,.F.);
#64781=ORIENTED_EDGE('',*,*,#47526,.T.);
#64782=ORIENTED_EDGE('',*,*,#47527,.F.);
#64783=ORIENTED_EDGE('',*,*,#47528,.F.);
#64784=ORIENTED_EDGE('',*,*,#46602,.F.);
#64785=ORIENTED_EDGE('',*,*,#47529,.F.);
#64786=ORIENTED_EDGE('',*,*,#46788,.T.);
#64787=ORIENTED_EDGE('',*,*,#46603,.F.);
#64788=ORIENTED_EDGE('',*,*,#47528,.T.);
#64789=ORIENTED_EDGE('',*,*,#47530,.T.);
#64790=ORIENTED_EDGE('',*,*,#47531,.F.);
#64791=ORIENTED_EDGE('',*,*,#46785,.F.);
#64792=ORIENTED_EDGE('',*,*,#47532,.F.);
#64793=ORIENTED_EDGE('',*,*,#47533,.T.);
#64794=ORIENTED_EDGE('',*,*,#47507,.T.);
#64795=ORIENTED_EDGE('',*,*,#46783,.F.);
#64796=ORIENTED_EDGE('',*,*,#47530,.F.);
#64797=ORIENTED_EDGE('',*,*,#47533,.F.);
#64798=ORIENTED_EDGE('',*,*,#47534,.F.);
#64799=ORIENTED_EDGE('',*,*,#47535,.F.);
#64800=ORIENTED_EDGE('',*,*,#47390,.T.);
#64801=ORIENTED_EDGE('',*,*,#46606,.F.);
#64802=ORIENTED_EDGE('',*,*,#47536,.F.);
#64803=ORIENTED_EDGE('',*,*,#47391,.T.);
#64804=ORIENTED_EDGE('',*,*,#47537,.F.);
#64805=ORIENTED_EDGE('',*,*,#47538,.F.);
#64806=ORIENTED_EDGE('',*,*,#47539,.F.);
#64807=ORIENTED_EDGE('',*,*,#47520,.T.);
#64808=ORIENTED_EDGE('',*,*,#47540,.F.);
#64809=ORIENTED_EDGE('',*,*,#47541,.F.);
#64810=ORIENTED_EDGE('',*,*,#47542,.F.);
#64811=ORIENTED_EDGE('',*,*,#46610,.F.);
#64812=ORIENTED_EDGE('',*,*,#47521,.T.);
#64813=ORIENTED_EDGE('',*,*,#47543,.F.);
#64814=ORIENTED_EDGE('',*,*,#47536,.T.);
#64815=ORIENTED_EDGE('',*,*,#47544,.T.);
#64816=ORIENTED_EDGE('',*,*,#46627,.F.);
#64817=ORIENTED_EDGE('',*,*,#47545,.F.);
#64818=ORIENTED_EDGE('',*,*,#47546,.F.);
#64819=ORIENTED_EDGE('',*,*,#47547,.T.);
#64820=ORIENTED_EDGE('',*,*,#46624,.F.);
#64821=ORIENTED_EDGE('',*,*,#47544,.F.);
#64822=ORIENTED_EDGE('',*,*,#47548,.F.);
#64823=ORIENTED_EDGE('',*,*,#47549,.T.);
#64824=ORIENTED_EDGE('',*,*,#46620,.F.);
#64825=ORIENTED_EDGE('',*,*,#47547,.F.);
#64826=ORIENTED_EDGE('',*,*,#47550,.F.);
#64827=ORIENTED_EDGE('',*,*,#47551,.T.);
#64828=ORIENTED_EDGE('',*,*,#47552,.F.);
#64829=ORIENTED_EDGE('',*,*,#47549,.F.);
#64830=ORIENTED_EDGE('',*,*,#47553,.F.);
#64831=ORIENTED_EDGE('',*,*,#47554,.T.);
#64832=ORIENTED_EDGE('',*,*,#47555,.F.);
#64833=ORIENTED_EDGE('',*,*,#47556,.F.);
#64834=ORIENTED_EDGE('',*,*,#46726,.F.);
#64835=ORIENTED_EDGE('',*,*,#47556,.T.);
#64836=ORIENTED_EDGE('',*,*,#47557,.F.);
#64837=ORIENTED_EDGE('',*,*,#47558,.F.);
#64838=ORIENTED_EDGE('',*,*,#46613,.F.);
#64839=ORIENTED_EDGE('',*,*,#47559,.F.);
#64840=ORIENTED_EDGE('',*,*,#46920,.T.);
#64841=ORIENTED_EDGE('',*,*,#46616,.F.);
#64842=ORIENTED_EDGE('',*,*,#47558,.T.);
#64843=ORIENTED_EDGE('',*,*,#47560,.T.);
#64844=ORIENTED_EDGE('',*,*,#47561,.F.);
#64845=ORIENTED_EDGE('',*,*,#46917,.F.);
#64846=ORIENTED_EDGE('',*,*,#47562,.F.);
#64847=ORIENTED_EDGE('',*,*,#47545,.T.);
#64848=ORIENTED_EDGE('',*,*,#46915,.F.);
#64849=ORIENTED_EDGE('',*,*,#47560,.F.);
#64850=ORIENTED_EDGE('',*,*,#47563,.F.);
#64851=ORIENTED_EDGE('',*,*,#47564,.T.);
#64852=ORIENTED_EDGE('',*,*,#47565,.F.);
#64853=ORIENTED_EDGE('',*,*,#47551,.F.);
#64854=ORIENTED_EDGE('',*,*,#47566,.F.);
#64855=ORIENTED_EDGE('',*,*,#46621,.F.);
#64856=ORIENTED_EDGE('',*,*,#47552,.T.);
#64857=ORIENTED_EDGE('',*,*,#47567,.F.);
#64858=ORIENTED_EDGE('',*,*,#47568,.T.);
#64859=ORIENTED_EDGE('',*,*,#47569,.T.);
#64860=ORIENTED_EDGE('',*,*,#47568,.F.);
#64861=ORIENTED_EDGE('',*,*,#47570,.F.);
#64862=ORIENTED_EDGE('',*,*,#47571,.F.);
#64863=ORIENTED_EDGE('',*,*,#47572,.T.);
#64864=ORIENTED_EDGE('',*,*,#46622,.F.);
#64865=ORIENTED_EDGE('',*,*,#47569,.F.);
#64866=ORIENTED_EDGE('',*,*,#47573,.F.);
#64867=ORIENTED_EDGE('',*,*,#47572,.F.);
#64868=ORIENTED_EDGE('',*,*,#47574,.F.);
#64869=ORIENTED_EDGE('',*,*,#47575,.F.);
#64870=ORIENTED_EDGE('',*,*,#46625,.F.);
#64871=ORIENTED_EDGE('',*,*,#47575,.T.);
#64872=ORIENTED_EDGE('',*,*,#47576,.F.);
#64873=ORIENTED_EDGE('',*,*,#47577,.F.);
#64874=ORIENTED_EDGE('',*,*,#46628,.F.);
#64875=ORIENTED_EDGE('',*,*,#47577,.T.);
#64876=ORIENTED_EDGE('',*,*,#47578,.F.);
#64877=ORIENTED_EDGE('',*,*,#47579,.F.);
#64878=ORIENTED_EDGE('',*,*,#46916,.F.);
#64879=ORIENTED_EDGE('',*,*,#47579,.T.);
#64880=ORIENTED_EDGE('',*,*,#47580,.F.);
#64881=ORIENTED_EDGE('',*,*,#46911,.F.);
#64882=ORIENTED_EDGE('',*,*,#47581,.F.);
#64883=ORIENTED_EDGE('',*,*,#46631,.F.);
#64884=ORIENTED_EDGE('',*,*,#46912,.T.);
#64885=ORIENTED_EDGE('',*,*,#47582,.F.);
#64886=ORIENTED_EDGE('',*,*,#47583,.F.);
#64887=ORIENTED_EDGE('',*,*,#47583,.T.);
#64888=ORIENTED_EDGE('',*,*,#47584,.F.);
#64889=ORIENTED_EDGE('',*,*,#47585,.F.);
#64890=ORIENTED_EDGE('',*,*,#46638,.F.);
#64891=ORIENTED_EDGE('',*,*,#47585,.T.);
#64892=ORIENTED_EDGE('',*,*,#47586,.F.);
#64893=ORIENTED_EDGE('',*,*,#47587,.F.);
#64894=ORIENTED_EDGE('',*,*,#46636,.F.);
#64895=ORIENTED_EDGE('',*,*,#47570,.T.);
#64896=ORIENTED_EDGE('',*,*,#47588,.F.);
#64897=ORIENTED_EDGE('',*,*,#47589,.F.);
#64898=ORIENTED_EDGE('',*,*,#47590,.F.);
#64899=ORIENTED_EDGE('',*,*,#47587,.T.);
#64900=ORIENTED_EDGE('',*,*,#47591,.F.);
#64901=ORIENTED_EDGE('',*,*,#47592,.F.);
#64902=ORIENTED_EDGE('',*,*,#47593,.F.);
#64903=ORIENTED_EDGE('',*,*,#47594,.F.);
#64904=ORIENTED_EDGE('',*,*,#47595,.T.);
#64905=ORIENTED_EDGE('',*,*,#46633,.F.);
#64906=ORIENTED_EDGE('',*,*,#47593,.T.);
#64907=ORIENTED_EDGE('',*,*,#47596,.T.);
#64908=ORIENTED_EDGE('',*,*,#47597,.F.);
#64909=ORIENTED_EDGE('',*,*,#47598,.F.);
#64910=ORIENTED_EDGE('',*,*,#47595,.F.);
#64911=ORIENTED_EDGE('',*,*,#47598,.T.);
#64912=ORIENTED_EDGE('',*,*,#47599,.F.);
#64913=ORIENTED_EDGE('',*,*,#47600,.F.);
#64914=ORIENTED_EDGE('',*,*,#46634,.F.);
#64915=ORIENTED_EDGE('',*,*,#47601,.F.);
#64916=ORIENTED_EDGE('',*,*,#46904,.T.);
#64917=ORIENTED_EDGE('',*,*,#46639,.F.);
#64918=ORIENTED_EDGE('',*,*,#46637,.F.);
#64919=ORIENTED_EDGE('',*,*,#47600,.T.);
#64920=ORIENTED_EDGE('',*,*,#46905,.T.);
#64921=ORIENTED_EDGE('',*,*,#47602,.F.);
#64922=ORIENTED_EDGE('',*,*,#47603,.F.);
#64923=ORIENTED_EDGE('',*,*,#47604,.F.);
#64924=ORIENTED_EDGE('',*,*,#47603,.T.);
#64925=ORIENTED_EDGE('',*,*,#47605,.F.);
#64926=ORIENTED_EDGE('',*,*,#47606,.F.);
#64927=ORIENTED_EDGE('',*,*,#46901,.F.);
#64928=ORIENTED_EDGE('',*,*,#47606,.T.);
#64929=ORIENTED_EDGE('',*,*,#47607,.F.);
#64930=ORIENTED_EDGE('',*,*,#47608,.F.);
#64931=ORIENTED_EDGE('',*,*,#46649,.F.);
#64932=ORIENTED_EDGE('',*,*,#47608,.T.);
#64933=ORIENTED_EDGE('',*,*,#47609,.F.);
#64934=ORIENTED_EDGE('',*,*,#47610,.F.);
#64935=ORIENTED_EDGE('',*,*,#46646,.F.);
#64936=ORIENTED_EDGE('',*,*,#47610,.T.);
#64937=ORIENTED_EDGE('',*,*,#47611,.F.);
#64938=ORIENTED_EDGE('',*,*,#47612,.F.);
#64939=ORIENTED_EDGE('',*,*,#46644,.F.);
#64940=ORIENTED_EDGE('',*,*,#47613,.T.);
#64941=ORIENTED_EDGE('',*,*,#47614,.F.);
#64942=ORIENTED_EDGE('',*,*,#47612,.T.);
#64943=ORIENTED_EDGE('',*,*,#47615,.F.);
#64944=ORIENTED_EDGE('',*,*,#47616,.T.);
#64945=ORIENTED_EDGE('',*,*,#47617,.F.);
#64946=ORIENTED_EDGE('',*,*,#47613,.F.);
#64947=ORIENTED_EDGE('',*,*,#47618,.F.);
#64948=ORIENTED_EDGE('',*,*,#46641,.F.);
#64949=ORIENTED_EDGE('',*,*,#47614,.T.);
#64950=ORIENTED_EDGE('',*,*,#47619,.F.);
#64951=ORIENTED_EDGE('',*,*,#47620,.T.);
#64952=ORIENTED_EDGE('',*,*,#47621,.T.);
#64953=ORIENTED_EDGE('',*,*,#47620,.F.);
#64954=ORIENTED_EDGE('',*,*,#47622,.F.);
#64955=ORIENTED_EDGE('',*,*,#47623,.F.);
#64956=ORIENTED_EDGE('',*,*,#47624,.T.);
#64957=ORIENTED_EDGE('',*,*,#46642,.F.);
#64958=ORIENTED_EDGE('',*,*,#47621,.F.);
#64959=ORIENTED_EDGE('',*,*,#47625,.F.);
#64960=ORIENTED_EDGE('',*,*,#47626,.T.);
#64961=ORIENTED_EDGE('',*,*,#46647,.F.);
#64962=ORIENTED_EDGE('',*,*,#47624,.F.);
#64963=ORIENTED_EDGE('',*,*,#47627,.F.);
#64964=ORIENTED_EDGE('',*,*,#47628,.T.);
#64965=ORIENTED_EDGE('',*,*,#46650,.F.);
#64966=ORIENTED_EDGE('',*,*,#47626,.F.);
#64967=ORIENTED_EDGE('',*,*,#47629,.F.);
#64968=ORIENTED_EDGE('',*,*,#47630,.T.);
#64969=ORIENTED_EDGE('',*,*,#46902,.F.);
#64970=ORIENTED_EDGE('',*,*,#47628,.F.);
#64971=ORIENTED_EDGE('',*,*,#47631,.F.);
#64972=ORIENTED_EDGE('',*,*,#46898,.T.);
#64973=ORIENTED_EDGE('',*,*,#47632,.F.);
#64974=ORIENTED_EDGE('',*,*,#47630,.F.);
#64975=ORIENTED_EDGE('',*,*,#47633,.F.);
#64976=ORIENTED_EDGE('',*,*,#46653,.F.);
#64977=ORIENTED_EDGE('',*,*,#46899,.T.);
#64978=ORIENTED_EDGE('',*,*,#47634,.F.);
#64979=ORIENTED_EDGE('',*,*,#47635,.T.);
#64980=ORIENTED_EDGE('',*,*,#47622,.T.);
#64981=ORIENTED_EDGE('',*,*,#47636,.F.);
#64982=ORIENTED_EDGE('',*,*,#47637,.F.);
#64983=ORIENTED_EDGE('',*,*,#47638,.F.);
#64984=ORIENTED_EDGE('',*,*,#47639,.T.);
#64985=ORIENTED_EDGE('',*,*,#47640,.F.);
#64986=ORIENTED_EDGE('',*,*,#47635,.F.);
#64987=ORIENTED_EDGE('',*,*,#47641,.F.);
#64988=ORIENTED_EDGE('',*,*,#47642,.T.);
#64989=ORIENTED_EDGE('',*,*,#47643,.T.);
#64990=ORIENTED_EDGE('',*,*,#46654,.T.);
#64991=ORIENTED_EDGE('',*,*,#47640,.T.);
#64992=ORIENTED_EDGE('',*,*,#47644,.T.);
#64993=ORIENTED_EDGE('',*,*,#47645,.F.);
#64994=ORIENTED_EDGE('',*,*,#47646,.F.);
#64995=ORIENTED_EDGE('',*,*,#47643,.F.);
#64996=ORIENTED_EDGE('',*,*,#47647,.F.);
#64997=ORIENTED_EDGE('',*,*,#46892,.T.);
#64998=ORIENTED_EDGE('',*,*,#46651,.F.);
#64999=ORIENTED_EDGE('',*,*,#47646,.T.);
#65000=ORIENTED_EDGE('',*,*,#46893,.T.);
#65001=ORIENTED_EDGE('',*,*,#47648,.F.);
#65002=ORIENTED_EDGE('',*,*,#47649,.F.);
#65003=ORIENTED_EDGE('',*,*,#47650,.F.);
#65004=ORIENTED_EDGE('',*,*,#47649,.T.);
#65005=ORIENTED_EDGE('',*,*,#47651,.F.);
#65006=ORIENTED_EDGE('',*,*,#47652,.F.);
#65007=ORIENTED_EDGE('',*,*,#46889,.F.);
#65008=ORIENTED_EDGE('',*,*,#47652,.T.);
#65009=ORIENTED_EDGE('',*,*,#47653,.F.);
#65010=ORIENTED_EDGE('',*,*,#47654,.F.);
#65011=ORIENTED_EDGE('',*,*,#46663,.F.);
#65012=ORIENTED_EDGE('',*,*,#47654,.T.);
#65013=ORIENTED_EDGE('',*,*,#47655,.F.);
#65014=ORIENTED_EDGE('',*,*,#47656,.F.);
#65015=ORIENTED_EDGE('',*,*,#46660,.F.);
#65016=ORIENTED_EDGE('',*,*,#47656,.T.);
#65017=ORIENTED_EDGE('',*,*,#47657,.F.);
#65018=ORIENTED_EDGE('',*,*,#47658,.F.);
#65019=ORIENTED_EDGE('',*,*,#46656,.F.);
#65020=ORIENTED_EDGE('',*,*,#47658,.T.);
#65021=ORIENTED_EDGE('',*,*,#47659,.F.);
#65022=ORIENTED_EDGE('',*,*,#47660,.F.);
#65023=ORIENTED_EDGE('',*,*,#47661,.F.);
#65024=ORIENTED_EDGE('',*,*,#47660,.T.);
#65025=ORIENTED_EDGE('',*,*,#47662,.F.);
#65026=ORIENTED_EDGE('',*,*,#47663,.F.);
#65027=ORIENTED_EDGE('',*,*,#47664,.F.);
#65028=ORIENTED_EDGE('',*,*,#46657,.F.);
#65029=ORIENTED_EDGE('',*,*,#47661,.T.);
#65030=ORIENTED_EDGE('',*,*,#47665,.F.);
#65031=ORIENTED_EDGE('',*,*,#47666,.T.);
#65032=ORIENTED_EDGE('',*,*,#47667,.T.);
#65033=ORIENTED_EDGE('',*,*,#47666,.F.);
#65034=ORIENTED_EDGE('',*,*,#47668,.F.);
#65035=ORIENTED_EDGE('',*,*,#47669,.F.);
#65036=ORIENTED_EDGE('',*,*,#47670,.T.);
#65037=ORIENTED_EDGE('',*,*,#46658,.F.);
#65038=ORIENTED_EDGE('',*,*,#47667,.F.);
#65039=ORIENTED_EDGE('',*,*,#47671,.F.);
#65040=ORIENTED_EDGE('',*,*,#47672,.T.);
#65041=ORIENTED_EDGE('',*,*,#46661,.F.);
#65042=ORIENTED_EDGE('',*,*,#47670,.F.);
#65043=ORIENTED_EDGE('',*,*,#47673,.F.);
#65044=ORIENTED_EDGE('',*,*,#47674,.T.);
#65045=ORIENTED_EDGE('',*,*,#46664,.F.);
#65046=ORIENTED_EDGE('',*,*,#47672,.F.);
#65047=ORIENTED_EDGE('',*,*,#47675,.F.);
#65048=ORIENTED_EDGE('',*,*,#47676,.T.);
#65049=ORIENTED_EDGE('',*,*,#46890,.F.);
#65050=ORIENTED_EDGE('',*,*,#47674,.F.);
#65051=ORIENTED_EDGE('',*,*,#47677,.F.);
#65052=ORIENTED_EDGE('',*,*,#46886,.T.);
#65053=ORIENTED_EDGE('',*,*,#47678,.F.);
#65054=ORIENTED_EDGE('',*,*,#47676,.F.);
#65055=ORIENTED_EDGE('',*,*,#47679,.F.);
#65056=ORIENTED_EDGE('',*,*,#46667,.F.);
#65057=ORIENTED_EDGE('',*,*,#46887,.T.);
#65058=ORIENTED_EDGE('',*,*,#47680,.F.);
#65059=ORIENTED_EDGE('',*,*,#47681,.T.);
#65060=ORIENTED_EDGE('',*,*,#47668,.T.);
#65061=ORIENTED_EDGE('',*,*,#47682,.F.);
#65062=ORIENTED_EDGE('',*,*,#47683,.F.);
#65063=ORIENTED_EDGE('',*,*,#47684,.F.);
#65064=ORIENTED_EDGE('',*,*,#47685,.T.);
#65065=ORIENTED_EDGE('',*,*,#47686,.F.);
#65066=ORIENTED_EDGE('',*,*,#47681,.F.);
#65067=ORIENTED_EDGE('',*,*,#47687,.F.);
#65068=ORIENTED_EDGE('',*,*,#47688,.T.);
#65069=ORIENTED_EDGE('',*,*,#47689,.T.);
#65070=ORIENTED_EDGE('',*,*,#46668,.T.);
#65071=ORIENTED_EDGE('',*,*,#47686,.T.);
#65072=ORIENTED_EDGE('',*,*,#47690,.T.);
#65073=ORIENTED_EDGE('',*,*,#47691,.F.);
#65074=ORIENTED_EDGE('',*,*,#47692,.F.);
#65075=ORIENTED_EDGE('',*,*,#47689,.F.);
#65076=ORIENTED_EDGE('',*,*,#47693,.F.);
#65077=ORIENTED_EDGE('',*,*,#46880,.T.);
#65078=ORIENTED_EDGE('',*,*,#46665,.F.);
#65079=ORIENTED_EDGE('',*,*,#47692,.T.);
#65080=ORIENTED_EDGE('',*,*,#46881,.T.);
#65081=ORIENTED_EDGE('',*,*,#47694,.F.);
#65082=ORIENTED_EDGE('',*,*,#47695,.F.);
#65083=ORIENTED_EDGE('',*,*,#47696,.F.);
#65084=ORIENTED_EDGE('',*,*,#47695,.T.);
#65085=ORIENTED_EDGE('',*,*,#47697,.F.);
#65086=ORIENTED_EDGE('',*,*,#47698,.F.);
#65087=ORIENTED_EDGE('',*,*,#46877,.F.);
#65088=ORIENTED_EDGE('',*,*,#47698,.T.);
#65089=ORIENTED_EDGE('',*,*,#47699,.F.);
#65090=ORIENTED_EDGE('',*,*,#47700,.F.);
#65091=ORIENTED_EDGE('',*,*,#46677,.F.);
#65092=ORIENTED_EDGE('',*,*,#47700,.T.);
#65093=ORIENTED_EDGE('',*,*,#47701,.F.);
#65094=ORIENTED_EDGE('',*,*,#47702,.F.);
#65095=ORIENTED_EDGE('',*,*,#46674,.F.);
#65096=ORIENTED_EDGE('',*,*,#47702,.T.);
#65097=ORIENTED_EDGE('',*,*,#47703,.F.);
#65098=ORIENTED_EDGE('',*,*,#47704,.F.);
#65099=ORIENTED_EDGE('',*,*,#46670,.F.);
#65100=ORIENTED_EDGE('',*,*,#47704,.T.);
#65101=ORIENTED_EDGE('',*,*,#47705,.F.);
#65102=ORIENTED_EDGE('',*,*,#47706,.F.);
#65103=ORIENTED_EDGE('',*,*,#47707,.F.);
#65104=ORIENTED_EDGE('',*,*,#47706,.T.);
#65105=ORIENTED_EDGE('',*,*,#47708,.F.);
#65106=ORIENTED_EDGE('',*,*,#47709,.F.);
#65107=ORIENTED_EDGE('',*,*,#47710,.F.);
#65108=ORIENTED_EDGE('',*,*,#46671,.F.);
#65109=ORIENTED_EDGE('',*,*,#47707,.T.);
#65110=ORIENTED_EDGE('',*,*,#47711,.F.);
#65111=ORIENTED_EDGE('',*,*,#47712,.T.);
#65112=ORIENTED_EDGE('',*,*,#47713,.T.);
#65113=ORIENTED_EDGE('',*,*,#47712,.F.);
#65114=ORIENTED_EDGE('',*,*,#47714,.F.);
#65115=ORIENTED_EDGE('',*,*,#47715,.F.);
#65116=ORIENTED_EDGE('',*,*,#47716,.T.);
#65117=ORIENTED_EDGE('',*,*,#46672,.F.);
#65118=ORIENTED_EDGE('',*,*,#47713,.F.);
#65119=ORIENTED_EDGE('',*,*,#47717,.F.);
#65120=ORIENTED_EDGE('',*,*,#47718,.T.);
#65121=ORIENTED_EDGE('',*,*,#46675,.F.);
#65122=ORIENTED_EDGE('',*,*,#47716,.F.);
#65123=ORIENTED_EDGE('',*,*,#47719,.F.);
#65124=ORIENTED_EDGE('',*,*,#47720,.T.);
#65125=ORIENTED_EDGE('',*,*,#46678,.F.);
#65126=ORIENTED_EDGE('',*,*,#47718,.F.);
#65127=ORIENTED_EDGE('',*,*,#47721,.F.);
#65128=ORIENTED_EDGE('',*,*,#47722,.T.);
#65129=ORIENTED_EDGE('',*,*,#46878,.F.);
#65130=ORIENTED_EDGE('',*,*,#47720,.F.);
#65131=ORIENTED_EDGE('',*,*,#47723,.F.);
#65132=ORIENTED_EDGE('',*,*,#46874,.T.);
#65133=ORIENTED_EDGE('',*,*,#47724,.F.);
#65134=ORIENTED_EDGE('',*,*,#47722,.F.);
#65135=ORIENTED_EDGE('',*,*,#47725,.F.);
#65136=ORIENTED_EDGE('',*,*,#46681,.F.);
#65137=ORIENTED_EDGE('',*,*,#46875,.T.);
#65138=ORIENTED_EDGE('',*,*,#47726,.F.);
#65139=ORIENTED_EDGE('',*,*,#47727,.F.);
#65140=ORIENTED_EDGE('',*,*,#47714,.T.);
#65141=ORIENTED_EDGE('',*,*,#47728,.F.);
#65142=ORIENTED_EDGE('',*,*,#47729,.F.);
#65143=ORIENTED_EDGE('',*,*,#47730,.F.);
#65144=ORIENTED_EDGE('',*,*,#47727,.T.);
#65145=ORIENTED_EDGE('',*,*,#47731,.F.);
#65146=ORIENTED_EDGE('',*,*,#47732,.F.);
#65147=ORIENTED_EDGE('',*,*,#47733,.F.);
#65148=ORIENTED_EDGE('',*,*,#47734,.T.);
#65149=ORIENTED_EDGE('',*,*,#47735,.T.);
#65150=ORIENTED_EDGE('',*,*,#46682,.T.);
#65151=ORIENTED_EDGE('',*,*,#47733,.T.);
#65152=ORIENTED_EDGE('',*,*,#47736,.T.);
#65153=ORIENTED_EDGE('',*,*,#47737,.F.);
#65154=ORIENTED_EDGE('',*,*,#47738,.F.);
#65155=ORIENTED_EDGE('',*,*,#47735,.F.);
#65156=ORIENTED_EDGE('',*,*,#47739,.F.);
#65157=ORIENTED_EDGE('',*,*,#46868,.T.);
#65158=ORIENTED_EDGE('',*,*,#46679,.F.);
#65159=ORIENTED_EDGE('',*,*,#47738,.T.);
#65160=ORIENTED_EDGE('',*,*,#46869,.T.);
#65161=ORIENTED_EDGE('',*,*,#47740,.F.);
#65162=ORIENTED_EDGE('',*,*,#47741,.F.);
#65163=ORIENTED_EDGE('',*,*,#47742,.F.);
#65164=ORIENTED_EDGE('',*,*,#47741,.T.);
#65165=ORIENTED_EDGE('',*,*,#47743,.F.);
#65166=ORIENTED_EDGE('',*,*,#47744,.F.);
#65167=ORIENTED_EDGE('',*,*,#46865,.F.);
#65168=ORIENTED_EDGE('',*,*,#47744,.T.);
#65169=ORIENTED_EDGE('',*,*,#47745,.F.);
#65170=ORIENTED_EDGE('',*,*,#47746,.F.);
#65171=ORIENTED_EDGE('',*,*,#46691,.F.);
#65172=ORIENTED_EDGE('',*,*,#47746,.T.);
#65173=ORIENTED_EDGE('',*,*,#47747,.F.);
#65174=ORIENTED_EDGE('',*,*,#47748,.F.);
#65175=ORIENTED_EDGE('',*,*,#46688,.F.);
#65176=ORIENTED_EDGE('',*,*,#47748,.T.);
#65177=ORIENTED_EDGE('',*,*,#47749,.F.);
#65178=ORIENTED_EDGE('',*,*,#47750,.F.);
#65179=ORIENTED_EDGE('',*,*,#46684,.F.);
#65180=ORIENTED_EDGE('',*,*,#47750,.T.);
#65181=ORIENTED_EDGE('',*,*,#47751,.F.);
#65182=ORIENTED_EDGE('',*,*,#47752,.F.);
#65183=ORIENTED_EDGE('',*,*,#47753,.F.);
#65184=ORIENTED_EDGE('',*,*,#47752,.T.);
#65185=ORIENTED_EDGE('',*,*,#47754,.F.);
#65186=ORIENTED_EDGE('',*,*,#47755,.F.);
#65187=ORIENTED_EDGE('',*,*,#47756,.F.);
#65188=ORIENTED_EDGE('',*,*,#46685,.F.);
#65189=ORIENTED_EDGE('',*,*,#47753,.T.);
#65190=ORIENTED_EDGE('',*,*,#47757,.F.);
#65191=ORIENTED_EDGE('',*,*,#47758,.T.);
#65192=ORIENTED_EDGE('',*,*,#47759,.T.);
#65193=ORIENTED_EDGE('',*,*,#47758,.F.);
#65194=ORIENTED_EDGE('',*,*,#47760,.F.);
#65195=ORIENTED_EDGE('',*,*,#47761,.F.);
#65196=ORIENTED_EDGE('',*,*,#47762,.T.);
#65197=ORIENTED_EDGE('',*,*,#46686,.F.);
#65198=ORIENTED_EDGE('',*,*,#47759,.F.);
#65199=ORIENTED_EDGE('',*,*,#47763,.F.);
#65200=ORIENTED_EDGE('',*,*,#47762,.F.);
#65201=ORIENTED_EDGE('',*,*,#47764,.F.);
#65202=ORIENTED_EDGE('',*,*,#47765,.F.);
#65203=ORIENTED_EDGE('',*,*,#46689,.F.);
#65204=ORIENTED_EDGE('',*,*,#47765,.T.);
#65205=ORIENTED_EDGE('',*,*,#47766,.F.);
#65206=ORIENTED_EDGE('',*,*,#47767,.F.);
#65207=ORIENTED_EDGE('',*,*,#46692,.F.);
#65208=ORIENTED_EDGE('',*,*,#47767,.T.);
#65209=ORIENTED_EDGE('',*,*,#47768,.F.);
#65210=ORIENTED_EDGE('',*,*,#47769,.F.);
#65211=ORIENTED_EDGE('',*,*,#46866,.F.);
#65212=ORIENTED_EDGE('',*,*,#47769,.T.);
#65213=ORIENTED_EDGE('',*,*,#47770,.F.);
#65214=ORIENTED_EDGE('',*,*,#46861,.F.);
#65215=ORIENTED_EDGE('',*,*,#47771,.F.);
#65216=ORIENTED_EDGE('',*,*,#46695,.T.);
#65217=ORIENTED_EDGE('',*,*,#46862,.T.);
#65218=ORIENTED_EDGE('',*,*,#47772,.F.);
#65219=ORIENTED_EDGE('',*,*,#47773,.F.);
#65220=ORIENTED_EDGE('',*,*,#46702,.F.);
#65221=ORIENTED_EDGE('',*,*,#47773,.T.);
#65222=ORIENTED_EDGE('',*,*,#47774,.F.);
#65223=ORIENTED_EDGE('',*,*,#47775,.F.);
#65224=ORIENTED_EDGE('',*,*,#46699,.F.);
#65225=ORIENTED_EDGE('',*,*,#47760,.T.);
#65226=ORIENTED_EDGE('',*,*,#47776,.F.);
#65227=ORIENTED_EDGE('',*,*,#47777,.F.);
#65228=ORIENTED_EDGE('',*,*,#47778,.F.);
#65229=ORIENTED_EDGE('',*,*,#47775,.T.);
#65230=ORIENTED_EDGE('',*,*,#47779,.F.);
#65231=ORIENTED_EDGE('',*,*,#47780,.F.);
#65232=ORIENTED_EDGE('',*,*,#47781,.F.);
#65233=ORIENTED_EDGE('',*,*,#47782,.F.);
#65234=ORIENTED_EDGE('',*,*,#47783,.T.);
#65235=ORIENTED_EDGE('',*,*,#46696,.F.);
#65236=ORIENTED_EDGE('',*,*,#47781,.T.);
#65237=ORIENTED_EDGE('',*,*,#47784,.T.);
#65238=ORIENTED_EDGE('',*,*,#47785,.F.);
#65239=ORIENTED_EDGE('',*,*,#47786,.F.);
#65240=ORIENTED_EDGE('',*,*,#47783,.F.);
#65241=ORIENTED_EDGE('',*,*,#47786,.T.);
#65242=ORIENTED_EDGE('',*,*,#47787,.F.);
#65243=ORIENTED_EDGE('',*,*,#47788,.F.);
#65244=ORIENTED_EDGE('',*,*,#46697,.F.);
#65245=ORIENTED_EDGE('',*,*,#47788,.T.);
#65246=ORIENTED_EDGE('',*,*,#47789,.F.);
#65247=ORIENTED_EDGE('',*,*,#47790,.F.);
#65248=ORIENTED_EDGE('',*,*,#46700,.F.);
#65249=ORIENTED_EDGE('',*,*,#47791,.F.);
#65250=ORIENTED_EDGE('',*,*,#46854,.T.);
#65251=ORIENTED_EDGE('',*,*,#46703,.F.);
#65252=ORIENTED_EDGE('',*,*,#47790,.T.);
#65253=ORIENTED_EDGE('',*,*,#46855,.T.);
#65254=ORIENTED_EDGE('',*,*,#47792,.F.);
#65255=ORIENTED_EDGE('',*,*,#47793,.F.);
#65256=ORIENTED_EDGE('',*,*,#47794,.F.);
#65257=ORIENTED_EDGE('',*,*,#47793,.T.);
#65258=ORIENTED_EDGE('',*,*,#47795,.F.);
#65259=ORIENTED_EDGE('',*,*,#47796,.F.);
#65260=ORIENTED_EDGE('',*,*,#46851,.F.);
#65261=ORIENTED_EDGE('',*,*,#47796,.T.);
#65262=ORIENTED_EDGE('',*,*,#47797,.F.);
#65263=ORIENTED_EDGE('',*,*,#47798,.F.);
#65264=ORIENTED_EDGE('',*,*,#46717,.F.);
#65265=ORIENTED_EDGE('',*,*,#47798,.T.);
#65266=ORIENTED_EDGE('',*,*,#47799,.F.);
#65267=ORIENTED_EDGE('',*,*,#47800,.F.);
#65268=ORIENTED_EDGE('',*,*,#46714,.F.);
#65269=ORIENTED_EDGE('',*,*,#47800,.T.);
#65270=ORIENTED_EDGE('',*,*,#47801,.F.);
#65271=ORIENTED_EDGE('',*,*,#47802,.F.);
#65272=ORIENTED_EDGE('',*,*,#46712,.F.);
#65273=ORIENTED_EDGE('',*,*,#47803,.T.);
#65274=ORIENTED_EDGE('',*,*,#47804,.F.);
#65275=ORIENTED_EDGE('',*,*,#47802,.T.);
#65276=ORIENTED_EDGE('',*,*,#47805,.F.);
#65277=ORIENTED_EDGE('',*,*,#47806,.T.);
#65278=ORIENTED_EDGE('',*,*,#47807,.F.);
#65279=ORIENTED_EDGE('',*,*,#47803,.F.);
#65280=ORIENTED_EDGE('',*,*,#47808,.F.);
#65281=ORIENTED_EDGE('',*,*,#46709,.F.);
#65282=ORIENTED_EDGE('',*,*,#47804,.T.);
#65283=ORIENTED_EDGE('',*,*,#47809,.F.);
#65284=ORIENTED_EDGE('',*,*,#47810,.T.);
#65285=ORIENTED_EDGE('',*,*,#47811,.T.);
#65286=ORIENTED_EDGE('',*,*,#47812,.F.);
#65287=ORIENTED_EDGE('',*,*,#47813,.F.);
#65288=ORIENTED_EDGE('',*,*,#46708,.F.);
#65289=ORIENTED_EDGE('',*,*,#47813,.T.);
#65290=ORIENTED_EDGE('',*,*,#47814,.F.);
#65291=ORIENTED_EDGE('',*,*,#47815,.F.);
#65292=ORIENTED_EDGE('',*,*,#46724,.F.);
#65293=ORIENTED_EDGE('',*,*,#47816,.T.);
#65294=ORIENTED_EDGE('',*,*,#47817,.F.);
#65295=ORIENTED_EDGE('',*,*,#47818,.F.);
#65296=ORIENTED_EDGE('',*,*,#47819,.F.);
#65297=ORIENTED_EDGE('',*,*,#47818,.T.);
#65298=ORIENTED_EDGE('',*,*,#47820,.F.);
#65299=ORIENTED_EDGE('',*,*,#47821,.F.);
#65300=ORIENTED_EDGE('',*,*,#47810,.F.);
#65301=ORIENTED_EDGE('',*,*,#47821,.T.);
#65302=ORIENTED_EDGE('',*,*,#47822,.F.);
#65303=ORIENTED_EDGE('',*,*,#47823,.F.);
#65304=ORIENTED_EDGE('',*,*,#46710,.F.);
#65305=ORIENTED_EDGE('',*,*,#47823,.T.);
#65306=ORIENTED_EDGE('',*,*,#47824,.F.);
#65307=ORIENTED_EDGE('',*,*,#47825,.F.);
#65308=ORIENTED_EDGE('',*,*,#46715,.F.);
#65309=ORIENTED_EDGE('',*,*,#47825,.T.);
#65310=ORIENTED_EDGE('',*,*,#47826,.F.);
#65311=ORIENTED_EDGE('',*,*,#47827,.F.);
#65312=ORIENTED_EDGE('',*,*,#46718,.F.);
#65313=ORIENTED_EDGE('',*,*,#47827,.T.);
#65314=ORIENTED_EDGE('',*,*,#47828,.F.);
#65315=ORIENTED_EDGE('',*,*,#47829,.F.);
#65316=ORIENTED_EDGE('',*,*,#46852,.F.);
#65317=ORIENTED_EDGE('',*,*,#47829,.T.);
#65318=ORIENTED_EDGE('',*,*,#47830,.F.);
#65319=ORIENTED_EDGE('',*,*,#46847,.F.);
#65320=ORIENTED_EDGE('',*,*,#47831,.F.);
#65321=ORIENTED_EDGE('',*,*,#46721,.F.);
#65322=ORIENTED_EDGE('',*,*,#46848,.T.);
#65323=ORIENTED_EDGE('',*,*,#47832,.F.);
#65324=ORIENTED_EDGE('',*,*,#47811,.F.);
#65325=ORIENTED_EDGE('',*,*,#47815,.T.);
#65326=ORIENTED_EDGE('',*,*,#47833,.F.);
#65327=ORIENTED_EDGE('',*,*,#47834,.F.);
#65328=ORIENTED_EDGE('',*,*,#47835,.F.);
#65329=ORIENTED_EDGE('',*,*,#47836,.F.);
#65330=ORIENTED_EDGE('',*,*,#47837,.T.);
#65331=ORIENTED_EDGE('',*,*,#46722,.F.);
#65332=ORIENTED_EDGE('',*,*,#47835,.T.);
#65333=ORIENTED_EDGE('',*,*,#47838,.T.);
#65334=ORIENTED_EDGE('',*,*,#47839,.F.);
#65335=ORIENTED_EDGE('',*,*,#47138,.F.);
#65336=ORIENTED_EDGE('',*,*,#47837,.F.);
#65337=ORIENTED_EDGE('',*,*,#47227,.T.);
#65338=ORIENTED_EDGE('',*,*,#47840,.F.);
#65339=ORIENTED_EDGE('',*,*,#47841,.F.);
#65340=ORIENTED_EDGE('',*,*,#47842,.F.);
#65341=ORIENTED_EDGE('',*,*,#47843,.F.);
#65342=ORIENTED_EDGE('',*,*,#47844,.T.);
#65343=ORIENTED_EDGE('',*,*,#46725,.F.);
#65344=ORIENTED_EDGE('',*,*,#47842,.T.);
#65345=ORIENTED_EDGE('',*,*,#47845,.T.);
#65346=ORIENTED_EDGE('',*,*,#47846,.F.);
#65347=ORIENTED_EDGE('',*,*,#47554,.F.);
#65348=ORIENTED_EDGE('',*,*,#47844,.F.);
#65349=ORIENTED_EDGE('',*,*,#47847,.T.);
#65350=ORIENTED_EDGE('',*,*,#47848,.F.);
#65351=ORIENTED_EDGE('',*,*,#47849,.F.);
#65352=ORIENTED_EDGE('',*,*,#47850,.F.);
#65353=ORIENTED_EDGE('',*,*,#47851,.T.);
#65354=ORIENTED_EDGE('',*,*,#47852,.F.);
#65355=ORIENTED_EDGE('',*,*,#47853,.F.);
#65356=ORIENTED_EDGE('',*,*,#47854,.F.);
#65357=ORIENTED_EDGE('',*,*,#47855,.T.);
#65358=ORIENTED_EDGE('',*,*,#47856,.F.);
#65359=ORIENTED_EDGE('',*,*,#47857,.F.);
#65360=ORIENTED_EDGE('',*,*,#47858,.F.);
#65361=ORIENTED_EDGE('',*,*,#47859,.T.);
#65362=ORIENTED_EDGE('',*,*,#47860,.F.);
#65363=ORIENTED_EDGE('',*,*,#47855,.F.);
#65364=ORIENTED_EDGE('',*,*,#47861,.F.);
#65365=ORIENTED_EDGE('',*,*,#47862,.T.);
#65366=ORIENTED_EDGE('',*,*,#47863,.F.);
#65367=ORIENTED_EDGE('',*,*,#47864,.F.);
#65368=ORIENTED_EDGE('',*,*,#47865,.F.);
#65369=ORIENTED_EDGE('',*,*,#47864,.T.);
#65370=ORIENTED_EDGE('',*,*,#47866,.F.);
#65371=ORIENTED_EDGE('',*,*,#47867,.F.);
#65372=ORIENTED_EDGE('',*,*,#47868,.F.);
#65373=ORIENTED_EDGE('',*,*,#47867,.T.);
#65374=ORIENTED_EDGE('',*,*,#47869,.F.);
#65375=ORIENTED_EDGE('',*,*,#47870,.F.);
#65376=ORIENTED_EDGE('',*,*,#47871,.F.);
#65377=ORIENTED_EDGE('',*,*,#47872,.T.);
#65378=ORIENTED_EDGE('',*,*,#47873,.F.);
#65379=ORIENTED_EDGE('',*,*,#47874,.F.);
#65380=ORIENTED_EDGE('',*,*,#47875,.F.);
#65381=ORIENTED_EDGE('',*,*,#47876,.F.);
#65382=ORIENTED_EDGE('',*,*,#47875,.T.);
#65383=ORIENTED_EDGE('',*,*,#47877,.F.);
#65384=ORIENTED_EDGE('',*,*,#47878,.T.);
#65385=ORIENTED_EDGE('',*,*,#47879,.T.);
#65386=ORIENTED_EDGE('',*,*,#47880,.F.);
#65387=ORIENTED_EDGE('',*,*,#47881,.F.);
#65388=ORIENTED_EDGE('',*,*,#47878,.F.);
#65389=ORIENTED_EDGE('',*,*,#47882,.T.);
#65390=ORIENTED_EDGE('',*,*,#47883,.F.);
#65391=ORIENTED_EDGE('',*,*,#47884,.F.);
#65392=ORIENTED_EDGE('',*,*,#47885,.F.);
#65393=ORIENTED_EDGE('',*,*,#47886,.T.);
#65394=ORIENTED_EDGE('',*,*,#46980,.F.);
#65395=ORIENTED_EDGE('',*,*,#47882,.F.);
#65396=ORIENTED_EDGE('',*,*,#47887,.F.);
#65397=ORIENTED_EDGE('',*,*,#47888,.T.);
#65398=ORIENTED_EDGE('',*,*,#47889,.F.);
#65399=ORIENTED_EDGE('',*,*,#47886,.F.);
#65400=ORIENTED_EDGE('',*,*,#47890,.F.);
#65401=ORIENTED_EDGE('',*,*,#47891,.T.);
#65402=ORIENTED_EDGE('',*,*,#47892,.F.);
#65403=ORIENTED_EDGE('',*,*,#47347,.F.);
#65404=ORIENTED_EDGE('',*,*,#47893,.F.);
#65405=ORIENTED_EDGE('',*,*,#47894,.T.);
#65406=ORIENTED_EDGE('',*,*,#47895,.F.);
#65407=ORIENTED_EDGE('',*,*,#47888,.F.);
#65408=ORIENTED_EDGE('',*,*,#47896,.F.);
#65409=ORIENTED_EDGE('',*,*,#46981,.T.);
#65410=ORIENTED_EDGE('',*,*,#47889,.T.);
#65411=ORIENTED_EDGE('',*,*,#47897,.T.);
#65412=ORIENTED_EDGE('',*,*,#47350,.T.);
#65413=ORIENTED_EDGE('',*,*,#47898,.T.);
#65414=ORIENTED_EDGE('',*,*,#47899,.F.);
#65415=ORIENTED_EDGE('',*,*,#47900,.F.);
#65416=ORIENTED_EDGE('',*,*,#47901,.F.);
#65417=ORIENTED_EDGE('',*,*,#47900,.T.);
#65418=ORIENTED_EDGE('',*,*,#47902,.F.);
#65419=ORIENTED_EDGE('',*,*,#47903,.F.);
#65420=ORIENTED_EDGE('',*,*,#46984,.F.);
#65421=ORIENTED_EDGE('',*,*,#47903,.T.);
#65422=ORIENTED_EDGE('',*,*,#47904,.F.);
#65423=ORIENTED_EDGE('',*,*,#47905,.F.);
#65424=ORIENTED_EDGE('',*,*,#46745,.F.);
#65425=ORIENTED_EDGE('',*,*,#47906,.T.);
#65426=ORIENTED_EDGE('',*,*,#47907,.F.);
#65427=ORIENTED_EDGE('',*,*,#47908,.F.);
#65428=ORIENTED_EDGE('',*,*,#47909,.F.);
#65429=ORIENTED_EDGE('',*,*,#47908,.T.);
#65430=ORIENTED_EDGE('',*,*,#47910,.F.);
#65431=ORIENTED_EDGE('',*,*,#47911,.F.);
#65432=ORIENTED_EDGE('',*,*,#46762,.F.);
#65433=ORIENTED_EDGE('',*,*,#47911,.T.);
#65434=ORIENTED_EDGE('',*,*,#47912,.F.);
#65435=ORIENTED_EDGE('',*,*,#47913,.F.);
#65436=ORIENTED_EDGE('',*,*,#46729,.F.);
#65437=ORIENTED_EDGE('',*,*,#47913,.T.);
#65438=ORIENTED_EDGE('',*,*,#47914,.F.);
#65439=ORIENTED_EDGE('',*,*,#47915,.F.);
#65440=ORIENTED_EDGE('',*,*,#47916,.F.);
#65441=ORIENTED_EDGE('',*,*,#47915,.T.);
#65442=ORIENTED_EDGE('',*,*,#47917,.F.);
#65443=ORIENTED_EDGE('',*,*,#47918,.F.);
#65444=ORIENTED_EDGE('',*,*,#47919,.F.);
#65445=ORIENTED_EDGE('',*,*,#46730,.F.);
#65446=ORIENTED_EDGE('',*,*,#47916,.T.);
#65447=ORIENTED_EDGE('',*,*,#47920,.F.);
#65448=ORIENTED_EDGE('',*,*,#47921,.T.);
#65449=ORIENTED_EDGE('',*,*,#47922,.T.);
#65450=ORIENTED_EDGE('',*,*,#47923,.F.);
#65451=ORIENTED_EDGE('',*,*,#47924,.F.);
#65452=ORIENTED_EDGE('',*,*,#46760,.F.);
#65453=ORIENTED_EDGE('',*,*,#47924,.T.);
#65454=ORIENTED_EDGE('',*,*,#47925,.F.);
#65455=ORIENTED_EDGE('',*,*,#47926,.F.);
#65456=ORIENTED_EDGE('',*,*,#46735,.F.);
#65457=ORIENTED_EDGE('',*,*,#47927,.T.);
#65458=ORIENTED_EDGE('',*,*,#47921,.F.);
#65459=ORIENTED_EDGE('',*,*,#47928,.F.);
#65460=ORIENTED_EDGE('',*,*,#47929,.F.);
#65461=ORIENTED_EDGE('',*,*,#47930,.T.);
#65462=ORIENTED_EDGE('',*,*,#46731,.F.);
#65463=ORIENTED_EDGE('',*,*,#47927,.F.);
#65464=ORIENTED_EDGE('',*,*,#47931,.F.);
#65465=ORIENTED_EDGE('',*,*,#47932,.T.);
#65466=ORIENTED_EDGE('',*,*,#46763,.F.);
#65467=ORIENTED_EDGE('',*,*,#47930,.F.);
#65468=ORIENTED_EDGE('',*,*,#47933,.F.);
#65469=ORIENTED_EDGE('',*,*,#47934,.T.);
#65470=ORIENTED_EDGE('',*,*,#47935,.F.);
#65471=ORIENTED_EDGE('',*,*,#47932,.F.);
#65472=ORIENTED_EDGE('',*,*,#47936,.F.);
#65473=ORIENTED_EDGE('',*,*,#47928,.T.);
#65474=ORIENTED_EDGE('',*,*,#47937,.F.);
#65475=ORIENTED_EDGE('',*,*,#47938,.F.);
#65476=ORIENTED_EDGE('',*,*,#47939,.F.);
#65477=ORIENTED_EDGE('',*,*,#47926,.T.);
#65478=ORIENTED_EDGE('',*,*,#47940,.F.);
#65479=ORIENTED_EDGE('',*,*,#47941,.F.);
#65480=ORIENTED_EDGE('',*,*,#47942,.F.);
#65481=ORIENTED_EDGE('',*,*,#47943,.F.);
#65482=ORIENTED_EDGE('',*,*,#47944,.T.);
#65483=ORIENTED_EDGE('',*,*,#46732,.F.);
#65484=ORIENTED_EDGE('',*,*,#47942,.T.);
#65485=ORIENTED_EDGE('',*,*,#47945,.T.);
#65486=ORIENTED_EDGE('',*,*,#47946,.F.);
#65487=ORIENTED_EDGE('',*,*,#47947,.F.);
#65488=ORIENTED_EDGE('',*,*,#47944,.F.);
#65489=ORIENTED_EDGE('',*,*,#47947,.T.);
#65490=ORIENTED_EDGE('',*,*,#47948,.F.);
#65491=ORIENTED_EDGE('',*,*,#47949,.F.);
#65492=ORIENTED_EDGE('',*,*,#46733,.F.);
#65493=ORIENTED_EDGE('',*,*,#47949,.T.);
#65494=ORIENTED_EDGE('',*,*,#47950,.F.);
#65495=ORIENTED_EDGE('',*,*,#47951,.F.);
#65496=ORIENTED_EDGE('',*,*,#46758,.F.);
#65497=ORIENTED_EDGE('',*,*,#47952,.T.);
#65498=ORIENTED_EDGE('',*,*,#47953,.F.);
#65499=ORIENTED_EDGE('',*,*,#47954,.F.);
#65500=ORIENTED_EDGE('',*,*,#47955,.F.);
#65501=ORIENTED_EDGE('',*,*,#47954,.T.);
#65502=ORIENTED_EDGE('',*,*,#47956,.F.);
#65503=ORIENTED_EDGE('',*,*,#47957,.F.);
#65504=ORIENTED_EDGE('',*,*,#46756,.F.);
#65505=ORIENTED_EDGE('',*,*,#47957,.T.);
#65506=ORIENTED_EDGE('',*,*,#47958,.F.);
#65507=ORIENTED_EDGE('',*,*,#47959,.F.);
#65508=ORIENTED_EDGE('',*,*,#46737,.F.);
#65509=ORIENTED_EDGE('',*,*,#47959,.T.);
#65510=ORIENTED_EDGE('',*,*,#47960,.F.);
#65511=ORIENTED_EDGE('',*,*,#47961,.F.);
#65512=ORIENTED_EDGE('',*,*,#47962,.F.);
#65513=ORIENTED_EDGE('',*,*,#47961,.T.);
#65514=ORIENTED_EDGE('',*,*,#47963,.F.);
#65515=ORIENTED_EDGE('',*,*,#47964,.F.);
#65516=ORIENTED_EDGE('',*,*,#47965,.F.);
#65517=ORIENTED_EDGE('',*,*,#46738,.F.);
#65518=ORIENTED_EDGE('',*,*,#47962,.T.);
#65519=ORIENTED_EDGE('',*,*,#47966,.F.);
#65520=ORIENTED_EDGE('',*,*,#47967,.T.);
#65521=ORIENTED_EDGE('',*,*,#47968,.T.);
#65522=ORIENTED_EDGE('',*,*,#47967,.F.);
#65523=ORIENTED_EDGE('',*,*,#47969,.F.);
#65524=ORIENTED_EDGE('',*,*,#47970,.F.);
#65525=ORIENTED_EDGE('',*,*,#47971,.T.);
#65526=ORIENTED_EDGE('',*,*,#46739,.F.);
#65527=ORIENTED_EDGE('',*,*,#47968,.F.);
#65528=ORIENTED_EDGE('',*,*,#47972,.F.);
#65529=ORIENTED_EDGE('',*,*,#47973,.T.);
#65530=ORIENTED_EDGE('',*,*,#46757,.F.);
#65531=ORIENTED_EDGE('',*,*,#47971,.F.);
#65532=ORIENTED_EDGE('',*,*,#47974,.F.);
#65533=ORIENTED_EDGE('',*,*,#47975,.T.);
#65534=ORIENTED_EDGE('',*,*,#47976,.F.);
#65535=ORIENTED_EDGE('',*,*,#47973,.F.);
#65536=ORIENTED_EDGE('',*,*,#47977,.F.);
#65537=ORIENTED_EDGE('',*,*,#47969,.T.);
#65538=ORIENTED_EDGE('',*,*,#47978,.F.);
#65539=ORIENTED_EDGE('',*,*,#47979,.F.);
#65540=ORIENTED_EDGE('',*,*,#47980,.F.);
#65541=ORIENTED_EDGE('',*,*,#47981,.T.);
#65542=ORIENTED_EDGE('',*,*,#47982,.F.);
#65543=ORIENTED_EDGE('',*,*,#47983,.F.);
#65544=ORIENTED_EDGE('',*,*,#47984,.F.);
#65545=ORIENTED_EDGE('',*,*,#47985,.T.);
#65546=ORIENTED_EDGE('',*,*,#47986,.T.);
#65547=ORIENTED_EDGE('',*,*,#47987,.T.);
#65548=ORIENTED_EDGE('',*,*,#47984,.T.);
#65549=ORIENTED_EDGE('',*,*,#47988,.T.);
#65550=ORIENTED_EDGE('',*,*,#47989,.F.);
#65551=ORIENTED_EDGE('',*,*,#47990,.F.);
#65552=ORIENTED_EDGE('',*,*,#47986,.F.);
#65553=ORIENTED_EDGE('',*,*,#47991,.T.);
#65554=ORIENTED_EDGE('',*,*,#47992,.F.);
#65555=ORIENTED_EDGE('',*,*,#47993,.F.);
#65556=ORIENTED_EDGE('',*,*,#47994,.F.);
#65557=ORIENTED_EDGE('',*,*,#47993,.T.);
#65558=ORIENTED_EDGE('',*,*,#47995,.F.);
#65559=ORIENTED_EDGE('',*,*,#47996,.F.);
#65560=ORIENTED_EDGE('',*,*,#46753,.F.);
#65561=ORIENTED_EDGE('',*,*,#47996,.T.);
#65562=ORIENTED_EDGE('',*,*,#47997,.F.);
#65563=ORIENTED_EDGE('',*,*,#47998,.F.);
#65564=ORIENTED_EDGE('',*,*,#46741,.F.);
#65565=ORIENTED_EDGE('',*,*,#47998,.T.);
#65566=ORIENTED_EDGE('',*,*,#47999,.F.);
#65567=ORIENTED_EDGE('',*,*,#48000,.F.);
#65568=ORIENTED_EDGE('',*,*,#48001,.F.);
#65569=ORIENTED_EDGE('',*,*,#48000,.T.);
#65570=ORIENTED_EDGE('',*,*,#48002,.F.);
#65571=ORIENTED_EDGE('',*,*,#48003,.F.);
#65572=ORIENTED_EDGE('',*,*,#48004,.F.);
#65573=ORIENTED_EDGE('',*,*,#46742,.F.);
#65574=ORIENTED_EDGE('',*,*,#48001,.T.);
#65575=ORIENTED_EDGE('',*,*,#48005,.F.);
#65576=ORIENTED_EDGE('',*,*,#48006,.T.);
#65577=ORIENTED_EDGE('',*,*,#48007,.T.);
#65578=ORIENTED_EDGE('',*,*,#48006,.F.);
#65579=ORIENTED_EDGE('',*,*,#48008,.F.);
#65580=ORIENTED_EDGE('',*,*,#48009,.F.);
#65581=ORIENTED_EDGE('',*,*,#48010,.T.);
#65582=ORIENTED_EDGE('',*,*,#46743,.F.);
#65583=ORIENTED_EDGE('',*,*,#48007,.F.);
#65584=ORIENTED_EDGE('',*,*,#48011,.F.);
#65585=ORIENTED_EDGE('',*,*,#48012,.T.);
#65586=ORIENTED_EDGE('',*,*,#46754,.F.);
#65587=ORIENTED_EDGE('',*,*,#48010,.F.);
#65588=ORIENTED_EDGE('',*,*,#48013,.F.);
#65589=ORIENTED_EDGE('',*,*,#48014,.T.);
#65590=ORIENTED_EDGE('',*,*,#48015,.F.);
#65591=ORIENTED_EDGE('',*,*,#48012,.F.);
#65592=ORIENTED_EDGE('',*,*,#48016,.F.);
#65593=ORIENTED_EDGE('',*,*,#48008,.T.);
#65594=ORIENTED_EDGE('',*,*,#48017,.F.);
#65595=ORIENTED_EDGE('',*,*,#48018,.F.);
#65596=ORIENTED_EDGE('',*,*,#48019,.F.);
#65597=ORIENTED_EDGE('',*,*,#48020,.T.);
#65598=ORIENTED_EDGE('',*,*,#48021,.T.);
#65599=ORIENTED_EDGE('',*,*,#48022,.T.);
#65600=ORIENTED_EDGE('',*,*,#46746,.T.);
#65601=ORIENTED_EDGE('',*,*,#48022,.F.);
#65602=ORIENTED_EDGE('',*,*,#48023,.T.);
#65603=ORIENTED_EDGE('',*,*,#48024,.T.);
#65604=ORIENTED_EDGE('',*,*,#48025,.F.);
#65605=ORIENTED_EDGE('',*,*,#47453,.F.);
#65606=ORIENTED_EDGE('',*,*,#46750,.F.);
#65607=ORIENTED_EDGE('',*,*,#47472,.T.);
#65608=ORIENTED_EDGE('',*,*,#48026,.F.);
#65609=ORIENTED_EDGE('',*,*,#46769,.T.);
#65610=ORIENTED_EDGE('',*,*,#48027,.T.);
#65611=ORIENTED_EDGE('',*,*,#48028,.F.);
#65612=ORIENTED_EDGE('',*,*,#48029,.F.);
#65613=ORIENTED_EDGE('',*,*,#48024,.F.);
#65614=ORIENTED_EDGE('',*,*,#48029,.T.);
#65615=ORIENTED_EDGE('',*,*,#48030,.F.);
#65616=ORIENTED_EDGE('',*,*,#47471,.F.);
#65617=ORIENTED_EDGE('',*,*,#48031,.F.);
#65618=ORIENTED_EDGE('',*,*,#48032,.T.);
#65619=ORIENTED_EDGE('',*,*,#48033,.F.);
#65620=ORIENTED_EDGE('',*,*,#48014,.F.);
#65621=ORIENTED_EDGE('',*,*,#48034,.F.);
#65622=ORIENTED_EDGE('',*,*,#48035,.T.);
#65623=ORIENTED_EDGE('',*,*,#47994,.T.);
#65624=ORIENTED_EDGE('',*,*,#46752,.T.);
#65625=ORIENTED_EDGE('',*,*,#48015,.T.);
#65626=ORIENTED_EDGE('',*,*,#48036,.T.);
#65627=ORIENTED_EDGE('',*,*,#48037,.F.);
#65628=ORIENTED_EDGE('',*,*,#47991,.F.);
#65629=ORIENTED_EDGE('',*,*,#48038,.F.);
#65630=ORIENTED_EDGE('',*,*,#48039,.F.);
#65631=ORIENTED_EDGE('',*,*,#48040,.T.);
#65632=ORIENTED_EDGE('',*,*,#48041,.F.);
#65633=ORIENTED_EDGE('',*,*,#47990,.T.);
#65634=ORIENTED_EDGE('',*,*,#48041,.T.);
#65635=ORIENTED_EDGE('',*,*,#48042,.T.);
#65636=ORIENTED_EDGE('',*,*,#48043,.T.);
#65637=ORIENTED_EDGE('',*,*,#47987,.F.);
#65638=ORIENTED_EDGE('',*,*,#48043,.F.);
#65639=ORIENTED_EDGE('',*,*,#48044,.T.);
#65640=ORIENTED_EDGE('',*,*,#48045,.F.);
#65641=ORIENTED_EDGE('',*,*,#47981,.F.);
#65642=ORIENTED_EDGE('',*,*,#48046,.T.);
#65643=ORIENTED_EDGE('',*,*,#48047,.F.);
#65644=ORIENTED_EDGE('',*,*,#47975,.F.);
#65645=ORIENTED_EDGE('',*,*,#48048,.F.);
#65646=ORIENTED_EDGE('',*,*,#48049,.T.);
#65647=ORIENTED_EDGE('',*,*,#47955,.T.);
#65648=ORIENTED_EDGE('',*,*,#46755,.T.);
#65649=ORIENTED_EDGE('',*,*,#47976,.T.);
#65650=ORIENTED_EDGE('',*,*,#48050,.T.);
#65651=ORIENTED_EDGE('',*,*,#48051,.F.);
#65652=ORIENTED_EDGE('',*,*,#47952,.F.);
#65653=ORIENTED_EDGE('',*,*,#48052,.F.);
#65654=ORIENTED_EDGE('',*,*,#48053,.F.);
#65655=ORIENTED_EDGE('',*,*,#48054,.T.);
#65656=ORIENTED_EDGE('',*,*,#48055,.F.);
#65657=ORIENTED_EDGE('',*,*,#47951,.T.);
#65658=ORIENTED_EDGE('',*,*,#48055,.T.);
#65659=ORIENTED_EDGE('',*,*,#48056,.T.);
#65660=ORIENTED_EDGE('',*,*,#48057,.T.);
#65661=ORIENTED_EDGE('',*,*,#46759,.T.);
#65662=ORIENTED_EDGE('',*,*,#48057,.F.);
#65663=ORIENTED_EDGE('',*,*,#48058,.T.);
#65664=ORIENTED_EDGE('',*,*,#48059,.F.);
#65665=ORIENTED_EDGE('',*,*,#47922,.F.);
#65666=ORIENTED_EDGE('',*,*,#48060,.T.);
#65667=ORIENTED_EDGE('',*,*,#48061,.F.);
#65668=ORIENTED_EDGE('',*,*,#47934,.F.);
#65669=ORIENTED_EDGE('',*,*,#48062,.F.);
#65670=ORIENTED_EDGE('',*,*,#48063,.T.);
#65671=ORIENTED_EDGE('',*,*,#47909,.T.);
#65672=ORIENTED_EDGE('',*,*,#46761,.T.);
#65673=ORIENTED_EDGE('',*,*,#47935,.T.);
#65674=ORIENTED_EDGE('',*,*,#48064,.T.);
#65675=ORIENTED_EDGE('',*,*,#48065,.F.);
#65676=ORIENTED_EDGE('',*,*,#47906,.F.);
#65677=ORIENTED_EDGE('',*,*,#48066,.F.);
#65678=ORIENTED_EDGE('',*,*,#48067,.F.);
#65679=ORIENTED_EDGE('',*,*,#48068,.T.);
#65680=ORIENTED_EDGE('',*,*,#48020,.F.);
#65681=ORIENTED_EDGE('',*,*,#47905,.T.);
#65682=ORIENTED_EDGE('',*,*,#48069,.T.);
#65683=ORIENTED_EDGE('',*,*,#48070,.T.);
#65684=ORIENTED_EDGE('',*,*,#47252,.T.);
#65685=ORIENTED_EDGE('',*,*,#46972,.T.);
#65686=ORIENTED_EDGE('',*,*,#48071,.T.);
#65687=ORIENTED_EDGE('',*,*,#48072,.T.);
#65688=ORIENTED_EDGE('',*,*,#47256,.T.);
#65689=ORIENTED_EDGE('',*,*,#46957,.T.);
#65690=ORIENTED_EDGE('',*,*,#46963,.T.);
#65691=ORIENTED_EDGE('',*,*,#46966,.T.);
#65692=ORIENTED_EDGE('',*,*,#46969,.T.);
#65693=ORIENTED_EDGE('',*,*,#47257,.T.);
#65694=ORIENTED_EDGE('',*,*,#48073,.T.);
#65695=ORIENTED_EDGE('',*,*,#48074,.T.);
#65696=ORIENTED_EDGE('',*,*,#47254,.F.);
#65697=ORIENTED_EDGE('',*,*,#48075,.F.);
#65698=ORIENTED_EDGE('',*,*,#48076,.T.);
#65699=ORIENTED_EDGE('',*,*,#47104,.T.);
#65700=ORIENTED_EDGE('',*,*,#46765,.T.);
#65701=ORIENTED_EDGE('',*,*,#47499,.T.);
#65702=ORIENTED_EDGE('',*,*,#47105,.T.);
#65703=ORIENTED_EDGE('',*,*,#48077,.T.);
#65704=ORIENTED_EDGE('',*,*,#47100,.F.);
#65705=ORIENTED_EDGE('',*,*,#48078,.F.);
#65706=ORIENTED_EDGE('',*,*,#46823,.T.);
#65707=ORIENTED_EDGE('',*,*,#47101,.T.);
#65708=ORIENTED_EDGE('',*,*,#48079,.T.);
#65709=ORIENTED_EDGE('',*,*,#48080,.T.);
#65710=ORIENTED_EDGE('',*,*,#47478,.T.);
#65711=ORIENTED_EDGE('',*,*,#46794,.T.);
#65712=ORIENTED_EDGE('',*,*,#46800,.T.);
#65713=ORIENTED_EDGE('',*,*,#46803,.T.);
#65714=ORIENTED_EDGE('',*,*,#46806,.T.);
#65715=ORIENTED_EDGE('',*,*,#47479,.T.);
#65716=ORIENTED_EDGE('',*,*,#48081,.T.);
#65717=ORIENTED_EDGE('',*,*,#47498,.F.);
#65718=ORIENTED_EDGE('',*,*,#48082,.F.);
#65719=ORIENTED_EDGE('',*,*,#46796,.T.);
#65720=ORIENTED_EDGE('',*,*,#47483,.T.);
#65721=ORIENTED_EDGE('',*,*,#46791,.T.);
#65722=ORIENTED_EDGE('',*,*,#46789,.T.);
#65723=ORIENTED_EDGE('',*,*,#46786,.T.);
#65724=ORIENTED_EDGE('',*,*,#47531,.T.);
#65725=ORIENTED_EDGE('',*,*,#46782,.T.);
#65726=ORIENTED_EDGE('',*,*,#47409,.T.);
#65727=ORIENTED_EDGE('',*,*,#46779,.T.);
#65728=ORIENTED_EDGE('',*,*,#46777,.T.);
#65729=ORIENTED_EDGE('',*,*,#46776,.T.);
#65730=ORIENTED_EDGE('',*,*,#47427,.T.);
#65731=ORIENTED_EDGE('',*,*,#46771,.T.);
#65732=ORIENTED_EDGE('',*,*,#46770,.T.);
#65733=ORIENTED_EDGE('',*,*,#48083,.T.);
#65734=ORIENTED_EDGE('',*,*,#48084,.T.);
#65735=ORIENTED_EDGE('',*,*,#48085,.T.);
#65736=ORIENTED_EDGE('',*,*,#48085,.F.);
#65737=ORIENTED_EDGE('',*,*,#48086,.T.);
#65738=ORIENTED_EDGE('',*,*,#48087,.F.);
#65739=ORIENTED_EDGE('',*,*,#46798,.T.);
#65740=ORIENTED_EDGE('',*,*,#48087,.T.);
#65741=ORIENTED_EDGE('',*,*,#48088,.T.);
#65742=ORIENTED_EDGE('',*,*,#48089,.T.);
#65743=ORIENTED_EDGE('',*,*,#46801,.T.);
#65744=ORIENTED_EDGE('',*,*,#48089,.F.);
#65745=ORIENTED_EDGE('',*,*,#48090,.T.);
#65746=ORIENTED_EDGE('',*,*,#48091,.F.);
#65747=ORIENTED_EDGE('',*,*,#46804,.T.);
#65748=ORIENTED_EDGE('',*,*,#46833,.T.);
#65749=ORIENTED_EDGE('',*,*,#47093,.T.);
#65750=ORIENTED_EDGE('',*,*,#46830,.T.);
#65751=ORIENTED_EDGE('',*,*,#46828,.T.);
#65752=ORIENTED_EDGE('',*,*,#46825,.T.);
#65753=ORIENTED_EDGE('',*,*,#47121,.T.);
#65754=ORIENTED_EDGE('',*,*,#46821,.T.);
#65755=ORIENTED_EDGE('',*,*,#48091,.T.);
#65756=ORIENTED_EDGE('',*,*,#48092,.T.);
#65757=ORIENTED_EDGE('',*,*,#48093,.T.);
#65758=ORIENTED_EDGE('',*,*,#46819,.T.);
#65759=ORIENTED_EDGE('',*,*,#46817,.T.);
#65760=ORIENTED_EDGE('',*,*,#47018,.T.);
#65761=ORIENTED_EDGE('',*,*,#46813,.T.);
#65762=ORIENTED_EDGE('',*,*,#46811,.T.);
#65763=ORIENTED_EDGE('',*,*,#46810,.T.);
#65764=ORIENTED_EDGE('',*,*,#47039,.T.);
#65765=ORIENTED_EDGE('',*,*,#48094,.F.);
#65766=ORIENTED_EDGE('',*,*,#46839,.T.);
#65767=ORIENTED_EDGE('',*,*,#47145,.T.);
#65768=ORIENTED_EDGE('',*,*,#46836,.T.);
#65769=ORIENTED_EDGE('',*,*,#48093,.F.);
#65770=ORIENTED_EDGE('',*,*,#48095,.T.);
#65771=ORIENTED_EDGE('',*,*,#48096,.T.);
#65772=ORIENTED_EDGE('',*,*,#46923,.T.);
#65773=ORIENTED_EDGE('',*,*,#46921,.T.);
#65774=ORIENTED_EDGE('',*,*,#46918,.T.);
#65775=ORIENTED_EDGE('',*,*,#47561,.T.);
#65776=ORIENTED_EDGE('',*,*,#46914,.T.);
#65777=ORIENTED_EDGE('',*,*,#47581,.T.);
#65778=ORIENTED_EDGE('',*,*,#46913,.T.);
#65779=ORIENTED_EDGE('',*,*,#46910,.T.);
#65780=ORIENTED_EDGE('',*,*,#46908,.T.);
#65781=ORIENTED_EDGE('',*,*,#46906,.T.);
#65782=ORIENTED_EDGE('',*,*,#47604,.T.);
#65783=ORIENTED_EDGE('',*,*,#46900,.T.);
#65784=ORIENTED_EDGE('',*,*,#47632,.T.);
#65785=ORIENTED_EDGE('',*,*,#46897,.T.);
#65786=ORIENTED_EDGE('',*,*,#46895,.T.);
#65787=ORIENTED_EDGE('',*,*,#46894,.T.);
#65788=ORIENTED_EDGE('',*,*,#47650,.T.);
#65789=ORIENTED_EDGE('',*,*,#46888,.T.);
#65790=ORIENTED_EDGE('',*,*,#47678,.T.);
#65791=ORIENTED_EDGE('',*,*,#46885,.T.);
#65792=ORIENTED_EDGE('',*,*,#46883,.T.);
#65793=ORIENTED_EDGE('',*,*,#46882,.T.);
#65794=ORIENTED_EDGE('',*,*,#47696,.T.);
#65795=ORIENTED_EDGE('',*,*,#46876,.T.);
#65796=ORIENTED_EDGE('',*,*,#47724,.T.);
#65797=ORIENTED_EDGE('',*,*,#46873,.T.);
#65798=ORIENTED_EDGE('',*,*,#46871,.T.);
#65799=ORIENTED_EDGE('',*,*,#46870,.T.);
#65800=ORIENTED_EDGE('',*,*,#47742,.T.);
#65801=ORIENTED_EDGE('',*,*,#46864,.T.);
#65802=ORIENTED_EDGE('',*,*,#47771,.T.);
#65803=ORIENTED_EDGE('',*,*,#46863,.T.);
#65804=ORIENTED_EDGE('',*,*,#46860,.T.);
#65805=ORIENTED_EDGE('',*,*,#46858,.T.);
#65806=ORIENTED_EDGE('',*,*,#46856,.T.);
#65807=ORIENTED_EDGE('',*,*,#47794,.T.);
#65808=ORIENTED_EDGE('',*,*,#46850,.T.);
#65809=ORIENTED_EDGE('',*,*,#47831,.T.);
#65810=ORIENTED_EDGE('',*,*,#46849,.T.);
#65811=ORIENTED_EDGE('',*,*,#46845,.T.);
#65812=ORIENTED_EDGE('',*,*,#46842,.T.);
#65813=ORIENTED_EDGE('',*,*,#48094,.T.);
#65814=ORIENTED_EDGE('',*,*,#48097,.T.);
#65815=ORIENTED_EDGE('',*,*,#47250,.T.);
#65816=ORIENTED_EDGE('',*,*,#46931,.T.);
#65817=ORIENTED_EDGE('',*,*,#48096,.F.);
#65818=ORIENTED_EDGE('',*,*,#48098,.T.);
#65819=ORIENTED_EDGE('',*,*,#48099,.F.);
#65820=ORIENTED_EDGE('',*,*,#46927,.T.);
#65821=ORIENTED_EDGE('',*,*,#46959,.T.);
#65822=ORIENTED_EDGE('',*,*,#47261,.T.);
#65823=ORIENTED_EDGE('',*,*,#46954,.T.);
#65824=ORIENTED_EDGE('',*,*,#46952,.T.);
#65825=ORIENTED_EDGE('',*,*,#46949,.T.);
#65826=ORIENTED_EDGE('',*,*,#47309,.T.);
#65827=ORIENTED_EDGE('',*,*,#46945,.T.);
#65828=ORIENTED_EDGE('',*,*,#47179,.T.);
#65829=ORIENTED_EDGE('',*,*,#46942,.T.);
#65830=ORIENTED_EDGE('',*,*,#46940,.T.);
#65831=ORIENTED_EDGE('',*,*,#46939,.T.);
#65832=ORIENTED_EDGE('',*,*,#47197,.T.);
#65833=ORIENTED_EDGE('',*,*,#46934,.T.);
#65834=ORIENTED_EDGE('',*,*,#46933,.T.);
#65835=ORIENTED_EDGE('',*,*,#48099,.T.);
#65836=ORIENTED_EDGE('',*,*,#48100,.T.);
#65837=ORIENTED_EDGE('',*,*,#48101,.T.);
#65838=ORIENTED_EDGE('',*,*,#48101,.F.);
#65839=ORIENTED_EDGE('',*,*,#48102,.T.);
#65840=ORIENTED_EDGE('',*,*,#48103,.F.);
#65841=ORIENTED_EDGE('',*,*,#46961,.T.);
#65842=ORIENTED_EDGE('',*,*,#48103,.T.);
#65843=ORIENTED_EDGE('',*,*,#48104,.T.);
#65844=ORIENTED_EDGE('',*,*,#48105,.T.);
#65845=ORIENTED_EDGE('',*,*,#46964,.T.);
#65846=ORIENTED_EDGE('',*,*,#48105,.F.);
#65847=ORIENTED_EDGE('',*,*,#48106,.T.);
#65848=ORIENTED_EDGE('',*,*,#48107,.F.);
#65849=ORIENTED_EDGE('',*,*,#46967,.T.);
#65850=ORIENTED_EDGE('',*,*,#48108,.T.);
#65851=ORIENTED_EDGE('',*,*,#48109,.T.);
#65852=ORIENTED_EDGE('',*,*,#48110,.T.);
#65853=ORIENTED_EDGE('',*,*,#48111,.T.);
#65854=ORIENTED_EDGE('',*,*,#46970,.T.);
#65855=ORIENTED_EDGE('',*,*,#48107,.T.);
#65856=ORIENTED_EDGE('',*,*,#48112,.T.);
#65857=ORIENTED_EDGE('',*,*,#48113,.T.);
#65858=ORIENTED_EDGE('',*,*,#48110,.F.);
#65859=ORIENTED_EDGE('',*,*,#48114,.F.);
#65860=ORIENTED_EDGE('',*,*,#48115,.F.);
#65861=ORIENTED_EDGE('',*,*,#48116,.T.);
#65862=ORIENTED_EDGE('',*,*,#48111,.F.);
#65863=ORIENTED_EDGE('',*,*,#48113,.F.);
#65864=ORIENTED_EDGE('',*,*,#48117,.F.);
#65865=ORIENTED_EDGE('',*,*,#48118,.T.);
#65866=ORIENTED_EDGE('',*,*,#46971,.F.);
#65867=ORIENTED_EDGE('',*,*,#48116,.F.);
#65868=ORIENTED_EDGE('',*,*,#48119,.F.);
#65869=ORIENTED_EDGE('',*,*,#48120,.T.);
#65870=ORIENTED_EDGE('',*,*,#48071,.F.);
#65871=ORIENTED_EDGE('',*,*,#48118,.F.);
#65872=ORIENTED_EDGE('',*,*,#48121,.F.);
#65873=ORIENTED_EDGE('',*,*,#48122,.T.);
#65874=ORIENTED_EDGE('',*,*,#48123,.T.);
#65875=ORIENTED_EDGE('',*,*,#48120,.F.);
#65876=ORIENTED_EDGE('',*,*,#48124,.F.);
#65877=ORIENTED_EDGE('',*,*,#46975,.T.);
#65878=ORIENTED_EDGE('',*,*,#48070,.F.);
#65879=ORIENTED_EDGE('',*,*,#48122,.F.);
#65880=ORIENTED_EDGE('',*,*,#48125,.F.);
#65881=ORIENTED_EDGE('',*,*,#48126,.F.);
#65882=ORIENTED_EDGE('',*,*,#46973,.T.);
#65883=ORIENTED_EDGE('',*,*,#48127,.F.);
#65884=ORIENTED_EDGE('',*,*,#48128,.T.);
#65885=ORIENTED_EDGE('',*,*,#47329,.T.);
#65886=ORIENTED_EDGE('',*,*,#48129,.F.);
#65887=ORIENTED_EDGE('',*,*,#48130,.F.);
#65888=ORIENTED_EDGE('',*,*,#48131,.F.);
#65889=ORIENTED_EDGE('',*,*,#48132,.T.);
#65890=ORIENTED_EDGE('',*,*,#47367,.T.);
#65891=ORIENTED_EDGE('',*,*,#46976,.T.);
#65892=ORIENTED_EDGE('',*,*,#47330,.T.);
#65893=ORIENTED_EDGE('',*,*,#47368,.T.);
#65894=ORIENTED_EDGE('',*,*,#48133,.F.);
#65895=ORIENTED_EDGE('',*,*,#48134,.T.);
#65896=ORIENTED_EDGE('',*,*,#48135,.F.);
#65897=ORIENTED_EDGE('',*,*,#48136,.F.);
#65898=ORIENTED_EDGE('',*,*,#48137,.T.);
#65899=ORIENTED_EDGE('',*,*,#48138,.F.);
#65900=ORIENTED_EDGE('',*,*,#47365,.T.);
#65901=ORIENTED_EDGE('',*,*,#48138,.T.);
#65902=ORIENTED_EDGE('',*,*,#48139,.T.);
#65903=ORIENTED_EDGE('',*,*,#48140,.T.);
#65904=ORIENTED_EDGE('',*,*,#47360,.T.);
#65905=ORIENTED_EDGE('',*,*,#48140,.F.);
#65906=ORIENTED_EDGE('',*,*,#48141,.T.);
#65907=ORIENTED_EDGE('',*,*,#48142,.F.);
#65908=ORIENTED_EDGE('',*,*,#47356,.F.);
#65909=ORIENTED_EDGE('',*,*,#47354,.T.);
#65910=ORIENTED_EDGE('',*,*,#48143,.F.);
#65911=ORIENTED_EDGE('',*,*,#48144,.F.);
#65912=ORIENTED_EDGE('',*,*,#48145,.F.);
#65913=ORIENTED_EDGE('',*,*,#48146,.T.);
#65914=ORIENTED_EDGE('',*,*,#47883,.T.);
#65915=ORIENTED_EDGE('',*,*,#46979,.T.);
#65916=ORIENTED_EDGE('',*,*,#47355,.T.);
#65917=ORIENTED_EDGE('',*,*,#47884,.T.);
#65918=ORIENTED_EDGE('',*,*,#48147,.F.);
#65919=ORIENTED_EDGE('',*,*,#48148,.T.);
#65920=ORIENTED_EDGE('',*,*,#48149,.F.);
#65921=ORIENTED_EDGE('',*,*,#48150,.F.);
#65922=ORIENTED_EDGE('',*,*,#48151,.T.);
#65923=ORIENTED_EDGE('',*,*,#48152,.F.);
#65924=ORIENTED_EDGE('',*,*,#47881,.T.);
#65925=ORIENTED_EDGE('',*,*,#48152,.T.);
#65926=ORIENTED_EDGE('',*,*,#48153,.T.);
#65927=ORIENTED_EDGE('',*,*,#48154,.T.);
#65928=ORIENTED_EDGE('',*,*,#47876,.T.);
#65929=ORIENTED_EDGE('',*,*,#48154,.F.);
#65930=ORIENTED_EDGE('',*,*,#48155,.T.);
#65931=ORIENTED_EDGE('',*,*,#48156,.F.);
#65932=ORIENTED_EDGE('',*,*,#47872,.F.);
#65933=ORIENTED_EDGE('',*,*,#47870,.T.);
#65934=ORIENTED_EDGE('',*,*,#48157,.F.);
#65935=ORIENTED_EDGE('',*,*,#48158,.F.);
#65936=ORIENTED_EDGE('',*,*,#48159,.F.);
#65937=ORIENTED_EDGE('',*,*,#48160,.T.);
#65938=ORIENTED_EDGE('',*,*,#47871,.T.);
#65939=ORIENTED_EDGE('',*,*,#48161,.T.);
#65940=ORIENTED_EDGE('',*,*,#48162,.T.);
#65941=ORIENTED_EDGE('',*,*,#47856,.T.);
#65942=ORIENTED_EDGE('',*,*,#48163,.F.);
#65943=ORIENTED_EDGE('',*,*,#47868,.T.);
#65944=ORIENTED_EDGE('',*,*,#48160,.F.);
#65945=ORIENTED_EDGE('',*,*,#47857,.T.);
#65946=ORIENTED_EDGE('',*,*,#48164,.F.);
#65947=ORIENTED_EDGE('',*,*,#48165,.T.);
#65948=ORIENTED_EDGE('',*,*,#48166,.F.);
#65949=ORIENTED_EDGE('',*,*,#48167,.T.);
#65950=ORIENTED_EDGE('',*,*,#48168,.F.);
#65951=ORIENTED_EDGE('',*,*,#48165,.F.);
#65952=ORIENTED_EDGE('',*,*,#48169,.F.);
#65953=ORIENTED_EDGE('',*,*,#48170,.F.);
#65954=ORIENTED_EDGE('',*,*,#48171,.T.);
#65955=ORIENTED_EDGE('',*,*,#48172,.F.);
#65956=ORIENTED_EDGE('',*,*,#48173,.T.);
#65957=ORIENTED_EDGE('',*,*,#48172,.T.);
#65958=ORIENTED_EDGE('',*,*,#48174,.T.);
#65959=ORIENTED_EDGE('',*,*,#48175,.T.);
#65960=ORIENTED_EDGE('',*,*,#48176,.T.);
#65961=ORIENTED_EDGE('',*,*,#48175,.F.);
#65962=ORIENTED_EDGE('',*,*,#48177,.T.);
#65963=ORIENTED_EDGE('',*,*,#48178,.F.);
#65964=ORIENTED_EDGE('',*,*,#48179,.T.);
#65965=ORIENTED_EDGE('',*,*,#47853,.T.);
#65966=ORIENTED_EDGE('',*,*,#48180,.F.);
#65967=ORIENTED_EDGE('',*,*,#48181,.F.);
#65968=ORIENTED_EDGE('',*,*,#48182,.F.);
#65969=ORIENTED_EDGE('',*,*,#48183,.F.);
#65970=ORIENTED_EDGE('',*,*,#47849,.T.);
#65971=ORIENTED_EDGE('',*,*,#48184,.F.);
#65972=ORIENTED_EDGE('',*,*,#48185,.F.);
#65973=ORIENTED_EDGE('',*,*,#48186,.T.);
#65974=ORIENTED_EDGE('',*,*,#48187,.F.);
#65975=ORIENTED_EDGE('',*,*,#48188,.F.);
#65976=ORIENTED_EDGE('',*,*,#48189,.T.);
#65977=ORIENTED_EDGE('',*,*,#48190,.F.);
#65978=ORIENTED_EDGE('',*,*,#48191,.T.);
#65979=ORIENTED_EDGE('',*,*,#48190,.T.);
#65980=ORIENTED_EDGE('',*,*,#48192,.T.);
#65981=ORIENTED_EDGE('',*,*,#48193,.T.);
#65982=ORIENTED_EDGE('',*,*,#48194,.T.);
#65983=ORIENTED_EDGE('',*,*,#48193,.F.);
#65984=ORIENTED_EDGE('',*,*,#48195,.T.);
#65985=ORIENTED_EDGE('',*,*,#48196,.F.);
#65986=ORIENTED_EDGE('',*,*,#48197,.T.);
#65987=ORIENTED_EDGE('',*,*,#48198,.T.);
#65988=ORIENTED_EDGE('',*,*,#46987,.F.);
#65989=ORIENTED_EDGE('',*,*,#48199,.F.);
#65990=ORIENTED_EDGE('',*,*,#48200,.F.);
#65991=ORIENTED_EDGE('',*,*,#48201,.T.);
#65992=ORIENTED_EDGE('',*,*,#47344,.F.);
#65993=ORIENTED_EDGE('',*,*,#48198,.F.);
#65994=ORIENTED_EDGE('',*,*,#48202,.F.);
#65995=ORIENTED_EDGE('',*,*,#48203,.T.);
#65996=ORIENTED_EDGE('',*,*,#48204,.F.);
#65997=ORIENTED_EDGE('',*,*,#48201,.F.);
#65998=ORIENTED_EDGE('',*,*,#48205,.F.);
#65999=ORIENTED_EDGE('',*,*,#48206,.T.);
#66000=ORIENTED_EDGE('',*,*,#48207,.F.);
#66001=ORIENTED_EDGE('',*,*,#48128,.F.);
#66002=ORIENTED_EDGE('',*,*,#48208,.F.);
#66003=ORIENTED_EDGE('',*,*,#48199,.T.);
#66004=ORIENTED_EDGE('',*,*,#47275,.F.);
#66005=ORIENTED_EDGE('',*,*,#48206,.F.);
#66006=ORIENTED_EDGE('',*,*,#48209,.F.);
#66007=ORIENTED_EDGE('',*,*,#48210,.T.);
#66008=ORIENTED_EDGE('',*,*,#47342,.F.);
#66009=ORIENTED_EDGE('',*,*,#48203,.F.);
#66010=ORIENTED_EDGE('',*,*,#48211,.F.);
#66011=ORIENTED_EDGE('',*,*,#47343,.T.);
#66012=ORIENTED_EDGE('',*,*,#48212,.T.);
#66013=ORIENTED_EDGE('',*,*,#48213,.T.);
#66014=ORIENTED_EDGE('',*,*,#47337,.T.);
#66015=ORIENTED_EDGE('',*,*,#48213,.F.);
#66016=ORIENTED_EDGE('',*,*,#48214,.T.);
#66017=ORIENTED_EDGE('',*,*,#48215,.F.);
#66018=ORIENTED_EDGE('',*,*,#47331,.F.);
#66019=ORIENTED_EDGE('',*,*,#47457,.T.);
#66020=ORIENTED_EDGE('',*,*,#48216,.F.);
#66021=ORIENTED_EDGE('',*,*,#48217,.F.);
#66022=ORIENTED_EDGE('',*,*,#48218,.F.);
#66023=ORIENTED_EDGE('',*,*,#48219,.F.);
#66024=ORIENTED_EDGE('',*,*,#47901,.T.);
#66025=ORIENTED_EDGE('',*,*,#46983,.F.);
#66026=ORIENTED_EDGE('',*,*,#48218,.T.);
#66027=ORIENTED_EDGE('',*,*,#47110,.T.);
#66028=ORIENTED_EDGE('',*,*,#48220,.F.);
#66029=ORIENTED_EDGE('',*,*,#48221,.F.);
#66030=ORIENTED_EDGE('',*,*,#48222,.F.);
#66031=ORIENTED_EDGE('',*,*,#48223,.F.);
#66032=ORIENTED_EDGE('',*,*,#48224,.T.);
#66033=ORIENTED_EDGE('',*,*,#48225,.T.);
#66034=ORIENTED_EDGE('',*,*,#47494,.T.);
#66035=ORIENTED_EDGE('',*,*,#46990,.T.);
#66036=ORIENTED_EDGE('',*,*,#47111,.T.);
#66037=ORIENTED_EDGE('',*,*,#48226,.T.);
#66038=ORIENTED_EDGE('',*,*,#48224,.F.);
#66039=ORIENTED_EDGE('',*,*,#48223,.T.);
#66040=ORIENTED_EDGE('',*,*,#48227,.F.);
#66041=ORIENTED_EDGE('',*,*,#48228,.T.);
#66042=ORIENTED_EDGE('',*,*,#48229,.T.);
#66043=ORIENTED_EDGE('',*,*,#48227,.T.);
#66044=ORIENTED_EDGE('',*,*,#48229,.F.);
#66045=ORIENTED_EDGE('',*,*,#48230,.T.);
#66046=ORIENTED_EDGE('',*,*,#48231,.F.);
#66047=ORIENTED_EDGE('',*,*,#47491,.F.);
#66048=ORIENTED_EDGE('',*,*,#48232,.F.);
#66049=ORIENTED_EDGE('',*,*,#48233,.T.);
#66050=ORIENTED_EDGE('',*,*,#48234,.F.);
#66051=ORIENTED_EDGE('',*,*,#48235,.F.);
#66052=ORIENTED_EDGE('',*,*,#48236,.F.);
#66053=ORIENTED_EDGE('',*,*,#48237,.T.);
#66054=ORIENTED_EDGE('',*,*,#47346,.F.);
#66055=ORIENTED_EDGE('',*,*,#48233,.F.);
#66056=ORIENTED_EDGE('',*,*,#48238,.F.);
#66057=ORIENTED_EDGE('',*,*,#48239,.T.);
#66058=ORIENTED_EDGE('',*,*,#46989,.F.);
#66059=ORIENTED_EDGE('',*,*,#48237,.F.);
#66060=ORIENTED_EDGE('',*,*,#48240,.F.);
#66061=ORIENTED_EDGE('',*,*,#48241,.T.);
#66062=ORIENTED_EDGE('',*,*,#47276,.F.);
#66063=ORIENTED_EDGE('',*,*,#48239,.F.);
#66064=ORIENTED_EDGE('',*,*,#48242,.F.);
#66065=ORIENTED_EDGE('',*,*,#47271,.T.);
#66066=ORIENTED_EDGE('',*,*,#48243,.F.);
#66067=ORIENTED_EDGE('',*,*,#48241,.F.);
#66068=ORIENTED_EDGE('',*,*,#48244,.F.);
#66069=ORIENTED_EDGE('',*,*,#48245,.F.);
#66070=ORIENTED_EDGE('',*,*,#48246,.T.);
#66071=ORIENTED_EDGE('',*,*,#47272,.T.);
#66072=ORIENTED_EDGE('',*,*,#48247,.T.);
#66073=ORIENTED_EDGE('',*,*,#47273,.T.);
#66074=ORIENTED_EDGE('',*,*,#48246,.F.);
#66075=ORIENTED_EDGE('',*,*,#48245,.T.);
#66076=ORIENTED_EDGE('',*,*,#48248,.F.);
#66077=ORIENTED_EDGE('',*,*,#48249,.T.);
#66078=ORIENTED_EDGE('',*,*,#48250,.T.);
#66079=ORIENTED_EDGE('',*,*,#48248,.T.);
#66080=ORIENTED_EDGE('',*,*,#48250,.F.);
#66081=ORIENTED_EDGE('',*,*,#47269,.T.);
#66082=ORIENTED_EDGE('',*,*,#48251,.F.);
#66083=ORIENTED_EDGE('',*,*,#48252,.F.);
#66084=ORIENTED_EDGE('',*,*,#48253,.F.);
#66085=ORIENTED_EDGE('',*,*,#48254,.T.);
#66086=ORIENTED_EDGE('',*,*,#47021,.T.);
#66087=ORIENTED_EDGE('',*,*,#48255,.T.);
#66088=ORIENTED_EDGE('',*,*,#47019,.T.);
#66089=ORIENTED_EDGE('',*,*,#47017,.T.);
#66090=ORIENTED_EDGE('',*,*,#47016,.T.);
#66091=ORIENTED_EDGE('',*,*,#47013,.T.);
#66092=ORIENTED_EDGE('',*,*,#47011,.T.);
#66093=ORIENTED_EDGE('',*,*,#47009,.T.);
#66094=ORIENTED_EDGE('',*,*,#47007,.T.);
#66095=ORIENTED_EDGE('',*,*,#47005,.T.);
#66096=ORIENTED_EDGE('',*,*,#47003,.T.);
#66097=ORIENTED_EDGE('',*,*,#47001,.T.);
#66098=ORIENTED_EDGE('',*,*,#47149,.T.);
#66099=ORIENTED_EDGE('',*,*,#47023,.T.);
#66100=ORIENTED_EDGE('',*,*,#48256,.T.);
#66101=ORIENTED_EDGE('',*,*,#48257,.T.);
#66102=ORIENTED_EDGE('',*,*,#48258,.T.);
#66103=ORIENTED_EDGE('',*,*,#47024,.T.);
#66104=ORIENTED_EDGE('',*,*,#46996,.T.);
#66105=ORIENTED_EDGE('',*,*,#46994,.T.);
#66106=ORIENTED_EDGE('',*,*,#47022,.T.);
#66107=ORIENTED_EDGE('',*,*,#48259,.F.);
#66108=ORIENTED_EDGE('',*,*,#48260,.F.);
#66109=ORIENTED_EDGE('',*,*,#48261,.F.);
#66110=ORIENTED_EDGE('',*,*,#48256,.F.);
#66111=ORIENTED_EDGE('',*,*,#48258,.F.);
#66112=ORIENTED_EDGE('',*,*,#48262,.T.);
#66113=ORIENTED_EDGE('',*,*,#48263,.F.);
#66114=ORIENTED_EDGE('',*,*,#47025,.T.);
#66115=ORIENTED_EDGE('',*,*,#48263,.T.);
#66116=ORIENTED_EDGE('',*,*,#48264,.T.);
#66117=ORIENTED_EDGE('',*,*,#48265,.T.);
#66118=ORIENTED_EDGE('',*,*,#47027,.T.);
#66119=ORIENTED_EDGE('',*,*,#48265,.F.);
#66120=ORIENTED_EDGE('',*,*,#48266,.T.);
#66121=ORIENTED_EDGE('',*,*,#48267,.F.);
#66122=ORIENTED_EDGE('',*,*,#47029,.F.);
#66123=ORIENTED_EDGE('',*,*,#48267,.T.);
#66124=ORIENTED_EDGE('',*,*,#48268,.T.);
#66125=ORIENTED_EDGE('',*,*,#48269,.T.);
#66126=ORIENTED_EDGE('',*,*,#47059,.T.);
#66127=ORIENTED_EDGE('',*,*,#47056,.T.);
#66128=ORIENTED_EDGE('',*,*,#47054,.T.);
#66129=ORIENTED_EDGE('',*,*,#47052,.T.);
#66130=ORIENTED_EDGE('',*,*,#47050,.T.);
#66131=ORIENTED_EDGE('',*,*,#47048,.T.);
#66132=ORIENTED_EDGE('',*,*,#47046,.T.);
#66133=ORIENTED_EDGE('',*,*,#47044,.T.);
#66134=ORIENTED_EDGE('',*,*,#47042,.T.);
#66135=ORIENTED_EDGE('',*,*,#47040,.T.);
#66136=ORIENTED_EDGE('',*,*,#47037,.T.);
#66137=ORIENTED_EDGE('',*,*,#47036,.T.);
#66138=ORIENTED_EDGE('',*,*,#47034,.T.);
#66139=ORIENTED_EDGE('',*,*,#47032,.T.);
#66140=ORIENTED_EDGE('',*,*,#47030,.T.);
#66141=ORIENTED_EDGE('',*,*,#47060,.T.);
#66142=ORIENTED_EDGE('',*,*,#48269,.F.);
#66143=ORIENTED_EDGE('',*,*,#48270,.F.);
#66144=ORIENTED_EDGE('',*,*,#48271,.F.);
#66145=ORIENTED_EDGE('',*,*,#47062,.T.);
#66146=ORIENTED_EDGE('',*,*,#47061,.T.);
#66147=ORIENTED_EDGE('',*,*,#48272,.T.);
#66148=ORIENTED_EDGE('',*,*,#47072,.T.);
#66149=ORIENTED_EDGE('',*,*,#48273,.T.);
#66150=ORIENTED_EDGE('',*,*,#48274,.F.);
#66151=ORIENTED_EDGE('',*,*,#47069,.F.);
#66152=ORIENTED_EDGE('',*,*,#48275,.F.);
#66153=ORIENTED_EDGE('',*,*,#47094,.T.);
#66154=ORIENTED_EDGE('',*,*,#47092,.T.);
#66155=ORIENTED_EDGE('',*,*,#47091,.T.);
#66156=ORIENTED_EDGE('',*,*,#47088,.T.);
#66157=ORIENTED_EDGE('',*,*,#47086,.T.);
#66158=ORIENTED_EDGE('',*,*,#47084,.T.);
#66159=ORIENTED_EDGE('',*,*,#47082,.T.);
#66160=ORIENTED_EDGE('',*,*,#47079,.T.);
#66161=ORIENTED_EDGE('',*,*,#47077,.T.);
#66162=ORIENTED_EDGE('',*,*,#47075,.T.);
#66163=ORIENTED_EDGE('',*,*,#47073,.T.);
#66164=ORIENTED_EDGE('',*,*,#47070,.T.);
#66165=ORIENTED_EDGE('',*,*,#48274,.T.);
#66166=ORIENTED_EDGE('',*,*,#48276,.T.);
#66167=ORIENTED_EDGE('',*,*,#48277,.T.);
#66168=ORIENTED_EDGE('',*,*,#47095,.T.);
#66169=ORIENTED_EDGE('',*,*,#47067,.T.);
#66170=ORIENTED_EDGE('',*,*,#47065,.T.);
#66171=ORIENTED_EDGE('',*,*,#48277,.F.);
#66172=ORIENTED_EDGE('',*,*,#48278,.T.);
#66173=ORIENTED_EDGE('',*,*,#48279,.F.);
#66174=ORIENTED_EDGE('',*,*,#47096,.T.);
#66175=ORIENTED_EDGE('',*,*,#48279,.T.);
#66176=ORIENTED_EDGE('',*,*,#48280,.T.);
#66177=ORIENTED_EDGE('',*,*,#48281,.T.);
#66178=ORIENTED_EDGE('',*,*,#47098,.T.);
#66179=ORIENTED_EDGE('',*,*,#48281,.F.);
#66180=ORIENTED_EDGE('',*,*,#48282,.T.);
#66181=ORIENTED_EDGE('',*,*,#48283,.F.);
#66182=ORIENTED_EDGE('',*,*,#47113,.T.);
#66183=ORIENTED_EDGE('',*,*,#47123,.T.);
#66184=ORIENTED_EDGE('',*,*,#47122,.T.);
#66185=ORIENTED_EDGE('',*,*,#47119,.T.);
#66186=ORIENTED_EDGE('',*,*,#47118,.T.);
#66187=ORIENTED_EDGE('',*,*,#47116,.T.);
#66188=ORIENTED_EDGE('',*,*,#47114,.T.);
#66189=ORIENTED_EDGE('',*,*,#48283,.T.);
#66190=ORIENTED_EDGE('',*,*,#48284,.T.);
#66191=ORIENTED_EDGE('',*,*,#48285,.T.);
#66192=ORIENTED_EDGE('',*,*,#48220,.T.);
#66193=ORIENTED_EDGE('',*,*,#47109,.T.);
#66194=ORIENTED_EDGE('',*,*,#47107,.T.);
#66195=ORIENTED_EDGE('',*,*,#47497,.T.);
#66196=ORIENTED_EDGE('',*,*,#47106,.T.);
#66197=ORIENTED_EDGE('',*,*,#48078,.T.);
#66198=ORIENTED_EDGE('',*,*,#47103,.T.);
#66199=ORIENTED_EDGE('',*,*,#48221,.T.);
#66200=ORIENTED_EDGE('',*,*,#48285,.F.);
#66201=ORIENTED_EDGE('',*,*,#48286,.F.);
#66202=ORIENTED_EDGE('',*,*,#48287,.F.);
#66203=ORIENTED_EDGE('',*,*,#47147,.T.);
#66204=ORIENTED_EDGE('',*,*,#47146,.T.);
#66205=ORIENTED_EDGE('',*,*,#47143,.T.);
#66206=ORIENTED_EDGE('',*,*,#47141,.T.);
#66207=ORIENTED_EDGE('',*,*,#47139,.T.);
#66208=ORIENTED_EDGE('',*,*,#47839,.T.);
#66209=ORIENTED_EDGE('',*,*,#48288,.T.);
#66210=ORIENTED_EDGE('',*,*,#48289,.T.);
#66211=ORIENTED_EDGE('',*,*,#48290,.T.);
#66212=ORIENTED_EDGE('',*,*,#47152,.T.);
#66213=ORIENTED_EDGE('',*,*,#47137,.T.);
#66214=ORIENTED_EDGE('',*,*,#47134,.T.);
#66215=ORIENTED_EDGE('',*,*,#47132,.T.);
#66216=ORIENTED_EDGE('',*,*,#47130,.T.);
#66217=ORIENTED_EDGE('',*,*,#47128,.T.);
#66218=ORIENTED_EDGE('',*,*,#47126,.T.);
#66219=ORIENTED_EDGE('',*,*,#48291,.T.);
#66220=ORIENTED_EDGE('',*,*,#48292,.F.);
#66221=ORIENTED_EDGE('',*,*,#47150,.F.);
#66222=ORIENTED_EDGE('',*,*,#48290,.F.);
#66223=ORIENTED_EDGE('',*,*,#47153,.F.);
#66224=ORIENTED_EDGE('',*,*,#47151,.T.);
#66225=ORIENTED_EDGE('',*,*,#48293,.T.);
#66226=ORIENTED_EDGE('',*,*,#48255,.F.);
#66227=ORIENTED_EDGE('',*,*,#47148,.T.);
#66228=ORIENTED_EDGE('',*,*,#47181,.T.);
#66229=ORIENTED_EDGE('',*,*,#47180,.T.);
#66230=ORIENTED_EDGE('',*,*,#47178,.T.);
#66231=ORIENTED_EDGE('',*,*,#47176,.T.);
#66232=ORIENTED_EDGE('',*,*,#47174,.T.);
#66233=ORIENTED_EDGE('',*,*,#47172,.T.);
#66234=ORIENTED_EDGE('',*,*,#47170,.T.);
#66235=ORIENTED_EDGE('',*,*,#47168,.T.);
#66236=ORIENTED_EDGE('',*,*,#47166,.T.);
#66237=ORIENTED_EDGE('',*,*,#47164,.T.);
#66238=ORIENTED_EDGE('',*,*,#47162,.T.);
#66239=ORIENTED_EDGE('',*,*,#47315,.T.);
#66240=ORIENTED_EDGE('',*,*,#48294,.T.);
#66241=ORIENTED_EDGE('',*,*,#48295,.T.);
#66242=ORIENTED_EDGE('',*,*,#48296,.T.);
#66243=ORIENTED_EDGE('',*,*,#47182,.T.);
#66244=ORIENTED_EDGE('',*,*,#47157,.T.);
#66245=ORIENTED_EDGE('',*,*,#47155,.T.);
#66246=ORIENTED_EDGE('',*,*,#48296,.F.);
#66247=ORIENTED_EDGE('',*,*,#48297,.T.);
#66248=ORIENTED_EDGE('',*,*,#48298,.F.);
#66249=ORIENTED_EDGE('',*,*,#47183,.T.);
#66250=ORIENTED_EDGE('',*,*,#48298,.T.);
#66251=ORIENTED_EDGE('',*,*,#48299,.T.);
#66252=ORIENTED_EDGE('',*,*,#48300,.T.);
#66253=ORIENTED_EDGE('',*,*,#47185,.T.);
#66254=ORIENTED_EDGE('',*,*,#48300,.F.);
#66255=ORIENTED_EDGE('',*,*,#48301,.T.);
#66256=ORIENTED_EDGE('',*,*,#48302,.F.);
#66257=ORIENTED_EDGE('',*,*,#47187,.F.);
#66258=ORIENTED_EDGE('',*,*,#48302,.T.);
#66259=ORIENTED_EDGE('',*,*,#48303,.T.);
#66260=ORIENTED_EDGE('',*,*,#48304,.T.);
#66261=ORIENTED_EDGE('',*,*,#47216,.T.);
#66262=ORIENTED_EDGE('',*,*,#47219,.T.);
#66263=ORIENTED_EDGE('',*,*,#47212,.T.);
#66264=ORIENTED_EDGE('',*,*,#47210,.T.);
#66265=ORIENTED_EDGE('',*,*,#47208,.T.);
#66266=ORIENTED_EDGE('',*,*,#47206,.T.);
#66267=ORIENTED_EDGE('',*,*,#47204,.T.);
#66268=ORIENTED_EDGE('',*,*,#47202,.T.);
#66269=ORIENTED_EDGE('',*,*,#47200,.T.);
#66270=ORIENTED_EDGE('',*,*,#47198,.T.);
#66271=ORIENTED_EDGE('',*,*,#47195,.T.);
#66272=ORIENTED_EDGE('',*,*,#47194,.T.);
#66273=ORIENTED_EDGE('',*,*,#47192,.T.);
#66274=ORIENTED_EDGE('',*,*,#47190,.T.);
#66275=ORIENTED_EDGE('',*,*,#47188,.T.);
#66276=ORIENTED_EDGE('',*,*,#47217,.T.);
#66277=ORIENTED_EDGE('',*,*,#48304,.F.);
#66278=ORIENTED_EDGE('',*,*,#48305,.F.);
#66279=ORIENTED_EDGE('',*,*,#48306,.F.);
#66280=ORIENTED_EDGE('',*,*,#48307,.T.);
#66281=ORIENTED_EDGE('',*,*,#47218,.T.);
#66282=ORIENTED_EDGE('',*,*,#48308,.T.);
#66283=ORIENTED_EDGE('',*,*,#47221,.F.);
#66284=ORIENTED_EDGE('',*,*,#47220,.T.);
#66285=ORIENTED_EDGE('',*,*,#48307,.F.);
#66286=ORIENTED_EDGE('',*,*,#48309,.T.);
#66287=ORIENTED_EDGE('',*,*,#48310,.T.);
#66288=ORIENTED_EDGE('',*,*,#47234,.T.);
#66289=ORIENTED_EDGE('',*,*,#48311,.T.);
#66290=ORIENTED_EDGE('',*,*,#47231,.T.);
#66291=ORIENTED_EDGE('',*,*,#48310,.F.);
#66292=ORIENTED_EDGE('',*,*,#48312,.T.);
#66293=ORIENTED_EDGE('',*,*,#48313,.F.);
#66294=ORIENTED_EDGE('',*,*,#47228,.F.);
#66295=ORIENTED_EDGE('',*,*,#48314,.F.);
#66296=ORIENTED_EDGE('',*,*,#47251,.T.);
#66297=ORIENTED_EDGE('',*,*,#47249,.T.);
#66298=ORIENTED_EDGE('',*,*,#47247,.T.);
#66299=ORIENTED_EDGE('',*,*,#47245,.T.);
#66300=ORIENTED_EDGE('',*,*,#47243,.T.);
#66301=ORIENTED_EDGE('',*,*,#47241,.T.);
#66302=ORIENTED_EDGE('',*,*,#47239,.T.);
#66303=ORIENTED_EDGE('',*,*,#47237,.T.);
#66304=ORIENTED_EDGE('',*,*,#47235,.T.);
#66305=ORIENTED_EDGE('',*,*,#47232,.T.);
#66306=ORIENTED_EDGE('',*,*,#47229,.T.);
#66307=ORIENTED_EDGE('',*,*,#48313,.T.);
#66308=ORIENTED_EDGE('',*,*,#48315,.T.);
#66309=ORIENTED_EDGE('',*,*,#48316,.T.);
#66310=ORIENTED_EDGE('',*,*,#47840,.T.);
#66311=ORIENTED_EDGE('',*,*,#47226,.T.);
#66312=ORIENTED_EDGE('',*,*,#47224,.T.);
#66313=ORIENTED_EDGE('',*,*,#48126,.T.);
#66314=ORIENTED_EDGE('',*,*,#48207,.T.);
#66315=ORIENTED_EDGE('',*,*,#47274,.T.);
#66316=ORIENTED_EDGE('',*,*,#48243,.T.);
#66317=ORIENTED_EDGE('',*,*,#47270,.T.);
#66318=ORIENTED_EDGE('',*,*,#48253,.T.);
#66319=ORIENTED_EDGE('',*,*,#48317,.T.);
#66320=ORIENTED_EDGE('',*,*,#48318,.T.);
#66321=ORIENTED_EDGE('',*,*,#48319,.T.);
#66322=ORIENTED_EDGE('',*,*,#47277,.T.);
#66323=ORIENTED_EDGE('',*,*,#47267,.T.);
#66324=ORIENTED_EDGE('',*,*,#47265,.T.);
#66325=ORIENTED_EDGE('',*,*,#47263,.T.);
#66326=ORIENTED_EDGE('',*,*,#47262,.T.);
#66327=ORIENTED_EDGE('',*,*,#47260,.T.);
#66328=ORIENTED_EDGE('',*,*,#47258,.T.);
#66329=ORIENTED_EDGE('',*,*,#48075,.T.);
#66330=ORIENTED_EDGE('',*,*,#47253,.T.);
#66331=ORIENTED_EDGE('',*,*,#48252,.T.);
#66332=ORIENTED_EDGE('',*,*,#48320,.F.);
#66333=ORIENTED_EDGE('',*,*,#48321,.F.);
#66334=ORIENTED_EDGE('',*,*,#48317,.F.);
#66335=ORIENTED_EDGE('',*,*,#48319,.F.);
#66336=ORIENTED_EDGE('',*,*,#48322,.T.);
#66337=ORIENTED_EDGE('',*,*,#48323,.F.);
#66338=ORIENTED_EDGE('',*,*,#47278,.T.);
#66339=ORIENTED_EDGE('',*,*,#48323,.T.);
#66340=ORIENTED_EDGE('',*,*,#48324,.T.);
#66341=ORIENTED_EDGE('',*,*,#48325,.T.);
#66342=ORIENTED_EDGE('',*,*,#47280,.T.);
#66343=ORIENTED_EDGE('',*,*,#48325,.F.);
#66344=ORIENTED_EDGE('',*,*,#48326,.T.);
#66345=ORIENTED_EDGE('',*,*,#48327,.F.);
#66346=ORIENTED_EDGE('',*,*,#47300,.F.);
#66347=ORIENTED_EDGE('',*,*,#47312,.T.);
#66348=ORIENTED_EDGE('',*,*,#47310,.T.);
#66349=ORIENTED_EDGE('',*,*,#47307,.T.);
#66350=ORIENTED_EDGE('',*,*,#47305,.T.);
#66351=ORIENTED_EDGE('',*,*,#47303,.T.);
#66352=ORIENTED_EDGE('',*,*,#47301,.T.);
#66353=ORIENTED_EDGE('',*,*,#48327,.T.);
#66354=ORIENTED_EDGE('',*,*,#48328,.T.);
#66355=ORIENTED_EDGE('',*,*,#48329,.T.);
#66356=ORIENTED_EDGE('',*,*,#47318,.T.);
#66357=ORIENTED_EDGE('',*,*,#47299,.T.);
#66358=ORIENTED_EDGE('',*,*,#47296,.T.);
#66359=ORIENTED_EDGE('',*,*,#47294,.T.);
#66360=ORIENTED_EDGE('',*,*,#47292,.T.);
#66361=ORIENTED_EDGE('',*,*,#47290,.T.);
#66362=ORIENTED_EDGE('',*,*,#47288,.T.);
#66363=ORIENTED_EDGE('',*,*,#47286,.T.);
#66364=ORIENTED_EDGE('',*,*,#47284,.T.);
#66365=ORIENTED_EDGE('',*,*,#47314,.T.);
#66366=ORIENTED_EDGE('',*,*,#48330,.F.);
#66367=ORIENTED_EDGE('',*,*,#48331,.F.);
#66368=ORIENTED_EDGE('',*,*,#48294,.F.);
#66369=ORIENTED_EDGE('',*,*,#48332,.T.);
#66370=ORIENTED_EDGE('',*,*,#48333,.F.);
#66371=ORIENTED_EDGE('',*,*,#47316,.F.);
#66372=ORIENTED_EDGE('',*,*,#48329,.F.);
#66373=ORIENTED_EDGE('',*,*,#47319,.T.);
#66374=ORIENTED_EDGE('',*,*,#47317,.T.);
#66375=ORIENTED_EDGE('',*,*,#48334,.T.);
#66376=ORIENTED_EDGE('',*,*,#47313,.T.);
#66377=ORIENTED_EDGE('',*,*,#48215,.T.);
#66378=ORIENTED_EDGE('',*,*,#48335,.T.);
#66379=ORIENTED_EDGE('',*,*,#48129,.T.);
#66380=ORIENTED_EDGE('',*,*,#47328,.T.);
#66381=ORIENTED_EDGE('',*,*,#47326,.T.);
#66382=ORIENTED_EDGE('',*,*,#47324,.T.);
#66383=ORIENTED_EDGE('',*,*,#47321,.T.);
#66384=ORIENTED_EDGE('',*,*,#47378,.T.);
#66385=ORIENTED_EDGE('',*,*,#48336,.T.);
#66386=ORIENTED_EDGE('',*,*,#48337,.T.);
#66387=ORIENTED_EDGE('',*,*,#48338,.T.);
#66388=ORIENTED_EDGE('',*,*,#47332,.T.);
#66389=ORIENTED_EDGE('',*,*,#48338,.F.);
#66390=ORIENTED_EDGE('',*,*,#48339,.T.);
#66391=ORIENTED_EDGE('',*,*,#48340,.F.);
#66392=ORIENTED_EDGE('',*,*,#47333,.T.);
#66393=ORIENTED_EDGE('',*,*,#48340,.T.);
#66394=ORIENTED_EDGE('',*,*,#48341,.T.);
#66395=ORIENTED_EDGE('',*,*,#48342,.T.);
#66396=ORIENTED_EDGE('',*,*,#47335,.T.);
#66397=ORIENTED_EDGE('',*,*,#48342,.F.);
#66398=ORIENTED_EDGE('',*,*,#48343,.T.);
#66399=ORIENTED_EDGE('',*,*,#48344,.F.);
#66400=ORIENTED_EDGE('',*,*,#47338,.F.);
#66401=ORIENTED_EDGE('',*,*,#47345,.T.);
#66402=ORIENTED_EDGE('',*,*,#48204,.T.);
#66403=ORIENTED_EDGE('',*,*,#47341,.T.);
#66404=ORIENTED_EDGE('',*,*,#47339,.T.);
#66405=ORIENTED_EDGE('',*,*,#48344,.T.);
#66406=ORIENTED_EDGE('',*,*,#48345,.T.);
#66407=ORIENTED_EDGE('',*,*,#48346,.T.);
#66408=ORIENTED_EDGE('',*,*,#48234,.T.);
#66409=ORIENTED_EDGE('',*,*,#48235,.T.);
#66410=ORIENTED_EDGE('',*,*,#48346,.F.);
#66411=ORIENTED_EDGE('',*,*,#48347,.F.);
#66412=ORIENTED_EDGE('',*,*,#48348,.F.);
#66413=ORIENTED_EDGE('',*,*,#48349,.T.);
#66414=ORIENTED_EDGE('',*,*,#48350,.F.);
#66415=ORIENTED_EDGE('',*,*,#47891,.F.);
#66416=ORIENTED_EDGE('',*,*,#48351,.F.);
#66417=ORIENTED_EDGE('',*,*,#48350,.T.);
#66418=ORIENTED_EDGE('',*,*,#48352,.T.);
#66419=ORIENTED_EDGE('',*,*,#48353,.T.);
#66420=ORIENTED_EDGE('',*,*,#47357,.T.);
#66421=ORIENTED_EDGE('',*,*,#48142,.T.);
#66422=ORIENTED_EDGE('',*,*,#48354,.T.);
#66423=ORIENTED_EDGE('',*,*,#48143,.T.);
#66424=ORIENTED_EDGE('',*,*,#47353,.T.);
#66425=ORIENTED_EDGE('',*,*,#47351,.T.);
#66426=ORIENTED_EDGE('',*,*,#47348,.T.);
#66427=ORIENTED_EDGE('',*,*,#47892,.T.);
#66428=ORIENTED_EDGE('',*,*,#48353,.F.);
#66429=ORIENTED_EDGE('',*,*,#48355,.T.);
#66430=ORIENTED_EDGE('',*,*,#48356,.F.);
#66431=ORIENTED_EDGE('',*,*,#47358,.T.);
#66432=ORIENTED_EDGE('',*,*,#48356,.T.);
#66433=ORIENTED_EDGE('',*,*,#48357,.T.);
#66434=ORIENTED_EDGE('',*,*,#48358,.T.);
#66435=ORIENTED_EDGE('',*,*,#47361,.T.);
#66436=ORIENTED_EDGE('',*,*,#48358,.F.);
#66437=ORIENTED_EDGE('',*,*,#48359,.T.);
#66438=ORIENTED_EDGE('',*,*,#48360,.F.);
#66439=ORIENTED_EDGE('',*,*,#47363,.F.);
#66440=ORIENTED_EDGE('',*,*,#48360,.T.);
#66441=ORIENTED_EDGE('',*,*,#48361,.T.);
#66442=ORIENTED_EDGE('',*,*,#48362,.T.);
#66443=ORIENTED_EDGE('',*,*,#47382,.T.);
#66444=ORIENTED_EDGE('',*,*,#47376,.T.);
#66445=ORIENTED_EDGE('',*,*,#47373,.T.);
#66446=ORIENTED_EDGE('',*,*,#47371,.T.);
#66447=ORIENTED_EDGE('',*,*,#47369,.T.);
#66448=ORIENTED_EDGE('',*,*,#48135,.T.);
#66449=ORIENTED_EDGE('',*,*,#48363,.T.);
#66450=ORIENTED_EDGE('',*,*,#48136,.T.);
#66451=ORIENTED_EDGE('',*,*,#47364,.T.);
#66452=ORIENTED_EDGE('',*,*,#48364,.T.);
#66453=ORIENTED_EDGE('',*,*,#48336,.F.);
#66454=ORIENTED_EDGE('',*,*,#47377,.F.);
#66455=ORIENTED_EDGE('',*,*,#48365,.F.);
#66456=ORIENTED_EDGE('',*,*,#48366,.T.);
#66457=ORIENTED_EDGE('',*,*,#48367,.F.);
#66458=ORIENTED_EDGE('',*,*,#47380,.F.);
#66459=ORIENTED_EDGE('',*,*,#48362,.F.);
#66460=ORIENTED_EDGE('',*,*,#47383,.T.);
#66461=ORIENTED_EDGE('',*,*,#47381,.T.);
#66462=ORIENTED_EDGE('',*,*,#48368,.T.);
#66463=ORIENTED_EDGE('',*,*,#47379,.T.);
#66464=ORIENTED_EDGE('',*,*,#47411,.T.);
#66465=ORIENTED_EDGE('',*,*,#47410,.T.);
#66466=ORIENTED_EDGE('',*,*,#47408,.T.);
#66467=ORIENTED_EDGE('',*,*,#47406,.T.);
#66468=ORIENTED_EDGE('',*,*,#47404,.T.);
#66469=ORIENTED_EDGE('',*,*,#47402,.T.);
#66470=ORIENTED_EDGE('',*,*,#47400,.T.);
#66471=ORIENTED_EDGE('',*,*,#47398,.T.);
#66472=ORIENTED_EDGE('',*,*,#47396,.T.);
#66473=ORIENTED_EDGE('',*,*,#47394,.T.);
#66474=ORIENTED_EDGE('',*,*,#47392,.T.);
#66475=ORIENTED_EDGE('',*,*,#47539,.T.);
#66476=ORIENTED_EDGE('',*,*,#48369,.T.);
#66477=ORIENTED_EDGE('',*,*,#48370,.T.);
#66478=ORIENTED_EDGE('',*,*,#48371,.T.);
#66479=ORIENTED_EDGE('',*,*,#47412,.T.);
#66480=ORIENTED_EDGE('',*,*,#47387,.T.);
#66481=ORIENTED_EDGE('',*,*,#47385,.T.);
#66482=ORIENTED_EDGE('',*,*,#48371,.F.);
#66483=ORIENTED_EDGE('',*,*,#48372,.T.);
#66484=ORIENTED_EDGE('',*,*,#48373,.F.);
#66485=ORIENTED_EDGE('',*,*,#47413,.T.);
#66486=ORIENTED_EDGE('',*,*,#48373,.T.);
#66487=ORIENTED_EDGE('',*,*,#48374,.T.);
#66488=ORIENTED_EDGE('',*,*,#48375,.T.);
#66489=ORIENTED_EDGE('',*,*,#47415,.T.);
#66490=ORIENTED_EDGE('',*,*,#48375,.F.);
#66491=ORIENTED_EDGE('',*,*,#48376,.T.);
#66492=ORIENTED_EDGE('',*,*,#48377,.F.);
#66493=ORIENTED_EDGE('',*,*,#47417,.F.);
#66494=ORIENTED_EDGE('',*,*,#48377,.T.);
#66495=ORIENTED_EDGE('',*,*,#48378,.T.);
#66496=ORIENTED_EDGE('',*,*,#48379,.T.);
#66497=ORIENTED_EDGE('',*,*,#47446,.T.);
#66498=ORIENTED_EDGE('',*,*,#47449,.T.);
#66499=ORIENTED_EDGE('',*,*,#47442,.T.);
#66500=ORIENTED_EDGE('',*,*,#47440,.T.);
#66501=ORIENTED_EDGE('',*,*,#47438,.T.);
#66502=ORIENTED_EDGE('',*,*,#47436,.T.);
#66503=ORIENTED_EDGE('',*,*,#47434,.T.);
#66504=ORIENTED_EDGE('',*,*,#47432,.T.);
#66505=ORIENTED_EDGE('',*,*,#47430,.T.);
#66506=ORIENTED_EDGE('',*,*,#47428,.T.);
#66507=ORIENTED_EDGE('',*,*,#47425,.T.);
#66508=ORIENTED_EDGE('',*,*,#47424,.T.);
#66509=ORIENTED_EDGE('',*,*,#47422,.T.);
#66510=ORIENTED_EDGE('',*,*,#47420,.T.);
#66511=ORIENTED_EDGE('',*,*,#47418,.T.);
#66512=ORIENTED_EDGE('',*,*,#47447,.T.);
#66513=ORIENTED_EDGE('',*,*,#48379,.F.);
#66514=ORIENTED_EDGE('',*,*,#48380,.F.);
#66515=ORIENTED_EDGE('',*,*,#48381,.F.);
#66516=ORIENTED_EDGE('',*,*,#48382,.T.);
#66517=ORIENTED_EDGE('',*,*,#47448,.T.);
#66518=ORIENTED_EDGE('',*,*,#48383,.T.);
#66519=ORIENTED_EDGE('',*,*,#47451,.F.);
#66520=ORIENTED_EDGE('',*,*,#47450,.T.);
#66521=ORIENTED_EDGE('',*,*,#48382,.F.);
#66522=ORIENTED_EDGE('',*,*,#48384,.T.);
#66523=ORIENTED_EDGE('',*,*,#47474,.T.);
#66524=ORIENTED_EDGE('',*,*,#48025,.T.);
#66525=ORIENTED_EDGE('',*,*,#48031,.T.);
#66526=ORIENTED_EDGE('',*,*,#47473,.T.);
#66527=ORIENTED_EDGE('',*,*,#47470,.T.);
#66528=ORIENTED_EDGE('',*,*,#47468,.T.);
#66529=ORIENTED_EDGE('',*,*,#47466,.T.);
#66530=ORIENTED_EDGE('',*,*,#47464,.T.);
#66531=ORIENTED_EDGE('',*,*,#47462,.T.);
#66532=ORIENTED_EDGE('',*,*,#47460,.T.);
#66533=ORIENTED_EDGE('',*,*,#47476,.T.);
#66534=ORIENTED_EDGE('',*,*,#48385,.T.);
#66535=ORIENTED_EDGE('',*,*,#48386,.T.);
#66536=ORIENTED_EDGE('',*,*,#48387,.T.);
#66537=ORIENTED_EDGE('',*,*,#48216,.T.);
#66538=ORIENTED_EDGE('',*,*,#47456,.T.);
#66539=ORIENTED_EDGE('',*,*,#47454,.T.);
#66540=ORIENTED_EDGE('',*,*,#47475,.T.);
#66541=ORIENTED_EDGE('',*,*,#48388,.F.);
#66542=ORIENTED_EDGE('',*,*,#48389,.F.);
#66543=ORIENTED_EDGE('',*,*,#48385,.F.);
#66544=ORIENTED_EDGE('',*,*,#48390,.T.);
#66545=ORIENTED_EDGE('',*,*,#48391,.F.);
#66546=ORIENTED_EDGE('',*,*,#48230,.F.);
#66547=ORIENTED_EDGE('',*,*,#48392,.F.);
#66548=ORIENTED_EDGE('',*,*,#48082,.T.);
#66549=ORIENTED_EDGE('',*,*,#47500,.T.);
#66550=ORIENTED_EDGE('',*,*,#47496,.T.);
#66551=ORIENTED_EDGE('',*,*,#47495,.T.);
#66552=ORIENTED_EDGE('',*,*,#47492,.T.);
#66553=ORIENTED_EDGE('',*,*,#48231,.T.);
#66554=ORIENTED_EDGE('',*,*,#48391,.T.);
#66555=ORIENTED_EDGE('',*,*,#48393,.T.);
#66556=ORIENTED_EDGE('',*,*,#48394,.T.);
#66557=ORIENTED_EDGE('',*,*,#47503,.T.);
#66558=ORIENTED_EDGE('',*,*,#47490,.T.);
#66559=ORIENTED_EDGE('',*,*,#47488,.T.);
#66560=ORIENTED_EDGE('',*,*,#47485,.T.);
#66561=ORIENTED_EDGE('',*,*,#47484,.T.);
#66562=ORIENTED_EDGE('',*,*,#47482,.T.);
#66563=ORIENTED_EDGE('',*,*,#47480,.T.);
#66564=ORIENTED_EDGE('',*,*,#48394,.F.);
#66565=ORIENTED_EDGE('',*,*,#48395,.T.);
#66566=ORIENTED_EDGE('',*,*,#48396,.F.);
#66567=ORIENTED_EDGE('',*,*,#47501,.F.);
#66568=ORIENTED_EDGE('',*,*,#48396,.T.);
#66569=ORIENTED_EDGE('',*,*,#48397,.T.);
#66570=ORIENTED_EDGE('',*,*,#48398,.T.);
#66571=ORIENTED_EDGE('',*,*,#47504,.T.);
#66572=ORIENTED_EDGE('',*,*,#48398,.F.);
#66573=ORIENTED_EDGE('',*,*,#48399,.T.);
#66574=ORIENTED_EDGE('',*,*,#48400,.F.);
#66575=ORIENTED_EDGE('',*,*,#47522,.F.);
#66576=ORIENTED_EDGE('',*,*,#47534,.T.);
#66577=ORIENTED_EDGE('',*,*,#47532,.T.);
#66578=ORIENTED_EDGE('',*,*,#47529,.T.);
#66579=ORIENTED_EDGE('',*,*,#47527,.T.);
#66580=ORIENTED_EDGE('',*,*,#47525,.T.);
#66581=ORIENTED_EDGE('',*,*,#47523,.T.);
#66582=ORIENTED_EDGE('',*,*,#48400,.T.);
#66583=ORIENTED_EDGE('',*,*,#48401,.T.);
#66584=ORIENTED_EDGE('',*,*,#48402,.T.);
#66585=ORIENTED_EDGE('',*,*,#47540,.T.);
#66586=ORIENTED_EDGE('',*,*,#47519,.T.);
#66587=ORIENTED_EDGE('',*,*,#47517,.T.);
#66588=ORIENTED_EDGE('',*,*,#47515,.T.);
#66589=ORIENTED_EDGE('',*,*,#47514,.T.);
#66590=ORIENTED_EDGE('',*,*,#47512,.T.);
#66591=ORIENTED_EDGE('',*,*,#47510,.T.);
#66592=ORIENTED_EDGE('',*,*,#47508,.T.);
#66593=ORIENTED_EDGE('',*,*,#47538,.T.);
#66594=ORIENTED_EDGE('',*,*,#48403,.F.);
#66595=ORIENTED_EDGE('',*,*,#48404,.F.);
#66596=ORIENTED_EDGE('',*,*,#48369,.F.);
#66597=ORIENTED_EDGE('',*,*,#47541,.T.);
#66598=ORIENTED_EDGE('',*,*,#48402,.F.);
#66599=ORIENTED_EDGE('',*,*,#48405,.F.);
#66600=ORIENTED_EDGE('',*,*,#48406,.F.);
#66601=ORIENTED_EDGE('',*,*,#47543,.T.);
#66602=ORIENTED_EDGE('',*,*,#47542,.T.);
#66603=ORIENTED_EDGE('',*,*,#48407,.T.);
#66604=ORIENTED_EDGE('',*,*,#47537,.T.);
#66605=ORIENTED_EDGE('',*,*,#47535,.T.);
#66606=ORIENTED_EDGE('',*,*,#47563,.T.);
#66607=ORIENTED_EDGE('',*,*,#47562,.T.);
#66608=ORIENTED_EDGE('',*,*,#47559,.T.);
#66609=ORIENTED_EDGE('',*,*,#47557,.T.);
#66610=ORIENTED_EDGE('',*,*,#47555,.T.);
#66611=ORIENTED_EDGE('',*,*,#47846,.T.);
#66612=ORIENTED_EDGE('',*,*,#48408,.T.);
#66613=ORIENTED_EDGE('',*,*,#48409,.T.);
#66614=ORIENTED_EDGE('',*,*,#48410,.T.);
#66615=ORIENTED_EDGE('',*,*,#47566,.T.);
#66616=ORIENTED_EDGE('',*,*,#47553,.T.);
#66617=ORIENTED_EDGE('',*,*,#47550,.T.);
#66618=ORIENTED_EDGE('',*,*,#47548,.T.);
#66619=ORIENTED_EDGE('',*,*,#47546,.T.);
#66620=ORIENTED_EDGE('',*,*,#48411,.T.);
#66621=ORIENTED_EDGE('',*,*,#48412,.F.);
#66622=ORIENTED_EDGE('',*,*,#47564,.F.);
#66623=ORIENTED_EDGE('',*,*,#48410,.F.);
#66624=ORIENTED_EDGE('',*,*,#47567,.T.);
#66625=ORIENTED_EDGE('',*,*,#47565,.T.);
#66626=ORIENTED_EDGE('',*,*,#48413,.T.);
#66627=ORIENTED_EDGE('',*,*,#47588,.T.);
#66628=ORIENTED_EDGE('',*,*,#48414,.T.);
#66629=ORIENTED_EDGE('',*,*,#48415,.T.);
#66630=ORIENTED_EDGE('',*,*,#48416,.T.);
#66631=ORIENTED_EDGE('',*,*,#47591,.T.);
#66632=ORIENTED_EDGE('',*,*,#47586,.T.);
#66633=ORIENTED_EDGE('',*,*,#47584,.T.);
#66634=ORIENTED_EDGE('',*,*,#47582,.T.);
#66635=ORIENTED_EDGE('',*,*,#47580,.T.);
#66636=ORIENTED_EDGE('',*,*,#47578,.T.);
#66637=ORIENTED_EDGE('',*,*,#47576,.T.);
#66638=ORIENTED_EDGE('',*,*,#47574,.T.);
#66639=ORIENTED_EDGE('',*,*,#47573,.T.);
#66640=ORIENTED_EDGE('',*,*,#47571,.T.);
#66641=ORIENTED_EDGE('',*,*,#47590,.T.);
#66642=ORIENTED_EDGE('',*,*,#47589,.T.);
#66643=ORIENTED_EDGE('',*,*,#48417,.F.);
#66644=ORIENTED_EDGE('',*,*,#48418,.F.);
#66645=ORIENTED_EDGE('',*,*,#48414,.F.);
#66646=ORIENTED_EDGE('',*,*,#48416,.F.);
#66647=ORIENTED_EDGE('',*,*,#48419,.T.);
#66648=ORIENTED_EDGE('',*,*,#48420,.F.);
#66649=ORIENTED_EDGE('',*,*,#47592,.T.);
#66650=ORIENTED_EDGE('',*,*,#48420,.T.);
#66651=ORIENTED_EDGE('',*,*,#48421,.T.);
#66652=ORIENTED_EDGE('',*,*,#48422,.T.);
#66653=ORIENTED_EDGE('',*,*,#47594,.T.);
#66654=ORIENTED_EDGE('',*,*,#48422,.F.);
#66655=ORIENTED_EDGE('',*,*,#48423,.T.);
#66656=ORIENTED_EDGE('',*,*,#48424,.F.);
#66657=ORIENTED_EDGE('',*,*,#47596,.F.);
#66658=ORIENTED_EDGE('',*,*,#48424,.T.);
#66659=ORIENTED_EDGE('',*,*,#48425,.T.);
#66660=ORIENTED_EDGE('',*,*,#48426,.T.);
#66661=ORIENTED_EDGE('',*,*,#47618,.T.);
#66662=ORIENTED_EDGE('',*,*,#47615,.T.);
#66663=ORIENTED_EDGE('',*,*,#47611,.T.);
#66664=ORIENTED_EDGE('',*,*,#47609,.T.);
#66665=ORIENTED_EDGE('',*,*,#47607,.T.);
#66666=ORIENTED_EDGE('',*,*,#47605,.T.);
#66667=ORIENTED_EDGE('',*,*,#47602,.T.);
#66668=ORIENTED_EDGE('',*,*,#47601,.T.);
#66669=ORIENTED_EDGE('',*,*,#47599,.T.);
#66670=ORIENTED_EDGE('',*,*,#47597,.T.);
#66671=ORIENTED_EDGE('',*,*,#48427,.T.);
#66672=ORIENTED_EDGE('',*,*,#48428,.F.);
#66673=ORIENTED_EDGE('',*,*,#47616,.F.);
#66674=ORIENTED_EDGE('',*,*,#48426,.F.);
#66675=ORIENTED_EDGE('',*,*,#47619,.T.);
#66676=ORIENTED_EDGE('',*,*,#47617,.T.);
#66677=ORIENTED_EDGE('',*,*,#48429,.T.);
#66678=ORIENTED_EDGE('',*,*,#47636,.T.);
#66679=ORIENTED_EDGE('',*,*,#48430,.T.);
#66680=ORIENTED_EDGE('',*,*,#48431,.T.);
#66681=ORIENTED_EDGE('',*,*,#48432,.T.);
#66682=ORIENTED_EDGE('',*,*,#47641,.T.);
#66683=ORIENTED_EDGE('',*,*,#47634,.T.);
#66684=ORIENTED_EDGE('',*,*,#47633,.T.);
#66685=ORIENTED_EDGE('',*,*,#47631,.T.);
#66686=ORIENTED_EDGE('',*,*,#47629,.T.);
#66687=ORIENTED_EDGE('',*,*,#47627,.T.);
#66688=ORIENTED_EDGE('',*,*,#47625,.T.);
#66689=ORIENTED_EDGE('',*,*,#47623,.T.);
#66690=ORIENTED_EDGE('',*,*,#47638,.T.);
#66691=ORIENTED_EDGE('',*,*,#47637,.T.);
#66692=ORIENTED_EDGE('',*,*,#48433,.F.);
#66693=ORIENTED_EDGE('',*,*,#48434,.F.);
#66694=ORIENTED_EDGE('',*,*,#48430,.F.);
#66695=ORIENTED_EDGE('',*,*,#48432,.F.);
#66696=ORIENTED_EDGE('',*,*,#48435,.T.);
#66697=ORIENTED_EDGE('',*,*,#48436,.F.);
#66698=ORIENTED_EDGE('',*,*,#47639,.F.);
#66699=ORIENTED_EDGE('',*,*,#48436,.T.);
#66700=ORIENTED_EDGE('',*,*,#48437,.T.);
#66701=ORIENTED_EDGE('',*,*,#48438,.T.);
#66702=ORIENTED_EDGE('',*,*,#47642,.F.);
#66703=ORIENTED_EDGE('',*,*,#48438,.F.);
#66704=ORIENTED_EDGE('',*,*,#48439,.T.);
#66705=ORIENTED_EDGE('',*,*,#48440,.F.);
#66706=ORIENTED_EDGE('',*,*,#47644,.F.);
#66707=ORIENTED_EDGE('',*,*,#48440,.T.);
#66708=ORIENTED_EDGE('',*,*,#48441,.T.);
#66709=ORIENTED_EDGE('',*,*,#48442,.T.);
#66710=ORIENTED_EDGE('',*,*,#47662,.T.);
#66711=ORIENTED_EDGE('',*,*,#47659,.T.);
#66712=ORIENTED_EDGE('',*,*,#47657,.T.);
#66713=ORIENTED_EDGE('',*,*,#47655,.T.);
#66714=ORIENTED_EDGE('',*,*,#47653,.T.);
#66715=ORIENTED_EDGE('',*,*,#47651,.T.);
#66716=ORIENTED_EDGE('',*,*,#47648,.T.);
#66717=ORIENTED_EDGE('',*,*,#47647,.T.);
#66718=ORIENTED_EDGE('',*,*,#47645,.T.);
#66719=ORIENTED_EDGE('',*,*,#47663,.T.);
#66720=ORIENTED_EDGE('',*,*,#48442,.F.);
#66721=ORIENTED_EDGE('',*,*,#48443,.F.);
#66722=ORIENTED_EDGE('',*,*,#48444,.F.);
#66723=ORIENTED_EDGE('',*,*,#47665,.T.);
#66724=ORIENTED_EDGE('',*,*,#47664,.T.);
#66725=ORIENTED_EDGE('',*,*,#48445,.T.);
#66726=ORIENTED_EDGE('',*,*,#47682,.T.);
#66727=ORIENTED_EDGE('',*,*,#48446,.T.);
#66728=ORIENTED_EDGE('',*,*,#48447,.T.);
#66729=ORIENTED_EDGE('',*,*,#48448,.T.);
#66730=ORIENTED_EDGE('',*,*,#47687,.T.);
#66731=ORIENTED_EDGE('',*,*,#47680,.T.);
#66732=ORIENTED_EDGE('',*,*,#47679,.T.);
#66733=ORIENTED_EDGE('',*,*,#47677,.T.);
#66734=ORIENTED_EDGE('',*,*,#47675,.T.);
#66735=ORIENTED_EDGE('',*,*,#47673,.T.);
#66736=ORIENTED_EDGE('',*,*,#47671,.T.);
#66737=ORIENTED_EDGE('',*,*,#47669,.T.);
#66738=ORIENTED_EDGE('',*,*,#47684,.T.);
#66739=ORIENTED_EDGE('',*,*,#47683,.T.);
#66740=ORIENTED_EDGE('',*,*,#48449,.F.);
#66741=ORIENTED_EDGE('',*,*,#48450,.F.);
#66742=ORIENTED_EDGE('',*,*,#48446,.F.);
#66743=ORIENTED_EDGE('',*,*,#48448,.F.);
#66744=ORIENTED_EDGE('',*,*,#48451,.T.);
#66745=ORIENTED_EDGE('',*,*,#48452,.F.);
#66746=ORIENTED_EDGE('',*,*,#47685,.F.);
#66747=ORIENTED_EDGE('',*,*,#48452,.T.);
#66748=ORIENTED_EDGE('',*,*,#48453,.T.);
#66749=ORIENTED_EDGE('',*,*,#48454,.T.);
#66750=ORIENTED_EDGE('',*,*,#47688,.F.);
#66751=ORIENTED_EDGE('',*,*,#48454,.F.);
#66752=ORIENTED_EDGE('',*,*,#48455,.T.);
#66753=ORIENTED_EDGE('',*,*,#48456,.F.);
#66754=ORIENTED_EDGE('',*,*,#47690,.F.);
#66755=ORIENTED_EDGE('',*,*,#48456,.T.);
#66756=ORIENTED_EDGE('',*,*,#48457,.T.);
#66757=ORIENTED_EDGE('',*,*,#48458,.T.);
#66758=ORIENTED_EDGE('',*,*,#47708,.T.);
#66759=ORIENTED_EDGE('',*,*,#47705,.T.);
#66760=ORIENTED_EDGE('',*,*,#47703,.T.);
#66761=ORIENTED_EDGE('',*,*,#47701,.T.);
#66762=ORIENTED_EDGE('',*,*,#47699,.T.);
#66763=ORIENTED_EDGE('',*,*,#47697,.T.);
#66764=ORIENTED_EDGE('',*,*,#47694,.T.);
#66765=ORIENTED_EDGE('',*,*,#47693,.T.);
#66766=ORIENTED_EDGE('',*,*,#47691,.T.);
#66767=ORIENTED_EDGE('',*,*,#47709,.T.);
#66768=ORIENTED_EDGE('',*,*,#48458,.F.);
#66769=ORIENTED_EDGE('',*,*,#48459,.F.);
#66770=ORIENTED_EDGE('',*,*,#48460,.F.);
#66771=ORIENTED_EDGE('',*,*,#47711,.T.);
#66772=ORIENTED_EDGE('',*,*,#47710,.T.);
#66773=ORIENTED_EDGE('',*,*,#48461,.T.);
#66774=ORIENTED_EDGE('',*,*,#47728,.T.);
#66775=ORIENTED_EDGE('',*,*,#47726,.T.);
#66776=ORIENTED_EDGE('',*,*,#47725,.T.);
#66777=ORIENTED_EDGE('',*,*,#47723,.T.);
#66778=ORIENTED_EDGE('',*,*,#47721,.T.);
#66779=ORIENTED_EDGE('',*,*,#47719,.T.);
#66780=ORIENTED_EDGE('',*,*,#47717,.T.);
#66781=ORIENTED_EDGE('',*,*,#47715,.T.);
#66782=ORIENTED_EDGE('',*,*,#47730,.T.);
#66783=ORIENTED_EDGE('',*,*,#48462,.T.);
#66784=ORIENTED_EDGE('',*,*,#48463,.T.);
#66785=ORIENTED_EDGE('',*,*,#48464,.T.);
#66786=ORIENTED_EDGE('',*,*,#47731,.T.);
#66787=ORIENTED_EDGE('',*,*,#47729,.T.);
#66788=ORIENTED_EDGE('',*,*,#48465,.F.);
#66789=ORIENTED_EDGE('',*,*,#48466,.F.);
#66790=ORIENTED_EDGE('',*,*,#48462,.F.);
#66791=ORIENTED_EDGE('',*,*,#48464,.F.);
#66792=ORIENTED_EDGE('',*,*,#48467,.T.);
#66793=ORIENTED_EDGE('',*,*,#48468,.F.);
#66794=ORIENTED_EDGE('',*,*,#47732,.T.);
#66795=ORIENTED_EDGE('',*,*,#48468,.T.);
#66796=ORIENTED_EDGE('',*,*,#48469,.T.);
#66797=ORIENTED_EDGE('',*,*,#48470,.T.);
#66798=ORIENTED_EDGE('',*,*,#47734,.F.);
#66799=ORIENTED_EDGE('',*,*,#48470,.F.);
#66800=ORIENTED_EDGE('',*,*,#48471,.T.);
#66801=ORIENTED_EDGE('',*,*,#48472,.F.);
#66802=ORIENTED_EDGE('',*,*,#47736,.F.);
#66803=ORIENTED_EDGE('',*,*,#48472,.T.);
#66804=ORIENTED_EDGE('',*,*,#48473,.T.);
#66805=ORIENTED_EDGE('',*,*,#48474,.T.);
#66806=ORIENTED_EDGE('',*,*,#47754,.T.);
#66807=ORIENTED_EDGE('',*,*,#47751,.T.);
#66808=ORIENTED_EDGE('',*,*,#47749,.T.);
#66809=ORIENTED_EDGE('',*,*,#47747,.T.);
#66810=ORIENTED_EDGE('',*,*,#47745,.T.);
#66811=ORIENTED_EDGE('',*,*,#47743,.T.);
#66812=ORIENTED_EDGE('',*,*,#47740,.T.);
#66813=ORIENTED_EDGE('',*,*,#47739,.T.);
#66814=ORIENTED_EDGE('',*,*,#47737,.T.);
#66815=ORIENTED_EDGE('',*,*,#47755,.T.);
#66816=ORIENTED_EDGE('',*,*,#48474,.F.);
#66817=ORIENTED_EDGE('',*,*,#48475,.F.);
#66818=ORIENTED_EDGE('',*,*,#48476,.F.);
#66819=ORIENTED_EDGE('',*,*,#47757,.T.);
#66820=ORIENTED_EDGE('',*,*,#47756,.T.);
#66821=ORIENTED_EDGE('',*,*,#48477,.T.);
#66822=ORIENTED_EDGE('',*,*,#47776,.T.);
#66823=ORIENTED_EDGE('',*,*,#48478,.T.);
#66824=ORIENTED_EDGE('',*,*,#48479,.T.);
#66825=ORIENTED_EDGE('',*,*,#48480,.T.);
#66826=ORIENTED_EDGE('',*,*,#47779,.T.);
#66827=ORIENTED_EDGE('',*,*,#47774,.T.);
#66828=ORIENTED_EDGE('',*,*,#47772,.T.);
#66829=ORIENTED_EDGE('',*,*,#47770,.T.);
#66830=ORIENTED_EDGE('',*,*,#47768,.T.);
#66831=ORIENTED_EDGE('',*,*,#47766,.T.);
#66832=ORIENTED_EDGE('',*,*,#47764,.T.);
#66833=ORIENTED_EDGE('',*,*,#47763,.T.);
#66834=ORIENTED_EDGE('',*,*,#47761,.T.);
#66835=ORIENTED_EDGE('',*,*,#47778,.T.);
#66836=ORIENTED_EDGE('',*,*,#47777,.T.);
#66837=ORIENTED_EDGE('',*,*,#48481,.F.);
#66838=ORIENTED_EDGE('',*,*,#48482,.F.);
#66839=ORIENTED_EDGE('',*,*,#48478,.F.);
#66840=ORIENTED_EDGE('',*,*,#48480,.F.);
#66841=ORIENTED_EDGE('',*,*,#48483,.T.);
#66842=ORIENTED_EDGE('',*,*,#48484,.F.);
#66843=ORIENTED_EDGE('',*,*,#47780,.T.);
#66844=ORIENTED_EDGE('',*,*,#48484,.T.);
#66845=ORIENTED_EDGE('',*,*,#48485,.T.);
#66846=ORIENTED_EDGE('',*,*,#48486,.T.);
#66847=ORIENTED_EDGE('',*,*,#47782,.T.);
#66848=ORIENTED_EDGE('',*,*,#48486,.F.);
#66849=ORIENTED_EDGE('',*,*,#48487,.T.);
#66850=ORIENTED_EDGE('',*,*,#48488,.F.);
#66851=ORIENTED_EDGE('',*,*,#47784,.F.);
#66852=ORIENTED_EDGE('',*,*,#48488,.T.);
#66853=ORIENTED_EDGE('',*,*,#48489,.T.);
#66854=ORIENTED_EDGE('',*,*,#48490,.T.);
#66855=ORIENTED_EDGE('',*,*,#47808,.T.);
#66856=ORIENTED_EDGE('',*,*,#47805,.T.);
#66857=ORIENTED_EDGE('',*,*,#47801,.T.);
#66858=ORIENTED_EDGE('',*,*,#47799,.T.);
#66859=ORIENTED_EDGE('',*,*,#47797,.T.);
#66860=ORIENTED_EDGE('',*,*,#47795,.T.);
#66861=ORIENTED_EDGE('',*,*,#47792,.T.);
#66862=ORIENTED_EDGE('',*,*,#47791,.T.);
#66863=ORIENTED_EDGE('',*,*,#47789,.T.);
#66864=ORIENTED_EDGE('',*,*,#47787,.T.);
#66865=ORIENTED_EDGE('',*,*,#47785,.T.);
#66866=ORIENTED_EDGE('',*,*,#48491,.T.);
#66867=ORIENTED_EDGE('',*,*,#48492,.F.);
#66868=ORIENTED_EDGE('',*,*,#47806,.F.);
#66869=ORIENTED_EDGE('',*,*,#48490,.F.);
#66870=ORIENTED_EDGE('',*,*,#47809,.T.);
#66871=ORIENTED_EDGE('',*,*,#47807,.T.);
#66872=ORIENTED_EDGE('',*,*,#48493,.T.);
#66873=ORIENTED_EDGE('',*,*,#47819,.T.);
#66874=ORIENTED_EDGE('',*,*,#48494,.T.);
#66875=ORIENTED_EDGE('',*,*,#48495,.F.);
#66876=ORIENTED_EDGE('',*,*,#47816,.F.);
#66877=ORIENTED_EDGE('',*,*,#48496,.F.);
#66878=ORIENTED_EDGE('',*,*,#47832,.T.);
#66879=ORIENTED_EDGE('',*,*,#47830,.T.);
#66880=ORIENTED_EDGE('',*,*,#47828,.T.);
#66881=ORIENTED_EDGE('',*,*,#47826,.T.);
#66882=ORIENTED_EDGE('',*,*,#47824,.T.);
#66883=ORIENTED_EDGE('',*,*,#47822,.T.);
#66884=ORIENTED_EDGE('',*,*,#47820,.T.);
#66885=ORIENTED_EDGE('',*,*,#47817,.T.);
#66886=ORIENTED_EDGE('',*,*,#48495,.T.);
#66887=ORIENTED_EDGE('',*,*,#48497,.T.);
#66888=ORIENTED_EDGE('',*,*,#48498,.T.);
#66889=ORIENTED_EDGE('',*,*,#47833,.T.);
#66890=ORIENTED_EDGE('',*,*,#47814,.T.);
#66891=ORIENTED_EDGE('',*,*,#47812,.T.);
#66892=ORIENTED_EDGE('',*,*,#48498,.F.);
#66893=ORIENTED_EDGE('',*,*,#48499,.T.);
#66894=ORIENTED_EDGE('',*,*,#48500,.T.);
#66895=ORIENTED_EDGE('',*,*,#48501,.F.);
#66896=ORIENTED_EDGE('',*,*,#47834,.T.);
#66897=ORIENTED_EDGE('',*,*,#48501,.T.);
#66898=ORIENTED_EDGE('',*,*,#48502,.T.);
#66899=ORIENTED_EDGE('',*,*,#48503,.T.);
#66900=ORIENTED_EDGE('',*,*,#47836,.T.);
#66901=ORIENTED_EDGE('',*,*,#48503,.F.);
#66902=ORIENTED_EDGE('',*,*,#48504,.T.);
#66903=ORIENTED_EDGE('',*,*,#48505,.T.);
#66904=ORIENTED_EDGE('',*,*,#48288,.F.);
#66905=ORIENTED_EDGE('',*,*,#47838,.F.);
#66906=ORIENTED_EDGE('',*,*,#48316,.F.);
#66907=ORIENTED_EDGE('',*,*,#48506,.T.);
#66908=ORIENTED_EDGE('',*,*,#48507,.T.);
#66909=ORIENTED_EDGE('',*,*,#48508,.F.);
#66910=ORIENTED_EDGE('',*,*,#47841,.T.);
#66911=ORIENTED_EDGE('',*,*,#48508,.T.);
#66912=ORIENTED_EDGE('',*,*,#48509,.T.);
#66913=ORIENTED_EDGE('',*,*,#48510,.T.);
#66914=ORIENTED_EDGE('',*,*,#47843,.T.);
#66915=ORIENTED_EDGE('',*,*,#48511,.T.);
#66916=ORIENTED_EDGE('',*,*,#48512,.T.);
#66917=ORIENTED_EDGE('',*,*,#48408,.F.);
#66918=ORIENTED_EDGE('',*,*,#47845,.F.);
#66919=ORIENTED_EDGE('',*,*,#48510,.F.);
#66920=ORIENTED_EDGE('',*,*,#48513,.T.);
#66921=ORIENTED_EDGE('',*,*,#48514,.T.);
#66922=ORIENTED_EDGE('',*,*,#48515,.T.);
#66923=ORIENTED_EDGE('',*,*,#48196,.T.);
#66924=ORIENTED_EDGE('',*,*,#48516,.T.);
#66925=ORIENTED_EDGE('',*,*,#48517,.T.);
#66926=ORIENTED_EDGE('',*,*,#48518,.T.);
#66927=ORIENTED_EDGE('',*,*,#48515,.F.);
#66928=ORIENTED_EDGE('',*,*,#48519,.T.);
#66929=ORIENTED_EDGE('',*,*,#48520,.F.);
#66930=ORIENTED_EDGE('',*,*,#48197,.F.);
#66931=ORIENTED_EDGE('',*,*,#48520,.T.);
#66932=ORIENTED_EDGE('',*,*,#48521,.T.);
#66933=ORIENTED_EDGE('',*,*,#48522,.T.);
#66934=ORIENTED_EDGE('',*,*,#48194,.F.);
#66935=ORIENTED_EDGE('',*,*,#48522,.F.);
#66936=ORIENTED_EDGE('',*,*,#48523,.T.);
#66937=ORIENTED_EDGE('',*,*,#48524,.F.);
#66938=ORIENTED_EDGE('',*,*,#48191,.F.);
#66939=ORIENTED_EDGE('',*,*,#48524,.T.);
#66940=ORIENTED_EDGE('',*,*,#48525,.T.);
#66941=ORIENTED_EDGE('',*,*,#48526,.T.);
#66942=ORIENTED_EDGE('',*,*,#47850,.T.);
#66943=ORIENTED_EDGE('',*,*,#48187,.T.);
#66944=ORIENTED_EDGE('',*,*,#48527,.T.);
#66945=ORIENTED_EDGE('',*,*,#48188,.T.);
#66946=ORIENTED_EDGE('',*,*,#48528,.T.);
#66947=ORIENTED_EDGE('',*,*,#48529,.F.);
#66948=ORIENTED_EDGE('',*,*,#47847,.F.);
#66949=ORIENTED_EDGE('',*,*,#48526,.F.);
#66950=ORIENTED_EDGE('',*,*,#48530,.T.);
#66951=ORIENTED_EDGE('',*,*,#47848,.T.);
#66952=ORIENTED_EDGE('',*,*,#48531,.T.);
#66953=ORIENTED_EDGE('',*,*,#47854,.T.);
#66954=ORIENTED_EDGE('',*,*,#48532,.T.);
#66955=ORIENTED_EDGE('',*,*,#48533,.T.);
#66956=ORIENTED_EDGE('',*,*,#48534,.T.);
#66957=ORIENTED_EDGE('',*,*,#48178,.T.);
#66958=ORIENTED_EDGE('',*,*,#48535,.T.);
#66959=ORIENTED_EDGE('',*,*,#48180,.T.);
#66960=ORIENTED_EDGE('',*,*,#47852,.T.);
#66961=ORIENTED_EDGE('',*,*,#47851,.F.);
#66962=ORIENTED_EDGE('',*,*,#48536,.F.);
#66963=ORIENTED_EDGE('',*,*,#48537,.F.);
#66964=ORIENTED_EDGE('',*,*,#48532,.F.);
#66965=ORIENTED_EDGE('',*,*,#48534,.F.);
#66966=ORIENTED_EDGE('',*,*,#48538,.T.);
#66967=ORIENTED_EDGE('',*,*,#48539,.F.);
#66968=ORIENTED_EDGE('',*,*,#48179,.F.);
#66969=ORIENTED_EDGE('',*,*,#48539,.T.);
#66970=ORIENTED_EDGE('',*,*,#48540,.T.);
#66971=ORIENTED_EDGE('',*,*,#48541,.T.);
#66972=ORIENTED_EDGE('',*,*,#48176,.F.);
#66973=ORIENTED_EDGE('',*,*,#48541,.F.);
#66974=ORIENTED_EDGE('',*,*,#48542,.T.);
#66975=ORIENTED_EDGE('',*,*,#48543,.F.);
#66976=ORIENTED_EDGE('',*,*,#48173,.F.);
#66977=ORIENTED_EDGE('',*,*,#48543,.T.);
#66978=ORIENTED_EDGE('',*,*,#48544,.T.);
#66979=ORIENTED_EDGE('',*,*,#48545,.T.);
#66980=ORIENTED_EDGE('',*,*,#47861,.T.);
#66981=ORIENTED_EDGE('',*,*,#47858,.T.);
#66982=ORIENTED_EDGE('',*,*,#48166,.T.);
#66983=ORIENTED_EDGE('',*,*,#48168,.T.);
#66984=ORIENTED_EDGE('',*,*,#48546,.T.);
#66985=ORIENTED_EDGE('',*,*,#48170,.T.);
#66986=ORIENTED_EDGE('',*,*,#48547,.T.);
#66987=ORIENTED_EDGE('',*,*,#48548,.F.);
#66988=ORIENTED_EDGE('',*,*,#47859,.F.);
#66989=ORIENTED_EDGE('',*,*,#48545,.F.);
#66990=ORIENTED_EDGE('',*,*,#48163,.T.);
#66991=ORIENTED_EDGE('',*,*,#47860,.T.);
#66992=ORIENTED_EDGE('',*,*,#48549,.T.);
#66993=ORIENTED_EDGE('',*,*,#47865,.T.);
#66994=ORIENTED_EDGE('',*,*,#48550,.T.);
#66995=ORIENTED_EDGE('',*,*,#48551,.F.);
#66996=ORIENTED_EDGE('',*,*,#47862,.F.);
#66997=ORIENTED_EDGE('',*,*,#48552,.F.);
#66998=ORIENTED_EDGE('',*,*,#48551,.T.);
#66999=ORIENTED_EDGE('',*,*,#48553,.T.);
#67000=ORIENTED_EDGE('',*,*,#48554,.T.);
#67001=ORIENTED_EDGE('',*,*,#47873,.T.);
#67002=ORIENTED_EDGE('',*,*,#48156,.T.);
#67003=ORIENTED_EDGE('',*,*,#48555,.T.);
#67004=ORIENTED_EDGE('',*,*,#48157,.T.);
#67005=ORIENTED_EDGE('',*,*,#47869,.T.);
#67006=ORIENTED_EDGE('',*,*,#47866,.T.);
#67007=ORIENTED_EDGE('',*,*,#47863,.T.);
#67008=ORIENTED_EDGE('',*,*,#48554,.F.);
#67009=ORIENTED_EDGE('',*,*,#48556,.T.);
#67010=ORIENTED_EDGE('',*,*,#48557,.F.);
#67011=ORIENTED_EDGE('',*,*,#47874,.T.);
#67012=ORIENTED_EDGE('',*,*,#48557,.T.);
#67013=ORIENTED_EDGE('',*,*,#48558,.T.);
#67014=ORIENTED_EDGE('',*,*,#48559,.T.);
#67015=ORIENTED_EDGE('',*,*,#47877,.T.);
#67016=ORIENTED_EDGE('',*,*,#48559,.F.);
#67017=ORIENTED_EDGE('',*,*,#48560,.T.);
#67018=ORIENTED_EDGE('',*,*,#48561,.F.);
#67019=ORIENTED_EDGE('',*,*,#47879,.F.);
#67020=ORIENTED_EDGE('',*,*,#48561,.T.);
#67021=ORIENTED_EDGE('',*,*,#48562,.T.);
#67022=ORIENTED_EDGE('',*,*,#48563,.T.);
#67023=ORIENTED_EDGE('',*,*,#47896,.T.);
#67024=ORIENTED_EDGE('',*,*,#47890,.T.);
#67025=ORIENTED_EDGE('',*,*,#47887,.T.);
#67026=ORIENTED_EDGE('',*,*,#47885,.T.);
#67027=ORIENTED_EDGE('',*,*,#48149,.T.);
#67028=ORIENTED_EDGE('',*,*,#48564,.T.);
#67029=ORIENTED_EDGE('',*,*,#48150,.T.);
#67030=ORIENTED_EDGE('',*,*,#47880,.T.);
#67031=ORIENTED_EDGE('',*,*,#48565,.T.);
#67032=ORIENTED_EDGE('',*,*,#48566,.F.);
#67033=ORIENTED_EDGE('',*,*,#47894,.F.);
#67034=ORIENTED_EDGE('',*,*,#48563,.F.);
#67035=ORIENTED_EDGE('',*,*,#47897,.F.);
#67036=ORIENTED_EDGE('',*,*,#47895,.T.);
#67037=ORIENTED_EDGE('',*,*,#48567,.T.);
#67038=ORIENTED_EDGE('',*,*,#48568,.T.);
#67039=ORIENTED_EDGE('',*,*,#48569,.T.);
#67040=ORIENTED_EDGE('',*,*,#47893,.T.);
#67041=ORIENTED_EDGE('',*,*,#48570,.F.);
#67042=ORIENTED_EDGE('',*,*,#48571,.T.);
#67043=ORIENTED_EDGE('',*,*,#48572,.F.);
#67044=ORIENTED_EDGE('',*,*,#47898,.F.);
#67045=ORIENTED_EDGE('',*,*,#48572,.T.);
#67046=ORIENTED_EDGE('',*,*,#48573,.T.);
#67047=ORIENTED_EDGE('',*,*,#48574,.T.);
#67048=ORIENTED_EDGE('',*,*,#47917,.T.);
#67049=ORIENTED_EDGE('',*,*,#47914,.T.);
#67050=ORIENTED_EDGE('',*,*,#47912,.T.);
#67051=ORIENTED_EDGE('',*,*,#47910,.T.);
#67052=ORIENTED_EDGE('',*,*,#47907,.T.);
#67053=ORIENTED_EDGE('',*,*,#48065,.T.);
#67054=ORIENTED_EDGE('',*,*,#48575,.T.);
#67055=ORIENTED_EDGE('',*,*,#48067,.T.);
#67056=ORIENTED_EDGE('',*,*,#47904,.T.);
#67057=ORIENTED_EDGE('',*,*,#47902,.T.);
#67058=ORIENTED_EDGE('',*,*,#47899,.T.);
#67059=ORIENTED_EDGE('',*,*,#47918,.T.);
#67060=ORIENTED_EDGE('',*,*,#48574,.F.);
#67061=ORIENTED_EDGE('',*,*,#48576,.F.);
#67062=ORIENTED_EDGE('',*,*,#48577,.F.);
#67063=ORIENTED_EDGE('',*,*,#47920,.T.);
#67064=ORIENTED_EDGE('',*,*,#47919,.T.);
#67065=ORIENTED_EDGE('',*,*,#48578,.T.);
#67066=ORIENTED_EDGE('',*,*,#47937,.T.);
#67067=ORIENTED_EDGE('',*,*,#48059,.T.);
#67068=ORIENTED_EDGE('',*,*,#48579,.T.);
#67069=ORIENTED_EDGE('',*,*,#48062,.T.);
#67070=ORIENTED_EDGE('',*,*,#47936,.T.);
#67071=ORIENTED_EDGE('',*,*,#47933,.T.);
#67072=ORIENTED_EDGE('',*,*,#47931,.T.);
#67073=ORIENTED_EDGE('',*,*,#47929,.T.);
#67074=ORIENTED_EDGE('',*,*,#47939,.T.);
#67075=ORIENTED_EDGE('',*,*,#48580,.T.);
#67076=ORIENTED_EDGE('',*,*,#48581,.T.);
#67077=ORIENTED_EDGE('',*,*,#48582,.T.);
#67078=ORIENTED_EDGE('',*,*,#47940,.T.);
#67079=ORIENTED_EDGE('',*,*,#47925,.T.);
#67080=ORIENTED_EDGE('',*,*,#47923,.T.);
#67081=ORIENTED_EDGE('',*,*,#47938,.T.);
#67082=ORIENTED_EDGE('',*,*,#48583,.F.);
#67083=ORIENTED_EDGE('',*,*,#48584,.F.);
#67084=ORIENTED_EDGE('',*,*,#48580,.F.);
#67085=ORIENTED_EDGE('',*,*,#48582,.F.);
#67086=ORIENTED_EDGE('',*,*,#48585,.T.);
#67087=ORIENTED_EDGE('',*,*,#48586,.F.);
#67088=ORIENTED_EDGE('',*,*,#47941,.T.);
#67089=ORIENTED_EDGE('',*,*,#48586,.T.);
#67090=ORIENTED_EDGE('',*,*,#48587,.T.);
#67091=ORIENTED_EDGE('',*,*,#48588,.T.);
#67092=ORIENTED_EDGE('',*,*,#47943,.T.);
#67093=ORIENTED_EDGE('',*,*,#48588,.F.);
#67094=ORIENTED_EDGE('',*,*,#48589,.T.);
#67095=ORIENTED_EDGE('',*,*,#48590,.F.);
#67096=ORIENTED_EDGE('',*,*,#47945,.F.);
#67097=ORIENTED_EDGE('',*,*,#48590,.T.);
#67098=ORIENTED_EDGE('',*,*,#48591,.T.);
#67099=ORIENTED_EDGE('',*,*,#48592,.T.);
#67100=ORIENTED_EDGE('',*,*,#47963,.T.);
#67101=ORIENTED_EDGE('',*,*,#47960,.T.);
#67102=ORIENTED_EDGE('',*,*,#47958,.T.);
#67103=ORIENTED_EDGE('',*,*,#47956,.T.);
#67104=ORIENTED_EDGE('',*,*,#47953,.T.);
#67105=ORIENTED_EDGE('',*,*,#48051,.T.);
#67106=ORIENTED_EDGE('',*,*,#48593,.T.);
#67107=ORIENTED_EDGE('',*,*,#48053,.T.);
#67108=ORIENTED_EDGE('',*,*,#47950,.T.);
#67109=ORIENTED_EDGE('',*,*,#47948,.T.);
#67110=ORIENTED_EDGE('',*,*,#47946,.T.);
#67111=ORIENTED_EDGE('',*,*,#47964,.T.);
#67112=ORIENTED_EDGE('',*,*,#48592,.F.);
#67113=ORIENTED_EDGE('',*,*,#48594,.F.);
#67114=ORIENTED_EDGE('',*,*,#48595,.F.);
#67115=ORIENTED_EDGE('',*,*,#48596,.F.);
#67116=ORIENTED_EDGE('',*,*,#47966,.T.);
#67117=ORIENTED_EDGE('',*,*,#47965,.T.);
#67118=ORIENTED_EDGE('',*,*,#48597,.T.);
#67119=ORIENTED_EDGE('',*,*,#47978,.T.);
#67120=ORIENTED_EDGE('',*,*,#48045,.T.);
#67121=ORIENTED_EDGE('',*,*,#48598,.T.);
#67122=ORIENTED_EDGE('',*,*,#48048,.T.);
#67123=ORIENTED_EDGE('',*,*,#47977,.T.);
#67124=ORIENTED_EDGE('',*,*,#47974,.T.);
#67125=ORIENTED_EDGE('',*,*,#47972,.T.);
#67126=ORIENTED_EDGE('',*,*,#47970,.T.);
#67127=ORIENTED_EDGE('',*,*,#47980,.T.);
#67128=ORIENTED_EDGE('',*,*,#48599,.T.);
#67129=ORIENTED_EDGE('',*,*,#48600,.T.);
#67130=ORIENTED_EDGE('',*,*,#48601,.T.);
#67131=ORIENTED_EDGE('',*,*,#47982,.T.);
#67132=ORIENTED_EDGE('',*,*,#47979,.T.);
#67133=ORIENTED_EDGE('',*,*,#48602,.F.);
#67134=ORIENTED_EDGE('',*,*,#48603,.F.);
#67135=ORIENTED_EDGE('',*,*,#48599,.F.);
#67136=ORIENTED_EDGE('',*,*,#48601,.F.);
#67137=ORIENTED_EDGE('',*,*,#48604,.T.);
#67138=ORIENTED_EDGE('',*,*,#48605,.F.);
#67139=ORIENTED_EDGE('',*,*,#47983,.T.);
#67140=ORIENTED_EDGE('',*,*,#48605,.T.);
#67141=ORIENTED_EDGE('',*,*,#48606,.T.);
#67142=ORIENTED_EDGE('',*,*,#48607,.T.);
#67143=ORIENTED_EDGE('',*,*,#47985,.F.);
#67144=ORIENTED_EDGE('',*,*,#48607,.F.);
#67145=ORIENTED_EDGE('',*,*,#48608,.T.);
#67146=ORIENTED_EDGE('',*,*,#48609,.F.);
#67147=ORIENTED_EDGE('',*,*,#47988,.F.);
#67148=ORIENTED_EDGE('',*,*,#48609,.T.);
#67149=ORIENTED_EDGE('',*,*,#48610,.T.);
#67150=ORIENTED_EDGE('',*,*,#48611,.T.);
#67151=ORIENTED_EDGE('',*,*,#48002,.T.);
#67152=ORIENTED_EDGE('',*,*,#47999,.T.);
#67153=ORIENTED_EDGE('',*,*,#47997,.T.);
#67154=ORIENTED_EDGE('',*,*,#47995,.T.);
#67155=ORIENTED_EDGE('',*,*,#47992,.T.);
#67156=ORIENTED_EDGE('',*,*,#48037,.T.);
#67157=ORIENTED_EDGE('',*,*,#48612,.T.);
#67158=ORIENTED_EDGE('',*,*,#48039,.T.);
#67159=ORIENTED_EDGE('',*,*,#47989,.T.);
#67160=ORIENTED_EDGE('',*,*,#48003,.T.);
#67161=ORIENTED_EDGE('',*,*,#48611,.F.);
#67162=ORIENTED_EDGE('',*,*,#48613,.F.);
#67163=ORIENTED_EDGE('',*,*,#48614,.F.);
#67164=ORIENTED_EDGE('',*,*,#48615,.F.);
#67165=ORIENTED_EDGE('',*,*,#48005,.T.);
#67166=ORIENTED_EDGE('',*,*,#48004,.T.);
#67167=ORIENTED_EDGE('',*,*,#48616,.T.);
#67168=ORIENTED_EDGE('',*,*,#48017,.T.);
#67169=ORIENTED_EDGE('',*,*,#48617,.T.);
#67170=ORIENTED_EDGE('',*,*,#48618,.T.);
#67171=ORIENTED_EDGE('',*,*,#48034,.T.);
#67172=ORIENTED_EDGE('',*,*,#48016,.T.);
#67173=ORIENTED_EDGE('',*,*,#48013,.T.);
#67174=ORIENTED_EDGE('',*,*,#48011,.T.);
#67175=ORIENTED_EDGE('',*,*,#48009,.T.);
#67176=ORIENTED_EDGE('',*,*,#48019,.T.);
#67177=ORIENTED_EDGE('',*,*,#48619,.T.);
#67178=ORIENTED_EDGE('',*,*,#48620,.T.);
#67179=ORIENTED_EDGE('',*,*,#48621,.T.);
#67180=ORIENTED_EDGE('',*,*,#48622,.T.);
#67181=ORIENTED_EDGE('',*,*,#48018,.T.);
#67182=ORIENTED_EDGE('',*,*,#48623,.F.);
#67183=ORIENTED_EDGE('',*,*,#48624,.F.);
#67184=ORIENTED_EDGE('',*,*,#48619,.F.);
#67185=ORIENTED_EDGE('',*,*,#48621,.F.);
#67186=ORIENTED_EDGE('',*,*,#48625,.T.);
#67187=ORIENTED_EDGE('',*,*,#48626,.F.);
#67188=ORIENTED_EDGE('',*,*,#48627,.T.);
#67189=ORIENTED_EDGE('',*,*,#48628,.T.);
#67190=ORIENTED_EDGE('',*,*,#48622,.F.);
#67191=ORIENTED_EDGE('',*,*,#48627,.F.);
#67192=ORIENTED_EDGE('',*,*,#48629,.F.);
#67193=ORIENTED_EDGE('',*,*,#48630,.F.);
#67194=ORIENTED_EDGE('',*,*,#48631,.T.);
#67195=ORIENTED_EDGE('',*,*,#48617,.F.);
#67196=ORIENTED_EDGE('',*,*,#48628,.F.);
#67197=ORIENTED_EDGE('',*,*,#48632,.T.);
#67198=ORIENTED_EDGE('',*,*,#48633,.F.);
#67199=ORIENTED_EDGE('',*,*,#48634,.F.);
#67200=ORIENTED_EDGE('',*,*,#48021,.F.);
#67201=ORIENTED_EDGE('',*,*,#48634,.T.);
#67202=ORIENTED_EDGE('',*,*,#48635,.F.);
#67203=ORIENTED_EDGE('',*,*,#48027,.F.);
#67204=ORIENTED_EDGE('',*,*,#48023,.F.);
#67205=ORIENTED_EDGE('',*,*,#48030,.T.);
#67206=ORIENTED_EDGE('',*,*,#48028,.T.);
#67207=ORIENTED_EDGE('',*,*,#48636,.F.);
#67208=ORIENTED_EDGE('',*,*,#48637,.T.);
#67209=ORIENTED_EDGE('',*,*,#48083,.F.);
#67210=ORIENTED_EDGE('',*,*,#48026,.T.);
#67211=ORIENTED_EDGE('',*,*,#48638,.T.);
#67212=ORIENTED_EDGE('',*,*,#48639,.F.);
#67213=ORIENTED_EDGE('',*,*,#48640,.F.);
#67214=ORIENTED_EDGE('',*,*,#48631,.F.);
#67215=ORIENTED_EDGE('',*,*,#48640,.T.);
#67216=ORIENTED_EDGE('',*,*,#48641,.F.);
#67217=ORIENTED_EDGE('',*,*,#48032,.F.);
#67218=ORIENTED_EDGE('',*,*,#48618,.F.);
#67219=ORIENTED_EDGE('',*,*,#48642,.F.);
#67220=ORIENTED_EDGE('',*,*,#48038,.T.);
#67221=ORIENTED_EDGE('',*,*,#48035,.F.);
#67222=ORIENTED_EDGE('',*,*,#48033,.T.);
#67223=ORIENTED_EDGE('',*,*,#48643,.T.);
#67224=ORIENTED_EDGE('',*,*,#48612,.F.);
#67225=ORIENTED_EDGE('',*,*,#48036,.F.);
#67226=ORIENTED_EDGE('',*,*,#48644,.F.);
#67227=ORIENTED_EDGE('',*,*,#48645,.F.);
#67228=ORIENTED_EDGE('',*,*,#48040,.F.);
#67229=ORIENTED_EDGE('',*,*,#48643,.F.);
#67230=ORIENTED_EDGE('',*,*,#48646,.F.);
#67231=ORIENTED_EDGE('',*,*,#48645,.T.);
#67232=ORIENTED_EDGE('',*,*,#48647,.F.);
#67233=ORIENTED_EDGE('',*,*,#48648,.F.);
#67234=ORIENTED_EDGE('',*,*,#48042,.F.);
#67235=ORIENTED_EDGE('',*,*,#48648,.T.);
#67236=ORIENTED_EDGE('',*,*,#48649,.F.);
#67237=ORIENTED_EDGE('',*,*,#48650,.F.);
#67238=ORIENTED_EDGE('',*,*,#48044,.F.);
#67239=ORIENTED_EDGE('',*,*,#48650,.T.);
#67240=ORIENTED_EDGE('',*,*,#48651,.F.);
#67241=ORIENTED_EDGE('',*,*,#48046,.F.);
#67242=ORIENTED_EDGE('',*,*,#48598,.F.);
#67243=ORIENTED_EDGE('',*,*,#48652,.F.);
#67244=ORIENTED_EDGE('',*,*,#48052,.T.);
#67245=ORIENTED_EDGE('',*,*,#48049,.F.);
#67246=ORIENTED_EDGE('',*,*,#48047,.T.);
#67247=ORIENTED_EDGE('',*,*,#48653,.T.);
#67248=ORIENTED_EDGE('',*,*,#48593,.F.);
#67249=ORIENTED_EDGE('',*,*,#48050,.F.);
#67250=ORIENTED_EDGE('',*,*,#48654,.F.);
#67251=ORIENTED_EDGE('',*,*,#48655,.F.);
#67252=ORIENTED_EDGE('',*,*,#48054,.F.);
#67253=ORIENTED_EDGE('',*,*,#48653,.F.);
#67254=ORIENTED_EDGE('',*,*,#48656,.F.);
#67255=ORIENTED_EDGE('',*,*,#48655,.T.);
#67256=ORIENTED_EDGE('',*,*,#48657,.F.);
#67257=ORIENTED_EDGE('',*,*,#48658,.F.);
#67258=ORIENTED_EDGE('',*,*,#48056,.F.);
#67259=ORIENTED_EDGE('',*,*,#48658,.T.);
#67260=ORIENTED_EDGE('',*,*,#48659,.F.);
#67261=ORIENTED_EDGE('',*,*,#48660,.F.);
#67262=ORIENTED_EDGE('',*,*,#48058,.F.);
#67263=ORIENTED_EDGE('',*,*,#48660,.T.);
#67264=ORIENTED_EDGE('',*,*,#48661,.F.);
#67265=ORIENTED_EDGE('',*,*,#48060,.F.);
#67266=ORIENTED_EDGE('',*,*,#48579,.F.);
#67267=ORIENTED_EDGE('',*,*,#48662,.F.);
#67268=ORIENTED_EDGE('',*,*,#48066,.T.);
#67269=ORIENTED_EDGE('',*,*,#48063,.F.);
#67270=ORIENTED_EDGE('',*,*,#48061,.T.);
#67271=ORIENTED_EDGE('',*,*,#48663,.T.);
#67272=ORIENTED_EDGE('',*,*,#48575,.F.);
#67273=ORIENTED_EDGE('',*,*,#48064,.F.);
#67274=ORIENTED_EDGE('',*,*,#48664,.F.);
#67275=ORIENTED_EDGE('',*,*,#48663,.F.);
#67276=ORIENTED_EDGE('',*,*,#48665,.F.);
#67277=ORIENTED_EDGE('',*,*,#48632,.F.);
#67278=ORIENTED_EDGE('',*,*,#48068,.F.);
#67279=ORIENTED_EDGE('',*,*,#48072,.F.);
#67280=ORIENTED_EDGE('',*,*,#48123,.F.);
#67281=ORIENTED_EDGE('',*,*,#48069,.F.);
#67282=ORIENTED_EDGE('',*,*,#48074,.F.);
#67283=ORIENTED_EDGE('',*,*,#48666,.T.);
#67284=ORIENTED_EDGE('',*,*,#48667,.T.);
#67285=ORIENTED_EDGE('',*,*,#48666,.F.);
#67286=ORIENTED_EDGE('',*,*,#48073,.F.);
#67287=ORIENTED_EDGE('',*,*,#48077,.F.);
#67288=ORIENTED_EDGE('',*,*,#48076,.F.);
#67289=ORIENTED_EDGE('',*,*,#48081,.F.);
#67290=ORIENTED_EDGE('',*,*,#48080,.F.);
#67291=ORIENTED_EDGE('',*,*,#48668,.T.);
#67292=ORIENTED_EDGE('',*,*,#48669,.T.);
#67293=ORIENTED_EDGE('',*,*,#48668,.F.);
#67294=ORIENTED_EDGE('',*,*,#48079,.F.);
#67295=ORIENTED_EDGE('',*,*,#48670,.T.);
#67296=ORIENTED_EDGE('',*,*,#48671,.F.);
#67297=ORIENTED_EDGE('',*,*,#48672,.F.);
#67298=ORIENTED_EDGE('',*,*,#48637,.F.);
#67299=ORIENTED_EDGE('',*,*,#48672,.T.);
#67300=ORIENTED_EDGE('',*,*,#48673,.F.);
#67301=ORIENTED_EDGE('',*,*,#48674,.F.);
#67302=ORIENTED_EDGE('',*,*,#48084,.F.);
#67303=ORIENTED_EDGE('',*,*,#48674,.T.);
#67304=ORIENTED_EDGE('',*,*,#48675,.F.);
#67305=ORIENTED_EDGE('',*,*,#48676,.F.);
#67306=ORIENTED_EDGE('',*,*,#48086,.F.);
#67307=ORIENTED_EDGE('',*,*,#48676,.T.);
#67308=ORIENTED_EDGE('',*,*,#48677,.F.);
#67309=ORIENTED_EDGE('',*,*,#48678,.F.);
#67310=ORIENTED_EDGE('',*,*,#48088,.F.);
#67311=ORIENTED_EDGE('',*,*,#48678,.T.);
#67312=ORIENTED_EDGE('',*,*,#48679,.F.);
#67313=ORIENTED_EDGE('',*,*,#48680,.F.);
#67314=ORIENTED_EDGE('',*,*,#48090,.F.);
#67315=ORIENTED_EDGE('',*,*,#48680,.T.);
#67316=ORIENTED_EDGE('',*,*,#48681,.F.);
#67317=ORIENTED_EDGE('',*,*,#48682,.F.);
#67318=ORIENTED_EDGE('',*,*,#48092,.F.);
#67319=ORIENTED_EDGE('',*,*,#48682,.T.);
#67320=ORIENTED_EDGE('',*,*,#48683,.F.);
#67321=ORIENTED_EDGE('',*,*,#48684,.F.);
#67322=ORIENTED_EDGE('',*,*,#48095,.F.);
#67323=ORIENTED_EDGE('',*,*,#48684,.T.);
#67324=ORIENTED_EDGE('',*,*,#48685,.F.);
#67325=ORIENTED_EDGE('',*,*,#48686,.F.);
#67326=ORIENTED_EDGE('',*,*,#48097,.F.);
#67327=ORIENTED_EDGE('',*,*,#48686,.T.);
#67328=ORIENTED_EDGE('',*,*,#48687,.F.);
#67329=ORIENTED_EDGE('',*,*,#48688,.F.);
#67330=ORIENTED_EDGE('',*,*,#48098,.F.);
#67331=ORIENTED_EDGE('',*,*,#48688,.T.);
#67332=ORIENTED_EDGE('',*,*,#48689,.F.);
#67333=ORIENTED_EDGE('',*,*,#48690,.F.);
#67334=ORIENTED_EDGE('',*,*,#48100,.F.);
#67335=ORIENTED_EDGE('',*,*,#48690,.T.);
#67336=ORIENTED_EDGE('',*,*,#48691,.F.);
#67337=ORIENTED_EDGE('',*,*,#48692,.F.);
#67338=ORIENTED_EDGE('',*,*,#48102,.F.);
#67339=ORIENTED_EDGE('',*,*,#48692,.T.);
#67340=ORIENTED_EDGE('',*,*,#48693,.F.);
#67341=ORIENTED_EDGE('',*,*,#48694,.F.);
#67342=ORIENTED_EDGE('',*,*,#48104,.F.);
#67343=ORIENTED_EDGE('',*,*,#48694,.T.);
#67344=ORIENTED_EDGE('',*,*,#48695,.F.);
#67345=ORIENTED_EDGE('',*,*,#48696,.F.);
#67346=ORIENTED_EDGE('',*,*,#48106,.F.);
#67347=ORIENTED_EDGE('',*,*,#48696,.T.);
#67348=ORIENTED_EDGE('',*,*,#48697,.F.);
#67349=ORIENTED_EDGE('',*,*,#48698,.F.);
#67350=ORIENTED_EDGE('',*,*,#48112,.F.);
#67351=ORIENTED_EDGE('',*,*,#48698,.T.);
#67352=ORIENTED_EDGE('',*,*,#48699,.F.);
#67353=ORIENTED_EDGE('',*,*,#48700,.F.);
#67354=ORIENTED_EDGE('',*,*,#48701,.F.);
#67355=ORIENTED_EDGE('',*,*,#48702,.F.);
#67356=ORIENTED_EDGE('',*,*,#48703,.T.);
#67357=ORIENTED_EDGE('',*,*,#48108,.F.);
#67358=ORIENTED_EDGE('',*,*,#48701,.T.);
#67359=ORIENTED_EDGE('',*,*,#48114,.T.);
#67360=ORIENTED_EDGE('',*,*,#48109,.F.);
#67361=ORIENTED_EDGE('',*,*,#48704,.F.);
#67362=ORIENTED_EDGE('',*,*,#48705,.F.);
#67363=ORIENTED_EDGE('',*,*,#48704,.T.);
#67364=ORIENTED_EDGE('',*,*,#48703,.F.);
#67365=ORIENTED_EDGE('',*,*,#48706,.F.);
#67366=ORIENTED_EDGE('',*,*,#48707,.F.);
#67367=ORIENTED_EDGE('',*,*,#48708,.F.);
#67368=ORIENTED_EDGE('',*,*,#48115,.T.);
#67369=ORIENTED_EDGE('',*,*,#48709,.F.);
#67370=ORIENTED_EDGE('',*,*,#48710,.F.);
#67371=ORIENTED_EDGE('',*,*,#48127,.T.);
#67372=ORIENTED_EDGE('',*,*,#48125,.T.);
#67373=ORIENTED_EDGE('',*,*,#48124,.T.);
#67374=ORIENTED_EDGE('',*,*,#48121,.T.);
#67375=ORIENTED_EDGE('',*,*,#48119,.T.);
#67376=ORIENTED_EDGE('',*,*,#48117,.T.);
#67377=ORIENTED_EDGE('',*,*,#48708,.T.);
#67378=ORIENTED_EDGE('',*,*,#48711,.F.);
#67379=ORIENTED_EDGE('',*,*,#48712,.T.);
#67380=ORIENTED_EDGE('',*,*,#48130,.T.);
#67381=ORIENTED_EDGE('',*,*,#48335,.F.);
#67382=ORIENTED_EDGE('',*,*,#48713,.F.);
#67383=ORIENTED_EDGE('',*,*,#48714,.F.);
#67384=ORIENTED_EDGE('',*,*,#48715,.F.);
#67385=ORIENTED_EDGE('',*,*,#48133,.T.);
#67386=ORIENTED_EDGE('',*,*,#48132,.F.);
#67387=ORIENTED_EDGE('',*,*,#48131,.T.);
#67388=ORIENTED_EDGE('',*,*,#48716,.T.);
#67389=ORIENTED_EDGE('',*,*,#48363,.F.);
#67390=ORIENTED_EDGE('',*,*,#48134,.F.);
#67391=ORIENTED_EDGE('',*,*,#48717,.F.);
#67392=ORIENTED_EDGE('',*,*,#48718,.T.);
#67393=ORIENTED_EDGE('',*,*,#48137,.F.);
#67394=ORIENTED_EDGE('',*,*,#48716,.F.);
#67395=ORIENTED_EDGE('',*,*,#48719,.F.);
#67396=ORIENTED_EDGE('',*,*,#48720,.T.);
#67397=ORIENTED_EDGE('',*,*,#48139,.F.);
#67398=ORIENTED_EDGE('',*,*,#48718,.F.);
#67399=ORIENTED_EDGE('',*,*,#48721,.F.);
#67400=ORIENTED_EDGE('',*,*,#48722,.T.);
#67401=ORIENTED_EDGE('',*,*,#48141,.F.);
#67402=ORIENTED_EDGE('',*,*,#48720,.F.);
#67403=ORIENTED_EDGE('',*,*,#48723,.F.);
#67404=ORIENTED_EDGE('',*,*,#48144,.T.);
#67405=ORIENTED_EDGE('',*,*,#48354,.F.);
#67406=ORIENTED_EDGE('',*,*,#48722,.F.);
#67407=ORIENTED_EDGE('',*,*,#48724,.F.);
#67408=ORIENTED_EDGE('',*,*,#48725,.F.);
#67409=ORIENTED_EDGE('',*,*,#48147,.T.);
#67410=ORIENTED_EDGE('',*,*,#48146,.F.);
#67411=ORIENTED_EDGE('',*,*,#48145,.T.);
#67412=ORIENTED_EDGE('',*,*,#48726,.T.);
#67413=ORIENTED_EDGE('',*,*,#48564,.F.);
#67414=ORIENTED_EDGE('',*,*,#48148,.F.);
#67415=ORIENTED_EDGE('',*,*,#48727,.F.);
#67416=ORIENTED_EDGE('',*,*,#48728,.T.);
#67417=ORIENTED_EDGE('',*,*,#48151,.F.);
#67418=ORIENTED_EDGE('',*,*,#48726,.F.);
#67419=ORIENTED_EDGE('',*,*,#48729,.F.);
#67420=ORIENTED_EDGE('',*,*,#48730,.T.);
#67421=ORIENTED_EDGE('',*,*,#48153,.F.);
#67422=ORIENTED_EDGE('',*,*,#48728,.F.);
#67423=ORIENTED_EDGE('',*,*,#48731,.F.);
#67424=ORIENTED_EDGE('',*,*,#48732,.T.);
#67425=ORIENTED_EDGE('',*,*,#48155,.F.);
#67426=ORIENTED_EDGE('',*,*,#48730,.F.);
#67427=ORIENTED_EDGE('',*,*,#48733,.F.);
#67428=ORIENTED_EDGE('',*,*,#48158,.T.);
#67429=ORIENTED_EDGE('',*,*,#48555,.F.);
#67430=ORIENTED_EDGE('',*,*,#48732,.F.);
#67431=ORIENTED_EDGE('',*,*,#48734,.F.);
#67432=ORIENTED_EDGE('',*,*,#48161,.F.);
#67433=ORIENTED_EDGE('',*,*,#48159,.T.);
#67434=ORIENTED_EDGE('',*,*,#48735,.F.);
#67435=ORIENTED_EDGE('',*,*,#48736,.F.);
#67436=ORIENTED_EDGE('',*,*,#48737,.F.);
#67437=ORIENTED_EDGE('',*,*,#48164,.T.);
#67438=ORIENTED_EDGE('',*,*,#48162,.F.);
#67439=ORIENTED_EDGE('',*,*,#48736,.T.);
#67440=ORIENTED_EDGE('',*,*,#48738,.F.);
#67441=ORIENTED_EDGE('',*,*,#48739,.F.);
#67442=ORIENTED_EDGE('',*,*,#48169,.T.);
#67443=ORIENTED_EDGE('',*,*,#48737,.T.);
#67444=ORIENTED_EDGE('',*,*,#48740,.T.);
#67445=ORIENTED_EDGE('',*,*,#48546,.F.);
#67446=ORIENTED_EDGE('',*,*,#48167,.F.);
#67447=ORIENTED_EDGE('',*,*,#48741,.F.);
#67448=ORIENTED_EDGE('',*,*,#48742,.T.);
#67449=ORIENTED_EDGE('',*,*,#48171,.F.);
#67450=ORIENTED_EDGE('',*,*,#48740,.F.);
#67451=ORIENTED_EDGE('',*,*,#48743,.F.);
#67452=ORIENTED_EDGE('',*,*,#48744,.T.);
#67453=ORIENTED_EDGE('',*,*,#48174,.F.);
#67454=ORIENTED_EDGE('',*,*,#48742,.F.);
#67455=ORIENTED_EDGE('',*,*,#48745,.F.);
#67456=ORIENTED_EDGE('',*,*,#48746,.T.);
#67457=ORIENTED_EDGE('',*,*,#48177,.F.);
#67458=ORIENTED_EDGE('',*,*,#48744,.F.);
#67459=ORIENTED_EDGE('',*,*,#48747,.F.);
#67460=ORIENTED_EDGE('',*,*,#48181,.T.);
#67461=ORIENTED_EDGE('',*,*,#48535,.F.);
#67462=ORIENTED_EDGE('',*,*,#48746,.F.);
#67463=ORIENTED_EDGE('',*,*,#48748,.F.);
#67464=ORIENTED_EDGE('',*,*,#48184,.T.);
#67465=ORIENTED_EDGE('',*,*,#48530,.F.);
#67466=ORIENTED_EDGE('',*,*,#48183,.T.);
#67467=ORIENTED_EDGE('',*,*,#48182,.T.);
#67468=ORIENTED_EDGE('',*,*,#48749,.F.);
#67469=ORIENTED_EDGE('',*,*,#48185,.T.);
#67470=ORIENTED_EDGE('',*,*,#48750,.T.);
#67471=ORIENTED_EDGE('',*,*,#48527,.F.);
#67472=ORIENTED_EDGE('',*,*,#48186,.F.);
#67473=ORIENTED_EDGE('',*,*,#48751,.F.);
#67474=ORIENTED_EDGE('',*,*,#48752,.T.);
#67475=ORIENTED_EDGE('',*,*,#48189,.F.);
#67476=ORIENTED_EDGE('',*,*,#48750,.F.);
#67477=ORIENTED_EDGE('',*,*,#48753,.F.);
#67478=ORIENTED_EDGE('',*,*,#48754,.T.);
#67479=ORIENTED_EDGE('',*,*,#48192,.F.);
#67480=ORIENTED_EDGE('',*,*,#48752,.F.);
#67481=ORIENTED_EDGE('',*,*,#48755,.F.);
#67482=ORIENTED_EDGE('',*,*,#48756,.T.);
#67483=ORIENTED_EDGE('',*,*,#48195,.F.);
#67484=ORIENTED_EDGE('',*,*,#48754,.F.);
#67485=ORIENTED_EDGE('',*,*,#48757,.F.);
#67486=ORIENTED_EDGE('',*,*,#48758,.T.);
#67487=ORIENTED_EDGE('',*,*,#48516,.F.);
#67488=ORIENTED_EDGE('',*,*,#48756,.F.);
#67489=ORIENTED_EDGE('',*,*,#48759,.F.);
#67490=ORIENTED_EDGE('',*,*,#48209,.T.);
#67491=ORIENTED_EDGE('',*,*,#48208,.T.);
#67492=ORIENTED_EDGE('',*,*,#48712,.F.);
#67493=ORIENTED_EDGE('',*,*,#48760,.F.);
#67494=ORIENTED_EDGE('',*,*,#48761,.F.);
#67495=ORIENTED_EDGE('',*,*,#48211,.T.);
#67496=ORIENTED_EDGE('',*,*,#48205,.T.);
#67497=ORIENTED_EDGE('',*,*,#48202,.T.);
#67498=ORIENTED_EDGE('',*,*,#48200,.T.);
#67499=ORIENTED_EDGE('',*,*,#48762,.T.);
#67500=ORIENTED_EDGE('',*,*,#48212,.F.);
#67501=ORIENTED_EDGE('',*,*,#48210,.F.);
#67502=ORIENTED_EDGE('',*,*,#48763,.F.);
#67503=ORIENTED_EDGE('',*,*,#48713,.T.);
#67504=ORIENTED_EDGE('',*,*,#48214,.F.);
#67505=ORIENTED_EDGE('',*,*,#48762,.F.);
#67506=ORIENTED_EDGE('',*,*,#48764,.F.);
#67507=ORIENTED_EDGE('',*,*,#48765,.T.);
#67508=ORIENTED_EDGE('',*,*,#48517,.F.);
#67509=ORIENTED_EDGE('',*,*,#48758,.F.);
#67510=ORIENTED_EDGE('',*,*,#48766,.F.);
#67511=ORIENTED_EDGE('',*,*,#48767,.F.);
#67512=ORIENTED_EDGE('',*,*,#48768,.T.);
#67513=ORIENTED_EDGE('',*,*,#48518,.F.);
#67514=ORIENTED_EDGE('',*,*,#48765,.F.);
#67515=ORIENTED_EDGE('',*,*,#48769,.F.);
#67516=ORIENTED_EDGE('',*,*,#48768,.F.);
#67517=ORIENTED_EDGE('',*,*,#48770,.F.);
#67518=ORIENTED_EDGE('',*,*,#48771,.F.);
#67519=ORIENTED_EDGE('',*,*,#48513,.F.);
#67520=ORIENTED_EDGE('',*,*,#48387,.F.);
#67521=ORIENTED_EDGE('',*,*,#48772,.T.);
#67522=ORIENTED_EDGE('',*,*,#48773,.T.);
#67523=ORIENTED_EDGE('',*,*,#48774,.F.);
#67524=ORIENTED_EDGE('',*,*,#48217,.T.);
#67525=ORIENTED_EDGE('',*,*,#48774,.T.);
#67526=ORIENTED_EDGE('',*,*,#48775,.T.);
#67527=ORIENTED_EDGE('',*,*,#48776,.T.);
#67528=ORIENTED_EDGE('',*,*,#48570,.T.);
#67529=ORIENTED_EDGE('',*,*,#48219,.T.);
#67530=ORIENTED_EDGE('',*,*,#48777,.T.);
#67531=ORIENTED_EDGE('',*,*,#48232,.T.);
#67532=ORIENTED_EDGE('',*,*,#48225,.F.);
#67533=ORIENTED_EDGE('',*,*,#48226,.F.);
#67534=ORIENTED_EDGE('',*,*,#48222,.T.);
#67535=ORIENTED_EDGE('',*,*,#48778,.T.);
#67536=ORIENTED_EDGE('',*,*,#48779,.T.);
#67537=ORIENTED_EDGE('',*,*,#48780,.T.);
#67538=ORIENTED_EDGE('',*,*,#48781,.T.);
#67539=ORIENTED_EDGE('',*,*,#48782,.T.);
#67540=ORIENTED_EDGE('',*,*,#48251,.T.);
#67541=ORIENTED_EDGE('',*,*,#48247,.F.);
#67542=ORIENTED_EDGE('',*,*,#48244,.T.);
#67543=ORIENTED_EDGE('',*,*,#48242,.T.);
#67544=ORIENTED_EDGE('',*,*,#48240,.T.);
#67545=ORIENTED_EDGE('',*,*,#48238,.T.);
#67546=ORIENTED_EDGE('',*,*,#48236,.T.);
#67547=ORIENTED_EDGE('',*,*,#48783,.T.);
#67548=ORIENTED_EDGE('',*,*,#48784,.T.);
#67549=ORIENTED_EDGE('',*,*,#48785,.T.);
#67550=ORIENTED_EDGE('',*,*,#48786,.T.);
#67551=ORIENTED_EDGE('',*,*,#48787,.F.);
#67552=ORIENTED_EDGE('',*,*,#48259,.T.);
#67553=ORIENTED_EDGE('',*,*,#48254,.F.);
#67554=ORIENTED_EDGE('',*,*,#48788,.F.);
#67555=ORIENTED_EDGE('',*,*,#48789,.F.);
#67556=ORIENTED_EDGE('',*,*,#48257,.F.);
#67557=ORIENTED_EDGE('',*,*,#48261,.T.);
#67558=ORIENTED_EDGE('',*,*,#48260,.T.);
#67559=ORIENTED_EDGE('',*,*,#48790,.F.);
#67560=ORIENTED_EDGE('',*,*,#48791,.F.);
#67561=ORIENTED_EDGE('',*,*,#48792,.T.);
#67562=ORIENTED_EDGE('',*,*,#48262,.F.);
#67563=ORIENTED_EDGE('',*,*,#48789,.T.);
#67564=ORIENTED_EDGE('',*,*,#48791,.T.);
#67565=ORIENTED_EDGE('',*,*,#48793,.F.);
#67566=ORIENTED_EDGE('',*,*,#48794,.T.);
#67567=ORIENTED_EDGE('',*,*,#48264,.F.);
#67568=ORIENTED_EDGE('',*,*,#48792,.F.);
#67569=ORIENTED_EDGE('',*,*,#48795,.F.);
#67570=ORIENTED_EDGE('',*,*,#48796,.T.);
#67571=ORIENTED_EDGE('',*,*,#48266,.F.);
#67572=ORIENTED_EDGE('',*,*,#48794,.F.);
#67573=ORIENTED_EDGE('',*,*,#48797,.F.);
#67574=ORIENTED_EDGE('',*,*,#48270,.T.);
#67575=ORIENTED_EDGE('',*,*,#48268,.F.);
#67576=ORIENTED_EDGE('',*,*,#48796,.F.);
#67577=ORIENTED_EDGE('',*,*,#48798,.F.);
#67578=ORIENTED_EDGE('',*,*,#48272,.F.);
#67579=ORIENTED_EDGE('',*,*,#48271,.T.);
#67580=ORIENTED_EDGE('',*,*,#48799,.F.);
#67581=ORIENTED_EDGE('',*,*,#48275,.T.);
#67582=ORIENTED_EDGE('',*,*,#48800,.T.);
#67583=ORIENTED_EDGE('',*,*,#48276,.F.);
#67584=ORIENTED_EDGE('',*,*,#48273,.F.);
#67585=ORIENTED_EDGE('',*,*,#48801,.F.);
#67586=ORIENTED_EDGE('',*,*,#48802,.T.);
#67587=ORIENTED_EDGE('',*,*,#48278,.F.);
#67588=ORIENTED_EDGE('',*,*,#48800,.F.);
#67589=ORIENTED_EDGE('',*,*,#48803,.F.);
#67590=ORIENTED_EDGE('',*,*,#48804,.T.);
#67591=ORIENTED_EDGE('',*,*,#48280,.F.);
#67592=ORIENTED_EDGE('',*,*,#48802,.F.);
#67593=ORIENTED_EDGE('',*,*,#48805,.F.);
#67594=ORIENTED_EDGE('',*,*,#48806,.T.);
#67595=ORIENTED_EDGE('',*,*,#48282,.F.);
#67596=ORIENTED_EDGE('',*,*,#48804,.F.);
#67597=ORIENTED_EDGE('',*,*,#48807,.F.);
#67598=ORIENTED_EDGE('',*,*,#48286,.T.);
#67599=ORIENTED_EDGE('',*,*,#48284,.F.);
#67600=ORIENTED_EDGE('',*,*,#48806,.F.);
#67601=ORIENTED_EDGE('',*,*,#48808,.F.);
#67602=ORIENTED_EDGE('',*,*,#48778,.F.);
#67603=ORIENTED_EDGE('',*,*,#48287,.T.);
#67604=ORIENTED_EDGE('',*,*,#48809,.F.);
#67605=ORIENTED_EDGE('',*,*,#48810,.T.);
#67606=ORIENTED_EDGE('',*,*,#48811,.F.);
#67607=ORIENTED_EDGE('',*,*,#48812,.F.);
#67608=ORIENTED_EDGE('',*,*,#48813,.F.);
#67609=ORIENTED_EDGE('',*,*,#48505,.F.);
#67610=ORIENTED_EDGE('',*,*,#48813,.T.);
#67611=ORIENTED_EDGE('',*,*,#48814,.F.);
#67612=ORIENTED_EDGE('',*,*,#48291,.F.);
#67613=ORIENTED_EDGE('',*,*,#48289,.F.);
#67614=ORIENTED_EDGE('',*,*,#48293,.F.);
#67615=ORIENTED_EDGE('',*,*,#48292,.T.);
#67616=ORIENTED_EDGE('',*,*,#48815,.F.);
#67617=ORIENTED_EDGE('',*,*,#48788,.T.);
#67618=ORIENTED_EDGE('',*,*,#48331,.T.);
#67619=ORIENTED_EDGE('',*,*,#48816,.F.);
#67620=ORIENTED_EDGE('',*,*,#48817,.F.);
#67621=ORIENTED_EDGE('',*,*,#48295,.F.);
#67622=ORIENTED_EDGE('',*,*,#48818,.T.);
#67623=ORIENTED_EDGE('',*,*,#48297,.F.);
#67624=ORIENTED_EDGE('',*,*,#48817,.T.);
#67625=ORIENTED_EDGE('',*,*,#48819,.F.);
#67626=ORIENTED_EDGE('',*,*,#48820,.T.);
#67627=ORIENTED_EDGE('',*,*,#48299,.F.);
#67628=ORIENTED_EDGE('',*,*,#48818,.F.);
#67629=ORIENTED_EDGE('',*,*,#48821,.F.);
#67630=ORIENTED_EDGE('',*,*,#48822,.T.);
#67631=ORIENTED_EDGE('',*,*,#48301,.F.);
#67632=ORIENTED_EDGE('',*,*,#48820,.F.);
#67633=ORIENTED_EDGE('',*,*,#48823,.F.);
#67634=ORIENTED_EDGE('',*,*,#48305,.T.);
#67635=ORIENTED_EDGE('',*,*,#48303,.F.);
#67636=ORIENTED_EDGE('',*,*,#48822,.F.);
#67637=ORIENTED_EDGE('',*,*,#48824,.F.);
#67638=ORIENTED_EDGE('',*,*,#48308,.F.);
#67639=ORIENTED_EDGE('',*,*,#48306,.T.);
#67640=ORIENTED_EDGE('',*,*,#48825,.F.);
#67641=ORIENTED_EDGE('',*,*,#48826,.F.);
#67642=ORIENTED_EDGE('',*,*,#48827,.F.);
#67643=ORIENTED_EDGE('',*,*,#48314,.T.);
#67644=ORIENTED_EDGE('',*,*,#48311,.F.);
#67645=ORIENTED_EDGE('',*,*,#48309,.F.);
#67646=ORIENTED_EDGE('',*,*,#48826,.T.);
#67647=ORIENTED_EDGE('',*,*,#48828,.T.);
#67648=ORIENTED_EDGE('',*,*,#48315,.F.);
#67649=ORIENTED_EDGE('',*,*,#48312,.F.);
#67650=ORIENTED_EDGE('',*,*,#48829,.F.);
#67651=ORIENTED_EDGE('',*,*,#48830,.T.);
#67652=ORIENTED_EDGE('',*,*,#48506,.F.);
#67653=ORIENTED_EDGE('',*,*,#48828,.F.);
#67654=ORIENTED_EDGE('',*,*,#48831,.F.);
#67655=ORIENTED_EDGE('',*,*,#48832,.F.);
#67656=ORIENTED_EDGE('',*,*,#48320,.T.);
#67657=ORIENTED_EDGE('',*,*,#48782,.F.);
#67658=ORIENTED_EDGE('',*,*,#48833,.F.);
#67659=ORIENTED_EDGE('',*,*,#48321,.T.);
#67660=ORIENTED_EDGE('',*,*,#48834,.F.);
#67661=ORIENTED_EDGE('',*,*,#48835,.F.);
#67662=ORIENTED_EDGE('',*,*,#48318,.F.);
#67663=ORIENTED_EDGE('',*,*,#48835,.T.);
#67664=ORIENTED_EDGE('',*,*,#48836,.F.);
#67665=ORIENTED_EDGE('',*,*,#48837,.F.);
#67666=ORIENTED_EDGE('',*,*,#48322,.F.);
#67667=ORIENTED_EDGE('',*,*,#48837,.T.);
#67668=ORIENTED_EDGE('',*,*,#48838,.F.);
#67669=ORIENTED_EDGE('',*,*,#48839,.F.);
#67670=ORIENTED_EDGE('',*,*,#48324,.F.);
#67671=ORIENTED_EDGE('',*,*,#48839,.T.);
#67672=ORIENTED_EDGE('',*,*,#48840,.F.);
#67673=ORIENTED_EDGE('',*,*,#48841,.F.);
#67674=ORIENTED_EDGE('',*,*,#48326,.F.);
#67675=ORIENTED_EDGE('',*,*,#48841,.T.);
#67676=ORIENTED_EDGE('',*,*,#48842,.F.);
#67677=ORIENTED_EDGE('',*,*,#48332,.F.);
#67678=ORIENTED_EDGE('',*,*,#48328,.F.);
#67679=ORIENTED_EDGE('',*,*,#48334,.F.);
#67680=ORIENTED_EDGE('',*,*,#48333,.T.);
#67681=ORIENTED_EDGE('',*,*,#48843,.F.);
#67682=ORIENTED_EDGE('',*,*,#48330,.T.);
#67683=ORIENTED_EDGE('',*,*,#48844,.T.);
#67684=ORIENTED_EDGE('',*,*,#48785,.F.);
#67685=ORIENTED_EDGE('',*,*,#48845,.F.);
#67686=ORIENTED_EDGE('',*,*,#48846,.F.);
#67687=ORIENTED_EDGE('',*,*,#48847,.T.);
#67688=ORIENTED_EDGE('',*,*,#48337,.F.);
#67689=ORIENTED_EDGE('',*,*,#48364,.F.);
#67690=ORIENTED_EDGE('',*,*,#48848,.F.);
#67691=ORIENTED_EDGE('',*,*,#48849,.T.);
#67692=ORIENTED_EDGE('',*,*,#48339,.F.);
#67693=ORIENTED_EDGE('',*,*,#48847,.F.);
#67694=ORIENTED_EDGE('',*,*,#48850,.F.);
#67695=ORIENTED_EDGE('',*,*,#48851,.T.);
#67696=ORIENTED_EDGE('',*,*,#48341,.F.);
#67697=ORIENTED_EDGE('',*,*,#48849,.F.);
#67698=ORIENTED_EDGE('',*,*,#48852,.F.);
#67699=ORIENTED_EDGE('',*,*,#48853,.T.);
#67700=ORIENTED_EDGE('',*,*,#48343,.F.);
#67701=ORIENTED_EDGE('',*,*,#48851,.F.);
#67702=ORIENTED_EDGE('',*,*,#48854,.F.);
#67703=ORIENTED_EDGE('',*,*,#48347,.T.);
#67704=ORIENTED_EDGE('',*,*,#48345,.F.);
#67705=ORIENTED_EDGE('',*,*,#48853,.F.);
#67706=ORIENTED_EDGE('',*,*,#48855,.F.);
#67707=ORIENTED_EDGE('',*,*,#48783,.F.);
#67708=ORIENTED_EDGE('',*,*,#48348,.T.);
#67709=ORIENTED_EDGE('',*,*,#48856,.F.);
#67710=ORIENTED_EDGE('',*,*,#48857,.T.);
#67711=ORIENTED_EDGE('',*,*,#48858,.F.);
#67712=ORIENTED_EDGE('',*,*,#48351,.T.);
#67713=ORIENTED_EDGE('',*,*,#48569,.F.);
#67714=ORIENTED_EDGE('',*,*,#48859,.F.);
#67715=ORIENTED_EDGE('',*,*,#48860,.F.);
#67716=ORIENTED_EDGE('',*,*,#48352,.F.);
#67717=ORIENTED_EDGE('',*,*,#48349,.F.);
#67718=ORIENTED_EDGE('',*,*,#48861,.F.);
#67719=ORIENTED_EDGE('',*,*,#48860,.T.);
#67720=ORIENTED_EDGE('',*,*,#48862,.F.);
#67721=ORIENTED_EDGE('',*,*,#48863,.F.);
#67722=ORIENTED_EDGE('',*,*,#48355,.F.);
#67723=ORIENTED_EDGE('',*,*,#48863,.T.);
#67724=ORIENTED_EDGE('',*,*,#48864,.F.);
#67725=ORIENTED_EDGE('',*,*,#48865,.F.);
#67726=ORIENTED_EDGE('',*,*,#48357,.F.);
#67727=ORIENTED_EDGE('',*,*,#48865,.T.);
#67728=ORIENTED_EDGE('',*,*,#48866,.F.);
#67729=ORIENTED_EDGE('',*,*,#48867,.F.);
#67730=ORIENTED_EDGE('',*,*,#48359,.F.);
#67731=ORIENTED_EDGE('',*,*,#48867,.T.);
#67732=ORIENTED_EDGE('',*,*,#48868,.F.);
#67733=ORIENTED_EDGE('',*,*,#48366,.F.);
#67734=ORIENTED_EDGE('',*,*,#48361,.F.);
#67735=ORIENTED_EDGE('',*,*,#48368,.F.);
#67736=ORIENTED_EDGE('',*,*,#48367,.T.);
#67737=ORIENTED_EDGE('',*,*,#48869,.F.);
#67738=ORIENTED_EDGE('',*,*,#48365,.T.);
#67739=ORIENTED_EDGE('',*,*,#48859,.T.);
#67740=ORIENTED_EDGE('',*,*,#48568,.F.);
#67741=ORIENTED_EDGE('',*,*,#48870,.F.);
#67742=ORIENTED_EDGE('',*,*,#48871,.F.);
#67743=ORIENTED_EDGE('',*,*,#48872,.T.);
#67744=ORIENTED_EDGE('',*,*,#48780,.F.);
#67745=ORIENTED_EDGE('',*,*,#48873,.F.);
#67746=ORIENTED_EDGE('',*,*,#48874,.F.);
#67747=ORIENTED_EDGE('',*,*,#48404,.T.);
#67748=ORIENTED_EDGE('',*,*,#48875,.F.);
#67749=ORIENTED_EDGE('',*,*,#48876,.F.);
#67750=ORIENTED_EDGE('',*,*,#48370,.F.);
#67751=ORIENTED_EDGE('',*,*,#48877,.T.);
#67752=ORIENTED_EDGE('',*,*,#48372,.F.);
#67753=ORIENTED_EDGE('',*,*,#48876,.T.);
#67754=ORIENTED_EDGE('',*,*,#48878,.F.);
#67755=ORIENTED_EDGE('',*,*,#48879,.T.);
#67756=ORIENTED_EDGE('',*,*,#48374,.F.);
#67757=ORIENTED_EDGE('',*,*,#48877,.F.);
#67758=ORIENTED_EDGE('',*,*,#48880,.F.);
#67759=ORIENTED_EDGE('',*,*,#48881,.T.);
#67760=ORIENTED_EDGE('',*,*,#48376,.F.);
#67761=ORIENTED_EDGE('',*,*,#48879,.F.);
#67762=ORIENTED_EDGE('',*,*,#48882,.F.);
#67763=ORIENTED_EDGE('',*,*,#48380,.T.);
#67764=ORIENTED_EDGE('',*,*,#48378,.F.);
#67765=ORIENTED_EDGE('',*,*,#48881,.F.);
#67766=ORIENTED_EDGE('',*,*,#48883,.F.);
#67767=ORIENTED_EDGE('',*,*,#48383,.F.);
#67768=ORIENTED_EDGE('',*,*,#48381,.T.);
#67769=ORIENTED_EDGE('',*,*,#48884,.F.);
#67770=ORIENTED_EDGE('',*,*,#48885,.F.);
#67771=ORIENTED_EDGE('',*,*,#48886,.F.);
#67772=ORIENTED_EDGE('',*,*,#48388,.T.);
#67773=ORIENTED_EDGE('',*,*,#48384,.F.);
#67774=ORIENTED_EDGE('',*,*,#48885,.T.);
#67775=ORIENTED_EDGE('',*,*,#48389,.T.);
#67776=ORIENTED_EDGE('',*,*,#48887,.F.);
#67777=ORIENTED_EDGE('',*,*,#48888,.F.);
#67778=ORIENTED_EDGE('',*,*,#48386,.F.);
#67779=ORIENTED_EDGE('',*,*,#48889,.T.);
#67780=ORIENTED_EDGE('',*,*,#48772,.F.);
#67781=ORIENTED_EDGE('',*,*,#48888,.T.);
#67782=ORIENTED_EDGE('',*,*,#48890,.F.);
#67783=ORIENTED_EDGE('',*,*,#48891,.F.);
#67784=ORIENTED_EDGE('',*,*,#48392,.T.);
#67785=ORIENTED_EDGE('',*,*,#48777,.F.);
#67786=ORIENTED_EDGE('',*,*,#48892,.F.);
#67787=ORIENTED_EDGE('',*,*,#48893,.T.);
#67788=ORIENTED_EDGE('',*,*,#48393,.F.);
#67789=ORIENTED_EDGE('',*,*,#48390,.F.);
#67790=ORIENTED_EDGE('',*,*,#48894,.F.);
#67791=ORIENTED_EDGE('',*,*,#48895,.T.);
#67792=ORIENTED_EDGE('',*,*,#48395,.F.);
#67793=ORIENTED_EDGE('',*,*,#48893,.F.);
#67794=ORIENTED_EDGE('',*,*,#48896,.F.);
#67795=ORIENTED_EDGE('',*,*,#48897,.T.);
#67796=ORIENTED_EDGE('',*,*,#48397,.F.);
#67797=ORIENTED_EDGE('',*,*,#48895,.F.);
#67798=ORIENTED_EDGE('',*,*,#48898,.F.);
#67799=ORIENTED_EDGE('',*,*,#48899,.T.);
#67800=ORIENTED_EDGE('',*,*,#48399,.F.);
#67801=ORIENTED_EDGE('',*,*,#48897,.F.);
#67802=ORIENTED_EDGE('',*,*,#48900,.F.);
#67803=ORIENTED_EDGE('',*,*,#48405,.T.);
#67804=ORIENTED_EDGE('',*,*,#48401,.F.);
#67805=ORIENTED_EDGE('',*,*,#48899,.F.);
#67806=ORIENTED_EDGE('',*,*,#48901,.F.);
#67807=ORIENTED_EDGE('',*,*,#48407,.F.);
#67808=ORIENTED_EDGE('',*,*,#48406,.T.);
#67809=ORIENTED_EDGE('',*,*,#48902,.F.);
#67810=ORIENTED_EDGE('',*,*,#48403,.T.);
#67811=ORIENTED_EDGE('',*,*,#48903,.T.);
#67812=ORIENTED_EDGE('',*,*,#48904,.F.);
#67813=ORIENTED_EDGE('',*,*,#48905,.F.);
#67814=ORIENTED_EDGE('',*,*,#48512,.F.);
#67815=ORIENTED_EDGE('',*,*,#48905,.T.);
#67816=ORIENTED_EDGE('',*,*,#48906,.F.);
#67817=ORIENTED_EDGE('',*,*,#48411,.F.);
#67818=ORIENTED_EDGE('',*,*,#48409,.F.);
#67819=ORIENTED_EDGE('',*,*,#48413,.F.);
#67820=ORIENTED_EDGE('',*,*,#48412,.T.);
#67821=ORIENTED_EDGE('',*,*,#48907,.F.);
#67822=ORIENTED_EDGE('',*,*,#48417,.T.);
#67823=ORIENTED_EDGE('',*,*,#48418,.T.);
#67824=ORIENTED_EDGE('',*,*,#48908,.F.);
#67825=ORIENTED_EDGE('',*,*,#48909,.F.);
#67826=ORIENTED_EDGE('',*,*,#48415,.F.);
#67827=ORIENTED_EDGE('',*,*,#48909,.T.);
#67828=ORIENTED_EDGE('',*,*,#48910,.F.);
#67829=ORIENTED_EDGE('',*,*,#48911,.F.);
#67830=ORIENTED_EDGE('',*,*,#48419,.F.);
#67831=ORIENTED_EDGE('',*,*,#48911,.T.);
#67832=ORIENTED_EDGE('',*,*,#48912,.F.);
#67833=ORIENTED_EDGE('',*,*,#48913,.F.);
#67834=ORIENTED_EDGE('',*,*,#48421,.F.);
#67835=ORIENTED_EDGE('',*,*,#48913,.T.);
#67836=ORIENTED_EDGE('',*,*,#48914,.F.);
#67837=ORIENTED_EDGE('',*,*,#48915,.F.);
#67838=ORIENTED_EDGE('',*,*,#48423,.F.);
#67839=ORIENTED_EDGE('',*,*,#48915,.T.);
#67840=ORIENTED_EDGE('',*,*,#48916,.F.);
#67841=ORIENTED_EDGE('',*,*,#48427,.F.);
#67842=ORIENTED_EDGE('',*,*,#48425,.F.);
#67843=ORIENTED_EDGE('',*,*,#48429,.F.);
#67844=ORIENTED_EDGE('',*,*,#48428,.T.);
#67845=ORIENTED_EDGE('',*,*,#48917,.F.);
#67846=ORIENTED_EDGE('',*,*,#48433,.T.);
#67847=ORIENTED_EDGE('',*,*,#48434,.T.);
#67848=ORIENTED_EDGE('',*,*,#48918,.F.);
#67849=ORIENTED_EDGE('',*,*,#48919,.F.);
#67850=ORIENTED_EDGE('',*,*,#48431,.F.);
#67851=ORIENTED_EDGE('',*,*,#48920,.T.);
#67852=ORIENTED_EDGE('',*,*,#48435,.F.);
#67853=ORIENTED_EDGE('',*,*,#48919,.T.);
#67854=ORIENTED_EDGE('',*,*,#48921,.F.);
#67855=ORIENTED_EDGE('',*,*,#48922,.T.);
#67856=ORIENTED_EDGE('',*,*,#48437,.F.);
#67857=ORIENTED_EDGE('',*,*,#48920,.F.);
#67858=ORIENTED_EDGE('',*,*,#48923,.F.);
#67859=ORIENTED_EDGE('',*,*,#48924,.T.);
#67860=ORIENTED_EDGE('',*,*,#48439,.F.);
#67861=ORIENTED_EDGE('',*,*,#48922,.F.);
#67862=ORIENTED_EDGE('',*,*,#48925,.F.);
#67863=ORIENTED_EDGE('',*,*,#48443,.T.);
#67864=ORIENTED_EDGE('',*,*,#48441,.F.);
#67865=ORIENTED_EDGE('',*,*,#48924,.F.);
#67866=ORIENTED_EDGE('',*,*,#48926,.F.);
#67867=ORIENTED_EDGE('',*,*,#48445,.F.);
#67868=ORIENTED_EDGE('',*,*,#48444,.T.);
#67869=ORIENTED_EDGE('',*,*,#48927,.F.);
#67870=ORIENTED_EDGE('',*,*,#48449,.T.);
#67871=ORIENTED_EDGE('',*,*,#48450,.T.);
#67872=ORIENTED_EDGE('',*,*,#48928,.F.);
#67873=ORIENTED_EDGE('',*,*,#48929,.F.);
#67874=ORIENTED_EDGE('',*,*,#48447,.F.);
#67875=ORIENTED_EDGE('',*,*,#48930,.T.);
#67876=ORIENTED_EDGE('',*,*,#48451,.F.);
#67877=ORIENTED_EDGE('',*,*,#48929,.T.);
#67878=ORIENTED_EDGE('',*,*,#48931,.F.);
#67879=ORIENTED_EDGE('',*,*,#48932,.T.);
#67880=ORIENTED_EDGE('',*,*,#48453,.F.);
#67881=ORIENTED_EDGE('',*,*,#48930,.F.);
#67882=ORIENTED_EDGE('',*,*,#48933,.F.);
#67883=ORIENTED_EDGE('',*,*,#48934,.T.);
#67884=ORIENTED_EDGE('',*,*,#48455,.F.);
#67885=ORIENTED_EDGE('',*,*,#48932,.F.);
#67886=ORIENTED_EDGE('',*,*,#48935,.F.);
#67887=ORIENTED_EDGE('',*,*,#48459,.T.);
#67888=ORIENTED_EDGE('',*,*,#48457,.F.);
#67889=ORIENTED_EDGE('',*,*,#48934,.F.);
#67890=ORIENTED_EDGE('',*,*,#48936,.F.);
#67891=ORIENTED_EDGE('',*,*,#48461,.F.);
#67892=ORIENTED_EDGE('',*,*,#48460,.T.);
#67893=ORIENTED_EDGE('',*,*,#48937,.F.);
#67894=ORIENTED_EDGE('',*,*,#48465,.T.);
#67895=ORIENTED_EDGE('',*,*,#48466,.T.);
#67896=ORIENTED_EDGE('',*,*,#48938,.F.);
#67897=ORIENTED_EDGE('',*,*,#48939,.F.);
#67898=ORIENTED_EDGE('',*,*,#48463,.F.);
#67899=ORIENTED_EDGE('',*,*,#48940,.T.);
#67900=ORIENTED_EDGE('',*,*,#48467,.F.);
#67901=ORIENTED_EDGE('',*,*,#48939,.T.);
#67902=ORIENTED_EDGE('',*,*,#48941,.F.);
#67903=ORIENTED_EDGE('',*,*,#48942,.T.);
#67904=ORIENTED_EDGE('',*,*,#48469,.F.);
#67905=ORIENTED_EDGE('',*,*,#48940,.F.);
#67906=ORIENTED_EDGE('',*,*,#48943,.F.);
#67907=ORIENTED_EDGE('',*,*,#48944,.T.);
#67908=ORIENTED_EDGE('',*,*,#48471,.F.);
#67909=ORIENTED_EDGE('',*,*,#48942,.F.);
#67910=ORIENTED_EDGE('',*,*,#48945,.F.);
#67911=ORIENTED_EDGE('',*,*,#48475,.T.);
#67912=ORIENTED_EDGE('',*,*,#48473,.F.);
#67913=ORIENTED_EDGE('',*,*,#48944,.F.);
#67914=ORIENTED_EDGE('',*,*,#48946,.F.);
#67915=ORIENTED_EDGE('',*,*,#48477,.F.);
#67916=ORIENTED_EDGE('',*,*,#48476,.T.);
#67917=ORIENTED_EDGE('',*,*,#48947,.F.);
#67918=ORIENTED_EDGE('',*,*,#48481,.T.);
#67919=ORIENTED_EDGE('',*,*,#48482,.T.);
#67920=ORIENTED_EDGE('',*,*,#48948,.F.);
#67921=ORIENTED_EDGE('',*,*,#48949,.F.);
#67922=ORIENTED_EDGE('',*,*,#48479,.F.);
#67923=ORIENTED_EDGE('',*,*,#48949,.T.);
#67924=ORIENTED_EDGE('',*,*,#48950,.F.);
#67925=ORIENTED_EDGE('',*,*,#48951,.F.);
#67926=ORIENTED_EDGE('',*,*,#48483,.F.);
#67927=ORIENTED_EDGE('',*,*,#48951,.T.);
#67928=ORIENTED_EDGE('',*,*,#48952,.F.);
#67929=ORIENTED_EDGE('',*,*,#48953,.F.);
#67930=ORIENTED_EDGE('',*,*,#48485,.F.);
#67931=ORIENTED_EDGE('',*,*,#48953,.T.);
#67932=ORIENTED_EDGE('',*,*,#48954,.F.);
#67933=ORIENTED_EDGE('',*,*,#48955,.F.);
#67934=ORIENTED_EDGE('',*,*,#48487,.F.);
#67935=ORIENTED_EDGE('',*,*,#48955,.T.);
#67936=ORIENTED_EDGE('',*,*,#48956,.F.);
#67937=ORIENTED_EDGE('',*,*,#48491,.F.);
#67938=ORIENTED_EDGE('',*,*,#48489,.F.);
#67939=ORIENTED_EDGE('',*,*,#48493,.F.);
#67940=ORIENTED_EDGE('',*,*,#48492,.T.);
#67941=ORIENTED_EDGE('',*,*,#48957,.F.);
#67942=ORIENTED_EDGE('',*,*,#48496,.T.);
#67943=ORIENTED_EDGE('',*,*,#48958,.T.);
#67944=ORIENTED_EDGE('',*,*,#48497,.F.);
#67945=ORIENTED_EDGE('',*,*,#48494,.F.);
#67946=ORIENTED_EDGE('',*,*,#48959,.F.);
#67947=ORIENTED_EDGE('',*,*,#48960,.T.);
#67948=ORIENTED_EDGE('',*,*,#48499,.F.);
#67949=ORIENTED_EDGE('',*,*,#48958,.F.);
#67950=ORIENTED_EDGE('',*,*,#48961,.F.);
#67951=ORIENTED_EDGE('',*,*,#48869,.T.);
#67952=ORIENTED_EDGE('',*,*,#48868,.T.);
#67953=ORIENTED_EDGE('',*,*,#48866,.T.);
#67954=ORIENTED_EDGE('',*,*,#48864,.T.);
#67955=ORIENTED_EDGE('',*,*,#48862,.T.);
#67956=ORIENTED_EDGE('',*,*,#48861,.T.);
#67957=ORIENTED_EDGE('',*,*,#48858,.T.);
#67958=ORIENTED_EDGE('',*,*,#48962,.T.);
#67959=ORIENTED_EDGE('',*,*,#48963,.T.);
#67960=ORIENTED_EDGE('',*,*,#48964,.T.);
#67961=ORIENTED_EDGE('',*,*,#48856,.T.);
#67962=ORIENTED_EDGE('',*,*,#48855,.T.);
#67963=ORIENTED_EDGE('',*,*,#48854,.T.);
#67964=ORIENTED_EDGE('',*,*,#48852,.T.);
#67965=ORIENTED_EDGE('',*,*,#48850,.T.);
#67966=ORIENTED_EDGE('',*,*,#48848,.T.);
#67967=ORIENTED_EDGE('',*,*,#48845,.T.);
#67968=ORIENTED_EDGE('',*,*,#48784,.F.);
#67969=ORIENTED_EDGE('',*,*,#48857,.F.);
#67970=ORIENTED_EDGE('',*,*,#48965,.F.);
#67971=ORIENTED_EDGE('',*,*,#48966,.T.);
#67972=ORIENTED_EDGE('',*,*,#48846,.T.);
#67973=ORIENTED_EDGE('',*,*,#48967,.T.);
#67974=ORIENTED_EDGE('',*,*,#48968,.T.);
#67975=ORIENTED_EDGE('',*,*,#48967,.F.);
#67976=ORIENTED_EDGE('',*,*,#48965,.T.);
#67977=ORIENTED_EDGE('',*,*,#48964,.F.);
#67978=ORIENTED_EDGE('',*,*,#48969,.F.);
#67979=ORIENTED_EDGE('',*,*,#48833,.T.);
#67980=ORIENTED_EDGE('',*,*,#48786,.F.);
#67981=ORIENTED_EDGE('',*,*,#48844,.F.);
#67982=ORIENTED_EDGE('',*,*,#48970,.F.);
#67983=ORIENTED_EDGE('',*,*,#48843,.T.);
#67984=ORIENTED_EDGE('',*,*,#48842,.T.);
#67985=ORIENTED_EDGE('',*,*,#48840,.T.);
#67986=ORIENTED_EDGE('',*,*,#48838,.T.);
#67987=ORIENTED_EDGE('',*,*,#48836,.T.);
#67988=ORIENTED_EDGE('',*,*,#48834,.T.);
#67989=ORIENTED_EDGE('',*,*,#48832,.T.);
#67990=ORIENTED_EDGE('',*,*,#48971,.T.);
#67991=ORIENTED_EDGE('',*,*,#48972,.T.);
#67992=ORIENTED_EDGE('',*,*,#48973,.T.);
#67993=ORIENTED_EDGE('',*,*,#48831,.T.);
#67994=ORIENTED_EDGE('',*,*,#48829,.T.);
#67995=ORIENTED_EDGE('',*,*,#48827,.T.);
#67996=ORIENTED_EDGE('',*,*,#48825,.T.);
#67997=ORIENTED_EDGE('',*,*,#48824,.T.);
#67998=ORIENTED_EDGE('',*,*,#48823,.T.);
#67999=ORIENTED_EDGE('',*,*,#48821,.T.);
#68000=ORIENTED_EDGE('',*,*,#48819,.T.);
#68001=ORIENTED_EDGE('',*,*,#48816,.T.);
#68002=ORIENTED_EDGE('',*,*,#48971,.F.);
#68003=ORIENTED_EDGE('',*,*,#48970,.T.);
#68004=ORIENTED_EDGE('',*,*,#48966,.F.);
#68005=ORIENTED_EDGE('',*,*,#48974,.F.);
#68006=ORIENTED_EDGE('',*,*,#48975,.T.);
#68007=ORIENTED_EDGE('',*,*,#48507,.F.);
#68008=ORIENTED_EDGE('',*,*,#48830,.F.);
#68009=ORIENTED_EDGE('',*,*,#48976,.F.);
#68010=ORIENTED_EDGE('',*,*,#48977,.F.);
#68011=ORIENTED_EDGE('',*,*,#48509,.F.);
#68012=ORIENTED_EDGE('',*,*,#48975,.F.);
#68013=ORIENTED_EDGE('',*,*,#48978,.F.);
#68014=ORIENTED_EDGE('',*,*,#48977,.T.);
#68015=ORIENTED_EDGE('',*,*,#48979,.F.);
#68016=ORIENTED_EDGE('',*,*,#48903,.F.);
#68017=ORIENTED_EDGE('',*,*,#48511,.F.);
#68018=ORIENTED_EDGE('',*,*,#48980,.F.);
#68019=ORIENTED_EDGE('',*,*,#48981,.T.);
#68020=ORIENTED_EDGE('',*,*,#48961,.T.);
#68021=ORIENTED_EDGE('',*,*,#48959,.T.);
#68022=ORIENTED_EDGE('',*,*,#48957,.T.);
#68023=ORIENTED_EDGE('',*,*,#48956,.T.);
#68024=ORIENTED_EDGE('',*,*,#48954,.T.);
#68025=ORIENTED_EDGE('',*,*,#48952,.T.);
#68026=ORIENTED_EDGE('',*,*,#48950,.T.);
#68027=ORIENTED_EDGE('',*,*,#48948,.T.);
#68028=ORIENTED_EDGE('',*,*,#48947,.T.);
#68029=ORIENTED_EDGE('',*,*,#48946,.T.);
#68030=ORIENTED_EDGE('',*,*,#48945,.T.);
#68031=ORIENTED_EDGE('',*,*,#48943,.T.);
#68032=ORIENTED_EDGE('',*,*,#48941,.T.);
#68033=ORIENTED_EDGE('',*,*,#48938,.T.);
#68034=ORIENTED_EDGE('',*,*,#48937,.T.);
#68035=ORIENTED_EDGE('',*,*,#48936,.T.);
#68036=ORIENTED_EDGE('',*,*,#48935,.T.);
#68037=ORIENTED_EDGE('',*,*,#48933,.T.);
#68038=ORIENTED_EDGE('',*,*,#48931,.T.);
#68039=ORIENTED_EDGE('',*,*,#48928,.T.);
#68040=ORIENTED_EDGE('',*,*,#48927,.T.);
#68041=ORIENTED_EDGE('',*,*,#48926,.T.);
#68042=ORIENTED_EDGE('',*,*,#48925,.T.);
#68043=ORIENTED_EDGE('',*,*,#48923,.T.);
#68044=ORIENTED_EDGE('',*,*,#48921,.T.);
#68045=ORIENTED_EDGE('',*,*,#48918,.T.);
#68046=ORIENTED_EDGE('',*,*,#48917,.T.);
#68047=ORIENTED_EDGE('',*,*,#48916,.T.);
#68048=ORIENTED_EDGE('',*,*,#48914,.T.);
#68049=ORIENTED_EDGE('',*,*,#48912,.T.);
#68050=ORIENTED_EDGE('',*,*,#48910,.T.);
#68051=ORIENTED_EDGE('',*,*,#48908,.T.);
#68052=ORIENTED_EDGE('',*,*,#48907,.T.);
#68053=ORIENTED_EDGE('',*,*,#48906,.T.);
#68054=ORIENTED_EDGE('',*,*,#48904,.T.);
#68055=ORIENTED_EDGE('',*,*,#48982,.T.);
#68056=ORIENTED_EDGE('',*,*,#48982,.F.);
#68057=ORIENTED_EDGE('',*,*,#48979,.T.);
#68058=ORIENTED_EDGE('',*,*,#48978,.T.);
#68059=ORIENTED_EDGE('',*,*,#48976,.T.);
#68060=ORIENTED_EDGE('',*,*,#48973,.F.);
#68061=ORIENTED_EDGE('',*,*,#48983,.F.);
#68062=ORIENTED_EDGE('',*,*,#48984,.T.);
#68063=ORIENTED_EDGE('',*,*,#48500,.F.);
#68064=ORIENTED_EDGE('',*,*,#48960,.F.);
#68065=ORIENTED_EDGE('',*,*,#48985,.F.);
#68066=ORIENTED_EDGE('',*,*,#48986,.T.);
#68067=ORIENTED_EDGE('',*,*,#48502,.F.);
#68068=ORIENTED_EDGE('',*,*,#48984,.F.);
#68069=ORIENTED_EDGE('',*,*,#48987,.F.);
#68070=ORIENTED_EDGE('',*,*,#48811,.T.);
#68071=ORIENTED_EDGE('',*,*,#48504,.F.);
#68072=ORIENTED_EDGE('',*,*,#48986,.F.);
#68073=ORIENTED_EDGE('',*,*,#48988,.F.);
#68074=ORIENTED_EDGE('',*,*,#48771,.T.);
#68075=ORIENTED_EDGE('',*,*,#48989,.F.);
#68076=ORIENTED_EDGE('',*,*,#48990,.F.);
#68077=ORIENTED_EDGE('',*,*,#48514,.F.);
#68078=ORIENTED_EDGE('',*,*,#48990,.T.);
#68079=ORIENTED_EDGE('',*,*,#48991,.F.);
#68080=ORIENTED_EDGE('',*,*,#48992,.F.);
#68081=ORIENTED_EDGE('',*,*,#48519,.F.);
#68082=ORIENTED_EDGE('',*,*,#48992,.T.);
#68083=ORIENTED_EDGE('',*,*,#48993,.F.);
#68084=ORIENTED_EDGE('',*,*,#48994,.F.);
#68085=ORIENTED_EDGE('',*,*,#48521,.F.);
#68086=ORIENTED_EDGE('',*,*,#48994,.T.);
#68087=ORIENTED_EDGE('',*,*,#48995,.F.);
#68088=ORIENTED_EDGE('',*,*,#48996,.F.);
#68089=ORIENTED_EDGE('',*,*,#48523,.F.);
#68090=ORIENTED_EDGE('',*,*,#48996,.T.);
#68091=ORIENTED_EDGE('',*,*,#48997,.F.);
#68092=ORIENTED_EDGE('',*,*,#48528,.F.);
#68093=ORIENTED_EDGE('',*,*,#48525,.F.);
#68094=ORIENTED_EDGE('',*,*,#48531,.F.);
#68095=ORIENTED_EDGE('',*,*,#48529,.T.);
#68096=ORIENTED_EDGE('',*,*,#48998,.F.);
#68097=ORIENTED_EDGE('',*,*,#48536,.T.);
#68098=ORIENTED_EDGE('',*,*,#48537,.T.);
#68099=ORIENTED_EDGE('',*,*,#48999,.F.);
#68100=ORIENTED_EDGE('',*,*,#49000,.F.);
#68101=ORIENTED_EDGE('',*,*,#48533,.F.);
#68102=ORIENTED_EDGE('',*,*,#49000,.T.);
#68103=ORIENTED_EDGE('',*,*,#49001,.F.);
#68104=ORIENTED_EDGE('',*,*,#49002,.F.);
#68105=ORIENTED_EDGE('',*,*,#48538,.F.);
#68106=ORIENTED_EDGE('',*,*,#49002,.T.);
#68107=ORIENTED_EDGE('',*,*,#49003,.F.);
#68108=ORIENTED_EDGE('',*,*,#49004,.F.);
#68109=ORIENTED_EDGE('',*,*,#48540,.F.);
#68110=ORIENTED_EDGE('',*,*,#49004,.T.);
#68111=ORIENTED_EDGE('',*,*,#49005,.F.);
#68112=ORIENTED_EDGE('',*,*,#49006,.F.);
#68113=ORIENTED_EDGE('',*,*,#48542,.F.);
#68114=ORIENTED_EDGE('',*,*,#49006,.T.);
#68115=ORIENTED_EDGE('',*,*,#49007,.F.);
#68116=ORIENTED_EDGE('',*,*,#48547,.F.);
#68117=ORIENTED_EDGE('',*,*,#48544,.F.);
#68118=ORIENTED_EDGE('',*,*,#48549,.F.);
#68119=ORIENTED_EDGE('',*,*,#48548,.T.);
#68120=ORIENTED_EDGE('',*,*,#49008,.F.);
#68121=ORIENTED_EDGE('',*,*,#48552,.T.);
#68122=ORIENTED_EDGE('',*,*,#49009,.F.);
#68123=ORIENTED_EDGE('',*,*,#48553,.F.);
#68124=ORIENTED_EDGE('',*,*,#48550,.F.);
#68125=ORIENTED_EDGE('',*,*,#49010,.F.);
#68126=ORIENTED_EDGE('',*,*,#49009,.T.);
#68127=ORIENTED_EDGE('',*,*,#49011,.F.);
#68128=ORIENTED_EDGE('',*,*,#49012,.F.);
#68129=ORIENTED_EDGE('',*,*,#48556,.F.);
#68130=ORIENTED_EDGE('',*,*,#49012,.T.);
#68131=ORIENTED_EDGE('',*,*,#49013,.F.);
#68132=ORIENTED_EDGE('',*,*,#49014,.F.);
#68133=ORIENTED_EDGE('',*,*,#48558,.F.);
#68134=ORIENTED_EDGE('',*,*,#49014,.T.);
#68135=ORIENTED_EDGE('',*,*,#49015,.F.);
#68136=ORIENTED_EDGE('',*,*,#49016,.F.);
#68137=ORIENTED_EDGE('',*,*,#48560,.F.);
#68138=ORIENTED_EDGE('',*,*,#49016,.T.);
#68139=ORIENTED_EDGE('',*,*,#49017,.F.);
#68140=ORIENTED_EDGE('',*,*,#48565,.F.);
#68141=ORIENTED_EDGE('',*,*,#48562,.F.);
#68142=ORIENTED_EDGE('',*,*,#48567,.F.);
#68143=ORIENTED_EDGE('',*,*,#48566,.T.);
#68144=ORIENTED_EDGE('',*,*,#49018,.F.);
#68145=ORIENTED_EDGE('',*,*,#48870,.T.);
#68146=ORIENTED_EDGE('',*,*,#48962,.F.);
#68147=ORIENTED_EDGE('',*,*,#48871,.T.);
#68148=ORIENTED_EDGE('',*,*,#49019,.F.);
#68149=ORIENTED_EDGE('',*,*,#49020,.F.);
#68150=ORIENTED_EDGE('',*,*,#49021,.T.);
#68151=ORIENTED_EDGE('',*,*,#48776,.F.);
#68152=ORIENTED_EDGE('',*,*,#49022,.F.);
#68153=ORIENTED_EDGE('',*,*,#49023,.F.);
#68154=ORIENTED_EDGE('',*,*,#49024,.T.);
#68155=ORIENTED_EDGE('',*,*,#48571,.F.);
#68156=ORIENTED_EDGE('',*,*,#49021,.F.);
#68157=ORIENTED_EDGE('',*,*,#49025,.F.);
#68158=ORIENTED_EDGE('',*,*,#49024,.F.);
#68159=ORIENTED_EDGE('',*,*,#49026,.F.);
#68160=ORIENTED_EDGE('',*,*,#48576,.T.);
#68161=ORIENTED_EDGE('',*,*,#48573,.F.);
#68162=ORIENTED_EDGE('',*,*,#48578,.F.);
#68163=ORIENTED_EDGE('',*,*,#48577,.T.);
#68164=ORIENTED_EDGE('',*,*,#49027,.F.);
#68165=ORIENTED_EDGE('',*,*,#48583,.T.);
#68166=ORIENTED_EDGE('',*,*,#48584,.T.);
#68167=ORIENTED_EDGE('',*,*,#49028,.F.);
#68168=ORIENTED_EDGE('',*,*,#49029,.F.);
#68169=ORIENTED_EDGE('',*,*,#48581,.F.);
#68170=ORIENTED_EDGE('',*,*,#49030,.T.);
#68171=ORIENTED_EDGE('',*,*,#48585,.F.);
#68172=ORIENTED_EDGE('',*,*,#49029,.T.);
#68173=ORIENTED_EDGE('',*,*,#49031,.F.);
#68174=ORIENTED_EDGE('',*,*,#49032,.T.);
#68175=ORIENTED_EDGE('',*,*,#48587,.F.);
#68176=ORIENTED_EDGE('',*,*,#49030,.F.);
#68177=ORIENTED_EDGE('',*,*,#49033,.F.);
#68178=ORIENTED_EDGE('',*,*,#49034,.T.);
#68179=ORIENTED_EDGE('',*,*,#48589,.F.);
#68180=ORIENTED_EDGE('',*,*,#49032,.F.);
#68181=ORIENTED_EDGE('',*,*,#49035,.F.);
#68182=ORIENTED_EDGE('',*,*,#49034,.F.);
#68183=ORIENTED_EDGE('',*,*,#49036,.F.);
#68184=ORIENTED_EDGE('',*,*,#48595,.T.);
#68185=ORIENTED_EDGE('',*,*,#48594,.T.);
#68186=ORIENTED_EDGE('',*,*,#48591,.F.);
#68187=ORIENTED_EDGE('',*,*,#48597,.F.);
#68188=ORIENTED_EDGE('',*,*,#48596,.T.);
#68189=ORIENTED_EDGE('',*,*,#49037,.F.);
#68190=ORIENTED_EDGE('',*,*,#48602,.T.);
#68191=ORIENTED_EDGE('',*,*,#48603,.T.);
#68192=ORIENTED_EDGE('',*,*,#49038,.F.);
#68193=ORIENTED_EDGE('',*,*,#49039,.F.);
#68194=ORIENTED_EDGE('',*,*,#48600,.F.);
#68195=ORIENTED_EDGE('',*,*,#49040,.T.);
#68196=ORIENTED_EDGE('',*,*,#48604,.F.);
#68197=ORIENTED_EDGE('',*,*,#49039,.T.);
#68198=ORIENTED_EDGE('',*,*,#49041,.F.);
#68199=ORIENTED_EDGE('',*,*,#49042,.T.);
#68200=ORIENTED_EDGE('',*,*,#48606,.F.);
#68201=ORIENTED_EDGE('',*,*,#49040,.F.);
#68202=ORIENTED_EDGE('',*,*,#49043,.F.);
#68203=ORIENTED_EDGE('',*,*,#49044,.T.);
#68204=ORIENTED_EDGE('',*,*,#49045,.T.);
#68205=ORIENTED_EDGE('',*,*,#48608,.F.);
#68206=ORIENTED_EDGE('',*,*,#49042,.F.);
#68207=ORIENTED_EDGE('',*,*,#49046,.F.);
#68208=ORIENTED_EDGE('',*,*,#49044,.F.);
#68209=ORIENTED_EDGE('',*,*,#49047,.F.);
#68210=ORIENTED_EDGE('',*,*,#48614,.T.);
#68211=ORIENTED_EDGE('',*,*,#48613,.T.);
#68212=ORIENTED_EDGE('',*,*,#48610,.F.);
#68213=ORIENTED_EDGE('',*,*,#49045,.F.);
#68214=ORIENTED_EDGE('',*,*,#48616,.F.);
#68215=ORIENTED_EDGE('',*,*,#48615,.T.);
#68216=ORIENTED_EDGE('',*,*,#49048,.F.);
#68217=ORIENTED_EDGE('',*,*,#48623,.T.);
#68218=ORIENTED_EDGE('',*,*,#48624,.T.);
#68219=ORIENTED_EDGE('',*,*,#49049,.F.);
#68220=ORIENTED_EDGE('',*,*,#49050,.F.);
#68221=ORIENTED_EDGE('',*,*,#48620,.F.);
#68222=ORIENTED_EDGE('',*,*,#49050,.T.);
#68223=ORIENTED_EDGE('',*,*,#49051,.F.);
#68224=ORIENTED_EDGE('',*,*,#49052,.F.);
#68225=ORIENTED_EDGE('',*,*,#48625,.F.);
#68226=ORIENTED_EDGE('',*,*,#49053,.F.);
#68227=ORIENTED_EDGE('',*,*,#43775,.F.);
#68228=ORIENTED_EDGE('',*,*,#43895,.F.);
#68229=ORIENTED_EDGE('',*,*,#43892,.F.);
#68230=ORIENTED_EDGE('',*,*,#43891,.F.);
#68231=ORIENTED_EDGE('',*,*,#43886,.F.);
#68232=ORIENTED_EDGE('',*,*,#43883,.F.);
#68233=ORIENTED_EDGE('',*,*,#43878,.F.);
#68234=ORIENTED_EDGE('',*,*,#43875,.F.);
#68235=ORIENTED_EDGE('',*,*,#43872,.F.);
#68236=ORIENTED_EDGE('',*,*,#43871,.F.);
#68237=ORIENTED_EDGE('',*,*,#43865,.F.);
#68238=ORIENTED_EDGE('',*,*,#43862,.F.);
#68239=ORIENTED_EDGE('',*,*,#43857,.F.);
#68240=ORIENTED_EDGE('',*,*,#43854,.F.);
#68241=ORIENTED_EDGE('',*,*,#43851,.F.);
#68242=ORIENTED_EDGE('',*,*,#43849,.F.);
#68243=ORIENTED_EDGE('',*,*,#43843,.F.);
#68244=ORIENTED_EDGE('',*,*,#43840,.F.);
#68245=ORIENTED_EDGE('',*,*,#43837,.F.);
#68246=ORIENTED_EDGE('',*,*,#49054,.T.);
#68247=ORIENTED_EDGE('',*,*,#49051,.T.);
#68248=ORIENTED_EDGE('',*,*,#49049,.T.);
#68249=ORIENTED_EDGE('',*,*,#49048,.T.);
#68250=ORIENTED_EDGE('',*,*,#49047,.T.);
#68251=ORIENTED_EDGE('',*,*,#49046,.T.);
#68252=ORIENTED_EDGE('',*,*,#49043,.T.);
#68253=ORIENTED_EDGE('',*,*,#49041,.T.);
#68254=ORIENTED_EDGE('',*,*,#49038,.T.);
#68255=ORIENTED_EDGE('',*,*,#49037,.T.);
#68256=ORIENTED_EDGE('',*,*,#49036,.T.);
#68257=ORIENTED_EDGE('',*,*,#49035,.T.);
#68258=ORIENTED_EDGE('',*,*,#49033,.T.);
#68259=ORIENTED_EDGE('',*,*,#49031,.T.);
#68260=ORIENTED_EDGE('',*,*,#49028,.T.);
#68261=ORIENTED_EDGE('',*,*,#49027,.T.);
#68262=ORIENTED_EDGE('',*,*,#49026,.T.);
#68263=ORIENTED_EDGE('',*,*,#49025,.T.);
#68264=ORIENTED_EDGE('',*,*,#49023,.T.);
#68265=ORIENTED_EDGE('',*,*,#49055,.T.);
#68266=ORIENTED_EDGE('',*,*,#48815,.T.);
#68267=ORIENTED_EDGE('',*,*,#48814,.T.);
#68268=ORIENTED_EDGE('',*,*,#48812,.T.);
#68269=ORIENTED_EDGE('',*,*,#49056,.T.);
#68270=ORIENTED_EDGE('',*,*,#49057,.T.);
#68271=ORIENTED_EDGE('',*,*,#49058,.T.);
#68272=ORIENTED_EDGE('',*,*,#48809,.T.);
#68273=ORIENTED_EDGE('',*,*,#48808,.T.);
#68274=ORIENTED_EDGE('',*,*,#48807,.T.);
#68275=ORIENTED_EDGE('',*,*,#48805,.T.);
#68276=ORIENTED_EDGE('',*,*,#48803,.T.);
#68277=ORIENTED_EDGE('',*,*,#48801,.T.);
#68278=ORIENTED_EDGE('',*,*,#48799,.T.);
#68279=ORIENTED_EDGE('',*,*,#48798,.T.);
#68280=ORIENTED_EDGE('',*,*,#48797,.T.);
#68281=ORIENTED_EDGE('',*,*,#48795,.T.);
#68282=ORIENTED_EDGE('',*,*,#48793,.T.);
#68283=ORIENTED_EDGE('',*,*,#48790,.T.);
#68284=ORIENTED_EDGE('',*,*,#48787,.T.);
#68285=ORIENTED_EDGE('',*,*,#48873,.T.);
#68286=ORIENTED_EDGE('',*,*,#48779,.F.);
#68287=ORIENTED_EDGE('',*,*,#48810,.F.);
#68288=ORIENTED_EDGE('',*,*,#49059,.F.);
#68289=ORIENTED_EDGE('',*,*,#49060,.T.);
#68290=ORIENTED_EDGE('',*,*,#48874,.T.);
#68291=ORIENTED_EDGE('',*,*,#49061,.T.);
#68292=ORIENTED_EDGE('',*,*,#49062,.T.);
#68293=ORIENTED_EDGE('',*,*,#49061,.F.);
#68294=ORIENTED_EDGE('',*,*,#49059,.T.);
#68295=ORIENTED_EDGE('',*,*,#49058,.F.);
#68296=ORIENTED_EDGE('',*,*,#49063,.F.);
#68297=ORIENTED_EDGE('',*,*,#48892,.T.);
#68298=ORIENTED_EDGE('',*,*,#48781,.F.);
#68299=ORIENTED_EDGE('',*,*,#48872,.F.);
#68300=ORIENTED_EDGE('',*,*,#49064,.F.);
#68301=ORIENTED_EDGE('',*,*,#48902,.T.);
#68302=ORIENTED_EDGE('',*,*,#48901,.T.);
#68303=ORIENTED_EDGE('',*,*,#48900,.T.);
#68304=ORIENTED_EDGE('',*,*,#48898,.T.);
#68305=ORIENTED_EDGE('',*,*,#48896,.T.);
#68306=ORIENTED_EDGE('',*,*,#48894,.T.);
#68307=ORIENTED_EDGE('',*,*,#48891,.T.);
#68308=ORIENTED_EDGE('',*,*,#49065,.T.);
#68309=ORIENTED_EDGE('',*,*,#49066,.T.);
#68310=ORIENTED_EDGE('',*,*,#49067,.T.);
#68311=ORIENTED_EDGE('',*,*,#48890,.T.);
#68312=ORIENTED_EDGE('',*,*,#48887,.T.);
#68313=ORIENTED_EDGE('',*,*,#48886,.T.);
#68314=ORIENTED_EDGE('',*,*,#48884,.T.);
#68315=ORIENTED_EDGE('',*,*,#48883,.T.);
#68316=ORIENTED_EDGE('',*,*,#48882,.T.);
#68317=ORIENTED_EDGE('',*,*,#48880,.T.);
#68318=ORIENTED_EDGE('',*,*,#48878,.T.);
#68319=ORIENTED_EDGE('',*,*,#48875,.T.);
#68320=ORIENTED_EDGE('',*,*,#49065,.F.);
#68321=ORIENTED_EDGE('',*,*,#49064,.T.);
#68322=ORIENTED_EDGE('',*,*,#49060,.F.);
#68323=ORIENTED_EDGE('',*,*,#49068,.F.);
#68324=ORIENTED_EDGE('',*,*,#49069,.T.);
#68325=ORIENTED_EDGE('',*,*,#48773,.F.);
#68326=ORIENTED_EDGE('',*,*,#48889,.F.);
#68327=ORIENTED_EDGE('',*,*,#49070,.F.);
#68328=ORIENTED_EDGE('',*,*,#49022,.T.);
#68329=ORIENTED_EDGE('',*,*,#48775,.F.);
#68330=ORIENTED_EDGE('',*,*,#49069,.F.);
#68331=ORIENTED_EDGE('',*,*,#49071,.F.);
#68332=ORIENTED_EDGE('',*,*,#49071,.T.);
#68333=ORIENTED_EDGE('',*,*,#49070,.T.);
#68334=ORIENTED_EDGE('',*,*,#49067,.F.);
#68335=ORIENTED_EDGE('',*,*,#49072,.F.);
#68336=ORIENTED_EDGE('',*,*,#49055,.F.);
#68337=ORIENTED_EDGE('',*,*,#49054,.F.);
#68338=ORIENTED_EDGE('',*,*,#43836,.F.);
#68339=ORIENTED_EDGE('',*,*,#49073,.F.);
#68340=ORIENTED_EDGE('',*,*,#49052,.T.);
#68341=ORIENTED_EDGE('',*,*,#48626,.T.);
#68342=ORIENTED_EDGE('',*,*,#49073,.T.);
#68343=ORIENTED_EDGE('',*,*,#44577,.F.);
#68344=ORIENTED_EDGE('',*,*,#49074,.F.);
#68345=ORIENTED_EDGE('',*,*,#49075,.T.);
#68346=ORIENTED_EDGE('',*,*,#48629,.T.);
#68347=ORIENTED_EDGE('',*,*,#49074,.T.);
#68348=ORIENTED_EDGE('',*,*,#44573,.F.);
#68349=ORIENTED_EDGE('',*,*,#49075,.F.);
#68350=ORIENTED_EDGE('',*,*,#44570,.F.);
#68351=ORIENTED_EDGE('',*,*,#49076,.T.);
#68352=ORIENTED_EDGE('',*,*,#48630,.T.);
#68353=ORIENTED_EDGE('',*,*,#49076,.F.);
#68354=ORIENTED_EDGE('',*,*,#44556,.T.);
#68355=ORIENTED_EDGE('',*,*,#49077,.F.);
#68356=ORIENTED_EDGE('',*,*,#48638,.F.);
#68357=ORIENTED_EDGE('',*,*,#49078,.T.);
#68358=ORIENTED_EDGE('',*,*,#48636,.T.);
#68359=ORIENTED_EDGE('',*,*,#48635,.T.);
#68360=ORIENTED_EDGE('',*,*,#48633,.T.);
#68361=ORIENTED_EDGE('',*,*,#48665,.T.);
#68362=ORIENTED_EDGE('',*,*,#48664,.T.);
#68363=ORIENTED_EDGE('',*,*,#48662,.T.);
#68364=ORIENTED_EDGE('',*,*,#48661,.T.);
#68365=ORIENTED_EDGE('',*,*,#48659,.T.);
#68366=ORIENTED_EDGE('',*,*,#48657,.T.);
#68367=ORIENTED_EDGE('',*,*,#48656,.T.);
#68368=ORIENTED_EDGE('',*,*,#48654,.T.);
#68369=ORIENTED_EDGE('',*,*,#48652,.T.);
#68370=ORIENTED_EDGE('',*,*,#48651,.T.);
#68371=ORIENTED_EDGE('',*,*,#48649,.T.);
#68372=ORIENTED_EDGE('',*,*,#48647,.T.);
#68373=ORIENTED_EDGE('',*,*,#48646,.T.);
#68374=ORIENTED_EDGE('',*,*,#48644,.T.);
#68375=ORIENTED_EDGE('',*,*,#48642,.T.);
#68376=ORIENTED_EDGE('',*,*,#48641,.T.);
#68377=ORIENTED_EDGE('',*,*,#48639,.T.);
#68378=ORIENTED_EDGE('',*,*,#49077,.T.);
#68379=ORIENTED_EDGE('',*,*,#44558,.F.);
#68380=ORIENTED_EDGE('',*,*,#44555,.F.);
#68381=ORIENTED_EDGE('',*,*,#44548,.F.);
#68382=ORIENTED_EDGE('',*,*,#44545,.F.);
#68383=ORIENTED_EDGE('',*,*,#44542,.F.);
#68384=ORIENTED_EDGE('',*,*,#44541,.F.);
#68385=ORIENTED_EDGE('',*,*,#44538,.F.);
#68386=ORIENTED_EDGE('',*,*,#44535,.F.);
#68387=ORIENTED_EDGE('',*,*,#44528,.F.);
#68388=ORIENTED_EDGE('',*,*,#44525,.F.);
#68389=ORIENTED_EDGE('',*,*,#44522,.F.);
#68390=ORIENTED_EDGE('',*,*,#44521,.F.);
#68391=ORIENTED_EDGE('',*,*,#44518,.F.);
#68392=ORIENTED_EDGE('',*,*,#44515,.F.);
#68393=ORIENTED_EDGE('',*,*,#44508,.F.);
#68394=ORIENTED_EDGE('',*,*,#44505,.F.);
#68395=ORIENTED_EDGE('',*,*,#44504,.F.);
#68396=ORIENTED_EDGE('',*,*,#44569,.F.);
#68397=ORIENTED_EDGE('',*,*,#44567,.F.);
#68398=ORIENTED_EDGE('',*,*,#44562,.F.);
#68399=ORIENTED_EDGE('',*,*,#49079,.F.);
#68400=ORIENTED_EDGE('',*,*,#48670,.F.);
#68401=ORIENTED_EDGE('',*,*,#49078,.F.);
#68402=ORIENTED_EDGE('',*,*,#44484,.T.);
#68403=ORIENTED_EDGE('',*,*,#49079,.T.);
#68404=ORIENTED_EDGE('',*,*,#44486,.F.);
#68405=ORIENTED_EDGE('',*,*,#44483,.F.);
#68406=ORIENTED_EDGE('',*,*,#44480,.F.);
#68407=ORIENTED_EDGE('',*,*,#44477,.F.);
#68408=ORIENTED_EDGE('',*,*,#44474,.F.);
#68409=ORIENTED_EDGE('',*,*,#44471,.F.);
#68410=ORIENTED_EDGE('',*,*,#44468,.F.);
#68411=ORIENTED_EDGE('',*,*,#44465,.F.);
#68412=ORIENTED_EDGE('',*,*,#44462,.F.);
#68413=ORIENTED_EDGE('',*,*,#44459,.F.);
#68414=ORIENTED_EDGE('',*,*,#44456,.F.);
#68415=ORIENTED_EDGE('',*,*,#44453,.F.);
#68416=ORIENTED_EDGE('',*,*,#44450,.F.);
#68417=ORIENTED_EDGE('',*,*,#44447,.F.);
#68418=ORIENTED_EDGE('',*,*,#44444,.F.);
#68419=ORIENTED_EDGE('',*,*,#49080,.T.);
#68420=ORIENTED_EDGE('',*,*,#48699,.T.);
#68421=ORIENTED_EDGE('',*,*,#48697,.T.);
#68422=ORIENTED_EDGE('',*,*,#48695,.T.);
#68423=ORIENTED_EDGE('',*,*,#48693,.T.);
#68424=ORIENTED_EDGE('',*,*,#48691,.T.);
#68425=ORIENTED_EDGE('',*,*,#48689,.T.);
#68426=ORIENTED_EDGE('',*,*,#48687,.T.);
#68427=ORIENTED_EDGE('',*,*,#48685,.T.);
#68428=ORIENTED_EDGE('',*,*,#48683,.T.);
#68429=ORIENTED_EDGE('',*,*,#48681,.T.);
#68430=ORIENTED_EDGE('',*,*,#48679,.T.);
#68431=ORIENTED_EDGE('',*,*,#48677,.T.);
#68432=ORIENTED_EDGE('',*,*,#48675,.T.);
#68433=ORIENTED_EDGE('',*,*,#48673,.T.);
#68434=ORIENTED_EDGE('',*,*,#48671,.T.);
#68435=ORIENTED_EDGE('',*,*,#44497,.T.);
#68436=ORIENTED_EDGE('',*,*,#44490,.T.);
#68437=ORIENTED_EDGE('',*,*,#48667,.F.);
#68438=ORIENTED_EDGE('',*,*,#48669,.F.);
#68439=ORIENTED_EDGE('',*,*,#49080,.F.);
#68440=ORIENTED_EDGE('',*,*,#44443,.F.);
#68441=ORIENTED_EDGE('',*,*,#49081,.F.);
#68442=ORIENTED_EDGE('',*,*,#48700,.T.);
#68443=ORIENTED_EDGE('',*,*,#49081,.T.);
#68444=ORIENTED_EDGE('',*,*,#44439,.F.);
#68445=ORIENTED_EDGE('',*,*,#49082,.T.);
#68446=ORIENTED_EDGE('',*,*,#48702,.T.);
#68447=ORIENTED_EDGE('',*,*,#48706,.T.);
#68448=ORIENTED_EDGE('',*,*,#49082,.F.);
#68449=ORIENTED_EDGE('',*,*,#44434,.F.);
#68450=ORIENTED_EDGE('',*,*,#49083,.F.);
#68451=ORIENTED_EDGE('',*,*,#48707,.T.);
#68452=ORIENTED_EDGE('',*,*,#49083,.T.);
#68453=ORIENTED_EDGE('',*,*,#44433,.F.);
#68454=ORIENTED_EDGE('',*,*,#44437,.F.);
#68455=ORIENTED_EDGE('',*,*,#44430,.F.);
#68456=ORIENTED_EDGE('',*,*,#49084,.F.);
#68457=ORIENTED_EDGE('',*,*,#48709,.T.);
#68458=ORIENTED_EDGE('',*,*,#48705,.T.);
#68459=ORIENTED_EDGE('',*,*,#49084,.T.);
#68460=ORIENTED_EDGE('',*,*,#44429,.F.);
#68461=ORIENTED_EDGE('',*,*,#44422,.F.);
#68462=ORIENTED_EDGE('',*,*,#44328,.F.);
#68463=ORIENTED_EDGE('',*,*,#49085,.T.);
#68464=ORIENTED_EDGE('',*,*,#48760,.T.);
#68465=ORIENTED_EDGE('',*,*,#48711,.T.);
#68466=ORIENTED_EDGE('',*,*,#48710,.T.);
#68467=ORIENTED_EDGE('',*,*,#48764,.T.);
#68468=ORIENTED_EDGE('',*,*,#48763,.T.);
#68469=ORIENTED_EDGE('',*,*,#48761,.T.);
#68470=ORIENTED_EDGE('',*,*,#49085,.F.);
#68471=ORIENTED_EDGE('',*,*,#44327,.F.);
#68472=ORIENTED_EDGE('',*,*,#44319,.F.);
#68473=ORIENTED_EDGE('',*,*,#44316,.F.);
#68474=ORIENTED_EDGE('',*,*,#44419,.F.);
#68475=ORIENTED_EDGE('',*,*,#44414,.F.);
#68476=ORIENTED_EDGE('',*,*,#44411,.F.);
#68477=ORIENTED_EDGE('',*,*,#44408,.F.);
#68478=ORIENTED_EDGE('',*,*,#44405,.F.);
#68479=ORIENTED_EDGE('',*,*,#44402,.F.);
#68480=ORIENTED_EDGE('',*,*,#44399,.F.);
#68481=ORIENTED_EDGE('',*,*,#44394,.F.);
#68482=ORIENTED_EDGE('',*,*,#44391,.F.);
#68483=ORIENTED_EDGE('',*,*,#44388,.F.);
#68484=ORIENTED_EDGE('',*,*,#44385,.F.);
#68485=ORIENTED_EDGE('',*,*,#44382,.F.);
#68486=ORIENTED_EDGE('',*,*,#44379,.F.);
#68487=ORIENTED_EDGE('',*,*,#44376,.F.);
#68488=ORIENTED_EDGE('',*,*,#44371,.F.);
#68489=ORIENTED_EDGE('',*,*,#44368,.F.);
#68490=ORIENTED_EDGE('',*,*,#44365,.F.);
#68491=ORIENTED_EDGE('',*,*,#44362,.F.);
#68492=ORIENTED_EDGE('',*,*,#44359,.F.);
#68493=ORIENTED_EDGE('',*,*,#44356,.F.);
#68494=ORIENTED_EDGE('',*,*,#44353,.F.);
#68495=ORIENTED_EDGE('',*,*,#44350,.F.);
#68496=ORIENTED_EDGE('',*,*,#44343,.F.);
#68497=ORIENTED_EDGE('',*,*,#44340,.F.);
#68498=ORIENTED_EDGE('',*,*,#44337,.F.);
#68499=ORIENTED_EDGE('',*,*,#44334,.F.);
#68500=ORIENTED_EDGE('',*,*,#44331,.F.);
#68501=ORIENTED_EDGE('',*,*,#49086,.T.);
#68502=ORIENTED_EDGE('',*,*,#48759,.T.);
#68503=ORIENTED_EDGE('',*,*,#48757,.T.);
#68504=ORIENTED_EDGE('',*,*,#48755,.T.);
#68505=ORIENTED_EDGE('',*,*,#48753,.T.);
#68506=ORIENTED_EDGE('',*,*,#48751,.T.);
#68507=ORIENTED_EDGE('',*,*,#48749,.T.);
#68508=ORIENTED_EDGE('',*,*,#48748,.T.);
#68509=ORIENTED_EDGE('',*,*,#48747,.T.);
#68510=ORIENTED_EDGE('',*,*,#48745,.T.);
#68511=ORIENTED_EDGE('',*,*,#48743,.T.);
#68512=ORIENTED_EDGE('',*,*,#48741,.T.);
#68513=ORIENTED_EDGE('',*,*,#48739,.T.);
#68514=ORIENTED_EDGE('',*,*,#48738,.T.);
#68515=ORIENTED_EDGE('',*,*,#48735,.T.);
#68516=ORIENTED_EDGE('',*,*,#48734,.T.);
#68517=ORIENTED_EDGE('',*,*,#48733,.T.);
#68518=ORIENTED_EDGE('',*,*,#48731,.T.);
#68519=ORIENTED_EDGE('',*,*,#48729,.T.);
#68520=ORIENTED_EDGE('',*,*,#48727,.T.);
#68521=ORIENTED_EDGE('',*,*,#48725,.T.);
#68522=ORIENTED_EDGE('',*,*,#48724,.T.);
#68523=ORIENTED_EDGE('',*,*,#48723,.T.);
#68524=ORIENTED_EDGE('',*,*,#48721,.T.);
#68525=ORIENTED_EDGE('',*,*,#48719,.T.);
#68526=ORIENTED_EDGE('',*,*,#48717,.T.);
#68527=ORIENTED_EDGE('',*,*,#48715,.T.);
#68528=ORIENTED_EDGE('',*,*,#48714,.T.);
#68529=ORIENTED_EDGE('',*,*,#44311,.F.);
#68530=ORIENTED_EDGE('',*,*,#49087,.F.);
#68531=ORIENTED_EDGE('',*,*,#48767,.T.);
#68532=ORIENTED_EDGE('',*,*,#48766,.T.);
#68533=ORIENTED_EDGE('',*,*,#49086,.F.);
#68534=ORIENTED_EDGE('',*,*,#44312,.F.);
#68535=ORIENTED_EDGE('',*,*,#49087,.T.);
#68536=ORIENTED_EDGE('',*,*,#44308,.F.);
#68537=ORIENTED_EDGE('',*,*,#49088,.T.);
#68538=ORIENTED_EDGE('',*,*,#48769,.T.);
#68539=ORIENTED_EDGE('',*,*,#49089,.F.);
#68540=ORIENTED_EDGE('',*,*,#48770,.T.);
#68541=ORIENTED_EDGE('',*,*,#49088,.F.);
#68542=ORIENTED_EDGE('',*,*,#44307,.F.);
#68543=ORIENTED_EDGE('',*,*,#49090,.F.);
#68544=ORIENTED_EDGE('',*,*,#49019,.T.);
#68545=ORIENTED_EDGE('',*,*,#49018,.T.);
#68546=ORIENTED_EDGE('',*,*,#49017,.T.);
#68547=ORIENTED_EDGE('',*,*,#49015,.T.);
#68548=ORIENTED_EDGE('',*,*,#49013,.T.);
#68549=ORIENTED_EDGE('',*,*,#49011,.T.);
#68550=ORIENTED_EDGE('',*,*,#49010,.T.);
#68551=ORIENTED_EDGE('',*,*,#49008,.T.);
#68552=ORIENTED_EDGE('',*,*,#49007,.T.);
#68553=ORIENTED_EDGE('',*,*,#49005,.T.);
#68554=ORIENTED_EDGE('',*,*,#49003,.T.);
#68555=ORIENTED_EDGE('',*,*,#49001,.T.);
#68556=ORIENTED_EDGE('',*,*,#48999,.T.);
#68557=ORIENTED_EDGE('',*,*,#48998,.T.);
#68558=ORIENTED_EDGE('',*,*,#48997,.T.);
#68559=ORIENTED_EDGE('',*,*,#48995,.T.);
#68560=ORIENTED_EDGE('',*,*,#48993,.T.);
#68561=ORIENTED_EDGE('',*,*,#48991,.T.);
#68562=ORIENTED_EDGE('',*,*,#48989,.T.);
#68563=ORIENTED_EDGE('',*,*,#49089,.T.);
#68564=ORIENTED_EDGE('',*,*,#43960,.F.);
#68565=ORIENTED_EDGE('',*,*,#43957,.F.);
#68566=ORIENTED_EDGE('',*,*,#43954,.F.);
#68567=ORIENTED_EDGE('',*,*,#43951,.F.);
#68568=ORIENTED_EDGE('',*,*,#43948,.F.);
#68569=ORIENTED_EDGE('',*,*,#43943,.F.);
#68570=ORIENTED_EDGE('',*,*,#43940,.F.);
#68571=ORIENTED_EDGE('',*,*,#43937,.F.);
#68572=ORIENTED_EDGE('',*,*,#43934,.F.);
#68573=ORIENTED_EDGE('',*,*,#43931,.F.);
#68574=ORIENTED_EDGE('',*,*,#43928,.F.);
#68575=ORIENTED_EDGE('',*,*,#43923,.F.);
#68576=ORIENTED_EDGE('',*,*,#43918,.F.);
#68577=ORIENTED_EDGE('',*,*,#43917,.F.);
#68578=ORIENTED_EDGE('',*,*,#43914,.F.);
#68579=ORIENTED_EDGE('',*,*,#43911,.F.);
#68580=ORIENTED_EDGE('',*,*,#43908,.F.);
#68581=ORIENTED_EDGE('',*,*,#43903,.F.);
#68582=ORIENTED_EDGE('',*,*,#43899,.F.);
#68583=ORIENTED_EDGE('',*,*,#49056,.F.);
#68584=ORIENTED_EDGE('',*,*,#48988,.T.);
#68585=ORIENTED_EDGE('',*,*,#48987,.T.);
#68586=ORIENTED_EDGE('',*,*,#48985,.T.);
#68587=ORIENTED_EDGE('',*,*,#48981,.F.);
#68588=ORIENTED_EDGE('',*,*,#49091,.F.);
#68589=ORIENTED_EDGE('',*,*,#49020,.T.);
#68590=ORIENTED_EDGE('',*,*,#49090,.T.);
#68591=ORIENTED_EDGE('',*,*,#43898,.F.);
#68592=ORIENTED_EDGE('',*,*,#44057,.T.);
#68593=ORIENTED_EDGE('',*,*,#44042,.F.);
#68594=ORIENTED_EDGE('',*,*,#44045,.T.);
#68595=ORIENTED_EDGE('',*,*,#44018,.F.);
#68596=ORIENTED_EDGE('',*,*,#44031,.T.);
#68597=ORIENTED_EDGE('',*,*,#43969,.F.);
#68598=ORIENTED_EDGE('',*,*,#43974,.F.);
#68599=ORIENTED_EDGE('',*,*,#43769,.F.);
#68600=ORIENTED_EDGE('',*,*,#43831,.T.);
#68601=ORIENTED_EDGE('',*,*,#43809,.F.);
#68602=ORIENTED_EDGE('',*,*,#43812,.T.);
#68603=ORIENTED_EDGE('',*,*,#43785,.F.);
#68604=ORIENTED_EDGE('',*,*,#43798,.T.);
#68605=ORIENTED_EDGE('',*,*,#43776,.F.);
#68606=ORIENTED_EDGE('',*,*,#49053,.T.);
#68607=ORIENTED_EDGE('',*,*,#49072,.T.);
#68608=ORIENTED_EDGE('',*,*,#49066,.F.);
#68609=ORIENTED_EDGE('',*,*,#49068,.T.);
#68610=ORIENTED_EDGE('',*,*,#49062,.F.);
#68611=ORIENTED_EDGE('',*,*,#49063,.T.);
#68612=ORIENTED_EDGE('',*,*,#49057,.F.);
#68613=ORIENTED_EDGE('',*,*,#49091,.T.);
#68614=ORIENTED_EDGE('',*,*,#48980,.T.);
#68615=ORIENTED_EDGE('',*,*,#48983,.T.);
#68616=ORIENTED_EDGE('',*,*,#48972,.F.);
#68617=ORIENTED_EDGE('',*,*,#48974,.T.);
#68618=ORIENTED_EDGE('',*,*,#48968,.F.);
#68619=ORIENTED_EDGE('',*,*,#48969,.T.);
#68620=ORIENTED_EDGE('',*,*,#48963,.F.);
#68621=ORIENTED_EDGE('',*,*,#45308,.T.);
#68622=ORIENTED_EDGE('',*,*,#45324,.T.);
#68623=ORIENTED_EDGE('',*,*,#48249,.F.);
#68624=ORIENTED_EDGE('',*,*,#48228,.F.);
#68625=ORIENTED_EDGE('',*,*,#49092,.T.);
#68626=ORIENTED_EDGE('',*,*,#49093,.T.);
#68627=ORIENTED_EDGE('',*,*,#49094,.F.);
#68628=ORIENTED_EDGE('',*,*,#49095,.T.);
#68629=ORIENTED_EDGE('',*,*,#49096,.T.);
#68630=ORIENTED_EDGE('',*,*,#49097,.T.);
#68631=ORIENTED_EDGE('',*,*,#49092,.F.);
#68632=ORIENTED_EDGE('',*,*,#49098,.T.);
#68633=ORIENTED_EDGE('',*,*,#49099,.T.);
#68634=ORIENTED_EDGE('',*,*,#49100,.T.);
#68635=ORIENTED_EDGE('',*,*,#49096,.F.);
#68636=ORIENTED_EDGE('',*,*,#49101,.T.);
#68637=ORIENTED_EDGE('',*,*,#49102,.T.);
#68638=ORIENTED_EDGE('',*,*,#49103,.T.);
#68639=ORIENTED_EDGE('',*,*,#49099,.F.);
#68640=ORIENTED_EDGE('',*,*,#49104,.T.);
#68641=ORIENTED_EDGE('',*,*,#49105,.T.);
#68642=ORIENTED_EDGE('',*,*,#49106,.T.);
#68643=ORIENTED_EDGE('',*,*,#49102,.F.);
#68644=ORIENTED_EDGE('',*,*,#49107,.T.);
#68645=ORIENTED_EDGE('',*,*,#49094,.T.);
#68646=ORIENTED_EDGE('',*,*,#49108,.T.);
#68647=ORIENTED_EDGE('',*,*,#49105,.F.);
#68648=ORIENTED_EDGE('',*,*,#49109,.T.);
#68649=ORIENTED_EDGE('',*,*,#49110,.T.);
#68650=ORIENTED_EDGE('',*,*,#49101,.F.);
#68651=ORIENTED_EDGE('',*,*,#49098,.F.);
#68652=ORIENTED_EDGE('',*,*,#49095,.F.);
#68653=ORIENTED_EDGE('',*,*,#49109,.F.);
#68654=ORIENTED_EDGE('',*,*,#49107,.F.);
#68655=ORIENTED_EDGE('',*,*,#49104,.F.);
#68656=ORIENTED_EDGE('',*,*,#49110,.F.);
#68657=ORIENTED_EDGE('',*,*,#49111,.T.);
#68658=ORIENTED_EDGE('',*,*,#49093,.F.);
#68659=ORIENTED_EDGE('',*,*,#49112,.T.);
#68660=ORIENTED_EDGE('',*,*,#49097,.F.);
#68661=ORIENTED_EDGE('',*,*,#49113,.T.);
#68662=ORIENTED_EDGE('',*,*,#49100,.F.);
#68663=ORIENTED_EDGE('',*,*,#49114,.T.);
#68664=ORIENTED_EDGE('',*,*,#49103,.F.);
#68665=ORIENTED_EDGE('',*,*,#49115,.T.);
#68666=ORIENTED_EDGE('',*,*,#49106,.F.);
#68667=ORIENTED_EDGE('',*,*,#49116,.T.);
#68668=ORIENTED_EDGE('',*,*,#49108,.F.);
#68669=ORIENTED_EDGE('',*,*,#49117,.F.);
#68670=ORIENTED_EDGE('',*,*,#49118,.T.);
#68671=ORIENTED_EDGE('',*,*,#49119,.F.);
#68672=ORIENTED_EDGE('',*,*,#49120,.F.);
#68673=ORIENTED_EDGE('',*,*,#49118,.F.);
#68674=ORIENTED_EDGE('',*,*,#49121,.F.);
#68675=ORIENTED_EDGE('',*,*,#49117,.T.);
#68676=ORIENTED_EDGE('',*,*,#49116,.F.);
#68677=ORIENTED_EDGE('',*,*,#49111,.F.);
#68678=ORIENTED_EDGE('',*,*,#49112,.F.);
#68679=ORIENTED_EDGE('',*,*,#49113,.F.);
#68680=ORIENTED_EDGE('',*,*,#49114,.F.);
#68681=ORIENTED_EDGE('',*,*,#49115,.F.);
#68682=ORIENTED_EDGE('',*,*,#49121,.T.);
#68683=ORIENTED_EDGE('',*,*,#49122,.T.);
#68684=ORIENTED_EDGE('',*,*,#49119,.T.);
#68685=ORIENTED_EDGE('',*,*,#49120,.T.);
#68686=ORIENTED_EDGE('',*,*,#49122,.F.);
#68687=ORIENTED_EDGE('',*,*,#49123,.F.);
#68688=ORIENTED_EDGE('',*,*,#49124,.T.);
#68689=ORIENTED_EDGE('',*,*,#49125,.F.);
#68690=ORIENTED_EDGE('',*,*,#49124,.F.);
#68691=ORIENTED_EDGE('',*,*,#49125,.T.);
#68692=ORIENTED_EDGE('',*,*,#49126,.T.);
#68693=ORIENTED_EDGE('',*,*,#49127,.T.);
#68694=ORIENTED_EDGE('',*,*,#49123,.T.);
#68695=ORIENTED_EDGE('',*,*,#49127,.F.);
#68696=ORIENTED_EDGE('',*,*,#49128,.F.);
#68697=ORIENTED_EDGE('',*,*,#49126,.F.);
#68698=ORIENTED_EDGE('',*,*,#49129,.T.);
#68699=ORIENTED_EDGE('',*,*,#49130,.T.);
#68700=ORIENTED_EDGE('',*,*,#49128,.T.);
#68701=ORIENTED_EDGE('',*,*,#49130,.F.);
#68702=ORIENTED_EDGE('',*,*,#49129,.F.);
#68703=ORIENTED_EDGE('',*,*,#49131,.F.);
#68704=ORIENTED_EDGE('',*,*,#49132,.T.);
#68705=ORIENTED_EDGE('',*,*,#49133,.F.);
#68706=ORIENTED_EDGE('',*,*,#49134,.T.);
#68707=ORIENTED_EDGE('',*,*,#49135,.T.);
#68708=ORIENTED_EDGE('',*,*,#49136,.T.);
#68709=ORIENTED_EDGE('',*,*,#49137,.T.);
#68710=ORIENTED_EDGE('',*,*,#49138,.T.);
#68711=ORIENTED_EDGE('',*,*,#49136,.F.);
#68712=ORIENTED_EDGE('',*,*,#49139,.F.);
#68713=ORIENTED_EDGE('',*,*,#49140,.T.);
#68714=ORIENTED_EDGE('',*,*,#49141,.F.);
#68715=ORIENTED_EDGE('',*,*,#49142,.T.);
#68716=ORIENTED_EDGE('',*,*,#49143,.F.);
#68717=ORIENTED_EDGE('',*,*,#49144,.T.);
#68718=ORIENTED_EDGE('',*,*,#49141,.T.);
#68719=ORIENTED_EDGE('',*,*,#49145,.T.);
#68720=ORIENTED_EDGE('',*,*,#49146,.T.);
#68721=ORIENTED_EDGE('',*,*,#49139,.T.);
#68722=ORIENTED_EDGE('',*,*,#49147,.F.);
#68723=ORIENTED_EDGE('',*,*,#49148,.F.);
#68724=ORIENTED_EDGE('',*,*,#49149,.T.);
#68725=ORIENTED_EDGE('',*,*,#49143,.T.);
#68726=ORIENTED_EDGE('',*,*,#49150,.T.);
#68727=ORIENTED_EDGE('',*,*,#49151,.F.);
#68728=ORIENTED_EDGE('',*,*,#49152,.T.);
#68729=ORIENTED_EDGE('',*,*,#49147,.T.);
#68730=ORIENTED_EDGE('',*,*,#49153,.T.);
#68731=ORIENTED_EDGE('',*,*,#49154,.F.);
#68732=ORIENTED_EDGE('',*,*,#49155,.T.);
#68733=ORIENTED_EDGE('',*,*,#49148,.T.);
#68734=ORIENTED_EDGE('',*,*,#49156,.T.);
#68735=ORIENTED_EDGE('',*,*,#49157,.F.);
#68736=ORIENTED_EDGE('',*,*,#49158,.T.);
#68737=ORIENTED_EDGE('',*,*,#49151,.T.);
#68738=ORIENTED_EDGE('',*,*,#49159,.T.);
#68739=ORIENTED_EDGE('',*,*,#49160,.F.);
#68740=ORIENTED_EDGE('',*,*,#49161,.T.);
#68741=ORIENTED_EDGE('',*,*,#49154,.T.);
#68742=ORIENTED_EDGE('',*,*,#49162,.T.);
#68743=ORIENTED_EDGE('',*,*,#49163,.F.);
#68744=ORIENTED_EDGE('',*,*,#49164,.T.);
#68745=ORIENTED_EDGE('',*,*,#49157,.T.);
#68746=ORIENTED_EDGE('',*,*,#49165,.T.);
#68747=ORIENTED_EDGE('',*,*,#49166,.F.);
#68748=ORIENTED_EDGE('',*,*,#49167,.T.);
#68749=ORIENTED_EDGE('',*,*,#49160,.T.);
#68750=ORIENTED_EDGE('',*,*,#49168,.T.);
#68751=ORIENTED_EDGE('',*,*,#49169,.F.);
#68752=ORIENTED_EDGE('',*,*,#49170,.T.);
#68753=ORIENTED_EDGE('',*,*,#49163,.T.);
#68754=ORIENTED_EDGE('',*,*,#49171,.T.);
#68755=ORIENTED_EDGE('',*,*,#49172,.F.);
#68756=ORIENTED_EDGE('',*,*,#49173,.T.);
#68757=ORIENTED_EDGE('',*,*,#49174,.T.);
#68758=ORIENTED_EDGE('',*,*,#49166,.T.);
#68759=ORIENTED_EDGE('',*,*,#49175,.T.);
#68760=ORIENTED_EDGE('',*,*,#49169,.T.);
#68761=ORIENTED_EDGE('',*,*,#49172,.T.);
#68762=ORIENTED_EDGE('',*,*,#49176,.T.);
#68763=ORIENTED_EDGE('',*,*,#49177,.F.);
#68764=ORIENTED_EDGE('',*,*,#49178,.T.);
#68765=ORIENTED_EDGE('',*,*,#49179,.F.);
#68766=ORIENTED_EDGE('',*,*,#49180,.T.);
#68767=ORIENTED_EDGE('',*,*,#49181,.F.);
#68768=ORIENTED_EDGE('',*,*,#49182,.T.);
#68769=ORIENTED_EDGE('',*,*,#49179,.T.);
#68770=ORIENTED_EDGE('',*,*,#49183,.T.);
#68771=ORIENTED_EDGE('',*,*,#49184,.F.);
#68772=ORIENTED_EDGE('',*,*,#49185,.T.);
#68773=ORIENTED_EDGE('',*,*,#49177,.T.);
#68774=ORIENTED_EDGE('',*,*,#49186,.T.);
#68775=ORIENTED_EDGE('',*,*,#49187,.F.);
#68776=ORIENTED_EDGE('',*,*,#49188,.T.);
#68777=ORIENTED_EDGE('',*,*,#49181,.T.);
#68778=ORIENTED_EDGE('',*,*,#49189,.T.);
#68779=ORIENTED_EDGE('',*,*,#49190,.F.);
#68780=ORIENTED_EDGE('',*,*,#49191,.T.);
#68781=ORIENTED_EDGE('',*,*,#49184,.T.);
#68782=ORIENTED_EDGE('',*,*,#49192,.T.);
#68783=ORIENTED_EDGE('',*,*,#49193,.F.);
#68784=ORIENTED_EDGE('',*,*,#49187,.T.);
#68785=ORIENTED_EDGE('',*,*,#49194,.T.);
#68786=ORIENTED_EDGE('',*,*,#49195,.F.);
#68787=ORIENTED_EDGE('',*,*,#49196,.T.);
#68788=ORIENTED_EDGE('',*,*,#49190,.T.);
#68789=ORIENTED_EDGE('',*,*,#49197,.T.);
#68790=ORIENTED_EDGE('',*,*,#49198,.F.);
#68791=ORIENTED_EDGE('',*,*,#49199,.T.);
#68792=ORIENTED_EDGE('',*,*,#49193,.T.);
#68793=ORIENTED_EDGE('',*,*,#49200,.T.);
#68794=ORIENTED_EDGE('',*,*,#49201,.F.);
#68795=ORIENTED_EDGE('',*,*,#49202,.T.);
#68796=ORIENTED_EDGE('',*,*,#49195,.T.);
#68797=ORIENTED_EDGE('',*,*,#49203,.T.);
#68798=ORIENTED_EDGE('',*,*,#49204,.F.);
#68799=ORIENTED_EDGE('',*,*,#49205,.T.);
#68800=ORIENTED_EDGE('',*,*,#49198,.T.);
#68801=ORIENTED_EDGE('',*,*,#49206,.T.);
#68802=ORIENTED_EDGE('',*,*,#49207,.T.);
#68803=ORIENTED_EDGE('',*,*,#49201,.T.);
#68804=ORIENTED_EDGE('',*,*,#49208,.F.);
#68805=ORIENTED_EDGE('',*,*,#49209,.F.);
#68806=ORIENTED_EDGE('',*,*,#49210,.T.);
#68807=ORIENTED_EDGE('',*,*,#49204,.T.);
#68808=ORIENTED_EDGE('',*,*,#49211,.T.);
#68809=ORIENTED_EDGE('',*,*,#49212,.F.);
#68810=ORIENTED_EDGE('',*,*,#49213,.T.);
#68811=ORIENTED_EDGE('',*,*,#49208,.T.);
#68812=ORIENTED_EDGE('',*,*,#49214,.T.);
#68813=ORIENTED_EDGE('',*,*,#49209,.T.);
#68814=ORIENTED_EDGE('',*,*,#49215,.T.);
#68815=ORIENTED_EDGE('',*,*,#49212,.T.);
#68816=ORIENTED_EDGE('',*,*,#49216,.T.);
#68817=ORIENTED_EDGE('',*,*,#49217,.F.);
#68818=ORIENTED_EDGE('',*,*,#49218,.T.);
#68819=ORIENTED_EDGE('',*,*,#49219,.T.);
#68820=ORIENTED_EDGE('',*,*,#49220,.T.);
#68821=ORIENTED_EDGE('',*,*,#49221,.F.);
#68822=ORIENTED_EDGE('',*,*,#49222,.T.);
#68823=ORIENTED_EDGE('',*,*,#49217,.T.);
#68824=ORIENTED_EDGE('',*,*,#49223,.T.);
#68825=ORIENTED_EDGE('',*,*,#49224,.F.);
#68826=ORIENTED_EDGE('',*,*,#49225,.T.);
#68827=ORIENTED_EDGE('',*,*,#49221,.T.);
#68828=ORIENTED_EDGE('',*,*,#49226,.T.);
#68829=ORIENTED_EDGE('',*,*,#49227,.F.);
#68830=ORIENTED_EDGE('',*,*,#49228,.T.);
#68831=ORIENTED_EDGE('',*,*,#49224,.T.);
#68832=ORIENTED_EDGE('',*,*,#49229,.T.);
#68833=ORIENTED_EDGE('',*,*,#49230,.F.);
#68834=ORIENTED_EDGE('',*,*,#49231,.T.);
#68835=ORIENTED_EDGE('',*,*,#49227,.T.);
#68836=ORIENTED_EDGE('',*,*,#49232,.T.);
#68837=ORIENTED_EDGE('',*,*,#49233,.F.);
#68838=ORIENTED_EDGE('',*,*,#49234,.T.);
#68839=ORIENTED_EDGE('',*,*,#49230,.T.);
#68840=ORIENTED_EDGE('',*,*,#49235,.T.);
#68841=ORIENTED_EDGE('',*,*,#49236,.F.);
#68842=ORIENTED_EDGE('',*,*,#49237,.T.);
#68843=ORIENTED_EDGE('',*,*,#49233,.T.);
#68844=ORIENTED_EDGE('',*,*,#49238,.T.);
#68845=ORIENTED_EDGE('',*,*,#49239,.T.);
#68846=ORIENTED_EDGE('',*,*,#49240,.F.);
#68847=ORIENTED_EDGE('',*,*,#49241,.T.);
#68848=ORIENTED_EDGE('',*,*,#49146,.F.);
#68849=ORIENTED_EDGE('',*,*,#49242,.F.);
#68850=ORIENTED_EDGE('',*,*,#49243,.T.);
#68851=ORIENTED_EDGE('',*,*,#49240,.T.);
#68852=ORIENTED_EDGE('',*,*,#49244,.T.);
#68853=ORIENTED_EDGE('',*,*,#49245,.T.);
#68854=ORIENTED_EDGE('',*,*,#49246,.F.);
#68855=ORIENTED_EDGE('',*,*,#49247,.T.);
#68856=ORIENTED_EDGE('',*,*,#49176,.F.);
#68857=ORIENTED_EDGE('',*,*,#49248,.F.);
#68858=ORIENTED_EDGE('',*,*,#49249,.T.);
#68859=ORIENTED_EDGE('',*,*,#49242,.T.);
#68860=ORIENTED_EDGE('',*,*,#49250,.T.);
#68861=ORIENTED_EDGE('',*,*,#49251,.F.);
#68862=ORIENTED_EDGE('',*,*,#49252,.T.);
#68863=ORIENTED_EDGE('',*,*,#49246,.T.);
#68864=ORIENTED_EDGE('',*,*,#49253,.T.);
#68865=ORIENTED_EDGE('',*,*,#49254,.F.);
#68866=ORIENTED_EDGE('',*,*,#49255,.T.);
#68867=ORIENTED_EDGE('',*,*,#49248,.T.);
#68868=ORIENTED_EDGE('',*,*,#49256,.T.);
#68869=ORIENTED_EDGE('',*,*,#49257,.F.);
#68870=ORIENTED_EDGE('',*,*,#49258,.T.);
#68871=ORIENTED_EDGE('',*,*,#49251,.T.);
#68872=ORIENTED_EDGE('',*,*,#49259,.T.);
#68873=ORIENTED_EDGE('',*,*,#49260,.F.);
#68874=ORIENTED_EDGE('',*,*,#49261,.T.);
#68875=ORIENTED_EDGE('',*,*,#49254,.T.);
#68876=ORIENTED_EDGE('',*,*,#49262,.T.);
#68877=ORIENTED_EDGE('',*,*,#49263,.F.);
#68878=ORIENTED_EDGE('',*,*,#49264,.T.);
#68879=ORIENTED_EDGE('',*,*,#49257,.T.);
#68880=ORIENTED_EDGE('',*,*,#49265,.T.);
#68881=ORIENTED_EDGE('',*,*,#49266,.F.);
#68882=ORIENTED_EDGE('',*,*,#49267,.T.);
#68883=ORIENTED_EDGE('',*,*,#49260,.T.);
#68884=ORIENTED_EDGE('',*,*,#49268,.T.);
#68885=ORIENTED_EDGE('',*,*,#49269,.F.);
#68886=ORIENTED_EDGE('',*,*,#49270,.T.);
#68887=ORIENTED_EDGE('',*,*,#49263,.T.);
#68888=ORIENTED_EDGE('',*,*,#49271,.T.);
#68889=ORIENTED_EDGE('',*,*,#49272,.F.);
#68890=ORIENTED_EDGE('',*,*,#49273,.T.);
#68891=ORIENTED_EDGE('',*,*,#49266,.T.);
#68892=ORIENTED_EDGE('',*,*,#49274,.T.);
#68893=ORIENTED_EDGE('',*,*,#49269,.T.);
#68894=ORIENTED_EDGE('',*,*,#49275,.T.);
#68895=ORIENTED_EDGE('',*,*,#49272,.T.);
#68896=ORIENTED_EDGE('',*,*,#49276,.T.);
#68897=ORIENTED_EDGE('',*,*,#49277,.F.);
#68898=ORIENTED_EDGE('',*,*,#49278,.T.);
#68899=ORIENTED_EDGE('',*,*,#49279,.F.);
#68900=ORIENTED_EDGE('',*,*,#49280,.T.);
#68901=ORIENTED_EDGE('',*,*,#49281,.F.);
#68902=ORIENTED_EDGE('',*,*,#49282,.T.);
#68903=ORIENTED_EDGE('',*,*,#49279,.T.);
#68904=ORIENTED_EDGE('',*,*,#49283,.T.);
#68905=ORIENTED_EDGE('',*,*,#49284,.F.);
#68906=ORIENTED_EDGE('',*,*,#49285,.T.);
#68907=ORIENTED_EDGE('',*,*,#49277,.T.);
#68908=ORIENTED_EDGE('',*,*,#49286,.T.);
#68909=ORIENTED_EDGE('',*,*,#49287,.F.);
#68910=ORIENTED_EDGE('',*,*,#49288,.T.);
#68911=ORIENTED_EDGE('',*,*,#49281,.T.);
#68912=ORIENTED_EDGE('',*,*,#49289,.T.);
#68913=ORIENTED_EDGE('',*,*,#49290,.F.);
#68914=ORIENTED_EDGE('',*,*,#49291,.T.);
#68915=ORIENTED_EDGE('',*,*,#49284,.T.);
#68916=ORIENTED_EDGE('',*,*,#49292,.T.);
#68917=ORIENTED_EDGE('',*,*,#49293,.F.);
#68918=ORIENTED_EDGE('',*,*,#49294,.T.);
#68919=ORIENTED_EDGE('',*,*,#49295,.T.);
#68920=ORIENTED_EDGE('',*,*,#49287,.T.);
#68921=ORIENTED_EDGE('',*,*,#49296,.T.);
#68922=ORIENTED_EDGE('',*,*,#49297,.F.);
#68923=ORIENTED_EDGE('',*,*,#49298,.T.);
#68924=ORIENTED_EDGE('',*,*,#49290,.T.);
#68925=ORIENTED_EDGE('',*,*,#49299,.T.);
#68926=ORIENTED_EDGE('',*,*,#49300,.F.);
#68927=ORIENTED_EDGE('',*,*,#49301,.T.);
#68928=ORIENTED_EDGE('',*,*,#49293,.T.);
#68929=ORIENTED_EDGE('',*,*,#49302,.T.);
#68930=ORIENTED_EDGE('',*,*,#49303,.T.);
#68931=ORIENTED_EDGE('',*,*,#49297,.T.);
#68932=ORIENTED_EDGE('',*,*,#49304,.T.);
#68933=ORIENTED_EDGE('',*,*,#49194,.F.);
#68934=ORIENTED_EDGE('',*,*,#49305,.F.);
#68935=ORIENTED_EDGE('',*,*,#49306,.T.);
#68936=ORIENTED_EDGE('',*,*,#49300,.T.);
#68937=ORIENTED_EDGE('',*,*,#49307,.T.);
#68938=ORIENTED_EDGE('',*,*,#49308,.T.);
#68939=ORIENTED_EDGE('',*,*,#49305,.T.);
#68940=ORIENTED_EDGE('',*,*,#49309,.T.);
#68941=ORIENTED_EDGE('',*,*,#49207,.F.);
#68942=ORIENTED_EDGE('',*,*,#49310,.T.);
#68943=ORIENTED_EDGE('',*,*,#49311,.F.);
#68944=ORIENTED_EDGE('',*,*,#49312,.T.);
#68945=ORIENTED_EDGE('',*,*,#49192,.F.);
#68946=ORIENTED_EDGE('',*,*,#49313,.T.);
#68947=ORIENTED_EDGE('',*,*,#49311,.T.);
#68948=ORIENTED_EDGE('',*,*,#49314,.T.);
#68949=ORIENTED_EDGE('',*,*,#49315,.F.);
#68950=ORIENTED_EDGE('',*,*,#49316,.T.);
#68951=ORIENTED_EDGE('',*,*,#49317,.F.);
#68952=ORIENTED_EDGE('',*,*,#49318,.T.);
#68953=ORIENTED_EDGE('',*,*,#49315,.T.);
#68954=ORIENTED_EDGE('',*,*,#49319,.T.);
#68955=ORIENTED_EDGE('',*,*,#49132,.F.);
#68956=ORIENTED_EDGE('',*,*,#49320,.F.);
#68957=ORIENTED_EDGE('',*,*,#49321,.T.);
#68958=ORIENTED_EDGE('',*,*,#49317,.T.);
#68959=ORIENTED_EDGE('',*,*,#49322,.T.);
#68960=ORIENTED_EDGE('',*,*,#49323,.T.);
#68961=ORIENTED_EDGE('',*,*,#49320,.T.);
#68962=ORIENTED_EDGE('',*,*,#49324,.T.);
#68963=ORIENTED_EDGE('',*,*,#49180,.F.);
#68964=ORIENTED_EDGE('',*,*,#49325,.T.);
#68965=ORIENTED_EDGE('',*,*,#49326,.F.);
#68966=ORIENTED_EDGE('',*,*,#49327,.T.);
#68967=ORIENTED_EDGE('',*,*,#49308,.F.);
#68968=ORIENTED_EDGE('',*,*,#49213,.F.);
#68969=ORIENTED_EDGE('',*,*,#49328,.T.);
#68970=ORIENTED_EDGE('',*,*,#49326,.T.);
#68971=ORIENTED_EDGE('',*,*,#49329,.T.);
#68972=ORIENTED_EDGE('',*,*,#49330,.F.);
#68973=ORIENTED_EDGE('',*,*,#49331,.F.);
#68974=ORIENTED_EDGE('',*,*,#49332,.T.);
#68975=ORIENTED_EDGE('',*,*,#49330,.T.);
#68976=ORIENTED_EDGE('',*,*,#49333,.T.);
#68977=ORIENTED_EDGE('',*,*,#49334,.F.);
#68978=ORIENTED_EDGE('',*,*,#49335,.T.);
#68979=ORIENTED_EDGE('',*,*,#49331,.T.);
#68980=ORIENTED_EDGE('',*,*,#49336,.T.);
#68981=ORIENTED_EDGE('',*,*,#49304,.F.);
#68982=ORIENTED_EDGE('',*,*,#49337,.T.);
#68983=ORIENTED_EDGE('',*,*,#49334,.T.);
#68984=ORIENTED_EDGE('',*,*,#49338,.T.);
#68985=ORIENTED_EDGE('',*,*,#49200,.F.);
#68986=ORIENTED_EDGE('',*,*,#49339,.T.);
#68987=ORIENTED_EDGE('',*,*,#49340,.F.);
#68988=ORIENTED_EDGE('',*,*,#49341,.T.);
#68989=ORIENTED_EDGE('',*,*,#49250,.F.);
#68990=ORIENTED_EDGE('',*,*,#49342,.F.);
#68991=ORIENTED_EDGE('',*,*,#49343,.T.);
#68992=ORIENTED_EDGE('',*,*,#49340,.T.);
#68993=ORIENTED_EDGE('',*,*,#49344,.T.);
#68994=ORIENTED_EDGE('',*,*,#49345,.F.);
#68995=ORIENTED_EDGE('',*,*,#49346,.T.);
#68996=ORIENTED_EDGE('',*,*,#49342,.T.);
#68997=ORIENTED_EDGE('',*,*,#49347,.T.);
#68998=ORIENTED_EDGE('',*,*,#49348,.T.);
#68999=ORIENTED_EDGE('',*,*,#49349,.F.);
#69000=ORIENTED_EDGE('',*,*,#49350,.T.);
#69001=ORIENTED_EDGE('',*,*,#49345,.T.);
#69002=ORIENTED_EDGE('',*,*,#49247,.F.);
#69003=ORIENTED_EDGE('',*,*,#49351,.T.);
#69004=ORIENTED_EDGE('',*,*,#49349,.T.);
#69005=ORIENTED_EDGE('',*,*,#49352,.T.);
#69006=ORIENTED_EDGE('',*,*,#49170,.F.);
#69007=ORIENTED_EDGE('',*,*,#49353,.T.);
#69008=ORIENTED_EDGE('',*,*,#49354,.F.);
#69009=ORIENTED_EDGE('',*,*,#49355,.T.);
#69010=ORIENTED_EDGE('',*,*,#49149,.F.);
#69011=ORIENTED_EDGE('',*,*,#49356,.F.);
#69012=ORIENTED_EDGE('',*,*,#49357,.T.);
#69013=ORIENTED_EDGE('',*,*,#49354,.T.);
#69014=ORIENTED_EDGE('',*,*,#49358,.T.);
#69015=ORIENTED_EDGE('',*,*,#49359,.F.);
#69016=ORIENTED_EDGE('',*,*,#49360,.T.);
#69017=ORIENTED_EDGE('',*,*,#49356,.T.);
#69018=ORIENTED_EDGE('',*,*,#49361,.T.);
#69019=ORIENTED_EDGE('',*,*,#49362,.T.);
#69020=ORIENTED_EDGE('',*,*,#49363,.F.);
#69021=ORIENTED_EDGE('',*,*,#49364,.T.);
#69022=ORIENTED_EDGE('',*,*,#49359,.T.);
#69023=ORIENTED_EDGE('',*,*,#49365,.T.);
#69024=ORIENTED_EDGE('',*,*,#49363,.T.);
#69025=ORIENTED_EDGE('',*,*,#49366,.T.);
#69026=ORIENTED_EDGE('',*,*,#49161,.F.);
#69027=ORIENTED_EDGE('',*,*,#49367,.T.);
#69028=ORIENTED_EDGE('',*,*,#49335,.F.);
#69029=ORIENTED_EDGE('',*,*,#49368,.T.);
#69030=ORIENTED_EDGE('',*,*,#49286,.F.);
#69031=ORIENTED_EDGE('',*,*,#49280,.F.);
#69032=ORIENTED_EDGE('',*,*,#49294,.F.);
#69033=ORIENTED_EDGE('',*,*,#49369,.T.);
#69034=ORIENTED_EDGE('',*,*,#49328,.F.);
#69035=ORIENTED_EDGE('',*,*,#49370,.T.);
#69036=ORIENTED_EDGE('',*,*,#49288,.F.);
#69037=ORIENTED_EDGE('',*,*,#49295,.F.);
#69038=ORIENTED_EDGE('',*,*,#49371,.T.);
#69039=ORIENTED_EDGE('',*,*,#49321,.F.);
#69040=ORIENTED_EDGE('',*,*,#49372,.T.);
#69041=ORIENTED_EDGE('',*,*,#49188,.F.);
#69042=ORIENTED_EDGE('',*,*,#49199,.F.);
#69043=ORIENTED_EDGE('',*,*,#49205,.F.);
#69044=ORIENTED_EDGE('',*,*,#49373,.T.);
#69045=ORIENTED_EDGE('',*,*,#49313,.F.);
#69046=ORIENTED_EDGE('',*,*,#49374,.T.);
#69047=ORIENTED_EDGE('',*,*,#49216,.F.);
#69048=ORIENTED_EDGE('',*,*,#49214,.F.);
#69049=ORIENTED_EDGE('',*,*,#49203,.F.);
#69050=ORIENTED_EDGE('',*,*,#49375,.T.);
#69051=ORIENTED_EDGE('',*,*,#49357,.F.);
#69052=ORIENTED_EDGE('',*,*,#49376,.T.);
#69053=ORIENTED_EDGE('',*,*,#49153,.F.);
#69054=ORIENTED_EDGE('',*,*,#49142,.F.);
#69055=ORIENTED_EDGE('',*,*,#49364,.F.);
#69056=ORIENTED_EDGE('',*,*,#49377,.T.);
#69057=ORIENTED_EDGE('',*,*,#49174,.F.);
#69058=ORIENTED_EDGE('',*,*,#49173,.F.);
#69059=ORIENTED_EDGE('',*,*,#49171,.F.);
#69060=ORIENTED_EDGE('',*,*,#49165,.F.);
#69061=ORIENTED_EDGE('',*,*,#49378,.T.);
#69062=ORIENTED_EDGE('',*,*,#49270,.F.);
#69063=ORIENTED_EDGE('',*,*,#49379,.T.);
#69064=ORIENTED_EDGE('',*,*,#49350,.F.);
#69065=ORIENTED_EDGE('',*,*,#49380,.T.);
#69066=ORIENTED_EDGE('',*,*,#49264,.F.);
#69067=ORIENTED_EDGE('',*,*,#49268,.F.);
#69068=ORIENTED_EDGE('',*,*,#49381,.T.);
#69069=ORIENTED_EDGE('',*,*,#49343,.F.);
#69070=ORIENTED_EDGE('',*,*,#49382,.T.);
#69071=ORIENTED_EDGE('',*,*,#49274,.F.);
#69072=ORIENTED_EDGE('',*,*,#49383,.T.);
#69073=ORIENTED_EDGE('',*,*,#49384,.F.);
#69074=ORIENTED_EDGE('',*,*,#49385,.T.);
#69075=ORIENTED_EDGE('',*,*,#49386,.F.);
#69076=ORIENTED_EDGE('',*,*,#49387,.F.);
#69077=ORIENTED_EDGE('',*,*,#49388,.T.);
#69078=ORIENTED_EDGE('',*,*,#49384,.T.);
#69079=ORIENTED_EDGE('',*,*,#49389,.T.);
#69080=ORIENTED_EDGE('',*,*,#49390,.F.);
#69081=ORIENTED_EDGE('',*,*,#49391,.T.);
#69082=ORIENTED_EDGE('',*,*,#49386,.T.);
#69083=ORIENTED_EDGE('',*,*,#49392,.T.);
#69084=ORIENTED_EDGE('',*,*,#49393,.F.);
#69085=ORIENTED_EDGE('',*,*,#49394,.T.);
#69086=ORIENTED_EDGE('',*,*,#49387,.T.);
#69087=ORIENTED_EDGE('',*,*,#49395,.T.);
#69088=ORIENTED_EDGE('',*,*,#49396,.F.);
#69089=ORIENTED_EDGE('',*,*,#49397,.T.);
#69090=ORIENTED_EDGE('',*,*,#49390,.T.);
#69091=ORIENTED_EDGE('',*,*,#49398,.T.);
#69092=ORIENTED_EDGE('',*,*,#49399,.F.);
#69093=ORIENTED_EDGE('',*,*,#49400,.T.);
#69094=ORIENTED_EDGE('',*,*,#49393,.T.);
#69095=ORIENTED_EDGE('',*,*,#49401,.T.);
#69096=ORIENTED_EDGE('',*,*,#49402,.F.);
#69097=ORIENTED_EDGE('',*,*,#49403,.T.);
#69098=ORIENTED_EDGE('',*,*,#49396,.T.);
#69099=ORIENTED_EDGE('',*,*,#49404,.T.);
#69100=ORIENTED_EDGE('',*,*,#49405,.F.);
#69101=ORIENTED_EDGE('',*,*,#49406,.T.);
#69102=ORIENTED_EDGE('',*,*,#49399,.T.);
#69103=ORIENTED_EDGE('',*,*,#49407,.T.);
#69104=ORIENTED_EDGE('',*,*,#49408,.F.);
#69105=ORIENTED_EDGE('',*,*,#49409,.T.);
#69106=ORIENTED_EDGE('',*,*,#49402,.T.);
#69107=ORIENTED_EDGE('',*,*,#49410,.T.);
#69108=ORIENTED_EDGE('',*,*,#49405,.T.);
#69109=ORIENTED_EDGE('',*,*,#49411,.T.);
#69110=ORIENTED_EDGE('',*,*,#49408,.T.);
#69111=ORIENTED_EDGE('',*,*,#49412,.T.);
#69112=ORIENTED_EDGE('',*,*,#49413,.T.);
#69113=ORIENTED_EDGE('',*,*,#49414,.F.);
#69114=ORIENTED_EDGE('',*,*,#49415,.T.);
#69115=ORIENTED_EDGE('',*,*,#49416,.F.);
#69116=ORIENTED_EDGE('',*,*,#49417,.F.);
#69117=ORIENTED_EDGE('',*,*,#49418,.T.);
#69118=ORIENTED_EDGE('',*,*,#49414,.T.);
#69119=ORIENTED_EDGE('',*,*,#49419,.T.);
#69120=ORIENTED_EDGE('',*,*,#49420,.F.);
#69121=ORIENTED_EDGE('',*,*,#49421,.T.);
#69122=ORIENTED_EDGE('',*,*,#49416,.T.);
#69123=ORIENTED_EDGE('',*,*,#49422,.T.);
#69124=ORIENTED_EDGE('',*,*,#49423,.F.);
#69125=ORIENTED_EDGE('',*,*,#49424,.T.);
#69126=ORIENTED_EDGE('',*,*,#49417,.T.);
#69127=ORIENTED_EDGE('',*,*,#49425,.T.);
#69128=ORIENTED_EDGE('',*,*,#49426,.F.);
#69129=ORIENTED_EDGE('',*,*,#49427,.T.);
#69130=ORIENTED_EDGE('',*,*,#49420,.T.);
#69131=ORIENTED_EDGE('',*,*,#49428,.T.);
#69132=ORIENTED_EDGE('',*,*,#49429,.F.);
#69133=ORIENTED_EDGE('',*,*,#49430,.T.);
#69134=ORIENTED_EDGE('',*,*,#49423,.T.);
#69135=ORIENTED_EDGE('',*,*,#49431,.T.);
#69136=ORIENTED_EDGE('',*,*,#49432,.F.);
#69137=ORIENTED_EDGE('',*,*,#49433,.T.);
#69138=ORIENTED_EDGE('',*,*,#49426,.T.);
#69139=ORIENTED_EDGE('',*,*,#49434,.T.);
#69140=ORIENTED_EDGE('',*,*,#49429,.T.);
#69141=ORIENTED_EDGE('',*,*,#49435,.T.);
#69142=ORIENTED_EDGE('',*,*,#49432,.T.);
#69143=ORIENTED_EDGE('',*,*,#49436,.T.);
#69144=ORIENTED_EDGE('',*,*,#49437,.T.);
#69145=ORIENTED_EDGE('',*,*,#49438,.F.);
#69146=ORIENTED_EDGE('',*,*,#49439,.T.);
#69147=ORIENTED_EDGE('',*,*,#49440,.F.);
#69148=ORIENTED_EDGE('',*,*,#49441,.F.);
#69149=ORIENTED_EDGE('',*,*,#49442,.T.);
#69150=ORIENTED_EDGE('',*,*,#49438,.T.);
#69151=ORIENTED_EDGE('',*,*,#49443,.T.);
#69152=ORIENTED_EDGE('',*,*,#49444,.F.);
#69153=ORIENTED_EDGE('',*,*,#49445,.T.);
#69154=ORIENTED_EDGE('',*,*,#49440,.T.);
#69155=ORIENTED_EDGE('',*,*,#49446,.T.);
#69156=ORIENTED_EDGE('',*,*,#49447,.F.);
#69157=ORIENTED_EDGE('',*,*,#49448,.T.);
#69158=ORIENTED_EDGE('',*,*,#49441,.T.);
#69159=ORIENTED_EDGE('',*,*,#49449,.T.);
#69160=ORIENTED_EDGE('',*,*,#49450,.F.);
#69161=ORIENTED_EDGE('',*,*,#49451,.T.);
#69162=ORIENTED_EDGE('',*,*,#49444,.T.);
#69163=ORIENTED_EDGE('',*,*,#49452,.T.);
#69164=ORIENTED_EDGE('',*,*,#49453,.F.);
#69165=ORIENTED_EDGE('',*,*,#49454,.T.);
#69166=ORIENTED_EDGE('',*,*,#49447,.T.);
#69167=ORIENTED_EDGE('',*,*,#49455,.T.);
#69168=ORIENTED_EDGE('',*,*,#49456,.F.);
#69169=ORIENTED_EDGE('',*,*,#49457,.T.);
#69170=ORIENTED_EDGE('',*,*,#49450,.T.);
#69171=ORIENTED_EDGE('',*,*,#49458,.T.);
#69172=ORIENTED_EDGE('',*,*,#49453,.T.);
#69173=ORIENTED_EDGE('',*,*,#49459,.T.);
#69174=ORIENTED_EDGE('',*,*,#49456,.T.);
#69175=ORIENTED_EDGE('',*,*,#49460,.T.);
#69176=ORIENTED_EDGE('',*,*,#49461,.F.);
#69177=ORIENTED_EDGE('',*,*,#49462,.T.);
#69178=ORIENTED_EDGE('',*,*,#49463,.F.);
#69179=ORIENTED_EDGE('',*,*,#49464,.T.);
#69180=ORIENTED_EDGE('',*,*,#49465,.F.);
#69181=ORIENTED_EDGE('',*,*,#49466,.T.);
#69182=ORIENTED_EDGE('',*,*,#49463,.T.);
#69183=ORIENTED_EDGE('',*,*,#49467,.T.);
#69184=ORIENTED_EDGE('',*,*,#49468,.F.);
#69185=ORIENTED_EDGE('',*,*,#49469,.T.);
#69186=ORIENTED_EDGE('',*,*,#49461,.T.);
#69187=ORIENTED_EDGE('',*,*,#49470,.T.);
#69188=ORIENTED_EDGE('',*,*,#49471,.F.);
#69189=ORIENTED_EDGE('',*,*,#49472,.T.);
#69190=ORIENTED_EDGE('',*,*,#49465,.T.);
#69191=ORIENTED_EDGE('',*,*,#49473,.T.);
#69192=ORIENTED_EDGE('',*,*,#49474,.F.);
#69193=ORIENTED_EDGE('',*,*,#49475,.T.);
#69194=ORIENTED_EDGE('',*,*,#49468,.T.);
#69195=ORIENTED_EDGE('',*,*,#49476,.T.);
#69196=ORIENTED_EDGE('',*,*,#49477,.F.);
#69197=ORIENTED_EDGE('',*,*,#49478,.T.);
#69198=ORIENTED_EDGE('',*,*,#49471,.T.);
#69199=ORIENTED_EDGE('',*,*,#49479,.T.);
#69200=ORIENTED_EDGE('',*,*,#49480,.F.);
#69201=ORIENTED_EDGE('',*,*,#49481,.T.);
#69202=ORIENTED_EDGE('',*,*,#49474,.T.);
#69203=ORIENTED_EDGE('',*,*,#49482,.T.);
#69204=ORIENTED_EDGE('',*,*,#49477,.T.);
#69205=ORIENTED_EDGE('',*,*,#49483,.T.);
#69206=ORIENTED_EDGE('',*,*,#49480,.T.);
#69207=ORIENTED_EDGE('',*,*,#49484,.T.);
#69208=ORIENTED_EDGE('',*,*,#49485,.F.);
#69209=ORIENTED_EDGE('',*,*,#49486,.T.);
#69210=ORIENTED_EDGE('',*,*,#49487,.F.);
#69211=ORIENTED_EDGE('',*,*,#49488,.T.);
#69212=ORIENTED_EDGE('',*,*,#49489,.F.);
#69213=ORIENTED_EDGE('',*,*,#49490,.T.);
#69214=ORIENTED_EDGE('',*,*,#49487,.T.);
#69215=ORIENTED_EDGE('',*,*,#49491,.T.);
#69216=ORIENTED_EDGE('',*,*,#49492,.F.);
#69217=ORIENTED_EDGE('',*,*,#49493,.T.);
#69218=ORIENTED_EDGE('',*,*,#49485,.T.);
#69219=ORIENTED_EDGE('',*,*,#49494,.T.);
#69220=ORIENTED_EDGE('',*,*,#49495,.F.);
#69221=ORIENTED_EDGE('',*,*,#49496,.T.);
#69222=ORIENTED_EDGE('',*,*,#49489,.T.);
#69223=ORIENTED_EDGE('',*,*,#49497,.T.);
#69224=ORIENTED_EDGE('',*,*,#49498,.F.);
#69225=ORIENTED_EDGE('',*,*,#49499,.T.);
#69226=ORIENTED_EDGE('',*,*,#49492,.T.);
#69227=ORIENTED_EDGE('',*,*,#49500,.T.);
#69228=ORIENTED_EDGE('',*,*,#49501,.F.);
#69229=ORIENTED_EDGE('',*,*,#49502,.T.);
#69230=ORIENTED_EDGE('',*,*,#49495,.T.);
#69231=ORIENTED_EDGE('',*,*,#49503,.T.);
#69232=ORIENTED_EDGE('',*,*,#49504,.F.);
#69233=ORIENTED_EDGE('',*,*,#49505,.T.);
#69234=ORIENTED_EDGE('',*,*,#49498,.T.);
#69235=ORIENTED_EDGE('',*,*,#49506,.T.);
#69236=ORIENTED_EDGE('',*,*,#49507,.F.);
#69237=ORIENTED_EDGE('',*,*,#49508,.T.);
#69238=ORIENTED_EDGE('',*,*,#49501,.T.);
#69239=ORIENTED_EDGE('',*,*,#49509,.T.);
#69240=ORIENTED_EDGE('',*,*,#49504,.T.);
#69241=ORIENTED_EDGE('',*,*,#49510,.T.);
#69242=ORIENTED_EDGE('',*,*,#49507,.T.);
#69243=ORIENTED_EDGE('',*,*,#49511,.T.);
#69244=ORIENTED_EDGE('',*,*,#49512,.F.);
#69245=ORIENTED_EDGE('',*,*,#49513,.T.);
#69246=ORIENTED_EDGE('',*,*,#49514,.F.);
#69247=ORIENTED_EDGE('',*,*,#49515,.T.);
#69248=ORIENTED_EDGE('',*,*,#49516,.F.);
#69249=ORIENTED_EDGE('',*,*,#49517,.T.);
#69250=ORIENTED_EDGE('',*,*,#49514,.T.);
#69251=ORIENTED_EDGE('',*,*,#49518,.T.);
#69252=ORIENTED_EDGE('',*,*,#49519,.F.);
#69253=ORIENTED_EDGE('',*,*,#49520,.T.);
#69254=ORIENTED_EDGE('',*,*,#49512,.T.);
#69255=ORIENTED_EDGE('',*,*,#49521,.T.);
#69256=ORIENTED_EDGE('',*,*,#49522,.F.);
#69257=ORIENTED_EDGE('',*,*,#49523,.T.);
#69258=ORIENTED_EDGE('',*,*,#49516,.T.);
#69259=ORIENTED_EDGE('',*,*,#49524,.T.);
#69260=ORIENTED_EDGE('',*,*,#49525,.F.);
#69261=ORIENTED_EDGE('',*,*,#49526,.T.);
#69262=ORIENTED_EDGE('',*,*,#49519,.T.);
#69263=ORIENTED_EDGE('',*,*,#49527,.T.);
#69264=ORIENTED_EDGE('',*,*,#49528,.F.);
#69265=ORIENTED_EDGE('',*,*,#49529,.T.);
#69266=ORIENTED_EDGE('',*,*,#49522,.T.);
#69267=ORIENTED_EDGE('',*,*,#49530,.T.);
#69268=ORIENTED_EDGE('',*,*,#49531,.F.);
#69269=ORIENTED_EDGE('',*,*,#49532,.T.);
#69270=ORIENTED_EDGE('',*,*,#49525,.T.);
#69271=ORIENTED_EDGE('',*,*,#49533,.T.);
#69272=ORIENTED_EDGE('',*,*,#49528,.T.);
#69273=ORIENTED_EDGE('',*,*,#49534,.T.);
#69274=ORIENTED_EDGE('',*,*,#49531,.T.);
#69275=ORIENTED_EDGE('',*,*,#49535,.T.);
#69276=ORIENTED_EDGE('',*,*,#49536,.F.);
#69277=ORIENTED_EDGE('',*,*,#49537,.T.);
#69278=ORIENTED_EDGE('',*,*,#49538,.F.);
#69279=ORIENTED_EDGE('',*,*,#49539,.T.);
#69280=ORIENTED_EDGE('',*,*,#49540,.F.);
#69281=ORIENTED_EDGE('',*,*,#49541,.T.);
#69282=ORIENTED_EDGE('',*,*,#49538,.T.);
#69283=ORIENTED_EDGE('',*,*,#49542,.T.);
#69284=ORIENTED_EDGE('',*,*,#49543,.F.);
#69285=ORIENTED_EDGE('',*,*,#49544,.T.);
#69286=ORIENTED_EDGE('',*,*,#49536,.T.);
#69287=ORIENTED_EDGE('',*,*,#49545,.T.);
#69288=ORIENTED_EDGE('',*,*,#49546,.F.);
#69289=ORIENTED_EDGE('',*,*,#49547,.T.);
#69290=ORIENTED_EDGE('',*,*,#49540,.T.);
#69291=ORIENTED_EDGE('',*,*,#49548,.T.);
#69292=ORIENTED_EDGE('',*,*,#49549,.F.);
#69293=ORIENTED_EDGE('',*,*,#49550,.T.);
#69294=ORIENTED_EDGE('',*,*,#49543,.T.);
#69295=ORIENTED_EDGE('',*,*,#49551,.T.);
#69296=ORIENTED_EDGE('',*,*,#49552,.F.);
#69297=ORIENTED_EDGE('',*,*,#49553,.T.);
#69298=ORIENTED_EDGE('',*,*,#49546,.T.);
#69299=ORIENTED_EDGE('',*,*,#49554,.T.);
#69300=ORIENTED_EDGE('',*,*,#49555,.F.);
#69301=ORIENTED_EDGE('',*,*,#49556,.T.);
#69302=ORIENTED_EDGE('',*,*,#49549,.T.);
#69303=ORIENTED_EDGE('',*,*,#49557,.T.);
#69304=ORIENTED_EDGE('',*,*,#49552,.T.);
#69305=ORIENTED_EDGE('',*,*,#49558,.T.);
#69306=ORIENTED_EDGE('',*,*,#49555,.T.);
#69307=ORIENTED_EDGE('',*,*,#49559,.T.);
#69308=ORIENTED_EDGE('',*,*,#49560,.F.);
#69309=ORIENTED_EDGE('',*,*,#49561,.T.);
#69310=ORIENTED_EDGE('',*,*,#49562,.F.);
#69311=ORIENTED_EDGE('',*,*,#49563,.T.);
#69312=ORIENTED_EDGE('',*,*,#49564,.F.);
#69313=ORIENTED_EDGE('',*,*,#49565,.T.);
#69314=ORIENTED_EDGE('',*,*,#49562,.T.);
#69315=ORIENTED_EDGE('',*,*,#49566,.T.);
#69316=ORIENTED_EDGE('',*,*,#49567,.F.);
#69317=ORIENTED_EDGE('',*,*,#49568,.T.);
#69318=ORIENTED_EDGE('',*,*,#49560,.T.);
#69319=ORIENTED_EDGE('',*,*,#49569,.T.);
#69320=ORIENTED_EDGE('',*,*,#49570,.F.);
#69321=ORIENTED_EDGE('',*,*,#49571,.T.);
#69322=ORIENTED_EDGE('',*,*,#49564,.T.);
#69323=ORIENTED_EDGE('',*,*,#49572,.T.);
#69324=ORIENTED_EDGE('',*,*,#49573,.F.);
#69325=ORIENTED_EDGE('',*,*,#49574,.T.);
#69326=ORIENTED_EDGE('',*,*,#49567,.T.);
#69327=ORIENTED_EDGE('',*,*,#49575,.T.);
#69328=ORIENTED_EDGE('',*,*,#49576,.F.);
#69329=ORIENTED_EDGE('',*,*,#49577,.T.);
#69330=ORIENTED_EDGE('',*,*,#49570,.T.);
#69331=ORIENTED_EDGE('',*,*,#49578,.T.);
#69332=ORIENTED_EDGE('',*,*,#49579,.F.);
#69333=ORIENTED_EDGE('',*,*,#49580,.T.);
#69334=ORIENTED_EDGE('',*,*,#49573,.T.);
#69335=ORIENTED_EDGE('',*,*,#49581,.T.);
#69336=ORIENTED_EDGE('',*,*,#49576,.T.);
#69337=ORIENTED_EDGE('',*,*,#49582,.T.);
#69338=ORIENTED_EDGE('',*,*,#49579,.T.);
#69339=ORIENTED_EDGE('',*,*,#49583,.T.);
#69340=ORIENTED_EDGE('',*,*,#49584,.F.);
#69341=ORIENTED_EDGE('',*,*,#49585,.T.);
#69342=ORIENTED_EDGE('',*,*,#49586,.F.);
#69343=ORIENTED_EDGE('',*,*,#49587,.T.);
#69344=ORIENTED_EDGE('',*,*,#49588,.F.);
#69345=ORIENTED_EDGE('',*,*,#49589,.T.);
#69346=ORIENTED_EDGE('',*,*,#49586,.T.);
#69347=ORIENTED_EDGE('',*,*,#49590,.T.);
#69348=ORIENTED_EDGE('',*,*,#49591,.F.);
#69349=ORIENTED_EDGE('',*,*,#49592,.T.);
#69350=ORIENTED_EDGE('',*,*,#49584,.T.);
#69351=ORIENTED_EDGE('',*,*,#49593,.T.);
#69352=ORIENTED_EDGE('',*,*,#49594,.F.);
#69353=ORIENTED_EDGE('',*,*,#49595,.T.);
#69354=ORIENTED_EDGE('',*,*,#49588,.T.);
#69355=ORIENTED_EDGE('',*,*,#49596,.T.);
#69356=ORIENTED_EDGE('',*,*,#49597,.F.);
#69357=ORIENTED_EDGE('',*,*,#49598,.T.);
#69358=ORIENTED_EDGE('',*,*,#49591,.T.);
#69359=ORIENTED_EDGE('',*,*,#49599,.T.);
#69360=ORIENTED_EDGE('',*,*,#49600,.F.);
#69361=ORIENTED_EDGE('',*,*,#49601,.T.);
#69362=ORIENTED_EDGE('',*,*,#49594,.T.);
#69363=ORIENTED_EDGE('',*,*,#49602,.T.);
#69364=ORIENTED_EDGE('',*,*,#49603,.F.);
#69365=ORIENTED_EDGE('',*,*,#49604,.T.);
#69366=ORIENTED_EDGE('',*,*,#49597,.T.);
#69367=ORIENTED_EDGE('',*,*,#49605,.T.);
#69368=ORIENTED_EDGE('',*,*,#49600,.T.);
#69369=ORIENTED_EDGE('',*,*,#49606,.T.);
#69370=ORIENTED_EDGE('',*,*,#49603,.T.);
#69371=ORIENTED_EDGE('',*,*,#49607,.T.);
#69372=ORIENTED_EDGE('',*,*,#49608,.F.);
#69373=ORIENTED_EDGE('',*,*,#49609,.T.);
#69374=ORIENTED_EDGE('',*,*,#49610,.F.);
#69375=ORIENTED_EDGE('',*,*,#49611,.T.);
#69376=ORIENTED_EDGE('',*,*,#49612,.F.);
#69377=ORIENTED_EDGE('',*,*,#49613,.T.);
#69378=ORIENTED_EDGE('',*,*,#49610,.T.);
#69379=ORIENTED_EDGE('',*,*,#49614,.T.);
#69380=ORIENTED_EDGE('',*,*,#49615,.F.);
#69381=ORIENTED_EDGE('',*,*,#49616,.T.);
#69382=ORIENTED_EDGE('',*,*,#49608,.T.);
#69383=ORIENTED_EDGE('',*,*,#49617,.T.);
#69384=ORIENTED_EDGE('',*,*,#49618,.F.);
#69385=ORIENTED_EDGE('',*,*,#49619,.T.);
#69386=ORIENTED_EDGE('',*,*,#49612,.T.);
#69387=ORIENTED_EDGE('',*,*,#49620,.T.);
#69388=ORIENTED_EDGE('',*,*,#49621,.F.);
#69389=ORIENTED_EDGE('',*,*,#49622,.T.);
#69390=ORIENTED_EDGE('',*,*,#49615,.T.);
#69391=ORIENTED_EDGE('',*,*,#49623,.T.);
#69392=ORIENTED_EDGE('',*,*,#49624,.F.);
#69393=ORIENTED_EDGE('',*,*,#49625,.T.);
#69394=ORIENTED_EDGE('',*,*,#49618,.T.);
#69395=ORIENTED_EDGE('',*,*,#49626,.T.);
#69396=ORIENTED_EDGE('',*,*,#49627,.F.);
#69397=ORIENTED_EDGE('',*,*,#49628,.T.);
#69398=ORIENTED_EDGE('',*,*,#49621,.T.);
#69399=ORIENTED_EDGE('',*,*,#49629,.T.);
#69400=ORIENTED_EDGE('',*,*,#49624,.T.);
#69401=ORIENTED_EDGE('',*,*,#49630,.T.);
#69402=ORIENTED_EDGE('',*,*,#49627,.T.);
#69403=ORIENTED_EDGE('',*,*,#49631,.T.);
#69404=ORIENTED_EDGE('',*,*,#49632,.F.);
#69405=ORIENTED_EDGE('',*,*,#49633,.T.);
#69406=ORIENTED_EDGE('',*,*,#49634,.F.);
#69407=ORIENTED_EDGE('',*,*,#49635,.T.);
#69408=ORIENTED_EDGE('',*,*,#49636,.F.);
#69409=ORIENTED_EDGE('',*,*,#49637,.T.);
#69410=ORIENTED_EDGE('',*,*,#49634,.T.);
#69411=ORIENTED_EDGE('',*,*,#49638,.T.);
#69412=ORIENTED_EDGE('',*,*,#49639,.F.);
#69413=ORIENTED_EDGE('',*,*,#49640,.T.);
#69414=ORIENTED_EDGE('',*,*,#49632,.T.);
#69415=ORIENTED_EDGE('',*,*,#49641,.T.);
#69416=ORIENTED_EDGE('',*,*,#49642,.F.);
#69417=ORIENTED_EDGE('',*,*,#49643,.T.);
#69418=ORIENTED_EDGE('',*,*,#49636,.T.);
#69419=ORIENTED_EDGE('',*,*,#49644,.T.);
#69420=ORIENTED_EDGE('',*,*,#49645,.F.);
#69421=ORIENTED_EDGE('',*,*,#49646,.T.);
#69422=ORIENTED_EDGE('',*,*,#49639,.T.);
#69423=ORIENTED_EDGE('',*,*,#49647,.T.);
#69424=ORIENTED_EDGE('',*,*,#49648,.F.);
#69425=ORIENTED_EDGE('',*,*,#49649,.T.);
#69426=ORIENTED_EDGE('',*,*,#49642,.T.);
#69427=ORIENTED_EDGE('',*,*,#49650,.T.);
#69428=ORIENTED_EDGE('',*,*,#49651,.F.);
#69429=ORIENTED_EDGE('',*,*,#49652,.T.);
#69430=ORIENTED_EDGE('',*,*,#49645,.T.);
#69431=ORIENTED_EDGE('',*,*,#49653,.T.);
#69432=ORIENTED_EDGE('',*,*,#49654,.F.);
#69433=ORIENTED_EDGE('',*,*,#49655,.T.);
#69434=ORIENTED_EDGE('',*,*,#49648,.T.);
#69435=ORIENTED_EDGE('',*,*,#49656,.T.);
#69436=ORIENTED_EDGE('',*,*,#49657,.F.);
#69437=ORIENTED_EDGE('',*,*,#49658,.T.);
#69438=ORIENTED_EDGE('',*,*,#49651,.T.);
#69439=ORIENTED_EDGE('',*,*,#49659,.T.);
#69440=ORIENTED_EDGE('',*,*,#49654,.T.);
#69441=ORIENTED_EDGE('',*,*,#49660,.T.);
#69442=ORIENTED_EDGE('',*,*,#49657,.T.);
#69443=ORIENTED_EDGE('',*,*,#49661,.T.);
#69444=ORIENTED_EDGE('',*,*,#49662,.F.);
#69445=ORIENTED_EDGE('',*,*,#49663,.T.);
#69446=ORIENTED_EDGE('',*,*,#49664,.F.);
#69447=ORIENTED_EDGE('',*,*,#49665,.T.);
#69448=ORIENTED_EDGE('',*,*,#49666,.F.);
#69449=ORIENTED_EDGE('',*,*,#49667,.T.);
#69450=ORIENTED_EDGE('',*,*,#49664,.T.);
#69451=ORIENTED_EDGE('',*,*,#49668,.T.);
#69452=ORIENTED_EDGE('',*,*,#49669,.F.);
#69453=ORIENTED_EDGE('',*,*,#49670,.T.);
#69454=ORIENTED_EDGE('',*,*,#49662,.T.);
#69455=ORIENTED_EDGE('',*,*,#49671,.T.);
#69456=ORIENTED_EDGE('',*,*,#49672,.F.);
#69457=ORIENTED_EDGE('',*,*,#49673,.T.);
#69458=ORIENTED_EDGE('',*,*,#49666,.T.);
#69459=ORIENTED_EDGE('',*,*,#49674,.T.);
#69460=ORIENTED_EDGE('',*,*,#49675,.F.);
#69461=ORIENTED_EDGE('',*,*,#49676,.T.);
#69462=ORIENTED_EDGE('',*,*,#49669,.T.);
#69463=ORIENTED_EDGE('',*,*,#49677,.T.);
#69464=ORIENTED_EDGE('',*,*,#49678,.F.);
#69465=ORIENTED_EDGE('',*,*,#49679,.T.);
#69466=ORIENTED_EDGE('',*,*,#49672,.T.);
#69467=ORIENTED_EDGE('',*,*,#49680,.T.);
#69468=ORIENTED_EDGE('',*,*,#49681,.F.);
#69469=ORIENTED_EDGE('',*,*,#49682,.T.);
#69470=ORIENTED_EDGE('',*,*,#49675,.T.);
#69471=ORIENTED_EDGE('',*,*,#49683,.T.);
#69472=ORIENTED_EDGE('',*,*,#49678,.T.);
#69473=ORIENTED_EDGE('',*,*,#49684,.T.);
#69474=ORIENTED_EDGE('',*,*,#49681,.T.);
#69475=ORIENTED_EDGE('',*,*,#49685,.T.);
#69476=ORIENTED_EDGE('',*,*,#49686,.F.);
#69477=ORIENTED_EDGE('',*,*,#49687,.T.);
#69478=ORIENTED_EDGE('',*,*,#49688,.F.);
#69479=ORIENTED_EDGE('',*,*,#49689,.T.);
#69480=ORIENTED_EDGE('',*,*,#49690,.F.);
#69481=ORIENTED_EDGE('',*,*,#49691,.T.);
#69482=ORIENTED_EDGE('',*,*,#49688,.T.);
#69483=ORIENTED_EDGE('',*,*,#49692,.T.);
#69484=ORIENTED_EDGE('',*,*,#49693,.F.);
#69485=ORIENTED_EDGE('',*,*,#49694,.T.);
#69486=ORIENTED_EDGE('',*,*,#49686,.T.);
#69487=ORIENTED_EDGE('',*,*,#49695,.T.);
#69488=ORIENTED_EDGE('',*,*,#49696,.F.);
#69489=ORIENTED_EDGE('',*,*,#49697,.T.);
#69490=ORIENTED_EDGE('',*,*,#49690,.T.);
#69491=ORIENTED_EDGE('',*,*,#49698,.T.);
#69492=ORIENTED_EDGE('',*,*,#49699,.F.);
#69493=ORIENTED_EDGE('',*,*,#49700,.T.);
#69494=ORIENTED_EDGE('',*,*,#49693,.T.);
#69495=ORIENTED_EDGE('',*,*,#49701,.T.);
#69496=ORIENTED_EDGE('',*,*,#49702,.F.);
#69497=ORIENTED_EDGE('',*,*,#49703,.T.);
#69498=ORIENTED_EDGE('',*,*,#49696,.T.);
#69499=ORIENTED_EDGE('',*,*,#49704,.T.);
#69500=ORIENTED_EDGE('',*,*,#49705,.F.);
#69501=ORIENTED_EDGE('',*,*,#49706,.T.);
#69502=ORIENTED_EDGE('',*,*,#49699,.T.);
#69503=ORIENTED_EDGE('',*,*,#49707,.T.);
#69504=ORIENTED_EDGE('',*,*,#49702,.T.);
#69505=ORIENTED_EDGE('',*,*,#49708,.T.);
#69506=ORIENTED_EDGE('',*,*,#49705,.T.);
#69507=ORIENTED_EDGE('',*,*,#49709,.T.);
#69508=ORIENTED_EDGE('',*,*,#49710,.F.);
#69509=ORIENTED_EDGE('',*,*,#49711,.T.);
#69510=ORIENTED_EDGE('',*,*,#49712,.F.);
#69511=ORIENTED_EDGE('',*,*,#49713,.T.);
#69512=ORIENTED_EDGE('',*,*,#49714,.F.);
#69513=ORIENTED_EDGE('',*,*,#49715,.T.);
#69514=ORIENTED_EDGE('',*,*,#49712,.T.);
#69515=ORIENTED_EDGE('',*,*,#49716,.T.);
#69516=ORIENTED_EDGE('',*,*,#49717,.F.);
#69517=ORIENTED_EDGE('',*,*,#49718,.T.);
#69518=ORIENTED_EDGE('',*,*,#49710,.T.);
#69519=ORIENTED_EDGE('',*,*,#49719,.T.);
#69520=ORIENTED_EDGE('',*,*,#49720,.F.);
#69521=ORIENTED_EDGE('',*,*,#49721,.T.);
#69522=ORIENTED_EDGE('',*,*,#49714,.T.);
#69523=ORIENTED_EDGE('',*,*,#49722,.T.);
#69524=ORIENTED_EDGE('',*,*,#49723,.F.);
#69525=ORIENTED_EDGE('',*,*,#49724,.T.);
#69526=ORIENTED_EDGE('',*,*,#49717,.T.);
#69527=ORIENTED_EDGE('',*,*,#49725,.T.);
#69528=ORIENTED_EDGE('',*,*,#49726,.F.);
#69529=ORIENTED_EDGE('',*,*,#49727,.T.);
#69530=ORIENTED_EDGE('',*,*,#49720,.T.);
#69531=ORIENTED_EDGE('',*,*,#49728,.T.);
#69532=ORIENTED_EDGE('',*,*,#49729,.F.);
#69533=ORIENTED_EDGE('',*,*,#49730,.T.);
#69534=ORIENTED_EDGE('',*,*,#49723,.T.);
#69535=ORIENTED_EDGE('',*,*,#49731,.T.);
#69536=ORIENTED_EDGE('',*,*,#49732,.F.);
#69537=ORIENTED_EDGE('',*,*,#49733,.T.);
#69538=ORIENTED_EDGE('',*,*,#49726,.T.);
#69539=ORIENTED_EDGE('',*,*,#49734,.T.);
#69540=ORIENTED_EDGE('',*,*,#49735,.F.);
#69541=ORIENTED_EDGE('',*,*,#49736,.T.);
#69542=ORIENTED_EDGE('',*,*,#49729,.T.);
#69543=ORIENTED_EDGE('',*,*,#49737,.T.);
#69544=ORIENTED_EDGE('',*,*,#49732,.T.);
#69545=ORIENTED_EDGE('',*,*,#49738,.T.);
#69546=ORIENTED_EDGE('',*,*,#49735,.T.);
#69547=ORIENTED_EDGE('',*,*,#49739,.T.);
#69548=ORIENTED_EDGE('',*,*,#49740,.F.);
#69549=ORIENTED_EDGE('',*,*,#49741,.T.);
#69550=ORIENTED_EDGE('',*,*,#49742,.F.);
#69551=ORIENTED_EDGE('',*,*,#49743,.T.);
#69552=ORIENTED_EDGE('',*,*,#49744,.F.);
#69553=ORIENTED_EDGE('',*,*,#49745,.T.);
#69554=ORIENTED_EDGE('',*,*,#49742,.T.);
#69555=ORIENTED_EDGE('',*,*,#49746,.T.);
#69556=ORIENTED_EDGE('',*,*,#49747,.F.);
#69557=ORIENTED_EDGE('',*,*,#49748,.T.);
#69558=ORIENTED_EDGE('',*,*,#49740,.T.);
#69559=ORIENTED_EDGE('',*,*,#49749,.T.);
#69560=ORIENTED_EDGE('',*,*,#49750,.F.);
#69561=ORIENTED_EDGE('',*,*,#49751,.T.);
#69562=ORIENTED_EDGE('',*,*,#49744,.T.);
#69563=ORIENTED_EDGE('',*,*,#49752,.T.);
#69564=ORIENTED_EDGE('',*,*,#49753,.F.);
#69565=ORIENTED_EDGE('',*,*,#49754,.T.);
#69566=ORIENTED_EDGE('',*,*,#49747,.T.);
#69567=ORIENTED_EDGE('',*,*,#49755,.T.);
#69568=ORIENTED_EDGE('',*,*,#49756,.F.);
#69569=ORIENTED_EDGE('',*,*,#49757,.T.);
#69570=ORIENTED_EDGE('',*,*,#49750,.T.);
#69571=ORIENTED_EDGE('',*,*,#49758,.T.);
#69572=ORIENTED_EDGE('',*,*,#49759,.F.);
#69573=ORIENTED_EDGE('',*,*,#49760,.T.);
#69574=ORIENTED_EDGE('',*,*,#49753,.T.);
#69575=ORIENTED_EDGE('',*,*,#49761,.T.);
#69576=ORIENTED_EDGE('',*,*,#49762,.F.);
#69577=ORIENTED_EDGE('',*,*,#49763,.T.);
#69578=ORIENTED_EDGE('',*,*,#49756,.T.);
#69579=ORIENTED_EDGE('',*,*,#49764,.T.);
#69580=ORIENTED_EDGE('',*,*,#49765,.F.);
#69581=ORIENTED_EDGE('',*,*,#49766,.T.);
#69582=ORIENTED_EDGE('',*,*,#49759,.T.);
#69583=ORIENTED_EDGE('',*,*,#49767,.T.);
#69584=ORIENTED_EDGE('',*,*,#49762,.T.);
#69585=ORIENTED_EDGE('',*,*,#49768,.T.);
#69586=ORIENTED_EDGE('',*,*,#49765,.T.);
#69587=ORIENTED_EDGE('',*,*,#49769,.T.);
#69588=ORIENTED_EDGE('',*,*,#49770,.F.);
#69589=ORIENTED_EDGE('',*,*,#49771,.T.);
#69590=ORIENTED_EDGE('',*,*,#49772,.F.);
#69591=ORIENTED_EDGE('',*,*,#49773,.T.);
#69592=ORIENTED_EDGE('',*,*,#49774,.F.);
#69593=ORIENTED_EDGE('',*,*,#49775,.T.);
#69594=ORIENTED_EDGE('',*,*,#49772,.T.);
#69595=ORIENTED_EDGE('',*,*,#49776,.T.);
#69596=ORIENTED_EDGE('',*,*,#49777,.F.);
#69597=ORIENTED_EDGE('',*,*,#49778,.T.);
#69598=ORIENTED_EDGE('',*,*,#49770,.T.);
#69599=ORIENTED_EDGE('',*,*,#49779,.T.);
#69600=ORIENTED_EDGE('',*,*,#49780,.F.);
#69601=ORIENTED_EDGE('',*,*,#49781,.T.);
#69602=ORIENTED_EDGE('',*,*,#49774,.T.);
#69603=ORIENTED_EDGE('',*,*,#49782,.T.);
#69604=ORIENTED_EDGE('',*,*,#49783,.F.);
#69605=ORIENTED_EDGE('',*,*,#49784,.T.);
#69606=ORIENTED_EDGE('',*,*,#49777,.T.);
#69607=ORIENTED_EDGE('',*,*,#49785,.T.);
#69608=ORIENTED_EDGE('',*,*,#49786,.F.);
#69609=ORIENTED_EDGE('',*,*,#49787,.T.);
#69610=ORIENTED_EDGE('',*,*,#49780,.T.);
#69611=ORIENTED_EDGE('',*,*,#49788,.T.);
#69612=ORIENTED_EDGE('',*,*,#49789,.F.);
#69613=ORIENTED_EDGE('',*,*,#49790,.T.);
#69614=ORIENTED_EDGE('',*,*,#49783,.T.);
#69615=ORIENTED_EDGE('',*,*,#49791,.T.);
#69616=ORIENTED_EDGE('',*,*,#49786,.T.);
#69617=ORIENTED_EDGE('',*,*,#49792,.T.);
#69618=ORIENTED_EDGE('',*,*,#49789,.T.);
#69619=ORIENTED_EDGE('',*,*,#49793,.T.);
#69620=ORIENTED_EDGE('',*,*,#49794,.F.);
#69621=ORIENTED_EDGE('',*,*,#49795,.T.);
#69622=ORIENTED_EDGE('',*,*,#49796,.F.);
#69623=ORIENTED_EDGE('',*,*,#49797,.T.);
#69624=ORIENTED_EDGE('',*,*,#49798,.F.);
#69625=ORIENTED_EDGE('',*,*,#49799,.T.);
#69626=ORIENTED_EDGE('',*,*,#49796,.T.);
#69627=ORIENTED_EDGE('',*,*,#49800,.T.);
#69628=ORIENTED_EDGE('',*,*,#49801,.F.);
#69629=ORIENTED_EDGE('',*,*,#49802,.T.);
#69630=ORIENTED_EDGE('',*,*,#49794,.T.);
#69631=ORIENTED_EDGE('',*,*,#49803,.T.);
#69632=ORIENTED_EDGE('',*,*,#49804,.F.);
#69633=ORIENTED_EDGE('',*,*,#49805,.T.);
#69634=ORIENTED_EDGE('',*,*,#49798,.T.);
#69635=ORIENTED_EDGE('',*,*,#49806,.T.);
#69636=ORIENTED_EDGE('',*,*,#49807,.F.);
#69637=ORIENTED_EDGE('',*,*,#49808,.T.);
#69638=ORIENTED_EDGE('',*,*,#49801,.T.);
#69639=ORIENTED_EDGE('',*,*,#49809,.T.);
#69640=ORIENTED_EDGE('',*,*,#49810,.F.);
#69641=ORIENTED_EDGE('',*,*,#49811,.T.);
#69642=ORIENTED_EDGE('',*,*,#49804,.T.);
#69643=ORIENTED_EDGE('',*,*,#49812,.T.);
#69644=ORIENTED_EDGE('',*,*,#49813,.F.);
#69645=ORIENTED_EDGE('',*,*,#49814,.T.);
#69646=ORIENTED_EDGE('',*,*,#49807,.T.);
#69647=ORIENTED_EDGE('',*,*,#49815,.T.);
#69648=ORIENTED_EDGE('',*,*,#49810,.T.);
#69649=ORIENTED_EDGE('',*,*,#49816,.T.);
#69650=ORIENTED_EDGE('',*,*,#49813,.T.);
#69651=ORIENTED_EDGE('',*,*,#49817,.T.);
#69652=ORIENTED_EDGE('',*,*,#49818,.F.);
#69653=ORIENTED_EDGE('',*,*,#49819,.T.);
#69654=ORIENTED_EDGE('',*,*,#49820,.F.);
#69655=ORIENTED_EDGE('',*,*,#49821,.T.);
#69656=ORIENTED_EDGE('',*,*,#49822,.F.);
#69657=ORIENTED_EDGE('',*,*,#49823,.T.);
#69658=ORIENTED_EDGE('',*,*,#49820,.T.);
#69659=ORIENTED_EDGE('',*,*,#49824,.T.);
#69660=ORIENTED_EDGE('',*,*,#49825,.F.);
#69661=ORIENTED_EDGE('',*,*,#49826,.T.);
#69662=ORIENTED_EDGE('',*,*,#49818,.T.);
#69663=ORIENTED_EDGE('',*,*,#49827,.T.);
#69664=ORIENTED_EDGE('',*,*,#49828,.F.);
#69665=ORIENTED_EDGE('',*,*,#49829,.T.);
#69666=ORIENTED_EDGE('',*,*,#49822,.T.);
#69667=ORIENTED_EDGE('',*,*,#49830,.T.);
#69668=ORIENTED_EDGE('',*,*,#49831,.F.);
#69669=ORIENTED_EDGE('',*,*,#49832,.T.);
#69670=ORIENTED_EDGE('',*,*,#49825,.T.);
#69671=ORIENTED_EDGE('',*,*,#49833,.T.);
#69672=ORIENTED_EDGE('',*,*,#49834,.F.);
#69673=ORIENTED_EDGE('',*,*,#49835,.T.);
#69674=ORIENTED_EDGE('',*,*,#49828,.T.);
#69675=ORIENTED_EDGE('',*,*,#49836,.T.);
#69676=ORIENTED_EDGE('',*,*,#49837,.F.);
#69677=ORIENTED_EDGE('',*,*,#49838,.T.);
#69678=ORIENTED_EDGE('',*,*,#49831,.T.);
#69679=ORIENTED_EDGE('',*,*,#49839,.T.);
#69680=ORIENTED_EDGE('',*,*,#49834,.T.);
#69681=ORIENTED_EDGE('',*,*,#49840,.T.);
#69682=ORIENTED_EDGE('',*,*,#49837,.T.);
#69683=ORIENTED_EDGE('',*,*,#49841,.T.);
#69684=ORIENTED_EDGE('',*,*,#49842,.F.);
#69685=ORIENTED_EDGE('',*,*,#49843,.T.);
#69686=ORIENTED_EDGE('',*,*,#49844,.F.);
#69687=ORIENTED_EDGE('',*,*,#49845,.T.);
#69688=ORIENTED_EDGE('',*,*,#49846,.F.);
#69689=ORIENTED_EDGE('',*,*,#49847,.T.);
#69690=ORIENTED_EDGE('',*,*,#49844,.T.);
#69691=ORIENTED_EDGE('',*,*,#49848,.T.);
#69692=ORIENTED_EDGE('',*,*,#49849,.F.);
#69693=ORIENTED_EDGE('',*,*,#49850,.T.);
#69694=ORIENTED_EDGE('',*,*,#49842,.T.);
#69695=ORIENTED_EDGE('',*,*,#49851,.T.);
#69696=ORIENTED_EDGE('',*,*,#49852,.F.);
#69697=ORIENTED_EDGE('',*,*,#49853,.T.);
#69698=ORIENTED_EDGE('',*,*,#49846,.T.);
#69699=ORIENTED_EDGE('',*,*,#49854,.T.);
#69700=ORIENTED_EDGE('',*,*,#49855,.F.);
#69701=ORIENTED_EDGE('',*,*,#49856,.T.);
#69702=ORIENTED_EDGE('',*,*,#49849,.T.);
#69703=ORIENTED_EDGE('',*,*,#49857,.T.);
#69704=ORIENTED_EDGE('',*,*,#49858,.F.);
#69705=ORIENTED_EDGE('',*,*,#49859,.T.);
#69706=ORIENTED_EDGE('',*,*,#49852,.T.);
#69707=ORIENTED_EDGE('',*,*,#49860,.T.);
#69708=ORIENTED_EDGE('',*,*,#49861,.F.);
#69709=ORIENTED_EDGE('',*,*,#49862,.T.);
#69710=ORIENTED_EDGE('',*,*,#49855,.T.);
#69711=ORIENTED_EDGE('',*,*,#49863,.T.);
#69712=ORIENTED_EDGE('',*,*,#49858,.T.);
#69713=ORIENTED_EDGE('',*,*,#49864,.T.);
#69714=ORIENTED_EDGE('',*,*,#49861,.T.);
#69715=ORIENTED_EDGE('',*,*,#49865,.T.);
#69716=ORIENTED_EDGE('',*,*,#49866,.F.);
#69717=ORIENTED_EDGE('',*,*,#49867,.T.);
#69718=ORIENTED_EDGE('',*,*,#49868,.F.);
#69719=ORIENTED_EDGE('',*,*,#49869,.T.);
#69720=ORIENTED_EDGE('',*,*,#49870,.F.);
#69721=ORIENTED_EDGE('',*,*,#49871,.T.);
#69722=ORIENTED_EDGE('',*,*,#49868,.T.);
#69723=ORIENTED_EDGE('',*,*,#49872,.T.);
#69724=ORIENTED_EDGE('',*,*,#49873,.F.);
#69725=ORIENTED_EDGE('',*,*,#49874,.T.);
#69726=ORIENTED_EDGE('',*,*,#49866,.T.);
#69727=ORIENTED_EDGE('',*,*,#49875,.T.);
#69728=ORIENTED_EDGE('',*,*,#49876,.F.);
#69729=ORIENTED_EDGE('',*,*,#49877,.T.);
#69730=ORIENTED_EDGE('',*,*,#49870,.T.);
#69731=ORIENTED_EDGE('',*,*,#49878,.T.);
#69732=ORIENTED_EDGE('',*,*,#49879,.F.);
#69733=ORIENTED_EDGE('',*,*,#49880,.T.);
#69734=ORIENTED_EDGE('',*,*,#49873,.T.);
#69735=ORIENTED_EDGE('',*,*,#49881,.T.);
#69736=ORIENTED_EDGE('',*,*,#49882,.F.);
#69737=ORIENTED_EDGE('',*,*,#49883,.T.);
#69738=ORIENTED_EDGE('',*,*,#49876,.T.);
#69739=ORIENTED_EDGE('',*,*,#49884,.T.);
#69740=ORIENTED_EDGE('',*,*,#49885,.F.);
#69741=ORIENTED_EDGE('',*,*,#49886,.T.);
#69742=ORIENTED_EDGE('',*,*,#49879,.T.);
#69743=ORIENTED_EDGE('',*,*,#49887,.T.);
#69744=ORIENTED_EDGE('',*,*,#49888,.T.);
#69745=ORIENTED_EDGE('',*,*,#49889,.F.);
#69746=ORIENTED_EDGE('',*,*,#49890,.T.);
#69747=ORIENTED_EDGE('',*,*,#49882,.T.);
#69748=ORIENTED_EDGE('',*,*,#49885,.T.);
#69749=ORIENTED_EDGE('',*,*,#49891,.T.);
#69750=ORIENTED_EDGE('',*,*,#49889,.T.);
#69751=ORIENTED_EDGE('',*,*,#49892,.T.);
#69752=ORIENTED_EDGE('',*,*,#49893,.F.);
#69753=ORIENTED_EDGE('',*,*,#49894,.T.);
#69754=ORIENTED_EDGE('',*,*,#49895,.F.);
#69755=ORIENTED_EDGE('',*,*,#49896,.T.);
#69756=ORIENTED_EDGE('',*,*,#49897,.F.);
#69757=ORIENTED_EDGE('',*,*,#49898,.T.);
#69758=ORIENTED_EDGE('',*,*,#49895,.T.);
#69759=ORIENTED_EDGE('',*,*,#49899,.T.);
#69760=ORIENTED_EDGE('',*,*,#49900,.F.);
#69761=ORIENTED_EDGE('',*,*,#49901,.T.);
#69762=ORIENTED_EDGE('',*,*,#49893,.T.);
#69763=ORIENTED_EDGE('',*,*,#49902,.T.);
#69764=ORIENTED_EDGE('',*,*,#49903,.F.);
#69765=ORIENTED_EDGE('',*,*,#49904,.T.);
#69766=ORIENTED_EDGE('',*,*,#49897,.T.);
#69767=ORIENTED_EDGE('',*,*,#49905,.T.);
#69768=ORIENTED_EDGE('',*,*,#49906,.F.);
#69769=ORIENTED_EDGE('',*,*,#49907,.T.);
#69770=ORIENTED_EDGE('',*,*,#49900,.T.);
#69771=ORIENTED_EDGE('',*,*,#49908,.T.);
#69772=ORIENTED_EDGE('',*,*,#49909,.F.);
#69773=ORIENTED_EDGE('',*,*,#49910,.T.);
#69774=ORIENTED_EDGE('',*,*,#49903,.T.);
#69775=ORIENTED_EDGE('',*,*,#49911,.T.);
#69776=ORIENTED_EDGE('',*,*,#49912,.F.);
#69777=ORIENTED_EDGE('',*,*,#49913,.T.);
#69778=ORIENTED_EDGE('',*,*,#49906,.T.);
#69779=ORIENTED_EDGE('',*,*,#49914,.T.);
#69780=ORIENTED_EDGE('',*,*,#49909,.T.);
#69781=ORIENTED_EDGE('',*,*,#49915,.T.);
#69782=ORIENTED_EDGE('',*,*,#49912,.T.);
#69783=ORIENTED_EDGE('',*,*,#49916,.T.);
#69784=ORIENTED_EDGE('',*,*,#49917,.F.);
#69785=ORIENTED_EDGE('',*,*,#49918,.T.);
#69786=ORIENTED_EDGE('',*,*,#49919,.F.);
#69787=ORIENTED_EDGE('',*,*,#49920,.T.);
#69788=ORIENTED_EDGE('',*,*,#49921,.F.);
#69789=ORIENTED_EDGE('',*,*,#49922,.T.);
#69790=ORIENTED_EDGE('',*,*,#49919,.T.);
#69791=ORIENTED_EDGE('',*,*,#49923,.T.);
#69792=ORIENTED_EDGE('',*,*,#49924,.F.);
#69793=ORIENTED_EDGE('',*,*,#49925,.T.);
#69794=ORIENTED_EDGE('',*,*,#49917,.T.);
#69795=ORIENTED_EDGE('',*,*,#49926,.T.);
#69796=ORIENTED_EDGE('',*,*,#49927,.F.);
#69797=ORIENTED_EDGE('',*,*,#49928,.T.);
#69798=ORIENTED_EDGE('',*,*,#49921,.T.);
#69799=ORIENTED_EDGE('',*,*,#49929,.T.);
#69800=ORIENTED_EDGE('',*,*,#49930,.F.);
#69801=ORIENTED_EDGE('',*,*,#49931,.T.);
#69802=ORIENTED_EDGE('',*,*,#49924,.T.);
#69803=ORIENTED_EDGE('',*,*,#49932,.T.);
#69804=ORIENTED_EDGE('',*,*,#49933,.F.);
#69805=ORIENTED_EDGE('',*,*,#49934,.T.);
#69806=ORIENTED_EDGE('',*,*,#49927,.T.);
#69807=ORIENTED_EDGE('',*,*,#49935,.T.);
#69808=ORIENTED_EDGE('',*,*,#49936,.F.);
#69809=ORIENTED_EDGE('',*,*,#49937,.T.);
#69810=ORIENTED_EDGE('',*,*,#49930,.T.);
#69811=ORIENTED_EDGE('',*,*,#49938,.T.);
#69812=ORIENTED_EDGE('',*,*,#49939,.F.);
#69813=ORIENTED_EDGE('',*,*,#49940,.T.);
#69814=ORIENTED_EDGE('',*,*,#49933,.T.);
#69815=ORIENTED_EDGE('',*,*,#49941,.T.);
#69816=ORIENTED_EDGE('',*,*,#49942,.F.);
#69817=ORIENTED_EDGE('',*,*,#49943,.T.);
#69818=ORIENTED_EDGE('',*,*,#49936,.T.);
#69819=ORIENTED_EDGE('',*,*,#49944,.T.);
#69820=ORIENTED_EDGE('',*,*,#49939,.T.);
#69821=ORIENTED_EDGE('',*,*,#49945,.T.);
#69822=ORIENTED_EDGE('',*,*,#49942,.T.);
#69823=ORIENTED_EDGE('',*,*,#49946,.T.);
#69824=ORIENTED_EDGE('',*,*,#49947,.F.);
#69825=ORIENTED_EDGE('',*,*,#49948,.T.);
#69826=ORIENTED_EDGE('',*,*,#49949,.F.);
#69827=ORIENTED_EDGE('',*,*,#49950,.T.);
#69828=ORIENTED_EDGE('',*,*,#49951,.F.);
#69829=ORIENTED_EDGE('',*,*,#49952,.T.);
#69830=ORIENTED_EDGE('',*,*,#49949,.T.);
#69831=ORIENTED_EDGE('',*,*,#49953,.T.);
#69832=ORIENTED_EDGE('',*,*,#49954,.F.);
#69833=ORIENTED_EDGE('',*,*,#49955,.T.);
#69834=ORIENTED_EDGE('',*,*,#49947,.T.);
#69835=ORIENTED_EDGE('',*,*,#49956,.T.);
#69836=ORIENTED_EDGE('',*,*,#49957,.F.);
#69837=ORIENTED_EDGE('',*,*,#49958,.T.);
#69838=ORIENTED_EDGE('',*,*,#49951,.T.);
#69839=ORIENTED_EDGE('',*,*,#49959,.T.);
#69840=ORIENTED_EDGE('',*,*,#49960,.F.);
#69841=ORIENTED_EDGE('',*,*,#49961,.T.);
#69842=ORIENTED_EDGE('',*,*,#49954,.T.);
#69843=ORIENTED_EDGE('',*,*,#49962,.T.);
#69844=ORIENTED_EDGE('',*,*,#49963,.F.);
#69845=ORIENTED_EDGE('',*,*,#49964,.T.);
#69846=ORIENTED_EDGE('',*,*,#49957,.T.);
#69847=ORIENTED_EDGE('',*,*,#49965,.T.);
#69848=ORIENTED_EDGE('',*,*,#49966,.F.);
#69849=ORIENTED_EDGE('',*,*,#49967,.T.);
#69850=ORIENTED_EDGE('',*,*,#49960,.T.);
#69851=ORIENTED_EDGE('',*,*,#49968,.T.);
#69852=ORIENTED_EDGE('',*,*,#49963,.T.);
#69853=ORIENTED_EDGE('',*,*,#49969,.T.);
#69854=ORIENTED_EDGE('',*,*,#49966,.T.);
#69855=ORIENTED_EDGE('',*,*,#49970,.T.);
#69856=ORIENTED_EDGE('',*,*,#49971,.F.);
#69857=ORIENTED_EDGE('',*,*,#49972,.T.);
#69858=ORIENTED_EDGE('',*,*,#49973,.F.);
#69859=ORIENTED_EDGE('',*,*,#49974,.T.);
#69860=ORIENTED_EDGE('',*,*,#49975,.F.);
#69861=ORIENTED_EDGE('',*,*,#49976,.T.);
#69862=ORIENTED_EDGE('',*,*,#49973,.T.);
#69863=ORIENTED_EDGE('',*,*,#49977,.T.);
#69864=ORIENTED_EDGE('',*,*,#49978,.F.);
#69865=ORIENTED_EDGE('',*,*,#49979,.T.);
#69866=ORIENTED_EDGE('',*,*,#49971,.T.);
#69867=ORIENTED_EDGE('',*,*,#49980,.T.);
#69868=ORIENTED_EDGE('',*,*,#49981,.F.);
#69869=ORIENTED_EDGE('',*,*,#49982,.T.);
#69870=ORIENTED_EDGE('',*,*,#49975,.T.);
#69871=ORIENTED_EDGE('',*,*,#49983,.T.);
#69872=ORIENTED_EDGE('',*,*,#49984,.F.);
#69873=ORIENTED_EDGE('',*,*,#49985,.T.);
#69874=ORIENTED_EDGE('',*,*,#49978,.T.);
#69875=ORIENTED_EDGE('',*,*,#49986,.T.);
#69876=ORIENTED_EDGE('',*,*,#49987,.F.);
#69877=ORIENTED_EDGE('',*,*,#49988,.T.);
#69878=ORIENTED_EDGE('',*,*,#49981,.T.);
#69879=ORIENTED_EDGE('',*,*,#49989,.T.);
#69880=ORIENTED_EDGE('',*,*,#49990,.F.);
#69881=ORIENTED_EDGE('',*,*,#49991,.T.);
#69882=ORIENTED_EDGE('',*,*,#49984,.T.);
#69883=ORIENTED_EDGE('',*,*,#49992,.T.);
#69884=ORIENTED_EDGE('',*,*,#49993,.F.);
#69885=ORIENTED_EDGE('',*,*,#49994,.T.);
#69886=ORIENTED_EDGE('',*,*,#49987,.T.);
#69887=ORIENTED_EDGE('',*,*,#49995,.T.);
#69888=ORIENTED_EDGE('',*,*,#49996,.F.);
#69889=ORIENTED_EDGE('',*,*,#49997,.T.);
#69890=ORIENTED_EDGE('',*,*,#49990,.T.);
#69891=ORIENTED_EDGE('',*,*,#49998,.T.);
#69892=ORIENTED_EDGE('',*,*,#49993,.T.);
#69893=ORIENTED_EDGE('',*,*,#49999,.T.);
#69894=ORIENTED_EDGE('',*,*,#49996,.T.);
#69895=ORIENTED_EDGE('',*,*,#50000,.T.);
#69896=ORIENTED_EDGE('',*,*,#50001,.F.);
#69897=ORIENTED_EDGE('',*,*,#50002,.T.);
#69898=ORIENTED_EDGE('',*,*,#50003,.F.);
#69899=ORIENTED_EDGE('',*,*,#50004,.T.);
#69900=ORIENTED_EDGE('',*,*,#50005,.F.);
#69901=ORIENTED_EDGE('',*,*,#50006,.T.);
#69902=ORIENTED_EDGE('',*,*,#50003,.T.);
#69903=ORIENTED_EDGE('',*,*,#50007,.T.);
#69904=ORIENTED_EDGE('',*,*,#50008,.F.);
#69905=ORIENTED_EDGE('',*,*,#50009,.T.);
#69906=ORIENTED_EDGE('',*,*,#50001,.T.);
#69907=ORIENTED_EDGE('',*,*,#50010,.T.);
#69908=ORIENTED_EDGE('',*,*,#50011,.F.);
#69909=ORIENTED_EDGE('',*,*,#50012,.T.);
#69910=ORIENTED_EDGE('',*,*,#50005,.T.);
#69911=ORIENTED_EDGE('',*,*,#50013,.T.);
#69912=ORIENTED_EDGE('',*,*,#50014,.F.);
#69913=ORIENTED_EDGE('',*,*,#50015,.T.);
#69914=ORIENTED_EDGE('',*,*,#50008,.T.);
#69915=ORIENTED_EDGE('',*,*,#50016,.T.);
#69916=ORIENTED_EDGE('',*,*,#50017,.F.);
#69917=ORIENTED_EDGE('',*,*,#50018,.T.);
#69918=ORIENTED_EDGE('',*,*,#50011,.T.);
#69919=ORIENTED_EDGE('',*,*,#50019,.T.);
#69920=ORIENTED_EDGE('',*,*,#50020,.F.);
#69921=ORIENTED_EDGE('',*,*,#50021,.T.);
#69922=ORIENTED_EDGE('',*,*,#50014,.T.);
#69923=ORIENTED_EDGE('',*,*,#50022,.T.);
#69924=ORIENTED_EDGE('',*,*,#50017,.T.);
#69925=ORIENTED_EDGE('',*,*,#50023,.T.);
#69926=ORIENTED_EDGE('',*,*,#50020,.T.);
#69927=ORIENTED_EDGE('',*,*,#50024,.T.);
#69928=ORIENTED_EDGE('',*,*,#50025,.F.);
#69929=ORIENTED_EDGE('',*,*,#50026,.T.);
#69930=ORIENTED_EDGE('',*,*,#50027,.F.);
#69931=ORIENTED_EDGE('',*,*,#50028,.T.);
#69932=ORIENTED_EDGE('',*,*,#50029,.F.);
#69933=ORIENTED_EDGE('',*,*,#50030,.T.);
#69934=ORIENTED_EDGE('',*,*,#50027,.T.);
#69935=ORIENTED_EDGE('',*,*,#50031,.T.);
#69936=ORIENTED_EDGE('',*,*,#50032,.F.);
#69937=ORIENTED_EDGE('',*,*,#50033,.T.);
#69938=ORIENTED_EDGE('',*,*,#50025,.T.);
#69939=ORIENTED_EDGE('',*,*,#50034,.T.);
#69940=ORIENTED_EDGE('',*,*,#50035,.F.);
#69941=ORIENTED_EDGE('',*,*,#50036,.T.);
#69942=ORIENTED_EDGE('',*,*,#50029,.T.);
#69943=ORIENTED_EDGE('',*,*,#50037,.T.);
#69944=ORIENTED_EDGE('',*,*,#50038,.F.);
#69945=ORIENTED_EDGE('',*,*,#50039,.T.);
#69946=ORIENTED_EDGE('',*,*,#50032,.T.);
#69947=ORIENTED_EDGE('',*,*,#50040,.T.);
#69948=ORIENTED_EDGE('',*,*,#50041,.F.);
#69949=ORIENTED_EDGE('',*,*,#50042,.T.);
#69950=ORIENTED_EDGE('',*,*,#50035,.T.);
#69951=ORIENTED_EDGE('',*,*,#50043,.T.);
#69952=ORIENTED_EDGE('',*,*,#50044,.F.);
#69953=ORIENTED_EDGE('',*,*,#50045,.T.);
#69954=ORIENTED_EDGE('',*,*,#50038,.T.);
#69955=ORIENTED_EDGE('',*,*,#50046,.T.);
#69956=ORIENTED_EDGE('',*,*,#50041,.T.);
#69957=ORIENTED_EDGE('',*,*,#50047,.T.);
#69958=ORIENTED_EDGE('',*,*,#50044,.T.);
#69959=ORIENTED_EDGE('',*,*,#50048,.T.);
#69960=ORIENTED_EDGE('',*,*,#50049,.F.);
#69961=ORIENTED_EDGE('',*,*,#50050,.T.);
#69962=ORIENTED_EDGE('',*,*,#50051,.F.);
#69963=ORIENTED_EDGE('',*,*,#50052,.T.);
#69964=ORIENTED_EDGE('',*,*,#50053,.F.);
#69965=ORIENTED_EDGE('',*,*,#50054,.T.);
#69966=ORIENTED_EDGE('',*,*,#50051,.T.);
#69967=ORIENTED_EDGE('',*,*,#50055,.T.);
#69968=ORIENTED_EDGE('',*,*,#50056,.F.);
#69969=ORIENTED_EDGE('',*,*,#50057,.T.);
#69970=ORIENTED_EDGE('',*,*,#50049,.T.);
#69971=ORIENTED_EDGE('',*,*,#50058,.T.);
#69972=ORIENTED_EDGE('',*,*,#50059,.F.);
#69973=ORIENTED_EDGE('',*,*,#50060,.T.);
#69974=ORIENTED_EDGE('',*,*,#50053,.T.);
#69975=ORIENTED_EDGE('',*,*,#50061,.T.);
#69976=ORIENTED_EDGE('',*,*,#50062,.F.);
#69977=ORIENTED_EDGE('',*,*,#50063,.T.);
#69978=ORIENTED_EDGE('',*,*,#50056,.T.);
#69979=ORIENTED_EDGE('',*,*,#50064,.T.);
#69980=ORIENTED_EDGE('',*,*,#50065,.F.);
#69981=ORIENTED_EDGE('',*,*,#50066,.T.);
#69982=ORIENTED_EDGE('',*,*,#50059,.T.);
#69983=ORIENTED_EDGE('',*,*,#50067,.T.);
#69984=ORIENTED_EDGE('',*,*,#50068,.F.);
#69985=ORIENTED_EDGE('',*,*,#50069,.T.);
#69986=ORIENTED_EDGE('',*,*,#50062,.T.);
#69987=ORIENTED_EDGE('',*,*,#50070,.T.);
#69988=ORIENTED_EDGE('',*,*,#50065,.T.);
#69989=ORIENTED_EDGE('',*,*,#50071,.T.);
#69990=ORIENTED_EDGE('',*,*,#50068,.T.);
#69991=ORIENTED_EDGE('',*,*,#50072,.T.);
#69992=ORIENTED_EDGE('',*,*,#50073,.F.);
#69993=ORIENTED_EDGE('',*,*,#50074,.T.);
#69994=ORIENTED_EDGE('',*,*,#50075,.F.);
#69995=ORIENTED_EDGE('',*,*,#50076,.T.);
#69996=ORIENTED_EDGE('',*,*,#50077,.F.);
#69997=ORIENTED_EDGE('',*,*,#50078,.T.);
#69998=ORIENTED_EDGE('',*,*,#50075,.T.);
#69999=ORIENTED_EDGE('',*,*,#50079,.T.);
#70000=ORIENTED_EDGE('',*,*,#50080,.F.);
#70001=ORIENTED_EDGE('',*,*,#50081,.T.);
#70002=ORIENTED_EDGE('',*,*,#50073,.T.);
#70003=ORIENTED_EDGE('',*,*,#50082,.T.);
#70004=ORIENTED_EDGE('',*,*,#50083,.F.);
#70005=ORIENTED_EDGE('',*,*,#50084,.T.);
#70006=ORIENTED_EDGE('',*,*,#50077,.T.);
#70007=ORIENTED_EDGE('',*,*,#50085,.T.);
#70008=ORIENTED_EDGE('',*,*,#50086,.F.);
#70009=ORIENTED_EDGE('',*,*,#50087,.T.);
#70010=ORIENTED_EDGE('',*,*,#50080,.T.);
#70011=ORIENTED_EDGE('',*,*,#50088,.T.);
#70012=ORIENTED_EDGE('',*,*,#50089,.F.);
#70013=ORIENTED_EDGE('',*,*,#50090,.T.);
#70014=ORIENTED_EDGE('',*,*,#50083,.T.);
#70015=ORIENTED_EDGE('',*,*,#50091,.T.);
#70016=ORIENTED_EDGE('',*,*,#50092,.F.);
#70017=ORIENTED_EDGE('',*,*,#50093,.T.);
#70018=ORIENTED_EDGE('',*,*,#50086,.T.);
#70019=ORIENTED_EDGE('',*,*,#50094,.T.);
#70020=ORIENTED_EDGE('',*,*,#50089,.T.);
#70021=ORIENTED_EDGE('',*,*,#50095,.T.);
#70022=ORIENTED_EDGE('',*,*,#50092,.T.);
#70023=ORIENTED_EDGE('',*,*,#50096,.T.);
#70024=ORIENTED_EDGE('',*,*,#50097,.F.);
#70025=ORIENTED_EDGE('',*,*,#50098,.T.);
#70026=ORIENTED_EDGE('',*,*,#50099,.F.);
#70027=ORIENTED_EDGE('',*,*,#50100,.T.);
#70028=ORIENTED_EDGE('',*,*,#50101,.F.);
#70029=ORIENTED_EDGE('',*,*,#50102,.T.);
#70030=ORIENTED_EDGE('',*,*,#50099,.T.);
#70031=ORIENTED_EDGE('',*,*,#50103,.T.);
#70032=ORIENTED_EDGE('',*,*,#50104,.F.);
#70033=ORIENTED_EDGE('',*,*,#50105,.T.);
#70034=ORIENTED_EDGE('',*,*,#50097,.T.);
#70035=ORIENTED_EDGE('',*,*,#50106,.T.);
#70036=ORIENTED_EDGE('',*,*,#50107,.F.);
#70037=ORIENTED_EDGE('',*,*,#50108,.T.);
#70038=ORIENTED_EDGE('',*,*,#50101,.T.);
#70039=ORIENTED_EDGE('',*,*,#50109,.T.);
#70040=ORIENTED_EDGE('',*,*,#50110,.F.);
#70041=ORIENTED_EDGE('',*,*,#50111,.T.);
#70042=ORIENTED_EDGE('',*,*,#50104,.T.);
#70043=ORIENTED_EDGE('',*,*,#50112,.T.);
#70044=ORIENTED_EDGE('',*,*,#50107,.T.);
#70045=ORIENTED_EDGE('',*,*,#50113,.T.);
#70046=ORIENTED_EDGE('',*,*,#50110,.T.);
#70047=ORIENTED_EDGE('',*,*,#50114,.T.);
#70048=ORIENTED_EDGE('',*,*,#50115,.T.);
#70049=ORIENTED_EDGE('',*,*,#50116,.F.);
#70050=ORIENTED_EDGE('',*,*,#50117,.T.);
#70051=ORIENTED_EDGE('',*,*,#50118,.F.);
#70052=ORIENTED_EDGE('',*,*,#50119,.F.);
#70053=ORIENTED_EDGE('',*,*,#50120,.T.);
#70054=ORIENTED_EDGE('',*,*,#50116,.T.);
#70055=ORIENTED_EDGE('',*,*,#50121,.T.);
#70056=ORIENTED_EDGE('',*,*,#50122,.F.);
#70057=ORIENTED_EDGE('',*,*,#50123,.T.);
#70058=ORIENTED_EDGE('',*,*,#50118,.T.);
#70059=ORIENTED_EDGE('',*,*,#50124,.T.);
#70060=ORIENTED_EDGE('',*,*,#50125,.F.);
#70061=ORIENTED_EDGE('',*,*,#50126,.T.);
#70062=ORIENTED_EDGE('',*,*,#50119,.T.);
#70063=ORIENTED_EDGE('',*,*,#50127,.T.);
#70064=ORIENTED_EDGE('',*,*,#50128,.F.);
#70065=ORIENTED_EDGE('',*,*,#50129,.T.);
#70066=ORIENTED_EDGE('',*,*,#50122,.T.);
#70067=ORIENTED_EDGE('',*,*,#50130,.T.);
#70068=ORIENTED_EDGE('',*,*,#50125,.T.);
#70069=ORIENTED_EDGE('',*,*,#50131,.T.);
#70070=ORIENTED_EDGE('',*,*,#50128,.T.);
#70071=ORIENTED_EDGE('',*,*,#50132,.T.);
#70072=ORIENTED_EDGE('',*,*,#50133,.F.);
#70073=ORIENTED_EDGE('',*,*,#50134,.T.);
#70074=ORIENTED_EDGE('',*,*,#50135,.T.);
#70075=ORIENTED_EDGE('',*,*,#50136,.T.);
#70076=ORIENTED_EDGE('',*,*,#50137,.F.);
#70077=ORIENTED_EDGE('',*,*,#50138,.T.);
#70078=ORIENTED_EDGE('',*,*,#50133,.T.);
#70079=ORIENTED_EDGE('',*,*,#50139,.T.);
#70080=ORIENTED_EDGE('',*,*,#50140,.F.);
#70081=ORIENTED_EDGE('',*,*,#50141,.T.);
#70082=ORIENTED_EDGE('',*,*,#50137,.T.);
#70083=ORIENTED_EDGE('',*,*,#50142,.T.);
#70084=ORIENTED_EDGE('',*,*,#50143,.F.);
#70085=ORIENTED_EDGE('',*,*,#50144,.T.);
#70086=ORIENTED_EDGE('',*,*,#50140,.T.);
#70087=ORIENTED_EDGE('',*,*,#50145,.T.);
#70088=ORIENTED_EDGE('',*,*,#50146,.F.);
#70089=ORIENTED_EDGE('',*,*,#50147,.T.);
#70090=ORIENTED_EDGE('',*,*,#50143,.T.);
#70091=ORIENTED_EDGE('',*,*,#50148,.T.);
#70092=ORIENTED_EDGE('',*,*,#50149,.F.);
#70093=ORIENTED_EDGE('',*,*,#50150,.T.);
#70094=ORIENTED_EDGE('',*,*,#50146,.T.);
#70095=ORIENTED_EDGE('',*,*,#50151,.T.);
#70096=ORIENTED_EDGE('',*,*,#50152,.F.);
#70097=ORIENTED_EDGE('',*,*,#50153,.T.);
#70098=ORIENTED_EDGE('',*,*,#50149,.T.);
#70099=ORIENTED_EDGE('',*,*,#50154,.T.);
#70100=ORIENTED_EDGE('',*,*,#50155,.F.);
#70101=ORIENTED_EDGE('',*,*,#50156,.T.);
#70102=ORIENTED_EDGE('',*,*,#50157,.T.);
#70103=ORIENTED_EDGE('',*,*,#50158,.T.);
#70104=ORIENTED_EDGE('',*,*,#50159,.F.);
#70105=ORIENTED_EDGE('',*,*,#50160,.T.);
#70106=ORIENTED_EDGE('',*,*,#50155,.T.);
#70107=ORIENTED_EDGE('',*,*,#50161,.T.);
#70108=ORIENTED_EDGE('',*,*,#50162,.F.);
#70109=ORIENTED_EDGE('',*,*,#50163,.T.);
#70110=ORIENTED_EDGE('',*,*,#50159,.T.);
#70111=ORIENTED_EDGE('',*,*,#50164,.T.);
#70112=ORIENTED_EDGE('',*,*,#50165,.F.);
#70113=ORIENTED_EDGE('',*,*,#50166,.T.);
#70114=ORIENTED_EDGE('',*,*,#50162,.T.);
#70115=ORIENTED_EDGE('',*,*,#50167,.T.);
#70116=ORIENTED_EDGE('',*,*,#50168,.F.);
#70117=ORIENTED_EDGE('',*,*,#50169,.T.);
#70118=ORIENTED_EDGE('',*,*,#50165,.T.);
#70119=ORIENTED_EDGE('',*,*,#50170,.T.);
#70120=ORIENTED_EDGE('',*,*,#50171,.F.);
#70121=ORIENTED_EDGE('',*,*,#50172,.T.);
#70122=ORIENTED_EDGE('',*,*,#50168,.T.);
#70123=ORIENTED_EDGE('',*,*,#50173,.T.);
#70124=ORIENTED_EDGE('',*,*,#50174,.F.);
#70125=ORIENTED_EDGE('',*,*,#50175,.T.);
#70126=ORIENTED_EDGE('',*,*,#50171,.T.);
#70127=ORIENTED_EDGE('',*,*,#50176,.T.);
#70128=ORIENTED_EDGE('',*,*,#50177,.F.);
#70129=ORIENTED_EDGE('',*,*,#50178,.T.);
#70130=ORIENTED_EDGE('',*,*,#50179,.T.);
#70131=ORIENTED_EDGE('',*,*,#50180,.T.);
#70132=ORIENTED_EDGE('',*,*,#50181,.F.);
#70133=ORIENTED_EDGE('',*,*,#50182,.T.);
#70134=ORIENTED_EDGE('',*,*,#50177,.T.);
#70135=ORIENTED_EDGE('',*,*,#50183,.T.);
#70136=ORIENTED_EDGE('',*,*,#50184,.T.);
#70137=ORIENTED_EDGE('',*,*,#50181,.T.);
#70138=ORIENTED_EDGE('',*,*,#50185,.T.);
#70139=ORIENTED_EDGE('',*,*,#50186,.F.);
#70140=ORIENTED_EDGE('',*,*,#50187,.F.);
#70141=ORIENTED_EDGE('',*,*,#50188,.T.);
#70142=ORIENTED_EDGE('',*,*,#50186,.T.);
#70143=ORIENTED_EDGE('',*,*,#50189,.T.);
#70144=ORIENTED_EDGE('',*,*,#50190,.F.);
#70145=ORIENTED_EDGE('',*,*,#50191,.T.);
#70146=ORIENTED_EDGE('',*,*,#50187,.T.);
#70147=ORIENTED_EDGE('',*,*,#50192,.T.);
#70148=ORIENTED_EDGE('',*,*,#50193,.F.);
#70149=ORIENTED_EDGE('',*,*,#50194,.T.);
#70150=ORIENTED_EDGE('',*,*,#50190,.T.);
#70151=ORIENTED_EDGE('',*,*,#50195,.T.);
#70152=ORIENTED_EDGE('',*,*,#50196,.T.);
#70153=ORIENTED_EDGE('',*,*,#50197,.T.);
#70154=ORIENTED_EDGE('',*,*,#50193,.T.);
#70155=ORIENTED_EDGE('',*,*,#50198,.T.);
#70156=ORIENTED_EDGE('',*,*,#50199,.F.);
#70157=ORIENTED_EDGE('',*,*,#50200,.T.);
#70158=ORIENTED_EDGE('',*,*,#50201,.T.);
#70159=ORIENTED_EDGE('',*,*,#50202,.T.);
#70160=ORIENTED_EDGE('',*,*,#50203,.F.);
#70161=ORIENTED_EDGE('',*,*,#50204,.T.);
#70162=ORIENTED_EDGE('',*,*,#50199,.T.);
#70163=ORIENTED_EDGE('',*,*,#50205,.T.);
#70164=ORIENTED_EDGE('',*,*,#50206,.F.);
#70165=ORIENTED_EDGE('',*,*,#50207,.T.);
#70166=ORIENTED_EDGE('',*,*,#50203,.T.);
#70167=ORIENTED_EDGE('',*,*,#50208,.T.);
#70168=ORIENTED_EDGE('',*,*,#50209,.F.);
#70169=ORIENTED_EDGE('',*,*,#50210,.T.);
#70170=ORIENTED_EDGE('',*,*,#50206,.T.);
#70171=ORIENTED_EDGE('',*,*,#50211,.T.);
#70172=ORIENTED_EDGE('',*,*,#50212,.F.);
#70173=ORIENTED_EDGE('',*,*,#50213,.T.);
#70174=ORIENTED_EDGE('',*,*,#50209,.T.);
#70175=ORIENTED_EDGE('',*,*,#50214,.T.);
#70176=ORIENTED_EDGE('',*,*,#50215,.F.);
#70177=ORIENTED_EDGE('',*,*,#50216,.T.);
#70178=ORIENTED_EDGE('',*,*,#50212,.T.);
#70179=ORIENTED_EDGE('',*,*,#50217,.T.);
#70180=ORIENTED_EDGE('',*,*,#50218,.T.);
#70181=ORIENTED_EDGE('',*,*,#50219,.T.);
#70182=ORIENTED_EDGE('',*,*,#50215,.T.);
#70183=ORIENTED_EDGE('',*,*,#50220,.T.);
#70184=ORIENTED_EDGE('',*,*,#50221,.F.);
#70185=ORIENTED_EDGE('',*,*,#50222,.T.);
#70186=ORIENTED_EDGE('',*,*,#50223,.T.);
#70187=ORIENTED_EDGE('',*,*,#50224,.T.);
#70188=ORIENTED_EDGE('',*,*,#50225,.F.);
#70189=ORIENTED_EDGE('',*,*,#50226,.T.);
#70190=ORIENTED_EDGE('',*,*,#50221,.T.);
#70191=ORIENTED_EDGE('',*,*,#50227,.T.);
#70192=ORIENTED_EDGE('',*,*,#50228,.T.);
#70193=ORIENTED_EDGE('',*,*,#50225,.T.);
#70194=ORIENTED_EDGE('',*,*,#50229,.T.);
#70195=ORIENTED_EDGE('',*,*,#50230,.F.);
#70196=ORIENTED_EDGE('',*,*,#50231,.F.);
#70197=ORIENTED_EDGE('',*,*,#50232,.T.);
#70198=ORIENTED_EDGE('',*,*,#50230,.T.);
#70199=ORIENTED_EDGE('',*,*,#50233,.T.);
#70200=ORIENTED_EDGE('',*,*,#50234,.F.);
#70201=ORIENTED_EDGE('',*,*,#50235,.T.);
#70202=ORIENTED_EDGE('',*,*,#50231,.T.);
#70203=ORIENTED_EDGE('',*,*,#50236,.T.);
#70204=ORIENTED_EDGE('',*,*,#50237,.F.);
#70205=ORIENTED_EDGE('',*,*,#50238,.T.);
#70206=ORIENTED_EDGE('',*,*,#50234,.T.);
#70207=ORIENTED_EDGE('',*,*,#50239,.T.);
#70208=ORIENTED_EDGE('',*,*,#50240,.T.);
#70209=ORIENTED_EDGE('',*,*,#50241,.T.);
#70210=ORIENTED_EDGE('',*,*,#50237,.T.);
#70211=ORIENTED_EDGE('',*,*,#50242,.T.);
#70212=ORIENTED_EDGE('',*,*,#50243,.T.);
#70213=ORIENTED_EDGE('',*,*,#50244,.T.);
#70214=ORIENTED_EDGE('',*,*,#50245,.F.);
#70215=ORIENTED_EDGE('',*,*,#50246,.T.);
#70216=ORIENTED_EDGE('',*,*,#50247,.F.);
#70217=ORIENTED_EDGE('',*,*,#50248,.T.);
#70218=ORIENTED_EDGE('',*,*,#50245,.T.);
#70219=ORIENTED_EDGE('',*,*,#50249,.T.);
#70220=ORIENTED_EDGE('',*,*,#50250,.F.);
#70221=ORIENTED_EDGE('',*,*,#50251,.T.);
#70222=ORIENTED_EDGE('',*,*,#50247,.T.);
#70223=ORIENTED_EDGE('',*,*,#50252,.T.);
#70224=ORIENTED_EDGE('',*,*,#50253,.F.);
#70225=ORIENTED_EDGE('',*,*,#50254,.T.);
#70226=ORIENTED_EDGE('',*,*,#50250,.T.);
#70227=ORIENTED_EDGE('',*,*,#50255,.T.);
#70228=ORIENTED_EDGE('',*,*,#50256,.F.);
#70229=ORIENTED_EDGE('',*,*,#50257,.T.);
#70230=ORIENTED_EDGE('',*,*,#50253,.T.);
#70231=ORIENTED_EDGE('',*,*,#50258,.T.);
#70232=ORIENTED_EDGE('',*,*,#50259,.F.);
#70233=ORIENTED_EDGE('',*,*,#50260,.T.);
#70234=ORIENTED_EDGE('',*,*,#50256,.T.);
#70235=ORIENTED_EDGE('',*,*,#50261,.T.);
#70236=ORIENTED_EDGE('',*,*,#50262,.T.);
#70237=ORIENTED_EDGE('',*,*,#50263,.T.);
#70238=ORIENTED_EDGE('',*,*,#50259,.T.);
#70239=ORIENTED_EDGE('',*,*,#50264,.T.);
#70240=ORIENTED_EDGE('',*,*,#50265,.F.);
#70241=ORIENTED_EDGE('',*,*,#50266,.T.);
#70242=ORIENTED_EDGE('',*,*,#50267,.T.);
#70243=ORIENTED_EDGE('',*,*,#50268,.T.);
#70244=ORIENTED_EDGE('',*,*,#50269,.F.);
#70245=ORIENTED_EDGE('',*,*,#50270,.T.);
#70246=ORIENTED_EDGE('',*,*,#50265,.T.);
#70247=ORIENTED_EDGE('',*,*,#50271,.T.);
#70248=ORIENTED_EDGE('',*,*,#50272,.F.);
#70249=ORIENTED_EDGE('',*,*,#50273,.T.);
#70250=ORIENTED_EDGE('',*,*,#50269,.T.);
#70251=ORIENTED_EDGE('',*,*,#50274,.T.);
#70252=ORIENTED_EDGE('',*,*,#50275,.F.);
#70253=ORIENTED_EDGE('',*,*,#50276,.T.);
#70254=ORIENTED_EDGE('',*,*,#50272,.T.);
#70255=ORIENTED_EDGE('',*,*,#50277,.T.);
#70256=ORIENTED_EDGE('',*,*,#50278,.F.);
#70257=ORIENTED_EDGE('',*,*,#50279,.T.);
#70258=ORIENTED_EDGE('',*,*,#50275,.T.);
#70259=ORIENTED_EDGE('',*,*,#50280,.T.);
#70260=ORIENTED_EDGE('',*,*,#50281,.F.);
#70261=ORIENTED_EDGE('',*,*,#50282,.T.);
#70262=ORIENTED_EDGE('',*,*,#50278,.T.);
#70263=ORIENTED_EDGE('',*,*,#50283,.T.);
#70264=ORIENTED_EDGE('',*,*,#50284,.F.);
#70265=ORIENTED_EDGE('',*,*,#50285,.T.);
#70266=ORIENTED_EDGE('',*,*,#50281,.T.);
#70267=ORIENTED_EDGE('',*,*,#50286,.T.);
#70268=ORIENTED_EDGE('',*,*,#50287,.T.);
#70269=ORIENTED_EDGE('',*,*,#50288,.T.);
#70270=ORIENTED_EDGE('',*,*,#50289,.T.);
#70271=ORIENTED_EDGE('',*,*,#50290,.T.);
#70272=ORIENTED_EDGE('',*,*,#50291,.F.);
#70273=ORIENTED_EDGE('',*,*,#50292,.T.);
#70274=ORIENTED_EDGE('',*,*,#50293,.F.);
#70275=ORIENTED_EDGE('',*,*,#50294,.T.);
#70276=ORIENTED_EDGE('',*,*,#50291,.T.);
#70277=ORIENTED_EDGE('',*,*,#50295,.T.);
#70278=ORIENTED_EDGE('',*,*,#50296,.F.);
#70279=ORIENTED_EDGE('',*,*,#50297,.T.);
#70280=ORIENTED_EDGE('',*,*,#50293,.T.);
#70281=ORIENTED_EDGE('',*,*,#50298,.T.);
#70282=ORIENTED_EDGE('',*,*,#50299,.F.);
#70283=ORIENTED_EDGE('',*,*,#50300,.T.);
#70284=ORIENTED_EDGE('',*,*,#50296,.T.);
#70285=ORIENTED_EDGE('',*,*,#50301,.T.);
#70286=ORIENTED_EDGE('',*,*,#50302,.F.);
#70287=ORIENTED_EDGE('',*,*,#50303,.T.);
#70288=ORIENTED_EDGE('',*,*,#50299,.T.);
#70289=ORIENTED_EDGE('',*,*,#50304,.T.);
#70290=ORIENTED_EDGE('',*,*,#50305,.F.);
#70291=ORIENTED_EDGE('',*,*,#50306,.T.);
#70292=ORIENTED_EDGE('',*,*,#50302,.T.);
#70293=ORIENTED_EDGE('',*,*,#50307,.T.);
#70294=ORIENTED_EDGE('',*,*,#50308,.F.);
#70295=ORIENTED_EDGE('',*,*,#50309,.T.);
#70296=ORIENTED_EDGE('',*,*,#50305,.T.);
#70297=ORIENTED_EDGE('',*,*,#50310,.T.);
#70298=ORIENTED_EDGE('',*,*,#50311,.F.);
#70299=ORIENTED_EDGE('',*,*,#50312,.T.);
#70300=ORIENTED_EDGE('',*,*,#50308,.T.);
#70301=ORIENTED_EDGE('',*,*,#50313,.T.);
#70302=ORIENTED_EDGE('',*,*,#50314,.F.);
#70303=ORIENTED_EDGE('',*,*,#50315,.T.);
#70304=ORIENTED_EDGE('',*,*,#50316,.T.);
#70305=ORIENTED_EDGE('',*,*,#50317,.T.);
#70306=ORIENTED_EDGE('',*,*,#50318,.T.);
#70307=ORIENTED_EDGE('',*,*,#50319,.T.);
#70308=ORIENTED_EDGE('',*,*,#50320,.T.);
#70309=ORIENTED_EDGE('',*,*,#50311,.T.);
#70310=ORIENTED_EDGE('',*,*,#50321,.T.);
#70311=ORIENTED_EDGE('',*,*,#50322,.F.);
#70312=ORIENTED_EDGE('',*,*,#50323,.T.);
#70313=ORIENTED_EDGE('',*,*,#50314,.T.);
#70314=ORIENTED_EDGE('',*,*,#50324,.T.);
#70315=ORIENTED_EDGE('',*,*,#50325,.F.);
#70316=ORIENTED_EDGE('',*,*,#50326,.T.);
#70317=ORIENTED_EDGE('',*,*,#50322,.T.);
#70318=ORIENTED_EDGE('',*,*,#50327,.T.);
#70319=ORIENTED_EDGE('',*,*,#50328,.F.);
#70320=ORIENTED_EDGE('',*,*,#50329,.T.);
#70321=ORIENTED_EDGE('',*,*,#50325,.T.);
#70322=ORIENTED_EDGE('',*,*,#50330,.T.);
#70323=ORIENTED_EDGE('',*,*,#50331,.F.);
#70324=ORIENTED_EDGE('',*,*,#50332,.T.);
#70325=ORIENTED_EDGE('',*,*,#50328,.T.);
#70326=ORIENTED_EDGE('',*,*,#50333,.T.);
#70327=ORIENTED_EDGE('',*,*,#50334,.F.);
#70328=ORIENTED_EDGE('',*,*,#50335,.T.);
#70329=ORIENTED_EDGE('',*,*,#50331,.T.);
#70330=ORIENTED_EDGE('',*,*,#50336,.T.);
#70331=ORIENTED_EDGE('',*,*,#50337,.F.);
#70332=ORIENTED_EDGE('',*,*,#50338,.T.);
#70333=ORIENTED_EDGE('',*,*,#50334,.T.);
#70334=ORIENTED_EDGE('',*,*,#50339,.T.);
#70335=ORIENTED_EDGE('',*,*,#50340,.F.);
#70336=ORIENTED_EDGE('',*,*,#50341,.T.);
#70337=ORIENTED_EDGE('',*,*,#50337,.T.);
#70338=ORIENTED_EDGE('',*,*,#50342,.T.);
#70339=ORIENTED_EDGE('',*,*,#50343,.T.);
#70340=ORIENTED_EDGE('',*,*,#50344,.F.);
#70341=ORIENTED_EDGE('',*,*,#50345,.T.);
#70342=ORIENTED_EDGE('',*,*,#49261,.F.);
#70343=ORIENTED_EDGE('',*,*,#49267,.F.);
#70344=ORIENTED_EDGE('',*,*,#50346,.F.);
#70345=ORIENTED_EDGE('',*,*,#50347,.T.);
#70346=ORIENTED_EDGE('',*,*,#50344,.T.);
#70347=ORIENTED_EDGE('',*,*,#50348,.T.);
#70348=ORIENTED_EDGE('',*,*,#50349,.F.);
#70349=ORIENTED_EDGE('',*,*,#50350,.T.);
#70350=ORIENTED_EDGE('',*,*,#50346,.T.);
#70351=ORIENTED_EDGE('',*,*,#50351,.T.);
#70352=ORIENTED_EDGE('',*,*,#50352,.F.);
#70353=ORIENTED_EDGE('',*,*,#50353,.T.);
#70354=ORIENTED_EDGE('',*,*,#50349,.T.);
#70355=ORIENTED_EDGE('',*,*,#50354,.T.);
#70356=ORIENTED_EDGE('',*,*,#50355,.F.);
#70357=ORIENTED_EDGE('',*,*,#50356,.F.);
#70358=ORIENTED_EDGE('',*,*,#50357,.T.);
#70359=ORIENTED_EDGE('',*,*,#50352,.T.);
#70360=ORIENTED_EDGE('',*,*,#50358,.T.);
#70361=ORIENTED_EDGE('',*,*,#50359,.T.);
#70362=ORIENTED_EDGE('',*,*,#50360,.T.);
#70363=ORIENTED_EDGE('',*,*,#50356,.T.);
#70364=ORIENTED_EDGE('',*,*,#50361,.F.);
#70365=ORIENTED_EDGE('',*,*,#50361,.T.);
#70366=ORIENTED_EDGE('',*,*,#50355,.T.);
#70367=ORIENTED_EDGE('',*,*,#50362,.F.);
#70368=ORIENTED_EDGE('',*,*,#50363,.F.);
#70369=ORIENTED_EDGE('',*,*,#50364,.T.);
#70370=ORIENTED_EDGE('',*,*,#50365,.T.);
#70371=ORIENTED_EDGE('',*,*,#50366,.T.);
#70372=ORIENTED_EDGE('',*,*,#50367,.T.);
#70373=ORIENTED_EDGE('',*,*,#50368,.T.);
#70374=ORIENTED_EDGE('',*,*,#50369,.T.);
#70375=ORIENTED_EDGE('',*,*,#50370,.T.);
#70376=ORIENTED_EDGE('',*,*,#50362,.T.);
#70377=ORIENTED_EDGE('',*,*,#50371,.T.);
#70378=ORIENTED_EDGE('',*,*,#50372,.F.);
#70379=ORIENTED_EDGE('',*,*,#50363,.T.);
#70380=ORIENTED_EDGE('',*,*,#50373,.F.);
#70381=ORIENTED_EDGE('',*,*,#50374,.T.);
#70382=ORIENTED_EDGE('',*,*,#50375,.T.);
#70383=ORIENTED_EDGE('',*,*,#50372,.T.);
#70384=ORIENTED_EDGE('',*,*,#50376,.F.);
#70385=ORIENTED_EDGE('',*,*,#50376,.T.);
#70386=ORIENTED_EDGE('',*,*,#50373,.T.);
#70387=ORIENTED_EDGE('',*,*,#50377,.T.);
#70388=ORIENTED_EDGE('',*,*,#50378,.F.);
#70389=ORIENTED_EDGE('',*,*,#50379,.T.);
#70390=ORIENTED_EDGE('',*,*,#50380,.F.);
#70391=ORIENTED_EDGE('',*,*,#50381,.T.);
#70392=ORIENTED_EDGE('',*,*,#50378,.T.);
#70393=ORIENTED_EDGE('',*,*,#50382,.T.);
#70394=ORIENTED_EDGE('',*,*,#50383,.F.);
#70395=ORIENTED_EDGE('',*,*,#50384,.T.);
#70396=ORIENTED_EDGE('',*,*,#50380,.T.);
#70397=ORIENTED_EDGE('',*,*,#50385,.T.);
#70398=ORIENTED_EDGE('',*,*,#50386,.F.);
#70399=ORIENTED_EDGE('',*,*,#50387,.T.);
#70400=ORIENTED_EDGE('',*,*,#50383,.T.);
#70401=ORIENTED_EDGE('',*,*,#50388,.T.);
#70402=ORIENTED_EDGE('',*,*,#49291,.F.);
#70403=ORIENTED_EDGE('',*,*,#50389,.T.);
#70404=ORIENTED_EDGE('',*,*,#50386,.T.);
#70405=ORIENTED_EDGE('',*,*,#50390,.T.);
#70406=ORIENTED_EDGE('',*,*,#49285,.F.);
#70407=ORIENTED_EDGE('',*,*,#50391,.F.);
#70408=ORIENTED_EDGE('',*,*,#50392,.T.);
#70409=ORIENTED_EDGE('',*,*,#50393,.F.);
#70410=ORIENTED_EDGE('',*,*,#50394,.T.);
#70411=ORIENTED_EDGE('',*,*,#50395,.T.);
#70412=ORIENTED_EDGE('',*,*,#50391,.T.);
#70413=ORIENTED_EDGE('',*,*,#50396,.F.);
#70414=ORIENTED_EDGE('',*,*,#50396,.T.);
#70415=ORIENTED_EDGE('',*,*,#50393,.T.);
#70416=ORIENTED_EDGE('',*,*,#50397,.T.);
#70417=ORIENTED_EDGE('',*,*,#50398,.F.);
#70418=ORIENTED_EDGE('',*,*,#50399,.T.);
#70419=ORIENTED_EDGE('',*,*,#50400,.F.);
#70420=ORIENTED_EDGE('',*,*,#50401,.T.);
#70421=ORIENTED_EDGE('',*,*,#50398,.T.);
#70422=ORIENTED_EDGE('',*,*,#50402,.T.);
#70423=ORIENTED_EDGE('',*,*,#50403,.F.);
#70424=ORIENTED_EDGE('',*,*,#50404,.T.);
#70425=ORIENTED_EDGE('',*,*,#50400,.T.);
#70426=ORIENTED_EDGE('',*,*,#50405,.T.);
#70427=ORIENTED_EDGE('',*,*,#50406,.F.);
#70428=ORIENTED_EDGE('',*,*,#50407,.T.);
#70429=ORIENTED_EDGE('',*,*,#50403,.T.);
#70430=ORIENTED_EDGE('',*,*,#50408,.T.);
#70431=ORIENTED_EDGE('',*,*,#50409,.T.);
#70432=ORIENTED_EDGE('',*,*,#50406,.T.);
#70433=ORIENTED_EDGE('',*,*,#50410,.T.);
#70434=ORIENTED_EDGE('',*,*,#49265,.F.);
#70435=ORIENTED_EDGE('',*,*,#49259,.F.);
#70436=ORIENTED_EDGE('',*,*,#50411,.T.);
#70437=ORIENTED_EDGE('',*,*,#50412,.T.);
#70438=ORIENTED_EDGE('',*,*,#50413,.F.);
#70439=ORIENTED_EDGE('',*,*,#50414,.T.);
#70440=ORIENTED_EDGE('',*,*,#50415,.T.);
#70441=ORIENTED_EDGE('',*,*,#50416,.T.);
#70442=ORIENTED_EDGE('',*,*,#50417,.T.);
#70443=ORIENTED_EDGE('',*,*,#50418,.F.);
#70444=ORIENTED_EDGE('',*,*,#50419,.T.);
#70445=ORIENTED_EDGE('',*,*,#50413,.T.);
#70446=ORIENTED_EDGE('',*,*,#50420,.T.);
#70447=ORIENTED_EDGE('',*,*,#50421,.F.);
#70448=ORIENTED_EDGE('',*,*,#50418,.T.);
#70449=ORIENTED_EDGE('',*,*,#50422,.F.);
#70450=ORIENTED_EDGE('',*,*,#50423,.T.);
#70451=ORIENTED_EDGE('',*,*,#50424,.F.);
#70452=ORIENTED_EDGE('',*,*,#50425,.T.);
#70453=ORIENTED_EDGE('',*,*,#50421,.T.);
#70454=ORIENTED_EDGE('',*,*,#50426,.F.);
#70455=ORIENTED_EDGE('',*,*,#50426,.T.);
#70456=ORIENTED_EDGE('',*,*,#50422,.T.);
#70457=ORIENTED_EDGE('',*,*,#50427,.T.);
#70458=ORIENTED_EDGE('',*,*,#50428,.T.);
#70459=ORIENTED_EDGE('',*,*,#50429,.F.);
#70460=ORIENTED_EDGE('',*,*,#50430,.T.);
#70461=ORIENTED_EDGE('',*,*,#50424,.T.);
#70462=ORIENTED_EDGE('',*,*,#50431,.T.);
#70463=ORIENTED_EDGE('',*,*,#50432,.F.);
#70464=ORIENTED_EDGE('',*,*,#50433,.T.);
#70465=ORIENTED_EDGE('',*,*,#50429,.T.);
#70466=ORIENTED_EDGE('',*,*,#50434,.T.);
#70467=ORIENTED_EDGE('',*,*,#50435,.F.);
#70468=ORIENTED_EDGE('',*,*,#50436,.T.);
#70469=ORIENTED_EDGE('',*,*,#50432,.T.);
#70470=ORIENTED_EDGE('',*,*,#50437,.T.);
#70471=ORIENTED_EDGE('',*,*,#49296,.F.);
#70472=ORIENTED_EDGE('',*,*,#50438,.T.);
#70473=ORIENTED_EDGE('',*,*,#50435,.T.);
#70474=ORIENTED_EDGE('',*,*,#50439,.T.);
#70475=ORIENTED_EDGE('',*,*,#49302,.F.);
#70476=ORIENTED_EDGE('',*,*,#50440,.T.);
#70477=ORIENTED_EDGE('',*,*,#50394,.F.);
#70478=ORIENTED_EDGE('',*,*,#50441,.T.);
#70479=ORIENTED_EDGE('',*,*,#50341,.F.);
#70480=ORIENTED_EDGE('',*,*,#50442,.T.);
#70481=ORIENTED_EDGE('',*,*,#50360,.F.);
#70482=ORIENTED_EDGE('',*,*,#50443,.T.);
#70483=ORIENTED_EDGE('',*,*,#50323,.F.);
#70484=ORIENTED_EDGE('',*,*,#50444,.T.);
#70485=ORIENTED_EDGE('',*,*,#50374,.F.);
#70486=ORIENTED_EDGE('',*,*,#50445,.T.);
#70487=ORIENTED_EDGE('',*,*,#50312,.F.);
#70488=ORIENTED_EDGE('',*,*,#50446,.T.);
#70489=ORIENTED_EDGE('',*,*,#50428,.F.);
#70490=ORIENTED_EDGE('',*,*,#50447,.T.);
#70491=ORIENTED_EDGE('',*,*,#50294,.F.);
#70492=ORIENTED_EDGE('',*,*,#50448,.T.);
#70493=ORIENTED_EDGE('',*,*,#50449,.T.);
#70494=ORIENTED_EDGE('',*,*,#50185,.F.);
#70495=ORIENTED_EDGE('',*,*,#50450,.T.);
#70496=ORIENTED_EDGE('',*,*,#50451,.T.);
#70497=ORIENTED_EDGE('',*,*,#50452,.T.);
#70498=ORIENTED_EDGE('',*,*,#50453,.T.);
#70499=ORIENTED_EDGE('',*,*,#50264,.F.);
#70500=ORIENTED_EDGE('',*,*,#50454,.T.);
#70501=ORIENTED_EDGE('',*,*,#50455,.T.);
#70502=ORIENTED_EDGE('',*,*,#50456,.T.);
#70503=ORIENTED_EDGE('',*,*,#50208,.F.);
#70504=ORIENTED_EDGE('',*,*,#50457,.T.);
#70505=ORIENTED_EDGE('',*,*,#50458,.T.);
#70506=ORIENTED_EDGE('',*,*,#50459,.T.);
#70507=ORIENTED_EDGE('',*,*,#50202,.F.);
#70508=ORIENTED_EDGE('',*,*,#50460,.T.);
#70509=ORIENTED_EDGE('',*,*,#50461,.T.);
#70510=ORIENTED_EDGE('',*,*,#50462,.T.);
#70511=ORIENTED_EDGE('',*,*,#50198,.F.);
#70512=ORIENTED_EDGE('',*,*,#50463,.T.);
#70513=ORIENTED_EDGE('',*,*,#50464,.T.);
#70514=ORIENTED_EDGE('',*,*,#50465,.T.);
#70515=ORIENTED_EDGE('',*,*,#50192,.F.);
#70516=ORIENTED_EDGE('',*,*,#50466,.T.);
#70517=ORIENTED_EDGE('',*,*,#50467,.T.);
#70518=ORIENTED_EDGE('',*,*,#50468,.T.);
#70519=ORIENTED_EDGE('',*,*,#50180,.F.);
#70520=ORIENTED_EDGE('',*,*,#50469,.T.);
#70521=ORIENTED_EDGE('',*,*,#50470,.T.);
#70522=ORIENTED_EDGE('',*,*,#50471,.T.);
#70523=ORIENTED_EDGE('',*,*,#50242,.F.);
#70524=ORIENTED_EDGE('',*,*,#50472,.T.);
#70525=ORIENTED_EDGE('',*,*,#50473,.T.);
#70526=ORIENTED_EDGE('',*,*,#50474,.T.);
#70527=ORIENTED_EDGE('',*,*,#50224,.F.);
#70528=ORIENTED_EDGE('',*,*,#50475,.T.);
#70529=ORIENTED_EDGE('',*,*,#50476,.T.);
#70530=ORIENTED_EDGE('',*,*,#49890,.F.);
#70531=ORIENTED_EDGE('',*,*,#50477,.T.);
#70532=ORIENTED_EDGE('',*,*,#50478,.T.);
#70533=ORIENTED_EDGE('',*,*,#50479,.T.);
#70534=ORIENTED_EDGE('',*,*,#50480,.T.);
#70535=ORIENTED_EDGE('',*,*,#49767,.F.);
#70536=ORIENTED_EDGE('',*,*,#50481,.T.);
#70537=ORIENTED_EDGE('',*,*,#50482,.T.);
#70538=ORIENTED_EDGE('',*,*,#50483,.T.);
#70539=ORIENTED_EDGE('',*,*,#49743,.F.);
#70540=ORIENTED_EDGE('',*,*,#50484,.T.);
#70541=ORIENTED_EDGE('',*,*,#50485,.T.);
#70542=ORIENTED_EDGE('',*,*,#50486,.T.);
#70543=ORIENTED_EDGE('',*,*,#49751,.F.);
#70544=ORIENTED_EDGE('',*,*,#50487,.T.);
#70545=ORIENTED_EDGE('',*,*,#50488,.T.);
#70546=ORIENTED_EDGE('',*,*,#50489,.T.);
#70547=ORIENTED_EDGE('',*,*,#49763,.F.);
#70548=ORIENTED_EDGE('',*,*,#50490,.T.);
#70549=ORIENTED_EDGE('',*,*,#50491,.T.);
#70550=ORIENTED_EDGE('',*,*,#50492,.T.);
#70551=ORIENTED_EDGE('',*,*,#49713,.F.);
#70552=ORIENTED_EDGE('',*,*,#50493,.T.);
#70553=ORIENTED_EDGE('',*,*,#50494,.T.);
#70554=ORIENTED_EDGE('',*,*,#50495,.T.);
#70555=ORIENTED_EDGE('',*,*,#49721,.F.);
#70556=ORIENTED_EDGE('',*,*,#50496,.T.);
#70557=ORIENTED_EDGE('',*,*,#50497,.T.);
#70558=ORIENTED_EDGE('',*,*,#50498,.T.);
#70559=ORIENTED_EDGE('',*,*,#49733,.F.);
#70560=ORIENTED_EDGE('',*,*,#50499,.T.);
#70561=ORIENTED_EDGE('',*,*,#50500,.T.);
#70562=ORIENTED_EDGE('',*,*,#50501,.T.);
#70563=ORIENTED_EDGE('',*,*,#49737,.F.);
#70564=ORIENTED_EDGE('',*,*,#50502,.T.);
#70565=ORIENTED_EDGE('',*,*,#50503,.T.);
#70566=ORIENTED_EDGE('',*,*,#50504,.T.);
#70567=ORIENTED_EDGE('',*,*,#49510,.F.);
#70568=ORIENTED_EDGE('',*,*,#50505,.T.);
#70569=ORIENTED_EDGE('',*,*,#50506,.T.);
#70570=ORIENTED_EDGE('',*,*,#50507,.T.);
#70571=ORIENTED_EDGE('',*,*,#49500,.F.);
#70572=ORIENTED_EDGE('',*,*,#50508,.T.);
#70573=ORIENTED_EDGE('',*,*,#50509,.T.);
#70574=ORIENTED_EDGE('',*,*,#50510,.T.);
#70575=ORIENTED_EDGE('',*,*,#49488,.F.);
#70576=ORIENTED_EDGE('',*,*,#50511,.T.);
#70577=ORIENTED_EDGE('',*,*,#50512,.T.);
#70578=ORIENTED_EDGE('',*,*,#50513,.T.);
#70579=ORIENTED_EDGE('',*,*,#49496,.F.);
#70580=ORIENTED_EDGE('',*,*,#50514,.T.);
#70581=ORIENTED_EDGE('',*,*,#50515,.T.);
#70582=ORIENTED_EDGE('',*,*,#50516,.T.);
#70583=ORIENTED_EDGE('',*,*,#49881,.F.);
#70584=ORIENTED_EDGE('',*,*,#50517,.T.);
#70585=ORIENTED_EDGE('',*,*,#50518,.T.);
#70586=ORIENTED_EDGE('',*,*,#50519,.T.);
#70587=ORIENTED_EDGE('',*,*,#49869,.F.);
#70588=ORIENTED_EDGE('',*,*,#50520,.T.);
#70589=ORIENTED_EDGE('',*,*,#50521,.T.);
#70590=ORIENTED_EDGE('',*,*,#50522,.T.);
#70591=ORIENTED_EDGE('',*,*,#49877,.F.);
#70592=ORIENTED_EDGE('',*,*,#50523,.T.);
#70593=ORIENTED_EDGE('',*,*,#50524,.T.);
#70594=ORIENTED_EDGE('',*,*,#50525,.T.);
#70595=ORIENTED_EDGE('',*,*,#50126,.F.);
#70596=ORIENTED_EDGE('',*,*,#50526,.T.);
#70597=ORIENTED_EDGE('',*,*,#50527,.T.);
#70598=ORIENTED_EDGE('',*,*,#50528,.T.);
#70599=ORIENTED_EDGE('',*,*,#50130,.F.);
#70600=ORIENTED_EDGE('',*,*,#50529,.T.);
#70601=ORIENTED_EDGE('',*,*,#50530,.T.);
#70602=ORIENTED_EDGE('',*,*,#50117,.F.);
#70603=ORIENTED_EDGE('',*,*,#50531,.T.);
#70604=ORIENTED_EDGE('',*,*,#50532,.T.);
#70605=ORIENTED_EDGE('',*,*,#50533,.T.);
#70606=ORIENTED_EDGE('',*,*,#50534,.T.);
#70607=ORIENTED_EDGE('',*,*,#49575,.F.);
#70608=ORIENTED_EDGE('',*,*,#50535,.T.);
#70609=ORIENTED_EDGE('',*,*,#50536,.T.);
#70610=ORIENTED_EDGE('',*,*,#50537,.T.);
#70611=ORIENTED_EDGE('',*,*,#49563,.F.);
#70612=ORIENTED_EDGE('',*,*,#50538,.T.);
#70613=ORIENTED_EDGE('',*,*,#50539,.T.);
#70614=ORIENTED_EDGE('',*,*,#50540,.T.);
#70615=ORIENTED_EDGE('',*,*,#49571,.F.);
#70616=ORIENTED_EDGE('',*,*,#50541,.T.);
#70617=ORIENTED_EDGE('',*,*,#50542,.T.);
#70618=ORIENTED_EDGE('',*,*,#50543,.T.);
#70619=ORIENTED_EDGE('',*,*,#49583,.F.);
#70620=ORIENTED_EDGE('',*,*,#50544,.T.);
#70621=ORIENTED_EDGE('',*,*,#50545,.T.);
#70622=ORIENTED_EDGE('',*,*,#50546,.T.);
#70623=ORIENTED_EDGE('',*,*,#49599,.F.);
#70624=ORIENTED_EDGE('',*,*,#50547,.T.);
#70625=ORIENTED_EDGE('',*,*,#50548,.T.);
#70626=ORIENTED_EDGE('',*,*,#50549,.T.);
#70627=ORIENTED_EDGE('',*,*,#49587,.F.);
#70628=ORIENTED_EDGE('',*,*,#50550,.T.);
#70629=ORIENTED_EDGE('',*,*,#50551,.T.);
#70630=ORIENTED_EDGE('',*,*,#50552,.T.);
#70631=ORIENTED_EDGE('',*,*,#49595,.F.);
#70632=ORIENTED_EDGE('',*,*,#50553,.T.);
#70633=ORIENTED_EDGE('',*,*,#50554,.T.);
#70634=ORIENTED_EDGE('',*,*,#50555,.T.);
#70635=ORIENTED_EDGE('',*,*,#49607,.F.);
#70636=ORIENTED_EDGE('',*,*,#50556,.T.);
#70637=ORIENTED_EDGE('',*,*,#50557,.T.);
#70638=ORIENTED_EDGE('',*,*,#50558,.T.);
#70639=ORIENTED_EDGE('',*,*,#49974,.F.);
#70640=ORIENTED_EDGE('',*,*,#50559,.T.);
#70641=ORIENTED_EDGE('',*,*,#50560,.T.);
#70642=ORIENTED_EDGE('',*,*,#50561,.T.);
#70643=ORIENTED_EDGE('',*,*,#49982,.F.);
#70644=ORIENTED_EDGE('',*,*,#50562,.T.);
#70645=ORIENTED_EDGE('',*,*,#50563,.T.);
#70646=ORIENTED_EDGE('',*,*,#50564,.T.);
#70647=ORIENTED_EDGE('',*,*,#49994,.F.);
#70648=ORIENTED_EDGE('',*,*,#50565,.T.);
#70649=ORIENTED_EDGE('',*,*,#50566,.T.);
#70650=ORIENTED_EDGE('',*,*,#50567,.T.);
#70651=ORIENTED_EDGE('',*,*,#49986,.F.);
#70652=ORIENTED_EDGE('',*,*,#50568,.T.);
#70653=ORIENTED_EDGE('',*,*,#50569,.T.);
#70654=ORIENTED_EDGE('',*,*,#50570,.T.);
#70655=ORIENTED_EDGE('',*,*,#49920,.F.);
#70656=ORIENTED_EDGE('',*,*,#50571,.T.);
#70657=ORIENTED_EDGE('',*,*,#50572,.T.);
#70658=ORIENTED_EDGE('',*,*,#50573,.T.);
#70659=ORIENTED_EDGE('',*,*,#49928,.F.);
#70660=ORIENTED_EDGE('',*,*,#50574,.T.);
#70661=ORIENTED_EDGE('',*,*,#50575,.T.);
#70662=ORIENTED_EDGE('',*,*,#50576,.T.);
#70663=ORIENTED_EDGE('',*,*,#49944,.F.);
#70664=ORIENTED_EDGE('',*,*,#50577,.T.);
#70665=ORIENTED_EDGE('',*,*,#50578,.T.);
#70666=ORIENTED_EDGE('',*,*,#50579,.T.);
#70667=ORIENTED_EDGE('',*,*,#49932,.F.);
#70668=ORIENTED_EDGE('',*,*,#50580,.T.);
#70669=ORIENTED_EDGE('',*,*,#50581,.T.);
#70670=ORIENTED_EDGE('',*,*,#50582,.T.);
#70671=ORIENTED_EDGE('',*,*,#49701,.F.);
#70672=ORIENTED_EDGE('',*,*,#50583,.T.);
#70673=ORIENTED_EDGE('',*,*,#50584,.T.);
#70674=ORIENTED_EDGE('',*,*,#50585,.T.);
#70675=ORIENTED_EDGE('',*,*,#49689,.F.);
#70676=ORIENTED_EDGE('',*,*,#50586,.T.);
#70677=ORIENTED_EDGE('',*,*,#50587,.T.);
#70678=ORIENTED_EDGE('',*,*,#50588,.T.);
#70679=ORIENTED_EDGE('',*,*,#49697,.F.);
#70680=ORIENTED_EDGE('',*,*,#50589,.T.);
#70681=ORIENTED_EDGE('',*,*,#50590,.T.);
#70682=ORIENTED_EDGE('',*,*,#50591,.T.);
#70683=ORIENTED_EDGE('',*,*,#49709,.F.);
#70684=ORIENTED_EDGE('',*,*,#50592,.T.);
#70685=ORIENTED_EDGE('',*,*,#50593,.T.);
#70686=ORIENTED_EDGE('',*,*,#50594,.T.);
#70687=ORIENTED_EDGE('',*,*,#49793,.F.);
#70688=ORIENTED_EDGE('',*,*,#50595,.T.);
#70689=ORIENTED_EDGE('',*,*,#50596,.T.);
#70690=ORIENTED_EDGE('',*,*,#50597,.T.);
#70691=ORIENTED_EDGE('',*,*,#49785,.F.);
#70692=ORIENTED_EDGE('',*,*,#50598,.T.);
#70693=ORIENTED_EDGE('',*,*,#50599,.T.);
#70694=ORIENTED_EDGE('',*,*,#50600,.T.);
#70695=ORIENTED_EDGE('',*,*,#49773,.F.);
#70696=ORIENTED_EDGE('',*,*,#50601,.T.);
#70697=ORIENTED_EDGE('',*,*,#50602,.T.);
#70698=ORIENTED_EDGE('',*,*,#50603,.T.);
#70699=ORIENTED_EDGE('',*,*,#49781,.F.);
#70700=ORIENTED_EDGE('',*,*,#50604,.T.);
#70701=ORIENTED_EDGE('',*,*,#50605,.T.);
#70702=ORIENTED_EDGE('',*,*,#50606,.T.);
#70703=ORIENTED_EDGE('',*,*,#49821,.F.);
#70704=ORIENTED_EDGE('',*,*,#50607,.T.);
#70705=ORIENTED_EDGE('',*,*,#50608,.T.);
#70706=ORIENTED_EDGE('',*,*,#50609,.T.);
#70707=ORIENTED_EDGE('',*,*,#49829,.F.);
#70708=ORIENTED_EDGE('',*,*,#50610,.T.);
#70709=ORIENTED_EDGE('',*,*,#50611,.T.);
#70710=ORIENTED_EDGE('',*,*,#50612,.T.);
#70711=ORIENTED_EDGE('',*,*,#49841,.F.);
#70712=ORIENTED_EDGE('',*,*,#50613,.T.);
#70713=ORIENTED_EDGE('',*,*,#50614,.T.);
#70714=ORIENTED_EDGE('',*,*,#50615,.T.);
#70715=ORIENTED_EDGE('',*,*,#49833,.F.);
#70716=ORIENTED_EDGE('',*,*,#50616,.T.);
#70717=ORIENTED_EDGE('',*,*,#50617,.T.);
#70718=ORIENTED_EDGE('',*,*,#50618,.T.);
#70719=ORIENTED_EDGE('',*,*,#50108,.F.);
#70720=ORIENTED_EDGE('',*,*,#50619,.T.);
#70721=ORIENTED_EDGE('',*,*,#50620,.T.);
#70722=ORIENTED_EDGE('',*,*,#50621,.T.);
#70723=ORIENTED_EDGE('',*,*,#50112,.F.);
#70724=ORIENTED_EDGE('',*,*,#50622,.T.);
#70725=ORIENTED_EDGE('',*,*,#50623,.T.);
#70726=ORIENTED_EDGE('',*,*,#50624,.T.);
#70727=ORIENTED_EDGE('',*,*,#50100,.F.);
#70728=ORIENTED_EDGE('',*,*,#50625,.T.);
#70729=ORIENTED_EDGE('',*,*,#50626,.T.);
#70730=ORIENTED_EDGE('',*,*,#50627,.T.);
#70731=ORIENTED_EDGE('',*,*,#49958,.F.);
#70732=ORIENTED_EDGE('',*,*,#50628,.T.);
#70733=ORIENTED_EDGE('',*,*,#50629,.T.);
#70734=ORIENTED_EDGE('',*,*,#50630,.T.);
#70735=ORIENTED_EDGE('',*,*,#49970,.F.);
#70736=ORIENTED_EDGE('',*,*,#50631,.T.);
#70737=ORIENTED_EDGE('',*,*,#50632,.T.);
#70738=ORIENTED_EDGE('',*,*,#50633,.T.);
#70739=ORIENTED_EDGE('',*,*,#49962,.F.);
#70740=ORIENTED_EDGE('',*,*,#50634,.T.);
#70741=ORIENTED_EDGE('',*,*,#50635,.T.);
#70742=ORIENTED_EDGE('',*,*,#50636,.T.);
#70743=ORIENTED_EDGE('',*,*,#49950,.F.);
#70744=ORIENTED_EDGE('',*,*,#50637,.T.);
#70745=ORIENTED_EDGE('',*,*,#50638,.T.);
#70746=ORIENTED_EDGE('',*,*,#50639,.T.);
#70747=ORIENTED_EDGE('',*,*,#49908,.F.);
#70748=ORIENTED_EDGE('',*,*,#50640,.T.);
#70749=ORIENTED_EDGE('',*,*,#50641,.T.);
#70750=ORIENTED_EDGE('',*,*,#50642,.T.);
#70751=ORIENTED_EDGE('',*,*,#49896,.F.);
#70752=ORIENTED_EDGE('',*,*,#50643,.T.);
#70753=ORIENTED_EDGE('',*,*,#50644,.T.);
#70754=ORIENTED_EDGE('',*,*,#50645,.T.);
#70755=ORIENTED_EDGE('',*,*,#49904,.F.);
#70756=ORIENTED_EDGE('',*,*,#50646,.T.);
#70757=ORIENTED_EDGE('',*,*,#50647,.T.);
#70758=ORIENTED_EDGE('',*,*,#50648,.T.);
#70759=ORIENTED_EDGE('',*,*,#49916,.F.);
#70760=ORIENTED_EDGE('',*,*,#50649,.T.);
#70761=ORIENTED_EDGE('',*,*,#50650,.T.);
#70762=ORIENTED_EDGE('',*,*,#50651,.T.);
#70763=ORIENTED_EDGE('',*,*,#49809,.F.);
#70764=ORIENTED_EDGE('',*,*,#50652,.T.);
#70765=ORIENTED_EDGE('',*,*,#50653,.T.);
#70766=ORIENTED_EDGE('',*,*,#50654,.T.);
#70767=ORIENTED_EDGE('',*,*,#49797,.F.);
#70768=ORIENTED_EDGE('',*,*,#50655,.T.);
#70769=ORIENTED_EDGE('',*,*,#50656,.T.);
#70770=ORIENTED_EDGE('',*,*,#50657,.T.);
#70771=ORIENTED_EDGE('',*,*,#49805,.F.);
#70772=ORIENTED_EDGE('',*,*,#50658,.T.);
#70773=ORIENTED_EDGE('',*,*,#50659,.T.);
#70774=ORIENTED_EDGE('',*,*,#50660,.T.);
#70775=ORIENTED_EDGE('',*,*,#49817,.F.);
#70776=ORIENTED_EDGE('',*,*,#50661,.T.);
#70777=ORIENTED_EDGE('',*,*,#50662,.T.);
#70778=ORIENTED_EDGE('',*,*,#50663,.T.);
#70779=ORIENTED_EDGE('',*,*,#49665,.F.);
#70780=ORIENTED_EDGE('',*,*,#50664,.T.);
#70781=ORIENTED_EDGE('',*,*,#50665,.T.);
#70782=ORIENTED_EDGE('',*,*,#50666,.T.);
#70783=ORIENTED_EDGE('',*,*,#49673,.F.);
#70784=ORIENTED_EDGE('',*,*,#50667,.T.);
#70785=ORIENTED_EDGE('',*,*,#50668,.T.);
#70786=ORIENTED_EDGE('',*,*,#50669,.T.);
#70787=ORIENTED_EDGE('',*,*,#49685,.F.);
#70788=ORIENTED_EDGE('',*,*,#50670,.T.);
#70789=ORIENTED_EDGE('',*,*,#50671,.T.);
#70790=ORIENTED_EDGE('',*,*,#50672,.T.);
#70791=ORIENTED_EDGE('',*,*,#49677,.F.);
#70792=ORIENTED_EDGE('',*,*,#50673,.T.);
#70793=ORIENTED_EDGE('',*,*,#50674,.T.);
#70794=ORIENTED_EDGE('',*,*,#50675,.T.);
#70795=ORIENTED_EDGE('',*,*,#49611,.F.);
#70796=ORIENTED_EDGE('',*,*,#50676,.T.);
#70797=ORIENTED_EDGE('',*,*,#50677,.T.);
#70798=ORIENTED_EDGE('',*,*,#50678,.T.);
#70799=ORIENTED_EDGE('',*,*,#49619,.F.);
#70800=ORIENTED_EDGE('',*,*,#50679,.T.);
#70801=ORIENTED_EDGE('',*,*,#50680,.T.);
#70802=ORIENTED_EDGE('',*,*,#50681,.T.);
#70803=ORIENTED_EDGE('',*,*,#49631,.F.);
#70804=ORIENTED_EDGE('',*,*,#50682,.T.);
#70805=ORIENTED_EDGE('',*,*,#50683,.T.);
#70806=ORIENTED_EDGE('',*,*,#50684,.T.);
#70807=ORIENTED_EDGE('',*,*,#49623,.F.);
#70808=ORIENTED_EDGE('',*,*,#50685,.T.);
#70809=ORIENTED_EDGE('',*,*,#50686,.T.);
#70810=ORIENTED_EDGE('',*,*,#50687,.T.);
#70811=ORIENTED_EDGE('',*,*,#49635,.F.);
#70812=ORIENTED_EDGE('',*,*,#50688,.T.);
#70813=ORIENTED_EDGE('',*,*,#50689,.T.);
#70814=ORIENTED_EDGE('',*,*,#50690,.T.);
#70815=ORIENTED_EDGE('',*,*,#49643,.F.);
#70816=ORIENTED_EDGE('',*,*,#50691,.T.);
#70817=ORIENTED_EDGE('',*,*,#50692,.T.);
#70818=ORIENTED_EDGE('',*,*,#50693,.T.);
#70819=ORIENTED_EDGE('',*,*,#49655,.F.);
#70820=ORIENTED_EDGE('',*,*,#50694,.T.);
#70821=ORIENTED_EDGE('',*,*,#50695,.T.);
#70822=ORIENTED_EDGE('',*,*,#50696,.T.);
#70823=ORIENTED_EDGE('',*,*,#49647,.F.);
#70824=ORIENTED_EDGE('',*,*,#50697,.T.);
#70825=ORIENTED_EDGE('',*,*,#50698,.T.);
#70826=ORIENTED_EDGE('',*,*,#50699,.T.);
#70827=ORIENTED_EDGE('',*,*,#49406,.F.);
#70828=ORIENTED_EDGE('',*,*,#50700,.T.);
#70829=ORIENTED_EDGE('',*,*,#50701,.T.);
#70830=ORIENTED_EDGE('',*,*,#50702,.T.);
#70831=ORIENTED_EDGE('',*,*,#49410,.F.);
#70832=ORIENTED_EDGE('',*,*,#50703,.T.);
#70833=ORIENTED_EDGE('',*,*,#50704,.T.);
#70834=ORIENTED_EDGE('',*,*,#49385,.F.);
#70835=ORIENTED_EDGE('',*,*,#50705,.T.);
#70836=ORIENTED_EDGE('',*,*,#50706,.T.);
#70837=ORIENTED_EDGE('',*,*,#50707,.T.);
#70838=ORIENTED_EDGE('',*,*,#50708,.T.);
#70839=ORIENTED_EDGE('',*,*,#49394,.F.);
#70840=ORIENTED_EDGE('',*,*,#50709,.T.);
#70841=ORIENTED_EDGE('',*,*,#50710,.T.);
#70842=ORIENTED_EDGE('',*,*,#50711,.T.);
#70843=ORIENTED_EDGE('',*,*,#50016,.F.);
#70844=ORIENTED_EDGE('',*,*,#50712,.T.);
#70845=ORIENTED_EDGE('',*,*,#50713,.T.);
#70846=ORIENTED_EDGE('',*,*,#50714,.T.);
#70847=ORIENTED_EDGE('',*,*,#50004,.F.);
#70848=ORIENTED_EDGE('',*,*,#50715,.T.);
#70849=ORIENTED_EDGE('',*,*,#50716,.T.);
#70850=ORIENTED_EDGE('',*,*,#50717,.T.);
#70851=ORIENTED_EDGE('',*,*,#50012,.F.);
#70852=ORIENTED_EDGE('',*,*,#50718,.T.);
#70853=ORIENTED_EDGE('',*,*,#50719,.T.);
#70854=ORIENTED_EDGE('',*,*,#50720,.T.);
#70855=ORIENTED_EDGE('',*,*,#50024,.F.);
#70856=ORIENTED_EDGE('',*,*,#50721,.T.);
#70857=ORIENTED_EDGE('',*,*,#50722,.T.);
#70858=ORIENTED_EDGE('',*,*,#50723,.T.);
#70859=ORIENTED_EDGE('',*,*,#49551,.F.);
#70860=ORIENTED_EDGE('',*,*,#50724,.T.);
#70861=ORIENTED_EDGE('',*,*,#50725,.T.);
#70862=ORIENTED_EDGE('',*,*,#50726,.T.);
#70863=ORIENTED_EDGE('',*,*,#49539,.F.);
#70864=ORIENTED_EDGE('',*,*,#50727,.T.);
#70865=ORIENTED_EDGE('',*,*,#50728,.T.);
#70866=ORIENTED_EDGE('',*,*,#50729,.T.);
#70867=ORIENTED_EDGE('',*,*,#49547,.F.);
#70868=ORIENTED_EDGE('',*,*,#50730,.T.);
#70869=ORIENTED_EDGE('',*,*,#50731,.T.);
#70870=ORIENTED_EDGE('',*,*,#50732,.T.);
#70871=ORIENTED_EDGE('',*,*,#49559,.F.);
#70872=ORIENTED_EDGE('',*,*,#50733,.T.);
#70873=ORIENTED_EDGE('',*,*,#50734,.T.);
#70874=ORIENTED_EDGE('',*,*,#50735,.T.);
#70875=ORIENTED_EDGE('',*,*,#49527,.F.);
#70876=ORIENTED_EDGE('',*,*,#50736,.T.);
#70877=ORIENTED_EDGE('',*,*,#50737,.T.);
#70878=ORIENTED_EDGE('',*,*,#50738,.T.);
#70879=ORIENTED_EDGE('',*,*,#49515,.F.);
#70880=ORIENTED_EDGE('',*,*,#50739,.T.);
#70881=ORIENTED_EDGE('',*,*,#50740,.T.);
#70882=ORIENTED_EDGE('',*,*,#50741,.T.);
#70883=ORIENTED_EDGE('',*,*,#49523,.F.);
#70884=ORIENTED_EDGE('',*,*,#50742,.T.);
#70885=ORIENTED_EDGE('',*,*,#50743,.T.);
#70886=ORIENTED_EDGE('',*,*,#50744,.T.);
#70887=ORIENTED_EDGE('',*,*,#49535,.F.);
#70888=ORIENTED_EDGE('',*,*,#50745,.T.);
#70889=ORIENTED_EDGE('',*,*,#50746,.T.);
#70890=ORIENTED_EDGE('',*,*,#50747,.T.);
#70891=ORIENTED_EDGE('',*,*,#49845,.F.);
#70892=ORIENTED_EDGE('',*,*,#50748,.T.);
#70893=ORIENTED_EDGE('',*,*,#50749,.T.);
#70894=ORIENTED_EDGE('',*,*,#50750,.T.);
#70895=ORIENTED_EDGE('',*,*,#49853,.F.);
#70896=ORIENTED_EDGE('',*,*,#50751,.T.);
#70897=ORIENTED_EDGE('',*,*,#50752,.T.);
#70898=ORIENTED_EDGE('',*,*,#50753,.T.);
#70899=ORIENTED_EDGE('',*,*,#49865,.F.);
#70900=ORIENTED_EDGE('',*,*,#50754,.T.);
#70901=ORIENTED_EDGE('',*,*,#50755,.T.);
#70902=ORIENTED_EDGE('',*,*,#50756,.T.);
#70903=ORIENTED_EDGE('',*,*,#49857,.F.);
#70904=ORIENTED_EDGE('',*,*,#50757,.T.);
#70905=ORIENTED_EDGE('',*,*,#50758,.T.);
#70906=ORIENTED_EDGE('',*,*,#50759,.T.);
#70907=ORIENTED_EDGE('',*,*,#50036,.F.);
#70908=ORIENTED_EDGE('',*,*,#50760,.T.);
#70909=ORIENTED_EDGE('',*,*,#50761,.T.);
#70910=ORIENTED_EDGE('',*,*,#50762,.T.);
#70911=ORIENTED_EDGE('',*,*,#50048,.F.);
#70912=ORIENTED_EDGE('',*,*,#50763,.T.);
#70913=ORIENTED_EDGE('',*,*,#50764,.T.);
#70914=ORIENTED_EDGE('',*,*,#50765,.T.);
#70915=ORIENTED_EDGE('',*,*,#50040,.F.);
#70916=ORIENTED_EDGE('',*,*,#50766,.T.);
#70917=ORIENTED_EDGE('',*,*,#50767,.T.);
#70918=ORIENTED_EDGE('',*,*,#50768,.T.);
#70919=ORIENTED_EDGE('',*,*,#50028,.F.);
#70920=ORIENTED_EDGE('',*,*,#50769,.T.);
#70921=ORIENTED_EDGE('',*,*,#50770,.T.);
#70922=ORIENTED_EDGE('',*,*,#50771,.T.);
#70923=ORIENTED_EDGE('',*,*,#49436,.F.);
#70924=ORIENTED_EDGE('',*,*,#50772,.T.);
#70925=ORIENTED_EDGE('',*,*,#50773,.T.);
#70926=ORIENTED_EDGE('',*,*,#50774,.T.);
#70927=ORIENTED_EDGE('',*,*,#49428,.F.);
#70928=ORIENTED_EDGE('',*,*,#50775,.T.);
#70929=ORIENTED_EDGE('',*,*,#50776,.T.);
#70930=ORIENTED_EDGE('',*,*,#49415,.F.);
#70931=ORIENTED_EDGE('',*,*,#50777,.T.);
#70932=ORIENTED_EDGE('',*,*,#50778,.T.);
#70933=ORIENTED_EDGE('',*,*,#50779,.T.);
#70934=ORIENTED_EDGE('',*,*,#50780,.T.);
#70935=ORIENTED_EDGE('',*,*,#49424,.F.);
#70936=ORIENTED_EDGE('',*,*,#50781,.T.);
#70937=ORIENTED_EDGE('',*,*,#50782,.T.);
#70938=ORIENTED_EDGE('',*,*,#50783,.T.);
#70939=ORIENTED_EDGE('',*,*,#50064,.F.);
#70940=ORIENTED_EDGE('',*,*,#50784,.T.);
#70941=ORIENTED_EDGE('',*,*,#50785,.T.);
#70942=ORIENTED_EDGE('',*,*,#50786,.T.);
#70943=ORIENTED_EDGE('',*,*,#50052,.F.);
#70944=ORIENTED_EDGE('',*,*,#50787,.T.);
#70945=ORIENTED_EDGE('',*,*,#50788,.T.);
#70946=ORIENTED_EDGE('',*,*,#50789,.T.);
#70947=ORIENTED_EDGE('',*,*,#50060,.F.);
#70948=ORIENTED_EDGE('',*,*,#50790,.T.);
#70949=ORIENTED_EDGE('',*,*,#50791,.T.);
#70950=ORIENTED_EDGE('',*,*,#50792,.T.);
#70951=ORIENTED_EDGE('',*,*,#50072,.F.);
#70952=ORIENTED_EDGE('',*,*,#50793,.T.);
#70953=ORIENTED_EDGE('',*,*,#50794,.T.);
#70954=ORIENTED_EDGE('',*,*,#50795,.T.);
#70955=ORIENTED_EDGE('',*,*,#49476,.F.);
#70956=ORIENTED_EDGE('',*,*,#50796,.T.);
#70957=ORIENTED_EDGE('',*,*,#50797,.T.);
#70958=ORIENTED_EDGE('',*,*,#50798,.T.);
#70959=ORIENTED_EDGE('',*,*,#49464,.F.);
#70960=ORIENTED_EDGE('',*,*,#50799,.T.);
#70961=ORIENTED_EDGE('',*,*,#50800,.T.);
#70962=ORIENTED_EDGE('',*,*,#50801,.T.);
#70963=ORIENTED_EDGE('',*,*,#49472,.F.);
#70964=ORIENTED_EDGE('',*,*,#50802,.T.);
#70965=ORIENTED_EDGE('',*,*,#50803,.T.);
#70966=ORIENTED_EDGE('',*,*,#50804,.T.);
#70967=ORIENTED_EDGE('',*,*,#49484,.F.);
#70968=ORIENTED_EDGE('',*,*,#50805,.T.);
#70969=ORIENTED_EDGE('',*,*,#50806,.T.);
#70970=ORIENTED_EDGE('',*,*,#50807,.T.);
#70971=ORIENTED_EDGE('',*,*,#50084,.F.);
#70972=ORIENTED_EDGE('',*,*,#50808,.T.);
#70973=ORIENTED_EDGE('',*,*,#50809,.T.);
#70974=ORIENTED_EDGE('',*,*,#50810,.T.);
#70975=ORIENTED_EDGE('',*,*,#50096,.F.);
#70976=ORIENTED_EDGE('',*,*,#50811,.T.);
#70977=ORIENTED_EDGE('',*,*,#50812,.T.);
#70978=ORIENTED_EDGE('',*,*,#50813,.T.);
#70979=ORIENTED_EDGE('',*,*,#50088,.F.);
#70980=ORIENTED_EDGE('',*,*,#50814,.T.);
#70981=ORIENTED_EDGE('',*,*,#50815,.T.);
#70982=ORIENTED_EDGE('',*,*,#50816,.T.);
#70983=ORIENTED_EDGE('',*,*,#50076,.F.);
#70984=ORIENTED_EDGE('',*,*,#50817,.T.);
#70985=ORIENTED_EDGE('',*,*,#50818,.T.);
#70986=ORIENTED_EDGE('',*,*,#50819,.T.);
#70987=ORIENTED_EDGE('',*,*,#49460,.F.);
#70988=ORIENTED_EDGE('',*,*,#50820,.T.);
#70989=ORIENTED_EDGE('',*,*,#50821,.T.);
#70990=ORIENTED_EDGE('',*,*,#50822,.T.);
#70991=ORIENTED_EDGE('',*,*,#49452,.F.);
#70992=ORIENTED_EDGE('',*,*,#50823,.T.);
#70993=ORIENTED_EDGE('',*,*,#50824,.T.);
#70994=ORIENTED_EDGE('',*,*,#49439,.F.);
#70995=ORIENTED_EDGE('',*,*,#50825,.T.);
#70996=ORIENTED_EDGE('',*,*,#50826,.T.);
#70997=ORIENTED_EDGE('',*,*,#50827,.T.);
#70998=ORIENTED_EDGE('',*,*,#50828,.T.);
#70999=ORIENTED_EDGE('',*,*,#49448,.F.);
#71000=ORIENTED_EDGE('',*,*,#50829,.T.);
#71001=ORIENTED_EDGE('',*,*,#50830,.T.);
#71002=ORIENTED_EDGE('',*,*,#50831,.T.);
#71003=ORIENTED_EDGE('',*,*,#50214,.F.);
#71004=ORIENTED_EDGE('',*,*,#50832,.T.);
#71005=ORIENTED_EDGE('',*,*,#50833,.T.);
#71006=ORIENTED_EDGE('',*,*,#50834,.T.);
#71007=ORIENTED_EDGE('',*,*,#50252,.F.);
#71008=ORIENTED_EDGE('',*,*,#50835,.T.);
#71009=ORIENTED_EDGE('',*,*,#50836,.T.);
#71010=ORIENTED_EDGE('',*,*,#50837,.T.);
#71011=ORIENTED_EDGE('',*,*,#50236,.F.);
#71012=ORIENTED_EDGE('',*,*,#50838,.T.);
#71013=ORIENTED_EDGE('',*,*,#50839,.T.);
#71014=ORIENTED_EDGE('',*,*,#50229,.F.);
#71015=ORIENTED_EDGE('',*,*,#50840,.T.);
#71016=ORIENTED_EDGE('',*,*,#50841,.T.);
#71017=ORIENTED_EDGE('',*,*,#50842,.T.);
#71018=ORIENTED_EDGE('',*,*,#50843,.T.);
#71019=ORIENTED_EDGE('',*,*,#50258,.F.);
#71020=ORIENTED_EDGE('',*,*,#50844,.T.);
#71021=ORIENTED_EDGE('',*,*,#50845,.T.);
#71022=ORIENTED_EDGE('',*,*,#50244,.F.);
#71023=ORIENTED_EDGE('',*,*,#50846,.T.);
#71024=ORIENTED_EDGE('',*,*,#50847,.T.);
#71025=ORIENTED_EDGE('',*,*,#50848,.T.);
#71026=ORIENTED_EDGE('',*,*,#50849,.T.);
#71027=ORIENTED_EDGE('',*,*,#50220,.F.);
#71028=ORIENTED_EDGE('',*,*,#50850,.T.);
#71029=ORIENTED_EDGE('',*,*,#50851,.T.);
#71030=ORIENTED_EDGE('',*,*,#50852,.T.);
#71031=ORIENTED_EDGE('',*,*,#49725,.F.);
#71032=ORIENTED_EDGE('',*,*,#50853,.T.);
#71033=ORIENTED_EDGE('',*,*,#50854,.T.);
#71034=ORIENTED_EDGE('',*,*,#50855,.T.);
#71035=ORIENTED_EDGE('',*,*,#49755,.F.);
#71036=ORIENTED_EDGE('',*,*,#50856,.T.);
#71037=ORIENTED_EDGE('',*,*,#50857,.T.);
#71038=ORIENTED_EDGE('',*,*,#50477,.F.);
#71039=ORIENTED_EDGE('',*,*,#49891,.F.);
#71040=ORIENTED_EDGE('',*,*,#50504,.F.);
#71041=ORIENTED_EDGE('',*,*,#50858,.T.);
#71042=ORIENTED_EDGE('',*,*,#50859,.T.);
#71043=ORIENTED_EDGE('',*,*,#49508,.F.);
#71044=ORIENTED_EDGE('',*,*,#50516,.F.);
#71045=ORIENTED_EDGE('',*,*,#50860,.T.);
#71046=ORIENTED_EDGE('',*,*,#50856,.F.);
#71047=ORIENTED_EDGE('',*,*,#49887,.F.);
#71048=ORIENTED_EDGE('',*,*,#50859,.F.);
#71049=ORIENTED_EDGE('',*,*,#50861,.T.);
#71050=ORIENTED_EDGE('',*,*,#50511,.F.);
#71051=ORIENTED_EDGE('',*,*,#49502,.F.);
#71052=ORIENTED_EDGE('',*,*,#50834,.F.);
#71053=ORIENTED_EDGE('',*,*,#50862,.F.);
#71054=ORIENTED_EDGE('',*,*,#50841,.F.);
#71055=ORIENTED_EDGE('',*,*,#50255,.F.);
#71056=ORIENTED_EDGE('',*,*,#50845,.F.);
#71057=ORIENTED_EDGE('',*,*,#50863,.F.);
#71058=ORIENTED_EDGE('',*,*,#50832,.F.);
#71059=ORIENTED_EDGE('',*,*,#50249,.F.);
#71060=ORIENTED_EDGE('',*,*,#50831,.F.);
#71061=ORIENTED_EDGE('',*,*,#50864,.F.);
#71062=ORIENTED_EDGE('',*,*,#50847,.F.);
#71063=ORIENTED_EDGE('',*,*,#50217,.F.);
#71064=ORIENTED_EDGE('',*,*,#50456,.F.);
#71065=ORIENTED_EDGE('',*,*,#50865,.F.);
#71066=ORIENTED_EDGE('',*,*,#50829,.F.);
#71067=ORIENTED_EDGE('',*,*,#50211,.F.);
#71068=ORIENTED_EDGE('',*,*,#50855,.F.);
#71069=ORIENTED_EDGE('',*,*,#50866,.T.);
#71070=ORIENTED_EDGE('',*,*,#50478,.F.);
#71071=ORIENTED_EDGE('',*,*,#49761,.F.);
#71072=ORIENTED_EDGE('',*,*,#50839,.F.);
#71073=ORIENTED_EDGE('',*,*,#50867,.F.);
#71074=ORIENTED_EDGE('',*,*,#50835,.F.);
#71075=ORIENTED_EDGE('',*,*,#50233,.F.);
#71076=ORIENTED_EDGE('',*,*,#50837,.F.);
#71077=ORIENTED_EDGE('',*,*,#50868,.T.);
#71078=ORIENTED_EDGE('',*,*,#50469,.F.);
#71079=ORIENTED_EDGE('',*,*,#50239,.F.);
#71080=ORIENTED_EDGE('',*,*,#50468,.F.);
#71081=ORIENTED_EDGE('',*,*,#50869,.T.);
#71082=ORIENTED_EDGE('',*,*,#50450,.F.);
#71083=ORIENTED_EDGE('',*,*,#50183,.F.);
#71084=ORIENTED_EDGE('',*,*,#50449,.F.);
#71085=ORIENTED_EDGE('',*,*,#50870,.F.);
#71086=ORIENTED_EDGE('',*,*,#50463,.F.);
#71087=ORIENTED_EDGE('',*,*,#50189,.F.);
#71088=ORIENTED_EDGE('',*,*,#50492,.F.);
#71089=ORIENTED_EDGE('',*,*,#50871,.T.);
#71090=ORIENTED_EDGE('',*,*,#50850,.F.);
#71091=ORIENTED_EDGE('',*,*,#49719,.F.);
#71092=ORIENTED_EDGE('',*,*,#50534,.F.);
#71093=ORIENTED_EDGE('',*,*,#50872,.F.);
#71094=ORIENTED_EDGE('',*,*,#50541,.F.);
#71095=ORIENTED_EDGE('',*,*,#49581,.F.);
#71096=ORIENTED_EDGE('',*,*,#50690,.F.);
#71097=ORIENTED_EDGE('',*,*,#50873,.F.);
#71098=ORIENTED_EDGE('',*,*,#50685,.F.);
#71099=ORIENTED_EDGE('',*,*,#49637,.F.);
#71100=ORIENTED_EDGE('',*,*,#50678,.F.);
#71101=ORIENTED_EDGE('',*,*,#50874,.F.);
#71102=ORIENTED_EDGE('',*,*,#50673,.F.);
#71103=ORIENTED_EDGE('',*,*,#49613,.F.);
#71104=ORIENTED_EDGE('',*,*,#50546,.F.);
#71105=ORIENTED_EDGE('',*,*,#50875,.F.);
#71106=ORIENTED_EDGE('',*,*,#50553,.F.);
#71107=ORIENTED_EDGE('',*,*,#49605,.F.);
#71108=ORIENTED_EDGE('',*,*,#50666,.F.);
#71109=ORIENTED_EDGE('',*,*,#50876,.F.);
#71110=ORIENTED_EDGE('',*,*,#50661,.F.);
#71111=ORIENTED_EDGE('',*,*,#49667,.F.);
#71112=ORIENTED_EDGE('',*,*,#50582,.F.);
#71113=ORIENTED_EDGE('',*,*,#50877,.F.);
#71114=ORIENTED_EDGE('',*,*,#50589,.F.);
#71115=ORIENTED_EDGE('',*,*,#49707,.F.);
#71116=ORIENTED_EDGE('',*,*,#50654,.F.);
#71117=ORIENTED_EDGE('',*,*,#50878,.F.);
#71118=ORIENTED_EDGE('',*,*,#50649,.F.);
#71119=ORIENTED_EDGE('',*,*,#49803,.F.);
#71120=ORIENTED_EDGE('',*,*,#50594,.F.);
#71121=ORIENTED_EDGE('',*,*,#50879,.F.);
#71122=ORIENTED_EDGE('',*,*,#50601,.F.);
#71123=ORIENTED_EDGE('',*,*,#49787,.F.);
#71124=ORIENTED_EDGE('',*,*,#50570,.F.);
#71125=ORIENTED_EDGE('',*,*,#50880,.F.);
#71126=ORIENTED_EDGE('',*,*,#50577,.F.);
#71127=ORIENTED_EDGE('',*,*,#49926,.F.);
#71128=ORIENTED_EDGE('',*,*,#50630,.F.);
#71129=ORIENTED_EDGE('',*,*,#50881,.F.);
#71130=ORIENTED_EDGE('',*,*,#50625,.F.);
#71131=ORIENTED_EDGE('',*,*,#49964,.F.);
#71132=ORIENTED_EDGE('',*,*,#50642,.F.);
#71133=ORIENTED_EDGE('',*,*,#50882,.F.);
#71134=ORIENTED_EDGE('',*,*,#50637,.F.);
#71135=ORIENTED_EDGE('',*,*,#49902,.F.);
#71136=ORIENTED_EDGE('',*,*,#50606,.F.);
#71137=ORIENTED_EDGE('',*,*,#50883,.F.);
#71138=ORIENTED_EDGE('',*,*,#50613,.F.);
#71139=ORIENTED_EDGE('',*,*,#49827,.F.);
#71140=ORIENTED_EDGE('',*,*,#50621,.F.);
#71141=ORIENTED_EDGE('',*,*,#50884,.F.);
#71142=ORIENTED_EDGE('',*,*,#50616,.F.);
#71143=ORIENTED_EDGE('',*,*,#50114,.F.);
#71144=ORIENTED_EDGE('',*,*,#50558,.F.);
#71145=ORIENTED_EDGE('',*,*,#50885,.F.);
#71146=ORIENTED_EDGE('',*,*,#50565,.F.);
#71147=ORIENTED_EDGE('',*,*,#49980,.F.);
#71148=ORIENTED_EDGE('',*,*,#50525,.F.);
#71149=ORIENTED_EDGE('',*,*,#50886,.F.);
#71150=ORIENTED_EDGE('',*,*,#50531,.F.);
#71151=ORIENTED_EDGE('',*,*,#50120,.F.);
#71152=ORIENTED_EDGE('',*,*,#50702,.F.);
#71153=ORIENTED_EDGE('',*,*,#50887,.F.);
#71154=ORIENTED_EDGE('',*,*,#50697,.F.);
#71155=ORIENTED_EDGE('',*,*,#49412,.F.);
#71156=ORIENTED_EDGE('',*,*,#50774,.F.);
#71157=ORIENTED_EDGE('',*,*,#50888,.F.);
#71158=ORIENTED_EDGE('',*,*,#50769,.F.);
#71159=ORIENTED_EDGE('',*,*,#49434,.F.);
#71160=ORIENTED_EDGE('',*,*,#50708,.F.);
#71161=ORIENTED_EDGE('',*,*,#50889,.F.);
#71162=ORIENTED_EDGE('',*,*,#50705,.F.);
#71163=ORIENTED_EDGE('',*,*,#49388,.F.);
#71164=ORIENTED_EDGE('',*,*,#50540,.F.);
#71165=ORIENTED_EDGE('',*,*,#50890,.F.);
#71166=ORIENTED_EDGE('',*,*,#50535,.F.);
#71167=ORIENTED_EDGE('',*,*,#49565,.F.);
#71168=ORIENTED_EDGE('',*,*,#50723,.F.);
#71169=ORIENTED_EDGE('',*,*,#50891,.F.);
#71170=ORIENTED_EDGE('',*,*,#50730,.F.);
#71171=ORIENTED_EDGE('',*,*,#49557,.F.);
#71172=ORIENTED_EDGE('',*,*,#50564,.F.);
#71173=ORIENTED_EDGE('',*,*,#50892,.F.);
#71174=ORIENTED_EDGE('',*,*,#50559,.F.);
#71175=ORIENTED_EDGE('',*,*,#49988,.F.);
#71176=ORIENTED_EDGE('',*,*,#50714,.F.);
#71177=ORIENTED_EDGE('',*,*,#50893,.F.);
#71178=ORIENTED_EDGE('',*,*,#50709,.F.);
#71179=ORIENTED_EDGE('',*,*,#50010,.F.);
#71180=ORIENTED_EDGE('',*,*,#50552,.F.);
#71181=ORIENTED_EDGE('',*,*,#50894,.F.);
#71182=ORIENTED_EDGE('',*,*,#50547,.F.);
#71183=ORIENTED_EDGE('',*,*,#49589,.F.);
#71184=ORIENTED_EDGE('',*,*,#50735,.F.);
#71185=ORIENTED_EDGE('',*,*,#50895,.F.);
#71186=ORIENTED_EDGE('',*,*,#50742,.F.);
#71187=ORIENTED_EDGE('',*,*,#49533,.F.);
#71188=ORIENTED_EDGE('',*,*,#50588,.F.);
#71189=ORIENTED_EDGE('',*,*,#50896,.F.);
#71190=ORIENTED_EDGE('',*,*,#50583,.F.);
#71191=ORIENTED_EDGE('',*,*,#49691,.F.);
#71192=ORIENTED_EDGE('',*,*,#50498,.F.);
#71193=ORIENTED_EDGE('',*,*,#50897,.F.);
#71194=ORIENTED_EDGE('',*,*,#50493,.F.);
#71195=ORIENTED_EDGE('',*,*,#49727,.F.);
#71196=ORIENTED_EDGE('',*,*,#50600,.F.);
#71197=ORIENTED_EDGE('',*,*,#50898,.F.);
#71198=ORIENTED_EDGE('',*,*,#50595,.F.);
#71199=ORIENTED_EDGE('',*,*,#49779,.F.);
#71200=ORIENTED_EDGE('',*,*,#50489,.F.);
#71201=ORIENTED_EDGE('',*,*,#50899,.F.);
#71202=ORIENTED_EDGE('',*,*,#50484,.F.);
#71203=ORIENTED_EDGE('',*,*,#49757,.F.);
#71204=ORIENTED_EDGE('',*,*,#50636,.F.);
#71205=ORIENTED_EDGE('',*,*,#50900,.F.);
#71206=ORIENTED_EDGE('',*,*,#50631,.F.);
#71207=ORIENTED_EDGE('',*,*,#49956,.F.);
#71208=ORIENTED_EDGE('',*,*,#50762,.F.);
#71209=ORIENTED_EDGE('',*,*,#50901,.F.);
#71210=ORIENTED_EDGE('',*,*,#50757,.F.);
#71211=ORIENTED_EDGE('',*,*,#50042,.F.);
#71212=ORIENTED_EDGE('',*,*,#50612,.F.);
#71213=ORIENTED_EDGE('',*,*,#50902,.F.);
#71214=ORIENTED_EDGE('',*,*,#50607,.F.);
#71215=ORIENTED_EDGE('',*,*,#49835,.F.);
#71216=ORIENTED_EDGE('',*,*,#50747,.F.);
#71217=ORIENTED_EDGE('',*,*,#50903,.F.);
#71218=ORIENTED_EDGE('',*,*,#50754,.F.);
#71219=ORIENTED_EDGE('',*,*,#49851,.F.);
#71220=ORIENTED_EDGE('',*,*,#50904,.T.);
#71221=ORIENTED_EDGE('',*,*,#50905,.F.);
#71222=ORIENTED_EDGE('',*,*,#50906,.F.);
#71223=ORIENTED_EDGE('',*,*,#50907,.F.);
#71224=ORIENTED_EDGE('',*,*,#50908,.T.);
#71225=ORIENTED_EDGE('',*,*,#50909,.F.);
#71226=ORIENTED_EDGE('',*,*,#50904,.F.);
#71227=ORIENTED_EDGE('',*,*,#50910,.F.);
#71228=ORIENTED_EDGE('',*,*,#50906,.T.);
#71229=ORIENTED_EDGE('',*,*,#50911,.F.);
#71230=ORIENTED_EDGE('',*,*,#50912,.T.);
#71231=ORIENTED_EDGE('',*,*,#50913,.F.);
#71232=ORIENTED_EDGE('',*,*,#50822,.F.);
#71233=ORIENTED_EDGE('',*,*,#50914,.F.);
#71234=ORIENTED_EDGE('',*,*,#50817,.F.);
#71235=ORIENTED_EDGE('',*,*,#49458,.F.);
#71236=ORIENTED_EDGE('',*,*,#50780,.F.);
#71237=ORIENTED_EDGE('',*,*,#50915,.F.);
#71238=ORIENTED_EDGE('',*,*,#50777,.F.);
#71239=ORIENTED_EDGE('',*,*,#49418,.F.);
#71240=ORIENTED_EDGE('',*,*,#50729,.F.);
#71241=ORIENTED_EDGE('',*,*,#50916,.F.);
#71242=ORIENTED_EDGE('',*,*,#50724,.F.);
#71243=ORIENTED_EDGE('',*,*,#49541,.F.);
#71244=ORIENTED_EDGE('',*,*,#50795,.F.);
#71245=ORIENTED_EDGE('',*,*,#50917,.F.);
#71246=ORIENTED_EDGE('',*,*,#50802,.F.);
#71247=ORIENTED_EDGE('',*,*,#49482,.F.);
#71248=ORIENTED_EDGE('',*,*,#50720,.F.);
#71249=ORIENTED_EDGE('',*,*,#50918,.F.);
#71250=ORIENTED_EDGE('',*,*,#50715,.F.);
#71251=ORIENTED_EDGE('',*,*,#50018,.F.);
#71252=ORIENTED_EDGE('',*,*,#50786,.F.);
#71253=ORIENTED_EDGE('',*,*,#50919,.F.);
#71254=ORIENTED_EDGE('',*,*,#50781,.F.);
#71255=ORIENTED_EDGE('',*,*,#50058,.F.);
#71256=ORIENTED_EDGE('',*,*,#50741,.F.);
#71257=ORIENTED_EDGE('',*,*,#50920,.F.);
#71258=ORIENTED_EDGE('',*,*,#50736,.F.);
#71259=ORIENTED_EDGE('',*,*,#49517,.F.);
#71260=ORIENTED_EDGE('',*,*,#50507,.F.);
#71261=ORIENTED_EDGE('',*,*,#50921,.F.);
#71262=ORIENTED_EDGE('',*,*,#50502,.F.);
#71263=ORIENTED_EDGE('',*,*,#49506,.F.);
#71264=ORIENTED_EDGE('',*,*,#50852,.F.);
#71265=ORIENTED_EDGE('',*,*,#50922,.F.);
#71266=ORIENTED_EDGE('',*,*,#50499,.F.);
#71267=ORIENTED_EDGE('',*,*,#49731,.F.);
#71268=ORIENTED_EDGE('',*,*,#50483,.F.);
#71269=ORIENTED_EDGE('',*,*,#50923,.F.);
#71270=ORIENTED_EDGE('',*,*,#50853,.F.);
#71271=ORIENTED_EDGE('',*,*,#49749,.F.);
#71272=ORIENTED_EDGE('',*,*,#50768,.F.);
#71273=ORIENTED_EDGE('',*,*,#50924,.F.);
#71274=ORIENTED_EDGE('',*,*,#50763,.F.);
#71275=ORIENTED_EDGE('',*,*,#50034,.F.);
#71276=ORIENTED_EDGE('',*,*,#50810,.F.);
#71277=ORIENTED_EDGE('',*,*,#50925,.F.);
#71278=ORIENTED_EDGE('',*,*,#50805,.F.);
#71279=ORIENTED_EDGE('',*,*,#50090,.F.);
#71280=ORIENTED_EDGE('',*,*,#50753,.F.);
#71281=ORIENTED_EDGE('',*,*,#50926,.F.);
#71282=ORIENTED_EDGE('',*,*,#50748,.F.);
#71283=ORIENTED_EDGE('',*,*,#49859,.F.);
#71284=ORIENTED_EDGE('',*,*,#50476,.F.);
#71285=ORIENTED_EDGE('',*,*,#50927,.F.);
#71286=ORIENTED_EDGE('',*,*,#50520,.F.);
#71287=ORIENTED_EDGE('',*,*,#49883,.F.);
#71288=ORIENTED_EDGE('',*,*,#50513,.F.);
#71289=ORIENTED_EDGE('',*,*,#50928,.F.);
#71290=ORIENTED_EDGE('',*,*,#50508,.F.);
#71291=ORIENTED_EDGE('',*,*,#49490,.F.);
#71292=ORIENTED_EDGE('',*,*,#50816,.F.);
#71293=ORIENTED_EDGE('',*,*,#50929,.F.);
#71294=ORIENTED_EDGE('',*,*,#50811,.F.);
#71295=ORIENTED_EDGE('',*,*,#50082,.F.);
#71296=ORIENTED_EDGE('',*,*,#50519,.F.);
#71297=ORIENTED_EDGE('',*,*,#50930,.F.);
#71298=ORIENTED_EDGE('',*,*,#50514,.F.);
#71299=ORIENTED_EDGE('',*,*,#49875,.F.);
#71300=ORIENTED_EDGE('',*,*,#50843,.F.);
#71301=ORIENTED_EDGE('',*,*,#50931,.F.);
#71302=ORIENTED_EDGE('',*,*,#50451,.F.);
#71303=ORIENTED_EDGE('',*,*,#50261,.F.);
#71304=ORIENTED_EDGE('',*,*,#50474,.F.);
#71305=ORIENTED_EDGE('',*,*,#50932,.F.);
#71306=ORIENTED_EDGE('',*,*,#50840,.F.);
#71307=ORIENTED_EDGE('',*,*,#50227,.F.);
#71308=ORIENTED_EDGE('',*,*,#50801,.F.);
#71309=ORIENTED_EDGE('',*,*,#50933,.F.);
#71310=ORIENTED_EDGE('',*,*,#50796,.F.);
#71311=ORIENTED_EDGE('',*,*,#49466,.F.);
#71312=ORIENTED_EDGE('',*,*,#50828,.F.);
#71313=ORIENTED_EDGE('',*,*,#50934,.F.);
#71314=ORIENTED_EDGE('',*,*,#50825,.F.);
#71315=ORIENTED_EDGE('',*,*,#49442,.F.);
#71316=ORIENTED_EDGE('',*,*,#50792,.F.);
#71317=ORIENTED_EDGE('',*,*,#50935,.F.);
#71318=ORIENTED_EDGE('',*,*,#50787,.F.);
#71319=ORIENTED_EDGE('',*,*,#50066,.F.);
#71320=ORIENTED_EDGE('',*,*,#50936,.T.);
#71321=ORIENTED_EDGE('',*,*,#50937,.T.);
#71322=ORIENTED_EDGE('',*,*,#50938,.F.);
#71323=ORIENTED_EDGE('',*,*,#50939,.F.);
#71324=ORIENTED_EDGE('',*,*,#50940,.F.);
#71325=ORIENTED_EDGE('',*,*,#50941,.F.);
#71326=ORIENTED_EDGE('',*,*,#50942,.F.);
#71327=ORIENTED_EDGE('',*,*,#50938,.T.);
#71328=ORIENTED_EDGE('',*,*,#50941,.T.);
#71329=ORIENTED_EDGE('',*,*,#50943,.T.);
#71330=ORIENTED_EDGE('',*,*,#50944,.F.);
#71331=ORIENTED_EDGE('',*,*,#50945,.F.);
#71332=ORIENTED_EDGE('',*,*,#50944,.T.);
#71333=ORIENTED_EDGE('',*,*,#50946,.T.);
#71334=ORIENTED_EDGE('',*,*,#50947,.F.);
#71335=ORIENTED_EDGE('',*,*,#50948,.F.);
#71336=ORIENTED_EDGE('',*,*,#50947,.T.);
#71337=ORIENTED_EDGE('',*,*,#50949,.T.);
#71338=ORIENTED_EDGE('',*,*,#50950,.F.);
#71339=ORIENTED_EDGE('',*,*,#50951,.F.);
#71340=ORIENTED_EDGE('',*,*,#50952,.F.);
#71341=ORIENTED_EDGE('',*,*,#50953,.F.);
#71342=ORIENTED_EDGE('',*,*,#50954,.F.);
#71343=ORIENTED_EDGE('',*,*,#50950,.T.);
#71344=ORIENTED_EDGE('',*,*,#50953,.T.);
#71345=ORIENTED_EDGE('',*,*,#50955,.T.);
#71346=ORIENTED_EDGE('',*,*,#50956,.F.);
#71347=ORIENTED_EDGE('',*,*,#50957,.F.);
#71348=ORIENTED_EDGE('',*,*,#50958,.T.);
#71349=ORIENTED_EDGE('',*,*,#50959,.F.);
#71350=ORIENTED_EDGE('',*,*,#50960,.T.);
#71351=ORIENTED_EDGE('',*,*,#50961,.F.);
#71352=ORIENTED_EDGE('',*,*,#50962,.F.);
#71353=ORIENTED_EDGE('',*,*,#50963,.T.);
#71354=ORIENTED_EDGE('',*,*,#50958,.F.);
#71355=ORIENTED_EDGE('',*,*,#50964,.T.);
#71356=ORIENTED_EDGE('',*,*,#50965,.T.);
#71357=ORIENTED_EDGE('',*,*,#50966,.T.);
#71358=ORIENTED_EDGE('',*,*,#50967,.F.);
#71359=ORIENTED_EDGE('',*,*,#50968,.T.);
#71360=ORIENTED_EDGE('',*,*,#50966,.F.);
#71361=ORIENTED_EDGE('',*,*,#50969,.F.);
#71362=ORIENTED_EDGE('',*,*,#50970,.T.);
#71363=ORIENTED_EDGE('',*,*,#50971,.F.);
#71364=ORIENTED_EDGE('',*,*,#50972,.T.);
#71365=ORIENTED_EDGE('',*,*,#50973,.F.);
#71366=ORIENTED_EDGE('',*,*,#50974,.T.);
#71367=ORIENTED_EDGE('',*,*,#50975,.F.);
#71368=ORIENTED_EDGE('',*,*,#50976,.F.);
#71369=ORIENTED_EDGE('',*,*,#50977,.F.);
#71370=ORIENTED_EDGE('',*,*,#50976,.T.);
#71371=ORIENTED_EDGE('',*,*,#50978,.F.);
#71372=ORIENTED_EDGE('',*,*,#50970,.F.);
#71373=ORIENTED_EDGE('',*,*,#50979,.F.);
#71374=ORIENTED_EDGE('',*,*,#50980,.T.);
#71375=ORIENTED_EDGE('',*,*,#50981,.F.);
#71376=ORIENTED_EDGE('',*,*,#50982,.F.);
#71377=ORIENTED_EDGE('',*,*,#50983,.F.);
#71378=ORIENTED_EDGE('',*,*,#50984,.T.);
#71379=ORIENTED_EDGE('',*,*,#50985,.F.);
#71380=ORIENTED_EDGE('',*,*,#50986,.T.);
#71381=ORIENTED_EDGE('',*,*,#50987,.F.);
#71382=ORIENTED_EDGE('',*,*,#50982,.T.);
#71383=ORIENTED_EDGE('',*,*,#50988,.F.);
#71384=ORIENTED_EDGE('',*,*,#50984,.F.);
#71385=ORIENTED_EDGE('',*,*,#50989,.T.);
#71386=ORIENTED_EDGE('',*,*,#50990,.F.);
#71387=ORIENTED_EDGE('',*,*,#50991,.F.);
#71388=ORIENTED_EDGE('',*,*,#50992,.T.);
#71389=ORIENTED_EDGE('',*,*,#50993,.T.);
#71390=ORIENTED_EDGE('',*,*,#50994,.F.);
#71391=ORIENTED_EDGE('',*,*,#50995,.F.);
#71392=ORIENTED_EDGE('',*,*,#50996,.T.);
#71393=ORIENTED_EDGE('',*,*,#50997,.T.);
#71394=ORIENTED_EDGE('',*,*,#50998,.F.);
#71395=ORIENTED_EDGE('',*,*,#50999,.F.);
#71396=ORIENTED_EDGE('',*,*,#50994,.T.);
#71397=ORIENTED_EDGE('',*,*,#51000,.T.);
#71398=ORIENTED_EDGE('',*,*,#51001,.F.);
#71399=ORIENTED_EDGE('',*,*,#51002,.F.);
#71400=ORIENTED_EDGE('',*,*,#50998,.T.);
#71401=ORIENTED_EDGE('',*,*,#51003,.F.);
#71402=ORIENTED_EDGE('',*,*,#51004,.F.);
#71403=ORIENTED_EDGE('',*,*,#51001,.T.);
#71404=ORIENTED_EDGE('',*,*,#51005,.T.);
#71405=ORIENTED_EDGE('',*,*,#51006,.T.);
#71406=ORIENTED_EDGE('',*,*,#51007,.F.);
#71407=ORIENTED_EDGE('',*,*,#51008,.F.);
#71408=ORIENTED_EDGE('',*,*,#51009,.T.);
#71409=ORIENTED_EDGE('',*,*,#51010,.T.);
#71410=ORIENTED_EDGE('',*,*,#50992,.F.);
#71411=ORIENTED_EDGE('',*,*,#51011,.F.);
#71412=ORIENTED_EDGE('',*,*,#51007,.T.);
#71413=ORIENTED_EDGE('',*,*,#51012,.F.);
#71414=ORIENTED_EDGE('',*,*,#51013,.T.);
#71415=ORIENTED_EDGE('',*,*,#51014,.F.);
#71416=ORIENTED_EDGE('',*,*,#51015,.T.);
#71417=ORIENTED_EDGE('',*,*,#51016,.F.);
#71418=ORIENTED_EDGE('',*,*,#51017,.F.);
#71419=ORIENTED_EDGE('',*,*,#51018,.T.);
#71420=ORIENTED_EDGE('',*,*,#51019,.T.);
#71421=ORIENTED_EDGE('',*,*,#51020,.T.);
#71422=ORIENTED_EDGE('',*,*,#51021,.F.);
#71423=ORIENTED_EDGE('',*,*,#51022,.F.);
#71424=ORIENTED_EDGE('',*,*,#51023,.T.);
#71425=ORIENTED_EDGE('',*,*,#51024,.F.);
#71426=ORIENTED_EDGE('',*,*,#51025,.T.);
#71427=ORIENTED_EDGE('',*,*,#51026,.F.);
#71428=ORIENTED_EDGE('',*,*,#51027,.F.);
#71429=ORIENTED_EDGE('',*,*,#51028,.T.);
#71430=ORIENTED_EDGE('',*,*,#51029,.T.);
#71431=ORIENTED_EDGE('',*,*,#51030,.T.);
#71432=ORIENTED_EDGE('',*,*,#51031,.T.);
#71433=ORIENTED_EDGE('',*,*,#51032,.T.);
#71434=ORIENTED_EDGE('',*,*,#51033,.F.);
#71435=ORIENTED_EDGE('',*,*,#51019,.F.);
#71436=ORIENTED_EDGE('',*,*,#51034,.F.);
#71437=ORIENTED_EDGE('',*,*,#51035,.T.);
#71438=ORIENTED_EDGE('',*,*,#51036,.F.);
#71439=ORIENTED_EDGE('',*,*,#50973,.T.);
#71440=ORIENTED_EDGE('',*,*,#50977,.T.);
#71441=ORIENTED_EDGE('',*,*,#50969,.T.);
#71442=ORIENTED_EDGE('',*,*,#51037,.F.);
#71443=ORIENTED_EDGE('',*,*,#51038,.T.);
#71444=ORIENTED_EDGE('',*,*,#51039,.T.);
#71445=ORIENTED_EDGE('',*,*,#51035,.F.);
#71446=ORIENTED_EDGE('',*,*,#51040,.T.);
#71447=ORIENTED_EDGE('',*,*,#51038,.F.);
#71448=ORIENTED_EDGE('',*,*,#51041,.T.);
#71449=ORIENTED_EDGE('',*,*,#51015,.F.);
#71450=ORIENTED_EDGE('',*,*,#51042,.T.);
#71451=ORIENTED_EDGE('',*,*,#51043,.T.);
#71452=ORIENTED_EDGE('',*,*,#51044,.F.);
#71453=ORIENTED_EDGE('',*,*,#51029,.F.);
#71454=ORIENTED_EDGE('',*,*,#51045,.F.);
#71455=ORIENTED_EDGE('',*,*,#51046,.T.);
#71456=ORIENTED_EDGE('',*,*,#50987,.T.);
#71457=ORIENTED_EDGE('',*,*,#50983,.T.);
#71458=ORIENTED_EDGE('',*,*,#51047,.F.);
#71459=ORIENTED_EDGE('',*,*,#51048,.T.);
#71460=ORIENTED_EDGE('',*,*,#51049,.T.);
#71461=ORIENTED_EDGE('',*,*,#51046,.F.);
#71462=ORIENTED_EDGE('',*,*,#51050,.F.);
#71463=ORIENTED_EDGE('',*,*,#50979,.T.);
#71464=ORIENTED_EDGE('',*,*,#51051,.T.);
#71465=ORIENTED_EDGE('',*,*,#51048,.F.);
#71466=ORIENTED_EDGE('',*,*,#51052,.T.);
#71467=ORIENTED_EDGE('',*,*,#51025,.F.);
#71468=ORIENTED_EDGE('',*,*,#51053,.T.);
#71469=ORIENTED_EDGE('',*,*,#51054,.T.);
#71470=ORIENTED_EDGE('',*,*,#51055,.F.);
#71471=ORIENTED_EDGE('',*,*,#51056,.F.);
#71472=ORIENTED_EDGE('',*,*,#51057,.T.);
#71473=ORIENTED_EDGE('',*,*,#51058,.T.);
#71474=ORIENTED_EDGE('',*,*,#51057,.F.);
#71475=ORIENTED_EDGE('',*,*,#51059,.F.);
#71476=ORIENTED_EDGE('',*,*,#51060,.T.);
#71477=ORIENTED_EDGE('',*,*,#51061,.T.);
#71478=ORIENTED_EDGE('',*,*,#51060,.F.);
#71479=ORIENTED_EDGE('',*,*,#51062,.F.);
#71480=ORIENTED_EDGE('',*,*,#51063,.T.);
#71481=ORIENTED_EDGE('',*,*,#51064,.T.);
#71482=ORIENTED_EDGE('',*,*,#51063,.F.);
#71483=ORIENTED_EDGE('',*,*,#51065,.F.);
#71484=ORIENTED_EDGE('',*,*,#51066,.T.);
#71485=ORIENTED_EDGE('',*,*,#51067,.T.);
#71486=ORIENTED_EDGE('',*,*,#51068,.F.);
#71487=ORIENTED_EDGE('',*,*,#51069,.F.);
#71488=ORIENTED_EDGE('',*,*,#51070,.T.);
#71489=ORIENTED_EDGE('',*,*,#51071,.T.);
#71490=ORIENTED_EDGE('',*,*,#51070,.F.);
#71491=ORIENTED_EDGE('',*,*,#51072,.F.);
#71492=ORIENTED_EDGE('',*,*,#51073,.T.);
#71493=ORIENTED_EDGE('',*,*,#51074,.T.);
#71494=ORIENTED_EDGE('',*,*,#51073,.F.);
#71495=ORIENTED_EDGE('',*,*,#51075,.F.);
#71496=ORIENTED_EDGE('',*,*,#51055,.T.);
#71497=ORIENTED_EDGE('',*,*,#51076,.F.);
#71498=ORIENTED_EDGE('',*,*,#51077,.T.);
#71499=ORIENTED_EDGE('',*,*,#51078,.T.);
#71500=ORIENTED_EDGE('',*,*,#51013,.F.);
#71501=ORIENTED_EDGE('',*,*,#51079,.T.);
#71502=ORIENTED_EDGE('',*,*,#51080,.T.);
#71503=ORIENTED_EDGE('',*,*,#51081,.F.);
#71504=ORIENTED_EDGE('',*,*,#51031,.F.);
#71505=ORIENTED_EDGE('',*,*,#51082,.F.);
#71506=ORIENTED_EDGE('',*,*,#51079,.F.);
#71507=ORIENTED_EDGE('',*,*,#51030,.F.);
#71508=ORIENTED_EDGE('',*,*,#51044,.T.);
#71509=ORIENTED_EDGE('',*,*,#51083,.T.);
#71510=ORIENTED_EDGE('',*,*,#51042,.F.);
#71511=ORIENTED_EDGE('',*,*,#51014,.T.);
#71512=ORIENTED_EDGE('',*,*,#51078,.F.);
#71513=ORIENTED_EDGE('',*,*,#51084,.F.);
#71514=ORIENTED_EDGE('',*,*,#51085,.T.);
#71515=ORIENTED_EDGE('',*,*,#51086,.T.);
#71516=ORIENTED_EDGE('',*,*,#51023,.F.);
#71517=ORIENTED_EDGE('',*,*,#51087,.F.);
#71518=ORIENTED_EDGE('',*,*,#51088,.T.);
#71519=ORIENTED_EDGE('',*,*,#51076,.T.);
#71520=ORIENTED_EDGE('',*,*,#51012,.T.);
#71521=ORIENTED_EDGE('',*,*,#51089,.T.);
#71522=ORIENTED_EDGE('',*,*,#51017,.T.);
#71523=ORIENTED_EDGE('',*,*,#51090,.T.);
#71524=ORIENTED_EDGE('',*,*,#51091,.F.);
#71525=ORIENTED_EDGE('',*,*,#51092,.F.);
#71526=ORIENTED_EDGE('',*,*,#50989,.F.);
#71527=ORIENTED_EDGE('',*,*,#51010,.F.);
#71528=ORIENTED_EDGE('',*,*,#51006,.F.);
#71529=ORIENTED_EDGE('',*,*,#51093,.F.);
#71530=ORIENTED_EDGE('',*,*,#51090,.F.);
#71531=ORIENTED_EDGE('',*,*,#51021,.T.);
#71532=ORIENTED_EDGE('',*,*,#51094,.T.);
#71533=ORIENTED_EDGE('',*,*,#51095,.F.);
#71534=ORIENTED_EDGE('',*,*,#50985,.T.);
#71535=ORIENTED_EDGE('',*,*,#50988,.T.);
#71536=ORIENTED_EDGE('',*,*,#50981,.T.);
#71537=ORIENTED_EDGE('',*,*,#51096,.F.);
#71538=ORIENTED_EDGE('',*,*,#51097,.T.);
#71539=ORIENTED_EDGE('',*,*,#51098,.F.);
#71540=ORIENTED_EDGE('',*,*,#51096,.T.);
#71541=ORIENTED_EDGE('',*,*,#50980,.F.);
#71542=ORIENTED_EDGE('',*,*,#51050,.T.);
#71543=ORIENTED_EDGE('',*,*,#51045,.T.);
#71544=ORIENTED_EDGE('',*,*,#51028,.F.);
#71545=ORIENTED_EDGE('',*,*,#51099,.F.);
#71546=ORIENTED_EDGE('',*,*,#51026,.T.);
#71547=ORIENTED_EDGE('',*,*,#51052,.F.);
#71548=ORIENTED_EDGE('',*,*,#51047,.T.);
#71549=ORIENTED_EDGE('',*,*,#50986,.F.);
#71550=ORIENTED_EDGE('',*,*,#51095,.T.);
#71551=ORIENTED_EDGE('',*,*,#51100,.T.);
#71552=ORIENTED_EDGE('',*,*,#50967,.T.);
#71553=ORIENTED_EDGE('',*,*,#50965,.F.);
#71554=ORIENTED_EDGE('',*,*,#51101,.F.);
#71555=ORIENTED_EDGE('',*,*,#51102,.F.);
#71556=ORIENTED_EDGE('',*,*,#51103,.T.);
#71557=ORIENTED_EDGE('',*,*,#50975,.T.);
#71558=ORIENTED_EDGE('',*,*,#51104,.F.);
#71559=ORIENTED_EDGE('',*,*,#51105,.T.);
#71560=ORIENTED_EDGE('',*,*,#51106,.F.);
#71561=ORIENTED_EDGE('',*,*,#50971,.T.);
#71562=ORIENTED_EDGE('',*,*,#50978,.T.);
#71563=ORIENTED_EDGE('',*,*,#51107,.F.);
#71564=ORIENTED_EDGE('',*,*,#51104,.T.);
#71565=ORIENTED_EDGE('',*,*,#50974,.F.);
#71566=ORIENTED_EDGE('',*,*,#51036,.T.);
#71567=ORIENTED_EDGE('',*,*,#51034,.T.);
#71568=ORIENTED_EDGE('',*,*,#51018,.F.);
#71569=ORIENTED_EDGE('',*,*,#51089,.F.);
#71570=ORIENTED_EDGE('',*,*,#51016,.T.);
#71571=ORIENTED_EDGE('',*,*,#51041,.F.);
#71572=ORIENTED_EDGE('',*,*,#51037,.T.);
#71573=ORIENTED_EDGE('',*,*,#50972,.F.);
#71574=ORIENTED_EDGE('',*,*,#51106,.T.);
#71575=ORIENTED_EDGE('',*,*,#51108,.F.);
#71576=ORIENTED_EDGE('',*,*,#50962,.T.);
#71577=ORIENTED_EDGE('',*,*,#50961,.T.);
#71578=ORIENTED_EDGE('',*,*,#51109,.T.);
#71579=ORIENTED_EDGE('',*,*,#51110,.F.);
#71580=ORIENTED_EDGE('',*,*,#51111,.T.);
#71581=ORIENTED_EDGE('',*,*,#51112,.T.);
#71582=ORIENTED_EDGE('',*,*,#51005,.F.);
#71583=ORIENTED_EDGE('',*,*,#51000,.F.);
#71584=ORIENTED_EDGE('',*,*,#50997,.F.);
#71585=ORIENTED_EDGE('',*,*,#50993,.F.);
#71586=ORIENTED_EDGE('',*,*,#51113,.F.);
#71587=ORIENTED_EDGE('',*,*,#51114,.T.);
#71588=ORIENTED_EDGE('',*,*,#51084,.T.);
#71589=ORIENTED_EDGE('',*,*,#51022,.T.);
#71590=ORIENTED_EDGE('',*,*,#51099,.T.);
#71591=ORIENTED_EDGE('',*,*,#51027,.T.);
#71592=ORIENTED_EDGE('',*,*,#51081,.T.);
#71593=ORIENTED_EDGE('',*,*,#51115,.F.);
#71594=ORIENTED_EDGE('',*,*,#51116,.T.);
#71595=ORIENTED_EDGE('',*,*,#51117,.F.);
#71596=ORIENTED_EDGE('',*,*,#51118,.T.);
#71597=ORIENTED_EDGE('',*,*,#51119,.F.);
#71598=ORIENTED_EDGE('',*,*,#51120,.T.);
#71599=ORIENTED_EDGE('',*,*,#51121,.F.);
#71600=ORIENTED_EDGE('',*,*,#51122,.F.);
#71601=ORIENTED_EDGE('',*,*,#51102,.T.);
#71602=ORIENTED_EDGE('',*,*,#51123,.T.);
#71603=ORIENTED_EDGE('',*,*,#51124,.T.);
#71604=ORIENTED_EDGE('',*,*,#51125,.F.);
#71605=ORIENTED_EDGE('',*,*,#51126,.F.);
#71606=ORIENTED_EDGE('',*,*,#51127,.T.);
#71607=ORIENTED_EDGE('',*,*,#51117,.T.);
#71608=ORIENTED_EDGE('',*,*,#51128,.F.);
#71609=ORIENTED_EDGE('',*,*,#51129,.T.);
#71610=ORIENTED_EDGE('',*,*,#51115,.T.);
#71611=ORIENTED_EDGE('',*,*,#51130,.T.);
#71612=ORIENTED_EDGE('',*,*,#51131,.F.);
#71613=ORIENTED_EDGE('',*,*,#51132,.T.);
#71614=ORIENTED_EDGE('',*,*,#51087,.T.);
#71615=ORIENTED_EDGE('',*,*,#51009,.F.);
#71616=ORIENTED_EDGE('',*,*,#51133,.F.);
#71617=ORIENTED_EDGE('',*,*,#51134,.T.);
#71618=ORIENTED_EDGE('',*,*,#51119,.T.);
#71619=ORIENTED_EDGE('',*,*,#51135,.T.);
#71620=ORIENTED_EDGE('',*,*,#51136,.F.);
#71621=ORIENTED_EDGE('',*,*,#51122,.T.);
#71622=ORIENTED_EDGE('',*,*,#51137,.T.);
#71623=ORIENTED_EDGE('',*,*,#51138,.F.);
#71624=ORIENTED_EDGE('',*,*,#50990,.T.);
#71625=ORIENTED_EDGE('',*,*,#51092,.T.);
#71626=ORIENTED_EDGE('',*,*,#50960,.F.);
#71627=ORIENTED_EDGE('',*,*,#51139,.T.);
#71628=ORIENTED_EDGE('',*,*,#51109,.F.);
#71629=ORIENTED_EDGE('',*,*,#51140,.F.);
#71630=ORIENTED_EDGE('',*,*,#51123,.F.);
#71631=ORIENTED_EDGE('',*,*,#51101,.T.);
#71632=ORIENTED_EDGE('',*,*,#50964,.F.);
#71633=ORIENTED_EDGE('',*,*,#50968,.F.);
#71634=ORIENTED_EDGE('',*,*,#51100,.F.);
#71635=ORIENTED_EDGE('',*,*,#51097,.F.);
#71636=ORIENTED_EDGE('',*,*,#51098,.T.);
#71637=ORIENTED_EDGE('',*,*,#51124,.F.);
#71638=ORIENTED_EDGE('',*,*,#51140,.T.);
#71639=ORIENTED_EDGE('',*,*,#51103,.F.);
#71640=ORIENTED_EDGE('',*,*,#51141,.F.);
#71641=ORIENTED_EDGE('',*,*,#51142,.T.);
#71642=ORIENTED_EDGE('',*,*,#51003,.T.);
#71643=ORIENTED_EDGE('',*,*,#51112,.F.);
#71644=ORIENTED_EDGE('',*,*,#51080,.F.);
#71645=ORIENTED_EDGE('',*,*,#51082,.T.);
#71646=ORIENTED_EDGE('',*,*,#51077,.F.);
#71647=ORIENTED_EDGE('',*,*,#51088,.F.);
#71648=ORIENTED_EDGE('',*,*,#51132,.F.);
#71649=ORIENTED_EDGE('',*,*,#51143,.F.);
#71650=ORIENTED_EDGE('',*,*,#51144,.F.);
#71651=ORIENTED_EDGE('',*,*,#51135,.F.);
#71652=ORIENTED_EDGE('',*,*,#51120,.F.);
#71653=ORIENTED_EDGE('',*,*,#51134,.F.);
#71654=ORIENTED_EDGE('',*,*,#51145,.F.);
#71655=ORIENTED_EDGE('',*,*,#51125,.T.);
#71656=ORIENTED_EDGE('',*,*,#51118,.F.);
#71657=ORIENTED_EDGE('',*,*,#51127,.F.);
#71658=ORIENTED_EDGE('',*,*,#51146,.F.);
#71659=ORIENTED_EDGE('',*,*,#51130,.F.);
#71660=ORIENTED_EDGE('',*,*,#51116,.F.);
#71661=ORIENTED_EDGE('',*,*,#51129,.F.);
#71662=ORIENTED_EDGE('',*,*,#51105,.F.);
#71663=ORIENTED_EDGE('',*,*,#51107,.T.);
#71664=ORIENTED_EDGE('',*,*,#51139,.F.);
#71665=ORIENTED_EDGE('',*,*,#50959,.T.);
#71666=ORIENTED_EDGE('',*,*,#50963,.F.);
#71667=ORIENTED_EDGE('',*,*,#51108,.T.);
#71668=ORIENTED_EDGE('',*,*,#51147,.F.);
#71669=ORIENTED_EDGE('',*,*,#51148,.T.);
#71670=ORIENTED_EDGE('',*,*,#51149,.T.);
#71671=ORIENTED_EDGE('',*,*,#49398,.F.);
#71672=ORIENTED_EDGE('',*,*,#50696,.F.);
#71673=ORIENTED_EDGE('',*,*,#51150,.T.);
#71674=ORIENTED_EDGE('',*,*,#51151,.T.);
#71675=ORIENTED_EDGE('',*,*,#49653,.F.);
#71676=ORIENTED_EDGE('',*,*,#51151,.F.);
#71677=ORIENTED_EDGE('',*,*,#51152,.T.);
#71678=ORIENTED_EDGE('',*,*,#51153,.T.);
#71679=ORIENTED_EDGE('',*,*,#49659,.F.);
#71680=ORIENTED_EDGE('',*,*,#50684,.F.);
#71681=ORIENTED_EDGE('',*,*,#51154,.T.);
#71682=ORIENTED_EDGE('',*,*,#50679,.F.);
#71683=ORIENTED_EDGE('',*,*,#49629,.F.);
#71684=ORIENTED_EDGE('',*,*,#51155,.F.);
#71685=ORIENTED_EDGE('',*,*,#51156,.T.);
#71686=ORIENTED_EDGE('',*,*,#51157,.T.);
#71687=ORIENTED_EDGE('',*,*,#49940,.F.);
#71688=ORIENTED_EDGE('',*,*,#51157,.F.);
#71689=ORIENTED_EDGE('',*,*,#51158,.T.);
#71690=ORIENTED_EDGE('',*,*,#50571,.F.);
#71691=ORIENTED_EDGE('',*,*,#49934,.F.);
#71692=ORIENTED_EDGE('',*,*,#51159,.F.);
#71693=ORIENTED_EDGE('',*,*,#51160,.T.);
#71694=ORIENTED_EDGE('',*,*,#51161,.T.);
#71695=ORIENTED_EDGE('',*,*,#49998,.F.);
#71696=ORIENTED_EDGE('',*,*,#51162,.F.);
#71697=ORIENTED_EDGE('',*,*,#51162,.T.);
#71698=ORIENTED_EDGE('',*,*,#51163,.T.);
#71699=ORIENTED_EDGE('',*,*,#51164,.F.);
#71700=ORIENTED_EDGE('',*,*,#49134,.F.);
#71701=ORIENTED_EDGE('',*,*,#51165,.F.);
#71702=ORIENTED_EDGE('',*,*,#51163,.F.);
#71703=ORIENTED_EDGE('',*,*,#51166,.F.);
#71704=ORIENTED_EDGE('',*,*,#51166,.T.);
#71705=ORIENTED_EDGE('',*,*,#51167,.T.);
#71706=ORIENTED_EDGE('',*,*,#49137,.F.);
#71707=ORIENTED_EDGE('',*,*,#49138,.F.);
#71708=ORIENTED_EDGE('',*,*,#51167,.F.);
#71709=ORIENTED_EDGE('',*,*,#49366,.F.);
#71710=ORIENTED_EDGE('',*,*,#49362,.F.);
#71711=ORIENTED_EDGE('',*,*,#49361,.F.);
#71712=ORIENTED_EDGE('',*,*,#49358,.F.);
#71713=ORIENTED_EDGE('',*,*,#49353,.F.);
#71714=ORIENTED_EDGE('',*,*,#49155,.F.);
#71715=ORIENTED_EDGE('',*,*,#49135,.F.);
#71716=ORIENTED_EDGE('',*,*,#49355,.F.);
#71717=ORIENTED_EDGE('',*,*,#49375,.F.);
#71718=ORIENTED_EDGE('',*,*,#49144,.F.);
#71719=ORIENTED_EDGE('',*,*,#49377,.F.);
#71720=ORIENTED_EDGE('',*,*,#49365,.F.);
#71721=ORIENTED_EDGE('',*,*,#49167,.F.);
#71722=ORIENTED_EDGE('',*,*,#49376,.F.);
#71723=ORIENTED_EDGE('',*,*,#49360,.F.);
#71724=ORIENTED_EDGE('',*,*,#49378,.F.);
#71725=ORIENTED_EDGE('',*,*,#49159,.F.);
#71726=ORIENTED_EDGE('',*,*,#49324,.F.);
#71727=ORIENTED_EDGE('',*,*,#49322,.F.);
#71728=ORIENTED_EDGE('',*,*,#49316,.F.);
#71729=ORIENTED_EDGE('',*,*,#51168,.F.);
#71730=ORIENTED_EDGE('',*,*,#49319,.F.);
#71731=ORIENTED_EDGE('',*,*,#49314,.F.);
#71732=ORIENTED_EDGE('',*,*,#49310,.F.);
#71733=ORIENTED_EDGE('',*,*,#49186,.F.);
#71734=ORIENTED_EDGE('',*,*,#49312,.F.);
#71735=ORIENTED_EDGE('',*,*,#49373,.F.);
#71736=ORIENTED_EDGE('',*,*,#49197,.F.);
#71737=ORIENTED_EDGE('',*,*,#49372,.F.);
#71738=ORIENTED_EDGE('',*,*,#49323,.F.);
#71739=ORIENTED_EDGE('',*,*,#49182,.F.);
#71740=ORIENTED_EDGE('',*,*,#49374,.F.);
#71741=ORIENTED_EDGE('',*,*,#49318,.F.);
#71742=ORIENTED_EDGE('',*,*,#49371,.F.);
#71743=ORIENTED_EDGE('',*,*,#49210,.F.);
#71744=ORIENTED_EDGE('',*,*,#49341,.F.);
#71745=ORIENTED_EDGE('',*,*,#49381,.F.);
#71746=ORIENTED_EDGE('',*,*,#49262,.F.);
#71747=ORIENTED_EDGE('',*,*,#49256,.F.);
#71748=ORIENTED_EDGE('',*,*,#49258,.F.);
#71749=ORIENTED_EDGE('',*,*,#49380,.F.);
#71750=ORIENTED_EDGE('',*,*,#49351,.F.);
#71751=ORIENTED_EDGE('',*,*,#49252,.F.);
#71752=ORIENTED_EDGE('',*,*,#49382,.F.);
#71753=ORIENTED_EDGE('',*,*,#49346,.F.);
#71754=ORIENTED_EDGE('',*,*,#49379,.F.);
#71755=ORIENTED_EDGE('',*,*,#49276,.F.);
#71756=ORIENTED_EDGE('',*,*,#49368,.F.);
#71757=ORIENTED_EDGE('',*,*,#49337,.F.);
#71758=ORIENTED_EDGE('',*,*,#49299,.F.);
#71759=ORIENTED_EDGE('',*,*,#49292,.F.);
#71760=ORIENTED_EDGE('',*,*,#49327,.F.);
#71761=ORIENTED_EDGE('',*,*,#49369,.F.);
#71762=ORIENTED_EDGE('',*,*,#49301,.F.);
#71763=ORIENTED_EDGE('',*,*,#49306,.F.);
#71764=ORIENTED_EDGE('',*,*,#49370,.F.);
#71765=ORIENTED_EDGE('',*,*,#49332,.F.);
#71766=ORIENTED_EDGE('',*,*,#49367,.F.);
#71767=ORIENTED_EDGE('',*,*,#49282,.F.);
#71768=ORIENTED_EDGE('',*,*,#50443,.F.);
#71769=ORIENTED_EDGE('',*,*,#50359,.F.);
#71770=ORIENTED_EDGE('',*,*,#50370,.F.);
#71771=ORIENTED_EDGE('',*,*,#50369,.F.);
#71772=ORIENTED_EDGE('',*,*,#50368,.F.);
#71773=ORIENTED_EDGE('',*,*,#50367,.F.);
#71774=ORIENTED_EDGE('',*,*,#50366,.F.);
#71775=ORIENTED_EDGE('',*,*,#50365,.F.);
#71776=ORIENTED_EDGE('',*,*,#50364,.F.);
#71777=ORIENTED_EDGE('',*,*,#50375,.F.);
#71778=ORIENTED_EDGE('',*,*,#50444,.F.);
#71779=ORIENTED_EDGE('',*,*,#50320,.F.);
#71780=ORIENTED_EDGE('',*,*,#50319,.F.);
#71781=ORIENTED_EDGE('',*,*,#50318,.F.);
#71782=ORIENTED_EDGE('',*,*,#50317,.F.);
#71783=ORIENTED_EDGE('',*,*,#50316,.F.);
#71784=ORIENTED_EDGE('',*,*,#50315,.F.);
#71785=ORIENTED_EDGE('',*,*,#51169,.F.);
#71786=ORIENTED_EDGE('',*,*,#51170,.F.);
#71787=ORIENTED_EDGE('',*,*,#51171,.T.);
#71788=ORIENTED_EDGE('',*,*,#50173,.F.);
#71789=ORIENTED_EDGE('',*,*,#51172,.F.);
#71790=ORIENTED_EDGE('',*,*,#51173,.F.);
#71791=ORIENTED_EDGE('',*,*,#51169,.T.);
#71792=ORIENTED_EDGE('',*,*,#50170,.F.);
#71793=ORIENTED_EDGE('',*,*,#51174,.F.);
#71794=ORIENTED_EDGE('',*,*,#51175,.F.);
#71795=ORIENTED_EDGE('',*,*,#51172,.T.);
#71796=ORIENTED_EDGE('',*,*,#50167,.F.);
#71797=ORIENTED_EDGE('',*,*,#51176,.F.);
#71798=ORIENTED_EDGE('',*,*,#51177,.F.);
#71799=ORIENTED_EDGE('',*,*,#51174,.T.);
#71800=ORIENTED_EDGE('',*,*,#50164,.F.);
#71801=ORIENTED_EDGE('',*,*,#51178,.F.);
#71802=ORIENTED_EDGE('',*,*,#51179,.F.);
#71803=ORIENTED_EDGE('',*,*,#51176,.T.);
#71804=ORIENTED_EDGE('',*,*,#50161,.F.);
#71805=ORIENTED_EDGE('',*,*,#51180,.F.);
#71806=ORIENTED_EDGE('',*,*,#51181,.F.);
#71807=ORIENTED_EDGE('',*,*,#51178,.T.);
#71808=ORIENTED_EDGE('',*,*,#50158,.F.);
#71809=ORIENTED_EDGE('',*,*,#51171,.F.);
#71810=ORIENTED_EDGE('',*,*,#51182,.F.);
#71811=ORIENTED_EDGE('',*,*,#51183,.T.);
#71812=ORIENTED_EDGE('',*,*,#50176,.F.);
#71813=ORIENTED_EDGE('',*,*,#51184,.F.);
#71814=ORIENTED_EDGE('',*,*,#51185,.T.);
#71815=ORIENTED_EDGE('',*,*,#51186,.T.);
#71816=ORIENTED_EDGE('',*,*,#50134,.F.);
#71817=ORIENTED_EDGE('',*,*,#51187,.F.);
#71818=ORIENTED_EDGE('',*,*,#51188,.T.);
#71819=ORIENTED_EDGE('',*,*,#51189,.T.);
#71820=ORIENTED_EDGE('',*,*,#50153,.F.);
#71821=ORIENTED_EDGE('',*,*,#51189,.F.);
#71822=ORIENTED_EDGE('',*,*,#51190,.T.);
#71823=ORIENTED_EDGE('',*,*,#51191,.T.);
#71824=ORIENTED_EDGE('',*,*,#50150,.F.);
#71825=ORIENTED_EDGE('',*,*,#51191,.F.);
#71826=ORIENTED_EDGE('',*,*,#51192,.T.);
#71827=ORIENTED_EDGE('',*,*,#51193,.T.);
#71828=ORIENTED_EDGE('',*,*,#50147,.F.);
#71829=ORIENTED_EDGE('',*,*,#51193,.F.);
#71830=ORIENTED_EDGE('',*,*,#51194,.T.);
#71831=ORIENTED_EDGE('',*,*,#51195,.T.);
#71832=ORIENTED_EDGE('',*,*,#50144,.F.);
#71833=ORIENTED_EDGE('',*,*,#51195,.F.);
#71834=ORIENTED_EDGE('',*,*,#51196,.T.);
#71835=ORIENTED_EDGE('',*,*,#51197,.T.);
#71836=ORIENTED_EDGE('',*,*,#50141,.F.);
#71837=ORIENTED_EDGE('',*,*,#51197,.F.);
#71838=ORIENTED_EDGE('',*,*,#51198,.T.);
#71839=ORIENTED_EDGE('',*,*,#51184,.T.);
#71840=ORIENTED_EDGE('',*,*,#50138,.F.);
#71841=ORIENTED_EDGE('',*,*,#51199,.T.);
#71842=ORIENTED_EDGE('',*,*,#50350,.F.);
#71843=ORIENTED_EDGE('',*,*,#50353,.F.);
#71844=ORIENTED_EDGE('',*,*,#51200,.F.);
#71845=ORIENTED_EDGE('',*,*,#50329,.F.);
#71846=ORIENTED_EDGE('',*,*,#51201,.T.);
#71847=ORIENTED_EDGE('',*,*,#50401,.F.);
#71848=ORIENTED_EDGE('',*,*,#50404,.F.);
#71849=ORIENTED_EDGE('',*,*,#51202,.F.);
#71850=ORIENTED_EDGE('',*,*,#50335,.F.);
#71851=ORIENTED_EDGE('',*,*,#51203,.T.);
#71852=ORIENTED_EDGE('',*,*,#50434,.F.);
#71853=ORIENTED_EDGE('',*,*,#50431,.F.);
#71854=ORIENTED_EDGE('',*,*,#51204,.F.);
#71855=ORIENTED_EDGE('',*,*,#50300,.F.);
#71856=ORIENTED_EDGE('',*,*,#51205,.F.);
#71857=ORIENTED_EDGE('',*,*,#50381,.F.);
#71858=ORIENTED_EDGE('',*,*,#50384,.F.);
#71859=ORIENTED_EDGE('',*,*,#51206,.F.);
#71860=ORIENTED_EDGE('',*,*,#50306,.F.);
#71861=ORIENTED_EDGE('',*,*,#51207,.F.);
#71862=ORIENTED_EDGE('',*,*,#50408,.F.);
#71863=ORIENTED_EDGE('',*,*,#50405,.F.);
#71864=ORIENTED_EDGE('',*,*,#51208,.T.);
#71865=ORIENTED_EDGE('',*,*,#49238,.F.);
#71866=ORIENTED_EDGE('',*,*,#51209,.F.);
#71867=ORIENTED_EDGE('',*,*,#50343,.F.);
#71868=ORIENTED_EDGE('',*,*,#49273,.F.);
#71869=ORIENTED_EDGE('',*,*,#49275,.F.);
#71870=ORIENTED_EDGE('',*,*,#49271,.F.);
#71871=ORIENTED_EDGE('',*,*,#50410,.F.);
#71872=ORIENTED_EDGE('',*,*,#51207,.T.);
#71873=ORIENTED_EDGE('',*,*,#49235,.F.);
#71874=ORIENTED_EDGE('',*,*,#51210,.F.);
#71875=ORIENTED_EDGE('',*,*,#50351,.F.);
#71876=ORIENTED_EDGE('',*,*,#50348,.F.);
#71877=ORIENTED_EDGE('',*,*,#51209,.T.);
#71878=ORIENTED_EDGE('',*,*,#49232,.F.);
#71879=ORIENTED_EDGE('',*,*,#51211,.F.);
#71880=ORIENTED_EDGE('',*,*,#50388,.F.);
#71881=ORIENTED_EDGE('',*,*,#50385,.F.);
#71882=ORIENTED_EDGE('',*,*,#51212,.T.);
#71883=ORIENTED_EDGE('',*,*,#49226,.F.);
#71884=ORIENTED_EDGE('',*,*,#51213,.F.);
#71885=ORIENTED_EDGE('',*,*,#50438,.F.);
#71886=ORIENTED_EDGE('',*,*,#49289,.F.);
#71887=ORIENTED_EDGE('',*,*,#49283,.F.);
#71888=ORIENTED_EDGE('',*,*,#49278,.F.);
#71889=ORIENTED_EDGE('',*,*,#50390,.F.);
#71890=ORIENTED_EDGE('',*,*,#51211,.T.);
#71891=ORIENTED_EDGE('',*,*,#49223,.F.);
#71892=ORIENTED_EDGE('',*,*,#51214,.F.);
#71893=ORIENTED_EDGE('',*,*,#50433,.F.);
#71894=ORIENTED_EDGE('',*,*,#50436,.F.);
#71895=ORIENTED_EDGE('',*,*,#51213,.T.);
#71896=ORIENTED_EDGE('',*,*,#49220,.F.);
#71897=ORIENTED_EDGE('',*,*,#51215,.T.);
#71898=ORIENTED_EDGE('',*,*,#51216,.F.);
#71899=ORIENTED_EDGE('',*,*,#51217,.F.);
#71900=ORIENTED_EDGE('',*,*,#50276,.F.);
#71901=ORIENTED_EDGE('',*,*,#51217,.T.);
#71902=ORIENTED_EDGE('',*,*,#51218,.F.);
#71903=ORIENTED_EDGE('',*,*,#51219,.F.);
#71904=ORIENTED_EDGE('',*,*,#50273,.F.);
#71905=ORIENTED_EDGE('',*,*,#51219,.T.);
#71906=ORIENTED_EDGE('',*,*,#51220,.F.);
#71907=ORIENTED_EDGE('',*,*,#51221,.F.);
#71908=ORIENTED_EDGE('',*,*,#50270,.F.);
#71909=ORIENTED_EDGE('',*,*,#51221,.T.);
#71910=ORIENTED_EDGE('',*,*,#51222,.F.);
#71911=ORIENTED_EDGE('',*,*,#51223,.F.);
#71912=ORIENTED_EDGE('',*,*,#50266,.F.);
#71913=ORIENTED_EDGE('',*,*,#51224,.T.);
#71914=ORIENTED_EDGE('',*,*,#51225,.F.);
#71915=ORIENTED_EDGE('',*,*,#51226,.F.);
#71916=ORIENTED_EDGE('',*,*,#50285,.F.);
#71917=ORIENTED_EDGE('',*,*,#51226,.T.);
#71918=ORIENTED_EDGE('',*,*,#51227,.F.);
#71919=ORIENTED_EDGE('',*,*,#51228,.F.);
#71920=ORIENTED_EDGE('',*,*,#50282,.F.);
#71921=ORIENTED_EDGE('',*,*,#51228,.T.);
#71922=ORIENTED_EDGE('',*,*,#51229,.F.);
#71923=ORIENTED_EDGE('',*,*,#51215,.F.);
#71924=ORIENTED_EDGE('',*,*,#50279,.F.);
#71925=ORIENTED_EDGE('',*,*,#51200,.T.);
#71926=ORIENTED_EDGE('',*,*,#50357,.F.);
#71927=ORIENTED_EDGE('',*,*,#50442,.F.);
#71928=ORIENTED_EDGE('',*,*,#50326,.F.);
#71929=ORIENTED_EDGE('',*,*,#50445,.F.);
#71930=ORIENTED_EDGE('',*,*,#50379,.F.);
#71931=ORIENTED_EDGE('',*,*,#51205,.T.);
#71932=ORIENTED_EDGE('',*,*,#50309,.F.);
#71933=ORIENTED_EDGE('',*,*,#51212,.F.);
#71934=ORIENTED_EDGE('',*,*,#50382,.F.);
#71935=ORIENTED_EDGE('',*,*,#50377,.F.);
#71936=ORIENTED_EDGE('',*,*,#50371,.F.);
#71937=ORIENTED_EDGE('',*,*,#50358,.F.);
#71938=ORIENTED_EDGE('',*,*,#50354,.F.);
#71939=ORIENTED_EDGE('',*,*,#51210,.T.);
#71940=ORIENTED_EDGE('',*,*,#49229,.F.);
#71941=ORIENTED_EDGE('',*,*,#51204,.T.);
#71942=ORIENTED_EDGE('',*,*,#50423,.F.);
#71943=ORIENTED_EDGE('',*,*,#50446,.F.);
#71944=ORIENTED_EDGE('',*,*,#50297,.F.);
#71945=ORIENTED_EDGE('',*,*,#50441,.F.);
#71946=ORIENTED_EDGE('',*,*,#50399,.F.);
#71947=ORIENTED_EDGE('',*,*,#51201,.F.);
#71948=ORIENTED_EDGE('',*,*,#50338,.F.);
#71949=ORIENTED_EDGE('',*,*,#49338,.F.);
#71950=ORIENTED_EDGE('',*,*,#49336,.F.);
#71951=ORIENTED_EDGE('',*,*,#49333,.F.);
#71952=ORIENTED_EDGE('',*,*,#49329,.F.);
#71953=ORIENTED_EDGE('',*,*,#49325,.F.);
#71954=ORIENTED_EDGE('',*,*,#49215,.F.);
#71955=ORIENTED_EDGE('',*,*,#49211,.F.);
#71956=ORIENTED_EDGE('',*,*,#49206,.F.);
#71957=ORIENTED_EDGE('',*,*,#49309,.F.);
#71958=ORIENTED_EDGE('',*,*,#49307,.F.);
#71959=ORIENTED_EDGE('',*,*,#50439,.F.);
#71960=ORIENTED_EDGE('',*,*,#50437,.F.);
#71961=ORIENTED_EDGE('',*,*,#51203,.F.);
#71962=ORIENTED_EDGE('',*,*,#50303,.F.);
#71963=ORIENTED_EDGE('',*,*,#51206,.T.);
#71964=ORIENTED_EDGE('',*,*,#50387,.F.);
#71965=ORIENTED_EDGE('',*,*,#50389,.F.);
#71966=ORIENTED_EDGE('',*,*,#49298,.F.);
#71967=ORIENTED_EDGE('',*,*,#49303,.F.);
#71968=ORIENTED_EDGE('',*,*,#49189,.F.);
#71969=ORIENTED_EDGE('',*,*,#49183,.F.);
#71970=ORIENTED_EDGE('',*,*,#49178,.F.);
#71971=ORIENTED_EDGE('',*,*,#49185,.F.);
#71972=ORIENTED_EDGE('',*,*,#49191,.F.);
#71973=ORIENTED_EDGE('',*,*,#49196,.F.);
#71974=ORIENTED_EDGE('',*,*,#49202,.F.);
#71975=ORIENTED_EDGE('',*,*,#49158,.F.);
#71976=ORIENTED_EDGE('',*,*,#49164,.F.);
#71977=ORIENTED_EDGE('',*,*,#49352,.F.);
#71978=ORIENTED_EDGE('',*,*,#49348,.F.);
#71979=ORIENTED_EDGE('',*,*,#49347,.F.);
#71980=ORIENTED_EDGE('',*,*,#49344,.F.);
#71981=ORIENTED_EDGE('',*,*,#49339,.F.);
#71982=ORIENTED_EDGE('',*,*,#49244,.F.);
#71983=ORIENTED_EDGE('',*,*,#49239,.F.);
#71984=ORIENTED_EDGE('',*,*,#49152,.F.);
#71985=ORIENTED_EDGE('',*,*,#49241,.F.);
#71986=ORIENTED_EDGE('',*,*,#49243,.F.);
#71987=ORIENTED_EDGE('',*,*,#49249,.F.);
#71988=ORIENTED_EDGE('',*,*,#49255,.F.);
#71989=ORIENTED_EDGE('',*,*,#50345,.F.);
#71990=ORIENTED_EDGE('',*,*,#50347,.F.);
#71991=ORIENTED_EDGE('',*,*,#51199,.F.);
#71992=ORIENTED_EDGE('',*,*,#50332,.F.);
#71993=ORIENTED_EDGE('',*,*,#51202,.T.);
#71994=ORIENTED_EDGE('',*,*,#50407,.F.);
#71995=ORIENTED_EDGE('',*,*,#50409,.F.);
#71996=ORIENTED_EDGE('',*,*,#49253,.F.);
#71997=ORIENTED_EDGE('',*,*,#49245,.F.);
#71998=ORIENTED_EDGE('',*,*,#49175,.F.);
#71999=ORIENTED_EDGE('',*,*,#49168,.F.);
#72000=ORIENTED_EDGE('',*,*,#49162,.F.);
#72001=ORIENTED_EDGE('',*,*,#49156,.F.);
#72002=ORIENTED_EDGE('',*,*,#49150,.F.);
#72003=ORIENTED_EDGE('',*,*,#49145,.F.);
#72004=ORIENTED_EDGE('',*,*,#49140,.F.);
#72005=ORIENTED_EDGE('',*,*,#51153,.F.);
#72006=ORIENTED_EDGE('',*,*,#51230,.T.);
#72007=ORIENTED_EDGE('',*,*,#50691,.F.);
#72008=ORIENTED_EDGE('',*,*,#49661,.F.);
#72009=ORIENTED_EDGE('',*,*,#50672,.F.);
#72010=ORIENTED_EDGE('',*,*,#51231,.T.);
#72011=ORIENTED_EDGE('',*,*,#50667,.F.);
#72012=ORIENTED_EDGE('',*,*,#49683,.F.);
#72013=ORIENTED_EDGE('',*,*,#50660,.F.);
#72014=ORIENTED_EDGE('',*,*,#51232,.T.);
#72015=ORIENTED_EDGE('',*,*,#50655,.F.);
#72016=ORIENTED_EDGE('',*,*,#49811,.F.);
#72017=ORIENTED_EDGE('',*,*,#50648,.F.);
#72018=ORIENTED_EDGE('',*,*,#51233,.T.);
#72019=ORIENTED_EDGE('',*,*,#50643,.F.);
#72020=ORIENTED_EDGE('',*,*,#49910,.F.);
#72021=ORIENTED_EDGE('',*,*,#50576,.F.);
#72022=ORIENTED_EDGE('',*,*,#51234,.T.);
#72023=ORIENTED_EDGE('',*,*,#51155,.T.);
#72024=ORIENTED_EDGE('',*,*,#49946,.F.);
#72025=ORIENTED_EDGE('',*,*,#50522,.F.);
#72026=ORIENTED_EDGE('',*,*,#51235,.F.);
#72027=ORIENTED_EDGE('',*,*,#50517,.F.);
#72028=ORIENTED_EDGE('',*,*,#49871,.F.);
#72029=ORIENTED_EDGE('',*,*,#50813,.F.);
#72030=ORIENTED_EDGE('',*,*,#51236,.F.);
#72031=ORIENTED_EDGE('',*,*,#50808,.F.);
#72032=ORIENTED_EDGE('',*,*,#50094,.F.);
#72033=ORIENTED_EDGE('',*,*,#50465,.F.);
#72034=ORIENTED_EDGE('',*,*,#51237,.F.);
#72035=ORIENTED_EDGE('',*,*,#50460,.F.);
#72036=ORIENTED_EDGE('',*,*,#50195,.F.);
#72037=ORIENTED_EDGE('',*,*,#50459,.F.);
#72038=ORIENTED_EDGE('',*,*,#51238,.F.);
#72039=ORIENTED_EDGE('',*,*,#50454,.F.);
#72040=ORIENTED_EDGE('',*,*,#50205,.F.);
#72041=ORIENTED_EDGE('',*,*,#50807,.F.);
#72042=ORIENTED_EDGE('',*,*,#51239,.F.);
#72043=ORIENTED_EDGE('',*,*,#50814,.F.);
#72044=ORIENTED_EDGE('',*,*,#50078,.F.);
#72045=ORIENTED_EDGE('',*,*,#50789,.F.);
#72046=ORIENTED_EDGE('',*,*,#51240,.F.);
#72047=ORIENTED_EDGE('',*,*,#50784,.F.);
#72048=ORIENTED_EDGE('',*,*,#50054,.F.);
#72049=ORIENTED_EDGE('',*,*,#50510,.F.);
#72050=ORIENTED_EDGE('',*,*,#51241,.F.);
#72051=ORIENTED_EDGE('',*,*,#50505,.F.);
#72052=ORIENTED_EDGE('',*,*,#49494,.F.);
#72053=ORIENTED_EDGE('',*,*,#50804,.F.);
#72054=ORIENTED_EDGE('',*,*,#51242,.F.);
#72055=ORIENTED_EDGE('',*,*,#50799,.F.);
#72056=ORIENTED_EDGE('',*,*,#49478,.F.);
#72057=ORIENTED_EDGE('',*,*,#50798,.F.);
#72058=ORIENTED_EDGE('',*,*,#51243,.F.);
#72059=ORIENTED_EDGE('',*,*,#50793,.F.);
#72060=ORIENTED_EDGE('',*,*,#49470,.F.);
#72061=ORIENTED_EDGE('',*,*,#50819,.F.);
#72062=ORIENTED_EDGE('',*,*,#51244,.F.);
#72063=ORIENTED_EDGE('',*,*,#50826,.F.);
#72064=ORIENTED_EDGE('',*,*,#49454,.F.);
#72065=ORIENTED_EDGE('',*,*,#50824,.F.);
#72066=ORIENTED_EDGE('',*,*,#51245,.T.);
#72067=ORIENTED_EDGE('',*,*,#50820,.F.);
#72068=ORIENTED_EDGE('',*,*,#49446,.F.);
#72069=ORIENTED_EDGE('',*,*,#50783,.F.);
#72070=ORIENTED_EDGE('',*,*,#51246,.T.);
#72071=ORIENTED_EDGE('',*,*,#50790,.F.);
#72072=ORIENTED_EDGE('',*,*,#50070,.F.);
#72073=ORIENTED_EDGE('',*,*,#51247,.F.);
#72074=ORIENTED_EDGE('',*,*,#50936,.F.);
#72075=ORIENTED_EDGE('',*,*,#51248,.F.);
#72076=ORIENTED_EDGE('',*,*,#50908,.F.);
#72077=ORIENTED_EDGE('',*,*,#50756,.F.);
#72078=ORIENTED_EDGE('',*,*,#51249,.F.);
#72079=ORIENTED_EDGE('',*,*,#50751,.F.);
#72080=ORIENTED_EDGE('',*,*,#49863,.F.);
#72081=ORIENTED_EDGE('',*,*,#50765,.F.);
#72082=ORIENTED_EDGE('',*,*,#51250,.F.);
#72083=ORIENTED_EDGE('',*,*,#50760,.F.);
#72084=ORIENTED_EDGE('',*,*,#50046,.F.);
#72085=ORIENTED_EDGE('',*,*,#50486,.F.);
#72086=ORIENTED_EDGE('',*,*,#51251,.F.);
#72087=ORIENTED_EDGE('',*,*,#50481,.F.);
#72088=ORIENTED_EDGE('',*,*,#49745,.F.);
#72089=ORIENTED_EDGE('',*,*,#50750,.F.);
#72090=ORIENTED_EDGE('',*,*,#51252,.F.);
#72091=ORIENTED_EDGE('',*,*,#50745,.F.);
#72092=ORIENTED_EDGE('',*,*,#49847,.F.);
#72093=ORIENTED_EDGE('',*,*,#50495,.F.);
#72094=ORIENTED_EDGE('',*,*,#51253,.F.);
#72095=ORIENTED_EDGE('',*,*,#50490,.F.);
#72096=ORIENTED_EDGE('',*,*,#49715,.F.);
#72097=ORIENTED_EDGE('',*,*,#50480,.F.);
#72098=ORIENTED_EDGE('',*,*,#51254,.F.);
#72099=ORIENTED_EDGE('',*,*,#50487,.F.);
#72100=ORIENTED_EDGE('',*,*,#49769,.F.);
#72101=ORIENTED_EDGE('',*,*,#50744,.F.);
#72102=ORIENTED_EDGE('',*,*,#51255,.F.);
#72103=ORIENTED_EDGE('',*,*,#50739,.F.);
#72104=ORIENTED_EDGE('',*,*,#49529,.F.);
#72105=ORIENTED_EDGE('',*,*,#50501,.F.);
#72106=ORIENTED_EDGE('',*,*,#51256,.F.);
#72107=ORIENTED_EDGE('',*,*,#50496,.F.);
#72108=ORIENTED_EDGE('',*,*,#49739,.F.);
#72109=ORIENTED_EDGE('',*,*,#50759,.F.);
#72110=ORIENTED_EDGE('',*,*,#51257,.F.);
#72111=ORIENTED_EDGE('',*,*,#50766,.F.);
#72112=ORIENTED_EDGE('',*,*,#50030,.F.);
#72113=ORIENTED_EDGE('',*,*,#50717,.F.);
#72114=ORIENTED_EDGE('',*,*,#51258,.F.);
#72115=ORIENTED_EDGE('',*,*,#50712,.F.);
#72116=ORIENTED_EDGE('',*,*,#50006,.F.);
#72117=ORIENTED_EDGE('',*,*,#50738,.F.);
#72118=ORIENTED_EDGE('',*,*,#51259,.F.);
#72119=ORIENTED_EDGE('',*,*,#50733,.F.);
#72120=ORIENTED_EDGE('',*,*,#49521,.F.);
#72121=ORIENTED_EDGE('',*,*,#50732,.F.);
#72122=ORIENTED_EDGE('',*,*,#51260,.F.);
#72123=ORIENTED_EDGE('',*,*,#50727,.F.);
#72124=ORIENTED_EDGE('',*,*,#49553,.F.);
#72125=ORIENTED_EDGE('',*,*,#50726,.F.);
#72126=ORIENTED_EDGE('',*,*,#51261,.F.);
#72127=ORIENTED_EDGE('',*,*,#50721,.F.);
#72128=ORIENTED_EDGE('',*,*,#49545,.F.);
#72129=ORIENTED_EDGE('',*,*,#50771,.F.);
#72130=ORIENTED_EDGE('',*,*,#51262,.F.);
#72131=ORIENTED_EDGE('',*,*,#50778,.F.);
#72132=ORIENTED_EDGE('',*,*,#49430,.F.);
#72133=ORIENTED_EDGE('',*,*,#50776,.F.);
#72134=ORIENTED_EDGE('',*,*,#51263,.T.);
#72135=ORIENTED_EDGE('',*,*,#50772,.F.);
#72136=ORIENTED_EDGE('',*,*,#49422,.F.);
#72137=ORIENTED_EDGE('',*,*,#50704,.F.);
#72138=ORIENTED_EDGE('',*,*,#51264,.T.);
#72139=ORIENTED_EDGE('',*,*,#51147,.T.);
#72140=ORIENTED_EDGE('',*,*,#49392,.F.);
#72141=ORIENTED_EDGE('',*,*,#50711,.F.);
#72142=ORIENTED_EDGE('',*,*,#51265,.T.);
#72143=ORIENTED_EDGE('',*,*,#50718,.F.);
#72144=ORIENTED_EDGE('',*,*,#50022,.F.);
#72145=ORIENTED_EDGE('',*,*,#51161,.F.);
#72146=ORIENTED_EDGE('',*,*,#51266,.T.);
#72147=ORIENTED_EDGE('',*,*,#50562,.F.);
#72148=ORIENTED_EDGE('',*,*,#50000,.F.);
#72149=ORIENTED_EDGE('',*,*,#51149,.F.);
#72150=ORIENTED_EDGE('',*,*,#51267,.T.);
#72151=ORIENTED_EDGE('',*,*,#50700,.F.);
#72152=ORIENTED_EDGE('',*,*,#49404,.F.);
#72153=ORIENTED_EDGE('',*,*,#50530,.F.);
#72154=ORIENTED_EDGE('',*,*,#51268,.T.);
#72155=ORIENTED_EDGE('',*,*,#50526,.F.);
#72156=ORIENTED_EDGE('',*,*,#50124,.F.);
#72157=ORIENTED_EDGE('',*,*,#50567,.F.);
#72158=ORIENTED_EDGE('',*,*,#51269,.T.);
#72159=ORIENTED_EDGE('',*,*,#51159,.T.);
#72160=ORIENTED_EDGE('',*,*,#49992,.F.);
#72161=ORIENTED_EDGE('',*,*,#50624,.F.);
#72162=ORIENTED_EDGE('',*,*,#51270,.T.);
#72163=ORIENTED_EDGE('',*,*,#50619,.F.);
#72164=ORIENTED_EDGE('',*,*,#50106,.F.);
#72165=ORIENTED_EDGE('',*,*,#50615,.F.);
#72166=ORIENTED_EDGE('',*,*,#51271,.F.);
#72167=ORIENTED_EDGE('',*,*,#50610,.F.);
#72168=ORIENTED_EDGE('',*,*,#49839,.F.);
#72169=ORIENTED_EDGE('',*,*,#50645,.F.);
#72170=ORIENTED_EDGE('',*,*,#51272,.F.);
#72171=ORIENTED_EDGE('',*,*,#50640,.F.);
#72172=ORIENTED_EDGE('',*,*,#49898,.F.);
#72173=ORIENTED_EDGE('',*,*,#50633,.F.);
#72174=ORIENTED_EDGE('',*,*,#51273,.F.);
#72175=ORIENTED_EDGE('',*,*,#50628,.F.);
#72176=ORIENTED_EDGE('',*,*,#49968,.F.);
#72177=ORIENTED_EDGE('',*,*,#50579,.F.);
#72178=ORIENTED_EDGE('',*,*,#51274,.F.);
#72179=ORIENTED_EDGE('',*,*,#50574,.F.);
#72180=ORIENTED_EDGE('',*,*,#49938,.F.);
#72181=ORIENTED_EDGE('',*,*,#50603,.F.);
#72182=ORIENTED_EDGE('',*,*,#51275,.F.);
#72183=ORIENTED_EDGE('',*,*,#50598,.F.);
#72184=ORIENTED_EDGE('',*,*,#49775,.F.);
#72185=ORIENTED_EDGE('',*,*,#50657,.F.);
#72186=ORIENTED_EDGE('',*,*,#51276,.F.);
#72187=ORIENTED_EDGE('',*,*,#50652,.F.);
#72188=ORIENTED_EDGE('',*,*,#49799,.F.);
#72189=ORIENTED_EDGE('',*,*,#50609,.F.);
#72190=ORIENTED_EDGE('',*,*,#51277,.F.);
#72191=ORIENTED_EDGE('',*,*,#50604,.F.);
#72192=ORIENTED_EDGE('',*,*,#49823,.F.);
#72193=ORIENTED_EDGE('',*,*,#50639,.F.);
#72194=ORIENTED_EDGE('',*,*,#51278,.F.);
#72195=ORIENTED_EDGE('',*,*,#50646,.F.);
#72196=ORIENTED_EDGE('',*,*,#49914,.F.);
#72197=ORIENTED_EDGE('',*,*,#50591,.F.);
#72198=ORIENTED_EDGE('',*,*,#51279,.F.);
#72199=ORIENTED_EDGE('',*,*,#50586,.F.);
#72200=ORIENTED_EDGE('',*,*,#49703,.F.);
#72201=ORIENTED_EDGE('',*,*,#50669,.F.);
#72202=ORIENTED_EDGE('',*,*,#51280,.F.);
#72203=ORIENTED_EDGE('',*,*,#50664,.F.);
#72204=ORIENTED_EDGE('',*,*,#49679,.F.);
#72205=ORIENTED_EDGE('',*,*,#50597,.F.);
#72206=ORIENTED_EDGE('',*,*,#51281,.F.);
#72207=ORIENTED_EDGE('',*,*,#50592,.F.);
#72208=ORIENTED_EDGE('',*,*,#49791,.F.);
#72209=ORIENTED_EDGE('',*,*,#50651,.F.);
#72210=ORIENTED_EDGE('',*,*,#51282,.F.);
#72211=ORIENTED_EDGE('',*,*,#50658,.F.);
#72212=ORIENTED_EDGE('',*,*,#49815,.F.);
#72213=ORIENTED_EDGE('',*,*,#50555,.F.);
#72214=ORIENTED_EDGE('',*,*,#51283,.F.);
#72215=ORIENTED_EDGE('',*,*,#50550,.F.);
#72216=ORIENTED_EDGE('',*,*,#49601,.F.);
#72217=ORIENTED_EDGE('',*,*,#50681,.F.);
#72218=ORIENTED_EDGE('',*,*,#51284,.F.);
#72219=ORIENTED_EDGE('',*,*,#50676,.F.);
#72220=ORIENTED_EDGE('',*,*,#49625,.F.);
#72221=ORIENTED_EDGE('',*,*,#50585,.F.);
#72222=ORIENTED_EDGE('',*,*,#51285,.F.);
#72223=ORIENTED_EDGE('',*,*,#50580,.F.);
#72224=ORIENTED_EDGE('',*,*,#49695,.F.);
#72225=ORIENTED_EDGE('',*,*,#50663,.F.);
#72226=ORIENTED_EDGE('',*,*,#51286,.F.);
#72227=ORIENTED_EDGE('',*,*,#50670,.F.);
#72228=ORIENTED_EDGE('',*,*,#49671,.F.);
#72229=ORIENTED_EDGE('',*,*,#50627,.F.);
#72230=ORIENTED_EDGE('',*,*,#51287,.F.);
#72231=ORIENTED_EDGE('',*,*,#50634,.F.);
#72232=ORIENTED_EDGE('',*,*,#49952,.F.);
#72233=ORIENTED_EDGE('',*,*,#50573,.F.);
#72234=ORIENTED_EDGE('',*,*,#51288,.F.);
#72235=ORIENTED_EDGE('',*,*,#50568,.F.);
#72236=ORIENTED_EDGE('',*,*,#49922,.F.);
#72237=ORIENTED_EDGE('',*,*,#50561,.F.);
#72238=ORIENTED_EDGE('',*,*,#51289,.F.);
#72239=ORIENTED_EDGE('',*,*,#50556,.F.);
#72240=ORIENTED_EDGE('',*,*,#49976,.F.);
#72241=ORIENTED_EDGE('',*,*,#50618,.F.);
#72242=ORIENTED_EDGE('',*,*,#51290,.F.);
#72243=ORIENTED_EDGE('',*,*,#50622,.F.);
#72244=ORIENTED_EDGE('',*,*,#50102,.F.);
#72245=ORIENTED_EDGE('',*,*,#50549,.F.);
#72246=ORIENTED_EDGE('',*,*,#51291,.F.);
#72247=ORIENTED_EDGE('',*,*,#50544,.F.);
#72248=ORIENTED_EDGE('',*,*,#49593,.F.);
#72249=ORIENTED_EDGE('',*,*,#50675,.F.);
#72250=ORIENTED_EDGE('',*,*,#51292,.F.);
#72251=ORIENTED_EDGE('',*,*,#50682,.F.);
#72252=ORIENTED_EDGE('',*,*,#49617,.F.);
#72253=ORIENTED_EDGE('',*,*,#50543,.F.);
#72254=ORIENTED_EDGE('',*,*,#51293,.F.);
#72255=ORIENTED_EDGE('',*,*,#50538,.F.);
#72256=ORIENTED_EDGE('',*,*,#49577,.F.);
#72257=ORIENTED_EDGE('',*,*,#50693,.F.);
#72258=ORIENTED_EDGE('',*,*,#51294,.F.);
#72259=ORIENTED_EDGE('',*,*,#50688,.F.);
#72260=ORIENTED_EDGE('',*,*,#49649,.F.);
#72261=ORIENTED_EDGE('',*,*,#50537,.F.);
#72262=ORIENTED_EDGE('',*,*,#51295,.F.);
#72263=ORIENTED_EDGE('',*,*,#50532,.F.);
#72264=ORIENTED_EDGE('',*,*,#49569,.F.);
#72265=ORIENTED_EDGE('',*,*,#50687,.F.);
#72266=ORIENTED_EDGE('',*,*,#51296,.F.);
#72267=ORIENTED_EDGE('',*,*,#50694,.F.);
#72268=ORIENTED_EDGE('',*,*,#49641,.F.);
#72269=ORIENTED_EDGE('',*,*,#50699,.F.);
#72270=ORIENTED_EDGE('',*,*,#51297,.F.);
#72271=ORIENTED_EDGE('',*,*,#50706,.F.);
#72272=ORIENTED_EDGE('',*,*,#49400,.F.);
#72273=ORIENTED_EDGE('',*,*,#50528,.F.);
#72274=ORIENTED_EDGE('',*,*,#51298,.F.);
#72275=ORIENTED_EDGE('',*,*,#50523,.F.);
#72276=ORIENTED_EDGE('',*,*,#50132,.F.);
#72277=ORIENTED_EDGE('',*,*,#51299,.T.);
#72278=ORIENTED_EDGE('',*,*,#51300,.F.);
#72279=ORIENTED_EDGE('',*,*,#51301,.T.);
#72280=ORIENTED_EDGE('',*,*,#51302,.F.);
#72281=ORIENTED_EDGE('',*,*,#51303,.F.);
#72282=ORIENTED_EDGE('',*,*,#51301,.F.);
#72283=ORIENTED_EDGE('',*,*,#51304,.F.);
#72284=ORIENTED_EDGE('',*,*,#51305,.F.);
#72285=ORIENTED_EDGE('',*,*,#51299,.F.);
#72286=ORIENTED_EDGE('',*,*,#51306,.F.);
#72287=ORIENTED_EDGE('',*,*,#51307,.T.);
#72288=ORIENTED_EDGE('',*,*,#51308,.F.);
#72289=ORIENTED_EDGE('',*,*,#51309,.F.);
#72290=ORIENTED_EDGE('',*,*,#51307,.F.);
#72291=ORIENTED_EDGE('',*,*,#51310,.T.);
#72292=ORIENTED_EDGE('',*,*,#51311,.F.);
#72293=ORIENTED_EDGE('',*,*,#51312,.T.);
#72294=ORIENTED_EDGE('',*,*,#51313,.F.);
#72295=ORIENTED_EDGE('',*,*,#51314,.T.);
#72296=ORIENTED_EDGE('',*,*,#51315,.F.);
#72297=ORIENTED_EDGE('',*,*,#51312,.F.);
#72298=ORIENTED_EDGE('',*,*,#51316,.F.);
#72299=ORIENTED_EDGE('',*,*,#51317,.F.);
#72300=ORIENTED_EDGE('',*,*,#51318,.T.);
#72301=ORIENTED_EDGE('',*,*,#51310,.F.);
#72302=ORIENTED_EDGE('',*,*,#51319,.T.);
#72303=ORIENTED_EDGE('',*,*,#51320,.F.);
#72304=ORIENTED_EDGE('',*,*,#51314,.F.);
#72305=ORIENTED_EDGE('',*,*,#51321,.F.);
#72306=ORIENTED_EDGE('',*,*,#51322,.T.);
#72307=ORIENTED_EDGE('',*,*,#51323,.F.);
#72308=ORIENTED_EDGE('',*,*,#51318,.F.);
#72309=ORIENTED_EDGE('',*,*,#51324,.F.);
#72310=ORIENTED_EDGE('',*,*,#51325,.T.);
#72311=ORIENTED_EDGE('',*,*,#51326,.F.);
#72312=ORIENTED_EDGE('',*,*,#51319,.F.);
#72313=ORIENTED_EDGE('',*,*,#51327,.F.);
#72314=ORIENTED_EDGE('',*,*,#51328,.T.);
#72315=ORIENTED_EDGE('',*,*,#51329,.F.);
#72316=ORIENTED_EDGE('',*,*,#51322,.F.);
#72317=ORIENTED_EDGE('',*,*,#51330,.F.);
#72318=ORIENTED_EDGE('',*,*,#51331,.T.);
#72319=ORIENTED_EDGE('',*,*,#51332,.F.);
#72320=ORIENTED_EDGE('',*,*,#51325,.F.);
#72321=ORIENTED_EDGE('',*,*,#51333,.F.);
#72322=ORIENTED_EDGE('',*,*,#51334,.T.);
#72323=ORIENTED_EDGE('',*,*,#51335,.F.);
#72324=ORIENTED_EDGE('',*,*,#51328,.F.);
#72325=ORIENTED_EDGE('',*,*,#51336,.F.);
#72326=ORIENTED_EDGE('',*,*,#51337,.T.);
#72327=ORIENTED_EDGE('',*,*,#51338,.F.);
#72328=ORIENTED_EDGE('',*,*,#51331,.F.);
#72329=ORIENTED_EDGE('',*,*,#51339,.F.);
#72330=ORIENTED_EDGE('',*,*,#51340,.T.);
#72331=ORIENTED_EDGE('',*,*,#51341,.F.);
#72332=ORIENTED_EDGE('',*,*,#51334,.F.);
#72333=ORIENTED_EDGE('',*,*,#51342,.F.);
#72334=ORIENTED_EDGE('',*,*,#51343,.T.);
#72335=ORIENTED_EDGE('',*,*,#51344,.F.);
#72336=ORIENTED_EDGE('',*,*,#51337,.F.);
#72337=ORIENTED_EDGE('',*,*,#51345,.F.);
#72338=ORIENTED_EDGE('',*,*,#51346,.F.);
#72339=ORIENTED_EDGE('',*,*,#51340,.F.);
#72340=ORIENTED_EDGE('',*,*,#51347,.F.);
#72341=ORIENTED_EDGE('',*,*,#51343,.F.);
#72342=ORIENTED_EDGE('',*,*,#51348,.T.);
#72343=ORIENTED_EDGE('',*,*,#51349,.F.);
#72344=ORIENTED_EDGE('',*,*,#51350,.T.);
#72345=ORIENTED_EDGE('',*,*,#51351,.F.);
#72346=ORIENTED_EDGE('',*,*,#51352,.T.);
#72347=ORIENTED_EDGE('',*,*,#51353,.F.);
#72348=ORIENTED_EDGE('',*,*,#51350,.F.);
#72349=ORIENTED_EDGE('',*,*,#51354,.F.);
#72350=ORIENTED_EDGE('',*,*,#51355,.T.);
#72351=ORIENTED_EDGE('',*,*,#51356,.F.);
#72352=ORIENTED_EDGE('',*,*,#51348,.F.);
#72353=ORIENTED_EDGE('',*,*,#51357,.F.);
#72354=ORIENTED_EDGE('',*,*,#51358,.T.);
#72355=ORIENTED_EDGE('',*,*,#51359,.F.);
#72356=ORIENTED_EDGE('',*,*,#51352,.F.);
#72357=ORIENTED_EDGE('',*,*,#51360,.F.);
#72358=ORIENTED_EDGE('',*,*,#51361,.T.);
#72359=ORIENTED_EDGE('',*,*,#51362,.F.);
#72360=ORIENTED_EDGE('',*,*,#51355,.F.);
#72361=ORIENTED_EDGE('',*,*,#51363,.F.);
#72362=ORIENTED_EDGE('',*,*,#51364,.T.);
#72363=ORIENTED_EDGE('',*,*,#51365,.F.);
#72364=ORIENTED_EDGE('',*,*,#51358,.F.);
#72365=ORIENTED_EDGE('',*,*,#51366,.T.);
#72366=ORIENTED_EDGE('',*,*,#51367,.F.);
#72367=ORIENTED_EDGE('',*,*,#51361,.F.);
#72368=ORIENTED_EDGE('',*,*,#51368,.F.);
#72369=ORIENTED_EDGE('',*,*,#51369,.T.);
#72370=ORIENTED_EDGE('',*,*,#51370,.F.);
#72371=ORIENTED_EDGE('',*,*,#51364,.F.);
#72372=ORIENTED_EDGE('',*,*,#51371,.F.);
#72373=ORIENTED_EDGE('',*,*,#51372,.T.);
#72374=ORIENTED_EDGE('',*,*,#51373,.F.);
#72375=ORIENTED_EDGE('',*,*,#51366,.F.);
#72376=ORIENTED_EDGE('',*,*,#51374,.F.);
#72377=ORIENTED_EDGE('',*,*,#51375,.T.);
#72378=ORIENTED_EDGE('',*,*,#51376,.F.);
#72379=ORIENTED_EDGE('',*,*,#51369,.F.);
#72380=ORIENTED_EDGE('',*,*,#51377,.F.);
#72381=ORIENTED_EDGE('',*,*,#51378,.F.);
#72382=ORIENTED_EDGE('',*,*,#51379,.T.);
#72383=ORIENTED_EDGE('',*,*,#51372,.F.);
#72384=ORIENTED_EDGE('',*,*,#51380,.T.);
#72385=ORIENTED_EDGE('',*,*,#51381,.F.);
#72386=ORIENTED_EDGE('',*,*,#51375,.F.);
#72387=ORIENTED_EDGE('',*,*,#51382,.F.);
#72388=ORIENTED_EDGE('',*,*,#51383,.T.);
#72389=ORIENTED_EDGE('',*,*,#51384,.F.);
#72390=ORIENTED_EDGE('',*,*,#51379,.F.);
#72391=ORIENTED_EDGE('',*,*,#51385,.F.);
#72392=ORIENTED_EDGE('',*,*,#51380,.F.);
#72393=ORIENTED_EDGE('',*,*,#51386,.F.);
#72394=ORIENTED_EDGE('',*,*,#51383,.F.);
#72395=ORIENTED_EDGE('',*,*,#51387,.F.);
#72396=ORIENTED_EDGE('',*,*,#51388,.F.);
#72397=ORIENTED_EDGE('',*,*,#49219,.F.);
#72398=ORIENTED_EDGE('',*,*,#51389,.F.);
#72399=ORIENTED_EDGE('',*,*,#51390,.T.);
#72400=ORIENTED_EDGE('',*,*,#51391,.T.);
#72401=ORIENTED_EDGE('',*,*,#51392,.F.);
#72402=ORIENTED_EDGE('',*,*,#51390,.F.);
#72403=ORIENTED_EDGE('',*,*,#51393,.F.);
#72404=ORIENTED_EDGE('',*,*,#51394,.T.);
#72405=ORIENTED_EDGE('',*,*,#51395,.F.);
#72406=ORIENTED_EDGE('',*,*,#51391,.F.);
#72407=ORIENTED_EDGE('',*,*,#51396,.F.);
#72408=ORIENTED_EDGE('',*,*,#51397,.T.);
#72409=ORIENTED_EDGE('',*,*,#51398,.F.);
#72410=ORIENTED_EDGE('',*,*,#51394,.F.);
#72411=ORIENTED_EDGE('',*,*,#51399,.F.);
#72412=ORIENTED_EDGE('',*,*,#51400,.T.);
#72413=ORIENTED_EDGE('',*,*,#51401,.F.);
#72414=ORIENTED_EDGE('',*,*,#51397,.F.);
#72415=ORIENTED_EDGE('',*,*,#51402,.F.);
#72416=ORIENTED_EDGE('',*,*,#51403,.T.);
#72417=ORIENTED_EDGE('',*,*,#51404,.F.);
#72418=ORIENTED_EDGE('',*,*,#51400,.F.);
#72419=ORIENTED_EDGE('',*,*,#51405,.F.);
#72420=ORIENTED_EDGE('',*,*,#51406,.T.);
#72421=ORIENTED_EDGE('',*,*,#51407,.F.);
#72422=ORIENTED_EDGE('',*,*,#51403,.F.);
#72423=ORIENTED_EDGE('',*,*,#51408,.F.);
#72424=ORIENTED_EDGE('',*,*,#51409,.T.);
#72425=ORIENTED_EDGE('',*,*,#51410,.F.);
#72426=ORIENTED_EDGE('',*,*,#51406,.F.);
#72427=ORIENTED_EDGE('',*,*,#51411,.F.);
#72428=ORIENTED_EDGE('',*,*,#51412,.F.);
#72429=ORIENTED_EDGE('',*,*,#49236,.T.);
#72430=ORIENTED_EDGE('',*,*,#51413,.F.);
#72431=ORIENTED_EDGE('',*,*,#51409,.F.);
#72432=ORIENTED_EDGE('',*,*,#51414,.F.);
#72433=ORIENTED_EDGE('',*,*,#51317,.T.);
#72434=ORIENTED_EDGE('',*,*,#51415,.F.);
#72435=ORIENTED_EDGE('',*,*,#51416,.T.);
#72436=ORIENTED_EDGE('',*,*,#51417,.T.);
#72437=ORIENTED_EDGE('',*,*,#51418,.F.);
#72438=ORIENTED_EDGE('',*,*,#51416,.F.);
#72439=ORIENTED_EDGE('',*,*,#51419,.F.);
#72440=ORIENTED_EDGE('',*,*,#51420,.F.);
#72441=ORIENTED_EDGE('',*,*,#51347,.T.);
#72442=ORIENTED_EDGE('',*,*,#51421,.F.);
#72443=ORIENTED_EDGE('',*,*,#51422,.T.);
#72444=ORIENTED_EDGE('',*,*,#51423,.T.);
#72445=ORIENTED_EDGE('',*,*,#51424,.F.);
#72446=ORIENTED_EDGE('',*,*,#51417,.F.);
#72447=ORIENTED_EDGE('',*,*,#51425,.F.);
#72448=ORIENTED_EDGE('',*,*,#51426,.T.);
#72449=ORIENTED_EDGE('',*,*,#51427,.F.);
#72450=ORIENTED_EDGE('',*,*,#51422,.F.);
#72451=ORIENTED_EDGE('',*,*,#51428,.F.);
#72452=ORIENTED_EDGE('',*,*,#51429,.T.);
#72453=ORIENTED_EDGE('',*,*,#51430,.F.);
#72454=ORIENTED_EDGE('',*,*,#51423,.F.);
#72455=ORIENTED_EDGE('',*,*,#51431,.F.);
#72456=ORIENTED_EDGE('',*,*,#51432,.T.);
#72457=ORIENTED_EDGE('',*,*,#51433,.F.);
#72458=ORIENTED_EDGE('',*,*,#51426,.F.);
#72459=ORIENTED_EDGE('',*,*,#51434,.F.);
#72460=ORIENTED_EDGE('',*,*,#51435,.T.);
#72461=ORIENTED_EDGE('',*,*,#51436,.F.);
#72462=ORIENTED_EDGE('',*,*,#51429,.F.);
#72463=ORIENTED_EDGE('',*,*,#51437,.F.);
#72464=ORIENTED_EDGE('',*,*,#51438,.T.);
#72465=ORIENTED_EDGE('',*,*,#51439,.F.);
#72466=ORIENTED_EDGE('',*,*,#51432,.F.);
#72467=ORIENTED_EDGE('',*,*,#51440,.F.);
#72468=ORIENTED_EDGE('',*,*,#51441,.T.);
#72469=ORIENTED_EDGE('',*,*,#51442,.F.);
#72470=ORIENTED_EDGE('',*,*,#51435,.F.);
#72471=ORIENTED_EDGE('',*,*,#51443,.F.);
#72472=ORIENTED_EDGE('',*,*,#51444,.T.);
#72473=ORIENTED_EDGE('',*,*,#51445,.F.);
#72474=ORIENTED_EDGE('',*,*,#51438,.F.);
#72475=ORIENTED_EDGE('',*,*,#51446,.F.);
#72476=ORIENTED_EDGE('',*,*,#51447,.T.);
#72477=ORIENTED_EDGE('',*,*,#51448,.F.);
#72478=ORIENTED_EDGE('',*,*,#51441,.F.);
#72479=ORIENTED_EDGE('',*,*,#51449,.F.);
#72480=ORIENTED_EDGE('',*,*,#51444,.F.);
#72481=ORIENTED_EDGE('',*,*,#51450,.F.);
#72482=ORIENTED_EDGE('',*,*,#51447,.F.);
#72483=ORIENTED_EDGE('',*,*,#51451,.F.);
#72484=ORIENTED_EDGE('',*,*,#51452,.T.);
#72485=ORIENTED_EDGE('',*,*,#51453,.F.);
#72486=ORIENTED_EDGE('',*,*,#51454,.T.);
#72487=ORIENTED_EDGE('',*,*,#51455,.F.);
#72488=ORIENTED_EDGE('',*,*,#51456,.T.);
#72489=ORIENTED_EDGE('',*,*,#51457,.F.);
#72490=ORIENTED_EDGE('',*,*,#51454,.F.);
#72491=ORIENTED_EDGE('',*,*,#51458,.F.);
#72492=ORIENTED_EDGE('',*,*,#51459,.T.);
#72493=ORIENTED_EDGE('',*,*,#51460,.F.);
#72494=ORIENTED_EDGE('',*,*,#51452,.F.);
#72495=ORIENTED_EDGE('',*,*,#51461,.F.);
#72496=ORIENTED_EDGE('',*,*,#51462,.T.);
#72497=ORIENTED_EDGE('',*,*,#51463,.F.);
#72498=ORIENTED_EDGE('',*,*,#51456,.F.);
#72499=ORIENTED_EDGE('',*,*,#51464,.F.);
#72500=ORIENTED_EDGE('',*,*,#51465,.T.);
#72501=ORIENTED_EDGE('',*,*,#51466,.F.);
#72502=ORIENTED_EDGE('',*,*,#51459,.F.);
#72503=ORIENTED_EDGE('',*,*,#51467,.F.);
#72504=ORIENTED_EDGE('',*,*,#51468,.T.);
#72505=ORIENTED_EDGE('',*,*,#51469,.F.);
#72506=ORIENTED_EDGE('',*,*,#51462,.F.);
#72507=ORIENTED_EDGE('',*,*,#51470,.F.);
#72508=ORIENTED_EDGE('',*,*,#51471,.F.);
#72509=ORIENTED_EDGE('',*,*,#51472,.T.);
#72510=ORIENTED_EDGE('',*,*,#51473,.F.);
#72511=ORIENTED_EDGE('',*,*,#51465,.F.);
#72512=ORIENTED_EDGE('',*,*,#51474,.F.);
#72513=ORIENTED_EDGE('',*,*,#51475,.T.);
#72514=ORIENTED_EDGE('',*,*,#51476,.F.);
#72515=ORIENTED_EDGE('',*,*,#51468,.F.);
#72516=ORIENTED_EDGE('',*,*,#51477,.F.);
#72517=ORIENTED_EDGE('',*,*,#51478,.F.);
#72518=ORIENTED_EDGE('',*,*,#51365,.T.);
#72519=ORIENTED_EDGE('',*,*,#51479,.F.);
#72520=ORIENTED_EDGE('',*,*,#51472,.F.);
#72521=ORIENTED_EDGE('',*,*,#51480,.T.);
#72522=ORIENTED_EDGE('',*,*,#51481,.F.);
#72523=ORIENTED_EDGE('',*,*,#51475,.F.);
#72524=ORIENTED_EDGE('',*,*,#51482,.F.);
#72525=ORIENTED_EDGE('',*,*,#51483,.F.);
#72526=ORIENTED_EDGE('',*,*,#51378,.T.);
#72527=ORIENTED_EDGE('',*,*,#51484,.F.);
#72528=ORIENTED_EDGE('',*,*,#51480,.F.);
#72529=ORIENTED_EDGE('',*,*,#51485,.F.);
#72530=ORIENTED_EDGE('',*,*,#51362,.T.);
#72531=ORIENTED_EDGE('',*,*,#51486,.F.);
#72532=ORIENTED_EDGE('',*,*,#51487,.T.);
#72533=ORIENTED_EDGE('',*,*,#51488,.F.);
#72534=ORIENTED_EDGE('',*,*,#51489,.T.);
#72535=ORIENTED_EDGE('',*,*,#51490,.F.);
#72536=ORIENTED_EDGE('',*,*,#51487,.F.);
#72537=ORIENTED_EDGE('',*,*,#51491,.F.);
#72538=ORIENTED_EDGE('',*,*,#51302,.T.);
#72539=ORIENTED_EDGE('',*,*,#51492,.F.);
#72540=ORIENTED_EDGE('',*,*,#51489,.F.);
#72541=ORIENTED_EDGE('',*,*,#51493,.F.);
#72542=ORIENTED_EDGE('',*,*,#51494,.T.);
#72543=ORIENTED_EDGE('',*,*,#51495,.T.);
#72544=ORIENTED_EDGE('',*,*,#51496,.F.);
#72545=ORIENTED_EDGE('',*,*,#51494,.F.);
#72546=ORIENTED_EDGE('',*,*,#51497,.F.);
#72547=ORIENTED_EDGE('',*,*,#51498,.F.);
#72548=ORIENTED_EDGE('',*,*,#51349,.T.);
#72549=ORIENTED_EDGE('',*,*,#51499,.F.);
#72550=ORIENTED_EDGE('',*,*,#51495,.F.);
#72551=ORIENTED_EDGE('',*,*,#51500,.F.);
#72552=ORIENTED_EDGE('',*,*,#51385,.T.);
#72553=ORIENTED_EDGE('',*,*,#51483,.T.);
#72554=ORIENTED_EDGE('',*,*,#51501,.F.);
#72555=ORIENTED_EDGE('',*,*,#51502,.T.);
#72556=ORIENTED_EDGE('',*,*,#51503,.F.);
#72557=ORIENTED_EDGE('',*,*,#51504,.T.);
#72558=ORIENTED_EDGE('',*,*,#51505,.F.);
#72559=ORIENTED_EDGE('',*,*,#51502,.F.);
#72560=ORIENTED_EDGE('',*,*,#51506,.T.);
#72561=ORIENTED_EDGE('',*,*,#51507,.F.);
#72562=ORIENTED_EDGE('',*,*,#51504,.F.);
#72563=ORIENTED_EDGE('',*,*,#51508,.F.);
#72564=ORIENTED_EDGE('',*,*,#51509,.T.);
#72565=ORIENTED_EDGE('',*,*,#51510,.F.);
#72566=ORIENTED_EDGE('',*,*,#51506,.F.);
#72567=ORIENTED_EDGE('',*,*,#51511,.F.);
#72568=ORIENTED_EDGE('',*,*,#51479,.T.);
#72569=ORIENTED_EDGE('',*,*,#51370,.T.);
#72570=ORIENTED_EDGE('',*,*,#51512,.F.);
#72571=ORIENTED_EDGE('',*,*,#51509,.F.);
#72572=ORIENTED_EDGE('',*,*,#51513,.F.);
#72573=ORIENTED_EDGE('',*,*,#51514,.F.);
#72574=ORIENTED_EDGE('',*,*,#51424,.T.);
#72575=ORIENTED_EDGE('',*,*,#51515,.F.);
#72576=ORIENTED_EDGE('',*,*,#51516,.T.);
#72577=ORIENTED_EDGE('',*,*,#51517,.T.);
#72578=ORIENTED_EDGE('',*,*,#51518,.F.);
#72579=ORIENTED_EDGE('',*,*,#51516,.F.);
#72580=ORIENTED_EDGE('',*,*,#51519,.F.);
#72581=ORIENTED_EDGE('',*,*,#51520,.T.);
#72582=ORIENTED_EDGE('',*,*,#51521,.F.);
#72583=ORIENTED_EDGE('',*,*,#51517,.F.);
#72584=ORIENTED_EDGE('',*,*,#51522,.F.);
#72585=ORIENTED_EDGE('',*,*,#51523,.F.);
#72586=ORIENTED_EDGE('',*,*,#51520,.F.);
#72587=ORIENTED_EDGE('',*,*,#51524,.F.);
#72588=ORIENTED_EDGE('',*,*,#51525,.T.);
#72589=ORIENTED_EDGE('',*,*,#51421,.T.);
#72590=ORIENTED_EDGE('',*,*,#51342,.T.);
#72591=ORIENTED_EDGE('',*,*,#51526,.F.);
#72592=ORIENTED_EDGE('',*,*,#51525,.F.);
#72593=ORIENTED_EDGE('',*,*,#51527,.F.);
#72594=ORIENTED_EDGE('',*,*,#51528,.F.);
#72595=ORIENTED_EDGE('',*,*,#51321,.T.);
#72596=ORIENTED_EDGE('',*,*,#51529,.F.);
#72597=ORIENTED_EDGE('',*,*,#51530,.T.);
#72598=ORIENTED_EDGE('',*,*,#51531,.T.);
#72599=ORIENTED_EDGE('',*,*,#51532,.F.);
#72600=ORIENTED_EDGE('',*,*,#51530,.F.);
#72601=ORIENTED_EDGE('',*,*,#51533,.F.);
#72602=ORIENTED_EDGE('',*,*,#51534,.T.);
#72603=ORIENTED_EDGE('',*,*,#51535,.F.);
#72604=ORIENTED_EDGE('',*,*,#51531,.F.);
#72605=ORIENTED_EDGE('',*,*,#51536,.F.);
#72606=ORIENTED_EDGE('',*,*,#51537,.F.);
#72607=ORIENTED_EDGE('',*,*,#51534,.F.);
#72608=ORIENTED_EDGE('',*,*,#51538,.F.);
#72609=ORIENTED_EDGE('',*,*,#51539,.T.);
#72610=ORIENTED_EDGE('',*,*,#51540,.F.);
#72611=ORIENTED_EDGE('',*,*,#51333,.T.);
#72612=ORIENTED_EDGE('',*,*,#51541,.F.);
#72613=ORIENTED_EDGE('',*,*,#51539,.F.);
#72614=ORIENTED_EDGE('',*,*,#51542,.F.);
#72615=ORIENTED_EDGE('',*,*,#51453,.T.);
#72616=ORIENTED_EDGE('',*,*,#51460,.T.);
#72617=ORIENTED_EDGE('',*,*,#51543,.F.);
#72618=ORIENTED_EDGE('',*,*,#51511,.T.);
#72619=ORIENTED_EDGE('',*,*,#51470,.T.);
#72620=ORIENTED_EDGE('',*,*,#51464,.T.);
#72621=ORIENTED_EDGE('',*,*,#51544,.F.);
#72622=ORIENTED_EDGE('',*,*,#51503,.T.);
#72623=ORIENTED_EDGE('',*,*,#51545,.F.);
#72624=ORIENTED_EDGE('',*,*,#51471,.T.);
#72625=ORIENTED_EDGE('',*,*,#51546,.F.);
#72626=ORIENTED_EDGE('',*,*,#51377,.T.);
#72627=ORIENTED_EDGE('',*,*,#51371,.T.);
#72628=ORIENTED_EDGE('',*,*,#51360,.T.);
#72629=ORIENTED_EDGE('',*,*,#51547,.F.);
#72630=ORIENTED_EDGE('',*,*,#51497,.T.);
#72631=ORIENTED_EDGE('',*,*,#51548,.F.);
#72632=ORIENTED_EDGE('',*,*,#51373,.T.);
#72633=ORIENTED_EDGE('',*,*,#51384,.T.);
#72634=ORIENTED_EDGE('',*,*,#51386,.T.);
#72635=ORIENTED_EDGE('',*,*,#51549,.F.);
#72636=ORIENTED_EDGE('',*,*,#51488,.T.);
#72637=ORIENTED_EDGE('',*,*,#51550,.F.);
#72638=ORIENTED_EDGE('',*,*,#51311,.T.);
#72639=ORIENTED_EDGE('',*,*,#51323,.T.);
#72640=ORIENTED_EDGE('',*,*,#51551,.F.);
#72641=ORIENTED_EDGE('',*,*,#51533,.T.);
#72642=ORIENTED_EDGE('',*,*,#51538,.T.);
#72643=ORIENTED_EDGE('',*,*,#51552,.F.);
#72644=ORIENTED_EDGE('',*,*,#51335,.T.);
#72645=ORIENTED_EDGE('',*,*,#51341,.T.);
#72646=ORIENTED_EDGE('',*,*,#51346,.T.);
#72647=ORIENTED_EDGE('',*,*,#51345,.T.);
#72648=ORIENTED_EDGE('',*,*,#51553,.F.);
#72649=ORIENTED_EDGE('',*,*,#51446,.T.);
#72650=ORIENTED_EDGE('',*,*,#51440,.T.);
#72651=ORIENTED_EDGE('',*,*,#51554,.F.);
#72652=ORIENTED_EDGE('',*,*,#51524,.T.);
#72653=ORIENTED_EDGE('',*,*,#51555,.F.);
#72654=ORIENTED_EDGE('',*,*,#51442,.T.);
#72655=ORIENTED_EDGE('',*,*,#51448,.T.);
#72656=ORIENTED_EDGE('',*,*,#51556,.F.);
#72657=ORIENTED_EDGE('',*,*,#51519,.T.);
#72658=ORIENTED_EDGE('',*,*,#51557,.F.);
#72659=ORIENTED_EDGE('',*,*,#51558,.F.);
#72660=ORIENTED_EDGE('',*,*,#51559,.T.);
#72661=ORIENTED_EDGE('',*,*,#51560,.F.);
#72662=ORIENTED_EDGE('',*,*,#51561,.T.);
#72663=ORIENTED_EDGE('',*,*,#51562,.T.);
#72664=ORIENTED_EDGE('',*,*,#51563,.F.);
#72665=ORIENTED_EDGE('',*,*,#51561,.F.);
#72666=ORIENTED_EDGE('',*,*,#51564,.F.);
#72667=ORIENTED_EDGE('',*,*,#51565,.T.);
#72668=ORIENTED_EDGE('',*,*,#51566,.F.);
#72669=ORIENTED_EDGE('',*,*,#51559,.F.);
#72670=ORIENTED_EDGE('',*,*,#51567,.F.);
#72671=ORIENTED_EDGE('',*,*,#51568,.T.);
#72672=ORIENTED_EDGE('',*,*,#51569,.F.);
#72673=ORIENTED_EDGE('',*,*,#51562,.F.);
#72674=ORIENTED_EDGE('',*,*,#51570,.F.);
#72675=ORIENTED_EDGE('',*,*,#51571,.T.);
#72676=ORIENTED_EDGE('',*,*,#51572,.F.);
#72677=ORIENTED_EDGE('',*,*,#51565,.F.);
#72678=ORIENTED_EDGE('',*,*,#51573,.F.);
#72679=ORIENTED_EDGE('',*,*,#51574,.T.);
#72680=ORIENTED_EDGE('',*,*,#51575,.F.);
#72681=ORIENTED_EDGE('',*,*,#51568,.F.);
#72682=ORIENTED_EDGE('',*,*,#51576,.F.);
#72683=ORIENTED_EDGE('',*,*,#51577,.T.);
#72684=ORIENTED_EDGE('',*,*,#51578,.F.);
#72685=ORIENTED_EDGE('',*,*,#51571,.F.);
#72686=ORIENTED_EDGE('',*,*,#51579,.F.);
#72687=ORIENTED_EDGE('',*,*,#51580,.T.);
#72688=ORIENTED_EDGE('',*,*,#51581,.F.);
#72689=ORIENTED_EDGE('',*,*,#51574,.F.);
#72690=ORIENTED_EDGE('',*,*,#51582,.F.);
#72691=ORIENTED_EDGE('',*,*,#51583,.T.);
#72692=ORIENTED_EDGE('',*,*,#51584,.F.);
#72693=ORIENTED_EDGE('',*,*,#51577,.F.);
#72694=ORIENTED_EDGE('',*,*,#51585,.F.);
#72695=ORIENTED_EDGE('',*,*,#51580,.F.);
#72696=ORIENTED_EDGE('',*,*,#51586,.F.);
#72697=ORIENTED_EDGE('',*,*,#51583,.F.);
#72698=ORIENTED_EDGE('',*,*,#51587,.F.);
#72699=ORIENTED_EDGE('',*,*,#51588,.F.);
#72700=ORIENTED_EDGE('',*,*,#51589,.T.);
#72701=ORIENTED_EDGE('',*,*,#51590,.F.);
#72702=ORIENTED_EDGE('',*,*,#51591,.T.);
#72703=ORIENTED_EDGE('',*,*,#51592,.T.);
#72704=ORIENTED_EDGE('',*,*,#51593,.F.);
#72705=ORIENTED_EDGE('',*,*,#51591,.F.);
#72706=ORIENTED_EDGE('',*,*,#51594,.F.);
#72707=ORIENTED_EDGE('',*,*,#51595,.T.);
#72708=ORIENTED_EDGE('',*,*,#51596,.F.);
#72709=ORIENTED_EDGE('',*,*,#51589,.F.);
#72710=ORIENTED_EDGE('',*,*,#51597,.F.);
#72711=ORIENTED_EDGE('',*,*,#51598,.T.);
#72712=ORIENTED_EDGE('',*,*,#51599,.F.);
#72713=ORIENTED_EDGE('',*,*,#51592,.F.);
#72714=ORIENTED_EDGE('',*,*,#51600,.F.);
#72715=ORIENTED_EDGE('',*,*,#51601,.T.);
#72716=ORIENTED_EDGE('',*,*,#51602,.F.);
#72717=ORIENTED_EDGE('',*,*,#51595,.F.);
#72718=ORIENTED_EDGE('',*,*,#51603,.F.);
#72719=ORIENTED_EDGE('',*,*,#51604,.T.);
#72720=ORIENTED_EDGE('',*,*,#51605,.F.);
#72721=ORIENTED_EDGE('',*,*,#51598,.F.);
#72722=ORIENTED_EDGE('',*,*,#51606,.F.);
#72723=ORIENTED_EDGE('',*,*,#51607,.T.);
#72724=ORIENTED_EDGE('',*,*,#51608,.F.);
#72725=ORIENTED_EDGE('',*,*,#51601,.F.);
#72726=ORIENTED_EDGE('',*,*,#51609,.F.);
#72727=ORIENTED_EDGE('',*,*,#51604,.F.);
#72728=ORIENTED_EDGE('',*,*,#51610,.F.);
#72729=ORIENTED_EDGE('',*,*,#51607,.F.);
#72730=ORIENTED_EDGE('',*,*,#51611,.F.);
#72731=ORIENTED_EDGE('',*,*,#51612,.F.);
#72732=ORIENTED_EDGE('',*,*,#51613,.T.);
#72733=ORIENTED_EDGE('',*,*,#51614,.F.);
#72734=ORIENTED_EDGE('',*,*,#51615,.T.);
#72735=ORIENTED_EDGE('',*,*,#51616,.T.);
#72736=ORIENTED_EDGE('',*,*,#51617,.F.);
#72737=ORIENTED_EDGE('',*,*,#51615,.F.);
#72738=ORIENTED_EDGE('',*,*,#51618,.F.);
#72739=ORIENTED_EDGE('',*,*,#51619,.T.);
#72740=ORIENTED_EDGE('',*,*,#51620,.F.);
#72741=ORIENTED_EDGE('',*,*,#51613,.F.);
#72742=ORIENTED_EDGE('',*,*,#51621,.F.);
#72743=ORIENTED_EDGE('',*,*,#51622,.T.);
#72744=ORIENTED_EDGE('',*,*,#51623,.F.);
#72745=ORIENTED_EDGE('',*,*,#51616,.F.);
#72746=ORIENTED_EDGE('',*,*,#51624,.F.);
#72747=ORIENTED_EDGE('',*,*,#51625,.T.);
#72748=ORIENTED_EDGE('',*,*,#51626,.F.);
#72749=ORIENTED_EDGE('',*,*,#51619,.F.);
#72750=ORIENTED_EDGE('',*,*,#51627,.F.);
#72751=ORIENTED_EDGE('',*,*,#51628,.T.);
#72752=ORIENTED_EDGE('',*,*,#51629,.F.);
#72753=ORIENTED_EDGE('',*,*,#51622,.F.);
#72754=ORIENTED_EDGE('',*,*,#51630,.F.);
#72755=ORIENTED_EDGE('',*,*,#51631,.T.);
#72756=ORIENTED_EDGE('',*,*,#51632,.F.);
#72757=ORIENTED_EDGE('',*,*,#51625,.F.);
#72758=ORIENTED_EDGE('',*,*,#51633,.F.);
#72759=ORIENTED_EDGE('',*,*,#51628,.F.);
#72760=ORIENTED_EDGE('',*,*,#51634,.F.);
#72761=ORIENTED_EDGE('',*,*,#51631,.F.);
#72762=ORIENTED_EDGE('',*,*,#51635,.F.);
#72763=ORIENTED_EDGE('',*,*,#51636,.T.);
#72764=ORIENTED_EDGE('',*,*,#51637,.F.);
#72765=ORIENTED_EDGE('',*,*,#51638,.T.);
#72766=ORIENTED_EDGE('',*,*,#51639,.F.);
#72767=ORIENTED_EDGE('',*,*,#51640,.T.);
#72768=ORIENTED_EDGE('',*,*,#51641,.F.);
#72769=ORIENTED_EDGE('',*,*,#51638,.F.);
#72770=ORIENTED_EDGE('',*,*,#51642,.F.);
#72771=ORIENTED_EDGE('',*,*,#51643,.T.);
#72772=ORIENTED_EDGE('',*,*,#51644,.F.);
#72773=ORIENTED_EDGE('',*,*,#51636,.F.);
#72774=ORIENTED_EDGE('',*,*,#51645,.F.);
#72775=ORIENTED_EDGE('',*,*,#51646,.T.);
#72776=ORIENTED_EDGE('',*,*,#51647,.F.);
#72777=ORIENTED_EDGE('',*,*,#51640,.F.);
#72778=ORIENTED_EDGE('',*,*,#51648,.F.);
#72779=ORIENTED_EDGE('',*,*,#51649,.T.);
#72780=ORIENTED_EDGE('',*,*,#51650,.F.);
#72781=ORIENTED_EDGE('',*,*,#51643,.F.);
#72782=ORIENTED_EDGE('',*,*,#51651,.F.);
#72783=ORIENTED_EDGE('',*,*,#51652,.T.);
#72784=ORIENTED_EDGE('',*,*,#51653,.F.);
#72785=ORIENTED_EDGE('',*,*,#51646,.F.);
#72786=ORIENTED_EDGE('',*,*,#51654,.F.);
#72787=ORIENTED_EDGE('',*,*,#51655,.T.);
#72788=ORIENTED_EDGE('',*,*,#51656,.F.);
#72789=ORIENTED_EDGE('',*,*,#51649,.F.);
#72790=ORIENTED_EDGE('',*,*,#51657,.F.);
#72791=ORIENTED_EDGE('',*,*,#51652,.F.);
#72792=ORIENTED_EDGE('',*,*,#51658,.F.);
#72793=ORIENTED_EDGE('',*,*,#51655,.F.);
#72794=ORIENTED_EDGE('',*,*,#51659,.F.);
#72795=ORIENTED_EDGE('',*,*,#51660,.T.);
#72796=ORIENTED_EDGE('',*,*,#51661,.F.);
#72797=ORIENTED_EDGE('',*,*,#51662,.T.);
#72798=ORIENTED_EDGE('',*,*,#51663,.F.);
#72799=ORIENTED_EDGE('',*,*,#51664,.T.);
#72800=ORIENTED_EDGE('',*,*,#51665,.F.);
#72801=ORIENTED_EDGE('',*,*,#51662,.F.);
#72802=ORIENTED_EDGE('',*,*,#51666,.F.);
#72803=ORIENTED_EDGE('',*,*,#51667,.T.);
#72804=ORIENTED_EDGE('',*,*,#51668,.F.);
#72805=ORIENTED_EDGE('',*,*,#51660,.F.);
#72806=ORIENTED_EDGE('',*,*,#51669,.F.);
#72807=ORIENTED_EDGE('',*,*,#51670,.T.);
#72808=ORIENTED_EDGE('',*,*,#51671,.F.);
#72809=ORIENTED_EDGE('',*,*,#51664,.F.);
#72810=ORIENTED_EDGE('',*,*,#51672,.F.);
#72811=ORIENTED_EDGE('',*,*,#51673,.T.);
#72812=ORIENTED_EDGE('',*,*,#51674,.F.);
#72813=ORIENTED_EDGE('',*,*,#51667,.F.);
#72814=ORIENTED_EDGE('',*,*,#51675,.F.);
#72815=ORIENTED_EDGE('',*,*,#51676,.T.);
#72816=ORIENTED_EDGE('',*,*,#51677,.F.);
#72817=ORIENTED_EDGE('',*,*,#51670,.F.);
#72818=ORIENTED_EDGE('',*,*,#51678,.F.);
#72819=ORIENTED_EDGE('',*,*,#51679,.T.);
#72820=ORIENTED_EDGE('',*,*,#51680,.F.);
#72821=ORIENTED_EDGE('',*,*,#51673,.F.);
#72822=ORIENTED_EDGE('',*,*,#51681,.F.);
#72823=ORIENTED_EDGE('',*,*,#51682,.T.);
#72824=ORIENTED_EDGE('',*,*,#51683,.F.);
#72825=ORIENTED_EDGE('',*,*,#51676,.F.);
#72826=ORIENTED_EDGE('',*,*,#51684,.F.);
#72827=ORIENTED_EDGE('',*,*,#51679,.F.);
#72828=ORIENTED_EDGE('',*,*,#51685,.F.);
#72829=ORIENTED_EDGE('',*,*,#51682,.F.);
#72830=ORIENTED_EDGE('',*,*,#51686,.F.);
#72831=ORIENTED_EDGE('',*,*,#51687,.T.);
#72832=ORIENTED_EDGE('',*,*,#51688,.F.);
#72833=ORIENTED_EDGE('',*,*,#51689,.T.);
#72834=ORIENTED_EDGE('',*,*,#51690,.F.);
#72835=ORIENTED_EDGE('',*,*,#51691,.T.);
#72836=ORIENTED_EDGE('',*,*,#51692,.F.);
#72837=ORIENTED_EDGE('',*,*,#51689,.F.);
#72838=ORIENTED_EDGE('',*,*,#51693,.F.);
#72839=ORIENTED_EDGE('',*,*,#51694,.T.);
#72840=ORIENTED_EDGE('',*,*,#51695,.F.);
#72841=ORIENTED_EDGE('',*,*,#51687,.F.);
#72842=ORIENTED_EDGE('',*,*,#51696,.F.);
#72843=ORIENTED_EDGE('',*,*,#51697,.T.);
#72844=ORIENTED_EDGE('',*,*,#51698,.F.);
#72845=ORIENTED_EDGE('',*,*,#51691,.F.);
#72846=ORIENTED_EDGE('',*,*,#51699,.F.);
#72847=ORIENTED_EDGE('',*,*,#51700,.T.);
#72848=ORIENTED_EDGE('',*,*,#51701,.F.);
#72849=ORIENTED_EDGE('',*,*,#51694,.F.);
#72850=ORIENTED_EDGE('',*,*,#51702,.F.);
#72851=ORIENTED_EDGE('',*,*,#51703,.T.);
#72852=ORIENTED_EDGE('',*,*,#51704,.F.);
#72853=ORIENTED_EDGE('',*,*,#51697,.F.);
#72854=ORIENTED_EDGE('',*,*,#51705,.F.);
#72855=ORIENTED_EDGE('',*,*,#51706,.T.);
#72856=ORIENTED_EDGE('',*,*,#51707,.F.);
#72857=ORIENTED_EDGE('',*,*,#51700,.F.);
#72858=ORIENTED_EDGE('',*,*,#51708,.F.);
#72859=ORIENTED_EDGE('',*,*,#51703,.F.);
#72860=ORIENTED_EDGE('',*,*,#51709,.F.);
#72861=ORIENTED_EDGE('',*,*,#51706,.F.);
#72862=ORIENTED_EDGE('',*,*,#51710,.F.);
#72863=ORIENTED_EDGE('',*,*,#51711,.T.);
#72864=ORIENTED_EDGE('',*,*,#51712,.F.);
#72865=ORIENTED_EDGE('',*,*,#51713,.T.);
#72866=ORIENTED_EDGE('',*,*,#51714,.F.);
#72867=ORIENTED_EDGE('',*,*,#51715,.T.);
#72868=ORIENTED_EDGE('',*,*,#51716,.F.);
#72869=ORIENTED_EDGE('',*,*,#51713,.F.);
#72870=ORIENTED_EDGE('',*,*,#51717,.F.);
#72871=ORIENTED_EDGE('',*,*,#51718,.T.);
#72872=ORIENTED_EDGE('',*,*,#51719,.F.);
#72873=ORIENTED_EDGE('',*,*,#51711,.F.);
#72874=ORIENTED_EDGE('',*,*,#51720,.F.);
#72875=ORIENTED_EDGE('',*,*,#51721,.T.);
#72876=ORIENTED_EDGE('',*,*,#51722,.F.);
#72877=ORIENTED_EDGE('',*,*,#51715,.F.);
#72878=ORIENTED_EDGE('',*,*,#51723,.F.);
#72879=ORIENTED_EDGE('',*,*,#51724,.T.);
#72880=ORIENTED_EDGE('',*,*,#51725,.F.);
#72881=ORIENTED_EDGE('',*,*,#51718,.F.);
#72882=ORIENTED_EDGE('',*,*,#51726,.F.);
#72883=ORIENTED_EDGE('',*,*,#51727,.T.);
#72884=ORIENTED_EDGE('',*,*,#51728,.F.);
#72885=ORIENTED_EDGE('',*,*,#51721,.F.);
#72886=ORIENTED_EDGE('',*,*,#51729,.F.);
#72887=ORIENTED_EDGE('',*,*,#51730,.T.);
#72888=ORIENTED_EDGE('',*,*,#51731,.F.);
#72889=ORIENTED_EDGE('',*,*,#51724,.F.);
#72890=ORIENTED_EDGE('',*,*,#51732,.F.);
#72891=ORIENTED_EDGE('',*,*,#51727,.F.);
#72892=ORIENTED_EDGE('',*,*,#51733,.F.);
#72893=ORIENTED_EDGE('',*,*,#51730,.F.);
#72894=ORIENTED_EDGE('',*,*,#51734,.F.);
#72895=ORIENTED_EDGE('',*,*,#51735,.T.);
#72896=ORIENTED_EDGE('',*,*,#51736,.F.);
#72897=ORIENTED_EDGE('',*,*,#51737,.T.);
#72898=ORIENTED_EDGE('',*,*,#51738,.F.);
#72899=ORIENTED_EDGE('',*,*,#51739,.T.);
#72900=ORIENTED_EDGE('',*,*,#51740,.F.);
#72901=ORIENTED_EDGE('',*,*,#51737,.F.);
#72902=ORIENTED_EDGE('',*,*,#51741,.F.);
#72903=ORIENTED_EDGE('',*,*,#51742,.T.);
#72904=ORIENTED_EDGE('',*,*,#51743,.F.);
#72905=ORIENTED_EDGE('',*,*,#51735,.F.);
#72906=ORIENTED_EDGE('',*,*,#51744,.F.);
#72907=ORIENTED_EDGE('',*,*,#51745,.T.);
#72908=ORIENTED_EDGE('',*,*,#51746,.F.);
#72909=ORIENTED_EDGE('',*,*,#51739,.F.);
#72910=ORIENTED_EDGE('',*,*,#51747,.F.);
#72911=ORIENTED_EDGE('',*,*,#51748,.T.);
#72912=ORIENTED_EDGE('',*,*,#51749,.F.);
#72913=ORIENTED_EDGE('',*,*,#51742,.F.);
#72914=ORIENTED_EDGE('',*,*,#51750,.F.);
#72915=ORIENTED_EDGE('',*,*,#51751,.T.);
#72916=ORIENTED_EDGE('',*,*,#51752,.F.);
#72917=ORIENTED_EDGE('',*,*,#51745,.F.);
#72918=ORIENTED_EDGE('',*,*,#51753,.F.);
#72919=ORIENTED_EDGE('',*,*,#51754,.T.);
#72920=ORIENTED_EDGE('',*,*,#51755,.F.);
#72921=ORIENTED_EDGE('',*,*,#51748,.F.);
#72922=ORIENTED_EDGE('',*,*,#51756,.F.);
#72923=ORIENTED_EDGE('',*,*,#51751,.F.);
#72924=ORIENTED_EDGE('',*,*,#51757,.F.);
#72925=ORIENTED_EDGE('',*,*,#51754,.F.);
#72926=ORIENTED_EDGE('',*,*,#51758,.F.);
#72927=ORIENTED_EDGE('',*,*,#51759,.T.);
#72928=ORIENTED_EDGE('',*,*,#51760,.F.);
#72929=ORIENTED_EDGE('',*,*,#51761,.T.);
#72930=ORIENTED_EDGE('',*,*,#51762,.F.);
#72931=ORIENTED_EDGE('',*,*,#51763,.T.);
#72932=ORIENTED_EDGE('',*,*,#51764,.F.);
#72933=ORIENTED_EDGE('',*,*,#51761,.F.);
#72934=ORIENTED_EDGE('',*,*,#51765,.F.);
#72935=ORIENTED_EDGE('',*,*,#51766,.T.);
#72936=ORIENTED_EDGE('',*,*,#51767,.F.);
#72937=ORIENTED_EDGE('',*,*,#51759,.F.);
#72938=ORIENTED_EDGE('',*,*,#51768,.F.);
#72939=ORIENTED_EDGE('',*,*,#51769,.T.);
#72940=ORIENTED_EDGE('',*,*,#51770,.F.);
#72941=ORIENTED_EDGE('',*,*,#51763,.F.);
#72942=ORIENTED_EDGE('',*,*,#51771,.F.);
#72943=ORIENTED_EDGE('',*,*,#51772,.T.);
#72944=ORIENTED_EDGE('',*,*,#51773,.F.);
#72945=ORIENTED_EDGE('',*,*,#51766,.F.);
#72946=ORIENTED_EDGE('',*,*,#51774,.F.);
#72947=ORIENTED_EDGE('',*,*,#51775,.T.);
#72948=ORIENTED_EDGE('',*,*,#51776,.F.);
#72949=ORIENTED_EDGE('',*,*,#51769,.F.);
#72950=ORIENTED_EDGE('',*,*,#51777,.F.);
#72951=ORIENTED_EDGE('',*,*,#51778,.T.);
#72952=ORIENTED_EDGE('',*,*,#51779,.F.);
#72953=ORIENTED_EDGE('',*,*,#51772,.F.);
#72954=ORIENTED_EDGE('',*,*,#51780,.F.);
#72955=ORIENTED_EDGE('',*,*,#51775,.F.);
#72956=ORIENTED_EDGE('',*,*,#51781,.F.);
#72957=ORIENTED_EDGE('',*,*,#51778,.F.);
#72958=ORIENTED_EDGE('',*,*,#51782,.F.);
#72959=ORIENTED_EDGE('',*,*,#51783,.T.);
#72960=ORIENTED_EDGE('',*,*,#51784,.F.);
#72961=ORIENTED_EDGE('',*,*,#51785,.T.);
#72962=ORIENTED_EDGE('',*,*,#51786,.F.);
#72963=ORIENTED_EDGE('',*,*,#51787,.T.);
#72964=ORIENTED_EDGE('',*,*,#51788,.F.);
#72965=ORIENTED_EDGE('',*,*,#51785,.F.);
#72966=ORIENTED_EDGE('',*,*,#51789,.F.);
#72967=ORIENTED_EDGE('',*,*,#51790,.T.);
#72968=ORIENTED_EDGE('',*,*,#51791,.F.);
#72969=ORIENTED_EDGE('',*,*,#51783,.F.);
#72970=ORIENTED_EDGE('',*,*,#51792,.F.);
#72971=ORIENTED_EDGE('',*,*,#51793,.T.);
#72972=ORIENTED_EDGE('',*,*,#51794,.F.);
#72973=ORIENTED_EDGE('',*,*,#51787,.F.);
#72974=ORIENTED_EDGE('',*,*,#51795,.F.);
#72975=ORIENTED_EDGE('',*,*,#51796,.T.);
#72976=ORIENTED_EDGE('',*,*,#51797,.F.);
#72977=ORIENTED_EDGE('',*,*,#51790,.F.);
#72978=ORIENTED_EDGE('',*,*,#51798,.F.);
#72979=ORIENTED_EDGE('',*,*,#51799,.T.);
#72980=ORIENTED_EDGE('',*,*,#51800,.F.);
#72981=ORIENTED_EDGE('',*,*,#51793,.F.);
#72982=ORIENTED_EDGE('',*,*,#51801,.F.);
#72983=ORIENTED_EDGE('',*,*,#51802,.T.);
#72984=ORIENTED_EDGE('',*,*,#51803,.F.);
#72985=ORIENTED_EDGE('',*,*,#51796,.F.);
#72986=ORIENTED_EDGE('',*,*,#51804,.F.);
#72987=ORIENTED_EDGE('',*,*,#51799,.F.);
#72988=ORIENTED_EDGE('',*,*,#51805,.F.);
#72989=ORIENTED_EDGE('',*,*,#51802,.F.);
#72990=ORIENTED_EDGE('',*,*,#51806,.F.);
#72991=ORIENTED_EDGE('',*,*,#51807,.T.);
#72992=ORIENTED_EDGE('',*,*,#51808,.F.);
#72993=ORIENTED_EDGE('',*,*,#51809,.T.);
#72994=ORIENTED_EDGE('',*,*,#51810,.F.);
#72995=ORIENTED_EDGE('',*,*,#51811,.T.);
#72996=ORIENTED_EDGE('',*,*,#51812,.F.);
#72997=ORIENTED_EDGE('',*,*,#51809,.F.);
#72998=ORIENTED_EDGE('',*,*,#51813,.F.);
#72999=ORIENTED_EDGE('',*,*,#51814,.T.);
#73000=ORIENTED_EDGE('',*,*,#51815,.F.);
#73001=ORIENTED_EDGE('',*,*,#51807,.F.);
#73002=ORIENTED_EDGE('',*,*,#51816,.F.);
#73003=ORIENTED_EDGE('',*,*,#51817,.T.);
#73004=ORIENTED_EDGE('',*,*,#51818,.F.);
#73005=ORIENTED_EDGE('',*,*,#51811,.F.);
#73006=ORIENTED_EDGE('',*,*,#51819,.F.);
#73007=ORIENTED_EDGE('',*,*,#51820,.T.);
#73008=ORIENTED_EDGE('',*,*,#51821,.F.);
#73009=ORIENTED_EDGE('',*,*,#51814,.F.);
#73010=ORIENTED_EDGE('',*,*,#51822,.F.);
#73011=ORIENTED_EDGE('',*,*,#51823,.T.);
#73012=ORIENTED_EDGE('',*,*,#51824,.F.);
#73013=ORIENTED_EDGE('',*,*,#51817,.F.);
#73014=ORIENTED_EDGE('',*,*,#51825,.F.);
#73015=ORIENTED_EDGE('',*,*,#51826,.T.);
#73016=ORIENTED_EDGE('',*,*,#51827,.F.);
#73017=ORIENTED_EDGE('',*,*,#51820,.F.);
#73018=ORIENTED_EDGE('',*,*,#51828,.F.);
#73019=ORIENTED_EDGE('',*,*,#51829,.T.);
#73020=ORIENTED_EDGE('',*,*,#51830,.F.);
#73021=ORIENTED_EDGE('',*,*,#51823,.F.);
#73022=ORIENTED_EDGE('',*,*,#51831,.F.);
#73023=ORIENTED_EDGE('',*,*,#51832,.T.);
#73024=ORIENTED_EDGE('',*,*,#51833,.F.);
#73025=ORIENTED_EDGE('',*,*,#51826,.F.);
#73026=ORIENTED_EDGE('',*,*,#51834,.F.);
#73027=ORIENTED_EDGE('',*,*,#51829,.F.);
#73028=ORIENTED_EDGE('',*,*,#51835,.F.);
#73029=ORIENTED_EDGE('',*,*,#51832,.F.);
#73030=ORIENTED_EDGE('',*,*,#51836,.F.);
#73031=ORIENTED_EDGE('',*,*,#51837,.T.);
#73032=ORIENTED_EDGE('',*,*,#51838,.F.);
#73033=ORIENTED_EDGE('',*,*,#51839,.T.);
#73034=ORIENTED_EDGE('',*,*,#51840,.F.);
#73035=ORIENTED_EDGE('',*,*,#51841,.T.);
#73036=ORIENTED_EDGE('',*,*,#51842,.F.);
#73037=ORIENTED_EDGE('',*,*,#51839,.F.);
#73038=ORIENTED_EDGE('',*,*,#51843,.F.);
#73039=ORIENTED_EDGE('',*,*,#51844,.T.);
#73040=ORIENTED_EDGE('',*,*,#51845,.F.);
#73041=ORIENTED_EDGE('',*,*,#51837,.F.);
#73042=ORIENTED_EDGE('',*,*,#51846,.F.);
#73043=ORIENTED_EDGE('',*,*,#51847,.T.);
#73044=ORIENTED_EDGE('',*,*,#51848,.F.);
#73045=ORIENTED_EDGE('',*,*,#51841,.F.);
#73046=ORIENTED_EDGE('',*,*,#51849,.F.);
#73047=ORIENTED_EDGE('',*,*,#51850,.T.);
#73048=ORIENTED_EDGE('',*,*,#51851,.F.);
#73049=ORIENTED_EDGE('',*,*,#51844,.F.);
#73050=ORIENTED_EDGE('',*,*,#51852,.F.);
#73051=ORIENTED_EDGE('',*,*,#51853,.T.);
#73052=ORIENTED_EDGE('',*,*,#51854,.F.);
#73053=ORIENTED_EDGE('',*,*,#51847,.F.);
#73054=ORIENTED_EDGE('',*,*,#51855,.F.);
#73055=ORIENTED_EDGE('',*,*,#51856,.T.);
#73056=ORIENTED_EDGE('',*,*,#51857,.F.);
#73057=ORIENTED_EDGE('',*,*,#51850,.F.);
#73058=ORIENTED_EDGE('',*,*,#51858,.F.);
#73059=ORIENTED_EDGE('',*,*,#51853,.F.);
#73060=ORIENTED_EDGE('',*,*,#51859,.F.);
#73061=ORIENTED_EDGE('',*,*,#51856,.F.);
#73062=ORIENTED_EDGE('',*,*,#51860,.F.);
#73063=ORIENTED_EDGE('',*,*,#51861,.T.);
#73064=ORIENTED_EDGE('',*,*,#51862,.F.);
#73065=ORIENTED_EDGE('',*,*,#51863,.T.);
#73066=ORIENTED_EDGE('',*,*,#51864,.F.);
#73067=ORIENTED_EDGE('',*,*,#51865,.T.);
#73068=ORIENTED_EDGE('',*,*,#51866,.F.);
#73069=ORIENTED_EDGE('',*,*,#51863,.F.);
#73070=ORIENTED_EDGE('',*,*,#51867,.F.);
#73071=ORIENTED_EDGE('',*,*,#51868,.T.);
#73072=ORIENTED_EDGE('',*,*,#51869,.F.);
#73073=ORIENTED_EDGE('',*,*,#51861,.F.);
#73074=ORIENTED_EDGE('',*,*,#51870,.F.);
#73075=ORIENTED_EDGE('',*,*,#51871,.T.);
#73076=ORIENTED_EDGE('',*,*,#51872,.F.);
#73077=ORIENTED_EDGE('',*,*,#51865,.F.);
#73078=ORIENTED_EDGE('',*,*,#51873,.F.);
#73079=ORIENTED_EDGE('',*,*,#51874,.T.);
#73080=ORIENTED_EDGE('',*,*,#51875,.F.);
#73081=ORIENTED_EDGE('',*,*,#51868,.F.);
#73082=ORIENTED_EDGE('',*,*,#51876,.F.);
#73083=ORIENTED_EDGE('',*,*,#51877,.T.);
#73084=ORIENTED_EDGE('',*,*,#51878,.F.);
#73085=ORIENTED_EDGE('',*,*,#51871,.F.);
#73086=ORIENTED_EDGE('',*,*,#51879,.F.);
#73087=ORIENTED_EDGE('',*,*,#51880,.T.);
#73088=ORIENTED_EDGE('',*,*,#51881,.F.);
#73089=ORIENTED_EDGE('',*,*,#51874,.F.);
#73090=ORIENTED_EDGE('',*,*,#51882,.F.);
#73091=ORIENTED_EDGE('',*,*,#51877,.F.);
#73092=ORIENTED_EDGE('',*,*,#51883,.F.);
#73093=ORIENTED_EDGE('',*,*,#51880,.F.);
#73094=ORIENTED_EDGE('',*,*,#51884,.F.);
#73095=ORIENTED_EDGE('',*,*,#51885,.T.);
#73096=ORIENTED_EDGE('',*,*,#51886,.F.);
#73097=ORIENTED_EDGE('',*,*,#51887,.T.);
#73098=ORIENTED_EDGE('',*,*,#51888,.F.);
#73099=ORIENTED_EDGE('',*,*,#51889,.T.);
#73100=ORIENTED_EDGE('',*,*,#51890,.F.);
#73101=ORIENTED_EDGE('',*,*,#51887,.F.);
#73102=ORIENTED_EDGE('',*,*,#51891,.F.);
#73103=ORIENTED_EDGE('',*,*,#51892,.T.);
#73104=ORIENTED_EDGE('',*,*,#51893,.F.);
#73105=ORIENTED_EDGE('',*,*,#51885,.F.);
#73106=ORIENTED_EDGE('',*,*,#51894,.F.);
#73107=ORIENTED_EDGE('',*,*,#51895,.T.);
#73108=ORIENTED_EDGE('',*,*,#51896,.F.);
#73109=ORIENTED_EDGE('',*,*,#51889,.F.);
#73110=ORIENTED_EDGE('',*,*,#51897,.F.);
#73111=ORIENTED_EDGE('',*,*,#51898,.T.);
#73112=ORIENTED_EDGE('',*,*,#51899,.F.);
#73113=ORIENTED_EDGE('',*,*,#51892,.F.);
#73114=ORIENTED_EDGE('',*,*,#51900,.F.);
#73115=ORIENTED_EDGE('',*,*,#51901,.T.);
#73116=ORIENTED_EDGE('',*,*,#51902,.F.);
#73117=ORIENTED_EDGE('',*,*,#51895,.F.);
#73118=ORIENTED_EDGE('',*,*,#51903,.F.);
#73119=ORIENTED_EDGE('',*,*,#51904,.T.);
#73120=ORIENTED_EDGE('',*,*,#51905,.F.);
#73121=ORIENTED_EDGE('',*,*,#51898,.F.);
#73122=ORIENTED_EDGE('',*,*,#51906,.F.);
#73123=ORIENTED_EDGE('',*,*,#51907,.T.);
#73124=ORIENTED_EDGE('',*,*,#51908,.F.);
#73125=ORIENTED_EDGE('',*,*,#51901,.F.);
#73126=ORIENTED_EDGE('',*,*,#51909,.F.);
#73127=ORIENTED_EDGE('',*,*,#51910,.T.);
#73128=ORIENTED_EDGE('',*,*,#51911,.F.);
#73129=ORIENTED_EDGE('',*,*,#51904,.F.);
#73130=ORIENTED_EDGE('',*,*,#51912,.F.);
#73131=ORIENTED_EDGE('',*,*,#51907,.F.);
#73132=ORIENTED_EDGE('',*,*,#51913,.F.);
#73133=ORIENTED_EDGE('',*,*,#51910,.F.);
#73134=ORIENTED_EDGE('',*,*,#51914,.F.);
#73135=ORIENTED_EDGE('',*,*,#51915,.T.);
#73136=ORIENTED_EDGE('',*,*,#51916,.F.);
#73137=ORIENTED_EDGE('',*,*,#51917,.T.);
#73138=ORIENTED_EDGE('',*,*,#51918,.F.);
#73139=ORIENTED_EDGE('',*,*,#51919,.T.);
#73140=ORIENTED_EDGE('',*,*,#51920,.F.);
#73141=ORIENTED_EDGE('',*,*,#51917,.F.);
#73142=ORIENTED_EDGE('',*,*,#51921,.F.);
#73143=ORIENTED_EDGE('',*,*,#51922,.T.);
#73144=ORIENTED_EDGE('',*,*,#51923,.F.);
#73145=ORIENTED_EDGE('',*,*,#51915,.F.);
#73146=ORIENTED_EDGE('',*,*,#51924,.F.);
#73147=ORIENTED_EDGE('',*,*,#51925,.T.);
#73148=ORIENTED_EDGE('',*,*,#51926,.F.);
#73149=ORIENTED_EDGE('',*,*,#51919,.F.);
#73150=ORIENTED_EDGE('',*,*,#51927,.F.);
#73151=ORIENTED_EDGE('',*,*,#51928,.T.);
#73152=ORIENTED_EDGE('',*,*,#51929,.F.);
#73153=ORIENTED_EDGE('',*,*,#51922,.F.);
#73154=ORIENTED_EDGE('',*,*,#51930,.F.);
#73155=ORIENTED_EDGE('',*,*,#51931,.T.);
#73156=ORIENTED_EDGE('',*,*,#51932,.F.);
#73157=ORIENTED_EDGE('',*,*,#51925,.F.);
#73158=ORIENTED_EDGE('',*,*,#51933,.F.);
#73159=ORIENTED_EDGE('',*,*,#51934,.T.);
#73160=ORIENTED_EDGE('',*,*,#51935,.F.);
#73161=ORIENTED_EDGE('',*,*,#51928,.F.);
#73162=ORIENTED_EDGE('',*,*,#51936,.F.);
#73163=ORIENTED_EDGE('',*,*,#51937,.T.);
#73164=ORIENTED_EDGE('',*,*,#51938,.F.);
#73165=ORIENTED_EDGE('',*,*,#51931,.F.);
#73166=ORIENTED_EDGE('',*,*,#51939,.F.);
#73167=ORIENTED_EDGE('',*,*,#51940,.T.);
#73168=ORIENTED_EDGE('',*,*,#51941,.F.);
#73169=ORIENTED_EDGE('',*,*,#51934,.F.);
#73170=ORIENTED_EDGE('',*,*,#51942,.F.);
#73171=ORIENTED_EDGE('',*,*,#51937,.F.);
#73172=ORIENTED_EDGE('',*,*,#51943,.F.);
#73173=ORIENTED_EDGE('',*,*,#51940,.F.);
#73174=ORIENTED_EDGE('',*,*,#51944,.F.);
#73175=ORIENTED_EDGE('',*,*,#51945,.T.);
#73176=ORIENTED_EDGE('',*,*,#51946,.F.);
#73177=ORIENTED_EDGE('',*,*,#51947,.T.);
#73178=ORIENTED_EDGE('',*,*,#51948,.F.);
#73179=ORIENTED_EDGE('',*,*,#51949,.T.);
#73180=ORIENTED_EDGE('',*,*,#51950,.F.);
#73181=ORIENTED_EDGE('',*,*,#51947,.F.);
#73182=ORIENTED_EDGE('',*,*,#51951,.F.);
#73183=ORIENTED_EDGE('',*,*,#51952,.T.);
#73184=ORIENTED_EDGE('',*,*,#51953,.F.);
#73185=ORIENTED_EDGE('',*,*,#51945,.F.);
#73186=ORIENTED_EDGE('',*,*,#51954,.F.);
#73187=ORIENTED_EDGE('',*,*,#51955,.T.);
#73188=ORIENTED_EDGE('',*,*,#51956,.F.);
#73189=ORIENTED_EDGE('',*,*,#51949,.F.);
#73190=ORIENTED_EDGE('',*,*,#51957,.F.);
#73191=ORIENTED_EDGE('',*,*,#51958,.T.);
#73192=ORIENTED_EDGE('',*,*,#51959,.F.);
#73193=ORIENTED_EDGE('',*,*,#51952,.F.);
#73194=ORIENTED_EDGE('',*,*,#51960,.F.);
#73195=ORIENTED_EDGE('',*,*,#51961,.T.);
#73196=ORIENTED_EDGE('',*,*,#51962,.F.);
#73197=ORIENTED_EDGE('',*,*,#51955,.F.);
#73198=ORIENTED_EDGE('',*,*,#51963,.F.);
#73199=ORIENTED_EDGE('',*,*,#51964,.T.);
#73200=ORIENTED_EDGE('',*,*,#51965,.F.);
#73201=ORIENTED_EDGE('',*,*,#51958,.F.);
#73202=ORIENTED_EDGE('',*,*,#51966,.F.);
#73203=ORIENTED_EDGE('',*,*,#51961,.F.);
#73204=ORIENTED_EDGE('',*,*,#51967,.F.);
#73205=ORIENTED_EDGE('',*,*,#51964,.F.);
#73206=ORIENTED_EDGE('',*,*,#51968,.F.);
#73207=ORIENTED_EDGE('',*,*,#51969,.T.);
#73208=ORIENTED_EDGE('',*,*,#51970,.F.);
#73209=ORIENTED_EDGE('',*,*,#51971,.T.);
#73210=ORIENTED_EDGE('',*,*,#51972,.F.);
#73211=ORIENTED_EDGE('',*,*,#51973,.T.);
#73212=ORIENTED_EDGE('',*,*,#51974,.F.);
#73213=ORIENTED_EDGE('',*,*,#51971,.F.);
#73214=ORIENTED_EDGE('',*,*,#51975,.F.);
#73215=ORIENTED_EDGE('',*,*,#51976,.T.);
#73216=ORIENTED_EDGE('',*,*,#51977,.F.);
#73217=ORIENTED_EDGE('',*,*,#51969,.F.);
#73218=ORIENTED_EDGE('',*,*,#51978,.F.);
#73219=ORIENTED_EDGE('',*,*,#51979,.T.);
#73220=ORIENTED_EDGE('',*,*,#51980,.F.);
#73221=ORIENTED_EDGE('',*,*,#51973,.F.);
#73222=ORIENTED_EDGE('',*,*,#51981,.F.);
#73223=ORIENTED_EDGE('',*,*,#51982,.T.);
#73224=ORIENTED_EDGE('',*,*,#51983,.F.);
#73225=ORIENTED_EDGE('',*,*,#51976,.F.);
#73226=ORIENTED_EDGE('',*,*,#51984,.F.);
#73227=ORIENTED_EDGE('',*,*,#51985,.T.);
#73228=ORIENTED_EDGE('',*,*,#51986,.F.);
#73229=ORIENTED_EDGE('',*,*,#51979,.F.);
#73230=ORIENTED_EDGE('',*,*,#51987,.F.);
#73231=ORIENTED_EDGE('',*,*,#51988,.T.);
#73232=ORIENTED_EDGE('',*,*,#51989,.F.);
#73233=ORIENTED_EDGE('',*,*,#51982,.F.);
#73234=ORIENTED_EDGE('',*,*,#51990,.F.);
#73235=ORIENTED_EDGE('',*,*,#51985,.F.);
#73236=ORIENTED_EDGE('',*,*,#51991,.F.);
#73237=ORIENTED_EDGE('',*,*,#51988,.F.);
#73238=ORIENTED_EDGE('',*,*,#51992,.F.);
#73239=ORIENTED_EDGE('',*,*,#51993,.T.);
#73240=ORIENTED_EDGE('',*,*,#51994,.F.);
#73241=ORIENTED_EDGE('',*,*,#51995,.T.);
#73242=ORIENTED_EDGE('',*,*,#51996,.F.);
#73243=ORIENTED_EDGE('',*,*,#51997,.T.);
#73244=ORIENTED_EDGE('',*,*,#51998,.F.);
#73245=ORIENTED_EDGE('',*,*,#51995,.F.);
#73246=ORIENTED_EDGE('',*,*,#51999,.F.);
#73247=ORIENTED_EDGE('',*,*,#52000,.T.);
#73248=ORIENTED_EDGE('',*,*,#52001,.F.);
#73249=ORIENTED_EDGE('',*,*,#51993,.F.);
#73250=ORIENTED_EDGE('',*,*,#52002,.F.);
#73251=ORIENTED_EDGE('',*,*,#52003,.T.);
#73252=ORIENTED_EDGE('',*,*,#52004,.F.);
#73253=ORIENTED_EDGE('',*,*,#51997,.F.);
#73254=ORIENTED_EDGE('',*,*,#52005,.F.);
#73255=ORIENTED_EDGE('',*,*,#52006,.T.);
#73256=ORIENTED_EDGE('',*,*,#52007,.F.);
#73257=ORIENTED_EDGE('',*,*,#52000,.F.);
#73258=ORIENTED_EDGE('',*,*,#52008,.F.);
#73259=ORIENTED_EDGE('',*,*,#52009,.T.);
#73260=ORIENTED_EDGE('',*,*,#52010,.F.);
#73261=ORIENTED_EDGE('',*,*,#52003,.F.);
#73262=ORIENTED_EDGE('',*,*,#52011,.F.);
#73263=ORIENTED_EDGE('',*,*,#52012,.T.);
#73264=ORIENTED_EDGE('',*,*,#52013,.F.);
#73265=ORIENTED_EDGE('',*,*,#52006,.F.);
#73266=ORIENTED_EDGE('',*,*,#52014,.F.);
#73267=ORIENTED_EDGE('',*,*,#52009,.F.);
#73268=ORIENTED_EDGE('',*,*,#52015,.F.);
#73269=ORIENTED_EDGE('',*,*,#52012,.F.);
#73270=ORIENTED_EDGE('',*,*,#52016,.F.);
#73271=ORIENTED_EDGE('',*,*,#52017,.T.);
#73272=ORIENTED_EDGE('',*,*,#52018,.F.);
#73273=ORIENTED_EDGE('',*,*,#52019,.T.);
#73274=ORIENTED_EDGE('',*,*,#52020,.F.);
#73275=ORIENTED_EDGE('',*,*,#52021,.T.);
#73276=ORIENTED_EDGE('',*,*,#52022,.F.);
#73277=ORIENTED_EDGE('',*,*,#52019,.F.);
#73278=ORIENTED_EDGE('',*,*,#52023,.F.);
#73279=ORIENTED_EDGE('',*,*,#52024,.T.);
#73280=ORIENTED_EDGE('',*,*,#52025,.F.);
#73281=ORIENTED_EDGE('',*,*,#52017,.F.);
#73282=ORIENTED_EDGE('',*,*,#52026,.F.);
#73283=ORIENTED_EDGE('',*,*,#52027,.T.);
#73284=ORIENTED_EDGE('',*,*,#52028,.F.);
#73285=ORIENTED_EDGE('',*,*,#52021,.F.);
#73286=ORIENTED_EDGE('',*,*,#52029,.F.);
#73287=ORIENTED_EDGE('',*,*,#52030,.T.);
#73288=ORIENTED_EDGE('',*,*,#52031,.F.);
#73289=ORIENTED_EDGE('',*,*,#52024,.F.);
#73290=ORIENTED_EDGE('',*,*,#52032,.F.);
#73291=ORIENTED_EDGE('',*,*,#52033,.T.);
#73292=ORIENTED_EDGE('',*,*,#52034,.F.);
#73293=ORIENTED_EDGE('',*,*,#52027,.F.);
#73294=ORIENTED_EDGE('',*,*,#52035,.F.);
#73295=ORIENTED_EDGE('',*,*,#52036,.T.);
#73296=ORIENTED_EDGE('',*,*,#52037,.F.);
#73297=ORIENTED_EDGE('',*,*,#52030,.F.);
#73298=ORIENTED_EDGE('',*,*,#52038,.F.);
#73299=ORIENTED_EDGE('',*,*,#52033,.F.);
#73300=ORIENTED_EDGE('',*,*,#52039,.F.);
#73301=ORIENTED_EDGE('',*,*,#52036,.F.);
#73302=ORIENTED_EDGE('',*,*,#52040,.F.);
#73303=ORIENTED_EDGE('',*,*,#52041,.T.);
#73304=ORIENTED_EDGE('',*,*,#52042,.F.);
#73305=ORIENTED_EDGE('',*,*,#52043,.T.);
#73306=ORIENTED_EDGE('',*,*,#52044,.F.);
#73307=ORIENTED_EDGE('',*,*,#52045,.T.);
#73308=ORIENTED_EDGE('',*,*,#52046,.F.);
#73309=ORIENTED_EDGE('',*,*,#52043,.F.);
#73310=ORIENTED_EDGE('',*,*,#52047,.F.);
#73311=ORIENTED_EDGE('',*,*,#52048,.T.);
#73312=ORIENTED_EDGE('',*,*,#52049,.F.);
#73313=ORIENTED_EDGE('',*,*,#52041,.F.);
#73314=ORIENTED_EDGE('',*,*,#52050,.F.);
#73315=ORIENTED_EDGE('',*,*,#52051,.T.);
#73316=ORIENTED_EDGE('',*,*,#52052,.F.);
#73317=ORIENTED_EDGE('',*,*,#52045,.F.);
#73318=ORIENTED_EDGE('',*,*,#52053,.F.);
#73319=ORIENTED_EDGE('',*,*,#52054,.T.);
#73320=ORIENTED_EDGE('',*,*,#52055,.F.);
#73321=ORIENTED_EDGE('',*,*,#52048,.F.);
#73322=ORIENTED_EDGE('',*,*,#52056,.F.);
#73323=ORIENTED_EDGE('',*,*,#52057,.T.);
#73324=ORIENTED_EDGE('',*,*,#52058,.F.);
#73325=ORIENTED_EDGE('',*,*,#52051,.F.);
#73326=ORIENTED_EDGE('',*,*,#52059,.F.);
#73327=ORIENTED_EDGE('',*,*,#52060,.T.);
#73328=ORIENTED_EDGE('',*,*,#52061,.F.);
#73329=ORIENTED_EDGE('',*,*,#52054,.F.);
#73330=ORIENTED_EDGE('',*,*,#52062,.F.);
#73331=ORIENTED_EDGE('',*,*,#52063,.F.);
#73332=ORIENTED_EDGE('',*,*,#52057,.F.);
#73333=ORIENTED_EDGE('',*,*,#52064,.F.);
#73334=ORIENTED_EDGE('',*,*,#52065,.T.);
#73335=ORIENTED_EDGE('',*,*,#52060,.F.);
#73336=ORIENTED_EDGE('',*,*,#52066,.F.);
#73337=ORIENTED_EDGE('',*,*,#52065,.F.);
#73338=ORIENTED_EDGE('',*,*,#52067,.F.);
#73339=ORIENTED_EDGE('',*,*,#52068,.T.);
#73340=ORIENTED_EDGE('',*,*,#52069,.F.);
#73341=ORIENTED_EDGE('',*,*,#52070,.T.);
#73342=ORIENTED_EDGE('',*,*,#52071,.F.);
#73343=ORIENTED_EDGE('',*,*,#52072,.T.);
#73344=ORIENTED_EDGE('',*,*,#52073,.F.);
#73345=ORIENTED_EDGE('',*,*,#52070,.F.);
#73346=ORIENTED_EDGE('',*,*,#52074,.F.);
#73347=ORIENTED_EDGE('',*,*,#52075,.T.);
#73348=ORIENTED_EDGE('',*,*,#52076,.F.);
#73349=ORIENTED_EDGE('',*,*,#52068,.F.);
#73350=ORIENTED_EDGE('',*,*,#52077,.F.);
#73351=ORIENTED_EDGE('',*,*,#52078,.T.);
#73352=ORIENTED_EDGE('',*,*,#52079,.F.);
#73353=ORIENTED_EDGE('',*,*,#52072,.F.);
#73354=ORIENTED_EDGE('',*,*,#52080,.F.);
#73355=ORIENTED_EDGE('',*,*,#52081,.T.);
#73356=ORIENTED_EDGE('',*,*,#52082,.F.);
#73357=ORIENTED_EDGE('',*,*,#52075,.F.);
#73358=ORIENTED_EDGE('',*,*,#52083,.F.);
#73359=ORIENTED_EDGE('',*,*,#52084,.T.);
#73360=ORIENTED_EDGE('',*,*,#52085,.F.);
#73361=ORIENTED_EDGE('',*,*,#52078,.F.);
#73362=ORIENTED_EDGE('',*,*,#52086,.F.);
#73363=ORIENTED_EDGE('',*,*,#52087,.T.);
#73364=ORIENTED_EDGE('',*,*,#52088,.F.);
#73365=ORIENTED_EDGE('',*,*,#52081,.F.);
#73366=ORIENTED_EDGE('',*,*,#52089,.F.);
#73367=ORIENTED_EDGE('',*,*,#52084,.F.);
#73368=ORIENTED_EDGE('',*,*,#52090,.F.);
#73369=ORIENTED_EDGE('',*,*,#52087,.F.);
#73370=ORIENTED_EDGE('',*,*,#52091,.F.);
#73371=ORIENTED_EDGE('',*,*,#52092,.T.);
#73372=ORIENTED_EDGE('',*,*,#52093,.F.);
#73373=ORIENTED_EDGE('',*,*,#52094,.T.);
#73374=ORIENTED_EDGE('',*,*,#52095,.F.);
#73375=ORIENTED_EDGE('',*,*,#52096,.T.);
#73376=ORIENTED_EDGE('',*,*,#52097,.F.);
#73377=ORIENTED_EDGE('',*,*,#52094,.F.);
#73378=ORIENTED_EDGE('',*,*,#52098,.F.);
#73379=ORIENTED_EDGE('',*,*,#52099,.T.);
#73380=ORIENTED_EDGE('',*,*,#52100,.F.);
#73381=ORIENTED_EDGE('',*,*,#52092,.F.);
#73382=ORIENTED_EDGE('',*,*,#52101,.F.);
#73383=ORIENTED_EDGE('',*,*,#52102,.T.);
#73384=ORIENTED_EDGE('',*,*,#52103,.F.);
#73385=ORIENTED_EDGE('',*,*,#52096,.F.);
#73386=ORIENTED_EDGE('',*,*,#52104,.F.);
#73387=ORIENTED_EDGE('',*,*,#52105,.T.);
#73388=ORIENTED_EDGE('',*,*,#52106,.F.);
#73389=ORIENTED_EDGE('',*,*,#52099,.F.);
#73390=ORIENTED_EDGE('',*,*,#52107,.F.);
#73391=ORIENTED_EDGE('',*,*,#52108,.T.);
#73392=ORIENTED_EDGE('',*,*,#52109,.F.);
#73393=ORIENTED_EDGE('',*,*,#52102,.F.);
#73394=ORIENTED_EDGE('',*,*,#52110,.F.);
#73395=ORIENTED_EDGE('',*,*,#52111,.T.);
#73396=ORIENTED_EDGE('',*,*,#52112,.F.);
#73397=ORIENTED_EDGE('',*,*,#52105,.F.);
#73398=ORIENTED_EDGE('',*,*,#52113,.F.);
#73399=ORIENTED_EDGE('',*,*,#52114,.T.);
#73400=ORIENTED_EDGE('',*,*,#52115,.F.);
#73401=ORIENTED_EDGE('',*,*,#52108,.F.);
#73402=ORIENTED_EDGE('',*,*,#52116,.F.);
#73403=ORIENTED_EDGE('',*,*,#52117,.T.);
#73404=ORIENTED_EDGE('',*,*,#52118,.F.);
#73405=ORIENTED_EDGE('',*,*,#52111,.F.);
#73406=ORIENTED_EDGE('',*,*,#52119,.F.);
#73407=ORIENTED_EDGE('',*,*,#52114,.F.);
#73408=ORIENTED_EDGE('',*,*,#52120,.F.);
#73409=ORIENTED_EDGE('',*,*,#52117,.F.);
#73410=ORIENTED_EDGE('',*,*,#52121,.F.);
#73411=ORIENTED_EDGE('',*,*,#52122,.T.);
#73412=ORIENTED_EDGE('',*,*,#52123,.F.);
#73413=ORIENTED_EDGE('',*,*,#52124,.T.);
#73414=ORIENTED_EDGE('',*,*,#52125,.F.);
#73415=ORIENTED_EDGE('',*,*,#52126,.T.);
#73416=ORIENTED_EDGE('',*,*,#52127,.F.);
#73417=ORIENTED_EDGE('',*,*,#52124,.F.);
#73418=ORIENTED_EDGE('',*,*,#52128,.F.);
#73419=ORIENTED_EDGE('',*,*,#52129,.T.);
#73420=ORIENTED_EDGE('',*,*,#52130,.F.);
#73421=ORIENTED_EDGE('',*,*,#52122,.F.);
#73422=ORIENTED_EDGE('',*,*,#52131,.F.);
#73423=ORIENTED_EDGE('',*,*,#52132,.T.);
#73424=ORIENTED_EDGE('',*,*,#52133,.F.);
#73425=ORIENTED_EDGE('',*,*,#52126,.F.);
#73426=ORIENTED_EDGE('',*,*,#52134,.F.);
#73427=ORIENTED_EDGE('',*,*,#52135,.T.);
#73428=ORIENTED_EDGE('',*,*,#52136,.F.);
#73429=ORIENTED_EDGE('',*,*,#52129,.F.);
#73430=ORIENTED_EDGE('',*,*,#52137,.F.);
#73431=ORIENTED_EDGE('',*,*,#52138,.T.);
#73432=ORIENTED_EDGE('',*,*,#52139,.F.);
#73433=ORIENTED_EDGE('',*,*,#52132,.F.);
#73434=ORIENTED_EDGE('',*,*,#52140,.F.);
#73435=ORIENTED_EDGE('',*,*,#52141,.T.);
#73436=ORIENTED_EDGE('',*,*,#52142,.F.);
#73437=ORIENTED_EDGE('',*,*,#52135,.F.);
#73438=ORIENTED_EDGE('',*,*,#52143,.F.);
#73439=ORIENTED_EDGE('',*,*,#52138,.F.);
#73440=ORIENTED_EDGE('',*,*,#52144,.F.);
#73441=ORIENTED_EDGE('',*,*,#52141,.F.);
#73442=ORIENTED_EDGE('',*,*,#52145,.F.);
#73443=ORIENTED_EDGE('',*,*,#52146,.T.);
#73444=ORIENTED_EDGE('',*,*,#52147,.F.);
#73445=ORIENTED_EDGE('',*,*,#52148,.T.);
#73446=ORIENTED_EDGE('',*,*,#52149,.F.);
#73447=ORIENTED_EDGE('',*,*,#52150,.T.);
#73448=ORIENTED_EDGE('',*,*,#52151,.F.);
#73449=ORIENTED_EDGE('',*,*,#52148,.F.);
#73450=ORIENTED_EDGE('',*,*,#52152,.F.);
#73451=ORIENTED_EDGE('',*,*,#52153,.T.);
#73452=ORIENTED_EDGE('',*,*,#52154,.F.);
#73453=ORIENTED_EDGE('',*,*,#52146,.F.);
#73454=ORIENTED_EDGE('',*,*,#52155,.F.);
#73455=ORIENTED_EDGE('',*,*,#52156,.T.);
#73456=ORIENTED_EDGE('',*,*,#52157,.F.);
#73457=ORIENTED_EDGE('',*,*,#52150,.F.);
#73458=ORIENTED_EDGE('',*,*,#52158,.F.);
#73459=ORIENTED_EDGE('',*,*,#52159,.T.);
#73460=ORIENTED_EDGE('',*,*,#52160,.F.);
#73461=ORIENTED_EDGE('',*,*,#52153,.F.);
#73462=ORIENTED_EDGE('',*,*,#52161,.F.);
#73463=ORIENTED_EDGE('',*,*,#52162,.T.);
#73464=ORIENTED_EDGE('',*,*,#52163,.F.);
#73465=ORIENTED_EDGE('',*,*,#52156,.F.);
#73466=ORIENTED_EDGE('',*,*,#52164,.F.);
#73467=ORIENTED_EDGE('',*,*,#52165,.T.);
#73468=ORIENTED_EDGE('',*,*,#52166,.F.);
#73469=ORIENTED_EDGE('',*,*,#52159,.F.);
#73470=ORIENTED_EDGE('',*,*,#52167,.F.);
#73471=ORIENTED_EDGE('',*,*,#52168,.T.);
#73472=ORIENTED_EDGE('',*,*,#52169,.F.);
#73473=ORIENTED_EDGE('',*,*,#52162,.F.);
#73474=ORIENTED_EDGE('',*,*,#52170,.F.);
#73475=ORIENTED_EDGE('',*,*,#52171,.T.);
#73476=ORIENTED_EDGE('',*,*,#52172,.F.);
#73477=ORIENTED_EDGE('',*,*,#52165,.F.);
#73478=ORIENTED_EDGE('',*,*,#52173,.F.);
#73479=ORIENTED_EDGE('',*,*,#52168,.F.);
#73480=ORIENTED_EDGE('',*,*,#52174,.F.);
#73481=ORIENTED_EDGE('',*,*,#52171,.F.);
#73482=ORIENTED_EDGE('',*,*,#52175,.F.);
#73483=ORIENTED_EDGE('',*,*,#52176,.T.);
#73484=ORIENTED_EDGE('',*,*,#52177,.F.);
#73485=ORIENTED_EDGE('',*,*,#52178,.T.);
#73486=ORIENTED_EDGE('',*,*,#52179,.F.);
#73487=ORIENTED_EDGE('',*,*,#52180,.T.);
#73488=ORIENTED_EDGE('',*,*,#52181,.F.);
#73489=ORIENTED_EDGE('',*,*,#52178,.F.);
#73490=ORIENTED_EDGE('',*,*,#52182,.F.);
#73491=ORIENTED_EDGE('',*,*,#52183,.T.);
#73492=ORIENTED_EDGE('',*,*,#52184,.F.);
#73493=ORIENTED_EDGE('',*,*,#52176,.F.);
#73494=ORIENTED_EDGE('',*,*,#52185,.F.);
#73495=ORIENTED_EDGE('',*,*,#52186,.T.);
#73496=ORIENTED_EDGE('',*,*,#52187,.F.);
#73497=ORIENTED_EDGE('',*,*,#52180,.F.);
#73498=ORIENTED_EDGE('',*,*,#52188,.F.);
#73499=ORIENTED_EDGE('',*,*,#52189,.T.);
#73500=ORIENTED_EDGE('',*,*,#52190,.F.);
#73501=ORIENTED_EDGE('',*,*,#52183,.F.);
#73502=ORIENTED_EDGE('',*,*,#52191,.F.);
#73503=ORIENTED_EDGE('',*,*,#52192,.T.);
#73504=ORIENTED_EDGE('',*,*,#52193,.F.);
#73505=ORIENTED_EDGE('',*,*,#52186,.F.);
#73506=ORIENTED_EDGE('',*,*,#52194,.F.);
#73507=ORIENTED_EDGE('',*,*,#52195,.T.);
#73508=ORIENTED_EDGE('',*,*,#52196,.F.);
#73509=ORIENTED_EDGE('',*,*,#52189,.F.);
#73510=ORIENTED_EDGE('',*,*,#52197,.F.);
#73511=ORIENTED_EDGE('',*,*,#52192,.F.);
#73512=ORIENTED_EDGE('',*,*,#52198,.F.);
#73513=ORIENTED_EDGE('',*,*,#52195,.F.);
#73514=ORIENTED_EDGE('',*,*,#52199,.F.);
#73515=ORIENTED_EDGE('',*,*,#52200,.T.);
#73516=ORIENTED_EDGE('',*,*,#52201,.F.);
#73517=ORIENTED_EDGE('',*,*,#52202,.T.);
#73518=ORIENTED_EDGE('',*,*,#52203,.F.);
#73519=ORIENTED_EDGE('',*,*,#52204,.T.);
#73520=ORIENTED_EDGE('',*,*,#52205,.F.);
#73521=ORIENTED_EDGE('',*,*,#52202,.F.);
#73522=ORIENTED_EDGE('',*,*,#52206,.F.);
#73523=ORIENTED_EDGE('',*,*,#52207,.T.);
#73524=ORIENTED_EDGE('',*,*,#52208,.F.);
#73525=ORIENTED_EDGE('',*,*,#52200,.F.);
#73526=ORIENTED_EDGE('',*,*,#52209,.F.);
#73527=ORIENTED_EDGE('',*,*,#52210,.T.);
#73528=ORIENTED_EDGE('',*,*,#52211,.F.);
#73529=ORIENTED_EDGE('',*,*,#52204,.F.);
#73530=ORIENTED_EDGE('',*,*,#52212,.F.);
#73531=ORIENTED_EDGE('',*,*,#52213,.T.);
#73532=ORIENTED_EDGE('',*,*,#52214,.F.);
#73533=ORIENTED_EDGE('',*,*,#52207,.F.);
#73534=ORIENTED_EDGE('',*,*,#52215,.F.);
#73535=ORIENTED_EDGE('',*,*,#52216,.T.);
#73536=ORIENTED_EDGE('',*,*,#52217,.F.);
#73537=ORIENTED_EDGE('',*,*,#52210,.F.);
#73538=ORIENTED_EDGE('',*,*,#52218,.F.);
#73539=ORIENTED_EDGE('',*,*,#52219,.T.);
#73540=ORIENTED_EDGE('',*,*,#52220,.F.);
#73541=ORIENTED_EDGE('',*,*,#52213,.F.);
#73542=ORIENTED_EDGE('',*,*,#52221,.F.);
#73543=ORIENTED_EDGE('',*,*,#52216,.F.);
#73544=ORIENTED_EDGE('',*,*,#52222,.F.);
#73545=ORIENTED_EDGE('',*,*,#52219,.F.);
#73546=ORIENTED_EDGE('',*,*,#52223,.F.);
#73547=ORIENTED_EDGE('',*,*,#52224,.T.);
#73548=ORIENTED_EDGE('',*,*,#52225,.F.);
#73549=ORIENTED_EDGE('',*,*,#52226,.T.);
#73550=ORIENTED_EDGE('',*,*,#52227,.F.);
#73551=ORIENTED_EDGE('',*,*,#52228,.T.);
#73552=ORIENTED_EDGE('',*,*,#52229,.F.);
#73553=ORIENTED_EDGE('',*,*,#52226,.F.);
#73554=ORIENTED_EDGE('',*,*,#52230,.F.);
#73555=ORIENTED_EDGE('',*,*,#52231,.T.);
#73556=ORIENTED_EDGE('',*,*,#52232,.F.);
#73557=ORIENTED_EDGE('',*,*,#52224,.F.);
#73558=ORIENTED_EDGE('',*,*,#52233,.F.);
#73559=ORIENTED_EDGE('',*,*,#52234,.T.);
#73560=ORIENTED_EDGE('',*,*,#52235,.F.);
#73561=ORIENTED_EDGE('',*,*,#52228,.F.);
#73562=ORIENTED_EDGE('',*,*,#52236,.F.);
#73563=ORIENTED_EDGE('',*,*,#52237,.T.);
#73564=ORIENTED_EDGE('',*,*,#52238,.F.);
#73565=ORIENTED_EDGE('',*,*,#52231,.F.);
#73566=ORIENTED_EDGE('',*,*,#52239,.F.);
#73567=ORIENTED_EDGE('',*,*,#52240,.T.);
#73568=ORIENTED_EDGE('',*,*,#52241,.F.);
#73569=ORIENTED_EDGE('',*,*,#52234,.F.);
#73570=ORIENTED_EDGE('',*,*,#52242,.F.);
#73571=ORIENTED_EDGE('',*,*,#52243,.T.);
#73572=ORIENTED_EDGE('',*,*,#52244,.F.);
#73573=ORIENTED_EDGE('',*,*,#52237,.F.);
#73574=ORIENTED_EDGE('',*,*,#52245,.F.);
#73575=ORIENTED_EDGE('',*,*,#52240,.F.);
#73576=ORIENTED_EDGE('',*,*,#52246,.F.);
#73577=ORIENTED_EDGE('',*,*,#52243,.F.);
#73578=ORIENTED_EDGE('',*,*,#52247,.F.);
#73579=ORIENTED_EDGE('',*,*,#52248,.T.);
#73580=ORIENTED_EDGE('',*,*,#52249,.F.);
#73581=ORIENTED_EDGE('',*,*,#52250,.T.);
#73582=ORIENTED_EDGE('',*,*,#52251,.F.);
#73583=ORIENTED_EDGE('',*,*,#52252,.T.);
#73584=ORIENTED_EDGE('',*,*,#52253,.F.);
#73585=ORIENTED_EDGE('',*,*,#52250,.F.);
#73586=ORIENTED_EDGE('',*,*,#52254,.F.);
#73587=ORIENTED_EDGE('',*,*,#52255,.T.);
#73588=ORIENTED_EDGE('',*,*,#52256,.F.);
#73589=ORIENTED_EDGE('',*,*,#52248,.F.);
#73590=ORIENTED_EDGE('',*,*,#52257,.F.);
#73591=ORIENTED_EDGE('',*,*,#52258,.T.);
#73592=ORIENTED_EDGE('',*,*,#52259,.F.);
#73593=ORIENTED_EDGE('',*,*,#52252,.F.);
#73594=ORIENTED_EDGE('',*,*,#52260,.F.);
#73595=ORIENTED_EDGE('',*,*,#52261,.T.);
#73596=ORIENTED_EDGE('',*,*,#52262,.F.);
#73597=ORIENTED_EDGE('',*,*,#52255,.F.);
#73598=ORIENTED_EDGE('',*,*,#52263,.F.);
#73599=ORIENTED_EDGE('',*,*,#52264,.T.);
#73600=ORIENTED_EDGE('',*,*,#52265,.F.);
#73601=ORIENTED_EDGE('',*,*,#52258,.F.);
#73602=ORIENTED_EDGE('',*,*,#52266,.F.);
#73603=ORIENTED_EDGE('',*,*,#52267,.T.);
#73604=ORIENTED_EDGE('',*,*,#52268,.F.);
#73605=ORIENTED_EDGE('',*,*,#52261,.F.);
#73606=ORIENTED_EDGE('',*,*,#52269,.F.);
#73607=ORIENTED_EDGE('',*,*,#52264,.F.);
#73608=ORIENTED_EDGE('',*,*,#52270,.F.);
#73609=ORIENTED_EDGE('',*,*,#52267,.F.);
#73610=ORIENTED_EDGE('',*,*,#52271,.F.);
#73611=ORIENTED_EDGE('',*,*,#52272,.T.);
#73612=ORIENTED_EDGE('',*,*,#52273,.F.);
#73613=ORIENTED_EDGE('',*,*,#52274,.T.);
#73614=ORIENTED_EDGE('',*,*,#52275,.F.);
#73615=ORIENTED_EDGE('',*,*,#52276,.T.);
#73616=ORIENTED_EDGE('',*,*,#52277,.F.);
#73617=ORIENTED_EDGE('',*,*,#52274,.F.);
#73618=ORIENTED_EDGE('',*,*,#52278,.F.);
#73619=ORIENTED_EDGE('',*,*,#52279,.T.);
#73620=ORIENTED_EDGE('',*,*,#52280,.F.);
#73621=ORIENTED_EDGE('',*,*,#52272,.F.);
#73622=ORIENTED_EDGE('',*,*,#52281,.F.);
#73623=ORIENTED_EDGE('',*,*,#52282,.T.);
#73624=ORIENTED_EDGE('',*,*,#52283,.F.);
#73625=ORIENTED_EDGE('',*,*,#52276,.F.);
#73626=ORIENTED_EDGE('',*,*,#52284,.F.);
#73627=ORIENTED_EDGE('',*,*,#52285,.T.);
#73628=ORIENTED_EDGE('',*,*,#52286,.F.);
#73629=ORIENTED_EDGE('',*,*,#52279,.F.);
#73630=ORIENTED_EDGE('',*,*,#52287,.F.);
#73631=ORIENTED_EDGE('',*,*,#52282,.F.);
#73632=ORIENTED_EDGE('',*,*,#52288,.F.);
#73633=ORIENTED_EDGE('',*,*,#52285,.F.);
#73634=ORIENTED_EDGE('',*,*,#52289,.F.);
#73635=ORIENTED_EDGE('',*,*,#52290,.F.);
#73636=ORIENTED_EDGE('',*,*,#52291,.T.);
#73637=ORIENTED_EDGE('',*,*,#52292,.F.);
#73638=ORIENTED_EDGE('',*,*,#52293,.T.);
#73639=ORIENTED_EDGE('',*,*,#52294,.T.);
#73640=ORIENTED_EDGE('',*,*,#52295,.F.);
#73641=ORIENTED_EDGE('',*,*,#52293,.F.);
#73642=ORIENTED_EDGE('',*,*,#52296,.F.);
#73643=ORIENTED_EDGE('',*,*,#52297,.T.);
#73644=ORIENTED_EDGE('',*,*,#52298,.F.);
#73645=ORIENTED_EDGE('',*,*,#52291,.F.);
#73646=ORIENTED_EDGE('',*,*,#52299,.F.);
#73647=ORIENTED_EDGE('',*,*,#52300,.T.);
#73648=ORIENTED_EDGE('',*,*,#52301,.F.);
#73649=ORIENTED_EDGE('',*,*,#52294,.F.);
#73650=ORIENTED_EDGE('',*,*,#52302,.F.);
#73651=ORIENTED_EDGE('',*,*,#52303,.T.);
#73652=ORIENTED_EDGE('',*,*,#52304,.F.);
#73653=ORIENTED_EDGE('',*,*,#52297,.F.);
#73654=ORIENTED_EDGE('',*,*,#52305,.F.);
#73655=ORIENTED_EDGE('',*,*,#52300,.F.);
#73656=ORIENTED_EDGE('',*,*,#52306,.F.);
#73657=ORIENTED_EDGE('',*,*,#52303,.F.);
#73658=ORIENTED_EDGE('',*,*,#52307,.F.);
#73659=ORIENTED_EDGE('',*,*,#52308,.F.);
#73660=ORIENTED_EDGE('',*,*,#52309,.T.);
#73661=ORIENTED_EDGE('',*,*,#52310,.F.);
#73662=ORIENTED_EDGE('',*,*,#52309,.F.);
#73663=ORIENTED_EDGE('',*,*,#52311,.F.);
#73664=ORIENTED_EDGE('',*,*,#52312,.T.);
#73665=ORIENTED_EDGE('',*,*,#52313,.F.);
#73666=ORIENTED_EDGE('',*,*,#52312,.F.);
#73667=ORIENTED_EDGE('',*,*,#52314,.T.);
#73668=ORIENTED_EDGE('',*,*,#52315,.F.);
#73669=ORIENTED_EDGE('',*,*,#50135,.F.);
#73670=ORIENTED_EDGE('',*,*,#52316,.F.);
#73671=ORIENTED_EDGE('',*,*,#52317,.T.);
#73672=ORIENTED_EDGE('',*,*,#52318,.F.);
#73673=ORIENTED_EDGE('',*,*,#52314,.F.);
#73674=ORIENTED_EDGE('',*,*,#52319,.F.);
#73675=ORIENTED_EDGE('',*,*,#52320,.T.);
#73676=ORIENTED_EDGE('',*,*,#52321,.F.);
#73677=ORIENTED_EDGE('',*,*,#52317,.F.);
#73678=ORIENTED_EDGE('',*,*,#52322,.F.);
#73679=ORIENTED_EDGE('',*,*,#52323,.T.);
#73680=ORIENTED_EDGE('',*,*,#52324,.F.);
#73681=ORIENTED_EDGE('',*,*,#52320,.F.);
#73682=ORIENTED_EDGE('',*,*,#52325,.F.);
#73683=ORIENTED_EDGE('',*,*,#52326,.T.);
#73684=ORIENTED_EDGE('',*,*,#52327,.F.);
#73685=ORIENTED_EDGE('',*,*,#52323,.F.);
#73686=ORIENTED_EDGE('',*,*,#52328,.F.);
#73687=ORIENTED_EDGE('',*,*,#52329,.T.);
#73688=ORIENTED_EDGE('',*,*,#52330,.F.);
#73689=ORIENTED_EDGE('',*,*,#52326,.F.);
#73690=ORIENTED_EDGE('',*,*,#52331,.F.);
#73691=ORIENTED_EDGE('',*,*,#52332,.T.);
#73692=ORIENTED_EDGE('',*,*,#52333,.F.);
#73693=ORIENTED_EDGE('',*,*,#52329,.F.);
#73694=ORIENTED_EDGE('',*,*,#52334,.F.);
#73695=ORIENTED_EDGE('',*,*,#52335,.T.);
#73696=ORIENTED_EDGE('',*,*,#52336,.F.);
#73697=ORIENTED_EDGE('',*,*,#52332,.F.);
#73698=ORIENTED_EDGE('',*,*,#52337,.F.);
#73699=ORIENTED_EDGE('',*,*,#52338,.F.);
#73700=ORIENTED_EDGE('',*,*,#52335,.F.);
#73701=ORIENTED_EDGE('',*,*,#52339,.F.);
#73702=ORIENTED_EDGE('',*,*,#50152,.T.);
#73703=ORIENTED_EDGE('',*,*,#52340,.T.);
#73704=ORIENTED_EDGE('',*,*,#52341,.F.);
#73705=ORIENTED_EDGE('',*,*,#50157,.F.);
#73706=ORIENTED_EDGE('',*,*,#52342,.F.);
#73707=ORIENTED_EDGE('',*,*,#52343,.T.);
#73708=ORIENTED_EDGE('',*,*,#52344,.F.);
#73709=ORIENTED_EDGE('',*,*,#52340,.F.);
#73710=ORIENTED_EDGE('',*,*,#52345,.F.);
#73711=ORIENTED_EDGE('',*,*,#52346,.T.);
#73712=ORIENTED_EDGE('',*,*,#52347,.F.);
#73713=ORIENTED_EDGE('',*,*,#52343,.F.);
#73714=ORIENTED_EDGE('',*,*,#52348,.F.);
#73715=ORIENTED_EDGE('',*,*,#52349,.T.);
#73716=ORIENTED_EDGE('',*,*,#52350,.F.);
#73717=ORIENTED_EDGE('',*,*,#52346,.F.);
#73718=ORIENTED_EDGE('',*,*,#52351,.F.);
#73719=ORIENTED_EDGE('',*,*,#52352,.T.);
#73720=ORIENTED_EDGE('',*,*,#52353,.F.);
#73721=ORIENTED_EDGE('',*,*,#52349,.F.);
#73722=ORIENTED_EDGE('',*,*,#52354,.F.);
#73723=ORIENTED_EDGE('',*,*,#52355,.T.);
#73724=ORIENTED_EDGE('',*,*,#52356,.F.);
#73725=ORIENTED_EDGE('',*,*,#52352,.F.);
#73726=ORIENTED_EDGE('',*,*,#52357,.F.);
#73727=ORIENTED_EDGE('',*,*,#52358,.T.);
#73728=ORIENTED_EDGE('',*,*,#52359,.F.);
#73729=ORIENTED_EDGE('',*,*,#52355,.F.);
#73730=ORIENTED_EDGE('',*,*,#52360,.F.);
#73731=ORIENTED_EDGE('',*,*,#52361,.T.);
#73732=ORIENTED_EDGE('',*,*,#52362,.F.);
#73733=ORIENTED_EDGE('',*,*,#52358,.F.);
#73734=ORIENTED_EDGE('',*,*,#52363,.F.);
#73735=ORIENTED_EDGE('',*,*,#52364,.F.);
#73736=ORIENTED_EDGE('',*,*,#52361,.F.);
#73737=ORIENTED_EDGE('',*,*,#52365,.F.);
#73738=ORIENTED_EDGE('',*,*,#50174,.T.);
#73739=ORIENTED_EDGE('',*,*,#52366,.T.);
#73740=ORIENTED_EDGE('',*,*,#52367,.F.);
#73741=ORIENTED_EDGE('',*,*,#52368,.F.);
#73742=ORIENTED_EDGE('',*,*,#52369,.F.);
#73743=ORIENTED_EDGE('',*,*,#52370,.T.);
#73744=ORIENTED_EDGE('',*,*,#52371,.F.);
#73745=ORIENTED_EDGE('',*,*,#52366,.F.);
#73746=ORIENTED_EDGE('',*,*,#52372,.F.);
#73747=ORIENTED_EDGE('',*,*,#52373,.F.);
#73748=ORIENTED_EDGE('',*,*,#52374,.T.);
#73749=ORIENTED_EDGE('',*,*,#52375,.F.);
#73750=ORIENTED_EDGE('',*,*,#52370,.F.);
#73751=ORIENTED_EDGE('',*,*,#52376,.T.);
#73752=ORIENTED_EDGE('',*,*,#52377,.F.);
#73753=ORIENTED_EDGE('',*,*,#52374,.F.);
#73754=ORIENTED_EDGE('',*,*,#52378,.F.);
#73755=ORIENTED_EDGE('',*,*,#52379,.T.);
#73756=ORIENTED_EDGE('',*,*,#52380,.F.);
#73757=ORIENTED_EDGE('',*,*,#52376,.F.);
#73758=ORIENTED_EDGE('',*,*,#52381,.F.);
#73759=ORIENTED_EDGE('',*,*,#52382,.T.);
#73760=ORIENTED_EDGE('',*,*,#52383,.F.);
#73761=ORIENTED_EDGE('',*,*,#52379,.F.);
#73762=ORIENTED_EDGE('',*,*,#52384,.F.);
#73763=ORIENTED_EDGE('',*,*,#52385,.F.);
#73764=ORIENTED_EDGE('',*,*,#52386,.F.);
#73765=ORIENTED_EDGE('',*,*,#52382,.F.);
#73766=ORIENTED_EDGE('',*,*,#52387,.F.);
#73767=ORIENTED_EDGE('',*,*,#52388,.T.);
#73768=ORIENTED_EDGE('',*,*,#52389,.F.);
#73769=ORIENTED_EDGE('',*,*,#52390,.F.);
#73770=ORIENTED_EDGE('',*,*,#52391,.F.);
#73771=ORIENTED_EDGE('',*,*,#52392,.T.);
#73772=ORIENTED_EDGE('',*,*,#52393,.F.);
#73773=ORIENTED_EDGE('',*,*,#52388,.F.);
#73774=ORIENTED_EDGE('',*,*,#52394,.F.);
#73775=ORIENTED_EDGE('',*,*,#52395,.T.);
#73776=ORIENTED_EDGE('',*,*,#52396,.F.);
#73777=ORIENTED_EDGE('',*,*,#52392,.F.);
#73778=ORIENTED_EDGE('',*,*,#52397,.F.);
#73779=ORIENTED_EDGE('',*,*,#52398,.T.);
#73780=ORIENTED_EDGE('',*,*,#52399,.F.);
#73781=ORIENTED_EDGE('',*,*,#52395,.F.);
#73782=ORIENTED_EDGE('',*,*,#52400,.F.);
#73783=ORIENTED_EDGE('',*,*,#52401,.T.);
#73784=ORIENTED_EDGE('',*,*,#52402,.F.);
#73785=ORIENTED_EDGE('',*,*,#52398,.F.);
#73786=ORIENTED_EDGE('',*,*,#52403,.F.);
#73787=ORIENTED_EDGE('',*,*,#52404,.T.);
#73788=ORIENTED_EDGE('',*,*,#52405,.F.);
#73789=ORIENTED_EDGE('',*,*,#52401,.F.);
#73790=ORIENTED_EDGE('',*,*,#52406,.F.);
#73791=ORIENTED_EDGE('',*,*,#52407,.F.);
#73792=ORIENTED_EDGE('',*,*,#52408,.F.);
#73793=ORIENTED_EDGE('',*,*,#52404,.F.);
#73794=ORIENTED_EDGE('',*,*,#52409,.F.);
#73795=ORIENTED_EDGE('',*,*,#52410,.T.);
#73796=ORIENTED_EDGE('',*,*,#52411,.F.);
#73797=ORIENTED_EDGE('',*,*,#52412,.F.);
#73798=ORIENTED_EDGE('',*,*,#52413,.F.);
#73799=ORIENTED_EDGE('',*,*,#52414,.T.);
#73800=ORIENTED_EDGE('',*,*,#52415,.F.);
#73801=ORIENTED_EDGE('',*,*,#52410,.F.);
#73802=ORIENTED_EDGE('',*,*,#52416,.F.);
#73803=ORIENTED_EDGE('',*,*,#52417,.F.);
#73804=ORIENTED_EDGE('',*,*,#52418,.T.);
#73805=ORIENTED_EDGE('',*,*,#52419,.F.);
#73806=ORIENTED_EDGE('',*,*,#52414,.F.);
#73807=ORIENTED_EDGE('',*,*,#52420,.T.);
#73808=ORIENTED_EDGE('',*,*,#52421,.F.);
#73809=ORIENTED_EDGE('',*,*,#52418,.F.);
#73810=ORIENTED_EDGE('',*,*,#52422,.F.);
#73811=ORIENTED_EDGE('',*,*,#52423,.T.);
#73812=ORIENTED_EDGE('',*,*,#52424,.F.);
#73813=ORIENTED_EDGE('',*,*,#52420,.F.);
#73814=ORIENTED_EDGE('',*,*,#52425,.F.);
#73815=ORIENTED_EDGE('',*,*,#52426,.T.);
#73816=ORIENTED_EDGE('',*,*,#52427,.F.);
#73817=ORIENTED_EDGE('',*,*,#52423,.F.);
#73818=ORIENTED_EDGE('',*,*,#52428,.F.);
#73819=ORIENTED_EDGE('',*,*,#52429,.F.);
#73820=ORIENTED_EDGE('',*,*,#52430,.F.);
#73821=ORIENTED_EDGE('',*,*,#52426,.F.);
#73822=ORIENTED_EDGE('',*,*,#52431,.F.);
#73823=ORIENTED_EDGE('',*,*,#52432,.F.);
#73824=ORIENTED_EDGE('',*,*,#52433,.F.);
#73825=ORIENTED_EDGE('',*,*,#52434,.T.);
#73826=ORIENTED_EDGE('',*,*,#52435,.F.);
#73827=ORIENTED_EDGE('',*,*,#52436,.T.);
#73828=ORIENTED_EDGE('',*,*,#52437,.F.);
#73829=ORIENTED_EDGE('',*,*,#52434,.F.);
#73830=ORIENTED_EDGE('',*,*,#52438,.F.);
#73831=ORIENTED_EDGE('',*,*,#52439,.T.);
#73832=ORIENTED_EDGE('',*,*,#52440,.F.);
#73833=ORIENTED_EDGE('',*,*,#52436,.F.);
#73834=ORIENTED_EDGE('',*,*,#52441,.F.);
#73835=ORIENTED_EDGE('',*,*,#52442,.T.);
#73836=ORIENTED_EDGE('',*,*,#52443,.F.);
#73837=ORIENTED_EDGE('',*,*,#52439,.F.);
#73838=ORIENTED_EDGE('',*,*,#52444,.F.);
#73839=ORIENTED_EDGE('',*,*,#52445,.T.);
#73840=ORIENTED_EDGE('',*,*,#52446,.F.);
#73841=ORIENTED_EDGE('',*,*,#52442,.F.);
#73842=ORIENTED_EDGE('',*,*,#52447,.F.);
#73843=ORIENTED_EDGE('',*,*,#52448,.T.);
#73844=ORIENTED_EDGE('',*,*,#52449,.F.);
#73845=ORIENTED_EDGE('',*,*,#52445,.F.);
#73846=ORIENTED_EDGE('',*,*,#52450,.F.);
#73847=ORIENTED_EDGE('',*,*,#52451,.F.);
#73848=ORIENTED_EDGE('',*,*,#52452,.F.);
#73849=ORIENTED_EDGE('',*,*,#52448,.F.);
#73850=ORIENTED_EDGE('',*,*,#52453,.F.);
#73851=ORIENTED_EDGE('',*,*,#52454,.F.);
#73852=ORIENTED_EDGE('',*,*,#50267,.F.);
#73853=ORIENTED_EDGE('',*,*,#52455,.F.);
#73854=ORIENTED_EDGE('',*,*,#52456,.T.);
#73855=ORIENTED_EDGE('',*,*,#52457,.T.);
#73856=ORIENTED_EDGE('',*,*,#52458,.F.);
#73857=ORIENTED_EDGE('',*,*,#52456,.F.);
#73858=ORIENTED_EDGE('',*,*,#52459,.F.);
#73859=ORIENTED_EDGE('',*,*,#52460,.T.);
#73860=ORIENTED_EDGE('',*,*,#52461,.F.);
#73861=ORIENTED_EDGE('',*,*,#52457,.F.);
#73862=ORIENTED_EDGE('',*,*,#52462,.F.);
#73863=ORIENTED_EDGE('',*,*,#52463,.T.);
#73864=ORIENTED_EDGE('',*,*,#52464,.F.);
#73865=ORIENTED_EDGE('',*,*,#52460,.F.);
#73866=ORIENTED_EDGE('',*,*,#52465,.F.);
#73867=ORIENTED_EDGE('',*,*,#52466,.T.);
#73868=ORIENTED_EDGE('',*,*,#52467,.F.);
#73869=ORIENTED_EDGE('',*,*,#52463,.F.);
#73870=ORIENTED_EDGE('',*,*,#52468,.F.);
#73871=ORIENTED_EDGE('',*,*,#52469,.T.);
#73872=ORIENTED_EDGE('',*,*,#52470,.F.);
#73873=ORIENTED_EDGE('',*,*,#52466,.F.);
#73874=ORIENTED_EDGE('',*,*,#52471,.F.);
#73875=ORIENTED_EDGE('',*,*,#52472,.T.);
#73876=ORIENTED_EDGE('',*,*,#52473,.F.);
#73877=ORIENTED_EDGE('',*,*,#52469,.F.);
#73878=ORIENTED_EDGE('',*,*,#52474,.F.);
#73879=ORIENTED_EDGE('',*,*,#52475,.T.);
#73880=ORIENTED_EDGE('',*,*,#52476,.F.);
#73881=ORIENTED_EDGE('',*,*,#52472,.F.);
#73882=ORIENTED_EDGE('',*,*,#52477,.F.);
#73883=ORIENTED_EDGE('',*,*,#52478,.F.);
#73884=ORIENTED_EDGE('',*,*,#52475,.F.);
#73885=ORIENTED_EDGE('',*,*,#52479,.F.);
#73886=ORIENTED_EDGE('',*,*,#50284,.T.);
#73887=ORIENTED_EDGE('',*,*,#52480,.F.);
#73888=ORIENTED_EDGE('',*,*,#52481,.F.);
#73889=ORIENTED_EDGE('',*,*,#52482,.T.);
#73890=ORIENTED_EDGE('',*,*,#52483,.F.);
#73891=ORIENTED_EDGE('',*,*,#50289,.F.);
#73892=ORIENTED_EDGE('',*,*,#52484,.F.);
#73893=ORIENTED_EDGE('',*,*,#52485,.T.);
#73894=ORIENTED_EDGE('',*,*,#52486,.F.);
#73895=ORIENTED_EDGE('',*,*,#52482,.F.);
#73896=ORIENTED_EDGE('',*,*,#52487,.F.);
#73897=ORIENTED_EDGE('',*,*,#52488,.T.);
#73898=ORIENTED_EDGE('',*,*,#52489,.F.);
#73899=ORIENTED_EDGE('',*,*,#52485,.F.);
#73900=ORIENTED_EDGE('',*,*,#52490,.F.);
#73901=ORIENTED_EDGE('',*,*,#52491,.T.);
#73902=ORIENTED_EDGE('',*,*,#52492,.F.);
#73903=ORIENTED_EDGE('',*,*,#52488,.F.);
#73904=ORIENTED_EDGE('',*,*,#52493,.F.);
#73905=ORIENTED_EDGE('',*,*,#52494,.T.);
#73906=ORIENTED_EDGE('',*,*,#52495,.F.);
#73907=ORIENTED_EDGE('',*,*,#52491,.F.);
#73908=ORIENTED_EDGE('',*,*,#52496,.F.);
#73909=ORIENTED_EDGE('',*,*,#52497,.T.);
#73910=ORIENTED_EDGE('',*,*,#52498,.F.);
#73911=ORIENTED_EDGE('',*,*,#52494,.F.);
#73912=ORIENTED_EDGE('',*,*,#52499,.F.);
#73913=ORIENTED_EDGE('',*,*,#52500,.T.);
#73914=ORIENTED_EDGE('',*,*,#52501,.F.);
#73915=ORIENTED_EDGE('',*,*,#52497,.F.);
#73916=ORIENTED_EDGE('',*,*,#52502,.F.);
#73917=ORIENTED_EDGE('',*,*,#52503,.T.);
#73918=ORIENTED_EDGE('',*,*,#52504,.F.);
#73919=ORIENTED_EDGE('',*,*,#52500,.F.);
#73920=ORIENTED_EDGE('',*,*,#52505,.F.);
#73921=ORIENTED_EDGE('',*,*,#52506,.T.);
#73922=ORIENTED_EDGE('',*,*,#52507,.F.);
#73923=ORIENTED_EDGE('',*,*,#52503,.F.);
#73924=ORIENTED_EDGE('',*,*,#52508,.F.);
#73925=ORIENTED_EDGE('',*,*,#52509,.F.);
#73926=ORIENTED_EDGE('',*,*,#52510,.F.);
#73927=ORIENTED_EDGE('',*,*,#52511,.F.);
#73928=ORIENTED_EDGE('',*,*,#52512,.F.);
#73929=ORIENTED_EDGE('',*,*,#52513,.F.);
#73930=ORIENTED_EDGE('',*,*,#52514,.T.);
#73931=ORIENTED_EDGE('',*,*,#52515,.F.);
#73932=ORIENTED_EDGE('',*,*,#52506,.F.);
#73933=ORIENTED_EDGE('',*,*,#52516,.F.);
#73934=ORIENTED_EDGE('',*,*,#52517,.T.);
#73935=ORIENTED_EDGE('',*,*,#52518,.F.);
#73936=ORIENTED_EDGE('',*,*,#52514,.F.);
#73937=ORIENTED_EDGE('',*,*,#52519,.F.);
#73938=ORIENTED_EDGE('',*,*,#52520,.T.);
#73939=ORIENTED_EDGE('',*,*,#52521,.F.);
#73940=ORIENTED_EDGE('',*,*,#52517,.F.);
#73941=ORIENTED_EDGE('',*,*,#52522,.F.);
#73942=ORIENTED_EDGE('',*,*,#52523,.T.);
#73943=ORIENTED_EDGE('',*,*,#52524,.F.);
#73944=ORIENTED_EDGE('',*,*,#52520,.F.);
#73945=ORIENTED_EDGE('',*,*,#52525,.F.);
#73946=ORIENTED_EDGE('',*,*,#52526,.T.);
#73947=ORIENTED_EDGE('',*,*,#52527,.F.);
#73948=ORIENTED_EDGE('',*,*,#52523,.F.);
#73949=ORIENTED_EDGE('',*,*,#52528,.F.);
#73950=ORIENTED_EDGE('',*,*,#52529,.T.);
#73951=ORIENTED_EDGE('',*,*,#52530,.F.);
#73952=ORIENTED_EDGE('',*,*,#52526,.F.);
#73953=ORIENTED_EDGE('',*,*,#52531,.F.);
#73954=ORIENTED_EDGE('',*,*,#52532,.T.);
#73955=ORIENTED_EDGE('',*,*,#52533,.F.);
#73956=ORIENTED_EDGE('',*,*,#52529,.F.);
#73957=ORIENTED_EDGE('',*,*,#52534,.F.);
#73958=ORIENTED_EDGE('',*,*,#52535,.F.);
#73959=ORIENTED_EDGE('',*,*,#52536,.T.);
#73960=ORIENTED_EDGE('',*,*,#52537,.T.);
#73961=ORIENTED_EDGE('',*,*,#52538,.T.);
#73962=ORIENTED_EDGE('',*,*,#50340,.T.);
#73963=ORIENTED_EDGE('',*,*,#52539,.F.);
#73964=ORIENTED_EDGE('',*,*,#52532,.F.);
#73965=ORIENTED_EDGE('',*,*,#52540,.F.);
#73966=ORIENTED_EDGE('',*,*,#52541,.F.);
#73967=ORIENTED_EDGE('',*,*,#52542,.F.);
#73968=ORIENTED_EDGE('',*,*,#51443,.T.);
#73969=ORIENTED_EDGE('',*,*,#51437,.T.);
#73970=ORIENTED_EDGE('',*,*,#52543,.F.);
#73971=ORIENTED_EDGE('',*,*,#52544,.T.);
#73972=ORIENTED_EDGE('',*,*,#52545,.T.);
#73973=ORIENTED_EDGE('',*,*,#52546,.F.);
#73974=ORIENTED_EDGE('',*,*,#52544,.F.);
#73975=ORIENTED_EDGE('',*,*,#52547,.F.);
#73976=ORIENTED_EDGE('',*,*,#52548,.T.);
#73977=ORIENTED_EDGE('',*,*,#52549,.F.);
#73978=ORIENTED_EDGE('',*,*,#52545,.F.);
#73979=ORIENTED_EDGE('',*,*,#52550,.F.);
#73980=ORIENTED_EDGE('',*,*,#52551,.T.);
#73981=ORIENTED_EDGE('',*,*,#52552,.F.);
#73982=ORIENTED_EDGE('',*,*,#52548,.F.);
#73983=ORIENTED_EDGE('',*,*,#52553,.F.);
#73984=ORIENTED_EDGE('',*,*,#52554,.T.);
#73985=ORIENTED_EDGE('',*,*,#52555,.F.);
#73986=ORIENTED_EDGE('',*,*,#52551,.F.);
#73987=ORIENTED_EDGE('',*,*,#52556,.F.);
#73988=ORIENTED_EDGE('',*,*,#52557,.T.);
#73989=ORIENTED_EDGE('',*,*,#52558,.F.);
#73990=ORIENTED_EDGE('',*,*,#52559,.T.);
#73991=ORIENTED_EDGE('',*,*,#52557,.F.);
#73992=ORIENTED_EDGE('',*,*,#52560,.F.);
#73993=ORIENTED_EDGE('',*,*,#52559,.F.);
#73994=ORIENTED_EDGE('',*,*,#52561,.T.);
#73995=ORIENTED_EDGE('',*,*,#52554,.F.);
#73996=ORIENTED_EDGE('',*,*,#52562,.T.);
#73997=ORIENTED_EDGE('',*,*,#52563,.F.);
#73998=ORIENTED_EDGE('',*,*,#52561,.F.);
#73999=ORIENTED_EDGE('',*,*,#52564,.F.);
#74000=ORIENTED_EDGE('',*,*,#52565,.F.);
#74001=ORIENTED_EDGE('',*,*,#52566,.F.);
#74002=ORIENTED_EDGE('',*,*,#52567,.F.);
#74003=ORIENTED_EDGE('',*,*,#52568,.F.);
#74004=ORIENTED_EDGE('',*,*,#52569,.F.);
#74005=ORIENTED_EDGE('',*,*,#52570,.F.);
#74006=ORIENTED_EDGE('',*,*,#52571,.T.);
#74007=ORIENTED_EDGE('',*,*,#52572,.T.);
#74008=ORIENTED_EDGE('',*,*,#52562,.F.);
#74009=ORIENTED_EDGE('',*,*,#52573,.F.);
#74010=ORIENTED_EDGE('',*,*,#52574,.T.);
#74011=ORIENTED_EDGE('',*,*,#52571,.F.);
#74012=ORIENTED_EDGE('',*,*,#52575,.F.);
#74013=ORIENTED_EDGE('',*,*,#52574,.F.);
#74014=ORIENTED_EDGE('',*,*,#52576,.F.);
#74015=ORIENTED_EDGE('',*,*,#52577,.T.);
#74016=ORIENTED_EDGE('',*,*,#52578,.F.);
#74017=ORIENTED_EDGE('',*,*,#52572,.F.);
#74018=ORIENTED_EDGE('',*,*,#52579,.T.);
#74019=ORIENTED_EDGE('',*,*,#52580,.F.);
#74020=ORIENTED_EDGE('',*,*,#52577,.F.);
#74021=ORIENTED_EDGE('',*,*,#52581,.F.);
#74022=ORIENTED_EDGE('',*,*,#52582,.T.);
#74023=ORIENTED_EDGE('',*,*,#52583,.F.);
#74024=ORIENTED_EDGE('',*,*,#52579,.F.);
#74025=ORIENTED_EDGE('',*,*,#52584,.F.);
#74026=ORIENTED_EDGE('',*,*,#52585,.T.);
#74027=ORIENTED_EDGE('',*,*,#52586,.F.);
#74028=ORIENTED_EDGE('',*,*,#52582,.F.);
#74029=ORIENTED_EDGE('',*,*,#52587,.F.);
#74030=ORIENTED_EDGE('',*,*,#51467,.T.);
#74031=ORIENTED_EDGE('',*,*,#51461,.T.);
#74032=ORIENTED_EDGE('',*,*,#52588,.F.);
#74033=ORIENTED_EDGE('',*,*,#52585,.F.);
#74034=ORIENTED_EDGE('',*,*,#52589,.F.);
#74035=ORIENTED_EDGE('',*,*,#52590,.F.);
#74036=ORIENTED_EDGE('',*,*,#52591,.F.);
#74037=ORIENTED_EDGE('',*,*,#52592,.T.);
#74038=ORIENTED_EDGE('',*,*,#52593,.F.);
#74039=ORIENTED_EDGE('',*,*,#50392,.F.);
#74040=ORIENTED_EDGE('',*,*,#52594,.T.);
#74041=ORIENTED_EDGE('',*,*,#52595,.T.);
#74042=ORIENTED_EDGE('',*,*,#52596,.T.);
#74043=ORIENTED_EDGE('',*,*,#52597,.T.);
#74044=ORIENTED_EDGE('',*,*,#52598,.F.);
#74045=ORIENTED_EDGE('',*,*,#52599,.F.);
#74046=ORIENTED_EDGE('',*,*,#52600,.T.);
#74047=ORIENTED_EDGE('',*,*,#52601,.T.);
#74048=ORIENTED_EDGE('',*,*,#52592,.F.);
#74049=ORIENTED_EDGE('',*,*,#52602,.F.);
#74050=ORIENTED_EDGE('',*,*,#52603,.T.);
#74051=ORIENTED_EDGE('',*,*,#52600,.F.);
#74052=ORIENTED_EDGE('',*,*,#52604,.F.);
#74053=ORIENTED_EDGE('',*,*,#52603,.F.);
#74054=ORIENTED_EDGE('',*,*,#52605,.F.);
#74055=ORIENTED_EDGE('',*,*,#52606,.T.);
#74056=ORIENTED_EDGE('',*,*,#52607,.F.);
#74057=ORIENTED_EDGE('',*,*,#52601,.F.);
#74058=ORIENTED_EDGE('',*,*,#52608,.T.);
#74059=ORIENTED_EDGE('',*,*,#52609,.F.);
#74060=ORIENTED_EDGE('',*,*,#52606,.F.);
#74061=ORIENTED_EDGE('',*,*,#52610,.F.);
#74062=ORIENTED_EDGE('',*,*,#52611,.T.);
#74063=ORIENTED_EDGE('',*,*,#52612,.F.);
#74064=ORIENTED_EDGE('',*,*,#52608,.F.);
#74065=ORIENTED_EDGE('',*,*,#52613,.F.);
#74066=ORIENTED_EDGE('',*,*,#52614,.T.);
#74067=ORIENTED_EDGE('',*,*,#52615,.F.);
#74068=ORIENTED_EDGE('',*,*,#52611,.F.);
#74069=ORIENTED_EDGE('',*,*,#52616,.F.);
#74070=ORIENTED_EDGE('',*,*,#52617,.F.);
#74071=ORIENTED_EDGE('',*,*,#51433,.T.);
#74072=ORIENTED_EDGE('',*,*,#51439,.T.);
#74073=ORIENTED_EDGE('',*,*,#52618,.F.);
#74074=ORIENTED_EDGE('',*,*,#52614,.F.);
#74075=ORIENTED_EDGE('',*,*,#50411,.F.);
#74076=ORIENTED_EDGE('',*,*,#52619,.F.);
#74077=ORIENTED_EDGE('',*,*,#52620,.T.);
#74078=ORIENTED_EDGE('',*,*,#52621,.F.);
#74079=ORIENTED_EDGE('',*,*,#52622,.F.);
#74080=ORIENTED_EDGE('',*,*,#52623,.F.);
#74081=ORIENTED_EDGE('',*,*,#52620,.F.);
#74082=ORIENTED_EDGE('',*,*,#52624,.F.);
#74083=ORIENTED_EDGE('',*,*,#52625,.T.);
#74084=ORIENTED_EDGE('',*,*,#52626,.F.);
#74085=ORIENTED_EDGE('',*,*,#52627,.F.);
#74086=ORIENTED_EDGE('',*,*,#52628,.T.);
#74087=ORIENTED_EDGE('',*,*,#52629,.T.);
#74088=ORIENTED_EDGE('',*,*,#52625,.F.);
#74089=ORIENTED_EDGE('',*,*,#52630,.F.);
#74090=ORIENTED_EDGE('',*,*,#52631,.T.);
#74091=ORIENTED_EDGE('',*,*,#52628,.F.);
#74092=ORIENTED_EDGE('',*,*,#52632,.F.);
#74093=ORIENTED_EDGE('',*,*,#52633,.T.);
#74094=ORIENTED_EDGE('',*,*,#52631,.F.);
#74095=ORIENTED_EDGE('',*,*,#52634,.F.);
#74096=ORIENTED_EDGE('',*,*,#52635,.F.);
#74097=ORIENTED_EDGE('',*,*,#52629,.F.);
#74098=ORIENTED_EDGE('',*,*,#52636,.T.);
#74099=ORIENTED_EDGE('',*,*,#52637,.F.);
#74100=ORIENTED_EDGE('',*,*,#52633,.F.);
#74101=ORIENTED_EDGE('',*,*,#52638,.F.);
#74102=ORIENTED_EDGE('',*,*,#52639,.T.);
#74103=ORIENTED_EDGE('',*,*,#52640,.F.);
#74104=ORIENTED_EDGE('',*,*,#52636,.F.);
#74105=ORIENTED_EDGE('',*,*,#52641,.F.);
#74106=ORIENTED_EDGE('',*,*,#52642,.T.);
#74107=ORIENTED_EDGE('',*,*,#52643,.F.);
#74108=ORIENTED_EDGE('',*,*,#52639,.F.);
#74109=ORIENTED_EDGE('',*,*,#52644,.F.);
#74110=ORIENTED_EDGE('',*,*,#51469,.T.);
#74111=ORIENTED_EDGE('',*,*,#51476,.T.);
#74112=ORIENTED_EDGE('',*,*,#52645,.F.);
#74113=ORIENTED_EDGE('',*,*,#52642,.F.);
#74114=ORIENTED_EDGE('',*,*,#52646,.F.);
#74115=ORIENTED_EDGE('',*,*,#52647,.F.);
#74116=ORIENTED_EDGE('',*,*,#52534,.T.);
#74117=ORIENTED_EDGE('',*,*,#52648,.F.);
#74118=ORIENTED_EDGE('',*,*,#52602,.T.);
#74119=ORIENTED_EDGE('',*,*,#52649,.F.);
#74120=ORIENTED_EDGE('',*,*,#52516,.T.);
#74121=ORIENTED_EDGE('',*,*,#52650,.F.);
#74122=ORIENTED_EDGE('',*,*,#52560,.T.);
#74123=ORIENTED_EDGE('',*,*,#52651,.F.);
#74124=ORIENTED_EDGE('',*,*,#52505,.T.);
#74125=ORIENTED_EDGE('',*,*,#52652,.F.);
#74126=ORIENTED_EDGE('',*,*,#52573,.T.);
#74127=ORIENTED_EDGE('',*,*,#52653,.F.);
#74128=ORIENTED_EDGE('',*,*,#52487,.T.);
#74129=ORIENTED_EDGE('',*,*,#52654,.F.);
#74130=ORIENTED_EDGE('',*,*,#52634,.T.);
#74131=ORIENTED_EDGE('',*,*,#52655,.F.);
#74132=ORIENTED_EDGE('',*,*,#52656,.F.);
#74133=ORIENTED_EDGE('',*,*,#52375,.T.);
#74134=ORIENTED_EDGE('',*,*,#52657,.F.);
#74135=ORIENTED_EDGE('',*,*,#52658,.F.);
#74136=ORIENTED_EDGE('',*,*,#52452,.T.);
#74137=ORIENTED_EDGE('',*,*,#52659,.F.);
#74138=ORIENTED_EDGE('',*,*,#52660,.F.);
#74139=ORIENTED_EDGE('',*,*,#52661,.F.);
#74140=ORIENTED_EDGE('',*,*,#52396,.T.);
#74141=ORIENTED_EDGE('',*,*,#52662,.F.);
#74142=ORIENTED_EDGE('',*,*,#52663,.F.);
#74143=ORIENTED_EDGE('',*,*,#52664,.F.);
#74144=ORIENTED_EDGE('',*,*,#52389,.T.);
#74145=ORIENTED_EDGE('',*,*,#52665,.F.);
#74146=ORIENTED_EDGE('',*,*,#52666,.F.);
#74147=ORIENTED_EDGE('',*,*,#52667,.F.);
#74148=ORIENTED_EDGE('',*,*,#52386,.T.);
#74149=ORIENTED_EDGE('',*,*,#52668,.F.);
#74150=ORIENTED_EDGE('',*,*,#52669,.F.);
#74151=ORIENTED_EDGE('',*,*,#52670,.F.);
#74152=ORIENTED_EDGE('',*,*,#52380,.T.);
#74153=ORIENTED_EDGE('',*,*,#52671,.F.);
#74154=ORIENTED_EDGE('',*,*,#52672,.F.);
#74155=ORIENTED_EDGE('',*,*,#52673,.F.);
#74156=ORIENTED_EDGE('',*,*,#52367,.T.);
#74157=ORIENTED_EDGE('',*,*,#52674,.F.);
#74158=ORIENTED_EDGE('',*,*,#52675,.F.);
#74159=ORIENTED_EDGE('',*,*,#52676,.F.);
#74160=ORIENTED_EDGE('',*,*,#52430,.T.);
#74161=ORIENTED_EDGE('',*,*,#52677,.F.);
#74162=ORIENTED_EDGE('',*,*,#52678,.F.);
#74163=ORIENTED_EDGE('',*,*,#52679,.F.);
#74164=ORIENTED_EDGE('',*,*,#52411,.T.);
#74165=ORIENTED_EDGE('',*,*,#52680,.F.);
#74166=ORIENTED_EDGE('',*,*,#52681,.F.);
#74167=ORIENTED_EDGE('',*,*,#52682,.F.);
#74168=ORIENTED_EDGE('',*,*,#52683,.F.);
#74169=ORIENTED_EDGE('',*,*,#52064,.T.);
#74170=ORIENTED_EDGE('',*,*,#52684,.F.);
#74171=ORIENTED_EDGE('',*,*,#52685,.F.);
#74172=ORIENTED_EDGE('',*,*,#51941,.T.);
#74173=ORIENTED_EDGE('',*,*,#52686,.F.);
#74174=ORIENTED_EDGE('',*,*,#52687,.F.);
#74175=ORIENTED_EDGE('',*,*,#52688,.F.);
#74176=ORIENTED_EDGE('',*,*,#51916,.T.);
#74177=ORIENTED_EDGE('',*,*,#52689,.F.);
#74178=ORIENTED_EDGE('',*,*,#52690,.F.);
#74179=ORIENTED_EDGE('',*,*,#52691,.F.);
#74180=ORIENTED_EDGE('',*,*,#51927,.T.);
#74181=ORIENTED_EDGE('',*,*,#52692,.F.);
#74182=ORIENTED_EDGE('',*,*,#52693,.F.);
#74183=ORIENTED_EDGE('',*,*,#52694,.F.);
#74184=ORIENTED_EDGE('',*,*,#51939,.T.);
#74185=ORIENTED_EDGE('',*,*,#52695,.F.);
#74186=ORIENTED_EDGE('',*,*,#52696,.F.);
#74187=ORIENTED_EDGE('',*,*,#52697,.F.);
#74188=ORIENTED_EDGE('',*,*,#51886,.T.);
#74189=ORIENTED_EDGE('',*,*,#52698,.F.);
#74190=ORIENTED_EDGE('',*,*,#52699,.F.);
#74191=ORIENTED_EDGE('',*,*,#52700,.F.);
#74192=ORIENTED_EDGE('',*,*,#51897,.T.);
#74193=ORIENTED_EDGE('',*,*,#52701,.F.);
#74194=ORIENTED_EDGE('',*,*,#52702,.F.);
#74195=ORIENTED_EDGE('',*,*,#52703,.F.);
#74196=ORIENTED_EDGE('',*,*,#51909,.T.);
#74197=ORIENTED_EDGE('',*,*,#52704,.F.);
#74198=ORIENTED_EDGE('',*,*,#52705,.F.);
#74199=ORIENTED_EDGE('',*,*,#52706,.F.);
#74200=ORIENTED_EDGE('',*,*,#51911,.T.);
#74201=ORIENTED_EDGE('',*,*,#52707,.F.);
#74202=ORIENTED_EDGE('',*,*,#52708,.F.);
#74203=ORIENTED_EDGE('',*,*,#52709,.F.);
#74204=ORIENTED_EDGE('',*,*,#51686,.T.);
#74205=ORIENTED_EDGE('',*,*,#52710,.F.);
#74206=ORIENTED_EDGE('',*,*,#52711,.F.);
#74207=ORIENTED_EDGE('',*,*,#52712,.F.);
#74208=ORIENTED_EDGE('',*,*,#51674,.T.);
#74209=ORIENTED_EDGE('',*,*,#52713,.F.);
#74210=ORIENTED_EDGE('',*,*,#52714,.F.);
#74211=ORIENTED_EDGE('',*,*,#52715,.F.);
#74212=ORIENTED_EDGE('',*,*,#51661,.T.);
#74213=ORIENTED_EDGE('',*,*,#52716,.F.);
#74214=ORIENTED_EDGE('',*,*,#52717,.F.);
#74215=ORIENTED_EDGE('',*,*,#52718,.F.);
#74216=ORIENTED_EDGE('',*,*,#51672,.T.);
#74217=ORIENTED_EDGE('',*,*,#52719,.F.);
#74218=ORIENTED_EDGE('',*,*,#52720,.F.);
#74219=ORIENTED_EDGE('',*,*,#52721,.F.);
#74220=ORIENTED_EDGE('',*,*,#52055,.T.);
#74221=ORIENTED_EDGE('',*,*,#52722,.F.);
#74222=ORIENTED_EDGE('',*,*,#52723,.F.);
#74223=ORIENTED_EDGE('',*,*,#52724,.F.);
#74224=ORIENTED_EDGE('',*,*,#52042,.T.);
#74225=ORIENTED_EDGE('',*,*,#52725,.F.);
#74226=ORIENTED_EDGE('',*,*,#52726,.F.);
#74227=ORIENTED_EDGE('',*,*,#52727,.F.);
#74228=ORIENTED_EDGE('',*,*,#52053,.T.);
#74229=ORIENTED_EDGE('',*,*,#52728,.F.);
#74230=ORIENTED_EDGE('',*,*,#52729,.F.);
#74231=ORIENTED_EDGE('',*,*,#52730,.F.);
#74232=ORIENTED_EDGE('',*,*,#52302,.T.);
#74233=ORIENTED_EDGE('',*,*,#52731,.F.);
#74234=ORIENTED_EDGE('',*,*,#52732,.F.);
#74235=ORIENTED_EDGE('',*,*,#52733,.F.);
#74236=ORIENTED_EDGE('',*,*,#52304,.T.);
#74237=ORIENTED_EDGE('',*,*,#52734,.F.);
#74238=ORIENTED_EDGE('',*,*,#52735,.F.);
#74239=ORIENTED_EDGE('',*,*,#52736,.F.);
#74240=ORIENTED_EDGE('',*,*,#52737,.F.);
#74241=ORIENTED_EDGE('',*,*,#52292,.T.);
#74242=ORIENTED_EDGE('',*,*,#52738,.F.);
#74243=ORIENTED_EDGE('',*,*,#52739,.F.);
#74244=ORIENTED_EDGE('',*,*,#51749,.T.);
#74245=ORIENTED_EDGE('',*,*,#52740,.F.);
#74246=ORIENTED_EDGE('',*,*,#52741,.F.);
#74247=ORIENTED_EDGE('',*,*,#52742,.F.);
#74248=ORIENTED_EDGE('',*,*,#51736,.T.);
#74249=ORIENTED_EDGE('',*,*,#52743,.F.);
#74250=ORIENTED_EDGE('',*,*,#52744,.F.);
#74251=ORIENTED_EDGE('',*,*,#52745,.F.);
#74252=ORIENTED_EDGE('',*,*,#51747,.T.);
#74253=ORIENTED_EDGE('',*,*,#52746,.F.);
#74254=ORIENTED_EDGE('',*,*,#52747,.F.);
#74255=ORIENTED_EDGE('',*,*,#52748,.F.);
#74256=ORIENTED_EDGE('',*,*,#51757,.T.);
#74257=ORIENTED_EDGE('',*,*,#52749,.F.);
#74258=ORIENTED_EDGE('',*,*,#52750,.F.);
#74259=ORIENTED_EDGE('',*,*,#52751,.F.);
#74260=ORIENTED_EDGE('',*,*,#51773,.T.);
#74261=ORIENTED_EDGE('',*,*,#52752,.F.);
#74262=ORIENTED_EDGE('',*,*,#52753,.F.);
#74263=ORIENTED_EDGE('',*,*,#52754,.F.);
#74264=ORIENTED_EDGE('',*,*,#51760,.T.);
#74265=ORIENTED_EDGE('',*,*,#52755,.F.);
#74266=ORIENTED_EDGE('',*,*,#52756,.F.);
#74267=ORIENTED_EDGE('',*,*,#52757,.F.);
#74268=ORIENTED_EDGE('',*,*,#51771,.T.);
#74269=ORIENTED_EDGE('',*,*,#52758,.F.);
#74270=ORIENTED_EDGE('',*,*,#52759,.F.);
#74271=ORIENTED_EDGE('',*,*,#52760,.F.);
#74272=ORIENTED_EDGE('',*,*,#51781,.T.);
#74273=ORIENTED_EDGE('',*,*,#52761,.F.);
#74274=ORIENTED_EDGE('',*,*,#52762,.F.);
#74275=ORIENTED_EDGE('',*,*,#52763,.F.);
#74276=ORIENTED_EDGE('',*,*,#52147,.T.);
#74277=ORIENTED_EDGE('',*,*,#52764,.F.);
#74278=ORIENTED_EDGE('',*,*,#52765,.F.);
#74279=ORIENTED_EDGE('',*,*,#52766,.F.);
#74280=ORIENTED_EDGE('',*,*,#52158,.T.);
#74281=ORIENTED_EDGE('',*,*,#52767,.F.);
#74282=ORIENTED_EDGE('',*,*,#52768,.F.);
#74283=ORIENTED_EDGE('',*,*,#52769,.F.);
#74284=ORIENTED_EDGE('',*,*,#52170,.T.);
#74285=ORIENTED_EDGE('',*,*,#52770,.F.);
#74286=ORIENTED_EDGE('',*,*,#52771,.F.);
#74287=ORIENTED_EDGE('',*,*,#52772,.F.);
#74288=ORIENTED_EDGE('',*,*,#52160,.T.);
#74289=ORIENTED_EDGE('',*,*,#52773,.F.);
#74290=ORIENTED_EDGE('',*,*,#52774,.F.);
#74291=ORIENTED_EDGE('',*,*,#52775,.F.);
#74292=ORIENTED_EDGE('',*,*,#52093,.T.);
#74293=ORIENTED_EDGE('',*,*,#52776,.F.);
#74294=ORIENTED_EDGE('',*,*,#52777,.F.);
#74295=ORIENTED_EDGE('',*,*,#52778,.F.);
#74296=ORIENTED_EDGE('',*,*,#52104,.T.);
#74297=ORIENTED_EDGE('',*,*,#52779,.F.);
#74298=ORIENTED_EDGE('',*,*,#52780,.F.);
#74299=ORIENTED_EDGE('',*,*,#52781,.F.);
#74300=ORIENTED_EDGE('',*,*,#52118,.T.);
#74301=ORIENTED_EDGE('',*,*,#52782,.F.);
#74302=ORIENTED_EDGE('',*,*,#52783,.F.);
#74303=ORIENTED_EDGE('',*,*,#52784,.F.);
#74304=ORIENTED_EDGE('',*,*,#52106,.T.);
#74305=ORIENTED_EDGE('',*,*,#52785,.F.);
#74306=ORIENTED_EDGE('',*,*,#52786,.F.);
#74307=ORIENTED_EDGE('',*,*,#52787,.F.);
#74308=ORIENTED_EDGE('',*,*,#51875,.T.);
#74309=ORIENTED_EDGE('',*,*,#52788,.F.);
#74310=ORIENTED_EDGE('',*,*,#52789,.F.);
#74311=ORIENTED_EDGE('',*,*,#52790,.F.);
#74312=ORIENTED_EDGE('',*,*,#51862,.T.);
#74313=ORIENTED_EDGE('',*,*,#52791,.F.);
#74314=ORIENTED_EDGE('',*,*,#52792,.F.);
#74315=ORIENTED_EDGE('',*,*,#52793,.F.);
#74316=ORIENTED_EDGE('',*,*,#51873,.T.);
#74317=ORIENTED_EDGE('',*,*,#52794,.F.);
#74318=ORIENTED_EDGE('',*,*,#52795,.F.);
#74319=ORIENTED_EDGE('',*,*,#52796,.F.);
#74320=ORIENTED_EDGE('',*,*,#51883,.T.);
#74321=ORIENTED_EDGE('',*,*,#52797,.F.);
#74322=ORIENTED_EDGE('',*,*,#52798,.F.);
#74323=ORIENTED_EDGE('',*,*,#52799,.F.);
#74324=ORIENTED_EDGE('',*,*,#51967,.T.);
#74325=ORIENTED_EDGE('',*,*,#52800,.F.);
#74326=ORIENTED_EDGE('',*,*,#52801,.F.);
#74327=ORIENTED_EDGE('',*,*,#52802,.F.);
#74328=ORIENTED_EDGE('',*,*,#51959,.T.);
#74329=ORIENTED_EDGE('',*,*,#52803,.F.);
#74330=ORIENTED_EDGE('',*,*,#52804,.F.);
#74331=ORIENTED_EDGE('',*,*,#52805,.F.);
#74332=ORIENTED_EDGE('',*,*,#51946,.T.);
#74333=ORIENTED_EDGE('',*,*,#52806,.F.);
#74334=ORIENTED_EDGE('',*,*,#52807,.F.);
#74335=ORIENTED_EDGE('',*,*,#52808,.F.);
#74336=ORIENTED_EDGE('',*,*,#51957,.T.);
#74337=ORIENTED_EDGE('',*,*,#52809,.F.);
#74338=ORIENTED_EDGE('',*,*,#52810,.F.);
#74339=ORIENTED_EDGE('',*,*,#52811,.F.);
#74340=ORIENTED_EDGE('',*,*,#51994,.T.);
#74341=ORIENTED_EDGE('',*,*,#52812,.F.);
#74342=ORIENTED_EDGE('',*,*,#52813,.F.);
#74343=ORIENTED_EDGE('',*,*,#52814,.F.);
#74344=ORIENTED_EDGE('',*,*,#52005,.T.);
#74345=ORIENTED_EDGE('',*,*,#52815,.F.);
#74346=ORIENTED_EDGE('',*,*,#52816,.F.);
#74347=ORIENTED_EDGE('',*,*,#52817,.F.);
#74348=ORIENTED_EDGE('',*,*,#52015,.T.);
#74349=ORIENTED_EDGE('',*,*,#52818,.F.);
#74350=ORIENTED_EDGE('',*,*,#52819,.F.);
#74351=ORIENTED_EDGE('',*,*,#52820,.F.);
#74352=ORIENTED_EDGE('',*,*,#52007,.T.);
#74353=ORIENTED_EDGE('',*,*,#52821,.F.);
#74354=ORIENTED_EDGE('',*,*,#52822,.F.);
#74355=ORIENTED_EDGE('',*,*,#52823,.F.);
#74356=ORIENTED_EDGE('',*,*,#52284,.T.);
#74357=ORIENTED_EDGE('',*,*,#52824,.F.);
#74358=ORIENTED_EDGE('',*,*,#52825,.F.);
#74359=ORIENTED_EDGE('',*,*,#52826,.F.);
#74360=ORIENTED_EDGE('',*,*,#52286,.T.);
#74361=ORIENTED_EDGE('',*,*,#52827,.F.);
#74362=ORIENTED_EDGE('',*,*,#52828,.F.);
#74363=ORIENTED_EDGE('',*,*,#52829,.F.);
#74364=ORIENTED_EDGE('',*,*,#52273,.T.);
#74365=ORIENTED_EDGE('',*,*,#52830,.F.);
#74366=ORIENTED_EDGE('',*,*,#52831,.F.);
#74367=ORIENTED_EDGE('',*,*,#52832,.F.);
#74368=ORIENTED_EDGE('',*,*,#52134,.T.);
#74369=ORIENTED_EDGE('',*,*,#52833,.F.);
#74370=ORIENTED_EDGE('',*,*,#52834,.F.);
#74371=ORIENTED_EDGE('',*,*,#52835,.F.);
#74372=ORIENTED_EDGE('',*,*,#52144,.T.);
#74373=ORIENTED_EDGE('',*,*,#52836,.F.);
#74374=ORIENTED_EDGE('',*,*,#52837,.F.);
#74375=ORIENTED_EDGE('',*,*,#52838,.F.);
#74376=ORIENTED_EDGE('',*,*,#52136,.T.);
#74377=ORIENTED_EDGE('',*,*,#52839,.F.);
#74378=ORIENTED_EDGE('',*,*,#52840,.F.);
#74379=ORIENTED_EDGE('',*,*,#52841,.F.);
#74380=ORIENTED_EDGE('',*,*,#52123,.T.);
#74381=ORIENTED_EDGE('',*,*,#52842,.F.);
#74382=ORIENTED_EDGE('',*,*,#52843,.F.);
#74383=ORIENTED_EDGE('',*,*,#52844,.F.);
#74384=ORIENTED_EDGE('',*,*,#52082,.T.);
#74385=ORIENTED_EDGE('',*,*,#52845,.F.);
#74386=ORIENTED_EDGE('',*,*,#52846,.F.);
#74387=ORIENTED_EDGE('',*,*,#52847,.F.);
#74388=ORIENTED_EDGE('',*,*,#52069,.T.);
#74389=ORIENTED_EDGE('',*,*,#52848,.F.);
#74390=ORIENTED_EDGE('',*,*,#52849,.F.);
#74391=ORIENTED_EDGE('',*,*,#52850,.F.);
#74392=ORIENTED_EDGE('',*,*,#52080,.T.);
#74393=ORIENTED_EDGE('',*,*,#52851,.F.);
#74394=ORIENTED_EDGE('',*,*,#52852,.F.);
#74395=ORIENTED_EDGE('',*,*,#52853,.F.);
#74396=ORIENTED_EDGE('',*,*,#52090,.T.);
#74397=ORIENTED_EDGE('',*,*,#52854,.F.);
#74398=ORIENTED_EDGE('',*,*,#52855,.F.);
#74399=ORIENTED_EDGE('',*,*,#52856,.F.);
#74400=ORIENTED_EDGE('',*,*,#51983,.T.);
#74401=ORIENTED_EDGE('',*,*,#52857,.F.);
#74402=ORIENTED_EDGE('',*,*,#52858,.F.);
#74403=ORIENTED_EDGE('',*,*,#52859,.F.);
#74404=ORIENTED_EDGE('',*,*,#51970,.T.);
#74405=ORIENTED_EDGE('',*,*,#52860,.F.);
#74406=ORIENTED_EDGE('',*,*,#52861,.F.);
#74407=ORIENTED_EDGE('',*,*,#52862,.F.);
#74408=ORIENTED_EDGE('',*,*,#51981,.T.);
#74409=ORIENTED_EDGE('',*,*,#52863,.F.);
#74410=ORIENTED_EDGE('',*,*,#52864,.F.);
#74411=ORIENTED_EDGE('',*,*,#52865,.F.);
#74412=ORIENTED_EDGE('',*,*,#51991,.T.);
#74413=ORIENTED_EDGE('',*,*,#52866,.F.);
#74414=ORIENTED_EDGE('',*,*,#52867,.F.);
#74415=ORIENTED_EDGE('',*,*,#52868,.F.);
#74416=ORIENTED_EDGE('',*,*,#51838,.T.);
#74417=ORIENTED_EDGE('',*,*,#52869,.F.);
#74418=ORIENTED_EDGE('',*,*,#52870,.F.);
#74419=ORIENTED_EDGE('',*,*,#52871,.F.);
#74420=ORIENTED_EDGE('',*,*,#51849,.T.);
#74421=ORIENTED_EDGE('',*,*,#52872,.F.);
#74422=ORIENTED_EDGE('',*,*,#52873,.F.);
#74423=ORIENTED_EDGE('',*,*,#52874,.F.);
#74424=ORIENTED_EDGE('',*,*,#51859,.T.);
#74425=ORIENTED_EDGE('',*,*,#52875,.F.);
#74426=ORIENTED_EDGE('',*,*,#52876,.F.);
#74427=ORIENTED_EDGE('',*,*,#52877,.F.);
#74428=ORIENTED_EDGE('',*,*,#51851,.T.);
#74429=ORIENTED_EDGE('',*,*,#52878,.F.);
#74430=ORIENTED_EDGE('',*,*,#52879,.F.);
#74431=ORIENTED_EDGE('',*,*,#52880,.F.);
#74432=ORIENTED_EDGE('',*,*,#51784,.T.);
#74433=ORIENTED_EDGE('',*,*,#52881,.F.);
#74434=ORIENTED_EDGE('',*,*,#52882,.F.);
#74435=ORIENTED_EDGE('',*,*,#52883,.F.);
#74436=ORIENTED_EDGE('',*,*,#51795,.T.);
#74437=ORIENTED_EDGE('',*,*,#52884,.F.);
#74438=ORIENTED_EDGE('',*,*,#52885,.F.);
#74439=ORIENTED_EDGE('',*,*,#52886,.F.);
#74440=ORIENTED_EDGE('',*,*,#51805,.T.);
#74441=ORIENTED_EDGE('',*,*,#52887,.F.);
#74442=ORIENTED_EDGE('',*,*,#52888,.F.);
#74443=ORIENTED_EDGE('',*,*,#52889,.F.);
#74444=ORIENTED_EDGE('',*,*,#51797,.T.);
#74445=ORIENTED_EDGE('',*,*,#52890,.F.);
#74446=ORIENTED_EDGE('',*,*,#52891,.F.);
#74447=ORIENTED_EDGE('',*,*,#52892,.F.);
#74448=ORIENTED_EDGE('',*,*,#51808,.T.);
#74449=ORIENTED_EDGE('',*,*,#52893,.F.);
#74450=ORIENTED_EDGE('',*,*,#52894,.F.);
#74451=ORIENTED_EDGE('',*,*,#52895,.F.);
#74452=ORIENTED_EDGE('',*,*,#51819,.T.);
#74453=ORIENTED_EDGE('',*,*,#52896,.F.);
#74454=ORIENTED_EDGE('',*,*,#52897,.F.);
#74455=ORIENTED_EDGE('',*,*,#52898,.F.);
#74456=ORIENTED_EDGE('',*,*,#51831,.T.);
#74457=ORIENTED_EDGE('',*,*,#52899,.F.);
#74458=ORIENTED_EDGE('',*,*,#52900,.F.);
#74459=ORIENTED_EDGE('',*,*,#52901,.F.);
#74460=ORIENTED_EDGE('',*,*,#51821,.T.);
#74461=ORIENTED_EDGE('',*,*,#52902,.F.);
#74462=ORIENTED_EDGE('',*,*,#52903,.F.);
#74463=ORIENTED_EDGE('',*,*,#52904,.F.);
#74464=ORIENTED_EDGE('',*,*,#51582,.T.);
#74465=ORIENTED_EDGE('',*,*,#52905,.F.);
#74466=ORIENTED_EDGE('',*,*,#52906,.F.);
#74467=ORIENTED_EDGE('',*,*,#52907,.F.);
#74468=ORIENTED_EDGE('',*,*,#51584,.T.);
#74469=ORIENTED_EDGE('',*,*,#52908,.F.);
#74470=ORIENTED_EDGE('',*,*,#52909,.F.);
#74471=ORIENTED_EDGE('',*,*,#52910,.F.);
#74472=ORIENTED_EDGE('',*,*,#52911,.F.);
#74473=ORIENTED_EDGE('',*,*,#51560,.T.);
#74474=ORIENTED_EDGE('',*,*,#52912,.F.);
#74475=ORIENTED_EDGE('',*,*,#52913,.F.);
#74476=ORIENTED_EDGE('',*,*,#51570,.T.);
#74477=ORIENTED_EDGE('',*,*,#52914,.F.);
#74478=ORIENTED_EDGE('',*,*,#52915,.F.);
#74479=ORIENTED_EDGE('',*,*,#52916,.F.);
#74480=ORIENTED_EDGE('',*,*,#52190,.T.);
#74481=ORIENTED_EDGE('',*,*,#52917,.F.);
#74482=ORIENTED_EDGE('',*,*,#52918,.F.);
#74483=ORIENTED_EDGE('',*,*,#52919,.F.);
#74484=ORIENTED_EDGE('',*,*,#52177,.T.);
#74485=ORIENTED_EDGE('',*,*,#52920,.F.);
#74486=ORIENTED_EDGE('',*,*,#52921,.F.);
#74487=ORIENTED_EDGE('',*,*,#52922,.F.);
#74488=ORIENTED_EDGE('',*,*,#52188,.T.);
#74489=ORIENTED_EDGE('',*,*,#52923,.F.);
#74490=ORIENTED_EDGE('',*,*,#52924,.F.);
#74491=ORIENTED_EDGE('',*,*,#52925,.F.);
#74492=ORIENTED_EDGE('',*,*,#52198,.T.);
#74493=ORIENTED_EDGE('',*,*,#52926,.F.);
#74494=ORIENTED_EDGE('',*,*,#52927,.F.);
#74495=ORIENTED_EDGE('',*,*,#52928,.F.);
#74496=ORIENTED_EDGE('',*,*,#51725,.T.);
#74497=ORIENTED_EDGE('',*,*,#52929,.F.);
#74498=ORIENTED_EDGE('',*,*,#52930,.F.);
#74499=ORIENTED_EDGE('',*,*,#52931,.F.);
#74500=ORIENTED_EDGE('',*,*,#51712,.T.);
#74501=ORIENTED_EDGE('',*,*,#52932,.F.);
#74502=ORIENTED_EDGE('',*,*,#52933,.F.);
#74503=ORIENTED_EDGE('',*,*,#52934,.F.);
#74504=ORIENTED_EDGE('',*,*,#51723,.T.);
#74505=ORIENTED_EDGE('',*,*,#52935,.F.);
#74506=ORIENTED_EDGE('',*,*,#52936,.F.);
#74507=ORIENTED_EDGE('',*,*,#52937,.F.);
#74508=ORIENTED_EDGE('',*,*,#51733,.T.);
#74509=ORIENTED_EDGE('',*,*,#52938,.F.);
#74510=ORIENTED_EDGE('',*,*,#52939,.F.);
#74511=ORIENTED_EDGE('',*,*,#52940,.F.);
#74512=ORIENTED_EDGE('',*,*,#51701,.T.);
#74513=ORIENTED_EDGE('',*,*,#52941,.F.);
#74514=ORIENTED_EDGE('',*,*,#52942,.F.);
#74515=ORIENTED_EDGE('',*,*,#52943,.F.);
#74516=ORIENTED_EDGE('',*,*,#51688,.T.);
#74517=ORIENTED_EDGE('',*,*,#52944,.F.);
#74518=ORIENTED_EDGE('',*,*,#52945,.F.);
#74519=ORIENTED_EDGE('',*,*,#52946,.F.);
#74520=ORIENTED_EDGE('',*,*,#51699,.T.);
#74521=ORIENTED_EDGE('',*,*,#52947,.F.);
#74522=ORIENTED_EDGE('',*,*,#52948,.F.);
#74523=ORIENTED_EDGE('',*,*,#52949,.F.);
#74524=ORIENTED_EDGE('',*,*,#51709,.T.);
#74525=ORIENTED_EDGE('',*,*,#52950,.F.);
#74526=ORIENTED_EDGE('',*,*,#52951,.F.);
#74527=ORIENTED_EDGE('',*,*,#52952,.F.);
#74528=ORIENTED_EDGE('',*,*,#52018,.T.);
#74529=ORIENTED_EDGE('',*,*,#52953,.F.);
#74530=ORIENTED_EDGE('',*,*,#52954,.F.);
#74531=ORIENTED_EDGE('',*,*,#52955,.F.);
#74532=ORIENTED_EDGE('',*,*,#52029,.T.);
#74533=ORIENTED_EDGE('',*,*,#52956,.F.);
#74534=ORIENTED_EDGE('',*,*,#52957,.F.);
#74535=ORIENTED_EDGE('',*,*,#52958,.F.);
#74536=ORIENTED_EDGE('',*,*,#52039,.T.);
#74537=ORIENTED_EDGE('',*,*,#52959,.F.);
#74538=ORIENTED_EDGE('',*,*,#52960,.F.);
#74539=ORIENTED_EDGE('',*,*,#52961,.F.);
#74540=ORIENTED_EDGE('',*,*,#52031,.T.);
#74541=ORIENTED_EDGE('',*,*,#52962,.F.);
#74542=ORIENTED_EDGE('',*,*,#52963,.F.);
#74543=ORIENTED_EDGE('',*,*,#52964,.F.);
#74544=ORIENTED_EDGE('',*,*,#52212,.T.);
#74545=ORIENTED_EDGE('',*,*,#52965,.F.);
#74546=ORIENTED_EDGE('',*,*,#52966,.F.);
#74547=ORIENTED_EDGE('',*,*,#52967,.F.);
#74548=ORIENTED_EDGE('',*,*,#52222,.T.);
#74549=ORIENTED_EDGE('',*,*,#52968,.F.);
#74550=ORIENTED_EDGE('',*,*,#52969,.F.);
#74551=ORIENTED_EDGE('',*,*,#52970,.F.);
#74552=ORIENTED_EDGE('',*,*,#52214,.T.);
#74553=ORIENTED_EDGE('',*,*,#52971,.F.);
#74554=ORIENTED_EDGE('',*,*,#52972,.F.);
#74555=ORIENTED_EDGE('',*,*,#52973,.F.);
#74556=ORIENTED_EDGE('',*,*,#52201,.T.);
#74557=ORIENTED_EDGE('',*,*,#52974,.F.);
#74558=ORIENTED_EDGE('',*,*,#52975,.F.);
#74559=ORIENTED_EDGE('',*,*,#52976,.F.);
#74560=ORIENTED_EDGE('',*,*,#51610,.T.);
#74561=ORIENTED_EDGE('',*,*,#52977,.F.);
#74562=ORIENTED_EDGE('',*,*,#52978,.F.);
#74563=ORIENTED_EDGE('',*,*,#52979,.F.);
#74564=ORIENTED_EDGE('',*,*,#51602,.T.);
#74565=ORIENTED_EDGE('',*,*,#52980,.F.);
#74566=ORIENTED_EDGE('',*,*,#52981,.F.);
#74567=ORIENTED_EDGE('',*,*,#52982,.F.);
#74568=ORIENTED_EDGE('',*,*,#52983,.F.);
#74569=ORIENTED_EDGE('',*,*,#51590,.T.);
#74570=ORIENTED_EDGE('',*,*,#52984,.F.);
#74571=ORIENTED_EDGE('',*,*,#52985,.F.);
#74572=ORIENTED_EDGE('',*,*,#51600,.T.);
#74573=ORIENTED_EDGE('',*,*,#52986,.F.);
#74574=ORIENTED_EDGE('',*,*,#52987,.F.);
#74575=ORIENTED_EDGE('',*,*,#52988,.F.);
#74576=ORIENTED_EDGE('',*,*,#52238,.T.);
#74577=ORIENTED_EDGE('',*,*,#52989,.F.);
#74578=ORIENTED_EDGE('',*,*,#52990,.F.);
#74579=ORIENTED_EDGE('',*,*,#52991,.F.);
#74580=ORIENTED_EDGE('',*,*,#52225,.T.);
#74581=ORIENTED_EDGE('',*,*,#52992,.F.);
#74582=ORIENTED_EDGE('',*,*,#52993,.F.);
#74583=ORIENTED_EDGE('',*,*,#52994,.F.);
#74584=ORIENTED_EDGE('',*,*,#52236,.T.);
#74585=ORIENTED_EDGE('',*,*,#52995,.F.);
#74586=ORIENTED_EDGE('',*,*,#52996,.F.);
#74587=ORIENTED_EDGE('',*,*,#52997,.F.);
#74588=ORIENTED_EDGE('',*,*,#52246,.T.);
#74589=ORIENTED_EDGE('',*,*,#52998,.F.);
#74590=ORIENTED_EDGE('',*,*,#52999,.F.);
#74591=ORIENTED_EDGE('',*,*,#53000,.F.);
#74592=ORIENTED_EDGE('',*,*,#51650,.T.);
#74593=ORIENTED_EDGE('',*,*,#53001,.F.);
#74594=ORIENTED_EDGE('',*,*,#53002,.F.);
#74595=ORIENTED_EDGE('',*,*,#53003,.F.);
#74596=ORIENTED_EDGE('',*,*,#51637,.T.);
#74597=ORIENTED_EDGE('',*,*,#53004,.F.);
#74598=ORIENTED_EDGE('',*,*,#53005,.F.);
#74599=ORIENTED_EDGE('',*,*,#53006,.F.);
#74600=ORIENTED_EDGE('',*,*,#51648,.T.);
#74601=ORIENTED_EDGE('',*,*,#53007,.F.);
#74602=ORIENTED_EDGE('',*,*,#53008,.F.);
#74603=ORIENTED_EDGE('',*,*,#53009,.F.);
#74604=ORIENTED_EDGE('',*,*,#51658,.T.);
#74605=ORIENTED_EDGE('',*,*,#53010,.F.);
#74606=ORIENTED_EDGE('',*,*,#53011,.F.);
#74607=ORIENTED_EDGE('',*,*,#53012,.F.);
#74608=ORIENTED_EDGE('',*,*,#52260,.T.);
#74609=ORIENTED_EDGE('',*,*,#53013,.F.);
#74610=ORIENTED_EDGE('',*,*,#53014,.F.);
#74611=ORIENTED_EDGE('',*,*,#53015,.F.);
#74612=ORIENTED_EDGE('',*,*,#52270,.T.);
#74613=ORIENTED_EDGE('',*,*,#53016,.F.);
#74614=ORIENTED_EDGE('',*,*,#53017,.F.);
#74615=ORIENTED_EDGE('',*,*,#53018,.F.);
#74616=ORIENTED_EDGE('',*,*,#52262,.T.);
#74617=ORIENTED_EDGE('',*,*,#53019,.F.);
#74618=ORIENTED_EDGE('',*,*,#53020,.F.);
#74619=ORIENTED_EDGE('',*,*,#53021,.F.);
#74620=ORIENTED_EDGE('',*,*,#52249,.T.);
#74621=ORIENTED_EDGE('',*,*,#53022,.F.);
#74622=ORIENTED_EDGE('',*,*,#53023,.F.);
#74623=ORIENTED_EDGE('',*,*,#53024,.F.);
#74624=ORIENTED_EDGE('',*,*,#51634,.T.);
#74625=ORIENTED_EDGE('',*,*,#53025,.F.);
#74626=ORIENTED_EDGE('',*,*,#53026,.F.);
#74627=ORIENTED_EDGE('',*,*,#53027,.F.);
#74628=ORIENTED_EDGE('',*,*,#51626,.T.);
#74629=ORIENTED_EDGE('',*,*,#53028,.F.);
#74630=ORIENTED_EDGE('',*,*,#53029,.F.);
#74631=ORIENTED_EDGE('',*,*,#53030,.F.);
#74632=ORIENTED_EDGE('',*,*,#53031,.F.);
#74633=ORIENTED_EDGE('',*,*,#51614,.T.);
#74634=ORIENTED_EDGE('',*,*,#53032,.F.);
#74635=ORIENTED_EDGE('',*,*,#53033,.F.);
#74636=ORIENTED_EDGE('',*,*,#51624,.T.);
#74637=ORIENTED_EDGE('',*,*,#53034,.F.);
#74638=ORIENTED_EDGE('',*,*,#53035,.F.);
#74639=ORIENTED_EDGE('',*,*,#53036,.F.);
#74640=ORIENTED_EDGE('',*,*,#52402,.T.);
#74641=ORIENTED_EDGE('',*,*,#53037,.F.);
#74642=ORIENTED_EDGE('',*,*,#53038,.F.);
#74643=ORIENTED_EDGE('',*,*,#53039,.F.);
#74644=ORIENTED_EDGE('',*,*,#52440,.T.);
#74645=ORIENTED_EDGE('',*,*,#53040,.F.);
#74646=ORIENTED_EDGE('',*,*,#53041,.F.);
#74647=ORIENTED_EDGE('',*,*,#53042,.F.);
#74648=ORIENTED_EDGE('',*,*,#52424,.T.);
#74649=ORIENTED_EDGE('',*,*,#53043,.F.);
#74650=ORIENTED_EDGE('',*,*,#53044,.F.);
#74651=ORIENTED_EDGE('',*,*,#53045,.F.);
#74652=ORIENTED_EDGE('',*,*,#53046,.F.);
#74653=ORIENTED_EDGE('',*,*,#52419,.T.);
#74654=ORIENTED_EDGE('',*,*,#53047,.F.);
#74655=ORIENTED_EDGE('',*,*,#53048,.F.);
#74656=ORIENTED_EDGE('',*,*,#52446,.T.);
#74657=ORIENTED_EDGE('',*,*,#53049,.F.);
#74658=ORIENTED_EDGE('',*,*,#53050,.F.);
#74659=ORIENTED_EDGE('',*,*,#53051,.F.);
#74660=ORIENTED_EDGE('',*,*,#53052,.F.);
#74661=ORIENTED_EDGE('',*,*,#52435,.T.);
#74662=ORIENTED_EDGE('',*,*,#53053,.F.);
#74663=ORIENTED_EDGE('',*,*,#53054,.F.);
#74664=ORIENTED_EDGE('',*,*,#52408,.T.);
#74665=ORIENTED_EDGE('',*,*,#53055,.F.);
#74666=ORIENTED_EDGE('',*,*,#53056,.F.);
#74667=ORIENTED_EDGE('',*,*,#53057,.F.);
#74668=ORIENTED_EDGE('',*,*,#51899,.T.);
#74669=ORIENTED_EDGE('',*,*,#53058,.F.);
#74670=ORIENTED_EDGE('',*,*,#53059,.F.);
#74671=ORIENTED_EDGE('',*,*,#53060,.F.);
#74672=ORIENTED_EDGE('',*,*,#51929,.T.);
#74673=ORIENTED_EDGE('',*,*,#53061,.F.);
#74674=ORIENTED_EDGE('',*,*,#53062,.F.);
#74675=ORIENTED_EDGE('',*,*,#53063,.F.);
#74676=ORIENTED_EDGE('',*,*,#52067,.T.);
#74677=ORIENTED_EDGE('',*,*,#52683,.T.);
#74678=ORIENTED_EDGE('',*,*,#53064,.F.);
#74679=ORIENTED_EDGE('',*,*,#52710,.T.);
#74680=ORIENTED_EDGE('',*,*,#51684,.T.);
#74681=ORIENTED_EDGE('',*,*,#53065,.F.);
#74682=ORIENTED_EDGE('',*,*,#53066,.F.);
#74683=ORIENTED_EDGE('',*,*,#53067,.T.);
#74684=ORIENTED_EDGE('',*,*,#53067,.F.);
#74685=ORIENTED_EDGE('',*,*,#53068,.T.);
#74686=ORIENTED_EDGE('',*,*,#52311,.T.);
#74687=ORIENTED_EDGE('',*,*,#53068,.F.);
#74688=ORIENTED_EDGE('',*,*,#52308,.T.);
#74689=ORIENTED_EDGE('',*,*,#52313,.T.);
#74690=ORIENTED_EDGE('',*,*,#52722,.T.);
#74691=ORIENTED_EDGE('',*,*,#52061,.T.);
#74692=ORIENTED_EDGE('',*,*,#53063,.T.);
#74693=ORIENTED_EDGE('',*,*,#53069,.F.);
#74694=ORIENTED_EDGE('',*,*,#53065,.T.);
#74695=ORIENTED_EDGE('',*,*,#51678,.T.);
#74696=ORIENTED_EDGE('',*,*,#52718,.T.);
#74697=ORIENTED_EDGE('',*,*,#53070,.F.);
#74698=ORIENTED_EDGE('',*,*,#52310,.T.);
#74699=ORIENTED_EDGE('',*,*,#53071,.T.);
#74700=ORIENTED_EDGE('',*,*,#53072,.T.);
#74701=ORIENTED_EDGE('',*,*,#50262,.F.);
#74702=ORIENTED_EDGE('',*,*,#50453,.F.);
#74703=ORIENTED_EDGE('',*,*,#53073,.T.);
#74704=ORIENTED_EDGE('',*,*,#50846,.F.);
#74705=ORIENTED_EDGE('',*,*,#50243,.F.);
#74706=ORIENTED_EDGE('',*,*,#53074,.F.);
#74707=ORIENTED_EDGE('',*,*,#50218,.F.);
#74708=ORIENTED_EDGE('',*,*,#50849,.F.);
#74709=ORIENTED_EDGE('',*,*,#53075,.T.);
#74710=ORIENTED_EDGE('',*,*,#50457,.F.);
#74711=ORIENTED_EDGE('',*,*,#50201,.F.);
#74712=ORIENTED_EDGE('',*,*,#53076,.F.);
#74713=ORIENTED_EDGE('',*,*,#50196,.F.);
#74714=ORIENTED_EDGE('',*,*,#50462,.F.);
#74715=ORIENTED_EDGE('',*,*,#53077,.T.);
#74716=ORIENTED_EDGE('',*,*,#50466,.F.);
#74717=ORIENTED_EDGE('',*,*,#50179,.F.);
#74718=ORIENTED_EDGE('',*,*,#53078,.F.);
#74719=ORIENTED_EDGE('',*,*,#50240,.F.);
#74720=ORIENTED_EDGE('',*,*,#50471,.F.);
#74721=ORIENTED_EDGE('',*,*,#53079,.T.);
#74722=ORIENTED_EDGE('',*,*,#50472,.F.);
#74723=ORIENTED_EDGE('',*,*,#50223,.F.);
#74724=ORIENTED_EDGE('',*,*,#53080,.T.);
#74725=ORIENTED_EDGE('',*,*,#52412,.T.);
#74726=ORIENTED_EDGE('',*,*,#52679,.T.);
#74727=ORIENTED_EDGE('',*,*,#53081,.F.);
#74728=ORIENTED_EDGE('',*,*,#52677,.T.);
#74729=ORIENTED_EDGE('',*,*,#52429,.T.);
#74730=ORIENTED_EDGE('',*,*,#53082,.T.);
#74731=ORIENTED_EDGE('',*,*,#52368,.T.);
#74732=ORIENTED_EDGE('',*,*,#52673,.T.);
#74733=ORIENTED_EDGE('',*,*,#53083,.F.);
#74734=ORIENTED_EDGE('',*,*,#52668,.T.);
#74735=ORIENTED_EDGE('',*,*,#52385,.T.);
#74736=ORIENTED_EDGE('',*,*,#53084,.T.);
#74737=ORIENTED_EDGE('',*,*,#52390,.T.);
#74738=ORIENTED_EDGE('',*,*,#52664,.T.);
#74739=ORIENTED_EDGE('',*,*,#53085,.F.);
#74740=ORIENTED_EDGE('',*,*,#53055,.T.);
#74741=ORIENTED_EDGE('',*,*,#52407,.T.);
#74742=ORIENTED_EDGE('',*,*,#53086,.T.);
#74743=ORIENTED_EDGE('',*,*,#52432,.T.);
#74744=ORIENTED_EDGE('',*,*,#53052,.T.);
#74745=ORIENTED_EDGE('',*,*,#53087,.F.);
#74746=ORIENTED_EDGE('',*,*,#52659,.T.);
#74747=ORIENTED_EDGE('',*,*,#52451,.T.);
#74748=ORIENTED_EDGE('',*,*,#53088,.T.);
#74749=ORIENTED_EDGE('',*,*,#53071,.F.);
#74750=ORIENTED_EDGE('',*,*,#53040,.T.);
#74751=ORIENTED_EDGE('',*,*,#52443,.T.);
#74752=ORIENTED_EDGE('',*,*,#53048,.T.);
#74753=ORIENTED_EDGE('',*,*,#53089,.T.);
#74754=ORIENTED_EDGE('',*,*,#53053,.T.);
#74755=ORIENTED_EDGE('',*,*,#52437,.T.);
#74756=ORIENTED_EDGE('',*,*,#53039,.T.);
#74757=ORIENTED_EDGE('',*,*,#53090,.T.);
#74758=ORIENTED_EDGE('',*,*,#53037,.T.);
#74759=ORIENTED_EDGE('',*,*,#52405,.T.);
#74760=ORIENTED_EDGE('',*,*,#53054,.T.);
#74761=ORIENTED_EDGE('',*,*,#53091,.T.);
#74762=ORIENTED_EDGE('',*,*,#52662,.T.);
#74763=ORIENTED_EDGE('',*,*,#52399,.T.);
#74764=ORIENTED_EDGE('',*,*,#53036,.T.);
#74765=ORIENTED_EDGE('',*,*,#53092,.T.);
#74766=ORIENTED_EDGE('',*,*,#53061,.T.);
#74767=ORIENTED_EDGE('',*,*,#51935,.T.);
#74768=ORIENTED_EDGE('',*,*,#52685,.T.);
#74769=ORIENTED_EDGE('',*,*,#53093,.F.);
#74770=ORIENTED_EDGE('',*,*,#53047,.T.);
#74771=ORIENTED_EDGE('',*,*,#52421,.T.);
#74772=ORIENTED_EDGE('',*,*,#53042,.T.);
#74773=ORIENTED_EDGE('',*,*,#53094,.T.);
#74774=ORIENTED_EDGE('',*,*,#53043,.T.);
#74775=ORIENTED_EDGE('',*,*,#52427,.T.);
#74776=ORIENTED_EDGE('',*,*,#52676,.T.);
#74777=ORIENTED_EDGE('',*,*,#53095,.F.);
#74778=ORIENTED_EDGE('',*,*,#52674,.T.);
#74779=ORIENTED_EDGE('',*,*,#52371,.T.);
#74780=ORIENTED_EDGE('',*,*,#52656,.T.);
#74781=ORIENTED_EDGE('',*,*,#53096,.F.);
#74782=ORIENTED_EDGE('',*,*,#52657,.T.);
#74783=ORIENTED_EDGE('',*,*,#52377,.T.);
#74784=ORIENTED_EDGE('',*,*,#52670,.T.);
#74785=ORIENTED_EDGE('',*,*,#53097,.T.);
#74786=ORIENTED_EDGE('',*,*,#52698,.T.);
#74787=ORIENTED_EDGE('',*,*,#51893,.T.);
#74788=ORIENTED_EDGE('',*,*,#53057,.T.);
#74789=ORIENTED_EDGE('',*,*,#53098,.F.);
#74790=ORIENTED_EDGE('',*,*,#52740,.T.);
#74791=ORIENTED_EDGE('',*,*,#51755,.T.);
#74792=ORIENTED_EDGE('',*,*,#52748,.T.);
#74793=ORIENTED_EDGE('',*,*,#53099,.T.);
#74794=ORIENTED_EDGE('',*,*,#52896,.T.);
#74795=ORIENTED_EDGE('',*,*,#51813,.T.);
#74796=ORIENTED_EDGE('',*,*,#52892,.T.);
#74797=ORIENTED_EDGE('',*,*,#53100,.T.);
#74798=ORIENTED_EDGE('',*,*,#52884,.T.);
#74799=ORIENTED_EDGE('',*,*,#51789,.T.);
#74800=ORIENTED_EDGE('',*,*,#52880,.T.);
#74801=ORIENTED_EDGE('',*,*,#53101,.T.);
#74802=ORIENTED_EDGE('',*,*,#52752,.T.);
#74803=ORIENTED_EDGE('',*,*,#51779,.T.);
#74804=ORIENTED_EDGE('',*,*,#52760,.T.);
#74805=ORIENTED_EDGE('',*,*,#53102,.T.);
#74806=ORIENTED_EDGE('',*,*,#52872,.T.);
#74807=ORIENTED_EDGE('',*,*,#51843,.T.);
#74808=ORIENTED_EDGE('',*,*,#52868,.T.);
#74809=ORIENTED_EDGE('',*,*,#53103,.T.);
#74810=ORIENTED_EDGE('',*,*,#52788,.T.);
#74811=ORIENTED_EDGE('',*,*,#51881,.T.);
#74812=ORIENTED_EDGE('',*,*,#52796,.T.);
#74813=ORIENTED_EDGE('',*,*,#53104,.T.);
#74814=ORIENTED_EDGE('',*,*,#52860,.T.);
#74815=ORIENTED_EDGE('',*,*,#51977,.T.);
#74816=ORIENTED_EDGE('',*,*,#52856,.T.);
#74817=ORIENTED_EDGE('',*,*,#53105,.T.);
#74818=ORIENTED_EDGE('',*,*,#52800,.T.);
#74819=ORIENTED_EDGE('',*,*,#51963,.T.);
#74820=ORIENTED_EDGE('',*,*,#52808,.T.);
#74821=ORIENTED_EDGE('',*,*,#53106,.T.);
#74822=ORIENTED_EDGE('',*,*,#52776,.T.);
#74823=ORIENTED_EDGE('',*,*,#52100,.T.);
#74824=ORIENTED_EDGE('',*,*,#52784,.T.);
#74825=ORIENTED_EDGE('',*,*,#53107,.T.);
#74826=ORIENTED_EDGE('',*,*,#52836,.T.);
#74827=ORIENTED_EDGE('',*,*,#52140,.T.);
#74828=ORIENTED_EDGE('',*,*,#52832,.T.);
#74829=ORIENTED_EDGE('',*,*,#53108,.T.);
#74830=ORIENTED_EDGE('',*,*,#52848,.T.);
#74831=ORIENTED_EDGE('',*,*,#52076,.T.);
#74832=ORIENTED_EDGE('',*,*,#52844,.T.);
#74833=ORIENTED_EDGE('',*,*,#53109,.T.);
#74834=ORIENTED_EDGE('',*,*,#52812,.T.);
#74835=ORIENTED_EDGE('',*,*,#52001,.T.);
#74836=ORIENTED_EDGE('',*,*,#52820,.T.);
#74837=ORIENTED_EDGE('',*,*,#53110,.T.);
#74838=ORIENTED_EDGE('',*,*,#52827,.T.);
#74839=ORIENTED_EDGE('',*,*,#52288,.T.);
#74840=ORIENTED_EDGE('',*,*,#52823,.T.);
#74841=ORIENTED_EDGE('',*,*,#53111,.T.);
#74842=ORIENTED_EDGE('',*,*,#52764,.T.);
#74843=ORIENTED_EDGE('',*,*,#52154,.T.);
#74844=ORIENTED_EDGE('',*,*,#52772,.T.);
#74845=ORIENTED_EDGE('',*,*,#53112,.T.);
#74846=ORIENTED_EDGE('',*,*,#52731,.T.);
#74847=ORIENTED_EDGE('',*,*,#52296,.T.);
#74848=ORIENTED_EDGE('',*,*,#52737,.T.);
#74849=ORIENTED_EDGE('',*,*,#53113,.T.);
#74850=ORIENTED_EDGE('',*,*,#52908,.T.);
#74851=ORIENTED_EDGE('',*,*,#51586,.T.);
#74852=ORIENTED_EDGE('',*,*,#52904,.T.);
#74853=ORIENTED_EDGE('',*,*,#53114,.T.);
#74854=ORIENTED_EDGE('',*,*,#52980,.T.);
#74855=ORIENTED_EDGE('',*,*,#51608,.T.);
#74856=ORIENTED_EDGE('',*,*,#52976,.T.);
#74857=ORIENTED_EDGE('',*,*,#53115,.T.);
#74858=ORIENTED_EDGE('',*,*,#52914,.T.);
#74859=ORIENTED_EDGE('',*,*,#51564,.T.);
#74860=ORIENTED_EDGE('',*,*,#52911,.T.);
#74861=ORIENTED_EDGE('',*,*,#53116,.T.);
#74862=ORIENTED_EDGE('',*,*,#52746,.T.);
#74863=ORIENTED_EDGE('',*,*,#51741,.T.);
#74864=ORIENTED_EDGE('',*,*,#52742,.T.);
#74865=ORIENTED_EDGE('',*,*,#53117,.T.);
#74866=ORIENTED_EDGE('',*,*,#52929,.T.);
#74867=ORIENTED_EDGE('',*,*,#51731,.T.);
#74868=ORIENTED_EDGE('',*,*,#52937,.T.);
#74869=ORIENTED_EDGE('',*,*,#53118,.T.);
#74870=ORIENTED_EDGE('',*,*,#52770,.T.);
#74871=ORIENTED_EDGE('',*,*,#52164,.T.);
#74872=ORIENTED_EDGE('',*,*,#52766,.T.);
#74873=ORIENTED_EDGE('',*,*,#53119,.T.);
#74874=ORIENTED_EDGE('',*,*,#52920,.T.);
#74875=ORIENTED_EDGE('',*,*,#52184,.T.);
#74876=ORIENTED_EDGE('',*,*,#52916,.T.);
#74877=ORIENTED_EDGE('',*,*,#53120,.T.);
#74878=ORIENTED_EDGE('',*,*,#52758,.T.);
#74879=ORIENTED_EDGE('',*,*,#51765,.T.);
#74880=ORIENTED_EDGE('',*,*,#52754,.T.);
#74881=ORIENTED_EDGE('',*,*,#53121,.T.);
#74882=ORIENTED_EDGE('',*,*,#52941,.T.);
#74883=ORIENTED_EDGE('',*,*,#51707,.T.);
#74884=ORIENTED_EDGE('',*,*,#52949,.T.);
#74885=ORIENTED_EDGE('',*,*,#53122,.T.);
#74886=ORIENTED_EDGE('',*,*,#52794,.T.);
#74887=ORIENTED_EDGE('',*,*,#51867,.T.);
#74888=ORIENTED_EDGE('',*,*,#52790,.T.);
#74889=ORIENTED_EDGE('',*,*,#53123,.T.);
#74890=ORIENTED_EDGE('',*,*,#52704,.T.);
#74891=ORIENTED_EDGE('',*,*,#51903,.T.);
#74892=ORIENTED_EDGE('',*,*,#52700,.T.);
#74893=ORIENTED_EDGE('',*,*,#53124,.T.);
#74894=ORIENTED_EDGE('',*,*,#52806,.T.);
#74895=ORIENTED_EDGE('',*,*,#51953,.T.);
#74896=ORIENTED_EDGE('',*,*,#52802,.T.);
#74897=ORIENTED_EDGE('',*,*,#53125,.T.);
#74898=ORIENTED_EDGE('',*,*,#52695,.T.);
#74899=ORIENTED_EDGE('',*,*,#51933,.T.);
#74900=ORIENTED_EDGE('',*,*,#52691,.T.);
#74901=ORIENTED_EDGE('',*,*,#53126,.T.);
#74902=ORIENTED_EDGE('',*,*,#52842,.T.);
#74903=ORIENTED_EDGE('',*,*,#52130,.T.);
#74904=ORIENTED_EDGE('',*,*,#52838,.T.);
#74905=ORIENTED_EDGE('',*,*,#53127,.T.);
#74906=ORIENTED_EDGE('',*,*,#52968,.T.);
#74907=ORIENTED_EDGE('',*,*,#52218,.T.);
#74908=ORIENTED_EDGE('',*,*,#52964,.T.);
#74909=ORIENTED_EDGE('',*,*,#53128,.T.);
#74910=ORIENTED_EDGE('',*,*,#52818,.T.);
#74911=ORIENTED_EDGE('',*,*,#52011,.T.);
#74912=ORIENTED_EDGE('',*,*,#52814,.T.);
#74913=ORIENTED_EDGE('',*,*,#53129,.T.);
#74914=ORIENTED_EDGE('',*,*,#52953,.T.);
#74915=ORIENTED_EDGE('',*,*,#52025,.T.);
#74916=ORIENTED_EDGE('',*,*,#52961,.T.);
#74917=ORIENTED_EDGE('',*,*,#53130,.T.);
#74918=ORIENTED_EDGE('',*,*,#53131,.F.);
#74919=ORIENTED_EDGE('',*,*,#53132,.T.);
#74920=ORIENTED_EDGE('',*,*,#53133,.T.);
#74921=ORIENTED_EDGE('',*,*,#53134,.T.);
#74922=ORIENTED_EDGE('',*,*,#53135,.F.);
#74923=ORIENTED_EDGE('',*,*,#53136,.T.);
#74924=ORIENTED_EDGE('',*,*,#53131,.T.);
#74925=ORIENTED_EDGE('',*,*,#53137,.T.);
#74926=ORIENTED_EDGE('',*,*,#53133,.F.);
#74927=ORIENTED_EDGE('',*,*,#53138,.T.);
#74928=ORIENTED_EDGE('',*,*,#53139,.F.);
#74929=ORIENTED_EDGE('',*,*,#53140,.T.);
#74930=ORIENTED_EDGE('',*,*,#53028,.T.);
#74931=ORIENTED_EDGE('',*,*,#51632,.T.);
#74932=ORIENTED_EDGE('',*,*,#53024,.T.);
#74933=ORIENTED_EDGE('',*,*,#53141,.T.);
#74934=ORIENTED_EDGE('',*,*,#52986,.T.);
#74935=ORIENTED_EDGE('',*,*,#51594,.T.);
#74936=ORIENTED_EDGE('',*,*,#52983,.T.);
#74937=ORIENTED_EDGE('',*,*,#53142,.T.);
#74938=ORIENTED_EDGE('',*,*,#52935,.T.);
#74939=ORIENTED_EDGE('',*,*,#51717,.T.);
#74940=ORIENTED_EDGE('',*,*,#52931,.T.);
#74941=ORIENTED_EDGE('',*,*,#53143,.T.);
#74942=ORIENTED_EDGE('',*,*,#53001,.T.);
#74943=ORIENTED_EDGE('',*,*,#51656,.T.);
#74944=ORIENTED_EDGE('',*,*,#53009,.T.);
#74945=ORIENTED_EDGE('',*,*,#53144,.T.);
#74946=ORIENTED_EDGE('',*,*,#52926,.T.);
#74947=ORIENTED_EDGE('',*,*,#52194,.T.);
#74948=ORIENTED_EDGE('',*,*,#52922,.T.);
#74949=ORIENTED_EDGE('',*,*,#53145,.T.);
#74950=ORIENTED_EDGE('',*,*,#52992,.T.);
#74951=ORIENTED_EDGE('',*,*,#52232,.T.);
#74952=ORIENTED_EDGE('',*,*,#52988,.T.);
#74953=ORIENTED_EDGE('',*,*,#53146,.T.);
#74954=ORIENTED_EDGE('',*,*,#52947,.T.);
#74955=ORIENTED_EDGE('',*,*,#51693,.T.);
#74956=ORIENTED_EDGE('',*,*,#52943,.T.);
#74957=ORIENTED_EDGE('',*,*,#53147,.T.);
#74958=ORIENTED_EDGE('',*,*,#52713,.T.);
#74959=ORIENTED_EDGE('',*,*,#51680,.T.);
#74960=ORIENTED_EDGE('',*,*,#52709,.T.);
#74961=ORIENTED_EDGE('',*,*,#53148,.T.);
#74962=ORIENTED_EDGE('',*,*,#53058,.T.);
#74963=ORIENTED_EDGE('',*,*,#51905,.T.);
#74964=ORIENTED_EDGE('',*,*,#52706,.T.);
#74965=ORIENTED_EDGE('',*,*,#53149,.T.);
#74966=ORIENTED_EDGE('',*,*,#52689,.T.);
#74967=ORIENTED_EDGE('',*,*,#51923,.T.);
#74968=ORIENTED_EDGE('',*,*,#53060,.T.);
#74969=ORIENTED_EDGE('',*,*,#53150,.T.);
#74970=ORIENTED_EDGE('',*,*,#52974,.T.);
#74971=ORIENTED_EDGE('',*,*,#52208,.T.);
#74972=ORIENTED_EDGE('',*,*,#52970,.T.);
#74973=ORIENTED_EDGE('',*,*,#53151,.T.);
#74974=ORIENTED_EDGE('',*,*,#53016,.T.);
#74975=ORIENTED_EDGE('',*,*,#52266,.T.);
#74976=ORIENTED_EDGE('',*,*,#53012,.T.);
#74977=ORIENTED_EDGE('',*,*,#53152,.T.);
#74978=ORIENTED_EDGE('',*,*,#52959,.T.);
#74979=ORIENTED_EDGE('',*,*,#52035,.T.);
#74980=ORIENTED_EDGE('',*,*,#52955,.T.);
#74981=ORIENTED_EDGE('',*,*,#53153,.T.);
#74982=ORIENTED_EDGE('',*,*,#52684,.T.);
#74983=ORIENTED_EDGE('',*,*,#52059,.T.);
#74984=ORIENTED_EDGE('',*,*,#52727,.T.);
#74985=ORIENTED_EDGE('',*,*,#53154,.T.);
#74986=ORIENTED_EDGE('',*,*,#52719,.T.);
#74987=ORIENTED_EDGE('',*,*,#51666,.T.);
#74988=ORIENTED_EDGE('',*,*,#52715,.T.);
#74989=ORIENTED_EDGE('',*,*,#53155,.T.);
#74990=ORIENTED_EDGE('',*,*,#53022,.T.);
#74991=ORIENTED_EDGE('',*,*,#52256,.T.);
#74992=ORIENTED_EDGE('',*,*,#53018,.T.);
#74993=ORIENTED_EDGE('',*,*,#53156,.T.);
#74994=ORIENTED_EDGE('',*,*,#52725,.T.);
#74995=ORIENTED_EDGE('',*,*,#52049,.T.);
#74996=ORIENTED_EDGE('',*,*,#52721,.T.);
#74997=ORIENTED_EDGE('',*,*,#53157,.T.);
#74998=ORIENTED_EDGE('',*,*,#53049,.T.);
#74999=ORIENTED_EDGE('',*,*,#52449,.T.);
#75000=ORIENTED_EDGE('',*,*,#52658,.T.);
#75001=ORIENTED_EDGE('',*,*,#53158,.T.);
#75002=ORIENTED_EDGE('',*,*,#52680,.T.);
#75003=ORIENTED_EDGE('',*,*,#52415,.T.);
#75004=ORIENTED_EDGE('',*,*,#53046,.T.);
#75005=ORIENTED_EDGE('',*,*,#53159,.T.);
#75006=ORIENTED_EDGE('',*,*,#53007,.T.);
#75007=ORIENTED_EDGE('',*,*,#51642,.T.);
#75008=ORIENTED_EDGE('',*,*,#53003,.T.);
#75009=ORIENTED_EDGE('',*,*,#53160,.T.);
#75010=ORIENTED_EDGE('',*,*,#53034,.T.);
#75011=ORIENTED_EDGE('',*,*,#51618,.T.);
#75012=ORIENTED_EDGE('',*,*,#53031,.T.);
#75013=ORIENTED_EDGE('',*,*,#53161,.T.);
#75014=ORIENTED_EDGE('',*,*,#52998,.T.);
#75015=ORIENTED_EDGE('',*,*,#52242,.T.);
#75016=ORIENTED_EDGE('',*,*,#52994,.T.);
#75017=ORIENTED_EDGE('',*,*,#53162,.T.);
#75018=ORIENTED_EDGE('',*,*,#53163,.F.);
#75019=ORIENTED_EDGE('',*,*,#50911,.T.);
#75020=ORIENTED_EDGE('',*,*,#50905,.T.);
#75021=ORIENTED_EDGE('',*,*,#50909,.T.);
#75022=ORIENTED_EDGE('',*,*,#51248,.T.);
#75023=ORIENTED_EDGE('',*,*,#50939,.T.);
#75024=ORIENTED_EDGE('',*,*,#50942,.T.);
#75025=ORIENTED_EDGE('',*,*,#50945,.T.);
#75026=ORIENTED_EDGE('',*,*,#50948,.T.);
#75027=ORIENTED_EDGE('',*,*,#50951,.T.);
#75028=ORIENTED_EDGE('',*,*,#50954,.T.);
#75029=ORIENTED_EDGE('',*,*,#50957,.T.);
#75030=ORIENTED_EDGE('',*,*,#53164,.F.);
#75031=ORIENTED_EDGE('',*,*,#53165,.F.);
#75032=ORIENTED_EDGE('',*,*,#53166,.F.);
#75033=ORIENTED_EDGE('',*,*,#53167,.F.);
#75034=ORIENTED_EDGE('',*,*,#53168,.F.);
#75035=ORIENTED_EDGE('',*,*,#53169,.F.);
#75036=ORIENTED_EDGE('',*,*,#53170,.F.);
#75037=ORIENTED_EDGE('',*,*,#53171,.F.);
#75038=ORIENTED_EDGE('',*,*,#53172,.F.);
#75039=ORIENTED_EDGE('',*,*,#53137,.F.);
#75040=ORIENTED_EDGE('',*,*,#53134,.F.);
#75041=ORIENTED_EDGE('',*,*,#53140,.F.);
#75042=ORIENTED_EDGE('',*,*,#50893,.T.);
#75043=ORIENTED_EDGE('',*,*,#50713,.F.);
#75044=ORIENTED_EDGE('',*,*,#51258,.T.);
#75045=ORIENTED_EDGE('',*,*,#50716,.F.);
#75046=ORIENTED_EDGE('',*,*,#50918,.T.);
#75047=ORIENTED_EDGE('',*,*,#50719,.F.);
#75048=ORIENTED_EDGE('',*,*,#51265,.F.);
#75049=ORIENTED_EDGE('',*,*,#50710,.F.);
#75050=ORIENTED_EDGE('',*,*,#51261,.T.);
#75051=ORIENTED_EDGE('',*,*,#50725,.F.);
#75052=ORIENTED_EDGE('',*,*,#50916,.T.);
#75053=ORIENTED_EDGE('',*,*,#50728,.F.);
#75054=ORIENTED_EDGE('',*,*,#51260,.T.);
#75055=ORIENTED_EDGE('',*,*,#50731,.F.);
#75056=ORIENTED_EDGE('',*,*,#50891,.T.);
#75057=ORIENTED_EDGE('',*,*,#50722,.F.);
#75058=ORIENTED_EDGE('',*,*,#51259,.T.);
#75059=ORIENTED_EDGE('',*,*,#50737,.F.);
#75060=ORIENTED_EDGE('',*,*,#50920,.T.);
#75061=ORIENTED_EDGE('',*,*,#50740,.F.);
#75062=ORIENTED_EDGE('',*,*,#51255,.T.);
#75063=ORIENTED_EDGE('',*,*,#50743,.F.);
#75064=ORIENTED_EDGE('',*,*,#50895,.T.);
#75065=ORIENTED_EDGE('',*,*,#50734,.F.);
#75066=ORIENTED_EDGE('',*,*,#51252,.T.);
#75067=ORIENTED_EDGE('',*,*,#50749,.F.);
#75068=ORIENTED_EDGE('',*,*,#50926,.T.);
#75069=ORIENTED_EDGE('',*,*,#50752,.F.);
#75070=ORIENTED_EDGE('',*,*,#51249,.T.);
#75071=ORIENTED_EDGE('',*,*,#50755,.F.);
#75072=ORIENTED_EDGE('',*,*,#50903,.T.);
#75073=ORIENTED_EDGE('',*,*,#50746,.F.);
#75074=ORIENTED_EDGE('',*,*,#50901,.T.);
#75075=ORIENTED_EDGE('',*,*,#50761,.F.);
#75076=ORIENTED_EDGE('',*,*,#51250,.T.);
#75077=ORIENTED_EDGE('',*,*,#50764,.F.);
#75078=ORIENTED_EDGE('',*,*,#50924,.T.);
#75079=ORIENTED_EDGE('',*,*,#50767,.F.);
#75080=ORIENTED_EDGE('',*,*,#51257,.T.);
#75081=ORIENTED_EDGE('',*,*,#50758,.F.);
#75082=ORIENTED_EDGE('',*,*,#50915,.T.);
#75083=ORIENTED_EDGE('',*,*,#50779,.F.);
#75084=ORIENTED_EDGE('',*,*,#51262,.T.);
#75085=ORIENTED_EDGE('',*,*,#50770,.F.);
#75086=ORIENTED_EDGE('',*,*,#50888,.T.);
#75087=ORIENTED_EDGE('',*,*,#50773,.F.);
#75088=ORIENTED_EDGE('',*,*,#51263,.F.);
#75089=ORIENTED_EDGE('',*,*,#50775,.F.);
#75090=ORIENTED_EDGE('',*,*,#50934,.T.);
#75091=ORIENTED_EDGE('',*,*,#50827,.F.);
#75092=ORIENTED_EDGE('',*,*,#51244,.T.);
#75093=ORIENTED_EDGE('',*,*,#50818,.F.);
#75094=ORIENTED_EDGE('',*,*,#50914,.T.);
#75095=ORIENTED_EDGE('',*,*,#50821,.F.);
#75096=ORIENTED_EDGE('',*,*,#51245,.F.);
#75097=ORIENTED_EDGE('',*,*,#50823,.F.);
#75098=ORIENTED_EDGE('',*,*,#50925,.T.);
#75099=ORIENTED_EDGE('',*,*,#50809,.F.);
#75100=ORIENTED_EDGE('',*,*,#51236,.T.);
#75101=ORIENTED_EDGE('',*,*,#50812,.F.);
#75102=ORIENTED_EDGE('',*,*,#50929,.T.);
#75103=ORIENTED_EDGE('',*,*,#50815,.F.);
#75104=ORIENTED_EDGE('',*,*,#51239,.T.);
#75105=ORIENTED_EDGE('',*,*,#50806,.F.);
#75106=ORIENTED_EDGE('',*,*,#51243,.T.);
#75107=ORIENTED_EDGE('',*,*,#50797,.F.);
#75108=ORIENTED_EDGE('',*,*,#50933,.T.);
#75109=ORIENTED_EDGE('',*,*,#50800,.F.);
#75110=ORIENTED_EDGE('',*,*,#51242,.T.);
#75111=ORIENTED_EDGE('',*,*,#50803,.F.);
#75112=ORIENTED_EDGE('',*,*,#50917,.T.);
#75113=ORIENTED_EDGE('',*,*,#50794,.F.);
#75114=ORIENTED_EDGE('',*,*,#50919,.T.);
#75115=ORIENTED_EDGE('',*,*,#50785,.F.);
#75116=ORIENTED_EDGE('',*,*,#51240,.T.);
#75117=ORIENTED_EDGE('',*,*,#50788,.F.);
#75118=ORIENTED_EDGE('',*,*,#50935,.T.);
#75119=ORIENTED_EDGE('',*,*,#50791,.F.);
#75120=ORIENTED_EDGE('',*,*,#51246,.F.);
#75121=ORIENTED_EDGE('',*,*,#50782,.F.);
#75122=ORIENTED_EDGE('',*,*,#50887,.T.);
#75123=ORIENTED_EDGE('',*,*,#50701,.F.);
#75124=ORIENTED_EDGE('',*,*,#51267,.F.);
#75125=ORIENTED_EDGE('',*,*,#51148,.F.);
#75126=ORIENTED_EDGE('',*,*,#51264,.F.);
#75127=ORIENTED_EDGE('',*,*,#50703,.F.);
#75128=ORIENTED_EDGE('',*,*,#50889,.T.);
#75129=ORIENTED_EDGE('',*,*,#50707,.F.);
#75130=ORIENTED_EDGE('',*,*,#51297,.T.);
#75131=ORIENTED_EDGE('',*,*,#50698,.F.);
#75132=ORIENTED_EDGE('',*,*,#51294,.T.);
#75133=ORIENTED_EDGE('',*,*,#50692,.F.);
#75134=ORIENTED_EDGE('',*,*,#51230,.F.);
#75135=ORIENTED_EDGE('',*,*,#51152,.F.);
#75136=ORIENTED_EDGE('',*,*,#51150,.F.);
#75137=ORIENTED_EDGE('',*,*,#50695,.F.);
#75138=ORIENTED_EDGE('',*,*,#51296,.T.);
#75139=ORIENTED_EDGE('',*,*,#50686,.F.);
#75140=ORIENTED_EDGE('',*,*,#50873,.T.);
#75141=ORIENTED_EDGE('',*,*,#50689,.F.);
#75142=ORIENTED_EDGE('',*,*,#51284,.T.);
#75143=ORIENTED_EDGE('',*,*,#50680,.F.);
#75144=ORIENTED_EDGE('',*,*,#51154,.F.);
#75145=ORIENTED_EDGE('',*,*,#50683,.F.);
#75146=ORIENTED_EDGE('',*,*,#51292,.T.);
#75147=ORIENTED_EDGE('',*,*,#50674,.F.);
#75148=ORIENTED_EDGE('',*,*,#50874,.T.);
#75149=ORIENTED_EDGE('',*,*,#50677,.F.);
#75150=ORIENTED_EDGE('',*,*,#51280,.T.);
#75151=ORIENTED_EDGE('',*,*,#50668,.F.);
#75152=ORIENTED_EDGE('',*,*,#51231,.F.);
#75153=ORIENTED_EDGE('',*,*,#50671,.F.);
#75154=ORIENTED_EDGE('',*,*,#51286,.T.);
#75155=ORIENTED_EDGE('',*,*,#50662,.F.);
#75156=ORIENTED_EDGE('',*,*,#50876,.T.);
#75157=ORIENTED_EDGE('',*,*,#50665,.F.);
#75158=ORIENTED_EDGE('',*,*,#51276,.T.);
#75159=ORIENTED_EDGE('',*,*,#50656,.F.);
#75160=ORIENTED_EDGE('',*,*,#51232,.F.);
#75161=ORIENTED_EDGE('',*,*,#50659,.F.);
#75162=ORIENTED_EDGE('',*,*,#51282,.T.);
#75163=ORIENTED_EDGE('',*,*,#50650,.F.);
#75164=ORIENTED_EDGE('',*,*,#50878,.T.);
#75165=ORIENTED_EDGE('',*,*,#50653,.F.);
#75166=ORIENTED_EDGE('',*,*,#51272,.T.);
#75167=ORIENTED_EDGE('',*,*,#50644,.F.);
#75168=ORIENTED_EDGE('',*,*,#51233,.F.);
#75169=ORIENTED_EDGE('',*,*,#50647,.F.);
#75170=ORIENTED_EDGE('',*,*,#51278,.T.);
#75171=ORIENTED_EDGE('',*,*,#50638,.F.);
#75172=ORIENTED_EDGE('',*,*,#50882,.T.);
#75173=ORIENTED_EDGE('',*,*,#50641,.F.);
#75174=ORIENTED_EDGE('',*,*,#50881,.T.);
#75175=ORIENTED_EDGE('',*,*,#50629,.F.);
#75176=ORIENTED_EDGE('',*,*,#51273,.T.);
#75177=ORIENTED_EDGE('',*,*,#50632,.F.);
#75178=ORIENTED_EDGE('',*,*,#50900,.T.);
#75179=ORIENTED_EDGE('',*,*,#50635,.F.);
#75180=ORIENTED_EDGE('',*,*,#51287,.T.);
#75181=ORIENTED_EDGE('',*,*,#50626,.F.);
#75182=ORIENTED_EDGE('',*,*,#51290,.T.);
#75183=ORIENTED_EDGE('',*,*,#50617,.F.);
#75184=ORIENTED_EDGE('',*,*,#50884,.T.);
#75185=ORIENTED_EDGE('',*,*,#50620,.F.);
#75186=ORIENTED_EDGE('',*,*,#51270,.F.);
#75187=ORIENTED_EDGE('',*,*,#50623,.F.);
#75188=ORIENTED_EDGE('',*,*,#51277,.T.);
#75189=ORIENTED_EDGE('',*,*,#50608,.F.);
#75190=ORIENTED_EDGE('',*,*,#50902,.T.);
#75191=ORIENTED_EDGE('',*,*,#50611,.F.);
#75192=ORIENTED_EDGE('',*,*,#51271,.T.);
#75193=ORIENTED_EDGE('',*,*,#50614,.F.);
#75194=ORIENTED_EDGE('',*,*,#50883,.T.);
#75195=ORIENTED_EDGE('',*,*,#50605,.F.);
#75196=ORIENTED_EDGE('',*,*,#51281,.T.);
#75197=ORIENTED_EDGE('',*,*,#50596,.F.);
#75198=ORIENTED_EDGE('',*,*,#50898,.T.);
#75199=ORIENTED_EDGE('',*,*,#50599,.F.);
#75200=ORIENTED_EDGE('',*,*,#51275,.T.);
#75201=ORIENTED_EDGE('',*,*,#50602,.F.);
#75202=ORIENTED_EDGE('',*,*,#50879,.T.);
#75203=ORIENTED_EDGE('',*,*,#50593,.F.);
#75204=ORIENTED_EDGE('',*,*,#51285,.T.);
#75205=ORIENTED_EDGE('',*,*,#50584,.F.);
#75206=ORIENTED_EDGE('',*,*,#50896,.T.);
#75207=ORIENTED_EDGE('',*,*,#50587,.F.);
#75208=ORIENTED_EDGE('',*,*,#51279,.T.);
#75209=ORIENTED_EDGE('',*,*,#50590,.F.);
#75210=ORIENTED_EDGE('',*,*,#50877,.T.);
#75211=ORIENTED_EDGE('',*,*,#50581,.F.);
#75212=ORIENTED_EDGE('',*,*,#51288,.T.);
#75213=ORIENTED_EDGE('',*,*,#50572,.F.);
#75214=ORIENTED_EDGE('',*,*,#51158,.F.);
#75215=ORIENTED_EDGE('',*,*,#51156,.F.);
#75216=ORIENTED_EDGE('',*,*,#51234,.F.);
#75217=ORIENTED_EDGE('',*,*,#50575,.F.);
#75218=ORIENTED_EDGE('',*,*,#51274,.T.);
#75219=ORIENTED_EDGE('',*,*,#50578,.F.);
#75220=ORIENTED_EDGE('',*,*,#50880,.T.);
#75221=ORIENTED_EDGE('',*,*,#50569,.F.);
#75222=ORIENTED_EDGE('',*,*,#51289,.T.);
#75223=ORIENTED_EDGE('',*,*,#50560,.F.);
#75224=ORIENTED_EDGE('',*,*,#50892,.T.);
#75225=ORIENTED_EDGE('',*,*,#50563,.F.);
#75226=ORIENTED_EDGE('',*,*,#51266,.F.);
#75227=ORIENTED_EDGE('',*,*,#51160,.F.);
#75228=ORIENTED_EDGE('',*,*,#51269,.F.);
#75229=ORIENTED_EDGE('',*,*,#50566,.F.);
#75230=ORIENTED_EDGE('',*,*,#50885,.T.);
#75231=ORIENTED_EDGE('',*,*,#50557,.F.);
#75232=ORIENTED_EDGE('',*,*,#51291,.T.);
#75233=ORIENTED_EDGE('',*,*,#50548,.F.);
#75234=ORIENTED_EDGE('',*,*,#50894,.T.);
#75235=ORIENTED_EDGE('',*,*,#50551,.F.);
#75236=ORIENTED_EDGE('',*,*,#51283,.T.);
#75237=ORIENTED_EDGE('',*,*,#50554,.F.);
#75238=ORIENTED_EDGE('',*,*,#50875,.T.);
#75239=ORIENTED_EDGE('',*,*,#50545,.F.);
#75240=ORIENTED_EDGE('',*,*,#51295,.T.);
#75241=ORIENTED_EDGE('',*,*,#50536,.F.);
#75242=ORIENTED_EDGE('',*,*,#50890,.T.);
#75243=ORIENTED_EDGE('',*,*,#50539,.F.);
#75244=ORIENTED_EDGE('',*,*,#51293,.T.);
#75245=ORIENTED_EDGE('',*,*,#50542,.F.);
#75246=ORIENTED_EDGE('',*,*,#50872,.T.);
#75247=ORIENTED_EDGE('',*,*,#50533,.F.);
#75248=ORIENTED_EDGE('',*,*,#51298,.T.);
#75249=ORIENTED_EDGE('',*,*,#50527,.F.);
#75250=ORIENTED_EDGE('',*,*,#51268,.F.);
#75251=ORIENTED_EDGE('',*,*,#50529,.F.);
#75252=ORIENTED_EDGE('',*,*,#50886,.T.);
#75253=ORIENTED_EDGE('',*,*,#50524,.F.);
#75254=ORIENTED_EDGE('',*,*,#51253,.T.);
#75255=ORIENTED_EDGE('',*,*,#50494,.F.);
#75256=ORIENTED_EDGE('',*,*,#50897,.T.);
#75257=ORIENTED_EDGE('',*,*,#50497,.F.);
#75258=ORIENTED_EDGE('',*,*,#51256,.T.);
#75259=ORIENTED_EDGE('',*,*,#50500,.F.);
#75260=ORIENTED_EDGE('',*,*,#50922,.T.);
#75261=ORIENTED_EDGE('',*,*,#50851,.F.);
#75262=ORIENTED_EDGE('',*,*,#50871,.F.);
#75263=ORIENTED_EDGE('',*,*,#50491,.F.);
#75264=ORIENTED_EDGE('',*,*,#50932,.T.);
#75265=ORIENTED_EDGE('',*,*,#50473,.F.);
#75266=ORIENTED_EDGE('',*,*,#53079,.F.);
#75267=ORIENTED_EDGE('',*,*,#50470,.F.);
#75268=ORIENTED_EDGE('',*,*,#50868,.F.);
#75269=ORIENTED_EDGE('',*,*,#50836,.F.);
#75270=ORIENTED_EDGE('',*,*,#50867,.T.);
#75271=ORIENTED_EDGE('',*,*,#50838,.F.);
#75272=ORIENTED_EDGE('',*,*,#50862,.T.);
#75273=ORIENTED_EDGE('',*,*,#50833,.F.);
#75274=ORIENTED_EDGE('',*,*,#50863,.T.);
#75275=ORIENTED_EDGE('',*,*,#50844,.F.);
#75276=ORIENTED_EDGE('',*,*,#53073,.F.);
#75277=ORIENTED_EDGE('',*,*,#50452,.F.);
#75278=ORIENTED_EDGE('',*,*,#50931,.T.);
#75279=ORIENTED_EDGE('',*,*,#50842,.F.);
#75280=ORIENTED_EDGE('',*,*,#50930,.T.);
#75281=ORIENTED_EDGE('',*,*,#50518,.F.);
#75282=ORIENTED_EDGE('',*,*,#51235,.T.);
#75283=ORIENTED_EDGE('',*,*,#50521,.F.);
#75284=ORIENTED_EDGE('',*,*,#50927,.T.);
#75285=ORIENTED_EDGE('',*,*,#50475,.F.);
#75286=ORIENTED_EDGE('',*,*,#50857,.F.);
#75287=ORIENTED_EDGE('',*,*,#50860,.F.);
#75288=ORIENTED_EDGE('',*,*,#50515,.F.);
#75289=ORIENTED_EDGE('',*,*,#50864,.T.);
#75290=ORIENTED_EDGE('',*,*,#50830,.F.);
#75291=ORIENTED_EDGE('',*,*,#50865,.T.);
#75292=ORIENTED_EDGE('',*,*,#50455,.F.);
#75293=ORIENTED_EDGE('',*,*,#51238,.T.);
#75294=ORIENTED_EDGE('',*,*,#50458,.F.);
#75295=ORIENTED_EDGE('',*,*,#53075,.F.);
#75296=ORIENTED_EDGE('',*,*,#50848,.F.);
#75297=ORIENTED_EDGE('',*,*,#50921,.T.);
#75298=ORIENTED_EDGE('',*,*,#50506,.F.);
#75299=ORIENTED_EDGE('',*,*,#51241,.T.);
#75300=ORIENTED_EDGE('',*,*,#50509,.F.);
#75301=ORIENTED_EDGE('',*,*,#50928,.T.);
#75302=ORIENTED_EDGE('',*,*,#50512,.F.);
#75303=ORIENTED_EDGE('',*,*,#50861,.F.);
#75304=ORIENTED_EDGE('',*,*,#50858,.F.);
#75305=ORIENTED_EDGE('',*,*,#50503,.F.);
#75306=ORIENTED_EDGE('',*,*,#50870,.T.);
#75307=ORIENTED_EDGE('',*,*,#50448,.F.);
#75308=ORIENTED_EDGE('',*,*,#50869,.F.);
#75309=ORIENTED_EDGE('',*,*,#50467,.F.);
#75310=ORIENTED_EDGE('',*,*,#53077,.F.);
#75311=ORIENTED_EDGE('',*,*,#50461,.F.);
#75312=ORIENTED_EDGE('',*,*,#51237,.T.);
#75313=ORIENTED_EDGE('',*,*,#50464,.F.);
#75314=ORIENTED_EDGE('',*,*,#50923,.T.);
#75315=ORIENTED_EDGE('',*,*,#50482,.F.);
#75316=ORIENTED_EDGE('',*,*,#51251,.T.);
#75317=ORIENTED_EDGE('',*,*,#50485,.F.);
#75318=ORIENTED_EDGE('',*,*,#50899,.T.);
#75319=ORIENTED_EDGE('',*,*,#50488,.F.);
#75320=ORIENTED_EDGE('',*,*,#51254,.T.);
#75321=ORIENTED_EDGE('',*,*,#50479,.F.);
#75322=ORIENTED_EDGE('',*,*,#50866,.F.);
#75323=ORIENTED_EDGE('',*,*,#50854,.F.);
#75324=ORIENTED_EDGE('',*,*,#53120,.F.);
#75325=ORIENTED_EDGE('',*,*,#52918,.T.);
#75326=ORIENTED_EDGE('',*,*,#53173,.T.);
#75327=ORIENTED_EDGE('',*,*,#52927,.T.);
#75328=ORIENTED_EDGE('',*,*,#53145,.F.);
#75329=ORIENTED_EDGE('',*,*,#52924,.T.);
#75330=ORIENTED_EDGE('',*,*,#53174,.F.);
#75331=ORIENTED_EDGE('',*,*,#52921,.T.);
#75332=ORIENTED_EDGE('',*,*,#53175,.F.);
#75333=ORIENTED_EDGE('',*,*,#52930,.T.);
#75334=ORIENTED_EDGE('',*,*,#53118,.F.);
#75335=ORIENTED_EDGE('',*,*,#52939,.T.);
#75336=ORIENTED_EDGE('',*,*,#53176,.F.);
#75337=ORIENTED_EDGE('',*,*,#52936,.T.);
#75338=ORIENTED_EDGE('',*,*,#53143,.F.);
#75339=ORIENTED_EDGE('',*,*,#52933,.T.);
#75340=ORIENTED_EDGE('',*,*,#53177,.F.);
#75341=ORIENTED_EDGE('',*,*,#52942,.T.);
#75342=ORIENTED_EDGE('',*,*,#53122,.F.);
#75343=ORIENTED_EDGE('',*,*,#52951,.T.);
#75344=ORIENTED_EDGE('',*,*,#53178,.F.);
#75345=ORIENTED_EDGE('',*,*,#52948,.T.);
#75346=ORIENTED_EDGE('',*,*,#53147,.F.);
#75347=ORIENTED_EDGE('',*,*,#52945,.T.);
#75348=ORIENTED_EDGE('',*,*,#53179,.F.);
#75349=ORIENTED_EDGE('',*,*,#52954,.T.);
#75350=ORIENTED_EDGE('',*,*,#53130,.F.);
#75351=ORIENTED_EDGE('',*,*,#52963,.T.);
#75352=ORIENTED_EDGE('',*,*,#53180,.F.);
#75353=ORIENTED_EDGE('',*,*,#52960,.T.);
#75354=ORIENTED_EDGE('',*,*,#53153,.F.);
#75355=ORIENTED_EDGE('',*,*,#52957,.T.);
#75356=ORIENTED_EDGE('',*,*,#53128,.F.);
#75357=ORIENTED_EDGE('',*,*,#52966,.T.);
#75358=ORIENTED_EDGE('',*,*,#53181,.F.);
#75359=ORIENTED_EDGE('',*,*,#52975,.T.);
#75360=ORIENTED_EDGE('',*,*,#53151,.F.);
#75361=ORIENTED_EDGE('',*,*,#52972,.T.);
#75362=ORIENTED_EDGE('',*,*,#53182,.F.);
#75363=ORIENTED_EDGE('',*,*,#52969,.T.);
#75364=ORIENTED_EDGE('',*,*,#53142,.F.);
#75365=ORIENTED_EDGE('',*,*,#52982,.T.);
#75366=ORIENTED_EDGE('',*,*,#53183,.T.);
#75367=ORIENTED_EDGE('',*,*,#52981,.T.);
#75368=ORIENTED_EDGE('',*,*,#53115,.F.);
#75369=ORIENTED_EDGE('',*,*,#52978,.T.);
#75370=ORIENTED_EDGE('',*,*,#53184,.F.);
#75371=ORIENTED_EDGE('',*,*,#52987,.T.);
#75372=ORIENTED_EDGE('',*,*,#53161,.F.);
#75373=ORIENTED_EDGE('',*,*,#53030,.T.);
#75374=ORIENTED_EDGE('',*,*,#53185,.T.);
#75375=ORIENTED_EDGE('',*,*,#53029,.T.);
#75376=ORIENTED_EDGE('',*,*,#53141,.F.);
#75377=ORIENTED_EDGE('',*,*,#53026,.T.);
#75378=ORIENTED_EDGE('',*,*,#53186,.F.);
#75379=ORIENTED_EDGE('',*,*,#53035,.T.);
#75380=ORIENTED_EDGE('',*,*,#53152,.F.);
#75381=ORIENTED_EDGE('',*,*,#53014,.T.);
#75382=ORIENTED_EDGE('',*,*,#53187,.F.);
#75383=ORIENTED_EDGE('',*,*,#53023,.T.);
#75384=ORIENTED_EDGE('',*,*,#53156,.F.);
#75385=ORIENTED_EDGE('',*,*,#53020,.T.);
#75386=ORIENTED_EDGE('',*,*,#53188,.F.);
#75387=ORIENTED_EDGE('',*,*,#53017,.T.);
#75388=ORIENTED_EDGE('',*,*,#53189,.F.);
#75389=ORIENTED_EDGE('',*,*,#53002,.T.);
#75390=ORIENTED_EDGE('',*,*,#53144,.F.);
#75391=ORIENTED_EDGE('',*,*,#53011,.T.);
#75392=ORIENTED_EDGE('',*,*,#53190,.F.);
#75393=ORIENTED_EDGE('',*,*,#53008,.T.);
#75394=ORIENTED_EDGE('',*,*,#53160,.F.);
#75395=ORIENTED_EDGE('',*,*,#53005,.T.);
#75396=ORIENTED_EDGE('',*,*,#53146,.F.);
#75397=ORIENTED_EDGE('',*,*,#52990,.T.);
#75398=ORIENTED_EDGE('',*,*,#53191,.T.);
#75399=ORIENTED_EDGE('',*,*,#52999,.T.);
#75400=ORIENTED_EDGE('',*,*,#53162,.F.);
#75401=ORIENTED_EDGE('',*,*,#52996,.T.);
#75402=ORIENTED_EDGE('',*,*,#53192,.F.);
#75403=ORIENTED_EDGE('',*,*,#52993,.T.);
#75404=ORIENTED_EDGE('',*,*,#53114,.F.);
#75405=ORIENTED_EDGE('',*,*,#52906,.T.);
#75406=ORIENTED_EDGE('',*,*,#53193,.F.);
#75407=ORIENTED_EDGE('',*,*,#52915,.T.);
#75408=ORIENTED_EDGE('',*,*,#53116,.F.);
#75409=ORIENTED_EDGE('',*,*,#52910,.T.);
#75410=ORIENTED_EDGE('',*,*,#53194,.T.);
#75411=ORIENTED_EDGE('',*,*,#53195,.T.);
#75412=ORIENTED_EDGE('',*,*,#53196,.T.);
#75413=ORIENTED_EDGE('',*,*,#52909,.T.);
#75414=ORIENTED_EDGE('',*,*,#53197,.F.);
#75415=ORIENTED_EDGE('',*,*,#52897,.T.);
#75416=ORIENTED_EDGE('',*,*,#53100,.F.);
#75417=ORIENTED_EDGE('',*,*,#52894,.T.);
#75418=ORIENTED_EDGE('',*,*,#53198,.F.);
#75419=ORIENTED_EDGE('',*,*,#52903,.T.);
#75420=ORIENTED_EDGE('',*,*,#53199,.T.);
#75421=ORIENTED_EDGE('',*,*,#53200,.T.);
#75422=ORIENTED_EDGE('',*,*,#53201,.T.);
#75423=ORIENTED_EDGE('',*,*,#52900,.T.);
#75424=ORIENTED_EDGE('',*,*,#53202,.F.);
#75425=ORIENTED_EDGE('',*,*,#52885,.T.);
#75426=ORIENTED_EDGE('',*,*,#53101,.F.);
#75427=ORIENTED_EDGE('',*,*,#52882,.T.);
#75428=ORIENTED_EDGE('',*,*,#53203,.F.);
#75429=ORIENTED_EDGE('',*,*,#52891,.T.);
#75430=ORIENTED_EDGE('',*,*,#53204,.T.);
#75431=ORIENTED_EDGE('',*,*,#52888,.T.);
#75432=ORIENTED_EDGE('',*,*,#53205,.F.);
#75433=ORIENTED_EDGE('',*,*,#52873,.T.);
#75434=ORIENTED_EDGE('',*,*,#53103,.F.);
#75435=ORIENTED_EDGE('',*,*,#52870,.T.);
#75436=ORIENTED_EDGE('',*,*,#53206,.F.);
#75437=ORIENTED_EDGE('',*,*,#52879,.T.);
#75438=ORIENTED_EDGE('',*,*,#53207,.T.);
#75439=ORIENTED_EDGE('',*,*,#52876,.T.);
#75440=ORIENTED_EDGE('',*,*,#53208,.F.);
#75441=ORIENTED_EDGE('',*,*,#52861,.T.);
#75442=ORIENTED_EDGE('',*,*,#53105,.F.);
#75443=ORIENTED_EDGE('',*,*,#52858,.T.);
#75444=ORIENTED_EDGE('',*,*,#53209,.F.);
#75445=ORIENTED_EDGE('',*,*,#52867,.T.);
#75446=ORIENTED_EDGE('',*,*,#53210,.T.);
#75447=ORIENTED_EDGE('',*,*,#52864,.T.);
#75448=ORIENTED_EDGE('',*,*,#53211,.F.);
#75449=ORIENTED_EDGE('',*,*,#52849,.T.);
#75450=ORIENTED_EDGE('',*,*,#53109,.F.);
#75451=ORIENTED_EDGE('',*,*,#52846,.T.);
#75452=ORIENTED_EDGE('',*,*,#53212,.F.);
#75453=ORIENTED_EDGE('',*,*,#52855,.T.);
#75454=ORIENTED_EDGE('',*,*,#53213,.T.);
#75455=ORIENTED_EDGE('',*,*,#52852,.T.);
#75456=ORIENTED_EDGE('',*,*,#53108,.F.);
#75457=ORIENTED_EDGE('',*,*,#52834,.T.);
#75458=ORIENTED_EDGE('',*,*,#53214,.F.);
#75459=ORIENTED_EDGE('',*,*,#52843,.T.);
#75460=ORIENTED_EDGE('',*,*,#53127,.F.);
#75461=ORIENTED_EDGE('',*,*,#52840,.T.);
#75462=ORIENTED_EDGE('',*,*,#53215,.F.);
#75463=ORIENTED_EDGE('',*,*,#52837,.T.);
#75464=ORIENTED_EDGE('',*,*,#53216,.F.);
#75465=ORIENTED_EDGE('',*,*,#52831,.T.);
#75466=ORIENTED_EDGE('',*,*,#53217,.T.);
#75467=ORIENTED_EDGE('',*,*,#52828,.T.);
#75468=ORIENTED_EDGE('',*,*,#53111,.F.);
#75469=ORIENTED_EDGE('',*,*,#52825,.T.);
#75470=ORIENTED_EDGE('',*,*,#53218,.F.);
#75471=ORIENTED_EDGE('',*,*,#52813,.T.);
#75472=ORIENTED_EDGE('',*,*,#53110,.F.);
#75473=ORIENTED_EDGE('',*,*,#52822,.T.);
#75474=ORIENTED_EDGE('',*,*,#53219,.F.);
#75475=ORIENTED_EDGE('',*,*,#52819,.T.);
#75476=ORIENTED_EDGE('',*,*,#53129,.F.);
#75477=ORIENTED_EDGE('',*,*,#52816,.T.);
#75478=ORIENTED_EDGE('',*,*,#53220,.F.);
#75479=ORIENTED_EDGE('',*,*,#52801,.T.);
#75480=ORIENTED_EDGE('',*,*,#53106,.F.);
#75481=ORIENTED_EDGE('',*,*,#52810,.T.);
#75482=ORIENTED_EDGE('',*,*,#53221,.F.);
#75483=ORIENTED_EDGE('',*,*,#52807,.T.);
#75484=ORIENTED_EDGE('',*,*,#53125,.F.);
#75485=ORIENTED_EDGE('',*,*,#52804,.T.);
#75486=ORIENTED_EDGE('',*,*,#53222,.F.);
#75487=ORIENTED_EDGE('',*,*,#52789,.T.);
#75488=ORIENTED_EDGE('',*,*,#53104,.F.);
#75489=ORIENTED_EDGE('',*,*,#52798,.T.);
#75490=ORIENTED_EDGE('',*,*,#53223,.F.);
#75491=ORIENTED_EDGE('',*,*,#52795,.T.);
#75492=ORIENTED_EDGE('',*,*,#53123,.F.);
#75493=ORIENTED_EDGE('',*,*,#52792,.T.);
#75494=ORIENTED_EDGE('',*,*,#53224,.F.);
#75495=ORIENTED_EDGE('',*,*,#52777,.T.);
#75496=ORIENTED_EDGE('',*,*,#53107,.F.);
#75497=ORIENTED_EDGE('',*,*,#52786,.T.);
#75498=ORIENTED_EDGE('',*,*,#53225,.F.);
#75499=ORIENTED_EDGE('',*,*,#52783,.T.);
#75500=ORIENTED_EDGE('',*,*,#53226,.T.);
#75501=ORIENTED_EDGE('',*,*,#53227,.T.);
#75502=ORIENTED_EDGE('',*,*,#53228,.T.);
#75503=ORIENTED_EDGE('',*,*,#52780,.T.);
#75504=ORIENTED_EDGE('',*,*,#53229,.F.);
#75505=ORIENTED_EDGE('',*,*,#52765,.T.);
#75506=ORIENTED_EDGE('',*,*,#53112,.F.);
#75507=ORIENTED_EDGE('',*,*,#52774,.T.);
#75508=ORIENTED_EDGE('',*,*,#53230,.T.);
#75509=ORIENTED_EDGE('',*,*,#53231,.T.);
#75510=ORIENTED_EDGE('',*,*,#53232,.T.);
#75511=ORIENTED_EDGE('',*,*,#52771,.T.);
#75512=ORIENTED_EDGE('',*,*,#53119,.F.);
#75513=ORIENTED_EDGE('',*,*,#52768,.T.);
#75514=ORIENTED_EDGE('',*,*,#53233,.F.);
#75515=ORIENTED_EDGE('',*,*,#52753,.T.);
#75516=ORIENTED_EDGE('',*,*,#53102,.F.);
#75517=ORIENTED_EDGE('',*,*,#52762,.T.);
#75518=ORIENTED_EDGE('',*,*,#53234,.F.);
#75519=ORIENTED_EDGE('',*,*,#52759,.T.);
#75520=ORIENTED_EDGE('',*,*,#53121,.F.);
#75521=ORIENTED_EDGE('',*,*,#52756,.T.);
#75522=ORIENTED_EDGE('',*,*,#53235,.F.);
#75523=ORIENTED_EDGE('',*,*,#52741,.T.);
#75524=ORIENTED_EDGE('',*,*,#53099,.F.);
#75525=ORIENTED_EDGE('',*,*,#52750,.T.);
#75526=ORIENTED_EDGE('',*,*,#53236,.F.);
#75527=ORIENTED_EDGE('',*,*,#52747,.T.);
#75528=ORIENTED_EDGE('',*,*,#53117,.F.);
#75529=ORIENTED_EDGE('',*,*,#52744,.T.);
#75530=ORIENTED_EDGE('',*,*,#53237,.F.);
#75531=ORIENTED_EDGE('',*,*,#52732,.T.);
#75532=ORIENTED_EDGE('',*,*,#53113,.F.);
#75533=ORIENTED_EDGE('',*,*,#52736,.T.);
#75534=ORIENTED_EDGE('',*,*,#53238,.T.);
#75535=ORIENTED_EDGE('',*,*,#52735,.T.);
#75536=ORIENTED_EDGE('',*,*,#53239,.F.);
#75537=ORIENTED_EDGE('',*,*,#52699,.T.);
#75538=ORIENTED_EDGE('',*,*,#53098,.T.);
#75539=ORIENTED_EDGE('',*,*,#53059,.T.);
#75540=ORIENTED_EDGE('',*,*,#53149,.F.);
#75541=ORIENTED_EDGE('',*,*,#52708,.T.);
#75542=ORIENTED_EDGE('',*,*,#53240,.F.);
#75543=ORIENTED_EDGE('',*,*,#52705,.T.);
#75544=ORIENTED_EDGE('',*,*,#53124,.F.);
#75545=ORIENTED_EDGE('',*,*,#52702,.T.);
#75546=ORIENTED_EDGE('',*,*,#53159,.F.);
#75547=ORIENTED_EDGE('',*,*,#53045,.T.);
#75548=ORIENTED_EDGE('',*,*,#53094,.F.);
#75549=ORIENTED_EDGE('',*,*,#53044,.T.);
#75550=ORIENTED_EDGE('',*,*,#53095,.T.);
#75551=ORIENTED_EDGE('',*,*,#52678,.T.);
#75552=ORIENTED_EDGE('',*,*,#53081,.T.);
#75553=ORIENTED_EDGE('',*,*,#52681,.T.);
#75554=ORIENTED_EDGE('',*,*,#53089,.F.);
#75555=ORIENTED_EDGE('',*,*,#53050,.T.);
#75556=ORIENTED_EDGE('',*,*,#53158,.F.);
#75557=ORIENTED_EDGE('',*,*,#52660,.T.);
#75558=ORIENTED_EDGE('',*,*,#53087,.T.);
#75559=ORIENTED_EDGE('',*,*,#53051,.T.);
#75560=ORIENTED_EDGE('',*,*,#53090,.F.);
#75561=ORIENTED_EDGE('',*,*,#53041,.T.);
#75562=ORIENTED_EDGE('',*,*,#53157,.F.);
#75563=ORIENTED_EDGE('',*,*,#52723,.T.);
#75564=ORIENTED_EDGE('',*,*,#53069,.T.);
#75565=ORIENTED_EDGE('',*,*,#53064,.T.);
#75566=ORIENTED_EDGE('',*,*,#52682,.T.);
#75567=ORIENTED_EDGE('',*,*,#53154,.F.);
#75568=ORIENTED_EDGE('',*,*,#52729,.T.);
#75569=ORIENTED_EDGE('',*,*,#53241,.F.);
#75570=ORIENTED_EDGE('',*,*,#52726,.T.);
#75571=ORIENTED_EDGE('',*,*,#53091,.F.);
#75572=ORIENTED_EDGE('',*,*,#53056,.T.);
#75573=ORIENTED_EDGE('',*,*,#53085,.T.);
#75574=ORIENTED_EDGE('',*,*,#52666,.T.);
#75575=ORIENTED_EDGE('',*,*,#53242,.F.);
#75576=ORIENTED_EDGE('',*,*,#52663,.T.);
#75577=ORIENTED_EDGE('',*,*,#53092,.F.);
#75578=ORIENTED_EDGE('',*,*,#53038,.T.);
#75579=ORIENTED_EDGE('',*,*,#53148,.F.);
#75580=ORIENTED_EDGE('',*,*,#52711,.T.);
#75581=ORIENTED_EDGE('',*,*,#53066,.T.);
#75582=ORIENTED_EDGE('',*,*,#53070,.T.);
#75583=ORIENTED_EDGE('',*,*,#52720,.T.);
#75584=ORIENTED_EDGE('',*,*,#53155,.F.);
#75585=ORIENTED_EDGE('',*,*,#52717,.T.);
#75586=ORIENTED_EDGE('',*,*,#53243,.F.);
#75587=ORIENTED_EDGE('',*,*,#52714,.T.);
#75588=ORIENTED_EDGE('',*,*,#53097,.F.);
#75589=ORIENTED_EDGE('',*,*,#52672,.T.);
#75590=ORIENTED_EDGE('',*,*,#53244,.F.);
#75591=ORIENTED_EDGE('',*,*,#52669,.T.);
#75592=ORIENTED_EDGE('',*,*,#53083,.T.);
#75593=ORIENTED_EDGE('',*,*,#52675,.T.);
#75594=ORIENTED_EDGE('',*,*,#53096,.T.);
#75595=ORIENTED_EDGE('',*,*,#52655,.T.);
#75596=ORIENTED_EDGE('',*,*,#53150,.F.);
#75597=ORIENTED_EDGE('',*,*,#53062,.T.);
#75598=ORIENTED_EDGE('',*,*,#53093,.T.);
#75599=ORIENTED_EDGE('',*,*,#52687,.T.);
#75600=ORIENTED_EDGE('',*,*,#53245,.F.);
#75601=ORIENTED_EDGE('',*,*,#52696,.T.);
#75602=ORIENTED_EDGE('',*,*,#53126,.F.);
#75603=ORIENTED_EDGE('',*,*,#52693,.T.);
#75604=ORIENTED_EDGE('',*,*,#53246,.F.);
#75605=ORIENTED_EDGE('',*,*,#52690,.T.);
#75606=ORIENTED_EDGE('',*,*,#53247,.F.);
#75607=ORIENTED_EDGE('',*,*,#53171,.T.);
#75608=ORIENTED_EDGE('',*,*,#53248,.T.);
#75609=ORIENTED_EDGE('',*,*,#53249,.F.);
#75610=ORIENTED_EDGE('',*,*,#53250,.T.);
#75611=ORIENTED_EDGE('',*,*,#53248,.F.);
#75612=ORIENTED_EDGE('',*,*,#53170,.T.);
#75613=ORIENTED_EDGE('',*,*,#53251,.T.);
#75614=ORIENTED_EDGE('',*,*,#53251,.F.);
#75615=ORIENTED_EDGE('',*,*,#53169,.T.);
#75616=ORIENTED_EDGE('',*,*,#53252,.T.);
#75617=ORIENTED_EDGE('',*,*,#53253,.F.);
#75618=ORIENTED_EDGE('',*,*,#53252,.F.);
#75619=ORIENTED_EDGE('',*,*,#53168,.T.);
#75620=ORIENTED_EDGE('',*,*,#53254,.T.);
#75621=ORIENTED_EDGE('',*,*,#53255,.F.);
#75622=ORIENTED_EDGE('',*,*,#53254,.F.);
#75623=ORIENTED_EDGE('',*,*,#53167,.T.);
#75624=ORIENTED_EDGE('',*,*,#53256,.T.);
#75625=ORIENTED_EDGE('',*,*,#53257,.F.);
#75626=ORIENTED_EDGE('',*,*,#53258,.T.);
#75627=ORIENTED_EDGE('',*,*,#53256,.F.);
#75628=ORIENTED_EDGE('',*,*,#53166,.T.);
#75629=ORIENTED_EDGE('',*,*,#53259,.T.);
#75630=ORIENTED_EDGE('',*,*,#53259,.F.);
#75631=ORIENTED_EDGE('',*,*,#53165,.T.);
#75632=ORIENTED_EDGE('',*,*,#53260,.T.);
#75633=ORIENTED_EDGE('',*,*,#53261,.F.);
#75634=ORIENTED_EDGE('',*,*,#53260,.F.);
#75635=ORIENTED_EDGE('',*,*,#53164,.T.);
#75636=ORIENTED_EDGE('',*,*,#50956,.T.);
#75637=ORIENTED_EDGE('',*,*,#53262,.F.);
#75638=ORIENTED_EDGE('',*,*,#53263,.F.);
#75639=ORIENTED_EDGE('',*,*,#53264,.T.);
#75640=ORIENTED_EDGE('',*,*,#53265,.F.);
#75641=ORIENTED_EDGE('',*,*,#53266,.T.);
#75642=ORIENTED_EDGE('',*,*,#53267,.T.);
#75643=ORIENTED_EDGE('',*,*,#53263,.T.);
#75644=ORIENTED_EDGE('',*,*,#53268,.F.);
#75645=ORIENTED_EDGE('',*,*,#53269,.F.);
#75646=ORIENTED_EDGE('',*,*,#53270,.F.);
#75647=ORIENTED_EDGE('',*,*,#53271,.F.);
#75648=ORIENTED_EDGE('',*,*,#53272,.T.);
#75649=ORIENTED_EDGE('',*,*,#53270,.T.);
#75650=ORIENTED_EDGE('',*,*,#53273,.F.);
#75651=ORIENTED_EDGE('',*,*,#53274,.T.);
#75652=ORIENTED_EDGE('',*,*,#53275,.F.);
#75653=ORIENTED_EDGE('',*,*,#53276,.T.);
#75654=ORIENTED_EDGE('',*,*,#53277,.F.);
#75655=ORIENTED_EDGE('',*,*,#53278,.T.);
#75656=ORIENTED_EDGE('',*,*,#53279,.T.);
#75657=ORIENTED_EDGE('',*,*,#53280,.T.);
#75658=ORIENTED_EDGE('',*,*,#53281,.F.);
#75659=ORIENTED_EDGE('',*,*,#53282,.T.);
#75660=ORIENTED_EDGE('',*,*,#53277,.T.);
#75661=ORIENTED_EDGE('',*,*,#53283,.T.);
#75662=ORIENTED_EDGE('',*,*,#53279,.F.);
#75663=ORIENTED_EDGE('',*,*,#53284,.T.);
#75664=ORIENTED_EDGE('',*,*,#53285,.T.);
#75665=ORIENTED_EDGE('',*,*,#53286,.T.);
#75666=ORIENTED_EDGE('',*,*,#53287,.F.);
#75667=ORIENTED_EDGE('',*,*,#53288,.T.);
#75668=ORIENTED_EDGE('',*,*,#53289,.F.);
#75669=ORIENTED_EDGE('',*,*,#53290,.T.);
#75670=ORIENTED_EDGE('',*,*,#53291,.F.);
#75671=ORIENTED_EDGE('',*,*,#53292,.T.);
#75672=ORIENTED_EDGE('',*,*,#53291,.T.);
#75673=ORIENTED_EDGE('',*,*,#53293,.T.);
#75674=ORIENTED_EDGE('',*,*,#53285,.F.);
#75675=ORIENTED_EDGE('',*,*,#53294,.F.);
#75676=ORIENTED_EDGE('',*,*,#53295,.F.);
#75677=ORIENTED_EDGE('',*,*,#53296,.T.);
#75678=ORIENTED_EDGE('',*,*,#53297,.T.);
#75679=ORIENTED_EDGE('',*,*,#51137,.F.);
#75680=ORIENTED_EDGE('',*,*,#51121,.T.);
#75681=ORIENTED_EDGE('',*,*,#51136,.T.);
#75682=ORIENTED_EDGE('',*,*,#51091,.T.);
#75683=ORIENTED_EDGE('',*,*,#51093,.T.);
#75684=ORIENTED_EDGE('',*,*,#53298,.T.);
#75685=ORIENTED_EDGE('',*,*,#53299,.F.);
#75686=ORIENTED_EDGE('',*,*,#53300,.F.);
#75687=ORIENTED_EDGE('',*,*,#53301,.F.);
#75688=ORIENTED_EDGE('',*,*,#53302,.F.);
#75689=ORIENTED_EDGE('',*,*,#53303,.T.);
#75690=ORIENTED_EDGE('',*,*,#53304,.F.);
#75691=ORIENTED_EDGE('',*,*,#53305,.T.);
#75692=ORIENTED_EDGE('',*,*,#53306,.T.);
#75693=ORIENTED_EDGE('',*,*,#53307,.F.);
#75694=ORIENTED_EDGE('',*,*,#51085,.F.);
#75695=ORIENTED_EDGE('',*,*,#51114,.F.);
#75696=ORIENTED_EDGE('',*,*,#53308,.T.);
#75697=ORIENTED_EDGE('',*,*,#51111,.F.);
#75698=ORIENTED_EDGE('',*,*,#53309,.T.);
#75699=ORIENTED_EDGE('',*,*,#53310,.F.);
#75700=ORIENTED_EDGE('',*,*,#53311,.F.);
#75701=ORIENTED_EDGE('',*,*,#53312,.T.);
#75702=ORIENTED_EDGE('',*,*,#53313,.F.);
#75703=ORIENTED_EDGE('',*,*,#53314,.F.);
#75704=ORIENTED_EDGE('',*,*,#53315,.F.);
#75705=ORIENTED_EDGE('',*,*,#53316,.T.);
#75706=ORIENTED_EDGE('',*,*,#53317,.T.);
#75707=ORIENTED_EDGE('',*,*,#53294,.T.);
#75708=ORIENTED_EDGE('',*,*,#53318,.T.);
#75709=ORIENTED_EDGE('',*,*,#53296,.F.);
#75710=ORIENTED_EDGE('',*,*,#53319,.F.);
#75711=ORIENTED_EDGE('',*,*,#53320,.T.);
#75712=ORIENTED_EDGE('',*,*,#53321,.T.);
#75713=ORIENTED_EDGE('',*,*,#53322,.F.);
#75714=ORIENTED_EDGE('',*,*,#53313,.T.);
#75715=ORIENTED_EDGE('',*,*,#53323,.F.);
#75716=ORIENTED_EDGE('',*,*,#53311,.T.);
#75717=ORIENTED_EDGE('',*,*,#53324,.F.);
#75718=ORIENTED_EDGE('',*,*,#53309,.F.);
#75719=ORIENTED_EDGE('',*,*,#51110,.T.);
#75720=ORIENTED_EDGE('',*,*,#53308,.F.);
#75721=ORIENTED_EDGE('',*,*,#51113,.T.);
#75722=ORIENTED_EDGE('',*,*,#50996,.F.);
#75723=ORIENTED_EDGE('',*,*,#53325,.F.);
#75724=ORIENTED_EDGE('',*,*,#53321,.F.);
#75725=ORIENTED_EDGE('',*,*,#53326,.T.);
#75726=ORIENTED_EDGE('',*,*,#53327,.T.);
#75727=ORIENTED_EDGE('',*,*,#53328,.F.);
#75728=ORIENTED_EDGE('',*,*,#53327,.F.);
#75729=ORIENTED_EDGE('',*,*,#53329,.T.);
#75730=ORIENTED_EDGE('',*,*,#53330,.T.);
#75731=ORIENTED_EDGE('',*,*,#53331,.F.);
#75732=ORIENTED_EDGE('',*,*,#53330,.F.);
#75733=ORIENTED_EDGE('',*,*,#53332,.T.);
#75734=ORIENTED_EDGE('',*,*,#53333,.T.);
#75735=ORIENTED_EDGE('',*,*,#53334,.T.);
#75736=ORIENTED_EDGE('',*,*,#53335,.T.);
#75737=ORIENTED_EDGE('',*,*,#53336,.F.);
#75738=ORIENTED_EDGE('',*,*,#53333,.F.);
#75739=ORIENTED_EDGE('',*,*,#53337,.F.);
#75740=ORIENTED_EDGE('',*,*,#53338,.F.);
#75741=ORIENTED_EDGE('',*,*,#53339,.T.);
#75742=ORIENTED_EDGE('',*,*,#53340,.T.);
#75743=ORIENTED_EDGE('',*,*,#53341,.F.);
#75744=ORIENTED_EDGE('',*,*,#53340,.F.);
#75745=ORIENTED_EDGE('',*,*,#53342,.T.);
#75746=ORIENTED_EDGE('',*,*,#53315,.T.);
#75747=ORIENTED_EDGE('',*,*,#53343,.T.);
#75748=ORIENTED_EDGE('',*,*,#53344,.T.);
#75749=ORIENTED_EDGE('',*,*,#53345,.F.);
#75750=ORIENTED_EDGE('',*,*,#53346,.T.);
#75751=ORIENTED_EDGE('',*,*,#53347,.F.);
#75752=ORIENTED_EDGE('',*,*,#53348,.T.);
#75753=ORIENTED_EDGE('',*,*,#53349,.T.);
#75754=ORIENTED_EDGE('',*,*,#53350,.F.);
#75755=ORIENTED_EDGE('',*,*,#53351,.F.);
#75756=ORIENTED_EDGE('',*,*,#53352,.F.);
#75757=ORIENTED_EDGE('',*,*,#53353,.T.);
#75758=ORIENTED_EDGE('',*,*,#53354,.T.);
#75759=ORIENTED_EDGE('',*,*,#53355,.F.);
#75760=ORIENTED_EDGE('',*,*,#53356,.T.);
#75761=ORIENTED_EDGE('',*,*,#53357,.F.);
#75762=ORIENTED_EDGE('',*,*,#53358,.T.);
#75763=ORIENTED_EDGE('',*,*,#53359,.F.);
#75764=ORIENTED_EDGE('',*,*,#53360,.F.);
#75765=ORIENTED_EDGE('',*,*,#53361,.F.);
#75766=ORIENTED_EDGE('',*,*,#53362,.F.);
#75767=ORIENTED_EDGE('',*,*,#53363,.F.);
#75768=ORIENTED_EDGE('',*,*,#53364,.F.);
#75769=ORIENTED_EDGE('',*,*,#53365,.T.);
#75770=ORIENTED_EDGE('',*,*,#53351,.T.);
#75771=ORIENTED_EDGE('',*,*,#53366,.T.);
#75772=ORIENTED_EDGE('',*,*,#53367,.T.);
#75773=ORIENTED_EDGE('',*,*,#53364,.T.);
#75774=ORIENTED_EDGE('',*,*,#53368,.F.);
#75775=ORIENTED_EDGE('',*,*,#53369,.F.);
#75776=ORIENTED_EDGE('',*,*,#53370,.T.);
#75777=ORIENTED_EDGE('',*,*,#53274,.F.);
#75778=ORIENTED_EDGE('',*,*,#53282,.F.);
#75779=ORIENTED_EDGE('',*,*,#53278,.F.);
#75780=ORIENTED_EDGE('',*,*,#53371,.F.);
#75781=ORIENTED_EDGE('',*,*,#53372,.F.);
#75782=ORIENTED_EDGE('',*,*,#53345,.T.);
#75783=ORIENTED_EDGE('',*,*,#53373,.F.);
#75784=ORIENTED_EDGE('',*,*,#53369,.T.);
#75785=ORIENTED_EDGE('',*,*,#53374,.F.);
#75786=ORIENTED_EDGE('',*,*,#53375,.F.);
#75787=ORIENTED_EDGE('',*,*,#53376,.T.);
#75788=ORIENTED_EDGE('',*,*,#53361,.T.);
#75789=ORIENTED_EDGE('',*,*,#53377,.T.);
#75790=ORIENTED_EDGE('',*,*,#53292,.F.);
#75791=ORIENTED_EDGE('',*,*,#53284,.F.);
#75792=ORIENTED_EDGE('',*,*,#53378,.T.);
#75793=ORIENTED_EDGE('',*,*,#53375,.T.);
#75794=ORIENTED_EDGE('',*,*,#53379,.F.);
#75795=ORIENTED_EDGE('',*,*,#53380,.F.);
#75796=ORIENTED_EDGE('',*,*,#53381,.T.);
#75797=ORIENTED_EDGE('',*,*,#53288,.F.);
#75798=ORIENTED_EDGE('',*,*,#53382,.F.);
#75799=ORIENTED_EDGE('',*,*,#53383,.F.);
#75800=ORIENTED_EDGE('',*,*,#53355,.T.);
#75801=ORIENTED_EDGE('',*,*,#53384,.F.);
#75802=ORIENTED_EDGE('',*,*,#53380,.T.);
#75803=ORIENTED_EDGE('',*,*,#53385,.F.);
#75804=ORIENTED_EDGE('',*,*,#53366,.F.);
#75805=ORIENTED_EDGE('',*,*,#53350,.T.);
#75806=ORIENTED_EDGE('',*,*,#53386,.T.);
#75807=ORIENTED_EDGE('',*,*,#53298,.F.);
#75808=ORIENTED_EDGE('',*,*,#51094,.F.);
#75809=ORIENTED_EDGE('',*,*,#51020,.F.);
#75810=ORIENTED_EDGE('',*,*,#51033,.T.);
#75811=ORIENTED_EDGE('',*,*,#53387,.F.);
#75812=ORIENTED_EDGE('',*,*,#51065,.T.);
#75813=ORIENTED_EDGE('',*,*,#51062,.T.);
#75814=ORIENTED_EDGE('',*,*,#51059,.T.);
#75815=ORIENTED_EDGE('',*,*,#51056,.T.);
#75816=ORIENTED_EDGE('',*,*,#51075,.T.);
#75817=ORIENTED_EDGE('',*,*,#51072,.T.);
#75818=ORIENTED_EDGE('',*,*,#51069,.T.);
#75819=ORIENTED_EDGE('',*,*,#53388,.F.);
#75820=ORIENTED_EDGE('',*,*,#53389,.F.);
#75821=ORIENTED_EDGE('',*,*,#53390,.F.);
#75822=ORIENTED_EDGE('',*,*,#53391,.F.);
#75823=ORIENTED_EDGE('',*,*,#53392,.F.);
#75824=ORIENTED_EDGE('',*,*,#53393,.F.);
#75825=ORIENTED_EDGE('',*,*,#53394,.F.);
#75826=ORIENTED_EDGE('',*,*,#53395,.F.);
#75827=ORIENTED_EDGE('',*,*,#51051,.F.);
#75828=ORIENTED_EDGE('',*,*,#53396,.T.);
#75829=ORIENTED_EDGE('',*,*,#53382,.T.);
#75830=ORIENTED_EDGE('',*,*,#53379,.T.);
#75831=ORIENTED_EDGE('',*,*,#53374,.T.);
#75832=ORIENTED_EDGE('',*,*,#53397,.T.);
#75833=ORIENTED_EDGE('',*,*,#53371,.T.);
#75834=ORIENTED_EDGE('',*,*,#53368,.T.);
#75835=ORIENTED_EDGE('',*,*,#53363,.T.);
#75836=ORIENTED_EDGE('',*,*,#53385,.T.);
#75837=ORIENTED_EDGE('',*,*,#51032,.F.);
#75838=ORIENTED_EDGE('',*,*,#51039,.F.);
#75839=ORIENTED_EDGE('',*,*,#51040,.F.);
#75840=ORIENTED_EDGE('',*,*,#51083,.F.);
#75841=ORIENTED_EDGE('',*,*,#51043,.F.);
#75842=ORIENTED_EDGE('',*,*,#51049,.F.);
#75843=ORIENTED_EDGE('',*,*,#53398,.F.);
#75844=ORIENTED_EDGE('',*,*,#53399,.F.);
#75845=ORIENTED_EDGE('',*,*,#53392,.T.);
#75846=ORIENTED_EDGE('',*,*,#53400,.T.);
#75847=ORIENTED_EDGE('',*,*,#53401,.F.);
#75848=ORIENTED_EDGE('',*,*,#53402,.F.);
#75849=ORIENTED_EDGE('',*,*,#53393,.T.);
#75850=ORIENTED_EDGE('',*,*,#53399,.T.);
#75851=ORIENTED_EDGE('',*,*,#53403,.F.);
#75852=ORIENTED_EDGE('',*,*,#53404,.F.);
#75853=ORIENTED_EDGE('',*,*,#53394,.T.);
#75854=ORIENTED_EDGE('',*,*,#53402,.T.);
#75855=ORIENTED_EDGE('',*,*,#53405,.F.);
#75856=ORIENTED_EDGE('',*,*,#53406,.F.);
#75857=ORIENTED_EDGE('',*,*,#53395,.T.);
#75858=ORIENTED_EDGE('',*,*,#53404,.T.);
#75859=ORIENTED_EDGE('',*,*,#53387,.T.);
#75860=ORIENTED_EDGE('',*,*,#53406,.T.);
#75861=ORIENTED_EDGE('',*,*,#53407,.F.);
#75862=ORIENTED_EDGE('',*,*,#51066,.F.);
#75863=ORIENTED_EDGE('',*,*,#53408,.F.);
#75864=ORIENTED_EDGE('',*,*,#53409,.F.);
#75865=ORIENTED_EDGE('',*,*,#53388,.T.);
#75866=ORIENTED_EDGE('',*,*,#51068,.T.);
#75867=ORIENTED_EDGE('',*,*,#53410,.F.);
#75868=ORIENTED_EDGE('',*,*,#53411,.F.);
#75869=ORIENTED_EDGE('',*,*,#53389,.T.);
#75870=ORIENTED_EDGE('',*,*,#53409,.T.);
#75871=ORIENTED_EDGE('',*,*,#53412,.F.);
#75872=ORIENTED_EDGE('',*,*,#53413,.F.);
#75873=ORIENTED_EDGE('',*,*,#53390,.T.);
#75874=ORIENTED_EDGE('',*,*,#53411,.T.);
#75875=ORIENTED_EDGE('',*,*,#53414,.F.);
#75876=ORIENTED_EDGE('',*,*,#53400,.F.);
#75877=ORIENTED_EDGE('',*,*,#53391,.T.);
#75878=ORIENTED_EDGE('',*,*,#53413,.T.);
#75879=ORIENTED_EDGE('',*,*,#53415,.T.);
#75880=ORIENTED_EDGE('',*,*,#53347,.T.);
#75881=ORIENTED_EDGE('',*,*,#53416,.F.);
#75882=ORIENTED_EDGE('',*,*,#53417,.F.);
#75883=ORIENTED_EDGE('',*,*,#53418,.F.);
#75884=ORIENTED_EDGE('',*,*,#53359,.T.);
#75885=ORIENTED_EDGE('',*,*,#53419,.T.);
#75886=ORIENTED_EDGE('',*,*,#53420,.F.);
#75887=ORIENTED_EDGE('',*,*,#53421,.T.);
#75888=ORIENTED_EDGE('',*,*,#53416,.T.);
#75889=ORIENTED_EDGE('',*,*,#53346,.F.);
#75890=ORIENTED_EDGE('',*,*,#53372,.T.);
#75891=ORIENTED_EDGE('',*,*,#53397,.F.);
#75892=ORIENTED_EDGE('',*,*,#53377,.F.);
#75893=ORIENTED_EDGE('',*,*,#53360,.T.);
#75894=ORIENTED_EDGE('',*,*,#53418,.T.);
#75895=ORIENTED_EDGE('',*,*,#53422,.T.);
#75896=ORIENTED_EDGE('',*,*,#53357,.T.);
#75897=ORIENTED_EDGE('',*,*,#53423,.F.);
#75898=ORIENTED_EDGE('',*,*,#53306,.F.);
#75899=ORIENTED_EDGE('',*,*,#53307,.T.);
#75900=ORIENTED_EDGE('',*,*,#53423,.T.);
#75901=ORIENTED_EDGE('',*,*,#53356,.F.);
#75902=ORIENTED_EDGE('',*,*,#53383,.T.);
#75903=ORIENTED_EDGE('',*,*,#53396,.F.);
#75904=ORIENTED_EDGE('',*,*,#51053,.F.);
#75905=ORIENTED_EDGE('',*,*,#51024,.T.);
#75906=ORIENTED_EDGE('',*,*,#51086,.F.);
#75907=ORIENTED_EDGE('',*,*,#53424,.T.);
#75908=ORIENTED_EDGE('',*,*,#53337,.T.);
#75909=ORIENTED_EDGE('',*,*,#53341,.T.);
#75910=ORIENTED_EDGE('',*,*,#53314,.T.);
#75911=ORIENTED_EDGE('',*,*,#53425,.T.);
#75912=ORIENTED_EDGE('',*,*,#53300,.T.);
#75913=ORIENTED_EDGE('',*,*,#53426,.F.);
#75914=ORIENTED_EDGE('',*,*,#53348,.F.);
#75915=ORIENTED_EDGE('',*,*,#53427,.F.);
#75916=ORIENTED_EDGE('',*,*,#53343,.F.);
#75917=ORIENTED_EDGE('',*,*,#53415,.F.);
#75918=ORIENTED_EDGE('',*,*,#53428,.F.);
#75919=ORIENTED_EDGE('',*,*,#53299,.T.);
#75920=ORIENTED_EDGE('',*,*,#53386,.F.);
#75921=ORIENTED_EDGE('',*,*,#53349,.F.);
#75922=ORIENTED_EDGE('',*,*,#53426,.T.);
#75923=ORIENTED_EDGE('',*,*,#53429,.T.);
#75924=ORIENTED_EDGE('',*,*,#53430,.F.);
#75925=ORIENTED_EDGE('',*,*,#53431,.T.);
#75926=ORIENTED_EDGE('',*,*,#53286,.F.);
#75927=ORIENTED_EDGE('',*,*,#53293,.F.);
#75928=ORIENTED_EDGE('',*,*,#53290,.F.);
#75929=ORIENTED_EDGE('',*,*,#53432,.T.);
#75930=ORIENTED_EDGE('',*,*,#53433,.F.);
#75931=ORIENTED_EDGE('',*,*,#53434,.T.);
#75932=ORIENTED_EDGE('',*,*,#53435,.T.);
#75933=ORIENTED_EDGE('',*,*,#53271,.T.);
#75934=ORIENTED_EDGE('',*,*,#53272,.F.);
#75935=ORIENTED_EDGE('',*,*,#53436,.F.);
#75936=ORIENTED_EDGE('',*,*,#53429,.F.);
#75937=ORIENTED_EDGE('',*,*,#53289,.T.);
#75938=ORIENTED_EDGE('',*,*,#53381,.F.);
#75939=ORIENTED_EDGE('',*,*,#53384,.T.);
#75940=ORIENTED_EDGE('',*,*,#53354,.F.);
#75941=ORIENTED_EDGE('',*,*,#53437,.T.);
#75942=ORIENTED_EDGE('',*,*,#53362,.T.);
#75943=ORIENTED_EDGE('',*,*,#53376,.F.);
#75944=ORIENTED_EDGE('',*,*,#53378,.F.);
#75945=ORIENTED_EDGE('',*,*,#53287,.T.);
#75946=ORIENTED_EDGE('',*,*,#53431,.F.);
#75947=ORIENTED_EDGE('',*,*,#53280,.F.);
#75948=ORIENTED_EDGE('',*,*,#53283,.F.);
#75949=ORIENTED_EDGE('',*,*,#53276,.F.);
#75950=ORIENTED_EDGE('',*,*,#53438,.T.);
#75951=ORIENTED_EDGE('',*,*,#53439,.F.);
#75952=ORIENTED_EDGE('',*,*,#53440,.T.);
#75953=ORIENTED_EDGE('',*,*,#53441,.T.);
#75954=ORIENTED_EDGE('',*,*,#53442,.F.);
#75955=ORIENTED_EDGE('',*,*,#53264,.F.);
#75956=ORIENTED_EDGE('',*,*,#53267,.F.);
#75957=ORIENTED_EDGE('',*,*,#53443,.T.);
#75958=ORIENTED_EDGE('',*,*,#53438,.F.);
#75959=ORIENTED_EDGE('',*,*,#53275,.T.);
#75960=ORIENTED_EDGE('',*,*,#53370,.F.);
#75961=ORIENTED_EDGE('',*,*,#53373,.T.);
#75962=ORIENTED_EDGE('',*,*,#53344,.F.);
#75963=ORIENTED_EDGE('',*,*,#53427,.T.);
#75964=ORIENTED_EDGE('',*,*,#53352,.T.);
#75965=ORIENTED_EDGE('',*,*,#53365,.F.);
#75966=ORIENTED_EDGE('',*,*,#53367,.F.);
#75967=ORIENTED_EDGE('',*,*,#53281,.T.);
#75968=ORIENTED_EDGE('',*,*,#53440,.F.);
#75969=ORIENTED_EDGE('',*,*,#53310,.T.);
#75970=ORIENTED_EDGE('',*,*,#53324,.T.);
#75971=ORIENTED_EDGE('',*,*,#53323,.T.);
#75972=ORIENTED_EDGE('',*,*,#53312,.F.);
#75973=ORIENTED_EDGE('',*,*,#53444,.F.);
#75974=ORIENTED_EDGE('',*,*,#53419,.F.);
#75975=ORIENTED_EDGE('',*,*,#53358,.F.);
#75976=ORIENTED_EDGE('',*,*,#53437,.F.);
#75977=ORIENTED_EDGE('',*,*,#53353,.F.);
#75978=ORIENTED_EDGE('',*,*,#53422,.F.);
#75979=ORIENTED_EDGE('',*,*,#53305,.F.);
#75980=ORIENTED_EDGE('',*,*,#53322,.T.);
#75981=ORIENTED_EDGE('',*,*,#53325,.T.);
#75982=ORIENTED_EDGE('',*,*,#53328,.T.);
#75983=ORIENTED_EDGE('',*,*,#53331,.T.);
#75984=ORIENTED_EDGE('',*,*,#53336,.T.);
#75985=ORIENTED_EDGE('',*,*,#53445,.T.);
#75986=ORIENTED_EDGE('',*,*,#53446,.F.);
#75987=ORIENTED_EDGE('',*,*,#53447,.T.);
#75988=ORIENTED_EDGE('',*,*,#53448,.F.);
#75989=ORIENTED_EDGE('',*,*,#53449,.T.);
#75990=ORIENTED_EDGE('',*,*,#53450,.F.);
#75991=ORIENTED_EDGE('',*,*,#53319,.T.);
#75992=ORIENTED_EDGE('',*,*,#53295,.T.);
#75993=ORIENTED_EDGE('',*,*,#53302,.T.);
#75994=ORIENTED_EDGE('',*,*,#53451,.T.);
#75995=ORIENTED_EDGE('',*,*,#53434,.F.);
#75996=ORIENTED_EDGE('',*,*,#53452,.F.);
#75997=ORIENTED_EDGE('',*,*,#53453,.F.);
#75998=ORIENTED_EDGE('',*,*,#53454,.T.);
#75999=ORIENTED_EDGE('',*,*,#53447,.F.);
#76000=ORIENTED_EDGE('',*,*,#53455,.F.);
#76001=ORIENTED_EDGE('',*,*,#53456,.T.);
#76002=ORIENTED_EDGE('',*,*,#53457,.T.);
#76003=ORIENTED_EDGE('',*,*,#53458,.F.);
#76004=ORIENTED_EDGE('',*,*,#53445,.F.);
#76005=ORIENTED_EDGE('',*,*,#53459,.F.);
#76006=ORIENTED_EDGE('',*,*,#53460,.F.);
#76007=ORIENTED_EDGE('',*,*,#53461,.T.);
#76008=ORIENTED_EDGE('',*,*,#53338,.T.);
#76009=ORIENTED_EDGE('',*,*,#53424,.F.);
#76010=ORIENTED_EDGE('',*,*,#53462,.T.);
#76011=ORIENTED_EDGE('',*,*,#53463,.F.);
#76012=ORIENTED_EDGE('',*,*,#53449,.F.);
#76013=ORIENTED_EDGE('',*,*,#53464,.F.);
#76014=ORIENTED_EDGE('',*,*,#53301,.T.);
#76015=ORIENTED_EDGE('',*,*,#53425,.F.);
#76016=ORIENTED_EDGE('',*,*,#53317,.F.);
#76017=ORIENTED_EDGE('',*,*,#53465,.T.);
#76018=ORIENTED_EDGE('',*,*,#53303,.F.);
#76019=ORIENTED_EDGE('',*,*,#53451,.F.);
#76020=ORIENTED_EDGE('',*,*,#53265,.T.);
#76021=ORIENTED_EDGE('',*,*,#53442,.T.);
#76022=ORIENTED_EDGE('',*,*,#53466,.F.);
#76023=ORIENTED_EDGE('',*,*,#53467,.T.);
#76024=ORIENTED_EDGE('',*,*,#53432,.F.);
#76025=ORIENTED_EDGE('',*,*,#53430,.T.);
#76026=ORIENTED_EDGE('',*,*,#53436,.T.);
#76027=ORIENTED_EDGE('',*,*,#53273,.T.);
#76028=ORIENTED_EDGE('',*,*,#53269,.T.);
#76029=ORIENTED_EDGE('',*,*,#53435,.F.);
#76030=ORIENTED_EDGE('',*,*,#53453,.T.);
#76031=ORIENTED_EDGE('',*,*,#53452,.T.);
#76032=ORIENTED_EDGE('',*,*,#53433,.T.);
#76033=ORIENTED_EDGE('',*,*,#53467,.F.);
#76034=ORIENTED_EDGE('',*,*,#53468,.T.);
#76035=ORIENTED_EDGE('',*,*,#53459,.T.);
#76036=ORIENTED_EDGE('',*,*,#53446,.T.);
#76037=ORIENTED_EDGE('',*,*,#53458,.T.);
#76038=ORIENTED_EDGE('',*,*,#53469,.T.);
#76039=ORIENTED_EDGE('',*,*,#53455,.T.);
#76040=ORIENTED_EDGE('',*,*,#53448,.T.);
#76041=ORIENTED_EDGE('',*,*,#53454,.F.);
#76042=ORIENTED_EDGE('',*,*,#53470,.T.);
#76043=ORIENTED_EDGE('',*,*,#53464,.T.);
#76044=ORIENTED_EDGE('',*,*,#53450,.T.);
#76045=ORIENTED_EDGE('',*,*,#53463,.T.);
#76046=ORIENTED_EDGE('',*,*,#53471,.T.);
#76047=ORIENTED_EDGE('',*,*,#53472,.T.);
#76048=ORIENTED_EDGE('',*,*,#53460,.T.);
#76049=ORIENTED_EDGE('',*,*,#53428,.T.);
#76050=ORIENTED_EDGE('',*,*,#53417,.T.);
#76051=ORIENTED_EDGE('',*,*,#53421,.F.);
#76052=ORIENTED_EDGE('',*,*,#53420,.T.);
#76053=ORIENTED_EDGE('',*,*,#53444,.T.);
#76054=ORIENTED_EDGE('',*,*,#53335,.F.);
#76055=ORIENTED_EDGE('',*,*,#53473,.T.);
#76056=ORIENTED_EDGE('',*,*,#53439,.T.);
#76057=ORIENTED_EDGE('',*,*,#53443,.F.);
#76058=ORIENTED_EDGE('',*,*,#53268,.T.);
#76059=ORIENTED_EDGE('',*,*,#53266,.F.);
#76060=ORIENTED_EDGE('',*,*,#53466,.T.);
#76061=ORIENTED_EDGE('',*,*,#53441,.F.);
#76062=ORIENTED_EDGE('',*,*,#53474,.T.);
#76063=ORIENTED_EDGE('',*,*,#51572,.T.);
#76064=ORIENTED_EDGE('',*,*,#53475,.F.);
#76065=ORIENTED_EDGE('',*,*,#53195,.F.);
#76066=ORIENTED_EDGE('',*,*,#52902,.T.);
#76067=ORIENTED_EDGE('',*,*,#51827,.T.);
#76068=ORIENTED_EDGE('',*,*,#53476,.F.);
#76069=ORIENTED_EDGE('',*,*,#53199,.F.);
#76070=ORIENTED_EDGE('',*,*,#53476,.T.);
#76071=ORIENTED_EDGE('',*,*,#51833,.T.);
#76072=ORIENTED_EDGE('',*,*,#53477,.F.);
#76073=ORIENTED_EDGE('',*,*,#53200,.F.);
#76074=ORIENTED_EDGE('',*,*,#52890,.T.);
#76075=ORIENTED_EDGE('',*,*,#51803,.T.);
#76076=ORIENTED_EDGE('',*,*,#52886,.T.);
#76077=ORIENTED_EDGE('',*,*,#53204,.F.);
#76078=ORIENTED_EDGE('',*,*,#53478,.T.);
#76079=ORIENTED_EDGE('',*,*,#52116,.T.);
#76080=ORIENTED_EDGE('',*,*,#53479,.F.);
#76081=ORIENTED_EDGE('',*,*,#53227,.F.);
#76082=ORIENTED_EDGE('',*,*,#53479,.T.);
#76083=ORIENTED_EDGE('',*,*,#52110,.T.);
#76084=ORIENTED_EDGE('',*,*,#52778,.T.);
#76085=ORIENTED_EDGE('',*,*,#53228,.F.);
#76086=ORIENTED_EDGE('',*,*,#53480,.T.);
#76087=ORIENTED_EDGE('',*,*,#52172,.T.);
#76088=ORIENTED_EDGE('',*,*,#53481,.F.);
#76089=ORIENTED_EDGE('',*,*,#53231,.F.);
#76090=ORIENTED_EDGE('',*,*,#53482,.T.);
#76091=ORIENTED_EDGE('',*,*,#53482,.F.);
#76092=ORIENTED_EDGE('',*,*,#53483,.T.);
#76093=ORIENTED_EDGE('',*,*,#51304,.T.);
#76094=ORIENTED_EDGE('',*,*,#51300,.T.);
#76095=ORIENTED_EDGE('',*,*,#51305,.T.);
#76096=ORIENTED_EDGE('',*,*,#53483,.F.);
#76097=ORIENTED_EDGE('',*,*,#53484,.T.);
#76098=ORIENTED_EDGE('',*,*,#53484,.F.);
#76099=ORIENTED_EDGE('',*,*,#53485,.T.);
#76100=ORIENTED_EDGE('',*,*,#51308,.T.);
#76101=ORIENTED_EDGE('',*,*,#51309,.T.);
#76102=ORIENTED_EDGE('',*,*,#53485,.F.);
#76103=ORIENTED_EDGE('',*,*,#51541,.T.);
#76104=ORIENTED_EDGE('',*,*,#51327,.T.);
#76105=ORIENTED_EDGE('',*,*,#51528,.T.);
#76106=ORIENTED_EDGE('',*,*,#51532,.T.);
#76107=ORIENTED_EDGE('',*,*,#51535,.T.);
#76108=ORIENTED_EDGE('',*,*,#51537,.T.);
#76109=ORIENTED_EDGE('',*,*,#51306,.T.);
#76110=ORIENTED_EDGE('',*,*,#51529,.T.);
#76111=ORIENTED_EDGE('',*,*,#51316,.T.);
#76112=ORIENTED_EDGE('',*,*,#51550,.T.);
#76113=ORIENTED_EDGE('',*,*,#51553,.T.);
#76114=ORIENTED_EDGE('',*,*,#51339,.T.);
#76115=ORIENTED_EDGE('',*,*,#51540,.T.);
#76116=ORIENTED_EDGE('',*,*,#51551,.T.);
#76117=ORIENTED_EDGE('',*,*,#51329,.T.);
#76118=ORIENTED_EDGE('',*,*,#51552,.T.);
#76119=ORIENTED_EDGE('',*,*,#51536,.T.);
#76120=ORIENTED_EDGE('',*,*,#51499,.T.);
#76121=ORIENTED_EDGE('',*,*,#51356,.T.);
#76122=ORIENTED_EDGE('',*,*,#51485,.T.);
#76123=ORIENTED_EDGE('',*,*,#51490,.T.);
#76124=ORIENTED_EDGE('',*,*,#51492,.T.);
#76125=ORIENTED_EDGE('',*,*,#51303,.T.);
#76126=ORIENTED_EDGE('',*,*,#51491,.T.);
#76127=ORIENTED_EDGE('',*,*,#51496,.T.);
#76128=ORIENTED_EDGE('',*,*,#51486,.T.);
#76129=ORIENTED_EDGE('',*,*,#51367,.T.);
#76130=ORIENTED_EDGE('',*,*,#51548,.T.);
#76131=ORIENTED_EDGE('',*,*,#51547,.T.);
#76132=ORIENTED_EDGE('',*,*,#51354,.T.);
#76133=ORIENTED_EDGE('',*,*,#51498,.T.);
#76134=ORIENTED_EDGE('',*,*,#51549,.T.);
#76135=ORIENTED_EDGE('',*,*,#51382,.T.);
#76136=ORIENTED_EDGE('',*,*,#51546,.T.);
#76137=ORIENTED_EDGE('',*,*,#51493,.T.);
#76138=ORIENTED_EDGE('',*,*,#51515,.T.);
#76139=ORIENTED_EDGE('',*,*,#51430,.T.);
#76140=ORIENTED_EDGE('',*,*,#51436,.T.);
#76141=ORIENTED_EDGE('',*,*,#51557,.T.);
#76142=ORIENTED_EDGE('',*,*,#51434,.T.);
#76143=ORIENTED_EDGE('',*,*,#51428,.T.);
#76144=ORIENTED_EDGE('',*,*,#51527,.T.);
#76145=ORIENTED_EDGE('',*,*,#51554,.T.);
#76146=ORIENTED_EDGE('',*,*,#51556,.T.);
#76147=ORIENTED_EDGE('',*,*,#51450,.T.);
#76148=ORIENTED_EDGE('',*,*,#51555,.T.);
#76149=ORIENTED_EDGE('',*,*,#51522,.T.);
#76150=ORIENTED_EDGE('',*,*,#51543,.T.);
#76151=ORIENTED_EDGE('',*,*,#51466,.T.);
#76152=ORIENTED_EDGE('',*,*,#51473,.T.);
#76153=ORIENTED_EDGE('',*,*,#51513,.T.);
#76154=ORIENTED_EDGE('',*,*,#51501,.T.);
#76155=ORIENTED_EDGE('',*,*,#51482,.T.);
#76156=ORIENTED_EDGE('',*,*,#51477,.T.);
#76157=ORIENTED_EDGE('',*,*,#51545,.T.);
#76158=ORIENTED_EDGE('',*,*,#51544,.T.);
#76159=ORIENTED_EDGE('',*,*,#51458,.T.);
#76160=ORIENTED_EDGE('',*,*,#51542,.T.);
#76161=ORIENTED_EDGE('',*,*,#51508,.T.);
#76162=ORIENTED_EDGE('',*,*,#52598,.T.);
#76163=ORIENTED_EDGE('',*,*,#52597,.F.);
#76164=ORIENTED_EDGE('',*,*,#52596,.F.);
#76165=ORIENTED_EDGE('',*,*,#52595,.F.);
#76166=ORIENTED_EDGE('',*,*,#52594,.F.);
#76167=ORIENTED_EDGE('',*,*,#50395,.F.);
#76168=ORIENTED_EDGE('',*,*,#50440,.F.);
#76169=ORIENTED_EDGE('',*,*,#52538,.F.);
#76170=ORIENTED_EDGE('',*,*,#52537,.F.);
#76171=ORIENTED_EDGE('',*,*,#52536,.F.);
#76172=ORIENTED_EDGE('',*,*,#52535,.T.);
#76173=ORIENTED_EDGE('',*,*,#52541,.T.);
#76174=ORIENTED_EDGE('',*,*,#52540,.T.);
#76175=ORIENTED_EDGE('',*,*,#52647,.T.);
#76176=ORIENTED_EDGE('',*,*,#52604,.T.);
#76177=ORIENTED_EDGE('',*,*,#52591,.T.);
#76178=ORIENTED_EDGE('',*,*,#52590,.T.);
#76179=ORIENTED_EDGE('',*,*,#52599,.T.);
#76180=ORIENTED_EDGE('',*,*,#52654,.T.);
#76181=ORIENTED_EDGE('',*,*,#52481,.T.);
#76182=ORIENTED_EDGE('',*,*,#52480,.T.);
#76183=ORIENTED_EDGE('',*,*,#52484,.T.);
#76184=ORIENTED_EDGE('',*,*,#50288,.F.);
#76185=ORIENTED_EDGE('',*,*,#50287,.F.);
#76186=ORIENTED_EDGE('',*,*,#50292,.F.);
#76187=ORIENTED_EDGE('',*,*,#50447,.F.);
#76188=ORIENTED_EDGE('',*,*,#50427,.F.);
#76189=ORIENTED_EDGE('',*,*,#50417,.F.);
#76190=ORIENTED_EDGE('',*,*,#50416,.F.);
#76191=ORIENTED_EDGE('',*,*,#50415,.F.);
#76192=ORIENTED_EDGE('',*,*,#50420,.F.);
#76193=ORIENTED_EDGE('',*,*,#50412,.F.);
#76194=ORIENTED_EDGE('',*,*,#52621,.T.);
#76195=ORIENTED_EDGE('',*,*,#52623,.T.);
#76196=ORIENTED_EDGE('',*,*,#52622,.T.);
#76197=ORIENTED_EDGE('',*,*,#52627,.T.);
#76198=ORIENTED_EDGE('',*,*,#52626,.T.);
#76199=ORIENTED_EDGE('',*,*,#52635,.T.);
#76200=ORIENTED_EDGE('',*,*,#52650,.T.);
#76201=ORIENTED_EDGE('',*,*,#52513,.T.);
#76202=ORIENTED_EDGE('',*,*,#52512,.T.);
#76203=ORIENTED_EDGE('',*,*,#52511,.T.);
#76204=ORIENTED_EDGE('',*,*,#52510,.T.);
#76205=ORIENTED_EDGE('',*,*,#52509,.T.);
#76206=ORIENTED_EDGE('',*,*,#52508,.T.);
#76207=ORIENTED_EDGE('',*,*,#52651,.T.);
#76208=ORIENTED_EDGE('',*,*,#52575,.T.);
#76209=ORIENTED_EDGE('',*,*,#52570,.T.);
#76210=ORIENTED_EDGE('',*,*,#52569,.T.);
#76211=ORIENTED_EDGE('',*,*,#52568,.T.);
#76212=ORIENTED_EDGE('',*,*,#52567,.T.);
#76213=ORIENTED_EDGE('',*,*,#52566,.T.);
#76214=ORIENTED_EDGE('',*,*,#52565,.T.);
#76215=ORIENTED_EDGE('',*,*,#52564,.T.);
#76216=ORIENTED_EDGE('',*,*,#52558,.T.);
#76217=ORIENTED_EDGE('',*,*,#52342,.T.);
#76218=ORIENTED_EDGE('',*,*,#50156,.F.);
#76219=ORIENTED_EDGE('',*,*,#50160,.F.);
#76220=ORIENTED_EDGE('',*,*,#50163,.F.);
#76221=ORIENTED_EDGE('',*,*,#50166,.F.);
#76222=ORIENTED_EDGE('',*,*,#50169,.F.);
#76223=ORIENTED_EDGE('',*,*,#50172,.F.);
#76224=ORIENTED_EDGE('',*,*,#50175,.F.);
#76225=ORIENTED_EDGE('',*,*,#52365,.T.);
#76226=ORIENTED_EDGE('',*,*,#52363,.T.);
#76227=ORIENTED_EDGE('',*,*,#52360,.T.);
#76228=ORIENTED_EDGE('',*,*,#52357,.T.);
#76229=ORIENTED_EDGE('',*,*,#52354,.T.);
#76230=ORIENTED_EDGE('',*,*,#52351,.T.);
#76231=ORIENTED_EDGE('',*,*,#52348,.T.);
#76232=ORIENTED_EDGE('',*,*,#52345,.T.);
#76233=ORIENTED_EDGE('',*,*,#49391,.F.);
#76234=ORIENTED_EDGE('',*,*,#49397,.F.);
#76235=ORIENTED_EDGE('',*,*,#49403,.F.);
#76236=ORIENTED_EDGE('',*,*,#49409,.F.);
#76237=ORIENTED_EDGE('',*,*,#49411,.F.);
#76238=ORIENTED_EDGE('',*,*,#49407,.F.);
#76239=ORIENTED_EDGE('',*,*,#49401,.F.);
#76240=ORIENTED_EDGE('',*,*,#49395,.F.);
#76241=ORIENTED_EDGE('',*,*,#49389,.F.);
#76242=ORIENTED_EDGE('',*,*,#49383,.F.);
#76243=ORIENTED_EDGE('',*,*,#49421,.F.);
#76244=ORIENTED_EDGE('',*,*,#49427,.F.);
#76245=ORIENTED_EDGE('',*,*,#49433,.F.);
#76246=ORIENTED_EDGE('',*,*,#49435,.F.);
#76247=ORIENTED_EDGE('',*,*,#49431,.F.);
#76248=ORIENTED_EDGE('',*,*,#49425,.F.);
#76249=ORIENTED_EDGE('',*,*,#49419,.F.);
#76250=ORIENTED_EDGE('',*,*,#49413,.F.);
#76251=ORIENTED_EDGE('',*,*,#49445,.F.);
#76252=ORIENTED_EDGE('',*,*,#49451,.F.);
#76253=ORIENTED_EDGE('',*,*,#49457,.F.);
#76254=ORIENTED_EDGE('',*,*,#49459,.F.);
#76255=ORIENTED_EDGE('',*,*,#49455,.F.);
#76256=ORIENTED_EDGE('',*,*,#49449,.F.);
#76257=ORIENTED_EDGE('',*,*,#49443,.F.);
#76258=ORIENTED_EDGE('',*,*,#49437,.F.);
#76259=ORIENTED_EDGE('',*,*,#49469,.F.);
#76260=ORIENTED_EDGE('',*,*,#49475,.F.);
#76261=ORIENTED_EDGE('',*,*,#49481,.F.);
#76262=ORIENTED_EDGE('',*,*,#49483,.F.);
#76263=ORIENTED_EDGE('',*,*,#49479,.F.);
#76264=ORIENTED_EDGE('',*,*,#49473,.F.);
#76265=ORIENTED_EDGE('',*,*,#49467,.F.);
#76266=ORIENTED_EDGE('',*,*,#49462,.F.);
#76267=ORIENTED_EDGE('',*,*,#49493,.F.);
#76268=ORIENTED_EDGE('',*,*,#49499,.F.);
#76269=ORIENTED_EDGE('',*,*,#49505,.F.);
#76270=ORIENTED_EDGE('',*,*,#49511,.F.);
#76271=ORIENTED_EDGE('',*,*,#49509,.F.);
#76272=ORIENTED_EDGE('',*,*,#49503,.F.);
#76273=ORIENTED_EDGE('',*,*,#49497,.F.);
#76274=ORIENTED_EDGE('',*,*,#49491,.F.);
#76275=ORIENTED_EDGE('',*,*,#49486,.F.);
#76276=ORIENTED_EDGE('',*,*,#49520,.F.);
#76277=ORIENTED_EDGE('',*,*,#49526,.F.);
#76278=ORIENTED_EDGE('',*,*,#49532,.F.);
#76279=ORIENTED_EDGE('',*,*,#49534,.F.);
#76280=ORIENTED_EDGE('',*,*,#49530,.F.);
#76281=ORIENTED_EDGE('',*,*,#49524,.F.);
#76282=ORIENTED_EDGE('',*,*,#49518,.F.);
#76283=ORIENTED_EDGE('',*,*,#49513,.F.);
#76284=ORIENTED_EDGE('',*,*,#49544,.F.);
#76285=ORIENTED_EDGE('',*,*,#49550,.F.);
#76286=ORIENTED_EDGE('',*,*,#49556,.F.);
#76287=ORIENTED_EDGE('',*,*,#49558,.F.);
#76288=ORIENTED_EDGE('',*,*,#49554,.F.);
#76289=ORIENTED_EDGE('',*,*,#49548,.F.);
#76290=ORIENTED_EDGE('',*,*,#49542,.F.);
#76291=ORIENTED_EDGE('',*,*,#49537,.F.);
#76292=ORIENTED_EDGE('',*,*,#49568,.F.);
#76293=ORIENTED_EDGE('',*,*,#49574,.F.);
#76294=ORIENTED_EDGE('',*,*,#49580,.F.);
#76295=ORIENTED_EDGE('',*,*,#49582,.F.);
#76296=ORIENTED_EDGE('',*,*,#49578,.F.);
#76297=ORIENTED_EDGE('',*,*,#49572,.F.);
#76298=ORIENTED_EDGE('',*,*,#49566,.F.);
#76299=ORIENTED_EDGE('',*,*,#49561,.F.);
#76300=ORIENTED_EDGE('',*,*,#49592,.F.);
#76301=ORIENTED_EDGE('',*,*,#49598,.F.);
#76302=ORIENTED_EDGE('',*,*,#49604,.F.);
#76303=ORIENTED_EDGE('',*,*,#49606,.F.);
#76304=ORIENTED_EDGE('',*,*,#49602,.F.);
#76305=ORIENTED_EDGE('',*,*,#49596,.F.);
#76306=ORIENTED_EDGE('',*,*,#49590,.F.);
#76307=ORIENTED_EDGE('',*,*,#49585,.F.);
#76308=ORIENTED_EDGE('',*,*,#49616,.F.);
#76309=ORIENTED_EDGE('',*,*,#49622,.F.);
#76310=ORIENTED_EDGE('',*,*,#49628,.F.);
#76311=ORIENTED_EDGE('',*,*,#49630,.F.);
#76312=ORIENTED_EDGE('',*,*,#49626,.F.);
#76313=ORIENTED_EDGE('',*,*,#49620,.F.);
#76314=ORIENTED_EDGE('',*,*,#49614,.F.);
#76315=ORIENTED_EDGE('',*,*,#49609,.F.);
#76316=ORIENTED_EDGE('',*,*,#49640,.F.);
#76317=ORIENTED_EDGE('',*,*,#49646,.F.);
#76318=ORIENTED_EDGE('',*,*,#49652,.F.);
#76319=ORIENTED_EDGE('',*,*,#49658,.F.);
#76320=ORIENTED_EDGE('',*,*,#49660,.F.);
#76321=ORIENTED_EDGE('',*,*,#49656,.F.);
#76322=ORIENTED_EDGE('',*,*,#49650,.F.);
#76323=ORIENTED_EDGE('',*,*,#49644,.F.);
#76324=ORIENTED_EDGE('',*,*,#49638,.F.);
#76325=ORIENTED_EDGE('',*,*,#49633,.F.);
#76326=ORIENTED_EDGE('',*,*,#49670,.F.);
#76327=ORIENTED_EDGE('',*,*,#49676,.F.);
#76328=ORIENTED_EDGE('',*,*,#49682,.F.);
#76329=ORIENTED_EDGE('',*,*,#49684,.F.);
#76330=ORIENTED_EDGE('',*,*,#49680,.F.);
#76331=ORIENTED_EDGE('',*,*,#49674,.F.);
#76332=ORIENTED_EDGE('',*,*,#49668,.F.);
#76333=ORIENTED_EDGE('',*,*,#49663,.F.);
#76334=ORIENTED_EDGE('',*,*,#49694,.F.);
#76335=ORIENTED_EDGE('',*,*,#49700,.F.);
#76336=ORIENTED_EDGE('',*,*,#49706,.F.);
#76337=ORIENTED_EDGE('',*,*,#49708,.F.);
#76338=ORIENTED_EDGE('',*,*,#49704,.F.);
#76339=ORIENTED_EDGE('',*,*,#49698,.F.);
#76340=ORIENTED_EDGE('',*,*,#49692,.F.);
#76341=ORIENTED_EDGE('',*,*,#49687,.F.);
#76342=ORIENTED_EDGE('',*,*,#49718,.F.);
#76343=ORIENTED_EDGE('',*,*,#49724,.F.);
#76344=ORIENTED_EDGE('',*,*,#49730,.F.);
#76345=ORIENTED_EDGE('',*,*,#49736,.F.);
#76346=ORIENTED_EDGE('',*,*,#49738,.F.);
#76347=ORIENTED_EDGE('',*,*,#49734,.F.);
#76348=ORIENTED_EDGE('',*,*,#49728,.F.);
#76349=ORIENTED_EDGE('',*,*,#49722,.F.);
#76350=ORIENTED_EDGE('',*,*,#49716,.F.);
#76351=ORIENTED_EDGE('',*,*,#49711,.F.);
#76352=ORIENTED_EDGE('',*,*,#49748,.F.);
#76353=ORIENTED_EDGE('',*,*,#49754,.F.);
#76354=ORIENTED_EDGE('',*,*,#49760,.F.);
#76355=ORIENTED_EDGE('',*,*,#49766,.F.);
#76356=ORIENTED_EDGE('',*,*,#49768,.F.);
#76357=ORIENTED_EDGE('',*,*,#49764,.F.);
#76358=ORIENTED_EDGE('',*,*,#49758,.F.);
#76359=ORIENTED_EDGE('',*,*,#49752,.F.);
#76360=ORIENTED_EDGE('',*,*,#49746,.F.);
#76361=ORIENTED_EDGE('',*,*,#49741,.F.);
#76362=ORIENTED_EDGE('',*,*,#49778,.F.);
#76363=ORIENTED_EDGE('',*,*,#49784,.F.);
#76364=ORIENTED_EDGE('',*,*,#49790,.F.);
#76365=ORIENTED_EDGE('',*,*,#49792,.F.);
#76366=ORIENTED_EDGE('',*,*,#49788,.F.);
#76367=ORIENTED_EDGE('',*,*,#49782,.F.);
#76368=ORIENTED_EDGE('',*,*,#49776,.F.);
#76369=ORIENTED_EDGE('',*,*,#49771,.F.);
#76370=ORIENTED_EDGE('',*,*,#49802,.F.);
#76371=ORIENTED_EDGE('',*,*,#49808,.F.);
#76372=ORIENTED_EDGE('',*,*,#49814,.F.);
#76373=ORIENTED_EDGE('',*,*,#49816,.F.);
#76374=ORIENTED_EDGE('',*,*,#49812,.F.);
#76375=ORIENTED_EDGE('',*,*,#49806,.F.);
#76376=ORIENTED_EDGE('',*,*,#49800,.F.);
#76377=ORIENTED_EDGE('',*,*,#49795,.F.);
#76378=ORIENTED_EDGE('',*,*,#49826,.F.);
#76379=ORIENTED_EDGE('',*,*,#49832,.F.);
#76380=ORIENTED_EDGE('',*,*,#49838,.F.);
#76381=ORIENTED_EDGE('',*,*,#49840,.F.);
#76382=ORIENTED_EDGE('',*,*,#49836,.F.);
#76383=ORIENTED_EDGE('',*,*,#49830,.F.);
#76384=ORIENTED_EDGE('',*,*,#49824,.F.);
#76385=ORIENTED_EDGE('',*,*,#49819,.F.);
#76386=ORIENTED_EDGE('',*,*,#49850,.F.);
#76387=ORIENTED_EDGE('',*,*,#49856,.F.);
#76388=ORIENTED_EDGE('',*,*,#49862,.F.);
#76389=ORIENTED_EDGE('',*,*,#49864,.F.);
#76390=ORIENTED_EDGE('',*,*,#49860,.F.);
#76391=ORIENTED_EDGE('',*,*,#49854,.F.);
#76392=ORIENTED_EDGE('',*,*,#49848,.F.);
#76393=ORIENTED_EDGE('',*,*,#49843,.F.);
#76394=ORIENTED_EDGE('',*,*,#49874,.F.);
#76395=ORIENTED_EDGE('',*,*,#49880,.F.);
#76396=ORIENTED_EDGE('',*,*,#49886,.F.);
#76397=ORIENTED_EDGE('',*,*,#49892,.F.);
#76398=ORIENTED_EDGE('',*,*,#49888,.F.);
#76399=ORIENTED_EDGE('',*,*,#49884,.F.);
#76400=ORIENTED_EDGE('',*,*,#49878,.F.);
#76401=ORIENTED_EDGE('',*,*,#49872,.F.);
#76402=ORIENTED_EDGE('',*,*,#49867,.F.);
#76403=ORIENTED_EDGE('',*,*,#49901,.F.);
#76404=ORIENTED_EDGE('',*,*,#49907,.F.);
#76405=ORIENTED_EDGE('',*,*,#49913,.F.);
#76406=ORIENTED_EDGE('',*,*,#49915,.F.);
#76407=ORIENTED_EDGE('',*,*,#49911,.F.);
#76408=ORIENTED_EDGE('',*,*,#49905,.F.);
#76409=ORIENTED_EDGE('',*,*,#49899,.F.);
#76410=ORIENTED_EDGE('',*,*,#49894,.F.);
#76411=ORIENTED_EDGE('',*,*,#49925,.F.);
#76412=ORIENTED_EDGE('',*,*,#49931,.F.);
#76413=ORIENTED_EDGE('',*,*,#49937,.F.);
#76414=ORIENTED_EDGE('',*,*,#49943,.F.);
#76415=ORIENTED_EDGE('',*,*,#49945,.F.);
#76416=ORIENTED_EDGE('',*,*,#49941,.F.);
#76417=ORIENTED_EDGE('',*,*,#49935,.F.);
#76418=ORIENTED_EDGE('',*,*,#49929,.F.);
#76419=ORIENTED_EDGE('',*,*,#49923,.F.);
#76420=ORIENTED_EDGE('',*,*,#49918,.F.);
#76421=ORIENTED_EDGE('',*,*,#49955,.F.);
#76422=ORIENTED_EDGE('',*,*,#49961,.F.);
#76423=ORIENTED_EDGE('',*,*,#49967,.F.);
#76424=ORIENTED_EDGE('',*,*,#49969,.F.);
#76425=ORIENTED_EDGE('',*,*,#49965,.F.);
#76426=ORIENTED_EDGE('',*,*,#49959,.F.);
#76427=ORIENTED_EDGE('',*,*,#49953,.F.);
#76428=ORIENTED_EDGE('',*,*,#49948,.F.);
#76429=ORIENTED_EDGE('',*,*,#49979,.F.);
#76430=ORIENTED_EDGE('',*,*,#49985,.F.);
#76431=ORIENTED_EDGE('',*,*,#49991,.F.);
#76432=ORIENTED_EDGE('',*,*,#49997,.F.);
#76433=ORIENTED_EDGE('',*,*,#49999,.F.);
#76434=ORIENTED_EDGE('',*,*,#49995,.F.);
#76435=ORIENTED_EDGE('',*,*,#49989,.F.);
#76436=ORIENTED_EDGE('',*,*,#49983,.F.);
#76437=ORIENTED_EDGE('',*,*,#49977,.F.);
#76438=ORIENTED_EDGE('',*,*,#49972,.F.);
#76439=ORIENTED_EDGE('',*,*,#50009,.F.);
#76440=ORIENTED_EDGE('',*,*,#50015,.F.);
#76441=ORIENTED_EDGE('',*,*,#50021,.F.);
#76442=ORIENTED_EDGE('',*,*,#50023,.F.);
#76443=ORIENTED_EDGE('',*,*,#50019,.F.);
#76444=ORIENTED_EDGE('',*,*,#50013,.F.);
#76445=ORIENTED_EDGE('',*,*,#50007,.F.);
#76446=ORIENTED_EDGE('',*,*,#50002,.F.);
#76447=ORIENTED_EDGE('',*,*,#50033,.F.);
#76448=ORIENTED_EDGE('',*,*,#50039,.F.);
#76449=ORIENTED_EDGE('',*,*,#50045,.F.);
#76450=ORIENTED_EDGE('',*,*,#50047,.F.);
#76451=ORIENTED_EDGE('',*,*,#50043,.F.);
#76452=ORIENTED_EDGE('',*,*,#50037,.F.);
#76453=ORIENTED_EDGE('',*,*,#50031,.F.);
#76454=ORIENTED_EDGE('',*,*,#50026,.F.);
#76455=ORIENTED_EDGE('',*,*,#50057,.F.);
#76456=ORIENTED_EDGE('',*,*,#50063,.F.);
#76457=ORIENTED_EDGE('',*,*,#50069,.F.);
#76458=ORIENTED_EDGE('',*,*,#50071,.F.);
#76459=ORIENTED_EDGE('',*,*,#50067,.F.);
#76460=ORIENTED_EDGE('',*,*,#50061,.F.);
#76461=ORIENTED_EDGE('',*,*,#50055,.F.);
#76462=ORIENTED_EDGE('',*,*,#50050,.F.);
#76463=ORIENTED_EDGE('',*,*,#50081,.F.);
#76464=ORIENTED_EDGE('',*,*,#50087,.F.);
#76465=ORIENTED_EDGE('',*,*,#50093,.F.);
#76466=ORIENTED_EDGE('',*,*,#50095,.F.);
#76467=ORIENTED_EDGE('',*,*,#50091,.F.);
#76468=ORIENTED_EDGE('',*,*,#50085,.F.);
#76469=ORIENTED_EDGE('',*,*,#50079,.F.);
#76470=ORIENTED_EDGE('',*,*,#50074,.F.);
#76471=ORIENTED_EDGE('',*,*,#50105,.F.);
#76472=ORIENTED_EDGE('',*,*,#50111,.F.);
#76473=ORIENTED_EDGE('',*,*,#50113,.F.);
#76474=ORIENTED_EDGE('',*,*,#50109,.F.);
#76475=ORIENTED_EDGE('',*,*,#50103,.F.);
#76476=ORIENTED_EDGE('',*,*,#50098,.F.);
#76477=ORIENTED_EDGE('',*,*,#50123,.F.);
#76478=ORIENTED_EDGE('',*,*,#50129,.F.);
#76479=ORIENTED_EDGE('',*,*,#50131,.F.);
#76480=ORIENTED_EDGE('',*,*,#50127,.F.);
#76481=ORIENTED_EDGE('',*,*,#50121,.F.);
#76482=ORIENTED_EDGE('',*,*,#50115,.F.);
#76483=ORIENTED_EDGE('',*,*,#52438,.T.);
#76484=ORIENTED_EDGE('',*,*,#52433,.T.);
#76485=ORIENTED_EDGE('',*,*,#53086,.F.);
#76486=ORIENTED_EDGE('',*,*,#52409,.T.);
#76487=ORIENTED_EDGE('',*,*,#52406,.T.);
#76488=ORIENTED_EDGE('',*,*,#52403,.T.);
#76489=ORIENTED_EDGE('',*,*,#52400,.T.);
#76490=ORIENTED_EDGE('',*,*,#52397,.T.);
#76491=ORIENTED_EDGE('',*,*,#52394,.T.);
#76492=ORIENTED_EDGE('',*,*,#52391,.T.);
#76493=ORIENTED_EDGE('',*,*,#53084,.F.);
#76494=ORIENTED_EDGE('',*,*,#52387,.T.);
#76495=ORIENTED_EDGE('',*,*,#52384,.T.);
#76496=ORIENTED_EDGE('',*,*,#52381,.T.);
#76497=ORIENTED_EDGE('',*,*,#52378,.T.);
#76498=ORIENTED_EDGE('',*,*,#52373,.T.);
#76499=ORIENTED_EDGE('',*,*,#52372,.T.);
#76500=ORIENTED_EDGE('',*,*,#52369,.T.);
#76501=ORIENTED_EDGE('',*,*,#53082,.F.);
#76502=ORIENTED_EDGE('',*,*,#52431,.T.);
#76503=ORIENTED_EDGE('',*,*,#52428,.T.);
#76504=ORIENTED_EDGE('',*,*,#52425,.T.);
#76505=ORIENTED_EDGE('',*,*,#52422,.T.);
#76506=ORIENTED_EDGE('',*,*,#52417,.T.);
#76507=ORIENTED_EDGE('',*,*,#52416,.T.);
#76508=ORIENTED_EDGE('',*,*,#52413,.T.);
#76509=ORIENTED_EDGE('',*,*,#53080,.F.);
#76510=ORIENTED_EDGE('',*,*,#50222,.F.);
#76511=ORIENTED_EDGE('',*,*,#50226,.F.);
#76512=ORIENTED_EDGE('',*,*,#50228,.F.);
#76513=ORIENTED_EDGE('',*,*,#50232,.F.);
#76514=ORIENTED_EDGE('',*,*,#50235,.F.);
#76515=ORIENTED_EDGE('',*,*,#50238,.F.);
#76516=ORIENTED_EDGE('',*,*,#50241,.F.);
#76517=ORIENTED_EDGE('',*,*,#53078,.T.);
#76518=ORIENTED_EDGE('',*,*,#50178,.F.);
#76519=ORIENTED_EDGE('',*,*,#50182,.F.);
#76520=ORIENTED_EDGE('',*,*,#50184,.F.);
#76521=ORIENTED_EDGE('',*,*,#50188,.F.);
#76522=ORIENTED_EDGE('',*,*,#50191,.F.);
#76523=ORIENTED_EDGE('',*,*,#50194,.F.);
#76524=ORIENTED_EDGE('',*,*,#50197,.F.);
#76525=ORIENTED_EDGE('',*,*,#53076,.T.);
#76526=ORIENTED_EDGE('',*,*,#50200,.F.);
#76527=ORIENTED_EDGE('',*,*,#50204,.F.);
#76528=ORIENTED_EDGE('',*,*,#50207,.F.);
#76529=ORIENTED_EDGE('',*,*,#50210,.F.);
#76530=ORIENTED_EDGE('',*,*,#50213,.F.);
#76531=ORIENTED_EDGE('',*,*,#50216,.F.);
#76532=ORIENTED_EDGE('',*,*,#50219,.F.);
#76533=ORIENTED_EDGE('',*,*,#53074,.T.);
#76534=ORIENTED_EDGE('',*,*,#50246,.F.);
#76535=ORIENTED_EDGE('',*,*,#50248,.F.);
#76536=ORIENTED_EDGE('',*,*,#50251,.F.);
#76537=ORIENTED_EDGE('',*,*,#50254,.F.);
#76538=ORIENTED_EDGE('',*,*,#50257,.F.);
#76539=ORIENTED_EDGE('',*,*,#50260,.F.);
#76540=ORIENTED_EDGE('',*,*,#50263,.F.);
#76541=ORIENTED_EDGE('',*,*,#53072,.F.);
#76542=ORIENTED_EDGE('',*,*,#53088,.F.);
#76543=ORIENTED_EDGE('',*,*,#52453,.T.);
#76544=ORIENTED_EDGE('',*,*,#52450,.T.);
#76545=ORIENTED_EDGE('',*,*,#52447,.T.);
#76546=ORIENTED_EDGE('',*,*,#52444,.T.);
#76547=ORIENTED_EDGE('',*,*,#52441,.T.);
#76548=ORIENTED_EDGE('',*,*,#51567,.T.);
#76549=ORIENTED_EDGE('',*,*,#51558,.T.);
#76550=ORIENTED_EDGE('',*,*,#51563,.T.);
#76551=ORIENTED_EDGE('',*,*,#51569,.T.);
#76552=ORIENTED_EDGE('',*,*,#51575,.T.);
#76553=ORIENTED_EDGE('',*,*,#51581,.T.);
#76554=ORIENTED_EDGE('',*,*,#51587,.T.);
#76555=ORIENTED_EDGE('',*,*,#51585,.T.);
#76556=ORIENTED_EDGE('',*,*,#51579,.T.);
#76557=ORIENTED_EDGE('',*,*,#51573,.T.);
#76558=ORIENTED_EDGE('',*,*,#51597,.T.);
#76559=ORIENTED_EDGE('',*,*,#51588,.T.);
#76560=ORIENTED_EDGE('',*,*,#51593,.T.);
#76561=ORIENTED_EDGE('',*,*,#51599,.T.);
#76562=ORIENTED_EDGE('',*,*,#51605,.T.);
#76563=ORIENTED_EDGE('',*,*,#51611,.T.);
#76564=ORIENTED_EDGE('',*,*,#51609,.T.);
#76565=ORIENTED_EDGE('',*,*,#51603,.T.);
#76566=ORIENTED_EDGE('',*,*,#51621,.T.);
#76567=ORIENTED_EDGE('',*,*,#51612,.T.);
#76568=ORIENTED_EDGE('',*,*,#51617,.T.);
#76569=ORIENTED_EDGE('',*,*,#51623,.T.);
#76570=ORIENTED_EDGE('',*,*,#51629,.T.);
#76571=ORIENTED_EDGE('',*,*,#51635,.T.);
#76572=ORIENTED_EDGE('',*,*,#51633,.T.);
#76573=ORIENTED_EDGE('',*,*,#51627,.T.);
#76574=ORIENTED_EDGE('',*,*,#51645,.T.);
#76575=ORIENTED_EDGE('',*,*,#51639,.T.);
#76576=ORIENTED_EDGE('',*,*,#51641,.T.);
#76577=ORIENTED_EDGE('',*,*,#51647,.T.);
#76578=ORIENTED_EDGE('',*,*,#51653,.T.);
#76579=ORIENTED_EDGE('',*,*,#51659,.T.);
#76580=ORIENTED_EDGE('',*,*,#51657,.T.);
#76581=ORIENTED_EDGE('',*,*,#51651,.T.);
#76582=ORIENTED_EDGE('',*,*,#51669,.T.);
#76583=ORIENTED_EDGE('',*,*,#51663,.T.);
#76584=ORIENTED_EDGE('',*,*,#51665,.T.);
#76585=ORIENTED_EDGE('',*,*,#51671,.T.);
#76586=ORIENTED_EDGE('',*,*,#51677,.T.);
#76587=ORIENTED_EDGE('',*,*,#51683,.T.);
#76588=ORIENTED_EDGE('',*,*,#51685,.T.);
#76589=ORIENTED_EDGE('',*,*,#51681,.T.);
#76590=ORIENTED_EDGE('',*,*,#51675,.T.);
#76591=ORIENTED_EDGE('',*,*,#51696,.T.);
#76592=ORIENTED_EDGE('',*,*,#51690,.T.);
#76593=ORIENTED_EDGE('',*,*,#51692,.T.);
#76594=ORIENTED_EDGE('',*,*,#51698,.T.);
#76595=ORIENTED_EDGE('',*,*,#51704,.T.);
#76596=ORIENTED_EDGE('',*,*,#51710,.T.);
#76597=ORIENTED_EDGE('',*,*,#51708,.T.);
#76598=ORIENTED_EDGE('',*,*,#51702,.T.);
#76599=ORIENTED_EDGE('',*,*,#51720,.T.);
#76600=ORIENTED_EDGE('',*,*,#51714,.T.);
#76601=ORIENTED_EDGE('',*,*,#51716,.T.);
#76602=ORIENTED_EDGE('',*,*,#51722,.T.);
#76603=ORIENTED_EDGE('',*,*,#51728,.T.);
#76604=ORIENTED_EDGE('',*,*,#51734,.T.);
#76605=ORIENTED_EDGE('',*,*,#51732,.T.);
#76606=ORIENTED_EDGE('',*,*,#51726,.T.);
#76607=ORIENTED_EDGE('',*,*,#51744,.T.);
#76608=ORIENTED_EDGE('',*,*,#51738,.T.);
#76609=ORIENTED_EDGE('',*,*,#51740,.T.);
#76610=ORIENTED_EDGE('',*,*,#51746,.T.);
#76611=ORIENTED_EDGE('',*,*,#51752,.T.);
#76612=ORIENTED_EDGE('',*,*,#51758,.T.);
#76613=ORIENTED_EDGE('',*,*,#51756,.T.);
#76614=ORIENTED_EDGE('',*,*,#51750,.T.);
#76615=ORIENTED_EDGE('',*,*,#51768,.T.);
#76616=ORIENTED_EDGE('',*,*,#51762,.T.);
#76617=ORIENTED_EDGE('',*,*,#51764,.T.);
#76618=ORIENTED_EDGE('',*,*,#51770,.T.);
#76619=ORIENTED_EDGE('',*,*,#51776,.T.);
#76620=ORIENTED_EDGE('',*,*,#51782,.T.);
#76621=ORIENTED_EDGE('',*,*,#51780,.T.);
#76622=ORIENTED_EDGE('',*,*,#51774,.T.);
#76623=ORIENTED_EDGE('',*,*,#51792,.T.);
#76624=ORIENTED_EDGE('',*,*,#51786,.T.);
#76625=ORIENTED_EDGE('',*,*,#51788,.T.);
#76626=ORIENTED_EDGE('',*,*,#51794,.T.);
#76627=ORIENTED_EDGE('',*,*,#51800,.T.);
#76628=ORIENTED_EDGE('',*,*,#51806,.T.);
#76629=ORIENTED_EDGE('',*,*,#51804,.T.);
#76630=ORIENTED_EDGE('',*,*,#51798,.T.);
#76631=ORIENTED_EDGE('',*,*,#51816,.T.);
#76632=ORIENTED_EDGE('',*,*,#51810,.T.);
#76633=ORIENTED_EDGE('',*,*,#51812,.T.);
#76634=ORIENTED_EDGE('',*,*,#51818,.T.);
#76635=ORIENTED_EDGE('',*,*,#51824,.T.);
#76636=ORIENTED_EDGE('',*,*,#51830,.T.);
#76637=ORIENTED_EDGE('',*,*,#51836,.T.);
#76638=ORIENTED_EDGE('',*,*,#51834,.T.);
#76639=ORIENTED_EDGE('',*,*,#51828,.T.);
#76640=ORIENTED_EDGE('',*,*,#51822,.T.);
#76641=ORIENTED_EDGE('',*,*,#51846,.T.);
#76642=ORIENTED_EDGE('',*,*,#51840,.T.);
#76643=ORIENTED_EDGE('',*,*,#51842,.T.);
#76644=ORIENTED_EDGE('',*,*,#51848,.T.);
#76645=ORIENTED_EDGE('',*,*,#51854,.T.);
#76646=ORIENTED_EDGE('',*,*,#51860,.T.);
#76647=ORIENTED_EDGE('',*,*,#51858,.T.);
#76648=ORIENTED_EDGE('',*,*,#51852,.T.);
#76649=ORIENTED_EDGE('',*,*,#51870,.T.);
#76650=ORIENTED_EDGE('',*,*,#51864,.T.);
#76651=ORIENTED_EDGE('',*,*,#51866,.T.);
#76652=ORIENTED_EDGE('',*,*,#51872,.T.);
#76653=ORIENTED_EDGE('',*,*,#51878,.T.);
#76654=ORIENTED_EDGE('',*,*,#51884,.T.);
#76655=ORIENTED_EDGE('',*,*,#51882,.T.);
#76656=ORIENTED_EDGE('',*,*,#51876,.T.);
#76657=ORIENTED_EDGE('',*,*,#51894,.T.);
#76658=ORIENTED_EDGE('',*,*,#51888,.T.);
#76659=ORIENTED_EDGE('',*,*,#51890,.T.);
#76660=ORIENTED_EDGE('',*,*,#51896,.T.);
#76661=ORIENTED_EDGE('',*,*,#51902,.T.);
#76662=ORIENTED_EDGE('',*,*,#51908,.T.);
#76663=ORIENTED_EDGE('',*,*,#51914,.T.);
#76664=ORIENTED_EDGE('',*,*,#51912,.T.);
#76665=ORIENTED_EDGE('',*,*,#51906,.T.);
#76666=ORIENTED_EDGE('',*,*,#51900,.T.);
#76667=ORIENTED_EDGE('',*,*,#51924,.T.);
#76668=ORIENTED_EDGE('',*,*,#51918,.T.);
#76669=ORIENTED_EDGE('',*,*,#51920,.T.);
#76670=ORIENTED_EDGE('',*,*,#51926,.T.);
#76671=ORIENTED_EDGE('',*,*,#51932,.T.);
#76672=ORIENTED_EDGE('',*,*,#51938,.T.);
#76673=ORIENTED_EDGE('',*,*,#51944,.T.);
#76674=ORIENTED_EDGE('',*,*,#51942,.T.);
#76675=ORIENTED_EDGE('',*,*,#51936,.T.);
#76676=ORIENTED_EDGE('',*,*,#51930,.T.);
#76677=ORIENTED_EDGE('',*,*,#51954,.T.);
#76678=ORIENTED_EDGE('',*,*,#51948,.T.);
#76679=ORIENTED_EDGE('',*,*,#51950,.T.);
#76680=ORIENTED_EDGE('',*,*,#51956,.T.);
#76681=ORIENTED_EDGE('',*,*,#51962,.T.);
#76682=ORIENTED_EDGE('',*,*,#51968,.T.);
#76683=ORIENTED_EDGE('',*,*,#51966,.T.);
#76684=ORIENTED_EDGE('',*,*,#51960,.T.);
#76685=ORIENTED_EDGE('',*,*,#51978,.T.);
#76686=ORIENTED_EDGE('',*,*,#51972,.T.);
#76687=ORIENTED_EDGE('',*,*,#51974,.T.);
#76688=ORIENTED_EDGE('',*,*,#51980,.T.);
#76689=ORIENTED_EDGE('',*,*,#51986,.T.);
#76690=ORIENTED_EDGE('',*,*,#51992,.T.);
#76691=ORIENTED_EDGE('',*,*,#51990,.T.);
#76692=ORIENTED_EDGE('',*,*,#51984,.T.);
#76693=ORIENTED_EDGE('',*,*,#52002,.T.);
#76694=ORIENTED_EDGE('',*,*,#51996,.T.);
#76695=ORIENTED_EDGE('',*,*,#51998,.T.);
#76696=ORIENTED_EDGE('',*,*,#52004,.T.);
#76697=ORIENTED_EDGE('',*,*,#52010,.T.);
#76698=ORIENTED_EDGE('',*,*,#52016,.T.);
#76699=ORIENTED_EDGE('',*,*,#52014,.T.);
#76700=ORIENTED_EDGE('',*,*,#52008,.T.);
#76701=ORIENTED_EDGE('',*,*,#52026,.T.);
#76702=ORIENTED_EDGE('',*,*,#52020,.T.);
#76703=ORIENTED_EDGE('',*,*,#52022,.T.);
#76704=ORIENTED_EDGE('',*,*,#52028,.T.);
#76705=ORIENTED_EDGE('',*,*,#52034,.T.);
#76706=ORIENTED_EDGE('',*,*,#52040,.T.);
#76707=ORIENTED_EDGE('',*,*,#52038,.T.);
#76708=ORIENTED_EDGE('',*,*,#52032,.T.);
#76709=ORIENTED_EDGE('',*,*,#52050,.T.);
#76710=ORIENTED_EDGE('',*,*,#52044,.T.);
#76711=ORIENTED_EDGE('',*,*,#52046,.T.);
#76712=ORIENTED_EDGE('',*,*,#52052,.T.);
#76713=ORIENTED_EDGE('',*,*,#52058,.T.);
#76714=ORIENTED_EDGE('',*,*,#52063,.T.);
#76715=ORIENTED_EDGE('',*,*,#52066,.T.);
#76716=ORIENTED_EDGE('',*,*,#52062,.T.);
#76717=ORIENTED_EDGE('',*,*,#52056,.T.);
#76718=ORIENTED_EDGE('',*,*,#52077,.T.);
#76719=ORIENTED_EDGE('',*,*,#52071,.T.);
#76720=ORIENTED_EDGE('',*,*,#52073,.T.);
#76721=ORIENTED_EDGE('',*,*,#52079,.T.);
#76722=ORIENTED_EDGE('',*,*,#52085,.T.);
#76723=ORIENTED_EDGE('',*,*,#52091,.T.);
#76724=ORIENTED_EDGE('',*,*,#52089,.T.);
#76725=ORIENTED_EDGE('',*,*,#52083,.T.);
#76726=ORIENTED_EDGE('',*,*,#52101,.T.);
#76727=ORIENTED_EDGE('',*,*,#52095,.T.);
#76728=ORIENTED_EDGE('',*,*,#52097,.T.);
#76729=ORIENTED_EDGE('',*,*,#52103,.T.);
#76730=ORIENTED_EDGE('',*,*,#52109,.T.);
#76731=ORIENTED_EDGE('',*,*,#52115,.T.);
#76732=ORIENTED_EDGE('',*,*,#52121,.T.);
#76733=ORIENTED_EDGE('',*,*,#52119,.T.);
#76734=ORIENTED_EDGE('',*,*,#52113,.T.);
#76735=ORIENTED_EDGE('',*,*,#52107,.T.);
#76736=ORIENTED_EDGE('',*,*,#52131,.T.);
#76737=ORIENTED_EDGE('',*,*,#52125,.T.);
#76738=ORIENTED_EDGE('',*,*,#52127,.T.);
#76739=ORIENTED_EDGE('',*,*,#52133,.T.);
#76740=ORIENTED_EDGE('',*,*,#52139,.T.);
#76741=ORIENTED_EDGE('',*,*,#52145,.T.);
#76742=ORIENTED_EDGE('',*,*,#52143,.T.);
#76743=ORIENTED_EDGE('',*,*,#52137,.T.);
#76744=ORIENTED_EDGE('',*,*,#52155,.T.);
#76745=ORIENTED_EDGE('',*,*,#52149,.T.);
#76746=ORIENTED_EDGE('',*,*,#52151,.T.);
#76747=ORIENTED_EDGE('',*,*,#52157,.T.);
#76748=ORIENTED_EDGE('',*,*,#52163,.T.);
#76749=ORIENTED_EDGE('',*,*,#52169,.T.);
#76750=ORIENTED_EDGE('',*,*,#52175,.T.);
#76751=ORIENTED_EDGE('',*,*,#52173,.T.);
#76752=ORIENTED_EDGE('',*,*,#52167,.T.);
#76753=ORIENTED_EDGE('',*,*,#52161,.T.);
#76754=ORIENTED_EDGE('',*,*,#52185,.T.);
#76755=ORIENTED_EDGE('',*,*,#52179,.T.);
#76756=ORIENTED_EDGE('',*,*,#52181,.T.);
#76757=ORIENTED_EDGE('',*,*,#52187,.T.);
#76758=ORIENTED_EDGE('',*,*,#52193,.T.);
#76759=ORIENTED_EDGE('',*,*,#52199,.T.);
#76760=ORIENTED_EDGE('',*,*,#52197,.T.);
#76761=ORIENTED_EDGE('',*,*,#52191,.T.);
#76762=ORIENTED_EDGE('',*,*,#52209,.T.);
#76763=ORIENTED_EDGE('',*,*,#52203,.T.);
#76764=ORIENTED_EDGE('',*,*,#52205,.T.);
#76765=ORIENTED_EDGE('',*,*,#52211,.T.);
#76766=ORIENTED_EDGE('',*,*,#52217,.T.);
#76767=ORIENTED_EDGE('',*,*,#52223,.T.);
#76768=ORIENTED_EDGE('',*,*,#52221,.T.);
#76769=ORIENTED_EDGE('',*,*,#52215,.T.);
#76770=ORIENTED_EDGE('',*,*,#52233,.T.);
#76771=ORIENTED_EDGE('',*,*,#52227,.T.);
#76772=ORIENTED_EDGE('',*,*,#52229,.T.);
#76773=ORIENTED_EDGE('',*,*,#52235,.T.);
#76774=ORIENTED_EDGE('',*,*,#52241,.T.);
#76775=ORIENTED_EDGE('',*,*,#52247,.T.);
#76776=ORIENTED_EDGE('',*,*,#52245,.T.);
#76777=ORIENTED_EDGE('',*,*,#52239,.T.);
#76778=ORIENTED_EDGE('',*,*,#52257,.T.);
#76779=ORIENTED_EDGE('',*,*,#52251,.T.);
#76780=ORIENTED_EDGE('',*,*,#52253,.T.);
#76781=ORIENTED_EDGE('',*,*,#52259,.T.);
#76782=ORIENTED_EDGE('',*,*,#52265,.T.);
#76783=ORIENTED_EDGE('',*,*,#52271,.T.);
#76784=ORIENTED_EDGE('',*,*,#52269,.T.);
#76785=ORIENTED_EDGE('',*,*,#52263,.T.);
#76786=ORIENTED_EDGE('',*,*,#52281,.T.);
#76787=ORIENTED_EDGE('',*,*,#52275,.T.);
#76788=ORIENTED_EDGE('',*,*,#52277,.T.);
#76789=ORIENTED_EDGE('',*,*,#52283,.T.);
#76790=ORIENTED_EDGE('',*,*,#52289,.T.);
#76791=ORIENTED_EDGE('',*,*,#52287,.T.);
#76792=ORIENTED_EDGE('',*,*,#52299,.T.);
#76793=ORIENTED_EDGE('',*,*,#52290,.T.);
#76794=ORIENTED_EDGE('',*,*,#52295,.T.);
#76795=ORIENTED_EDGE('',*,*,#52301,.T.);
#76796=ORIENTED_EDGE('',*,*,#52307,.T.);
#76797=ORIENTED_EDGE('',*,*,#52305,.T.);
#76798=ORIENTED_EDGE('',*,*,#53486,.T.);
#76799=ORIENTED_EDGE('',*,*,#52359,.T.);
#76800=ORIENTED_EDGE('',*,*,#53487,.F.);
#76801=ORIENTED_EDGE('',*,*,#53488,.T.);
#76802=ORIENTED_EDGE('',*,*,#53489,.T.);
#76803=ORIENTED_EDGE('',*,*,#52356,.T.);
#76804=ORIENTED_EDGE('',*,*,#53486,.F.);
#76805=ORIENTED_EDGE('',*,*,#53490,.T.);
#76806=ORIENTED_EDGE('',*,*,#53491,.T.);
#76807=ORIENTED_EDGE('',*,*,#52353,.T.);
#76808=ORIENTED_EDGE('',*,*,#53489,.F.);
#76809=ORIENTED_EDGE('',*,*,#53492,.T.);
#76810=ORIENTED_EDGE('',*,*,#53493,.T.);
#76811=ORIENTED_EDGE('',*,*,#52350,.T.);
#76812=ORIENTED_EDGE('',*,*,#53491,.F.);
#76813=ORIENTED_EDGE('',*,*,#53494,.T.);
#76814=ORIENTED_EDGE('',*,*,#53495,.T.);
#76815=ORIENTED_EDGE('',*,*,#52347,.T.);
#76816=ORIENTED_EDGE('',*,*,#53493,.F.);
#76817=ORIENTED_EDGE('',*,*,#53496,.T.);
#76818=ORIENTED_EDGE('',*,*,#53497,.T.);
#76819=ORIENTED_EDGE('',*,*,#52344,.T.);
#76820=ORIENTED_EDGE('',*,*,#53495,.F.);
#76821=ORIENTED_EDGE('',*,*,#53498,.T.);
#76822=ORIENTED_EDGE('',*,*,#53499,.T.);
#76823=ORIENTED_EDGE('',*,*,#51180,.T.);
#76824=ORIENTED_EDGE('',*,*,#52341,.T.);
#76825=ORIENTED_EDGE('',*,*,#53497,.F.);
#76826=ORIENTED_EDGE('',*,*,#53500,.T.);
#76827=ORIENTED_EDGE('',*,*,#53501,.T.);
#76828=ORIENTED_EDGE('',*,*,#52364,.T.);
#76829=ORIENTED_EDGE('',*,*,#51183,.F.);
#76830=ORIENTED_EDGE('',*,*,#53487,.T.);
#76831=ORIENTED_EDGE('',*,*,#52362,.T.);
#76832=ORIENTED_EDGE('',*,*,#53501,.F.);
#76833=ORIENTED_EDGE('',*,*,#53502,.T.);
#76834=ORIENTED_EDGE('',*,*,#53503,.T.);
#76835=ORIENTED_EDGE('',*,*,#51185,.F.);
#76836=ORIENTED_EDGE('',*,*,#51198,.F.);
#76837=ORIENTED_EDGE('',*,*,#51196,.F.);
#76838=ORIENTED_EDGE('',*,*,#51194,.F.);
#76839=ORIENTED_EDGE('',*,*,#51192,.F.);
#76840=ORIENTED_EDGE('',*,*,#51190,.F.);
#76841=ORIENTED_EDGE('',*,*,#51188,.F.);
#76842=ORIENTED_EDGE('',*,*,#53504,.T.);
#76843=ORIENTED_EDGE('',*,*,#53505,.T.);
#76844=ORIENTED_EDGE('',*,*,#53506,.T.);
#76845=ORIENTED_EDGE('',*,*,#53507,.T.);
#76846=ORIENTED_EDGE('',*,*,#53508,.T.);
#76847=ORIENTED_EDGE('',*,*,#53509,.T.);
#76848=ORIENTED_EDGE('',*,*,#53510,.T.);
#76849=ORIENTED_EDGE('',*,*,#53511,.T.);
#76850=ORIENTED_EDGE('',*,*,#53500,.F.);
#76851=ORIENTED_EDGE('',*,*,#51182,.T.);
#76852=ORIENTED_EDGE('',*,*,#51170,.T.);
#76853=ORIENTED_EDGE('',*,*,#51173,.T.);
#76854=ORIENTED_EDGE('',*,*,#51175,.T.);
#76855=ORIENTED_EDGE('',*,*,#51177,.T.);
#76856=ORIENTED_EDGE('',*,*,#51179,.T.);
#76857=ORIENTED_EDGE('',*,*,#51181,.T.);
#76858=ORIENTED_EDGE('',*,*,#53499,.F.);
#76859=ORIENTED_EDGE('',*,*,#53498,.F.);
#76860=ORIENTED_EDGE('',*,*,#53496,.F.);
#76861=ORIENTED_EDGE('',*,*,#53494,.F.);
#76862=ORIENTED_EDGE('',*,*,#53492,.F.);
#76863=ORIENTED_EDGE('',*,*,#53490,.F.);
#76864=ORIENTED_EDGE('',*,*,#53488,.F.);
#76865=ORIENTED_EDGE('',*,*,#53502,.F.);
#76866=ORIENTED_EDGE('',*,*,#53512,.T.);
#76867=ORIENTED_EDGE('',*,*,#52319,.T.);
#76868=ORIENTED_EDGE('',*,*,#53513,.F.);
#76869=ORIENTED_EDGE('',*,*,#53511,.F.);
#76870=ORIENTED_EDGE('',*,*,#53513,.T.);
#76871=ORIENTED_EDGE('',*,*,#52316,.T.);
#76872=ORIENTED_EDGE('',*,*,#51186,.F.);
#76873=ORIENTED_EDGE('',*,*,#53503,.F.);
#76874=ORIENTED_EDGE('',*,*,#53504,.F.);
#76875=ORIENTED_EDGE('',*,*,#51187,.T.);
#76876=ORIENTED_EDGE('',*,*,#52339,.T.);
#76877=ORIENTED_EDGE('',*,*,#53514,.F.);
#76878=ORIENTED_EDGE('',*,*,#53514,.T.);
#76879=ORIENTED_EDGE('',*,*,#52337,.T.);
#76880=ORIENTED_EDGE('',*,*,#53515,.F.);
#76881=ORIENTED_EDGE('',*,*,#53505,.F.);
#76882=ORIENTED_EDGE('',*,*,#53515,.T.);
#76883=ORIENTED_EDGE('',*,*,#52334,.T.);
#76884=ORIENTED_EDGE('',*,*,#53516,.F.);
#76885=ORIENTED_EDGE('',*,*,#53506,.F.);
#76886=ORIENTED_EDGE('',*,*,#53516,.T.);
#76887=ORIENTED_EDGE('',*,*,#52331,.T.);
#76888=ORIENTED_EDGE('',*,*,#53517,.F.);
#76889=ORIENTED_EDGE('',*,*,#53507,.F.);
#76890=ORIENTED_EDGE('',*,*,#53517,.T.);
#76891=ORIENTED_EDGE('',*,*,#52328,.T.);
#76892=ORIENTED_EDGE('',*,*,#53518,.F.);
#76893=ORIENTED_EDGE('',*,*,#53508,.F.);
#76894=ORIENTED_EDGE('',*,*,#53518,.T.);
#76895=ORIENTED_EDGE('',*,*,#52325,.T.);
#76896=ORIENTED_EDGE('',*,*,#53519,.F.);
#76897=ORIENTED_EDGE('',*,*,#53509,.F.);
#76898=ORIENTED_EDGE('',*,*,#53519,.T.);
#76899=ORIENTED_EDGE('',*,*,#52322,.T.);
#76900=ORIENTED_EDGE('',*,*,#53512,.F.);
#76901=ORIENTED_EDGE('',*,*,#53510,.F.);
#76902=ORIENTED_EDGE('',*,*,#53520,.F.);
#76903=ORIENTED_EDGE('',*,*,#52522,.T.);
#76904=ORIENTED_EDGE('',*,*,#53521,.T.);
#76905=ORIENTED_EDGE('',*,*,#52553,.T.);
#76906=ORIENTED_EDGE('',*,*,#52550,.T.);
#76907=ORIENTED_EDGE('',*,*,#53522,.F.);
#76908=ORIENTED_EDGE('',*,*,#52528,.T.);
#76909=ORIENTED_EDGE('',*,*,#53523,.T.);
#76910=ORIENTED_EDGE('',*,*,#52613,.T.);
#76911=ORIENTED_EDGE('',*,*,#52610,.T.);
#76912=ORIENTED_EDGE('',*,*,#53524,.F.);
#76913=ORIENTED_EDGE('',*,*,#52493,.T.);
#76914=ORIENTED_EDGE('',*,*,#53525,.T.);
#76915=ORIENTED_EDGE('',*,*,#52637,.T.);
#76916=ORIENTED_EDGE('',*,*,#52640,.T.);
#76917=ORIENTED_EDGE('',*,*,#53526,.T.);
#76918=ORIENTED_EDGE('',*,*,#52499,.T.);
#76919=ORIENTED_EDGE('',*,*,#53527,.T.);
#76920=ORIENTED_EDGE('',*,*,#52584,.T.);
#76921=ORIENTED_EDGE('',*,*,#52581,.T.);
#76922=ORIENTED_EDGE('',*,*,#53528,.T.);
#76923=ORIENTED_EDGE('',*,*,#51410,.T.);
#76924=ORIENTED_EDGE('',*,*,#53529,.F.);
#76925=ORIENTED_EDGE('',*,*,#52612,.T.);
#76926=ORIENTED_EDGE('',*,*,#52615,.T.);
#76927=ORIENTED_EDGE('',*,*,#53530,.T.);
#76928=ORIENTED_EDGE('',*,*,#51407,.T.);
#76929=ORIENTED_EDGE('',*,*,#53528,.F.);
#76930=ORIENTED_EDGE('',*,*,#52618,.T.);
#76931=ORIENTED_EDGE('',*,*,#51445,.T.);
#76932=ORIENTED_EDGE('',*,*,#51451,.T.);
#76933=ORIENTED_EDGE('',*,*,#51449,.T.);
#76934=ORIENTED_EDGE('',*,*,#52542,.T.);
#76935=ORIENTED_EDGE('',*,*,#53531,.T.);
#76936=ORIENTED_EDGE('',*,*,#51404,.T.);
#76937=ORIENTED_EDGE('',*,*,#53530,.F.);
#76938=ORIENTED_EDGE('',*,*,#52546,.T.);
#76939=ORIENTED_EDGE('',*,*,#52549,.T.);
#76940=ORIENTED_EDGE('',*,*,#53532,.T.);
#76941=ORIENTED_EDGE('',*,*,#51398,.T.);
#76942=ORIENTED_EDGE('',*,*,#53533,.F.);
#76943=ORIENTED_EDGE('',*,*,#52583,.T.);
#76944=ORIENTED_EDGE('',*,*,#52586,.T.);
#76945=ORIENTED_EDGE('',*,*,#53534,.T.);
#76946=ORIENTED_EDGE('',*,*,#51395,.T.);
#76947=ORIENTED_EDGE('',*,*,#53532,.F.);
#76948=ORIENTED_EDGE('',*,*,#52588,.T.);
#76949=ORIENTED_EDGE('',*,*,#51455,.T.);
#76950=ORIENTED_EDGE('',*,*,#51457,.T.);
#76951=ORIENTED_EDGE('',*,*,#51463,.T.);
#76952=ORIENTED_EDGE('',*,*,#52646,.T.);
#76953=ORIENTED_EDGE('',*,*,#53535,.T.);
#76954=ORIENTED_EDGE('',*,*,#51392,.T.);
#76955=ORIENTED_EDGE('',*,*,#53534,.F.);
#76956=ORIENTED_EDGE('',*,*,#52644,.T.);
#76957=ORIENTED_EDGE('',*,*,#52641,.T.);
#76958=ORIENTED_EDGE('',*,*,#53529,.T.);
#76959=ORIENTED_EDGE('',*,*,#51413,.T.);
#76960=ORIENTED_EDGE('',*,*,#51208,.F.);
#76961=ORIENTED_EDGE('',*,*,#50402,.F.);
#76962=ORIENTED_EDGE('',*,*,#50397,.F.);
#76963=ORIENTED_EDGE('',*,*,#52593,.T.);
#76964=ORIENTED_EDGE('',*,*,#52607,.T.);
#76965=ORIENTED_EDGE('',*,*,#52609,.T.);
#76966=ORIENTED_EDGE('',*,*,#53536,.F.);
#76967=ORIENTED_EDGE('',*,*,#51222,.T.);
#76968=ORIENTED_EDGE('',*,*,#51220,.T.);
#76969=ORIENTED_EDGE('',*,*,#51218,.T.);
#76970=ORIENTED_EDGE('',*,*,#51216,.T.);
#76971=ORIENTED_EDGE('',*,*,#51229,.T.);
#76972=ORIENTED_EDGE('',*,*,#51227,.T.);
#76973=ORIENTED_EDGE('',*,*,#51225,.T.);
#76974=ORIENTED_EDGE('',*,*,#53537,.F.);
#76975=ORIENTED_EDGE('',*,*,#53538,.F.);
#76976=ORIENTED_EDGE('',*,*,#53539,.F.);
#76977=ORIENTED_EDGE('',*,*,#53540,.F.);
#76978=ORIENTED_EDGE('',*,*,#53541,.F.);
#76979=ORIENTED_EDGE('',*,*,#53542,.F.);
#76980=ORIENTED_EDGE('',*,*,#53543,.F.);
#76981=ORIENTED_EDGE('',*,*,#53544,.F.);
#76982=ORIENTED_EDGE('',*,*,#53410,.T.);
#76983=ORIENTED_EDGE('',*,*,#53408,.T.);
#76984=ORIENTED_EDGE('',*,*,#51067,.F.);
#76985=ORIENTED_EDGE('',*,*,#51071,.F.);
#76986=ORIENTED_EDGE('',*,*,#51074,.F.);
#76987=ORIENTED_EDGE('',*,*,#51054,.F.);
#76988=ORIENTED_EDGE('',*,*,#51058,.F.);
#76989=ORIENTED_EDGE('',*,*,#51061,.F.);
#76990=ORIENTED_EDGE('',*,*,#51064,.F.);
#76991=ORIENTED_EDGE('',*,*,#53407,.T.);
#76992=ORIENTED_EDGE('',*,*,#53405,.T.);
#76993=ORIENTED_EDGE('',*,*,#53403,.T.);
#76994=ORIENTED_EDGE('',*,*,#53401,.T.);
#76995=ORIENTED_EDGE('',*,*,#53398,.T.);
#76996=ORIENTED_EDGE('',*,*,#53414,.T.);
#76997=ORIENTED_EDGE('',*,*,#53412,.T.);
#76998=ORIENTED_EDGE('',*,*,#50268,.F.);
#76999=ORIENTED_EDGE('',*,*,#52454,.T.);
#77000=ORIENTED_EDGE('',*,*,#52458,.T.);
#77001=ORIENTED_EDGE('',*,*,#52461,.T.);
#77002=ORIENTED_EDGE('',*,*,#52464,.T.);
#77003=ORIENTED_EDGE('',*,*,#52467,.T.);
#77004=ORIENTED_EDGE('',*,*,#52470,.T.);
#77005=ORIENTED_EDGE('',*,*,#52473,.T.);
#77006=ORIENTED_EDGE('',*,*,#52476,.T.);
#77007=ORIENTED_EDGE('',*,*,#52478,.T.);
#77008=ORIENTED_EDGE('',*,*,#50286,.F.);
#77009=ORIENTED_EDGE('',*,*,#50283,.F.);
#77010=ORIENTED_EDGE('',*,*,#50280,.F.);
#77011=ORIENTED_EDGE('',*,*,#50277,.F.);
#77012=ORIENTED_EDGE('',*,*,#50274,.F.);
#77013=ORIENTED_EDGE('',*,*,#50271,.F.);
#77014=ORIENTED_EDGE('',*,*,#51393,.T.);
#77015=ORIENTED_EDGE('',*,*,#51389,.T.);
#77016=ORIENTED_EDGE('',*,*,#49218,.F.);
#77017=ORIENTED_EDGE('',*,*,#49222,.F.);
#77018=ORIENTED_EDGE('',*,*,#49225,.F.);
#77019=ORIENTED_EDGE('',*,*,#49228,.F.);
#77020=ORIENTED_EDGE('',*,*,#49231,.F.);
#77021=ORIENTED_EDGE('',*,*,#49234,.F.);
#77022=ORIENTED_EDGE('',*,*,#49237,.F.);
#77023=ORIENTED_EDGE('',*,*,#51412,.T.);
#77024=ORIENTED_EDGE('',*,*,#51411,.T.);
#77025=ORIENTED_EDGE('',*,*,#51408,.T.);
#77026=ORIENTED_EDGE('',*,*,#51405,.T.);
#77027=ORIENTED_EDGE('',*,*,#51402,.T.);
#77028=ORIENTED_EDGE('',*,*,#51399,.T.);
#77029=ORIENTED_EDGE('',*,*,#51396,.T.);
#77030=ORIENTED_EDGE('',*,*,#53545,.F.);
#77031=ORIENTED_EDGE('',*,*,#52468,.T.);
#77032=ORIENTED_EDGE('',*,*,#53546,.T.);
#77033=ORIENTED_EDGE('',*,*,#53541,.T.);
#77034=ORIENTED_EDGE('',*,*,#53546,.F.);
#77035=ORIENTED_EDGE('',*,*,#52465,.T.);
#77036=ORIENTED_EDGE('',*,*,#53547,.T.);
#77037=ORIENTED_EDGE('',*,*,#53542,.T.);
#77038=ORIENTED_EDGE('',*,*,#53547,.F.);
#77039=ORIENTED_EDGE('',*,*,#52462,.T.);
#77040=ORIENTED_EDGE('',*,*,#53548,.T.);
#77041=ORIENTED_EDGE('',*,*,#53543,.T.);
#77042=ORIENTED_EDGE('',*,*,#53548,.F.);
#77043=ORIENTED_EDGE('',*,*,#52459,.T.);
#77044=ORIENTED_EDGE('',*,*,#53549,.T.);
#77045=ORIENTED_EDGE('',*,*,#53544,.T.);
#77046=ORIENTED_EDGE('',*,*,#52455,.T.);
#77047=ORIENTED_EDGE('',*,*,#51223,.T.);
#77048=ORIENTED_EDGE('',*,*,#53536,.T.);
#77049=ORIENTED_EDGE('',*,*,#53549,.F.);
#77050=ORIENTED_EDGE('',*,*,#53537,.T.);
#77051=ORIENTED_EDGE('',*,*,#51224,.F.);
#77052=ORIENTED_EDGE('',*,*,#52479,.T.);
#77053=ORIENTED_EDGE('',*,*,#53550,.T.);
#77054=ORIENTED_EDGE('',*,*,#53550,.F.);
#77055=ORIENTED_EDGE('',*,*,#52477,.T.);
#77056=ORIENTED_EDGE('',*,*,#53551,.T.);
#77057=ORIENTED_EDGE('',*,*,#53538,.T.);
#77058=ORIENTED_EDGE('',*,*,#53551,.F.);
#77059=ORIENTED_EDGE('',*,*,#52474,.T.);
#77060=ORIENTED_EDGE('',*,*,#53552,.T.);
#77061=ORIENTED_EDGE('',*,*,#53539,.T.);
#77062=ORIENTED_EDGE('',*,*,#53552,.F.);
#77063=ORIENTED_EDGE('',*,*,#52471,.T.);
#77064=ORIENTED_EDGE('',*,*,#53545,.T.);
#77065=ORIENTED_EDGE('',*,*,#53540,.T.);
#77066=ORIENTED_EDGE('',*,*,#53521,.F.);
#77067=ORIENTED_EDGE('',*,*,#52519,.T.);
#77068=ORIENTED_EDGE('',*,*,#52649,.T.);
#77069=ORIENTED_EDGE('',*,*,#52556,.T.);
#77070=ORIENTED_EDGE('',*,*,#52652,.T.);
#77071=ORIENTED_EDGE('',*,*,#52502,.T.);
#77072=ORIENTED_EDGE('',*,*,#53526,.F.);
#77073=ORIENTED_EDGE('',*,*,#52576,.T.);
#77074=ORIENTED_EDGE('',*,*,#53533,.T.);
#77075=ORIENTED_EDGE('',*,*,#51401,.T.);
#77076=ORIENTED_EDGE('',*,*,#53531,.F.);
#77077=ORIENTED_EDGE('',*,*,#52552,.T.);
#77078=ORIENTED_EDGE('',*,*,#52555,.T.);
#77079=ORIENTED_EDGE('',*,*,#52563,.T.);
#77080=ORIENTED_EDGE('',*,*,#52578,.T.);
#77081=ORIENTED_EDGE('',*,*,#52580,.T.);
#77082=ORIENTED_EDGE('',*,*,#53525,.F.);
#77083=ORIENTED_EDGE('',*,*,#52490,.T.);
#77084=ORIENTED_EDGE('',*,*,#52653,.T.);
#77085=ORIENTED_EDGE('',*,*,#52630,.T.);
#77086=ORIENTED_EDGE('',*,*,#50414,.F.);
#77087=ORIENTED_EDGE('',*,*,#50419,.F.);
#77088=ORIENTED_EDGE('',*,*,#50425,.F.);
#77089=ORIENTED_EDGE('',*,*,#50430,.F.);
#77090=ORIENTED_EDGE('',*,*,#51214,.T.);
#77091=ORIENTED_EDGE('',*,*,#51388,.T.);
#77092=ORIENTED_EDGE('',*,*,#53535,.F.);
#77093=ORIENTED_EDGE('',*,*,#52638,.T.);
#77094=ORIENTED_EDGE('',*,*,#52632,.T.);
#77095=ORIENTED_EDGE('',*,*,#52624,.T.);
#77096=ORIENTED_EDGE('',*,*,#52619,.T.);
#77097=ORIENTED_EDGE('',*,*,#52539,.T.);
#77098=ORIENTED_EDGE('',*,*,#50342,.F.);
#77099=ORIENTED_EDGE('',*,*,#50339,.F.);
#77100=ORIENTED_EDGE('',*,*,#50336,.F.);
#77101=ORIENTED_EDGE('',*,*,#50333,.F.);
#77102=ORIENTED_EDGE('',*,*,#50330,.F.);
#77103=ORIENTED_EDGE('',*,*,#50327,.F.);
#77104=ORIENTED_EDGE('',*,*,#50324,.F.);
#77105=ORIENTED_EDGE('',*,*,#50321,.F.);
#77106=ORIENTED_EDGE('',*,*,#50313,.F.);
#77107=ORIENTED_EDGE('',*,*,#50310,.F.);
#77108=ORIENTED_EDGE('',*,*,#50307,.F.);
#77109=ORIENTED_EDGE('',*,*,#50304,.F.);
#77110=ORIENTED_EDGE('',*,*,#50301,.F.);
#77111=ORIENTED_EDGE('',*,*,#50298,.F.);
#77112=ORIENTED_EDGE('',*,*,#50295,.F.);
#77113=ORIENTED_EDGE('',*,*,#50290,.F.);
#77114=ORIENTED_EDGE('',*,*,#52483,.T.);
#77115=ORIENTED_EDGE('',*,*,#52486,.T.);
#77116=ORIENTED_EDGE('',*,*,#52489,.T.);
#77117=ORIENTED_EDGE('',*,*,#52492,.T.);
#77118=ORIENTED_EDGE('',*,*,#52495,.T.);
#77119=ORIENTED_EDGE('',*,*,#52498,.T.);
#77120=ORIENTED_EDGE('',*,*,#52501,.T.);
#77121=ORIENTED_EDGE('',*,*,#52504,.T.);
#77122=ORIENTED_EDGE('',*,*,#52507,.T.);
#77123=ORIENTED_EDGE('',*,*,#52515,.T.);
#77124=ORIENTED_EDGE('',*,*,#52518,.T.);
#77125=ORIENTED_EDGE('',*,*,#52521,.T.);
#77126=ORIENTED_EDGE('',*,*,#52524,.T.);
#77127=ORIENTED_EDGE('',*,*,#52527,.T.);
#77128=ORIENTED_EDGE('',*,*,#52530,.T.);
#77129=ORIENTED_EDGE('',*,*,#52533,.T.);
#77130=ORIENTED_EDGE('',*,*,#50136,.F.);
#77131=ORIENTED_EDGE('',*,*,#52315,.T.);
#77132=ORIENTED_EDGE('',*,*,#52318,.T.);
#77133=ORIENTED_EDGE('',*,*,#52321,.T.);
#77134=ORIENTED_EDGE('',*,*,#52324,.T.);
#77135=ORIENTED_EDGE('',*,*,#52327,.T.);
#77136=ORIENTED_EDGE('',*,*,#52330,.T.);
#77137=ORIENTED_EDGE('',*,*,#52333,.T.);
#77138=ORIENTED_EDGE('',*,*,#52336,.T.);
#77139=ORIENTED_EDGE('',*,*,#52338,.T.);
#77140=ORIENTED_EDGE('',*,*,#50154,.F.);
#77141=ORIENTED_EDGE('',*,*,#50151,.F.);
#77142=ORIENTED_EDGE('',*,*,#50148,.F.);
#77143=ORIENTED_EDGE('',*,*,#50145,.F.);
#77144=ORIENTED_EDGE('',*,*,#50142,.F.);
#77145=ORIENTED_EDGE('',*,*,#50139,.F.);
#77146=ORIENTED_EDGE('',*,*,#52648,.T.);
#77147=ORIENTED_EDGE('',*,*,#52531,.T.);
#77148=ORIENTED_EDGE('',*,*,#53522,.T.);
#77149=ORIENTED_EDGE('',*,*,#52605,.T.);
#77150=ORIENTED_EDGE('',*,*,#51512,.T.);
#77151=ORIENTED_EDGE('',*,*,#51376,.T.);
#77152=ORIENTED_EDGE('',*,*,#51381,.T.);
#77153=ORIENTED_EDGE('',*,*,#51387,.T.);
#77154=ORIENTED_EDGE('',*,*,#51500,.T.);
#77155=ORIENTED_EDGE('',*,*,#51505,.T.);
#77156=ORIENTED_EDGE('',*,*,#51507,.T.);
#77157=ORIENTED_EDGE('',*,*,#51510,.T.);
#77158=ORIENTED_EDGE('',*,*,#51484,.T.);
#77159=ORIENTED_EDGE('',*,*,#51374,.T.);
#77160=ORIENTED_EDGE('',*,*,#51368,.T.);
#77161=ORIENTED_EDGE('',*,*,#51363,.T.);
#77162=ORIENTED_EDGE('',*,*,#51357,.T.);
#77163=ORIENTED_EDGE('',*,*,#51351,.T.);
#77164=ORIENTED_EDGE('',*,*,#51353,.T.);
#77165=ORIENTED_EDGE('',*,*,#51359,.T.);
#77166=ORIENTED_EDGE('',*,*,#51478,.T.);
#77167=ORIENTED_EDGE('',*,*,#51474,.T.);
#77168=ORIENTED_EDGE('',*,*,#52589,.T.);
#77169=ORIENTED_EDGE('',*,*,#52587,.T.);
#77170=ORIENTED_EDGE('',*,*,#53527,.F.);
#77171=ORIENTED_EDGE('',*,*,#52496,.T.);
#77172=ORIENTED_EDGE('',*,*,#53524,.T.);
#77173=ORIENTED_EDGE('',*,*,#52643,.T.);
#77174=ORIENTED_EDGE('',*,*,#52645,.T.);
#77175=ORIENTED_EDGE('',*,*,#51481,.T.);
#77176=ORIENTED_EDGE('',*,*,#51330,.T.);
#77177=ORIENTED_EDGE('',*,*,#51324,.T.);
#77178=ORIENTED_EDGE('',*,*,#51414,.T.);
#77179=ORIENTED_EDGE('',*,*,#51418,.T.);
#77180=ORIENTED_EDGE('',*,*,#51514,.T.);
#77181=ORIENTED_EDGE('',*,*,#51518,.T.);
#77182=ORIENTED_EDGE('',*,*,#51521,.T.);
#77183=ORIENTED_EDGE('',*,*,#51523,.T.);
#77184=ORIENTED_EDGE('',*,*,#51526,.T.);
#77185=ORIENTED_EDGE('',*,*,#51336,.T.);
#77186=ORIENTED_EDGE('',*,*,#51415,.T.);
#77187=ORIENTED_EDGE('',*,*,#51313,.T.);
#77188=ORIENTED_EDGE('',*,*,#51315,.T.);
#77189=ORIENTED_EDGE('',*,*,#51320,.T.);
#77190=ORIENTED_EDGE('',*,*,#51326,.T.);
#77191=ORIENTED_EDGE('',*,*,#51332,.T.);
#77192=ORIENTED_EDGE('',*,*,#51338,.T.);
#77193=ORIENTED_EDGE('',*,*,#51344,.T.);
#77194=ORIENTED_EDGE('',*,*,#51420,.T.);
#77195=ORIENTED_EDGE('',*,*,#51427,.T.);
#77196=ORIENTED_EDGE('',*,*,#52617,.T.);
#77197=ORIENTED_EDGE('',*,*,#52616,.T.);
#77198=ORIENTED_EDGE('',*,*,#53523,.F.);
#77199=ORIENTED_EDGE('',*,*,#52525,.T.);
#77200=ORIENTED_EDGE('',*,*,#53520,.T.);
#77201=ORIENTED_EDGE('',*,*,#52547,.T.);
#77202=ORIENTED_EDGE('',*,*,#52543,.T.);
#77203=ORIENTED_EDGE('',*,*,#51431,.T.);
#77204=ORIENTED_EDGE('',*,*,#51425,.T.);
#77205=ORIENTED_EDGE('',*,*,#51419,.T.);
#77206=ORIENTED_EDGE('',*,*,#53477,.T.);
#77207=ORIENTED_EDGE('',*,*,#51835,.T.);
#77208=ORIENTED_EDGE('',*,*,#52898,.T.);
#77209=ORIENTED_EDGE('',*,*,#53201,.F.);
#77210=ORIENTED_EDGE('',*,*,#52878,.T.);
#77211=ORIENTED_EDGE('',*,*,#51857,.T.);
#77212=ORIENTED_EDGE('',*,*,#52874,.T.);
#77213=ORIENTED_EDGE('',*,*,#53207,.F.);
#77214=ORIENTED_EDGE('',*,*,#52866,.T.);
#77215=ORIENTED_EDGE('',*,*,#51987,.T.);
#77216=ORIENTED_EDGE('',*,*,#52862,.T.);
#77217=ORIENTED_EDGE('',*,*,#53210,.F.);
#77218=ORIENTED_EDGE('',*,*,#52854,.T.);
#77219=ORIENTED_EDGE('',*,*,#52086,.T.);
#77220=ORIENTED_EDGE('',*,*,#52850,.T.);
#77221=ORIENTED_EDGE('',*,*,#53213,.F.);
#77222=ORIENTED_EDGE('',*,*,#52782,.T.);
#77223=ORIENTED_EDGE('',*,*,#52120,.T.);
#77224=ORIENTED_EDGE('',*,*,#53478,.F.);
#77225=ORIENTED_EDGE('',*,*,#53226,.F.);
#77226=ORIENTED_EDGE('',*,*,#52728,.T.);
#77227=ORIENTED_EDGE('',*,*,#52047,.T.);
#77228=ORIENTED_EDGE('',*,*,#52724,.T.);
#77229=ORIENTED_EDGE('',*,*,#53241,.T.);
#77230=ORIENTED_EDGE('',*,*,#53019,.T.);
#77231=ORIENTED_EDGE('',*,*,#52268,.T.);
#77232=ORIENTED_EDGE('',*,*,#53015,.T.);
#77233=ORIENTED_EDGE('',*,*,#53188,.T.);
#77234=ORIENTED_EDGE('',*,*,#52671,.T.);
#77235=ORIENTED_EDGE('',*,*,#52383,.T.);
#77236=ORIENTED_EDGE('',*,*,#52667,.T.);
#77237=ORIENTED_EDGE('',*,*,#53244,.T.);
#77238=ORIENTED_EDGE('',*,*,#52665,.T.);
#77239=ORIENTED_EDGE('',*,*,#52393,.T.);
#77240=ORIENTED_EDGE('',*,*,#52661,.T.);
#77241=ORIENTED_EDGE('',*,*,#53242,.T.);
#77242=ORIENTED_EDGE('',*,*,#53013,.T.);
#77243=ORIENTED_EDGE('',*,*,#52254,.T.);
#77244=ORIENTED_EDGE('',*,*,#53021,.T.);
#77245=ORIENTED_EDGE('',*,*,#53187,.T.);
#77246=ORIENTED_EDGE('',*,*,#52995,.T.);
#77247=ORIENTED_EDGE('',*,*,#52230,.T.);
#77248=ORIENTED_EDGE('',*,*,#52991,.T.);
#77249=ORIENTED_EDGE('',*,*,#53192,.T.);
#77250=ORIENTED_EDGE('',*,*,#52716,.T.);
#77251=ORIENTED_EDGE('',*,*,#51668,.T.);
#77252=ORIENTED_EDGE('',*,*,#52712,.T.);
#77253=ORIENTED_EDGE('',*,*,#53243,.T.);
#77254=ORIENTED_EDGE('',*,*,#53010,.T.);
#77255=ORIENTED_EDGE('',*,*,#51654,.T.);
#77256=ORIENTED_EDGE('',*,*,#53006,.T.);
#77257=ORIENTED_EDGE('',*,*,#53190,.T.);
#77258=ORIENTED_EDGE('',*,*,#53004,.T.);
#77259=ORIENTED_EDGE('',*,*,#51644,.T.);
#77260=ORIENTED_EDGE('',*,*,#53000,.T.);
#77261=ORIENTED_EDGE('',*,*,#53189,.T.);
#77262=ORIENTED_EDGE('',*,*,#53025,.T.);
#77263=ORIENTED_EDGE('',*,*,#51630,.T.);
#77264=ORIENTED_EDGE('',*,*,#53033,.T.);
#77265=ORIENTED_EDGE('',*,*,#53186,.T.);
#77266=ORIENTED_EDGE('',*,*,#53032,.T.);
#77267=ORIENTED_EDGE('',*,*,#51620,.T.);
#77268=ORIENTED_EDGE('',*,*,#53027,.T.);
#77269=ORIENTED_EDGE('',*,*,#53185,.F.);
#77270=ORIENTED_EDGE('',*,*,#52989,.T.);
#77271=ORIENTED_EDGE('',*,*,#52244,.T.);
#77272=ORIENTED_EDGE('',*,*,#52997,.T.);
#77273=ORIENTED_EDGE('',*,*,#53191,.F.);
#77274=ORIENTED_EDGE('',*,*,#53163,.T.);
#77275=ORIENTED_EDGE('',*,*,#53139,.T.);
#77276=ORIENTED_EDGE('',*,*,#53553,.T.);
#77277=ORIENTED_EDGE('',*,*,#50912,.F.);
#77278=ORIENTED_EDGE('',*,*,#53554,.T.);
#77279=ORIENTED_EDGE('',*,*,#53135,.T.);
#77280=ORIENTED_EDGE('',*,*,#53172,.T.);
#77281=ORIENTED_EDGE('',*,*,#53247,.T.);
#77282=ORIENTED_EDGE('',*,*,#53297,.F.);
#77283=ORIENTED_EDGE('',*,*,#53318,.F.);
#77284=ORIENTED_EDGE('',*,*,#53304,.T.);
#77285=ORIENTED_EDGE('',*,*,#53465,.F.);
#77286=ORIENTED_EDGE('',*,*,#53316,.F.);
#77287=ORIENTED_EDGE('',*,*,#53342,.F.);
#77288=ORIENTED_EDGE('',*,*,#53339,.F.);
#77289=ORIENTED_EDGE('',*,*,#53461,.F.);
#77290=ORIENTED_EDGE('',*,*,#53472,.F.);
#77291=ORIENTED_EDGE('',*,*,#53471,.F.);
#77292=ORIENTED_EDGE('',*,*,#53462,.F.);
#77293=ORIENTED_EDGE('',*,*,#53470,.F.);
#77294=ORIENTED_EDGE('',*,*,#53456,.F.);
#77295=ORIENTED_EDGE('',*,*,#53469,.F.);
#77296=ORIENTED_EDGE('',*,*,#53457,.F.);
#77297=ORIENTED_EDGE('',*,*,#53468,.F.);
#77298=ORIENTED_EDGE('',*,*,#53473,.F.);
#77299=ORIENTED_EDGE('',*,*,#53334,.F.);
#77300=ORIENTED_EDGE('',*,*,#53332,.F.);
#77301=ORIENTED_EDGE('',*,*,#53329,.F.);
#77302=ORIENTED_EDGE('',*,*,#53326,.F.);
#77303=ORIENTED_EDGE('',*,*,#53320,.F.);
#77304=ORIENTED_EDGE('',*,*,#50995,.T.);
#77305=ORIENTED_EDGE('',*,*,#50999,.T.);
#77306=ORIENTED_EDGE('',*,*,#51002,.T.);
#77307=ORIENTED_EDGE('',*,*,#51004,.T.);
#77308=ORIENTED_EDGE('',*,*,#51142,.F.);
#77309=ORIENTED_EDGE('',*,*,#51141,.T.);
#77310=ORIENTED_EDGE('',*,*,#51128,.T.);
#77311=ORIENTED_EDGE('',*,*,#51146,.T.);
#77312=ORIENTED_EDGE('',*,*,#51126,.T.);
#77313=ORIENTED_EDGE('',*,*,#51145,.T.);
#77314=ORIENTED_EDGE('',*,*,#51133,.T.);
#77315=ORIENTED_EDGE('',*,*,#51144,.T.);
#77316=ORIENTED_EDGE('',*,*,#51143,.T.);
#77317=ORIENTED_EDGE('',*,*,#51131,.T.);
#77318=ORIENTED_EDGE('',*,*,#51008,.T.);
#77319=ORIENTED_EDGE('',*,*,#51011,.T.);
#77320=ORIENTED_EDGE('',*,*,#50991,.T.);
#77321=ORIENTED_EDGE('',*,*,#51138,.T.);
#77322=ORIENTED_EDGE('',*,*,#53136,.F.);
#77323=ORIENTED_EDGE('',*,*,#53554,.F.);
#77324=ORIENTED_EDGE('',*,*,#53249,.T.);
#77325=ORIENTED_EDGE('',*,*,#53250,.F.);
#77326=ORIENTED_EDGE('',*,*,#53253,.T.);
#77327=ORIENTED_EDGE('',*,*,#53255,.T.);
#77328=ORIENTED_EDGE('',*,*,#53257,.T.);
#77329=ORIENTED_EDGE('',*,*,#53258,.F.);
#77330=ORIENTED_EDGE('',*,*,#53261,.T.);
#77331=ORIENTED_EDGE('',*,*,#53262,.T.);
#77332=ORIENTED_EDGE('',*,*,#50955,.F.);
#77333=ORIENTED_EDGE('',*,*,#50952,.T.);
#77334=ORIENTED_EDGE('',*,*,#50949,.F.);
#77335=ORIENTED_EDGE('',*,*,#50946,.F.);
#77336=ORIENTED_EDGE('',*,*,#50943,.F.);
#77337=ORIENTED_EDGE('',*,*,#50940,.T.);
#77338=ORIENTED_EDGE('',*,*,#50937,.F.);
#77339=ORIENTED_EDGE('',*,*,#51247,.T.);
#77340=ORIENTED_EDGE('',*,*,#50910,.T.);
#77341=ORIENTED_EDGE('',*,*,#50907,.T.);
#77342=ORIENTED_EDGE('',*,*,#50913,.T.);
#77343=ORIENTED_EDGE('',*,*,#53553,.F.);
#77344=ORIENTED_EDGE('',*,*,#53138,.F.);
#77345=ORIENTED_EDGE('',*,*,#53132,.F.);
#77346=ORIENTED_EDGE('',*,*,#52962,.T.);
#77347=ORIENTED_EDGE('',*,*,#52037,.T.);
#77348=ORIENTED_EDGE('',*,*,#52958,.T.);
#77349=ORIENTED_EDGE('',*,*,#53180,.T.);
#77350=ORIENTED_EDGE('',*,*,#52971,.T.);
#77351=ORIENTED_EDGE('',*,*,#52220,.T.);
#77352=ORIENTED_EDGE('',*,*,#52967,.T.);
#77353=ORIENTED_EDGE('',*,*,#53182,.T.);
#77354=ORIENTED_EDGE('',*,*,#52692,.T.);
#77355=ORIENTED_EDGE('',*,*,#51921,.T.);
#77356=ORIENTED_EDGE('',*,*,#52688,.T.);
#77357=ORIENTED_EDGE('',*,*,#53246,.T.);
#77358=ORIENTED_EDGE('',*,*,#52956,.T.);
#77359=ORIENTED_EDGE('',*,*,#52023,.T.);
#77360=ORIENTED_EDGE('',*,*,#52952,.T.);
#77361=ORIENTED_EDGE('',*,*,#53179,.T.);
#77362=ORIENTED_EDGE('',*,*,#52701,.T.);
#77363=ORIENTED_EDGE('',*,*,#51891,.T.);
#77364=ORIENTED_EDGE('',*,*,#52697,.T.);
#77365=ORIENTED_EDGE('',*,*,#53239,.T.);
#77366=ORIENTED_EDGE('',*,*,#52686,.T.);
#77367=ORIENTED_EDGE('',*,*,#51943,.T.);
#77368=ORIENTED_EDGE('',*,*,#52694,.T.);
#77369=ORIENTED_EDGE('',*,*,#53245,.T.);
#77370=ORIENTED_EDGE('',*,*,#52950,.T.);
#77371=ORIENTED_EDGE('',*,*,#51705,.T.);
#77372=ORIENTED_EDGE('',*,*,#52946,.T.);
#77373=ORIENTED_EDGE('',*,*,#53178,.T.);
#77374=ORIENTED_EDGE('',*,*,#52707,.T.);
#77375=ORIENTED_EDGE('',*,*,#51913,.T.);
#77376=ORIENTED_EDGE('',*,*,#52703,.T.);
#77377=ORIENTED_EDGE('',*,*,#53240,.T.);
#77378=ORIENTED_EDGE('',*,*,#52965,.T.);
#77379=ORIENTED_EDGE('',*,*,#52206,.T.);
#77380=ORIENTED_EDGE('',*,*,#52973,.T.);
#77381=ORIENTED_EDGE('',*,*,#53181,.T.);
#77382=ORIENTED_EDGE('',*,*,#52923,.T.);
#77383=ORIENTED_EDGE('',*,*,#52182,.T.);
#77384=ORIENTED_EDGE('',*,*,#52919,.T.);
#77385=ORIENTED_EDGE('',*,*,#53174,.T.);
#77386=ORIENTED_EDGE('',*,*,#52944,.T.);
#77387=ORIENTED_EDGE('',*,*,#51695,.T.);
#77388=ORIENTED_EDGE('',*,*,#52940,.T.);
#77389=ORIENTED_EDGE('',*,*,#53177,.T.);
#77390=ORIENTED_EDGE('',*,*,#52938,.T.);
#77391=ORIENTED_EDGE('',*,*,#51729,.T.);
#77392=ORIENTED_EDGE('',*,*,#52934,.T.);
#77393=ORIENTED_EDGE('',*,*,#53176,.T.);
#77394=ORIENTED_EDGE('',*,*,#52932,.T.);
#77395=ORIENTED_EDGE('',*,*,#51719,.T.);
#77396=ORIENTED_EDGE('',*,*,#52928,.T.);
#77397=ORIENTED_EDGE('',*,*,#53175,.T.);
#77398=ORIENTED_EDGE('',*,*,#52977,.T.);
#77399=ORIENTED_EDGE('',*,*,#51606,.T.);
#77400=ORIENTED_EDGE('',*,*,#52985,.T.);
#77401=ORIENTED_EDGE('',*,*,#53184,.T.);
#77402=ORIENTED_EDGE('',*,*,#52984,.T.);
#77403=ORIENTED_EDGE('',*,*,#51596,.T.);
#77404=ORIENTED_EDGE('',*,*,#52979,.T.);
#77405=ORIENTED_EDGE('',*,*,#53183,.F.);
#77406=ORIENTED_EDGE('',*,*,#52912,.T.);
#77407=ORIENTED_EDGE('',*,*,#51566,.T.);
#77408=ORIENTED_EDGE('',*,*,#53474,.F.);
#77409=ORIENTED_EDGE('',*,*,#53194,.F.);
#77410=ORIENTED_EDGE('',*,*,#52917,.T.);
#77411=ORIENTED_EDGE('',*,*,#52196,.T.);
#77412=ORIENTED_EDGE('',*,*,#52925,.T.);
#77413=ORIENTED_EDGE('',*,*,#53173,.F.);
#77414=ORIENTED_EDGE('',*,*,#53481,.T.);
#77415=ORIENTED_EDGE('',*,*,#52174,.T.);
#77416=ORIENTED_EDGE('',*,*,#52769,.T.);
#77417=ORIENTED_EDGE('',*,*,#53232,.F.);
#77418=ORIENTED_EDGE('',*,*,#53475,.T.);
#77419=ORIENTED_EDGE('',*,*,#51578,.T.);
#77420=ORIENTED_EDGE('',*,*,#52907,.T.);
#77421=ORIENTED_EDGE('',*,*,#53196,.F.);
#77422=ORIENTED_EDGE('',*,*,#52738,.T.);
#77423=ORIENTED_EDGE('',*,*,#52298,.T.);
#77424=ORIENTED_EDGE('',*,*,#52733,.T.);
#77425=ORIENTED_EDGE('',*,*,#53238,.F.);
#77426=ORIENTED_EDGE('',*,*,#52773,.T.);
#77427=ORIENTED_EDGE('',*,*,#52166,.T.);
#77428=ORIENTED_EDGE('',*,*,#53480,.F.);
#77429=ORIENTED_EDGE('',*,*,#53230,.F.);
#77430=ORIENTED_EDGE('',*,*,#52830,.T.);
#77431=ORIENTED_EDGE('',*,*,#52280,.T.);
#77432=ORIENTED_EDGE('',*,*,#52826,.T.);
#77433=ORIENTED_EDGE('',*,*,#53217,.F.);
#77434=ORIENTED_EDGE('',*,*,#52821,.T.);
#77435=ORIENTED_EDGE('',*,*,#52013,.T.);
#77436=ORIENTED_EDGE('',*,*,#52817,.T.);
#77437=ORIENTED_EDGE('',*,*,#53219,.T.);
#77438=ORIENTED_EDGE('',*,*,#52851,.T.);
#77439=ORIENTED_EDGE('',*,*,#52074,.T.);
#77440=ORIENTED_EDGE('',*,*,#52847,.T.);
#77441=ORIENTED_EDGE('',*,*,#53211,.T.);
#77442=ORIENTED_EDGE('',*,*,#52839,.T.);
#77443=ORIENTED_EDGE('',*,*,#52142,.T.);
#77444=ORIENTED_EDGE('',*,*,#52835,.T.);
#77445=ORIENTED_EDGE('',*,*,#53215,.T.);
#77446=ORIENTED_EDGE('',*,*,#52785,.T.);
#77447=ORIENTED_EDGE('',*,*,#52112,.T.);
#77448=ORIENTED_EDGE('',*,*,#52781,.T.);
#77449=ORIENTED_EDGE('',*,*,#53225,.T.);
#77450=ORIENTED_EDGE('',*,*,#52809,.T.);
#77451=ORIENTED_EDGE('',*,*,#51951,.T.);
#77452=ORIENTED_EDGE('',*,*,#52805,.T.);
#77453=ORIENTED_EDGE('',*,*,#53221,.T.);
#77454=ORIENTED_EDGE('',*,*,#52863,.T.);
#77455=ORIENTED_EDGE('',*,*,#51975,.T.);
#77456=ORIENTED_EDGE('',*,*,#52859,.T.);
#77457=ORIENTED_EDGE('',*,*,#53208,.T.);
#77458=ORIENTED_EDGE('',*,*,#52815,.T.);
#77459=ORIENTED_EDGE('',*,*,#51999,.T.);
#77460=ORIENTED_EDGE('',*,*,#52811,.T.);
#77461=ORIENTED_EDGE('',*,*,#53218,.T.);
#77462=ORIENTED_EDGE('',*,*,#52845,.T.);
#77463=ORIENTED_EDGE('',*,*,#52088,.T.);
#77464=ORIENTED_EDGE('',*,*,#52853,.T.);
#77465=ORIENTED_EDGE('',*,*,#53212,.T.);
#77466=ORIENTED_EDGE('',*,*,#52797,.T.);
#77467=ORIENTED_EDGE('',*,*,#51879,.T.);
#77468=ORIENTED_EDGE('',*,*,#52793,.T.);
#77469=ORIENTED_EDGE('',*,*,#53223,.T.);
#77470=ORIENTED_EDGE('',*,*,#52875,.T.);
#77471=ORIENTED_EDGE('',*,*,#51855,.T.);
#77472=ORIENTED_EDGE('',*,*,#52871,.T.);
#77473=ORIENTED_EDGE('',*,*,#53205,.T.);
#77474=ORIENTED_EDGE('',*,*,#52803,.T.);
#77475=ORIENTED_EDGE('',*,*,#51965,.T.);
#77476=ORIENTED_EDGE('',*,*,#52799,.T.);
#77477=ORIENTED_EDGE('',*,*,#53220,.T.);
#77478=ORIENTED_EDGE('',*,*,#52857,.T.);
#77479=ORIENTED_EDGE('',*,*,#51989,.T.);
#77480=ORIENTED_EDGE('',*,*,#52865,.T.);
#77481=ORIENTED_EDGE('',*,*,#53209,.T.);
#77482=ORIENTED_EDGE('',*,*,#52761,.T.);
#77483=ORIENTED_EDGE('',*,*,#51777,.T.);
#77484=ORIENTED_EDGE('',*,*,#52757,.T.);
#77485=ORIENTED_EDGE('',*,*,#53234,.T.);
#77486=ORIENTED_EDGE('',*,*,#52887,.T.);
#77487=ORIENTED_EDGE('',*,*,#51801,.T.);
#77488=ORIENTED_EDGE('',*,*,#52883,.T.);
#77489=ORIENTED_EDGE('',*,*,#53202,.T.);
#77490=ORIENTED_EDGE('',*,*,#52791,.T.);
#77491=ORIENTED_EDGE('',*,*,#51869,.T.);
#77492=ORIENTED_EDGE('',*,*,#52787,.T.);
#77493=ORIENTED_EDGE('',*,*,#53222,.T.);
#77494=ORIENTED_EDGE('',*,*,#52869,.T.);
#77495=ORIENTED_EDGE('',*,*,#51845,.T.);
#77496=ORIENTED_EDGE('',*,*,#52877,.T.);
#77497=ORIENTED_EDGE('',*,*,#53206,.T.);
#77498=ORIENTED_EDGE('',*,*,#52833,.T.);
#77499=ORIENTED_EDGE('',*,*,#52128,.T.);
#77500=ORIENTED_EDGE('',*,*,#52841,.T.);
#77501=ORIENTED_EDGE('',*,*,#53214,.T.);
#77502=ORIENTED_EDGE('',*,*,#52779,.T.);
#77503=ORIENTED_EDGE('',*,*,#52098,.T.);
#77504=ORIENTED_EDGE('',*,*,#52775,.T.);
#77505=ORIENTED_EDGE('',*,*,#53224,.T.);
#77506=ORIENTED_EDGE('',*,*,#52767,.T.);
#77507=ORIENTED_EDGE('',*,*,#52152,.T.);
#77508=ORIENTED_EDGE('',*,*,#52763,.T.);
#77509=ORIENTED_EDGE('',*,*,#53229,.T.);
#77510=ORIENTED_EDGE('',*,*,#52824,.T.);
#77511=ORIENTED_EDGE('',*,*,#52278,.T.);
#77512=ORIENTED_EDGE('',*,*,#52829,.T.);
#77513=ORIENTED_EDGE('',*,*,#53216,.T.);
#77514=ORIENTED_EDGE('',*,*,#52755,.T.);
#77515=ORIENTED_EDGE('',*,*,#51767,.T.);
#77516=ORIENTED_EDGE('',*,*,#52751,.T.);
#77517=ORIENTED_EDGE('',*,*,#53233,.T.);
#77518=ORIENTED_EDGE('',*,*,#52881,.T.);
#77519=ORIENTED_EDGE('',*,*,#51791,.T.);
#77520=ORIENTED_EDGE('',*,*,#52889,.T.);
#77521=ORIENTED_EDGE('',*,*,#53203,.T.);
#77522=ORIENTED_EDGE('',*,*,#52749,.T.);
#77523=ORIENTED_EDGE('',*,*,#51753,.T.);
#77524=ORIENTED_EDGE('',*,*,#52745,.T.);
#77525=ORIENTED_EDGE('',*,*,#53236,.T.);
#77526=ORIENTED_EDGE('',*,*,#52899,.T.);
#77527=ORIENTED_EDGE('',*,*,#51825,.T.);
#77528=ORIENTED_EDGE('',*,*,#52895,.T.);
#77529=ORIENTED_EDGE('',*,*,#53197,.T.);
#77530=ORIENTED_EDGE('',*,*,#52743,.T.);
#77531=ORIENTED_EDGE('',*,*,#51743,.T.);
#77532=ORIENTED_EDGE('',*,*,#52739,.T.);
#77533=ORIENTED_EDGE('',*,*,#53235,.T.);
#77534=ORIENTED_EDGE('',*,*,#52893,.T.);
#77535=ORIENTED_EDGE('',*,*,#51815,.T.);
#77536=ORIENTED_EDGE('',*,*,#52901,.T.);
#77537=ORIENTED_EDGE('',*,*,#53198,.T.);
#77538=ORIENTED_EDGE('',*,*,#52905,.T.);
#77539=ORIENTED_EDGE('',*,*,#51576,.T.);
#77540=ORIENTED_EDGE('',*,*,#52913,.T.);
#77541=ORIENTED_EDGE('',*,*,#53193,.T.);
#77542=ORIENTED_EDGE('',*,*,#52734,.T.);
#77543=ORIENTED_EDGE('',*,*,#52306,.T.);
#77544=ORIENTED_EDGE('',*,*,#52730,.T.);
#77545=ORIENTED_EDGE('',*,*,#53237,.T.);
#77546=ORIENTED_EDGE('',*,*,#51168,.T.);
#77547=ORIENTED_EDGE('',*,*,#49131,.T.);
#77548=ORIENTED_EDGE('',*,*,#51164,.T.);
#77549=ORIENTED_EDGE('',*,*,#51165,.T.);
#77550=ORIENTED_EDGE('',*,*,#49133,.T.);
#77551=ORIENTED_EDGE('',*,*,#53555,.F.);
#77552=ORIENTED_EDGE('',*,*,#53556,.F.);
#77553=ORIENTED_EDGE('',*,*,#53557,.T.);
#77554=ORIENTED_EDGE('',*,*,#53558,.F.);
#77555=ORIENTED_EDGE('',*,*,#53559,.F.);
#77556=ORIENTED_EDGE('',*,*,#53560,.F.);
#77557=ORIENTED_EDGE('',*,*,#53555,.T.);
#77558=ORIENTED_EDGE('',*,*,#53561,.F.);
#77559=ORIENTED_EDGE('',*,*,#53562,.F.);
#77560=ORIENTED_EDGE('',*,*,#53563,.F.);
#77561=ORIENTED_EDGE('',*,*,#53559,.T.);
#77562=ORIENTED_EDGE('',*,*,#53564,.F.);
#77563=ORIENTED_EDGE('',*,*,#53565,.F.);
#77564=ORIENTED_EDGE('',*,*,#53566,.F.);
#77565=ORIENTED_EDGE('',*,*,#53562,.T.);
#77566=ORIENTED_EDGE('',*,*,#53567,.F.);
#77567=ORIENTED_EDGE('',*,*,#53568,.F.);
#77568=ORIENTED_EDGE('',*,*,#53569,.F.);
#77569=ORIENTED_EDGE('',*,*,#53565,.T.);
#77570=ORIENTED_EDGE('',*,*,#53570,.F.);
#77571=ORIENTED_EDGE('',*,*,#53557,.F.);
#77572=ORIENTED_EDGE('',*,*,#53571,.F.);
#77573=ORIENTED_EDGE('',*,*,#53568,.T.);
#77574=ORIENTED_EDGE('',*,*,#53572,.F.);
#77575=ORIENTED_EDGE('',*,*,#53573,.T.);
#77576=ORIENTED_EDGE('',*,*,#53566,.T.);
#77577=ORIENTED_EDGE('',*,*,#53569,.T.);
#77578=ORIENTED_EDGE('',*,*,#53571,.T.);
#77579=ORIENTED_EDGE('',*,*,#53556,.T.);
#77580=ORIENTED_EDGE('',*,*,#53560,.T.);
#77581=ORIENTED_EDGE('',*,*,#53563,.T.);
#77582=ORIENTED_EDGE('',*,*,#53573,.F.);
#77583=ORIENTED_EDGE('',*,*,#53574,.F.);
#77584=ORIENTED_EDGE('',*,*,#53558,.T.);
#77585=ORIENTED_EDGE('',*,*,#53575,.F.);
#77586=ORIENTED_EDGE('',*,*,#53561,.T.);
#77587=ORIENTED_EDGE('',*,*,#53576,.F.);
#77588=ORIENTED_EDGE('',*,*,#53564,.T.);
#77589=ORIENTED_EDGE('',*,*,#53577,.F.);
#77590=ORIENTED_EDGE('',*,*,#53567,.T.);
#77591=ORIENTED_EDGE('',*,*,#53578,.F.);
#77592=ORIENTED_EDGE('',*,*,#53570,.T.);
#77593=ORIENTED_EDGE('',*,*,#53579,.F.);
#77594=ORIENTED_EDGE('',*,*,#53572,.T.);
#77595=ORIENTED_EDGE('',*,*,#53580,.T.);
#77596=ORIENTED_EDGE('',*,*,#53581,.T.);
#77597=ORIENTED_EDGE('',*,*,#53582,.T.);
#77598=ORIENTED_EDGE('',*,*,#53583,.T.);
#77599=ORIENTED_EDGE('',*,*,#53581,.F.);
#77600=ORIENTED_EDGE('',*,*,#53584,.T.);
#77601=ORIENTED_EDGE('',*,*,#53580,.F.);
#77602=ORIENTED_EDGE('',*,*,#53579,.T.);
#77603=ORIENTED_EDGE('',*,*,#53578,.T.);
#77604=ORIENTED_EDGE('',*,*,#53577,.T.);
#77605=ORIENTED_EDGE('',*,*,#53576,.T.);
#77606=ORIENTED_EDGE('',*,*,#53575,.T.);
#77607=ORIENTED_EDGE('',*,*,#53574,.T.);
#77608=ORIENTED_EDGE('',*,*,#53584,.F.);
#77609=ORIENTED_EDGE('',*,*,#53585,.T.);
#77610=ORIENTED_EDGE('',*,*,#53582,.F.);
#77611=ORIENTED_EDGE('',*,*,#53583,.F.);
#77612=ORIENTED_EDGE('',*,*,#53585,.F.);
#77613=ORIENTED_EDGE('',*,*,#53586,.T.);
#77614=ORIENTED_EDGE('',*,*,#53587,.T.);
#77615=ORIENTED_EDGE('',*,*,#53588,.T.);
#77616=ORIENTED_EDGE('',*,*,#53589,.T.);
#77617=ORIENTED_EDGE('',*,*,#53590,.T.);
#77618=ORIENTED_EDGE('',*,*,#53591,.T.);
#77619=ORIENTED_EDGE('',*,*,#53592,.T.);
#77620=ORIENTED_EDGE('',*,*,#53587,.F.);
#77621=ORIENTED_EDGE('',*,*,#53593,.T.);
#77622=ORIENTED_EDGE('',*,*,#53594,.T.);
#77623=ORIENTED_EDGE('',*,*,#53595,.T.);
#77624=ORIENTED_EDGE('',*,*,#53588,.F.);
#77625=ORIENTED_EDGE('',*,*,#53596,.T.);
#77626=ORIENTED_EDGE('',*,*,#53597,.T.);
#77627=ORIENTED_EDGE('',*,*,#53589,.F.);
#77628=ORIENTED_EDGE('',*,*,#53598,.T.);
#77629=ORIENTED_EDGE('',*,*,#53599,.T.);
#77630=ORIENTED_EDGE('',*,*,#53590,.F.);
#77631=ORIENTED_EDGE('',*,*,#53600,.T.);
#77632=ORIENTED_EDGE('',*,*,#53601,.T.);
#77633=ORIENTED_EDGE('',*,*,#53591,.F.);
#77634=ORIENTED_EDGE('',*,*,#53602,.T.);
#77635=ORIENTED_EDGE('',*,*,#53603,.T.);
#77636=ORIENTED_EDGE('',*,*,#53586,.F.);
#77637=ORIENTED_EDGE('',*,*,#53604,.F.);
#77638=ORIENTED_EDGE('',*,*,#53605,.T.);
#77639=ORIENTED_EDGE('',*,*,#53606,.T.);
#77640=ORIENTED_EDGE('',*,*,#53607,.T.);
#77641=ORIENTED_EDGE('',*,*,#53608,.T.);
#77642=ORIENTED_EDGE('',*,*,#53609,.T.);
#77643=ORIENTED_EDGE('',*,*,#53605,.F.);
#77644=ORIENTED_EDGE('',*,*,#53610,.F.);
#77645=ORIENTED_EDGE('',*,*,#53611,.F.);
#77646=ORIENTED_EDGE('',*,*,#53606,.F.);
#77647=ORIENTED_EDGE('',*,*,#53612,.F.);
#77648=ORIENTED_EDGE('',*,*,#53613,.F.);
#77649=ORIENTED_EDGE('',*,*,#53607,.F.);
#77650=ORIENTED_EDGE('',*,*,#53614,.F.);
#77651=ORIENTED_EDGE('',*,*,#53615,.F.);
#77652=ORIENTED_EDGE('',*,*,#53608,.F.);
#77653=ORIENTED_EDGE('',*,*,#53616,.F.);
#77654=ORIENTED_EDGE('',*,*,#53617,.F.);
#77655=ORIENTED_EDGE('',*,*,#53609,.F.);
#77656=ORIENTED_EDGE('',*,*,#53618,.F.);
#77657=ORIENTED_EDGE('',*,*,#53619,.F.);
#77658=ORIENTED_EDGE('',*,*,#53620,.F.);
#77659=ORIENTED_EDGE('',*,*,#53604,.T.);
#77660=ORIENTED_EDGE('',*,*,#53621,.F.);
#77661=ORIENTED_EDGE('',*,*,#53603,.F.);
#77662=ORIENTED_EDGE('',*,*,#53622,.T.);
#77663=ORIENTED_EDGE('',*,*,#53610,.T.);
#77664=ORIENTED_EDGE('',*,*,#53620,.T.);
#77665=ORIENTED_EDGE('',*,*,#53623,.F.);
#77666=ORIENTED_EDGE('',*,*,#53593,.F.);
#77667=ORIENTED_EDGE('',*,*,#53601,.F.);
#77668=ORIENTED_EDGE('',*,*,#53624,.T.);
#77669=ORIENTED_EDGE('',*,*,#53612,.T.);
#77670=ORIENTED_EDGE('',*,*,#53611,.T.);
#77671=ORIENTED_EDGE('',*,*,#53622,.F.);
#77672=ORIENTED_EDGE('',*,*,#53602,.F.);
#77673=ORIENTED_EDGE('',*,*,#53599,.F.);
#77674=ORIENTED_EDGE('',*,*,#53625,.T.);
#77675=ORIENTED_EDGE('',*,*,#53614,.T.);
#77676=ORIENTED_EDGE('',*,*,#53613,.T.);
#77677=ORIENTED_EDGE('',*,*,#53624,.F.);
#77678=ORIENTED_EDGE('',*,*,#53600,.F.);
#77679=ORIENTED_EDGE('',*,*,#53597,.F.);
#77680=ORIENTED_EDGE('',*,*,#53626,.T.);
#77681=ORIENTED_EDGE('',*,*,#53616,.T.);
#77682=ORIENTED_EDGE('',*,*,#53615,.T.);
#77683=ORIENTED_EDGE('',*,*,#53625,.F.);
#77684=ORIENTED_EDGE('',*,*,#53598,.F.);
#77685=ORIENTED_EDGE('',*,*,#53595,.F.);
#77686=ORIENTED_EDGE('',*,*,#53627,.T.);
#77687=ORIENTED_EDGE('',*,*,#53618,.T.);
#77688=ORIENTED_EDGE('',*,*,#53617,.T.);
#77689=ORIENTED_EDGE('',*,*,#53626,.F.);
#77690=ORIENTED_EDGE('',*,*,#53596,.F.);
#77691=ORIENTED_EDGE('',*,*,#53592,.F.);
#77692=ORIENTED_EDGE('',*,*,#53623,.T.);
#77693=ORIENTED_EDGE('',*,*,#53621,.T.);
#77694=ORIENTED_EDGE('',*,*,#53619,.T.);
#77695=ORIENTED_EDGE('',*,*,#53627,.F.);
#77696=ORIENTED_EDGE('',*,*,#53594,.F.);
#77697=ORIENTED_EDGE('',*,*,#53628,.T.);
#77698=ORIENTED_EDGE('',*,*,#53629,.T.);
#77699=ORIENTED_EDGE('',*,*,#53630,.T.);
#77700=ORIENTED_EDGE('',*,*,#53631,.T.);
#77701=ORIENTED_EDGE('',*,*,#53632,.T.);
#77702=ORIENTED_EDGE('',*,*,#53633,.T.);
#77703=ORIENTED_EDGE('',*,*,#53634,.T.);
#77704=ORIENTED_EDGE('',*,*,#53629,.F.);
#77705=ORIENTED_EDGE('',*,*,#53635,.T.);
#77706=ORIENTED_EDGE('',*,*,#53636,.T.);
#77707=ORIENTED_EDGE('',*,*,#53637,.T.);
#77708=ORIENTED_EDGE('',*,*,#53630,.F.);
#77709=ORIENTED_EDGE('',*,*,#53638,.T.);
#77710=ORIENTED_EDGE('',*,*,#53639,.T.);
#77711=ORIENTED_EDGE('',*,*,#53631,.F.);
#77712=ORIENTED_EDGE('',*,*,#53640,.T.);
#77713=ORIENTED_EDGE('',*,*,#53641,.T.);
#77714=ORIENTED_EDGE('',*,*,#53632,.F.);
#77715=ORIENTED_EDGE('',*,*,#53642,.T.);
#77716=ORIENTED_EDGE('',*,*,#53643,.T.);
#77717=ORIENTED_EDGE('',*,*,#53633,.F.);
#77718=ORIENTED_EDGE('',*,*,#53644,.T.);
#77719=ORIENTED_EDGE('',*,*,#53645,.T.);
#77720=ORIENTED_EDGE('',*,*,#53628,.F.);
#77721=ORIENTED_EDGE('',*,*,#53646,.F.);
#77722=ORIENTED_EDGE('',*,*,#53647,.T.);
#77723=ORIENTED_EDGE('',*,*,#53648,.T.);
#77724=ORIENTED_EDGE('',*,*,#53649,.T.);
#77725=ORIENTED_EDGE('',*,*,#53650,.T.);
#77726=ORIENTED_EDGE('',*,*,#53651,.T.);
#77727=ORIENTED_EDGE('',*,*,#53647,.F.);
#77728=ORIENTED_EDGE('',*,*,#53652,.F.);
#77729=ORIENTED_EDGE('',*,*,#53653,.F.);
#77730=ORIENTED_EDGE('',*,*,#53648,.F.);
#77731=ORIENTED_EDGE('',*,*,#53654,.F.);
#77732=ORIENTED_EDGE('',*,*,#53655,.F.);
#77733=ORIENTED_EDGE('',*,*,#53649,.F.);
#77734=ORIENTED_EDGE('',*,*,#53656,.F.);
#77735=ORIENTED_EDGE('',*,*,#53657,.F.);
#77736=ORIENTED_EDGE('',*,*,#53650,.F.);
#77737=ORIENTED_EDGE('',*,*,#53658,.F.);
#77738=ORIENTED_EDGE('',*,*,#53659,.F.);
#77739=ORIENTED_EDGE('',*,*,#53651,.F.);
#77740=ORIENTED_EDGE('',*,*,#53660,.F.);
#77741=ORIENTED_EDGE('',*,*,#53661,.F.);
#77742=ORIENTED_EDGE('',*,*,#53662,.F.);
#77743=ORIENTED_EDGE('',*,*,#53646,.T.);
#77744=ORIENTED_EDGE('',*,*,#53663,.F.);
#77745=ORIENTED_EDGE('',*,*,#53645,.F.);
#77746=ORIENTED_EDGE('',*,*,#53664,.T.);
#77747=ORIENTED_EDGE('',*,*,#53652,.T.);
#77748=ORIENTED_EDGE('',*,*,#53662,.T.);
#77749=ORIENTED_EDGE('',*,*,#53665,.F.);
#77750=ORIENTED_EDGE('',*,*,#53635,.F.);
#77751=ORIENTED_EDGE('',*,*,#53643,.F.);
#77752=ORIENTED_EDGE('',*,*,#53666,.T.);
#77753=ORIENTED_EDGE('',*,*,#53654,.T.);
#77754=ORIENTED_EDGE('',*,*,#53653,.T.);
#77755=ORIENTED_EDGE('',*,*,#53664,.F.);
#77756=ORIENTED_EDGE('',*,*,#53644,.F.);
#77757=ORIENTED_EDGE('',*,*,#53641,.F.);
#77758=ORIENTED_EDGE('',*,*,#53667,.T.);
#77759=ORIENTED_EDGE('',*,*,#53656,.T.);
#77760=ORIENTED_EDGE('',*,*,#53655,.T.);
#77761=ORIENTED_EDGE('',*,*,#53666,.F.);
#77762=ORIENTED_EDGE('',*,*,#53642,.F.);
#77763=ORIENTED_EDGE('',*,*,#53639,.F.);
#77764=ORIENTED_EDGE('',*,*,#53668,.T.);
#77765=ORIENTED_EDGE('',*,*,#53658,.T.);
#77766=ORIENTED_EDGE('',*,*,#53657,.T.);
#77767=ORIENTED_EDGE('',*,*,#53667,.F.);
#77768=ORIENTED_EDGE('',*,*,#53640,.F.);
#77769=ORIENTED_EDGE('',*,*,#53637,.F.);
#77770=ORIENTED_EDGE('',*,*,#53669,.T.);
#77771=ORIENTED_EDGE('',*,*,#53660,.T.);
#77772=ORIENTED_EDGE('',*,*,#53659,.T.);
#77773=ORIENTED_EDGE('',*,*,#53668,.F.);
#77774=ORIENTED_EDGE('',*,*,#53638,.F.);
#77775=ORIENTED_EDGE('',*,*,#53634,.F.);
#77776=ORIENTED_EDGE('',*,*,#53665,.T.);
#77777=ORIENTED_EDGE('',*,*,#53663,.T.);
#77778=ORIENTED_EDGE('',*,*,#53661,.T.);
#77779=ORIENTED_EDGE('',*,*,#53669,.F.);
#77780=ORIENTED_EDGE('',*,*,#53636,.F.);
#77781=ORIENTED_EDGE('',*,*,#53670,.T.);
#77782=ORIENTED_EDGE('',*,*,#53671,.T.);
#77783=ORIENTED_EDGE('',*,*,#53672,.F.);
#77784=ORIENTED_EDGE('',*,*,#53673,.T.);
#77785=ORIENTED_EDGE('',*,*,#53674,.T.);
#77786=ORIENTED_EDGE('',*,*,#53675,.T.);
#77787=ORIENTED_EDGE('',*,*,#53670,.F.);
#77788=ORIENTED_EDGE('',*,*,#53676,.T.);
#77789=ORIENTED_EDGE('',*,*,#53677,.T.);
#77790=ORIENTED_EDGE('',*,*,#53678,.T.);
#77791=ORIENTED_EDGE('',*,*,#53674,.F.);
#77792=ORIENTED_EDGE('',*,*,#53679,.T.);
#77793=ORIENTED_EDGE('',*,*,#53680,.T.);
#77794=ORIENTED_EDGE('',*,*,#53681,.T.);
#77795=ORIENTED_EDGE('',*,*,#53677,.F.);
#77796=ORIENTED_EDGE('',*,*,#53682,.T.);
#77797=ORIENTED_EDGE('',*,*,#53683,.T.);
#77798=ORIENTED_EDGE('',*,*,#53684,.T.);
#77799=ORIENTED_EDGE('',*,*,#53680,.F.);
#77800=ORIENTED_EDGE('',*,*,#53685,.T.);
#77801=ORIENTED_EDGE('',*,*,#53672,.T.);
#77802=ORIENTED_EDGE('',*,*,#53686,.T.);
#77803=ORIENTED_EDGE('',*,*,#53683,.F.);
#77804=ORIENTED_EDGE('',*,*,#53687,.T.);
#77805=ORIENTED_EDGE('',*,*,#53688,.T.);
#77806=ORIENTED_EDGE('',*,*,#53679,.F.);
#77807=ORIENTED_EDGE('',*,*,#53676,.F.);
#77808=ORIENTED_EDGE('',*,*,#53673,.F.);
#77809=ORIENTED_EDGE('',*,*,#53687,.F.);
#77810=ORIENTED_EDGE('',*,*,#53685,.F.);
#77811=ORIENTED_EDGE('',*,*,#53682,.F.);
#77812=ORIENTED_EDGE('',*,*,#53688,.F.);
#77813=ORIENTED_EDGE('',*,*,#53689,.T.);
#77814=ORIENTED_EDGE('',*,*,#53671,.F.);
#77815=ORIENTED_EDGE('',*,*,#53690,.T.);
#77816=ORIENTED_EDGE('',*,*,#53675,.F.);
#77817=ORIENTED_EDGE('',*,*,#53691,.T.);
#77818=ORIENTED_EDGE('',*,*,#53678,.F.);
#77819=ORIENTED_EDGE('',*,*,#53692,.T.);
#77820=ORIENTED_EDGE('',*,*,#53681,.F.);
#77821=ORIENTED_EDGE('',*,*,#53693,.T.);
#77822=ORIENTED_EDGE('',*,*,#53684,.F.);
#77823=ORIENTED_EDGE('',*,*,#53694,.T.);
#77824=ORIENTED_EDGE('',*,*,#53686,.F.);
#77825=ORIENTED_EDGE('',*,*,#53695,.F.);
#77826=ORIENTED_EDGE('',*,*,#53696,.T.);
#77827=ORIENTED_EDGE('',*,*,#53697,.F.);
#77828=ORIENTED_EDGE('',*,*,#53698,.F.);
#77829=ORIENTED_EDGE('',*,*,#53696,.F.);
#77830=ORIENTED_EDGE('',*,*,#53699,.F.);
#77831=ORIENTED_EDGE('',*,*,#53695,.T.);
#77832=ORIENTED_EDGE('',*,*,#53694,.F.);
#77833=ORIENTED_EDGE('',*,*,#53689,.F.);
#77834=ORIENTED_EDGE('',*,*,#53690,.F.);
#77835=ORIENTED_EDGE('',*,*,#53691,.F.);
#77836=ORIENTED_EDGE('',*,*,#53692,.F.);
#77837=ORIENTED_EDGE('',*,*,#53693,.F.);
#77838=ORIENTED_EDGE('',*,*,#53699,.T.);
#77839=ORIENTED_EDGE('',*,*,#53700,.T.);
#77840=ORIENTED_EDGE('',*,*,#53697,.T.);
#77841=ORIENTED_EDGE('',*,*,#53698,.T.);
#77842=ORIENTED_EDGE('',*,*,#53700,.F.);
#77843=ORIENTED_EDGE('',*,*,#53701,.T.);
#77844=ORIENTED_EDGE('',*,*,#53702,.F.);
#77845=ORIENTED_EDGE('',*,*,#53703,.F.);
#77846=ORIENTED_EDGE('',*,*,#53704,.F.);
#77847=ORIENTED_EDGE('',*,*,#53705,.F.);
#77848=ORIENTED_EDGE('',*,*,#53706,.F.);
#77849=ORIENTED_EDGE('',*,*,#53707,.F.);
#77850=ORIENTED_EDGE('',*,*,#53708,.T.);
#77851=ORIENTED_EDGE('',*,*,#53701,.F.);
#77852=ORIENTED_EDGE('',*,*,#53708,.F.);
#77853=ORIENTED_EDGE('',*,*,#53709,.F.);
#77854=ORIENTED_EDGE('',*,*,#53710,.T.);
#77855=ORIENTED_EDGE('',*,*,#53711,.F.);
#77856=ORIENTED_EDGE('',*,*,#53712,.F.);
#77857=ORIENTED_EDGE('',*,*,#53710,.F.);
#77858=ORIENTED_EDGE('',*,*,#53713,.F.);
#77859=ORIENTED_EDGE('',*,*,#53714,.F.);
#77860=ORIENTED_EDGE('',*,*,#53715,.F.);
#77861=ORIENTED_EDGE('',*,*,#53716,.F.);
#77862=ORIENTED_EDGE('',*,*,#53702,.T.);
#77863=ORIENTED_EDGE('',*,*,#53717,.T.);
#77864=ORIENTED_EDGE('',*,*,#53716,.T.);
#77865=ORIENTED_EDGE('',*,*,#53718,.F.);
#77866=ORIENTED_EDGE('',*,*,#53703,.T.);
#77867=ORIENTED_EDGE('',*,*,#53718,.T.);
#77868=ORIENTED_EDGE('',*,*,#53715,.T.);
#77869=ORIENTED_EDGE('',*,*,#53719,.F.);
#77870=ORIENTED_EDGE('',*,*,#53704,.T.);
#77871=ORIENTED_EDGE('',*,*,#53719,.T.);
#77872=ORIENTED_EDGE('',*,*,#53714,.T.);
#77873=ORIENTED_EDGE('',*,*,#53720,.F.);
#77874=ORIENTED_EDGE('',*,*,#53705,.T.);
#77875=ORIENTED_EDGE('',*,*,#53720,.T.);
#77876=ORIENTED_EDGE('',*,*,#53713,.T.);
#77877=ORIENTED_EDGE('',*,*,#53717,.F.);
#77878=ORIENTED_EDGE('',*,*,#53721,.T.);
#77879=ORIENTED_EDGE('',*,*,#53722,.T.);
#77880=ORIENTED_EDGE('',*,*,#53723,.T.);
#77881=ORIENTED_EDGE('',*,*,#53721,.F.);
#77882=ORIENTED_EDGE('',*,*,#53723,.F.);
#77883=ORIENTED_EDGE('',*,*,#53706,.T.);
#77884=ORIENTED_EDGE('',*,*,#53707,.T.);
#77885=ORIENTED_EDGE('',*,*,#53724,.T.);
#77886=ORIENTED_EDGE('',*,*,#53711,.T.);
#77887=ORIENTED_EDGE('',*,*,#53712,.T.);
#77888=ORIENTED_EDGE('',*,*,#53724,.F.);
#77889=ORIENTED_EDGE('',*,*,#53709,.T.);
#77890=ORIENTED_EDGE('',*,*,#53722,.F.);
#77891=ORIENTED_EDGE('',*,*,#53725,.T.);
#77892=ORIENTED_EDGE('',*,*,#53726,.T.);
#77893=ORIENTED_EDGE('',*,*,#53727,.T.);
#77894=ORIENTED_EDGE('',*,*,#53726,.F.);
#77895=ORIENTED_EDGE('',*,*,#53727,.F.);
#77896=ORIENTED_EDGE('',*,*,#53728,.F.);
#77897=ORIENTED_EDGE('',*,*,#53729,.T.);
#77898=ORIENTED_EDGE('',*,*,#53725,.F.);
#77899=ORIENTED_EDGE('',*,*,#53729,.F.);
#77900=ORIENTED_EDGE('',*,*,#53730,.T.);
#77901=ORIENTED_EDGE('',*,*,#53728,.T.);
#77902=ORIENTED_EDGE('',*,*,#53731,.F.);
#77903=ORIENTED_EDGE('',*,*,#53732,.T.);
#77904=ORIENTED_EDGE('',*,*,#53730,.F.);
#77905=ORIENTED_EDGE('',*,*,#53732,.F.);
#77906=ORIENTED_EDGE('',*,*,#53731,.T.);
#77907=ORIENTED_EDGE('',*,*,#53733,.T.);
#77908=ORIENTED_EDGE('',*,*,#53734,.F.);
#77909=ORIENTED_EDGE('',*,*,#53735,.T.);
#77910=ORIENTED_EDGE('',*,*,#53736,.F.);
#77911=ORIENTED_EDGE('',*,*,#53737,.T.);
#77912=ORIENTED_EDGE('',*,*,#53738,.F.);
#77913=ORIENTED_EDGE('',*,*,#53735,.F.);
#77914=ORIENTED_EDGE('',*,*,#53739,.F.);
#77915=ORIENTED_EDGE('',*,*,#53740,.T.);
#77916=ORIENTED_EDGE('',*,*,#53741,.F.);
#77917=ORIENTED_EDGE('',*,*,#53733,.F.);
#77918=ORIENTED_EDGE('',*,*,#53742,.F.);
#77919=ORIENTED_EDGE('',*,*,#53743,.T.);
#77920=ORIENTED_EDGE('',*,*,#53744,.F.);
#77921=ORIENTED_EDGE('',*,*,#53737,.F.);
#77922=ORIENTED_EDGE('',*,*,#53745,.F.);
#77923=ORIENTED_EDGE('',*,*,#53746,.T.);
#77924=ORIENTED_EDGE('',*,*,#53747,.F.);
#77925=ORIENTED_EDGE('',*,*,#53740,.F.);
#77926=ORIENTED_EDGE('',*,*,#53748,.F.);
#77927=ORIENTED_EDGE('',*,*,#53749,.T.);
#77928=ORIENTED_EDGE('',*,*,#53750,.F.);
#77929=ORIENTED_EDGE('',*,*,#53743,.F.);
#77930=ORIENTED_EDGE('',*,*,#53751,.F.);
#77931=ORIENTED_EDGE('',*,*,#53752,.T.);
#77932=ORIENTED_EDGE('',*,*,#53753,.F.);
#77933=ORIENTED_EDGE('',*,*,#53746,.F.);
#77934=ORIENTED_EDGE('',*,*,#53754,.F.);
#77935=ORIENTED_EDGE('',*,*,#53749,.F.);
#77936=ORIENTED_EDGE('',*,*,#53755,.F.);
#77937=ORIENTED_EDGE('',*,*,#53752,.F.);
#77938=ORIENTED_EDGE('',*,*,#53756,.F.);
#77939=ORIENTED_EDGE('',*,*,#53757,.T.);
#77940=ORIENTED_EDGE('',*,*,#53754,.T.);
#77941=ORIENTED_EDGE('',*,*,#53758,.F.);
#77942=ORIENTED_EDGE('',*,*,#53759,.F.);
#77943=ORIENTED_EDGE('',*,*,#53760,.T.);
#77944=ORIENTED_EDGE('',*,*,#53756,.T.);
#77945=ORIENTED_EDGE('',*,*,#53757,.F.);
#77946=ORIENTED_EDGE('',*,*,#53761,.F.);
#77947=ORIENTED_EDGE('',*,*,#53758,.T.);
#77948=ORIENTED_EDGE('',*,*,#53748,.T.);
#77949=ORIENTED_EDGE('',*,*,#53762,.F.);
#77950=ORIENTED_EDGE('',*,*,#53763,.F.);
#77951=ORIENTED_EDGE('',*,*,#53764,.F.);
#77952=ORIENTED_EDGE('',*,*,#53765,.F.);
#77953=ORIENTED_EDGE('',*,*,#53766,.F.);
#77954=ORIENTED_EDGE('',*,*,#53767,.F.);
#77955=ORIENTED_EDGE('',*,*,#53768,.F.);
#77956=ORIENTED_EDGE('',*,*,#53769,.F.);
#77957=ORIENTED_EDGE('',*,*,#53770,.F.);
#77958=ORIENTED_EDGE('',*,*,#53771,.T.);
#77959=ORIENTED_EDGE('',*,*,#53772,.T.);
#77960=ORIENTED_EDGE('',*,*,#53773,.T.);
#77961=ORIENTED_EDGE('',*,*,#53774,.F.);
#77962=ORIENTED_EDGE('',*,*,#53765,.T.);
#77963=ORIENTED_EDGE('',*,*,#53770,.T.);
#77964=ORIENTED_EDGE('',*,*,#53775,.T.);
#77965=ORIENTED_EDGE('',*,*,#53776,.F.);
#77966=ORIENTED_EDGE('',*,*,#53777,.T.);
#77967=ORIENTED_EDGE('',*,*,#53774,.T.);
#77968=ORIENTED_EDGE('',*,*,#53778,.T.);
#77969=ORIENTED_EDGE('',*,*,#53766,.T.);
#77970=ORIENTED_EDGE('',*,*,#53777,.F.);
#77971=ORIENTED_EDGE('',*,*,#53779,.T.);
#77972=ORIENTED_EDGE('',*,*,#53780,.F.);
#77973=ORIENTED_EDGE('',*,*,#53781,.F.);
#77974=ORIENTED_EDGE('',*,*,#53782,.T.);
#77975=ORIENTED_EDGE('',*,*,#53783,.T.);
#77976=ORIENTED_EDGE('',*,*,#53780,.T.);
#77977=ORIENTED_EDGE('',*,*,#53784,.F.);
#77978=ORIENTED_EDGE('',*,*,#53785,.T.);
#77979=ORIENTED_EDGE('',*,*,#53786,.T.);
#77980=ORIENTED_EDGE('',*,*,#53787,.T.);
#77981=ORIENTED_EDGE('',*,*,#53783,.F.);
#77982=ORIENTED_EDGE('',*,*,#53788,.T.);
#77983=ORIENTED_EDGE('',*,*,#53784,.T.);
#77984=ORIENTED_EDGE('',*,*,#53767,.T.);
#77985=ORIENTED_EDGE('',*,*,#53789,.T.);
#77986=ORIENTED_EDGE('',*,*,#53771,.F.);
#77987=ORIENTED_EDGE('',*,*,#53764,.T.);
#77988=ORIENTED_EDGE('',*,*,#53787,.F.);
#77989=ORIENTED_EDGE('',*,*,#53790,.F.);
#77990=ORIENTED_EDGE('',*,*,#53791,.T.);
#77991=ORIENTED_EDGE('',*,*,#53792,.F.);
#77992=ORIENTED_EDGE('',*,*,#53793,.T.);
#77993=ORIENTED_EDGE('',*,*,#53794,.T.);
#77994=ORIENTED_EDGE('',*,*,#53795,.F.);
#77995=ORIENTED_EDGE('',*,*,#53796,.F.);
#77996=ORIENTED_EDGE('',*,*,#53797,.F.);
#77997=ORIENTED_EDGE('',*,*,#53796,.T.);
#77998=ORIENTED_EDGE('',*,*,#53791,.F.);
#77999=ORIENTED_EDGE('',*,*,#53798,.F.);
#78000=ORIENTED_EDGE('',*,*,#53799,.F.);
#78001=ORIENTED_EDGE('',*,*,#53800,.T.);
#78002=ORIENTED_EDGE('',*,*,#53801,.F.);
#78003=ORIENTED_EDGE('',*,*,#53794,.F.);
#78004=ORIENTED_EDGE('',*,*,#53802,.F.);
#78005=ORIENTED_EDGE('',*,*,#53803,.F.);
#78006=ORIENTED_EDGE('',*,*,#53801,.T.);
#78007=ORIENTED_EDGE('',*,*,#53804,.F.);
#78008=ORIENTED_EDGE('',*,*,#53805,.T.);
#78009=ORIENTED_EDGE('',*,*,#53806,.T.);
#78010=ORIENTED_EDGE('',*,*,#53807,.F.);
#78011=ORIENTED_EDGE('',*,*,#53808,.F.);
#78012=ORIENTED_EDGE('',*,*,#53805,.F.);
#78013=ORIENTED_EDGE('',*,*,#53808,.T.);
#78014=ORIENTED_EDGE('',*,*,#53809,.F.);
#78015=ORIENTED_EDGE('',*,*,#53810,.F.);
#78016=ORIENTED_EDGE('',*,*,#53811,.F.);
#78017=ORIENTED_EDGE('',*,*,#53810,.T.);
#78018=ORIENTED_EDGE('',*,*,#53812,.F.);
#78019=ORIENTED_EDGE('',*,*,#53813,.F.);
#78020=ORIENTED_EDGE('',*,*,#53793,.F.);
#78021=ORIENTED_EDGE('',*,*,#53792,.T.);
#78022=ORIENTED_EDGE('',*,*,#53795,.T.);
#78023=ORIENTED_EDGE('',*,*,#53803,.T.);
#78024=ORIENTED_EDGE('',*,*,#53811,.T.);
#78025=ORIENTED_EDGE('',*,*,#53814,.T.);
#78026=ORIENTED_EDGE('',*,*,#53815,.T.);
#78027=ORIENTED_EDGE('',*,*,#53816,.T.);
#78028=ORIENTED_EDGE('',*,*,#53736,.T.);
#78029=ORIENTED_EDGE('',*,*,#53817,.F.);
#78030=ORIENTED_EDGE('',*,*,#53818,.T.);
#78031=ORIENTED_EDGE('',*,*,#53819,.T.);
#78032=ORIENTED_EDGE('',*,*,#53744,.T.);
#78033=ORIENTED_EDGE('',*,*,#53820,.F.);
#78034=ORIENTED_EDGE('',*,*,#53821,.T.);
#78035=ORIENTED_EDGE('',*,*,#53822,.F.);
#78036=ORIENTED_EDGE('',*,*,#53772,.F.);
#78037=ORIENTED_EDGE('',*,*,#53823,.F.);
#78038=ORIENTED_EDGE('',*,*,#53813,.T.);
#78039=ORIENTED_EDGE('',*,*,#53823,.T.);
#78040=ORIENTED_EDGE('',*,*,#53789,.F.);
#78041=ORIENTED_EDGE('',*,*,#53824,.T.);
#78042=ORIENTED_EDGE('',*,*,#53790,.T.);
#78043=ORIENTED_EDGE('',*,*,#53824,.F.);
#78044=ORIENTED_EDGE('',*,*,#53786,.F.);
#78045=ORIENTED_EDGE('',*,*,#53825,.F.);
#78046=ORIENTED_EDGE('',*,*,#53798,.T.);
#78047=ORIENTED_EDGE('',*,*,#53799,.T.);
#78048=ORIENTED_EDGE('',*,*,#53825,.T.);
#78049=ORIENTED_EDGE('',*,*,#53785,.F.);
#78050=ORIENTED_EDGE('',*,*,#53788,.F.);
#78051=ORIENTED_EDGE('',*,*,#53782,.F.);
#78052=ORIENTED_EDGE('',*,*,#53826,.T.);
#78053=ORIENTED_EDGE('',*,*,#53802,.T.);
#78054=ORIENTED_EDGE('',*,*,#53797,.T.);
#78055=ORIENTED_EDGE('',*,*,#53826,.F.);
#78056=ORIENTED_EDGE('',*,*,#53781,.T.);
#78057=ORIENTED_EDGE('',*,*,#53827,.F.);
#78058=ORIENTED_EDGE('',*,*,#53800,.F.);
#78059=ORIENTED_EDGE('',*,*,#53804,.T.);
#78060=ORIENTED_EDGE('',*,*,#53827,.T.);
#78061=ORIENTED_EDGE('',*,*,#53779,.F.);
#78062=ORIENTED_EDGE('',*,*,#53828,.T.);
#78063=ORIENTED_EDGE('',*,*,#53828,.F.);
#78064=ORIENTED_EDGE('',*,*,#53776,.T.);
#78065=ORIENTED_EDGE('',*,*,#53829,.F.);
#78066=ORIENTED_EDGE('',*,*,#53806,.F.);
#78067=ORIENTED_EDGE('',*,*,#53739,.T.);
#78068=ORIENTED_EDGE('',*,*,#53734,.T.);
#78069=ORIENTED_EDGE('',*,*,#53741,.T.);
#78070=ORIENTED_EDGE('',*,*,#53747,.T.);
#78071=ORIENTED_EDGE('',*,*,#53753,.T.);
#78072=ORIENTED_EDGE('',*,*,#53755,.T.);
#78073=ORIENTED_EDGE('',*,*,#53751,.T.);
#78074=ORIENTED_EDGE('',*,*,#53745,.T.);
#78075=ORIENTED_EDGE('',*,*,#53829,.T.);
#78076=ORIENTED_EDGE('',*,*,#53778,.F.);
#78077=ORIENTED_EDGE('',*,*,#53775,.F.);
#78078=ORIENTED_EDGE('',*,*,#53773,.F.);
#78079=ORIENTED_EDGE('',*,*,#53822,.T.);
#78080=ORIENTED_EDGE('',*,*,#53812,.T.);
#78081=ORIENTED_EDGE('',*,*,#53809,.T.);
#78082=ORIENTED_EDGE('',*,*,#53807,.T.);
#78083=ORIENTED_EDGE('',*,*,#53820,.T.);
#78084=ORIENTED_EDGE('',*,*,#53750,.T.);
#78085=ORIENTED_EDGE('',*,*,#53760,.F.);
#78086=ORIENTED_EDGE('',*,*,#53830,.T.);
#78087=ORIENTED_EDGE('',*,*,#53762,.T.);
#78088=ORIENTED_EDGE('',*,*,#53742,.T.);
#78089=ORIENTED_EDGE('',*,*,#53816,.F.);
#78090=ORIENTED_EDGE('',*,*,#53831,.T.);
#78091=ORIENTED_EDGE('',*,*,#53814,.F.);
#78092=ORIENTED_EDGE('',*,*,#53832,.T.);
#78093=ORIENTED_EDGE('',*,*,#53768,.T.);
#78094=ORIENTED_EDGE('',*,*,#53832,.F.);
#78095=ORIENTED_EDGE('',*,*,#53815,.F.);
#78096=ORIENTED_EDGE('',*,*,#53833,.T.);
#78097=ORIENTED_EDGE('',*,*,#53769,.T.);
#78098=ORIENTED_EDGE('',*,*,#53833,.F.);
#78099=ORIENTED_EDGE('',*,*,#53817,.T.);
#78100=ORIENTED_EDGE('',*,*,#53738,.T.);
#78101=ORIENTED_EDGE('',*,*,#53819,.F.);
#78102=ORIENTED_EDGE('',*,*,#53834,.T.);
#78103=ORIENTED_EDGE('',*,*,#53830,.F.);
#78104=ORIENTED_EDGE('',*,*,#53761,.T.);
#78105=ORIENTED_EDGE('',*,*,#53759,.T.);
#78106=ORIENTED_EDGE('',*,*,#53763,.T.);
#78107=ORIENTED_EDGE('',*,*,#53831,.F.);
#78108=ORIENTED_EDGE('',*,*,#53818,.F.);
#78109=ORIENTED_EDGE('',*,*,#53834,.F.);
#78110=ORIENTED_EDGE('',*,*,#53821,.F.);
#78111=ORIENTED_EDGE('',*,*,#53835,.T.);
#78112=ORIENTED_EDGE('',*,*,#53836,.F.);
#78113=ORIENTED_EDGE('',*,*,#53837,.F.);
#78114=ORIENTED_EDGE('',*,*,#53838,.F.);
#78115=ORIENTED_EDGE('',*,*,#53839,.F.);
#78116=ORIENTED_EDGE('',*,*,#53840,.F.);
#78117=ORIENTED_EDGE('',*,*,#53841,.F.);
#78118=ORIENTED_EDGE('',*,*,#53842,.T.);
#78119=ORIENTED_EDGE('',*,*,#53835,.F.);
#78120=ORIENTED_EDGE('',*,*,#53842,.F.);
#78121=ORIENTED_EDGE('',*,*,#53843,.F.);
#78122=ORIENTED_EDGE('',*,*,#53844,.T.);
#78123=ORIENTED_EDGE('',*,*,#53845,.F.);
#78124=ORIENTED_EDGE('',*,*,#53846,.F.);
#78125=ORIENTED_EDGE('',*,*,#53844,.F.);
#78126=ORIENTED_EDGE('',*,*,#53847,.F.);
#78127=ORIENTED_EDGE('',*,*,#53848,.F.);
#78128=ORIENTED_EDGE('',*,*,#53849,.F.);
#78129=ORIENTED_EDGE('',*,*,#53850,.F.);
#78130=ORIENTED_EDGE('',*,*,#53836,.T.);
#78131=ORIENTED_EDGE('',*,*,#53851,.T.);
#78132=ORIENTED_EDGE('',*,*,#53850,.T.);
#78133=ORIENTED_EDGE('',*,*,#53852,.F.);
#78134=ORIENTED_EDGE('',*,*,#53837,.T.);
#78135=ORIENTED_EDGE('',*,*,#53852,.T.);
#78136=ORIENTED_EDGE('',*,*,#53849,.T.);
#78137=ORIENTED_EDGE('',*,*,#53853,.F.);
#78138=ORIENTED_EDGE('',*,*,#53838,.T.);
#78139=ORIENTED_EDGE('',*,*,#53853,.T.);
#78140=ORIENTED_EDGE('',*,*,#53848,.T.);
#78141=ORIENTED_EDGE('',*,*,#53854,.F.);
#78142=ORIENTED_EDGE('',*,*,#53839,.T.);
#78143=ORIENTED_EDGE('',*,*,#53854,.T.);
#78144=ORIENTED_EDGE('',*,*,#53847,.T.);
#78145=ORIENTED_EDGE('',*,*,#53851,.F.);
#78146=ORIENTED_EDGE('',*,*,#53855,.T.);
#78147=ORIENTED_EDGE('',*,*,#53856,.T.);
#78148=ORIENTED_EDGE('',*,*,#53857,.T.);
#78149=ORIENTED_EDGE('',*,*,#53855,.F.);
#78150=ORIENTED_EDGE('',*,*,#53857,.F.);
#78151=ORIENTED_EDGE('',*,*,#53840,.T.);
#78152=ORIENTED_EDGE('',*,*,#53841,.T.);
#78153=ORIENTED_EDGE('',*,*,#53858,.T.);
#78154=ORIENTED_EDGE('',*,*,#53845,.T.);
#78155=ORIENTED_EDGE('',*,*,#53846,.T.);
#78156=ORIENTED_EDGE('',*,*,#53858,.F.);
#78157=ORIENTED_EDGE('',*,*,#53843,.T.);
#78158=ORIENTED_EDGE('',*,*,#53856,.F.);
#78159=ORIENTED_EDGE('',*,*,#53859,.T.);
#78160=ORIENTED_EDGE('',*,*,#53860,.F.);
#78161=ORIENTED_EDGE('',*,*,#53861,.F.);
#78162=ORIENTED_EDGE('',*,*,#53862,.F.);
#78163=ORIENTED_EDGE('',*,*,#53863,.T.);
#78164=ORIENTED_EDGE('',*,*,#53864,.F.);
#78165=ORIENTED_EDGE('',*,*,#53859,.F.);
#78166=ORIENTED_EDGE('',*,*,#53865,.F.);
#78167=ORIENTED_EDGE('',*,*,#53866,.T.);
#78168=ORIENTED_EDGE('',*,*,#53867,.F.);
#78169=ORIENTED_EDGE('',*,*,#53863,.F.);
#78170=ORIENTED_EDGE('',*,*,#53868,.F.);
#78171=ORIENTED_EDGE('',*,*,#53869,.T.);
#78172=ORIENTED_EDGE('',*,*,#53870,.F.);
#78173=ORIENTED_EDGE('',*,*,#53866,.F.);
#78174=ORIENTED_EDGE('',*,*,#53871,.F.);
#78175=ORIENTED_EDGE('',*,*,#53872,.F.);
#78176=ORIENTED_EDGE('',*,*,#53873,.F.);
#78177=ORIENTED_EDGE('',*,*,#53869,.F.);
#78178=ORIENTED_EDGE('',*,*,#53874,.F.);
#78179=ORIENTED_EDGE('',*,*,#53875,.T.);
#78180=ORIENTED_EDGE('',*,*,#53876,.F.);
#78181=ORIENTED_EDGE('',*,*,#53877,.F.);
#78182=ORIENTED_EDGE('',*,*,#53878,.F.);
#78183=ORIENTED_EDGE('',*,*,#53879,.T.);
#78184=ORIENTED_EDGE('',*,*,#53880,.F.);
#78185=ORIENTED_EDGE('',*,*,#53875,.F.);
#78186=ORIENTED_EDGE('',*,*,#53881,.F.);
#78187=ORIENTED_EDGE('',*,*,#53882,.T.);
#78188=ORIENTED_EDGE('',*,*,#53883,.F.);
#78189=ORIENTED_EDGE('',*,*,#53879,.F.);
#78190=ORIENTED_EDGE('',*,*,#53884,.F.);
#78191=ORIENTED_EDGE('',*,*,#53885,.T.);
#78192=ORIENTED_EDGE('',*,*,#53886,.F.);
#78193=ORIENTED_EDGE('',*,*,#53882,.F.);
#78194=ORIENTED_EDGE('',*,*,#53887,.F.);
#78195=ORIENTED_EDGE('',*,*,#53888,.F.);
#78196=ORIENTED_EDGE('',*,*,#53889,.F.);
#78197=ORIENTED_EDGE('',*,*,#53885,.F.);
#78198=ORIENTED_EDGE('',*,*,#53890,.F.);
#78199=ORIENTED_EDGE('',*,*,#53891,.T.);
#78200=ORIENTED_EDGE('',*,*,#53892,.F.);
#78201=ORIENTED_EDGE('',*,*,#53893,.F.);
#78202=ORIENTED_EDGE('',*,*,#53894,.F.);
#78203=ORIENTED_EDGE('',*,*,#53895,.T.);
#78204=ORIENTED_EDGE('',*,*,#53896,.F.);
#78205=ORIENTED_EDGE('',*,*,#53891,.F.);
#78206=ORIENTED_EDGE('',*,*,#53897,.F.);
#78207=ORIENTED_EDGE('',*,*,#53898,.T.);
#78208=ORIENTED_EDGE('',*,*,#53899,.F.);
#78209=ORIENTED_EDGE('',*,*,#53895,.F.);
#78210=ORIENTED_EDGE('',*,*,#53900,.F.);
#78211=ORIENTED_EDGE('',*,*,#53901,.T.);
#78212=ORIENTED_EDGE('',*,*,#53902,.F.);
#78213=ORIENTED_EDGE('',*,*,#53898,.F.);
#78214=ORIENTED_EDGE('',*,*,#53903,.F.);
#78215=ORIENTED_EDGE('',*,*,#53904,.T.);
#78216=ORIENTED_EDGE('',*,*,#53905,.F.);
#78217=ORIENTED_EDGE('',*,*,#53901,.F.);
#78218=ORIENTED_EDGE('',*,*,#53906,.F.);
#78219=ORIENTED_EDGE('',*,*,#53907,.T.);
#78220=ORIENTED_EDGE('',*,*,#53908,.F.);
#78221=ORIENTED_EDGE('',*,*,#53904,.F.);
#78222=ORIENTED_EDGE('',*,*,#53909,.F.);
#78223=ORIENTED_EDGE('',*,*,#53910,.T.);
#78224=ORIENTED_EDGE('',*,*,#53911,.F.);
#78225=ORIENTED_EDGE('',*,*,#53907,.F.);
#78226=ORIENTED_EDGE('',*,*,#53912,.F.);
#78227=ORIENTED_EDGE('',*,*,#53913,.T.);
#78228=ORIENTED_EDGE('',*,*,#53914,.F.);
#78229=ORIENTED_EDGE('',*,*,#53910,.F.);
#78230=ORIENTED_EDGE('',*,*,#53915,.F.);
#78231=ORIENTED_EDGE('',*,*,#53916,.F.);
#78232=ORIENTED_EDGE('',*,*,#53917,.F.);
#78233=ORIENTED_EDGE('',*,*,#53913,.F.);
#78234=ORIENTED_EDGE('',*,*,#53918,.F.);
#78235=ORIENTED_EDGE('',*,*,#53919,.F.);
#78236=ORIENTED_EDGE('',*,*,#53920,.F.);
#78237=ORIENTED_EDGE('',*,*,#53921,.T.);
#78238=ORIENTED_EDGE('',*,*,#53922,.F.);
#78239=ORIENTED_EDGE('',*,*,#53923,.T.);
#78240=ORIENTED_EDGE('',*,*,#53924,.F.);
#78241=ORIENTED_EDGE('',*,*,#53921,.F.);
#78242=ORIENTED_EDGE('',*,*,#53925,.F.);
#78243=ORIENTED_EDGE('',*,*,#53926,.T.);
#78244=ORIENTED_EDGE('',*,*,#53927,.F.);
#78245=ORIENTED_EDGE('',*,*,#53923,.F.);
#78246=ORIENTED_EDGE('',*,*,#53928,.F.);
#78247=ORIENTED_EDGE('',*,*,#53929,.T.);
#78248=ORIENTED_EDGE('',*,*,#53930,.F.);
#78249=ORIENTED_EDGE('',*,*,#53926,.F.);
#78250=ORIENTED_EDGE('',*,*,#53931,.F.);
#78251=ORIENTED_EDGE('',*,*,#53932,.F.);
#78252=ORIENTED_EDGE('',*,*,#53933,.F.);
#78253=ORIENTED_EDGE('',*,*,#53929,.F.);
#78254=ORIENTED_EDGE('',*,*,#53934,.F.);
#78255=ORIENTED_EDGE('',*,*,#53935,.T.);
#78256=ORIENTED_EDGE('',*,*,#53936,.F.);
#78257=ORIENTED_EDGE('',*,*,#53937,.F.);
#78258=ORIENTED_EDGE('',*,*,#53938,.F.);
#78259=ORIENTED_EDGE('',*,*,#53939,.T.);
#78260=ORIENTED_EDGE('',*,*,#53940,.F.);
#78261=ORIENTED_EDGE('',*,*,#53935,.F.);
#78262=ORIENTED_EDGE('',*,*,#53941,.F.);
#78263=ORIENTED_EDGE('',*,*,#53942,.T.);
#78264=ORIENTED_EDGE('',*,*,#53943,.F.);
#78265=ORIENTED_EDGE('',*,*,#53939,.F.);
#78266=ORIENTED_EDGE('',*,*,#53944,.F.);
#78267=ORIENTED_EDGE('',*,*,#53945,.T.);
#78268=ORIENTED_EDGE('',*,*,#53946,.F.);
#78269=ORIENTED_EDGE('',*,*,#53942,.F.);
#78270=ORIENTED_EDGE('',*,*,#53947,.F.);
#78271=ORIENTED_EDGE('',*,*,#53948,.T.);
#78272=ORIENTED_EDGE('',*,*,#53949,.F.);
#78273=ORIENTED_EDGE('',*,*,#53945,.F.);
#78274=ORIENTED_EDGE('',*,*,#53950,.F.);
#78275=ORIENTED_EDGE('',*,*,#53951,.T.);
#78276=ORIENTED_EDGE('',*,*,#53952,.F.);
#78277=ORIENTED_EDGE('',*,*,#53948,.F.);
#78278=ORIENTED_EDGE('',*,*,#53953,.F.);
#78279=ORIENTED_EDGE('',*,*,#53954,.T.);
#78280=ORIENTED_EDGE('',*,*,#53955,.F.);
#78281=ORIENTED_EDGE('',*,*,#53951,.F.);
#78282=ORIENTED_EDGE('',*,*,#53956,.F.);
#78283=ORIENTED_EDGE('',*,*,#53957,.T.);
#78284=ORIENTED_EDGE('',*,*,#53958,.F.);
#78285=ORIENTED_EDGE('',*,*,#53954,.F.);
#78286=ORIENTED_EDGE('',*,*,#53959,.F.);
#78287=ORIENTED_EDGE('',*,*,#53960,.T.);
#78288=ORIENTED_EDGE('',*,*,#53961,.F.);
#78289=ORIENTED_EDGE('',*,*,#53957,.F.);
#78290=ORIENTED_EDGE('',*,*,#53962,.F.);
#78291=ORIENTED_EDGE('',*,*,#53963,.F.);
#78292=ORIENTED_EDGE('',*,*,#53964,.F.);
#78293=ORIENTED_EDGE('',*,*,#53960,.F.);
#78294=ORIENTED_EDGE('',*,*,#53965,.F.);
#78295=ORIENTED_EDGE('',*,*,#53966,.T.);
#78296=ORIENTED_EDGE('',*,*,#53967,.F.);
#78297=ORIENTED_EDGE('',*,*,#53968,.F.);
#78298=ORIENTED_EDGE('',*,*,#53969,.F.);
#78299=ORIENTED_EDGE('',*,*,#53970,.T.);
#78300=ORIENTED_EDGE('',*,*,#53971,.F.);
#78301=ORIENTED_EDGE('',*,*,#53966,.F.);
#78302=ORIENTED_EDGE('',*,*,#53972,.F.);
#78303=ORIENTED_EDGE('',*,*,#53973,.T.);
#78304=ORIENTED_EDGE('',*,*,#53974,.F.);
#78305=ORIENTED_EDGE('',*,*,#53970,.F.);
#78306=ORIENTED_EDGE('',*,*,#53975,.F.);
#78307=ORIENTED_EDGE('',*,*,#53976,.T.);
#78308=ORIENTED_EDGE('',*,*,#53977,.F.);
#78309=ORIENTED_EDGE('',*,*,#53973,.F.);
#78310=ORIENTED_EDGE('',*,*,#53978,.F.);
#78311=ORIENTED_EDGE('',*,*,#53979,.T.);
#78312=ORIENTED_EDGE('',*,*,#53980,.F.);
#78313=ORIENTED_EDGE('',*,*,#53976,.F.);
#78314=ORIENTED_EDGE('',*,*,#53981,.F.);
#78315=ORIENTED_EDGE('',*,*,#53982,.T.);
#78316=ORIENTED_EDGE('',*,*,#53983,.F.);
#78317=ORIENTED_EDGE('',*,*,#53979,.F.);
#78318=ORIENTED_EDGE('',*,*,#53984,.F.);
#78319=ORIENTED_EDGE('',*,*,#53985,.T.);
#78320=ORIENTED_EDGE('',*,*,#53986,.F.);
#78321=ORIENTED_EDGE('',*,*,#53982,.F.);
#78322=ORIENTED_EDGE('',*,*,#53987,.F.);
#78323=ORIENTED_EDGE('',*,*,#53988,.T.);
#78324=ORIENTED_EDGE('',*,*,#53989,.F.);
#78325=ORIENTED_EDGE('',*,*,#53985,.F.);
#78326=ORIENTED_EDGE('',*,*,#53990,.F.);
#78327=ORIENTED_EDGE('',*,*,#53991,.F.);
#78328=ORIENTED_EDGE('',*,*,#53992,.F.);
#78329=ORIENTED_EDGE('',*,*,#53988,.F.);
#78330=ORIENTED_EDGE('',*,*,#53993,.F.);
#78331=ORIENTED_EDGE('',*,*,#53994,.T.);
#78332=ORIENTED_EDGE('',*,*,#53995,.F.);
#78333=ORIENTED_EDGE('',*,*,#53996,.F.);
#78334=ORIENTED_EDGE('',*,*,#53997,.F.);
#78335=ORIENTED_EDGE('',*,*,#53998,.T.);
#78336=ORIENTED_EDGE('',*,*,#53999,.F.);
#78337=ORIENTED_EDGE('',*,*,#53994,.F.);
#78338=ORIENTED_EDGE('',*,*,#54000,.F.);
#78339=ORIENTED_EDGE('',*,*,#54001,.T.);
#78340=ORIENTED_EDGE('',*,*,#54002,.F.);
#78341=ORIENTED_EDGE('',*,*,#53998,.F.);
#78342=ORIENTED_EDGE('',*,*,#54003,.F.);
#78343=ORIENTED_EDGE('',*,*,#54004,.T.);
#78344=ORIENTED_EDGE('',*,*,#54005,.F.);
#78345=ORIENTED_EDGE('',*,*,#54001,.F.);
#78346=ORIENTED_EDGE('',*,*,#54006,.F.);
#78347=ORIENTED_EDGE('',*,*,#54007,.T.);
#78348=ORIENTED_EDGE('',*,*,#54008,.F.);
#78349=ORIENTED_EDGE('',*,*,#54004,.F.);
#78350=ORIENTED_EDGE('',*,*,#54009,.F.);
#78351=ORIENTED_EDGE('',*,*,#54010,.T.);
#78352=ORIENTED_EDGE('',*,*,#54011,.F.);
#78353=ORIENTED_EDGE('',*,*,#54007,.F.);
#78354=ORIENTED_EDGE('',*,*,#54012,.F.);
#78355=ORIENTED_EDGE('',*,*,#54013,.T.);
#78356=ORIENTED_EDGE('',*,*,#54014,.F.);
#78357=ORIENTED_EDGE('',*,*,#54010,.F.);
#78358=ORIENTED_EDGE('',*,*,#54015,.F.);
#78359=ORIENTED_EDGE('',*,*,#54016,.T.);
#78360=ORIENTED_EDGE('',*,*,#54017,.F.);
#78361=ORIENTED_EDGE('',*,*,#54013,.F.);
#78362=ORIENTED_EDGE('',*,*,#54018,.F.);
#78363=ORIENTED_EDGE('',*,*,#54019,.F.);
#78364=ORIENTED_EDGE('',*,*,#54020,.F.);
#78365=ORIENTED_EDGE('',*,*,#54016,.F.);
#78366=ORIENTED_EDGE('',*,*,#54021,.F.);
#78367=ORIENTED_EDGE('',*,*,#54022,.T.);
#78368=ORIENTED_EDGE('',*,*,#54023,.F.);
#78369=ORIENTED_EDGE('',*,*,#54024,.F.);
#78370=ORIENTED_EDGE('',*,*,#54025,.F.);
#78371=ORIENTED_EDGE('',*,*,#54026,.T.);
#78372=ORIENTED_EDGE('',*,*,#54027,.F.);
#78373=ORIENTED_EDGE('',*,*,#54022,.F.);
#78374=ORIENTED_EDGE('',*,*,#54028,.F.);
#78375=ORIENTED_EDGE('',*,*,#54029,.T.);
#78376=ORIENTED_EDGE('',*,*,#54030,.F.);
#78377=ORIENTED_EDGE('',*,*,#54026,.F.);
#78378=ORIENTED_EDGE('',*,*,#54031,.F.);
#78379=ORIENTED_EDGE('',*,*,#54032,.T.);
#78380=ORIENTED_EDGE('',*,*,#54033,.F.);
#78381=ORIENTED_EDGE('',*,*,#54029,.F.);
#78382=ORIENTED_EDGE('',*,*,#54034,.F.);
#78383=ORIENTED_EDGE('',*,*,#54035,.T.);
#78384=ORIENTED_EDGE('',*,*,#54036,.F.);
#78385=ORIENTED_EDGE('',*,*,#54032,.F.);
#78386=ORIENTED_EDGE('',*,*,#54037,.F.);
#78387=ORIENTED_EDGE('',*,*,#54038,.T.);
#78388=ORIENTED_EDGE('',*,*,#54039,.F.);
#78389=ORIENTED_EDGE('',*,*,#54035,.F.);
#78390=ORIENTED_EDGE('',*,*,#54040,.F.);
#78391=ORIENTED_EDGE('',*,*,#54041,.T.);
#78392=ORIENTED_EDGE('',*,*,#54042,.F.);
#78393=ORIENTED_EDGE('',*,*,#54038,.F.);
#78394=ORIENTED_EDGE('',*,*,#54043,.F.);
#78395=ORIENTED_EDGE('',*,*,#54044,.T.);
#78396=ORIENTED_EDGE('',*,*,#54045,.F.);
#78397=ORIENTED_EDGE('',*,*,#54041,.F.);
#78398=ORIENTED_EDGE('',*,*,#54046,.F.);
#78399=ORIENTED_EDGE('',*,*,#54047,.F.);
#78400=ORIENTED_EDGE('',*,*,#54048,.F.);
#78401=ORIENTED_EDGE('',*,*,#54044,.F.);
#78402=ORIENTED_EDGE('',*,*,#54049,.F.);
#78403=ORIENTED_EDGE('',*,*,#54050,.T.);
#78404=ORIENTED_EDGE('',*,*,#54051,.F.);
#78405=ORIENTED_EDGE('',*,*,#54052,.F.);
#78406=ORIENTED_EDGE('',*,*,#54053,.F.);
#78407=ORIENTED_EDGE('',*,*,#54054,.T.);
#78408=ORIENTED_EDGE('',*,*,#54055,.F.);
#78409=ORIENTED_EDGE('',*,*,#54050,.F.);
#78410=ORIENTED_EDGE('',*,*,#54056,.F.);
#78411=ORIENTED_EDGE('',*,*,#54057,.T.);
#78412=ORIENTED_EDGE('',*,*,#54058,.F.);
#78413=ORIENTED_EDGE('',*,*,#54054,.F.);
#78414=ORIENTED_EDGE('',*,*,#54059,.F.);
#78415=ORIENTED_EDGE('',*,*,#54060,.T.);
#78416=ORIENTED_EDGE('',*,*,#54061,.F.);
#78417=ORIENTED_EDGE('',*,*,#54057,.F.);
#78418=ORIENTED_EDGE('',*,*,#54062,.F.);
#78419=ORIENTED_EDGE('',*,*,#54063,.T.);
#78420=ORIENTED_EDGE('',*,*,#54064,.F.);
#78421=ORIENTED_EDGE('',*,*,#54060,.F.);
#78422=ORIENTED_EDGE('',*,*,#54065,.F.);
#78423=ORIENTED_EDGE('',*,*,#54066,.T.);
#78424=ORIENTED_EDGE('',*,*,#54067,.F.);
#78425=ORIENTED_EDGE('',*,*,#54063,.F.);
#78426=ORIENTED_EDGE('',*,*,#54068,.F.);
#78427=ORIENTED_EDGE('',*,*,#54069,.T.);
#78428=ORIENTED_EDGE('',*,*,#54070,.F.);
#78429=ORIENTED_EDGE('',*,*,#54066,.F.);
#78430=ORIENTED_EDGE('',*,*,#54071,.F.);
#78431=ORIENTED_EDGE('',*,*,#54072,.T.);
#78432=ORIENTED_EDGE('',*,*,#54073,.F.);
#78433=ORIENTED_EDGE('',*,*,#54069,.F.);
#78434=ORIENTED_EDGE('',*,*,#54074,.F.);
#78435=ORIENTED_EDGE('',*,*,#54075,.F.);
#78436=ORIENTED_EDGE('',*,*,#54076,.F.);
#78437=ORIENTED_EDGE('',*,*,#54072,.F.);
#78438=ORIENTED_EDGE('',*,*,#54077,.F.);
#78439=ORIENTED_EDGE('',*,*,#54078,.T.);
#78440=ORIENTED_EDGE('',*,*,#54079,.F.);
#78441=ORIENTED_EDGE('',*,*,#54080,.F.);
#78442=ORIENTED_EDGE('',*,*,#54081,.F.);
#78443=ORIENTED_EDGE('',*,*,#54082,.T.);
#78444=ORIENTED_EDGE('',*,*,#54083,.F.);
#78445=ORIENTED_EDGE('',*,*,#54078,.F.);
#78446=ORIENTED_EDGE('',*,*,#54084,.F.);
#78447=ORIENTED_EDGE('',*,*,#54085,.T.);
#78448=ORIENTED_EDGE('',*,*,#54086,.F.);
#78449=ORIENTED_EDGE('',*,*,#54082,.F.);
#78450=ORIENTED_EDGE('',*,*,#54087,.F.);
#78451=ORIENTED_EDGE('',*,*,#54088,.T.);
#78452=ORIENTED_EDGE('',*,*,#54089,.F.);
#78453=ORIENTED_EDGE('',*,*,#54085,.F.);
#78454=ORIENTED_EDGE('',*,*,#54090,.F.);
#78455=ORIENTED_EDGE('',*,*,#54091,.T.);
#78456=ORIENTED_EDGE('',*,*,#54092,.F.);
#78457=ORIENTED_EDGE('',*,*,#54088,.F.);
#78458=ORIENTED_EDGE('',*,*,#54093,.F.);
#78459=ORIENTED_EDGE('',*,*,#54094,.T.);
#78460=ORIENTED_EDGE('',*,*,#54095,.F.);
#78461=ORIENTED_EDGE('',*,*,#54091,.F.);
#78462=ORIENTED_EDGE('',*,*,#54096,.F.);
#78463=ORIENTED_EDGE('',*,*,#54097,.T.);
#78464=ORIENTED_EDGE('',*,*,#54098,.F.);
#78465=ORIENTED_EDGE('',*,*,#54094,.F.);
#78466=ORIENTED_EDGE('',*,*,#54099,.F.);
#78467=ORIENTED_EDGE('',*,*,#54100,.T.);
#78468=ORIENTED_EDGE('',*,*,#54101,.F.);
#78469=ORIENTED_EDGE('',*,*,#54097,.F.);
#78470=ORIENTED_EDGE('',*,*,#54102,.F.);
#78471=ORIENTED_EDGE('',*,*,#54103,.F.);
#78472=ORIENTED_EDGE('',*,*,#54104,.F.);
#78473=ORIENTED_EDGE('',*,*,#54100,.F.);
#78474=ORIENTED_EDGE('',*,*,#54105,.F.);
#78475=ORIENTED_EDGE('',*,*,#54106,.T.);
#78476=ORIENTED_EDGE('',*,*,#54107,.F.);
#78477=ORIENTED_EDGE('',*,*,#54108,.F.);
#78478=ORIENTED_EDGE('',*,*,#54109,.F.);
#78479=ORIENTED_EDGE('',*,*,#54110,.T.);
#78480=ORIENTED_EDGE('',*,*,#54111,.F.);
#78481=ORIENTED_EDGE('',*,*,#54106,.F.);
#78482=ORIENTED_EDGE('',*,*,#54112,.F.);
#78483=ORIENTED_EDGE('',*,*,#54113,.T.);
#78484=ORIENTED_EDGE('',*,*,#54114,.F.);
#78485=ORIENTED_EDGE('',*,*,#54110,.F.);
#78486=ORIENTED_EDGE('',*,*,#54115,.F.);
#78487=ORIENTED_EDGE('',*,*,#54116,.T.);
#78488=ORIENTED_EDGE('',*,*,#54117,.F.);
#78489=ORIENTED_EDGE('',*,*,#54113,.F.);
#78490=ORIENTED_EDGE('',*,*,#54118,.F.);
#78491=ORIENTED_EDGE('',*,*,#54119,.T.);
#78492=ORIENTED_EDGE('',*,*,#54120,.F.);
#78493=ORIENTED_EDGE('',*,*,#54116,.F.);
#78494=ORIENTED_EDGE('',*,*,#54121,.F.);
#78495=ORIENTED_EDGE('',*,*,#54122,.T.);
#78496=ORIENTED_EDGE('',*,*,#54123,.F.);
#78497=ORIENTED_EDGE('',*,*,#54119,.F.);
#78498=ORIENTED_EDGE('',*,*,#54124,.F.);
#78499=ORIENTED_EDGE('',*,*,#54125,.T.);
#78500=ORIENTED_EDGE('',*,*,#54126,.F.);
#78501=ORIENTED_EDGE('',*,*,#54122,.F.);
#78502=ORIENTED_EDGE('',*,*,#54127,.F.);
#78503=ORIENTED_EDGE('',*,*,#54128,.T.);
#78504=ORIENTED_EDGE('',*,*,#54129,.F.);
#78505=ORIENTED_EDGE('',*,*,#54125,.F.);
#78506=ORIENTED_EDGE('',*,*,#54130,.F.);
#78507=ORIENTED_EDGE('',*,*,#54131,.F.);
#78508=ORIENTED_EDGE('',*,*,#54132,.F.);
#78509=ORIENTED_EDGE('',*,*,#54128,.F.);
#78510=ORIENTED_EDGE('',*,*,#54133,.F.);
#78511=ORIENTED_EDGE('',*,*,#54134,.T.);
#78512=ORIENTED_EDGE('',*,*,#54135,.F.);
#78513=ORIENTED_EDGE('',*,*,#54136,.F.);
#78514=ORIENTED_EDGE('',*,*,#54137,.F.);
#78515=ORIENTED_EDGE('',*,*,#54138,.T.);
#78516=ORIENTED_EDGE('',*,*,#54139,.F.);
#78517=ORIENTED_EDGE('',*,*,#54134,.F.);
#78518=ORIENTED_EDGE('',*,*,#54140,.F.);
#78519=ORIENTED_EDGE('',*,*,#54141,.T.);
#78520=ORIENTED_EDGE('',*,*,#54142,.F.);
#78521=ORIENTED_EDGE('',*,*,#54138,.F.);
#78522=ORIENTED_EDGE('',*,*,#54143,.F.);
#78523=ORIENTED_EDGE('',*,*,#54144,.T.);
#78524=ORIENTED_EDGE('',*,*,#54145,.F.);
#78525=ORIENTED_EDGE('',*,*,#54141,.F.);
#78526=ORIENTED_EDGE('',*,*,#54146,.F.);
#78527=ORIENTED_EDGE('',*,*,#54147,.T.);
#78528=ORIENTED_EDGE('',*,*,#54148,.F.);
#78529=ORIENTED_EDGE('',*,*,#54144,.F.);
#78530=ORIENTED_EDGE('',*,*,#54149,.F.);
#78531=ORIENTED_EDGE('',*,*,#54150,.T.);
#78532=ORIENTED_EDGE('',*,*,#54151,.F.);
#78533=ORIENTED_EDGE('',*,*,#54147,.F.);
#78534=ORIENTED_EDGE('',*,*,#54152,.F.);
#78535=ORIENTED_EDGE('',*,*,#54153,.T.);
#78536=ORIENTED_EDGE('',*,*,#54154,.F.);
#78537=ORIENTED_EDGE('',*,*,#54150,.F.);
#78538=ORIENTED_EDGE('',*,*,#54155,.F.);
#78539=ORIENTED_EDGE('',*,*,#54156,.T.);
#78540=ORIENTED_EDGE('',*,*,#54157,.F.);
#78541=ORIENTED_EDGE('',*,*,#54153,.F.);
#78542=ORIENTED_EDGE('',*,*,#54158,.F.);
#78543=ORIENTED_EDGE('',*,*,#54159,.T.);
#78544=ORIENTED_EDGE('',*,*,#54160,.F.);
#78545=ORIENTED_EDGE('',*,*,#54156,.F.);
#78546=ORIENTED_EDGE('',*,*,#54161,.F.);
#78547=ORIENTED_EDGE('',*,*,#54162,.F.);
#78548=ORIENTED_EDGE('',*,*,#54163,.F.);
#78549=ORIENTED_EDGE('',*,*,#54159,.F.);
#78550=ORIENTED_EDGE('',*,*,#54164,.F.);
#78551=ORIENTED_EDGE('',*,*,#54165,.T.);
#78552=ORIENTED_EDGE('',*,*,#54166,.F.);
#78553=ORIENTED_EDGE('',*,*,#54167,.F.);
#78554=ORIENTED_EDGE('',*,*,#54168,.F.);
#78555=ORIENTED_EDGE('',*,*,#54169,.T.);
#78556=ORIENTED_EDGE('',*,*,#54170,.F.);
#78557=ORIENTED_EDGE('',*,*,#54165,.F.);
#78558=ORIENTED_EDGE('',*,*,#54171,.F.);
#78559=ORIENTED_EDGE('',*,*,#54172,.T.);
#78560=ORIENTED_EDGE('',*,*,#54173,.F.);
#78561=ORIENTED_EDGE('',*,*,#54169,.F.);
#78562=ORIENTED_EDGE('',*,*,#54174,.F.);
#78563=ORIENTED_EDGE('',*,*,#54175,.T.);
#78564=ORIENTED_EDGE('',*,*,#54176,.F.);
#78565=ORIENTED_EDGE('',*,*,#54172,.F.);
#78566=ORIENTED_EDGE('',*,*,#54177,.F.);
#78567=ORIENTED_EDGE('',*,*,#54178,.T.);
#78568=ORIENTED_EDGE('',*,*,#54179,.F.);
#78569=ORIENTED_EDGE('',*,*,#54175,.F.);
#78570=ORIENTED_EDGE('',*,*,#54180,.F.);
#78571=ORIENTED_EDGE('',*,*,#54181,.T.);
#78572=ORIENTED_EDGE('',*,*,#54182,.F.);
#78573=ORIENTED_EDGE('',*,*,#54178,.F.);
#78574=ORIENTED_EDGE('',*,*,#54183,.F.);
#78575=ORIENTED_EDGE('',*,*,#54184,.T.);
#78576=ORIENTED_EDGE('',*,*,#54185,.F.);
#78577=ORIENTED_EDGE('',*,*,#54181,.F.);
#78578=ORIENTED_EDGE('',*,*,#54186,.F.);
#78579=ORIENTED_EDGE('',*,*,#54187,.T.);
#78580=ORIENTED_EDGE('',*,*,#54188,.F.);
#78581=ORIENTED_EDGE('',*,*,#54184,.F.);
#78582=ORIENTED_EDGE('',*,*,#54189,.F.);
#78583=ORIENTED_EDGE('',*,*,#54190,.F.);
#78584=ORIENTED_EDGE('',*,*,#54191,.F.);
#78585=ORIENTED_EDGE('',*,*,#54187,.F.);
#78586=ORIENTED_EDGE('',*,*,#54192,.F.);
#78587=ORIENTED_EDGE('',*,*,#54193,.F.);
#78588=ORIENTED_EDGE('',*,*,#54194,.F.);
#78589=ORIENTED_EDGE('',*,*,#54195,.T.);
#78590=ORIENTED_EDGE('',*,*,#54196,.F.);
#78591=ORIENTED_EDGE('',*,*,#54197,.T.);
#78592=ORIENTED_EDGE('',*,*,#54198,.F.);
#78593=ORIENTED_EDGE('',*,*,#54195,.F.);
#78594=ORIENTED_EDGE('',*,*,#54199,.F.);
#78595=ORIENTED_EDGE('',*,*,#54200,.T.);
#78596=ORIENTED_EDGE('',*,*,#54201,.F.);
#78597=ORIENTED_EDGE('',*,*,#54197,.F.);
#78598=ORIENTED_EDGE('',*,*,#54202,.F.);
#78599=ORIENTED_EDGE('',*,*,#54203,.T.);
#78600=ORIENTED_EDGE('',*,*,#54204,.F.);
#78601=ORIENTED_EDGE('',*,*,#54200,.F.);
#78602=ORIENTED_EDGE('',*,*,#54205,.F.);
#78603=ORIENTED_EDGE('',*,*,#54206,.F.);
#78604=ORIENTED_EDGE('',*,*,#54207,.F.);
#78605=ORIENTED_EDGE('',*,*,#54203,.F.);
#78606=ORIENTED_EDGE('',*,*,#54208,.F.);
#78607=ORIENTED_EDGE('',*,*,#54209,.F.);
#78608=ORIENTED_EDGE('',*,*,#53930,.T.);
#78609=ORIENTED_EDGE('',*,*,#54210,.F.);
#78610=ORIENTED_EDGE('',*,*,#54211,.F.);
#78611=ORIENTED_EDGE('',*,*,#54212,.F.);
#78612=ORIENTED_EDGE('',*,*,#53887,.T.);
#78613=ORIENTED_EDGE('',*,*,#54213,.F.);
#78614=ORIENTED_EDGE('',*,*,#54214,.F.);
#78615=ORIENTED_EDGE('',*,*,#54215,.F.);
#78616=ORIENTED_EDGE('',*,*,#54198,.T.);
#78617=ORIENTED_EDGE('',*,*,#54216,.F.);
#78618=ORIENTED_EDGE('',*,*,#54217,.F.);
#78619=ORIENTED_EDGE('',*,*,#54218,.F.);
#78620=ORIENTED_EDGE('',*,*,#53865,.T.);
#78621=ORIENTED_EDGE('',*,*,#54219,.F.);
#78622=ORIENTED_EDGE('',*,*,#54220,.F.);
#78623=ORIENTED_EDGE('',*,*,#54221,.F.);
#78624=ORIENTED_EDGE('',*,*,#53871,.T.);
#78625=ORIENTED_EDGE('',*,*,#54222,.F.);
#78626=ORIENTED_EDGE('',*,*,#54223,.F.);
#78627=ORIENTED_EDGE('',*,*,#54224,.F.);
#78628=ORIENTED_EDGE('',*,*,#54176,.T.);
#78629=ORIENTED_EDGE('',*,*,#54225,.F.);
#78630=ORIENTED_EDGE('',*,*,#54226,.F.);
#78631=ORIENTED_EDGE('',*,*,#54227,.F.);
#78632=ORIENTED_EDGE('',*,*,#54145,.T.);
#78633=ORIENTED_EDGE('',*,*,#54228,.F.);
#78634=ORIENTED_EDGE('',*,*,#54229,.F.);
#78635=ORIENTED_EDGE('',*,*,#54230,.F.);
#78636=ORIENTED_EDGE('',*,*,#54117,.T.);
#78637=ORIENTED_EDGE('',*,*,#54231,.F.);
#78638=ORIENTED_EDGE('',*,*,#54232,.F.);
#78639=ORIENTED_EDGE('',*,*,#54233,.F.);
#78640=ORIENTED_EDGE('',*,*,#54089,.T.);
#78641=ORIENTED_EDGE('',*,*,#54234,.F.);
#78642=ORIENTED_EDGE('',*,*,#54235,.F.);
#78643=ORIENTED_EDGE('',*,*,#54236,.F.);
#78644=ORIENTED_EDGE('',*,*,#54061,.T.);
#78645=ORIENTED_EDGE('',*,*,#54237,.F.);
#78646=ORIENTED_EDGE('',*,*,#54238,.F.);
#78647=ORIENTED_EDGE('',*,*,#54239,.F.);
#78648=ORIENTED_EDGE('',*,*,#54033,.T.);
#78649=ORIENTED_EDGE('',*,*,#54240,.F.);
#78650=ORIENTED_EDGE('',*,*,#54241,.F.);
#78651=ORIENTED_EDGE('',*,*,#54242,.F.);
#78652=ORIENTED_EDGE('',*,*,#54067,.T.);
#78653=ORIENTED_EDGE('',*,*,#54243,.F.);
#78654=ORIENTED_EDGE('',*,*,#54244,.F.);
#78655=ORIENTED_EDGE('',*,*,#54245,.F.);
#78656=ORIENTED_EDGE('',*,*,#54095,.T.);
#78657=ORIENTED_EDGE('',*,*,#54246,.F.);
#78658=ORIENTED_EDGE('',*,*,#54247,.F.);
#78659=ORIENTED_EDGE('',*,*,#54248,.F.);
#78660=ORIENTED_EDGE('',*,*,#54123,.T.);
#78661=ORIENTED_EDGE('',*,*,#54249,.F.);
#78662=ORIENTED_EDGE('',*,*,#54250,.F.);
#78663=ORIENTED_EDGE('',*,*,#54251,.F.);
#78664=ORIENTED_EDGE('',*,*,#54154,.T.);
#78665=ORIENTED_EDGE('',*,*,#54252,.F.);
#78666=ORIENTED_EDGE('',*,*,#54253,.F.);
#78667=ORIENTED_EDGE('',*,*,#54254,.F.);
#78668=ORIENTED_EDGE('',*,*,#54182,.T.);
#78669=ORIENTED_EDGE('',*,*,#54255,.F.);
#78670=ORIENTED_EDGE('',*,*,#54256,.F.);
#78671=ORIENTED_EDGE('',*,*,#54257,.F.);
#78672=ORIENTED_EDGE('',*,*,#54039,.T.);
#78673=ORIENTED_EDGE('',*,*,#54258,.F.);
#78674=ORIENTED_EDGE('',*,*,#54259,.F.);
#78675=ORIENTED_EDGE('',*,*,#54260,.F.);
#78676=ORIENTED_EDGE('',*,*,#54005,.T.);
#78677=ORIENTED_EDGE('',*,*,#54261,.F.);
#78678=ORIENTED_EDGE('',*,*,#54262,.F.);
#78679=ORIENTED_EDGE('',*,*,#54263,.F.);
#78680=ORIENTED_EDGE('',*,*,#54011,.T.);
#78681=ORIENTED_EDGE('',*,*,#54264,.F.);
#78682=ORIENTED_EDGE('',*,*,#54265,.F.);
#78683=ORIENTED_EDGE('',*,*,#54266,.F.);
#78684=ORIENTED_EDGE('',*,*,#53977,.T.);
#78685=ORIENTED_EDGE('',*,*,#54267,.F.);
#78686=ORIENTED_EDGE('',*,*,#54268,.F.);
#78687=ORIENTED_EDGE('',*,*,#54269,.F.);
#78688=ORIENTED_EDGE('',*,*,#53946,.T.);
#78689=ORIENTED_EDGE('',*,*,#54270,.F.);
#78690=ORIENTED_EDGE('',*,*,#54271,.F.);
#78691=ORIENTED_EDGE('',*,*,#54272,.F.);
#78692=ORIENTED_EDGE('',*,*,#53983,.T.);
#78693=ORIENTED_EDGE('',*,*,#54273,.F.);
#78694=ORIENTED_EDGE('',*,*,#54274,.F.);
#78695=ORIENTED_EDGE('',*,*,#54275,.F.);
#78696=ORIENTED_EDGE('',*,*,#53955,.T.);
#78697=ORIENTED_EDGE('',*,*,#54276,.F.);
#78698=ORIENTED_EDGE('',*,*,#54277,.F.);
#78699=ORIENTED_EDGE('',*,*,#54278,.F.);
#78700=ORIENTED_EDGE('',*,*,#53902,.T.);
#78701=ORIENTED_EDGE('',*,*,#54279,.F.);
#78702=ORIENTED_EDGE('',*,*,#54280,.F.);
#78703=ORIENTED_EDGE('',*,*,#54281,.F.);
#78704=ORIENTED_EDGE('',*,*,#53908,.T.);
#78705=ORIENTED_EDGE('',*,*,#54282,.F.);
#78706=ORIENTED_EDGE('',*,*,#54283,.F.);
#78707=ORIENTED_EDGE('',*,*,#54284,.F.);
#78708=ORIENTED_EDGE('',*,*,#53881,.T.);
#78709=ORIENTED_EDGE('',*,*,#54285,.F.);
#78710=ORIENTED_EDGE('',*,*,#54286,.F.);
#78711=ORIENTED_EDGE('',*,*,#54199,.T.);
#78712=ORIENTED_EDGE('',*,*,#54194,.T.);
#78713=ORIENTED_EDGE('',*,*,#54287,.F.);
#78714=ORIENTED_EDGE('',*,*,#53860,.T.);
#78715=ORIENTED_EDGE('',*,*,#53864,.T.);
#78716=ORIENTED_EDGE('',*,*,#53867,.T.);
#78717=ORIENTED_EDGE('',*,*,#53870,.T.);
#78718=ORIENTED_EDGE('',*,*,#53873,.T.);
#78719=ORIENTED_EDGE('',*,*,#54288,.F.);
#78720=ORIENTED_EDGE('',*,*,#54289,.F.);
#78721=ORIENTED_EDGE('',*,*,#54290,.F.);
#78722=ORIENTED_EDGE('',*,*,#53876,.T.);
#78723=ORIENTED_EDGE('',*,*,#53880,.T.);
#78724=ORIENTED_EDGE('',*,*,#53883,.T.);
#78725=ORIENTED_EDGE('',*,*,#53886,.T.);
#78726=ORIENTED_EDGE('',*,*,#53889,.T.);
#78727=ORIENTED_EDGE('',*,*,#54291,.F.);
#78728=ORIENTED_EDGE('',*,*,#53934,.T.);
#78729=ORIENTED_EDGE('',*,*,#53931,.T.);
#78730=ORIENTED_EDGE('',*,*,#53928,.T.);
#78731=ORIENTED_EDGE('',*,*,#54292,.T.);
#78732=ORIENTED_EDGE('',*,*,#53912,.T.);
#78733=ORIENTED_EDGE('',*,*,#53909,.T.);
#78734=ORIENTED_EDGE('',*,*,#53906,.T.);
#78735=ORIENTED_EDGE('',*,*,#53903,.T.);
#78736=ORIENTED_EDGE('',*,*,#53900,.T.);
#78737=ORIENTED_EDGE('',*,*,#54293,.T.);
#78738=ORIENTED_EDGE('',*,*,#53959,.T.);
#78739=ORIENTED_EDGE('',*,*,#53956,.T.);
#78740=ORIENTED_EDGE('',*,*,#53953,.T.);
#78741=ORIENTED_EDGE('',*,*,#53950,.T.);
#78742=ORIENTED_EDGE('',*,*,#53947,.T.);
#78743=ORIENTED_EDGE('',*,*,#53944,.T.);
#78744=ORIENTED_EDGE('',*,*,#54294,.T.);
#78745=ORIENTED_EDGE('',*,*,#53987,.T.);
#78746=ORIENTED_EDGE('',*,*,#53984,.T.);
#78747=ORIENTED_EDGE('',*,*,#53981,.T.);
#78748=ORIENTED_EDGE('',*,*,#53978,.T.);
#78749=ORIENTED_EDGE('',*,*,#53975,.T.);
#78750=ORIENTED_EDGE('',*,*,#54295,.T.);
#78751=ORIENTED_EDGE('',*,*,#54015,.T.);
#78752=ORIENTED_EDGE('',*,*,#54012,.T.);
#78753=ORIENTED_EDGE('',*,*,#54009,.T.);
#78754=ORIENTED_EDGE('',*,*,#54006,.T.);
#78755=ORIENTED_EDGE('',*,*,#54003,.T.);
#78756=ORIENTED_EDGE('',*,*,#54296,.T.);
#78757=ORIENTED_EDGE('',*,*,#54043,.T.);
#78758=ORIENTED_EDGE('',*,*,#54040,.T.);
#78759=ORIENTED_EDGE('',*,*,#54037,.T.);
#78760=ORIENTED_EDGE('',*,*,#54034,.T.);
#78761=ORIENTED_EDGE('',*,*,#54031,.T.);
#78762=ORIENTED_EDGE('',*,*,#54297,.T.);
#78763=ORIENTED_EDGE('',*,*,#54071,.T.);
#78764=ORIENTED_EDGE('',*,*,#54068,.T.);
#78765=ORIENTED_EDGE('',*,*,#54065,.T.);
#78766=ORIENTED_EDGE('',*,*,#54062,.T.);
#78767=ORIENTED_EDGE('',*,*,#54059,.T.);
#78768=ORIENTED_EDGE('',*,*,#54298,.T.);
#78769=ORIENTED_EDGE('',*,*,#54099,.T.);
#78770=ORIENTED_EDGE('',*,*,#54096,.T.);
#78771=ORIENTED_EDGE('',*,*,#54093,.T.);
#78772=ORIENTED_EDGE('',*,*,#54090,.T.);
#78773=ORIENTED_EDGE('',*,*,#54087,.T.);
#78774=ORIENTED_EDGE('',*,*,#54299,.T.);
#78775=ORIENTED_EDGE('',*,*,#54127,.T.);
#78776=ORIENTED_EDGE('',*,*,#54124,.T.);
#78777=ORIENTED_EDGE('',*,*,#54121,.T.);
#78778=ORIENTED_EDGE('',*,*,#54118,.T.);
#78779=ORIENTED_EDGE('',*,*,#54115,.T.);
#78780=ORIENTED_EDGE('',*,*,#54300,.T.);
#78781=ORIENTED_EDGE('',*,*,#54158,.T.);
#78782=ORIENTED_EDGE('',*,*,#54155,.T.);
#78783=ORIENTED_EDGE('',*,*,#54152,.T.);
#78784=ORIENTED_EDGE('',*,*,#54149,.T.);
#78785=ORIENTED_EDGE('',*,*,#54146,.T.);
#78786=ORIENTED_EDGE('',*,*,#54143,.T.);
#78787=ORIENTED_EDGE('',*,*,#54301,.T.);
#78788=ORIENTED_EDGE('',*,*,#54186,.T.);
#78789=ORIENTED_EDGE('',*,*,#54183,.T.);
#78790=ORIENTED_EDGE('',*,*,#54180,.T.);
#78791=ORIENTED_EDGE('',*,*,#54177,.T.);
#78792=ORIENTED_EDGE('',*,*,#54174,.T.);
#78793=ORIENTED_EDGE('',*,*,#54302,.T.);
#78794=ORIENTED_EDGE('',*,*,#54202,.T.);
#78795=ORIENTED_EDGE('',*,*,#54303,.F.);
#78796=ORIENTED_EDGE('',*,*,#53922,.T.);
#78797=ORIENTED_EDGE('',*,*,#53924,.T.);
#78798=ORIENTED_EDGE('',*,*,#53927,.T.);
#78799=ORIENTED_EDGE('',*,*,#54209,.T.);
#78800=ORIENTED_EDGE('',*,*,#54288,.T.);
#78801=ORIENTED_EDGE('',*,*,#53872,.T.);
#78802=ORIENTED_EDGE('',*,*,#54304,.F.);
#78803=ORIENTED_EDGE('',*,*,#54305,.F.);
#78804=ORIENTED_EDGE('',*,*,#54306,.T.);
#78805=ORIENTED_EDGE('',*,*,#54304,.T.);
#78806=ORIENTED_EDGE('',*,*,#53874,.T.);
#78807=ORIENTED_EDGE('',*,*,#54221,.T.);
#78808=ORIENTED_EDGE('',*,*,#54307,.F.);
#78809=ORIENTED_EDGE('',*,*,#54213,.T.);
#78810=ORIENTED_EDGE('',*,*,#53884,.T.);
#78811=ORIENTED_EDGE('',*,*,#54284,.T.);
#78812=ORIENTED_EDGE('',*,*,#54308,.F.);
#78813=ORIENTED_EDGE('',*,*,#54285,.T.);
#78814=ORIENTED_EDGE('',*,*,#53878,.T.);
#78815=ORIENTED_EDGE('',*,*,#54309,.F.);
#78816=ORIENTED_EDGE('',*,*,#54310,.F.);
#78817=ORIENTED_EDGE('',*,*,#54282,.T.);
#78818=ORIENTED_EDGE('',*,*,#53911,.T.);
#78819=ORIENTED_EDGE('',*,*,#53914,.T.);
#78820=ORIENTED_EDGE('',*,*,#53917,.T.);
#78821=ORIENTED_EDGE('',*,*,#54311,.F.);
#78822=ORIENTED_EDGE('',*,*,#54312,.F.);
#78823=ORIENTED_EDGE('',*,*,#53892,.T.);
#78824=ORIENTED_EDGE('',*,*,#53896,.T.);
#78825=ORIENTED_EDGE('',*,*,#53899,.T.);
#78826=ORIENTED_EDGE('',*,*,#54278,.T.);
#78827=ORIENTED_EDGE('',*,*,#54246,.T.);
#78828=ORIENTED_EDGE('',*,*,#54098,.T.);
#78829=ORIENTED_EDGE('',*,*,#54101,.T.);
#78830=ORIENTED_EDGE('',*,*,#54104,.T.);
#78831=ORIENTED_EDGE('',*,*,#54313,.F.);
#78832=ORIENTED_EDGE('',*,*,#54314,.F.);
#78833=ORIENTED_EDGE('',*,*,#54079,.T.);
#78834=ORIENTED_EDGE('',*,*,#54083,.T.);
#78835=ORIENTED_EDGE('',*,*,#54086,.T.);
#78836=ORIENTED_EDGE('',*,*,#54233,.T.);
#78837=ORIENTED_EDGE('',*,*,#54249,.T.);
#78838=ORIENTED_EDGE('',*,*,#54126,.T.);
#78839=ORIENTED_EDGE('',*,*,#54129,.T.);
#78840=ORIENTED_EDGE('',*,*,#54132,.T.);
#78841=ORIENTED_EDGE('',*,*,#54315,.F.);
#78842=ORIENTED_EDGE('',*,*,#54316,.F.);
#78843=ORIENTED_EDGE('',*,*,#54107,.T.);
#78844=ORIENTED_EDGE('',*,*,#54111,.T.);
#78845=ORIENTED_EDGE('',*,*,#54114,.T.);
#78846=ORIENTED_EDGE('',*,*,#54230,.T.);
#78847=ORIENTED_EDGE('',*,*,#54317,.F.);
#78848=ORIENTED_EDGE('',*,*,#54135,.T.);
#78849=ORIENTED_EDGE('',*,*,#54139,.T.);
#78850=ORIENTED_EDGE('',*,*,#54142,.T.);
#78851=ORIENTED_EDGE('',*,*,#54227,.T.);
#78852=ORIENTED_EDGE('',*,*,#54276,.T.);
#78853=ORIENTED_EDGE('',*,*,#53958,.T.);
#78854=ORIENTED_EDGE('',*,*,#53961,.T.);
#78855=ORIENTED_EDGE('',*,*,#53964,.T.);
#78856=ORIENTED_EDGE('',*,*,#54318,.F.);
#78857=ORIENTED_EDGE('',*,*,#54243,.T.);
#78858=ORIENTED_EDGE('',*,*,#54070,.T.);
#78859=ORIENTED_EDGE('',*,*,#54073,.T.);
#78860=ORIENTED_EDGE('',*,*,#54076,.T.);
#78861=ORIENTED_EDGE('',*,*,#54319,.F.);
#78862=ORIENTED_EDGE('',*,*,#54320,.F.);
#78863=ORIENTED_EDGE('',*,*,#54051,.T.);
#78864=ORIENTED_EDGE('',*,*,#54055,.T.);
#78865=ORIENTED_EDGE('',*,*,#54058,.T.);
#78866=ORIENTED_EDGE('',*,*,#54236,.T.);
#78867=ORIENTED_EDGE('',*,*,#54321,.F.);
#78868=ORIENTED_EDGE('',*,*,#54105,.T.);
#78869=ORIENTED_EDGE('',*,*,#54322,.T.);
#78870=ORIENTED_EDGE('',*,*,#54053,.T.);
#78871=ORIENTED_EDGE('',*,*,#54322,.F.);
#78872=ORIENTED_EDGE('',*,*,#54102,.T.);
#78873=ORIENTED_EDGE('',*,*,#54298,.F.);
#78874=ORIENTED_EDGE('',*,*,#54056,.T.);
#78875=ORIENTED_EDGE('',*,*,#54237,.T.);
#78876=ORIENTED_EDGE('',*,*,#54064,.T.);
#78877=ORIENTED_EDGE('',*,*,#54242,.T.);
#78878=ORIENTED_EDGE('',*,*,#54323,.F.);
#78879=ORIENTED_EDGE('',*,*,#54258,.T.);
#78880=ORIENTED_EDGE('',*,*,#54042,.T.);
#78881=ORIENTED_EDGE('',*,*,#54045,.T.);
#78882=ORIENTED_EDGE('',*,*,#54048,.T.);
#78883=ORIENTED_EDGE('',*,*,#54324,.F.);
#78884=ORIENTED_EDGE('',*,*,#54325,.F.);
#78885=ORIENTED_EDGE('',*,*,#54023,.T.);
#78886=ORIENTED_EDGE('',*,*,#54027,.T.);
#78887=ORIENTED_EDGE('',*,*,#54030,.T.);
#78888=ORIENTED_EDGE('',*,*,#54239,.T.);
#78889=ORIENTED_EDGE('',*,*,#54326,.F.);
#78890=ORIENTED_EDGE('',*,*,#54077,.T.);
#78891=ORIENTED_EDGE('',*,*,#54327,.T.);
#78892=ORIENTED_EDGE('',*,*,#54025,.T.);
#78893=ORIENTED_EDGE('',*,*,#54327,.F.);
#78894=ORIENTED_EDGE('',*,*,#54074,.T.);
#78895=ORIENTED_EDGE('',*,*,#54297,.F.);
#78896=ORIENTED_EDGE('',*,*,#54028,.T.);
#78897=ORIENTED_EDGE('',*,*,#54240,.T.);
#78898=ORIENTED_EDGE('',*,*,#54036,.T.);
#78899=ORIENTED_EDGE('',*,*,#54257,.T.);
#78900=ORIENTED_EDGE('',*,*,#54328,.F.);
#78901=ORIENTED_EDGE('',*,*,#54264,.T.);
#78902=ORIENTED_EDGE('',*,*,#54014,.T.);
#78903=ORIENTED_EDGE('',*,*,#54017,.T.);
#78904=ORIENTED_EDGE('',*,*,#54020,.T.);
#78905=ORIENTED_EDGE('',*,*,#54329,.F.);
#78906=ORIENTED_EDGE('',*,*,#54330,.F.);
#78907=ORIENTED_EDGE('',*,*,#53995,.T.);
#78908=ORIENTED_EDGE('',*,*,#53999,.T.);
#78909=ORIENTED_EDGE('',*,*,#54002,.T.);
#78910=ORIENTED_EDGE('',*,*,#54260,.T.);
#78911=ORIENTED_EDGE('',*,*,#54331,.F.);
#78912=ORIENTED_EDGE('',*,*,#54049,.T.);
#78913=ORIENTED_EDGE('',*,*,#54332,.T.);
#78914=ORIENTED_EDGE('',*,*,#53997,.T.);
#78915=ORIENTED_EDGE('',*,*,#54332,.F.);
#78916=ORIENTED_EDGE('',*,*,#54046,.T.);
#78917=ORIENTED_EDGE('',*,*,#54296,.F.);
#78918=ORIENTED_EDGE('',*,*,#54000,.T.);
#78919=ORIENTED_EDGE('',*,*,#54261,.T.);
#78920=ORIENTED_EDGE('',*,*,#54008,.T.);
#78921=ORIENTED_EDGE('',*,*,#54263,.T.);
#78922=ORIENTED_EDGE('',*,*,#54333,.F.);
#78923=ORIENTED_EDGE('',*,*,#54273,.T.);
#78924=ORIENTED_EDGE('',*,*,#53986,.T.);
#78925=ORIENTED_EDGE('',*,*,#53989,.T.);
#78926=ORIENTED_EDGE('',*,*,#53992,.T.);
#78927=ORIENTED_EDGE('',*,*,#54334,.F.);
#78928=ORIENTED_EDGE('',*,*,#54335,.F.);
#78929=ORIENTED_EDGE('',*,*,#53967,.T.);
#78930=ORIENTED_EDGE('',*,*,#53971,.T.);
#78931=ORIENTED_EDGE('',*,*,#53974,.T.);
#78932=ORIENTED_EDGE('',*,*,#54266,.T.);
#78933=ORIENTED_EDGE('',*,*,#54336,.F.);
#78934=ORIENTED_EDGE('',*,*,#54021,.T.);
#78935=ORIENTED_EDGE('',*,*,#54337,.T.);
#78936=ORIENTED_EDGE('',*,*,#53969,.T.);
#78937=ORIENTED_EDGE('',*,*,#54337,.F.);
#78938=ORIENTED_EDGE('',*,*,#54018,.T.);
#78939=ORIENTED_EDGE('',*,*,#54295,.F.);
#78940=ORIENTED_EDGE('',*,*,#53972,.T.);
#78941=ORIENTED_EDGE('',*,*,#54267,.T.);
#78942=ORIENTED_EDGE('',*,*,#53980,.T.);
#78943=ORIENTED_EDGE('',*,*,#54272,.T.);
#78944=ORIENTED_EDGE('',*,*,#54338,.F.);
#78945=ORIENTED_EDGE('',*,*,#54255,.T.);
#78946=ORIENTED_EDGE('',*,*,#54185,.T.);
#78947=ORIENTED_EDGE('',*,*,#54188,.T.);
#78948=ORIENTED_EDGE('',*,*,#54191,.T.);
#78949=ORIENTED_EDGE('',*,*,#54339,.F.);
#78950=ORIENTED_EDGE('',*,*,#54340,.F.);
#78951=ORIENTED_EDGE('',*,*,#54166,.T.);
#78952=ORIENTED_EDGE('',*,*,#54170,.T.);
#78953=ORIENTED_EDGE('',*,*,#54173,.T.);
#78954=ORIENTED_EDGE('',*,*,#54224,.T.);
#78955=ORIENTED_EDGE('',*,*,#54341,.F.);
#78956=ORIENTED_EDGE('',*,*,#54208,.T.);
#78957=ORIENTED_EDGE('',*,*,#54342,.T.);
#78958=ORIENTED_EDGE('',*,*,#54168,.T.);
#78959=ORIENTED_EDGE('',*,*,#54342,.F.);
#78960=ORIENTED_EDGE('',*,*,#54205,.T.);
#78961=ORIENTED_EDGE('',*,*,#54302,.F.);
#78962=ORIENTED_EDGE('',*,*,#54171,.T.);
#78963=ORIENTED_EDGE('',*,*,#54225,.T.);
#78964=ORIENTED_EDGE('',*,*,#54179,.T.);
#78965=ORIENTED_EDGE('',*,*,#54254,.T.);
#78966=ORIENTED_EDGE('',*,*,#54343,.F.);
#78967=ORIENTED_EDGE('',*,*,#54270,.T.);
#78968=ORIENTED_EDGE('',*,*,#53949,.T.);
#78969=ORIENTED_EDGE('',*,*,#54344,.F.);
#78970=ORIENTED_EDGE('',*,*,#54345,.F.);
#78971=ORIENTED_EDGE('',*,*,#54344,.T.);
#78972=ORIENTED_EDGE('',*,*,#53952,.T.);
#78973=ORIENTED_EDGE('',*,*,#54275,.T.);
#78974=ORIENTED_EDGE('',*,*,#54346,.F.);
#78975=ORIENTED_EDGE('',*,*,#54347,.F.);
#78976=ORIENTED_EDGE('',*,*,#54151,.T.);
#78977=ORIENTED_EDGE('',*,*,#54251,.T.);
#78978=ORIENTED_EDGE('',*,*,#54348,.F.);
#78979=ORIENTED_EDGE('',*,*,#54252,.T.);
#78980=ORIENTED_EDGE('',*,*,#54157,.T.);
#78981=ORIENTED_EDGE('',*,*,#54160,.T.);
#78982=ORIENTED_EDGE('',*,*,#54163,.T.);
#78983=ORIENTED_EDGE('',*,*,#54349,.F.);
#78984=ORIENTED_EDGE('',*,*,#54350,.T.);
#78985=ORIENTED_EDGE('',*,*,#54206,.T.);
#78986=ORIENTED_EDGE('',*,*,#54341,.T.);
#78987=ORIENTED_EDGE('',*,*,#54167,.T.);
#78988=ORIENTED_EDGE('',*,*,#54340,.T.);
#78989=ORIENTED_EDGE('',*,*,#54226,.T.);
#78990=ORIENTED_EDGE('',*,*,#54343,.T.);
#78991=ORIENTED_EDGE('',*,*,#54256,.T.);
#78992=ORIENTED_EDGE('',*,*,#54339,.T.);
#78993=ORIENTED_EDGE('',*,*,#54190,.T.);
#78994=ORIENTED_EDGE('',*,*,#54351,.T.);
#78995=ORIENTED_EDGE('',*,*,#54136,.T.);
#78996=ORIENTED_EDGE('',*,*,#54317,.T.);
#78997=ORIENTED_EDGE('',*,*,#54229,.T.);
#78998=ORIENTED_EDGE('',*,*,#54352,.T.);
#78999=ORIENTED_EDGE('',*,*,#54348,.T.);
#79000=ORIENTED_EDGE('',*,*,#54253,.T.);
#79001=ORIENTED_EDGE('',*,*,#54349,.T.);
#79002=ORIENTED_EDGE('',*,*,#54162,.T.);
#79003=ORIENTED_EDGE('',*,*,#54353,.T.);
#79004=ORIENTED_EDGE('',*,*,#54108,.T.);
#79005=ORIENTED_EDGE('',*,*,#54316,.T.);
#79006=ORIENTED_EDGE('',*,*,#54232,.T.);
#79007=ORIENTED_EDGE('',*,*,#54354,.T.);
#79008=ORIENTED_EDGE('',*,*,#54250,.T.);
#79009=ORIENTED_EDGE('',*,*,#54315,.T.);
#79010=ORIENTED_EDGE('',*,*,#54131,.T.);
#79011=ORIENTED_EDGE('',*,*,#54355,.T.);
#79012=ORIENTED_EDGE('',*,*,#54080,.T.);
#79013=ORIENTED_EDGE('',*,*,#54314,.T.);
#79014=ORIENTED_EDGE('',*,*,#54235,.T.);
#79015=ORIENTED_EDGE('',*,*,#54356,.T.);
#79016=ORIENTED_EDGE('',*,*,#54247,.T.);
#79017=ORIENTED_EDGE('',*,*,#54313,.T.);
#79018=ORIENTED_EDGE('',*,*,#54103,.T.);
#79019=ORIENTED_EDGE('',*,*,#54321,.T.);
#79020=ORIENTED_EDGE('',*,*,#54052,.T.);
#79021=ORIENTED_EDGE('',*,*,#54320,.T.);
#79022=ORIENTED_EDGE('',*,*,#54238,.T.);
#79023=ORIENTED_EDGE('',*,*,#54323,.T.);
#79024=ORIENTED_EDGE('',*,*,#54244,.T.);
#79025=ORIENTED_EDGE('',*,*,#54319,.T.);
#79026=ORIENTED_EDGE('',*,*,#54075,.T.);
#79027=ORIENTED_EDGE('',*,*,#54326,.T.);
#79028=ORIENTED_EDGE('',*,*,#54024,.T.);
#79029=ORIENTED_EDGE('',*,*,#54325,.T.);
#79030=ORIENTED_EDGE('',*,*,#54241,.T.);
#79031=ORIENTED_EDGE('',*,*,#54328,.T.);
#79032=ORIENTED_EDGE('',*,*,#54259,.T.);
#79033=ORIENTED_EDGE('',*,*,#54324,.T.);
#79034=ORIENTED_EDGE('',*,*,#54047,.T.);
#79035=ORIENTED_EDGE('',*,*,#54331,.T.);
#79036=ORIENTED_EDGE('',*,*,#53996,.T.);
#79037=ORIENTED_EDGE('',*,*,#54330,.T.);
#79038=ORIENTED_EDGE('',*,*,#54262,.T.);
#79039=ORIENTED_EDGE('',*,*,#54333,.T.);
#79040=ORIENTED_EDGE('',*,*,#54265,.T.);
#79041=ORIENTED_EDGE('',*,*,#54329,.T.);
#79042=ORIENTED_EDGE('',*,*,#54019,.T.);
#79043=ORIENTED_EDGE('',*,*,#54336,.T.);
#79044=ORIENTED_EDGE('',*,*,#53968,.T.);
#79045=ORIENTED_EDGE('',*,*,#54335,.T.);
#79046=ORIENTED_EDGE('',*,*,#54268,.T.);
#79047=ORIENTED_EDGE('',*,*,#54338,.T.);
#79048=ORIENTED_EDGE('',*,*,#54274,.T.);
#79049=ORIENTED_EDGE('',*,*,#54334,.T.);
#79050=ORIENTED_EDGE('',*,*,#53991,.T.);
#79051=ORIENTED_EDGE('',*,*,#54357,.T.);
#79052=ORIENTED_EDGE('',*,*,#53937,.T.);
#79053=ORIENTED_EDGE('',*,*,#54358,.T.);
#79054=ORIENTED_EDGE('',*,*,#54271,.T.);
#79055=ORIENTED_EDGE('',*,*,#54345,.T.);
#79056=ORIENTED_EDGE('',*,*,#54346,.T.);
#79057=ORIENTED_EDGE('',*,*,#54277,.T.);
#79058=ORIENTED_EDGE('',*,*,#54318,.T.);
#79059=ORIENTED_EDGE('',*,*,#53963,.T.);
#79060=ORIENTED_EDGE('',*,*,#54359,.T.);
#79061=ORIENTED_EDGE('',*,*,#53893,.T.);
#79062=ORIENTED_EDGE('',*,*,#54312,.T.);
#79063=ORIENTED_EDGE('',*,*,#54280,.T.);
#79064=ORIENTED_EDGE('',*,*,#54360,.T.);
#79065=ORIENTED_EDGE('',*,*,#54283,.T.);
#79066=ORIENTED_EDGE('',*,*,#54311,.T.);
#79067=ORIENTED_EDGE('',*,*,#53916,.T.);
#79068=ORIENTED_EDGE('',*,*,#54361,.T.);
#79069=ORIENTED_EDGE('',*,*,#53919,.T.);
#79070=ORIENTED_EDGE('',*,*,#54303,.T.);
#79071=ORIENTED_EDGE('',*,*,#54211,.T.);
#79072=ORIENTED_EDGE('',*,*,#54362,.T.);
#79073=ORIENTED_EDGE('',*,*,#54363,.T.);
#79074=ORIENTED_EDGE('',*,*,#54364,.T.);
#79075=ORIENTED_EDGE('',*,*,#54214,.T.);
#79076=ORIENTED_EDGE('',*,*,#54308,.T.);
#79077=ORIENTED_EDGE('',*,*,#54286,.T.);
#79078=ORIENTED_EDGE('',*,*,#54310,.T.);
#79079=ORIENTED_EDGE('',*,*,#54365,.T.);
#79080=ORIENTED_EDGE('',*,*,#54366,.T.);
#79081=ORIENTED_EDGE('',*,*,#54305,.T.);
#79082=ORIENTED_EDGE('',*,*,#54307,.T.);
#79083=ORIENTED_EDGE('',*,*,#54223,.T.);
#79084=ORIENTED_EDGE('',*,*,#54367,.T.);
#79085=ORIENTED_EDGE('',*,*,#54220,.T.);
#79086=ORIENTED_EDGE('',*,*,#54368,.T.);
#79087=ORIENTED_EDGE('',*,*,#54369,.T.);
#79088=ORIENTED_EDGE('',*,*,#54370,.T.);
#79089=ORIENTED_EDGE('',*,*,#54217,.T.);
#79090=ORIENTED_EDGE('',*,*,#54228,.T.);
#79091=ORIENTED_EDGE('',*,*,#54148,.T.);
#79092=ORIENTED_EDGE('',*,*,#54347,.T.);
#79093=ORIENTED_EDGE('',*,*,#54352,.F.);
#79094=ORIENTED_EDGE('',*,*,#54358,.F.);
#79095=ORIENTED_EDGE('',*,*,#53936,.T.);
#79096=ORIENTED_EDGE('',*,*,#53940,.T.);
#79097=ORIENTED_EDGE('',*,*,#53943,.T.);
#79098=ORIENTED_EDGE('',*,*,#54269,.T.);
#79099=ORIENTED_EDGE('',*,*,#54301,.F.);
#79100=ORIENTED_EDGE('',*,*,#54140,.T.);
#79101=ORIENTED_EDGE('',*,*,#54371,.F.);
#79102=ORIENTED_EDGE('',*,*,#54189,.T.);
#79103=ORIENTED_EDGE('',*,*,#54351,.F.);
#79104=ORIENTED_EDGE('',*,*,#54192,.T.);
#79105=ORIENTED_EDGE('',*,*,#54371,.T.);
#79106=ORIENTED_EDGE('',*,*,#54137,.T.);
#79107=ORIENTED_EDGE('',*,*,#54294,.F.);
#79108=ORIENTED_EDGE('',*,*,#53941,.T.);
#79109=ORIENTED_EDGE('',*,*,#54372,.F.);
#79110=ORIENTED_EDGE('',*,*,#53990,.T.);
#79111=ORIENTED_EDGE('',*,*,#54357,.F.);
#79112=ORIENTED_EDGE('',*,*,#53993,.T.);
#79113=ORIENTED_EDGE('',*,*,#54372,.T.);
#79114=ORIENTED_EDGE('',*,*,#53938,.T.);
#79115=ORIENTED_EDGE('',*,*,#54293,.F.);
#79116=ORIENTED_EDGE('',*,*,#53897,.T.);
#79117=ORIENTED_EDGE('',*,*,#54373,.F.);
#79118=ORIENTED_EDGE('',*,*,#53962,.T.);
#79119=ORIENTED_EDGE('',*,*,#54359,.F.);
#79120=ORIENTED_EDGE('',*,*,#53965,.T.);
#79121=ORIENTED_EDGE('',*,*,#54373,.T.);
#79122=ORIENTED_EDGE('',*,*,#53894,.T.);
#79123=ORIENTED_EDGE('',*,*,#54300,.F.);
#79124=ORIENTED_EDGE('',*,*,#54112,.T.);
#79125=ORIENTED_EDGE('',*,*,#54374,.F.);
#79126=ORIENTED_EDGE('',*,*,#54161,.T.);
#79127=ORIENTED_EDGE('',*,*,#54353,.F.);
#79128=ORIENTED_EDGE('',*,*,#54164,.T.);
#79129=ORIENTED_EDGE('',*,*,#54374,.T.);
#79130=ORIENTED_EDGE('',*,*,#54109,.T.);
#79131=ORIENTED_EDGE('',*,*,#54231,.T.);
#79132=ORIENTED_EDGE('',*,*,#54120,.T.);
#79133=ORIENTED_EDGE('',*,*,#54248,.T.);
#79134=ORIENTED_EDGE('',*,*,#54354,.F.);
#79135=ORIENTED_EDGE('',*,*,#54299,.F.);
#79136=ORIENTED_EDGE('',*,*,#54084,.T.);
#79137=ORIENTED_EDGE('',*,*,#54375,.F.);
#79138=ORIENTED_EDGE('',*,*,#54130,.T.);
#79139=ORIENTED_EDGE('',*,*,#54355,.F.);
#79140=ORIENTED_EDGE('',*,*,#54133,.T.);
#79141=ORIENTED_EDGE('',*,*,#54375,.T.);
#79142=ORIENTED_EDGE('',*,*,#54081,.T.);
#79143=ORIENTED_EDGE('',*,*,#54234,.T.);
#79144=ORIENTED_EDGE('',*,*,#54092,.T.);
#79145=ORIENTED_EDGE('',*,*,#54245,.T.);
#79146=ORIENTED_EDGE('',*,*,#54356,.F.);
#79147=ORIENTED_EDGE('',*,*,#54279,.T.);
#79148=ORIENTED_EDGE('',*,*,#53905,.T.);
#79149=ORIENTED_EDGE('',*,*,#54281,.T.);
#79150=ORIENTED_EDGE('',*,*,#54360,.F.);
#79151=ORIENTED_EDGE('',*,*,#54292,.F.);
#79152=ORIENTED_EDGE('',*,*,#53925,.T.);
#79153=ORIENTED_EDGE('',*,*,#54376,.F.);
#79154=ORIENTED_EDGE('',*,*,#53915,.T.);
#79155=ORIENTED_EDGE('',*,*,#54376,.T.);
#79156=ORIENTED_EDGE('',*,*,#53920,.T.);
#79157=ORIENTED_EDGE('',*,*,#54361,.F.);
#79158=ORIENTED_EDGE('',*,*,#53918,.T.);
#79159=ORIENTED_EDGE('',*,*,#54377,.T.);
#79160=ORIENTED_EDGE('',*,*,#53890,.T.);
#79161=ORIENTED_EDGE('',*,*,#54212,.T.);
#79162=ORIENTED_EDGE('',*,*,#54364,.F.);
#79163=ORIENTED_EDGE('',*,*,#54309,.T.);
#79164=ORIENTED_EDGE('',*,*,#53877,.T.);
#79165=ORIENTED_EDGE('',*,*,#54290,.T.);
#79166=ORIENTED_EDGE('',*,*,#54378,.F.);
#79167=ORIENTED_EDGE('',*,*,#54365,.F.);
#79168=ORIENTED_EDGE('',*,*,#54378,.T.);
#79169=ORIENTED_EDGE('',*,*,#54289,.T.);
#79170=ORIENTED_EDGE('',*,*,#54306,.F.);
#79171=ORIENTED_EDGE('',*,*,#54366,.F.);
#79172=ORIENTED_EDGE('',*,*,#54222,.T.);
#79173=ORIENTED_EDGE('',*,*,#53868,.T.);
#79174=ORIENTED_EDGE('',*,*,#54218,.T.);
#79175=ORIENTED_EDGE('',*,*,#54367,.F.);
#79176=ORIENTED_EDGE('',*,*,#54219,.T.);
#79177=ORIENTED_EDGE('',*,*,#53862,.T.);
#79178=ORIENTED_EDGE('',*,*,#54379,.F.);
#79179=ORIENTED_EDGE('',*,*,#54368,.F.);
#79180=ORIENTED_EDGE('',*,*,#54287,.T.);
#79181=ORIENTED_EDGE('',*,*,#54193,.T.);
#79182=ORIENTED_EDGE('',*,*,#54380,.F.);
#79183=ORIENTED_EDGE('',*,*,#54369,.F.);
#79184=ORIENTED_EDGE('',*,*,#54379,.T.);
#79185=ORIENTED_EDGE('',*,*,#53861,.T.);
#79186=ORIENTED_EDGE('',*,*,#54380,.T.);
#79187=ORIENTED_EDGE('',*,*,#54196,.T.);
#79188=ORIENTED_EDGE('',*,*,#54215,.T.);
#79189=ORIENTED_EDGE('',*,*,#54370,.F.);
#79190=ORIENTED_EDGE('',*,*,#54216,.T.);
#79191=ORIENTED_EDGE('',*,*,#54201,.T.);
#79192=ORIENTED_EDGE('',*,*,#54204,.T.);
#79193=ORIENTED_EDGE('',*,*,#54207,.T.);
#79194=ORIENTED_EDGE('',*,*,#54350,.F.);
#79195=ORIENTED_EDGE('',*,*,#54210,.T.);
#79196=ORIENTED_EDGE('',*,*,#53933,.T.);
#79197=ORIENTED_EDGE('',*,*,#54381,.F.);
#79198=ORIENTED_EDGE('',*,*,#54362,.F.);
#79199=ORIENTED_EDGE('',*,*,#54381,.T.);
#79200=ORIENTED_EDGE('',*,*,#53932,.T.);
#79201=ORIENTED_EDGE('',*,*,#54291,.T.);
#79202=ORIENTED_EDGE('',*,*,#53888,.T.);
#79203=ORIENTED_EDGE('',*,*,#54377,.F.);
#79204=ORIENTED_EDGE('',*,*,#54363,.F.);
#79205=ORIENTED_EDGE('',*,*,#54382,.T.);
#79206=ORIENTED_EDGE('',*,*,#54383,.T.);
#79207=ORIENTED_EDGE('',*,*,#54384,.T.);
#79208=ORIENTED_EDGE('',*,*,#54385,.T.);
#79209=ORIENTED_EDGE('',*,*,#54386,.T.);
#79210=ORIENTED_EDGE('',*,*,#54387,.T.);
#79211=ORIENTED_EDGE('',*,*,#54388,.T.);
#79212=ORIENTED_EDGE('',*,*,#54383,.F.);
#79213=ORIENTED_EDGE('',*,*,#54389,.T.);
#79214=ORIENTED_EDGE('',*,*,#54390,.T.);
#79215=ORIENTED_EDGE('',*,*,#54391,.T.);
#79216=ORIENTED_EDGE('',*,*,#54384,.F.);
#79217=ORIENTED_EDGE('',*,*,#54392,.T.);
#79218=ORIENTED_EDGE('',*,*,#54393,.T.);
#79219=ORIENTED_EDGE('',*,*,#54385,.F.);
#79220=ORIENTED_EDGE('',*,*,#54394,.T.);
#79221=ORIENTED_EDGE('',*,*,#54395,.T.);
#79222=ORIENTED_EDGE('',*,*,#54386,.F.);
#79223=ORIENTED_EDGE('',*,*,#54396,.T.);
#79224=ORIENTED_EDGE('',*,*,#54397,.T.);
#79225=ORIENTED_EDGE('',*,*,#54387,.F.);
#79226=ORIENTED_EDGE('',*,*,#54398,.T.);
#79227=ORIENTED_EDGE('',*,*,#54399,.T.);
#79228=ORIENTED_EDGE('',*,*,#54382,.F.);
#79229=ORIENTED_EDGE('',*,*,#54400,.F.);
#79230=ORIENTED_EDGE('',*,*,#54401,.T.);
#79231=ORIENTED_EDGE('',*,*,#54402,.T.);
#79232=ORIENTED_EDGE('',*,*,#54403,.T.);
#79233=ORIENTED_EDGE('',*,*,#54404,.T.);
#79234=ORIENTED_EDGE('',*,*,#54405,.T.);
#79235=ORIENTED_EDGE('',*,*,#54401,.F.);
#79236=ORIENTED_EDGE('',*,*,#54406,.F.);
#79237=ORIENTED_EDGE('',*,*,#54407,.F.);
#79238=ORIENTED_EDGE('',*,*,#54402,.F.);
#79239=ORIENTED_EDGE('',*,*,#54408,.F.);
#79240=ORIENTED_EDGE('',*,*,#54409,.F.);
#79241=ORIENTED_EDGE('',*,*,#54403,.F.);
#79242=ORIENTED_EDGE('',*,*,#54410,.F.);
#79243=ORIENTED_EDGE('',*,*,#54411,.F.);
#79244=ORIENTED_EDGE('',*,*,#54404,.F.);
#79245=ORIENTED_EDGE('',*,*,#54412,.F.);
#79246=ORIENTED_EDGE('',*,*,#54413,.F.);
#79247=ORIENTED_EDGE('',*,*,#54405,.F.);
#79248=ORIENTED_EDGE('',*,*,#54414,.F.);
#79249=ORIENTED_EDGE('',*,*,#54415,.F.);
#79250=ORIENTED_EDGE('',*,*,#54416,.F.);
#79251=ORIENTED_EDGE('',*,*,#54400,.T.);
#79252=ORIENTED_EDGE('',*,*,#54417,.F.);
#79253=ORIENTED_EDGE('',*,*,#54399,.F.);
#79254=ORIENTED_EDGE('',*,*,#54418,.T.);
#79255=ORIENTED_EDGE('',*,*,#54406,.T.);
#79256=ORIENTED_EDGE('',*,*,#54416,.T.);
#79257=ORIENTED_EDGE('',*,*,#54419,.F.);
#79258=ORIENTED_EDGE('',*,*,#54389,.F.);
#79259=ORIENTED_EDGE('',*,*,#54397,.F.);
#79260=ORIENTED_EDGE('',*,*,#54420,.T.);
#79261=ORIENTED_EDGE('',*,*,#54408,.T.);
#79262=ORIENTED_EDGE('',*,*,#54407,.T.);
#79263=ORIENTED_EDGE('',*,*,#54418,.F.);
#79264=ORIENTED_EDGE('',*,*,#54398,.F.);
#79265=ORIENTED_EDGE('',*,*,#54395,.F.);
#79266=ORIENTED_EDGE('',*,*,#54421,.T.);
#79267=ORIENTED_EDGE('',*,*,#54410,.T.);
#79268=ORIENTED_EDGE('',*,*,#54409,.T.);
#79269=ORIENTED_EDGE('',*,*,#54420,.F.);
#79270=ORIENTED_EDGE('',*,*,#54396,.F.);
#79271=ORIENTED_EDGE('',*,*,#54393,.F.);
#79272=ORIENTED_EDGE('',*,*,#54422,.T.);
#79273=ORIENTED_EDGE('',*,*,#54412,.T.);
#79274=ORIENTED_EDGE('',*,*,#54411,.T.);
#79275=ORIENTED_EDGE('',*,*,#54421,.F.);
#79276=ORIENTED_EDGE('',*,*,#54394,.F.);
#79277=ORIENTED_EDGE('',*,*,#54391,.F.);
#79278=ORIENTED_EDGE('',*,*,#54423,.T.);
#79279=ORIENTED_EDGE('',*,*,#54414,.T.);
#79280=ORIENTED_EDGE('',*,*,#54413,.T.);
#79281=ORIENTED_EDGE('',*,*,#54422,.F.);
#79282=ORIENTED_EDGE('',*,*,#54392,.F.);
#79283=ORIENTED_EDGE('',*,*,#54388,.F.);
#79284=ORIENTED_EDGE('',*,*,#54419,.T.);
#79285=ORIENTED_EDGE('',*,*,#54417,.T.);
#79286=ORIENTED_EDGE('',*,*,#54415,.T.);
#79287=ORIENTED_EDGE('',*,*,#54423,.F.);
#79288=ORIENTED_EDGE('',*,*,#54390,.F.);
#79289=ORIENTED_EDGE('',*,*,#54424,.T.);
#79290=ORIENTED_EDGE('',*,*,#54425,.T.);
#79291=ORIENTED_EDGE('',*,*,#54426,.T.);
#79292=ORIENTED_EDGE('',*,*,#54427,.T.);
#79293=ORIENTED_EDGE('',*,*,#54428,.T.);
#79294=ORIENTED_EDGE('',*,*,#54429,.T.);
#79295=ORIENTED_EDGE('',*,*,#54430,.T.);
#79296=ORIENTED_EDGE('',*,*,#54425,.F.);
#79297=ORIENTED_EDGE('',*,*,#54431,.T.);
#79298=ORIENTED_EDGE('',*,*,#54432,.T.);
#79299=ORIENTED_EDGE('',*,*,#54433,.T.);
#79300=ORIENTED_EDGE('',*,*,#54426,.F.);
#79301=ORIENTED_EDGE('',*,*,#54434,.T.);
#79302=ORIENTED_EDGE('',*,*,#54435,.T.);
#79303=ORIENTED_EDGE('',*,*,#54427,.F.);
#79304=ORIENTED_EDGE('',*,*,#54436,.T.);
#79305=ORIENTED_EDGE('',*,*,#54437,.T.);
#79306=ORIENTED_EDGE('',*,*,#54428,.F.);
#79307=ORIENTED_EDGE('',*,*,#54438,.T.);
#79308=ORIENTED_EDGE('',*,*,#54439,.T.);
#79309=ORIENTED_EDGE('',*,*,#54429,.F.);
#79310=ORIENTED_EDGE('',*,*,#54440,.T.);
#79311=ORIENTED_EDGE('',*,*,#54441,.T.);
#79312=ORIENTED_EDGE('',*,*,#54424,.F.);
#79313=ORIENTED_EDGE('',*,*,#54442,.F.);
#79314=ORIENTED_EDGE('',*,*,#54443,.T.);
#79315=ORIENTED_EDGE('',*,*,#54444,.T.);
#79316=ORIENTED_EDGE('',*,*,#54445,.T.);
#79317=ORIENTED_EDGE('',*,*,#54446,.T.);
#79318=ORIENTED_EDGE('',*,*,#54447,.T.);
#79319=ORIENTED_EDGE('',*,*,#54443,.F.);
#79320=ORIENTED_EDGE('',*,*,#54448,.F.);
#79321=ORIENTED_EDGE('',*,*,#54449,.F.);
#79322=ORIENTED_EDGE('',*,*,#54444,.F.);
#79323=ORIENTED_EDGE('',*,*,#54450,.F.);
#79324=ORIENTED_EDGE('',*,*,#54451,.F.);
#79325=ORIENTED_EDGE('',*,*,#54445,.F.);
#79326=ORIENTED_EDGE('',*,*,#54452,.F.);
#79327=ORIENTED_EDGE('',*,*,#54453,.F.);
#79328=ORIENTED_EDGE('',*,*,#54446,.F.);
#79329=ORIENTED_EDGE('',*,*,#54454,.F.);
#79330=ORIENTED_EDGE('',*,*,#54455,.F.);
#79331=ORIENTED_EDGE('',*,*,#54447,.F.);
#79332=ORIENTED_EDGE('',*,*,#54456,.F.);
#79333=ORIENTED_EDGE('',*,*,#54457,.F.);
#79334=ORIENTED_EDGE('',*,*,#54458,.F.);
#79335=ORIENTED_EDGE('',*,*,#54442,.T.);
#79336=ORIENTED_EDGE('',*,*,#54459,.F.);
#79337=ORIENTED_EDGE('',*,*,#54441,.F.);
#79338=ORIENTED_EDGE('',*,*,#54460,.T.);
#79339=ORIENTED_EDGE('',*,*,#54448,.T.);
#79340=ORIENTED_EDGE('',*,*,#54458,.T.);
#79341=ORIENTED_EDGE('',*,*,#54461,.F.);
#79342=ORIENTED_EDGE('',*,*,#54431,.F.);
#79343=ORIENTED_EDGE('',*,*,#54439,.F.);
#79344=ORIENTED_EDGE('',*,*,#54462,.T.);
#79345=ORIENTED_EDGE('',*,*,#54450,.T.);
#79346=ORIENTED_EDGE('',*,*,#54449,.T.);
#79347=ORIENTED_EDGE('',*,*,#54460,.F.);
#79348=ORIENTED_EDGE('',*,*,#54440,.F.);
#79349=ORIENTED_EDGE('',*,*,#54437,.F.);
#79350=ORIENTED_EDGE('',*,*,#54463,.T.);
#79351=ORIENTED_EDGE('',*,*,#54452,.T.);
#79352=ORIENTED_EDGE('',*,*,#54451,.T.);
#79353=ORIENTED_EDGE('',*,*,#54462,.F.);
#79354=ORIENTED_EDGE('',*,*,#54438,.F.);
#79355=ORIENTED_EDGE('',*,*,#54435,.F.);
#79356=ORIENTED_EDGE('',*,*,#54464,.T.);
#79357=ORIENTED_EDGE('',*,*,#54454,.T.);
#79358=ORIENTED_EDGE('',*,*,#54453,.T.);
#79359=ORIENTED_EDGE('',*,*,#54463,.F.);
#79360=ORIENTED_EDGE('',*,*,#54436,.F.);
#79361=ORIENTED_EDGE('',*,*,#54433,.F.);
#79362=ORIENTED_EDGE('',*,*,#54465,.T.);
#79363=ORIENTED_EDGE('',*,*,#54456,.T.);
#79364=ORIENTED_EDGE('',*,*,#54455,.T.);
#79365=ORIENTED_EDGE('',*,*,#54464,.F.);
#79366=ORIENTED_EDGE('',*,*,#54434,.F.);
#79367=ORIENTED_EDGE('',*,*,#54430,.F.);
#79368=ORIENTED_EDGE('',*,*,#54461,.T.);
#79369=ORIENTED_EDGE('',*,*,#54459,.T.);
#79370=ORIENTED_EDGE('',*,*,#54457,.T.);
#79371=ORIENTED_EDGE('',*,*,#54465,.F.);
#79372=ORIENTED_EDGE('',*,*,#54432,.F.);
#79373=ORIENTED_EDGE('',*,*,#54466,.F.);
#79374=ORIENTED_EDGE('',*,*,#54467,.F.);
#79375=ORIENTED_EDGE('',*,*,#54468,.T.);
#79376=ORIENTED_EDGE('',*,*,#54469,.F.);
#79377=ORIENTED_EDGE('',*,*,#54470,.F.);
#79378=ORIENTED_EDGE('',*,*,#54471,.F.);
#79379=ORIENTED_EDGE('',*,*,#54466,.T.);
#79380=ORIENTED_EDGE('',*,*,#54472,.F.);
#79381=ORIENTED_EDGE('',*,*,#54473,.F.);
#79382=ORIENTED_EDGE('',*,*,#54474,.F.);
#79383=ORIENTED_EDGE('',*,*,#54470,.T.);
#79384=ORIENTED_EDGE('',*,*,#54475,.F.);
#79385=ORIENTED_EDGE('',*,*,#54476,.F.);
#79386=ORIENTED_EDGE('',*,*,#54477,.F.);
#79387=ORIENTED_EDGE('',*,*,#54473,.T.);
#79388=ORIENTED_EDGE('',*,*,#54478,.F.);
#79389=ORIENTED_EDGE('',*,*,#54479,.F.);
#79390=ORIENTED_EDGE('',*,*,#54480,.F.);
#79391=ORIENTED_EDGE('',*,*,#54476,.T.);
#79392=ORIENTED_EDGE('',*,*,#54481,.F.);
#79393=ORIENTED_EDGE('',*,*,#54468,.F.);
#79394=ORIENTED_EDGE('',*,*,#54482,.F.);
#79395=ORIENTED_EDGE('',*,*,#54479,.T.);
#79396=ORIENTED_EDGE('',*,*,#54483,.F.);
#79397=ORIENTED_EDGE('',*,*,#54484,.T.);
#79398=ORIENTED_EDGE('',*,*,#54477,.T.);
#79399=ORIENTED_EDGE('',*,*,#54480,.T.);
#79400=ORIENTED_EDGE('',*,*,#54482,.T.);
#79401=ORIENTED_EDGE('',*,*,#54467,.T.);
#79402=ORIENTED_EDGE('',*,*,#54471,.T.);
#79403=ORIENTED_EDGE('',*,*,#54474,.T.);
#79404=ORIENTED_EDGE('',*,*,#54484,.F.);
#79405=ORIENTED_EDGE('',*,*,#54485,.F.);
#79406=ORIENTED_EDGE('',*,*,#54469,.T.);
#79407=ORIENTED_EDGE('',*,*,#54486,.F.);
#79408=ORIENTED_EDGE('',*,*,#54472,.T.);
#79409=ORIENTED_EDGE('',*,*,#54487,.F.);
#79410=ORIENTED_EDGE('',*,*,#54475,.T.);
#79411=ORIENTED_EDGE('',*,*,#54488,.F.);
#79412=ORIENTED_EDGE('',*,*,#54478,.T.);
#79413=ORIENTED_EDGE('',*,*,#54489,.F.);
#79414=ORIENTED_EDGE('',*,*,#54481,.T.);
#79415=ORIENTED_EDGE('',*,*,#54490,.F.);
#79416=ORIENTED_EDGE('',*,*,#54483,.T.);
#79417=ORIENTED_EDGE('',*,*,#54491,.T.);
#79418=ORIENTED_EDGE('',*,*,#54492,.T.);
#79419=ORIENTED_EDGE('',*,*,#54493,.T.);
#79420=ORIENTED_EDGE('',*,*,#54494,.T.);
#79421=ORIENTED_EDGE('',*,*,#54492,.F.);
#79422=ORIENTED_EDGE('',*,*,#54495,.T.);
#79423=ORIENTED_EDGE('',*,*,#54491,.F.);
#79424=ORIENTED_EDGE('',*,*,#54490,.T.);
#79425=ORIENTED_EDGE('',*,*,#54489,.T.);
#79426=ORIENTED_EDGE('',*,*,#54488,.T.);
#79427=ORIENTED_EDGE('',*,*,#54487,.T.);
#79428=ORIENTED_EDGE('',*,*,#54486,.T.);
#79429=ORIENTED_EDGE('',*,*,#54485,.T.);
#79430=ORIENTED_EDGE('',*,*,#54495,.F.);
#79431=ORIENTED_EDGE('',*,*,#54496,.T.);
#79432=ORIENTED_EDGE('',*,*,#54493,.F.);
#79433=ORIENTED_EDGE('',*,*,#54494,.F.);
#79434=ORIENTED_EDGE('',*,*,#54496,.F.);
#79435=ORIENTED_EDGE('',*,*,#54497,.T.);
#79436=ORIENTED_EDGE('',*,*,#54498,.T.);
#79437=ORIENTED_EDGE('',*,*,#54499,.T.);
#79438=ORIENTED_EDGE('',*,*,#54500,.T.);
#79439=ORIENTED_EDGE('',*,*,#54501,.T.);
#79440=ORIENTED_EDGE('',*,*,#54502,.F.);
#79441=ORIENTED_EDGE('',*,*,#54502,.T.);
#79442=ORIENTED_EDGE('',*,*,#54503,.T.);
#79443=ORIENTED_EDGE('',*,*,#54504,.F.);
#79444=ORIENTED_EDGE('',*,*,#54505,.F.);
#79445=ORIENTED_EDGE('',*,*,#54504,.T.);
#79446=ORIENTED_EDGE('',*,*,#54506,.T.);
#79447=ORIENTED_EDGE('',*,*,#54507,.F.);
#79448=ORIENTED_EDGE('',*,*,#54508,.T.);
#79449=ORIENTED_EDGE('',*,*,#54507,.T.);
#79450=ORIENTED_EDGE('',*,*,#54509,.T.);
#79451=ORIENTED_EDGE('',*,*,#54510,.T.);
#79452=ORIENTED_EDGE('',*,*,#54511,.F.);
#79453=ORIENTED_EDGE('',*,*,#54512,.T.);
#79454=ORIENTED_EDGE('',*,*,#54513,.F.);
#79455=ORIENTED_EDGE('',*,*,#54514,.T.);
#79456=ORIENTED_EDGE('',*,*,#54515,.F.);
#79457=ORIENTED_EDGE('',*,*,#54516,.T.);
#79458=ORIENTED_EDGE('',*,*,#54511,.T.);
#79459=ORIENTED_EDGE('',*,*,#54517,.T.);
#79460=ORIENTED_EDGE('',*,*,#54518,.T.);
#79461=ORIENTED_EDGE('',*,*,#54515,.T.);
#79462=ORIENTED_EDGE('',*,*,#54519,.F.);
#79463=ORIENTED_EDGE('',*,*,#54520,.T.);
#79464=ORIENTED_EDGE('',*,*,#54521,.T.);
#79465=ORIENTED_EDGE('',*,*,#54522,.F.);
#79466=ORIENTED_EDGE('',*,*,#54523,.T.);
#79467=ORIENTED_EDGE('',*,*,#54519,.T.);
#79468=ORIENTED_EDGE('',*,*,#54524,.F.);
#79469=ORIENTED_EDGE('',*,*,#54525,.T.);
#79470=ORIENTED_EDGE('',*,*,#54522,.T.);
#79471=ORIENTED_EDGE('',*,*,#54526,.T.);
#79472=ORIENTED_EDGE('',*,*,#54527,.T.);
#79473=ORIENTED_EDGE('',*,*,#54528,.T.);
#79474=ORIENTED_EDGE('',*,*,#54529,.T.);
#79475=ORIENTED_EDGE('',*,*,#54510,.F.);
#79476=ORIENTED_EDGE('',*,*,#54530,.T.);
#79477=ORIENTED_EDGE('',*,*,#54531,.T.);
#79478=ORIENTED_EDGE('',*,*,#54532,.T.);
#79479=ORIENTED_EDGE('',*,*,#54533,.F.);
#79480=ORIENTED_EDGE('',*,*,#54534,.T.);
#79481=ORIENTED_EDGE('',*,*,#54535,.T.);
#79482=ORIENTED_EDGE('',*,*,#54536,.T.);
#79483=ORIENTED_EDGE('',*,*,#54537,.F.);
#79484=ORIENTED_EDGE('',*,*,#54538,.T.);
#79485=ORIENTED_EDGE('',*,*,#54539,.F.);
#79486=ORIENTED_EDGE('',*,*,#54540,.T.);
#79487=ORIENTED_EDGE('',*,*,#54541,.F.);
#79488=ORIENTED_EDGE('',*,*,#54500,.F.);
#79489=ORIENTED_EDGE('',*,*,#54542,.F.);
#79490=ORIENTED_EDGE('',*,*,#54538,.F.);
#79491=ORIENTED_EDGE('',*,*,#54543,.F.);
#79492=ORIENTED_EDGE('',*,*,#54536,.F.);
#79493=ORIENTED_EDGE('',*,*,#54544,.T.);
#79494=ORIENTED_EDGE('',*,*,#54499,.F.);
#79495=ORIENTED_EDGE('',*,*,#54545,.F.);
#79496=ORIENTED_EDGE('',*,*,#54517,.F.);
#79497=ORIENTED_EDGE('',*,*,#54514,.F.);
#79498=ORIENTED_EDGE('',*,*,#54546,.F.);
#79499=ORIENTED_EDGE('',*,*,#54547,.T.);
#79500=ORIENTED_EDGE('',*,*,#54548,.T.);
#79501=ORIENTED_EDGE('',*,*,#54549,.F.);
#79502=ORIENTED_EDGE('',*,*,#54550,.F.);
#79503=ORIENTED_EDGE('',*,*,#54526,.F.);
#79504=ORIENTED_EDGE('',*,*,#54521,.F.);
#79505=ORIENTED_EDGE('',*,*,#54551,.F.);
#79506=ORIENTED_EDGE('',*,*,#54552,.T.);
#79507=ORIENTED_EDGE('',*,*,#54553,.F.);
#79508=ORIENTED_EDGE('',*,*,#54554,.T.);
#79509=ORIENTED_EDGE('',*,*,#54555,.T.);
#79510=ORIENTED_EDGE('',*,*,#54556,.F.);
#79511=ORIENTED_EDGE('',*,*,#54557,.T.);
#79512=ORIENTED_EDGE('',*,*,#54558,.T.);
#79513=ORIENTED_EDGE('',*,*,#54554,.F.);
#79514=ORIENTED_EDGE('',*,*,#54559,.T.);
#79515=ORIENTED_EDGE('',*,*,#54560,.T.);
#79516=ORIENTED_EDGE('',*,*,#54561,.T.);
#79517=ORIENTED_EDGE('',*,*,#54557,.F.);
#79518=ORIENTED_EDGE('',*,*,#54562,.F.);
#79519=ORIENTED_EDGE('',*,*,#54563,.F.);
#79520=ORIENTED_EDGE('',*,*,#54564,.T.);
#79521=ORIENTED_EDGE('',*,*,#54560,.F.);
#79522=ORIENTED_EDGE('',*,*,#54565,.T.);
#79523=ORIENTED_EDGE('',*,*,#54566,.T.);
#79524=ORIENTED_EDGE('',*,*,#54567,.T.);
#79525=ORIENTED_EDGE('',*,*,#54568,.F.);
#79526=ORIENTED_EDGE('',*,*,#54567,.F.);
#79527=ORIENTED_EDGE('',*,*,#54569,.T.);
#79528=ORIENTED_EDGE('',*,*,#54570,.T.);
#79529=ORIENTED_EDGE('',*,*,#54570,.F.);
#79530=ORIENTED_EDGE('',*,*,#54571,.T.);
#79531=ORIENTED_EDGE('',*,*,#54572,.F.);
#79532=ORIENTED_EDGE('',*,*,#54573,.F.);
#79533=ORIENTED_EDGE('',*,*,#54574,.T.);
#79534=ORIENTED_EDGE('',*,*,#54575,.T.);
#79535=ORIENTED_EDGE('',*,*,#54575,.F.);
#79536=ORIENTED_EDGE('',*,*,#54576,.T.);
#79537=ORIENTED_EDGE('',*,*,#54577,.T.);
#79538=ORIENTED_EDGE('',*,*,#54577,.F.);
#79539=ORIENTED_EDGE('',*,*,#54578,.T.);
#79540=ORIENTED_EDGE('',*,*,#54579,.T.);
#79541=ORIENTED_EDGE('',*,*,#54580,.F.);
#79542=ORIENTED_EDGE('',*,*,#54581,.F.);
#79543=ORIENTED_EDGE('',*,*,#54582,.T.);
#79544=ORIENTED_EDGE('',*,*,#54583,.F.);
#79545=ORIENTED_EDGE('',*,*,#54584,.F.);
#79546=ORIENTED_EDGE('',*,*,#54585,.T.);
#79547=ORIENTED_EDGE('',*,*,#54563,.T.);
#79548=ORIENTED_EDGE('',*,*,#54586,.F.);
#79549=ORIENTED_EDGE('',*,*,#54587,.F.);
#79550=ORIENTED_EDGE('',*,*,#54588,.F.);
#79551=ORIENTED_EDGE('',*,*,#54589,.F.);
#79552=ORIENTED_EDGE('',*,*,#54590,.F.);
#79553=ORIENTED_EDGE('',*,*,#54591,.F.);
#79554=ORIENTED_EDGE('',*,*,#54592,.F.);
#79555=ORIENTED_EDGE('',*,*,#54593,.T.);
#79556=ORIENTED_EDGE('',*,*,#54594,.F.);
#79557=ORIENTED_EDGE('',*,*,#54595,.F.);
#79558=ORIENTED_EDGE('',*,*,#54551,.T.);
#79559=ORIENTED_EDGE('',*,*,#54596,.F.);
#79560=ORIENTED_EDGE('',*,*,#54588,.T.);
#79561=ORIENTED_EDGE('',*,*,#54597,.F.);
#79562=ORIENTED_EDGE('',*,*,#54594,.T.);
#79563=ORIENTED_EDGE('',*,*,#54598,.T.);
#79564=ORIENTED_EDGE('',*,*,#54556,.T.);
#79565=ORIENTED_EDGE('',*,*,#54534,.F.);
#79566=ORIENTED_EDGE('',*,*,#54599,.T.);
#79567=ORIENTED_EDGE('',*,*,#54590,.T.);
#79568=ORIENTED_EDGE('',*,*,#54600,.T.);
#79569=ORIENTED_EDGE('',*,*,#54592,.T.);
#79570=ORIENTED_EDGE('',*,*,#54601,.T.);
#79571=ORIENTED_EDGE('',*,*,#54540,.F.);
#79572=ORIENTED_EDGE('',*,*,#54602,.T.);
#79573=ORIENTED_EDGE('',*,*,#54603,.F.);
#79574=ORIENTED_EDGE('',*,*,#54573,.T.);
#79575=ORIENTED_EDGE('',*,*,#54580,.T.);
#79576=ORIENTED_EDGE('',*,*,#54604,.T.);
#79577=ORIENTED_EDGE('',*,*,#54605,.T.);
#79578=ORIENTED_EDGE('',*,*,#54606,.F.);
#79579=ORIENTED_EDGE('',*,*,#54607,.F.);
#79580=ORIENTED_EDGE('',*,*,#54608,.T.);
#79581=ORIENTED_EDGE('',*,*,#54568,.T.);
#79582=ORIENTED_EDGE('',*,*,#54572,.T.);
#79583=ORIENTED_EDGE('',*,*,#54609,.F.);
#79584=ORIENTED_EDGE('',*,*,#54542,.T.);
#79585=ORIENTED_EDGE('',*,*,#54505,.T.);
#79586=ORIENTED_EDGE('',*,*,#54610,.T.);
#79587=ORIENTED_EDGE('',*,*,#54611,.F.);
#79588=ORIENTED_EDGE('',*,*,#54539,.T.);
#79589=ORIENTED_EDGE('',*,*,#54609,.T.);
#79590=ORIENTED_EDGE('',*,*,#54612,.T.);
#79591=ORIENTED_EDGE('',*,*,#54613,.F.);
#79592=ORIENTED_EDGE('',*,*,#54546,.T.);
#79593=ORIENTED_EDGE('',*,*,#54513,.T.);
#79594=ORIENTED_EDGE('',*,*,#54614,.T.);
#79595=ORIENTED_EDGE('',*,*,#54615,.F.);
#79596=ORIENTED_EDGE('',*,*,#54616,.T.);
#79597=ORIENTED_EDGE('',*,*,#54613,.T.);
#79598=ORIENTED_EDGE('',*,*,#54617,.T.);
#79599=ORIENTED_EDGE('',*,*,#54527,.F.);
#79600=ORIENTED_EDGE('',*,*,#54618,.T.);
#79601=ORIENTED_EDGE('',*,*,#54615,.T.);
#79602=ORIENTED_EDGE('',*,*,#54619,.T.);
#79603=ORIENTED_EDGE('',*,*,#54620,.F.);
#79604=ORIENTED_EDGE('',*,*,#54621,.T.);
#79605=ORIENTED_EDGE('',*,*,#54524,.T.);
#79606=ORIENTED_EDGE('',*,*,#54550,.T.);
#79607=ORIENTED_EDGE('',*,*,#54622,.F.);
#79608=ORIENTED_EDGE('',*,*,#54623,.T.);
#79609=ORIENTED_EDGE('',*,*,#54620,.T.);
#79610=ORIENTED_EDGE('',*,*,#54624,.T.);
#79611=ORIENTED_EDGE('',*,*,#54531,.F.);
#79612=ORIENTED_EDGE('',*,*,#54625,.T.);
#79613=ORIENTED_EDGE('',*,*,#54622,.T.);
#79614=ORIENTED_EDGE('',*,*,#54626,.T.);
#79615=ORIENTED_EDGE('',*,*,#54627,.T.);
#79616=ORIENTED_EDGE('',*,*,#54628,.F.);
#79617=ORIENTED_EDGE('',*,*,#54624,.F.);
#79618=ORIENTED_EDGE('',*,*,#54549,.T.);
#79619=ORIENTED_EDGE('',*,*,#54629,.T.);
#79620=ORIENTED_EDGE('',*,*,#54547,.F.);
#79621=ORIENTED_EDGE('',*,*,#54616,.F.);
#79622=ORIENTED_EDGE('',*,*,#54630,.T.);
#79623=ORIENTED_EDGE('',*,*,#54631,.T.);
#79624=ORIENTED_EDGE('',*,*,#54632,.T.);
#79625=ORIENTED_EDGE('',*,*,#54606,.T.);
#79626=ORIENTED_EDGE('',*,*,#54633,.T.);
#79627=ORIENTED_EDGE('',*,*,#54634,.T.);
#79628=ORIENTED_EDGE('',*,*,#54627,.F.);
#79629=ORIENTED_EDGE('',*,*,#54548,.F.);
#79630=ORIENTED_EDGE('',*,*,#54629,.F.);
#79631=ORIENTED_EDGE('',*,*,#54635,.T.);
#79632=ORIENTED_EDGE('',*,*,#54636,.F.);
#79633=ORIENTED_EDGE('',*,*,#54559,.F.);
#79634=ORIENTED_EDGE('',*,*,#54598,.F.);
#79635=ORIENTED_EDGE('',*,*,#54637,.T.);
#79636=ORIENTED_EDGE('',*,*,#54638,.F.);
#79637=ORIENTED_EDGE('',*,*,#54635,.F.);
#79638=ORIENTED_EDGE('',*,*,#54593,.F.);
#79639=ORIENTED_EDGE('',*,*,#54602,.F.);
#79640=ORIENTED_EDGE('',*,*,#54611,.T.);
#79641=ORIENTED_EDGE('',*,*,#54639,.F.);
#79642=ORIENTED_EDGE('',*,*,#54637,.F.);
#79643=ORIENTED_EDGE('',*,*,#54640,.T.);
#79644=ORIENTED_EDGE('',*,*,#54641,.F.);
#79645=ORIENTED_EDGE('',*,*,#54565,.F.);
#79646=ORIENTED_EDGE('',*,*,#54608,.F.);
#79647=ORIENTED_EDGE('',*,*,#54642,.T.);
#79648=ORIENTED_EDGE('',*,*,#54643,.F.);
#79649=ORIENTED_EDGE('',*,*,#54640,.F.);
#79650=ORIENTED_EDGE('',*,*,#54644,.F.);
#79651=ORIENTED_EDGE('',*,*,#54583,.T.);
#79652=ORIENTED_EDGE('',*,*,#54645,.F.);
#79653=ORIENTED_EDGE('',*,*,#54642,.F.);
#79654=ORIENTED_EDGE('',*,*,#54646,.F.);
#79655=ORIENTED_EDGE('',*,*,#54647,.T.);
#79656=ORIENTED_EDGE('',*,*,#54604,.F.);
#79657=ORIENTED_EDGE('',*,*,#54579,.F.);
#79658=ORIENTED_EDGE('',*,*,#54648,.F.);
#79659=ORIENTED_EDGE('',*,*,#54649,.T.);
#79660=ORIENTED_EDGE('',*,*,#54650,.F.);
#79661=ORIENTED_EDGE('',*,*,#54647,.F.);
#79662=ORIENTED_EDGE('',*,*,#54651,.F.);
#79663=ORIENTED_EDGE('',*,*,#54584,.T.);
#79664=ORIENTED_EDGE('',*,*,#54652,.F.);
#79665=ORIENTED_EDGE('',*,*,#54649,.F.);
#79666=ORIENTED_EDGE('',*,*,#54653,.F.);
#79667=ORIENTED_EDGE('',*,*,#54625,.F.);
#79668=ORIENTED_EDGE('',*,*,#54530,.F.);
#79669=ORIENTED_EDGE('',*,*,#54509,.F.);
#79670=ORIENTED_EDGE('',*,*,#54506,.F.);
#79671=ORIENTED_EDGE('',*,*,#54503,.F.);
#79672=ORIENTED_EDGE('',*,*,#54501,.F.);
#79673=ORIENTED_EDGE('',*,*,#54541,.T.);
#79674=ORIENTED_EDGE('',*,*,#54537,.T.);
#79675=ORIENTED_EDGE('',*,*,#54601,.F.);
#79676=ORIENTED_EDGE('',*,*,#54591,.T.);
#79677=ORIENTED_EDGE('',*,*,#54597,.T.);
#79678=ORIENTED_EDGE('',*,*,#54555,.F.);
#79679=ORIENTED_EDGE('',*,*,#54558,.F.);
#79680=ORIENTED_EDGE('',*,*,#54561,.F.);
#79681=ORIENTED_EDGE('',*,*,#54564,.F.);
#79682=ORIENTED_EDGE('',*,*,#54585,.F.);
#79683=ORIENTED_EDGE('',*,*,#54653,.T.);
#79684=ORIENTED_EDGE('',*,*,#54651,.T.);
#79685=ORIENTED_EDGE('',*,*,#54648,.T.);
#79686=ORIENTED_EDGE('',*,*,#54578,.F.);
#79687=ORIENTED_EDGE('',*,*,#54576,.F.);
#79688=ORIENTED_EDGE('',*,*,#54574,.F.);
#79689=ORIENTED_EDGE('',*,*,#54603,.T.);
#79690=ORIENTED_EDGE('',*,*,#54571,.F.);
#79691=ORIENTED_EDGE('',*,*,#54569,.F.);
#79692=ORIENTED_EDGE('',*,*,#54566,.F.);
#79693=ORIENTED_EDGE('',*,*,#54641,.T.);
#79694=ORIENTED_EDGE('',*,*,#54643,.T.);
#79695=ORIENTED_EDGE('',*,*,#54645,.T.);
#79696=ORIENTED_EDGE('',*,*,#54582,.F.);
#79697=ORIENTED_EDGE('',*,*,#54654,.F.);
#79698=ORIENTED_EDGE('',*,*,#54552,.F.);
#79699=ORIENTED_EDGE('',*,*,#54595,.T.);
#79700=ORIENTED_EDGE('',*,*,#54587,.T.);
#79701=ORIENTED_EDGE('',*,*,#54599,.F.);
#79702=ORIENTED_EDGE('',*,*,#54533,.T.);
#79703=ORIENTED_EDGE('',*,*,#54543,.T.);
#79704=ORIENTED_EDGE('',*,*,#54498,.F.);
#79705=ORIENTED_EDGE('',*,*,#54655,.T.);
#79706=ORIENTED_EDGE('',*,*,#54528,.F.);
#79707=ORIENTED_EDGE('',*,*,#54619,.F.);
#79708=ORIENTED_EDGE('',*,*,#54617,.F.);
#79709=ORIENTED_EDGE('',*,*,#54614,.F.);
#79710=ORIENTED_EDGE('',*,*,#54512,.F.);
#79711=ORIENTED_EDGE('',*,*,#54516,.F.);
#79712=ORIENTED_EDGE('',*,*,#54518,.F.);
#79713=ORIENTED_EDGE('',*,*,#54545,.T.);
#79714=ORIENTED_EDGE('',*,*,#54520,.F.);
#79715=ORIENTED_EDGE('',*,*,#54523,.F.);
#79716=ORIENTED_EDGE('',*,*,#54525,.F.);
#79717=ORIENTED_EDGE('',*,*,#54621,.F.);
#79718=ORIENTED_EDGE('',*,*,#54623,.F.);
#79719=ORIENTED_EDGE('',*,*,#54631,.F.);
#79720=ORIENTED_EDGE('',*,*,#54630,.F.);
#79721=ORIENTED_EDGE('',*,*,#54618,.F.);
#79722=ORIENTED_EDGE('',*,*,#54529,.F.);
#79723=ORIENTED_EDGE('',*,*,#54655,.F.);
#79724=ORIENTED_EDGE('',*,*,#54497,.F.);
#79725=ORIENTED_EDGE('',*,*,#54544,.F.);
#79726=ORIENTED_EDGE('',*,*,#54535,.F.);
#79727=ORIENTED_EDGE('',*,*,#54600,.F.);
#79728=ORIENTED_EDGE('',*,*,#54589,.T.);
#79729=ORIENTED_EDGE('',*,*,#54596,.T.);
#79730=ORIENTED_EDGE('',*,*,#54553,.T.);
#79731=ORIENTED_EDGE('',*,*,#54654,.T.);
#79732=ORIENTED_EDGE('',*,*,#54581,.T.);
#79733=ORIENTED_EDGE('',*,*,#54646,.T.);
#79734=ORIENTED_EDGE('',*,*,#54656,.T.);
#79735=ORIENTED_EDGE('',*,*,#54634,.F.);
#79736=ORIENTED_EDGE('',*,*,#54657,.F.);
#79737=ORIENTED_EDGE('',*,*,#54652,.T.);
#79738=ORIENTED_EDGE('',*,*,#54586,.T.);
#79739=ORIENTED_EDGE('',*,*,#54562,.T.);
#79740=ORIENTED_EDGE('',*,*,#54636,.T.);
#79741=ORIENTED_EDGE('',*,*,#54638,.T.);
#79742=ORIENTED_EDGE('',*,*,#54639,.T.);
#79743=ORIENTED_EDGE('',*,*,#54612,.F.);
#79744=ORIENTED_EDGE('',*,*,#54610,.F.);
#79745=ORIENTED_EDGE('',*,*,#54508,.F.);
#79746=ORIENTED_EDGE('',*,*,#54532,.F.);
#79747=ORIENTED_EDGE('',*,*,#54626,.F.);
#79748=ORIENTED_EDGE('',*,*,#54628,.T.);
#79749=ORIENTED_EDGE('',*,*,#54633,.F.);
#79750=ORIENTED_EDGE('',*,*,#54605,.F.);
#79751=ORIENTED_EDGE('',*,*,#54650,.T.);
#79752=ORIENTED_EDGE('',*,*,#54657,.T.);
#79753=ORIENTED_EDGE('',*,*,#54632,.F.);
#79754=ORIENTED_EDGE('',*,*,#54656,.F.);
#79755=ORIENTED_EDGE('',*,*,#54644,.T.);
#79756=ORIENTED_EDGE('',*,*,#54607,.T.);
#79757=ORIENTED_EDGE('',*,*,#54658,.T.);
#79758=ORIENTED_EDGE('',*,*,#54659,.T.);
#79759=ORIENTED_EDGE('',*,*,#54660,.F.);
#79760=ORIENTED_EDGE('',*,*,#54661,.T.);
#79761=ORIENTED_EDGE('',*,*,#54662,.T.);
#79762=ORIENTED_EDGE('',*,*,#54663,.T.);
#79763=ORIENTED_EDGE('',*,*,#54658,.F.);
#79764=ORIENTED_EDGE('',*,*,#54664,.T.);
#79765=ORIENTED_EDGE('',*,*,#54665,.T.);
#79766=ORIENTED_EDGE('',*,*,#54666,.T.);
#79767=ORIENTED_EDGE('',*,*,#54662,.F.);
#79768=ORIENTED_EDGE('',*,*,#54667,.T.);
#79769=ORIENTED_EDGE('',*,*,#54668,.T.);
#79770=ORIENTED_EDGE('',*,*,#54669,.T.);
#79771=ORIENTED_EDGE('',*,*,#54665,.F.);
#79772=ORIENTED_EDGE('',*,*,#54670,.T.);
#79773=ORIENTED_EDGE('',*,*,#54671,.T.);
#79774=ORIENTED_EDGE('',*,*,#54672,.T.);
#79775=ORIENTED_EDGE('',*,*,#54668,.F.);
#79776=ORIENTED_EDGE('',*,*,#54673,.T.);
#79777=ORIENTED_EDGE('',*,*,#54674,.T.);
#79778=ORIENTED_EDGE('',*,*,#54675,.T.);
#79779=ORIENTED_EDGE('',*,*,#54671,.F.);
#79780=ORIENTED_EDGE('',*,*,#54676,.T.);
#79781=ORIENTED_EDGE('',*,*,#54677,.T.);
#79782=ORIENTED_EDGE('',*,*,#54678,.T.);
#79783=ORIENTED_EDGE('',*,*,#54674,.F.);
#79784=ORIENTED_EDGE('',*,*,#54679,.T.);
#79785=ORIENTED_EDGE('',*,*,#54680,.T.);
#79786=ORIENTED_EDGE('',*,*,#54681,.T.);
#79787=ORIENTED_EDGE('',*,*,#54677,.F.);
#79788=ORIENTED_EDGE('',*,*,#54682,.T.);
#79789=ORIENTED_EDGE('',*,*,#54683,.T.);
#79790=ORIENTED_EDGE('',*,*,#54684,.T.);
#79791=ORIENTED_EDGE('',*,*,#54680,.F.);
#79792=ORIENTED_EDGE('',*,*,#54685,.T.);
#79793=ORIENTED_EDGE('',*,*,#54686,.T.);
#79794=ORIENTED_EDGE('',*,*,#54687,.T.);
#79795=ORIENTED_EDGE('',*,*,#54683,.F.);
#79796=ORIENTED_EDGE('',*,*,#54688,.T.);
#79797=ORIENTED_EDGE('',*,*,#54689,.T.);
#79798=ORIENTED_EDGE('',*,*,#54690,.T.);
#79799=ORIENTED_EDGE('',*,*,#54686,.F.);
#79800=ORIENTED_EDGE('',*,*,#54691,.T.);
#79801=ORIENTED_EDGE('',*,*,#54692,.T.);
#79802=ORIENTED_EDGE('',*,*,#54693,.T.);
#79803=ORIENTED_EDGE('',*,*,#54689,.F.);
#79804=ORIENTED_EDGE('',*,*,#54694,.T.);
#79805=ORIENTED_EDGE('',*,*,#54695,.T.);
#79806=ORIENTED_EDGE('',*,*,#54696,.T.);
#79807=ORIENTED_EDGE('',*,*,#54692,.F.);
#79808=ORIENTED_EDGE('',*,*,#54697,.T.);
#79809=ORIENTED_EDGE('',*,*,#54698,.T.);
#79810=ORIENTED_EDGE('',*,*,#54699,.T.);
#79811=ORIENTED_EDGE('',*,*,#54695,.F.);
#79812=ORIENTED_EDGE('',*,*,#54700,.T.);
#79813=ORIENTED_EDGE('',*,*,#54701,.T.);
#79814=ORIENTED_EDGE('',*,*,#54702,.T.);
#79815=ORIENTED_EDGE('',*,*,#54698,.F.);
#79816=ORIENTED_EDGE('',*,*,#54703,.T.);
#79817=ORIENTED_EDGE('',*,*,#54704,.T.);
#79818=ORIENTED_EDGE('',*,*,#54705,.T.);
#79819=ORIENTED_EDGE('',*,*,#54701,.F.);
#79820=ORIENTED_EDGE('',*,*,#54706,.T.);
#79821=ORIENTED_EDGE('',*,*,#54707,.T.);
#79822=ORIENTED_EDGE('',*,*,#54708,.T.);
#79823=ORIENTED_EDGE('',*,*,#54704,.F.);
#79824=ORIENTED_EDGE('',*,*,#54709,.T.);
#79825=ORIENTED_EDGE('',*,*,#54710,.T.);
#79826=ORIENTED_EDGE('',*,*,#54711,.T.);
#79827=ORIENTED_EDGE('',*,*,#54707,.F.);
#79828=ORIENTED_EDGE('',*,*,#54712,.T.);
#79829=ORIENTED_EDGE('',*,*,#54713,.F.);
#79830=ORIENTED_EDGE('',*,*,#54714,.T.);
#79831=ORIENTED_EDGE('',*,*,#54715,.T.);
#79832=ORIENTED_EDGE('',*,*,#54716,.T.);
#79833=ORIENTED_EDGE('',*,*,#54717,.T.);
#79834=ORIENTED_EDGE('',*,*,#54718,.T.);
#79835=ORIENTED_EDGE('',*,*,#54719,.T.);
#79836=ORIENTED_EDGE('',*,*,#54720,.T.);
#79837=ORIENTED_EDGE('',*,*,#54721,.T.);
#79838=ORIENTED_EDGE('',*,*,#54722,.T.);
#79839=ORIENTED_EDGE('',*,*,#54717,.F.);
#79840=ORIENTED_EDGE('',*,*,#54723,.T.);
#79841=ORIENTED_EDGE('',*,*,#54724,.T.);
#79842=ORIENTED_EDGE('',*,*,#54725,.T.);
#79843=ORIENTED_EDGE('',*,*,#54721,.F.);
#79844=ORIENTED_EDGE('',*,*,#54726,.T.);
#79845=ORIENTED_EDGE('',*,*,#54727,.T.);
#79846=ORIENTED_EDGE('',*,*,#54728,.T.);
#79847=ORIENTED_EDGE('',*,*,#54724,.F.);
#79848=ORIENTED_EDGE('',*,*,#54729,.T.);
#79849=ORIENTED_EDGE('',*,*,#54730,.T.);
#79850=ORIENTED_EDGE('',*,*,#54731,.T.);
#79851=ORIENTED_EDGE('',*,*,#54727,.F.);
#79852=ORIENTED_EDGE('',*,*,#54732,.T.);
#79853=ORIENTED_EDGE('',*,*,#54733,.T.);
#79854=ORIENTED_EDGE('',*,*,#54734,.T.);
#79855=ORIENTED_EDGE('',*,*,#54730,.F.);
#79856=ORIENTED_EDGE('',*,*,#54735,.T.);
#79857=ORIENTED_EDGE('',*,*,#54736,.T.);
#79858=ORIENTED_EDGE('',*,*,#54737,.T.);
#79859=ORIENTED_EDGE('',*,*,#54733,.F.);
#79860=ORIENTED_EDGE('',*,*,#54738,.T.);
#79861=ORIENTED_EDGE('',*,*,#54739,.T.);
#79862=ORIENTED_EDGE('',*,*,#54740,.T.);
#79863=ORIENTED_EDGE('',*,*,#54736,.F.);
#79864=ORIENTED_EDGE('',*,*,#54741,.T.);
#79865=ORIENTED_EDGE('',*,*,#54742,.T.);
#79866=ORIENTED_EDGE('',*,*,#54743,.T.);
#79867=ORIENTED_EDGE('',*,*,#54739,.F.);
#79868=ORIENTED_EDGE('',*,*,#54744,.T.);
#79869=ORIENTED_EDGE('',*,*,#54745,.T.);
#79870=ORIENTED_EDGE('',*,*,#54746,.T.);
#79871=ORIENTED_EDGE('',*,*,#54742,.F.);
#79872=ORIENTED_EDGE('',*,*,#54747,.T.);
#79873=ORIENTED_EDGE('',*,*,#54748,.T.);
#79874=ORIENTED_EDGE('',*,*,#54749,.T.);
#79875=ORIENTED_EDGE('',*,*,#54745,.F.);
#79876=ORIENTED_EDGE('',*,*,#54750,.T.);
#79877=ORIENTED_EDGE('',*,*,#54751,.T.);
#79878=ORIENTED_EDGE('',*,*,#54752,.T.);
#79879=ORIENTED_EDGE('',*,*,#54748,.F.);
#79880=ORIENTED_EDGE('',*,*,#54753,.T.);
#79881=ORIENTED_EDGE('',*,*,#54754,.T.);
#79882=ORIENTED_EDGE('',*,*,#54755,.T.);
#79883=ORIENTED_EDGE('',*,*,#54751,.F.);
#79884=ORIENTED_EDGE('',*,*,#54756,.T.);
#79885=ORIENTED_EDGE('',*,*,#54757,.T.);
#79886=ORIENTED_EDGE('',*,*,#54758,.T.);
#79887=ORIENTED_EDGE('',*,*,#54754,.F.);
#79888=ORIENTED_EDGE('',*,*,#54759,.T.);
#79889=ORIENTED_EDGE('',*,*,#54760,.T.);
#79890=ORIENTED_EDGE('',*,*,#54761,.T.);
#79891=ORIENTED_EDGE('',*,*,#54757,.F.);
#79892=ORIENTED_EDGE('',*,*,#54762,.T.);
#79893=ORIENTED_EDGE('',*,*,#54763,.T.);
#79894=ORIENTED_EDGE('',*,*,#54764,.T.);
#79895=ORIENTED_EDGE('',*,*,#54760,.F.);
#79896=ORIENTED_EDGE('',*,*,#54765,.T.);
#79897=ORIENTED_EDGE('',*,*,#54766,.T.);
#79898=ORIENTED_EDGE('',*,*,#54767,.T.);
#79899=ORIENTED_EDGE('',*,*,#54763,.F.);
#79900=ORIENTED_EDGE('',*,*,#54768,.T.);
#79901=ORIENTED_EDGE('',*,*,#54769,.T.);
#79902=ORIENTED_EDGE('',*,*,#54770,.T.);
#79903=ORIENTED_EDGE('',*,*,#54766,.F.);
#79904=ORIENTED_EDGE('',*,*,#54771,.T.);
#79905=ORIENTED_EDGE('',*,*,#54772,.F.);
#79906=ORIENTED_EDGE('',*,*,#54773,.T.);
#79907=ORIENTED_EDGE('',*,*,#54774,.F.);
#79908=ORIENTED_EDGE('',*,*,#54775,.T.);
#79909=ORIENTED_EDGE('',*,*,#54776,.T.);
#79910=ORIENTED_EDGE('',*,*,#54777,.T.);
#79911=ORIENTED_EDGE('',*,*,#54778,.F.);
#79912=ORIENTED_EDGE('',*,*,#54779,.F.);
#79913=ORIENTED_EDGE('',*,*,#54780,.T.);
#79914=ORIENTED_EDGE('',*,*,#54781,.T.);
#79915=ORIENTED_EDGE('',*,*,#54782,.F.);
#79916=ORIENTED_EDGE('',*,*,#54783,.T.);
#79917=ORIENTED_EDGE('',*,*,#54776,.F.);
#79918=ORIENTED_EDGE('',*,*,#54784,.F.);
#79919=ORIENTED_EDGE('',*,*,#54785,.T.);
#79920=ORIENTED_EDGE('',*,*,#54786,.T.);
#79921=ORIENTED_EDGE('',*,*,#54780,.F.);
#79922=ORIENTED_EDGE('',*,*,#54787,.F.);
#79923=ORIENTED_EDGE('',*,*,#54788,.T.);
#79924=ORIENTED_EDGE('',*,*,#54789,.T.);
#79925=ORIENTED_EDGE('',*,*,#54785,.F.);
#79926=ORIENTED_EDGE('',*,*,#54790,.F.);
#79927=ORIENTED_EDGE('',*,*,#54791,.T.);
#79928=ORIENTED_EDGE('',*,*,#54792,.T.);
#79929=ORIENTED_EDGE('',*,*,#54788,.F.);
#79930=ORIENTED_EDGE('',*,*,#54793,.F.);
#79931=ORIENTED_EDGE('',*,*,#54794,.T.);
#79932=ORIENTED_EDGE('',*,*,#54795,.T.);
#79933=ORIENTED_EDGE('',*,*,#54791,.F.);
#79934=ORIENTED_EDGE('',*,*,#54796,.F.);
#79935=ORIENTED_EDGE('',*,*,#54797,.T.);
#79936=ORIENTED_EDGE('',*,*,#54798,.T.);
#79937=ORIENTED_EDGE('',*,*,#54794,.F.);
#79938=ORIENTED_EDGE('',*,*,#54799,.F.);
#79939=ORIENTED_EDGE('',*,*,#54800,.T.);
#79940=ORIENTED_EDGE('',*,*,#54801,.T.);
#79941=ORIENTED_EDGE('',*,*,#54797,.F.);
#79942=ORIENTED_EDGE('',*,*,#54802,.F.);
#79943=ORIENTED_EDGE('',*,*,#54803,.T.);
#79944=ORIENTED_EDGE('',*,*,#54804,.T.);
#79945=ORIENTED_EDGE('',*,*,#54800,.F.);
#79946=ORIENTED_EDGE('',*,*,#54805,.F.);
#79947=ORIENTED_EDGE('',*,*,#54806,.T.);
#79948=ORIENTED_EDGE('',*,*,#54807,.T.);
#79949=ORIENTED_EDGE('',*,*,#54803,.F.);
#79950=ORIENTED_EDGE('',*,*,#54808,.F.);
#79951=ORIENTED_EDGE('',*,*,#54809,.T.);
#79952=ORIENTED_EDGE('',*,*,#54810,.T.);
#79953=ORIENTED_EDGE('',*,*,#54806,.F.);
#79954=ORIENTED_EDGE('',*,*,#54811,.F.);
#79955=ORIENTED_EDGE('',*,*,#54812,.T.);
#79956=ORIENTED_EDGE('',*,*,#54813,.T.);
#79957=ORIENTED_EDGE('',*,*,#54809,.F.);
#79958=ORIENTED_EDGE('',*,*,#54814,.F.);
#79959=ORIENTED_EDGE('',*,*,#54815,.T.);
#79960=ORIENTED_EDGE('',*,*,#54816,.T.);
#79961=ORIENTED_EDGE('',*,*,#54812,.F.);
#79962=ORIENTED_EDGE('',*,*,#54817,.F.);
#79963=ORIENTED_EDGE('',*,*,#54818,.T.);
#79964=ORIENTED_EDGE('',*,*,#54819,.T.);
#79965=ORIENTED_EDGE('',*,*,#54815,.F.);
#79966=ORIENTED_EDGE('',*,*,#54820,.F.);
#79967=ORIENTED_EDGE('',*,*,#54821,.T.);
#79968=ORIENTED_EDGE('',*,*,#54822,.T.);
#79969=ORIENTED_EDGE('',*,*,#54818,.F.);
#79970=ORIENTED_EDGE('',*,*,#54823,.F.);
#79971=ORIENTED_EDGE('',*,*,#54824,.T.);
#79972=ORIENTED_EDGE('',*,*,#54825,.T.);
#79973=ORIENTED_EDGE('',*,*,#54821,.F.);
#79974=ORIENTED_EDGE('',*,*,#54826,.F.);
#79975=ORIENTED_EDGE('',*,*,#54827,.T.);
#79976=ORIENTED_EDGE('',*,*,#54828,.T.);
#79977=ORIENTED_EDGE('',*,*,#54824,.F.);
#79978=ORIENTED_EDGE('',*,*,#54829,.F.);
#79979=ORIENTED_EDGE('',*,*,#54830,.T.);
#79980=ORIENTED_EDGE('',*,*,#54831,.T.);
#79981=ORIENTED_EDGE('',*,*,#54827,.F.);
#79982=ORIENTED_EDGE('',*,*,#54832,.F.);
#79983=ORIENTED_EDGE('',*,*,#54833,.F.);
#79984=ORIENTED_EDGE('',*,*,#54834,.F.);
#79985=ORIENTED_EDGE('',*,*,#54835,.T.);
#79986=ORIENTED_EDGE('',*,*,#54836,.T.);
#79987=ORIENTED_EDGE('',*,*,#54837,.T.);
#79988=ORIENTED_EDGE('',*,*,#54838,.F.);
#79989=ORIENTED_EDGE('',*,*,#54839,.T.);
#79990=ORIENTED_EDGE('',*,*,#54840,.T.);
#79991=ORIENTED_EDGE('',*,*,#54841,.T.);
#79992=ORIENTED_EDGE('',*,*,#54836,.F.);
#79993=ORIENTED_EDGE('',*,*,#54842,.T.);
#79994=ORIENTED_EDGE('',*,*,#54843,.T.);
#79995=ORIENTED_EDGE('',*,*,#54844,.T.);
#79996=ORIENTED_EDGE('',*,*,#54840,.F.);
#79997=ORIENTED_EDGE('',*,*,#54845,.T.);
#79998=ORIENTED_EDGE('',*,*,#54846,.T.);
#79999=ORIENTED_EDGE('',*,*,#54847,.T.);
#80000=ORIENTED_EDGE('',*,*,#54843,.F.);
#80001=ORIENTED_EDGE('',*,*,#54848,.T.);
#80002=ORIENTED_EDGE('',*,*,#54849,.T.);
#80003=ORIENTED_EDGE('',*,*,#54850,.T.);
#80004=ORIENTED_EDGE('',*,*,#54846,.F.);
#80005=ORIENTED_EDGE('',*,*,#54851,.T.);
#80006=ORIENTED_EDGE('',*,*,#54852,.T.);
#80007=ORIENTED_EDGE('',*,*,#54853,.T.);
#80008=ORIENTED_EDGE('',*,*,#54849,.F.);
#80009=ORIENTED_EDGE('',*,*,#54854,.T.);
#80010=ORIENTED_EDGE('',*,*,#54855,.T.);
#80011=ORIENTED_EDGE('',*,*,#54856,.T.);
#80012=ORIENTED_EDGE('',*,*,#54852,.F.);
#80013=ORIENTED_EDGE('',*,*,#54857,.T.);
#80014=ORIENTED_EDGE('',*,*,#54858,.T.);
#80015=ORIENTED_EDGE('',*,*,#54859,.T.);
#80016=ORIENTED_EDGE('',*,*,#54855,.F.);
#80017=ORIENTED_EDGE('',*,*,#54860,.T.);
#80018=ORIENTED_EDGE('',*,*,#54861,.T.);
#80019=ORIENTED_EDGE('',*,*,#54862,.T.);
#80020=ORIENTED_EDGE('',*,*,#54858,.F.);
#80021=ORIENTED_EDGE('',*,*,#54863,.T.);
#80022=ORIENTED_EDGE('',*,*,#54864,.T.);
#80023=ORIENTED_EDGE('',*,*,#54865,.T.);
#80024=ORIENTED_EDGE('',*,*,#54861,.F.);
#80025=ORIENTED_EDGE('',*,*,#54866,.T.);
#80026=ORIENTED_EDGE('',*,*,#54867,.T.);
#80027=ORIENTED_EDGE('',*,*,#54868,.T.);
#80028=ORIENTED_EDGE('',*,*,#54864,.F.);
#80029=ORIENTED_EDGE('',*,*,#54869,.T.);
#80030=ORIENTED_EDGE('',*,*,#54870,.T.);
#80031=ORIENTED_EDGE('',*,*,#54871,.T.);
#80032=ORIENTED_EDGE('',*,*,#54867,.F.);
#80033=ORIENTED_EDGE('',*,*,#54872,.T.);
#80034=ORIENTED_EDGE('',*,*,#54873,.T.);
#80035=ORIENTED_EDGE('',*,*,#54874,.T.);
#80036=ORIENTED_EDGE('',*,*,#54870,.F.);
#80037=ORIENTED_EDGE('',*,*,#54875,.T.);
#80038=ORIENTED_EDGE('',*,*,#54876,.T.);
#80039=ORIENTED_EDGE('',*,*,#54877,.T.);
#80040=ORIENTED_EDGE('',*,*,#54873,.F.);
#80041=ORIENTED_EDGE('',*,*,#54878,.T.);
#80042=ORIENTED_EDGE('',*,*,#54879,.T.);
#80043=ORIENTED_EDGE('',*,*,#54880,.T.);
#80044=ORIENTED_EDGE('',*,*,#54876,.F.);
#80045=ORIENTED_EDGE('',*,*,#54881,.T.);
#80046=ORIENTED_EDGE('',*,*,#54882,.T.);
#80047=ORIENTED_EDGE('',*,*,#54883,.T.);
#80048=ORIENTED_EDGE('',*,*,#54879,.F.);
#80049=ORIENTED_EDGE('',*,*,#54884,.T.);
#80050=ORIENTED_EDGE('',*,*,#54885,.T.);
#80051=ORIENTED_EDGE('',*,*,#54886,.T.);
#80052=ORIENTED_EDGE('',*,*,#54882,.F.);
#80053=ORIENTED_EDGE('',*,*,#54887,.T.);
#80054=ORIENTED_EDGE('',*,*,#54888,.F.);
#80055=ORIENTED_EDGE('',*,*,#54889,.T.);
#80056=ORIENTED_EDGE('',*,*,#54890,.T.);
#80057=ORIENTED_EDGE('',*,*,#54891,.T.);
#80058=ORIENTED_EDGE('',*,*,#54892,.T.);
#80059=ORIENTED_EDGE('',*,*,#54893,.T.);
#80060=ORIENTED_EDGE('',*,*,#54894,.T.);
#80061=ORIENTED_EDGE('',*,*,#54895,.T.);
#80062=ORIENTED_EDGE('',*,*,#54896,.F.);
#80063=ORIENTED_EDGE('',*,*,#54897,.F.);
#80064=ORIENTED_EDGE('',*,*,#54898,.T.);
#80065=ORIENTED_EDGE('',*,*,#54899,.T.);
#80066=ORIENTED_EDGE('',*,*,#54900,.F.);
#80067=ORIENTED_EDGE('',*,*,#54901,.T.);
#80068=ORIENTED_EDGE('',*,*,#54894,.F.);
#80069=ORIENTED_EDGE('',*,*,#54902,.F.);
#80070=ORIENTED_EDGE('',*,*,#54903,.T.);
#80071=ORIENTED_EDGE('',*,*,#54904,.T.);
#80072=ORIENTED_EDGE('',*,*,#54898,.F.);
#80073=ORIENTED_EDGE('',*,*,#54905,.F.);
#80074=ORIENTED_EDGE('',*,*,#54906,.T.);
#80075=ORIENTED_EDGE('',*,*,#54907,.T.);
#80076=ORIENTED_EDGE('',*,*,#54903,.F.);
#80077=ORIENTED_EDGE('',*,*,#54908,.F.);
#80078=ORIENTED_EDGE('',*,*,#54909,.T.);
#80079=ORIENTED_EDGE('',*,*,#54910,.T.);
#80080=ORIENTED_EDGE('',*,*,#54906,.F.);
#80081=ORIENTED_EDGE('',*,*,#54911,.F.);
#80082=ORIENTED_EDGE('',*,*,#54912,.T.);
#80083=ORIENTED_EDGE('',*,*,#54913,.T.);
#80084=ORIENTED_EDGE('',*,*,#54909,.F.);
#80085=ORIENTED_EDGE('',*,*,#54914,.F.);
#80086=ORIENTED_EDGE('',*,*,#54915,.T.);
#80087=ORIENTED_EDGE('',*,*,#54916,.T.);
#80088=ORIENTED_EDGE('',*,*,#54912,.F.);
#80089=ORIENTED_EDGE('',*,*,#54917,.F.);
#80090=ORIENTED_EDGE('',*,*,#54918,.T.);
#80091=ORIENTED_EDGE('',*,*,#54919,.T.);
#80092=ORIENTED_EDGE('',*,*,#54915,.F.);
#80093=ORIENTED_EDGE('',*,*,#54920,.F.);
#80094=ORIENTED_EDGE('',*,*,#54921,.T.);
#80095=ORIENTED_EDGE('',*,*,#54922,.T.);
#80096=ORIENTED_EDGE('',*,*,#54918,.F.);
#80097=ORIENTED_EDGE('',*,*,#54923,.F.);
#80098=ORIENTED_EDGE('',*,*,#54924,.T.);
#80099=ORIENTED_EDGE('',*,*,#54925,.T.);
#80100=ORIENTED_EDGE('',*,*,#54921,.F.);
#80101=ORIENTED_EDGE('',*,*,#54926,.F.);
#80102=ORIENTED_EDGE('',*,*,#54927,.T.);
#80103=ORIENTED_EDGE('',*,*,#54928,.T.);
#80104=ORIENTED_EDGE('',*,*,#54924,.F.);
#80105=ORIENTED_EDGE('',*,*,#54929,.F.);
#80106=ORIENTED_EDGE('',*,*,#54930,.T.);
#80107=ORIENTED_EDGE('',*,*,#54931,.T.);
#80108=ORIENTED_EDGE('',*,*,#54927,.F.);
#80109=ORIENTED_EDGE('',*,*,#54932,.F.);
#80110=ORIENTED_EDGE('',*,*,#54933,.T.);
#80111=ORIENTED_EDGE('',*,*,#54934,.T.);
#80112=ORIENTED_EDGE('',*,*,#54930,.F.);
#80113=ORIENTED_EDGE('',*,*,#54935,.F.);
#80114=ORIENTED_EDGE('',*,*,#54936,.T.);
#80115=ORIENTED_EDGE('',*,*,#54937,.T.);
#80116=ORIENTED_EDGE('',*,*,#54933,.F.);
#80117=ORIENTED_EDGE('',*,*,#54938,.F.);
#80118=ORIENTED_EDGE('',*,*,#54939,.T.);
#80119=ORIENTED_EDGE('',*,*,#54940,.T.);
#80120=ORIENTED_EDGE('',*,*,#54936,.F.);
#80121=ORIENTED_EDGE('',*,*,#54941,.F.);
#80122=ORIENTED_EDGE('',*,*,#54942,.T.);
#80123=ORIENTED_EDGE('',*,*,#54943,.T.);
#80124=ORIENTED_EDGE('',*,*,#54939,.F.);
#80125=ORIENTED_EDGE('',*,*,#54944,.F.);
#80126=ORIENTED_EDGE('',*,*,#54945,.T.);
#80127=ORIENTED_EDGE('',*,*,#54946,.T.);
#80128=ORIENTED_EDGE('',*,*,#54942,.F.);
#80129=ORIENTED_EDGE('',*,*,#54947,.F.);
#80130=ORIENTED_EDGE('',*,*,#54948,.T.);
#80131=ORIENTED_EDGE('',*,*,#54949,.T.);
#80132=ORIENTED_EDGE('',*,*,#54945,.F.);
#80133=ORIENTED_EDGE('',*,*,#54950,.F.);
#80134=ORIENTED_EDGE('',*,*,#54951,.F.);
#80135=ORIENTED_EDGE('',*,*,#54952,.F.);
#80136=ORIENTED_EDGE('',*,*,#54953,.T.);
#80137=ORIENTED_EDGE('',*,*,#54954,.T.);
#80138=ORIENTED_EDGE('',*,*,#54955,.T.);
#80139=ORIENTED_EDGE('',*,*,#54956,.T.);
#80140=ORIENTED_EDGE('',*,*,#54957,.T.);
#80141=ORIENTED_EDGE('',*,*,#54958,.T.);
#80142=ORIENTED_EDGE('',*,*,#54954,.F.);
#80143=ORIENTED_EDGE('',*,*,#54959,.T.);
#80144=ORIENTED_EDGE('',*,*,#54960,.T.);
#80145=ORIENTED_EDGE('',*,*,#54961,.T.);
#80146=ORIENTED_EDGE('',*,*,#54957,.F.);
#80147=ORIENTED_EDGE('',*,*,#54962,.T.);
#80148=ORIENTED_EDGE('',*,*,#54963,.T.);
#80149=ORIENTED_EDGE('',*,*,#54964,.T.);
#80150=ORIENTED_EDGE('',*,*,#54960,.F.);
#80151=ORIENTED_EDGE('',*,*,#54965,.T.);
#80152=ORIENTED_EDGE('',*,*,#54966,.T.);
#80153=ORIENTED_EDGE('',*,*,#54967,.T.);
#80154=ORIENTED_EDGE('',*,*,#54963,.F.);
#80155=ORIENTED_EDGE('',*,*,#54968,.T.);
#80156=ORIENTED_EDGE('',*,*,#54969,.T.);
#80157=ORIENTED_EDGE('',*,*,#54970,.T.);
#80158=ORIENTED_EDGE('',*,*,#54966,.F.);
#80159=ORIENTED_EDGE('',*,*,#54971,.T.);
#80160=ORIENTED_EDGE('',*,*,#54972,.T.);
#80161=ORIENTED_EDGE('',*,*,#54973,.T.);
#80162=ORIENTED_EDGE('',*,*,#54969,.F.);
#80163=ORIENTED_EDGE('',*,*,#54974,.T.);
#80164=ORIENTED_EDGE('',*,*,#54975,.T.);
#80165=ORIENTED_EDGE('',*,*,#54976,.T.);
#80166=ORIENTED_EDGE('',*,*,#54972,.F.);
#80167=ORIENTED_EDGE('',*,*,#54977,.T.);
#80168=ORIENTED_EDGE('',*,*,#54978,.T.);
#80169=ORIENTED_EDGE('',*,*,#54979,.T.);
#80170=ORIENTED_EDGE('',*,*,#54975,.F.);
#80171=ORIENTED_EDGE('',*,*,#54980,.T.);
#80172=ORIENTED_EDGE('',*,*,#54981,.T.);
#80173=ORIENTED_EDGE('',*,*,#54982,.T.);
#80174=ORIENTED_EDGE('',*,*,#54978,.F.);
#80175=ORIENTED_EDGE('',*,*,#54983,.T.);
#80176=ORIENTED_EDGE('',*,*,#54984,.T.);
#80177=ORIENTED_EDGE('',*,*,#54985,.T.);
#80178=ORIENTED_EDGE('',*,*,#54981,.F.);
#80179=ORIENTED_EDGE('',*,*,#54986,.T.);
#80180=ORIENTED_EDGE('',*,*,#54987,.T.);
#80181=ORIENTED_EDGE('',*,*,#54988,.T.);
#80182=ORIENTED_EDGE('',*,*,#54984,.F.);
#80183=ORIENTED_EDGE('',*,*,#54989,.T.);
#80184=ORIENTED_EDGE('',*,*,#54990,.T.);
#80185=ORIENTED_EDGE('',*,*,#54991,.T.);
#80186=ORIENTED_EDGE('',*,*,#54987,.F.);
#80187=ORIENTED_EDGE('',*,*,#54992,.T.);
#80188=ORIENTED_EDGE('',*,*,#54993,.T.);
#80189=ORIENTED_EDGE('',*,*,#54994,.T.);
#80190=ORIENTED_EDGE('',*,*,#54990,.F.);
#80191=ORIENTED_EDGE('',*,*,#54995,.T.);
#80192=ORIENTED_EDGE('',*,*,#54996,.T.);
#80193=ORIENTED_EDGE('',*,*,#54997,.T.);
#80194=ORIENTED_EDGE('',*,*,#54993,.F.);
#80195=ORIENTED_EDGE('',*,*,#54998,.T.);
#80196=ORIENTED_EDGE('',*,*,#54999,.T.);
#80197=ORIENTED_EDGE('',*,*,#55000,.T.);
#80198=ORIENTED_EDGE('',*,*,#54996,.F.);
#80199=ORIENTED_EDGE('',*,*,#55001,.T.);
#80200=ORIENTED_EDGE('',*,*,#55002,.T.);
#80201=ORIENTED_EDGE('',*,*,#55003,.T.);
#80202=ORIENTED_EDGE('',*,*,#54999,.F.);
#80203=ORIENTED_EDGE('',*,*,#55004,.T.);
#80204=ORIENTED_EDGE('',*,*,#55005,.T.);
#80205=ORIENTED_EDGE('',*,*,#55006,.T.);
#80206=ORIENTED_EDGE('',*,*,#55002,.F.);
#80207=ORIENTED_EDGE('',*,*,#55007,.T.);
#80208=ORIENTED_EDGE('',*,*,#55008,.F.);
#80209=ORIENTED_EDGE('',*,*,#55009,.T.);
#80210=ORIENTED_EDGE('',*,*,#55010,.F.);
#80211=ORIENTED_EDGE('',*,*,#55011,.T.);
#80212=ORIENTED_EDGE('',*,*,#55012,.T.);
#80213=ORIENTED_EDGE('',*,*,#55013,.T.);
#80214=ORIENTED_EDGE('',*,*,#55014,.F.);
#80215=ORIENTED_EDGE('',*,*,#55015,.F.);
#80216=ORIENTED_EDGE('',*,*,#55016,.T.);
#80217=ORIENTED_EDGE('',*,*,#55017,.T.);
#80218=ORIENTED_EDGE('',*,*,#55018,.F.);
#80219=ORIENTED_EDGE('',*,*,#55019,.T.);
#80220=ORIENTED_EDGE('',*,*,#55012,.F.);
#80221=ORIENTED_EDGE('',*,*,#55020,.F.);
#80222=ORIENTED_EDGE('',*,*,#55021,.T.);
#80223=ORIENTED_EDGE('',*,*,#55022,.T.);
#80224=ORIENTED_EDGE('',*,*,#55016,.F.);
#80225=ORIENTED_EDGE('',*,*,#55023,.F.);
#80226=ORIENTED_EDGE('',*,*,#55024,.T.);
#80227=ORIENTED_EDGE('',*,*,#55025,.T.);
#80228=ORIENTED_EDGE('',*,*,#55021,.F.);
#80229=ORIENTED_EDGE('',*,*,#55026,.F.);
#80230=ORIENTED_EDGE('',*,*,#55027,.T.);
#80231=ORIENTED_EDGE('',*,*,#55028,.T.);
#80232=ORIENTED_EDGE('',*,*,#55024,.F.);
#80233=ORIENTED_EDGE('',*,*,#55029,.F.);
#80234=ORIENTED_EDGE('',*,*,#55030,.T.);
#80235=ORIENTED_EDGE('',*,*,#55031,.T.);
#80236=ORIENTED_EDGE('',*,*,#55027,.F.);
#80237=ORIENTED_EDGE('',*,*,#55032,.F.);
#80238=ORIENTED_EDGE('',*,*,#55033,.T.);
#80239=ORIENTED_EDGE('',*,*,#55034,.T.);
#80240=ORIENTED_EDGE('',*,*,#55030,.F.);
#80241=ORIENTED_EDGE('',*,*,#55035,.F.);
#80242=ORIENTED_EDGE('',*,*,#55036,.T.);
#80243=ORIENTED_EDGE('',*,*,#55037,.T.);
#80244=ORIENTED_EDGE('',*,*,#55033,.F.);
#80245=ORIENTED_EDGE('',*,*,#55038,.F.);
#80246=ORIENTED_EDGE('',*,*,#55039,.T.);
#80247=ORIENTED_EDGE('',*,*,#55040,.T.);
#80248=ORIENTED_EDGE('',*,*,#55036,.F.);
#80249=ORIENTED_EDGE('',*,*,#55041,.F.);
#80250=ORIENTED_EDGE('',*,*,#55042,.T.);
#80251=ORIENTED_EDGE('',*,*,#55043,.T.);
#80252=ORIENTED_EDGE('',*,*,#55039,.F.);
#80253=ORIENTED_EDGE('',*,*,#55044,.F.);
#80254=ORIENTED_EDGE('',*,*,#55045,.T.);
#80255=ORIENTED_EDGE('',*,*,#55046,.T.);
#80256=ORIENTED_EDGE('',*,*,#55042,.F.);
#80257=ORIENTED_EDGE('',*,*,#55047,.F.);
#80258=ORIENTED_EDGE('',*,*,#55048,.T.);
#80259=ORIENTED_EDGE('',*,*,#55049,.T.);
#80260=ORIENTED_EDGE('',*,*,#55045,.F.);
#80261=ORIENTED_EDGE('',*,*,#55050,.F.);
#80262=ORIENTED_EDGE('',*,*,#55051,.T.);
#80263=ORIENTED_EDGE('',*,*,#55052,.T.);
#80264=ORIENTED_EDGE('',*,*,#55048,.F.);
#80265=ORIENTED_EDGE('',*,*,#55053,.F.);
#80266=ORIENTED_EDGE('',*,*,#55054,.T.);
#80267=ORIENTED_EDGE('',*,*,#55055,.T.);
#80268=ORIENTED_EDGE('',*,*,#55051,.F.);
#80269=ORIENTED_EDGE('',*,*,#55056,.F.);
#80270=ORIENTED_EDGE('',*,*,#55057,.T.);
#80271=ORIENTED_EDGE('',*,*,#55058,.T.);
#80272=ORIENTED_EDGE('',*,*,#55054,.F.);
#80273=ORIENTED_EDGE('',*,*,#55059,.F.);
#80274=ORIENTED_EDGE('',*,*,#55060,.T.);
#80275=ORIENTED_EDGE('',*,*,#55061,.T.);
#80276=ORIENTED_EDGE('',*,*,#55057,.F.);
#80277=ORIENTED_EDGE('',*,*,#55062,.F.);
#80278=ORIENTED_EDGE('',*,*,#55063,.T.);
#80279=ORIENTED_EDGE('',*,*,#55064,.T.);
#80280=ORIENTED_EDGE('',*,*,#55060,.F.);
#80281=ORIENTED_EDGE('',*,*,#55065,.F.);
#80282=ORIENTED_EDGE('',*,*,#55066,.T.);
#80283=ORIENTED_EDGE('',*,*,#55067,.T.);
#80284=ORIENTED_EDGE('',*,*,#55063,.F.);
#80285=ORIENTED_EDGE('',*,*,#55068,.F.);
#80286=ORIENTED_EDGE('',*,*,#55069,.F.);
#80287=ORIENTED_EDGE('',*,*,#55070,.F.);
#80288=ORIENTED_EDGE('',*,*,#55071,.T.);
#80289=ORIENTED_EDGE('',*,*,#55072,.T.);
#80290=ORIENTED_EDGE('',*,*,#55073,.T.);
#80291=ORIENTED_EDGE('',*,*,#55074,.F.);
#80292=ORIENTED_EDGE('',*,*,#55075,.F.);
#80293=ORIENTED_EDGE('',*,*,#55076,.T.);
#80294=ORIENTED_EDGE('',*,*,#55077,.T.);
#80295=ORIENTED_EDGE('',*,*,#55078,.F.);
#80296=ORIENTED_EDGE('',*,*,#55079,.T.);
#80297=ORIENTED_EDGE('',*,*,#55072,.F.);
#80298=ORIENTED_EDGE('',*,*,#55080,.F.);
#80299=ORIENTED_EDGE('',*,*,#55081,.T.);
#80300=ORIENTED_EDGE('',*,*,#55082,.T.);
#80301=ORIENTED_EDGE('',*,*,#55076,.F.);
#80302=ORIENTED_EDGE('',*,*,#55083,.F.);
#80303=ORIENTED_EDGE('',*,*,#55084,.T.);
#80304=ORIENTED_EDGE('',*,*,#55085,.T.);
#80305=ORIENTED_EDGE('',*,*,#55081,.F.);
#80306=ORIENTED_EDGE('',*,*,#55086,.F.);
#80307=ORIENTED_EDGE('',*,*,#55087,.T.);
#80308=ORIENTED_EDGE('',*,*,#55088,.T.);
#80309=ORIENTED_EDGE('',*,*,#55084,.F.);
#80310=ORIENTED_EDGE('',*,*,#55089,.F.);
#80311=ORIENTED_EDGE('',*,*,#55090,.T.);
#80312=ORIENTED_EDGE('',*,*,#55091,.T.);
#80313=ORIENTED_EDGE('',*,*,#55087,.F.);
#80314=ORIENTED_EDGE('',*,*,#55092,.F.);
#80315=ORIENTED_EDGE('',*,*,#55093,.T.);
#80316=ORIENTED_EDGE('',*,*,#55094,.T.);
#80317=ORIENTED_EDGE('',*,*,#55090,.F.);
#80318=ORIENTED_EDGE('',*,*,#55095,.F.);
#80319=ORIENTED_EDGE('',*,*,#55096,.T.);
#80320=ORIENTED_EDGE('',*,*,#55097,.T.);
#80321=ORIENTED_EDGE('',*,*,#55093,.F.);
#80322=ORIENTED_EDGE('',*,*,#55098,.F.);
#80323=ORIENTED_EDGE('',*,*,#55099,.T.);
#80324=ORIENTED_EDGE('',*,*,#55100,.T.);
#80325=ORIENTED_EDGE('',*,*,#55096,.F.);
#80326=ORIENTED_EDGE('',*,*,#55101,.F.);
#80327=ORIENTED_EDGE('',*,*,#55102,.T.);
#80328=ORIENTED_EDGE('',*,*,#55103,.T.);
#80329=ORIENTED_EDGE('',*,*,#55099,.F.);
#80330=ORIENTED_EDGE('',*,*,#55104,.F.);
#80331=ORIENTED_EDGE('',*,*,#55105,.T.);
#80332=ORIENTED_EDGE('',*,*,#55106,.T.);
#80333=ORIENTED_EDGE('',*,*,#55102,.F.);
#80334=ORIENTED_EDGE('',*,*,#55107,.F.);
#80335=ORIENTED_EDGE('',*,*,#55108,.T.);
#80336=ORIENTED_EDGE('',*,*,#55109,.T.);
#80337=ORIENTED_EDGE('',*,*,#55105,.F.);
#80338=ORIENTED_EDGE('',*,*,#55110,.F.);
#80339=ORIENTED_EDGE('',*,*,#55111,.T.);
#80340=ORIENTED_EDGE('',*,*,#55112,.T.);
#80341=ORIENTED_EDGE('',*,*,#55108,.F.);
#80342=ORIENTED_EDGE('',*,*,#55113,.F.);
#80343=ORIENTED_EDGE('',*,*,#55114,.T.);
#80344=ORIENTED_EDGE('',*,*,#55115,.T.);
#80345=ORIENTED_EDGE('',*,*,#55111,.F.);
#80346=ORIENTED_EDGE('',*,*,#55116,.F.);
#80347=ORIENTED_EDGE('',*,*,#55117,.T.);
#80348=ORIENTED_EDGE('',*,*,#55118,.T.);
#80349=ORIENTED_EDGE('',*,*,#55114,.F.);
#80350=ORIENTED_EDGE('',*,*,#55119,.F.);
#80351=ORIENTED_EDGE('',*,*,#55120,.T.);
#80352=ORIENTED_EDGE('',*,*,#55121,.T.);
#80353=ORIENTED_EDGE('',*,*,#55117,.F.);
#80354=ORIENTED_EDGE('',*,*,#55122,.F.);
#80355=ORIENTED_EDGE('',*,*,#55123,.T.);
#80356=ORIENTED_EDGE('',*,*,#55124,.T.);
#80357=ORIENTED_EDGE('',*,*,#55120,.F.);
#80358=ORIENTED_EDGE('',*,*,#55125,.F.);
#80359=ORIENTED_EDGE('',*,*,#55126,.T.);
#80360=ORIENTED_EDGE('',*,*,#55127,.T.);
#80361=ORIENTED_EDGE('',*,*,#55123,.F.);
#80362=ORIENTED_EDGE('',*,*,#55128,.F.);
#80363=ORIENTED_EDGE('',*,*,#55129,.F.);
#80364=ORIENTED_EDGE('',*,*,#55130,.F.);
#80365=ORIENTED_EDGE('',*,*,#55131,.T.);
#80366=ORIENTED_EDGE('',*,*,#55132,.T.);
#80367=ORIENTED_EDGE('',*,*,#55133,.T.);
#80368=ORIENTED_EDGE('',*,*,#55134,.F.);
#80369=ORIENTED_EDGE('',*,*,#55135,.F.);
#80370=ORIENTED_EDGE('',*,*,#55136,.F.);
#80371=ORIENTED_EDGE('',*,*,#55137,.F.);
#80372=ORIENTED_EDGE('',*,*,#55138,.F.);
#80373=ORIENTED_EDGE('',*,*,#55139,.T.);
#80374=ORIENTED_EDGE('',*,*,#55140,.T.);
#80375=ORIENTED_EDGE('',*,*,#55141,.T.);
#80376=ORIENTED_EDGE('',*,*,#55142,.T.);
#80377=ORIENTED_EDGE('',*,*,#55139,.F.);
#80378=ORIENTED_EDGE('',*,*,#55143,.F.);
#80379=ORIENTED_EDGE('',*,*,#55144,.T.);
#80380=ORIENTED_EDGE('',*,*,#55145,.T.);
#80381=ORIENTED_EDGE('',*,*,#55146,.T.);
#80382=ORIENTED_EDGE('',*,*,#55140,.F.);
#80383=ORIENTED_EDGE('',*,*,#55147,.T.);
#80384=ORIENTED_EDGE('',*,*,#55148,.T.);
#80385=ORIENTED_EDGE('',*,*,#55149,.T.);
#80386=ORIENTED_EDGE('',*,*,#55150,.T.);
#80387=ORIENTED_EDGE('',*,*,#55151,.T.);
#80388=ORIENTED_EDGE('',*,*,#55152,.T.);
#80389=ORIENTED_EDGE('',*,*,#55153,.T.);
#80390=ORIENTED_EDGE('',*,*,#55154,.T.);
#80391=ORIENTED_EDGE('',*,*,#55155,.F.);
#80392=ORIENTED_EDGE('',*,*,#55156,.F.);
#80393=ORIENTED_EDGE('',*,*,#55157,.T.);
#80394=ORIENTED_EDGE('',*,*,#55135,.T.);
#80395=ORIENTED_EDGE('',*,*,#55158,.F.);
#80396=ORIENTED_EDGE('',*,*,#55137,.T.);
#80397=ORIENTED_EDGE('',*,*,#55159,.F.);
#80398=ORIENTED_EDGE('',*,*,#55160,.F.);
#80399=ORIENTED_EDGE('',*,*,#55156,.T.);
#80400=ORIENTED_EDGE('',*,*,#55161,.F.);
#80401=ORIENTED_EDGE('',*,*,#55160,.T.);
#80402=ORIENTED_EDGE('',*,*,#55162,.T.);
#80403=ORIENTED_EDGE('',*,*,#55142,.F.);
#80404=ORIENTED_EDGE('',*,*,#55163,.T.);
#80405=ORIENTED_EDGE('',*,*,#55164,.F.);
#80406=ORIENTED_EDGE('',*,*,#55165,.T.);
#80407=ORIENTED_EDGE('',*,*,#55166,.T.);
#80408=ORIENTED_EDGE('',*,*,#55167,.F.);
#80409=ORIENTED_EDGE('',*,*,#55168,.T.);
#80410=ORIENTED_EDGE('',*,*,#55132,.F.);
#80411=ORIENTED_EDGE('',*,*,#55169,.F.);
#80412=ORIENTED_EDGE('',*,*,#55170,.F.);
#80413=ORIENTED_EDGE('',*,*,#55171,.T.);
#80414=ORIENTED_EDGE('',*,*,#55172,.F.);
#80415=ORIENTED_EDGE('',*,*,#55173,.F.);
#80416=ORIENTED_EDGE('',*,*,#55174,.F.);
#80417=ORIENTED_EDGE('',*,*,#55175,.F.);
#80418=ORIENTED_EDGE('',*,*,#55176,.T.);
#80419=ORIENTED_EDGE('',*,*,#55177,.T.);
#80420=ORIENTED_EDGE('',*,*,#55178,.T.);
#80421=ORIENTED_EDGE('',*,*,#55179,.F.);
#80422=ORIENTED_EDGE('',*,*,#55180,.F.);
#80423=ORIENTED_EDGE('',*,*,#55181,.F.);
#80424=ORIENTED_EDGE('',*,*,#55182,.F.);
#80425=ORIENTED_EDGE('',*,*,#55183,.T.);
#80426=ORIENTED_EDGE('',*,*,#55184,.T.);
#80427=ORIENTED_EDGE('',*,*,#55185,.T.);
#80428=ORIENTED_EDGE('',*,*,#55186,.F.);
#80429=ORIENTED_EDGE('',*,*,#55186,.T.);
#80430=ORIENTED_EDGE('',*,*,#55187,.T.);
#80431=ORIENTED_EDGE('',*,*,#55188,.F.);
#80432=ORIENTED_EDGE('',*,*,#55187,.F.);
#80433=ORIENTED_EDGE('',*,*,#55170,.T.);
#80434=ORIENTED_EDGE('',*,*,#55189,.T.);
#80435=ORIENTED_EDGE('',*,*,#55185,.F.);
#80436=ORIENTED_EDGE('',*,*,#55189,.F.);
#80437=ORIENTED_EDGE('',*,*,#55188,.T.);
#80438=ORIENTED_EDGE('',*,*,#55190,.T.);
#80439=ORIENTED_EDGE('',*,*,#55191,.F.);
#80440=ORIENTED_EDGE('',*,*,#55191,.T.);
#80441=ORIENTED_EDGE('',*,*,#55192,.T.);
#80442=ORIENTED_EDGE('',*,*,#55193,.F.);
#80443=ORIENTED_EDGE('',*,*,#55192,.F.);
#80444=ORIENTED_EDGE('',*,*,#55169,.T.);
#80445=ORIENTED_EDGE('',*,*,#55194,.T.);
#80446=ORIENTED_EDGE('',*,*,#55190,.F.);
#80447=ORIENTED_EDGE('',*,*,#55194,.F.);
#80448=ORIENTED_EDGE('',*,*,#55193,.T.);
#80449=ORIENTED_EDGE('',*,*,#55195,.T.);
#80450=ORIENTED_EDGE('',*,*,#55196,.F.);
#80451=ORIENTED_EDGE('',*,*,#55196,.T.);
#80452=ORIENTED_EDGE('',*,*,#55197,.T.);
#80453=ORIENTED_EDGE('',*,*,#55198,.F.);
#80454=ORIENTED_EDGE('',*,*,#55197,.F.);
#80455=ORIENTED_EDGE('',*,*,#55167,.T.);
#80456=ORIENTED_EDGE('',*,*,#55199,.T.);
#80457=ORIENTED_EDGE('',*,*,#55200,.T.);
#80458=ORIENTED_EDGE('',*,*,#55195,.F.);
#80459=ORIENTED_EDGE('',*,*,#55200,.F.);
#80460=ORIENTED_EDGE('',*,*,#55201,.T.);
#80461=ORIENTED_EDGE('',*,*,#55198,.T.);
#80462=ORIENTED_EDGE('',*,*,#55202,.T.);
#80463=ORIENTED_EDGE('',*,*,#55203,.F.);
#80464=ORIENTED_EDGE('',*,*,#55203,.T.);
#80465=ORIENTED_EDGE('',*,*,#55204,.T.);
#80466=ORIENTED_EDGE('',*,*,#55205,.F.);
#80467=ORIENTED_EDGE('',*,*,#55204,.F.);
#80468=ORIENTED_EDGE('',*,*,#55164,.T.);
#80469=ORIENTED_EDGE('',*,*,#55206,.T.);
#80470=ORIENTED_EDGE('',*,*,#55207,.T.);
#80471=ORIENTED_EDGE('',*,*,#55202,.F.);
#80472=ORIENTED_EDGE('',*,*,#55207,.F.);
#80473=ORIENTED_EDGE('',*,*,#55208,.T.);
#80474=ORIENTED_EDGE('',*,*,#55205,.T.);
#80475=ORIENTED_EDGE('',*,*,#55171,.F.);
#80476=ORIENTED_EDGE('',*,*,#55209,.F.);
#80477=ORIENTED_EDGE('',*,*,#55210,.F.);
#80478=ORIENTED_EDGE('',*,*,#55183,.F.);
#80479=ORIENTED_EDGE('',*,*,#55211,.F.);
#80480=ORIENTED_EDGE('',*,*,#55212,.F.);
#80481=ORIENTED_EDGE('',*,*,#55213,.T.);
#80482=ORIENTED_EDGE('',*,*,#55214,.F.);
#80483=ORIENTED_EDGE('',*,*,#55215,.F.);
#80484=ORIENTED_EDGE('',*,*,#55213,.F.);
#80485=ORIENTED_EDGE('',*,*,#55216,.F.);
#80486=ORIENTED_EDGE('',*,*,#55217,.F.);
#80487=ORIENTED_EDGE('',*,*,#55218,.T.);
#80488=ORIENTED_EDGE('',*,*,#55219,.F.);
#80489=ORIENTED_EDGE('',*,*,#55220,.F.);
#80490=ORIENTED_EDGE('',*,*,#55218,.F.);
#80491=ORIENTED_EDGE('',*,*,#55221,.T.);
#80492=ORIENTED_EDGE('',*,*,#55222,.T.);
#80493=ORIENTED_EDGE('',*,*,#55223,.F.);
#80494=ORIENTED_EDGE('',*,*,#55224,.T.);
#80495=ORIENTED_EDGE('',*,*,#55225,.T.);
#80496=ORIENTED_EDGE('',*,*,#55226,.T.);
#80497=ORIENTED_EDGE('',*,*,#55221,.F.);
#80498=ORIENTED_EDGE('',*,*,#55227,.T.);
#80499=ORIENTED_EDGE('',*,*,#55228,.T.);
#80500=ORIENTED_EDGE('',*,*,#55229,.T.);
#80501=ORIENTED_EDGE('',*,*,#55225,.F.);
#80502=ORIENTED_EDGE('',*,*,#55230,.T.);
#80503=ORIENTED_EDGE('',*,*,#55231,.T.);
#80504=ORIENTED_EDGE('',*,*,#55232,.T.);
#80505=ORIENTED_EDGE('',*,*,#55228,.F.);
#80506=ORIENTED_EDGE('',*,*,#55233,.T.);
#80507=ORIENTED_EDGE('',*,*,#55234,.T.);
#80508=ORIENTED_EDGE('',*,*,#55235,.T.);
#80509=ORIENTED_EDGE('',*,*,#55231,.F.);
#80510=ORIENTED_EDGE('',*,*,#55236,.T.);
#80511=ORIENTED_EDGE('',*,*,#55223,.T.);
#80512=ORIENTED_EDGE('',*,*,#55237,.T.);
#80513=ORIENTED_EDGE('',*,*,#55234,.F.);
#80514=ORIENTED_EDGE('',*,*,#55238,.T.);
#80515=ORIENTED_EDGE('',*,*,#55239,.T.);
#80516=ORIENTED_EDGE('',*,*,#55238,.F.);
#80517=ORIENTED_EDGE('',*,*,#55236,.F.);
#80518=ORIENTED_EDGE('',*,*,#55233,.F.);
#80519=ORIENTED_EDGE('',*,*,#55230,.F.);
#80520=ORIENTED_EDGE('',*,*,#55227,.F.);
#80521=ORIENTED_EDGE('',*,*,#55224,.F.);
#80522=ORIENTED_EDGE('',*,*,#55239,.F.);
#80523=ORIENTED_EDGE('',*,*,#55240,.T.);
#80524=ORIENTED_EDGE('',*,*,#55222,.F.);
#80525=ORIENTED_EDGE('',*,*,#55241,.T.);
#80526=ORIENTED_EDGE('',*,*,#55226,.F.);
#80527=ORIENTED_EDGE('',*,*,#55242,.T.);
#80528=ORIENTED_EDGE('',*,*,#55229,.F.);
#80529=ORIENTED_EDGE('',*,*,#55243,.T.);
#80530=ORIENTED_EDGE('',*,*,#55232,.F.);
#80531=ORIENTED_EDGE('',*,*,#55244,.T.);
#80532=ORIENTED_EDGE('',*,*,#55235,.F.);
#80533=ORIENTED_EDGE('',*,*,#55245,.T.);
#80534=ORIENTED_EDGE('',*,*,#55237,.F.);
#80535=ORIENTED_EDGE('',*,*,#55216,.T.);
#80536=ORIENTED_EDGE('',*,*,#55217,.T.);
#80537=ORIENTED_EDGE('',*,*,#55246,.T.);
#80538=ORIENTED_EDGE('',*,*,#55214,.T.);
#80539=ORIENTED_EDGE('',*,*,#55215,.T.);
#80540=ORIENTED_EDGE('',*,*,#55246,.F.);
#80541=ORIENTED_EDGE('',*,*,#55212,.T.);
#80542=ORIENTED_EDGE('',*,*,#55242,.F.);
#80543=ORIENTED_EDGE('',*,*,#55243,.F.);
#80544=ORIENTED_EDGE('',*,*,#55244,.F.);
#80545=ORIENTED_EDGE('',*,*,#55245,.F.);
#80546=ORIENTED_EDGE('',*,*,#55240,.F.);
#80547=ORIENTED_EDGE('',*,*,#55241,.F.);
#80548=ORIENTED_EDGE('',*,*,#55210,.T.);
#80549=ORIENTED_EDGE('',*,*,#55247,.T.);
#80550=ORIENTED_EDGE('',*,*,#55219,.T.);
#80551=ORIENTED_EDGE('',*,*,#55220,.T.);
#80552=ORIENTED_EDGE('',*,*,#55247,.F.);
#80553=ORIENTED_EDGE('',*,*,#55209,.T.);
#80554=ORIENTED_EDGE('',*,*,#55184,.F.);
#80555=ORIENTED_EDGE('',*,*,#55248,.F.);
#80556=ORIENTED_EDGE('',*,*,#55249,.T.);
#80557=ORIENTED_EDGE('',*,*,#55249,.F.);
#80558=ORIENTED_EDGE('',*,*,#55250,.T.);
#80559=ORIENTED_EDGE('',*,*,#55251,.T.);
#80560=ORIENTED_EDGE('',*,*,#55252,.T.);
#80561=ORIENTED_EDGE('',*,*,#55252,.F.);
#80562=ORIENTED_EDGE('',*,*,#55253,.T.);
#80563=ORIENTED_EDGE('',*,*,#55254,.F.);
#80564=ORIENTED_EDGE('',*,*,#55255,.F.);
#80565=ORIENTED_EDGE('',*,*,#55256,.T.);
#80566=ORIENTED_EDGE('',*,*,#55257,.T.);
#80567=ORIENTED_EDGE('',*,*,#55258,.F.);
#80568=ORIENTED_EDGE('',*,*,#55256,.F.);
#80569=ORIENTED_EDGE('',*,*,#55259,.F.);
#80570=ORIENTED_EDGE('',*,*,#55260,.F.);
#80571=ORIENTED_EDGE('',*,*,#55261,.F.);
#80572=ORIENTED_EDGE('',*,*,#55262,.T.);
#80573=ORIENTED_EDGE('',*,*,#55263,.F.);
#80574=ORIENTED_EDGE('',*,*,#55257,.F.);
#80575=ORIENTED_EDGE('',*,*,#55264,.F.);
#80576=ORIENTED_EDGE('',*,*,#55265,.T.);
#80577=ORIENTED_EDGE('',*,*,#55266,.F.);
#80578=ORIENTED_EDGE('',*,*,#55262,.F.);
#80579=ORIENTED_EDGE('',*,*,#55267,.F.);
#80580=ORIENTED_EDGE('',*,*,#55268,.T.);
#80581=ORIENTED_EDGE('',*,*,#55269,.F.);
#80582=ORIENTED_EDGE('',*,*,#55265,.F.);
#80583=ORIENTED_EDGE('',*,*,#55270,.F.);
#80584=ORIENTED_EDGE('',*,*,#55271,.F.);
#80585=ORIENTED_EDGE('',*,*,#55272,.F.);
#80586=ORIENTED_EDGE('',*,*,#55268,.F.);
#80587=ORIENTED_EDGE('',*,*,#55273,.F.);
#80588=ORIENTED_EDGE('',*,*,#55274,.F.);
#80589=ORIENTED_EDGE('',*,*,#55275,.F.);
#80590=ORIENTED_EDGE('',*,*,#55175,.T.);
#80591=ORIENTED_EDGE('',*,*,#55276,.T.);
#80592=ORIENTED_EDGE('',*,*,#55276,.F.);
#80593=ORIENTED_EDGE('',*,*,#55174,.T.);
#80594=ORIENTED_EDGE('',*,*,#55277,.T.);
#80595=ORIENTED_EDGE('',*,*,#55278,.F.);
#80596=ORIENTED_EDGE('',*,*,#55277,.F.);
#80597=ORIENTED_EDGE('',*,*,#55173,.T.);
#80598=ORIENTED_EDGE('',*,*,#55279,.F.);
#80599=ORIENTED_EDGE('',*,*,#55280,.F.);
#80600=ORIENTED_EDGE('',*,*,#55181,.T.);
#80601=ORIENTED_EDGE('',*,*,#55281,.T.);
#80602=ORIENTED_EDGE('',*,*,#55281,.F.);
#80603=ORIENTED_EDGE('',*,*,#55180,.T.);
#80604=ORIENTED_EDGE('',*,*,#55282,.T.);
#80605=ORIENTED_EDGE('',*,*,#55283,.F.);
#80606=ORIENTED_EDGE('',*,*,#55282,.F.);
#80607=ORIENTED_EDGE('',*,*,#55179,.T.);
#80608=ORIENTED_EDGE('',*,*,#55284,.F.);
#80609=ORIENTED_EDGE('',*,*,#55285,.F.);
#80610=ORIENTED_EDGE('',*,*,#55260,.T.);
#80611=ORIENTED_EDGE('',*,*,#55286,.F.);
#80612=ORIENTED_EDGE('',*,*,#55287,.F.);
#80613=ORIENTED_EDGE('',*,*,#55288,.F.);
#80614=ORIENTED_EDGE('',*,*,#55289,.T.);
#80615=ORIENTED_EDGE('',*,*,#55290,.F.);
#80616=ORIENTED_EDGE('',*,*,#55291,.F.);
#80617=ORIENTED_EDGE('',*,*,#55271,.T.);
#80618=ORIENTED_EDGE('',*,*,#55292,.F.);
#80619=ORIENTED_EDGE('',*,*,#55293,.T.);
#80620=ORIENTED_EDGE('',*,*,#55294,.F.);
#80621=ORIENTED_EDGE('',*,*,#55289,.F.);
#80622=ORIENTED_EDGE('',*,*,#55295,.F.);
#80623=ORIENTED_EDGE('',*,*,#55296,.T.);
#80624=ORIENTED_EDGE('',*,*,#55297,.F.);
#80625=ORIENTED_EDGE('',*,*,#55283,.T.);
#80626=ORIENTED_EDGE('',*,*,#55284,.T.);
#80627=ORIENTED_EDGE('',*,*,#55298,.F.);
#80628=ORIENTED_EDGE('',*,*,#55293,.F.);
#80629=ORIENTED_EDGE('',*,*,#55296,.F.);
#80630=ORIENTED_EDGE('',*,*,#55299,.F.);
#80631=ORIENTED_EDGE('',*,*,#55300,.F.);
#80632=ORIENTED_EDGE('',*,*,#55301,.T.);
#80633=ORIENTED_EDGE('',*,*,#55302,.F.);
#80634=ORIENTED_EDGE('',*,*,#55303,.F.);
#80635=ORIENTED_EDGE('',*,*,#55288,.T.);
#80636=ORIENTED_EDGE('',*,*,#55304,.T.);
#80637=ORIENTED_EDGE('',*,*,#55305,.F.);
#80638=ORIENTED_EDGE('',*,*,#55301,.F.);
#80639=ORIENTED_EDGE('',*,*,#55306,.F.);
#80640=ORIENTED_EDGE('',*,*,#55307,.F.);
#80641=ORIENTED_EDGE('',*,*,#55275,.T.);
#80642=ORIENTED_EDGE('',*,*,#55278,.T.);
#80643=ORIENTED_EDGE('',*,*,#55308,.F.);
#80644=ORIENTED_EDGE('',*,*,#55304,.F.);
#80645=ORIENTED_EDGE('',*,*,#55309,.F.);
#80646=ORIENTED_EDGE('',*,*,#55290,.T.);
#80647=ORIENTED_EDGE('',*,*,#55310,.F.);
#80648=ORIENTED_EDGE('',*,*,#55311,.T.);
#80649=ORIENTED_EDGE('',*,*,#55312,.T.);
#80650=ORIENTED_EDGE('',*,*,#55313,.F.);
#80651=ORIENTED_EDGE('',*,*,#55311,.F.);
#80652=ORIENTED_EDGE('',*,*,#55314,.F.);
#80653=ORIENTED_EDGE('',*,*,#55315,.T.);
#80654=ORIENTED_EDGE('',*,*,#55316,.F.);
#80655=ORIENTED_EDGE('',*,*,#55312,.F.);
#80656=ORIENTED_EDGE('',*,*,#55317,.T.);
#80657=ORIENTED_EDGE('',*,*,#55318,.F.);
#80658=ORIENTED_EDGE('',*,*,#55315,.F.);
#80659=ORIENTED_EDGE('',*,*,#55319,.F.);
#80660=ORIENTED_EDGE('',*,*,#55320,.T.);
#80661=ORIENTED_EDGE('',*,*,#55321,.F.);
#80662=ORIENTED_EDGE('',*,*,#55317,.F.);
#80663=ORIENTED_EDGE('',*,*,#55322,.F.);
#80664=ORIENTED_EDGE('',*,*,#55323,.F.);
#80665=ORIENTED_EDGE('',*,*,#55298,.T.);
#80666=ORIENTED_EDGE('',*,*,#55178,.F.);
#80667=ORIENTED_EDGE('',*,*,#55320,.F.);
#80668=ORIENTED_EDGE('',*,*,#55324,.F.);
#80669=ORIENTED_EDGE('',*,*,#55300,.T.);
#80670=ORIENTED_EDGE('',*,*,#55325,.F.);
#80671=ORIENTED_EDGE('',*,*,#55326,.T.);
#80672=ORIENTED_EDGE('',*,*,#55327,.F.);
#80673=ORIENTED_EDGE('',*,*,#55328,.T.);
#80674=ORIENTED_EDGE('',*,*,#55326,.F.);
#80675=ORIENTED_EDGE('',*,*,#55329,.T.);
#80676=ORIENTED_EDGE('',*,*,#55330,.F.);
#80677=ORIENTED_EDGE('',*,*,#55328,.F.);
#80678=ORIENTED_EDGE('',*,*,#55331,.F.);
#80679=ORIENTED_EDGE('',*,*,#55332,.T.);
#80680=ORIENTED_EDGE('',*,*,#55333,.F.);
#80681=ORIENTED_EDGE('',*,*,#55329,.F.);
#80682=ORIENTED_EDGE('',*,*,#55334,.F.);
#80683=ORIENTED_EDGE('',*,*,#55176,.F.);
#80684=ORIENTED_EDGE('',*,*,#55307,.T.);
#80685=ORIENTED_EDGE('',*,*,#55335,.F.);
#80686=ORIENTED_EDGE('',*,*,#55332,.F.);
#80687=ORIENTED_EDGE('',*,*,#55286,.T.);
#80688=ORIENTED_EDGE('',*,*,#55259,.T.);
#80689=ORIENTED_EDGE('',*,*,#55255,.T.);
#80690=ORIENTED_EDGE('',*,*,#55336,.F.);
#80691=ORIENTED_EDGE('',*,*,#55264,.T.);
#80692=ORIENTED_EDGE('',*,*,#55261,.T.);
#80693=ORIENTED_EDGE('',*,*,#55285,.T.);
#80694=ORIENTED_EDGE('',*,*,#55303,.T.);
#80695=ORIENTED_EDGE('',*,*,#55337,.F.);
#80696=ORIENTED_EDGE('',*,*,#55273,.T.);
#80697=ORIENTED_EDGE('',*,*,#55270,.T.);
#80698=ORIENTED_EDGE('',*,*,#55267,.T.);
#80699=ORIENTED_EDGE('',*,*,#55335,.T.);
#80700=ORIENTED_EDGE('',*,*,#55306,.T.);
#80701=ORIENTED_EDGE('',*,*,#55324,.T.);
#80702=ORIENTED_EDGE('',*,*,#55330,.T.);
#80703=ORIENTED_EDGE('',*,*,#55333,.T.);
#80704=ORIENTED_EDGE('',*,*,#55310,.T.);
#80705=ORIENTED_EDGE('',*,*,#55294,.T.);
#80706=ORIENTED_EDGE('',*,*,#55323,.T.);
#80707=ORIENTED_EDGE('',*,*,#55322,.T.);
#80708=ORIENTED_EDGE('',*,*,#55319,.T.);
#80709=ORIENTED_EDGE('',*,*,#55314,.T.);
#80710=ORIENTED_EDGE('',*,*,#55172,.T.);
#80711=ORIENTED_EDGE('',*,*,#55211,.T.);
#80712=ORIENTED_EDGE('',*,*,#55182,.T.);
#80713=ORIENTED_EDGE('',*,*,#55280,.T.);
#80714=ORIENTED_EDGE('',*,*,#55297,.T.);
#80715=ORIENTED_EDGE('',*,*,#55295,.T.);
#80716=ORIENTED_EDGE('',*,*,#55292,.T.);
#80717=ORIENTED_EDGE('',*,*,#55274,.T.);
#80718=ORIENTED_EDGE('',*,*,#55337,.T.);
#80719=ORIENTED_EDGE('',*,*,#55302,.T.);
#80720=ORIENTED_EDGE('',*,*,#55305,.T.);
#80721=ORIENTED_EDGE('',*,*,#55308,.T.);
#80722=ORIENTED_EDGE('',*,*,#55279,.T.);
#80723=ORIENTED_EDGE('',*,*,#55338,.T.);
#80724=ORIENTED_EDGE('',*,*,#55339,.T.);
#80725=ORIENTED_EDGE('',*,*,#55340,.T.);
#80726=ORIENTED_EDGE('',*,*,#55341,.F.);
#80727=ORIENTED_EDGE('',*,*,#55342,.T.);
#80728=ORIENTED_EDGE('',*,*,#55343,.T.);
#80729=ORIENTED_EDGE('',*,*,#55344,.T.);
#80730=ORIENTED_EDGE('',*,*,#55345,.F.);
#80731=ORIENTED_EDGE('',*,*,#55346,.T.);
#80732=ORIENTED_EDGE('',*,*,#55347,.T.);
#80733=ORIENTED_EDGE('',*,*,#55348,.T.);
#80734=ORIENTED_EDGE('',*,*,#55349,.F.);
#80735=ORIENTED_EDGE('',*,*,#55350,.F.);
#80736=ORIENTED_EDGE('',*,*,#55349,.T.);
#80737=ORIENTED_EDGE('',*,*,#55351,.T.);
#80738=ORIENTED_EDGE('',*,*,#55352,.T.);
#80739=ORIENTED_EDGE('',*,*,#55353,.T.);
#80740=ORIENTED_EDGE('',*,*,#55354,.T.);
#80741=ORIENTED_EDGE('',*,*,#55355,.T.);
#80742=ORIENTED_EDGE('',*,*,#55356,.F.);
#80743=ORIENTED_EDGE('',*,*,#55357,.T.);
#80744=ORIENTED_EDGE('',*,*,#55358,.T.);
#80745=ORIENTED_EDGE('',*,*,#55359,.T.);
#80746=ORIENTED_EDGE('',*,*,#55360,.F.);
#80747=ORIENTED_EDGE('',*,*,#55348,.F.);
#80748=ORIENTED_EDGE('',*,*,#55361,.F.);
#80749=ORIENTED_EDGE('',*,*,#55357,.F.);
#80750=ORIENTED_EDGE('',*,*,#55362,.F.);
#80751=ORIENTED_EDGE('',*,*,#55363,.F.);
#80752=ORIENTED_EDGE('',*,*,#55360,.T.);
#80753=ORIENTED_EDGE('',*,*,#55364,.T.);
#80754=ORIENTED_EDGE('',*,*,#55365,.T.);
#80755=ORIENTED_EDGE('',*,*,#55359,.F.);
#80756=ORIENTED_EDGE('',*,*,#55366,.F.);
#80757=ORIENTED_EDGE('',*,*,#55353,.F.);
#80758=ORIENTED_EDGE('',*,*,#55367,.F.);
#80759=ORIENTED_EDGE('',*,*,#55368,.F.);
#80760=ORIENTED_EDGE('',*,*,#55356,.T.);
#80761=ORIENTED_EDGE('',*,*,#55369,.T.);
#80762=ORIENTED_EDGE('',*,*,#55370,.T.);
#80763=ORIENTED_EDGE('',*,*,#55355,.F.);
#80764=ORIENTED_EDGE('',*,*,#55371,.F.);
#80765=ORIENTED_EDGE('',*,*,#55342,.F.);
#80766=ORIENTED_EDGE('',*,*,#55372,.F.);
#80767=ORIENTED_EDGE('',*,*,#55373,.F.);
#80768=ORIENTED_EDGE('',*,*,#55345,.T.);
#80769=ORIENTED_EDGE('',*,*,#55374,.T.);
#80770=ORIENTED_EDGE('',*,*,#55375,.T.);
#80771=ORIENTED_EDGE('',*,*,#55376,.T.);
#80772=ORIENTED_EDGE('',*,*,#55377,.T.);
#80773=ORIENTED_EDGE('',*,*,#55378,.T.);
#80774=ORIENTED_EDGE('',*,*,#55379,.F.);
#80775=ORIENTED_EDGE('',*,*,#55380,.T.);
#80776=ORIENTED_EDGE('',*,*,#55381,.T.);
#80777=ORIENTED_EDGE('',*,*,#55382,.T.);
#80778=ORIENTED_EDGE('',*,*,#55383,.F.);
#80779=ORIENTED_EDGE('',*,*,#55384,.F.);
#80780=ORIENTED_EDGE('',*,*,#55263,.T.);
#80781=ORIENTED_EDGE('',*,*,#55385,.F.);
#80782=ORIENTED_EDGE('',*,*,#55386,.F.);
#80783=ORIENTED_EDGE('',*,*,#55380,.F.);
#80784=ORIENTED_EDGE('',*,*,#55387,.F.);
#80785=ORIENTED_EDGE('',*,*,#55383,.T.);
#80786=ORIENTED_EDGE('',*,*,#55388,.T.);
#80787=ORIENTED_EDGE('',*,*,#55389,.T.);
#80788=ORIENTED_EDGE('',*,*,#55382,.F.);
#80789=ORIENTED_EDGE('',*,*,#55390,.F.);
#80790=ORIENTED_EDGE('',*,*,#55376,.F.);
#80791=ORIENTED_EDGE('',*,*,#55391,.F.);
#80792=ORIENTED_EDGE('',*,*,#55392,.F.);
#80793=ORIENTED_EDGE('',*,*,#55379,.T.);
#80794=ORIENTED_EDGE('',*,*,#55393,.T.);
#80795=ORIENTED_EDGE('',*,*,#55394,.T.);
#80796=ORIENTED_EDGE('',*,*,#55378,.F.);
#80797=ORIENTED_EDGE('',*,*,#55395,.F.);
#80798=ORIENTED_EDGE('',*,*,#55338,.F.);
#80799=ORIENTED_EDGE('',*,*,#55396,.F.);
#80800=ORIENTED_EDGE('',*,*,#55397,.F.);
#80801=ORIENTED_EDGE('',*,*,#55341,.T.);
#80802=ORIENTED_EDGE('',*,*,#55398,.T.);
#80803=ORIENTED_EDGE('',*,*,#55399,.T.);
#80804=ORIENTED_EDGE('',*,*,#55393,.F.);
#80805=ORIENTED_EDGE('',*,*,#55396,.T.);
#80806=ORIENTED_EDGE('',*,*,#55397,.T.);
#80807=ORIENTED_EDGE('',*,*,#55400,.T.);
#80808=ORIENTED_EDGE('',*,*,#55388,.F.);
#80809=ORIENTED_EDGE('',*,*,#55391,.T.);
#80810=ORIENTED_EDGE('',*,*,#55392,.T.);
#80811=ORIENTED_EDGE('',*,*,#55401,.T.);
#80812=ORIENTED_EDGE('',*,*,#55369,.F.);
#80813=ORIENTED_EDGE('',*,*,#55372,.T.);
#80814=ORIENTED_EDGE('',*,*,#55373,.T.);
#80815=ORIENTED_EDGE('',*,*,#55402,.T.);
#80816=ORIENTED_EDGE('',*,*,#55364,.F.);
#80817=ORIENTED_EDGE('',*,*,#55367,.T.);
#80818=ORIENTED_EDGE('',*,*,#55368,.T.);
#80819=ORIENTED_EDGE('',*,*,#55403,.T.);
#80820=ORIENTED_EDGE('',*,*,#55351,.F.);
#80821=ORIENTED_EDGE('',*,*,#55362,.T.);
#80822=ORIENTED_EDGE('',*,*,#55363,.T.);
#80823=ORIENTED_EDGE('',*,*,#55404,.T.);
#80824=ORIENTED_EDGE('',*,*,#55405,.F.);
#80825=ORIENTED_EDGE('',*,*,#55406,.T.);
#80826=ORIENTED_EDGE('',*,*,#55407,.F.);
#80827=ORIENTED_EDGE('',*,*,#55408,.F.);
#80828=ORIENTED_EDGE('',*,*,#55409,.F.);
#80829=ORIENTED_EDGE('',*,*,#55410,.T.);
#80830=ORIENTED_EDGE('',*,*,#55411,.F.);
#80831=ORIENTED_EDGE('',*,*,#55412,.F.);
#80832=ORIENTED_EDGE('',*,*,#55413,.F.);
#80833=ORIENTED_EDGE('',*,*,#55414,.T.);
#80834=ORIENTED_EDGE('',*,*,#55415,.F.);
#80835=ORIENTED_EDGE('',*,*,#55416,.F.);
#80836=ORIENTED_EDGE('',*,*,#55417,.F.);
#80837=ORIENTED_EDGE('',*,*,#55418,.T.);
#80838=ORIENTED_EDGE('',*,*,#55419,.F.);
#80839=ORIENTED_EDGE('',*,*,#55420,.F.);
#80840=ORIENTED_EDGE('',*,*,#55421,.T.);
#80841=ORIENTED_EDGE('',*,*,#55417,.T.);
#80842=ORIENTED_EDGE('',*,*,#55422,.T.);
#80843=ORIENTED_EDGE('',*,*,#55346,.F.);
#80844=ORIENTED_EDGE('',*,*,#55423,.T.);
#80845=ORIENTED_EDGE('',*,*,#55424,.F.);
#80846=ORIENTED_EDGE('',*,*,#55425,.F.);
#80847=ORIENTED_EDGE('',*,*,#55418,.F.);
#80848=ORIENTED_EDGE('',*,*,#55426,.F.);
#80849=ORIENTED_EDGE('',*,*,#55427,.T.);
#80850=ORIENTED_EDGE('',*,*,#55428,.F.);
#80851=ORIENTED_EDGE('',*,*,#55429,.F.);
#80852=ORIENTED_EDGE('',*,*,#55430,.F.);
#80853=ORIENTED_EDGE('',*,*,#55431,.T.);
#80854=ORIENTED_EDGE('',*,*,#55432,.F.);
#80855=ORIENTED_EDGE('',*,*,#55433,.F.);
#80856=ORIENTED_EDGE('',*,*,#55419,.T.);
#80857=ORIENTED_EDGE('',*,*,#55434,.T.);
#80858=ORIENTED_EDGE('',*,*,#55430,.T.);
#80859=ORIENTED_EDGE('',*,*,#55435,.T.);
#80860=ORIENTED_EDGE('',*,*,#55436,.T.);
#80861=ORIENTED_EDGE('',*,*,#55437,.F.);
#80862=ORIENTED_EDGE('',*,*,#55438,.F.);
#80863=ORIENTED_EDGE('',*,*,#55431,.F.);
#80864=ORIENTED_EDGE('',*,*,#55432,.T.);
#80865=ORIENTED_EDGE('',*,*,#55439,.T.);
#80866=ORIENTED_EDGE('',*,*,#55426,.T.);
#80867=ORIENTED_EDGE('',*,*,#55440,.T.);
#80868=ORIENTED_EDGE('',*,*,#55441,.T.);
#80869=ORIENTED_EDGE('',*,*,#55442,.F.);
#80870=ORIENTED_EDGE('',*,*,#55443,.F.);
#80871=ORIENTED_EDGE('',*,*,#55427,.F.);
#80872=ORIENTED_EDGE('',*,*,#55428,.T.);
#80873=ORIENTED_EDGE('',*,*,#55444,.T.);
#80874=ORIENTED_EDGE('',*,*,#55413,.T.);
#80875=ORIENTED_EDGE('',*,*,#55445,.T.);
#80876=ORIENTED_EDGE('',*,*,#55446,.T.);
#80877=ORIENTED_EDGE('',*,*,#55447,.F.);
#80878=ORIENTED_EDGE('',*,*,#55448,.F.);
#80879=ORIENTED_EDGE('',*,*,#55414,.F.);
#80880=ORIENTED_EDGE('',*,*,#55449,.T.);
#80881=ORIENTED_EDGE('',*,*,#55415,.T.);
#80882=ORIENTED_EDGE('',*,*,#55450,.T.);
#80883=ORIENTED_EDGE('',*,*,#55409,.T.);
#80884=ORIENTED_EDGE('',*,*,#55451,.T.);
#80885=ORIENTED_EDGE('',*,*,#55452,.F.);
#80886=ORIENTED_EDGE('',*,*,#55453,.F.);
#80887=ORIENTED_EDGE('',*,*,#55410,.F.);
#80888=ORIENTED_EDGE('',*,*,#55454,.F.);
#80889=ORIENTED_EDGE('',*,*,#55455,.T.);
#80890=ORIENTED_EDGE('',*,*,#55456,.F.);
#80891=ORIENTED_EDGE('',*,*,#55457,.F.);
#80892=ORIENTED_EDGE('',*,*,#55458,.F.);
#80893=ORIENTED_EDGE('',*,*,#55459,.T.);
#80894=ORIENTED_EDGE('',*,*,#55460,.F.);
#80895=ORIENTED_EDGE('',*,*,#55461,.F.);
#80896=ORIENTED_EDGE('',*,*,#55411,.T.);
#80897=ORIENTED_EDGE('',*,*,#55462,.T.);
#80898=ORIENTED_EDGE('',*,*,#55458,.T.);
#80899=ORIENTED_EDGE('',*,*,#55463,.T.);
#80900=ORIENTED_EDGE('',*,*,#55464,.T.);
#80901=ORIENTED_EDGE('',*,*,#55465,.F.);
#80902=ORIENTED_EDGE('',*,*,#55466,.F.);
#80903=ORIENTED_EDGE('',*,*,#55459,.F.);
#80904=ORIENTED_EDGE('',*,*,#55460,.T.);
#80905=ORIENTED_EDGE('',*,*,#55467,.T.);
#80906=ORIENTED_EDGE('',*,*,#55454,.T.);
#80907=ORIENTED_EDGE('',*,*,#55468,.T.);
#80908=ORIENTED_EDGE('',*,*,#55469,.T.);
#80909=ORIENTED_EDGE('',*,*,#55470,.F.);
#80910=ORIENTED_EDGE('',*,*,#55471,.F.);
#80911=ORIENTED_EDGE('',*,*,#55455,.F.);
#80912=ORIENTED_EDGE('',*,*,#55456,.T.);
#80913=ORIENTED_EDGE('',*,*,#55472,.T.);
#80914=ORIENTED_EDGE('',*,*,#55405,.T.);
#80915=ORIENTED_EDGE('',*,*,#55473,.T.);
#80916=ORIENTED_EDGE('',*,*,#55474,.T.);
#80917=ORIENTED_EDGE('',*,*,#55475,.F.);
#80918=ORIENTED_EDGE('',*,*,#55476,.F.);
#80919=ORIENTED_EDGE('',*,*,#55406,.F.);
#80920=ORIENTED_EDGE('',*,*,#55477,.T.);
#80921=ORIENTED_EDGE('',*,*,#55340,.F.);
#80922=ORIENTED_EDGE('',*,*,#55478,.T.);
#80923=ORIENTED_EDGE('',*,*,#55407,.T.);
#80924=ORIENTED_EDGE('',*,*,#55477,.F.);
#80925=ORIENTED_EDGE('',*,*,#55476,.T.);
#80926=ORIENTED_EDGE('',*,*,#55479,.F.);
#80927=ORIENTED_EDGE('',*,*,#55398,.F.);
#80928=ORIENTED_EDGE('',*,*,#55480,.F.);
#80929=ORIENTED_EDGE('',*,*,#55316,.T.);
#80930=ORIENTED_EDGE('',*,*,#55481,.F.);
#80931=ORIENTED_EDGE('',*,*,#55327,.T.);
#80932=ORIENTED_EDGE('',*,*,#55482,.F.);
#80933=ORIENTED_EDGE('',*,*,#55321,.T.);
#80934=ORIENTED_EDGE('',*,*,#55177,.F.);
#80935=ORIENTED_EDGE('',*,*,#55334,.T.);
#80936=ORIENTED_EDGE('',*,*,#55421,.F.);
#80937=ORIENTED_EDGE('',*,*,#55350,.T.);
#80938=ORIENTED_EDGE('',*,*,#55483,.F.);
#80939=ORIENTED_EDGE('',*,*,#55423,.F.);
#80940=ORIENTED_EDGE('',*,*,#55448,.T.);
#80941=ORIENTED_EDGE('',*,*,#55484,.F.);
#80942=ORIENTED_EDGE('',*,*,#55451,.F.);
#80943=ORIENTED_EDGE('',*,*,#55450,.F.);
#80944=ORIENTED_EDGE('',*,*,#55471,.T.);
#80945=ORIENTED_EDGE('',*,*,#55485,.F.);
#80946=ORIENTED_EDGE('',*,*,#55474,.F.);
#80947=ORIENTED_EDGE('',*,*,#55472,.F.);
#80948=ORIENTED_EDGE('',*,*,#55466,.T.);
#80949=ORIENTED_EDGE('',*,*,#55486,.F.);
#80950=ORIENTED_EDGE('',*,*,#55469,.F.);
#80951=ORIENTED_EDGE('',*,*,#55467,.F.);
#80952=ORIENTED_EDGE('',*,*,#55453,.T.);
#80953=ORIENTED_EDGE('',*,*,#55487,.F.);
#80954=ORIENTED_EDGE('',*,*,#55464,.F.);
#80955=ORIENTED_EDGE('',*,*,#55462,.F.);
#80956=ORIENTED_EDGE('',*,*,#55443,.T.);
#80957=ORIENTED_EDGE('',*,*,#55488,.F.);
#80958=ORIENTED_EDGE('',*,*,#55446,.F.);
#80959=ORIENTED_EDGE('',*,*,#55444,.F.);
#80960=ORIENTED_EDGE('',*,*,#55438,.T.);
#80961=ORIENTED_EDGE('',*,*,#55489,.F.);
#80962=ORIENTED_EDGE('',*,*,#55441,.F.);
#80963=ORIENTED_EDGE('',*,*,#55439,.F.);
#80964=ORIENTED_EDGE('',*,*,#55425,.T.);
#80965=ORIENTED_EDGE('',*,*,#55490,.F.);
#80966=ORIENTED_EDGE('',*,*,#55436,.F.);
#80967=ORIENTED_EDGE('',*,*,#55434,.F.);
#80968=ORIENTED_EDGE('',*,*,#55385,.T.);
#80969=ORIENTED_EDGE('',*,*,#55266,.T.);
#80970=ORIENTED_EDGE('',*,*,#55491,.T.);
#80971=ORIENTED_EDGE('',*,*,#55492,.T.);
#80972=ORIENTED_EDGE('',*,*,#55491,.F.);
#80973=ORIENTED_EDGE('',*,*,#55269,.T.);
#80974=ORIENTED_EDGE('',*,*,#55493,.F.);
#80975=ORIENTED_EDGE('',*,*,#55344,.F.);
#80976=ORIENTED_EDGE('',*,*,#55494,.F.);
#80977=ORIENTED_EDGE('',*,*,#55493,.T.);
#80978=ORIENTED_EDGE('',*,*,#55272,.T.);
#80979=ORIENTED_EDGE('',*,*,#55291,.T.);
#80980=ORIENTED_EDGE('',*,*,#55309,.T.);
#80981=ORIENTED_EDGE('',*,*,#55495,.T.);
#80982=ORIENTED_EDGE('',*,*,#55374,.F.);
#80983=ORIENTED_EDGE('',*,*,#55496,.T.);
#80984=ORIENTED_EDGE('',*,*,#55258,.T.);
#80985=ORIENTED_EDGE('',*,*,#55384,.T.);
#80986=ORIENTED_EDGE('',*,*,#55387,.T.);
#80987=ORIENTED_EDGE('',*,*,#55497,.T.);
#80988=ORIENTED_EDGE('',*,*,#55498,.T.);
#80989=ORIENTED_EDGE('',*,*,#55499,.F.);
#80990=ORIENTED_EDGE('',*,*,#55498,.F.);
#80991=ORIENTED_EDGE('',*,*,#55500,.T.);
#80992=ORIENTED_EDGE('',*,*,#55501,.T.);
#80993=ORIENTED_EDGE('',*,*,#55502,.T.);
#80994=ORIENTED_EDGE('',*,*,#55499,.T.);
#80995=ORIENTED_EDGE('',*,*,#55503,.T.);
#80996=ORIENTED_EDGE('',*,*,#55078,.T.);
#80997=ORIENTED_EDGE('',*,*,#55504,.F.);
#80998=ORIENTED_EDGE('',*,*,#55505,.T.);
#80999=ORIENTED_EDGE('',*,*,#55506,.T.);
#81000=ORIENTED_EDGE('',*,*,#55507,.F.);
#81001=ORIENTED_EDGE('',*,*,#55508,.T.);
#81002=ORIENTED_EDGE('',*,*,#55509,.T.);
#81003=ORIENTED_EDGE('',*,*,#55510,.T.);
#81004=ORIENTED_EDGE('',*,*,#55511,.T.);
#81005=ORIENTED_EDGE('',*,*,#55512,.F.);
#81006=ORIENTED_EDGE('',*,*,#55513,.F.);
#81007=ORIENTED_EDGE('',*,*,#55514,.T.);
#81008=ORIENTED_EDGE('',*,*,#55515,.F.);
#81009=ORIENTED_EDGE('',*,*,#54715,.F.);
#81010=ORIENTED_EDGE('',*,*,#55510,.F.);
#81011=ORIENTED_EDGE('',*,*,#55500,.F.);
#81012=ORIENTED_EDGE('',*,*,#55497,.F.);
#81013=ORIENTED_EDGE('',*,*,#55502,.F.);
#81014=ORIENTED_EDGE('',*,*,#55508,.F.);
#81015=ORIENTED_EDGE('',*,*,#55129,.T.);
#81016=ORIENTED_EDGE('',*,*,#55516,.T.);
#81017=ORIENTED_EDGE('',*,*,#55126,.F.);
#81018=ORIENTED_EDGE('',*,*,#55517,.F.);
#81019=ORIENTED_EDGE('',*,*,#55501,.F.);
#81020=ORIENTED_EDGE('',*,*,#55509,.F.);
#81021=ORIENTED_EDGE('',*,*,#54716,.F.);
#81022=ORIENTED_EDGE('',*,*,#55518,.F.);
#81023=ORIENTED_EDGE('',*,*,#55073,.F.);
#81024=ORIENTED_EDGE('',*,*,#55079,.F.);
#81025=ORIENTED_EDGE('',*,*,#55503,.F.);
#81026=ORIENTED_EDGE('',*,*,#55077,.F.);
#81027=ORIENTED_EDGE('',*,*,#55082,.F.);
#81028=ORIENTED_EDGE('',*,*,#55085,.F.);
#81029=ORIENTED_EDGE('',*,*,#55088,.F.);
#81030=ORIENTED_EDGE('',*,*,#55091,.F.);
#81031=ORIENTED_EDGE('',*,*,#55094,.F.);
#81032=ORIENTED_EDGE('',*,*,#55097,.F.);
#81033=ORIENTED_EDGE('',*,*,#55100,.F.);
#81034=ORIENTED_EDGE('',*,*,#55103,.F.);
#81035=ORIENTED_EDGE('',*,*,#55106,.F.);
#81036=ORIENTED_EDGE('',*,*,#55109,.F.);
#81037=ORIENTED_EDGE('',*,*,#55112,.F.);
#81038=ORIENTED_EDGE('',*,*,#55115,.F.);
#81039=ORIENTED_EDGE('',*,*,#55118,.F.);
#81040=ORIENTED_EDGE('',*,*,#55121,.F.);
#81041=ORIENTED_EDGE('',*,*,#55124,.F.);
#81042=ORIENTED_EDGE('',*,*,#55127,.F.);
#81043=ORIENTED_EDGE('',*,*,#55516,.F.);
#81044=ORIENTED_EDGE('',*,*,#55131,.F.);
#81045=ORIENTED_EDGE('',*,*,#55519,.F.);
#81046=ORIENTED_EDGE('',*,*,#54659,.F.);
#81047=ORIENTED_EDGE('',*,*,#54663,.F.);
#81048=ORIENTED_EDGE('',*,*,#54666,.F.);
#81049=ORIENTED_EDGE('',*,*,#54669,.F.);
#81050=ORIENTED_EDGE('',*,*,#54672,.F.);
#81051=ORIENTED_EDGE('',*,*,#54675,.F.);
#81052=ORIENTED_EDGE('',*,*,#54678,.F.);
#81053=ORIENTED_EDGE('',*,*,#54681,.F.);
#81054=ORIENTED_EDGE('',*,*,#54684,.F.);
#81055=ORIENTED_EDGE('',*,*,#54687,.F.);
#81056=ORIENTED_EDGE('',*,*,#54690,.F.);
#81057=ORIENTED_EDGE('',*,*,#54693,.F.);
#81058=ORIENTED_EDGE('',*,*,#54696,.F.);
#81059=ORIENTED_EDGE('',*,*,#54699,.F.);
#81060=ORIENTED_EDGE('',*,*,#54702,.F.);
#81061=ORIENTED_EDGE('',*,*,#54705,.F.);
#81062=ORIENTED_EDGE('',*,*,#54708,.F.);
#81063=ORIENTED_EDGE('',*,*,#54711,.F.);
#81064=ORIENTED_EDGE('',*,*,#55520,.F.);
#81065=ORIENTED_EDGE('',*,*,#55521,.F.);
#81066=ORIENTED_EDGE('',*,*,#55522,.F.);
#81067=ORIENTED_EDGE('',*,*,#55511,.F.);
#81068=ORIENTED_EDGE('',*,*,#54714,.F.);
#81069=ORIENTED_EDGE('',*,*,#54661,.F.);
#81070=ORIENTED_EDGE('',*,*,#55523,.F.);
#81071=ORIENTED_EDGE('',*,*,#55517,.T.);
#81072=ORIENTED_EDGE('',*,*,#55128,.T.);
#81073=ORIENTED_EDGE('',*,*,#55125,.T.);
#81074=ORIENTED_EDGE('',*,*,#55122,.T.);
#81075=ORIENTED_EDGE('',*,*,#55119,.T.);
#81076=ORIENTED_EDGE('',*,*,#55116,.T.);
#81077=ORIENTED_EDGE('',*,*,#55113,.T.);
#81078=ORIENTED_EDGE('',*,*,#55110,.T.);
#81079=ORIENTED_EDGE('',*,*,#55107,.T.);
#81080=ORIENTED_EDGE('',*,*,#55104,.T.);
#81081=ORIENTED_EDGE('',*,*,#55101,.T.);
#81082=ORIENTED_EDGE('',*,*,#55098,.T.);
#81083=ORIENTED_EDGE('',*,*,#55095,.T.);
#81084=ORIENTED_EDGE('',*,*,#55092,.T.);
#81085=ORIENTED_EDGE('',*,*,#55089,.T.);
#81086=ORIENTED_EDGE('',*,*,#55086,.T.);
#81087=ORIENTED_EDGE('',*,*,#55083,.T.);
#81088=ORIENTED_EDGE('',*,*,#55080,.T.);
#81089=ORIENTED_EDGE('',*,*,#55075,.T.);
#81090=ORIENTED_EDGE('',*,*,#55524,.F.);
#81091=ORIENTED_EDGE('',*,*,#55506,.F.);
#81092=ORIENTED_EDGE('',*,*,#55525,.F.);
#81093=ORIENTED_EDGE('',*,*,#54712,.F.);
#81094=ORIENTED_EDGE('',*,*,#54709,.F.);
#81095=ORIENTED_EDGE('',*,*,#54706,.F.);
#81096=ORIENTED_EDGE('',*,*,#54703,.F.);
#81097=ORIENTED_EDGE('',*,*,#54700,.F.);
#81098=ORIENTED_EDGE('',*,*,#54697,.F.);
#81099=ORIENTED_EDGE('',*,*,#54694,.F.);
#81100=ORIENTED_EDGE('',*,*,#54691,.F.);
#81101=ORIENTED_EDGE('',*,*,#54688,.F.);
#81102=ORIENTED_EDGE('',*,*,#54685,.F.);
#81103=ORIENTED_EDGE('',*,*,#54682,.F.);
#81104=ORIENTED_EDGE('',*,*,#54679,.F.);
#81105=ORIENTED_EDGE('',*,*,#54676,.F.);
#81106=ORIENTED_EDGE('',*,*,#54673,.F.);
#81107=ORIENTED_EDGE('',*,*,#54670,.F.);
#81108=ORIENTED_EDGE('',*,*,#54667,.F.);
#81109=ORIENTED_EDGE('',*,*,#54664,.F.);
#81110=ORIENTED_EDGE('',*,*,#55526,.F.);
#81111=ORIENTED_EDGE('',*,*,#55527,.T.);
#81112=ORIENTED_EDGE('',*,*,#55528,.T.);
#81113=ORIENTED_EDGE('',*,*,#55018,.T.);
#81114=ORIENTED_EDGE('',*,*,#55529,.T.);
#81115=ORIENTED_EDGE('',*,*,#55530,.T.);
#81116=ORIENTED_EDGE('',*,*,#55014,.T.);
#81117=ORIENTED_EDGE('',*,*,#55531,.T.);
#81118=ORIENTED_EDGE('',*,*,#55532,.F.);
#81119=ORIENTED_EDGE('',*,*,#55533,.T.);
#81120=ORIENTED_EDGE('',*,*,#55534,.T.);
#81121=ORIENTED_EDGE('',*,*,#55535,.F.);
#81122=ORIENTED_EDGE('',*,*,#55536,.T.);
#81123=ORIENTED_EDGE('',*,*,#55537,.T.);
#81124=ORIENTED_EDGE('',*,*,#55538,.F.);
#81125=ORIENTED_EDGE('',*,*,#55539,.T.);
#81126=ORIENTED_EDGE('',*,*,#55529,.F.);
#81127=ORIENTED_EDGE('',*,*,#54774,.T.);
#81128=ORIENTED_EDGE('',*,*,#55533,.F.);
#81129=ORIENTED_EDGE('',*,*,#55069,.T.);
#81130=ORIENTED_EDGE('',*,*,#55540,.T.);
#81131=ORIENTED_EDGE('',*,*,#55066,.F.);
#81132=ORIENTED_EDGE('',*,*,#55541,.F.);
#81133=ORIENTED_EDGE('',*,*,#55527,.F.);
#81134=ORIENTED_EDGE('',*,*,#55542,.F.);
#81135=ORIENTED_EDGE('',*,*,#54775,.F.);
#81136=ORIENTED_EDGE('',*,*,#55531,.F.);
#81137=ORIENTED_EDGE('',*,*,#55013,.F.);
#81138=ORIENTED_EDGE('',*,*,#55019,.F.);
#81139=ORIENTED_EDGE('',*,*,#55528,.F.);
#81140=ORIENTED_EDGE('',*,*,#55017,.F.);
#81141=ORIENTED_EDGE('',*,*,#55022,.F.);
#81142=ORIENTED_EDGE('',*,*,#55025,.F.);
#81143=ORIENTED_EDGE('',*,*,#55028,.F.);
#81144=ORIENTED_EDGE('',*,*,#55031,.F.);
#81145=ORIENTED_EDGE('',*,*,#55034,.F.);
#81146=ORIENTED_EDGE('',*,*,#55037,.F.);
#81147=ORIENTED_EDGE('',*,*,#55040,.F.);
#81148=ORIENTED_EDGE('',*,*,#55043,.F.);
#81149=ORIENTED_EDGE('',*,*,#55046,.F.);
#81150=ORIENTED_EDGE('',*,*,#55049,.F.);
#81151=ORIENTED_EDGE('',*,*,#55052,.F.);
#81152=ORIENTED_EDGE('',*,*,#55055,.F.);
#81153=ORIENTED_EDGE('',*,*,#55058,.F.);
#81154=ORIENTED_EDGE('',*,*,#55061,.F.);
#81155=ORIENTED_EDGE('',*,*,#55064,.F.);
#81156=ORIENTED_EDGE('',*,*,#55067,.F.);
#81157=ORIENTED_EDGE('',*,*,#55540,.F.);
#81158=ORIENTED_EDGE('',*,*,#55071,.F.);
#81159=ORIENTED_EDGE('',*,*,#55543,.F.);
#81160=ORIENTED_EDGE('',*,*,#54718,.F.);
#81161=ORIENTED_EDGE('',*,*,#54722,.F.);
#81162=ORIENTED_EDGE('',*,*,#54725,.F.);
#81163=ORIENTED_EDGE('',*,*,#54728,.F.);
#81164=ORIENTED_EDGE('',*,*,#54731,.F.);
#81165=ORIENTED_EDGE('',*,*,#54734,.F.);
#81166=ORIENTED_EDGE('',*,*,#54737,.F.);
#81167=ORIENTED_EDGE('',*,*,#54740,.F.);
#81168=ORIENTED_EDGE('',*,*,#54743,.F.);
#81169=ORIENTED_EDGE('',*,*,#54746,.F.);
#81170=ORIENTED_EDGE('',*,*,#54749,.F.);
#81171=ORIENTED_EDGE('',*,*,#54752,.F.);
#81172=ORIENTED_EDGE('',*,*,#54755,.F.);
#81173=ORIENTED_EDGE('',*,*,#54758,.F.);
#81174=ORIENTED_EDGE('',*,*,#54761,.F.);
#81175=ORIENTED_EDGE('',*,*,#54764,.F.);
#81176=ORIENTED_EDGE('',*,*,#54767,.F.);
#81177=ORIENTED_EDGE('',*,*,#54770,.F.);
#81178=ORIENTED_EDGE('',*,*,#55544,.F.);
#81179=ORIENTED_EDGE('',*,*,#55545,.F.);
#81180=ORIENTED_EDGE('',*,*,#55546,.F.);
#81181=ORIENTED_EDGE('',*,*,#55547,.F.);
#81182=ORIENTED_EDGE('',*,*,#55534,.F.);
#81183=ORIENTED_EDGE('',*,*,#54773,.F.);
#81184=ORIENTED_EDGE('',*,*,#54720,.F.);
#81185=ORIENTED_EDGE('',*,*,#55548,.F.);
#81186=ORIENTED_EDGE('',*,*,#55541,.T.);
#81187=ORIENTED_EDGE('',*,*,#55068,.T.);
#81188=ORIENTED_EDGE('',*,*,#55065,.T.);
#81189=ORIENTED_EDGE('',*,*,#55062,.T.);
#81190=ORIENTED_EDGE('',*,*,#55059,.T.);
#81191=ORIENTED_EDGE('',*,*,#55056,.T.);
#81192=ORIENTED_EDGE('',*,*,#55053,.T.);
#81193=ORIENTED_EDGE('',*,*,#55050,.T.);
#81194=ORIENTED_EDGE('',*,*,#55047,.T.);
#81195=ORIENTED_EDGE('',*,*,#55044,.T.);
#81196=ORIENTED_EDGE('',*,*,#55041,.T.);
#81197=ORIENTED_EDGE('',*,*,#55038,.T.);
#81198=ORIENTED_EDGE('',*,*,#55035,.T.);
#81199=ORIENTED_EDGE('',*,*,#55032,.T.);
#81200=ORIENTED_EDGE('',*,*,#55029,.T.);
#81201=ORIENTED_EDGE('',*,*,#55026,.T.);
#81202=ORIENTED_EDGE('',*,*,#55023,.T.);
#81203=ORIENTED_EDGE('',*,*,#55020,.T.);
#81204=ORIENTED_EDGE('',*,*,#55015,.T.);
#81205=ORIENTED_EDGE('',*,*,#55530,.F.);
#81206=ORIENTED_EDGE('',*,*,#55549,.F.);
#81207=ORIENTED_EDGE('',*,*,#54771,.F.);
#81208=ORIENTED_EDGE('',*,*,#54768,.F.);
#81209=ORIENTED_EDGE('',*,*,#54765,.F.);
#81210=ORIENTED_EDGE('',*,*,#54762,.F.);
#81211=ORIENTED_EDGE('',*,*,#54759,.F.);
#81212=ORIENTED_EDGE('',*,*,#54756,.F.);
#81213=ORIENTED_EDGE('',*,*,#54753,.F.);
#81214=ORIENTED_EDGE('',*,*,#54750,.F.);
#81215=ORIENTED_EDGE('',*,*,#54747,.F.);
#81216=ORIENTED_EDGE('',*,*,#54744,.F.);
#81217=ORIENTED_EDGE('',*,*,#54741,.F.);
#81218=ORIENTED_EDGE('',*,*,#54738,.F.);
#81219=ORIENTED_EDGE('',*,*,#54735,.F.);
#81220=ORIENTED_EDGE('',*,*,#54732,.F.);
#81221=ORIENTED_EDGE('',*,*,#54729,.F.);
#81222=ORIENTED_EDGE('',*,*,#54726,.F.);
#81223=ORIENTED_EDGE('',*,*,#54723,.F.);
#81224=ORIENTED_EDGE('',*,*,#55550,.F.);
#81225=ORIENTED_EDGE('',*,*,#55551,.T.);
#81226=ORIENTED_EDGE('',*,*,#55552,.F.);
#81227=ORIENTED_EDGE('',*,*,#55250,.F.);
#81228=ORIENTED_EDGE('',*,*,#55008,.T.);
#81229=ORIENTED_EDGE('',*,*,#55553,.T.);
#81230=ORIENTED_EDGE('',*,*,#55005,.F.);
#81231=ORIENTED_EDGE('',*,*,#55554,.T.);
#81232=ORIENTED_EDGE('',*,*,#55555,.F.);
#81233=ORIENTED_EDGE('',*,*,#55556,.T.);
#81234=ORIENTED_EDGE('',*,*,#55557,.T.);
#81235=ORIENTED_EDGE('',*,*,#54900,.T.);
#81236=ORIENTED_EDGE('',*,*,#55558,.T.);
#81237=ORIENTED_EDGE('',*,*,#55559,.T.);
#81238=ORIENTED_EDGE('',*,*,#54896,.T.);
#81239=ORIENTED_EDGE('',*,*,#55560,.T.);
#81240=ORIENTED_EDGE('',*,*,#55561,.F.);
#81241=ORIENTED_EDGE('',*,*,#55562,.T.);
#81242=ORIENTED_EDGE('',*,*,#55563,.T.);
#81243=ORIENTED_EDGE('',*,*,#55564,.F.);
#81244=ORIENTED_EDGE('',*,*,#55565,.T.);
#81245=ORIENTED_EDGE('',*,*,#55566,.T.);
#81246=ORIENTED_EDGE('',*,*,#55567,.F.);
#81247=ORIENTED_EDGE('',*,*,#55555,.T.);
#81248=ORIENTED_EDGE('',*,*,#55558,.F.);
#81249=ORIENTED_EDGE('',*,*,#55010,.T.);
#81250=ORIENTED_EDGE('',*,*,#55562,.F.);
#81251=ORIENTED_EDGE('',*,*,#54951,.T.);
#81252=ORIENTED_EDGE('',*,*,#55568,.T.);
#81253=ORIENTED_EDGE('',*,*,#54948,.F.);
#81254=ORIENTED_EDGE('',*,*,#55569,.F.);
#81255=ORIENTED_EDGE('',*,*,#55551,.F.);
#81256=ORIENTED_EDGE('',*,*,#55570,.F.);
#81257=ORIENTED_EDGE('',*,*,#55011,.F.);
#81258=ORIENTED_EDGE('',*,*,#55560,.F.);
#81259=ORIENTED_EDGE('',*,*,#54895,.F.);
#81260=ORIENTED_EDGE('',*,*,#54901,.F.);
#81261=ORIENTED_EDGE('',*,*,#55557,.F.);
#81262=ORIENTED_EDGE('',*,*,#54899,.F.);
#81263=ORIENTED_EDGE('',*,*,#54904,.F.);
#81264=ORIENTED_EDGE('',*,*,#54907,.F.);
#81265=ORIENTED_EDGE('',*,*,#54910,.F.);
#81266=ORIENTED_EDGE('',*,*,#54913,.F.);
#81267=ORIENTED_EDGE('',*,*,#54916,.F.);
#81268=ORIENTED_EDGE('',*,*,#54919,.F.);
#81269=ORIENTED_EDGE('',*,*,#54922,.F.);
#81270=ORIENTED_EDGE('',*,*,#54925,.F.);
#81271=ORIENTED_EDGE('',*,*,#54928,.F.);
#81272=ORIENTED_EDGE('',*,*,#54931,.F.);
#81273=ORIENTED_EDGE('',*,*,#54934,.F.);
#81274=ORIENTED_EDGE('',*,*,#54937,.F.);
#81275=ORIENTED_EDGE('',*,*,#54940,.F.);
#81276=ORIENTED_EDGE('',*,*,#54943,.F.);
#81277=ORIENTED_EDGE('',*,*,#54946,.F.);
#81278=ORIENTED_EDGE('',*,*,#54949,.F.);
#81279=ORIENTED_EDGE('',*,*,#55568,.F.);
#81280=ORIENTED_EDGE('',*,*,#54953,.F.);
#81281=ORIENTED_EDGE('',*,*,#55571,.F.);
#81282=ORIENTED_EDGE('',*,*,#54958,.F.);
#81283=ORIENTED_EDGE('',*,*,#54961,.F.);
#81284=ORIENTED_EDGE('',*,*,#54964,.F.);
#81285=ORIENTED_EDGE('',*,*,#54967,.F.);
#81286=ORIENTED_EDGE('',*,*,#54970,.F.);
#81287=ORIENTED_EDGE('',*,*,#54973,.F.);
#81288=ORIENTED_EDGE('',*,*,#54976,.F.);
#81289=ORIENTED_EDGE('',*,*,#54979,.F.);
#81290=ORIENTED_EDGE('',*,*,#54982,.F.);
#81291=ORIENTED_EDGE('',*,*,#54985,.F.);
#81292=ORIENTED_EDGE('',*,*,#54988,.F.);
#81293=ORIENTED_EDGE('',*,*,#54991,.F.);
#81294=ORIENTED_EDGE('',*,*,#54994,.F.);
#81295=ORIENTED_EDGE('',*,*,#54997,.F.);
#81296=ORIENTED_EDGE('',*,*,#55000,.F.);
#81297=ORIENTED_EDGE('',*,*,#55003,.F.);
#81298=ORIENTED_EDGE('',*,*,#55006,.F.);
#81299=ORIENTED_EDGE('',*,*,#55553,.F.);
#81300=ORIENTED_EDGE('',*,*,#55556,.F.);
#81301=ORIENTED_EDGE('',*,*,#55572,.F.);
#81302=ORIENTED_EDGE('',*,*,#55573,.F.);
#81303=ORIENTED_EDGE('',*,*,#55563,.F.);
#81304=ORIENTED_EDGE('',*,*,#55009,.F.);
#81305=ORIENTED_EDGE('',*,*,#54956,.F.);
#81306=ORIENTED_EDGE('',*,*,#55574,.F.);
#81307=ORIENTED_EDGE('',*,*,#55569,.T.);
#81308=ORIENTED_EDGE('',*,*,#54950,.T.);
#81309=ORIENTED_EDGE('',*,*,#54947,.T.);
#81310=ORIENTED_EDGE('',*,*,#54944,.T.);
#81311=ORIENTED_EDGE('',*,*,#54941,.T.);
#81312=ORIENTED_EDGE('',*,*,#54938,.T.);
#81313=ORIENTED_EDGE('',*,*,#54935,.T.);
#81314=ORIENTED_EDGE('',*,*,#54932,.T.);
#81315=ORIENTED_EDGE('',*,*,#54929,.T.);
#81316=ORIENTED_EDGE('',*,*,#54926,.T.);
#81317=ORIENTED_EDGE('',*,*,#54923,.T.);
#81318=ORIENTED_EDGE('',*,*,#54920,.T.);
#81319=ORIENTED_EDGE('',*,*,#54917,.T.);
#81320=ORIENTED_EDGE('',*,*,#54914,.T.);
#81321=ORIENTED_EDGE('',*,*,#54911,.T.);
#81322=ORIENTED_EDGE('',*,*,#54908,.T.);
#81323=ORIENTED_EDGE('',*,*,#54905,.T.);
#81324=ORIENTED_EDGE('',*,*,#54902,.T.);
#81325=ORIENTED_EDGE('',*,*,#54897,.T.);
#81326=ORIENTED_EDGE('',*,*,#55559,.F.);
#81327=ORIENTED_EDGE('',*,*,#55554,.F.);
#81328=ORIENTED_EDGE('',*,*,#55007,.F.);
#81329=ORIENTED_EDGE('',*,*,#55004,.F.);
#81330=ORIENTED_EDGE('',*,*,#55001,.F.);
#81331=ORIENTED_EDGE('',*,*,#54998,.F.);
#81332=ORIENTED_EDGE('',*,*,#54995,.F.);
#81333=ORIENTED_EDGE('',*,*,#54992,.F.);
#81334=ORIENTED_EDGE('',*,*,#54989,.F.);
#81335=ORIENTED_EDGE('',*,*,#54986,.F.);
#81336=ORIENTED_EDGE('',*,*,#54983,.F.);
#81337=ORIENTED_EDGE('',*,*,#54980,.F.);
#81338=ORIENTED_EDGE('',*,*,#54977,.F.);
#81339=ORIENTED_EDGE('',*,*,#54974,.F.);
#81340=ORIENTED_EDGE('',*,*,#54971,.F.);
#81341=ORIENTED_EDGE('',*,*,#54968,.F.);
#81342=ORIENTED_EDGE('',*,*,#54965,.F.);
#81343=ORIENTED_EDGE('',*,*,#54962,.F.);
#81344=ORIENTED_EDGE('',*,*,#54959,.F.);
#81345=ORIENTED_EDGE('',*,*,#55575,.T.);
#81346=ORIENTED_EDGE('',*,*,#55253,.F.);
#81347=ORIENTED_EDGE('',*,*,#55576,.T.);
#81348=ORIENTED_EDGE('',*,*,#55577,.T.);
#81349=ORIENTED_EDGE('',*,*,#54888,.T.);
#81350=ORIENTED_EDGE('',*,*,#55578,.T.);
#81351=ORIENTED_EDGE('',*,*,#54885,.F.);
#81352=ORIENTED_EDGE('',*,*,#55579,.T.);
#81353=ORIENTED_EDGE('',*,*,#55580,.T.);
#81354=ORIENTED_EDGE('',*,*,#54782,.T.);
#81355=ORIENTED_EDGE('',*,*,#55581,.F.);
#81356=ORIENTED_EDGE('',*,*,#55582,.T.);
#81357=ORIENTED_EDGE('',*,*,#55583,.T.);
#81358=ORIENTED_EDGE('',*,*,#55584,.F.);
#81359=ORIENTED_EDGE('',*,*,#55585,.T.);
#81360=ORIENTED_EDGE('',*,*,#55586,.T.);
#81361=ORIENTED_EDGE('',*,*,#55587,.T.);
#81362=ORIENTED_EDGE('',*,*,#55588,.T.);
#81363=ORIENTED_EDGE('',*,*,#55589,.F.);
#81364=ORIENTED_EDGE('',*,*,#55590,.F.);
#81365=ORIENTED_EDGE('',*,*,#55591,.T.);
#81366=ORIENTED_EDGE('',*,*,#55592,.F.);
#81367=ORIENTED_EDGE('',*,*,#54892,.F.);
#81368=ORIENTED_EDGE('',*,*,#55587,.F.);
#81369=ORIENTED_EDGE('',*,*,#55576,.F.);
#81370=ORIENTED_EDGE('',*,*,#55251,.F.);
#81371=ORIENTED_EDGE('',*,*,#55575,.F.);
#81372=ORIENTED_EDGE('',*,*,#55585,.F.);
#81373=ORIENTED_EDGE('',*,*,#55468,.F.);
#81374=ORIENTED_EDGE('',*,*,#55457,.T.);
#81375=ORIENTED_EDGE('',*,*,#55473,.F.);
#81376=ORIENTED_EDGE('',*,*,#55408,.T.);
#81377=ORIENTED_EDGE('',*,*,#55478,.F.);
#81378=ORIENTED_EDGE('',*,*,#55339,.F.);
#81379=ORIENTED_EDGE('',*,*,#55395,.T.);
#81380=ORIENTED_EDGE('',*,*,#55377,.F.);
#81381=ORIENTED_EDGE('',*,*,#55390,.T.);
#81382=ORIENTED_EDGE('',*,*,#55381,.F.);
#81383=ORIENTED_EDGE('',*,*,#55386,.T.);
#81384=ORIENTED_EDGE('',*,*,#55492,.F.);
#81385=ORIENTED_EDGE('',*,*,#55494,.T.);
#81386=ORIENTED_EDGE('',*,*,#55343,.F.);
#81387=ORIENTED_EDGE('',*,*,#55371,.T.);
#81388=ORIENTED_EDGE('',*,*,#55354,.F.);
#81389=ORIENTED_EDGE('',*,*,#55366,.T.);
#81390=ORIENTED_EDGE('',*,*,#55358,.F.);
#81391=ORIENTED_EDGE('',*,*,#55361,.T.);
#81392=ORIENTED_EDGE('',*,*,#55347,.F.);
#81393=ORIENTED_EDGE('',*,*,#55422,.F.);
#81394=ORIENTED_EDGE('',*,*,#55420,.T.);
#81395=ORIENTED_EDGE('',*,*,#55435,.F.);
#81396=ORIENTED_EDGE('',*,*,#55433,.T.);
#81397=ORIENTED_EDGE('',*,*,#55440,.F.);
#81398=ORIENTED_EDGE('',*,*,#55429,.T.);
#81399=ORIENTED_EDGE('',*,*,#55445,.F.);
#81400=ORIENTED_EDGE('',*,*,#55416,.T.);
#81401=ORIENTED_EDGE('',*,*,#55449,.F.);
#81402=ORIENTED_EDGE('',*,*,#55412,.T.);
#81403=ORIENTED_EDGE('',*,*,#55463,.F.);
#81404=ORIENTED_EDGE('',*,*,#55461,.T.);
#81405=ORIENTED_EDGE('',*,*,#54955,.F.);
#81406=ORIENTED_EDGE('',*,*,#55571,.T.);
#81407=ORIENTED_EDGE('',*,*,#54952,.T.);
#81408=ORIENTED_EDGE('',*,*,#55574,.T.);
#81409=ORIENTED_EDGE('',*,*,#55523,.T.);
#81410=ORIENTED_EDGE('',*,*,#54660,.T.);
#81411=ORIENTED_EDGE('',*,*,#55519,.T.);
#81412=ORIENTED_EDGE('',*,*,#55130,.T.);
#81413=ORIENTED_EDGE('',*,*,#54719,.F.);
#81414=ORIENTED_EDGE('',*,*,#55543,.T.);
#81415=ORIENTED_EDGE('',*,*,#55070,.T.);
#81416=ORIENTED_EDGE('',*,*,#55548,.T.);
#81417=ORIENTED_EDGE('',*,*,#55593,.T.);
#81418=ORIENTED_EDGE('',*,*,#54838,.T.);
#81419=ORIENTED_EDGE('',*,*,#55594,.T.);
#81420=ORIENTED_EDGE('',*,*,#54834,.T.);
#81421=ORIENTED_EDGE('',*,*,#54833,.T.);
#81422=ORIENTED_EDGE('',*,*,#55595,.T.);
#81423=ORIENTED_EDGE('',*,*,#54830,.F.);
#81424=ORIENTED_EDGE('',*,*,#55596,.F.);
#81425=ORIENTED_EDGE('',*,*,#55577,.F.);
#81426=ORIENTED_EDGE('',*,*,#55586,.F.);
#81427=ORIENTED_EDGE('',*,*,#54893,.F.);
#81428=ORIENTED_EDGE('',*,*,#55597,.F.);
#81429=ORIENTED_EDGE('',*,*,#54777,.F.);
#81430=ORIENTED_EDGE('',*,*,#54783,.F.);
#81431=ORIENTED_EDGE('',*,*,#55580,.F.);
#81432=ORIENTED_EDGE('',*,*,#54781,.F.);
#81433=ORIENTED_EDGE('',*,*,#54786,.F.);
#81434=ORIENTED_EDGE('',*,*,#54789,.F.);
#81435=ORIENTED_EDGE('',*,*,#54792,.F.);
#81436=ORIENTED_EDGE('',*,*,#54795,.F.);
#81437=ORIENTED_EDGE('',*,*,#54798,.F.);
#81438=ORIENTED_EDGE('',*,*,#54801,.F.);
#81439=ORIENTED_EDGE('',*,*,#54804,.F.);
#81440=ORIENTED_EDGE('',*,*,#54807,.F.);
#81441=ORIENTED_EDGE('',*,*,#54810,.F.);
#81442=ORIENTED_EDGE('',*,*,#54813,.F.);
#81443=ORIENTED_EDGE('',*,*,#54816,.F.);
#81444=ORIENTED_EDGE('',*,*,#54819,.F.);
#81445=ORIENTED_EDGE('',*,*,#54822,.F.);
#81446=ORIENTED_EDGE('',*,*,#54825,.F.);
#81447=ORIENTED_EDGE('',*,*,#54828,.F.);
#81448=ORIENTED_EDGE('',*,*,#54831,.F.);
#81449=ORIENTED_EDGE('',*,*,#55595,.F.);
#81450=ORIENTED_EDGE('',*,*,#54835,.F.);
#81451=ORIENTED_EDGE('',*,*,#55594,.F.);
#81452=ORIENTED_EDGE('',*,*,#54837,.F.);
#81453=ORIENTED_EDGE('',*,*,#54841,.F.);
#81454=ORIENTED_EDGE('',*,*,#54844,.F.);
#81455=ORIENTED_EDGE('',*,*,#54847,.F.);
#81456=ORIENTED_EDGE('',*,*,#54850,.F.);
#81457=ORIENTED_EDGE('',*,*,#54853,.F.);
#81458=ORIENTED_EDGE('',*,*,#54856,.F.);
#81459=ORIENTED_EDGE('',*,*,#54859,.F.);
#81460=ORIENTED_EDGE('',*,*,#54862,.F.);
#81461=ORIENTED_EDGE('',*,*,#54865,.F.);
#81462=ORIENTED_EDGE('',*,*,#54868,.F.);
#81463=ORIENTED_EDGE('',*,*,#54871,.F.);
#81464=ORIENTED_EDGE('',*,*,#54874,.F.);
#81465=ORIENTED_EDGE('',*,*,#54877,.F.);
#81466=ORIENTED_EDGE('',*,*,#54880,.F.);
#81467=ORIENTED_EDGE('',*,*,#54883,.F.);
#81468=ORIENTED_EDGE('',*,*,#54886,.F.);
#81469=ORIENTED_EDGE('',*,*,#55578,.F.);
#81470=ORIENTED_EDGE('',*,*,#54891,.F.);
#81471=ORIENTED_EDGE('',*,*,#55598,.F.);
#81472=ORIENTED_EDGE('',*,*,#55588,.F.);
#81473=ORIENTED_EDGE('',*,*,#54839,.F.);
#81474=ORIENTED_EDGE('',*,*,#55593,.F.);
#81475=ORIENTED_EDGE('',*,*,#55596,.T.);
#81476=ORIENTED_EDGE('',*,*,#54832,.T.);
#81477=ORIENTED_EDGE('',*,*,#54829,.T.);
#81478=ORIENTED_EDGE('',*,*,#54826,.T.);
#81479=ORIENTED_EDGE('',*,*,#54823,.T.);
#81480=ORIENTED_EDGE('',*,*,#54820,.T.);
#81481=ORIENTED_EDGE('',*,*,#54817,.T.);
#81482=ORIENTED_EDGE('',*,*,#54814,.T.);
#81483=ORIENTED_EDGE('',*,*,#54811,.T.);
#81484=ORIENTED_EDGE('',*,*,#54808,.T.);
#81485=ORIENTED_EDGE('',*,*,#54805,.T.);
#81486=ORIENTED_EDGE('',*,*,#54802,.T.);
#81487=ORIENTED_EDGE('',*,*,#54799,.T.);
#81488=ORIENTED_EDGE('',*,*,#54796,.T.);
#81489=ORIENTED_EDGE('',*,*,#54793,.T.);
#81490=ORIENTED_EDGE('',*,*,#54790,.T.);
#81491=ORIENTED_EDGE('',*,*,#54787,.T.);
#81492=ORIENTED_EDGE('',*,*,#54784,.T.);
#81493=ORIENTED_EDGE('',*,*,#54779,.T.);
#81494=ORIENTED_EDGE('',*,*,#55599,.F.);
#81495=ORIENTED_EDGE('',*,*,#55583,.F.);
#81496=ORIENTED_EDGE('',*,*,#54889,.F.);
#81497=ORIENTED_EDGE('',*,*,#55579,.F.);
#81498=ORIENTED_EDGE('',*,*,#54887,.F.);
#81499=ORIENTED_EDGE('',*,*,#54884,.F.);
#81500=ORIENTED_EDGE('',*,*,#54881,.F.);
#81501=ORIENTED_EDGE('',*,*,#54878,.F.);
#81502=ORIENTED_EDGE('',*,*,#54875,.F.);
#81503=ORIENTED_EDGE('',*,*,#54872,.F.);
#81504=ORIENTED_EDGE('',*,*,#54869,.F.);
#81505=ORIENTED_EDGE('',*,*,#54866,.F.);
#81506=ORIENTED_EDGE('',*,*,#54863,.F.);
#81507=ORIENTED_EDGE('',*,*,#54860,.F.);
#81508=ORIENTED_EDGE('',*,*,#54857,.F.);
#81509=ORIENTED_EDGE('',*,*,#54854,.F.);
#81510=ORIENTED_EDGE('',*,*,#54851,.F.);
#81511=ORIENTED_EDGE('',*,*,#54848,.F.);
#81512=ORIENTED_EDGE('',*,*,#54845,.F.);
#81513=ORIENTED_EDGE('',*,*,#54842,.F.);
#81514=ORIENTED_EDGE('',*,*,#54772,.T.);
#81515=ORIENTED_EDGE('',*,*,#55544,.T.);
#81516=ORIENTED_EDGE('',*,*,#54769,.F.);
#81517=ORIENTED_EDGE('',*,*,#55549,.T.);
#81518=ORIENTED_EDGE('',*,*,#55539,.F.);
#81519=ORIENTED_EDGE('',*,*,#55545,.T.);
#81520=ORIENTED_EDGE('',*,*,#54713,.T.);
#81521=ORIENTED_EDGE('',*,*,#55520,.T.);
#81522=ORIENTED_EDGE('',*,*,#54710,.F.);
#81523=ORIENTED_EDGE('',*,*,#55525,.T.);
#81524=ORIENTED_EDGE('',*,*,#55600,.T.);
#81525=ORIENTED_EDGE('',*,*,#55521,.T.);
#81526=ORIENTED_EDGE('',*,*,#55480,.T.);
#81527=ORIENTED_EDGE('',*,*,#55325,.T.);
#81528=ORIENTED_EDGE('',*,*,#55299,.T.);
#81529=ORIENTED_EDGE('',*,*,#55287,.T.);
#81530=ORIENTED_EDGE('',*,*,#55336,.T.);
#81531=ORIENTED_EDGE('',*,*,#55254,.T.);
#81532=ORIENTED_EDGE('',*,*,#55496,.F.);
#81533=ORIENTED_EDGE('',*,*,#55389,.F.);
#81534=ORIENTED_EDGE('',*,*,#55401,.F.);
#81535=ORIENTED_EDGE('',*,*,#55394,.F.);
#81536=ORIENTED_EDGE('',*,*,#55400,.F.);
#81537=ORIENTED_EDGE('',*,*,#55399,.F.);
#81538=ORIENTED_EDGE('',*,*,#55479,.T.);
#81539=ORIENTED_EDGE('',*,*,#55475,.T.);
#81540=ORIENTED_EDGE('',*,*,#55485,.T.);
#81541=ORIENTED_EDGE('',*,*,#55470,.T.);
#81542=ORIENTED_EDGE('',*,*,#55486,.T.);
#81543=ORIENTED_EDGE('',*,*,#55465,.T.);
#81544=ORIENTED_EDGE('',*,*,#55487,.T.);
#81545=ORIENTED_EDGE('',*,*,#55452,.T.);
#81546=ORIENTED_EDGE('',*,*,#55484,.T.);
#81547=ORIENTED_EDGE('',*,*,#55447,.T.);
#81548=ORIENTED_EDGE('',*,*,#55488,.T.);
#81549=ORIENTED_EDGE('',*,*,#55442,.T.);
#81550=ORIENTED_EDGE('',*,*,#55489,.T.);
#81551=ORIENTED_EDGE('',*,*,#55437,.T.);
#81552=ORIENTED_EDGE('',*,*,#55490,.T.);
#81553=ORIENTED_EDGE('',*,*,#55424,.T.);
#81554=ORIENTED_EDGE('',*,*,#55483,.T.);
#81555=ORIENTED_EDGE('',*,*,#55352,.F.);
#81556=ORIENTED_EDGE('',*,*,#55404,.F.);
#81557=ORIENTED_EDGE('',*,*,#55365,.F.);
#81558=ORIENTED_EDGE('',*,*,#55403,.F.);
#81559=ORIENTED_EDGE('',*,*,#55370,.F.);
#81560=ORIENTED_EDGE('',*,*,#55402,.F.);
#81561=ORIENTED_EDGE('',*,*,#55375,.F.);
#81562=ORIENTED_EDGE('',*,*,#55495,.F.);
#81563=ORIENTED_EDGE('',*,*,#55313,.T.);
#81564=ORIENTED_EDGE('',*,*,#55601,.F.);
#81565=ORIENTED_EDGE('',*,*,#55565,.F.);
#81566=ORIENTED_EDGE('',*,*,#55590,.T.);
#81567=ORIENTED_EDGE('',*,*,#55602,.T.);
#81568=ORIENTED_EDGE('',*,*,#55513,.T.);
#81569=ORIENTED_EDGE('',*,*,#55603,.T.);
#81570=ORIENTED_EDGE('',*,*,#55604,.F.);
#81571=ORIENTED_EDGE('',*,*,#55536,.F.);
#81572=ORIENTED_EDGE('',*,*,#55482,.T.);
#81573=ORIENTED_EDGE('',*,*,#55331,.T.);
#81574=ORIENTED_EDGE('',*,*,#55481,.T.);
#81575=ORIENTED_EDGE('',*,*,#55318,.T.);
#81576=ORIENTED_EDGE('',*,*,#55602,.F.);
#81577=ORIENTED_EDGE('',*,*,#55589,.T.);
#81578=ORIENTED_EDGE('',*,*,#55605,.F.);
#81579=ORIENTED_EDGE('',*,*,#54890,.F.);
#81580=ORIENTED_EDGE('',*,*,#55582,.F.);
#81581=ORIENTED_EDGE('',*,*,#55591,.F.);
#81582=ORIENTED_EDGE('',*,*,#55605,.T.);
#81583=ORIENTED_EDGE('',*,*,#55584,.T.);
#81584=ORIENTED_EDGE('',*,*,#55598,.T.);
#81585=ORIENTED_EDGE('',*,*,#55592,.T.);
#81586=ORIENTED_EDGE('',*,*,#55581,.T.);
#81587=ORIENTED_EDGE('',*,*,#55599,.T.);
#81588=ORIENTED_EDGE('',*,*,#54778,.T.);
#81589=ORIENTED_EDGE('',*,*,#55597,.T.);
#81590=ORIENTED_EDGE('',*,*,#55601,.T.);
#81591=ORIENTED_EDGE('',*,*,#55564,.T.);
#81592=ORIENTED_EDGE('',*,*,#55606,.F.);
#81593=ORIENTED_EDGE('',*,*,#55550,.T.);
#81594=ORIENTED_EDGE('',*,*,#55248,.T.);
#81595=ORIENTED_EDGE('',*,*,#55552,.T.);
#81596=ORIENTED_EDGE('',*,*,#55607,.F.);
#81597=ORIENTED_EDGE('',*,*,#55566,.F.);
#81598=ORIENTED_EDGE('',*,*,#55567,.T.);
#81599=ORIENTED_EDGE('',*,*,#55608,.T.);
#81600=ORIENTED_EDGE('',*,*,#55572,.T.);
#81601=ORIENTED_EDGE('',*,*,#55606,.T.);
#81602=ORIENTED_EDGE('',*,*,#55561,.T.);
#81603=ORIENTED_EDGE('',*,*,#55573,.T.);
#81604=ORIENTED_EDGE('',*,*,#55608,.F.);
#81605=ORIENTED_EDGE('',*,*,#55607,.T.);
#81606=ORIENTED_EDGE('',*,*,#55570,.T.);
#81607=ORIENTED_EDGE('',*,*,#55604,.T.);
#81608=ORIENTED_EDGE('',*,*,#55535,.T.);
#81609=ORIENTED_EDGE('',*,*,#55609,.F.);
#81610=ORIENTED_EDGE('',*,*,#55526,.T.);
#81611=ORIENTED_EDGE('',*,*,#55610,.F.);
#81612=ORIENTED_EDGE('',*,*,#55537,.F.);
#81613=ORIENTED_EDGE('',*,*,#55538,.T.);
#81614=ORIENTED_EDGE('',*,*,#55611,.T.);
#81615=ORIENTED_EDGE('',*,*,#55546,.T.);
#81616=ORIENTED_EDGE('',*,*,#55609,.T.);
#81617=ORIENTED_EDGE('',*,*,#55532,.T.);
#81618=ORIENTED_EDGE('',*,*,#55547,.T.);
#81619=ORIENTED_EDGE('',*,*,#55611,.F.);
#81620=ORIENTED_EDGE('',*,*,#55610,.T.);
#81621=ORIENTED_EDGE('',*,*,#55542,.T.);
#81622=ORIENTED_EDGE('',*,*,#55603,.F.);
#81623=ORIENTED_EDGE('',*,*,#55512,.T.);
#81624=ORIENTED_EDGE('',*,*,#55612,.F.);
#81625=ORIENTED_EDGE('',*,*,#55600,.F.);
#81626=ORIENTED_EDGE('',*,*,#55505,.F.);
#81627=ORIENTED_EDGE('',*,*,#55514,.F.);
#81628=ORIENTED_EDGE('',*,*,#55612,.T.);
#81629=ORIENTED_EDGE('',*,*,#55507,.T.);
#81630=ORIENTED_EDGE('',*,*,#55522,.T.);
#81631=ORIENTED_EDGE('',*,*,#55515,.T.);
#81632=ORIENTED_EDGE('',*,*,#55504,.T.);
#81633=ORIENTED_EDGE('',*,*,#55524,.T.);
#81634=ORIENTED_EDGE('',*,*,#55074,.T.);
#81635=ORIENTED_EDGE('',*,*,#55518,.T.);
#81636=ORIENTED_EDGE('',*,*,#55162,.F.);
#81637=ORIENTED_EDGE('',*,*,#55159,.T.);
#81638=ORIENTED_EDGE('',*,*,#55136,.T.);
#81639=ORIENTED_EDGE('',*,*,#55157,.F.);
#81640=ORIENTED_EDGE('',*,*,#55613,.T.);
#81641=ORIENTED_EDGE('',*,*,#55614,.T.);
#81642=ORIENTED_EDGE('',*,*,#55143,.T.);
#81643=ORIENTED_EDGE('',*,*,#55138,.T.);
#81644=ORIENTED_EDGE('',*,*,#55158,.T.);
#81645=ORIENTED_EDGE('',*,*,#55161,.T.);
#81646=ORIENTED_EDGE('',*,*,#55155,.T.);
#81647=ORIENTED_EDGE('',*,*,#55134,.T.);
#81648=ORIENTED_EDGE('',*,*,#55141,.F.);
#81649=ORIENTED_EDGE('',*,*,#55146,.F.);
#81650=ORIENTED_EDGE('',*,*,#55615,.F.);
#81651=ORIENTED_EDGE('',*,*,#55163,.F.);
#81652=ORIENTED_EDGE('',*,*,#55615,.T.);
#81653=ORIENTED_EDGE('',*,*,#55145,.F.);
#81654=ORIENTED_EDGE('',*,*,#55616,.F.);
#81655=ORIENTED_EDGE('',*,*,#55206,.F.);
#81656=ORIENTED_EDGE('',*,*,#55616,.T.);
#81657=ORIENTED_EDGE('',*,*,#55150,.F.);
#81658=ORIENTED_EDGE('',*,*,#55617,.F.);
#81659=ORIENTED_EDGE('',*,*,#55208,.F.);
#81660=ORIENTED_EDGE('',*,*,#55144,.F.);
#81661=ORIENTED_EDGE('',*,*,#55614,.F.);
#81662=ORIENTED_EDGE('',*,*,#55618,.F.);
#81663=ORIENTED_EDGE('',*,*,#55147,.F.);
#81664=ORIENTED_EDGE('',*,*,#55619,.F.);
#81665=ORIENTED_EDGE('',*,*,#55148,.F.);
#81666=ORIENTED_EDGE('',*,*,#55620,.F.);
#81667=ORIENTED_EDGE('',*,*,#55154,.F.);
#81668=ORIENTED_EDGE('',*,*,#55617,.T.);
#81669=ORIENTED_EDGE('',*,*,#55149,.F.);
#81670=ORIENTED_EDGE('',*,*,#55621,.F.);
#81671=ORIENTED_EDGE('',*,*,#55165,.F.);
#81672=ORIENTED_EDGE('',*,*,#55620,.T.);
#81673=ORIENTED_EDGE('',*,*,#55618,.T.);
#81674=ORIENTED_EDGE('',*,*,#55622,.F.);
#81675=ORIENTED_EDGE('',*,*,#55621,.T.);
#81676=ORIENTED_EDGE('',*,*,#55619,.T.);
#81677=ORIENTED_EDGE('',*,*,#55623,.F.);
#81678=ORIENTED_EDGE('',*,*,#55622,.T.);
#81679=ORIENTED_EDGE('',*,*,#55613,.F.);
#81680=ORIENTED_EDGE('',*,*,#55624,.F.);
#81681=ORIENTED_EDGE('',*,*,#55151,.F.);
#81682=ORIENTED_EDGE('',*,*,#55623,.T.);
#81683=ORIENTED_EDGE('',*,*,#55153,.F.);
#81684=ORIENTED_EDGE('',*,*,#55625,.F.);
#81685=ORIENTED_EDGE('',*,*,#55168,.F.);
#81686=ORIENTED_EDGE('',*,*,#55201,.F.);
#81687=ORIENTED_EDGE('',*,*,#55199,.F.);
#81688=ORIENTED_EDGE('',*,*,#55166,.F.);
#81689=ORIENTED_EDGE('',*,*,#55624,.T.);
#81690=ORIENTED_EDGE('',*,*,#55133,.F.);
#81691=ORIENTED_EDGE('',*,*,#55625,.T.);
#81692=ORIENTED_EDGE('',*,*,#55152,.F.);
#81693=ORIENTED_EDGE('',*,*,#55626,.T.);
#81694=ORIENTED_EDGE('',*,*,#55627,.F.);
#81695=ORIENTED_EDGE('',*,*,#55628,.F.);
#81696=ORIENTED_EDGE('',*,*,#55629,.T.);
#81697=ORIENTED_EDGE('',*,*,#55630,.T.);
#81698=ORIENTED_EDGE('',*,*,#55631,.F.);
#81699=ORIENTED_EDGE('',*,*,#55632,.F.);
#81700=ORIENTED_EDGE('',*,*,#55627,.T.);
#81701=ORIENTED_EDGE('',*,*,#55633,.T.);
#81702=ORIENTED_EDGE('',*,*,#55634,.F.);
#81703=ORIENTED_EDGE('',*,*,#55635,.F.);
#81704=ORIENTED_EDGE('',*,*,#55631,.T.);
#81705=ORIENTED_EDGE('',*,*,#55636,.T.);
#81706=ORIENTED_EDGE('',*,*,#55629,.F.);
#81707=ORIENTED_EDGE('',*,*,#55637,.F.);
#81708=ORIENTED_EDGE('',*,*,#55634,.T.);
#81709=ORIENTED_EDGE('',*,*,#55628,.T.);
#81710=ORIENTED_EDGE('',*,*,#55632,.T.);
#81711=ORIENTED_EDGE('',*,*,#55635,.T.);
#81712=ORIENTED_EDGE('',*,*,#55637,.T.);
#81713=ORIENTED_EDGE('',*,*,#55626,.F.);
#81714=ORIENTED_EDGE('',*,*,#55636,.F.);
#81715=ORIENTED_EDGE('',*,*,#55633,.F.);
#81716=ORIENTED_EDGE('',*,*,#55630,.F.);
#81717=ORIENTED_EDGE('',*,*,#55638,.F.);
#81718=ORIENTED_EDGE('',*,*,#55639,.T.);
#81719=ORIENTED_EDGE('',*,*,#55640,.F.);
#81720=ORIENTED_EDGE('',*,*,#55639,.F.);
#81721=ORIENTED_EDGE('',*,*,#55640,.T.);
#81722=ORIENTED_EDGE('',*,*,#55641,.T.);
#81723=ORIENTED_EDGE('',*,*,#55642,.F.);
#81724=ORIENTED_EDGE('',*,*,#55641,.F.);
#81725=ORIENTED_EDGE('',*,*,#55643,.T.);
#81726=ORIENTED_EDGE('',*,*,#55644,.T.);
#81727=ORIENTED_EDGE('',*,*,#55645,.T.);
#81728=ORIENTED_EDGE('',*,*,#55646,.T.);
#81729=ORIENTED_EDGE('',*,*,#55647,.T.);
#81730=ORIENTED_EDGE('',*,*,#55648,.T.);
#81731=ORIENTED_EDGE('',*,*,#55649,.T.);
#81732=ORIENTED_EDGE('',*,*,#55650,.T.);
#81733=ORIENTED_EDGE('',*,*,#55651,.T.);
#81734=ORIENTED_EDGE('',*,*,#55652,.F.);
#81735=ORIENTED_EDGE('',*,*,#55653,.T.);
#81736=ORIENTED_EDGE('',*,*,#55654,.T.);
#81737=ORIENTED_EDGE('',*,*,#55655,.T.);
#81738=ORIENTED_EDGE('',*,*,#55656,.T.);
#81739=ORIENTED_EDGE('',*,*,#55657,.T.);
#81740=ORIENTED_EDGE('',*,*,#55658,.T.);
#81741=ORIENTED_EDGE('',*,*,#55659,.T.);
#81742=ORIENTED_EDGE('',*,*,#55660,.T.);
#81743=ORIENTED_EDGE('',*,*,#55661,.F.);
#81744=ORIENTED_EDGE('',*,*,#55662,.T.);
#81745=ORIENTED_EDGE('',*,*,#55663,.T.);
#81746=ORIENTED_EDGE('',*,*,#55664,.T.);
#81747=ORIENTED_EDGE('',*,*,#55665,.T.);
#81748=ORIENTED_EDGE('',*,*,#55666,.T.);
#81749=ORIENTED_EDGE('',*,*,#55667,.T.);
#81750=ORIENTED_EDGE('',*,*,#55668,.T.);
#81751=ORIENTED_EDGE('',*,*,#55669,.F.);
#81752=ORIENTED_EDGE('',*,*,#55670,.T.);
#81753=ORIENTED_EDGE('',*,*,#55671,.T.);
#81754=ORIENTED_EDGE('',*,*,#55672,.T.);
#81755=ORIENTED_EDGE('',*,*,#55673,.T.);
#81756=ORIENTED_EDGE('',*,*,#55674,.T.);
#81757=ORIENTED_EDGE('',*,*,#55675,.T.);
#81758=ORIENTED_EDGE('',*,*,#55676,.T.);
#81759=ORIENTED_EDGE('',*,*,#55677,.T.);
#81760=ORIENTED_EDGE('',*,*,#55678,.F.);
#81761=ORIENTED_EDGE('',*,*,#55679,.T.);
#81762=ORIENTED_EDGE('',*,*,#55680,.T.);
#81763=ORIENTED_EDGE('',*,*,#55681,.T.);
#81764=ORIENTED_EDGE('',*,*,#55682,.T.);
#81765=ORIENTED_EDGE('',*,*,#55683,.T.);
#81766=ORIENTED_EDGE('',*,*,#55684,.T.);
#81767=ORIENTED_EDGE('',*,*,#55685,.F.);
#81768=ORIENTED_EDGE('',*,*,#55686,.T.);
#81769=ORIENTED_EDGE('',*,*,#55687,.T.);
#81770=ORIENTED_EDGE('',*,*,#55688,.T.);
#81771=ORIENTED_EDGE('',*,*,#55689,.T.);
#81772=ORIENTED_EDGE('',*,*,#55690,.T.);
#81773=ORIENTED_EDGE('',*,*,#55691,.T.);
#81774=ORIENTED_EDGE('',*,*,#55692,.T.);
#81775=ORIENTED_EDGE('',*,*,#55693,.F.);
#81776=ORIENTED_EDGE('',*,*,#55694,.T.);
#81777=ORIENTED_EDGE('',*,*,#55695,.T.);
#81778=ORIENTED_EDGE('',*,*,#55696,.T.);
#81779=ORIENTED_EDGE('',*,*,#55697,.T.);
#81780=ORIENTED_EDGE('',*,*,#55698,.F.);
#81781=ORIENTED_EDGE('',*,*,#55699,.T.);
#81782=ORIENTED_EDGE('',*,*,#55700,.T.);
#81783=ORIENTED_EDGE('',*,*,#55701,.F.);
#81784=ORIENTED_EDGE('',*,*,#55702,.T.);
#81785=ORIENTED_EDGE('',*,*,#55703,.F.);
#81786=ORIENTED_EDGE('',*,*,#55704,.F.);
#81787=ORIENTED_EDGE('',*,*,#55705,.F.);
#81788=ORIENTED_EDGE('',*,*,#55706,.F.);
#81789=ORIENTED_EDGE('',*,*,#55707,.F.);
#81790=ORIENTED_EDGE('',*,*,#55708,.F.);
#81791=ORIENTED_EDGE('',*,*,#55709,.F.);
#81792=ORIENTED_EDGE('',*,*,#55710,.F.);
#81793=ORIENTED_EDGE('',*,*,#55711,.F.);
#81794=ORIENTED_EDGE('',*,*,#55712,.F.);
#81795=ORIENTED_EDGE('',*,*,#55654,.F.);
#81796=ORIENTED_EDGE('',*,*,#55713,.F.);
#81797=ORIENTED_EDGE('',*,*,#55655,.F.);
#81798=ORIENTED_EDGE('',*,*,#55714,.F.);
#81799=ORIENTED_EDGE('',*,*,#55687,.F.);
#81800=ORIENTED_EDGE('',*,*,#55715,.F.);
#81801=ORIENTED_EDGE('',*,*,#55679,.F.);
#81802=ORIENTED_EDGE('',*,*,#55716,.F.);
#81803=ORIENTED_EDGE('',*,*,#55663,.F.);
#81804=ORIENTED_EDGE('',*,*,#55717,.F.);
#81805=ORIENTED_EDGE('',*,*,#55672,.F.);
#81806=ORIENTED_EDGE('',*,*,#55718,.F.);
#81807=ORIENTED_EDGE('',*,*,#55719,.F.);
#81808=ORIENTED_EDGE('',*,*,#55720,.F.);
#81809=ORIENTED_EDGE('',*,*,#55721,.F.);
#81810=ORIENTED_EDGE('',*,*,#55722,.F.);
#81811=ORIENTED_EDGE('',*,*,#55723,.F.);
#81812=ORIENTED_EDGE('',*,*,#55724,.F.);
#81813=ORIENTED_EDGE('',*,*,#55725,.F.);
#81814=ORIENTED_EDGE('',*,*,#55726,.F.);
#81815=ORIENTED_EDGE('',*,*,#55727,.F.);
#81816=ORIENTED_EDGE('',*,*,#55699,.F.);
#81817=ORIENTED_EDGE('',*,*,#55728,.F.);
#81818=ORIENTED_EDGE('',*,*,#55729,.F.);
#81819=ORIENTED_EDGE('',*,*,#55642,.T.);
#81820=ORIENTED_EDGE('',*,*,#55701,.T.);
#81821=ORIENTED_EDGE('',*,*,#55730,.T.);
#81822=ORIENTED_EDGE('',*,*,#55731,.T.);
#81823=ORIENTED_EDGE('',*,*,#55732,.T.);
#81824=ORIENTED_EDGE('',*,*,#55733,.F.);
#81825=ORIENTED_EDGE('',*,*,#55734,.F.);
#81826=ORIENTED_EDGE('',*,*,#55735,.F.);
#81827=ORIENTED_EDGE('',*,*,#55736,.F.);
#81828=ORIENTED_EDGE('',*,*,#55704,.T.);
#81829=ORIENTED_EDGE('',*,*,#55737,.F.);
#81830=ORIENTED_EDGE('',*,*,#55738,.F.);
#81831=ORIENTED_EDGE('',*,*,#55726,.T.);
#81832=ORIENTED_EDGE('',*,*,#55739,.F.);
#81833=ORIENTED_EDGE('',*,*,#55740,.F.);
#81834=ORIENTED_EDGE('',*,*,#55741,.F.);
#81835=ORIENTED_EDGE('',*,*,#55742,.F.);
#81836=ORIENTED_EDGE('',*,*,#55743,.F.);
#81837=ORIENTED_EDGE('',*,*,#55724,.T.);
#81838=ORIENTED_EDGE('',*,*,#55744,.F.);
#81839=ORIENTED_EDGE('',*,*,#55745,.F.);
#81840=ORIENTED_EDGE('',*,*,#55746,.F.);
#81841=ORIENTED_EDGE('',*,*,#55747,.F.);
#81842=ORIENTED_EDGE('',*,*,#55748,.F.);
#81843=ORIENTED_EDGE('',*,*,#55722,.T.);
#81844=ORIENTED_EDGE('',*,*,#55749,.F.);
#81845=ORIENTED_EDGE('',*,*,#55750,.F.);
#81846=ORIENTED_EDGE('',*,*,#55751,.F.);
#81847=ORIENTED_EDGE('',*,*,#55752,.F.);
#81848=ORIENTED_EDGE('',*,*,#55643,.F.);
#81849=ORIENTED_EDGE('',*,*,#55753,.F.);
#81850=ORIENTED_EDGE('',*,*,#55754,.F.);
#81851=ORIENTED_EDGE('',*,*,#55755,.F.);
#81852=ORIENTED_EDGE('',*,*,#55708,.T.);
#81853=ORIENTED_EDGE('',*,*,#55756,.F.);
#81854=ORIENTED_EDGE('',*,*,#55757,.F.);
#81855=ORIENTED_EDGE('',*,*,#55706,.T.);
#81856=ORIENTED_EDGE('',*,*,#55758,.F.);
#81857=ORIENTED_EDGE('',*,*,#55759,.F.);
#81858=ORIENTED_EDGE('',*,*,#55760,.F.);
#81859=ORIENTED_EDGE('',*,*,#55761,.F.);
#81860=ORIENTED_EDGE('',*,*,#55762,.F.);
#81861=ORIENTED_EDGE('',*,*,#55763,.F.);
#81862=ORIENTED_EDGE('',*,*,#55764,.F.);
#81863=ORIENTED_EDGE('',*,*,#55765,.F.);
#81864=ORIENTED_EDGE('',*,*,#55710,.T.);
#81865=ORIENTED_EDGE('',*,*,#55766,.F.);
#81866=ORIENTED_EDGE('',*,*,#55767,.F.);
#81867=ORIENTED_EDGE('',*,*,#55768,.F.);
#81868=ORIENTED_EDGE('',*,*,#55769,.F.);
#81869=ORIENTED_EDGE('',*,*,#55656,.F.);
#81870=ORIENTED_EDGE('',*,*,#55713,.T.);
#81871=ORIENTED_EDGE('',*,*,#55653,.F.);
#81872=ORIENTED_EDGE('',*,*,#55647,.F.);
#81873=ORIENTED_EDGE('',*,*,#55712,.T.);
#81874=ORIENTED_EDGE('',*,*,#55770,.F.);
#81875=ORIENTED_EDGE('',*,*,#55771,.F.);
#81876=ORIENTED_EDGE('',*,*,#55772,.F.);
#81877=ORIENTED_EDGE('',*,*,#55773,.F.);
#81878=ORIENTED_EDGE('',*,*,#55774,.F.);
#81879=ORIENTED_EDGE('',*,*,#55775,.F.);
#81880=ORIENTED_EDGE('',*,*,#55776,.F.);
#81881=ORIENTED_EDGE('',*,*,#55688,.F.);
#81882=ORIENTED_EDGE('',*,*,#55714,.T.);
#81883=ORIENTED_EDGE('',*,*,#55662,.F.);
#81884=ORIENTED_EDGE('',*,*,#55777,.F.);
#81885=ORIENTED_EDGE('',*,*,#55778,.F.);
#81886=ORIENTED_EDGE('',*,*,#55779,.F.);
#81887=ORIENTED_EDGE('',*,*,#55673,.F.);
#81888=ORIENTED_EDGE('',*,*,#55717,.T.);
#81889=ORIENTED_EDGE('',*,*,#55670,.F.);
#81890=ORIENTED_EDGE('',*,*,#55664,.F.);
#81891=ORIENTED_EDGE('',*,*,#55716,.T.);
#81892=ORIENTED_EDGE('',*,*,#55686,.F.);
#81893=ORIENTED_EDGE('',*,*,#55780,.F.);
#81894=ORIENTED_EDGE('',*,*,#55781,.F.);
#81895=ORIENTED_EDGE('',*,*,#55782,.F.);
#81896=ORIENTED_EDGE('',*,*,#55783,.F.);
#81897=ORIENTED_EDGE('',*,*,#55784,.F.);
#81898=ORIENTED_EDGE('',*,*,#55785,.F.);
#81899=ORIENTED_EDGE('',*,*,#55786,.F.);
#81900=ORIENTED_EDGE('',*,*,#55718,.T.);
#81901=ORIENTED_EDGE('',*,*,#55671,.F.);
#81902=ORIENTED_EDGE('',*,*,#55680,.F.);
#81903=ORIENTED_EDGE('',*,*,#55715,.T.);
#81904=ORIENTED_EDGE('',*,*,#55694,.F.);
#81905=ORIENTED_EDGE('',*,*,#55787,.F.);
#81906=ORIENTED_EDGE('',*,*,#55788,.F.);
#81907=ORIENTED_EDGE('',*,*,#55789,.F.);
#81908=ORIENTED_EDGE('',*,*,#55790,.F.);
#81909=ORIENTED_EDGE('',*,*,#55791,.F.);
#81910=ORIENTED_EDGE('',*,*,#55792,.F.);
#81911=ORIENTED_EDGE('',*,*,#55734,.T.);
#81912=ORIENTED_EDGE('',*,*,#55793,.F.);
#81913=ORIENTED_EDGE('',*,*,#55741,.T.);
#81914=ORIENTED_EDGE('',*,*,#55794,.F.);
#81915=ORIENTED_EDGE('',*,*,#55795,.F.);
#81916=ORIENTED_EDGE('',*,*,#55796,.F.);
#81917=ORIENTED_EDGE('',*,*,#55746,.T.);
#81918=ORIENTED_EDGE('',*,*,#55797,.F.);
#81919=ORIENTED_EDGE('',*,*,#55798,.F.);
#81920=ORIENTED_EDGE('',*,*,#55799,.F.);
#81921=ORIENTED_EDGE('',*,*,#55751,.T.);
#81922=ORIENTED_EDGE('',*,*,#55800,.F.);
#81923=ORIENTED_EDGE('',*,*,#55801,.F.);
#81924=ORIENTED_EDGE('',*,*,#55646,.F.);
#81925=ORIENTED_EDGE('',*,*,#55802,.F.);
#81926=ORIENTED_EDGE('',*,*,#55803,.F.);
#81927=ORIENTED_EDGE('',*,*,#55753,.T.);
#81928=ORIENTED_EDGE('',*,*,#55804,.F.);
#81929=ORIENTED_EDGE('',*,*,#55760,.T.);
#81930=ORIENTED_EDGE('',*,*,#55805,.F.);
#81931=ORIENTED_EDGE('',*,*,#55806,.F.);
#81932=ORIENTED_EDGE('',*,*,#55807,.F.);
#81933=ORIENTED_EDGE('',*,*,#55808,.F.);
#81934=ORIENTED_EDGE('',*,*,#55809,.F.);
#81935=ORIENTED_EDGE('',*,*,#55763,.T.);
#81936=ORIENTED_EDGE('',*,*,#55810,.F.);
#81937=ORIENTED_EDGE('',*,*,#55811,.F.);
#81938=ORIENTED_EDGE('',*,*,#55812,.F.);
#81939=ORIENTED_EDGE('',*,*,#55768,.T.);
#81940=ORIENTED_EDGE('',*,*,#55813,.F.);
#81941=ORIENTED_EDGE('',*,*,#55772,.T.);
#81942=ORIENTED_EDGE('',*,*,#55814,.F.);
#81943=ORIENTED_EDGE('',*,*,#55815,.F.);
#81944=ORIENTED_EDGE('',*,*,#55816,.F.);
#81945=ORIENTED_EDGE('',*,*,#55817,.F.);
#81946=ORIENTED_EDGE('',*,*,#55818,.F.);
#81947=ORIENTED_EDGE('',*,*,#55775,.T.);
#81948=ORIENTED_EDGE('',*,*,#55819,.F.);
#81949=ORIENTED_EDGE('',*,*,#55820,.F.);
#81950=ORIENTED_EDGE('',*,*,#55821,.F.);
#81951=ORIENTED_EDGE('',*,*,#55778,.T.);
#81952=ORIENTED_EDGE('',*,*,#55822,.F.);
#81953=ORIENTED_EDGE('',*,*,#55781,.T.);
#81954=ORIENTED_EDGE('',*,*,#55823,.F.);
#81955=ORIENTED_EDGE('',*,*,#55824,.F.);
#81956=ORIENTED_EDGE('',*,*,#55825,.F.);
#81957=ORIENTED_EDGE('',*,*,#55826,.F.);
#81958=ORIENTED_EDGE('',*,*,#55827,.F.);
#81959=ORIENTED_EDGE('',*,*,#55784,.T.);
#81960=ORIENTED_EDGE('',*,*,#55828,.F.);
#81961=ORIENTED_EDGE('',*,*,#55788,.T.);
#81962=ORIENTED_EDGE('',*,*,#55829,.F.);
#81963=ORIENTED_EDGE('',*,*,#55830,.F.);
#81964=ORIENTED_EDGE('',*,*,#55831,.F.);
#81965=ORIENTED_EDGE('',*,*,#55832,.F.);
#81966=ORIENTED_EDGE('',*,*,#55833,.F.);
#81967=ORIENTED_EDGE('',*,*,#55834,.F.);
#81968=ORIENTED_EDGE('',*,*,#55835,.F.);
#81969=ORIENTED_EDGE('',*,*,#55791,.T.);
#81970=ORIENTED_EDGE('',*,*,#55836,.F.);
#81971=ORIENTED_EDGE('',*,*,#55837,.F.);
#81972=ORIENTED_EDGE('',*,*,#55795,.T.);
#81973=ORIENTED_EDGE('',*,*,#55838,.F.);
#81974=ORIENTED_EDGE('',*,*,#55839,.F.);
#81975=ORIENTED_EDGE('',*,*,#55840,.F.);
#81976=ORIENTED_EDGE('',*,*,#55841,.F.);
#81977=ORIENTED_EDGE('',*,*,#55842,.F.);
#81978=ORIENTED_EDGE('',*,*,#55798,.T.);
#81979=ORIENTED_EDGE('',*,*,#55843,.F.);
#81980=ORIENTED_EDGE('',*,*,#55844,.F.);
#81981=ORIENTED_EDGE('',*,*,#55845,.F.);
#81982=ORIENTED_EDGE('',*,*,#55846,.F.);
#81983=ORIENTED_EDGE('',*,*,#55847,.F.);
#81984=ORIENTED_EDGE('',*,*,#55801,.T.);
#81985=ORIENTED_EDGE('',*,*,#55848,.F.);
#81986=ORIENTED_EDGE('',*,*,#55849,.F.);
#81987=ORIENTED_EDGE('',*,*,#55850,.F.);
#81988=ORIENTED_EDGE('',*,*,#55645,.F.);
#81989=ORIENTED_EDGE('',*,*,#55851,.F.);
#81990=ORIENTED_EDGE('',*,*,#55852,.F.);
#81991=ORIENTED_EDGE('',*,*,#55853,.F.);
#81992=ORIENTED_EDGE('',*,*,#55854,.F.);
#81993=ORIENTED_EDGE('',*,*,#55802,.T.);
#81994=ORIENTED_EDGE('',*,*,#55855,.F.);
#81995=ORIENTED_EDGE('',*,*,#55856,.F.);
#81996=ORIENTED_EDGE('',*,*,#55806,.T.);
#81997=ORIENTED_EDGE('',*,*,#55857,.F.);
#81998=ORIENTED_EDGE('',*,*,#55858,.F.);
#81999=ORIENTED_EDGE('',*,*,#55859,.F.);
#82000=ORIENTED_EDGE('',*,*,#55860,.F.);
#82001=ORIENTED_EDGE('',*,*,#55861,.F.);
#82002=ORIENTED_EDGE('',*,*,#55862,.F.);
#82003=ORIENTED_EDGE('',*,*,#55863,.F.);
#82004=ORIENTED_EDGE('',*,*,#55864,.F.);
#82005=ORIENTED_EDGE('',*,*,#55808,.T.);
#82006=ORIENTED_EDGE('',*,*,#55865,.F.);
#82007=ORIENTED_EDGE('',*,*,#55651,.F.);
#82008=ORIENTED_EDGE('',*,*,#55866,.F.);
#82009=ORIENTED_EDGE('',*,*,#55658,.F.);
#82010=ORIENTED_EDGE('',*,*,#55867,.F.);
#82011=ORIENTED_EDGE('',*,*,#55811,.T.);
#82012=ORIENTED_EDGE('',*,*,#55649,.F.);
#82013=ORIENTED_EDGE('',*,*,#55868,.F.);
#82014=ORIENTED_EDGE('',*,*,#55815,.T.);
#82015=ORIENTED_EDGE('',*,*,#55869,.F.);
#82016=ORIENTED_EDGE('',*,*,#55870,.F.);
#82017=ORIENTED_EDGE('',*,*,#55871,.F.);
#82018=ORIENTED_EDGE('',*,*,#55872,.F.);
#82019=ORIENTED_EDGE('',*,*,#55660,.F.);
#82020=ORIENTED_EDGE('',*,*,#55873,.F.);
#82021=ORIENTED_EDGE('',*,*,#55690,.F.);
#82022=ORIENTED_EDGE('',*,*,#55874,.F.);
#82023=ORIENTED_EDGE('',*,*,#55817,.T.);
#82024=ORIENTED_EDGE('',*,*,#55875,.F.);
#82025=ORIENTED_EDGE('',*,*,#55668,.F.);
#82026=ORIENTED_EDGE('',*,*,#55876,.F.);
#82027=ORIENTED_EDGE('',*,*,#55675,.F.);
#82028=ORIENTED_EDGE('',*,*,#55877,.F.);
#82029=ORIENTED_EDGE('',*,*,#55820,.T.);
#82030=ORIENTED_EDGE('',*,*,#55666,.F.);
#82031=ORIENTED_EDGE('',*,*,#55878,.F.);
#82032=ORIENTED_EDGE('',*,*,#55824,.T.);
#82033=ORIENTED_EDGE('',*,*,#55879,.F.);
#82034=ORIENTED_EDGE('',*,*,#55684,.F.);
#82035=ORIENTED_EDGE('',*,*,#55880,.F.);
#82036=ORIENTED_EDGE('',*,*,#55881,.F.);
#82037=ORIENTED_EDGE('',*,*,#55677,.F.);
#82038=ORIENTED_EDGE('',*,*,#55882,.F.);
#82039=ORIENTED_EDGE('',*,*,#55883,.F.);
#82040=ORIENTED_EDGE('',*,*,#55884,.F.);
#82041=ORIENTED_EDGE('',*,*,#55826,.T.);
#82042=ORIENTED_EDGE('',*,*,#55682,.F.);
#82043=ORIENTED_EDGE('',*,*,#55885,.F.);
#82044=ORIENTED_EDGE('',*,*,#55830,.T.);
#82045=ORIENTED_EDGE('',*,*,#55886,.F.);
#82046=ORIENTED_EDGE('',*,*,#55692,.F.);
#82047=ORIENTED_EDGE('',*,*,#55887,.F.);
#82048=ORIENTED_EDGE('',*,*,#55888,.F.);
#82049=ORIENTED_EDGE('',*,*,#55720,.T.);
#82050=ORIENTED_EDGE('',*,*,#55889,.F.);
#82051=ORIENTED_EDGE('',*,*,#55890,.F.);
#82052=ORIENTED_EDGE('',*,*,#55891,.F.);
#82053=ORIENTED_EDGE('',*,*,#55695,.F.);
#82054=ORIENTED_EDGE('',*,*,#55696,.F.);
#82055=ORIENTED_EDGE('',*,*,#55891,.T.);
#82056=ORIENTED_EDGE('',*,*,#55892,.F.);
#82057=ORIENTED_EDGE('',*,*,#55893,.F.);
#82058=ORIENTED_EDGE('',*,*,#55894,.F.);
#82059=ORIENTED_EDGE('',*,*,#55697,.F.);
#82060=ORIENTED_EDGE('',*,*,#55893,.T.);
#82061=ORIENTED_EDGE('',*,*,#55895,.F.);
#82062=ORIENTED_EDGE('',*,*,#55896,.F.);
#82063=ORIENTED_EDGE('',*,*,#55897,.F.);
#82064=ORIENTED_EDGE('',*,*,#55898,.F.);
#82065=ORIENTED_EDGE('',*,*,#55840,.T.);
#82066=ORIENTED_EDGE('',*,*,#55899,.F.);
#82067=ORIENTED_EDGE('',*,*,#55845,.T.);
#82068=ORIENTED_EDGE('',*,*,#55900,.F.);
#82069=ORIENTED_EDGE('',*,*,#55850,.T.);
#82070=ORIENTED_EDGE('',*,*,#55901,.F.);
#82071=ORIENTED_EDGE('',*,*,#55897,.T.);
#82072=ORIENTED_EDGE('',*,*,#55902,.F.);
#82073=ORIENTED_EDGE('',*,*,#55882,.T.);
#82074=ORIENTED_EDGE('',*,*,#55676,.F.);
#82075=ORIENTED_EDGE('',*,*,#55876,.T.);
#82076=ORIENTED_EDGE('',*,*,#55667,.F.);
#82077=ORIENTED_EDGE('',*,*,#55880,.T.);
#82078=ORIENTED_EDGE('',*,*,#55683,.F.);
#82079=ORIENTED_EDGE('',*,*,#55887,.T.);
#82080=ORIENTED_EDGE('',*,*,#55691,.F.);
#82081=ORIENTED_EDGE('',*,*,#55873,.T.);
#82082=ORIENTED_EDGE('',*,*,#55659,.F.);
#82083=ORIENTED_EDGE('',*,*,#55866,.T.);
#82084=ORIENTED_EDGE('',*,*,#55650,.F.);
#82085=ORIENTED_EDGE('',*,*,#55871,.T.);
#82086=ORIENTED_EDGE('',*,*,#55903,.F.);
#82087=ORIENTED_EDGE('',*,*,#55862,.T.);
#82088=ORIENTED_EDGE('',*,*,#55904,.F.);
#82089=ORIENTED_EDGE('',*,*,#55852,.T.);
#82090=ORIENTED_EDGE('',*,*,#55905,.F.);
#82091=ORIENTED_EDGE('',*,*,#55859,.T.);
#82092=ORIENTED_EDGE('',*,*,#55906,.F.);
#82093=ORIENTED_EDGE('',*,*,#55833,.T.);
#82094=ORIENTED_EDGE('',*,*,#55638,.T.);
#82095=ORIENTED_EDGE('',*,*,#55890,.T.);
#82096=ORIENTED_EDGE('',*,*,#55907,.T.);
#82097=ORIENTED_EDGE('',*,*,#55895,.T.);
#82098=ORIENTED_EDGE('',*,*,#55892,.T.);
#82099=ORIENTED_EDGE('',*,*,#55785,.T.);
#82100=ORIENTED_EDGE('',*,*,#55827,.T.);
#82101=ORIENTED_EDGE('',*,*,#55884,.T.);
#82102=ORIENTED_EDGE('',*,*,#55908,.F.);
#82103=ORIENTED_EDGE('',*,*,#55889,.T.);
#82104=ORIENTED_EDGE('',*,*,#55719,.T.);
#82105=ORIENTED_EDGE('',*,*,#55786,.T.);
#82106=ORIENTED_EDGE('',*,*,#55908,.T.);
#82107=ORIENTED_EDGE('',*,*,#55883,.T.);
#82108=ORIENTED_EDGE('',*,*,#55902,.T.);
#82109=ORIENTED_EDGE('',*,*,#55896,.T.);
#82110=ORIENTED_EDGE('',*,*,#55907,.F.);
#82111=ORIENTED_EDGE('',*,*,#55750,.T.);
#82112=ORIENTED_EDGE('',*,*,#55909,.T.);
#82113=ORIENTED_EDGE('',*,*,#55848,.T.);
#82114=ORIENTED_EDGE('',*,*,#55800,.T.);
#82115=ORIENTED_EDGE('',*,*,#55749,.T.);
#82116=ORIENTED_EDGE('',*,*,#55721,.T.);
#82117=ORIENTED_EDGE('',*,*,#55888,.T.);
#82118=ORIENTED_EDGE('',*,*,#55698,.T.);
#82119=ORIENTED_EDGE('',*,*,#55894,.T.);
#82120=ORIENTED_EDGE('',*,*,#55901,.T.);
#82121=ORIENTED_EDGE('',*,*,#55849,.T.);
#82122=ORIENTED_EDGE('',*,*,#55909,.F.);
#82123=ORIENTED_EDGE('',*,*,#55787,.T.);
#82124=ORIENTED_EDGE('',*,*,#55693,.T.);
#82125=ORIENTED_EDGE('',*,*,#55886,.T.);
#82126=ORIENTED_EDGE('',*,*,#55829,.T.);
#82127=ORIENTED_EDGE('',*,*,#55776,.T.);
#82128=ORIENTED_EDGE('',*,*,#55818,.T.);
#82129=ORIENTED_EDGE('',*,*,#55874,.T.);
#82130=ORIENTED_EDGE('',*,*,#55689,.F.);
#82131=ORIENTED_EDGE('',*,*,#55780,.T.);
#82132=ORIENTED_EDGE('',*,*,#55685,.T.);
#82133=ORIENTED_EDGE('',*,*,#55879,.T.);
#82134=ORIENTED_EDGE('',*,*,#55823,.T.);
#82135=ORIENTED_EDGE('',*,*,#55789,.T.);
#82136=ORIENTED_EDGE('',*,*,#55828,.T.);
#82137=ORIENTED_EDGE('',*,*,#55885,.T.);
#82138=ORIENTED_EDGE('',*,*,#55681,.F.);
#82139=ORIENTED_EDGE('',*,*,#55783,.T.);
#82140=ORIENTED_EDGE('',*,*,#55678,.T.);
#82141=ORIENTED_EDGE('',*,*,#55881,.T.);
#82142=ORIENTED_EDGE('',*,*,#55825,.T.);
#82143=ORIENTED_EDGE('',*,*,#55779,.T.);
#82144=ORIENTED_EDGE('',*,*,#55821,.T.);
#82145=ORIENTED_EDGE('',*,*,#55877,.T.);
#82146=ORIENTED_EDGE('',*,*,#55674,.F.);
#82147=ORIENTED_EDGE('',*,*,#55777,.T.);
#82148=ORIENTED_EDGE('',*,*,#55669,.T.);
#82149=ORIENTED_EDGE('',*,*,#55875,.T.);
#82150=ORIENTED_EDGE('',*,*,#55819,.T.);
#82151=ORIENTED_EDGE('',*,*,#55782,.T.);
#82152=ORIENTED_EDGE('',*,*,#55822,.T.);
#82153=ORIENTED_EDGE('',*,*,#55878,.T.);
#82154=ORIENTED_EDGE('',*,*,#55665,.F.);
#82155=ORIENTED_EDGE('',*,*,#55771,.T.);
#82156=ORIENTED_EDGE('',*,*,#55910,.T.);
#82157=ORIENTED_EDGE('',*,*,#55869,.T.);
#82158=ORIENTED_EDGE('',*,*,#55814,.T.);
#82159=ORIENTED_EDGE('',*,*,#55764,.T.);
#82160=ORIENTED_EDGE('',*,*,#55809,.T.);
#82161=ORIENTED_EDGE('',*,*,#55864,.T.);
#82162=ORIENTED_EDGE('',*,*,#55911,.F.);
#82163=ORIENTED_EDGE('',*,*,#55770,.T.);
#82164=ORIENTED_EDGE('',*,*,#55711,.T.);
#82165=ORIENTED_EDGE('',*,*,#55765,.T.);
#82166=ORIENTED_EDGE('',*,*,#55911,.T.);
#82167=ORIENTED_EDGE('',*,*,#55863,.T.);
#82168=ORIENTED_EDGE('',*,*,#55903,.T.);
#82169=ORIENTED_EDGE('',*,*,#55870,.T.);
#82170=ORIENTED_EDGE('',*,*,#55910,.F.);
#82171=ORIENTED_EDGE('',*,*,#55774,.T.);
#82172=ORIENTED_EDGE('',*,*,#55661,.T.);
#82173=ORIENTED_EDGE('',*,*,#55872,.T.);
#82174=ORIENTED_EDGE('',*,*,#55816,.T.);
#82175=ORIENTED_EDGE('',*,*,#55769,.T.);
#82176=ORIENTED_EDGE('',*,*,#55812,.T.);
#82177=ORIENTED_EDGE('',*,*,#55867,.T.);
#82178=ORIENTED_EDGE('',*,*,#55657,.F.);
#82179=ORIENTED_EDGE('',*,*,#55767,.T.);
#82180=ORIENTED_EDGE('',*,*,#55652,.T.);
#82181=ORIENTED_EDGE('',*,*,#55865,.T.);
#82182=ORIENTED_EDGE('',*,*,#55810,.T.);
#82183=ORIENTED_EDGE('',*,*,#55773,.T.);
#82184=ORIENTED_EDGE('',*,*,#55813,.T.);
#82185=ORIENTED_EDGE('',*,*,#55868,.T.);
#82186=ORIENTED_EDGE('',*,*,#55648,.F.);
#82187=ORIENTED_EDGE('',*,*,#55759,.T.);
#82188=ORIENTED_EDGE('',*,*,#55912,.T.);
#82189=ORIENTED_EDGE('',*,*,#55857,.T.);
#82190=ORIENTED_EDGE('',*,*,#55805,.T.);
#82191=ORIENTED_EDGE('',*,*,#55735,.T.);
#82192=ORIENTED_EDGE('',*,*,#55792,.T.);
#82193=ORIENTED_EDGE('',*,*,#55835,.T.);
#82194=ORIENTED_EDGE('',*,*,#55913,.F.);
#82195=ORIENTED_EDGE('',*,*,#55758,.T.);
#82196=ORIENTED_EDGE('',*,*,#55705,.T.);
#82197=ORIENTED_EDGE('',*,*,#55736,.T.);
#82198=ORIENTED_EDGE('',*,*,#55913,.T.);
#82199=ORIENTED_EDGE('',*,*,#55834,.T.);
#82200=ORIENTED_EDGE('',*,*,#55906,.T.);
#82201=ORIENTED_EDGE('',*,*,#55858,.T.);
#82202=ORIENTED_EDGE('',*,*,#55912,.F.);
#82203=ORIENTED_EDGE('',*,*,#55762,.T.);
#82204=ORIENTED_EDGE('',*,*,#55914,.T.);
#82205=ORIENTED_EDGE('',*,*,#55860,.T.);
#82206=ORIENTED_EDGE('',*,*,#55807,.T.);
#82207=ORIENTED_EDGE('',*,*,#55754,.T.);
#82208=ORIENTED_EDGE('',*,*,#55803,.T.);
#82209=ORIENTED_EDGE('',*,*,#55854,.T.);
#82210=ORIENTED_EDGE('',*,*,#55915,.F.);
#82211=ORIENTED_EDGE('',*,*,#55766,.T.);
#82212=ORIENTED_EDGE('',*,*,#55709,.T.);
#82213=ORIENTED_EDGE('',*,*,#55755,.T.);
#82214=ORIENTED_EDGE('',*,*,#55915,.T.);
#82215=ORIENTED_EDGE('',*,*,#55853,.T.);
#82216=ORIENTED_EDGE('',*,*,#55904,.T.);
#82217=ORIENTED_EDGE('',*,*,#55861,.T.);
#82218=ORIENTED_EDGE('',*,*,#55914,.F.);
#82219=ORIENTED_EDGE('',*,*,#55761,.T.);
#82220=ORIENTED_EDGE('',*,*,#55804,.T.);
#82221=ORIENTED_EDGE('',*,*,#55856,.T.);
#82222=ORIENTED_EDGE('',*,*,#55916,.F.);
#82223=ORIENTED_EDGE('',*,*,#55756,.T.);
#82224=ORIENTED_EDGE('',*,*,#55707,.T.);
#82225=ORIENTED_EDGE('',*,*,#55757,.T.);
#82226=ORIENTED_EDGE('',*,*,#55916,.T.);
#82227=ORIENTED_EDGE('',*,*,#55855,.T.);
#82228=ORIENTED_EDGE('',*,*,#55905,.T.);
#82229=ORIENTED_EDGE('',*,*,#55851,.T.);
#82230=ORIENTED_EDGE('',*,*,#55644,.F.);
#82231=ORIENTED_EDGE('',*,*,#55745,.T.);
#82232=ORIENTED_EDGE('',*,*,#55917,.T.);
#82233=ORIENTED_EDGE('',*,*,#55843,.T.);
#82234=ORIENTED_EDGE('',*,*,#55797,.T.);
#82235=ORIENTED_EDGE('',*,*,#55752,.T.);
#82236=ORIENTED_EDGE('',*,*,#55799,.T.);
#82237=ORIENTED_EDGE('',*,*,#55847,.T.);
#82238=ORIENTED_EDGE('',*,*,#55918,.F.);
#82239=ORIENTED_EDGE('',*,*,#55744,.T.);
#82240=ORIENTED_EDGE('',*,*,#55723,.T.);
#82241=ORIENTED_EDGE('',*,*,#55748,.T.);
#82242=ORIENTED_EDGE('',*,*,#55918,.T.);
#82243=ORIENTED_EDGE('',*,*,#55846,.T.);
#82244=ORIENTED_EDGE('',*,*,#55900,.T.);
#82245=ORIENTED_EDGE('',*,*,#55844,.T.);
#82246=ORIENTED_EDGE('',*,*,#55917,.F.);
#82247=ORIENTED_EDGE('',*,*,#55740,.T.);
#82248=ORIENTED_EDGE('',*,*,#55919,.T.);
#82249=ORIENTED_EDGE('',*,*,#55838,.T.);
#82250=ORIENTED_EDGE('',*,*,#55794,.T.);
#82251=ORIENTED_EDGE('',*,*,#55747,.T.);
#82252=ORIENTED_EDGE('',*,*,#55796,.T.);
#82253=ORIENTED_EDGE('',*,*,#55842,.T.);
#82254=ORIENTED_EDGE('',*,*,#55920,.F.);
#82255=ORIENTED_EDGE('',*,*,#55739,.T.);
#82256=ORIENTED_EDGE('',*,*,#55725,.T.);
#82257=ORIENTED_EDGE('',*,*,#55743,.T.);
#82258=ORIENTED_EDGE('',*,*,#55920,.T.);
#82259=ORIENTED_EDGE('',*,*,#55841,.T.);
#82260=ORIENTED_EDGE('',*,*,#55899,.T.);
#82261=ORIENTED_EDGE('',*,*,#55839,.T.);
#82262=ORIENTED_EDGE('',*,*,#55919,.F.);
#82263=ORIENTED_EDGE('',*,*,#55733,.T.);
#82264=ORIENTED_EDGE('',*,*,#55921,.T.);
#82265=ORIENTED_EDGE('',*,*,#55831,.T.);
#82266=ORIENTED_EDGE('',*,*,#55790,.T.);
#82267=ORIENTED_EDGE('',*,*,#55742,.T.);
#82268=ORIENTED_EDGE('',*,*,#55793,.T.);
#82269=ORIENTED_EDGE('',*,*,#55837,.T.);
#82270=ORIENTED_EDGE('',*,*,#55922,.F.);
#82271=ORIENTED_EDGE('',*,*,#55737,.T.);
#82272=ORIENTED_EDGE('',*,*,#55703,.T.);
#82273=ORIENTED_EDGE('',*,*,#55738,.T.);
#82274=ORIENTED_EDGE('',*,*,#55922,.T.);
#82275=ORIENTED_EDGE('',*,*,#55836,.T.);
#82276=ORIENTED_EDGE('',*,*,#55898,.T.);
#82277=ORIENTED_EDGE('',*,*,#55832,.T.);
#82278=ORIENTED_EDGE('',*,*,#55921,.F.);
#82279=ORIENTED_EDGE('',*,*,#55729,.T.);
#82280=ORIENTED_EDGE('',*,*,#55923,.T.);
#82281=ORIENTED_EDGE('',*,*,#55731,.F.);
#82282=ORIENTED_EDGE('',*,*,#55924,.F.);
#82283=ORIENTED_EDGE('',*,*,#55727,.T.);
#82284=ORIENTED_EDGE('',*,*,#55924,.T.);
#82285=ORIENTED_EDGE('',*,*,#55730,.F.);
#82286=ORIENTED_EDGE('',*,*,#55700,.F.);
#82287=ORIENTED_EDGE('',*,*,#55728,.T.);
#82288=ORIENTED_EDGE('',*,*,#55702,.F.);
#82289=ORIENTED_EDGE('',*,*,#55732,.F.);
#82290=ORIENTED_EDGE('',*,*,#55923,.F.);
#82291=ORIENTED_EDGE('',*,*,#55925,.T.);
#82292=ORIENTED_EDGE('',*,*,#55926,.T.);
#82293=ORIENTED_EDGE('',*,*,#55927,.T.);
#82294=ORIENTED_EDGE('',*,*,#55926,.F.);
#82295=ORIENTED_EDGE('',*,*,#55928,.F.);
#82296=ORIENTED_EDGE('',*,*,#55929,.T.);
#82297=ORIENTED_EDGE('',*,*,#55930,.F.);
#82298=ORIENTED_EDGE('',*,*,#55931,.F.);
#82299=ORIENTED_EDGE('',*,*,#55932,.F.);
#82300=ORIENTED_EDGE('',*,*,#55933,.T.);
#82301=ORIENTED_EDGE('',*,*,#55934,.F.);
#82302=ORIENTED_EDGE('',*,*,#55929,.F.);
#82303=ORIENTED_EDGE('',*,*,#55935,.F.);
#82304=ORIENTED_EDGE('',*,*,#55936,.T.);
#82305=ORIENTED_EDGE('',*,*,#55937,.F.);
#82306=ORIENTED_EDGE('',*,*,#55933,.F.);
#82307=ORIENTED_EDGE('',*,*,#55938,.F.);
#82308=ORIENTED_EDGE('',*,*,#55931,.T.);
#82309=ORIENTED_EDGE('',*,*,#55939,.F.);
#82310=ORIENTED_EDGE('',*,*,#55936,.F.);
#82311=ORIENTED_EDGE('',*,*,#55930,.T.);
#82312=ORIENTED_EDGE('',*,*,#55934,.T.);
#82313=ORIENTED_EDGE('',*,*,#55937,.T.);
#82314=ORIENTED_EDGE('',*,*,#55939,.T.);
#82315=ORIENTED_EDGE('',*,*,#55927,.F.);
#82316=ORIENTED_EDGE('',*,*,#55928,.T.);
#82317=ORIENTED_EDGE('',*,*,#55938,.T.);
#82318=ORIENTED_EDGE('',*,*,#55935,.T.);
#82319=ORIENTED_EDGE('',*,*,#55932,.T.);
#82320=ORIENTED_EDGE('',*,*,#55925,.F.);
#82321=ORIENTED_EDGE('',*,*,#55940,.F.);
#82322=ORIENTED_EDGE('',*,*,#55941,.T.);
#82323=ORIENTED_EDGE('',*,*,#55942,.F.);
#82324=ORIENTED_EDGE('',*,*,#55941,.F.);
#82325=ORIENTED_EDGE('',*,*,#55942,.T.);
#82326=ORIENTED_EDGE('',*,*,#55943,.T.);
#82327=ORIENTED_EDGE('',*,*,#55944,.F.);
#82328=ORIENTED_EDGE('',*,*,#55943,.F.);
#82329=ORIENTED_EDGE('',*,*,#55945,.T.);
#82330=ORIENTED_EDGE('',*,*,#55946,.T.);
#82331=ORIENTED_EDGE('',*,*,#55947,.T.);
#82332=ORIENTED_EDGE('',*,*,#55948,.F.);
#82333=ORIENTED_EDGE('',*,*,#55949,.T.);
#82334=ORIENTED_EDGE('',*,*,#55950,.T.);
#82335=ORIENTED_EDGE('',*,*,#55951,.T.);
#82336=ORIENTED_EDGE('',*,*,#55952,.T.);
#82337=ORIENTED_EDGE('',*,*,#55953,.T.);
#82338=ORIENTED_EDGE('',*,*,#55954,.T.);
#82339=ORIENTED_EDGE('',*,*,#55955,.T.);
#82340=ORIENTED_EDGE('',*,*,#55956,.T.);
#82341=ORIENTED_EDGE('',*,*,#55957,.T.);
#82342=ORIENTED_EDGE('',*,*,#55958,.T.);
#82343=ORIENTED_EDGE('',*,*,#55959,.F.);
#82344=ORIENTED_EDGE('',*,*,#55960,.T.);
#82345=ORIENTED_EDGE('',*,*,#55961,.T.);
#82346=ORIENTED_EDGE('',*,*,#55962,.T.);
#82347=ORIENTED_EDGE('',*,*,#55963,.T.);
#82348=ORIENTED_EDGE('',*,*,#55964,.T.);
#82349=ORIENTED_EDGE('',*,*,#55965,.T.);
#82350=ORIENTED_EDGE('',*,*,#55966,.T.);
#82351=ORIENTED_EDGE('',*,*,#55967,.F.);
#82352=ORIENTED_EDGE('',*,*,#55968,.T.);
#82353=ORIENTED_EDGE('',*,*,#55969,.T.);
#82354=ORIENTED_EDGE('',*,*,#55970,.T.);
#82355=ORIENTED_EDGE('',*,*,#55971,.T.);
#82356=ORIENTED_EDGE('',*,*,#55972,.T.);
#82357=ORIENTED_EDGE('',*,*,#55973,.T.);
#82358=ORIENTED_EDGE('',*,*,#55974,.T.);
#82359=ORIENTED_EDGE('',*,*,#55975,.F.);
#82360=ORIENTED_EDGE('',*,*,#55976,.T.);
#82361=ORIENTED_EDGE('',*,*,#55977,.T.);
#82362=ORIENTED_EDGE('',*,*,#55978,.T.);
#82363=ORIENTED_EDGE('',*,*,#55979,.T.);
#82364=ORIENTED_EDGE('',*,*,#55980,.T.);
#82365=ORIENTED_EDGE('',*,*,#55981,.T.);
#82366=ORIENTED_EDGE('',*,*,#55982,.T.);
#82367=ORIENTED_EDGE('',*,*,#55983,.F.);
#82368=ORIENTED_EDGE('',*,*,#55984,.T.);
#82369=ORIENTED_EDGE('',*,*,#55985,.T.);
#82370=ORIENTED_EDGE('',*,*,#55986,.T.);
#82371=ORIENTED_EDGE('',*,*,#55987,.T.);
#82372=ORIENTED_EDGE('',*,*,#55988,.T.);
#82373=ORIENTED_EDGE('',*,*,#55989,.T.);
#82374=ORIENTED_EDGE('',*,*,#55990,.F.);
#82375=ORIENTED_EDGE('',*,*,#55991,.T.);
#82376=ORIENTED_EDGE('',*,*,#55992,.T.);
#82377=ORIENTED_EDGE('',*,*,#55993,.T.);
#82378=ORIENTED_EDGE('',*,*,#55994,.T.);
#82379=ORIENTED_EDGE('',*,*,#55995,.T.);
#82380=ORIENTED_EDGE('',*,*,#55996,.T.);
#82381=ORIENTED_EDGE('',*,*,#55997,.T.);
#82382=ORIENTED_EDGE('',*,*,#55998,.F.);
#82383=ORIENTED_EDGE('',*,*,#55999,.T.);
#82384=ORIENTED_EDGE('',*,*,#56000,.T.);
#82385=ORIENTED_EDGE('',*,*,#56001,.T.);
#82386=ORIENTED_EDGE('',*,*,#56002,.T.);
#82387=ORIENTED_EDGE('',*,*,#56003,.T.);
#82388=ORIENTED_EDGE('',*,*,#56004,.T.);
#82389=ORIENTED_EDGE('',*,*,#56005,.T.);
#82390=ORIENTED_EDGE('',*,*,#56006,.T.);
#82391=ORIENTED_EDGE('',*,*,#56007,.T.);
#82392=ORIENTED_EDGE('',*,*,#56008,.F.);
#82393=ORIENTED_EDGE('',*,*,#56009,.T.);
#82394=ORIENTED_EDGE('',*,*,#56010,.T.);
#82395=ORIENTED_EDGE('',*,*,#56011,.T.);
#82396=ORIENTED_EDGE('',*,*,#56012,.T.);
#82397=ORIENTED_EDGE('',*,*,#56013,.T.);
#82398=ORIENTED_EDGE('',*,*,#56014,.T.);
#82399=ORIENTED_EDGE('',*,*,#56015,.F.);
#82400=ORIENTED_EDGE('',*,*,#56016,.T.);
#82401=ORIENTED_EDGE('',*,*,#56017,.T.);
#82402=ORIENTED_EDGE('',*,*,#56018,.T.);
#82403=ORIENTED_EDGE('',*,*,#56019,.T.);
#82404=ORIENTED_EDGE('',*,*,#56020,.T.);
#82405=ORIENTED_EDGE('',*,*,#56021,.T.);
#82406=ORIENTED_EDGE('',*,*,#56022,.T.);
#82407=ORIENTED_EDGE('',*,*,#56023,.T.);
#82408=ORIENTED_EDGE('',*,*,#56024,.F.);
#82409=ORIENTED_EDGE('',*,*,#56025,.T.);
#82410=ORIENTED_EDGE('',*,*,#56026,.T.);
#82411=ORIENTED_EDGE('',*,*,#56027,.T.);
#82412=ORIENTED_EDGE('',*,*,#56028,.T.);
#82413=ORIENTED_EDGE('',*,*,#56029,.T.);
#82414=ORIENTED_EDGE('',*,*,#56030,.T.);
#82415=ORIENTED_EDGE('',*,*,#56031,.F.);
#82416=ORIENTED_EDGE('',*,*,#56032,.T.);
#82417=ORIENTED_EDGE('',*,*,#56033,.T.);
#82418=ORIENTED_EDGE('',*,*,#56034,.T.);
#82419=ORIENTED_EDGE('',*,*,#56035,.T.);
#82420=ORIENTED_EDGE('',*,*,#56036,.T.);
#82421=ORIENTED_EDGE('',*,*,#56037,.T.);
#82422=ORIENTED_EDGE('',*,*,#56038,.T.);
#82423=ORIENTED_EDGE('',*,*,#56039,.F.);
#82424=ORIENTED_EDGE('',*,*,#56040,.T.);
#82425=ORIENTED_EDGE('',*,*,#56041,.T.);
#82426=ORIENTED_EDGE('',*,*,#56042,.T.);
#82427=ORIENTED_EDGE('',*,*,#56043,.T.);
#82428=ORIENTED_EDGE('',*,*,#56044,.T.);
#82429=ORIENTED_EDGE('',*,*,#56045,.T.);
#82430=ORIENTED_EDGE('',*,*,#56046,.T.);
#82431=ORIENTED_EDGE('',*,*,#56047,.F.);
#82432=ORIENTED_EDGE('',*,*,#56048,.T.);
#82433=ORIENTED_EDGE('',*,*,#56049,.T.);
#82434=ORIENTED_EDGE('',*,*,#56050,.F.);
#82435=ORIENTED_EDGE('',*,*,#56051,.F.);
#82436=ORIENTED_EDGE('',*,*,#56052,.F.);
#82437=ORIENTED_EDGE('',*,*,#56053,.F.);
#82438=ORIENTED_EDGE('',*,*,#56054,.F.);
#82439=ORIENTED_EDGE('',*,*,#56055,.T.);
#82440=ORIENTED_EDGE('',*,*,#56056,.F.);
#82441=ORIENTED_EDGE('',*,*,#56049,.F.);
#82442=ORIENTED_EDGE('',*,*,#56057,.F.);
#82443=ORIENTED_EDGE('',*,*,#56058,.T.);
#82444=ORIENTED_EDGE('',*,*,#56059,.F.);
#82445=ORIENTED_EDGE('',*,*,#56060,.F.);
#82446=ORIENTED_EDGE('',*,*,#56055,.F.);
#82447=ORIENTED_EDGE('',*,*,#56061,.F.);
#82448=ORIENTED_EDGE('',*,*,#56062,.F.);
#82449=ORIENTED_EDGE('',*,*,#56063,.T.);
#82450=ORIENTED_EDGE('',*,*,#56064,.T.);
#82451=ORIENTED_EDGE('',*,*,#56065,.F.);
#82452=ORIENTED_EDGE('',*,*,#56066,.T.);
#82453=ORIENTED_EDGE('',*,*,#56067,.F.);
#82454=ORIENTED_EDGE('',*,*,#56068,.F.);
#82455=ORIENTED_EDGE('',*,*,#56069,.F.);
#82456=ORIENTED_EDGE('',*,*,#56070,.F.);
#82457=ORIENTED_EDGE('',*,*,#56071,.F.);
#82458=ORIENTED_EDGE('',*,*,#56072,.F.);
#82459=ORIENTED_EDGE('',*,*,#56073,.F.);
#82460=ORIENTED_EDGE('',*,*,#56074,.F.);
#82461=ORIENTED_EDGE('',*,*,#56075,.F.);
#82462=ORIENTED_EDGE('',*,*,#56076,.F.);
#82463=ORIENTED_EDGE('',*,*,#56077,.F.);
#82464=ORIENTED_EDGE('',*,*,#56078,.F.);
#82465=ORIENTED_EDGE('',*,*,#56079,.F.);
#82466=ORIENTED_EDGE('',*,*,#56080,.F.);
#82467=ORIENTED_EDGE('',*,*,#56081,.F.);
#82468=ORIENTED_EDGE('',*,*,#56082,.F.);
#82469=ORIENTED_EDGE('',*,*,#56083,.F.);
#82470=ORIENTED_EDGE('',*,*,#56084,.F.);
#82471=ORIENTED_EDGE('',*,*,#55992,.F.);
#82472=ORIENTED_EDGE('',*,*,#56085,.F.);
#82473=ORIENTED_EDGE('',*,*,#56000,.F.);
#82474=ORIENTED_EDGE('',*,*,#56086,.F.);
#82475=ORIENTED_EDGE('',*,*,#55969,.F.);
#82476=ORIENTED_EDGE('',*,*,#56087,.F.);
#82477=ORIENTED_EDGE('',*,*,#55977,.F.);
#82478=ORIENTED_EDGE('',*,*,#56088,.F.);
#82479=ORIENTED_EDGE('',*,*,#55961,.F.);
#82480=ORIENTED_EDGE('',*,*,#56089,.F.);
#82481=ORIENTED_EDGE('',*,*,#55953,.F.);
#82482=ORIENTED_EDGE('',*,*,#56090,.F.);
#82483=ORIENTED_EDGE('',*,*,#56041,.F.);
#82484=ORIENTED_EDGE('',*,*,#56091,.F.);
#82485=ORIENTED_EDGE('',*,*,#56033,.F.);
#82486=ORIENTED_EDGE('',*,*,#56092,.F.);
#82487=ORIENTED_EDGE('',*,*,#56025,.F.);
#82488=ORIENTED_EDGE('',*,*,#56093,.F.);
#82489=ORIENTED_EDGE('',*,*,#56009,.F.);
#82490=ORIENTED_EDGE('',*,*,#56094,.F.);
#82491=ORIENTED_EDGE('',*,*,#56002,.F.);
#82492=ORIENTED_EDGE('',*,*,#56095,.F.);
#82493=ORIENTED_EDGE('',*,*,#56018,.F.);
#82494=ORIENTED_EDGE('',*,*,#56096,.F.);
#82495=ORIENTED_EDGE('',*,*,#56097,.F.);
#82496=ORIENTED_EDGE('',*,*,#56098,.F.);
#82497=ORIENTED_EDGE('',*,*,#56099,.F.);
#82498=ORIENTED_EDGE('',*,*,#56100,.F.);
#82499=ORIENTED_EDGE('',*,*,#56101,.F.);
#82500=ORIENTED_EDGE('',*,*,#56102,.F.);
#82501=ORIENTED_EDGE('',*,*,#56103,.F.);
#82502=ORIENTED_EDGE('',*,*,#56104,.F.);
#82503=ORIENTED_EDGE('',*,*,#56105,.F.);
#82504=ORIENTED_EDGE('',*,*,#56106,.F.);
#82505=ORIENTED_EDGE('',*,*,#56107,.F.);
#82506=ORIENTED_EDGE('',*,*,#56108,.F.);
#82507=ORIENTED_EDGE('',*,*,#56109,.F.);
#82508=ORIENTED_EDGE('',*,*,#56110,.F.);
#82509=ORIENTED_EDGE('',*,*,#56111,.F.);
#82510=ORIENTED_EDGE('',*,*,#56112,.F.);
#82511=ORIENTED_EDGE('',*,*,#56113,.F.);
#82512=ORIENTED_EDGE('',*,*,#56058,.F.);
#82513=ORIENTED_EDGE('',*,*,#56114,.F.);
#82514=ORIENTED_EDGE('',*,*,#56063,.F.);
#82515=ORIENTED_EDGE('',*,*,#56115,.F.);
#82516=ORIENTED_EDGE('',*,*,#56116,.F.);
#82517=ORIENTED_EDGE('',*,*,#55944,.T.);
#82518=ORIENTED_EDGE('',*,*,#56065,.T.);
#82519=ORIENTED_EDGE('',*,*,#56117,.T.);
#82520=ORIENTED_EDGE('',*,*,#56118,.T.);
#82521=ORIENTED_EDGE('',*,*,#56119,.T.);
#82522=ORIENTED_EDGE('',*,*,#56120,.F.);
#82523=ORIENTED_EDGE('',*,*,#56121,.F.);
#82524=ORIENTED_EDGE('',*,*,#56122,.F.);
#82525=ORIENTED_EDGE('',*,*,#56123,.F.);
#82526=ORIENTED_EDGE('',*,*,#56068,.T.);
#82527=ORIENTED_EDGE('',*,*,#56124,.F.);
#82528=ORIENTED_EDGE('',*,*,#56125,.F.);
#82529=ORIENTED_EDGE('',*,*,#56112,.T.);
#82530=ORIENTED_EDGE('',*,*,#56126,.F.);
#82531=ORIENTED_EDGE('',*,*,#56127,.F.);
#82532=ORIENTED_EDGE('',*,*,#56128,.F.);
#82533=ORIENTED_EDGE('',*,*,#56129,.F.);
#82534=ORIENTED_EDGE('',*,*,#56130,.F.);
#82535=ORIENTED_EDGE('',*,*,#56110,.T.);
#82536=ORIENTED_EDGE('',*,*,#56131,.F.);
#82537=ORIENTED_EDGE('',*,*,#56132,.F.);
#82538=ORIENTED_EDGE('',*,*,#56133,.F.);
#82539=ORIENTED_EDGE('',*,*,#56134,.F.);
#82540=ORIENTED_EDGE('',*,*,#56135,.F.);
#82541=ORIENTED_EDGE('',*,*,#56108,.T.);
#82542=ORIENTED_EDGE('',*,*,#56136,.F.);
#82543=ORIENTED_EDGE('',*,*,#56137,.F.);
#82544=ORIENTED_EDGE('',*,*,#56138,.F.);
#82545=ORIENTED_EDGE('',*,*,#56139,.F.);
#82546=ORIENTED_EDGE('',*,*,#56140,.F.);
#82547=ORIENTED_EDGE('',*,*,#56141,.F.);
#82548=ORIENTED_EDGE('',*,*,#56142,.F.);
#82549=ORIENTED_EDGE('',*,*,#56143,.F.);
#82550=ORIENTED_EDGE('',*,*,#56104,.T.);
#82551=ORIENTED_EDGE('',*,*,#56144,.F.);
#82552=ORIENTED_EDGE('',*,*,#56145,.F.);
#82553=ORIENTED_EDGE('',*,*,#56102,.T.);
#82554=ORIENTED_EDGE('',*,*,#56146,.F.);
#82555=ORIENTED_EDGE('',*,*,#56147,.F.);
#82556=ORIENTED_EDGE('',*,*,#56148,.F.);
#82557=ORIENTED_EDGE('',*,*,#55945,.F.);
#82558=ORIENTED_EDGE('',*,*,#56149,.F.);
#82559=ORIENTED_EDGE('',*,*,#56106,.T.);
#82560=ORIENTED_EDGE('',*,*,#56150,.F.);
#82561=ORIENTED_EDGE('',*,*,#56151,.F.);
#82562=ORIENTED_EDGE('',*,*,#56152,.F.);
#82563=ORIENTED_EDGE('',*,*,#56153,.F.);
#82564=ORIENTED_EDGE('',*,*,#56154,.F.);
#82565=ORIENTED_EDGE('',*,*,#56155,.F.);
#82566=ORIENTED_EDGE('',*,*,#56156,.F.);
#82567=ORIENTED_EDGE('',*,*,#56157,.F.);
#82568=ORIENTED_EDGE('',*,*,#56082,.T.);
#82569=ORIENTED_EDGE('',*,*,#56158,.F.);
#82570=ORIENTED_EDGE('',*,*,#56159,.F.);
#82571=ORIENTED_EDGE('',*,*,#56080,.T.);
#82572=ORIENTED_EDGE('',*,*,#56160,.F.);
#82573=ORIENTED_EDGE('',*,*,#56161,.F.);
#82574=ORIENTED_EDGE('',*,*,#56162,.F.);
#82575=ORIENTED_EDGE('',*,*,#56163,.F.);
#82576=ORIENTED_EDGE('',*,*,#56164,.F.);
#82577=ORIENTED_EDGE('',*,*,#56078,.T.);
#82578=ORIENTED_EDGE('',*,*,#56165,.F.);
#82579=ORIENTED_EDGE('',*,*,#55949,.F.);
#82580=ORIENTED_EDGE('',*,*,#56166,.F.);
#82581=ORIENTED_EDGE('',*,*,#56167,.F.);
#82582=ORIENTED_EDGE('',*,*,#56168,.F.);
#82583=ORIENTED_EDGE('',*,*,#56169,.F.);
#82584=ORIENTED_EDGE('',*,*,#56170,.F.);
#82585=ORIENTED_EDGE('',*,*,#56171,.F.);
#82586=ORIENTED_EDGE('',*,*,#56076,.T.);
#82587=ORIENTED_EDGE('',*,*,#56172,.F.);
#82588=ORIENTED_EDGE('',*,*,#56173,.F.);
#82589=ORIENTED_EDGE('',*,*,#56074,.T.);
#82590=ORIENTED_EDGE('',*,*,#56174,.F.);
#82591=ORIENTED_EDGE('',*,*,#56175,.F.);
#82592=ORIENTED_EDGE('',*,*,#56176,.F.);
#82593=ORIENTED_EDGE('',*,*,#56177,.F.);
#82594=ORIENTED_EDGE('',*,*,#56178,.F.);
#82595=ORIENTED_EDGE('',*,*,#56179,.F.);
#82596=ORIENTED_EDGE('',*,*,#56180,.F.);
#82597=ORIENTED_EDGE('',*,*,#56181,.F.);
#82598=ORIENTED_EDGE('',*,*,#56072,.T.);
#82599=ORIENTED_EDGE('',*,*,#56182,.F.);
#82600=ORIENTED_EDGE('',*,*,#56183,.F.);
#82601=ORIENTED_EDGE('',*,*,#56070,.T.);
#82602=ORIENTED_EDGE('',*,*,#56184,.F.);
#82603=ORIENTED_EDGE('',*,*,#56185,.F.);
#82604=ORIENTED_EDGE('',*,*,#56186,.F.);
#82605=ORIENTED_EDGE('',*,*,#56187,.F.);
#82606=ORIENTED_EDGE('',*,*,#56188,.F.);
#82607=ORIENTED_EDGE('',*,*,#56189,.F.);
#82608=ORIENTED_EDGE('',*,*,#56190,.F.);
#82609=ORIENTED_EDGE('',*,*,#56042,.F.);
#82610=ORIENTED_EDGE('',*,*,#56090,.T.);
#82611=ORIENTED_EDGE('',*,*,#55960,.F.);
#82612=ORIENTED_EDGE('',*,*,#55954,.F.);
#82613=ORIENTED_EDGE('',*,*,#56089,.T.);
#82614=ORIENTED_EDGE('',*,*,#55968,.F.);
#82615=ORIENTED_EDGE('',*,*,#56191,.F.);
#82616=ORIENTED_EDGE('',*,*,#56192,.F.);
#82617=ORIENTED_EDGE('',*,*,#56193,.F.);
#82618=ORIENTED_EDGE('',*,*,#55962,.F.);
#82619=ORIENTED_EDGE('',*,*,#56088,.T.);
#82620=ORIENTED_EDGE('',*,*,#55984,.F.);
#82621=ORIENTED_EDGE('',*,*,#56194,.F.);
#82622=ORIENTED_EDGE('',*,*,#56195,.F.);
#82623=ORIENTED_EDGE('',*,*,#56196,.F.);
#82624=ORIENTED_EDGE('',*,*,#56197,.F.);
#82625=ORIENTED_EDGE('',*,*,#56198,.F.);
#82626=ORIENTED_EDGE('',*,*,#56199,.F.);
#82627=ORIENTED_EDGE('',*,*,#55978,.F.);
#82628=ORIENTED_EDGE('',*,*,#56087,.T.);
#82629=ORIENTED_EDGE('',*,*,#55976,.F.);
#82630=ORIENTED_EDGE('',*,*,#55970,.F.);
#82631=ORIENTED_EDGE('',*,*,#56086,.T.);
#82632=ORIENTED_EDGE('',*,*,#55999,.F.);
#82633=ORIENTED_EDGE('',*,*,#56200,.F.);
#82634=ORIENTED_EDGE('',*,*,#56201,.F.);
#82635=ORIENTED_EDGE('',*,*,#56202,.F.);
#82636=ORIENTED_EDGE('',*,*,#56203,.F.);
#82637=ORIENTED_EDGE('',*,*,#56204,.F.);
#82638=ORIENTED_EDGE('',*,*,#56205,.F.);
#82639=ORIENTED_EDGE('',*,*,#55993,.F.);
#82640=ORIENTED_EDGE('',*,*,#56085,.T.);
#82641=ORIENTED_EDGE('',*,*,#55991,.F.);
#82642=ORIENTED_EDGE('',*,*,#55985,.F.);
#82643=ORIENTED_EDGE('',*,*,#56084,.T.);
#82644=ORIENTED_EDGE('',*,*,#56206,.F.);
#82645=ORIENTED_EDGE('',*,*,#56207,.F.);
#82646=ORIENTED_EDGE('',*,*,#56208,.F.);
#82647=ORIENTED_EDGE('',*,*,#56209,.F.);
#82648=ORIENTED_EDGE('',*,*,#56210,.F.);
#82649=ORIENTED_EDGE('',*,*,#56211,.F.);
#82650=ORIENTED_EDGE('',*,*,#56212,.F.);
#82651=ORIENTED_EDGE('',*,*,#56019,.F.);
#82652=ORIENTED_EDGE('',*,*,#56095,.T.);
#82653=ORIENTED_EDGE('',*,*,#56001,.F.);
#82654=ORIENTED_EDGE('',*,*,#56003,.F.);
#82655=ORIENTED_EDGE('',*,*,#56094,.T.);
#82656=ORIENTED_EDGE('',*,*,#56016,.F.);
#82657=ORIENTED_EDGE('',*,*,#56213,.F.);
#82658=ORIENTED_EDGE('',*,*,#56214,.F.);
#82659=ORIENTED_EDGE('',*,*,#56215,.F.);
#82660=ORIENTED_EDGE('',*,*,#56010,.F.);
#82661=ORIENTED_EDGE('',*,*,#56093,.T.);
#82662=ORIENTED_EDGE('',*,*,#56032,.F.);
#82663=ORIENTED_EDGE('',*,*,#56216,.F.);
#82664=ORIENTED_EDGE('',*,*,#56217,.F.);
#82665=ORIENTED_EDGE('',*,*,#56218,.F.);
#82666=ORIENTED_EDGE('',*,*,#56219,.F.);
#82667=ORIENTED_EDGE('',*,*,#56220,.F.);
#82668=ORIENTED_EDGE('',*,*,#56221,.F.);
#82669=ORIENTED_EDGE('',*,*,#56222,.F.);
#82670=ORIENTED_EDGE('',*,*,#56096,.T.);
#82671=ORIENTED_EDGE('',*,*,#56017,.F.);
#82672=ORIENTED_EDGE('',*,*,#56223,.F.);
#82673=ORIENTED_EDGE('',*,*,#56224,.F.);
#82674=ORIENTED_EDGE('',*,*,#56225,.F.);
#82675=ORIENTED_EDGE('',*,*,#56226,.F.);
#82676=ORIENTED_EDGE('',*,*,#56098,.T.);
#82677=ORIENTED_EDGE('',*,*,#56227,.F.);
#82678=ORIENTED_EDGE('',*,*,#56026,.F.);
#82679=ORIENTED_EDGE('',*,*,#56092,.T.);
#82680=ORIENTED_EDGE('',*,*,#56040,.F.);
#82681=ORIENTED_EDGE('',*,*,#56228,.F.);
#82682=ORIENTED_EDGE('',*,*,#56229,.F.);
#82683=ORIENTED_EDGE('',*,*,#56230,.F.);
#82684=ORIENTED_EDGE('',*,*,#56034,.F.);
#82685=ORIENTED_EDGE('',*,*,#56091,.T.);
#82686=ORIENTED_EDGE('',*,*,#56048,.F.);
#82687=ORIENTED_EDGE('',*,*,#56231,.F.);
#82688=ORIENTED_EDGE('',*,*,#56232,.F.);
#82689=ORIENTED_EDGE('',*,*,#56233,.F.);
#82690=ORIENTED_EDGE('',*,*,#56234,.F.);
#82691=ORIENTED_EDGE('',*,*,#56235,.F.);
#82692=ORIENTED_EDGE('',*,*,#56236,.F.);
#82693=ORIENTED_EDGE('',*,*,#56121,.T.);
#82694=ORIENTED_EDGE('',*,*,#56237,.F.);
#82695=ORIENTED_EDGE('',*,*,#56128,.T.);
#82696=ORIENTED_EDGE('',*,*,#56238,.F.);
#82697=ORIENTED_EDGE('',*,*,#56239,.F.);
#82698=ORIENTED_EDGE('',*,*,#56240,.F.);
#82699=ORIENTED_EDGE('',*,*,#56133,.T.);
#82700=ORIENTED_EDGE('',*,*,#56241,.F.);
#82701=ORIENTED_EDGE('',*,*,#56242,.F.);
#82702=ORIENTED_EDGE('',*,*,#56243,.F.);
#82703=ORIENTED_EDGE('',*,*,#56138,.T.);
#82704=ORIENTED_EDGE('',*,*,#56244,.F.);
#82705=ORIENTED_EDGE('',*,*,#56245,.F.);
#82706=ORIENTED_EDGE('',*,*,#56246,.F.);
#82707=ORIENTED_EDGE('',*,*,#56247,.F.);
#82708=ORIENTED_EDGE('',*,*,#56248,.F.);
#82709=ORIENTED_EDGE('',*,*,#56141,.T.);
#82710=ORIENTED_EDGE('',*,*,#55946,.F.);
#82711=ORIENTED_EDGE('',*,*,#56148,.T.);
#82712=ORIENTED_EDGE('',*,*,#56249,.F.);
#82713=ORIENTED_EDGE('',*,*,#56250,.F.);
#82714=ORIENTED_EDGE('',*,*,#56251,.F.);
#82715=ORIENTED_EDGE('',*,*,#56152,.T.);
#82716=ORIENTED_EDGE('',*,*,#56252,.F.);
#82717=ORIENTED_EDGE('',*,*,#56253,.F.);
#82718=ORIENTED_EDGE('',*,*,#56254,.F.);
#82719=ORIENTED_EDGE('',*,*,#56255,.F.);
#82720=ORIENTED_EDGE('',*,*,#56256,.F.);
#82721=ORIENTED_EDGE('',*,*,#56155,.T.);
#82722=ORIENTED_EDGE('',*,*,#56257,.F.);
#82723=ORIENTED_EDGE('',*,*,#56162,.T.);
#82724=ORIENTED_EDGE('',*,*,#56258,.F.);
#82725=ORIENTED_EDGE('',*,*,#56259,.F.);
#82726=ORIENTED_EDGE('',*,*,#56260,.F.);
#82727=ORIENTED_EDGE('',*,*,#56166,.T.);
#82728=ORIENTED_EDGE('',*,*,#55952,.F.);
#82729=ORIENTED_EDGE('',*,*,#56261,.F.);
#82730=ORIENTED_EDGE('',*,*,#56262,.F.);
#82731=ORIENTED_EDGE('',*,*,#56263,.F.);
#82732=ORIENTED_EDGE('',*,*,#56264,.F.);
#82733=ORIENTED_EDGE('',*,*,#56169,.T.);
#82734=ORIENTED_EDGE('',*,*,#56265,.F.);
#82735=ORIENTED_EDGE('',*,*,#56176,.T.);
#82736=ORIENTED_EDGE('',*,*,#56266,.F.);
#82737=ORIENTED_EDGE('',*,*,#56267,.F.);
#82738=ORIENTED_EDGE('',*,*,#56268,.F.);
#82739=ORIENTED_EDGE('',*,*,#56269,.F.);
#82740=ORIENTED_EDGE('',*,*,#56270,.F.);
#82741=ORIENTED_EDGE('',*,*,#56179,.T.);
#82742=ORIENTED_EDGE('',*,*,#56271,.F.);
#82743=ORIENTED_EDGE('',*,*,#56186,.T.);
#82744=ORIENTED_EDGE('',*,*,#56272,.F.);
#82745=ORIENTED_EDGE('',*,*,#56273,.F.);
#82746=ORIENTED_EDGE('',*,*,#56274,.F.);
#82747=ORIENTED_EDGE('',*,*,#56275,.F.);
#82748=ORIENTED_EDGE('',*,*,#56276,.F.);
#82749=ORIENTED_EDGE('',*,*,#56189,.T.);
#82750=ORIENTED_EDGE('',*,*,#56277,.F.);
#82751=ORIENTED_EDGE('',*,*,#56192,.T.);
#82752=ORIENTED_EDGE('',*,*,#56278,.F.);
#82753=ORIENTED_EDGE('',*,*,#56279,.F.);
#82754=ORIENTED_EDGE('',*,*,#56280,.F.);
#82755=ORIENTED_EDGE('',*,*,#56195,.T.);
#82756=ORIENTED_EDGE('',*,*,#56281,.F.);
#82757=ORIENTED_EDGE('',*,*,#56282,.F.);
#82758=ORIENTED_EDGE('',*,*,#56283,.F.);
#82759=ORIENTED_EDGE('',*,*,#56284,.F.);
#82760=ORIENTED_EDGE('',*,*,#56285,.F.);
#82761=ORIENTED_EDGE('',*,*,#56198,.T.);
#82762=ORIENTED_EDGE('',*,*,#56286,.F.);
#82763=ORIENTED_EDGE('',*,*,#56201,.T.);
#82764=ORIENTED_EDGE('',*,*,#56287,.F.);
#82765=ORIENTED_EDGE('',*,*,#56288,.F.);
#82766=ORIENTED_EDGE('',*,*,#56289,.F.);
#82767=ORIENTED_EDGE('',*,*,#56290,.F.);
#82768=ORIENTED_EDGE('',*,*,#56291,.F.);
#82769=ORIENTED_EDGE('',*,*,#56204,.T.);
#82770=ORIENTED_EDGE('',*,*,#56292,.F.);
#82771=ORIENTED_EDGE('',*,*,#56208,.T.);
#82772=ORIENTED_EDGE('',*,*,#56293,.F.);
#82773=ORIENTED_EDGE('',*,*,#56294,.F.);
#82774=ORIENTED_EDGE('',*,*,#56295,.F.);
#82775=ORIENTED_EDGE('',*,*,#56296,.F.);
#82776=ORIENTED_EDGE('',*,*,#56297,.F.);
#82777=ORIENTED_EDGE('',*,*,#56211,.T.);
#82778=ORIENTED_EDGE('',*,*,#56298,.F.);
#82779=ORIENTED_EDGE('',*,*,#56214,.T.);
#82780=ORIENTED_EDGE('',*,*,#56299,.F.);
#82781=ORIENTED_EDGE('',*,*,#56300,.F.);
#82782=ORIENTED_EDGE('',*,*,#56301,.F.);
#82783=ORIENTED_EDGE('',*,*,#56217,.T.);
#82784=ORIENTED_EDGE('',*,*,#56302,.F.);
#82785=ORIENTED_EDGE('',*,*,#56303,.F.);
#82786=ORIENTED_EDGE('',*,*,#56304,.F.);
#82787=ORIENTED_EDGE('',*,*,#56305,.F.);
#82788=ORIENTED_EDGE('',*,*,#56306,.F.);
#82789=ORIENTED_EDGE('',*,*,#56220,.T.);
#82790=ORIENTED_EDGE('',*,*,#56307,.F.);
#82791=ORIENTED_EDGE('',*,*,#56308,.F.);
#82792=ORIENTED_EDGE('',*,*,#56309,.F.);
#82793=ORIENTED_EDGE('',*,*,#56224,.T.);
#82794=ORIENTED_EDGE('',*,*,#56310,.F.);
#82795=ORIENTED_EDGE('',*,*,#56229,.T.);
#82796=ORIENTED_EDGE('',*,*,#56311,.F.);
#82797=ORIENTED_EDGE('',*,*,#56312,.F.);
#82798=ORIENTED_EDGE('',*,*,#56313,.F.);
#82799=ORIENTED_EDGE('',*,*,#56232,.T.);
#82800=ORIENTED_EDGE('',*,*,#56314,.F.);
#82801=ORIENTED_EDGE('',*,*,#56315,.F.);
#82802=ORIENTED_EDGE('',*,*,#56316,.F.);
#82803=ORIENTED_EDGE('',*,*,#56317,.F.);
#82804=ORIENTED_EDGE('',*,*,#56318,.F.);
#82805=ORIENTED_EDGE('',*,*,#56319,.F.);
#82806=ORIENTED_EDGE('',*,*,#56320,.F.);
#82807=ORIENTED_EDGE('',*,*,#56235,.T.);
#82808=ORIENTED_EDGE('',*,*,#56321,.F.);
#82809=ORIENTED_EDGE('',*,*,#56322,.F.);
#82810=ORIENTED_EDGE('',*,*,#56239,.T.);
#82811=ORIENTED_EDGE('',*,*,#56323,.F.);
#82812=ORIENTED_EDGE('',*,*,#56324,.F.);
#82813=ORIENTED_EDGE('',*,*,#56325,.F.);
#82814=ORIENTED_EDGE('',*,*,#56326,.F.);
#82815=ORIENTED_EDGE('',*,*,#56327,.F.);
#82816=ORIENTED_EDGE('',*,*,#56242,.T.);
#82817=ORIENTED_EDGE('',*,*,#56328,.F.);
#82818=ORIENTED_EDGE('',*,*,#56329,.F.);
#82819=ORIENTED_EDGE('',*,*,#56330,.F.);
#82820=ORIENTED_EDGE('',*,*,#56331,.F.);
#82821=ORIENTED_EDGE('',*,*,#56332,.F.);
#82822=ORIENTED_EDGE('',*,*,#56245,.T.);
#82823=ORIENTED_EDGE('',*,*,#56333,.F.);
#82824=ORIENTED_EDGE('',*,*,#56334,.F.);
#82825=ORIENTED_EDGE('',*,*,#56335,.F.);
#82826=ORIENTED_EDGE('',*,*,#56336,.F.);
#82827=ORIENTED_EDGE('',*,*,#56337,.F.);
#82828=ORIENTED_EDGE('',*,*,#56338,.F.);
#82829=ORIENTED_EDGE('',*,*,#56339,.F.);
#82830=ORIENTED_EDGE('',*,*,#56340,.F.);
#82831=ORIENTED_EDGE('',*,*,#56247,.T.);
#82832=ORIENTED_EDGE('',*,*,#56341,.F.);
#82833=ORIENTED_EDGE('',*,*,#55947,.F.);
#82834=ORIENTED_EDGE('',*,*,#56250,.T.);
#82835=ORIENTED_EDGE('',*,*,#56342,.F.);
#82836=ORIENTED_EDGE('',*,*,#56343,.F.);
#82837=ORIENTED_EDGE('',*,*,#56344,.F.);
#82838=ORIENTED_EDGE('',*,*,#56345,.F.);
#82839=ORIENTED_EDGE('',*,*,#56346,.F.);
#82840=ORIENTED_EDGE('',*,*,#56253,.T.);
#82841=ORIENTED_EDGE('',*,*,#56347,.F.);
#82842=ORIENTED_EDGE('',*,*,#56348,.F.);
#82843=ORIENTED_EDGE('',*,*,#56349,.F.);
#82844=ORIENTED_EDGE('',*,*,#56350,.F.);
#82845=ORIENTED_EDGE('',*,*,#56351,.F.);
#82846=ORIENTED_EDGE('',*,*,#56352,.F.);
#82847=ORIENTED_EDGE('',*,*,#56353,.F.);
#82848=ORIENTED_EDGE('',*,*,#56354,.F.);
#82849=ORIENTED_EDGE('',*,*,#56255,.T.);
#82850=ORIENTED_EDGE('',*,*,#56355,.F.);
#82851=ORIENTED_EDGE('',*,*,#56356,.F.);
#82852=ORIENTED_EDGE('',*,*,#56259,.T.);
#82853=ORIENTED_EDGE('',*,*,#56357,.F.);
#82854=ORIENTED_EDGE('',*,*,#56358,.F.);
#82855=ORIENTED_EDGE('',*,*,#56359,.F.);
#82856=ORIENTED_EDGE('',*,*,#56360,.F.);
#82857=ORIENTED_EDGE('',*,*,#56361,.F.);
#82858=ORIENTED_EDGE('',*,*,#56261,.T.);
#82859=ORIENTED_EDGE('',*,*,#55951,.F.);
#82860=ORIENTED_EDGE('',*,*,#56362,.F.);
#82861=ORIENTED_EDGE('',*,*,#56363,.F.);
#82862=ORIENTED_EDGE('',*,*,#56364,.F.);
#82863=ORIENTED_EDGE('',*,*,#56365,.F.);
#82864=ORIENTED_EDGE('',*,*,#56366,.F.);
#82865=ORIENTED_EDGE('',*,*,#56367,.F.);
#82866=ORIENTED_EDGE('',*,*,#56368,.F.);
#82867=ORIENTED_EDGE('',*,*,#56263,.T.);
#82868=ORIENTED_EDGE('',*,*,#56369,.F.);
#82869=ORIENTED_EDGE('',*,*,#56370,.F.);
#82870=ORIENTED_EDGE('',*,*,#56267,.T.);
#82871=ORIENTED_EDGE('',*,*,#56371,.F.);
#82872=ORIENTED_EDGE('',*,*,#56372,.F.);
#82873=ORIENTED_EDGE('',*,*,#56373,.F.);
#82874=ORIENTED_EDGE('',*,*,#56374,.F.);
#82875=ORIENTED_EDGE('',*,*,#56375,.F.);
#82876=ORIENTED_EDGE('',*,*,#56376,.F.);
#82877=ORIENTED_EDGE('',*,*,#56377,.F.);
#82878=ORIENTED_EDGE('',*,*,#56378,.F.);
#82879=ORIENTED_EDGE('',*,*,#56269,.T.);
#82880=ORIENTED_EDGE('',*,*,#56379,.F.);
#82881=ORIENTED_EDGE('',*,*,#56380,.F.);
#82882=ORIENTED_EDGE('',*,*,#56273,.T.);
#82883=ORIENTED_EDGE('',*,*,#56381,.F.);
#82884=ORIENTED_EDGE('',*,*,#56382,.F.);
#82885=ORIENTED_EDGE('',*,*,#56383,.F.);
#82886=ORIENTED_EDGE('',*,*,#56384,.F.);
#82887=ORIENTED_EDGE('',*,*,#55958,.F.);
#82888=ORIENTED_EDGE('',*,*,#56385,.F.);
#82889=ORIENTED_EDGE('',*,*,#56044,.F.);
#82890=ORIENTED_EDGE('',*,*,#56386,.F.);
#82891=ORIENTED_EDGE('',*,*,#56275,.T.);
#82892=ORIENTED_EDGE('',*,*,#55956,.F.);
#82893=ORIENTED_EDGE('',*,*,#56387,.F.);
#82894=ORIENTED_EDGE('',*,*,#56279,.T.);
#82895=ORIENTED_EDGE('',*,*,#56388,.F.);
#82896=ORIENTED_EDGE('',*,*,#55966,.F.);
#82897=ORIENTED_EDGE('',*,*,#56389,.F.);
#82898=ORIENTED_EDGE('',*,*,#55964,.F.);
#82899=ORIENTED_EDGE('',*,*,#56390,.F.);
#82900=ORIENTED_EDGE('',*,*,#56282,.T.);
#82901=ORIENTED_EDGE('',*,*,#56391,.F.);
#82902=ORIENTED_EDGE('',*,*,#55982,.F.);
#82903=ORIENTED_EDGE('',*,*,#56392,.F.);
#82904=ORIENTED_EDGE('',*,*,#56393,.F.);
#82905=ORIENTED_EDGE('',*,*,#55974,.F.);
#82906=ORIENTED_EDGE('',*,*,#56394,.F.);
#82907=ORIENTED_EDGE('',*,*,#55980,.F.);
#82908=ORIENTED_EDGE('',*,*,#56395,.F.);
#82909=ORIENTED_EDGE('',*,*,#56284,.T.);
#82910=ORIENTED_EDGE('',*,*,#55972,.F.);
#82911=ORIENTED_EDGE('',*,*,#56396,.F.);
#82912=ORIENTED_EDGE('',*,*,#56288,.T.);
#82913=ORIENTED_EDGE('',*,*,#56397,.F.);
#82914=ORIENTED_EDGE('',*,*,#55997,.F.);
#82915=ORIENTED_EDGE('',*,*,#56398,.F.);
#82916=ORIENTED_EDGE('',*,*,#56399,.F.);
#82917=ORIENTED_EDGE('',*,*,#55989,.F.);
#82918=ORIENTED_EDGE('',*,*,#56400,.F.);
#82919=ORIENTED_EDGE('',*,*,#55995,.F.);
#82920=ORIENTED_EDGE('',*,*,#56401,.F.);
#82921=ORIENTED_EDGE('',*,*,#56290,.T.);
#82922=ORIENTED_EDGE('',*,*,#55987,.F.);
#82923=ORIENTED_EDGE('',*,*,#56402,.F.);
#82924=ORIENTED_EDGE('',*,*,#56294,.T.);
#82925=ORIENTED_EDGE('',*,*,#56403,.F.);
#82926=ORIENTED_EDGE('',*,*,#56404,.F.);
#82927=ORIENTED_EDGE('',*,*,#56405,.F.);
#82928=ORIENTED_EDGE('',*,*,#56406,.F.);
#82929=ORIENTED_EDGE('',*,*,#56007,.F.);
#82930=ORIENTED_EDGE('',*,*,#56407,.F.);
#82931=ORIENTED_EDGE('',*,*,#56021,.F.);
#82932=ORIENTED_EDGE('',*,*,#56408,.F.);
#82933=ORIENTED_EDGE('',*,*,#56296,.T.);
#82934=ORIENTED_EDGE('',*,*,#56005,.F.);
#82935=ORIENTED_EDGE('',*,*,#56409,.F.);
#82936=ORIENTED_EDGE('',*,*,#56300,.T.);
#82937=ORIENTED_EDGE('',*,*,#56410,.F.);
#82938=ORIENTED_EDGE('',*,*,#56014,.F.);
#82939=ORIENTED_EDGE('',*,*,#56411,.F.);
#82940=ORIENTED_EDGE('',*,*,#56012,.F.);
#82941=ORIENTED_EDGE('',*,*,#56412,.F.);
#82942=ORIENTED_EDGE('',*,*,#56303,.T.);
#82943=ORIENTED_EDGE('',*,*,#56413,.F.);
#82944=ORIENTED_EDGE('',*,*,#56030,.F.);
#82945=ORIENTED_EDGE('',*,*,#56414,.F.);
#82946=ORIENTED_EDGE('',*,*,#56415,.F.);
#82947=ORIENTED_EDGE('',*,*,#56023,.F.);
#82948=ORIENTED_EDGE('',*,*,#56416,.F.);
#82949=ORIENTED_EDGE('',*,*,#56417,.F.);
#82950=ORIENTED_EDGE('',*,*,#56418,.F.);
#82951=ORIENTED_EDGE('',*,*,#56305,.T.);
#82952=ORIENTED_EDGE('',*,*,#56419,.F.);
#82953=ORIENTED_EDGE('',*,*,#56420,.F.);
#82954=ORIENTED_EDGE('',*,*,#56421,.F.);
#82955=ORIENTED_EDGE('',*,*,#56422,.F.);
#82956=ORIENTED_EDGE('',*,*,#56423,.F.);
#82957=ORIENTED_EDGE('',*,*,#56308,.T.);
#82958=ORIENTED_EDGE('',*,*,#56028,.F.);
#82959=ORIENTED_EDGE('',*,*,#56424,.F.);
#82960=ORIENTED_EDGE('',*,*,#56312,.T.);
#82961=ORIENTED_EDGE('',*,*,#56425,.F.);
#82962=ORIENTED_EDGE('',*,*,#56038,.F.);
#82963=ORIENTED_EDGE('',*,*,#56426,.F.);
#82964=ORIENTED_EDGE('',*,*,#56036,.F.);
#82965=ORIENTED_EDGE('',*,*,#56427,.F.);
#82966=ORIENTED_EDGE('',*,*,#56315,.T.);
#82967=ORIENTED_EDGE('',*,*,#56428,.F.);
#82968=ORIENTED_EDGE('',*,*,#56046,.F.);
#82969=ORIENTED_EDGE('',*,*,#56429,.F.);
#82970=ORIENTED_EDGE('',*,*,#56430,.F.);
#82971=ORIENTED_EDGE('',*,*,#56100,.T.);
#82972=ORIENTED_EDGE('',*,*,#56431,.F.);
#82973=ORIENTED_EDGE('',*,*,#56432,.F.);
#82974=ORIENTED_EDGE('',*,*,#56433,.F.);
#82975=ORIENTED_EDGE('',*,*,#56434,.F.);
#82976=ORIENTED_EDGE('',*,*,#56435,.F.);
#82977=ORIENTED_EDGE('',*,*,#56433,.T.);
#82978=ORIENTED_EDGE('',*,*,#56436,.F.);
#82979=ORIENTED_EDGE('',*,*,#56437,.F.);
#82980=ORIENTED_EDGE('',*,*,#56438,.F.);
#82981=ORIENTED_EDGE('',*,*,#56439,.F.);
#82982=ORIENTED_EDGE('',*,*,#56437,.T.);
#82983=ORIENTED_EDGE('',*,*,#56440,.F.);
#82984=ORIENTED_EDGE('',*,*,#56441,.F.);
#82985=ORIENTED_EDGE('',*,*,#56442,.F.);
#82986=ORIENTED_EDGE('',*,*,#56443,.F.);
#82987=ORIENTED_EDGE('',*,*,#56052,.T.);
#82988=ORIENTED_EDGE('',*,*,#56444,.F.);
#82989=ORIENTED_EDGE('',*,*,#56325,.T.);
#82990=ORIENTED_EDGE('',*,*,#56445,.F.);
#82991=ORIENTED_EDGE('',*,*,#56330,.T.);
#82992=ORIENTED_EDGE('',*,*,#56446,.F.);
#82993=ORIENTED_EDGE('',*,*,#56335,.T.);
#82994=ORIENTED_EDGE('',*,*,#56447,.F.);
#82995=ORIENTED_EDGE('',*,*,#56349,.T.);
#82996=ORIENTED_EDGE('',*,*,#56448,.F.);
#82997=ORIENTED_EDGE('',*,*,#56338,.T.);
#82998=ORIENTED_EDGE('',*,*,#56449,.F.);
#82999=ORIENTED_EDGE('',*,*,#56344,.T.);
#83000=ORIENTED_EDGE('',*,*,#56450,.F.);
#83001=ORIENTED_EDGE('',*,*,#56442,.T.);
#83002=ORIENTED_EDGE('',*,*,#56451,.F.);
#83003=ORIENTED_EDGE('',*,*,#56421,.T.);
#83004=ORIENTED_EDGE('',*,*,#56452,.F.);
#83005=ORIENTED_EDGE('',*,*,#56416,.T.);
#83006=ORIENTED_EDGE('',*,*,#56022,.F.);
#83007=ORIENTED_EDGE('',*,*,#56407,.T.);
#83008=ORIENTED_EDGE('',*,*,#56006,.F.);
#83009=ORIENTED_EDGE('',*,*,#56411,.T.);
#83010=ORIENTED_EDGE('',*,*,#56013,.F.);
#83011=ORIENTED_EDGE('',*,*,#56414,.T.);
#83012=ORIENTED_EDGE('',*,*,#56029,.F.);
#83013=ORIENTED_EDGE('',*,*,#56426,.T.);
#83014=ORIENTED_EDGE('',*,*,#56037,.F.);
#83015=ORIENTED_EDGE('',*,*,#56429,.T.);
#83016=ORIENTED_EDGE('',*,*,#56045,.F.);
#83017=ORIENTED_EDGE('',*,*,#56385,.T.);
#83018=ORIENTED_EDGE('',*,*,#55957,.F.);
#83019=ORIENTED_EDGE('',*,*,#56389,.T.);
#83020=ORIENTED_EDGE('',*,*,#55965,.F.);
#83021=ORIENTED_EDGE('',*,*,#56392,.T.);
#83022=ORIENTED_EDGE('',*,*,#55981,.F.);
#83023=ORIENTED_EDGE('',*,*,#56394,.T.);
#83024=ORIENTED_EDGE('',*,*,#55973,.F.);
#83025=ORIENTED_EDGE('',*,*,#56398,.T.);
#83026=ORIENTED_EDGE('',*,*,#55996,.F.);
#83027=ORIENTED_EDGE('',*,*,#56400,.T.);
#83028=ORIENTED_EDGE('',*,*,#55988,.F.);
#83029=ORIENTED_EDGE('',*,*,#56405,.T.);
#83030=ORIENTED_EDGE('',*,*,#56453,.F.);
#83031=ORIENTED_EDGE('',*,*,#56352,.T.);
#83032=ORIENTED_EDGE('',*,*,#56454,.F.);
#83033=ORIENTED_EDGE('',*,*,#56359,.T.);
#83034=ORIENTED_EDGE('',*,*,#56455,.F.);
#83035=ORIENTED_EDGE('',*,*,#56363,.T.);
#83036=ORIENTED_EDGE('',*,*,#56456,.F.);
#83037=ORIENTED_EDGE('',*,*,#56366,.T.);
#83038=ORIENTED_EDGE('',*,*,#56457,.F.);
#83039=ORIENTED_EDGE('',*,*,#56373,.T.);
#83040=ORIENTED_EDGE('',*,*,#56458,.F.);
#83041=ORIENTED_EDGE('',*,*,#56376,.T.);
#83042=ORIENTED_EDGE('',*,*,#56459,.F.);
#83043=ORIENTED_EDGE('',*,*,#56383,.T.);
#83044=ORIENTED_EDGE('',*,*,#56460,.F.);
#83045=ORIENTED_EDGE('',*,*,#56318,.T.);
#83046=ORIENTED_EDGE('',*,*,#55940,.T.);
#83047=ORIENTED_EDGE('',*,*,#56432,.T.);
#83048=ORIENTED_EDGE('',*,*,#56461,.T.);
#83049=ORIENTED_EDGE('',*,*,#56440,.T.);
#83050=ORIENTED_EDGE('',*,*,#56436,.T.);
#83051=ORIENTED_EDGE('',*,*,#56225,.T.);
#83052=ORIENTED_EDGE('',*,*,#56309,.T.);
#83053=ORIENTED_EDGE('',*,*,#56423,.T.);
#83054=ORIENTED_EDGE('',*,*,#56462,.F.);
#83055=ORIENTED_EDGE('',*,*,#56431,.T.);
#83056=ORIENTED_EDGE('',*,*,#56099,.T.);
#83057=ORIENTED_EDGE('',*,*,#56226,.T.);
#83058=ORIENTED_EDGE('',*,*,#56462,.T.);
#83059=ORIENTED_EDGE('',*,*,#56422,.T.);
#83060=ORIENTED_EDGE('',*,*,#56451,.T.);
#83061=ORIENTED_EDGE('',*,*,#56441,.T.);
#83062=ORIENTED_EDGE('',*,*,#56461,.F.);
#83063=ORIENTED_EDGE('',*,*,#56147,.T.);
#83064=ORIENTED_EDGE('',*,*,#56463,.T.);
#83065=ORIENTED_EDGE('',*,*,#56342,.T.);
#83066=ORIENTED_EDGE('',*,*,#56249,.T.);
#83067=ORIENTED_EDGE('',*,*,#56434,.T.);
#83068=ORIENTED_EDGE('',*,*,#56435,.T.);
#83069=ORIENTED_EDGE('',*,*,#56439,.T.);
#83070=ORIENTED_EDGE('',*,*,#56464,.F.);
#83071=ORIENTED_EDGE('',*,*,#56146,.T.);
#83072=ORIENTED_EDGE('',*,*,#56101,.T.);
#83073=ORIENTED_EDGE('',*,*,#56430,.T.);
#83074=ORIENTED_EDGE('',*,*,#56464,.T.);
#83075=ORIENTED_EDGE('',*,*,#56438,.T.);
#83076=ORIENTED_EDGE('',*,*,#56450,.T.);
#83077=ORIENTED_EDGE('',*,*,#56343,.T.);
#83078=ORIENTED_EDGE('',*,*,#56463,.F.);
#83079=ORIENTED_EDGE('',*,*,#56231,.T.);
#83080=ORIENTED_EDGE('',*,*,#56047,.T.);
#83081=ORIENTED_EDGE('',*,*,#56428,.T.);
#83082=ORIENTED_EDGE('',*,*,#56314,.T.);
#83083=ORIENTED_EDGE('',*,*,#56190,.T.);
#83084=ORIENTED_EDGE('',*,*,#56276,.T.);
#83085=ORIENTED_EDGE('',*,*,#56386,.T.);
#83086=ORIENTED_EDGE('',*,*,#56043,.F.);
#83087=ORIENTED_EDGE('',*,*,#56228,.T.);
#83088=ORIENTED_EDGE('',*,*,#56039,.T.);
#83089=ORIENTED_EDGE('',*,*,#56425,.T.);
#83090=ORIENTED_EDGE('',*,*,#56311,.T.);
#83091=ORIENTED_EDGE('',*,*,#56233,.T.);
#83092=ORIENTED_EDGE('',*,*,#56313,.T.);
#83093=ORIENTED_EDGE('',*,*,#56427,.T.);
#83094=ORIENTED_EDGE('',*,*,#56035,.F.);
#83095=ORIENTED_EDGE('',*,*,#56216,.T.);
#83096=ORIENTED_EDGE('',*,*,#56031,.T.);
#83097=ORIENTED_EDGE('',*,*,#56413,.T.);
#83098=ORIENTED_EDGE('',*,*,#56302,.T.);
#83099=ORIENTED_EDGE('',*,*,#56230,.T.);
#83100=ORIENTED_EDGE('',*,*,#56310,.T.);
#83101=ORIENTED_EDGE('',*,*,#56424,.T.);
#83102=ORIENTED_EDGE('',*,*,#56027,.F.);
#83103=ORIENTED_EDGE('',*,*,#56223,.T.);
#83104=ORIENTED_EDGE('',*,*,#56465,.T.);
#83105=ORIENTED_EDGE('',*,*,#56419,.T.);
#83106=ORIENTED_EDGE('',*,*,#56307,.T.);
#83107=ORIENTED_EDGE('',*,*,#56221,.T.);
#83108=ORIENTED_EDGE('',*,*,#56306,.T.);
#83109=ORIENTED_EDGE('',*,*,#56418,.T.);
#83110=ORIENTED_EDGE('',*,*,#56466,.F.);
#83111=ORIENTED_EDGE('',*,*,#56227,.T.);
#83112=ORIENTED_EDGE('',*,*,#56097,.T.);
#83113=ORIENTED_EDGE('',*,*,#56222,.T.);
#83114=ORIENTED_EDGE('',*,*,#56466,.T.);
#83115=ORIENTED_EDGE('',*,*,#56417,.T.);
#83116=ORIENTED_EDGE('',*,*,#56452,.T.);
#83117=ORIENTED_EDGE('',*,*,#56420,.T.);
#83118=ORIENTED_EDGE('',*,*,#56465,.F.);
#83119=ORIENTED_EDGE('',*,*,#56219,.T.);
#83120=ORIENTED_EDGE('',*,*,#56024,.T.);
#83121=ORIENTED_EDGE('',*,*,#56415,.T.);
#83122=ORIENTED_EDGE('',*,*,#56304,.T.);
#83123=ORIENTED_EDGE('',*,*,#56212,.T.);
#83124=ORIENTED_EDGE('',*,*,#56297,.T.);
#83125=ORIENTED_EDGE('',*,*,#56408,.T.);
#83126=ORIENTED_EDGE('',*,*,#56020,.F.);
#83127=ORIENTED_EDGE('',*,*,#56213,.T.);
#83128=ORIENTED_EDGE('',*,*,#56015,.T.);
#83129=ORIENTED_EDGE('',*,*,#56410,.T.);
#83130=ORIENTED_EDGE('',*,*,#56299,.T.);
#83131=ORIENTED_EDGE('',*,*,#56218,.T.);
#83132=ORIENTED_EDGE('',*,*,#56301,.T.);
#83133=ORIENTED_EDGE('',*,*,#56412,.T.);
#83134=ORIENTED_EDGE('',*,*,#56011,.F.);
#83135=ORIENTED_EDGE('',*,*,#56210,.T.);
#83136=ORIENTED_EDGE('',*,*,#56008,.T.);
#83137=ORIENTED_EDGE('',*,*,#56406,.T.);
#83138=ORIENTED_EDGE('',*,*,#56295,.T.);
#83139=ORIENTED_EDGE('',*,*,#56215,.T.);
#83140=ORIENTED_EDGE('',*,*,#56298,.T.);
#83141=ORIENTED_EDGE('',*,*,#56409,.T.);
#83142=ORIENTED_EDGE('',*,*,#56004,.F.);
#83143=ORIENTED_EDGE('',*,*,#56207,.T.);
#83144=ORIENTED_EDGE('',*,*,#56467,.T.);
#83145=ORIENTED_EDGE('',*,*,#56403,.T.);
#83146=ORIENTED_EDGE('',*,*,#56293,.T.);
#83147=ORIENTED_EDGE('',*,*,#56156,.T.);
#83148=ORIENTED_EDGE('',*,*,#56256,.T.);
#83149=ORIENTED_EDGE('',*,*,#56354,.T.);
#83150=ORIENTED_EDGE('',*,*,#56468,.F.);
#83151=ORIENTED_EDGE('',*,*,#56206,.T.);
#83152=ORIENTED_EDGE('',*,*,#56083,.T.);
#83153=ORIENTED_EDGE('',*,*,#56157,.T.);
#83154=ORIENTED_EDGE('',*,*,#56468,.T.);
#83155=ORIENTED_EDGE('',*,*,#56353,.T.);
#83156=ORIENTED_EDGE('',*,*,#56453,.T.);
#83157=ORIENTED_EDGE('',*,*,#56404,.T.);
#83158=ORIENTED_EDGE('',*,*,#56467,.F.);
#83159=ORIENTED_EDGE('',*,*,#56200,.T.);
#83160=ORIENTED_EDGE('',*,*,#55998,.T.);
#83161=ORIENTED_EDGE('',*,*,#56397,.T.);
#83162=ORIENTED_EDGE('',*,*,#56287,.T.);
#83163=ORIENTED_EDGE('',*,*,#56205,.T.);
#83164=ORIENTED_EDGE('',*,*,#56291,.T.);
#83165=ORIENTED_EDGE('',*,*,#56401,.T.);
#83166=ORIENTED_EDGE('',*,*,#55994,.F.);
#83167=ORIENTED_EDGE('',*,*,#56203,.T.);
#83168=ORIENTED_EDGE('',*,*,#55990,.T.);
#83169=ORIENTED_EDGE('',*,*,#56399,.T.);
#83170=ORIENTED_EDGE('',*,*,#56289,.T.);
#83171=ORIENTED_EDGE('',*,*,#56209,.T.);
#83172=ORIENTED_EDGE('',*,*,#56292,.T.);
#83173=ORIENTED_EDGE('',*,*,#56402,.T.);
#83174=ORIENTED_EDGE('',*,*,#55986,.F.);
#83175=ORIENTED_EDGE('',*,*,#56194,.T.);
#83176=ORIENTED_EDGE('',*,*,#55983,.T.);
#83177=ORIENTED_EDGE('',*,*,#56391,.T.);
#83178=ORIENTED_EDGE('',*,*,#56281,.T.);
#83179=ORIENTED_EDGE('',*,*,#56199,.T.);
#83180=ORIENTED_EDGE('',*,*,#56285,.T.);
#83181=ORIENTED_EDGE('',*,*,#56395,.T.);
#83182=ORIENTED_EDGE('',*,*,#55979,.F.);
#83183=ORIENTED_EDGE('',*,*,#56197,.T.);
#83184=ORIENTED_EDGE('',*,*,#55975,.T.);
#83185=ORIENTED_EDGE('',*,*,#56393,.T.);
#83186=ORIENTED_EDGE('',*,*,#56283,.T.);
#83187=ORIENTED_EDGE('',*,*,#56202,.T.);
#83188=ORIENTED_EDGE('',*,*,#56286,.T.);
#83189=ORIENTED_EDGE('',*,*,#56396,.T.);
#83190=ORIENTED_EDGE('',*,*,#55971,.F.);
#83191=ORIENTED_EDGE('',*,*,#56191,.T.);
#83192=ORIENTED_EDGE('',*,*,#55967,.T.);
#83193=ORIENTED_EDGE('',*,*,#56388,.T.);
#83194=ORIENTED_EDGE('',*,*,#56278,.T.);
#83195=ORIENTED_EDGE('',*,*,#56196,.T.);
#83196=ORIENTED_EDGE('',*,*,#56280,.T.);
#83197=ORIENTED_EDGE('',*,*,#56390,.T.);
#83198=ORIENTED_EDGE('',*,*,#55963,.F.);
#83199=ORIENTED_EDGE('',*,*,#56188,.T.);
#83200=ORIENTED_EDGE('',*,*,#55959,.T.);
#83201=ORIENTED_EDGE('',*,*,#56384,.T.);
#83202=ORIENTED_EDGE('',*,*,#56274,.T.);
#83203=ORIENTED_EDGE('',*,*,#56193,.T.);
#83204=ORIENTED_EDGE('',*,*,#56277,.T.);
#83205=ORIENTED_EDGE('',*,*,#56387,.T.);
#83206=ORIENTED_EDGE('',*,*,#55955,.F.);
#83207=ORIENTED_EDGE('',*,*,#56185,.T.);
#83208=ORIENTED_EDGE('',*,*,#56469,.T.);
#83209=ORIENTED_EDGE('',*,*,#56381,.T.);
#83210=ORIENTED_EDGE('',*,*,#56272,.T.);
#83211=ORIENTED_EDGE('',*,*,#56122,.T.);
#83212=ORIENTED_EDGE('',*,*,#56236,.T.);
#83213=ORIENTED_EDGE('',*,*,#56320,.T.);
#83214=ORIENTED_EDGE('',*,*,#56470,.F.);
#83215=ORIENTED_EDGE('',*,*,#56184,.T.);
#83216=ORIENTED_EDGE('',*,*,#56069,.T.);
#83217=ORIENTED_EDGE('',*,*,#56123,.T.);
#83218=ORIENTED_EDGE('',*,*,#56470,.T.);
#83219=ORIENTED_EDGE('',*,*,#56319,.T.);
#83220=ORIENTED_EDGE('',*,*,#56460,.T.);
#83221=ORIENTED_EDGE('',*,*,#56382,.T.);
#83222=ORIENTED_EDGE('',*,*,#56469,.F.);
#83223=ORIENTED_EDGE('',*,*,#56175,.T.);
#83224=ORIENTED_EDGE('',*,*,#56471,.T.);
#83225=ORIENTED_EDGE('',*,*,#56371,.T.);
#83226=ORIENTED_EDGE('',*,*,#56266,.T.);
#83227=ORIENTED_EDGE('',*,*,#56180,.T.);
#83228=ORIENTED_EDGE('',*,*,#56270,.T.);
#83229=ORIENTED_EDGE('',*,*,#56378,.T.);
#83230=ORIENTED_EDGE('',*,*,#56472,.F.);
#83231=ORIENTED_EDGE('',*,*,#56174,.T.);
#83232=ORIENTED_EDGE('',*,*,#56073,.T.);
#83233=ORIENTED_EDGE('',*,*,#56181,.T.);
#83234=ORIENTED_EDGE('',*,*,#56472,.T.);
#83235=ORIENTED_EDGE('',*,*,#56377,.T.);
#83236=ORIENTED_EDGE('',*,*,#56458,.T.);
#83237=ORIENTED_EDGE('',*,*,#56372,.T.);
#83238=ORIENTED_EDGE('',*,*,#56471,.F.);
#83239=ORIENTED_EDGE('',*,*,#56178,.T.);
#83240=ORIENTED_EDGE('',*,*,#56473,.T.);
#83241=ORIENTED_EDGE('',*,*,#56374,.T.);
#83242=ORIENTED_EDGE('',*,*,#56268,.T.);
#83243=ORIENTED_EDGE('',*,*,#56187,.T.);
#83244=ORIENTED_EDGE('',*,*,#56271,.T.);
#83245=ORIENTED_EDGE('',*,*,#56380,.T.);
#83246=ORIENTED_EDGE('',*,*,#56474,.F.);
#83247=ORIENTED_EDGE('',*,*,#56182,.T.);
#83248=ORIENTED_EDGE('',*,*,#56071,.T.);
#83249=ORIENTED_EDGE('',*,*,#56183,.T.);
#83250=ORIENTED_EDGE('',*,*,#56474,.T.);
#83251=ORIENTED_EDGE('',*,*,#56379,.T.);
#83252=ORIENTED_EDGE('',*,*,#56459,.T.);
#83253=ORIENTED_EDGE('',*,*,#56375,.T.);
#83254=ORIENTED_EDGE('',*,*,#56473,.F.);
#83255=ORIENTED_EDGE('',*,*,#56170,.T.);
#83256=ORIENTED_EDGE('',*,*,#56264,.T.);
#83257=ORIENTED_EDGE('',*,*,#56368,.T.);
#83258=ORIENTED_EDGE('',*,*,#56475,.F.);
#83259=ORIENTED_EDGE('',*,*,#56165,.T.);
#83260=ORIENTED_EDGE('',*,*,#56077,.T.);
#83261=ORIENTED_EDGE('',*,*,#56171,.T.);
#83262=ORIENTED_EDGE('',*,*,#56475,.T.);
#83263=ORIENTED_EDGE('',*,*,#56367,.T.);
#83264=ORIENTED_EDGE('',*,*,#56456,.T.);
#83265=ORIENTED_EDGE('',*,*,#56362,.T.);
#83266=ORIENTED_EDGE('',*,*,#55950,.F.);
#83267=ORIENTED_EDGE('',*,*,#56168,.T.);
#83268=ORIENTED_EDGE('',*,*,#56476,.T.);
#83269=ORIENTED_EDGE('',*,*,#56364,.T.);
#83270=ORIENTED_EDGE('',*,*,#56262,.T.);
#83271=ORIENTED_EDGE('',*,*,#56177,.T.);
#83272=ORIENTED_EDGE('',*,*,#56265,.T.);
#83273=ORIENTED_EDGE('',*,*,#56370,.T.);
#83274=ORIENTED_EDGE('',*,*,#56477,.F.);
#83275=ORIENTED_EDGE('',*,*,#56172,.T.);
#83276=ORIENTED_EDGE('',*,*,#56075,.T.);
#83277=ORIENTED_EDGE('',*,*,#56173,.T.);
#83278=ORIENTED_EDGE('',*,*,#56477,.T.);
#83279=ORIENTED_EDGE('',*,*,#56369,.T.);
#83280=ORIENTED_EDGE('',*,*,#56457,.T.);
#83281=ORIENTED_EDGE('',*,*,#56365,.T.);
#83282=ORIENTED_EDGE('',*,*,#56476,.F.);
#83283=ORIENTED_EDGE('',*,*,#56161,.T.);
#83284=ORIENTED_EDGE('',*,*,#56478,.T.);
#83285=ORIENTED_EDGE('',*,*,#56357,.T.);
#83286=ORIENTED_EDGE('',*,*,#56258,.T.);
#83287=ORIENTED_EDGE('',*,*,#56167,.T.);
#83288=ORIENTED_EDGE('',*,*,#56260,.T.);
#83289=ORIENTED_EDGE('',*,*,#56361,.T.);
#83290=ORIENTED_EDGE('',*,*,#56479,.F.);
#83291=ORIENTED_EDGE('',*,*,#56160,.T.);
#83292=ORIENTED_EDGE('',*,*,#56079,.T.);
#83293=ORIENTED_EDGE('',*,*,#56164,.T.);
#83294=ORIENTED_EDGE('',*,*,#56479,.T.);
#83295=ORIENTED_EDGE('',*,*,#56360,.T.);
#83296=ORIENTED_EDGE('',*,*,#56455,.T.);
#83297=ORIENTED_EDGE('',*,*,#56358,.T.);
#83298=ORIENTED_EDGE('',*,*,#56478,.F.);
#83299=ORIENTED_EDGE('',*,*,#56154,.T.);
#83300=ORIENTED_EDGE('',*,*,#56480,.T.);
#83301=ORIENTED_EDGE('',*,*,#56350,.T.);
#83302=ORIENTED_EDGE('',*,*,#56254,.T.);
#83303=ORIENTED_EDGE('',*,*,#56163,.T.);
#83304=ORIENTED_EDGE('',*,*,#56257,.T.);
#83305=ORIENTED_EDGE('',*,*,#56356,.T.);
#83306=ORIENTED_EDGE('',*,*,#56481,.F.);
#83307=ORIENTED_EDGE('',*,*,#56158,.T.);
#83308=ORIENTED_EDGE('',*,*,#56081,.T.);
#83309=ORIENTED_EDGE('',*,*,#56159,.T.);
#83310=ORIENTED_EDGE('',*,*,#56481,.T.);
#83311=ORIENTED_EDGE('',*,*,#56355,.T.);
#83312=ORIENTED_EDGE('',*,*,#56454,.T.);
#83313=ORIENTED_EDGE('',*,*,#56351,.T.);
#83314=ORIENTED_EDGE('',*,*,#56480,.F.);
#83315=ORIENTED_EDGE('',*,*,#56151,.T.);
#83316=ORIENTED_EDGE('',*,*,#56482,.T.);
#83317=ORIENTED_EDGE('',*,*,#56347,.T.);
#83318=ORIENTED_EDGE('',*,*,#56252,.T.);
#83319=ORIENTED_EDGE('',*,*,#56142,.T.);
#83320=ORIENTED_EDGE('',*,*,#56248,.T.);
#83321=ORIENTED_EDGE('',*,*,#56340,.T.);
#83322=ORIENTED_EDGE('',*,*,#56483,.F.);
#83323=ORIENTED_EDGE('',*,*,#56150,.T.);
#83324=ORIENTED_EDGE('',*,*,#56105,.T.);
#83325=ORIENTED_EDGE('',*,*,#56143,.T.);
#83326=ORIENTED_EDGE('',*,*,#56483,.T.);
#83327=ORIENTED_EDGE('',*,*,#56339,.T.);
#83328=ORIENTED_EDGE('',*,*,#56448,.T.);
#83329=ORIENTED_EDGE('',*,*,#56348,.T.);
#83330=ORIENTED_EDGE('',*,*,#56482,.F.);
#83331=ORIENTED_EDGE('',*,*,#56137,.T.);
#83332=ORIENTED_EDGE('',*,*,#56484,.T.);
#83333=ORIENTED_EDGE('',*,*,#56333,.T.);
#83334=ORIENTED_EDGE('',*,*,#56244,.T.);
#83335=ORIENTED_EDGE('',*,*,#56153,.T.);
#83336=ORIENTED_EDGE('',*,*,#56251,.T.);
#83337=ORIENTED_EDGE('',*,*,#56346,.T.);
#83338=ORIENTED_EDGE('',*,*,#56485,.F.);
#83339=ORIENTED_EDGE('',*,*,#56136,.T.);
#83340=ORIENTED_EDGE('',*,*,#56107,.T.);
#83341=ORIENTED_EDGE('',*,*,#56149,.T.);
#83342=ORIENTED_EDGE('',*,*,#56485,.T.);
#83343=ORIENTED_EDGE('',*,*,#56345,.T.);
#83344=ORIENTED_EDGE('',*,*,#56447,.T.);
#83345=ORIENTED_EDGE('',*,*,#56334,.T.);
#83346=ORIENTED_EDGE('',*,*,#56484,.F.);
#83347=ORIENTED_EDGE('',*,*,#56140,.T.);
#83348=ORIENTED_EDGE('',*,*,#56486,.T.);
#83349=ORIENTED_EDGE('',*,*,#56336,.T.);
#83350=ORIENTED_EDGE('',*,*,#56246,.T.);
#83351=ORIENTED_EDGE('',*,*,#56144,.T.);
#83352=ORIENTED_EDGE('',*,*,#56103,.T.);
#83353=ORIENTED_EDGE('',*,*,#56145,.T.);
#83354=ORIENTED_EDGE('',*,*,#55948,.T.);
#83355=ORIENTED_EDGE('',*,*,#56341,.T.);
#83356=ORIENTED_EDGE('',*,*,#56449,.T.);
#83357=ORIENTED_EDGE('',*,*,#56337,.T.);
#83358=ORIENTED_EDGE('',*,*,#56486,.F.);
#83359=ORIENTED_EDGE('',*,*,#56132,.T.);
#83360=ORIENTED_EDGE('',*,*,#56487,.T.);
#83361=ORIENTED_EDGE('',*,*,#56328,.T.);
#83362=ORIENTED_EDGE('',*,*,#56241,.T.);
#83363=ORIENTED_EDGE('',*,*,#56139,.T.);
#83364=ORIENTED_EDGE('',*,*,#56243,.T.);
#83365=ORIENTED_EDGE('',*,*,#56332,.T.);
#83366=ORIENTED_EDGE('',*,*,#56488,.F.);
#83367=ORIENTED_EDGE('',*,*,#56131,.T.);
#83368=ORIENTED_EDGE('',*,*,#56109,.T.);
#83369=ORIENTED_EDGE('',*,*,#56135,.T.);
#83370=ORIENTED_EDGE('',*,*,#56488,.T.);
#83371=ORIENTED_EDGE('',*,*,#56331,.T.);
#83372=ORIENTED_EDGE('',*,*,#56446,.T.);
#83373=ORIENTED_EDGE('',*,*,#56329,.T.);
#83374=ORIENTED_EDGE('',*,*,#56487,.F.);
#83375=ORIENTED_EDGE('',*,*,#56127,.T.);
#83376=ORIENTED_EDGE('',*,*,#56489,.T.);
#83377=ORIENTED_EDGE('',*,*,#56323,.T.);
#83378=ORIENTED_EDGE('',*,*,#56238,.T.);
#83379=ORIENTED_EDGE('',*,*,#56134,.T.);
#83380=ORIENTED_EDGE('',*,*,#56240,.T.);
#83381=ORIENTED_EDGE('',*,*,#56327,.T.);
#83382=ORIENTED_EDGE('',*,*,#56490,.F.);
#83383=ORIENTED_EDGE('',*,*,#56126,.T.);
#83384=ORIENTED_EDGE('',*,*,#56111,.T.);
#83385=ORIENTED_EDGE('',*,*,#56130,.T.);
#83386=ORIENTED_EDGE('',*,*,#56490,.T.);
#83387=ORIENTED_EDGE('',*,*,#56326,.T.);
#83388=ORIENTED_EDGE('',*,*,#56445,.T.);
#83389=ORIENTED_EDGE('',*,*,#56324,.T.);
#83390=ORIENTED_EDGE('',*,*,#56489,.F.);
#83391=ORIENTED_EDGE('',*,*,#56060,.T.);
#83392=ORIENTED_EDGE('',*,*,#56491,.T.);
#83393=ORIENTED_EDGE('',*,*,#56050,.T.);
#83394=ORIENTED_EDGE('',*,*,#56056,.T.);
#83395=ORIENTED_EDGE('',*,*,#56129,.T.);
#83396=ORIENTED_EDGE('',*,*,#56237,.T.);
#83397=ORIENTED_EDGE('',*,*,#56322,.T.);
#83398=ORIENTED_EDGE('',*,*,#56492,.F.);
#83399=ORIENTED_EDGE('',*,*,#56059,.T.);
#83400=ORIENTED_EDGE('',*,*,#56113,.T.);
#83401=ORIENTED_EDGE('',*,*,#56125,.T.);
#83402=ORIENTED_EDGE('',*,*,#56492,.T.);
#83403=ORIENTED_EDGE('',*,*,#56321,.T.);
#83404=ORIENTED_EDGE('',*,*,#56444,.T.);
#83405=ORIENTED_EDGE('',*,*,#56051,.T.);
#83406=ORIENTED_EDGE('',*,*,#56491,.F.);
#83407=ORIENTED_EDGE('',*,*,#56120,.T.);
#83408=ORIENTED_EDGE('',*,*,#56493,.T.);
#83409=ORIENTED_EDGE('',*,*,#56316,.T.);
#83410=ORIENTED_EDGE('',*,*,#56234,.T.);
#83411=ORIENTED_EDGE('',*,*,#56061,.T.);
#83412=ORIENTED_EDGE('',*,*,#56057,.T.);
#83413=ORIENTED_EDGE('',*,*,#56054,.T.);
#83414=ORIENTED_EDGE('',*,*,#56494,.F.);
#83415=ORIENTED_EDGE('',*,*,#56124,.T.);
#83416=ORIENTED_EDGE('',*,*,#56067,.T.);
#83417=ORIENTED_EDGE('',*,*,#56062,.T.);
#83418=ORIENTED_EDGE('',*,*,#56494,.T.);
#83419=ORIENTED_EDGE('',*,*,#56053,.T.);
#83420=ORIENTED_EDGE('',*,*,#56443,.T.);
#83421=ORIENTED_EDGE('',*,*,#56317,.T.);
#83422=ORIENTED_EDGE('',*,*,#56493,.F.);
#83423=ORIENTED_EDGE('',*,*,#56116,.T.);
#83424=ORIENTED_EDGE('',*,*,#56495,.T.);
#83425=ORIENTED_EDGE('',*,*,#56118,.F.);
#83426=ORIENTED_EDGE('',*,*,#56496,.F.);
#83427=ORIENTED_EDGE('',*,*,#56114,.T.);
#83428=ORIENTED_EDGE('',*,*,#56496,.T.);
#83429=ORIENTED_EDGE('',*,*,#56117,.F.);
#83430=ORIENTED_EDGE('',*,*,#56064,.F.);
#83431=ORIENTED_EDGE('',*,*,#56115,.T.);
#83432=ORIENTED_EDGE('',*,*,#56066,.F.);
#83433=ORIENTED_EDGE('',*,*,#56119,.F.);
#83434=ORIENTED_EDGE('',*,*,#56495,.F.);
#83435=ORIENTED_EDGE('',*,*,#56497,.T.);
#83436=ORIENTED_EDGE('',*,*,#56498,.T.);
#83437=ORIENTED_EDGE('',*,*,#56499,.F.);
#83438=ORIENTED_EDGE('',*,*,#56498,.F.);
#83439=ORIENTED_EDGE('',*,*,#56500,.F.);
#83440=ORIENTED_EDGE('',*,*,#56501,.T.);
#83441=ORIENTED_EDGE('',*,*,#56502,.T.);
#83442=ORIENTED_EDGE('',*,*,#56503,.F.);
#83443=ORIENTED_EDGE('',*,*,#56504,.T.);
#83444=ORIENTED_EDGE('',*,*,#56505,.T.);
#83445=ORIENTED_EDGE('',*,*,#56506,.F.);
#83446=ORIENTED_EDGE('',*,*,#56505,.F.);
#83447=ORIENTED_EDGE('',*,*,#56507,.T.);
#83448=ORIENTED_EDGE('',*,*,#56508,.F.);
#83449=ORIENTED_EDGE('',*,*,#56509,.F.);
#83450=ORIENTED_EDGE('',*,*,#56503,.T.);
#83451=ORIENTED_EDGE('',*,*,#56510,.T.);
#83452=ORIENTED_EDGE('',*,*,#56511,.F.);
#83453=ORIENTED_EDGE('',*,*,#56512,.F.);
#83454=ORIENTED_EDGE('',*,*,#56508,.T.);
#83455=ORIENTED_EDGE('',*,*,#56513,.F.);
#83456=ORIENTED_EDGE('',*,*,#56501,.F.);
#83457=ORIENTED_EDGE('',*,*,#56514,.T.);
#83458=ORIENTED_EDGE('',*,*,#56511,.T.);
#83459=ORIENTED_EDGE('',*,*,#56509,.T.);
#83460=ORIENTED_EDGE('',*,*,#56512,.T.);
#83461=ORIENTED_EDGE('',*,*,#56514,.F.);
#83462=ORIENTED_EDGE('',*,*,#56500,.T.);
#83463=ORIENTED_EDGE('',*,*,#56504,.F.);
#83464=ORIENTED_EDGE('',*,*,#56497,.F.);
#83465=ORIENTED_EDGE('',*,*,#56507,.F.);
#83466=ORIENTED_EDGE('',*,*,#56502,.F.);
#83467=ORIENTED_EDGE('',*,*,#56513,.T.);
#83468=ORIENTED_EDGE('',*,*,#56510,.F.);
#83469=ORIENTED_EDGE('',*,*,#56506,.T.);
#83470=ORIENTED_EDGE('',*,*,#56499,.T.);
#83471=ORIENTED_EDGE('',*,*,#56515,.T.);
#83472=ORIENTED_EDGE('',*,*,#56516,.T.);
#83473=ORIENTED_EDGE('',*,*,#56517,.F.);
#83474=ORIENTED_EDGE('',*,*,#56516,.F.);
#83475=ORIENTED_EDGE('',*,*,#56518,.T.);
#83476=ORIENTED_EDGE('',*,*,#56519,.T.);
#83477=ORIENTED_EDGE('',*,*,#56520,.F.);
#83478=ORIENTED_EDGE('',*,*,#56519,.F.);
#83479=ORIENTED_EDGE('',*,*,#56521,.F.);
#83480=ORIENTED_EDGE('',*,*,#56522,.T.);
#83481=ORIENTED_EDGE('',*,*,#56523,.T.);
#83482=ORIENTED_EDGE('',*,*,#56524,.F.);
#83483=ORIENTED_EDGE('',*,*,#56525,.T.);
#83484=ORIENTED_EDGE('',*,*,#56526,.T.);
#83485=ORIENTED_EDGE('',*,*,#56527,.T.);
#83486=ORIENTED_EDGE('',*,*,#56521,.T.);
#83487=ORIENTED_EDGE('',*,*,#56515,.F.);
#83488=ORIENTED_EDGE('',*,*,#56518,.F.);
#83489=ORIENTED_EDGE('',*,*,#56528,.F.);
#83490=ORIENTED_EDGE('',*,*,#56523,.F.);
#83491=ORIENTED_EDGE('',*,*,#56529,.F.);
#83492=ORIENTED_EDGE('',*,*,#56530,.F.);
#83493=ORIENTED_EDGE('',*,*,#56520,.T.);
#83494=ORIENTED_EDGE('',*,*,#56517,.T.);
#83495=ORIENTED_EDGE('',*,*,#56528,.T.);
#83496=ORIENTED_EDGE('',*,*,#56531,.F.);
#83497=ORIENTED_EDGE('',*,*,#56525,.F.);
#83498=ORIENTED_EDGE('',*,*,#56524,.T.);
#83499=ORIENTED_EDGE('',*,*,#56530,.T.);
#83500=ORIENTED_EDGE('',*,*,#56532,.F.);
#83501=ORIENTED_EDGE('',*,*,#56526,.F.);
#83502=ORIENTED_EDGE('',*,*,#56531,.T.);
#83503=ORIENTED_EDGE('',*,*,#56529,.T.);
#83504=ORIENTED_EDGE('',*,*,#56522,.F.);
#83505=ORIENTED_EDGE('',*,*,#56527,.F.);
#83506=ORIENTED_EDGE('',*,*,#56532,.T.);
#83507=ORIENTED_EDGE('',*,*,#56533,.T.);
#83508=ORIENTED_EDGE('',*,*,#56534,.T.);
#83509=ORIENTED_EDGE('',*,*,#56535,.F.);
#83510=ORIENTED_EDGE('',*,*,#56534,.F.);
#83511=ORIENTED_EDGE('',*,*,#56535,.T.);
#83512=ORIENTED_EDGE('',*,*,#56533,.F.);
#83513=ORIENTED_EDGE('',*,*,#56536,.T.);
#83514=ORIENTED_EDGE('',*,*,#56537,.T.);
#83515=ORIENTED_EDGE('',*,*,#56538,.F.);
#83516=ORIENTED_EDGE('',*,*,#56537,.F.);
#83517=ORIENTED_EDGE('',*,*,#56538,.T.);
#83518=ORIENTED_EDGE('',*,*,#56536,.F.);
#83519=ORIENTED_EDGE('',*,*,#56539,.T.);
#83520=ORIENTED_EDGE('',*,*,#56540,.T.);
#83521=ORIENTED_EDGE('',*,*,#56541,.F.);
#83522=ORIENTED_EDGE('',*,*,#56540,.F.);
#83523=ORIENTED_EDGE('',*,*,#56542,.F.);
#83524=ORIENTED_EDGE('',*,*,#56543,.T.);
#83525=ORIENTED_EDGE('',*,*,#56544,.T.);
#83526=ORIENTED_EDGE('',*,*,#56543,.F.);
#83527=ORIENTED_EDGE('',*,*,#56545,.T.);
#83528=ORIENTED_EDGE('',*,*,#56546,.T.);
#83529=ORIENTED_EDGE('',*,*,#56547,.F.);
#83530=ORIENTED_EDGE('',*,*,#56546,.F.);
#83531=ORIENTED_EDGE('',*,*,#56548,.T.);
#83532=ORIENTED_EDGE('',*,*,#56549,.T.);
#83533=ORIENTED_EDGE('',*,*,#56550,.T.);
#83534=ORIENTED_EDGE('',*,*,#56549,.F.);
#83535=ORIENTED_EDGE('',*,*,#56547,.T.);
#83536=ORIENTED_EDGE('',*,*,#56544,.F.);
#83537=ORIENTED_EDGE('',*,*,#56545,.F.);
#83538=ORIENTED_EDGE('',*,*,#56541,.T.);
#83539=ORIENTED_EDGE('',*,*,#56542,.T.);
#83540=ORIENTED_EDGE('',*,*,#56548,.F.);
#83541=ORIENTED_EDGE('',*,*,#56539,.F.);
#83542=ORIENTED_EDGE('',*,*,#56550,.F.);
#83543=ORIENTED_EDGE('',*,*,#56551,.F.);
#83544=ORIENTED_EDGE('',*,*,#56552,.T.);
#83545=ORIENTED_EDGE('',*,*,#56553,.T.);
#83546=ORIENTED_EDGE('',*,*,#56552,.F.);
#83547=ORIENTED_EDGE('',*,*,#56554,.F.);
#83548=ORIENTED_EDGE('',*,*,#56555,.T.);
#83549=ORIENTED_EDGE('',*,*,#56556,.T.);
#83550=ORIENTED_EDGE('',*,*,#56555,.F.);
#83551=ORIENTED_EDGE('',*,*,#56557,.F.);
#83552=ORIENTED_EDGE('',*,*,#56558,.T.);
#83553=ORIENTED_EDGE('',*,*,#56559,.T.);
#83554=ORIENTED_EDGE('',*,*,#56558,.F.);
#83555=ORIENTED_EDGE('',*,*,#56553,.F.);
#83556=ORIENTED_EDGE('',*,*,#56560,.T.);
#83557=ORIENTED_EDGE('',*,*,#56561,.T.);
#83558=ORIENTED_EDGE('',*,*,#56560,.F.);
#83559=ORIENTED_EDGE('',*,*,#56561,.F.);
#83560=ORIENTED_EDGE('',*,*,#56562,.T.);
#83561=ORIENTED_EDGE('',*,*,#56563,.T.);
#83562=ORIENTED_EDGE('',*,*,#56562,.F.);
#83563=ORIENTED_EDGE('',*,*,#56564,.F.);
#83564=ORIENTED_EDGE('',*,*,#56565,.T.);
#83565=ORIENTED_EDGE('',*,*,#56566,.T.);
#83566=ORIENTED_EDGE('',*,*,#56565,.F.);
#83567=ORIENTED_EDGE('',*,*,#56566,.F.);
#83568=ORIENTED_EDGE('',*,*,#56567,.T.);
#83569=ORIENTED_EDGE('',*,*,#56554,.T.);
#83570=ORIENTED_EDGE('',*,*,#56567,.F.);
#83571=ORIENTED_EDGE('',*,*,#56556,.F.);
#83572=ORIENTED_EDGE('',*,*,#56568,.T.);
#83573=ORIENTED_EDGE('',*,*,#56557,.T.);
#83574=ORIENTED_EDGE('',*,*,#56568,.F.);
#83575=ORIENTED_EDGE('',*,*,#56559,.F.);
#83576=ORIENTED_EDGE('',*,*,#56569,.T.);
#83577=ORIENTED_EDGE('',*,*,#56570,.T.);
#83578=ORIENTED_EDGE('',*,*,#56569,.F.);
#83579=ORIENTED_EDGE('',*,*,#56570,.F.);
#83580=ORIENTED_EDGE('',*,*,#56571,.T.);
#83581=ORIENTED_EDGE('',*,*,#56572,.T.);
#83582=ORIENTED_EDGE('',*,*,#56571,.F.);
#83583=ORIENTED_EDGE('',*,*,#56564,.T.);
#83584=ORIENTED_EDGE('',*,*,#56563,.F.);
#83585=ORIENTED_EDGE('',*,*,#56572,.F.);
#83586=ORIENTED_EDGE('',*,*,#56551,.T.);
#83587=ORIENTED_EDGE('',*,*,#56573,.T.);
#83588=ORIENTED_EDGE('',*,*,#56573,.F.);
#83589=ORIENTED_EDGE('',*,*,#56574,.F.);
#83590=ORIENTED_EDGE('',*,*,#56575,.T.);
#83591=ORIENTED_EDGE('',*,*,#56576,.F.);
#83592=ORIENTED_EDGE('',*,*,#56577,.T.);
#83593=ORIENTED_EDGE('',*,*,#56578,.T.);
#83594=ORIENTED_EDGE('',*,*,#56577,.F.);
#83595=ORIENTED_EDGE('',*,*,#56578,.F.);
#83596=ORIENTED_EDGE('',*,*,#56579,.T.);
#83597=ORIENTED_EDGE('',*,*,#56580,.T.);
#83598=ORIENTED_EDGE('',*,*,#56579,.F.);
#83599=ORIENTED_EDGE('',*,*,#56580,.F.);
#83600=ORIENTED_EDGE('',*,*,#56581,.T.);
#83601=ORIENTED_EDGE('',*,*,#56582,.T.);
#83602=ORIENTED_EDGE('',*,*,#56581,.F.);
#83603=ORIENTED_EDGE('',*,*,#56576,.T.);
#83604=ORIENTED_EDGE('',*,*,#56575,.F.);
#83605=ORIENTED_EDGE('',*,*,#56582,.F.);
#83606=ORIENTED_EDGE('',*,*,#56574,.T.);
#83607=ORIENTED_EDGE('',*,*,#56583,.T.);
#83608=ORIENTED_EDGE('',*,*,#56583,.F.);
#83609=ORIENTED_EDGE('',*,*,#56584,.T.);
#83610=ORIENTED_EDGE('',*,*,#56584,.F.);
#83611=ORIENTED_EDGE('',*,*,#56585,.T.);
#83612=ORIENTED_EDGE('',*,*,#56585,.F.);
#83613=ORIENTED_EDGE('',*,*,#56586,.T.);
#83614=ORIENTED_EDGE('',*,*,#56586,.F.);
#83615=ORIENTED_EDGE('',*,*,#56587,.T.);
#83616=ORIENTED_EDGE('',*,*,#56587,.F.);
#83617=ORIENTED_EDGE('',*,*,#56588,.T.);
#83618=ORIENTED_EDGE('',*,*,#56588,.F.);
#83619=ORIENTED_EDGE('',*,*,#56589,.T.);
#83620=ORIENTED_EDGE('',*,*,#56589,.F.);
#83621=ORIENTED_EDGE('',*,*,#56590,.T.);
#83622=ORIENTED_EDGE('',*,*,#56590,.F.);
#83623=ORIENTED_EDGE('',*,*,#56591,.T.);
#83624=ORIENTED_EDGE('',*,*,#56591,.F.);
#83625=ORIENTED_EDGE('',*,*,#56592,.T.);
#83626=ORIENTED_EDGE('',*,*,#56592,.F.);
#83627=ORIENTED_EDGE('',*,*,#56593,.T.);
#83628=ORIENTED_EDGE('',*,*,#56593,.F.);
#83629=ORIENTED_EDGE('',*,*,#56594,.T.);
#83630=ORIENTED_EDGE('',*,*,#56594,.F.);
#83631=ORIENTED_EDGE('',*,*,#56595,.T.);
#83632=ORIENTED_EDGE('',*,*,#56595,.F.);
#83633=ORIENTED_EDGE('',*,*,#56596,.T.);
#83634=ORIENTED_EDGE('',*,*,#56596,.F.);
#83635=ORIENTED_EDGE('',*,*,#56597,.T.);
#83636=ORIENTED_EDGE('',*,*,#56597,.F.);
#83637=ORIENTED_EDGE('',*,*,#56598,.T.);
#83638=ORIENTED_EDGE('',*,*,#56598,.F.);
#83639=ORIENTED_EDGE('',*,*,#56599,.T.);
#83640=ORIENTED_EDGE('',*,*,#56599,.F.);
#83641=ORIENTED_EDGE('',*,*,#56600,.T.);
#83642=ORIENTED_EDGE('',*,*,#56600,.F.);
#83643=ORIENTED_EDGE('',*,*,#56601,.T.);
#83644=ORIENTED_EDGE('',*,*,#56601,.F.);
#83645=ORIENTED_EDGE('',*,*,#56602,.T.);
#83646=ORIENTED_EDGE('',*,*,#56602,.F.);
#83647=ORIENTED_EDGE('',*,*,#56603,.T.);
#83648=ORIENTED_EDGE('',*,*,#56603,.F.);
#83649=ORIENTED_EDGE('',*,*,#56604,.T.);
#83650=ORIENTED_EDGE('',*,*,#56604,.F.);
#83651=ORIENTED_EDGE('',*,*,#56605,.T.);
#83652=ORIENTED_EDGE('',*,*,#56605,.F.);
#83653=ORIENTED_EDGE('',*,*,#56606,.T.);
#83654=ORIENTED_EDGE('',*,*,#56606,.F.);
#83655=ORIENTED_EDGE('',*,*,#56607,.F.);
#83656=ORIENTED_EDGE('',*,*,#56608,.T.);
#83657=ORIENTED_EDGE('',*,*,#56609,.T.);
#83658=ORIENTED_EDGE('',*,*,#56608,.F.);
#83659=ORIENTED_EDGE('',*,*,#56610,.F.);
#83660=ORIENTED_EDGE('',*,*,#56611,.T.);
#83661=ORIENTED_EDGE('',*,*,#56612,.T.);
#83662=ORIENTED_EDGE('',*,*,#56611,.F.);
#83663=ORIENTED_EDGE('',*,*,#56613,.T.);
#83664=ORIENTED_EDGE('',*,*,#56614,.T.);
#83665=ORIENTED_EDGE('',*,*,#56615,.F.);
#83666=ORIENTED_EDGE('',*,*,#56614,.F.);
#83667=ORIENTED_EDGE('',*,*,#56616,.T.);
#83668=ORIENTED_EDGE('',*,*,#56617,.T.);
#83669=ORIENTED_EDGE('',*,*,#56618,.F.);
#83670=ORIENTED_EDGE('',*,*,#56617,.F.);
#83671=ORIENTED_EDGE('',*,*,#56619,.T.);
#83672=ORIENTED_EDGE('',*,*,#56620,.F.);
#83673=ORIENTED_EDGE('',*,*,#56621,.F.);
#83674=ORIENTED_EDGE('',*,*,#56622,.T.);
#83675=ORIENTED_EDGE('',*,*,#56623,.T.);
#83676=ORIENTED_EDGE('',*,*,#56624,.F.);
#83677=ORIENTED_EDGE('',*,*,#56625,.F.);
#83678=ORIENTED_EDGE('',*,*,#56620,.T.);
#83679=ORIENTED_EDGE('',*,*,#56626,.T.);
#83680=ORIENTED_EDGE('',*,*,#56627,.F.);
#83681=ORIENTED_EDGE('',*,*,#56628,.F.);
#83682=ORIENTED_EDGE('',*,*,#56624,.T.);
#83683=ORIENTED_EDGE('',*,*,#56629,.T.);
#83684=ORIENTED_EDGE('',*,*,#56630,.F.);
#83685=ORIENTED_EDGE('',*,*,#56631,.F.);
#83686=ORIENTED_EDGE('',*,*,#56627,.T.);
#83687=ORIENTED_EDGE('',*,*,#56632,.T.);
#83688=ORIENTED_EDGE('',*,*,#56633,.F.);
#83689=ORIENTED_EDGE('',*,*,#56634,.F.);
#83690=ORIENTED_EDGE('',*,*,#56630,.T.);
#83691=ORIENTED_EDGE('',*,*,#56635,.T.);
#83692=ORIENTED_EDGE('',*,*,#56622,.F.);
#83693=ORIENTED_EDGE('',*,*,#56636,.F.);
#83694=ORIENTED_EDGE('',*,*,#56633,.T.);
#83695=ORIENTED_EDGE('',*,*,#56621,.T.);
#83696=ORIENTED_EDGE('',*,*,#56625,.T.);
#83697=ORIENTED_EDGE('',*,*,#56628,.T.);
#83698=ORIENTED_EDGE('',*,*,#56631,.T.);
#83699=ORIENTED_EDGE('',*,*,#56634,.T.);
#83700=ORIENTED_EDGE('',*,*,#56636,.T.);
#83701=ORIENTED_EDGE('',*,*,#56616,.F.);
#83702=ORIENTED_EDGE('',*,*,#56619,.F.);
#83703=ORIENTED_EDGE('',*,*,#56635,.F.);
#83704=ORIENTED_EDGE('',*,*,#56632,.F.);
#83705=ORIENTED_EDGE('',*,*,#56629,.F.);
#83706=ORIENTED_EDGE('',*,*,#56626,.F.);
#83707=ORIENTED_EDGE('',*,*,#56623,.F.);
#83708=ORIENTED_EDGE('',*,*,#56610,.T.);
#83709=ORIENTED_EDGE('',*,*,#56618,.T.);
#83710=ORIENTED_EDGE('',*,*,#56613,.F.);
#83711=ORIENTED_EDGE('',*,*,#56615,.T.);
#83712=ORIENTED_EDGE('',*,*,#56612,.F.);
#83713=ORIENTED_EDGE('',*,*,#56607,.T.);
#83714=ORIENTED_EDGE('',*,*,#56609,.F.);
#83715=ORIENTED_EDGE('',*,*,#56637,.T.);
#83716=ORIENTED_EDGE('',*,*,#56638,.F.);
#83717=ORIENTED_EDGE('',*,*,#56639,.F.);
#83718=ORIENTED_EDGE('',*,*,#56640,.T.);
#83719=ORIENTED_EDGE('',*,*,#56641,.T.);
#83720=ORIENTED_EDGE('',*,*,#56642,.F.);
#83721=ORIENTED_EDGE('',*,*,#56637,.F.);
#83722=ORIENTED_EDGE('',*,*,#56643,.F.);
#83723=ORIENTED_EDGE('',*,*,#56644,.T.);
#83724=ORIENTED_EDGE('',*,*,#56645,.T.);
#83725=ORIENTED_EDGE('',*,*,#56640,.F.);
#83726=ORIENTED_EDGE('',*,*,#56646,.F.);
#83727=ORIENTED_EDGE('',*,*,#56647,.T.);
#83728=ORIENTED_EDGE('',*,*,#56648,.T.);
#83729=ORIENTED_EDGE('',*,*,#56644,.F.);
#83730=ORIENTED_EDGE('',*,*,#56649,.F.);
#83731=ORIENTED_EDGE('',*,*,#56650,.F.);
#83732=ORIENTED_EDGE('',*,*,#56651,.F.);
#83733=ORIENTED_EDGE('',*,*,#56652,.F.);
#83734=ORIENTED_EDGE('',*,*,#56653,.T.);
#83735=ORIENTED_EDGE('',*,*,#56654,.F.);
#83736=ORIENTED_EDGE('',*,*,#56642,.T.);
#83737=ORIENTED_EDGE('',*,*,#56655,.T.);
#83738=ORIENTED_EDGE('',*,*,#56656,.F.);
#83739=ORIENTED_EDGE('',*,*,#56657,.T.);
#83740=ORIENTED_EDGE('',*,*,#56652,.T.);
#83741=ORIENTED_EDGE('',*,*,#56658,.T.);
#83742=ORIENTED_EDGE('',*,*,#56659,.T.);
#83743=ORIENTED_EDGE('',*,*,#56660,.F.);
#83744=ORIENTED_EDGE('',*,*,#56661,.F.);
#83745=ORIENTED_EDGE('',*,*,#56662,.T.);
#83746=ORIENTED_EDGE('',*,*,#56663,.F.);
#83747=ORIENTED_EDGE('',*,*,#56664,.F.);
#83748=ORIENTED_EDGE('',*,*,#56659,.F.);
#83749=ORIENTED_EDGE('',*,*,#56665,.F.);
#83750=ORIENTED_EDGE('',*,*,#56666,.T.);
#83751=ORIENTED_EDGE('',*,*,#56667,.F.);
#83752=ORIENTED_EDGE('',*,*,#56662,.F.);
#83753=ORIENTED_EDGE('',*,*,#56668,.F.);
#83754=ORIENTED_EDGE('',*,*,#56669,.T.);
#83755=ORIENTED_EDGE('',*,*,#56670,.F.);
#83756=ORIENTED_EDGE('',*,*,#56666,.F.);
#83757=ORIENTED_EDGE('',*,*,#56671,.F.);
#83758=ORIENTED_EDGE('',*,*,#56672,.T.);
#83759=ORIENTED_EDGE('',*,*,#56673,.F.);
#83760=ORIENTED_EDGE('',*,*,#56669,.F.);
#83761=ORIENTED_EDGE('',*,*,#56674,.F.);
#83762=ORIENTED_EDGE('',*,*,#56675,.F.);
#83763=ORIENTED_EDGE('',*,*,#56676,.F.);
#83764=ORIENTED_EDGE('',*,*,#56677,.F.);
#83765=ORIENTED_EDGE('',*,*,#56678,.F.);
#83766=ORIENTED_EDGE('',*,*,#56675,.T.);
#83767=ORIENTED_EDGE('',*,*,#56679,.F.);
#83768=ORIENTED_EDGE('',*,*,#56672,.F.);
#83769=ORIENTED_EDGE('',*,*,#56680,.F.);
#83770=ORIENTED_EDGE('',*,*,#56656,.T.);
#83771=ORIENTED_EDGE('',*,*,#56681,.T.);
#83772=ORIENTED_EDGE('',*,*,#56660,.T.);
#83773=ORIENTED_EDGE('',*,*,#56682,.T.);
#83774=ORIENTED_EDGE('',*,*,#56683,.F.);
#83775=ORIENTED_EDGE('',*,*,#56682,.F.);
#83776=ORIENTED_EDGE('',*,*,#56664,.T.);
#83777=ORIENTED_EDGE('',*,*,#56684,.T.);
#83778=ORIENTED_EDGE('',*,*,#56654,.T.);
#83779=ORIENTED_EDGE('',*,*,#56685,.T.);
#83780=ORIENTED_EDGE('',*,*,#56677,.T.);
#83781=ORIENTED_EDGE('',*,*,#56686,.T.);
#83782=ORIENTED_EDGE('',*,*,#56687,.T.);
#83783=ORIENTED_EDGE('',*,*,#56688,.F.);
#83784=ORIENTED_EDGE('',*,*,#56687,.F.);
#83785=ORIENTED_EDGE('',*,*,#56689,.T.);
#83786=ORIENTED_EDGE('',*,*,#56638,.T.);
#83787=ORIENTED_EDGE('',*,*,#56690,.F.);
#83788=ORIENTED_EDGE('',*,*,#56691,.T.);
#83789=ORIENTED_EDGE('',*,*,#56692,.T.);
#83790=ORIENTED_EDGE('',*,*,#56693,.T.);
#83791=ORIENTED_EDGE('',*,*,#56694,.T.);
#83792=ORIENTED_EDGE('',*,*,#56695,.T.);
#83793=ORIENTED_EDGE('',*,*,#56683,.T.);
#83794=ORIENTED_EDGE('',*,*,#56696,.F.);
#83795=ORIENTED_EDGE('',*,*,#56697,.T.);
#83796=ORIENTED_EDGE('',*,*,#56698,.T.);
#83797=ORIENTED_EDGE('',*,*,#56699,.T.);
#83798=ORIENTED_EDGE('',*,*,#56700,.F.);
#83799=ORIENTED_EDGE('',*,*,#56701,.F.);
#83800=ORIENTED_EDGE('',*,*,#56702,.F.);
#83801=ORIENTED_EDGE('',*,*,#56700,.T.);
#83802=ORIENTED_EDGE('',*,*,#56703,.T.);
#83803=ORIENTED_EDGE('',*,*,#56704,.T.);
#83804=ORIENTED_EDGE('',*,*,#56705,.F.);
#83805=ORIENTED_EDGE('',*,*,#56706,.F.);
#83806=ORIENTED_EDGE('',*,*,#56707,.F.);
#83807=ORIENTED_EDGE('',*,*,#56705,.T.);
#83808=ORIENTED_EDGE('',*,*,#56708,.T.);
#83809=ORIENTED_EDGE('',*,*,#56709,.T.);
#83810=ORIENTED_EDGE('',*,*,#56710,.F.);
#83811=ORIENTED_EDGE('',*,*,#56711,.F.);
#83812=ORIENTED_EDGE('',*,*,#56712,.F.);
#83813=ORIENTED_EDGE('',*,*,#56710,.T.);
#83814=ORIENTED_EDGE('',*,*,#56713,.T.);
#83815=ORIENTED_EDGE('',*,*,#56714,.T.);
#83816=ORIENTED_EDGE('',*,*,#56715,.F.);
#83817=ORIENTED_EDGE('',*,*,#56716,.F.);
#83818=ORIENTED_EDGE('',*,*,#56717,.F.);
#83819=ORIENTED_EDGE('',*,*,#56715,.T.);
#83820=ORIENTED_EDGE('',*,*,#56718,.T.);
#83821=ORIENTED_EDGE('',*,*,#56719,.T.);
#83822=ORIENTED_EDGE('',*,*,#56720,.F.);
#83823=ORIENTED_EDGE('',*,*,#56721,.F.);
#83824=ORIENTED_EDGE('',*,*,#56722,.F.);
#83825=ORIENTED_EDGE('',*,*,#56720,.T.);
#83826=ORIENTED_EDGE('',*,*,#56723,.T.);
#83827=ORIENTED_EDGE('',*,*,#56724,.T.);
#83828=ORIENTED_EDGE('',*,*,#56697,.F.);
#83829=ORIENTED_EDGE('',*,*,#56725,.F.);
#83830=ORIENTED_EDGE('',*,*,#56726,.T.);
#83831=ORIENTED_EDGE('',*,*,#56727,.T.);
#83832=ORIENTED_EDGE('',*,*,#56728,.T.);
#83833=ORIENTED_EDGE('',*,*,#56729,.T.);
#83834=ORIENTED_EDGE('',*,*,#56730,.T.);
#83835=ORIENTED_EDGE('',*,*,#56731,.T.);
#83836=ORIENTED_EDGE('',*,*,#56688,.T.);
#83837=ORIENTED_EDGE('',*,*,#56724,.F.);
#83838=ORIENTED_EDGE('',*,*,#56726,.F.);
#83839=ORIENTED_EDGE('',*,*,#56698,.F.);
#83840=ORIENTED_EDGE('',*,*,#56731,.F.);
#83841=ORIENTED_EDGE('',*,*,#56703,.F.);
#83842=ORIENTED_EDGE('',*,*,#56699,.F.);
#83843=ORIENTED_EDGE('',*,*,#56730,.F.);
#83844=ORIENTED_EDGE('',*,*,#56708,.F.);
#83845=ORIENTED_EDGE('',*,*,#56704,.F.);
#83846=ORIENTED_EDGE('',*,*,#56729,.F.);
#83847=ORIENTED_EDGE('',*,*,#56713,.F.);
#83848=ORIENTED_EDGE('',*,*,#56709,.F.);
#83849=ORIENTED_EDGE('',*,*,#56728,.F.);
#83850=ORIENTED_EDGE('',*,*,#56718,.F.);
#83851=ORIENTED_EDGE('',*,*,#56714,.F.);
#83852=ORIENTED_EDGE('',*,*,#56727,.F.);
#83853=ORIENTED_EDGE('',*,*,#56723,.F.);
#83854=ORIENTED_EDGE('',*,*,#56719,.F.);
#83855=ORIENTED_EDGE('',*,*,#56721,.T.);
#83856=ORIENTED_EDGE('',*,*,#56722,.T.);
#83857=ORIENTED_EDGE('',*,*,#56690,.T.);
#83858=ORIENTED_EDGE('',*,*,#56716,.T.);
#83859=ORIENTED_EDGE('',*,*,#56717,.T.);
#83860=ORIENTED_EDGE('',*,*,#56695,.F.);
#83861=ORIENTED_EDGE('',*,*,#56711,.T.);
#83862=ORIENTED_EDGE('',*,*,#56712,.T.);
#83863=ORIENTED_EDGE('',*,*,#56694,.F.);
#83864=ORIENTED_EDGE('',*,*,#56706,.T.);
#83865=ORIENTED_EDGE('',*,*,#56707,.T.);
#83866=ORIENTED_EDGE('',*,*,#56693,.F.);
#83867=ORIENTED_EDGE('',*,*,#56701,.T.);
#83868=ORIENTED_EDGE('',*,*,#56702,.T.);
#83869=ORIENTED_EDGE('',*,*,#56692,.F.);
#83870=ORIENTED_EDGE('',*,*,#56696,.T.);
#83871=ORIENTED_EDGE('',*,*,#56691,.F.);
#83872=ORIENTED_EDGE('',*,*,#56725,.T.);
#83873=ORIENTED_EDGE('',*,*,#56653,.F.);
#83874=ORIENTED_EDGE('',*,*,#56657,.F.);
#83875=ORIENTED_EDGE('',*,*,#56684,.F.);
#83876=ORIENTED_EDGE('',*,*,#56663,.T.);
#83877=ORIENTED_EDGE('',*,*,#56667,.T.);
#83878=ORIENTED_EDGE('',*,*,#56670,.T.);
#83879=ORIENTED_EDGE('',*,*,#56673,.T.);
#83880=ORIENTED_EDGE('',*,*,#56679,.T.);
#83881=ORIENTED_EDGE('',*,*,#56678,.T.);
#83882=ORIENTED_EDGE('',*,*,#56685,.F.);
#83883=ORIENTED_EDGE('',*,*,#56655,.F.);
#83884=ORIENTED_EDGE('',*,*,#56641,.F.);
#83885=ORIENTED_EDGE('',*,*,#56645,.F.);
#83886=ORIENTED_EDGE('',*,*,#56648,.F.);
#83887=ORIENTED_EDGE('',*,*,#56732,.F.);
#83888=ORIENTED_EDGE('',*,*,#56676,.T.);
#83889=ORIENTED_EDGE('',*,*,#56680,.T.);
#83890=ORIENTED_EDGE('',*,*,#56674,.T.);
#83891=ORIENTED_EDGE('',*,*,#56671,.T.);
#83892=ORIENTED_EDGE('',*,*,#56668,.T.);
#83893=ORIENTED_EDGE('',*,*,#56665,.T.);
#83894=ORIENTED_EDGE('',*,*,#56661,.T.);
#83895=ORIENTED_EDGE('',*,*,#56681,.F.);
#83896=ORIENTED_EDGE('',*,*,#56658,.F.);
#83897=ORIENTED_EDGE('',*,*,#56651,.T.);
#83898=ORIENTED_EDGE('',*,*,#56733,.T.);
#83899=ORIENTED_EDGE('',*,*,#56649,.T.);
#83900=ORIENTED_EDGE('',*,*,#56646,.T.);
#83901=ORIENTED_EDGE('',*,*,#56643,.T.);
#83902=ORIENTED_EDGE('',*,*,#56639,.T.);
#83903=ORIENTED_EDGE('',*,*,#56689,.F.);
#83904=ORIENTED_EDGE('',*,*,#56686,.F.);
#83905=ORIENTED_EDGE('',*,*,#56650,.T.);
#83906=ORIENTED_EDGE('',*,*,#56732,.T.);
#83907=ORIENTED_EDGE('',*,*,#56647,.F.);
#83908=ORIENTED_EDGE('',*,*,#56733,.F.);
#83909=ORIENTED_EDGE('',*,*,#56734,.T.);
#83910=ORIENTED_EDGE('',*,*,#56735,.T.);
#83911=ORIENTED_EDGE('',*,*,#56736,.F.);
#83912=ORIENTED_EDGE('',*,*,#56737,.F.);
#83913=ORIENTED_EDGE('',*,*,#56738,.T.);
#83914=ORIENTED_EDGE('',*,*,#56739,.T.);
#83915=ORIENTED_EDGE('',*,*,#56734,.F.);
#83916=ORIENTED_EDGE('',*,*,#56740,.F.);
#83917=ORIENTED_EDGE('',*,*,#56741,.T.);
#83918=ORIENTED_EDGE('',*,*,#56742,.T.);
#83919=ORIENTED_EDGE('',*,*,#56738,.F.);
#83920=ORIENTED_EDGE('',*,*,#56743,.F.);
#83921=ORIENTED_EDGE('',*,*,#56744,.T.);
#83922=ORIENTED_EDGE('',*,*,#56745,.T.);
#83923=ORIENTED_EDGE('',*,*,#56741,.F.);
#83924=ORIENTED_EDGE('',*,*,#56746,.F.);
#83925=ORIENTED_EDGE('',*,*,#56747,.T.);
#83926=ORIENTED_EDGE('',*,*,#56748,.T.);
#83927=ORIENTED_EDGE('',*,*,#56744,.F.);
#83928=ORIENTED_EDGE('',*,*,#56749,.F.);
#83929=ORIENTED_EDGE('',*,*,#56750,.F.);
#83930=ORIENTED_EDGE('',*,*,#56751,.F.);
#83931=ORIENTED_EDGE('',*,*,#56752,.T.);
#83932=ORIENTED_EDGE('',*,*,#56753,.T.);
#83933=ORIENTED_EDGE('',*,*,#56754,.F.);
#83934=ORIENTED_EDGE('',*,*,#56755,.F.);
#83935=ORIENTED_EDGE('',*,*,#56756,.T.);
#83936=ORIENTED_EDGE('',*,*,#56757,.F.);
#83937=ORIENTED_EDGE('',*,*,#56753,.F.);
#83938=ORIENTED_EDGE('',*,*,#56758,.F.);
#83939=ORIENTED_EDGE('',*,*,#56759,.T.);
#83940=ORIENTED_EDGE('',*,*,#56760,.F.);
#83941=ORIENTED_EDGE('',*,*,#56756,.F.);
#83942=ORIENTED_EDGE('',*,*,#56761,.F.);
#83943=ORIENTED_EDGE('',*,*,#56762,.T.);
#83944=ORIENTED_EDGE('',*,*,#56763,.F.);
#83945=ORIENTED_EDGE('',*,*,#56759,.F.);
#83946=ORIENTED_EDGE('',*,*,#56764,.F.);
#83947=ORIENTED_EDGE('',*,*,#56765,.T.);
#83948=ORIENTED_EDGE('',*,*,#56766,.F.);
#83949=ORIENTED_EDGE('',*,*,#56762,.F.);
#83950=ORIENTED_EDGE('',*,*,#56767,.F.);
#83951=ORIENTED_EDGE('',*,*,#56768,.T.);
#83952=ORIENTED_EDGE('',*,*,#56769,.F.);
#83953=ORIENTED_EDGE('',*,*,#56765,.F.);
#83954=ORIENTED_EDGE('',*,*,#56770,.F.);
#83955=ORIENTED_EDGE('',*,*,#56771,.F.);
#83956=ORIENTED_EDGE('',*,*,#56772,.F.);
#83957=ORIENTED_EDGE('',*,*,#56773,.F.);
#83958=ORIENTED_EDGE('',*,*,#56774,.F.);
#83959=ORIENTED_EDGE('',*,*,#56771,.T.);
#83960=ORIENTED_EDGE('',*,*,#56775,.F.);
#83961=ORIENTED_EDGE('',*,*,#56768,.F.);
#83962=ORIENTED_EDGE('',*,*,#56776,.F.);
#83963=ORIENTED_EDGE('',*,*,#56777,.F.);
#83964=ORIENTED_EDGE('',*,*,#56778,.T.);
#83965=ORIENTED_EDGE('',*,*,#56779,.F.);
#83966=ORIENTED_EDGE('',*,*,#56780,.F.);
#83967=ORIENTED_EDGE('',*,*,#56781,.F.);
#83968=ORIENTED_EDGE('',*,*,#56782,.F.);
#83969=ORIENTED_EDGE('',*,*,#56783,.F.);
#83970=ORIENTED_EDGE('',*,*,#56784,.F.);
#83971=ORIENTED_EDGE('',*,*,#56785,.T.);
#83972=ORIENTED_EDGE('',*,*,#56786,.T.);
#83973=ORIENTED_EDGE('',*,*,#56787,.T.);
#83974=ORIENTED_EDGE('',*,*,#56788,.T.);
#83975=ORIENTED_EDGE('',*,*,#56789,.T.);
#83976=ORIENTED_EDGE('',*,*,#56790,.F.);
#83977=ORIENTED_EDGE('',*,*,#56789,.F.);
#83978=ORIENTED_EDGE('',*,*,#56791,.T.);
#83979=ORIENTED_EDGE('',*,*,#56792,.T.);
#83980=ORIENTED_EDGE('',*,*,#56793,.T.);
#83981=ORIENTED_EDGE('',*,*,#56794,.T.);
#83982=ORIENTED_EDGE('',*,*,#56795,.T.);
#83983=ORIENTED_EDGE('',*,*,#56796,.F.);
#83984=ORIENTED_EDGE('',*,*,#56795,.F.);
#83985=ORIENTED_EDGE('',*,*,#56797,.T.);
#83986=ORIENTED_EDGE('',*,*,#56736,.T.);
#83987=ORIENTED_EDGE('',*,*,#56798,.T.);
#83988=ORIENTED_EDGE('',*,*,#56773,.T.);
#83989=ORIENTED_EDGE('',*,*,#56790,.T.);
#83990=ORIENTED_EDGE('',*,*,#56796,.T.);
#83991=ORIENTED_EDGE('',*,*,#56799,.T.);
#83992=ORIENTED_EDGE('',*,*,#56779,.T.);
#83993=ORIENTED_EDGE('',*,*,#56800,.F.);
#83994=ORIENTED_EDGE('',*,*,#56792,.F.);
#83995=ORIENTED_EDGE('',*,*,#56800,.T.);
#83996=ORIENTED_EDGE('',*,*,#56784,.T.);
#83997=ORIENTED_EDGE('',*,*,#56801,.F.);
#83998=ORIENTED_EDGE('',*,*,#56793,.F.);
#83999=ORIENTED_EDGE('',*,*,#56801,.T.);
#84000=ORIENTED_EDGE('',*,*,#56783,.T.);
#84001=ORIENTED_EDGE('',*,*,#56802,.F.);
#84002=ORIENTED_EDGE('',*,*,#56785,.F.);
#84003=ORIENTED_EDGE('',*,*,#56802,.T.);
#84004=ORIENTED_EDGE('',*,*,#56782,.T.);
#84005=ORIENTED_EDGE('',*,*,#56803,.F.);
#84006=ORIENTED_EDGE('',*,*,#56786,.F.);
#84007=ORIENTED_EDGE('',*,*,#56803,.T.);
#84008=ORIENTED_EDGE('',*,*,#56781,.T.);
#84009=ORIENTED_EDGE('',*,*,#56804,.F.);
#84010=ORIENTED_EDGE('',*,*,#56787,.F.);
#84011=ORIENTED_EDGE('',*,*,#56804,.T.);
#84012=ORIENTED_EDGE('',*,*,#56780,.T.);
#84013=ORIENTED_EDGE('',*,*,#56799,.F.);
#84014=ORIENTED_EDGE('',*,*,#56791,.F.);
#84015=ORIENTED_EDGE('',*,*,#56788,.F.);
#84016=ORIENTED_EDGE('',*,*,#56777,.T.);
#84017=ORIENTED_EDGE('',*,*,#56778,.F.);
#84018=ORIENTED_EDGE('',*,*,#56751,.T.);
#84019=ORIENTED_EDGE('',*,*,#56805,.T.);
#84020=ORIENTED_EDGE('',*,*,#56754,.T.);
#84021=ORIENTED_EDGE('',*,*,#56806,.T.);
#84022=ORIENTED_EDGE('',*,*,#56752,.F.);
#84023=ORIENTED_EDGE('',*,*,#56806,.F.);
#84024=ORIENTED_EDGE('',*,*,#56757,.T.);
#84025=ORIENTED_EDGE('',*,*,#56760,.T.);
#84026=ORIENTED_EDGE('',*,*,#56763,.T.);
#84027=ORIENTED_EDGE('',*,*,#56766,.T.);
#84028=ORIENTED_EDGE('',*,*,#56769,.T.);
#84029=ORIENTED_EDGE('',*,*,#56775,.T.);
#84030=ORIENTED_EDGE('',*,*,#56774,.T.);
#84031=ORIENTED_EDGE('',*,*,#56798,.F.);
#84032=ORIENTED_EDGE('',*,*,#56735,.F.);
#84033=ORIENTED_EDGE('',*,*,#56739,.F.);
#84034=ORIENTED_EDGE('',*,*,#56742,.F.);
#84035=ORIENTED_EDGE('',*,*,#56745,.F.);
#84036=ORIENTED_EDGE('',*,*,#56748,.F.);
#84037=ORIENTED_EDGE('',*,*,#56807,.F.);
#84038=ORIENTED_EDGE('',*,*,#56772,.T.);
#84039=ORIENTED_EDGE('',*,*,#56776,.T.);
#84040=ORIENTED_EDGE('',*,*,#56770,.T.);
#84041=ORIENTED_EDGE('',*,*,#56767,.T.);
#84042=ORIENTED_EDGE('',*,*,#56764,.T.);
#84043=ORIENTED_EDGE('',*,*,#56761,.T.);
#84044=ORIENTED_EDGE('',*,*,#56758,.T.);
#84045=ORIENTED_EDGE('',*,*,#56755,.T.);
#84046=ORIENTED_EDGE('',*,*,#56805,.F.);
#84047=ORIENTED_EDGE('',*,*,#56808,.T.);
#84048=ORIENTED_EDGE('',*,*,#56749,.T.);
#84049=ORIENTED_EDGE('',*,*,#56746,.T.);
#84050=ORIENTED_EDGE('',*,*,#56743,.T.);
#84051=ORIENTED_EDGE('',*,*,#56740,.T.);
#84052=ORIENTED_EDGE('',*,*,#56737,.T.);
#84053=ORIENTED_EDGE('',*,*,#56797,.F.);
#84054=ORIENTED_EDGE('',*,*,#56794,.F.);
#84055=ORIENTED_EDGE('',*,*,#56750,.T.);
#84056=ORIENTED_EDGE('',*,*,#56807,.T.);
#84057=ORIENTED_EDGE('',*,*,#56747,.F.);
#84058=ORIENTED_EDGE('',*,*,#56808,.F.);
#84059=ORIENTED_EDGE('',*,*,#56809,.F.);
#84060=ORIENTED_EDGE('',*,*,#56810,.F.);
#84061=ORIENTED_EDGE('',*,*,#56811,.F.);
#84062=ORIENTED_EDGE('',*,*,#56812,.T.);
#84063=ORIENTED_EDGE('',*,*,#56813,.T.);
#84064=ORIENTED_EDGE('',*,*,#56814,.T.);
#84065=ORIENTED_EDGE('',*,*,#56815,.T.);
#84066=ORIENTED_EDGE('',*,*,#56814,.F.);
#84067=ORIENTED_EDGE('',*,*,#56816,.T.);
#84068=ORIENTED_EDGE('',*,*,#56811,.T.);
#84069=ORIENTED_EDGE('',*,*,#56817,.T.);
#84070=ORIENTED_EDGE('',*,*,#56818,.T.);
#84071=ORIENTED_EDGE('',*,*,#56819,.T.);
#84072=ORIENTED_EDGE('',*,*,#56820,.T.);
#84073=ORIENTED_EDGE('',*,*,#56818,.F.);
#84074=ORIENTED_EDGE('',*,*,#56821,.T.);
#84075=ORIENTED_EDGE('',*,*,#56821,.F.);
#84076=ORIENTED_EDGE('',*,*,#56817,.F.);
#84077=ORIENTED_EDGE('',*,*,#56810,.T.);
#84078=ORIENTED_EDGE('',*,*,#56822,.T.);
#84079=ORIENTED_EDGE('',*,*,#56823,.T.);
#84080=ORIENTED_EDGE('',*,*,#56812,.F.);
#84081=ORIENTED_EDGE('',*,*,#56816,.F.);
#84082=ORIENTED_EDGE('',*,*,#56813,.F.);
#84083=ORIENTED_EDGE('',*,*,#56820,.F.);
#84084=ORIENTED_EDGE('',*,*,#56824,.T.);
#84085=ORIENTED_EDGE('',*,*,#56825,.F.);
#84086=ORIENTED_EDGE('',*,*,#56809,.T.);
#84087=ORIENTED_EDGE('',*,*,#56825,.T.);
#84088=ORIENTED_EDGE('',*,*,#56826,.T.);
#84089=ORIENTED_EDGE('',*,*,#56822,.F.);
#84090=ORIENTED_EDGE('',*,*,#56815,.F.);
#84091=ORIENTED_EDGE('',*,*,#56819,.F.);
#84092=ORIENTED_EDGE('',*,*,#56823,.F.);
#84093=ORIENTED_EDGE('',*,*,#56826,.F.);
#84094=ORIENTED_EDGE('',*,*,#56824,.F.);
#84095=ORIENTED_EDGE('',*,*,#56827,.F.);
#84096=ORIENTED_EDGE('',*,*,#56828,.F.);
#84097=ORIENTED_EDGE('',*,*,#56829,.T.);
#84098=ORIENTED_EDGE('',*,*,#56830,.F.);
#84099=ORIENTED_EDGE('',*,*,#56831,.F.);
#84100=ORIENTED_EDGE('',*,*,#56827,.T.);
#84101=ORIENTED_EDGE('',*,*,#56832,.T.);
#84102=ORIENTED_EDGE('',*,*,#56833,.F.);
#84103=ORIENTED_EDGE('',*,*,#56834,.F.);
#84104=ORIENTED_EDGE('',*,*,#56830,.T.);
#84105=ORIENTED_EDGE('',*,*,#56835,.T.);
#84106=ORIENTED_EDGE('',*,*,#56836,.F.);
#84107=ORIENTED_EDGE('',*,*,#56837,.F.);
#84108=ORIENTED_EDGE('',*,*,#56833,.T.);
#84109=ORIENTED_EDGE('',*,*,#56838,.T.);
#84110=ORIENTED_EDGE('',*,*,#56839,.F.);
#84111=ORIENTED_EDGE('',*,*,#56840,.F.);
#84112=ORIENTED_EDGE('',*,*,#56836,.T.);
#84113=ORIENTED_EDGE('',*,*,#56841,.T.);
#84114=ORIENTED_EDGE('',*,*,#56842,.F.);
#84115=ORIENTED_EDGE('',*,*,#56843,.F.);
#84116=ORIENTED_EDGE('',*,*,#56839,.T.);
#84117=ORIENTED_EDGE('',*,*,#56844,.T.);
#84118=ORIENTED_EDGE('',*,*,#56845,.F.);
#84119=ORIENTED_EDGE('',*,*,#56846,.F.);
#84120=ORIENTED_EDGE('',*,*,#56842,.T.);
#84121=ORIENTED_EDGE('',*,*,#56847,.T.);
#84122=ORIENTED_EDGE('',*,*,#56848,.F.);
#84123=ORIENTED_EDGE('',*,*,#56849,.F.);
#84124=ORIENTED_EDGE('',*,*,#56845,.T.);
#84125=ORIENTED_EDGE('',*,*,#56850,.T.);
#84126=ORIENTED_EDGE('',*,*,#56851,.F.);
#84127=ORIENTED_EDGE('',*,*,#56852,.F.);
#84128=ORIENTED_EDGE('',*,*,#56848,.T.);
#84129=ORIENTED_EDGE('',*,*,#56853,.T.);
#84130=ORIENTED_EDGE('',*,*,#56854,.F.);
#84131=ORIENTED_EDGE('',*,*,#56855,.F.);
#84132=ORIENTED_EDGE('',*,*,#56851,.T.);
#84133=ORIENTED_EDGE('',*,*,#56856,.T.);
#84134=ORIENTED_EDGE('',*,*,#56857,.F.);
#84135=ORIENTED_EDGE('',*,*,#56858,.F.);
#84136=ORIENTED_EDGE('',*,*,#56854,.T.);
#84137=ORIENTED_EDGE('',*,*,#56859,.T.);
#84138=ORIENTED_EDGE('',*,*,#56860,.F.);
#84139=ORIENTED_EDGE('',*,*,#56861,.F.);
#84140=ORIENTED_EDGE('',*,*,#56857,.T.);
#84141=ORIENTED_EDGE('',*,*,#56862,.T.);
#84142=ORIENTED_EDGE('',*,*,#56863,.F.);
#84143=ORIENTED_EDGE('',*,*,#56864,.F.);
#84144=ORIENTED_EDGE('',*,*,#56860,.T.);
#84145=ORIENTED_EDGE('',*,*,#56865,.T.);
#84146=ORIENTED_EDGE('',*,*,#56866,.F.);
#84147=ORIENTED_EDGE('',*,*,#56867,.F.);
#84148=ORIENTED_EDGE('',*,*,#56863,.T.);
#84149=ORIENTED_EDGE('',*,*,#56868,.T.);
#84150=ORIENTED_EDGE('',*,*,#56869,.F.);
#84151=ORIENTED_EDGE('',*,*,#56870,.F.);
#84152=ORIENTED_EDGE('',*,*,#56866,.T.);
#84153=ORIENTED_EDGE('',*,*,#56871,.T.);
#84154=ORIENTED_EDGE('',*,*,#56872,.F.);
#84155=ORIENTED_EDGE('',*,*,#56873,.F.);
#84156=ORIENTED_EDGE('',*,*,#56869,.T.);
#84157=ORIENTED_EDGE('',*,*,#56874,.T.);
#84158=ORIENTED_EDGE('',*,*,#56875,.F.);
#84159=ORIENTED_EDGE('',*,*,#56876,.F.);
#84160=ORIENTED_EDGE('',*,*,#56872,.T.);
#84161=ORIENTED_EDGE('',*,*,#56877,.T.);
#84162=ORIENTED_EDGE('',*,*,#56878,.F.);
#84163=ORIENTED_EDGE('',*,*,#56879,.F.);
#84164=ORIENTED_EDGE('',*,*,#56875,.T.);
#84165=ORIENTED_EDGE('',*,*,#56880,.T.);
#84166=ORIENTED_EDGE('',*,*,#56881,.F.);
#84167=ORIENTED_EDGE('',*,*,#56882,.F.);
#84168=ORIENTED_EDGE('',*,*,#56878,.T.);
#84169=ORIENTED_EDGE('',*,*,#56883,.T.);
#84170=ORIENTED_EDGE('',*,*,#56884,.F.);
#84171=ORIENTED_EDGE('',*,*,#56885,.F.);
#84172=ORIENTED_EDGE('',*,*,#56881,.T.);
#84173=ORIENTED_EDGE('',*,*,#56886,.T.);
#84174=ORIENTED_EDGE('',*,*,#56887,.F.);
#84175=ORIENTED_EDGE('',*,*,#56888,.F.);
#84176=ORIENTED_EDGE('',*,*,#56889,.F.);
#84177=ORIENTED_EDGE('',*,*,#56890,.T.);
#84178=ORIENTED_EDGE('',*,*,#56891,.F.);
#84179=ORIENTED_EDGE('',*,*,#56892,.F.);
#84180=ORIENTED_EDGE('',*,*,#56887,.T.);
#84181=ORIENTED_EDGE('',*,*,#56893,.T.);
#84182=ORIENTED_EDGE('',*,*,#56894,.F.);
#84183=ORIENTED_EDGE('',*,*,#56895,.F.);
#84184=ORIENTED_EDGE('',*,*,#56891,.T.);
#84185=ORIENTED_EDGE('',*,*,#56896,.T.);
#84186=ORIENTED_EDGE('',*,*,#56897,.F.);
#84187=ORIENTED_EDGE('',*,*,#56898,.F.);
#84188=ORIENTED_EDGE('',*,*,#56894,.T.);
#84189=ORIENTED_EDGE('',*,*,#56899,.T.);
#84190=ORIENTED_EDGE('',*,*,#56900,.F.);
#84191=ORIENTED_EDGE('',*,*,#56901,.F.);
#84192=ORIENTED_EDGE('',*,*,#56897,.T.);
#84193=ORIENTED_EDGE('',*,*,#56902,.T.);
#84194=ORIENTED_EDGE('',*,*,#56903,.F.);
#84195=ORIENTED_EDGE('',*,*,#56904,.F.);
#84196=ORIENTED_EDGE('',*,*,#56900,.T.);
#84197=ORIENTED_EDGE('',*,*,#56905,.T.);
#84198=ORIENTED_EDGE('',*,*,#56906,.F.);
#84199=ORIENTED_EDGE('',*,*,#56907,.F.);
#84200=ORIENTED_EDGE('',*,*,#56903,.T.);
#84201=ORIENTED_EDGE('',*,*,#56908,.T.);
#84202=ORIENTED_EDGE('',*,*,#56909,.F.);
#84203=ORIENTED_EDGE('',*,*,#56910,.F.);
#84204=ORIENTED_EDGE('',*,*,#56906,.T.);
#84205=ORIENTED_EDGE('',*,*,#56911,.T.);
#84206=ORIENTED_EDGE('',*,*,#56912,.F.);
#84207=ORIENTED_EDGE('',*,*,#56913,.F.);
#84208=ORIENTED_EDGE('',*,*,#56909,.T.);
#84209=ORIENTED_EDGE('',*,*,#56914,.T.);
#84210=ORIENTED_EDGE('',*,*,#56915,.F.);
#84211=ORIENTED_EDGE('',*,*,#56916,.F.);
#84212=ORIENTED_EDGE('',*,*,#56912,.T.);
#84213=ORIENTED_EDGE('',*,*,#56917,.T.);
#84214=ORIENTED_EDGE('',*,*,#56918,.F.);
#84215=ORIENTED_EDGE('',*,*,#56919,.F.);
#84216=ORIENTED_EDGE('',*,*,#56915,.T.);
#84217=ORIENTED_EDGE('',*,*,#56920,.T.);
#84218=ORIENTED_EDGE('',*,*,#56921,.F.);
#84219=ORIENTED_EDGE('',*,*,#56922,.F.);
#84220=ORIENTED_EDGE('',*,*,#56918,.T.);
#84221=ORIENTED_EDGE('',*,*,#56923,.T.);
#84222=ORIENTED_EDGE('',*,*,#56924,.F.);
#84223=ORIENTED_EDGE('',*,*,#56925,.F.);
#84224=ORIENTED_EDGE('',*,*,#56921,.T.);
#84225=ORIENTED_EDGE('',*,*,#56926,.T.);
#84226=ORIENTED_EDGE('',*,*,#56927,.F.);
#84227=ORIENTED_EDGE('',*,*,#56928,.T.);
#84228=ORIENTED_EDGE('',*,*,#56929,.T.);
#84229=ORIENTED_EDGE('',*,*,#56930,.T.);
#84230=ORIENTED_EDGE('',*,*,#56931,.F.);
#84231=ORIENTED_EDGE('',*,*,#56932,.T.);
#84232=ORIENTED_EDGE('',*,*,#56927,.T.);
#84233=ORIENTED_EDGE('',*,*,#56933,.T.);
#84234=ORIENTED_EDGE('',*,*,#56934,.F.);
#84235=ORIENTED_EDGE('',*,*,#56935,.T.);
#84236=ORIENTED_EDGE('',*,*,#56931,.T.);
#84237=ORIENTED_EDGE('',*,*,#56936,.T.);
#84238=ORIENTED_EDGE('',*,*,#56937,.F.);
#84239=ORIENTED_EDGE('',*,*,#56938,.T.);
#84240=ORIENTED_EDGE('',*,*,#56934,.T.);
#84241=ORIENTED_EDGE('',*,*,#56939,.T.);
#84242=ORIENTED_EDGE('',*,*,#56940,.F.);
#84243=ORIENTED_EDGE('',*,*,#56941,.T.);
#84244=ORIENTED_EDGE('',*,*,#56937,.T.);
#84245=ORIENTED_EDGE('',*,*,#56942,.T.);
#84246=ORIENTED_EDGE('',*,*,#56943,.F.);
#84247=ORIENTED_EDGE('',*,*,#56944,.T.);
#84248=ORIENTED_EDGE('',*,*,#56940,.T.);
#84249=ORIENTED_EDGE('',*,*,#56945,.T.);
#84250=ORIENTED_EDGE('',*,*,#56946,.F.);
#84251=ORIENTED_EDGE('',*,*,#56947,.T.);
#84252=ORIENTED_EDGE('',*,*,#56943,.T.);
#84253=ORIENTED_EDGE('',*,*,#56948,.T.);
#84254=ORIENTED_EDGE('',*,*,#56949,.F.);
#84255=ORIENTED_EDGE('',*,*,#56950,.T.);
#84256=ORIENTED_EDGE('',*,*,#56946,.T.);
#84257=ORIENTED_EDGE('',*,*,#56951,.T.);
#84258=ORIENTED_EDGE('',*,*,#56952,.F.);
#84259=ORIENTED_EDGE('',*,*,#56953,.T.);
#84260=ORIENTED_EDGE('',*,*,#56949,.T.);
#84261=ORIENTED_EDGE('',*,*,#56954,.T.);
#84262=ORIENTED_EDGE('',*,*,#56955,.F.);
#84263=ORIENTED_EDGE('',*,*,#56956,.T.);
#84264=ORIENTED_EDGE('',*,*,#56952,.T.);
#84265=ORIENTED_EDGE('',*,*,#56957,.T.);
#84266=ORIENTED_EDGE('',*,*,#56958,.F.);
#84267=ORIENTED_EDGE('',*,*,#56959,.T.);
#84268=ORIENTED_EDGE('',*,*,#56955,.T.);
#84269=ORIENTED_EDGE('',*,*,#56960,.T.);
#84270=ORIENTED_EDGE('',*,*,#56961,.F.);
#84271=ORIENTED_EDGE('',*,*,#56962,.T.);
#84272=ORIENTED_EDGE('',*,*,#56958,.T.);
#84273=ORIENTED_EDGE('',*,*,#56963,.T.);
#84274=ORIENTED_EDGE('',*,*,#56964,.F.);
#84275=ORIENTED_EDGE('',*,*,#56965,.T.);
#84276=ORIENTED_EDGE('',*,*,#56961,.T.);
#84277=ORIENTED_EDGE('',*,*,#56966,.T.);
#84278=ORIENTED_EDGE('',*,*,#56967,.F.);
#84279=ORIENTED_EDGE('',*,*,#56968,.T.);
#84280=ORIENTED_EDGE('',*,*,#56969,.F.);
#84281=ORIENTED_EDGE('',*,*,#56970,.T.);
#84282=ORIENTED_EDGE('',*,*,#56971,.F.);
#84283=ORIENTED_EDGE('',*,*,#56972,.T.);
#84284=ORIENTED_EDGE('',*,*,#56967,.T.);
#84285=ORIENTED_EDGE('',*,*,#56973,.T.);
#84286=ORIENTED_EDGE('',*,*,#56974,.F.);
#84287=ORIENTED_EDGE('',*,*,#56975,.T.);
#84288=ORIENTED_EDGE('',*,*,#56971,.T.);
#84289=ORIENTED_EDGE('',*,*,#56976,.T.);
#84290=ORIENTED_EDGE('',*,*,#56977,.F.);
#84291=ORIENTED_EDGE('',*,*,#56978,.T.);
#84292=ORIENTED_EDGE('',*,*,#56974,.T.);
#84293=ORIENTED_EDGE('',*,*,#56979,.T.);
#84294=ORIENTED_EDGE('',*,*,#56980,.F.);
#84295=ORIENTED_EDGE('',*,*,#56981,.T.);
#84296=ORIENTED_EDGE('',*,*,#56977,.T.);
#84297=ORIENTED_EDGE('',*,*,#56982,.T.);
#84298=ORIENTED_EDGE('',*,*,#56983,.F.);
#84299=ORIENTED_EDGE('',*,*,#56984,.T.);
#84300=ORIENTED_EDGE('',*,*,#56980,.T.);
#84301=ORIENTED_EDGE('',*,*,#56985,.T.);
#84302=ORIENTED_EDGE('',*,*,#56986,.F.);
#84303=ORIENTED_EDGE('',*,*,#56987,.T.);
#84304=ORIENTED_EDGE('',*,*,#56983,.T.);
#84305=ORIENTED_EDGE('',*,*,#56988,.T.);
#84306=ORIENTED_EDGE('',*,*,#56989,.F.);
#84307=ORIENTED_EDGE('',*,*,#56990,.T.);
#84308=ORIENTED_EDGE('',*,*,#56986,.T.);
#84309=ORIENTED_EDGE('',*,*,#56991,.T.);
#84310=ORIENTED_EDGE('',*,*,#56992,.F.);
#84311=ORIENTED_EDGE('',*,*,#56993,.T.);
#84312=ORIENTED_EDGE('',*,*,#56989,.T.);
#84313=ORIENTED_EDGE('',*,*,#56994,.T.);
#84314=ORIENTED_EDGE('',*,*,#56995,.F.);
#84315=ORIENTED_EDGE('',*,*,#56996,.T.);
#84316=ORIENTED_EDGE('',*,*,#56992,.T.);
#84317=ORIENTED_EDGE('',*,*,#56997,.T.);
#84318=ORIENTED_EDGE('',*,*,#56998,.F.);
#84319=ORIENTED_EDGE('',*,*,#56999,.T.);
#84320=ORIENTED_EDGE('',*,*,#56995,.T.);
#84321=ORIENTED_EDGE('',*,*,#57000,.T.);
#84322=ORIENTED_EDGE('',*,*,#57001,.F.);
#84323=ORIENTED_EDGE('',*,*,#57002,.T.);
#84324=ORIENTED_EDGE('',*,*,#56998,.T.);
#84325=ORIENTED_EDGE('',*,*,#57003,.T.);
#84326=ORIENTED_EDGE('',*,*,#57004,.F.);
#84327=ORIENTED_EDGE('',*,*,#57005,.T.);
#84328=ORIENTED_EDGE('',*,*,#57001,.T.);
#84329=ORIENTED_EDGE('',*,*,#57006,.T.);
#84330=ORIENTED_EDGE('',*,*,#57007,.F.);
#84331=ORIENTED_EDGE('',*,*,#57008,.T.);
#84332=ORIENTED_EDGE('',*,*,#57004,.T.);
#84333=ORIENTED_EDGE('',*,*,#57009,.T.);
#84334=ORIENTED_EDGE('',*,*,#57010,.F.);
#84335=ORIENTED_EDGE('',*,*,#57011,.T.);
#84336=ORIENTED_EDGE('',*,*,#57007,.T.);
#84337=ORIENTED_EDGE('',*,*,#57012,.T.);
#84338=ORIENTED_EDGE('',*,*,#57013,.F.);
#84339=ORIENTED_EDGE('',*,*,#57014,.T.);
#84340=ORIENTED_EDGE('',*,*,#57010,.T.);
#84341=ORIENTED_EDGE('',*,*,#57015,.T.);
#84342=ORIENTED_EDGE('',*,*,#57016,.F.);
#84343=ORIENTED_EDGE('',*,*,#57017,.T.);
#84344=ORIENTED_EDGE('',*,*,#57013,.T.);
#84345=ORIENTED_EDGE('',*,*,#57018,.T.);
#84346=ORIENTED_EDGE('',*,*,#57019,.F.);
#84347=ORIENTED_EDGE('',*,*,#57020,.T.);
#84348=ORIENTED_EDGE('',*,*,#57016,.T.);
#84349=ORIENTED_EDGE('',*,*,#57021,.T.);
#84350=ORIENTED_EDGE('',*,*,#57022,.F.);
#84351=ORIENTED_EDGE('',*,*,#57023,.T.);
#84352=ORIENTED_EDGE('',*,*,#57019,.T.);
#84353=ORIENTED_EDGE('',*,*,#57024,.T.);
#84354=ORIENTED_EDGE('',*,*,#57022,.T.);
#84355=ORIENTED_EDGE('',*,*,#57025,.T.);
#84356=ORIENTED_EDGE('',*,*,#57026,.T.);
#84357=ORIENTED_EDGE('',*,*,#56969,.T.);
#84358=ORIENTED_EDGE('',*,*,#57027,.T.);
#84359=ORIENTED_EDGE('',*,*,#57028,.T.);
#84360=ORIENTED_EDGE('',*,*,#57029,.F.);
#84361=ORIENTED_EDGE('',*,*,#57028,.F.);
#84362=ORIENTED_EDGE('',*,*,#57030,.T.);
#84363=ORIENTED_EDGE('',*,*,#57031,.T.);
#84364=ORIENTED_EDGE('',*,*,#57032,.T.);
#84365=ORIENTED_EDGE('',*,*,#57033,.F.);
#84366=ORIENTED_EDGE('',*,*,#57034,.F.);
#84367=ORIENTED_EDGE('',*,*,#57035,.F.);
#84368=ORIENTED_EDGE('',*,*,#56929,.F.);
#84369=ORIENTED_EDGE('',*,*,#57036,.F.);
#84370=ORIENTED_EDGE('',*,*,#57037,.T.);
#84371=ORIENTED_EDGE('',*,*,#57038,.F.);
#84372=ORIENTED_EDGE('',*,*,#57037,.F.);
#84373=ORIENTED_EDGE('',*,*,#56964,.T.);
#84374=ORIENTED_EDGE('',*,*,#57039,.T.);
#84375=ORIENTED_EDGE('',*,*,#57040,.F.);
#84376=ORIENTED_EDGE('',*,*,#57041,.T.);
#84377=ORIENTED_EDGE('',*,*,#57042,.F.);
#84378=ORIENTED_EDGE('',*,*,#56888,.T.);
#84379=ORIENTED_EDGE('',*,*,#56892,.T.);
#84380=ORIENTED_EDGE('',*,*,#56895,.T.);
#84381=ORIENTED_EDGE('',*,*,#56898,.T.);
#84382=ORIENTED_EDGE('',*,*,#56901,.T.);
#84383=ORIENTED_EDGE('',*,*,#56904,.T.);
#84384=ORIENTED_EDGE('',*,*,#56907,.T.);
#84385=ORIENTED_EDGE('',*,*,#56910,.T.);
#84386=ORIENTED_EDGE('',*,*,#56913,.T.);
#84387=ORIENTED_EDGE('',*,*,#56916,.T.);
#84388=ORIENTED_EDGE('',*,*,#56919,.T.);
#84389=ORIENTED_EDGE('',*,*,#56922,.T.);
#84390=ORIENTED_EDGE('',*,*,#56925,.T.);
#84391=ORIENTED_EDGE('',*,*,#57043,.T.);
#84392=ORIENTED_EDGE('',*,*,#57033,.T.);
#84393=ORIENTED_EDGE('',*,*,#57036,.T.);
#84394=ORIENTED_EDGE('',*,*,#56928,.F.);
#84395=ORIENTED_EDGE('',*,*,#56932,.F.);
#84396=ORIENTED_EDGE('',*,*,#56935,.F.);
#84397=ORIENTED_EDGE('',*,*,#56938,.F.);
#84398=ORIENTED_EDGE('',*,*,#56941,.F.);
#84399=ORIENTED_EDGE('',*,*,#56944,.F.);
#84400=ORIENTED_EDGE('',*,*,#56947,.F.);
#84401=ORIENTED_EDGE('',*,*,#56950,.F.);
#84402=ORIENTED_EDGE('',*,*,#56953,.F.);
#84403=ORIENTED_EDGE('',*,*,#56956,.F.);
#84404=ORIENTED_EDGE('',*,*,#56959,.F.);
#84405=ORIENTED_EDGE('',*,*,#56962,.F.);
#84406=ORIENTED_EDGE('',*,*,#56965,.F.);
#84407=ORIENTED_EDGE('',*,*,#57041,.F.);
#84408=ORIENTED_EDGE('',*,*,#57044,.F.);
#84409=ORIENTED_EDGE('',*,*,#57039,.F.);
#84410=ORIENTED_EDGE('',*,*,#56966,.F.);
#84411=ORIENTED_EDGE('',*,*,#56963,.F.);
#84412=ORIENTED_EDGE('',*,*,#56960,.F.);
#84413=ORIENTED_EDGE('',*,*,#56957,.F.);
#84414=ORIENTED_EDGE('',*,*,#56954,.F.);
#84415=ORIENTED_EDGE('',*,*,#56951,.F.);
#84416=ORIENTED_EDGE('',*,*,#56948,.F.);
#84417=ORIENTED_EDGE('',*,*,#56945,.F.);
#84418=ORIENTED_EDGE('',*,*,#56942,.F.);
#84419=ORIENTED_EDGE('',*,*,#56939,.F.);
#84420=ORIENTED_EDGE('',*,*,#56936,.F.);
#84421=ORIENTED_EDGE('',*,*,#56933,.F.);
#84422=ORIENTED_EDGE('',*,*,#56930,.F.);
#84423=ORIENTED_EDGE('',*,*,#57035,.T.);
#84424=ORIENTED_EDGE('',*,*,#57045,.F.);
#84425=ORIENTED_EDGE('',*,*,#56926,.F.);
#84426=ORIENTED_EDGE('',*,*,#56923,.F.);
#84427=ORIENTED_EDGE('',*,*,#56920,.F.);
#84428=ORIENTED_EDGE('',*,*,#56917,.F.);
#84429=ORIENTED_EDGE('',*,*,#56914,.F.);
#84430=ORIENTED_EDGE('',*,*,#56911,.F.);
#84431=ORIENTED_EDGE('',*,*,#56908,.F.);
#84432=ORIENTED_EDGE('',*,*,#56905,.F.);
#84433=ORIENTED_EDGE('',*,*,#56902,.F.);
#84434=ORIENTED_EDGE('',*,*,#56899,.F.);
#84435=ORIENTED_EDGE('',*,*,#56896,.F.);
#84436=ORIENTED_EDGE('',*,*,#56893,.F.);
#84437=ORIENTED_EDGE('',*,*,#56890,.F.);
#84438=ORIENTED_EDGE('',*,*,#56924,.T.);
#84439=ORIENTED_EDGE('',*,*,#57045,.T.);
#84440=ORIENTED_EDGE('',*,*,#57034,.T.);
#84441=ORIENTED_EDGE('',*,*,#57043,.F.);
#84442=ORIENTED_EDGE('',*,*,#57038,.T.);
#84443=ORIENTED_EDGE('',*,*,#57046,.T.);
#84444=ORIENTED_EDGE('',*,*,#57047,.T.);
#84445=ORIENTED_EDGE('',*,*,#57048,.T.);
#84446=ORIENTED_EDGE('',*,*,#57049,.T.);
#84447=ORIENTED_EDGE('',*,*,#57042,.T.);
#84448=ORIENTED_EDGE('',*,*,#57040,.T.);
#84449=ORIENTED_EDGE('',*,*,#57044,.T.);
#84450=ORIENTED_EDGE('',*,*,#56889,.T.);
#84451=ORIENTED_EDGE('',*,*,#57050,.F.);
#84452=ORIENTED_EDGE('',*,*,#57051,.F.);
#84453=ORIENTED_EDGE('',*,*,#57052,.F.);
#84454=ORIENTED_EDGE('',*,*,#57053,.F.);
#84455=ORIENTED_EDGE('',*,*,#57054,.T.);
#84456=ORIENTED_EDGE('',*,*,#57055,.T.);
#84457=ORIENTED_EDGE('',*,*,#57056,.T.);
#84458=ORIENTED_EDGE('',*,*,#57057,.T.);
#84459=ORIENTED_EDGE('',*,*,#57058,.T.);
#84460=ORIENTED_EDGE('',*,*,#57059,.T.);
#84461=ORIENTED_EDGE('',*,*,#57050,.T.);
#84462=ORIENTED_EDGE('',*,*,#57060,.F.);
#84463=ORIENTED_EDGE('',*,*,#57046,.F.);
#84464=ORIENTED_EDGE('',*,*,#57061,.T.);
#84465=ORIENTED_EDGE('',*,*,#57053,.T.);
#84466=ORIENTED_EDGE('',*,*,#57062,.F.);
#84467=ORIENTED_EDGE('',*,*,#57047,.F.);
#84468=ORIENTED_EDGE('',*,*,#57060,.T.);
#84469=ORIENTED_EDGE('',*,*,#57052,.T.);
#84470=ORIENTED_EDGE('',*,*,#57063,.F.);
#84471=ORIENTED_EDGE('',*,*,#57048,.F.);
#84472=ORIENTED_EDGE('',*,*,#57062,.T.);
#84473=ORIENTED_EDGE('',*,*,#57051,.T.);
#84474=ORIENTED_EDGE('',*,*,#57061,.F.);
#84475=ORIENTED_EDGE('',*,*,#57049,.F.);
#84476=ORIENTED_EDGE('',*,*,#57063,.T.);
#84477=ORIENTED_EDGE('',*,*,#57064,.T.);
#84478=ORIENTED_EDGE('',*,*,#57065,.T.);
#84479=ORIENTED_EDGE('',*,*,#57066,.T.);
#84480=ORIENTED_EDGE('',*,*,#57067,.F.);
#84481=ORIENTED_EDGE('',*,*,#57068,.F.);
#84482=ORIENTED_EDGE('',*,*,#57069,.F.);
#84483=ORIENTED_EDGE('',*,*,#57067,.T.);
#84484=ORIENTED_EDGE('',*,*,#57070,.T.);
#84485=ORIENTED_EDGE('',*,*,#57071,.T.);
#84486=ORIENTED_EDGE('',*,*,#57072,.F.);
#84487=ORIENTED_EDGE('',*,*,#57073,.F.);
#84488=ORIENTED_EDGE('',*,*,#57074,.F.);
#84489=ORIENTED_EDGE('',*,*,#57072,.T.);
#84490=ORIENTED_EDGE('',*,*,#57075,.T.);
#84491=ORIENTED_EDGE('',*,*,#57076,.T.);
#84492=ORIENTED_EDGE('',*,*,#57077,.F.);
#84493=ORIENTED_EDGE('',*,*,#57078,.F.);
#84494=ORIENTED_EDGE('',*,*,#57079,.F.);
#84495=ORIENTED_EDGE('',*,*,#57077,.T.);
#84496=ORIENTED_EDGE('',*,*,#57080,.T.);
#84497=ORIENTED_EDGE('',*,*,#57081,.T.);
#84498=ORIENTED_EDGE('',*,*,#57082,.F.);
#84499=ORIENTED_EDGE('',*,*,#57083,.F.);
#84500=ORIENTED_EDGE('',*,*,#57084,.F.);
#84501=ORIENTED_EDGE('',*,*,#57082,.T.);
#84502=ORIENTED_EDGE('',*,*,#57085,.T.);
#84503=ORIENTED_EDGE('',*,*,#57086,.T.);
#84504=ORIENTED_EDGE('',*,*,#57087,.F.);
#84505=ORIENTED_EDGE('',*,*,#57088,.F.);
#84506=ORIENTED_EDGE('',*,*,#57089,.F.);
#84507=ORIENTED_EDGE('',*,*,#57087,.T.);
#84508=ORIENTED_EDGE('',*,*,#57090,.T.);
#84509=ORIENTED_EDGE('',*,*,#57091,.T.);
#84510=ORIENTED_EDGE('',*,*,#57064,.F.);
#84511=ORIENTED_EDGE('',*,*,#57092,.F.);
#84512=ORIENTED_EDGE('',*,*,#57093,.F.);
#84513=ORIENTED_EDGE('',*,*,#57094,.F.);
#84514=ORIENTED_EDGE('',*,*,#57095,.T.);
#84515=ORIENTED_EDGE('',*,*,#57096,.T.);
#84516=ORIENTED_EDGE('',*,*,#57097,.T.);
#84517=ORIENTED_EDGE('',*,*,#57098,.T.);
#84518=ORIENTED_EDGE('',*,*,#57099,.T.);
#84519=ORIENTED_EDGE('',*,*,#57029,.T.);
#84520=ORIENTED_EDGE('',*,*,#57068,.T.);
#84521=ORIENTED_EDGE('',*,*,#57074,.T.);
#84522=ORIENTED_EDGE('',*,*,#57094,.T.);
#84523=ORIENTED_EDGE('',*,*,#57069,.T.);
#84524=ORIENTED_EDGE('',*,*,#57099,.F.);
#84525=ORIENTED_EDGE('',*,*,#57092,.T.);
#84526=ORIENTED_EDGE('',*,*,#57088,.T.);
#84527=ORIENTED_EDGE('',*,*,#57093,.T.);
#84528=ORIENTED_EDGE('',*,*,#57098,.F.);
#84529=ORIENTED_EDGE('',*,*,#57083,.T.);
#84530=ORIENTED_EDGE('',*,*,#57089,.T.);
#84531=ORIENTED_EDGE('',*,*,#57097,.F.);
#84532=ORIENTED_EDGE('',*,*,#57078,.T.);
#84533=ORIENTED_EDGE('',*,*,#57084,.T.);
#84534=ORIENTED_EDGE('',*,*,#57096,.F.);
#84535=ORIENTED_EDGE('',*,*,#57073,.T.);
#84536=ORIENTED_EDGE('',*,*,#57079,.T.);
#84537=ORIENTED_EDGE('',*,*,#57095,.F.);
#84538=ORIENTED_EDGE('',*,*,#57054,.F.);
#84539=ORIENTED_EDGE('',*,*,#57075,.F.);
#84540=ORIENTED_EDGE('',*,*,#57071,.F.);
#84541=ORIENTED_EDGE('',*,*,#57059,.F.);
#84542=ORIENTED_EDGE('',*,*,#57080,.F.);
#84543=ORIENTED_EDGE('',*,*,#57076,.F.);
#84544=ORIENTED_EDGE('',*,*,#57058,.F.);
#84545=ORIENTED_EDGE('',*,*,#57085,.F.);
#84546=ORIENTED_EDGE('',*,*,#57081,.F.);
#84547=ORIENTED_EDGE('',*,*,#57057,.F.);
#84548=ORIENTED_EDGE('',*,*,#57090,.F.);
#84549=ORIENTED_EDGE('',*,*,#57086,.F.);
#84550=ORIENTED_EDGE('',*,*,#57091,.F.);
#84551=ORIENTED_EDGE('',*,*,#57056,.F.);
#84552=ORIENTED_EDGE('',*,*,#57065,.F.);
#84553=ORIENTED_EDGE('',*,*,#57055,.F.);
#84554=ORIENTED_EDGE('',*,*,#57070,.F.);
#84555=ORIENTED_EDGE('',*,*,#57066,.F.);
#84556=ORIENTED_EDGE('',*,*,#56829,.F.);
#84557=ORIENTED_EDGE('',*,*,#57100,.F.);
#84558=ORIENTED_EDGE('',*,*,#57026,.F.);
#84559=ORIENTED_EDGE('',*,*,#57101,.F.);
#84560=ORIENTED_EDGE('',*,*,#56828,.T.);
#84561=ORIENTED_EDGE('',*,*,#56831,.T.);
#84562=ORIENTED_EDGE('',*,*,#56834,.T.);
#84563=ORIENTED_EDGE('',*,*,#56837,.T.);
#84564=ORIENTED_EDGE('',*,*,#56840,.T.);
#84565=ORIENTED_EDGE('',*,*,#56843,.T.);
#84566=ORIENTED_EDGE('',*,*,#56846,.T.);
#84567=ORIENTED_EDGE('',*,*,#56849,.T.);
#84568=ORIENTED_EDGE('',*,*,#56852,.T.);
#84569=ORIENTED_EDGE('',*,*,#56855,.T.);
#84570=ORIENTED_EDGE('',*,*,#56858,.T.);
#84571=ORIENTED_EDGE('',*,*,#56861,.T.);
#84572=ORIENTED_EDGE('',*,*,#56864,.T.);
#84573=ORIENTED_EDGE('',*,*,#56867,.T.);
#84574=ORIENTED_EDGE('',*,*,#56870,.T.);
#84575=ORIENTED_EDGE('',*,*,#56873,.T.);
#84576=ORIENTED_EDGE('',*,*,#56876,.T.);
#84577=ORIENTED_EDGE('',*,*,#56879,.T.);
#84578=ORIENTED_EDGE('',*,*,#56882,.T.);
#84579=ORIENTED_EDGE('',*,*,#56885,.T.);
#84580=ORIENTED_EDGE('',*,*,#57102,.T.);
#84581=ORIENTED_EDGE('',*,*,#57030,.F.);
#84582=ORIENTED_EDGE('',*,*,#57027,.F.);
#84583=ORIENTED_EDGE('',*,*,#56968,.F.);
#84584=ORIENTED_EDGE('',*,*,#56972,.F.);
#84585=ORIENTED_EDGE('',*,*,#56975,.F.);
#84586=ORIENTED_EDGE('',*,*,#56978,.F.);
#84587=ORIENTED_EDGE('',*,*,#56981,.F.);
#84588=ORIENTED_EDGE('',*,*,#56984,.F.);
#84589=ORIENTED_EDGE('',*,*,#56987,.F.);
#84590=ORIENTED_EDGE('',*,*,#56990,.F.);
#84591=ORIENTED_EDGE('',*,*,#56993,.F.);
#84592=ORIENTED_EDGE('',*,*,#56996,.F.);
#84593=ORIENTED_EDGE('',*,*,#56999,.F.);
#84594=ORIENTED_EDGE('',*,*,#57002,.F.);
#84595=ORIENTED_EDGE('',*,*,#57005,.F.);
#84596=ORIENTED_EDGE('',*,*,#57008,.F.);
#84597=ORIENTED_EDGE('',*,*,#57011,.F.);
#84598=ORIENTED_EDGE('',*,*,#57014,.F.);
#84599=ORIENTED_EDGE('',*,*,#57017,.F.);
#84600=ORIENTED_EDGE('',*,*,#57020,.F.);
#84601=ORIENTED_EDGE('',*,*,#57023,.F.);
#84602=ORIENTED_EDGE('',*,*,#57100,.T.);
#84603=ORIENTED_EDGE('',*,*,#56970,.F.);
#84604=ORIENTED_EDGE('',*,*,#57032,.F.);
#84605=ORIENTED_EDGE('',*,*,#57103,.F.);
#84606=ORIENTED_EDGE('',*,*,#56886,.F.);
#84607=ORIENTED_EDGE('',*,*,#56883,.F.);
#84608=ORIENTED_EDGE('',*,*,#56880,.F.);
#84609=ORIENTED_EDGE('',*,*,#56877,.F.);
#84610=ORIENTED_EDGE('',*,*,#56874,.F.);
#84611=ORIENTED_EDGE('',*,*,#56871,.F.);
#84612=ORIENTED_EDGE('',*,*,#56868,.F.);
#84613=ORIENTED_EDGE('',*,*,#56865,.F.);
#84614=ORIENTED_EDGE('',*,*,#56862,.F.);
#84615=ORIENTED_EDGE('',*,*,#56859,.F.);
#84616=ORIENTED_EDGE('',*,*,#56856,.F.);
#84617=ORIENTED_EDGE('',*,*,#56853,.F.);
#84618=ORIENTED_EDGE('',*,*,#56850,.F.);
#84619=ORIENTED_EDGE('',*,*,#56847,.F.);
#84620=ORIENTED_EDGE('',*,*,#56844,.F.);
#84621=ORIENTED_EDGE('',*,*,#56841,.F.);
#84622=ORIENTED_EDGE('',*,*,#56838,.F.);
#84623=ORIENTED_EDGE('',*,*,#56835,.F.);
#84624=ORIENTED_EDGE('',*,*,#56832,.F.);
#84625=ORIENTED_EDGE('',*,*,#57101,.T.);
#84626=ORIENTED_EDGE('',*,*,#57025,.F.);
#84627=ORIENTED_EDGE('',*,*,#57024,.F.);
#84628=ORIENTED_EDGE('',*,*,#57021,.F.);
#84629=ORIENTED_EDGE('',*,*,#57018,.F.);
#84630=ORIENTED_EDGE('',*,*,#57015,.F.);
#84631=ORIENTED_EDGE('',*,*,#57012,.F.);
#84632=ORIENTED_EDGE('',*,*,#57009,.F.);
#84633=ORIENTED_EDGE('',*,*,#57006,.F.);
#84634=ORIENTED_EDGE('',*,*,#57003,.F.);
#84635=ORIENTED_EDGE('',*,*,#57000,.F.);
#84636=ORIENTED_EDGE('',*,*,#56997,.F.);
#84637=ORIENTED_EDGE('',*,*,#56994,.F.);
#84638=ORIENTED_EDGE('',*,*,#56991,.F.);
#84639=ORIENTED_EDGE('',*,*,#56988,.F.);
#84640=ORIENTED_EDGE('',*,*,#56985,.F.);
#84641=ORIENTED_EDGE('',*,*,#56982,.F.);
#84642=ORIENTED_EDGE('',*,*,#56979,.F.);
#84643=ORIENTED_EDGE('',*,*,#56976,.F.);
#84644=ORIENTED_EDGE('',*,*,#56973,.F.);
#84645=ORIENTED_EDGE('',*,*,#56884,.T.);
#84646=ORIENTED_EDGE('',*,*,#57103,.T.);
#84647=ORIENTED_EDGE('',*,*,#57031,.F.);
#84648=ORIENTED_EDGE('',*,*,#57102,.F.);
#84649=ORIENTED_EDGE('',*,*,#57104,.F.);
#84650=ORIENTED_EDGE('',*,*,#57105,.T.);
#84651=ORIENTED_EDGE('',*,*,#57106,.T.);
#84652=ORIENTED_EDGE('',*,*,#57105,.F.);
#84653=ORIENTED_EDGE('',*,*,#57107,.F.);
#84654=ORIENTED_EDGE('',*,*,#57108,.T.);
#84655=ORIENTED_EDGE('',*,*,#57109,.T.);
#84656=ORIENTED_EDGE('',*,*,#57108,.F.);
#84657=ORIENTED_EDGE('',*,*,#57110,.F.);
#84658=ORIENTED_EDGE('',*,*,#57111,.T.);
#84659=ORIENTED_EDGE('',*,*,#57112,.T.);
#84660=ORIENTED_EDGE('',*,*,#57111,.F.);
#84661=ORIENTED_EDGE('',*,*,#57113,.F.);
#84662=ORIENTED_EDGE('',*,*,#57114,.T.);
#84663=ORIENTED_EDGE('',*,*,#57115,.T.);
#84664=ORIENTED_EDGE('',*,*,#57114,.F.);
#84665=ORIENTED_EDGE('',*,*,#57116,.F.);
#84666=ORIENTED_EDGE('',*,*,#57117,.T.);
#84667=ORIENTED_EDGE('',*,*,#57118,.T.);
#84668=ORIENTED_EDGE('',*,*,#57117,.F.);
#84669=ORIENTED_EDGE('',*,*,#57119,.F.);
#84670=ORIENTED_EDGE('',*,*,#57120,.T.);
#84671=ORIENTED_EDGE('',*,*,#57121,.T.);
#84672=ORIENTED_EDGE('',*,*,#57120,.F.);
#84673=ORIENTED_EDGE('',*,*,#57122,.F.);
#84674=ORIENTED_EDGE('',*,*,#57123,.T.);
#84675=ORIENTED_EDGE('',*,*,#57124,.T.);
#84676=ORIENTED_EDGE('',*,*,#57123,.F.);
#84677=ORIENTED_EDGE('',*,*,#57125,.F.);
#84678=ORIENTED_EDGE('',*,*,#57126,.T.);
#84679=ORIENTED_EDGE('',*,*,#57127,.T.);
#84680=ORIENTED_EDGE('',*,*,#57126,.F.);
#84681=ORIENTED_EDGE('',*,*,#57128,.F.);
#84682=ORIENTED_EDGE('',*,*,#57129,.T.);
#84683=ORIENTED_EDGE('',*,*,#57130,.T.);
#84684=ORIENTED_EDGE('',*,*,#57129,.F.);
#84685=ORIENTED_EDGE('',*,*,#57131,.F.);
#84686=ORIENTED_EDGE('',*,*,#57132,.T.);
#84687=ORIENTED_EDGE('',*,*,#57133,.F.);
#84688=ORIENTED_EDGE('',*,*,#57132,.F.);
#84689=ORIENTED_EDGE('',*,*,#57134,.F.);
#84690=ORIENTED_EDGE('',*,*,#57135,.T.);
#84691=ORIENTED_EDGE('',*,*,#57136,.T.);
#84692=ORIENTED_EDGE('',*,*,#57135,.F.);
#84693=ORIENTED_EDGE('',*,*,#57137,.F.);
#84694=ORIENTED_EDGE('',*,*,#57138,.T.);
#84695=ORIENTED_EDGE('',*,*,#57139,.F.);
#84696=ORIENTED_EDGE('',*,*,#57140,.T.);
#84697=ORIENTED_EDGE('',*,*,#57141,.F.);
#84698=ORIENTED_EDGE('',*,*,#57140,.F.);
#84699=ORIENTED_EDGE('',*,*,#57142,.F.);
#84700=ORIENTED_EDGE('',*,*,#57143,.T.);
#84701=ORIENTED_EDGE('',*,*,#57144,.F.);
#84702=ORIENTED_EDGE('',*,*,#57145,.F.);
#84703=ORIENTED_EDGE('',*,*,#57143,.F.);
#84704=ORIENTED_EDGE('',*,*,#57138,.F.);
#84705=ORIENTED_EDGE('',*,*,#57146,.T.);
#84706=ORIENTED_EDGE('',*,*,#57144,.T.);
#84707=ORIENTED_EDGE('',*,*,#57145,.T.);
#84708=ORIENTED_EDGE('',*,*,#57146,.F.);
#84709=ORIENTED_EDGE('',*,*,#57147,.F.);
#84710=ORIENTED_EDGE('',*,*,#57148,.T.);
#84711=ORIENTED_EDGE('',*,*,#57149,.T.);
#84712=ORIENTED_EDGE('',*,*,#57148,.F.);
#84713=ORIENTED_EDGE('',*,*,#57149,.F.);
#84714=ORIENTED_EDGE('',*,*,#57150,.T.);
#84715=ORIENTED_EDGE('',*,*,#57139,.T.);
#84716=ORIENTED_EDGE('',*,*,#57150,.F.);
#84717=ORIENTED_EDGE('',*,*,#57133,.T.);
#84718=ORIENTED_EDGE('',*,*,#57141,.T.);
#84719=ORIENTED_EDGE('',*,*,#57147,.T.);
#84720=ORIENTED_EDGE('',*,*,#57142,.T.);
#84721=ORIENTED_EDGE('',*,*,#57134,.T.);
#84722=ORIENTED_EDGE('',*,*,#57136,.F.);
#84723=ORIENTED_EDGE('',*,*,#57137,.T.);
#84724=ORIENTED_EDGE('',*,*,#57128,.T.);
#84725=ORIENTED_EDGE('',*,*,#57125,.T.);
#84726=ORIENTED_EDGE('',*,*,#57122,.T.);
#84727=ORIENTED_EDGE('',*,*,#57119,.T.);
#84728=ORIENTED_EDGE('',*,*,#57116,.T.);
#84729=ORIENTED_EDGE('',*,*,#57113,.T.);
#84730=ORIENTED_EDGE('',*,*,#57110,.T.);
#84731=ORIENTED_EDGE('',*,*,#57107,.T.);
#84732=ORIENTED_EDGE('',*,*,#57104,.T.);
#84733=ORIENTED_EDGE('',*,*,#57131,.T.);
#84734=ORIENTED_EDGE('',*,*,#57106,.F.);
#84735=ORIENTED_EDGE('',*,*,#57109,.F.);
#84736=ORIENTED_EDGE('',*,*,#57112,.F.);
#84737=ORIENTED_EDGE('',*,*,#57115,.F.);
#84738=ORIENTED_EDGE('',*,*,#57118,.F.);
#84739=ORIENTED_EDGE('',*,*,#57121,.F.);
#84740=ORIENTED_EDGE('',*,*,#57124,.F.);
#84741=ORIENTED_EDGE('',*,*,#57127,.F.);
#84742=ORIENTED_EDGE('',*,*,#57130,.F.);
#84743=ORIENTED_EDGE('',*,*,#57151,.T.);
#84744=ORIENTED_EDGE('',*,*,#57152,.T.);
#84745=ORIENTED_EDGE('',*,*,#57153,.T.);
#84746=ORIENTED_EDGE('',*,*,#57154,.T.);
#84747=ORIENTED_EDGE('',*,*,#57155,.F.);
#84748=ORIENTED_EDGE('',*,*,#57156,.F.);
#84749=ORIENTED_EDGE('',*,*,#57157,.F.);
#84750=ORIENTED_EDGE('',*,*,#57158,.F.);
#84751=ORIENTED_EDGE('',*,*,#57159,.F.);
#84752=ORIENTED_EDGE('',*,*,#57160,.F.);
#84753=ORIENTED_EDGE('',*,*,#57161,.F.);
#84754=ORIENTED_EDGE('',*,*,#57162,.F.);
#84755=ORIENTED_EDGE('',*,*,#57163,.T.);
#84756=ORIENTED_EDGE('',*,*,#57164,.T.);
#84757=ORIENTED_EDGE('',*,*,#57165,.T.);
#84758=ORIENTED_EDGE('',*,*,#57166,.T.);
#84759=ORIENTED_EDGE('',*,*,#57159,.T.);
#84760=ORIENTED_EDGE('',*,*,#57167,.F.);
#84761=ORIENTED_EDGE('',*,*,#57151,.F.);
#84762=ORIENTED_EDGE('',*,*,#57168,.T.);
#84763=ORIENTED_EDGE('',*,*,#57162,.T.);
#84764=ORIENTED_EDGE('',*,*,#57169,.F.);
#84765=ORIENTED_EDGE('',*,*,#57152,.F.);
#84766=ORIENTED_EDGE('',*,*,#57167,.T.);
#84767=ORIENTED_EDGE('',*,*,#57161,.T.);
#84768=ORIENTED_EDGE('',*,*,#57170,.F.);
#84769=ORIENTED_EDGE('',*,*,#57153,.F.);
#84770=ORIENTED_EDGE('',*,*,#57169,.T.);
#84771=ORIENTED_EDGE('',*,*,#57160,.T.);
#84772=ORIENTED_EDGE('',*,*,#57168,.F.);
#84773=ORIENTED_EDGE('',*,*,#57154,.F.);
#84774=ORIENTED_EDGE('',*,*,#57170,.T.);
#84775=ORIENTED_EDGE('',*,*,#57164,.F.);
#84776=ORIENTED_EDGE('',*,*,#57171,.F.);
#84777=ORIENTED_EDGE('',*,*,#57155,.T.);
#84778=ORIENTED_EDGE('',*,*,#57172,.T.);
#84779=ORIENTED_EDGE('',*,*,#57165,.F.);
#84780=ORIENTED_EDGE('',*,*,#57172,.F.);
#84781=ORIENTED_EDGE('',*,*,#57158,.T.);
#84782=ORIENTED_EDGE('',*,*,#57173,.T.);
#84783=ORIENTED_EDGE('',*,*,#57166,.F.);
#84784=ORIENTED_EDGE('',*,*,#57173,.F.);
#84785=ORIENTED_EDGE('',*,*,#57157,.T.);
#84786=ORIENTED_EDGE('',*,*,#57174,.T.);
#84787=ORIENTED_EDGE('',*,*,#57163,.F.);
#84788=ORIENTED_EDGE('',*,*,#57174,.F.);
#84789=ORIENTED_EDGE('',*,*,#57156,.T.);
#84790=ORIENTED_EDGE('',*,*,#57171,.T.);
#84791=ORIENTED_EDGE('',*,*,#57175,.T.);
#84792=ORIENTED_EDGE('',*,*,#57176,.F.);
#84793=ORIENTED_EDGE('',*,*,#57177,.F.);
#84794=ORIENTED_EDGE('',*,*,#57178,.T.);
#84795=ORIENTED_EDGE('',*,*,#57179,.T.);
#84796=ORIENTED_EDGE('',*,*,#57180,.F.);
#84797=ORIENTED_EDGE('',*,*,#57181,.F.);
#84798=ORIENTED_EDGE('',*,*,#57176,.T.);
#84799=ORIENTED_EDGE('',*,*,#57182,.T.);
#84800=ORIENTED_EDGE('',*,*,#57183,.F.);
#84801=ORIENTED_EDGE('',*,*,#57184,.F.);
#84802=ORIENTED_EDGE('',*,*,#57180,.T.);
#84803=ORIENTED_EDGE('',*,*,#57185,.T.);
#84804=ORIENTED_EDGE('',*,*,#57178,.F.);
#84805=ORIENTED_EDGE('',*,*,#57186,.F.);
#84806=ORIENTED_EDGE('',*,*,#57183,.T.);
#84807=ORIENTED_EDGE('',*,*,#57177,.T.);
#84808=ORIENTED_EDGE('',*,*,#57181,.T.);
#84809=ORIENTED_EDGE('',*,*,#57184,.T.);
#84810=ORIENTED_EDGE('',*,*,#57186,.T.);
#84811=ORIENTED_EDGE('',*,*,#57175,.F.);
#84812=ORIENTED_EDGE('',*,*,#57185,.F.);
#84813=ORIENTED_EDGE('',*,*,#57182,.F.);
#84814=ORIENTED_EDGE('',*,*,#57179,.F.);
#84815=ORIENTED_EDGE('',*,*,#57187,.F.);
#84816=ORIENTED_EDGE('',*,*,#57188,.T.);
#84817=ORIENTED_EDGE('',*,*,#57189,.T.);
#84818=ORIENTED_EDGE('',*,*,#57188,.F.);
#84819=ORIENTED_EDGE('',*,*,#57190,.F.);
#84820=ORIENTED_EDGE('',*,*,#57191,.T.);
#84821=ORIENTED_EDGE('',*,*,#57192,.T.);
#84822=ORIENTED_EDGE('',*,*,#57191,.F.);
#84823=ORIENTED_EDGE('',*,*,#57193,.T.);
#84824=ORIENTED_EDGE('',*,*,#57194,.T.);
#84825=ORIENTED_EDGE('',*,*,#57195,.T.);
#84826=ORIENTED_EDGE('',*,*,#57194,.F.);
#84827=ORIENTED_EDGE('',*,*,#57196,.T.);
#84828=ORIENTED_EDGE('',*,*,#57197,.T.);
#84829=ORIENTED_EDGE('',*,*,#57198,.T.);
#84830=ORIENTED_EDGE('',*,*,#57197,.F.);
#84831=ORIENTED_EDGE('',*,*,#57199,.T.);
#84832=ORIENTED_EDGE('',*,*,#57200,.T.);
#84833=ORIENTED_EDGE('',*,*,#57201,.T.);
#84834=ORIENTED_EDGE('',*,*,#57200,.F.);
#84835=ORIENTED_EDGE('',*,*,#57202,.F.);
#84836=ORIENTED_EDGE('',*,*,#57203,.T.);
#84837=ORIENTED_EDGE('',*,*,#57204,.T.);
#84838=ORIENTED_EDGE('',*,*,#57203,.F.);
#84839=ORIENTED_EDGE('',*,*,#57205,.F.);
#84840=ORIENTED_EDGE('',*,*,#57206,.T.);
#84841=ORIENTED_EDGE('',*,*,#57207,.T.);
#84842=ORIENTED_EDGE('',*,*,#57206,.F.);
#84843=ORIENTED_EDGE('',*,*,#57208,.F.);
#84844=ORIENTED_EDGE('',*,*,#57209,.T.);
#84845=ORIENTED_EDGE('',*,*,#57210,.T.);
#84846=ORIENTED_EDGE('',*,*,#57209,.F.);
#84847=ORIENTED_EDGE('',*,*,#57211,.T.);
#84848=ORIENTED_EDGE('',*,*,#57212,.T.);
#84849=ORIENTED_EDGE('',*,*,#57213,.T.);
#84850=ORIENTED_EDGE('',*,*,#57214,.F.);
#84851=ORIENTED_EDGE('',*,*,#57215,.F.);
#84852=ORIENTED_EDGE('',*,*,#57216,.T.);
#84853=ORIENTED_EDGE('',*,*,#57217,.T.);
#84854=ORIENTED_EDGE('',*,*,#57218,.T.);
#84855=ORIENTED_EDGE('',*,*,#57219,.F.);
#84856=ORIENTED_EDGE('',*,*,#57220,.T.);
#84857=ORIENTED_EDGE('',*,*,#57221,.T.);
#84858=ORIENTED_EDGE('',*,*,#57222,.T.);
#84859=ORIENTED_EDGE('',*,*,#57223,.F.);
#84860=ORIENTED_EDGE('',*,*,#57224,.T.);
#84861=ORIENTED_EDGE('',*,*,#57225,.T.);
#84862=ORIENTED_EDGE('',*,*,#57226,.F.);
#84863=ORIENTED_EDGE('',*,*,#57213,.F.);
#84864=ORIENTED_EDGE('',*,*,#57227,.T.);
#84865=ORIENTED_EDGE('',*,*,#57219,.T.);
#84866=ORIENTED_EDGE('',*,*,#57228,.F.);
#84867=ORIENTED_EDGE('',*,*,#57223,.T.);
#84868=ORIENTED_EDGE('',*,*,#57229,.T.);
#84869=ORIENTED_EDGE('',*,*,#57217,.F.);
#84870=ORIENTED_EDGE('',*,*,#57230,.T.);
#84871=ORIENTED_EDGE('',*,*,#57231,.F.);
#84872=ORIENTED_EDGE('',*,*,#57225,.F.);
#84873=ORIENTED_EDGE('',*,*,#57232,.T.);
#84874=ORIENTED_EDGE('',*,*,#57215,.T.);
#84875=ORIENTED_EDGE('',*,*,#57187,.T.);
#84876=ORIENTED_EDGE('',*,*,#57190,.T.);
#84877=ORIENTED_EDGE('',*,*,#57216,.F.);
#84878=ORIENTED_EDGE('',*,*,#57232,.F.);
#84879=ORIENTED_EDGE('',*,*,#57224,.F.);
#84880=ORIENTED_EDGE('',*,*,#57230,.F.);
#84881=ORIENTED_EDGE('',*,*,#57202,.T.);
#84882=ORIENTED_EDGE('',*,*,#57205,.T.);
#84883=ORIENTED_EDGE('',*,*,#57208,.T.);
#84884=ORIENTED_EDGE('',*,*,#57214,.T.);
#84885=ORIENTED_EDGE('',*,*,#57228,.T.);
#84886=ORIENTED_EDGE('',*,*,#57226,.T.);
#84887=ORIENTED_EDGE('',*,*,#57231,.T.);
#84888=ORIENTED_EDGE('',*,*,#57195,.F.);
#84889=ORIENTED_EDGE('',*,*,#57198,.F.);
#84890=ORIENTED_EDGE('',*,*,#57201,.F.);
#84891=ORIENTED_EDGE('',*,*,#57233,.T.);
#84892=ORIENTED_EDGE('',*,*,#57220,.F.);
#84893=ORIENTED_EDGE('',*,*,#57227,.F.);
#84894=ORIENTED_EDGE('',*,*,#57212,.F.);
#84895=ORIENTED_EDGE('',*,*,#57193,.F.);
#84896=ORIENTED_EDGE('',*,*,#57196,.F.);
#84897=ORIENTED_EDGE('',*,*,#57199,.F.);
#84898=ORIENTED_EDGE('',*,*,#57234,.T.);
#84899=ORIENTED_EDGE('',*,*,#57221,.F.);
#84900=ORIENTED_EDGE('',*,*,#57233,.F.);
#84901=ORIENTED_EDGE('',*,*,#57211,.F.);
#84902=ORIENTED_EDGE('',*,*,#57189,.F.);
#84903=ORIENTED_EDGE('',*,*,#57192,.F.);
#84904=ORIENTED_EDGE('',*,*,#57229,.F.);
#84905=ORIENTED_EDGE('',*,*,#57222,.F.);
#84906=ORIENTED_EDGE('',*,*,#57234,.F.);
#84907=ORIENTED_EDGE('',*,*,#57218,.F.);
#84908=ORIENTED_EDGE('',*,*,#57204,.F.);
#84909=ORIENTED_EDGE('',*,*,#57207,.F.);
#84910=ORIENTED_EDGE('',*,*,#57210,.F.);
#84911=ORIENTED_EDGE('',*,*,#57235,.F.);
#84912=ORIENTED_EDGE('',*,*,#57236,.T.);
#84913=ORIENTED_EDGE('',*,*,#57237,.T.);
#84914=ORIENTED_EDGE('',*,*,#57236,.F.);
#84915=ORIENTED_EDGE('',*,*,#57238,.F.);
#84916=ORIENTED_EDGE('',*,*,#57239,.T.);
#84917=ORIENTED_EDGE('',*,*,#57240,.T.);
#84918=ORIENTED_EDGE('',*,*,#57239,.F.);
#84919=ORIENTED_EDGE('',*,*,#57241,.F.);
#84920=ORIENTED_EDGE('',*,*,#57242,.T.);
#84921=ORIENTED_EDGE('',*,*,#57243,.T.);
#84922=ORIENTED_EDGE('',*,*,#57244,.T.);
#84923=ORIENTED_EDGE('',*,*,#57245,.T.);
#84924=ORIENTED_EDGE('',*,*,#57246,.T.);
#84925=ORIENTED_EDGE('',*,*,#57247,.F.);
#84926=ORIENTED_EDGE('',*,*,#57248,.T.);
#84927=ORIENTED_EDGE('',*,*,#57249,.F.);
#84928=ORIENTED_EDGE('',*,*,#57245,.F.);
#84929=ORIENTED_EDGE('',*,*,#57250,.T.);
#84930=ORIENTED_EDGE('',*,*,#57251,.T.);
#84931=ORIENTED_EDGE('',*,*,#57247,.T.);
#84932=ORIENTED_EDGE('',*,*,#57252,.T.);
#84933=ORIENTED_EDGE('',*,*,#57253,.F.);
#84934=ORIENTED_EDGE('',*,*,#57254,.F.);
#84935=ORIENTED_EDGE('',*,*,#57243,.F.);
#84936=ORIENTED_EDGE('',*,*,#57255,.T.);
#84937=ORIENTED_EDGE('',*,*,#57256,.T.);
#84938=ORIENTED_EDGE('',*,*,#57257,.T.);
#84939=ORIENTED_EDGE('',*,*,#57258,.F.);
#84940=ORIENTED_EDGE('',*,*,#57241,.T.);
#84941=ORIENTED_EDGE('',*,*,#57259,.F.);
#84942=ORIENTED_EDGE('',*,*,#57260,.F.);
#84943=ORIENTED_EDGE('',*,*,#57256,.F.);
#84944=ORIENTED_EDGE('',*,*,#57261,.T.);
#84945=ORIENTED_EDGE('',*,*,#57260,.T.);
#84946=ORIENTED_EDGE('',*,*,#57262,.T.);
#84947=ORIENTED_EDGE('',*,*,#57263,.F.);
#84948=ORIENTED_EDGE('',*,*,#57251,.F.);
#84949=ORIENTED_EDGE('',*,*,#57264,.T.);
#84950=ORIENTED_EDGE('',*,*,#57253,.T.);
#84951=ORIENTED_EDGE('',*,*,#57265,.F.);
#84952=ORIENTED_EDGE('',*,*,#57266,.F.);
#84953=ORIENTED_EDGE('',*,*,#57262,.F.);
#84954=ORIENTED_EDGE('',*,*,#57267,.T.);
#84955=ORIENTED_EDGE('',*,*,#57268,.F.);
#84956=ORIENTED_EDGE('',*,*,#57265,.T.);
#84957=ORIENTED_EDGE('',*,*,#57269,.T.);
#84958=ORIENTED_EDGE('',*,*,#57270,.T.);
#84959=ORIENTED_EDGE('',*,*,#57244,.F.);
#84960=ORIENTED_EDGE('',*,*,#57271,.T.);
#84961=ORIENTED_EDGE('',*,*,#57272,.F.);
#84962=ORIENTED_EDGE('',*,*,#57273,.F.);
#84963=ORIENTED_EDGE('',*,*,#57248,.F.);
#84964=ORIENTED_EDGE('',*,*,#57274,.F.);
#84965=ORIENTED_EDGE('',*,*,#57270,.F.);
#84966=ORIENTED_EDGE('',*,*,#57275,.T.);
#84967=ORIENTED_EDGE('',*,*,#57276,.F.);
#84968=ORIENTED_EDGE('',*,*,#57277,.T.);
#84969=ORIENTED_EDGE('',*,*,#57264,.F.);
#84970=ORIENTED_EDGE('',*,*,#57278,.F.);
#84971=ORIENTED_EDGE('',*,*,#57279,.T.);
#84972=ORIENTED_EDGE('',*,*,#57276,.T.);
#84973=ORIENTED_EDGE('',*,*,#57280,.F.);
#84974=ORIENTED_EDGE('',*,*,#57272,.T.);
#84975=ORIENTED_EDGE('',*,*,#57277,.F.);
#84976=ORIENTED_EDGE('',*,*,#57281,.F.);
#84977=ORIENTED_EDGE('',*,*,#57274,.T.);
#84978=ORIENTED_EDGE('',*,*,#57254,.T.);
#84979=ORIENTED_EDGE('',*,*,#57279,.F.);
#84980=ORIENTED_EDGE('',*,*,#57282,.F.);
#84981=ORIENTED_EDGE('',*,*,#57268,.T.);
#84982=ORIENTED_EDGE('',*,*,#57281,.T.);
#84983=ORIENTED_EDGE('',*,*,#57237,.F.);
#84984=ORIENTED_EDGE('',*,*,#57240,.F.);
#84985=ORIENTED_EDGE('',*,*,#57271,.F.);
#84986=ORIENTED_EDGE('',*,*,#57257,.F.);
#84987=ORIENTED_EDGE('',*,*,#57266,.T.);
#84988=ORIENTED_EDGE('',*,*,#57282,.T.);
#84989=ORIENTED_EDGE('',*,*,#57273,.T.);
#84990=ORIENTED_EDGE('',*,*,#57283,.F.);
#84991=ORIENTED_EDGE('',*,*,#57267,.F.);
#84992=ORIENTED_EDGE('',*,*,#57259,.T.);
#84993=ORIENTED_EDGE('',*,*,#57280,.T.);
#84994=ORIENTED_EDGE('',*,*,#57284,.F.);
#84995=ORIENTED_EDGE('',*,*,#57269,.F.);
#84996=ORIENTED_EDGE('',*,*,#57283,.T.);
#84997=ORIENTED_EDGE('',*,*,#57235,.T.);
#84998=ORIENTED_EDGE('',*,*,#57238,.T.);
#84999=ORIENTED_EDGE('',*,*,#57278,.T.);
#85000=ORIENTED_EDGE('',*,*,#57250,.F.);
#85001=ORIENTED_EDGE('',*,*,#57275,.F.);
#85002=ORIENTED_EDGE('',*,*,#57284,.T.);
#85003=ORIENTED_EDGE('',*,*,#57249,.T.);
#85004=ORIENTED_EDGE('',*,*,#57263,.T.);
#85005=ORIENTED_EDGE('',*,*,#57252,.F.);
#85006=ORIENTED_EDGE('',*,*,#57246,.F.);
#85007=ORIENTED_EDGE('',*,*,#57258,.T.);
#85008=ORIENTED_EDGE('',*,*,#57261,.F.);
#85009=ORIENTED_EDGE('',*,*,#57255,.F.);
#85010=ORIENTED_EDGE('',*,*,#57242,.F.);
#85011=ORIENTED_EDGE('',*,*,#57285,.F.);
#85012=ORIENTED_EDGE('',*,*,#57286,.T.);
#85013=ORIENTED_EDGE('',*,*,#57287,.T.);
#85014=ORIENTED_EDGE('',*,*,#57288,.T.);
#85015=ORIENTED_EDGE('',*,*,#57289,.T.);
#85016=ORIENTED_EDGE('',*,*,#57290,.F.);
#85017=ORIENTED_EDGE('',*,*,#57291,.T.);
#85018=ORIENTED_EDGE('',*,*,#57292,.T.);
#85019=ORIENTED_EDGE('',*,*,#57285,.T.);
#85020=ORIENTED_EDGE('',*,*,#57293,.T.);
#85021=ORIENTED_EDGE('',*,*,#57294,.F.);
#85022=ORIENTED_EDGE('',*,*,#57295,.T.);
#85023=ORIENTED_EDGE('',*,*,#57296,.T.);
#85024=ORIENTED_EDGE('',*,*,#57297,.T.);
#85025=ORIENTED_EDGE('',*,*,#57298,.F.);
#85026=ORIENTED_EDGE('',*,*,#57299,.T.);
#85027=ORIENTED_EDGE('',*,*,#57294,.T.);
#85028=ORIENTED_EDGE('',*,*,#57300,.T.);
#85029=ORIENTED_EDGE('',*,*,#57301,.F.);
#85030=ORIENTED_EDGE('',*,*,#57302,.T.);
#85031=ORIENTED_EDGE('',*,*,#57298,.T.);
#85032=ORIENTED_EDGE('',*,*,#57303,.T.);
#85033=ORIENTED_EDGE('',*,*,#57304,.F.);
#85034=ORIENTED_EDGE('',*,*,#57305,.T.);
#85035=ORIENTED_EDGE('',*,*,#57301,.T.);
#85036=ORIENTED_EDGE('',*,*,#57306,.T.);
#85037=ORIENTED_EDGE('',*,*,#57307,.F.);
#85038=ORIENTED_EDGE('',*,*,#57308,.T.);
#85039=ORIENTED_EDGE('',*,*,#57304,.T.);
#85040=ORIENTED_EDGE('',*,*,#57309,.T.);
#85041=ORIENTED_EDGE('',*,*,#57310,.F.);
#85042=ORIENTED_EDGE('',*,*,#57311,.T.);
#85043=ORIENTED_EDGE('',*,*,#57307,.T.);
#85044=ORIENTED_EDGE('',*,*,#57312,.T.);
#85045=ORIENTED_EDGE('',*,*,#57313,.F.);
#85046=ORIENTED_EDGE('',*,*,#57314,.T.);
#85047=ORIENTED_EDGE('',*,*,#57310,.T.);
#85048=ORIENTED_EDGE('',*,*,#57315,.T.);
#85049=ORIENTED_EDGE('',*,*,#57316,.F.);
#85050=ORIENTED_EDGE('',*,*,#57317,.T.);
#85051=ORIENTED_EDGE('',*,*,#57313,.T.);
#85052=ORIENTED_EDGE('',*,*,#57318,.T.);
#85053=ORIENTED_EDGE('',*,*,#57319,.F.);
#85054=ORIENTED_EDGE('',*,*,#57320,.T.);
#85055=ORIENTED_EDGE('',*,*,#57316,.T.);
#85056=ORIENTED_EDGE('',*,*,#57321,.T.);
#85057=ORIENTED_EDGE('',*,*,#57322,.F.);
#85058=ORIENTED_EDGE('',*,*,#57323,.T.);
#85059=ORIENTED_EDGE('',*,*,#57319,.T.);
#85060=ORIENTED_EDGE('',*,*,#57324,.T.);
#85061=ORIENTED_EDGE('',*,*,#57325,.F.);
#85062=ORIENTED_EDGE('',*,*,#57326,.T.);
#85063=ORIENTED_EDGE('',*,*,#57322,.T.);
#85064=ORIENTED_EDGE('',*,*,#57327,.T.);
#85065=ORIENTED_EDGE('',*,*,#57328,.F.);
#85066=ORIENTED_EDGE('',*,*,#57329,.T.);
#85067=ORIENTED_EDGE('',*,*,#57325,.T.);
#85068=ORIENTED_EDGE('',*,*,#57330,.T.);
#85069=ORIENTED_EDGE('',*,*,#57331,.F.);
#85070=ORIENTED_EDGE('',*,*,#57332,.T.);
#85071=ORIENTED_EDGE('',*,*,#57328,.T.);
#85072=ORIENTED_EDGE('',*,*,#57333,.T.);
#85073=ORIENTED_EDGE('',*,*,#57334,.F.);
#85074=ORIENTED_EDGE('',*,*,#57335,.T.);
#85075=ORIENTED_EDGE('',*,*,#57331,.T.);
#85076=ORIENTED_EDGE('',*,*,#57336,.T.);
#85077=ORIENTED_EDGE('',*,*,#57337,.F.);
#85078=ORIENTED_EDGE('',*,*,#57338,.T.);
#85079=ORIENTED_EDGE('',*,*,#57334,.T.);
#85080=ORIENTED_EDGE('',*,*,#57339,.T.);
#85081=ORIENTED_EDGE('',*,*,#57340,.F.);
#85082=ORIENTED_EDGE('',*,*,#57341,.T.);
#85083=ORIENTED_EDGE('',*,*,#57337,.T.);
#85084=ORIENTED_EDGE('',*,*,#57342,.T.);
#85085=ORIENTED_EDGE('',*,*,#57343,.F.);
#85086=ORIENTED_EDGE('',*,*,#57344,.T.);
#85087=ORIENTED_EDGE('',*,*,#57345,.F.);
#85088=ORIENTED_EDGE('',*,*,#57346,.T.);
#85089=ORIENTED_EDGE('',*,*,#57347,.T.);
#85090=ORIENTED_EDGE('',*,*,#57348,.T.);
#85091=ORIENTED_EDGE('',*,*,#57291,.F.);
#85092=ORIENTED_EDGE('',*,*,#57349,.F.);
#85093=ORIENTED_EDGE('',*,*,#57344,.F.);
#85094=ORIENTED_EDGE('',*,*,#57350,.F.);
#85095=ORIENTED_EDGE('',*,*,#57351,.T.);
#85096=ORIENTED_EDGE('',*,*,#57288,.F.);
#85097=ORIENTED_EDGE('',*,*,#57352,.F.);
#85098=ORIENTED_EDGE('',*,*,#57353,.T.);
#85099=ORIENTED_EDGE('',*,*,#57350,.T.);
#85100=ORIENTED_EDGE('',*,*,#57287,.F.);
#85101=ORIENTED_EDGE('',*,*,#57354,.F.);
#85102=ORIENTED_EDGE('',*,*,#57355,.F.);
#85103=ORIENTED_EDGE('',*,*,#57356,.T.);
#85104=ORIENTED_EDGE('',*,*,#57352,.T.);
#85105=ORIENTED_EDGE('',*,*,#57357,.F.);
#85106=ORIENTED_EDGE('',*,*,#57358,.F.);
#85107=ORIENTED_EDGE('',*,*,#57359,.T.);
#85108=ORIENTED_EDGE('',*,*,#57355,.T.);
#85109=ORIENTED_EDGE('',*,*,#57360,.F.);
#85110=ORIENTED_EDGE('',*,*,#57361,.F.);
#85111=ORIENTED_EDGE('',*,*,#57362,.T.);
#85112=ORIENTED_EDGE('',*,*,#57358,.T.);
#85113=ORIENTED_EDGE('',*,*,#57363,.F.);
#85114=ORIENTED_EDGE('',*,*,#57364,.F.);
#85115=ORIENTED_EDGE('',*,*,#57365,.T.);
#85116=ORIENTED_EDGE('',*,*,#57361,.T.);
#85117=ORIENTED_EDGE('',*,*,#57366,.F.);
#85118=ORIENTED_EDGE('',*,*,#57367,.F.);
#85119=ORIENTED_EDGE('',*,*,#57368,.T.);
#85120=ORIENTED_EDGE('',*,*,#57364,.T.);
#85121=ORIENTED_EDGE('',*,*,#57369,.F.);
#85122=ORIENTED_EDGE('',*,*,#57370,.F.);
#85123=ORIENTED_EDGE('',*,*,#57371,.T.);
#85124=ORIENTED_EDGE('',*,*,#57367,.T.);
#85125=ORIENTED_EDGE('',*,*,#57372,.F.);
#85126=ORIENTED_EDGE('',*,*,#57373,.F.);
#85127=ORIENTED_EDGE('',*,*,#57374,.T.);
#85128=ORIENTED_EDGE('',*,*,#57370,.T.);
#85129=ORIENTED_EDGE('',*,*,#57375,.F.);
#85130=ORIENTED_EDGE('',*,*,#57376,.F.);
#85131=ORIENTED_EDGE('',*,*,#57377,.T.);
#85132=ORIENTED_EDGE('',*,*,#57373,.T.);
#85133=ORIENTED_EDGE('',*,*,#57378,.F.);
#85134=ORIENTED_EDGE('',*,*,#57379,.F.);
#85135=ORIENTED_EDGE('',*,*,#57380,.T.);
#85136=ORIENTED_EDGE('',*,*,#57376,.T.);
#85137=ORIENTED_EDGE('',*,*,#57381,.F.);
#85138=ORIENTED_EDGE('',*,*,#57382,.F.);
#85139=ORIENTED_EDGE('',*,*,#57383,.T.);
#85140=ORIENTED_EDGE('',*,*,#57379,.T.);
#85141=ORIENTED_EDGE('',*,*,#57384,.F.);
#85142=ORIENTED_EDGE('',*,*,#57385,.F.);
#85143=ORIENTED_EDGE('',*,*,#57386,.T.);
#85144=ORIENTED_EDGE('',*,*,#57382,.T.);
#85145=ORIENTED_EDGE('',*,*,#57387,.F.);
#85146=ORIENTED_EDGE('',*,*,#57388,.F.);
#85147=ORIENTED_EDGE('',*,*,#57389,.T.);
#85148=ORIENTED_EDGE('',*,*,#57385,.T.);
#85149=ORIENTED_EDGE('',*,*,#57390,.F.);
#85150=ORIENTED_EDGE('',*,*,#57391,.F.);
#85151=ORIENTED_EDGE('',*,*,#57392,.T.);
#85152=ORIENTED_EDGE('',*,*,#57388,.T.);
#85153=ORIENTED_EDGE('',*,*,#57393,.F.);
#85154=ORIENTED_EDGE('',*,*,#57394,.F.);
#85155=ORIENTED_EDGE('',*,*,#57395,.T.);
#85156=ORIENTED_EDGE('',*,*,#57391,.T.);
#85157=ORIENTED_EDGE('',*,*,#57396,.F.);
#85158=ORIENTED_EDGE('',*,*,#57397,.F.);
#85159=ORIENTED_EDGE('',*,*,#57398,.T.);
#85160=ORIENTED_EDGE('',*,*,#57399,.T.);
#85161=ORIENTED_EDGE('',*,*,#57394,.T.);
#85162=ORIENTED_EDGE('',*,*,#57400,.F.);
#85163=ORIENTED_EDGE('',*,*,#57401,.F.);
#85164=ORIENTED_EDGE('',*,*,#57402,.F.);
#85165=ORIENTED_EDGE('',*,*,#57403,.F.);
#85166=ORIENTED_EDGE('',*,*,#57296,.F.);
#85167=ORIENTED_EDGE('',*,*,#57404,.F.);
#85168=ORIENTED_EDGE('',*,*,#57405,.T.);
#85169=ORIENTED_EDGE('',*,*,#57401,.T.);
#85170=ORIENTED_EDGE('',*,*,#57405,.F.);
#85171=ORIENTED_EDGE('',*,*,#57406,.F.);
#85172=ORIENTED_EDGE('',*,*,#57398,.F.);
#85173=ORIENTED_EDGE('',*,*,#57292,.F.);
#85174=ORIENTED_EDGE('',*,*,#57348,.F.);
#85175=ORIENTED_EDGE('',*,*,#57407,.F.);
#85176=ORIENTED_EDGE('',*,*,#57342,.F.);
#85177=ORIENTED_EDGE('',*,*,#57339,.F.);
#85178=ORIENTED_EDGE('',*,*,#57336,.F.);
#85179=ORIENTED_EDGE('',*,*,#57333,.F.);
#85180=ORIENTED_EDGE('',*,*,#57330,.F.);
#85181=ORIENTED_EDGE('',*,*,#57327,.F.);
#85182=ORIENTED_EDGE('',*,*,#57324,.F.);
#85183=ORIENTED_EDGE('',*,*,#57321,.F.);
#85184=ORIENTED_EDGE('',*,*,#57318,.F.);
#85185=ORIENTED_EDGE('',*,*,#57315,.F.);
#85186=ORIENTED_EDGE('',*,*,#57312,.F.);
#85187=ORIENTED_EDGE('',*,*,#57309,.F.);
#85188=ORIENTED_EDGE('',*,*,#57306,.F.);
#85189=ORIENTED_EDGE('',*,*,#57303,.F.);
#85190=ORIENTED_EDGE('',*,*,#57300,.F.);
#85191=ORIENTED_EDGE('',*,*,#57297,.F.);
#85192=ORIENTED_EDGE('',*,*,#57403,.T.);
#85193=ORIENTED_EDGE('',*,*,#57408,.T.);
#85194=ORIENTED_EDGE('',*,*,#57400,.T.);
#85195=ORIENTED_EDGE('',*,*,#57396,.T.);
#85196=ORIENTED_EDGE('',*,*,#57393,.T.);
#85197=ORIENTED_EDGE('',*,*,#57390,.T.);
#85198=ORIENTED_EDGE('',*,*,#57387,.T.);
#85199=ORIENTED_EDGE('',*,*,#57384,.T.);
#85200=ORIENTED_EDGE('',*,*,#57381,.T.);
#85201=ORIENTED_EDGE('',*,*,#57378,.T.);
#85202=ORIENTED_EDGE('',*,*,#57375,.T.);
#85203=ORIENTED_EDGE('',*,*,#57372,.T.);
#85204=ORIENTED_EDGE('',*,*,#57369,.T.);
#85205=ORIENTED_EDGE('',*,*,#57366,.T.);
#85206=ORIENTED_EDGE('',*,*,#57363,.T.);
#85207=ORIENTED_EDGE('',*,*,#57360,.T.);
#85208=ORIENTED_EDGE('',*,*,#57357,.T.);
#85209=ORIENTED_EDGE('',*,*,#57354,.T.);
#85210=ORIENTED_EDGE('',*,*,#57286,.F.);
#85211=ORIENTED_EDGE('',*,*,#57289,.F.);
#85212=ORIENTED_EDGE('',*,*,#57351,.F.);
#85213=ORIENTED_EDGE('',*,*,#57353,.F.);
#85214=ORIENTED_EDGE('',*,*,#57356,.F.);
#85215=ORIENTED_EDGE('',*,*,#57359,.F.);
#85216=ORIENTED_EDGE('',*,*,#57362,.F.);
#85217=ORIENTED_EDGE('',*,*,#57365,.F.);
#85218=ORIENTED_EDGE('',*,*,#57368,.F.);
#85219=ORIENTED_EDGE('',*,*,#57371,.F.);
#85220=ORIENTED_EDGE('',*,*,#57374,.F.);
#85221=ORIENTED_EDGE('',*,*,#57377,.F.);
#85222=ORIENTED_EDGE('',*,*,#57380,.F.);
#85223=ORIENTED_EDGE('',*,*,#57383,.F.);
#85224=ORIENTED_EDGE('',*,*,#57386,.F.);
#85225=ORIENTED_EDGE('',*,*,#57389,.F.);
#85226=ORIENTED_EDGE('',*,*,#57392,.F.);
#85227=ORIENTED_EDGE('',*,*,#57395,.F.);
#85228=ORIENTED_EDGE('',*,*,#57399,.F.);
#85229=ORIENTED_EDGE('',*,*,#57406,.T.);
#85230=ORIENTED_EDGE('',*,*,#57404,.T.);
#85231=ORIENTED_EDGE('',*,*,#57295,.F.);
#85232=ORIENTED_EDGE('',*,*,#57299,.F.);
#85233=ORIENTED_EDGE('',*,*,#57302,.F.);
#85234=ORIENTED_EDGE('',*,*,#57305,.F.);
#85235=ORIENTED_EDGE('',*,*,#57308,.F.);
#85236=ORIENTED_EDGE('',*,*,#57311,.F.);
#85237=ORIENTED_EDGE('',*,*,#57314,.F.);
#85238=ORIENTED_EDGE('',*,*,#57317,.F.);
#85239=ORIENTED_EDGE('',*,*,#57320,.F.);
#85240=ORIENTED_EDGE('',*,*,#57323,.F.);
#85241=ORIENTED_EDGE('',*,*,#57326,.F.);
#85242=ORIENTED_EDGE('',*,*,#57329,.F.);
#85243=ORIENTED_EDGE('',*,*,#57332,.F.);
#85244=ORIENTED_EDGE('',*,*,#57335,.F.);
#85245=ORIENTED_EDGE('',*,*,#57338,.F.);
#85246=ORIENTED_EDGE('',*,*,#57341,.F.);
#85247=ORIENTED_EDGE('',*,*,#57409,.F.);
#85248=ORIENTED_EDGE('',*,*,#57346,.F.);
#85249=ORIENTED_EDGE('',*,*,#57410,.F.);
#85250=ORIENTED_EDGE('',*,*,#57293,.F.);
#85251=ORIENTED_EDGE('',*,*,#57397,.T.);
#85252=ORIENTED_EDGE('',*,*,#57408,.F.);
#85253=ORIENTED_EDGE('',*,*,#57402,.T.);
#85254=ORIENTED_EDGE('',*,*,#57411,.T.);
#85255=ORIENTED_EDGE('',*,*,#57412,.T.);
#85256=ORIENTED_EDGE('',*,*,#57413,.T.);
#85257=ORIENTED_EDGE('',*,*,#57414,.T.);
#85258=ORIENTED_EDGE('',*,*,#57415,.T.);
#85259=ORIENTED_EDGE('',*,*,#57416,.T.);
#85260=ORIENTED_EDGE('',*,*,#57417,.T.);
#85261=ORIENTED_EDGE('',*,*,#57418,.T.);
#85262=ORIENTED_EDGE('',*,*,#57419,.T.);
#85263=ORIENTED_EDGE('',*,*,#57420,.T.);
#85264=ORIENTED_EDGE('',*,*,#57421,.T.);
#85265=ORIENTED_EDGE('',*,*,#57422,.T.);
#85266=ORIENTED_EDGE('',*,*,#57423,.T.);
#85267=ORIENTED_EDGE('',*,*,#57424,.T.);
#85268=ORIENTED_EDGE('',*,*,#57425,.T.);
#85269=ORIENTED_EDGE('',*,*,#57426,.T.);
#85270=ORIENTED_EDGE('',*,*,#57427,.F.);
#85271=ORIENTED_EDGE('',*,*,#57428,.F.);
#85272=ORIENTED_EDGE('',*,*,#57429,.T.);
#85273=ORIENTED_EDGE('',*,*,#57413,.F.);
#85274=ORIENTED_EDGE('',*,*,#57429,.F.);
#85275=ORIENTED_EDGE('',*,*,#57430,.F.);
#85276=ORIENTED_EDGE('',*,*,#57431,.T.);
#85277=ORIENTED_EDGE('',*,*,#57414,.F.);
#85278=ORIENTED_EDGE('',*,*,#57431,.F.);
#85279=ORIENTED_EDGE('',*,*,#57432,.F.);
#85280=ORIENTED_EDGE('',*,*,#57433,.T.);
#85281=ORIENTED_EDGE('',*,*,#57411,.F.);
#85282=ORIENTED_EDGE('',*,*,#57433,.F.);
#85283=ORIENTED_EDGE('',*,*,#57434,.F.);
#85284=ORIENTED_EDGE('',*,*,#57427,.T.);
#85285=ORIENTED_EDGE('',*,*,#57412,.F.);
#85286=ORIENTED_EDGE('',*,*,#57435,.F.);
#85287=ORIENTED_EDGE('',*,*,#57436,.F.);
#85288=ORIENTED_EDGE('',*,*,#57437,.T.);
#85289=ORIENTED_EDGE('',*,*,#57417,.F.);
#85290=ORIENTED_EDGE('',*,*,#57437,.F.);
#85291=ORIENTED_EDGE('',*,*,#57438,.F.);
#85292=ORIENTED_EDGE('',*,*,#57439,.T.);
#85293=ORIENTED_EDGE('',*,*,#57418,.F.);
#85294=ORIENTED_EDGE('',*,*,#57439,.F.);
#85295=ORIENTED_EDGE('',*,*,#57440,.F.);
#85296=ORIENTED_EDGE('',*,*,#57441,.T.);
#85297=ORIENTED_EDGE('',*,*,#57415,.F.);
#85298=ORIENTED_EDGE('',*,*,#57441,.F.);
#85299=ORIENTED_EDGE('',*,*,#57442,.F.);
#85300=ORIENTED_EDGE('',*,*,#57435,.T.);
#85301=ORIENTED_EDGE('',*,*,#57416,.F.);
#85302=ORIENTED_EDGE('',*,*,#57443,.F.);
#85303=ORIENTED_EDGE('',*,*,#57444,.F.);
#85304=ORIENTED_EDGE('',*,*,#57445,.T.);
#85305=ORIENTED_EDGE('',*,*,#57421,.F.);
#85306=ORIENTED_EDGE('',*,*,#57445,.F.);
#85307=ORIENTED_EDGE('',*,*,#57446,.F.);
#85308=ORIENTED_EDGE('',*,*,#57447,.T.);
#85309=ORIENTED_EDGE('',*,*,#57422,.F.);
#85310=ORIENTED_EDGE('',*,*,#57447,.F.);
#85311=ORIENTED_EDGE('',*,*,#57448,.F.);
#85312=ORIENTED_EDGE('',*,*,#57449,.T.);
#85313=ORIENTED_EDGE('',*,*,#57419,.F.);
#85314=ORIENTED_EDGE('',*,*,#57449,.F.);
#85315=ORIENTED_EDGE('',*,*,#57450,.F.);
#85316=ORIENTED_EDGE('',*,*,#57443,.T.);
#85317=ORIENTED_EDGE('',*,*,#57420,.F.);
#85318=ORIENTED_EDGE('',*,*,#57451,.F.);
#85319=ORIENTED_EDGE('',*,*,#57452,.F.);
#85320=ORIENTED_EDGE('',*,*,#57453,.T.);
#85321=ORIENTED_EDGE('',*,*,#57425,.F.);
#85322=ORIENTED_EDGE('',*,*,#57453,.F.);
#85323=ORIENTED_EDGE('',*,*,#57454,.F.);
#85324=ORIENTED_EDGE('',*,*,#57455,.T.);
#85325=ORIENTED_EDGE('',*,*,#57426,.F.);
#85326=ORIENTED_EDGE('',*,*,#57455,.F.);
#85327=ORIENTED_EDGE('',*,*,#57456,.F.);
#85328=ORIENTED_EDGE('',*,*,#57457,.T.);
#85329=ORIENTED_EDGE('',*,*,#57423,.F.);
#85330=ORIENTED_EDGE('',*,*,#57457,.F.);
#85331=ORIENTED_EDGE('',*,*,#57458,.F.);
#85332=ORIENTED_EDGE('',*,*,#57451,.T.);
#85333=ORIENTED_EDGE('',*,*,#57424,.F.);
#85334=ORIENTED_EDGE('',*,*,#57459,.T.);
#85335=ORIENTED_EDGE('',*,*,#57460,.T.);
#85336=ORIENTED_EDGE('',*,*,#57461,.T.);
#85337=ORIENTED_EDGE('',*,*,#57462,.T.);
#85338=ORIENTED_EDGE('',*,*,#57463,.T.);
#85339=ORIENTED_EDGE('',*,*,#57464,.T.);
#85340=ORIENTED_EDGE('',*,*,#57465,.T.);
#85341=ORIENTED_EDGE('',*,*,#57466,.T.);
#85342=ORIENTED_EDGE('',*,*,#57434,.T.);
#85343=ORIENTED_EDGE('',*,*,#57432,.T.);
#85344=ORIENTED_EDGE('',*,*,#57430,.T.);
#85345=ORIENTED_EDGE('',*,*,#57428,.T.);
#85346=ORIENTED_EDGE('',*,*,#57442,.T.);
#85347=ORIENTED_EDGE('',*,*,#57440,.T.);
#85348=ORIENTED_EDGE('',*,*,#57438,.T.);
#85349=ORIENTED_EDGE('',*,*,#57436,.T.);
#85350=ORIENTED_EDGE('',*,*,#57467,.T.);
#85351=ORIENTED_EDGE('',*,*,#57468,.T.);
#85352=ORIENTED_EDGE('',*,*,#57469,.T.);
#85353=ORIENTED_EDGE('',*,*,#57470,.T.);
#85354=ORIENTED_EDGE('',*,*,#57471,.T.);
#85355=ORIENTED_EDGE('',*,*,#57472,.T.);
#85356=ORIENTED_EDGE('',*,*,#57473,.T.);
#85357=ORIENTED_EDGE('',*,*,#57474,.T.);
#85358=ORIENTED_EDGE('',*,*,#57450,.T.);
#85359=ORIENTED_EDGE('',*,*,#57448,.T.);
#85360=ORIENTED_EDGE('',*,*,#57446,.T.);
#85361=ORIENTED_EDGE('',*,*,#57444,.T.);
#85362=ORIENTED_EDGE('',*,*,#57458,.T.);
#85363=ORIENTED_EDGE('',*,*,#57456,.T.);
#85364=ORIENTED_EDGE('',*,*,#57454,.T.);
#85365=ORIENTED_EDGE('',*,*,#57452,.T.);
#85366=ORIENTED_EDGE('',*,*,#57475,.T.);
#85367=ORIENTED_EDGE('',*,*,#57476,.T.);
#85368=ORIENTED_EDGE('',*,*,#57477,.T.);
#85369=ORIENTED_EDGE('',*,*,#57478,.T.);
#85370=ORIENTED_EDGE('',*,*,#57479,.F.);
#85371=ORIENTED_EDGE('',*,*,#57463,.F.);
#85372=ORIENTED_EDGE('',*,*,#57480,.T.);
#85373=ORIENTED_EDGE('',*,*,#57481,.F.);
#85374=ORIENTED_EDGE('',*,*,#57482,.F.);
#85375=ORIENTED_EDGE('',*,*,#57464,.F.);
#85376=ORIENTED_EDGE('',*,*,#57479,.T.);
#85377=ORIENTED_EDGE('',*,*,#57483,.F.);
#85378=ORIENTED_EDGE('',*,*,#57484,.F.);
#85379=ORIENTED_EDGE('',*,*,#57465,.F.);
#85380=ORIENTED_EDGE('',*,*,#57482,.T.);
#85381=ORIENTED_EDGE('',*,*,#57485,.F.);
#85382=ORIENTED_EDGE('',*,*,#57486,.F.);
#85383=ORIENTED_EDGE('',*,*,#57466,.F.);
#85384=ORIENTED_EDGE('',*,*,#57484,.T.);
#85385=ORIENTED_EDGE('',*,*,#57487,.F.);
#85386=ORIENTED_EDGE('',*,*,#57488,.F.);
#85387=ORIENTED_EDGE('',*,*,#57459,.F.);
#85388=ORIENTED_EDGE('',*,*,#57486,.T.);
#85389=ORIENTED_EDGE('',*,*,#57489,.F.);
#85390=ORIENTED_EDGE('',*,*,#57490,.F.);
#85391=ORIENTED_EDGE('',*,*,#57460,.F.);
#85392=ORIENTED_EDGE('',*,*,#57488,.T.);
#85393=ORIENTED_EDGE('',*,*,#57491,.F.);
#85394=ORIENTED_EDGE('',*,*,#57492,.F.);
#85395=ORIENTED_EDGE('',*,*,#57461,.F.);
#85396=ORIENTED_EDGE('',*,*,#57490,.T.);
#85397=ORIENTED_EDGE('',*,*,#57493,.F.);
#85398=ORIENTED_EDGE('',*,*,#57480,.F.);
#85399=ORIENTED_EDGE('',*,*,#57462,.F.);
#85400=ORIENTED_EDGE('',*,*,#57492,.T.);
#85401=ORIENTED_EDGE('',*,*,#57494,.F.);
#85402=ORIENTED_EDGE('',*,*,#57495,.F.);
#85403=ORIENTED_EDGE('',*,*,#57471,.F.);
#85404=ORIENTED_EDGE('',*,*,#57496,.T.);
#85405=ORIENTED_EDGE('',*,*,#57497,.F.);
#85406=ORIENTED_EDGE('',*,*,#57498,.F.);
#85407=ORIENTED_EDGE('',*,*,#57472,.F.);
#85408=ORIENTED_EDGE('',*,*,#57495,.T.);
#85409=ORIENTED_EDGE('',*,*,#57499,.F.);
#85410=ORIENTED_EDGE('',*,*,#57500,.F.);
#85411=ORIENTED_EDGE('',*,*,#57473,.F.);
#85412=ORIENTED_EDGE('',*,*,#57498,.T.);
#85413=ORIENTED_EDGE('',*,*,#57501,.F.);
#85414=ORIENTED_EDGE('',*,*,#57502,.F.);
#85415=ORIENTED_EDGE('',*,*,#57474,.F.);
#85416=ORIENTED_EDGE('',*,*,#57500,.T.);
#85417=ORIENTED_EDGE('',*,*,#57503,.F.);
#85418=ORIENTED_EDGE('',*,*,#57504,.F.);
#85419=ORIENTED_EDGE('',*,*,#57467,.F.);
#85420=ORIENTED_EDGE('',*,*,#57502,.T.);
#85421=ORIENTED_EDGE('',*,*,#57505,.F.);
#85422=ORIENTED_EDGE('',*,*,#57506,.F.);
#85423=ORIENTED_EDGE('',*,*,#57468,.F.);
#85424=ORIENTED_EDGE('',*,*,#57504,.T.);
#85425=ORIENTED_EDGE('',*,*,#57507,.F.);
#85426=ORIENTED_EDGE('',*,*,#57508,.F.);
#85427=ORIENTED_EDGE('',*,*,#57469,.F.);
#85428=ORIENTED_EDGE('',*,*,#57506,.T.);
#85429=ORIENTED_EDGE('',*,*,#57509,.F.);
#85430=ORIENTED_EDGE('',*,*,#57496,.F.);
#85431=ORIENTED_EDGE('',*,*,#57470,.F.);
#85432=ORIENTED_EDGE('',*,*,#57508,.T.);
#85433=ORIENTED_EDGE('',*,*,#57510,.F.);
#85434=ORIENTED_EDGE('',*,*,#57511,.F.);
#85435=ORIENTED_EDGE('',*,*,#57475,.F.);
#85436=ORIENTED_EDGE('',*,*,#57512,.T.);
#85437=ORIENTED_EDGE('',*,*,#57513,.F.);
#85438=ORIENTED_EDGE('',*,*,#57514,.F.);
#85439=ORIENTED_EDGE('',*,*,#57476,.F.);
#85440=ORIENTED_EDGE('',*,*,#57511,.T.);
#85441=ORIENTED_EDGE('',*,*,#57515,.F.);
#85442=ORIENTED_EDGE('',*,*,#57516,.F.);
#85443=ORIENTED_EDGE('',*,*,#57477,.F.);
#85444=ORIENTED_EDGE('',*,*,#57514,.T.);
#85445=ORIENTED_EDGE('',*,*,#57517,.F.);
#85446=ORIENTED_EDGE('',*,*,#57512,.F.);
#85447=ORIENTED_EDGE('',*,*,#57478,.F.);
#85448=ORIENTED_EDGE('',*,*,#57516,.T.);
#85449=ORIENTED_EDGE('',*,*,#57518,.F.);
#85450=ORIENTED_EDGE('',*,*,#57519,.T.);
#85451=ORIENTED_EDGE('',*,*,#57520,.T.);
#85452=ORIENTED_EDGE('',*,*,#57521,.T.);
#85453=ORIENTED_EDGE('',*,*,#57522,.T.);
#85454=ORIENTED_EDGE('',*,*,#57523,.T.);
#85455=ORIENTED_EDGE('',*,*,#57524,.T.);
#85456=ORIENTED_EDGE('',*,*,#57494,.T.);
#85457=ORIENTED_EDGE('',*,*,#57493,.T.);
#85458=ORIENTED_EDGE('',*,*,#57491,.T.);
#85459=ORIENTED_EDGE('',*,*,#57489,.T.);
#85460=ORIENTED_EDGE('',*,*,#57487,.T.);
#85461=ORIENTED_EDGE('',*,*,#57485,.T.);
#85462=ORIENTED_EDGE('',*,*,#57483,.T.);
#85463=ORIENTED_EDGE('',*,*,#57481,.T.);
#85464=ORIENTED_EDGE('',*,*,#57510,.T.);
#85465=ORIENTED_EDGE('',*,*,#57509,.T.);
#85466=ORIENTED_EDGE('',*,*,#57507,.T.);
#85467=ORIENTED_EDGE('',*,*,#57505,.T.);
#85468=ORIENTED_EDGE('',*,*,#57503,.T.);
#85469=ORIENTED_EDGE('',*,*,#57501,.T.);
#85470=ORIENTED_EDGE('',*,*,#57499,.T.);
#85471=ORIENTED_EDGE('',*,*,#57497,.T.);
#85472=ORIENTED_EDGE('',*,*,#57518,.T.);
#85473=ORIENTED_EDGE('',*,*,#57517,.T.);
#85474=ORIENTED_EDGE('',*,*,#57515,.T.);
#85475=ORIENTED_EDGE('',*,*,#57513,.T.);
#85476=ORIENTED_EDGE('',*,*,#57525,.T.);
#85477=ORIENTED_EDGE('',*,*,#57526,.T.);
#85478=ORIENTED_EDGE('',*,*,#57524,.F.);
#85479=ORIENTED_EDGE('',*,*,#57527,.T.);
#85480=ORIENTED_EDGE('',*,*,#57528,.T.);
#85481=ORIENTED_EDGE('',*,*,#57519,.F.);
#85482=ORIENTED_EDGE('',*,*,#57529,.T.);
#85483=ORIENTED_EDGE('',*,*,#57530,.T.);
#85484=ORIENTED_EDGE('',*,*,#57520,.F.);
#85485=ORIENTED_EDGE('',*,*,#57531,.T.);
#85486=ORIENTED_EDGE('',*,*,#57532,.T.);
#85487=ORIENTED_EDGE('',*,*,#57521,.F.);
#85488=ORIENTED_EDGE('',*,*,#57533,.T.);
#85489=ORIENTED_EDGE('',*,*,#57534,.T.);
#85490=ORIENTED_EDGE('',*,*,#57523,.F.);
#85491=ORIENTED_EDGE('',*,*,#57535,.T.);
#85492=ORIENTED_EDGE('',*,*,#57522,.F.);
#85493=ORIENTED_EDGE('',*,*,#57536,.T.);
#85494=ORIENTED_EDGE('',*,*,#57534,.F.);
#85495=ORIENTED_EDGE('',*,*,#57537,.T.);
#85496=ORIENTED_EDGE('',*,*,#57538,.T.);
#85497=ORIENTED_EDGE('',*,*,#57539,.F.);
#85498=ORIENTED_EDGE('',*,*,#57525,.F.);
#85499=ORIENTED_EDGE('',*,*,#57526,.F.);
#85500=ORIENTED_EDGE('',*,*,#57539,.T.);
#85501=ORIENTED_EDGE('',*,*,#57540,.T.);
#85502=ORIENTED_EDGE('',*,*,#57541,.F.);
#85503=ORIENTED_EDGE('',*,*,#57527,.F.);
#85504=ORIENTED_EDGE('',*,*,#57528,.F.);
#85505=ORIENTED_EDGE('',*,*,#57541,.T.);
#85506=ORIENTED_EDGE('',*,*,#57542,.T.);
#85507=ORIENTED_EDGE('',*,*,#57543,.F.);
#85508=ORIENTED_EDGE('',*,*,#57529,.F.);
#85509=ORIENTED_EDGE('',*,*,#57530,.F.);
#85510=ORIENTED_EDGE('',*,*,#57543,.T.);
#85511=ORIENTED_EDGE('',*,*,#57544,.T.);
#85512=ORIENTED_EDGE('',*,*,#57545,.F.);
#85513=ORIENTED_EDGE('',*,*,#57531,.F.);
#85514=ORIENTED_EDGE('',*,*,#57532,.F.);
#85515=ORIENTED_EDGE('',*,*,#57545,.T.);
#85516=ORIENTED_EDGE('',*,*,#57546,.T.);
#85517=ORIENTED_EDGE('',*,*,#57547,.F.);
#85518=ORIENTED_EDGE('',*,*,#57536,.F.);
#85519=ORIENTED_EDGE('',*,*,#57535,.F.);
#85520=ORIENTED_EDGE('',*,*,#57547,.T.);
#85521=ORIENTED_EDGE('',*,*,#57548,.T.);
#85522=ORIENTED_EDGE('',*,*,#57537,.F.);
#85523=ORIENTED_EDGE('',*,*,#57533,.F.);
#85524=ORIENTED_EDGE('',*,*,#57548,.F.);
#85525=ORIENTED_EDGE('',*,*,#57546,.F.);
#85526=ORIENTED_EDGE('',*,*,#57544,.F.);
#85527=ORIENTED_EDGE('',*,*,#57542,.F.);
#85528=ORIENTED_EDGE('',*,*,#57540,.F.);
#85529=ORIENTED_EDGE('',*,*,#57538,.F.);
#85530=ORIENTED_EDGE('',*,*,#57343,.T.);
#85531=ORIENTED_EDGE('',*,*,#57347,.F.);
#85532=ORIENTED_EDGE('',*,*,#57409,.T.);
#85533=ORIENTED_EDGE('',*,*,#57340,.T.);
#85534=ORIENTED_EDGE('',*,*,#57407,.T.);
#85535=ORIENTED_EDGE('',*,*,#57290,.T.);
#85536=ORIENTED_EDGE('',*,*,#57410,.T.);
#85537=ORIENTED_EDGE('',*,*,#57345,.T.);
#85538=ORIENTED_EDGE('',*,*,#57349,.T.);
#85539=ORIENTED_EDGE('',*,*,#57549,.F.);
#85540=ORIENTED_EDGE('',*,*,#57550,.F.);
#85541=ORIENTED_EDGE('',*,*,#57551,.F.);
#85542=ORIENTED_EDGE('',*,*,#57552,.F.);
#85543=ORIENTED_EDGE('',*,*,#57553,.T.);
#85544=ORIENTED_EDGE('',*,*,#57554,.F.);
#85545=ORIENTED_EDGE('',*,*,#57555,.T.);
#85546=ORIENTED_EDGE('',*,*,#57556,.F.);
#85547=ORIENTED_EDGE('',*,*,#57557,.T.);
#85548=ORIENTED_EDGE('',*,*,#57558,.F.);
#85549=ORIENTED_EDGE('',*,*,#57553,.F.);
#85550=ORIENTED_EDGE('',*,*,#57559,.F.);
#85551=ORIENTED_EDGE('',*,*,#57560,.T.);
#85552=ORIENTED_EDGE('',*,*,#57561,.F.);
#85553=ORIENTED_EDGE('',*,*,#57557,.F.);
#85554=ORIENTED_EDGE('',*,*,#57562,.F.);
#85555=ORIENTED_EDGE('',*,*,#57563,.T.);
#85556=ORIENTED_EDGE('',*,*,#57564,.F.);
#85557=ORIENTED_EDGE('',*,*,#57560,.F.);
#85558=ORIENTED_EDGE('',*,*,#57565,.F.);
#85559=ORIENTED_EDGE('',*,*,#57566,.F.);
#85560=ORIENTED_EDGE('',*,*,#57567,.F.);
#85561=ORIENTED_EDGE('',*,*,#57568,.T.);
#85562=ORIENTED_EDGE('',*,*,#57569,.T.);
#85563=ORIENTED_EDGE('',*,*,#57570,.F.);
#85564=ORIENTED_EDGE('',*,*,#57571,.T.);
#85565=ORIENTED_EDGE('',*,*,#57572,.T.);
#85566=ORIENTED_EDGE('',*,*,#57551,.T.);
#85567=ORIENTED_EDGE('',*,*,#57573,.F.);
#85568=ORIENTED_EDGE('',*,*,#57574,.T.);
#85569=ORIENTED_EDGE('',*,*,#57575,.T.);
#85570=ORIENTED_EDGE('',*,*,#57571,.F.);
#85571=ORIENTED_EDGE('',*,*,#57576,.F.);
#85572=ORIENTED_EDGE('',*,*,#57577,.T.);
#85573=ORIENTED_EDGE('',*,*,#57578,.T.);
#85574=ORIENTED_EDGE('',*,*,#57574,.F.);
#85575=ORIENTED_EDGE('',*,*,#57579,.F.);
#85576=ORIENTED_EDGE('',*,*,#57580,.F.);
#85577=ORIENTED_EDGE('',*,*,#57581,.T.);
#85578=ORIENTED_EDGE('',*,*,#57582,.T.);
#85579=ORIENTED_EDGE('',*,*,#57554,.T.);
#85580=ORIENTED_EDGE('',*,*,#57558,.T.);
#85581=ORIENTED_EDGE('',*,*,#57561,.T.);
#85582=ORIENTED_EDGE('',*,*,#57564,.T.);
#85583=ORIENTED_EDGE('',*,*,#57583,.T.);
#85584=ORIENTED_EDGE('',*,*,#57570,.T.);
#85585=ORIENTED_EDGE('',*,*,#57584,.T.);
#85586=ORIENTED_EDGE('',*,*,#57552,.T.);
#85587=ORIENTED_EDGE('',*,*,#57572,.F.);
#85588=ORIENTED_EDGE('',*,*,#57575,.F.);
#85589=ORIENTED_EDGE('',*,*,#57578,.F.);
#85590=ORIENTED_EDGE('',*,*,#57585,.F.);
#85591=ORIENTED_EDGE('',*,*,#57582,.F.);
#85592=ORIENTED_EDGE('',*,*,#57586,.T.);
#85593=ORIENTED_EDGE('',*,*,#57587,.T.);
#85594=ORIENTED_EDGE('',*,*,#57580,.T.);
#85595=ORIENTED_EDGE('',*,*,#57585,.T.);
#85596=ORIENTED_EDGE('',*,*,#57577,.F.);
#85597=ORIENTED_EDGE('',*,*,#57588,.F.);
#85598=ORIENTED_EDGE('',*,*,#57589,.T.);
#85599=ORIENTED_EDGE('',*,*,#57588,.T.);
#85600=ORIENTED_EDGE('',*,*,#57579,.T.);
#85601=ORIENTED_EDGE('',*,*,#57576,.T.);
#85602=ORIENTED_EDGE('',*,*,#57573,.T.);
#85603=ORIENTED_EDGE('',*,*,#57550,.T.);
#85604=ORIENTED_EDGE('',*,*,#57590,.T.);
#85605=ORIENTED_EDGE('',*,*,#57567,.T.);
#85606=ORIENTED_EDGE('',*,*,#57591,.T.);
#85607=ORIENTED_EDGE('',*,*,#57565,.T.);
#85608=ORIENTED_EDGE('',*,*,#57562,.T.);
#85609=ORIENTED_EDGE('',*,*,#57559,.T.);
#85610=ORIENTED_EDGE('',*,*,#57556,.T.);
#85611=ORIENTED_EDGE('',*,*,#57592,.T.);
#85612=ORIENTED_EDGE('',*,*,#57593,.F.);
#85613=ORIENTED_EDGE('',*,*,#57594,.F.);
#85614=ORIENTED_EDGE('',*,*,#57595,.F.);
#85615=ORIENTED_EDGE('',*,*,#57596,.F.);
#85616=ORIENTED_EDGE('',*,*,#57597,.F.);
#85617=ORIENTED_EDGE('',*,*,#57598,.F.);
#85618=ORIENTED_EDGE('',*,*,#57599,.F.);
#85619=ORIENTED_EDGE('',*,*,#57600,.F.);
#85620=ORIENTED_EDGE('',*,*,#57601,.F.);
#85621=ORIENTED_EDGE('',*,*,#57602,.F.);
#85622=ORIENTED_EDGE('',*,*,#57603,.F.);
#85623=ORIENTED_EDGE('',*,*,#57604,.F.);
#85624=ORIENTED_EDGE('',*,*,#57605,.F.);
#85625=ORIENTED_EDGE('',*,*,#57606,.F.);
#85626=ORIENTED_EDGE('',*,*,#57607,.F.);
#85627=ORIENTED_EDGE('',*,*,#57608,.F.);
#85628=ORIENTED_EDGE('',*,*,#57609,.F.);
#85629=ORIENTED_EDGE('',*,*,#57610,.F.);
#85630=ORIENTED_EDGE('',*,*,#57611,.F.);
#85631=ORIENTED_EDGE('',*,*,#57612,.F.);
#85632=ORIENTED_EDGE('',*,*,#57613,.F.);
#85633=ORIENTED_EDGE('',*,*,#57614,.F.);
#85634=ORIENTED_EDGE('',*,*,#57615,.F.);
#85635=ORIENTED_EDGE('',*,*,#57616,.F.);
#85636=ORIENTED_EDGE('',*,*,#57617,.F.);
#85637=ORIENTED_EDGE('',*,*,#57615,.T.);
#85638=ORIENTED_EDGE('',*,*,#57618,.F.);
#85639=ORIENTED_EDGE('',*,*,#57619,.F.);
#85640=ORIENTED_EDGE('',*,*,#57620,.F.);
#85641=ORIENTED_EDGE('',*,*,#57611,.T.);
#85642=ORIENTED_EDGE('',*,*,#57621,.F.);
#85643=ORIENTED_EDGE('',*,*,#57622,.F.);
#85644=ORIENTED_EDGE('',*,*,#57623,.F.);
#85645=ORIENTED_EDGE('',*,*,#57607,.T.);
#85646=ORIENTED_EDGE('',*,*,#57624,.F.);
#85647=ORIENTED_EDGE('',*,*,#57625,.F.);
#85648=ORIENTED_EDGE('',*,*,#57626,.F.);
#85649=ORIENTED_EDGE('',*,*,#57603,.T.);
#85650=ORIENTED_EDGE('',*,*,#57627,.F.);
#85651=ORIENTED_EDGE('',*,*,#57628,.F.);
#85652=ORIENTED_EDGE('',*,*,#57629,.F.);
#85653=ORIENTED_EDGE('',*,*,#57599,.T.);
#85654=ORIENTED_EDGE('',*,*,#57630,.F.);
#85655=ORIENTED_EDGE('',*,*,#57631,.F.);
#85656=ORIENTED_EDGE('',*,*,#57632,.F.);
#85657=ORIENTED_EDGE('',*,*,#57595,.T.);
#85658=ORIENTED_EDGE('',*,*,#57633,.F.);
#85659=ORIENTED_EDGE('',*,*,#57634,.T.);
#85660=ORIENTED_EDGE('',*,*,#57635,.T.);
#85661=ORIENTED_EDGE('',*,*,#57597,.T.);
#85662=ORIENTED_EDGE('',*,*,#57636,.T.);
#85663=ORIENTED_EDGE('',*,*,#57637,.F.);
#85664=ORIENTED_EDGE('',*,*,#57638,.T.);
#85665=ORIENTED_EDGE('',*,*,#57601,.T.);
#85666=ORIENTED_EDGE('',*,*,#57639,.T.);
#85667=ORIENTED_EDGE('',*,*,#57640,.F.);
#85668=ORIENTED_EDGE('',*,*,#57641,.T.);
#85669=ORIENTED_EDGE('',*,*,#57605,.T.);
#85670=ORIENTED_EDGE('',*,*,#57642,.T.);
#85671=ORIENTED_EDGE('',*,*,#57643,.F.);
#85672=ORIENTED_EDGE('',*,*,#57644,.T.);
#85673=ORIENTED_EDGE('',*,*,#57609,.T.);
#85674=ORIENTED_EDGE('',*,*,#57645,.T.);
#85675=ORIENTED_EDGE('',*,*,#57646,.F.);
#85676=ORIENTED_EDGE('',*,*,#57647,.T.);
#85677=ORIENTED_EDGE('',*,*,#57613,.T.);
#85678=ORIENTED_EDGE('',*,*,#57648,.T.);
#85679=ORIENTED_EDGE('',*,*,#57649,.F.);
#85680=ORIENTED_EDGE('',*,*,#57650,.T.);
#85681=ORIENTED_EDGE('',*,*,#57593,.T.);
#85682=ORIENTED_EDGE('',*,*,#57651,.T.);
#85683=ORIENTED_EDGE('',*,*,#57652,.F.);
#85684=ORIENTED_EDGE('',*,*,#57566,.T.);
#85685=ORIENTED_EDGE('',*,*,#57583,.F.);
#85686=ORIENTED_EDGE('',*,*,#57563,.F.);
#85687=ORIENTED_EDGE('',*,*,#57591,.F.);
#85688=ORIENTED_EDGE('',*,*,#57648,.F.);
#85689=ORIENTED_EDGE('',*,*,#57616,.T.);
#85690=ORIENTED_EDGE('',*,*,#57617,.T.);
#85691=ORIENTED_EDGE('',*,*,#57633,.T.);
#85692=ORIENTED_EDGE('',*,*,#57594,.T.);
#85693=ORIENTED_EDGE('',*,*,#57650,.F.);
#85694=ORIENTED_EDGE('',*,*,#57618,.T.);
#85695=ORIENTED_EDGE('',*,*,#57614,.T.);
#85696=ORIENTED_EDGE('',*,*,#57647,.F.);
#85697=ORIENTED_EDGE('',*,*,#57645,.F.);
#85698=ORIENTED_EDGE('',*,*,#57612,.T.);
#85699=ORIENTED_EDGE('',*,*,#57620,.T.);
#85700=ORIENTED_EDGE('',*,*,#57621,.T.);
#85701=ORIENTED_EDGE('',*,*,#57610,.T.);
#85702=ORIENTED_EDGE('',*,*,#57644,.F.);
#85703=ORIENTED_EDGE('',*,*,#57642,.F.);
#85704=ORIENTED_EDGE('',*,*,#57608,.T.);
#85705=ORIENTED_EDGE('',*,*,#57623,.T.);
#85706=ORIENTED_EDGE('',*,*,#57624,.T.);
#85707=ORIENTED_EDGE('',*,*,#57606,.T.);
#85708=ORIENTED_EDGE('',*,*,#57641,.F.);
#85709=ORIENTED_EDGE('',*,*,#57639,.F.);
#85710=ORIENTED_EDGE('',*,*,#57604,.T.);
#85711=ORIENTED_EDGE('',*,*,#57626,.T.);
#85712=ORIENTED_EDGE('',*,*,#57627,.T.);
#85713=ORIENTED_EDGE('',*,*,#57602,.T.);
#85714=ORIENTED_EDGE('',*,*,#57638,.F.);
#85715=ORIENTED_EDGE('',*,*,#57636,.F.);
#85716=ORIENTED_EDGE('',*,*,#57600,.T.);
#85717=ORIENTED_EDGE('',*,*,#57629,.T.);
#85718=ORIENTED_EDGE('',*,*,#57630,.T.);
#85719=ORIENTED_EDGE('',*,*,#57598,.T.);
#85720=ORIENTED_EDGE('',*,*,#57635,.F.);
#85721=ORIENTED_EDGE('',*,*,#57651,.F.);
#85722=ORIENTED_EDGE('',*,*,#57596,.T.);
#85723=ORIENTED_EDGE('',*,*,#57632,.T.);
#85724=ORIENTED_EDGE('',*,*,#57649,.T.);
#85725=ORIENTED_EDGE('',*,*,#57652,.T.);
#85726=ORIENTED_EDGE('',*,*,#57637,.T.);
#85727=ORIENTED_EDGE('',*,*,#57640,.T.);
#85728=ORIENTED_EDGE('',*,*,#57643,.T.);
#85729=ORIENTED_EDGE('',*,*,#57646,.T.);
#85730=ORIENTED_EDGE('',*,*,#57653,.T.);
#85731=ORIENTED_EDGE('',*,*,#57634,.F.);
#85732=ORIENTED_EDGE('',*,*,#57619,.T.);
#85733=ORIENTED_EDGE('',*,*,#57622,.T.);
#85734=ORIENTED_EDGE('',*,*,#57625,.T.);
#85735=ORIENTED_EDGE('',*,*,#57628,.T.);
#85736=ORIENTED_EDGE('',*,*,#57631,.T.);
#85737=ORIENTED_EDGE('',*,*,#57654,.T.);
#85738=ORIENTED_EDGE('',*,*,#57586,.F.);
#85739=ORIENTED_EDGE('',*,*,#57581,.F.);
#85740=ORIENTED_EDGE('',*,*,#57589,.F.);
#85741=ORIENTED_EDGE('',*,*,#57592,.F.);
#85742=ORIENTED_EDGE('',*,*,#57555,.F.);
#85743=ORIENTED_EDGE('',*,*,#57587,.F.);
#85744=ORIENTED_EDGE('',*,*,#57655,.T.);
#85745=ORIENTED_EDGE('',*,*,#57654,.F.);
#85746=ORIENTED_EDGE('',*,*,#57655,.F.);
#85747=ORIENTED_EDGE('',*,*,#57549,.T.);
#85748=ORIENTED_EDGE('',*,*,#57584,.F.);
#85749=ORIENTED_EDGE('',*,*,#57569,.F.);
#85750=ORIENTED_EDGE('',*,*,#57656,.T.);
#85751=ORIENTED_EDGE('',*,*,#57653,.F.);
#85752=ORIENTED_EDGE('',*,*,#57656,.F.);
#85753=ORIENTED_EDGE('',*,*,#57568,.F.);
#85754=ORIENTED_EDGE('',*,*,#57590,.F.);
#85755=CYLINDRICAL_SURFACE('',#93965,7.5);
#85756=CYLINDRICAL_SURFACE('',#93968,7.5);
#85757=CYLINDRICAL_SURFACE('',#93971,7.50000000000001);
#85758=CYLINDRICAL_SURFACE('',#93974,7.5);
#85759=CYLINDRICAL_SURFACE('',#93977,7.50000000000001);
#85760=CYLINDRICAL_SURFACE('',#93980,7.5);
#85761=CYLINDRICAL_SURFACE('',#93983,7.5);
#85762=CYLINDRICAL_SURFACE('',#93986,7.5);
#85763=CYLINDRICAL_SURFACE('',#93989,7.5);
#85764=CYLINDRICAL_SURFACE('',#93992,7.5);
#85765=CYLINDRICAL_SURFACE('',#93995,7.5);
#85766=CYLINDRICAL_SURFACE('',#93998,7.50000000000001);
#85767=CYLINDRICAL_SURFACE('',#94019,2.);
#85768=CYLINDRICAL_SURFACE('',#94020,2.);
#85769=CYLINDRICAL_SURFACE('',#94021,2.);
#85770=CYLINDRICAL_SURFACE('',#94022,2.);
#85771=CYLINDRICAL_SURFACE('',#94024,7.50000000000001);
#85772=CYLINDRICAL_SURFACE('',#94027,7.50000000000001);
#85773=CYLINDRICAL_SURFACE('',#94030,7.50000000000001);
#85774=CYLINDRICAL_SURFACE('',#94033,7.50000000000001);
#85775=CYLINDRICAL_SURFACE('',#94036,7.50000000000001);
#85776=CYLINDRICAL_SURFACE('',#94039,7.50000000000001);
#85777=CYLINDRICAL_SURFACE('',#94042,7.50000000000001);
#85778=CYLINDRICAL_SURFACE('',#94045,7.50000000000001);
#85779=CYLINDRICAL_SURFACE('',#94048,7.5);
#85780=CYLINDRICAL_SURFACE('',#94051,7.50000000000001);
#85781=CYLINDRICAL_SURFACE('',#94054,7.50000000000001);
#85782=CYLINDRICAL_SURFACE('',#94057,7.50000000000001);
#85783=CYLINDRICAL_SURFACE('',#94078,2.);
#85784=CYLINDRICAL_SURFACE('',#94079,2.);
#85785=CYLINDRICAL_SURFACE('',#94080,2.);
#85786=CYLINDRICAL_SURFACE('',#94081,2.);
#85787=CYLINDRICAL_SURFACE('',#94087,2.);
#85788=CYLINDRICAL_SURFACE('',#94091,2.5);
#85789=CYLINDRICAL_SURFACE('',#94098,2.);
#85790=CYLINDRICAL_SURFACE('',#94102,2.5);
#85791=CYLINDRICAL_SURFACE('',#94105,5.);
#85792=CYLINDRICAL_SURFACE('',#94108,3.);
#85793=CYLINDRICAL_SURFACE('',#94116,3.);
#85794=CYLINDRICAL_SURFACE('',#94124,3.);
#85795=CYLINDRICAL_SURFACE('',#94136,0.5);
#85796=CYLINDRICAL_SURFACE('',#94143,0.5);
#85797=CYLINDRICAL_SURFACE('',#94153,0.5);
#85798=CYLINDRICAL_SURFACE('',#94160,0.5);
#85799=CYLINDRICAL_SURFACE('',#94170,0.5);
#85800=CYLINDRICAL_SURFACE('',#94177,0.5);
#85801=CYLINDRICAL_SURFACE('',#94184,5.);
#85802=CYLINDRICAL_SURFACE('',#94190,0.5);
#85803=CYLINDRICAL_SURFACE('',#94199,0.5);
#85804=CYLINDRICAL_SURFACE('',#94206,0.5);
#85805=CYLINDRICAL_SURFACE('',#94214,0.5);
#85806=CYLINDRICAL_SURFACE('',#94221,0.5);
#85807=CYLINDRICAL_SURFACE('',#94229,0.5);
#85808=CYLINDRICAL_SURFACE('',#94237,5.);
#85809=CYLINDRICAL_SURFACE('',#94241,58.3875000000282);
#85810=CYLINDRICAL_SURFACE('',#94260,3.);
#85811=CYLINDRICAL_SURFACE('',#94269,3.);
#85812=CYLINDRICAL_SURFACE('',#94279,0.5);
#85813=CYLINDRICAL_SURFACE('',#94285,0.5);
#85814=CYLINDRICAL_SURFACE('',#94293,0.5);
#85815=CYLINDRICAL_SURFACE('',#94299,0.5);
#85816=CYLINDRICAL_SURFACE('',#94306,0.5);
#85817=CYLINDRICAL_SURFACE('',#94312,0.5);
#85818=CYLINDRICAL_SURFACE('',#94319,0.5);
#85819=CYLINDRICAL_SURFACE('',#94325,0.5);
#85820=CYLINDRICAL_SURFACE('',#94332,0.5);
#85821=CYLINDRICAL_SURFACE('',#94338,0.5);
#85822=CYLINDRICAL_SURFACE('',#94346,0.5);
#85823=CYLINDRICAL_SURFACE('',#94352,0.5);
#85824=CYLINDRICAL_SURFACE('',#94355,0.999999999999996);
#85825=CYLINDRICAL_SURFACE('',#94356,0.5);
#85826=CYLINDRICAL_SURFACE('',#94360,0.500000000000005);
#85827=CYLINDRICAL_SURFACE('',#94363,0.5);
#85828=CYLINDRICAL_SURFACE('',#94365,0.999999999999996);
#85829=CYLINDRICAL_SURFACE('',#94367,0.5);
#85830=CYLINDRICAL_SURFACE('',#94370,0.999999999999996);
#85831=CYLINDRICAL_SURFACE('',#94371,0.5);
#85832=CYLINDRICAL_SURFACE('',#94375,0.500000000000005);
#85833=CYLINDRICAL_SURFACE('',#94378,0.5);
#85834=CYLINDRICAL_SURFACE('',#94380,0.999999999999996);
#85835=CYLINDRICAL_SURFACE('',#94382,0.999999999999997);
#85836=CYLINDRICAL_SURFACE('',#94383,0.5);
#85837=CYLINDRICAL_SURFACE('',#94387,0.499999999999999);
#85838=CYLINDRICAL_SURFACE('',#94390,0.5);
#85839=CYLINDRICAL_SURFACE('',#94392,0.999999999999997);
#85840=CYLINDRICAL_SURFACE('',#94393,0.5);
#85841=CYLINDRICAL_SURFACE('',#94397,0.499999999999999);
#85842=CYLINDRICAL_SURFACE('',#94400,0.5);
#85843=CYLINDRICAL_SURFACE('',#94402,0.999999999999996);
#85844=CYLINDRICAL_SURFACE('',#94403,0.999999999999997);
#85845=CYLINDRICAL_SURFACE('',#94404,0.5);
#85846=CYLINDRICAL_SURFACE('',#94408,0.499999999999999);
#85847=CYLINDRICAL_SURFACE('',#94411,0.5);
#85848=CYLINDRICAL_SURFACE('',#94413,0.999999999999997);
#85849=CYLINDRICAL_SURFACE('',#94416,0.5);
#85850=CYLINDRICAL_SURFACE('',#94420,0.999999999999997);
#85851=CYLINDRICAL_SURFACE('',#94421,0.5);
#85852=CYLINDRICAL_SURFACE('',#94425,0.499999999999999);
#85853=CYLINDRICAL_SURFACE('',#94428,0.5);
#85854=CYLINDRICAL_SURFACE('',#94431,0.5);
#85855=CYLINDRICAL_SURFACE('',#94435,1.);
#85856=CYLINDRICAL_SURFACE('',#94436,0.5);
#85857=CYLINDRICAL_SURFACE('',#94440,0.499999999999998);
#85858=CYLINDRICAL_SURFACE('',#94443,0.5);
#85859=CYLINDRICAL_SURFACE('',#94445,1.);
#85860=CYLINDRICAL_SURFACE('',#94446,0.5);
#85861=CYLINDRICAL_SURFACE('',#94450,0.499999999999998);
#85862=CYLINDRICAL_SURFACE('',#94454,0.5);
#85863=CYLINDRICAL_SURFACE('',#94457,1.);
#85864=CYLINDRICAL_SURFACE('',#94467,0.5);
#85865=CYLINDRICAL_SURFACE('',#94479,0.5);
#85866=CYLINDRICAL_SURFACE('',#94481,3.);
#85867=CYLINDRICAL_SURFACE('',#94484,0.5);
#85868=CYLINDRICAL_SURFACE('',#94490,0.5);
#85869=CYLINDRICAL_SURFACE('',#94496,0.5);
#85870=CYLINDRICAL_SURFACE('',#94503,0.5);
#85871=CYLINDRICAL_SURFACE('',#94510,0.5);
#85872=CYLINDRICAL_SURFACE('',#94516,0.5);
#85873=CYLINDRICAL_SURFACE('',#94523,1.);
#85874=CYLINDRICAL_SURFACE('',#94525,0.5);
#85875=CYLINDRICAL_SURFACE('',#94532,0.5);
#85876=CYLINDRICAL_SURFACE('',#94538,0.5);
#85877=CYLINDRICAL_SURFACE('',#94540,1.);
#85878=CYLINDRICAL_SURFACE('',#94543,0.5);
#85879=CYLINDRICAL_SURFACE('',#94550,0.5);
#85880=CYLINDRICAL_SURFACE('',#94556,0.5);
#85881=CYLINDRICAL_SURFACE('',#94558,1.);
#85882=CYLINDRICAL_SURFACE('',#94561,0.5);
#85883=CYLINDRICAL_SURFACE('',#94564,3.);
#85884=CYLINDRICAL_SURFACE('',#94571,0.499999999999999);
#85885=CYLINDRICAL_SURFACE('',#94573,5.);
#85886=CYLINDRICAL_SURFACE('',#94579,0.250000000000003);
#85887=CYLINDRICAL_SURFACE('',#94593,0.249999999999997);
#85888=CYLINDRICAL_SURFACE('',#94607,0.250000000000003);
#85889=CYLINDRICAL_SURFACE('',#94621,0.250000000000003);
#85890=CYLINDRICAL_SURFACE('',#94627,2.75);
#85891=CYLINDRICAL_SURFACE('',#94632,2.75);
#85892=CYLINDRICAL_SURFACE('',#94638,0.5);
#85893=CYLINDRICAL_SURFACE('',#94645,0.5);
#85894=CYLINDRICAL_SURFACE('',#94654,0.5);
#85895=CYLINDRICAL_SURFACE('',#94661,0.5);
#85896=CYLINDRICAL_SURFACE('',#94669,0.5);
#85897=CYLINDRICAL_SURFACE('',#94676,0.5);
#85898=CYLINDRICAL_SURFACE('',#94680,3.);
#85899=CYLINDRICAL_SURFACE('',#94687,0.5);
#85900=CYLINDRICAL_SURFACE('',#94713,0.5);
#85901=CYLINDRICAL_SURFACE('',#94716,0.5);
#85902=CYLINDRICAL_SURFACE('',#94731,0.5);
#85903=CYLINDRICAL_SURFACE('',#94742,0.5);
#85904=CYLINDRICAL_SURFACE('',#94745,0.5);
#85905=CYLINDRICAL_SURFACE('',#94770,0.5);
#85906=CYLINDRICAL_SURFACE('',#94773,0.5);
#85907=CYLINDRICAL_SURFACE('',#94775,0.5);
#85908=CYLINDRICAL_SURFACE('',#94778,0.5);
#85909=CYLINDRICAL_SURFACE('',#94793,0.5);
#85910=CYLINDRICAL_SURFACE('',#94796,0.5);
#85911=CYLINDRICAL_SURFACE('',#94849,0.5);
#85912=CYLINDRICAL_SURFACE('',#94852,0.5);
#85913=CYLINDRICAL_SURFACE('',#94874,0.5);
#85914=CYLINDRICAL_SURFACE('',#94877,0.5);
#85915=CYLINDRICAL_SURFACE('',#94897,0.5);
#85916=CYLINDRICAL_SURFACE('',#94900,0.5);
#85917=CYLINDRICAL_SURFACE('',#94912,0.5);
#85918=CYLINDRICAL_SURFACE('',#94915,0.5);
#85919=CYLINDRICAL_SURFACE('',#94924,0.5);
#85920=CYLINDRICAL_SURFACE('',#94927,0.5);
#85921=CYLINDRICAL_SURFACE('',#94939,0.5);
#85922=CYLINDRICAL_SURFACE('',#94942,0.5);
#85923=CYLINDRICAL_SURFACE('',#94965,0.5);
#85924=CYLINDRICAL_SURFACE('',#94968,0.5);
#85925=CYLINDRICAL_SURFACE('',#94986,0.5);
#85926=CYLINDRICAL_SURFACE('',#94989,0.5);
#85927=CYLINDRICAL_SURFACE('',#95001,0.5);
#85928=CYLINDRICAL_SURFACE('',#95004,0.5);
#85929=CYLINDRICAL_SURFACE('',#95011,0.5);
#85930=CYLINDRICAL_SURFACE('',#95013,2.);
#85931=CYLINDRICAL_SURFACE('',#95018,2.75);
#85932=CYLINDRICAL_SURFACE('',#95019,0.5);
#85933=CYLINDRICAL_SURFACE('',#95029,0.5);
#85934=CYLINDRICAL_SURFACE('',#95030,0.5);
#85935=CYLINDRICAL_SURFACE('',#95032,2.);
#85936=CYLINDRICAL_SURFACE('',#95037,2.75);
#85937=CYLINDRICAL_SURFACE('',#95039,0.5);
#85938=CYLINDRICAL_SURFACE('',#95041,3.);
#85939=CYLINDRICAL_SURFACE('',#95046,0.5);
#85940=CYLINDRICAL_SURFACE('',#95054,0.5);
#85941=CYLINDRICAL_SURFACE('',#95057,0.5);
#85942=CYLINDRICAL_SURFACE('',#95059,0.5);
#85943=CYLINDRICAL_SURFACE('',#95062,0.5);
#85944=CYLINDRICAL_SURFACE('',#95064,0.5);
#85945=CYLINDRICAL_SURFACE('',#95071,0.5);
#85946=CYLINDRICAL_SURFACE('',#95074,0.5);
#85947=CYLINDRICAL_SURFACE('',#95079,0.5);
#85948=CYLINDRICAL_SURFACE('',#95082,0.5);
#85949=CYLINDRICAL_SURFACE('',#95087,0.5);
#85950=CYLINDRICAL_SURFACE('',#95089,0.5);
#85951=CYLINDRICAL_SURFACE('',#95093,0.5);
#85952=CYLINDRICAL_SURFACE('',#95096,0.5);
#85953=CYLINDRICAL_SURFACE('',#95099,3.);
#85954=CYLINDRICAL_SURFACE('',#95101,67.5);
#85955=CYLINDRICAL_SURFACE('',#95103,3.);
#85956=CYLINDRICAL_SURFACE('',#95106,5.);
#85957=CYLINDRICAL_SURFACE('',#95107,58.5);
#85958=CYLINDRICAL_SURFACE('',#95123,5.);
#85959=CYLINDRICAL_SURFACE('',#95125,3.);
#85960=CYLINDRICAL_SURFACE('',#95127,67.5);
#85961=CYLINDRICAL_SURFACE('',#95129,3.);
#85962=CYLINDRICAL_SURFACE('',#95149,0.5);
#85963=CYLINDRICAL_SURFACE('',#95154,0.5);
#85964=CYLINDRICAL_SURFACE('',#95157,0.5);
#85965=CYLINDRICAL_SURFACE('',#95167,0.5);
#85966=CYLINDRICAL_SURFACE('',#95171,0.5);
#85967=CYLINDRICAL_SURFACE('',#95178,0.5);
#85968=CYLINDRICAL_SURFACE('',#95183,0.5);
#85969=CYLINDRICAL_SURFACE('',#95186,0.5);
#85970=CYLINDRICAL_SURFACE('',#95188,0.5);
#85971=CYLINDRICAL_SURFACE('',#95192,0.5);
#85972=CYLINDRICAL_SURFACE('',#95196,0.5);
#85973=CYLINDRICAL_SURFACE('',#95202,0.5);
#85974=CYLINDRICAL_SURFACE('',#95206,3.);
#85975=CYLINDRICAL_SURFACE('',#95213,0.5);
#85976=CYLINDRICAL_SURFACE('',#95215,0.5);
#85977=CYLINDRICAL_SURFACE('',#95221,0.5);
#85978=CYLINDRICAL_SURFACE('',#95227,0.5);
#85979=CYLINDRICAL_SURFACE('',#95235,0.5);
#85980=CYLINDRICAL_SURFACE('',#95238,3.);
#85981=CYLINDRICAL_SURFACE('',#95241,0.5);
#85982=CYLINDRICAL_SURFACE('',#95248,3.);
#85983=CYLINDRICAL_SURFACE('',#95255,3.);
#85984=CYLINDRICAL_SURFACE('',#95259,0.5);
#85985=CYLINDRICAL_SURFACE('',#95261,0.5);
#85986=CYLINDRICAL_SURFACE('',#95268,0.5);
#85987=CYLINDRICAL_SURFACE('',#95271,0.5);
#85988=CYLINDRICAL_SURFACE('',#95277,0.5);
#85989=CYLINDRICAL_SURFACE('',#95283,0.5);
#85990=CYLINDRICAL_SURFACE('',#95285,0.5);
#85991=CYLINDRICAL_SURFACE('',#95290,0.5);
#85992=CYLINDRICAL_SURFACE('',#95294,3.);
#85993=CYLINDRICAL_SURFACE('',#95299,0.5);
#85994=CYLINDRICAL_SURFACE('',#95304,0.5);
#85995=CYLINDRICAL_SURFACE('',#95311,0.5);
#85996=CYLINDRICAL_SURFACE('',#95315,0.5);
#85997=CYLINDRICAL_SURFACE('',#95321,0.5);
#85998=CYLINDRICAL_SURFACE('',#95324,0.5);
#85999=CYLINDRICAL_SURFACE('',#95326,0.5);
#86000=CYLINDRICAL_SURFACE('',#95329,0.5);
#86001=CYLINDRICAL_SURFACE('',#95336,0.5);
#86002=CYLINDRICAL_SURFACE('',#95341,0.5);
#86003=CYLINDRICAL_SURFACE('',#95348,0.5);
#86004=CYLINDRICAL_SURFACE('',#95351,0.5);
#86005=CYLINDRICAL_SURFACE('',#95354,0.5);
#86006=CYLINDRICAL_SURFACE('',#95357,0.5);
#86007=CYLINDRICAL_SURFACE('',#95365,0.5);
#86008=CYLINDRICAL_SURFACE('',#95370,0.5);
#86009=CYLINDRICAL_SURFACE('',#95376,0.5);
#86010=CYLINDRICAL_SURFACE('',#95379,0.5);
#86011=CYLINDRICAL_SURFACE('',#95381,0.5);
#86012=CYLINDRICAL_SURFACE('',#95384,0.5);
#86013=CYLINDRICAL_SURFACE('',#95391,0.5);
#86014=CYLINDRICAL_SURFACE('',#95395,0.5);
#86015=CYLINDRICAL_SURFACE('',#95401,0.5);
#86016=CYLINDRICAL_SURFACE('',#95407,0.5);
#86017=CYLINDRICAL_SURFACE('',#95411,3.);
#86018=CYLINDRICAL_SURFACE('',#95416,0.5);
#86019=CYLINDRICAL_SURFACE('',#95421,0.5);
#86020=CYLINDRICAL_SURFACE('',#95422,0.5);
#86021=CYLINDRICAL_SURFACE('',#95429,0.5);
#86022=CYLINDRICAL_SURFACE('',#95435,0.5);
#86023=CYLINDRICAL_SURFACE('',#95437,0.5);
#86024=CYLINDRICAL_SURFACE('',#95442,0.5);
#86025=CYLINDRICAL_SURFACE('',#95444,0.5);
#86026=CYLINDRICAL_SURFACE('',#95448,0.5);
#86027=CYLINDRICAL_SURFACE('',#95450,0.5);
#86028=CYLINDRICAL_SURFACE('',#95457,0.5);
#86029=CYLINDRICAL_SURFACE('',#95459,0.5);
#86030=CYLINDRICAL_SURFACE('',#95464,0.5);
#86031=CYLINDRICAL_SURFACE('',#95470,0.5);
#86032=CYLINDRICAL_SURFACE('',#95476,0.5);
#86033=CYLINDRICAL_SURFACE('',#95477,3.);
#86034=CYLINDRICAL_SURFACE('',#95481,0.5);
#86035=CYLINDRICAL_SURFACE('',#95483,1.);
#86036=CYLINDRICAL_SURFACE('',#95486,0.5);
#86037=CYLINDRICAL_SURFACE('',#95489,0.5);
#86038=CYLINDRICAL_SURFACE('',#95494,0.5);
#86039=CYLINDRICAL_SURFACE('',#95495,0.5);
#86040=CYLINDRICAL_SURFACE('',#95499,0.5);
#86041=CYLINDRICAL_SURFACE('',#95506,0.5);
#86042=CYLINDRICAL_SURFACE('',#95509,0.5);
#86043=CYLINDRICAL_SURFACE('',#95516,0.5);
#86044=CYLINDRICAL_SURFACE('',#95519,0.5);
#86045=CYLINDRICAL_SURFACE('',#95524,0.5);
#86046=CYLINDRICAL_SURFACE('',#95527,0.5);
#86047=CYLINDRICAL_SURFACE('',#95529,0.5);
#86048=CYLINDRICAL_SURFACE('',#95534,0.5);
#86049=CYLINDRICAL_SURFACE('',#95538,3.);
#86050=CYLINDRICAL_SURFACE('',#95542,0.5);
#86051=CYLINDRICAL_SURFACE('',#95544,0.5);
#86052=CYLINDRICAL_SURFACE('',#95548,0.5);
#86053=CYLINDRICAL_SURFACE('',#95553,0.5);
#86054=CYLINDRICAL_SURFACE('',#95557,0.5);
#86055=CYLINDRICAL_SURFACE('',#95563,0.5);
#86056=CYLINDRICAL_SURFACE('',#95565,0.5);
#86057=CYLINDRICAL_SURFACE('',#95570,0.5);
#86058=CYLINDRICAL_SURFACE('',#95573,3.);
#86059=CYLINDRICAL_SURFACE('',#95576,0.5);
#86060=CYLINDRICAL_SURFACE('',#95579,1.);
#86061=CYLINDRICAL_SURFACE('',#95580,0.5);
#86062=CYLINDRICAL_SURFACE('',#95584,3.);
#86063=CYLINDRICAL_SURFACE('',#95587,0.5);
#86064=CYLINDRICAL_SURFACE('',#95593,0.5);
#86065=CYLINDRICAL_SURFACE('',#95595,0.5);
#86066=CYLINDRICAL_SURFACE('',#95600,0.5);
#86067=CYLINDRICAL_SURFACE('',#95602,0.5);
#86068=CYLINDRICAL_SURFACE('',#95607,0.5);
#86069=CYLINDRICAL_SURFACE('',#95614,0.5);
#86070=CYLINDRICAL_SURFACE('',#95619,0.5);
#86071=CYLINDRICAL_SURFACE('',#95620,3.);
#86072=CYLINDRICAL_SURFACE('',#95624,1.);
#86073=CYLINDRICAL_SURFACE('',#95625,0.5);
#86074=CYLINDRICAL_SURFACE('',#95630,0.5);
#86075=CYLINDRICAL_SURFACE('',#95631,0.5);
#86076=CYLINDRICAL_SURFACE('',#95635,0.5);
#86077=CYLINDRICAL_SURFACE('',#95636,0.5);
#86078=CYLINDRICAL_SURFACE('',#95638,0.5);
#86079=CYLINDRICAL_SURFACE('',#95640,0.5);
#86080=CYLINDRICAL_SURFACE('',#95648,0.5);
#86081=CYLINDRICAL_SURFACE('',#95653,0.5);
#86082=CYLINDRICAL_SURFACE('',#95660,0.5);
#86083=CYLINDRICAL_SURFACE('',#95663,0.5);
#86084=CYLINDRICAL_SURFACE('',#95668,0.5);
#86085=CYLINDRICAL_SURFACE('',#95671,0.5);
#86086=CYLINDRICAL_SURFACE('',#95673,0.5);
#86087=CYLINDRICAL_SURFACE('',#95678,0.5);
#86088=CYLINDRICAL_SURFACE('',#95682,3.);
#86089=CYLINDRICAL_SURFACE('',#95686,0.5);
#86090=CYLINDRICAL_SURFACE('',#95688,0.5);
#86091=CYLINDRICAL_SURFACE('',#95692,0.5);
#86092=CYLINDRICAL_SURFACE('',#95697,0.5);
#86093=CYLINDRICAL_SURFACE('',#95701,0.5);
#86094=CYLINDRICAL_SURFACE('',#95711,0.5);
#86095=CYLINDRICAL_SURFACE('',#95713,0.5);
#86096=CYLINDRICAL_SURFACE('',#95719,0.5);
#86097=CYLINDRICAL_SURFACE('',#95722,0.5);
#86098=CYLINDRICAL_SURFACE('',#95729,0.5);
#86099=CYLINDRICAL_SURFACE('',#95731,0.5);
#86100=CYLINDRICAL_SURFACE('',#95736,0.5);
#86101=CYLINDRICAL_SURFACE('',#95741,0.5);
#86102=CYLINDRICAL_SURFACE('',#95743,0.5);
#86103=CYLINDRICAL_SURFACE('',#95745,0.5);
#86104=CYLINDRICAL_SURFACE('',#95746,3.);
#86105=CYLINDRICAL_SURFACE('',#95750,0.5);
#86106=CYLINDRICAL_SURFACE('',#95752,0.5);
#86107=CYLINDRICAL_SURFACE('',#95757,0.5);
#86108=CYLINDRICAL_SURFACE('',#95762,0.5);
#86109=CYLINDRICAL_SURFACE('',#95767,0.5);
#86110=CYLINDRICAL_SURFACE('',#95768,0.5);
#86111=CYLINDRICAL_SURFACE('',#95774,0.5);
#86112=CYLINDRICAL_SURFACE('',#95779,0.5);
#86113=CYLINDRICAL_SURFACE('',#95784,0.5);
#86114=CYLINDRICAL_SURFACE('',#95787,0.5);
#86115=CYLINDRICAL_SURFACE('',#95789,0.5);
#86116=CYLINDRICAL_SURFACE('',#95794,0.5);
#86117=CYLINDRICAL_SURFACE('',#95798,3.);
#86118=CYLINDRICAL_SURFACE('',#95802,0.5);
#86119=CYLINDRICAL_SURFACE('',#95803,0.5);
#86120=CYLINDRICAL_SURFACE('',#95805,0.5);
#86121=CYLINDRICAL_SURFACE('',#95810,0.5);
#86122=CYLINDRICAL_SURFACE('',#95815,0.5);
#86123=CYLINDRICAL_SURFACE('',#95818,0.5);
#86124=CYLINDRICAL_SURFACE('',#95824,58.5);
#86125=CYLINDRICAL_SURFACE('',#95827,0.999999999999999);
#86126=CYLINDRICAL_SURFACE('',#95835,1.);
#86127=CYLINDRICAL_SURFACE('',#95837,0.5);
#86128=CYLINDRICAL_SURFACE('',#95839,1.);
#86129=CYLINDRICAL_SURFACE('',#95841,0.5);
#86130=CYLINDRICAL_SURFACE('',#95843,1.);
#86131=CYLINDRICAL_SURFACE('',#95888,1.);
#86132=CYLINDRICAL_SURFACE('',#95890,0.5);
#86133=CYLINDRICAL_SURFACE('',#95892,1.);
#86134=CYLINDRICAL_SURFACE('',#95895,1.);
#86135=CYLINDRICAL_SURFACE('',#95897,0.5);
#86136=CYLINDRICAL_SURFACE('',#95905,0.999999999999999);
#86137=CYLINDRICAL_SURFACE('',#95907,0.500000000000006);
#86138=CYLINDRICAL_SURFACE('',#95909,0.999999999999999);
#86139=CYLINDRICAL_SURFACE('',#95911,0.500000000000006);
#86140=CYLINDRICAL_SURFACE('',#95913,0.999999999999999);
#86141=CYLINDRICAL_SURFACE('',#95915,3.);
#86142=CYLINDRICAL_SURFACE('',#95919,3.);
#86143=CYLINDRICAL_SURFACE('',#95929,3.);
#86144=CYLINDRICAL_SURFACE('',#95931,3.);
#86145=CYLINDRICAL_SURFACE('',#95933,0.5);
#86146=CYLINDRICAL_SURFACE('',#95942,0.5);
#86147=CYLINDRICAL_SURFACE('',#95943,3.);
#86148=CYLINDRICAL_SURFACE('',#95949,3.);
#86149=CYLINDRICAL_SURFACE('',#95952,3.);
#86150=CYLINDRICAL_SURFACE('',#95965,3.);
#86151=CYLINDRICAL_SURFACE('',#95971,3.);
#86152=CYLINDRICAL_SURFACE('',#95986,3.);
#86153=CYLINDRICAL_SURFACE('',#95994,3.);
#86154=CYLINDRICAL_SURFACE('',#96004,3.);
#86155=CYLINDRICAL_SURFACE('',#96010,3.);
#86156=CYLINDRICAL_SURFACE('',#96023,3.);
#86157=CYLINDRICAL_SURFACE('',#96033,3.);
#86158=CYLINDRICAL_SURFACE('',#96051,3.);
#86159=CYLINDRICAL_SURFACE('',#96062,3.);
#86160=CYLINDRICAL_SURFACE('',#96083,3.);
#86161=CYLINDRICAL_SURFACE('',#96089,3.);
#86162=CYLINDRICAL_SURFACE('',#96100,3.);
#86163=CYLINDRICAL_SURFACE('',#96103,0.5);
#86164=CYLINDRICAL_SURFACE('',#96123,0.5);
#86165=CYLINDRICAL_SURFACE('',#96126,3.);
#86166=CYLINDRICAL_SURFACE('',#96131,3.);
#86167=CYLINDRICAL_SURFACE('',#96145,3.);
#86168=CYLINDRICAL_SURFACE('',#96151,3.);
#86169=CYLINDRICAL_SURFACE('',#96160,0.999999999999999);
#86170=CYLINDRICAL_SURFACE('',#96163,0.500000000000006);
#86171=CYLINDRICAL_SURFACE('',#96166,0.999999999999999);
#86172=CYLINDRICAL_SURFACE('',#96169,0.500000000000006);
#86173=CYLINDRICAL_SURFACE('',#96172,0.999999999999999);
#86174=CYLINDRICAL_SURFACE('',#96188,0.5);
#86175=CYLINDRICAL_SURFACE('',#96191,1.);
#86176=CYLINDRICAL_SURFACE('',#96194,1.);
#86177=CYLINDRICAL_SURFACE('',#96197,0.5);
#86178=CYLINDRICAL_SURFACE('',#96200,1.);
#86179=CYLINDRICAL_SURFACE('',#96273,1.);
#86180=CYLINDRICAL_SURFACE('',#96276,0.5);
#86181=CYLINDRICAL_SURFACE('',#96279,1.);
#86182=CYLINDRICAL_SURFACE('',#96282,0.5);
#86183=CYLINDRICAL_SURFACE('',#96285,1.);
#86184=CYLINDRICAL_SURFACE('',#96299,0.999999999999999);
#86185=CYLINDRICAL_SURFACE('',#96305,58.5);
#86186=CYLINDRICAL_SURFACE('',#96313,0.5);
#86187=CYLINDRICAL_SURFACE('',#96318,0.5);
#86188=CYLINDRICAL_SURFACE('',#96323,0.5);
#86189=CYLINDRICAL_SURFACE('',#96327,0.5);
#86190=CYLINDRICAL_SURFACE('',#96328,0.5);
#86191=CYLINDRICAL_SURFACE('',#96329,0.5);
#86192=CYLINDRICAL_SURFACE('',#96336,3.);
#86193=CYLINDRICAL_SURFACE('',#96342,0.5);
#86194=CYLINDRICAL_SURFACE('',#96347,0.5);
#86195=CYLINDRICAL_SURFACE('',#96348,0.5);
#86196=CYLINDRICAL_SURFACE('',#96351,0.5);
#86197=CYLINDRICAL_SURFACE('',#96356,0.5);
#86198=CYLINDRICAL_SURFACE('',#96361,0.5);
#86199=CYLINDRICAL_SURFACE('',#96369,0.5);
#86200=CYLINDRICAL_SURFACE('',#96371,0.5);
#86201=CYLINDRICAL_SURFACE('',#96377,0.5);
#86202=CYLINDRICAL_SURFACE('',#96382,0.5);
#86203=CYLINDRICAL_SURFACE('',#96386,0.5);
#86204=CYLINDRICAL_SURFACE('',#96387,0.5);
#86205=CYLINDRICAL_SURFACE('',#96392,3.);
#86206=CYLINDRICAL_SURFACE('',#96394,0.5);
#86207=CYLINDRICAL_SURFACE('',#96397,0.5);
#86208=CYLINDRICAL_SURFACE('',#96399,0.5);
#86209=CYLINDRICAL_SURFACE('',#96406,0.5);
#86210=CYLINDRICAL_SURFACE('',#96411,0.5);
#86211=CYLINDRICAL_SURFACE('',#96412,0.5);
#86212=CYLINDRICAL_SURFACE('',#96418,0.5);
#86213=CYLINDRICAL_SURFACE('',#96422,0.5);
#86214=CYLINDRICAL_SURFACE('',#96428,0.5);
#86215=CYLINDRICAL_SURFACE('',#96429,0.5);
#86216=CYLINDRICAL_SURFACE('',#96440,0.5);
#86217=CYLINDRICAL_SURFACE('',#96446,0.5);
#86218=CYLINDRICAL_SURFACE('',#96451,0.5);
#86219=CYLINDRICAL_SURFACE('',#96454,0.5);
#86220=CYLINDRICAL_SURFACE('',#96455,0.5);
#86221=CYLINDRICAL_SURFACE('',#96460,3.);
#86222=CYLINDRICAL_SURFACE('',#96466,0.5);
#86223=CYLINDRICAL_SURFACE('',#96471,0.5);
#86224=CYLINDRICAL_SURFACE('',#96472,0.5);
#86225=CYLINDRICAL_SURFACE('',#96475,0.5);
#86226=CYLINDRICAL_SURFACE('',#96480,0.5);
#86227=CYLINDRICAL_SURFACE('',#96484,0.5);
#86228=CYLINDRICAL_SURFACE('',#96493,0.5);
#86229=CYLINDRICAL_SURFACE('',#96503,0.5);
#86230=CYLINDRICAL_SURFACE('',#96509,0.5);
#86231=CYLINDRICAL_SURFACE('',#96510,0.5);
#86232=CYLINDRICAL_SURFACE('',#96511,0.5);
#86233=CYLINDRICAL_SURFACE('',#96513,0.5);
#86234=CYLINDRICAL_SURFACE('',#96517,0.5);
#86235=CYLINDRICAL_SURFACE('',#96518,0.5);
#86236=CYLINDRICAL_SURFACE('',#96523,0.5);
#86237=CYLINDRICAL_SURFACE('',#96527,1.);
#86238=CYLINDRICAL_SURFACE('',#96533,3.);
#86239=CYLINDRICAL_SURFACE('',#96535,0.5);
#86240=CYLINDRICAL_SURFACE('',#96541,0.5);
#86241=CYLINDRICAL_SURFACE('',#96550,0.5);
#86242=CYLINDRICAL_SURFACE('',#96555,0.5);
#86243=CYLINDRICAL_SURFACE('',#96556,0.5);
#86244=CYLINDRICAL_SURFACE('',#96559,0.5);
#86245=CYLINDRICAL_SURFACE('',#96561,0.5);
#86246=CYLINDRICAL_SURFACE('',#96569,0.5);
#86247=CYLINDRICAL_SURFACE('',#96576,3.);
#86248=CYLINDRICAL_SURFACE('',#96582,0.5);
#86249=CYLINDRICAL_SURFACE('',#96583,1.);
#86250=CYLINDRICAL_SURFACE('',#96588,0.5);
#86251=CYLINDRICAL_SURFACE('',#96595,3.);
#86252=CYLINDRICAL_SURFACE('',#96601,0.5);
#86253=CYLINDRICAL_SURFACE('',#96607,0.5);
#86254=CYLINDRICAL_SURFACE('',#96609,0.5);
#86255=CYLINDRICAL_SURFACE('',#96617,0.5);
#86256=CYLINDRICAL_SURFACE('',#96623,0.5);
#86257=CYLINDRICAL_SURFACE('',#96628,0.5);
#86258=CYLINDRICAL_SURFACE('',#96631,0.5);
#86259=CYLINDRICAL_SURFACE('',#96632,0.5);
#86260=CYLINDRICAL_SURFACE('',#96637,3.);
#86261=CYLINDRICAL_SURFACE('',#96643,0.5);
#86262=CYLINDRICAL_SURFACE('',#96648,0.5);
#86263=CYLINDRICAL_SURFACE('',#96649,0.5);
#86264=CYLINDRICAL_SURFACE('',#96652,0.5);
#86265=CYLINDRICAL_SURFACE('',#96657,0.5);
#86266=CYLINDRICAL_SURFACE('',#96661,0.5);
#86267=CYLINDRICAL_SURFACE('',#96670,0.5);
#86268=CYLINDRICAL_SURFACE('',#96675,0.5);
#86269=CYLINDRICAL_SURFACE('',#96683,0.5);
#86270=CYLINDRICAL_SURFACE('',#96687,0.5);
#86271=CYLINDRICAL_SURFACE('',#96688,0.5);
#86272=CYLINDRICAL_SURFACE('',#96693,0.5);
#86273=CYLINDRICAL_SURFACE('',#96697,0.5);
#86274=CYLINDRICAL_SURFACE('',#96698,1.);
#86275=CYLINDRICAL_SURFACE('',#96699,0.5);
#86276=CYLINDRICAL_SURFACE('',#96705,3.);
#86277=CYLINDRICAL_SURFACE('',#96707,0.5);
#86278=CYLINDRICAL_SURFACE('',#96713,0.5);
#86279=CYLINDRICAL_SURFACE('',#96721,0.5);
#86280=CYLINDRICAL_SURFACE('',#96726,0.5);
#86281=CYLINDRICAL_SURFACE('',#96727,0.5);
#86282=CYLINDRICAL_SURFACE('',#96733,0.5);
#86283=CYLINDRICAL_SURFACE('',#96735,0.5);
#86284=CYLINDRICAL_SURFACE('',#96740,0.5);
#86285=CYLINDRICAL_SURFACE('',#96743,0.5);
#86286=CYLINDRICAL_SURFACE('',#96749,0.5);
#86287=CYLINDRICAL_SURFACE('',#96750,0.5);
#86288=CYLINDRICAL_SURFACE('',#96756,0.5);
#86289=CYLINDRICAL_SURFACE('',#96762,0.5);
#86290=CYLINDRICAL_SURFACE('',#96763,0.5);
#86291=CYLINDRICAL_SURFACE('',#96768,0.5);
#86292=CYLINDRICAL_SURFACE('',#96775,3.);
#86293=CYLINDRICAL_SURFACE('',#96781,0.5);
#86294=CYLINDRICAL_SURFACE('',#96785,0.5);
#86295=CYLINDRICAL_SURFACE('',#96791,0.5);
#86296=CYLINDRICAL_SURFACE('',#96797,0.5);
#86297=CYLINDRICAL_SURFACE('',#96803,0.5);
#86298=CYLINDRICAL_SURFACE('',#96806,0.5);
#86299=CYLINDRICAL_SURFACE('',#96809,0.5);
#86300=CYLINDRICAL_SURFACE('',#96812,0.5);
#86301=CYLINDRICAL_SURFACE('',#96818,0.5);
#86302=CYLINDRICAL_SURFACE('',#96826,0.5);
#86303=CYLINDRICAL_SURFACE('',#96833,0.5);
#86304=CYLINDRICAL_SURFACE('',#96836,0.5);
#86305=CYLINDRICAL_SURFACE('',#96840,0.5);
#86306=CYLINDRICAL_SURFACE('',#96843,0.5);
#86307=CYLINDRICAL_SURFACE('',#96850,0.5);
#86308=CYLINDRICAL_SURFACE('',#96858,0.5);
#86309=CYLINDRICAL_SURFACE('',#96864,0.5);
#86310=CYLINDRICAL_SURFACE('',#96867,0.5);
#86311=CYLINDRICAL_SURFACE('',#96870,0.5);
#86312=CYLINDRICAL_SURFACE('',#96873,0.5);
#86313=CYLINDRICAL_SURFACE('',#96879,0.5);
#86314=CYLINDRICAL_SURFACE('',#96885,0.5);
#86315=CYLINDRICAL_SURFACE('',#96891,0.5);
#86316=CYLINDRICAL_SURFACE('',#96895,0.5);
#86317=CYLINDRICAL_SURFACE('',#96902,3.);
#86318=CYLINDRICAL_SURFACE('',#96908,0.5);
#86319=CYLINDRICAL_SURFACE('',#96913,0.5);
#86320=CYLINDRICAL_SURFACE('',#96914,0.5);
#86321=CYLINDRICAL_SURFACE('',#96920,0.5);
#86322=CYLINDRICAL_SURFACE('',#96928,0.5);
#86323=CYLINDRICAL_SURFACE('',#96933,0.5);
#86324=CYLINDRICAL_SURFACE('',#96939,0.5);
#86325=CYLINDRICAL_SURFACE('',#96940,0.5);
#86326=CYLINDRICAL_SURFACE('',#96945,3.);
#86327=CYLINDRICAL_SURFACE('',#96954,3.);
#86328=CYLINDRICAL_SURFACE('',#96970,0.5);
#86329=CYLINDRICAL_SURFACE('',#96977,3.);
#86330=CYLINDRICAL_SURFACE('',#96983,0.5);
#86331=CYLINDRICAL_SURFACE('',#96999,0.5);
#86332=CYLINDRICAL_SURFACE('',#97007,0.5);
#86333=CYLINDRICAL_SURFACE('',#97015,0.5);
#86334=CYLINDRICAL_SURFACE('',#97019,0.5);
#86335=CYLINDRICAL_SURFACE('',#97028,3.);
#86336=CYLINDRICAL_SURFACE('',#97034,0.5);
#86337=CYLINDRICAL_SURFACE('',#97042,0.5);
#86338=CYLINDRICAL_SURFACE('',#97048,0.5);
#86339=CYLINDRICAL_SURFACE('',#97053,0.5);
#86340=CYLINDRICAL_SURFACE('',#97057,0.5);
#86341=CYLINDRICAL_SURFACE('',#97063,0.5);
#86342=CYLINDRICAL_SURFACE('',#97071,0.5);
#86343=CYLINDRICAL_SURFACE('',#97079,0.5);
#86344=CYLINDRICAL_SURFACE('',#97082,0.5);
#86345=CYLINDRICAL_SURFACE('',#97100,0.5);
#86346=CYLINDRICAL_SURFACE('',#97103,0.5);
#86347=CYLINDRICAL_SURFACE('',#97112,0.5);
#86348=CYLINDRICAL_SURFACE('',#97123,3.);
#86349=CYLINDRICAL_SURFACE('',#97125,67.5);
#86350=CYLINDRICAL_SURFACE('',#97127,3.);
#86351=CYLINDRICAL_SURFACE('',#97130,5.);
#86352=CYLINDRICAL_SURFACE('',#97132,58.5);
#86353=CYLINDRICAL_SURFACE('',#97134,5.);
#86354=CYLINDRICAL_SURFACE('',#97137,3.);
#86355=CYLINDRICAL_SURFACE('',#97139,67.5);
#86356=CYLINDRICAL_SURFACE('',#97141,3.);
#86357=CYLINDRICAL_SURFACE('',#97146,0.5);
#86358=CYLINDRICAL_SURFACE('',#97149,0.5);
#86359=CYLINDRICAL_SURFACE('',#97152,0.5);
#86360=CYLINDRICAL_SURFACE('',#97153,0.5);
#86361=CYLINDRICAL_SURFACE('',#97162,0.5);
#86362=CYLINDRICAL_SURFACE('',#97165,0.5);
#86363=CYLINDRICAL_SURFACE('',#97174,0.5);
#86364=CYLINDRICAL_SURFACE('',#97177,0.5);
#86365=CYLINDRICAL_SURFACE('',#97188,0.5);
#86366=CYLINDRICAL_SURFACE('',#97193,0.5);
#86367=CYLINDRICAL_SURFACE('',#97200,0.5);
#86368=CYLINDRICAL_SURFACE('',#97204,0.5);
#86369=CYLINDRICAL_SURFACE('',#97210,0.5);
#86370=CYLINDRICAL_SURFACE('',#97218,0.5);
#86371=CYLINDRICAL_SURFACE('',#97224,3.);
#86372=CYLINDRICAL_SURFACE('',#97225,0.5);
#86373=CYLINDRICAL_SURFACE('',#97227,2.75);
#86374=CYLINDRICAL_SURFACE('',#97233,2.);
#86375=CYLINDRICAL_SURFACE('',#97235,0.5);
#86376=CYLINDRICAL_SURFACE('',#97237,0.5);
#86377=CYLINDRICAL_SURFACE('',#97247,0.5);
#86378=CYLINDRICAL_SURFACE('',#97248,2.75);
#86379=CYLINDRICAL_SURFACE('',#97253,2.);
#86380=CYLINDRICAL_SURFACE('',#97255,0.5);
#86381=CYLINDRICAL_SURFACE('',#97262,0.5);
#86382=CYLINDRICAL_SURFACE('',#97264,0.5);
#86383=CYLINDRICAL_SURFACE('',#97270,0.5);
#86384=CYLINDRICAL_SURFACE('',#97272,0.5);
#86385=CYLINDRICAL_SURFACE('',#97279,0.5);
#86386=CYLINDRICAL_SURFACE('',#97281,0.5);
#86387=CYLINDRICAL_SURFACE('',#97293,0.5);
#86388=CYLINDRICAL_SURFACE('',#97295,0.5);
#86389=CYLINDRICAL_SURFACE('',#97301,0.5);
#86390=CYLINDRICAL_SURFACE('',#97303,0.5);
#86391=CYLINDRICAL_SURFACE('',#97308,0.5);
#86392=CYLINDRICAL_SURFACE('',#97310,0.5);
#86393=CYLINDRICAL_SURFACE('',#97316,0.5);
#86394=CYLINDRICAL_SURFACE('',#97318,0.5);
#86395=CYLINDRICAL_SURFACE('',#97328,0.5);
#86396=CYLINDRICAL_SURFACE('',#97330,0.5);
#86397=CYLINDRICAL_SURFACE('',#97345,0.5);
#86398=CYLINDRICAL_SURFACE('',#97348,0.5);
#86399=CYLINDRICAL_SURFACE('',#97392,0.5);
#86400=CYLINDRICAL_SURFACE('',#97395,0.5);
#86401=CYLINDRICAL_SURFACE('',#97405,0.5);
#86402=CYLINDRICAL_SURFACE('',#97408,0.5);
#86403=CYLINDRICAL_SURFACE('',#97410,0.5);
#86404=CYLINDRICAL_SURFACE('',#97414,0.5);
#86405=CYLINDRICAL_SURFACE('',#97440,0.5);
#86406=CYLINDRICAL_SURFACE('',#97443,0.5);
#86407=CYLINDRICAL_SURFACE('',#97449,0.5);
#86408=CYLINDRICAL_SURFACE('',#97460,0.5);
#86409=CYLINDRICAL_SURFACE('',#97463,0.5);
#86410=CYLINDRICAL_SURFACE('',#97488,0.5);
#86411=CYLINDRICAL_SURFACE('',#97494,3.);
#86412=CYLINDRICAL_SURFACE('',#97498,0.5);
#86413=CYLINDRICAL_SURFACE('',#97501,0.5);
#86414=CYLINDRICAL_SURFACE('',#97507,0.5);
#86415=CYLINDRICAL_SURFACE('',#97510,0.5);
#86416=CYLINDRICAL_SURFACE('',#97517,0.5);
#86417=CYLINDRICAL_SURFACE('',#97520,0.5);
#86418=CYLINDRICAL_SURFACE('',#97522,2.75);
#86419=CYLINDRICAL_SURFACE('',#97524,2.75);
#86420=CYLINDRICAL_SURFACE('',#97530,0.250000000000003);
#86421=CYLINDRICAL_SURFACE('',#97541,0.250000000000003);
#86422=CYLINDRICAL_SURFACE('',#97552,0.249999999999997);
#86423=CYLINDRICAL_SURFACE('',#97563,0.250000000000003);
#86424=CYLINDRICAL_SURFACE('',#97569,5.);
#86425=CYLINDRICAL_SURFACE('',#97571,0.499999999999999);
#86426=CYLINDRICAL_SURFACE('',#97576,3.);
#86427=CYLINDRICAL_SURFACE('',#97579,0.5);
#86428=CYLINDRICAL_SURFACE('',#97581,1.);
#86429=CYLINDRICAL_SURFACE('',#97582,0.5);
#86430=CYLINDRICAL_SURFACE('',#97587,0.5);
#86431=CYLINDRICAL_SURFACE('',#97592,0.5);
#86432=CYLINDRICAL_SURFACE('',#97593,1.);
#86433=CYLINDRICAL_SURFACE('',#97594,0.5);
#86434=CYLINDRICAL_SURFACE('',#97599,0.5);
#86435=CYLINDRICAL_SURFACE('',#97604,0.5);
#86436=CYLINDRICAL_SURFACE('',#97605,1.);
#86437=CYLINDRICAL_SURFACE('',#97610,0.5);
#86438=CYLINDRICAL_SURFACE('',#97615,0.5);
#86439=CYLINDRICAL_SURFACE('',#97620,0.5);
#86440=CYLINDRICAL_SURFACE('',#97623,0.5);
#86441=CYLINDRICAL_SURFACE('',#97628,0.5);
#86442=CYLINDRICAL_SURFACE('',#97633,0.5);
#86443=CYLINDRICAL_SURFACE('',#97635,3.);
#86444=CYLINDRICAL_SURFACE('',#97637,0.5);
#86445=CYLINDRICAL_SURFACE('',#97646,0.5);
#86446=CYLINDRICAL_SURFACE('',#97656,1.);
#86447=CYLINDRICAL_SURFACE('',#97658,0.5);
#86448=CYLINDRICAL_SURFACE('',#97662,0.499999999999998);
#86449=CYLINDRICAL_SURFACE('',#97665,0.5);
#86450=CYLINDRICAL_SURFACE('',#97666,1.);
#86451=CYLINDRICAL_SURFACE('',#97667,0.5);
#86452=CYLINDRICAL_SURFACE('',#97670,0.499999999999998);
#86453=CYLINDRICAL_SURFACE('',#97673,0.5);
#86454=CYLINDRICAL_SURFACE('',#97674,1.);
#86455=CYLINDRICAL_SURFACE('',#97679,0.5);
#86456=CYLINDRICAL_SURFACE('',#97680,0.5);
#86457=CYLINDRICAL_SURFACE('',#97683,0.499999999999999);
#86458=CYLINDRICAL_SURFACE('',#97686,0.5);
#86459=CYLINDRICAL_SURFACE('',#97687,0.999999999999997);
#86460=CYLINDRICAL_SURFACE('',#97689,0.5);
#86461=CYLINDRICAL_SURFACE('',#97693,0.999999999999997);
#86462=CYLINDRICAL_SURFACE('',#97695,0.5);
#86463=CYLINDRICAL_SURFACE('',#97698,0.499999999999999);
#86464=CYLINDRICAL_SURFACE('',#97701,0.5);
#86465=CYLINDRICAL_SURFACE('',#97702,0.999999999999997);
#86466=CYLINDRICAL_SURFACE('',#97703,0.999999999999996);
#86467=CYLINDRICAL_SURFACE('',#97706,0.5);
#86468=CYLINDRICAL_SURFACE('',#97709,0.499999999999999);
#86469=CYLINDRICAL_SURFACE('',#97712,0.5);
#86470=CYLINDRICAL_SURFACE('',#97713,0.999999999999997);
#86471=CYLINDRICAL_SURFACE('',#97716,0.5);
#86472=CYLINDRICAL_SURFACE('',#97719,0.499999999999999);
#86473=CYLINDRICAL_SURFACE('',#97722,0.5);
#86474=CYLINDRICAL_SURFACE('',#97723,0.999999999999997);
#86475=CYLINDRICAL_SURFACE('',#97725,0.999999999999996);
#86476=CYLINDRICAL_SURFACE('',#97728,0.5);
#86477=CYLINDRICAL_SURFACE('',#97731,0.500000000000005);
#86478=CYLINDRICAL_SURFACE('',#97734,0.5);
#86479=CYLINDRICAL_SURFACE('',#97735,0.999999999999996);
#86480=CYLINDRICAL_SURFACE('',#97737,0.5);
#86481=CYLINDRICAL_SURFACE('',#97740,0.999999999999996);
#86482=CYLINDRICAL_SURFACE('',#97742,0.5);
#86483=CYLINDRICAL_SURFACE('',#97745,0.500000000000005);
#86484=CYLINDRICAL_SURFACE('',#97748,0.5);
#86485=CYLINDRICAL_SURFACE('',#97749,0.999999999999996);
#86486=CYLINDRICAL_SURFACE('',#97752,0.5);
#86487=CYLINDRICAL_SURFACE('',#97755,0.5);
#86488=CYLINDRICAL_SURFACE('',#97762,0.5);
#86489=CYLINDRICAL_SURFACE('',#97765,0.5);
#86490=CYLINDRICAL_SURFACE('',#97771,0.5);
#86491=CYLINDRICAL_SURFACE('',#97774,0.5);
#86492=CYLINDRICAL_SURFACE('',#97780,0.5);
#86493=CYLINDRICAL_SURFACE('',#97783,0.5);
#86494=CYLINDRICAL_SURFACE('',#97789,0.5);
#86495=CYLINDRICAL_SURFACE('',#97792,0.5);
#86496=CYLINDRICAL_SURFACE('',#97799,0.5);
#86497=CYLINDRICAL_SURFACE('',#97802,0.5);
#86498=CYLINDRICAL_SURFACE('',#97809,3.);
#86499=CYLINDRICAL_SURFACE('',#97814,3.);
#86500=CYLINDRICAL_SURFACE('',#97821,58.3875000000282);
#86501=CYLINDRICAL_SURFACE('',#97823,5.);
#86502=CYLINDRICAL_SURFACE('',#97829,0.5);
#86503=CYLINDRICAL_SURFACE('',#97835,0.5);
#86504=CYLINDRICAL_SURFACE('',#97838,0.5);
#86505=CYLINDRICAL_SURFACE('',#97844,0.5);
#86506=CYLINDRICAL_SURFACE('',#97847,0.5);
#86507=CYLINDRICAL_SURFACE('',#97854,0.5);
#86508=CYLINDRICAL_SURFACE('',#97857,5.);
#86509=CYLINDRICAL_SURFACE('',#97864,0.5);
#86510=CYLINDRICAL_SURFACE('',#97867,0.5);
#86511=CYLINDRICAL_SURFACE('',#97874,0.5);
#86512=CYLINDRICAL_SURFACE('',#97877,0.5);
#86513=CYLINDRICAL_SURFACE('',#97884,0.5);
#86514=CYLINDRICAL_SURFACE('',#97887,0.5);
#86515=CYLINDRICAL_SURFACE('',#97890,58.3875000000282);
#86516=CYLINDRICAL_SURFACE('',#97897,3.);
#86517=CYLINDRICAL_SURFACE('',#97902,3.);
#86518=CYLINDRICAL_SURFACE('',#97907,3.);
#86519=CYLINDRICAL_SURFACE('',#97915,58.5);
#86520=CYLINDRICAL_SURFACE('',#97923,58.5);
#86521=CYLINDRICAL_SURFACE('',#97937,58.3875000000282);
#86522=CYLINDRICAL_SURFACE('',#97939,5.);
#86523=CYLINDRICAL_SURFACE('',#97969,3.25);
#86524=CYLINDRICAL_SURFACE('',#97974,2.);
#86525=CYLINDRICAL_SURFACE('',#97978,2.5);
#86526=CYLINDRICAL_SURFACE('',#98110,0.75);
#86527=CYLINDRICAL_SURFACE('',#98123,0.75);
#86528=CYLINDRICAL_SURFACE('',#98124,0.75);
#86529=CYLINDRICAL_SURFACE('',#98136,0.750000000000001);
#86530=CYLINDRICAL_SURFACE('',#98137,0.750000000000001);
#86531=CYLINDRICAL_SURFACE('',#98149,0.749999999999998);
#86532=CYLINDRICAL_SURFACE('',#98150,0.749999999999999);
#86533=CYLINDRICAL_SURFACE('',#98162,0.75);
#86534=CYLINDRICAL_SURFACE('',#98163,1.5);
#86535=CYLINDRICAL_SURFACE('',#98164,1.5);
#86536=CYLINDRICAL_SURFACE('',#98165,1.5);
#86537=CYLINDRICAL_SURFACE('',#98166,1.5);
#86538=CYLINDRICAL_SURFACE('',#98167,1.49999999999999);
#86539=CYLINDRICAL_SURFACE('',#98168,1.5);
#86540=CYLINDRICAL_SURFACE('',#98169,1.5);
#86541=CYLINDRICAL_SURFACE('',#98170,1.5);
#86542=CYLINDRICAL_SURFACE('',#98176,0.450000000000006);
#86543=CYLINDRICAL_SURFACE('',#98190,0.449999999999999);
#86544=CYLINDRICAL_SURFACE('',#98204,0.450000000000006);
#86545=CYLINDRICAL_SURFACE('',#98210,0.450000000000006);
#86546=CYLINDRICAL_SURFACE('',#98224,0.449999999999999);
#86547=CYLINDRICAL_SURFACE('',#98226,0.450000000000006);
#86548=CYLINDRICAL_SURFACE('',#98236,0.450000000000006);
#86549=CYLINDRICAL_SURFACE('',#98250,0.449999999999999);
#86550=CYLINDRICAL_SURFACE('',#98252,0.450000000000001);
#86551=CYLINDRICAL_SURFACE('',#98262,0.450000000000006);
#86552=CYLINDRICAL_SURFACE('',#98264,0.449999999999999);
#86553=CYLINDRICAL_SURFACE('',#98274,0.450000000000001);
#86554=CYLINDRICAL_SURFACE('',#98276,0.450000000000001);
#86555=CYLINDRICAL_SURFACE('',#98286,0.450000000000006);
#86556=CYLINDRICAL_SURFACE('',#98288,0.450000000000001);
#86557=CYLINDRICAL_SURFACE('',#98302,0.450000000000001);
#86558=CYLINDRICAL_SURFACE('',#98316,0.450000000000006);
#86559=CYLINDRICAL_SURFACE('',#98318,0.450000000000001);
#86560=CYLINDRICAL_SURFACE('',#98328,0.45);
#86561=CYLINDRICAL_SURFACE('',#98330,0.450000000000006);
#86562=CYLINDRICAL_SURFACE('',#98340,0.450000000000006);
#86563=CYLINDRICAL_SURFACE('',#98342,0.449999999999999);
#86564=CYLINDRICAL_SURFACE('',#98352,0.450000000000001);
#86565=CYLINDRICAL_SURFACE('',#98354,0.450000000000006);
#86566=CYLINDRICAL_SURFACE('',#98364,0.450000000000006);
#86567=CYLINDRICAL_SURFACE('',#98366,0.449999999999999);
#86568=CYLINDRICAL_SURFACE('',#98376,0.450000000000001);
#86569=CYLINDRICAL_SURFACE('',#98378,0.450000000000006);
#86570=CYLINDRICAL_SURFACE('',#98388,0.450000000000006);
#86571=CYLINDRICAL_SURFACE('',#98390,0.450000000000001);
#86572=CYLINDRICAL_SURFACE('',#98400,0.45);
#86573=CYLINDRICAL_SURFACE('',#98402,0.450000000000006);
#86574=CYLINDRICAL_SURFACE('',#98412,0.450000000000006);
#86575=CYLINDRICAL_SURFACE('',#98414,0.450000000000001);
#86576=CYLINDRICAL_SURFACE('',#98424,0.45);
#86577=CYLINDRICAL_SURFACE('',#98438,0.450000000000006);
#86578=CYLINDRICAL_SURFACE('',#98440,0.449999999999999);
#86579=CYLINDRICAL_SURFACE('',#98450,0.450000000000001);
#86580=CYLINDRICAL_SURFACE('',#98472,0.450000000000006);
#86581=CYLINDRICAL_SURFACE('',#98474,0.45);
#86582=CYLINDRICAL_SURFACE('',#98484,0.450000000000001);
#86583=CYLINDRICAL_SURFACE('',#98498,0.450000000000006);
#86584=CYLINDRICAL_SURFACE('',#98500,0.45);
#86585=CYLINDRICAL_SURFACE('',#98510,0.450000000000001);
#86586=CYLINDRICAL_SURFACE('',#98512,0.450000000000006);
#86587=CYLINDRICAL_SURFACE('',#98522,0.450000000000001);
#86588=CYLINDRICAL_SURFACE('',#98536,0.450000000000006);
#86589=CYLINDRICAL_SURFACE('',#98538,0.450000000000006);
#86590=CYLINDRICAL_SURFACE('',#98548,0.45);
#86591=CYLINDRICAL_SURFACE('',#98554,0.449999999999999);
#86592=CYLINDRICAL_SURFACE('',#98556,0.450000000000006);
#86593=CYLINDRICAL_SURFACE('',#98566,0.450000000000006);
#86594=CYLINDRICAL_SURFACE('',#98580,0.450000000000001);
#86595=CYLINDRICAL_SURFACE('',#98586,0.449999999999999);
#86596=CYLINDRICAL_SURFACE('',#98588,0.450000000000006);
#86597=CYLINDRICAL_SURFACE('',#98598,0.450000000000006);
#86598=CYLINDRICAL_SURFACE('',#98600,0.450000000000001);
#86599=CYLINDRICAL_SURFACE('',#98610,0.449999999999999);
#86600=CYLINDRICAL_SURFACE('',#98612,0.450000000000006);
#86601=CYLINDRICAL_SURFACE('',#98626,0.450000000000001);
#86602=CYLINDRICAL_SURFACE('',#98636,0.449999999999999);
#86603=CYLINDRICAL_SURFACE('',#98638,0.450000000000006);
#86604=CYLINDRICAL_SURFACE('',#98648,0.450000000000006);
#86605=CYLINDRICAL_SURFACE('',#98650,0.449999999999999);
#86606=CYLINDRICAL_SURFACE('',#98660,0.449999999999999);
#86607=CYLINDRICAL_SURFACE('',#98662,0.450000000000006);
#86608=CYLINDRICAL_SURFACE('',#98672,0.450000000000006);
#86609=CYLINDRICAL_SURFACE('',#98674,0.449999999999999);
#86610=CYLINDRICAL_SURFACE('',#98684,0.449999999999999);
#86611=CYLINDRICAL_SURFACE('',#98686,0.450000000000006);
#86612=CYLINDRICAL_SURFACE('',#98696,0.450000000000001);
#86613=CYLINDRICAL_SURFACE('',#98714,0.449999999999999);
#86614=CYLINDRICAL_SURFACE('',#98716,0.450000000000006);
#86615=CYLINDRICAL_SURFACE('',#98730,0.449999999999999);
#86616=CYLINDRICAL_SURFACE('',#98740,0.449999999999999);
#86617=CYLINDRICAL_SURFACE('',#98742,0.450000000000006);
#86618=CYLINDRICAL_SURFACE('',#98756,0.449999999999999);
#86619=CYLINDRICAL_SURFACE('',#98774,0.449999999999999);
#86620=CYLINDRICAL_SURFACE('',#98776,0.450000000000006);
#86621=CYLINDRICAL_SURFACE('',#98786,0.450000000000006);
#86622=CYLINDRICAL_SURFACE('',#98788,0.449999999999999);
#86623=CYLINDRICAL_SURFACE('',#98798,0.449999999999999);
#86624=CYLINDRICAL_SURFACE('',#98800,0.450000000000006);
#86625=CYLINDRICAL_SURFACE('',#98810,0.450000000000006);
#86626=CYLINDRICAL_SURFACE('',#98832,0.449999999999999);
#86627=CYLINDRICAL_SURFACE('',#98834,0.450000000000006);
#86628=CYLINDRICAL_SURFACE('',#98844,0.450000000000006);
#86629=CYLINDRICAL_SURFACE('',#98858,0.449999999999999);
#86630=CYLINDRICAL_SURFACE('',#98860,0.450000000000006);
#86631=CYLINDRICAL_SURFACE('',#98870,0.450000000000006);
#86632=CYLINDRICAL_SURFACE('',#98872,0.449999999999999);
#86633=CYLINDRICAL_SURFACE('',#98882,0.449999999999999);
#86634=CYLINDRICAL_SURFACE('',#98884,0.450000000000001);
#86635=CYLINDRICAL_SURFACE('',#98894,0.450000000000006);
#86636=CYLINDRICAL_SURFACE('',#98908,0.449999999999999);
#86637=CYLINDRICAL_SURFACE('',#98910,0.450000000000006);
#86638=CYLINDRICAL_SURFACE('',#98920,0.450000000000001);
#86639=CYLINDRICAL_SURFACE('',#98922,0.449999999999999);
#86640=CYLINDRICAL_SURFACE('',#98932,0.449999999999999);
#86641=CYLINDRICAL_SURFACE('',#98946,0.450000000000006);
#86642=CYLINDRICAL_SURFACE('',#98952,0.450000000000006);
#86643=CYLINDRICAL_SURFACE('',#98966,0.449999999999999);
#86644=CYLINDRICAL_SURFACE('',#99029,0.44999999999999);
#86645=CYLINDRICAL_SURFACE('',#99043,0.450000000000001);
#86646=CYLINDRICAL_SURFACE('',#99052,0.450000000000001);
#86647=CYLINDRICAL_SURFACE('',#99066,0.45);
#86648=CYLINDRICAL_SURFACE('',#99075,0.450000000000006);
#86649=CYLINDRICAL_SURFACE('',#99089,0.44999999999999);
#86650=CYLINDRICAL_SURFACE('',#99098,0.45);
#86651=CYLINDRICAL_SURFACE('',#99112,0.450000000000006);
#86652=CYLINDRICAL_SURFACE('',#99220,0.75);
#86653=CYLINDRICAL_SURFACE('',#99222,0.750000000000001);
#86654=CYLINDRICAL_SURFACE('',#99224,0.750000000000001);
#86655=CYLINDRICAL_SURFACE('',#99226,0.750000000000001);
#86656=CYLINDRICAL_SURFACE('',#99228,0.750000000000001);
#86657=CYLINDRICAL_SURFACE('',#99230,0.750000000000001);
#86658=CYLINDRICAL_SURFACE('',#99232,0.75);
#86659=CYLINDRICAL_SURFACE('',#99234,0.75);
#86660=CYLINDRICAL_SURFACE('',#99236,0.75);
#86661=CYLINDRICAL_SURFACE('',#99238,0.750000000000001);
#86662=CYLINDRICAL_SURFACE('',#99240,0.750000000000001);
#86663=CYLINDRICAL_SURFACE('',#99242,0.750000000000001);
#86664=CYLINDRICAL_SURFACE('',#99244,0.750000000000001);
#86665=CYLINDRICAL_SURFACE('',#99246,0.750000000000001);
#86666=CYLINDRICAL_SURFACE('',#99248,0.750000000000001);
#86667=CYLINDRICAL_SURFACE('',#99250,0.750000000000001);
#86668=CYLINDRICAL_SURFACE('',#99252,0.75);
#86669=CYLINDRICAL_SURFACE('',#99254,0.75);
#86670=CYLINDRICAL_SURFACE('',#99256,0.75);
#86671=CYLINDRICAL_SURFACE('',#99258,0.75);
#86672=CYLINDRICAL_SURFACE('',#99260,0.750000000000001);
#86673=CYLINDRICAL_SURFACE('',#99262,0.75);
#86674=CYLINDRICAL_SURFACE('',#99264,0.750000000000001);
#86675=CYLINDRICAL_SURFACE('',#99266,0.750000000000001);
#86676=CYLINDRICAL_SURFACE('',#99268,0.750000000000001);
#86677=CYLINDRICAL_SURFACE('',#99270,0.750000000000001);
#86678=CYLINDRICAL_SURFACE('',#99272,0.750000000000001);
#86679=CYLINDRICAL_SURFACE('',#99274,0.750000000000001);
#86680=CYLINDRICAL_SURFACE('',#99276,0.750000000000001);
#86681=CYLINDRICAL_SURFACE('',#99278,0.750000000000001);
#86682=CYLINDRICAL_SURFACE('',#99280,0.750000000000001);
#86683=CYLINDRICAL_SURFACE('',#99282,0.750000000000001);
#86684=CYLINDRICAL_SURFACE('',#99284,0.75);
#86685=CYLINDRICAL_SURFACE('',#99286,0.750000000000001);
#86686=CYLINDRICAL_SURFACE('',#99288,0.75);
#86687=CYLINDRICAL_SURFACE('',#99290,0.75);
#86688=CYLINDRICAL_SURFACE('',#99292,0.750000000000001);
#86689=CYLINDRICAL_SURFACE('',#99294,0.750000000000001);
#86690=CYLINDRICAL_SURFACE('',#99296,0.750000000000001);
#86691=CYLINDRICAL_SURFACE('',#99298,0.750000000000001);
#86692=CYLINDRICAL_SURFACE('',#99300,0.750000000000001);
#86693=CYLINDRICAL_SURFACE('',#99302,0.750000000000001);
#86694=CYLINDRICAL_SURFACE('',#99304,0.750000000000001);
#86695=CYLINDRICAL_SURFACE('',#99306,0.750000000000001);
#86696=CYLINDRICAL_SURFACE('',#99308,0.75);
#86697=CYLINDRICAL_SURFACE('',#99310,0.75);
#86698=CYLINDRICAL_SURFACE('',#99312,0.750000000000001);
#86699=CYLINDRICAL_SURFACE('',#99314,0.750000000000001);
#86700=CYLINDRICAL_SURFACE('',#99316,0.750000000000001);
#86701=CYLINDRICAL_SURFACE('',#99318,0.750000000000001);
#86702=CYLINDRICAL_SURFACE('',#99320,0.750000000000001);
#86703=CYLINDRICAL_SURFACE('',#99322,0.750000000000001);
#86704=CYLINDRICAL_SURFACE('',#99324,0.750000000000001);
#86705=CYLINDRICAL_SURFACE('',#99326,0.750000000000001);
#86706=CYLINDRICAL_SURFACE('',#99328,0.750000000000001);
#86707=CYLINDRICAL_SURFACE('',#99330,0.750000000000001);
#86708=CYLINDRICAL_SURFACE('',#99332,0.750000000000001);
#86709=CYLINDRICAL_SURFACE('',#99334,0.750000000000001);
#86710=CYLINDRICAL_SURFACE('',#99336,0.750000000000001);
#86711=CYLINDRICAL_SURFACE('',#99338,0.750000000000001);
#86712=CYLINDRICAL_SURFACE('',#99340,0.750000000000001);
#86713=CYLINDRICAL_SURFACE('',#99342,0.750000000000001);
#86714=CYLINDRICAL_SURFACE('',#99344,0.750000000000001);
#86715=CYLINDRICAL_SURFACE('',#99346,0.750000000000001);
#86716=CYLINDRICAL_SURFACE('',#99348,0.750000000000001);
#86717=CYLINDRICAL_SURFACE('',#99350,0.750000000000001);
#86718=CYLINDRICAL_SURFACE('',#99352,0.750000000000001);
#86719=CYLINDRICAL_SURFACE('',#99354,0.750000000000001);
#86720=CYLINDRICAL_SURFACE('',#99356,0.750000000000001);
#86721=CYLINDRICAL_SURFACE('',#99358,0.750000000000001);
#86722=CYLINDRICAL_SURFACE('',#99360,0.750000000000001);
#86723=CYLINDRICAL_SURFACE('',#99362,0.75);
#86724=CYLINDRICAL_SURFACE('',#99364,0.750000000000001);
#86725=CYLINDRICAL_SURFACE('',#99366,0.750000000000001);
#86726=CYLINDRICAL_SURFACE('',#99368,0.75);
#86727=CYLINDRICAL_SURFACE('',#99370,0.750000000000001);
#86728=CYLINDRICAL_SURFACE('',#99372,0.75);
#86729=CYLINDRICAL_SURFACE('',#99374,0.75);
#86730=CYLINDRICAL_SURFACE('',#99376,0.750000000000001);
#86731=CYLINDRICAL_SURFACE('',#99378,0.750000000000001);
#86732=CYLINDRICAL_SURFACE('',#99380,0.750000000000001);
#86733=CYLINDRICAL_SURFACE('',#99382,0.750000000000001);
#86734=CYLINDRICAL_SURFACE('',#99384,0.750000000000001);
#86735=CYLINDRICAL_SURFACE('',#99386,0.750000000000001);
#86736=CYLINDRICAL_SURFACE('',#99388,0.750000000000001);
#86737=CYLINDRICAL_SURFACE('',#99390,0.750000000000001);
#86738=CYLINDRICAL_SURFACE('',#99392,0.750000000000001);
#86739=CYLINDRICAL_SURFACE('',#99394,0.750000000000001);
#86740=CYLINDRICAL_SURFACE('',#99396,0.750000000000001);
#86741=CYLINDRICAL_SURFACE('',#99398,0.750000000000001);
#86742=CYLINDRICAL_SURFACE('',#99400,0.750000000000001);
#86743=CYLINDRICAL_SURFACE('',#99402,0.750000000000001);
#86744=CYLINDRICAL_SURFACE('',#99404,0.750000000000001);
#86745=CYLINDRICAL_SURFACE('',#99406,0.750000000000001);
#86746=CYLINDRICAL_SURFACE('',#99408,0.750000000000001);
#86747=CYLINDRICAL_SURFACE('',#99410,0.75);
#86748=CYLINDRICAL_SURFACE('',#99412,0.750000000000001);
#86749=CYLINDRICAL_SURFACE('',#99414,0.75);
#86750=CYLINDRICAL_SURFACE('',#99416,0.75);
#86751=CYLINDRICAL_SURFACE('',#99418,0.750000000000001);
#86752=CYLINDRICAL_SURFACE('',#99420,0.750000000000001);
#86753=CYLINDRICAL_SURFACE('',#99422,0.750000000000001);
#86754=CYLINDRICAL_SURFACE('',#99424,0.750000000000001);
#86755=CYLINDRICAL_SURFACE('',#99426,0.750000000000001);
#86756=CYLINDRICAL_SURFACE('',#99428,0.750000000000001);
#86757=CYLINDRICAL_SURFACE('',#99430,0.750000000000001);
#86758=CYLINDRICAL_SURFACE('',#99432,0.750000000000001);
#86759=CYLINDRICAL_SURFACE('',#99434,0.750000000000001);
#86760=CYLINDRICAL_SURFACE('',#99436,0.750000000000001);
#86761=CYLINDRICAL_SURFACE('',#99438,0.750000000000001);
#86762=CYLINDRICAL_SURFACE('',#99440,0.750000000000001);
#86763=CYLINDRICAL_SURFACE('',#99442,0.750000000000001);
#86764=CYLINDRICAL_SURFACE('',#99444,0.750000000000001);
#86765=CYLINDRICAL_SURFACE('',#99446,0.750000000000001);
#86766=CYLINDRICAL_SURFACE('',#99448,0.750000000000001);
#86767=CYLINDRICAL_SURFACE('',#99450,0.750000000000001);
#86768=CYLINDRICAL_SURFACE('',#99452,0.750000000000001);
#86769=CYLINDRICAL_SURFACE('',#99454,0.750000000000001);
#86770=CYLINDRICAL_SURFACE('',#99456,0.750000000000001);
#86771=CYLINDRICAL_SURFACE('',#99458,0.750000000000001);
#86772=CYLINDRICAL_SURFACE('',#99460,0.750000000000001);
#86773=CYLINDRICAL_SURFACE('',#99462,0.750000000000001);
#86774=CYLINDRICAL_SURFACE('',#99464,0.750000000000001);
#86775=CYLINDRICAL_SURFACE('',#99466,0.750000000000001);
#86776=CYLINDRICAL_SURFACE('',#99468,0.750000000000001);
#86777=CYLINDRICAL_SURFACE('',#99470,0.750000000000001);
#86778=CYLINDRICAL_SURFACE('',#99472,0.750000000000001);
#86779=CYLINDRICAL_SURFACE('',#99474,0.750000000000001);
#86780=CYLINDRICAL_SURFACE('',#99476,0.750000000000001);
#86781=CYLINDRICAL_SURFACE('',#99478,0.75);
#86782=CYLINDRICAL_SURFACE('',#99480,0.75);
#86783=CYLINDRICAL_SURFACE('',#99482,0.750000000000001);
#86784=CYLINDRICAL_SURFACE('',#99484,0.750000000000001);
#86785=CYLINDRICAL_SURFACE('',#99486,0.750000000000001);
#86786=CYLINDRICAL_SURFACE('',#99488,10.);
#86787=CYLINDRICAL_SURFACE('',#99490,10.);
#86788=CYLINDRICAL_SURFACE('',#99492,10.);
#86789=CYLINDRICAL_SURFACE('',#99494,10.);
#86790=CYLINDRICAL_SURFACE('',#99496,13.1055395526668);
#86791=CYLINDRICAL_SURFACE('',#99498,13.1055395526668);
#86792=CYLINDRICAL_SURFACE('',#99500,11.1055395526669);
#86793=CYLINDRICAL_SURFACE('',#99504,11.1055395526669);
#86794=CYLINDRICAL_SURFACE('',#99506,12.1055395526668);
#86795=CYLINDRICAL_SURFACE('',#99508,11.1055395526669);
#86796=CYLINDRICAL_SURFACE('',#99512,11.1055395526669);
#86797=CYLINDRICAL_SURFACE('',#99514,12.1055395526668);
#86798=CYLINDRICAL_SURFACE('',#99573,3.5);
#86799=CYLINDRICAL_SURFACE('',#99576,50.5);
#86800=CYLINDRICAL_SURFACE('',#99579,3.5);
#86801=CYLINDRICAL_SURFACE('',#99582,679.934816028482);
#86802=CYLINDRICAL_SURFACE('',#99585,3.5);
#86803=CYLINDRICAL_SURFACE('',#99588,50.5);
#86804=CYLINDRICAL_SURFACE('',#99591,3.49999999999996);
#86805=CYLINDRICAL_SURFACE('',#99602,74.6139048513169);
#86806=CYLINDRICAL_SURFACE('',#99607,74.6139048513167);
#86807=CYLINDRICAL_SURFACE('',#99610,8.5);
#86808=CYLINDRICAL_SURFACE('',#99613,8.5);
#86809=CYLINDRICAL_SURFACE('',#99616,55.5);
#86810=CYLINDRICAL_SURFACE('',#99619,8.5);
#86811=CYLINDRICAL_SURFACE('',#99622,684.934816028482);
#86812=CYLINDRICAL_SURFACE('',#99625,8.5);
#86813=CYLINDRICAL_SURFACE('',#99628,55.5);
#86814=CYLINDRICAL_SURFACE('',#99692,684.934816028482);
#86815=CYLINDRICAL_SURFACE('',#99694,684.934816028482);
#86816=CYLINDRICAL_SURFACE('',#99696,684.934816028482);
#86817=CYLINDRICAL_SURFACE('',#99698,684.934816028482);
#86818=CYLINDRICAL_SURFACE('',#99700,684.934816028482);
#86819=CYLINDRICAL_SURFACE('',#99706,1.);
#86820=CYLINDRICAL_SURFACE('',#99708,48.);
#86821=CYLINDRICAL_SURFACE('',#99710,0.999999999999999);
#86822=CYLINDRICAL_SURFACE('',#99712,677.434816028482);
#86823=CYLINDRICAL_SURFACE('',#99714,1.);
#86824=CYLINDRICAL_SURFACE('',#99716,48.);
#86825=CYLINDRICAL_SURFACE('',#99718,0.999999999999959);
#86826=CYLINDRICAL_SURFACE('',#99731,73.8);
#86827=CYLINDRICAL_SURFACE('',#99736,73.8);
#86828=CYLINDRICAL_SURFACE('',#99739,77.1139048513169);
#86829=CYLINDRICAL_SURFACE('',#99742,77.1139048513167);
#86830=CYLINDRICAL_SURFACE('',#99743,51.8);
#86831=CYLINDRICAL_SURFACE('',#99745,4.8);
#86832=CYLINDRICAL_SURFACE('',#99747,681.234816028482);
#86833=CYLINDRICAL_SURFACE('',#99749,4.8);
#86834=CYLINDRICAL_SURFACE('',#99751,51.8);
#86835=CYLINDRICAL_SURFACE('',#99753,4.8);
#86836=CYLINDRICAL_SURFACE('',#99755,4.8);
#86837=CYLINDRICAL_SURFACE('',#99757,5.99999999999992);
#86838=CYLINDRICAL_SURFACE('',#99759,6.);
#86839=CYLINDRICAL_SURFACE('',#99761,53.);
#86840=CYLINDRICAL_SURFACE('',#99763,6.);
#86841=CYLINDRICAL_SURFACE('',#99765,682.434816028482);
#86842=CYLINDRICAL_SURFACE('',#99767,6.);
#86843=CYLINDRICAL_SURFACE('',#99769,53.);
#86844=CYLINDRICAL_SURFACE('',#99794,677.434816028482);
#86845=CYLINDRICAL_SURFACE('',#99796,677.434816028482);
#86846=CYLINDRICAL_SURFACE('',#99798,677.434816028482);
#86847=CYLINDRICAL_SURFACE('',#99800,677.434816028482);
#86848=CYLINDRICAL_SURFACE('',#99802,677.434816028482);
#86849=CYLINDRICAL_SURFACE('',#99814,204.49569081556);
#86850=CYLINDRICAL_SURFACE('',#99816,677.434816028482);
#86851=CYLINDRICAL_SURFACE('',#99818,206.99569081556);
#86852=CYLINDRICAL_SURFACE('',#99835,204.49569081556);
#86853=CYLINDRICAL_SURFACE('',#99837,204.49569081556);
#86854=CYLINDRICAL_SURFACE('',#99839,677.434816028482);
#86855=CYLINDRICAL_SURFACE('',#99841,677.434816028482);
#86856=CYLINDRICAL_SURFACE('',#99843,48.);
#86857=CYLINDRICAL_SURFACE('',#99845,48.);
#86858=CYLINDRICAL_SURFACE('',#99847,48.);
#86859=CYLINDRICAL_SURFACE('',#99849,48.);
#86860=CYLINDRICAL_SURFACE('',#100018,0.75);
#86861=CYLINDRICAL_SURFACE('',#100031,0.75);
#86862=CYLINDRICAL_SURFACE('',#100032,0.75);
#86863=CYLINDRICAL_SURFACE('',#100044,0.750000000000001);
#86864=CYLINDRICAL_SURFACE('',#100045,0.750000000000001);
#86865=CYLINDRICAL_SURFACE('',#100057,0.749999999999998);
#86866=CYLINDRICAL_SURFACE('',#100058,0.749999999999999);
#86867=CYLINDRICAL_SURFACE('',#100070,0.75);
#86868=CYLINDRICAL_SURFACE('',#100071,1.5);
#86869=CYLINDRICAL_SURFACE('',#100072,1.5);
#86870=CYLINDRICAL_SURFACE('',#100073,1.5);
#86871=CYLINDRICAL_SURFACE('',#100074,1.5);
#86872=CYLINDRICAL_SURFACE('',#100075,1.49999999999999);
#86873=CYLINDRICAL_SURFACE('',#100076,1.5);
#86874=CYLINDRICAL_SURFACE('',#100077,1.5);
#86875=CYLINDRICAL_SURFACE('',#100078,1.5);
#86876=CYLINDRICAL_SURFACE('',#100084,0.450000000000006);
#86877=CYLINDRICAL_SURFACE('',#100098,0.449999999999999);
#86878=CYLINDRICAL_SURFACE('',#100112,0.450000000000006);
#86879=CYLINDRICAL_SURFACE('',#100118,0.450000000000006);
#86880=CYLINDRICAL_SURFACE('',#100132,0.449999999999999);
#86881=CYLINDRICAL_SURFACE('',#100134,0.450000000000006);
#86882=CYLINDRICAL_SURFACE('',#100144,0.450000000000006);
#86883=CYLINDRICAL_SURFACE('',#100158,0.449999999999999);
#86884=CYLINDRICAL_SURFACE('',#100160,0.450000000000001);
#86885=CYLINDRICAL_SURFACE('',#100170,0.450000000000006);
#86886=CYLINDRICAL_SURFACE('',#100172,0.449999999999999);
#86887=CYLINDRICAL_SURFACE('',#100182,0.450000000000001);
#86888=CYLINDRICAL_SURFACE('',#100184,0.450000000000001);
#86889=CYLINDRICAL_SURFACE('',#100194,0.450000000000006);
#86890=CYLINDRICAL_SURFACE('',#100196,0.450000000000001);
#86891=CYLINDRICAL_SURFACE('',#100210,0.450000000000001);
#86892=CYLINDRICAL_SURFACE('',#100224,0.450000000000006);
#86893=CYLINDRICAL_SURFACE('',#100226,0.450000000000001);
#86894=CYLINDRICAL_SURFACE('',#100236,0.45);
#86895=CYLINDRICAL_SURFACE('',#100238,0.450000000000006);
#86896=CYLINDRICAL_SURFACE('',#100248,0.450000000000006);
#86897=CYLINDRICAL_SURFACE('',#100250,0.449999999999999);
#86898=CYLINDRICAL_SURFACE('',#100260,0.450000000000001);
#86899=CYLINDRICAL_SURFACE('',#100262,0.450000000000006);
#86900=CYLINDRICAL_SURFACE('',#100272,0.450000000000006);
#86901=CYLINDRICAL_SURFACE('',#100274,0.449999999999999);
#86902=CYLINDRICAL_SURFACE('',#100284,0.450000000000001);
#86903=CYLINDRICAL_SURFACE('',#100286,0.450000000000006);
#86904=CYLINDRICAL_SURFACE('',#100296,0.450000000000006);
#86905=CYLINDRICAL_SURFACE('',#100298,0.450000000000001);
#86906=CYLINDRICAL_SURFACE('',#100308,0.45);
#86907=CYLINDRICAL_SURFACE('',#100310,0.450000000000006);
#86908=CYLINDRICAL_SURFACE('',#100320,0.450000000000006);
#86909=CYLINDRICAL_SURFACE('',#100322,0.450000000000001);
#86910=CYLINDRICAL_SURFACE('',#100332,0.45);
#86911=CYLINDRICAL_SURFACE('',#100346,0.450000000000006);
#86912=CYLINDRICAL_SURFACE('',#100348,0.449999999999999);
#86913=CYLINDRICAL_SURFACE('',#100358,0.450000000000001);
#86914=CYLINDRICAL_SURFACE('',#100380,0.450000000000006);
#86915=CYLINDRICAL_SURFACE('',#100382,0.45);
#86916=CYLINDRICAL_SURFACE('',#100392,0.450000000000001);
#86917=CYLINDRICAL_SURFACE('',#100406,0.450000000000006);
#86918=CYLINDRICAL_SURFACE('',#100408,0.45);
#86919=CYLINDRICAL_SURFACE('',#100418,0.450000000000001);
#86920=CYLINDRICAL_SURFACE('',#100420,0.450000000000006);
#86921=CYLINDRICAL_SURFACE('',#100430,0.450000000000001);
#86922=CYLINDRICAL_SURFACE('',#100444,0.450000000000006);
#86923=CYLINDRICAL_SURFACE('',#100446,0.450000000000006);
#86924=CYLINDRICAL_SURFACE('',#100456,0.45);
#86925=CYLINDRICAL_SURFACE('',#100462,0.449999999999999);
#86926=CYLINDRICAL_SURFACE('',#100464,0.450000000000006);
#86927=CYLINDRICAL_SURFACE('',#100474,0.450000000000006);
#86928=CYLINDRICAL_SURFACE('',#100488,0.450000000000001);
#86929=CYLINDRICAL_SURFACE('',#100494,0.449999999999999);
#86930=CYLINDRICAL_SURFACE('',#100496,0.450000000000006);
#86931=CYLINDRICAL_SURFACE('',#100506,0.450000000000006);
#86932=CYLINDRICAL_SURFACE('',#100508,0.450000000000001);
#86933=CYLINDRICAL_SURFACE('',#100518,0.449999999999999);
#86934=CYLINDRICAL_SURFACE('',#100520,0.450000000000006);
#86935=CYLINDRICAL_SURFACE('',#100534,0.450000000000001);
#86936=CYLINDRICAL_SURFACE('',#100544,0.449999999999999);
#86937=CYLINDRICAL_SURFACE('',#100546,0.450000000000006);
#86938=CYLINDRICAL_SURFACE('',#100556,0.450000000000006);
#86939=CYLINDRICAL_SURFACE('',#100558,0.449999999999999);
#86940=CYLINDRICAL_SURFACE('',#100568,0.449999999999999);
#86941=CYLINDRICAL_SURFACE('',#100570,0.450000000000006);
#86942=CYLINDRICAL_SURFACE('',#100580,0.450000000000006);
#86943=CYLINDRICAL_SURFACE('',#100582,0.449999999999999);
#86944=CYLINDRICAL_SURFACE('',#100592,0.449999999999999);
#86945=CYLINDRICAL_SURFACE('',#100594,0.450000000000006);
#86946=CYLINDRICAL_SURFACE('',#100604,0.450000000000001);
#86947=CYLINDRICAL_SURFACE('',#100622,0.449999999999999);
#86948=CYLINDRICAL_SURFACE('',#100624,0.450000000000006);
#86949=CYLINDRICAL_SURFACE('',#100638,0.449999999999999);
#86950=CYLINDRICAL_SURFACE('',#100648,0.449999999999999);
#86951=CYLINDRICAL_SURFACE('',#100650,0.450000000000006);
#86952=CYLINDRICAL_SURFACE('',#100664,0.449999999999999);
#86953=CYLINDRICAL_SURFACE('',#100682,0.449999999999999);
#86954=CYLINDRICAL_SURFACE('',#100684,0.450000000000006);
#86955=CYLINDRICAL_SURFACE('',#100694,0.450000000000006);
#86956=CYLINDRICAL_SURFACE('',#100696,0.449999999999999);
#86957=CYLINDRICAL_SURFACE('',#100706,0.449999999999999);
#86958=CYLINDRICAL_SURFACE('',#100708,0.450000000000006);
#86959=CYLINDRICAL_SURFACE('',#100718,0.450000000000006);
#86960=CYLINDRICAL_SURFACE('',#100740,0.449999999999999);
#86961=CYLINDRICAL_SURFACE('',#100742,0.450000000000006);
#86962=CYLINDRICAL_SURFACE('',#100752,0.450000000000006);
#86963=CYLINDRICAL_SURFACE('',#100766,0.449999999999999);
#86964=CYLINDRICAL_SURFACE('',#100768,0.450000000000006);
#86965=CYLINDRICAL_SURFACE('',#100778,0.450000000000006);
#86966=CYLINDRICAL_SURFACE('',#100780,0.449999999999999);
#86967=CYLINDRICAL_SURFACE('',#100790,0.449999999999999);
#86968=CYLINDRICAL_SURFACE('',#100792,0.450000000000001);
#86969=CYLINDRICAL_SURFACE('',#100802,0.450000000000006);
#86970=CYLINDRICAL_SURFACE('',#100816,0.449999999999999);
#86971=CYLINDRICAL_SURFACE('',#100818,0.450000000000006);
#86972=CYLINDRICAL_SURFACE('',#100828,0.450000000000001);
#86973=CYLINDRICAL_SURFACE('',#100830,0.449999999999999);
#86974=CYLINDRICAL_SURFACE('',#100840,0.449999999999999);
#86975=CYLINDRICAL_SURFACE('',#100854,0.450000000000006);
#86976=CYLINDRICAL_SURFACE('',#100860,0.450000000000006);
#86977=CYLINDRICAL_SURFACE('',#100874,0.449999999999999);
#86978=CYLINDRICAL_SURFACE('',#100957,0.44999999999999);
#86979=CYLINDRICAL_SURFACE('',#100971,0.450000000000001);
#86980=CYLINDRICAL_SURFACE('',#100980,0.450000000000001);
#86981=CYLINDRICAL_SURFACE('',#100994,0.45);
#86982=CYLINDRICAL_SURFACE('',#101003,0.450000000000006);
#86983=CYLINDRICAL_SURFACE('',#101017,0.44999999999999);
#86984=CYLINDRICAL_SURFACE('',#101026,0.45);
#86985=CYLINDRICAL_SURFACE('',#101040,0.450000000000006);
#86986=CYLINDRICAL_SURFACE('',#101154,0.75);
#86987=CYLINDRICAL_SURFACE('',#101156,0.750000000000001);
#86988=CYLINDRICAL_SURFACE('',#101158,0.750000000000001);
#86989=CYLINDRICAL_SURFACE('',#101160,0.750000000000001);
#86990=CYLINDRICAL_SURFACE('',#101162,0.750000000000001);
#86991=CYLINDRICAL_SURFACE('',#101164,0.750000000000001);
#86992=CYLINDRICAL_SURFACE('',#101166,0.75);
#86993=CYLINDRICAL_SURFACE('',#101168,0.75);
#86994=CYLINDRICAL_SURFACE('',#101170,0.75);
#86995=CYLINDRICAL_SURFACE('',#101172,0.750000000000001);
#86996=CYLINDRICAL_SURFACE('',#101174,0.750000000000001);
#86997=CYLINDRICAL_SURFACE('',#101176,0.750000000000001);
#86998=CYLINDRICAL_SURFACE('',#101178,0.750000000000001);
#86999=CYLINDRICAL_SURFACE('',#101180,0.750000000000001);
#87000=CYLINDRICAL_SURFACE('',#101182,0.750000000000001);
#87001=CYLINDRICAL_SURFACE('',#101184,0.750000000000001);
#87002=CYLINDRICAL_SURFACE('',#101186,0.75);
#87003=CYLINDRICAL_SURFACE('',#101188,0.75);
#87004=CYLINDRICAL_SURFACE('',#101190,0.75);
#87005=CYLINDRICAL_SURFACE('',#101192,0.75);
#87006=CYLINDRICAL_SURFACE('',#101194,0.750000000000001);
#87007=CYLINDRICAL_SURFACE('',#101196,0.75);
#87008=CYLINDRICAL_SURFACE('',#101198,0.750000000000001);
#87009=CYLINDRICAL_SURFACE('',#101200,0.750000000000001);
#87010=CYLINDRICAL_SURFACE('',#101202,0.750000000000001);
#87011=CYLINDRICAL_SURFACE('',#101204,0.750000000000001);
#87012=CYLINDRICAL_SURFACE('',#101206,0.750000000000001);
#87013=CYLINDRICAL_SURFACE('',#101208,0.750000000000001);
#87014=CYLINDRICAL_SURFACE('',#101210,0.750000000000001);
#87015=CYLINDRICAL_SURFACE('',#101212,0.750000000000001);
#87016=CYLINDRICAL_SURFACE('',#101214,0.750000000000001);
#87017=CYLINDRICAL_SURFACE('',#101216,0.750000000000001);
#87018=CYLINDRICAL_SURFACE('',#101218,0.75);
#87019=CYLINDRICAL_SURFACE('',#101220,0.750000000000001);
#87020=CYLINDRICAL_SURFACE('',#101222,0.75);
#87021=CYLINDRICAL_SURFACE('',#101224,0.75);
#87022=CYLINDRICAL_SURFACE('',#101226,0.750000000000001);
#87023=CYLINDRICAL_SURFACE('',#101228,0.750000000000001);
#87024=CYLINDRICAL_SURFACE('',#101230,0.750000000000001);
#87025=CYLINDRICAL_SURFACE('',#101232,0.750000000000001);
#87026=CYLINDRICAL_SURFACE('',#101234,0.750000000000001);
#87027=CYLINDRICAL_SURFACE('',#101236,0.750000000000001);
#87028=CYLINDRICAL_SURFACE('',#101238,0.750000000000001);
#87029=CYLINDRICAL_SURFACE('',#101240,0.750000000000001);
#87030=CYLINDRICAL_SURFACE('',#101242,0.75);
#87031=CYLINDRICAL_SURFACE('',#101244,0.75);
#87032=CYLINDRICAL_SURFACE('',#101246,0.750000000000001);
#87033=CYLINDRICAL_SURFACE('',#101248,0.750000000000001);
#87034=CYLINDRICAL_SURFACE('',#101250,0.750000000000001);
#87035=CYLINDRICAL_SURFACE('',#101252,0.750000000000001);
#87036=CYLINDRICAL_SURFACE('',#101254,0.750000000000001);
#87037=CYLINDRICAL_SURFACE('',#101256,0.750000000000001);
#87038=CYLINDRICAL_SURFACE('',#101258,0.750000000000001);
#87039=CYLINDRICAL_SURFACE('',#101260,0.750000000000001);
#87040=CYLINDRICAL_SURFACE('',#101262,0.750000000000001);
#87041=CYLINDRICAL_SURFACE('',#101264,0.750000000000001);
#87042=CYLINDRICAL_SURFACE('',#101266,0.750000000000001);
#87043=CYLINDRICAL_SURFACE('',#101268,0.750000000000001);
#87044=CYLINDRICAL_SURFACE('',#101270,0.750000000000001);
#87045=CYLINDRICAL_SURFACE('',#101272,0.750000000000001);
#87046=CYLINDRICAL_SURFACE('',#101274,0.750000000000001);
#87047=CYLINDRICAL_SURFACE('',#101276,0.750000000000001);
#87048=CYLINDRICAL_SURFACE('',#101278,0.750000000000001);
#87049=CYLINDRICAL_SURFACE('',#101280,0.750000000000001);
#87050=CYLINDRICAL_SURFACE('',#101282,0.750000000000001);
#87051=CYLINDRICAL_SURFACE('',#101284,0.750000000000001);
#87052=CYLINDRICAL_SURFACE('',#101286,0.750000000000001);
#87053=CYLINDRICAL_SURFACE('',#101288,0.750000000000001);
#87054=CYLINDRICAL_SURFACE('',#101290,0.750000000000001);
#87055=CYLINDRICAL_SURFACE('',#101292,0.750000000000001);
#87056=CYLINDRICAL_SURFACE('',#101294,0.750000000000001);
#87057=CYLINDRICAL_SURFACE('',#101296,0.75);
#87058=CYLINDRICAL_SURFACE('',#101298,0.750000000000001);
#87059=CYLINDRICAL_SURFACE('',#101300,0.750000000000001);
#87060=CYLINDRICAL_SURFACE('',#101302,0.75);
#87061=CYLINDRICAL_SURFACE('',#101304,0.750000000000001);
#87062=CYLINDRICAL_SURFACE('',#101306,0.75);
#87063=CYLINDRICAL_SURFACE('',#101308,0.75);
#87064=CYLINDRICAL_SURFACE('',#101310,0.750000000000001);
#87065=CYLINDRICAL_SURFACE('',#101312,0.750000000000001);
#87066=CYLINDRICAL_SURFACE('',#101314,0.750000000000001);
#87067=CYLINDRICAL_SURFACE('',#101316,0.750000000000001);
#87068=CYLINDRICAL_SURFACE('',#101318,0.750000000000001);
#87069=CYLINDRICAL_SURFACE('',#101320,0.750000000000001);
#87070=CYLINDRICAL_SURFACE('',#101322,0.750000000000001);
#87071=CYLINDRICAL_SURFACE('',#101324,0.750000000000001);
#87072=CYLINDRICAL_SURFACE('',#101326,0.750000000000001);
#87073=CYLINDRICAL_SURFACE('',#101328,0.750000000000001);
#87074=CYLINDRICAL_SURFACE('',#101330,0.750000000000001);
#87075=CYLINDRICAL_SURFACE('',#101332,0.750000000000001);
#87076=CYLINDRICAL_SURFACE('',#101334,0.750000000000001);
#87077=CYLINDRICAL_SURFACE('',#101336,0.750000000000001);
#87078=CYLINDRICAL_SURFACE('',#101338,0.750000000000001);
#87079=CYLINDRICAL_SURFACE('',#101340,0.750000000000001);
#87080=CYLINDRICAL_SURFACE('',#101342,0.750000000000001);
#87081=CYLINDRICAL_SURFACE('',#101344,0.75);
#87082=CYLINDRICAL_SURFACE('',#101346,0.750000000000001);
#87083=CYLINDRICAL_SURFACE('',#101348,0.75);
#87084=CYLINDRICAL_SURFACE('',#101350,0.75);
#87085=CYLINDRICAL_SURFACE('',#101352,0.750000000000001);
#87086=CYLINDRICAL_SURFACE('',#101354,0.750000000000001);
#87087=CYLINDRICAL_SURFACE('',#101356,0.750000000000001);
#87088=CYLINDRICAL_SURFACE('',#101358,0.750000000000001);
#87089=CYLINDRICAL_SURFACE('',#101360,0.750000000000001);
#87090=CYLINDRICAL_SURFACE('',#101362,0.750000000000001);
#87091=CYLINDRICAL_SURFACE('',#101364,0.750000000000001);
#87092=CYLINDRICAL_SURFACE('',#101366,0.750000000000001);
#87093=CYLINDRICAL_SURFACE('',#101368,0.750000000000001);
#87094=CYLINDRICAL_SURFACE('',#101370,0.750000000000001);
#87095=CYLINDRICAL_SURFACE('',#101372,0.750000000000001);
#87096=CYLINDRICAL_SURFACE('',#101374,0.750000000000001);
#87097=CYLINDRICAL_SURFACE('',#101376,0.750000000000001);
#87098=CYLINDRICAL_SURFACE('',#101378,0.750000000000001);
#87099=CYLINDRICAL_SURFACE('',#101380,0.750000000000001);
#87100=CYLINDRICAL_SURFACE('',#101382,0.750000000000001);
#87101=CYLINDRICAL_SURFACE('',#101384,0.750000000000001);
#87102=CYLINDRICAL_SURFACE('',#101386,0.750000000000001);
#87103=CYLINDRICAL_SURFACE('',#101388,0.750000000000001);
#87104=CYLINDRICAL_SURFACE('',#101390,0.750000000000001);
#87105=CYLINDRICAL_SURFACE('',#101392,0.750000000000001);
#87106=CYLINDRICAL_SURFACE('',#101394,0.750000000000001);
#87107=CYLINDRICAL_SURFACE('',#101396,0.750000000000001);
#87108=CYLINDRICAL_SURFACE('',#101398,0.750000000000001);
#87109=CYLINDRICAL_SURFACE('',#101400,0.750000000000001);
#87110=CYLINDRICAL_SURFACE('',#101402,0.750000000000001);
#87111=CYLINDRICAL_SURFACE('',#101404,0.750000000000001);
#87112=CYLINDRICAL_SURFACE('',#101406,0.750000000000001);
#87113=CYLINDRICAL_SURFACE('',#101408,0.750000000000001);
#87114=CYLINDRICAL_SURFACE('',#101410,0.750000000000001);
#87115=CYLINDRICAL_SURFACE('',#101412,0.75);
#87116=CYLINDRICAL_SURFACE('',#101414,0.75);
#87117=CYLINDRICAL_SURFACE('',#101416,0.750000000000001);
#87118=CYLINDRICAL_SURFACE('',#101418,0.750000000000001);
#87119=CYLINDRICAL_SURFACE('',#101420,0.750000000000001);
#87120=CYLINDRICAL_SURFACE('',#101422,10.);
#87121=CYLINDRICAL_SURFACE('',#101424,10.);
#87122=CYLINDRICAL_SURFACE('',#101426,10.);
#87123=CYLINDRICAL_SURFACE('',#101428,10.);
#87124=CYLINDRICAL_SURFACE('',#101432,4.62535);
#87125=CYLINDRICAL_SURFACE('',#101434,13.1055395526668);
#87126=CYLINDRICAL_SURFACE('',#101436,13.1055395526668);
#87127=CYLINDRICAL_SURFACE('',#101438,8.10553955266686);
#87128=CYLINDRICAL_SURFACE('',#101456,11.1055395526669);
#87129=CYLINDRICAL_SURFACE('',#101460,11.1055395526669);
#87130=CYLINDRICAL_SURFACE('',#101462,12.1055395526668);
#87131=CYLINDRICAL_SURFACE('',#101464,11.1055395526669);
#87132=CYLINDRICAL_SURFACE('',#101468,11.1055395526669);
#87133=CYLINDRICAL_SURFACE('',#101470,12.1055395526668);
#87134=CYLINDRICAL_SURFACE('',#101562,3.5);
#87135=CYLINDRICAL_SURFACE('',#101564,50.5);
#87136=CYLINDRICAL_SURFACE('',#101566,3.5);
#87137=CYLINDRICAL_SURFACE('',#101568,679.934816028482);
#87138=CYLINDRICAL_SURFACE('',#101570,3.5);
#87139=CYLINDRICAL_SURFACE('',#101572,50.5);
#87140=CYLINDRICAL_SURFACE('',#101574,3.49999999999996);
#87141=CYLINDRICAL_SURFACE('',#101576,679.934816028482);
#87142=CYLINDRICAL_SURFACE('',#101586,74.6139048513169);
#87143=CYLINDRICAL_SURFACE('',#101591,74.6139048513167);
#87144=CYLINDRICAL_SURFACE('',#101594,8.5);
#87145=CYLINDRICAL_SURFACE('',#101597,684.934816028482);
#87146=CYLINDRICAL_SURFACE('',#101600,211.99569081556);
#87147=CYLINDRICAL_SURFACE('',#101605,8.5);
#87148=CYLINDRICAL_SURFACE('',#101608,55.5);
#87149=CYLINDRICAL_SURFACE('',#101611,8.5);
#87150=CYLINDRICAL_SURFACE('',#101614,684.934816028482);
#87151=CYLINDRICAL_SURFACE('',#101617,8.5);
#87152=CYLINDRICAL_SURFACE('',#101620,55.5);
#87153=CYLINDRICAL_SURFACE('',#101695,684.934816028482);
#87154=CYLINDRICAL_SURFACE('',#101697,684.934816028482);
#87155=CYLINDRICAL_SURFACE('',#101699,684.934816028482);
#87156=CYLINDRICAL_SURFACE('',#101701,684.934816028482);
#87157=CYLINDRICAL_SURFACE('',#101703,684.934816028482);
#87158=CYLINDRICAL_SURFACE('',#101709,1.);
#87159=CYLINDRICAL_SURFACE('',#101710,48.);
#87160=CYLINDRICAL_SURFACE('',#101711,0.999999999999999);
#87161=CYLINDRICAL_SURFACE('',#101712,677.434816028482);
#87162=CYLINDRICAL_SURFACE('',#101713,1.);
#87163=CYLINDRICAL_SURFACE('',#101714,48.);
#87164=CYLINDRICAL_SURFACE('',#101715,0.999999999999959);
#87165=CYLINDRICAL_SURFACE('',#101725,73.8);
#87166=CYLINDRICAL_SURFACE('',#101729,73.8);
#87167=CYLINDRICAL_SURFACE('',#101732,77.1139048513169);
#87168=CYLINDRICAL_SURFACE('',#101735,77.1139048513167);
#87169=CYLINDRICAL_SURFACE('',#101737,51.8);
#87170=CYLINDRICAL_SURFACE('',#101739,4.8);
#87171=CYLINDRICAL_SURFACE('',#101741,681.234816028482);
#87172=CYLINDRICAL_SURFACE('',#101743,4.8);
#87173=CYLINDRICAL_SURFACE('',#101745,51.8);
#87174=CYLINDRICAL_SURFACE('',#101747,4.8);
#87175=CYLINDRICAL_SURFACE('',#101749,681.234816028482);
#87176=CYLINDRICAL_SURFACE('',#101751,208.29569081556);
#87177=CYLINDRICAL_SURFACE('',#101753,4.8);
#87178=CYLINDRICAL_SURFACE('',#101765,5.99999999999992);
#87179=CYLINDRICAL_SURFACE('',#101766,682.434816028482);
#87180=CYLINDRICAL_SURFACE('',#101767,209.495690815561);
#87181=CYLINDRICAL_SURFACE('',#101768,6.);
#87182=CYLINDRICAL_SURFACE('',#101769,53.);
#87183=CYLINDRICAL_SURFACE('',#101770,6.);
#87184=CYLINDRICAL_SURFACE('',#101771,682.434816028482);
#87185=CYLINDRICAL_SURFACE('',#101772,6.);
#87186=CYLINDRICAL_SURFACE('',#101773,53.);
#87187=CYLINDRICAL_SURFACE('',#101806,677.434816028482);
#87188=CYLINDRICAL_SURFACE('',#101807,677.434816028482);
#87189=CYLINDRICAL_SURFACE('',#101808,677.434816028482);
#87190=CYLINDRICAL_SURFACE('',#101809,677.434816028482);
#87191=CYLINDRICAL_SURFACE('',#101810,677.434816028482);
#87192=CYLINDRICAL_SURFACE('',#101821,204.49569081556);
#87193=CYLINDRICAL_SURFACE('',#101822,677.434816028482);
#87194=CYLINDRICAL_SURFACE('',#101823,206.99569081556);
#87195=CYLINDRICAL_SURFACE('',#101825,206.99569081556);
#87196=CYLINDRICAL_SURFACE('',#101842,204.49569081556);
#87197=CYLINDRICAL_SURFACE('',#101843,204.49569081556);
#87198=CYLINDRICAL_SURFACE('',#101844,677.434816028482);
#87199=CYLINDRICAL_SURFACE('',#101845,677.434816028482);
#87200=CYLINDRICAL_SURFACE('',#101846,48.);
#87201=CYLINDRICAL_SURFACE('',#101847,48.);
#87202=CYLINDRICAL_SURFACE('',#101848,48.);
#87203=CYLINDRICAL_SURFACE('',#101849,48.);
#87204=CYLINDRICAL_SURFACE('',#101906,3.25);
#87205=CYLINDRICAL_SURFACE('',#101998,3.25);
#87206=CYLINDRICAL_SURFACE('',#102021,7.8);
#87207=CYLINDRICAL_SURFACE('',#102023,8.8);
#87208=CYLINDRICAL_SURFACE('',#102029,2.);
#87209=CYLINDRICAL_SURFACE('',#102033,2.5);
#87210=CYLINDRICAL_SURFACE('',#102041,0.5);
#87211=CYLINDRICAL_SURFACE('',#102043,0.5);
#87212=CYLINDRICAL_SURFACE('',#102053,0.5);
#87213=CYLINDRICAL_SURFACE('',#102055,0.5);
#87214=CYLINDRICAL_SURFACE('',#102061,7.00000000000001);
#87215=CYLINDRICAL_SURFACE('',#102063,7.00000000000001);
#87216=CYLINDRICAL_SURFACE('',#102073,1.);
#87217=CYLINDRICAL_SURFACE('',#102079,4.);
#87218=CYLINDRICAL_SURFACE('',#102090,1.);
#87219=CYLINDRICAL_SURFACE('',#102091,4.);
#87220=CYLINDRICAL_SURFACE('',#102092,4.);
#87221=CYLINDRICAL_SURFACE('',#102095,1.);
#87222=CYLINDRICAL_SURFACE('',#102105,4.);
#87223=CYLINDRICAL_SURFACE('',#102111,1.);
#87224=CYLINDRICAL_SURFACE('',#102119,7.00000000000001);
#87225=CYLINDRICAL_SURFACE('',#102121,7.00000000000001);
#87226=CYLINDRICAL_SURFACE('',#102123,1.);
#87227=CYLINDRICAL_SURFACE('',#102125,1.);
#87228=CYLINDRICAL_SURFACE('',#102127,1.);
#87229=CYLINDRICAL_SURFACE('',#102129,1.);
#87230=CYLINDRICAL_SURFACE('',#102133,7.8);
#87231=CYLINDRICAL_SURFACE('',#102134,7.8);
#87232=CYLINDRICAL_SURFACE('',#102159,7.8);
#87233=CYLINDRICAL_SURFACE('',#102161,8.8);
#87234=CYLINDRICAL_SURFACE('',#102163,0.499999999999998);
#87235=CYLINDRICAL_SURFACE('',#102169,0.5);
#87236=CYLINDRICAL_SURFACE('',#102175,0.5);
#87237=CYLINDRICAL_SURFACE('',#102176,0.5);
#87238=CYLINDRICAL_SURFACE('',#102183,0.5);
#87239=CYLINDRICAL_SURFACE('',#102189,0.499999999999998);
#87240=CYLINDRICAL_SURFACE('',#102190,0.5);
#87241=CYLINDRICAL_SURFACE('',#102197,0.5);
#87242=CYLINDRICAL_SURFACE('',#102203,0.5);
#87243=CYLINDRICAL_SURFACE('',#102209,0.5);
#87244=CYLINDRICAL_SURFACE('',#102215,0.5);
#87245=CYLINDRICAL_SURFACE('',#102217,0.5);
#87246=CYLINDRICAL_SURFACE('',#102224,0.5);
#87247=CYLINDRICAL_SURFACE('',#102230,0.500000000000003);
#87248=CYLINDRICAL_SURFACE('',#102231,0.5);
#87249=CYLINDRICAL_SURFACE('',#102238,0.5);
#87250=CYLINDRICAL_SURFACE('',#102248,0.5);
#87251=CYLINDRICAL_SURFACE('',#102254,0.5);
#87252=CYLINDRICAL_SURFACE('',#102260,0.5);
#87253=CYLINDRICAL_SURFACE('',#102262,0.5);
#87254=CYLINDRICAL_SURFACE('',#102269,0.5);
#87255=CYLINDRICAL_SURFACE('',#102283,0.5);
#87256=CYLINDRICAL_SURFACE('',#102289,0.5);
#87257=CYLINDRICAL_SURFACE('',#102291,0.5);
#87258=CYLINDRICAL_SURFACE('',#102298,0.5);
#87259=CYLINDRICAL_SURFACE('',#102312,0.5);
#87260=CYLINDRICAL_SURFACE('',#102318,0.5);
#87261=CYLINDRICAL_SURFACE('',#102320,0.5);
#87262=CYLINDRICAL_SURFACE('',#102327,0.5);
#87263=CYLINDRICAL_SURFACE('',#102341,0.5);
#87264=CYLINDRICAL_SURFACE('',#102347,0.5);
#87265=CYLINDRICAL_SURFACE('',#102349,0.5);
#87266=CYLINDRICAL_SURFACE('',#102356,0.5);
#87267=CYLINDRICAL_SURFACE('',#102370,0.5);
#87268=CYLINDRICAL_SURFACE('',#102376,0.5);
#87269=CYLINDRICAL_SURFACE('',#102378,0.5);
#87270=CYLINDRICAL_SURFACE('',#102385,0.5);
#87271=CYLINDRICAL_SURFACE('',#102399,0.5);
#87272=CYLINDRICAL_SURFACE('',#102405,0.5);
#87273=CYLINDRICAL_SURFACE('',#102407,0.5);
#87274=CYLINDRICAL_SURFACE('',#102414,0.5);
#87275=CYLINDRICAL_SURFACE('',#102428,0.5);
#87276=CYLINDRICAL_SURFACE('',#102434,0.5);
#87277=CYLINDRICAL_SURFACE('',#102436,0.5);
#87278=CYLINDRICAL_SURFACE('',#102443,0.5);
#87279=CYLINDRICAL_SURFACE('',#102449,0.5);
#87280=CYLINDRICAL_SURFACE('',#102459,0.5);
#87281=CYLINDRICAL_SURFACE('',#102465,0.5);
#87282=CYLINDRICAL_SURFACE('',#102467,0.5);
#87283=CYLINDRICAL_SURFACE('',#102474,0.5);
#87284=CYLINDRICAL_SURFACE('',#102480,0.5);
#87285=CYLINDRICAL_SURFACE('',#102486,0.5);
#87286=CYLINDRICAL_SURFACE('',#102492,0.5);
#87287=CYLINDRICAL_SURFACE('',#102494,0.499999999999998);
#87288=CYLINDRICAL_SURFACE('',#102500,0.5);
#87289=CYLINDRICAL_SURFACE('',#102506,0.5);
#87290=CYLINDRICAL_SURFACE('',#102508,0.5);
#87291=CYLINDRICAL_SURFACE('',#102510,0.5);
#87292=CYLINDRICAL_SURFACE('',#102512,0.5);
#87293=CYLINDRICAL_SURFACE('',#102514,0.5);
#87294=CYLINDRICAL_SURFACE('',#102516,0.5);
#87295=CYLINDRICAL_SURFACE('',#102518,0.5);
#87296=CYLINDRICAL_SURFACE('',#102520,0.5);
#87297=CYLINDRICAL_SURFACE('',#102522,0.5);
#87298=CYLINDRICAL_SURFACE('',#102524,0.5);
#87299=CYLINDRICAL_SURFACE('',#102526,0.5);
#87300=CYLINDRICAL_SURFACE('',#102528,0.5);
#87301=CYLINDRICAL_SURFACE('',#102530,0.5);
#87302=CYLINDRICAL_SURFACE('',#102532,0.5);
#87303=CYLINDRICAL_SURFACE('',#102534,0.5);
#87304=CYLINDRICAL_SURFACE('',#102536,0.5);
#87305=CYLINDRICAL_SURFACE('',#102538,0.5);
#87306=CYLINDRICAL_SURFACE('',#102540,0.5);
#87307=CYLINDRICAL_SURFACE('',#102542,0.5);
#87308=CYLINDRICAL_SURFACE('',#102544,0.5);
#87309=CYLINDRICAL_SURFACE('',#102546,0.5);
#87310=CYLINDRICAL_SURFACE('',#102548,0.5);
#87311=CYLINDRICAL_SURFACE('',#102550,0.5);
#87312=CYLINDRICAL_SURFACE('',#102552,0.5);
#87313=CYLINDRICAL_SURFACE('',#102554,0.5);
#87314=CYLINDRICAL_SURFACE('',#102556,0.5);
#87315=CYLINDRICAL_SURFACE('',#102558,0.5);
#87316=CYLINDRICAL_SURFACE('',#102565,231.99961917989);
#87317=CYLINDRICAL_SURFACE('',#102581,3.);
#87318=CYLINDRICAL_SURFACE('',#102582,58.5);
#87319=CYLINDRICAL_SURFACE('',#102587,3.);
#87320=CYLINDRICAL_SURFACE('',#102588,58.5);
#87321=CYLINDRICAL_SURFACE('',#102593,3.);
#87322=CYLINDRICAL_SURFACE('',#102594,58.5);
#87323=CYLINDRICAL_SURFACE('',#102599,3.);
#87324=CYLINDRICAL_SURFACE('',#102600,58.5);
#87325=CYLINDRICAL_SURFACE('',#102605,3.);
#87326=CYLINDRICAL_SURFACE('',#102607,5.);
#87327=CYLINDRICAL_SURFACE('',#102610,5.);
#87328=CYLINDRICAL_SURFACE('',#102620,3.);
#87329=CYLINDRICAL_SURFACE('',#102622,3.);
#87330=CYLINDRICAL_SURFACE('',#102624,3.);
#87331=CYLINDRICAL_SURFACE('',#102626,3.);
#87332=CYLINDRICAL_SURFACE('',#102628,58.5);
#87333=CYLINDRICAL_SURFACE('',#102629,3.);
#87334=CYLINDRICAL_SURFACE('',#102631,58.5);
#87335=CYLINDRICAL_SURFACE('',#102633,3.);
#87336=CYLINDRICAL_SURFACE('',#102640,77.1121191998622);
#87337=CYLINDRICAL_SURFACE('',#102644,77.1121191998622);
#87338=CYLINDRICAL_SURFACE('',#102736,3.25);
#87339=CYLINDRICAL_SURFACE('',#102737,0.749999999999997);
#87340=CYLINDRICAL_SURFACE('',#102740,0.75);
#87341=CYLINDRICAL_SURFACE('',#102747,0.750000000000001);
#87342=CYLINDRICAL_SURFACE('',#102776,0.499999999999987);
#87343=CYLINDRICAL_SURFACE('',#102779,0.500000000000001);
#87344=CYLINDRICAL_SURFACE('',#102784,0.749999999999997);
#87345=CYLINDRICAL_SURFACE('',#102787,0.75);
#87346=CYLINDRICAL_SURFACE('',#102794,0.750000000000001);
#87347=CYLINDRICAL_SURFACE('',#102823,0.499999999999987);
#87348=CYLINDRICAL_SURFACE('',#102826,0.500000000000001);
#87349=CYLINDRICAL_SURFACE('',#102833,0.750000000000001);
#87350=CYLINDRICAL_SURFACE('',#102836,0.750000000000001);
#87351=CYLINDRICAL_SURFACE('',#102842,0.750000000000001);
#87352=CYLINDRICAL_SURFACE('',#102843,0.750000000000001);
#87353=CYLINDRICAL_SURFACE('',#102849,0.750000000000001);
#87354=CYLINDRICAL_SURFACE('',#102850,7.00000000000001);
#87355=CYLINDRICAL_SURFACE('',#102852,7.00000000000001);
#87356=CYLINDRICAL_SURFACE('',#102857,0.750000000000001);
#87357=CYLINDRICAL_SURFACE('',#102860,0.750000000000001);
#87358=CYLINDRICAL_SURFACE('',#102861,0.750000000000001);
#87359=CYLINDRICAL_SURFACE('',#102867,0.750000000000001);
#87360=CYLINDRICAL_SURFACE('',#102868,0.750000000000001);
#87361=CYLINDRICAL_SURFACE('',#102874,0.750000000000001);
#87362=CYLINDRICAL_SURFACE('',#102878,7.00000000000001);
#87363=CYLINDRICAL_SURFACE('',#102879,7.00000000000001);
#87364=CYLINDRICAL_SURFACE('',#102880,2.);
#87365=CYLINDRICAL_SURFACE('',#102882,2.);
#87366=CYLINDRICAL_SURFACE('',#102883,2.);
#87367=CYLINDRICAL_SURFACE('',#102884,2.);
#87368=CYLINDRICAL_SURFACE('',#102885,2.);
#87369=CYLINDRICAL_SURFACE('',#102886,2.);
#87370=CYLINDRICAL_SURFACE('',#102887,2.);
#87371=CYLINDRICAL_SURFACE('',#102888,2.);
#87372=CYLINDRICAL_SURFACE('',#102889,2.);
#87373=CYLINDRICAL_SURFACE('',#102890,2.);
#87374=CYLINDRICAL_SURFACE('',#102891,2.);
#87375=CYLINDRICAL_SURFACE('',#102892,2.);
#87376=CYLINDRICAL_SURFACE('',#102893,2.);
#87377=CYLINDRICAL_SURFACE('',#102894,2.);
#87378=CYLINDRICAL_SURFACE('',#102895,2.);
#87379=CYLINDRICAL_SURFACE('',#102896,2.);
#87380=CYLINDRICAL_SURFACE('',#102897,2.);
#87381=CYLINDRICAL_SURFACE('',#102898,2.);
#87382=CYLINDRICAL_SURFACE('',#102899,2.);
#87383=CYLINDRICAL_SURFACE('',#102900,2.);
#87384=CYLINDRICAL_SURFACE('',#102902,2.);
#87385=CYLINDRICAL_SURFACE('',#102903,2.);
#87386=CYLINDRICAL_SURFACE('',#102904,2.);
#87387=CYLINDRICAL_SURFACE('',#102905,2.);
#87388=CYLINDRICAL_SURFACE('',#102906,2.);
#87389=CYLINDRICAL_SURFACE('',#102907,2.);
#87390=CYLINDRICAL_SURFACE('',#102908,2.);
#87391=CYLINDRICAL_SURFACE('',#102909,2.);
#87392=CYLINDRICAL_SURFACE('',#102910,2.);
#87393=CYLINDRICAL_SURFACE('',#102911,2.);
#87394=CYLINDRICAL_SURFACE('',#102912,2.);
#87395=CYLINDRICAL_SURFACE('',#102913,2.);
#87396=CYLINDRICAL_SURFACE('',#102914,2.);
#87397=CYLINDRICAL_SURFACE('',#102915,2.);
#87398=CYLINDRICAL_SURFACE('',#102916,2.);
#87399=CYLINDRICAL_SURFACE('',#102917,2.);
#87400=CYLINDRICAL_SURFACE('',#102918,2.);
#87401=CYLINDRICAL_SURFACE('',#102919,2.);
#87402=CYLINDRICAL_SURFACE('',#102920,1.66874528305244);
#87403=CYLINDRICAL_SURFACE('',#102921,1.66874528305244);
#87404=CYLINDRICAL_SURFACE('',#102922,1.66874528305244);
#87405=CYLINDRICAL_SURFACE('',#102923,1.66874528305244);
#87406=CYLINDRICAL_SURFACE('',#102924,1.66874528305244);
#87407=CYLINDRICAL_SURFACE('',#102925,1.66874528305244);
#87408=CYLINDRICAL_SURFACE('',#102926,1.66874528305244);
#87409=CYLINDRICAL_SURFACE('',#102927,1.66874528305244);
#87410=CYLINDRICAL_SURFACE('',#102928,1.66874528305244);
#87411=CYLINDRICAL_SURFACE('',#102929,1.66874528305244);
#87412=CYLINDRICAL_SURFACE('',#102930,1.66874528305244);
#87413=CYLINDRICAL_SURFACE('',#102931,1.66874528305244);
#87414=CYLINDRICAL_SURFACE('',#102932,1.66874528305244);
#87415=CYLINDRICAL_SURFACE('',#102933,1.66874528305244);
#87416=CYLINDRICAL_SURFACE('',#102934,1.66874528305244);
#87417=CYLINDRICAL_SURFACE('',#102935,1.66874528305244);
#87418=CYLINDRICAL_SURFACE('',#102936,1.66874528305244);
#87419=CYLINDRICAL_SURFACE('',#102937,1.66874528305244);
#87420=CYLINDRICAL_SURFACE('',#102938,1.66874528305244);
#87421=CYLINDRICAL_SURFACE('',#102940,2.);
#87422=CYLINDRICAL_SURFACE('',#102942,2.);
#87423=CYLINDRICAL_SURFACE('',#102943,2.);
#87424=CYLINDRICAL_SURFACE('',#102944,2.);
#87425=CYLINDRICAL_SURFACE('',#102945,2.);
#87426=CYLINDRICAL_SURFACE('',#102946,2.);
#87427=CYLINDRICAL_SURFACE('',#102947,2.);
#87428=CYLINDRICAL_SURFACE('',#102948,2.);
#87429=CYLINDRICAL_SURFACE('',#102949,2.);
#87430=CYLINDRICAL_SURFACE('',#102950,2.);
#87431=CYLINDRICAL_SURFACE('',#102951,2.);
#87432=CYLINDRICAL_SURFACE('',#102952,2.);
#87433=CYLINDRICAL_SURFACE('',#102953,2.);
#87434=CYLINDRICAL_SURFACE('',#102954,2.);
#87435=CYLINDRICAL_SURFACE('',#102955,2.);
#87436=CYLINDRICAL_SURFACE('',#102956,2.);
#87437=CYLINDRICAL_SURFACE('',#102957,2.);
#87438=CYLINDRICAL_SURFACE('',#102958,2.);
#87439=CYLINDRICAL_SURFACE('',#102960,1.66874528305248);
#87440=CYLINDRICAL_SURFACE('',#102961,1.66874528305248);
#87441=CYLINDRICAL_SURFACE('',#102962,1.66874528305248);
#87442=CYLINDRICAL_SURFACE('',#102963,1.66874528305248);
#87443=CYLINDRICAL_SURFACE('',#102964,1.66874528305248);
#87444=CYLINDRICAL_SURFACE('',#102965,1.66874528305248);
#87445=CYLINDRICAL_SURFACE('',#102966,1.66874528305248);
#87446=CYLINDRICAL_SURFACE('',#102967,1.66874528305248);
#87447=CYLINDRICAL_SURFACE('',#102968,1.66874528305248);
#87448=CYLINDRICAL_SURFACE('',#102969,1.66874528305248);
#87449=CYLINDRICAL_SURFACE('',#102970,1.66874528305248);
#87450=CYLINDRICAL_SURFACE('',#102971,1.66874528305248);
#87451=CYLINDRICAL_SURFACE('',#102972,1.66874528305248);
#87452=CYLINDRICAL_SURFACE('',#102973,1.66874528305248);
#87453=CYLINDRICAL_SURFACE('',#102974,1.66874528305248);
#87454=CYLINDRICAL_SURFACE('',#102975,1.66874528305248);
#87455=CYLINDRICAL_SURFACE('',#102976,1.66874528305248);
#87456=CYLINDRICAL_SURFACE('',#102977,1.66874528305248);
#87457=CYLINDRICAL_SURFACE('',#102978,1.66874528305248);
#87458=CYLINDRICAL_SURFACE('',#102980,2.);
#87459=CYLINDRICAL_SURFACE('',#102982,2.);
#87460=CYLINDRICAL_SURFACE('',#102983,2.);
#87461=CYLINDRICAL_SURFACE('',#102984,2.);
#87462=CYLINDRICAL_SURFACE('',#102985,2.);
#87463=CYLINDRICAL_SURFACE('',#102986,2.);
#87464=CYLINDRICAL_SURFACE('',#102987,2.);
#87465=CYLINDRICAL_SURFACE('',#102988,2.);
#87466=CYLINDRICAL_SURFACE('',#102989,2.);
#87467=CYLINDRICAL_SURFACE('',#102990,2.);
#87468=CYLINDRICAL_SURFACE('',#102991,2.);
#87469=CYLINDRICAL_SURFACE('',#102992,2.);
#87470=CYLINDRICAL_SURFACE('',#102993,2.);
#87471=CYLINDRICAL_SURFACE('',#102994,2.);
#87472=CYLINDRICAL_SURFACE('',#102995,2.);
#87473=CYLINDRICAL_SURFACE('',#102996,2.);
#87474=CYLINDRICAL_SURFACE('',#102997,2.);
#87475=CYLINDRICAL_SURFACE('',#102998,2.);
#87476=CYLINDRICAL_SURFACE('',#102999,2.);
#87477=CYLINDRICAL_SURFACE('',#103000,1.66874528305242);
#87478=CYLINDRICAL_SURFACE('',#103001,1.66874528305242);
#87479=CYLINDRICAL_SURFACE('',#103002,1.66874528305242);
#87480=CYLINDRICAL_SURFACE('',#103003,1.66874528305242);
#87481=CYLINDRICAL_SURFACE('',#103004,1.66874528305242);
#87482=CYLINDRICAL_SURFACE('',#103005,1.66874528305242);
#87483=CYLINDRICAL_SURFACE('',#103006,1.66874528305242);
#87484=CYLINDRICAL_SURFACE('',#103007,1.66874528305242);
#87485=CYLINDRICAL_SURFACE('',#103008,1.66874528305242);
#87486=CYLINDRICAL_SURFACE('',#103009,1.66874528305242);
#87487=CYLINDRICAL_SURFACE('',#103010,1.66874528305242);
#87488=CYLINDRICAL_SURFACE('',#103011,1.66874528305242);
#87489=CYLINDRICAL_SURFACE('',#103012,1.66874528305242);
#87490=CYLINDRICAL_SURFACE('',#103013,1.66874528305242);
#87491=CYLINDRICAL_SURFACE('',#103014,1.66874528305242);
#87492=CYLINDRICAL_SURFACE('',#103015,1.66874528305242);
#87493=CYLINDRICAL_SURFACE('',#103016,1.66874528305242);
#87494=CYLINDRICAL_SURFACE('',#103017,1.66874528305242);
#87495=CYLINDRICAL_SURFACE('',#103018,1.66874528305242);
#87496=CYLINDRICAL_SURFACE('',#103020,1.66874528305242);
#87497=CYLINDRICAL_SURFACE('',#103021,1.66874528305242);
#87498=CYLINDRICAL_SURFACE('',#103022,1.66874528305242);
#87499=CYLINDRICAL_SURFACE('',#103023,1.66874528305242);
#87500=CYLINDRICAL_SURFACE('',#103024,1.66874528305242);
#87501=CYLINDRICAL_SURFACE('',#103025,1.66874528305242);
#87502=CYLINDRICAL_SURFACE('',#103026,1.66874528305242);
#87503=CYLINDRICAL_SURFACE('',#103027,1.66874528305242);
#87504=CYLINDRICAL_SURFACE('',#103028,1.66874528305242);
#87505=CYLINDRICAL_SURFACE('',#103029,1.66874528305242);
#87506=CYLINDRICAL_SURFACE('',#103030,1.66874528305242);
#87507=CYLINDRICAL_SURFACE('',#103031,1.66874528305242);
#87508=CYLINDRICAL_SURFACE('',#103032,1.66874528305242);
#87509=CYLINDRICAL_SURFACE('',#103033,1.66874528305242);
#87510=CYLINDRICAL_SURFACE('',#103034,1.66874528305242);
#87511=CYLINDRICAL_SURFACE('',#103035,1.66874528305242);
#87512=CYLINDRICAL_SURFACE('',#103036,1.66874528305242);
#87513=CYLINDRICAL_SURFACE('',#103037,1.66874528305242);
#87514=CYLINDRICAL_SURFACE('',#103038,1.66874528305242);
#87515=CYLINDRICAL_SURFACE('',#103059,3.);
#87516=CYLINDRICAL_SURFACE('',#103061,6.);
#87517=CYLINDRICAL_SURFACE('',#103066,3.);
#87518=CYLINDRICAL_SURFACE('',#103068,6.);
#87519=CYLINDRICAL_SURFACE('',#103073,3.);
#87520=CYLINDRICAL_SURFACE('',#103075,6.);
#87521=CYLINDRICAL_SURFACE('',#103080,3.);
#87522=CYLINDRICAL_SURFACE('',#103082,6.00000000000001);
#87523=CYLINDRICAL_SURFACE('',#103122,7.);
#87524=CYLINDRICAL_SURFACE('',#103138,0.999999999999999);
#87525=CYLINDRICAL_SURFACE('',#103143,0.999999999999997);
#87526=CYLINDRICAL_SURFACE('',#103154,1.);
#87527=CYLINDRICAL_SURFACE('',#103157,1.);
#87528=CYLINDRICAL_SURFACE('',#103164,1.);
#87529=CYLINDRICAL_SURFACE('',#103167,1.);
#87530=CYLINDRICAL_SURFACE('',#103169,20.);
#87531=CYLINDRICAL_SURFACE('',#103174,3.);
#87532=CYLINDRICAL_SURFACE('',#103176,3.);
#87533=CYLINDRICAL_SURFACE('',#103178,3.);
#87534=CYLINDRICAL_SURFACE('',#103182,3.);
#87535=CYLINDRICAL_SURFACE('',#103184,3.);
#87536=CYLINDRICAL_SURFACE('',#103189,67.5);
#87537=CYLINDRICAL_SURFACE('',#103197,3.);
#87538=CYLINDRICAL_SURFACE('',#103199,3.);
#87539=CYLINDRICAL_SURFACE('',#103204,67.5);
#87540=CYLINDRICAL_SURFACE('',#103216,3.);
#87541=CYLINDRICAL_SURFACE('',#103218,3.);
#87542=CYLINDRICAL_SURFACE('',#103220,3.);
#87543=CYLINDRICAL_SURFACE('',#103222,3.);
#87544=CYLINDRICAL_SURFACE('',#103224,58.3875000000282);
#87545=CYLINDRICAL_SURFACE('',#103229,3.);
#87546=CYLINDRICAL_SURFACE('',#103231,3.);
#87547=CYLINDRICAL_SURFACE('',#103236,67.5);
#87548=CYLINDRICAL_SURFACE('',#103244,58.3875000000282);
#87549=CYLINDRICAL_SURFACE('',#103249,3.);
#87550=CYLINDRICAL_SURFACE('',#103251,3.);
#87551=CYLINDRICAL_SURFACE('',#103256,67.5);
#87552=CYLINDRICAL_SURFACE('',#103264,58.3875000000282);
#87553=CYLINDRICAL_SURFACE('',#103282,3.);
#87554=CYLINDRICAL_SURFACE('',#103284,58.3875000000282);
#87555=CYLINDRICAL_SURFACE('',#103289,2.);
#87556=CYLINDRICAL_SURFACE('',#103292,1.66874528305242);
#87557=CYLINDRICAL_SURFACE('',#103293,2.);
#87558=CYLINDRICAL_SURFACE('',#103295,1.66874528305242);
#87559=CYLINDRICAL_SURFACE('',#103296,2.);
#87560=CYLINDRICAL_SURFACE('',#103297,2.);
#87561=CYLINDRICAL_SURFACE('',#103299,1.66874528305248);
#87562=CYLINDRICAL_SURFACE('',#103300,2.);
#87563=CYLINDRICAL_SURFACE('',#103301,2.);
#87564=CYLINDRICAL_SURFACE('',#103305,1.66874528305244);
#87565=CYLINDRICAL_SURFACE('',#103306,2.);
#87566=CYLINDRICAL_SURFACE('',#103307,2.);
#87567=CYLINDRICAL_SURFACE('',#103309,53.8875000000282);
#87568=CYLINDRICAL_SURFACE('',#103312,10.);
#87569=CYLINDRICAL_SURFACE('',#103316,10.);
#87570=CYLINDRICAL_SURFACE('',#103318,10.);
#87571=CYLINDRICAL_SURFACE('',#103321,10.);
#87572=CYLINDRICAL_SURFACE('',#103327,10.);
#87573=CYLINDRICAL_SURFACE('',#103329,10.);
#87574=CYLINDRICAL_SURFACE('',#103331,10.);
#87575=CYLINDRICAL_SURFACE('',#103345,32.4);
#87576=CYLINDRICAL_SURFACE('',#103347,23.324544);
#87577=CYLINDRICAL_SURFACE('',#103348,5.77396800000001);
#87578=CYLINDRICAL_SURFACE('',#103351,5.77396800000001);
#87579=CYLINDRICAL_SURFACE('',#103354,5.77396800000001);
#87580=CYLINDRICAL_SURFACE('',#103357,5.77396800000001);
#87581=CYLINDRICAL_SURFACE('',#103360,5.77396800000001);
#87582=CYLINDRICAL_SURFACE('',#103363,5.77396800000001);
#87583=CYLINDRICAL_SURFACE('',#103366,23.324544);
#87584=CYLINDRICAL_SURFACE('',#103367,15.12);
#87585=CYLINDRICAL_SURFACE('',#103424,49.6934108978581);
#87586=CYLINDRICAL_SURFACE('',#103426,49.6934108978581);
#87587=CYLINDRICAL_SURFACE('',#103428,49.6934108978581);
#87588=CYLINDRICAL_SURFACE('',#103430,49.6934108978581);
#87589=CYLINDRICAL_SURFACE('',#103432,49.6934108978581);
#87590=CYLINDRICAL_SURFACE('',#103434,49.6934108978581);
#87591=CYLINDRICAL_SURFACE('',#103436,49.6934108978581);
#87592=CYLINDRICAL_SURFACE('',#103438,49.6934108978581);
#87593=CYLINDRICAL_SURFACE('',#103440,49.6934108978581);
#87594=CYLINDRICAL_SURFACE('',#103442,49.6934108978581);
#87595=CYLINDRICAL_SURFACE('',#103444,49.6934108978581);
#87596=CYLINDRICAL_SURFACE('',#103446,49.6934108978581);
#87597=CYLINDRICAL_SURFACE('',#103448,49.6934108978581);
#87598=CYLINDRICAL_SURFACE('',#103450,49.6934108978581);
#87599=CYLINDRICAL_SURFACE('',#103482,49.6934108978581);
#87600=CYLINDRICAL_SURFACE('',#103496,23.324544);
#87601=CYLINDRICAL_SURFACE('',#103497,23.324544);
#87602=CYLINDRICAL_SURFACE('',#103498,5.77396800000001);
#87603=CYLINDRICAL_SURFACE('',#103499,23.324544);
#87604=CYLINDRICAL_SURFACE('',#103500,5.773968);
#87605=CYLINDRICAL_SURFACE('',#103501,23.324544);
#87606=CYLINDRICAL_SURFACE('',#103502,23.324544);
#87607=CYLINDRICAL_SURFACE('',#103503,23.324544);
#87608=CYLINDRICAL_SURFACE('',#103504,23.324544);
#87609=CYLINDRICAL_SURFACE('',#103505,23.324544);
#87610=CYLINDRICAL_SURFACE('',#103506,23.324544);
#87611=CYLINDRICAL_SURFACE('',#103507,23.324544);
#87612=CYLINDRICAL_SURFACE('',#103508,23.324544);
#87613=CYLINDRICAL_SURFACE('',#103509,23.324544);
#87614=CYLINDRICAL_SURFACE('',#103510,23.324544);
#87615=CYLINDRICAL_SURFACE('',#103511,5.773968);
#87616=CYLINDRICAL_SURFACE('',#103512,23.324544);
#87617=CYLINDRICAL_SURFACE('',#103513,23.324544);
#87618=CYLINDRICAL_SURFACE('',#103514,23.324544);
#87619=CYLINDRICAL_SURFACE('',#103515,23.324544);
#87620=CYLINDRICAL_SURFACE('',#103516,23.324544);
#87621=CYLINDRICAL_SURFACE('',#103517,23.324544);
#87622=CYLINDRICAL_SURFACE('',#103518,5.773968);
#87623=CYLINDRICAL_SURFACE('',#103519,23.324544);
#87624=CYLINDRICAL_SURFACE('',#103520,23.324544);
#87625=CYLINDRICAL_SURFACE('',#103521,5.77396800000001);
#87626=CYLINDRICAL_SURFACE('',#103522,23.324544);
#87627=CYLINDRICAL_SURFACE('',#103523,5.773968);
#87628=CYLINDRICAL_SURFACE('',#103524,23.324544);
#87629=CYLINDRICAL_SURFACE('',#103525,23.324544);
#87630=CYLINDRICAL_SURFACE('',#103526,5.773968);
#87631=CYLINDRICAL_SURFACE('',#103527,23.324544);
#87632=CYLINDRICAL_SURFACE('',#103528,23.324544);
#87633=CYLINDRICAL_SURFACE('',#103529,5.773968);
#87634=CYLINDRICAL_SURFACE('',#103530,23.324544);
#87635=CYLINDRICAL_SURFACE('',#103531,23.324544);
#87636=CYLINDRICAL_SURFACE('',#103532,5.773968);
#87637=CYLINDRICAL_SURFACE('',#103536,10.12);
#87638=CYLINDRICAL_SURFACE('',#103539,15.12);
#87639=CYLINDRICAL_SURFACE('',#103552,25.2);
#87640=CYLINDRICAL_SURFACE('',#103554,25.611264);
#87641=CYLINDRICAL_SURFACE('',#103555,25.611264);
#87642=CYLINDRICAL_SURFACE('',#103556,3.36814799999999);
#87643=CYLINDRICAL_SURFACE('',#103559,3.36814799999999);
#87644=CYLINDRICAL_SURFACE('',#103562,3.36814799999999);
#87645=CYLINDRICAL_SURFACE('',#103565,3.36814799999999);
#87646=CYLINDRICAL_SURFACE('',#103568,3.36814799999999);
#87647=CYLINDRICAL_SURFACE('',#103571,3.36814799999999);
#87648=CYLINDRICAL_SURFACE('',#103574,3.36814799999999);
#87649=CYLINDRICAL_SURFACE('',#103577,3.36814799999999);
#87650=CYLINDRICAL_SURFACE('',#103580,3.36814799999999);
#87651=CYLINDRICAL_SURFACE('',#103583,3.36814799999999);
#87652=CYLINDRICAL_SURFACE('',#103586,3.36814799999999);
#87653=CYLINDRICAL_SURFACE('',#103589,3.36814799999999);
#87654=CYLINDRICAL_SURFACE('',#103595,54.361863151615);
#87655=CYLINDRICAL_SURFACE('',#103599,8.82);
#87656=CYLINDRICAL_SURFACE('',#103707,54.361863151615);
#87657=CYLINDRICAL_SURFACE('',#103709,54.361863151615);
#87658=CYLINDRICAL_SURFACE('',#103711,54.361863151615);
#87659=CYLINDRICAL_SURFACE('',#103713,54.361863151615);
#87660=CYLINDRICAL_SURFACE('',#103715,54.361863151615);
#87661=CYLINDRICAL_SURFACE('',#103717,54.361863151615);
#87662=CYLINDRICAL_SURFACE('',#103719,54.361863151615);
#87663=CYLINDRICAL_SURFACE('',#103721,54.361863151615);
#87664=CYLINDRICAL_SURFACE('',#103723,54.361863151615);
#87665=CYLINDRICAL_SURFACE('',#103725,54.361863151615);
#87666=CYLINDRICAL_SURFACE('',#103727,54.361863151615);
#87667=CYLINDRICAL_SURFACE('',#103729,54.361863151615);
#87668=CYLINDRICAL_SURFACE('',#103731,54.361863151615);
#87669=CYLINDRICAL_SURFACE('',#103733,54.361863151615);
#87670=CYLINDRICAL_SURFACE('',#103735,54.361863151615);
#87671=CYLINDRICAL_SURFACE('',#103737,54.361863151615);
#87672=CYLINDRICAL_SURFACE('',#103739,54.361863151615);
#87673=CYLINDRICAL_SURFACE('',#103741,54.361863151615);
#87674=CYLINDRICAL_SURFACE('',#103743,54.361863151615);
#87675=CYLINDRICAL_SURFACE('',#103745,54.361863151615);
#87676=CYLINDRICAL_SURFACE('',#103747,54.361863151615);
#87677=CYLINDRICAL_SURFACE('',#103749,54.361863151615);
#87678=CYLINDRICAL_SURFACE('',#103751,54.361863151615);
#87679=CYLINDRICAL_SURFACE('',#103753,54.361863151615);
#87680=CYLINDRICAL_SURFACE('',#103755,54.361863151615);
#87681=CYLINDRICAL_SURFACE('',#103757,54.361863151615);
#87682=CYLINDRICAL_SURFACE('',#103759,54.361863151615);
#87683=CYLINDRICAL_SURFACE('',#103761,54.361863151615);
#87684=CYLINDRICAL_SURFACE('',#103821,54.361863151615);
#87685=CYLINDRICAL_SURFACE('',#103844,25.611264);
#87686=CYLINDRICAL_SURFACE('',#103845,25.611264);
#87687=CYLINDRICAL_SURFACE('',#103846,3.36814799999999);
#87688=CYLINDRICAL_SURFACE('',#103847,25.611264);
#87689=CYLINDRICAL_SURFACE('',#103848,25.611264);
#87690=CYLINDRICAL_SURFACE('',#103849,3.36814799999999);
#87691=CYLINDRICAL_SURFACE('',#103850,25.611264);
#87692=CYLINDRICAL_SURFACE('',#103851,25.611264);
#87693=CYLINDRICAL_SURFACE('',#103852,25.611264);
#87694=CYLINDRICAL_SURFACE('',#103853,25.611264);
#87695=CYLINDRICAL_SURFACE('',#103854,25.611264);
#87696=CYLINDRICAL_SURFACE('',#103855,25.611264);
#87697=CYLINDRICAL_SURFACE('',#103856,25.611264);
#87698=CYLINDRICAL_SURFACE('',#103857,25.611264);
#87699=CYLINDRICAL_SURFACE('',#103858,3.36814799999999);
#87700=CYLINDRICAL_SURFACE('',#103859,25.611264);
#87701=CYLINDRICAL_SURFACE('',#103860,25.611264);
#87702=CYLINDRICAL_SURFACE('',#103861,25.611264);
#87703=CYLINDRICAL_SURFACE('',#103862,25.611264);
#87704=CYLINDRICAL_SURFACE('',#103863,25.611264);
#87705=CYLINDRICAL_SURFACE('',#103864,25.611264);
#87706=CYLINDRICAL_SURFACE('',#103865,25.611264);
#87707=CYLINDRICAL_SURFACE('',#103866,25.611264);
#87708=CYLINDRICAL_SURFACE('',#103867,3.36814799999999);
#87709=CYLINDRICAL_SURFACE('',#103868,25.611264);
#87710=CYLINDRICAL_SURFACE('',#103869,25.611264);
#87711=CYLINDRICAL_SURFACE('',#103870,25.611264);
#87712=CYLINDRICAL_SURFACE('',#103871,25.611264);
#87713=CYLINDRICAL_SURFACE('',#103872,25.611264);
#87714=CYLINDRICAL_SURFACE('',#103873,25.611264);
#87715=CYLINDRICAL_SURFACE('',#103874,25.611264);
#87716=CYLINDRICAL_SURFACE('',#103875,25.611264);
#87717=CYLINDRICAL_SURFACE('',#103876,25.611264);
#87718=CYLINDRICAL_SURFACE('',#103877,25.611264);
#87719=CYLINDRICAL_SURFACE('',#103878,25.611264);
#87720=CYLINDRICAL_SURFACE('',#103879,25.611264);
#87721=CYLINDRICAL_SURFACE('',#103880,25.611264);
#87722=CYLINDRICAL_SURFACE('',#103881,25.611264);
#87723=CYLINDRICAL_SURFACE('',#103882,3.36814799999999);
#87724=CYLINDRICAL_SURFACE('',#103883,25.611264);
#87725=CYLINDRICAL_SURFACE('',#103884,25.611264);
#87726=CYLINDRICAL_SURFACE('',#103885,3.36814799999999);
#87727=CYLINDRICAL_SURFACE('',#103886,25.611264);
#87728=CYLINDRICAL_SURFACE('',#103887,25.611264);
#87729=CYLINDRICAL_SURFACE('',#103888,3.36814799999999);
#87730=CYLINDRICAL_SURFACE('',#103889,25.611264);
#87731=CYLINDRICAL_SURFACE('',#103890,3.36814799999999);
#87732=CYLINDRICAL_SURFACE('',#103891,25.611264);
#87733=CYLINDRICAL_SURFACE('',#103892,25.611264);
#87734=CYLINDRICAL_SURFACE('',#103893,3.36814799999999);
#87735=CYLINDRICAL_SURFACE('',#103894,25.611264);
#87736=CYLINDRICAL_SURFACE('',#103895,25.611264);
#87737=CYLINDRICAL_SURFACE('',#103896,3.36814799999999);
#87738=CYLINDRICAL_SURFACE('',#103897,25.611264);
#87739=CYLINDRICAL_SURFACE('',#103898,25.611264);
#87740=CYLINDRICAL_SURFACE('',#103899,3.368148);
#87741=CYLINDRICAL_SURFACE('',#103900,25.611264);
#87742=CYLINDRICAL_SURFACE('',#103901,25.611264);
#87743=CYLINDRICAL_SURFACE('',#103902,3.368148);
#87744=CYLINDRICAL_SURFACE('',#103903,25.611264);
#87745=CYLINDRICAL_SURFACE('',#103904,25.611264);
#87746=CYLINDRICAL_SURFACE('',#103905,3.36814799999999);
#87747=CYLINDRICAL_SURFACE('',#103906,25.611264);
#87748=CYLINDRICAL_SURFACE('',#103907,3.36814799999999);
#87749=CYLINDRICAL_SURFACE('',#103908,25.611264);
#87750=CYLINDRICAL_SURFACE('',#103909,25.611264);
#87751=CYLINDRICAL_SURFACE('',#103910,3.36814799999999);
#87752=CYLINDRICAL_SURFACE('',#103911,25.611264);
#87753=CYLINDRICAL_SURFACE('',#103912,25.611264);
#87754=CYLINDRICAL_SURFACE('',#103913,3.36814799999999);
#87755=CYLINDRICAL_SURFACE('',#103914,25.611264);
#87756=CYLINDRICAL_SURFACE('',#103915,25.611264);
#87757=CYLINDRICAL_SURFACE('',#103916,3.36814799999999);
#87758=CYLINDRICAL_SURFACE('',#103917,25.611264);
#87759=CYLINDRICAL_SURFACE('',#103918,25.611264);
#87760=CYLINDRICAL_SURFACE('',#103919,3.36814799999999);
#87761=CYLINDRICAL_SURFACE('',#103924,3.95);
#87762=CYLINDRICAL_SURFACE('',#103927,10.5);
#87763=CYLINDRICAL_SURFACE('',#103930,3.95);
#87764=CYLINDRICAL_SURFACE('',#103933,10.5);
#87765=CYLINDRICAL_SURFACE('',#103936,10.5);
#87766=CYLINDRICAL_SURFACE('',#103939,10.5);
#87767=CYLINDRICAL_SURFACE('',#103944,3.95);
#87768=CYLINDRICAL_SURFACE('',#103947,3.95);
#87769=CYLINDRICAL_SURFACE('',#103950,10.5);
#87770=CYLINDRICAL_SURFACE('',#103961,10.5);
#87771=CYLINDRICAL_SURFACE('',#103962,10.5);
#87772=CYLINDRICAL_SURFACE('',#103963,10.5);
#87773=CYLINDRICAL_SURFACE('',#103964,3.95);
#87774=CYLINDRICAL_SURFACE('',#103969,3.95);
#87775=CYLINDRICAL_SURFACE('',#104113,36.25);
#87776=CYLINDRICAL_SURFACE('',#104116,36.25);
#87777=CYLINDRICAL_SURFACE('',#104119,45.);
#87778=CYLINDRICAL_SURFACE('',#104122,30.);
#87779=CYLINDRICAL_SURFACE('',#104151,23.4);
#87780=CYLINDRICAL_SURFACE('',#104152,23.4);
#87781=CYLINDRICAL_SURFACE('',#104153,23.4);
#87782=CYLINDRICAL_SURFACE('',#104168,36.);
#87783=CYLINDRICAL_SURFACE('',#104224,7.25);
#87784=CYLINDRICAL_SURFACE('',#104227,16.);
#87785=CYLINDRICAL_SURFACE('',#104230,7.25);
#87786=CYLINDRICAL_SURFACE('',#104233,16.);
#87787=CYLINDRICAL_SURFACE('',#104249,10.0514428414941);
#87788=CYLINDRICAL_SURFACE('',#104251,10.0514428414941);
#87789=CYLINDRICAL_SURFACE('',#104253,10.0514428414941);
#87790=CYLINDRICAL_SURFACE('',#104254,10.0514428414941);
#87791=CYLINDRICAL_SURFACE('',#104255,10.0514428414941);
#87792=CYLINDRICAL_SURFACE('',#104259,12.);
#87793=CYLINDRICAL_SURFACE('',#104261,12.);
#87794=CYLINDRICAL_SURFACE('',#104263,12.);
#87795=CYLINDRICAL_SURFACE('',#104264,12.);
#87796=CYLINDRICAL_SURFACE('',#104265,12.);
#87797=CYLINDRICAL_SURFACE('',#104266,12.);
#87798=CYLINDRICAL_SURFACE('',#104268,12.);
#87799=CYLINDRICAL_SURFACE('',#104305,10.0514428414941);
#87800=CYLINDRICAL_SURFACE('',#104306,10.0514428414941);
#87801=CYLINDRICAL_SURFACE('',#104308,10.0514428414941);
#87802=CYLINDRICAL_SURFACE('',#104309,10.0514428414941);
#87803=CYLINDRICAL_SURFACE('',#104310,10.0514428414941);
#87804=CYLINDRICAL_SURFACE('',#104311,10.0514428414941);
#87805=CYLINDRICAL_SURFACE('',#104312,10.0514428414941);
#87806=CYLINDRICAL_SURFACE('',#104314,12.);
#87807=CYLINDRICAL_SURFACE('',#104316,12.);
#87808=CYLINDRICAL_SURFACE('',#104317,12.);
#87809=CYLINDRICAL_SURFACE('',#104318,12.);
#87810=CYLINDRICAL_SURFACE('',#104319,12.);
#87811=CYLINDRICAL_SURFACE('',#104320,12.);
#87812=CYLINDRICAL_SURFACE('',#104321,12.);
#87813=CYLINDRICAL_SURFACE('',#104323,12.);
#87814=CYLINDRICAL_SURFACE('',#104347,10.0514428414941);
#87815=CYLINDRICAL_SURFACE('',#104348,10.0514428414941);
#87816=CYLINDRICAL_SURFACE('',#104353,12.);
#87817=CYLINDRICAL_SURFACE('',#104355,10.0514428414941);
#87818=CYLINDRICAL_SURFACE('',#104358,10.0514428414941);
#87819=CYLINDRICAL_SURFACE('',#104360,10.0514428414941);
#87820=CYLINDRICAL_SURFACE('',#104361,10.0514428414941);
#87821=CYLINDRICAL_SURFACE('',#104362,10.0514428414941);
#87822=CYLINDRICAL_SURFACE('',#104363,10.0514428414941);
#87823=CYLINDRICAL_SURFACE('',#104364,10.0514428414941);
#87824=CYLINDRICAL_SURFACE('',#104365,10.0514428414941);
#87825=CYLINDRICAL_SURFACE('',#104366,10.0514428414941);
#87826=CYLINDRICAL_SURFACE('',#104367,10.0514428414941);
#87827=CYLINDRICAL_SURFACE('',#104368,10.0514428414941);
#87828=CYLINDRICAL_SURFACE('',#104369,10.0514428414941);
#87829=CYLINDRICAL_SURFACE('',#104370,10.0514428414941);
#87830=CYLINDRICAL_SURFACE('',#104371,10.0514428414941);
#87831=CYLINDRICAL_SURFACE('',#104372,10.0514428414941);
#87832=CYLINDRICAL_SURFACE('',#104373,10.0514428414941);
#87833=CYLINDRICAL_SURFACE('',#104374,10.0514428414941);
#87834=CYLINDRICAL_SURFACE('',#104375,10.0514428414941);
#87835=CYLINDRICAL_SURFACE('',#104376,10.0514428414941);
#87836=CYLINDRICAL_SURFACE('',#104377,10.0514428414941);
#87837=CYLINDRICAL_SURFACE('',#104378,10.0514428414941);
#87838=CYLINDRICAL_SURFACE('',#104379,10.0514428414941);
#87839=CYLINDRICAL_SURFACE('',#104381,10.0514428414941);
#87840=CYLINDRICAL_SURFACE('',#104382,10.0514428414941);
#87841=CYLINDRICAL_SURFACE('',#104383,10.0514428414941);
#87842=CYLINDRICAL_SURFACE('',#104384,10.0514428414941);
#87843=CYLINDRICAL_SURFACE('',#104385,10.0514428414941);
#87844=CYLINDRICAL_SURFACE('',#104386,10.0514428414941);
#87845=CYLINDRICAL_SURFACE('',#104387,10.0514428414941);
#87846=CYLINDRICAL_SURFACE('',#104388,10.0514428414941);
#87847=CYLINDRICAL_SURFACE('',#104389,10.0514428414941);
#87848=CYLINDRICAL_SURFACE('',#104390,10.0514428414941);
#87849=CYLINDRICAL_SURFACE('',#104391,10.0514428414941);
#87850=CYLINDRICAL_SURFACE('',#104392,10.0514428414941);
#87851=CYLINDRICAL_SURFACE('',#104393,12.);
#87852=CYLINDRICAL_SURFACE('',#104395,12.);
#87853=CYLINDRICAL_SURFACE('',#104396,12.);
#87854=CYLINDRICAL_SURFACE('',#104397,12.);
#87855=CYLINDRICAL_SURFACE('',#104398,12.);
#87856=CYLINDRICAL_SURFACE('',#104399,12.);
#87857=CYLINDRICAL_SURFACE('',#104400,12.);
#87858=CYLINDRICAL_SURFACE('',#104401,12.);
#87859=CYLINDRICAL_SURFACE('',#104402,12.);
#87860=CYLINDRICAL_SURFACE('',#104403,12.);
#87861=CYLINDRICAL_SURFACE('',#104404,12.);
#87862=CYLINDRICAL_SURFACE('',#104405,12.);
#87863=CYLINDRICAL_SURFACE('',#104406,12.);
#87864=CYLINDRICAL_SURFACE('',#104407,12.);
#87865=CYLINDRICAL_SURFACE('',#104409,12.);
#87866=CYLINDRICAL_SURFACE('',#104410,12.);
#87867=CYLINDRICAL_SURFACE('',#104411,12.);
#87868=CYLINDRICAL_SURFACE('',#104412,12.);
#87869=CYLINDRICAL_SURFACE('',#104413,12.);
#87870=CYLINDRICAL_SURFACE('',#104414,12.);
#87871=CYLINDRICAL_SURFACE('',#104415,12.);
#87872=CYLINDRICAL_SURFACE('',#104416,12.);
#87873=CYLINDRICAL_SURFACE('',#104417,12.);
#87874=CYLINDRICAL_SURFACE('',#104418,12.);
#87875=CYLINDRICAL_SURFACE('',#104419,12.);
#87876=CYLINDRICAL_SURFACE('',#104420,12.);
#87877=CYLINDRICAL_SURFACE('',#104421,12.);
#87878=CYLINDRICAL_SURFACE('',#104422,12.);
#87879=CYLINDRICAL_SURFACE('',#104423,12.);
#87880=CYLINDRICAL_SURFACE('',#104424,12.);
#87881=CYLINDRICAL_SURFACE('',#104425,12.);
#87882=CYLINDRICAL_SURFACE('',#104426,12.);
#87883=CYLINDRICAL_SURFACE('',#104427,12.);
#87884=CYLINDRICAL_SURFACE('',#104435,12.);
#87885=CYLINDRICAL_SURFACE('',#104437,10.0514428414941);
#87886=CYLINDRICAL_SURFACE('',#104477,10.0514428414941);
#87887=CYLINDRICAL_SURFACE('',#104478,1.190625);
#87888=CYLINDRICAL_SURFACE('',#104481,1.190625);
#87889=CYLINDRICAL_SURFACE('',#104484,1.190625);
#87890=CYLINDRICAL_SURFACE('',#104487,1.19062499999999);
#87891=CYLINDRICAL_SURFACE('',#104490,1.190625);
#87892=CYLINDRICAL_SURFACE('',#104493,1.190625);
#87893=CYLINDRICAL_SURFACE('',#104496,1.190625);
#87894=CYLINDRICAL_SURFACE('',#104499,1.190625);
#87895=CYLINDRICAL_SURFACE('',#104502,1.190625);
#87896=CYLINDRICAL_SURFACE('',#104505,55.2538194444444);
#87897=CYLINDRICAL_SURFACE('',#104508,44.5707880434783);
#87898=CYLINDRICAL_SURFACE('',#104523,16.8332621659243);
#87899=CYLINDRICAL_SURFACE('',#104528,44.5707880434783);
#87900=CYLINDRICAL_SURFACE('',#104563,6.00000000000001);
#87901=CYLINDRICAL_SURFACE('',#104566,6.00000000000001);
#87902=CYLINDRICAL_SURFACE('',#104569,6.00000000000001);
#87903=CYLINDRICAL_SURFACE('',#104572,6.00000000000001);
#87904=CYLINDRICAL_SURFACE('',#104575,6.00000000000001);
#87905=CYLINDRICAL_SURFACE('',#104578,6.00000000000001);
#87906=CYLINDRICAL_SURFACE('',#104581,6.00000000000001);
#87907=CYLINDRICAL_SURFACE('',#104584,6.00000000000001);
#87908=CYLINDRICAL_SURFACE('',#104598,7.00000000000001);
#87909=CYLINDRICAL_SURFACE('',#104601,7.);
#87910=CYLINDRICAL_SURFACE('',#104626,6.4732);
#87911=CYLINDRICAL_SURFACE('',#104628,6.4732);
#87912=CYLINDRICAL_SURFACE('',#104629,0.7366);
#87913=CYLINDRICAL_SURFACE('',#104631,0.736599999999997);
#87914=CYLINDRICAL_SURFACE('',#104643,6.);
#87915=CYLINDRICAL_SURFACE('',#104645,6.);
#87916=CYLINDRICAL_SURFACE('',#104646,6.);
#87917=CYLINDRICAL_SURFACE('',#104647,6.);
#87918=CYLINDRICAL_SURFACE('',#104648,6.);
#87919=CYLINDRICAL_SURFACE('',#104649,6.);
#87920=CYLINDRICAL_SURFACE('',#104650,6.);
#87921=CYLINDRICAL_SURFACE('',#104651,6.);
#87922=CYLINDRICAL_SURFACE('',#104652,6.);
#87923=CYLINDRICAL_SURFACE('',#104653,6.);
#87924=CYLINDRICAL_SURFACE('',#104654,6.);
#87925=CYLINDRICAL_SURFACE('',#104655,6.);
#87926=CYLINDRICAL_SURFACE('',#104656,6.);
#87927=CYLINDRICAL_SURFACE('',#104657,6.);
#87928=CYLINDRICAL_SURFACE('',#104658,6.);
#87929=CYLINDRICAL_SURFACE('',#104659,6.);
#87930=CYLINDRICAL_SURFACE('',#104660,6.);
#87931=CYLINDRICAL_SURFACE('',#104664,4.86334165753294);
#87932=CYLINDRICAL_SURFACE('',#104665,4.86334165753294);
#87933=CYLINDRICAL_SURFACE('',#104666,4.86334165753294);
#87934=CYLINDRICAL_SURFACE('',#104667,4.86334165753294);
#87935=CYLINDRICAL_SURFACE('',#104668,4.86334165753294);
#87936=CYLINDRICAL_SURFACE('',#104669,4.86334165753294);
#87937=CYLINDRICAL_SURFACE('',#104670,4.86334165753294);
#87938=CYLINDRICAL_SURFACE('',#104671,4.86334165753294);
#87939=CYLINDRICAL_SURFACE('',#104672,4.86334165753294);
#87940=CYLINDRICAL_SURFACE('',#104673,4.86334165753294);
#87941=CYLINDRICAL_SURFACE('',#104674,4.86334165753294);
#87942=CYLINDRICAL_SURFACE('',#104675,4.86334165753294);
#87943=CYLINDRICAL_SURFACE('',#104676,4.86334165753294);
#87944=CYLINDRICAL_SURFACE('',#104677,4.86334165753294);
#87945=CYLINDRICAL_SURFACE('',#104678,4.86334165753294);
#87946=CYLINDRICAL_SURFACE('',#104679,4.86334165753294);
#87947=CYLINDRICAL_SURFACE('',#104680,4.86334165753294);
#87948=CYLINDRICAL_SURFACE('',#104686,4.86334165753294);
#87949=CYLINDRICAL_SURFACE('',#104718,6.);
#87950=CYLINDRICAL_SURFACE('',#104723,6.);
#87951=CYLINDRICAL_SURFACE('',#104725,6.);
#87952=CYLINDRICAL_SURFACE('',#104726,6.);
#87953=CYLINDRICAL_SURFACE('',#104727,6.);
#87954=CYLINDRICAL_SURFACE('',#104728,6.);
#87955=CYLINDRICAL_SURFACE('',#104731,4.86334165753295);
#87956=CYLINDRICAL_SURFACE('',#104732,4.86334165753295);
#87957=CYLINDRICAL_SURFACE('',#104733,4.86334165753295);
#87958=CYLINDRICAL_SURFACE('',#104734,4.86334165753295);
#87959=CYLINDRICAL_SURFACE('',#104736,4.86334165753295);
#87960=CYLINDRICAL_SURFACE('',#104738,0.285000000000001);
#87961=CYLINDRICAL_SURFACE('',#104739,0.285);
#87962=CYLINDRICAL_SURFACE('',#104740,0.285000000000001);
#87963=CYLINDRICAL_SURFACE('',#104741,0.285000000000001);
#87964=CYLINDRICAL_SURFACE('',#104742,0.285);
#87965=CYLINDRICAL_SURFACE('',#104743,0.285000000000001);
#87966=CYLINDRICAL_SURFACE('',#104768,6.);
#87967=ADVANCED_FACE('',(#8688),#85755,.F.);
#87968=ADVANCED_FACE('',(#8689),#85756,.F.);
#87969=ADVANCED_FACE('',(#8690),#85757,.F.);
#87970=ADVANCED_FACE('',(#8691),#85758,.F.);
#87971=ADVANCED_FACE('',(#8692),#85759,.F.);
#87972=ADVANCED_FACE('',(#8693),#85760,.F.);
#87973=ADVANCED_FACE('',(#8694),#85761,.F.);
#87974=ADVANCED_FACE('',(#8695),#85762,.F.);
#87975=ADVANCED_FACE('',(#8696),#85763,.F.);
#87976=ADVANCED_FACE('',(#8697),#85764,.F.);
#87977=ADVANCED_FACE('',(#8698),#85765,.F.);
#87978=ADVANCED_FACE('',(#8699),#85766,.F.);
#87979=ADVANCED_FACE('',(#8700),#7706,.F.);
#87980=ADVANCED_FACE('',(#8701),#7707,.F.);
#87981=ADVANCED_FACE('',(#8702,#7391,#7392,#7393,#7394,#7395,#7396,#7397,
#7398,#7399,#7400,#7401,#7402),#7708,.F.);
#87982=ADVANCED_FACE('',(#8703),#7709,.F.);
#87983=ADVANCED_FACE('',(#8704),#7710,.F.);
#87984=ADVANCED_FACE('',(#8705),#7711,.F.);
#87985=ADVANCED_FACE('',(#8706,#7403,#7404,#7405,#7406,#7407,#7408,#7409,
#7410,#7411,#7412,#7413,#7414),#7712,.F.);
#87986=ADVANCED_FACE('',(#8707),#7713,.F.);
#87987=ADVANCED_FACE('',(#8708),#7714,.T.);
#87988=ADVANCED_FACE('',(#8709),#7715,.F.);
#87989=ADVANCED_FACE('',(#8710),#85767,.T.);
#87990=ADVANCED_FACE('',(#8711),#85768,.T.);
#87991=ADVANCED_FACE('',(#8712),#85769,.F.);
#87992=ADVANCED_FACE('',(#8713),#85770,.F.);
#87993=ADVANCED_FACE('',(#8714),#85771,.F.);
#87994=ADVANCED_FACE('',(#8715),#85772,.F.);
#87995=ADVANCED_FACE('',(#8716),#85773,.F.);
#87996=ADVANCED_FACE('',(#8717),#85774,.F.);
#87997=ADVANCED_FACE('',(#8718),#85775,.F.);
#87998=ADVANCED_FACE('',(#8719),#85776,.F.);
#87999=ADVANCED_FACE('',(#8720),#85777,.F.);
#88000=ADVANCED_FACE('',(#8721),#85778,.F.);
#88001=ADVANCED_FACE('',(#8722),#85779,.F.);
#88002=ADVANCED_FACE('',(#8723),#85780,.F.);
#88003=ADVANCED_FACE('',(#8724),#85781,.F.);
#88004=ADVANCED_FACE('',(#8725),#85782,.F.);
#88005=ADVANCED_FACE('',(#8726),#7716,.F.);
#88006=ADVANCED_FACE('',(#8727),#7717,.F.);
#88007=ADVANCED_FACE('',(#8728,#7415,#7416,#7417,#7418,#7419,#7420,#7421,
#7422,#7423,#7424,#7425,#7426),#7718,.F.);
#88008=ADVANCED_FACE('',(#8729),#7719,.F.);
#88009=ADVANCED_FACE('',(#8730),#7720,.F.);
#88010=ADVANCED_FACE('',(#8731),#7721,.F.);
#88011=ADVANCED_FACE('',(#8732,#7427,#7428,#7429,#7430,#7431,#7432,#7433,
#7434,#7435,#7436,#7437,#7438),#7722,.F.);
#88012=ADVANCED_FACE('',(#8733),#7723,.F.);
#88013=ADVANCED_FACE('',(#8734),#7724,.T.);
#88014=ADVANCED_FACE('',(#8735),#7725,.F.);
#88015=ADVANCED_FACE('',(#8736),#85783,.T.);
#88016=ADVANCED_FACE('',(#8737),#85784,.T.);
#88017=ADVANCED_FACE('',(#8738),#85785,.F.);
#88018=ADVANCED_FACE('',(#8739),#85786,.F.);
#88019=ADVANCED_FACE('',(#8740),#6929,.T.);
#88020=ADVANCED_FACE('',(#8741),#7726,.T.);
#88021=ADVANCED_FACE('',(#8742),#85787,.T.);
#88022=ADVANCED_FACE('',(#8743,#7439),#7727,.F.);
#88023=ADVANCED_FACE('',(#8744),#85788,.T.);
#88024=ADVANCED_FACE('',(#8745),#7728,.F.);
#88025=ADVANCED_FACE('',(#8746),#6930,.T.);
#88026=ADVANCED_FACE('',(#8747),#7729,.T.);
#88027=ADVANCED_FACE('',(#8748),#85789,.T.);
#88028=ADVANCED_FACE('',(#8749,#7440),#7730,.F.);
#88029=ADVANCED_FACE('',(#8750),#85790,.T.);
#88030=ADVANCED_FACE('',(#8751),#7731,.F.);
#88031=ADVANCED_FACE('',(#8752),#85791,.F.);
#88032=ADVANCED_FACE('',(#8753),#85792,.F.);
#88033=ADVANCED_FACE('',(#8754),#3206,.F.);
#88034=ADVANCED_FACE('',(#8755),#2038,.F.);
#88035=ADVANCED_FACE('',(#8756),#85793,.T.);
#88036=ADVANCED_FACE('',(#8757),#7732,.T.);
#88037=ADVANCED_FACE('',(#8758),#3207,.T.);
#88038=ADVANCED_FACE('',(#8759),#85794,.T.);
#88039=ADVANCED_FACE('',(#8760),#7733,.T.);
#88040=ADVANCED_FACE('',(#8761),#3208,.T.);
#88041=ADVANCED_FACE('',(#8762),#7734,.T.);
#88042=ADVANCED_FACE('',(#8763),#2039,.F.);
#88043=ADVANCED_FACE('',(#8764),#85795,.F.);
#88044=ADVANCED_FACE('',(#8765),#3209,.T.);
#88045=ADVANCED_FACE('',(#8766),#85796,.F.);
#88046=ADVANCED_FACE('',(#8767),#2040,.F.);
#88047=ADVANCED_FACE('',(#8768),#2041,.F.);
#88048=ADVANCED_FACE('',(#8769),#2042,.F.);
#88049=ADVANCED_FACE('',(#8770),#85797,.F.);
#88050=ADVANCED_FACE('',(#8771),#3210,.T.);
#88051=ADVANCED_FACE('',(#8772),#85798,.F.);
#88052=ADVANCED_FACE('',(#8773),#2043,.F.);
#88053=ADVANCED_FACE('',(#8774),#3211,.F.);
#88054=ADVANCED_FACE('',(#8775),#2044,.F.);
#88055=ADVANCED_FACE('',(#8776),#85799,.F.);
#88056=ADVANCED_FACE('',(#8777),#3212,.T.);
#88057=ADVANCED_FACE('',(#8778),#85800,.F.);
#88058=ADVANCED_FACE('',(#8779),#2045,.F.);
#88059=ADVANCED_FACE('',(#8780),#3213,.F.);
#88060=ADVANCED_FACE('',(#8781),#85801,.F.);
#88061=ADVANCED_FACE('',(#8782),#3214,.T.);
#88062=ADVANCED_FACE('',(#8783),#85802,.F.);
#88063=ADVANCED_FACE('',(#8784),#2046,.F.);
#88064=ADVANCED_FACE('',(#8785),#3215,.F.);
#88065=ADVANCED_FACE('',(#8786),#2047,.F.);
#88066=ADVANCED_FACE('',(#8787),#85803,.F.);
#88067=ADVANCED_FACE('',(#8788),#3216,.T.);
#88068=ADVANCED_FACE('',(#8789),#85804,.F.);
#88069=ADVANCED_FACE('',(#8790),#2048,.F.);
#88070=ADVANCED_FACE('',(#8791),#2049,.F.);
#88071=ADVANCED_FACE('',(#8792),#2050,.F.);
#88072=ADVANCED_FACE('',(#8793),#85805,.F.);
#88073=ADVANCED_FACE('',(#8794),#3217,.T.);
#88074=ADVANCED_FACE('',(#8795),#85806,.F.);
#88075=ADVANCED_FACE('',(#8796),#2051,.F.);
#88076=ADVANCED_FACE('',(#8797),#2052,.F.);
#88077=ADVANCED_FACE('',(#8798),#2053,.F.);
#88078=ADVANCED_FACE('',(#8799),#85807,.F.);
#88079=ADVANCED_FACE('',(#8800),#2054,.F.);
#88080=ADVANCED_FACE('',(#8801),#3218,.F.);
#88081=ADVANCED_FACE('',(#8802),#2055,.F.);
#88082=ADVANCED_FACE('',(#8803),#85808,.F.);
#88083=ADVANCED_FACE('',(#8804),#85809,.T.);
#88084=ADVANCED_FACE('',(#8805),#2056,.F.);
#88085=ADVANCED_FACE('',(#8806),#3219,.F.);
#88086=ADVANCED_FACE('',(#8807),#2057,.F.);
#88087=ADVANCED_FACE('',(#8808),#85810,.T.);
#88088=ADVANCED_FACE('',(#8809),#7735,.T.);
#88089=ADVANCED_FACE('',(#8810),#3220,.T.);
#88090=ADVANCED_FACE('',(#8811),#85811,.T.);
#88091=ADVANCED_FACE('',(#8812),#7736,.T.);
#88092=ADVANCED_FACE('',(#8813),#3221,.T.);
#88093=ADVANCED_FACE('',(#8814),#7737,.T.);
#88094=ADVANCED_FACE('',(#8815),#2058,.F.);
#88095=ADVANCED_FACE('',(#8816),#85812,.F.);
#88096=ADVANCED_FACE('',(#8817),#3222,.T.);
#88097=ADVANCED_FACE('',(#8818),#85813,.F.);
#88098=ADVANCED_FACE('',(#8819),#2059,.F.);
#88099=ADVANCED_FACE('',(#8820),#3223,.F.);
#88100=ADVANCED_FACE('',(#8821),#2060,.F.);
#88101=ADVANCED_FACE('',(#8822),#85814,.F.);
#88102=ADVANCED_FACE('',(#8823),#3224,.T.);
#88103=ADVANCED_FACE('',(#8824),#85815,.F.);
#88104=ADVANCED_FACE('',(#8825),#2061,.F.);
#88105=ADVANCED_FACE('',(#8826),#2062,.F.);
#88106=ADVANCED_FACE('',(#8827),#2063,.F.);
#88107=ADVANCED_FACE('',(#8828),#85816,.F.);
#88108=ADVANCED_FACE('',(#8829),#3225,.T.);
#88109=ADVANCED_FACE('',(#8830),#85817,.F.);
#88110=ADVANCED_FACE('',(#8831),#2064,.F.);
#88111=ADVANCED_FACE('',(#8832),#2065,.F.);
#88112=ADVANCED_FACE('',(#8833),#2066,.F.);
#88113=ADVANCED_FACE('',(#8834),#85818,.F.);
#88114=ADVANCED_FACE('',(#8835),#3226,.T.);
#88115=ADVANCED_FACE('',(#8836),#85819,.F.);
#88116=ADVANCED_FACE('',(#8837),#2067,.F.);
#88117=ADVANCED_FACE('',(#8838),#2068,.F.);
#88118=ADVANCED_FACE('',(#8839),#2069,.F.);
#88119=ADVANCED_FACE('',(#8840),#85820,.F.);
#88120=ADVANCED_FACE('',(#8841),#3227,.T.);
#88121=ADVANCED_FACE('',(#8842),#85821,.F.);
#88122=ADVANCED_FACE('',(#8843),#2070,.F.);
#88123=ADVANCED_FACE('',(#8844),#3228,.F.);
#88124=ADVANCED_FACE('',(#8845),#2071,.F.);
#88125=ADVANCED_FACE('',(#8846),#85822,.F.);
#88126=ADVANCED_FACE('',(#8847),#3229,.T.);
#88127=ADVANCED_FACE('',(#8848),#85823,.F.);
#88128=ADVANCED_FACE('',(#8849),#2072,.F.);
#88129=ADVANCED_FACE('',(#8850),#85824,.T.);
#88130=ADVANCED_FACE('',(#8851),#85825,.F.);
#88131=ADVANCED_FACE('',(#8852),#2073,.F.);
#88132=ADVANCED_FACE('',(#8853),#85826,.F.);
#88133=ADVANCED_FACE('',(#8854),#2074,.F.);
#88134=ADVANCED_FACE('',(#8855),#85827,.F.);
#88135=ADVANCED_FACE('',(#8856),#85828,.T.);
#88136=ADVANCED_FACE('',(#8857),#2075,.F.);
#88137=ADVANCED_FACE('',(#8858),#85829,.F.);
#88138=ADVANCED_FACE('',(#8859),#2076,.T.);
#88139=ADVANCED_FACE('',(#8860),#85830,.T.);
#88140=ADVANCED_FACE('',(#8861),#85831,.F.);
#88141=ADVANCED_FACE('',(#8862),#2077,.F.);
#88142=ADVANCED_FACE('',(#8863),#85832,.F.);
#88143=ADVANCED_FACE('',(#8864),#2078,.F.);
#88144=ADVANCED_FACE('',(#8865),#85833,.F.);
#88145=ADVANCED_FACE('',(#8866),#85834,.T.);
#88146=ADVANCED_FACE('',(#8867),#2079,.T.);
#88147=ADVANCED_FACE('',(#8868),#85835,.T.);
#88148=ADVANCED_FACE('',(#8869),#85836,.F.);
#88149=ADVANCED_FACE('',(#8870),#2080,.F.);
#88150=ADVANCED_FACE('',(#8871),#85837,.F.);
#88151=ADVANCED_FACE('',(#8872),#2081,.F.);
#88152=ADVANCED_FACE('',(#8873),#85838,.F.);
#88153=ADVANCED_FACE('',(#8874),#2082,.T.);
#88154=ADVANCED_FACE('',(#8875),#85839,.T.);
#88155=ADVANCED_FACE('',(#8876),#85840,.F.);
#88156=ADVANCED_FACE('',(#8877),#2083,.F.);
#88157=ADVANCED_FACE('',(#8878),#85841,.F.);
#88158=ADVANCED_FACE('',(#8879),#2084,.F.);
#88159=ADVANCED_FACE('',(#8880),#85842,.F.);
#88160=ADVANCED_FACE('',(#8881),#85843,.T.);
#88161=ADVANCED_FACE('',(#8882),#85844,.T.);
#88162=ADVANCED_FACE('',(#8883),#85845,.F.);
#88163=ADVANCED_FACE('',(#8884),#2085,.F.);
#88164=ADVANCED_FACE('',(#8885),#85846,.F.);
#88165=ADVANCED_FACE('',(#8886),#2086,.F.);
#88166=ADVANCED_FACE('',(#8887),#85847,.F.);
#88167=ADVANCED_FACE('',(#8888),#85848,.T.);
#88168=ADVANCED_FACE('',(#8889),#2087,.F.);
#88169=ADVANCED_FACE('',(#8890),#85849,.F.);
#88170=ADVANCED_FACE('',(#8891),#2088,.T.);
#88171=ADVANCED_FACE('',(#8892),#85850,.T.);
#88172=ADVANCED_FACE('',(#8893),#85851,.F.);
#88173=ADVANCED_FACE('',(#8894),#2089,.F.);
#88174=ADVANCED_FACE('',(#8895),#85852,.F.);
#88175=ADVANCED_FACE('',(#8896),#2090,.F.);
#88176=ADVANCED_FACE('',(#8897),#85853,.F.);
#88177=ADVANCED_FACE('',(#8898),#2091,.T.);
#88178=ADVANCED_FACE('',(#8899),#85854,.F.);
#88179=ADVANCED_FACE('',(#8900),#2092,.F.);
#88180=ADVANCED_FACE('',(#8901),#85855,.T.);
#88181=ADVANCED_FACE('',(#8902),#85856,.F.);
#88182=ADVANCED_FACE('',(#8903),#2093,.F.);
#88183=ADVANCED_FACE('',(#8904),#85857,.F.);
#88184=ADVANCED_FACE('',(#8905),#2094,.F.);
#88185=ADVANCED_FACE('',(#8906),#85858,.F.);
#88186=ADVANCED_FACE('',(#8907),#85859,.T.);
#88187=ADVANCED_FACE('',(#8908),#85860,.F.);
#88188=ADVANCED_FACE('',(#8909),#2095,.F.);
#88189=ADVANCED_FACE('',(#8910),#85861,.F.);
#88190=ADVANCED_FACE('',(#8911),#2096,.F.);
#88191=ADVANCED_FACE('',(#8912),#85862,.F.);
#88192=ADVANCED_FACE('',(#8913),#85863,.T.);
#88193=ADVANCED_FACE('',(#8914),#7738,.T.);
#88194=ADVANCED_FACE('',(#8915),#7739,.T.);
#88195=ADVANCED_FACE('',(#8916),#7740,.F.);
#88196=ADVANCED_FACE('',(#8917),#85864,.T.);
#88197=ADVANCED_FACE('',(#8918),#2097,.F.);
#88198=ADVANCED_FACE('',(#8919),#2098,.F.);
#88199=ADVANCED_FACE('',(#8920),#2099,.F.);
#88200=ADVANCED_FACE('',(#8921),#3230,.F.);
#88201=ADVANCED_FACE('',(#8922),#85865,.F.);
#88202=ADVANCED_FACE('',(#8923),#85866,.T.);
#88203=ADVANCED_FACE('',(#8924),#85867,.F.);
#88204=ADVANCED_FACE('',(#8925),#3231,.F.);
#88205=ADVANCED_FACE('',(#8926),#85868,.F.);
#88206=ADVANCED_FACE('',(#8927),#3232,.F.);
#88207=ADVANCED_FACE('',(#8928),#85869,.F.);
#88208=ADVANCED_FACE('',(#8929),#3233,.F.);
#88209=ADVANCED_FACE('',(#8930),#85870,.F.);
#88210=ADVANCED_FACE('',(#8931),#3234,.F.);
#88211=ADVANCED_FACE('',(#8932),#85871,.F.);
#88212=ADVANCED_FACE('',(#8933),#3235,.F.);
#88213=ADVANCED_FACE('',(#8934),#85872,.F.);
#88214=ADVANCED_FACE('',(#8935),#3236,.F.);
#88215=ADVANCED_FACE('',(#8936),#2100,.F.);
#88216=ADVANCED_FACE('',(#8937),#85873,.F.);
#88217=ADVANCED_FACE('',(#8938),#85874,.F.);
#88218=ADVANCED_FACE('',(#8939),#3237,.F.);
#88219=ADVANCED_FACE('',(#8940),#85875,.F.);
#88220=ADVANCED_FACE('',(#8941),#3238,.F.);
#88221=ADVANCED_FACE('',(#8942),#85876,.F.);
#88222=ADVANCED_FACE('',(#8943),#85877,.F.);
#88223=ADVANCED_FACE('',(#8944),#85878,.F.);
#88224=ADVANCED_FACE('',(#8945),#3239,.F.);
#88225=ADVANCED_FACE('',(#8946),#85879,.F.);
#88226=ADVANCED_FACE('',(#8947),#3240,.F.);
#88227=ADVANCED_FACE('',(#8948),#85880,.F.);
#88228=ADVANCED_FACE('',(#8949),#85881,.F.);
#88229=ADVANCED_FACE('',(#8950),#85882,.F.);
#88230=ADVANCED_FACE('',(#8951),#7741,.F.);
#88231=ADVANCED_FACE('',(#8952),#85883,.T.);
#88232=ADVANCED_FACE('',(#8953),#3241,.F.);
#88233=ADVANCED_FACE('',(#8954),#85884,.F.);
#88234=ADVANCED_FACE('',(#8955),#85885,.F.);
#88235=ADVANCED_FACE('',(#8956),#3242,.T.);
#88236=ADVANCED_FACE('',(#8957),#85886,.T.);
#88237=ADVANCED_FACE('',(#8958),#3243,.T.);
#88238=ADVANCED_FACE('',(#8959),#3244,.T.);
#88239=ADVANCED_FACE('',(#8960),#3245,.T.);
#88240=ADVANCED_FACE('',(#8961),#85887,.T.);
#88241=ADVANCED_FACE('',(#8962),#3246,.T.);
#88242=ADVANCED_FACE('',(#8963),#3247,.T.);
#88243=ADVANCED_FACE('',(#8964),#3248,.T.);
#88244=ADVANCED_FACE('',(#8965),#85888,.T.);
#88245=ADVANCED_FACE('',(#8966),#3249,.T.);
#88246=ADVANCED_FACE('',(#8967),#3250,.T.);
#88247=ADVANCED_FACE('',(#8968),#3251,.T.);
#88248=ADVANCED_FACE('',(#8969),#85889,.T.);
#88249=ADVANCED_FACE('',(#8970),#3252,.T.);
#88250=ADVANCED_FACE('',(#8971),#85890,.F.);
#88251=ADVANCED_FACE('',(#8972),#85891,.F.);
#88252=ADVANCED_FACE('',(#8973),#2101,.F.);
#88253=ADVANCED_FACE('',(#8974),#85892,.F.);
#88254=ADVANCED_FACE('',(#8975),#3253,.T.);
#88255=ADVANCED_FACE('',(#8976),#85893,.F.);
#88256=ADVANCED_FACE('',(#8977),#2102,.F.);
#88257=ADVANCED_FACE('',(#8978),#3254,.F.);
#88258=ADVANCED_FACE('',(#8979),#2103,.F.);
#88259=ADVANCED_FACE('',(#8980),#85894,.F.);
#88260=ADVANCED_FACE('',(#8981),#3255,.T.);
#88261=ADVANCED_FACE('',(#8982),#85895,.F.);
#88262=ADVANCED_FACE('',(#8983),#2104,.F.);
#88263=ADVANCED_FACE('',(#8984),#2105,.F.);
#88264=ADVANCED_FACE('',(#8985),#2106,.F.);
#88265=ADVANCED_FACE('',(#8986),#85896,.F.);
#88266=ADVANCED_FACE('',(#8987),#3256,.T.);
#88267=ADVANCED_FACE('',(#8988),#85897,.F.);
#88268=ADVANCED_FACE('',(#8989),#2107,.F.);
#88269=ADVANCED_FACE('',(#8990),#85898,.F.);
#88270=ADVANCED_FACE('',(#8991),#2108,.F.);
#88271=ADVANCED_FACE('',(#8992),#3257,.F.);
#88272=ADVANCED_FACE('',(#8993),#2109,.T.);
#88273=ADVANCED_FACE('',(#8994),#85899,.T.);
#88274=ADVANCED_FACE('',(#8995),#2110,.T.);
#88275=ADVANCED_FACE('',(#8996),#2111,.F.);
#88276=ADVANCED_FACE('',(#8997),#7742,.F.);
#88277=ADVANCED_FACE('',(#8998),#6931,.T.);
#88278=ADVANCED_FACE('',(#8999),#2112,.F.);
#88279=ADVANCED_FACE('',(#9000),#7743,.F.);
#88280=ADVANCED_FACE('',(#9001),#2113,.T.);
#88281=ADVANCED_FACE('',(#9002),#2114,.T.);
#88282=ADVANCED_FACE('',(#9003),#2115,.T.);
#88283=ADVANCED_FACE('',(#9004),#2116,.F.);
#88284=ADVANCED_FACE('',(#9005),#7744,.F.);
#88285=ADVANCED_FACE('',(#9006),#6932,.T.);
#88286=ADVANCED_FACE('',(#9007),#2117,.F.);
#88287=ADVANCED_FACE('',(#9008),#7745,.F.);
#88288=ADVANCED_FACE('',(#9009),#85900,.T.);
#88289=ADVANCED_FACE('',(#9010),#7746,.F.);
#88290=ADVANCED_FACE('',(#9011),#85901,.T.);
#88291=ADVANCED_FACE('',(#9012),#2118,.F.);
#88292=ADVANCED_FACE('',(#9013),#7747,.F.);
#88293=ADVANCED_FACE('',(#9014),#6933,.T.);
#88294=ADVANCED_FACE('',(#9015),#2119,.F.);
#88295=ADVANCED_FACE('',(#9016),#7748,.F.);
#88296=ADVANCED_FACE('',(#9017),#85902,.T.);
#88297=ADVANCED_FACE('',(#9018),#3258,.F.);
#88298=ADVANCED_FACE('',(#9019),#2120,.F.);
#88299=ADVANCED_FACE('',(#9020),#7749,.F.);
#88300=ADVANCED_FACE('',(#9021),#85903,.T.);
#88301=ADVANCED_FACE('',(#9022),#7750,.T.);
#88302=ADVANCED_FACE('',(#9023),#85904,.T.);
#88303=ADVANCED_FACE('',(#9024),#7751,.F.);
#88304=ADVANCED_FACE('',(#9025),#2121,.F.);
#88305=ADVANCED_FACE('',(#9026),#6934,.T.);
#88306=ADVANCED_FACE('',(#9027),#2122,.F.);
#88307=ADVANCED_FACE('',(#9028),#7752,.F.);
#88308=ADVANCED_FACE('',(#9029),#2123,.T.);
#88309=ADVANCED_FACE('',(#9030),#2124,.T.);
#88310=ADVANCED_FACE('',(#9031),#2125,.T.);
#88311=ADVANCED_FACE('',(#9032),#2126,.F.);
#88312=ADVANCED_FACE('',(#9033),#7753,.F.);
#88313=ADVANCED_FACE('',(#9034),#6935,.T.);
#88314=ADVANCED_FACE('',(#9035),#2127,.F.);
#88315=ADVANCED_FACE('',(#9036),#7754,.F.);
#88316=ADVANCED_FACE('',(#9037),#2128,.T.);
#88317=ADVANCED_FACE('',(#9038),#2129,.T.);
#88318=ADVANCED_FACE('',(#9039),#2130,.T.);
#88319=ADVANCED_FACE('',(#9040),#7755,.F.);
#88320=ADVANCED_FACE('',(#9041),#85905,.T.);
#88321=ADVANCED_FACE('',(#9042),#7756,.F.);
#88322=ADVANCED_FACE('',(#9043),#85906,.T.);
#88323=ADVANCED_FACE('',(#9044),#85907,.T.);
#88324=ADVANCED_FACE('',(#9045),#7757,.F.);
#88325=ADVANCED_FACE('',(#9046),#85908,.T.);
#88326=ADVANCED_FACE('',(#9047),#7758,.F.);
#88327=ADVANCED_FACE('',(#9048),#2131,.F.);
#88328=ADVANCED_FACE('',(#9049),#6936,.T.);
#88329=ADVANCED_FACE('',(#9050),#2132,.F.);
#88330=ADVANCED_FACE('',(#9051),#7759,.F.);
#88331=ADVANCED_FACE('',(#9052),#85909,.T.);
#88332=ADVANCED_FACE('',(#9053),#7760,.F.);
#88333=ADVANCED_FACE('',(#9054),#85910,.T.);
#88334=ADVANCED_FACE('',(#9055),#2133,.F.);
#88335=ADVANCED_FACE('',(#9056),#7761,.F.);
#88336=ADVANCED_FACE('',(#9057),#6937,.T.);
#88337=ADVANCED_FACE('',(#9058),#2134,.F.);
#88338=ADVANCED_FACE('',(#9059),#7762,.F.);
#88339=ADVANCED_FACE('',(#9060),#2135,.T.);
#88340=ADVANCED_FACE('',(#9061),#2136,.T.);
#88341=ADVANCED_FACE('',(#9062),#2137,.T.);
#88342=ADVANCED_FACE('',(#9063),#2138,.F.);
#88343=ADVANCED_FACE('',(#9064),#7763,.F.);
#88344=ADVANCED_FACE('',(#9065),#6938,.T.);
#88345=ADVANCED_FACE('',(#9066),#2139,.F.);
#88346=ADVANCED_FACE('',(#9067),#7764,.F.);
#88347=ADVANCED_FACE('',(#9068),#2140,.T.);
#88348=ADVANCED_FACE('',(#9069),#2141,.T.);
#88349=ADVANCED_FACE('',(#9070),#2142,.T.);
#88350=ADVANCED_FACE('',(#9071),#2143,.F.);
#88351=ADVANCED_FACE('',(#9072),#7765,.F.);
#88352=ADVANCED_FACE('',(#9073),#6939,.T.);
#88353=ADVANCED_FACE('',(#9074),#2144,.F.);
#88354=ADVANCED_FACE('',(#9075),#7766,.F.);
#88355=ADVANCED_FACE('',(#9076),#2145,.T.);
#88356=ADVANCED_FACE('',(#9077),#2146,.T.);
#88357=ADVANCED_FACE('',(#9078),#2147,.T.);
#88358=ADVANCED_FACE('',(#9079),#2148,.F.);
#88359=ADVANCED_FACE('',(#9080),#7767,.F.);
#88360=ADVANCED_FACE('',(#9081),#6940,.T.);
#88361=ADVANCED_FACE('',(#9082),#2149,.F.);
#88362=ADVANCED_FACE('',(#9083),#7768,.F.);
#88363=ADVANCED_FACE('',(#9084),#85911,.T.);
#88364=ADVANCED_FACE('',(#9085),#7769,.F.);
#88365=ADVANCED_FACE('',(#9086),#85912,.T.);
#88366=ADVANCED_FACE('',(#9087),#2150,.F.);
#88367=ADVANCED_FACE('',(#9088),#7770,.F.);
#88368=ADVANCED_FACE('',(#9089),#6941,.T.);
#88369=ADVANCED_FACE('',(#9090),#2151,.F.);
#88370=ADVANCED_FACE('',(#9091),#7771,.F.);
#88371=ADVANCED_FACE('',(#9092),#7772,.T.);
#88372=ADVANCED_FACE('',(#9093),#2152,.F.);
#88373=ADVANCED_FACE('',(#9094),#2153,.F.);
#88374=ADVANCED_FACE('',(#9095),#7773,.F.);
#88375=ADVANCED_FACE('',(#9096),#85913,.T.);
#88376=ADVANCED_FACE('',(#9097),#7774,.F.);
#88377=ADVANCED_FACE('',(#9098),#85914,.T.);
#88378=ADVANCED_FACE('',(#9099),#7775,.F.);
#88379=ADVANCED_FACE('',(#9100),#2154,.F.);
#88380=ADVANCED_FACE('',(#9101),#2155,.F.);
#88381=ADVANCED_FACE('',(#9102),#7776,.F.);
#88382=ADVANCED_FACE('',(#9103),#3259,.F.);
#88383=ADVANCED_FACE('',(#9104),#7777,.T.);
#88384=ADVANCED_FACE('',(#9105),#2156,.F.);
#88385=ADVANCED_FACE('',(#9106),#7778,.F.);
#88386=ADVANCED_FACE('',(#9107),#85915,.T.);
#88387=ADVANCED_FACE('',(#9108),#7779,.F.);
#88388=ADVANCED_FACE('',(#9109),#85916,.T.);
#88389=ADVANCED_FACE('',(#9110),#7780,.F.);
#88390=ADVANCED_FACE('',(#9111),#7781,.T.);
#88391=ADVANCED_FACE('',(#9112),#2157,.F.);
#88392=ADVANCED_FACE('',(#9113),#2158,.F.);
#88393=ADVANCED_FACE('',(#9114),#7782,.F.);
#88394=ADVANCED_FACE('',(#9115),#85917,.T.);
#88395=ADVANCED_FACE('',(#9116),#7783,.T.);
#88396=ADVANCED_FACE('',(#9117),#85918,.T.);
#88397=ADVANCED_FACE('',(#9118),#7784,.F.);
#88398=ADVANCED_FACE('',(#9119),#2159,.F.);
#88399=ADVANCED_FACE('',(#9120),#2160,.F.);
#88400=ADVANCED_FACE('',(#9121),#7785,.T.);
#88401=ADVANCED_FACE('',(#9122),#85919,.T.);
#88402=ADVANCED_FACE('',(#9123),#7786,.T.);
#88403=ADVANCED_FACE('',(#9124),#85920,.T.);
#88404=ADVANCED_FACE('',(#9125),#7787,.F.);
#88405=ADVANCED_FACE('',(#9126),#7788,.T.);
#88406=ADVANCED_FACE('',(#9127),#2161,.F.);
#88407=ADVANCED_FACE('',(#9128),#2162,.F.);
#88408=ADVANCED_FACE('',(#9129),#7789,.F.);
#88409=ADVANCED_FACE('',(#9130),#85921,.T.);
#88410=ADVANCED_FACE('',(#9131),#7790,.F.);
#88411=ADVANCED_FACE('',(#9132),#85922,.T.);
#88412=ADVANCED_FACE('',(#9133),#2163,.F.);
#88413=ADVANCED_FACE('',(#9134),#7791,.F.);
#88414=ADVANCED_FACE('',(#9135),#7792,.F.);
#88415=ADVANCED_FACE('',(#9136),#2164,.F.);
#88416=ADVANCED_FACE('',(#9137),#2165,.T.);
#88417=ADVANCED_FACE('',(#9138),#3260,.F.);
#88418=ADVANCED_FACE('',(#9139),#7793,.T.);
#88419=ADVANCED_FACE('',(#9140),#2166,.F.);
#88420=ADVANCED_FACE('',(#9141),#7794,.F.);
#88421=ADVANCED_FACE('',(#9142),#85923,.T.);
#88422=ADVANCED_FACE('',(#9143),#7795,.F.);
#88423=ADVANCED_FACE('',(#9144),#85924,.T.);
#88424=ADVANCED_FACE('',(#9145),#7796,.F.);
#88425=ADVANCED_FACE('',(#9146),#3261,.F.);
#88426=ADVANCED_FACE('',(#9147),#2167,.F.);
#88427=ADVANCED_FACE('',(#9148),#7797,.F.);
#88428=ADVANCED_FACE('',(#9149),#2168,.F.);
#88429=ADVANCED_FACE('',(#9150),#7798,.F.);
#88430=ADVANCED_FACE('',(#9151),#85925,.T.);
#88431=ADVANCED_FACE('',(#9152),#7799,.F.);
#88432=ADVANCED_FACE('',(#9153),#85926,.T.);
#88433=ADVANCED_FACE('',(#9154),#7800,.F.);
#88434=ADVANCED_FACE('',(#9155),#2169,.F.);
#88435=ADVANCED_FACE('',(#9156),#7801,.T.);
#88436=ADVANCED_FACE('',(#9157),#2170,.F.);
#88437=ADVANCED_FACE('',(#9158),#7802,.F.);
#88438=ADVANCED_FACE('',(#9159),#85927,.T.);
#88439=ADVANCED_FACE('',(#9160),#7803,.F.);
#88440=ADVANCED_FACE('',(#9161),#85928,.T.);
#88441=ADVANCED_FACE('',(#9162),#2171,.F.);
#88442=ADVANCED_FACE('',(#9163),#7804,.F.);
#88443=ADVANCED_FACE('',(#9164),#7805,.T.);
#88444=ADVANCED_FACE('',(#9165),#85929,.F.);
#88445=ADVANCED_FACE('',(#9166),#85930,.F.);
#88446=ADVANCED_FACE('',(#9167,#7441),#7806,.T.);
#88447=ADVANCED_FACE('',(#9168),#85931,.F.);
#88448=ADVANCED_FACE('',(#9169),#85932,.F.);
#88449=ADVANCED_FACE('',(#9170),#2172,.T.);
#88450=ADVANCED_FACE('',(#9171),#3262,.F.);
#88451=ADVANCED_FACE('',(#9172),#2173,.T.);
#88452=ADVANCED_FACE('',(#9173),#85933,.F.);
#88453=ADVANCED_FACE('',(#9174),#85934,.F.);
#88454=ADVANCED_FACE('',(#9175),#85935,.F.);
#88455=ADVANCED_FACE('',(#9176,#7442),#7807,.T.);
#88456=ADVANCED_FACE('',(#9177),#85936,.F.);
#88457=ADVANCED_FACE('',(#9178),#85937,.F.);
#88458=ADVANCED_FACE('',(#9179),#85938,.T.);
#88459=ADVANCED_FACE('',(#9180),#3263,.T.);
#88460=ADVANCED_FACE('',(#9181),#85939,.T.);
#88461=ADVANCED_FACE('',(#9182),#7808,.T.);
#88462=ADVANCED_FACE('',(#9183),#2174,.F.);
#88463=ADVANCED_FACE('',(#9184),#2175,.F.);
#88464=ADVANCED_FACE('',(#9185),#3264,.F.);
#88465=ADVANCED_FACE('',(#9186),#85940,.F.);
#88466=ADVANCED_FACE('',(#9187),#2176,.F.);
#88467=ADVANCED_FACE('',(#9188),#2177,.F.);
#88468=ADVANCED_FACE('',(#9189),#85941,.T.);
#88469=ADVANCED_FACE('',(#9190),#7809,.T.);
#88470=ADVANCED_FACE('',(#9191),#85942,.T.);
#88471=ADVANCED_FACE('',(#9192),#2178,.F.);
#88472=ADVANCED_FACE('',(#9193),#2179,.F.);
#88473=ADVANCED_FACE('',(#9194),#85943,.T.);
#88474=ADVANCED_FACE('',(#9195),#7810,.T.);
#88475=ADVANCED_FACE('',(#9196),#85944,.T.);
#88476=ADVANCED_FACE('',(#9197),#2180,.F.);
#88477=ADVANCED_FACE('',(#9198),#2181,.F.);
#88478=ADVANCED_FACE('',(#9199),#2182,.F.);
#88479=ADVANCED_FACE('',(#9200),#7811,.F.);
#88480=ADVANCED_FACE('',(#9201),#2183,.T.);
#88481=ADVANCED_FACE('',(#9202),#85945,.T.);
#88482=ADVANCED_FACE('',(#9203),#7812,.T.);
#88483=ADVANCED_FACE('',(#9204),#85946,.T.);
#88484=ADVANCED_FACE('',(#9205),#2184,.T.);
#88485=ADVANCED_FACE('',(#9206),#7813,.F.);
#88486=ADVANCED_FACE('',(#9207),#2185,.T.);
#88487=ADVANCED_FACE('',(#9208),#85947,.T.);
#88488=ADVANCED_FACE('',(#9209),#7814,.T.);
#88489=ADVANCED_FACE('',(#9210),#85948,.T.);
#88490=ADVANCED_FACE('',(#9211),#2186,.T.);
#88491=ADVANCED_FACE('',(#9212),#7815,.F.);
#88492=ADVANCED_FACE('',(#9213),#2187,.T.);
#88493=ADVANCED_FACE('',(#9214),#85949,.F.);
#88494=ADVANCED_FACE('',(#9215),#85950,.F.);
#88495=ADVANCED_FACE('',(#9216),#2188,.F.);
#88496=ADVANCED_FACE('',(#9217),#85951,.F.);
#88497=ADVANCED_FACE('',(#9218),#2189,.F.);
#88498=ADVANCED_FACE('',(#9219),#85952,.F.);
#88499=ADVANCED_FACE('',(#9220),#2190,.F.);
#88500=ADVANCED_FACE('',(#9221),#7816,.T.);
#88501=ADVANCED_FACE('',(#9222),#85953,.T.);
#88502=ADVANCED_FACE('',(#9223),#85954,.T.);
#88503=ADVANCED_FACE('',(#9224),#85955,.T.);
#88504=ADVANCED_FACE('',(#9225),#7817,.T.);
#88505=ADVANCED_FACE('',(#9226),#85956,.F.);
#88506=ADVANCED_FACE('',(#9227),#85957,.T.);
#88507=ADVANCED_FACE('',(#9228),#85958,.F.);
#88508=ADVANCED_FACE('',(#9229),#7818,.T.);
#88509=ADVANCED_FACE('',(#9230),#85959,.T.);
#88510=ADVANCED_FACE('',(#9231),#85960,.T.);
#88511=ADVANCED_FACE('',(#9232),#85961,.T.);
#88512=ADVANCED_FACE('',(#9233),#7819,.T.);
#88513=ADVANCED_FACE('',(#9234),#2191,.F.);
#88514=ADVANCED_FACE('',(#9235),#7820,.F.);
#88515=ADVANCED_FACE('',(#9236),#2192,.F.);
#88516=ADVANCED_FACE('',(#9237),#7821,.F.);
#88517=ADVANCED_FACE('',(#9238),#2193,.F.);
#88518=ADVANCED_FACE('',(#9239),#7822,.F.);
#88519=ADVANCED_FACE('',(#9240),#7823,.F.);
#88520=ADVANCED_FACE('',(#9241),#85962,.T.);
#88521=ADVANCED_FACE('',(#9242),#2194,.F.);
#88522=ADVANCED_FACE('',(#9243),#6942,.T.);
#88523=ADVANCED_FACE('',(#9244),#2195,.F.);
#88524=ADVANCED_FACE('',(#9245),#85963,.T.);
#88525=ADVANCED_FACE('',(#9246),#7824,.F.);
#88526=ADVANCED_FACE('',(#9247),#85964,.T.);
#88527=ADVANCED_FACE('',(#9248),#2196,.F.);
#88528=ADVANCED_FACE('',(#9249),#6943,.T.);
#88529=ADVANCED_FACE('',(#9250),#2197,.F.);
#88530=ADVANCED_FACE('',(#9251),#2198,.T.);
#88531=ADVANCED_FACE('',(#9252),#2199,.T.);
#88532=ADVANCED_FACE('',(#9253),#2200,.T.);
#88533=ADVANCED_FACE('',(#9254),#2201,.F.);
#88534=ADVANCED_FACE('',(#9255),#6944,.T.);
#88535=ADVANCED_FACE('',(#9256),#2202,.F.);
#88536=ADVANCED_FACE('',(#9257),#85965,.F.);
#88537=ADVANCED_FACE('',(#9258),#2203,.F.);
#88538=ADVANCED_FACE('',(#9259),#2204,.T.);
#88539=ADVANCED_FACE('',(#9260),#85966,.T.);
#88540=ADVANCED_FACE('',(#9261),#7825,.F.);
#88541=ADVANCED_FACE('',(#9262),#2205,.F.);
#88542=ADVANCED_FACE('',(#9263),#2206,.F.);
#88543=ADVANCED_FACE('',(#9264),#2207,.F.);
#88544=ADVANCED_FACE('',(#9265),#85967,.F.);
#88545=ADVANCED_FACE('',(#9266),#2208,.F.);
#88546=ADVANCED_FACE('',(#9267),#2209,.F.);
#88547=ADVANCED_FACE('',(#9268),#2210,.F.);
#88548=ADVANCED_FACE('',(#9269),#2211,.F.);
#88549=ADVANCED_FACE('',(#9270),#85968,.F.);
#88550=ADVANCED_FACE('',(#9271),#2212,.F.);
#88551=ADVANCED_FACE('',(#9272),#2213,.F.);
#88552=ADVANCED_FACE('',(#9273),#85969,.T.);
#88553=ADVANCED_FACE('',(#9274),#7826,.T.);
#88554=ADVANCED_FACE('',(#9275),#85970,.T.);
#88555=ADVANCED_FACE('',(#9276),#2214,.F.);
#88556=ADVANCED_FACE('',(#9277),#2215,.F.);
#88557=ADVANCED_FACE('',(#9278),#2216,.F.);
#88558=ADVANCED_FACE('',(#9279),#85971,.F.);
#88559=ADVANCED_FACE('',(#9280),#2217,.F.);
#88560=ADVANCED_FACE('',(#9281),#2218,.F.);
#88561=ADVANCED_FACE('',(#9282),#2219,.F.);
#88562=ADVANCED_FACE('',(#9283),#2220,.F.);
#88563=ADVANCED_FACE('',(#9284),#85972,.F.);
#88564=ADVANCED_FACE('',(#9285),#2221,.F.);
#88565=ADVANCED_FACE('',(#9286),#2222,.F.);
#88566=ADVANCED_FACE('',(#9287),#3265,.T.);
#88567=ADVANCED_FACE('',(#9288),#85973,.T.);
#88568=ADVANCED_FACE('',(#9289),#3266,.T.);
#88569=ADVANCED_FACE('',(#9290),#85974,.T.);
#88570=ADVANCED_FACE('',(#9291),#3267,.T.);
#88571=ADVANCED_FACE('',(#9292),#2223,.F.);
#88572=ADVANCED_FACE('',(#9293),#2224,.F.);
#88573=ADVANCED_FACE('',(#9294),#2225,.F.);
#88574=ADVANCED_FACE('',(#9295),#85975,.F.);
#88575=ADVANCED_FACE('',(#9296),#2226,.F.);
#88576=ADVANCED_FACE('',(#9297),#85976,.T.);
#88577=ADVANCED_FACE('',(#9298),#3268,.T.);
#88578=ADVANCED_FACE('',(#9299),#2227,.F.);
#88579=ADVANCED_FACE('',(#9300),#2228,.F.);
#88580=ADVANCED_FACE('',(#9301),#2229,.F.);
#88581=ADVANCED_FACE('',(#9302),#85977,.F.);
#88582=ADVANCED_FACE('',(#9303),#2230,.F.);
#88583=ADVANCED_FACE('',(#9304),#2231,.F.);
#88584=ADVANCED_FACE('',(#9305),#3269,.T.);
#88585=ADVANCED_FACE('',(#9306),#85978,.T.);
#88586=ADVANCED_FACE('',(#9307),#3270,.T.);
#88587=ADVANCED_FACE('',(#9308),#6945,.T.);
#88588=ADVANCED_FACE('',(#9309),#2232,.F.);
#88589=ADVANCED_FACE('',(#9310),#2233,.F.);
#88590=ADVANCED_FACE('',(#9311),#2234,.F.);
#88591=ADVANCED_FACE('',(#9312),#2235,.F.);
#88592=ADVANCED_FACE('',(#9313),#85979,.F.);
#88593=ADVANCED_FACE('',(#9314),#3271,.T.);
#88594=ADVANCED_FACE('',(#9315),#85980,.T.);
#88595=ADVANCED_FACE('',(#9316),#3272,.T.);
#88596=ADVANCED_FACE('',(#9317),#85981,.F.);
#88597=ADVANCED_FACE('',(#9318),#2236,.F.);
#88598=ADVANCED_FACE('',(#9319),#2237,.F.);
#88599=ADVANCED_FACE('',(#9320),#2238,.F.);
#88600=ADVANCED_FACE('',(#9321),#2239,.F.);
#88601=ADVANCED_FACE('',(#9322),#2240,.F.);
#88602=ADVANCED_FACE('',(#9323),#2241,.F.);
#88603=ADVANCED_FACE('',(#9324),#3273,.T.);
#88604=ADVANCED_FACE('',(#9325),#85982,.T.);
#88605=ADVANCED_FACE('',(#9326),#3274,.T.);
#88606=ADVANCED_FACE('',(#9327),#3275,.T.);
#88607=ADVANCED_FACE('',(#9328),#85983,.T.);
#88608=ADVANCED_FACE('',(#9329),#3276,.T.);
#88609=ADVANCED_FACE('',(#9330),#85984,.T.);
#88610=ADVANCED_FACE('',(#9331),#85985,.F.);
#88611=ADVANCED_FACE('',(#9332),#2242,.F.);
#88612=ADVANCED_FACE('',(#9333),#2243,.F.);
#88613=ADVANCED_FACE('',(#9334),#2244,.F.);
#88614=ADVANCED_FACE('',(#9335),#85986,.F.);
#88615=ADVANCED_FACE('',(#9336),#2245,.F.);
#88616=ADVANCED_FACE('',(#9337),#2246,.F.);
#88617=ADVANCED_FACE('',(#9338),#85987,.T.);
#88618=ADVANCED_FACE('',(#9339),#3277,.T.);
#88619=ADVANCED_FACE('',(#9340),#2247,.F.);
#88620=ADVANCED_FACE('',(#9341),#2248,.F.);
#88621=ADVANCED_FACE('',(#9342),#2249,.F.);
#88622=ADVANCED_FACE('',(#9343),#85988,.F.);
#88623=ADVANCED_FACE('',(#9344),#2250,.F.);
#88624=ADVANCED_FACE('',(#9345),#2251,.F.);
#88625=ADVANCED_FACE('',(#9346),#2252,.F.);
#88626=ADVANCED_FACE('',(#9347),#85989,.F.);
#88627=ADVANCED_FACE('',(#9348),#85990,.T.);
#88628=ADVANCED_FACE('',(#9349),#3278,.T.);
#88629=ADVANCED_FACE('',(#9350),#85991,.T.);
#88630=ADVANCED_FACE('',(#9351),#3279,.T.);
#88631=ADVANCED_FACE('',(#9352),#85992,.T.);
#88632=ADVANCED_FACE('',(#9353),#3280,.T.);
#88633=ADVANCED_FACE('',(#9354),#2253,.F.);
#88634=ADVANCED_FACE('',(#9355),#85993,.T.);
#88635=ADVANCED_FACE('',(#9356),#3281,.T.);
#88636=ADVANCED_FACE('',(#9357),#85994,.F.);
#88637=ADVANCED_FACE('',(#9358),#2254,.F.);
#88638=ADVANCED_FACE('',(#9359),#2255,.F.);
#88639=ADVANCED_FACE('',(#9360),#2256,.F.);
#88640=ADVANCED_FACE('',(#9361),#85995,.F.);
#88641=ADVANCED_FACE('',(#9362),#2257,.F.);
#88642=ADVANCED_FACE('',(#9363),#2258,.F.);
#88643=ADVANCED_FACE('',(#9364),#2259,.F.);
#88644=ADVANCED_FACE('',(#9365),#2260,.F.);
#88645=ADVANCED_FACE('',(#9366),#85996,.F.);
#88646=ADVANCED_FACE('',(#9367),#2261,.F.);
#88647=ADVANCED_FACE('',(#9368),#2262,.F.);
#88648=ADVANCED_FACE('',(#9369),#2263,.F.);
#88649=ADVANCED_FACE('',(#9370),#85997,.F.);
#88650=ADVANCED_FACE('',(#9371),#2264,.T.);
#88651=ADVANCED_FACE('',(#9372),#85998,.T.);
#88652=ADVANCED_FACE('',(#9373),#7827,.T.);
#88653=ADVANCED_FACE('',(#9374),#85999,.T.);
#88654=ADVANCED_FACE('',(#9375),#2265,.F.);
#88655=ADVANCED_FACE('',(#9376),#2266,.T.);
#88656=ADVANCED_FACE('',(#9377),#86000,.F.);
#88657=ADVANCED_FACE('',(#9378),#2267,.F.);
#88658=ADVANCED_FACE('',(#9379),#2268,.F.);
#88659=ADVANCED_FACE('',(#9380),#2269,.F.);
#88660=ADVANCED_FACE('',(#9381),#86001,.F.);
#88661=ADVANCED_FACE('',(#9382),#2270,.F.);
#88662=ADVANCED_FACE('',(#9383),#2271,.F.);
#88663=ADVANCED_FACE('',(#9384),#2272,.F.);
#88664=ADVANCED_FACE('',(#9385),#2273,.F.);
#88665=ADVANCED_FACE('',(#9386),#86002,.F.);
#88666=ADVANCED_FACE('',(#9387),#2274,.F.);
#88667=ADVANCED_FACE('',(#9388),#2275,.F.);
#88668=ADVANCED_FACE('',(#9389),#2276,.F.);
#88669=ADVANCED_FACE('',(#9390),#86003,.F.);
#88670=ADVANCED_FACE('',(#9391),#2277,.T.);
#88671=ADVANCED_FACE('',(#9392),#86004,.T.);
#88672=ADVANCED_FACE('',(#9393),#7828,.T.);
#88673=ADVANCED_FACE('',(#9394),#86005,.T.);
#88674=ADVANCED_FACE('',(#9395),#2278,.F.);
#88675=ADVANCED_FACE('',(#9396),#2279,.T.);
#88676=ADVANCED_FACE('',(#9397),#86006,.F.);
#88677=ADVANCED_FACE('',(#9398),#2280,.F.);
#88678=ADVANCED_FACE('',(#9399),#2281,.F.);
#88679=ADVANCED_FACE('',(#9400),#2282,.F.);
#88680=ADVANCED_FACE('',(#9401),#86007,.F.);
#88681=ADVANCED_FACE('',(#9402),#2283,.F.);
#88682=ADVANCED_FACE('',(#9403),#2284,.F.);
#88683=ADVANCED_FACE('',(#9404),#2285,.F.);
#88684=ADVANCED_FACE('',(#9405),#2286,.F.);
#88685=ADVANCED_FACE('',(#9406),#86008,.F.);
#88686=ADVANCED_FACE('',(#9407),#2287,.F.);
#88687=ADVANCED_FACE('',(#9408),#2288,.F.);
#88688=ADVANCED_FACE('',(#9409),#2289,.F.);
#88689=ADVANCED_FACE('',(#9410),#86009,.F.);
#88690=ADVANCED_FACE('',(#9411),#2290,.T.);
#88691=ADVANCED_FACE('',(#9412),#86010,.T.);
#88692=ADVANCED_FACE('',(#9413),#7829,.T.);
#88693=ADVANCED_FACE('',(#9414),#86011,.T.);
#88694=ADVANCED_FACE('',(#9415),#2291,.F.);
#88695=ADVANCED_FACE('',(#9416),#2292,.T.);
#88696=ADVANCED_FACE('',(#9417),#86012,.F.);
#88697=ADVANCED_FACE('',(#9418),#2293,.F.);
#88698=ADVANCED_FACE('',(#9419),#2294,.F.);
#88699=ADVANCED_FACE('',(#9420),#2295,.F.);
#88700=ADVANCED_FACE('',(#9421),#86013,.F.);
#88701=ADVANCED_FACE('',(#9422),#2296,.F.);
#88702=ADVANCED_FACE('',(#9423),#2297,.F.);
#88703=ADVANCED_FACE('',(#9424),#2298,.F.);
#88704=ADVANCED_FACE('',(#9425),#2299,.F.);
#88705=ADVANCED_FACE('',(#9426),#86014,.F.);
#88706=ADVANCED_FACE('',(#9427),#2300,.F.);
#88707=ADVANCED_FACE('',(#9428),#2301,.F.);
#88708=ADVANCED_FACE('',(#9429),#2302,.F.);
#88709=ADVANCED_FACE('',(#9430),#86015,.F.);
#88710=ADVANCED_FACE('',(#9431),#3282,.T.);
#88711=ADVANCED_FACE('',(#9432),#86016,.T.);
#88712=ADVANCED_FACE('',(#9433),#3283,.T.);
#88713=ADVANCED_FACE('',(#9434),#86017,.T.);
#88714=ADVANCED_FACE('',(#9435),#3284,.T.);
#88715=ADVANCED_FACE('',(#9436),#2303,.F.);
#88716=ADVANCED_FACE('',(#9437),#86018,.T.);
#88717=ADVANCED_FACE('',(#9438),#3285,.T.);
#88718=ADVANCED_FACE('',(#9439),#86019,.T.);
#88719=ADVANCED_FACE('',(#9440),#86020,.F.);
#88720=ADVANCED_FACE('',(#9441),#2304,.F.);
#88721=ADVANCED_FACE('',(#9442),#2305,.F.);
#88722=ADVANCED_FACE('',(#9443),#2306,.F.);
#88723=ADVANCED_FACE('',(#9444),#86021,.F.);
#88724=ADVANCED_FACE('',(#9445),#2307,.F.);
#88725=ADVANCED_FACE('',(#9446),#2308,.F.);
#88726=ADVANCED_FACE('',(#9447),#2309,.F.);
#88727=ADVANCED_FACE('',(#9448),#2310,.F.);
#88728=ADVANCED_FACE('',(#9449),#86022,.F.);
#88729=ADVANCED_FACE('',(#9450),#86023,.T.);
#88730=ADVANCED_FACE('',(#9451),#3286,.T.);
#88731=ADVANCED_FACE('',(#9452),#86024,.T.);
#88732=ADVANCED_FACE('',(#9453),#2311,.F.);
#88733=ADVANCED_FACE('',(#9454),#86025,.F.);
#88734=ADVANCED_FACE('',(#9455),#2312,.F.);
#88735=ADVANCED_FACE('',(#9456),#2313,.F.);
#88736=ADVANCED_FACE('',(#9457),#2314,.F.);
#88737=ADVANCED_FACE('',(#9458),#86026,.F.);
#88738=ADVANCED_FACE('',(#9459),#86027,.F.);
#88739=ADVANCED_FACE('',(#9460),#3287,.F.);
#88740=ADVANCED_FACE('',(#9461),#2315,.F.);
#88741=ADVANCED_FACE('',(#9462),#86028,.F.);
#88742=ADVANCED_FACE('',(#9463),#86029,.T.);
#88743=ADVANCED_FACE('',(#9464),#3288,.T.);
#88744=ADVANCED_FACE('',(#9465),#86030,.T.);
#88745=ADVANCED_FACE('',(#9466),#3289,.T.);
#88746=ADVANCED_FACE('',(#9467),#2316,.F.);
#88747=ADVANCED_FACE('',(#9468),#2317,.F.);
#88748=ADVANCED_FACE('',(#9469),#86031,.F.);
#88749=ADVANCED_FACE('',(#9470),#2318,.F.);
#88750=ADVANCED_FACE('',(#9471),#2319,.F.);
#88751=ADVANCED_FACE('',(#9472),#2320,.F.);
#88752=ADVANCED_FACE('',(#9473),#86032,.F.);
#88753=ADVANCED_FACE('',(#9474),#86033,.T.);
#88754=ADVANCED_FACE('',(#9475),#3290,.T.);
#88755=ADVANCED_FACE('',(#9476),#86034,.F.);
#88756=ADVANCED_FACE('',(#9477),#86035,.F.);
#88757=ADVANCED_FACE('',(#9478),#86036,.F.);
#88758=ADVANCED_FACE('',(#9479),#2321,.F.);
#88759=ADVANCED_FACE('',(#9480),#86037,.T.);
#88760=ADVANCED_FACE('',(#9481),#3291,.T.);
#88761=ADVANCED_FACE('',(#9482),#86038,.T.);
#88762=ADVANCED_FACE('',(#9483),#86039,.F.);
#88763=ADVANCED_FACE('',(#9484),#2322,.F.);
#88764=ADVANCED_FACE('',(#9485),#86040,.F.);
#88765=ADVANCED_FACE('',(#9486),#2323,.F.);
#88766=ADVANCED_FACE('',(#9487),#2324,.F.);
#88767=ADVANCED_FACE('',(#9488),#2325,.F.);
#88768=ADVANCED_FACE('',(#9489),#2326,.F.);
#88769=ADVANCED_FACE('',(#9490),#2327,.F.);
#88770=ADVANCED_FACE('',(#9491),#86041,.F.);
#88771=ADVANCED_FACE('',(#9492),#2328,.F.);
#88772=ADVANCED_FACE('',(#9493),#2329,.F.);
#88773=ADVANCED_FACE('',(#9494),#86042,.T.);
#88774=ADVANCED_FACE('',(#9495),#3292,.T.);
#88775=ADVANCED_FACE('',(#9496),#6946,.T.);
#88776=ADVANCED_FACE('',(#9497),#2330,.F.);
#88777=ADVANCED_FACE('',(#9498),#86043,.F.);
#88778=ADVANCED_FACE('',(#9499),#2331,.F.);
#88779=ADVANCED_FACE('',(#9500),#2332,.F.);
#88780=ADVANCED_FACE('',(#9501),#86044,.F.);
#88781=ADVANCED_FACE('',(#9502),#2333,.F.);
#88782=ADVANCED_FACE('',(#9503),#2334,.F.);
#88783=ADVANCED_FACE('',(#9504),#2335,.F.);
#88784=ADVANCED_FACE('',(#9505),#86045,.F.);
#88785=ADVANCED_FACE('',(#9506),#2336,.F.);
#88786=ADVANCED_FACE('',(#9507),#86046,.F.);
#88787=ADVANCED_FACE('',(#9508),#86047,.T.);
#88788=ADVANCED_FACE('',(#9509),#3293,.T.);
#88789=ADVANCED_FACE('',(#9510),#86048,.T.);
#88790=ADVANCED_FACE('',(#9511),#3294,.T.);
#88791=ADVANCED_FACE('',(#9512),#86049,.T.);
#88792=ADVANCED_FACE('',(#9513),#3295,.T.);
#88793=ADVANCED_FACE('',(#9514),#86050,.T.);
#88794=ADVANCED_FACE('',(#9515),#86051,.F.);
#88795=ADVANCED_FACE('',(#9516),#2337,.F.);
#88796=ADVANCED_FACE('',(#9517),#86052,.F.);
#88797=ADVANCED_FACE('',(#9518),#2338,.F.);
#88798=ADVANCED_FACE('',(#9519),#2339,.F.);
#88799=ADVANCED_FACE('',(#9520),#2340,.F.);
#88800=ADVANCED_FACE('',(#9521),#86053,.F.);
#88801=ADVANCED_FACE('',(#9522),#2341,.F.);
#88802=ADVANCED_FACE('',(#9523),#2342,.F.);
#88803=ADVANCED_FACE('',(#9524),#2343,.F.);
#88804=ADVANCED_FACE('',(#9525),#86054,.T.);
#88805=ADVANCED_FACE('',(#9526),#3296,.T.);
#88806=ADVANCED_FACE('',(#9527),#3297,.F.);
#88807=ADVANCED_FACE('',(#9528),#86055,.F.);
#88808=ADVANCED_FACE('',(#9529),#86056,.F.);
#88809=ADVANCED_FACE('',(#9530),#2344,.F.);
#88810=ADVANCED_FACE('',(#9531),#2345,.F.);
#88811=ADVANCED_FACE('',(#9532),#2346,.F.);
#88812=ADVANCED_FACE('',(#9533),#86057,.F.);
#88813=ADVANCED_FACE('',(#9534),#3298,.T.);
#88814=ADVANCED_FACE('',(#9535),#86058,.T.);
#88815=ADVANCED_FACE('',(#9536),#3299,.T.);
#88816=ADVANCED_FACE('',(#9537),#86059,.F.);
#88817=ADVANCED_FACE('',(#9538),#2347,.F.);
#88818=ADVANCED_FACE('',(#9539),#2348,.F.);
#88819=ADVANCED_FACE('',(#9540),#86060,.F.);
#88820=ADVANCED_FACE('',(#9541),#86061,.T.);
#88821=ADVANCED_FACE('',(#9542),#3300,.T.);
#88822=ADVANCED_FACE('',(#9543),#86062,.T.);
#88823=ADVANCED_FACE('',(#9544),#3301,.T.);
#88824=ADVANCED_FACE('',(#9545),#86063,.F.);
#88825=ADVANCED_FACE('',(#9546),#2349,.F.);
#88826=ADVANCED_FACE('',(#9547),#2350,.F.);
#88827=ADVANCED_FACE('',(#9548),#2351,.F.);
#88828=ADVANCED_FACE('',(#9549),#3302,.F.);
#88829=ADVANCED_FACE('',(#9550),#86064,.F.);
#88830=ADVANCED_FACE('',(#9551),#86065,.F.);
#88831=ADVANCED_FACE('',(#9552),#2352,.F.);
#88832=ADVANCED_FACE('',(#9553),#86066,.F.);
#88833=ADVANCED_FACE('',(#9554),#86067,.T.);
#88834=ADVANCED_FACE('',(#9555),#3303,.T.);
#88835=ADVANCED_FACE('',(#9556),#86068,.T.);
#88836=ADVANCED_FACE('',(#9557),#3304,.T.);
#88837=ADVANCED_FACE('',(#9558),#2353,.F.);
#88838=ADVANCED_FACE('',(#9559),#2354,.F.);
#88839=ADVANCED_FACE('',(#9560),#2355,.F.);
#88840=ADVANCED_FACE('',(#9561),#86069,.F.);
#88841=ADVANCED_FACE('',(#9562),#2356,.F.);
#88842=ADVANCED_FACE('',(#9563),#2357,.F.);
#88843=ADVANCED_FACE('',(#9564),#2358,.F.);
#88844=ADVANCED_FACE('',(#9565),#86070,.F.);
#88845=ADVANCED_FACE('',(#9566),#86071,.T.);
#88846=ADVANCED_FACE('',(#9567),#3305,.T.);
#88847=ADVANCED_FACE('',(#9568),#86072,.F.);
#88848=ADVANCED_FACE('',(#9569),#2359,.F.);
#88849=ADVANCED_FACE('',(#9570),#86073,.T.);
#88850=ADVANCED_FACE('',(#9571),#3306,.T.);
#88851=ADVANCED_FACE('',(#9572),#86074,.T.);
#88852=ADVANCED_FACE('',(#9573),#86075,.F.);
#88853=ADVANCED_FACE('',(#9574),#2360,.F.);
#88854=ADVANCED_FACE('',(#9575),#86076,.F.);
#88855=ADVANCED_FACE('',(#9576),#86077,.F.);
#88856=ADVANCED_FACE('',(#9577),#86078,.T.);
#88857=ADVANCED_FACE('',(#9578),#86079,.F.);
#88858=ADVANCED_FACE('',(#9579),#2361,.F.);
#88859=ADVANCED_FACE('',(#9580),#2362,.F.);
#88860=ADVANCED_FACE('',(#9581),#2363,.F.);
#88861=ADVANCED_FACE('',(#9582),#2364,.F.);
#88862=ADVANCED_FACE('',(#9583),#86080,.F.);
#88863=ADVANCED_FACE('',(#9584),#2365,.F.);
#88864=ADVANCED_FACE('',(#9585),#2366,.F.);
#88865=ADVANCED_FACE('',(#9586),#2367,.F.);
#88866=ADVANCED_FACE('',(#9587),#2368,.F.);
#88867=ADVANCED_FACE('',(#9588),#86081,.T.);
#88868=ADVANCED_FACE('',(#9589),#3307,.T.);
#88869=ADVANCED_FACE('',(#9590),#6947,.T.);
#88870=ADVANCED_FACE('',(#9591),#2369,.F.);
#88871=ADVANCED_FACE('',(#9592),#86082,.F.);
#88872=ADVANCED_FACE('',(#9593),#2370,.F.);
#88873=ADVANCED_FACE('',(#9594),#2371,.F.);
#88874=ADVANCED_FACE('',(#9595),#86083,.F.);
#88875=ADVANCED_FACE('',(#9596),#2372,.F.);
#88876=ADVANCED_FACE('',(#9597),#2373,.F.);
#88877=ADVANCED_FACE('',(#9598),#2374,.F.);
#88878=ADVANCED_FACE('',(#9599),#86084,.F.);
#88879=ADVANCED_FACE('',(#9600),#2375,.F.);
#88880=ADVANCED_FACE('',(#9601),#86085,.F.);
#88881=ADVANCED_FACE('',(#9602),#86086,.T.);
#88882=ADVANCED_FACE('',(#9603),#3308,.T.);
#88883=ADVANCED_FACE('',(#9604),#86087,.T.);
#88884=ADVANCED_FACE('',(#9605),#3309,.T.);
#88885=ADVANCED_FACE('',(#9606),#86088,.T.);
#88886=ADVANCED_FACE('',(#9607),#3310,.T.);
#88887=ADVANCED_FACE('',(#9608),#86089,.T.);
#88888=ADVANCED_FACE('',(#9609),#86090,.F.);
#88889=ADVANCED_FACE('',(#9610),#2376,.F.);
#88890=ADVANCED_FACE('',(#9611),#86091,.F.);
#88891=ADVANCED_FACE('',(#9612),#2377,.F.);
#88892=ADVANCED_FACE('',(#9613),#2378,.F.);
#88893=ADVANCED_FACE('',(#9614),#2379,.F.);
#88894=ADVANCED_FACE('',(#9615),#86092,.F.);
#88895=ADVANCED_FACE('',(#9616),#2380,.F.);
#88896=ADVANCED_FACE('',(#9617),#2381,.F.);
#88897=ADVANCED_FACE('',(#9618),#2382,.F.);
#88898=ADVANCED_FACE('',(#9619),#86093,.T.);
#88899=ADVANCED_FACE('',(#9620),#3311,.T.);
#88900=ADVANCED_FACE('',(#9621),#6948,.T.);
#88901=ADVANCED_FACE('',(#9622),#2383,.F.);
#88902=ADVANCED_FACE('',(#9623),#2384,.F.);
#88903=ADVANCED_FACE('',(#9624),#2385,.F.);
#88904=ADVANCED_FACE('',(#9625),#86094,.F.);
#88905=ADVANCED_FACE('',(#9626),#86095,.T.);
#88906=ADVANCED_FACE('',(#9627),#3312,.T.);
#88907=ADVANCED_FACE('',(#9628),#86096,.T.);
#88908=ADVANCED_FACE('',(#9629),#2386,.F.);
#88909=ADVANCED_FACE('',(#9630),#2387,.F.);
#88910=ADVANCED_FACE('',(#9631),#86097,.F.);
#88911=ADVANCED_FACE('',(#9632),#2388,.F.);
#88912=ADVANCED_FACE('',(#9633),#2389,.F.);
#88913=ADVANCED_FACE('',(#9634),#2390,.F.);
#88914=ADVANCED_FACE('',(#9635),#2391,.F.);
#88915=ADVANCED_FACE('',(#9636),#86098,.F.);
#88916=ADVANCED_FACE('',(#9637),#86099,.T.);
#88917=ADVANCED_FACE('',(#9638),#3313,.T.);
#88918=ADVANCED_FACE('',(#9639),#86100,.T.);
#88919=ADVANCED_FACE('',(#9640),#3314,.T.);
#88920=ADVANCED_FACE('',(#9641),#2392,.F.);
#88921=ADVANCED_FACE('',(#9642),#86101,.F.);
#88922=ADVANCED_FACE('',(#9643),#86102,.F.);
#88923=ADVANCED_FACE('',(#9644),#86103,.F.);
#88924=ADVANCED_FACE('',(#9645),#86104,.T.);
#88925=ADVANCED_FACE('',(#9646),#3315,.T.);
#88926=ADVANCED_FACE('',(#9647),#86105,.T.);
#88927=ADVANCED_FACE('',(#9648),#86106,.F.);
#88928=ADVANCED_FACE('',(#9649),#2393,.F.);
#88929=ADVANCED_FACE('',(#9650),#86107,.F.);
#88930=ADVANCED_FACE('',(#9651),#2394,.F.);
#88931=ADVANCED_FACE('',(#9652),#2395,.F.);
#88932=ADVANCED_FACE('',(#9653),#2396,.F.);
#88933=ADVANCED_FACE('',(#9654),#86108,.F.);
#88934=ADVANCED_FACE('',(#9655),#2397,.F.);
#88935=ADVANCED_FACE('',(#9656),#2398,.F.);
#88936=ADVANCED_FACE('',(#9657),#2399,.F.);
#88937=ADVANCED_FACE('',(#9658),#86109,.F.);
#88938=ADVANCED_FACE('',(#9659),#86110,.T.);
#88939=ADVANCED_FACE('',(#9660),#3316,.T.);
#88940=ADVANCED_FACE('',(#9661),#3317,.F.);
#88941=ADVANCED_FACE('',(#9662),#86111,.F.);
#88942=ADVANCED_FACE('',(#9663),#2400,.F.);
#88943=ADVANCED_FACE('',(#9664),#2401,.F.);
#88944=ADVANCED_FACE('',(#9665),#2402,.F.);
#88945=ADVANCED_FACE('',(#9666),#86112,.F.);
#88946=ADVANCED_FACE('',(#9667),#2403,.F.);
#88947=ADVANCED_FACE('',(#9668),#2404,.F.);
#88948=ADVANCED_FACE('',(#9669),#2405,.F.);
#88949=ADVANCED_FACE('',(#9670),#86113,.F.);
#88950=ADVANCED_FACE('',(#9671),#2406,.F.);
#88951=ADVANCED_FACE('',(#9672),#86114,.F.);
#88952=ADVANCED_FACE('',(#9673),#86115,.T.);
#88953=ADVANCED_FACE('',(#9674),#3318,.T.);
#88954=ADVANCED_FACE('',(#9675),#86116,.T.);
#88955=ADVANCED_FACE('',(#9676),#3319,.T.);
#88956=ADVANCED_FACE('',(#9677),#86117,.T.);
#88957=ADVANCED_FACE('',(#9678),#3320,.T.);
#88958=ADVANCED_FACE('',(#9679),#86118,.F.);
#88959=ADVANCED_FACE('',(#9680),#86119,.T.);
#88960=ADVANCED_FACE('',(#9681),#86120,.F.);
#88961=ADVANCED_FACE('',(#9682),#2407,.F.);
#88962=ADVANCED_FACE('',(#9683),#86121,.F.);
#88963=ADVANCED_FACE('',(#9684),#2408,.F.);
#88964=ADVANCED_FACE('',(#9685),#2409,.F.);
#88965=ADVANCED_FACE('',(#9686),#2410,.F.);
#88966=ADVANCED_FACE('',(#9687),#86122,.F.);
#88967=ADVANCED_FACE('',(#9688),#2411,.F.);
#88968=ADVANCED_FACE('',(#9689),#2412,.F.);
#88969=ADVANCED_FACE('',(#9690),#86123,.T.);
#88970=ADVANCED_FACE('',(#9691),#3321,.T.);
#88971=ADVANCED_FACE('',(#9692),#7830,.T.);
#88972=ADVANCED_FACE('',(#9693),#86124,.T.);
#88973=ADVANCED_FACE('',(#9694),#7831,.T.);
#88974=ADVANCED_FACE('',(#9695),#2413,.F.);
#88975=ADVANCED_FACE('',(#9696),#2414,.F.);
#88976=ADVANCED_FACE('',(#9697),#1016,.F.);
#88977=ADVANCED_FACE('',(#9698),#86125,.T.);
#88978=ADVANCED_FACE('',(#9699),#3322,.T.);
#88979=ADVANCED_FACE('',(#9700),#3323,.T.);
#88980=ADVANCED_FACE('',(#9701),#3324,.T.);
#88981=ADVANCED_FACE('',(#9702),#86126,.T.);
#88982=ADVANCED_FACE('',(#9703),#2415,.F.);
#88983=ADVANCED_FACE('',(#9704),#86127,.F.);
#88984=ADVANCED_FACE('',(#9705),#2416,.F.);
#88985=ADVANCED_FACE('',(#9706),#86128,.T.);
#88986=ADVANCED_FACE('',(#9707),#2417,.F.);
#88987=ADVANCED_FACE('',(#9708),#86129,.F.);
#88988=ADVANCED_FACE('',(#9709),#2418,.F.);
#88989=ADVANCED_FACE('',(#9710),#86130,.T.);
#88990=ADVANCED_FACE('',(#9711),#2419,.T.);
#88991=ADVANCED_FACE('',(#9712),#2420,.F.);
#88992=ADVANCED_FACE('',(#9713),#2421,.T.);
#88993=ADVANCED_FACE('',(#9714),#2422,.F.);
#88994=ADVANCED_FACE('',(#9715),#3325,.F.);
#88995=ADVANCED_FACE('',(#9716),#2423,.F.);
#88996=ADVANCED_FACE('',(#9717),#3326,.T.);
#88997=ADVANCED_FACE('',(#9718),#2424,.F.);
#88998=ADVANCED_FACE('',(#9719),#3327,.F.);
#88999=ADVANCED_FACE('',(#9720),#2425,.F.);
#89000=ADVANCED_FACE('',(#9721),#2426,.F.);
#89001=ADVANCED_FACE('',(#9722),#3328,.T.);
#89002=ADVANCED_FACE('',(#9723),#2427,.F.);
#89003=ADVANCED_FACE('',(#9724),#2428,.F.);
#89004=ADVANCED_FACE('',(#9725),#2429,.F.);
#89005=ADVANCED_FACE('',(#9726),#3329,.T.);
#89006=ADVANCED_FACE('',(#9727),#2430,.F.);
#89007=ADVANCED_FACE('',(#9728),#2431,.F.);
#89008=ADVANCED_FACE('',(#9729),#2432,.F.);
#89009=ADVANCED_FACE('',(#9730),#3330,.T.);
#89010=ADVANCED_FACE('',(#9731),#2433,.F.);
#89011=ADVANCED_FACE('',(#9732),#2434,.F.);
#89012=ADVANCED_FACE('',(#9733),#2435,.F.);
#89013=ADVANCED_FACE('',(#9734),#3331,.T.);
#89014=ADVANCED_FACE('',(#9735),#2436,.F.);
#89015=ADVANCED_FACE('',(#9736),#2437,.F.);
#89016=ADVANCED_FACE('',(#9737),#3332,.F.);
#89017=ADVANCED_FACE('',(#9738),#2438,.F.);
#89018=ADVANCED_FACE('',(#9739),#3333,.T.);
#89019=ADVANCED_FACE('',(#9740),#2439,.F.);
#89020=ADVANCED_FACE('',(#9741),#3334,.F.);
#89021=ADVANCED_FACE('',(#9742),#2440,.F.);
#89022=ADVANCED_FACE('',(#9743),#2441,.F.);
#89023=ADVANCED_FACE('',(#9744),#2442,.T.);
#89024=ADVANCED_FACE('',(#9745),#86131,.T.);
#89025=ADVANCED_FACE('',(#9746),#2443,.F.);
#89026=ADVANCED_FACE('',(#9747),#86132,.F.);
#89027=ADVANCED_FACE('',(#9748),#2444,.F.);
#89028=ADVANCED_FACE('',(#9749),#86133,.T.);
#89029=ADVANCED_FACE('',(#9750),#2445,.T.);
#89030=ADVANCED_FACE('',(#9751),#86134,.T.);
#89031=ADVANCED_FACE('',(#9752),#2446,.F.);
#89032=ADVANCED_FACE('',(#9753),#86135,.F.);
#89033=ADVANCED_FACE('',(#9754),#2447,.F.);
#89034=ADVANCED_FACE('',(#9755),#3335,.T.);
#89035=ADVANCED_FACE('',(#9756),#3336,.T.);
#89036=ADVANCED_FACE('',(#9757),#3337,.T.);
#89037=ADVANCED_FACE('',(#9758),#86136,.T.);
#89038=ADVANCED_FACE('',(#9759),#2448,.F.);
#89039=ADVANCED_FACE('',(#9760),#86137,.F.);
#89040=ADVANCED_FACE('',(#9761),#2449,.F.);
#89041=ADVANCED_FACE('',(#9762),#86138,.T.);
#89042=ADVANCED_FACE('',(#9763),#2450,.F.);
#89043=ADVANCED_FACE('',(#9764),#86139,.F.);
#89044=ADVANCED_FACE('',(#9765),#2451,.F.);
#89045=ADVANCED_FACE('',(#9766),#86140,.T.);
#89046=ADVANCED_FACE('',(#9767),#2452,.T.);
#89047=ADVANCED_FACE('',(#9768),#2453,.T.);
#89048=ADVANCED_FACE('',(#9769),#2454,.F.);
#89049=ADVANCED_FACE('',(#9770),#86141,.T.);
#89050=ADVANCED_FACE('',(#9771),#2455,.F.);
#89051=ADVANCED_FACE('',(#9772),#2456,.F.);
#89052=ADVANCED_FACE('',(#9773),#3338,.F.);
#89053=ADVANCED_FACE('',(#9774),#86142,.T.);
#89054=ADVANCED_FACE('',(#9775),#7832,.F.);
#89055=ADVANCED_FACE('',(#9776),#7833,.F.);
#89056=ADVANCED_FACE('',(#9777),#7834,.T.);
#89057=ADVANCED_FACE('',(#9778),#7835,.F.);
#89058=ADVANCED_FACE('',(#9779),#7836,.T.);
#89059=ADVANCED_FACE('',(#9780),#7837,.T.);
#89060=ADVANCED_FACE('',(#9781),#7838,.F.);
#89061=ADVANCED_FACE('',(#9782),#6949,.T.);
#89062=ADVANCED_FACE('',(#9783),#2457,.F.);
#89063=ADVANCED_FACE('',(#9784),#7839,.T.);
#89064=ADVANCED_FACE('',(#9785),#86143,.T.);
#89065=ADVANCED_FACE('',(#9786),#7840,.F.);
#89066=ADVANCED_FACE('',(#9787),#86144,.T.);
#89067=ADVANCED_FACE('',(#9788),#7841,.T.);
#89068=ADVANCED_FACE('',(#9789),#86145,.T.);
#89069=ADVANCED_FACE('',(#9790),#6950,.T.);
#89070=ADVANCED_FACE('',(#9791),#2458,.F.);
#89071=ADVANCED_FACE('',(#9792),#7842,.T.);
#89072=ADVANCED_FACE('',(#9793),#2459,.T.);
#89073=ADVANCED_FACE('',(#9794),#6951,.T.);
#89074=ADVANCED_FACE('',(#9795),#2460,.F.);
#89075=ADVANCED_FACE('',(#9796),#7843,.T.);
#89076=ADVANCED_FACE('',(#9797),#2461,.T.);
#89077=ADVANCED_FACE('',(#9798),#6952,.T.);
#89078=ADVANCED_FACE('',(#9799),#2462,.F.);
#89079=ADVANCED_FACE('',(#9800),#7844,.T.);
#89080=ADVANCED_FACE('',(#9801),#2463,.T.);
#89081=ADVANCED_FACE('',(#9802),#6953,.T.);
#89082=ADVANCED_FACE('',(#9803),#2464,.F.);
#89083=ADVANCED_FACE('',(#9804),#7845,.T.);
#89084=ADVANCED_FACE('',(#9805),#86146,.T.);
#89085=ADVANCED_FACE('',(#9806),#86147,.T.);
#89086=ADVANCED_FACE('',(#9807),#7846,.T.);
#89087=ADVANCED_FACE('',(#9808),#7847,.F.);
#89088=ADVANCED_FACE('',(#9809),#6954,.T.);
#89089=ADVANCED_FACE('',(#9810),#2465,.F.);
#89090=ADVANCED_FACE('',(#9811),#7848,.T.);
#89091=ADVANCED_FACE('',(#9812),#7849,.F.);
#89092=ADVANCED_FACE('',(#9813),#86148,.T.);
#89093=ADVANCED_FACE('',(#9814),#2466,.F.);
#89094=ADVANCED_FACE('',(#9815),#6955,.T.);
#89095=ADVANCED_FACE('',(#9816),#7850,.F.);
#89096=ADVANCED_FACE('',(#9817),#86149,.T.);
#89097=ADVANCED_FACE('',(#9818),#7851,.T.);
#89098=ADVANCED_FACE('',(#9819),#7852,.F.);
#89099=ADVANCED_FACE('',(#9820),#2467,.F.);
#89100=ADVANCED_FACE('',(#9821),#2468,.F.);
#89101=ADVANCED_FACE('',(#9822),#3339,.F.);
#89102=ADVANCED_FACE('',(#9823),#7853,.F.);
#89103=ADVANCED_FACE('',(#9824),#2469,.T.);
#89104=ADVANCED_FACE('',(#9825),#6956,.T.);
#89105=ADVANCED_FACE('',(#9826),#2470,.F.);
#89106=ADVANCED_FACE('',(#9827),#7854,.F.);
#89107=ADVANCED_FACE('',(#9828),#2471,.F.);
#89108=ADVANCED_FACE('',(#9829),#7855,.F.);
#89109=ADVANCED_FACE('',(#9830),#7856,.F.);
#89110=ADVANCED_FACE('',(#9831),#86150,.T.);
#89111=ADVANCED_FACE('',(#9832),#7857,.T.);
#89112=ADVANCED_FACE('',(#9833),#6957,.T.);
#89113=ADVANCED_FACE('',(#9834),#6958,.T.);
#89114=ADVANCED_FACE('',(#9835),#6959,.T.);
#89115=ADVANCED_FACE('',(#9836),#7858,.F.);
#89116=ADVANCED_FACE('',(#9837),#86151,.T.);
#89117=ADVANCED_FACE('',(#9838),#7859,.T.);
#89118=ADVANCED_FACE('',(#9839),#2472,.F.);
#89119=ADVANCED_FACE('',(#9840),#7860,.T.);
#89120=ADVANCED_FACE('',(#9841),#2473,.F.);
#89121=ADVANCED_FACE('',(#9842),#6960,.T.);
#89122=ADVANCED_FACE('',(#9843),#3340,.F.);
#89123=ADVANCED_FACE('',(#9844),#7861,.F.);
#89124=ADVANCED_FACE('',(#9845),#3341,.F.);
#89125=ADVANCED_FACE('',(#9846),#6961,.T.);
#89126=ADVANCED_FACE('',(#9847),#2474,.F.);
#89127=ADVANCED_FACE('',(#9848),#7862,.T.);
#89128=ADVANCED_FACE('',(#9849),#2475,.F.);
#89129=ADVANCED_FACE('',(#9850),#7863,.F.);
#89130=ADVANCED_FACE('',(#9851),#7864,.F.);
#89131=ADVANCED_FACE('',(#9852),#86152,.T.);
#89132=ADVANCED_FACE('',(#9853),#7865,.T.);
#89133=ADVANCED_FACE('',(#9854),#2476,.F.);
#89134=ADVANCED_FACE('',(#9855),#7866,.T.);
#89135=ADVANCED_FACE('',(#9856),#2477,.F.);
#89136=ADVANCED_FACE('',(#9857),#6962,.T.);
#89137=ADVANCED_FACE('',(#9858),#3342,.F.);
#89138=ADVANCED_FACE('',(#9859),#7867,.F.);
#89139=ADVANCED_FACE('',(#9860),#86153,.T.);
#89140=ADVANCED_FACE('',(#9861),#7868,.T.);
#89141=ADVANCED_FACE('',(#9862),#7869,.F.);
#89142=ADVANCED_FACE('',(#9863),#3343,.F.);
#89143=ADVANCED_FACE('',(#9864),#6963,.T.);
#89144=ADVANCED_FACE('',(#9865),#2478,.F.);
#89145=ADVANCED_FACE('',(#9866),#7870,.T.);
#89146=ADVANCED_FACE('',(#9867),#2479,.F.);
#89147=ADVANCED_FACE('',(#9868),#6964,.T.);
#89148=ADVANCED_FACE('',(#9869),#7871,.F.);
#89149=ADVANCED_FACE('',(#9870),#86154,.T.);
#89150=ADVANCED_FACE('',(#9871),#7872,.T.);
#89151=ADVANCED_FACE('',(#9872),#7873,.F.);
#89152=ADVANCED_FACE('',(#9873),#7874,.F.);
#89153=ADVANCED_FACE('',(#9874),#7875,.T.);
#89154=ADVANCED_FACE('',(#9875),#86155,.T.);
#89155=ADVANCED_FACE('',(#9876),#7876,.F.);
#89156=ADVANCED_FACE('',(#9877),#6965,.T.);
#89157=ADVANCED_FACE('',(#9878),#2480,.F.);
#89158=ADVANCED_FACE('',(#9879),#7877,.T.);
#89159=ADVANCED_FACE('',(#9880),#2481,.F.);
#89160=ADVANCED_FACE('',(#9881),#6966,.T.);
#89161=ADVANCED_FACE('',(#9882),#3344,.F.);
#89162=ADVANCED_FACE('',(#9883),#7878,.F.);
#89163=ADVANCED_FACE('',(#9884),#7879,.T.);
#89164=ADVANCED_FACE('',(#9885),#86156,.T.);
#89165=ADVANCED_FACE('',(#9886),#7880,.F.);
#89166=ADVANCED_FACE('',(#9887),#3345,.F.);
#89167=ADVANCED_FACE('',(#9888),#6967,.T.);
#89168=ADVANCED_FACE('',(#9889),#2482,.F.);
#89169=ADVANCED_FACE('',(#9890),#7881,.T.);
#89170=ADVANCED_FACE('',(#9891),#2483,.F.);
#89171=ADVANCED_FACE('',(#9892),#7882,.T.);
#89172=ADVANCED_FACE('',(#9893),#86157,.T.);
#89173=ADVANCED_FACE('',(#9894),#7883,.F.);
#89174=ADVANCED_FACE('',(#9895),#7884,.F.);
#89175=ADVANCED_FACE('',(#9896),#2484,.F.);
#89176=ADVANCED_FACE('',(#9897),#7885,.T.);
#89177=ADVANCED_FACE('',(#9898),#2485,.F.);
#89178=ADVANCED_FACE('',(#9899),#6968,.T.);
#89179=ADVANCED_FACE('',(#9900),#3346,.F.);
#89180=ADVANCED_FACE('',(#9901),#7886,.F.);
#89181=ADVANCED_FACE('',(#9902),#3347,.F.);
#89182=ADVANCED_FACE('',(#9903),#6969,.T.);
#89183=ADVANCED_FACE('',(#9904),#2486,.F.);
#89184=ADVANCED_FACE('',(#9905),#7887,.T.);
#89185=ADVANCED_FACE('',(#9906),#2487,.F.);
#89186=ADVANCED_FACE('',(#9907),#7888,.T.);
#89187=ADVANCED_FACE('',(#9908),#86158,.T.);
#89188=ADVANCED_FACE('',(#9909),#7889,.F.);
#89189=ADVANCED_FACE('',(#9910),#6970,.T.);
#89190=ADVANCED_FACE('',(#9911),#6971,.T.);
#89191=ADVANCED_FACE('',(#9912),#6972,.T.);
#89192=ADVANCED_FACE('',(#9913),#7890,.T.);
#89193=ADVANCED_FACE('',(#9914),#86159,.T.);
#89194=ADVANCED_FACE('',(#9915),#7891,.F.);
#89195=ADVANCED_FACE('',(#9916),#7892,.F.);
#89196=ADVANCED_FACE('',(#9917),#2488,.F.);
#89197=ADVANCED_FACE('',(#9918),#7893,.F.);
#89198=ADVANCED_FACE('',(#9919),#2489,.F.);
#89199=ADVANCED_FACE('',(#9920),#6973,.T.);
#89200=ADVANCED_FACE('',(#9921),#2490,.T.);
#89201=ADVANCED_FACE('',(#9922),#7894,.F.);
#89202=ADVANCED_FACE('',(#9923),#3348,.F.);
#89203=ADVANCED_FACE('',(#9924),#2491,.F.);
#89204=ADVANCED_FACE('',(#9925),#2492,.F.);
#89205=ADVANCED_FACE('',(#9926),#7895,.F.);
#89206=ADVANCED_FACE('',(#9927),#7896,.T.);
#89207=ADVANCED_FACE('',(#9928),#86160,.T.);
#89208=ADVANCED_FACE('',(#9929),#7897,.F.);
#89209=ADVANCED_FACE('',(#9930),#6974,.T.);
#89210=ADVANCED_FACE('',(#9931),#2493,.F.);
#89211=ADVANCED_FACE('',(#9932),#86161,.T.);
#89212=ADVANCED_FACE('',(#9933),#7898,.F.);
#89213=ADVANCED_FACE('',(#9934),#7899,.T.);
#89214=ADVANCED_FACE('',(#9935),#2494,.F.);
#89215=ADVANCED_FACE('',(#9936),#6975,.T.);
#89216=ADVANCED_FACE('',(#9937),#7900,.F.);
#89217=ADVANCED_FACE('',(#9938),#7901,.T.);
#89218=ADVANCED_FACE('',(#9939),#86162,.T.);
#89219=ADVANCED_FACE('',(#9940),#86163,.T.);
#89220=ADVANCED_FACE('',(#9941),#7902,.T.);
#89221=ADVANCED_FACE('',(#9942),#2495,.F.);
#89222=ADVANCED_FACE('',(#9943),#6976,.T.);
#89223=ADVANCED_FACE('',(#9944),#2496,.T.);
#89224=ADVANCED_FACE('',(#9945),#7903,.T.);
#89225=ADVANCED_FACE('',(#9946),#2497,.F.);
#89226=ADVANCED_FACE('',(#9947),#6977,.T.);
#89227=ADVANCED_FACE('',(#9948),#2498,.T.);
#89228=ADVANCED_FACE('',(#9949),#7904,.T.);
#89229=ADVANCED_FACE('',(#9950),#2499,.F.);
#89230=ADVANCED_FACE('',(#9951),#6978,.T.);
#89231=ADVANCED_FACE('',(#9952),#2500,.T.);
#89232=ADVANCED_FACE('',(#9953),#7905,.T.);
#89233=ADVANCED_FACE('',(#9954),#2501,.F.);
#89234=ADVANCED_FACE('',(#9955),#6979,.T.);
#89235=ADVANCED_FACE('',(#9956),#86164,.T.);
#89236=ADVANCED_FACE('',(#9957),#7906,.T.);
#89237=ADVANCED_FACE('',(#9958),#86165,.T.);
#89238=ADVANCED_FACE('',(#9959),#7907,.F.);
#89239=ADVANCED_FACE('',(#9960),#86166,.T.);
#89240=ADVANCED_FACE('',(#9961),#7908,.T.);
#89241=ADVANCED_FACE('',(#9962),#2502,.F.);
#89242=ADVANCED_FACE('',(#9963),#6980,.T.);
#89243=ADVANCED_FACE('',(#9964),#7909,.F.);
#89244=ADVANCED_FACE('',(#9965),#7910,.T.);
#89245=ADVANCED_FACE('',(#9966),#7911,.T.);
#89246=ADVANCED_FACE('',(#9967),#7912,.F.);
#89247=ADVANCED_FACE('',(#9968),#7913,.T.);
#89248=ADVANCED_FACE('',(#9969),#7914,.F.);
#89249=ADVANCED_FACE('',(#9970),#7915,.F.);
#89250=ADVANCED_FACE('',(#9971),#86167,.T.);
#89251=ADVANCED_FACE('',(#9972),#3349,.F.);
#89252=ADVANCED_FACE('',(#9973),#2503,.F.);
#89253=ADVANCED_FACE('',(#9974),#2504,.F.);
#89254=ADVANCED_FACE('',(#9975),#86168,.T.);
#89255=ADVANCED_FACE('',(#9976),#2505,.F.);
#89256=ADVANCED_FACE('',(#9977),#2506,.T.);
#89257=ADVANCED_FACE('',(#9978),#2507,.T.);
#89258=ADVANCED_FACE('',(#9979),#86169,.T.);
#89259=ADVANCED_FACE('',(#9980),#2508,.F.);
#89260=ADVANCED_FACE('',(#9981),#86170,.F.);
#89261=ADVANCED_FACE('',(#9982),#2509,.F.);
#89262=ADVANCED_FACE('',(#9983),#86171,.T.);
#89263=ADVANCED_FACE('',(#9984),#2510,.F.);
#89264=ADVANCED_FACE('',(#9985),#86172,.F.);
#89265=ADVANCED_FACE('',(#9986),#2511,.F.);
#89266=ADVANCED_FACE('',(#9987),#86173,.T.);
#89267=ADVANCED_FACE('',(#9988),#3350,.T.);
#89268=ADVANCED_FACE('',(#9989),#3351,.T.);
#89269=ADVANCED_FACE('',(#9990),#3352,.T.);
#89270=ADVANCED_FACE('',(#9991),#2512,.F.);
#89271=ADVANCED_FACE('',(#9992),#86174,.F.);
#89272=ADVANCED_FACE('',(#9993),#2513,.F.);
#89273=ADVANCED_FACE('',(#9994),#86175,.T.);
#89274=ADVANCED_FACE('',(#9995),#2514,.T.);
#89275=ADVANCED_FACE('',(#9996),#86176,.T.);
#89276=ADVANCED_FACE('',(#9997),#2515,.F.);
#89277=ADVANCED_FACE('',(#9998),#86177,.F.);
#89278=ADVANCED_FACE('',(#9999),#2516,.F.);
#89279=ADVANCED_FACE('',(#10000),#86178,.T.);
#89280=ADVANCED_FACE('',(#10001),#2517,.T.);
#89281=ADVANCED_FACE('',(#10002),#2518,.F.);
#89282=ADVANCED_FACE('',(#10003),#2519,.F.);
#89283=ADVANCED_FACE('',(#10004),#3353,.F.);
#89284=ADVANCED_FACE('',(#10005),#2520,.F.);
#89285=ADVANCED_FACE('',(#10006),#3354,.T.);
#89286=ADVANCED_FACE('',(#10007),#2521,.F.);
#89287=ADVANCED_FACE('',(#10008),#3355,.F.);
#89288=ADVANCED_FACE('',(#10009),#2522,.F.);
#89289=ADVANCED_FACE('',(#10010),#2523,.F.);
#89290=ADVANCED_FACE('',(#10011),#3356,.T.);
#89291=ADVANCED_FACE('',(#10012),#2524,.F.);
#89292=ADVANCED_FACE('',(#10013),#2525,.F.);
#89293=ADVANCED_FACE('',(#10014),#2526,.F.);
#89294=ADVANCED_FACE('',(#10015),#3357,.T.);
#89295=ADVANCED_FACE('',(#10016),#2527,.F.);
#89296=ADVANCED_FACE('',(#10017),#2528,.F.);
#89297=ADVANCED_FACE('',(#10018),#2529,.F.);
#89298=ADVANCED_FACE('',(#10019),#3358,.T.);
#89299=ADVANCED_FACE('',(#10020),#2530,.F.);
#89300=ADVANCED_FACE('',(#10021),#2531,.F.);
#89301=ADVANCED_FACE('',(#10022),#2532,.F.);
#89302=ADVANCED_FACE('',(#10023),#3359,.T.);
#89303=ADVANCED_FACE('',(#10024),#2533,.F.);
#89304=ADVANCED_FACE('',(#10025),#2534,.F.);
#89305=ADVANCED_FACE('',(#10026),#3360,.F.);
#89306=ADVANCED_FACE('',(#10027),#2535,.F.);
#89307=ADVANCED_FACE('',(#10028),#3361,.T.);
#89308=ADVANCED_FACE('',(#10029),#2536,.F.);
#89309=ADVANCED_FACE('',(#10030),#3362,.F.);
#89310=ADVANCED_FACE('',(#10031),#2537,.F.);
#89311=ADVANCED_FACE('',(#10032),#2538,.T.);
#89312=ADVANCED_FACE('',(#10033),#2539,.F.);
#89313=ADVANCED_FACE('',(#10034),#2540,.T.);
#89314=ADVANCED_FACE('',(#10035),#86179,.T.);
#89315=ADVANCED_FACE('',(#10036),#2541,.F.);
#89316=ADVANCED_FACE('',(#10037),#86180,.F.);
#89317=ADVANCED_FACE('',(#10038),#2542,.F.);
#89318=ADVANCED_FACE('',(#10039),#86181,.T.);
#89319=ADVANCED_FACE('',(#10040),#2543,.F.);
#89320=ADVANCED_FACE('',(#10041),#86182,.F.);
#89321=ADVANCED_FACE('',(#10042),#2544,.F.);
#89322=ADVANCED_FACE('',(#10043),#86183,.T.);
#89323=ADVANCED_FACE('',(#10044),#3363,.T.);
#89324=ADVANCED_FACE('',(#10045),#3364,.T.);
#89325=ADVANCED_FACE('',(#10046),#3365,.T.);
#89326=ADVANCED_FACE('',(#10047),#86184,.T.);
#89327=ADVANCED_FACE('',(#10048),#1017,.F.);
#89328=ADVANCED_FACE('',(#10049),#2545,.F.);
#89329=ADVANCED_FACE('',(#10050),#2546,.F.);
#89330=ADVANCED_FACE('',(#10051),#7916,.T.);
#89331=ADVANCED_FACE('',(#10052),#86185,.T.);
#89332=ADVANCED_FACE('',(#10053),#7917,.T.);
#89333=ADVANCED_FACE('',(#10054),#3366,.T.);
#89334=ADVANCED_FACE('',(#10055),#86186,.T.);
#89335=ADVANCED_FACE('',(#10056),#2547,.F.);
#89336=ADVANCED_FACE('',(#10057),#2548,.F.);
#89337=ADVANCED_FACE('',(#10058),#86187,.F.);
#89338=ADVANCED_FACE('',(#10059),#2549,.F.);
#89339=ADVANCED_FACE('',(#10060),#2550,.F.);
#89340=ADVANCED_FACE('',(#10061),#2551,.F.);
#89341=ADVANCED_FACE('',(#10062),#86188,.F.);
#89342=ADVANCED_FACE('',(#10063),#2552,.F.);
#89343=ADVANCED_FACE('',(#10064),#86189,.F.);
#89344=ADVANCED_FACE('',(#10065),#86190,.T.);
#89345=ADVANCED_FACE('',(#10066),#86191,.F.);
#89346=ADVANCED_FACE('',(#10067),#3367,.T.);
#89347=ADVANCED_FACE('',(#10068),#86192,.T.);
#89348=ADVANCED_FACE('',(#10069),#3368,.T.);
#89349=ADVANCED_FACE('',(#10070),#86193,.T.);
#89350=ADVANCED_FACE('',(#10071),#3369,.T.);
#89351=ADVANCED_FACE('',(#10072),#86194,.T.);
#89352=ADVANCED_FACE('',(#10073),#86195,.F.);
#89353=ADVANCED_FACE('',(#10074),#2553,.F.);
#89354=ADVANCED_FACE('',(#10075),#86196,.F.);
#89355=ADVANCED_FACE('',(#10076),#2554,.F.);
#89356=ADVANCED_FACE('',(#10077),#2555,.F.);
#89357=ADVANCED_FACE('',(#10078),#2556,.F.);
#89358=ADVANCED_FACE('',(#10079),#86197,.F.);
#89359=ADVANCED_FACE('',(#10080),#2557,.F.);
#89360=ADVANCED_FACE('',(#10081),#2558,.F.);
#89361=ADVANCED_FACE('',(#10082),#2559,.F.);
#89362=ADVANCED_FACE('',(#10083),#86198,.F.);
#89363=ADVANCED_FACE('',(#10084),#3370,.F.);
#89364=ADVANCED_FACE('',(#10085),#3371,.T.);
#89365=ADVANCED_FACE('',(#10086),#86199,.T.);
#89366=ADVANCED_FACE('',(#10087),#86200,.F.);
#89367=ADVANCED_FACE('',(#10088),#2560,.F.);
#89368=ADVANCED_FACE('',(#10089),#2561,.F.);
#89369=ADVANCED_FACE('',(#10090),#2562,.F.);
#89370=ADVANCED_FACE('',(#10091),#86201,.F.);
#89371=ADVANCED_FACE('',(#10092),#2563,.F.);
#89372=ADVANCED_FACE('',(#10093),#2564,.F.);
#89373=ADVANCED_FACE('',(#10094),#2565,.F.);
#89374=ADVANCED_FACE('',(#10095),#86202,.F.);
#89375=ADVANCED_FACE('',(#10096),#2566,.F.);
#89376=ADVANCED_FACE('',(#10097),#86203,.F.);
#89377=ADVANCED_FACE('',(#10098),#86204,.T.);
#89378=ADVANCED_FACE('',(#10099),#3372,.T.);
#89379=ADVANCED_FACE('',(#10100),#86205,.T.);
#89380=ADVANCED_FACE('',(#10101),#86206,.F.);
#89381=ADVANCED_FACE('',(#10102),#86207,.F.);
#89382=ADVANCED_FACE('',(#10103),#86208,.F.);
#89383=ADVANCED_FACE('',(#10104),#2567,.F.);
#89384=ADVANCED_FACE('',(#10105),#3373,.T.);
#89385=ADVANCED_FACE('',(#10106),#86209,.T.);
#89386=ADVANCED_FACE('',(#10107),#3374,.T.);
#89387=ADVANCED_FACE('',(#10108),#86210,.T.);
#89388=ADVANCED_FACE('',(#10109),#86211,.F.);
#89389=ADVANCED_FACE('',(#10110),#2568,.F.);
#89390=ADVANCED_FACE('',(#10111),#2569,.F.);
#89391=ADVANCED_FACE('',(#10112),#2570,.F.);
#89392=ADVANCED_FACE('',(#10113),#2571,.F.);
#89393=ADVANCED_FACE('',(#10114),#86212,.F.);
#89394=ADVANCED_FACE('',(#10115),#2572,.F.);
#89395=ADVANCED_FACE('',(#10116),#2573,.F.);
#89396=ADVANCED_FACE('',(#10117),#86213,.T.);
#89397=ADVANCED_FACE('',(#10118),#3375,.T.);
#89398=ADVANCED_FACE('',(#10119),#86214,.T.);
#89399=ADVANCED_FACE('',(#10120),#86215,.F.);
#89400=ADVANCED_FACE('',(#10121),#2574,.F.);
#89401=ADVANCED_FACE('',(#10122),#2575,.F.);
#89402=ADVANCED_FACE('',(#10123),#2576,.F.);
#89403=ADVANCED_FACE('',(#10124),#6981,.T.);
#89404=ADVANCED_FACE('',(#10125),#3376,.T.);
#89405=ADVANCED_FACE('',(#10126),#86216,.T.);
#89406=ADVANCED_FACE('',(#10127),#2577,.F.);
#89407=ADVANCED_FACE('',(#10128),#2578,.F.);
#89408=ADVANCED_FACE('',(#10129),#2579,.F.);
#89409=ADVANCED_FACE('',(#10130),#86217,.F.);
#89410=ADVANCED_FACE('',(#10131),#2580,.F.);
#89411=ADVANCED_FACE('',(#10132),#2581,.F.);
#89412=ADVANCED_FACE('',(#10133),#2582,.F.);
#89413=ADVANCED_FACE('',(#10134),#86218,.F.);
#89414=ADVANCED_FACE('',(#10135),#2583,.F.);
#89415=ADVANCED_FACE('',(#10136),#86219,.F.);
#89416=ADVANCED_FACE('',(#10137),#86220,.T.);
#89417=ADVANCED_FACE('',(#10138),#3377,.T.);
#89418=ADVANCED_FACE('',(#10139),#86221,.T.);
#89419=ADVANCED_FACE('',(#10140),#3378,.T.);
#89420=ADVANCED_FACE('',(#10141),#86222,.T.);
#89421=ADVANCED_FACE('',(#10142),#3379,.T.);
#89422=ADVANCED_FACE('',(#10143),#86223,.T.);
#89423=ADVANCED_FACE('',(#10144),#86224,.F.);
#89424=ADVANCED_FACE('',(#10145),#2584,.F.);
#89425=ADVANCED_FACE('',(#10146),#86225,.F.);
#89426=ADVANCED_FACE('',(#10147),#2585,.F.);
#89427=ADVANCED_FACE('',(#10148),#2586,.F.);
#89428=ADVANCED_FACE('',(#10149),#2587,.F.);
#89429=ADVANCED_FACE('',(#10150),#86226,.F.);
#89430=ADVANCED_FACE('',(#10151),#2588,.F.);
#89431=ADVANCED_FACE('',(#10152),#2589,.F.);
#89432=ADVANCED_FACE('',(#10153),#86227,.F.);
#89433=ADVANCED_FACE('',(#10154),#2590,.F.);
#89434=ADVANCED_FACE('',(#10155),#6982,.T.);
#89435=ADVANCED_FACE('',(#10156),#3380,.T.);
#89436=ADVANCED_FACE('',(#10157),#86228,.T.);
#89437=ADVANCED_FACE('',(#10158),#2591,.F.);
#89438=ADVANCED_FACE('',(#10159),#2592,.F.);
#89439=ADVANCED_FACE('',(#10160),#2593,.F.);
#89440=ADVANCED_FACE('',(#10161),#2594,.F.);
#89441=ADVANCED_FACE('',(#10162),#86229,.F.);
#89442=ADVANCED_FACE('',(#10163),#2595,.F.);
#89443=ADVANCED_FACE('',(#10164),#2596,.F.);
#89444=ADVANCED_FACE('',(#10165),#2597,.F.);
#89445=ADVANCED_FACE('',(#10166),#2598,.F.);
#89446=ADVANCED_FACE('',(#10167),#86230,.F.);
#89447=ADVANCED_FACE('',(#10168),#86231,.T.);
#89448=ADVANCED_FACE('',(#10169),#86232,.F.);
#89449=ADVANCED_FACE('',(#10170),#86233,.F.);
#89450=ADVANCED_FACE('',(#10171),#2599,.F.);
#89451=ADVANCED_FACE('',(#10172),#86234,.F.);
#89452=ADVANCED_FACE('',(#10173),#86235,.T.);
#89453=ADVANCED_FACE('',(#10174),#3381,.T.);
#89454=ADVANCED_FACE('',(#10175),#86236,.T.);
#89455=ADVANCED_FACE('',(#10176),#2600,.F.);
#89456=ADVANCED_FACE('',(#10177),#86237,.F.);
#89457=ADVANCED_FACE('',(#10178),#3382,.T.);
#89458=ADVANCED_FACE('',(#10179),#86238,.T.);
#89459=ADVANCED_FACE('',(#10180),#86239,.F.);
#89460=ADVANCED_FACE('',(#10181),#2601,.F.);
#89461=ADVANCED_FACE('',(#10182),#2602,.F.);
#89462=ADVANCED_FACE('',(#10183),#2603,.F.);
#89463=ADVANCED_FACE('',(#10184),#86240,.F.);
#89464=ADVANCED_FACE('',(#10185),#2604,.F.);
#89465=ADVANCED_FACE('',(#10186),#2605,.F.);
#89466=ADVANCED_FACE('',(#10187),#2606,.F.);
#89467=ADVANCED_FACE('',(#10188),#3383,.T.);
#89468=ADVANCED_FACE('',(#10189),#86241,.T.);
#89469=ADVANCED_FACE('',(#10190),#3384,.T.);
#89470=ADVANCED_FACE('',(#10191),#86242,.T.);
#89471=ADVANCED_FACE('',(#10192),#86243,.F.);
#89472=ADVANCED_FACE('',(#10193),#2607,.F.);
#89473=ADVANCED_FACE('',(#10194),#86244,.F.);
#89474=ADVANCED_FACE('',(#10195),#86245,.F.);
#89475=ADVANCED_FACE('',(#10196),#3385,.F.);
#89476=ADVANCED_FACE('',(#10197),#2608,.F.);
#89477=ADVANCED_FACE('',(#10198),#2609,.F.);
#89478=ADVANCED_FACE('',(#10199),#2610,.F.);
#89479=ADVANCED_FACE('',(#10200),#86246,.F.);
#89480=ADVANCED_FACE('',(#10201),#3386,.T.);
#89481=ADVANCED_FACE('',(#10202),#86247,.T.);
#89482=ADVANCED_FACE('',(#10203),#3387,.T.);
#89483=ADVANCED_FACE('',(#10204),#86248,.T.);
#89484=ADVANCED_FACE('',(#10205),#86249,.F.);
#89485=ADVANCED_FACE('',(#10206),#2611,.F.);
#89486=ADVANCED_FACE('',(#10207),#2612,.F.);
#89487=ADVANCED_FACE('',(#10208),#86250,.F.);
#89488=ADVANCED_FACE('',(#10209),#3388,.T.);
#89489=ADVANCED_FACE('',(#10210),#86251,.T.);
#89490=ADVANCED_FACE('',(#10211),#3389,.T.);
#89491=ADVANCED_FACE('',(#10212),#86252,.F.);
#89492=ADVANCED_FACE('',(#10213),#2613,.F.);
#89493=ADVANCED_FACE('',(#10214),#2614,.F.);
#89494=ADVANCED_FACE('',(#10215),#2615,.F.);
#89495=ADVANCED_FACE('',(#10216),#86253,.F.);
#89496=ADVANCED_FACE('',(#10217),#86254,.F.);
#89497=ADVANCED_FACE('',(#10218),#3390,.F.);
#89498=ADVANCED_FACE('',(#10219),#3391,.T.);
#89499=ADVANCED_FACE('',(#10220),#86255,.T.);
#89500=ADVANCED_FACE('',(#10221),#2616,.F.);
#89501=ADVANCED_FACE('',(#10222),#2617,.F.);
#89502=ADVANCED_FACE('',(#10223),#2618,.F.);
#89503=ADVANCED_FACE('',(#10224),#86256,.F.);
#89504=ADVANCED_FACE('',(#10225),#2619,.F.);
#89505=ADVANCED_FACE('',(#10226),#2620,.F.);
#89506=ADVANCED_FACE('',(#10227),#2621,.F.);
#89507=ADVANCED_FACE('',(#10228),#86257,.F.);
#89508=ADVANCED_FACE('',(#10229),#2622,.F.);
#89509=ADVANCED_FACE('',(#10230),#86258,.F.);
#89510=ADVANCED_FACE('',(#10231),#86259,.T.);
#89511=ADVANCED_FACE('',(#10232),#3392,.T.);
#89512=ADVANCED_FACE('',(#10233),#86260,.T.);
#89513=ADVANCED_FACE('',(#10234),#3393,.T.);
#89514=ADVANCED_FACE('',(#10235),#86261,.T.);
#89515=ADVANCED_FACE('',(#10236),#3394,.T.);
#89516=ADVANCED_FACE('',(#10237),#86262,.T.);
#89517=ADVANCED_FACE('',(#10238),#86263,.F.);
#89518=ADVANCED_FACE('',(#10239),#2623,.F.);
#89519=ADVANCED_FACE('',(#10240),#86264,.F.);
#89520=ADVANCED_FACE('',(#10241),#2624,.F.);
#89521=ADVANCED_FACE('',(#10242),#2625,.F.);
#89522=ADVANCED_FACE('',(#10243),#2626,.F.);
#89523=ADVANCED_FACE('',(#10244),#86265,.F.);
#89524=ADVANCED_FACE('',(#10245),#2627,.F.);
#89525=ADVANCED_FACE('',(#10246),#2628,.F.);
#89526=ADVANCED_FACE('',(#10247),#86266,.F.);
#89527=ADVANCED_FACE('',(#10248),#2629,.F.);
#89528=ADVANCED_FACE('',(#10249),#6983,.T.);
#89529=ADVANCED_FACE('',(#10250),#3395,.T.);
#89530=ADVANCED_FACE('',(#10251),#86267,.T.);
#89531=ADVANCED_FACE('',(#10252),#2630,.F.);
#89532=ADVANCED_FACE('',(#10253),#2631,.F.);
#89533=ADVANCED_FACE('',(#10254),#86268,.F.);
#89534=ADVANCED_FACE('',(#10255),#2632,.F.);
#89535=ADVANCED_FACE('',(#10256),#2633,.F.);
#89536=ADVANCED_FACE('',(#10257),#2634,.F.);
#89537=ADVANCED_FACE('',(#10258),#2635,.F.);
#89538=ADVANCED_FACE('',(#10259),#2636,.F.);
#89539=ADVANCED_FACE('',(#10260),#86269,.F.);
#89540=ADVANCED_FACE('',(#10261),#2637,.F.);
#89541=ADVANCED_FACE('',(#10262),#86270,.F.);
#89542=ADVANCED_FACE('',(#10263),#86271,.T.);
#89543=ADVANCED_FACE('',(#10264),#3396,.T.);
#89544=ADVANCED_FACE('',(#10265),#86272,.T.);
#89545=ADVANCED_FACE('',(#10266),#2638,.F.);
#89546=ADVANCED_FACE('',(#10267),#86273,.F.);
#89547=ADVANCED_FACE('',(#10268),#86274,.F.);
#89548=ADVANCED_FACE('',(#10269),#86275,.F.);
#89549=ADVANCED_FACE('',(#10270),#3397,.T.);
#89550=ADVANCED_FACE('',(#10271),#86276,.T.);
#89551=ADVANCED_FACE('',(#10272),#86277,.F.);
#89552=ADVANCED_FACE('',(#10273),#2639,.F.);
#89553=ADVANCED_FACE('',(#10274),#2640,.F.);
#89554=ADVANCED_FACE('',(#10275),#2641,.F.);
#89555=ADVANCED_FACE('',(#10276),#86278,.F.);
#89556=ADVANCED_FACE('',(#10277),#2642,.F.);
#89557=ADVANCED_FACE('',(#10278),#2643,.F.);
#89558=ADVANCED_FACE('',(#10279),#3398,.T.);
#89559=ADVANCED_FACE('',(#10280),#86279,.T.);
#89560=ADVANCED_FACE('',(#10281),#3399,.T.);
#89561=ADVANCED_FACE('',(#10282),#86280,.T.);
#89562=ADVANCED_FACE('',(#10283),#86281,.F.);
#89563=ADVANCED_FACE('',(#10284),#2644,.F.);
#89564=ADVANCED_FACE('',(#10285),#3400,.F.);
#89565=ADVANCED_FACE('',(#10286),#86282,.F.);
#89566=ADVANCED_FACE('',(#10287),#86283,.F.);
#89567=ADVANCED_FACE('',(#10288),#2645,.F.);
#89568=ADVANCED_FACE('',(#10289),#2646,.F.);
#89569=ADVANCED_FACE('',(#10290),#2647,.F.);
#89570=ADVANCED_FACE('',(#10291),#86284,.F.);
#89571=ADVANCED_FACE('',(#10292),#2648,.F.);
#89572=ADVANCED_FACE('',(#10293),#86285,.T.);
#89573=ADVANCED_FACE('',(#10294),#3401,.T.);
#89574=ADVANCED_FACE('',(#10295),#86286,.T.);
#89575=ADVANCED_FACE('',(#10296),#86287,.F.);
#89576=ADVANCED_FACE('',(#10297),#2649,.F.);
#89577=ADVANCED_FACE('',(#10298),#2650,.F.);
#89578=ADVANCED_FACE('',(#10299),#2651,.F.);
#89579=ADVANCED_FACE('',(#10300),#2652,.F.);
#89580=ADVANCED_FACE('',(#10301),#86288,.F.);
#89581=ADVANCED_FACE('',(#10302),#2653,.F.);
#89582=ADVANCED_FACE('',(#10303),#2654,.F.);
#89583=ADVANCED_FACE('',(#10304),#2655,.F.);
#89584=ADVANCED_FACE('',(#10305),#86289,.F.);
#89585=ADVANCED_FACE('',(#10306),#86290,.T.);
#89586=ADVANCED_FACE('',(#10307),#3402,.T.);
#89587=ADVANCED_FACE('',(#10308),#86291,.T.);
#89588=ADVANCED_FACE('',(#10309),#2656,.F.);
#89589=ADVANCED_FACE('',(#10310),#3403,.T.);
#89590=ADVANCED_FACE('',(#10311),#86292,.T.);
#89591=ADVANCED_FACE('',(#10312),#3404,.T.);
#89592=ADVANCED_FACE('',(#10313),#86293,.T.);
#89593=ADVANCED_FACE('',(#10314),#3405,.T.);
#89594=ADVANCED_FACE('',(#10315),#86294,.F.);
#89595=ADVANCED_FACE('',(#10316),#2657,.F.);
#89596=ADVANCED_FACE('',(#10317),#2658,.F.);
#89597=ADVANCED_FACE('',(#10318),#2659,.F.);
#89598=ADVANCED_FACE('',(#10319),#86295,.F.);
#89599=ADVANCED_FACE('',(#10320),#2660,.F.);
#89600=ADVANCED_FACE('',(#10321),#2661,.F.);
#89601=ADVANCED_FACE('',(#10322),#2662,.F.);
#89602=ADVANCED_FACE('',(#10323),#2663,.F.);
#89603=ADVANCED_FACE('',(#10324),#86296,.F.);
#89604=ADVANCED_FACE('',(#10325),#2664,.F.);
#89605=ADVANCED_FACE('',(#10326),#2665,.F.);
#89606=ADVANCED_FACE('',(#10327),#2666,.F.);
#89607=ADVANCED_FACE('',(#10328),#86297,.F.);
#89608=ADVANCED_FACE('',(#10329),#2667,.T.);
#89609=ADVANCED_FACE('',(#10330),#2668,.F.);
#89610=ADVANCED_FACE('',(#10331),#86298,.T.);
#89611=ADVANCED_FACE('',(#10332),#7918,.T.);
#89612=ADVANCED_FACE('',(#10333),#86299,.T.);
#89613=ADVANCED_FACE('',(#10334),#2669,.T.);
#89614=ADVANCED_FACE('',(#10335),#86300,.F.);
#89615=ADVANCED_FACE('',(#10336),#2670,.F.);
#89616=ADVANCED_FACE('',(#10337),#2671,.F.);
#89617=ADVANCED_FACE('',(#10338),#2672,.F.);
#89618=ADVANCED_FACE('',(#10339),#86301,.F.);
#89619=ADVANCED_FACE('',(#10340),#2673,.F.);
#89620=ADVANCED_FACE('',(#10341),#2674,.F.);
#89621=ADVANCED_FACE('',(#10342),#2675,.F.);
#89622=ADVANCED_FACE('',(#10343),#2676,.F.);
#89623=ADVANCED_FACE('',(#10344),#86302,.F.);
#89624=ADVANCED_FACE('',(#10345),#2677,.F.);
#89625=ADVANCED_FACE('',(#10346),#2678,.F.);
#89626=ADVANCED_FACE('',(#10347),#2679,.F.);
#89627=ADVANCED_FACE('',(#10348),#86303,.F.);
#89628=ADVANCED_FACE('',(#10349),#2680,.T.);
#89629=ADVANCED_FACE('',(#10350),#2681,.F.);
#89630=ADVANCED_FACE('',(#10351),#86304,.T.);
#89631=ADVANCED_FACE('',(#10352),#7919,.T.);
#89632=ADVANCED_FACE('',(#10353),#86305,.T.);
#89633=ADVANCED_FACE('',(#10354),#2682,.T.);
#89634=ADVANCED_FACE('',(#10355),#86306,.F.);
#89635=ADVANCED_FACE('',(#10356),#2683,.F.);
#89636=ADVANCED_FACE('',(#10357),#2684,.F.);
#89637=ADVANCED_FACE('',(#10358),#2685,.F.);
#89638=ADVANCED_FACE('',(#10359),#86307,.F.);
#89639=ADVANCED_FACE('',(#10360),#2686,.F.);
#89640=ADVANCED_FACE('',(#10361),#2687,.F.);
#89641=ADVANCED_FACE('',(#10362),#2688,.F.);
#89642=ADVANCED_FACE('',(#10363),#2689,.F.);
#89643=ADVANCED_FACE('',(#10364),#86308,.F.);
#89644=ADVANCED_FACE('',(#10365),#2690,.F.);
#89645=ADVANCED_FACE('',(#10366),#2691,.F.);
#89646=ADVANCED_FACE('',(#10367),#2692,.F.);
#89647=ADVANCED_FACE('',(#10368),#86309,.F.);
#89648=ADVANCED_FACE('',(#10369),#2693,.T.);
#89649=ADVANCED_FACE('',(#10370),#2694,.F.);
#89650=ADVANCED_FACE('',(#10371),#86310,.T.);
#89651=ADVANCED_FACE('',(#10372),#7920,.T.);
#89652=ADVANCED_FACE('',(#10373),#86311,.T.);
#89653=ADVANCED_FACE('',(#10374),#2695,.T.);
#89654=ADVANCED_FACE('',(#10375),#86312,.F.);
#89655=ADVANCED_FACE('',(#10376),#2696,.F.);
#89656=ADVANCED_FACE('',(#10377),#2697,.F.);
#89657=ADVANCED_FACE('',(#10378),#2698,.F.);
#89658=ADVANCED_FACE('',(#10379),#86313,.F.);
#89659=ADVANCED_FACE('',(#10380),#2699,.F.);
#89660=ADVANCED_FACE('',(#10381),#2700,.F.);
#89661=ADVANCED_FACE('',(#10382),#2701,.F.);
#89662=ADVANCED_FACE('',(#10383),#2702,.F.);
#89663=ADVANCED_FACE('',(#10384),#86314,.F.);
#89664=ADVANCED_FACE('',(#10385),#2703,.F.);
#89665=ADVANCED_FACE('',(#10386),#2704,.F.);
#89666=ADVANCED_FACE('',(#10387),#2705,.F.);
#89667=ADVANCED_FACE('',(#10388),#86315,.F.);
#89668=ADVANCED_FACE('',(#10389),#3406,.T.);
#89669=ADVANCED_FACE('',(#10390),#86316,.T.);
#89670=ADVANCED_FACE('',(#10391),#2706,.F.);
#89671=ADVANCED_FACE('',(#10392),#3407,.T.);
#89672=ADVANCED_FACE('',(#10393),#86317,.T.);
#89673=ADVANCED_FACE('',(#10394),#3408,.T.);
#89674=ADVANCED_FACE('',(#10395),#86318,.T.);
#89675=ADVANCED_FACE('',(#10396),#3409,.T.);
#89676=ADVANCED_FACE('',(#10397),#86319,.T.);
#89677=ADVANCED_FACE('',(#10398),#86320,.F.);
#89678=ADVANCED_FACE('',(#10399),#2707,.F.);
#89679=ADVANCED_FACE('',(#10400),#2708,.F.);
#89680=ADVANCED_FACE('',(#10401),#2709,.F.);
#89681=ADVANCED_FACE('',(#10402),#86321,.F.);
#89682=ADVANCED_FACE('',(#10403),#2710,.F.);
#89683=ADVANCED_FACE('',(#10404),#2711,.F.);
#89684=ADVANCED_FACE('',(#10405),#2712,.F.);
#89685=ADVANCED_FACE('',(#10406),#3410,.T.);
#89686=ADVANCED_FACE('',(#10407),#86322,.T.);
#89687=ADVANCED_FACE('',(#10408),#2713,.F.);
#89688=ADVANCED_FACE('',(#10409),#2714,.F.);
#89689=ADVANCED_FACE('',(#10410),#86323,.F.);
#89690=ADVANCED_FACE('',(#10411),#2715,.F.);
#89691=ADVANCED_FACE('',(#10412),#2716,.F.);
#89692=ADVANCED_FACE('',(#10413),#2717,.F.);
#89693=ADVANCED_FACE('',(#10414),#86324,.F.);
#89694=ADVANCED_FACE('',(#10415),#86325,.T.);
#89695=ADVANCED_FACE('',(#10416),#3411,.T.);
#89696=ADVANCED_FACE('',(#10417),#86326,.T.);
#89697=ADVANCED_FACE('',(#10418),#3412,.T.);
#89698=ADVANCED_FACE('',(#10419),#3413,.T.);
#89699=ADVANCED_FACE('',(#10420),#86327,.T.);
#89700=ADVANCED_FACE('',(#10421),#3414,.T.);
#89701=ADVANCED_FACE('',(#10422),#2718,.F.);
#89702=ADVANCED_FACE('',(#10423),#2719,.F.);
#89703=ADVANCED_FACE('',(#10424),#2720,.F.);
#89704=ADVANCED_FACE('',(#10425),#2721,.F.);
#89705=ADVANCED_FACE('',(#10426),#2722,.F.);
#89706=ADVANCED_FACE('',(#10427),#2723,.F.);
#89707=ADVANCED_FACE('',(#10428),#86328,.F.);
#89708=ADVANCED_FACE('',(#10429),#3415,.T.);
#89709=ADVANCED_FACE('',(#10430),#86329,.T.);
#89710=ADVANCED_FACE('',(#10431),#3416,.T.);
#89711=ADVANCED_FACE('',(#10432),#86330,.F.);
#89712=ADVANCED_FACE('',(#10433),#2724,.F.);
#89713=ADVANCED_FACE('',(#10434),#2725,.F.);
#89714=ADVANCED_FACE('',(#10435),#2726,.F.);
#89715=ADVANCED_FACE('',(#10436),#2727,.F.);
#89716=ADVANCED_FACE('',(#10437),#6984,.T.);
#89717=ADVANCED_FACE('',(#10438),#3417,.T.);
#89718=ADVANCED_FACE('',(#10439),#86331,.T.);
#89719=ADVANCED_FACE('',(#10440),#3418,.T.);
#89720=ADVANCED_FACE('',(#10441),#2728,.F.);
#89721=ADVANCED_FACE('',(#10442),#2729,.F.);
#89722=ADVANCED_FACE('',(#10443),#86332,.F.);
#89723=ADVANCED_FACE('',(#10444),#2730,.F.);
#89724=ADVANCED_FACE('',(#10445),#2731,.F.);
#89725=ADVANCED_FACE('',(#10446),#2732,.F.);
#89726=ADVANCED_FACE('',(#10447),#3419,.T.);
#89727=ADVANCED_FACE('',(#10448),#86333,.T.);
#89728=ADVANCED_FACE('',(#10449),#2733,.F.);
#89729=ADVANCED_FACE('',(#10450),#86334,.F.);
#89730=ADVANCED_FACE('',(#10451),#2734,.F.);
#89731=ADVANCED_FACE('',(#10452),#2735,.F.);
#89732=ADVANCED_FACE('',(#10453),#2736,.F.);
#89733=ADVANCED_FACE('',(#10454),#3420,.T.);
#89734=ADVANCED_FACE('',(#10455),#86335,.T.);
#89735=ADVANCED_FACE('',(#10456),#3421,.T.);
#89736=ADVANCED_FACE('',(#10457),#86336,.T.);
#89737=ADVANCED_FACE('',(#10458),#3422,.T.);
#89738=ADVANCED_FACE('',(#10459),#2737,.F.);
#89739=ADVANCED_FACE('',(#10460),#2738,.F.);
#89740=ADVANCED_FACE('',(#10461),#86337,.F.);
#89741=ADVANCED_FACE('',(#10462),#2739,.F.);
#89742=ADVANCED_FACE('',(#10463),#2740,.F.);
#89743=ADVANCED_FACE('',(#10464),#2741,.F.);
#89744=ADVANCED_FACE('',(#10465),#2742,.F.);
#89745=ADVANCED_FACE('',(#10466),#86338,.F.);
#89746=ADVANCED_FACE('',(#10467),#2743,.F.);
#89747=ADVANCED_FACE('',(#10468),#2744,.F.);
#89748=ADVANCED_FACE('',(#10469),#2745,.F.);
#89749=ADVANCED_FACE('',(#10470),#86339,.T.);
#89750=ADVANCED_FACE('',(#10471),#7921,.T.);
#89751=ADVANCED_FACE('',(#10472),#86340,.T.);
#89752=ADVANCED_FACE('',(#10473),#2746,.F.);
#89753=ADVANCED_FACE('',(#10474),#2747,.F.);
#89754=ADVANCED_FACE('',(#10475),#86341,.F.);
#89755=ADVANCED_FACE('',(#10476),#2748,.F.);
#89756=ADVANCED_FACE('',(#10477),#2749,.F.);
#89757=ADVANCED_FACE('',(#10478),#2750,.F.);
#89758=ADVANCED_FACE('',(#10479),#2751,.F.);
#89759=ADVANCED_FACE('',(#10480),#86342,.F.);
#89760=ADVANCED_FACE('',(#10481),#2752,.F.);
#89761=ADVANCED_FACE('',(#10482),#2753,.F.);
#89762=ADVANCED_FACE('',(#10483),#2754,.F.);
#89763=ADVANCED_FACE('',(#10484),#7922,.F.);
#89764=ADVANCED_FACE('',(#10485),#86343,.T.);
#89765=ADVANCED_FACE('',(#10486),#2755,.T.);
#89766=ADVANCED_FACE('',(#10487),#2756,.F.);
#89767=ADVANCED_FACE('',(#10488),#86344,.F.);
#89768=ADVANCED_FACE('',(#10489),#2757,.F.);
#89769=ADVANCED_FACE('',(#10490),#6985,.T.);
#89770=ADVANCED_FACE('',(#10491),#2758,.F.);
#89771=ADVANCED_FACE('',(#10492),#2759,.T.);
#89772=ADVANCED_FACE('',(#10493),#2760,.T.);
#89773=ADVANCED_FACE('',(#10494),#2761,.T.);
#89774=ADVANCED_FACE('',(#10495),#2762,.F.);
#89775=ADVANCED_FACE('',(#10496),#6986,.T.);
#89776=ADVANCED_FACE('',(#10497),#2763,.F.);
#89777=ADVANCED_FACE('',(#10498),#86345,.T.);
#89778=ADVANCED_FACE('',(#10499),#7923,.F.);
#89779=ADVANCED_FACE('',(#10500),#86346,.T.);
#89780=ADVANCED_FACE('',(#10501),#2764,.F.);
#89781=ADVANCED_FACE('',(#10502),#6987,.T.);
#89782=ADVANCED_FACE('',(#10503),#2765,.F.);
#89783=ADVANCED_FACE('',(#10504),#86347,.T.);
#89784=ADVANCED_FACE('',(#10505),#7924,.F.);
#89785=ADVANCED_FACE('',(#10506),#7925,.F.);
#89786=ADVANCED_FACE('',(#10507),#2766,.F.);
#89787=ADVANCED_FACE('',(#10508),#7926,.F.);
#89788=ADVANCED_FACE('',(#10509),#2767,.F.);
#89789=ADVANCED_FACE('',(#10510),#7927,.F.);
#89790=ADVANCED_FACE('',(#10511),#2768,.F.);
#89791=ADVANCED_FACE('',(#10512),#7928,.T.);
#89792=ADVANCED_FACE('',(#10513),#86348,.T.);
#89793=ADVANCED_FACE('',(#10514),#86349,.T.);
#89794=ADVANCED_FACE('',(#10515),#86350,.T.);
#89795=ADVANCED_FACE('',(#10516),#7929,.T.);
#89796=ADVANCED_FACE('',(#10517),#86351,.F.);
#89797=ADVANCED_FACE('',(#10518),#86352,.T.);
#89798=ADVANCED_FACE('',(#10519),#86353,.F.);
#89799=ADVANCED_FACE('',(#10520),#7930,.T.);
#89800=ADVANCED_FACE('',(#10521),#86354,.T.);
#89801=ADVANCED_FACE('',(#10522),#86355,.T.);
#89802=ADVANCED_FACE('',(#10523),#86356,.T.);
#89803=ADVANCED_FACE('',(#10524),#7931,.T.);
#89804=ADVANCED_FACE('',(#10525),#2769,.F.);
#89805=ADVANCED_FACE('',(#10526),#86357,.F.);
#89806=ADVANCED_FACE('',(#10527),#2770,.F.);
#89807=ADVANCED_FACE('',(#10528),#86358,.F.);
#89808=ADVANCED_FACE('',(#10529),#2771,.F.);
#89809=ADVANCED_FACE('',(#10530),#86359,.F.);
#89810=ADVANCED_FACE('',(#10531),#86360,.F.);
#89811=ADVANCED_FACE('',(#10532),#2772,.T.);
#89812=ADVANCED_FACE('',(#10533),#7932,.F.);
#89813=ADVANCED_FACE('',(#10534),#2773,.T.);
#89814=ADVANCED_FACE('',(#10535),#86361,.T.);
#89815=ADVANCED_FACE('',(#10536),#7933,.T.);
#89816=ADVANCED_FACE('',(#10537),#86362,.T.);
#89817=ADVANCED_FACE('',(#10538),#2774,.T.);
#89818=ADVANCED_FACE('',(#10539),#7934,.F.);
#89819=ADVANCED_FACE('',(#10540),#2775,.T.);
#89820=ADVANCED_FACE('',(#10541),#86363,.T.);
#89821=ADVANCED_FACE('',(#10542),#7935,.T.);
#89822=ADVANCED_FACE('',(#10543),#86364,.T.);
#89823=ADVANCED_FACE('',(#10544),#2776,.T.);
#89824=ADVANCED_FACE('',(#10545),#7936,.F.);
#89825=ADVANCED_FACE('',(#10546),#2777,.F.);
#89826=ADVANCED_FACE('',(#10547),#2778,.F.);
#89827=ADVANCED_FACE('',(#10548),#2779,.F.);
#89828=ADVANCED_FACE('',(#10549),#86365,.T.);
#89829=ADVANCED_FACE('',(#10550),#7937,.T.);
#89830=ADVANCED_FACE('',(#10551),#86366,.T.);
#89831=ADVANCED_FACE('',(#10552),#2780,.F.);
#89832=ADVANCED_FACE('',(#10553),#2781,.F.);
#89833=ADVANCED_FACE('',(#10554),#86367,.T.);
#89834=ADVANCED_FACE('',(#10555),#7938,.T.);
#89835=ADVANCED_FACE('',(#10556),#86368,.T.);
#89836=ADVANCED_FACE('',(#10557),#2782,.F.);
#89837=ADVANCED_FACE('',(#10558),#2783,.F.);
#89838=ADVANCED_FACE('',(#10559),#86369,.F.);
#89839=ADVANCED_FACE('',(#10560),#3423,.F.);
#89840=ADVANCED_FACE('',(#10561),#2784,.F.);
#89841=ADVANCED_FACE('',(#10562),#2785,.F.);
#89842=ADVANCED_FACE('',(#10563),#7939,.T.);
#89843=ADVANCED_FACE('',(#10564),#86370,.T.);
#89844=ADVANCED_FACE('',(#10565),#3424,.T.);
#89845=ADVANCED_FACE('',(#10566),#86371,.T.);
#89846=ADVANCED_FACE('',(#10567),#86372,.F.);
#89847=ADVANCED_FACE('',(#10568),#86373,.F.);
#89848=ADVANCED_FACE('',(#10569,#7443),#7940,.T.);
#89849=ADVANCED_FACE('',(#10570),#86374,.F.);
#89850=ADVANCED_FACE('',(#10571),#86375,.F.);
#89851=ADVANCED_FACE('',(#10572),#86376,.F.);
#89852=ADVANCED_FACE('',(#10573),#2786,.T.);
#89853=ADVANCED_FACE('',(#10574),#3425,.F.);
#89854=ADVANCED_FACE('',(#10575),#2787,.T.);
#89855=ADVANCED_FACE('',(#10576),#86377,.F.);
#89856=ADVANCED_FACE('',(#10577),#86378,.F.);
#89857=ADVANCED_FACE('',(#10578,#7444),#7941,.T.);
#89858=ADVANCED_FACE('',(#10579),#86379,.F.);
#89859=ADVANCED_FACE('',(#10580),#86380,.F.);
#89860=ADVANCED_FACE('',(#10581),#7942,.T.);
#89861=ADVANCED_FACE('',(#10582),#7943,.F.);
#89862=ADVANCED_FACE('',(#10583),#2788,.F.);
#89863=ADVANCED_FACE('',(#10584),#86381,.T.);
#89864=ADVANCED_FACE('',(#10585),#7944,.F.);
#89865=ADVANCED_FACE('',(#10586),#86382,.T.);
#89866=ADVANCED_FACE('',(#10587),#7945,.F.);
#89867=ADVANCED_FACE('',(#10588),#2789,.F.);
#89868=ADVANCED_FACE('',(#10589),#7946,.T.);
#89869=ADVANCED_FACE('',(#10590),#2790,.F.);
#89870=ADVANCED_FACE('',(#10591),#7947,.F.);
#89871=ADVANCED_FACE('',(#10592),#86383,.T.);
#89872=ADVANCED_FACE('',(#10593),#7948,.F.);
#89873=ADVANCED_FACE('',(#10594),#86384,.T.);
#89874=ADVANCED_FACE('',(#10595),#7949,.F.);
#89875=ADVANCED_FACE('',(#10596),#2791,.F.);
#89876=ADVANCED_FACE('',(#10597),#7950,.F.);
#89877=ADVANCED_FACE('',(#10598),#2792,.F.);
#89878=ADVANCED_FACE('',(#10599),#3426,.F.);
#89879=ADVANCED_FACE('',(#10600),#7951,.F.);
#89880=ADVANCED_FACE('',(#10601),#86385,.T.);
#89881=ADVANCED_FACE('',(#10602),#7952,.F.);
#89882=ADVANCED_FACE('',(#10603),#86386,.T.);
#89883=ADVANCED_FACE('',(#10604),#7953,.F.);
#89884=ADVANCED_FACE('',(#10605),#2793,.F.);
#89885=ADVANCED_FACE('',(#10606),#7954,.T.);
#89886=ADVANCED_FACE('',(#10607),#3427,.F.);
#89887=ADVANCED_FACE('',(#10608),#2794,.T.);
#89888=ADVANCED_FACE('',(#10609),#2795,.F.);
#89889=ADVANCED_FACE('',(#10610),#7955,.F.);
#89890=ADVANCED_FACE('',(#10611),#7956,.F.);
#89891=ADVANCED_FACE('',(#10612),#2796,.F.);
#89892=ADVANCED_FACE('',(#10613),#86387,.T.);
#89893=ADVANCED_FACE('',(#10614),#7957,.F.);
#89894=ADVANCED_FACE('',(#10615),#86388,.T.);
#89895=ADVANCED_FACE('',(#10616),#7958,.F.);
#89896=ADVANCED_FACE('',(#10617),#2797,.F.);
#89897=ADVANCED_FACE('',(#10618),#2798,.F.);
#89898=ADVANCED_FACE('',(#10619),#7959,.T.);
#89899=ADVANCED_FACE('',(#10620),#7960,.F.);
#89900=ADVANCED_FACE('',(#10621),#86389,.T.);
#89901=ADVANCED_FACE('',(#10622),#7961,.T.);
#89902=ADVANCED_FACE('',(#10623),#86390,.T.);
#89903=ADVANCED_FACE('',(#10624),#7962,.T.);
#89904=ADVANCED_FACE('',(#10625),#2799,.F.);
#89905=ADVANCED_FACE('',(#10626),#2800,.F.);
#89906=ADVANCED_FACE('',(#10627),#7963,.F.);
#89907=ADVANCED_FACE('',(#10628),#86391,.T.);
#89908=ADVANCED_FACE('',(#10629),#7964,.T.);
#89909=ADVANCED_FACE('',(#10630),#86392,.T.);
#89910=ADVANCED_FACE('',(#10631),#7965,.F.);
#89911=ADVANCED_FACE('',(#10632),#2801,.F.);
#89912=ADVANCED_FACE('',(#10633),#2802,.F.);
#89913=ADVANCED_FACE('',(#10634),#7966,.T.);
#89914=ADVANCED_FACE('',(#10635),#7967,.F.);
#89915=ADVANCED_FACE('',(#10636),#86393,.T.);
#89916=ADVANCED_FACE('',(#10637),#7968,.F.);
#89917=ADVANCED_FACE('',(#10638),#86394,.T.);
#89918=ADVANCED_FACE('',(#10639),#7969,.F.);
#89919=ADVANCED_FACE('',(#10640),#2803,.F.);
#89920=ADVANCED_FACE('',(#10641),#7970,.T.);
#89921=ADVANCED_FACE('',(#10642),#3428,.F.);
#89922=ADVANCED_FACE('',(#10643),#7971,.F.);
#89923=ADVANCED_FACE('',(#10644),#2804,.F.);
#89924=ADVANCED_FACE('',(#10645),#2805,.F.);
#89925=ADVANCED_FACE('',(#10646),#7972,.F.);
#89926=ADVANCED_FACE('',(#10647),#86395,.T.);
#89927=ADVANCED_FACE('',(#10648),#7973,.F.);
#89928=ADVANCED_FACE('',(#10649),#86396,.T.);
#89929=ADVANCED_FACE('',(#10650),#7974,.F.);
#89930=ADVANCED_FACE('',(#10651),#2806,.F.);
#89931=ADVANCED_FACE('',(#10652),#2807,.F.);
#89932=ADVANCED_FACE('',(#10653),#7975,.T.);
#89933=ADVANCED_FACE('',(#10654),#7976,.F.);
#89934=ADVANCED_FACE('',(#10655),#2808,.F.);
#89935=ADVANCED_FACE('',(#10656),#6988,.T.);
#89936=ADVANCED_FACE('',(#10657),#7977,.F.);
#89937=ADVANCED_FACE('',(#10658),#2809,.F.);
#89938=ADVANCED_FACE('',(#10659),#86397,.T.);
#89939=ADVANCED_FACE('',(#10660),#7978,.F.);
#89940=ADVANCED_FACE('',(#10661),#86398,.T.);
#89941=ADVANCED_FACE('',(#10662),#7979,.F.);
#89942=ADVANCED_FACE('',(#10663),#2810,.F.);
#89943=ADVANCED_FACE('',(#10664),#6989,.T.);
#89944=ADVANCED_FACE('',(#10665),#7980,.F.);
#89945=ADVANCED_FACE('',(#10666),#2811,.F.);
#89946=ADVANCED_FACE('',(#10667),#2812,.T.);
#89947=ADVANCED_FACE('',(#10668),#2813,.T.);
#89948=ADVANCED_FACE('',(#10669),#2814,.T.);
#89949=ADVANCED_FACE('',(#10670),#7981,.F.);
#89950=ADVANCED_FACE('',(#10671),#2815,.F.);
#89951=ADVANCED_FACE('',(#10672),#6990,.T.);
#89952=ADVANCED_FACE('',(#10673),#7982,.F.);
#89953=ADVANCED_FACE('',(#10674),#2816,.F.);
#89954=ADVANCED_FACE('',(#10675),#2817,.T.);
#89955=ADVANCED_FACE('',(#10676),#2818,.T.);
#89956=ADVANCED_FACE('',(#10677),#2819,.T.);
#89957=ADVANCED_FACE('',(#10678),#7983,.F.);
#89958=ADVANCED_FACE('',(#10679),#2820,.F.);
#89959=ADVANCED_FACE('',(#10680),#6991,.T.);
#89960=ADVANCED_FACE('',(#10681),#7984,.F.);
#89961=ADVANCED_FACE('',(#10682),#2821,.F.);
#89962=ADVANCED_FACE('',(#10683),#2822,.T.);
#89963=ADVANCED_FACE('',(#10684),#2823,.T.);
#89964=ADVANCED_FACE('',(#10685),#2824,.T.);
#89965=ADVANCED_FACE('',(#10686),#7985,.F.);
#89966=ADVANCED_FACE('',(#10687),#2825,.F.);
#89967=ADVANCED_FACE('',(#10688),#6992,.T.);
#89968=ADVANCED_FACE('',(#10689),#7986,.F.);
#89969=ADVANCED_FACE('',(#10690),#2826,.F.);
#89970=ADVANCED_FACE('',(#10691),#86399,.T.);
#89971=ADVANCED_FACE('',(#10692),#7987,.F.);
#89972=ADVANCED_FACE('',(#10693),#86400,.T.);
#89973=ADVANCED_FACE('',(#10694),#7988,.F.);
#89974=ADVANCED_FACE('',(#10695),#2827,.F.);
#89975=ADVANCED_FACE('',(#10696),#6993,.T.);
#89976=ADVANCED_FACE('',(#10697),#2828,.F.);
#89977=ADVANCED_FACE('',(#10698),#7989,.F.);
#89978=ADVANCED_FACE('',(#10699),#86401,.T.);
#89979=ADVANCED_FACE('',(#10700),#7990,.F.);
#89980=ADVANCED_FACE('',(#10701),#86402,.T.);
#89981=ADVANCED_FACE('',(#10702),#86403,.T.);
#89982=ADVANCED_FACE('',(#10703),#7991,.F.);
#89983=ADVANCED_FACE('',(#10704),#86404,.T.);
#89984=ADVANCED_FACE('',(#10705),#7992,.F.);
#89985=ADVANCED_FACE('',(#10706),#2829,.T.);
#89986=ADVANCED_FACE('',(#10707),#2830,.T.);
#89987=ADVANCED_FACE('',(#10708),#2831,.T.);
#89988=ADVANCED_FACE('',(#10709),#7993,.F.);
#89989=ADVANCED_FACE('',(#10710),#2832,.F.);
#89990=ADVANCED_FACE('',(#10711),#6994,.T.);
#89991=ADVANCED_FACE('',(#10712),#7994,.F.);
#89992=ADVANCED_FACE('',(#10713),#2833,.F.);
#89993=ADVANCED_FACE('',(#10714),#2834,.T.);
#89994=ADVANCED_FACE('',(#10715),#2835,.T.);
#89995=ADVANCED_FACE('',(#10716),#2836,.T.);
#89996=ADVANCED_FACE('',(#10717),#7995,.F.);
#89997=ADVANCED_FACE('',(#10718),#2837,.F.);
#89998=ADVANCED_FACE('',(#10719),#6995,.T.);
#89999=ADVANCED_FACE('',(#10720),#2838,.F.);
#90000=ADVANCED_FACE('',(#10721),#7996,.F.);
#90001=ADVANCED_FACE('',(#10722),#86405,.T.);
#90002=ADVANCED_FACE('',(#10723),#7997,.T.);
#90003=ADVANCED_FACE('',(#10724),#86406,.T.);
#90004=ADVANCED_FACE('',(#10725),#7998,.F.);
#90005=ADVANCED_FACE('',(#10726),#2839,.F.);
#90006=ADVANCED_FACE('',(#10727),#3429,.F.);
#90007=ADVANCED_FACE('',(#10728),#86407,.T.);
#90008=ADVANCED_FACE('',(#10729),#7999,.F.);
#90009=ADVANCED_FACE('',(#10730),#2840,.F.);
#90010=ADVANCED_FACE('',(#10731),#6996,.T.);
#90011=ADVANCED_FACE('',(#10732),#8000,.F.);
#90012=ADVANCED_FACE('',(#10733),#2841,.F.);
#90013=ADVANCED_FACE('',(#10734),#86408,.T.);
#90014=ADVANCED_FACE('',(#10735),#8001,.F.);
#90015=ADVANCED_FACE('',(#10736),#86409,.T.);
#90016=ADVANCED_FACE('',(#10737),#8002,.F.);
#90017=ADVANCED_FACE('',(#10738),#2842,.F.);
#90018=ADVANCED_FACE('',(#10739),#6997,.T.);
#90019=ADVANCED_FACE('',(#10740),#8003,.F.);
#90020=ADVANCED_FACE('',(#10741),#2843,.F.);
#90021=ADVANCED_FACE('',(#10742),#2844,.T.);
#90022=ADVANCED_FACE('',(#10743),#2845,.T.);
#90023=ADVANCED_FACE('',(#10744),#2846,.T.);
#90024=ADVANCED_FACE('',(#10745),#8004,.F.);
#90025=ADVANCED_FACE('',(#10746),#2847,.F.);
#90026=ADVANCED_FACE('',(#10747),#6998,.T.);
#90027=ADVANCED_FACE('',(#10748),#8005,.F.);
#90028=ADVANCED_FACE('',(#10749),#2848,.F.);
#90029=ADVANCED_FACE('',(#10750),#2849,.T.);
#90030=ADVANCED_FACE('',(#10751),#86410,.T.);
#90031=ADVANCED_FACE('',(#10752),#2850,.T.);
#90032=ADVANCED_FACE('',(#10753),#3430,.F.);
#90033=ADVANCED_FACE('',(#10754),#2851,.F.);
#90034=ADVANCED_FACE('',(#10755),#86411,.F.);
#90035=ADVANCED_FACE('',(#10756),#2852,.F.);
#90036=ADVANCED_FACE('',(#10757),#86412,.F.);
#90037=ADVANCED_FACE('',(#10758),#3431,.T.);
#90038=ADVANCED_FACE('',(#10759),#86413,.F.);
#90039=ADVANCED_FACE('',(#10760),#2853,.F.);
#90040=ADVANCED_FACE('',(#10761),#2854,.F.);
#90041=ADVANCED_FACE('',(#10762),#2855,.F.);
#90042=ADVANCED_FACE('',(#10763),#86414,.F.);
#90043=ADVANCED_FACE('',(#10764),#3432,.T.);
#90044=ADVANCED_FACE('',(#10765),#86415,.F.);
#90045=ADVANCED_FACE('',(#10766),#2856,.F.);
#90046=ADVANCED_FACE('',(#10767),#3433,.F.);
#90047=ADVANCED_FACE('',(#10768),#2857,.F.);
#90048=ADVANCED_FACE('',(#10769),#86416,.F.);
#90049=ADVANCED_FACE('',(#10770),#3434,.T.);
#90050=ADVANCED_FACE('',(#10771),#86417,.F.);
#90051=ADVANCED_FACE('',(#10772),#2858,.F.);
#90052=ADVANCED_FACE('',(#10773),#86418,.F.);
#90053=ADVANCED_FACE('',(#10774),#86419,.F.);
#90054=ADVANCED_FACE('',(#10775),#3435,.T.);
#90055=ADVANCED_FACE('',(#10776),#86420,.T.);
#90056=ADVANCED_FACE('',(#10777),#3436,.T.);
#90057=ADVANCED_FACE('',(#10778),#3437,.T.);
#90058=ADVANCED_FACE('',(#10779),#3438,.T.);
#90059=ADVANCED_FACE('',(#10780),#86421,.T.);
#90060=ADVANCED_FACE('',(#10781),#3439,.T.);
#90061=ADVANCED_FACE('',(#10782),#3440,.T.);
#90062=ADVANCED_FACE('',(#10783),#3441,.T.);
#90063=ADVANCED_FACE('',(#10784),#86422,.T.);
#90064=ADVANCED_FACE('',(#10785),#3442,.T.);
#90065=ADVANCED_FACE('',(#10786),#3443,.T.);
#90066=ADVANCED_FACE('',(#10787),#3444,.T.);
#90067=ADVANCED_FACE('',(#10788),#86423,.T.);
#90068=ADVANCED_FACE('',(#10789),#3445,.T.);
#90069=ADVANCED_FACE('',(#10790),#86424,.F.);
#90070=ADVANCED_FACE('',(#10791),#86425,.F.);
#90071=ADVANCED_FACE('',(#10792),#3446,.F.);
#90072=ADVANCED_FACE('',(#10793),#86426,.T.);
#90073=ADVANCED_FACE('',(#10794),#8006,.F.);
#90074=ADVANCED_FACE('',(#10795),#86427,.F.);
#90075=ADVANCED_FACE('',(#10796),#86428,.F.);
#90076=ADVANCED_FACE('',(#10797),#86429,.F.);
#90077=ADVANCED_FACE('',(#10798),#3447,.F.);
#90078=ADVANCED_FACE('',(#10799),#86430,.F.);
#90079=ADVANCED_FACE('',(#10800),#3448,.F.);
#90080=ADVANCED_FACE('',(#10801),#86431,.F.);
#90081=ADVANCED_FACE('',(#10802),#86432,.F.);
#90082=ADVANCED_FACE('',(#10803),#86433,.F.);
#90083=ADVANCED_FACE('',(#10804),#3449,.F.);
#90084=ADVANCED_FACE('',(#10805),#86434,.F.);
#90085=ADVANCED_FACE('',(#10806),#3450,.F.);
#90086=ADVANCED_FACE('',(#10807),#86435,.F.);
#90087=ADVANCED_FACE('',(#10808),#86436,.F.);
#90088=ADVANCED_FACE('',(#10809),#2859,.F.);
#90089=ADVANCED_FACE('',(#10810),#3451,.F.);
#90090=ADVANCED_FACE('',(#10811),#86437,.F.);
#90091=ADVANCED_FACE('',(#10812),#3452,.F.);
#90092=ADVANCED_FACE('',(#10813),#86438,.F.);
#90093=ADVANCED_FACE('',(#10814),#3453,.F.);
#90094=ADVANCED_FACE('',(#10815),#86439,.F.);
#90095=ADVANCED_FACE('',(#10816),#3454,.F.);
#90096=ADVANCED_FACE('',(#10817),#86440,.F.);
#90097=ADVANCED_FACE('',(#10818),#3455,.F.);
#90098=ADVANCED_FACE('',(#10819),#86441,.F.);
#90099=ADVANCED_FACE('',(#10820),#3456,.F.);
#90100=ADVANCED_FACE('',(#10821),#86442,.F.);
#90101=ADVANCED_FACE('',(#10822),#86443,.T.);
#90102=ADVANCED_FACE('',(#10823),#86444,.F.);
#90103=ADVANCED_FACE('',(#10824),#3457,.F.);
#90104=ADVANCED_FACE('',(#10825),#2860,.F.);
#90105=ADVANCED_FACE('',(#10826),#2861,.F.);
#90106=ADVANCED_FACE('',(#10827),#2862,.F.);
#90107=ADVANCED_FACE('',(#10828),#86445,.T.);
#90108=ADVANCED_FACE('',(#10829),#8007,.F.);
#90109=ADVANCED_FACE('',(#10830),#8008,.T.);
#90110=ADVANCED_FACE('',(#10831),#8009,.T.);
#90111=ADVANCED_FACE('',(#10832),#86446,.T.);
#90112=ADVANCED_FACE('',(#10833),#86447,.F.);
#90113=ADVANCED_FACE('',(#10834),#2863,.F.);
#90114=ADVANCED_FACE('',(#10835),#86448,.F.);
#90115=ADVANCED_FACE('',(#10836),#2864,.F.);
#90116=ADVANCED_FACE('',(#10837),#86449,.F.);
#90117=ADVANCED_FACE('',(#10838),#86450,.T.);
#90118=ADVANCED_FACE('',(#10839),#86451,.F.);
#90119=ADVANCED_FACE('',(#10840),#2865,.F.);
#90120=ADVANCED_FACE('',(#10841),#86452,.F.);
#90121=ADVANCED_FACE('',(#10842),#2866,.F.);
#90122=ADVANCED_FACE('',(#10843),#86453,.F.);
#90123=ADVANCED_FACE('',(#10844),#86454,.T.);
#90124=ADVANCED_FACE('',(#10845),#2867,.F.);
#90125=ADVANCED_FACE('',(#10846),#86455,.F.);
#90126=ADVANCED_FACE('',(#10847),#2868,.T.);
#90127=ADVANCED_FACE('',(#10848),#86456,.F.);
#90128=ADVANCED_FACE('',(#10849),#2869,.F.);
#90129=ADVANCED_FACE('',(#10850),#86457,.F.);
#90130=ADVANCED_FACE('',(#10851),#2870,.F.);
#90131=ADVANCED_FACE('',(#10852),#86458,.F.);
#90132=ADVANCED_FACE('',(#10853),#86459,.T.);
#90133=ADVANCED_FACE('',(#10854),#2871,.T.);
#90134=ADVANCED_FACE('',(#10855),#86460,.F.);
#90135=ADVANCED_FACE('',(#10856),#2872,.F.);
#90136=ADVANCED_FACE('',(#10857),#86461,.T.);
#90137=ADVANCED_FACE('',(#10858),#86462,.F.);
#90138=ADVANCED_FACE('',(#10859),#2873,.F.);
#90139=ADVANCED_FACE('',(#10860),#86463,.F.);
#90140=ADVANCED_FACE('',(#10861),#2874,.F.);
#90141=ADVANCED_FACE('',(#10862),#86464,.F.);
#90142=ADVANCED_FACE('',(#10863),#86465,.T.);
#90143=ADVANCED_FACE('',(#10864),#86466,.T.);
#90144=ADVANCED_FACE('',(#10865),#86467,.F.);
#90145=ADVANCED_FACE('',(#10866),#2875,.F.);
#90146=ADVANCED_FACE('',(#10867),#86468,.F.);
#90147=ADVANCED_FACE('',(#10868),#2876,.F.);
#90148=ADVANCED_FACE('',(#10869),#86469,.F.);
#90149=ADVANCED_FACE('',(#10870),#86470,.T.);
#90150=ADVANCED_FACE('',(#10871),#2877,.T.);
#90151=ADVANCED_FACE('',(#10872),#86471,.F.);
#90152=ADVANCED_FACE('',(#10873),#2878,.F.);
#90153=ADVANCED_FACE('',(#10874),#86472,.F.);
#90154=ADVANCED_FACE('',(#10875),#2879,.F.);
#90155=ADVANCED_FACE('',(#10876),#86473,.F.);
#90156=ADVANCED_FACE('',(#10877),#86474,.T.);
#90157=ADVANCED_FACE('',(#10878),#2880,.T.);
#90158=ADVANCED_FACE('',(#10879),#86475,.T.);
#90159=ADVANCED_FACE('',(#10880),#86476,.F.);
#90160=ADVANCED_FACE('',(#10881),#2881,.F.);
#90161=ADVANCED_FACE('',(#10882),#86477,.F.);
#90162=ADVANCED_FACE('',(#10883),#2882,.F.);
#90163=ADVANCED_FACE('',(#10884),#86478,.F.);
#90164=ADVANCED_FACE('',(#10885),#86479,.T.);
#90165=ADVANCED_FACE('',(#10886),#2883,.T.);
#90166=ADVANCED_FACE('',(#10887),#86480,.F.);
#90167=ADVANCED_FACE('',(#10888),#2884,.F.);
#90168=ADVANCED_FACE('',(#10889),#86481,.T.);
#90169=ADVANCED_FACE('',(#10890),#86482,.F.);
#90170=ADVANCED_FACE('',(#10891),#2885,.F.);
#90171=ADVANCED_FACE('',(#10892),#86483,.F.);
#90172=ADVANCED_FACE('',(#10893),#2886,.F.);
#90173=ADVANCED_FACE('',(#10894),#86484,.F.);
#90174=ADVANCED_FACE('',(#10895),#86485,.T.);
#90175=ADVANCED_FACE('',(#10896),#2887,.F.);
#90176=ADVANCED_FACE('',(#10897),#86486,.F.);
#90177=ADVANCED_FACE('',(#10898),#3458,.T.);
#90178=ADVANCED_FACE('',(#10899),#86487,.F.);
#90179=ADVANCED_FACE('',(#10900),#2888,.F.);
#90180=ADVANCED_FACE('',(#10901),#3459,.F.);
#90181=ADVANCED_FACE('',(#10902),#2889,.F.);
#90182=ADVANCED_FACE('',(#10903),#86488,.F.);
#90183=ADVANCED_FACE('',(#10904),#3460,.T.);
#90184=ADVANCED_FACE('',(#10905),#86489,.F.);
#90185=ADVANCED_FACE('',(#10906),#2890,.F.);
#90186=ADVANCED_FACE('',(#10907),#2891,.F.);
#90187=ADVANCED_FACE('',(#10908),#2892,.F.);
#90188=ADVANCED_FACE('',(#10909),#86490,.F.);
#90189=ADVANCED_FACE('',(#10910),#3461,.T.);
#90190=ADVANCED_FACE('',(#10911),#86491,.F.);
#90191=ADVANCED_FACE('',(#10912),#2893,.F.);
#90192=ADVANCED_FACE('',(#10913),#2894,.F.);
#90193=ADVANCED_FACE('',(#10914),#2895,.F.);
#90194=ADVANCED_FACE('',(#10915),#86492,.F.);
#90195=ADVANCED_FACE('',(#10916),#3462,.T.);
#90196=ADVANCED_FACE('',(#10917),#86493,.F.);
#90197=ADVANCED_FACE('',(#10918),#2896,.F.);
#90198=ADVANCED_FACE('',(#10919),#2897,.F.);
#90199=ADVANCED_FACE('',(#10920),#2898,.F.);
#90200=ADVANCED_FACE('',(#10921),#86494,.F.);
#90201=ADVANCED_FACE('',(#10922),#3463,.T.);
#90202=ADVANCED_FACE('',(#10923),#86495,.F.);
#90203=ADVANCED_FACE('',(#10924),#2899,.F.);
#90204=ADVANCED_FACE('',(#10925),#3464,.F.);
#90205=ADVANCED_FACE('',(#10926),#2900,.F.);
#90206=ADVANCED_FACE('',(#10927),#86496,.F.);
#90207=ADVANCED_FACE('',(#10928),#3465,.T.);
#90208=ADVANCED_FACE('',(#10929),#86497,.F.);
#90209=ADVANCED_FACE('',(#10930),#2901,.F.);
#90210=ADVANCED_FACE('',(#10931),#8010,.T.);
#90211=ADVANCED_FACE('',(#10932),#3466,.T.);
#90212=ADVANCED_FACE('',(#10933),#8011,.T.);
#90213=ADVANCED_FACE('',(#10934),#86498,.T.);
#90214=ADVANCED_FACE('',(#10935),#3467,.T.);
#90215=ADVANCED_FACE('',(#10936),#8012,.T.);
#90216=ADVANCED_FACE('',(#10937),#86499,.T.);
#90217=ADVANCED_FACE('',(#10938),#2902,.F.);
#90218=ADVANCED_FACE('',(#10939),#3468,.F.);
#90219=ADVANCED_FACE('',(#10940),#2903,.F.);
#90220=ADVANCED_FACE('',(#10941),#86500,.T.);
#90221=ADVANCED_FACE('',(#10942),#86501,.F.);
#90222=ADVANCED_FACE('',(#10943),#2904,.F.);
#90223=ADVANCED_FACE('',(#10944),#3469,.F.);
#90224=ADVANCED_FACE('',(#10945),#2905,.F.);
#90225=ADVANCED_FACE('',(#10946),#86502,.F.);
#90226=ADVANCED_FACE('',(#10947),#2906,.F.);
#90227=ADVANCED_FACE('',(#10948),#2907,.F.);
#90228=ADVANCED_FACE('',(#10949),#2908,.F.);
#90229=ADVANCED_FACE('',(#10950),#86503,.F.);
#90230=ADVANCED_FACE('',(#10951),#3470,.T.);
#90231=ADVANCED_FACE('',(#10952),#86504,.F.);
#90232=ADVANCED_FACE('',(#10953),#2909,.F.);
#90233=ADVANCED_FACE('',(#10954),#2910,.F.);
#90234=ADVANCED_FACE('',(#10955),#2911,.F.);
#90235=ADVANCED_FACE('',(#10956),#86505,.F.);
#90236=ADVANCED_FACE('',(#10957),#3471,.T.);
#90237=ADVANCED_FACE('',(#10958),#86506,.F.);
#90238=ADVANCED_FACE('',(#10959),#2912,.F.);
#90239=ADVANCED_FACE('',(#10960),#3472,.F.);
#90240=ADVANCED_FACE('',(#10961),#2913,.F.);
#90241=ADVANCED_FACE('',(#10962),#86507,.F.);
#90242=ADVANCED_FACE('',(#10963),#3473,.T.);
#90243=ADVANCED_FACE('',(#10964),#86508,.F.);
#90244=ADVANCED_FACE('',(#10965),#3474,.F.);
#90245=ADVANCED_FACE('',(#10966),#2914,.F.);
#90246=ADVANCED_FACE('',(#10967),#86509,.F.);
#90247=ADVANCED_FACE('',(#10968),#3475,.T.);
#90248=ADVANCED_FACE('',(#10969),#86510,.F.);
#90249=ADVANCED_FACE('',(#10970),#2915,.F.);
#90250=ADVANCED_FACE('',(#10971),#3476,.F.);
#90251=ADVANCED_FACE('',(#10972),#2916,.F.);
#90252=ADVANCED_FACE('',(#10973),#86511,.F.);
#90253=ADVANCED_FACE('',(#10974),#3477,.T.);
#90254=ADVANCED_FACE('',(#10975),#86512,.F.);
#90255=ADVANCED_FACE('',(#10976),#2917,.F.);
#90256=ADVANCED_FACE('',(#10977),#2918,.F.);
#90257=ADVANCED_FACE('',(#10978),#2919,.F.);
#90258=ADVANCED_FACE('',(#10979),#86513,.F.);
#90259=ADVANCED_FACE('',(#10980),#3478,.T.);
#90260=ADVANCED_FACE('',(#10981),#86514,.F.);
#90261=ADVANCED_FACE('',(#10982),#2920,.F.);
#90262=ADVANCED_FACE('',(#10983),#86515,.T.);
#90263=ADVANCED_FACE('',(#10984),#8013,.T.);
#90264=ADVANCED_FACE('',(#10985),#3479,.T.);
#90265=ADVANCED_FACE('',(#10986),#8014,.T.);
#90266=ADVANCED_FACE('',(#10987),#86516,.T.);
#90267=ADVANCED_FACE('',(#10988),#3480,.T.);
#90268=ADVANCED_FACE('',(#10989),#8015,.T.);
#90269=ADVANCED_FACE('',(#10990),#86517,.T.);
#90270=ADVANCED_FACE('',(#10991),#2921,.F.);
#90271=ADVANCED_FACE('',(#10992),#3481,.F.);
#90272=ADVANCED_FACE('',(#10993),#86518,.F.);
#90273=ADVANCED_FACE('',(#10994),#2922,.F.);
#90274=ADVANCED_FACE('',(#10995),#2923,.T.);
#90275=ADVANCED_FACE('',(#10996),#8016,.T.);
#90276=ADVANCED_FACE('',(#10997),#2924,.T.);
#90277=ADVANCED_FACE('',(#10998),#2925,.F.);
#90278=ADVANCED_FACE('',(#10999),#86519,.T.);
#90279=ADVANCED_FACE('',(#11000),#3482,.T.);
#90280=ADVANCED_FACE('',(#11001,#7445,#7446,#7447,#7448),#8017,.F.);
#90281=ADVANCED_FACE('',(#11002),#3483,.T.);
#90282=ADVANCED_FACE('',(#11003),#86520,.T.);
#90283=ADVANCED_FACE('',(#11004),#3484,.F.);
#90284=ADVANCED_FACE('',(#11005),#8018,.F.);
#90285=ADVANCED_FACE('',(#11006),#8019,.F.);
#90286=ADVANCED_FACE('',(#11007),#8020,.F.);
#90287=ADVANCED_FACE('',(#11008),#3485,.F.);
#90288=ADVANCED_FACE('',(#11009),#6999,.T.);
#90289=ADVANCED_FACE('',(#11010),#3486,.T.);
#90290=ADVANCED_FACE('',(#11011),#86521,.T.);
#90291=ADVANCED_FACE('',(#11012),#86522,.F.);
#90292=ADVANCED_FACE('',(#11013,#7449,#7450,#7451,#7452),#8021,.F.);
#90293=ADVANCED_FACE('',(#11014),#8022,.F.);
#90294=ADVANCED_FACE('',(#11015),#8023,.F.);
#90295=ADVANCED_FACE('',(#11016),#8024,.F.);
#90296=ADVANCED_FACE('',(#11017),#8025,.F.);
#90297=ADVANCED_FACE('',(#11018),#8026,.F.);
#90298=ADVANCED_FACE('',(#11019),#8027,.F.);
#90299=ADVANCED_FACE('',(#11020),#7000,.F.);
#90300=ADVANCED_FACE('',(#11021),#7001,.F.);
#90301=ADVANCED_FACE('',(#11022),#7002,.F.);
#90302=ADVANCED_FACE('',(#11023),#7003,.F.);
#90303=ADVANCED_FACE('',(#11024),#7004,.F.);
#90304=ADVANCED_FACE('',(#11025),#7005,.F.);
#90305=ADVANCED_FACE('',(#11026),#7006,.F.);
#90306=ADVANCED_FACE('',(#11027),#3487,.T.);
#90307=ADVANCED_FACE('',(#11028),#8028,.F.);
#90308=ADVANCED_FACE('',(#11029,#7453),#8029,.T.);
#90309=ADVANCED_FACE('',(#11030),#86523,.T.);
#90310=ADVANCED_FACE('',(#11031),#7007,.T.);
#90311=ADVANCED_FACE('',(#11032),#8030,.T.);
#90312=ADVANCED_FACE('',(#11033),#86524,.T.);
#90313=ADVANCED_FACE('',(#11034,#7454),#8031,.F.);
#90314=ADVANCED_FACE('',(#11035),#86525,.T.);
#90315=ADVANCED_FACE('',(#11036),#8032,.F.);
#90316=ADVANCED_FACE('',(#11037),#2926,.T.);
#90317=ADVANCED_FACE('',(#11038),#3488,.T.);
#90318=ADVANCED_FACE('',(#11039),#2927,.F.);
#90319=ADVANCED_FACE('',(#11040),#2928,.F.);
#90320=ADVANCED_FACE('',(#11041),#1018,.F.);
#90321=ADVANCED_FACE('',(#11042),#2929,.F.);
#90322=ADVANCED_FACE('',(#11043),#3489,.F.);
#90323=ADVANCED_FACE('',(#11044),#2930,.F.);
#90324=ADVANCED_FACE('',(#11045),#3490,.F.);
#90325=ADVANCED_FACE('',(#11046),#2931,.F.);
#90326=ADVANCED_FACE('',(#11047),#3491,.F.);
#90327=ADVANCED_FACE('',(#11048),#2932,.F.);
#90328=ADVANCED_FACE('',(#11049),#2933,.F.);
#90329=ADVANCED_FACE('',(#11050),#2934,.F.);
#90330=ADVANCED_FACE('',(#11051),#1019,.F.);
#90331=ADVANCED_FACE('',(#11052),#2935,.F.);
#90332=ADVANCED_FACE('',(#11053),#2936,.F.);
#90333=ADVANCED_FACE('',(#11054),#2937,.F.);
#90334=ADVANCED_FACE('',(#11055),#2938,.F.);
#90335=ADVANCED_FACE('',(#11056),#2939,.F.);
#90336=ADVANCED_FACE('',(#11057),#1020,.F.);
#90337=ADVANCED_FACE('',(#11058),#2940,.F.);
#90338=ADVANCED_FACE('',(#11059),#2941,.F.);
#90339=ADVANCED_FACE('',(#11060),#2942,.F.);
#90340=ADVANCED_FACE('',(#11061),#3492,.F.);
#90341=ADVANCED_FACE('',(#11062),#1021,.F.);
#90342=ADVANCED_FACE('',(#11063),#3493,.F.);
#90343=ADVANCED_FACE('',(#11064),#2943,.F.);
#90344=ADVANCED_FACE('',(#11065),#3494,.F.);
#90345=ADVANCED_FACE('',(#11066),#3495,.F.);
#90346=ADVANCED_FACE('',(#11067),#3496,.F.);
#90347=ADVANCED_FACE('',(#11068),#3497,.F.);
#90348=ADVANCED_FACE('',(#11069),#3498,.F.);
#90349=ADVANCED_FACE('',(#11070),#3499,.F.);
#90350=ADVANCED_FACE('',(#11071),#3500,.F.);
#90351=ADVANCED_FACE('',(#11072),#3501,.F.);
#90352=ADVANCED_FACE('',(#11073),#2944,.F.);
#90353=ADVANCED_FACE('',(#11074),#2945,.F.);
#90354=ADVANCED_FACE('',(#11075),#2946,.F.);
#90355=ADVANCED_FACE('',(#11076),#2947,.F.);
#90356=ADVANCED_FACE('',(#11077),#2948,.F.);
#90357=ADVANCED_FACE('',(#11078),#2949,.F.);
#90358=ADVANCED_FACE('',(#11079),#2950,.F.);
#90359=ADVANCED_FACE('',(#11080),#2951,.F.);
#90360=ADVANCED_FACE('',(#11081),#2952,.F.);
#90361=ADVANCED_FACE('',(#11082),#2953,.F.);
#90362=ADVANCED_FACE('',(#11083),#2954,.F.);
#90363=ADVANCED_FACE('',(#11084),#2955,.F.);
#90364=ADVANCED_FACE('',(#11085),#3502,.F.);
#90365=ADVANCED_FACE('',(#11086),#2956,.F.);
#90366=ADVANCED_FACE('',(#11087),#3503,.F.);
#90367=ADVANCED_FACE('',(#11088),#2957,.F.);
#90368=ADVANCED_FACE('',(#11089),#2958,.F.);
#90369=ADVANCED_FACE('',(#11090),#2959,.F.);
#90370=ADVANCED_FACE('',(#11091),#2960,.F.);
#90371=ADVANCED_FACE('',(#11092),#2961,.F.);
#90372=ADVANCED_FACE('',(#11093),#2962,.F.);
#90373=ADVANCED_FACE('',(#11094),#2963,.F.);
#90374=ADVANCED_FACE('',(#11095),#2964,.F.);
#90375=ADVANCED_FACE('',(#11096),#2965,.F.);
#90376=ADVANCED_FACE('',(#11097),#86526,.T.);
#90377=ADVANCED_FACE('',(#11098),#2966,.F.);
#90378=ADVANCED_FACE('',(#11099),#3504,.T.);
#90379=ADVANCED_FACE('',(#11100),#2967,.F.);
#90380=ADVANCED_FACE('',(#11101),#86527,.T.);
#90381=ADVANCED_FACE('',(#11102),#86528,.T.);
#90382=ADVANCED_FACE('',(#11103),#2968,.F.);
#90383=ADVANCED_FACE('',(#11104),#3505,.T.);
#90384=ADVANCED_FACE('',(#11105),#2969,.F.);
#90385=ADVANCED_FACE('',(#11106),#86529,.T.);
#90386=ADVANCED_FACE('',(#11107),#86530,.T.);
#90387=ADVANCED_FACE('',(#11108),#2970,.F.);
#90388=ADVANCED_FACE('',(#11109),#3506,.T.);
#90389=ADVANCED_FACE('',(#11110),#2971,.F.);
#90390=ADVANCED_FACE('',(#11111),#86531,.T.);
#90391=ADVANCED_FACE('',(#11112),#86532,.T.);
#90392=ADVANCED_FACE('',(#11113),#2972,.F.);
#90393=ADVANCED_FACE('',(#11114),#3507,.T.);
#90394=ADVANCED_FACE('',(#11115),#2973,.F.);
#90395=ADVANCED_FACE('',(#11116),#86533,.T.);
#90396=ADVANCED_FACE('',(#11117),#86534,.T.);
#90397=ADVANCED_FACE('',(#11118),#86535,.T.);
#90398=ADVANCED_FACE('',(#11119),#86536,.T.);
#90399=ADVANCED_FACE('',(#11120),#86537,.T.);
#90400=ADVANCED_FACE('',(#11121),#86538,.T.);
#90401=ADVANCED_FACE('',(#11122),#86539,.T.);
#90402=ADVANCED_FACE('',(#11123),#86540,.T.);
#90403=ADVANCED_FACE('',(#11124),#86541,.T.);
#90404=ADVANCED_FACE('',(#11125),#3508,.T.);
#90405=ADVANCED_FACE('',(#11126),#86542,.T.);
#90406=ADVANCED_FACE('',(#11127),#3509,.T.);
#90407=ADVANCED_FACE('',(#11128),#3510,.T.);
#90408=ADVANCED_FACE('',(#11129),#3511,.T.);
#90409=ADVANCED_FACE('',(#11130),#86543,.T.);
#90410=ADVANCED_FACE('',(#11131),#3512,.T.);
#90411=ADVANCED_FACE('',(#11132),#3513,.T.);
#90412=ADVANCED_FACE('',(#11133),#3514,.T.);
#90413=ADVANCED_FACE('',(#11134),#86544,.T.);
#90414=ADVANCED_FACE('',(#11135),#3515,.T.);
#90415=ADVANCED_FACE('',(#11136),#86545,.T.);
#90416=ADVANCED_FACE('',(#11137),#3516,.T.);
#90417=ADVANCED_FACE('',(#11138),#3517,.T.);
#90418=ADVANCED_FACE('',(#11139),#3518,.T.);
#90419=ADVANCED_FACE('',(#11140),#86546,.T.);
#90420=ADVANCED_FACE('',(#11141),#86547,.T.);
#90421=ADVANCED_FACE('',(#11142),#3519,.T.);
#90422=ADVANCED_FACE('',(#11143),#3520,.T.);
#90423=ADVANCED_FACE('',(#11144),#86548,.T.);
#90424=ADVANCED_FACE('',(#11145),#3521,.T.);
#90425=ADVANCED_FACE('',(#11146),#3522,.T.);
#90426=ADVANCED_FACE('',(#11147),#3523,.T.);
#90427=ADVANCED_FACE('',(#11148),#86549,.T.);
#90428=ADVANCED_FACE('',(#11149),#86550,.T.);
#90429=ADVANCED_FACE('',(#11150),#3524,.T.);
#90430=ADVANCED_FACE('',(#11151),#3525,.T.);
#90431=ADVANCED_FACE('',(#11152),#86551,.T.);
#90432=ADVANCED_FACE('',(#11153),#86552,.T.);
#90433=ADVANCED_FACE('',(#11154),#3526,.T.);
#90434=ADVANCED_FACE('',(#11155),#3527,.T.);
#90435=ADVANCED_FACE('',(#11156),#86553,.T.);
#90436=ADVANCED_FACE('',(#11157),#86554,.T.);
#90437=ADVANCED_FACE('',(#11158),#3528,.T.);
#90438=ADVANCED_FACE('',(#11159),#3529,.T.);
#90439=ADVANCED_FACE('',(#11160),#86555,.T.);
#90440=ADVANCED_FACE('',(#11161),#86556,.T.);
#90441=ADVANCED_FACE('',(#11162),#3530,.T.);
#90442=ADVANCED_FACE('',(#11163),#3531,.T.);
#90443=ADVANCED_FACE('',(#11164),#3532,.T.);
#90444=ADVANCED_FACE('',(#11165),#86557,.T.);
#90445=ADVANCED_FACE('',(#11166),#3533,.T.);
#90446=ADVANCED_FACE('',(#11167),#3534,.T.);
#90447=ADVANCED_FACE('',(#11168),#3535,.T.);
#90448=ADVANCED_FACE('',(#11169),#86558,.T.);
#90449=ADVANCED_FACE('',(#11170),#86559,.T.);
#90450=ADVANCED_FACE('',(#11171),#3536,.T.);
#90451=ADVANCED_FACE('',(#11172),#3537,.T.);
#90452=ADVANCED_FACE('',(#11173),#86560,.T.);
#90453=ADVANCED_FACE('',(#11174),#86561,.T.);
#90454=ADVANCED_FACE('',(#11175),#3538,.T.);
#90455=ADVANCED_FACE('',(#11176),#3539,.T.);
#90456=ADVANCED_FACE('',(#11177),#86562,.T.);
#90457=ADVANCED_FACE('',(#11178),#86563,.T.);
#90458=ADVANCED_FACE('',(#11179),#3540,.T.);
#90459=ADVANCED_FACE('',(#11180),#3541,.T.);
#90460=ADVANCED_FACE('',(#11181),#86564,.T.);
#90461=ADVANCED_FACE('',(#11182),#86565,.T.);
#90462=ADVANCED_FACE('',(#11183),#3542,.T.);
#90463=ADVANCED_FACE('',(#11184),#3543,.T.);
#90464=ADVANCED_FACE('',(#11185),#86566,.T.);
#90465=ADVANCED_FACE('',(#11186),#86567,.T.);
#90466=ADVANCED_FACE('',(#11187),#3544,.T.);
#90467=ADVANCED_FACE('',(#11188),#3545,.T.);
#90468=ADVANCED_FACE('',(#11189),#86568,.T.);
#90469=ADVANCED_FACE('',(#11190),#86569,.T.);
#90470=ADVANCED_FACE('',(#11191),#3546,.T.);
#90471=ADVANCED_FACE('',(#11192),#3547,.T.);
#90472=ADVANCED_FACE('',(#11193),#86570,.T.);
#90473=ADVANCED_FACE('',(#11194),#86571,.T.);
#90474=ADVANCED_FACE('',(#11195),#3548,.T.);
#90475=ADVANCED_FACE('',(#11196),#3549,.T.);
#90476=ADVANCED_FACE('',(#11197),#86572,.T.);
#90477=ADVANCED_FACE('',(#11198),#86573,.T.);
#90478=ADVANCED_FACE('',(#11199),#3550,.T.);
#90479=ADVANCED_FACE('',(#11200),#3551,.T.);
#90480=ADVANCED_FACE('',(#11201),#86574,.T.);
#90481=ADVANCED_FACE('',(#11202),#86575,.T.);
#90482=ADVANCED_FACE('',(#11203),#3552,.T.);
#90483=ADVANCED_FACE('',(#11204),#3553,.T.);
#90484=ADVANCED_FACE('',(#11205),#86576,.T.);
#90485=ADVANCED_FACE('',(#11206),#3554,.T.);
#90486=ADVANCED_FACE('',(#11207),#3555,.T.);
#90487=ADVANCED_FACE('',(#11208),#3556,.T.);
#90488=ADVANCED_FACE('',(#11209),#86577,.T.);
#90489=ADVANCED_FACE('',(#11210),#86578,.T.);
#90490=ADVANCED_FACE('',(#11211),#3557,.T.);
#90491=ADVANCED_FACE('',(#11212),#3558,.T.);
#90492=ADVANCED_FACE('',(#11213),#86579,.T.);
#90493=ADVANCED_FACE('',(#11214),#3559,.T.);
#90494=ADVANCED_FACE('',(#11215),#3560,.T.);
#90495=ADVANCED_FACE('',(#11216),#3561,.T.);
#90496=ADVANCED_FACE('',(#11217),#3562,.T.);
#90497=ADVANCED_FACE('',(#11218),#3563,.T.);
#90498=ADVANCED_FACE('',(#11219),#86580,.T.);
#90499=ADVANCED_FACE('',(#11220),#86581,.T.);
#90500=ADVANCED_FACE('',(#11221),#3564,.T.);
#90501=ADVANCED_FACE('',(#11222),#3565,.T.);
#90502=ADVANCED_FACE('',(#11223),#86582,.T.);
#90503=ADVANCED_FACE('',(#11224),#3566,.T.);
#90504=ADVANCED_FACE('',(#11225),#3567,.T.);
#90505=ADVANCED_FACE('',(#11226),#3568,.T.);
#90506=ADVANCED_FACE('',(#11227),#86583,.T.);
#90507=ADVANCED_FACE('',(#11228),#86584,.T.);
#90508=ADVANCED_FACE('',(#11229),#3569,.T.);
#90509=ADVANCED_FACE('',(#11230),#3570,.T.);
#90510=ADVANCED_FACE('',(#11231),#86585,.T.);
#90511=ADVANCED_FACE('',(#11232),#86586,.T.);
#90512=ADVANCED_FACE('',(#11233),#3571,.T.);
#90513=ADVANCED_FACE('',(#11234),#3572,.T.);
#90514=ADVANCED_FACE('',(#11235),#86587,.T.);
#90515=ADVANCED_FACE('',(#11236),#3573,.T.);
#90516=ADVANCED_FACE('',(#11237),#3574,.T.);
#90517=ADVANCED_FACE('',(#11238),#3575,.T.);
#90518=ADVANCED_FACE('',(#11239),#86588,.T.);
#90519=ADVANCED_FACE('',(#11240),#86589,.T.);
#90520=ADVANCED_FACE('',(#11241),#3576,.T.);
#90521=ADVANCED_FACE('',(#11242),#3577,.T.);
#90522=ADVANCED_FACE('',(#11243),#86590,.T.);
#90523=ADVANCED_FACE('',(#11244),#3578,.T.);
#90524=ADVANCED_FACE('',(#11245),#86591,.T.);
#90525=ADVANCED_FACE('',(#11246),#86592,.T.);
#90526=ADVANCED_FACE('',(#11247),#3579,.T.);
#90527=ADVANCED_FACE('',(#11248),#3580,.T.);
#90528=ADVANCED_FACE('',(#11249),#86593,.T.);
#90529=ADVANCED_FACE('',(#11250),#3581,.T.);
#90530=ADVANCED_FACE('',(#11251),#3582,.T.);
#90531=ADVANCED_FACE('',(#11252),#3583,.T.);
#90532=ADVANCED_FACE('',(#11253),#86594,.T.);
#90533=ADVANCED_FACE('',(#11254),#3584,.T.);
#90534=ADVANCED_FACE('',(#11255),#86595,.T.);
#90535=ADVANCED_FACE('',(#11256),#86596,.T.);
#90536=ADVANCED_FACE('',(#11257),#3585,.T.);
#90537=ADVANCED_FACE('',(#11258),#3586,.T.);
#90538=ADVANCED_FACE('',(#11259),#86597,.T.);
#90539=ADVANCED_FACE('',(#11260),#86598,.T.);
#90540=ADVANCED_FACE('',(#11261),#3587,.T.);
#90541=ADVANCED_FACE('',(#11262),#3588,.T.);
#90542=ADVANCED_FACE('',(#11263),#86599,.T.);
#90543=ADVANCED_FACE('',(#11264),#86600,.T.);
#90544=ADVANCED_FACE('',(#11265),#3589,.T.);
#90545=ADVANCED_FACE('',(#11266),#3590,.T.);
#90546=ADVANCED_FACE('',(#11267),#3591,.T.);
#90547=ADVANCED_FACE('',(#11268),#86601,.T.);
#90548=ADVANCED_FACE('',(#11269),#3592,.T.);
#90549=ADVANCED_FACE('',(#11270),#3593,.T.);
#90550=ADVANCED_FACE('',(#11271),#86602,.T.);
#90551=ADVANCED_FACE('',(#11272),#86603,.T.);
#90552=ADVANCED_FACE('',(#11273),#3594,.T.);
#90553=ADVANCED_FACE('',(#11274),#3595,.T.);
#90554=ADVANCED_FACE('',(#11275),#86604,.T.);
#90555=ADVANCED_FACE('',(#11276),#86605,.T.);
#90556=ADVANCED_FACE('',(#11277),#3596,.T.);
#90557=ADVANCED_FACE('',(#11278),#3597,.T.);
#90558=ADVANCED_FACE('',(#11279),#86606,.T.);
#90559=ADVANCED_FACE('',(#11280),#86607,.T.);
#90560=ADVANCED_FACE('',(#11281),#3598,.T.);
#90561=ADVANCED_FACE('',(#11282),#3599,.T.);
#90562=ADVANCED_FACE('',(#11283),#86608,.T.);
#90563=ADVANCED_FACE('',(#11284),#86609,.T.);
#90564=ADVANCED_FACE('',(#11285),#3600,.T.);
#90565=ADVANCED_FACE('',(#11286),#3601,.T.);
#90566=ADVANCED_FACE('',(#11287),#86610,.T.);
#90567=ADVANCED_FACE('',(#11288),#86611,.T.);
#90568=ADVANCED_FACE('',(#11289),#3602,.T.);
#90569=ADVANCED_FACE('',(#11290),#3603,.T.);
#90570=ADVANCED_FACE('',(#11291),#86612,.T.);
#90571=ADVANCED_FACE('',(#11292),#3604,.T.);
#90572=ADVANCED_FACE('',(#11293),#3605,.T.);
#90573=ADVANCED_FACE('',(#11294),#3606,.T.);
#90574=ADVANCED_FACE('',(#11295),#3607,.T.);
#90575=ADVANCED_FACE('',(#11296),#86613,.T.);
#90576=ADVANCED_FACE('',(#11297),#86614,.T.);
#90577=ADVANCED_FACE('',(#11298),#3608,.T.);
#90578=ADVANCED_FACE('',(#11299),#3609,.T.);
#90579=ADVANCED_FACE('',(#11300),#3610,.T.);
#90580=ADVANCED_FACE('',(#11301),#86615,.T.);
#90581=ADVANCED_FACE('',(#11302),#3611,.T.);
#90582=ADVANCED_FACE('',(#11303),#3612,.T.);
#90583=ADVANCED_FACE('',(#11304),#86616,.T.);
#90584=ADVANCED_FACE('',(#11305),#86617,.T.);
#90585=ADVANCED_FACE('',(#11306),#3613,.T.);
#90586=ADVANCED_FACE('',(#11307),#3614,.T.);
#90587=ADVANCED_FACE('',(#11308),#3615,.T.);
#90588=ADVANCED_FACE('',(#11309),#86618,.T.);
#90589=ADVANCED_FACE('',(#11310),#3616,.T.);
#90590=ADVANCED_FACE('',(#11311),#3617,.T.);
#90591=ADVANCED_FACE('',(#11312),#3618,.T.);
#90592=ADVANCED_FACE('',(#11313),#3619,.T.);
#90593=ADVANCED_FACE('',(#11314),#86619,.T.);
#90594=ADVANCED_FACE('',(#11315),#86620,.T.);
#90595=ADVANCED_FACE('',(#11316),#3620,.T.);
#90596=ADVANCED_FACE('',(#11317),#3621,.T.);
#90597=ADVANCED_FACE('',(#11318),#86621,.T.);
#90598=ADVANCED_FACE('',(#11319),#86622,.T.);
#90599=ADVANCED_FACE('',(#11320),#3622,.T.);
#90600=ADVANCED_FACE('',(#11321),#3623,.T.);
#90601=ADVANCED_FACE('',(#11322),#86623,.T.);
#90602=ADVANCED_FACE('',(#11323),#86624,.T.);
#90603=ADVANCED_FACE('',(#11324),#3624,.T.);
#90604=ADVANCED_FACE('',(#11325),#3625,.T.);
#90605=ADVANCED_FACE('',(#11326),#86625,.T.);
#90606=ADVANCED_FACE('',(#11327),#3626,.T.);
#90607=ADVANCED_FACE('',(#11328),#3627,.T.);
#90608=ADVANCED_FACE('',(#11329),#3628,.T.);
#90609=ADVANCED_FACE('',(#11330),#3629,.T.);
#90610=ADVANCED_FACE('',(#11331),#3630,.T.);
#90611=ADVANCED_FACE('',(#11332),#86626,.T.);
#90612=ADVANCED_FACE('',(#11333),#86627,.T.);
#90613=ADVANCED_FACE('',(#11334),#3631,.T.);
#90614=ADVANCED_FACE('',(#11335),#3632,.T.);
#90615=ADVANCED_FACE('',(#11336),#86628,.T.);
#90616=ADVANCED_FACE('',(#11337),#3633,.T.);
#90617=ADVANCED_FACE('',(#11338),#3634,.T.);
#90618=ADVANCED_FACE('',(#11339),#3635,.T.);
#90619=ADVANCED_FACE('',(#11340),#86629,.T.);
#90620=ADVANCED_FACE('',(#11341),#86630,.T.);
#90621=ADVANCED_FACE('',(#11342),#3636,.T.);
#90622=ADVANCED_FACE('',(#11343),#3637,.T.);
#90623=ADVANCED_FACE('',(#11344),#86631,.T.);
#90624=ADVANCED_FACE('',(#11345),#86632,.T.);
#90625=ADVANCED_FACE('',(#11346),#3638,.T.);
#90626=ADVANCED_FACE('',(#11347),#3639,.T.);
#90627=ADVANCED_FACE('',(#11348),#86633,.T.);
#90628=ADVANCED_FACE('',(#11349),#86634,.T.);
#90629=ADVANCED_FACE('',(#11350),#3640,.T.);
#90630=ADVANCED_FACE('',(#11351),#3641,.T.);
#90631=ADVANCED_FACE('',(#11352),#86635,.T.);
#90632=ADVANCED_FACE('',(#11353),#3642,.T.);
#90633=ADVANCED_FACE('',(#11354),#3643,.T.);
#90634=ADVANCED_FACE('',(#11355),#3644,.T.);
#90635=ADVANCED_FACE('',(#11356),#86636,.T.);
#90636=ADVANCED_FACE('',(#11357),#86637,.T.);
#90637=ADVANCED_FACE('',(#11358),#3645,.T.);
#90638=ADVANCED_FACE('',(#11359),#3646,.T.);
#90639=ADVANCED_FACE('',(#11360),#86638,.T.);
#90640=ADVANCED_FACE('',(#11361),#86639,.T.);
#90641=ADVANCED_FACE('',(#11362),#3647,.T.);
#90642=ADVANCED_FACE('',(#11363),#3648,.T.);
#90643=ADVANCED_FACE('',(#11364),#86640,.T.);
#90644=ADVANCED_FACE('',(#11365),#3649,.T.);
#90645=ADVANCED_FACE('',(#11366),#3650,.T.);
#90646=ADVANCED_FACE('',(#11367),#3651,.T.);
#90647=ADVANCED_FACE('',(#11368),#86641,.T.);
#90648=ADVANCED_FACE('',(#11369),#3652,.T.);
#90649=ADVANCED_FACE('',(#11370),#86642,.T.);
#90650=ADVANCED_FACE('',(#11371),#3653,.T.);
#90651=ADVANCED_FACE('',(#11372),#3654,.T.);
#90652=ADVANCED_FACE('',(#11373),#3655,.T.);
#90653=ADVANCED_FACE('',(#11374),#86643,.T.);
#90654=ADVANCED_FACE('',(#11375),#3656,.T.);
#90655=ADVANCED_FACE('',(#11376),#3657,.T.);
#90656=ADVANCED_FACE('',(#11377),#3658,.T.);
#90657=ADVANCED_FACE('',(#11378),#3659,.T.);
#90658=ADVANCED_FACE('',(#11379),#3660,.T.);
#90659=ADVANCED_FACE('',(#11380),#3661,.T.);
#90660=ADVANCED_FACE('',(#11381),#3662,.T.);
#90661=ADVANCED_FACE('',(#11382),#3663,.T.);
#90662=ADVANCED_FACE('',(#11383),#3664,.T.);
#90663=ADVANCED_FACE('',(#11384),#3665,.T.);
#90664=ADVANCED_FACE('',(#11385),#3666,.T.);
#90665=ADVANCED_FACE('',(#11386),#3667,.T.);
#90666=ADVANCED_FACE('',(#11387),#3668,.T.);
#90667=ADVANCED_FACE('',(#11388),#3669,.T.);
#90668=ADVANCED_FACE('',(#11389),#3670,.T.);
#90669=ADVANCED_FACE('',(#11390),#86644,.T.);
#90670=ADVANCED_FACE('',(#11391),#3671,.T.);
#90671=ADVANCED_FACE('',(#11392),#3672,.T.);
#90672=ADVANCED_FACE('',(#11393),#3673,.T.);
#90673=ADVANCED_FACE('',(#11394),#86645,.T.);
#90674=ADVANCED_FACE('',(#11395),#3674,.T.);
#90675=ADVANCED_FACE('',(#11396),#3675,.T.);
#90676=ADVANCED_FACE('',(#11397),#86646,.T.);
#90677=ADVANCED_FACE('',(#11398),#3676,.T.);
#90678=ADVANCED_FACE('',(#11399),#3677,.T.);
#90679=ADVANCED_FACE('',(#11400),#3678,.T.);
#90680=ADVANCED_FACE('',(#11401),#86647,.T.);
#90681=ADVANCED_FACE('',(#11402),#3679,.T.);
#90682=ADVANCED_FACE('',(#11403),#3680,.T.);
#90683=ADVANCED_FACE('',(#11404),#86648,.T.);
#90684=ADVANCED_FACE('',(#11405),#3681,.T.);
#90685=ADVANCED_FACE('',(#11406),#3682,.T.);
#90686=ADVANCED_FACE('',(#11407),#3683,.T.);
#90687=ADVANCED_FACE('',(#11408),#86649,.T.);
#90688=ADVANCED_FACE('',(#11409),#3684,.T.);
#90689=ADVANCED_FACE('',(#11410),#3685,.T.);
#90690=ADVANCED_FACE('',(#11411),#86650,.T.);
#90691=ADVANCED_FACE('',(#11412),#3686,.T.);
#90692=ADVANCED_FACE('',(#11413),#3687,.T.);
#90693=ADVANCED_FACE('',(#11414),#3688,.T.);
#90694=ADVANCED_FACE('',(#11415),#86651,.T.);
#90695=ADVANCED_FACE('',(#11416),#3689,.T.);
#90696=ADVANCED_FACE('',(#11417),#3690,.T.);
#90697=ADVANCED_FACE('',(#11418),#3691,.T.);
#90698=ADVANCED_FACE('',(#11419),#3692,.T.);
#90699=ADVANCED_FACE('',(#11420),#3693,.T.);
#90700=ADVANCED_FACE('',(#11421),#3694,.T.);
#90701=ADVANCED_FACE('',(#11422),#3695,.T.);
#90702=ADVANCED_FACE('',(#11423),#3696,.T.);
#90703=ADVANCED_FACE('',(#11424),#2974,.T.);
#90704=ADVANCED_FACE('',(#11425),#2975,.T.);
#90705=ADVANCED_FACE('',(#11426),#2976,.T.);
#90706=ADVANCED_FACE('',(#11427),#2977,.T.);
#90707=ADVANCED_FACE('',(#11428),#2978,.T.);
#90708=ADVANCED_FACE('',(#11429),#2979,.T.);
#90709=ADVANCED_FACE('',(#11430),#2980,.T.);
#90710=ADVANCED_FACE('',(#11431),#2981,.T.);
#90711=ADVANCED_FACE('',(#11432),#2982,.T.);
#90712=ADVANCED_FACE('',(#11433),#2983,.T.);
#90713=ADVANCED_FACE('',(#11434),#2984,.T.);
#90714=ADVANCED_FACE('',(#11435),#2985,.T.);
#90715=ADVANCED_FACE('',(#11436),#2986,.T.);
#90716=ADVANCED_FACE('',(#11437),#2987,.T.);
#90717=ADVANCED_FACE('',(#11438),#2988,.T.);
#90718=ADVANCED_FACE('',(#11439),#2989,.T.);
#90719=ADVANCED_FACE('',(#11440),#2990,.T.);
#90720=ADVANCED_FACE('',(#11441),#2991,.T.);
#90721=ADVANCED_FACE('',(#11442),#2992,.T.);
#90722=ADVANCED_FACE('',(#11443),#2993,.T.);
#90723=ADVANCED_FACE('',(#11444),#2994,.T.);
#90724=ADVANCED_FACE('',(#11445),#2995,.T.);
#90725=ADVANCED_FACE('',(#11446),#2996,.T.);
#90726=ADVANCED_FACE('',(#11447),#2997,.T.);
#90727=ADVANCED_FACE('',(#11448),#2998,.T.);
#90728=ADVANCED_FACE('',(#11449),#2999,.T.);
#90729=ADVANCED_FACE('',(#11450),#3000,.T.);
#90730=ADVANCED_FACE('',(#11451),#3001,.T.);
#90731=ADVANCED_FACE('',(#11452),#3002,.T.);
#90732=ADVANCED_FACE('',(#11453),#3003,.T.);
#90733=ADVANCED_FACE('',(#11454),#3004,.T.);
#90734=ADVANCED_FACE('',(#11455),#3005,.T.);
#90735=ADVANCED_FACE('',(#11456),#3006,.T.);
#90736=ADVANCED_FACE('',(#11457),#3007,.T.);
#90737=ADVANCED_FACE('',(#11458),#3008,.T.);
#90738=ADVANCED_FACE('',(#11459),#3009,.T.);
#90739=ADVANCED_FACE('',(#11460),#3010,.T.);
#90740=ADVANCED_FACE('',(#11461),#3011,.T.);
#90741=ADVANCED_FACE('',(#11462),#3697,.T.);
#90742=ADVANCED_FACE('',(#11463),#3012,.T.);
#90743=ADVANCED_FACE('',(#11464),#3013,.T.);
#90744=ADVANCED_FACE('',(#11465),#3014,.T.);
#90745=ADVANCED_FACE('',(#11466),#3015,.T.);
#90746=ADVANCED_FACE('',(#11467),#3016,.T.);
#90747=ADVANCED_FACE('',(#11468),#3017,.T.);
#90748=ADVANCED_FACE('',(#11469),#3018,.T.);
#90749=ADVANCED_FACE('',(#11470),#3019,.T.);
#90750=ADVANCED_FACE('',(#11471),#3020,.T.);
#90751=ADVANCED_FACE('',(#11472),#3021,.T.);
#90752=ADVANCED_FACE('',(#11473),#3022,.T.);
#90753=ADVANCED_FACE('',(#11474),#3023,.T.);
#90754=ADVANCED_FACE('',(#11475),#86652,.F.);
#90755=ADVANCED_FACE('',(#11476),#86653,.F.);
#90756=ADVANCED_FACE('',(#11477),#86654,.F.);
#90757=ADVANCED_FACE('',(#11478),#86655,.F.);
#90758=ADVANCED_FACE('',(#11479),#86656,.F.);
#90759=ADVANCED_FACE('',(#11480),#86657,.F.);
#90760=ADVANCED_FACE('',(#11481),#86658,.F.);
#90761=ADVANCED_FACE('',(#11482),#86659,.F.);
#90762=ADVANCED_FACE('',(#11483),#86660,.F.);
#90763=ADVANCED_FACE('',(#11484),#86661,.F.);
#90764=ADVANCED_FACE('',(#11485),#86662,.F.);
#90765=ADVANCED_FACE('',(#11486),#86663,.F.);
#90766=ADVANCED_FACE('',(#11487),#86664,.F.);
#90767=ADVANCED_FACE('',(#11488),#86665,.F.);
#90768=ADVANCED_FACE('',(#11489),#86666,.F.);
#90769=ADVANCED_FACE('',(#11490),#86667,.F.);
#90770=ADVANCED_FACE('',(#11491),#86668,.F.);
#90771=ADVANCED_FACE('',(#11492),#86669,.F.);
#90772=ADVANCED_FACE('',(#11493),#86670,.F.);
#90773=ADVANCED_FACE('',(#11494),#86671,.F.);
#90774=ADVANCED_FACE('',(#11495),#86672,.F.);
#90775=ADVANCED_FACE('',(#11496),#86673,.F.);
#90776=ADVANCED_FACE('',(#11497),#86674,.F.);
#90777=ADVANCED_FACE('',(#11498),#86675,.F.);
#90778=ADVANCED_FACE('',(#11499),#86676,.F.);
#90779=ADVANCED_FACE('',(#11500),#86677,.F.);
#90780=ADVANCED_FACE('',(#11501),#86678,.F.);
#90781=ADVANCED_FACE('',(#11502),#86679,.F.);
#90782=ADVANCED_FACE('',(#11503),#86680,.F.);
#90783=ADVANCED_FACE('',(#11504),#86681,.F.);
#90784=ADVANCED_FACE('',(#11505),#86682,.F.);
#90785=ADVANCED_FACE('',(#11506),#86683,.F.);
#90786=ADVANCED_FACE('',(#11507),#86684,.F.);
#90787=ADVANCED_FACE('',(#11508),#86685,.F.);
#90788=ADVANCED_FACE('',(#11509),#86686,.F.);
#90789=ADVANCED_FACE('',(#11510),#86687,.F.);
#90790=ADVANCED_FACE('',(#11511),#86688,.F.);
#90791=ADVANCED_FACE('',(#11512),#86689,.F.);
#90792=ADVANCED_FACE('',(#11513),#86690,.F.);
#90793=ADVANCED_FACE('',(#11514),#86691,.F.);
#90794=ADVANCED_FACE('',(#11515),#86692,.F.);
#90795=ADVANCED_FACE('',(#11516),#86693,.F.);
#90796=ADVANCED_FACE('',(#11517),#86694,.F.);
#90797=ADVANCED_FACE('',(#11518),#86695,.F.);
#90798=ADVANCED_FACE('',(#11519),#86696,.F.);
#90799=ADVANCED_FACE('',(#11520),#86697,.F.);
#90800=ADVANCED_FACE('',(#11521),#86698,.F.);
#90801=ADVANCED_FACE('',(#11522),#86699,.F.);
#90802=ADVANCED_FACE('',(#11523),#86700,.F.);
#90803=ADVANCED_FACE('',(#11524),#86701,.F.);
#90804=ADVANCED_FACE('',(#11525),#86702,.F.);
#90805=ADVANCED_FACE('',(#11526),#86703,.F.);
#90806=ADVANCED_FACE('',(#11527),#86704,.F.);
#90807=ADVANCED_FACE('',(#11528),#86705,.F.);
#90808=ADVANCED_FACE('',(#11529),#86706,.F.);
#90809=ADVANCED_FACE('',(#11530),#86707,.F.);
#90810=ADVANCED_FACE('',(#11531),#86708,.F.);
#90811=ADVANCED_FACE('',(#11532),#86709,.F.);
#90812=ADVANCED_FACE('',(#11533),#86710,.F.);
#90813=ADVANCED_FACE('',(#11534),#86711,.F.);
#90814=ADVANCED_FACE('',(#11535),#86712,.F.);
#90815=ADVANCED_FACE('',(#11536),#86713,.F.);
#90816=ADVANCED_FACE('',(#11537),#86714,.F.);
#90817=ADVANCED_FACE('',(#11538),#86715,.F.);
#90818=ADVANCED_FACE('',(#11539),#86716,.F.);
#90819=ADVANCED_FACE('',(#11540),#86717,.F.);
#90820=ADVANCED_FACE('',(#11541),#86718,.F.);
#90821=ADVANCED_FACE('',(#11542),#86719,.F.);
#90822=ADVANCED_FACE('',(#11543),#86720,.F.);
#90823=ADVANCED_FACE('',(#11544),#86721,.F.);
#90824=ADVANCED_FACE('',(#11545),#86722,.F.);
#90825=ADVANCED_FACE('',(#11546),#86723,.F.);
#90826=ADVANCED_FACE('',(#11547),#86724,.F.);
#90827=ADVANCED_FACE('',(#11548),#86725,.F.);
#90828=ADVANCED_FACE('',(#11549),#86726,.F.);
#90829=ADVANCED_FACE('',(#11550),#86727,.F.);
#90830=ADVANCED_FACE('',(#11551),#86728,.F.);
#90831=ADVANCED_FACE('',(#11552),#86729,.F.);
#90832=ADVANCED_FACE('',(#11553),#86730,.F.);
#90833=ADVANCED_FACE('',(#11554),#86731,.F.);
#90834=ADVANCED_FACE('',(#11555),#86732,.F.);
#90835=ADVANCED_FACE('',(#11556),#86733,.F.);
#90836=ADVANCED_FACE('',(#11557),#86734,.F.);
#90837=ADVANCED_FACE('',(#11558),#86735,.F.);
#90838=ADVANCED_FACE('',(#11559),#86736,.F.);
#90839=ADVANCED_FACE('',(#11560),#86737,.F.);
#90840=ADVANCED_FACE('',(#11561),#86738,.F.);
#90841=ADVANCED_FACE('',(#11562),#86739,.F.);
#90842=ADVANCED_FACE('',(#11563),#86740,.F.);
#90843=ADVANCED_FACE('',(#11564),#86741,.F.);
#90844=ADVANCED_FACE('',(#11565),#86742,.F.);
#90845=ADVANCED_FACE('',(#11566),#86743,.F.);
#90846=ADVANCED_FACE('',(#11567),#86744,.F.);
#90847=ADVANCED_FACE('',(#11568),#86745,.F.);
#90848=ADVANCED_FACE('',(#11569),#86746,.F.);
#90849=ADVANCED_FACE('',(#11570),#86747,.F.);
#90850=ADVANCED_FACE('',(#11571),#86748,.F.);
#90851=ADVANCED_FACE('',(#11572),#86749,.F.);
#90852=ADVANCED_FACE('',(#11573),#86750,.F.);
#90853=ADVANCED_FACE('',(#11574),#86751,.F.);
#90854=ADVANCED_FACE('',(#11575),#86752,.F.);
#90855=ADVANCED_FACE('',(#11576),#86753,.F.);
#90856=ADVANCED_FACE('',(#11577),#86754,.F.);
#90857=ADVANCED_FACE('',(#11578),#86755,.F.);
#90858=ADVANCED_FACE('',(#11579),#86756,.F.);
#90859=ADVANCED_FACE('',(#11580),#86757,.F.);
#90860=ADVANCED_FACE('',(#11581),#86758,.F.);
#90861=ADVANCED_FACE('',(#11582),#86759,.F.);
#90862=ADVANCED_FACE('',(#11583),#86760,.F.);
#90863=ADVANCED_FACE('',(#11584),#86761,.F.);
#90864=ADVANCED_FACE('',(#11585),#86762,.F.);
#90865=ADVANCED_FACE('',(#11586),#86763,.F.);
#90866=ADVANCED_FACE('',(#11587),#86764,.F.);
#90867=ADVANCED_FACE('',(#11588),#86765,.F.);
#90868=ADVANCED_FACE('',(#11589),#86766,.F.);
#90869=ADVANCED_FACE('',(#11590),#86767,.F.);
#90870=ADVANCED_FACE('',(#11591),#86768,.F.);
#90871=ADVANCED_FACE('',(#11592),#86769,.F.);
#90872=ADVANCED_FACE('',(#11593),#86770,.F.);
#90873=ADVANCED_FACE('',(#11594),#86771,.F.);
#90874=ADVANCED_FACE('',(#11595),#86772,.F.);
#90875=ADVANCED_FACE('',(#11596),#86773,.F.);
#90876=ADVANCED_FACE('',(#11597),#86774,.F.);
#90877=ADVANCED_FACE('',(#11598),#86775,.F.);
#90878=ADVANCED_FACE('',(#11599),#86776,.F.);
#90879=ADVANCED_FACE('',(#11600),#86777,.F.);
#90880=ADVANCED_FACE('',(#11601),#86778,.F.);
#90881=ADVANCED_FACE('',(#11602),#86779,.F.);
#90882=ADVANCED_FACE('',(#11603),#86780,.F.);
#90883=ADVANCED_FACE('',(#11604),#86781,.F.);
#90884=ADVANCED_FACE('',(#11605),#86782,.F.);
#90885=ADVANCED_FACE('',(#11606),#86783,.F.);
#90886=ADVANCED_FACE('',(#11607),#86784,.F.);
#90887=ADVANCED_FACE('',(#11608),#86785,.F.);
#90888=ADVANCED_FACE('',(#11609),#86786,.F.);
#90889=ADVANCED_FACE('',(#11610),#86787,.F.);
#90890=ADVANCED_FACE('',(#11611),#86788,.F.);
#90891=ADVANCED_FACE('',(#11612),#86789,.F.);
#90892=ADVANCED_FACE('',(#11613),#86790,.T.);
#90893=ADVANCED_FACE('',(#11614),#86791,.T.);
#90894=ADVANCED_FACE('',(#11615),#86792,.F.);
#90895=ADVANCED_FACE('',(#11616),#8033,.F.);
#90896=ADVANCED_FACE('',(#11617),#8034,.F.);
#90897=ADVANCED_FACE('',(#11618),#86793,.F.);
#90898=ADVANCED_FACE('',(#11619),#86794,.T.);
#90899=ADVANCED_FACE('',(#11620),#86795,.F.);
#90900=ADVANCED_FACE('',(#11621),#8035,.T.);
#90901=ADVANCED_FACE('',(#11622),#8036,.T.);
#90902=ADVANCED_FACE('',(#11623),#86796,.F.);
#90903=ADVANCED_FACE('',(#11624),#86797,.T.);
#90904=ADVANCED_FACE('',(#11625),#8037,.F.);
#90905=ADVANCED_FACE('',(#11626),#8038,.F.);
#90906=ADVANCED_FACE('',(#11627),#8039,.F.);
#90907=ADVANCED_FACE('',(#11628),#8040,.F.);
#90908=ADVANCED_FACE('',(#11629),#8041,.F.);
#90909=ADVANCED_FACE('',(#11630),#8042,.F.);
#90910=ADVANCED_FACE('',(#11631),#8043,.F.);
#90911=ADVANCED_FACE('',(#11632),#8044,.F.);
#90912=ADVANCED_FACE('',(#11633),#8045,.F.);
#90913=ADVANCED_FACE('',(#11634),#8046,.F.);
#90914=ADVANCED_FACE('',(#11635),#8047,.F.);
#90915=ADVANCED_FACE('',(#11636),#8048,.F.);
#90916=ADVANCED_FACE('',(#11637),#8049,.F.);
#90917=ADVANCED_FACE('',(#11638),#8050,.F.);
#90918=ADVANCED_FACE('',(#11639),#8051,.F.);
#90919=ADVANCED_FACE('',(#11640),#8052,.F.);
#90920=ADVANCED_FACE('',(#11641),#8053,.F.);
#90921=ADVANCED_FACE('',(#11642),#8054,.F.);
#90922=ADVANCED_FACE('',(#11643),#8055,.F.);
#90923=ADVANCED_FACE('',(#11644),#8056,.F.);
#90924=ADVANCED_FACE('',(#11645),#8057,.F.);
#90925=ADVANCED_FACE('',(#11646),#8058,.F.);
#90926=ADVANCED_FACE('',(#11647),#8059,.F.);
#90927=ADVANCED_FACE('',(#11648),#8060,.F.);
#90928=ADVANCED_FACE('',(#11649),#8061,.F.);
#90929=ADVANCED_FACE('',(#11650),#8062,.F.);
#90930=ADVANCED_FACE('',(#11651),#8063,.F.);
#90931=ADVANCED_FACE('',(#11652),#8064,.F.);
#90932=ADVANCED_FACE('',(#11653),#8065,.F.);
#90933=ADVANCED_FACE('',(#11654),#8066,.F.);
#90934=ADVANCED_FACE('',(#11655),#8067,.F.);
#90935=ADVANCED_FACE('',(#11656),#8068,.F.);
#90936=ADVANCED_FACE('',(#11657),#8069,.F.);
#90937=ADVANCED_FACE('',(#11658),#8070,.F.);
#90938=ADVANCED_FACE('',(#11659),#8071,.F.);
#90939=ADVANCED_FACE('',(#11660),#8072,.F.);
#90940=ADVANCED_FACE('',(#11661),#8073,.F.);
#90941=ADVANCED_FACE('',(#11662),#8074,.F.);
#90942=ADVANCED_FACE('',(#11663),#8075,.F.);
#90943=ADVANCED_FACE('',(#11664),#8076,.F.);
#90944=ADVANCED_FACE('',(#11665),#8077,.F.);
#90945=ADVANCED_FACE('',(#11666),#8078,.F.);
#90946=ADVANCED_FACE('',(#11667),#8079,.F.);
#90947=ADVANCED_FACE('',(#11668),#8080,.F.);
#90948=ADVANCED_FACE('',(#11669),#8081,.F.);
#90949=ADVANCED_FACE('',(#11670),#8082,.F.);
#90950=ADVANCED_FACE('',(#11671),#8083,.F.);
#90951=ADVANCED_FACE('',(#11672),#8084,.F.);
#90952=ADVANCED_FACE('',(#11673),#8085,.F.);
#90953=ADVANCED_FACE('',(#11674),#8086,.F.);
#90954=ADVANCED_FACE('',(#11675),#8087,.F.);
#90955=ADVANCED_FACE('',(#11676),#8088,.F.);
#90956=ADVANCED_FACE('',(#11677),#8089,.F.);
#90957=ADVANCED_FACE('',(#11678),#8090,.F.);
#90958=ADVANCED_FACE('',(#11679),#8091,.F.);
#90959=ADVANCED_FACE('',(#11680),#8092,.F.);
#90960=ADVANCED_FACE('',(#11681),#8093,.F.);
#90961=ADVANCED_FACE('',(#11682),#86798,.T.);
#90962=ADVANCED_FACE('',(#11683),#86799,.T.);
#90963=ADVANCED_FACE('',(#11684),#86800,.T.);
#90964=ADVANCED_FACE('',(#11685),#86801,.T.);
#90965=ADVANCED_FACE('',(#11686),#86802,.T.);
#90966=ADVANCED_FACE('',(#11687),#86803,.T.);
#90967=ADVANCED_FACE('',(#11688),#86804,.T.);
#90968=ADVANCED_FACE('',(#11689),#8094,.T.);
#90969=ADVANCED_FACE('',(#11690),#8095,.T.);
#90970=ADVANCED_FACE('',(#11691),#8096,.F.);
#90971=ADVANCED_FACE('',(#11692),#8097,.T.);
#90972=ADVANCED_FACE('',(#11693),#8098,.F.);
#90973=ADVANCED_FACE('',(#11694),#8099,.F.);
#90974=ADVANCED_FACE('',(#11695),#86805,.F.);
#90975=ADVANCED_FACE('',(#11696),#8100,.F.);
#90976=ADVANCED_FACE('',(#11697),#8101,.F.);
#90977=ADVANCED_FACE('',(#11698),#86806,.F.);
#90978=ADVANCED_FACE('',(#11699),#86807,.T.);
#90979=ADVANCED_FACE('',(#11700),#86808,.T.);
#90980=ADVANCED_FACE('',(#11701),#86809,.T.);
#90981=ADVANCED_FACE('',(#11702),#86810,.T.);
#90982=ADVANCED_FACE('',(#11703),#86811,.T.);
#90983=ADVANCED_FACE('',(#11704),#86812,.T.);
#90984=ADVANCED_FACE('',(#11705),#86813,.T.);
#90985=ADVANCED_FACE('',(#11706),#905,.F.);
#90986=ADVANCED_FACE('',(#11707),#906,.F.);
#90987=ADVANCED_FACE('',(#11708),#907,.F.);
#90988=ADVANCED_FACE('',(#11709),#908,.F.);
#90989=ADVANCED_FACE('',(#11710),#7008,.F.);
#90990=ADVANCED_FACE('',(#11711),#7009,.F.);
#90991=ADVANCED_FACE('',(#11712),#7010,.F.);
#90992=ADVANCED_FACE('',(#11713),#7011,.F.);
#90993=ADVANCED_FACE('',(#11714),#7012,.F.);
#90994=ADVANCED_FACE('',(#11715),#7013,.F.);
#90995=ADVANCED_FACE('',(#11716),#7014,.F.);
#90996=ADVANCED_FACE('',(#11717),#7015,.F.);
#90997=ADVANCED_FACE('',(#11718),#7016,.F.);
#90998=ADVANCED_FACE('',(#11719),#7017,.F.);
#90999=ADVANCED_FACE('',(#11720),#7018,.F.);
#91000=ADVANCED_FACE('',(#11721),#7019,.F.);
#91001=ADVANCED_FACE('',(#11722),#7020,.F.);
#91002=ADVANCED_FACE('',(#11723),#909,.F.);
#91003=ADVANCED_FACE('',(#11724),#910,.F.);
#91004=ADVANCED_FACE('',(#11725),#7021,.F.);
#91005=ADVANCED_FACE('',(#11726),#911,.F.);
#91006=ADVANCED_FACE('',(#11727),#8102,.F.);
#91007=ADVANCED_FACE('',(#11728),#912,.F.);
#91008=ADVANCED_FACE('',(#11729),#8103,.F.);
#91009=ADVANCED_FACE('',(#11730),#913,.F.);
#91010=ADVANCED_FACE('',(#11731),#8104,.T.);
#91011=ADVANCED_FACE('',(#11732),#914,.F.);
#91012=ADVANCED_FACE('',(#11733),#8105,.F.);
#91013=ADVANCED_FACE('',(#11734),#8106,.F.);
#91014=ADVANCED_FACE('',(#11735),#8107,.F.);
#91015=ADVANCED_FACE('',(#11736),#8108,.F.);
#91016=ADVANCED_FACE('',(#11737),#8109,.F.);
#91017=ADVANCED_FACE('',(#11738),#8110,.F.);
#91018=ADVANCED_FACE('',(#11739),#8111,.F.);
#91019=ADVANCED_FACE('',(#11740),#86814,.T.);
#91020=ADVANCED_FACE('',(#11741),#86815,.T.);
#91021=ADVANCED_FACE('',(#11742),#86816,.T.);
#91022=ADVANCED_FACE('',(#11743),#86817,.T.);
#91023=ADVANCED_FACE('',(#11744),#86818,.T.);
#91024=ADVANCED_FACE('',(#11745),#8112,.T.);
#91025=ADVANCED_FACE('',(#11746),#7022,.T.);
#91026=ADVANCED_FACE('',(#11747),#8113,.T.);
#91027=ADVANCED_FACE('',(#11748),#915,.F.);
#91028=ADVANCED_FACE('',(#11749),#7023,.T.);
#91029=ADVANCED_FACE('',(#11750),#86819,.F.);
#91030=ADVANCED_FACE('',(#11751),#86820,.F.);
#91031=ADVANCED_FACE('',(#11752),#86821,.F.);
#91032=ADVANCED_FACE('',(#11753),#86822,.F.);
#91033=ADVANCED_FACE('',(#11754),#86823,.F.);
#91034=ADVANCED_FACE('',(#11755),#86824,.F.);
#91035=ADVANCED_FACE('',(#11756),#86825,.F.);
#91036=ADVANCED_FACE('',(#11757),#8114,.T.);
#91037=ADVANCED_FACE('',(#11758),#7024,.F.);
#91038=ADVANCED_FACE('',(#11759),#8115,.T.);
#91039=ADVANCED_FACE('',(#11760),#7025,.F.);
#91040=ADVANCED_FACE('',(#11761,#7455),#8116,.F.);
#91041=ADVANCED_FACE('',(#11762),#8117,.F.);
#91042=ADVANCED_FACE('',(#11763),#8118,.F.);
#91043=ADVANCED_FACE('',(#11764),#86826,.T.);
#91044=ADVANCED_FACE('',(#11765),#8119,.T.);
#91045=ADVANCED_FACE('',(#11766),#8120,.F.);
#91046=ADVANCED_FACE('',(#11767),#8121,.F.);
#91047=ADVANCED_FACE('',(#11768),#86827,.T.);
#91048=ADVANCED_FACE('',(#11769),#8122,.T.);
#91049=ADVANCED_FACE('',(#11770),#8123,.T.);
#91050=ADVANCED_FACE('',(#11771),#86828,.T.);
#91051=ADVANCED_FACE('',(#11772),#8124,.T.);
#91052=ADVANCED_FACE('',(#11773),#8125,.T.);
#91053=ADVANCED_FACE('',(#11774),#86829,.T.);
#91054=ADVANCED_FACE('',(#11775),#916,.F.);
#91055=ADVANCED_FACE('',(#11776),#86830,.T.);
#91056=ADVANCED_FACE('',(#11777),#86831,.T.);
#91057=ADVANCED_FACE('',(#11778),#86832,.T.);
#91058=ADVANCED_FACE('',(#11779),#86833,.T.);
#91059=ADVANCED_FACE('',(#11780),#86834,.T.);
#91060=ADVANCED_FACE('',(#11781),#86835,.T.);
#91061=ADVANCED_FACE('',(#11782),#86836,.T.);
#91062=ADVANCED_FACE('',(#11783),#86837,.F.);
#91063=ADVANCED_FACE('',(#11784),#86838,.F.);
#91064=ADVANCED_FACE('',(#11785),#86839,.F.);
#91065=ADVANCED_FACE('',(#11786),#86840,.F.);
#91066=ADVANCED_FACE('',(#11787),#86841,.F.);
#91067=ADVANCED_FACE('',(#11788),#86842,.F.);
#91068=ADVANCED_FACE('',(#11789),#86843,.F.);
#91069=ADVANCED_FACE('',(#11790),#917,.F.);
#91070=ADVANCED_FACE('',(#11791),#918,.F.);
#91071=ADVANCED_FACE('',(#11792),#919,.F.);
#91072=ADVANCED_FACE('',(#11793),#920,.F.);
#91073=ADVANCED_FACE('',(#11794),#7026,.T.);
#91074=ADVANCED_FACE('',(#11795),#7027,.T.);
#91075=ADVANCED_FACE('',(#11796),#7028,.T.);
#91076=ADVANCED_FACE('',(#11797),#7029,.T.);
#91077=ADVANCED_FACE('',(#11798),#7030,.T.);
#91078=ADVANCED_FACE('',(#11799),#7031,.T.);
#91079=ADVANCED_FACE('',(#11800),#7032,.T.);
#91080=ADVANCED_FACE('',(#11801),#7033,.T.);
#91081=ADVANCED_FACE('',(#11802),#7034,.T.);
#91082=ADVANCED_FACE('',(#11803),#7035,.T.);
#91083=ADVANCED_FACE('',(#11804),#7036,.T.);
#91084=ADVANCED_FACE('',(#11805),#7037,.T.);
#91085=ADVANCED_FACE('',(#11806),#7038,.T.);
#91086=ADVANCED_FACE('',(#11807),#921,.F.);
#91087=ADVANCED_FACE('',(#11808),#922,.F.);
#91088=ADVANCED_FACE('',(#11809),#7039,.T.);
#91089=ADVANCED_FACE('',(#11810),#923,.F.);
#91090=ADVANCED_FACE('',(#11811),#924,.F.);
#91091=ADVANCED_FACE('',(#11812),#8126,.T.);
#91092=ADVANCED_FACE('',(#11813),#925,.F.);
#91093=ADVANCED_FACE('',(#11814),#8127,.F.);
#91094=ADVANCED_FACE('',(#11815),#926,.F.);
#91095=ADVANCED_FACE('',(#11816),#86844,.F.);
#91096=ADVANCED_FACE('',(#11817),#86845,.F.);
#91097=ADVANCED_FACE('',(#11818),#86846,.F.);
#91098=ADVANCED_FACE('',(#11819),#86847,.F.);
#91099=ADVANCED_FACE('',(#11820),#86848,.F.);
#91100=ADVANCED_FACE('',(#11821),#8128,.T.);
#91101=ADVANCED_FACE('',(#11822),#8129,.T.);
#91102=ADVANCED_FACE('',(#11823),#8130,.T.);
#91103=ADVANCED_FACE('',(#11824),#8131,.T.);
#91104=ADVANCED_FACE('',(#11825),#8132,.T.);
#91105=ADVANCED_FACE('',(#11826),#8133,.T.);
#91106=ADVANCED_FACE('',(#11827),#8134,.T.);
#91107=ADVANCED_FACE('',(#11828),#8135,.T.);
#91108=ADVANCED_FACE('',(#11829),#8136,.T.);
#91109=ADVANCED_FACE('',(#11830),#8137,.T.);
#91110=ADVANCED_FACE('',(#11831),#86849,.F.);
#91111=ADVANCED_FACE('',(#11832),#86850,.F.);
#91112=ADVANCED_FACE('',(#11833),#86851,.T.);
#91113=ADVANCED_FACE('',(#11834),#8138,.T.);
#91114=ADVANCED_FACE('',(#11835),#8139,.T.);
#91115=ADVANCED_FACE('',(#11836),#8140,.T.);
#91116=ADVANCED_FACE('',(#11837),#8141,.T.);
#91117=ADVANCED_FACE('',(#11838),#8142,.T.);
#91118=ADVANCED_FACE('',(#11839),#8143,.T.);
#91119=ADVANCED_FACE('',(#11840),#8144,.T.);
#91120=ADVANCED_FACE('',(#11841),#8145,.T.);
#91121=ADVANCED_FACE('',(#11842),#8146,.T.);
#91122=ADVANCED_FACE('',(#11843),#8147,.T.);
#91123=ADVANCED_FACE('',(#11844),#8148,.T.);
#91124=ADVANCED_FACE('',(#11845),#8149,.T.);
#91125=ADVANCED_FACE('',(#11846),#8150,.T.);
#91126=ADVANCED_FACE('',(#11847),#8151,.T.);
#91127=ADVANCED_FACE('',(#11848),#86852,.F.);
#91128=ADVANCED_FACE('',(#11849),#86853,.F.);
#91129=ADVANCED_FACE('',(#11850),#86854,.F.);
#91130=ADVANCED_FACE('',(#11851),#86855,.F.);
#91131=ADVANCED_FACE('',(#11852),#86856,.F.);
#91132=ADVANCED_FACE('',(#11853),#86857,.F.);
#91133=ADVANCED_FACE('',(#11854),#86858,.F.);
#91134=ADVANCED_FACE('',(#11855),#86859,.F.);
#91135=ADVANCED_FACE('',(#11856),#8152,.T.);
#91136=ADVANCED_FACE('',(#11857),#8153,.T.);
#91137=ADVANCED_FACE('',(#11858),#8154,.T.);
#91138=ADVANCED_FACE('',(#11859),#8155,.T.);
#91139=ADVANCED_FACE('',(#11860),#8156,.T.);
#91140=ADVANCED_FACE('',(#11861),#8157,.T.);
#91141=ADVANCED_FACE('',(#11862),#8158,.T.);
#91142=ADVANCED_FACE('',(#11863),#8159,.T.);
#91143=ADVANCED_FACE('',(#11864),#8160,.T.);
#91144=ADVANCED_FACE('',(#11865),#8161,.T.);
#91145=ADVANCED_FACE('',(#11866),#8162,.T.);
#91146=ADVANCED_FACE('',(#11867),#8163,.T.);
#91147=ADVANCED_FACE('',(#11868),#8164,.T.);
#91148=ADVANCED_FACE('',(#11869),#8165,.T.);
#91149=ADVANCED_FACE('',(#11870),#8166,.T.);
#91150=ADVANCED_FACE('',(#11871),#8167,.T.);
#91151=ADVANCED_FACE('',(#11872),#8168,.T.);
#91152=ADVANCED_FACE('',(#11873),#8169,.T.);
#91153=ADVANCED_FACE('',(#11874),#8170,.T.);
#91154=ADVANCED_FACE('',(#11875),#8171,.T.);
#91155=ADVANCED_FACE('',(#11876),#8172,.T.);
#91156=ADVANCED_FACE('',(#11877),#8173,.T.);
#91157=ADVANCED_FACE('',(#11878),#8174,.T.);
#91158=ADVANCED_FACE('',(#11879),#8175,.T.);
#91159=ADVANCED_FACE('',(#11880),#8176,.T.);
#91160=ADVANCED_FACE('',(#11881),#8177,.T.);
#91161=ADVANCED_FACE('',(#11882),#8178,.T.);
#91162=ADVANCED_FACE('',(#11883),#8179,.T.);
#91163=ADVANCED_FACE('',(#11884),#3024,.T.);
#91164=ADVANCED_FACE('',(#11885),#3698,.T.);
#91165=ADVANCED_FACE('',(#11886),#3699,.T.);
#91166=ADVANCED_FACE('',(#11887),#3025,.F.);
#91167=ADVANCED_FACE('',(#11888),#3026,.F.);
#91168=ADVANCED_FACE('',(#11889),#1022,.F.);
#91169=ADVANCED_FACE('',(#11890),#3027,.F.);
#91170=ADVANCED_FACE('',(#11891),#3700,.F.);
#91171=ADVANCED_FACE('',(#11892),#3028,.F.);
#91172=ADVANCED_FACE('',(#11893),#3701,.F.);
#91173=ADVANCED_FACE('',(#11894),#3029,.F.);
#91174=ADVANCED_FACE('',(#11895),#3702,.F.);
#91175=ADVANCED_FACE('',(#11896),#3030,.F.);
#91176=ADVANCED_FACE('',(#11897),#3031,.F.);
#91177=ADVANCED_FACE('',(#11898),#3032,.F.);
#91178=ADVANCED_FACE('',(#11899),#1023,.F.);
#91179=ADVANCED_FACE('',(#11900),#3033,.F.);
#91180=ADVANCED_FACE('',(#11901),#3034,.F.);
#91181=ADVANCED_FACE('',(#11902),#3035,.F.);
#91182=ADVANCED_FACE('',(#11903),#3036,.F.);
#91183=ADVANCED_FACE('',(#11904),#3037,.F.);
#91184=ADVANCED_FACE('',(#11905),#1024,.F.);
#91185=ADVANCED_FACE('',(#11906),#3038,.F.);
#91186=ADVANCED_FACE('',(#11907),#3039,.F.);
#91187=ADVANCED_FACE('',(#11908),#3040,.F.);
#91188=ADVANCED_FACE('',(#11909),#3703,.F.);
#91189=ADVANCED_FACE('',(#11910),#1025,.F.);
#91190=ADVANCED_FACE('',(#11911),#3704,.F.);
#91191=ADVANCED_FACE('',(#11912),#3041,.F.);
#91192=ADVANCED_FACE('',(#11913),#3705,.F.);
#91193=ADVANCED_FACE('',(#11914),#3706,.F.);
#91194=ADVANCED_FACE('',(#11915),#3707,.F.);
#91195=ADVANCED_FACE('',(#11916),#3708,.F.);
#91196=ADVANCED_FACE('',(#11917),#3709,.F.);
#91197=ADVANCED_FACE('',(#11918),#3710,.F.);
#91198=ADVANCED_FACE('',(#11919),#3711,.F.);
#91199=ADVANCED_FACE('',(#11920),#3712,.F.);
#91200=ADVANCED_FACE('',(#11921),#3713,.F.);
#91201=ADVANCED_FACE('',(#11922),#3714,.F.);
#91202=ADVANCED_FACE('',(#11923),#3042,.F.);
#91203=ADVANCED_FACE('',(#11924),#3043,.F.);
#91204=ADVANCED_FACE('',(#11925),#3044,.F.);
#91205=ADVANCED_FACE('',(#11926),#3045,.F.);
#91206=ADVANCED_FACE('',(#11927),#3046,.F.);
#91207=ADVANCED_FACE('',(#11928),#3047,.F.);
#91208=ADVANCED_FACE('',(#11929),#3048,.F.);
#91209=ADVANCED_FACE('',(#11930),#3049,.F.);
#91210=ADVANCED_FACE('',(#11931),#3050,.F.);
#91211=ADVANCED_FACE('',(#11932),#3051,.F.);
#91212=ADVANCED_FACE('',(#11933),#3052,.F.);
#91213=ADVANCED_FACE('',(#11934),#3053,.F.);
#91214=ADVANCED_FACE('',(#11935),#3715,.F.);
#91215=ADVANCED_FACE('',(#11936),#3054,.F.);
#91216=ADVANCED_FACE('',(#11937),#3716,.F.);
#91217=ADVANCED_FACE('',(#11938),#3055,.F.);
#91218=ADVANCED_FACE('',(#11939),#3056,.F.);
#91219=ADVANCED_FACE('',(#11940),#3057,.F.);
#91220=ADVANCED_FACE('',(#11941),#3058,.F.);
#91221=ADVANCED_FACE('',(#11942),#3059,.F.);
#91222=ADVANCED_FACE('',(#11943),#3060,.F.);
#91223=ADVANCED_FACE('',(#11944),#3061,.F.);
#91224=ADVANCED_FACE('',(#11945),#3062,.F.);
#91225=ADVANCED_FACE('',(#11946),#3063,.F.);
#91226=ADVANCED_FACE('',(#11947),#86860,.T.);
#91227=ADVANCED_FACE('',(#11948),#3064,.F.);
#91228=ADVANCED_FACE('',(#11949),#3717,.T.);
#91229=ADVANCED_FACE('',(#11950),#3065,.F.);
#91230=ADVANCED_FACE('',(#11951),#86861,.T.);
#91231=ADVANCED_FACE('',(#11952),#86862,.T.);
#91232=ADVANCED_FACE('',(#11953),#3066,.F.);
#91233=ADVANCED_FACE('',(#11954),#3718,.T.);
#91234=ADVANCED_FACE('',(#11955),#3067,.F.);
#91235=ADVANCED_FACE('',(#11956),#86863,.T.);
#91236=ADVANCED_FACE('',(#11957),#86864,.T.);
#91237=ADVANCED_FACE('',(#11958),#3068,.F.);
#91238=ADVANCED_FACE('',(#11959),#3719,.T.);
#91239=ADVANCED_FACE('',(#11960),#3069,.F.);
#91240=ADVANCED_FACE('',(#11961),#86865,.T.);
#91241=ADVANCED_FACE('',(#11962),#86866,.T.);
#91242=ADVANCED_FACE('',(#11963),#3070,.F.);
#91243=ADVANCED_FACE('',(#11964),#3720,.T.);
#91244=ADVANCED_FACE('',(#11965),#3071,.F.);
#91245=ADVANCED_FACE('',(#11966),#86867,.T.);
#91246=ADVANCED_FACE('',(#11967),#86868,.T.);
#91247=ADVANCED_FACE('',(#11968),#86869,.T.);
#91248=ADVANCED_FACE('',(#11969),#86870,.T.);
#91249=ADVANCED_FACE('',(#11970),#86871,.T.);
#91250=ADVANCED_FACE('',(#11971),#86872,.T.);
#91251=ADVANCED_FACE('',(#11972),#86873,.T.);
#91252=ADVANCED_FACE('',(#11973),#86874,.T.);
#91253=ADVANCED_FACE('',(#11974),#86875,.T.);
#91254=ADVANCED_FACE('',(#11975),#3721,.T.);
#91255=ADVANCED_FACE('',(#11976),#86876,.T.);
#91256=ADVANCED_FACE('',(#11977),#3722,.T.);
#91257=ADVANCED_FACE('',(#11978),#3723,.T.);
#91258=ADVANCED_FACE('',(#11979),#3724,.T.);
#91259=ADVANCED_FACE('',(#11980),#86877,.T.);
#91260=ADVANCED_FACE('',(#11981),#3725,.T.);
#91261=ADVANCED_FACE('',(#11982),#3726,.T.);
#91262=ADVANCED_FACE('',(#11983),#3727,.T.);
#91263=ADVANCED_FACE('',(#11984),#86878,.T.);
#91264=ADVANCED_FACE('',(#11985),#3728,.T.);
#91265=ADVANCED_FACE('',(#11986),#86879,.T.);
#91266=ADVANCED_FACE('',(#11987),#3729,.T.);
#91267=ADVANCED_FACE('',(#11988),#3730,.T.);
#91268=ADVANCED_FACE('',(#11989),#3731,.T.);
#91269=ADVANCED_FACE('',(#11990),#86880,.T.);
#91270=ADVANCED_FACE('',(#11991),#86881,.T.);
#91271=ADVANCED_FACE('',(#11992),#3732,.T.);
#91272=ADVANCED_FACE('',(#11993),#3733,.T.);
#91273=ADVANCED_FACE('',(#11994),#86882,.T.);
#91274=ADVANCED_FACE('',(#11995),#3734,.T.);
#91275=ADVANCED_FACE('',(#11996),#3735,.T.);
#91276=ADVANCED_FACE('',(#11997),#3736,.T.);
#91277=ADVANCED_FACE('',(#11998),#86883,.T.);
#91278=ADVANCED_FACE('',(#11999),#86884,.T.);
#91279=ADVANCED_FACE('',(#12000),#3737,.T.);
#91280=ADVANCED_FACE('',(#12001),#3738,.T.);
#91281=ADVANCED_FACE('',(#12002),#86885,.T.);
#91282=ADVANCED_FACE('',(#12003),#86886,.T.);
#91283=ADVANCED_FACE('',(#12004),#3739,.T.);
#91284=ADVANCED_FACE('',(#12005),#3740,.T.);
#91285=ADVANCED_FACE('',(#12006),#86887,.T.);
#91286=ADVANCED_FACE('',(#12007),#86888,.T.);
#91287=ADVANCED_FACE('',(#12008),#3741,.T.);
#91288=ADVANCED_FACE('',(#12009),#3742,.T.);
#91289=ADVANCED_FACE('',(#12010),#86889,.T.);
#91290=ADVANCED_FACE('',(#12011),#86890,.T.);
#91291=ADVANCED_FACE('',(#12012),#3743,.T.);
#91292=ADVANCED_FACE('',(#12013),#3744,.T.);
#91293=ADVANCED_FACE('',(#12014),#3745,.T.);
#91294=ADVANCED_FACE('',(#12015),#86891,.T.);
#91295=ADVANCED_FACE('',(#12016),#3746,.T.);
#91296=ADVANCED_FACE('',(#12017),#3747,.T.);
#91297=ADVANCED_FACE('',(#12018),#3748,.T.);
#91298=ADVANCED_FACE('',(#12019),#86892,.T.);
#91299=ADVANCED_FACE('',(#12020),#86893,.T.);
#91300=ADVANCED_FACE('',(#12021),#3749,.T.);
#91301=ADVANCED_FACE('',(#12022),#3750,.T.);
#91302=ADVANCED_FACE('',(#12023),#86894,.T.);
#91303=ADVANCED_FACE('',(#12024),#86895,.T.);
#91304=ADVANCED_FACE('',(#12025),#3751,.T.);
#91305=ADVANCED_FACE('',(#12026),#3752,.T.);
#91306=ADVANCED_FACE('',(#12027),#86896,.T.);
#91307=ADVANCED_FACE('',(#12028),#86897,.T.);
#91308=ADVANCED_FACE('',(#12029),#3753,.T.);
#91309=ADVANCED_FACE('',(#12030),#3754,.T.);
#91310=ADVANCED_FACE('',(#12031),#86898,.T.);
#91311=ADVANCED_FACE('',(#12032),#86899,.T.);
#91312=ADVANCED_FACE('',(#12033),#3755,.T.);
#91313=ADVANCED_FACE('',(#12034),#3756,.T.);
#91314=ADVANCED_FACE('',(#12035),#86900,.T.);
#91315=ADVANCED_FACE('',(#12036),#86901,.T.);
#91316=ADVANCED_FACE('',(#12037),#3757,.T.);
#91317=ADVANCED_FACE('',(#12038),#3758,.T.);
#91318=ADVANCED_FACE('',(#12039),#86902,.T.);
#91319=ADVANCED_FACE('',(#12040),#86903,.T.);
#91320=ADVANCED_FACE('',(#12041),#3759,.T.);
#91321=ADVANCED_FACE('',(#12042),#3760,.T.);
#91322=ADVANCED_FACE('',(#12043),#86904,.T.);
#91323=ADVANCED_FACE('',(#12044),#86905,.T.);
#91324=ADVANCED_FACE('',(#12045),#3761,.T.);
#91325=ADVANCED_FACE('',(#12046),#3762,.T.);
#91326=ADVANCED_FACE('',(#12047),#86906,.T.);
#91327=ADVANCED_FACE('',(#12048),#86907,.T.);
#91328=ADVANCED_FACE('',(#12049),#3763,.T.);
#91329=ADVANCED_FACE('',(#12050),#3764,.T.);
#91330=ADVANCED_FACE('',(#12051),#86908,.T.);
#91331=ADVANCED_FACE('',(#12052),#86909,.T.);
#91332=ADVANCED_FACE('',(#12053),#3765,.T.);
#91333=ADVANCED_FACE('',(#12054),#3766,.T.);
#91334=ADVANCED_FACE('',(#12055),#86910,.T.);
#91335=ADVANCED_FACE('',(#12056),#3767,.T.);
#91336=ADVANCED_FACE('',(#12057),#3768,.T.);
#91337=ADVANCED_FACE('',(#12058),#3769,.T.);
#91338=ADVANCED_FACE('',(#12059),#86911,.T.);
#91339=ADVANCED_FACE('',(#12060),#86912,.T.);
#91340=ADVANCED_FACE('',(#12061),#3770,.T.);
#91341=ADVANCED_FACE('',(#12062),#3771,.T.);
#91342=ADVANCED_FACE('',(#12063),#86913,.T.);
#91343=ADVANCED_FACE('',(#12064),#3772,.T.);
#91344=ADVANCED_FACE('',(#12065),#3773,.T.);
#91345=ADVANCED_FACE('',(#12066),#3774,.T.);
#91346=ADVANCED_FACE('',(#12067),#3775,.T.);
#91347=ADVANCED_FACE('',(#12068),#3776,.T.);
#91348=ADVANCED_FACE('',(#12069),#86914,.T.);
#91349=ADVANCED_FACE('',(#12070),#86915,.T.);
#91350=ADVANCED_FACE('',(#12071),#3777,.T.);
#91351=ADVANCED_FACE('',(#12072),#3778,.T.);
#91352=ADVANCED_FACE('',(#12073),#86916,.T.);
#91353=ADVANCED_FACE('',(#12074),#3779,.T.);
#91354=ADVANCED_FACE('',(#12075),#3780,.T.);
#91355=ADVANCED_FACE('',(#12076),#3781,.T.);
#91356=ADVANCED_FACE('',(#12077),#86917,.T.);
#91357=ADVANCED_FACE('',(#12078),#86918,.T.);
#91358=ADVANCED_FACE('',(#12079),#3782,.T.);
#91359=ADVANCED_FACE('',(#12080),#3783,.T.);
#91360=ADVANCED_FACE('',(#12081),#86919,.T.);
#91361=ADVANCED_FACE('',(#12082),#86920,.T.);
#91362=ADVANCED_FACE('',(#12083),#3784,.T.);
#91363=ADVANCED_FACE('',(#12084),#3785,.T.);
#91364=ADVANCED_FACE('',(#12085),#86921,.T.);
#91365=ADVANCED_FACE('',(#12086),#3786,.T.);
#91366=ADVANCED_FACE('',(#12087),#3787,.T.);
#91367=ADVANCED_FACE('',(#12088),#3788,.T.);
#91368=ADVANCED_FACE('',(#12089),#86922,.T.);
#91369=ADVANCED_FACE('',(#12090),#86923,.T.);
#91370=ADVANCED_FACE('',(#12091),#3789,.T.);
#91371=ADVANCED_FACE('',(#12092),#3790,.T.);
#91372=ADVANCED_FACE('',(#12093),#86924,.T.);
#91373=ADVANCED_FACE('',(#12094),#3791,.T.);
#91374=ADVANCED_FACE('',(#12095),#86925,.T.);
#91375=ADVANCED_FACE('',(#12096),#86926,.T.);
#91376=ADVANCED_FACE('',(#12097),#3792,.T.);
#91377=ADVANCED_FACE('',(#12098),#3793,.T.);
#91378=ADVANCED_FACE('',(#12099),#86927,.T.);
#91379=ADVANCED_FACE('',(#12100),#3794,.T.);
#91380=ADVANCED_FACE('',(#12101),#3795,.T.);
#91381=ADVANCED_FACE('',(#12102),#3796,.T.);
#91382=ADVANCED_FACE('',(#12103),#86928,.T.);
#91383=ADVANCED_FACE('',(#12104),#3797,.T.);
#91384=ADVANCED_FACE('',(#12105),#86929,.T.);
#91385=ADVANCED_FACE('',(#12106),#86930,.T.);
#91386=ADVANCED_FACE('',(#12107),#3798,.T.);
#91387=ADVANCED_FACE('',(#12108),#3799,.T.);
#91388=ADVANCED_FACE('',(#12109),#86931,.T.);
#91389=ADVANCED_FACE('',(#12110),#86932,.T.);
#91390=ADVANCED_FACE('',(#12111),#3800,.T.);
#91391=ADVANCED_FACE('',(#12112),#3801,.T.);
#91392=ADVANCED_FACE('',(#12113),#86933,.T.);
#91393=ADVANCED_FACE('',(#12114),#86934,.T.);
#91394=ADVANCED_FACE('',(#12115),#3802,.T.);
#91395=ADVANCED_FACE('',(#12116),#3803,.T.);
#91396=ADVANCED_FACE('',(#12117),#3804,.T.);
#91397=ADVANCED_FACE('',(#12118),#86935,.T.);
#91398=ADVANCED_FACE('',(#12119),#3805,.T.);
#91399=ADVANCED_FACE('',(#12120),#3806,.T.);
#91400=ADVANCED_FACE('',(#12121),#86936,.T.);
#91401=ADVANCED_FACE('',(#12122),#86937,.T.);
#91402=ADVANCED_FACE('',(#12123),#3807,.T.);
#91403=ADVANCED_FACE('',(#12124),#3808,.T.);
#91404=ADVANCED_FACE('',(#12125),#86938,.T.);
#91405=ADVANCED_FACE('',(#12126),#86939,.T.);
#91406=ADVANCED_FACE('',(#12127),#3809,.T.);
#91407=ADVANCED_FACE('',(#12128),#3810,.T.);
#91408=ADVANCED_FACE('',(#12129),#86940,.T.);
#91409=ADVANCED_FACE('',(#12130),#86941,.T.);
#91410=ADVANCED_FACE('',(#12131),#3811,.T.);
#91411=ADVANCED_FACE('',(#12132),#3812,.T.);
#91412=ADVANCED_FACE('',(#12133),#86942,.T.);
#91413=ADVANCED_FACE('',(#12134),#86943,.T.);
#91414=ADVANCED_FACE('',(#12135),#3813,.T.);
#91415=ADVANCED_FACE('',(#12136),#3814,.T.);
#91416=ADVANCED_FACE('',(#12137),#86944,.T.);
#91417=ADVANCED_FACE('',(#12138),#86945,.T.);
#91418=ADVANCED_FACE('',(#12139),#3815,.T.);
#91419=ADVANCED_FACE('',(#12140),#3816,.T.);
#91420=ADVANCED_FACE('',(#12141),#86946,.T.);
#91421=ADVANCED_FACE('',(#12142),#3817,.T.);
#91422=ADVANCED_FACE('',(#12143),#3818,.T.);
#91423=ADVANCED_FACE('',(#12144),#3819,.T.);
#91424=ADVANCED_FACE('',(#12145),#3820,.T.);
#91425=ADVANCED_FACE('',(#12146),#86947,.T.);
#91426=ADVANCED_FACE('',(#12147),#86948,.T.);
#91427=ADVANCED_FACE('',(#12148),#3821,.T.);
#91428=ADVANCED_FACE('',(#12149),#3822,.T.);
#91429=ADVANCED_FACE('',(#12150),#3823,.T.);
#91430=ADVANCED_FACE('',(#12151),#86949,.T.);
#91431=ADVANCED_FACE('',(#12152),#3824,.T.);
#91432=ADVANCED_FACE('',(#12153),#3825,.T.);
#91433=ADVANCED_FACE('',(#12154),#86950,.T.);
#91434=ADVANCED_FACE('',(#12155),#86951,.T.);
#91435=ADVANCED_FACE('',(#12156),#3826,.T.);
#91436=ADVANCED_FACE('',(#12157),#3827,.T.);
#91437=ADVANCED_FACE('',(#12158),#3828,.T.);
#91438=ADVANCED_FACE('',(#12159),#86952,.T.);
#91439=ADVANCED_FACE('',(#12160),#3829,.T.);
#91440=ADVANCED_FACE('',(#12161),#3830,.T.);
#91441=ADVANCED_FACE('',(#12162),#3831,.T.);
#91442=ADVANCED_FACE('',(#12163),#3832,.T.);
#91443=ADVANCED_FACE('',(#12164),#86953,.T.);
#91444=ADVANCED_FACE('',(#12165),#86954,.T.);
#91445=ADVANCED_FACE('',(#12166),#3833,.T.);
#91446=ADVANCED_FACE('',(#12167),#3834,.T.);
#91447=ADVANCED_FACE('',(#12168),#86955,.T.);
#91448=ADVANCED_FACE('',(#12169),#86956,.T.);
#91449=ADVANCED_FACE('',(#12170),#3835,.T.);
#91450=ADVANCED_FACE('',(#12171),#3836,.T.);
#91451=ADVANCED_FACE('',(#12172),#86957,.T.);
#91452=ADVANCED_FACE('',(#12173),#86958,.T.);
#91453=ADVANCED_FACE('',(#12174),#3837,.T.);
#91454=ADVANCED_FACE('',(#12175),#3838,.T.);
#91455=ADVANCED_FACE('',(#12176),#86959,.T.);
#91456=ADVANCED_FACE('',(#12177),#3839,.T.);
#91457=ADVANCED_FACE('',(#12178),#3840,.T.);
#91458=ADVANCED_FACE('',(#12179),#3841,.T.);
#91459=ADVANCED_FACE('',(#12180),#3842,.T.);
#91460=ADVANCED_FACE('',(#12181),#3843,.T.);
#91461=ADVANCED_FACE('',(#12182),#86960,.T.);
#91462=ADVANCED_FACE('',(#12183),#86961,.T.);
#91463=ADVANCED_FACE('',(#12184),#3844,.T.);
#91464=ADVANCED_FACE('',(#12185),#3845,.T.);
#91465=ADVANCED_FACE('',(#12186),#86962,.T.);
#91466=ADVANCED_FACE('',(#12187),#3846,.T.);
#91467=ADVANCED_FACE('',(#12188),#3847,.T.);
#91468=ADVANCED_FACE('',(#12189),#3848,.T.);
#91469=ADVANCED_FACE('',(#12190),#86963,.T.);
#91470=ADVANCED_FACE('',(#12191),#86964,.T.);
#91471=ADVANCED_FACE('',(#12192),#3849,.T.);
#91472=ADVANCED_FACE('',(#12193),#3850,.T.);
#91473=ADVANCED_FACE('',(#12194),#86965,.T.);
#91474=ADVANCED_FACE('',(#12195),#86966,.T.);
#91475=ADVANCED_FACE('',(#12196),#3851,.T.);
#91476=ADVANCED_FACE('',(#12197),#3852,.T.);
#91477=ADVANCED_FACE('',(#12198),#86967,.T.);
#91478=ADVANCED_FACE('',(#12199),#86968,.T.);
#91479=ADVANCED_FACE('',(#12200),#3853,.T.);
#91480=ADVANCED_FACE('',(#12201),#3854,.T.);
#91481=ADVANCED_FACE('',(#12202),#86969,.T.);
#91482=ADVANCED_FACE('',(#12203),#3855,.T.);
#91483=ADVANCED_FACE('',(#12204),#3856,.T.);
#91484=ADVANCED_FACE('',(#12205),#3857,.T.);
#91485=ADVANCED_FACE('',(#12206),#86970,.T.);
#91486=ADVANCED_FACE('',(#12207),#86971,.T.);
#91487=ADVANCED_FACE('',(#12208),#3858,.T.);
#91488=ADVANCED_FACE('',(#12209),#3859,.T.);
#91489=ADVANCED_FACE('',(#12210),#86972,.T.);
#91490=ADVANCED_FACE('',(#12211),#86973,.T.);
#91491=ADVANCED_FACE('',(#12212),#3860,.T.);
#91492=ADVANCED_FACE('',(#12213),#3861,.T.);
#91493=ADVANCED_FACE('',(#12214),#86974,.T.);
#91494=ADVANCED_FACE('',(#12215),#3862,.T.);
#91495=ADVANCED_FACE('',(#12216),#3863,.T.);
#91496=ADVANCED_FACE('',(#12217),#3864,.T.);
#91497=ADVANCED_FACE('',(#12218),#86975,.T.);
#91498=ADVANCED_FACE('',(#12219),#3865,.T.);
#91499=ADVANCED_FACE('',(#12220),#86976,.T.);
#91500=ADVANCED_FACE('',(#12221),#3866,.T.);
#91501=ADVANCED_FACE('',(#12222),#3867,.T.);
#91502=ADVANCED_FACE('',(#12223),#3868,.T.);
#91503=ADVANCED_FACE('',(#12224),#86977,.T.);
#91504=ADVANCED_FACE('',(#12225),#3869,.T.);
#91505=ADVANCED_FACE('',(#12226),#3870,.T.);
#91506=ADVANCED_FACE('',(#12227),#3871,.T.);
#91507=ADVANCED_FACE('',(#12228),#3872,.T.);
#91508=ADVANCED_FACE('',(#12229),#3873,.T.);
#91509=ADVANCED_FACE('',(#12230),#3874,.T.);
#91510=ADVANCED_FACE('',(#12231),#3875,.T.);
#91511=ADVANCED_FACE('',(#12232),#3876,.T.);
#91512=ADVANCED_FACE('',(#12233),#3877,.T.);
#91513=ADVANCED_FACE('',(#12234),#3878,.T.);
#91514=ADVANCED_FACE('',(#12235),#3879,.T.);
#91515=ADVANCED_FACE('',(#12236),#3880,.T.);
#91516=ADVANCED_FACE('',(#12237),#3881,.T.);
#91517=ADVANCED_FACE('',(#12238),#3882,.T.);
#91518=ADVANCED_FACE('',(#12239),#3883,.T.);
#91519=ADVANCED_FACE('',(#12240),#3884,.T.);
#91520=ADVANCED_FACE('',(#12241),#3885,.T.);
#91521=ADVANCED_FACE('',(#12242),#3886,.T.);
#91522=ADVANCED_FACE('',(#12243),#3887,.T.);
#91523=ADVANCED_FACE('',(#12244),#3888,.T.);
#91524=ADVANCED_FACE('',(#12245),#3889,.T.);
#91525=ADVANCED_FACE('',(#12246),#86978,.T.);
#91526=ADVANCED_FACE('',(#12247),#3890,.T.);
#91527=ADVANCED_FACE('',(#12248),#3891,.T.);
#91528=ADVANCED_FACE('',(#12249),#3892,.T.);
#91529=ADVANCED_FACE('',(#12250),#86979,.T.);
#91530=ADVANCED_FACE('',(#12251),#3893,.T.);
#91531=ADVANCED_FACE('',(#12252),#3894,.T.);
#91532=ADVANCED_FACE('',(#12253),#86980,.T.);
#91533=ADVANCED_FACE('',(#12254),#3895,.T.);
#91534=ADVANCED_FACE('',(#12255),#3896,.T.);
#91535=ADVANCED_FACE('',(#12256),#3897,.T.);
#91536=ADVANCED_FACE('',(#12257),#86981,.T.);
#91537=ADVANCED_FACE('',(#12258),#3898,.T.);
#91538=ADVANCED_FACE('',(#12259),#3899,.T.);
#91539=ADVANCED_FACE('',(#12260),#86982,.T.);
#91540=ADVANCED_FACE('',(#12261),#3900,.T.);
#91541=ADVANCED_FACE('',(#12262),#3901,.T.);
#91542=ADVANCED_FACE('',(#12263),#3902,.T.);
#91543=ADVANCED_FACE('',(#12264),#86983,.T.);
#91544=ADVANCED_FACE('',(#12265),#3903,.T.);
#91545=ADVANCED_FACE('',(#12266),#3904,.T.);
#91546=ADVANCED_FACE('',(#12267),#86984,.T.);
#91547=ADVANCED_FACE('',(#12268),#3905,.T.);
#91548=ADVANCED_FACE('',(#12269),#3906,.T.);
#91549=ADVANCED_FACE('',(#12270),#3907,.T.);
#91550=ADVANCED_FACE('',(#12271),#86985,.T.);
#91551=ADVANCED_FACE('',(#12272),#3908,.T.);
#91552=ADVANCED_FACE('',(#12273),#3909,.T.);
#91553=ADVANCED_FACE('',(#12274),#3910,.T.);
#91554=ADVANCED_FACE('',(#12275),#3911,.T.);
#91555=ADVANCED_FACE('',(#12276),#3912,.T.);
#91556=ADVANCED_FACE('',(#12277),#3913,.T.);
#91557=ADVANCED_FACE('',(#12278),#3914,.T.);
#91558=ADVANCED_FACE('',(#12279),#3915,.T.);
#91559=ADVANCED_FACE('',(#12280),#3916,.T.);
#91560=ADVANCED_FACE('',(#12281),#3917,.T.);
#91561=ADVANCED_FACE('',(#12282),#3072,.T.);
#91562=ADVANCED_FACE('',(#12283),#3073,.T.);
#91563=ADVANCED_FACE('',(#12284),#3074,.T.);
#91564=ADVANCED_FACE('',(#12285),#3075,.T.);
#91565=ADVANCED_FACE('',(#12286),#3076,.T.);
#91566=ADVANCED_FACE('',(#12287),#3077,.T.);
#91567=ADVANCED_FACE('',(#12288),#3078,.T.);
#91568=ADVANCED_FACE('',(#12289),#3079,.T.);
#91569=ADVANCED_FACE('',(#12290),#3080,.T.);
#91570=ADVANCED_FACE('',(#12291),#3081,.T.);
#91571=ADVANCED_FACE('',(#12292),#3082,.T.);
#91572=ADVANCED_FACE('',(#12293),#3083,.T.);
#91573=ADVANCED_FACE('',(#12294),#3084,.T.);
#91574=ADVANCED_FACE('',(#12295),#3085,.T.);
#91575=ADVANCED_FACE('',(#12296),#3086,.T.);
#91576=ADVANCED_FACE('',(#12297),#3087,.T.);
#91577=ADVANCED_FACE('',(#12298),#3088,.T.);
#91578=ADVANCED_FACE('',(#12299),#3089,.T.);
#91579=ADVANCED_FACE('',(#12300),#3090,.T.);
#91580=ADVANCED_FACE('',(#12301),#3091,.T.);
#91581=ADVANCED_FACE('',(#12302),#3092,.T.);
#91582=ADVANCED_FACE('',(#12303),#3093,.T.);
#91583=ADVANCED_FACE('',(#12304),#3094,.T.);
#91584=ADVANCED_FACE('',(#12305),#3095,.T.);
#91585=ADVANCED_FACE('',(#12306),#3096,.T.);
#91586=ADVANCED_FACE('',(#12307),#3097,.T.);
#91587=ADVANCED_FACE('',(#12308),#3098,.T.);
#91588=ADVANCED_FACE('',(#12309),#3099,.T.);
#91589=ADVANCED_FACE('',(#12310),#3100,.T.);
#91590=ADVANCED_FACE('',(#12311),#3101,.T.);
#91591=ADVANCED_FACE('',(#12312),#3102,.T.);
#91592=ADVANCED_FACE('',(#12313),#3103,.T.);
#91593=ADVANCED_FACE('',(#12314),#3104,.T.);
#91594=ADVANCED_FACE('',(#12315),#3105,.T.);
#91595=ADVANCED_FACE('',(#12316),#3106,.T.);
#91596=ADVANCED_FACE('',(#12317),#3107,.T.);
#91597=ADVANCED_FACE('',(#12318),#3108,.T.);
#91598=ADVANCED_FACE('',(#12319),#3109,.T.);
#91599=ADVANCED_FACE('',(#12320),#3110,.T.);
#91600=ADVANCED_FACE('',(#12321),#3111,.T.);
#91601=ADVANCED_FACE('',(#12322),#3918,.T.);
#91602=ADVANCED_FACE('',(#12323),#3112,.T.);
#91603=ADVANCED_FACE('',(#12324),#3113,.T.);
#91604=ADVANCED_FACE('',(#12325),#3114,.T.);
#91605=ADVANCED_FACE('',(#12326),#3115,.T.);
#91606=ADVANCED_FACE('',(#12327),#3116,.T.);
#91607=ADVANCED_FACE('',(#12328),#3117,.T.);
#91608=ADVANCED_FACE('',(#12329),#3118,.T.);
#91609=ADVANCED_FACE('',(#12330),#3119,.T.);
#91610=ADVANCED_FACE('',(#12331),#3120,.T.);
#91611=ADVANCED_FACE('',(#12332),#3121,.T.);
#91612=ADVANCED_FACE('',(#12333),#3122,.T.);
#91613=ADVANCED_FACE('',(#12334),#3123,.T.);
#91614=ADVANCED_FACE('',(#12335),#86986,.F.);
#91615=ADVANCED_FACE('',(#12336),#86987,.F.);
#91616=ADVANCED_FACE('',(#12337),#86988,.F.);
#91617=ADVANCED_FACE('',(#12338),#86989,.F.);
#91618=ADVANCED_FACE('',(#12339),#86990,.F.);
#91619=ADVANCED_FACE('',(#12340),#86991,.F.);
#91620=ADVANCED_FACE('',(#12341),#86992,.F.);
#91621=ADVANCED_FACE('',(#12342),#86993,.F.);
#91622=ADVANCED_FACE('',(#12343),#86994,.F.);
#91623=ADVANCED_FACE('',(#12344),#86995,.F.);
#91624=ADVANCED_FACE('',(#12345),#86996,.F.);
#91625=ADVANCED_FACE('',(#12346),#86997,.F.);
#91626=ADVANCED_FACE('',(#12347),#86998,.F.);
#91627=ADVANCED_FACE('',(#12348),#86999,.F.);
#91628=ADVANCED_FACE('',(#12349),#87000,.F.);
#91629=ADVANCED_FACE('',(#12350),#87001,.F.);
#91630=ADVANCED_FACE('',(#12351),#87002,.F.);
#91631=ADVANCED_FACE('',(#12352),#87003,.F.);
#91632=ADVANCED_FACE('',(#12353),#87004,.F.);
#91633=ADVANCED_FACE('',(#12354),#87005,.F.);
#91634=ADVANCED_FACE('',(#12355),#87006,.F.);
#91635=ADVANCED_FACE('',(#12356),#87007,.F.);
#91636=ADVANCED_FACE('',(#12357),#87008,.F.);
#91637=ADVANCED_FACE('',(#12358),#87009,.F.);
#91638=ADVANCED_FACE('',(#12359),#87010,.F.);
#91639=ADVANCED_FACE('',(#12360),#87011,.F.);
#91640=ADVANCED_FACE('',(#12361),#87012,.F.);
#91641=ADVANCED_FACE('',(#12362),#87013,.F.);
#91642=ADVANCED_FACE('',(#12363),#87014,.F.);
#91643=ADVANCED_FACE('',(#12364),#87015,.F.);
#91644=ADVANCED_FACE('',(#12365),#87016,.F.);
#91645=ADVANCED_FACE('',(#12366),#87017,.F.);
#91646=ADVANCED_FACE('',(#12367),#87018,.F.);
#91647=ADVANCED_FACE('',(#12368),#87019,.F.);
#91648=ADVANCED_FACE('',(#12369),#87020,.F.);
#91649=ADVANCED_FACE('',(#12370),#87021,.F.);
#91650=ADVANCED_FACE('',(#12371),#87022,.F.);
#91651=ADVANCED_FACE('',(#12372),#87023,.F.);
#91652=ADVANCED_FACE('',(#12373),#87024,.F.);
#91653=ADVANCED_FACE('',(#12374),#87025,.F.);
#91654=ADVANCED_FACE('',(#12375),#87026,.F.);
#91655=ADVANCED_FACE('',(#12376),#87027,.F.);
#91656=ADVANCED_FACE('',(#12377),#87028,.F.);
#91657=ADVANCED_FACE('',(#12378),#87029,.F.);
#91658=ADVANCED_FACE('',(#12379),#87030,.F.);
#91659=ADVANCED_FACE('',(#12380),#87031,.F.);
#91660=ADVANCED_FACE('',(#12381),#87032,.F.);
#91661=ADVANCED_FACE('',(#12382),#87033,.F.);
#91662=ADVANCED_FACE('',(#12383),#87034,.F.);
#91663=ADVANCED_FACE('',(#12384),#87035,.F.);
#91664=ADVANCED_FACE('',(#12385),#87036,.F.);
#91665=ADVANCED_FACE('',(#12386),#87037,.F.);
#91666=ADVANCED_FACE('',(#12387),#87038,.F.);
#91667=ADVANCED_FACE('',(#12388),#87039,.F.);
#91668=ADVANCED_FACE('',(#12389),#87040,.F.);
#91669=ADVANCED_FACE('',(#12390),#87041,.F.);
#91670=ADVANCED_FACE('',(#12391),#87042,.F.);
#91671=ADVANCED_FACE('',(#12392),#87043,.F.);
#91672=ADVANCED_FACE('',(#12393),#87044,.F.);
#91673=ADVANCED_FACE('',(#12394),#87045,.F.);
#91674=ADVANCED_FACE('',(#12395),#87046,.F.);
#91675=ADVANCED_FACE('',(#12396),#87047,.F.);
#91676=ADVANCED_FACE('',(#12397),#87048,.F.);
#91677=ADVANCED_FACE('',(#12398),#87049,.F.);
#91678=ADVANCED_FACE('',(#12399),#87050,.F.);
#91679=ADVANCED_FACE('',(#12400),#87051,.F.);
#91680=ADVANCED_FACE('',(#12401),#87052,.F.);
#91681=ADVANCED_FACE('',(#12402),#87053,.F.);
#91682=ADVANCED_FACE('',(#12403),#87054,.F.);
#91683=ADVANCED_FACE('',(#12404),#87055,.F.);
#91684=ADVANCED_FACE('',(#12405),#87056,.F.);
#91685=ADVANCED_FACE('',(#12406),#87057,.F.);
#91686=ADVANCED_FACE('',(#12407),#87058,.F.);
#91687=ADVANCED_FACE('',(#12408),#87059,.F.);
#91688=ADVANCED_FACE('',(#12409),#87060,.F.);
#91689=ADVANCED_FACE('',(#12410),#87061,.F.);
#91690=ADVANCED_FACE('',(#12411),#87062,.F.);
#91691=ADVANCED_FACE('',(#12412),#87063,.F.);
#91692=ADVANCED_FACE('',(#12413),#87064,.F.);
#91693=ADVANCED_FACE('',(#12414),#87065,.F.);
#91694=ADVANCED_FACE('',(#12415),#87066,.F.);
#91695=ADVANCED_FACE('',(#12416),#87067,.F.);
#91696=ADVANCED_FACE('',(#12417),#87068,.F.);
#91697=ADVANCED_FACE('',(#12418),#87069,.F.);
#91698=ADVANCED_FACE('',(#12419),#87070,.F.);
#91699=ADVANCED_FACE('',(#12420),#87071,.F.);
#91700=ADVANCED_FACE('',(#12421),#87072,.F.);
#91701=ADVANCED_FACE('',(#12422),#87073,.F.);
#91702=ADVANCED_FACE('',(#12423),#87074,.F.);
#91703=ADVANCED_FACE('',(#12424),#87075,.F.);
#91704=ADVANCED_FACE('',(#12425),#87076,.F.);
#91705=ADVANCED_FACE('',(#12426),#87077,.F.);
#91706=ADVANCED_FACE('',(#12427),#87078,.F.);
#91707=ADVANCED_FACE('',(#12428),#87079,.F.);
#91708=ADVANCED_FACE('',(#12429),#87080,.F.);
#91709=ADVANCED_FACE('',(#12430),#87081,.F.);
#91710=ADVANCED_FACE('',(#12431),#87082,.F.);
#91711=ADVANCED_FACE('',(#12432),#87083,.F.);
#91712=ADVANCED_FACE('',(#12433),#87084,.F.);
#91713=ADVANCED_FACE('',(#12434),#87085,.F.);
#91714=ADVANCED_FACE('',(#12435),#87086,.F.);
#91715=ADVANCED_FACE('',(#12436),#87087,.F.);
#91716=ADVANCED_FACE('',(#12437),#87088,.F.);
#91717=ADVANCED_FACE('',(#12438),#87089,.F.);
#91718=ADVANCED_FACE('',(#12439),#87090,.F.);
#91719=ADVANCED_FACE('',(#12440),#87091,.F.);
#91720=ADVANCED_FACE('',(#12441),#87092,.F.);
#91721=ADVANCED_FACE('',(#12442),#87093,.F.);
#91722=ADVANCED_FACE('',(#12443),#87094,.F.);
#91723=ADVANCED_FACE('',(#12444),#87095,.F.);
#91724=ADVANCED_FACE('',(#12445),#87096,.F.);
#91725=ADVANCED_FACE('',(#12446),#87097,.F.);
#91726=ADVANCED_FACE('',(#12447),#87098,.F.);
#91727=ADVANCED_FACE('',(#12448),#87099,.F.);
#91728=ADVANCED_FACE('',(#12449),#87100,.F.);
#91729=ADVANCED_FACE('',(#12450),#87101,.F.);
#91730=ADVANCED_FACE('',(#12451),#87102,.F.);
#91731=ADVANCED_FACE('',(#12452),#87103,.F.);
#91732=ADVANCED_FACE('',(#12453),#87104,.F.);
#91733=ADVANCED_FACE('',(#12454),#87105,.F.);
#91734=ADVANCED_FACE('',(#12455),#87106,.F.);
#91735=ADVANCED_FACE('',(#12456),#87107,.F.);
#91736=ADVANCED_FACE('',(#12457),#87108,.F.);
#91737=ADVANCED_FACE('',(#12458),#87109,.F.);
#91738=ADVANCED_FACE('',(#12459),#87110,.F.);
#91739=ADVANCED_FACE('',(#12460),#87111,.F.);
#91740=ADVANCED_FACE('',(#12461),#87112,.F.);
#91741=ADVANCED_FACE('',(#12462),#87113,.F.);
#91742=ADVANCED_FACE('',(#12463),#87114,.F.);
#91743=ADVANCED_FACE('',(#12464),#87115,.F.);
#91744=ADVANCED_FACE('',(#12465),#87116,.F.);
#91745=ADVANCED_FACE('',(#12466),#87117,.F.);
#91746=ADVANCED_FACE('',(#12467),#87118,.F.);
#91747=ADVANCED_FACE('',(#12468),#87119,.F.);
#91748=ADVANCED_FACE('',(#12469),#87120,.F.);
#91749=ADVANCED_FACE('',(#12470),#87121,.F.);
#91750=ADVANCED_FACE('',(#12471),#87122,.F.);
#91751=ADVANCED_FACE('',(#12472),#87123,.F.);
#91752=ADVANCED_FACE('',(#12473),#8180,.T.);
#91753=ADVANCED_FACE('',(#12474),#87124,.F.);
#91754=ADVANCED_FACE('',(#12475,#7456),#8181,.T.);
#91755=ADVANCED_FACE('',(#12476),#87125,.T.);
#91756=ADVANCED_FACE('',(#12477),#87126,.T.);
#91757=ADVANCED_FACE('',(#12478),#87127,.T.);
#91758=ADVANCED_FACE('',(#12479),#87128,.F.);
#91759=ADVANCED_FACE('',(#12480),#8182,.F.);
#91760=ADVANCED_FACE('',(#12481),#8183,.F.);
#91761=ADVANCED_FACE('',(#12482),#87129,.F.);
#91762=ADVANCED_FACE('',(#12483),#87130,.T.);
#91763=ADVANCED_FACE('',(#12484),#87131,.F.);
#91764=ADVANCED_FACE('',(#12485),#8184,.T.);
#91765=ADVANCED_FACE('',(#12486),#8185,.T.);
#91766=ADVANCED_FACE('',(#12487),#87132,.F.);
#91767=ADVANCED_FACE('',(#12488),#87133,.T.);
#91768=ADVANCED_FACE('',(#12489),#8186,.F.);
#91769=ADVANCED_FACE('',(#12490),#8187,.F.);
#91770=ADVANCED_FACE('',(#12491),#8188,.F.);
#91771=ADVANCED_FACE('',(#12492),#8189,.F.);
#91772=ADVANCED_FACE('',(#12493),#8190,.F.);
#91773=ADVANCED_FACE('',(#12494),#8191,.F.);
#91774=ADVANCED_FACE('',(#12495),#8192,.F.);
#91775=ADVANCED_FACE('',(#12496),#8193,.F.);
#91776=ADVANCED_FACE('',(#12497),#8194,.F.);
#91777=ADVANCED_FACE('',(#12498),#8195,.F.);
#91778=ADVANCED_FACE('',(#12499),#8196,.F.);
#91779=ADVANCED_FACE('',(#12500),#8197,.F.);
#91780=ADVANCED_FACE('',(#12501),#8198,.F.);
#91781=ADVANCED_FACE('',(#12502),#8199,.F.);
#91782=ADVANCED_FACE('',(#12503),#8200,.F.);
#91783=ADVANCED_FACE('',(#12504),#8201,.F.);
#91784=ADVANCED_FACE('',(#12505),#8202,.F.);
#91785=ADVANCED_FACE('',(#12506),#8203,.F.);
#91786=ADVANCED_FACE('',(#12507),#8204,.F.);
#91787=ADVANCED_FACE('',(#12508),#8205,.F.);
#91788=ADVANCED_FACE('',(#12509),#8206,.F.);
#91789=ADVANCED_FACE('',(#12510),#8207,.F.);
#91790=ADVANCED_FACE('',(#12511),#8208,.F.);
#91791=ADVANCED_FACE('',(#12512),#8209,.F.);
#91792=ADVANCED_FACE('',(#12513),#8210,.F.);
#91793=ADVANCED_FACE('',(#12514),#8211,.F.);
#91794=ADVANCED_FACE('',(#12515),#8212,.F.);
#91795=ADVANCED_FACE('',(#12516),#8213,.F.);
#91796=ADVANCED_FACE('',(#12517),#8214,.F.);
#91797=ADVANCED_FACE('',(#12518),#8215,.F.);
#91798=ADVANCED_FACE('',(#12519),#8216,.F.);
#91799=ADVANCED_FACE('',(#12520),#8217,.F.);
#91800=ADVANCED_FACE('',(#12521),#8218,.F.);
#91801=ADVANCED_FACE('',(#12522),#8219,.F.);
#91802=ADVANCED_FACE('',(#12523),#8220,.F.);
#91803=ADVANCED_FACE('',(#12524),#8221,.F.);
#91804=ADVANCED_FACE('',(#12525),#8222,.F.);
#91805=ADVANCED_FACE('',(#12526),#8223,.F.);
#91806=ADVANCED_FACE('',(#12527),#8224,.F.);
#91807=ADVANCED_FACE('',(#12528),#8225,.F.);
#91808=ADVANCED_FACE('',(#12529),#8226,.F.);
#91809=ADVANCED_FACE('',(#12530),#8227,.F.);
#91810=ADVANCED_FACE('',(#12531),#8228,.F.);
#91811=ADVANCED_FACE('',(#12532),#8229,.F.);
#91812=ADVANCED_FACE('',(#12533),#8230,.F.);
#91813=ADVANCED_FACE('',(#12534),#8231,.F.);
#91814=ADVANCED_FACE('',(#12535),#8232,.F.);
#91815=ADVANCED_FACE('',(#12536),#8233,.F.);
#91816=ADVANCED_FACE('',(#12537),#8234,.F.);
#91817=ADVANCED_FACE('',(#12538),#8235,.F.);
#91818=ADVANCED_FACE('',(#12539),#8236,.F.);
#91819=ADVANCED_FACE('',(#12540),#8237,.F.);
#91820=ADVANCED_FACE('',(#12541),#8238,.F.);
#91821=ADVANCED_FACE('',(#12542),#8239,.F.);
#91822=ADVANCED_FACE('',(#12543),#8240,.F.);
#91823=ADVANCED_FACE('',(#12544),#8241,.F.);
#91824=ADVANCED_FACE('',(#12545),#8242,.F.);
#91825=ADVANCED_FACE('',(#12546,#7457,#7458,#7459,#7460,#7461,#7462,#7463,
#7464,#7465,#7466,#7467,#7468,#7469,#7470,#7471,#7472,#7473,#7474,#7475,
#7476,#7477,#7478,#7479,#7480,#7481,#7482,#7483,#7484,#7485,#7486,#7487,
#7488,#7489,#7490,#7491,#7492,#7493,#7494,#7495,#7496,#7497,#7498,#7499,
#7500,#7501,#7502,#7503,#7504,#7505,#7506,#7507,#7508,#7509,#7510,#7511,
#7512,#7513,#7514,#7515,#7516,#7517,#7518,#7519,#7520,#7521,#7522,#7523,
#7524),#8243,.F.);
#91826=ADVANCED_FACE('',(#12547),#87134,.T.);
#91827=ADVANCED_FACE('',(#12548),#87135,.T.);
#91828=ADVANCED_FACE('',(#12549),#87136,.T.);
#91829=ADVANCED_FACE('',(#12550),#87137,.T.);
#91830=ADVANCED_FACE('',(#12551),#87138,.T.);
#91831=ADVANCED_FACE('',(#12552),#87139,.T.);
#91832=ADVANCED_FACE('',(#12553),#87140,.T.);
#91833=ADVANCED_FACE('',(#12554),#87141,.T.);
#91834=ADVANCED_FACE('',(#12555),#8244,.T.);
#91835=ADVANCED_FACE('',(#12556),#8245,.T.);
#91836=ADVANCED_FACE('',(#12557),#8246,.F.);
#91837=ADVANCED_FACE('',(#12558),#8247,.T.);
#91838=ADVANCED_FACE('',(#12559),#8248,.F.);
#91839=ADVANCED_FACE('',(#12560),#8249,.F.);
#91840=ADVANCED_FACE('',(#12561),#87142,.F.);
#91841=ADVANCED_FACE('',(#12562),#8250,.F.);
#91842=ADVANCED_FACE('',(#12563),#8251,.F.);
#91843=ADVANCED_FACE('',(#12564),#87143,.F.);
#91844=ADVANCED_FACE('',(#12565),#927,.T.);
#91845=ADVANCED_FACE('',(#12566),#928,.F.);
#91846=ADVANCED_FACE('',(#12567),#87144,.T.);
#91847=ADVANCED_FACE('',(#12568),#87145,.T.);
#91848=ADVANCED_FACE('',(#12569),#87146,.T.);
#91849=ADVANCED_FACE('',(#12570),#87147,.T.);
#91850=ADVANCED_FACE('',(#12571),#87148,.T.);
#91851=ADVANCED_FACE('',(#12572),#87149,.T.);
#91852=ADVANCED_FACE('',(#12573),#87150,.T.);
#91853=ADVANCED_FACE('',(#12574),#87151,.T.);
#91854=ADVANCED_FACE('',(#12575),#87152,.T.);
#91855=ADVANCED_FACE('',(#12576),#929,.F.);
#91856=ADVANCED_FACE('',(#12577),#930,.F.);
#91857=ADVANCED_FACE('',(#12578),#931,.F.);
#91858=ADVANCED_FACE('',(#12579),#932,.F.);
#91859=ADVANCED_FACE('',(#12580),#7040,.F.);
#91860=ADVANCED_FACE('',(#12581),#7041,.F.);
#91861=ADVANCED_FACE('',(#12582),#7042,.F.);
#91862=ADVANCED_FACE('',(#12583),#7043,.F.);
#91863=ADVANCED_FACE('',(#12584),#7044,.F.);
#91864=ADVANCED_FACE('',(#12585),#7045,.F.);
#91865=ADVANCED_FACE('',(#12586),#7046,.F.);
#91866=ADVANCED_FACE('',(#12587,#7525),#8252,.T.);
#91867=ADVANCED_FACE('',(#12588),#7047,.F.);
#91868=ADVANCED_FACE('',(#12589),#7048,.F.);
#91869=ADVANCED_FACE('',(#12590),#7049,.F.);
#91870=ADVANCED_FACE('',(#12591),#7050,.F.);
#91871=ADVANCED_FACE('',(#12592),#7051,.F.);
#91872=ADVANCED_FACE('',(#12593),#7052,.F.);
#91873=ADVANCED_FACE('',(#12594),#7053,.F.);
#91874=ADVANCED_FACE('',(#12595),#7054,.F.);
#91875=ADVANCED_FACE('',(#12596),#7055,.F.);
#91876=ADVANCED_FACE('',(#12597),#933,.F.);
#91877=ADVANCED_FACE('',(#12598),#934,.F.);
#91878=ADVANCED_FACE('',(#12599),#7056,.F.);
#91879=ADVANCED_FACE('',(#12600),#935,.F.);
#91880=ADVANCED_FACE('',(#12601),#7057,.F.);
#91881=ADVANCED_FACE('',(#12602),#8253,.F.);
#91882=ADVANCED_FACE('',(#12603),#936,.F.);
#91883=ADVANCED_FACE('',(#12604),#8254,.F.);
#91884=ADVANCED_FACE('',(#12605),#937,.F.);
#91885=ADVANCED_FACE('',(#12606),#8255,.T.);
#91886=ADVANCED_FACE('',(#12607),#938,.F.);
#91887=ADVANCED_FACE('',(#12608),#8256,.F.);
#91888=ADVANCED_FACE('',(#12609),#8257,.F.);
#91889=ADVANCED_FACE('',(#12610),#8258,.F.);
#91890=ADVANCED_FACE('',(#12611),#8259,.F.);
#91891=ADVANCED_FACE('',(#12612),#8260,.F.);
#91892=ADVANCED_FACE('',(#12613),#8261,.F.);
#91893=ADVANCED_FACE('',(#12614),#8262,.F.);
#91894=ADVANCED_FACE('',(#12615),#8263,.F.);
#91895=ADVANCED_FACE('',(#12616),#8264,.F.);
#91896=ADVANCED_FACE('',(#12617),#87153,.T.);
#91897=ADVANCED_FACE('',(#12618),#87154,.T.);
#91898=ADVANCED_FACE('',(#12619),#87155,.T.);
#91899=ADVANCED_FACE('',(#12620),#87156,.T.);
#91900=ADVANCED_FACE('',(#12621),#87157,.T.);
#91901=ADVANCED_FACE('',(#12622),#8265,.T.);
#91902=ADVANCED_FACE('',(#12623),#7058,.T.);
#91903=ADVANCED_FACE('',(#12624),#8266,.T.);
#91904=ADVANCED_FACE('',(#12625),#939,.F.);
#91905=ADVANCED_FACE('',(#12626),#7059,.T.);
#91906=ADVANCED_FACE('',(#12627),#87158,.F.);
#91907=ADVANCED_FACE('',(#12628),#87159,.F.);
#91908=ADVANCED_FACE('',(#12629),#87160,.F.);
#91909=ADVANCED_FACE('',(#12630),#87161,.F.);
#91910=ADVANCED_FACE('',(#12631),#87162,.F.);
#91911=ADVANCED_FACE('',(#12632),#87163,.F.);
#91912=ADVANCED_FACE('',(#12633),#87164,.F.);
#91913=ADVANCED_FACE('',(#12634),#8267,.T.);
#91914=ADVANCED_FACE('',(#12635),#7060,.F.);
#91915=ADVANCED_FACE('',(#12636),#8268,.T.);
#91916=ADVANCED_FACE('',(#12637),#7061,.F.);
#91917=ADVANCED_FACE('',(#12638,#7526),#8269,.F.);
#91918=ADVANCED_FACE('',(#12639),#8270,.F.);
#91919=ADVANCED_FACE('',(#12640),#8271,.F.);
#91920=ADVANCED_FACE('',(#12641),#87165,.T.);
#91921=ADVANCED_FACE('',(#12642),#8272,.T.);
#91922=ADVANCED_FACE('',(#12643),#8273,.F.);
#91923=ADVANCED_FACE('',(#12644),#8274,.F.);
#91924=ADVANCED_FACE('',(#12645),#87166,.T.);
#91925=ADVANCED_FACE('',(#12646),#8275,.T.);
#91926=ADVANCED_FACE('',(#12647),#8276,.T.);
#91927=ADVANCED_FACE('',(#12648),#87167,.T.);
#91928=ADVANCED_FACE('',(#12649),#8277,.T.);
#91929=ADVANCED_FACE('',(#12650),#8278,.T.);
#91930=ADVANCED_FACE('',(#12651),#87168,.T.);
#91931=ADVANCED_FACE('',(#12652),#940,.F.);
#91932=ADVANCED_FACE('',(#12653),#941,.T.);
#91933=ADVANCED_FACE('',(#12654),#942,.T.);
#91934=ADVANCED_FACE('',(#12655,#7527,#7528,#7529,#7530,#7531,#7532,#7533,
#7534,#7535,#7536,#7537,#7538,#7539,#7540,#7541,#7542,#7543,#7544,#7545,
#7546,#7547,#7548,#7549,#7550,#7551,#7552,#7553,#7554,#7555,#7556,#7557,
#7558,#7559,#7560,#7561,#7562,#7563,#7564,#7565,#7566,#7567,#7568,#7569,
#7570,#7571,#7572,#7573,#7574,#7575,#7576,#7577,#7578,#7579,#7580,#7581,
#7582,#7583,#7584,#7585,#7586,#7587),#8279,.T.);
#91935=ADVANCED_FACE('',(#12656),#87169,.T.);
#91936=ADVANCED_FACE('',(#12657),#87170,.T.);
#91937=ADVANCED_FACE('',(#12658),#87171,.T.);
#91938=ADVANCED_FACE('',(#12659),#87172,.T.);
#91939=ADVANCED_FACE('',(#12660),#87173,.T.);
#91940=ADVANCED_FACE('',(#12661),#87174,.T.);
#91941=ADVANCED_FACE('',(#12662),#87175,.T.);
#91942=ADVANCED_FACE('',(#12663),#87176,.T.);
#91943=ADVANCED_FACE('',(#12664),#87177,.T.);
#91944=ADVANCED_FACE('',(#12665,#7588),#8280,.T.);
#91945=ADVANCED_FACE('',(#12666),#87178,.F.);
#91946=ADVANCED_FACE('',(#12667),#87179,.F.);
#91947=ADVANCED_FACE('',(#12668),#87180,.F.);
#91948=ADVANCED_FACE('',(#12669),#87181,.F.);
#91949=ADVANCED_FACE('',(#12670),#87182,.F.);
#91950=ADVANCED_FACE('',(#12671),#87183,.F.);
#91951=ADVANCED_FACE('',(#12672),#87184,.F.);
#91952=ADVANCED_FACE('',(#12673),#87185,.F.);
#91953=ADVANCED_FACE('',(#12674),#87186,.F.);
#91954=ADVANCED_FACE('',(#12675),#943,.T.);
#91955=ADVANCED_FACE('',(#12676),#944,.T.);
#91956=ADVANCED_FACE('',(#12677),#945,.T.);
#91957=ADVANCED_FACE('',(#12678),#946,.T.);
#91958=ADVANCED_FACE('',(#12679),#7062,.T.);
#91959=ADVANCED_FACE('',(#12680),#7063,.T.);
#91960=ADVANCED_FACE('',(#12681),#7064,.T.);
#91961=ADVANCED_FACE('',(#12682),#7065,.T.);
#91962=ADVANCED_FACE('',(#12683),#7066,.T.);
#91963=ADVANCED_FACE('',(#12684),#7067,.T.);
#91964=ADVANCED_FACE('',(#12685),#7068,.T.);
#91965=ADVANCED_FACE('',(#12686,#7589),#8281,.T.);
#91966=ADVANCED_FACE('',(#12687,#7590),#8282,.F.);
#91967=ADVANCED_FACE('',(#12688),#7069,.T.);
#91968=ADVANCED_FACE('',(#12689),#7070,.T.);
#91969=ADVANCED_FACE('',(#12690),#7071,.T.);
#91970=ADVANCED_FACE('',(#12691),#7072,.T.);
#91971=ADVANCED_FACE('',(#12692),#7073,.T.);
#91972=ADVANCED_FACE('',(#12693),#7074,.T.);
#91973=ADVANCED_FACE('',(#12694),#7075,.T.);
#91974=ADVANCED_FACE('',(#12695),#7076,.T.);
#91975=ADVANCED_FACE('',(#12696),#7077,.T.);
#91976=ADVANCED_FACE('',(#12697),#947,.T.);
#91977=ADVANCED_FACE('',(#12698),#948,.T.);
#91978=ADVANCED_FACE('',(#12699),#7078,.T.);
#91979=ADVANCED_FACE('',(#12700),#949,.T.);
#91980=ADVANCED_FACE('',(#12701),#7079,.T.);
#91981=ADVANCED_FACE('',(#12702,#7591),#8283,.T.);
#91982=ADVANCED_FACE('',(#12703),#950,.T.);
#91983=ADVANCED_FACE('',(#12704),#8284,.T.);
#91984=ADVANCED_FACE('',(#12705),#951,.T.);
#91985=ADVANCED_FACE('',(#12706),#8285,.F.);
#91986=ADVANCED_FACE('',(#12707),#952,.T.);
#91987=ADVANCED_FACE('',(#12708),#87187,.F.);
#91988=ADVANCED_FACE('',(#12709),#87188,.F.);
#91989=ADVANCED_FACE('',(#12710),#87189,.F.);
#91990=ADVANCED_FACE('',(#12711),#87190,.F.);
#91991=ADVANCED_FACE('',(#12712),#87191,.F.);
#91992=ADVANCED_FACE('',(#12713),#8286,.T.);
#91993=ADVANCED_FACE('',(#12714),#8287,.T.);
#91994=ADVANCED_FACE('',(#12715),#8288,.T.);
#91995=ADVANCED_FACE('',(#12716),#8289,.T.);
#91996=ADVANCED_FACE('',(#12717),#8290,.T.);
#91997=ADVANCED_FACE('',(#12718),#8291,.T.);
#91998=ADVANCED_FACE('',(#12719),#8292,.T.);
#91999=ADVANCED_FACE('',(#12720),#8293,.T.);
#92000=ADVANCED_FACE('',(#12721),#8294,.T.);
#92001=ADVANCED_FACE('',(#12722),#8295,.T.);
#92002=ADVANCED_FACE('',(#12723),#87192,.F.);
#92003=ADVANCED_FACE('',(#12724),#87193,.F.);
#92004=ADVANCED_FACE('',(#12725),#87194,.T.);
#92005=ADVANCED_FACE('',(#12726),#87195,.T.);
#92006=ADVANCED_FACE('',(#12727,#7592),#8296,.F.);
#92007=ADVANCED_FACE('',(#12728),#8297,.T.);
#92008=ADVANCED_FACE('',(#12729),#8298,.T.);
#92009=ADVANCED_FACE('',(#12730),#8299,.T.);
#92010=ADVANCED_FACE('',(#12731),#8300,.T.);
#92011=ADVANCED_FACE('',(#12732),#8301,.T.);
#92012=ADVANCED_FACE('',(#12733),#8302,.T.);
#92013=ADVANCED_FACE('',(#12734),#8303,.T.);
#92014=ADVANCED_FACE('',(#12735),#8304,.T.);
#92015=ADVANCED_FACE('',(#12736),#8305,.T.);
#92016=ADVANCED_FACE('',(#12737),#8306,.T.);
#92017=ADVANCED_FACE('',(#12738),#8307,.T.);
#92018=ADVANCED_FACE('',(#12739),#8308,.T.);
#92019=ADVANCED_FACE('',(#12740),#8309,.T.);
#92020=ADVANCED_FACE('',(#12741),#8310,.T.);
#92021=ADVANCED_FACE('',(#12742),#87196,.F.);
#92022=ADVANCED_FACE('',(#12743),#87197,.F.);
#92023=ADVANCED_FACE('',(#12744),#87198,.F.);
#92024=ADVANCED_FACE('',(#12745),#87199,.F.);
#92025=ADVANCED_FACE('',(#12746),#87200,.F.);
#92026=ADVANCED_FACE('',(#12747),#87201,.F.);
#92027=ADVANCED_FACE('',(#12748),#87202,.F.);
#92028=ADVANCED_FACE('',(#12749),#87203,.F.);
#92029=ADVANCED_FACE('',(#12750),#8311,.T.);
#92030=ADVANCED_FACE('',(#12751),#8312,.T.);
#92031=ADVANCED_FACE('',(#12752),#8313,.T.);
#92032=ADVANCED_FACE('',(#12753),#8314,.T.);
#92033=ADVANCED_FACE('',(#12754),#8315,.T.);
#92034=ADVANCED_FACE('',(#12755),#8316,.T.);
#92035=ADVANCED_FACE('',(#12756),#8317,.T.);
#92036=ADVANCED_FACE('',(#12757),#8318,.T.);
#92037=ADVANCED_FACE('',(#12758),#8319,.T.);
#92038=ADVANCED_FACE('',(#12759),#8320,.T.);
#92039=ADVANCED_FACE('',(#12760),#8321,.T.);
#92040=ADVANCED_FACE('',(#12761),#8322,.T.);
#92041=ADVANCED_FACE('',(#12762),#8323,.T.);
#92042=ADVANCED_FACE('',(#12763),#8324,.T.);
#92043=ADVANCED_FACE('',(#12764),#8325,.T.);
#92044=ADVANCED_FACE('',(#12765),#8326,.T.);
#92045=ADVANCED_FACE('',(#12766),#8327,.T.);
#92046=ADVANCED_FACE('',(#12767),#8328,.T.);
#92047=ADVANCED_FACE('',(#12768),#8329,.T.);
#92048=ADVANCED_FACE('',(#12769),#8330,.T.);
#92049=ADVANCED_FACE('',(#12770),#8331,.T.);
#92050=ADVANCED_FACE('',(#12771),#8332,.T.);
#92051=ADVANCED_FACE('',(#12772),#8333,.T.);
#92052=ADVANCED_FACE('',(#12773),#8334,.T.);
#92053=ADVANCED_FACE('',(#12774),#8335,.T.);
#92054=ADVANCED_FACE('',(#12775),#8336,.T.);
#92055=ADVANCED_FACE('',(#12776),#8337,.T.);
#92056=ADVANCED_FACE('',(#12777),#8338,.T.);
#92057=ADVANCED_FACE('',(#12778),#3919,.T.);
#92058=ADVANCED_FACE('',(#12779),#8339,.F.);
#92059=ADVANCED_FACE('',(#12780),#8340,.F.);
#92060=ADVANCED_FACE('',(#12781),#8341,.F.);
#92061=ADVANCED_FACE('',(#12782),#8342,.F.);
#92062=ADVANCED_FACE('',(#12783),#8343,.F.);
#92063=ADVANCED_FACE('',(#12784),#8344,.F.);
#92064=ADVANCED_FACE('',(#12785),#7080,.F.);
#92065=ADVANCED_FACE('',(#12786),#7081,.F.);
#92066=ADVANCED_FACE('',(#12787),#7082,.F.);
#92067=ADVANCED_FACE('',(#12788),#7083,.F.);
#92068=ADVANCED_FACE('',(#12789),#7084,.F.);
#92069=ADVANCED_FACE('',(#12790),#7085,.F.);
#92070=ADVANCED_FACE('',(#12791),#7086,.F.);
#92071=ADVANCED_FACE('',(#12792),#3920,.T.);
#92072=ADVANCED_FACE('',(#12793),#8345,.F.);
#92073=ADVANCED_FACE('',(#12794,#7593),#8346,.T.);
#92074=ADVANCED_FACE('',(#12795),#87204,.T.);
#92075=ADVANCED_FACE('',(#12796),#8347,.T.);
#92076=ADVANCED_FACE('',(#12797),#7087,.T.);
#92077=ADVANCED_FACE('',(#12798),#7088,.T.);
#92078=ADVANCED_FACE('',(#12799),#7089,.T.);
#92079=ADVANCED_FACE('',(#12800),#7090,.T.);
#92080=ADVANCED_FACE('',(#12801),#7091,.T.);
#92081=ADVANCED_FACE('',(#12802),#7092,.T.);
#92082=ADVANCED_FACE('',(#12803),#8348,.F.);
#92083=ADVANCED_FACE('',(#12804),#7093,.T.);
#92084=ADVANCED_FACE('',(#12805),#7094,.T.);
#92085=ADVANCED_FACE('',(#12806),#7095,.T.);
#92086=ADVANCED_FACE('',(#12807),#7096,.T.);
#92087=ADVANCED_FACE('',(#12808),#7097,.T.);
#92088=ADVANCED_FACE('',(#12809),#7098,.T.);
#92089=ADVANCED_FACE('',(#12810),#8349,.F.);
#92090=ADVANCED_FACE('',(#12811),#8350,.F.);
#92091=ADVANCED_FACE('',(#12812),#8351,.F.);
#92092=ADVANCED_FACE('',(#12813),#8352,.F.);
#92093=ADVANCED_FACE('',(#12814),#8353,.F.);
#92094=ADVANCED_FACE('',(#12815),#8354,.F.);
#92095=ADVANCED_FACE('',(#12816),#8355,.T.);
#92096=ADVANCED_FACE('',(#12817),#7099,.T.);
#92097=ADVANCED_FACE('',(#12818),#7100,.T.);
#92098=ADVANCED_FACE('',(#12819),#7101,.T.);
#92099=ADVANCED_FACE('',(#12820),#7102,.T.);
#92100=ADVANCED_FACE('',(#12821),#7103,.T.);
#92101=ADVANCED_FACE('',(#12822),#7104,.T.);
#92102=ADVANCED_FACE('',(#12823),#8356,.F.);
#92103=ADVANCED_FACE('',(#12824),#7105,.T.);
#92104=ADVANCED_FACE('',(#12825),#7106,.T.);
#92105=ADVANCED_FACE('',(#12826),#7107,.T.);
#92106=ADVANCED_FACE('',(#12827),#7108,.T.);
#92107=ADVANCED_FACE('',(#12828),#7109,.T.);
#92108=ADVANCED_FACE('',(#12829),#7110,.T.);
#92109=ADVANCED_FACE('',(#12830),#8357,.F.);
#92110=ADVANCED_FACE('',(#12831),#8358,.F.);
#92111=ADVANCED_FACE('',(#12832),#8359,.F.);
#92112=ADVANCED_FACE('',(#12833),#8360,.F.);
#92113=ADVANCED_FACE('',(#12834),#8361,.F.);
#92114=ADVANCED_FACE('',(#12835),#8362,.F.);
#92115=ADVANCED_FACE('',(#12836),#8363,.F.);
#92116=ADVANCED_FACE('',(#12837),#8364,.F.);
#92117=ADVANCED_FACE('',(#12838),#8365,.F.);
#92118=ADVANCED_FACE('',(#12839),#8366,.F.);
#92119=ADVANCED_FACE('',(#12840),#8367,.F.);
#92120=ADVANCED_FACE('',(#12841),#8368,.F.);
#92121=ADVANCED_FACE('',(#12842),#7111,.F.);
#92122=ADVANCED_FACE('',(#12843),#7112,.F.);
#92123=ADVANCED_FACE('',(#12844),#7113,.F.);
#92124=ADVANCED_FACE('',(#12845),#7114,.F.);
#92125=ADVANCED_FACE('',(#12846),#7115,.F.);
#92126=ADVANCED_FACE('',(#12847),#7116,.F.);
#92127=ADVANCED_FACE('',(#12848),#7117,.F.);
#92128=ADVANCED_FACE('',(#12849),#3921,.T.);
#92129=ADVANCED_FACE('',(#12850),#8369,.F.);
#92130=ADVANCED_FACE('',(#12851,#7594),#8370,.T.);
#92131=ADVANCED_FACE('',(#12852),#87205,.T.);
#92132=ADVANCED_FACE('',(#12853,#7595),#1026,.T.);
#92133=ADVANCED_FACE('',(#12854),#3922,.T.);
#92134=ADVANCED_FACE('',(#12855),#3923,.T.);
#92135=ADVANCED_FACE('',(#12856),#8371,.F.);
#92136=ADVANCED_FACE('',(#12857),#8372,.F.);
#92137=ADVANCED_FACE('',(#12858),#7118,.F.);
#92138=ADVANCED_FACE('',(#12859),#8373,.F.);
#92139=ADVANCED_FACE('',(#12860),#7119,.F.);
#92140=ADVANCED_FACE('',(#12861),#8374,.T.);
#92141=ADVANCED_FACE('',(#12862),#87206,.T.);
#92142=ADVANCED_FACE('',(#12863),#87207,.T.);
#92143=ADVANCED_FACE('',(#12864,#7596),#8375,.T.);
#92144=ADVANCED_FACE('',(#12865),#7120,.T.);
#92145=ADVANCED_FACE('',(#12866),#8376,.T.);
#92146=ADVANCED_FACE('',(#12867),#87208,.T.);
#92147=ADVANCED_FACE('',(#12868,#7597),#8377,.F.);
#92148=ADVANCED_FACE('',(#12869),#87209,.T.);
#92149=ADVANCED_FACE('',(#12870),#8378,.F.);
#92150=ADVANCED_FACE('',(#12871),#3924,.T.);
#92151=ADVANCED_FACE('',(#12872),#87210,.T.);
#92152=ADVANCED_FACE('',(#12873),#87211,.T.);
#92153=ADVANCED_FACE('',(#12874),#3925,.T.);
#92154=ADVANCED_FACE('',(#12875),#3926,.T.);
#92155=ADVANCED_FACE('',(#12876),#87212,.T.);
#92156=ADVANCED_FACE('',(#12877),#87213,.T.);
#92157=ADVANCED_FACE('',(#12878),#3927,.T.);
#92158=ADVANCED_FACE('',(#12879),#8379,.F.);
#92159=ADVANCED_FACE('',(#12880),#87214,.T.);
#92160=ADVANCED_FACE('',(#12881),#87215,.T.);
#92161=ADVANCED_FACE('',(#12882,#7598,#7599),#8380,.F.);
#92162=ADVANCED_FACE('',(#12883),#3928,.F.);
#92163=ADVANCED_FACE('',(#12884),#87216,.F.);
#92164=ADVANCED_FACE('',(#12885),#3929,.F.);
#92165=ADVANCED_FACE('',(#12886),#87217,.T.);
#92166=ADVANCED_FACE('',(#12887),#3930,.T.);
#92167=ADVANCED_FACE('',(#12888),#3931,.T.);
#92168=ADVANCED_FACE('',(#12889),#87218,.T.);
#92169=ADVANCED_FACE('',(#12890),#87219,.T.);
#92170=ADVANCED_FACE('',(#12891),#87220,.T.);
#92171=ADVANCED_FACE('',(#12892),#87221,.T.);
#92172=ADVANCED_FACE('',(#12893),#3932,.T.);
#92173=ADVANCED_FACE('',(#12894),#3933,.T.);
#92174=ADVANCED_FACE('',(#12895),#87222,.T.);
#92175=ADVANCED_FACE('',(#12896),#3934,.F.);
#92176=ADVANCED_FACE('',(#12897),#87223,.F.);
#92177=ADVANCED_FACE('',(#12898),#3935,.F.);
#92178=ADVANCED_FACE('',(#12899,#7600,#7601),#8381,.F.);
#92179=ADVANCED_FACE('',(#12900),#87224,.T.);
#92180=ADVANCED_FACE('',(#12901),#87225,.T.);
#92181=ADVANCED_FACE('',(#12902),#87226,.F.);
#92182=ADVANCED_FACE('',(#12903),#8382,.F.);
#92183=ADVANCED_FACE('',(#12904),#87227,.T.);
#92184=ADVANCED_FACE('',(#12905),#8383,.T.);
#92185=ADVANCED_FACE('',(#12906),#87228,.T.);
#92186=ADVANCED_FACE('',(#12907),#8384,.F.);
#92187=ADVANCED_FACE('',(#12908),#87229,.F.);
#92188=ADVANCED_FACE('',(#12909,#7602),#8385,.F.);
#92189=ADVANCED_FACE('',(#12910),#8386,.F.);
#92190=ADVANCED_FACE('',(#12911),#8387,.F.);
#92191=ADVANCED_FACE('',(#12912),#87230,.F.);
#92192=ADVANCED_FACE('',(#12913),#87231,.F.);
#92193=ADVANCED_FACE('',(#12914),#8388,.F.);
#92194=ADVANCED_FACE('',(#12915),#8389,.F.);
#92195=ADVANCED_FACE('',(#12916,#7603),#1027,.T.);
#92196=ADVANCED_FACE('',(#12917),#3936,.T.);
#92197=ADVANCED_FACE('',(#12918),#3937,.T.);
#92198=ADVANCED_FACE('',(#12919),#8390,.F.);
#92199=ADVANCED_FACE('',(#12920),#8391,.F.);
#92200=ADVANCED_FACE('',(#12921),#7121,.F.);
#92201=ADVANCED_FACE('',(#12922),#8392,.F.);
#92202=ADVANCED_FACE('',(#12923),#7122,.F.);
#92203=ADVANCED_FACE('',(#12924),#8393,.T.);
#92204=ADVANCED_FACE('',(#12925),#87232,.T.);
#92205=ADVANCED_FACE('',(#12926),#87233,.T.);
#92206=ADVANCED_FACE('',(#12927,#7604),#8394,.T.);
#92207=ADVANCED_FACE('',(#12928),#87234,.T.);
#92208=ADVANCED_FACE('',(#12929),#3938,.T.);
#92209=ADVANCED_FACE('',(#12930),#87235,.T.);
#92210=ADVANCED_FACE('',(#12931),#3939,.T.);
#92211=ADVANCED_FACE('',(#12932),#87236,.T.);
#92212=ADVANCED_FACE('',(#12933),#87237,.T.);
#92213=ADVANCED_FACE('',(#12934),#3940,.T.);
#92214=ADVANCED_FACE('',(#12935),#87238,.T.);
#92215=ADVANCED_FACE('',(#12936),#3941,.T.);
#92216=ADVANCED_FACE('',(#12937),#87239,.T.);
#92217=ADVANCED_FACE('',(#12938),#87240,.T.);
#92218=ADVANCED_FACE('',(#12939),#3942,.T.);
#92219=ADVANCED_FACE('',(#12940),#87241,.T.);
#92220=ADVANCED_FACE('',(#12941),#3943,.T.);
#92221=ADVANCED_FACE('',(#12942),#87242,.T.);
#92222=ADVANCED_FACE('',(#12943),#3944,.T.);
#92223=ADVANCED_FACE('',(#12944),#87243,.T.);
#92224=ADVANCED_FACE('',(#12945),#3945,.T.);
#92225=ADVANCED_FACE('',(#12946),#87244,.T.);
#92226=ADVANCED_FACE('',(#12947),#87245,.T.);
#92227=ADVANCED_FACE('',(#12948),#3946,.T.);
#92228=ADVANCED_FACE('',(#12949),#87246,.T.);
#92229=ADVANCED_FACE('',(#12950),#3947,.T.);
#92230=ADVANCED_FACE('',(#12951),#87247,.T.);
#92231=ADVANCED_FACE('',(#12952),#87248,.T.);
#92232=ADVANCED_FACE('',(#12953),#3948,.T.);
#92233=ADVANCED_FACE('',(#12954),#87249,.T.);
#92234=ADVANCED_FACE('',(#12955),#3949,.T.);
#92235=ADVANCED_FACE('',(#12956),#3950,.T.);
#92236=ADVANCED_FACE('',(#12957),#87250,.T.);
#92237=ADVANCED_FACE('',(#12958),#3951,.T.);
#92238=ADVANCED_FACE('',(#12959),#87251,.T.);
#92239=ADVANCED_FACE('',(#12960),#3952,.T.);
#92240=ADVANCED_FACE('',(#12961),#87252,.T.);
#92241=ADVANCED_FACE('',(#12962),#87253,.T.);
#92242=ADVANCED_FACE('',(#12963),#3953,.T.);
#92243=ADVANCED_FACE('',(#12964),#87254,.T.);
#92244=ADVANCED_FACE('',(#12965),#3954,.T.);
#92245=ADVANCED_FACE('',(#12966),#3955,.T.);
#92246=ADVANCED_FACE('',(#12967),#3956,.T.);
#92247=ADVANCED_FACE('',(#12968),#87255,.T.);
#92248=ADVANCED_FACE('',(#12969),#3957,.T.);
#92249=ADVANCED_FACE('',(#12970),#87256,.T.);
#92250=ADVANCED_FACE('',(#12971),#87257,.T.);
#92251=ADVANCED_FACE('',(#12972),#3958,.T.);
#92252=ADVANCED_FACE('',(#12973),#87258,.T.);
#92253=ADVANCED_FACE('',(#12974),#3959,.T.);
#92254=ADVANCED_FACE('',(#12975),#3960,.T.);
#92255=ADVANCED_FACE('',(#12976),#3961,.T.);
#92256=ADVANCED_FACE('',(#12977),#87259,.T.);
#92257=ADVANCED_FACE('',(#12978),#3962,.T.);
#92258=ADVANCED_FACE('',(#12979),#87260,.T.);
#92259=ADVANCED_FACE('',(#12980),#87261,.T.);
#92260=ADVANCED_FACE('',(#12981),#3963,.T.);
#92261=ADVANCED_FACE('',(#12982),#87262,.T.);
#92262=ADVANCED_FACE('',(#12983),#3964,.T.);
#92263=ADVANCED_FACE('',(#12984),#3965,.T.);
#92264=ADVANCED_FACE('',(#12985),#3966,.T.);
#92265=ADVANCED_FACE('',(#12986),#87263,.T.);
#92266=ADVANCED_FACE('',(#12987),#3967,.T.);
#92267=ADVANCED_FACE('',(#12988),#87264,.T.);
#92268=ADVANCED_FACE('',(#12989),#87265,.T.);
#92269=ADVANCED_FACE('',(#12990),#3968,.T.);
#92270=ADVANCED_FACE('',(#12991),#87266,.T.);
#92271=ADVANCED_FACE('',(#12992),#3969,.T.);
#92272=ADVANCED_FACE('',(#12993),#3970,.T.);
#92273=ADVANCED_FACE('',(#12994),#3971,.T.);
#92274=ADVANCED_FACE('',(#12995),#87267,.T.);
#92275=ADVANCED_FACE('',(#12996),#3972,.T.);
#92276=ADVANCED_FACE('',(#12997),#87268,.T.);
#92277=ADVANCED_FACE('',(#12998),#87269,.T.);
#92278=ADVANCED_FACE('',(#12999),#3973,.T.);
#92279=ADVANCED_FACE('',(#13000),#87270,.T.);
#92280=ADVANCED_FACE('',(#13001),#3974,.T.);
#92281=ADVANCED_FACE('',(#13002),#3975,.T.);
#92282=ADVANCED_FACE('',(#13003),#3976,.T.);
#92283=ADVANCED_FACE('',(#13004),#87271,.T.);
#92284=ADVANCED_FACE('',(#13005),#3977,.T.);
#92285=ADVANCED_FACE('',(#13006),#87272,.T.);
#92286=ADVANCED_FACE('',(#13007),#87273,.T.);
#92287=ADVANCED_FACE('',(#13008),#3978,.T.);
#92288=ADVANCED_FACE('',(#13009),#87274,.T.);
#92289=ADVANCED_FACE('',(#13010),#3979,.T.);
#92290=ADVANCED_FACE('',(#13011),#3980,.T.);
#92291=ADVANCED_FACE('',(#13012),#3981,.T.);
#92292=ADVANCED_FACE('',(#13013),#87275,.T.);
#92293=ADVANCED_FACE('',(#13014),#3982,.T.);
#92294=ADVANCED_FACE('',(#13015),#87276,.T.);
#92295=ADVANCED_FACE('',(#13016),#87277,.T.);
#92296=ADVANCED_FACE('',(#13017),#3983,.T.);
#92297=ADVANCED_FACE('',(#13018),#87278,.T.);
#92298=ADVANCED_FACE('',(#13019),#3984,.T.);
#92299=ADVANCED_FACE('',(#13020),#87279,.T.);
#92300=ADVANCED_FACE('',(#13021),#3985,.T.);
#92301=ADVANCED_FACE('',(#13022),#3986,.T.);
#92302=ADVANCED_FACE('',(#13023),#87280,.T.);
#92303=ADVANCED_FACE('',(#13024),#3987,.T.);
#92304=ADVANCED_FACE('',(#13025),#87281,.T.);
#92305=ADVANCED_FACE('',(#13026),#87282,.T.);
#92306=ADVANCED_FACE('',(#13027),#3988,.T.);
#92307=ADVANCED_FACE('',(#13028),#87283,.T.);
#92308=ADVANCED_FACE('',(#13029),#3989,.T.);
#92309=ADVANCED_FACE('',(#13030),#87284,.T.);
#92310=ADVANCED_FACE('',(#13031),#3990,.T.);
#92311=ADVANCED_FACE('',(#13032),#87285,.T.);
#92312=ADVANCED_FACE('',(#13033),#3991,.T.);
#92313=ADVANCED_FACE('',(#13034),#87286,.T.);
#92314=ADVANCED_FACE('',(#13035),#87287,.T.);
#92315=ADVANCED_FACE('',(#13036),#3992,.T.);
#92316=ADVANCED_FACE('',(#13037),#87288,.T.);
#92317=ADVANCED_FACE('',(#13038),#3993,.T.);
#92318=ADVANCED_FACE('',(#13039),#87289,.T.);
#92319=ADVANCED_FACE('',(#13040),#87290,.F.);
#92320=ADVANCED_FACE('',(#13041),#87291,.F.);
#92321=ADVANCED_FACE('',(#13042),#87292,.F.);
#92322=ADVANCED_FACE('',(#13043),#87293,.F.);
#92323=ADVANCED_FACE('',(#13044),#87294,.F.);
#92324=ADVANCED_FACE('',(#13045),#87295,.F.);
#92325=ADVANCED_FACE('',(#13046),#87296,.F.);
#92326=ADVANCED_FACE('',(#13047),#87297,.F.);
#92327=ADVANCED_FACE('',(#13048),#87298,.F.);
#92328=ADVANCED_FACE('',(#13049),#87299,.F.);
#92329=ADVANCED_FACE('',(#13050),#87300,.F.);
#92330=ADVANCED_FACE('',(#13051),#87301,.F.);
#92331=ADVANCED_FACE('',(#13052),#87302,.F.);
#92332=ADVANCED_FACE('',(#13053),#87303,.F.);
#92333=ADVANCED_FACE('',(#13054),#87304,.F.);
#92334=ADVANCED_FACE('',(#13055),#87305,.F.);
#92335=ADVANCED_FACE('',(#13056),#87306,.F.);
#92336=ADVANCED_FACE('',(#13057),#87307,.F.);
#92337=ADVANCED_FACE('',(#13058),#87308,.F.);
#92338=ADVANCED_FACE('',(#13059),#87309,.F.);
#92339=ADVANCED_FACE('',(#13060),#87310,.F.);
#92340=ADVANCED_FACE('',(#13061),#87311,.F.);
#92341=ADVANCED_FACE('',(#13062),#87312,.F.);
#92342=ADVANCED_FACE('',(#13063),#87313,.F.);
#92343=ADVANCED_FACE('',(#13064),#87314,.F.);
#92344=ADVANCED_FACE('',(#13065),#87315,.F.);
#92345=ADVANCED_FACE('',(#13066),#8395,.T.);
#92346=ADVANCED_FACE('',(#13067),#8396,.F.);
#92347=ADVANCED_FACE('',(#13068),#87316,.T.);
#92348=ADVANCED_FACE('',(#13069),#8397,.F.);
#92349=ADVANCED_FACE('',(#13070),#8398,.F.);
#92350=ADVANCED_FACE('',(#13071),#8399,.F.);
#92351=ADVANCED_FACE('',(#13072),#8400,.F.);
#92352=ADVANCED_FACE('',(#13073),#8401,.F.);
#92353=ADVANCED_FACE('',(#13074),#8402,.F.);
#92354=ADVANCED_FACE('',(#13075),#8403,.F.);
#92355=ADVANCED_FACE('',(#13076),#8404,.F.);
#92356=ADVANCED_FACE('',(#13077),#8405,.F.);
#92357=ADVANCED_FACE('',(#13078),#8406,.F.);
#92358=ADVANCED_FACE('',(#13079),#8407,.F.);
#92359=ADVANCED_FACE('',(#13080),#8408,.F.);
#92360=ADVANCED_FACE('',(#13081),#8409,.F.);
#92361=ADVANCED_FACE('',(#13082),#8410,.F.);
#92362=ADVANCED_FACE('',(#13083),#87317,.T.);
#92363=ADVANCED_FACE('',(#13084),#87318,.T.);
#92364=ADVANCED_FACE('',(#13085),#8411,.F.);
#92365=ADVANCED_FACE('',(#13086),#8412,.F.);
#92366=ADVANCED_FACE('',(#13087),#8413,.F.);
#92367=ADVANCED_FACE('',(#13088),#87319,.T.);
#92368=ADVANCED_FACE('',(#13089),#87320,.T.);
#92369=ADVANCED_FACE('',(#13090),#8414,.F.);
#92370=ADVANCED_FACE('',(#13091),#8415,.F.);
#92371=ADVANCED_FACE('',(#13092),#8416,.F.);
#92372=ADVANCED_FACE('',(#13093),#87321,.T.);
#92373=ADVANCED_FACE('',(#13094),#87322,.T.);
#92374=ADVANCED_FACE('',(#13095),#8417,.F.);
#92375=ADVANCED_FACE('',(#13096),#8418,.F.);
#92376=ADVANCED_FACE('',(#13097),#8419,.F.);
#92377=ADVANCED_FACE('',(#13098),#87323,.T.);
#92378=ADVANCED_FACE('',(#13099),#87324,.T.);
#92379=ADVANCED_FACE('',(#13100),#8420,.F.);
#92380=ADVANCED_FACE('',(#13101),#8421,.F.);
#92381=ADVANCED_FACE('',(#13102),#8422,.F.);
#92382=ADVANCED_FACE('',(#13103),#87325,.T.);
#92383=ADVANCED_FACE('',(#13104),#8423,.T.);
#92384=ADVANCED_FACE('',(#13105),#87326,.F.);
#92385=ADVANCED_FACE('',(#13106),#8424,.T.);
#92386=ADVANCED_FACE('',(#13107),#87327,.F.);
#92387=ADVANCED_FACE('',(#13108),#8425,.F.);
#92388=ADVANCED_FACE('',(#13109),#8426,.F.);
#92389=ADVANCED_FACE('',(#13110),#8427,.T.);
#92390=ADVANCED_FACE('',(#13111),#8428,.F.);
#92391=ADVANCED_FACE('',(#13112),#87328,.T.);
#92392=ADVANCED_FACE('',(#13113),#8429,.F.);
#92393=ADVANCED_FACE('',(#13114),#87329,.T.);
#92394=ADVANCED_FACE('',(#13115),#8430,.F.);
#92395=ADVANCED_FACE('',(#13116),#87330,.T.);
#92396=ADVANCED_FACE('',(#13117),#8431,.F.);
#92397=ADVANCED_FACE('',(#13118),#87331,.T.);
#92398=ADVANCED_FACE('',(#13119),#8432,.F.);
#92399=ADVANCED_FACE('',(#13120),#87332,.T.);
#92400=ADVANCED_FACE('',(#13121),#87333,.T.);
#92401=ADVANCED_FACE('',(#13122),#8433,.F.);
#92402=ADVANCED_FACE('',(#13123),#87334,.T.);
#92403=ADVANCED_FACE('',(#13124),#8434,.T.);
#92404=ADVANCED_FACE('',(#13125),#87335,.T.);
#92405=ADVANCED_FACE('',(#13126),#8435,.F.);
#92406=ADVANCED_FACE('',(#13127),#8436,.F.);
#92407=ADVANCED_FACE('',(#13128),#8437,.F.);
#92408=ADVANCED_FACE('',(#13129),#8438,.T.);
#92409=ADVANCED_FACE('',(#13130),#8439,.F.);
#92410=ADVANCED_FACE('',(#13131),#8440,.F.);
#92411=ADVANCED_FACE('',(#13132),#87336,.T.);
#92412=ADVANCED_FACE('',(#13133),#8441,.F.);
#92413=ADVANCED_FACE('',(#13134),#8442,.F.);
#92414=ADVANCED_FACE('',(#13135),#8443,.F.);
#92415=ADVANCED_FACE('',(#13136),#87337,.T.);
#92416=ADVANCED_FACE('',(#13137),#8444,.T.);
#92417=ADVANCED_FACE('',(#13138),#7123,.T.);
#92418=ADVANCED_FACE('',(#13139),#7124,.T.);
#92419=ADVANCED_FACE('',(#13140),#7125,.T.);
#92420=ADVANCED_FACE('',(#13141),#7126,.T.);
#92421=ADVANCED_FACE('',(#13142),#7127,.T.);
#92422=ADVANCED_FACE('',(#13143),#7128,.T.);
#92423=ADVANCED_FACE('',(#13144),#8445,.F.);
#92424=ADVANCED_FACE('',(#13145),#7129,.T.);
#92425=ADVANCED_FACE('',(#13146),#7130,.T.);
#92426=ADVANCED_FACE('',(#13147),#7131,.T.);
#92427=ADVANCED_FACE('',(#13148),#7132,.T.);
#92428=ADVANCED_FACE('',(#13149),#7133,.T.);
#92429=ADVANCED_FACE('',(#13150),#7134,.T.);
#92430=ADVANCED_FACE('',(#13151),#8446,.F.);
#92431=ADVANCED_FACE('',(#13152),#8447,.F.);
#92432=ADVANCED_FACE('',(#13153),#8448,.F.);
#92433=ADVANCED_FACE('',(#13154),#8449,.F.);
#92434=ADVANCED_FACE('',(#13155),#8450,.F.);
#92435=ADVANCED_FACE('',(#13156),#8451,.F.);
#92436=ADVANCED_FACE('',(#13157),#8452,.T.);
#92437=ADVANCED_FACE('',(#13158),#7135,.T.);
#92438=ADVANCED_FACE('',(#13159),#7136,.T.);
#92439=ADVANCED_FACE('',(#13160),#7137,.T.);
#92440=ADVANCED_FACE('',(#13161),#7138,.T.);
#92441=ADVANCED_FACE('',(#13162),#7139,.T.);
#92442=ADVANCED_FACE('',(#13163),#7140,.T.);
#92443=ADVANCED_FACE('',(#13164),#8453,.F.);
#92444=ADVANCED_FACE('',(#13165),#7141,.T.);
#92445=ADVANCED_FACE('',(#13166),#7142,.T.);
#92446=ADVANCED_FACE('',(#13167),#7143,.T.);
#92447=ADVANCED_FACE('',(#13168),#7144,.T.);
#92448=ADVANCED_FACE('',(#13169),#7145,.T.);
#92449=ADVANCED_FACE('',(#13170),#7146,.T.);
#92450=ADVANCED_FACE('',(#13171),#8454,.F.);
#92451=ADVANCED_FACE('',(#13172),#8455,.F.);
#92452=ADVANCED_FACE('',(#13173),#8456,.F.);
#92453=ADVANCED_FACE('',(#13174),#8457,.F.);
#92454=ADVANCED_FACE('',(#13175),#8458,.F.);
#92455=ADVANCED_FACE('',(#13176),#8459,.F.);
#92456=ADVANCED_FACE('',(#13177),#8460,.F.);
#92457=ADVANCED_FACE('',(#13178),#8461,.F.);
#92458=ADVANCED_FACE('',(#13179),#8462,.F.);
#92459=ADVANCED_FACE('',(#13180),#8463,.F.);
#92460=ADVANCED_FACE('',(#13181),#8464,.F.);
#92461=ADVANCED_FACE('',(#13182),#8465,.F.);
#92462=ADVANCED_FACE('',(#13183),#7147,.F.);
#92463=ADVANCED_FACE('',(#13184),#7148,.F.);
#92464=ADVANCED_FACE('',(#13185),#7149,.F.);
#92465=ADVANCED_FACE('',(#13186),#7150,.F.);
#92466=ADVANCED_FACE('',(#13187),#7151,.F.);
#92467=ADVANCED_FACE('',(#13188),#7152,.F.);
#92468=ADVANCED_FACE('',(#13189),#7153,.F.);
#92469=ADVANCED_FACE('',(#13190),#3994,.T.);
#92470=ADVANCED_FACE('',(#13191),#8466,.F.);
#92471=ADVANCED_FACE('',(#13192,#7605),#8467,.T.);
#92472=ADVANCED_FACE('',(#13193),#87338,.T.);
#92473=ADVANCED_FACE('',(#13194),#87339,.T.);
#92474=ADVANCED_FACE('',(#13195),#87340,.T.);
#92475=ADVANCED_FACE('',(#13196),#1028,.T.);
#92476=ADVANCED_FACE('',(#13197),#87341,.T.);
#92477=ADVANCED_FACE('',(#13198),#1029,.T.);
#92478=ADVANCED_FACE('',(#13199),#3995,.T.);
#92479=ADVANCED_FACE('',(#13200),#1030,.T.);
#92480=ADVANCED_FACE('',(#13201),#3996,.T.);
#92481=ADVANCED_FACE('',(#13202),#3997,.T.);
#92482=ADVANCED_FACE('',(#13203),#1031,.T.);
#92483=ADVANCED_FACE('',(#13204),#3998,.T.);
#92484=ADVANCED_FACE('',(#13205),#3999,.T.);
#92485=ADVANCED_FACE('',(#13206),#4000,.T.);
#92486=ADVANCED_FACE('',(#13207),#87342,.F.);
#92487=ADVANCED_FACE('',(#13208),#87343,.F.);
#92488=ADVANCED_FACE('',(#13209),#8468,.F.);
#92489=ADVANCED_FACE('',(#13210),#8469,.F.);
#92490=ADVANCED_FACE('',(#13211),#8470,.F.);
#92491=ADVANCED_FACE('',(#13212),#87344,.T.);
#92492=ADVANCED_FACE('',(#13213),#87345,.T.);
#92493=ADVANCED_FACE('',(#13214),#1032,.T.);
#92494=ADVANCED_FACE('',(#13215),#87346,.T.);
#92495=ADVANCED_FACE('',(#13216),#1033,.T.);
#92496=ADVANCED_FACE('',(#13217),#4001,.T.);
#92497=ADVANCED_FACE('',(#13218),#1034,.T.);
#92498=ADVANCED_FACE('',(#13219),#4002,.T.);
#92499=ADVANCED_FACE('',(#13220),#4003,.T.);
#92500=ADVANCED_FACE('',(#13221),#1035,.T.);
#92501=ADVANCED_FACE('',(#13222),#4004,.T.);
#92502=ADVANCED_FACE('',(#13223),#4005,.T.);
#92503=ADVANCED_FACE('',(#13224),#4006,.T.);
#92504=ADVANCED_FACE('',(#13225),#87347,.F.);
#92505=ADVANCED_FACE('',(#13226),#87348,.F.);
#92506=ADVANCED_FACE('',(#13227),#8471,.F.);
#92507=ADVANCED_FACE('',(#13228),#8472,.F.);
#92508=ADVANCED_FACE('',(#13229),#8473,.T.);
#92509=ADVANCED_FACE('',(#13230),#8474,.T.);
#92510=ADVANCED_FACE('',(#13231),#8475,.F.);
#92511=ADVANCED_FACE('',(#13232),#87349,.T.);
#92512=ADVANCED_FACE('',(#13233),#3124,.T.);
#92513=ADVANCED_FACE('',(#13234),#87350,.T.);
#92514=ADVANCED_FACE('',(#13235),#4007,.T.);
#92515=ADVANCED_FACE('',(#13236),#87351,.T.);
#92516=ADVANCED_FACE('',(#13237),#87352,.T.);
#92517=ADVANCED_FACE('',(#13238),#4008,.T.);
#92518=ADVANCED_FACE('',(#13239),#87353,.T.);
#92519=ADVANCED_FACE('',(#13240),#87354,.T.);
#92520=ADVANCED_FACE('',(#13241),#87355,.T.);
#92521=ADVANCED_FACE('',(#13242),#8476,.T.);
#92522=ADVANCED_FACE('',(#13243),#87356,.T.);
#92523=ADVANCED_FACE('',(#13244),#3125,.T.);
#92524=ADVANCED_FACE('',(#13245),#87357,.T.);
#92525=ADVANCED_FACE('',(#13246),#87358,.T.);
#92526=ADVANCED_FACE('',(#13247),#4009,.T.);
#92527=ADVANCED_FACE('',(#13248),#87359,.T.);
#92528=ADVANCED_FACE('',(#13249),#87360,.T.);
#92529=ADVANCED_FACE('',(#13250),#4010,.T.);
#92530=ADVANCED_FACE('',(#13251),#87361,.T.);
#92531=ADVANCED_FACE('',(#13252),#8477,.T.);
#92532=ADVANCED_FACE('',(#13253),#8478,.F.);
#92533=ADVANCED_FACE('',(#13254),#8479,.F.);
#92534=ADVANCED_FACE('',(#13255),#87362,.T.);
#92535=ADVANCED_FACE('',(#13256),#87363,.T.);
#92536=ADVANCED_FACE('',(#13257),#87364,.F.);
#92537=ADVANCED_FACE('',(#13258),#87365,.F.);
#92538=ADVANCED_FACE('',(#13259),#87366,.F.);
#92539=ADVANCED_FACE('',(#13260),#87367,.F.);
#92540=ADVANCED_FACE('',(#13261),#87368,.F.);
#92541=ADVANCED_FACE('',(#13262),#87369,.F.);
#92542=ADVANCED_FACE('',(#13263),#87370,.F.);
#92543=ADVANCED_FACE('',(#13264),#87371,.F.);
#92544=ADVANCED_FACE('',(#13265),#87372,.F.);
#92545=ADVANCED_FACE('',(#13266),#87373,.F.);
#92546=ADVANCED_FACE('',(#13267),#87374,.F.);
#92547=ADVANCED_FACE('',(#13268),#87375,.F.);
#92548=ADVANCED_FACE('',(#13269),#87376,.F.);
#92549=ADVANCED_FACE('',(#13270),#87377,.F.);
#92550=ADVANCED_FACE('',(#13271),#87378,.F.);
#92551=ADVANCED_FACE('',(#13272),#87379,.F.);
#92552=ADVANCED_FACE('',(#13273),#87380,.F.);
#92553=ADVANCED_FACE('',(#13274),#87381,.F.);
#92554=ADVANCED_FACE('',(#13275),#87382,.F.);
#92555=ADVANCED_FACE('',(#13276),#87383,.F.);
#92556=ADVANCED_FACE('',(#13277),#87384,.F.);
#92557=ADVANCED_FACE('',(#13278),#87385,.F.);
#92558=ADVANCED_FACE('',(#13279),#87386,.F.);
#92559=ADVANCED_FACE('',(#13280),#87387,.F.);
#92560=ADVANCED_FACE('',(#13281),#87388,.F.);
#92561=ADVANCED_FACE('',(#13282),#87389,.F.);
#92562=ADVANCED_FACE('',(#13283),#87390,.F.);
#92563=ADVANCED_FACE('',(#13284),#87391,.F.);
#92564=ADVANCED_FACE('',(#13285),#87392,.F.);
#92565=ADVANCED_FACE('',(#13286),#87393,.F.);
#92566=ADVANCED_FACE('',(#13287),#87394,.F.);
#92567=ADVANCED_FACE('',(#13288),#87395,.F.);
#92568=ADVANCED_FACE('',(#13289),#87396,.F.);
#92569=ADVANCED_FACE('',(#13290),#87397,.F.);
#92570=ADVANCED_FACE('',(#13291),#87398,.F.);
#92571=ADVANCED_FACE('',(#13292),#87399,.F.);
#92572=ADVANCED_FACE('',(#13293),#87400,.F.);
#92573=ADVANCED_FACE('',(#13294),#87401,.F.);
#92574=ADVANCED_FACE('',(#13295),#87402,.F.);
#92575=ADVANCED_FACE('',(#13296),#87403,.F.);
#92576=ADVANCED_FACE('',(#13297),#87404,.F.);
#92577=ADVANCED_FACE('',(#13298),#87405,.F.);
#92578=ADVANCED_FACE('',(#13299),#87406,.F.);
#92579=ADVANCED_FACE('',(#13300),#87407,.F.);
#92580=ADVANCED_FACE('',(#13301),#87408,.F.);
#92581=ADVANCED_FACE('',(#13302),#87409,.F.);
#92582=ADVANCED_FACE('',(#13303),#87410,.F.);
#92583=ADVANCED_FACE('',(#13304),#87411,.F.);
#92584=ADVANCED_FACE('',(#13305),#87412,.F.);
#92585=ADVANCED_FACE('',(#13306),#87413,.F.);
#92586=ADVANCED_FACE('',(#13307),#87414,.F.);
#92587=ADVANCED_FACE('',(#13308),#87415,.F.);
#92588=ADVANCED_FACE('',(#13309),#87416,.F.);
#92589=ADVANCED_FACE('',(#13310),#87417,.F.);
#92590=ADVANCED_FACE('',(#13311),#87418,.F.);
#92591=ADVANCED_FACE('',(#13312),#87419,.F.);
#92592=ADVANCED_FACE('',(#13313),#87420,.F.);
#92593=ADVANCED_FACE('',(#13314),#87421,.F.);
#92594=ADVANCED_FACE('',(#13315),#87422,.F.);
#92595=ADVANCED_FACE('',(#13316),#87423,.F.);
#92596=ADVANCED_FACE('',(#13317),#87424,.F.);
#92597=ADVANCED_FACE('',(#13318),#87425,.F.);
#92598=ADVANCED_FACE('',(#13319),#87426,.F.);
#92599=ADVANCED_FACE('',(#13320),#87427,.F.);
#92600=ADVANCED_FACE('',(#13321),#87428,.F.);
#92601=ADVANCED_FACE('',(#13322),#87429,.F.);
#92602=ADVANCED_FACE('',(#13323),#87430,.F.);
#92603=ADVANCED_FACE('',(#13324),#87431,.F.);
#92604=ADVANCED_FACE('',(#13325),#87432,.F.);
#92605=ADVANCED_FACE('',(#13326),#87433,.F.);
#92606=ADVANCED_FACE('',(#13327),#87434,.F.);
#92607=ADVANCED_FACE('',(#13328),#87435,.F.);
#92608=ADVANCED_FACE('',(#13329),#87436,.F.);
#92609=ADVANCED_FACE('',(#13330),#87437,.F.);
#92610=ADVANCED_FACE('',(#13331),#87438,.F.);
#92611=ADVANCED_FACE('',(#13332),#87439,.F.);
#92612=ADVANCED_FACE('',(#13333),#87440,.F.);
#92613=ADVANCED_FACE('',(#13334),#87441,.F.);
#92614=ADVANCED_FACE('',(#13335),#87442,.F.);
#92615=ADVANCED_FACE('',(#13336),#87443,.F.);
#92616=ADVANCED_FACE('',(#13337),#87444,.F.);
#92617=ADVANCED_FACE('',(#13338),#87445,.F.);
#92618=ADVANCED_FACE('',(#13339),#87446,.F.);
#92619=ADVANCED_FACE('',(#13340),#87447,.F.);
#92620=ADVANCED_FACE('',(#13341),#87448,.F.);
#92621=ADVANCED_FACE('',(#13342),#87449,.F.);
#92622=ADVANCED_FACE('',(#13343),#87450,.F.);
#92623=ADVANCED_FACE('',(#13344),#87451,.F.);
#92624=ADVANCED_FACE('',(#13345),#87452,.F.);
#92625=ADVANCED_FACE('',(#13346),#87453,.F.);
#92626=ADVANCED_FACE('',(#13347),#87454,.F.);
#92627=ADVANCED_FACE('',(#13348),#87455,.F.);
#92628=ADVANCED_FACE('',(#13349),#87456,.F.);
#92629=ADVANCED_FACE('',(#13350),#87457,.F.);
#92630=ADVANCED_FACE('',(#13351),#87458,.F.);
#92631=ADVANCED_FACE('',(#13352),#87459,.F.);
#92632=ADVANCED_FACE('',(#13353),#87460,.F.);
#92633=ADVANCED_FACE('',(#13354),#87461,.F.);
#92634=ADVANCED_FACE('',(#13355),#87462,.F.);
#92635=ADVANCED_FACE('',(#13356),#87463,.F.);
#92636=ADVANCED_FACE('',(#13357),#87464,.F.);
#92637=ADVANCED_FACE('',(#13358),#87465,.F.);
#92638=ADVANCED_FACE('',(#13359),#87466,.F.);
#92639=ADVANCED_FACE('',(#13360),#87467,.F.);
#92640=ADVANCED_FACE('',(#13361),#87468,.F.);
#92641=ADVANCED_FACE('',(#13362),#87469,.F.);
#92642=ADVANCED_FACE('',(#13363),#87470,.F.);
#92643=ADVANCED_FACE('',(#13364),#87471,.F.);
#92644=ADVANCED_FACE('',(#13365),#87472,.F.);
#92645=ADVANCED_FACE('',(#13366),#87473,.F.);
#92646=ADVANCED_FACE('',(#13367),#87474,.F.);
#92647=ADVANCED_FACE('',(#13368),#87475,.F.);
#92648=ADVANCED_FACE('',(#13369),#87476,.F.);
#92649=ADVANCED_FACE('',(#13370),#87477,.F.);
#92650=ADVANCED_FACE('',(#13371),#87478,.F.);
#92651=ADVANCED_FACE('',(#13372),#87479,.F.);
#92652=ADVANCED_FACE('',(#13373),#87480,.F.);
#92653=ADVANCED_FACE('',(#13374),#87481,.F.);
#92654=ADVANCED_FACE('',(#13375),#87482,.F.);
#92655=ADVANCED_FACE('',(#13376),#87483,.F.);
#92656=ADVANCED_FACE('',(#13377),#87484,.F.);
#92657=ADVANCED_FACE('',(#13378),#87485,.F.);
#92658=ADVANCED_FACE('',(#13379),#87486,.F.);
#92659=ADVANCED_FACE('',(#13380),#87487,.F.);
#92660=ADVANCED_FACE('',(#13381),#87488,.F.);
#92661=ADVANCED_FACE('',(#13382),#87489,.F.);
#92662=ADVANCED_FACE('',(#13383),#87490,.F.);
#92663=ADVANCED_FACE('',(#13384),#87491,.F.);
#92664=ADVANCED_FACE('',(#13385),#87492,.F.);
#92665=ADVANCED_FACE('',(#13386),#87493,.F.);
#92666=ADVANCED_FACE('',(#13387),#87494,.F.);
#92667=ADVANCED_FACE('',(#13388),#87495,.F.);
#92668=ADVANCED_FACE('',(#13389),#87496,.F.);
#92669=ADVANCED_FACE('',(#13390),#87497,.F.);
#92670=ADVANCED_FACE('',(#13391),#87498,.F.);
#92671=ADVANCED_FACE('',(#13392),#87499,.F.);
#92672=ADVANCED_FACE('',(#13393),#87500,.F.);
#92673=ADVANCED_FACE('',(#13394),#87501,.F.);
#92674=ADVANCED_FACE('',(#13395),#87502,.F.);
#92675=ADVANCED_FACE('',(#13396),#87503,.F.);
#92676=ADVANCED_FACE('',(#13397),#87504,.F.);
#92677=ADVANCED_FACE('',(#13398),#87505,.F.);
#92678=ADVANCED_FACE('',(#13399),#87506,.F.);
#92679=ADVANCED_FACE('',(#13400),#87507,.F.);
#92680=ADVANCED_FACE('',(#13401),#87508,.F.);
#92681=ADVANCED_FACE('',(#13402),#87509,.F.);
#92682=ADVANCED_FACE('',(#13403),#87510,.F.);
#92683=ADVANCED_FACE('',(#13404),#87511,.F.);
#92684=ADVANCED_FACE('',(#13405),#87512,.F.);
#92685=ADVANCED_FACE('',(#13406),#87513,.F.);
#92686=ADVANCED_FACE('',(#13407),#87514,.F.);
#92687=ADVANCED_FACE('',(#13408),#8480,.F.);
#92688=ADVANCED_FACE('',(#13409),#8481,.F.);
#92689=ADVANCED_FACE('',(#13410),#8482,.F.);
#92690=ADVANCED_FACE('',(#13411),#8483,.F.);
#92691=ADVANCED_FACE('',(#13412),#8484,.F.);
#92692=ADVANCED_FACE('',(#13413),#8485,.F.);
#92693=ADVANCED_FACE('',(#13414),#8486,.T.);
#92694=ADVANCED_FACE('',(#13415,#7606,#7607,#7608),#8487,.T.);
#92695=ADVANCED_FACE('',(#13416,#7609),#8488,.T.);
#92696=ADVANCED_FACE('',(#13417),#87515,.F.);
#92697=ADVANCED_FACE('',(#13418),#87516,.T.);
#92698=ADVANCED_FACE('',(#13419),#8489,.T.);
#92699=ADVANCED_FACE('',(#13420,#7610),#8490,.T.);
#92700=ADVANCED_FACE('',(#13421),#87517,.F.);
#92701=ADVANCED_FACE('',(#13422),#87518,.T.);
#92702=ADVANCED_FACE('',(#13423),#8491,.T.);
#92703=ADVANCED_FACE('',(#13424,#7611),#8492,.T.);
#92704=ADVANCED_FACE('',(#13425),#87519,.F.);
#92705=ADVANCED_FACE('',(#13426),#87520,.T.);
#92706=ADVANCED_FACE('',(#13427),#8493,.T.);
#92707=ADVANCED_FACE('',(#13428,#7612),#8494,.T.);
#92708=ADVANCED_FACE('',(#13429),#87521,.F.);
#92709=ADVANCED_FACE('',(#13430),#87522,.T.);
#92710=ADVANCED_FACE('',(#13431),#8495,.T.);
#92711=ADVANCED_FACE('',(#13432),#4011,.T.);
#92712=ADVANCED_FACE('',(#13433),#4012,.T.);
#92713=ADVANCED_FACE('',(#13434),#4013,.T.);
#92714=ADVANCED_FACE('',(#13435),#8496,.F.);
#92715=ADVANCED_FACE('',(#13436),#8497,.F.);
#92716=ADVANCED_FACE('',(#13437),#8498,.F.);
#92717=ADVANCED_FACE('',(#13438),#8499,.F.);
#92718=ADVANCED_FACE('',(#13439),#8500,.F.);
#92719=ADVANCED_FACE('',(#13440),#8501,.F.);
#92720=ADVANCED_FACE('',(#13441),#7154,.F.);
#92721=ADVANCED_FACE('',(#13442),#7155,.F.);
#92722=ADVANCED_FACE('',(#13443),#7156,.F.);
#92723=ADVANCED_FACE('',(#13444),#7157,.F.);
#92724=ADVANCED_FACE('',(#13445),#7158,.F.);
#92725=ADVANCED_FACE('',(#13446),#7159,.F.);
#92726=ADVANCED_FACE('',(#13447),#7160,.F.);
#92727=ADVANCED_FACE('',(#13448),#7161,.T.);
#92728=ADVANCED_FACE('',(#13449,#7613),#8502,.T.);
#92729=ADVANCED_FACE('',(#13450),#87523,.T.);
#92730=ADVANCED_FACE('',(#13451),#953,.F.);
#92731=ADVANCED_FACE('',(#13452),#3126,.F.);
#92732=ADVANCED_FACE('',(#13453),#954,.T.);
#92733=ADVANCED_FACE('',(#13454),#3127,.F.);
#92734=ADVANCED_FACE('',(#13455),#3128,.T.);
#92735=ADVANCED_FACE('',(#13456),#3129,.T.);
#92736=ADVANCED_FACE('',(#13457),#3130,.T.);
#92737=ADVANCED_FACE('',(#13458),#3131,.T.);
#92738=ADVANCED_FACE('',(#13459),#3132,.T.);
#92739=ADVANCED_FACE('',(#13460),#3133,.T.);
#92740=ADVANCED_FACE('',(#13461),#3134,.F.);
#92741=ADVANCED_FACE('',(#13462),#3135,.F.);
#92742=ADVANCED_FACE('',(#13463),#3136,.F.);
#92743=ADVANCED_FACE('',(#13464),#3137,.F.);
#92744=ADVANCED_FACE('',(#13465),#3138,.F.);
#92745=ADVANCED_FACE('',(#13466),#3139,.F.);
#92746=ADVANCED_FACE('',(#13467),#3140,.T.);
#92747=ADVANCED_FACE('',(#13468),#3141,.T.);
#92748=ADVANCED_FACE('',(#13469),#87524,.T.);
#92749=ADVANCED_FACE('',(#13470),#3142,.T.);
#92750=ADVANCED_FACE('',(#13471),#3143,.T.);
#92751=ADVANCED_FACE('',(#13472),#87525,.T.);
#92752=ADVANCED_FACE('',(#13473),#3144,.T.);
#92753=ADVANCED_FACE('',(#13474),#3145,.F.);
#92754=ADVANCED_FACE('',(#13475),#3146,.F.);
#92755=ADVANCED_FACE('',(#13476),#1036,.F.);
#92756=ADVANCED_FACE('',(#13477),#87526,.F.);
#92757=ADVANCED_FACE('',(#13478),#3147,.F.);
#92758=ADVANCED_FACE('',(#13479),#87527,.F.);
#92759=ADVANCED_FACE('',(#13480),#3148,.F.);
#92760=ADVANCED_FACE('',(#13481),#1037,.F.);
#92761=ADVANCED_FACE('',(#13482),#87528,.F.);
#92762=ADVANCED_FACE('',(#13483),#3149,.F.);
#92763=ADVANCED_FACE('',(#13484),#87529,.F.);
#92764=ADVANCED_FACE('',(#13485),#8503,.T.);
#92765=ADVANCED_FACE('',(#13486),#87530,.F.);
#92766=ADVANCED_FACE('',(#13487),#8504,.F.);
#92767=ADVANCED_FACE('',(#13488),#8505,.T.);
#92768=ADVANCED_FACE('',(#13489),#8506,.F.);
#92769=ADVANCED_FACE('',(#13490),#87531,.F.);
#92770=ADVANCED_FACE('',(#13491),#87532,.F.);
#92771=ADVANCED_FACE('',(#13492),#87533,.F.);
#92772=ADVANCED_FACE('',(#13493),#3150,.T.);
#92773=ADVANCED_FACE('',(#13494),#87534,.T.);
#92774=ADVANCED_FACE('',(#13495),#87535,.T.);
#92775=ADVANCED_FACE('',(#13496),#8507,.T.);
#92776=ADVANCED_FACE('',(#13497),#3151,.T.);
#92777=ADVANCED_FACE('',(#13498),#87536,.T.);
#92778=ADVANCED_FACE('',(#13499),#3152,.T.);
#92779=ADVANCED_FACE('',(#13500),#8508,.T.);
#92780=ADVANCED_FACE('',(#13501),#3153,.T.);
#92781=ADVANCED_FACE('',(#13502),#87537,.T.);
#92782=ADVANCED_FACE('',(#13503),#87538,.T.);
#92783=ADVANCED_FACE('',(#13504),#8509,.T.);
#92784=ADVANCED_FACE('',(#13505),#3154,.T.);
#92785=ADVANCED_FACE('',(#13506),#87539,.T.);
#92786=ADVANCED_FACE('',(#13507),#3155,.T.);
#92787=ADVANCED_FACE('',(#13508),#8510,.T.);
#92788=ADVANCED_FACE('',(#13509),#3156,.T.);
#92789=ADVANCED_FACE('',(#13510),#3157,.T.);
#92790=ADVANCED_FACE('',(#13511),#4014,.T.);
#92791=ADVANCED_FACE('',(#13512),#3158,.T.);
#92792=ADVANCED_FACE('',(#13513),#4015,.T.);
#92793=ADVANCED_FACE('',(#13514),#3159,.T.);
#92794=ADVANCED_FACE('',(#13515),#87540,.F.);
#92795=ADVANCED_FACE('',(#13516),#87541,.F.);
#92796=ADVANCED_FACE('',(#13517),#87542,.F.);
#92797=ADVANCED_FACE('',(#13518),#87543,.F.);
#92798=ADVANCED_FACE('',(#13519),#87544,.T.);
#92799=ADVANCED_FACE('',(#13520),#3160,.T.);
#92800=ADVANCED_FACE('',(#13521),#87545,.T.);
#92801=ADVANCED_FACE('',(#13522),#87546,.T.);
#92802=ADVANCED_FACE('',(#13523),#8511,.T.);
#92803=ADVANCED_FACE('',(#13524),#3161,.T.);
#92804=ADVANCED_FACE('',(#13525),#87547,.T.);
#92805=ADVANCED_FACE('',(#13526),#3162,.T.);
#92806=ADVANCED_FACE('',(#13527),#8512,.T.);
#92807=ADVANCED_FACE('',(#13528),#3163,.T.);
#92808=ADVANCED_FACE('',(#13529),#87548,.T.);
#92809=ADVANCED_FACE('',(#13530),#3164,.T.);
#92810=ADVANCED_FACE('',(#13531),#87549,.T.);
#92811=ADVANCED_FACE('',(#13532),#87550,.T.);
#92812=ADVANCED_FACE('',(#13533),#8513,.T.);
#92813=ADVANCED_FACE('',(#13534),#3165,.T.);
#92814=ADVANCED_FACE('',(#13535),#87551,.T.);
#92815=ADVANCED_FACE('',(#13536),#3166,.T.);
#92816=ADVANCED_FACE('',(#13537),#8514,.T.);
#92817=ADVANCED_FACE('',(#13538),#3167,.T.);
#92818=ADVANCED_FACE('',(#13539),#87552,.T.);
#92819=ADVANCED_FACE('',(#13540),#4016,.T.);
#92820=ADVANCED_FACE('',(#13541),#4017,.F.);
#92821=ADVANCED_FACE('',(#13542),#4018,.F.);
#92822=ADVANCED_FACE('',(#13543),#4019,.T.);
#92823=ADVANCED_FACE('',(#13544),#4020,.T.);
#92824=ADVANCED_FACE('',(#13545),#3168,.T.);
#92825=ADVANCED_FACE('',(#13546),#4021,.T.);
#92826=ADVANCED_FACE('',(#13547),#3169,.T.);
#92827=ADVANCED_FACE('',(#13548),#3170,.T.);
#92828=ADVANCED_FACE('',(#13549),#4022,.T.);
#92829=ADVANCED_FACE('',(#13550),#3171,.T.);
#92830=ADVANCED_FACE('',(#13551),#87553,.F.);
#92831=ADVANCED_FACE('',(#13552),#87554,.T.);
#92832=ADVANCED_FACE('',(#13553),#4023,.T.);
#92833=ADVANCED_FACE('',(#13554),#3172,.T.);
#92834=ADVANCED_FACE('',(#13555),#955,.T.);
#92835=ADVANCED_FACE('',(#13556),#3173,.F.);
#92836=ADVANCED_FACE('',(#13557),#87555,.F.);
#92837=ADVANCED_FACE('',(#13558),#956,.T.);
#92838=ADVANCED_FACE('',(#13559),#957,.T.);
#92839=ADVANCED_FACE('',(#13560),#958,.T.);
#92840=ADVANCED_FACE('',(#13561),#959,.T.);
#92841=ADVANCED_FACE('',(#13562),#87556,.F.);
#92842=ADVANCED_FACE('',(#13563),#3174,.F.);
#92843=ADVANCED_FACE('',(#13564),#3175,.F.);
#92844=ADVANCED_FACE('',(#13565),#3176,.F.);
#92845=ADVANCED_FACE('',(#13566),#3177,.F.);
#92846=ADVANCED_FACE('',(#13567),#87557,.F.);
#92847=ADVANCED_FACE('',(#13568),#960,.F.);
#92848=ADVANCED_FACE('',(#13569),#961,.F.);
#92849=ADVANCED_FACE('',(#13570),#962,.F.);
#92850=ADVANCED_FACE('',(#13571),#963,.F.);
#92851=ADVANCED_FACE('',(#13572),#87558,.F.);
#92852=ADVANCED_FACE('',(#13573),#3178,.F.);
#92853=ADVANCED_FACE('',(#13574),#3179,.F.);
#92854=ADVANCED_FACE('',(#13575),#3180,.F.);
#92855=ADVANCED_FACE('',(#13576),#3181,.F.);
#92856=ADVANCED_FACE('',(#13577),#87559,.F.);
#92857=ADVANCED_FACE('',(#13578),#87560,.F.);
#92858=ADVANCED_FACE('',(#13579),#964,.F.);
#92859=ADVANCED_FACE('',(#13580),#965,.F.);
#92860=ADVANCED_FACE('',(#13581),#966,.F.);
#92861=ADVANCED_FACE('',(#13582),#967,.F.);
#92862=ADVANCED_FACE('',(#13583),#87561,.F.);
#92863=ADVANCED_FACE('',(#13584),#3182,.F.);
#92864=ADVANCED_FACE('',(#13585),#3183,.F.);
#92865=ADVANCED_FACE('',(#13586),#3184,.F.);
#92866=ADVANCED_FACE('',(#13587),#3185,.F.);
#92867=ADVANCED_FACE('',(#13588),#87562,.F.);
#92868=ADVANCED_FACE('',(#13589),#87563,.F.);
#92869=ADVANCED_FACE('',(#13590),#968,.T.);
#92870=ADVANCED_FACE('',(#13591),#969,.T.);
#92871=ADVANCED_FACE('',(#13592),#970,.T.);
#92872=ADVANCED_FACE('',(#13593),#971,.T.);
#92873=ADVANCED_FACE('',(#13594,#7614,#7615,#7616,#7617),#8515,.T.);
#92874=ADVANCED_FACE('',(#13595),#87564,.F.);
#92875=ADVANCED_FACE('',(#13596),#3186,.F.);
#92876=ADVANCED_FACE('',(#13597),#3187,.F.);
#92877=ADVANCED_FACE('',(#13598),#3188,.F.);
#92878=ADVANCED_FACE('',(#13599),#3189,.F.);
#92879=ADVANCED_FACE('',(#13600),#87565,.F.);
#92880=ADVANCED_FACE('',(#13601),#87566,.F.);
#92881=ADVANCED_FACE('',(#13602,#7618,#7619,#7620,#7621),#7162,.T.);
#92882=ADVANCED_FACE('',(#13603),#87567,.T.);
#92883=ADVANCED_FACE('',(#13604),#972,.T.);
#92884=ADVANCED_FACE('',(#13605),#973,.T.);
#92885=ADVANCED_FACE('',(#13606),#974,.T.);
#92886=ADVANCED_FACE('',(#13607),#975,.F.);
#92887=ADVANCED_FACE('',(#13608),#976,.F.);
#92888=ADVANCED_FACE('',(#13609),#977,.F.);
#92889=ADVANCED_FACE('',(#13610),#978,.F.);
#92890=ADVANCED_FACE('',(#13611),#979,.F.);
#92891=ADVANCED_FACE('',(#13612),#980,.F.);
#92892=ADVANCED_FACE('',(#13613),#981,.T.);
#92893=ADVANCED_FACE('',(#13614),#982,.T.);
#92894=ADVANCED_FACE('',(#13615),#983,.T.);
#92895=ADVANCED_FACE('',(#13616),#8516,.F.);
#92896=ADVANCED_FACE('',(#13617),#8517,.T.);
#92897=ADVANCED_FACE('',(#13618),#87568,.T.);
#92898=ADVANCED_FACE('',(#13619),#3190,.T.);
#92899=ADVANCED_FACE('',(#13620),#3191,.T.);
#92900=ADVANCED_FACE('',(#13621),#87569,.T.);
#92901=ADVANCED_FACE('',(#13622),#87570,.T.);
#92902=ADVANCED_FACE('',(#13623),#87571,.T.);
#92903=ADVANCED_FACE('',(#13624),#1038,.T.);
#92904=ADVANCED_FACE('',(#13625),#1039,.T.);
#92905=ADVANCED_FACE('',(#13626),#87572,.T.);
#92906=ADVANCED_FACE('',(#13627),#87573,.T.);
#92907=ADVANCED_FACE('',(#13628),#87574,.T.);
#92908=ADVANCED_FACE('',(#13629),#8518,.F.);
#92909=ADVANCED_FACE('',(#13630),#8519,.F.);
#92910=ADVANCED_FACE('',(#13631),#8520,.F.);
#92911=ADVANCED_FACE('',(#13632),#8521,.F.);
#92912=ADVANCED_FACE('',(#13633),#8522,.T.);
#92913=ADVANCED_FACE('',(#13634),#8523,.F.);
#92914=ADVANCED_FACE('',(#13635),#4024,.F.);
#92915=ADVANCED_FACE('',(#13636),#87575,.T.);
#92916=ADVANCED_FACE('',(#13637),#87576,.T.);
#92917=ADVANCED_FACE('',(#13638),#87577,.F.);
#92918=ADVANCED_FACE('',(#13639),#87578,.F.);
#92919=ADVANCED_FACE('',(#13640),#87579,.F.);
#92920=ADVANCED_FACE('',(#13641),#87580,.F.);
#92921=ADVANCED_FACE('',(#13642),#87581,.F.);
#92922=ADVANCED_FACE('',(#13643),#87582,.F.);
#92923=ADVANCED_FACE('',(#13644),#87583,.T.);
#92924=ADVANCED_FACE('',(#13645),#87584,.F.);
#92925=ADVANCED_FACE('',(#13646,#7622),#8524,.F.);
#92926=ADVANCED_FACE('',(#13647,#7623),#8525,.T.);
#92927=ADVANCED_FACE('',(#13648),#4025,.T.);
#92928=ADVANCED_FACE('',(#13649),#4026,.T.);
#92929=ADVANCED_FACE('',(#13650),#4027,.T.);
#92930=ADVANCED_FACE('',(#13651),#4028,.T.);
#92931=ADVANCED_FACE('',(#13652),#4029,.T.);
#92932=ADVANCED_FACE('',(#13653),#4030,.T.);
#92933=ADVANCED_FACE('',(#13654),#4031,.T.);
#92934=ADVANCED_FACE('',(#13655),#4032,.T.);
#92935=ADVANCED_FACE('',(#13656),#4033,.T.);
#92936=ADVANCED_FACE('',(#13657),#4034,.T.);
#92937=ADVANCED_FACE('',(#13658),#4035,.T.);
#92938=ADVANCED_FACE('',(#13659),#4036,.T.);
#92939=ADVANCED_FACE('',(#13660),#4037,.T.);
#92940=ADVANCED_FACE('',(#13661),#4038,.T.);
#92941=ADVANCED_FACE('',(#13662),#87585,.T.);
#92942=ADVANCED_FACE('',(#13663),#87586,.T.);
#92943=ADVANCED_FACE('',(#13664),#87587,.T.);
#92944=ADVANCED_FACE('',(#13665),#87588,.T.);
#92945=ADVANCED_FACE('',(#13666),#87589,.T.);
#92946=ADVANCED_FACE('',(#13667),#87590,.T.);
#92947=ADVANCED_FACE('',(#13668),#87591,.T.);
#92948=ADVANCED_FACE('',(#13669),#87592,.T.);
#92949=ADVANCED_FACE('',(#13670),#87593,.T.);
#92950=ADVANCED_FACE('',(#13671),#87594,.T.);
#92951=ADVANCED_FACE('',(#13672),#87595,.T.);
#92952=ADVANCED_FACE('',(#13673),#87596,.T.);
#92953=ADVANCED_FACE('',(#13674),#87597,.T.);
#92954=ADVANCED_FACE('',(#13675),#87598,.T.);
#92955=ADVANCED_FACE('',(#13676),#4039,.T.);
#92956=ADVANCED_FACE('',(#13677),#4040,.T.);
#92957=ADVANCED_FACE('',(#13678),#4041,.T.);
#92958=ADVANCED_FACE('',(#13679),#4042,.T.);
#92959=ADVANCED_FACE('',(#13680),#4043,.T.);
#92960=ADVANCED_FACE('',(#13681),#4044,.T.);
#92961=ADVANCED_FACE('',(#13682),#4045,.T.);
#92962=ADVANCED_FACE('',(#13683),#4046,.T.);
#92963=ADVANCED_FACE('',(#13684),#4047,.T.);
#92964=ADVANCED_FACE('',(#13685),#4048,.T.);
#92965=ADVANCED_FACE('',(#13686),#4049,.T.);
#92966=ADVANCED_FACE('',(#13687),#4050,.T.);
#92967=ADVANCED_FACE('',(#13688),#4051,.T.);
#92968=ADVANCED_FACE('',(#13689),#4052,.T.);
#92969=ADVANCED_FACE('',(#13690),#4053,.T.);
#92970=ADVANCED_FACE('',(#13691),#87599,.T.);
#92971=ADVANCED_FACE('',(#13692),#4054,.T.);
#92972=ADVANCED_FACE('',(#13693,#7624),#8526,.F.);
#92973=ADVANCED_FACE('',(#13694),#87600,.T.);
#92974=ADVANCED_FACE('',(#13695),#87601,.T.);
#92975=ADVANCED_FACE('',(#13696),#87602,.F.);
#92976=ADVANCED_FACE('',(#13697),#87603,.T.);
#92977=ADVANCED_FACE('',(#13698),#87604,.F.);
#92978=ADVANCED_FACE('',(#13699),#87605,.T.);
#92979=ADVANCED_FACE('',(#13700),#87606,.T.);
#92980=ADVANCED_FACE('',(#13701),#87607,.T.);
#92981=ADVANCED_FACE('',(#13702),#87608,.T.);
#92982=ADVANCED_FACE('',(#13703),#87609,.T.);
#92983=ADVANCED_FACE('',(#13704),#87610,.T.);
#92984=ADVANCED_FACE('',(#13705),#87611,.T.);
#92985=ADVANCED_FACE('',(#13706),#87612,.T.);
#92986=ADVANCED_FACE('',(#13707),#87613,.T.);
#92987=ADVANCED_FACE('',(#13708),#87614,.T.);
#92988=ADVANCED_FACE('',(#13709),#87615,.F.);
#92989=ADVANCED_FACE('',(#13710),#87616,.T.);
#92990=ADVANCED_FACE('',(#13711),#87617,.T.);
#92991=ADVANCED_FACE('',(#13712),#87618,.T.);
#92992=ADVANCED_FACE('',(#13713),#87619,.T.);
#92993=ADVANCED_FACE('',(#13714),#87620,.T.);
#92994=ADVANCED_FACE('',(#13715),#87621,.T.);
#92995=ADVANCED_FACE('',(#13716),#87622,.F.);
#92996=ADVANCED_FACE('',(#13717),#87623,.T.);
#92997=ADVANCED_FACE('',(#13718),#87624,.T.);
#92998=ADVANCED_FACE('',(#13719),#87625,.F.);
#92999=ADVANCED_FACE('',(#13720),#87626,.T.);
#93000=ADVANCED_FACE('',(#13721),#87627,.F.);
#93001=ADVANCED_FACE('',(#13722),#87628,.T.);
#93002=ADVANCED_FACE('',(#13723),#87629,.T.);
#93003=ADVANCED_FACE('',(#13724),#87630,.F.);
#93004=ADVANCED_FACE('',(#13725),#87631,.T.);
#93005=ADVANCED_FACE('',(#13726),#87632,.T.);
#93006=ADVANCED_FACE('',(#13727),#87633,.F.);
#93007=ADVANCED_FACE('',(#13728),#87634,.T.);
#93008=ADVANCED_FACE('',(#13729),#87635,.T.);
#93009=ADVANCED_FACE('',(#13730),#87636,.F.);
#93010=ADVANCED_FACE('',(#13731),#8527,.T.);
#93011=ADVANCED_FACE('',(#13732),#8528,.T.);
#93012=ADVANCED_FACE('',(#13733),#8529,.T.);
#93013=ADVANCED_FACE('',(#13734),#87637,.F.);
#93014=ADVANCED_FACE('',(#13735),#87638,.T.);
#93015=ADVANCED_FACE('',(#13736),#8530,.T.);
#93016=ADVANCED_FACE('',(#13737),#8531,.T.);
#93017=ADVANCED_FACE('',(#13738),#8532,.T.);
#93018=ADVANCED_FACE('',(#13739,#7625),#8533,.T.);
#93019=ADVANCED_FACE('',(#13740,#7626),#8534,.F.);
#93020=ADVANCED_FACE('',(#13741),#4055,.F.);
#93021=ADVANCED_FACE('',(#13742),#87639,.T.);
#93022=ADVANCED_FACE('',(#13743),#87640,.T.);
#93023=ADVANCED_FACE('',(#13744),#87641,.T.);
#93024=ADVANCED_FACE('',(#13745),#87642,.F.);
#93025=ADVANCED_FACE('',(#13746),#87643,.F.);
#93026=ADVANCED_FACE('',(#13747),#87644,.F.);
#93027=ADVANCED_FACE('',(#13748),#87645,.F.);
#93028=ADVANCED_FACE('',(#13749),#87646,.F.);
#93029=ADVANCED_FACE('',(#13750),#87647,.F.);
#93030=ADVANCED_FACE('',(#13751),#87648,.F.);
#93031=ADVANCED_FACE('',(#13752),#87649,.F.);
#93032=ADVANCED_FACE('',(#13753),#87650,.F.);
#93033=ADVANCED_FACE('',(#13754),#87651,.F.);
#93034=ADVANCED_FACE('',(#13755),#87652,.F.);
#93035=ADVANCED_FACE('',(#13756),#87653,.F.);
#93036=ADVANCED_FACE('',(#13757),#4056,.T.);
#93037=ADVANCED_FACE('',(#13758),#87654,.T.);
#93038=ADVANCED_FACE('',(#13759),#4057,.T.);
#93039=ADVANCED_FACE('',(#13760),#87655,.F.);
#93040=ADVANCED_FACE('',(#13761,#7627),#8535,.F.);
#93041=ADVANCED_FACE('',(#13762,#7628),#8536,.T.);
#93042=ADVANCED_FACE('',(#13763),#4058,.T.);
#93043=ADVANCED_FACE('',(#13764),#4059,.T.);
#93044=ADVANCED_FACE('',(#13765),#4060,.T.);
#93045=ADVANCED_FACE('',(#13766),#4061,.T.);
#93046=ADVANCED_FACE('',(#13767),#4062,.T.);
#93047=ADVANCED_FACE('',(#13768),#4063,.T.);
#93048=ADVANCED_FACE('',(#13769),#4064,.T.);
#93049=ADVANCED_FACE('',(#13770),#4065,.T.);
#93050=ADVANCED_FACE('',(#13771),#4066,.T.);
#93051=ADVANCED_FACE('',(#13772),#4067,.T.);
#93052=ADVANCED_FACE('',(#13773),#4068,.T.);
#93053=ADVANCED_FACE('',(#13774),#4069,.T.);
#93054=ADVANCED_FACE('',(#13775),#4070,.T.);
#93055=ADVANCED_FACE('',(#13776),#4071,.T.);
#93056=ADVANCED_FACE('',(#13777),#4072,.T.);
#93057=ADVANCED_FACE('',(#13778),#4073,.T.);
#93058=ADVANCED_FACE('',(#13779),#4074,.T.);
#93059=ADVANCED_FACE('',(#13780),#4075,.T.);
#93060=ADVANCED_FACE('',(#13781),#4076,.T.);
#93061=ADVANCED_FACE('',(#13782),#4077,.T.);
#93062=ADVANCED_FACE('',(#13783),#4078,.T.);
#93063=ADVANCED_FACE('',(#13784),#4079,.T.);
#93064=ADVANCED_FACE('',(#13785),#4080,.T.);
#93065=ADVANCED_FACE('',(#13786),#4081,.T.);
#93066=ADVANCED_FACE('',(#13787),#4082,.T.);
#93067=ADVANCED_FACE('',(#13788),#4083,.T.);
#93068=ADVANCED_FACE('',(#13789),#4084,.T.);
#93069=ADVANCED_FACE('',(#13790),#4085,.T.);
#93070=ADVANCED_FACE('',(#13791),#87656,.T.);
#93071=ADVANCED_FACE('',(#13792),#87657,.T.);
#93072=ADVANCED_FACE('',(#13793),#87658,.T.);
#93073=ADVANCED_FACE('',(#13794),#87659,.T.);
#93074=ADVANCED_FACE('',(#13795),#87660,.T.);
#93075=ADVANCED_FACE('',(#13796),#87661,.T.);
#93076=ADVANCED_FACE('',(#13797),#87662,.T.);
#93077=ADVANCED_FACE('',(#13798),#87663,.T.);
#93078=ADVANCED_FACE('',(#13799),#87664,.T.);
#93079=ADVANCED_FACE('',(#13800),#87665,.T.);
#93080=ADVANCED_FACE('',(#13801),#87666,.T.);
#93081=ADVANCED_FACE('',(#13802),#87667,.T.);
#93082=ADVANCED_FACE('',(#13803),#87668,.T.);
#93083=ADVANCED_FACE('',(#13804),#87669,.T.);
#93084=ADVANCED_FACE('',(#13805),#87670,.T.);
#93085=ADVANCED_FACE('',(#13806),#87671,.T.);
#93086=ADVANCED_FACE('',(#13807),#87672,.T.);
#93087=ADVANCED_FACE('',(#13808),#87673,.T.);
#93088=ADVANCED_FACE('',(#13809),#87674,.T.);
#93089=ADVANCED_FACE('',(#13810),#87675,.T.);
#93090=ADVANCED_FACE('',(#13811),#87676,.T.);
#93091=ADVANCED_FACE('',(#13812),#87677,.T.);
#93092=ADVANCED_FACE('',(#13813),#87678,.T.);
#93093=ADVANCED_FACE('',(#13814),#87679,.T.);
#93094=ADVANCED_FACE('',(#13815),#87680,.T.);
#93095=ADVANCED_FACE('',(#13816),#87681,.T.);
#93096=ADVANCED_FACE('',(#13817),#87682,.T.);
#93097=ADVANCED_FACE('',(#13818),#87683,.T.);
#93098=ADVANCED_FACE('',(#13819),#4086,.T.);
#93099=ADVANCED_FACE('',(#13820),#4087,.T.);
#93100=ADVANCED_FACE('',(#13821),#4088,.T.);
#93101=ADVANCED_FACE('',(#13822),#4089,.T.);
#93102=ADVANCED_FACE('',(#13823),#4090,.T.);
#93103=ADVANCED_FACE('',(#13824),#4091,.T.);
#93104=ADVANCED_FACE('',(#13825),#4092,.T.);
#93105=ADVANCED_FACE('',(#13826),#4093,.T.);
#93106=ADVANCED_FACE('',(#13827),#4094,.T.);
#93107=ADVANCED_FACE('',(#13828),#4095,.T.);
#93108=ADVANCED_FACE('',(#13829),#4096,.T.);
#93109=ADVANCED_FACE('',(#13830),#4097,.T.);
#93110=ADVANCED_FACE('',(#13831),#4098,.T.);
#93111=ADVANCED_FACE('',(#13832),#4099,.T.);
#93112=ADVANCED_FACE('',(#13833),#4100,.T.);
#93113=ADVANCED_FACE('',(#13834),#4101,.T.);
#93114=ADVANCED_FACE('',(#13835),#4102,.T.);
#93115=ADVANCED_FACE('',(#13836),#4103,.T.);
#93116=ADVANCED_FACE('',(#13837),#4104,.T.);
#93117=ADVANCED_FACE('',(#13838),#4105,.T.);
#93118=ADVANCED_FACE('',(#13839),#4106,.T.);
#93119=ADVANCED_FACE('',(#13840),#4107,.T.);
#93120=ADVANCED_FACE('',(#13841),#4108,.T.);
#93121=ADVANCED_FACE('',(#13842),#4109,.T.);
#93122=ADVANCED_FACE('',(#13843),#4110,.T.);
#93123=ADVANCED_FACE('',(#13844),#4111,.T.);
#93124=ADVANCED_FACE('',(#13845),#4112,.T.);
#93125=ADVANCED_FACE('',(#13846),#4113,.T.);
#93126=ADVANCED_FACE('',(#13847),#4114,.T.);
#93127=ADVANCED_FACE('',(#13848),#87684,.T.);
#93128=ADVANCED_FACE('',(#13849),#4115,.T.);
#93129=ADVANCED_FACE('',(#13850,#7629),#8537,.F.);
#93130=ADVANCED_FACE('',(#13851),#87685,.T.);
#93131=ADVANCED_FACE('',(#13852),#87686,.T.);
#93132=ADVANCED_FACE('',(#13853),#87687,.F.);
#93133=ADVANCED_FACE('',(#13854),#87688,.T.);
#93134=ADVANCED_FACE('',(#13855),#87689,.T.);
#93135=ADVANCED_FACE('',(#13856),#87690,.F.);
#93136=ADVANCED_FACE('',(#13857),#87691,.T.);
#93137=ADVANCED_FACE('',(#13858),#87692,.T.);
#93138=ADVANCED_FACE('',(#13859),#87693,.T.);
#93139=ADVANCED_FACE('',(#13860),#87694,.T.);
#93140=ADVANCED_FACE('',(#13861),#87695,.T.);
#93141=ADVANCED_FACE('',(#13862),#87696,.T.);
#93142=ADVANCED_FACE('',(#13863),#87697,.T.);
#93143=ADVANCED_FACE('',(#13864),#87698,.T.);
#93144=ADVANCED_FACE('',(#13865),#87699,.F.);
#93145=ADVANCED_FACE('',(#13866),#87700,.T.);
#93146=ADVANCED_FACE('',(#13867),#87701,.T.);
#93147=ADVANCED_FACE('',(#13868),#87702,.T.);
#93148=ADVANCED_FACE('',(#13869),#87703,.T.);
#93149=ADVANCED_FACE('',(#13870),#87704,.T.);
#93150=ADVANCED_FACE('',(#13871),#87705,.T.);
#93151=ADVANCED_FACE('',(#13872),#87706,.T.);
#93152=ADVANCED_FACE('',(#13873),#87707,.T.);
#93153=ADVANCED_FACE('',(#13874),#87708,.F.);
#93154=ADVANCED_FACE('',(#13875),#87709,.T.);
#93155=ADVANCED_FACE('',(#13876),#87710,.T.);
#93156=ADVANCED_FACE('',(#13877),#87711,.T.);
#93157=ADVANCED_FACE('',(#13878),#87712,.T.);
#93158=ADVANCED_FACE('',(#13879),#87713,.T.);
#93159=ADVANCED_FACE('',(#13880),#87714,.T.);
#93160=ADVANCED_FACE('',(#13881),#87715,.T.);
#93161=ADVANCED_FACE('',(#13882),#87716,.T.);
#93162=ADVANCED_FACE('',(#13883),#87717,.T.);
#93163=ADVANCED_FACE('',(#13884),#87718,.T.);
#93164=ADVANCED_FACE('',(#13885),#87719,.T.);
#93165=ADVANCED_FACE('',(#13886),#87720,.T.);
#93166=ADVANCED_FACE('',(#13887),#87721,.T.);
#93167=ADVANCED_FACE('',(#13888),#87722,.T.);
#93168=ADVANCED_FACE('',(#13889),#87723,.F.);
#93169=ADVANCED_FACE('',(#13890),#87724,.T.);
#93170=ADVANCED_FACE('',(#13891),#87725,.T.);
#93171=ADVANCED_FACE('',(#13892),#87726,.F.);
#93172=ADVANCED_FACE('',(#13893),#87727,.T.);
#93173=ADVANCED_FACE('',(#13894),#87728,.T.);
#93174=ADVANCED_FACE('',(#13895),#87729,.F.);
#93175=ADVANCED_FACE('',(#13896),#87730,.T.);
#93176=ADVANCED_FACE('',(#13897),#87731,.F.);
#93177=ADVANCED_FACE('',(#13898),#87732,.T.);
#93178=ADVANCED_FACE('',(#13899),#87733,.T.);
#93179=ADVANCED_FACE('',(#13900),#87734,.F.);
#93180=ADVANCED_FACE('',(#13901),#87735,.T.);
#93181=ADVANCED_FACE('',(#13902),#87736,.T.);
#93182=ADVANCED_FACE('',(#13903),#87737,.F.);
#93183=ADVANCED_FACE('',(#13904),#87738,.T.);
#93184=ADVANCED_FACE('',(#13905),#87739,.T.);
#93185=ADVANCED_FACE('',(#13906),#87740,.F.);
#93186=ADVANCED_FACE('',(#13907),#87741,.T.);
#93187=ADVANCED_FACE('',(#13908),#87742,.T.);
#93188=ADVANCED_FACE('',(#13909),#87743,.F.);
#93189=ADVANCED_FACE('',(#13910),#87744,.T.);
#93190=ADVANCED_FACE('',(#13911),#87745,.T.);
#93191=ADVANCED_FACE('',(#13912),#87746,.F.);
#93192=ADVANCED_FACE('',(#13913),#87747,.T.);
#93193=ADVANCED_FACE('',(#13914),#87748,.F.);
#93194=ADVANCED_FACE('',(#13915),#87749,.T.);
#93195=ADVANCED_FACE('',(#13916),#87750,.T.);
#93196=ADVANCED_FACE('',(#13917),#87751,.F.);
#93197=ADVANCED_FACE('',(#13918),#87752,.T.);
#93198=ADVANCED_FACE('',(#13919),#87753,.T.);
#93199=ADVANCED_FACE('',(#13920),#87754,.F.);
#93200=ADVANCED_FACE('',(#13921),#87755,.T.);
#93201=ADVANCED_FACE('',(#13922),#87756,.T.);
#93202=ADVANCED_FACE('',(#13923),#87757,.F.);
#93203=ADVANCED_FACE('',(#13924),#87758,.T.);
#93204=ADVANCED_FACE('',(#13925),#87759,.T.);
#93205=ADVANCED_FACE('',(#13926),#87760,.F.);
#93206=ADVANCED_FACE('',(#13927),#8538,.T.);
#93207=ADVANCED_FACE('',(#13928),#8539,.T.);
#93208=ADVANCED_FACE('',(#13929),#8540,.T.);
#93209=ADVANCED_FACE('',(#13930),#87761,.F.);
#93210=ADVANCED_FACE('',(#13931),#87762,.T.);
#93211=ADVANCED_FACE('',(#13932),#87763,.F.);
#93212=ADVANCED_FACE('',(#13933),#87764,.F.);
#93213=ADVANCED_FACE('',(#13934),#87765,.T.);
#93214=ADVANCED_FACE('',(#13935),#87766,.F.);
#93215=ADVANCED_FACE('',(#13936,#7630,#7631),#8541,.T.);
#93216=ADVANCED_FACE('',(#13937,#7632,#7633),#8542,.F.);
#93217=ADVANCED_FACE('',(#13938),#87767,.F.);
#93218=ADVANCED_FACE('',(#13939),#87768,.F.);
#93219=ADVANCED_FACE('',(#13940),#87769,.T.);
#93220=ADVANCED_FACE('',(#13941,#7634,#7635),#8543,.T.);
#93221=ADVANCED_FACE('',(#13942,#7636,#7637),#8544,.F.);
#93222=ADVANCED_FACE('',(#13943),#87770,.F.);
#93223=ADVANCED_FACE('',(#13944),#87771,.T.);
#93224=ADVANCED_FACE('',(#13945),#87772,.F.);
#93225=ADVANCED_FACE('',(#13946),#87773,.T.);
#93226=ADVANCED_FACE('',(#13947),#8545,.T.);
#93227=ADVANCED_FACE('',(#13948),#8546,.F.);
#93228=ADVANCED_FACE('',(#13949),#87774,.T.);
#93229=ADVANCED_FACE('',(#13950),#8547,.T.);
#93230=ADVANCED_FACE('',(#13951),#8548,.F.);
#93231=ADVANCED_FACE('',(#13952),#87775,.F.);
#93232=ADVANCED_FACE('',(#13953),#87776,.F.);
#93233=ADVANCED_FACE('',(#13954),#87777,.T.);
#93234=ADVANCED_FACE('',(#13955),#87778,.F.);
#93235=ADVANCED_FACE('',(#13956,#7638),#8549,.T.);
#93236=ADVANCED_FACE('',(#13957,#7639),#8550,.F.);
#93237=ADVANCED_FACE('',(#13958,#7640),#8551,.T.);
#93238=ADVANCED_FACE('',(#13959,#7641),#8552,.T.);
#93239=ADVANCED_FACE('',(#13960),#4116,.T.);
#93240=ADVANCED_FACE('',(#13961),#4117,.F.);
#93241=ADVANCED_FACE('',(#13962),#4118,.F.);
#93242=ADVANCED_FACE('',(#13963),#7163,.F.);
#93243=ADVANCED_FACE('',(#13964),#4119,.T.);
#93244=ADVANCED_FACE('',(#13965),#4120,.T.);
#93245=ADVANCED_FACE('',(#13966),#87779,.T.);
#93246=ADVANCED_FACE('',(#13967),#87780,.T.);
#93247=ADVANCED_FACE('',(#13968),#87781,.T.);
#93248=ADVANCED_FACE('',(#13969),#4121,.T.);
#93249=ADVANCED_FACE('',(#13970,#7642),#8553,.F.);
#93250=ADVANCED_FACE('',(#13971,#7643),#8554,.F.);
#93251=ADVANCED_FACE('',(#13972,#7644,#7645),#1040,.F.);
#93252=ADVANCED_FACE('',(#13973),#4122,.T.);
#93253=ADVANCED_FACE('',(#13974),#87782,.T.);
#93254=ADVANCED_FACE('',(#13975),#4123,.T.);
#93255=ADVANCED_FACE('',(#13976,#7646),#8555,.F.);
#93256=ADVANCED_FACE('',(#13977,#7647),#8556,.F.);
#93257=ADVANCED_FACE('',(#13978),#1041,.T.);
#93258=ADVANCED_FACE('',(#13979),#1042,.T.);
#93259=ADVANCED_FACE('',(#13980),#1043,.T.);
#93260=ADVANCED_FACE('',(#13981),#1044,.T.);
#93261=ADVANCED_FACE('',(#13982),#1045,.T.);
#93262=ADVANCED_FACE('',(#13983),#1046,.T.);
#93263=ADVANCED_FACE('',(#13984),#1047,.T.);
#93264=ADVANCED_FACE('',(#13985),#1048,.T.);
#93265=ADVANCED_FACE('',(#13986),#1049,.T.);
#93266=ADVANCED_FACE('',(#13987),#1050,.T.);
#93267=ADVANCED_FACE('',(#13988),#1051,.T.);
#93268=ADVANCED_FACE('',(#13989),#1052,.T.);
#93269=ADVANCED_FACE('',(#13990),#1053,.T.);
#93270=ADVANCED_FACE('',(#13991),#1054,.T.);
#93271=ADVANCED_FACE('',(#13992),#1055,.T.);
#93272=ADVANCED_FACE('',(#13993),#1056,.T.);
#93273=ADVANCED_FACE('',(#13994),#1057,.T.);
#93274=ADVANCED_FACE('',(#13995),#1058,.T.);
#93275=ADVANCED_FACE('',(#13996),#1059,.T.);
#93276=ADVANCED_FACE('',(#13997),#1060,.T.);
#93277=ADVANCED_FACE('',(#13998),#1061,.T.);
#93278=ADVANCED_FACE('',(#13999),#1062,.T.);
#93279=ADVANCED_FACE('',(#14000),#1063,.T.);
#93280=ADVANCED_FACE('',(#14001),#1064,.T.);
#93281=ADVANCED_FACE('',(#14002),#87783,.T.);
#93282=ADVANCED_FACE('',(#14003),#87784,.T.);
#93283=ADVANCED_FACE('',(#14004),#87785,.T.);
#93284=ADVANCED_FACE('',(#14005),#87786,.T.);
#93285=ADVANCED_FACE('',(#14006),#8557,.F.);
#93286=ADVANCED_FACE('',(#14007),#8558,.F.);
#93287=ADVANCED_FACE('',(#14008),#8559,.F.);
#93288=ADVANCED_FACE('',(#14009),#8560,.F.);
#93289=ADVANCED_FACE('',(#14010),#8561,.F.);
#93290=ADVANCED_FACE('',(#14011),#8562,.F.);
#93291=ADVANCED_FACE('',(#14012,#7648),#8563,.T.);
#93292=ADVANCED_FACE('',(#14013,#7649),#8564,.F.);
#93293=ADVANCED_FACE('',(#14014,#7650),#8565,.T.);
#93294=ADVANCED_FACE('',(#14015),#8566,.T.);
#93295=ADVANCED_FACE('',(#14016,#7651),#8567,.T.);
#93296=ADVANCED_FACE('',(#14017),#8568,.T.);
#93297=ADVANCED_FACE('',(#14018),#87787,.F.);
#93298=ADVANCED_FACE('',(#14019),#87788,.F.);
#93299=ADVANCED_FACE('',(#14020),#87789,.F.);
#93300=ADVANCED_FACE('',(#14021),#87790,.F.);
#93301=ADVANCED_FACE('',(#14022),#87791,.F.);
#93302=ADVANCED_FACE('',(#14023),#7164,.F.);
#93303=ADVANCED_FACE('',(#14024),#7165,.F.);
#93304=ADVANCED_FACE('',(#14025),#87792,.F.);
#93305=ADVANCED_FACE('',(#14026),#87793,.F.);
#93306=ADVANCED_FACE('',(#14027),#87794,.F.);
#93307=ADVANCED_FACE('',(#14028),#87795,.F.);
#93308=ADVANCED_FACE('',(#14029),#87796,.F.);
#93309=ADVANCED_FACE('',(#14030),#87797,.F.);
#93310=ADVANCED_FACE('',(#14031),#87798,.F.);
#93311=ADVANCED_FACE('',(#14032),#7166,.F.);
#93312=ADVANCED_FACE('',(#14033),#7167,.F.);
#93313=ADVANCED_FACE('',(#14034,#7652),#8569,.F.);
#93314=ADVANCED_FACE('',(#14035),#8570,.T.);
#93315=ADVANCED_FACE('',(#14036),#8571,.T.);
#93316=ADVANCED_FACE('',(#14037),#8572,.T.);
#93317=ADVANCED_FACE('',(#14038),#8573,.T.);
#93318=ADVANCED_FACE('',(#14039),#8574,.T.);
#93319=ADVANCED_FACE('',(#14040),#8575,.T.);
#93320=ADVANCED_FACE('',(#14041,#7653),#8576,.T.);
#93321=ADVANCED_FACE('',(#14042),#7168,.T.);
#93322=ADVANCED_FACE('',(#14043),#7169,.T.);
#93323=ADVANCED_FACE('',(#14044),#7170,.T.);
#93324=ADVANCED_FACE('',(#14045),#7171,.T.);
#93325=ADVANCED_FACE('',(#14046),#7172,.T.);
#93326=ADVANCED_FACE('',(#14047),#7173,.T.);
#93327=ADVANCED_FACE('',(#14048),#7174,.T.);
#93328=ADVANCED_FACE('',(#14049),#7175,.T.);
#93329=ADVANCED_FACE('',(#14050),#7176,.T.);
#93330=ADVANCED_FACE('',(#14051),#7177,.T.);
#93331=ADVANCED_FACE('',(#14052),#7178,.T.);
#93332=ADVANCED_FACE('',(#14053),#7179,.T.);
#93333=ADVANCED_FACE('',(#14054),#3192,.T.);
#93334=ADVANCED_FACE('',(#14055),#3193,.T.);
#93335=ADVANCED_FACE('',(#14056),#87799,.F.);
#93336=ADVANCED_FACE('',(#14057),#87800,.F.);
#93337=ADVANCED_FACE('',(#14058),#87801,.F.);
#93338=ADVANCED_FACE('',(#14059),#87802,.F.);
#93339=ADVANCED_FACE('',(#14060),#87803,.F.);
#93340=ADVANCED_FACE('',(#14061),#87804,.F.);
#93341=ADVANCED_FACE('',(#14062),#87805,.F.);
#93342=ADVANCED_FACE('',(#14063),#87806,.F.);
#93343=ADVANCED_FACE('',(#14064),#87807,.F.);
#93344=ADVANCED_FACE('',(#14065),#87808,.F.);
#93345=ADVANCED_FACE('',(#14066),#87809,.F.);
#93346=ADVANCED_FACE('',(#14067),#87810,.F.);
#93347=ADVANCED_FACE('',(#14068),#87811,.F.);
#93348=ADVANCED_FACE('',(#14069),#87812,.F.);
#93349=ADVANCED_FACE('',(#14070),#87813,.F.);
#93350=ADVANCED_FACE('',(#14071),#1065,.T.);
#93351=ADVANCED_FACE('',(#14072,#7654),#1066,.T.);
#93352=ADVANCED_FACE('',(#14073),#7180,.T.);
#93353=ADVANCED_FACE('',(#14074),#7181,.F.);
#93354=ADVANCED_FACE('',(#14075,#7655),#8577,.T.);
#93355=ADVANCED_FACE('',(#14076),#8578,.F.);
#93356=ADVANCED_FACE('',(#14077),#8579,.F.);
#93357=ADVANCED_FACE('',(#14078),#8580,.F.);
#93358=ADVANCED_FACE('',(#14079),#8581,.F.);
#93359=ADVANCED_FACE('',(#14080),#8582,.F.);
#93360=ADVANCED_FACE('',(#14081),#8583,.F.);
#93361=ADVANCED_FACE('',(#14082,#7656),#8584,.T.);
#93362=ADVANCED_FACE('',(#14083),#8585,.T.);
#93363=ADVANCED_FACE('',(#14084),#3194,.T.);
#93364=ADVANCED_FACE('',(#14085),#3195,.T.);
#93365=ADVANCED_FACE('',(#14086),#87814,.F.);
#93366=ADVANCED_FACE('',(#14087),#87815,.T.);
#93367=ADVANCED_FACE('',(#14088),#7182,.F.);
#93368=ADVANCED_FACE('',(#14089),#87816,.T.);
#93369=ADVANCED_FACE('',(#14090),#3196,.F.);
#93370=ADVANCED_FACE('',(#14091),#3197,.F.);
#93371=ADVANCED_FACE('',(#14092),#87817,.T.);
#93372=ADVANCED_FACE('',(#14093,#7657),#8586,.T.);
#93373=ADVANCED_FACE('',(#14094),#87818,.T.);
#93374=ADVANCED_FACE('',(#14095),#87819,.T.);
#93375=ADVANCED_FACE('',(#14096),#87820,.T.);
#93376=ADVANCED_FACE('',(#14097),#87821,.T.);
#93377=ADVANCED_FACE('',(#14098),#87822,.T.);
#93378=ADVANCED_FACE('',(#14099),#87823,.T.);
#93379=ADVANCED_FACE('',(#14100),#87824,.T.);
#93380=ADVANCED_FACE('',(#14101),#87825,.T.);
#93381=ADVANCED_FACE('',(#14102),#87826,.T.);
#93382=ADVANCED_FACE('',(#14103),#87827,.T.);
#93383=ADVANCED_FACE('',(#14104),#87828,.T.);
#93384=ADVANCED_FACE('',(#14105),#87829,.T.);
#93385=ADVANCED_FACE('',(#14106),#87830,.T.);
#93386=ADVANCED_FACE('',(#14107),#87831,.T.);
#93387=ADVANCED_FACE('',(#14108),#87832,.T.);
#93388=ADVANCED_FACE('',(#14109),#87833,.T.);
#93389=ADVANCED_FACE('',(#14110),#87834,.T.);
#93390=ADVANCED_FACE('',(#14111),#87835,.T.);
#93391=ADVANCED_FACE('',(#14112),#87836,.T.);
#93392=ADVANCED_FACE('',(#14113),#87837,.T.);
#93393=ADVANCED_FACE('',(#14114),#87838,.T.);
#93394=ADVANCED_FACE('',(#14115),#87839,.T.);
#93395=ADVANCED_FACE('',(#14116),#87840,.T.);
#93396=ADVANCED_FACE('',(#14117),#87841,.T.);
#93397=ADVANCED_FACE('',(#14118),#87842,.T.);
#93398=ADVANCED_FACE('',(#14119),#87843,.T.);
#93399=ADVANCED_FACE('',(#14120),#87844,.T.);
#93400=ADVANCED_FACE('',(#14121),#87845,.T.);
#93401=ADVANCED_FACE('',(#14122),#87846,.T.);
#93402=ADVANCED_FACE('',(#14123),#87847,.T.);
#93403=ADVANCED_FACE('',(#14124),#87848,.T.);
#93404=ADVANCED_FACE('',(#14125),#87849,.T.);
#93405=ADVANCED_FACE('',(#14126),#87850,.T.);
#93406=ADVANCED_FACE('',(#14127),#87851,.T.);
#93407=ADVANCED_FACE('',(#14128),#87852,.T.);
#93408=ADVANCED_FACE('',(#14129),#87853,.T.);
#93409=ADVANCED_FACE('',(#14130),#87854,.T.);
#93410=ADVANCED_FACE('',(#14131),#87855,.T.);
#93411=ADVANCED_FACE('',(#14132),#87856,.T.);
#93412=ADVANCED_FACE('',(#14133),#87857,.T.);
#93413=ADVANCED_FACE('',(#14134),#87858,.T.);
#93414=ADVANCED_FACE('',(#14135),#87859,.T.);
#93415=ADVANCED_FACE('',(#14136),#87860,.T.);
#93416=ADVANCED_FACE('',(#14137),#87861,.T.);
#93417=ADVANCED_FACE('',(#14138),#87862,.T.);
#93418=ADVANCED_FACE('',(#14139),#87863,.T.);
#93419=ADVANCED_FACE('',(#14140),#87864,.T.);
#93420=ADVANCED_FACE('',(#14141),#87865,.T.);
#93421=ADVANCED_FACE('',(#14142),#87866,.T.);
#93422=ADVANCED_FACE('',(#14143),#87867,.T.);
#93423=ADVANCED_FACE('',(#14144),#87868,.T.);
#93424=ADVANCED_FACE('',(#14145),#87869,.T.);
#93425=ADVANCED_FACE('',(#14146),#87870,.T.);
#93426=ADVANCED_FACE('',(#14147),#87871,.T.);
#93427=ADVANCED_FACE('',(#14148),#87872,.T.);
#93428=ADVANCED_FACE('',(#14149),#87873,.T.);
#93429=ADVANCED_FACE('',(#14150),#87874,.T.);
#93430=ADVANCED_FACE('',(#14151),#87875,.T.);
#93431=ADVANCED_FACE('',(#14152),#87876,.T.);
#93432=ADVANCED_FACE('',(#14153),#87877,.T.);
#93433=ADVANCED_FACE('',(#14154),#87878,.T.);
#93434=ADVANCED_FACE('',(#14155),#87879,.T.);
#93435=ADVANCED_FACE('',(#14156),#87880,.T.);
#93436=ADVANCED_FACE('',(#14157),#87881,.T.);
#93437=ADVANCED_FACE('',(#14158),#87882,.T.);
#93438=ADVANCED_FACE('',(#14159),#87883,.T.);
#93439=ADVANCED_FACE('',(#14160),#7183,.F.);
#93440=ADVANCED_FACE('',(#14161),#7184,.T.);
#93441=ADVANCED_FACE('',(#14162),#87884,.T.);
#93442=ADVANCED_FACE('',(#14163),#3198,.F.);
#93443=ADVANCED_FACE('',(#14164),#3199,.F.);
#93444=ADVANCED_FACE('',(#14165),#87885,.T.);
#93445=ADVANCED_FACE('',(#14166),#8587,.T.);
#93446=ADVANCED_FACE('',(#14167,#7658),#8588,.F.);
#93447=ADVANCED_FACE('',(#14168,#7659),#8589,.T.);
#93448=ADVANCED_FACE('',(#14169),#8590,.F.);
#93449=ADVANCED_FACE('',(#14170),#8591,.F.);
#93450=ADVANCED_FACE('',(#14171),#8592,.F.);
#93451=ADVANCED_FACE('',(#14172),#8593,.F.);
#93452=ADVANCED_FACE('',(#14173),#8594,.T.);
#93453=ADVANCED_FACE('',(#14174),#8595,.T.);
#93454=ADVANCED_FACE('',(#14175),#8596,.T.);
#93455=ADVANCED_FACE('',(#14176),#8597,.T.);
#93456=ADVANCED_FACE('',(#14177),#8598,.T.);
#93457=ADVANCED_FACE('',(#14178),#8599,.T.);
#93458=ADVANCED_FACE('',(#14179,#7660),#8600,.F.);
#93459=ADVANCED_FACE('',(#14180),#7185,.T.);
#93460=ADVANCED_FACE('',(#14181),#7186,.T.);
#93461=ADVANCED_FACE('',(#14182),#7187,.T.);
#93462=ADVANCED_FACE('',(#14183),#7188,.T.);
#93463=ADVANCED_FACE('',(#14184),#7189,.T.);
#93464=ADVANCED_FACE('',(#14185),#7190,.T.);
#93465=ADVANCED_FACE('',(#14186),#7191,.T.);
#93466=ADVANCED_FACE('',(#14187),#7192,.T.);
#93467=ADVANCED_FACE('',(#14188),#7193,.T.);
#93468=ADVANCED_FACE('',(#14189),#7194,.T.);
#93469=ADVANCED_FACE('',(#14190),#7195,.T.);
#93470=ADVANCED_FACE('',(#14191),#7196,.T.);
#93471=ADVANCED_FACE('',(#14192),#8601,.F.);
#93472=ADVANCED_FACE('',(#14193),#3200,.F.);
#93473=ADVANCED_FACE('',(#14194),#3201,.F.);
#93474=ADVANCED_FACE('',(#14195),#87886,.T.);
#93475=ADVANCED_FACE('',(#14196),#87887,.F.);
#93476=ADVANCED_FACE('',(#14197),#87888,.F.);
#93477=ADVANCED_FACE('',(#14198),#87889,.F.);
#93478=ADVANCED_FACE('',(#14199),#87890,.F.);
#93479=ADVANCED_FACE('',(#14200),#87891,.F.);
#93480=ADVANCED_FACE('',(#14201),#87892,.F.);
#93481=ADVANCED_FACE('',(#14202),#87893,.F.);
#93482=ADVANCED_FACE('',(#14203),#87894,.F.);
#93483=ADVANCED_FACE('',(#14204),#87895,.F.);
#93484=ADVANCED_FACE('',(#14205),#87896,.T.);
#93485=ADVANCED_FACE('',(#14206),#87897,.F.);
#93486=ADVANCED_FACE('',(#14207,#7661),#1067,.F.);
#93487=ADVANCED_FACE('',(#14208),#4124,.T.);
#93488=ADVANCED_FACE('',(#14209),#4125,.T.);
#93489=ADVANCED_FACE('',(#14210),#87898,.F.);
#93490=ADVANCED_FACE('',(#14211),#4126,.F.);
#93491=ADVANCED_FACE('',(#14212),#87899,.F.);
#93492=ADVANCED_FACE('',(#14213,#7662),#8602,.T.);
#93493=ADVANCED_FACE('',(#14214,#7663),#8603,.F.);
#93494=ADVANCED_FACE('',(#14215),#8604,.F.);
#93495=ADVANCED_FACE('',(#14216,#7664),#8605,.F.);
#93496=ADVANCED_FACE('',(#14217),#8606,.T.);
#93497=ADVANCED_FACE('',(#14218),#8607,.T.);
#93498=ADVANCED_FACE('',(#14219),#8608,.T.);
#93499=ADVANCED_FACE('',(#14220),#8609,.T.);
#93500=ADVANCED_FACE('',(#14221),#8610,.T.);
#93501=ADVANCED_FACE('',(#14222),#8611,.T.);
#93502=ADVANCED_FACE('',(#14223),#8612,.T.);
#93503=ADVANCED_FACE('',(#14224),#8613,.T.);
#93504=ADVANCED_FACE('',(#14225),#8614,.T.);
#93505=ADVANCED_FACE('',(#14226,#7665,#7666,#7667,#7668,#7669,#7670,#7671,
#7672,#7673),#8615,.F.);
#93506=ADVANCED_FACE('',(#14227,#7674),#8616,.F.);
#93507=ADVANCED_FACE('',(#14228,#7675),#8617,.T.);
#93508=ADVANCED_FACE('',(#14229),#8618,.F.);
#93509=ADVANCED_FACE('',(#14230),#8619,.F.);
#93510=ADVANCED_FACE('',(#14231),#8620,.F.);
#93511=ADVANCED_FACE('',(#14232),#8621,.F.);
#93512=ADVANCED_FACE('',(#14233),#8622,.T.);
#93513=ADVANCED_FACE('',(#14234),#8623,.T.);
#93514=ADVANCED_FACE('',(#14235),#8624,.T.);
#93515=ADVANCED_FACE('',(#14236),#8625,.T.);
#93516=ADVANCED_FACE('',(#14237),#8626,.F.);
#93517=ADVANCED_FACE('',(#14238),#8627,.F.);
#93518=ADVANCED_FACE('',(#14239),#8628,.F.);
#93519=ADVANCED_FACE('',(#14240),#8629,.F.);
#93520=ADVANCED_FACE('',(#14241),#8630,.F.);
#93521=ADVANCED_FACE('',(#14242),#8631,.T.);
#93522=ADVANCED_FACE('',(#14243),#87900,.F.);
#93523=ADVANCED_FACE('',(#14244),#87901,.F.);
#93524=ADVANCED_FACE('',(#14245),#87902,.F.);
#93525=ADVANCED_FACE('',(#14246),#87903,.F.);
#93526=ADVANCED_FACE('',(#14247),#87904,.F.);
#93527=ADVANCED_FACE('',(#14248),#87905,.F.);
#93528=ADVANCED_FACE('',(#14249),#87906,.F.);
#93529=ADVANCED_FACE('',(#14250),#87907,.F.);
#93530=ADVANCED_FACE('',(#14251),#8632,.T.);
#93531=ADVANCED_FACE('',(#14252),#8633,.T.);
#93532=ADVANCED_FACE('',(#14253),#8634,.T.);
#93533=ADVANCED_FACE('',(#14254),#8635,.T.);
#93534=ADVANCED_FACE('',(#14255,#7676,#7677),#8636,.T.);
#93535=ADVANCED_FACE('',(#14256,#7678,#7679,#7680),#8637,.T.);
#93536=ADVANCED_FACE('',(#14257,#7681,#7682,#7683),#8638,.F.);
#93537=ADVANCED_FACE('',(#14258,#7684,#7685,#7686),#8639,.T.);
#93538=ADVANCED_FACE('',(#14259,#7687,#7688),#8640,.T.);
#93539=ADVANCED_FACE('',(#14260,#7689,#7690,#7691),#8641,.T.);
#93540=ADVANCED_FACE('',(#14261),#87908,.F.);
#93541=ADVANCED_FACE('',(#14262),#87909,.F.);
#93542=ADVANCED_FACE('',(#14263),#8642,.T.);
#93543=ADVANCED_FACE('',(#14264),#8643,.T.);
#93544=ADVANCED_FACE('',(#14265),#8644,.F.);
#93545=ADVANCED_FACE('',(#14266),#8645,.T.);
#93546=ADVANCED_FACE('',(#14267),#8646,.T.);
#93547=ADVANCED_FACE('',(#14268),#8647,.F.);
#93548=ADVANCED_FACE('',(#14269),#8648,.T.);
#93549=ADVANCED_FACE('',(#14270),#8649,.F.);
#93550=ADVANCED_FACE('',(#14271),#8650,.T.);
#93551=ADVANCED_FACE('',(#14272),#8651,.T.);
#93552=ADVANCED_FACE('',(#14273),#8652,.T.);
#93553=ADVANCED_FACE('',(#14274),#8653,.T.);
#93554=ADVANCED_FACE('',(#14275),#8654,.T.);
#93555=ADVANCED_FACE('',(#14276),#8655,.T.);
#93556=ADVANCED_FACE('',(#14277),#87910,.T.);
#93557=ADVANCED_FACE('',(#14278,#7692,#7693),#8656,.T.);
#93558=ADVANCED_FACE('',(#14279),#87911,.T.);
#93559=ADVANCED_FACE('',(#14280),#87912,.F.);
#93560=ADVANCED_FACE('',(#14281,#7694,#7695),#8657,.F.);
#93561=ADVANCED_FACE('',(#14282),#87913,.F.);
#93562=ADVANCED_FACE('',(#14283),#8658,.T.);
#93563=ADVANCED_FACE('',(#14284),#8659,.T.);
#93564=ADVANCED_FACE('',(#14285),#7197,.T.);
#93565=ADVANCED_FACE('',(#14286),#7198,.T.);
#93566=ADVANCED_FACE('',(#14287),#87914,.T.);
#93567=ADVANCED_FACE('',(#14288),#87915,.T.);
#93568=ADVANCED_FACE('',(#14289),#87916,.T.);
#93569=ADVANCED_FACE('',(#14290),#87917,.T.);
#93570=ADVANCED_FACE('',(#14291),#87918,.T.);
#93571=ADVANCED_FACE('',(#14292),#87919,.T.);
#93572=ADVANCED_FACE('',(#14293),#87920,.T.);
#93573=ADVANCED_FACE('',(#14294),#87921,.T.);
#93574=ADVANCED_FACE('',(#14295),#87922,.T.);
#93575=ADVANCED_FACE('',(#14296),#87923,.T.);
#93576=ADVANCED_FACE('',(#14297),#87924,.T.);
#93577=ADVANCED_FACE('',(#14298),#87925,.T.);
#93578=ADVANCED_FACE('',(#14299),#87926,.T.);
#93579=ADVANCED_FACE('',(#14300),#87927,.T.);
#93580=ADVANCED_FACE('',(#14301),#87928,.T.);
#93581=ADVANCED_FACE('',(#14302),#87929,.T.);
#93582=ADVANCED_FACE('',(#14303),#87930,.T.);
#93583=ADVANCED_FACE('',(#14304),#87931,.T.);
#93584=ADVANCED_FACE('',(#14305),#87932,.T.);
#93585=ADVANCED_FACE('',(#14306),#87933,.T.);
#93586=ADVANCED_FACE('',(#14307),#87934,.T.);
#93587=ADVANCED_FACE('',(#14308),#87935,.T.);
#93588=ADVANCED_FACE('',(#14309),#87936,.T.);
#93589=ADVANCED_FACE('',(#14310),#87937,.T.);
#93590=ADVANCED_FACE('',(#14311),#87938,.T.);
#93591=ADVANCED_FACE('',(#14312),#87939,.T.);
#93592=ADVANCED_FACE('',(#14313),#87940,.T.);
#93593=ADVANCED_FACE('',(#14314),#87941,.T.);
#93594=ADVANCED_FACE('',(#14315),#87942,.T.);
#93595=ADVANCED_FACE('',(#14316),#87943,.T.);
#93596=ADVANCED_FACE('',(#14317),#87944,.T.);
#93597=ADVANCED_FACE('',(#14318),#87945,.T.);
#93598=ADVANCED_FACE('',(#14319),#87946,.T.);
#93599=ADVANCED_FACE('',(#14320),#87947,.T.);
#93600=ADVANCED_FACE('',(#14321),#8660,.F.);
#93601=ADVANCED_FACE('',(#14322),#7199,.T.);
#93602=ADVANCED_FACE('',(#14323),#3202,.T.);
#93603=ADVANCED_FACE('',(#14324),#3203,.T.);
#93604=ADVANCED_FACE('',(#14325),#87948,.T.);
#93605=ADVANCED_FACE('',(#14326),#8661,.T.);
#93606=ADVANCED_FACE('',(#14327),#8662,.T.);
#93607=ADVANCED_FACE('',(#14328),#8663,.T.);
#93608=ADVANCED_FACE('',(#14329),#8664,.T.);
#93609=ADVANCED_FACE('',(#14330),#984,.T.);
#93610=ADVANCED_FACE('',(#14331),#985,.T.);
#93611=ADVANCED_FACE('',(#14332),#986,.T.);
#93612=ADVANCED_FACE('',(#14333),#987,.T.);
#93613=ADVANCED_FACE('',(#14334),#988,.T.);
#93614=ADVANCED_FACE('',(#14335),#989,.T.);
#93615=ADVANCED_FACE('',(#14336),#990,.T.);
#93616=ADVANCED_FACE('',(#14337),#991,.T.);
#93617=ADVANCED_FACE('',(#14338),#992,.T.);
#93618=ADVANCED_FACE('',(#14339),#993,.T.);
#93619=ADVANCED_FACE('',(#14340),#994,.T.);
#93620=ADVANCED_FACE('',(#14341),#995,.T.);
#93621=ADVANCED_FACE('',(#14342),#996,.T.);
#93622=ADVANCED_FACE('',(#14343),#997,.T.);
#93623=ADVANCED_FACE('',(#14344),#998,.T.);
#93624=ADVANCED_FACE('',(#14345),#999,.T.);
#93625=ADVANCED_FACE('',(#14346,#7696,#7697),#8665,.T.);
#93626=ADVANCED_FACE('',(#14347,#7698,#7699),#8666,.T.);
#93627=ADVANCED_FACE('',(#14348),#8667,.T.);
#93628=ADVANCED_FACE('',(#14349),#1000,.T.);
#93629=ADVANCED_FACE('',(#14350),#1001,.T.);
#93630=ADVANCED_FACE('',(#14351),#1002,.T.);
#93631=ADVANCED_FACE('',(#14352),#1003,.T.);
#93632=ADVANCED_FACE('',(#14353),#1004,.T.);
#93633=ADVANCED_FACE('',(#14354),#1005,.T.);
#93634=ADVANCED_FACE('',(#14355),#1006,.T.);
#93635=ADVANCED_FACE('',(#14356),#1007,.T.);
#93636=ADVANCED_FACE('',(#14357),#1008,.T.);
#93637=ADVANCED_FACE('',(#14358),#1009,.T.);
#93638=ADVANCED_FACE('',(#14359),#1010,.T.);
#93639=ADVANCED_FACE('',(#14360),#1011,.T.);
#93640=ADVANCED_FACE('',(#14361),#1012,.T.);
#93641=ADVANCED_FACE('',(#14362),#1013,.T.);
#93642=ADVANCED_FACE('',(#14363),#1014,.T.);
#93643=ADVANCED_FACE('',(#14364),#1015,.T.);
#93644=ADVANCED_FACE('',(#14365),#8668,.T.);
#93645=ADVANCED_FACE('',(#14366),#8669,.T.);
#93646=ADVANCED_FACE('',(#14367),#8670,.T.);
#93647=ADVANCED_FACE('',(#14368),#8671,.T.);
#93648=ADVANCED_FACE('',(#14369,#7700,#7701,#7702),#8672,.T.);
#93649=ADVANCED_FACE('',(#14370),#7200,.T.);
#93650=ADVANCED_FACE('',(#14371),#7201,.T.);
#93651=ADVANCED_FACE('',(#14372),#7202,.T.);
#93652=ADVANCED_FACE('',(#14373),#7203,.T.);
#93653=ADVANCED_FACE('',(#14374),#7204,.T.);
#93654=ADVANCED_FACE('',(#14375),#7205,.T.);
#93655=ADVANCED_FACE('',(#14376),#8673,.F.);
#93656=ADVANCED_FACE('',(#14377),#8674,.F.);
#93657=ADVANCED_FACE('',(#14378),#8675,.F.);
#93658=ADVANCED_FACE('',(#14379),#8676,.F.);
#93659=ADVANCED_FACE('',(#14380),#8677,.F.);
#93660=ADVANCED_FACE('',(#14381),#8678,.F.);
#93661=ADVANCED_FACE('',(#14382,#7703),#8679,.F.);
#93662=ADVANCED_FACE('',(#14383),#87949,.T.);
#93663=ADVANCED_FACE('',(#14384),#7206,.T.);
#93664=ADVANCED_FACE('',(#14385),#7207,.F.);
#93665=ADVANCED_FACE('',(#14386),#87950,.F.);
#93666=ADVANCED_FACE('',(#14387),#87951,.F.);
#93667=ADVANCED_FACE('',(#14388),#87952,.F.);
#93668=ADVANCED_FACE('',(#14389),#87953,.F.);
#93669=ADVANCED_FACE('',(#14390),#87954,.F.);
#93670=ADVANCED_FACE('',(#14391),#87955,.F.);
#93671=ADVANCED_FACE('',(#14392),#87956,.F.);
#93672=ADVANCED_FACE('',(#14393),#87957,.F.);
#93673=ADVANCED_FACE('',(#14394),#87958,.F.);
#93674=ADVANCED_FACE('',(#14395),#3204,.F.);
#93675=ADVANCED_FACE('',(#14396),#87959,.F.);
#93676=ADVANCED_FACE('',(#14397),#3205,.F.);
#93677=ADVANCED_FACE('',(#14398),#87960,.T.);
#93678=ADVANCED_FACE('',(#14399),#87961,.T.);
#93679=ADVANCED_FACE('',(#14400),#87962,.T.);
#93680=ADVANCED_FACE('',(#14401),#87963,.T.);
#93681=ADVANCED_FACE('',(#14402),#87964,.T.);
#93682=ADVANCED_FACE('',(#14403),#87965,.T.);
#93683=ADVANCED_FACE('',(#14404),#7208,.T.);
#93684=ADVANCED_FACE('',(#14405),#7209,.T.);
#93685=ADVANCED_FACE('',(#14406),#7210,.T.);
#93686=ADVANCED_FACE('',(#14407),#7211,.T.);
#93687=ADVANCED_FACE('',(#14408),#7212,.T.);
#93688=ADVANCED_FACE('',(#14409),#7213,.T.);
#93689=ADVANCED_FACE('',(#14410),#7214,.T.);
#93690=ADVANCED_FACE('',(#14411),#7215,.T.);
#93691=ADVANCED_FACE('',(#14412),#7216,.T.);
#93692=ADVANCED_FACE('',(#14413),#7217,.T.);
#93693=ADVANCED_FACE('',(#14414),#7218,.T.);
#93694=ADVANCED_FACE('',(#14415),#7219,.T.);
#93695=ADVANCED_FACE('',(#14416),#87966,.F.);
#93696=ADVANCED_FACE('',(#14417),#8680,.F.);
#93697=ADVANCED_FACE('',(#14418),#8681,.F.);
#93698=ADVANCED_FACE('',(#14419),#8682,.F.);
#93699=ADVANCED_FACE('',(#14420),#8683,.F.);
#93700=ADVANCED_FACE('',(#14421),#8684,.F.);
#93701=ADVANCED_FACE('',(#14422),#8685,.F.);
#93702=ADVANCED_FACE('',(#14423,#7704),#8686,.T.);
#93703=ADVANCED_FACE('',(#14424,#7705),#8687,.F.);
#93704=ADVANCED_FACE('',(#14425),#7220,.F.);
#93705=ADVANCED_FACE('',(#14426),#7221,.F.);
#93706=CLOSED_SHELL('',(#87967,#87968,#87969,#87970,#87971,#87972,#87973,
#87974,#87975,#87976,#87977,#87978,#87979,#87980,#87981,#87982,#87983,#87984,
#87985,#87986,#87987,#87988,#87989,#87990,#87991,#87992));
#93707=CLOSED_SHELL('',(#87993,#87994,#87995,#87996,#87997,#87998,#87999,
#88000,#88001,#88002,#88003,#88004,#88005,#88006,#88007,#88008,#88009,#88010,
#88011,#88012,#88013,#88014,#88015,#88016,#88017,#88018));
#93708=CLOSED_SHELL('',(#88019,#88020,#88021,#88022,#88023,#88024));
#93709=CLOSED_SHELL('',(#88025,#88026,#88027,#88028,#88029,#88030));
#93710=CLOSED_SHELL('',(#88031,#88032,#88033,#88034,#88035,#88036,#88037,
#88038,#88039,#88040,#88041,#88042,#88043,#88044,#88045,#88046,#88047,#88048,
#88049,#88050,#88051,#88052,#88053,#88054,#88055,#88056,#88057,#88058,#88059,
#88060,#88061,#88062,#88063,#88064,#88065,#88066,#88067,#88068,#88069,#88070,
#88071,#88072,#88073,#88074,#88075,#88076,#88077,#88078,#88079,#88080,#88081,
#88082,#88083,#88084,#88085,#88086,#88087,#88088,#88089,#88090,#88091,#88092,
#88093,#88094,#88095,#88096,#88097,#88098,#88099,#88100,#88101,#88102,#88103,
#88104,#88105,#88106,#88107,#88108,#88109,#88110,#88111,#88112,#88113,#88114,
#88115,#88116,#88117,#88118,#88119,#88120,#88121,#88122,#88123,#88124,#88125,
#88126,#88127,#88128,#88129,#88130,#88131,#88132,#88133,#88134,#88135,#88136,
#88137,#88138,#88139,#88140,#88141,#88142,#88143,#88144,#88145,#88146,#88147,
#88148,#88149,#88150,#88151,#88152,#88153,#88154,#88155,#88156,#88157,#88158,
#88159,#88160,#88161,#88162,#88163,#88164,#88165,#88166,#88167,#88168,#88169,
#88170,#88171,#88172,#88173,#88174,#88175,#88176,#88177,#88178,#88179,#88180,
#88181,#88182,#88183,#88184,#88185,#88186,#88187,#88188,#88189,#88190,#88191,
#88192,#88193,#88194,#88195,#88196,#88197,#88198,#88199,#88200,#88201,#88202,
#88203,#88204,#88205,#88206,#88207,#88208,#88209,#88210,#88211,#88212,#88213,
#88214,#88215,#88216,#88217,#88218,#88219,#88220,#88221,#88222,#88223,#88224,
#88225,#88226,#88227,#88228,#88229,#88230,#88231,#88232,#88233,#88234,#88235,
#88236,#88237,#88238,#88239,#88240,#88241,#88242,#88243,#88244,#88245,#88246,
#88247,#88248,#88249,#88250,#88251,#88252,#88253,#88254,#88255,#88256,#88257,
#88258,#88259,#88260,#88261,#88262,#88263,#88264,#88265,#88266,#88267,#88268,
#88269,#88270,#88271,#88272,#88273,#88274,#88275,#88276,#88277,#88278,#88279,
#88280,#88281,#88282,#88283,#88284,#88285,#88286,#88287,#88288,#88289,#88290,
#88291,#88292,#88293,#88294,#88295,#88296,#88297,#88298,#88299,#88300,#88301,
#88302,#88303,#88304,#88305,#88306,#88307,#88308,#88309,#88310,#88311,#88312,
#88313,#88314,#88315,#88316,#88317,#88318,#88319,#88320,#88321,#88322,#88323,
#88324,#88325,#88326,#88327,#88328,#88329,#88330,#88331,#88332,#88333,#88334,
#88335,#88336,#88337,#88338,#88339,#88340,#88341,#88342,#88343,#88344,#88345,
#88346,#88347,#88348,#88349,#88350,#88351,#88352,#88353,#88354,#88355,#88356,
#88357,#88358,#88359,#88360,#88361,#88362,#88363,#88364,#88365,#88366,#88367,
#88368,#88369,#88370,#88371,#88372,#88373,#88374,#88375,#88376,#88377,#88378,
#88379,#88380,#88381,#88382,#88383,#88384,#88385,#88386,#88387,#88388,#88389,
#88390,#88391,#88392,#88393,#88394,#88395,#88396,#88397,#88398,#88399,#88400,
#88401,#88402,#88403,#88404,#88405,#88406,#88407,#88408,#88409,#88410,#88411,
#88412,#88413,#88414,#88415,#88416,#88417,#88418,#88419,#88420,#88421,#88422,
#88423,#88424,#88425,#88426,#88427,#88428,#88429,#88430,#88431,#88432,#88433,
#88434,#88435,#88436,#88437,#88438,#88439,#88440,#88441,#88442,#88443,#88444,
#88445,#88446,#88447,#88448,#88449,#88450,#88451,#88452,#88453,#88454,#88455,
#88456,#88457,#88458,#88459,#88460,#88461,#88462,#88463,#88464,#88465,#88466,
#88467,#88468,#88469,#88470,#88471,#88472,#88473,#88474,#88475,#88476,#88477,
#88478,#88479,#88480,#88481,#88482,#88483,#88484,#88485,#88486,#88487,#88488,
#88489,#88490,#88491,#88492,#88493,#88494,#88495,#88496,#88497,#88498,#88499,
#88500,#88501,#88502,#88503,#88504,#88505,#88506,#88507,#88508,#88509,#88510,
#88511,#88512,#88513,#88514,#88515,#88516,#88517,#88518,#88519,#88520,#88521,
#88522,#88523,#88524,#88525,#88526,#88527,#88528,#88529,#88530,#88531,#88532,
#88533,#88534,#88535,#88536,#88537,#88538,#88539,#88540,#88541,#88542,#88543,
#88544,#88545,#88546,#88547,#88548,#88549,#88550,#88551,#88552,#88553,#88554,
#88555,#88556,#88557,#88558,#88559,#88560,#88561,#88562,#88563,#88564,#88565,
#88566,#88567,#88568,#88569,#88570,#88571,#88572,#88573,#88574,#88575,#88576,
#88577,#88578,#88579,#88580,#88581,#88582,#88583,#88584,#88585,#88586,#88587,
#88588,#88589,#88590,#88591,#88592,#88593,#88594,#88595,#88596,#88597,#88598,
#88599,#88600,#88601,#88602,#88603,#88604,#88605,#88606,#88607,#88608,#88609,
#88610,#88611,#88612,#88613,#88614,#88615,#88616,#88617,#88618,#88619,#88620,
#88621,#88622,#88623,#88624,#88625,#88626,#88627,#88628,#88629,#88630,#88631,
#88632,#88633,#88634,#88635,#88636,#88637,#88638,#88639,#88640,#88641,#88642,
#88643,#88644,#88645,#88646,#88647,#88648,#88649,#88650,#88651,#88652,#88653,
#88654,#88655,#88656,#88657,#88658,#88659,#88660,#88661,#88662,#88663,#88664,
#88665,#88666,#88667,#88668,#88669,#88670,#88671,#88672,#88673,#88674,#88675,
#88676,#88677,#88678,#88679,#88680,#88681,#88682,#88683,#88684,#88685,#88686,
#88687,#88688,#88689,#88690,#88691,#88692,#88693,#88694,#88695,#88696,#88697,
#88698,#88699,#88700,#88701,#88702,#88703,#88704,#88705,#88706,#88707,#88708,
#88709,#88710,#88711,#88712,#88713,#88714,#88715,#88716,#88717,#88718,#88719,
#88720,#88721,#88722,#88723,#88724,#88725,#88726,#88727,#88728,#88729,#88730,
#88731,#88732,#88733,#88734,#88735,#88736,#88737,#88738,#88739,#88740,#88741,
#88742,#88743,#88744,#88745,#88746,#88747,#88748,#88749,#88750,#88751,#88752,
#88753,#88754,#88755,#88756,#88757,#88758,#88759,#88760,#88761,#88762,#88763,
#88764,#88765,#88766,#88767,#88768,#88769,#88770,#88771,#88772,#88773,#88774,
#88775,#88776,#88777,#88778,#88779,#88780,#88781,#88782,#88783,#88784,#88785,
#88786,#88787,#88788,#88789,#88790,#88791,#88792,#88793,#88794,#88795,#88796,
#88797,#88798,#88799,#88800,#88801,#88802,#88803,#88804,#88805,#88806,#88807,
#88808,#88809,#88810,#88811,#88812,#88813,#88814,#88815,#88816,#88817,#88818,
#88819,#88820,#88821,#88822,#88823,#88824,#88825,#88826,#88827,#88828,#88829,
#88830,#88831,#88832,#88833,#88834,#88835,#88836,#88837,#88838,#88839,#88840,
#88841,#88842,#88843,#88844,#88845,#88846,#88847,#88848,#88849,#88850,#88851,
#88852,#88853,#88854,#88855,#88856,#88857,#88858,#88859,#88860,#88861,#88862,
#88863,#88864,#88865,#88866,#88867,#88868,#88869,#88870,#88871,#88872,#88873,
#88874,#88875,#88876,#88877,#88878,#88879,#88880,#88881,#88882,#88883,#88884,
#88885,#88886,#88887,#88888,#88889,#88890,#88891,#88892,#88893,#88894,#88895,
#88896,#88897,#88898,#88899,#88900,#88901,#88902,#88903,#88904,#88905,#88906,
#88907,#88908,#88909,#88910,#88911,#88912,#88913,#88914,#88915,#88916,#88917,
#88918,#88919,#88920,#88921,#88922,#88923,#88924,#88925,#88926,#88927,#88928,
#88929,#88930,#88931,#88932,#88933,#88934,#88935,#88936,#88937,#88938,#88939,
#88940,#88941,#88942,#88943,#88944,#88945,#88946,#88947,#88948,#88949,#88950,
#88951,#88952,#88953,#88954,#88955,#88956,#88957,#88958,#88959,#88960,#88961,
#88962,#88963,#88964,#88965,#88966,#88967,#88968,#88969,#88970,#88971,#88972,
#88973,#88974,#88975,#88976,#88977,#88978,#88979,#88980,#88981,#88982,#88983,
#88984,#88985,#88986,#88987,#88988,#88989,#88990,#88991,#88992,#88993,#88994,
#88995,#88996,#88997,#88998,#88999,#89000,#89001,#89002,#89003,#89004,#89005,
#89006,#89007,#89008,#89009,#89010,#89011,#89012,#89013,#89014,#89015,#89016,
#89017,#89018,#89019,#89020,#89021,#89022,#89023,#89024,#89025,#89026,#89027,
#89028,#89029,#89030,#89031,#89032,#89033,#89034,#89035,#89036,#89037,#89038,
#89039,#89040,#89041,#89042,#89043,#89044,#89045,#89046,#89047,#89048,#89049,
#89050,#89051,#89052,#89053,#89054,#89055,#89056,#89057,#89058,#89059,#89060,
#89061,#89062,#89063,#89064,#89065,#89066,#89067,#89068,#89069,#89070,#89071,
#89072,#89073,#89074,#89075,#89076,#89077,#89078,#89079,#89080,#89081,#89082,
#89083,#89084,#89085,#89086,#89087,#89088,#89089,#89090,#89091,#89092,#89093,
#89094,#89095,#89096,#89097,#89098,#89099,#89100,#89101,#89102,#89103,#89104,
#89105,#89106,#89107,#89108,#89109,#89110,#89111,#89112,#89113,#89114,#89115,
#89116,#89117,#89118,#89119,#89120,#89121,#89122,#89123,#89124,#89125,#89126,
#89127,#89128,#89129,#89130,#89131,#89132,#89133,#89134,#89135,#89136,#89137,
#89138,#89139,#89140,#89141,#89142,#89143,#89144,#89145,#89146,#89147,#89148,
#89149,#89150,#89151,#89152,#89153,#89154,#89155,#89156,#89157,#89158,#89159,
#89160,#89161,#89162,#89163,#89164,#89165,#89166,#89167,#89168,#89169,#89170,
#89171,#89172,#89173,#89174,#89175,#89176,#89177,#89178,#89179,#89180,#89181,
#89182,#89183,#89184,#89185,#89186,#89187,#89188,#89189,#89190,#89191,#89192,
#89193,#89194,#89195,#89196,#89197,#89198,#89199,#89200,#89201,#89202,#89203,
#89204,#89205,#89206,#89207,#89208,#89209,#89210,#89211,#89212,#89213,#89214,
#89215,#89216,#89217,#89218,#89219,#89220,#89221,#89222,#89223,#89224,#89225,
#89226,#89227,#89228,#89229,#89230,#89231,#89232,#89233,#89234,#89235,#89236,
#89237,#89238,#89239,#89240,#89241,#89242,#89243,#89244,#89245,#89246,#89247,
#89248,#89249,#89250,#89251,#89252,#89253,#89254,#89255,#89256,#89257,#89258,
#89259,#89260,#89261,#89262,#89263,#89264,#89265,#89266,#89267,#89268,#89269,
#89270,#89271,#89272,#89273,#89274,#89275,#89276,#89277,#89278,#89279,#89280,
#89281,#89282,#89283,#89284,#89285,#89286,#89287,#89288,#89289,#89290,#89291,
#89292,#89293,#89294,#89295,#89296,#89297,#89298,#89299,#89300,#89301,#89302,
#89303,#89304,#89305,#89306,#89307,#89308,#89309,#89310,#89311,#89312,#89313,
#89314,#89315,#89316,#89317,#89318,#89319,#89320,#89321,#89322,#89323,#89324,
#89325,#89326,#89327,#89328,#89329,#89330,#89331,#89332,#89333,#89334,#89335,
#89336,#89337,#89338,#89339,#89340,#89341,#89342,#89343,#89344,#89345,#89346,
#89347,#89348,#89349,#89350,#89351,#89352,#89353,#89354,#89355,#89356,#89357,
#89358,#89359,#89360,#89361,#89362,#89363,#89364,#89365,#89366,#89367,#89368,
#89369,#89370,#89371,#89372,#89373,#89374,#89375,#89376,#89377,#89378,#89379,
#89380,#89381,#89382,#89383,#89384,#89385,#89386,#89387,#89388,#89389,#89390,
#89391,#89392,#89393,#89394,#89395,#89396,#89397,#89398,#89399,#89400,#89401,
#89402,#89403,#89404,#89405,#89406,#89407,#89408,#89409,#89410,#89411,#89412,
#89413,#89414,#89415,#89416,#89417,#89418,#89419,#89420,#89421,#89422,#89423,
#89424,#89425,#89426,#89427,#89428,#89429,#89430,#89431,#89432,#89433,#89434,
#89435,#89436,#89437,#89438,#89439,#89440,#89441,#89442,#89443,#89444,#89445,
#89446,#89447,#89448,#89449,#89450,#89451,#89452,#89453,#89454,#89455,#89456,
#89457,#89458,#89459,#89460,#89461,#89462,#89463,#89464,#89465,#89466,#89467,
#89468,#89469,#89470,#89471,#89472,#89473,#89474,#89475,#89476,#89477,#89478,
#89479,#89480,#89481,#89482,#89483,#89484,#89485,#89486,#89487,#89488,#89489,
#89490,#89491,#89492,#89493,#89494,#89495,#89496,#89497,#89498,#89499,#89500,
#89501,#89502,#89503,#89504,#89505,#89506,#89507,#89508,#89509,#89510,#89511,
#89512,#89513,#89514,#89515,#89516,#89517,#89518,#89519,#89520,#89521,#89522,
#89523,#89524,#89525,#89526,#89527,#89528,#89529,#89530,#89531,#89532,#89533,
#89534,#89535,#89536,#89537,#89538,#89539,#89540,#89541,#89542,#89543,#89544,
#89545,#89546,#89547,#89548,#89549,#89550,#89551,#89552,#89553,#89554,#89555,
#89556,#89557,#89558,#89559,#89560,#89561,#89562,#89563,#89564,#89565,#89566,
#89567,#89568,#89569,#89570,#89571,#89572,#89573,#89574,#89575,#89576,#89577,
#89578,#89579,#89580,#89581,#89582,#89583,#89584,#89585,#89586,#89587,#89588,
#89589,#89590,#89591,#89592,#89593,#89594,#89595,#89596,#89597,#89598,#89599,
#89600,#89601,#89602,#89603,#89604,#89605,#89606,#89607,#89608,#89609,#89610,
#89611,#89612,#89613,#89614,#89615,#89616,#89617,#89618,#89619,#89620,#89621,
#89622,#89623,#89624,#89625,#89626,#89627,#89628,#89629,#89630,#89631,#89632,
#89633,#89634,#89635,#89636,#89637,#89638,#89639,#89640,#89641,#89642,#89643,
#89644,#89645,#89646,#89647,#89648,#89649,#89650,#89651,#89652,#89653,#89654,
#89655,#89656,#89657,#89658,#89659,#89660,#89661,#89662,#89663,#89664,#89665,
#89666,#89667,#89668,#89669,#89670,#89671,#89672,#89673,#89674,#89675,#89676,
#89677,#89678,#89679,#89680,#89681,#89682,#89683,#89684,#89685,#89686,#89687,
#89688,#89689,#89690,#89691,#89692,#89693,#89694,#89695,#89696,#89697,#89698,
#89699,#89700,#89701,#89702,#89703,#89704,#89705,#89706,#89707,#89708,#89709,
#89710,#89711,#89712,#89713,#89714,#89715,#89716,#89717,#89718,#89719,#89720,
#89721,#89722,#89723,#89724,#89725,#89726,#89727,#89728,#89729,#89730,#89731,
#89732,#89733,#89734,#89735,#89736,#89737,#89738,#89739,#89740,#89741,#89742,
#89743,#89744,#89745,#89746,#89747,#89748,#89749,#89750,#89751,#89752,#89753,
#89754,#89755,#89756,#89757,#89758,#89759,#89760,#89761,#89762,#89763,#89764,
#89765,#89766,#89767,#89768,#89769,#89770,#89771,#89772,#89773,#89774,#89775,
#89776,#89777,#89778,#89779,#89780,#89781,#89782,#89783,#89784,#89785,#89786,
#89787,#89788,#89789,#89790,#89791,#89792,#89793,#89794,#89795,#89796,#89797,
#89798,#89799,#89800,#89801,#89802,#89803,#89804,#89805,#89806,#89807,#89808,
#89809,#89810,#89811,#89812,#89813,#89814,#89815,#89816,#89817,#89818,#89819,
#89820,#89821,#89822,#89823,#89824,#89825,#89826,#89827,#89828,#89829,#89830,
#89831,#89832,#89833,#89834,#89835,#89836,#89837,#89838,#89839,#89840,#89841,
#89842,#89843,#89844,#89845,#89846,#89847,#89848,#89849,#89850,#89851,#89852,
#89853,#89854,#89855,#89856,#89857,#89858,#89859,#89860,#89861,#89862,#89863,
#89864,#89865,#89866,#89867,#89868,#89869,#89870,#89871,#89872,#89873,#89874,
#89875,#89876,#89877,#89878,#89879,#89880,#89881,#89882,#89883,#89884,#89885,
#89886,#89887,#89888,#89889,#89890,#89891,#89892,#89893,#89894,#89895,#89896,
#89897,#89898,#89899,#89900,#89901,#89902,#89903,#89904,#89905,#89906,#89907,
#89908,#89909,#89910,#89911,#89912,#89913,#89914,#89915,#89916,#89917,#89918,
#89919,#89920,#89921,#89922,#89923,#89924,#89925,#89926,#89927,#89928,#89929,
#89930,#89931,#89932,#89933,#89934,#89935,#89936,#89937,#89938,#89939,#89940,
#89941,#89942,#89943,#89944,#89945,#89946,#89947,#89948,#89949,#89950,#89951,
#89952,#89953,#89954,#89955,#89956,#89957,#89958,#89959,#89960,#89961,#89962,
#89963,#89964,#89965,#89966,#89967,#89968,#89969,#89970,#89971,#89972,#89973,
#89974,#89975,#89976,#89977,#89978,#89979,#89980,#89981,#89982,#89983,#89984,
#89985,#89986,#89987,#89988,#89989,#89990,#89991,#89992,#89993,#89994,#89995,
#89996,#89997,#89998,#89999,#90000,#90001,#90002,#90003,#90004,#90005,#90006,
#90007,#90008,#90009,#90010,#90011,#90012,#90013,#90014,#90015,#90016,#90017,
#90018,#90019,#90020,#90021,#90022,#90023,#90024,#90025,#90026,#90027,#90028,
#90029,#90030,#90031,#90032,#90033,#90034,#90035,#90036,#90037,#90038,#90039,
#90040,#90041,#90042,#90043,#90044,#90045,#90046,#90047,#90048,#90049,#90050,
#90051,#90052,#90053,#90054,#90055,#90056,#90057,#90058,#90059,#90060,#90061,
#90062,#90063,#90064,#90065,#90066,#90067,#90068,#90069,#90070,#90071,#90072,
#90073,#90074,#90075,#90076,#90077,#90078,#90079,#90080,#90081,#90082,#90083,
#90084,#90085,#90086,#90087,#90088,#90089,#90090,#90091,#90092,#90093,#90094,
#90095,#90096,#90097,#90098,#90099,#90100,#90101,#90102,#90103,#90104,#90105,
#90106,#90107,#90108,#90109,#90110,#90111,#90112,#90113,#90114,#90115,#90116,
#90117,#90118,#90119,#90120,#90121,#90122,#90123,#90124,#90125,#90126,#90127,
#90128,#90129,#90130,#90131,#90132,#90133,#90134,#90135,#90136,#90137,#90138,
#90139,#90140,#90141,#90142,#90143,#90144,#90145,#90146,#90147,#90148,#90149,
#90150,#90151,#90152,#90153,#90154,#90155,#90156,#90157,#90158,#90159,#90160,
#90161,#90162,#90163,#90164,#90165,#90166,#90167,#90168,#90169,#90170,#90171,
#90172,#90173,#90174,#90175,#90176,#90177,#90178,#90179,#90180,#90181,#90182,
#90183,#90184,#90185,#90186,#90187,#90188,#90189,#90190,#90191,#90192,#90193,
#90194,#90195,#90196,#90197,#90198,#90199,#90200,#90201,#90202,#90203,#90204,
#90205,#90206,#90207,#90208,#90209,#90210,#90211,#90212,#90213,#90214,#90215,
#90216,#90217,#90218,#90219,#90220,#90221,#90222,#90223,#90224,#90225,#90226,
#90227,#90228,#90229,#90230,#90231,#90232,#90233,#90234,#90235,#90236,#90237,
#90238,#90239,#90240,#90241,#90242,#90243,#90244,#90245,#90246,#90247,#90248,
#90249,#90250,#90251,#90252,#90253,#90254,#90255,#90256,#90257,#90258,#90259,
#90260,#90261,#90262,#90263,#90264,#90265,#90266,#90267,#90268,#90269,#90270,
#90271,#90272,#90273,#90274,#90275,#90276,#90277,#90278,#90279,#90280,#90281,
#90282,#90283,#90284,#90285,#90286,#90287,#90288,#90289,#90290,#90291,#90292));
#93711=CLOSED_SHELL('',(#90293,#90294,#90295,#90296,#90297,#90298,#90299,
#90300,#90301,#90302,#90303,#90304,#90305,#90306,#90307,#90308,#90309));
#93712=CLOSED_SHELL('',(#90310,#90311,#90312,#90313,#90314,#90315));
#93713=CLOSED_SHELL('',(#90316,#90317,#90318,#90319,#90320,#90321,#90322,
#90323,#90324,#90325,#90326,#90327,#90328,#90329,#90330,#90331,#90332,#90333,
#90334,#90335,#90336,#90337,#90338,#90339,#90340,#90341,#90342,#90343,#90344,
#90345,#90346,#90347,#90348,#90349,#90350,#90351,#90352,#90353,#90354,#90355,
#90356,#90357,#90358,#90359,#90360,#90361,#90362,#90363,#90364,#90365,#90366,
#90367,#90368,#90369,#90370,#90371,#90372,#90373,#90374,#90375,#90376,#90377,
#90378,#90379,#90380,#90381,#90382,#90383,#90384,#90385,#90386,#90387,#90388,
#90389,#90390,#90391,#90392,#90393,#90394,#90395,#90396,#90397,#90398,#90399,
#90400,#90401,#90402,#90403,#90404,#90405,#90406,#90407,#90408,#90409,#90410,
#90411,#90412,#90413,#90414,#90415,#90416,#90417,#90418,#90419,#90420,#90421,
#90422,#90423,#90424,#90425,#90426,#90427,#90428,#90429,#90430,#90431,#90432,
#90433,#90434,#90435,#90436,#90437,#90438,#90439,#90440,#90441,#90442,#90443,
#90444,#90445,#90446,#90447,#90448,#90449,#90450,#90451,#90452,#90453,#90454,
#90455,#90456,#90457,#90458,#90459,#90460,#90461,#90462,#90463,#90464,#90465,
#90466,#90467,#90468,#90469,#90470,#90471,#90472,#90473,#90474,#90475,#90476,
#90477,#90478,#90479,#90480,#90481,#90482,#90483,#90484,#90485,#90486,#90487,
#90488,#90489,#90490,#90491,#90492,#90493,#90494,#90495,#90496,#90497,#90498,
#90499,#90500,#90501,#90502,#90503,#90504,#90505,#90506,#90507,#90508,#90509,
#90510,#90511,#90512,#90513,#90514,#90515,#90516,#90517,#90518,#90519,#90520,
#90521,#90522,#90523,#90524,#90525,#90526,#90527,#90528,#90529,#90530,#90531,
#90532,#90533,#90534,#90535,#90536,#90537,#90538,#90539,#90540,#90541,#90542,
#90543,#90544,#90545,#90546,#90547,#90548,#90549,#90550,#90551,#90552,#90553,
#90554,#90555,#90556,#90557,#90558,#90559,#90560,#90561,#90562,#90563,#90564,
#90565,#90566,#90567,#90568,#90569,#90570,#90571,#90572,#90573,#90574,#90575,
#90576,#90577,#90578,#90579,#90580,#90581,#90582,#90583,#90584,#90585,#90586,
#90587,#90588,#90589,#90590,#90591,#90592,#90593,#90594,#90595,#90596,#90597,
#90598,#90599,#90600,#90601,#90602,#90603,#90604,#90605,#90606,#90607,#90608,
#90609,#90610,#90611,#90612,#90613,#90614,#90615,#90616,#90617,#90618,#90619,
#90620,#90621,#90622,#90623,#90624,#90625,#90626,#90627,#90628,#90629,#90630,
#90631,#90632,#90633,#90634,#90635,#90636,#90637,#90638,#90639,#90640,#90641,
#90642,#90643,#90644,#90645,#90646,#90647,#90648,#90649,#90650,#90651,#90652,
#90653,#90654,#90655,#90656,#90657,#90658,#90659,#90660,#90661,#90662,#90663,
#90664,#90665,#90666,#90667,#90668,#90669,#90670,#90671,#90672,#90673,#90674,
#90675,#90676,#90677,#90678,#90679,#90680,#90681,#90682,#90683,#90684,#90685,
#90686,#90687,#90688,#90689,#90690,#90691,#90692,#90693,#90694,#90695,#90696,
#90697,#90698,#90699,#90700,#90701,#90702,#90703,#90704,#90705,#90706,#90707,
#90708,#90709,#90710,#90711,#90712,#90713,#90714,#90715,#90716,#90717,#90718,
#90719,#90720,#90721,#90722,#90723,#90724,#90725,#90726,#90727,#90728,#90729,
#90730,#90731,#90732,#90733,#90734,#90735,#90736,#90737,#90738,#90739,#90740,
#90741,#90742,#90743,#90744,#90745,#90746,#90747,#90748,#90749,#90750,#90751,
#90752,#90753,#90754,#90755,#90756,#90757,#90758,#90759,#90760,#90761,#90762,
#90763,#90764,#90765,#90766,#90767,#90768,#90769,#90770,#90771,#90772,#90773,
#90774,#90775,#90776,#90777,#90778,#90779,#90780,#90781,#90782,#90783,#90784,
#90785,#90786,#90787,#90788,#90789,#90790,#90791,#90792,#90793,#90794,#90795,
#90796,#90797,#90798,#90799,#90800,#90801,#90802,#90803,#90804,#90805,#90806,
#90807,#90808,#90809,#90810,#90811,#90812,#90813,#90814,#90815,#90816,#90817,
#90818,#90819,#90820,#90821,#90822,#90823,#90824,#90825,#90826,#90827,#90828,
#90829,#90830,#90831,#90832,#90833,#90834,#90835,#90836,#90837,#90838,#90839,
#90840,#90841,#90842,#90843,#90844,#90845,#90846,#90847,#90848,#90849,#90850,
#90851,#90852,#90853,#90854,#90855,#90856,#90857,#90858,#90859,#90860,#90861,
#90862,#90863,#90864,#90865,#90866,#90867,#90868,#90869,#90870,#90871,#90872,
#90873,#90874,#90875,#90876,#90877,#90878,#90879,#90880,#90881,#90882,#90883,
#90884,#90885,#90886,#90887,#90888,#90889,#90890,#90891,#90892,#90893,#90894,
#90895,#90896,#90897,#90898,#90899,#90900,#90901,#90902,#90903,#90904,#90905,
#90906,#90907,#90908,#90909,#90910,#90911,#90912,#90913,#90914,#90915,#90916,
#90917,#90918,#90919,#90920,#90921,#90922,#90923,#90924,#90925,#90926,#90927,
#90928,#90929,#90930,#90931,#90932,#90933,#90934,#90935,#90936,#90937,#90938,
#90939,#90940,#90941,#90942,#90943,#90944,#90945,#90946,#90947,#90948,#90949,
#90950,#90951,#90952,#90953,#90954,#90955,#90956,#90957,#90958,#90959,#90960,
#90961,#90962,#90963,#90964,#90965,#90966,#90967,#90968,#90969,#90970,#90971,
#90972,#90973,#90974,#90975,#90976,#90977,#90978,#90979,#90980,#90981,#90982,
#90983,#90984,#90985,#90986,#90987,#90988,#90989,#90990,#90991,#90992,#90993,
#90994,#90995,#90996,#90997,#90998,#90999,#91000,#91001,#91002,#91003,#91004,
#91005,#91006,#91007,#91008,#91009,#91010,#91011,#91012,#91013,#91014,#91015,
#91016,#91017,#91018,#91019,#91020,#91021,#91022,#91023,#91024,#91025,#91026,
#91027,#91028,#91029,#91030,#91031,#91032,#91033,#91034,#91035,#91036,#91037,
#91038,#91039,#91040,#91041,#91042,#91043,#91044,#91045,#91046,#91047,#91048,
#91049,#91050,#91051,#91052,#91053,#91054,#91055,#91056,#91057,#91058,#91059,
#91060,#91061,#91062,#91063,#91064,#91065,#91066,#91067,#91068,#91069,#91070,
#91071,#91072,#91073,#91074,#91075,#91076,#91077,#91078,#91079,#91080,#91081,
#91082,#91083,#91084,#91085,#91086,#91087,#91088,#91089,#91090,#91091,#91092,
#91093,#91094,#91095,#91096,#91097,#91098,#91099,#91100,#91101,#91102,#91103,
#91104,#91105,#91106,#91107,#91108,#91109,#91110,#91111,#91112,#91113,#91114,
#91115,#91116,#91117,#91118,#91119,#91120,#91121,#91122,#91123,#91124,#91125,
#91126,#91127,#91128,#91129,#91130,#91131,#91132,#91133,#91134,#91135,#91136,
#91137,#91138,#91139,#91140,#91141,#91142,#91143,#91144,#91145,#91146,#91147,
#91148,#91149,#91150,#91151,#91152,#91153,#91154,#91155,#91156,#91157,#91158,
#91159,#91160,#91161,#91162,#91163,#91164,#91165,#91166,#91167,#91168,#91169,
#91170,#91171,#91172,#91173,#91174,#91175,#91176,#91177,#91178,#91179,#91180,
#91181,#91182,#91183,#91184,#91185,#91186,#91187,#91188,#91189,#91190,#91191,
#91192,#91193,#91194,#91195,#91196,#91197,#91198,#91199,#91200,#91201,#91202,
#91203,#91204,#91205,#91206,#91207,#91208,#91209,#91210,#91211,#91212,#91213,
#91214,#91215,#91216,#91217,#91218,#91219,#91220,#91221,#91222,#91223,#91224,
#91225,#91226,#91227,#91228,#91229,#91230,#91231,#91232,#91233,#91234,#91235,
#91236,#91237,#91238,#91239,#91240,#91241,#91242,#91243,#91244,#91245,#91246,
#91247,#91248,#91249,#91250,#91251,#91252,#91253,#91254,#91255,#91256,#91257,
#91258,#91259,#91260,#91261,#91262,#91263,#91264,#91265,#91266,#91267,#91268,
#91269,#91270,#91271,#91272,#91273,#91274,#91275,#91276,#91277,#91278,#91279,
#91280,#91281,#91282,#91283,#91284,#91285,#91286,#91287,#91288,#91289,#91290,
#91291,#91292,#91293,#91294,#91295,#91296,#91297,#91298,#91299,#91300,#91301,
#91302,#91303,#91304,#91305,#91306,#91307,#91308,#91309,#91310,#91311,#91312,
#91313,#91314,#91315,#91316,#91317,#91318,#91319,#91320,#91321,#91322,#91323,
#91324,#91325,#91326,#91327,#91328,#91329,#91330,#91331,#91332,#91333,#91334,
#91335,#91336,#91337,#91338,#91339,#91340,#91341,#91342,#91343,#91344,#91345,
#91346,#91347,#91348,#91349,#91350,#91351,#91352,#91353,#91354,#91355,#91356,
#91357,#91358,#91359,#91360,#91361,#91362,#91363,#91364,#91365,#91366,#91367,
#91368,#91369,#91370,#91371,#91372,#91373,#91374,#91375,#91376,#91377,#91378,
#91379,#91380,#91381,#91382,#91383,#91384,#91385,#91386,#91387,#91388,#91389,
#91390,#91391,#91392,#91393,#91394,#91395,#91396,#91397,#91398,#91399,#91400,
#91401,#91402,#91403,#91404,#91405,#91406,#91407,#91408,#91409,#91410,#91411,
#91412,#91413,#91414,#91415,#91416,#91417,#91418,#91419,#91420,#91421,#91422,
#91423,#91424,#91425,#91426,#91427,#91428,#91429,#91430,#91431,#91432,#91433,
#91434,#91435,#91436,#91437,#91438,#91439,#91440,#91441,#91442,#91443,#91444,
#91445,#91446,#91447,#91448,#91449,#91450,#91451,#91452,#91453,#91454,#91455,
#91456,#91457,#91458,#91459,#91460,#91461,#91462,#91463,#91464,#91465,#91466,
#91467,#91468,#91469,#91470,#91471,#91472,#91473,#91474,#91475,#91476,#91477,
#91478,#91479,#91480,#91481,#91482,#91483,#91484,#91485,#91486,#91487,#91488,
#91489,#91490,#91491,#91492,#91493,#91494,#91495,#91496,#91497,#91498,#91499,
#91500,#91501,#91502,#91503,#91504,#91505,#91506,#91507,#91508,#91509,#91510,
#91511,#91512,#91513,#91514,#91515,#91516,#91517,#91518,#91519,#91520,#91521,
#91522,#91523,#91524,#91525,#91526,#91527,#91528,#91529,#91530,#91531,#91532,
#91533,#91534,#91535,#91536,#91537,#91538,#91539,#91540,#91541,#91542,#91543,
#91544,#91545,#91546,#91547,#91548,#91549,#91550,#91551,#91552,#91553,#91554,
#91555,#91556,#91557,#91558,#91559,#91560,#91561,#91562,#91563,#91564,#91565,
#91566,#91567,#91568,#91569,#91570,#91571,#91572,#91573,#91574,#91575,#91576,
#91577,#91578,#91579,#91580,#91581,#91582,#91583,#91584,#91585,#91586,#91587,
#91588,#91589,#91590,#91591,#91592,#91593,#91594,#91595,#91596,#91597,#91598,
#91599,#91600,#91601,#91602,#91603,#91604,#91605,#91606,#91607,#91608,#91609,
#91610,#91611,#91612,#91613,#91614,#91615,#91616,#91617,#91618,#91619,#91620,
#91621,#91622,#91623,#91624,#91625,#91626,#91627,#91628,#91629,#91630,#91631,
#91632,#91633,#91634,#91635,#91636,#91637,#91638,#91639,#91640,#91641,#91642,
#91643,#91644,#91645,#91646,#91647,#91648,#91649,#91650,#91651,#91652,#91653,
#91654,#91655,#91656,#91657,#91658,#91659,#91660,#91661,#91662,#91663,#91664,
#91665,#91666,#91667,#91668,#91669,#91670,#91671,#91672,#91673,#91674,#91675,
#91676,#91677,#91678,#91679,#91680,#91681,#91682,#91683,#91684,#91685,#91686,
#91687,#91688,#91689,#91690,#91691,#91692,#91693,#91694,#91695,#91696,#91697,
#91698,#91699,#91700,#91701,#91702,#91703,#91704,#91705,#91706,#91707,#91708,
#91709,#91710,#91711,#91712,#91713,#91714,#91715,#91716,#91717,#91718,#91719,
#91720,#91721,#91722,#91723,#91724,#91725,#91726,#91727,#91728,#91729,#91730,
#91731,#91732,#91733,#91734,#91735,#91736,#91737,#91738,#91739,#91740,#91741,
#91742,#91743,#91744,#91745,#91746,#91747,#91748,#91749,#91750,#91751,#91752,
#91753,#91754,#91755,#91756,#91757,#91758,#91759,#91760,#91761,#91762,#91763,
#91764,#91765,#91766,#91767,#91768,#91769,#91770,#91771,#91772,#91773,#91774,
#91775,#91776,#91777,#91778,#91779,#91780,#91781,#91782,#91783,#91784,#91785,
#91786,#91787,#91788,#91789,#91790,#91791,#91792,#91793,#91794,#91795,#91796,
#91797,#91798,#91799,#91800,#91801,#91802,#91803,#91804,#91805,#91806,#91807,
#91808,#91809,#91810,#91811,#91812,#91813,#91814,#91815,#91816,#91817,#91818,
#91819,#91820,#91821,#91822,#91823,#91824,#91825,#91826,#91827,#91828,#91829,
#91830,#91831,#91832,#91833,#91834,#91835,#91836,#91837,#91838,#91839,#91840,
#91841,#91842,#91843,#91844,#91845,#91846,#91847,#91848,#91849,#91850,#91851,
#91852,#91853,#91854,#91855,#91856,#91857,#91858,#91859,#91860,#91861,#91862,
#91863,#91864,#91865,#91866,#91867,#91868,#91869,#91870,#91871,#91872,#91873,
#91874,#91875,#91876,#91877,#91878,#91879,#91880,#91881,#91882,#91883,#91884,
#91885,#91886,#91887,#91888,#91889,#91890,#91891,#91892,#91893,#91894,#91895,
#91896,#91897,#91898,#91899,#91900,#91901,#91902,#91903,#91904,#91905,#91906,
#91907,#91908,#91909,#91910,#91911,#91912,#91913,#91914,#91915,#91916,#91917,
#91918,#91919,#91920,#91921,#91922,#91923,#91924,#91925,#91926,#91927,#91928,
#91929,#91930,#91931,#91932,#91933,#91934,#91935,#91936,#91937,#91938,#91939,
#91940,#91941,#91942,#91943,#91944,#91945,#91946,#91947,#91948,#91949,#91950,
#91951,#91952,#91953,#91954,#91955,#91956,#91957,#91958,#91959,#91960,#91961,
#91962,#91963,#91964,#91965,#91966,#91967,#91968,#91969,#91970,#91971,#91972,
#91973,#91974,#91975,#91976,#91977,#91978,#91979,#91980,#91981,#91982,#91983,
#91984,#91985,#91986,#91987,#91988,#91989,#91990,#91991,#91992,#91993,#91994,
#91995,#91996,#91997,#91998,#91999,#92000,#92001,#92002,#92003,#92004,#92005,
#92006,#92007,#92008,#92009,#92010,#92011,#92012,#92013,#92014,#92015,#92016,
#92017,#92018,#92019,#92020,#92021,#92022,#92023,#92024,#92025,#92026,#92027,
#92028,#92029,#92030,#92031,#92032,#92033,#92034,#92035,#92036,#92037,#92038,
#92039,#92040,#92041,#92042,#92043,#92044,#92045,#92046,#92047,#92048,#92049,
#92050,#92051,#92052,#92053,#92054,#92055,#92056,#92057));
#93714=CLOSED_SHELL('',(#92058,#92059,#92060,#92061,#92062,#92063,#92064,
#92065,#92066,#92067,#92068,#92069,#92070,#92071,#92072,#92073,#92074));
#93715=CLOSED_SHELL('',(#92075,#92076,#92077,#92078,#92079,#92080,#92081,
#92082,#92083,#92084,#92085,#92086,#92087,#92088,#92089,#92090,#92091,#92092,
#92093,#92094));
#93716=CLOSED_SHELL('',(#92095,#92096,#92097,#92098,#92099,#92100,#92101,
#92102,#92103,#92104,#92105,#92106,#92107,#92108,#92109,#92110,#92111,#92112,
#92113,#92114));
#93717=CLOSED_SHELL('',(#92115,#92116,#92117,#92118,#92119,#92120,#92121,
#92122,#92123,#92124,#92125,#92126,#92127,#92128,#92129,#92130,#92131));
#93718=CLOSED_SHELL('',(#92132,#92133,#92134,#92135,#92136,#92137,#92138,
#92139,#92140,#92141,#92142,#92143));
#93719=CLOSED_SHELL('',(#92144,#92145,#92146,#92147,#92148,#92149));
#93720=CLOSED_SHELL('',(#92150,#92151,#92152,#92153,#92154,#92155,#92156,
#92157,#92158,#92159,#92160,#92161,#92162,#92163,#92164,#92165,#92166,#92167,
#92168,#92169,#92170,#92171,#92172,#92173,#92174,#92175,#92176,#92177,#92178,
#92179,#92180,#92181,#92182,#92183,#92184,#92185,#92186,#92187,#92188,#92189,
#92190,#92191,#92192,#92193,#92194));
#93721=CLOSED_SHELL('',(#92195,#92196,#92197,#92198,#92199,#92200,#92201,
#92202,#92203,#92204,#92205,#92206));
#93722=CLOSED_SHELL('',(#92207,#92208,#92209,#92210,#92211,#92212,#92213,
#92214,#92215,#92216,#92217,#92218,#92219,#92220,#92221,#92222,#92223,#92224,
#92225,#92226,#92227,#92228,#92229,#92230,#92231,#92232,#92233,#92234,#92235,
#92236,#92237,#92238,#92239,#92240,#92241,#92242,#92243,#92244,#92245,#92246,
#92247,#92248,#92249,#92250,#92251,#92252,#92253,#92254,#92255,#92256,#92257,
#92258,#92259,#92260,#92261,#92262,#92263,#92264,#92265,#92266,#92267,#92268,
#92269,#92270,#92271,#92272,#92273,#92274,#92275,#92276,#92277,#92278,#92279,
#92280,#92281,#92282,#92283,#92284,#92285,#92286,#92287,#92288,#92289,#92290,
#92291,#92292,#92293,#92294,#92295,#92296,#92297,#92298,#92299,#92300,#92301,
#92302,#92303,#92304,#92305,#92306,#92307,#92308,#92309,#92310,#92311,#92312,
#92313,#92314,#92315,#92316,#92317,#92318,#92319,#92320,#92321,#92322,#92323,
#92324,#92325,#92326,#92327,#92328,#92329,#92330,#92331,#92332,#92333,#92334,
#92335,#92336,#92337,#92338,#92339,#92340,#92341,#92342,#92343,#92344,#92345,
#92346,#92347,#92348,#92349,#92350,#92351,#92352,#92353,#92354,#92355,#92356,
#92357,#92358,#92359,#92360,#92361,#92362,#92363,#92364,#92365,#92366,#92367,
#92368,#92369,#92370,#92371,#92372,#92373,#92374,#92375,#92376,#92377,#92378,
#92379,#92380,#92381,#92382,#92383,#92384,#92385,#92386,#92387,#92388,#92389,
#92390,#92391,#92392,#92393,#92394,#92395,#92396,#92397,#92398,#92399,#92400,
#92401,#92402,#92403,#92404,#92405,#92406,#92407,#92408,#92409,#92410,#92411,
#92412,#92413,#92414,#92415));
#93723=CLOSED_SHELL('',(#92416,#92417,#92418,#92419,#92420,#92421,#92422,
#92423,#92424,#92425,#92426,#92427,#92428,#92429,#92430,#92431,#92432,#92433,
#92434,#92435));
#93724=CLOSED_SHELL('',(#92436,#92437,#92438,#92439,#92440,#92441,#92442,
#92443,#92444,#92445,#92446,#92447,#92448,#92449,#92450,#92451,#92452,#92453,
#92454,#92455));
#93725=CLOSED_SHELL('',(#92456,#92457,#92458,#92459,#92460,#92461,#92462,
#92463,#92464,#92465,#92466,#92467,#92468,#92469,#92470,#92471,#92472));
#93726=CLOSED_SHELL('',(#92473,#92474,#92475,#92476,#92477,#92478,#92479,
#92480,#92481,#92482,#92483,#92484,#92485,#92486,#92487,#92488,#92489,#92490,
#92491,#92492,#92493,#92494,#92495,#92496,#92497,#92498,#92499,#92500,#92501,
#92502,#92503,#92504,#92505,#92506,#92507,#92508,#92509,#92510,#92511,#92512,
#92513,#92514,#92515,#92516,#92517,#92518,#92519,#92520,#92521,#92522,#92523,
#92524,#92525,#92526,#92527,#92528,#92529,#92530,#92531,#92532,#92533,#92534,
#92535));
#93727=CLOSED_SHELL('',(#92536,#92537,#92538,#92539,#92540,#92541,#92542,
#92543,#92544,#92545,#92546,#92547,#92548,#92549,#92550,#92551,#92552,#92553,
#92554,#92555,#92556,#92557,#92558,#92559,#92560,#92561,#92562,#92563,#92564,
#92565,#92566,#92567,#92568,#92569,#92570,#92571,#92572,#92573,#92574,#92575,
#92576,#92577,#92578,#92579,#92580,#92581,#92582,#92583,#92584,#92585,#92586,
#92587,#92588,#92589,#92590,#92591,#92592,#92593,#92594,#92595,#92596,#92597,
#92598,#92599,#92600,#92601,#92602,#92603,#92604,#92605,#92606,#92607,#92608,
#92609,#92610,#92611,#92612,#92613,#92614,#92615,#92616,#92617,#92618,#92619,
#92620,#92621,#92622,#92623,#92624,#92625,#92626,#92627,#92628,#92629,#92630,
#92631,#92632,#92633,#92634,#92635,#92636,#92637,#92638,#92639,#92640,#92641,
#92642,#92643,#92644,#92645,#92646,#92647,#92648,#92649,#92650,#92651,#92652,
#92653,#92654,#92655,#92656,#92657,#92658,#92659,#92660,#92661,#92662,#92663,
#92664,#92665,#92666,#92667,#92668,#92669,#92670,#92671,#92672,#92673,#92674,
#92675,#92676,#92677,#92678,#92679,#92680,#92681,#92682,#92683,#92684,#92685,
#92686,#92687,#92688,#92689,#92690,#92691,#92692,#92693,#92694,#92695,#92696,
#92697,#92698,#92699,#92700,#92701,#92702,#92703,#92704,#92705,#92706,#92707,
#92708,#92709,#92710,#92711,#92712,#92713,#92714,#92715,#92716,#92717,#92718,
#92719,#92720,#92721,#92722,#92723,#92724,#92725,#92726,#92727,#92728,#92729,
#92730,#92731,#92732,#92733,#92734,#92735,#92736,#92737,#92738,#92739,#92740,
#92741,#92742,#92743,#92744,#92745,#92746,#92747,#92748,#92749,#92750,#92751,
#92752,#92753,#92754,#92755,#92756,#92757,#92758,#92759,#92760,#92761,#92762,
#92763,#92764,#92765,#92766,#92767,#92768,#92769,#92770,#92771,#92772,#92773,
#92774,#92775,#92776,#92777,#92778,#92779,#92780,#92781,#92782,#92783,#92784,
#92785,#92786,#92787,#92788,#92789,#92790,#92791,#92792,#92793,#92794,#92795,
#92796,#92797,#92798,#92799,#92800,#92801,#92802,#92803,#92804,#92805,#92806,
#92807,#92808,#92809,#92810,#92811,#92812,#92813,#92814,#92815,#92816,#92817,
#92818,#92819,#92820,#92821,#92822,#92823,#92824,#92825,#92826,#92827,#92828,
#92829,#92830,#92831,#92832,#92833,#92834,#92835,#92836,#92837,#92838,#92839,
#92840,#92841,#92842,#92843,#92844,#92845,#92846,#92847,#92848,#92849,#92850,
#92851,#92852,#92853,#92854,#92855,#92856,#92857,#92858,#92859,#92860,#92861,
#92862,#92863,#92864,#92865,#92866,#92867,#92868,#92869,#92870,#92871,#92872,
#92873,#92874,#92875,#92876,#92877,#92878,#92879,#92880,#92881,#92882,#92883,
#92884,#92885,#92886,#92887,#92888,#92889,#92890,#92891,#92892,#92893,#92894,
#92895,#92896,#92897,#92898,#92899,#92900,#92901,#92902,#92903,#92904,#92905,
#92906,#92907));
#93728=CLOSED_SHELL('',(#92908,#92909,#92910,#92911,#92912,#92913));
#93729=CLOSED_SHELL('',(#92914,#92915,#92916,#92917,#92918,#92919,#92920,
#92921,#92922,#92923,#92924,#92925,#92926,#92927,#92928,#92929,#92930,#92931,
#92932,#92933,#92934,#92935,#92936,#92937,#92938,#92939,#92940,#92941,#92942,
#92943,#92944,#92945,#92946,#92947,#92948,#92949,#92950,#92951,#92952,#92953,
#92954,#92955,#92956,#92957,#92958,#92959,#92960,#92961,#92962,#92963,#92964,
#92965,#92966,#92967,#92968,#92969,#92970,#92971,#92972,#92973,#92974,#92975,
#92976,#92977,#92978,#92979,#92980,#92981,#92982,#92983,#92984,#92985,#92986,
#92987,#92988,#92989,#92990,#92991,#92992,#92993,#92994,#92995,#92996,#92997,
#92998,#92999,#93000,#93001,#93002,#93003,#93004,#93005,#93006,#93007,#93008,
#93009,#93010,#93011,#93012));
#93730=CLOSED_SHELL('',(#93013,#93014,#93015,#93016,#93017,#93018,#93019));
#93731=CLOSED_SHELL('',(#93020,#93021,#93022,#93023,#93024,#93025,#93026,
#93027,#93028,#93029,#93030,#93031,#93032,#93033,#93034,#93035,#93036,#93037,
#93038,#93039,#93040,#93041,#93042,#93043,#93044,#93045,#93046,#93047,#93048,
#93049,#93050,#93051,#93052,#93053,#93054,#93055,#93056,#93057,#93058,#93059,
#93060,#93061,#93062,#93063,#93064,#93065,#93066,#93067,#93068,#93069,#93070,
#93071,#93072,#93073,#93074,#93075,#93076,#93077,#93078,#93079,#93080,#93081,
#93082,#93083,#93084,#93085,#93086,#93087,#93088,#93089,#93090,#93091,#93092,
#93093,#93094,#93095,#93096,#93097,#93098,#93099,#93100,#93101,#93102,#93103,
#93104,#93105,#93106,#93107,#93108,#93109,#93110,#93111,#93112,#93113,#93114,
#93115,#93116,#93117,#93118,#93119,#93120,#93121,#93122,#93123,#93124,#93125,
#93126,#93127,#93128,#93129,#93130,#93131,#93132,#93133,#93134,#93135,#93136,
#93137,#93138,#93139,#93140,#93141,#93142,#93143,#93144,#93145,#93146,#93147,
#93148,#93149,#93150,#93151,#93152,#93153,#93154,#93155,#93156,#93157,#93158,
#93159,#93160,#93161,#93162,#93163,#93164,#93165,#93166,#93167,#93168,#93169,
#93170,#93171,#93172,#93173,#93174,#93175,#93176,#93177,#93178,#93179,#93180,
#93181,#93182,#93183,#93184,#93185,#93186,#93187,#93188,#93189,#93190,#93191,
#93192,#93193,#93194,#93195,#93196,#93197,#93198,#93199,#93200,#93201,#93202,
#93203,#93204,#93205,#93206,#93207,#93208));
#93732=CLOSED_SHELL('',(#93209,#93210,#93211,#93212,#93213,#93214,#93215,
#93216));
#93733=CLOSED_SHELL('',(#93217,#93218,#93219,#93220,#93221,#93222,#93223,
#93224));
#93734=CLOSED_SHELL('',(#93225,#93226,#93227));
#93735=CLOSED_SHELL('',(#93228,#93229,#93230));
#93736=CLOSED_SHELL('',(#93231,#93232,#93233,#93234,#93235,#93236,#93237,
#93238));
#93737=CLOSED_SHELL('',(#93239,#93240,#93241,#93242,#93243,#93244,#93245,
#93246,#93247,#93248,#93249,#93250));
#93738=CLOSED_SHELL('',(#93251,#93252,#93253,#93254,#93255,#93256));
#93739=CLOSED_SHELL('',(#93257));
#93740=CLOSED_SHELL('',(#93258));
#93741=CLOSED_SHELL('',(#93259));
#93742=CLOSED_SHELL('',(#93260));
#93743=CLOSED_SHELL('',(#93261));
#93744=CLOSED_SHELL('',(#93262));
#93745=CLOSED_SHELL('',(#93263));
#93746=CLOSED_SHELL('',(#93264));
#93747=CLOSED_SHELL('',(#93265));
#93748=CLOSED_SHELL('',(#93266));
#93749=CLOSED_SHELL('',(#93267));
#93750=CLOSED_SHELL('',(#93268));
#93751=CLOSED_SHELL('',(#93269));
#93752=CLOSED_SHELL('',(#93270));
#93753=CLOSED_SHELL('',(#93271));
#93754=CLOSED_SHELL('',(#93272));
#93755=CLOSED_SHELL('',(#93273));
#93756=CLOSED_SHELL('',(#93274));
#93757=CLOSED_SHELL('',(#93275));
#93758=CLOSED_SHELL('',(#93276));
#93759=CLOSED_SHELL('',(#93277));
#93760=CLOSED_SHELL('',(#93278));
#93761=CLOSED_SHELL('',(#93279));
#93762=CLOSED_SHELL('',(#93280));
#93763=CLOSED_SHELL('',(#93281,#93282,#93283,#93284,#93285,#93286,#93287,
#93288,#93289,#93290,#93291,#93292,#93293,#93294,#93295,#93296));
#93764=CLOSED_SHELL('',(#93297,#93298,#93299,#93300,#93301,#93302,#93303,
#93304,#93305,#93306,#93307,#93308,#93309,#93310,#93311,#93312,#93313,#93314,
#93315,#93316,#93317,#93318,#93319,#93320,#93321,#93322,#93323,#93324,#93325,
#93326,#93327,#93328,#93329,#93330,#93331,#93332,#93333,#93334,#93335));
#93765=CLOSED_SHELL('',(#93336,#93337,#93338,#93339,#93340,#93341,#93342,
#93343,#93344,#93345,#93346,#93347,#93348,#93349,#93350,#93351,#93352,#93353,
#93354,#93355,#93356,#93357,#93358,#93359,#93360,#93361,#93362,#93363,#93364,
#93365));
#93766=CLOSED_SHELL('',(#93366,#93367,#93368,#93369,#93370,#93371,#93372));
#93767=CLOSED_SHELL('',(#93373,#93374,#93375,#93376,#93377,#93378,#93379,
#93380,#93381,#93382,#93383,#93384,#93385,#93386,#93387,#93388,#93389,#93390,
#93391,#93392,#93393,#93394,#93395,#93396,#93397,#93398,#93399,#93400,#93401,
#93402,#93403,#93404,#93405,#93406,#93407,#93408,#93409,#93410,#93411,#93412,
#93413,#93414,#93415,#93416,#93417,#93418,#93419,#93420,#93421,#93422,#93423,
#93424,#93425,#93426,#93427,#93428,#93429,#93430,#93431,#93432,#93433,#93434,
#93435,#93436,#93437,#93438,#93439,#93440,#93441,#93442,#93443,#93444,#93445,
#93446,#93447,#93448,#93449,#93450,#93451,#93452,#93453,#93454,#93455,#93456,
#93457,#93458,#93459,#93460,#93461,#93462,#93463,#93464,#93465,#93466,#93467,
#93468,#93469,#93470,#93471,#93472,#93473,#93474));
#93768=CLOSED_SHELL('',(#93475,#93476,#93477,#93478,#93479,#93480,#93481,
#93482,#93483,#93484,#93485,#93486,#93487,#93488,#93489,#93490,#93491,#93492,
#93493,#93494,#93495,#93496,#93497,#93498,#93499,#93500,#93501,#93502,#93503,
#93504,#93505));
#93769=CLOSED_SHELL('',(#93506,#93507,#93508,#93509,#93510,#93511,#93512,
#93513,#93514,#93515));
#93770=CLOSED_SHELL('',(#93516,#93517,#93518,#93519,#93520,#93521));
#93771=CLOSED_SHELL('',(#93522,#93523,#93524,#93525,#93526,#93527,#93528,
#93529,#93530,#93531,#93532,#93533,#93534,#93535,#93536,#93537,#93538,#93539));
#93772=CLOSED_SHELL('',(#93540,#93541,#93542,#93543,#93544,#93545,#93546,
#93547,#93548,#93549,#93550,#93551,#93552,#93553,#93554,#93555,#93556,#93557,
#93558,#93559,#93560,#93561,#93562,#93563));
#93773=CLOSED_SHELL('',(#93564,#93565,#93566,#93567,#93568,#93569,#93570,
#93571,#93572,#93573,#93574,#93575,#93576,#93577,#93578,#93579,#93580,#93581,
#93582,#93583,#93584,#93585,#93586,#93587,#93588,#93589,#93590,#93591,#93592,
#93593,#93594,#93595,#93596,#93597,#93598,#93599,#93600,#93601,#93602,#93603,
#93604,#93605,#93606,#93607,#93608,#93609,#93610,#93611,#93612,#93613,#93614,
#93615,#93616,#93617,#93618,#93619,#93620,#93621,#93622,#93623,#93624,#93625,
#93626,#93627,#93628,#93629,#93630,#93631,#93632,#93633,#93634,#93635,#93636,
#93637,#93638,#93639,#93640,#93641,#93642,#93643,#93644,#93645,#93646,#93647,
#93648,#93649,#93650,#93651,#93652,#93653,#93654,#93655,#93656,#93657,#93658,
#93659,#93660,#93661,#93662,#93663));
#93774=CLOSED_SHELL('',(#93664,#93665,#93666,#93667,#93668,#93669,#93670,
#93671,#93672,#93673,#93674,#93675,#93676,#93677,#93678,#93679,#93680,#93681,
#93682,#93683,#93684,#93685,#93686,#93687,#93688,#93689,#93690,#93691,#93692,
#93693,#93694,#93695,#93696,#93697,#93698,#93699,#93700,#93701,#93702,#93703,
#93704,#93705));
#93775=DERIVED_UNIT_ELEMENT(#93809,1.);
#93776=DERIVED_UNIT_ELEMENT(#310625,-3.);
#93777=DERIVED_UNIT_ELEMENT(#93809,1.);
#93778=DERIVED_UNIT_ELEMENT(#310625,-3.);
#93779=DERIVED_UNIT_ELEMENT(#93809,1.);
#93780=DERIVED_UNIT_ELEMENT(#310625,-3.);
#93781=DERIVED_UNIT_ELEMENT(#93809,1.);
#93782=DERIVED_UNIT_ELEMENT(#310625,-3.);
#93783=DERIVED_UNIT_ELEMENT(#93809,1.);
#93784=DERIVED_UNIT_ELEMENT(#310625,-3.);
#93785=DERIVED_UNIT_ELEMENT(#93809,1.);
#93786=DERIVED_UNIT_ELEMENT(#310625,-3.);
#93787=DERIVED_UNIT_ELEMENT(#93809,1.);
#93788=DERIVED_UNIT_ELEMENT(#310625,-3.);
#93789=DERIVED_UNIT_ELEMENT(#93809,1.);
#93790=DERIVED_UNIT_ELEMENT(#310625,-3.);
#93791=DERIVED_UNIT_ELEMENT(#93809,1.);
#93792=DERIVED_UNIT_ELEMENT(#310625,-3.);
#93793=DERIVED_UNIT_ELEMENT(#93809,1.);
#93794=DERIVED_UNIT_ELEMENT(#310625,-3.);
#93795=DERIVED_UNIT_ELEMENT(#93809,1.);
#93796=DERIVED_UNIT_ELEMENT(#310625,-3.);
#93797=DERIVED_UNIT_ELEMENT(#93809,1.);
#93798=DERIVED_UNIT_ELEMENT(#310625,-3.);
#93799=DERIVED_UNIT_ELEMENT(#93809,1.);
#93800=DERIVED_UNIT_ELEMENT(#310625,-3.);
#93801=DERIVED_UNIT_ELEMENT(#93809,1.);
#93802=DERIVED_UNIT_ELEMENT(#310625,-3.);
#93803=DERIVED_UNIT_ELEMENT(#93809,1.);
#93804=DERIVED_UNIT_ELEMENT(#310625,-3.);
#93805=DERIVED_UNIT_ELEMENT(#93809,1.);
#93806=DERIVED_UNIT_ELEMENT(#310625,-3.);
#93807=DERIVED_UNIT_ELEMENT(#93809,1.);
#93808=DERIVED_UNIT_ELEMENT(#310625,-3.);
#93809=(
MASS_UNIT()
NAMED_UNIT(*)
SI_UNIT(.KILO.,.GRAM.)
);
#93810=DERIVED_UNIT((#93775,#93776));
#93811=DERIVED_UNIT((#93777,#93778));
#93812=DERIVED_UNIT((#93779,#93780));
#93813=DERIVED_UNIT((#93781,#93782));
#93814=DERIVED_UNIT((#93783,#93784));
#93815=DERIVED_UNIT((#93785,#93786));
#93816=DERIVED_UNIT((#93787,#93788));
#93817=DERIVED_UNIT((#93789,#93790));
#93818=DERIVED_UNIT((#93791,#93792));
#93819=DERIVED_UNIT((#93793,#93794));
#93820=DERIVED_UNIT((#93795,#93796));
#93821=DERIVED_UNIT((#93797,#93798));
#93822=DERIVED_UNIT((#93799,#93800));
#93823=DERIVED_UNIT((#93801,#93802));
#93824=DERIVED_UNIT((#93803,#93804));
#93825=DERIVED_UNIT((#93805,#93806));
#93826=DERIVED_UNIT((#93807,#93808));
#93827=MEASURE_REPRESENTATION_ITEM('density measure',
POSITIVE_RATIO_MEASURE(7850.),#93810);
#93828=MEASURE_REPRESENTATION_ITEM('density measure',
POSITIVE_RATIO_MEASURE(7850.),#93811);
#93829=MEASURE_REPRESENTATION_ITEM('density measure',
POSITIVE_RATIO_MEASURE(7850.),#93812);
#93830=MEASURE_REPRESENTATION_ITEM('density measure',
POSITIVE_RATIO_MEASURE(7850.),#93813);
#93831=MEASURE_REPRESENTATION_ITEM('density measure',
POSITIVE_RATIO_MEASURE(7850.),#93814);
#93832=MEASURE_REPRESENTATION_ITEM('density measure',
POSITIVE_RATIO_MEASURE(7850.),#93815);
#93833=MEASURE_REPRESENTATION_ITEM('density measure',
POSITIVE_RATIO_MEASURE(7850.),#93816);
#93834=MEASURE_REPRESENTATION_ITEM('density measure',
POSITIVE_RATIO_MEASURE(7850.),#93817);
#93835=MEASURE_REPRESENTATION_ITEM('density measure',
POSITIVE_RATIO_MEASURE(7850.),#93818);
#93836=MEASURE_REPRESENTATION_ITEM('density measure',
POSITIVE_RATIO_MEASURE(7850.),#93819);
#93837=MEASURE_REPRESENTATION_ITEM('density measure',
POSITIVE_RATIO_MEASURE(7850.),#93820);
#93838=MEASURE_REPRESENTATION_ITEM('density measure',
POSITIVE_RATIO_MEASURE(7850.),#93821);
#93839=MEASURE_REPRESENTATION_ITEM('density measure',
POSITIVE_RATIO_MEASURE(7850.),#93822);
#93840=MEASURE_REPRESENTATION_ITEM('density measure',
POSITIVE_RATIO_MEASURE(7850.),#93823);
#93841=MEASURE_REPRESENTATION_ITEM('density measure',
POSITIVE_RATIO_MEASURE(7850.),#93824);
#93842=MEASURE_REPRESENTATION_ITEM('density measure',
POSITIVE_RATIO_MEASURE(7850.),#93825);
#93843=MEASURE_REPRESENTATION_ITEM('density measure',
POSITIVE_RATIO_MEASURE(7850.),#93826);
#93844=PROPERTY_DEFINITION_REPRESENTATION(#93929,#93878);
#93845=PROPERTY_DEFINITION_REPRESENTATION(#93930,#93879);
#93846=PROPERTY_DEFINITION_REPRESENTATION(#93931,#93880);
#93847=PROPERTY_DEFINITION_REPRESENTATION(#93932,#93881);
#93848=PROPERTY_DEFINITION_REPRESENTATION(#93933,#93882);
#93849=PROPERTY_DEFINITION_REPRESENTATION(#93934,#93883);
#93850=PROPERTY_DEFINITION_REPRESENTATION(#93935,#93884);
#93851=PROPERTY_DEFINITION_REPRESENTATION(#93936,#93885);
#93852=PROPERTY_DEFINITION_REPRESENTATION(#93937,#93886);
#93853=PROPERTY_DEFINITION_REPRESENTATION(#93938,#93887);
#93854=PROPERTY_DEFINITION_REPRESENTATION(#93939,#93888);
#93855=PROPERTY_DEFINITION_REPRESENTATION(#93940,#93889);
#93856=PROPERTY_DEFINITION_REPRESENTATION(#93941,#93890);
#93857=PROPERTY_DEFINITION_REPRESENTATION(#93942,#93891);
#93858=PROPERTY_DEFINITION_REPRESENTATION(#93943,#93892);
#93859=PROPERTY_DEFINITION_REPRESENTATION(#93944,#93893);
#93860=PROPERTY_DEFINITION_REPRESENTATION(#93945,#93894);
#93861=PROPERTY_DEFINITION_REPRESENTATION(#93946,#93895);
#93862=PROPERTY_DEFINITION_REPRESENTATION(#93947,#93896);
#93863=PROPERTY_DEFINITION_REPRESENTATION(#93948,#93897);
#93864=PROPERTY_DEFINITION_REPRESENTATION(#93949,#93898);
#93865=PROPERTY_DEFINITION_REPRESENTATION(#93950,#93899);
#93866=PROPERTY_DEFINITION_REPRESENTATION(#93951,#93900);
#93867=PROPERTY_DEFINITION_REPRESENTATION(#93952,#93901);
#93868=PROPERTY_DEFINITION_REPRESENTATION(#93953,#93902);
#93869=PROPERTY_DEFINITION_REPRESENTATION(#93954,#93903);
#93870=PROPERTY_DEFINITION_REPRESENTATION(#93955,#93904);
#93871=PROPERTY_DEFINITION_REPRESENTATION(#93956,#93905);
#93872=PROPERTY_DEFINITION_REPRESENTATION(#93957,#93906);
#93873=PROPERTY_DEFINITION_REPRESENTATION(#93958,#93907);
#93874=PROPERTY_DEFINITION_REPRESENTATION(#93959,#93908);
#93875=PROPERTY_DEFINITION_REPRESENTATION(#93960,#93909);
#93876=PROPERTY_DEFINITION_REPRESENTATION(#93961,#93910);
#93877=PROPERTY_DEFINITION_REPRESENTATION(#93962,#93911);
#93878=REPRESENTATION('material name',(#93912),#310603);
#93879=REPRESENTATION('density',(#93827),#310603);
#93880=REPRESENTATION('material name',(#93913),#310604);
#93881=REPRESENTATION('density',(#93828),#310604);
#93882=REPRESENTATION('material name',(#93914),#310605);
#93883=REPRESENTATION('density',(#93829),#310605);
#93884=REPRESENTATION('material name',(#93915),#310606);
#93885=REPRESENTATION('density',(#93830),#310606);
#93886=REPRESENTATION('material name',(#93916),#310608);
#93887=REPRESENTATION('density',(#93831),#310608);
#93888=REPRESENTATION('material name',(#93917),#310609);
#93889=REPRESENTATION('density',(#93832),#310609);
#93890=REPRESENTATION('material name',(#93918),#310610);
#93891=REPRESENTATION('density',(#93833),#310610);
#93892=REPRESENTATION('material name',(#93919),#310611);
#93893=REPRESENTATION('density',(#93834),#310611);
#93894=REPRESENTATION('material name',(#93920),#310612);
#93895=REPRESENTATION('density',(#93835),#310612);
#93896=REPRESENTATION('material name',(#93921),#310613);
#93897=REPRESENTATION('density',(#93836),#310613);
#93898=REPRESENTATION('material name',(#93922),#310614);
#93899=REPRESENTATION('density',(#93837),#310614);
#93900=REPRESENTATION('material name',(#93923),#310615);
#93901=REPRESENTATION('density',(#93838),#310615);
#93902=REPRESENTATION('material name',(#93924),#310616);
#93903=REPRESENTATION('density',(#93839),#310616);
#93904=REPRESENTATION('material name',(#93925),#310618);
#93905=REPRESENTATION('density',(#93840),#310618);
#93906=REPRESENTATION('material name',(#93926),#310619);
#93907=REPRESENTATION('density',(#93841),#310619);
#93908=REPRESENTATION('material name',(#93927),#310621);
#93909=REPRESENTATION('density',(#93842),#310621);
#93910=REPRESENTATION('material name',(#93928),#310622);
#93911=REPRESENTATION('density',(#93843),#310622);
#93912=DESCRIPTIVE_REPRESENTATION_ITEM('Steel','Steel');
#93913=DESCRIPTIVE_REPRESENTATION_ITEM('Steel','Steel');
#93914=DESCRIPTIVE_REPRESENTATION_ITEM('Steel','Steel');
#93915=DESCRIPTIVE_REPRESENTATION_ITEM('Steel','Steel');
#93916=DESCRIPTIVE_REPRESENTATION_ITEM('Steel','Steel');
#93917=DESCRIPTIVE_REPRESENTATION_ITEM('Steel','Steel');
#93918=DESCRIPTIVE_REPRESENTATION_ITEM('Steel','Steel');
#93919=DESCRIPTIVE_REPRESENTATION_ITEM('Steel','Steel');
#93920=DESCRIPTIVE_REPRESENTATION_ITEM('Steel','Steel');
#93921=DESCRIPTIVE_REPRESENTATION_ITEM('Steel','Steel');
#93922=DESCRIPTIVE_REPRESENTATION_ITEM('Steel','Steel');
#93923=DESCRIPTIVE_REPRESENTATION_ITEM('Steel','Steel');
#93924=DESCRIPTIVE_REPRESENTATION_ITEM('Steel','Steel');
#93925=DESCRIPTIVE_REPRESENTATION_ITEM('Steel','Steel');
#93926=DESCRIPTIVE_REPRESENTATION_ITEM('Steel','Steel');
#93927=DESCRIPTIVE_REPRESENTATION_ITEM('Steel','Steel');
#93928=DESCRIPTIVE_REPRESENTATION_ITEM('Steel','Steel');
#93929=PROPERTY_DEFINITION('material property','material name',#310916);
#93930=PROPERTY_DEFINITION('material property','density of part',#310916);
#93931=PROPERTY_DEFINITION('material property','material name',#310917);
#93932=PROPERTY_DEFINITION('material property','density of part',#310917);
#93933=PROPERTY_DEFINITION('material property','material name',#310918);
#93934=PROPERTY_DEFINITION('material property','density of part',#310918);
#93935=PROPERTY_DEFINITION('material property','material name',#310919);
#93936=PROPERTY_DEFINITION('material property','density of part',#310919);
#93937=PROPERTY_DEFINITION('material property','material name',#310921);
#93938=PROPERTY_DEFINITION('material property','density of part',#310921);
#93939=PROPERTY_DEFINITION('material property','material name',#310922);
#93940=PROPERTY_DEFINITION('material property','density of part',#310922);
#93941=PROPERTY_DEFINITION('material property','material name',#310923);
#93942=PROPERTY_DEFINITION('material property','density of part',#310923);
#93943=PROPERTY_DEFINITION('material property','material name',#310924);
#93944=PROPERTY_DEFINITION('material property','density of part',#310924);
#93945=PROPERTY_DEFINITION('material property','material name',#310925);
#93946=PROPERTY_DEFINITION('material property','density of part',#310925);
#93947=PROPERTY_DEFINITION('material property','material name',#310926);
#93948=PROPERTY_DEFINITION('material property','density of part',#310926);
#93949=PROPERTY_DEFINITION('material property','material name',#310927);
#93950=PROPERTY_DEFINITION('material property','density of part',#310927);
#93951=PROPERTY_DEFINITION('material property','material name',#310928);
#93952=PROPERTY_DEFINITION('material property','density of part',#310928);
#93953=PROPERTY_DEFINITION('material property','material name',#310929);
#93954=PROPERTY_DEFINITION('material property','density of part',#310929);
#93955=PROPERTY_DEFINITION('material property','material name',#310931);
#93956=PROPERTY_DEFINITION('material property','density of part',#310931);
#93957=PROPERTY_DEFINITION('material property','material name',#310932);
#93958=PROPERTY_DEFINITION('material property','density of part',#310932);
#93959=PROPERTY_DEFINITION('material property','material name',#310934);
#93960=PROPERTY_DEFINITION('material property','density of part',#310934);
#93961=PROPERTY_DEFINITION('material property','material name',#310935);
#93962=PROPERTY_DEFINITION('material property','density of part',#310935);
#93963=AXIS2_PLACEMENT_3D('',#131013,#104864,#104865);
#93964=AXIS2_PLACEMENT_3D('',#131014,#104866,#104867);
#93965=AXIS2_PLACEMENT_3D('',#131015,#104868,#104869);
#93966=AXIS2_PLACEMENT_3D('',#131017,#104870,#104871);
#93967=AXIS2_PLACEMENT_3D('',#131020,#104873,#104874);
#93968=AXIS2_PLACEMENT_3D('',#131021,#104875,#104876);
#93969=AXIS2_PLACEMENT_3D('',#131023,#104877,#104878);
#93970=AXIS2_PLACEMENT_3D('',#131026,#104880,#104881);
#93971=AXIS2_PLACEMENT_3D('',#131027,#104882,#104883);
#93972=AXIS2_PLACEMENT_3D('',#131029,#104884,#104885);
#93973=AXIS2_PLACEMENT_3D('',#131032,#104887,#104888);
#93974=AXIS2_PLACEMENT_3D('',#131033,#104889,#104890);
#93975=AXIS2_PLACEMENT_3D('',#131035,#104891,#104892);
#93976=AXIS2_PLACEMENT_3D('',#131038,#104894,#104895);
#93977=AXIS2_PLACEMENT_3D('',#131039,#104896,#104897);
#93978=AXIS2_PLACEMENT_3D('',#131041,#104898,#104899);
#93979=AXIS2_PLACEMENT_3D('',#131044,#104901,#104902);
#93980=AXIS2_PLACEMENT_3D('',#131045,#104903,#104904);
#93981=AXIS2_PLACEMENT_3D('',#131047,#104905,#104906);
#93982=AXIS2_PLACEMENT_3D('',#131050,#104908,#104909);
#93983=AXIS2_PLACEMENT_3D('',#131051,#104910,#104911);
#93984=AXIS2_PLACEMENT_3D('',#131053,#104912,#104913);
#93985=AXIS2_PLACEMENT_3D('',#131056,#104915,#104916);
#93986=AXIS2_PLACEMENT_3D('',#131057,#104917,#104918);
#93987=AXIS2_PLACEMENT_3D('',#131059,#104919,#104920);
#93988=AXIS2_PLACEMENT_3D('',#131062,#104922,#104923);
#93989=AXIS2_PLACEMENT_3D('',#131063,#104924,#104925);
#93990=AXIS2_PLACEMENT_3D('',#131065,#104926,#104927);
#93991=AXIS2_PLACEMENT_3D('',#131068,#104929,#104930);
#93992=AXIS2_PLACEMENT_3D('',#131069,#104931,#104932);
#93993=AXIS2_PLACEMENT_3D('',#131071,#104933,#104934);
#93994=AXIS2_PLACEMENT_3D('',#131074,#104936,#104937);
#93995=AXIS2_PLACEMENT_3D('',#131075,#104938,#104939);
#93996=AXIS2_PLACEMENT_3D('',#131077,#104940,#104941);
#93997=AXIS2_PLACEMENT_3D('',#131080,#104943,#104944);
#93998=AXIS2_PLACEMENT_3D('',#131081,#104945,#104946);
#93999=AXIS2_PLACEMENT_3D('',#131083,#104947,#104948);
#94000=AXIS2_PLACEMENT_3D('',#131086,#104950,#104951);
#94001=AXIS2_PLACEMENT_3D('',#131087,#104952,#104953);
#94002=AXIS2_PLACEMENT_3D('',#131096,#104958,#104959);
#94003=AXIS2_PLACEMENT_3D('',#131102,#104963,#104964);
#94004=AXIS2_PLACEMENT_3D('',#131111,#104969,#104970);
#94005=AXIS2_PLACEMENT_3D('',#131120,#104975,#104976);
#94006=AXIS2_PLACEMENT_3D('',#131126,#104980,#104981);
#94007=AXIS2_PLACEMENT_3D('',#131132,#104985,#104986);
#94008=AXIS2_PLACEMENT_3D('',#131141,#104991,#104992);
#94009=AXIS2_PLACEMENT_3D('',#131147,#104996,#104997);
#94010=AXIS2_PLACEMENT_3D('',#131148,#104998,#104999);
#94011=AXIS2_PLACEMENT_3D('',#131149,#105000,#105001);
#94012=AXIS2_PLACEMENT_3D('',#131150,#105002,#105003);
#94013=AXIS2_PLACEMENT_3D('',#131151,#105004,#105005);
#94014=AXIS2_PLACEMENT_3D('',#131152,#105006,#105007);
#94015=AXIS2_PLACEMENT_3D('',#131153,#105008,#105009);
#94016=AXIS2_PLACEMENT_3D('',#131154,#105010,#105011);
#94017=AXIS2_PLACEMENT_3D('',#131155,#105012,#105013);
#94018=AXIS2_PLACEMENT_3D('',#131156,#105014,#105015);
#94019=AXIS2_PLACEMENT_3D('',#131157,#105016,#105017);
#94020=AXIS2_PLACEMENT_3D('',#131158,#105018,#105019);
#94021=AXIS2_PLACEMENT_3D('',#131159,#105020,#105021);
#94022=AXIS2_PLACEMENT_3D('',#131160,#105022,#105023);
#94023=AXIS2_PLACEMENT_3D('',#131161,#105024,#105025);
#94024=AXIS2_PLACEMENT_3D('',#131162,#105026,#105027);
#94025=AXIS2_PLACEMENT_3D('',#131164,#105028,#105029);
#94026=AXIS2_PLACEMENT_3D('',#131167,#105031,#105032);
#94027=AXIS2_PLACEMENT_3D('',#131168,#105033,#105034);
#94028=AXIS2_PLACEMENT_3D('',#131170,#105035,#105036);
#94029=AXIS2_PLACEMENT_3D('',#131173,#105038,#105039);
#94030=AXIS2_PLACEMENT_3D('',#131174,#105040,#105041);
#94031=AXIS2_PLACEMENT_3D('',#131176,#105042,#105043);
#94032=AXIS2_PLACEMENT_3D('',#131179,#105045,#105046);
#94033=AXIS2_PLACEMENT_3D('',#131180,#105047,#105048);
#94034=AXIS2_PLACEMENT_3D('',#131182,#105049,#105050);
#94035=AXIS2_PLACEMENT_3D('',#131185,#105052,#105053);
#94036=AXIS2_PLACEMENT_3D('',#131186,#105054,#105055);
#94037=AXIS2_PLACEMENT_3D('',#131188,#105056,#105057);
#94038=AXIS2_PLACEMENT_3D('',#131191,#105059,#105060);
#94039=AXIS2_PLACEMENT_3D('',#131192,#105061,#105062);
#94040=AXIS2_PLACEMENT_3D('',#131194,#105063,#105064);
#94041=AXIS2_PLACEMENT_3D('',#131197,#105066,#105067);
#94042=AXIS2_PLACEMENT_3D('',#131198,#105068,#105069);
#94043=AXIS2_PLACEMENT_3D('',#131200,#105070,#105071);
#94044=AXIS2_PLACEMENT_3D('',#131203,#105073,#105074);
#94045=AXIS2_PLACEMENT_3D('',#131204,#105075,#105076);
#94046=AXIS2_PLACEMENT_3D('',#131206,#105077,#105078);
#94047=AXIS2_PLACEMENT_3D('',#131209,#105080,#105081);
#94048=AXIS2_PLACEMENT_3D('',#131210,#105082,#105083);
#94049=AXIS2_PLACEMENT_3D('',#131212,#105084,#105085);
#94050=AXIS2_PLACEMENT_3D('',#131215,#105087,#105088);
#94051=AXIS2_PLACEMENT_3D('',#131216,#105089,#105090);
#94052=AXIS2_PLACEMENT_3D('',#131218,#105091,#105092);
#94053=AXIS2_PLACEMENT_3D('',#131221,#105094,#105095);
#94054=AXIS2_PLACEMENT_3D('',#131222,#105096,#105097);
#94055=AXIS2_PLACEMENT_3D('',#131224,#105098,#105099);
#94056=AXIS2_PLACEMENT_3D('',#131227,#105101,#105102);
#94057=AXIS2_PLACEMENT_3D('',#131228,#105103,#105104);
#94058=AXIS2_PLACEMENT_3D('',#131230,#105105,#105106);
#94059=AXIS2_PLACEMENT_3D('',#131233,#105108,#105109);
#94060=AXIS2_PLACEMENT_3D('',#131234,#105110,#105111);
#94061=AXIS2_PLACEMENT_3D('',#131243,#105116,#105117);
#94062=AXIS2_PLACEMENT_3D('',#131249,#105121,#105122);
#94063=AXIS2_PLACEMENT_3D('',#131258,#105127,#105128);
#94064=AXIS2_PLACEMENT_3D('',#131267,#105133,#105134);
#94065=AXIS2_PLACEMENT_3D('',#131273,#105138,#105139);
#94066=AXIS2_PLACEMENT_3D('',#131279,#105143,#105144);
#94067=AXIS2_PLACEMENT_3D('',#131288,#105149,#105150);
#94068=AXIS2_PLACEMENT_3D('',#131294,#105154,#105155);
#94069=AXIS2_PLACEMENT_3D('',#131295,#105156,#105157);
#94070=AXIS2_PLACEMENT_3D('',#131296,#105158,#105159);
#94071=AXIS2_PLACEMENT_3D('',#131297,#105160,#105161);
#94072=AXIS2_PLACEMENT_3D('',#131298,#105162,#105163);
#94073=AXIS2_PLACEMENT_3D('',#131299,#105164,#105165);
#94074=AXIS2_PLACEMENT_3D('',#131300,#105166,#105167);
#94075=AXIS2_PLACEMENT_3D('',#131301,#105168,#105169);
#94076=AXIS2_PLACEMENT_3D('',#131302,#105170,#105171);
#94077=AXIS2_PLACEMENT_3D('',#131303,#105172,#105173);
#94078=AXIS2_PLACEMENT_3D('',#131304,#105174,#105175);
#94079=AXIS2_PLACEMENT_3D('',#131305,#105176,#105177);
#94080=AXIS2_PLACEMENT_3D('',#131306,#105178,#105179);
#94081=AXIS2_PLACEMENT_3D('',#131307,#105180,#105181);
#94082=AXIS2_PLACEMENT_3D('',#131308,#105182,#105183);
#94083=AXIS2_PLACEMENT_3D('',#131309,#105184,#105185);
#94084=AXIS2_PLACEMENT_3D('',#131311,#105186,#105187);
#94085=AXIS2_PLACEMENT_3D('',#131314,#105189,#105190);
#94086=AXIS2_PLACEMENT_3D('',#131315,#105191,#105192);
#94087=AXIS2_PLACEMENT_3D('',#131316,#105193,#105194);
#94088=AXIS2_PLACEMENT_3D('',#131318,#105195,#105196);
#94089=AXIS2_PLACEMENT_3D('',#131320,#105198,#105199);
#94090=AXIS2_PLACEMENT_3D('',#131322,#105200,#105201);
#94091=AXIS2_PLACEMENT_3D('',#131323,#105202,#105203);
#94092=AXIS2_PLACEMENT_3D('',#131325,#105204,#105205);
#94093=AXIS2_PLACEMENT_3D('',#131327,#105207,#105208);
#94094=AXIS2_PLACEMENT_3D('',#131328,#105209,#105210);
#94095=AXIS2_PLACEMENT_3D('',#131330,#105211,#105212);
#94096=AXIS2_PLACEMENT_3D('',#131333,#105214,#105215);
#94097=AXIS2_PLACEMENT_3D('',#131334,#105216,#105217);
#94098=AXIS2_PLACEMENT_3D('',#131335,#105218,#105219);
#94099=AXIS2_PLACEMENT_3D('',#131337,#105220,#105221);
#94100=AXIS2_PLACEMENT_3D('',#131339,#105223,#105224);
#94101=AXIS2_PLACEMENT_3D('',#131341,#105225,#105226);
#94102=AXIS2_PLACEMENT_3D('',#131342,#105227,#105228);
#94103=AXIS2_PLACEMENT_3D('',#131344,#105229,#105230);
#94104=AXIS2_PLACEMENT_3D('',#131346,#105232,#105233);
#94105=AXIS2_PLACEMENT_3D('',#131347,#105234,#105235);
#94106=AXIS2_PLACEMENT_3D('',#131352,#105237,#105238);
#94107=AXIS2_PLACEMENT_3D('',#131364,#105240,#105241);
#94108=AXIS2_PLACEMENT_3D('',#131369,#105242,#105243);
#94109=AXIS2_PLACEMENT_3D('',#131372,#105244,#105245);
#94110=AXIS2_PLACEMENT_3D('',#131376,#105247,#105248);
#94111=AXIS2_PLACEMENT_3D('',#131383,#105250,#105251);
#94112=AXIS2_PLACEMENT_3D('',#131385,#105252,#105253);
#94113=AXIS2_PLACEMENT_3D('',#131387,#105254,#105255);
#94114=AXIS2_PLACEMENT_3D('',#131388,#105256,#105257);
#94115=AXIS2_PLACEMENT_3D('',#131402,#105258,#105259);
#94116=AXIS2_PLACEMENT_3D('',#131413,#105260,#105261);
#94117=AXIS2_PLACEMENT_3D('',#131418,#105263,#105264);
#94118=AXIS2_PLACEMENT_3D('',#131421,#105266,#105267);
#94119=AXIS2_PLACEMENT_3D('',#131422,#105268,#105269);
#94120=AXIS2_PLACEMENT_3D('',#131533,#105281,#105282);
#94121=AXIS2_PLACEMENT_3D('',#131535,#105283,#105284);
#94122=AXIS2_PLACEMENT_3D('',#131537,#105285,#105286);
#94123=AXIS2_PLACEMENT_3D('',#131538,#105287,#105288);
#94124=AXIS2_PLACEMENT_3D('',#131539,#105289,#105290);
#94125=AXIS2_PLACEMENT_3D('',#131544,#105292,#105293);
#94126=AXIS2_PLACEMENT_3D('',#131547,#105295,#105296);
#94127=AXIS2_PLACEMENT_3D('',#131548,#105297,#105298);
#94128=AXIS2_PLACEMENT_3D('',#131551,#105301,#105302);
#94129=AXIS2_PLACEMENT_3D('',#131553,#105303,#105304);
#94130=AXIS2_PLACEMENT_3D('',#131555,#105305,#105306);
#94131=AXIS2_PLACEMENT_3D('',#131556,#105307,#105308);
#94132=AXIS2_PLACEMENT_3D('',#131557,#105309,#105310);
#94133=AXIS2_PLACEMENT_3D('',#131630,#105321,#105322);
#94134=AXIS2_PLACEMENT_3D('',#131658,#105324,#105325);
#94135=AXIS2_PLACEMENT_3D('',#131669,#105326,#105327);
#94136=AXIS2_PLACEMENT_3D('',#131678,#105328,#105329);
#94137=AXIS2_PLACEMENT_3D('',#131681,#105330,#105331);
#94138=AXIS2_PLACEMENT_3D('',#131684,#105334,#105335);
#94139=AXIS2_PLACEMENT_3D('',#131687,#105336,#105337);
#94140=AXIS2_PLACEMENT_3D('',#131688,#105338,#105339);
#94141=AXIS2_PLACEMENT_3D('',#131690,#105340,#105341);
#94142=AXIS2_PLACEMENT_3D('',#131691,#105342,#105343);
#94143=AXIS2_PLACEMENT_3D('',#131692,#105344,#105345);
#94144=AXIS2_PLACEMENT_3D('',#131695,#105346,#105347);
#94145=AXIS2_PLACEMENT_3D('',#131699,#105349,#105350);
#94146=AXIS2_PLACEMENT_3D('',#131700,#105351,#105352);
#94147=AXIS2_PLACEMENT_3D('',#131703,#105354,#105355);
#94148=AXIS2_PLACEMENT_3D('',#131782,#105356,#105357);
#94149=AXIS2_PLACEMENT_3D('',#131806,#105358,#105359);
#94150=AXIS2_PLACEMENT_3D('',#131808,#105360,#105361);
#94151=AXIS2_PLACEMENT_3D('',#131809,#105362,#105363);
#94152=AXIS2_PLACEMENT_3D('',#131879,#105364,#105365);
#94153=AXIS2_PLACEMENT_3D('',#131890,#105366,#105367);
#94154=AXIS2_PLACEMENT_3D('',#131893,#105368,#105369);
#94155=AXIS2_PLACEMENT_3D('',#131896,#105372,#105373);
#94156=AXIS2_PLACEMENT_3D('',#131899,#105374,#105375);
#94157=AXIS2_PLACEMENT_3D('',#131900,#105376,#105377);
#94158=AXIS2_PLACEMENT_3D('',#131902,#105378,#105379);
#94159=AXIS2_PLACEMENT_3D('',#131903,#105380,#105381);
#94160=AXIS2_PLACEMENT_3D('',#131904,#105382,#105383);
#94161=AXIS2_PLACEMENT_3D('',#131907,#105384,#105385);
#94162=AXIS2_PLACEMENT_3D('',#131911,#105387,#105388);
#94163=AXIS2_PLACEMENT_3D('',#131912,#105389,#105390);
#94164=AXIS2_PLACEMENT_3D('',#131940,#105392,#105393);
#94165=AXIS2_PLACEMENT_3D('',#131947,#105394,#105395);
#94166=AXIS2_PLACEMENT_3D('',#131949,#105396,#105397);
#94167=AXIS2_PLACEMENT_3D('',#131951,#105398,#105399);
#94168=AXIS2_PLACEMENT_3D('',#131952,#105400,#105401);
#94169=AXIS2_PLACEMENT_3D('',#132028,#105402,#105403);
#94170=AXIS2_PLACEMENT_3D('',#132066,#105404,#105405);
#94171=AXIS2_PLACEMENT_3D('',#132069,#105406,#105407);
#94172=AXIS2_PLACEMENT_3D('',#132072,#105410,#105411);
#94173=AXIS2_PLACEMENT_3D('',#132075,#105412,#105413);
#94174=AXIS2_PLACEMENT_3D('',#132076,#105414,#105415);
#94175=AXIS2_PLACEMENT_3D('',#132078,#105416,#105417);
#94176=AXIS2_PLACEMENT_3D('',#132079,#105418,#105419);
#94177=AXIS2_PLACEMENT_3D('',#132080,#105420,#105421);
#94178=AXIS2_PLACEMENT_3D('',#132083,#105422,#105423);
#94179=AXIS2_PLACEMENT_3D('',#132086,#105425,#105426);
#94180=AXIS2_PLACEMENT_3D('',#132163,#105428,#105429);
#94181=AXIS2_PLACEMENT_3D('',#132174,#105430,#105431);
#94182=AXIS2_PLACEMENT_3D('',#132175,#105432,#105433);
#94183=AXIS2_PLACEMENT_3D('',#132176,#105434,#105435);
#94184=AXIS2_PLACEMENT_3D('',#132177,#105436,#105437);
#94185=AXIS2_PLACEMENT_3D('',#132182,#105439,#105440);
#94186=AXIS2_PLACEMENT_3D('',#132204,#105442,#105443);
#94187=AXIS2_PLACEMENT_3D('',#132207,#105444,#105445);
#94188=AXIS2_PLACEMENT_3D('',#132208,#105446,#105447);
#94189=AXIS2_PLACEMENT_3D('',#132210,#105448,#105449);
#94190=AXIS2_PLACEMENT_3D('',#132215,#105450,#105451);
#94191=AXIS2_PLACEMENT_3D('',#132218,#105452,#105453);
#94192=AXIS2_PLACEMENT_3D('',#132221,#105455,#105456);
#94193=AXIS2_PLACEMENT_3D('',#132243,#105458,#105459);
#94194=AXIS2_PLACEMENT_3D('',#132256,#105460,#105461);
#94195=AXIS2_PLACEMENT_3D('',#132259,#105462,#105463);
#94196=AXIS2_PLACEMENT_3D('',#132260,#105464,#105465);
#94197=AXIS2_PLACEMENT_3D('',#132261,#105466,#105467);
#94198=AXIS2_PLACEMENT_3D('',#132294,#105468,#105469);
#94199=AXIS2_PLACEMENT_3D('',#132351,#105470,#105471);
#94200=AXIS2_PLACEMENT_3D('',#132355,#105473,#105474);
#94201=AXIS2_PLACEMENT_3D('',#132357,#105476,#105477);
#94202=AXIS2_PLACEMENT_3D('',#132360,#105478,#105479);
#94203=AXIS2_PLACEMENT_3D('',#132361,#105480,#105481);
#94204=AXIS2_PLACEMENT_3D('',#132363,#105482,#105483);
#94205=AXIS2_PLACEMENT_3D('',#132364,#105484,#105485);
#94206=AXIS2_PLACEMENT_3D('',#132365,#105486,#105487);
#94207=AXIS2_PLACEMENT_3D('',#132368,#105488,#105489);
#94208=AXIS2_PLACEMENT_3D('',#132371,#105491,#105492);
#94209=AXIS2_PLACEMENT_3D('',#132405,#105494,#105495);
#94210=AXIS2_PLACEMENT_3D('',#132473,#105496,#105497);
#94211=AXIS2_PLACEMENT_3D('',#132474,#105498,#105499);
#94212=AXIS2_PLACEMENT_3D('',#132475,#105500,#105501);
#94213=AXIS2_PLACEMENT_3D('',#132496,#105502,#105503);
#94214=AXIS2_PLACEMENT_3D('',#132509,#105504,#105505);
#94215=AXIS2_PLACEMENT_3D('',#132512,#105506,#105507);
#94216=AXIS2_PLACEMENT_3D('',#132515,#105510,#105511);
#94217=AXIS2_PLACEMENT_3D('',#132518,#105512,#105513);
#94218=AXIS2_PLACEMENT_3D('',#132519,#105514,#105515);
#94219=AXIS2_PLACEMENT_3D('',#132521,#105516,#105517);
#94220=AXIS2_PLACEMENT_3D('',#132522,#105518,#105519);
#94221=AXIS2_PLACEMENT_3D('',#132523,#105520,#105521);
#94222=AXIS2_PLACEMENT_3D('',#132526,#105522,#105523);
#94223=AXIS2_PLACEMENT_3D('',#132529,#105525,#105526);
#94224=AXIS2_PLACEMENT_3D('',#132563,#105528,#105529);
#94225=AXIS2_PLACEMENT_3D('',#132600,#105530,#105531);
#94226=AXIS2_PLACEMENT_3D('',#132601,#105532,#105533);
#94227=AXIS2_PLACEMENT_3D('',#132602,#105534,#105535);
#94228=AXIS2_PLACEMENT_3D('',#132641,#105536,#105537);
#94229=AXIS2_PLACEMENT_3D('',#132697,#105538,#105539);
#94230=AXIS2_PLACEMENT_3D('',#132700,#105540,#105541);
#94231=AXIS2_PLACEMENT_3D('',#132716,#105544,#105545);
#94232=AXIS2_PLACEMENT_3D('',#132718,#105546,#105547);
#94233=AXIS2_PLACEMENT_3D('',#132723,#105548,#105549);
#94234=AXIS2_PLACEMENT_3D('',#132725,#105550,#105551);
#94235=AXIS2_PLACEMENT_3D('',#132726,#105552,#105553);
#94236=AXIS2_PLACEMENT_3D('',#132740,#105554,#105555);
#94237=AXIS2_PLACEMENT_3D('',#132751,#105556,#105557);
#94238=AXIS2_PLACEMENT_3D('',#132756,#105559,#105560);
#94239=AXIS2_PLACEMENT_3D('',#132767,#105562,#105563);
#94240=AXIS2_PLACEMENT_3D('',#132768,#105564,#105565);
#94241=AXIS2_PLACEMENT_3D('',#132769,#105566,#105567);
#94242=AXIS2_PLACEMENT_3D('',#132770,#105568,#105569);
#94243=AXIS2_PLACEMENT_3D('',#132783,#105571,#105572);
#94244=AXIS2_PLACEMENT_3D('',#132831,#105574,#105575);
#94245=AXIS2_PLACEMENT_3D('',#132842,#105577,#105578);
#94246=AXIS2_PLACEMENT_3D('',#132855,#105580,#105581);
#94247=AXIS2_PLACEMENT_3D('',#132912,#105583,#105584);
#94248=AXIS2_PLACEMENT_3D('',#132927,#105586,#105587);
#94249=AXIS2_PLACEMENT_3D('',#132954,#105589,#105590);
#94250=AXIS2_PLACEMENT_3D('',#133002,#105592,#105593);
#94251=AXIS2_PLACEMENT_3D('',#133053,#105595,#105596);
#94252=AXIS2_PLACEMENT_3D('',#133101,#105598,#105599);
#94253=AXIS2_PLACEMENT_3D('',#133114,#105601,#105602);
#94254=AXIS2_PLACEMENT_3D('',#133136,#105604,#105605);
#94255=AXIS2_PLACEMENT_3D('',#133142,#105606,#105607);
#94256=AXIS2_PLACEMENT_3D('',#133143,#105608,#105609);
#94257=AXIS2_PLACEMENT_3D('',#133145,#105610,#105611);
#94258=AXIS2_PLACEMENT_3D('',#133146,#105612,#105613);
#94259=AXIS2_PLACEMENT_3D('',#133166,#105614,#105615);
#94260=AXIS2_PLACEMENT_3D('',#133173,#105616,#105617);
#94261=AXIS2_PLACEMENT_3D('',#133178,#105619,#105620);
#94262=AXIS2_PLACEMENT_3D('',#133181,#105622,#105623);
#94263=AXIS2_PLACEMENT_3D('',#133182,#105624,#105625);
#94264=AXIS2_PLACEMENT_3D('',#133232,#105632,#105633);
#94265=AXIS2_PLACEMENT_3D('',#133257,#105639,#105640);
#94266=AXIS2_PLACEMENT_3D('',#133259,#105641,#105642);
#94267=AXIS2_PLACEMENT_3D('',#133261,#105643,#105644);
#94268=AXIS2_PLACEMENT_3D('',#133262,#105645,#105646);
#94269=AXIS2_PLACEMENT_3D('',#133263,#105647,#105648);
#94270=AXIS2_PLACEMENT_3D('',#133268,#105650,#105651);
#94271=AXIS2_PLACEMENT_3D('',#133271,#105653,#105654);
#94272=AXIS2_PLACEMENT_3D('',#133272,#105655,#105656);
#94273=AXIS2_PLACEMENT_3D('',#133275,#105659,#105660);
#94274=AXIS2_PLACEMENT_3D('',#133277,#105661,#105662);
#94275=AXIS2_PLACEMENT_3D('',#133279,#105663,#105664);
#94276=AXIS2_PLACEMENT_3D('',#133280,#105665,#105666);
#94277=AXIS2_PLACEMENT_3D('',#133281,#105667,#105668);
#94278=AXIS2_PLACEMENT_3D('',#133366,#105678,#105679);
#94279=AXIS2_PLACEMENT_3D('',#133373,#105680,#105681);
#94280=AXIS2_PLACEMENT_3D('',#133375,#105682,#105683);
#94281=AXIS2_PLACEMENT_3D('',#133377,#105685,#105686);
#94282=AXIS2_PLACEMENT_3D('',#133380,#105687,#105688);
#94283=AXIS2_PLACEMENT_3D('',#133381,#105689,#105690);
#94284=AXIS2_PLACEMENT_3D('',#133382,#105691,#105692);
#94285=AXIS2_PLACEMENT_3D('',#133383,#105693,#105694);
#94286=AXIS2_PLACEMENT_3D('',#133385,#105695,#105696);
#94287=AXIS2_PLACEMENT_3D('',#133388,#105698,#105699);
#94288=AXIS2_PLACEMENT_3D('',#133414,#105700,#105701);
#94289=AXIS2_PLACEMENT_3D('',#133423,#105702,#105703);
#94290=AXIS2_PLACEMENT_3D('',#133425,#105704,#105705);
#94291=AXIS2_PLACEMENT_3D('',#133426,#105706,#105707);
#94292=AXIS2_PLACEMENT_3D('',#133458,#105708,#105709);
#94293=AXIS2_PLACEMENT_3D('',#133469,#105710,#105711);
#94294=AXIS2_PLACEMENT_3D('',#133471,#105712,#105713);
#94295=AXIS2_PLACEMENT_3D('',#133473,#105715,#105716);
#94296=AXIS2_PLACEMENT_3D('',#133476,#105717,#105718);
#94297=AXIS2_PLACEMENT_3D('',#133477,#105719,#105720);
#94298=AXIS2_PLACEMENT_3D('',#133478,#105721,#105722);
#94299=AXIS2_PLACEMENT_3D('',#133479,#105723,#105724);
#94300=AXIS2_PLACEMENT_3D('',#133481,#105725,#105726);
#94301=AXIS2_PLACEMENT_3D('',#133483,#105727,#105728);
#94302=AXIS2_PLACEMENT_3D('',#133516,#105730,#105731);
#94303=AXIS2_PLACEMENT_3D('',#133540,#105732,#105733);
#94304=AXIS2_PLACEMENT_3D('',#133541,#105734,#105735);
#94305=AXIS2_PLACEMENT_3D('',#133579,#105736,#105737);
#94306=AXIS2_PLACEMENT_3D('',#133629,#105738,#105739);
#94307=AXIS2_PLACEMENT_3D('',#133631,#105740,#105741);
#94308=AXIS2_PLACEMENT_3D('',#133633,#105743,#105744);
#94309=AXIS2_PLACEMENT_3D('',#133636,#105745,#105746);
#94310=AXIS2_PLACEMENT_3D('',#133637,#105747,#105748);
#94311=AXIS2_PLACEMENT_3D('',#133638,#105749,#105750);
#94312=AXIS2_PLACEMENT_3D('',#133639,#105751,#105752);
#94313=AXIS2_PLACEMENT_3D('',#133641,#105753,#105754);
#94314=AXIS2_PLACEMENT_3D('',#133643,#105755,#105756);
#94315=AXIS2_PLACEMENT_3D('',#133676,#105758,#105759);
#94316=AXIS2_PLACEMENT_3D('',#133739,#105760,#105761);
#94317=AXIS2_PLACEMENT_3D('',#133740,#105762,#105763);
#94318=AXIS2_PLACEMENT_3D('',#133772,#105764,#105765);
#94319=AXIS2_PLACEMENT_3D('',#133822,#105766,#105767);
#94320=AXIS2_PLACEMENT_3D('',#133824,#105768,#105769);
#94321=AXIS2_PLACEMENT_3D('',#133826,#105771,#105772);
#94322=AXIS2_PLACEMENT_3D('',#133829,#105773,#105774);
#94323=AXIS2_PLACEMENT_3D('',#133830,#105775,#105776);
#94324=AXIS2_PLACEMENT_3D('',#133831,#105777,#105778);
#94325=AXIS2_PLACEMENT_3D('',#133832,#105779,#105780);
#94326=AXIS2_PLACEMENT_3D('',#133834,#105781,#105782);
#94327=AXIS2_PLACEMENT_3D('',#133836,#105783,#105784);
#94328=AXIS2_PLACEMENT_3D('',#133869,#105786,#105787);
#94329=AXIS2_PLACEMENT_3D('',#133893,#105788,#105789);
#94330=AXIS2_PLACEMENT_3D('',#133894,#105790,#105791);
#94331=AXIS2_PLACEMENT_3D('',#133920,#105792,#105793);
#94332=AXIS2_PLACEMENT_3D('',#133929,#105794,#105795);
#94333=AXIS2_PLACEMENT_3D('',#133931,#105796,#105797);
#94334=AXIS2_PLACEMENT_3D('',#133933,#105799,#105800);
#94335=AXIS2_PLACEMENT_3D('',#133936,#105801,#105802);
#94336=AXIS2_PLACEMENT_3D('',#133937,#105803,#105804);
#94337=AXIS2_PLACEMENT_3D('',#133938,#105805,#105806);
#94338=AXIS2_PLACEMENT_3D('',#133939,#105807,#105808);
#94339=AXIS2_PLACEMENT_3D('',#133941,#105809,#105810);
#94340=AXIS2_PLACEMENT_3D('',#133944,#105812,#105813);
#94341=AXIS2_PLACEMENT_3D('',#133964,#105814,#105815);
#94342=AXIS2_PLACEMENT_3D('',#133971,#105816,#105817);
#94343=AXIS2_PLACEMENT_3D('',#133973,#105818,#105819);
#94344=AXIS2_PLACEMENT_3D('',#133974,#105820,#105821);
#94345=AXIS2_PLACEMENT_3D('',#134006,#105822,#105823);
#94346=AXIS2_PLACEMENT_3D('',#134044,#105824,#105825);
#94347=AXIS2_PLACEMENT_3D('',#134046,#105826,#105827);
#94348=AXIS2_PLACEMENT_3D('',#134048,#105829,#105830);
#94349=AXIS2_PLACEMENT_3D('',#134051,#105831,#105832);
#94350=AXIS2_PLACEMENT_3D('',#134052,#105833,#105834);
#94351=AXIS2_PLACEMENT_3D('',#134053,#105835,#105836);
#94352=AXIS2_PLACEMENT_3D('',#134054,#105837,#105838);
#94353=AXIS2_PLACEMENT_3D('',#134056,#105839,#105840);
#94354=AXIS2_PLACEMENT_3D('',#134059,#105842,#105843);
#94355=AXIS2_PLACEMENT_3D('',#134092,#105844,#105845);
#94356=AXIS2_PLACEMENT_3D('',#134116,#105847,#105848);
#94357=AXIS2_PLACEMENT_3D('',#134118,#105849,#105850);
#94358=AXIS2_PLACEMENT_3D('',#134120,#105851,#105852);
#94359=AXIS2_PLACEMENT_3D('',#134141,#105854,#105855);
#94360=AXIS2_PLACEMENT_3D('',#134148,#105856,#105857);
#94361=AXIS2_PLACEMENT_3D('',#134150,#105858,#105859);
#94362=AXIS2_PLACEMENT_3D('',#134171,#105861,#105862);
#94363=AXIS2_PLACEMENT_3D('',#134178,#105863,#105864);
#94364=AXIS2_PLACEMENT_3D('',#134180,#105865,#105866);
#94365=AXIS2_PLACEMENT_3D('',#134182,#105868,#105869);
#94366=AXIS2_PLACEMENT_3D('',#134214,#105871,#105872);
#94367=AXIS2_PLACEMENT_3D('',#134221,#105873,#105874);
#94368=AXIS2_PLACEMENT_3D('',#134223,#105875,#105876);
#94369=AXIS2_PLACEMENT_3D('',#134244,#105878,#105879);
#94370=AXIS2_PLACEMENT_3D('',#134258,#105880,#105881);
#94371=AXIS2_PLACEMENT_3D('',#134271,#105883,#105884);
#94372=AXIS2_PLACEMENT_3D('',#134273,#105885,#105886);
#94373=AXIS2_PLACEMENT_3D('',#134275,#105887,#105888);
#94374=AXIS2_PLACEMENT_3D('',#134296,#105890,#105891);
#94375=AXIS2_PLACEMENT_3D('',#134303,#105892,#105893);
#94376=AXIS2_PLACEMENT_3D('',#134305,#105894,#105895);
#94377=AXIS2_PLACEMENT_3D('',#134326,#105897,#105898);
#94378=AXIS2_PLACEMENT_3D('',#134333,#105899,#105900);
#94379=AXIS2_PLACEMENT_3D('',#134335,#105901,#105902);
#94380=AXIS2_PLACEMENT_3D('',#134337,#105904,#105905);
#94381=AXIS2_PLACEMENT_3D('',#134358,#105907,#105908);
#94382=AXIS2_PLACEMENT_3D('',#134365,#105909,#105910);
#94383=AXIS2_PLACEMENT_3D('',#134389,#105912,#105913);
#94384=AXIS2_PLACEMENT_3D('',#134391,#105914,#105915);
#94385=AXIS2_PLACEMENT_3D('',#134394,#105917,#105918);
#94386=AXIS2_PLACEMENT_3D('',#134414,#105919,#105920);
#94387=AXIS2_PLACEMENT_3D('',#134421,#105921,#105922);
#94388=AXIS2_PLACEMENT_3D('',#134423,#105923,#105924);
#94389=AXIS2_PLACEMENT_3D('',#134444,#105926,#105927);
#94390=AXIS2_PLACEMENT_3D('',#134451,#105928,#105929);
#94391=AXIS2_PLACEMENT_3D('',#134453,#105930,#105931);
#94392=AXIS2_PLACEMENT_3D('',#134492,#105933,#105934);
#94393=AXIS2_PLACEMENT_3D('',#134505,#105936,#105937);
#94394=AXIS2_PLACEMENT_3D('',#134507,#105938,#105939);
#94395=AXIS2_PLACEMENT_3D('',#134509,#105940,#105941);
#94396=AXIS2_PLACEMENT_3D('',#134530,#105943,#105944);
#94397=AXIS2_PLACEMENT_3D('',#134537,#105945,#105946);
#94398=AXIS2_PLACEMENT_3D('',#134539,#105947,#105948);
#94399=AXIS2_PLACEMENT_3D('',#134560,#105950,#105951);
#94400=AXIS2_PLACEMENT_3D('',#134567,#105952,#105953);
#94401=AXIS2_PLACEMENT_3D('',#134569,#105954,#105955);
#94402=AXIS2_PLACEMENT_3D('',#134571,#105957,#105958);
#94403=AXIS2_PLACEMENT_3D('',#134573,#105960,#105961);
#94404=AXIS2_PLACEMENT_3D('',#134597,#105963,#105964);
#94405=AXIS2_PLACEMENT_3D('',#134599,#105965,#105966);
#94406=AXIS2_PLACEMENT_3D('',#134602,#105968,#105969);
#94407=AXIS2_PLACEMENT_3D('',#134622,#105970,#105971);
#94408=AXIS2_PLACEMENT_3D('',#134629,#105972,#105973);
#94409=AXIS2_PLACEMENT_3D('',#134631,#105974,#105975);
#94410=AXIS2_PLACEMENT_3D('',#134652,#105977,#105978);
#94411=AXIS2_PLACEMENT_3D('',#134659,#105979,#105980);
#94412=AXIS2_PLACEMENT_3D('',#134661,#105981,#105982);
#94413=AXIS2_PLACEMENT_3D('',#134663,#105984,#105985);
#94414=AXIS2_PLACEMENT_3D('',#134689,#105987,#105988);
#94415=AXIS2_PLACEMENT_3D('',#134690,#105989,#105990);
#94416=AXIS2_PLACEMENT_3D('',#134691,#105991,#105992);
#94417=AXIS2_PLACEMENT_3D('',#134693,#105993,#105994);
#94418=AXIS2_PLACEMENT_3D('',#134714,#105996,#105997);
#94419=AXIS2_PLACEMENT_3D('',#134723,#105998,#105999);
#94420=AXIS2_PLACEMENT_3D('',#134737,#106000,#106001);
#94421=AXIS2_PLACEMENT_3D('',#134750,#106003,#106004);
#94422=AXIS2_PLACEMENT_3D('',#134752,#106005,#106006);
#94423=AXIS2_PLACEMENT_3D('',#134754,#106007,#106008);
#94424=AXIS2_PLACEMENT_3D('',#134775,#106010,#106011);
#94425=AXIS2_PLACEMENT_3D('',#134782,#106012,#106013);
#94426=AXIS2_PLACEMENT_3D('',#134784,#106014,#106015);
#94427=AXIS2_PLACEMENT_3D('',#134805,#106017,#106018);
#94428=AXIS2_PLACEMENT_3D('',#134812,#106019,#106020);
#94429=AXIS2_PLACEMENT_3D('',#134814,#106021,#106022);
#94430=AXIS2_PLACEMENT_3D('',#134842,#106024,#106025);
#94431=AXIS2_PLACEMENT_3D('',#134849,#106026,#106027);
#94432=AXIS2_PLACEMENT_3D('',#134851,#106028,#106029);
#94433=AXIS2_PLACEMENT_3D('',#134854,#106031,#106032);
#94434=AXIS2_PLACEMENT_3D('',#134867,#106033,#106034);
#94435=AXIS2_PLACEMENT_3D('',#134868,#106035,#106036);
#94436=AXIS2_PLACEMENT_3D('',#134881,#106038,#106039);
#94437=AXIS2_PLACEMENT_3D('',#134883,#106040,#106041);
#94438=AXIS2_PLACEMENT_3D('',#134885,#106042,#106043);
#94439=AXIS2_PLACEMENT_3D('',#134906,#106045,#106046);
#94440=AXIS2_PLACEMENT_3D('',#134913,#106047,#106048);
#94441=AXIS2_PLACEMENT_3D('',#134915,#106049,#106050);
#94442=AXIS2_PLACEMENT_3D('',#134936,#106052,#106053);
#94443=AXIS2_PLACEMENT_3D('',#134943,#106054,#106055);
#94444=AXIS2_PLACEMENT_3D('',#134945,#106056,#106057);
#94445=AXIS2_PLACEMENT_3D('',#134947,#106059,#106060);
#94446=AXIS2_PLACEMENT_3D('',#134971,#106062,#106063);
#94447=AXIS2_PLACEMENT_3D('',#134973,#106064,#106065);
#94448=AXIS2_PLACEMENT_3D('',#134975,#106066,#106067);
#94449=AXIS2_PLACEMENT_3D('',#134996,#106069,#106070);
#94450=AXIS2_PLACEMENT_3D('',#135003,#106071,#106072);
#94451=AXIS2_PLACEMENT_3D('',#135005,#106073,#106074);
#94452=AXIS2_PLACEMENT_3D('',#135026,#106076,#106077);
#94453=AXIS2_PLACEMENT_3D('',#135028,#106078,#106079);
#94454=AXIS2_PLACEMENT_3D('',#135035,#106080,#106081);
#94455=AXIS2_PLACEMENT_3D('',#135037,#106082,#106083);
#94456=AXIS2_PLACEMENT_3D('',#135039,#106084,#106085);
#94457=AXIS2_PLACEMENT_3D('',#135041,#106087,#106088);
#94458=AXIS2_PLACEMENT_3D('',#135054,#106090,#106091);
#94459=AXIS2_PLACEMENT_3D('',#135058,#106093,#106094);
#94460=AXIS2_PLACEMENT_3D('',#135060,#106095,#106096);
#94461=AXIS2_PLACEMENT_3D('',#135062,#106097,#106098);
#94462=AXIS2_PLACEMENT_3D('',#135066,#106100,#106101);
#94463=AXIS2_PLACEMENT_3D('',#135068,#106103,#106104);
#94464=AXIS2_PLACEMENT_3D('',#135072,#106106,#106107);
#94465=AXIS2_PLACEMENT_3D('',#135074,#106108,#106109);
#94466=AXIS2_PLACEMENT_3D('',#135076,#106111,#106112);
#94467=AXIS2_PLACEMENT_3D('',#135082,#106116,#106117);
#94468=AXIS2_PLACEMENT_3D('',#135085,#106119,#106120);
#94469=AXIS2_PLACEMENT_3D('',#135100,#106121,#106122);
#94470=AXIS2_PLACEMENT_3D('',#135101,#106123,#106124);
#94471=AXIS2_PLACEMENT_3D('',#135102,#106125,#106126);
#94472=AXIS2_PLACEMENT_3D('',#135121,#106127,#106128);
#94473=AXIS2_PLACEMENT_3D('',#135225,#106129,#106130);
#94474=AXIS2_PLACEMENT_3D('',#135232,#106131,#106132);
#94475=AXIS2_PLACEMENT_3D('',#135235,#106133,#106134);
#94476=AXIS2_PLACEMENT_3D('',#135237,#106135,#106136);
#94477=AXIS2_PLACEMENT_3D('',#135239,#106137,#106138);
#94478=AXIS2_PLACEMENT_3D('',#135240,#106139,#106140);
#94479=AXIS2_PLACEMENT_3D('',#135241,#106141,#106142);
#94480=AXIS2_PLACEMENT_3D('',#135245,#106144,#106145);
#94481=AXIS2_PLACEMENT_3D('',#135247,#106147,#106148);
#94482=AXIS2_PLACEMENT_3D('',#135283,#106151,#106152);
#94483=AXIS2_PLACEMENT_3D('',#135286,#106154,#106155);
#94484=AXIS2_PLACEMENT_3D('',#135287,#106156,#106157);
#94485=AXIS2_PLACEMENT_3D('',#135291,#106159,#106160);
#94486=AXIS2_PLACEMENT_3D('',#135293,#106162,#106163);
#94487=AXIS2_PLACEMENT_3D('',#135295,#106164,#106165);
#94488=AXIS2_PLACEMENT_3D('',#135297,#106166,#106167);
#94489=AXIS2_PLACEMENT_3D('',#135298,#106168,#106169);
#94490=AXIS2_PLACEMENT_3D('',#135299,#106170,#106171);
#94491=AXIS2_PLACEMENT_3D('',#135303,#106173,#106174);
#94492=AXIS2_PLACEMENT_3D('',#135305,#106176,#106177);
#94493=AXIS2_PLACEMENT_3D('',#135307,#106178,#106179);
#94494=AXIS2_PLACEMENT_3D('',#135309,#106180,#106181);
#94495=AXIS2_PLACEMENT_3D('',#135310,#106182,#106183);
#94496=AXIS2_PLACEMENT_3D('',#135311,#106184,#106185);
#94497=AXIS2_PLACEMENT_3D('',#135315,#106187,#106188);
#94498=AXIS2_PLACEMENT_3D('',#135317,#106190,#106191);
#94499=AXIS2_PLACEMENT_3D('',#135320,#106192,#106193);
#94500=AXIS2_PLACEMENT_3D('',#135322,#106194,#106195);
#94501=AXIS2_PLACEMENT_3D('',#135324,#106196,#106197);
#94502=AXIS2_PLACEMENT_3D('',#135338,#106198,#106199);
#94503=AXIS2_PLACEMENT_3D('',#135382,#106200,#106201);
#94504=AXIS2_PLACEMENT_3D('',#135384,#106202,#106203);
#94505=AXIS2_PLACEMENT_3D('',#135388,#106205,#106206);
#94506=AXIS2_PLACEMENT_3D('',#135390,#106208,#106209);
#94507=AXIS2_PLACEMENT_3D('',#135392,#106210,#106211);
#94508=AXIS2_PLACEMENT_3D('',#135394,#106212,#106213);
#94509=AXIS2_PLACEMENT_3D('',#135395,#106214,#106215);
#94510=AXIS2_PLACEMENT_3D('',#135396,#106216,#106217);
#94511=AXIS2_PLACEMENT_3D('',#135400,#106219,#106220);
#94512=AXIS2_PLACEMENT_3D('',#135402,#106222,#106223);
#94513=AXIS2_PLACEMENT_3D('',#135404,#106224,#106225);
#94514=AXIS2_PLACEMENT_3D('',#135406,#106226,#106227);
#94515=AXIS2_PLACEMENT_3D('',#135407,#106228,#106229);
#94516=AXIS2_PLACEMENT_3D('',#135408,#106230,#106231);
#94517=AXIS2_PLACEMENT_3D('',#135412,#106233,#106234);
#94518=AXIS2_PLACEMENT_3D('',#135414,#106236,#106237);
#94519=AXIS2_PLACEMENT_3D('',#135416,#106238,#106239);
#94520=AXIS2_PLACEMENT_3D('',#135418,#106240,#106241);
#94521=AXIS2_PLACEMENT_3D('',#135419,#106242,#106243);
#94522=AXIS2_PLACEMENT_3D('',#135446,#106244,#106245);
#94523=AXIS2_PLACEMENT_3D('',#135464,#106246,#106247);
#94524=AXIS2_PLACEMENT_3D('',#135469,#106250,#106251);
#94525=AXIS2_PLACEMENT_3D('',#135470,#106252,#106253);
#94526=AXIS2_PLACEMENT_3D('',#135472,#106254,#106255);
#94527=AXIS2_PLACEMENT_3D('',#135476,#106257,#106258);
#94528=AXIS2_PLACEMENT_3D('',#135478,#106260,#106261);
#94529=AXIS2_PLACEMENT_3D('',#135480,#106262,#106263);
#94530=AXIS2_PLACEMENT_3D('',#135482,#106264,#106265);
#94531=AXIS2_PLACEMENT_3D('',#135483,#106266,#106267);
#94532=AXIS2_PLACEMENT_3D('',#135484,#106268,#106269);
#94533=AXIS2_PLACEMENT_3D('',#135488,#106271,#106272);
#94534=AXIS2_PLACEMENT_3D('',#135490,#106274,#106275);
#94535=AXIS2_PLACEMENT_3D('',#135492,#106276,#106277);
#94536=AXIS2_PLACEMENT_3D('',#135494,#106278,#106279);
#94537=AXIS2_PLACEMENT_3D('',#135495,#106280,#106281);
#94538=AXIS2_PLACEMENT_3D('',#135496,#106282,#106283);
#94539=AXIS2_PLACEMENT_3D('',#135500,#106285,#106286);
#94540=AXIS2_PLACEMENT_3D('',#135502,#106288,#106289);
#94541=AXIS2_PLACEMENT_3D('',#135506,#106291,#106292);
#94542=AXIS2_PLACEMENT_3D('',#135509,#106294,#106295);
#94543=AXIS2_PLACEMENT_3D('',#135510,#106296,#106297);
#94544=AXIS2_PLACEMENT_3D('',#135512,#106298,#106299);
#94545=AXIS2_PLACEMENT_3D('',#135516,#106301,#106302);
#94546=AXIS2_PLACEMENT_3D('',#135518,#106304,#106305);
#94547=AXIS2_PLACEMENT_3D('',#135520,#106306,#106307);
#94548=AXIS2_PLACEMENT_3D('',#135522,#106308,#106309);
#94549=AXIS2_PLACEMENT_3D('',#135523,#106310,#106311);
#94550=AXIS2_PLACEMENT_3D('',#135524,#106312,#106313);
#94551=AXIS2_PLACEMENT_3D('',#135528,#106315,#106316);
#94552=AXIS2_PLACEMENT_3D('',#135530,#106318,#106319);
#94553=AXIS2_PLACEMENT_3D('',#135532,#106320,#106321);
#94554=AXIS2_PLACEMENT_3D('',#135534,#106322,#106323);
#94555=AXIS2_PLACEMENT_3D('',#135535,#106324,#106325);
#94556=AXIS2_PLACEMENT_3D('',#135536,#106326,#106327);
#94557=AXIS2_PLACEMENT_3D('',#135540,#106329,#106330);
#94558=AXIS2_PLACEMENT_3D('',#135542,#106332,#106333);
#94559=AXIS2_PLACEMENT_3D('',#135546,#106335,#106336);
#94560=AXIS2_PLACEMENT_3D('',#135549,#106338,#106339);
#94561=AXIS2_PLACEMENT_3D('',#135550,#106340,#106341);
#94562=AXIS2_PLACEMENT_3D('',#135552,#106342,#106343);
#94563=AXIS2_PLACEMENT_3D('',#135555,#106346,#106347);
#94564=AXIS2_PLACEMENT_3D('',#135610,#106354,#106355);
#94565=AXIS2_PLACEMENT_3D('',#135612,#106356,#106357);
#94566=AXIS2_PLACEMENT_3D('',#135625,#106359,#106360);
#94567=AXIS2_PLACEMENT_3D('',#135628,#106361,#106362);
#94568=AXIS2_PLACEMENT_3D('',#135630,#106363,#106364);
#94569=AXIS2_PLACEMENT_3D('',#135632,#106365,#106366);
#94570=AXIS2_PLACEMENT_3D('',#135633,#106367,#106368);
#94571=AXIS2_PLACEMENT_3D('',#135634,#106369,#106370);
#94572=AXIS2_PLACEMENT_3D('',#135636,#106371,#106372);
#94573=AXIS2_PLACEMENT_3D('',#135639,#106375,#106376);
#94574=AXIS2_PLACEMENT_3D('',#135643,#106378,#106379);
#94575=AXIS2_PLACEMENT_3D('',#135645,#106381,#106382);
#94576=AXIS2_PLACEMENT_3D('',#135647,#106383,#106384);
#94577=AXIS2_PLACEMENT_3D('',#135649,#106385,#106386);
#94578=AXIS2_PLACEMENT_3D('',#135650,#106387,#106388);
#94579=AXIS2_PLACEMENT_3D('',#135651,#106389,#106390);
#94580=AXIS2_PLACEMENT_3D('',#135654,#106391,#106392);
#94581=AXIS2_PLACEMENT_3D('',#135657,#106395,#106396);
#94582=AXIS2_PLACEMENT_3D('',#135660,#106397,#106398);
#94583=AXIS2_PLACEMENT_3D('',#135661,#106399,#106400);
#94584=AXIS2_PLACEMENT_3D('',#135662,#106401,#106402);
#94585=AXIS2_PLACEMENT_3D('',#135663,#106403,#106404);
#94586=AXIS2_PLACEMENT_3D('',#135666,#106405,#106406);
#94587=AXIS2_PLACEMENT_3D('',#135667,#106407,#106408);
#94588=AXIS2_PLACEMENT_3D('',#135668,#106409,#106410);
#94589=AXIS2_PLACEMENT_3D('',#135669,#106411,#106412);
#94590=AXIS2_PLACEMENT_3D('',#135672,#106413,#106414);
#94591=AXIS2_PLACEMENT_3D('',#135673,#106415,#106416);
#94592=AXIS2_PLACEMENT_3D('',#135674,#106417,#106418);
#94593=AXIS2_PLACEMENT_3D('',#135675,#106419,#106420);
#94594=AXIS2_PLACEMENT_3D('',#135678,#106421,#106422);
#94595=AXIS2_PLACEMENT_3D('',#135681,#106425,#106426);
#94596=AXIS2_PLACEMENT_3D('',#135684,#106427,#106428);
#94597=AXIS2_PLACEMENT_3D('',#135685,#106429,#106430);
#94598=AXIS2_PLACEMENT_3D('',#135686,#106431,#106432);
#94599=AXIS2_PLACEMENT_3D('',#135687,#106433,#106434);
#94600=AXIS2_PLACEMENT_3D('',#135690,#106435,#106436);
#94601=AXIS2_PLACEMENT_3D('',#135691,#106437,#106438);
#94602=AXIS2_PLACEMENT_3D('',#135692,#106439,#106440);
#94603=AXIS2_PLACEMENT_3D('',#135693,#106441,#106442);
#94604=AXIS2_PLACEMENT_3D('',#135696,#106443,#106444);
#94605=AXIS2_PLACEMENT_3D('',#135697,#106445,#106446);
#94606=AXIS2_PLACEMENT_3D('',#135698,#106447,#106448);
#94607=AXIS2_PLACEMENT_3D('',#135699,#106449,#106450);
#94608=AXIS2_PLACEMENT_3D('',#135702,#106451,#106452);
#94609=AXIS2_PLACEMENT_3D('',#135705,#106455,#106456);
#94610=AXIS2_PLACEMENT_3D('',#135708,#106457,#106458);
#94611=AXIS2_PLACEMENT_3D('',#135709,#106459,#106460);
#94612=AXIS2_PLACEMENT_3D('',#135710,#106461,#106462);
#94613=AXIS2_PLACEMENT_3D('',#135711,#106463,#106464);
#94614=AXIS2_PLACEMENT_3D('',#135714,#106465,#106466);
#94615=AXIS2_PLACEMENT_3D('',#135715,#106467,#106468);
#94616=AXIS2_PLACEMENT_3D('',#135716,#106469,#106470);
#94617=AXIS2_PLACEMENT_3D('',#135717,#106471,#106472);
#94618=AXIS2_PLACEMENT_3D('',#135720,#106473,#106474);
#94619=AXIS2_PLACEMENT_3D('',#135721,#106475,#106476);
#94620=AXIS2_PLACEMENT_3D('',#135722,#106477,#106478);
#94621=AXIS2_PLACEMENT_3D('',#135723,#106479,#106480);
#94622=AXIS2_PLACEMENT_3D('',#135726,#106481,#106482);
#94623=AXIS2_PLACEMENT_3D('',#135729,#106485,#106486);
#94624=AXIS2_PLACEMENT_3D('',#135732,#106487,#106488);
#94625=AXIS2_PLACEMENT_3D('',#135733,#106489,#106490);
#94626=AXIS2_PLACEMENT_3D('',#135734,#106491,#106492);
#94627=AXIS2_PLACEMENT_3D('',#135735,#106493,#106494);
#94628=AXIS2_PLACEMENT_3D('',#135765,#106495,#106496);
#94629=AXIS2_PLACEMENT_3D('',#135768,#106498,#106499);
#94630=AXIS2_PLACEMENT_3D('',#135770,#106500,#106501);
#94631=AXIS2_PLACEMENT_3D('',#135790,#106502,#106503);
#94632=AXIS2_PLACEMENT_3D('',#135791,#106504,#106505);
#94633=AXIS2_PLACEMENT_3D('',#135794,#106506,#106507);
#94634=AXIS2_PLACEMENT_3D('',#135806,#106509,#106510);
#94635=AXIS2_PLACEMENT_3D('',#135817,#106511,#106512);
#94636=AXIS2_PLACEMENT_3D('',#135868,#106513,#106514);
#94637=AXIS2_PLACEMENT_3D('',#135881,#106515,#106516);
#94638=AXIS2_PLACEMENT_3D('',#135925,#106517,#106518);
#94639=AXIS2_PLACEMENT_3D('',#135929,#106520,#106521);
#94640=AXIS2_PLACEMENT_3D('',#135931,#106523,#106524);
#94641=AXIS2_PLACEMENT_3D('',#135933,#106525,#106526);
#94642=AXIS2_PLACEMENT_3D('',#135935,#106527,#106528);
#94643=AXIS2_PLACEMENT_3D('',#135937,#106529,#106530);
#94644=AXIS2_PLACEMENT_3D('',#135938,#106531,#106532);
#94645=AXIS2_PLACEMENT_3D('',#135939,#106533,#106534);
#94646=AXIS2_PLACEMENT_3D('',#135942,#106535,#106536);
#94647=AXIS2_PLACEMENT_3D('',#135945,#106538,#106539);
#94648=AXIS2_PLACEMENT_3D('',#135979,#106541,#106542);
#94649=AXIS2_PLACEMENT_3D('',#136063,#106543,#106544);
#94650=AXIS2_PLACEMENT_3D('',#136066,#106545,#106546);
#94651=AXIS2_PLACEMENT_3D('',#136067,#106547,#106548);
#94652=AXIS2_PLACEMENT_3D('',#136068,#106549,#106550);
#94653=AXIS2_PLACEMENT_3D('',#136095,#106551,#106552);
#94654=AXIS2_PLACEMENT_3D('',#136102,#106553,#106554);
#94655=AXIS2_PLACEMENT_3D('',#136106,#106556,#106557);
#94656=AXIS2_PLACEMENT_3D('',#136108,#106559,#106560);
#94657=AXIS2_PLACEMENT_3D('',#136110,#106561,#106562);
#94658=AXIS2_PLACEMENT_3D('',#136112,#106563,#106564);
#94659=AXIS2_PLACEMENT_3D('',#136114,#106565,#106566);
#94660=AXIS2_PLACEMENT_3D('',#136115,#106567,#106568);
#94661=AXIS2_PLACEMENT_3D('',#136116,#106569,#106570);
#94662=AXIS2_PLACEMENT_3D('',#136119,#106571,#106572);
#94663=AXIS2_PLACEMENT_3D('',#136122,#106574,#106575);
#94664=AXIS2_PLACEMENT_3D('',#136150,#106577,#106578);
#94665=AXIS2_PLACEMENT_3D('',#136181,#106579,#106580);
#94666=AXIS2_PLACEMENT_3D('',#136182,#106581,#106582);
#94667=AXIS2_PLACEMENT_3D('',#136183,#106583,#106584);
#94668=AXIS2_PLACEMENT_3D('',#136268,#106585,#106586);
#94669=AXIS2_PLACEMENT_3D('',#136279,#106587,#106588);
#94670=AXIS2_PLACEMENT_3D('',#136283,#106590,#106591);
#94671=AXIS2_PLACEMENT_3D('',#136285,#106593,#106594);
#94672=AXIS2_PLACEMENT_3D('',#136287,#106595,#106596);
#94673=AXIS2_PLACEMENT_3D('',#136289,#106597,#106598);
#94674=AXIS2_PLACEMENT_3D('',#136291,#106599,#106600);
#94675=AXIS2_PLACEMENT_3D('',#136292,#106601,#106602);
#94676=AXIS2_PLACEMENT_3D('',#136293,#106603,#106604);
#94677=AXIS2_PLACEMENT_3D('',#136296,#106605,#106606);
#94678=AXIS2_PLACEMENT_3D('',#136299,#106608,#106609);
#94679=AXIS2_PLACEMENT_3D('',#136333,#106611,#106612);
#94680=AXIS2_PLACEMENT_3D('',#136393,#106613,#106614);
#94681=AXIS2_PLACEMENT_3D('',#136425,#106618,#106619);
#94682=AXIS2_PLACEMENT_3D('',#136431,#106620,#106621);
#94683=AXIS2_PLACEMENT_3D('',#136436,#106622,#106623);
#94684=AXIS2_PLACEMENT_3D('',#136437,#106624,#106625);
#94685=AXIS2_PLACEMENT_3D('',#136438,#106626,#106627);
#94686=AXIS2_PLACEMENT_3D('',#136481,#106628,#106629);
#94687=AXIS2_PLACEMENT_3D('',#136510,#106630,#106631);
#94688=AXIS2_PLACEMENT_3D('',#136514,#106633,#106634);
#94689=AXIS2_PLACEMENT_3D('',#136614,#106636,#106637);
#94690=AXIS2_PLACEMENT_3D('',#136615,#106638,#106639);
#94691=AXIS2_PLACEMENT_3D('',#136616,#106640,#106641);
#94692=AXIS2_PLACEMENT_3D('',#136623,#106642,#106643);
#94693=AXIS2_PLACEMENT_3D('',#136627,#106645,#106646);
#94694=AXIS2_PLACEMENT_3D('',#136633,#106647,#106648);
#94695=AXIS2_PLACEMENT_3D('',#136634,#106649,#106650);
#94696=AXIS2_PLACEMENT_3D('',#136673,#106651,#106652);
#94697=AXIS2_PLACEMENT_3D('',#136674,#106653,#106654);
#94698=AXIS2_PLACEMENT_3D('',#136675,#106655,#106656);
#94699=AXIS2_PLACEMENT_3D('',#136754,#106658,#106659);
#94700=AXIS2_PLACEMENT_3D('',#136851,#106661,#106662);
#94701=AXIS2_PLACEMENT_3D('',#136964,#106663,#106664);
#94702=AXIS2_PLACEMENT_3D('',#136978,#106665,#106666);
#94703=AXIS2_PLACEMENT_3D('',#136979,#106667,#106668);
#94704=AXIS2_PLACEMENT_3D('',#136980,#106669,#106670);
#94705=AXIS2_PLACEMENT_3D('',#137072,#106673,#106674);
#94706=AXIS2_PLACEMENT_3D('',#137073,#106675,#106676);
#94707=AXIS2_PLACEMENT_3D('',#137103,#106677,#106678);
#94708=AXIS2_PLACEMENT_3D('',#137104,#106679,#106680);
#94709=AXIS2_PLACEMENT_3D('',#137105,#106681,#106682);
#94710=AXIS2_PLACEMENT_3D('',#137109,#106684,#106685);
#94711=AXIS2_PLACEMENT_3D('',#137113,#106687,#106688);
#94712=AXIS2_PLACEMENT_3D('',#137116,#106690,#106691);
#94713=AXIS2_PLACEMENT_3D('',#137159,#106693,#106694);
#94714=AXIS2_PLACEMENT_3D('',#137162,#106696,#106697);
#94715=AXIS2_PLACEMENT_3D('',#137163,#106698,#106699);
#94716=AXIS2_PLACEMENT_3D('',#137167,#106702,#106703);
#94717=AXIS2_PLACEMENT_3D('',#137170,#106705,#106706);
#94718=AXIS2_PLACEMENT_3D('',#137184,#106707,#106708);
#94719=AXIS2_PLACEMENT_3D('',#137185,#106709,#106710);
#94720=AXIS2_PLACEMENT_3D('',#137186,#106711,#106712);
#94721=AXIS2_PLACEMENT_3D('',#137190,#106714,#106715);
#94722=AXIS2_PLACEMENT_3D('',#137193,#106717,#106718);
#94723=AXIS2_PLACEMENT_3D('',#137237,#106720,#106721);
#94724=AXIS2_PLACEMENT_3D('',#137238,#106722,#106723);
#94725=AXIS2_PLACEMENT_3D('',#137269,#106724,#106725);
#94726=AXIS2_PLACEMENT_3D('',#137270,#106726,#106727);
#94727=AXIS2_PLACEMENT_3D('',#137271,#106728,#106729);
#94728=AXIS2_PLACEMENT_3D('',#137275,#106731,#106732);
#94729=AXIS2_PLACEMENT_3D('',#137279,#106734,#106735);
#94730=AXIS2_PLACEMENT_3D('',#137282,#106737,#106738);
#94731=AXIS2_PLACEMENT_3D('',#137340,#106740,#106741);
#94732=AXIS2_PLACEMENT_3D('',#137341,#106742,#106743);
#94733=AXIS2_PLACEMENT_3D('',#137342,#106744,#106745);
#94734=AXIS2_PLACEMENT_3D('',#137345,#106746,#106747);
#94735=AXIS2_PLACEMENT_3D('',#137354,#106748,#106749);
#94736=AXIS2_PLACEMENT_3D('',#137368,#106750,#106751);
#94737=AXIS2_PLACEMENT_3D('',#137369,#106752,#106753);
#94738=AXIS2_PLACEMENT_3D('',#137370,#106754,#106755);
#94739=AXIS2_PLACEMENT_3D('',#137374,#106757,#106758);
#94740=AXIS2_PLACEMENT_3D('',#137377,#106760,#106761);
#94741=AXIS2_PLACEMENT_3D('',#137402,#106763,#106764);
#94742=AXIS2_PLACEMENT_3D('',#137403,#106765,#106766);
#94743=AXIS2_PLACEMENT_3D('',#137406,#106768,#106769);
#94744=AXIS2_PLACEMENT_3D('',#137407,#106770,#106771);
#94745=AXIS2_PLACEMENT_3D('',#137411,#106774,#106775);
#94746=AXIS2_PLACEMENT_3D('',#137414,#106777,#106778);
#94747=AXIS2_PLACEMENT_3D('',#137415,#106779,#106780);
#94748=AXIS2_PLACEMENT_3D('',#137417,#106781,#106782);
#94749=AXIS2_PLACEMENT_3D('',#137434,#106784,#106785);
#94750=AXIS2_PLACEMENT_3D('',#137437,#106787,#106788);
#94751=AXIS2_PLACEMENT_3D('',#137450,#106789,#106790);
#94752=AXIS2_PLACEMENT_3D('',#137451,#106791,#106792);
#94753=AXIS2_PLACEMENT_3D('',#137481,#106793,#106794);
#94754=AXIS2_PLACEMENT_3D('',#137482,#106795,#106796);
#94755=AXIS2_PLACEMENT_3D('',#137483,#106797,#106798);
#94756=AXIS2_PLACEMENT_3D('',#137551,#106800,#106801);
#94757=AXIS2_PLACEMENT_3D('',#137653,#106802,#106803);
#94758=AXIS2_PLACEMENT_3D('',#137679,#106804,#106805);
#94759=AXIS2_PLACEMENT_3D('',#137778,#106806,#106807);
#94760=AXIS2_PLACEMENT_3D('',#137792,#106808,#106809);
#94761=AXIS2_PLACEMENT_3D('',#137793,#106810,#106811);
#94762=AXIS2_PLACEMENT_3D('',#137794,#106812,#106813);
#94763=AXIS2_PLACEMENT_3D('',#137835,#106815,#106816);
#94764=AXIS2_PLACEMENT_3D('',#137857,#106817,#106818);
#94765=AXIS2_PLACEMENT_3D('',#137858,#106819,#106820);
#94766=AXIS2_PLACEMENT_3D('',#137859,#106821,#106822);
#94767=AXIS2_PLACEMENT_3D('',#137953,#106824,#106825);
#94768=AXIS2_PLACEMENT_3D('',#138040,#106826,#106827);
#94769=AXIS2_PLACEMENT_3D('',#138041,#106828,#106829);
#94770=AXIS2_PLACEMENT_3D('',#138043,#106831,#106832);
#94771=AXIS2_PLACEMENT_3D('',#138047,#106834,#106835);
#94772=AXIS2_PLACEMENT_3D('',#138049,#106837,#106838);
#94773=AXIS2_PLACEMENT_3D('',#138053,#106841,#106842);
#94774=AXIS2_PLACEMENT_3D('',#138056,#106844,#106845);
#94775=AXIS2_PLACEMENT_3D('',#138057,#106846,#106847);
#94776=AXIS2_PLACEMENT_3D('',#138061,#106849,#106850);
#94777=AXIS2_PLACEMENT_3D('',#138063,#106852,#106853);
#94778=AXIS2_PLACEMENT_3D('',#138067,#106856,#106857);
#94779=AXIS2_PLACEMENT_3D('',#138070,#106859,#106860);
#94780=AXIS2_PLACEMENT_3D('',#138071,#106861,#106862);
#94781=AXIS2_PLACEMENT_3D('',#138076,#106864,#106865);
#94782=AXIS2_PLACEMENT_3D('',#138079,#106867,#106868);
#94783=AXIS2_PLACEMENT_3D('',#138081,#106869,#106870);
#94784=AXIS2_PLACEMENT_3D('',#138150,#106872,#106873);
#94785=AXIS2_PLACEMENT_3D('',#138164,#106875,#106876);
#94786=AXIS2_PLACEMENT_3D('',#138165,#106877,#106878);
#94787=AXIS2_PLACEMENT_3D('',#138200,#106879,#106880);
#94788=AXIS2_PLACEMENT_3D('',#138201,#106881,#106882);
#94789=AXIS2_PLACEMENT_3D('',#138202,#106883,#106884);
#94790=AXIS2_PLACEMENT_3D('',#138206,#106886,#106887);
#94791=AXIS2_PLACEMENT_3D('',#138210,#106889,#106890);
#94792=AXIS2_PLACEMENT_3D('',#138216,#106893,#106894);
#94793=AXIS2_PLACEMENT_3D('',#138260,#106896,#106897);
#94794=AXIS2_PLACEMENT_3D('',#138263,#106899,#106900);
#94795=AXIS2_PLACEMENT_3D('',#138264,#106901,#106902);
#94796=AXIS2_PLACEMENT_3D('',#138268,#106905,#106906);
#94797=AXIS2_PLACEMENT_3D('',#138271,#106908,#106909);
#94798=AXIS2_PLACEMENT_3D('',#138285,#106910,#106911);
#94799=AXIS2_PLACEMENT_3D('',#138286,#106912,#106913);
#94800=AXIS2_PLACEMENT_3D('',#138287,#106914,#106915);
#94801=AXIS2_PLACEMENT_3D('',#138338,#106917,#106918);
#94802=AXIS2_PLACEMENT_3D('',#138342,#106920,#106921);
#94803=AXIS2_PLACEMENT_3D('',#138345,#106923,#106924);
#94804=AXIS2_PLACEMENT_3D('',#138346,#106925,#106926);
#94805=AXIS2_PLACEMENT_3D('',#138382,#106927,#106928);
#94806=AXIS2_PLACEMENT_3D('',#138383,#106929,#106930);
#94807=AXIS2_PLACEMENT_3D('',#138384,#106931,#106932);
#94808=AXIS2_PLACEMENT_3D('',#138481,#106935,#106936);
#94809=AXIS2_PLACEMENT_3D('',#138578,#106938,#106939);
#94810=AXIS2_PLACEMENT_3D('',#138690,#106940,#106941);
#94811=AXIS2_PLACEMENT_3D('',#138704,#106942,#106943);
#94812=AXIS2_PLACEMENT_3D('',#138705,#106944,#106945);
#94813=AXIS2_PLACEMENT_3D('',#138706,#106946,#106947);
#94814=AXIS2_PLACEMENT_3D('',#138785,#106950,#106951);
#94815=AXIS2_PLACEMENT_3D('',#138787,#106953,#106954);
#94816=AXIS2_PLACEMENT_3D('',#138817,#106955,#106956);
#94817=AXIS2_PLACEMENT_3D('',#138818,#106957,#106958);
#94818=AXIS2_PLACEMENT_3D('',#138819,#106959,#106960);
#94819=AXIS2_PLACEMENT_3D('',#138880,#106963,#106964);
#94820=AXIS2_PLACEMENT_3D('',#138887,#106965,#106966);
#94821=AXIS2_PLACEMENT_3D('',#138891,#106968,#106969);
#94822=AXIS2_PLACEMENT_3D('',#138937,#106970,#106971);
#94823=AXIS2_PLACEMENT_3D('',#138961,#106972,#106973);
#94824=AXIS2_PLACEMENT_3D('',#139021,#106974,#106975);
#94825=AXIS2_PLACEMENT_3D('',#139035,#106976,#106977);
#94826=AXIS2_PLACEMENT_3D('',#139036,#106978,#106979);
#94827=AXIS2_PLACEMENT_3D('',#139037,#106980,#106981);
#94828=AXIS2_PLACEMENT_3D('',#139044,#106982,#106983);
#94829=AXIS2_PLACEMENT_3D('',#139048,#106985,#106986);
#94830=AXIS2_PLACEMENT_3D('',#139055,#106987,#106988);
#94831=AXIS2_PLACEMENT_3D('',#139085,#106991,#106992);
#94832=AXIS2_PLACEMENT_3D('',#139117,#106993,#106994);
#94833=AXIS2_PLACEMENT_3D('',#139118,#106995,#106996);
#94834=AXIS2_PLACEMENT_3D('',#139119,#106997,#106998);
#94835=AXIS2_PLACEMENT_3D('',#139201,#107001,#107002);
#94836=AXIS2_PLACEMENT_3D('',#139298,#107004,#107005);
#94837=AXIS2_PLACEMENT_3D('',#139410,#107006,#107007);
#94838=AXIS2_PLACEMENT_3D('',#139424,#107008,#107009);
#94839=AXIS2_PLACEMENT_3D('',#139425,#107010,#107011);
#94840=AXIS2_PLACEMENT_3D('',#139426,#107012,#107013);
#94841=AXIS2_PLACEMENT_3D('',#139468,#107015,#107016);
#94842=AXIS2_PLACEMENT_3D('',#139513,#107019,#107020);
#94843=AXIS2_PLACEMENT_3D('',#139547,#107021,#107022);
#94844=AXIS2_PLACEMENT_3D('',#139548,#107023,#107024);
#94845=AXIS2_PLACEMENT_3D('',#139549,#107025,#107026);
#94846=AXIS2_PLACEMENT_3D('',#139553,#107028,#107029);
#94847=AXIS2_PLACEMENT_3D('',#139557,#107031,#107032);
#94848=AXIS2_PLACEMENT_3D('',#139561,#107034,#107035);
#94849=AXIS2_PLACEMENT_3D('',#139610,#107037,#107038);
#94850=AXIS2_PLACEMENT_3D('',#139613,#107040,#107041);
#94851=AXIS2_PLACEMENT_3D('',#139614,#107042,#107043);
#94852=AXIS2_PLACEMENT_3D('',#139618,#107046,#107047);
#94853=AXIS2_PLACEMENT_3D('',#139621,#107049,#107050);
#94854=AXIS2_PLACEMENT_3D('',#139635,#107051,#107052);
#94855=AXIS2_PLACEMENT_3D('',#139636,#107053,#107054);
#94856=AXIS2_PLACEMENT_3D('',#139637,#107055,#107056);
#94857=AXIS2_PLACEMENT_3D('',#139683,#107058,#107059);
#94858=AXIS2_PLACEMENT_3D('',#139689,#107062,#107063);
#94859=AXIS2_PLACEMENT_3D('',#139692,#107065,#107066);
#94860=AXIS2_PLACEMENT_3D('',#139693,#107067,#107068);
#94861=AXIS2_PLACEMENT_3D('',#139728,#107069,#107070);
#94862=AXIS2_PLACEMENT_3D('',#139729,#107071,#107072);
#94863=AXIS2_PLACEMENT_3D('',#139730,#107073,#107074);
#94864=AXIS2_PLACEMENT_3D('',#139733,#107075,#107076);
#94865=AXIS2_PLACEMENT_3D('',#139801,#107078,#107079);
#94866=AXIS2_PLACEMENT_3D('',#139805,#107081,#107082);
#94867=AXIS2_PLACEMENT_3D('',#139809,#107085,#107086);
#94868=AXIS2_PLACEMENT_3D('',#139817,#107087,#107088);
#94869=AXIS2_PLACEMENT_3D('',#139851,#107091,#107092);
#94870=AXIS2_PLACEMENT_3D('',#139893,#107093,#107094);
#94871=AXIS2_PLACEMENT_3D('',#139904,#107095,#107096);
#94872=AXIS2_PLACEMENT_3D('',#140007,#107101,#107102);
#94873=AXIS2_PLACEMENT_3D('',#140011,#107104,#107105);
#94874=AXIS2_PLACEMENT_3D('',#140015,#107108,#107109);
#94875=AXIS2_PLACEMENT_3D('',#140018,#107111,#107112);
#94876=AXIS2_PLACEMENT_3D('',#140019,#107113,#107114);
#94877=AXIS2_PLACEMENT_3D('',#140023,#107117,#107118);
#94878=AXIS2_PLACEMENT_3D('',#140026,#107120,#107121);
#94879=AXIS2_PLACEMENT_3D('',#140027,#107122,#107123);
#94880=AXIS2_PLACEMENT_3D('',#140079,#107127,#107128);
#94881=AXIS2_PLACEMENT_3D('',#140082,#107130,#107131);
#94882=AXIS2_PLACEMENT_3D('',#140169,#107136,#107137);
#94883=AXIS2_PLACEMENT_3D('',#140189,#107138,#107139);
#94884=AXIS2_PLACEMENT_3D('',#140221,#107140,#107141);
#94885=AXIS2_PLACEMENT_3D('',#140226,#107143,#107144);
#94886=AXIS2_PLACEMENT_3D('',#140229,#107146,#107147);
#94887=AXIS2_PLACEMENT_3D('',#140231,#107148,#107149);
#94888=AXIS2_PLACEMENT_3D('',#140301,#107152,#107153);
#94889=AXIS2_PLACEMENT_3D('',#140304,#107154,#107155);
#94890=AXIS2_PLACEMENT_3D('',#140305,#107156,#107157);
#94891=AXIS2_PLACEMENT_3D('',#140307,#107158,#107159);
#94892=AXIS2_PLACEMENT_3D('',#140316,#107160,#107161);
#94893=AXIS2_PLACEMENT_3D('',#140349,#107163,#107164);
#94894=AXIS2_PLACEMENT_3D('',#140360,#107165,#107166);
#94895=AXIS2_PLACEMENT_3D('',#140364,#107168,#107169);
#94896=AXIS2_PLACEMENT_3D('',#140368,#107171,#107172);
#94897=AXIS2_PLACEMENT_3D('',#140464,#107178,#107179);
#94898=AXIS2_PLACEMENT_3D('',#140467,#107181,#107182);
#94899=AXIS2_PLACEMENT_3D('',#140468,#107183,#107184);
#94900=AXIS2_PLACEMENT_3D('',#140472,#107187,#107188);
#94901=AXIS2_PLACEMENT_3D('',#140475,#107190,#107191);
#94902=AXIS2_PLACEMENT_3D('',#140476,#107192,#107193);
#94903=AXIS2_PLACEMENT_3D('',#140481,#107195,#107196);
#94904=AXIS2_PLACEMENT_3D('',#140484,#107198,#107199);
#94905=AXIS2_PLACEMENT_3D('',#140596,#107204,#107205);
#94906=AXIS2_PLACEMENT_3D('',#140599,#107206,#107207);
#94907=AXIS2_PLACEMENT_3D('',#140643,#107210,#107211);
#94908=AXIS2_PLACEMENT_3D('',#140675,#107212,#107213);
#94909=AXIS2_PLACEMENT_3D('',#140686,#107214,#107215);
#94910=AXIS2_PLACEMENT_3D('',#140690,#107217,#107218);
#94911=AXIS2_PLACEMENT_3D('',#140693,#107220,#107221);
#94912=AXIS2_PLACEMENT_3D('',#140736,#107224,#107225);
#94913=AXIS2_PLACEMENT_3D('',#140739,#107227,#107228);
#94914=AXIS2_PLACEMENT_3D('',#140740,#107229,#107230);
#94915=AXIS2_PLACEMENT_3D('',#140744,#107233,#107234);
#94916=AXIS2_PLACEMENT_3D('',#140747,#107236,#107237);
#94917=AXIS2_PLACEMENT_3D('',#140748,#107238,#107239);
#94918=AXIS2_PLACEMENT_3D('',#140831,#107241,#107242);
#94919=AXIS2_PLACEMENT_3D('',#140834,#107244,#107245);
#94920=AXIS2_PLACEMENT_3D('',#140871,#107246,#107247);
#94921=AXIS2_PLACEMENT_3D('',#140903,#107248,#107249);
#94922=AXIS2_PLACEMENT_3D('',#140917,#107250,#107251);
#94923=AXIS2_PLACEMENT_3D('',#140925,#107255,#107256);
#94924=AXIS2_PLACEMENT_3D('',#140929,#107259,#107260);
#94925=AXIS2_PLACEMENT_3D('',#140932,#107262,#107263);
#94926=AXIS2_PLACEMENT_3D('',#140933,#107264,#107265);
#94927=AXIS2_PLACEMENT_3D('',#140937,#107268,#107269);
#94928=AXIS2_PLACEMENT_3D('',#140940,#107271,#107272);
#94929=AXIS2_PLACEMENT_3D('',#140941,#107273,#107274);
#94930=AXIS2_PLACEMENT_3D('',#140944,#107276,#107277);
#94931=AXIS2_PLACEMENT_3D('',#140991,#107280,#107281);
#94932=AXIS2_PLACEMENT_3D('',#140992,#107282,#107283);
#94933=AXIS2_PLACEMENT_3D('',#140995,#107284,#107285);
#94934=AXIS2_PLACEMENT_3D('',#141039,#107288,#107289);
#94935=AXIS2_PLACEMENT_3D('',#141071,#107290,#107291);
#94936=AXIS2_PLACEMENT_3D('',#141082,#107292,#107293);
#94937=AXIS2_PLACEMENT_3D('',#141184,#107298,#107299);
#94938=AXIS2_PLACEMENT_3D('',#141188,#107301,#107302);
#94939=AXIS2_PLACEMENT_3D('',#141192,#107305,#107306);
#94940=AXIS2_PLACEMENT_3D('',#141195,#107308,#107309);
#94941=AXIS2_PLACEMENT_3D('',#141196,#107310,#107311);
#94942=AXIS2_PLACEMENT_3D('',#141200,#107314,#107315);
#94943=AXIS2_PLACEMENT_3D('',#141203,#107317,#107318);
#94944=AXIS2_PLACEMENT_3D('',#141235,#107319,#107320);
#94945=AXIS2_PLACEMENT_3D('',#141246,#107321,#107322);
#94946=AXIS2_PLACEMENT_3D('',#141290,#107328,#107329);
#94947=AXIS2_PLACEMENT_3D('',#141293,#107331,#107332);
#94948=AXIS2_PLACEMENT_3D('',#141320,#107336,#107337);
#94949=AXIS2_PLACEMENT_3D('',#141321,#107338,#107339);
#94950=AXIS2_PLACEMENT_3D('',#141326,#107341,#107342);
#94951=AXIS2_PLACEMENT_3D('',#141329,#107344,#107345);
#94952=AXIS2_PLACEMENT_3D('',#141331,#107346,#107347);
#94953=AXIS2_PLACEMENT_3D('',#141333,#107348,#107349);
#94954=AXIS2_PLACEMENT_3D('',#141335,#107350,#107351);
#94955=AXIS2_PLACEMENT_3D('',#141429,#107354,#107355);
#94956=AXIS2_PLACEMENT_3D('',#141451,#107356,#107357);
#94957=AXIS2_PLACEMENT_3D('',#141454,#107358,#107359);
#94958=AXIS2_PLACEMENT_3D('',#141455,#107360,#107361);
#94959=AXIS2_PLACEMENT_3D('',#141457,#107362,#107363);
#94960=AXIS2_PLACEMENT_3D('',#141466,#107364,#107365);
#94961=AXIS2_PLACEMENT_3D('',#141499,#107367,#107368);
#94962=AXIS2_PLACEMENT_3D('',#141510,#107369,#107370);
#94963=AXIS2_PLACEMENT_3D('',#141514,#107372,#107373);
#94964=AXIS2_PLACEMENT_3D('',#141518,#107375,#107376);
#94965=AXIS2_PLACEMENT_3D('',#141617,#107382,#107383);
#94966=AXIS2_PLACEMENT_3D('',#141620,#107385,#107386);
#94967=AXIS2_PLACEMENT_3D('',#141621,#107387,#107388);
#94968=AXIS2_PLACEMENT_3D('',#141625,#107391,#107392);
#94969=AXIS2_PLACEMENT_3D('',#141628,#107394,#107395);
#94970=AXIS2_PLACEMENT_3D('',#141629,#107396,#107397);
#94971=AXIS2_PLACEMENT_3D('',#141634,#107399,#107400);
#94972=AXIS2_PLACEMENT_3D('',#141637,#107402,#107403);
#94973=AXIS2_PLACEMENT_3D('',#141743,#107408,#107409);
#94974=AXIS2_PLACEMENT_3D('',#141746,#107410,#107411);
#94975=AXIS2_PLACEMENT_3D('',#141758,#107412,#107413);
#94976=AXIS2_PLACEMENT_3D('',#141759,#107414,#107415);
#94977=AXIS2_PLACEMENT_3D('',#141810,#107416,#107417);
#94978=AXIS2_PLACEMENT_3D('',#141811,#107418,#107419);
#94979=AXIS2_PLACEMENT_3D('',#141893,#107421,#107422);
#94980=AXIS2_PLACEMENT_3D('',#141895,#107423,#107424);
#94981=AXIS2_PLACEMENT_3D('',#141899,#107426,#107427);
#94982=AXIS2_PLACEMENT_3D('',#141934,#107430,#107431);
#94983=AXIS2_PLACEMENT_3D('',#141945,#107432,#107433);
#94984=AXIS2_PLACEMENT_3D('',#142031,#107440,#107441);
#94985=AXIS2_PLACEMENT_3D('',#142035,#107443,#107444);
#94986=AXIS2_PLACEMENT_3D('',#142039,#107447,#107448);
#94987=AXIS2_PLACEMENT_3D('',#142042,#107450,#107451);
#94988=AXIS2_PLACEMENT_3D('',#142043,#107452,#107453);
#94989=AXIS2_PLACEMENT_3D('',#142047,#107456,#107457);
#94990=AXIS2_PLACEMENT_3D('',#142050,#107459,#107460);
#94991=AXIS2_PLACEMENT_3D('',#142051,#107461,#107462);
#94992=AXIS2_PLACEMENT_3D('',#142056,#107464,#107465);
#94993=AXIS2_PLACEMENT_3D('',#142059,#107467,#107468);
#94994=AXIS2_PLACEMENT_3D('',#142200,#107473,#107474);
#94995=AXIS2_PLACEMENT_3D('',#142201,#107475,#107476);
#94996=AXIS2_PLACEMENT_3D('',#142204,#107477,#107478);
#94997=AXIS2_PLACEMENT_3D('',#142238,#107481,#107482);
#94998=AXIS2_PLACEMENT_3D('',#142252,#107483,#107484);
#94999=AXIS2_PLACEMENT_3D('',#142256,#107486,#107487);
#95000=AXIS2_PLACEMENT_3D('',#142260,#107489,#107490);
#95001=AXIS2_PLACEMENT_3D('',#142368,#107496,#107497);
#95002=AXIS2_PLACEMENT_3D('',#142371,#107499,#107500);
#95003=AXIS2_PLACEMENT_3D('',#142372,#107501,#107502);
#95004=AXIS2_PLACEMENT_3D('',#142376,#107505,#107506);
#95005=AXIS2_PLACEMENT_3D('',#142379,#107508,#107509);
#95006=AXIS2_PLACEMENT_3D('',#142411,#107510,#107511);
#95007=AXIS2_PLACEMENT_3D('',#142422,#107512,#107513);
#95008=AXIS2_PLACEMENT_3D('',#142427,#107515,#107516);
#95009=AXIS2_PLACEMENT_3D('',#142430,#107518,#107519);
#95010=AXIS2_PLACEMENT_3D('',#142539,#107524,#107525);
#95011=AXIS2_PLACEMENT_3D('',#142541,#107527,#107528);
#95012=AXIS2_PLACEMENT_3D('',#142542,#107529,#107530);
#95013=AXIS2_PLACEMENT_3D('',#142543,#107531,#107532);
#95014=AXIS2_PLACEMENT_3D('',#142545,#107533,#107534);
#95015=AXIS2_PLACEMENT_3D('',#142548,#107536,#107537);
#95016=AXIS2_PLACEMENT_3D('',#142549,#107538,#107539);
#95017=AXIS2_PLACEMENT_3D('',#142551,#107540,#107541);
#95018=AXIS2_PLACEMENT_3D('',#142552,#107542,#107543);
#95019=AXIS2_PLACEMENT_3D('',#142571,#107545,#107546);
#95020=AXIS2_PLACEMENT_3D('',#142572,#107547,#107548);
#95021=AXIS2_PLACEMENT_3D('',#142573,#107549,#107550);
#95022=AXIS2_PLACEMENT_3D('',#142584,#107551,#107552);
#95023=AXIS2_PLACEMENT_3D('',#142585,#107553,#107554);
#95024=AXIS2_PLACEMENT_3D('',#142586,#107555,#107556);
#95025=AXIS2_PLACEMENT_3D('',#142588,#107557,#107558);
#95026=AXIS2_PLACEMENT_3D('',#142589,#107559,#107560);
#95027=AXIS2_PLACEMENT_3D('',#142599,#107561,#107562);
#95028=AXIS2_PLACEMENT_3D('',#142600,#107563,#107564);
#95029=AXIS2_PLACEMENT_3D('',#142601,#107565,#107566);
#95030=AXIS2_PLACEMENT_3D('',#142602,#107567,#107568);
#95031=AXIS2_PLACEMENT_3D('',#142603,#107569,#107570);
#95032=AXIS2_PLACEMENT_3D('',#142604,#107571,#107572);
#95033=AXIS2_PLACEMENT_3D('',#142606,#107573,#107574);
#95034=AXIS2_PLACEMENT_3D('',#142609,#107576,#107577);
#95035=AXIS2_PLACEMENT_3D('',#142610,#107578,#107579);
#95036=AXIS2_PLACEMENT_3D('',#142612,#107580,#107581);
#95037=AXIS2_PLACEMENT_3D('',#142613,#107582,#107583);
#95038=AXIS2_PLACEMENT_3D('',#142643,#107585,#107586);
#95039=AXIS2_PLACEMENT_3D('',#142662,#107587,#107588);
#95040=AXIS2_PLACEMENT_3D('',#142663,#107589,#107590);
#95041=AXIS2_PLACEMENT_3D('',#142664,#107591,#107592);
#95042=AXIS2_PLACEMENT_3D('',#142666,#107593,#107594);
#95043=AXIS2_PLACEMENT_3D('',#142669,#107596,#107597);
#95044=AXIS2_PLACEMENT_3D('',#142670,#107598,#107599);
#95045=AXIS2_PLACEMENT_3D('',#142671,#107600,#107601);
#95046=AXIS2_PLACEMENT_3D('',#142672,#107602,#107603);
#95047=AXIS2_PLACEMENT_3D('',#142675,#107605,#107606);
#95048=AXIS2_PLACEMENT_3D('',#142676,#107607,#107608);
#95049=AXIS2_PLACEMENT_3D('',#142710,#107611,#107612);
#95050=AXIS2_PLACEMENT_3D('',#142740,#107613,#107614);
#95051=AXIS2_PLACEMENT_3D('',#142741,#107615,#107616);
#95052=AXIS2_PLACEMENT_3D('',#142748,#107617,#107618);
#95053=AXIS2_PLACEMENT_3D('',#142749,#107619,#107620);
#95054=AXIS2_PLACEMENT_3D('',#142750,#107621,#107622);
#95055=AXIS2_PLACEMENT_3D('',#142751,#107623,#107624);
#95056=AXIS2_PLACEMENT_3D('',#142765,#107625,#107626);
#95057=AXIS2_PLACEMENT_3D('',#142794,#107627,#107628);
#95058=AXIS2_PLACEMENT_3D('',#142796,#107630,#107631);
#95059=AXIS2_PLACEMENT_3D('',#142798,#107633,#107634);
#95060=AXIS2_PLACEMENT_3D('',#142835,#107635,#107636);
#95061=AXIS2_PLACEMENT_3D('',#142872,#107637,#107638);
#95062=AXIS2_PLACEMENT_3D('',#142873,#107639,#107640);
#95063=AXIS2_PLACEMENT_3D('',#142875,#107642,#107643);
#95064=AXIS2_PLACEMENT_3D('',#142877,#107645,#107646);
#95065=AXIS2_PLACEMENT_3D('',#142890,#107647,#107648);
#95066=AXIS2_PLACEMENT_3D('',#142921,#107649,#107650);
#95067=AXIS2_PLACEMENT_3D('',#142941,#107651,#107652);
#95068=AXIS2_PLACEMENT_3D('',#142970,#107653,#107654);
#95069=AXIS2_PLACEMENT_3D('',#142971,#107655,#107656);
#95070=AXIS2_PLACEMENT_3D('',#142982,#107658,#107659);
#95071=AXIS2_PLACEMENT_3D('',#142983,#107660,#107661);
#95072=AXIS2_PLACEMENT_3D('',#142986,#107663,#107664);
#95073=AXIS2_PLACEMENT_3D('',#142987,#107665,#107666);
#95074=AXIS2_PLACEMENT_3D('',#142991,#107669,#107670);
#95075=AXIS2_PLACEMENT_3D('',#142992,#107671,#107672);
#95076=AXIS2_PLACEMENT_3D('',#143002,#107673,#107674);
#95077=AXIS2_PLACEMENT_3D('',#143003,#107675,#107676);
#95078=AXIS2_PLACEMENT_3D('',#143033,#107679,#107680);
#95079=AXIS2_PLACEMENT_3D('',#143034,#107681,#107682);
#95080=AXIS2_PLACEMENT_3D('',#143037,#107684,#107685);
#95081=AXIS2_PLACEMENT_3D('',#143038,#107686,#107687);
#95082=AXIS2_PLACEMENT_3D('',#143042,#107690,#107691);
#95083=AXIS2_PLACEMENT_3D('',#143043,#107692,#107693);
#95084=AXIS2_PLACEMENT_3D('',#143053,#107694,#107695);
#95085=AXIS2_PLACEMENT_3D('',#143054,#107696,#107697);
#95086=AXIS2_PLACEMENT_3D('',#143081,#107700,#107701);
#95087=AXIS2_PLACEMENT_3D('',#143082,#107702,#107703);
#95088=AXIS2_PLACEMENT_3D('',#143083,#107704,#107705);
#95089=AXIS2_PLACEMENT_3D('',#143084,#107706,#107707);
#95090=AXIS2_PLACEMENT_3D('',#143086,#107708,#107709);
#95091=AXIS2_PLACEMENT_3D('',#143087,#107710,#107711);
#95092=AXIS2_PLACEMENT_3D('',#143119,#107713,#107714);
#95093=AXIS2_PLACEMENT_3D('',#143120,#107715,#107716);
#95094=AXIS2_PLACEMENT_3D('',#143122,#107717,#107718);
#95095=AXIS2_PLACEMENT_3D('',#143155,#107720,#107721);
#95096=AXIS2_PLACEMENT_3D('',#143166,#107722,#107723);
#95097=AXIS2_PLACEMENT_3D('',#143168,#107724,#107725);
#95098=AXIS2_PLACEMENT_3D('',#143213,#107727,#107728);
#95099=AXIS2_PLACEMENT_3D('',#143217,#107731,#107732);
#95100=AXIS2_PLACEMENT_3D('',#143220,#107734,#107735);
#95101=AXIS2_PLACEMENT_3D('',#143221,#107736,#107737);
#95102=AXIS2_PLACEMENT_3D('',#143224,#107739,#107740);
#95103=AXIS2_PLACEMENT_3D('',#143225,#107741,#107742);
#95104=AXIS2_PLACEMENT_3D('',#143228,#107744,#107745);
#95105=AXIS2_PLACEMENT_3D('',#143229,#107746,#107747);
#95106=AXIS2_PLACEMENT_3D('',#143295,#107758,#107759);
#95107=AXIS2_PLACEMENT_3D('',#143311,#107762,#107763);
#95108=AXIS2_PLACEMENT_3D('',#143315,#107765,#107766);
#95109=AXIS2_PLACEMENT_3D('',#143317,#107767,#107768);
#95110=AXIS2_PLACEMENT_3D('',#143368,#107770,#107771);
#95111=AXIS2_PLACEMENT_3D('',#143381,#107773,#107774);
#95112=AXIS2_PLACEMENT_3D('',#143390,#107775,#107776);
#95113=AXIS2_PLACEMENT_3D('',#143394,#107778,#107779);
#95114=AXIS2_PLACEMENT_3D('',#143442,#107781,#107782);
#95115=AXIS2_PLACEMENT_3D('',#143455,#107784,#107785);
#95116=AXIS2_PLACEMENT_3D('',#143468,#107787,#107788);
#95117=AXIS2_PLACEMENT_3D('',#143513,#107790,#107791);
#95118=AXIS2_PLACEMENT_3D('',#143567,#107793,#107794);
#95119=AXIS2_PLACEMENT_3D('',#143578,#107796,#107797);
#95120=AXIS2_PLACEMENT_3D('',#143592,#107799,#107800);
#95121=AXIS2_PLACEMENT_3D('',#143643,#107802,#107803);
#95122=AXIS2_PLACEMENT_3D('',#143691,#107805,#107806);
#95123=AXIS2_PLACEMENT_3D('',#143696,#107807,#107808);
#95124=AXIS2_PLACEMENT_3D('',#143712,#107811,#107812);
#95125=AXIS2_PLACEMENT_3D('',#143778,#107823,#107824);
#95126=AXIS2_PLACEMENT_3D('',#143781,#107826,#107827);
#95127=AXIS2_PLACEMENT_3D('',#143782,#107828,#107829);
#95128=AXIS2_PLACEMENT_3D('',#143785,#107831,#107832);
#95129=AXIS2_PLACEMENT_3D('',#143786,#107833,#107834);
#95130=AXIS2_PLACEMENT_3D('',#143789,#107836,#107837);
#95131=AXIS2_PLACEMENT_3D('',#143790,#107838,#107839);
#95132=AXIS2_PLACEMENT_3D('',#143884,#107849,#107850);
#95133=AXIS2_PLACEMENT_3D('',#143885,#107851,#107852);
#95134=AXIS2_PLACEMENT_3D('',#143886,#107853,#107854);
#95135=AXIS2_PLACEMENT_3D('',#143891,#107856,#107857);
#95136=AXIS2_PLACEMENT_3D('',#143893,#107858,#107859);
#95137=AXIS2_PLACEMENT_3D('',#143895,#107860,#107861);
#95138=AXIS2_PLACEMENT_3D('',#143930,#107865,#107866);
#95139=AXIS2_PLACEMENT_3D('',#143931,#107867,#107868);
#95140=AXIS2_PLACEMENT_3D('',#143932,#107869,#107870);
#95141=AXIS2_PLACEMENT_3D('',#143936,#107872,#107873);
#95142=AXIS2_PLACEMENT_3D('',#143968,#107875,#107876);
#95143=AXIS2_PLACEMENT_3D('',#143969,#107877,#107878);
#95144=AXIS2_PLACEMENT_3D('',#143970,#107879,#107880);
#95145=AXIS2_PLACEMENT_3D('',#143974,#107882,#107883);
#95146=AXIS2_PLACEMENT_3D('',#143976,#107884,#107885);
#95147=AXIS2_PLACEMENT_3D('',#143978,#107886,#107887);
#95148=AXIS2_PLACEMENT_3D('',#143982,#107890,#107891);
#95149=AXIS2_PLACEMENT_3D('',#143984,#107893,#107894);
#95150=AXIS2_PLACEMENT_3D('',#143986,#107895,#107896);
#95151=AXIS2_PLACEMENT_3D('',#144000,#107898,#107899);
#95152=AXIS2_PLACEMENT_3D('',#144001,#107900,#107901);
#95153=AXIS2_PLACEMENT_3D('',#144031,#107902,#107903);
#95154=AXIS2_PLACEMENT_3D('',#144032,#107904,#107905);
#95155=AXIS2_PLACEMENT_3D('',#144035,#107907,#107908);
#95156=AXIS2_PLACEMENT_3D('',#144036,#107909,#107910);
#95157=AXIS2_PLACEMENT_3D('',#144040,#107913,#107914);
#95158=AXIS2_PLACEMENT_3D('',#144041,#107915,#107916);
#95159=AXIS2_PLACEMENT_3D('',#144054,#107917,#107918);
#95160=AXIS2_PLACEMENT_3D('',#144055,#107919,#107920);
#95161=AXIS2_PLACEMENT_3D('',#144084,#107921,#107922);
#95162=AXIS2_PLACEMENT_3D('',#144142,#107923,#107924);
#95163=AXIS2_PLACEMENT_3D('',#144216,#107925,#107926);
#95164=AXIS2_PLACEMENT_3D('',#144229,#107927,#107928);
#95165=AXIS2_PLACEMENT_3D('',#144230,#107929,#107930);
#95166=AXIS2_PLACEMENT_3D('',#144269,#107931,#107932);
#95167=AXIS2_PLACEMENT_3D('',#144270,#107933,#107934);
#95168=AXIS2_PLACEMENT_3D('',#144271,#107935,#107936);
#95169=AXIS2_PLACEMENT_3D('',#144272,#107937,#107938);
#95170=AXIS2_PLACEMENT_3D('',#144315,#107939,#107940);
#95171=AXIS2_PLACEMENT_3D('',#144322,#107941,#107942);
#95172=AXIS2_PLACEMENT_3D('',#144325,#107944,#107945);
#95173=AXIS2_PLACEMENT_3D('',#144326,#107946,#107947);
#95174=AXIS2_PLACEMENT_3D('',#144340,#107949,#107950);
#95175=AXIS2_PLACEMENT_3D('',#144353,#107951,#107952);
#95176=AXIS2_PLACEMENT_3D('',#144367,#107953,#107954);
#95177=AXIS2_PLACEMENT_3D('',#144368,#107955,#107956);
#95178=AXIS2_PLACEMENT_3D('',#144369,#107957,#107958);
#95179=AXIS2_PLACEMENT_3D('',#144371,#107959,#107960);
#95180=AXIS2_PLACEMENT_3D('',#144385,#107962,#107963);
#95181=AXIS2_PLACEMENT_3D('',#144449,#107964,#107965);
#95182=AXIS2_PLACEMENT_3D('',#144468,#107966,#107967);
#95183=AXIS2_PLACEMENT_3D('',#144469,#107968,#107969);
#95184=AXIS2_PLACEMENT_3D('',#144471,#107970,#107971);
#95185=AXIS2_PLACEMENT_3D('',#144491,#107973,#107974);
#95186=AXIS2_PLACEMENT_3D('',#144529,#107975,#107976);
#95187=AXIS2_PLACEMENT_3D('',#144531,#107978,#107979);
#95188=AXIS2_PLACEMENT_3D('',#144533,#107981,#107982);
#95189=AXIS2_PLACEMENT_3D('',#144546,#107983,#107984);
#95190=AXIS2_PLACEMENT_3D('',#144559,#107985,#107986);
#95191=AXIS2_PLACEMENT_3D('',#144579,#107987,#107988);
#95192=AXIS2_PLACEMENT_3D('',#144605,#107989,#107990);
#95193=AXIS2_PLACEMENT_3D('',#144607,#107991,#107992);
#95194=AXIS2_PLACEMENT_3D('',#144686,#107994,#107995);
#95195=AXIS2_PLACEMENT_3D('',#144705,#107996,#107997);
#95196=AXIS2_PLACEMENT_3D('',#144706,#107998,#107999);
#95197=AXIS2_PLACEMENT_3D('',#144708,#108000,#108001);
#95198=AXIS2_PLACEMENT_3D('',#144728,#108003,#108004);
#95199=AXIS2_PLACEMENT_3D('',#144769,#108005,#108006);
#95200=AXIS2_PLACEMENT_3D('',#144771,#108007,#108008);
#95201=AXIS2_PLACEMENT_3D('',#144772,#108009,#108010);
#95202=AXIS2_PLACEMENT_3D('',#144773,#108011,#108012);
#95203=AXIS2_PLACEMENT_3D('',#144775,#108013,#108014);
#95204=AXIS2_PLACEMENT_3D('',#144777,#108016,#108017);
#95205=AXIS2_PLACEMENT_3D('',#144778,#108018,#108019);
#95206=AXIS2_PLACEMENT_3D('',#144779,#108020,#108021);
#95207=AXIS2_PLACEMENT_3D('',#144781,#108022,#108023);
#95208=AXIS2_PLACEMENT_3D('',#144783,#108025,#108026);
#95209=AXIS2_PLACEMENT_3D('',#144784,#108027,#108028);
#95210=AXIS2_PLACEMENT_3D('',#144797,#108029,#108030);
#95211=AXIS2_PLACEMENT_3D('',#144810,#108031,#108032);
#95212=AXIS2_PLACEMENT_3D('',#144830,#108033,#108034);
#95213=AXIS2_PLACEMENT_3D('',#144859,#108035,#108036);
#95214=AXIS2_PLACEMENT_3D('',#144861,#108037,#108038);
#95215=AXIS2_PLACEMENT_3D('',#144887,#108040,#108041);
#95216=AXIS2_PLACEMENT_3D('',#144889,#108042,#108043);
#95217=AXIS2_PLACEMENT_3D('',#144891,#108045,#108046);
#95218=AXIS2_PLACEMENT_3D('',#144892,#108047,#108048);
#95219=AXIS2_PLACEMENT_3D('',#144946,#108049,#108050);
#95220=AXIS2_PLACEMENT_3D('',#144965,#108051,#108052);
#95221=AXIS2_PLACEMENT_3D('',#144966,#108053,#108054);
#95222=AXIS2_PLACEMENT_3D('',#144968,#108055,#108056);
#95223=AXIS2_PLACEMENT_3D('',#144988,#108058,#108059);
#95224=AXIS2_PLACEMENT_3D('',#145032,#108060,#108061);
#95225=AXIS2_PLACEMENT_3D('',#145034,#108062,#108063);
#95226=AXIS2_PLACEMENT_3D('',#145035,#108064,#108065);
#95227=AXIS2_PLACEMENT_3D('',#145036,#108066,#108067);
#95228=AXIS2_PLACEMENT_3D('',#145037,#108068,#108069);
#95229=AXIS2_PLACEMENT_3D('',#145039,#108071,#108072);
#95230=AXIS2_PLACEMENT_3D('',#145040,#108073,#108074);
#95231=AXIS2_PLACEMENT_3D('',#145070,#108075,#108076);
#95232=AXIS2_PLACEMENT_3D('',#145095,#108077,#108078);
#95233=AXIS2_PLACEMENT_3D('',#145108,#108079,#108080);
#95234=AXIS2_PLACEMENT_3D('',#145127,#108081,#108082);
#95235=AXIS2_PLACEMENT_3D('',#145159,#108083,#108084);
#95236=AXIS2_PLACEMENT_3D('',#145160,#108085,#108086);
#95237=AXIS2_PLACEMENT_3D('',#145161,#108087,#108088);
#95238=AXIS2_PLACEMENT_3D('',#145162,#108089,#108090);
#95239=AXIS2_PLACEMENT_3D('',#145163,#108091,#108092);
#95240=AXIS2_PLACEMENT_3D('',#145164,#108093,#108094);
#95241=AXIS2_PLACEMENT_3D('',#145165,#108095,#108096);
#95242=AXIS2_PLACEMENT_3D('',#145166,#108097,#108098);
#95243=AXIS2_PLACEMENT_3D('',#145185,#108099,#108100);
#95244=AXIS2_PLACEMENT_3D('',#145210,#108101,#108102);
#95245=AXIS2_PLACEMENT_3D('',#145247,#108103,#108104);
#95246=AXIS2_PLACEMENT_3D('',#145249,#108105,#108106);
#95247=AXIS2_PLACEMENT_3D('',#145250,#108107,#108108);
#95248=AXIS2_PLACEMENT_3D('',#145251,#108109,#108110);
#95249=AXIS2_PLACEMENT_3D('',#145253,#108111,#108112);
#95250=AXIS2_PLACEMENT_3D('',#145255,#108114,#108115);
#95251=AXIS2_PLACEMENT_3D('',#145256,#108116,#108117);
#95252=AXIS2_PLACEMENT_3D('',#145257,#108118,#108119);
#95253=AXIS2_PLACEMENT_3D('',#145259,#108120,#108121);
#95254=AXIS2_PLACEMENT_3D('',#145260,#108122,#108123);
#95255=AXIS2_PLACEMENT_3D('',#145261,#108124,#108125);
#95256=AXIS2_PLACEMENT_3D('',#145263,#108126,#108127);
#95257=AXIS2_PLACEMENT_3D('',#145265,#108129,#108130);
#95258=AXIS2_PLACEMENT_3D('',#145266,#108131,#108132);
#95259=AXIS2_PLACEMENT_3D('',#145267,#108133,#108134);
#95260=AXIS2_PLACEMENT_3D('',#145271,#108136,#108137);
#95261=AXIS2_PLACEMENT_3D('',#145282,#108138,#108139);
#95262=AXIS2_PLACEMENT_3D('',#145283,#108140,#108141);
#95263=AXIS2_PLACEMENT_3D('',#145284,#108142,#108143);
#95264=AXIS2_PLACEMENT_3D('',#145298,#108144,#108145);
#95265=AXIS2_PLACEMENT_3D('',#145299,#108146,#108147);
#95266=AXIS2_PLACEMENT_3D('',#145319,#108148,#108149);
#95267=AXIS2_PLACEMENT_3D('',#145345,#108150,#108151);
#95268=AXIS2_PLACEMENT_3D('',#145352,#108152,#108153);
#95269=AXIS2_PLACEMENT_3D('',#145354,#108154,#108155);
#95270=AXIS2_PLACEMENT_3D('',#145374,#108157,#108158);
#95271=AXIS2_PLACEMENT_3D('',#145424,#108159,#108160);
#95272=AXIS2_PLACEMENT_3D('',#145426,#108161,#108162);
#95273=AXIS2_PLACEMENT_3D('',#145428,#108164,#108165);
#95274=AXIS2_PLACEMENT_3D('',#145429,#108166,#108167);
#95275=AXIS2_PLACEMENT_3D('',#145517,#108168,#108169);
#95276=AXIS2_PLACEMENT_3D('',#145536,#108170,#108171);
#95277=AXIS2_PLACEMENT_3D('',#145537,#108172,#108173);
#95278=AXIS2_PLACEMENT_3D('',#145539,#108174,#108175);
#95279=AXIS2_PLACEMENT_3D('',#145560,#108177,#108178);
#95280=AXIS2_PLACEMENT_3D('',#145586,#108179,#108180);
#95281=AXIS2_PLACEMENT_3D('',#145605,#108181,#108182);
#95282=AXIS2_PLACEMENT_3D('',#145606,#108183,#108184);
#95283=AXIS2_PLACEMENT_3D('',#145607,#108185,#108186);
#95284=AXIS2_PLACEMENT_3D('',#145608,#108187,#108188);
#95285=AXIS2_PLACEMENT_3D('',#145609,#108189,#108190);
#95286=AXIS2_PLACEMENT_3D('',#145611,#108191,#108192);
#95287=AXIS2_PLACEMENT_3D('',#145622,#108194,#108195);
#95288=AXIS2_PLACEMENT_3D('',#145624,#108196,#108197);
#95289=AXIS2_PLACEMENT_3D('',#145625,#108198,#108199);
#95290=AXIS2_PLACEMENT_3D('',#145626,#108200,#108201);
#95291=AXIS2_PLACEMENT_3D('',#145628,#108202,#108203);
#95292=AXIS2_PLACEMENT_3D('',#145630,#108205,#108206);
#95293=AXIS2_PLACEMENT_3D('',#145631,#108207,#108208);
#95294=AXIS2_PLACEMENT_3D('',#145632,#108209,#108210);
#95295=AXIS2_PLACEMENT_3D('',#145634,#108211,#108212);
#95296=AXIS2_PLACEMENT_3D('',#145636,#108214,#108215);
#95297=AXIS2_PLACEMENT_3D('',#145637,#108216,#108217);
#95298=AXIS2_PLACEMENT_3D('',#145656,#108218,#108219);
#95299=AXIS2_PLACEMENT_3D('',#145657,#108220,#108221);
#95300=AXIS2_PLACEMENT_3D('',#145659,#108222,#108223);
#95301=AXIS2_PLACEMENT_3D('',#145661,#108225,#108226);
#95302=AXIS2_PLACEMENT_3D('',#145664,#108227,#108228);
#95303=AXIS2_PLACEMENT_3D('',#145665,#108229,#108230);
#95304=AXIS2_PLACEMENT_3D('',#145670,#108231,#108232);
#95305=AXIS2_PLACEMENT_3D('',#145671,#108233,#108234);
#95306=AXIS2_PLACEMENT_3D('',#145672,#108235,#108236);
#95307=AXIS2_PLACEMENT_3D('',#145686,#108237,#108238);
#95308=AXIS2_PLACEMENT_3D('',#145687,#108239,#108240);
#95309=AXIS2_PLACEMENT_3D('',#145707,#108241,#108242);
#95310=AXIS2_PLACEMENT_3D('',#145733,#108243,#108244);
#95311=AXIS2_PLACEMENT_3D('',#145740,#108245,#108246);
#95312=AXIS2_PLACEMENT_3D('',#145742,#108247,#108248);
#95313=AXIS2_PLACEMENT_3D('',#145871,#108250,#108251);
#95314=AXIS2_PLACEMENT_3D('',#145890,#108252,#108253);
#95315=AXIS2_PLACEMENT_3D('',#145891,#108254,#108255);
#95316=AXIS2_PLACEMENT_3D('',#145893,#108256,#108257);
#95317=AXIS2_PLACEMENT_3D('',#145914,#108259,#108260);
#95318=AXIS2_PLACEMENT_3D('',#145934,#108261,#108262);
#95319=AXIS2_PLACEMENT_3D('',#145951,#108263,#108264);
#95320=AXIS2_PLACEMENT_3D('',#145952,#108265,#108266);
#95321=AXIS2_PLACEMENT_3D('',#145953,#108267,#108268);
#95322=AXIS2_PLACEMENT_3D('',#145954,#108269,#108270);
#95323=AXIS2_PLACEMENT_3D('',#145998,#108271,#108272);
#95324=AXIS2_PLACEMENT_3D('',#146024,#108273,#108274);
#95325=AXIS2_PLACEMENT_3D('',#146026,#108276,#108277);
#95326=AXIS2_PLACEMENT_3D('',#146033,#108279,#108280);
#95327=AXIS2_PLACEMENT_3D('',#146034,#108281,#108282);
#95328=AXIS2_PLACEMENT_3D('',#146047,#108283,#108284);
#95329=AXIS2_PLACEMENT_3D('',#146148,#108285,#108286);
#95330=AXIS2_PLACEMENT_3D('',#146149,#108287,#108288);
#95331=AXIS2_PLACEMENT_3D('',#146150,#108289,#108290);
#95332=AXIS2_PLACEMENT_3D('',#146164,#108291,#108292);
#95333=AXIS2_PLACEMENT_3D('',#146165,#108293,#108294);
#95334=AXIS2_PLACEMENT_3D('',#146179,#108295,#108296);
#95335=AXIS2_PLACEMENT_3D('',#146203,#108297,#108298);
#95336=AXIS2_PLACEMENT_3D('',#146211,#108299,#108300);
#95337=AXIS2_PLACEMENT_3D('',#146213,#108301,#108302);
#95338=AXIS2_PLACEMENT_3D('',#146299,#108304,#108305);
#95339=AXIS2_PLACEMENT_3D('',#146312,#108306,#108307);
#95340=AXIS2_PLACEMENT_3D('',#146325,#108308,#108309);
#95341=AXIS2_PLACEMENT_3D('',#146326,#108310,#108311);
#95342=AXIS2_PLACEMENT_3D('',#146328,#108312,#108313);
#95343=AXIS2_PLACEMENT_3D('',#146343,#108315,#108316);
#95344=AXIS2_PLACEMENT_3D('',#146344,#108317,#108318);
#95345=AXIS2_PLACEMENT_3D('',#146358,#108319,#108320);
#95346=AXIS2_PLACEMENT_3D('',#146375,#108321,#108322);
#95347=AXIS2_PLACEMENT_3D('',#146376,#108323,#108324);
#95348=AXIS2_PLACEMENT_3D('',#146377,#108325,#108326);
#95349=AXIS2_PLACEMENT_3D('',#146378,#108327,#108328);
#95350=AXIS2_PLACEMENT_3D('',#146410,#108329,#108330);
#95351=AXIS2_PLACEMENT_3D('',#146468,#108331,#108332);
#95352=AXIS2_PLACEMENT_3D('',#146470,#108334,#108335);
#95353=AXIS2_PLACEMENT_3D('',#146473,#108337,#108338);
#95354=AXIS2_PLACEMENT_3D('',#146474,#108339,#108340);
#95355=AXIS2_PLACEMENT_3D('',#146475,#108341,#108342);
#95356=AXIS2_PLACEMENT_3D('',#146488,#108343,#108344);
#95357=AXIS2_PLACEMENT_3D('',#146542,#108345,#108346);
#95358=AXIS2_PLACEMENT_3D('',#146543,#108347,#108348);
#95359=AXIS2_PLACEMENT_3D('',#146544,#108349,#108350);
#95360=AXIS2_PLACEMENT_3D('',#146558,#108351,#108352);
#95361=AXIS2_PLACEMENT_3D('',#146559,#108353,#108354);
#95362=AXIS2_PLACEMENT_3D('',#146573,#108355,#108356);
#95363=AXIS2_PLACEMENT_3D('',#146591,#108357,#108358);
#95364=AXIS2_PLACEMENT_3D('',#146592,#108359,#108360);
#95365=AXIS2_PLACEMENT_3D('',#146593,#108361,#108362);
#95366=AXIS2_PLACEMENT_3D('',#146595,#108363,#108364);
#95367=AXIS2_PLACEMENT_3D('',#146609,#108366,#108367);
#95368=AXIS2_PLACEMENT_3D('',#146679,#108368,#108369);
#95369=AXIS2_PLACEMENT_3D('',#146698,#108370,#108371);
#95370=AXIS2_PLACEMENT_3D('',#146699,#108372,#108373);
#95371=AXIS2_PLACEMENT_3D('',#146701,#108374,#108375);
#95372=AXIS2_PLACEMENT_3D('',#146722,#108377,#108378);
#95373=AXIS2_PLACEMENT_3D('',#146761,#108379,#108380);
#95374=AXIS2_PLACEMENT_3D('',#146778,#108381,#108382);
#95375=AXIS2_PLACEMENT_3D('',#146779,#108383,#108384);
#95376=AXIS2_PLACEMENT_3D('',#146780,#108385,#108386);
#95377=AXIS2_PLACEMENT_3D('',#146781,#108387,#108388);
#95378=AXIS2_PLACEMENT_3D('',#146825,#108389,#108390);
#95379=AXIS2_PLACEMENT_3D('',#146884,#108391,#108392);
#95380=AXIS2_PLACEMENT_3D('',#146886,#108394,#108395);
#95381=AXIS2_PLACEMENT_3D('',#146893,#108397,#108398);
#95382=AXIS2_PLACEMENT_3D('',#146894,#108399,#108400);
#95383=AXIS2_PLACEMENT_3D('',#146907,#108401,#108402);
#95384=AXIS2_PLACEMENT_3D('',#146971,#108403,#108404);
#95385=AXIS2_PLACEMENT_3D('',#146972,#108405,#108406);
#95386=AXIS2_PLACEMENT_3D('',#146973,#108407,#108408);
#95387=AXIS2_PLACEMENT_3D('',#146987,#108409,#108410);
#95388=AXIS2_PLACEMENT_3D('',#146988,#108411,#108412);
#95389=AXIS2_PLACEMENT_3D('',#147002,#108413,#108414);
#95390=AXIS2_PLACEMENT_3D('',#147026,#108415,#108416);
#95391=AXIS2_PLACEMENT_3D('',#147052,#108417,#108418);
#95392=AXIS2_PLACEMENT_3D('',#147054,#108419,#108420);
#95393=AXIS2_PLACEMENT_3D('',#147148,#108422,#108423);
#95394=AXIS2_PLACEMENT_3D('',#147167,#108424,#108425);
#95395=AXIS2_PLACEMENT_3D('',#147168,#108426,#108427);
#95396=AXIS2_PLACEMENT_3D('',#147170,#108428,#108429);
#95397=AXIS2_PLACEMENT_3D('',#147191,#108431,#108432);
#95398=AXIS2_PLACEMENT_3D('',#147239,#108433,#108434);
#95399=AXIS2_PLACEMENT_3D('',#147258,#108435,#108436);
#95400=AXIS2_PLACEMENT_3D('',#147259,#108437,#108438);
#95401=AXIS2_PLACEMENT_3D('',#147260,#108439,#108440);
#95402=AXIS2_PLACEMENT_3D('',#147261,#108441,#108442);
#95403=AXIS2_PLACEMENT_3D('',#147262,#108443,#108444);
#95404=AXIS2_PLACEMENT_3D('',#147264,#108445,#108446);
#95405=AXIS2_PLACEMENT_3D('',#147266,#108447,#108448);
#95406=AXIS2_PLACEMENT_3D('',#147268,#108449,#108450);
#95407=AXIS2_PLACEMENT_3D('',#147273,#108451,#108452);
#95408=AXIS2_PLACEMENT_3D('',#147275,#108453,#108454);
#95409=AXIS2_PLACEMENT_3D('',#147277,#108456,#108457);
#95410=AXIS2_PLACEMENT_3D('',#147278,#108458,#108459);
#95411=AXIS2_PLACEMENT_3D('',#147279,#108460,#108461);
#95412=AXIS2_PLACEMENT_3D('',#147281,#108462,#108463);
#95413=AXIS2_PLACEMENT_3D('',#147283,#108465,#108466);
#95414=AXIS2_PLACEMENT_3D('',#147284,#108467,#108468);
#95415=AXIS2_PLACEMENT_3D('',#147303,#108469,#108470);
#95416=AXIS2_PLACEMENT_3D('',#147304,#108471,#108472);
#95417=AXIS2_PLACEMENT_3D('',#147306,#108473,#108474);
#95418=AXIS2_PLACEMENT_3D('',#147308,#108476,#108477);
#95419=AXIS2_PLACEMENT_3D('',#147310,#108478,#108479);
#95420=AXIS2_PLACEMENT_3D('',#147311,#108480,#108481);
#95421=AXIS2_PLACEMENT_3D('',#147312,#108482,#108483);
#95422=AXIS2_PLACEMENT_3D('',#147352,#108485,#108486);
#95423=AXIS2_PLACEMENT_3D('',#147353,#108487,#108488);
#95424=AXIS2_PLACEMENT_3D('',#147354,#108489,#108490);
#95425=AXIS2_PLACEMENT_3D('',#147368,#108491,#108492);
#95426=AXIS2_PLACEMENT_3D('',#147369,#108493,#108494);
#95427=AXIS2_PLACEMENT_3D('',#147389,#108495,#108496);
#95428=AXIS2_PLACEMENT_3D('',#147415,#108497,#108498);
#95429=AXIS2_PLACEMENT_3D('',#147444,#108499,#108500);
#95430=AXIS2_PLACEMENT_3D('',#147446,#108501,#108502);
#95431=AXIS2_PLACEMENT_3D('',#147535,#108504,#108505);
#95432=AXIS2_PLACEMENT_3D('',#147549,#108506,#108507);
#95433=AXIS2_PLACEMENT_3D('',#147550,#108508,#108509);
#95434=AXIS2_PLACEMENT_3D('',#147551,#108510,#108511);
#95435=AXIS2_PLACEMENT_3D('',#147552,#108512,#108513);
#95436=AXIS2_PLACEMENT_3D('',#147553,#108514,#108515);
#95437=AXIS2_PLACEMENT_3D('',#147554,#108516,#108517);
#95438=AXIS2_PLACEMENT_3D('',#147556,#108518,#108519);
#95439=AXIS2_PLACEMENT_3D('',#147569,#108521,#108522);
#95440=AXIS2_PLACEMENT_3D('',#147571,#108523,#108524);
#95441=AXIS2_PLACEMENT_3D('',#147572,#108525,#108526);
#95442=AXIS2_PLACEMENT_3D('',#147573,#108527,#108528);
#95443=AXIS2_PLACEMENT_3D('',#147593,#108530,#108531);
#95444=AXIS2_PLACEMENT_3D('',#147594,#108532,#108533);
#95445=AXIS2_PLACEMENT_3D('',#147596,#108534,#108535);
#95446=AXIS2_PLACEMENT_3D('',#147617,#108537,#108538);
#95447=AXIS2_PLACEMENT_3D('',#147691,#108539,#108540);
#95448=AXIS2_PLACEMENT_3D('',#147702,#108541,#108542);
#95449=AXIS2_PLACEMENT_3D('',#147703,#108543,#108544);
#95450=AXIS2_PLACEMENT_3D('',#147704,#108545,#108546);
#95451=AXIS2_PLACEMENT_3D('',#147705,#108547,#108548);
#95452=AXIS2_PLACEMENT_3D('',#147706,#108549,#108550);
#95453=AXIS2_PLACEMENT_3D('',#147708,#108551,#108552);
#95454=AXIS2_PLACEMENT_3D('',#147746,#108553,#108554);
#95455=AXIS2_PLACEMENT_3D('',#147748,#108555,#108556);
#95456=AXIS2_PLACEMENT_3D('',#147749,#108557,#108558);
#95457=AXIS2_PLACEMENT_3D('',#147760,#108559,#108560);
#95458=AXIS2_PLACEMENT_3D('',#147761,#108561,#108562);
#95459=AXIS2_PLACEMENT_3D('',#147762,#108563,#108564);
#95460=AXIS2_PLACEMENT_3D('',#147764,#108565,#108566);
#95461=AXIS2_PLACEMENT_3D('',#147773,#108568,#108569);
#95462=AXIS2_PLACEMENT_3D('',#147775,#108570,#108571);
#95463=AXIS2_PLACEMENT_3D('',#147776,#108572,#108573);
#95464=AXIS2_PLACEMENT_3D('',#147777,#108574,#108575);
#95465=AXIS2_PLACEMENT_3D('',#147779,#108576,#108577);
#95466=AXIS2_PLACEMENT_3D('',#147781,#108579,#108580);
#95467=AXIS2_PLACEMENT_3D('',#147782,#108581,#108582);
#95468=AXIS2_PLACEMENT_3D('',#147813,#108583,#108584);
#95469=AXIS2_PLACEMENT_3D('',#147839,#108585,#108586);
#95470=AXIS2_PLACEMENT_3D('',#147850,#108587,#108588);
#95471=AXIS2_PLACEMENT_3D('',#147852,#108589,#108590);
#95472=AXIS2_PLACEMENT_3D('',#147885,#108592,#108593);
#95473=AXIS2_PLACEMENT_3D('',#147948,#108594,#108595);
#95474=AXIS2_PLACEMENT_3D('',#147968,#108596,#108597);
#95475=AXIS2_PLACEMENT_3D('',#147969,#108598,#108599);
#95476=AXIS2_PLACEMENT_3D('',#147970,#108600,#108601);
#95477=AXIS2_PLACEMENT_3D('',#147972,#108603,#108604);
#95478=AXIS2_PLACEMENT_3D('',#147975,#108606,#108607);
#95479=AXIS2_PLACEMENT_3D('',#147976,#108608,#108609);
#95480=AXIS2_PLACEMENT_3D('',#147977,#108610,#108611);
#95481=AXIS2_PLACEMENT_3D('',#147978,#108612,#108613);
#95482=AXIS2_PLACEMENT_3D('',#147979,#108614,#108615);
#95483=AXIS2_PLACEMENT_3D('',#147980,#108616,#108617);
#95484=AXIS2_PLACEMENT_3D('',#147981,#108618,#108619);
#95485=AXIS2_PLACEMENT_3D('',#147982,#108620,#108621);
#95486=AXIS2_PLACEMENT_3D('',#147983,#108622,#108623);
#95487=AXIS2_PLACEMENT_3D('',#147984,#108624,#108625);
#95488=AXIS2_PLACEMENT_3D('',#147987,#108627,#108628);
#95489=AXIS2_PLACEMENT_3D('',#148018,#108629,#108630);
#95490=AXIS2_PLACEMENT_3D('',#148020,#108631,#108632);
#95491=AXIS2_PLACEMENT_3D('',#148022,#108634,#108635);
#95492=AXIS2_PLACEMENT_3D('',#148024,#108636,#108637);
#95493=AXIS2_PLACEMENT_3D('',#148025,#108638,#108639);
#95494=AXIS2_PLACEMENT_3D('',#148026,#108640,#108641);
#95495=AXIS2_PLACEMENT_3D('',#148035,#108643,#108644);
#95496=AXIS2_PLACEMENT_3D('',#148036,#108645,#108646);
#95497=AXIS2_PLACEMENT_3D('',#148037,#108647,#108648);
#95498=AXIS2_PLACEMENT_3D('',#148068,#108649,#108650);
#95499=AXIS2_PLACEMENT_3D('',#148079,#108651,#108652);
#95500=AXIS2_PLACEMENT_3D('',#148092,#108653,#108654);
#95501=AXIS2_PLACEMENT_3D('',#148111,#108655,#108656);
#95502=AXIS2_PLACEMENT_3D('',#148125,#108657,#108658);
#95503=AXIS2_PLACEMENT_3D('',#148126,#108659,#108660);
#95504=AXIS2_PLACEMENT_3D('',#148140,#108661,#108662);
#95505=AXIS2_PLACEMENT_3D('',#148164,#108663,#108664);
#95506=AXIS2_PLACEMENT_3D('',#148196,#108665,#108666);
#95507=AXIS2_PLACEMENT_3D('',#148198,#108667,#108668);
#95508=AXIS2_PLACEMENT_3D('',#148225,#108670,#108671);
#95509=AXIS2_PLACEMENT_3D('',#148250,#108672,#108673);
#95510=AXIS2_PLACEMENT_3D('',#148252,#108674,#108675);
#95511=AXIS2_PLACEMENT_3D('',#148254,#108677,#108678);
#95512=AXIS2_PLACEMENT_3D('',#148255,#108679,#108680);
#95513=AXIS2_PLACEMENT_3D('',#148256,#108681,#108682);
#95514=AXIS2_PLACEMENT_3D('',#148290,#108683,#108684);
#95515=AXIS2_PLACEMENT_3D('',#148291,#108685,#108686);
#95516=AXIS2_PLACEMENT_3D('',#148292,#108687,#108688);
#95517=AXIS2_PLACEMENT_3D('',#148305,#108689,#108690);
#95518=AXIS2_PLACEMENT_3D('',#148331,#108691,#108692);
#95519=AXIS2_PLACEMENT_3D('',#148342,#108693,#108694);
#95520=AXIS2_PLACEMENT_3D('',#148344,#108695,#108696);
#95521=AXIS2_PLACEMENT_3D('',#148377,#108698,#108699);
#95522=AXIS2_PLACEMENT_3D('',#148431,#108700,#108701);
#95523=AXIS2_PLACEMENT_3D('',#148467,#108702,#108703);
#95524=AXIS2_PLACEMENT_3D('',#148478,#108704,#108705);
#95525=AXIS2_PLACEMENT_3D('',#148480,#108706,#108707);
#95526=AXIS2_PLACEMENT_3D('',#148512,#108709,#108710);
#95527=AXIS2_PLACEMENT_3D('',#148523,#108711,#108712);
#95528=AXIS2_PLACEMENT_3D('',#148524,#108713,#108714);
#95529=AXIS2_PLACEMENT_3D('',#148525,#108715,#108716);
#95530=AXIS2_PLACEMENT_3D('',#148527,#108717,#108718);
#95531=AXIS2_PLACEMENT_3D('',#148536,#108720,#108721);
#95532=AXIS2_PLACEMENT_3D('',#148538,#108722,#108723);
#95533=AXIS2_PLACEMENT_3D('',#148539,#108724,#108725);
#95534=AXIS2_PLACEMENT_3D('',#148540,#108726,#108727);
#95535=AXIS2_PLACEMENT_3D('',#148542,#108728,#108729);
#95536=AXIS2_PLACEMENT_3D('',#148544,#108731,#108732);
#95537=AXIS2_PLACEMENT_3D('',#148545,#108733,#108734);
#95538=AXIS2_PLACEMENT_3D('',#148546,#108735,#108736);
#95539=AXIS2_PLACEMENT_3D('',#148548,#108737,#108738);
#95540=AXIS2_PLACEMENT_3D('',#148550,#108740,#108741);
#95541=AXIS2_PLACEMENT_3D('',#148551,#108742,#108743);
#95542=AXIS2_PLACEMENT_3D('',#148552,#108744,#108745);
#95543=AXIS2_PLACEMENT_3D('',#148556,#108747,#108748);
#95544=AXIS2_PLACEMENT_3D('',#148563,#108749,#108750);
#95545=AXIS2_PLACEMENT_3D('',#148564,#108751,#108752);
#95546=AXIS2_PLACEMENT_3D('',#148565,#108753,#108754);
#95547=AXIS2_PLACEMENT_3D('',#148597,#108755,#108756);
#95548=AXIS2_PLACEMENT_3D('',#148608,#108757,#108758);
#95549=AXIS2_PLACEMENT_3D('',#148610,#108759,#108760);
#95550=AXIS2_PLACEMENT_3D('',#148631,#108762,#108763);
#95551=AXIS2_PLACEMENT_3D('',#148651,#108764,#108765);
#95552=AXIS2_PLACEMENT_3D('',#148681,#108766,#108767);
#95553=AXIS2_PLACEMENT_3D('',#148722,#108768,#108769);
#95554=AXIS2_PLACEMENT_3D('',#148724,#108770,#108771);
#95555=AXIS2_PLACEMENT_3D('',#148751,#108773,#108774);
#95556=AXIS2_PLACEMENT_3D('',#148772,#108775,#108776);
#95557=AXIS2_PLACEMENT_3D('',#148795,#108777,#108778);
#95558=AXIS2_PLACEMENT_3D('',#148797,#108779,#108780);
#95559=AXIS2_PLACEMENT_3D('',#148799,#108782,#108783);
#95560=AXIS2_PLACEMENT_3D('',#148800,#108784,#108785);
#95561=AXIS2_PLACEMENT_3D('',#148801,#108786,#108787);
#95562=AXIS2_PLACEMENT_3D('',#148804,#108788,#108789);
#95563=AXIS2_PLACEMENT_3D('',#148819,#108790,#108791);
#95564=AXIS2_PLACEMENT_3D('',#148820,#108792,#108793);
#95565=AXIS2_PLACEMENT_3D('',#148821,#108794,#108795);
#95566=AXIS2_PLACEMENT_3D('',#148822,#108796,#108797);
#95567=AXIS2_PLACEMENT_3D('',#148841,#108798,#108799);
#95568=AXIS2_PLACEMENT_3D('',#148855,#108800,#108801);
#95569=AXIS2_PLACEMENT_3D('',#148884,#108802,#108803);
#95570=AXIS2_PLACEMENT_3D('',#148925,#108804,#108805);
#95571=AXIS2_PLACEMENT_3D('',#148926,#108806,#108807);
#95572=AXIS2_PLACEMENT_3D('',#148927,#108808,#108809);
#95573=AXIS2_PLACEMENT_3D('',#148928,#108810,#108811);
#95574=AXIS2_PLACEMENT_3D('',#148929,#108812,#108813);
#95575=AXIS2_PLACEMENT_3D('',#148930,#108814,#108815);
#95576=AXIS2_PLACEMENT_3D('',#148931,#108816,#108817);
#95577=AXIS2_PLACEMENT_3D('',#148932,#108818,#108819);
#95578=AXIS2_PLACEMENT_3D('',#148963,#108820,#108821);
#95579=AXIS2_PLACEMENT_3D('',#149016,#108822,#108823);
#95580=AXIS2_PLACEMENT_3D('',#149018,#108825,#108826);
#95581=AXIS2_PLACEMENT_3D('',#149019,#108827,#108828);
#95582=AXIS2_PLACEMENT_3D('',#149020,#108829,#108830);
#95583=AXIS2_PLACEMENT_3D('',#149021,#108831,#108832);
#95584=AXIS2_PLACEMENT_3D('',#149022,#108833,#108834);
#95585=AXIS2_PLACEMENT_3D('',#149023,#108835,#108836);
#95586=AXIS2_PLACEMENT_3D('',#149024,#108837,#108838);
#95587=AXIS2_PLACEMENT_3D('',#149025,#108839,#108840);
#95588=AXIS2_PLACEMENT_3D('',#149026,#108841,#108842);
#95589=AXIS2_PLACEMENT_3D('',#149052,#108843,#108844);
#95590=AXIS2_PLACEMENT_3D('',#149073,#108845,#108846);
#95591=AXIS2_PLACEMENT_3D('',#149102,#108847,#108848);
#95592=AXIS2_PLACEMENT_3D('',#149105,#108849,#108850);
#95593=AXIS2_PLACEMENT_3D('',#149122,#108851,#108852);
#95594=AXIS2_PLACEMENT_3D('',#149123,#108853,#108854);
#95595=AXIS2_PLACEMENT_3D('',#149124,#108855,#108856);
#95596=AXIS2_PLACEMENT_3D('',#149125,#108857,#108858);
#95597=AXIS2_PLACEMENT_3D('',#149157,#108859,#108860);
#95598=AXIS2_PLACEMENT_3D('',#149159,#108861,#108862);
#95599=AXIS2_PLACEMENT_3D('',#149160,#108863,#108864);
#95600=AXIS2_PLACEMENT_3D('',#149171,#108865,#108866);
#95601=AXIS2_PLACEMENT_3D('',#149172,#108867,#108868);
#95602=AXIS2_PLACEMENT_3D('',#149173,#108869,#108870);
#95603=AXIS2_PLACEMENT_3D('',#149175,#108871,#108872);
#95604=AXIS2_PLACEMENT_3D('',#149184,#108874,#108875);
#95605=AXIS2_PLACEMENT_3D('',#149186,#108876,#108877);
#95606=AXIS2_PLACEMENT_3D('',#149187,#108878,#108879);
#95607=AXIS2_PLACEMENT_3D('',#149188,#108880,#108881);
#95608=AXIS2_PLACEMENT_3D('',#149190,#108882,#108883);
#95609=AXIS2_PLACEMENT_3D('',#149192,#108885,#108886);
#95610=AXIS2_PLACEMENT_3D('',#149193,#108887,#108888);
#95611=AXIS2_PLACEMENT_3D('',#149224,#108889,#108890);
#95612=AXIS2_PLACEMENT_3D('',#149238,#108891,#108892);
#95613=AXIS2_PLACEMENT_3D('',#149274,#108893,#108894);
#95614=AXIS2_PLACEMENT_3D('',#149324,#108895,#108896);
#95615=AXIS2_PLACEMENT_3D('',#149326,#108897,#108898);
#95616=AXIS2_PLACEMENT_3D('',#149365,#108900,#108901);
#95617=AXIS2_PLACEMENT_3D('',#149428,#108902,#108903);
#95618=AXIS2_PLACEMENT_3D('',#149458,#108904,#108905);
#95619=AXIS2_PLACEMENT_3D('',#149467,#108906,#108907);
#95620=AXIS2_PLACEMENT_3D('',#149469,#108909,#108910);
#95621=AXIS2_PLACEMENT_3D('',#149472,#108912,#108913);
#95622=AXIS2_PLACEMENT_3D('',#149473,#108914,#108915);
#95623=AXIS2_PLACEMENT_3D('',#149474,#108916,#108917);
#95624=AXIS2_PLACEMENT_3D('',#149475,#108918,#108919);
#95625=AXIS2_PLACEMENT_3D('',#149507,#108921,#108922);
#95626=AXIS2_PLACEMENT_3D('',#149509,#108923,#108924);
#95627=AXIS2_PLACEMENT_3D('',#149511,#108926,#108927);
#95628=AXIS2_PLACEMENT_3D('',#149513,#108928,#108929);
#95629=AXIS2_PLACEMENT_3D('',#149514,#108930,#108931);
#95630=AXIS2_PLACEMENT_3D('',#149515,#108932,#108933);
#95631=AXIS2_PLACEMENT_3D('',#149524,#108935,#108936);
#95632=AXIS2_PLACEMENT_3D('',#149525,#108937,#108938);
#95633=AXIS2_PLACEMENT_3D('',#149526,#108939,#108940);
#95634=AXIS2_PLACEMENT_3D('',#149557,#108941,#108942);
#95635=AXIS2_PLACEMENT_3D('',#149568,#108943,#108944);
#95636=AXIS2_PLACEMENT_3D('',#149569,#108945,#108946);
#95637=AXIS2_PLACEMENT_3D('',#149570,#108947,#108948);
#95638=AXIS2_PLACEMENT_3D('',#149571,#108949,#108950);
#95639=AXIS2_PLACEMENT_3D('',#149586,#108952,#108953);
#95640=AXIS2_PLACEMENT_3D('',#149593,#108954,#108955);
#95641=AXIS2_PLACEMENT_3D('',#149594,#108956,#108957);
#95642=AXIS2_PLACEMENT_3D('',#149595,#108958,#108959);
#95643=AXIS2_PLACEMENT_3D('',#149615,#108960,#108961);
#95644=AXIS2_PLACEMENT_3D('',#149654,#108962,#108963);
#95645=AXIS2_PLACEMENT_3D('',#149655,#108964,#108965);
#95646=AXIS2_PLACEMENT_3D('',#149675,#108966,#108967);
#95647=AXIS2_PLACEMENT_3D('',#149701,#108968,#108969);
#95648=AXIS2_PLACEMENT_3D('',#149739,#108970,#108971);
#95649=AXIS2_PLACEMENT_3D('',#149741,#108972,#108973);
#95650=AXIS2_PLACEMENT_3D('',#149768,#108975,#108976);
#95651=AXIS2_PLACEMENT_3D('',#149797,#108977,#108978);
#95652=AXIS2_PLACEMENT_3D('',#149816,#108979,#108980);
#95653=AXIS2_PLACEMENT_3D('',#149829,#108981,#108982);
#95654=AXIS2_PLACEMENT_3D('',#149831,#108983,#108984);
#95655=AXIS2_PLACEMENT_3D('',#149833,#108986,#108987);
#95656=AXIS2_PLACEMENT_3D('',#149834,#108988,#108989);
#95657=AXIS2_PLACEMENT_3D('',#149835,#108990,#108991);
#95658=AXIS2_PLACEMENT_3D('',#149872,#108992,#108993);
#95659=AXIS2_PLACEMENT_3D('',#149873,#108994,#108995);
#95660=AXIS2_PLACEMENT_3D('',#149874,#108996,#108997);
#95661=AXIS2_PLACEMENT_3D('',#149887,#108998,#108999);
#95662=AXIS2_PLACEMENT_3D('',#149913,#109000,#109001);
#95663=AXIS2_PLACEMENT_3D('',#149924,#109002,#109003);
#95664=AXIS2_PLACEMENT_3D('',#149926,#109004,#109005);
#95665=AXIS2_PLACEMENT_3D('',#149959,#109007,#109008);
#95666=AXIS2_PLACEMENT_3D('',#149983,#109009,#109010);
#95667=AXIS2_PLACEMENT_3D('',#150019,#109011,#109012);
#95668=AXIS2_PLACEMENT_3D('',#150030,#109013,#109014);
#95669=AXIS2_PLACEMENT_3D('',#150032,#109015,#109016);
#95670=AXIS2_PLACEMENT_3D('',#150064,#109018,#109019);
#95671=AXIS2_PLACEMENT_3D('',#150075,#109020,#109021);
#95672=AXIS2_PLACEMENT_3D('',#150076,#109022,#109023);
#95673=AXIS2_PLACEMENT_3D('',#150077,#109024,#109025);
#95674=AXIS2_PLACEMENT_3D('',#150079,#109026,#109027);
#95675=AXIS2_PLACEMENT_3D('',#150088,#109029,#109030);
#95676=AXIS2_PLACEMENT_3D('',#150090,#109031,#109032);
#95677=AXIS2_PLACEMENT_3D('',#150091,#109033,#109034);
#95678=AXIS2_PLACEMENT_3D('',#150092,#109035,#109036);
#95679=AXIS2_PLACEMENT_3D('',#150094,#109037,#109038);
#95680=AXIS2_PLACEMENT_3D('',#150096,#109040,#109041);
#95681=AXIS2_PLACEMENT_3D('',#150097,#109042,#109043);
#95682=AXIS2_PLACEMENT_3D('',#150098,#109044,#109045);
#95683=AXIS2_PLACEMENT_3D('',#150100,#109046,#109047);
#95684=AXIS2_PLACEMENT_3D('',#150102,#109049,#109050);
#95685=AXIS2_PLACEMENT_3D('',#150103,#109051,#109052);
#95686=AXIS2_PLACEMENT_3D('',#150104,#109053,#109054);
#95687=AXIS2_PLACEMENT_3D('',#150108,#109056,#109057);
#95688=AXIS2_PLACEMENT_3D('',#150115,#109058,#109059);
#95689=AXIS2_PLACEMENT_3D('',#150116,#109060,#109061);
#95690=AXIS2_PLACEMENT_3D('',#150117,#109062,#109063);
#95691=AXIS2_PLACEMENT_3D('',#150149,#109064,#109065);
#95692=AXIS2_PLACEMENT_3D('',#150160,#109066,#109067);
#95693=AXIS2_PLACEMENT_3D('',#150162,#109068,#109069);
#95694=AXIS2_PLACEMENT_3D('',#150183,#109071,#109072);
#95695=AXIS2_PLACEMENT_3D('',#150203,#109073,#109074);
#95696=AXIS2_PLACEMENT_3D('',#150233,#109075,#109076);
#95697=AXIS2_PLACEMENT_3D('',#150274,#109077,#109078);
#95698=AXIS2_PLACEMENT_3D('',#150276,#109079,#109080);
#95699=AXIS2_PLACEMENT_3D('',#150303,#109082,#109083);
#95700=AXIS2_PLACEMENT_3D('',#150362,#109084,#109085);
#95701=AXIS2_PLACEMENT_3D('',#150385,#109086,#109087);
#95702=AXIS2_PLACEMENT_3D('',#150387,#109088,#109089);
#95703=AXIS2_PLACEMENT_3D('',#150389,#109091,#109092);
#95704=AXIS2_PLACEMENT_3D('',#150390,#109093,#109094);
#95705=AXIS2_PLACEMENT_3D('',#150391,#109095,#109096);
#95706=AXIS2_PLACEMENT_3D('',#150423,#109097,#109098);
#95707=AXIS2_PLACEMENT_3D('',#150454,#109099,#109100);
#95708=AXIS2_PLACEMENT_3D('',#150455,#109101,#109102);
#95709=AXIS2_PLACEMENT_3D('',#150475,#109103,#109104);
#95710=AXIS2_PLACEMENT_3D('',#150476,#109105,#109106);
#95711=AXIS2_PLACEMENT_3D('',#150483,#109107,#109108);
#95712=AXIS2_PLACEMENT_3D('',#150484,#109109,#109110);
#95713=AXIS2_PLACEMENT_3D('',#150485,#109111,#109112);
#95714=AXIS2_PLACEMENT_3D('',#150494,#109113,#109114);
#95715=AXIS2_PLACEMENT_3D('',#150497,#109116,#109117);
#95716=AXIS2_PLACEMENT_3D('',#150498,#109118,#109119);
#95717=AXIS2_PLACEMENT_3D('',#150500,#109120,#109121);
#95718=AXIS2_PLACEMENT_3D('',#150501,#109122,#109123);
#95719=AXIS2_PLACEMENT_3D('',#150502,#109124,#109125);
#95720=AXIS2_PLACEMENT_3D('',#150522,#109127,#109128);
#95721=AXIS2_PLACEMENT_3D('',#150542,#109129,#109130);
#95722=AXIS2_PLACEMENT_3D('',#150580,#109131,#109132);
#95723=AXIS2_PLACEMENT_3D('',#150582,#109133,#109134);
#95724=AXIS2_PLACEMENT_3D('',#150609,#109136,#109137);
#95725=AXIS2_PLACEMENT_3D('',#150639,#109138,#109139);
#95726=AXIS2_PLACEMENT_3D('',#150658,#109140,#109141);
#95727=AXIS2_PLACEMENT_3D('',#150689,#109142,#109143);
#95728=AXIS2_PLACEMENT_3D('',#150690,#109144,#109145);
#95729=AXIS2_PLACEMENT_3D('',#150701,#109146,#109147);
#95730=AXIS2_PLACEMENT_3D('',#150702,#109148,#109149);
#95731=AXIS2_PLACEMENT_3D('',#150703,#109150,#109151);
#95732=AXIS2_PLACEMENT_3D('',#150705,#109152,#109153);
#95733=AXIS2_PLACEMENT_3D('',#150714,#109155,#109156);
#95734=AXIS2_PLACEMENT_3D('',#150716,#109157,#109158);
#95735=AXIS2_PLACEMENT_3D('',#150717,#109159,#109160);
#95736=AXIS2_PLACEMENT_3D('',#150718,#109161,#109162);
#95737=AXIS2_PLACEMENT_3D('',#150720,#109163,#109164);
#95738=AXIS2_PLACEMENT_3D('',#150722,#109166,#109167);
#95739=AXIS2_PLACEMENT_3D('',#150723,#109168,#109169);
#95740=AXIS2_PLACEMENT_3D('',#150754,#109170,#109171);
#95741=AXIS2_PLACEMENT_3D('',#150755,#109172,#109173);
#95742=AXIS2_PLACEMENT_3D('',#150757,#109174,#109175);
#95743=AXIS2_PLACEMENT_3D('',#150759,#109177,#109178);
#95744=AXIS2_PLACEMENT_3D('',#150760,#109179,#109180);
#95745=AXIS2_PLACEMENT_3D('',#150761,#109181,#109182);
#95746=AXIS2_PLACEMENT_3D('',#150762,#109183,#109184);
#95747=AXIS2_PLACEMENT_3D('',#150764,#109185,#109186);
#95748=AXIS2_PLACEMENT_3D('',#150766,#109188,#109189);
#95749=AXIS2_PLACEMENT_3D('',#150767,#109190,#109191);
#95750=AXIS2_PLACEMENT_3D('',#150768,#109192,#109193);
#95751=AXIS2_PLACEMENT_3D('',#150772,#109195,#109196);
#95752=AXIS2_PLACEMENT_3D('',#150779,#109197,#109198);
#95753=AXIS2_PLACEMENT_3D('',#150781,#109199,#109200);
#95754=AXIS2_PLACEMENT_3D('',#150782,#109201,#109202);
#95755=AXIS2_PLACEMENT_3D('',#150783,#109203,#109204);
#95756=AXIS2_PLACEMENT_3D('',#150815,#109205,#109206);
#95757=AXIS2_PLACEMENT_3D('',#150826,#109207,#109208);
#95758=AXIS2_PLACEMENT_3D('',#150828,#109209,#109210);
#95759=AXIS2_PLACEMENT_3D('',#150861,#109212,#109213);
#95760=AXIS2_PLACEMENT_3D('',#150885,#109214,#109215);
#95761=AXIS2_PLACEMENT_3D('',#150921,#109216,#109217);
#95762=AXIS2_PLACEMENT_3D('',#150971,#109218,#109219);
#95763=AXIS2_PLACEMENT_3D('',#150973,#109220,#109221);
#95764=AXIS2_PLACEMENT_3D('',#151012,#109223,#109224);
#95765=AXIS2_PLACEMENT_3D('',#151075,#109225,#109226);
#95766=AXIS2_PLACEMENT_3D('',#151104,#109227,#109228);
#95767=AXIS2_PLACEMENT_3D('',#151113,#109229,#109230);
#95768=AXIS2_PLACEMENT_3D('',#151114,#109231,#109232);
#95769=AXIS2_PLACEMENT_3D('',#151116,#109233,#109234);
#95770=AXIS2_PLACEMENT_3D('',#151118,#109236,#109237);
#95771=AXIS2_PLACEMENT_3D('',#151119,#109238,#109239);
#95772=AXIS2_PLACEMENT_3D('',#151120,#109240,#109241);
#95773=AXIS2_PLACEMENT_3D('',#151122,#109242,#109243);
#95774=AXIS2_PLACEMENT_3D('',#151129,#109244,#109245);
#95775=AXIS2_PLACEMENT_3D('',#151130,#109246,#109247);
#95776=AXIS2_PLACEMENT_3D('',#151149,#109248,#109249);
#95777=AXIS2_PLACEMENT_3D('',#151163,#109250,#109251);
#95778=AXIS2_PLACEMENT_3D('',#151193,#109252,#109253);
#95779=AXIS2_PLACEMENT_3D('',#151237,#109254,#109255);
#95780=AXIS2_PLACEMENT_3D('',#151239,#109256,#109257);
#95781=AXIS2_PLACEMENT_3D('',#151266,#109259,#109260);
#95782=AXIS2_PLACEMENT_3D('',#151326,#109261,#109262);
#95783=AXIS2_PLACEMENT_3D('',#151350,#109263,#109264);
#95784=AXIS2_PLACEMENT_3D('',#151357,#109265,#109266);
#95785=AXIS2_PLACEMENT_3D('',#151359,#109267,#109268);
#95786=AXIS2_PLACEMENT_3D('',#151391,#109270,#109271);
#95787=AXIS2_PLACEMENT_3D('',#151402,#109272,#109273);
#95788=AXIS2_PLACEMENT_3D('',#151403,#109274,#109275);
#95789=AXIS2_PLACEMENT_3D('',#151404,#109276,#109277);
#95790=AXIS2_PLACEMENT_3D('',#151406,#109278,#109279);
#95791=AXIS2_PLACEMENT_3D('',#151415,#109281,#109282);
#95792=AXIS2_PLACEMENT_3D('',#151417,#109283,#109284);
#95793=AXIS2_PLACEMENT_3D('',#151418,#109285,#109286);
#95794=AXIS2_PLACEMENT_3D('',#151419,#109287,#109288);
#95795=AXIS2_PLACEMENT_3D('',#151421,#109289,#109290);
#95796=AXIS2_PLACEMENT_3D('',#151423,#109292,#109293);
#95797=AXIS2_PLACEMENT_3D('',#151424,#109294,#109295);
#95798=AXIS2_PLACEMENT_3D('',#151425,#109296,#109297);
#95799=AXIS2_PLACEMENT_3D('',#151427,#109298,#109299);
#95800=AXIS2_PLACEMENT_3D('',#151429,#109301,#109302);
#95801=AXIS2_PLACEMENT_3D('',#151430,#109303,#109304);
#95802=AXIS2_PLACEMENT_3D('',#151431,#109305,#109306);
#95803=AXIS2_PLACEMENT_3D('',#151432,#109307,#109308);
#95804=AXIS2_PLACEMENT_3D('',#151436,#109310,#109311);
#95805=AXIS2_PLACEMENT_3D('',#151443,#109312,#109313);
#95806=AXIS2_PLACEMENT_3D('',#151445,#109314,#109315);
#95807=AXIS2_PLACEMENT_3D('',#151446,#109316,#109317);
#95808=AXIS2_PLACEMENT_3D('',#151447,#109318,#109319);
#95809=AXIS2_PLACEMENT_3D('',#151479,#109320,#109321);
#95810=AXIS2_PLACEMENT_3D('',#151490,#109322,#109323);
#95811=AXIS2_PLACEMENT_3D('',#151492,#109324,#109325);
#95812=AXIS2_PLACEMENT_3D('',#151519,#109327,#109328);
#95813=AXIS2_PLACEMENT_3D('',#151541,#109329,#109330);
#95814=AXIS2_PLACEMENT_3D('',#151571,#109331,#109332);
#95815=AXIS2_PLACEMENT_3D('',#151582,#109333,#109334);
#95816=AXIS2_PLACEMENT_3D('',#151584,#109335,#109336);
#95817=AXIS2_PLACEMENT_3D('',#151610,#109338,#109339);
#95818=AXIS2_PLACEMENT_3D('',#151666,#109340,#109341);
#95819=AXIS2_PLACEMENT_3D('',#151668,#109342,#109343);
#95820=AXIS2_PLACEMENT_3D('',#151670,#109345,#109346);
#95821=AXIS2_PLACEMENT_3D('',#151671,#109347,#109348);
#95822=AXIS2_PLACEMENT_3D('',#151672,#109349,#109350);
#95823=AXIS2_PLACEMENT_3D('',#151673,#109351,#109352);
#95824=AXIS2_PLACEMENT_3D('',#151674,#109353,#109354);
#95825=AXIS2_PLACEMENT_3D('',#151675,#109355,#109356);
#95826=AXIS2_PLACEMENT_3D('',#151720,#109358,#109359);
#95827=AXIS2_PLACEMENT_3D('',#151721,#109360,#109361);
#95828=AXIS2_PLACEMENT_3D('',#151722,#109362,#109363);
#95829=AXIS2_PLACEMENT_3D('',#151723,#109364,#109365);
#95830=AXIS2_PLACEMENT_3D('',#151724,#109366,#109367);
#95831=AXIS2_PLACEMENT_3D('',#151725,#109368,#109369);
#95832=AXIS2_PLACEMENT_3D('',#151726,#109370,#109371);
#95833=AXIS2_PLACEMENT_3D('',#151727,#109372,#109373);
#95834=AXIS2_PLACEMENT_3D('',#151728,#109374,#109375);
#95835=AXIS2_PLACEMENT_3D('',#151729,#109376,#109377);
#95836=AXIS2_PLACEMENT_3D('',#151748,#109378,#109379);
#95837=AXIS2_PLACEMENT_3D('',#151749,#109380,#109381);
#95838=AXIS2_PLACEMENT_3D('',#151750,#109382,#109383);
#95839=AXIS2_PLACEMENT_3D('',#151770,#109385,#109386);
#95840=AXIS2_PLACEMENT_3D('',#151790,#109388,#109389);
#95841=AXIS2_PLACEMENT_3D('',#151791,#109390,#109391);
#95842=AXIS2_PLACEMENT_3D('',#151792,#109392,#109393);
#95843=AXIS2_PLACEMENT_3D('',#151812,#109395,#109396);
#95844=AXIS2_PLACEMENT_3D('',#151814,#109397,#109398);
#95845=AXIS2_PLACEMENT_3D('',#151835,#109400,#109401);
#95846=AXIS2_PLACEMENT_3D('',#151860,#109402,#109403);
#95847=AXIS2_PLACEMENT_3D('',#151889,#109404,#109405);
#95848=AXIS2_PLACEMENT_3D('',#151890,#109406,#109407);
#95849=AXIS2_PLACEMENT_3D('',#151891,#109408,#109409);
#95850=AXIS2_PLACEMENT_3D('',#151892,#109410,#109411);
#95851=AXIS2_PLACEMENT_3D('',#151923,#109412,#109413);
#95852=AXIS2_PLACEMENT_3D('',#151924,#109414,#109415);
#95853=AXIS2_PLACEMENT_3D('',#151955,#109416,#109417);
#95854=AXIS2_PLACEMENT_3D('',#151956,#109418,#109419);
#95855=AXIS2_PLACEMENT_3D('',#151958,#109420,#109421);
#95856=AXIS2_PLACEMENT_3D('',#151959,#109422,#109423);
#95857=AXIS2_PLACEMENT_3D('',#151972,#109424,#109425);
#95858=AXIS2_PLACEMENT_3D('',#151989,#109426,#109427);
#95859=AXIS2_PLACEMENT_3D('',#151990,#109428,#109429);
#95860=AXIS2_PLACEMENT_3D('',#152009,#109430,#109431);
#95861=AXIS2_PLACEMENT_3D('',#152022,#109432,#109433);
#95862=AXIS2_PLACEMENT_3D('',#152023,#109434,#109435);
#95863=AXIS2_PLACEMENT_3D('',#152054,#109436,#109437);
#95864=AXIS2_PLACEMENT_3D('',#152055,#109438,#109439);
#95865=AXIS2_PLACEMENT_3D('',#152092,#109440,#109441);
#95866=AXIS2_PLACEMENT_3D('',#152105,#109442,#109443);
#95867=AXIS2_PLACEMENT_3D('',#152106,#109444,#109445);
#95868=AXIS2_PLACEMENT_3D('',#152131,#109446,#109447);
#95869=AXIS2_PLACEMENT_3D('',#152132,#109448,#109449);
#95870=AXIS2_PLACEMENT_3D('',#152157,#109450,#109451);
#95871=AXIS2_PLACEMENT_3D('',#152170,#109452,#109453);
#95872=AXIS2_PLACEMENT_3D('',#152171,#109454,#109455);
#95873=AXIS2_PLACEMENT_3D('',#152202,#109456,#109457);
#95874=AXIS2_PLACEMENT_3D('',#152203,#109458,#109459);
#95875=AXIS2_PLACEMENT_3D('',#152216,#109460,#109461);
#95876=AXIS2_PLACEMENT_3D('',#152236,#109462,#109463);
#95877=AXIS2_PLACEMENT_3D('',#152243,#109464,#109465);
#95878=AXIS2_PLACEMENT_3D('',#152244,#109466,#109467);
#95879=AXIS2_PLACEMENT_3D('',#152245,#109468,#109469);
#95880=AXIS2_PLACEMENT_3D('',#152270,#109470,#109471);
#95881=AXIS2_PLACEMENT_3D('',#152271,#109472,#109473);
#95882=AXIS2_PLACEMENT_3D('',#152302,#109474,#109475);
#95883=AXIS2_PLACEMENT_3D('',#152303,#109476,#109477);
#95884=AXIS2_PLACEMENT_3D('',#152304,#109478,#109479);
#95885=AXIS2_PLACEMENT_3D('',#152305,#109480,#109481);
#95886=AXIS2_PLACEMENT_3D('',#152318,#109482,#109483);
#95887=AXIS2_PLACEMENT_3D('',#152350,#109484,#109485);
#95888=AXIS2_PLACEMENT_3D('',#152355,#109486,#109487);
#95889=AXIS2_PLACEMENT_3D('',#152375,#109489,#109490);
#95890=AXIS2_PLACEMENT_3D('',#152376,#109491,#109492);
#95891=AXIS2_PLACEMENT_3D('',#152377,#109493,#109494);
#95892=AXIS2_PLACEMENT_3D('',#152397,#109496,#109497);
#95893=AXIS2_PLACEMENT_3D('',#152398,#109498,#109499);
#95894=AXIS2_PLACEMENT_3D('',#152418,#109500,#109501);
#95895=AXIS2_PLACEMENT_3D('',#152425,#109502,#109503);
#95896=AXIS2_PLACEMENT_3D('',#152445,#109505,#109506);
#95897=AXIS2_PLACEMENT_3D('',#152446,#109507,#109508);
#95898=AXIS2_PLACEMENT_3D('',#152447,#109509,#109510);
#95899=AXIS2_PLACEMENT_3D('',#152467,#109512,#109513);
#95900=AXIS2_PLACEMENT_3D('',#152468,#109514,#109515);
#95901=AXIS2_PLACEMENT_3D('',#152469,#109516,#109517);
#95902=AXIS2_PLACEMENT_3D('',#152470,#109518,#109519);
#95903=AXIS2_PLACEMENT_3D('',#152471,#109520,#109521);
#95904=AXIS2_PLACEMENT_3D('',#152472,#109522,#109523);
#95905=AXIS2_PLACEMENT_3D('',#152473,#109524,#109525);
#95906=AXIS2_PLACEMENT_3D('',#152492,#109526,#109527);
#95907=AXIS2_PLACEMENT_3D('',#152493,#109528,#109529);
#95908=AXIS2_PLACEMENT_3D('',#152494,#109530,#109531);
#95909=AXIS2_PLACEMENT_3D('',#152514,#109533,#109534);
#95910=AXIS2_PLACEMENT_3D('',#152534,#109536,#109537);
#95911=AXIS2_PLACEMENT_3D('',#152535,#109538,#109539);
#95912=AXIS2_PLACEMENT_3D('',#152536,#109540,#109541);
#95913=AXIS2_PLACEMENT_3D('',#152556,#109543,#109544);
#95914=AXIS2_PLACEMENT_3D('',#152558,#109545,#109546);
#95915=AXIS2_PLACEMENT_3D('',#152638,#109548,#109549);
#95916=AXIS2_PLACEMENT_3D('',#152723,#109551,#109552);
#95917=AXIS2_PLACEMENT_3D('',#152724,#109553,#109554);
#95918=AXIS2_PLACEMENT_3D('',#152725,#109555,#109556);
#95919=AXIS2_PLACEMENT_3D('',#152726,#109557,#109558);
#95920=AXIS2_PLACEMENT_3D('',#152727,#109559,#109560);
#95921=AXIS2_PLACEMENT_3D('',#152728,#109561,#109562);
#95922=AXIS2_PLACEMENT_3D('',#152729,#109563,#109564);
#95923=AXIS2_PLACEMENT_3D('',#152730,#109565,#109566);
#95924=AXIS2_PLACEMENT_3D('',#152731,#109567,#109568);
#95925=AXIS2_PLACEMENT_3D('',#152733,#109570,#109571);
#95926=AXIS2_PLACEMENT_3D('',#152735,#109573,#109574);
#95927=AXIS2_PLACEMENT_3D('',#152737,#109576,#109577);
#95928=AXIS2_PLACEMENT_3D('',#152782,#109578,#109579);
#95929=AXIS2_PLACEMENT_3D('',#152783,#109580,#109581);
#95930=AXIS2_PLACEMENT_3D('',#152784,#109582,#109583);
#95931=AXIS2_PLACEMENT_3D('',#152787,#109586,#109587);
#95932=AXIS2_PLACEMENT_3D('',#152789,#109589,#109590);
#95933=AXIS2_PLACEMENT_3D('',#152790,#109591,#109592);
#95934=AXIS2_PLACEMENT_3D('',#152791,#109593,#109594);
#95935=AXIS2_PLACEMENT_3D('',#152832,#109595,#109596);
#95936=AXIS2_PLACEMENT_3D('',#152845,#109597,#109598);
#95937=AXIS2_PLACEMENT_3D('',#152903,#109599,#109600);
#95938=AXIS2_PLACEMENT_3D('',#152916,#109601,#109602);
#95939=AXIS2_PLACEMENT_3D('',#152960,#109603,#109604);
#95940=AXIS2_PLACEMENT_3D('',#152973,#109605,#109606);
#95941=AXIS2_PLACEMENT_3D('',#153025,#109607,#109608);
#95942=AXIS2_PLACEMENT_3D('',#153026,#109609,#109610);
#95943=AXIS2_PLACEMENT_3D('',#153028,#109612,#109613);
#95944=AXIS2_PLACEMENT_3D('',#153031,#109616,#109617);
#95945=AXIS2_PLACEMENT_3D('',#153032,#109618,#109619);
#95946=AXIS2_PLACEMENT_3D('',#153033,#109620,#109621);
#95947=AXIS2_PLACEMENT_3D('',#153078,#109622,#109623);
#95948=AXIS2_PLACEMENT_3D('',#153079,#109624,#109625);
#95949=AXIS2_PLACEMENT_3D('',#153081,#109627,#109628);
#95950=AXIS2_PLACEMENT_3D('',#153102,#109629,#109630);
#95951=AXIS2_PLACEMENT_3D('',#153103,#109631,#109632);
#95952=AXIS2_PLACEMENT_3D('',#153105,#109634,#109635);
#95953=AXIS2_PLACEMENT_3D('',#153107,#109637,#109638);
#95954=AXIS2_PLACEMENT_3D('',#153108,#109639,#109640);
#95955=AXIS2_PLACEMENT_3D('',#153126,#109641,#109642);
#95956=AXIS2_PLACEMENT_3D('',#153143,#109643,#109644);
#95957=AXIS2_PLACEMENT_3D('',#153144,#109645,#109646);
#95958=AXIS2_PLACEMENT_3D('',#153145,#109647,#109648);
#95959=AXIS2_PLACEMENT_3D('',#153146,#109649,#109650);
#95960=AXIS2_PLACEMENT_3D('',#153147,#109651,#109652);
#95961=AXIS2_PLACEMENT_3D('',#153157,#109653,#109654);
#95962=AXIS2_PLACEMENT_3D('',#153178,#109655,#109656);
#95963=AXIS2_PLACEMENT_3D('',#153195,#109657,#109658);
#95964=AXIS2_PLACEMENT_3D('',#153196,#109659,#109660);
#95965=AXIS2_PLACEMENT_3D('',#153198,#109662,#109663);
#95966=AXIS2_PLACEMENT_3D('',#153200,#109665,#109666);
#95967=AXIS2_PLACEMENT_3D('',#153201,#109667,#109668);
#95968=AXIS2_PLACEMENT_3D('',#153202,#109669,#109670);
#95969=AXIS2_PLACEMENT_3D('',#153203,#109671,#109672);
#95970=AXIS2_PLACEMENT_3D('',#153208,#109673,#109674);
#95971=AXIS2_PLACEMENT_3D('',#153210,#109676,#109677);
#95972=AXIS2_PLACEMENT_3D('',#153212,#109679,#109680);
#95973=AXIS2_PLACEMENT_3D('',#153229,#109681,#109682);
#95974=AXIS2_PLACEMENT_3D('',#153250,#109683,#109684);
#95975=AXIS2_PLACEMENT_3D('',#153251,#109685,#109686);
#95976=AXIS2_PLACEMENT_3D('',#153252,#109687,#109688);
#95977=AXIS2_PLACEMENT_3D('',#153253,#109689,#109690);
#95978=AXIS2_PLACEMENT_3D('',#153254,#109691,#109692);
#95979=AXIS2_PLACEMENT_3D('',#153255,#109693,#109694);
#95980=AXIS2_PLACEMENT_3D('',#153256,#109695,#109696);
#95981=AXIS2_PLACEMENT_3D('',#153257,#109697,#109698);
#95982=AXIS2_PLACEMENT_3D('',#153258,#109699,#109700);
#95983=AXIS2_PLACEMENT_3D('',#153297,#109701,#109702);
#95984=AXIS2_PLACEMENT_3D('',#153329,#109703,#109704);
#95985=AXIS2_PLACEMENT_3D('',#153330,#109705,#109706);
#95986=AXIS2_PLACEMENT_3D('',#153332,#109708,#109709);
#95987=AXIS2_PLACEMENT_3D('',#153334,#109711,#109712);
#95988=AXIS2_PLACEMENT_3D('',#153366,#109713,#109714);
#95989=AXIS2_PLACEMENT_3D('',#153405,#109715,#109716);
#95990=AXIS2_PLACEMENT_3D('',#153406,#109717,#109718);
#95991=AXIS2_PLACEMENT_3D('',#153407,#109719,#109720);
#95992=AXIS2_PLACEMENT_3D('',#153408,#109721,#109722);
#95993=AXIS2_PLACEMENT_3D('',#153409,#109723,#109724);
#95994=AXIS2_PLACEMENT_3D('',#153411,#109726,#109727);
#95995=AXIS2_PLACEMENT_3D('',#153413,#109729,#109730);
#95996=AXIS2_PLACEMENT_3D('',#153414,#109731,#109732);
#95997=AXIS2_PLACEMENT_3D('',#153415,#109733,#109734);
#95998=AXIS2_PLACEMENT_3D('',#153416,#109735,#109736);
#95999=AXIS2_PLACEMENT_3D('',#153417,#109737,#109738);
#96000=AXIS2_PLACEMENT_3D('',#153418,#109739,#109740);
#96001=AXIS2_PLACEMENT_3D('',#153439,#109741,#109742);
#96002=AXIS2_PLACEMENT_3D('',#153460,#109743,#109744);
#96003=AXIS2_PLACEMENT_3D('',#153461,#109745,#109746);
#96004=AXIS2_PLACEMENT_3D('',#153463,#109748,#109749);
#96005=AXIS2_PLACEMENT_3D('',#153465,#109751,#109752);
#96006=AXIS2_PLACEMENT_3D('',#153466,#109753,#109754);
#96007=AXIS2_PLACEMENT_3D('',#153467,#109755,#109756);
#96008=AXIS2_PLACEMENT_3D('',#153470,#109757,#109758);
#96009=AXIS2_PLACEMENT_3D('',#153474,#109761,#109762);
#96010=AXIS2_PLACEMENT_3D('',#153483,#109767,#109768);
#96011=AXIS2_PLACEMENT_3D('',#153485,#109769,#109770);
#96012=AXIS2_PLACEMENT_3D('',#153488,#109772,#109773);
#96013=AXIS2_PLACEMENT_3D('',#153489,#109774,#109775);
#96014=AXIS2_PLACEMENT_3D('',#153495,#109779,#109780);
#96015=AXIS2_PLACEMENT_3D('',#153532,#109781,#109782);
#96016=AXIS2_PLACEMENT_3D('',#153791,#109783,#109784);
#96017=AXIS2_PLACEMENT_3D('',#154066,#109787,#109788);
#96018=AXIS2_PLACEMENT_3D('',#154069,#109789,#109790);
#96019=AXIS2_PLACEMENT_3D('',#154090,#109791,#109792);
#96020=AXIS2_PLACEMENT_3D('',#154093,#109793,#109794);
#96021=AXIS2_PLACEMENT_3D('',#154228,#109795,#109796);
#96022=AXIS2_PLACEMENT_3D('',#154234,#109800,#109801);
#96023=AXIS2_PLACEMENT_3D('',#154243,#109806,#109807);
#96024=AXIS2_PLACEMENT_3D('',#154245,#109808,#109809);
#96025=AXIS2_PLACEMENT_3D('',#154248,#109811,#109812);
#96026=AXIS2_PLACEMENT_3D('',#154249,#109813,#109814);
#96027=AXIS2_PLACEMENT_3D('',#154255,#109818,#109819);
#96028=AXIS2_PLACEMENT_3D('',#154272,#109820,#109821);
#96029=AXIS2_PLACEMENT_3D('',#154274,#109822,#109823);
#96030=AXIS2_PLACEMENT_3D('',#154368,#109824,#109825);
#96031=AXIS2_PLACEMENT_3D('',#154601,#109826,#109827);
#96032=AXIS2_PLACEMENT_3D('',#154807,#109830,#109831);
#96033=AXIS2_PLACEMENT_3D('',#154816,#109836,#109837);
#96034=AXIS2_PLACEMENT_3D('',#154818,#109838,#109839);
#96035=AXIS2_PLACEMENT_3D('',#154821,#109841,#109842);
#96036=AXIS2_PLACEMENT_3D('',#154822,#109843,#109844);
#96037=AXIS2_PLACEMENT_3D('',#154828,#109848,#109849);
#96038=AXIS2_PLACEMENT_3D('',#154834,#109852,#109853);
#96039=AXIS2_PLACEMENT_3D('',#154981,#109854,#109855);
#96040=AXIS2_PLACEMENT_3D('',#155238,#109858,#109859);
#96041=AXIS2_PLACEMENT_3D('',#155241,#109860,#109861);
#96042=AXIS2_PLACEMENT_3D('',#155289,#109862,#109863);
#96043=AXIS2_PLACEMENT_3D('',#155307,#109864,#109865);
#96044=AXIS2_PLACEMENT_3D('',#155368,#109866,#109867);
#96045=AXIS2_PLACEMENT_3D('',#155375,#109870,#109871);
#96046=AXIS2_PLACEMENT_3D('',#155377,#109873,#109874);
#96047=AXIS2_PLACEMENT_3D('',#155450,#109875,#109876);
#96048=AXIS2_PLACEMENT_3D('',#155518,#109877,#109878);
#96049=AXIS2_PLACEMENT_3D('',#155808,#109879,#109880);
#96050=AXIS2_PLACEMENT_3D('',#156125,#109883,#109884);
#96051=AXIS2_PLACEMENT_3D('',#156134,#109889,#109890);
#96052=AXIS2_PLACEMENT_3D('',#156138,#109892,#109893);
#96053=AXIS2_PLACEMENT_3D('',#156139,#109894,#109895);
#96054=AXIS2_PLACEMENT_3D('',#156140,#109896,#109897);
#96055=AXIS2_PLACEMENT_3D('',#156146,#109901,#109902);
#96056=AXIS2_PLACEMENT_3D('',#156153,#109903,#109904);
#96057=AXIS2_PLACEMENT_3D('',#156170,#109905,#109906);
#96058=AXIS2_PLACEMENT_3D('',#156204,#109907,#109908);
#96059=AXIS2_PLACEMENT_3D('',#156209,#109909,#109910);
#96060=AXIS2_PLACEMENT_3D('',#156236,#109911,#109912);
#96061=AXIS2_PLACEMENT_3D('',#156237,#109913,#109914);
#96062=AXIS2_PLACEMENT_3D('',#156246,#109919,#109920);
#96063=AXIS2_PLACEMENT_3D('',#156248,#109921,#109922);
#96064=AXIS2_PLACEMENT_3D('',#156251,#109924,#109925);
#96065=AXIS2_PLACEMENT_3D('',#156252,#109926,#109927);
#96066=AXIS2_PLACEMENT_3D('',#156258,#109931,#109932);
#96067=AXIS2_PLACEMENT_3D('',#156264,#109935,#109936);
#96068=AXIS2_PLACEMENT_3D('',#156420,#109937,#109938);
#96069=AXIS2_PLACEMENT_3D('',#156656,#109941,#109942);
#96070=AXIS2_PLACEMENT_3D('',#156659,#109943,#109944);
#96071=AXIS2_PLACEMENT_3D('',#156700,#109945,#109946);
#96072=AXIS2_PLACEMENT_3D('',#156702,#109947,#109948);
#96073=AXIS2_PLACEMENT_3D('',#156704,#109949,#109950);
#96074=AXIS2_PLACEMENT_3D('',#156705,#109951,#109952);
#96075=AXIS2_PLACEMENT_3D('',#156706,#109953,#109954);
#96076=AXIS2_PLACEMENT_3D('',#156713,#109957,#109958);
#96077=AXIS2_PLACEMENT_3D('',#156715,#109960,#109961);
#96078=AXIS2_PLACEMENT_3D('',#156717,#109962,#109963);
#96079=AXIS2_PLACEMENT_3D('',#156718,#109964,#109965);
#96080=AXIS2_PLACEMENT_3D('',#156851,#109966,#109967);
#96081=AXIS2_PLACEMENT_3D('',#157088,#109968,#109969);
#96082=AXIS2_PLACEMENT_3D('',#157097,#109972,#109973);
#96083=AXIS2_PLACEMENT_3D('',#157106,#109978,#109979);
#96084=AXIS2_PLACEMENT_3D('',#157110,#109981,#109982);
#96085=AXIS2_PLACEMENT_3D('',#157111,#109983,#109984);
#96086=AXIS2_PLACEMENT_3D('',#157112,#109985,#109986);
#96087=AXIS2_PLACEMENT_3D('',#157118,#109990,#109991);
#96088=AXIS2_PLACEMENT_3D('',#157121,#109992,#109993);
#96089=AXIS2_PLACEMENT_3D('',#157341,#109994,#109995);
#96090=AXIS2_PLACEMENT_3D('',#157346,#109997,#109998);
#96091=AXIS2_PLACEMENT_3D('',#157349,#110000,#110001);
#96092=AXIS2_PLACEMENT_3D('',#157350,#110002,#110003);
#96093=AXIS2_PLACEMENT_3D('',#157354,#110005,#110006);
#96094=AXIS2_PLACEMENT_3D('',#157356,#110008,#110009);
#96095=AXIS2_PLACEMENT_3D('',#157569,#110012,#110013);
#96096=AXIS2_PLACEMENT_3D('',#157572,#110014,#110015);
#96097=AXIS2_PLACEMENT_3D('',#157644,#110016,#110017);
#96098=AXIS2_PLACEMENT_3D('',#157649,#110019,#110020);
#96099=AXIS2_PLACEMENT_3D('',#157653,#110023,#110024);
#96100=AXIS2_PLACEMENT_3D('',#157662,#110029,#110030);
#96101=AXIS2_PLACEMENT_3D('',#157663,#110031,#110032);
#96102=AXIS2_PLACEMENT_3D('',#157664,#110033,#110034);
#96103=AXIS2_PLACEMENT_3D('',#157665,#110035,#110036);
#96104=AXIS2_PLACEMENT_3D('',#157667,#110037,#110038);
#96105=AXIS2_PLACEMENT_3D('',#157699,#110039,#110040);
#96106=AXIS2_PLACEMENT_3D('',#157935,#110043,#110044);
#96107=AXIS2_PLACEMENT_3D('',#157938,#110045,#110046);
#96108=AXIS2_PLACEMENT_3D('',#158125,#110047,#110048);
#96109=AXIS2_PLACEMENT_3D('',#158231,#110049,#110050);
#96110=AXIS2_PLACEMENT_3D('',#158391,#110053,#110054);
#96111=AXIS2_PLACEMENT_3D('',#158392,#110055,#110056);
#96112=AXIS2_PLACEMENT_3D('',#158395,#110057,#110058);
#96113=AXIS2_PLACEMENT_3D('',#158497,#110059,#110060);
#96114=AXIS2_PLACEMENT_3D('',#158539,#110061,#110062);
#96115=AXIS2_PLACEMENT_3D('',#158540,#110063,#110064);
#96116=AXIS2_PLACEMENT_3D('',#158663,#110067,#110068);
#96117=AXIS2_PLACEMENT_3D('',#158725,#110069,#110070);
#96118=AXIS2_PLACEMENT_3D('',#158728,#110071,#110072);
#96119=AXIS2_PLACEMENT_3D('',#158818,#110073,#110074);
#96120=AXIS2_PLACEMENT_3D('',#158954,#110075,#110076);
#96121=AXIS2_PLACEMENT_3D('',#159211,#110079,#110080);
#96122=AXIS2_PLACEMENT_3D('',#159214,#110081,#110082);
#96123=AXIS2_PLACEMENT_3D('',#159247,#110083,#110084);
#96124=AXIS2_PLACEMENT_3D('',#159266,#110086,#110087);
#96125=AXIS2_PLACEMENT_3D('',#159267,#110088,#110089);
#96126=AXIS2_PLACEMENT_3D('',#159276,#110094,#110095);
#96127=AXIS2_PLACEMENT_3D('',#159278,#110096,#110097);
#96128=AXIS2_PLACEMENT_3D('',#159280,#110099,#110100);
#96129=AXIS2_PLACEMENT_3D('',#159281,#110101,#110102);
#96130=AXIS2_PLACEMENT_3D('',#159284,#110104,#110105);
#96131=AXIS2_PLACEMENT_3D('',#159285,#110106,#110107);
#96132=AXIS2_PLACEMENT_3D('',#159290,#110109,#110110);
#96133=AXIS2_PLACEMENT_3D('',#159293,#110112,#110113);
#96134=AXIS2_PLACEMENT_3D('',#159294,#110114,#110115);
#96135=AXIS2_PLACEMENT_3D('',#159500,#110118,#110119);
#96136=AXIS2_PLACEMENT_3D('',#159503,#110120,#110121);
#96137=AXIS2_PLACEMENT_3D('',#159551,#110122,#110123);
#96138=AXIS2_PLACEMENT_3D('',#159555,#110125,#110126);
#96139=AXIS2_PLACEMENT_3D('',#159557,#110128,#110129);
#96140=AXIS2_PLACEMENT_3D('',#159563,#110133,#110134);
#96141=AXIS2_PLACEMENT_3D('',#159569,#110138,#110139);
#96142=AXIS2_PLACEMENT_3D('',#159611,#110142,#110143);
#96143=AXIS2_PLACEMENT_3D('',#159620,#110148,#110149);
#96144=AXIS2_PLACEMENT_3D('',#159659,#110152,#110153);
#96145=AXIS2_PLACEMENT_3D('',#159716,#110156,#110157);
#96146=AXIS2_PLACEMENT_3D('',#159721,#110159,#110160);
#96147=AXIS2_PLACEMENT_3D('',#159724,#110162,#110163);
#96148=AXIS2_PLACEMENT_3D('',#159725,#110164,#110165);
#96149=AXIS2_PLACEMENT_3D('',#159743,#110166,#110167);
#96150=AXIS2_PLACEMENT_3D('',#159909,#110168,#110169);
#96151=AXIS2_PLACEMENT_3D('',#160101,#110170,#110171);
#96152=AXIS2_PLACEMENT_3D('',#160103,#110172,#110173);
#96153=AXIS2_PLACEMENT_3D('',#160106,#110175,#110176);
#96154=AXIS2_PLACEMENT_3D('',#160366,#110177,#110178);
#96155=AXIS2_PLACEMENT_3D('',#160368,#110179,#110180);
#96156=AXIS2_PLACEMENT_3D('',#160370,#110181,#110182);
#96157=AXIS2_PLACEMENT_3D('',#160371,#110183,#110184);
#96158=AXIS2_PLACEMENT_3D('',#160397,#110185,#110186);
#96159=AXIS2_PLACEMENT_3D('',#160399,#110187,#110188);
#96160=AXIS2_PLACEMENT_3D('',#160413,#110189,#110190);
#96161=AXIS2_PLACEMENT_3D('',#160508,#110192,#110193);
#96162=AXIS2_PLACEMENT_3D('',#160566,#110194,#110195);
#96163=AXIS2_PLACEMENT_3D('',#160574,#110196,#110197);
#96164=AXIS2_PLACEMENT_3D('',#160577,#110199,#110200);
#96165=AXIS2_PLACEMENT_3D('',#160605,#110201,#110202);
#96166=AXIS2_PLACEMENT_3D('',#160652,#110203,#110204);
#96167=AXIS2_PLACEMENT_3D('',#160819,#110206,#110207);
#96168=AXIS2_PLACEMENT_3D('',#160828,#110208,#110209);
#96169=AXIS2_PLACEMENT_3D('',#160884,#110210,#110211);
#96170=AXIS2_PLACEMENT_3D('',#160887,#110213,#110214);
#96171=AXIS2_PLACEMENT_3D('',#160915,#110215,#110216);
#96172=AXIS2_PLACEMENT_3D('',#160962,#110217,#110218);
#96173=AXIS2_PLACEMENT_3D('',#161039,#110221,#110222);
#96174=AXIS2_PLACEMENT_3D('',#161040,#110223,#110224);
#96175=AXIS2_PLACEMENT_3D('',#161042,#110225,#110226);
#96176=AXIS2_PLACEMENT_3D('',#161044,#110227,#110228);
#96177=AXIS2_PLACEMENT_3D('',#161045,#110229,#110230);
#96178=AXIS2_PLACEMENT_3D('',#161046,#110231,#110232);
#96179=AXIS2_PLACEMENT_3D('',#161048,#110233,#110234);
#96180=AXIS2_PLACEMENT_3D('',#161050,#110235,#110236);
#96181=AXIS2_PLACEMENT_3D('',#161051,#110237,#110238);
#96182=AXIS2_PLACEMENT_3D('',#161052,#110239,#110240);
#96183=AXIS2_PLACEMENT_3D('',#161054,#110241,#110242);
#96184=AXIS2_PLACEMENT_3D('',#161056,#110243,#110244);
#96185=AXIS2_PLACEMENT_3D('',#161057,#110245,#110246);
#96186=AXIS2_PLACEMENT_3D('',#161077,#110247,#110248);
#96187=AXIS2_PLACEMENT_3D('',#161129,#110249,#110250);
#96188=AXIS2_PLACEMENT_3D('',#161137,#110251,#110252);
#96189=AXIS2_PLACEMENT_3D('',#161140,#110254,#110255);
#96190=AXIS2_PLACEMENT_3D('',#161168,#110256,#110257);
#96191=AXIS2_PLACEMENT_3D('',#161221,#110258,#110259);
#96192=AXIS2_PLACEMENT_3D('',#161301,#110261,#110262);
#96193=AXIS2_PLACEMENT_3D('',#161334,#110263,#110264);
#96194=AXIS2_PLACEMENT_3D('',#161335,#110265,#110266);
#96195=AXIS2_PLACEMENT_3D('',#161430,#110269,#110270);
#96196=AXIS2_PLACEMENT_3D('',#161439,#110271,#110272);
#96197=AXIS2_PLACEMENT_3D('',#161489,#110273,#110274);
#96198=AXIS2_PLACEMENT_3D('',#161492,#110276,#110277);
#96199=AXIS2_PLACEMENT_3D('',#161520,#110278,#110279);
#96200=AXIS2_PLACEMENT_3D('',#161573,#110280,#110281);
#96201=AXIS2_PLACEMENT_3D('',#161827,#110283,#110284);
#96202=AXIS2_PLACEMENT_3D('',#161844,#110285,#110286);
#96203=AXIS2_PLACEMENT_3D('',#161886,#110287,#110288);
#96204=AXIS2_PLACEMENT_3D('',#161887,#110289,#110290);
#96205=AXIS2_PLACEMENT_3D('',#161888,#110291,#110292);
#96206=AXIS2_PLACEMENT_3D('',#161889,#110293,#110294);
#96207=AXIS2_PLACEMENT_3D('',#161891,#110295,#110296);
#96208=AXIS2_PLACEMENT_3D('',#161892,#110297,#110298);
#96209=AXIS2_PLACEMENT_3D('',#161925,#110299,#110300);
#96210=AXIS2_PLACEMENT_3D('',#162033,#110301,#110302);
#96211=AXIS2_PLACEMENT_3D('',#162036,#110303,#110304);
#96212=AXIS2_PLACEMENT_3D('',#162037,#110305,#110306);
#96213=AXIS2_PLACEMENT_3D('',#162038,#110307,#110308);
#96214=AXIS2_PLACEMENT_3D('',#162064,#110309,#110310);
#96215=AXIS2_PLACEMENT_3D('',#162140,#110311,#110312);
#96216=AXIS2_PLACEMENT_3D('',#162151,#110313,#110314);
#96217=AXIS2_PLACEMENT_3D('',#162153,#110315,#110316);
#96218=AXIS2_PLACEMENT_3D('',#162154,#110317,#110318);
#96219=AXIS2_PLACEMENT_3D('',#162174,#110319,#110320);
#96220=AXIS2_PLACEMENT_3D('',#162220,#110321,#110322);
#96221=AXIS2_PLACEMENT_3D('',#162231,#110323,#110324);
#96222=AXIS2_PLACEMENT_3D('',#162232,#110325,#110326);
#96223=AXIS2_PLACEMENT_3D('',#162235,#110327,#110328);
#96224=AXIS2_PLACEMENT_3D('',#162236,#110329,#110330);
#96225=AXIS2_PLACEMENT_3D('',#162237,#110331,#110332);
#96226=AXIS2_PLACEMENT_3D('',#162269,#110333,#110334);
#96227=AXIS2_PLACEMENT_3D('',#162336,#110335,#110336);
#96228=AXIS2_PLACEMENT_3D('',#162393,#110337,#110338);
#96229=AXIS2_PLACEMENT_3D('',#162394,#110339,#110340);
#96230=AXIS2_PLACEMENT_3D('',#162503,#110341,#110342);
#96231=AXIS2_PLACEMENT_3D('',#162519,#110343,#110344);
#96232=AXIS2_PLACEMENT_3D('',#162522,#110345,#110346);
#96233=AXIS2_PLACEMENT_3D('',#162523,#110347,#110348);
#96234=AXIS2_PLACEMENT_3D('',#162524,#110349,#110350);
#96235=AXIS2_PLACEMENT_3D('',#162550,#110351,#110352);
#96236=AXIS2_PLACEMENT_3D('',#162629,#110353,#110354);
#96237=AXIS2_PLACEMENT_3D('',#162660,#110355,#110356);
#96238=AXIS2_PLACEMENT_3D('',#162661,#110357,#110358);
#96239=AXIS2_PLACEMENT_3D('',#162740,#110359,#110360);
#96240=AXIS2_PLACEMENT_3D('',#162829,#110361,#110362);
#96241=AXIS2_PLACEMENT_3D('',#162832,#110363,#110364);
#96242=AXIS2_PLACEMENT_3D('',#162833,#110365,#110366);
#96243=AXIS2_PLACEMENT_3D('',#162834,#110367,#110368);
#96244=AXIS2_PLACEMENT_3D('',#162866,#110369,#110370);
#96245=AXIS2_PLACEMENT_3D('',#162939,#110371,#110372);
#96246=AXIS2_PLACEMENT_3D('',#163002,#110373,#110374);
#96247=AXIS2_PLACEMENT_3D('',#163003,#110375,#110376);
#96248=AXIS2_PLACEMENT_3D('',#163052,#110377,#110378);
#96249=AXIS2_PLACEMENT_3D('',#163102,#110379,#110380);
#96250=AXIS2_PLACEMENT_3D('',#163105,#110381,#110382);
#96251=AXIS2_PLACEMENT_3D('',#163106,#110383,#110384);
#96252=AXIS2_PLACEMENT_3D('',#163107,#110385,#110386);
#96253=AXIS2_PLACEMENT_3D('',#163121,#110387,#110388);
#96254=AXIS2_PLACEMENT_3D('',#163130,#110389,#110390);
#96255=AXIS2_PLACEMENT_3D('',#163181,#110391,#110392);
#96256=AXIS2_PLACEMENT_3D('',#163210,#110393,#110394);
#96257=AXIS2_PLACEMENT_3D('',#163212,#110395,#110396);
#96258=AXIS2_PLACEMENT_3D('',#163213,#110397,#110398);
#96259=AXIS2_PLACEMENT_3D('',#163246,#110399,#110400);
#96260=AXIS2_PLACEMENT_3D('',#163309,#110401,#110402);
#96261=AXIS2_PLACEMENT_3D('',#163312,#110403,#110404);
#96262=AXIS2_PLACEMENT_3D('',#163313,#110405,#110406);
#96263=AXIS2_PLACEMENT_3D('',#163314,#110407,#110408);
#96264=AXIS2_PLACEMENT_3D('',#163347,#110409,#110410);
#96265=AXIS2_PLACEMENT_3D('',#163392,#110411,#110412);
#96266=AXIS2_PLACEMENT_3D('',#163463,#110413,#110414);
#96267=AXIS2_PLACEMENT_3D('',#163465,#110415,#110416);
#96268=AXIS2_PLACEMENT_3D('',#163466,#110417,#110418);
#96269=AXIS2_PLACEMENT_3D('',#163488,#110419,#110420);
#96270=AXIS2_PLACEMENT_3D('',#163611,#110421,#110422);
#96271=AXIS2_PLACEMENT_3D('',#163632,#110423,#110424);
#96272=AXIS2_PLACEMENT_3D('',#163670,#110425,#110426);
#96273=AXIS2_PLACEMENT_3D('',#163684,#110427,#110428);
#96274=AXIS2_PLACEMENT_3D('',#163779,#110430,#110431);
#96275=AXIS2_PLACEMENT_3D('',#163837,#110432,#110433);
#96276=AXIS2_PLACEMENT_3D('',#163845,#110434,#110435);
#96277=AXIS2_PLACEMENT_3D('',#163848,#110437,#110438);
#96278=AXIS2_PLACEMENT_3D('',#163876,#110439,#110440);
#96279=AXIS2_PLACEMENT_3D('',#163923,#110441,#110442);
#96280=AXIS2_PLACEMENT_3D('',#164090,#110444,#110445);
#96281=AXIS2_PLACEMENT_3D('',#164099,#110446,#110447);
#96282=AXIS2_PLACEMENT_3D('',#164155,#110448,#110449);
#96283=AXIS2_PLACEMENT_3D('',#164158,#110451,#110452);
#96284=AXIS2_PLACEMENT_3D('',#164186,#110453,#110454);
#96285=AXIS2_PLACEMENT_3D('',#164233,#110455,#110456);
#96286=AXIS2_PLACEMENT_3D('',#164310,#110459,#110460);
#96287=AXIS2_PLACEMENT_3D('',#164311,#110461,#110462);
#96288=AXIS2_PLACEMENT_3D('',#164313,#110463,#110464);
#96289=AXIS2_PLACEMENT_3D('',#164315,#110465,#110466);
#96290=AXIS2_PLACEMENT_3D('',#164316,#110467,#110468);
#96291=AXIS2_PLACEMENT_3D('',#164317,#110469,#110470);
#96292=AXIS2_PLACEMENT_3D('',#164319,#110471,#110472);
#96293=AXIS2_PLACEMENT_3D('',#164321,#110473,#110474);
#96294=AXIS2_PLACEMENT_3D('',#164322,#110475,#110476);
#96295=AXIS2_PLACEMENT_3D('',#164323,#110477,#110478);
#96296=AXIS2_PLACEMENT_3D('',#164325,#110479,#110480);
#96297=AXIS2_PLACEMENT_3D('',#164327,#110481,#110482);
#96298=AXIS2_PLACEMENT_3D('',#164328,#110483,#110484);
#96299=AXIS2_PLACEMENT_3D('',#164329,#110485,#110486);
#96300=AXIS2_PLACEMENT_3D('',#164404,#110489,#110490);
#96301=AXIS2_PLACEMENT_3D('',#164407,#110491,#110492);
#96302=AXIS2_PLACEMENT_3D('',#164409,#110493,#110494);
#96303=AXIS2_PLACEMENT_3D('',#164410,#110495,#110496);
#96304=AXIS2_PLACEMENT_3D('',#164889,#110497,#110498);
#96305=AXIS2_PLACEMENT_3D('',#164895,#110502,#110503);
#96306=AXIS2_PLACEMENT_3D('',#164942,#110506,#110507);
#96307=AXIS2_PLACEMENT_3D('',#164943,#110508,#110509);
#96308=AXIS2_PLACEMENT_3D('',#164946,#110510,#110511);
#96309=AXIS2_PLACEMENT_3D('',#164949,#110514,#110515);
#96310=AXIS2_PLACEMENT_3D('',#164951,#110516,#110517);
#96311=AXIS2_PLACEMENT_3D('',#164953,#110518,#110519);
#96312=AXIS2_PLACEMENT_3D('',#164954,#110520,#110521);
#96313=AXIS2_PLACEMENT_3D('',#164955,#110522,#110523);
#96314=AXIS2_PLACEMENT_3D('',#164958,#110525,#110526);
#96315=AXIS2_PLACEMENT_3D('',#164972,#110527,#110528);
#96316=AXIS2_PLACEMENT_3D('',#164991,#110529,#110530);
#96317=AXIS2_PLACEMENT_3D('',#165021,#110531,#110532);
#96318=AXIS2_PLACEMENT_3D('',#165050,#110533,#110534);
#96319=AXIS2_PLACEMENT_3D('',#165052,#110535,#110536);
#96320=AXIS2_PLACEMENT_3D('',#165079,#110538,#110539);
#96321=AXIS2_PLACEMENT_3D('',#165109,#110540,#110541);
#96322=AXIS2_PLACEMENT_3D('',#165139,#110542,#110543);
#96323=AXIS2_PLACEMENT_3D('',#165153,#110544,#110545);
#96324=AXIS2_PLACEMENT_3D('',#165155,#110546,#110547);
#96325=AXIS2_PLACEMENT_3D('',#165189,#110549,#110550);
#96326=AXIS2_PLACEMENT_3D('',#165190,#110551,#110552);
#96327=AXIS2_PLACEMENT_3D('',#165201,#110553,#110554);
#96328=AXIS2_PLACEMENT_3D('',#165204,#110557,#110558);
#96329=AXIS2_PLACEMENT_3D('',#165206,#110560,#110561);
#96330=AXIS2_PLACEMENT_3D('',#165209,#110562,#110563);
#96331=AXIS2_PLACEMENT_3D('',#165213,#110565,#110566);
#96332=AXIS2_PLACEMENT_3D('',#165215,#110568,#110569);
#96333=AXIS2_PLACEMENT_3D('',#165217,#110570,#110571);
#96334=AXIS2_PLACEMENT_3D('',#165219,#110572,#110573);
#96335=AXIS2_PLACEMENT_3D('',#165220,#110574,#110575);
#96336=AXIS2_PLACEMENT_3D('',#165221,#110576,#110577);
#96337=AXIS2_PLACEMENT_3D('',#165224,#110579,#110580);
#96338=AXIS2_PLACEMENT_3D('',#165225,#110581,#110582);
#96339=AXIS2_PLACEMENT_3D('',#165227,#110583,#110584);
#96340=AXIS2_PLACEMENT_3D('',#165229,#110585,#110586);
#96341=AXIS2_PLACEMENT_3D('',#165230,#110587,#110588);
#96342=AXIS2_PLACEMENT_3D('',#165231,#110589,#110590);
#96343=AXIS2_PLACEMENT_3D('',#165234,#110592,#110593);
#96344=AXIS2_PLACEMENT_3D('',#165235,#110594,#110595);
#96345=AXIS2_PLACEMENT_3D('',#165237,#110596,#110597);
#96346=AXIS2_PLACEMENT_3D('',#165238,#110598,#110599);
#96347=AXIS2_PLACEMENT_3D('',#165239,#110600,#110601);
#96348=AXIS2_PLACEMENT_3D('',#165241,#110603,#110604);
#96349=AXIS2_PLACEMENT_3D('',#165244,#110606,#110607);
#96350=AXIS2_PLACEMENT_3D('',#165287,#110609,#110610);
#96351=AXIS2_PLACEMENT_3D('',#165288,#110611,#110612);
#96352=AXIS2_PLACEMENT_3D('',#165291,#110614,#110615);
#96353=AXIS2_PLACEMENT_3D('',#165333,#110616,#110617);
#96354=AXIS2_PLACEMENT_3D('',#165351,#110618,#110619);
#96355=AXIS2_PLACEMENT_3D('',#165396,#110620,#110621);
#96356=AXIS2_PLACEMENT_3D('',#165397,#110622,#110623);
#96357=AXIS2_PLACEMENT_3D('',#165400,#110625,#110626);
#96358=AXIS2_PLACEMENT_3D('',#165442,#110627,#110628);
#96359=AXIS2_PLACEMENT_3D('',#165460,#110629,#110630);
#96360=AXIS2_PLACEMENT_3D('',#165497,#110631,#110632);
#96361=AXIS2_PLACEMENT_3D('',#165574,#110633,#110634);
#96362=AXIS2_PLACEMENT_3D('',#165578,#110636,#110637);
#96363=AXIS2_PLACEMENT_3D('',#165580,#110639,#110640);
#96364=AXIS2_PLACEMENT_3D('',#165582,#110641,#110642);
#96365=AXIS2_PLACEMENT_3D('',#165653,#110643,#110644);
#96366=AXIS2_PLACEMENT_3D('',#165655,#110645,#110646);
#96367=AXIS2_PLACEMENT_3D('',#165657,#110647,#110648);
#96368=AXIS2_PLACEMENT_3D('',#165658,#110649,#110650);
#96369=AXIS2_PLACEMENT_3D('',#165659,#110651,#110652);
#96370=AXIS2_PLACEMENT_3D('',#165662,#110654,#110655);
#96371=AXIS2_PLACEMENT_3D('',#165663,#110656,#110657);
#96372=AXIS2_PLACEMENT_3D('',#165666,#110658,#110659);
#96373=AXIS2_PLACEMENT_3D('',#165669,#110661,#110662);
#96374=AXIS2_PLACEMENT_3D('',#165715,#110664,#110665);
#96375=AXIS2_PLACEMENT_3D('',#165733,#110666,#110667);
#96376=AXIS2_PLACEMENT_3D('',#165790,#110668,#110669);
#96377=AXIS2_PLACEMENT_3D('',#165791,#110670,#110671);
#96378=AXIS2_PLACEMENT_3D('',#165794,#110673,#110674);
#96379=AXIS2_PLACEMENT_3D('',#165826,#110675,#110676);
#96380=AXIS2_PLACEMENT_3D('',#165856,#110677,#110678);
#96381=AXIS2_PLACEMENT_3D('',#165892,#110679,#110680);
#96382=AXIS2_PLACEMENT_3D('',#165906,#110681,#110682);
#96383=AXIS2_PLACEMENT_3D('',#165908,#110683,#110684);
#96384=AXIS2_PLACEMENT_3D('',#165942,#110686,#110687);
#96385=AXIS2_PLACEMENT_3D('',#165943,#110688,#110689);
#96386=AXIS2_PLACEMENT_3D('',#165954,#110690,#110691);
#96387=AXIS2_PLACEMENT_3D('',#165957,#110694,#110695);
#96388=AXIS2_PLACEMENT_3D('',#165959,#110697,#110698);
#96389=AXIS2_PLACEMENT_3D('',#165961,#110699,#110700);
#96390=AXIS2_PLACEMENT_3D('',#165963,#110701,#110702);
#96391=AXIS2_PLACEMENT_3D('',#165964,#110703,#110704);
#96392=AXIS2_PLACEMENT_3D('',#165965,#110705,#110706);
#96393=AXIS2_PLACEMENT_3D('',#165968,#110708,#110709);
#96394=AXIS2_PLACEMENT_3D('',#165969,#110710,#110711);
#96395=AXIS2_PLACEMENT_3D('',#165972,#110712,#110713);
#96396=AXIS2_PLACEMENT_3D('',#165975,#110715,#110716);
#96397=AXIS2_PLACEMENT_3D('',#165977,#110718,#110719);
#96398=AXIS2_PLACEMENT_3D('',#165981,#110721,#110722);
#96399=AXIS2_PLACEMENT_3D('',#165983,#110724,#110725);
#96400=AXIS2_PLACEMENT_3D('',#165986,#110727,#110728);
#96401=AXIS2_PLACEMENT_3D('',#166047,#110729,#110730);
#96402=AXIS2_PLACEMENT_3D('',#166074,#110731,#110732);
#96403=AXIS2_PLACEMENT_3D('',#166076,#110733,#110734);
#96404=AXIS2_PLACEMENT_3D('',#166078,#110735,#110736);
#96405=AXIS2_PLACEMENT_3D('',#166079,#110737,#110738);
#96406=AXIS2_PLACEMENT_3D('',#166080,#110739,#110740);
#96407=AXIS2_PLACEMENT_3D('',#166082,#110741,#110742);
#96408=AXIS2_PLACEMENT_3D('',#166084,#110744,#110745);
#96409=AXIS2_PLACEMENT_3D('',#166086,#110746,#110747);
#96410=AXIS2_PLACEMENT_3D('',#166087,#110748,#110749);
#96411=AXIS2_PLACEMENT_3D('',#166088,#110750,#110751);
#96412=AXIS2_PLACEMENT_3D('',#166090,#110753,#110754);
#96413=AXIS2_PLACEMENT_3D('',#166092,#110755,#110756);
#96414=AXIS2_PLACEMENT_3D('',#166148,#110759,#110760);
#96415=AXIS2_PLACEMENT_3D('',#166150,#110761,#110762);
#96416=AXIS2_PLACEMENT_3D('',#166174,#110763,#110764);
#96417=AXIS2_PLACEMENT_3D('',#166207,#110765,#110766);
#96418=AXIS2_PLACEMENT_3D('',#166224,#110767,#110768);
#96419=AXIS2_PLACEMENT_3D('',#166226,#110769,#110770);
#96420=AXIS2_PLACEMENT_3D('',#166247,#110772,#110773);
#96421=AXIS2_PLACEMENT_3D('',#166293,#110774,#110775);
#96422=AXIS2_PLACEMENT_3D('',#166329,#110776,#110777);
#96423=AXIS2_PLACEMENT_3D('',#166331,#110778,#110779);
#96424=AXIS2_PLACEMENT_3D('',#166334,#110781,#110782);
#96425=AXIS2_PLACEMENT_3D('',#166335,#110783,#110784);
#96426=AXIS2_PLACEMENT_3D('',#166337,#110785,#110786);
#96427=AXIS2_PLACEMENT_3D('',#166338,#110787,#110788);
#96428=AXIS2_PLACEMENT_3D('',#166339,#110789,#110790);
#96429=AXIS2_PLACEMENT_3D('',#166341,#110792,#110793);
#96430=AXIS2_PLACEMENT_3D('',#166343,#110794,#110795);
#96431=AXIS2_PLACEMENT_3D('',#166456,#110798,#110799);
#96432=AXIS2_PLACEMENT_3D('',#166457,#110800,#110801);
#96433=AXIS2_PLACEMENT_3D('',#166458,#110802,#110803);
#96434=AXIS2_PLACEMENT_3D('',#166459,#110804,#110805);
#96435=AXIS2_PLACEMENT_3D('',#166460,#110806,#110807);
#96436=AXIS2_PLACEMENT_3D('',#166461,#110808,#110809);
#96437=AXIS2_PLACEMENT_3D('',#166463,#110810,#110811);
#96438=AXIS2_PLACEMENT_3D('',#166465,#110812,#110813);
#96439=AXIS2_PLACEMENT_3D('',#166466,#110814,#110815);
#96440=AXIS2_PLACEMENT_3D('',#166467,#110816,#110817);
#96441=AXIS2_PLACEMENT_3D('',#166470,#110819,#110820);
#96442=AXIS2_PLACEMENT_3D('',#166490,#110821,#110822);
#96443=AXIS2_PLACEMENT_3D('',#166548,#110823,#110824);
#96444=AXIS2_PLACEMENT_3D('',#166584,#110825,#110826);
#96445=AXIS2_PLACEMENT_3D('',#166614,#110827,#110828);
#96446=AXIS2_PLACEMENT_3D('',#166634,#110829,#110830);
#96447=AXIS2_PLACEMENT_3D('',#166636,#110831,#110832);
#96448=AXIS2_PLACEMENT_3D('',#166663,#110834,#110835);
#96449=AXIS2_PLACEMENT_3D('',#166693,#110836,#110837);
#96450=AXIS2_PLACEMENT_3D('',#166717,#110838,#110839);
#96451=AXIS2_PLACEMENT_3D('',#166734,#110840,#110841);
#96452=AXIS2_PLACEMENT_3D('',#166736,#110842,#110843);
#96453=AXIS2_PLACEMENT_3D('',#166769,#110845,#110846);
#96454=AXIS2_PLACEMENT_3D('',#166780,#110847,#110848);
#96455=AXIS2_PLACEMENT_3D('',#166783,#110851,#110852);
#96456=AXIS2_PLACEMENT_3D('',#166785,#110854,#110855);
#96457=AXIS2_PLACEMENT_3D('',#166787,#110856,#110857);
#96458=AXIS2_PLACEMENT_3D('',#166789,#110858,#110859);
#96459=AXIS2_PLACEMENT_3D('',#166790,#110860,#110861);
#96460=AXIS2_PLACEMENT_3D('',#166791,#110862,#110863);
#96461=AXIS2_PLACEMENT_3D('',#166794,#110865,#110866);
#96462=AXIS2_PLACEMENT_3D('',#166795,#110867,#110868);
#96463=AXIS2_PLACEMENT_3D('',#166797,#110869,#110870);
#96464=AXIS2_PLACEMENT_3D('',#166799,#110871,#110872);
#96465=AXIS2_PLACEMENT_3D('',#166800,#110873,#110874);
#96466=AXIS2_PLACEMENT_3D('',#166801,#110875,#110876);
#96467=AXIS2_PLACEMENT_3D('',#166804,#110878,#110879);
#96468=AXIS2_PLACEMENT_3D('',#166805,#110880,#110881);
#96469=AXIS2_PLACEMENT_3D('',#166807,#110882,#110883);
#96470=AXIS2_PLACEMENT_3D('',#166808,#110884,#110885);
#96471=AXIS2_PLACEMENT_3D('',#166809,#110886,#110887);
#96472=AXIS2_PLACEMENT_3D('',#166811,#110889,#110890);
#96473=AXIS2_PLACEMENT_3D('',#166814,#110892,#110893);
#96474=AXIS2_PLACEMENT_3D('',#166857,#110895,#110896);
#96475=AXIS2_PLACEMENT_3D('',#166858,#110897,#110898);
#96476=AXIS2_PLACEMENT_3D('',#166861,#110900,#110901);
#96477=AXIS2_PLACEMENT_3D('',#166912,#110902,#110903);
#96478=AXIS2_PLACEMENT_3D('',#166930,#110904,#110905);
#96479=AXIS2_PLACEMENT_3D('',#166978,#110906,#110907);
#96480=AXIS2_PLACEMENT_3D('',#166979,#110908,#110909);
#96481=AXIS2_PLACEMENT_3D('',#166982,#110911,#110912);
#96482=AXIS2_PLACEMENT_3D('',#167024,#110913,#110914);
#96483=AXIS2_PLACEMENT_3D('',#167043,#110915,#110916);
#96484=AXIS2_PLACEMENT_3D('',#167063,#110917,#110918);
#96485=AXIS2_PLACEMENT_3D('',#167066,#110919,#110920);
#96486=AXIS2_PLACEMENT_3D('',#167070,#110922,#110923);
#96487=AXIS2_PLACEMENT_3D('',#167185,#110925,#110926);
#96488=AXIS2_PLACEMENT_3D('',#167187,#110927,#110928);
#96489=AXIS2_PLACEMENT_3D('',#167216,#110929,#110930);
#96490=AXIS2_PLACEMENT_3D('',#167218,#110931,#110932);
#96491=AXIS2_PLACEMENT_3D('',#167220,#110933,#110934);
#96492=AXIS2_PLACEMENT_3D('',#167221,#110935,#110936);
#96493=AXIS2_PLACEMENT_3D('',#167222,#110937,#110938);
#96494=AXIS2_PLACEMENT_3D('',#167225,#110940,#110941);
#96495=AXIS2_PLACEMENT_3D('',#167240,#110942,#110943);
#96496=AXIS2_PLACEMENT_3D('',#167242,#110944,#110945);
#96497=AXIS2_PLACEMENT_3D('',#167244,#110946,#110947);
#96498=AXIS2_PLACEMENT_3D('',#167271,#110948,#110949);
#96499=AXIS2_PLACEMENT_3D('',#167272,#110950,#110951);
#96500=AXIS2_PLACEMENT_3D('',#167273,#110952,#110953);
#96501=AXIS2_PLACEMENT_3D('',#167300,#110954,#110955);
#96502=AXIS2_PLACEMENT_3D('',#167342,#110956,#110957);
#96503=AXIS2_PLACEMENT_3D('',#167343,#110958,#110959);
#96504=AXIS2_PLACEMENT_3D('',#167346,#110961,#110962);
#96505=AXIS2_PLACEMENT_3D('',#167391,#110963,#110964);
#96506=AXIS2_PLACEMENT_3D('',#167418,#110965,#110966);
#96507=AXIS2_PLACEMENT_3D('',#167436,#110967,#110968);
#96508=AXIS2_PLACEMENT_3D('',#167469,#110969,#110970);
#96509=AXIS2_PLACEMENT_3D('',#167470,#110971,#110972);
#96510=AXIS2_PLACEMENT_3D('',#167473,#110975,#110976);
#96511=AXIS2_PLACEMENT_3D('',#167475,#110978,#110979);
#96512=AXIS2_PLACEMENT_3D('',#167480,#110982,#110983);
#96513=AXIS2_PLACEMENT_3D('',#167481,#110984,#110985);
#96514=AXIS2_PLACEMENT_3D('',#167483,#110986,#110987);
#96515=AXIS2_PLACEMENT_3D('',#167487,#110989,#110990);
#96516=AXIS2_PLACEMENT_3D('',#167520,#110992,#110993);
#96517=AXIS2_PLACEMENT_3D('',#167531,#110994,#110995);
#96518=AXIS2_PLACEMENT_3D('',#167534,#110998,#110999);
#96519=AXIS2_PLACEMENT_3D('',#167537,#111001,#111002);
#96520=AXIS2_PLACEMENT_3D('',#167538,#111003,#111004);
#96521=AXIS2_PLACEMENT_3D('',#167540,#111005,#111006);
#96522=AXIS2_PLACEMENT_3D('',#167541,#111007,#111008);
#96523=AXIS2_PLACEMENT_3D('',#167542,#111009,#111010);
#96524=AXIS2_PLACEMENT_3D('',#167545,#111012,#111013);
#96525=AXIS2_PLACEMENT_3D('',#167578,#111014,#111015);
#96526=AXIS2_PLACEMENT_3D('',#167600,#111016,#111017);
#96527=AXIS2_PLACEMENT_3D('',#167618,#111018,#111019);
#96528=AXIS2_PLACEMENT_3D('',#167659,#111021,#111022);
#96529=AXIS2_PLACEMENT_3D('',#167660,#111023,#111024);
#96530=AXIS2_PLACEMENT_3D('',#167662,#111025,#111026);
#96531=AXIS2_PLACEMENT_3D('',#167664,#111027,#111028);
#96532=AXIS2_PLACEMENT_3D('',#167665,#111029,#111030);
#96533=AXIS2_PLACEMENT_3D('',#167666,#111031,#111032);
#96534=AXIS2_PLACEMENT_3D('',#167669,#111034,#111035);
#96535=AXIS2_PLACEMENT_3D('',#167670,#111036,#111037);
#96536=AXIS2_PLACEMENT_3D('',#167672,#111038,#111039);
#96537=AXIS2_PLACEMENT_3D('',#167674,#111040,#111041);
#96538=AXIS2_PLACEMENT_3D('',#167701,#111043,#111044);
#96539=AXIS2_PLACEMENT_3D('',#167734,#111045,#111046);
#96540=AXIS2_PLACEMENT_3D('',#167776,#111047,#111048);
#96541=AXIS2_PLACEMENT_3D('',#167796,#111049,#111050);
#96542=AXIS2_PLACEMENT_3D('',#167798,#111051,#111052);
#96543=AXIS2_PLACEMENT_3D('',#167831,#111054,#111055);
#96544=AXIS2_PLACEMENT_3D('',#167861,#111056,#111057);
#96545=AXIS2_PLACEMENT_3D('',#167898,#111058,#111059);
#96546=AXIS2_PLACEMENT_3D('',#167991,#111060,#111061);
#96547=AXIS2_PLACEMENT_3D('',#167993,#111062,#111063);
#96548=AXIS2_PLACEMENT_3D('',#167995,#111064,#111065);
#96549=AXIS2_PLACEMENT_3D('',#167996,#111066,#111067);
#96550=AXIS2_PLACEMENT_3D('',#167997,#111068,#111069);
#96551=AXIS2_PLACEMENT_3D('',#168000,#111071,#111072);
#96552=AXIS2_PLACEMENT_3D('',#168001,#111073,#111074);
#96553=AXIS2_PLACEMENT_3D('',#168003,#111075,#111076);
#96554=AXIS2_PLACEMENT_3D('',#168004,#111077,#111078);
#96555=AXIS2_PLACEMENT_3D('',#168005,#111079,#111080);
#96556=AXIS2_PLACEMENT_3D('',#168007,#111082,#111083);
#96557=AXIS2_PLACEMENT_3D('',#168009,#111084,#111085);
#96558=AXIS2_PLACEMENT_3D('',#168013,#111088,#111089);
#96559=AXIS2_PLACEMENT_3D('',#168054,#111090,#111091);
#96560=AXIS2_PLACEMENT_3D('',#168058,#111093,#111094);
#96561=AXIS2_PLACEMENT_3D('',#168060,#111096,#111097);
#96562=AXIS2_PLACEMENT_3D('',#168063,#111098,#111099);
#96563=AXIS2_PLACEMENT_3D('',#168066,#111102,#111103);
#96564=AXIS2_PLACEMENT_3D('',#168067,#111104,#111105);
#96565=AXIS2_PLACEMENT_3D('',#168094,#111106,#111107);
#96566=AXIS2_PLACEMENT_3D('',#168115,#111108,#111109);
#96567=AXIS2_PLACEMENT_3D('',#168206,#111110,#111111);
#96568=AXIS2_PLACEMENT_3D('',#168248,#111112,#111113);
#96569=AXIS2_PLACEMENT_3D('',#168249,#111114,#111115);
#96570=AXIS2_PLACEMENT_3D('',#168253,#111117,#111118);
#96571=AXIS2_PLACEMENT_3D('',#168255,#111120,#111121);
#96572=AXIS2_PLACEMENT_3D('',#168258,#111122,#111123);
#96573=AXIS2_PLACEMENT_3D('',#168260,#111124,#111125);
#96574=AXIS2_PLACEMENT_3D('',#168262,#111126,#111127);
#96575=AXIS2_PLACEMENT_3D('',#168263,#111128,#111129);
#96576=AXIS2_PLACEMENT_3D('',#168264,#111130,#111131);
#96577=AXIS2_PLACEMENT_3D('',#168268,#111133,#111134);
#96578=AXIS2_PLACEMENT_3D('',#168270,#111136,#111137);
#96579=AXIS2_PLACEMENT_3D('',#168272,#111138,#111139);
#96580=AXIS2_PLACEMENT_3D('',#168274,#111140,#111141);
#96581=AXIS2_PLACEMENT_3D('',#168275,#111142,#111143);
#96582=AXIS2_PLACEMENT_3D('',#168276,#111144,#111145);
#96583=AXIS2_PLACEMENT_3D('',#168375,#111148,#111149);
#96584=AXIS2_PLACEMENT_3D('',#168398,#111151,#111152);
#96585=AXIS2_PLACEMENT_3D('',#168413,#111153,#111154);
#96586=AXIS2_PLACEMENT_3D('',#168419,#111155,#111156);
#96587=AXIS2_PLACEMENT_3D('',#168480,#111157,#111158);
#96588=AXIS2_PLACEMENT_3D('',#168481,#111159,#111160);
#96589=AXIS2_PLACEMENT_3D('',#168485,#111162,#111163);
#96590=AXIS2_PLACEMENT_3D('',#168487,#111165,#111166);
#96591=AXIS2_PLACEMENT_3D('',#168490,#111167,#111168);
#96592=AXIS2_PLACEMENT_3D('',#168492,#111169,#111170);
#96593=AXIS2_PLACEMENT_3D('',#168494,#111171,#111172);
#96594=AXIS2_PLACEMENT_3D('',#168495,#111173,#111174);
#96595=AXIS2_PLACEMENT_3D('',#168496,#111175,#111176);
#96596=AXIS2_PLACEMENT_3D('',#168501,#111179,#111180);
#96597=AXIS2_PLACEMENT_3D('',#168502,#111181,#111182);
#96598=AXIS2_PLACEMENT_3D('',#168504,#111183,#111184);
#96599=AXIS2_PLACEMENT_3D('',#168506,#111185,#111186);
#96600=AXIS2_PLACEMENT_3D('',#168507,#111187,#111188);
#96601=AXIS2_PLACEMENT_3D('',#168508,#111189,#111190);
#96602=AXIS2_PLACEMENT_3D('',#168510,#111191,#111192);
#96603=AXIS2_PLACEMENT_3D('',#168514,#111194,#111195);
#96604=AXIS2_PLACEMENT_3D('',#168541,#111197,#111198);
#96605=AXIS2_PLACEMENT_3D('',#168568,#111199,#111200);
#96606=AXIS2_PLACEMENT_3D('',#168593,#111201,#111202);
#96607=AXIS2_PLACEMENT_3D('',#168689,#111203,#111204);
#96608=AXIS2_PLACEMENT_3D('',#168692,#111205,#111206);
#96609=AXIS2_PLACEMENT_3D('',#168695,#111209,#111210);
#96610=AXIS2_PLACEMENT_3D('',#168698,#111211,#111212);
#96611=AXIS2_PLACEMENT_3D('',#168701,#111215,#111216);
#96612=AXIS2_PLACEMENT_3D('',#168702,#111217,#111218);
#96613=AXIS2_PLACEMENT_3D('',#168703,#111219,#111220);
#96614=AXIS2_PLACEMENT_3D('',#168705,#111221,#111222);
#96615=AXIS2_PLACEMENT_3D('',#168707,#111223,#111224);
#96616=AXIS2_PLACEMENT_3D('',#168708,#111225,#111226);
#96617=AXIS2_PLACEMENT_3D('',#168709,#111227,#111228);
#96618=AXIS2_PLACEMENT_3D('',#168712,#111230,#111231);
#96619=AXIS2_PLACEMENT_3D('',#168732,#111232,#111233);
#96620=AXIS2_PLACEMENT_3D('',#168790,#111234,#111235);
#96621=AXIS2_PLACEMENT_3D('',#168826,#111236,#111237);
#96622=AXIS2_PLACEMENT_3D('',#168856,#111238,#111239);
#96623=AXIS2_PLACEMENT_3D('',#168882,#111240,#111241);
#96624=AXIS2_PLACEMENT_3D('',#168884,#111242,#111243);
#96625=AXIS2_PLACEMENT_3D('',#168911,#111245,#111246);
#96626=AXIS2_PLACEMENT_3D('',#168941,#111247,#111248);
#96627=AXIS2_PLACEMENT_3D('',#168965,#111249,#111250);
#96628=AXIS2_PLACEMENT_3D('',#168982,#111251,#111252);
#96629=AXIS2_PLACEMENT_3D('',#168984,#111253,#111254);
#96630=AXIS2_PLACEMENT_3D('',#169017,#111256,#111257);
#96631=AXIS2_PLACEMENT_3D('',#169028,#111258,#111259);
#96632=AXIS2_PLACEMENT_3D('',#169031,#111262,#111263);
#96633=AXIS2_PLACEMENT_3D('',#169033,#111265,#111266);
#96634=AXIS2_PLACEMENT_3D('',#169035,#111267,#111268);
#96635=AXIS2_PLACEMENT_3D('',#169037,#111269,#111270);
#96636=AXIS2_PLACEMENT_3D('',#169038,#111271,#111272);
#96637=AXIS2_PLACEMENT_3D('',#169039,#111273,#111274);
#96638=AXIS2_PLACEMENT_3D('',#169042,#111276,#111277);
#96639=AXIS2_PLACEMENT_3D('',#169043,#111278,#111279);
#96640=AXIS2_PLACEMENT_3D('',#169045,#111280,#111281);
#96641=AXIS2_PLACEMENT_3D('',#169047,#111282,#111283);
#96642=AXIS2_PLACEMENT_3D('',#169048,#111284,#111285);
#96643=AXIS2_PLACEMENT_3D('',#169049,#111286,#111287);
#96644=AXIS2_PLACEMENT_3D('',#169052,#111289,#111290);
#96645=AXIS2_PLACEMENT_3D('',#169053,#111291,#111292);
#96646=AXIS2_PLACEMENT_3D('',#169055,#111293,#111294);
#96647=AXIS2_PLACEMENT_3D('',#169056,#111295,#111296);
#96648=AXIS2_PLACEMENT_3D('',#169057,#111297,#111298);
#96649=AXIS2_PLACEMENT_3D('',#169059,#111300,#111301);
#96650=AXIS2_PLACEMENT_3D('',#169062,#111303,#111304);
#96651=AXIS2_PLACEMENT_3D('',#169105,#111306,#111307);
#96652=AXIS2_PLACEMENT_3D('',#169106,#111308,#111309);
#96653=AXIS2_PLACEMENT_3D('',#169109,#111311,#111312);
#96654=AXIS2_PLACEMENT_3D('',#169160,#111313,#111314);
#96655=AXIS2_PLACEMENT_3D('',#169178,#111315,#111316);
#96656=AXIS2_PLACEMENT_3D('',#169226,#111317,#111318);
#96657=AXIS2_PLACEMENT_3D('',#169227,#111319,#111320);
#96658=AXIS2_PLACEMENT_3D('',#169230,#111322,#111323);
#96659=AXIS2_PLACEMENT_3D('',#169269,#111324,#111325);
#96660=AXIS2_PLACEMENT_3D('',#169288,#111326,#111327);
#96661=AXIS2_PLACEMENT_3D('',#169302,#111328,#111329);
#96662=AXIS2_PLACEMENT_3D('',#169305,#111330,#111331);
#96663=AXIS2_PLACEMENT_3D('',#169309,#111333,#111334);
#96664=AXIS2_PLACEMENT_3D('',#169424,#111336,#111337);
#96665=AXIS2_PLACEMENT_3D('',#169426,#111338,#111339);
#96666=AXIS2_PLACEMENT_3D('',#169443,#111340,#111341);
#96667=AXIS2_PLACEMENT_3D('',#169445,#111342,#111343);
#96668=AXIS2_PLACEMENT_3D('',#169447,#111344,#111345);
#96669=AXIS2_PLACEMENT_3D('',#169448,#111346,#111347);
#96670=AXIS2_PLACEMENT_3D('',#169449,#111348,#111349);
#96671=AXIS2_PLACEMENT_3D('',#169452,#111351,#111352);
#96672=AXIS2_PLACEMENT_3D('',#169466,#111353,#111354);
#96673=AXIS2_PLACEMENT_3D('',#169468,#111355,#111356);
#96674=AXIS2_PLACEMENT_3D('',#169498,#111357,#111358);
#96675=AXIS2_PLACEMENT_3D('',#169512,#111359,#111360);
#96676=AXIS2_PLACEMENT_3D('',#169514,#111361,#111362);
#96677=AXIS2_PLACEMENT_3D('',#169535,#111364,#111365);
#96678=AXIS2_PLACEMENT_3D('',#169571,#111366,#111367);
#96679=AXIS2_PLACEMENT_3D('',#169589,#111368,#111369);
#96680=AXIS2_PLACEMENT_3D('',#169614,#111370,#111371);
#96681=AXIS2_PLACEMENT_3D('',#169689,#111372,#111373);
#96682=AXIS2_PLACEMENT_3D('',#169690,#111374,#111375);
#96683=AXIS2_PLACEMENT_3D('',#169691,#111376,#111377);
#96684=AXIS2_PLACEMENT_3D('',#169693,#111378,#111379);
#96685=AXIS2_PLACEMENT_3D('',#169697,#111381,#111382);
#96686=AXIS2_PLACEMENT_3D('',#169730,#111384,#111385);
#96687=AXIS2_PLACEMENT_3D('',#169741,#111386,#111387);
#96688=AXIS2_PLACEMENT_3D('',#169744,#111390,#111391);
#96689=AXIS2_PLACEMENT_3D('',#169747,#111393,#111394);
#96690=AXIS2_PLACEMENT_3D('',#169748,#111395,#111396);
#96691=AXIS2_PLACEMENT_3D('',#169750,#111397,#111398);
#96692=AXIS2_PLACEMENT_3D('',#169751,#111399,#111400);
#96693=AXIS2_PLACEMENT_3D('',#169752,#111401,#111402);
#96694=AXIS2_PLACEMENT_3D('',#169754,#111403,#111404);
#96695=AXIS2_PLACEMENT_3D('',#169788,#111406,#111407);
#96696=AXIS2_PLACEMENT_3D('',#169827,#111408,#111409);
#96697=AXIS2_PLACEMENT_3D('',#169846,#111410,#111411);
#96698=AXIS2_PLACEMENT_3D('',#169848,#111413,#111414);
#96699=AXIS2_PLACEMENT_3D('',#169851,#111417,#111418);
#96700=AXIS2_PLACEMENT_3D('',#169854,#111419,#111420);
#96701=AXIS2_PLACEMENT_3D('',#169857,#111423,#111424);
#96702=AXIS2_PLACEMENT_3D('',#169860,#111425,#111426);
#96703=AXIS2_PLACEMENT_3D('',#169861,#111427,#111428);
#96704=AXIS2_PLACEMENT_3D('',#169862,#111429,#111430);
#96705=AXIS2_PLACEMENT_3D('',#169863,#111431,#111432);
#96706=AXIS2_PLACEMENT_3D('',#169866,#111434,#111435);
#96707=AXIS2_PLACEMENT_3D('',#169867,#111436,#111437);
#96708=AXIS2_PLACEMENT_3D('',#169869,#111438,#111439);
#96709=AXIS2_PLACEMENT_3D('',#169871,#111440,#111441);
#96710=AXIS2_PLACEMENT_3D('',#169886,#111443,#111444);
#96711=AXIS2_PLACEMENT_3D('',#169910,#111445,#111446);
#96712=AXIS2_PLACEMENT_3D('',#169967,#111447,#111448);
#96713=AXIS2_PLACEMENT_3D('',#169984,#111449,#111450);
#96714=AXIS2_PLACEMENT_3D('',#169987,#111452,#111453);
#96715=AXIS2_PLACEMENT_3D('',#170026,#111454,#111455);
#96716=AXIS2_PLACEMENT_3D('',#170078,#111456,#111457);
#96717=AXIS2_PLACEMENT_3D('',#170104,#111458,#111459);
#96718=AXIS2_PLACEMENT_3D('',#170106,#111460,#111461);
#96719=AXIS2_PLACEMENT_3D('',#170108,#111462,#111463);
#96720=AXIS2_PLACEMENT_3D('',#170109,#111464,#111465);
#96721=AXIS2_PLACEMENT_3D('',#170110,#111466,#111467);
#96722=AXIS2_PLACEMENT_3D('',#170113,#111469,#111470);
#96723=AXIS2_PLACEMENT_3D('',#170114,#111471,#111472);
#96724=AXIS2_PLACEMENT_3D('',#170116,#111473,#111474);
#96725=AXIS2_PLACEMENT_3D('',#170117,#111475,#111476);
#96726=AXIS2_PLACEMENT_3D('',#170118,#111477,#111478);
#96727=AXIS2_PLACEMENT_3D('',#170120,#111480,#111481);
#96728=AXIS2_PLACEMENT_3D('',#170122,#111482,#111483);
#96729=AXIS2_PLACEMENT_3D('',#170126,#111486,#111487);
#96730=AXIS2_PLACEMENT_3D('',#170167,#111488,#111489);
#96731=AXIS2_PLACEMENT_3D('',#170169,#111490,#111491);
#96732=AXIS2_PLACEMENT_3D('',#170170,#111492,#111493);
#96733=AXIS2_PLACEMENT_3D('',#170171,#111494,#111495);
#96734=AXIS2_PLACEMENT_3D('',#170175,#111497,#111498);
#96735=AXIS2_PLACEMENT_3D('',#170177,#111500,#111501);
#96736=AXIS2_PLACEMENT_3D('',#170181,#111503,#111504);
#96737=AXIS2_PLACEMENT_3D('',#170218,#111506,#111507);
#96738=AXIS2_PLACEMENT_3D('',#170220,#111508,#111509);
#96739=AXIS2_PLACEMENT_3D('',#170247,#111510,#111511);
#96740=AXIS2_PLACEMENT_3D('',#170273,#111512,#111513);
#96741=AXIS2_PLACEMENT_3D('',#170275,#111514,#111515);
#96742=AXIS2_PLACEMENT_3D('',#170297,#111517,#111518);
#96743=AXIS2_PLACEMENT_3D('',#170359,#111519,#111520);
#96744=AXIS2_PLACEMENT_3D('',#170361,#111521,#111522);
#96745=AXIS2_PLACEMENT_3D('',#170364,#111524,#111525);
#96746=AXIS2_PLACEMENT_3D('',#170365,#111526,#111527);
#96747=AXIS2_PLACEMENT_3D('',#170367,#111528,#111529);
#96748=AXIS2_PLACEMENT_3D('',#170368,#111530,#111531);
#96749=AXIS2_PLACEMENT_3D('',#170369,#111532,#111533);
#96750=AXIS2_PLACEMENT_3D('',#170371,#111535,#111536);
#96751=AXIS2_PLACEMENT_3D('',#170373,#111537,#111538);
#96752=AXIS2_PLACEMENT_3D('',#170388,#111541,#111542);
#96753=AXIS2_PLACEMENT_3D('',#170409,#111543,#111544);
#96754=AXIS2_PLACEMENT_3D('',#170569,#111545,#111546);
#96755=AXIS2_PLACEMENT_3D('',#170571,#111547,#111548);
#96756=AXIS2_PLACEMENT_3D('',#170580,#111549,#111550);
#96757=AXIS2_PLACEMENT_3D('',#170582,#111551,#111552);
#96758=AXIS2_PLACEMENT_3D('',#170619,#111554,#111555);
#96759=AXIS2_PLACEMENT_3D('',#170646,#111556,#111557);
#96760=AXIS2_PLACEMENT_3D('',#170660,#111558,#111559);
#96761=AXIS2_PLACEMENT_3D('',#170661,#111560,#111561);
#96762=AXIS2_PLACEMENT_3D('',#170662,#111562,#111563);
#96763=AXIS2_PLACEMENT_3D('',#170665,#111566,#111567);
#96764=AXIS2_PLACEMENT_3D('',#170668,#111569,#111570);
#96765=AXIS2_PLACEMENT_3D('',#170669,#111571,#111572);
#96766=AXIS2_PLACEMENT_3D('',#170671,#111573,#111574);
#96767=AXIS2_PLACEMENT_3D('',#170672,#111575,#111576);
#96768=AXIS2_PLACEMENT_3D('',#170673,#111577,#111578);
#96769=AXIS2_PLACEMENT_3D('',#170676,#111580,#111581);
#96770=AXIS2_PLACEMENT_3D('',#170728,#111582,#111583);
#96771=AXIS2_PLACEMENT_3D('',#170736,#111584,#111585);
#96772=AXIS2_PLACEMENT_3D('',#170738,#111586,#111587);
#96773=AXIS2_PLACEMENT_3D('',#170740,#111588,#111589);
#96774=AXIS2_PLACEMENT_3D('',#170741,#111590,#111591);
#96775=AXIS2_PLACEMENT_3D('',#170742,#111592,#111593);
#96776=AXIS2_PLACEMENT_3D('',#170745,#111595,#111596);
#96777=AXIS2_PLACEMENT_3D('',#170746,#111597,#111598);
#96778=AXIS2_PLACEMENT_3D('',#170748,#111599,#111600);
#96779=AXIS2_PLACEMENT_3D('',#170750,#111601,#111602);
#96780=AXIS2_PLACEMENT_3D('',#170751,#111603,#111604);
#96781=AXIS2_PLACEMENT_3D('',#170752,#111605,#111606);
#96782=AXIS2_PLACEMENT_3D('',#170755,#111608,#111609);
#96783=AXIS2_PLACEMENT_3D('',#170756,#111610,#111611);
#96784=AXIS2_PLACEMENT_3D('',#170757,#111612,#111613);
#96785=AXIS2_PLACEMENT_3D('',#170758,#111614,#111615);
#96786=AXIS2_PLACEMENT_3D('',#170761,#111617,#111618);
#96787=AXIS2_PLACEMENT_3D('',#170776,#111620,#111621);
#96788=AXIS2_PLACEMENT_3D('',#170777,#111622,#111623);
#96789=AXIS2_PLACEMENT_3D('',#170804,#111624,#111625);
#96790=AXIS2_PLACEMENT_3D('',#170840,#111626,#111627);
#96791=AXIS2_PLACEMENT_3D('',#170841,#111628,#111629);
#96792=AXIS2_PLACEMENT_3D('',#170844,#111631,#111632);
#96793=AXIS2_PLACEMENT_3D('',#170865,#111633,#111634);
#96794=AXIS2_PLACEMENT_3D('',#171002,#111635,#111636);
#96795=AXIS2_PLACEMENT_3D('',#171174,#111637,#111638);
#96796=AXIS2_PLACEMENT_3D('',#171176,#111639,#111640);
#96797=AXIS2_PLACEMENT_3D('',#171190,#111641,#111642);
#96798=AXIS2_PLACEMENT_3D('',#171192,#111643,#111644);
#96799=AXIS2_PLACEMENT_3D('',#171213,#111646,#111647);
#96800=AXIS2_PLACEMENT_3D('',#171240,#111648,#111649);
#96801=AXIS2_PLACEMENT_3D('',#171258,#111650,#111651);
#96802=AXIS2_PLACEMENT_3D('',#171259,#111652,#111653);
#96803=AXIS2_PLACEMENT_3D('',#171260,#111654,#111655);
#96804=AXIS2_PLACEMENT_3D('',#171346,#111658,#111659);
#96805=AXIS2_PLACEMENT_3D('',#171377,#111660,#111661);
#96806=AXIS2_PLACEMENT_3D('',#171382,#111662,#111663);
#96807=AXIS2_PLACEMENT_3D('',#171385,#111664,#111665);
#96808=AXIS2_PLACEMENT_3D('',#171388,#111668,#111669);
#96809=AXIS2_PLACEMENT_3D('',#171395,#111671,#111672);
#96810=AXIS2_PLACEMENT_3D('',#171397,#111673,#111674);
#96811=AXIS2_PLACEMENT_3D('',#171400,#111676,#111677);
#96812=AXIS2_PLACEMENT_3D('',#171480,#111678,#111679);
#96813=AXIS2_PLACEMENT_3D('',#171483,#111681,#111682);
#96814=AXIS2_PLACEMENT_3D('',#171498,#111684,#111685);
#96815=AXIS2_PLACEMENT_3D('',#171499,#111686,#111687);
#96816=AXIS2_PLACEMENT_3D('',#171517,#111688,#111689);
#96817=AXIS2_PLACEMENT_3D('',#171550,#111690,#111691);
#96818=AXIS2_PLACEMENT_3D('',#171551,#111692,#111693);
#96819=AXIS2_PLACEMENT_3D('',#171554,#111695,#111696);
#96820=AXIS2_PLACEMENT_3D('',#171588,#111697,#111698);
#96821=AXIS2_PLACEMENT_3D('',#171671,#111699,#111700);
#96822=AXIS2_PLACEMENT_3D('',#171753,#111701,#111702);
#96823=AXIS2_PLACEMENT_3D('',#171767,#111703,#111704);
#96824=AXIS2_PLACEMENT_3D('',#171769,#111705,#111706);
#96825=AXIS2_PLACEMENT_3D('',#171770,#111707,#111708);
#96826=AXIS2_PLACEMENT_3D('',#171771,#111709,#111710);
#96827=AXIS2_PLACEMENT_3D('',#171773,#111711,#111712);
#96828=AXIS2_PLACEMENT_3D('',#171788,#111714,#111715);
#96829=AXIS2_PLACEMENT_3D('',#171789,#111716,#111717);
#96830=AXIS2_PLACEMENT_3D('',#171803,#111718,#111719);
#96831=AXIS2_PLACEMENT_3D('',#171821,#111720,#111721);
#96832=AXIS2_PLACEMENT_3D('',#171822,#111722,#111723);
#96833=AXIS2_PLACEMENT_3D('',#171823,#111724,#111725);
#96834=AXIS2_PLACEMENT_3D('',#171882,#111728,#111729);
#96835=AXIS2_PLACEMENT_3D('',#171907,#111730,#111731);
#96836=AXIS2_PLACEMENT_3D('',#171912,#111732,#111733);
#96837=AXIS2_PLACEMENT_3D('',#171915,#111734,#111735);
#96838=AXIS2_PLACEMENT_3D('',#171918,#111738,#111739);
#96839=AXIS2_PLACEMENT_3D('',#171920,#111740,#111741);
#96840=AXIS2_PLACEMENT_3D('',#171922,#111743,#111744);
#96841=AXIS2_PLACEMENT_3D('',#171924,#111745,#111746);
#96842=AXIS2_PLACEMENT_3D('',#171927,#111748,#111749);
#96843=AXIS2_PLACEMENT_3D('',#171983,#111750,#111751);
#96844=AXIS2_PLACEMENT_3D('',#171986,#111753,#111754);
#96845=AXIS2_PLACEMENT_3D('',#172001,#111756,#111757);
#96846=AXIS2_PLACEMENT_3D('',#172002,#111758,#111759);
#96847=AXIS2_PLACEMENT_3D('',#172020,#111760,#111761);
#96848=AXIS2_PLACEMENT_3D('',#172034,#111762,#111763);
#96849=AXIS2_PLACEMENT_3D('',#172035,#111764,#111765);
#96850=AXIS2_PLACEMENT_3D('',#172036,#111766,#111767);
#96851=AXIS2_PLACEMENT_3D('',#172039,#111769,#111770);
#96852=AXIS2_PLACEMENT_3D('',#172053,#111771,#111772);
#96853=AXIS2_PLACEMENT_3D('',#172055,#111773,#111774);
#96854=AXIS2_PLACEMENT_3D('',#172056,#111775,#111776);
#96855=AXIS2_PLACEMENT_3D('',#172075,#111777,#111778);
#96856=AXIS2_PLACEMENT_3D('',#172228,#111779,#111780);
#96857=AXIS2_PLACEMENT_3D('',#172230,#111781,#111782);
#96858=AXIS2_PLACEMENT_3D('',#172244,#111783,#111784);
#96859=AXIS2_PLACEMENT_3D('',#172246,#111785,#111786);
#96860=AXIS2_PLACEMENT_3D('',#172267,#111788,#111789);
#96861=AXIS2_PLACEMENT_3D('',#172294,#111790,#111791);
#96862=AXIS2_PLACEMENT_3D('',#172312,#111792,#111793);
#96863=AXIS2_PLACEMENT_3D('',#172313,#111794,#111795);
#96864=AXIS2_PLACEMENT_3D('',#172314,#111796,#111797);
#96865=AXIS2_PLACEMENT_3D('',#172394,#111800,#111801);
#96866=AXIS2_PLACEMENT_3D('',#172424,#111802,#111803);
#96867=AXIS2_PLACEMENT_3D('',#172429,#111804,#111805);
#96868=AXIS2_PLACEMENT_3D('',#172433,#111807,#111808);
#96869=AXIS2_PLACEMENT_3D('',#172435,#111810,#111811);
#96870=AXIS2_PLACEMENT_3D('',#172442,#111813,#111814);
#96871=AXIS2_PLACEMENT_3D('',#172444,#111815,#111816);
#96872=AXIS2_PLACEMENT_3D('',#172447,#111818,#111819);
#96873=AXIS2_PLACEMENT_3D('',#172527,#111820,#111821);
#96874=AXIS2_PLACEMENT_3D('',#172530,#111823,#111824);
#96875=AXIS2_PLACEMENT_3D('',#172545,#111826,#111827);
#96876=AXIS2_PLACEMENT_3D('',#172546,#111828,#111829);
#96877=AXIS2_PLACEMENT_3D('',#172564,#111830,#111831);
#96878=AXIS2_PLACEMENT_3D('',#172597,#111832,#111833);
#96879=AXIS2_PLACEMENT_3D('',#172598,#111834,#111835);
#96880=AXIS2_PLACEMENT_3D('',#172601,#111837,#111838);
#96881=AXIS2_PLACEMENT_3D('',#172635,#111839,#111840);
#96882=AXIS2_PLACEMENT_3D('',#172718,#111841,#111842);
#96883=AXIS2_PLACEMENT_3D('',#172883,#111843,#111844);
#96884=AXIS2_PLACEMENT_3D('',#172885,#111845,#111846);
#96885=AXIS2_PLACEMENT_3D('',#172902,#111847,#111848);
#96886=AXIS2_PLACEMENT_3D('',#172904,#111849,#111850);
#96887=AXIS2_PLACEMENT_3D('',#172938,#111852,#111853);
#96888=AXIS2_PLACEMENT_3D('',#172965,#111854,#111855);
#96889=AXIS2_PLACEMENT_3D('',#172979,#111856,#111857);
#96890=AXIS2_PLACEMENT_3D('',#172980,#111858,#111859);
#96891=AXIS2_PLACEMENT_3D('',#172981,#111860,#111861);
#96892=AXIS2_PLACEMENT_3D('',#172984,#111864,#111865);
#96893=AXIS2_PLACEMENT_3D('',#172986,#111866,#111867);
#96894=AXIS2_PLACEMENT_3D('',#172987,#111868,#111869);
#96895=AXIS2_PLACEMENT_3D('',#172988,#111870,#111871);
#96896=AXIS2_PLACEMENT_3D('',#172991,#111873,#111874);
#96897=AXIS2_PLACEMENT_3D('',#173055,#111875,#111876);
#96898=AXIS2_PLACEMENT_3D('',#173063,#111877,#111878);
#96899=AXIS2_PLACEMENT_3D('',#173065,#111879,#111880);
#96900=AXIS2_PLACEMENT_3D('',#173067,#111881,#111882);
#96901=AXIS2_PLACEMENT_3D('',#173068,#111883,#111884);
#96902=AXIS2_PLACEMENT_3D('',#173069,#111885,#111886);
#96903=AXIS2_PLACEMENT_3D('',#173072,#111888,#111889);
#96904=AXIS2_PLACEMENT_3D('',#173073,#111890,#111891);
#96905=AXIS2_PLACEMENT_3D('',#173075,#111892,#111893);
#96906=AXIS2_PLACEMENT_3D('',#173077,#111894,#111895);
#96907=AXIS2_PLACEMENT_3D('',#173078,#111896,#111897);
#96908=AXIS2_PLACEMENT_3D('',#173079,#111898,#111899);
#96909=AXIS2_PLACEMENT_3D('',#173082,#111901,#111902);
#96910=AXIS2_PLACEMENT_3D('',#173083,#111903,#111904);
#96911=AXIS2_PLACEMENT_3D('',#173085,#111905,#111906);
#96912=AXIS2_PLACEMENT_3D('',#173086,#111907,#111908);
#96913=AXIS2_PLACEMENT_3D('',#173087,#111909,#111910);
#96914=AXIS2_PLACEMENT_3D('',#173089,#111912,#111913);
#96915=AXIS2_PLACEMENT_3D('',#173092,#111915,#111916);
#96916=AXIS2_PLACEMENT_3D('',#173107,#111918,#111919);
#96917=AXIS2_PLACEMENT_3D('',#173108,#111920,#111921);
#96918=AXIS2_PLACEMENT_3D('',#173135,#111922,#111923);
#96919=AXIS2_PLACEMENT_3D('',#173163,#111924,#111925);
#96920=AXIS2_PLACEMENT_3D('',#173164,#111926,#111927);
#96921=AXIS2_PLACEMENT_3D('',#173167,#111929,#111930);
#96922=AXIS2_PLACEMENT_3D('',#173188,#111931,#111932);
#96923=AXIS2_PLACEMENT_3D('',#173322,#111933,#111934);
#96924=AXIS2_PLACEMENT_3D('',#173502,#111935,#111936);
#96925=AXIS2_PLACEMENT_3D('',#173504,#111937,#111938);
#96926=AXIS2_PLACEMENT_3D('',#173506,#111939,#111940);
#96927=AXIS2_PLACEMENT_3D('',#173507,#111941,#111942);
#96928=AXIS2_PLACEMENT_3D('',#173508,#111943,#111944);
#96929=AXIS2_PLACEMENT_3D('',#173511,#111946,#111947);
#96930=AXIS2_PLACEMENT_3D('',#173532,#111948,#111949);
#96931=AXIS2_PLACEMENT_3D('',#173541,#111950,#111951);
#96932=AXIS2_PLACEMENT_3D('',#173626,#111952,#111953);
#96933=AXIS2_PLACEMENT_3D('',#173627,#111954,#111955);
#96934=AXIS2_PLACEMENT_3D('',#173630,#111957,#111958);
#96935=AXIS2_PLACEMENT_3D('',#173672,#111959,#111960);
#96936=AXIS2_PLACEMENT_3D('',#173699,#111961,#111962);
#96937=AXIS2_PLACEMENT_3D('',#173713,#111963,#111964);
#96938=AXIS2_PLACEMENT_3D('',#173714,#111965,#111966);
#96939=AXIS2_PLACEMENT_3D('',#173715,#111967,#111968);
#96940=AXIS2_PLACEMENT_3D('',#173718,#111971,#111972);
#96941=AXIS2_PLACEMENT_3D('',#173720,#111974,#111975);
#96942=AXIS2_PLACEMENT_3D('',#173722,#111976,#111977);
#96943=AXIS2_PLACEMENT_3D('',#173724,#111978,#111979);
#96944=AXIS2_PLACEMENT_3D('',#173725,#111980,#111981);
#96945=AXIS2_PLACEMENT_3D('',#173726,#111982,#111983);
#96946=AXIS2_PLACEMENT_3D('',#173729,#111985,#111986);
#96947=AXIS2_PLACEMENT_3D('',#173730,#111987,#111988);
#96948=AXIS2_PLACEMENT_3D('',#173732,#111989,#111990);
#96949=AXIS2_PLACEMENT_3D('',#173733,#111991,#111992);
#96950=AXIS2_PLACEMENT_3D('',#173734,#111993,#111994);
#96951=AXIS2_PLACEMENT_3D('',#173736,#111995,#111996);
#96952=AXIS2_PLACEMENT_3D('',#173738,#111997,#111998);
#96953=AXIS2_PLACEMENT_3D('',#173739,#111999,#112000);
#96954=AXIS2_PLACEMENT_3D('',#173740,#112001,#112002);
#96955=AXIS2_PLACEMENT_3D('',#173743,#112004,#112005);
#96956=AXIS2_PLACEMENT_3D('',#173744,#112006,#112007);
#96957=AXIS2_PLACEMENT_3D('',#173746,#112008,#112009);
#96958=AXIS2_PLACEMENT_3D('',#173747,#112010,#112011);
#96959=AXIS2_PLACEMENT_3D('',#173762,#112012,#112013);
#96960=AXIS2_PLACEMENT_3D('',#173779,#112014,#112015);
#96961=AXIS2_PLACEMENT_3D('',#173798,#112016,#112017);
#96962=AXIS2_PLACEMENT_3D('',#173805,#112018,#112019);
#96963=AXIS2_PLACEMENT_3D('',#173834,#112020,#112021);
#96964=AXIS2_PLACEMENT_3D('',#173836,#112022,#112023);
#96965=AXIS2_PLACEMENT_3D('',#173838,#112024,#112025);
#96966=AXIS2_PLACEMENT_3D('',#173857,#112026,#112027);
#96967=AXIS2_PLACEMENT_3D('',#173895,#112028,#112029);
#96968=AXIS2_PLACEMENT_3D('',#173902,#112030,#112031);
#96969=AXIS2_PLACEMENT_3D('',#173950,#112032,#112033);
#96970=AXIS2_PLACEMENT_3D('',#174054,#112034,#112035);
#96971=AXIS2_PLACEMENT_3D('',#174058,#112037,#112038);
#96972=AXIS2_PLACEMENT_3D('',#174060,#112040,#112041);
#96973=AXIS2_PLACEMENT_3D('',#174063,#112042,#112043);
#96974=AXIS2_PLACEMENT_3D('',#174065,#112044,#112045);
#96975=AXIS2_PLACEMENT_3D('',#174067,#112046,#112047);
#96976=AXIS2_PLACEMENT_3D('',#174068,#112048,#112049);
#96977=AXIS2_PLACEMENT_3D('',#174069,#112050,#112051);
#96978=AXIS2_PLACEMENT_3D('',#174074,#112054,#112055);
#96979=AXIS2_PLACEMENT_3D('',#174075,#112056,#112057);
#96980=AXIS2_PLACEMENT_3D('',#174077,#112058,#112059);
#96981=AXIS2_PLACEMENT_3D('',#174079,#112060,#112061);
#96982=AXIS2_PLACEMENT_3D('',#174080,#112062,#112063);
#96983=AXIS2_PLACEMENT_3D('',#174081,#112064,#112065);
#96984=AXIS2_PLACEMENT_3D('',#174083,#112066,#112067);
#96985=AXIS2_PLACEMENT_3D('',#174087,#112069,#112070);
#96986=AXIS2_PLACEMENT_3D('',#174108,#112072,#112073);
#96987=AXIS2_PLACEMENT_3D('',#174139,#112074,#112075);
#96988=AXIS2_PLACEMENT_3D('',#174189,#112076,#112077);
#96989=AXIS2_PLACEMENT_3D('',#174278,#112078,#112079);
#96990=AXIS2_PLACEMENT_3D('',#174279,#112080,#112081);
#96991=AXIS2_PLACEMENT_3D('',#174280,#112082,#112083);
#96992=AXIS2_PLACEMENT_3D('',#174281,#112084,#112085);
#96993=AXIS2_PLACEMENT_3D('',#174282,#112086,#112087);
#96994=AXIS2_PLACEMENT_3D('',#174283,#112088,#112089);
#96995=AXIS2_PLACEMENT_3D('',#174286,#112090,#112091);
#96996=AXIS2_PLACEMENT_3D('',#174288,#112092,#112093);
#96997=AXIS2_PLACEMENT_3D('',#174289,#112094,#112095);
#96998=AXIS2_PLACEMENT_3D('',#174290,#112096,#112097);
#96999=AXIS2_PLACEMENT_3D('',#174291,#112098,#112099);
#97000=AXIS2_PLACEMENT_3D('',#174294,#112101,#112102);
#97001=AXIS2_PLACEMENT_3D('',#174295,#112103,#112104);
#97002=AXIS2_PLACEMENT_3D('',#174297,#112105,#112106);
#97003=AXIS2_PLACEMENT_3D('',#174298,#112107,#112108);
#97004=AXIS2_PLACEMENT_3D('',#174313,#112109,#112110);
#97005=AXIS2_PLACEMENT_3D('',#174319,#112111,#112112);
#97006=AXIS2_PLACEMENT_3D('',#174383,#112113,#112114);
#97007=AXIS2_PLACEMENT_3D('',#174384,#112115,#112116);
#97008=AXIS2_PLACEMENT_3D('',#174387,#112118,#112119);
#97009=AXIS2_PLACEMENT_3D('',#174427,#112120,#112121);
#97010=AXIS2_PLACEMENT_3D('',#174485,#112122,#112123);
#97011=AXIS2_PLACEMENT_3D('',#174579,#112124,#112125);
#97012=AXIS2_PLACEMENT_3D('',#174581,#112126,#112127);
#97013=AXIS2_PLACEMENT_3D('',#174583,#112128,#112129);
#97014=AXIS2_PLACEMENT_3D('',#174584,#112130,#112131);
#97015=AXIS2_PLACEMENT_3D('',#174585,#112132,#112133);
#97016=AXIS2_PLACEMENT_3D('',#174588,#112135,#112136);
#97017=AXIS2_PLACEMENT_3D('',#174608,#112137,#112138);
#97018=AXIS2_PLACEMENT_3D('',#174610,#112139,#112140);
#97019=AXIS2_PLACEMENT_3D('',#174627,#112141,#112142);
#97020=AXIS2_PLACEMENT_3D('',#174629,#112143,#112144);
#97021=AXIS2_PLACEMENT_3D('',#174650,#112146,#112147);
#97022=AXIS2_PLACEMENT_3D('',#174678,#112148,#112149);
#97023=AXIS2_PLACEMENT_3D('',#174735,#112150,#112151);
#97024=AXIS2_PLACEMENT_3D('',#174740,#112152,#112153);
#97025=AXIS2_PLACEMENT_3D('',#174742,#112154,#112155);
#97026=AXIS2_PLACEMENT_3D('',#174744,#112156,#112157);
#97027=AXIS2_PLACEMENT_3D('',#174745,#112158,#112159);
#97028=AXIS2_PLACEMENT_3D('',#174746,#112160,#112161);
#97029=AXIS2_PLACEMENT_3D('',#174749,#112163,#112164);
#97030=AXIS2_PLACEMENT_3D('',#174750,#112165,#112166);
#97031=AXIS2_PLACEMENT_3D('',#174752,#112167,#112168);
#97032=AXIS2_PLACEMENT_3D('',#174754,#112169,#112170);
#97033=AXIS2_PLACEMENT_3D('',#174755,#112171,#112172);
#97034=AXIS2_PLACEMENT_3D('',#174756,#112173,#112174);
#97035=AXIS2_PLACEMENT_3D('',#174759,#112176,#112177);
#97036=AXIS2_PLACEMENT_3D('',#174760,#112178,#112179);
#97037=AXIS2_PLACEMENT_3D('',#174762,#112180,#112181);
#97038=AXIS2_PLACEMENT_3D('',#174763,#112182,#112183);
#97039=AXIS2_PLACEMENT_3D('',#174778,#112184,#112185);
#97040=AXIS2_PLACEMENT_3D('',#174784,#112186,#112187);
#97041=AXIS2_PLACEMENT_3D('',#174839,#112188,#112189);
#97042=AXIS2_PLACEMENT_3D('',#174840,#112190,#112191);
#97043=AXIS2_PLACEMENT_3D('',#174843,#112193,#112194);
#97044=AXIS2_PLACEMENT_3D('',#174877,#112195,#112196);
#97045=AXIS2_PLACEMENT_3D('',#174993,#112197,#112198);
#97046=AXIS2_PLACEMENT_3D('',#175152,#112199,#112200);
#97047=AXIS2_PLACEMENT_3D('',#175154,#112201,#112202);
#97048=AXIS2_PLACEMENT_3D('',#175168,#112203,#112204);
#97049=AXIS2_PLACEMENT_3D('',#175170,#112205,#112206);
#97050=AXIS2_PLACEMENT_3D('',#175191,#112208,#112209);
#97051=AXIS2_PLACEMENT_3D('',#175219,#112210,#112211);
#97052=AXIS2_PLACEMENT_3D('',#175269,#112212,#112213);
#97053=AXIS2_PLACEMENT_3D('',#175274,#112214,#112215);
#97054=AXIS2_PLACEMENT_3D('',#175277,#112216,#112217);
#97055=AXIS2_PLACEMENT_3D('',#175281,#112219,#112220);
#97056=AXIS2_PLACEMENT_3D('',#175283,#112222,#112223);
#97057=AXIS2_PLACEMENT_3D('',#175295,#112225,#112226);
#97058=AXIS2_PLACEMENT_3D('',#175297,#112227,#112228);
#97059=AXIS2_PLACEMENT_3D('',#175300,#112230,#112231);
#97060=AXIS2_PLACEMENT_3D('',#175315,#112232,#112233);
#97061=AXIS2_PLACEMENT_3D('',#175321,#112234,#112235);
#97062=AXIS2_PLACEMENT_3D('',#175368,#112236,#112237);
#97063=AXIS2_PLACEMENT_3D('',#175369,#112238,#112239);
#97064=AXIS2_PLACEMENT_3D('',#175372,#112241,#112242);
#97065=AXIS2_PLACEMENT_3D('',#175406,#112243,#112244);
#97066=AXIS2_PLACEMENT_3D('',#175495,#112245,#112246);
#97067=AXIS2_PLACEMENT_3D('',#175586,#112247,#112248);
#97068=AXIS2_PLACEMENT_3D('',#175600,#112249,#112250);
#97069=AXIS2_PLACEMENT_3D('',#175602,#112251,#112252);
#97070=AXIS2_PLACEMENT_3D('',#175603,#112253,#112254);
#97071=AXIS2_PLACEMENT_3D('',#175604,#112255,#112256);
#97072=AXIS2_PLACEMENT_3D('',#175606,#112257,#112258);
#97073=AXIS2_PLACEMENT_3D('',#175621,#112260,#112261);
#97074=AXIS2_PLACEMENT_3D('',#175622,#112262,#112263);
#97075=AXIS2_PLACEMENT_3D('',#175637,#112264,#112265);
#97076=AXIS2_PLACEMENT_3D('',#175680,#112266,#112267);
#97077=AXIS2_PLACEMENT_3D('',#175685,#112268,#112269);
#97078=AXIS2_PLACEMENT_3D('',#175689,#112271,#112272);
#97079=AXIS2_PLACEMENT_3D('',#175691,#112274,#112275);
#97080=AXIS2_PLACEMENT_3D('',#175789,#112277,#112278);
#97081=AXIS2_PLACEMENT_3D('',#175803,#112279,#112280);
#97082=AXIS2_PLACEMENT_3D('',#175804,#112281,#112282);
#97083=AXIS2_PLACEMENT_3D('',#175821,#112285,#112286);
#97084=AXIS2_PLACEMENT_3D('',#175822,#112287,#112288);
#97085=AXIS2_PLACEMENT_3D('',#175823,#112289,#112290);
#97086=AXIS2_PLACEMENT_3D('',#175824,#112291,#112292);
#97087=AXIS2_PLACEMENT_3D('',#175825,#112293,#112294);
#97088=AXIS2_PLACEMENT_3D('',#175840,#112295,#112296);
#97089=AXIS2_PLACEMENT_3D('',#175841,#112297,#112298);
#97090=AXIS2_PLACEMENT_3D('',#175842,#112299,#112300);
#97091=AXIS2_PLACEMENT_3D('',#176037,#112301,#112302);
#97092=AXIS2_PLACEMENT_3D('',#176225,#112303,#112304);
#97093=AXIS2_PLACEMENT_3D('',#176226,#112305,#112306);
#97094=AXIS2_PLACEMENT_3D('',#176227,#112307,#112308);
#97095=AXIS2_PLACEMENT_3D('',#176228,#112309,#112310);
#97096=AXIS2_PLACEMENT_3D('',#176229,#112311,#112312);
#97097=AXIS2_PLACEMENT_3D('',#176244,#112313,#112314);
#97098=AXIS2_PLACEMENT_3D('',#176245,#112315,#112316);
#97099=AXIS2_PLACEMENT_3D('',#176246,#112317,#112318);
#97100=AXIS2_PLACEMENT_3D('',#176247,#112319,#112320);
#97101=AXIS2_PLACEMENT_3D('',#176268,#112323,#112324);
#97102=AXIS2_PLACEMENT_3D('',#176270,#112325,#112326);
#97103=AXIS2_PLACEMENT_3D('',#176272,#112328,#112329);
#97104=AXIS2_PLACEMENT_3D('',#176305,#112331,#112332);
#97105=AXIS2_PLACEMENT_3D('',#176306,#112333,#112334);
#97106=AXIS2_PLACEMENT_3D('',#176307,#112335,#112336);
#97107=AXIS2_PLACEMENT_3D('',#176308,#112337,#112338);
#97108=AXIS2_PLACEMENT_3D('',#176309,#112339,#112340);
#97109=AXIS2_PLACEMENT_3D('',#176324,#112341,#112342);
#97110=AXIS2_PLACEMENT_3D('',#176325,#112343,#112344);
#97111=AXIS2_PLACEMENT_3D('',#176326,#112345,#112346);
#97112=AXIS2_PLACEMENT_3D('',#176327,#112347,#112348);
#97113=AXIS2_PLACEMENT_3D('',#176400,#112350,#112351);
#97114=AXIS2_PLACEMENT_3D('',#176402,#112352,#112353);
#97115=AXIS2_PLACEMENT_3D('',#176404,#112355,#112356);
#97116=AXIS2_PLACEMENT_3D('',#176407,#112358,#112359);
#97117=AXIS2_PLACEMENT_3D('',#176474,#112360,#112361);
#97118=AXIS2_PLACEMENT_3D('',#176475,#112362,#112363);
#97119=AXIS2_PLACEMENT_3D('',#176563,#112364,#112365);
#97120=AXIS2_PLACEMENT_3D('',#176565,#112366,#112367);
#97121=AXIS2_PLACEMENT_3D('',#176566,#112368,#112369);
#97122=AXIS2_PLACEMENT_3D('',#176646,#112370,#112371);
#97123=AXIS2_PLACEMENT_3D('',#176652,#112375,#112376);
#97124=AXIS2_PLACEMENT_3D('',#176654,#112377,#112378);
#97125=AXIS2_PLACEMENT_3D('',#176656,#112380,#112381);
#97126=AXIS2_PLACEMENT_3D('',#176658,#112382,#112383);
#97127=AXIS2_PLACEMENT_3D('',#176660,#112385,#112386);
#97128=AXIS2_PLACEMENT_3D('',#176662,#112387,#112388);
#97129=AXIS2_PLACEMENT_3D('',#176664,#112390,#112391);
#97130=AXIS2_PLACEMENT_3D('',#176668,#112394,#112395);
#97131=AXIS2_PLACEMENT_3D('',#176671,#112397,#112398);
#97132=AXIS2_PLACEMENT_3D('',#176672,#112399,#112400);
#97133=AXIS2_PLACEMENT_3D('',#176675,#112402,#112403);
#97134=AXIS2_PLACEMENT_3D('',#176676,#112404,#112405);
#97135=AXIS2_PLACEMENT_3D('',#176678,#112406,#112407);
#97136=AXIS2_PLACEMENT_3D('',#176680,#112409,#112410);
#97137=AXIS2_PLACEMENT_3D('',#176684,#112413,#112414);
#97138=AXIS2_PLACEMENT_3D('',#176686,#112415,#112416);
#97139=AXIS2_PLACEMENT_3D('',#176688,#112418,#112419);
#97140=AXIS2_PLACEMENT_3D('',#176690,#112420,#112421);
#97141=AXIS2_PLACEMENT_3D('',#176692,#112423,#112424);
#97142=AXIS2_PLACEMENT_3D('',#176694,#112425,#112426);
#97143=AXIS2_PLACEMENT_3D('',#176696,#112428,#112429);
#97144=AXIS2_PLACEMENT_3D('',#176749,#112434,#112435);
#97145=AXIS2_PLACEMENT_3D('',#176751,#112436,#112437);
#97146=AXIS2_PLACEMENT_3D('',#176846,#112438,#112439);
#97147=AXIS2_PLACEMENT_3D('',#176848,#112440,#112441);
#97148=AXIS2_PLACEMENT_3D('',#176881,#112443,#112444);
#97149=AXIS2_PLACEMENT_3D('',#176892,#112445,#112446);
#97150=AXIS2_PLACEMENT_3D('',#176894,#112447,#112448);
#97151=AXIS2_PLACEMENT_3D('',#176927,#112450,#112451);
#97152=AXIS2_PLACEMENT_3D('',#176977,#112452,#112453);
#97153=AXIS2_PLACEMENT_3D('',#176979,#112455,#112456);
#97154=AXIS2_PLACEMENT_3D('',#176984,#112459,#112460);
#97155=AXIS2_PLACEMENT_3D('',#176995,#112461,#112462);
#97156=AXIS2_PLACEMENT_3D('',#176997,#112463,#112464);
#97157=AXIS2_PLACEMENT_3D('',#176998,#112465,#112466);
#97158=AXIS2_PLACEMENT_3D('',#176999,#112467,#112468);
#97159=AXIS2_PLACEMENT_3D('',#177011,#112470,#112471);
#97160=AXIS2_PLACEMENT_3D('',#177013,#112472,#112473);
#97161=AXIS2_PLACEMENT_3D('',#177014,#112474,#112475);
#97162=AXIS2_PLACEMENT_3D('',#177015,#112476,#112477);
#97163=AXIS2_PLACEMENT_3D('',#177019,#112479,#112480);
#97164=AXIS2_PLACEMENT_3D('',#177021,#112482,#112483);
#97165=AXIS2_PLACEMENT_3D('',#177025,#112486,#112487);
#97166=AXIS2_PLACEMENT_3D('',#177027,#112488,#112489);
#97167=AXIS2_PLACEMENT_3D('',#177039,#112491,#112492);
#97168=AXIS2_PLACEMENT_3D('',#177041,#112493,#112494);
#97169=AXIS2_PLACEMENT_3D('',#177042,#112495,#112496);
#97170=AXIS2_PLACEMENT_3D('',#177043,#112497,#112498);
#97171=AXIS2_PLACEMENT_3D('',#177055,#112500,#112501);
#97172=AXIS2_PLACEMENT_3D('',#177057,#112502,#112503);
#97173=AXIS2_PLACEMENT_3D('',#177058,#112504,#112505);
#97174=AXIS2_PLACEMENT_3D('',#177059,#112506,#112507);
#97175=AXIS2_PLACEMENT_3D('',#177063,#112509,#112510);
#97176=AXIS2_PLACEMENT_3D('',#177065,#112512,#112513);
#97177=AXIS2_PLACEMENT_3D('',#177069,#112516,#112517);
#97178=AXIS2_PLACEMENT_3D('',#177071,#112518,#112519);
#97179=AXIS2_PLACEMENT_3D('',#177083,#112521,#112522);
#97180=AXIS2_PLACEMENT_3D('',#177085,#112523,#112524);
#97181=AXIS2_PLACEMENT_3D('',#177086,#112525,#112526);
#97182=AXIS2_PLACEMENT_3D('',#177087,#112527,#112528);
#97183=AXIS2_PLACEMENT_3D('',#177089,#112529,#112530);
#97184=AXIS2_PLACEMENT_3D('',#177312,#112532,#112533);
#97185=AXIS2_PLACEMENT_3D('',#177361,#112534,#112535);
#97186=AXIS2_PLACEMENT_3D('',#177362,#112536,#112537);
#97187=AXIS2_PLACEMENT_3D('',#177363,#112538,#112539);
#97188=AXIS2_PLACEMENT_3D('',#177364,#112540,#112541);
#97189=AXIS2_PLACEMENT_3D('',#177369,#112543,#112544);
#97190=AXIS2_PLACEMENT_3D('',#177372,#112546,#112547);
#97191=AXIS2_PLACEMENT_3D('',#177373,#112548,#112549);
#97192=AXIS2_PLACEMENT_3D('',#177378,#112552,#112553);
#97193=AXIS2_PLACEMENT_3D('',#177379,#112554,#112555);
#97194=AXIS2_PLACEMENT_3D('',#177381,#112556,#112557);
#97195=AXIS2_PLACEMENT_3D('',#177384,#112559,#112560);
#97196=AXIS2_PLACEMENT_3D('',#177457,#112561,#112562);
#97197=AXIS2_PLACEMENT_3D('',#177477,#112563,#112564);
#97198=AXIS2_PLACEMENT_3D('',#177515,#112565,#112566);
#97199=AXIS2_PLACEMENT_3D('',#177579,#112567,#112568);
#97200=AXIS2_PLACEMENT_3D('',#177586,#112569,#112570);
#97201=AXIS2_PLACEMENT_3D('',#177591,#112572,#112573);
#97202=AXIS2_PLACEMENT_3D('',#177594,#112575,#112576);
#97203=AXIS2_PLACEMENT_3D('',#177595,#112577,#112578);
#97204=AXIS2_PLACEMENT_3D('',#177604,#112581,#112582);
#97205=AXIS2_PLACEMENT_3D('',#177606,#112583,#112584);
#97206=AXIS2_PLACEMENT_3D('',#177609,#112586,#112587);
#97207=AXIS2_PLACEMENT_3D('',#177629,#112588,#112589);
#97208=AXIS2_PLACEMENT_3D('',#177631,#112590,#112591);
#97209=AXIS2_PLACEMENT_3D('',#177691,#112592,#112593);
#97210=AXIS2_PLACEMENT_3D('',#177726,#112594,#112595);
#97211=AXIS2_PLACEMENT_3D('',#177728,#112596,#112597);
#97212=AXIS2_PLACEMENT_3D('',#177731,#112600,#112601);
#97213=AXIS2_PLACEMENT_3D('',#177733,#112602,#112603);
#97214=AXIS2_PLACEMENT_3D('',#177734,#112604,#112605);
#97215=AXIS2_PLACEMENT_3D('',#177735,#112606,#112607);
#97216=AXIS2_PLACEMENT_3D('',#177819,#112608,#112609);
#97217=AXIS2_PLACEMENT_3D('',#177836,#112610,#112611);
#97218=AXIS2_PLACEMENT_3D('',#177840,#112614,#112615);
#97219=AXIS2_PLACEMENT_3D('',#177842,#112616,#112617);
#97220=AXIS2_PLACEMENT_3D('',#177844,#112619,#112620);
#97221=AXIS2_PLACEMENT_3D('',#177846,#112621,#112622);
#97222=AXIS2_PLACEMENT_3D('',#177848,#112623,#112624);
#97223=AXIS2_PLACEMENT_3D('',#177849,#112625,#112626);
#97224=AXIS2_PLACEMENT_3D('',#177850,#112627,#112628);
#97225=AXIS2_PLACEMENT_3D('',#177852,#112630,#112631);
#97226=AXIS2_PLACEMENT_3D('',#177856,#112633,#112634);
#97227=AXIS2_PLACEMENT_3D('',#177858,#112636,#112637);
#97228=AXIS2_PLACEMENT_3D('',#177860,#112638,#112639);
#97229=AXIS2_PLACEMENT_3D('',#177863,#112641,#112642);
#97230=AXIS2_PLACEMENT_3D('',#177864,#112643,#112644);
#97231=AXIS2_PLACEMENT_3D('',#177865,#112645,#112646);
#97232=AXIS2_PLACEMENT_3D('',#177867,#112647,#112648);
#97233=AXIS2_PLACEMENT_3D('',#177868,#112649,#112650);
#97234=AXIS2_PLACEMENT_3D('',#177870,#112651,#112652);
#97235=AXIS2_PLACEMENT_3D('',#177872,#112654,#112655);
#97236=AXIS2_PLACEMENT_3D('',#177875,#112656,#112657);
#97237=AXIS2_PLACEMENT_3D('',#177878,#112660,#112661);
#97238=AXIS2_PLACEMENT_3D('',#177880,#112662,#112663);
#97239=AXIS2_PLACEMENT_3D('',#177884,#112665,#112666);
#97240=AXIS2_PLACEMENT_3D('',#177896,#112668,#112669);
#97241=AXIS2_PLACEMENT_3D('',#177897,#112670,#112671);
#97242=AXIS2_PLACEMENT_3D('',#177898,#112672,#112673);
#97243=AXIS2_PLACEMENT_3D('',#177900,#112674,#112675);
#97244=AXIS2_PLACEMENT_3D('',#177901,#112676,#112677);
#97245=AXIS2_PLACEMENT_3D('',#177912,#112678,#112679);
#97246=AXIS2_PLACEMENT_3D('',#177913,#112680,#112681);
#97247=AXIS2_PLACEMENT_3D('',#177914,#112682,#112683);
#97248=AXIS2_PLACEMENT_3D('',#177917,#112686,#112687);
#97249=AXIS2_PLACEMENT_3D('',#177919,#112688,#112689);
#97250=AXIS2_PLACEMENT_3D('',#177921,#112691,#112692);
#97251=AXIS2_PLACEMENT_3D('',#177922,#112693,#112694);
#97252=AXIS2_PLACEMENT_3D('',#177924,#112695,#112696);
#97253=AXIS2_PLACEMENT_3D('',#177925,#112697,#112698);
#97254=AXIS2_PLACEMENT_3D('',#177927,#112699,#112700);
#97255=AXIS2_PLACEMENT_3D('',#177929,#112702,#112703);
#97256=AXIS2_PLACEMENT_3D('',#177933,#112705,#112706);
#97257=AXIS2_PLACEMENT_3D('',#177935,#112708,#112709);
#97258=AXIS2_PLACEMENT_3D('',#177938,#112711,#112712);
#97259=AXIS2_PLACEMENT_3D('',#177939,#112713,#112714);
#97260=AXIS2_PLACEMENT_3D('',#178059,#112717,#112718);
#97261=AXIS2_PLACEMENT_3D('',#178060,#112719,#112720);
#97262=AXIS2_PLACEMENT_3D('',#178061,#112721,#112722);
#97263=AXIS2_PLACEMENT_3D('',#178119,#112724,#112725);
#97264=AXIS2_PLACEMENT_3D('',#178123,#112728,#112729);
#97265=AXIS2_PLACEMENT_3D('',#178172,#112731,#112732);
#97266=AXIS2_PLACEMENT_3D('',#178219,#112734,#112735);
#97267=AXIS2_PLACEMENT_3D('',#178290,#112736,#112737);
#97268=AXIS2_PLACEMENT_3D('',#178324,#112739,#112740);
#97269=AXIS2_PLACEMENT_3D('',#178408,#112741,#112742);
#97270=AXIS2_PLACEMENT_3D('',#178412,#112745,#112746);
#97271=AXIS2_PLACEMENT_3D('',#178470,#112748,#112749);
#97272=AXIS2_PLACEMENT_3D('',#178474,#112752,#112753);
#97273=AXIS2_PLACEMENT_3D('',#178523,#112755,#112756);
#97274=AXIS2_PLACEMENT_3D('',#178567,#112758,#112759);
#97275=AXIS2_PLACEMENT_3D('',#178638,#112760,#112761);
#97276=AXIS2_PLACEMENT_3D('',#178693,#112764,#112765);
#97277=AXIS2_PLACEMENT_3D('',#178764,#112766,#112767);
#97278=AXIS2_PLACEMENT_3D('',#178820,#112768,#112769);
#97279=AXIS2_PLACEMENT_3D('',#178835,#112772,#112773);
#97280=AXIS2_PLACEMENT_3D('',#178887,#112775,#112776);
#97281=AXIS2_PLACEMENT_3D('',#178891,#112779,#112780);
#97282=AXIS2_PLACEMENT_3D('',#178946,#112782,#112783);
#97283=AXIS2_PLACEMENT_3D('',#178990,#112785,#112786);
#97284=AXIS2_PLACEMENT_3D('',#179067,#112787,#112788);
#97285=AXIS2_PLACEMENT_3D('',#179069,#112789,#112790);
#97286=AXIS2_PLACEMENT_3D('',#179071,#112792,#112793);
#97287=AXIS2_PLACEMENT_3D('',#179110,#112794,#112795);
#97288=AXIS2_PLACEMENT_3D('',#179125,#112796,#112797);
#97289=AXIS2_PLACEMENT_3D('',#179126,#112798,#112799);
#97290=AXIS2_PLACEMENT_3D('',#179170,#112800,#112801);
#97291=AXIS2_PLACEMENT_3D('',#179174,#112804,#112805);
#97292=AXIS2_PLACEMENT_3D('',#179290,#112808,#112809);
#97293=AXIS2_PLACEMENT_3D('',#179291,#112810,#112811);
#97294=AXIS2_PLACEMENT_3D('',#179343,#112813,#112814);
#97295=AXIS2_PLACEMENT_3D('',#179347,#112817,#112818);
#97296=AXIS2_PLACEMENT_3D('',#179402,#112820,#112821);
#97297=AXIS2_PLACEMENT_3D('',#179516,#112823,#112824);
#97298=AXIS2_PLACEMENT_3D('',#179548,#112825,#112826);
#97299=AXIS2_PLACEMENT_3D('',#179625,#112827,#112828);
#97300=AXIS2_PLACEMENT_3D('',#179627,#112830,#112831);
#97301=AXIS2_PLACEMENT_3D('',#179643,#112835,#112836);
#97302=AXIS2_PLACEMENT_3D('',#179701,#112838,#112839);
#97303=AXIS2_PLACEMENT_3D('',#179705,#112842,#112843);
#97304=AXIS2_PLACEMENT_3D('',#179754,#112845,#112846);
#97305=AXIS2_PLACEMENT_3D('',#179801,#112848,#112849);
#97306=AXIS2_PLACEMENT_3D('',#179910,#112850,#112851);
#97307=AXIS2_PLACEMENT_3D('',#180021,#112852,#112853);
#97308=AXIS2_PLACEMENT_3D('',#180026,#112857,#112858);
#97309=AXIS2_PLACEMENT_3D('',#180084,#112860,#112861);
#97310=AXIS2_PLACEMENT_3D('',#180088,#112864,#112865);
#97311=AXIS2_PLACEMENT_3D('',#180137,#112867,#112868);
#97312=AXIS2_PLACEMENT_3D('',#180182,#112871,#112872);
#97313=AXIS2_PLACEMENT_3D('',#180287,#112873,#112874);
#97314=AXIS2_PLACEMENT_3D('',#180358,#112875,#112876);
#97315=AXIS2_PLACEMENT_3D('',#180360,#112878,#112879);
#97316=AXIS2_PLACEMENT_3D('',#180375,#112882,#112883);
#97317=AXIS2_PLACEMENT_3D('',#180427,#112885,#112886);
#97318=AXIS2_PLACEMENT_3D('',#180431,#112889,#112890);
#97319=AXIS2_PLACEMENT_3D('',#180486,#112892,#112893);
#97320=AXIS2_PLACEMENT_3D('',#180530,#112895,#112896);
#97321=AXIS2_PLACEMENT_3D('',#180607,#112897,#112898);
#97322=AXIS2_PLACEMENT_3D('',#180609,#112899,#112900);
#97323=AXIS2_PLACEMENT_3D('',#180611,#112902,#112903);
#97324=AXIS2_PLACEMENT_3D('',#180633,#112904,#112905);
#97325=AXIS2_PLACEMENT_3D('',#180704,#112908,#112909);
#97326=AXIS2_PLACEMENT_3D('',#180737,#112910,#112911);
#97327=AXIS2_PLACEMENT_3D('',#180818,#112912,#112913);
#97328=AXIS2_PLACEMENT_3D('',#180822,#112916,#112917);
#97329=AXIS2_PLACEMENT_3D('',#180874,#112919,#112920);
#97330=AXIS2_PLACEMENT_3D('',#180878,#112923,#112924);
#97331=AXIS2_PLACEMENT_3D('',#180933,#112926,#112927);
#97332=AXIS2_PLACEMENT_3D('',#181047,#112929,#112930);
#97333=AXIS2_PLACEMENT_3D('',#181079,#112931,#112932);
#97334=AXIS2_PLACEMENT_3D('',#181156,#112933,#112934);
#97335=AXIS2_PLACEMENT_3D('',#181158,#112936,#112937);
#97336=AXIS2_PLACEMENT_3D('',#181163,#112940,#112941);
#97337=AXIS2_PLACEMENT_3D('',#181177,#112942,#112943);
#97338=AXIS2_PLACEMENT_3D('',#181178,#112944,#112945);
#97339=AXIS2_PLACEMENT_3D('',#181179,#112946,#112947);
#97340=AXIS2_PLACEMENT_3D('',#181180,#112948,#112949);
#97341=AXIS2_PLACEMENT_3D('',#181181,#112950,#112951);
#97342=AXIS2_PLACEMENT_3D('',#181183,#112952,#112953);
#97343=AXIS2_PLACEMENT_3D('',#181200,#112956,#112957);
#97344=AXIS2_PLACEMENT_3D('',#181201,#112958,#112959);
#97345=AXIS2_PLACEMENT_3D('',#181202,#112960,#112961);
#97346=AXIS2_PLACEMENT_3D('',#181223,#112963,#112964);
#97347=AXIS2_PLACEMENT_3D('',#181225,#112965,#112966);
#97348=AXIS2_PLACEMENT_3D('',#181227,#112968,#112969);
#97349=AXIS2_PLACEMENT_3D('',#181282,#112971,#112972);
#97350=AXIS2_PLACEMENT_3D('',#181285,#112974,#112975);
#97351=AXIS2_PLACEMENT_3D('',#181299,#112976,#112977);
#97352=AXIS2_PLACEMENT_3D('',#181300,#112978,#112979);
#97353=AXIS2_PLACEMENT_3D('',#181301,#112980,#112981);
#97354=AXIS2_PLACEMENT_3D('',#181302,#112982,#112983);
#97355=AXIS2_PLACEMENT_3D('',#181303,#112984,#112985);
#97356=AXIS2_PLACEMENT_3D('',#181305,#112986,#112987);
#97357=AXIS2_PLACEMENT_3D('',#181358,#112989,#112990);
#97358=AXIS2_PLACEMENT_3D('',#181359,#112991,#112992);
#97359=AXIS2_PLACEMENT_3D('',#181460,#112993,#112994);
#97360=AXIS2_PLACEMENT_3D('',#181729,#112995,#112996);
#97361=AXIS2_PLACEMENT_3D('',#181732,#112998,#112999);
#97362=AXIS2_PLACEMENT_3D('',#181746,#113000,#113001);
#97363=AXIS2_PLACEMENT_3D('',#181747,#113002,#113003);
#97364=AXIS2_PLACEMENT_3D('',#181748,#113004,#113005);
#97365=AXIS2_PLACEMENT_3D('',#181749,#113006,#113007);
#97366=AXIS2_PLACEMENT_3D('',#181750,#113008,#113009);
#97367=AXIS2_PLACEMENT_3D('',#181752,#113010,#113011);
#97368=AXIS2_PLACEMENT_3D('',#181796,#113013,#113014);
#97369=AXIS2_PLACEMENT_3D('',#181797,#113015,#113016);
#97370=AXIS2_PLACEMENT_3D('',#181955,#113017,#113018);
#97371=AXIS2_PLACEMENT_3D('',#182146,#113019,#113020);
#97372=AXIS2_PLACEMENT_3D('',#182149,#113022,#113023);
#97373=AXIS2_PLACEMENT_3D('',#182163,#113024,#113025);
#97374=AXIS2_PLACEMENT_3D('',#182164,#113026,#113027);
#97375=AXIS2_PLACEMENT_3D('',#182165,#113028,#113029);
#97376=AXIS2_PLACEMENT_3D('',#182166,#113030,#113031);
#97377=AXIS2_PLACEMENT_3D('',#182167,#113032,#113033);
#97378=AXIS2_PLACEMENT_3D('',#182169,#113034,#113035);
#97379=AXIS2_PLACEMENT_3D('',#182222,#113037,#113038);
#97380=AXIS2_PLACEMENT_3D('',#182223,#113039,#113040);
#97381=AXIS2_PLACEMENT_3D('',#182386,#113041,#113042);
#97382=AXIS2_PLACEMENT_3D('',#182578,#113043,#113044);
#97383=AXIS2_PLACEMENT_3D('',#182581,#113046,#113047);
#97384=AXIS2_PLACEMENT_3D('',#182595,#113048,#113049);
#97385=AXIS2_PLACEMENT_3D('',#182596,#113050,#113051);
#97386=AXIS2_PLACEMENT_3D('',#182597,#113052,#113053);
#97387=AXIS2_PLACEMENT_3D('',#182598,#113054,#113055);
#97388=AXIS2_PLACEMENT_3D('',#182599,#113056,#113057);
#97389=AXIS2_PLACEMENT_3D('',#182601,#113058,#113059);
#97390=AXIS2_PLACEMENT_3D('',#182618,#113062,#113063);
#97391=AXIS2_PLACEMENT_3D('',#182619,#113064,#113065);
#97392=AXIS2_PLACEMENT_3D('',#182620,#113066,#113067);
#97393=AXIS2_PLACEMENT_3D('',#182672,#113069,#113070);
#97394=AXIS2_PLACEMENT_3D('',#182674,#113071,#113072);
#97395=AXIS2_PLACEMENT_3D('',#182676,#113074,#113075);
#97396=AXIS2_PLACEMENT_3D('',#182755,#113077,#113078);
#97397=AXIS2_PLACEMENT_3D('',#182758,#113080,#113081);
#97398=AXIS2_PLACEMENT_3D('',#182772,#113082,#113083);
#97399=AXIS2_PLACEMENT_3D('',#182773,#113084,#113085);
#97400=AXIS2_PLACEMENT_3D('',#182774,#113086,#113087);
#97401=AXIS2_PLACEMENT_3D('',#182775,#113088,#113089);
#97402=AXIS2_PLACEMENT_3D('',#182790,#113090,#113091);
#97403=AXIS2_PLACEMENT_3D('',#182791,#113092,#113093);
#97404=AXIS2_PLACEMENT_3D('',#182805,#113094,#113095);
#97405=AXIS2_PLACEMENT_3D('',#182809,#113098,#113099);
#97406=AXIS2_PLACEMENT_3D('',#182860,#113101,#113102);
#97407=AXIS2_PLACEMENT_3D('',#182862,#113103,#113104);
#97408=AXIS2_PLACEMENT_3D('',#182864,#113106,#113107);
#97409=AXIS2_PLACEMENT_3D('',#182879,#113108,#113109);
#97410=AXIS2_PLACEMENT_3D('',#182880,#113110,#113111);
#97411=AXIS2_PLACEMENT_3D('',#182882,#113112,#113113);
#97412=AXIS2_PLACEMENT_3D('',#182919,#113115,#113116);
#97413=AXIS2_PLACEMENT_3D('',#182921,#113117,#113118);
#97414=AXIS2_PLACEMENT_3D('',#182923,#113120,#113121);
#97415=AXIS2_PLACEMENT_3D('',#182978,#113122,#113123);
#97416=AXIS2_PLACEMENT_3D('',#182981,#113124,#113125);
#97417=AXIS2_PLACEMENT_3D('',#183224,#113128,#113129);
#97418=AXIS2_PLACEMENT_3D('',#183457,#113130,#113131);
#97419=AXIS2_PLACEMENT_3D('',#183460,#113133,#113134);
#97420=AXIS2_PLACEMENT_3D('',#183475,#113136,#113137);
#97421=AXIS2_PLACEMENT_3D('',#183476,#113138,#113139);
#97422=AXIS2_PLACEMENT_3D('',#183477,#113140,#113141);
#97423=AXIS2_PLACEMENT_3D('',#183478,#113142,#113143);
#97424=AXIS2_PLACEMENT_3D('',#183479,#113144,#113145);
#97425=AXIS2_PLACEMENT_3D('',#183480,#113146,#113147);
#97426=AXIS2_PLACEMENT_3D('',#183482,#113148,#113149);
#97427=AXIS2_PLACEMENT_3D('',#183560,#113152,#113153);
#97428=AXIS2_PLACEMENT_3D('',#183561,#113154,#113155);
#97429=AXIS2_PLACEMENT_3D('',#183782,#113156,#113157);
#97430=AXIS2_PLACEMENT_3D('',#184036,#113158,#113159);
#97431=AXIS2_PLACEMENT_3D('',#184039,#113161,#113162);
#97432=AXIS2_PLACEMENT_3D('',#184054,#113164,#113165);
#97433=AXIS2_PLACEMENT_3D('',#184055,#113166,#113167);
#97434=AXIS2_PLACEMENT_3D('',#184056,#113168,#113169);
#97435=AXIS2_PLACEMENT_3D('',#184057,#113170,#113171);
#97436=AXIS2_PLACEMENT_3D('',#184072,#113172,#113173);
#97437=AXIS2_PLACEMENT_3D('',#184073,#113174,#113175);
#97438=AXIS2_PLACEMENT_3D('',#184074,#113176,#113177);
#97439=AXIS2_PLACEMENT_3D('',#184075,#113178,#113179);
#97440=AXIS2_PLACEMENT_3D('',#184080,#113183,#113184);
#97441=AXIS2_PLACEMENT_3D('',#184165,#113186,#113187);
#97442=AXIS2_PLACEMENT_3D('',#184167,#113188,#113189);
#97443=AXIS2_PLACEMENT_3D('',#184169,#113191,#113192);
#97444=AXIS2_PLACEMENT_3D('',#184188,#113194,#113195);
#97445=AXIS2_PLACEMENT_3D('',#184191,#113197,#113198);
#97446=AXIS2_PLACEMENT_3D('',#184206,#113200,#113201);
#97447=AXIS2_PLACEMENT_3D('',#184223,#113202,#113203);
#97448=AXIS2_PLACEMENT_3D('',#184225,#113204,#113205);
#97449=AXIS2_PLACEMENT_3D('',#184292,#113206,#113207);
#97450=AXIS2_PLACEMENT_3D('',#184367,#113210,#113211);
#97451=AXIS2_PLACEMENT_3D('',#184370,#113213,#113214);
#97452=AXIS2_PLACEMENT_3D('',#184385,#113216,#113217);
#97453=AXIS2_PLACEMENT_3D('',#184386,#113218,#113219);
#97454=AXIS2_PLACEMENT_3D('',#184387,#113220,#113221);
#97455=AXIS2_PLACEMENT_3D('',#184388,#113222,#113223);
#97456=AXIS2_PLACEMENT_3D('',#184389,#113224,#113225);
#97457=AXIS2_PLACEMENT_3D('',#184392,#113227,#113228);
#97458=AXIS2_PLACEMENT_3D('',#184409,#113231,#113232);
#97459=AXIS2_PLACEMENT_3D('',#184410,#113233,#113234);
#97460=AXIS2_PLACEMENT_3D('',#184411,#113235,#113236);
#97461=AXIS2_PLACEMENT_3D('',#184432,#113238,#113239);
#97462=AXIS2_PLACEMENT_3D('',#184434,#113240,#113241);
#97463=AXIS2_PLACEMENT_3D('',#184436,#113243,#113244);
#97464=AXIS2_PLACEMENT_3D('',#184491,#113246,#113247);
#97465=AXIS2_PLACEMENT_3D('',#184494,#113249,#113250);
#97466=AXIS2_PLACEMENT_3D('',#184509,#113252,#113253);
#97467=AXIS2_PLACEMENT_3D('',#184511,#113254,#113255);
#97468=AXIS2_PLACEMENT_3D('',#184512,#113256,#113257);
#97469=AXIS2_PLACEMENT_3D('',#184513,#113258,#113259);
#97470=AXIS2_PLACEMENT_3D('',#184514,#113260,#113261);
#97471=AXIS2_PLACEMENT_3D('',#184515,#113262,#113263);
#97472=AXIS2_PLACEMENT_3D('',#184518,#113265,#113266);
#97473=AXIS2_PLACEMENT_3D('',#184580,#113268,#113269);
#97474=AXIS2_PLACEMENT_3D('',#184581,#113270,#113271);
#97475=AXIS2_PLACEMENT_3D('',#184778,#113272,#113273);
#97476=AXIS2_PLACEMENT_3D('',#185011,#113274,#113275);
#97477=AXIS2_PLACEMENT_3D('',#185014,#113277,#113278);
#97478=AXIS2_PLACEMENT_3D('',#185029,#113280,#113281);
#97479=AXIS2_PLACEMENT_3D('',#185031,#113282,#113283);
#97480=AXIS2_PLACEMENT_3D('',#185032,#113284,#113285);
#97481=AXIS2_PLACEMENT_3D('',#185033,#113286,#113287);
#97482=AXIS2_PLACEMENT_3D('',#185034,#113288,#113289);
#97483=AXIS2_PLACEMENT_3D('',#185035,#113290,#113291);
#97484=AXIS2_PLACEMENT_3D('',#185068,#113293,#113294);
#97485=AXIS2_PLACEMENT_3D('',#185123,#113297,#113298);
#97486=AXIS2_PLACEMENT_3D('',#185124,#113299,#113300);
#97487=AXIS2_PLACEMENT_3D('',#185270,#113301,#113302);
#97488=AXIS2_PLACEMENT_3D('',#185271,#113303,#113304);
#97489=AXIS2_PLACEMENT_3D('',#185273,#113305,#113306);
#97490=AXIS2_PLACEMENT_3D('',#185419,#113308,#113309);
#97491=AXIS2_PLACEMENT_3D('',#185421,#113310,#113311);
#97492=AXIS2_PLACEMENT_3D('',#185423,#113312,#113313);
#97493=AXIS2_PLACEMENT_3D('',#185424,#113314,#113315);
#97494=AXIS2_PLACEMENT_3D('',#185468,#113316,#113317);
#97495=AXIS2_PLACEMENT_3D('',#185471,#113319,#113320);
#97496=AXIS2_PLACEMENT_3D('',#185503,#113321,#113322);
#97497=AXIS2_PLACEMENT_3D('',#185523,#113323,#113324);
#97498=AXIS2_PLACEMENT_3D('',#185524,#113325,#113326);
#97499=AXIS2_PLACEMENT_3D('',#185526,#113328,#113329);
#97500=AXIS2_PLACEMENT_3D('',#185527,#113330,#113331);
#97501=AXIS2_PLACEMENT_3D('',#185528,#113332,#113333);
#97502=AXIS2_PLACEMENT_3D('',#185530,#113334,#113335);
#97503=AXIS2_PLACEMENT_3D('',#185563,#113337,#113338);
#97504=AXIS2_PLACEMENT_3D('',#185629,#113339,#113340);
#97505=AXIS2_PLACEMENT_3D('',#185630,#113341,#113342);
#97506=AXIS2_PLACEMENT_3D('',#185681,#113343,#113344);
#97507=AXIS2_PLACEMENT_3D('',#185682,#113345,#113346);
#97508=AXIS2_PLACEMENT_3D('',#185684,#113348,#113349);
#97509=AXIS2_PLACEMENT_3D('',#185685,#113350,#113351);
#97510=AXIS2_PLACEMENT_3D('',#185686,#113352,#113353);
#97511=AXIS2_PLACEMENT_3D('',#185688,#113354,#113355);
#97512=AXIS2_PLACEMENT_3D('',#185709,#113357,#113358);
#97513=AXIS2_PLACEMENT_3D('',#185732,#113359,#113360);
#97514=AXIS2_PLACEMENT_3D('',#185734,#113361,#113362);
#97515=AXIS2_PLACEMENT_3D('',#185735,#113363,#113364);
#97516=AXIS2_PLACEMENT_3D('',#185813,#113365,#113366);
#97517=AXIS2_PLACEMENT_3D('',#185814,#113367,#113368);
#97518=AXIS2_PLACEMENT_3D('',#185816,#113370,#113371);
#97519=AXIS2_PLACEMENT_3D('',#185817,#113372,#113373);
#97520=AXIS2_PLACEMENT_3D('',#185818,#113374,#113375);
#97521=AXIS2_PLACEMENT_3D('',#185820,#113376,#113377);
#97522=AXIS2_PLACEMENT_3D('',#185895,#113379,#113380);
#97523=AXIS2_PLACEMENT_3D('',#185898,#113382,#113383);
#97524=AXIS2_PLACEMENT_3D('',#185899,#113384,#113385);
#97525=AXIS2_PLACEMENT_3D('',#185902,#113387,#113388);
#97526=AXIS2_PLACEMENT_3D('',#185903,#113389,#113390);
#97527=AXIS2_PLACEMENT_3D('',#185905,#113391,#113392);
#97528=AXIS2_PLACEMENT_3D('',#185907,#113393,#113394);
#97529=AXIS2_PLACEMENT_3D('',#185908,#113395,#113396);
#97530=AXIS2_PLACEMENT_3D('',#185909,#113397,#113398);
#97531=AXIS2_PLACEMENT_3D('',#185912,#113400,#113401);
#97532=AXIS2_PLACEMENT_3D('',#185913,#113402,#113403);
#97533=AXIS2_PLACEMENT_3D('',#185915,#113404,#113405);
#97534=AXIS2_PLACEMENT_3D('',#185916,#113406,#113407);
#97535=AXIS2_PLACEMENT_3D('',#185917,#113408,#113409);
#97536=AXIS2_PLACEMENT_3D('',#185919,#113410,#113411);
#97537=AXIS2_PLACEMENT_3D('',#185920,#113412,#113413);
#97538=AXIS2_PLACEMENT_3D('',#185921,#113414,#113415);
#97539=AXIS2_PLACEMENT_3D('',#185923,#113416,#113417);
#97540=AXIS2_PLACEMENT_3D('',#185924,#113418,#113419);
#97541=AXIS2_PLACEMENT_3D('',#185925,#113420,#113421);
#97542=AXIS2_PLACEMENT_3D('',#185928,#113423,#113424);
#97543=AXIS2_PLACEMENT_3D('',#185929,#113425,#113426);
#97544=AXIS2_PLACEMENT_3D('',#185931,#113427,#113428);
#97545=AXIS2_PLACEMENT_3D('',#185932,#113429,#113430);
#97546=AXIS2_PLACEMENT_3D('',#185933,#113431,#113432);
#97547=AXIS2_PLACEMENT_3D('',#185935,#113433,#113434);
#97548=AXIS2_PLACEMENT_3D('',#185936,#113435,#113436);
#97549=AXIS2_PLACEMENT_3D('',#185937,#113437,#113438);
#97550=AXIS2_PLACEMENT_3D('',#185939,#113439,#113440);
#97551=AXIS2_PLACEMENT_3D('',#185940,#113441,#113442);
#97552=AXIS2_PLACEMENT_3D('',#185941,#113443,#113444);
#97553=AXIS2_PLACEMENT_3D('',#185944,#113446,#113447);
#97554=AXIS2_PLACEMENT_3D('',#185945,#113448,#113449);
#97555=AXIS2_PLACEMENT_3D('',#185947,#113450,#113451);
#97556=AXIS2_PLACEMENT_3D('',#185948,#113452,#113453);
#97557=AXIS2_PLACEMENT_3D('',#185949,#113454,#113455);
#97558=AXIS2_PLACEMENT_3D('',#185951,#113456,#113457);
#97559=AXIS2_PLACEMENT_3D('',#185952,#113458,#113459);
#97560=AXIS2_PLACEMENT_3D('',#185953,#113460,#113461);
#97561=AXIS2_PLACEMENT_3D('',#185955,#113462,#113463);
#97562=AXIS2_PLACEMENT_3D('',#185956,#113464,#113465);
#97563=AXIS2_PLACEMENT_3D('',#185957,#113466,#113467);
#97564=AXIS2_PLACEMENT_3D('',#185960,#113469,#113470);
#97565=AXIS2_PLACEMENT_3D('',#185961,#113471,#113472);
#97566=AXIS2_PLACEMENT_3D('',#185963,#113473,#113474);
#97567=AXIS2_PLACEMENT_3D('',#185965,#113475,#113476);
#97568=AXIS2_PLACEMENT_3D('',#185966,#113477,#113478);
#97569=AXIS2_PLACEMENT_3D('',#185967,#113479,#113480);
#97570=AXIS2_PLACEMENT_3D('',#185970,#113482,#113483);
#97571=AXIS2_PLACEMENT_3D('',#185971,#113484,#113485);
#97572=AXIS2_PLACEMENT_3D('',#185973,#113486,#113487);
#97573=AXIS2_PLACEMENT_3D('',#185975,#113489,#113490);
#97574=AXIS2_PLACEMENT_3D('',#185977,#113491,#113492);
#97575=AXIS2_PLACEMENT_3D('',#185978,#113493,#113494);
#97576=AXIS2_PLACEMENT_3D('',#185979,#113495,#113496);
#97577=AXIS2_PLACEMENT_3D('',#185984,#113499,#113500);
#97578=AXIS2_PLACEMENT_3D('',#185985,#113501,#113502);
#97579=AXIS2_PLACEMENT_3D('',#185989,#113505,#113506);
#97580=AXIS2_PLACEMENT_3D('',#185991,#113507,#113508);
#97581=AXIS2_PLACEMENT_3D('',#185993,#113510,#113511);
#97582=AXIS2_PLACEMENT_3D('',#185995,#113513,#113514);
#97583=AXIS2_PLACEMENT_3D('',#185997,#113515,#113516);
#97584=AXIS2_PLACEMENT_3D('',#185999,#113518,#113519);
#97585=AXIS2_PLACEMENT_3D('',#186001,#113520,#113521);
#97586=AXIS2_PLACEMENT_3D('',#186002,#113522,#113523);
#97587=AXIS2_PLACEMENT_3D('',#186003,#113524,#113525);
#97588=AXIS2_PLACEMENT_3D('',#186005,#113526,#113527);
#97589=AXIS2_PLACEMENT_3D('',#186007,#113529,#113530);
#97590=AXIS2_PLACEMENT_3D('',#186009,#113531,#113532);
#97591=AXIS2_PLACEMENT_3D('',#186010,#113533,#113534);
#97592=AXIS2_PLACEMENT_3D('',#186011,#113535,#113536);
#97593=AXIS2_PLACEMENT_3D('',#186013,#113538,#113539);
#97594=AXIS2_PLACEMENT_3D('',#186015,#113541,#113542);
#97595=AXIS2_PLACEMENT_3D('',#186017,#113543,#113544);
#97596=AXIS2_PLACEMENT_3D('',#186019,#113546,#113547);
#97597=AXIS2_PLACEMENT_3D('',#186021,#113548,#113549);
#97598=AXIS2_PLACEMENT_3D('',#186022,#113550,#113551);
#97599=AXIS2_PLACEMENT_3D('',#186023,#113552,#113553);
#97600=AXIS2_PLACEMENT_3D('',#186025,#113554,#113555);
#97601=AXIS2_PLACEMENT_3D('',#186027,#113557,#113558);
#97602=AXIS2_PLACEMENT_3D('',#186029,#113559,#113560);
#97603=AXIS2_PLACEMENT_3D('',#186030,#113561,#113562);
#97604=AXIS2_PLACEMENT_3D('',#186031,#113563,#113564);
#97605=AXIS2_PLACEMENT_3D('',#186033,#113566,#113567);
#97606=AXIS2_PLACEMENT_3D('',#186036,#113569,#113570);
#97607=AXIS2_PLACEMENT_3D('',#186056,#113571,#113572);
#97608=AXIS2_PLACEMENT_3D('',#186063,#113573,#113574);
#97609=AXIS2_PLACEMENT_3D('',#186064,#113575,#113576);
#97610=AXIS2_PLACEMENT_3D('',#186065,#113577,#113578);
#97611=AXIS2_PLACEMENT_3D('',#186067,#113579,#113580);
#97612=AXIS2_PLACEMENT_3D('',#186069,#113582,#113583);
#97613=AXIS2_PLACEMENT_3D('',#186071,#113584,#113585);
#97614=AXIS2_PLACEMENT_3D('',#186072,#113586,#113587);
#97615=AXIS2_PLACEMENT_3D('',#186073,#113588,#113589);
#97616=AXIS2_PLACEMENT_3D('',#186075,#113590,#113591);
#97617=AXIS2_PLACEMENT_3D('',#186077,#113593,#113594);
#97618=AXIS2_PLACEMENT_3D('',#186079,#113595,#113596);
#97619=AXIS2_PLACEMENT_3D('',#186080,#113597,#113598);
#97620=AXIS2_PLACEMENT_3D('',#186081,#113599,#113600);
#97621=AXIS2_PLACEMENT_3D('',#186083,#113602,#113603);
#97622=AXIS2_PLACEMENT_3D('',#186084,#113604,#113605);
#97623=AXIS2_PLACEMENT_3D('',#186085,#113606,#113607);
#97624=AXIS2_PLACEMENT_3D('',#186087,#113608,#113609);
#97625=AXIS2_PLACEMENT_3D('',#186089,#113611,#113612);
#97626=AXIS2_PLACEMENT_3D('',#186091,#113613,#113614);
#97627=AXIS2_PLACEMENT_3D('',#186092,#113615,#113616);
#97628=AXIS2_PLACEMENT_3D('',#186093,#113617,#113618);
#97629=AXIS2_PLACEMENT_3D('',#186095,#113619,#113620);
#97630=AXIS2_PLACEMENT_3D('',#186097,#113622,#113623);
#97631=AXIS2_PLACEMENT_3D('',#186099,#113624,#113625);
#97632=AXIS2_PLACEMENT_3D('',#186100,#113626,#113627);
#97633=AXIS2_PLACEMENT_3D('',#186101,#113628,#113629);
#97634=AXIS2_PLACEMENT_3D('',#186103,#113630,#113631);
#97635=AXIS2_PLACEMENT_3D('',#186105,#113633,#113634);
#97636=AXIS2_PLACEMENT_3D('',#186107,#113635,#113636);
#97637=AXIS2_PLACEMENT_3D('',#186109,#113638,#113639);
#97638=AXIS2_PLACEMENT_3D('',#186111,#113640,#113641);
#97639=AXIS2_PLACEMENT_3D('',#186113,#113643,#113644);
#97640=AXIS2_PLACEMENT_3D('',#186114,#113645,#113646);
#97641=AXIS2_PLACEMENT_3D('',#186158,#113647,#113648);
#97642=AXIS2_PLACEMENT_3D('',#186233,#113649,#113650);
#97643=AXIS2_PLACEMENT_3D('',#186247,#113651,#113652);
#97644=AXIS2_PLACEMENT_3D('',#186271,#113653,#113654);
#97645=AXIS2_PLACEMENT_3D('',#186272,#113655,#113656);
#97646=AXIS2_PLACEMENT_3D('',#186273,#113657,#113658);
#97647=AXIS2_PLACEMENT_3D('',#186327,#113660,#113661);
#97648=AXIS2_PLACEMENT_3D('',#186329,#113662,#113663);
#97649=AXIS2_PLACEMENT_3D('',#186330,#113664,#113665);
#97650=AXIS2_PLACEMENT_3D('',#186331,#113666,#113667);
#97651=AXIS2_PLACEMENT_3D('',#186337,#113670,#113671);
#97652=AXIS2_PLACEMENT_3D('',#186340,#113673,#113674);
#97653=AXIS2_PLACEMENT_3D('',#186341,#113675,#113676);
#97654=AXIS2_PLACEMENT_3D('',#186347,#113679,#113680);
#97655=AXIS2_PLACEMENT_3D('',#186350,#113682,#113683);
#97656=AXIS2_PLACEMENT_3D('',#186351,#113684,#113685);
#97657=AXIS2_PLACEMENT_3D('',#186354,#113687,#113688);
#97658=AXIS2_PLACEMENT_3D('',#186355,#113689,#113690);
#97659=AXIS2_PLACEMENT_3D('',#186357,#113691,#113692);
#97660=AXIS2_PLACEMENT_3D('',#186360,#113694,#113695);
#97661=AXIS2_PLACEMENT_3D('',#186380,#113696,#113697);
#97662=AXIS2_PLACEMENT_3D('',#186388,#113698,#113699);
#97663=AXIS2_PLACEMENT_3D('',#186390,#113700,#113701);
#97664=AXIS2_PLACEMENT_3D('',#186411,#113703,#113704);
#97665=AXIS2_PLACEMENT_3D('',#186419,#113705,#113706);
#97666=AXIS2_PLACEMENT_3D('',#186421,#113708,#113709);
#97667=AXIS2_PLACEMENT_3D('',#186423,#113711,#113712);
#97668=AXIS2_PLACEMENT_3D('',#186425,#113713,#113714);
#97669=AXIS2_PLACEMENT_3D('',#186446,#113716,#113717);
#97670=AXIS2_PLACEMENT_3D('',#186454,#113718,#113719);
#97671=AXIS2_PLACEMENT_3D('',#186456,#113720,#113721);
#97672=AXIS2_PLACEMENT_3D('',#186477,#113723,#113724);
#97673=AXIS2_PLACEMENT_3D('',#186485,#113725,#113726);
#97674=AXIS2_PLACEMENT_3D('',#186487,#113728,#113729);
#97675=AXIS2_PLACEMENT_3D('',#186490,#113731,#113732);
#97676=AXIS2_PLACEMENT_3D('',#186504,#113733,#113734);
#97677=AXIS2_PLACEMENT_3D('',#186506,#113735,#113736);
#97678=AXIS2_PLACEMENT_3D('',#186507,#113737,#113738);
#97679=AXIS2_PLACEMENT_3D('',#186508,#113739,#113740);
#97680=AXIS2_PLACEMENT_3D('',#186547,#113742,#113743);
#97681=AXIS2_PLACEMENT_3D('',#186550,#113745,#113746);
#97682=AXIS2_PLACEMENT_3D('',#186570,#113747,#113748);
#97683=AXIS2_PLACEMENT_3D('',#186578,#113749,#113750);
#97684=AXIS2_PLACEMENT_3D('',#186580,#113751,#113752);
#97685=AXIS2_PLACEMENT_3D('',#186601,#113754,#113755);
#97686=AXIS2_PLACEMENT_3D('',#186609,#113756,#113757);
#97687=AXIS2_PLACEMENT_3D('',#186611,#113759,#113760);
#97688=AXIS2_PLACEMENT_3D('',#186614,#113762,#113763);
#97689=AXIS2_PLACEMENT_3D('',#186652,#113764,#113765);
#97690=AXIS2_PLACEMENT_3D('',#186654,#113766,#113767);
#97691=AXIS2_PLACEMENT_3D('',#186669,#113769,#113770);
#97692=AXIS2_PLACEMENT_3D('',#186670,#113771,#113772);
#97693=AXIS2_PLACEMENT_3D('',#186671,#113773,#113774);
#97694=AXIS2_PLACEMENT_3D('',#186674,#113776,#113777);
#97695=AXIS2_PLACEMENT_3D('',#186675,#113778,#113779);
#97696=AXIS2_PLACEMENT_3D('',#186678,#113781,#113782);
#97697=AXIS2_PLACEMENT_3D('',#186705,#113783,#113784);
#97698=AXIS2_PLACEMENT_3D('',#186706,#113785,#113786);
#97699=AXIS2_PLACEMENT_3D('',#186709,#113788,#113789);
#97700=AXIS2_PLACEMENT_3D('',#186736,#113790,#113791);
#97701=AXIS2_PLACEMENT_3D('',#186737,#113792,#113793);
#97702=AXIS2_PLACEMENT_3D('',#186739,#113795,#113796);
#97703=AXIS2_PLACEMENT_3D('',#186741,#113798,#113799);
#97704=AXIS2_PLACEMENT_3D('',#186743,#113800,#113801);
#97705=AXIS2_PLACEMENT_3D('',#186745,#113802,#113803);
#97706=AXIS2_PLACEMENT_3D('',#186747,#113805,#113806);
#97707=AXIS2_PLACEMENT_3D('',#186749,#113807,#113808);
#97708=AXIS2_PLACEMENT_3D('',#186770,#113810,#113811);
#97709=AXIS2_PLACEMENT_3D('',#186778,#113812,#113813);
#97710=AXIS2_PLACEMENT_3D('',#186780,#113814,#113815);
#97711=AXIS2_PLACEMENT_3D('',#186801,#113817,#113818);
#97712=AXIS2_PLACEMENT_3D('',#186809,#113819,#113820);
#97713=AXIS2_PLACEMENT_3D('',#186811,#113822,#113823);
#97714=AXIS2_PLACEMENT_3D('',#186814,#113825,#113826);
#97715=AXIS2_PLACEMENT_3D('',#186850,#113827,#113828);
#97716=AXIS2_PLACEMENT_3D('',#186851,#113829,#113830);
#97717=AXIS2_PLACEMENT_3D('',#186853,#113831,#113832);
#97718=AXIS2_PLACEMENT_3D('',#186881,#113834,#113835);
#97719=AXIS2_PLACEMENT_3D('',#186882,#113836,#113837);
#97720=AXIS2_PLACEMENT_3D('',#186885,#113839,#113840);
#97721=AXIS2_PLACEMENT_3D('',#186912,#113841,#113842);
#97722=AXIS2_PLACEMENT_3D('',#186913,#113843,#113844);
#97723=AXIS2_PLACEMENT_3D('',#186915,#113846,#113847);
#97724=AXIS2_PLACEMENT_3D('',#186936,#113849,#113850);
#97725=AXIS2_PLACEMENT_3D('',#186995,#113851,#113852);
#97726=AXIS2_PLACEMENT_3D('',#186997,#113853,#113854);
#97727=AXIS2_PLACEMENT_3D('',#186999,#113855,#113856);
#97728=AXIS2_PLACEMENT_3D('',#187001,#113858,#113859);
#97729=AXIS2_PLACEMENT_3D('',#187004,#113861,#113862);
#97730=AXIS2_PLACEMENT_3D('',#187024,#113863,#113864);
#97731=AXIS2_PLACEMENT_3D('',#187032,#113865,#113866);
#97732=AXIS2_PLACEMENT_3D('',#187034,#113867,#113868);
#97733=AXIS2_PLACEMENT_3D('',#187055,#113870,#113871);
#97734=AXIS2_PLACEMENT_3D('',#187063,#113872,#113873);
#97735=AXIS2_PLACEMENT_3D('',#187065,#113875,#113876);
#97736=AXIS2_PLACEMENT_3D('',#187068,#113878,#113879);
#97737=AXIS2_PLACEMENT_3D('',#187106,#113880,#113881);
#97738=AXIS2_PLACEMENT_3D('',#187109,#113883,#113884);
#97739=AXIS2_PLACEMENT_3D('',#187129,#113885,#113886);
#97740=AXIS2_PLACEMENT_3D('',#187167,#113887,#113888);
#97741=AXIS2_PLACEMENT_3D('',#187170,#113890,#113891);
#97742=AXIS2_PLACEMENT_3D('',#187171,#113892,#113893);
#97743=AXIS2_PLACEMENT_3D('',#187173,#113894,#113895);
#97744=AXIS2_PLACEMENT_3D('',#187194,#113897,#113898);
#97745=AXIS2_PLACEMENT_3D('',#187202,#113899,#113900);
#97746=AXIS2_PLACEMENT_3D('',#187204,#113901,#113902);
#97747=AXIS2_PLACEMENT_3D('',#187225,#113904,#113905);
#97748=AXIS2_PLACEMENT_3D('',#187233,#113906,#113907);
#97749=AXIS2_PLACEMENT_3D('',#187235,#113909,#113910);
#97750=AXIS2_PLACEMENT_3D('',#187262,#113912,#113913);
#97751=AXIS2_PLACEMENT_3D('',#187331,#113914,#113915);
#97752=AXIS2_PLACEMENT_3D('',#187332,#113916,#113917);
#97753=AXIS2_PLACEMENT_3D('',#187334,#113919,#113920);
#97754=AXIS2_PLACEMENT_3D('',#187335,#113921,#113922);
#97755=AXIS2_PLACEMENT_3D('',#187336,#113923,#113924);
#97756=AXIS2_PLACEMENT_3D('',#187339,#113926,#113927);
#97757=AXIS2_PLACEMENT_3D('',#187414,#113928,#113929);
#97758=AXIS2_PLACEMENT_3D('',#187415,#113930,#113931);
#97759=AXIS2_PLACEMENT_3D('',#187417,#113932,#113933);
#97760=AXIS2_PLACEMENT_3D('',#187418,#113934,#113935);
#97761=AXIS2_PLACEMENT_3D('',#187457,#113936,#113937);
#97762=AXIS2_PLACEMENT_3D('',#187458,#113938,#113939);
#97763=AXIS2_PLACEMENT_3D('',#187460,#113941,#113942);
#97764=AXIS2_PLACEMENT_3D('',#187461,#113943,#113944);
#97765=AXIS2_PLACEMENT_3D('',#187462,#113945,#113946);
#97766=AXIS2_PLACEMENT_3D('',#187465,#113948,#113949);
#97767=AXIS2_PLACEMENT_3D('',#187491,#113950,#113951);
#97768=AXIS2_PLACEMENT_3D('',#187533,#113952,#113953);
#97769=AXIS2_PLACEMENT_3D('',#187534,#113954,#113955);
#97770=AXIS2_PLACEMENT_3D('',#187566,#113956,#113957);
#97771=AXIS2_PLACEMENT_3D('',#187619,#113958,#113959);
#97772=AXIS2_PLACEMENT_3D('',#187621,#113961,#113962);
#97773=AXIS2_PLACEMENT_3D('',#187622,#113963,#113964);
#97774=AXIS2_PLACEMENT_3D('',#187623,#113965,#113966);
#97775=AXIS2_PLACEMENT_3D('',#187626,#113968,#113969);
#97776=AXIS2_PLACEMENT_3D('',#187658,#113970,#113971);
#97777=AXIS2_PLACEMENT_3D('',#187689,#113972,#113973);
#97778=AXIS2_PLACEMENT_3D('',#187690,#113974,#113975);
#97779=AXIS2_PLACEMENT_3D('',#187722,#113976,#113977);
#97780=AXIS2_PLACEMENT_3D('',#187745,#113978,#113979);
#97781=AXIS2_PLACEMENT_3D('',#187747,#113981,#113982);
#97782=AXIS2_PLACEMENT_3D('',#187748,#113983,#113984);
#97783=AXIS2_PLACEMENT_3D('',#187749,#113985,#113986);
#97784=AXIS2_PLACEMENT_3D('',#187752,#113988,#113989);
#97785=AXIS2_PLACEMENT_3D('',#187790,#113990,#113991);
#97786=AXIS2_PLACEMENT_3D('',#187847,#113992,#113993);
#97787=AXIS2_PLACEMENT_3D('',#187848,#113994,#113995);
#97788=AXIS2_PLACEMENT_3D('',#187880,#113996,#113997);
#97789=AXIS2_PLACEMENT_3D('',#187927,#113998,#113999);
#97790=AXIS2_PLACEMENT_3D('',#187929,#114001,#114002);
#97791=AXIS2_PLACEMENT_3D('',#187930,#114003,#114004);
#97792=AXIS2_PLACEMENT_3D('',#187931,#114005,#114006);
#97793=AXIS2_PLACEMENT_3D('',#187934,#114008,#114009);
#97794=AXIS2_PLACEMENT_3D('',#188009,#114010,#114011);
#97795=AXIS2_PLACEMENT_3D('',#188010,#114012,#114013);
#97796=AXIS2_PLACEMENT_3D('',#188012,#114014,#114015);
#97797=AXIS2_PLACEMENT_3D('',#188013,#114016,#114017);
#97798=AXIS2_PLACEMENT_3D('',#188100,#114018,#114019);
#97799=AXIS2_PLACEMENT_3D('',#188101,#114020,#114021);
#97800=AXIS2_PLACEMENT_3D('',#188103,#114023,#114024);
#97801=AXIS2_PLACEMENT_3D('',#188104,#114025,#114026);
#97802=AXIS2_PLACEMENT_3D('',#188105,#114027,#114028);
#97803=AXIS2_PLACEMENT_3D('',#188107,#114029,#114030);
#97804=AXIS2_PLACEMENT_3D('',#188128,#114032,#114033);
#97805=AXIS2_PLACEMENT_3D('',#188181,#114034,#114035);
#97806=AXIS2_PLACEMENT_3D('',#188187,#114039,#114040);
#97807=AXIS2_PLACEMENT_3D('',#188188,#114041,#114042);
#97808=AXIS2_PLACEMENT_3D('',#188189,#114043,#114044);
#97809=AXIS2_PLACEMENT_3D('',#188195,#114048,#114049);
#97810=AXIS2_PLACEMENT_3D('',#188196,#114050,#114051);
#97811=AXIS2_PLACEMENT_3D('',#188197,#114052,#114053);
#97812=AXIS2_PLACEMENT_3D('',#188198,#114054,#114055);
#97813=AXIS2_PLACEMENT_3D('',#188199,#114056,#114057);
#97814=AXIS2_PLACEMENT_3D('',#188205,#114061,#114062);
#97815=AXIS2_PLACEMENT_3D('',#188206,#114063,#114064);
#97816=AXIS2_PLACEMENT_3D('',#188226,#114065,#114066);
#97817=AXIS2_PLACEMENT_3D('',#188238,#114067,#114068);
#97818=AXIS2_PLACEMENT_3D('',#188240,#114069,#114070);
#97819=AXIS2_PLACEMENT_3D('',#188241,#114071,#114072);
#97820=AXIS2_PLACEMENT_3D('',#188254,#114073,#114074);
#97821=AXIS2_PLACEMENT_3D('',#188255,#114075,#114076);
#97822=AXIS2_PLACEMENT_3D('',#188258,#114077,#114078);
#97823=AXIS2_PLACEMENT_3D('',#188261,#114081,#114082);
#97824=AXIS2_PLACEMENT_3D('',#188262,#114083,#114084);
#97825=AXIS2_PLACEMENT_3D('',#188276,#114085,#114086);
#97826=AXIS2_PLACEMENT_3D('',#188284,#114087,#114088);
#97827=AXIS2_PLACEMENT_3D('',#188286,#114089,#114090);
#97828=AXIS2_PLACEMENT_3D('',#188287,#114091,#114092);
#97829=AXIS2_PLACEMENT_3D('',#188331,#114093,#114094);
#97830=AXIS2_PLACEMENT_3D('',#188334,#114096,#114097);
#97831=AXIS2_PLACEMENT_3D('',#188415,#114098,#114099);
#97832=AXIS2_PLACEMENT_3D('',#188429,#114100,#114101);
#97833=AXIS2_PLACEMENT_3D('',#188430,#114102,#114103);
#97834=AXIS2_PLACEMENT_3D('',#188474,#114104,#114105);
#97835=AXIS2_PLACEMENT_3D('',#188475,#114106,#114107);
#97836=AXIS2_PLACEMENT_3D('',#188477,#114109,#114110);
#97837=AXIS2_PLACEMENT_3D('',#188478,#114111,#114112);
#97838=AXIS2_PLACEMENT_3D('',#188479,#114113,#114114);
#97839=AXIS2_PLACEMENT_3D('',#188482,#114116,#114117);
#97840=AXIS2_PLACEMENT_3D('',#188514,#114118,#114119);
#97841=AXIS2_PLACEMENT_3D('',#188528,#114120,#114121);
#97842=AXIS2_PLACEMENT_3D('',#188529,#114122,#114123);
#97843=AXIS2_PLACEMENT_3D('',#188604,#114124,#114125);
#97844=AXIS2_PLACEMENT_3D('',#188605,#114126,#114127);
#97845=AXIS2_PLACEMENT_3D('',#188607,#114129,#114130);
#97846=AXIS2_PLACEMENT_3D('',#188608,#114131,#114132);
#97847=AXIS2_PLACEMENT_3D('',#188609,#114133,#114134);
#97848=AXIS2_PLACEMENT_3D('',#188611,#114135,#114136);
#97849=AXIS2_PLACEMENT_3D('',#188690,#114138,#114139);
#97850=AXIS2_PLACEMENT_3D('',#188691,#114140,#114141);
#97851=AXIS2_PLACEMENT_3D('',#188693,#114142,#114143);
#97852=AXIS2_PLACEMENT_3D('',#188694,#114144,#114145);
#97853=AXIS2_PLACEMENT_3D('',#188728,#114146,#114147);
#97854=AXIS2_PLACEMENT_3D('',#188729,#114148,#114149);
#97855=AXIS2_PLACEMENT_3D('',#188731,#114151,#114152);
#97856=AXIS2_PLACEMENT_3D('',#188732,#114153,#114154);
#97857=AXIS2_PLACEMENT_3D('',#188733,#114155,#114156);
#97858=AXIS2_PLACEMENT_3D('',#188736,#114158,#114159);
#97859=AXIS2_PLACEMENT_3D('',#188737,#114160,#114161);
#97860=AXIS2_PLACEMENT_3D('',#188739,#114162,#114163);
#97861=AXIS2_PLACEMENT_3D('',#188741,#114164,#114165);
#97862=AXIS2_PLACEMENT_3D('',#188742,#114166,#114167);
#97863=AXIS2_PLACEMENT_3D('',#188774,#114168,#114169);
#97864=AXIS2_PLACEMENT_3D('',#188818,#114170,#114171);
#97865=AXIS2_PLACEMENT_3D('',#188820,#114173,#114174);
#97866=AXIS2_PLACEMENT_3D('',#188821,#114175,#114176);
#97867=AXIS2_PLACEMENT_3D('',#188822,#114177,#114178);
#97868=AXIS2_PLACEMENT_3D('',#188825,#114180,#114181);
#97869=AXIS2_PLACEMENT_3D('',#188857,#114182,#114183);
#97870=AXIS2_PLACEMENT_3D('',#188901,#114184,#114185);
#97871=AXIS2_PLACEMENT_3D('',#188903,#114186,#114187);
#97872=AXIS2_PLACEMENT_3D('',#188904,#114188,#114189);
#97873=AXIS2_PLACEMENT_3D('',#188924,#114190,#114191);
#97874=AXIS2_PLACEMENT_3D('',#188944,#114192,#114193);
#97875=AXIS2_PLACEMENT_3D('',#188946,#114195,#114196);
#97876=AXIS2_PLACEMENT_3D('',#188947,#114197,#114198);
#97877=AXIS2_PLACEMENT_3D('',#188948,#114199,#114200);
#97878=AXIS2_PLACEMENT_3D('',#188951,#114202,#114203);
#97879=AXIS2_PLACEMENT_3D('',#188983,#114204,#114205);
#97880=AXIS2_PLACEMENT_3D('',#189034,#114206,#114207);
#97881=AXIS2_PLACEMENT_3D('',#189035,#114208,#114209);
#97882=AXIS2_PLACEMENT_3D('',#189068,#114210,#114211);
#97883=AXIS2_PLACEMENT_3D('',#189069,#114212,#114213);
#97884=AXIS2_PLACEMENT_3D('',#189116,#114214,#114215);
#97885=AXIS2_PLACEMENT_3D('',#189118,#114217,#114218);
#97886=AXIS2_PLACEMENT_3D('',#189119,#114219,#114220);
#97887=AXIS2_PLACEMENT_3D('',#189120,#114221,#114222);
#97888=AXIS2_PLACEMENT_3D('',#189123,#114224,#114225);
#97889=AXIS2_PLACEMENT_3D('',#189164,#114226,#114227);
#97890=AXIS2_PLACEMENT_3D('',#189165,#114228,#114229);
#97891=AXIS2_PLACEMENT_3D('',#189167,#114230,#114231);
#97892=AXIS2_PLACEMENT_3D('',#189168,#114232,#114233);
#97893=AXIS2_PLACEMENT_3D('',#189170,#114235,#114236);
#97894=AXIS2_PLACEMENT_3D('',#189176,#114240,#114241);
#97895=AXIS2_PLACEMENT_3D('',#189177,#114242,#114243);
#97896=AXIS2_PLACEMENT_3D('',#189178,#114244,#114245);
#97897=AXIS2_PLACEMENT_3D('',#189184,#114249,#114250);
#97898=AXIS2_PLACEMENT_3D('',#189185,#114251,#114252);
#97899=AXIS2_PLACEMENT_3D('',#189186,#114253,#114254);
#97900=AXIS2_PLACEMENT_3D('',#189187,#114255,#114256);
#97901=AXIS2_PLACEMENT_3D('',#189188,#114257,#114258);
#97902=AXIS2_PLACEMENT_3D('',#189194,#114262,#114263);
#97903=AXIS2_PLACEMENT_3D('',#189195,#114264,#114265);
#97904=AXIS2_PLACEMENT_3D('',#189209,#114266,#114267);
#97905=AXIS2_PLACEMENT_3D('',#189223,#114268,#114269);
#97906=AXIS2_PLACEMENT_3D('',#189224,#114270,#114271);
#97907=AXIS2_PLACEMENT_3D('',#189225,#114272,#114273);
#97908=AXIS2_PLACEMENT_3D('',#189226,#114274,#114275);
#97909=AXIS2_PLACEMENT_3D('',#189239,#114276,#114277);
#97910=AXIS2_PLACEMENT_3D('',#189252,#114278,#114279);
#97911=AXIS2_PLACEMENT_3D('',#189253,#114280,#114281);
#97912=AXIS2_PLACEMENT_3D('',#189254,#114282,#114283);
#97913=AXIS2_PLACEMENT_3D('',#189267,#114284,#114285);
#97914=AXIS2_PLACEMENT_3D('',#189280,#114286,#114287);
#97915=AXIS2_PLACEMENT_3D('',#189281,#114288,#114289);
#97916=AXIS2_PLACEMENT_3D('',#189282,#114290,#114291);
#97917=AXIS2_PLACEMENT_3D('',#189283,#114292,#114293);
#97918=AXIS2_PLACEMENT_3D('',#189284,#114294,#114295);
#97919=AXIS2_PLACEMENT_3D('',#189285,#114296,#114297);
#97920=AXIS2_PLACEMENT_3D('',#189286,#114298,#114299);
#97921=AXIS2_PLACEMENT_3D('',#189287,#114300,#114301);
#97922=AXIS2_PLACEMENT_3D('',#189288,#114302,#114303);
#97923=AXIS2_PLACEMENT_3D('',#189289,#114304,#114305);
#97924=AXIS2_PLACEMENT_3D('',#189290,#114306,#114307);
#97925=AXIS2_PLACEMENT_3D('',#189291,#114308,#114309);
#97926=AXIS2_PLACEMENT_3D('',#189292,#114310,#114311);
#97927=AXIS2_PLACEMENT_3D('',#189293,#114312,#114313);
#97928=AXIS2_PLACEMENT_3D('',#189295,#114315,#114316);
#97929=AXIS2_PLACEMENT_3D('',#189297,#114318,#114319);
#97930=AXIS2_PLACEMENT_3D('',#189298,#114320,#114321);
#97931=AXIS2_PLACEMENT_3D('',#189299,#114322,#114323);
#97932=AXIS2_PLACEMENT_3D('',#189300,#114324,#114325);
#97933=AXIS2_PLACEMENT_3D('',#189301,#114326,#114327);
#97934=AXIS2_PLACEMENT_3D('',#189302,#114328,#114329);
#97935=AXIS2_PLACEMENT_3D('',#189303,#114330,#114331);
#97936=AXIS2_PLACEMENT_3D('',#189304,#114332,#114333);
#97937=AXIS2_PLACEMENT_3D('',#189305,#114334,#114335);
#97938=AXIS2_PLACEMENT_3D('',#189306,#114336,#114337);
#97939=AXIS2_PLACEMENT_3D('',#189307,#114338,#114339);
#97940=AXIS2_PLACEMENT_3D('',#189308,#114340,#114341);
#97941=AXIS2_PLACEMENT_3D('',#189309,#114342,#114343);
#97942=AXIS2_PLACEMENT_3D('',#189310,#114344,#114345);
#97943=AXIS2_PLACEMENT_3D('',#189323,#114348,#114349);
#97944=AXIS2_PLACEMENT_3D('',#189333,#114351,#114352);
#97945=AXIS2_PLACEMENT_3D('',#189343,#114354,#114355);
#97946=AXIS2_PLACEMENT_3D('',#189353,#114357,#114358);
#97947=AXIS2_PLACEMENT_3D('',#189363,#114360,#114361);
#97948=AXIS2_PLACEMENT_3D('',#189370,#114362,#114363);
#97949=AXIS2_PLACEMENT_3D('',#189373,#114365,#114366);
#97950=AXIS2_PLACEMENT_3D('',#189374,#114367,#114368);
#97951=AXIS2_PLACEMENT_3D('',#189375,#114369,#114370);
#97952=AXIS2_PLACEMENT_3D('',#189376,#114371,#114372);
#97953=AXIS2_PLACEMENT_3D('',#189377,#114373,#114374);
#97954=AXIS2_PLACEMENT_3D('',#189378,#114375,#114376);
#97955=AXIS2_PLACEMENT_3D('',#189379,#114377,#114378);
#97956=AXIS2_PLACEMENT_3D('',#189380,#114379,#114380);
#97957=AXIS2_PLACEMENT_3D('',#189381,#114381,#114382);
#97958=AXIS2_PLACEMENT_3D('',#189382,#114383,#114384);
#97959=AXIS2_PLACEMENT_3D('',#189383,#114385,#114386);
#97960=AXIS2_PLACEMENT_3D('',#189384,#114387,#114388);
#97961=AXIS2_PLACEMENT_3D('',#189385,#114389,#114390);
#97962=AXIS2_PLACEMENT_3D('',#189387,#114391,#114392);
#97963=AXIS2_PLACEMENT_3D('',#189389,#114393,#114394);
#97964=AXIS2_PLACEMENT_3D('',#189391,#114395,#114396);
#97965=AXIS2_PLACEMENT_3D('',#189392,#114397,#114398);
#97966=AXIS2_PLACEMENT_3D('',#189393,#114399,#114400);
#97967=AXIS2_PLACEMENT_3D('',#189395,#114401,#114402);
#97968=AXIS2_PLACEMENT_3D('',#189396,#114403,#114404);
#97969=AXIS2_PLACEMENT_3D('',#189397,#114405,#114406);
#97970=AXIS2_PLACEMENT_3D('',#189399,#114408,#114409);
#97971=AXIS2_PLACEMENT_3D('',#189401,#114410,#114411);
#97972=AXIS2_PLACEMENT_3D('',#189404,#114413,#114414);
#97973=AXIS2_PLACEMENT_3D('',#189405,#114415,#114416);
#97974=AXIS2_PLACEMENT_3D('',#189406,#114417,#114418);
#97975=AXIS2_PLACEMENT_3D('',#189408,#114419,#114420);
#97976=AXIS2_PLACEMENT_3D('',#189410,#114422,#114423);
#97977=AXIS2_PLACEMENT_3D('',#189412,#114424,#114425);
#97978=AXIS2_PLACEMENT_3D('',#189413,#114426,#114427);
#97979=AXIS2_PLACEMENT_3D('',#189415,#114428,#114429);
#97980=AXIS2_PLACEMENT_3D('',#189417,#114431,#114432);
#97981=AXIS2_PLACEMENT_3D('',#189438,#114433,#114434);
#97982=AXIS2_PLACEMENT_3D('',#189447,#114435,#114436);
#97983=AXIS2_PLACEMENT_3D('',#189454,#114437,#114438);
#97984=AXIS2_PLACEMENT_3D('',#189456,#114439,#114440);
#97985=AXIS2_PLACEMENT_3D('',#189458,#114441,#114442);
#97986=AXIS2_PLACEMENT_3D('',#189460,#114443,#114444);
#97987=AXIS2_PLACEMENT_3D('',#189461,#114445,#114446);
#97988=AXIS2_PLACEMENT_3D('',#189494,#114447,#114448);
#97989=AXIS2_PLACEMENT_3D('',#189528,#114449,#114450);
#97990=AXIS2_PLACEMENT_3D('',#189553,#114451,#114452);
#97991=AXIS2_PLACEMENT_3D('',#189577,#114453,#114454);
#97992=AXIS2_PLACEMENT_3D('',#189579,#114455,#114456);
#97993=AXIS2_PLACEMENT_3D('',#189580,#114457,#114458);
#97994=AXIS2_PLACEMENT_3D('',#189613,#114459,#114460);
#97995=AXIS2_PLACEMENT_3D('',#189676,#114461,#114462);
#97996=AXIS2_PLACEMENT_3D('',#189679,#114463,#114464);
#97997=AXIS2_PLACEMENT_3D('',#189680,#114465,#114466);
#97998=AXIS2_PLACEMENT_3D('',#189681,#114467,#114468);
#97999=AXIS2_PLACEMENT_3D('',#189702,#114469,#114470);
#98000=AXIS2_PLACEMENT_3D('',#189716,#114471,#114472);
#98001=AXIS2_PLACEMENT_3D('',#189719,#114473,#114474);
#98002=AXIS2_PLACEMENT_3D('',#189720,#114475,#114476);
#98003=AXIS2_PLACEMENT_3D('',#189721,#114477,#114478);
#98004=AXIS2_PLACEMENT_3D('',#189754,#114479,#114480);
#98005=AXIS2_PLACEMENT_3D('',#189814,#114481,#114482);
#98006=AXIS2_PLACEMENT_3D('',#189817,#114483,#114484);
#98007=AXIS2_PLACEMENT_3D('',#189818,#114485,#114486);
#98008=AXIS2_PLACEMENT_3D('',#189819,#114487,#114488);
#98009=AXIS2_PLACEMENT_3D('',#189834,#114489,#114490);
#98010=AXIS2_PLACEMENT_3D('',#189857,#114491,#114492);
#98011=AXIS2_PLACEMENT_3D('',#189885,#114493,#114494);
#98012=AXIS2_PLACEMENT_3D('',#189887,#114495,#114496);
#98013=AXIS2_PLACEMENT_3D('',#189919,#114497,#114498);
#98014=AXIS2_PLACEMENT_3D('',#189920,#114499,#114500);
#98015=AXIS2_PLACEMENT_3D('',#189959,#114501,#114502);
#98016=AXIS2_PLACEMENT_3D('',#189974,#114503,#114504);
#98017=AXIS2_PLACEMENT_3D('',#190044,#114505,#114506);
#98018=AXIS2_PLACEMENT_3D('',#190082,#114507,#114508);
#98019=AXIS2_PLACEMENT_3D('',#190135,#114509,#114510);
#98020=AXIS2_PLACEMENT_3D('',#190180,#114511,#114512);
#98021=AXIS2_PLACEMENT_3D('',#190243,#114513,#114514);
#98022=AXIS2_PLACEMENT_3D('',#190245,#114515,#114516);
#98023=AXIS2_PLACEMENT_3D('',#190246,#114517,#114518);
#98024=AXIS2_PLACEMENT_3D('',#190261,#114519,#114520);
#98025=AXIS2_PLACEMENT_3D('',#190299,#114521,#114522);
#98026=AXIS2_PLACEMENT_3D('',#190334,#114523,#114524);
#98027=AXIS2_PLACEMENT_3D('',#190351,#114525,#114526);
#98028=AXIS2_PLACEMENT_3D('',#190354,#114527,#114528);
#98029=AXIS2_PLACEMENT_3D('',#190355,#114529,#114530);
#98030=AXIS2_PLACEMENT_3D('',#190356,#114531,#114532);
#98031=AXIS2_PLACEMENT_3D('',#190357,#114533,#114534);
#98032=AXIS2_PLACEMENT_3D('',#190359,#114535,#114536);
#98033=AXIS2_PLACEMENT_3D('',#190360,#114537,#114538);
#98034=AXIS2_PLACEMENT_3D('',#190361,#114539,#114540);
#98035=AXIS2_PLACEMENT_3D('',#190364,#114541,#114542);
#98036=AXIS2_PLACEMENT_3D('',#190365,#114543,#114544);
#98037=AXIS2_PLACEMENT_3D('',#190366,#114545,#114546);
#98038=AXIS2_PLACEMENT_3D('',#190381,#114547,#114548);
#98039=AXIS2_PLACEMENT_3D('',#190390,#114549,#114550);
#98040=AXIS2_PLACEMENT_3D('',#190391,#114551,#114552);
#98041=AXIS2_PLACEMENT_3D('',#190392,#114553,#114554);
#98042=AXIS2_PLACEMENT_3D('',#190393,#114555,#114556);
#98043=AXIS2_PLACEMENT_3D('',#190396,#114557,#114558);
#98044=AXIS2_PLACEMENT_3D('',#190398,#114559,#114560);
#98045=AXIS2_PLACEMENT_3D('',#190400,#114561,#114562);
#98046=AXIS2_PLACEMENT_3D('',#190401,#114563,#114564);
#98047=AXIS2_PLACEMENT_3D('',#190402,#114565,#114566);
#98048=AXIS2_PLACEMENT_3D('',#190405,#114567,#114568);
#98049=AXIS2_PLACEMENT_3D('',#190406,#114569,#114570);
#98050=AXIS2_PLACEMENT_3D('',#190407,#114571,#114572);
#98051=AXIS2_PLACEMENT_3D('',#190408,#114573,#114574);
#98052=AXIS2_PLACEMENT_3D('',#190411,#114575,#114576);
#98053=AXIS2_PLACEMENT_3D('',#190412,#114577,#114578);
#98054=AXIS2_PLACEMENT_3D('',#190413,#114579,#114580);
#98055=AXIS2_PLACEMENT_3D('',#190414,#114581,#114582);
#98056=AXIS2_PLACEMENT_3D('',#190417,#114583,#114584);
#98057=AXIS2_PLACEMENT_3D('',#190418,#114585,#114586);
#98058=AXIS2_PLACEMENT_3D('',#190419,#114587,#114588);
#98059=AXIS2_PLACEMENT_3D('',#190420,#114589,#114590);
#98060=AXIS2_PLACEMENT_3D('',#190423,#114591,#114592);
#98061=AXIS2_PLACEMENT_3D('',#190424,#114593,#114594);
#98062=AXIS2_PLACEMENT_3D('',#190425,#114595,#114596);
#98063=AXIS2_PLACEMENT_3D('',#190426,#114597,#114598);
#98064=AXIS2_PLACEMENT_3D('',#190429,#114599,#114600);
#98065=AXIS2_PLACEMENT_3D('',#190430,#114601,#114602);
#98066=AXIS2_PLACEMENT_3D('',#190431,#114603,#114604);
#98067=AXIS2_PLACEMENT_3D('',#190432,#114605,#114606);
#98068=AXIS2_PLACEMENT_3D('',#190435,#114607,#114608);
#98069=AXIS2_PLACEMENT_3D('',#190436,#114609,#114610);
#98070=AXIS2_PLACEMENT_3D('',#190437,#114611,#114612);
#98071=AXIS2_PLACEMENT_3D('',#190451,#114613,#114614);
#98072=AXIS2_PLACEMENT_3D('',#190453,#114615,#114616);
#98073=AXIS2_PLACEMENT_3D('',#190454,#114617,#114618);
#98074=AXIS2_PLACEMENT_3D('',#190469,#114619,#114620);
#98075=AXIS2_PLACEMENT_3D('',#190470,#114621,#114622);
#98076=AXIS2_PLACEMENT_3D('',#190525,#114623,#114624);
#98077=AXIS2_PLACEMENT_3D('',#190576,#114625,#114626);
#98078=AXIS2_PLACEMENT_3D('',#190637,#114627,#114628);
#98079=AXIS2_PLACEMENT_3D('',#190638,#114629,#114630);
#98080=AXIS2_PLACEMENT_3D('',#190639,#114631,#114632);
#98081=AXIS2_PLACEMENT_3D('',#190654,#114633,#114634);
#98082=AXIS2_PLACEMENT_3D('',#190655,#114635,#114636);
#98083=AXIS2_PLACEMENT_3D('',#190656,#114637,#114638);
#98084=AXIS2_PLACEMENT_3D('',#190671,#114639,#114640);
#98085=AXIS2_PLACEMENT_3D('',#190709,#114641,#114642);
#98086=AXIS2_PLACEMENT_3D('',#190759,#114643,#114644);
#98087=AXIS2_PLACEMENT_3D('',#190802,#114645,#114646);
#98088=AXIS2_PLACEMENT_3D('',#190875,#114647,#114648);
#98089=AXIS2_PLACEMENT_3D('',#190968,#114649,#114650);
#98090=AXIS2_PLACEMENT_3D('',#191012,#114651,#114652);
#98091=AXIS2_PLACEMENT_3D('',#191013,#114653,#114654);
#98092=AXIS2_PLACEMENT_3D('',#191014,#114655,#114656);
#98093=AXIS2_PLACEMENT_3D('',#191071,#114657,#114658);
#98094=AXIS2_PLACEMENT_3D('',#191092,#114659,#114660);
#98095=AXIS2_PLACEMENT_3D('',#191111,#114661,#114662);
#98096=AXIS2_PLACEMENT_3D('',#191114,#114663,#114664);
#98097=AXIS2_PLACEMENT_3D('',#191115,#114665,#114666);
#98098=AXIS2_PLACEMENT_3D('',#191116,#114667,#114668);
#98099=AXIS2_PLACEMENT_3D('',#191143,#114669,#114670);
#98100=AXIS2_PLACEMENT_3D('',#191216,#114671,#114672);
#98101=AXIS2_PLACEMENT_3D('',#191274,#114673,#114674);
#98102=AXIS2_PLACEMENT_3D('',#191321,#114675,#114676);
#98103=AXIS2_PLACEMENT_3D('',#191362,#114677,#114678);
#98104=AXIS2_PLACEMENT_3D('',#191363,#114679,#114680);
#98105=AXIS2_PLACEMENT_3D('',#191364,#114681,#114682);
#98106=AXIS2_PLACEMENT_3D('',#191379,#114683,#114684);
#98107=AXIS2_PLACEMENT_3D('',#191551,#114685,#114686);
#98108=AXIS2_PLACEMENT_3D('',#191552,#114687,#114688);
#98109=AXIS2_PLACEMENT_3D('',#191553,#114689,#114690);
#98110=AXIS2_PLACEMENT_3D('',#191636,#114691,#114692);
#98111=AXIS2_PLACEMENT_3D('',#191640,#114694,#114695);
#98112=AXIS2_PLACEMENT_3D('',#191652,#114697,#114698);
#98113=AXIS2_PLACEMENT_3D('',#191654,#114699,#114700);
#98114=AXIS2_PLACEMENT_3D('',#191655,#114701,#114702);
#98115=AXIS2_PLACEMENT_3D('',#191656,#114703,#114704);
#98116=AXIS2_PLACEMENT_3D('',#191658,#114705,#114706);
#98117=AXIS2_PLACEMENT_3D('',#191660,#114707,#114708);
#98118=AXIS2_PLACEMENT_3D('',#191661,#114709,#114710);
#98119=AXIS2_PLACEMENT_3D('',#191662,#114711,#114712);
#98120=AXIS2_PLACEMENT_3D('',#191674,#114713,#114714);
#98121=AXIS2_PLACEMENT_3D('',#191675,#114715,#114716);
#98122=AXIS2_PLACEMENT_3D('',#191676,#114717,#114718);
#98123=AXIS2_PLACEMENT_3D('',#191677,#114719,#114720);
#98124=AXIS2_PLACEMENT_3D('',#191680,#114723,#114724);
#98125=AXIS2_PLACEMENT_3D('',#191684,#114726,#114727);
#98126=AXIS2_PLACEMENT_3D('',#191696,#114729,#114730);
#98127=AXIS2_PLACEMENT_3D('',#191698,#114731,#114732);
#98128=AXIS2_PLACEMENT_3D('',#191699,#114733,#114734);
#98129=AXIS2_PLACEMENT_3D('',#191700,#114735,#114736);
#98130=AXIS2_PLACEMENT_3D('',#191703,#114737,#114738);
#98131=AXIS2_PLACEMENT_3D('',#191704,#114739,#114740);
#98132=AXIS2_PLACEMENT_3D('',#191705,#114741,#114742);
#98133=AXIS2_PLACEMENT_3D('',#191717,#114743,#114744);
#98134=AXIS2_PLACEMENT_3D('',#191718,#114745,#114746);
#98135=AXIS2_PLACEMENT_3D('',#191719,#114747,#114748);
#98136=AXIS2_PLACEMENT_3D('',#191720,#114749,#114750);
#98137=AXIS2_PLACEMENT_3D('',#191723,#114753,#114754);
#98138=AXIS2_PLACEMENT_3D('',#191727,#114756,#114757);
#98139=AXIS2_PLACEMENT_3D('',#191740,#114759,#114760);
#98140=AXIS2_PLACEMENT_3D('',#191741,#114761,#114762);
#98141=AXIS2_PLACEMENT_3D('',#191742,#114763,#114764);
#98142=AXIS2_PLACEMENT_3D('',#191743,#114765,#114766);
#98143=AXIS2_PLACEMENT_3D('',#191746,#114767,#114768);
#98144=AXIS2_PLACEMENT_3D('',#191747,#114769,#114770);
#98145=AXIS2_PLACEMENT_3D('',#191748,#114771,#114772);
#98146=AXIS2_PLACEMENT_3D('',#191759,#114773,#114774);
#98147=AXIS2_PLACEMENT_3D('',#191761,#114775,#114776);
#98148=AXIS2_PLACEMENT_3D('',#191762,#114777,#114778);
#98149=AXIS2_PLACEMENT_3D('',#191763,#114779,#114780);
#98150=AXIS2_PLACEMENT_3D('',#191766,#114783,#114784);
#98151=AXIS2_PLACEMENT_3D('',#191770,#114786,#114787);
#98152=AXIS2_PLACEMENT_3D('',#191783,#114789,#114790);
#98153=AXIS2_PLACEMENT_3D('',#191784,#114791,#114792);
#98154=AXIS2_PLACEMENT_3D('',#191785,#114793,#114794);
#98155=AXIS2_PLACEMENT_3D('',#191786,#114795,#114796);
#98156=AXIS2_PLACEMENT_3D('',#191789,#114797,#114798);
#98157=AXIS2_PLACEMENT_3D('',#191790,#114799,#114800);
#98158=AXIS2_PLACEMENT_3D('',#191791,#114801,#114802);
#98159=AXIS2_PLACEMENT_3D('',#191802,#114803,#114804);
#98160=AXIS2_PLACEMENT_3D('',#191804,#114805,#114806);
#98161=AXIS2_PLACEMENT_3D('',#191805,#114807,#114808);
#98162=AXIS2_PLACEMENT_3D('',#191806,#114809,#114810);
#98163=AXIS2_PLACEMENT_3D('',#191809,#114813,#114814);
#98164=AXIS2_PLACEMENT_3D('',#191812,#114817,#114818);
#98165=AXIS2_PLACEMENT_3D('',#191815,#114821,#114822);
#98166=AXIS2_PLACEMENT_3D('',#191818,#114825,#114826);
#98167=AXIS2_PLACEMENT_3D('',#191821,#114829,#114830);
#98168=AXIS2_PLACEMENT_3D('',#191824,#114833,#114834);
#98169=AXIS2_PLACEMENT_3D('',#191827,#114837,#114838);
#98170=AXIS2_PLACEMENT_3D('',#191830,#114841,#114842);
#98171=AXIS2_PLACEMENT_3D('',#191833,#114845,#114846);
#98172=AXIS2_PLACEMENT_3D('',#191836,#114847,#114848);
#98173=AXIS2_PLACEMENT_3D('',#191838,#114849,#114850);
#98174=AXIS2_PLACEMENT_3D('',#191840,#114851,#114852);
#98175=AXIS2_PLACEMENT_3D('',#191841,#114853,#114854);
#98176=AXIS2_PLACEMENT_3D('',#191842,#114855,#114856);
#98177=AXIS2_PLACEMENT_3D('',#191845,#114857,#114858);
#98178=AXIS2_PLACEMENT_3D('',#191848,#114861,#114862);
#98179=AXIS2_PLACEMENT_3D('',#191851,#114863,#114864);
#98180=AXIS2_PLACEMENT_3D('',#191852,#114865,#114866);
#98181=AXIS2_PLACEMENT_3D('',#191853,#114867,#114868);
#98182=AXIS2_PLACEMENT_3D('',#191854,#114869,#114870);
#98183=AXIS2_PLACEMENT_3D('',#191857,#114871,#114872);
#98184=AXIS2_PLACEMENT_3D('',#191858,#114873,#114874);
#98185=AXIS2_PLACEMENT_3D('',#191859,#114875,#114876);
#98186=AXIS2_PLACEMENT_3D('',#191860,#114877,#114878);
#98187=AXIS2_PLACEMENT_3D('',#191863,#114879,#114880);
#98188=AXIS2_PLACEMENT_3D('',#191864,#114881,#114882);
#98189=AXIS2_PLACEMENT_3D('',#191865,#114883,#114884);
#98190=AXIS2_PLACEMENT_3D('',#191866,#114885,#114886);
#98191=AXIS2_PLACEMENT_3D('',#191869,#114887,#114888);
#98192=AXIS2_PLACEMENT_3D('',#191872,#114891,#114892);
#98193=AXIS2_PLACEMENT_3D('',#191875,#114893,#114894);
#98194=AXIS2_PLACEMENT_3D('',#191876,#114895,#114896);
#98195=AXIS2_PLACEMENT_3D('',#191877,#114897,#114898);
#98196=AXIS2_PLACEMENT_3D('',#191878,#114899,#114900);
#98197=AXIS2_PLACEMENT_3D('',#191881,#114901,#114902);
#98198=AXIS2_PLACEMENT_3D('',#191882,#114903,#114904);
#98199=AXIS2_PLACEMENT_3D('',#191883,#114905,#114906);
#98200=AXIS2_PLACEMENT_3D('',#191884,#114907,#114908);
#98201=AXIS2_PLACEMENT_3D('',#191887,#114909,#114910);
#98202=AXIS2_PLACEMENT_3D('',#191888,#114911,#114912);
#98203=AXIS2_PLACEMENT_3D('',#191889,#114913,#114914);
#98204=AXIS2_PLACEMENT_3D('',#191890,#114915,#114916);
#98205=AXIS2_PLACEMENT_3D('',#191893,#114919,#114920);
#98206=AXIS2_PLACEMENT_3D('',#191896,#114921,#114922);
#98207=AXIS2_PLACEMENT_3D('',#191898,#114923,#114924);
#98208=AXIS2_PLACEMENT_3D('',#191900,#114925,#114926);
#98209=AXIS2_PLACEMENT_3D('',#191901,#114927,#114928);
#98210=AXIS2_PLACEMENT_3D('',#191902,#114929,#114930);
#98211=AXIS2_PLACEMENT_3D('',#191905,#114931,#114932);
#98212=AXIS2_PLACEMENT_3D('',#191908,#114935,#114936);
#98213=AXIS2_PLACEMENT_3D('',#191911,#114937,#114938);
#98214=AXIS2_PLACEMENT_3D('',#191912,#114939,#114940);
#98215=AXIS2_PLACEMENT_3D('',#191913,#114941,#114942);
#98216=AXIS2_PLACEMENT_3D('',#191914,#114943,#114944);
#98217=AXIS2_PLACEMENT_3D('',#191917,#114945,#114946);
#98218=AXIS2_PLACEMENT_3D('',#191918,#114947,#114948);
#98219=AXIS2_PLACEMENT_3D('',#191919,#114949,#114950);
#98220=AXIS2_PLACEMENT_3D('',#191920,#114951,#114952);
#98221=AXIS2_PLACEMENT_3D('',#191923,#114953,#114954);
#98222=AXIS2_PLACEMENT_3D('',#191924,#114955,#114956);
#98223=AXIS2_PLACEMENT_3D('',#191925,#114957,#114958);
#98224=AXIS2_PLACEMENT_3D('',#191926,#114959,#114960);
#98225=AXIS2_PLACEMENT_3D('',#191929,#114961,#114962);
#98226=AXIS2_PLACEMENT_3D('',#191932,#114965,#114966);
#98227=AXIS2_PLACEMENT_3D('',#191935,#114967,#114968);
#98228=AXIS2_PLACEMENT_3D('',#191938,#114971,#114972);
#98229=AXIS2_PLACEMENT_3D('',#191939,#114973,#114974);
#98230=AXIS2_PLACEMENT_3D('',#191940,#114975,#114976);
#98231=AXIS2_PLACEMENT_3D('',#191941,#114977,#114978);
#98232=AXIS2_PLACEMENT_3D('',#191944,#114979,#114980);
#98233=AXIS2_PLACEMENT_3D('',#191946,#114981,#114982);
#98234=AXIS2_PLACEMENT_3D('',#191948,#114983,#114984);
#98235=AXIS2_PLACEMENT_3D('',#191949,#114985,#114986);
#98236=AXIS2_PLACEMENT_3D('',#191950,#114987,#114988);
#98237=AXIS2_PLACEMENT_3D('',#191953,#114989,#114990);
#98238=AXIS2_PLACEMENT_3D('',#191956,#114993,#114994);
#98239=AXIS2_PLACEMENT_3D('',#191959,#114995,#114996);
#98240=AXIS2_PLACEMENT_3D('',#191960,#114997,#114998);
#98241=AXIS2_PLACEMENT_3D('',#191961,#114999,#115000);
#98242=AXIS2_PLACEMENT_3D('',#191962,#115001,#115002);
#98243=AXIS2_PLACEMENT_3D('',#191965,#115003,#115004);
#98244=AXIS2_PLACEMENT_3D('',#191966,#115005,#115006);
#98245=AXIS2_PLACEMENT_3D('',#191967,#115007,#115008);
#98246=AXIS2_PLACEMENT_3D('',#191968,#115009,#115010);
#98247=AXIS2_PLACEMENT_3D('',#191971,#115011,#115012);
#98248=AXIS2_PLACEMENT_3D('',#191972,#115013,#115014);
#98249=AXIS2_PLACEMENT_3D('',#191973,#115015,#115016);
#98250=AXIS2_PLACEMENT_3D('',#191974,#115017,#115018);
#98251=AXIS2_PLACEMENT_3D('',#191977,#115019,#115020);
#98252=AXIS2_PLACEMENT_3D('',#191980,#115023,#115024);
#98253=AXIS2_PLACEMENT_3D('',#191983,#115025,#115026);
#98254=AXIS2_PLACEMENT_3D('',#191986,#115029,#115030);
#98255=AXIS2_PLACEMENT_3D('',#191987,#115031,#115032);
#98256=AXIS2_PLACEMENT_3D('',#191988,#115033,#115034);
#98257=AXIS2_PLACEMENT_3D('',#191989,#115035,#115036);
#98258=AXIS2_PLACEMENT_3D('',#191992,#115037,#115038);
#98259=AXIS2_PLACEMENT_3D('',#191994,#115039,#115040);
#98260=AXIS2_PLACEMENT_3D('',#191996,#115041,#115042);
#98261=AXIS2_PLACEMENT_3D('',#191997,#115043,#115044);
#98262=AXIS2_PLACEMENT_3D('',#191998,#115045,#115046);
#98263=AXIS2_PLACEMENT_3D('',#192001,#115047,#115048);
#98264=AXIS2_PLACEMENT_3D('',#192004,#115051,#115052);
#98265=AXIS2_PLACEMENT_3D('',#192007,#115053,#115054);
#98266=AXIS2_PLACEMENT_3D('',#192010,#115057,#115058);
#98267=AXIS2_PLACEMENT_3D('',#192013,#115059,#115060);
#98268=AXIS2_PLACEMENT_3D('',#192014,#115061,#115062);
#98269=AXIS2_PLACEMENT_3D('',#192015,#115063,#115064);
#98270=AXIS2_PLACEMENT_3D('',#192016,#115065,#115066);
#98271=AXIS2_PLACEMENT_3D('',#192019,#115067,#115068);
#98272=AXIS2_PLACEMENT_3D('',#192020,#115069,#115070);
#98273=AXIS2_PLACEMENT_3D('',#192021,#115071,#115072);
#98274=AXIS2_PLACEMENT_3D('',#192022,#115073,#115074);
#98275=AXIS2_PLACEMENT_3D('',#192025,#115075,#115076);
#98276=AXIS2_PLACEMENT_3D('',#192028,#115079,#115080);
#98277=AXIS2_PLACEMENT_3D('',#192031,#115081,#115082);
#98278=AXIS2_PLACEMENT_3D('',#192034,#115085,#115086);
#98279=AXIS2_PLACEMENT_3D('',#192035,#115087,#115088);
#98280=AXIS2_PLACEMENT_3D('',#192036,#115089,#115090);
#98281=AXIS2_PLACEMENT_3D('',#192037,#115091,#115092);
#98282=AXIS2_PLACEMENT_3D('',#192040,#115093,#115094);
#98283=AXIS2_PLACEMENT_3D('',#192042,#115095,#115096);
#98284=AXIS2_PLACEMENT_3D('',#192044,#115097,#115098);
#98285=AXIS2_PLACEMENT_3D('',#192045,#115099,#115100);
#98286=AXIS2_PLACEMENT_3D('',#192046,#115101,#115102);
#98287=AXIS2_PLACEMENT_3D('',#192049,#115103,#115104);
#98288=AXIS2_PLACEMENT_3D('',#192052,#115107,#115108);
#98289=AXIS2_PLACEMENT_3D('',#192055,#115109,#115110);
#98290=AXIS2_PLACEMENT_3D('',#192058,#115113,#115114);
#98291=AXIS2_PLACEMENT_3D('',#192061,#115115,#115116);
#98292=AXIS2_PLACEMENT_3D('',#192062,#115117,#115118);
#98293=AXIS2_PLACEMENT_3D('',#192063,#115119,#115120);
#98294=AXIS2_PLACEMENT_3D('',#192064,#115121,#115122);
#98295=AXIS2_PLACEMENT_3D('',#192067,#115123,#115124);
#98296=AXIS2_PLACEMENT_3D('',#192068,#115125,#115126);
#98297=AXIS2_PLACEMENT_3D('',#192069,#115127,#115128);
#98298=AXIS2_PLACEMENT_3D('',#192070,#115129,#115130);
#98299=AXIS2_PLACEMENT_3D('',#192073,#115131,#115132);
#98300=AXIS2_PLACEMENT_3D('',#192074,#115133,#115134);
#98301=AXIS2_PLACEMENT_3D('',#192075,#115135,#115136);
#98302=AXIS2_PLACEMENT_3D('',#192076,#115137,#115138);
#98303=AXIS2_PLACEMENT_3D('',#192079,#115139,#115140);
#98304=AXIS2_PLACEMENT_3D('',#192082,#115143,#115144);
#98305=AXIS2_PLACEMENT_3D('',#192085,#115145,#115146);
#98306=AXIS2_PLACEMENT_3D('',#192086,#115147,#115148);
#98307=AXIS2_PLACEMENT_3D('',#192087,#115149,#115150);
#98308=AXIS2_PLACEMENT_3D('',#192088,#115151,#115152);
#98309=AXIS2_PLACEMENT_3D('',#192089,#115153,#115154);
#98310=AXIS2_PLACEMENT_3D('',#192090,#115155,#115156);
#98311=AXIS2_PLACEMENT_3D('',#192091,#115157,#115158);
#98312=AXIS2_PLACEMENT_3D('',#192094,#115159,#115160);
#98313=AXIS2_PLACEMENT_3D('',#192096,#115161,#115162);
#98314=AXIS2_PLACEMENT_3D('',#192098,#115163,#115164);
#98315=AXIS2_PLACEMENT_3D('',#192099,#115165,#115166);
#98316=AXIS2_PLACEMENT_3D('',#192100,#115167,#115168);
#98317=AXIS2_PLACEMENT_3D('',#192103,#115169,#115170);
#98318=AXIS2_PLACEMENT_3D('',#192106,#115173,#115174);
#98319=AXIS2_PLACEMENT_3D('',#192109,#115175,#115176);
#98320=AXIS2_PLACEMENT_3D('',#192112,#115179,#115180);
#98321=AXIS2_PLACEMENT_3D('',#192115,#115181,#115182);
#98322=AXIS2_PLACEMENT_3D('',#192116,#115183,#115184);
#98323=AXIS2_PLACEMENT_3D('',#192117,#115185,#115186);
#98324=AXIS2_PLACEMENT_3D('',#192118,#115187,#115188);
#98325=AXIS2_PLACEMENT_3D('',#192121,#115189,#115190);
#98326=AXIS2_PLACEMENT_3D('',#192122,#115191,#115192);
#98327=AXIS2_PLACEMENT_3D('',#192123,#115193,#115194);
#98328=AXIS2_PLACEMENT_3D('',#192124,#115195,#115196);
#98329=AXIS2_PLACEMENT_3D('',#192127,#115197,#115198);
#98330=AXIS2_PLACEMENT_3D('',#192130,#115201,#115202);
#98331=AXIS2_PLACEMENT_3D('',#192133,#115203,#115204);
#98332=AXIS2_PLACEMENT_3D('',#192136,#115207,#115208);
#98333=AXIS2_PLACEMENT_3D('',#192137,#115209,#115210);
#98334=AXIS2_PLACEMENT_3D('',#192138,#115211,#115212);
#98335=AXIS2_PLACEMENT_3D('',#192139,#115213,#115214);
#98336=AXIS2_PLACEMENT_3D('',#192142,#115215,#115216);
#98337=AXIS2_PLACEMENT_3D('',#192144,#115217,#115218);
#98338=AXIS2_PLACEMENT_3D('',#192146,#115219,#115220);
#98339=AXIS2_PLACEMENT_3D('',#192147,#115221,#115222);
#98340=AXIS2_PLACEMENT_3D('',#192148,#115223,#115224);
#98341=AXIS2_PLACEMENT_3D('',#192151,#115225,#115226);
#98342=AXIS2_PLACEMENT_3D('',#192154,#115229,#115230);
#98343=AXIS2_PLACEMENT_3D('',#192157,#115231,#115232);
#98344=AXIS2_PLACEMENT_3D('',#192160,#115235,#115236);
#98345=AXIS2_PLACEMENT_3D('',#192163,#115237,#115238);
#98346=AXIS2_PLACEMENT_3D('',#192164,#115239,#115240);
#98347=AXIS2_PLACEMENT_3D('',#192165,#115241,#115242);
#98348=AXIS2_PLACEMENT_3D('',#192166,#115243,#115244);
#98349=AXIS2_PLACEMENT_3D('',#192169,#115245,#115246);
#98350=AXIS2_PLACEMENT_3D('',#192170,#115247,#115248);
#98351=AXIS2_PLACEMENT_3D('',#192171,#115249,#115250);
#98352=AXIS2_PLACEMENT_3D('',#192172,#115251,#115252);
#98353=AXIS2_PLACEMENT_3D('',#192175,#115253,#115254);
#98354=AXIS2_PLACEMENT_3D('',#192178,#115257,#115258);
#98355=AXIS2_PLACEMENT_3D('',#192181,#115259,#115260);
#98356=AXIS2_PLACEMENT_3D('',#192184,#115263,#115264);
#98357=AXIS2_PLACEMENT_3D('',#192185,#115265,#115266);
#98358=AXIS2_PLACEMENT_3D('',#192186,#115267,#115268);
#98359=AXIS2_PLACEMENT_3D('',#192187,#115269,#115270);
#98360=AXIS2_PLACEMENT_3D('',#192190,#115271,#115272);
#98361=AXIS2_PLACEMENT_3D('',#192192,#115273,#115274);
#98362=AXIS2_PLACEMENT_3D('',#192194,#115275,#115276);
#98363=AXIS2_PLACEMENT_3D('',#192195,#115277,#115278);
#98364=AXIS2_PLACEMENT_3D('',#192196,#115279,#115280);
#98365=AXIS2_PLACEMENT_3D('',#192199,#115281,#115282);
#98366=AXIS2_PLACEMENT_3D('',#192202,#115285,#115286);
#98367=AXIS2_PLACEMENT_3D('',#192205,#115287,#115288);
#98368=AXIS2_PLACEMENT_3D('',#192208,#115291,#115292);
#98369=AXIS2_PLACEMENT_3D('',#192211,#115293,#115294);
#98370=AXIS2_PLACEMENT_3D('',#192212,#115295,#115296);
#98371=AXIS2_PLACEMENT_3D('',#192213,#115297,#115298);
#98372=AXIS2_PLACEMENT_3D('',#192214,#115299,#115300);
#98373=AXIS2_PLACEMENT_3D('',#192217,#115301,#115302);
#98374=AXIS2_PLACEMENT_3D('',#192218,#115303,#115304);
#98375=AXIS2_PLACEMENT_3D('',#192219,#115305,#115306);
#98376=AXIS2_PLACEMENT_3D('',#192220,#115307,#115308);
#98377=AXIS2_PLACEMENT_3D('',#192223,#115309,#115310);
#98378=AXIS2_PLACEMENT_3D('',#192226,#115313,#115314);
#98379=AXIS2_PLACEMENT_3D('',#192229,#115315,#115316);
#98380=AXIS2_PLACEMENT_3D('',#192232,#115319,#115320);
#98381=AXIS2_PLACEMENT_3D('',#192233,#115321,#115322);
#98382=AXIS2_PLACEMENT_3D('',#192234,#115323,#115324);
#98383=AXIS2_PLACEMENT_3D('',#192235,#115325,#115326);
#98384=AXIS2_PLACEMENT_3D('',#192238,#115327,#115328);
#98385=AXIS2_PLACEMENT_3D('',#192240,#115329,#115330);
#98386=AXIS2_PLACEMENT_3D('',#192242,#115331,#115332);
#98387=AXIS2_PLACEMENT_3D('',#192243,#115333,#115334);
#98388=AXIS2_PLACEMENT_3D('',#192244,#115335,#115336);
#98389=AXIS2_PLACEMENT_3D('',#192247,#115337,#115338);
#98390=AXIS2_PLACEMENT_3D('',#192250,#115341,#115342);
#98391=AXIS2_PLACEMENT_3D('',#192253,#115343,#115344);
#98392=AXIS2_PLACEMENT_3D('',#192256,#115347,#115348);
#98393=AXIS2_PLACEMENT_3D('',#192259,#115349,#115350);
#98394=AXIS2_PLACEMENT_3D('',#192260,#115351,#115352);
#98395=AXIS2_PLACEMENT_3D('',#192261,#115353,#115354);
#98396=AXIS2_PLACEMENT_3D('',#192262,#115355,#115356);
#98397=AXIS2_PLACEMENT_3D('',#192265,#115357,#115358);
#98398=AXIS2_PLACEMENT_3D('',#192266,#115359,#115360);
#98399=AXIS2_PLACEMENT_3D('',#192267,#115361,#115362);
#98400=AXIS2_PLACEMENT_3D('',#192268,#115363,#115364);
#98401=AXIS2_PLACEMENT_3D('',#192271,#115365,#115366);
#98402=AXIS2_PLACEMENT_3D('',#192274,#115369,#115370);
#98403=AXIS2_PLACEMENT_3D('',#192277,#115371,#115372);
#98404=AXIS2_PLACEMENT_3D('',#192280,#115375,#115376);
#98405=AXIS2_PLACEMENT_3D('',#192281,#115377,#115378);
#98406=AXIS2_PLACEMENT_3D('',#192282,#115379,#115380);
#98407=AXIS2_PLACEMENT_3D('',#192283,#115381,#115382);
#98408=AXIS2_PLACEMENT_3D('',#192286,#115383,#115384);
#98409=AXIS2_PLACEMENT_3D('',#192288,#115385,#115386);
#98410=AXIS2_PLACEMENT_3D('',#192290,#115387,#115388);
#98411=AXIS2_PLACEMENT_3D('',#192291,#115389,#115390);
#98412=AXIS2_PLACEMENT_3D('',#192292,#115391,#115392);
#98413=AXIS2_PLACEMENT_3D('',#192295,#115393,#115394);
#98414=AXIS2_PLACEMENT_3D('',#192298,#115397,#115398);
#98415=AXIS2_PLACEMENT_3D('',#192301,#115399,#115400);
#98416=AXIS2_PLACEMENT_3D('',#192304,#115403,#115404);
#98417=AXIS2_PLACEMENT_3D('',#192307,#115405,#115406);
#98418=AXIS2_PLACEMENT_3D('',#192308,#115407,#115408);
#98419=AXIS2_PLACEMENT_3D('',#192309,#115409,#115410);
#98420=AXIS2_PLACEMENT_3D('',#192310,#115411,#115412);
#98421=AXIS2_PLACEMENT_3D('',#192313,#115413,#115414);
#98422=AXIS2_PLACEMENT_3D('',#192314,#115415,#115416);
#98423=AXIS2_PLACEMENT_3D('',#192315,#115417,#115418);
#98424=AXIS2_PLACEMENT_3D('',#192316,#115419,#115420);
#98425=AXIS2_PLACEMENT_3D('',#192319,#115421,#115422);
#98426=AXIS2_PLACEMENT_3D('',#192322,#115425,#115426);
#98427=AXIS2_PLACEMENT_3D('',#192325,#115427,#115428);
#98428=AXIS2_PLACEMENT_3D('',#192326,#115429,#115430);
#98429=AXIS2_PLACEMENT_3D('',#192327,#115431,#115432);
#98430=AXIS2_PLACEMENT_3D('',#192328,#115433,#115434);
#98431=AXIS2_PLACEMENT_3D('',#192329,#115435,#115436);
#98432=AXIS2_PLACEMENT_3D('',#192330,#115437,#115438);
#98433=AXIS2_PLACEMENT_3D('',#192331,#115439,#115440);
#98434=AXIS2_PLACEMENT_3D('',#192334,#115441,#115442);
#98435=AXIS2_PLACEMENT_3D('',#192336,#115443,#115444);
#98436=AXIS2_PLACEMENT_3D('',#192338,#115445,#115446);
#98437=AXIS2_PLACEMENT_3D('',#192339,#115447,#115448);
#98438=AXIS2_PLACEMENT_3D('',#192340,#115449,#115450);
#98439=AXIS2_PLACEMENT_3D('',#192343,#115451,#115452);
#98440=AXIS2_PLACEMENT_3D('',#192346,#115455,#115456);
#98441=AXIS2_PLACEMENT_3D('',#192349,#115457,#115458);
#98442=AXIS2_PLACEMENT_3D('',#192352,#115461,#115462);
#98443=AXIS2_PLACEMENT_3D('',#192355,#115463,#115464);
#98444=AXIS2_PLACEMENT_3D('',#192356,#115465,#115466);
#98445=AXIS2_PLACEMENT_3D('',#192357,#115467,#115468);
#98446=AXIS2_PLACEMENT_3D('',#192358,#115469,#115470);
#98447=AXIS2_PLACEMENT_3D('',#192361,#115471,#115472);
#98448=AXIS2_PLACEMENT_3D('',#192362,#115473,#115474);
#98449=AXIS2_PLACEMENT_3D('',#192363,#115475,#115476);
#98450=AXIS2_PLACEMENT_3D('',#192364,#115477,#115478);
#98451=AXIS2_PLACEMENT_3D('',#192367,#115479,#115480);
#98452=AXIS2_PLACEMENT_3D('',#192370,#115483,#115484);
#98453=AXIS2_PLACEMENT_3D('',#192373,#115485,#115486);
#98454=AXIS2_PLACEMENT_3D('',#192374,#115487,#115488);
#98455=AXIS2_PLACEMENT_3D('',#192375,#115489,#115490);
#98456=AXIS2_PLACEMENT_3D('',#192376,#115491,#115492);
#98457=AXIS2_PLACEMENT_3D('',#192379,#115493,#115494);
#98458=AXIS2_PLACEMENT_3D('',#192380,#115495,#115496);
#98459=AXIS2_PLACEMENT_3D('',#192381,#115497,#115498);
#98460=AXIS2_PLACEMENT_3D('',#192382,#115499,#115500);
#98461=AXIS2_PLACEMENT_3D('',#192385,#115501,#115502);
#98462=AXIS2_PLACEMENT_3D('',#192386,#115503,#115504);
#98463=AXIS2_PLACEMENT_3D('',#192387,#115505,#115506);
#98464=AXIS2_PLACEMENT_3D('',#192388,#115507,#115508);
#98465=AXIS2_PLACEMENT_3D('',#192389,#115509,#115510);
#98466=AXIS2_PLACEMENT_3D('',#192390,#115511,#115512);
#98467=AXIS2_PLACEMENT_3D('',#192391,#115513,#115514);
#98468=AXIS2_PLACEMENT_3D('',#192394,#115515,#115516);
#98469=AXIS2_PLACEMENT_3D('',#192396,#115517,#115518);
#98470=AXIS2_PLACEMENT_3D('',#192398,#115519,#115520);
#98471=AXIS2_PLACEMENT_3D('',#192399,#115521,#115522);
#98472=AXIS2_PLACEMENT_3D('',#192400,#115523,#115524);
#98473=AXIS2_PLACEMENT_3D('',#192403,#115525,#115526);
#98474=AXIS2_PLACEMENT_3D('',#192406,#115529,#115530);
#98475=AXIS2_PLACEMENT_3D('',#192409,#115531,#115532);
#98476=AXIS2_PLACEMENT_3D('',#192412,#115535,#115536);
#98477=AXIS2_PLACEMENT_3D('',#192415,#115537,#115538);
#98478=AXIS2_PLACEMENT_3D('',#192416,#115539,#115540);
#98479=AXIS2_PLACEMENT_3D('',#192417,#115541,#115542);
#98480=AXIS2_PLACEMENT_3D('',#192418,#115543,#115544);
#98481=AXIS2_PLACEMENT_3D('',#192421,#115545,#115546);
#98482=AXIS2_PLACEMENT_3D('',#192422,#115547,#115548);
#98483=AXIS2_PLACEMENT_3D('',#192423,#115549,#115550);
#98484=AXIS2_PLACEMENT_3D('',#192424,#115551,#115552);
#98485=AXIS2_PLACEMENT_3D('',#192427,#115553,#115554);
#98486=AXIS2_PLACEMENT_3D('',#192430,#115557,#115558);
#98487=AXIS2_PLACEMENT_3D('',#192433,#115559,#115560);
#98488=AXIS2_PLACEMENT_3D('',#192434,#115561,#115562);
#98489=AXIS2_PLACEMENT_3D('',#192435,#115563,#115564);
#98490=AXIS2_PLACEMENT_3D('',#192436,#115565,#115566);
#98491=AXIS2_PLACEMENT_3D('',#192437,#115567,#115568);
#98492=AXIS2_PLACEMENT_3D('',#192438,#115569,#115570);
#98493=AXIS2_PLACEMENT_3D('',#192439,#115571,#115572);
#98494=AXIS2_PLACEMENT_3D('',#192442,#115573,#115574);
#98495=AXIS2_PLACEMENT_3D('',#192444,#115575,#115576);
#98496=AXIS2_PLACEMENT_3D('',#192446,#115577,#115578);
#98497=AXIS2_PLACEMENT_3D('',#192447,#115579,#115580);
#98498=AXIS2_PLACEMENT_3D('',#192448,#115581,#115582);
#98499=AXIS2_PLACEMENT_3D('',#192451,#115583,#115584);
#98500=AXIS2_PLACEMENT_3D('',#192454,#115587,#115588);
#98501=AXIS2_PLACEMENT_3D('',#192457,#115589,#115590);
#98502=AXIS2_PLACEMENT_3D('',#192460,#115593,#115594);
#98503=AXIS2_PLACEMENT_3D('',#192463,#115595,#115596);
#98504=AXIS2_PLACEMENT_3D('',#192464,#115597,#115598);
#98505=AXIS2_PLACEMENT_3D('',#192465,#115599,#115600);
#98506=AXIS2_PLACEMENT_3D('',#192466,#115601,#115602);
#98507=AXIS2_PLACEMENT_3D('',#192469,#115603,#115604);
#98508=AXIS2_PLACEMENT_3D('',#192470,#115605,#115606);
#98509=AXIS2_PLACEMENT_3D('',#192471,#115607,#115608);
#98510=AXIS2_PLACEMENT_3D('',#192472,#115609,#115610);
#98511=AXIS2_PLACEMENT_3D('',#192475,#115611,#115612);
#98512=AXIS2_PLACEMENT_3D('',#192478,#115615,#115616);
#98513=AXIS2_PLACEMENT_3D('',#192481,#115617,#115618);
#98514=AXIS2_PLACEMENT_3D('',#192484,#115621,#115622);
#98515=AXIS2_PLACEMENT_3D('',#192485,#115623,#115624);
#98516=AXIS2_PLACEMENT_3D('',#192486,#115625,#115626);
#98517=AXIS2_PLACEMENT_3D('',#192487,#115627,#115628);
#98518=AXIS2_PLACEMENT_3D('',#192490,#115629,#115630);
#98519=AXIS2_PLACEMENT_3D('',#192492,#115631,#115632);
#98520=AXIS2_PLACEMENT_3D('',#192494,#115633,#115634);
#98521=AXIS2_PLACEMENT_3D('',#192495,#115635,#115636);
#98522=AXIS2_PLACEMENT_3D('',#192496,#115637,#115638);
#98523=AXIS2_PLACEMENT_3D('',#192499,#115639,#115640);
#98524=AXIS2_PLACEMENT_3D('',#192502,#115643,#115644);
#98525=AXIS2_PLACEMENT_3D('',#192505,#115645,#115646);
#98526=AXIS2_PLACEMENT_3D('',#192506,#115647,#115648);
#98527=AXIS2_PLACEMENT_3D('',#192507,#115649,#115650);
#98528=AXIS2_PLACEMENT_3D('',#192508,#115651,#115652);
#98529=AXIS2_PLACEMENT_3D('',#192511,#115653,#115654);
#98530=AXIS2_PLACEMENT_3D('',#192512,#115655,#115656);
#98531=AXIS2_PLACEMENT_3D('',#192513,#115657,#115658);
#98532=AXIS2_PLACEMENT_3D('',#192514,#115659,#115660);
#98533=AXIS2_PLACEMENT_3D('',#192517,#115661,#115662);
#98534=AXIS2_PLACEMENT_3D('',#192518,#115663,#115664);
#98535=AXIS2_PLACEMENT_3D('',#192519,#115665,#115666);
#98536=AXIS2_PLACEMENT_3D('',#192520,#115667,#115668);
#98537=AXIS2_PLACEMENT_3D('',#192523,#115669,#115670);
#98538=AXIS2_PLACEMENT_3D('',#192526,#115673,#115674);
#98539=AXIS2_PLACEMENT_3D('',#192529,#115675,#115676);
#98540=AXIS2_PLACEMENT_3D('',#192532,#115679,#115680);
#98541=AXIS2_PLACEMENT_3D('',#192535,#115681,#115682);
#98542=AXIS2_PLACEMENT_3D('',#192536,#115683,#115684);
#98543=AXIS2_PLACEMENT_3D('',#192537,#115685,#115686);
#98544=AXIS2_PLACEMENT_3D('',#192538,#115687,#115688);
#98545=AXIS2_PLACEMENT_3D('',#192541,#115689,#115690);
#98546=AXIS2_PLACEMENT_3D('',#192542,#115691,#115692);
#98547=AXIS2_PLACEMENT_3D('',#192543,#115693,#115694);
#98548=AXIS2_PLACEMENT_3D('',#192544,#115695,#115696);
#98549=AXIS2_PLACEMENT_3D('',#192547,#115699,#115700);
#98550=AXIS2_PLACEMENT_3D('',#192550,#115701,#115702);
#98551=AXIS2_PLACEMENT_3D('',#192552,#115703,#115704);
#98552=AXIS2_PLACEMENT_3D('',#192554,#115705,#115706);
#98553=AXIS2_PLACEMENT_3D('',#192555,#115707,#115708);
#98554=AXIS2_PLACEMENT_3D('',#192556,#115709,#115710);
#98555=AXIS2_PLACEMENT_3D('',#192559,#115711,#115712);
#98556=AXIS2_PLACEMENT_3D('',#192562,#115715,#115716);
#98557=AXIS2_PLACEMENT_3D('',#192565,#115717,#115718);
#98558=AXIS2_PLACEMENT_3D('',#192568,#115721,#115722);
#98559=AXIS2_PLACEMENT_3D('',#192571,#115723,#115724);
#98560=AXIS2_PLACEMENT_3D('',#192572,#115725,#115726);
#98561=AXIS2_PLACEMENT_3D('',#192573,#115727,#115728);
#98562=AXIS2_PLACEMENT_3D('',#192574,#115729,#115730);
#98563=AXIS2_PLACEMENT_3D('',#192577,#115731,#115732);
#98564=AXIS2_PLACEMENT_3D('',#192578,#115733,#115734);
#98565=AXIS2_PLACEMENT_3D('',#192579,#115735,#115736);
#98566=AXIS2_PLACEMENT_3D('',#192580,#115737,#115738);
#98567=AXIS2_PLACEMENT_3D('',#192583,#115739,#115740);
#98568=AXIS2_PLACEMENT_3D('',#192586,#115743,#115744);
#98569=AXIS2_PLACEMENT_3D('',#192589,#115745,#115746);
#98570=AXIS2_PLACEMENT_3D('',#192590,#115747,#115748);
#98571=AXIS2_PLACEMENT_3D('',#192591,#115749,#115750);
#98572=AXIS2_PLACEMENT_3D('',#192592,#115751,#115752);
#98573=AXIS2_PLACEMENT_3D('',#192595,#115753,#115754);
#98574=AXIS2_PLACEMENT_3D('',#192596,#115755,#115756);
#98575=AXIS2_PLACEMENT_3D('',#192597,#115757,#115758);
#98576=AXIS2_PLACEMENT_3D('',#192598,#115759,#115760);
#98577=AXIS2_PLACEMENT_3D('',#192601,#115761,#115762);
#98578=AXIS2_PLACEMENT_3D('',#192602,#115763,#115764);
#98579=AXIS2_PLACEMENT_3D('',#192603,#115765,#115766);
#98580=AXIS2_PLACEMENT_3D('',#192604,#115767,#115768);
#98581=AXIS2_PLACEMENT_3D('',#192607,#115771,#115772);
#98582=AXIS2_PLACEMENT_3D('',#192610,#115773,#115774);
#98583=AXIS2_PLACEMENT_3D('',#192612,#115775,#115776);
#98584=AXIS2_PLACEMENT_3D('',#192614,#115777,#115778);
#98585=AXIS2_PLACEMENT_3D('',#192615,#115779,#115780);
#98586=AXIS2_PLACEMENT_3D('',#192616,#115781,#115782);
#98587=AXIS2_PLACEMENT_3D('',#192619,#115783,#115784);
#98588=AXIS2_PLACEMENT_3D('',#192622,#115787,#115788);
#98589=AXIS2_PLACEMENT_3D('',#192625,#115789,#115790);
#98590=AXIS2_PLACEMENT_3D('',#192628,#115793,#115794);
#98591=AXIS2_PLACEMENT_3D('',#192631,#115795,#115796);
#98592=AXIS2_PLACEMENT_3D('',#192632,#115797,#115798);
#98593=AXIS2_PLACEMENT_3D('',#192633,#115799,#115800);
#98594=AXIS2_PLACEMENT_3D('',#192634,#115801,#115802);
#98595=AXIS2_PLACEMENT_3D('',#192637,#115803,#115804);
#98596=AXIS2_PLACEMENT_3D('',#192638,#115805,#115806);
#98597=AXIS2_PLACEMENT_3D('',#192639,#115807,#115808);
#98598=AXIS2_PLACEMENT_3D('',#192640,#115809,#115810);
#98599=AXIS2_PLACEMENT_3D('',#192643,#115811,#115812);
#98600=AXIS2_PLACEMENT_3D('',#192646,#115815,#115816);
#98601=AXIS2_PLACEMENT_3D('',#192649,#115817,#115818);
#98602=AXIS2_PLACEMENT_3D('',#192652,#115821,#115822);
#98603=AXIS2_PLACEMENT_3D('',#192653,#115823,#115824);
#98604=AXIS2_PLACEMENT_3D('',#192654,#115825,#115826);
#98605=AXIS2_PLACEMENT_3D('',#192655,#115827,#115828);
#98606=AXIS2_PLACEMENT_3D('',#192658,#115829,#115830);
#98607=AXIS2_PLACEMENT_3D('',#192660,#115831,#115832);
#98608=AXIS2_PLACEMENT_3D('',#192662,#115833,#115834);
#98609=AXIS2_PLACEMENT_3D('',#192663,#115835,#115836);
#98610=AXIS2_PLACEMENT_3D('',#192664,#115837,#115838);
#98611=AXIS2_PLACEMENT_3D('',#192667,#115839,#115840);
#98612=AXIS2_PLACEMENT_3D('',#192670,#115843,#115844);
#98613=AXIS2_PLACEMENT_3D('',#192673,#115845,#115846);
#98614=AXIS2_PLACEMENT_3D('',#192676,#115849,#115850);
#98615=AXIS2_PLACEMENT_3D('',#192679,#115851,#115852);
#98616=AXIS2_PLACEMENT_3D('',#192680,#115853,#115854);
#98617=AXIS2_PLACEMENT_3D('',#192681,#115855,#115856);
#98618=AXIS2_PLACEMENT_3D('',#192682,#115857,#115858);
#98619=AXIS2_PLACEMENT_3D('',#192685,#115859,#115860);
#98620=AXIS2_PLACEMENT_3D('',#192686,#115861,#115862);
#98621=AXIS2_PLACEMENT_3D('',#192687,#115863,#115864);
#98622=AXIS2_PLACEMENT_3D('',#192688,#115865,#115866);
#98623=AXIS2_PLACEMENT_3D('',#192691,#115867,#115868);
#98624=AXIS2_PLACEMENT_3D('',#192692,#115869,#115870);
#98625=AXIS2_PLACEMENT_3D('',#192693,#115871,#115872);
#98626=AXIS2_PLACEMENT_3D('',#192694,#115873,#115874);
#98627=AXIS2_PLACEMENT_3D('',#192697,#115875,#115876);
#98628=AXIS2_PLACEMENT_3D('',#192700,#115879,#115880);
#98629=AXIS2_PLACEMENT_3D('',#192701,#115881,#115882);
#98630=AXIS2_PLACEMENT_3D('',#192702,#115883,#115884);
#98631=AXIS2_PLACEMENT_3D('',#192703,#115885,#115886);
#98632=AXIS2_PLACEMENT_3D('',#192706,#115887,#115888);
#98633=AXIS2_PLACEMENT_3D('',#192708,#115889,#115890);
#98634=AXIS2_PLACEMENT_3D('',#192710,#115891,#115892);
#98635=AXIS2_PLACEMENT_3D('',#192711,#115893,#115894);
#98636=AXIS2_PLACEMENT_3D('',#192712,#115895,#115896);
#98637=AXIS2_PLACEMENT_3D('',#192715,#115897,#115898);
#98638=AXIS2_PLACEMENT_3D('',#192718,#115901,#115902);
#98639=AXIS2_PLACEMENT_3D('',#192721,#115903,#115904);
#98640=AXIS2_PLACEMENT_3D('',#192724,#115907,#115908);
#98641=AXIS2_PLACEMENT_3D('',#192727,#115909,#115910);
#98642=AXIS2_PLACEMENT_3D('',#192728,#115911,#115912);
#98643=AXIS2_PLACEMENT_3D('',#192729,#115913,#115914);
#98644=AXIS2_PLACEMENT_3D('',#192730,#115915,#115916);
#98645=AXIS2_PLACEMENT_3D('',#192733,#115917,#115918);
#98646=AXIS2_PLACEMENT_3D('',#192734,#115919,#115920);
#98647=AXIS2_PLACEMENT_3D('',#192735,#115921,#115922);
#98648=AXIS2_PLACEMENT_3D('',#192736,#115923,#115924);
#98649=AXIS2_PLACEMENT_3D('',#192739,#115925,#115926);
#98650=AXIS2_PLACEMENT_3D('',#192742,#115929,#115930);
#98651=AXIS2_PLACEMENT_3D('',#192745,#115931,#115932);
#98652=AXIS2_PLACEMENT_3D('',#192748,#115935,#115936);
#98653=AXIS2_PLACEMENT_3D('',#192749,#115937,#115938);
#98654=AXIS2_PLACEMENT_3D('',#192750,#115939,#115940);
#98655=AXIS2_PLACEMENT_3D('',#192751,#115941,#115942);
#98656=AXIS2_PLACEMENT_3D('',#192754,#115943,#115944);
#98657=AXIS2_PLACEMENT_3D('',#192756,#115945,#115946);
#98658=AXIS2_PLACEMENT_3D('',#192758,#115947,#115948);
#98659=AXIS2_PLACEMENT_3D('',#192759,#115949,#115950);
#98660=AXIS2_PLACEMENT_3D('',#192760,#115951,#115952);
#98661=AXIS2_PLACEMENT_3D('',#192763,#115953,#115954);
#98662=AXIS2_PLACEMENT_3D('',#192766,#115957,#115958);
#98663=AXIS2_PLACEMENT_3D('',#192769,#115959,#115960);
#98664=AXIS2_PLACEMENT_3D('',#192772,#115963,#115964);
#98665=AXIS2_PLACEMENT_3D('',#192775,#115965,#115966);
#98666=AXIS2_PLACEMENT_3D('',#192776,#115967,#115968);
#98667=AXIS2_PLACEMENT_3D('',#192777,#115969,#115970);
#98668=AXIS2_PLACEMENT_3D('',#192778,#115971,#115972);
#98669=AXIS2_PLACEMENT_3D('',#192781,#115973,#115974);
#98670=AXIS2_PLACEMENT_3D('',#192782,#115975,#115976);
#98671=AXIS2_PLACEMENT_3D('',#192783,#115977,#115978);
#98672=AXIS2_PLACEMENT_3D('',#192784,#115979,#115980);
#98673=AXIS2_PLACEMENT_3D('',#192787,#115981,#115982);
#98674=AXIS2_PLACEMENT_3D('',#192790,#115985,#115986);
#98675=AXIS2_PLACEMENT_3D('',#192793,#115987,#115988);
#98676=AXIS2_PLACEMENT_3D('',#192796,#115991,#115992);
#98677=AXIS2_PLACEMENT_3D('',#192797,#115993,#115994);
#98678=AXIS2_PLACEMENT_3D('',#192798,#115995,#115996);
#98679=AXIS2_PLACEMENT_3D('',#192799,#115997,#115998);
#98680=AXIS2_PLACEMENT_3D('',#192802,#115999,#116000);
#98681=AXIS2_PLACEMENT_3D('',#192804,#116001,#116002);
#98682=AXIS2_PLACEMENT_3D('',#192806,#116003,#116004);
#98683=AXIS2_PLACEMENT_3D('',#192807,#116005,#116006);
#98684=AXIS2_PLACEMENT_3D('',#192808,#116007,#116008);
#98685=AXIS2_PLACEMENT_3D('',#192811,#116009,#116010);
#98686=AXIS2_PLACEMENT_3D('',#192814,#116013,#116014);
#98687=AXIS2_PLACEMENT_3D('',#192817,#116015,#116016);
#98688=AXIS2_PLACEMENT_3D('',#192820,#116019,#116020);
#98689=AXIS2_PLACEMENT_3D('',#192823,#116021,#116022);
#98690=AXIS2_PLACEMENT_3D('',#192824,#116023,#116024);
#98691=AXIS2_PLACEMENT_3D('',#192825,#116025,#116026);
#98692=AXIS2_PLACEMENT_3D('',#192826,#116027,#116028);
#98693=AXIS2_PLACEMENT_3D('',#192829,#116029,#116030);
#98694=AXIS2_PLACEMENT_3D('',#192830,#116031,#116032);
#98695=AXIS2_PLACEMENT_3D('',#192831,#116033,#116034);
#98696=AXIS2_PLACEMENT_3D('',#192832,#116035,#116036);
#98697=AXIS2_PLACEMENT_3D('',#192835,#116037,#116038);
#98698=AXIS2_PLACEMENT_3D('',#192838,#116041,#116042);
#98699=AXIS2_PLACEMENT_3D('',#192841,#116043,#116044);
#98700=AXIS2_PLACEMENT_3D('',#192842,#116045,#116046);
#98701=AXIS2_PLACEMENT_3D('',#192843,#116047,#116048);
#98702=AXIS2_PLACEMENT_3D('',#192844,#116049,#116050);
#98703=AXIS2_PLACEMENT_3D('',#192846,#116051,#116052);
#98704=AXIS2_PLACEMENT_3D('',#192848,#116053,#116054);
#98705=AXIS2_PLACEMENT_3D('',#192849,#116055,#116056);
#98706=AXIS2_PLACEMENT_3D('',#192850,#116057,#116058);
#98707=AXIS2_PLACEMENT_3D('',#192851,#116059,#116060);
#98708=AXIS2_PLACEMENT_3D('',#192852,#116061,#116062);
#98709=AXIS2_PLACEMENT_3D('',#192853,#116063,#116064);
#98710=AXIS2_PLACEMENT_3D('',#192856,#116065,#116066);
#98711=AXIS2_PLACEMENT_3D('',#192858,#116067,#116068);
#98712=AXIS2_PLACEMENT_3D('',#192860,#116069,#116070);
#98713=AXIS2_PLACEMENT_3D('',#192861,#116071,#116072);
#98714=AXIS2_PLACEMENT_3D('',#192862,#116073,#116074);
#98715=AXIS2_PLACEMENT_3D('',#192865,#116075,#116076);
#98716=AXIS2_PLACEMENT_3D('',#192868,#116079,#116080);
#98717=AXIS2_PLACEMENT_3D('',#192871,#116081,#116082);
#98718=AXIS2_PLACEMENT_3D('',#192874,#116085,#116086);
#98719=AXIS2_PLACEMENT_3D('',#192877,#116087,#116088);
#98720=AXIS2_PLACEMENT_3D('',#192878,#116089,#116090);
#98721=AXIS2_PLACEMENT_3D('',#192879,#116091,#116092);
#98722=AXIS2_PLACEMENT_3D('',#192880,#116093,#116094);
#98723=AXIS2_PLACEMENT_3D('',#192883,#116095,#116096);
#98724=AXIS2_PLACEMENT_3D('',#192884,#116097,#116098);
#98725=AXIS2_PLACEMENT_3D('',#192885,#116099,#116100);
#98726=AXIS2_PLACEMENT_3D('',#192886,#116101,#116102);
#98727=AXIS2_PLACEMENT_3D('',#192889,#116103,#116104);
#98728=AXIS2_PLACEMENT_3D('',#192890,#116105,#116106);
#98729=AXIS2_PLACEMENT_3D('',#192891,#116107,#116108);
#98730=AXIS2_PLACEMENT_3D('',#192892,#116109,#116110);
#98731=AXIS2_PLACEMENT_3D('',#192895,#116111,#116112);
#98732=AXIS2_PLACEMENT_3D('',#192898,#116115,#116116);
#98733=AXIS2_PLACEMENT_3D('',#192899,#116117,#116118);
#98734=AXIS2_PLACEMENT_3D('',#192900,#116119,#116120);
#98735=AXIS2_PLACEMENT_3D('',#192901,#116121,#116122);
#98736=AXIS2_PLACEMENT_3D('',#192904,#116123,#116124);
#98737=AXIS2_PLACEMENT_3D('',#192906,#116125,#116126);
#98738=AXIS2_PLACEMENT_3D('',#192908,#116127,#116128);
#98739=AXIS2_PLACEMENT_3D('',#192909,#116129,#116130);
#98740=AXIS2_PLACEMENT_3D('',#192910,#116131,#116132);
#98741=AXIS2_PLACEMENT_3D('',#192913,#116133,#116134);
#98742=AXIS2_PLACEMENT_3D('',#192916,#116137,#116138);
#98743=AXIS2_PLACEMENT_3D('',#192919,#116139,#116140);
#98744=AXIS2_PLACEMENT_3D('',#192922,#116143,#116144);
#98745=AXIS2_PLACEMENT_3D('',#192925,#116145,#116146);
#98746=AXIS2_PLACEMENT_3D('',#192926,#116147,#116148);
#98747=AXIS2_PLACEMENT_3D('',#192927,#116149,#116150);
#98748=AXIS2_PLACEMENT_3D('',#192928,#116151,#116152);
#98749=AXIS2_PLACEMENT_3D('',#192931,#116153,#116154);
#98750=AXIS2_PLACEMENT_3D('',#192932,#116155,#116156);
#98751=AXIS2_PLACEMENT_3D('',#192933,#116157,#116158);
#98752=AXIS2_PLACEMENT_3D('',#192934,#116159,#116160);
#98753=AXIS2_PLACEMENT_3D('',#192937,#116161,#116162);
#98754=AXIS2_PLACEMENT_3D('',#192938,#116163,#116164);
#98755=AXIS2_PLACEMENT_3D('',#192939,#116165,#116166);
#98756=AXIS2_PLACEMENT_3D('',#192940,#116167,#116168);
#98757=AXIS2_PLACEMENT_3D('',#192943,#116169,#116170);
#98758=AXIS2_PLACEMENT_3D('',#192946,#116173,#116174);
#98759=AXIS2_PLACEMENT_3D('',#192949,#116175,#116176);
#98760=AXIS2_PLACEMENT_3D('',#192950,#116177,#116178);
#98761=AXIS2_PLACEMENT_3D('',#192951,#116179,#116180);
#98762=AXIS2_PLACEMENT_3D('',#192952,#116181,#116182);
#98763=AXIS2_PLACEMENT_3D('',#192955,#116183,#116184);
#98764=AXIS2_PLACEMENT_3D('',#192956,#116185,#116186);
#98765=AXIS2_PLACEMENT_3D('',#192957,#116187,#116188);
#98766=AXIS2_PLACEMENT_3D('',#192958,#116189,#116190);
#98767=AXIS2_PLACEMENT_3D('',#192959,#116191,#116192);
#98768=AXIS2_PLACEMENT_3D('',#192960,#116193,#116194);
#98769=AXIS2_PLACEMENT_3D('',#192961,#116195,#116196);
#98770=AXIS2_PLACEMENT_3D('',#192964,#116197,#116198);
#98771=AXIS2_PLACEMENT_3D('',#192966,#116199,#116200);
#98772=AXIS2_PLACEMENT_3D('',#192968,#116201,#116202);
#98773=AXIS2_PLACEMENT_3D('',#192969,#116203,#116204);
#98774=AXIS2_PLACEMENT_3D('',#192970,#116205,#116206);
#98775=AXIS2_PLACEMENT_3D('',#192973,#116207,#116208);
#98776=AXIS2_PLACEMENT_3D('',#192976,#116211,#116212);
#98777=AXIS2_PLACEMENT_3D('',#192979,#116213,#116214);
#98778=AXIS2_PLACEMENT_3D('',#192982,#116217,#116218);
#98779=AXIS2_PLACEMENT_3D('',#192985,#116219,#116220);
#98780=AXIS2_PLACEMENT_3D('',#192986,#116221,#116222);
#98781=AXIS2_PLACEMENT_3D('',#192987,#116223,#116224);
#98782=AXIS2_PLACEMENT_3D('',#192988,#116225,#116226);
#98783=AXIS2_PLACEMENT_3D('',#192991,#116227,#116228);
#98784=AXIS2_PLACEMENT_3D('',#192992,#116229,#116230);
#98785=AXIS2_PLACEMENT_3D('',#192993,#116231,#116232);
#98786=AXIS2_PLACEMENT_3D('',#192994,#116233,#116234);
#98787=AXIS2_PLACEMENT_3D('',#192997,#116235,#116236);
#98788=AXIS2_PLACEMENT_3D('',#193000,#116239,#116240);
#98789=AXIS2_PLACEMENT_3D('',#193003,#116241,#116242);
#98790=AXIS2_PLACEMENT_3D('',#193006,#116245,#116246);
#98791=AXIS2_PLACEMENT_3D('',#193007,#116247,#116248);
#98792=AXIS2_PLACEMENT_3D('',#193008,#116249,#116250);
#98793=AXIS2_PLACEMENT_3D('',#193009,#116251,#116252);
#98794=AXIS2_PLACEMENT_3D('',#193012,#116253,#116254);
#98795=AXIS2_PLACEMENT_3D('',#193014,#116255,#116256);
#98796=AXIS2_PLACEMENT_3D('',#193016,#116257,#116258);
#98797=AXIS2_PLACEMENT_3D('',#193017,#116259,#116260);
#98798=AXIS2_PLACEMENT_3D('',#193018,#116261,#116262);
#98799=AXIS2_PLACEMENT_3D('',#193021,#116263,#116264);
#98800=AXIS2_PLACEMENT_3D('',#193024,#116267,#116268);
#98801=AXIS2_PLACEMENT_3D('',#193027,#116269,#116270);
#98802=AXIS2_PLACEMENT_3D('',#193030,#116273,#116274);
#98803=AXIS2_PLACEMENT_3D('',#193033,#116275,#116276);
#98804=AXIS2_PLACEMENT_3D('',#193034,#116277,#116278);
#98805=AXIS2_PLACEMENT_3D('',#193035,#116279,#116280);
#98806=AXIS2_PLACEMENT_3D('',#193036,#116281,#116282);
#98807=AXIS2_PLACEMENT_3D('',#193039,#116283,#116284);
#98808=AXIS2_PLACEMENT_3D('',#193040,#116285,#116286);
#98809=AXIS2_PLACEMENT_3D('',#193041,#116287,#116288);
#98810=AXIS2_PLACEMENT_3D('',#193042,#116289,#116290);
#98811=AXIS2_PLACEMENT_3D('',#193045,#116291,#116292);
#98812=AXIS2_PLACEMENT_3D('',#193048,#116295,#116296);
#98813=AXIS2_PLACEMENT_3D('',#193051,#116297,#116298);
#98814=AXIS2_PLACEMENT_3D('',#193052,#116299,#116300);
#98815=AXIS2_PLACEMENT_3D('',#193053,#116301,#116302);
#98816=AXIS2_PLACEMENT_3D('',#193054,#116303,#116304);
#98817=AXIS2_PLACEMENT_3D('',#193057,#116305,#116306);
#98818=AXIS2_PLACEMENT_3D('',#193058,#116307,#116308);
#98819=AXIS2_PLACEMENT_3D('',#193059,#116309,#116310);
#98820=AXIS2_PLACEMENT_3D('',#193060,#116311,#116312);
#98821=AXIS2_PLACEMENT_3D('',#193063,#116313,#116314);
#98822=AXIS2_PLACEMENT_3D('',#193064,#116315,#116316);
#98823=AXIS2_PLACEMENT_3D('',#193065,#116317,#116318);
#98824=AXIS2_PLACEMENT_3D('',#193066,#116319,#116320);
#98825=AXIS2_PLACEMENT_3D('',#193067,#116321,#116322);
#98826=AXIS2_PLACEMENT_3D('',#193068,#116323,#116324);
#98827=AXIS2_PLACEMENT_3D('',#193069,#116325,#116326);
#98828=AXIS2_PLACEMENT_3D('',#193072,#116327,#116328);
#98829=AXIS2_PLACEMENT_3D('',#193074,#116329,#116330);
#98830=AXIS2_PLACEMENT_3D('',#193076,#116331,#116332);
#98831=AXIS2_PLACEMENT_3D('',#193077,#116333,#116334);
#98832=AXIS2_PLACEMENT_3D('',#193078,#116335,#116336);
#98833=AXIS2_PLACEMENT_3D('',#193081,#116337,#116338);
#98834=AXIS2_PLACEMENT_3D('',#193084,#116341,#116342);
#98835=AXIS2_PLACEMENT_3D('',#193087,#116343,#116344);
#98836=AXIS2_PLACEMENT_3D('',#193090,#116347,#116348);
#98837=AXIS2_PLACEMENT_3D('',#193093,#116349,#116350);
#98838=AXIS2_PLACEMENT_3D('',#193094,#116351,#116352);
#98839=AXIS2_PLACEMENT_3D('',#193095,#116353,#116354);
#98840=AXIS2_PLACEMENT_3D('',#193096,#116355,#116356);
#98841=AXIS2_PLACEMENT_3D('',#193099,#116357,#116358);
#98842=AXIS2_PLACEMENT_3D('',#193100,#116359,#116360);
#98843=AXIS2_PLACEMENT_3D('',#193101,#116361,#116362);
#98844=AXIS2_PLACEMENT_3D('',#193102,#116363,#116364);
#98845=AXIS2_PLACEMENT_3D('',#193105,#116365,#116366);
#98846=AXIS2_PLACEMENT_3D('',#193108,#116369,#116370);
#98847=AXIS2_PLACEMENT_3D('',#193111,#116371,#116372);
#98848=AXIS2_PLACEMENT_3D('',#193112,#116373,#116374);
#98849=AXIS2_PLACEMENT_3D('',#193113,#116375,#116376);
#98850=AXIS2_PLACEMENT_3D('',#193114,#116377,#116378);
#98851=AXIS2_PLACEMENT_3D('',#193115,#116379,#116380);
#98852=AXIS2_PLACEMENT_3D('',#193116,#116381,#116382);
#98853=AXIS2_PLACEMENT_3D('',#193117,#116383,#116384);
#98854=AXIS2_PLACEMENT_3D('',#193120,#116385,#116386);
#98855=AXIS2_PLACEMENT_3D('',#193122,#116387,#116388);
#98856=AXIS2_PLACEMENT_3D('',#193124,#116389,#116390);
#98857=AXIS2_PLACEMENT_3D('',#193125,#116391,#116392);
#98858=AXIS2_PLACEMENT_3D('',#193126,#116393,#116394);
#98859=AXIS2_PLACEMENT_3D('',#193129,#116395,#116396);
#98860=AXIS2_PLACEMENT_3D('',#193132,#116399,#116400);
#98861=AXIS2_PLACEMENT_3D('',#193135,#116401,#116402);
#98862=AXIS2_PLACEMENT_3D('',#193138,#116405,#116406);
#98863=AXIS2_PLACEMENT_3D('',#193141,#116407,#116408);
#98864=AXIS2_PLACEMENT_3D('',#193142,#116409,#116410);
#98865=AXIS2_PLACEMENT_3D('',#193143,#116411,#116412);
#98866=AXIS2_PLACEMENT_3D('',#193144,#116413,#116414);
#98867=AXIS2_PLACEMENT_3D('',#193147,#116415,#116416);
#98868=AXIS2_PLACEMENT_3D('',#193148,#116417,#116418);
#98869=AXIS2_PLACEMENT_3D('',#193149,#116419,#116420);
#98870=AXIS2_PLACEMENT_3D('',#193150,#116421,#116422);
#98871=AXIS2_PLACEMENT_3D('',#193153,#116423,#116424);
#98872=AXIS2_PLACEMENT_3D('',#193156,#116427,#116428);
#98873=AXIS2_PLACEMENT_3D('',#193159,#116429,#116430);
#98874=AXIS2_PLACEMENT_3D('',#193162,#116433,#116434);
#98875=AXIS2_PLACEMENT_3D('',#193163,#116435,#116436);
#98876=AXIS2_PLACEMENT_3D('',#193164,#116437,#116438);
#98877=AXIS2_PLACEMENT_3D('',#193165,#116439,#116440);
#98878=AXIS2_PLACEMENT_3D('',#193168,#116441,#116442);
#98879=AXIS2_PLACEMENT_3D('',#193170,#116443,#116444);
#98880=AXIS2_PLACEMENT_3D('',#193172,#116445,#116446);
#98881=AXIS2_PLACEMENT_3D('',#193173,#116447,#116448);
#98882=AXIS2_PLACEMENT_3D('',#193174,#116449,#116450);
#98883=AXIS2_PLACEMENT_3D('',#193177,#116451,#116452);
#98884=AXIS2_PLACEMENT_3D('',#193180,#116455,#116456);
#98885=AXIS2_PLACEMENT_3D('',#193183,#116457,#116458);
#98886=AXIS2_PLACEMENT_3D('',#193186,#116461,#116462);
#98887=AXIS2_PLACEMENT_3D('',#193189,#116463,#116464);
#98888=AXIS2_PLACEMENT_3D('',#193190,#116465,#116466);
#98889=AXIS2_PLACEMENT_3D('',#193191,#116467,#116468);
#98890=AXIS2_PLACEMENT_3D('',#193192,#116469,#116470);
#98891=AXIS2_PLACEMENT_3D('',#193195,#116471,#116472);
#98892=AXIS2_PLACEMENT_3D('',#193196,#116473,#116474);
#98893=AXIS2_PLACEMENT_3D('',#193197,#116475,#116476);
#98894=AXIS2_PLACEMENT_3D('',#193198,#116477,#116478);
#98895=AXIS2_PLACEMENT_3D('',#193201,#116479,#116480);
#98896=AXIS2_PLACEMENT_3D('',#193204,#116483,#116484);
#98897=AXIS2_PLACEMENT_3D('',#193207,#116485,#116486);
#98898=AXIS2_PLACEMENT_3D('',#193208,#116487,#116488);
#98899=AXIS2_PLACEMENT_3D('',#193209,#116489,#116490);
#98900=AXIS2_PLACEMENT_3D('',#193210,#116491,#116492);
#98901=AXIS2_PLACEMENT_3D('',#193211,#116493,#116494);
#98902=AXIS2_PLACEMENT_3D('',#193212,#116495,#116496);
#98903=AXIS2_PLACEMENT_3D('',#193213,#116497,#116498);
#98904=AXIS2_PLACEMENT_3D('',#193216,#116499,#116500);
#98905=AXIS2_PLACEMENT_3D('',#193218,#116501,#116502);
#98906=AXIS2_PLACEMENT_3D('',#193220,#116503,#116504);
#98907=AXIS2_PLACEMENT_3D('',#193221,#116505,#116506);
#98908=AXIS2_PLACEMENT_3D('',#193222,#116507,#116508);
#98909=AXIS2_PLACEMENT_3D('',#193225,#116509,#116510);
#98910=AXIS2_PLACEMENT_3D('',#193228,#116513,#116514);
#98911=AXIS2_PLACEMENT_3D('',#193231,#116515,#116516);
#98912=AXIS2_PLACEMENT_3D('',#193234,#116519,#116520);
#98913=AXIS2_PLACEMENT_3D('',#193237,#116521,#116522);
#98914=AXIS2_PLACEMENT_3D('',#193238,#116523,#116524);
#98915=AXIS2_PLACEMENT_3D('',#193239,#116525,#116526);
#98916=AXIS2_PLACEMENT_3D('',#193240,#116527,#116528);
#98917=AXIS2_PLACEMENT_3D('',#193243,#116529,#116530);
#98918=AXIS2_PLACEMENT_3D('',#193244,#116531,#116532);
#98919=AXIS2_PLACEMENT_3D('',#193245,#116533,#116534);
#98920=AXIS2_PLACEMENT_3D('',#193246,#116535,#116536);
#98921=AXIS2_PLACEMENT_3D('',#193249,#116537,#116538);
#98922=AXIS2_PLACEMENT_3D('',#193252,#116541,#116542);
#98923=AXIS2_PLACEMENT_3D('',#193255,#116543,#116544);
#98924=AXIS2_PLACEMENT_3D('',#193258,#116547,#116548);
#98925=AXIS2_PLACEMENT_3D('',#193259,#116549,#116550);
#98926=AXIS2_PLACEMENT_3D('',#193260,#116551,#116552);
#98927=AXIS2_PLACEMENT_3D('',#193261,#116553,#116554);
#98928=AXIS2_PLACEMENT_3D('',#193264,#116555,#116556);
#98929=AXIS2_PLACEMENT_3D('',#193266,#116557,#116558);
#98930=AXIS2_PLACEMENT_3D('',#193268,#116559,#116560);
#98931=AXIS2_PLACEMENT_3D('',#193269,#116561,#116562);
#98932=AXIS2_PLACEMENT_3D('',#193270,#116563,#116564);
#98933=AXIS2_PLACEMENT_3D('',#193273,#116565,#116566);
#98934=AXIS2_PLACEMENT_3D('',#193276,#116569,#116570);
#98935=AXIS2_PLACEMENT_3D('',#193279,#116571,#116572);
#98936=AXIS2_PLACEMENT_3D('',#193280,#116573,#116574);
#98937=AXIS2_PLACEMENT_3D('',#193281,#116575,#116576);
#98938=AXIS2_PLACEMENT_3D('',#193282,#116577,#116578);
#98939=AXIS2_PLACEMENT_3D('',#193285,#116579,#116580);
#98940=AXIS2_PLACEMENT_3D('',#193286,#116581,#116582);
#98941=AXIS2_PLACEMENT_3D('',#193287,#116583,#116584);
#98942=AXIS2_PLACEMENT_3D('',#193288,#116585,#116586);
#98943=AXIS2_PLACEMENT_3D('',#193291,#116587,#116588);
#98944=AXIS2_PLACEMENT_3D('',#193292,#116589,#116590);
#98945=AXIS2_PLACEMENT_3D('',#193293,#116591,#116592);
#98946=AXIS2_PLACEMENT_3D('',#193294,#116593,#116594);
#98947=AXIS2_PLACEMENT_3D('',#193297,#116597,#116598);
#98948=AXIS2_PLACEMENT_3D('',#193300,#116599,#116600);
#98949=AXIS2_PLACEMENT_3D('',#193302,#116601,#116602);
#98950=AXIS2_PLACEMENT_3D('',#193304,#116603,#116604);
#98951=AXIS2_PLACEMENT_3D('',#193305,#116605,#116606);
#98952=AXIS2_PLACEMENT_3D('',#193306,#116607,#116608);
#98953=AXIS2_PLACEMENT_3D('',#193309,#116609,#116610);
#98954=AXIS2_PLACEMENT_3D('',#193312,#116613,#116614);
#98955=AXIS2_PLACEMENT_3D('',#193315,#116615,#116616);
#98956=AXIS2_PLACEMENT_3D('',#193316,#116617,#116618);
#98957=AXIS2_PLACEMENT_3D('',#193317,#116619,#116620);
#98958=AXIS2_PLACEMENT_3D('',#193318,#116621,#116622);
#98959=AXIS2_PLACEMENT_3D('',#193321,#116623,#116624);
#98960=AXIS2_PLACEMENT_3D('',#193322,#116625,#116626);
#98961=AXIS2_PLACEMENT_3D('',#193323,#116627,#116628);
#98962=AXIS2_PLACEMENT_3D('',#193324,#116629,#116630);
#98963=AXIS2_PLACEMENT_3D('',#193327,#116631,#116632);
#98964=AXIS2_PLACEMENT_3D('',#193328,#116633,#116634);
#98965=AXIS2_PLACEMENT_3D('',#193329,#116635,#116636);
#98966=AXIS2_PLACEMENT_3D('',#193330,#116637,#116638);
#98967=AXIS2_PLACEMENT_3D('',#193333,#116641,#116642);
#98968=AXIS2_PLACEMENT_3D('',#193336,#116643,#116644);
#98969=AXIS2_PLACEMENT_3D('',#193338,#116645,#116646);
#98970=AXIS2_PLACEMENT_3D('',#193340,#116647,#116648);
#98971=AXIS2_PLACEMENT_3D('',#193341,#116649,#116650);
#98972=AXIS2_PLACEMENT_3D('',#193342,#116651,#116652);
#98973=AXIS2_PLACEMENT_3D('',#193345,#116653,#116654);
#98974=AXIS2_PLACEMENT_3D('',#193346,#116655,#116656);
#98975=AXIS2_PLACEMENT_3D('',#193347,#116657,#116658);
#98976=AXIS2_PLACEMENT_3D('',#193348,#116659,#116660);
#98977=AXIS2_PLACEMENT_3D('',#193351,#116661,#116662);
#98978=AXIS2_PLACEMENT_3D('',#193352,#116663,#116664);
#98979=AXIS2_PLACEMENT_3D('',#193353,#116665,#116666);
#98980=AXIS2_PLACEMENT_3D('',#193354,#116667,#116668);
#98981=AXIS2_PLACEMENT_3D('',#193357,#116669,#116670);
#98982=AXIS2_PLACEMENT_3D('',#193358,#116671,#116672);
#98983=AXIS2_PLACEMENT_3D('',#193359,#116673,#116674);
#98984=AXIS2_PLACEMENT_3D('',#193360,#116675,#116676);
#98985=AXIS2_PLACEMENT_3D('',#193363,#116677,#116678);
#98986=AXIS2_PLACEMENT_3D('',#193364,#116679,#116680);
#98987=AXIS2_PLACEMENT_3D('',#193365,#116681,#116682);
#98988=AXIS2_PLACEMENT_3D('',#193366,#116683,#116684);
#98989=AXIS2_PLACEMENT_3D('',#193369,#116685,#116686);
#98990=AXIS2_PLACEMENT_3D('',#193370,#116687,#116688);
#98991=AXIS2_PLACEMENT_3D('',#193371,#116689,#116690);
#98992=AXIS2_PLACEMENT_3D('',#193372,#116691,#116692);
#98993=AXIS2_PLACEMENT_3D('',#193375,#116693,#116694);
#98994=AXIS2_PLACEMENT_3D('',#193376,#116695,#116696);
#98995=AXIS2_PLACEMENT_3D('',#193377,#116697,#116698);
#98996=AXIS2_PLACEMENT_3D('',#193378,#116699,#116700);
#98997=AXIS2_PLACEMENT_3D('',#193381,#116701,#116702);
#98998=AXIS2_PLACEMENT_3D('',#193383,#116703,#116704);
#98999=AXIS2_PLACEMENT_3D('',#193385,#116705,#116706);
#99000=AXIS2_PLACEMENT_3D('',#193386,#116707,#116708);
#99001=AXIS2_PLACEMENT_3D('',#193387,#116709,#116710);
#99002=AXIS2_PLACEMENT_3D('',#193390,#116711,#116712);
#99003=AXIS2_PLACEMENT_3D('',#193391,#116713,#116714);
#99004=AXIS2_PLACEMENT_3D('',#193392,#116715,#116716);
#99005=AXIS2_PLACEMENT_3D('',#193393,#116717,#116718);
#99006=AXIS2_PLACEMENT_3D('',#193396,#116719,#116720);
#99007=AXIS2_PLACEMENT_3D('',#193397,#116721,#116722);
#99008=AXIS2_PLACEMENT_3D('',#193398,#116723,#116724);
#99009=AXIS2_PLACEMENT_3D('',#193399,#116725,#116726);
#99010=AXIS2_PLACEMENT_3D('',#193402,#116727,#116728);
#99011=AXIS2_PLACEMENT_3D('',#193403,#116729,#116730);
#99012=AXIS2_PLACEMENT_3D('',#193404,#116731,#116732);
#99013=AXIS2_PLACEMENT_3D('',#193405,#116733,#116734);
#99014=AXIS2_PLACEMENT_3D('',#193408,#116735,#116736);
#99015=AXIS2_PLACEMENT_3D('',#193409,#116737,#116738);
#99016=AXIS2_PLACEMENT_3D('',#193410,#116739,#116740);
#99017=AXIS2_PLACEMENT_3D('',#193411,#116741,#116742);
#99018=AXIS2_PLACEMENT_3D('',#193414,#116743,#116744);
#99019=AXIS2_PLACEMENT_3D('',#193415,#116745,#116746);
#99020=AXIS2_PLACEMENT_3D('',#193416,#116747,#116748);
#99021=AXIS2_PLACEMENT_3D('',#193417,#116749,#116750);
#99022=AXIS2_PLACEMENT_3D('',#193420,#116751,#116752);
#99023=AXIS2_PLACEMENT_3D('',#193421,#116753,#116754);
#99024=AXIS2_PLACEMENT_3D('',#193422,#116755,#116756);
#99025=AXIS2_PLACEMENT_3D('',#193423,#116757,#116758);
#99026=AXIS2_PLACEMENT_3D('',#193426,#116759,#116760);
#99027=AXIS2_PLACEMENT_3D('',#193428,#116761,#116762);
#99028=AXIS2_PLACEMENT_3D('',#193440,#116763,#116764);
#99029=AXIS2_PLACEMENT_3D('',#193441,#116765,#116766);
#99030=AXIS2_PLACEMENT_3D('',#193444,#116767,#116768);
#99031=AXIS2_PLACEMENT_3D('',#193447,#116771,#116772);
#99032=AXIS2_PLACEMENT_3D('',#193449,#116773,#116774);
#99033=AXIS2_PLACEMENT_3D('',#193451,#116775,#116776);
#99034=AXIS2_PLACEMENT_3D('',#193452,#116777,#116778);
#99035=AXIS2_PLACEMENT_3D('',#193453,#116779,#116780);
#99036=AXIS2_PLACEMENT_3D('',#193456,#116781,#116782);
#99037=AXIS2_PLACEMENT_3D('',#193457,#116783,#116784);
#99038=AXIS2_PLACEMENT_3D('',#193458,#116785,#116786);
#99039=AXIS2_PLACEMENT_3D('',#193459,#116787,#116788);
#99040=AXIS2_PLACEMENT_3D('',#193462,#116789,#116790);
#99041=AXIS2_PLACEMENT_3D('',#193463,#116791,#116792);
#99042=AXIS2_PLACEMENT_3D('',#193464,#116793,#116794);
#99043=AXIS2_PLACEMENT_3D('',#193465,#116795,#116796);
#99044=AXIS2_PLACEMENT_3D('',#193468,#116797,#116798);
#99045=AXIS2_PLACEMENT_3D('',#193471,#116801,#116802);
#99046=AXIS2_PLACEMENT_3D('',#193484,#116803,#116804);
#99047=AXIS2_PLACEMENT_3D('',#193485,#116805,#116806);
#99048=AXIS2_PLACEMENT_3D('',#193486,#116807,#116808);
#99049=AXIS2_PLACEMENT_3D('',#193489,#116809,#116810);
#99050=AXIS2_PLACEMENT_3D('',#193491,#116811,#116812);
#99051=AXIS2_PLACEMENT_3D('',#193503,#116813,#116814);
#99052=AXIS2_PLACEMENT_3D('',#193504,#116815,#116816);
#99053=AXIS2_PLACEMENT_3D('',#193507,#116817,#116818);
#99054=AXIS2_PLACEMENT_3D('',#193510,#116821,#116822);
#99055=AXIS2_PLACEMENT_3D('',#193513,#116823,#116824);
#99056=AXIS2_PLACEMENT_3D('',#193514,#116825,#116826);
#99057=AXIS2_PLACEMENT_3D('',#193515,#116827,#116828);
#99058=AXIS2_PLACEMENT_3D('',#193516,#116829,#116830);
#99059=AXIS2_PLACEMENT_3D('',#193519,#116831,#116832);
#99060=AXIS2_PLACEMENT_3D('',#193520,#116833,#116834);
#99061=AXIS2_PLACEMENT_3D('',#193521,#116835,#116836);
#99062=AXIS2_PLACEMENT_3D('',#193522,#116837,#116838);
#99063=AXIS2_PLACEMENT_3D('',#193525,#116839,#116840);
#99064=AXIS2_PLACEMENT_3D('',#193526,#116841,#116842);
#99065=AXIS2_PLACEMENT_3D('',#193527,#116843,#116844);
#99066=AXIS2_PLACEMENT_3D('',#193528,#116845,#116846);
#99067=AXIS2_PLACEMENT_3D('',#193531,#116847,#116848);
#99068=AXIS2_PLACEMENT_3D('',#193534,#116851,#116852);
#99069=AXIS2_PLACEMENT_3D('',#193547,#116853,#116854);
#99070=AXIS2_PLACEMENT_3D('',#193548,#116855,#116856);
#99071=AXIS2_PLACEMENT_3D('',#193549,#116857,#116858);
#99072=AXIS2_PLACEMENT_3D('',#193552,#116859,#116860);
#99073=AXIS2_PLACEMENT_3D('',#193554,#116861,#116862);
#99074=AXIS2_PLACEMENT_3D('',#193566,#116863,#116864);
#99075=AXIS2_PLACEMENT_3D('',#193567,#116865,#116866);
#99076=AXIS2_PLACEMENT_3D('',#193570,#116867,#116868);
#99077=AXIS2_PLACEMENT_3D('',#193573,#116871,#116872);
#99078=AXIS2_PLACEMENT_3D('',#193575,#116873,#116874);
#99079=AXIS2_PLACEMENT_3D('',#193577,#116875,#116876);
#99080=AXIS2_PLACEMENT_3D('',#193578,#116877,#116878);
#99081=AXIS2_PLACEMENT_3D('',#193579,#116879,#116880);
#99082=AXIS2_PLACEMENT_3D('',#193582,#116881,#116882);
#99083=AXIS2_PLACEMENT_3D('',#193583,#116883,#116884);
#99084=AXIS2_PLACEMENT_3D('',#193584,#116885,#116886);
#99085=AXIS2_PLACEMENT_3D('',#193585,#116887,#116888);
#99086=AXIS2_PLACEMENT_3D('',#193588,#116889,#116890);
#99087=AXIS2_PLACEMENT_3D('',#193589,#116891,#116892);
#99088=AXIS2_PLACEMENT_3D('',#193590,#116893,#116894);
#99089=AXIS2_PLACEMENT_3D('',#193591,#116895,#116896);
#99090=AXIS2_PLACEMENT_3D('',#193594,#116897,#116898);
#99091=AXIS2_PLACEMENT_3D('',#193597,#116901,#116902);
#99092=AXIS2_PLACEMENT_3D('',#193610,#116903,#116904);
#99093=AXIS2_PLACEMENT_3D('',#193611,#116905,#116906);
#99094=AXIS2_PLACEMENT_3D('',#193612,#116907,#116908);
#99095=AXIS2_PLACEMENT_3D('',#193626,#116909,#116910);
#99096=AXIS2_PLACEMENT_3D('',#193628,#116911,#116912);
#99097=AXIS2_PLACEMENT_3D('',#193629,#116913,#116914);
#99098=AXIS2_PLACEMENT_3D('',#193630,#116915,#116916);
#99099=AXIS2_PLACEMENT_3D('',#193633,#116917,#116918);
#99100=AXIS2_PLACEMENT_3D('',#193636,#116921,#116922);
#99101=AXIS2_PLACEMENT_3D('',#193639,#116923,#116924);
#99102=AXIS2_PLACEMENT_3D('',#193640,#116925,#116926);
#99103=AXIS2_PLACEMENT_3D('',#193641,#116927,#116928);
#99104=AXIS2_PLACEMENT_3D('',#193642,#116929,#116930);
#99105=AXIS2_PLACEMENT_3D('',#193645,#116931,#116932);
#99106=AXIS2_PLACEMENT_3D('',#193646,#116933,#116934);
#99107=AXIS2_PLACEMENT_3D('',#193647,#116935,#116936);
#99108=AXIS2_PLACEMENT_3D('',#193648,#116937,#116938);
#99109=AXIS2_PLACEMENT_3D('',#193651,#116939,#116940);
#99110=AXIS2_PLACEMENT_3D('',#193652,#116941,#116942);
#99111=AXIS2_PLACEMENT_3D('',#193653,#116943,#116944);
#99112=AXIS2_PLACEMENT_3D('',#193654,#116945,#116946);
#99113=AXIS2_PLACEMENT_3D('',#193657,#116947,#116948);
#99114=AXIS2_PLACEMENT_3D('',#193660,#116951,#116952);
#99115=AXIS2_PLACEMENT_3D('',#193673,#116953,#116954);
#99116=AXIS2_PLACEMENT_3D('',#193674,#116955,#116956);
#99117=AXIS2_PLACEMENT_3D('',#193675,#116957,#116958);
#99118=AXIS2_PLACEMENT_3D('',#193678,#116959,#116960);
#99119=AXIS2_PLACEMENT_3D('',#193680,#116961,#116962);
#99120=AXIS2_PLACEMENT_3D('',#193682,#116963,#116964);
#99121=AXIS2_PLACEMENT_3D('',#193683,#116965,#116966);
#99122=AXIS2_PLACEMENT_3D('',#193684,#116967,#116968);
#99123=AXIS2_PLACEMENT_3D('',#193687,#116969,#116970);
#99124=AXIS2_PLACEMENT_3D('',#193688,#116971,#116972);
#99125=AXIS2_PLACEMENT_3D('',#193689,#116973,#116974);
#99126=AXIS2_PLACEMENT_3D('',#193690,#116975,#116976);
#99127=AXIS2_PLACEMENT_3D('',#193693,#116977,#116978);
#99128=AXIS2_PLACEMENT_3D('',#193694,#116979,#116980);
#99129=AXIS2_PLACEMENT_3D('',#193695,#116981,#116982);
#99130=AXIS2_PLACEMENT_3D('',#193696,#116983,#116984);
#99131=AXIS2_PLACEMENT_3D('',#193699,#116985,#116986);
#99132=AXIS2_PLACEMENT_3D('',#193700,#116987,#116988);
#99133=AXIS2_PLACEMENT_3D('',#193701,#116989,#116990);
#99134=AXIS2_PLACEMENT_3D('',#193702,#116991,#116992);
#99135=AXIS2_PLACEMENT_3D('',#193705,#116993,#116994);
#99136=AXIS2_PLACEMENT_3D('',#193706,#116995,#116996);
#99137=AXIS2_PLACEMENT_3D('',#193707,#116997,#116998);
#99138=AXIS2_PLACEMENT_3D('',#193708,#116999,#117000);
#99139=AXIS2_PLACEMENT_3D('',#193711,#117001,#117002);
#99140=AXIS2_PLACEMENT_3D('',#193712,#117003,#117004);
#99141=AXIS2_PLACEMENT_3D('',#193713,#117005,#117006);
#99142=AXIS2_PLACEMENT_3D('',#193714,#117007,#117008);
#99143=AXIS2_PLACEMENT_3D('',#193717,#117009,#117010);
#99144=AXIS2_PLACEMENT_3D('',#193718,#117011,#117012);
#99145=AXIS2_PLACEMENT_3D('',#193719,#117013,#117014);
#99146=AXIS2_PLACEMENT_3D('',#193916,#117015,#117016);
#99147=AXIS2_PLACEMENT_3D('',#194031,#117017,#117018);
#99148=AXIS2_PLACEMENT_3D('',#194057,#117019,#117020);
#99149=AXIS2_PLACEMENT_3D('',#194080,#117021,#117022);
#99150=AXIS2_PLACEMENT_3D('',#194081,#117023,#117024);
#99151=AXIS2_PLACEMENT_3D('',#194082,#117025,#117026);
#99152=AXIS2_PLACEMENT_3D('',#194163,#117027,#117028);
#99153=AXIS2_PLACEMENT_3D('',#194265,#117029,#117030);
#99154=AXIS2_PLACEMENT_3D('',#194471,#117031,#117032);
#99155=AXIS2_PLACEMENT_3D('',#194569,#117033,#117034);
#99156=AXIS2_PLACEMENT_3D('',#194570,#117035,#117036);
#99157=AXIS2_PLACEMENT_3D('',#194571,#117037,#117038);
#99158=AXIS2_PLACEMENT_3D('',#194586,#117039,#117040);
#99159=AXIS2_PLACEMENT_3D('',#194909,#117041,#117042);
#99160=AXIS2_PLACEMENT_3D('',#195312,#117043,#117044);
#99161=AXIS2_PLACEMENT_3D('',#195335,#117045,#117046);
#99162=AXIS2_PLACEMENT_3D('',#195336,#117047,#117048);
#99163=AXIS2_PLACEMENT_3D('',#195337,#117049,#117050);
#99164=AXIS2_PLACEMENT_3D('',#195436,#117051,#117052);
#99165=AXIS2_PLACEMENT_3D('',#195553,#117053,#117054);
#99166=AXIS2_PLACEMENT_3D('',#195768,#117055,#117056);
#99167=AXIS2_PLACEMENT_3D('',#195866,#117057,#117058);
#99168=AXIS2_PLACEMENT_3D('',#195867,#117059,#117060);
#99169=AXIS2_PLACEMENT_3D('',#195868,#117061,#117062);
#99170=AXIS2_PLACEMENT_3D('',#195883,#117063,#117064);
#99171=AXIS2_PLACEMENT_3D('',#195910,#117065,#117066);
#99172=AXIS2_PLACEMENT_3D('',#195911,#117067,#117068);
#99173=AXIS2_PLACEMENT_3D('',#195926,#117069,#117070);
#99174=AXIS2_PLACEMENT_3D('',#195927,#117071,#117072);
#99175=AXIS2_PLACEMENT_3D('',#195928,#117073,#117074);
#99176=AXIS2_PLACEMENT_3D('',#196009,#117075,#117076);
#99177=AXIS2_PLACEMENT_3D('',#196088,#117077,#117078);
#99178=AXIS2_PLACEMENT_3D('',#196160,#117079,#117080);
#99179=AXIS2_PLACEMENT_3D('',#196161,#117081,#117082);
#99180=AXIS2_PLACEMENT_3D('',#196186,#117083,#117084);
#99181=AXIS2_PLACEMENT_3D('',#196187,#117085,#117086);
#99182=AXIS2_PLACEMENT_3D('',#197288,#117087,#117088);
#99183=AXIS2_PLACEMENT_3D('',#197317,#117089,#117090);
#99184=AXIS2_PLACEMENT_3D('',#197342,#117091,#117092);
#99185=AXIS2_PLACEMENT_3D('',#197344,#117093,#117094);
#99186=AXIS2_PLACEMENT_3D('',#197345,#117095,#117096);
#99187=AXIS2_PLACEMENT_3D('',#197366,#117097,#117098);
#99188=AXIS2_PLACEMENT_3D('',#197460,#117099,#117100);
#99189=AXIS2_PLACEMENT_3D('',#197634,#117101,#117102);
#99190=AXIS2_PLACEMENT_3D('',#197635,#117103,#117104);
#99191=AXIS2_PLACEMENT_3D('',#197636,#117105,#117106);
#99192=AXIS2_PLACEMENT_3D('',#197649,#117107,#117108);
#99193=AXIS2_PLACEMENT_3D('',#197668,#117109,#117110);
#99194=AXIS2_PLACEMENT_3D('',#197749,#117111,#117112);
#99195=AXIS2_PLACEMENT_3D('',#197750,#117113,#117114);
#99196=AXIS2_PLACEMENT_3D('',#197751,#117115,#117116);
#99197=AXIS2_PLACEMENT_3D('',#197765,#117117,#117118);
#99198=AXIS2_PLACEMENT_3D('',#197767,#117119,#117120);
#99199=AXIS2_PLACEMENT_3D('',#197768,#117121,#117122);
#99200=AXIS2_PLACEMENT_3D('',#197801,#117123,#117124);
#99201=AXIS2_PLACEMENT_3D('',#197905,#117125,#117126);
#99202=AXIS2_PLACEMENT_3D('',#197972,#117127,#117128);
#99203=AXIS2_PLACEMENT_3D('',#197983,#117129,#117130);
#99204=AXIS2_PLACEMENT_3D('',#197996,#117131,#117132);
#99205=AXIS2_PLACEMENT_3D('',#198001,#117133,#117134);
#99206=AXIS2_PLACEMENT_3D('',#198004,#117135,#117136);
#99207=AXIS2_PLACEMENT_3D('',#198006,#117137,#117138);
#99208=AXIS2_PLACEMENT_3D('',#198008,#117139,#117140);
#99209=AXIS2_PLACEMENT_3D('',#198009,#117141,#117142);
#99210=AXIS2_PLACEMENT_3D('',#198530,#117143,#117144);
#99211=AXIS2_PLACEMENT_3D('',#198550,#117145,#117146);
#99212=AXIS2_PLACEMENT_3D('',#198551,#117147,#117148);
#99213=AXIS2_PLACEMENT_3D('',#198552,#117149,#117150);
#99214=AXIS2_PLACEMENT_3D('',#198573,#117151,#117152);
#99215=AXIS2_PLACEMENT_3D('',#198606,#117153,#117154);
#99216=AXIS2_PLACEMENT_3D('',#198764,#117155,#117156);
#99217=AXIS2_PLACEMENT_3D('',#198926,#117157,#117158);
#99218=AXIS2_PLACEMENT_3D('',#198927,#117159,#117160);
#99219=AXIS2_PLACEMENT_3D('',#198928,#117161,#117162);
#99220=AXIS2_PLACEMENT_3D('',#199108,#117163,#117164);
#99221=AXIS2_PLACEMENT_3D('',#199111,#117165,#117166);
#99222=AXIS2_PLACEMENT_3D('',#199114,#117169,#117170);
#99223=AXIS2_PLACEMENT_3D('',#199118,#117172,#117173);
#99224=AXIS2_PLACEMENT_3D('',#199120,#117175,#117176);
#99225=AXIS2_PLACEMENT_3D('',#199124,#117178,#117179);
#99226=AXIS2_PLACEMENT_3D('',#199126,#117181,#117182);
#99227=AXIS2_PLACEMENT_3D('',#199130,#117184,#117185);
#99228=AXIS2_PLACEMENT_3D('',#199132,#117187,#117188);
#99229=AXIS2_PLACEMENT_3D('',#199136,#117190,#117191);
#99230=AXIS2_PLACEMENT_3D('',#199138,#117193,#117194);
#99231=AXIS2_PLACEMENT_3D('',#199142,#117196,#117197);
#99232=AXIS2_PLACEMENT_3D('',#199144,#117199,#117200);
#99233=AXIS2_PLACEMENT_3D('',#199148,#117202,#117203);
#99234=AXIS2_PLACEMENT_3D('',#199150,#117205,#117206);
#99235=AXIS2_PLACEMENT_3D('',#199154,#117208,#117209);
#99236=AXIS2_PLACEMENT_3D('',#199156,#117211,#117212);
#99237=AXIS2_PLACEMENT_3D('',#199160,#117214,#117215);
#99238=AXIS2_PLACEMENT_3D('',#199162,#117217,#117218);
#99239=AXIS2_PLACEMENT_3D('',#199165,#117219,#117220);
#99240=AXIS2_PLACEMENT_3D('',#199168,#117223,#117224);
#99241=AXIS2_PLACEMENT_3D('',#199172,#117226,#117227);
#99242=AXIS2_PLACEMENT_3D('',#199174,#117229,#117230);
#99243=AXIS2_PLACEMENT_3D('',#199178,#117232,#117233);
#99244=AXIS2_PLACEMENT_3D('',#199180,#117235,#117236);
#99245=AXIS2_PLACEMENT_3D('',#199184,#117238,#117239);
#99246=AXIS2_PLACEMENT_3D('',#199186,#117241,#117242);
#99247=AXIS2_PLACEMENT_3D('',#199190,#117244,#117245);
#99248=AXIS2_PLACEMENT_3D('',#199192,#117247,#117248);
#99249=AXIS2_PLACEMENT_3D('',#199196,#117250,#117251);
#99250=AXIS2_PLACEMENT_3D('',#199198,#117253,#117254);
#99251=AXIS2_PLACEMENT_3D('',#199202,#117256,#117257);
#99252=AXIS2_PLACEMENT_3D('',#199204,#117259,#117260);
#99253=AXIS2_PLACEMENT_3D('',#199208,#117262,#117263);
#99254=AXIS2_PLACEMENT_3D('',#199210,#117265,#117266);
#99255=AXIS2_PLACEMENT_3D('',#199214,#117268,#117269);
#99256=AXIS2_PLACEMENT_3D('',#199216,#117271,#117272);
#99257=AXIS2_PLACEMENT_3D('',#199220,#117274,#117275);
#99258=AXIS2_PLACEMENT_3D('',#199222,#117277,#117278);
#99259=AXIS2_PLACEMENT_3D('',#199226,#117280,#117281);
#99260=AXIS2_PLACEMENT_3D('',#199228,#117283,#117284);
#99261=AXIS2_PLACEMENT_3D('',#199232,#117286,#117287);
#99262=AXIS2_PLACEMENT_3D('',#199234,#117289,#117290);
#99263=AXIS2_PLACEMENT_3D('',#199238,#117292,#117293);
#99264=AXIS2_PLACEMENT_3D('',#199240,#117295,#117296);
#99265=AXIS2_PLACEMENT_3D('',#199244,#117298,#117299);
#99266=AXIS2_PLACEMENT_3D('',#199246,#117301,#117302);
#99267=AXIS2_PLACEMENT_3D('',#199250,#117304,#117305);
#99268=AXIS2_PLACEMENT_3D('',#199252,#117307,#117308);
#99269=AXIS2_PLACEMENT_3D('',#199256,#117310,#117311);
#99270=AXIS2_PLACEMENT_3D('',#199258,#117313,#117314);
#99271=AXIS2_PLACEMENT_3D('',#199262,#117316,#117317);
#99272=AXIS2_PLACEMENT_3D('',#199264,#117319,#117320);
#99273=AXIS2_PLACEMENT_3D('',#199268,#117322,#117323);
#99274=AXIS2_PLACEMENT_3D('',#199270,#117325,#117326);
#99275=AXIS2_PLACEMENT_3D('',#199273,#117327,#117328);
#99276=AXIS2_PLACEMENT_3D('',#199276,#117331,#117332);
#99277=AXIS2_PLACEMENT_3D('',#199280,#117334,#117335);
#99278=AXIS2_PLACEMENT_3D('',#199282,#117337,#117338);
#99279=AXIS2_PLACEMENT_3D('',#199286,#117340,#117341);
#99280=AXIS2_PLACEMENT_3D('',#199288,#117343,#117344);
#99281=AXIS2_PLACEMENT_3D('',#199292,#117346,#117347);
#99282=AXIS2_PLACEMENT_3D('',#199294,#117349,#117350);
#99283=AXIS2_PLACEMENT_3D('',#199298,#117352,#117353);
#99284=AXIS2_PLACEMENT_3D('',#199300,#117355,#117356);
#99285=AXIS2_PLACEMENT_3D('',#199304,#117358,#117359);
#99286=AXIS2_PLACEMENT_3D('',#199306,#117361,#117362);
#99287=AXIS2_PLACEMENT_3D('',#199310,#117364,#117365);
#99288=AXIS2_PLACEMENT_3D('',#199312,#117367,#117368);
#99289=AXIS2_PLACEMENT_3D('',#199316,#117370,#117371);
#99290=AXIS2_PLACEMENT_3D('',#199318,#117373,#117374);
#99291=AXIS2_PLACEMENT_3D('',#199322,#117376,#117377);
#99292=AXIS2_PLACEMENT_3D('',#199324,#117379,#117380);
#99293=AXIS2_PLACEMENT_3D('',#199328,#117382,#117383);
#99294=AXIS2_PLACEMENT_3D('',#199330,#117385,#117386);
#99295=AXIS2_PLACEMENT_3D('',#199334,#117388,#117389);
#99296=AXIS2_PLACEMENT_3D('',#199336,#117391,#117392);
#99297=AXIS2_PLACEMENT_3D('',#199340,#117394,#117395);
#99298=AXIS2_PLACEMENT_3D('',#199342,#117397,#117398);
#99299=AXIS2_PLACEMENT_3D('',#199346,#117400,#117401);
#99300=AXIS2_PLACEMENT_3D('',#199348,#117403,#117404);
#99301=AXIS2_PLACEMENT_3D('',#199352,#117406,#117407);
#99302=AXIS2_PLACEMENT_3D('',#199354,#117409,#117410);
#99303=AXIS2_PLACEMENT_3D('',#199358,#117412,#117413);
#99304=AXIS2_PLACEMENT_3D('',#199360,#117415,#117416);
#99305=AXIS2_PLACEMENT_3D('',#199364,#117418,#117419);
#99306=AXIS2_PLACEMENT_3D('',#199366,#117421,#117422);
#99307=AXIS2_PLACEMENT_3D('',#199370,#117424,#117425);
#99308=AXIS2_PLACEMENT_3D('',#199372,#117427,#117428);
#99309=AXIS2_PLACEMENT_3D('',#199376,#117430,#117431);
#99310=AXIS2_PLACEMENT_3D('',#199378,#117433,#117434);
#99311=AXIS2_PLACEMENT_3D('',#199382,#117436,#117437);
#99312=AXIS2_PLACEMENT_3D('',#199384,#117439,#117440);
#99313=AXIS2_PLACEMENT_3D('',#199388,#117442,#117443);
#99314=AXIS2_PLACEMENT_3D('',#199390,#117445,#117446);
#99315=AXIS2_PLACEMENT_3D('',#199394,#117448,#117449);
#99316=AXIS2_PLACEMENT_3D('',#199396,#117451,#117452);
#99317=AXIS2_PLACEMENT_3D('',#199400,#117454,#117455);
#99318=AXIS2_PLACEMENT_3D('',#199402,#117457,#117458);
#99319=AXIS2_PLACEMENT_3D('',#199406,#117460,#117461);
#99320=AXIS2_PLACEMENT_3D('',#199408,#117463,#117464);
#99321=AXIS2_PLACEMENT_3D('',#199412,#117466,#117467);
#99322=AXIS2_PLACEMENT_3D('',#199414,#117469,#117470);
#99323=AXIS2_PLACEMENT_3D('',#199418,#117472,#117473);
#99324=AXIS2_PLACEMENT_3D('',#199420,#117475,#117476);
#99325=AXIS2_PLACEMENT_3D('',#199424,#117478,#117479);
#99326=AXIS2_PLACEMENT_3D('',#199426,#117481,#117482);
#99327=AXIS2_PLACEMENT_3D('',#199430,#117484,#117485);
#99328=AXIS2_PLACEMENT_3D('',#199432,#117487,#117488);
#99329=AXIS2_PLACEMENT_3D('',#199436,#117490,#117491);
#99330=AXIS2_PLACEMENT_3D('',#199438,#117493,#117494);
#99331=AXIS2_PLACEMENT_3D('',#199442,#117496,#117497);
#99332=AXIS2_PLACEMENT_3D('',#199444,#117499,#117500);
#99333=AXIS2_PLACEMENT_3D('',#199448,#117502,#117503);
#99334=AXIS2_PLACEMENT_3D('',#199450,#117505,#117506);
#99335=AXIS2_PLACEMENT_3D('',#199454,#117508,#117509);
#99336=AXIS2_PLACEMENT_3D('',#199456,#117511,#117512);
#99337=AXIS2_PLACEMENT_3D('',#199460,#117514,#117515);
#99338=AXIS2_PLACEMENT_3D('',#199462,#117517,#117518);
#99339=AXIS2_PLACEMENT_3D('',#199466,#117520,#117521);
#99340=AXIS2_PLACEMENT_3D('',#199468,#117523,#117524);
#99341=AXIS2_PLACEMENT_3D('',#199472,#117526,#117527);
#99342=AXIS2_PLACEMENT_3D('',#199474,#117529,#117530);
#99343=AXIS2_PLACEMENT_3D('',#199478,#117532,#117533);
#99344=AXIS2_PLACEMENT_3D('',#199480,#117535,#117536);
#99345=AXIS2_PLACEMENT_3D('',#199484,#117538,#117539);
#99346=AXIS2_PLACEMENT_3D('',#199486,#117541,#117542);
#99347=AXIS2_PLACEMENT_3D('',#199490,#117544,#117545);
#99348=AXIS2_PLACEMENT_3D('',#199492,#117547,#117548);
#99349=AXIS2_PLACEMENT_3D('',#199496,#117550,#117551);
#99350=AXIS2_PLACEMENT_3D('',#199498,#117553,#117554);
#99351=AXIS2_PLACEMENT_3D('',#199502,#117556,#117557);
#99352=AXIS2_PLACEMENT_3D('',#199504,#117559,#117560);
#99353=AXIS2_PLACEMENT_3D('',#199508,#117562,#117563);
#99354=AXIS2_PLACEMENT_3D('',#199510,#117565,#117566);
#99355=AXIS2_PLACEMENT_3D('',#199514,#117568,#117569);
#99356=AXIS2_PLACEMENT_3D('',#199516,#117571,#117572);
#99357=AXIS2_PLACEMENT_3D('',#199520,#117574,#117575);
#99358=AXIS2_PLACEMENT_3D('',#199522,#117577,#117578);
#99359=AXIS2_PLACEMENT_3D('',#199526,#117580,#117581);
#99360=AXIS2_PLACEMENT_3D('',#199528,#117583,#117584);
#99361=AXIS2_PLACEMENT_3D('',#199532,#117586,#117587);
#99362=AXIS2_PLACEMENT_3D('',#199534,#117589,#117590);
#99363=AXIS2_PLACEMENT_3D('',#199538,#117592,#117593);
#99364=AXIS2_PLACEMENT_3D('',#199540,#117595,#117596);
#99365=AXIS2_PLACEMENT_3D('',#199544,#117598,#117599);
#99366=AXIS2_PLACEMENT_3D('',#199546,#117601,#117602);
#99367=AXIS2_PLACEMENT_3D('',#199550,#117604,#117605);
#99368=AXIS2_PLACEMENT_3D('',#199552,#117607,#117608);
#99369=AXIS2_PLACEMENT_3D('',#199556,#117610,#117611);
#99370=AXIS2_PLACEMENT_3D('',#199558,#117613,#117614);
#99371=AXIS2_PLACEMENT_3D('',#199562,#117616,#117617);
#99372=AXIS2_PLACEMENT_3D('',#199564,#117619,#117620);
#99373=AXIS2_PLACEMENT_3D('',#199568,#117622,#117623);
#99374=AXIS2_PLACEMENT_3D('',#199570,#117625,#117626);
#99375=AXIS2_PLACEMENT_3D('',#199574,#117628,#117629);
#99376=AXIS2_PLACEMENT_3D('',#199576,#117631,#117632);
#99377=AXIS2_PLACEMENT_3D('',#199580,#117634,#117635);
#99378=AXIS2_PLACEMENT_3D('',#199582,#117637,#117638);
#99379=AXIS2_PLACEMENT_3D('',#199586,#117640,#117641);
#99380=AXIS2_PLACEMENT_3D('',#199588,#117643,#117644);
#99381=AXIS2_PLACEMENT_3D('',#199592,#117646,#117647);
#99382=AXIS2_PLACEMENT_3D('',#199594,#117649,#117650);
#99383=AXIS2_PLACEMENT_3D('',#199598,#117652,#117653);
#99384=AXIS2_PLACEMENT_3D('',#199600,#117655,#117656);
#99385=AXIS2_PLACEMENT_3D('',#199604,#117658,#117659);
#99386=AXIS2_PLACEMENT_3D('',#199606,#117661,#117662);
#99387=AXIS2_PLACEMENT_3D('',#199610,#117664,#117665);
#99388=AXIS2_PLACEMENT_3D('',#199612,#117667,#117668);
#99389=AXIS2_PLACEMENT_3D('',#199616,#117670,#117671);
#99390=AXIS2_PLACEMENT_3D('',#199618,#117673,#117674);
#99391=AXIS2_PLACEMENT_3D('',#199621,#117675,#117676);
#99392=AXIS2_PLACEMENT_3D('',#199624,#117679,#117680);
#99393=AXIS2_PLACEMENT_3D('',#199628,#117682,#117683);
#99394=AXIS2_PLACEMENT_3D('',#199630,#117685,#117686);
#99395=AXIS2_PLACEMENT_3D('',#199634,#117688,#117689);
#99396=AXIS2_PLACEMENT_3D('',#199636,#117691,#117692);
#99397=AXIS2_PLACEMENT_3D('',#199640,#117694,#117695);
#99398=AXIS2_PLACEMENT_3D('',#199642,#117697,#117698);
#99399=AXIS2_PLACEMENT_3D('',#199646,#117700,#117701);
#99400=AXIS2_PLACEMENT_3D('',#199648,#117703,#117704);
#99401=AXIS2_PLACEMENT_3D('',#199652,#117706,#117707);
#99402=AXIS2_PLACEMENT_3D('',#199654,#117709,#117710);
#99403=AXIS2_PLACEMENT_3D('',#199658,#117712,#117713);
#99404=AXIS2_PLACEMENT_3D('',#199660,#117715,#117716);
#99405=AXIS2_PLACEMENT_3D('',#199664,#117718,#117719);
#99406=AXIS2_PLACEMENT_3D('',#199666,#117721,#117722);
#99407=AXIS2_PLACEMENT_3D('',#199670,#117724,#117725);
#99408=AXIS2_PLACEMENT_3D('',#199672,#117727,#117728);
#99409=AXIS2_PLACEMENT_3D('',#199676,#117730,#117731);
#99410=AXIS2_PLACEMENT_3D('',#199678,#117733,#117734);
#99411=AXIS2_PLACEMENT_3D('',#199682,#117736,#117737);
#99412=AXIS2_PLACEMENT_3D('',#199684,#117739,#117740);
#99413=AXIS2_PLACEMENT_3D('',#199688,#117742,#117743);
#99414=AXIS2_PLACEMENT_3D('',#199690,#117745,#117746);
#99415=AXIS2_PLACEMENT_3D('',#199694,#117748,#117749);
#99416=AXIS2_PLACEMENT_3D('',#199696,#117751,#117752);
#99417=AXIS2_PLACEMENT_3D('',#199700,#117754,#117755);
#99418=AXIS2_PLACEMENT_3D('',#199702,#117757,#117758);
#99419=AXIS2_PLACEMENT_3D('',#199706,#117760,#117761);
#99420=AXIS2_PLACEMENT_3D('',#199708,#117763,#117764);
#99421=AXIS2_PLACEMENT_3D('',#199712,#117766,#117767);
#99422=AXIS2_PLACEMENT_3D('',#199714,#117769,#117770);
#99423=AXIS2_PLACEMENT_3D('',#199718,#117772,#117773);
#99424=AXIS2_PLACEMENT_3D('',#199720,#117775,#117776);
#99425=AXIS2_PLACEMENT_3D('',#199724,#117778,#117779);
#99426=AXIS2_PLACEMENT_3D('',#199726,#117781,#117782);
#99427=AXIS2_PLACEMENT_3D('',#199730,#117784,#117785);
#99428=AXIS2_PLACEMENT_3D('',#199732,#117787,#117788);
#99429=AXIS2_PLACEMENT_3D('',#199736,#117790,#117791);
#99430=AXIS2_PLACEMENT_3D('',#199738,#117793,#117794);
#99431=AXIS2_PLACEMENT_3D('',#199742,#117796,#117797);
#99432=AXIS2_PLACEMENT_3D('',#199744,#117799,#117800);
#99433=AXIS2_PLACEMENT_3D('',#199748,#117802,#117803);
#99434=AXIS2_PLACEMENT_3D('',#199750,#117805,#117806);
#99435=AXIS2_PLACEMENT_3D('',#199754,#117808,#117809);
#99436=AXIS2_PLACEMENT_3D('',#199756,#117811,#117812);
#99437=AXIS2_PLACEMENT_3D('',#199760,#117814,#117815);
#99438=AXIS2_PLACEMENT_3D('',#199762,#117817,#117818);
#99439=AXIS2_PLACEMENT_3D('',#199765,#117819,#117820);
#99440=AXIS2_PLACEMENT_3D('',#199768,#117823,#117824);
#99441=AXIS2_PLACEMENT_3D('',#199772,#117826,#117827);
#99442=AXIS2_PLACEMENT_3D('',#199774,#117829,#117830);
#99443=AXIS2_PLACEMENT_3D('',#199778,#117832,#117833);
#99444=AXIS2_PLACEMENT_3D('',#199780,#117835,#117836);
#99445=AXIS2_PLACEMENT_3D('',#199784,#117838,#117839);
#99446=AXIS2_PLACEMENT_3D('',#199786,#117841,#117842);
#99447=AXIS2_PLACEMENT_3D('',#199790,#117844,#117845);
#99448=AXIS2_PLACEMENT_3D('',#199792,#117847,#117848);
#99449=AXIS2_PLACEMENT_3D('',#199796,#117850,#117851);
#99450=AXIS2_PLACEMENT_3D('',#199798,#117853,#117854);
#99451=AXIS2_PLACEMENT_3D('',#199802,#117856,#117857);
#99452=AXIS2_PLACEMENT_3D('',#199804,#117859,#117860);
#99453=AXIS2_PLACEMENT_3D('',#199808,#117862,#117863);
#99454=AXIS2_PLACEMENT_3D('',#199810,#117865,#117866);
#99455=AXIS2_PLACEMENT_3D('',#199814,#117868,#117869);
#99456=AXIS2_PLACEMENT_3D('',#199816,#117871,#117872);
#99457=AXIS2_PLACEMENT_3D('',#199820,#117874,#117875);
#99458=AXIS2_PLACEMENT_3D('',#199822,#117877,#117878);
#99459=AXIS2_PLACEMENT_3D('',#199826,#117880,#117881);
#99460=AXIS2_PLACEMENT_3D('',#199828,#117883,#117884);
#99461=AXIS2_PLACEMENT_3D('',#199832,#117886,#117887);
#99462=AXIS2_PLACEMENT_3D('',#199834,#117889,#117890);
#99463=AXIS2_PLACEMENT_3D('',#199838,#117892,#117893);
#99464=AXIS2_PLACEMENT_3D('',#199840,#117895,#117896);
#99465=AXIS2_PLACEMENT_3D('',#199844,#117898,#117899);
#99466=AXIS2_PLACEMENT_3D('',#199846,#117901,#117902);
#99467=AXIS2_PLACEMENT_3D('',#199850,#117904,#117905);
#99468=AXIS2_PLACEMENT_3D('',#199852,#117907,#117908);
#99469=AXIS2_PLACEMENT_3D('',#199856,#117910,#117911);
#99470=AXIS2_PLACEMENT_3D('',#199858,#117913,#117914);
#99471=AXIS2_PLACEMENT_3D('',#199861,#117915,#117916);
#99472=AXIS2_PLACEMENT_3D('',#199864,#117919,#117920);
#99473=AXIS2_PLACEMENT_3D('',#199868,#117922,#117923);
#99474=AXIS2_PLACEMENT_3D('',#199870,#117925,#117926);
#99475=AXIS2_PLACEMENT_3D('',#199874,#117928,#117929);
#99476=AXIS2_PLACEMENT_3D('',#199876,#117931,#117932);
#99477=AXIS2_PLACEMENT_3D('',#199880,#117934,#117935);
#99478=AXIS2_PLACEMENT_3D('',#199882,#117937,#117938);
#99479=AXIS2_PLACEMENT_3D('',#199886,#117940,#117941);
#99480=AXIS2_PLACEMENT_3D('',#199888,#117943,#117944);
#99481=AXIS2_PLACEMENT_3D('',#199891,#117945,#117946);
#99482=AXIS2_PLACEMENT_3D('',#199894,#117949,#117950);
#99483=AXIS2_PLACEMENT_3D('',#199898,#117952,#117953);
#99484=AXIS2_PLACEMENT_3D('',#199900,#117955,#117956);
#99485=AXIS2_PLACEMENT_3D('',#199903,#117957,#117958);
#99486=AXIS2_PLACEMENT_3D('',#199906,#117961,#117962);
#99487=AXIS2_PLACEMENT_3D('',#199910,#117964,#117965);
#99488=AXIS2_PLACEMENT_3D('',#199912,#117967,#117968);
#99489=AXIS2_PLACEMENT_3D('',#199916,#117970,#117971);
#99490=AXIS2_PLACEMENT_3D('',#199918,#117973,#117974);
#99491=AXIS2_PLACEMENT_3D('',#199922,#117976,#117977);
#99492=AXIS2_PLACEMENT_3D('',#199924,#117979,#117980);
#99493=AXIS2_PLACEMENT_3D('',#199927,#117982,#117983);
#99494=AXIS2_PLACEMENT_3D('',#199928,#117984,#117985);
#99495=AXIS2_PLACEMENT_3D('',#199930,#117986,#117987);
#99496=AXIS2_PLACEMENT_3D('',#199932,#117989,#117990);
#99497=AXIS2_PLACEMENT_3D('',#199933,#117991,#117992);
#99498=AXIS2_PLACEMENT_3D('',#199934,#117993,#117994);
#99499=AXIS2_PLACEMENT_3D('',#199935,#117995,#117996);
#99500=AXIS2_PLACEMENT_3D('',#199936,#117997,#117998);
#99501=AXIS2_PLACEMENT_3D('',#199937,#117999,#118000);
#99502=AXIS2_PLACEMENT_3D('',#199938,#118001,#118002);
#99503=AXIS2_PLACEMENT_3D('',#199940,#118004,#118005);
#99504=AXIS2_PLACEMENT_3D('',#199942,#118007,#118008);
#99505=AXIS2_PLACEMENT_3D('',#199943,#118009,#118010);
#99506=AXIS2_PLACEMENT_3D('',#199944,#118011,#118012);
#99507=AXIS2_PLACEMENT_3D('',#199945,#118013,#118014);
#99508=AXIS2_PLACEMENT_3D('',#199946,#118015,#118016);
#99509=AXIS2_PLACEMENT_3D('',#199947,#118017,#118018);
#99510=AXIS2_PLACEMENT_3D('',#199948,#118019,#118020);
#99511=AXIS2_PLACEMENT_3D('',#199950,#118022,#118023);
#99512=AXIS2_PLACEMENT_3D('',#199952,#118025,#118026);
#99513=AXIS2_PLACEMENT_3D('',#199953,#118027,#118028);
#99514=AXIS2_PLACEMENT_3D('',#199954,#118029,#118030);
#99515=AXIS2_PLACEMENT_3D('',#199955,#118031,#118032);
#99516=AXIS2_PLACEMENT_3D('',#199956,#118033,#118034);
#99517=AXIS2_PLACEMENT_3D('',#199958,#118036,#118037);
#99518=AXIS2_PLACEMENT_3D('',#199960,#118039,#118040);
#99519=AXIS2_PLACEMENT_3D('',#199962,#118042,#118043);
#99520=AXIS2_PLACEMENT_3D('',#199964,#118045,#118046);
#99521=AXIS2_PLACEMENT_3D('',#199966,#118048,#118049);
#99522=AXIS2_PLACEMENT_3D('',#199968,#118051,#118052);
#99523=AXIS2_PLACEMENT_3D('',#199970,#118054,#118055);
#99524=AXIS2_PLACEMENT_3D('',#199972,#118057,#118058);
#99525=AXIS2_PLACEMENT_3D('',#199974,#118060,#118061);
#99526=AXIS2_PLACEMENT_3D('',#199976,#118063,#118064);
#99527=AXIS2_PLACEMENT_3D('',#199978,#118066,#118067);
#99528=AXIS2_PLACEMENT_3D('',#199980,#118069,#118070);
#99529=AXIS2_PLACEMENT_3D('',#199982,#118072,#118073);
#99530=AXIS2_PLACEMENT_3D('',#199984,#118075,#118076);
#99531=AXIS2_PLACEMENT_3D('',#199986,#118078,#118079);
#99532=AXIS2_PLACEMENT_3D('',#199988,#118081,#118082);
#99533=AXIS2_PLACEMENT_3D('',#199990,#118084,#118085);
#99534=AXIS2_PLACEMENT_3D('',#199992,#118087,#118088);
#99535=AXIS2_PLACEMENT_3D('',#199994,#118090,#118091);
#99536=AXIS2_PLACEMENT_3D('',#199996,#118093,#118094);
#99537=AXIS2_PLACEMENT_3D('',#199998,#118096,#118097);
#99538=AXIS2_PLACEMENT_3D('',#200000,#118099,#118100);
#99539=AXIS2_PLACEMENT_3D('',#200002,#118102,#118103);
#99540=AXIS2_PLACEMENT_3D('',#200004,#118105,#118106);
#99541=AXIS2_PLACEMENT_3D('',#200006,#118108,#118109);
#99542=AXIS2_PLACEMENT_3D('',#200008,#118111,#118112);
#99543=AXIS2_PLACEMENT_3D('',#200010,#118114,#118115);
#99544=AXIS2_PLACEMENT_3D('',#200012,#118117,#118118);
#99545=AXIS2_PLACEMENT_3D('',#200014,#118120,#118121);
#99546=AXIS2_PLACEMENT_3D('',#200016,#118123,#118124);
#99547=AXIS2_PLACEMENT_3D('',#200018,#118126,#118127);
#99548=AXIS2_PLACEMENT_3D('',#200020,#118129,#118130);
#99549=AXIS2_PLACEMENT_3D('',#200029,#118135,#118136);
#99550=AXIS2_PLACEMENT_3D('',#200035,#118140,#118141);
#99551=AXIS2_PLACEMENT_3D('',#200041,#118145,#118146);
#99552=AXIS2_PLACEMENT_3D('',#200043,#118148,#118149);
#99553=AXIS2_PLACEMENT_3D('',#200045,#118151,#118152);
#99554=AXIS2_PLACEMENT_3D('',#200047,#118154,#118155);
#99555=AXIS2_PLACEMENT_3D('',#200049,#118157,#118158);
#99556=AXIS2_PLACEMENT_3D('',#200051,#118160,#118161);
#99557=AXIS2_PLACEMENT_3D('',#200053,#118163,#118164);
#99558=AXIS2_PLACEMENT_3D('',#200055,#118166,#118167);
#99559=AXIS2_PLACEMENT_3D('',#200057,#118169,#118170);
#99560=AXIS2_PLACEMENT_3D('',#200059,#118172,#118173);
#99561=AXIS2_PLACEMENT_3D('',#200061,#118175,#118176);
#99562=AXIS2_PLACEMENT_3D('',#200063,#118178,#118179);
#99563=AXIS2_PLACEMENT_3D('',#200065,#118181,#118182);
#99564=AXIS2_PLACEMENT_3D('',#200067,#118184,#118185);
#99565=AXIS2_PLACEMENT_3D('',#200069,#118187,#118188);
#99566=AXIS2_PLACEMENT_3D('',#200071,#118190,#118191);
#99567=AXIS2_PLACEMENT_3D('',#200073,#118193,#118194);
#99568=AXIS2_PLACEMENT_3D('',#200075,#118196,#118197);
#99569=AXIS2_PLACEMENT_3D('',#200077,#118199,#118200);
#99570=AXIS2_PLACEMENT_3D('',#200079,#118202,#118203);
#99571=AXIS2_PLACEMENT_3D('',#200081,#118205,#118206);
#99572=AXIS2_PLACEMENT_3D('',#200083,#118208,#118209);
#99573=AXIS2_PLACEMENT_3D('',#200085,#118211,#118212);
#99574=AXIS2_PLACEMENT_3D('',#200090,#118214,#118215);
#99575=AXIS2_PLACEMENT_3D('',#200093,#118217,#118218);
#99576=AXIS2_PLACEMENT_3D('',#200094,#118219,#118220);
#99577=AXIS2_PLACEMENT_3D('',#200096,#118221,#118222);
#99578=AXIS2_PLACEMENT_3D('',#200099,#118224,#118225);
#99579=AXIS2_PLACEMENT_3D('',#200100,#118226,#118227);
#99580=AXIS2_PLACEMENT_3D('',#200102,#118228,#118229);
#99581=AXIS2_PLACEMENT_3D('',#200105,#118231,#118232);
#99582=AXIS2_PLACEMENT_3D('',#200106,#118233,#118234);
#99583=AXIS2_PLACEMENT_3D('',#200108,#118235,#118236);
#99584=AXIS2_PLACEMENT_3D('',#200111,#118238,#118239);
#99585=AXIS2_PLACEMENT_3D('',#200112,#118240,#118241);
#99586=AXIS2_PLACEMENT_3D('',#200114,#118242,#118243);
#99587=AXIS2_PLACEMENT_3D('',#200117,#118245,#118246);
#99588=AXIS2_PLACEMENT_3D('',#200118,#118247,#118248);
#99589=AXIS2_PLACEMENT_3D('',#200120,#118249,#118250);
#99590=AXIS2_PLACEMENT_3D('',#200123,#118252,#118253);
#99591=AXIS2_PLACEMENT_3D('',#200124,#118254,#118255);
#99592=AXIS2_PLACEMENT_3D('',#200126,#118256,#118257);
#99593=AXIS2_PLACEMENT_3D('',#200129,#118259,#118260);
#99594=AXIS2_PLACEMENT_3D('',#200130,#118261,#118262);
#99595=AXIS2_PLACEMENT_3D('',#200135,#118264,#118265);
#99596=AXIS2_PLACEMENT_3D('',#200144,#118267,#118268);
#99597=AXIS2_PLACEMENT_3D('',#200153,#118270,#118271);
#99598=AXIS2_PLACEMENT_3D('',#200156,#118272,#118273);
#99599=AXIS2_PLACEMENT_3D('',#200165,#118275,#118276);
#99600=AXIS2_PLACEMENT_3D('',#200174,#118278,#118279);
#99601=AXIS2_PLACEMENT_3D('',#200190,#118282,#118283);
#99602=AXIS2_PLACEMENT_3D('',#200206,#118286,#118287);
#99603=AXIS2_PLACEMENT_3D('',#200207,#118288,#118289);
#99604=AXIS2_PLACEMENT_3D('',#200208,#118290,#118291);
#99605=AXIS2_PLACEMENT_3D('',#200209,#118292,#118293);
#99606=AXIS2_PLACEMENT_3D('',#200225,#118296,#118297);
#99607=AXIS2_PLACEMENT_3D('',#200241,#118300,#118301);
#99608=AXIS2_PLACEMENT_3D('',#200242,#118302,#118303);
#99609=AXIS2_PLACEMENT_3D('',#200243,#118304,#118305);
#99610=AXIS2_PLACEMENT_3D('',#200244,#118306,#118307);
#99611=AXIS2_PLACEMENT_3D('',#200247,#118308,#118309);
#99612=AXIS2_PLACEMENT_3D('',#200251,#118311,#118312);
#99613=AXIS2_PLACEMENT_3D('',#200253,#118314,#118315);
#99614=AXIS2_PLACEMENT_3D('',#200256,#118316,#118317);
#99615=AXIS2_PLACEMENT_3D('',#200260,#118319,#118320);
#99616=AXIS2_PLACEMENT_3D('',#200262,#118322,#118323);
#99617=AXIS2_PLACEMENT_3D('',#200264,#118324,#118325);
#99618=AXIS2_PLACEMENT_3D('',#200267,#118327,#118328);
#99619=AXIS2_PLACEMENT_3D('',#200268,#118329,#118330);
#99620=AXIS2_PLACEMENT_3D('',#200270,#118331,#118332);
#99621=AXIS2_PLACEMENT_3D('',#200273,#118334,#118335);
#99622=AXIS2_PLACEMENT_3D('',#200274,#118336,#118337);
#99623=AXIS2_PLACEMENT_3D('',#200283,#118338,#118339);
#99624=AXIS2_PLACEMENT_3D('',#200284,#118340,#118341);
#99625=AXIS2_PLACEMENT_3D('',#200285,#118342,#118343);
#99626=AXIS2_PLACEMENT_3D('',#200288,#118344,#118345);
#99627=AXIS2_PLACEMENT_3D('',#200292,#118347,#118348);
#99628=AXIS2_PLACEMENT_3D('',#200294,#118350,#118351);
#99629=AXIS2_PLACEMENT_3D('',#200295,#118352,#118353);
#99630=AXIS2_PLACEMENT_3D('',#200296,#118354,#118355);
#99631=AXIS2_PLACEMENT_3D('',#202382,#118356,#118357);
#99632=AXIS2_PLACEMENT_3D('',#202385,#118358,#118359);
#99633=AXIS2_PLACEMENT_3D('',#202395,#118362,#118363);
#99634=AXIS2_PLACEMENT_3D('',#202413,#118365,#118366);
#99635=AXIS2_PLACEMENT_3D('',#202414,#118367,#118368);
#99636=AXIS2_PLACEMENT_3D('',#202416,#118369,#118370);
#99637=AXIS2_PLACEMENT_3D('',#202417,#118371,#118372);
#99638=AXIS2_PLACEMENT_3D('',#202419,#118374,#118375);
#99639=AXIS2_PLACEMENT_3D('',#202422,#118376,#118377);
#99640=AXIS2_PLACEMENT_3D('',#202425,#118379,#118380);
#99641=AXIS2_PLACEMENT_3D('',#202427,#118382,#118383);
#99642=AXIS2_PLACEMENT_3D('',#202439,#118385,#118386);
#99643=AXIS2_PLACEMENT_3D('',#202448,#118387,#118388);
#99644=AXIS2_PLACEMENT_3D('',#202450,#118389,#118390);
#99645=AXIS2_PLACEMENT_3D('',#202451,#118391,#118392);
#99646=AXIS2_PLACEMENT_3D('',#202453,#118394,#118395);
#99647=AXIS2_PLACEMENT_3D('',#202456,#118396,#118397);
#99648=AXIS2_PLACEMENT_3D('',#202460,#118399,#118400);
#99649=AXIS2_PLACEMENT_3D('',#202462,#118402,#118403);
#99650=AXIS2_PLACEMENT_3D('',#202464,#118404,#118405);
#99651=AXIS2_PLACEMENT_3D('',#202466,#118406,#118407);
#99652=AXIS2_PLACEMENT_3D('',#202468,#118409,#118410);
#99653=AXIS2_PLACEMENT_3D('',#202470,#118411,#118412);
#99654=AXIS2_PLACEMENT_3D('',#202472,#118413,#118414);
#99655=AXIS2_PLACEMENT_3D('',#202474,#118416,#118417);
#99656=AXIS2_PLACEMENT_3D('',#202476,#118418,#118419);
#99657=AXIS2_PLACEMENT_3D('',#202478,#118420,#118421);
#99658=AXIS2_PLACEMENT_3D('',#202480,#118423,#118424);
#99659=AXIS2_PLACEMENT_3D('',#202483,#118425,#118426);
#99660=AXIS2_PLACEMENT_3D('',#202487,#118428,#118429);
#99661=AXIS2_PLACEMENT_3D('',#202489,#118431,#118432);
#99662=AXIS2_PLACEMENT_3D('',#202491,#118433,#118434);
#99663=AXIS2_PLACEMENT_3D('',#202493,#118435,#118436);
#99664=AXIS2_PLACEMENT_3D('',#202495,#118438,#118439);
#99665=AXIS2_PLACEMENT_3D('',#202496,#118440,#118441);
#99666=AXIS2_PLACEMENT_3D('',#202497,#118442,#118443);
#99667=AXIS2_PLACEMENT_3D('',#202570,#118444,#118445);
#99668=AXIS2_PLACEMENT_3D('',#202752,#118446,#118447);
#99669=AXIS2_PLACEMENT_3D('',#202770,#118448,#118449);
#99670=AXIS2_PLACEMENT_3D('',#202854,#118450,#118451);
#99671=AXIS2_PLACEMENT_3D('',#202856,#118452,#118453);
#99672=AXIS2_PLACEMENT_3D('',#202880,#118454,#118455);
#99673=AXIS2_PLACEMENT_3D('',#202888,#118456,#118457);
#99674=AXIS2_PLACEMENT_3D('',#202952,#118458,#118459);
#99675=AXIS2_PLACEMENT_3D('',#202967,#118460,#118461);
#99676=AXIS2_PLACEMENT_3D('',#203229,#118462,#118463);
#99677=AXIS2_PLACEMENT_3D('',#203238,#118464,#118465);
#99678=AXIS2_PLACEMENT_3D('',#203562,#118466,#118467);
#99679=AXIS2_PLACEMENT_3D('',#203565,#118468,#118469);
#99680=AXIS2_PLACEMENT_3D('',#203572,#118470,#118471);
#99681=AXIS2_PLACEMENT_3D('',#203580,#118472,#118473);
#99682=AXIS2_PLACEMENT_3D('',#203587,#118474,#118475);
#99683=AXIS2_PLACEMENT_3D('',#203590,#118476,#118477);
#99684=AXIS2_PLACEMENT_3D('',#203597,#118478,#118479);
#99685=AXIS2_PLACEMENT_3D('',#203600,#118480,#118481);
#99686=AXIS2_PLACEMENT_3D('',#203607,#118482,#118483);
#99687=AXIS2_PLACEMENT_3D('',#203610,#118484,#118485);
#99688=AXIS2_PLACEMENT_3D('',#203617,#118486,#118487);
#99689=AXIS2_PLACEMENT_3D('',#203626,#118488,#118489);
#99690=AXIS2_PLACEMENT_3D('',#203627,#118490,#118491);
#99691=AXIS2_PLACEMENT_3D('',#203629,#118492,#118493);
#99692=AXIS2_PLACEMENT_3D('',#203631,#118495,#118496);
#99693=AXIS2_PLACEMENT_3D('',#203642,#118497,#118498);
#99694=AXIS2_PLACEMENT_3D('',#203651,#118499,#118500);
#99695=AXIS2_PLACEMENT_3D('',#203654,#118501,#118502);
#99696=AXIS2_PLACEMENT_3D('',#203669,#118503,#118504);
#99697=AXIS2_PLACEMENT_3D('',#203671,#118505,#118506);
#99698=AXIS2_PLACEMENT_3D('',#203678,#118507,#118508);
#99699=AXIS2_PLACEMENT_3D('',#203681,#118509,#118510);
#99700=AXIS2_PLACEMENT_3D('',#203698,#118511,#118512);
#99701=AXIS2_PLACEMENT_3D('',#203726,#118513,#118514);
#99702=AXIS2_PLACEMENT_3D('',#203727,#118515,#118516);
#99703=AXIS2_PLACEMENT_3D('',#203729,#118518,#118519);
#99704=AXIS2_PLACEMENT_3D('',#203731,#118521,#118522);
#99705=AXIS2_PLACEMENT_3D('',#204865,#118523,#118524);
#99706=AXIS2_PLACEMENT_3D('',#204866,#118525,#118526);
#99707=AXIS2_PLACEMENT_3D('',#204870,#118528,#118529);
#99708=AXIS2_PLACEMENT_3D('',#204872,#118531,#118532);
#99709=AXIS2_PLACEMENT_3D('',#204874,#118533,#118534);
#99710=AXIS2_PLACEMENT_3D('',#204876,#118536,#118537);
#99711=AXIS2_PLACEMENT_3D('',#204878,#118538,#118539);
#99712=AXIS2_PLACEMENT_3D('',#204880,#118541,#118542);
#99713=AXIS2_PLACEMENT_3D('',#204881,#118543,#118544);
#99714=AXIS2_PLACEMENT_3D('',#204882,#118545,#118546);
#99715=AXIS2_PLACEMENT_3D('',#204886,#118548,#118549);
#99716=AXIS2_PLACEMENT_3D('',#204888,#118551,#118552);
#99717=AXIS2_PLACEMENT_3D('',#204889,#118553,#118554);
#99718=AXIS2_PLACEMENT_3D('',#204890,#118555,#118556);
#99719=AXIS2_PLACEMENT_3D('',#204894,#118558,#118559);
#99720=AXIS2_PLACEMENT_3D('',#204896,#118561,#118562);
#99721=AXIS2_PLACEMENT_3D('',#204898,#118563,#118564);
#99722=AXIS2_PLACEMENT_3D('',#204899,#118565,#118566);
#99723=AXIS2_PLACEMENT_3D('',#204902,#118568,#118569);
#99724=AXIS2_PLACEMENT_3D('',#204903,#118570,#118571);
#99725=AXIS2_PLACEMENT_3D('',#204904,#118572,#118573);
#99726=AXIS2_PLACEMENT_3D('',#204906,#118574,#118575);
#99727=AXIS2_PLACEMENT_3D('',#204907,#118576,#118577);
#99728=AXIS2_PLACEMENT_3D('',#204909,#118579,#118580);
#99729=AXIS2_PLACEMENT_3D('',#204910,#118581,#118582);
#99730=AXIS2_PLACEMENT_3D('',#204911,#118583,#118584);
#99731=AXIS2_PLACEMENT_3D('',#204912,#118585,#118586);
#99732=AXIS2_PLACEMENT_3D('',#204913,#118587,#118588);
#99733=AXIS2_PLACEMENT_3D('',#204914,#118589,#118590);
#99734=AXIS2_PLACEMENT_3D('',#204915,#118591,#118592);
#99735=AXIS2_PLACEMENT_3D('',#204916,#118593,#118594);
#99736=AXIS2_PLACEMENT_3D('',#204917,#118595,#118596);
#99737=AXIS2_PLACEMENT_3D('',#204918,#118597,#118598);
#99738=AXIS2_PLACEMENT_3D('',#204919,#118599,#118600);
#99739=AXIS2_PLACEMENT_3D('',#204920,#118601,#118602);
#99740=AXIS2_PLACEMENT_3D('',#204921,#118603,#118604);
#99741=AXIS2_PLACEMENT_3D('',#204922,#118605,#118606);
#99742=AXIS2_PLACEMENT_3D('',#204923,#118607,#118608);
#99743=AXIS2_PLACEMENT_3D('',#205008,#118609,#118610);
#99744=AXIS2_PLACEMENT_3D('',#205012,#118612,#118613);
#99745=AXIS2_PLACEMENT_3D('',#205014,#118615,#118616);
#99746=AXIS2_PLACEMENT_3D('',#205017,#118618,#118619);
#99747=AXIS2_PLACEMENT_3D('',#205018,#118620,#118621);
#99748=AXIS2_PLACEMENT_3D('',#205021,#118623,#118624);
#99749=AXIS2_PLACEMENT_3D('',#205022,#118625,#118626);
#99750=AXIS2_PLACEMENT_3D('',#205025,#118628,#118629);
#99751=AXIS2_PLACEMENT_3D('',#205026,#118630,#118631);
#99752=AXIS2_PLACEMENT_3D('',#205029,#118633,#118634);
#99753=AXIS2_PLACEMENT_3D('',#205030,#118635,#118636);
#99754=AXIS2_PLACEMENT_3D('',#205033,#118638,#118639);
#99755=AXIS2_PLACEMENT_3D('',#205034,#118640,#118641);
#99756=AXIS2_PLACEMENT_3D('',#205036,#118642,#118643);
#99757=AXIS2_PLACEMENT_3D('',#205038,#118645,#118646);
#99758=AXIS2_PLACEMENT_3D('',#205042,#118648,#118649);
#99759=AXIS2_PLACEMENT_3D('',#205044,#118651,#118652);
#99760=AXIS2_PLACEMENT_3D('',#205048,#118654,#118655);
#99761=AXIS2_PLACEMENT_3D('',#205050,#118657,#118658);
#99762=AXIS2_PLACEMENT_3D('',#205052,#118659,#118660);
#99763=AXIS2_PLACEMENT_3D('',#205054,#118662,#118663);
#99764=AXIS2_PLACEMENT_3D('',#205056,#118664,#118665);
#99765=AXIS2_PLACEMENT_3D('',#205058,#118667,#118668);
#99766=AXIS2_PLACEMENT_3D('',#205060,#118669,#118670);
#99767=AXIS2_PLACEMENT_3D('',#205062,#118672,#118673);
#99768=AXIS2_PLACEMENT_3D('',#205064,#118674,#118675);
#99769=AXIS2_PLACEMENT_3D('',#205066,#118677,#118678);
#99770=AXIS2_PLACEMENT_3D('',#205067,#118679,#118680);
#99771=AXIS2_PLACEMENT_3D('',#205459,#118685,#118686);
#99772=AXIS2_PLACEMENT_3D('',#205462,#118689,#118690);
#99773=AXIS2_PLACEMENT_3D('',#205464,#118692,#118693);
#99774=AXIS2_PLACEMENT_3D('',#205466,#118695,#118696);
#99775=AXIS2_PLACEMENT_3D('',#205469,#118699,#118700);
#99776=AXIS2_PLACEMENT_3D('',#205471,#118702,#118703);
#99777=AXIS2_PLACEMENT_3D('',#205473,#118705,#118706);
#99778=AXIS2_PLACEMENT_3D('',#205477,#118708,#118709);
#99779=AXIS2_PLACEMENT_3D('',#205479,#118711,#118712);
#99780=AXIS2_PLACEMENT_3D('',#205481,#118713,#118714);
#99781=AXIS2_PLACEMENT_3D('',#205483,#118716,#118717);
#99782=AXIS2_PLACEMENT_3D('',#205485,#118718,#118719);
#99783=AXIS2_PLACEMENT_3D('',#205487,#118721,#118722);
#99784=AXIS2_PLACEMENT_3D('',#205489,#118723,#118724);
#99785=AXIS2_PLACEMENT_3D('',#205491,#118726,#118727);
#99786=AXIS2_PLACEMENT_3D('',#205495,#118729,#118730);
#99787=AXIS2_PLACEMENT_3D('',#205497,#118732,#118733);
#99788=AXIS2_PLACEMENT_3D('',#205499,#118734,#118735);
#99789=AXIS2_PLACEMENT_3D('',#205501,#118737,#118738);
#99790=AXIS2_PLACEMENT_3D('',#205502,#118739,#118740);
#99791=AXIS2_PLACEMENT_3D('',#205580,#118741,#118742);
#99792=AXIS2_PLACEMENT_3D('',#205679,#118743,#118744);
#99793=AXIS2_PLACEMENT_3D('',#206368,#118745,#118746);
#99794=AXIS2_PLACEMENT_3D('',#206961,#118747,#118748);
#99795=AXIS2_PLACEMENT_3D('',#206962,#118749,#118750);
#99796=AXIS2_PLACEMENT_3D('',#206963,#118751,#118752);
#99797=AXIS2_PLACEMENT_3D('',#206964,#118753,#118754);
#99798=AXIS2_PLACEMENT_3D('',#206965,#118755,#118756);
#99799=AXIS2_PLACEMENT_3D('',#206966,#118757,#118758);
#99800=AXIS2_PLACEMENT_3D('',#206967,#118759,#118760);
#99801=AXIS2_PLACEMENT_3D('',#206968,#118761,#118762);
#99802=AXIS2_PLACEMENT_3D('',#206969,#118763,#118764);
#99803=AXIS2_PLACEMENT_3D('',#206970,#118765,#118766);
#99804=AXIS2_PLACEMENT_3D('',#206971,#118767,#118768);
#99805=AXIS2_PLACEMENT_3D('',#206973,#118770,#118771);
#99806=AXIS2_PLACEMENT_3D('',#206975,#118773,#118774);
#99807=AXIS2_PLACEMENT_3D('',#206977,#118776,#118777);
#99808=AXIS2_PLACEMENT_3D('',#206979,#118779,#118780);
#99809=AXIS2_PLACEMENT_3D('',#206981,#118782,#118783);
#99810=AXIS2_PLACEMENT_3D('',#206983,#118785,#118786);
#99811=AXIS2_PLACEMENT_3D('',#206985,#118788,#118789);
#99812=AXIS2_PLACEMENT_3D('',#206987,#118791,#118792);
#99813=AXIS2_PLACEMENT_3D('',#206989,#118794,#118795);
#99814=AXIS2_PLACEMENT_3D('',#206991,#118797,#118798);
#99815=AXIS2_PLACEMENT_3D('',#206992,#118799,#118800);
#99816=AXIS2_PLACEMENT_3D('',#206993,#118801,#118802);
#99817=AXIS2_PLACEMENT_3D('',#206994,#118803,#118804);
#99818=AXIS2_PLACEMENT_3D('',#206995,#118805,#118806);
#99819=AXIS2_PLACEMENT_3D('',#206996,#118807,#118808);
#99820=AXIS2_PLACEMENT_3D('',#206997,#118809,#118810);
#99821=AXIS2_PLACEMENT_3D('',#206998,#118811,#118812);
#99822=AXIS2_PLACEMENT_3D('',#207000,#118814,#118815);
#99823=AXIS2_PLACEMENT_3D('',#207002,#118817,#118818);
#99824=AXIS2_PLACEMENT_3D('',#207004,#118820,#118821);
#99825=AXIS2_PLACEMENT_3D('',#207006,#118823,#118824);
#99826=AXIS2_PLACEMENT_3D('',#207008,#118826,#118827);
#99827=AXIS2_PLACEMENT_3D('',#207010,#118829,#118830);
#99828=AXIS2_PLACEMENT_3D('',#207012,#118832,#118833);
#99829=AXIS2_PLACEMENT_3D('',#207014,#118835,#118836);
#99830=AXIS2_PLACEMENT_3D('',#207016,#118838,#118839);
#99831=AXIS2_PLACEMENT_3D('',#207018,#118841,#118842);
#99832=AXIS2_PLACEMENT_3D('',#207020,#118844,#118845);
#99833=AXIS2_PLACEMENT_3D('',#207022,#118847,#118848);
#99834=AXIS2_PLACEMENT_3D('',#207024,#118850,#118851);
#99835=AXIS2_PLACEMENT_3D('',#207026,#118853,#118854);
#99836=AXIS2_PLACEMENT_3D('',#207027,#118855,#118856);
#99837=AXIS2_PLACEMENT_3D('',#207028,#118857,#118858);
#99838=AXIS2_PLACEMENT_3D('',#207029,#118859,#118860);
#99839=AXIS2_PLACEMENT_3D('',#207030,#118861,#118862);
#99840=AXIS2_PLACEMENT_3D('',#207031,#118863,#118864);
#99841=AXIS2_PLACEMENT_3D('',#207032,#118865,#118866);
#99842=AXIS2_PLACEMENT_3D('',#207033,#118867,#118868);
#99843=AXIS2_PLACEMENT_3D('',#207034,#118869,#118870);
#99844=AXIS2_PLACEMENT_3D('',#207035,#118871,#118872);
#99845=AXIS2_PLACEMENT_3D('',#207036,#118873,#118874);
#99846=AXIS2_PLACEMENT_3D('',#207037,#118875,#118876);
#99847=AXIS2_PLACEMENT_3D('',#207038,#118877,#118878);
#99848=AXIS2_PLACEMENT_3D('',#207039,#118879,#118880);
#99849=AXIS2_PLACEMENT_3D('',#207040,#118881,#118882);
#99850=AXIS2_PLACEMENT_3D('',#207041,#118883,#118884);
#99851=AXIS2_PLACEMENT_3D('',#207042,#118885,#118886);
#99852=AXIS2_PLACEMENT_3D('',#207044,#118888,#118889);
#99853=AXIS2_PLACEMENT_3D('',#207046,#118891,#118892);
#99854=AXIS2_PLACEMENT_3D('',#207048,#118894,#118895);
#99855=AXIS2_PLACEMENT_3D('',#207050,#118897,#118898);
#99856=AXIS2_PLACEMENT_3D('',#207052,#118900,#118901);
#99857=AXIS2_PLACEMENT_3D('',#207054,#118903,#118904);
#99858=AXIS2_PLACEMENT_3D('',#207056,#118906,#118907);
#99859=AXIS2_PLACEMENT_3D('',#207058,#118909,#118910);
#99860=AXIS2_PLACEMENT_3D('',#207060,#118912,#118913);
#99861=AXIS2_PLACEMENT_3D('',#207062,#118915,#118916);
#99862=AXIS2_PLACEMENT_3D('',#207064,#118918,#118919);
#99863=AXIS2_PLACEMENT_3D('',#207066,#118921,#118922);
#99864=AXIS2_PLACEMENT_3D('',#207068,#118924,#118925);
#99865=AXIS2_PLACEMENT_3D('',#207070,#118927,#118928);
#99866=AXIS2_PLACEMENT_3D('',#207072,#118930,#118931);
#99867=AXIS2_PLACEMENT_3D('',#207074,#118933,#118934);
#99868=AXIS2_PLACEMENT_3D('',#207076,#118936,#118937);
#99869=AXIS2_PLACEMENT_3D('',#207078,#118939,#118940);
#99870=AXIS2_PLACEMENT_3D('',#207080,#118942,#118943);
#99871=AXIS2_PLACEMENT_3D('',#207082,#118945,#118946);
#99872=AXIS2_PLACEMENT_3D('',#207084,#118948,#118949);
#99873=AXIS2_PLACEMENT_3D('',#207086,#118951,#118952);
#99874=AXIS2_PLACEMENT_3D('',#207088,#118954,#118955);
#99875=AXIS2_PLACEMENT_3D('',#207090,#118957,#118958);
#99876=AXIS2_PLACEMENT_3D('',#207092,#118960,#118961);
#99877=AXIS2_PLACEMENT_3D('',#207094,#118963,#118964);
#99878=AXIS2_PLACEMENT_3D('',#207096,#118966,#118967);
#99879=AXIS2_PLACEMENT_3D('',#207118,#118969,#118970);
#99880=AXIS2_PLACEMENT_3D('',#207173,#118971,#118972);
#99881=AXIS2_PLACEMENT_3D('',#207199,#118973,#118974);
#99882=AXIS2_PLACEMENT_3D('',#207200,#118975,#118976);
#99883=AXIS2_PLACEMENT_3D('',#207202,#118977,#118978);
#99884=AXIS2_PLACEMENT_3D('',#207203,#118979,#118980);
#99885=AXIS2_PLACEMENT_3D('',#207204,#118981,#118982);
#99886=AXIS2_PLACEMENT_3D('',#207206,#118983,#118984);
#99887=AXIS2_PLACEMENT_3D('',#207208,#118985,#118986);
#99888=AXIS2_PLACEMENT_3D('',#207210,#118987,#118988);
#99889=AXIS2_PLACEMENT_3D('',#207211,#118989,#118990);
#99890=AXIS2_PLACEMENT_3D('',#207244,#118991,#118992);
#99891=AXIS2_PLACEMENT_3D('',#207326,#118993,#118994);
#99892=AXIS2_PLACEMENT_3D('',#207372,#118995,#118996);
#99893=AXIS2_PLACEMENT_3D('',#207423,#118997,#118998);
#99894=AXIS2_PLACEMENT_3D('',#207425,#118999,#119000);
#99895=AXIS2_PLACEMENT_3D('',#207426,#119001,#119002);
#99896=AXIS2_PLACEMENT_3D('',#207459,#119003,#119004);
#99897=AXIS2_PLACEMENT_3D('',#207523,#119005,#119006);
#99898=AXIS2_PLACEMENT_3D('',#207526,#119007,#119008);
#99899=AXIS2_PLACEMENT_3D('',#207527,#119009,#119010);
#99900=AXIS2_PLACEMENT_3D('',#207528,#119011,#119012);
#99901=AXIS2_PLACEMENT_3D('',#207549,#119013,#119014);
#99902=AXIS2_PLACEMENT_3D('',#207582,#119015,#119016);
#99903=AXIS2_PLACEMENT_3D('',#207585,#119017,#119018);
#99904=AXIS2_PLACEMENT_3D('',#207586,#119019,#119020);
#99905=AXIS2_PLACEMENT_3D('',#207587,#119021,#119022);
#99906=AXIS2_PLACEMENT_3D('',#207620,#119023,#119024);
#99907=AXIS2_PLACEMENT_3D('',#207743,#119025,#119026);
#99908=AXIS2_PLACEMENT_3D('',#207746,#119027,#119028);
#99909=AXIS2_PLACEMENT_3D('',#207747,#119029,#119030);
#99910=AXIS2_PLACEMENT_3D('',#207748,#119031,#119032);
#99911=AXIS2_PLACEMENT_3D('',#207763,#119033,#119034);
#99912=AXIS2_PLACEMENT_3D('',#207797,#119035,#119036);
#99913=AXIS2_PLACEMENT_3D('',#207855,#119037,#119038);
#99914=AXIS2_PLACEMENT_3D('',#207961,#119039,#119040);
#99915=AXIS2_PLACEMENT_3D('',#207962,#119041,#119042);
#99916=AXIS2_PLACEMENT_3D('',#207963,#119043,#119044);
#99917=AXIS2_PLACEMENT_3D('',#208002,#119045,#119046);
#99918=AXIS2_PLACEMENT_3D('',#208039,#119047,#119048);
#99919=AXIS2_PLACEMENT_3D('',#208081,#119049,#119050);
#99920=AXIS2_PLACEMENT_3D('',#208110,#119051,#119052);
#99921=AXIS2_PLACEMENT_3D('',#208160,#119053,#119054);
#99922=AXIS2_PLACEMENT_3D('',#208333,#119055,#119056);
#99923=AXIS2_PLACEMENT_3D('',#208397,#119057,#119058);
#99924=AXIS2_PLACEMENT_3D('',#208399,#119059,#119060);
#99925=AXIS2_PLACEMENT_3D('',#208400,#119061,#119062);
#99926=AXIS2_PLACEMENT_3D('',#208415,#119063,#119064);
#99927=AXIS2_PLACEMENT_3D('',#208449,#119065,#119066);
#99928=AXIS2_PLACEMENT_3D('',#208484,#119067,#119068);
#99929=AXIS2_PLACEMENT_3D('',#208589,#119069,#119070);
#99930=AXIS2_PLACEMENT_3D('',#208592,#119071,#119072);
#99931=AXIS2_PLACEMENT_3D('',#208593,#119073,#119074);
#99932=AXIS2_PLACEMENT_3D('',#208594,#119075,#119076);
#99933=AXIS2_PLACEMENT_3D('',#208595,#119077,#119078);
#99934=AXIS2_PLACEMENT_3D('',#208597,#119079,#119080);
#99935=AXIS2_PLACEMENT_3D('',#208598,#119081,#119082);
#99936=AXIS2_PLACEMENT_3D('',#208599,#119083,#119084);
#99937=AXIS2_PLACEMENT_3D('',#208602,#119085,#119086);
#99938=AXIS2_PLACEMENT_3D('',#208603,#119087,#119088);
#99939=AXIS2_PLACEMENT_3D('',#208604,#119089,#119090);
#99940=AXIS2_PLACEMENT_3D('',#208619,#119091,#119092);
#99941=AXIS2_PLACEMENT_3D('',#208628,#119093,#119094);
#99942=AXIS2_PLACEMENT_3D('',#208629,#119095,#119096);
#99943=AXIS2_PLACEMENT_3D('',#208630,#119097,#119098);
#99944=AXIS2_PLACEMENT_3D('',#208631,#119099,#119100);
#99945=AXIS2_PLACEMENT_3D('',#208633,#119101,#119102);
#99946=AXIS2_PLACEMENT_3D('',#208635,#119103,#119104);
#99947=AXIS2_PLACEMENT_3D('',#208636,#119105,#119106);
#99948=AXIS2_PLACEMENT_3D('',#208637,#119107,#119108);
#99949=AXIS2_PLACEMENT_3D('',#208640,#119109,#119110);
#99950=AXIS2_PLACEMENT_3D('',#208641,#119111,#119112);
#99951=AXIS2_PLACEMENT_3D('',#208642,#119113,#119114);
#99952=AXIS2_PLACEMENT_3D('',#208643,#119115,#119116);
#99953=AXIS2_PLACEMENT_3D('',#208646,#119117,#119118);
#99954=AXIS2_PLACEMENT_3D('',#208647,#119119,#119120);
#99955=AXIS2_PLACEMENT_3D('',#208648,#119121,#119122);
#99956=AXIS2_PLACEMENT_3D('',#208649,#119123,#119124);
#99957=AXIS2_PLACEMENT_3D('',#208652,#119125,#119126);
#99958=AXIS2_PLACEMENT_3D('',#208653,#119127,#119128);
#99959=AXIS2_PLACEMENT_3D('',#208654,#119129,#119130);
#99960=AXIS2_PLACEMENT_3D('',#208655,#119131,#119132);
#99961=AXIS2_PLACEMENT_3D('',#208658,#119133,#119134);
#99962=AXIS2_PLACEMENT_3D('',#208659,#119135,#119136);
#99963=AXIS2_PLACEMENT_3D('',#208660,#119137,#119138);
#99964=AXIS2_PLACEMENT_3D('',#208661,#119139,#119140);
#99965=AXIS2_PLACEMENT_3D('',#208664,#119141,#119142);
#99966=AXIS2_PLACEMENT_3D('',#208665,#119143,#119144);
#99967=AXIS2_PLACEMENT_3D('',#208666,#119145,#119146);
#99968=AXIS2_PLACEMENT_3D('',#208667,#119147,#119148);
#99969=AXIS2_PLACEMENT_3D('',#208670,#119149,#119150);
#99970=AXIS2_PLACEMENT_3D('',#208671,#119151,#119152);
#99971=AXIS2_PLACEMENT_3D('',#208672,#119153,#119154);
#99972=AXIS2_PLACEMENT_3D('',#208673,#119155,#119156);
#99973=AXIS2_PLACEMENT_3D('',#208676,#119157,#119158);
#99974=AXIS2_PLACEMENT_3D('',#208677,#119159,#119160);
#99975=AXIS2_PLACEMENT_3D('',#208678,#119161,#119162);
#99976=AXIS2_PLACEMENT_3D('',#208679,#119163,#119164);
#99977=AXIS2_PLACEMENT_3D('',#208680,#119165,#119166);
#99978=AXIS2_PLACEMENT_3D('',#208681,#119167,#119168);
#99979=AXIS2_PLACEMENT_3D('',#208695,#119169,#119170);
#99980=AXIS2_PLACEMENT_3D('',#208697,#119171,#119172);
#99981=AXIS2_PLACEMENT_3D('',#208698,#119173,#119174);
#99982=AXIS2_PLACEMENT_3D('',#208713,#119175,#119176);
#99983=AXIS2_PLACEMENT_3D('',#208718,#119177,#119178);
#99984=AXIS2_PLACEMENT_3D('',#208812,#119179,#119180);
#99985=AXIS2_PLACEMENT_3D('',#208851,#119181,#119182);
#99986=AXIS2_PLACEMENT_3D('',#209013,#119183,#119184);
#99987=AXIS2_PLACEMENT_3D('',#209014,#119185,#119186);
#99988=AXIS2_PLACEMENT_3D('',#209015,#119187,#119188);
#99989=AXIS2_PLACEMENT_3D('',#209030,#119189,#119190);
#99990=AXIS2_PLACEMENT_3D('',#209031,#119191,#119192);
#99991=AXIS2_PLACEMENT_3D('',#209032,#119193,#119194);
#99992=AXIS2_PLACEMENT_3D('',#209047,#119195,#119196);
#99993=AXIS2_PLACEMENT_3D('',#209121,#119197,#119198);
#99994=AXIS2_PLACEMENT_3D('',#209210,#119199,#119200);
#99995=AXIS2_PLACEMENT_3D('',#209379,#119201,#119202);
#99996=AXIS2_PLACEMENT_3D('',#209565,#119203,#119204);
#99997=AXIS2_PLACEMENT_3D('',#209737,#119205,#119206);
#99998=AXIS2_PLACEMENT_3D('',#209857,#119207,#119208);
#99999=AXIS2_PLACEMENT_3D('',#209858,#119209,#119210);
#100000=AXIS2_PLACEMENT_3D('',#209859,#119211,#119212);
#100001=AXIS2_PLACEMENT_3D('',#209916,#119213,#119214);
#100002=AXIS2_PLACEMENT_3D('',#210016,#119215,#119216);
#100003=AXIS2_PLACEMENT_3D('',#210035,#119217,#119218);
#100004=AXIS2_PLACEMENT_3D('',#210038,#119219,#119220);
#100005=AXIS2_PLACEMENT_3D('',#210039,#119221,#119222);
#100006=AXIS2_PLACEMENT_3D('',#210040,#119223,#119224);
#100007=AXIS2_PLACEMENT_3D('',#210067,#119225,#119226);
#100008=AXIS2_PLACEMENT_3D('',#210259,#119227,#119228);
#100009=AXIS2_PLACEMENT_3D('',#210393,#119229,#119230);
#100010=AXIS2_PLACEMENT_3D('',#210473,#119231,#119232);
#100011=AXIS2_PLACEMENT_3D('',#210556,#119233,#119234);
#100012=AXIS2_PLACEMENT_3D('',#210557,#119235,#119236);
#100013=AXIS2_PLACEMENT_3D('',#210558,#119237,#119238);
#100014=AXIS2_PLACEMENT_3D('',#210573,#119239,#119240);
#100015=AXIS2_PLACEMENT_3D('',#210734,#119241,#119242);
#100016=AXIS2_PLACEMENT_3D('',#210735,#119243,#119244);
#100017=AXIS2_PLACEMENT_3D('',#210736,#119245,#119246);
#100018=AXIS2_PLACEMENT_3D('',#210829,#119247,#119248);
#100019=AXIS2_PLACEMENT_3D('',#210834,#119251,#119252);
#100020=AXIS2_PLACEMENT_3D('',#210845,#119253,#119254);
#100021=AXIS2_PLACEMENT_3D('',#210847,#119255,#119256);
#100022=AXIS2_PLACEMENT_3D('',#210848,#119257,#119258);
#100023=AXIS2_PLACEMENT_3D('',#210849,#119259,#119260);
#100024=AXIS2_PLACEMENT_3D('',#210851,#119261,#119262);
#100025=AXIS2_PLACEMENT_3D('',#210852,#119263,#119264);
#100026=AXIS2_PLACEMENT_3D('',#210854,#119265,#119266);
#100027=AXIS2_PLACEMENT_3D('',#210855,#119267,#119268);
#100028=AXIS2_PLACEMENT_3D('',#210867,#119269,#119270);
#100029=AXIS2_PLACEMENT_3D('',#210868,#119271,#119272);
#100030=AXIS2_PLACEMENT_3D('',#210869,#119273,#119274);
#100031=AXIS2_PLACEMENT_3D('',#210870,#119275,#119276);
#100032=AXIS2_PLACEMENT_3D('',#210873,#119279,#119280);
#100033=AXIS2_PLACEMENT_3D('',#210878,#119283,#119284);
#100034=AXIS2_PLACEMENT_3D('',#210889,#119285,#119286);
#100035=AXIS2_PLACEMENT_3D('',#210891,#119287,#119288);
#100036=AXIS2_PLACEMENT_3D('',#210892,#119289,#119290);
#100037=AXIS2_PLACEMENT_3D('',#210893,#119291,#119292);
#100038=AXIS2_PLACEMENT_3D('',#210896,#119293,#119294);
#100039=AXIS2_PLACEMENT_3D('',#210897,#119295,#119296);
#100040=AXIS2_PLACEMENT_3D('',#210898,#119297,#119298);
#100041=AXIS2_PLACEMENT_3D('',#210910,#119299,#119300);
#100042=AXIS2_PLACEMENT_3D('',#210911,#119301,#119302);
#100043=AXIS2_PLACEMENT_3D('',#210912,#119303,#119304);
#100044=AXIS2_PLACEMENT_3D('',#210913,#119305,#119306);
#100045=AXIS2_PLACEMENT_3D('',#210916,#119309,#119310);
#100046=AXIS2_PLACEMENT_3D('',#210921,#119313,#119314);
#100047=AXIS2_PLACEMENT_3D('',#210933,#119315,#119316);
#100048=AXIS2_PLACEMENT_3D('',#210934,#119317,#119318);
#100049=AXIS2_PLACEMENT_3D('',#210935,#119319,#119320);
#100050=AXIS2_PLACEMENT_3D('',#210936,#119321,#119322);
#100051=AXIS2_PLACEMENT_3D('',#210939,#119323,#119324);
#100052=AXIS2_PLACEMENT_3D('',#210940,#119325,#119326);
#100053=AXIS2_PLACEMENT_3D('',#210941,#119327,#119328);
#100054=AXIS2_PLACEMENT_3D('',#210952,#119329,#119330);
#100055=AXIS2_PLACEMENT_3D('',#210954,#119331,#119332);
#100056=AXIS2_PLACEMENT_3D('',#210955,#119333,#119334);
#100057=AXIS2_PLACEMENT_3D('',#210956,#119335,#119336);
#100058=AXIS2_PLACEMENT_3D('',#210959,#119339,#119340);
#100059=AXIS2_PLACEMENT_3D('',#210964,#119343,#119344);
#100060=AXIS2_PLACEMENT_3D('',#210976,#119345,#119346);
#100061=AXIS2_PLACEMENT_3D('',#210977,#119347,#119348);
#100062=AXIS2_PLACEMENT_3D('',#210978,#119349,#119350);
#100063=AXIS2_PLACEMENT_3D('',#210979,#119351,#119352);
#100064=AXIS2_PLACEMENT_3D('',#210982,#119353,#119354);
#100065=AXIS2_PLACEMENT_3D('',#210983,#119355,#119356);
#100066=AXIS2_PLACEMENT_3D('',#210984,#119357,#119358);
#100067=AXIS2_PLACEMENT_3D('',#210995,#119359,#119360);
#100068=AXIS2_PLACEMENT_3D('',#210997,#119361,#119362);
#100069=AXIS2_PLACEMENT_3D('',#210998,#119363,#119364);
#100070=AXIS2_PLACEMENT_3D('',#210999,#119365,#119366);
#100071=AXIS2_PLACEMENT_3D('',#211002,#119369,#119370);
#100072=AXIS2_PLACEMENT_3D('',#211005,#119373,#119374);
#100073=AXIS2_PLACEMENT_3D('',#211008,#119377,#119378);
#100074=AXIS2_PLACEMENT_3D('',#211011,#119381,#119382);
#100075=AXIS2_PLACEMENT_3D('',#211014,#119385,#119386);
#100076=AXIS2_PLACEMENT_3D('',#211017,#119389,#119390);
#100077=AXIS2_PLACEMENT_3D('',#211020,#119393,#119394);
#100078=AXIS2_PLACEMENT_3D('',#211023,#119397,#119398);
#100079=AXIS2_PLACEMENT_3D('',#211026,#119401,#119402);
#100080=AXIS2_PLACEMENT_3D('',#211029,#119403,#119404);
#100081=AXIS2_PLACEMENT_3D('',#211031,#119405,#119406);
#100082=AXIS2_PLACEMENT_3D('',#211033,#119407,#119408);
#100083=AXIS2_PLACEMENT_3D('',#211034,#119409,#119410);
#100084=AXIS2_PLACEMENT_3D('',#211035,#119411,#119412);
#100085=AXIS2_PLACEMENT_3D('',#211038,#119413,#119414);
#100086=AXIS2_PLACEMENT_3D('',#211041,#119417,#119418);
#100087=AXIS2_PLACEMENT_3D('',#211044,#119419,#119420);
#100088=AXIS2_PLACEMENT_3D('',#211045,#119421,#119422);
#100089=AXIS2_PLACEMENT_3D('',#211046,#119423,#119424);
#100090=AXIS2_PLACEMENT_3D('',#211047,#119425,#119426);
#100091=AXIS2_PLACEMENT_3D('',#211050,#119427,#119428);
#100092=AXIS2_PLACEMENT_3D('',#211051,#119429,#119430);
#100093=AXIS2_PLACEMENT_3D('',#211052,#119431,#119432);
#100094=AXIS2_PLACEMENT_3D('',#211053,#119433,#119434);
#100095=AXIS2_PLACEMENT_3D('',#211056,#119435,#119436);
#100096=AXIS2_PLACEMENT_3D('',#211057,#119437,#119438);
#100097=AXIS2_PLACEMENT_3D('',#211058,#119439,#119440);
#100098=AXIS2_PLACEMENT_3D('',#211059,#119441,#119442);
#100099=AXIS2_PLACEMENT_3D('',#211062,#119443,#119444);
#100100=AXIS2_PLACEMENT_3D('',#211065,#119447,#119448);
#100101=AXIS2_PLACEMENT_3D('',#211068,#119449,#119450);
#100102=AXIS2_PLACEMENT_3D('',#211069,#119451,#119452);
#100103=AXIS2_PLACEMENT_3D('',#211070,#119453,#119454);
#100104=AXIS2_PLACEMENT_3D('',#211071,#119455,#119456);
#100105=AXIS2_PLACEMENT_3D('',#211074,#119457,#119458);
#100106=AXIS2_PLACEMENT_3D('',#211075,#119459,#119460);
#100107=AXIS2_PLACEMENT_3D('',#211076,#119461,#119462);
#100108=AXIS2_PLACEMENT_3D('',#211077,#119463,#119464);
#100109=AXIS2_PLACEMENT_3D('',#211080,#119465,#119466);
#100110=AXIS2_PLACEMENT_3D('',#211081,#119467,#119468);
#100111=AXIS2_PLACEMENT_3D('',#211082,#119469,#119470);
#100112=AXIS2_PLACEMENT_3D('',#211083,#119471,#119472);
#100113=AXIS2_PLACEMENT_3D('',#211086,#119475,#119476);
#100114=AXIS2_PLACEMENT_3D('',#211089,#119477,#119478);
#100115=AXIS2_PLACEMENT_3D('',#211091,#119479,#119480);
#100116=AXIS2_PLACEMENT_3D('',#211093,#119481,#119482);
#100117=AXIS2_PLACEMENT_3D('',#211094,#119483,#119484);
#100118=AXIS2_PLACEMENT_3D('',#211095,#119485,#119486);
#100119=AXIS2_PLACEMENT_3D('',#211098,#119487,#119488);
#100120=AXIS2_PLACEMENT_3D('',#211101,#119491,#119492);
#100121=AXIS2_PLACEMENT_3D('',#211104,#119493,#119494);
#100122=AXIS2_PLACEMENT_3D('',#211105,#119495,#119496);
#100123=AXIS2_PLACEMENT_3D('',#211106,#119497,#119498);
#100124=AXIS2_PLACEMENT_3D('',#211107,#119499,#119500);
#100125=AXIS2_PLACEMENT_3D('',#211110,#119501,#119502);
#100126=AXIS2_PLACEMENT_3D('',#211111,#119503,#119504);
#100127=AXIS2_PLACEMENT_3D('',#211112,#119505,#119506);
#100128=AXIS2_PLACEMENT_3D('',#211113,#119507,#119508);
#100129=AXIS2_PLACEMENT_3D('',#211116,#119509,#119510);
#100130=AXIS2_PLACEMENT_3D('',#211117,#119511,#119512);
#100131=AXIS2_PLACEMENT_3D('',#211118,#119513,#119514);
#100132=AXIS2_PLACEMENT_3D('',#211119,#119515,#119516);
#100133=AXIS2_PLACEMENT_3D('',#211122,#119517,#119518);
#100134=AXIS2_PLACEMENT_3D('',#211125,#119521,#119522);
#100135=AXIS2_PLACEMENT_3D('',#211128,#119523,#119524);
#100136=AXIS2_PLACEMENT_3D('',#211131,#119527,#119528);
#100137=AXIS2_PLACEMENT_3D('',#211132,#119529,#119530);
#100138=AXIS2_PLACEMENT_3D('',#211133,#119531,#119532);
#100139=AXIS2_PLACEMENT_3D('',#211134,#119533,#119534);
#100140=AXIS2_PLACEMENT_3D('',#211137,#119535,#119536);
#100141=AXIS2_PLACEMENT_3D('',#211139,#119537,#119538);
#100142=AXIS2_PLACEMENT_3D('',#211141,#119539,#119540);
#100143=AXIS2_PLACEMENT_3D('',#211142,#119541,#119542);
#100144=AXIS2_PLACEMENT_3D('',#211143,#119543,#119544);
#100145=AXIS2_PLACEMENT_3D('',#211146,#119545,#119546);
#100146=AXIS2_PLACEMENT_3D('',#211149,#119549,#119550);
#100147=AXIS2_PLACEMENT_3D('',#211152,#119551,#119552);
#100148=AXIS2_PLACEMENT_3D('',#211153,#119553,#119554);
#100149=AXIS2_PLACEMENT_3D('',#211154,#119555,#119556);
#100150=AXIS2_PLACEMENT_3D('',#211155,#119557,#119558);
#100151=AXIS2_PLACEMENT_3D('',#211158,#119559,#119560);
#100152=AXIS2_PLACEMENT_3D('',#211159,#119561,#119562);
#100153=AXIS2_PLACEMENT_3D('',#211160,#119563,#119564);
#100154=AXIS2_PLACEMENT_3D('',#211161,#119565,#119566);
#100155=AXIS2_PLACEMENT_3D('',#211164,#119567,#119568);
#100156=AXIS2_PLACEMENT_3D('',#211165,#119569,#119570);
#100157=AXIS2_PLACEMENT_3D('',#211166,#119571,#119572);
#100158=AXIS2_PLACEMENT_3D('',#211167,#119573,#119574);
#100159=AXIS2_PLACEMENT_3D('',#211170,#119575,#119576);
#100160=AXIS2_PLACEMENT_3D('',#211173,#119579,#119580);
#100161=AXIS2_PLACEMENT_3D('',#211176,#119581,#119582);
#100162=AXIS2_PLACEMENT_3D('',#211179,#119585,#119586);
#100163=AXIS2_PLACEMENT_3D('',#211180,#119587,#119588);
#100164=AXIS2_PLACEMENT_3D('',#211181,#119589,#119590);
#100165=AXIS2_PLACEMENT_3D('',#211182,#119591,#119592);
#100166=AXIS2_PLACEMENT_3D('',#211185,#119593,#119594);
#100167=AXIS2_PLACEMENT_3D('',#211187,#119595,#119596);
#100168=AXIS2_PLACEMENT_3D('',#211189,#119597,#119598);
#100169=AXIS2_PLACEMENT_3D('',#211190,#119599,#119600);
#100170=AXIS2_PLACEMENT_3D('',#211191,#119601,#119602);
#100171=AXIS2_PLACEMENT_3D('',#211194,#119603,#119604);
#100172=AXIS2_PLACEMENT_3D('',#211197,#119607,#119608);
#100173=AXIS2_PLACEMENT_3D('',#211200,#119609,#119610);
#100174=AXIS2_PLACEMENT_3D('',#211203,#119613,#119614);
#100175=AXIS2_PLACEMENT_3D('',#211206,#119615,#119616);
#100176=AXIS2_PLACEMENT_3D('',#211207,#119617,#119618);
#100177=AXIS2_PLACEMENT_3D('',#211208,#119619,#119620);
#100178=AXIS2_PLACEMENT_3D('',#211209,#119621,#119622);
#100179=AXIS2_PLACEMENT_3D('',#211212,#119623,#119624);
#100180=AXIS2_PLACEMENT_3D('',#211213,#119625,#119626);
#100181=AXIS2_PLACEMENT_3D('',#211214,#119627,#119628);
#100182=AXIS2_PLACEMENT_3D('',#211215,#119629,#119630);
#100183=AXIS2_PLACEMENT_3D('',#211218,#119631,#119632);
#100184=AXIS2_PLACEMENT_3D('',#211221,#119635,#119636);
#100185=AXIS2_PLACEMENT_3D('',#211224,#119637,#119638);
#100186=AXIS2_PLACEMENT_3D('',#211227,#119641,#119642);
#100187=AXIS2_PLACEMENT_3D('',#211228,#119643,#119644);
#100188=AXIS2_PLACEMENT_3D('',#211229,#119645,#119646);
#100189=AXIS2_PLACEMENT_3D('',#211230,#119647,#119648);
#100190=AXIS2_PLACEMENT_3D('',#211233,#119649,#119650);
#100191=AXIS2_PLACEMENT_3D('',#211235,#119651,#119652);
#100192=AXIS2_PLACEMENT_3D('',#211237,#119653,#119654);
#100193=AXIS2_PLACEMENT_3D('',#211238,#119655,#119656);
#100194=AXIS2_PLACEMENT_3D('',#211239,#119657,#119658);
#100195=AXIS2_PLACEMENT_3D('',#211242,#119659,#119660);
#100196=AXIS2_PLACEMENT_3D('',#211245,#119663,#119664);
#100197=AXIS2_PLACEMENT_3D('',#211248,#119665,#119666);
#100198=AXIS2_PLACEMENT_3D('',#211251,#119669,#119670);
#100199=AXIS2_PLACEMENT_3D('',#211254,#119671,#119672);
#100200=AXIS2_PLACEMENT_3D('',#211255,#119673,#119674);
#100201=AXIS2_PLACEMENT_3D('',#211256,#119675,#119676);
#100202=AXIS2_PLACEMENT_3D('',#211257,#119677,#119678);
#100203=AXIS2_PLACEMENT_3D('',#211260,#119679,#119680);
#100204=AXIS2_PLACEMENT_3D('',#211261,#119681,#119682);
#100205=AXIS2_PLACEMENT_3D('',#211262,#119683,#119684);
#100206=AXIS2_PLACEMENT_3D('',#211263,#119685,#119686);
#100207=AXIS2_PLACEMENT_3D('',#211266,#119687,#119688);
#100208=AXIS2_PLACEMENT_3D('',#211267,#119689,#119690);
#100209=AXIS2_PLACEMENT_3D('',#211268,#119691,#119692);
#100210=AXIS2_PLACEMENT_3D('',#211269,#119693,#119694);
#100211=AXIS2_PLACEMENT_3D('',#211272,#119695,#119696);
#100212=AXIS2_PLACEMENT_3D('',#211275,#119699,#119700);
#100213=AXIS2_PLACEMENT_3D('',#211278,#119701,#119702);
#100214=AXIS2_PLACEMENT_3D('',#211279,#119703,#119704);
#100215=AXIS2_PLACEMENT_3D('',#211280,#119705,#119706);
#100216=AXIS2_PLACEMENT_3D('',#211281,#119707,#119708);
#100217=AXIS2_PLACEMENT_3D('',#211282,#119709,#119710);
#100218=AXIS2_PLACEMENT_3D('',#211283,#119711,#119712);
#100219=AXIS2_PLACEMENT_3D('',#211284,#119713,#119714);
#100220=AXIS2_PLACEMENT_3D('',#211287,#119715,#119716);
#100221=AXIS2_PLACEMENT_3D('',#211289,#119717,#119718);
#100222=AXIS2_PLACEMENT_3D('',#211291,#119719,#119720);
#100223=AXIS2_PLACEMENT_3D('',#211292,#119721,#119722);
#100224=AXIS2_PLACEMENT_3D('',#211293,#119723,#119724);
#100225=AXIS2_PLACEMENT_3D('',#211296,#119725,#119726);
#100226=AXIS2_PLACEMENT_3D('',#211299,#119729,#119730);
#100227=AXIS2_PLACEMENT_3D('',#211302,#119731,#119732);
#100228=AXIS2_PLACEMENT_3D('',#211305,#119735,#119736);
#100229=AXIS2_PLACEMENT_3D('',#211308,#119737,#119738);
#100230=AXIS2_PLACEMENT_3D('',#211309,#119739,#119740);
#100231=AXIS2_PLACEMENT_3D('',#211310,#119741,#119742);
#100232=AXIS2_PLACEMENT_3D('',#211311,#119743,#119744);
#100233=AXIS2_PLACEMENT_3D('',#211314,#119745,#119746);
#100234=AXIS2_PLACEMENT_3D('',#211315,#119747,#119748);
#100235=AXIS2_PLACEMENT_3D('',#211316,#119749,#119750);
#100236=AXIS2_PLACEMENT_3D('',#211317,#119751,#119752);
#100237=AXIS2_PLACEMENT_3D('',#211320,#119753,#119754);
#100238=AXIS2_PLACEMENT_3D('',#211323,#119757,#119758);
#100239=AXIS2_PLACEMENT_3D('',#211326,#119759,#119760);
#100240=AXIS2_PLACEMENT_3D('',#211329,#119763,#119764);
#100241=AXIS2_PLACEMENT_3D('',#211330,#119765,#119766);
#100242=AXIS2_PLACEMENT_3D('',#211331,#119767,#119768);
#100243=AXIS2_PLACEMENT_3D('',#211332,#119769,#119770);
#100244=AXIS2_PLACEMENT_3D('',#211335,#119771,#119772);
#100245=AXIS2_PLACEMENT_3D('',#211337,#119773,#119774);
#100246=AXIS2_PLACEMENT_3D('',#211339,#119775,#119776);
#100247=AXIS2_PLACEMENT_3D('',#211340,#119777,#119778);
#100248=AXIS2_PLACEMENT_3D('',#211341,#119779,#119780);
#100249=AXIS2_PLACEMENT_3D('',#211344,#119781,#119782);
#100250=AXIS2_PLACEMENT_3D('',#211347,#119785,#119786);
#100251=AXIS2_PLACEMENT_3D('',#211350,#119787,#119788);
#100252=AXIS2_PLACEMENT_3D('',#211353,#119791,#119792);
#100253=AXIS2_PLACEMENT_3D('',#211356,#119793,#119794);
#100254=AXIS2_PLACEMENT_3D('',#211357,#119795,#119796);
#100255=AXIS2_PLACEMENT_3D('',#211358,#119797,#119798);
#100256=AXIS2_PLACEMENT_3D('',#211359,#119799,#119800);
#100257=AXIS2_PLACEMENT_3D('',#211362,#119801,#119802);
#100258=AXIS2_PLACEMENT_3D('',#211363,#119803,#119804);
#100259=AXIS2_PLACEMENT_3D('',#211364,#119805,#119806);
#100260=AXIS2_PLACEMENT_3D('',#211365,#119807,#119808);
#100261=AXIS2_PLACEMENT_3D('',#211368,#119809,#119810);
#100262=AXIS2_PLACEMENT_3D('',#211371,#119813,#119814);
#100263=AXIS2_PLACEMENT_3D('',#211374,#119815,#119816);
#100264=AXIS2_PLACEMENT_3D('',#211377,#119819,#119820);
#100265=AXIS2_PLACEMENT_3D('',#211378,#119821,#119822);
#100266=AXIS2_PLACEMENT_3D('',#211379,#119823,#119824);
#100267=AXIS2_PLACEMENT_3D('',#211380,#119825,#119826);
#100268=AXIS2_PLACEMENT_3D('',#211383,#119827,#119828);
#100269=AXIS2_PLACEMENT_3D('',#211385,#119829,#119830);
#100270=AXIS2_PLACEMENT_3D('',#211387,#119831,#119832);
#100271=AXIS2_PLACEMENT_3D('',#211388,#119833,#119834);
#100272=AXIS2_PLACEMENT_3D('',#211389,#119835,#119836);
#100273=AXIS2_PLACEMENT_3D('',#211392,#119837,#119838);
#100274=AXIS2_PLACEMENT_3D('',#211395,#119841,#119842);
#100275=AXIS2_PLACEMENT_3D('',#211398,#119843,#119844);
#100276=AXIS2_PLACEMENT_3D('',#211401,#119847,#119848);
#100277=AXIS2_PLACEMENT_3D('',#211404,#119849,#119850);
#100278=AXIS2_PLACEMENT_3D('',#211405,#119851,#119852);
#100279=AXIS2_PLACEMENT_3D('',#211406,#119853,#119854);
#100280=AXIS2_PLACEMENT_3D('',#211407,#119855,#119856);
#100281=AXIS2_PLACEMENT_3D('',#211410,#119857,#119858);
#100282=AXIS2_PLACEMENT_3D('',#211411,#119859,#119860);
#100283=AXIS2_PLACEMENT_3D('',#211412,#119861,#119862);
#100284=AXIS2_PLACEMENT_3D('',#211413,#119863,#119864);
#100285=AXIS2_PLACEMENT_3D('',#211416,#119865,#119866);
#100286=AXIS2_PLACEMENT_3D('',#211419,#119869,#119870);
#100287=AXIS2_PLACEMENT_3D('',#211422,#119871,#119872);
#100288=AXIS2_PLACEMENT_3D('',#211425,#119875,#119876);
#100289=AXIS2_PLACEMENT_3D('',#211426,#119877,#119878);
#100290=AXIS2_PLACEMENT_3D('',#211427,#119879,#119880);
#100291=AXIS2_PLACEMENT_3D('',#211428,#119881,#119882);
#100292=AXIS2_PLACEMENT_3D('',#211431,#119883,#119884);
#100293=AXIS2_PLACEMENT_3D('',#211433,#119885,#119886);
#100294=AXIS2_PLACEMENT_3D('',#211435,#119887,#119888);
#100295=AXIS2_PLACEMENT_3D('',#211436,#119889,#119890);
#100296=AXIS2_PLACEMENT_3D('',#211437,#119891,#119892);
#100297=AXIS2_PLACEMENT_3D('',#211440,#119893,#119894);
#100298=AXIS2_PLACEMENT_3D('',#211443,#119897,#119898);
#100299=AXIS2_PLACEMENT_3D('',#211446,#119899,#119900);
#100300=AXIS2_PLACEMENT_3D('',#211449,#119903,#119904);
#100301=AXIS2_PLACEMENT_3D('',#211452,#119905,#119906);
#100302=AXIS2_PLACEMENT_3D('',#211453,#119907,#119908);
#100303=AXIS2_PLACEMENT_3D('',#211454,#119909,#119910);
#100304=AXIS2_PLACEMENT_3D('',#211455,#119911,#119912);
#100305=AXIS2_PLACEMENT_3D('',#211458,#119913,#119914);
#100306=AXIS2_PLACEMENT_3D('',#211459,#119915,#119916);
#100307=AXIS2_PLACEMENT_3D('',#211460,#119917,#119918);
#100308=AXIS2_PLACEMENT_3D('',#211461,#119919,#119920);
#100309=AXIS2_PLACEMENT_3D('',#211464,#119921,#119922);
#100310=AXIS2_PLACEMENT_3D('',#211467,#119925,#119926);
#100311=AXIS2_PLACEMENT_3D('',#211470,#119927,#119928);
#100312=AXIS2_PLACEMENT_3D('',#211473,#119931,#119932);
#100313=AXIS2_PLACEMENT_3D('',#211474,#119933,#119934);
#100314=AXIS2_PLACEMENT_3D('',#211475,#119935,#119936);
#100315=AXIS2_PLACEMENT_3D('',#211476,#119937,#119938);
#100316=AXIS2_PLACEMENT_3D('',#211479,#119939,#119940);
#100317=AXIS2_PLACEMENT_3D('',#211481,#119941,#119942);
#100318=AXIS2_PLACEMENT_3D('',#211483,#119943,#119944);
#100319=AXIS2_PLACEMENT_3D('',#211484,#119945,#119946);
#100320=AXIS2_PLACEMENT_3D('',#211485,#119947,#119948);
#100321=AXIS2_PLACEMENT_3D('',#211488,#119949,#119950);
#100322=AXIS2_PLACEMENT_3D('',#211491,#119953,#119954);
#100323=AXIS2_PLACEMENT_3D('',#211494,#119955,#119956);
#100324=AXIS2_PLACEMENT_3D('',#211497,#119959,#119960);
#100325=AXIS2_PLACEMENT_3D('',#211500,#119961,#119962);
#100326=AXIS2_PLACEMENT_3D('',#211501,#119963,#119964);
#100327=AXIS2_PLACEMENT_3D('',#211502,#119965,#119966);
#100328=AXIS2_PLACEMENT_3D('',#211503,#119967,#119968);
#100329=AXIS2_PLACEMENT_3D('',#211506,#119969,#119970);
#100330=AXIS2_PLACEMENT_3D('',#211507,#119971,#119972);
#100331=AXIS2_PLACEMENT_3D('',#211508,#119973,#119974);
#100332=AXIS2_PLACEMENT_3D('',#211509,#119975,#119976);
#100333=AXIS2_PLACEMENT_3D('',#211512,#119977,#119978);
#100334=AXIS2_PLACEMENT_3D('',#211515,#119981,#119982);
#100335=AXIS2_PLACEMENT_3D('',#211518,#119983,#119984);
#100336=AXIS2_PLACEMENT_3D('',#211519,#119985,#119986);
#100337=AXIS2_PLACEMENT_3D('',#211520,#119987,#119988);
#100338=AXIS2_PLACEMENT_3D('',#211521,#119989,#119990);
#100339=AXIS2_PLACEMENT_3D('',#211522,#119991,#119992);
#100340=AXIS2_PLACEMENT_3D('',#211523,#119993,#119994);
#100341=AXIS2_PLACEMENT_3D('',#211524,#119995,#119996);
#100342=AXIS2_PLACEMENT_3D('',#211527,#119997,#119998);
#100343=AXIS2_PLACEMENT_3D('',#211529,#119999,#120000);
#100344=AXIS2_PLACEMENT_3D('',#211531,#120001,#120002);
#100345=AXIS2_PLACEMENT_3D('',#211532,#120003,#120004);
#100346=AXIS2_PLACEMENT_3D('',#211533,#120005,#120006);
#100347=AXIS2_PLACEMENT_3D('',#211536,#120007,#120008);
#100348=AXIS2_PLACEMENT_3D('',#211539,#120011,#120012);
#100349=AXIS2_PLACEMENT_3D('',#211542,#120013,#120014);
#100350=AXIS2_PLACEMENT_3D('',#211545,#120017,#120018);
#100351=AXIS2_PLACEMENT_3D('',#211548,#120019,#120020);
#100352=AXIS2_PLACEMENT_3D('',#211549,#120021,#120022);
#100353=AXIS2_PLACEMENT_3D('',#211550,#120023,#120024);
#100354=AXIS2_PLACEMENT_3D('',#211551,#120025,#120026);
#100355=AXIS2_PLACEMENT_3D('',#211554,#120027,#120028);
#100356=AXIS2_PLACEMENT_3D('',#211555,#120029,#120030);
#100357=AXIS2_PLACEMENT_3D('',#211556,#120031,#120032);
#100358=AXIS2_PLACEMENT_3D('',#211557,#120033,#120034);
#100359=AXIS2_PLACEMENT_3D('',#211560,#120035,#120036);
#100360=AXIS2_PLACEMENT_3D('',#211563,#120039,#120040);
#100361=AXIS2_PLACEMENT_3D('',#211566,#120041,#120042);
#100362=AXIS2_PLACEMENT_3D('',#211567,#120043,#120044);
#100363=AXIS2_PLACEMENT_3D('',#211568,#120045,#120046);
#100364=AXIS2_PLACEMENT_3D('',#211569,#120047,#120048);
#100365=AXIS2_PLACEMENT_3D('',#211572,#120049,#120050);
#100366=AXIS2_PLACEMENT_3D('',#211573,#120051,#120052);
#100367=AXIS2_PLACEMENT_3D('',#211574,#120053,#120054);
#100368=AXIS2_PLACEMENT_3D('',#211575,#120055,#120056);
#100369=AXIS2_PLACEMENT_3D('',#211578,#120057,#120058);
#100370=AXIS2_PLACEMENT_3D('',#211579,#120059,#120060);
#100371=AXIS2_PLACEMENT_3D('',#211580,#120061,#120062);
#100372=AXIS2_PLACEMENT_3D('',#211581,#120063,#120064);
#100373=AXIS2_PLACEMENT_3D('',#211582,#120065,#120066);
#100374=AXIS2_PLACEMENT_3D('',#211583,#120067,#120068);
#100375=AXIS2_PLACEMENT_3D('',#211584,#120069,#120070);
#100376=AXIS2_PLACEMENT_3D('',#211587,#120071,#120072);
#100377=AXIS2_PLACEMENT_3D('',#211589,#120073,#120074);
#100378=AXIS2_PLACEMENT_3D('',#211591,#120075,#120076);
#100379=AXIS2_PLACEMENT_3D('',#211592,#120077,#120078);
#100380=AXIS2_PLACEMENT_3D('',#211593,#120079,#120080);
#100381=AXIS2_PLACEMENT_3D('',#211596,#120081,#120082);
#100382=AXIS2_PLACEMENT_3D('',#211599,#120085,#120086);
#100383=AXIS2_PLACEMENT_3D('',#211602,#120087,#120088);
#100384=AXIS2_PLACEMENT_3D('',#211605,#120091,#120092);
#100385=AXIS2_PLACEMENT_3D('',#211608,#120093,#120094);
#100386=AXIS2_PLACEMENT_3D('',#211609,#120095,#120096);
#100387=AXIS2_PLACEMENT_3D('',#211610,#120097,#120098);
#100388=AXIS2_PLACEMENT_3D('',#211611,#120099,#120100);
#100389=AXIS2_PLACEMENT_3D('',#211614,#120101,#120102);
#100390=AXIS2_PLACEMENT_3D('',#211615,#120103,#120104);
#100391=AXIS2_PLACEMENT_3D('',#211616,#120105,#120106);
#100392=AXIS2_PLACEMENT_3D('',#211617,#120107,#120108);
#100393=AXIS2_PLACEMENT_3D('',#211620,#120109,#120110);
#100394=AXIS2_PLACEMENT_3D('',#211623,#120113,#120114);
#100395=AXIS2_PLACEMENT_3D('',#211626,#120115,#120116);
#100396=AXIS2_PLACEMENT_3D('',#211627,#120117,#120118);
#100397=AXIS2_PLACEMENT_3D('',#211628,#120119,#120120);
#100398=AXIS2_PLACEMENT_3D('',#211629,#120121,#120122);
#100399=AXIS2_PLACEMENT_3D('',#211630,#120123,#120124);
#100400=AXIS2_PLACEMENT_3D('',#211631,#120125,#120126);
#100401=AXIS2_PLACEMENT_3D('',#211632,#120127,#120128);
#100402=AXIS2_PLACEMENT_3D('',#211635,#120129,#120130);
#100403=AXIS2_PLACEMENT_3D('',#211637,#120131,#120132);
#100404=AXIS2_PLACEMENT_3D('',#211639,#120133,#120134);
#100405=AXIS2_PLACEMENT_3D('',#211640,#120135,#120136);
#100406=AXIS2_PLACEMENT_3D('',#211641,#120137,#120138);
#100407=AXIS2_PLACEMENT_3D('',#211644,#120139,#120140);
#100408=AXIS2_PLACEMENT_3D('',#211647,#120143,#120144);
#100409=AXIS2_PLACEMENT_3D('',#211650,#120145,#120146);
#100410=AXIS2_PLACEMENT_3D('',#211653,#120149,#120150);
#100411=AXIS2_PLACEMENT_3D('',#211656,#120151,#120152);
#100412=AXIS2_PLACEMENT_3D('',#211657,#120153,#120154);
#100413=AXIS2_PLACEMENT_3D('',#211658,#120155,#120156);
#100414=AXIS2_PLACEMENT_3D('',#211659,#120157,#120158);
#100415=AXIS2_PLACEMENT_3D('',#211662,#120159,#120160);
#100416=AXIS2_PLACEMENT_3D('',#211663,#120161,#120162);
#100417=AXIS2_PLACEMENT_3D('',#211664,#120163,#120164);
#100418=AXIS2_PLACEMENT_3D('',#211665,#120165,#120166);
#100419=AXIS2_PLACEMENT_3D('',#211668,#120167,#120168);
#100420=AXIS2_PLACEMENT_3D('',#211671,#120171,#120172);
#100421=AXIS2_PLACEMENT_3D('',#211674,#120173,#120174);
#100422=AXIS2_PLACEMENT_3D('',#211677,#120177,#120178);
#100423=AXIS2_PLACEMENT_3D('',#211678,#120179,#120180);
#100424=AXIS2_PLACEMENT_3D('',#211679,#120181,#120182);
#100425=AXIS2_PLACEMENT_3D('',#211680,#120183,#120184);
#100426=AXIS2_PLACEMENT_3D('',#211683,#120185,#120186);
#100427=AXIS2_PLACEMENT_3D('',#211685,#120187,#120188);
#100428=AXIS2_PLACEMENT_3D('',#211687,#120189,#120190);
#100429=AXIS2_PLACEMENT_3D('',#211688,#120191,#120192);
#100430=AXIS2_PLACEMENT_3D('',#211689,#120193,#120194);
#100431=AXIS2_PLACEMENT_3D('',#211692,#120195,#120196);
#100432=AXIS2_PLACEMENT_3D('',#211695,#120199,#120200);
#100433=AXIS2_PLACEMENT_3D('',#211698,#120201,#120202);
#100434=AXIS2_PLACEMENT_3D('',#211699,#120203,#120204);
#100435=AXIS2_PLACEMENT_3D('',#211700,#120205,#120206);
#100436=AXIS2_PLACEMENT_3D('',#211701,#120207,#120208);
#100437=AXIS2_PLACEMENT_3D('',#211704,#120209,#120210);
#100438=AXIS2_PLACEMENT_3D('',#211705,#120211,#120212);
#100439=AXIS2_PLACEMENT_3D('',#211706,#120213,#120214);
#100440=AXIS2_PLACEMENT_3D('',#211707,#120215,#120216);
#100441=AXIS2_PLACEMENT_3D('',#211710,#120217,#120218);
#100442=AXIS2_PLACEMENT_3D('',#211711,#120219,#120220);
#100443=AXIS2_PLACEMENT_3D('',#211712,#120221,#120222);
#100444=AXIS2_PLACEMENT_3D('',#211713,#120223,#120224);
#100445=AXIS2_PLACEMENT_3D('',#211716,#120225,#120226);
#100446=AXIS2_PLACEMENT_3D('',#211719,#120229,#120230);
#100447=AXIS2_PLACEMENT_3D('',#211722,#120231,#120232);
#100448=AXIS2_PLACEMENT_3D('',#211725,#120235,#120236);
#100449=AXIS2_PLACEMENT_3D('',#211728,#120237,#120238);
#100450=AXIS2_PLACEMENT_3D('',#211729,#120239,#120240);
#100451=AXIS2_PLACEMENT_3D('',#211730,#120241,#120242);
#100452=AXIS2_PLACEMENT_3D('',#211731,#120243,#120244);
#100453=AXIS2_PLACEMENT_3D('',#211734,#120245,#120246);
#100454=AXIS2_PLACEMENT_3D('',#211735,#120247,#120248);
#100455=AXIS2_PLACEMENT_3D('',#211736,#120249,#120250);
#100456=AXIS2_PLACEMENT_3D('',#211737,#120251,#120252);
#100457=AXIS2_PLACEMENT_3D('',#211740,#120255,#120256);
#100458=AXIS2_PLACEMENT_3D('',#211743,#120257,#120258);
#100459=AXIS2_PLACEMENT_3D('',#211745,#120259,#120260);
#100460=AXIS2_PLACEMENT_3D('',#211747,#120261,#120262);
#100461=AXIS2_PLACEMENT_3D('',#211748,#120263,#120264);
#100462=AXIS2_PLACEMENT_3D('',#211749,#120265,#120266);
#100463=AXIS2_PLACEMENT_3D('',#211752,#120267,#120268);
#100464=AXIS2_PLACEMENT_3D('',#211755,#120271,#120272);
#100465=AXIS2_PLACEMENT_3D('',#211758,#120273,#120274);
#100466=AXIS2_PLACEMENT_3D('',#211761,#120277,#120278);
#100467=AXIS2_PLACEMENT_3D('',#211764,#120279,#120280);
#100468=AXIS2_PLACEMENT_3D('',#211765,#120281,#120282);
#100469=AXIS2_PLACEMENT_3D('',#211766,#120283,#120284);
#100470=AXIS2_PLACEMENT_3D('',#211767,#120285,#120286);
#100471=AXIS2_PLACEMENT_3D('',#211770,#120287,#120288);
#100472=AXIS2_PLACEMENT_3D('',#211771,#120289,#120290);
#100473=AXIS2_PLACEMENT_3D('',#211772,#120291,#120292);
#100474=AXIS2_PLACEMENT_3D('',#211773,#120293,#120294);
#100475=AXIS2_PLACEMENT_3D('',#211776,#120295,#120296);
#100476=AXIS2_PLACEMENT_3D('',#211779,#120299,#120300);
#100477=AXIS2_PLACEMENT_3D('',#211782,#120301,#120302);
#100478=AXIS2_PLACEMENT_3D('',#211783,#120303,#120304);
#100479=AXIS2_PLACEMENT_3D('',#211784,#120305,#120306);
#100480=AXIS2_PLACEMENT_3D('',#211785,#120307,#120308);
#100481=AXIS2_PLACEMENT_3D('',#211788,#120309,#120310);
#100482=AXIS2_PLACEMENT_3D('',#211789,#120311,#120312);
#100483=AXIS2_PLACEMENT_3D('',#211790,#120313,#120314);
#100484=AXIS2_PLACEMENT_3D('',#211791,#120315,#120316);
#100485=AXIS2_PLACEMENT_3D('',#211794,#120317,#120318);
#100486=AXIS2_PLACEMENT_3D('',#211795,#120319,#120320);
#100487=AXIS2_PLACEMENT_3D('',#211796,#120321,#120322);
#100488=AXIS2_PLACEMENT_3D('',#211797,#120323,#120324);
#100489=AXIS2_PLACEMENT_3D('',#211800,#120327,#120328);
#100490=AXIS2_PLACEMENT_3D('',#211803,#120329,#120330);
#100491=AXIS2_PLACEMENT_3D('',#211805,#120331,#120332);
#100492=AXIS2_PLACEMENT_3D('',#211807,#120333,#120334);
#100493=AXIS2_PLACEMENT_3D('',#211808,#120335,#120336);
#100494=AXIS2_PLACEMENT_3D('',#211809,#120337,#120338);
#100495=AXIS2_PLACEMENT_3D('',#211812,#120339,#120340);
#100496=AXIS2_PLACEMENT_3D('',#211815,#120343,#120344);
#100497=AXIS2_PLACEMENT_3D('',#211818,#120345,#120346);
#100498=AXIS2_PLACEMENT_3D('',#211821,#120349,#120350);
#100499=AXIS2_PLACEMENT_3D('',#211824,#120351,#120352);
#100500=AXIS2_PLACEMENT_3D('',#211825,#120353,#120354);
#100501=AXIS2_PLACEMENT_3D('',#211826,#120355,#120356);
#100502=AXIS2_PLACEMENT_3D('',#211827,#120357,#120358);
#100503=AXIS2_PLACEMENT_3D('',#211830,#120359,#120360);
#100504=AXIS2_PLACEMENT_3D('',#211831,#120361,#120362);
#100505=AXIS2_PLACEMENT_3D('',#211832,#120363,#120364);
#100506=AXIS2_PLACEMENT_3D('',#211833,#120365,#120366);
#100507=AXIS2_PLACEMENT_3D('',#211836,#120367,#120368);
#100508=AXIS2_PLACEMENT_3D('',#211839,#120371,#120372);
#100509=AXIS2_PLACEMENT_3D('',#211842,#120373,#120374);
#100510=AXIS2_PLACEMENT_3D('',#211845,#120377,#120378);
#100511=AXIS2_PLACEMENT_3D('',#211846,#120379,#120380);
#100512=AXIS2_PLACEMENT_3D('',#211847,#120381,#120382);
#100513=AXIS2_PLACEMENT_3D('',#211848,#120383,#120384);
#100514=AXIS2_PLACEMENT_3D('',#211851,#120385,#120386);
#100515=AXIS2_PLACEMENT_3D('',#211853,#120387,#120388);
#100516=AXIS2_PLACEMENT_3D('',#211855,#120389,#120390);
#100517=AXIS2_PLACEMENT_3D('',#211856,#120391,#120392);
#100518=AXIS2_PLACEMENT_3D('',#211857,#120393,#120394);
#100519=AXIS2_PLACEMENT_3D('',#211860,#120395,#120396);
#100520=AXIS2_PLACEMENT_3D('',#211863,#120399,#120400);
#100521=AXIS2_PLACEMENT_3D('',#211866,#120401,#120402);
#100522=AXIS2_PLACEMENT_3D('',#211869,#120405,#120406);
#100523=AXIS2_PLACEMENT_3D('',#211872,#120407,#120408);
#100524=AXIS2_PLACEMENT_3D('',#211873,#120409,#120410);
#100525=AXIS2_PLACEMENT_3D('',#211874,#120411,#120412);
#100526=AXIS2_PLACEMENT_3D('',#211875,#120413,#120414);
#100527=AXIS2_PLACEMENT_3D('',#211878,#120415,#120416);
#100528=AXIS2_PLACEMENT_3D('',#211879,#120417,#120418);
#100529=AXIS2_PLACEMENT_3D('',#211880,#120419,#120420);
#100530=AXIS2_PLACEMENT_3D('',#211881,#120421,#120422);
#100531=AXIS2_PLACEMENT_3D('',#211884,#120423,#120424);
#100532=AXIS2_PLACEMENT_3D('',#211885,#120425,#120426);
#100533=AXIS2_PLACEMENT_3D('',#211886,#120427,#120428);
#100534=AXIS2_PLACEMENT_3D('',#211887,#120429,#120430);
#100535=AXIS2_PLACEMENT_3D('',#211890,#120431,#120432);
#100536=AXIS2_PLACEMENT_3D('',#211893,#120435,#120436);
#100537=AXIS2_PLACEMENT_3D('',#211894,#120437,#120438);
#100538=AXIS2_PLACEMENT_3D('',#211895,#120439,#120440);
#100539=AXIS2_PLACEMENT_3D('',#211896,#120441,#120442);
#100540=AXIS2_PLACEMENT_3D('',#211899,#120443,#120444);
#100541=AXIS2_PLACEMENT_3D('',#211901,#120445,#120446);
#100542=AXIS2_PLACEMENT_3D('',#211903,#120447,#120448);
#100543=AXIS2_PLACEMENT_3D('',#211904,#120449,#120450);
#100544=AXIS2_PLACEMENT_3D('',#211905,#120451,#120452);
#100545=AXIS2_PLACEMENT_3D('',#211908,#120453,#120454);
#100546=AXIS2_PLACEMENT_3D('',#211911,#120457,#120458);
#100547=AXIS2_PLACEMENT_3D('',#211914,#120459,#120460);
#100548=AXIS2_PLACEMENT_3D('',#211917,#120463,#120464);
#100549=AXIS2_PLACEMENT_3D('',#211920,#120465,#120466);
#100550=AXIS2_PLACEMENT_3D('',#211921,#120467,#120468);
#100551=AXIS2_PLACEMENT_3D('',#211922,#120469,#120470);
#100552=AXIS2_PLACEMENT_3D('',#211923,#120471,#120472);
#100553=AXIS2_PLACEMENT_3D('',#211926,#120473,#120474);
#100554=AXIS2_PLACEMENT_3D('',#211927,#120475,#120476);
#100555=AXIS2_PLACEMENT_3D('',#211928,#120477,#120478);
#100556=AXIS2_PLACEMENT_3D('',#211929,#120479,#120480);
#100557=AXIS2_PLACEMENT_3D('',#211932,#120481,#120482);
#100558=AXIS2_PLACEMENT_3D('',#211935,#120485,#120486);
#100559=AXIS2_PLACEMENT_3D('',#211938,#120487,#120488);
#100560=AXIS2_PLACEMENT_3D('',#211941,#120491,#120492);
#100561=AXIS2_PLACEMENT_3D('',#211942,#120493,#120494);
#100562=AXIS2_PLACEMENT_3D('',#211943,#120495,#120496);
#100563=AXIS2_PLACEMENT_3D('',#211944,#120497,#120498);
#100564=AXIS2_PLACEMENT_3D('',#211947,#120499,#120500);
#100565=AXIS2_PLACEMENT_3D('',#211949,#120501,#120502);
#100566=AXIS2_PLACEMENT_3D('',#211951,#120503,#120504);
#100567=AXIS2_PLACEMENT_3D('',#211952,#120505,#120506);
#100568=AXIS2_PLACEMENT_3D('',#211953,#120507,#120508);
#100569=AXIS2_PLACEMENT_3D('',#211956,#120509,#120510);
#100570=AXIS2_PLACEMENT_3D('',#211959,#120513,#120514);
#100571=AXIS2_PLACEMENT_3D('',#211962,#120515,#120516);
#100572=AXIS2_PLACEMENT_3D('',#211965,#120519,#120520);
#100573=AXIS2_PLACEMENT_3D('',#211968,#120521,#120522);
#100574=AXIS2_PLACEMENT_3D('',#211969,#120523,#120524);
#100575=AXIS2_PLACEMENT_3D('',#211970,#120525,#120526);
#100576=AXIS2_PLACEMENT_3D('',#211971,#120527,#120528);
#100577=AXIS2_PLACEMENT_3D('',#211974,#120529,#120530);
#100578=AXIS2_PLACEMENT_3D('',#211975,#120531,#120532);
#100579=AXIS2_PLACEMENT_3D('',#211976,#120533,#120534);
#100580=AXIS2_PLACEMENT_3D('',#211977,#120535,#120536);
#100581=AXIS2_PLACEMENT_3D('',#211980,#120537,#120538);
#100582=AXIS2_PLACEMENT_3D('',#211983,#120541,#120542);
#100583=AXIS2_PLACEMENT_3D('',#211986,#120543,#120544);
#100584=AXIS2_PLACEMENT_3D('',#211989,#120547,#120548);
#100585=AXIS2_PLACEMENT_3D('',#211990,#120549,#120550);
#100586=AXIS2_PLACEMENT_3D('',#211991,#120551,#120552);
#100587=AXIS2_PLACEMENT_3D('',#211992,#120553,#120554);
#100588=AXIS2_PLACEMENT_3D('',#211995,#120555,#120556);
#100589=AXIS2_PLACEMENT_3D('',#211997,#120557,#120558);
#100590=AXIS2_PLACEMENT_3D('',#211999,#120559,#120560);
#100591=AXIS2_PLACEMENT_3D('',#212000,#120561,#120562);
#100592=AXIS2_PLACEMENT_3D('',#212001,#120563,#120564);
#100593=AXIS2_PLACEMENT_3D('',#212004,#120565,#120566);
#100594=AXIS2_PLACEMENT_3D('',#212007,#120569,#120570);
#100595=AXIS2_PLACEMENT_3D('',#212010,#120571,#120572);
#100596=AXIS2_PLACEMENT_3D('',#212013,#120575,#120576);
#100597=AXIS2_PLACEMENT_3D('',#212016,#120577,#120578);
#100598=AXIS2_PLACEMENT_3D('',#212017,#120579,#120580);
#100599=AXIS2_PLACEMENT_3D('',#212018,#120581,#120582);
#100600=AXIS2_PLACEMENT_3D('',#212019,#120583,#120584);
#100601=AXIS2_PLACEMENT_3D('',#212022,#120585,#120586);
#100602=AXIS2_PLACEMENT_3D('',#212023,#120587,#120588);
#100603=AXIS2_PLACEMENT_3D('',#212024,#120589,#120590);
#100604=AXIS2_PLACEMENT_3D('',#212025,#120591,#120592);
#100605=AXIS2_PLACEMENT_3D('',#212028,#120593,#120594);
#100606=AXIS2_PLACEMENT_3D('',#212031,#120597,#120598);
#100607=AXIS2_PLACEMENT_3D('',#212034,#120599,#120600);
#100608=AXIS2_PLACEMENT_3D('',#212035,#120601,#120602);
#100609=AXIS2_PLACEMENT_3D('',#212036,#120603,#120604);
#100610=AXIS2_PLACEMENT_3D('',#212037,#120605,#120606);
#100611=AXIS2_PLACEMENT_3D('',#212039,#120607,#120608);
#100612=AXIS2_PLACEMENT_3D('',#212041,#120609,#120610);
#100613=AXIS2_PLACEMENT_3D('',#212042,#120611,#120612);
#100614=AXIS2_PLACEMENT_3D('',#212043,#120613,#120614);
#100615=AXIS2_PLACEMENT_3D('',#212044,#120615,#120616);
#100616=AXIS2_PLACEMENT_3D('',#212045,#120617,#120618);
#100617=AXIS2_PLACEMENT_3D('',#212046,#120619,#120620);
#100618=AXIS2_PLACEMENT_3D('',#212049,#120621,#120622);
#100619=AXIS2_PLACEMENT_3D('',#212051,#120623,#120624);
#100620=AXIS2_PLACEMENT_3D('',#212053,#120625,#120626);
#100621=AXIS2_PLACEMENT_3D('',#212054,#120627,#120628);
#100622=AXIS2_PLACEMENT_3D('',#212055,#120629,#120630);
#100623=AXIS2_PLACEMENT_3D('',#212058,#120631,#120632);
#100624=AXIS2_PLACEMENT_3D('',#212061,#120635,#120636);
#100625=AXIS2_PLACEMENT_3D('',#212064,#120637,#120638);
#100626=AXIS2_PLACEMENT_3D('',#212067,#120641,#120642);
#100627=AXIS2_PLACEMENT_3D('',#212070,#120643,#120644);
#100628=AXIS2_PLACEMENT_3D('',#212071,#120645,#120646);
#100629=AXIS2_PLACEMENT_3D('',#212072,#120647,#120648);
#100630=AXIS2_PLACEMENT_3D('',#212073,#120649,#120650);
#100631=AXIS2_PLACEMENT_3D('',#212076,#120651,#120652);
#100632=AXIS2_PLACEMENT_3D('',#212077,#120653,#120654);
#100633=AXIS2_PLACEMENT_3D('',#212078,#120655,#120656);
#100634=AXIS2_PLACEMENT_3D('',#212079,#120657,#120658);
#100635=AXIS2_PLACEMENT_3D('',#212082,#120659,#120660);
#100636=AXIS2_PLACEMENT_3D('',#212083,#120661,#120662);
#100637=AXIS2_PLACEMENT_3D('',#212084,#120663,#120664);
#100638=AXIS2_PLACEMENT_3D('',#212085,#120665,#120666);
#100639=AXIS2_PLACEMENT_3D('',#212088,#120667,#120668);
#100640=AXIS2_PLACEMENT_3D('',#212091,#120671,#120672);
#100641=AXIS2_PLACEMENT_3D('',#212092,#120673,#120674);
#100642=AXIS2_PLACEMENT_3D('',#212093,#120675,#120676);
#100643=AXIS2_PLACEMENT_3D('',#212094,#120677,#120678);
#100644=AXIS2_PLACEMENT_3D('',#212097,#120679,#120680);
#100645=AXIS2_PLACEMENT_3D('',#212099,#120681,#120682);
#100646=AXIS2_PLACEMENT_3D('',#212101,#120683,#120684);
#100647=AXIS2_PLACEMENT_3D('',#212102,#120685,#120686);
#100648=AXIS2_PLACEMENT_3D('',#212103,#120687,#120688);
#100649=AXIS2_PLACEMENT_3D('',#212106,#120689,#120690);
#100650=AXIS2_PLACEMENT_3D('',#212109,#120693,#120694);
#100651=AXIS2_PLACEMENT_3D('',#212112,#120695,#120696);
#100652=AXIS2_PLACEMENT_3D('',#212115,#120699,#120700);
#100653=AXIS2_PLACEMENT_3D('',#212118,#120701,#120702);
#100654=AXIS2_PLACEMENT_3D('',#212119,#120703,#120704);
#100655=AXIS2_PLACEMENT_3D('',#212120,#120705,#120706);
#100656=AXIS2_PLACEMENT_3D('',#212121,#120707,#120708);
#100657=AXIS2_PLACEMENT_3D('',#212124,#120709,#120710);
#100658=AXIS2_PLACEMENT_3D('',#212125,#120711,#120712);
#100659=AXIS2_PLACEMENT_3D('',#212126,#120713,#120714);
#100660=AXIS2_PLACEMENT_3D('',#212127,#120715,#120716);
#100661=AXIS2_PLACEMENT_3D('',#212130,#120717,#120718);
#100662=AXIS2_PLACEMENT_3D('',#212131,#120719,#120720);
#100663=AXIS2_PLACEMENT_3D('',#212132,#120721,#120722);
#100664=AXIS2_PLACEMENT_3D('',#212133,#120723,#120724);
#100665=AXIS2_PLACEMENT_3D('',#212136,#120725,#120726);
#100666=AXIS2_PLACEMENT_3D('',#212139,#120729,#120730);
#100667=AXIS2_PLACEMENT_3D('',#212142,#120731,#120732);
#100668=AXIS2_PLACEMENT_3D('',#212143,#120733,#120734);
#100669=AXIS2_PLACEMENT_3D('',#212144,#120735,#120736);
#100670=AXIS2_PLACEMENT_3D('',#212145,#120737,#120738);
#100671=AXIS2_PLACEMENT_3D('',#212148,#120739,#120740);
#100672=AXIS2_PLACEMENT_3D('',#212149,#120741,#120742);
#100673=AXIS2_PLACEMENT_3D('',#212150,#120743,#120744);
#100674=AXIS2_PLACEMENT_3D('',#212151,#120745,#120746);
#100675=AXIS2_PLACEMENT_3D('',#212152,#120747,#120748);
#100676=AXIS2_PLACEMENT_3D('',#212153,#120749,#120750);
#100677=AXIS2_PLACEMENT_3D('',#212154,#120751,#120752);
#100678=AXIS2_PLACEMENT_3D('',#212157,#120753,#120754);
#100679=AXIS2_PLACEMENT_3D('',#212159,#120755,#120756);
#100680=AXIS2_PLACEMENT_3D('',#212161,#120757,#120758);
#100681=AXIS2_PLACEMENT_3D('',#212162,#120759,#120760);
#100682=AXIS2_PLACEMENT_3D('',#212163,#120761,#120762);
#100683=AXIS2_PLACEMENT_3D('',#212166,#120763,#120764);
#100684=AXIS2_PLACEMENT_3D('',#212169,#120767,#120768);
#100685=AXIS2_PLACEMENT_3D('',#212172,#120769,#120770);
#100686=AXIS2_PLACEMENT_3D('',#212175,#120773,#120774);
#100687=AXIS2_PLACEMENT_3D('',#212178,#120775,#120776);
#100688=AXIS2_PLACEMENT_3D('',#212179,#120777,#120778);
#100689=AXIS2_PLACEMENT_3D('',#212180,#120779,#120780);
#100690=AXIS2_PLACEMENT_3D('',#212181,#120781,#120782);
#100691=AXIS2_PLACEMENT_3D('',#212184,#120783,#120784);
#100692=AXIS2_PLACEMENT_3D('',#212185,#120785,#120786);
#100693=AXIS2_PLACEMENT_3D('',#212186,#120787,#120788);
#100694=AXIS2_PLACEMENT_3D('',#212187,#120789,#120790);
#100695=AXIS2_PLACEMENT_3D('',#212190,#120791,#120792);
#100696=AXIS2_PLACEMENT_3D('',#212193,#120795,#120796);
#100697=AXIS2_PLACEMENT_3D('',#212196,#120797,#120798);
#100698=AXIS2_PLACEMENT_3D('',#212199,#120801,#120802);
#100699=AXIS2_PLACEMENT_3D('',#212200,#120803,#120804);
#100700=AXIS2_PLACEMENT_3D('',#212201,#120805,#120806);
#100701=AXIS2_PLACEMENT_3D('',#212202,#120807,#120808);
#100702=AXIS2_PLACEMENT_3D('',#212205,#120809,#120810);
#100703=AXIS2_PLACEMENT_3D('',#212207,#120811,#120812);
#100704=AXIS2_PLACEMENT_3D('',#212209,#120813,#120814);
#100705=AXIS2_PLACEMENT_3D('',#212210,#120815,#120816);
#100706=AXIS2_PLACEMENT_3D('',#212211,#120817,#120818);
#100707=AXIS2_PLACEMENT_3D('',#212214,#120819,#120820);
#100708=AXIS2_PLACEMENT_3D('',#212217,#120823,#120824);
#100709=AXIS2_PLACEMENT_3D('',#212220,#120825,#120826);
#100710=AXIS2_PLACEMENT_3D('',#212223,#120829,#120830);
#100711=AXIS2_PLACEMENT_3D('',#212226,#120831,#120832);
#100712=AXIS2_PLACEMENT_3D('',#212227,#120833,#120834);
#100713=AXIS2_PLACEMENT_3D('',#212228,#120835,#120836);
#100714=AXIS2_PLACEMENT_3D('',#212229,#120837,#120838);
#100715=AXIS2_PLACEMENT_3D('',#212232,#120839,#120840);
#100716=AXIS2_PLACEMENT_3D('',#212233,#120841,#120842);
#100717=AXIS2_PLACEMENT_3D('',#212234,#120843,#120844);
#100718=AXIS2_PLACEMENT_3D('',#212235,#120845,#120846);
#100719=AXIS2_PLACEMENT_3D('',#212238,#120847,#120848);
#100720=AXIS2_PLACEMENT_3D('',#212241,#120851,#120852);
#100721=AXIS2_PLACEMENT_3D('',#212244,#120853,#120854);
#100722=AXIS2_PLACEMENT_3D('',#212245,#120855,#120856);
#100723=AXIS2_PLACEMENT_3D('',#212246,#120857,#120858);
#100724=AXIS2_PLACEMENT_3D('',#212247,#120859,#120860);
#100725=AXIS2_PLACEMENT_3D('',#212250,#120861,#120862);
#100726=AXIS2_PLACEMENT_3D('',#212251,#120863,#120864);
#100727=AXIS2_PLACEMENT_3D('',#212252,#120865,#120866);
#100728=AXIS2_PLACEMENT_3D('',#212253,#120867,#120868);
#100729=AXIS2_PLACEMENT_3D('',#212256,#120869,#120870);
#100730=AXIS2_PLACEMENT_3D('',#212257,#120871,#120872);
#100731=AXIS2_PLACEMENT_3D('',#212258,#120873,#120874);
#100732=AXIS2_PLACEMENT_3D('',#212259,#120875,#120876);
#100733=AXIS2_PLACEMENT_3D('',#212260,#120877,#120878);
#100734=AXIS2_PLACEMENT_3D('',#212261,#120879,#120880);
#100735=AXIS2_PLACEMENT_3D('',#212262,#120881,#120882);
#100736=AXIS2_PLACEMENT_3D('',#212265,#120883,#120884);
#100737=AXIS2_PLACEMENT_3D('',#212267,#120885,#120886);
#100738=AXIS2_PLACEMENT_3D('',#212269,#120887,#120888);
#100739=AXIS2_PLACEMENT_3D('',#212270,#120889,#120890);
#100740=AXIS2_PLACEMENT_3D('',#212271,#120891,#120892);
#100741=AXIS2_PLACEMENT_3D('',#212274,#120893,#120894);
#100742=AXIS2_PLACEMENT_3D('',#212277,#120897,#120898);
#100743=AXIS2_PLACEMENT_3D('',#212280,#120899,#120900);
#100744=AXIS2_PLACEMENT_3D('',#212283,#120903,#120904);
#100745=AXIS2_PLACEMENT_3D('',#212286,#120905,#120906);
#100746=AXIS2_PLACEMENT_3D('',#212287,#120907,#120908);
#100747=AXIS2_PLACEMENT_3D('',#212288,#120909,#120910);
#100748=AXIS2_PLACEMENT_3D('',#212289,#120911,#120912);
#100749=AXIS2_PLACEMENT_3D('',#212292,#120913,#120914);
#100750=AXIS2_PLACEMENT_3D('',#212293,#120915,#120916);
#100751=AXIS2_PLACEMENT_3D('',#212294,#120917,#120918);
#100752=AXIS2_PLACEMENT_3D('',#212295,#120919,#120920);
#100753=AXIS2_PLACEMENT_3D('',#212298,#120921,#120922);
#100754=AXIS2_PLACEMENT_3D('',#212301,#120925,#120926);
#100755=AXIS2_PLACEMENT_3D('',#212304,#120927,#120928);
#100756=AXIS2_PLACEMENT_3D('',#212305,#120929,#120930);
#100757=AXIS2_PLACEMENT_3D('',#212306,#120931,#120932);
#100758=AXIS2_PLACEMENT_3D('',#212307,#120933,#120934);
#100759=AXIS2_PLACEMENT_3D('',#212308,#120935,#120936);
#100760=AXIS2_PLACEMENT_3D('',#212309,#120937,#120938);
#100761=AXIS2_PLACEMENT_3D('',#212310,#120939,#120940);
#100762=AXIS2_PLACEMENT_3D('',#212313,#120941,#120942);
#100763=AXIS2_PLACEMENT_3D('',#212315,#120943,#120944);
#100764=AXIS2_PLACEMENT_3D('',#212317,#120945,#120946);
#100765=AXIS2_PLACEMENT_3D('',#212318,#120947,#120948);
#100766=AXIS2_PLACEMENT_3D('',#212319,#120949,#120950);
#100767=AXIS2_PLACEMENT_3D('',#212322,#120951,#120952);
#100768=AXIS2_PLACEMENT_3D('',#212325,#120955,#120956);
#100769=AXIS2_PLACEMENT_3D('',#212328,#120957,#120958);
#100770=AXIS2_PLACEMENT_3D('',#212331,#120961,#120962);
#100771=AXIS2_PLACEMENT_3D('',#212334,#120963,#120964);
#100772=AXIS2_PLACEMENT_3D('',#212335,#120965,#120966);
#100773=AXIS2_PLACEMENT_3D('',#212336,#120967,#120968);
#100774=AXIS2_PLACEMENT_3D('',#212337,#120969,#120970);
#100775=AXIS2_PLACEMENT_3D('',#212340,#120971,#120972);
#100776=AXIS2_PLACEMENT_3D('',#212341,#120973,#120974);
#100777=AXIS2_PLACEMENT_3D('',#212342,#120975,#120976);
#100778=AXIS2_PLACEMENT_3D('',#212343,#120977,#120978);
#100779=AXIS2_PLACEMENT_3D('',#212346,#120979,#120980);
#100780=AXIS2_PLACEMENT_3D('',#212349,#120983,#120984);
#100781=AXIS2_PLACEMENT_3D('',#212352,#120985,#120986);
#100782=AXIS2_PLACEMENT_3D('',#212355,#120989,#120990);
#100783=AXIS2_PLACEMENT_3D('',#212356,#120991,#120992);
#100784=AXIS2_PLACEMENT_3D('',#212357,#120993,#120994);
#100785=AXIS2_PLACEMENT_3D('',#212358,#120995,#120996);
#100786=AXIS2_PLACEMENT_3D('',#212361,#120997,#120998);
#100787=AXIS2_PLACEMENT_3D('',#212363,#120999,#121000);
#100788=AXIS2_PLACEMENT_3D('',#212365,#121001,#121002);
#100789=AXIS2_PLACEMENT_3D('',#212366,#121003,#121004);
#100790=AXIS2_PLACEMENT_3D('',#212367,#121005,#121006);
#100791=AXIS2_PLACEMENT_3D('',#212370,#121007,#121008);
#100792=AXIS2_PLACEMENT_3D('',#212373,#121011,#121012);
#100793=AXIS2_PLACEMENT_3D('',#212376,#121013,#121014);
#100794=AXIS2_PLACEMENT_3D('',#212379,#121017,#121018);
#100795=AXIS2_PLACEMENT_3D('',#212382,#121019,#121020);
#100796=AXIS2_PLACEMENT_3D('',#212383,#121021,#121022);
#100797=AXIS2_PLACEMENT_3D('',#212384,#121023,#121024);
#100798=AXIS2_PLACEMENT_3D('',#212385,#121025,#121026);
#100799=AXIS2_PLACEMENT_3D('',#212388,#121027,#121028);
#100800=AXIS2_PLACEMENT_3D('',#212389,#121029,#121030);
#100801=AXIS2_PLACEMENT_3D('',#212390,#121031,#121032);
#100802=AXIS2_PLACEMENT_3D('',#212391,#121033,#121034);
#100803=AXIS2_PLACEMENT_3D('',#212394,#121035,#121036);
#100804=AXIS2_PLACEMENT_3D('',#212397,#121039,#121040);
#100805=AXIS2_PLACEMENT_3D('',#212400,#121041,#121042);
#100806=AXIS2_PLACEMENT_3D('',#212401,#121043,#121044);
#100807=AXIS2_PLACEMENT_3D('',#212402,#121045,#121046);
#100808=AXIS2_PLACEMENT_3D('',#212403,#121047,#121048);
#100809=AXIS2_PLACEMENT_3D('',#212404,#121049,#121050);
#100810=AXIS2_PLACEMENT_3D('',#212405,#121051,#121052);
#100811=AXIS2_PLACEMENT_3D('',#212406,#121053,#121054);
#100812=AXIS2_PLACEMENT_3D('',#212409,#121055,#121056);
#100813=AXIS2_PLACEMENT_3D('',#212411,#121057,#121058);
#100814=AXIS2_PLACEMENT_3D('',#212413,#121059,#121060);
#100815=AXIS2_PLACEMENT_3D('',#212414,#121061,#121062);
#100816=AXIS2_PLACEMENT_3D('',#212415,#121063,#121064);
#100817=AXIS2_PLACEMENT_3D('',#212418,#121065,#121066);
#100818=AXIS2_PLACEMENT_3D('',#212421,#121069,#121070);
#100819=AXIS2_PLACEMENT_3D('',#212424,#121071,#121072);
#100820=AXIS2_PLACEMENT_3D('',#212427,#121075,#121076);
#100821=AXIS2_PLACEMENT_3D('',#212430,#121077,#121078);
#100822=AXIS2_PLACEMENT_3D('',#212431,#121079,#121080);
#100823=AXIS2_PLACEMENT_3D('',#212432,#121081,#121082);
#100824=AXIS2_PLACEMENT_3D('',#212433,#121083,#121084);
#100825=AXIS2_PLACEMENT_3D('',#212436,#121085,#121086);
#100826=AXIS2_PLACEMENT_3D('',#212437,#121087,#121088);
#100827=AXIS2_PLACEMENT_3D('',#212438,#121089,#121090);
#100828=AXIS2_PLACEMENT_3D('',#212439,#121091,#121092);
#100829=AXIS2_PLACEMENT_3D('',#212442,#121093,#121094);
#100830=AXIS2_PLACEMENT_3D('',#212445,#121097,#121098);
#100831=AXIS2_PLACEMENT_3D('',#212448,#121099,#121100);
#100832=AXIS2_PLACEMENT_3D('',#212451,#121103,#121104);
#100833=AXIS2_PLACEMENT_3D('',#212452,#121105,#121106);
#100834=AXIS2_PLACEMENT_3D('',#212453,#121107,#121108);
#100835=AXIS2_PLACEMENT_3D('',#212454,#121109,#121110);
#100836=AXIS2_PLACEMENT_3D('',#212457,#121111,#121112);
#100837=AXIS2_PLACEMENT_3D('',#212459,#121113,#121114);
#100838=AXIS2_PLACEMENT_3D('',#212461,#121115,#121116);
#100839=AXIS2_PLACEMENT_3D('',#212462,#121117,#121118);
#100840=AXIS2_PLACEMENT_3D('',#212463,#121119,#121120);
#100841=AXIS2_PLACEMENT_3D('',#212466,#121121,#121122);
#100842=AXIS2_PLACEMENT_3D('',#212469,#121125,#121126);
#100843=AXIS2_PLACEMENT_3D('',#212472,#121127,#121128);
#100844=AXIS2_PLACEMENT_3D('',#212473,#121129,#121130);
#100845=AXIS2_PLACEMENT_3D('',#212474,#121131,#121132);
#100846=AXIS2_PLACEMENT_3D('',#212475,#121133,#121134);
#100847=AXIS2_PLACEMENT_3D('',#212478,#121135,#121136);
#100848=AXIS2_PLACEMENT_3D('',#212479,#121137,#121138);
#100849=AXIS2_PLACEMENT_3D('',#212480,#121139,#121140);
#100850=AXIS2_PLACEMENT_3D('',#212481,#121141,#121142);
#100851=AXIS2_PLACEMENT_3D('',#212484,#121143,#121144);
#100852=AXIS2_PLACEMENT_3D('',#212485,#121145,#121146);
#100853=AXIS2_PLACEMENT_3D('',#212486,#121147,#121148);
#100854=AXIS2_PLACEMENT_3D('',#212487,#121149,#121150);
#100855=AXIS2_PLACEMENT_3D('',#212490,#121153,#121154);
#100856=AXIS2_PLACEMENT_3D('',#212493,#121155,#121156);
#100857=AXIS2_PLACEMENT_3D('',#212495,#121157,#121158);
#100858=AXIS2_PLACEMENT_3D('',#212497,#121159,#121160);
#100859=AXIS2_PLACEMENT_3D('',#212498,#121161,#121162);
#100860=AXIS2_PLACEMENT_3D('',#212499,#121163,#121164);
#100861=AXIS2_PLACEMENT_3D('',#212502,#121165,#121166);
#100862=AXIS2_PLACEMENT_3D('',#212505,#121169,#121170);
#100863=AXIS2_PLACEMENT_3D('',#212508,#121171,#121172);
#100864=AXIS2_PLACEMENT_3D('',#212509,#121173,#121174);
#100865=AXIS2_PLACEMENT_3D('',#212510,#121175,#121176);
#100866=AXIS2_PLACEMENT_3D('',#212511,#121177,#121178);
#100867=AXIS2_PLACEMENT_3D('',#212514,#121179,#121180);
#100868=AXIS2_PLACEMENT_3D('',#212515,#121181,#121182);
#100869=AXIS2_PLACEMENT_3D('',#212516,#121183,#121184);
#100870=AXIS2_PLACEMENT_3D('',#212517,#121185,#121186);
#100871=AXIS2_PLACEMENT_3D('',#212520,#121187,#121188);
#100872=AXIS2_PLACEMENT_3D('',#212521,#121189,#121190);
#100873=AXIS2_PLACEMENT_3D('',#212522,#121191,#121192);
#100874=AXIS2_PLACEMENT_3D('',#212523,#121193,#121194);
#100875=AXIS2_PLACEMENT_3D('',#212526,#121197,#121198);
#100876=AXIS2_PLACEMENT_3D('',#212528,#121199,#121200);
#100877=AXIS2_PLACEMENT_3D('',#212530,#121201,#121202);
#100878=AXIS2_PLACEMENT_3D('',#212531,#121203,#121204);
#100879=AXIS2_PLACEMENT_3D('',#212532,#121205,#121206);
#100880=AXIS2_PLACEMENT_3D('',#212534,#121207,#121208);
#100881=AXIS2_PLACEMENT_3D('',#212536,#121209,#121210);
#100882=AXIS2_PLACEMENT_3D('',#212537,#121211,#121212);
#100883=AXIS2_PLACEMENT_3D('',#212538,#121213,#121214);
#100884=AXIS2_PLACEMENT_3D('',#212541,#121215,#121216);
#100885=AXIS2_PLACEMENT_3D('',#212542,#121217,#121218);
#100886=AXIS2_PLACEMENT_3D('',#212543,#121219,#121220);
#100887=AXIS2_PLACEMENT_3D('',#212544,#121221,#121222);
#100888=AXIS2_PLACEMENT_3D('',#212547,#121223,#121224);
#100889=AXIS2_PLACEMENT_3D('',#212548,#121225,#121226);
#100890=AXIS2_PLACEMENT_3D('',#212549,#121227,#121228);
#100891=AXIS2_PLACEMENT_3D('',#212550,#121229,#121230);
#100892=AXIS2_PLACEMENT_3D('',#212553,#121231,#121232);
#100893=AXIS2_PLACEMENT_3D('',#212554,#121233,#121234);
#100894=AXIS2_PLACEMENT_3D('',#212555,#121235,#121236);
#100895=AXIS2_PLACEMENT_3D('',#212556,#121237,#121238);
#100896=AXIS2_PLACEMENT_3D('',#212559,#121239,#121240);
#100897=AXIS2_PLACEMENT_3D('',#212560,#121241,#121242);
#100898=AXIS2_PLACEMENT_3D('',#212561,#121243,#121244);
#100899=AXIS2_PLACEMENT_3D('',#212562,#121245,#121246);
#100900=AXIS2_PLACEMENT_3D('',#212565,#121247,#121248);
#100901=AXIS2_PLACEMENT_3D('',#212566,#121249,#121250);
#100902=AXIS2_PLACEMENT_3D('',#212567,#121251,#121252);
#100903=AXIS2_PLACEMENT_3D('',#212568,#121253,#121254);
#100904=AXIS2_PLACEMENT_3D('',#212571,#121255,#121256);
#100905=AXIS2_PLACEMENT_3D('',#212572,#121257,#121258);
#100906=AXIS2_PLACEMENT_3D('',#212573,#121259,#121260);
#100907=AXIS2_PLACEMENT_3D('',#212574,#121261,#121262);
#100908=AXIS2_PLACEMENT_3D('',#212577,#121263,#121264);
#100909=AXIS2_PLACEMENT_3D('',#212578,#121265,#121266);
#100910=AXIS2_PLACEMENT_3D('',#212579,#121267,#121268);
#100911=AXIS2_PLACEMENT_3D('',#212580,#121269,#121270);
#100912=AXIS2_PLACEMENT_3D('',#212583,#121271,#121272);
#100913=AXIS2_PLACEMENT_3D('',#212584,#121273,#121274);
#100914=AXIS2_PLACEMENT_3D('',#212585,#121275,#121276);
#100915=AXIS2_PLACEMENT_3D('',#212586,#121277,#121278);
#100916=AXIS2_PLACEMENT_3D('',#212587,#121279,#121280);
#100917=AXIS2_PLACEMENT_3D('',#212588,#121281,#121282);
#100918=AXIS2_PLACEMENT_3D('',#212589,#121283,#121284);
#100919=AXIS2_PLACEMENT_3D('',#212592,#121285,#121286);
#100920=AXIS2_PLACEMENT_3D('',#212593,#121287,#121288);
#100921=AXIS2_PLACEMENT_3D('',#212594,#121289,#121290);
#100922=AXIS2_PLACEMENT_3D('',#212595,#121291,#121292);
#100923=AXIS2_PLACEMENT_3D('',#212598,#121293,#121294);
#100924=AXIS2_PLACEMENT_3D('',#212599,#121295,#121296);
#100925=AXIS2_PLACEMENT_3D('',#212600,#121297,#121298);
#100926=AXIS2_PLACEMENT_3D('',#212601,#121299,#121300);
#100927=AXIS2_PLACEMENT_3D('',#212604,#121301,#121302);
#100928=AXIS2_PLACEMENT_3D('',#212605,#121303,#121304);
#100929=AXIS2_PLACEMENT_3D('',#212606,#121305,#121306);
#100930=AXIS2_PLACEMENT_3D('',#212607,#121307,#121308);
#100931=AXIS2_PLACEMENT_3D('',#212610,#121309,#121310);
#100932=AXIS2_PLACEMENT_3D('',#212611,#121311,#121312);
#100933=AXIS2_PLACEMENT_3D('',#212612,#121313,#121314);
#100934=AXIS2_PLACEMENT_3D('',#212613,#121315,#121316);
#100935=AXIS2_PLACEMENT_3D('',#212616,#121317,#121318);
#100936=AXIS2_PLACEMENT_3D('',#212617,#121319,#121320);
#100937=AXIS2_PLACEMENT_3D('',#212618,#121321,#121322);
#100938=AXIS2_PLACEMENT_3D('',#212619,#121323,#121324);
#100939=AXIS2_PLACEMENT_3D('',#212622,#121325,#121326);
#100940=AXIS2_PLACEMENT_3D('',#212623,#121327,#121328);
#100941=AXIS2_PLACEMENT_3D('',#212624,#121329,#121330);
#100942=AXIS2_PLACEMENT_3D('',#212625,#121331,#121332);
#100943=AXIS2_PLACEMENT_3D('',#212628,#121333,#121334);
#100944=AXIS2_PLACEMENT_3D('',#212629,#121335,#121336);
#100945=AXIS2_PLACEMENT_3D('',#212630,#121337,#121338);
#100946=AXIS2_PLACEMENT_3D('',#212631,#121339,#121340);
#100947=AXIS2_PLACEMENT_3D('',#212634,#121341,#121342);
#100948=AXIS2_PLACEMENT_3D('',#212635,#121343,#121344);
#100949=AXIS2_PLACEMENT_3D('',#212636,#121345,#121346);
#100950=AXIS2_PLACEMENT_3D('',#212637,#121347,#121348);
#100951=AXIS2_PLACEMENT_3D('',#212638,#121349,#121350);
#100952=AXIS2_PLACEMENT_3D('',#212639,#121351,#121352);
#100953=AXIS2_PLACEMENT_3D('',#212640,#121353,#121354);
#100954=AXIS2_PLACEMENT_3D('',#212643,#121355,#121356);
#100955=AXIS2_PLACEMENT_3D('',#212645,#121357,#121358);
#100956=AXIS2_PLACEMENT_3D('',#212657,#121359,#121360);
#100957=AXIS2_PLACEMENT_3D('',#212658,#121361,#121362);
#100958=AXIS2_PLACEMENT_3D('',#212661,#121363,#121364);
#100959=AXIS2_PLACEMENT_3D('',#212664,#121367,#121368);
#100960=AXIS2_PLACEMENT_3D('',#212666,#121369,#121370);
#100961=AXIS2_PLACEMENT_3D('',#212668,#121371,#121372);
#100962=AXIS2_PLACEMENT_3D('',#212669,#121373,#121374);
#100963=AXIS2_PLACEMENT_3D('',#212670,#121375,#121376);
#100964=AXIS2_PLACEMENT_3D('',#212673,#121377,#121378);
#100965=AXIS2_PLACEMENT_3D('',#212674,#121379,#121380);
#100966=AXIS2_PLACEMENT_3D('',#212675,#121381,#121382);
#100967=AXIS2_PLACEMENT_3D('',#212676,#121383,#121384);
#100968=AXIS2_PLACEMENT_3D('',#212679,#121385,#121386);
#100969=AXIS2_PLACEMENT_3D('',#212680,#121387,#121388);
#100970=AXIS2_PLACEMENT_3D('',#212681,#121389,#121390);
#100971=AXIS2_PLACEMENT_3D('',#212682,#121391,#121392);
#100972=AXIS2_PLACEMENT_3D('',#212685,#121393,#121394);
#100973=AXIS2_PLACEMENT_3D('',#212688,#121397,#121398);
#100974=AXIS2_PLACEMENT_3D('',#212701,#121399,#121400);
#100975=AXIS2_PLACEMENT_3D('',#212702,#121401,#121402);
#100976=AXIS2_PLACEMENT_3D('',#212703,#121403,#121404);
#100977=AXIS2_PLACEMENT_3D('',#212706,#121405,#121406);
#100978=AXIS2_PLACEMENT_3D('',#212708,#121407,#121408);
#100979=AXIS2_PLACEMENT_3D('',#212720,#121409,#121410);
#100980=AXIS2_PLACEMENT_3D('',#212721,#121411,#121412);
#100981=AXIS2_PLACEMENT_3D('',#212724,#121413,#121414);
#100982=AXIS2_PLACEMENT_3D('',#212727,#121417,#121418);
#100983=AXIS2_PLACEMENT_3D('',#212730,#121419,#121420);
#100984=AXIS2_PLACEMENT_3D('',#212731,#121421,#121422);
#100985=AXIS2_PLACEMENT_3D('',#212732,#121423,#121424);
#100986=AXIS2_PLACEMENT_3D('',#212733,#121425,#121426);
#100987=AXIS2_PLACEMENT_3D('',#212736,#121427,#121428);
#100988=AXIS2_PLACEMENT_3D('',#212737,#121429,#121430);
#100989=AXIS2_PLACEMENT_3D('',#212738,#121431,#121432);
#100990=AXIS2_PLACEMENT_3D('',#212739,#121433,#121434);
#100991=AXIS2_PLACEMENT_3D('',#212742,#121435,#121436);
#100992=AXIS2_PLACEMENT_3D('',#212743,#121437,#121438);
#100993=AXIS2_PLACEMENT_3D('',#212744,#121439,#121440);
#100994=AXIS2_PLACEMENT_3D('',#212745,#121441,#121442);
#100995=AXIS2_PLACEMENT_3D('',#212748,#121443,#121444);
#100996=AXIS2_PLACEMENT_3D('',#212751,#121447,#121448);
#100997=AXIS2_PLACEMENT_3D('',#212764,#121449,#121450);
#100998=AXIS2_PLACEMENT_3D('',#212765,#121451,#121452);
#100999=AXIS2_PLACEMENT_3D('',#212766,#121453,#121454);
#101000=AXIS2_PLACEMENT_3D('',#212769,#121455,#121456);
#101001=AXIS2_PLACEMENT_3D('',#212771,#121457,#121458);
#101002=AXIS2_PLACEMENT_3D('',#212783,#121459,#121460);
#101003=AXIS2_PLACEMENT_3D('',#212784,#121461,#121462);
#101004=AXIS2_PLACEMENT_3D('',#212787,#121463,#121464);
#101005=AXIS2_PLACEMENT_3D('',#212790,#121467,#121468);
#101006=AXIS2_PLACEMENT_3D('',#212792,#121469,#121470);
#101007=AXIS2_PLACEMENT_3D('',#212794,#121471,#121472);
#101008=AXIS2_PLACEMENT_3D('',#212795,#121473,#121474);
#101009=AXIS2_PLACEMENT_3D('',#212796,#121475,#121476);
#101010=AXIS2_PLACEMENT_3D('',#212799,#121477,#121478);
#101011=AXIS2_PLACEMENT_3D('',#212800,#121479,#121480);
#101012=AXIS2_PLACEMENT_3D('',#212801,#121481,#121482);
#101013=AXIS2_PLACEMENT_3D('',#212802,#121483,#121484);
#101014=AXIS2_PLACEMENT_3D('',#212805,#121485,#121486);
#101015=AXIS2_PLACEMENT_3D('',#212806,#121487,#121488);
#101016=AXIS2_PLACEMENT_3D('',#212807,#121489,#121490);
#101017=AXIS2_PLACEMENT_3D('',#212808,#121491,#121492);
#101018=AXIS2_PLACEMENT_3D('',#212811,#121493,#121494);
#101019=AXIS2_PLACEMENT_3D('',#212814,#121497,#121498);
#101020=AXIS2_PLACEMENT_3D('',#212827,#121499,#121500);
#101021=AXIS2_PLACEMENT_3D('',#212828,#121501,#121502);
#101022=AXIS2_PLACEMENT_3D('',#212829,#121503,#121504);
#101023=AXIS2_PLACEMENT_3D('',#212843,#121505,#121506);
#101024=AXIS2_PLACEMENT_3D('',#212845,#121507,#121508);
#101025=AXIS2_PLACEMENT_3D('',#212846,#121509,#121510);
#101026=AXIS2_PLACEMENT_3D('',#212847,#121511,#121512);
#101027=AXIS2_PLACEMENT_3D('',#212850,#121513,#121514);
#101028=AXIS2_PLACEMENT_3D('',#212853,#121517,#121518);
#101029=AXIS2_PLACEMENT_3D('',#212856,#121519,#121520);
#101030=AXIS2_PLACEMENT_3D('',#212857,#121521,#121522);
#101031=AXIS2_PLACEMENT_3D('',#212858,#121523,#121524);
#101032=AXIS2_PLACEMENT_3D('',#212859,#121525,#121526);
#101033=AXIS2_PLACEMENT_3D('',#212862,#121527,#121528);
#101034=AXIS2_PLACEMENT_3D('',#212863,#121529,#121530);
#101035=AXIS2_PLACEMENT_3D('',#212864,#121531,#121532);
#101036=AXIS2_PLACEMENT_3D('',#212865,#121533,#121534);
#101037=AXIS2_PLACEMENT_3D('',#212868,#121535,#121536);
#101038=AXIS2_PLACEMENT_3D('',#212869,#121537,#121538);
#101039=AXIS2_PLACEMENT_3D('',#212870,#121539,#121540);
#101040=AXIS2_PLACEMENT_3D('',#212871,#121541,#121542);
#101041=AXIS2_PLACEMENT_3D('',#212874,#121543,#121544);
#101042=AXIS2_PLACEMENT_3D('',#212877,#121547,#121548);
#101043=AXIS2_PLACEMENT_3D('',#212890,#121549,#121550);
#101044=AXIS2_PLACEMENT_3D('',#212891,#121551,#121552);
#101045=AXIS2_PLACEMENT_3D('',#212892,#121553,#121554);
#101046=AXIS2_PLACEMENT_3D('',#212894,#121555,#121556);
#101047=AXIS2_PLACEMENT_3D('',#212896,#121557,#121558);
#101048=AXIS2_PLACEMENT_3D('',#212897,#121559,#121560);
#101049=AXIS2_PLACEMENT_3D('',#212898,#121561,#121562);
#101050=AXIS2_PLACEMENT_3D('',#212901,#121563,#121564);
#101051=AXIS2_PLACEMENT_3D('',#212902,#121565,#121566);
#101052=AXIS2_PLACEMENT_3D('',#212903,#121567,#121568);
#101053=AXIS2_PLACEMENT_3D('',#212904,#121569,#121570);
#101054=AXIS2_PLACEMENT_3D('',#212907,#121571,#121572);
#101055=AXIS2_PLACEMENT_3D('',#212908,#121573,#121574);
#101056=AXIS2_PLACEMENT_3D('',#212909,#121575,#121576);
#101057=AXIS2_PLACEMENT_3D('',#212910,#121577,#121578);
#101058=AXIS2_PLACEMENT_3D('',#212913,#121579,#121580);
#101059=AXIS2_PLACEMENT_3D('',#212914,#121581,#121582);
#101060=AXIS2_PLACEMENT_3D('',#212915,#121583,#121584);
#101061=AXIS2_PLACEMENT_3D('',#212916,#121585,#121586);
#101062=AXIS2_PLACEMENT_3D('',#212919,#121587,#121588);
#101063=AXIS2_PLACEMENT_3D('',#212920,#121589,#121590);
#101064=AXIS2_PLACEMENT_3D('',#212921,#121591,#121592);
#101065=AXIS2_PLACEMENT_3D('',#212922,#121593,#121594);
#101066=AXIS2_PLACEMENT_3D('',#212925,#121595,#121596);
#101067=AXIS2_PLACEMENT_3D('',#212926,#121597,#121598);
#101068=AXIS2_PLACEMENT_3D('',#212927,#121599,#121600);
#101069=AXIS2_PLACEMENT_3D('',#212928,#121601,#121602);
#101070=AXIS2_PLACEMENT_3D('',#212931,#121603,#121604);
#101071=AXIS2_PLACEMENT_3D('',#212932,#121605,#121606);
#101072=AXIS2_PLACEMENT_3D('',#212933,#121607,#121608);
#101073=AXIS2_PLACEMENT_3D('',#212934,#121609,#121610);
#101074=AXIS2_PLACEMENT_3D('',#212937,#121611,#121612);
#101075=AXIS2_PLACEMENT_3D('',#212938,#121613,#121614);
#101076=AXIS2_PLACEMENT_3D('',#212939,#121615,#121616);
#101077=AXIS2_PLACEMENT_3D('',#212940,#121617,#121618);
#101078=AXIS2_PLACEMENT_3D('',#212941,#121619,#121620);
#101079=AXIS2_PLACEMENT_3D('',#212942,#121621,#121622);
#101080=AXIS2_PLACEMENT_3D('',#213177,#121623,#121624);
#101081=AXIS2_PLACEMENT_3D('',#213410,#121625,#121626);
#101082=AXIS2_PLACEMENT_3D('',#213415,#121627,#121628);
#101083=AXIS2_PLACEMENT_3D('',#213430,#121629,#121630);
#101084=AXIS2_PLACEMENT_3D('',#213431,#121631,#121632);
#101085=AXIS2_PLACEMENT_3D('',#213432,#121633,#121634);
#101086=AXIS2_PLACEMENT_3D('',#213513,#121635,#121636);
#101087=AXIS2_PLACEMENT_3D('',#213664,#121637,#121638);
#101088=AXIS2_PLACEMENT_3D('',#213897,#121639,#121640);
#101089=AXIS2_PLACEMENT_3D('',#214054,#121641,#121642);
#101090=AXIS2_PLACEMENT_3D('',#214055,#121643,#121644);
#101091=AXIS2_PLACEMENT_3D('',#214056,#121645,#121646);
#101092=AXIS2_PLACEMENT_3D('',#214071,#121647,#121648);
#101093=AXIS2_PLACEMENT_3D('',#214403,#121649,#121650);
#101094=AXIS2_PLACEMENT_3D('',#214927,#121651,#121652);
#101095=AXIS2_PLACEMENT_3D('',#214962,#121653,#121654);
#101096=AXIS2_PLACEMENT_3D('',#214963,#121655,#121656);
#101097=AXIS2_PLACEMENT_3D('',#214964,#121657,#121658);
#101098=AXIS2_PLACEMENT_3D('',#215063,#121659,#121660);
#101099=AXIS2_PLACEMENT_3D('',#215392,#121661,#121662);
#101100=AXIS2_PLACEMENT_3D('',#215637,#121663,#121664);
#101101=AXIS2_PLACEMENT_3D('',#215775,#121665,#121666);
#101102=AXIS2_PLACEMENT_3D('',#215776,#121667,#121668);
#101103=AXIS2_PLACEMENT_3D('',#215777,#121669,#121670);
#101104=AXIS2_PLACEMENT_3D('',#215792,#121671,#121672);
#101105=AXIS2_PLACEMENT_3D('',#216763,#121673,#121674);
#101106=AXIS2_PLACEMENT_3D('',#216764,#121675,#121676);
#101107=AXIS2_PLACEMENT_3D('',#216779,#121677,#121678);
#101108=AXIS2_PLACEMENT_3D('',#216780,#121679,#121680);
#101109=AXIS2_PLACEMENT_3D('',#216781,#121681,#121682);
#101110=AXIS2_PLACEMENT_3D('',#216862,#121683,#121684);
#101111=AXIS2_PLACEMENT_3D('',#217215,#121685,#121686);
#101112=AXIS2_PLACEMENT_3D('',#217277,#121687,#121688);
#101113=AXIS2_PLACEMENT_3D('',#217279,#121689,#121690);
#101114=AXIS2_PLACEMENT_3D('',#217280,#121691,#121692);
#101115=AXIS2_PLACEMENT_3D('',#217305,#121693,#121694);
#101116=AXIS2_PLACEMENT_3D('',#217306,#121695,#121696);
#101117=AXIS2_PLACEMENT_3D('',#218572,#121697,#121698);
#101118=AXIS2_PLACEMENT_3D('',#218593,#121699,#121700);
#101119=AXIS2_PLACEMENT_3D('',#218618,#121701,#121702);
#101120=AXIS2_PLACEMENT_3D('',#218620,#121703,#121704);
#101121=AXIS2_PLACEMENT_3D('',#218621,#121705,#121706);
#101122=AXIS2_PLACEMENT_3D('',#218642,#121707,#121708);
#101123=AXIS2_PLACEMENT_3D('',#218743,#121709,#121710);
#101124=AXIS2_PLACEMENT_3D('',#219018,#121711,#121712);
#101125=AXIS2_PLACEMENT_3D('',#219019,#121713,#121714);
#101126=AXIS2_PLACEMENT_3D('',#219020,#121715,#121716);
#101127=AXIS2_PLACEMENT_3D('',#219067,#121717,#121718);
#101128=AXIS2_PLACEMENT_3D('',#220115,#121719,#121720);
#101129=AXIS2_PLACEMENT_3D('',#220116,#121721,#121722);
#101130=AXIS2_PLACEMENT_3D('',#220131,#121723,#121724);
#101131=AXIS2_PLACEMENT_3D('',#220132,#121725,#121726);
#101132=AXIS2_PLACEMENT_3D('',#220133,#121727,#121728);
#101133=AXIS2_PLACEMENT_3D('',#220147,#121729,#121730);
#101134=AXIS2_PLACEMENT_3D('',#220149,#121731,#121732);
#101135=AXIS2_PLACEMENT_3D('',#220150,#121733,#121734);
#101136=AXIS2_PLACEMENT_3D('',#220183,#121735,#121736);
#101137=AXIS2_PLACEMENT_3D('',#220398,#121737,#121738);
#101138=AXIS2_PLACEMENT_3D('',#220608,#121739,#121740);
#101139=AXIS2_PLACEMENT_3D('',#220609,#121741,#121742);
#101140=AXIS2_PLACEMENT_3D('',#220632,#121743,#121744);
#101141=AXIS2_PLACEMENT_3D('',#220643,#121745,#121746);
#101142=AXIS2_PLACEMENT_3D('',#220645,#121747,#121748);
#101143=AXIS2_PLACEMENT_3D('',#220647,#121749,#121750);
#101144=AXIS2_PLACEMENT_3D('',#220648,#121751,#121752);
#101145=AXIS2_PLACEMENT_3D('',#221316,#121753,#121754);
#101146=AXIS2_PLACEMENT_3D('',#221341,#121755,#121756);
#101147=AXIS2_PLACEMENT_3D('',#221343,#121757,#121758);
#101148=AXIS2_PLACEMENT_3D('',#221344,#121759,#121760);
#101149=AXIS2_PLACEMENT_3D('',#221358,#121761,#121762);
#101150=AXIS2_PLACEMENT_3D('',#221398,#121763,#121764);
#101151=AXIS2_PLACEMENT_3D('',#221501,#121765,#121766);
#101152=AXIS2_PLACEMENT_3D('',#221827,#121767,#121768);
#101153=AXIS2_PLACEMENT_3D('',#221841,#121769,#121770);
#101154=AXIS2_PLACEMENT_3D('',#222188,#121771,#121772);
#101155=AXIS2_PLACEMENT_3D('',#222191,#121773,#121774);
#101156=AXIS2_PLACEMENT_3D('',#222194,#121777,#121778);
#101157=AXIS2_PLACEMENT_3D('',#222199,#121781,#121782);
#101158=AXIS2_PLACEMENT_3D('',#222200,#121783,#121784);
#101159=AXIS2_PLACEMENT_3D('',#222205,#121787,#121788);
#101160=AXIS2_PLACEMENT_3D('',#222206,#121789,#121790);
#101161=AXIS2_PLACEMENT_3D('',#222211,#121793,#121794);
#101162=AXIS2_PLACEMENT_3D('',#222212,#121795,#121796);
#101163=AXIS2_PLACEMENT_3D('',#222217,#121799,#121800);
#101164=AXIS2_PLACEMENT_3D('',#222218,#121801,#121802);
#101165=AXIS2_PLACEMENT_3D('',#222223,#121805,#121806);
#101166=AXIS2_PLACEMENT_3D('',#222224,#121807,#121808);
#101167=AXIS2_PLACEMENT_3D('',#222229,#121811,#121812);
#101168=AXIS2_PLACEMENT_3D('',#222230,#121813,#121814);
#101169=AXIS2_PLACEMENT_3D('',#222235,#121817,#121818);
#101170=AXIS2_PLACEMENT_3D('',#222236,#121819,#121820);
#101171=AXIS2_PLACEMENT_3D('',#222241,#121823,#121824);
#101172=AXIS2_PLACEMENT_3D('',#222242,#121825,#121826);
#101173=AXIS2_PLACEMENT_3D('',#222245,#121827,#121828);
#101174=AXIS2_PLACEMENT_3D('',#222248,#121831,#121832);
#101175=AXIS2_PLACEMENT_3D('',#222253,#121835,#121836);
#101176=AXIS2_PLACEMENT_3D('',#222254,#121837,#121838);
#101177=AXIS2_PLACEMENT_3D('',#222259,#121841,#121842);
#101178=AXIS2_PLACEMENT_3D('',#222260,#121843,#121844);
#101179=AXIS2_PLACEMENT_3D('',#222265,#121847,#121848);
#101180=AXIS2_PLACEMENT_3D('',#222266,#121849,#121850);
#101181=AXIS2_PLACEMENT_3D('',#222271,#121853,#121854);
#101182=AXIS2_PLACEMENT_3D('',#222272,#121855,#121856);
#101183=AXIS2_PLACEMENT_3D('',#222277,#121859,#121860);
#101184=AXIS2_PLACEMENT_3D('',#222278,#121861,#121862);
#101185=AXIS2_PLACEMENT_3D('',#222283,#121865,#121866);
#101186=AXIS2_PLACEMENT_3D('',#222284,#121867,#121868);
#101187=AXIS2_PLACEMENT_3D('',#222289,#121871,#121872);
#101188=AXIS2_PLACEMENT_3D('',#222290,#121873,#121874);
#101189=AXIS2_PLACEMENT_3D('',#222295,#121877,#121878);
#101190=AXIS2_PLACEMENT_3D('',#222296,#121879,#121880);
#101191=AXIS2_PLACEMENT_3D('',#222301,#121883,#121884);
#101192=AXIS2_PLACEMENT_3D('',#222302,#121885,#121886);
#101193=AXIS2_PLACEMENT_3D('',#222307,#121889,#121890);
#101194=AXIS2_PLACEMENT_3D('',#222308,#121891,#121892);
#101195=AXIS2_PLACEMENT_3D('',#222313,#121895,#121896);
#101196=AXIS2_PLACEMENT_3D('',#222314,#121897,#121898);
#101197=AXIS2_PLACEMENT_3D('',#222319,#121901,#121902);
#101198=AXIS2_PLACEMENT_3D('',#222320,#121903,#121904);
#101199=AXIS2_PLACEMENT_3D('',#222325,#121907,#121908);
#101200=AXIS2_PLACEMENT_3D('',#222326,#121909,#121910);
#101201=AXIS2_PLACEMENT_3D('',#222331,#121913,#121914);
#101202=AXIS2_PLACEMENT_3D('',#222332,#121915,#121916);
#101203=AXIS2_PLACEMENT_3D('',#222337,#121919,#121920);
#101204=AXIS2_PLACEMENT_3D('',#222338,#121921,#121922);
#101205=AXIS2_PLACEMENT_3D('',#222343,#121925,#121926);
#101206=AXIS2_PLACEMENT_3D('',#222344,#121927,#121928);
#101207=AXIS2_PLACEMENT_3D('',#222349,#121931,#121932);
#101208=AXIS2_PLACEMENT_3D('',#222350,#121933,#121934);
#101209=AXIS2_PLACEMENT_3D('',#222353,#121935,#121936);
#101210=AXIS2_PLACEMENT_3D('',#222356,#121939,#121940);
#101211=AXIS2_PLACEMENT_3D('',#222361,#121943,#121944);
#101212=AXIS2_PLACEMENT_3D('',#222362,#121945,#121946);
#101213=AXIS2_PLACEMENT_3D('',#222367,#121949,#121950);
#101214=AXIS2_PLACEMENT_3D('',#222368,#121951,#121952);
#101215=AXIS2_PLACEMENT_3D('',#222373,#121955,#121956);
#101216=AXIS2_PLACEMENT_3D('',#222374,#121957,#121958);
#101217=AXIS2_PLACEMENT_3D('',#222379,#121961,#121962);
#101218=AXIS2_PLACEMENT_3D('',#222380,#121963,#121964);
#101219=AXIS2_PLACEMENT_3D('',#222385,#121967,#121968);
#101220=AXIS2_PLACEMENT_3D('',#222386,#121969,#121970);
#101221=AXIS2_PLACEMENT_3D('',#222391,#121973,#121974);
#101222=AXIS2_PLACEMENT_3D('',#222392,#121975,#121976);
#101223=AXIS2_PLACEMENT_3D('',#222397,#121979,#121980);
#101224=AXIS2_PLACEMENT_3D('',#222398,#121981,#121982);
#101225=AXIS2_PLACEMENT_3D('',#222403,#121985,#121986);
#101226=AXIS2_PLACEMENT_3D('',#222404,#121987,#121988);
#101227=AXIS2_PLACEMENT_3D('',#222409,#121991,#121992);
#101228=AXIS2_PLACEMENT_3D('',#222410,#121993,#121994);
#101229=AXIS2_PLACEMENT_3D('',#222415,#121997,#121998);
#101230=AXIS2_PLACEMENT_3D('',#222416,#121999,#122000);
#101231=AXIS2_PLACEMENT_3D('',#222421,#122003,#122004);
#101232=AXIS2_PLACEMENT_3D('',#222422,#122005,#122006);
#101233=AXIS2_PLACEMENT_3D('',#222427,#122009,#122010);
#101234=AXIS2_PLACEMENT_3D('',#222428,#122011,#122012);
#101235=AXIS2_PLACEMENT_3D('',#222433,#122015,#122016);
#101236=AXIS2_PLACEMENT_3D('',#222434,#122017,#122018);
#101237=AXIS2_PLACEMENT_3D('',#222439,#122021,#122022);
#101238=AXIS2_PLACEMENT_3D('',#222440,#122023,#122024);
#101239=AXIS2_PLACEMENT_3D('',#222445,#122027,#122028);
#101240=AXIS2_PLACEMENT_3D('',#222446,#122029,#122030);
#101241=AXIS2_PLACEMENT_3D('',#222451,#122033,#122034);
#101242=AXIS2_PLACEMENT_3D('',#222452,#122035,#122036);
#101243=AXIS2_PLACEMENT_3D('',#222457,#122039,#122040);
#101244=AXIS2_PLACEMENT_3D('',#222458,#122041,#122042);
#101245=AXIS2_PLACEMENT_3D('',#222463,#122045,#122046);
#101246=AXIS2_PLACEMENT_3D('',#222464,#122047,#122048);
#101247=AXIS2_PLACEMENT_3D('',#222469,#122051,#122052);
#101248=AXIS2_PLACEMENT_3D('',#222470,#122053,#122054);
#101249=AXIS2_PLACEMENT_3D('',#222475,#122057,#122058);
#101250=AXIS2_PLACEMENT_3D('',#222476,#122059,#122060);
#101251=AXIS2_PLACEMENT_3D('',#222481,#122063,#122064);
#101252=AXIS2_PLACEMENT_3D('',#222482,#122065,#122066);
#101253=AXIS2_PLACEMENT_3D('',#222487,#122069,#122070);
#101254=AXIS2_PLACEMENT_3D('',#222488,#122071,#122072);
#101255=AXIS2_PLACEMENT_3D('',#222493,#122075,#122076);
#101256=AXIS2_PLACEMENT_3D('',#222494,#122077,#122078);
#101257=AXIS2_PLACEMENT_3D('',#222499,#122081,#122082);
#101258=AXIS2_PLACEMENT_3D('',#222500,#122083,#122084);
#101259=AXIS2_PLACEMENT_3D('',#222505,#122087,#122088);
#101260=AXIS2_PLACEMENT_3D('',#222506,#122089,#122090);
#101261=AXIS2_PLACEMENT_3D('',#222511,#122093,#122094);
#101262=AXIS2_PLACEMENT_3D('',#222512,#122095,#122096);
#101263=AXIS2_PLACEMENT_3D('',#222517,#122099,#122100);
#101264=AXIS2_PLACEMENT_3D('',#222518,#122101,#122102);
#101265=AXIS2_PLACEMENT_3D('',#222523,#122105,#122106);
#101266=AXIS2_PLACEMENT_3D('',#222524,#122107,#122108);
#101267=AXIS2_PLACEMENT_3D('',#222529,#122111,#122112);
#101268=AXIS2_PLACEMENT_3D('',#222530,#122113,#122114);
#101269=AXIS2_PLACEMENT_3D('',#222535,#122117,#122118);
#101270=AXIS2_PLACEMENT_3D('',#222536,#122119,#122120);
#101271=AXIS2_PLACEMENT_3D('',#222541,#122123,#122124);
#101272=AXIS2_PLACEMENT_3D('',#222542,#122125,#122126);
#101273=AXIS2_PLACEMENT_3D('',#222547,#122129,#122130);
#101274=AXIS2_PLACEMENT_3D('',#222548,#122131,#122132);
#101275=AXIS2_PLACEMENT_3D('',#222553,#122135,#122136);
#101276=AXIS2_PLACEMENT_3D('',#222554,#122137,#122138);
#101277=AXIS2_PLACEMENT_3D('',#222559,#122141,#122142);
#101278=AXIS2_PLACEMENT_3D('',#222560,#122143,#122144);
#101279=AXIS2_PLACEMENT_3D('',#222565,#122147,#122148);
#101280=AXIS2_PLACEMENT_3D('',#222566,#122149,#122150);
#101281=AXIS2_PLACEMENT_3D('',#222571,#122153,#122154);
#101282=AXIS2_PLACEMENT_3D('',#222572,#122155,#122156);
#101283=AXIS2_PLACEMENT_3D('',#222577,#122159,#122160);
#101284=AXIS2_PLACEMENT_3D('',#222578,#122161,#122162);
#101285=AXIS2_PLACEMENT_3D('',#222583,#122165,#122166);
#101286=AXIS2_PLACEMENT_3D('',#222584,#122167,#122168);
#101287=AXIS2_PLACEMENT_3D('',#222589,#122171,#122172);
#101288=AXIS2_PLACEMENT_3D('',#222590,#122173,#122174);
#101289=AXIS2_PLACEMENT_3D('',#222595,#122177,#122178);
#101290=AXIS2_PLACEMENT_3D('',#222596,#122179,#122180);
#101291=AXIS2_PLACEMENT_3D('',#222601,#122183,#122184);
#101292=AXIS2_PLACEMENT_3D('',#222602,#122185,#122186);
#101293=AXIS2_PLACEMENT_3D('',#222607,#122189,#122190);
#101294=AXIS2_PLACEMENT_3D('',#222608,#122191,#122192);
#101295=AXIS2_PLACEMENT_3D('',#222613,#122195,#122196);
#101296=AXIS2_PLACEMENT_3D('',#222614,#122197,#122198);
#101297=AXIS2_PLACEMENT_3D('',#222619,#122201,#122202);
#101298=AXIS2_PLACEMENT_3D('',#222620,#122203,#122204);
#101299=AXIS2_PLACEMENT_3D('',#222625,#122207,#122208);
#101300=AXIS2_PLACEMENT_3D('',#222626,#122209,#122210);
#101301=AXIS2_PLACEMENT_3D('',#222631,#122213,#122214);
#101302=AXIS2_PLACEMENT_3D('',#222632,#122215,#122216);
#101303=AXIS2_PLACEMENT_3D('',#222637,#122219,#122220);
#101304=AXIS2_PLACEMENT_3D('',#222638,#122221,#122222);
#101305=AXIS2_PLACEMENT_3D('',#222643,#122225,#122226);
#101306=AXIS2_PLACEMENT_3D('',#222644,#122227,#122228);
#101307=AXIS2_PLACEMENT_3D('',#222649,#122231,#122232);
#101308=AXIS2_PLACEMENT_3D('',#222650,#122233,#122234);
#101309=AXIS2_PLACEMENT_3D('',#222655,#122237,#122238);
#101310=AXIS2_PLACEMENT_3D('',#222656,#122239,#122240);
#101311=AXIS2_PLACEMENT_3D('',#222661,#122243,#122244);
#101312=AXIS2_PLACEMENT_3D('',#222662,#122245,#122246);
#101313=AXIS2_PLACEMENT_3D('',#222667,#122249,#122250);
#101314=AXIS2_PLACEMENT_3D('',#222668,#122251,#122252);
#101315=AXIS2_PLACEMENT_3D('',#222673,#122255,#122256);
#101316=AXIS2_PLACEMENT_3D('',#222674,#122257,#122258);
#101317=AXIS2_PLACEMENT_3D('',#222679,#122261,#122262);
#101318=AXIS2_PLACEMENT_3D('',#222680,#122263,#122264);
#101319=AXIS2_PLACEMENT_3D('',#222685,#122267,#122268);
#101320=AXIS2_PLACEMENT_3D('',#222686,#122269,#122270);
#101321=AXIS2_PLACEMENT_3D('',#222691,#122273,#122274);
#101322=AXIS2_PLACEMENT_3D('',#222692,#122275,#122276);
#101323=AXIS2_PLACEMENT_3D('',#222697,#122279,#122280);
#101324=AXIS2_PLACEMENT_3D('',#222698,#122281,#122282);
#101325=AXIS2_PLACEMENT_3D('',#222701,#122283,#122284);
#101326=AXIS2_PLACEMENT_3D('',#222704,#122287,#122288);
#101327=AXIS2_PLACEMENT_3D('',#222709,#122291,#122292);
#101328=AXIS2_PLACEMENT_3D('',#222710,#122293,#122294);
#101329=AXIS2_PLACEMENT_3D('',#222715,#122297,#122298);
#101330=AXIS2_PLACEMENT_3D('',#222716,#122299,#122300);
#101331=AXIS2_PLACEMENT_3D('',#222721,#122303,#122304);
#101332=AXIS2_PLACEMENT_3D('',#222722,#122305,#122306);
#101333=AXIS2_PLACEMENT_3D('',#222727,#122309,#122310);
#101334=AXIS2_PLACEMENT_3D('',#222728,#122311,#122312);
#101335=AXIS2_PLACEMENT_3D('',#222733,#122315,#122316);
#101336=AXIS2_PLACEMENT_3D('',#222734,#122317,#122318);
#101337=AXIS2_PLACEMENT_3D('',#222739,#122321,#122322);
#101338=AXIS2_PLACEMENT_3D('',#222740,#122323,#122324);
#101339=AXIS2_PLACEMENT_3D('',#222745,#122327,#122328);
#101340=AXIS2_PLACEMENT_3D('',#222746,#122329,#122330);
#101341=AXIS2_PLACEMENT_3D('',#222751,#122333,#122334);
#101342=AXIS2_PLACEMENT_3D('',#222752,#122335,#122336);
#101343=AXIS2_PLACEMENT_3D('',#222757,#122339,#122340);
#101344=AXIS2_PLACEMENT_3D('',#222758,#122341,#122342);
#101345=AXIS2_PLACEMENT_3D('',#222763,#122345,#122346);
#101346=AXIS2_PLACEMENT_3D('',#222764,#122347,#122348);
#101347=AXIS2_PLACEMENT_3D('',#222769,#122351,#122352);
#101348=AXIS2_PLACEMENT_3D('',#222770,#122353,#122354);
#101349=AXIS2_PLACEMENT_3D('',#222775,#122357,#122358);
#101350=AXIS2_PLACEMENT_3D('',#222776,#122359,#122360);
#101351=AXIS2_PLACEMENT_3D('',#222781,#122363,#122364);
#101352=AXIS2_PLACEMENT_3D('',#222782,#122365,#122366);
#101353=AXIS2_PLACEMENT_3D('',#222787,#122369,#122370);
#101354=AXIS2_PLACEMENT_3D('',#222788,#122371,#122372);
#101355=AXIS2_PLACEMENT_3D('',#222793,#122375,#122376);
#101356=AXIS2_PLACEMENT_3D('',#222794,#122377,#122378);
#101357=AXIS2_PLACEMENT_3D('',#222799,#122381,#122382);
#101358=AXIS2_PLACEMENT_3D('',#222800,#122383,#122384);
#101359=AXIS2_PLACEMENT_3D('',#222805,#122387,#122388);
#101360=AXIS2_PLACEMENT_3D('',#222806,#122389,#122390);
#101361=AXIS2_PLACEMENT_3D('',#222811,#122393,#122394);
#101362=AXIS2_PLACEMENT_3D('',#222812,#122395,#122396);
#101363=AXIS2_PLACEMENT_3D('',#222817,#122399,#122400);
#101364=AXIS2_PLACEMENT_3D('',#222818,#122401,#122402);
#101365=AXIS2_PLACEMENT_3D('',#222823,#122405,#122406);
#101366=AXIS2_PLACEMENT_3D('',#222824,#122407,#122408);
#101367=AXIS2_PLACEMENT_3D('',#222829,#122411,#122412);
#101368=AXIS2_PLACEMENT_3D('',#222830,#122413,#122414);
#101369=AXIS2_PLACEMENT_3D('',#222835,#122417,#122418);
#101370=AXIS2_PLACEMENT_3D('',#222836,#122419,#122420);
#101371=AXIS2_PLACEMENT_3D('',#222841,#122423,#122424);
#101372=AXIS2_PLACEMENT_3D('',#222842,#122425,#122426);
#101373=AXIS2_PLACEMENT_3D('',#222845,#122427,#122428);
#101374=AXIS2_PLACEMENT_3D('',#222848,#122431,#122432);
#101375=AXIS2_PLACEMENT_3D('',#222853,#122435,#122436);
#101376=AXIS2_PLACEMENT_3D('',#222854,#122437,#122438);
#101377=AXIS2_PLACEMENT_3D('',#222859,#122441,#122442);
#101378=AXIS2_PLACEMENT_3D('',#222860,#122443,#122444);
#101379=AXIS2_PLACEMENT_3D('',#222865,#122447,#122448);
#101380=AXIS2_PLACEMENT_3D('',#222866,#122449,#122450);
#101381=AXIS2_PLACEMENT_3D('',#222871,#122453,#122454);
#101382=AXIS2_PLACEMENT_3D('',#222872,#122455,#122456);
#101383=AXIS2_PLACEMENT_3D('',#222877,#122459,#122460);
#101384=AXIS2_PLACEMENT_3D('',#222878,#122461,#122462);
#101385=AXIS2_PLACEMENT_3D('',#222883,#122465,#122466);
#101386=AXIS2_PLACEMENT_3D('',#222884,#122467,#122468);
#101387=AXIS2_PLACEMENT_3D('',#222889,#122471,#122472);
#101388=AXIS2_PLACEMENT_3D('',#222890,#122473,#122474);
#101389=AXIS2_PLACEMENT_3D('',#222895,#122477,#122478);
#101390=AXIS2_PLACEMENT_3D('',#222896,#122479,#122480);
#101391=AXIS2_PLACEMENT_3D('',#222901,#122483,#122484);
#101392=AXIS2_PLACEMENT_3D('',#222902,#122485,#122486);
#101393=AXIS2_PLACEMENT_3D('',#222907,#122489,#122490);
#101394=AXIS2_PLACEMENT_3D('',#222908,#122491,#122492);
#101395=AXIS2_PLACEMENT_3D('',#222913,#122495,#122496);
#101396=AXIS2_PLACEMENT_3D('',#222914,#122497,#122498);
#101397=AXIS2_PLACEMENT_3D('',#222919,#122501,#122502);
#101398=AXIS2_PLACEMENT_3D('',#222920,#122503,#122504);
#101399=AXIS2_PLACEMENT_3D('',#222925,#122507,#122508);
#101400=AXIS2_PLACEMENT_3D('',#222926,#122509,#122510);
#101401=AXIS2_PLACEMENT_3D('',#222931,#122513,#122514);
#101402=AXIS2_PLACEMENT_3D('',#222932,#122515,#122516);
#101403=AXIS2_PLACEMENT_3D('',#222937,#122519,#122520);
#101404=AXIS2_PLACEMENT_3D('',#222938,#122521,#122522);
#101405=AXIS2_PLACEMENT_3D('',#222941,#122523,#122524);
#101406=AXIS2_PLACEMENT_3D('',#222944,#122527,#122528);
#101407=AXIS2_PLACEMENT_3D('',#222949,#122531,#122532);
#101408=AXIS2_PLACEMENT_3D('',#222950,#122533,#122534);
#101409=AXIS2_PLACEMENT_3D('',#222955,#122537,#122538);
#101410=AXIS2_PLACEMENT_3D('',#222956,#122539,#122540);
#101411=AXIS2_PLACEMENT_3D('',#222961,#122543,#122544);
#101412=AXIS2_PLACEMENT_3D('',#222962,#122545,#122546);
#101413=AXIS2_PLACEMENT_3D('',#222967,#122549,#122550);
#101414=AXIS2_PLACEMENT_3D('',#222968,#122551,#122552);
#101415=AXIS2_PLACEMENT_3D('',#222971,#122553,#122554);
#101416=AXIS2_PLACEMENT_3D('',#222974,#122557,#122558);
#101417=AXIS2_PLACEMENT_3D('',#222979,#122561,#122562);
#101418=AXIS2_PLACEMENT_3D('',#222980,#122563,#122564);
#101419=AXIS2_PLACEMENT_3D('',#222983,#122565,#122566);
#101420=AXIS2_PLACEMENT_3D('',#222986,#122569,#122570);
#101421=AXIS2_PLACEMENT_3D('',#222991,#122573,#122574);
#101422=AXIS2_PLACEMENT_3D('',#222992,#122575,#122576);
#101423=AXIS2_PLACEMENT_3D('',#222997,#122579,#122580);
#101424=AXIS2_PLACEMENT_3D('',#222998,#122581,#122582);
#101425=AXIS2_PLACEMENT_3D('',#223003,#122585,#122586);
#101426=AXIS2_PLACEMENT_3D('',#223004,#122587,#122588);
#101427=AXIS2_PLACEMENT_3D('',#223007,#122590,#122591);
#101428=AXIS2_PLACEMENT_3D('',#223008,#122592,#122593);
#101429=AXIS2_PLACEMENT_3D('',#223011,#122595,#122596);
#101430=AXIS2_PLACEMENT_3D('',#223012,#122597,#122598);
#101431=AXIS2_PLACEMENT_3D('',#223014,#122599,#122600);
#101432=AXIS2_PLACEMENT_3D('',#223015,#122601,#122602);
#101433=AXIS2_PLACEMENT_3D('',#223017,#122604,#122605);
#101434=AXIS2_PLACEMENT_3D('',#223018,#122606,#122607);
#101435=AXIS2_PLACEMENT_3D('',#223019,#122608,#122609);
#101436=AXIS2_PLACEMENT_3D('',#223020,#122610,#122611);
#101437=AXIS2_PLACEMENT_3D('',#223021,#122612,#122613);
#101438=AXIS2_PLACEMENT_3D('',#223022,#122614,#122615);
#101439=AXIS2_PLACEMENT_3D('',#223025,#122617,#122618);
#101440=AXIS2_PLACEMENT_3D('',#223026,#122619,#122620);
#101441=AXIS2_PLACEMENT_3D('',#223027,#122621,#122622);
#101442=AXIS2_PLACEMENT_3D('',#223028,#122623,#122624);
#101443=AXIS2_PLACEMENT_3D('',#223029,#122625,#122626);
#101444=AXIS2_PLACEMENT_3D('',#223030,#122627,#122628);
#101445=AXIS2_PLACEMENT_3D('',#223031,#122629,#122630);
#101446=AXIS2_PLACEMENT_3D('',#223032,#122631,#122632);
#101447=AXIS2_PLACEMENT_3D('',#223033,#122633,#122634);
#101448=AXIS2_PLACEMENT_3D('',#223034,#122635,#122636);
#101449=AXIS2_PLACEMENT_3D('',#223035,#122637,#122638);
#101450=AXIS2_PLACEMENT_3D('',#223036,#122639,#122640);
#101451=AXIS2_PLACEMENT_3D('',#223037,#122641,#122642);
#101452=AXIS2_PLACEMENT_3D('',#223038,#122643,#122644);
#101453=AXIS2_PLACEMENT_3D('',#223039,#122645,#122646);
#101454=AXIS2_PLACEMENT_3D('',#223040,#122647,#122648);
#101455=AXIS2_PLACEMENT_3D('',#223041,#122649,#122650);
#101456=AXIS2_PLACEMENT_3D('',#223042,#122651,#122652);
#101457=AXIS2_PLACEMENT_3D('',#223043,#122653,#122654);
#101458=AXIS2_PLACEMENT_3D('',#223044,#122655,#122656);
#101459=AXIS2_PLACEMENT_3D('',#223046,#122658,#122659);
#101460=AXIS2_PLACEMENT_3D('',#223048,#122661,#122662);
#101461=AXIS2_PLACEMENT_3D('',#223049,#122663,#122664);
#101462=AXIS2_PLACEMENT_3D('',#223050,#122665,#122666);
#101463=AXIS2_PLACEMENT_3D('',#223051,#122667,#122668);
#101464=AXIS2_PLACEMENT_3D('',#223052,#122669,#122670);
#101465=AXIS2_PLACEMENT_3D('',#223053,#122671,#122672);
#101466=AXIS2_PLACEMENT_3D('',#223054,#122673,#122674);
#101467=AXIS2_PLACEMENT_3D('',#223056,#122676,#122677);
#101468=AXIS2_PLACEMENT_3D('',#223058,#122679,#122680);
#101469=AXIS2_PLACEMENT_3D('',#223059,#122681,#122682);
#101470=AXIS2_PLACEMENT_3D('',#223060,#122683,#122684);
#101471=AXIS2_PLACEMENT_3D('',#223061,#122685,#122686);
#101472=AXIS2_PLACEMENT_3D('',#223062,#122687,#122688);
#101473=AXIS2_PLACEMENT_3D('',#223064,#122690,#122691);
#101474=AXIS2_PLACEMENT_3D('',#223066,#122693,#122694);
#101475=AXIS2_PLACEMENT_3D('',#223068,#122696,#122697);
#101476=AXIS2_PLACEMENT_3D('',#223070,#122699,#122700);
#101477=AXIS2_PLACEMENT_3D('',#223072,#122702,#122703);
#101478=AXIS2_PLACEMENT_3D('',#223074,#122705,#122706);
#101479=AXIS2_PLACEMENT_3D('',#223076,#122708,#122709);
#101480=AXIS2_PLACEMENT_3D('',#223078,#122711,#122712);
#101481=AXIS2_PLACEMENT_3D('',#223080,#122714,#122715);
#101482=AXIS2_PLACEMENT_3D('',#223082,#122717,#122718);
#101483=AXIS2_PLACEMENT_3D('',#223084,#122720,#122721);
#101484=AXIS2_PLACEMENT_3D('',#223086,#122723,#122724);
#101485=AXIS2_PLACEMENT_3D('',#223088,#122726,#122727);
#101486=AXIS2_PLACEMENT_3D('',#223090,#122729,#122730);
#101487=AXIS2_PLACEMENT_3D('',#223092,#122732,#122733);
#101488=AXIS2_PLACEMENT_3D('',#223094,#122735,#122736);
#101489=AXIS2_PLACEMENT_3D('',#223096,#122738,#122739);
#101490=AXIS2_PLACEMENT_3D('',#223098,#122741,#122742);
#101491=AXIS2_PLACEMENT_3D('',#223100,#122744,#122745);
#101492=AXIS2_PLACEMENT_3D('',#223102,#122747,#122748);
#101493=AXIS2_PLACEMENT_3D('',#223104,#122750,#122751);
#101494=AXIS2_PLACEMENT_3D('',#223106,#122753,#122754);
#101495=AXIS2_PLACEMENT_3D('',#223108,#122756,#122757);
#101496=AXIS2_PLACEMENT_3D('',#223110,#122759,#122760);
#101497=AXIS2_PLACEMENT_3D('',#223112,#122762,#122763);
#101498=AXIS2_PLACEMENT_3D('',#223114,#122765,#122766);
#101499=AXIS2_PLACEMENT_3D('',#223116,#122768,#122769);
#101500=AXIS2_PLACEMENT_3D('',#223118,#122771,#122772);
#101501=AXIS2_PLACEMENT_3D('',#223120,#122774,#122775);
#101502=AXIS2_PLACEMENT_3D('',#223122,#122777,#122778);
#101503=AXIS2_PLACEMENT_3D('',#223124,#122780,#122781);
#101504=AXIS2_PLACEMENT_3D('',#223126,#122783,#122784);
#101505=AXIS2_PLACEMENT_3D('',#223135,#122789,#122790);
#101506=AXIS2_PLACEMENT_3D('',#223141,#122794,#122795);
#101507=AXIS2_PLACEMENT_3D('',#223147,#122799,#122800);
#101508=AXIS2_PLACEMENT_3D('',#223149,#122802,#122803);
#101509=AXIS2_PLACEMENT_3D('',#223151,#122805,#122806);
#101510=AXIS2_PLACEMENT_3D('',#223153,#122808,#122809);
#101511=AXIS2_PLACEMENT_3D('',#223155,#122811,#122812);
#101512=AXIS2_PLACEMENT_3D('',#223157,#122814,#122815);
#101513=AXIS2_PLACEMENT_3D('',#223159,#122817,#122818);
#101514=AXIS2_PLACEMENT_3D('',#223161,#122820,#122821);
#101515=AXIS2_PLACEMENT_3D('',#223163,#122823,#122824);
#101516=AXIS2_PLACEMENT_3D('',#223165,#122826,#122827);
#101517=AXIS2_PLACEMENT_3D('',#223167,#122829,#122830);
#101518=AXIS2_PLACEMENT_3D('',#223169,#122832,#122833);
#101519=AXIS2_PLACEMENT_3D('',#223171,#122835,#122836);
#101520=AXIS2_PLACEMENT_3D('',#223173,#122838,#122839);
#101521=AXIS2_PLACEMENT_3D('',#223175,#122841,#122842);
#101522=AXIS2_PLACEMENT_3D('',#223177,#122844,#122845);
#101523=AXIS2_PLACEMENT_3D('',#223179,#122847,#122848);
#101524=AXIS2_PLACEMENT_3D('',#223181,#122850,#122851);
#101525=AXIS2_PLACEMENT_3D('',#223183,#122853,#122854);
#101526=AXIS2_PLACEMENT_3D('',#223185,#122856,#122857);
#101527=AXIS2_PLACEMENT_3D('',#223187,#122859,#122860);
#101528=AXIS2_PLACEMENT_3D('',#223189,#122862,#122863);
#101529=AXIS2_PLACEMENT_3D('',#223191,#122865,#122866);
#101530=AXIS2_PLACEMENT_3D('',#223192,#122867,#122868);
#101531=AXIS2_PLACEMENT_3D('',#223194,#122869,#122870);
#101532=AXIS2_PLACEMENT_3D('',#223196,#122871,#122872);
#101533=AXIS2_PLACEMENT_3D('',#223198,#122873,#122874);
#101534=AXIS2_PLACEMENT_3D('',#223200,#122875,#122876);
#101535=AXIS2_PLACEMENT_3D('',#223202,#122877,#122878);
#101536=AXIS2_PLACEMENT_3D('',#223204,#122879,#122880);
#101537=AXIS2_PLACEMENT_3D('',#223206,#122881,#122882);
#101538=AXIS2_PLACEMENT_3D('',#223208,#122883,#122884);
#101539=AXIS2_PLACEMENT_3D('',#223209,#122885,#122886);
#101540=AXIS2_PLACEMENT_3D('',#223210,#122887,#122888);
#101541=AXIS2_PLACEMENT_3D('',#223220,#122898,#122899);
#101542=AXIS2_PLACEMENT_3D('',#223222,#122901,#122902);
#101543=AXIS2_PLACEMENT_3D('',#223228,#122908,#122909);
#101544=AXIS2_PLACEMENT_3D('',#223232,#122912,#122913);
#101545=AXIS2_PLACEMENT_3D('',#223234,#122914,#122915);
#101546=AXIS2_PLACEMENT_3D('',#223235,#122916,#122917);
#101547=AXIS2_PLACEMENT_3D('',#223239,#122920,#122921);
#101548=AXIS2_PLACEMENT_3D('',#223241,#122922,#122923);
#101549=AXIS2_PLACEMENT_3D('',#223242,#122924,#122925);
#101550=AXIS2_PLACEMENT_3D('',#223245,#122928,#122929);
#101551=AXIS2_PLACEMENT_3D('',#223248,#122932,#122933);
#101552=AXIS2_PLACEMENT_3D('',#223251,#122936,#122937);
#101553=AXIS2_PLACEMENT_3D('',#223254,#122940,#122941);
#101554=AXIS2_PLACEMENT_3D('',#223258,#122945,#122946);
#101555=AXIS2_PLACEMENT_3D('',#223268,#122955,#122956);
#101556=AXIS2_PLACEMENT_3D('',#223270,#122957,#122958);
#101557=AXIS2_PLACEMENT_3D('',#223271,#122959,#122960);
#101558=AXIS2_PLACEMENT_3D('',#223274,#122962,#122963);
#101559=AXIS2_PLACEMENT_3D('',#223276,#122964,#122965);
#101560=AXIS2_PLACEMENT_3D('',#223277,#122966,#122967);
#101561=AXIS2_PLACEMENT_3D('',#223283,#122973,#122974);
#101562=AXIS2_PLACEMENT_3D('',#223292,#122983,#122984);
#101563=AXIS2_PLACEMENT_3D('',#223297,#122987,#122988);
#101564=AXIS2_PLACEMENT_3D('',#223298,#122989,#122990);
#101565=AXIS2_PLACEMENT_3D('',#223300,#122991,#122992);
#101566=AXIS2_PLACEMENT_3D('',#223302,#122994,#122995);
#101567=AXIS2_PLACEMENT_3D('',#223305,#122997,#122998);
#101568=AXIS2_PLACEMENT_3D('',#223306,#122999,#123000);
#101569=AXIS2_PLACEMENT_3D('',#223309,#123002,#123003);
#101570=AXIS2_PLACEMENT_3D('',#223310,#123004,#123005);
#101571=AXIS2_PLACEMENT_3D('',#223313,#123007,#123008);
#101572=AXIS2_PLACEMENT_3D('',#223314,#123009,#123010);
#101573=AXIS2_PLACEMENT_3D('',#223316,#123011,#123012);
#101574=AXIS2_PLACEMENT_3D('',#223318,#123014,#123015);
#101575=AXIS2_PLACEMENT_3D('',#223321,#123017,#123018);
#101576=AXIS2_PLACEMENT_3D('',#223322,#123019,#123020);
#101577=AXIS2_PLACEMENT_3D('',#223323,#123021,#123022);
#101578=AXIS2_PLACEMENT_3D('',#223324,#123023,#123024);
#101579=AXIS2_PLACEMENT_3D('',#223337,#123027,#123028);
#101580=AXIS2_PLACEMENT_3D('',#223338,#123029,#123030);
#101581=AXIS2_PLACEMENT_3D('',#223342,#123033,#123034);
#101582=AXIS2_PLACEMENT_3D('',#223345,#123035,#123036);
#101583=AXIS2_PLACEMENT_3D('',#223354,#123038,#123039);
#101584=AXIS2_PLACEMENT_3D('',#223363,#123041,#123042);
#101585=AXIS2_PLACEMENT_3D('',#223379,#123045,#123046);
#101586=AXIS2_PLACEMENT_3D('',#223395,#123049,#123050);
#101587=AXIS2_PLACEMENT_3D('',#223396,#123051,#123052);
#101588=AXIS2_PLACEMENT_3D('',#223397,#123053,#123054);
#101589=AXIS2_PLACEMENT_3D('',#223398,#123055,#123056);
#101590=AXIS2_PLACEMENT_3D('',#223414,#123059,#123060);
#101591=AXIS2_PLACEMENT_3D('',#223430,#123063,#123064);
#101592=AXIS2_PLACEMENT_3D('',#223431,#123065,#123066);
#101593=AXIS2_PLACEMENT_3D('',#223432,#123067,#123068);
#101594=AXIS2_PLACEMENT_3D('',#225923,#123069,#123070);
#101595=AXIS2_PLACEMENT_3D('',#225926,#123071,#123072);
#101596=AXIS2_PLACEMENT_3D('',#225930,#123074,#123075);
#101597=AXIS2_PLACEMENT_3D('',#225932,#123077,#123078);
#101598=AXIS2_PLACEMENT_3D('',#225933,#123079,#123080);
#101599=AXIS2_PLACEMENT_3D('',#225934,#123081,#123082);
#101600=AXIS2_PLACEMENT_3D('',#225935,#123083,#123084);
#101601=AXIS2_PLACEMENT_3D('',#225937,#123085,#123086);
#101602=AXIS2_PLACEMENT_3D('',#225940,#123088,#123089);
#101603=AXIS2_PLACEMENT_3D('',#225941,#123090,#123091);
#101604=AXIS2_PLACEMENT_3D('',#225942,#123092,#123093);
#101605=AXIS2_PLACEMENT_3D('',#225943,#123094,#123095);
#101606=AXIS2_PLACEMENT_3D('',#225945,#123096,#123097);
#101607=AXIS2_PLACEMENT_3D('',#225947,#123098,#123099);
#101608=AXIS2_PLACEMENT_3D('',#225949,#123101,#123102);
#101609=AXIS2_PLACEMENT_3D('',#225951,#123103,#123104);
#101610=AXIS2_PLACEMENT_3D('',#225953,#123105,#123106);
#101611=AXIS2_PLACEMENT_3D('',#225955,#123108,#123109);
#101612=AXIS2_PLACEMENT_3D('',#225957,#123110,#123111);
#101613=AXIS2_PLACEMENT_3D('',#225959,#123112,#123113);
#101614=AXIS2_PLACEMENT_3D('',#225961,#123115,#123116);
#101615=AXIS2_PLACEMENT_3D('',#225963,#123117,#123118);
#101616=AXIS2_PLACEMENT_3D('',#225971,#123119,#123120);
#101617=AXIS2_PLACEMENT_3D('',#225972,#123121,#123122);
#101618=AXIS2_PLACEMENT_3D('',#225975,#123123,#123124);
#101619=AXIS2_PLACEMENT_3D('',#225979,#123126,#123127);
#101620=AXIS2_PLACEMENT_3D('',#225981,#123129,#123130);
#101621=AXIS2_PLACEMENT_3D('',#225982,#123131,#123132);
#101622=AXIS2_PLACEMENT_3D('',#225983,#123133,#123134);
#101623=AXIS2_PLACEMENT_3D('',#228076,#123135,#123136);
#101624=AXIS2_PLACEMENT_3D('',#228079,#123137,#123138);
#101625=AXIS2_PLACEMENT_3D('',#228089,#123141,#123142);
#101626=AXIS2_PLACEMENT_3D('',#228099,#123143,#123144);
#101627=AXIS2_PLACEMENT_3D('',#228108,#123146,#123147);
#101628=AXIS2_PLACEMENT_3D('',#228110,#123148,#123149);
#101629=AXIS2_PLACEMENT_3D('',#228112,#123151,#123152);
#101630=AXIS2_PLACEMENT_3D('',#228113,#123153,#123154);
#101631=AXIS2_PLACEMENT_3D('',#228116,#123155,#123156);
#101632=AXIS2_PLACEMENT_3D('',#228119,#123158,#123159);
#101633=AXIS2_PLACEMENT_3D('',#228121,#123161,#123162);
#101634=AXIS2_PLACEMENT_3D('',#228129,#123163,#123164);
#101635=AXIS2_PLACEMENT_3D('',#228140,#123166,#123167);
#101636=AXIS2_PLACEMENT_3D('',#228142,#123168,#123169);
#101637=AXIS2_PLACEMENT_3D('',#228144,#123171,#123172);
#101638=AXIS2_PLACEMENT_3D('',#228145,#123173,#123174);
#101639=AXIS2_PLACEMENT_3D('',#228146,#123175,#123176);
#101640=AXIS2_PLACEMENT_3D('',#228153,#123177,#123178);
#101641=AXIS2_PLACEMENT_3D('',#228155,#123179,#123180);
#101642=AXIS2_PLACEMENT_3D('',#228157,#123181,#123182);
#101643=AXIS2_PLACEMENT_3D('',#228159,#123183,#123184);
#101644=AXIS2_PLACEMENT_3D('',#228161,#123185,#123186);
#101645=AXIS2_PLACEMENT_3D('',#228163,#123187,#123188);
#101646=AXIS2_PLACEMENT_3D('',#228165,#123189,#123190);
#101647=AXIS2_PLACEMENT_3D('',#228167,#123191,#123192);
#101648=AXIS2_PLACEMENT_3D('',#228169,#123193,#123194);
#101649=AXIS2_PLACEMENT_3D('',#228170,#123195,#123196);
#101650=AXIS2_PLACEMENT_3D('',#228171,#123197,#123198);
#101651=AXIS2_PLACEMENT_3D('',#228172,#123199,#123200);
#101652=AXIS2_PLACEMENT_3D('',#228173,#123201,#123202);
#101653=AXIS2_PLACEMENT_3D('',#228176,#123203,#123204);
#101654=AXIS2_PLACEMENT_3D('',#228179,#123207,#123208);
#101655=AXIS2_PLACEMENT_3D('',#228181,#123209,#123210);
#101656=AXIS2_PLACEMENT_3D('',#228183,#123212,#123213);
#101657=AXIS2_PLACEMENT_3D('',#228185,#123214,#123215);
#101658=AXIS2_PLACEMENT_3D('',#228187,#123217,#123218);
#101659=AXIS2_PLACEMENT_3D('',#228189,#123219,#123220);
#101660=AXIS2_PLACEMENT_3D('',#228191,#123222,#123223);
#101661=AXIS2_PLACEMENT_3D('',#228192,#123224,#123225);
#101662=AXIS2_PLACEMENT_3D('',#228193,#123226,#123227);
#101663=AXIS2_PLACEMENT_3D('',#228195,#123228,#123229);
#101664=AXIS2_PLACEMENT_3D('',#228197,#123231,#123232);
#101665=AXIS2_PLACEMENT_3D('',#228199,#123233,#123234);
#101666=AXIS2_PLACEMENT_3D('',#228201,#123236,#123237);
#101667=AXIS2_PLACEMENT_3D('',#228203,#123238,#123239);
#101668=AXIS2_PLACEMENT_3D('',#228205,#123241,#123242);
#101669=AXIS2_PLACEMENT_3D('',#228206,#123243,#123244);
#101670=AXIS2_PLACEMENT_3D('',#228279,#123245,#123246);
#101671=AXIS2_PLACEMENT_3D('',#228477,#123247,#123248);
#101672=AXIS2_PLACEMENT_3D('',#228484,#123249,#123250);
#101673=AXIS2_PLACEMENT_3D('',#228485,#123251,#123252);
#101674=AXIS2_PLACEMENT_3D('',#228487,#123253,#123254);
#101675=AXIS2_PLACEMENT_3D('',#228488,#123255,#123256);
#101676=AXIS2_PLACEMENT_3D('',#228489,#123257,#123258);
#101677=AXIS2_PLACEMENT_3D('',#228528,#123259,#123260);
#101678=AXIS2_PLACEMENT_3D('',#228537,#123261,#123262);
#101679=AXIS2_PLACEMENT_3D('',#228805,#123263,#123264);
#101680=AXIS2_PLACEMENT_3D('',#228814,#123265,#123266);
#101681=AXIS2_PLACEMENT_3D('',#229138,#123267,#123268);
#101682=AXIS2_PLACEMENT_3D('',#229139,#123269,#123270);
#101683=AXIS2_PLACEMENT_3D('',#229140,#123271,#123272);
#101684=AXIS2_PLACEMENT_3D('',#229147,#123273,#123274);
#101685=AXIS2_PLACEMENT_3D('',#229150,#123275,#123276);
#101686=AXIS2_PLACEMENT_3D('',#229157,#123277,#123278);
#101687=AXIS2_PLACEMENT_3D('',#229160,#123279,#123280);
#101688=AXIS2_PLACEMENT_3D('',#229167,#123281,#123282);
#101689=AXIS2_PLACEMENT_3D('',#229170,#123283,#123284);
#101690=AXIS2_PLACEMENT_3D('',#229177,#123285,#123286);
#101691=AXIS2_PLACEMENT_3D('',#229178,#123287,#123288);
#101692=AXIS2_PLACEMENT_3D('',#229179,#123289,#123290);
#101693=AXIS2_PLACEMENT_3D('',#229180,#123291,#123292);
#101694=AXIS2_PLACEMENT_3D('',#229183,#123294,#123295);
#101695=AXIS2_PLACEMENT_3D('',#229184,#123296,#123297);
#101696=AXIS2_PLACEMENT_3D('',#229203,#123298,#123299);
#101697=AXIS2_PLACEMENT_3D('',#229204,#123300,#123301);
#101698=AXIS2_PLACEMENT_3D('',#229207,#123302,#123303);
#101699=AXIS2_PLACEMENT_3D('',#229222,#123304,#123305);
#101700=AXIS2_PLACEMENT_3D('',#229230,#123306,#123307);
#101701=AXIS2_PLACEMENT_3D('',#229231,#123308,#123309);
#101702=AXIS2_PLACEMENT_3D('',#229234,#123310,#123311);
#101703=AXIS2_PLACEMENT_3D('',#229251,#123312,#123313);
#101704=AXIS2_PLACEMENT_3D('',#229252,#123314,#123315);
#101705=AXIS2_PLACEMENT_3D('',#229253,#123316,#123317);
#101706=AXIS2_PLACEMENT_3D('',#229255,#123319,#123320);
#101707=AXIS2_PLACEMENT_3D('',#229257,#123322,#123323);
#101708=AXIS2_PLACEMENT_3D('',#230391,#123324,#123325);
#101709=AXIS2_PLACEMENT_3D('',#230392,#123326,#123327);
#101710=AXIS2_PLACEMENT_3D('',#230395,#123330,#123331);
#101711=AXIS2_PLACEMENT_3D('',#230397,#123333,#123334);
#101712=AXIS2_PLACEMENT_3D('',#230399,#123336,#123337);
#101713=AXIS2_PLACEMENT_3D('',#230400,#123338,#123339);
#101714=AXIS2_PLACEMENT_3D('',#230403,#123342,#123343);
#101715=AXIS2_PLACEMENT_3D('',#230404,#123344,#123345);
#101716=AXIS2_PLACEMENT_3D('',#230407,#123348,#123349);
#101717=AXIS2_PLACEMENT_3D('',#230409,#123350,#123351);
#101718=AXIS2_PLACEMENT_3D('',#230410,#123352,#123353);
#101719=AXIS2_PLACEMENT_3D('',#230412,#123355,#123356);
#101720=AXIS2_PLACEMENT_3D('',#230414,#123357,#123358);
#101721=AXIS2_PLACEMENT_3D('',#230415,#123359,#123360);
#101722=AXIS2_PLACEMENT_3D('',#230417,#123362,#123363);
#101723=AXIS2_PLACEMENT_3D('',#230418,#123364,#123365);
#101724=AXIS2_PLACEMENT_3D('',#230419,#123366,#123367);
#101725=AXIS2_PLACEMENT_3D('',#230420,#123368,#123369);
#101726=AXIS2_PLACEMENT_3D('',#230421,#123370,#123371);
#101727=AXIS2_PLACEMENT_3D('',#230422,#123372,#123373);
#101728=AXIS2_PLACEMENT_3D('',#230423,#123374,#123375);
#101729=AXIS2_PLACEMENT_3D('',#230424,#123376,#123377);
#101730=AXIS2_PLACEMENT_3D('',#230425,#123378,#123379);
#101731=AXIS2_PLACEMENT_3D('',#230426,#123380,#123381);
#101732=AXIS2_PLACEMENT_3D('',#230427,#123382,#123383);
#101733=AXIS2_PLACEMENT_3D('',#230428,#123384,#123385);
#101734=AXIS2_PLACEMENT_3D('',#230429,#123386,#123387);
#101735=AXIS2_PLACEMENT_3D('',#230430,#123388,#123389);
#101736=AXIS2_PLACEMENT_3D('',#230767,#123390,#123391);
#101737=AXIS2_PLACEMENT_3D('',#230768,#123392,#123393);
#101738=AXIS2_PLACEMENT_3D('',#230773,#123396,#123397);
#101739=AXIS2_PLACEMENT_3D('',#230774,#123398,#123399);
#101740=AXIS2_PLACEMENT_3D('',#230777,#123401,#123402);
#101741=AXIS2_PLACEMENT_3D('',#230778,#123403,#123404);
#101742=AXIS2_PLACEMENT_3D('',#230781,#123406,#123407);
#101743=AXIS2_PLACEMENT_3D('',#230782,#123408,#123409);
#101744=AXIS2_PLACEMENT_3D('',#230785,#123411,#123412);
#101745=AXIS2_PLACEMENT_3D('',#230786,#123413,#123414);
#101746=AXIS2_PLACEMENT_3D('',#230789,#123416,#123417);
#101747=AXIS2_PLACEMENT_3D('',#230790,#123418,#123419);
#101748=AXIS2_PLACEMENT_3D('',#230793,#123421,#123422);
#101749=AXIS2_PLACEMENT_3D('',#230794,#123423,#123424);
#101750=AXIS2_PLACEMENT_3D('',#230795,#123425,#123426);
#101751=AXIS2_PLACEMENT_3D('',#230796,#123427,#123428);
#101752=AXIS2_PLACEMENT_3D('',#230798,#123429,#123430);
#101753=AXIS2_PLACEMENT_3D('',#230800,#123432,#123433);
#101754=AXIS2_PLACEMENT_3D('',#230801,#123434,#123435);
#101755=AXIS2_PLACEMENT_3D('',#230802,#123436,#123437);
#101756=AXIS2_PLACEMENT_3D('',#230804,#123438,#123439);
#101757=AXIS2_PLACEMENT_3D('',#230806,#123440,#123441);
#101758=AXIS2_PLACEMENT_3D('',#230808,#123442,#123443);
#101759=AXIS2_PLACEMENT_3D('',#230810,#123444,#123445);
#101760=AXIS2_PLACEMENT_3D('',#230812,#123446,#123447);
#101761=AXIS2_PLACEMENT_3D('',#230814,#123448,#123449);
#101762=AXIS2_PLACEMENT_3D('',#230816,#123450,#123451);
#101763=AXIS2_PLACEMENT_3D('',#230818,#123452,#123453);
#101764=AXIS2_PLACEMENT_3D('',#230819,#123454,#123455);
#101765=AXIS2_PLACEMENT_3D('',#230820,#123456,#123457);
#101766=AXIS2_PLACEMENT_3D('',#230823,#123460,#123461);
#101767=AXIS2_PLACEMENT_3D('',#230824,#123462,#123463);
#101768=AXIS2_PLACEMENT_3D('',#230826,#123465,#123466);
#101769=AXIS2_PLACEMENT_3D('',#230828,#123468,#123469);
#101770=AXIS2_PLACEMENT_3D('',#230830,#123471,#123472);
#101771=AXIS2_PLACEMENT_3D('',#230832,#123474,#123475);
#101772=AXIS2_PLACEMENT_3D('',#230834,#123477,#123478);
#101773=AXIS2_PLACEMENT_3D('',#230836,#123480,#123481);
#101774=AXIS2_PLACEMENT_3D('',#231228,#123486,#123487);
#101775=AXIS2_PLACEMENT_3D('',#231231,#123490,#123491);
#101776=AXIS2_PLACEMENT_3D('',#231233,#123493,#123494);
#101777=AXIS2_PLACEMENT_3D('',#231235,#123496,#123497);
#101778=AXIS2_PLACEMENT_3D('',#231238,#123500,#123501);
#101779=AXIS2_PLACEMENT_3D('',#231240,#123503,#123504);
#101780=AXIS2_PLACEMENT_3D('',#231242,#123506,#123507);
#101781=AXIS2_PLACEMENT_3D('',#231243,#123508,#123509);
#101782=AXIS2_PLACEMENT_3D('',#231245,#123510,#123511);
#101783=AXIS2_PLACEMENT_3D('',#231247,#123512,#123513);
#101784=AXIS2_PLACEMENT_3D('',#231249,#123514,#123515);
#101785=AXIS2_PLACEMENT_3D('',#231251,#123516,#123517);
#101786=AXIS2_PLACEMENT_3D('',#231253,#123518,#123519);
#101787=AXIS2_PLACEMENT_3D('',#231255,#123520,#123521);
#101788=AXIS2_PLACEMENT_3D('',#231257,#123522,#123523);
#101789=AXIS2_PLACEMENT_3D('',#231259,#123524,#123525);
#101790=AXIS2_PLACEMENT_3D('',#231260,#123526,#123527);
#101791=AXIS2_PLACEMENT_3D('',#231261,#123528,#123529);
#101792=AXIS2_PLACEMENT_3D('',#231262,#123530,#123531);
#101793=AXIS2_PLACEMENT_3D('',#231265,#123534,#123535);
#101794=AXIS2_PLACEMENT_3D('',#231267,#123537,#123538);
#101795=AXIS2_PLACEMENT_3D('',#231269,#123540,#123541);
#101796=AXIS2_PLACEMENT_3D('',#231271,#123543,#123544);
#101797=AXIS2_PLACEMENT_3D('',#231272,#123545,#123546);
#101798=AXIS2_PLACEMENT_3D('',#231274,#123548,#123549);
#101799=AXIS2_PLACEMENT_3D('',#231276,#123551,#123552);
#101800=AXIS2_PLACEMENT_3D('',#231278,#123554,#123555);
#101801=AXIS2_PLACEMENT_3D('',#231356,#123556,#123557);
#101802=AXIS2_PLACEMENT_3D('',#231406,#123558,#123559);
#101803=AXIS2_PLACEMENT_3D('',#231407,#123560,#123561);
#101804=AXIS2_PLACEMENT_3D('',#231457,#123562,#123563);
#101805=AXIS2_PLACEMENT_3D('',#232146,#123564,#123565);
#101806=AXIS2_PLACEMENT_3D('',#232739,#123566,#123567);
#101807=AXIS2_PLACEMENT_3D('',#232740,#123568,#123569);
#101808=AXIS2_PLACEMENT_3D('',#232741,#123570,#123571);
#101809=AXIS2_PLACEMENT_3D('',#232742,#123572,#123573);
#101810=AXIS2_PLACEMENT_3D('',#232743,#123574,#123575);
#101811=AXIS2_PLACEMENT_3D('',#232744,#123576,#123577);
#101812=AXIS2_PLACEMENT_3D('',#232745,#123578,#123579);
#101813=AXIS2_PLACEMENT_3D('',#232746,#123580,#123581);
#101814=AXIS2_PLACEMENT_3D('',#232747,#123582,#123583);
#101815=AXIS2_PLACEMENT_3D('',#232748,#123584,#123585);
#101816=AXIS2_PLACEMENT_3D('',#232749,#123586,#123587);
#101817=AXIS2_PLACEMENT_3D('',#232750,#123588,#123589);
#101818=AXIS2_PLACEMENT_3D('',#232751,#123590,#123591);
#101819=AXIS2_PLACEMENT_3D('',#232752,#123592,#123593);
#101820=AXIS2_PLACEMENT_3D('',#232753,#123594,#123595);
#101821=AXIS2_PLACEMENT_3D('',#232754,#123596,#123597);
#101822=AXIS2_PLACEMENT_3D('',#232755,#123598,#123599);
#101823=AXIS2_PLACEMENT_3D('',#232756,#123600,#123601);
#101824=AXIS2_PLACEMENT_3D('',#232757,#123602,#123603);
#101825=AXIS2_PLACEMENT_3D('',#232758,#123604,#123605);
#101826=AXIS2_PLACEMENT_3D('',#232759,#123606,#123607);
#101827=AXIS2_PLACEMENT_3D('',#232760,#123608,#123609);
#101828=AXIS2_PLACEMENT_3D('',#232761,#123610,#123611);
#101829=AXIS2_PLACEMENT_3D('',#232762,#123612,#123613);
#101830=AXIS2_PLACEMENT_3D('',#232763,#123614,#123615);
#101831=AXIS2_PLACEMENT_3D('',#232764,#123616,#123617);
#101832=AXIS2_PLACEMENT_3D('',#232765,#123618,#123619);
#101833=AXIS2_PLACEMENT_3D('',#232766,#123620,#123621);
#101834=AXIS2_PLACEMENT_3D('',#232767,#123622,#123623);
#101835=AXIS2_PLACEMENT_3D('',#232768,#123624,#123625);
#101836=AXIS2_PLACEMENT_3D('',#232769,#123626,#123627);
#101837=AXIS2_PLACEMENT_3D('',#232770,#123628,#123629);
#101838=AXIS2_PLACEMENT_3D('',#232771,#123630,#123631);
#101839=AXIS2_PLACEMENT_3D('',#232772,#123632,#123633);
#101840=AXIS2_PLACEMENT_3D('',#232773,#123634,#123635);
#101841=AXIS2_PLACEMENT_3D('',#232774,#123636,#123637);
#101842=AXIS2_PLACEMENT_3D('',#232775,#123638,#123639);
#101843=AXIS2_PLACEMENT_3D('',#232776,#123640,#123641);
#101844=AXIS2_PLACEMENT_3D('',#232777,#123642,#123643);
#101845=AXIS2_PLACEMENT_3D('',#232778,#123644,#123645);
#101846=AXIS2_PLACEMENT_3D('',#232779,#123646,#123647);
#101847=AXIS2_PLACEMENT_3D('',#232780,#123648,#123649);
#101848=AXIS2_PLACEMENT_3D('',#232781,#123650,#123651);
#101849=AXIS2_PLACEMENT_3D('',#232782,#123652,#123653);
#101850=AXIS2_PLACEMENT_3D('',#232783,#123654,#123655);
#101851=AXIS2_PLACEMENT_3D('',#232784,#123656,#123657);
#101852=AXIS2_PLACEMENT_3D('',#232785,#123658,#123659);
#101853=AXIS2_PLACEMENT_3D('',#232786,#123660,#123661);
#101854=AXIS2_PLACEMENT_3D('',#232787,#123662,#123663);
#101855=AXIS2_PLACEMENT_3D('',#232788,#123664,#123665);
#101856=AXIS2_PLACEMENT_3D('',#232789,#123666,#123667);
#101857=AXIS2_PLACEMENT_3D('',#232790,#123668,#123669);
#101858=AXIS2_PLACEMENT_3D('',#232791,#123670,#123671);
#101859=AXIS2_PLACEMENT_3D('',#232792,#123672,#123673);
#101860=AXIS2_PLACEMENT_3D('',#232793,#123674,#123675);
#101861=AXIS2_PLACEMENT_3D('',#232794,#123676,#123677);
#101862=AXIS2_PLACEMENT_3D('',#232795,#123678,#123679);
#101863=AXIS2_PLACEMENT_3D('',#232796,#123680,#123681);
#101864=AXIS2_PLACEMENT_3D('',#232797,#123682,#123683);
#101865=AXIS2_PLACEMENT_3D('',#232798,#123684,#123685);
#101866=AXIS2_PLACEMENT_3D('',#232799,#123686,#123687);
#101867=AXIS2_PLACEMENT_3D('',#232800,#123688,#123689);
#101868=AXIS2_PLACEMENT_3D('',#232801,#123690,#123691);
#101869=AXIS2_PLACEMENT_3D('',#232802,#123692,#123693);
#101870=AXIS2_PLACEMENT_3D('',#232803,#123694,#123695);
#101871=AXIS2_PLACEMENT_3D('',#232804,#123696,#123697);
#101872=AXIS2_PLACEMENT_3D('',#232805,#123698,#123699);
#101873=AXIS2_PLACEMENT_3D('',#232806,#123700,#123701);
#101874=AXIS2_PLACEMENT_3D('',#232807,#123702,#123703);
#101875=AXIS2_PLACEMENT_3D('',#232808,#123704,#123705);
#101876=AXIS2_PLACEMENT_3D('',#232809,#123706,#123707);
#101877=AXIS2_PLACEMENT_3D('',#232810,#123708,#123709);
#101878=AXIS2_PLACEMENT_3D('',#232811,#123710,#123711);
#101879=AXIS2_PLACEMENT_3D('',#232812,#123712,#123713);
#101880=AXIS2_PLACEMENT_3D('',#232825,#123716,#123717);
#101881=AXIS2_PLACEMENT_3D('',#232835,#123719,#123720);
#101882=AXIS2_PLACEMENT_3D('',#232845,#123722,#123723);
#101883=AXIS2_PLACEMENT_3D('',#232855,#123725,#123726);
#101884=AXIS2_PLACEMENT_3D('',#232865,#123728,#123729);
#101885=AXIS2_PLACEMENT_3D('',#232872,#123730,#123731);
#101886=AXIS2_PLACEMENT_3D('',#232875,#123733,#123734);
#101887=AXIS2_PLACEMENT_3D('',#232876,#123735,#123736);
#101888=AXIS2_PLACEMENT_3D('',#232877,#123737,#123738);
#101889=AXIS2_PLACEMENT_3D('',#232878,#123739,#123740);
#101890=AXIS2_PLACEMENT_3D('',#232879,#123741,#123742);
#101891=AXIS2_PLACEMENT_3D('',#232880,#123743,#123744);
#101892=AXIS2_PLACEMENT_3D('',#232881,#123745,#123746);
#101893=AXIS2_PLACEMENT_3D('',#232882,#123747,#123748);
#101894=AXIS2_PLACEMENT_3D('',#232883,#123749,#123750);
#101895=AXIS2_PLACEMENT_3D('',#232884,#123751,#123752);
#101896=AXIS2_PLACEMENT_3D('',#232885,#123753,#123754);
#101897=AXIS2_PLACEMENT_3D('',#232886,#123755,#123756);
#101898=AXIS2_PLACEMENT_3D('',#232887,#123757,#123758);
#101899=AXIS2_PLACEMENT_3D('',#232889,#123759,#123760);
#101900=AXIS2_PLACEMENT_3D('',#232891,#123761,#123762);
#101901=AXIS2_PLACEMENT_3D('',#232893,#123763,#123764);
#101902=AXIS2_PLACEMENT_3D('',#232894,#123765,#123766);
#101903=AXIS2_PLACEMENT_3D('',#232895,#123767,#123768);
#101904=AXIS2_PLACEMENT_3D('',#232897,#123769,#123770);
#101905=AXIS2_PLACEMENT_3D('',#232898,#123771,#123772);
#101906=AXIS2_PLACEMENT_3D('',#232899,#123773,#123774);
#101907=AXIS2_PLACEMENT_3D('',#232901,#123776,#123777);
#101908=AXIS2_PLACEMENT_3D('',#232904,#123778,#123779);
#101909=AXIS2_PLACEMENT_3D('',#232906,#123780,#123781);
#101910=AXIS2_PLACEMENT_3D('',#232908,#123782,#123783);
#101911=AXIS2_PLACEMENT_3D('',#232910,#123784,#123785);
#101912=AXIS2_PLACEMENT_3D('',#232912,#123786,#123787);
#101913=AXIS2_PLACEMENT_3D('',#232913,#123788,#123789);
#101914=AXIS2_PLACEMENT_3D('',#232914,#123790,#123791);
#101915=AXIS2_PLACEMENT_3D('',#232922,#123792,#123793);
#101916=AXIS2_PLACEMENT_3D('',#232930,#123794,#123795);
#101917=AXIS2_PLACEMENT_3D('',#232938,#123796,#123797);
#101918=AXIS2_PLACEMENT_3D('',#232946,#123798,#123799);
#101919=AXIS2_PLACEMENT_3D('',#232954,#123800,#123801);
#101920=AXIS2_PLACEMENT_3D('',#232962,#123802,#123803);
#101921=AXIS2_PLACEMENT_3D('',#232965,#123804,#123805);
#101922=AXIS2_PLACEMENT_3D('',#232967,#123806,#123807);
#101923=AXIS2_PLACEMENT_3D('',#232969,#123808,#123809);
#101924=AXIS2_PLACEMENT_3D('',#232971,#123810,#123811);
#101925=AXIS2_PLACEMENT_3D('',#232973,#123812,#123813);
#101926=AXIS2_PLACEMENT_3D('',#232974,#123814,#123815);
#101927=AXIS2_PLACEMENT_3D('',#232975,#123816,#123817);
#101928=AXIS2_PLACEMENT_3D('',#232983,#123818,#123819);
#101929=AXIS2_PLACEMENT_3D('',#232991,#123820,#123821);
#101930=AXIS2_PLACEMENT_3D('',#232999,#123822,#123823);
#101931=AXIS2_PLACEMENT_3D('',#233007,#123824,#123825);
#101932=AXIS2_PLACEMENT_3D('',#233015,#123826,#123827);
#101933=AXIS2_PLACEMENT_3D('',#233023,#123828,#123829);
#101934=AXIS2_PLACEMENT_3D('',#233026,#123832,#123833);
#101935=AXIS2_PLACEMENT_3D('',#233028,#123835,#123836);
#101936=AXIS2_PLACEMENT_3D('',#233030,#123838,#123839);
#101937=AXIS2_PLACEMENT_3D('',#233032,#123841,#123842);
#101938=AXIS2_PLACEMENT_3D('',#233034,#123844,#123845);
#101939=AXIS2_PLACEMENT_3D('',#233035,#123846,#123847);
#101940=AXIS2_PLACEMENT_3D('',#233038,#123848,#123849);
#101941=AXIS2_PLACEMENT_3D('',#233040,#123850,#123851);
#101942=AXIS2_PLACEMENT_3D('',#233042,#123852,#123853);
#101943=AXIS2_PLACEMENT_3D('',#233044,#123854,#123855);
#101944=AXIS2_PLACEMENT_3D('',#233046,#123856,#123857);
#101945=AXIS2_PLACEMENT_3D('',#233047,#123858,#123859);
#101946=AXIS2_PLACEMENT_3D('',#233048,#123860,#123861);
#101947=AXIS2_PLACEMENT_3D('',#233056,#123862,#123863);
#101948=AXIS2_PLACEMENT_3D('',#233064,#123864,#123865);
#101949=AXIS2_PLACEMENT_3D('',#233072,#123866,#123867);
#101950=AXIS2_PLACEMENT_3D('',#233080,#123868,#123869);
#101951=AXIS2_PLACEMENT_3D('',#233088,#123870,#123871);
#101952=AXIS2_PLACEMENT_3D('',#233096,#123872,#123873);
#101953=AXIS2_PLACEMENT_3D('',#233099,#123874,#123875);
#101954=AXIS2_PLACEMENT_3D('',#233101,#123876,#123877);
#101955=AXIS2_PLACEMENT_3D('',#233103,#123878,#123879);
#101956=AXIS2_PLACEMENT_3D('',#233105,#123880,#123881);
#101957=AXIS2_PLACEMENT_3D('',#233107,#123882,#123883);
#101958=AXIS2_PLACEMENT_3D('',#233108,#123884,#123885);
#101959=AXIS2_PLACEMENT_3D('',#233109,#123886,#123887);
#101960=AXIS2_PLACEMENT_3D('',#233117,#123888,#123889);
#101961=AXIS2_PLACEMENT_3D('',#233125,#123890,#123891);
#101962=AXIS2_PLACEMENT_3D('',#233133,#123892,#123893);
#101963=AXIS2_PLACEMENT_3D('',#233141,#123894,#123895);
#101964=AXIS2_PLACEMENT_3D('',#233149,#123896,#123897);
#101965=AXIS2_PLACEMENT_3D('',#233157,#123898,#123899);
#101966=AXIS2_PLACEMENT_3D('',#233160,#123902,#123903);
#101967=AXIS2_PLACEMENT_3D('',#233162,#123905,#123906);
#101968=AXIS2_PLACEMENT_3D('',#233164,#123908,#123909);
#101969=AXIS2_PLACEMENT_3D('',#233166,#123911,#123912);
#101970=AXIS2_PLACEMENT_3D('',#233168,#123914,#123915);
#101971=AXIS2_PLACEMENT_3D('',#233169,#123916,#123917);
#101972=AXIS2_PLACEMENT_3D('',#233182,#123920,#123921);
#101973=AXIS2_PLACEMENT_3D('',#233192,#123923,#123924);
#101974=AXIS2_PLACEMENT_3D('',#233202,#123926,#123927);
#101975=AXIS2_PLACEMENT_3D('',#233212,#123929,#123930);
#101976=AXIS2_PLACEMENT_3D('',#233222,#123932,#123933);
#101977=AXIS2_PLACEMENT_3D('',#233229,#123934,#123935);
#101978=AXIS2_PLACEMENT_3D('',#233232,#123937,#123938);
#101979=AXIS2_PLACEMENT_3D('',#233233,#123939,#123940);
#101980=AXIS2_PLACEMENT_3D('',#233234,#123941,#123942);
#101981=AXIS2_PLACEMENT_3D('',#233235,#123943,#123944);
#101982=AXIS2_PLACEMENT_3D('',#233236,#123945,#123946);
#101983=AXIS2_PLACEMENT_3D('',#233237,#123947,#123948);
#101984=AXIS2_PLACEMENT_3D('',#233238,#123949,#123950);
#101985=AXIS2_PLACEMENT_3D('',#233239,#123951,#123952);
#101986=AXIS2_PLACEMENT_3D('',#233240,#123953,#123954);
#101987=AXIS2_PLACEMENT_3D('',#233241,#123955,#123956);
#101988=AXIS2_PLACEMENT_3D('',#233242,#123957,#123958);
#101989=AXIS2_PLACEMENT_3D('',#233243,#123959,#123960);
#101990=AXIS2_PLACEMENT_3D('',#233244,#123961,#123962);
#101991=AXIS2_PLACEMENT_3D('',#233246,#123963,#123964);
#101992=AXIS2_PLACEMENT_3D('',#233248,#123965,#123966);
#101993=AXIS2_PLACEMENT_3D('',#233250,#123967,#123968);
#101994=AXIS2_PLACEMENT_3D('',#233251,#123969,#123970);
#101995=AXIS2_PLACEMENT_3D('',#233252,#123971,#123972);
#101996=AXIS2_PLACEMENT_3D('',#233254,#123973,#123974);
#101997=AXIS2_PLACEMENT_3D('',#233255,#123975,#123976);
#101998=AXIS2_PLACEMENT_3D('',#233256,#123977,#123978);
#101999=AXIS2_PLACEMENT_3D('',#233258,#123980,#123981);
#102000=AXIS2_PLACEMENT_3D('',#233260,#123982,#123983);
#102001=AXIS2_PLACEMENT_3D('',#233263,#123984,#123985);
#102002=AXIS2_PLACEMENT_3D('',#233284,#123986,#123987);
#102003=AXIS2_PLACEMENT_3D('',#233303,#123988,#123989);
#102004=AXIS2_PLACEMENT_3D('',#233306,#123990,#123991);
#102005=AXIS2_PLACEMENT_3D('',#233307,#123992,#123993);
#102006=AXIS2_PLACEMENT_3D('',#233308,#123994,#123995);
#102007=AXIS2_PLACEMENT_3D('',#233309,#123996,#123997);
#102008=AXIS2_PLACEMENT_3D('',#233311,#123998,#123999);
#102009=AXIS2_PLACEMENT_3D('',#233313,#124000,#124001);
#102010=AXIS2_PLACEMENT_3D('',#233315,#124002,#124003);
#102011=AXIS2_PLACEMENT_3D('',#233316,#124004,#124005);
#102012=AXIS2_PLACEMENT_3D('',#233317,#124006,#124007);
#102013=AXIS2_PLACEMENT_3D('',#233320,#124008,#124009);
#102014=AXIS2_PLACEMENT_3D('',#233324,#124011,#124012);
#102015=AXIS2_PLACEMENT_3D('',#233326,#124014,#124015);
#102016=AXIS2_PLACEMENT_3D('',#233329,#124018,#124019);
#102017=AXIS2_PLACEMENT_3D('',#233331,#124021,#124022);
#102018=AXIS2_PLACEMENT_3D('',#233333,#124024,#124025);
#102019=AXIS2_PLACEMENT_3D('',#233334,#124026,#124027);
#102020=AXIS2_PLACEMENT_3D('',#233336,#124028,#124029);
#102021=AXIS2_PLACEMENT_3D('',#233337,#124030,#124031);
#102022=AXIS2_PLACEMENT_3D('',#233339,#124032,#124033);
#102023=AXIS2_PLACEMENT_3D('',#233341,#124035,#124036);
#102024=AXIS2_PLACEMENT_3D('',#233343,#124038,#124039);
#102025=AXIS2_PLACEMENT_3D('',#233344,#124040,#124041);
#102026=AXIS2_PLACEMENT_3D('',#233346,#124042,#124043);
#102027=AXIS2_PLACEMENT_3D('',#233349,#124045,#124046);
#102028=AXIS2_PLACEMENT_3D('',#233350,#124047,#124048);
#102029=AXIS2_PLACEMENT_3D('',#233351,#124049,#124050);
#102030=AXIS2_PLACEMENT_3D('',#233353,#124051,#124052);
#102031=AXIS2_PLACEMENT_3D('',#233355,#124054,#124055);
#102032=AXIS2_PLACEMENT_3D('',#233357,#124056,#124057);
#102033=AXIS2_PLACEMENT_3D('',#233358,#124058,#124059);
#102034=AXIS2_PLACEMENT_3D('',#233360,#124060,#124061);
#102035=AXIS2_PLACEMENT_3D('',#233362,#124063,#124064);
#102036=AXIS2_PLACEMENT_3D('',#233363,#124065,#124066);
#102037=AXIS2_PLACEMENT_3D('',#233366,#124067,#124068);
#102038=AXIS2_PLACEMENT_3D('',#233368,#124069,#124070);
#102039=AXIS2_PLACEMENT_3D('',#233370,#124071,#124072);
#102040=AXIS2_PLACEMENT_3D('',#233371,#124073,#124074);
#102041=AXIS2_PLACEMENT_3D('',#233372,#124075,#124076);
#102042=AXIS2_PLACEMENT_3D('',#233375,#124077,#124078);
#102043=AXIS2_PLACEMENT_3D('',#233378,#124081,#124082);
#102044=AXIS2_PLACEMENT_3D('',#233381,#124083,#124084);
#102045=AXIS2_PLACEMENT_3D('',#233384,#124087,#124088);
#102046=AXIS2_PLACEMENT_3D('',#233387,#124089,#124090);
#102047=AXIS2_PLACEMENT_3D('',#233388,#124091,#124092);
#102048=AXIS2_PLACEMENT_3D('',#233389,#124093,#124094);
#102049=AXIS2_PLACEMENT_3D('',#233390,#124095,#124096);
#102050=AXIS2_PLACEMENT_3D('',#233393,#124097,#124098);
#102051=AXIS2_PLACEMENT_3D('',#233394,#124099,#124100);
#102052=AXIS2_PLACEMENT_3D('',#233395,#124101,#124102);
#102053=AXIS2_PLACEMENT_3D('',#233396,#124103,#124104);
#102054=AXIS2_PLACEMENT_3D('',#233399,#124105,#124106);
#102055=AXIS2_PLACEMENT_3D('',#233402,#124109,#124110);
#102056=AXIS2_PLACEMENT_3D('',#233405,#124111,#124112);
#102057=AXIS2_PLACEMENT_3D('',#233408,#124115,#124116);
#102058=AXIS2_PLACEMENT_3D('',#233409,#124117,#124118);
#102059=AXIS2_PLACEMENT_3D('',#233410,#124119,#124120);
#102060=AXIS2_PLACEMENT_3D('',#233411,#124121,#124122);
#102061=AXIS2_PLACEMENT_3D('',#233417,#124126,#124127);
#102062=AXIS2_PLACEMENT_3D('',#233420,#124129,#124130);
#102063=AXIS2_PLACEMENT_3D('',#233421,#124131,#124132);
#102064=AXIS2_PLACEMENT_3D('',#233424,#124134,#124135);
#102065=AXIS2_PLACEMENT_3D('',#233425,#124136,#124137);
#102066=AXIS2_PLACEMENT_3D('',#233435,#124142,#124143);
#102067=AXIS2_PLACEMENT_3D('',#233437,#124144,#124145);
#102068=AXIS2_PLACEMENT_3D('',#233438,#124146,#124147);
#102069=AXIS2_PLACEMENT_3D('',#233440,#124148,#124149);
#102070=AXIS2_PLACEMENT_3D('',#233442,#124150,#124151);
#102071=AXIS2_PLACEMENT_3D('',#233444,#124152,#124153);
#102072=AXIS2_PLACEMENT_3D('',#233445,#124154,#124155);
#102073=AXIS2_PLACEMENT_3D('',#233446,#124156,#124157);
#102074=AXIS2_PLACEMENT_3D('',#233448,#124158,#124159);
#102075=AXIS2_PLACEMENT_3D('',#233450,#124161,#124162);
#102076=AXIS2_PLACEMENT_3D('',#233453,#124163,#124164);
#102077=AXIS2_PLACEMENT_3D('',#233454,#124165,#124166);
#102078=AXIS2_PLACEMENT_3D('',#233455,#124167,#124168);
#102079=AXIS2_PLACEMENT_3D('',#233456,#124169,#124170);
#102080=AXIS2_PLACEMENT_3D('',#233459,#124172,#124173);
#102081=AXIS2_PLACEMENT_3D('',#233460,#124174,#124175);
#102082=AXIS2_PLACEMENT_3D('',#233462,#124176,#124177);
#102083=AXIS2_PLACEMENT_3D('',#233464,#124178,#124179);
#102084=AXIS2_PLACEMENT_3D('',#233465,#124180,#124181);
#102085=AXIS2_PLACEMENT_3D('',#233466,#124182,#124183);
#102086=AXIS2_PLACEMENT_3D('',#233468,#124184,#124185);
#102087=AXIS2_PLACEMENT_3D('',#233470,#124186,#124187);
#102088=AXIS2_PLACEMENT_3D('',#233472,#124188,#124189);
#102089=AXIS2_PLACEMENT_3D('',#233473,#124190,#124191);
#102090=AXIS2_PLACEMENT_3D('',#233474,#124192,#124193);
#102091=AXIS2_PLACEMENT_3D('',#233476,#124195,#124196);
#102092=AXIS2_PLACEMENT_3D('',#233478,#124198,#124199);
#102093=AXIS2_PLACEMENT_3D('',#233483,#124201,#124202);
#102094=AXIS2_PLACEMENT_3D('',#233486,#124204,#124205);
#102095=AXIS2_PLACEMENT_3D('',#233487,#124206,#124207);
#102096=AXIS2_PLACEMENT_3D('',#233490,#124208,#124209);
#102097=AXIS2_PLACEMENT_3D('',#233493,#124211,#124212);
#102098=AXIS2_PLACEMENT_3D('',#233495,#124214,#124215);
#102099=AXIS2_PLACEMENT_3D('',#233497,#124216,#124217);
#102100=AXIS2_PLACEMENT_3D('',#233498,#124218,#124219);
#102101=AXIS2_PLACEMENT_3D('',#233499,#124220,#124221);
#102102=AXIS2_PLACEMENT_3D('',#233502,#124222,#124223);
#102103=AXIS2_PLACEMENT_3D('',#233503,#124224,#124225);
#102104=AXIS2_PLACEMENT_3D('',#233504,#124226,#124227);
#102105=AXIS2_PLACEMENT_3D('',#233505,#124228,#124229);
#102106=AXIS2_PLACEMENT_3D('',#233510,#124232,#124233);
#102107=AXIS2_PLACEMENT_3D('',#233511,#124234,#124235);
#102108=AXIS2_PLACEMENT_3D('',#233513,#124236,#124237);
#102109=AXIS2_PLACEMENT_3D('',#233515,#124238,#124239);
#102110=AXIS2_PLACEMENT_3D('',#233516,#124240,#124241);
#102111=AXIS2_PLACEMENT_3D('',#233517,#124242,#124243);
#102112=AXIS2_PLACEMENT_3D('',#233520,#124245,#124246);
#102113=AXIS2_PLACEMENT_3D('',#233522,#124248,#124249);
#102114=AXIS2_PLACEMENT_3D('',#233524,#124250,#124251);
#102115=AXIS2_PLACEMENT_3D('',#233525,#124252,#124253);
#102116=AXIS2_PLACEMENT_3D('',#233526,#124254,#124255);
#102117=AXIS2_PLACEMENT_3D('',#233528,#124256,#124257);
#102118=AXIS2_PLACEMENT_3D('',#233530,#124258,#124259);
#102119=AXIS2_PLACEMENT_3D('',#233531,#124260,#124261);
#102120=AXIS2_PLACEMENT_3D('',#233536,#124264,#124265);
#102121=AXIS2_PLACEMENT_3D('',#233537,#124266,#124267);
#102122=AXIS2_PLACEMENT_3D('',#233542,#124270,#124271);
#102123=AXIS2_PLACEMENT_3D('',#233543,#124272,#124273);
#102124=AXIS2_PLACEMENT_3D('',#233546,#124276,#124277);
#102125=AXIS2_PLACEMENT_3D('',#233548,#124279,#124280);
#102126=AXIS2_PLACEMENT_3D('',#233550,#124282,#124283);
#102127=AXIS2_PLACEMENT_3D('',#233552,#124285,#124286);
#102128=AXIS2_PLACEMENT_3D('',#233554,#124288,#124289);
#102129=AXIS2_PLACEMENT_3D('',#233556,#124291,#124292);
#102130=AXIS2_PLACEMENT_3D('',#233558,#124294,#124295);
#102131=AXIS2_PLACEMENT_3D('',#233559,#124296,#124297);
#102132=AXIS2_PLACEMENT_3D('',#233561,#124299,#124300);
#102133=AXIS2_PLACEMENT_3D('',#233563,#124302,#124303);
#102134=AXIS2_PLACEMENT_3D('',#233565,#124305,#124306);
#102135=AXIS2_PLACEMENT_3D('',#233567,#124308,#124309);
#102136=AXIS2_PLACEMENT_3D('',#233569,#124311,#124312);
#102137=AXIS2_PLACEMENT_3D('',#233570,#124313,#124314);
#102138=AXIS2_PLACEMENT_3D('',#233572,#124315,#124316);
#102139=AXIS2_PLACEMENT_3D('',#233575,#124317,#124318);
#102140=AXIS2_PLACEMENT_3D('',#233596,#124319,#124320);
#102141=AXIS2_PLACEMENT_3D('',#233615,#124321,#124322);
#102142=AXIS2_PLACEMENT_3D('',#233618,#124323,#124324);
#102143=AXIS2_PLACEMENT_3D('',#233619,#124325,#124326);
#102144=AXIS2_PLACEMENT_3D('',#233620,#124327,#124328);
#102145=AXIS2_PLACEMENT_3D('',#233621,#124329,#124330);
#102146=AXIS2_PLACEMENT_3D('',#233623,#124331,#124332);
#102147=AXIS2_PLACEMENT_3D('',#233625,#124333,#124334);
#102148=AXIS2_PLACEMENT_3D('',#233627,#124335,#124336);
#102149=AXIS2_PLACEMENT_3D('',#233628,#124337,#124338);
#102150=AXIS2_PLACEMENT_3D('',#233629,#124339,#124340);
#102151=AXIS2_PLACEMENT_3D('',#233632,#124341,#124342);
#102152=AXIS2_PLACEMENT_3D('',#233636,#124344,#124345);
#102153=AXIS2_PLACEMENT_3D('',#233638,#124347,#124348);
#102154=AXIS2_PLACEMENT_3D('',#233641,#124351,#124352);
#102155=AXIS2_PLACEMENT_3D('',#233643,#124354,#124355);
#102156=AXIS2_PLACEMENT_3D('',#233645,#124357,#124358);
#102157=AXIS2_PLACEMENT_3D('',#233646,#124359,#124360);
#102158=AXIS2_PLACEMENT_3D('',#233648,#124361,#124362);
#102159=AXIS2_PLACEMENT_3D('',#233649,#124363,#124364);
#102160=AXIS2_PLACEMENT_3D('',#233651,#124365,#124366);
#102161=AXIS2_PLACEMENT_3D('',#233653,#124368,#124369);
#102162=AXIS2_PLACEMENT_3D('',#233655,#124371,#124372);
#102163=AXIS2_PLACEMENT_3D('',#233656,#124373,#124374);
#102164=AXIS2_PLACEMENT_3D('',#233659,#124375,#124376);
#102165=AXIS2_PLACEMENT_3D('',#233674,#124379,#124380);
#102166=AXIS2_PLACEMENT_3D('',#233677,#124381,#124382);
#102167=AXIS2_PLACEMENT_3D('',#233678,#124383,#124384);
#102168=AXIS2_PLACEMENT_3D('',#233679,#124385,#124386);
#102169=AXIS2_PLACEMENT_3D('',#233680,#124387,#124388);
#102170=AXIS2_PLACEMENT_3D('',#233683,#124389,#124390);
#102171=AXIS2_PLACEMENT_3D('',#233686,#124393,#124394);
#102172=AXIS2_PLACEMENT_3D('',#233689,#124395,#124396);
#102173=AXIS2_PLACEMENT_3D('',#233690,#124397,#124398);
#102174=AXIS2_PLACEMENT_3D('',#233691,#124399,#124400);
#102175=AXIS2_PLACEMENT_3D('',#233692,#124401,#124402);
#102176=AXIS2_PLACEMENT_3D('',#233707,#124405,#124406);
#102177=AXIS2_PLACEMENT_3D('',#233710,#124407,#124408);
#102178=AXIS2_PLACEMENT_3D('',#233714,#124410,#124411);
#102179=AXIS2_PLACEMENT_3D('',#233716,#124413,#124414);
#102180=AXIS2_PLACEMENT_3D('',#233719,#124415,#124416);
#102181=AXIS2_PLACEMENT_3D('',#233720,#124417,#124418);
#102182=AXIS2_PLACEMENT_3D('',#233721,#124419,#124420);
#102183=AXIS2_PLACEMENT_3D('',#233722,#124421,#124422);
#102184=AXIS2_PLACEMENT_3D('',#233725,#124423,#124424);
#102185=AXIS2_PLACEMENT_3D('',#233728,#124427,#124428);
#102186=AXIS2_PLACEMENT_3D('',#233731,#124429,#124430);
#102187=AXIS2_PLACEMENT_3D('',#233732,#124431,#124432);
#102188=AXIS2_PLACEMENT_3D('',#233733,#124433,#124434);
#102189=AXIS2_PLACEMENT_3D('',#233734,#124435,#124436);
#102190=AXIS2_PLACEMENT_3D('',#233749,#124439,#124440);
#102191=AXIS2_PLACEMENT_3D('',#233752,#124441,#124442);
#102192=AXIS2_PLACEMENT_3D('',#233756,#124444,#124445);
#102193=AXIS2_PLACEMENT_3D('',#233758,#124447,#124448);
#102194=AXIS2_PLACEMENT_3D('',#233761,#124449,#124450);
#102195=AXIS2_PLACEMENT_3D('',#233762,#124451,#124452);
#102196=AXIS2_PLACEMENT_3D('',#233763,#124453,#124454);
#102197=AXIS2_PLACEMENT_3D('',#233764,#124455,#124456);
#102198=AXIS2_PLACEMENT_3D('',#233767,#124457,#124458);
#102199=AXIS2_PLACEMENT_3D('',#233770,#124461,#124462);
#102200=AXIS2_PLACEMENT_3D('',#233773,#124463,#124464);
#102201=AXIS2_PLACEMENT_3D('',#233774,#124465,#124466);
#102202=AXIS2_PLACEMENT_3D('',#233775,#124467,#124468);
#102203=AXIS2_PLACEMENT_3D('',#233776,#124469,#124470);
#102204=AXIS2_PLACEMENT_3D('',#233779,#124471,#124472);
#102205=AXIS2_PLACEMENT_3D('',#233782,#124475,#124476);
#102206=AXIS2_PLACEMENT_3D('',#233785,#124477,#124478);
#102207=AXIS2_PLACEMENT_3D('',#233786,#124479,#124480);
#102208=AXIS2_PLACEMENT_3D('',#233787,#124481,#124482);
#102209=AXIS2_PLACEMENT_3D('',#233788,#124483,#124484);
#102210=AXIS2_PLACEMENT_3D('',#233791,#124485,#124486);
#102211=AXIS2_PLACEMENT_3D('',#233794,#124489,#124490);
#102212=AXIS2_PLACEMENT_3D('',#233797,#124491,#124492);
#102213=AXIS2_PLACEMENT_3D('',#233798,#124493,#124494);
#102214=AXIS2_PLACEMENT_3D('',#233799,#124495,#124496);
#102215=AXIS2_PLACEMENT_3D('',#233800,#124497,#124498);
#102216=AXIS2_PLACEMENT_3D('',#233803,#124499,#124500);
#102217=AXIS2_PLACEMENT_3D('',#233806,#124503,#124504);
#102218=AXIS2_PLACEMENT_3D('',#233809,#124505,#124506);
#102219=AXIS2_PLACEMENT_3D('',#233813,#124508,#124509);
#102220=AXIS2_PLACEMENT_3D('',#233815,#124511,#124512);
#102221=AXIS2_PLACEMENT_3D('',#233818,#124513,#124514);
#102222=AXIS2_PLACEMENT_3D('',#233819,#124515,#124516);
#102223=AXIS2_PLACEMENT_3D('',#233820,#124517,#124518);
#102224=AXIS2_PLACEMENT_3D('',#233821,#124519,#124520);
#102225=AXIS2_PLACEMENT_3D('',#233824,#124521,#124522);
#102226=AXIS2_PLACEMENT_3D('',#233827,#124525,#124526);
#102227=AXIS2_PLACEMENT_3D('',#233830,#124527,#124528);
#102228=AXIS2_PLACEMENT_3D('',#233831,#124529,#124530);
#102229=AXIS2_PLACEMENT_3D('',#233832,#124531,#124532);
#102230=AXIS2_PLACEMENT_3D('',#233833,#124533,#124534);
#102231=AXIS2_PLACEMENT_3D('',#233848,#124537,#124538);
#102232=AXIS2_PLACEMENT_3D('',#233851,#124539,#124540);
#102233=AXIS2_PLACEMENT_3D('',#233855,#124542,#124543);
#102234=AXIS2_PLACEMENT_3D('',#233857,#124545,#124546);
#102235=AXIS2_PLACEMENT_3D('',#233860,#124547,#124548);
#102236=AXIS2_PLACEMENT_3D('',#233861,#124549,#124550);
#102237=AXIS2_PLACEMENT_3D('',#233862,#124551,#124552);
#102238=AXIS2_PLACEMENT_3D('',#233863,#124553,#124554);
#102239=AXIS2_PLACEMENT_3D('',#233866,#124555,#124556);
#102240=AXIS2_PLACEMENT_3D('',#233869,#124559,#124560);
#102241=AXIS2_PLACEMENT_3D('',#233872,#124561,#124562);
#102242=AXIS2_PLACEMENT_3D('',#233873,#124563,#124564);
#102243=AXIS2_PLACEMENT_3D('',#233874,#124565,#124566);
#102244=AXIS2_PLACEMENT_3D('',#233875,#124567,#124568);
#102245=AXIS2_PLACEMENT_3D('',#233878,#124569,#124570);
#102246=AXIS2_PLACEMENT_3D('',#233879,#124571,#124572);
#102247=AXIS2_PLACEMENT_3D('',#233880,#124573,#124574);
#102248=AXIS2_PLACEMENT_3D('',#233881,#124575,#124576);
#102249=AXIS2_PLACEMENT_3D('',#233884,#124577,#124578);
#102250=AXIS2_PLACEMENT_3D('',#233887,#124581,#124582);
#102251=AXIS2_PLACEMENT_3D('',#233890,#124583,#124584);
#102252=AXIS2_PLACEMENT_3D('',#233891,#124585,#124586);
#102253=AXIS2_PLACEMENT_3D('',#233892,#124587,#124588);
#102254=AXIS2_PLACEMENT_3D('',#233893,#124589,#124590);
#102255=AXIS2_PLACEMENT_3D('',#233896,#124591,#124592);
#102256=AXIS2_PLACEMENT_3D('',#233899,#124595,#124596);
#102257=AXIS2_PLACEMENT_3D('',#233902,#124597,#124598);
#102258=AXIS2_PLACEMENT_3D('',#233903,#124599,#124600);
#102259=AXIS2_PLACEMENT_3D('',#233904,#124601,#124602);
#102260=AXIS2_PLACEMENT_3D('',#233905,#124603,#124604);
#102261=AXIS2_PLACEMENT_3D('',#233908,#124605,#124606);
#102262=AXIS2_PLACEMENT_3D('',#233911,#124609,#124610);
#102263=AXIS2_PLACEMENT_3D('',#233914,#124611,#124612);
#102264=AXIS2_PLACEMENT_3D('',#233918,#124614,#124615);
#102265=AXIS2_PLACEMENT_3D('',#233920,#124617,#124618);
#102266=AXIS2_PLACEMENT_3D('',#233923,#124619,#124620);
#102267=AXIS2_PLACEMENT_3D('',#233924,#124621,#124622);
#102268=AXIS2_PLACEMENT_3D('',#233925,#124623,#124624);
#102269=AXIS2_PLACEMENT_3D('',#233926,#124625,#124626);
#102270=AXIS2_PLACEMENT_3D('',#233929,#124627,#124628);
#102271=AXIS2_PLACEMENT_3D('',#233932,#124631,#124632);
#102272=AXIS2_PLACEMENT_3D('',#233935,#124633,#124634);
#102273=AXIS2_PLACEMENT_3D('',#233936,#124635,#124636);
#102274=AXIS2_PLACEMENT_3D('',#233937,#124637,#124638);
#102275=AXIS2_PLACEMENT_3D('',#233938,#124639,#124640);
#102276=AXIS2_PLACEMENT_3D('',#233941,#124641,#124642);
#102277=AXIS2_PLACEMENT_3D('',#233942,#124643,#124644);
#102278=AXIS2_PLACEMENT_3D('',#233943,#124645,#124646);
#102279=AXIS2_PLACEMENT_3D('',#233944,#124647,#124648);
#102280=AXIS2_PLACEMENT_3D('',#233947,#124649,#124650);
#102281=AXIS2_PLACEMENT_3D('',#233948,#124651,#124652);
#102282=AXIS2_PLACEMENT_3D('',#233949,#124653,#124654);
#102283=AXIS2_PLACEMENT_3D('',#233950,#124655,#124656);
#102284=AXIS2_PLACEMENT_3D('',#233953,#124657,#124658);
#102285=AXIS2_PLACEMENT_3D('',#233956,#124661,#124662);
#102286=AXIS2_PLACEMENT_3D('',#233959,#124663,#124664);
#102287=AXIS2_PLACEMENT_3D('',#233960,#124665,#124666);
#102288=AXIS2_PLACEMENT_3D('',#233961,#124667,#124668);
#102289=AXIS2_PLACEMENT_3D('',#233962,#124669,#124670);
#102290=AXIS2_PLACEMENT_3D('',#233965,#124671,#124672);
#102291=AXIS2_PLACEMENT_3D('',#233968,#124675,#124676);
#102292=AXIS2_PLACEMENT_3D('',#233971,#124677,#124678);
#102293=AXIS2_PLACEMENT_3D('',#233975,#124680,#124681);
#102294=AXIS2_PLACEMENT_3D('',#233977,#124683,#124684);
#102295=AXIS2_PLACEMENT_3D('',#233980,#124685,#124686);
#102296=AXIS2_PLACEMENT_3D('',#233981,#124687,#124688);
#102297=AXIS2_PLACEMENT_3D('',#233982,#124689,#124690);
#102298=AXIS2_PLACEMENT_3D('',#233983,#124691,#124692);
#102299=AXIS2_PLACEMENT_3D('',#233986,#124693,#124694);
#102300=AXIS2_PLACEMENT_3D('',#233989,#124697,#124698);
#102301=AXIS2_PLACEMENT_3D('',#233992,#124699,#124700);
#102302=AXIS2_PLACEMENT_3D('',#233993,#124701,#124702);
#102303=AXIS2_PLACEMENT_3D('',#233994,#124703,#124704);
#102304=AXIS2_PLACEMENT_3D('',#233995,#124705,#124706);
#102305=AXIS2_PLACEMENT_3D('',#233998,#124707,#124708);
#102306=AXIS2_PLACEMENT_3D('',#233999,#124709,#124710);
#102307=AXIS2_PLACEMENT_3D('',#234000,#124711,#124712);
#102308=AXIS2_PLACEMENT_3D('',#234001,#124713,#124714);
#102309=AXIS2_PLACEMENT_3D('',#234004,#124715,#124716);
#102310=AXIS2_PLACEMENT_3D('',#234005,#124717,#124718);
#102311=AXIS2_PLACEMENT_3D('',#234006,#124719,#124720);
#102312=AXIS2_PLACEMENT_3D('',#234007,#124721,#124722);
#102313=AXIS2_PLACEMENT_3D('',#234010,#124723,#124724);
#102314=AXIS2_PLACEMENT_3D('',#234013,#124727,#124728);
#102315=AXIS2_PLACEMENT_3D('',#234016,#124729,#124730);
#102316=AXIS2_PLACEMENT_3D('',#234017,#124731,#124732);
#102317=AXIS2_PLACEMENT_3D('',#234018,#124733,#124734);
#102318=AXIS2_PLACEMENT_3D('',#234019,#124735,#124736);
#102319=AXIS2_PLACEMENT_3D('',#234022,#124737,#124738);
#102320=AXIS2_PLACEMENT_3D('',#234025,#124741,#124742);
#102321=AXIS2_PLACEMENT_3D('',#234028,#124743,#124744);
#102322=AXIS2_PLACEMENT_3D('',#234032,#124746,#124747);
#102323=AXIS2_PLACEMENT_3D('',#234034,#124749,#124750);
#102324=AXIS2_PLACEMENT_3D('',#234037,#124751,#124752);
#102325=AXIS2_PLACEMENT_3D('',#234038,#124753,#124754);
#102326=AXIS2_PLACEMENT_3D('',#234039,#124755,#124756);
#102327=AXIS2_PLACEMENT_3D('',#234040,#124757,#124758);
#102328=AXIS2_PLACEMENT_3D('',#234043,#124759,#124760);
#102329=AXIS2_PLACEMENT_3D('',#234046,#124763,#124764);
#102330=AXIS2_PLACEMENT_3D('',#234049,#124765,#124766);
#102331=AXIS2_PLACEMENT_3D('',#234050,#124767,#124768);
#102332=AXIS2_PLACEMENT_3D('',#234051,#124769,#124770);
#102333=AXIS2_PLACEMENT_3D('',#234052,#124771,#124772);
#102334=AXIS2_PLACEMENT_3D('',#234055,#124773,#124774);
#102335=AXIS2_PLACEMENT_3D('',#234056,#124775,#124776);
#102336=AXIS2_PLACEMENT_3D('',#234057,#124777,#124778);
#102337=AXIS2_PLACEMENT_3D('',#234058,#124779,#124780);
#102338=AXIS2_PLACEMENT_3D('',#234061,#124781,#124782);
#102339=AXIS2_PLACEMENT_3D('',#234062,#124783,#124784);
#102340=AXIS2_PLACEMENT_3D('',#234063,#124785,#124786);
#102341=AXIS2_PLACEMENT_3D('',#234064,#124787,#124788);
#102342=AXIS2_PLACEMENT_3D('',#234067,#124789,#124790);
#102343=AXIS2_PLACEMENT_3D('',#234070,#124793,#124794);
#102344=AXIS2_PLACEMENT_3D('',#234073,#124795,#124796);
#102345=AXIS2_PLACEMENT_3D('',#234074,#124797,#124798);
#102346=AXIS2_PLACEMENT_3D('',#234075,#124799,#124800);
#102347=AXIS2_PLACEMENT_3D('',#234076,#124801,#124802);
#102348=AXIS2_PLACEMENT_3D('',#234079,#124803,#124804);
#102349=AXIS2_PLACEMENT_3D('',#234082,#124807,#124808);
#102350=AXIS2_PLACEMENT_3D('',#234085,#124809,#124810);
#102351=AXIS2_PLACEMENT_3D('',#234089,#124812,#124813);
#102352=AXIS2_PLACEMENT_3D('',#234091,#124815,#124816);
#102353=AXIS2_PLACEMENT_3D('',#234094,#124817,#124818);
#102354=AXIS2_PLACEMENT_3D('',#234095,#124819,#124820);
#102355=AXIS2_PLACEMENT_3D('',#234096,#124821,#124822);
#102356=AXIS2_PLACEMENT_3D('',#234097,#124823,#124824);
#102357=AXIS2_PLACEMENT_3D('',#234100,#124825,#124826);
#102358=AXIS2_PLACEMENT_3D('',#234103,#124829,#124830);
#102359=AXIS2_PLACEMENT_3D('',#234106,#124831,#124832);
#102360=AXIS2_PLACEMENT_3D('',#234107,#124833,#124834);
#102361=AXIS2_PLACEMENT_3D('',#234108,#124835,#124836);
#102362=AXIS2_PLACEMENT_3D('',#234109,#124837,#124838);
#102363=AXIS2_PLACEMENT_3D('',#234112,#124839,#124840);
#102364=AXIS2_PLACEMENT_3D('',#234113,#124841,#124842);
#102365=AXIS2_PLACEMENT_3D('',#234114,#124843,#124844);
#102366=AXIS2_PLACEMENT_3D('',#234115,#124845,#124846);
#102367=AXIS2_PLACEMENT_3D('',#234118,#124847,#124848);
#102368=AXIS2_PLACEMENT_3D('',#234119,#124849,#124850);
#102369=AXIS2_PLACEMENT_3D('',#234120,#124851,#124852);
#102370=AXIS2_PLACEMENT_3D('',#234121,#124853,#124854);
#102371=AXIS2_PLACEMENT_3D('',#234124,#124855,#124856);
#102372=AXIS2_PLACEMENT_3D('',#234127,#124859,#124860);
#102373=AXIS2_PLACEMENT_3D('',#234130,#124861,#124862);
#102374=AXIS2_PLACEMENT_3D('',#234131,#124863,#124864);
#102375=AXIS2_PLACEMENT_3D('',#234132,#124865,#124866);
#102376=AXIS2_PLACEMENT_3D('',#234133,#124867,#124868);
#102377=AXIS2_PLACEMENT_3D('',#234136,#124869,#124870);
#102378=AXIS2_PLACEMENT_3D('',#234139,#124873,#124874);
#102379=AXIS2_PLACEMENT_3D('',#234142,#124875,#124876);
#102380=AXIS2_PLACEMENT_3D('',#234146,#124878,#124879);
#102381=AXIS2_PLACEMENT_3D('',#234148,#124881,#124882);
#102382=AXIS2_PLACEMENT_3D('',#234151,#124883,#124884);
#102383=AXIS2_PLACEMENT_3D('',#234152,#124885,#124886);
#102384=AXIS2_PLACEMENT_3D('',#234153,#124887,#124888);
#102385=AXIS2_PLACEMENT_3D('',#234154,#124889,#124890);
#102386=AXIS2_PLACEMENT_3D('',#234157,#124891,#124892);
#102387=AXIS2_PLACEMENT_3D('',#234160,#124895,#124896);
#102388=AXIS2_PLACEMENT_3D('',#234163,#124897,#124898);
#102389=AXIS2_PLACEMENT_3D('',#234164,#124899,#124900);
#102390=AXIS2_PLACEMENT_3D('',#234165,#124901,#124902);
#102391=AXIS2_PLACEMENT_3D('',#234166,#124903,#124904);
#102392=AXIS2_PLACEMENT_3D('',#234169,#124905,#124906);
#102393=AXIS2_PLACEMENT_3D('',#234170,#124907,#124908);
#102394=AXIS2_PLACEMENT_3D('',#234171,#124909,#124910);
#102395=AXIS2_PLACEMENT_3D('',#234172,#124911,#124912);
#102396=AXIS2_PLACEMENT_3D('',#234175,#124913,#124914);
#102397=AXIS2_PLACEMENT_3D('',#234176,#124915,#124916);
#102398=AXIS2_PLACEMENT_3D('',#234177,#124917,#124918);
#102399=AXIS2_PLACEMENT_3D('',#234178,#124919,#124920);
#102400=AXIS2_PLACEMENT_3D('',#234181,#124921,#124922);
#102401=AXIS2_PLACEMENT_3D('',#234184,#124925,#124926);
#102402=AXIS2_PLACEMENT_3D('',#234187,#124927,#124928);
#102403=AXIS2_PLACEMENT_3D('',#234188,#124929,#124930);
#102404=AXIS2_PLACEMENT_3D('',#234189,#124931,#124932);
#102405=AXIS2_PLACEMENT_3D('',#234190,#124933,#124934);
#102406=AXIS2_PLACEMENT_3D('',#234193,#124935,#124936);
#102407=AXIS2_PLACEMENT_3D('',#234196,#124939,#124940);
#102408=AXIS2_PLACEMENT_3D('',#234199,#124941,#124942);
#102409=AXIS2_PLACEMENT_3D('',#234203,#124944,#124945);
#102410=AXIS2_PLACEMENT_3D('',#234205,#124947,#124948);
#102411=AXIS2_PLACEMENT_3D('',#234208,#124949,#124950);
#102412=AXIS2_PLACEMENT_3D('',#234209,#124951,#124952);
#102413=AXIS2_PLACEMENT_3D('',#234210,#124953,#124954);
#102414=AXIS2_PLACEMENT_3D('',#234211,#124955,#124956);
#102415=AXIS2_PLACEMENT_3D('',#234214,#124957,#124958);
#102416=AXIS2_PLACEMENT_3D('',#234217,#124961,#124962);
#102417=AXIS2_PLACEMENT_3D('',#234220,#124963,#124964);
#102418=AXIS2_PLACEMENT_3D('',#234221,#124965,#124966);
#102419=AXIS2_PLACEMENT_3D('',#234222,#124967,#124968);
#102420=AXIS2_PLACEMENT_3D('',#234223,#124969,#124970);
#102421=AXIS2_PLACEMENT_3D('',#234226,#124971,#124972);
#102422=AXIS2_PLACEMENT_3D('',#234227,#124973,#124974);
#102423=AXIS2_PLACEMENT_3D('',#234228,#124975,#124976);
#102424=AXIS2_PLACEMENT_3D('',#234229,#124977,#124978);
#102425=AXIS2_PLACEMENT_3D('',#234232,#124979,#124980);
#102426=AXIS2_PLACEMENT_3D('',#234233,#124981,#124982);
#102427=AXIS2_PLACEMENT_3D('',#234234,#124983,#124984);
#102428=AXIS2_PLACEMENT_3D('',#234235,#124985,#124986);
#102429=AXIS2_PLACEMENT_3D('',#234238,#124987,#124988);
#102430=AXIS2_PLACEMENT_3D('',#234241,#124991,#124992);
#102431=AXIS2_PLACEMENT_3D('',#234244,#124993,#124994);
#102432=AXIS2_PLACEMENT_3D('',#234245,#124995,#124996);
#102433=AXIS2_PLACEMENT_3D('',#234246,#124997,#124998);
#102434=AXIS2_PLACEMENT_3D('',#234247,#124999,#125000);
#102435=AXIS2_PLACEMENT_3D('',#234250,#125001,#125002);
#102436=AXIS2_PLACEMENT_3D('',#234253,#125005,#125006);
#102437=AXIS2_PLACEMENT_3D('',#234256,#125007,#125008);
#102438=AXIS2_PLACEMENT_3D('',#234260,#125010,#125011);
#102439=AXIS2_PLACEMENT_3D('',#234262,#125013,#125014);
#102440=AXIS2_PLACEMENT_3D('',#234265,#125015,#125016);
#102441=AXIS2_PLACEMENT_3D('',#234266,#125017,#125018);
#102442=AXIS2_PLACEMENT_3D('',#234267,#125019,#125020);
#102443=AXIS2_PLACEMENT_3D('',#234268,#125021,#125022);
#102444=AXIS2_PLACEMENT_3D('',#234271,#125023,#125024);
#102445=AXIS2_PLACEMENT_3D('',#234274,#125027,#125028);
#102446=AXIS2_PLACEMENT_3D('',#234277,#125029,#125030);
#102447=AXIS2_PLACEMENT_3D('',#234278,#125031,#125032);
#102448=AXIS2_PLACEMENT_3D('',#234279,#125033,#125034);
#102449=AXIS2_PLACEMENT_3D('',#234280,#125035,#125036);
#102450=AXIS2_PLACEMENT_3D('',#234283,#125037,#125038);
#102451=AXIS2_PLACEMENT_3D('',#234286,#125041,#125042);
#102452=AXIS2_PLACEMENT_3D('',#234289,#125043,#125044);
#102453=AXIS2_PLACEMENT_3D('',#234290,#125045,#125046);
#102454=AXIS2_PLACEMENT_3D('',#234291,#125047,#125048);
#102455=AXIS2_PLACEMENT_3D('',#234292,#125049,#125050);
#102456=AXIS2_PLACEMENT_3D('',#234295,#125051,#125052);
#102457=AXIS2_PLACEMENT_3D('',#234296,#125053,#125054);
#102458=AXIS2_PLACEMENT_3D('',#234297,#125055,#125056);
#102459=AXIS2_PLACEMENT_3D('',#234298,#125057,#125058);
#102460=AXIS2_PLACEMENT_3D('',#234301,#125059,#125060);
#102461=AXIS2_PLACEMENT_3D('',#234304,#125063,#125064);
#102462=AXIS2_PLACEMENT_3D('',#234307,#125065,#125066);
#102463=AXIS2_PLACEMENT_3D('',#234308,#125067,#125068);
#102464=AXIS2_PLACEMENT_3D('',#234309,#125069,#125070);
#102465=AXIS2_PLACEMENT_3D('',#234310,#125071,#125072);
#102466=AXIS2_PLACEMENT_3D('',#234313,#125073,#125074);
#102467=AXIS2_PLACEMENT_3D('',#234316,#125077,#125078);
#102468=AXIS2_PLACEMENT_3D('',#234319,#125079,#125080);
#102469=AXIS2_PLACEMENT_3D('',#234323,#125082,#125083);
#102470=AXIS2_PLACEMENT_3D('',#234325,#125085,#125086);
#102471=AXIS2_PLACEMENT_3D('',#234328,#125087,#125088);
#102472=AXIS2_PLACEMENT_3D('',#234329,#125089,#125090);
#102473=AXIS2_PLACEMENT_3D('',#234330,#125091,#125092);
#102474=AXIS2_PLACEMENT_3D('',#234331,#125093,#125094);
#102475=AXIS2_PLACEMENT_3D('',#234334,#125095,#125096);
#102476=AXIS2_PLACEMENT_3D('',#234337,#125099,#125100);
#102477=AXIS2_PLACEMENT_3D('',#234340,#125101,#125102);
#102478=AXIS2_PLACEMENT_3D('',#234341,#125103,#125104);
#102479=AXIS2_PLACEMENT_3D('',#234342,#125105,#125106);
#102480=AXIS2_PLACEMENT_3D('',#234343,#125107,#125108);
#102481=AXIS2_PLACEMENT_3D('',#234346,#125109,#125110);
#102482=AXIS2_PLACEMENT_3D('',#234349,#125113,#125114);
#102483=AXIS2_PLACEMENT_3D('',#234352,#125115,#125116);
#102484=AXIS2_PLACEMENT_3D('',#234353,#125117,#125118);
#102485=AXIS2_PLACEMENT_3D('',#234354,#125119,#125120);
#102486=AXIS2_PLACEMENT_3D('',#234355,#125121,#125122);
#102487=AXIS2_PLACEMENT_3D('',#234358,#125123,#125124);
#102488=AXIS2_PLACEMENT_3D('',#234361,#125127,#125128);
#102489=AXIS2_PLACEMENT_3D('',#234364,#125129,#125130);
#102490=AXIS2_PLACEMENT_3D('',#234365,#125131,#125132);
#102491=AXIS2_PLACEMENT_3D('',#234366,#125133,#125134);
#102492=AXIS2_PLACEMENT_3D('',#234367,#125135,#125136);
#102493=AXIS2_PLACEMENT_3D('',#234370,#125137,#125138);
#102494=AXIS2_PLACEMENT_3D('',#234373,#125141,#125142);
#102495=AXIS2_PLACEMENT_3D('',#234389,#125144,#125145);
#102496=AXIS2_PLACEMENT_3D('',#234391,#125147,#125148);
#102497=AXIS2_PLACEMENT_3D('',#234394,#125149,#125150);
#102498=AXIS2_PLACEMENT_3D('',#234395,#125151,#125152);
#102499=AXIS2_PLACEMENT_3D('',#234396,#125153,#125154);
#102500=AXIS2_PLACEMENT_3D('',#234397,#125155,#125156);
#102501=AXIS2_PLACEMENT_3D('',#234400,#125157,#125158);
#102502=AXIS2_PLACEMENT_3D('',#234403,#125161,#125162);
#102503=AXIS2_PLACEMENT_3D('',#234406,#125163,#125164);
#102504=AXIS2_PLACEMENT_3D('',#234407,#125165,#125166);
#102505=AXIS2_PLACEMENT_3D('',#234408,#125167,#125168);
#102506=AXIS2_PLACEMENT_3D('',#234409,#125169,#125170);
#102507=AXIS2_PLACEMENT_3D('',#234412,#125171,#125172);
#102508=AXIS2_PLACEMENT_3D('',#234415,#125175,#125176);
#102509=AXIS2_PLACEMENT_3D('',#234420,#125179,#125180);
#102510=AXIS2_PLACEMENT_3D('',#234421,#125181,#125182);
#102511=AXIS2_PLACEMENT_3D('',#234426,#125185,#125186);
#102512=AXIS2_PLACEMENT_3D('',#234427,#125187,#125188);
#102513=AXIS2_PLACEMENT_3D('',#234432,#125191,#125192);
#102514=AXIS2_PLACEMENT_3D('',#234433,#125193,#125194);
#102515=AXIS2_PLACEMENT_3D('',#234438,#125197,#125198);
#102516=AXIS2_PLACEMENT_3D('',#234439,#125199,#125200);
#102517=AXIS2_PLACEMENT_3D('',#234444,#125203,#125204);
#102518=AXIS2_PLACEMENT_3D('',#234445,#125205,#125206);
#102519=AXIS2_PLACEMENT_3D('',#234450,#125209,#125210);
#102520=AXIS2_PLACEMENT_3D('',#234451,#125211,#125212);
#102521=AXIS2_PLACEMENT_3D('',#234456,#125215,#125216);
#102522=AXIS2_PLACEMENT_3D('',#234457,#125217,#125218);
#102523=AXIS2_PLACEMENT_3D('',#234462,#125221,#125222);
#102524=AXIS2_PLACEMENT_3D('',#234463,#125223,#125224);
#102525=AXIS2_PLACEMENT_3D('',#234468,#125227,#125228);
#102526=AXIS2_PLACEMENT_3D('',#234469,#125229,#125230);
#102527=AXIS2_PLACEMENT_3D('',#234474,#125233,#125234);
#102528=AXIS2_PLACEMENT_3D('',#234475,#125235,#125236);
#102529=AXIS2_PLACEMENT_3D('',#234480,#125239,#125240);
#102530=AXIS2_PLACEMENT_3D('',#234481,#125241,#125242);
#102531=AXIS2_PLACEMENT_3D('',#234486,#125245,#125246);
#102532=AXIS2_PLACEMENT_3D('',#234487,#125247,#125248);
#102533=AXIS2_PLACEMENT_3D('',#234492,#125251,#125252);
#102534=AXIS2_PLACEMENT_3D('',#234493,#125253,#125254);
#102535=AXIS2_PLACEMENT_3D('',#234498,#125257,#125258);
#102536=AXIS2_PLACEMENT_3D('',#234499,#125259,#125260);
#102537=AXIS2_PLACEMENT_3D('',#234504,#125263,#125264);
#102538=AXIS2_PLACEMENT_3D('',#234505,#125265,#125266);
#102539=AXIS2_PLACEMENT_3D('',#234510,#125269,#125270);
#102540=AXIS2_PLACEMENT_3D('',#234511,#125271,#125272);
#102541=AXIS2_PLACEMENT_3D('',#234516,#125275,#125276);
#102542=AXIS2_PLACEMENT_3D('',#234517,#125277,#125278);
#102543=AXIS2_PLACEMENT_3D('',#234522,#125281,#125282);
#102544=AXIS2_PLACEMENT_3D('',#234523,#125283,#125284);
#102545=AXIS2_PLACEMENT_3D('',#234528,#125287,#125288);
#102546=AXIS2_PLACEMENT_3D('',#234529,#125289,#125290);
#102547=AXIS2_PLACEMENT_3D('',#234534,#125293,#125294);
#102548=AXIS2_PLACEMENT_3D('',#234535,#125295,#125296);
#102549=AXIS2_PLACEMENT_3D('',#234540,#125299,#125300);
#102550=AXIS2_PLACEMENT_3D('',#234541,#125301,#125302);
#102551=AXIS2_PLACEMENT_3D('',#234546,#125305,#125306);
#102552=AXIS2_PLACEMENT_3D('',#234547,#125307,#125308);
#102553=AXIS2_PLACEMENT_3D('',#234552,#125311,#125312);
#102554=AXIS2_PLACEMENT_3D('',#234553,#125313,#125314);
#102555=AXIS2_PLACEMENT_3D('',#234558,#125317,#125318);
#102556=AXIS2_PLACEMENT_3D('',#234559,#125319,#125320);
#102557=AXIS2_PLACEMENT_3D('',#234564,#125323,#125324);
#102558=AXIS2_PLACEMENT_3D('',#234565,#125325,#125326);
#102559=AXIS2_PLACEMENT_3D('',#234570,#125329,#125330);
#102560=AXIS2_PLACEMENT_3D('',#234571,#125331,#125332);
#102561=AXIS2_PLACEMENT_3D('',#234572,#125333,#125334);
#102562=AXIS2_PLACEMENT_3D('',#234574,#125335,#125336);
#102563=AXIS2_PLACEMENT_3D('',#234578,#125339,#125340);
#102564=AXIS2_PLACEMENT_3D('',#234590,#125352,#125353);
#102565=AXIS2_PLACEMENT_3D('',#234592,#125355,#125356);
#102566=AXIS2_PLACEMENT_3D('',#234596,#125358,#125359);
#102567=AXIS2_PLACEMENT_3D('',#234598,#125361,#125362);
#102568=AXIS2_PLACEMENT_3D('',#234600,#125364,#125365);
#102569=AXIS2_PLACEMENT_3D('',#234602,#125367,#125368);
#102570=AXIS2_PLACEMENT_3D('',#234606,#125371,#125372);
#102571=AXIS2_PLACEMENT_3D('',#234608,#125374,#125375);
#102572=AXIS2_PLACEMENT_3D('',#234610,#125377,#125378);
#102573=AXIS2_PLACEMENT_3D('',#234612,#125380,#125381);
#102574=AXIS2_PLACEMENT_3D('',#234614,#125383,#125384);
#102575=AXIS2_PLACEMENT_3D('',#234616,#125386,#125387);
#102576=AXIS2_PLACEMENT_3D('',#234618,#125389,#125390);
#102577=AXIS2_PLACEMENT_3D('',#234620,#125392,#125393);
#102578=AXIS2_PLACEMENT_3D('',#234622,#125395,#125396);
#102579=AXIS2_PLACEMENT_3D('',#234624,#125398,#125399);
#102580=AXIS2_PLACEMENT_3D('',#234626,#125401,#125402);
#102581=AXIS2_PLACEMENT_3D('',#234629,#125405,#125406);
#102582=AXIS2_PLACEMENT_3D('',#234630,#125407,#125408);
#102583=AXIS2_PLACEMENT_3D('',#234631,#125409,#125410);
#102584=AXIS2_PLACEMENT_3D('',#234632,#125411,#125412);
#102585=AXIS2_PLACEMENT_3D('',#234634,#125414,#125415);
#102586=AXIS2_PLACEMENT_3D('',#234636,#125417,#125418);
#102587=AXIS2_PLACEMENT_3D('',#234639,#125421,#125422);
#102588=AXIS2_PLACEMENT_3D('',#234640,#125423,#125424);
#102589=AXIS2_PLACEMENT_3D('',#234641,#125425,#125426);
#102590=AXIS2_PLACEMENT_3D('',#234642,#125427,#125428);
#102591=AXIS2_PLACEMENT_3D('',#234644,#125430,#125431);
#102592=AXIS2_PLACEMENT_3D('',#234646,#125433,#125434);
#102593=AXIS2_PLACEMENT_3D('',#234649,#125437,#125438);
#102594=AXIS2_PLACEMENT_3D('',#234650,#125439,#125440);
#102595=AXIS2_PLACEMENT_3D('',#234651,#125441,#125442);
#102596=AXIS2_PLACEMENT_3D('',#234652,#125443,#125444);
#102597=AXIS2_PLACEMENT_3D('',#234654,#125446,#125447);
#102598=AXIS2_PLACEMENT_3D('',#234656,#125449,#125450);
#102599=AXIS2_PLACEMENT_3D('',#234659,#125453,#125454);
#102600=AXIS2_PLACEMENT_3D('',#234660,#125455,#125456);
#102601=AXIS2_PLACEMENT_3D('',#234661,#125457,#125458);
#102602=AXIS2_PLACEMENT_3D('',#234662,#125459,#125460);
#102603=AXIS2_PLACEMENT_3D('',#234664,#125462,#125463);
#102604=AXIS2_PLACEMENT_3D('',#234666,#125465,#125466);
#102605=AXIS2_PLACEMENT_3D('',#234669,#125469,#125470);
#102606=AXIS2_PLACEMENT_3D('',#234670,#125471,#125472);
#102607=AXIS2_PLACEMENT_3D('',#234672,#125474,#125475);
#102608=AXIS2_PLACEMENT_3D('',#234675,#125477,#125478);
#102609=AXIS2_PLACEMENT_3D('',#234676,#125479,#125480);
#102610=AXIS2_PLACEMENT_3D('',#234678,#125482,#125483);
#102611=AXIS2_PLACEMENT_3D('',#234681,#125485,#125486);
#102612=AXIS2_PLACEMENT_3D('',#234682,#125487,#125488);
#102613=AXIS2_PLACEMENT_3D('',#234684,#125490,#125491);
#102614=AXIS2_PLACEMENT_3D('',#234689,#125496,#125497);
#102615=AXIS2_PLACEMENT_3D('',#234691,#125499,#125500);
#102616=AXIS2_PLACEMENT_3D('',#234700,#125507,#125508);
#102617=AXIS2_PLACEMENT_3D('',#234709,#125514,#125515);
#102618=AXIS2_PLACEMENT_3D('',#234711,#125517,#125518);
#102619=AXIS2_PLACEMENT_3D('',#234712,#125519,#125520);
#102620=AXIS2_PLACEMENT_3D('',#234713,#125521,#125522);
#102621=AXIS2_PLACEMENT_3D('',#234715,#125524,#125525);
#102622=AXIS2_PLACEMENT_3D('',#234716,#125526,#125527);
#102623=AXIS2_PLACEMENT_3D('',#234718,#125529,#125530);
#102624=AXIS2_PLACEMENT_3D('',#234719,#125531,#125532);
#102625=AXIS2_PLACEMENT_3D('',#234721,#125534,#125535);
#102626=AXIS2_PLACEMENT_3D('',#234722,#125536,#125537);
#102627=AXIS2_PLACEMENT_3D('',#234724,#125539,#125540);
#102628=AXIS2_PLACEMENT_3D('',#234725,#125541,#125542);
#102629=AXIS2_PLACEMENT_3D('',#234726,#125543,#125544);
#102630=AXIS2_PLACEMENT_3D('',#234728,#125546,#125547);
#102631=AXIS2_PLACEMENT_3D('',#234729,#125548,#125549);
#102632=AXIS2_PLACEMENT_3D('',#234730,#125550,#125551);
#102633=AXIS2_PLACEMENT_3D('',#234731,#125552,#125553);
#102634=AXIS2_PLACEMENT_3D('',#234733,#125555,#125556);
#102635=AXIS2_PLACEMENT_3D('',#234734,#125557,#125558);
#102636=AXIS2_PLACEMENT_3D('',#234736,#125560,#125561);
#102637=AXIS2_PLACEMENT_3D('',#234738,#125563,#125564);
#102638=AXIS2_PLACEMENT_3D('',#234739,#125565,#125566);
#102639=AXIS2_PLACEMENT_3D('',#234740,#125567,#125568);
#102640=AXIS2_PLACEMENT_3D('',#234742,#125570,#125571);
#102641=AXIS2_PLACEMENT_3D('',#234744,#125573,#125574);
#102642=AXIS2_PLACEMENT_3D('',#234745,#125575,#125576);
#102643=AXIS2_PLACEMENT_3D('',#234746,#125577,#125578);
#102644=AXIS2_PLACEMENT_3D('',#234748,#125580,#125581);
#102645=AXIS2_PLACEMENT_3D('',#234749,#125582,#125583);
#102646=AXIS2_PLACEMENT_3D('',#234752,#125584,#125585);
#102647=AXIS2_PLACEMENT_3D('',#234754,#125586,#125587);
#102648=AXIS2_PLACEMENT_3D('',#234756,#125588,#125589);
#102649=AXIS2_PLACEMENT_3D('',#234758,#125590,#125591);
#102650=AXIS2_PLACEMENT_3D('',#234760,#125592,#125593);
#102651=AXIS2_PLACEMENT_3D('',#234761,#125594,#125595);
#102652=AXIS2_PLACEMENT_3D('',#234762,#125596,#125597);
#102653=AXIS2_PLACEMENT_3D('',#234770,#125598,#125599);
#102654=AXIS2_PLACEMENT_3D('',#234778,#125600,#125601);
#102655=AXIS2_PLACEMENT_3D('',#234786,#125602,#125603);
#102656=AXIS2_PLACEMENT_3D('',#234794,#125604,#125605);
#102657=AXIS2_PLACEMENT_3D('',#234802,#125606,#125607);
#102658=AXIS2_PLACEMENT_3D('',#234810,#125608,#125609);
#102659=AXIS2_PLACEMENT_3D('',#234813,#125610,#125611);
#102660=AXIS2_PLACEMENT_3D('',#234815,#125612,#125613);
#102661=AXIS2_PLACEMENT_3D('',#234817,#125614,#125615);
#102662=AXIS2_PLACEMENT_3D('',#234819,#125616,#125617);
#102663=AXIS2_PLACEMENT_3D('',#234821,#125618,#125619);
#102664=AXIS2_PLACEMENT_3D('',#234822,#125620,#125621);
#102665=AXIS2_PLACEMENT_3D('',#234823,#125622,#125623);
#102666=AXIS2_PLACEMENT_3D('',#234831,#125624,#125625);
#102667=AXIS2_PLACEMENT_3D('',#234839,#125626,#125627);
#102668=AXIS2_PLACEMENT_3D('',#234847,#125628,#125629);
#102669=AXIS2_PLACEMENT_3D('',#234855,#125630,#125631);
#102670=AXIS2_PLACEMENT_3D('',#234863,#125632,#125633);
#102671=AXIS2_PLACEMENT_3D('',#234871,#125634,#125635);
#102672=AXIS2_PLACEMENT_3D('',#234874,#125638,#125639);
#102673=AXIS2_PLACEMENT_3D('',#234876,#125641,#125642);
#102674=AXIS2_PLACEMENT_3D('',#234878,#125644,#125645);
#102675=AXIS2_PLACEMENT_3D('',#234880,#125647,#125648);
#102676=AXIS2_PLACEMENT_3D('',#234882,#125650,#125651);
#102677=AXIS2_PLACEMENT_3D('',#234883,#125652,#125653);
#102678=AXIS2_PLACEMENT_3D('',#234886,#125654,#125655);
#102679=AXIS2_PLACEMENT_3D('',#234888,#125656,#125657);
#102680=AXIS2_PLACEMENT_3D('',#234890,#125658,#125659);
#102681=AXIS2_PLACEMENT_3D('',#234892,#125660,#125661);
#102682=AXIS2_PLACEMENT_3D('',#234894,#125662,#125663);
#102683=AXIS2_PLACEMENT_3D('',#234895,#125664,#125665);
#102684=AXIS2_PLACEMENT_3D('',#234896,#125666,#125667);
#102685=AXIS2_PLACEMENT_3D('',#234904,#125668,#125669);
#102686=AXIS2_PLACEMENT_3D('',#234912,#125670,#125671);
#102687=AXIS2_PLACEMENT_3D('',#234920,#125672,#125673);
#102688=AXIS2_PLACEMENT_3D('',#234928,#125674,#125675);
#102689=AXIS2_PLACEMENT_3D('',#234936,#125676,#125677);
#102690=AXIS2_PLACEMENT_3D('',#234944,#125678,#125679);
#102691=AXIS2_PLACEMENT_3D('',#234947,#125680,#125681);
#102692=AXIS2_PLACEMENT_3D('',#234949,#125682,#125683);
#102693=AXIS2_PLACEMENT_3D('',#234951,#125684,#125685);
#102694=AXIS2_PLACEMENT_3D('',#234953,#125686,#125687);
#102695=AXIS2_PLACEMENT_3D('',#234955,#125688,#125689);
#102696=AXIS2_PLACEMENT_3D('',#234956,#125690,#125691);
#102697=AXIS2_PLACEMENT_3D('',#234957,#125692,#125693);
#102698=AXIS2_PLACEMENT_3D('',#234965,#125694,#125695);
#102699=AXIS2_PLACEMENT_3D('',#234973,#125696,#125697);
#102700=AXIS2_PLACEMENT_3D('',#234981,#125698,#125699);
#102701=AXIS2_PLACEMENT_3D('',#234989,#125700,#125701);
#102702=AXIS2_PLACEMENT_3D('',#234997,#125702,#125703);
#102703=AXIS2_PLACEMENT_3D('',#235005,#125704,#125705);
#102704=AXIS2_PLACEMENT_3D('',#235008,#125708,#125709);
#102705=AXIS2_PLACEMENT_3D('',#235010,#125711,#125712);
#102706=AXIS2_PLACEMENT_3D('',#235012,#125714,#125715);
#102707=AXIS2_PLACEMENT_3D('',#235014,#125717,#125718);
#102708=AXIS2_PLACEMENT_3D('',#235016,#125720,#125721);
#102709=AXIS2_PLACEMENT_3D('',#235017,#125722,#125723);
#102710=AXIS2_PLACEMENT_3D('',#235030,#125726,#125727);
#102711=AXIS2_PLACEMENT_3D('',#235040,#125729,#125730);
#102712=AXIS2_PLACEMENT_3D('',#235050,#125732,#125733);
#102713=AXIS2_PLACEMENT_3D('',#235060,#125735,#125736);
#102714=AXIS2_PLACEMENT_3D('',#235070,#125738,#125739);
#102715=AXIS2_PLACEMENT_3D('',#235077,#125740,#125741);
#102716=AXIS2_PLACEMENT_3D('',#235080,#125743,#125744);
#102717=AXIS2_PLACEMENT_3D('',#235081,#125745,#125746);
#102718=AXIS2_PLACEMENT_3D('',#235082,#125747,#125748);
#102719=AXIS2_PLACEMENT_3D('',#235083,#125749,#125750);
#102720=AXIS2_PLACEMENT_3D('',#235084,#125751,#125752);
#102721=AXIS2_PLACEMENT_3D('',#235085,#125753,#125754);
#102722=AXIS2_PLACEMENT_3D('',#235086,#125755,#125756);
#102723=AXIS2_PLACEMENT_3D('',#235087,#125757,#125758);
#102724=AXIS2_PLACEMENT_3D('',#235088,#125759,#125760);
#102725=AXIS2_PLACEMENT_3D('',#235089,#125761,#125762);
#102726=AXIS2_PLACEMENT_3D('',#235090,#125763,#125764);
#102727=AXIS2_PLACEMENT_3D('',#235091,#125765,#125766);
#102728=AXIS2_PLACEMENT_3D('',#235092,#125767,#125768);
#102729=AXIS2_PLACEMENT_3D('',#235094,#125769,#125770);
#102730=AXIS2_PLACEMENT_3D('',#235096,#125771,#125772);
#102731=AXIS2_PLACEMENT_3D('',#235098,#125773,#125774);
#102732=AXIS2_PLACEMENT_3D('',#235099,#125775,#125776);
#102733=AXIS2_PLACEMENT_3D('',#235100,#125777,#125778);
#102734=AXIS2_PLACEMENT_3D('',#235102,#125779,#125780);
#102735=AXIS2_PLACEMENT_3D('',#235103,#125781,#125782);
#102736=AXIS2_PLACEMENT_3D('',#235104,#125783,#125784);
#102737=AXIS2_PLACEMENT_3D('',#235106,#125786,#125787);
#102738=AXIS2_PLACEMENT_3D('',#235109,#125788,#125789);
#102739=AXIS2_PLACEMENT_3D('',#235111,#125790,#125791);
#102740=AXIS2_PLACEMENT_3D('',#235113,#125793,#125794);
#102741=AXIS2_PLACEMENT_3D('',#235118,#125796,#125797);
#102742=AXIS2_PLACEMENT_3D('',#235119,#125798,#125799);
#102743=AXIS2_PLACEMENT_3D('',#235120,#125800,#125801);
#102744=AXIS2_PLACEMENT_3D('',#235122,#125802,#125803);
#102745=AXIS2_PLACEMENT_3D('',#235124,#125804,#125805);
#102746=AXIS2_PLACEMENT_3D('',#235125,#125806,#125807);
#102747=AXIS2_PLACEMENT_3D('',#235126,#125808,#125809);
#102748=AXIS2_PLACEMENT_3D('',#235130,#125811,#125812);
#102749=AXIS2_PLACEMENT_3D('',#235132,#125814,#125815);
#102750=AXIS2_PLACEMENT_3D('',#235134,#125816,#125817);
#102751=AXIS2_PLACEMENT_3D('',#235135,#125818,#125819);
#102752=AXIS2_PLACEMENT_3D('',#235136,#125820,#125821);
#102753=AXIS2_PLACEMENT_3D('',#235139,#125822,#125823);
#102754=AXIS2_PLACEMENT_3D('',#235146,#125824,#125825);
#102755=AXIS2_PLACEMENT_3D('',#235147,#125826,#125827);
#102756=AXIS2_PLACEMENT_3D('',#235148,#125828,#125829);
#102757=AXIS2_PLACEMENT_3D('',#235150,#125830,#125831);
#102758=AXIS2_PLACEMENT_3D('',#235151,#125832,#125833);
#102759=AXIS2_PLACEMENT_3D('',#235152,#125834,#125835);
#102760=AXIS2_PLACEMENT_3D('',#235154,#125836,#125837);
#102761=AXIS2_PLACEMENT_3D('',#235161,#125838,#125839);
#102762=AXIS2_PLACEMENT_3D('',#235164,#125840,#125841);
#102763=AXIS2_PLACEMENT_3D('',#235172,#125842,#125843);
#102764=AXIS2_PLACEMENT_3D('',#235173,#125844,#125845);
#102765=AXIS2_PLACEMENT_3D('',#235175,#125846,#125847);
#102766=AXIS2_PLACEMENT_3D('',#235176,#125848,#125849);
#102767=AXIS2_PLACEMENT_3D('',#235177,#125850,#125851);
#102768=AXIS2_PLACEMENT_3D('',#235180,#125852,#125853);
#102769=AXIS2_PLACEMENT_3D('',#235185,#125854,#125855);
#102770=AXIS2_PLACEMENT_3D('',#235186,#125856,#125857);
#102771=AXIS2_PLACEMENT_3D('',#235189,#125858,#125859);
#102772=AXIS2_PLACEMENT_3D('',#235197,#125860,#125861);
#102773=AXIS2_PLACEMENT_3D('',#235198,#125862,#125863);
#102774=AXIS2_PLACEMENT_3D('',#235205,#125864,#125865);
#102775=AXIS2_PLACEMENT_3D('',#235206,#125866,#125867);
#102776=AXIS2_PLACEMENT_3D('',#235207,#125868,#125869);
#102777=AXIS2_PLACEMENT_3D('',#235210,#125870,#125871);
#102778=AXIS2_PLACEMENT_3D('',#235214,#125873,#125874);
#102779=AXIS2_PLACEMENT_3D('',#235216,#125876,#125877);
#102780=AXIS2_PLACEMENT_3D('',#235219,#125878,#125879);
#102781=AXIS2_PLACEMENT_3D('',#235234,#125882,#125883);
#102782=AXIS2_PLACEMENT_3D('',#235237,#125886,#125887);
#102783=AXIS2_PLACEMENT_3D('',#235240,#125890,#125891);
#102784=AXIS2_PLACEMENT_3D('',#235251,#125898,#125899);
#102785=AXIS2_PLACEMENT_3D('',#235256,#125901,#125902);
#102786=AXIS2_PLACEMENT_3D('',#235257,#125903,#125904);
#102787=AXIS2_PLACEMENT_3D('',#235258,#125905,#125906);
#102788=AXIS2_PLACEMENT_3D('',#235261,#125907,#125908);
#102789=AXIS2_PLACEMENT_3D('',#235263,#125909,#125910);
#102790=AXIS2_PLACEMENT_3D('',#235265,#125912,#125913);
#102791=AXIS2_PLACEMENT_3D('',#235268,#125914,#125915);
#102792=AXIS2_PLACEMENT_3D('',#235269,#125916,#125917);
#102793=AXIS2_PLACEMENT_3D('',#235270,#125918,#125919);
#102794=AXIS2_PLACEMENT_3D('',#235271,#125920,#125921);
#102795=AXIS2_PLACEMENT_3D('',#235274,#125922,#125923);
#102796=AXIS2_PLACEMENT_3D('',#235277,#125926,#125927);
#102797=AXIS2_PLACEMENT_3D('',#235279,#125928,#125929);
#102798=AXIS2_PLACEMENT_3D('',#235280,#125930,#125931);
#102799=AXIS2_PLACEMENT_3D('',#235281,#125932,#125933);
#102800=AXIS2_PLACEMENT_3D('',#235284,#125934,#125935);
#102801=AXIS2_PLACEMENT_3D('',#235291,#125936,#125937);
#102802=AXIS2_PLACEMENT_3D('',#235292,#125938,#125939);
#102803=AXIS2_PLACEMENT_3D('',#235293,#125940,#125941);
#102804=AXIS2_PLACEMENT_3D('',#235295,#125942,#125943);
#102805=AXIS2_PLACEMENT_3D('',#235296,#125944,#125945);
#102806=AXIS2_PLACEMENT_3D('',#235297,#125946,#125947);
#102807=AXIS2_PLACEMENT_3D('',#235305,#125948,#125949);
#102808=AXIS2_PLACEMENT_3D('',#235306,#125950,#125951);
#102809=AXIS2_PLACEMENT_3D('',#235309,#125952,#125953);
#102810=AXIS2_PLACEMENT_3D('',#235317,#125954,#125955);
#102811=AXIS2_PLACEMENT_3D('',#235318,#125956,#125957);
#102812=AXIS2_PLACEMENT_3D('',#235320,#125958,#125959);
#102813=AXIS2_PLACEMENT_3D('',#235321,#125960,#125961);
#102814=AXIS2_PLACEMENT_3D('',#235322,#125962,#125963);
#102815=AXIS2_PLACEMENT_3D('',#235329,#125964,#125965);
#102816=AXIS2_PLACEMENT_3D('',#235330,#125966,#125967);
#102817=AXIS2_PLACEMENT_3D('',#235331,#125968,#125969);
#102818=AXIS2_PLACEMENT_3D('',#235334,#125970,#125971);
#102819=AXIS2_PLACEMENT_3D('',#235342,#125972,#125973);
#102820=AXIS2_PLACEMENT_3D('',#235343,#125974,#125975);
#102821=AXIS2_PLACEMENT_3D('',#235346,#125976,#125977);
#102822=AXIS2_PLACEMENT_3D('',#235351,#125978,#125979);
#102823=AXIS2_PLACEMENT_3D('',#235352,#125980,#125981);
#102824=AXIS2_PLACEMENT_3D('',#235355,#125982,#125983);
#102825=AXIS2_PLACEMENT_3D('',#235359,#125985,#125986);
#102826=AXIS2_PLACEMENT_3D('',#235361,#125988,#125989);
#102827=AXIS2_PLACEMENT_3D('',#235364,#125990,#125991);
#102828=AXIS2_PLACEMENT_3D('',#235445,#125994,#125995);
#102829=AXIS2_PLACEMENT_3D('',#235448,#125998,#125999);
#102830=AXIS2_PLACEMENT_3D('',#235451,#126002,#126003);
#102831=AXIS2_PLACEMENT_3D('',#235454,#126006,#126007);
#102832=AXIS2_PLACEMENT_3D('',#235457,#126010,#126011);
#102833=AXIS2_PLACEMENT_3D('',#235468,#126018,#126019);
#102834=AXIS2_PLACEMENT_3D('',#235470,#126020,#126021);
#102835=AXIS2_PLACEMENT_3D('',#235503,#126023,#126024);
#102836=AXIS2_PLACEMENT_3D('',#235514,#126025,#126026);
#102837=AXIS2_PLACEMENT_3D('',#235516,#126027,#126028);
#102838=AXIS2_PLACEMENT_3D('',#235518,#126030,#126031);
#102839=AXIS2_PLACEMENT_3D('',#235521,#126032,#126033);
#102840=AXIS2_PLACEMENT_3D('',#235522,#126034,#126035);
#102841=AXIS2_PLACEMENT_3D('',#235523,#126036,#126037);
#102842=AXIS2_PLACEMENT_3D('',#235524,#126038,#126039);
#102843=AXIS2_PLACEMENT_3D('',#235527,#126042,#126043);
#102844=AXIS2_PLACEMENT_3D('',#235529,#126044,#126045);
#102845=AXIS2_PLACEMENT_3D('',#235531,#126047,#126048);
#102846=AXIS2_PLACEMENT_3D('',#235534,#126049,#126050);
#102847=AXIS2_PLACEMENT_3D('',#235535,#126051,#126052);
#102848=AXIS2_PLACEMENT_3D('',#235536,#126053,#126054);
#102849=AXIS2_PLACEMENT_3D('',#235537,#126055,#126056);
#102850=AXIS2_PLACEMENT_3D('',#235540,#126059,#126060);
#102851=AXIS2_PLACEMENT_3D('',#235542,#126061,#126062);
#102852=AXIS2_PLACEMENT_3D('',#235544,#126064,#126065);
#102853=AXIS2_PLACEMENT_3D('',#235546,#126066,#126067);
#102854=AXIS2_PLACEMENT_3D('',#235548,#126069,#126070);
#102855=AXIS2_PLACEMENT_3D('',#235551,#126072,#126073);
#102856=AXIS2_PLACEMENT_3D('',#235553,#126074,#126075);
#102857=AXIS2_PLACEMENT_3D('',#235555,#126077,#126078);
#102858=AXIS2_PLACEMENT_3D('',#235557,#126079,#126080);
#102859=AXIS2_PLACEMENT_3D('',#235590,#126082,#126083);
#102860=AXIS2_PLACEMENT_3D('',#235601,#126084,#126085);
#102861=AXIS2_PLACEMENT_3D('',#235603,#126087,#126088);
#102862=AXIS2_PLACEMENT_3D('',#235605,#126089,#126090);
#102863=AXIS2_PLACEMENT_3D('',#235607,#126092,#126093);
#102864=AXIS2_PLACEMENT_3D('',#235610,#126094,#126095);
#102865=AXIS2_PLACEMENT_3D('',#235611,#126096,#126097);
#102866=AXIS2_PLACEMENT_3D('',#235612,#126098,#126099);
#102867=AXIS2_PLACEMENT_3D('',#235613,#126100,#126101);
#102868=AXIS2_PLACEMENT_3D('',#235616,#126104,#126105);
#102869=AXIS2_PLACEMENT_3D('',#235618,#126106,#126107);
#102870=AXIS2_PLACEMENT_3D('',#235620,#126109,#126110);
#102871=AXIS2_PLACEMENT_3D('',#235623,#126111,#126112);
#102872=AXIS2_PLACEMENT_3D('',#235624,#126113,#126114);
#102873=AXIS2_PLACEMENT_3D('',#235625,#126115,#126116);
#102874=AXIS2_PLACEMENT_3D('',#235626,#126117,#126118);
#102875=AXIS2_PLACEMENT_3D('',#235629,#126121,#126122);
#102876=AXIS2_PLACEMENT_3D('',#235632,#126125,#126126);
#102877=AXIS2_PLACEMENT_3D('',#235634,#126128,#126129);
#102878=AXIS2_PLACEMENT_3D('',#235636,#126131,#126132);
#102879=AXIS2_PLACEMENT_3D('',#235637,#126133,#126134);
#102880=AXIS2_PLACEMENT_3D('',#235638,#126135,#126136);
#102881=AXIS2_PLACEMENT_3D('',#235664,#126138,#126139);
#102882=AXIS2_PLACEMENT_3D('',#235693,#126140,#126141);
#102883=AXIS2_PLACEMENT_3D('',#235769,#126143,#126144);
#102884=AXIS2_PLACEMENT_3D('',#235847,#126146,#126147);
#102885=AXIS2_PLACEMENT_3D('',#235925,#126149,#126150);
#102886=AXIS2_PLACEMENT_3D('',#236001,#126152,#126153);
#102887=AXIS2_PLACEMENT_3D('',#236077,#126155,#126156);
#102888=AXIS2_PLACEMENT_3D('',#236153,#126158,#126159);
#102889=AXIS2_PLACEMENT_3D('',#236229,#126161,#126162);
#102890=AXIS2_PLACEMENT_3D('',#236307,#126164,#126165);
#102891=AXIS2_PLACEMENT_3D('',#236385,#126167,#126168);
#102892=AXIS2_PLACEMENT_3D('',#236461,#126170,#126171);
#102893=AXIS2_PLACEMENT_3D('',#236537,#126173,#126174);
#102894=AXIS2_PLACEMENT_3D('',#236613,#126176,#126177);
#102895=AXIS2_PLACEMENT_3D('',#236689,#126179,#126180);
#102896=AXIS2_PLACEMENT_3D('',#236765,#126182,#126183);
#102897=AXIS2_PLACEMENT_3D('',#236843,#126185,#126186);
#102898=AXIS2_PLACEMENT_3D('',#236921,#126188,#126189);
#102899=AXIS2_PLACEMENT_3D('',#236997,#126191,#126192);
#102900=AXIS2_PLACEMENT_3D('',#237025,#126194,#126195);
#102901=AXIS2_PLACEMENT_3D('',#237043,#126197,#126198);
#102902=AXIS2_PLACEMENT_3D('',#237062,#126199,#126200);
#102903=AXIS2_PLACEMENT_3D('',#237138,#126202,#126203);
#102904=AXIS2_PLACEMENT_3D('',#237216,#126205,#126206);
#102905=AXIS2_PLACEMENT_3D('',#237292,#126208,#126209);
#102906=AXIS2_PLACEMENT_3D('',#237368,#126211,#126212);
#102907=AXIS2_PLACEMENT_3D('',#237444,#126214,#126215);
#102908=AXIS2_PLACEMENT_3D('',#237520,#126217,#126218);
#102909=AXIS2_PLACEMENT_3D('',#237598,#126220,#126221);
#102910=AXIS2_PLACEMENT_3D('',#237674,#126223,#126224);
#102911=AXIS2_PLACEMENT_3D('',#237752,#126226,#126227);
#102912=AXIS2_PLACEMENT_3D('',#237828,#126229,#126230);
#102913=AXIS2_PLACEMENT_3D('',#237904,#126232,#126233);
#102914=AXIS2_PLACEMENT_3D('',#237980,#126235,#126236);
#102915=AXIS2_PLACEMENT_3D('',#238056,#126238,#126239);
#102916=AXIS2_PLACEMENT_3D('',#238134,#126241,#126242);
#102917=AXIS2_PLACEMENT_3D('',#238210,#126244,#126245);
#102918=AXIS2_PLACEMENT_3D('',#238288,#126247,#126248);
#102919=AXIS2_PLACEMENT_3D('',#238364,#126250,#126251);
#102920=AXIS2_PLACEMENT_3D('',#238410,#126253,#126254);
#102921=AXIS2_PLACEMENT_3D('',#238428,#126256,#126257);
#102922=AXIS2_PLACEMENT_3D('',#238473,#126259,#126260);
#102923=AXIS2_PLACEMENT_3D('',#238503,#126262,#126263);
#102924=AXIS2_PLACEMENT_3D('',#238533,#126265,#126266);
#102925=AXIS2_PLACEMENT_3D('',#238563,#126268,#126269);
#102926=AXIS2_PLACEMENT_3D('',#238593,#126271,#126272);
#102927=AXIS2_PLACEMENT_3D('',#238623,#126274,#126275);
#102928=AXIS2_PLACEMENT_3D('',#238653,#126277,#126278);
#102929=AXIS2_PLACEMENT_3D('',#238683,#126280,#126281);
#102930=AXIS2_PLACEMENT_3D('',#238713,#126283,#126284);
#102931=AXIS2_PLACEMENT_3D('',#238743,#126286,#126287);
#102932=AXIS2_PLACEMENT_3D('',#238773,#126289,#126290);
#102933=AXIS2_PLACEMENT_3D('',#238803,#126292,#126293);
#102934=AXIS2_PLACEMENT_3D('',#238833,#126295,#126296);
#102935=AXIS2_PLACEMENT_3D('',#238863,#126298,#126299);
#102936=AXIS2_PLACEMENT_3D('',#238893,#126301,#126302);
#102937=AXIS2_PLACEMENT_3D('',#238923,#126304,#126305);
#102938=AXIS2_PLACEMENT_3D('',#238953,#126307,#126308);
#102939=AXIS2_PLACEMENT_3D('',#238958,#126310,#126311);
#102940=AXIS2_PLACEMENT_3D('',#238964,#126312,#126313);
#102941=AXIS2_PLACEMENT_3D('',#238998,#126315,#126316);
#102942=AXIS2_PLACEMENT_3D('',#239035,#126317,#126318);
#102943=AXIS2_PLACEMENT_3D('',#239111,#126320,#126321);
#102944=AXIS2_PLACEMENT_3D('',#239187,#126323,#126324);
#102945=AXIS2_PLACEMENT_3D('',#239265,#126326,#126327);
#102946=AXIS2_PLACEMENT_3D('',#239341,#126329,#126330);
#102947=AXIS2_PLACEMENT_3D('',#239417,#126332,#126333);
#102948=AXIS2_PLACEMENT_3D('',#239495,#126335,#126336);
#102949=AXIS2_PLACEMENT_3D('',#239571,#126338,#126339);
#102950=AXIS2_PLACEMENT_3D('',#239647,#126341,#126342);
#102951=AXIS2_PLACEMENT_3D('',#239723,#126344,#126345);
#102952=AXIS2_PLACEMENT_3D('',#239801,#126347,#126348);
#102953=AXIS2_PLACEMENT_3D('',#239877,#126350,#126351);
#102954=AXIS2_PLACEMENT_3D('',#239953,#126353,#126354);
#102955=AXIS2_PLACEMENT_3D('',#240031,#126356,#126357);
#102956=AXIS2_PLACEMENT_3D('',#240107,#126359,#126360);
#102957=AXIS2_PLACEMENT_3D('',#240183,#126362,#126363);
#102958=AXIS2_PLACEMENT_3D('',#240259,#126365,#126366);
#102959=AXIS2_PLACEMENT_3D('',#240309,#126368,#126369);
#102960=AXIS2_PLACEMENT_3D('',#240344,#126370,#126371);
#102961=AXIS2_PLACEMENT_3D('',#240372,#126373,#126374);
#102962=AXIS2_PLACEMENT_3D('',#240417,#126376,#126377);
#102963=AXIS2_PLACEMENT_3D('',#240447,#126379,#126380);
#102964=AXIS2_PLACEMENT_3D('',#240477,#126382,#126383);
#102965=AXIS2_PLACEMENT_3D('',#240507,#126385,#126386);
#102966=AXIS2_PLACEMENT_3D('',#240537,#126388,#126389);
#102967=AXIS2_PLACEMENT_3D('',#240567,#126391,#126392);
#102968=AXIS2_PLACEMENT_3D('',#240597,#126394,#126395);
#102969=AXIS2_PLACEMENT_3D('',#240627,#126397,#126398);
#102970=AXIS2_PLACEMENT_3D('',#240657,#126400,#126401);
#102971=AXIS2_PLACEMENT_3D('',#240687,#126403,#126404);
#102972=AXIS2_PLACEMENT_3D('',#240717,#126406,#126407);
#102973=AXIS2_PLACEMENT_3D('',#240747,#126409,#126410);
#102974=AXIS2_PLACEMENT_3D('',#240777,#126412,#126413);
#102975=AXIS2_PLACEMENT_3D('',#240807,#126415,#126416);
#102976=AXIS2_PLACEMENT_3D('',#240837,#126418,#126419);
#102977=AXIS2_PLACEMENT_3D('',#240867,#126421,#126422);
#102978=AXIS2_PLACEMENT_3D('',#240897,#126424,#126425);
#102979=AXIS2_PLACEMENT_3D('',#240902,#126427,#126428);
#102980=AXIS2_PLACEMENT_3D('',#240908,#126429,#126430);
#102981=AXIS2_PLACEMENT_3D('',#240913,#126432,#126433);
#102982=AXIS2_PLACEMENT_3D('',#240924,#126434,#126435);
#102983=AXIS2_PLACEMENT_3D('',#241002,#126437,#126438);
#102984=AXIS2_PLACEMENT_3D('',#241078,#126440,#126441);
#102985=AXIS2_PLACEMENT_3D('',#241154,#126443,#126444);
#102986=AXIS2_PLACEMENT_3D('',#241230,#126446,#126447);
#102987=AXIS2_PLACEMENT_3D('',#241306,#126449,#126450);
#102988=AXIS2_PLACEMENT_3D('',#241382,#126452,#126453);
#102989=AXIS2_PLACEMENT_3D('',#241460,#126455,#126456);
#102990=AXIS2_PLACEMENT_3D('',#241538,#126458,#126459);
#102991=AXIS2_PLACEMENT_3D('',#241614,#126461,#126462);
#102992=AXIS2_PLACEMENT_3D('',#241690,#126464,#126465);
#102993=AXIS2_PLACEMENT_3D('',#241766,#126467,#126468);
#102994=AXIS2_PLACEMENT_3D('',#241842,#126470,#126471);
#102995=AXIS2_PLACEMENT_3D('',#241918,#126473,#126474);
#102996=AXIS2_PLACEMENT_3D('',#241998,#126476,#126477);
#102997=AXIS2_PLACEMENT_3D('',#242074,#126479,#126480);
#102998=AXIS2_PLACEMENT_3D('',#242150,#126482,#126483);
#102999=AXIS2_PLACEMENT_3D('',#242226,#126485,#126486);
#103000=AXIS2_PLACEMENT_3D('',#242290,#126488,#126489);
#103001=AXIS2_PLACEMENT_3D('',#242308,#126491,#126492);
#103002=AXIS2_PLACEMENT_3D('',#242353,#126494,#126495);
#103003=AXIS2_PLACEMENT_3D('',#242383,#126497,#126498);
#103004=AXIS2_PLACEMENT_3D('',#242413,#126500,#126501);
#103005=AXIS2_PLACEMENT_3D('',#242443,#126503,#126504);
#103006=AXIS2_PLACEMENT_3D('',#242473,#126506,#126507);
#103007=AXIS2_PLACEMENT_3D('',#242503,#126509,#126510);
#103008=AXIS2_PLACEMENT_3D('',#242533,#126512,#126513);
#103009=AXIS2_PLACEMENT_3D('',#242563,#126515,#126516);
#103010=AXIS2_PLACEMENT_3D('',#242593,#126518,#126519);
#103011=AXIS2_PLACEMENT_3D('',#242623,#126521,#126522);
#103012=AXIS2_PLACEMENT_3D('',#242653,#126524,#126525);
#103013=AXIS2_PLACEMENT_3D('',#242683,#126527,#126528);
#103014=AXIS2_PLACEMENT_3D('',#242713,#126530,#126531);
#103015=AXIS2_PLACEMENT_3D('',#242743,#126533,#126534);
#103016=AXIS2_PLACEMENT_3D('',#242773,#126536,#126537);
#103017=AXIS2_PLACEMENT_3D('',#242803,#126539,#126540);
#103018=AXIS2_PLACEMENT_3D('',#242833,#126542,#126543);
#103019=AXIS2_PLACEMENT_3D('',#242838,#126545,#126546);
#103020=AXIS2_PLACEMENT_3D('',#242844,#126547,#126548);
#103021=AXIS2_PLACEMENT_3D('',#242862,#126550,#126551);
#103022=AXIS2_PLACEMENT_3D('',#242907,#126553,#126554);
#103023=AXIS2_PLACEMENT_3D('',#242937,#126556,#126557);
#103024=AXIS2_PLACEMENT_3D('',#242967,#126559,#126560);
#103025=AXIS2_PLACEMENT_3D('',#242997,#126562,#126563);
#103026=AXIS2_PLACEMENT_3D('',#243027,#126565,#126566);
#103027=AXIS2_PLACEMENT_3D('',#243057,#126568,#126569);
#103028=AXIS2_PLACEMENT_3D('',#243087,#126571,#126572);
#103029=AXIS2_PLACEMENT_3D('',#243117,#126574,#126575);
#103030=AXIS2_PLACEMENT_3D('',#243147,#126577,#126578);
#103031=AXIS2_PLACEMENT_3D('',#243177,#126580,#126581);
#103032=AXIS2_PLACEMENT_3D('',#243207,#126583,#126584);
#103033=AXIS2_PLACEMENT_3D('',#243237,#126586,#126587);
#103034=AXIS2_PLACEMENT_3D('',#243267,#126589,#126590);
#103035=AXIS2_PLACEMENT_3D('',#243297,#126592,#126593);
#103036=AXIS2_PLACEMENT_3D('',#243327,#126595,#126596);
#103037=AXIS2_PLACEMENT_3D('',#243357,#126598,#126599);
#103038=AXIS2_PLACEMENT_3D('',#243387,#126601,#126602);
#103039=AXIS2_PLACEMENT_3D('',#243392,#126604,#126605);
#103040=AXIS2_PLACEMENT_3D('',#243398,#126606,#126607);
#103041=AXIS2_PLACEMENT_3D('',#243415,#126616,#126617);
#103042=AXIS2_PLACEMENT_3D('',#243420,#126619,#126620);
#103043=AXIS2_PLACEMENT_3D('',#243424,#126623,#126624);
#103044=AXIS2_PLACEMENT_3D('',#243425,#126625,#126626);
#103045=AXIS2_PLACEMENT_3D('',#243518,#126631,#126632);
#103046=AXIS2_PLACEMENT_3D('',#243527,#126637,#126638);
#103047=AXIS2_PLACEMENT_3D('',#243533,#126642,#126643);
#103048=AXIS2_PLACEMENT_3D('',#243539,#126647,#126648);
#103049=AXIS2_PLACEMENT_3D('',#243542,#126651,#126652);
#103050=AXIS2_PLACEMENT_3D('',#243546,#126654,#126655);
#103051=AXIS2_PLACEMENT_3D('',#243552,#126658,#126659);
#103052=AXIS2_PLACEMENT_3D('',#243555,#126661,#126662);
#103053=AXIS2_PLACEMENT_3D('',#243557,#126663,#126664);
#103054=AXIS2_PLACEMENT_3D('',#243727,#126667,#126668);
#103055=AXIS2_PLACEMENT_3D('',#243832,#126671,#126672);
#103056=AXIS2_PLACEMENT_3D('',#243833,#126673,#126674);
#103057=AXIS2_PLACEMENT_3D('',#243835,#126675,#126676);
#103058=AXIS2_PLACEMENT_3D('',#243837,#126677,#126678);
#103059=AXIS2_PLACEMENT_3D('',#243838,#126679,#126680);
#103060=AXIS2_PLACEMENT_3D('',#243841,#126682,#126683);
#103061=AXIS2_PLACEMENT_3D('',#243842,#126684,#126685);
#103062=AXIS2_PLACEMENT_3D('',#243844,#126687,#126688);
#103063=AXIS2_PLACEMENT_3D('',#243845,#126689,#126690);
#103064=AXIS2_PLACEMENT_3D('',#243847,#126691,#126692);
#103065=AXIS2_PLACEMENT_3D('',#243849,#126693,#126694);
#103066=AXIS2_PLACEMENT_3D('',#243850,#126695,#126696);
#103067=AXIS2_PLACEMENT_3D('',#243853,#126698,#126699);
#103068=AXIS2_PLACEMENT_3D('',#243854,#126700,#126701);
#103069=AXIS2_PLACEMENT_3D('',#243856,#126703,#126704);
#103070=AXIS2_PLACEMENT_3D('',#243857,#126705,#126706);
#103071=AXIS2_PLACEMENT_3D('',#243859,#126707,#126708);
#103072=AXIS2_PLACEMENT_3D('',#243861,#126709,#126710);
#103073=AXIS2_PLACEMENT_3D('',#243862,#126711,#126712);
#103074=AXIS2_PLACEMENT_3D('',#243865,#126714,#126715);
#103075=AXIS2_PLACEMENT_3D('',#243866,#126716,#126717);
#103076=AXIS2_PLACEMENT_3D('',#243905,#126719,#126720);
#103077=AXIS2_PLACEMENT_3D('',#243906,#126721,#126722);
#103078=AXIS2_PLACEMENT_3D('',#243908,#126723,#126724);
#103079=AXIS2_PLACEMENT_3D('',#243910,#126725,#126726);
#103080=AXIS2_PLACEMENT_3D('',#243911,#126727,#126728);
#103081=AXIS2_PLACEMENT_3D('',#243914,#126730,#126731);
#103082=AXIS2_PLACEMENT_3D('',#243915,#126732,#126733);
#103083=AXIS2_PLACEMENT_3D('',#243917,#126734,#126735);
#103084=AXIS2_PLACEMENT_3D('',#243919,#126737,#126738);
#103085=AXIS2_PLACEMENT_3D('',#243920,#126739,#126740);
#103086=AXIS2_PLACEMENT_3D('',#243921,#126741,#126742);
#103087=AXIS2_PLACEMENT_3D('',#243923,#126743,#126744);
#103088=AXIS2_PLACEMENT_3D('',#243924,#126745,#126746);
#103089=AXIS2_PLACEMENT_3D('',#243925,#126747,#126748);
#103090=AXIS2_PLACEMENT_3D('',#243926,#126749,#126750);
#103091=AXIS2_PLACEMENT_3D('',#243928,#126751,#126752);
#103092=AXIS2_PLACEMENT_3D('',#243930,#126753,#126754);
#103093=AXIS2_PLACEMENT_3D('',#243932,#126755,#126756);
#103094=AXIS2_PLACEMENT_3D('',#243933,#126757,#126758);
#103095=AXIS2_PLACEMENT_3D('',#243934,#126759,#126760);
#103096=AXIS2_PLACEMENT_3D('',#243937,#126761,#126762);
#103097=AXIS2_PLACEMENT_3D('',#243938,#126763,#126764);
#103098=AXIS2_PLACEMENT_3D('',#243940,#126765,#126766);
#103099=AXIS2_PLACEMENT_3D('',#243942,#126767,#126768);
#103100=AXIS2_PLACEMENT_3D('',#243943,#126769,#126770);
#103101=AXIS2_PLACEMENT_3D('',#243944,#126771,#126772);
#103102=AXIS2_PLACEMENT_3D('',#243957,#126775,#126776);
#103103=AXIS2_PLACEMENT_3D('',#243967,#126778,#126779);
#103104=AXIS2_PLACEMENT_3D('',#243977,#126781,#126782);
#103105=AXIS2_PLACEMENT_3D('',#243987,#126784,#126785);
#103106=AXIS2_PLACEMENT_3D('',#243997,#126787,#126788);
#103107=AXIS2_PLACEMENT_3D('',#244004,#126789,#126790);
#103108=AXIS2_PLACEMENT_3D('',#244007,#126792,#126793);
#103109=AXIS2_PLACEMENT_3D('',#244008,#126794,#126795);
#103110=AXIS2_PLACEMENT_3D('',#244009,#126796,#126797);
#103111=AXIS2_PLACEMENT_3D('',#244010,#126798,#126799);
#103112=AXIS2_PLACEMENT_3D('',#244011,#126800,#126801);
#103113=AXIS2_PLACEMENT_3D('',#244012,#126802,#126803);
#103114=AXIS2_PLACEMENT_3D('',#244013,#126804,#126805);
#103115=AXIS2_PLACEMENT_3D('',#244014,#126806,#126807);
#103116=AXIS2_PLACEMENT_3D('',#244015,#126808,#126809);
#103117=AXIS2_PLACEMENT_3D('',#244016,#126810,#126811);
#103118=AXIS2_PLACEMENT_3D('',#244017,#126812,#126813);
#103119=AXIS2_PLACEMENT_3D('',#244018,#126814,#126815);
#103120=AXIS2_PLACEMENT_3D('',#244019,#126816,#126817);
#103121=AXIS2_PLACEMENT_3D('',#244021,#126819,#126820);
#103122=AXIS2_PLACEMENT_3D('',#244022,#126821,#126822);
#103123=AXIS2_PLACEMENT_3D('',#246035,#126824,#126825);
#103124=AXIS2_PLACEMENT_3D('',#246037,#126826,#126827);
#103125=AXIS2_PLACEMENT_3D('',#246038,#126828,#126829);
#103126=AXIS2_PLACEMENT_3D('',#246083,#126830,#126831);
#103127=AXIS2_PLACEMENT_3D('',#246250,#126832,#126833);
#103128=AXIS2_PLACEMENT_3D('',#246251,#126834,#126835);
#103129=AXIS2_PLACEMENT_3D('',#246252,#126836,#126837);
#103130=AXIS2_PLACEMENT_3D('',#246267,#126838,#126839);
#103131=AXIS2_PLACEMENT_3D('',#246329,#126840,#126841);
#103132=AXIS2_PLACEMENT_3D('',#246600,#126842,#126843);
#103133=AXIS2_PLACEMENT_3D('',#246620,#126844,#126845);
#103134=AXIS2_PLACEMENT_3D('',#246703,#126848,#126849);
#103135=AXIS2_PLACEMENT_3D('',#246723,#126850,#126851);
#103136=AXIS2_PLACEMENT_3D('',#246928,#126853,#126854);
#103137=AXIS2_PLACEMENT_3D('',#247109,#126855,#126856);
#103138=AXIS2_PLACEMENT_3D('',#247110,#126857,#126858);
#103139=AXIS2_PLACEMENT_3D('',#247113,#126859,#126860);
#103140=AXIS2_PLACEMENT_3D('',#247117,#126863,#126864);
#103141=AXIS2_PLACEMENT_3D('',#247476,#126865,#126866);
#103142=AXIS2_PLACEMENT_3D('',#247478,#126867,#126868);
#103143=AXIS2_PLACEMENT_3D('',#247485,#126869,#126870);
#103144=AXIS2_PLACEMENT_3D('',#247488,#126871,#126872);
#103145=AXIS2_PLACEMENT_3D('',#247644,#126875,#126876);
#103146=AXIS2_PLACEMENT_3D('',#247646,#126877,#126878);
#103147=AXIS2_PLACEMENT_3D('',#247647,#126879,#126880);
#103148=AXIS2_PLACEMENT_3D('',#247662,#126881,#126882);
#103149=AXIS2_PLACEMENT_3D('',#247663,#126883,#126884);
#103150=AXIS2_PLACEMENT_3D('',#247664,#126885,#126886);
#103151=AXIS2_PLACEMENT_3D('',#247665,#126887,#126888);
#103152=AXIS2_PLACEMENT_3D('',#247667,#126889,#126890);
#103153=AXIS2_PLACEMENT_3D('',#247668,#126891,#126892);
#103154=AXIS2_PLACEMENT_3D('',#247669,#126893,#126894);
#103155=AXIS2_PLACEMENT_3D('',#247672,#126895,#126896);
#103156=AXIS2_PLACEMENT_3D('',#247712,#126899,#126900);
#103157=AXIS2_PLACEMENT_3D('',#247838,#126901,#126902);
#103158=AXIS2_PLACEMENT_3D('',#247853,#126904,#126905);
#103159=AXIS2_PLACEMENT_3D('',#247855,#126906,#126907);
#103160=AXIS2_PLACEMENT_3D('',#247856,#126908,#126909);
#103161=AXIS2_PLACEMENT_3D('',#247857,#126910,#126911);
#103162=AXIS2_PLACEMENT_3D('',#247859,#126912,#126913);
#103163=AXIS2_PLACEMENT_3D('',#247860,#126914,#126915);
#103164=AXIS2_PLACEMENT_3D('',#247861,#126916,#126917);
#103165=AXIS2_PLACEMENT_3D('',#247864,#126918,#126919);
#103166=AXIS2_PLACEMENT_3D('',#247904,#126922,#126923);
#103167=AXIS2_PLACEMENT_3D('',#247961,#126924,#126925);
#103168=AXIS2_PLACEMENT_3D('',#247963,#126927,#126928);
#103169=AXIS2_PLACEMENT_3D('',#247967,#126929,#126930);
#103170=AXIS2_PLACEMENT_3D('',#247968,#126931,#126932);
#103171=AXIS2_PLACEMENT_3D('',#247969,#126933,#126934);
#103172=AXIS2_PLACEMENT_3D('',#247970,#126935,#126936);
#103173=AXIS2_PLACEMENT_3D('',#247971,#126937,#126938);
#103174=AXIS2_PLACEMENT_3D('',#247972,#126939,#126940);
#103175=AXIS2_PLACEMENT_3D('',#247977,#126942,#126943);
#103176=AXIS2_PLACEMENT_3D('',#247996,#126945,#126946);
#103177=AXIS2_PLACEMENT_3D('',#248001,#126948,#126949);
#103178=AXIS2_PLACEMENT_3D('',#248020,#126951,#126952);
#103179=AXIS2_PLACEMENT_3D('',#248025,#126954,#126955);
#103180=AXIS2_PLACEMENT_3D('',#248057,#126957,#126958);
#103181=AXIS2_PLACEMENT_3D('',#248059,#126959,#126960);
#103182=AXIS2_PLACEMENT_3D('',#248073,#126961,#126962);
#103183=AXIS2_PLACEMENT_3D('',#248078,#126964,#126965);
#103184=AXIS2_PLACEMENT_3D('',#248087,#126967,#126968);
#103185=AXIS2_PLACEMENT_3D('',#248092,#126970,#126971);
#103186=AXIS2_PLACEMENT_3D('',#248101,#126973,#126974);
#103187=AXIS2_PLACEMENT_3D('',#248126,#126976,#126977);
#103188=AXIS2_PLACEMENT_3D('',#248128,#126978,#126979);
#103189=AXIS2_PLACEMENT_3D('',#248145,#126980,#126981);
#103190=AXIS2_PLACEMENT_3D('',#248146,#126982,#126983);
#103191=AXIS2_PLACEMENT_3D('',#248147,#126984,#126985);
#103192=AXIS2_PLACEMENT_3D('',#248167,#126986,#126987);
#103193=AXIS2_PLACEMENT_3D('',#248169,#126988,#126989);
#103194=AXIS2_PLACEMENT_3D('',#248186,#126990,#126991);
#103195=AXIS2_PLACEMENT_3D('',#248205,#126993,#126994);
#103196=AXIS2_PLACEMENT_3D('',#248207,#126995,#126996);
#103197=AXIS2_PLACEMENT_3D('',#248221,#126997,#126998);
#103198=AXIS2_PLACEMENT_3D('',#248226,#127000,#127001);
#103199=AXIS2_PLACEMENT_3D('',#248235,#127003,#127004);
#103200=AXIS2_PLACEMENT_3D('',#248240,#127006,#127007);
#103201=AXIS2_PLACEMENT_3D('',#248249,#127009,#127010);
#103202=AXIS2_PLACEMENT_3D('',#248276,#127013,#127014);
#103203=AXIS2_PLACEMENT_3D('',#248278,#127015,#127016);
#103204=AXIS2_PLACEMENT_3D('',#248295,#127017,#127018);
#103205=AXIS2_PLACEMENT_3D('',#248296,#127019,#127020);
#103206=AXIS2_PLACEMENT_3D('',#248297,#127021,#127022);
#103207=AXIS2_PLACEMENT_3D('',#248317,#127023,#127024);
#103208=AXIS2_PLACEMENT_3D('',#248319,#127025,#127026);
#103209=AXIS2_PLACEMENT_3D('',#248336,#127027,#127028);
#103210=AXIS2_PLACEMENT_3D('',#248355,#127030,#127031);
#103211=AXIS2_PLACEMENT_3D('',#248357,#127032,#127033);
#103212=AXIS2_PLACEMENT_3D('',#248411,#127034,#127035);
#103213=AXIS2_PLACEMENT_3D('',#248412,#127036,#127037);
#103214=AXIS2_PLACEMENT_3D('',#248453,#127038,#127039);
#103215=AXIS2_PLACEMENT_3D('',#248454,#127040,#127041);
#103216=AXIS2_PLACEMENT_3D('',#248495,#127042,#127043);
#103217=AXIS2_PLACEMENT_3D('',#248521,#127046,#127047);
#103218=AXIS2_PLACEMENT_3D('',#248522,#127048,#127049);
#103219=AXIS2_PLACEMENT_3D('',#248548,#127052,#127053);
#103220=AXIS2_PLACEMENT_3D('',#248549,#127054,#127055);
#103221=AXIS2_PLACEMENT_3D('',#248575,#127058,#127059);
#103222=AXIS2_PLACEMENT_3D('',#248576,#127060,#127061);
#103223=AXIS2_PLACEMENT_3D('',#248602,#127064,#127065);
#103224=AXIS2_PLACEMENT_3D('',#248603,#127066,#127067);
#103225=AXIS2_PLACEMENT_3D('',#248604,#127068,#127069);
#103226=AXIS2_PLACEMENT_3D('',#248605,#127070,#127071);
#103227=AXIS2_PLACEMENT_3D('',#248619,#127072,#127073);
#103228=AXIS2_PLACEMENT_3D('',#248634,#127074,#127075);
#103229=AXIS2_PLACEMENT_3D('',#248635,#127076,#127077);
#103230=AXIS2_PLACEMENT_3D('',#248664,#127080,#127081);
#103231=AXIS2_PLACEMENT_3D('',#248665,#127082,#127083);
#103232=AXIS2_PLACEMENT_3D('',#248694,#127086,#127087);
#103233=AXIS2_PLACEMENT_3D('',#248695,#127088,#127089);
#103234=AXIS2_PLACEMENT_3D('',#248720,#127091,#127092);
#103235=AXIS2_PLACEMENT_3D('',#248738,#127093,#127094);
#103236=AXIS2_PLACEMENT_3D('',#248739,#127095,#127096);
#103237=AXIS2_PLACEMENT_3D('',#248740,#127097,#127098);
#103238=AXIS2_PLACEMENT_3D('',#248741,#127099,#127100);
#103239=AXIS2_PLACEMENT_3D('',#248761,#127101,#127102);
#103240=AXIS2_PLACEMENT_3D('',#248779,#127103,#127104);
#103241=AXIS2_PLACEMENT_3D('',#248780,#127105,#127106);
#103242=AXIS2_PLACEMENT_3D('',#248799,#127108,#127109);
#103243=AXIS2_PLACEMENT_3D('',#248814,#127110,#127111);
#103244=AXIS2_PLACEMENT_3D('',#248815,#127112,#127113);
#103245=AXIS2_PLACEMENT_3D('',#248816,#127114,#127115);
#103246=AXIS2_PLACEMENT_3D('',#248817,#127116,#127117);
#103247=AXIS2_PLACEMENT_3D('',#248831,#127118,#127119);
#103248=AXIS2_PLACEMENT_3D('',#248846,#127120,#127121);
#103249=AXIS2_PLACEMENT_3D('',#248847,#127122,#127123);
#103250=AXIS2_PLACEMENT_3D('',#248876,#127126,#127127);
#103251=AXIS2_PLACEMENT_3D('',#248877,#127128,#127129);
#103252=AXIS2_PLACEMENT_3D('',#248906,#127132,#127133);
#103253=AXIS2_PLACEMENT_3D('',#248907,#127134,#127135);
#103254=AXIS2_PLACEMENT_3D('',#248932,#127137,#127138);
#103255=AXIS2_PLACEMENT_3D('',#248950,#127139,#127140);
#103256=AXIS2_PLACEMENT_3D('',#248951,#127141,#127142);
#103257=AXIS2_PLACEMENT_3D('',#248952,#127143,#127144);
#103258=AXIS2_PLACEMENT_3D('',#248953,#127145,#127146);
#103259=AXIS2_PLACEMENT_3D('',#248973,#127147,#127148);
#103260=AXIS2_PLACEMENT_3D('',#248991,#127149,#127150);
#103261=AXIS2_PLACEMENT_3D('',#248992,#127151,#127152);
#103262=AXIS2_PLACEMENT_3D('',#249011,#127154,#127155);
#103263=AXIS2_PLACEMENT_3D('',#249026,#127156,#127157);
#103264=AXIS2_PLACEMENT_3D('',#249027,#127158,#127159);
#103265=AXIS2_PLACEMENT_3D('',#249028,#127160,#127161);
#103266=AXIS2_PLACEMENT_3D('',#249029,#127162,#127163);
#103267=AXIS2_PLACEMENT_3D('',#249030,#127164,#127165);
#103268=AXIS2_PLACEMENT_3D('',#249031,#127166,#127167);
#103269=AXIS2_PLACEMENT_3D('',#249032,#127168,#127169);
#103270=AXIS2_PLACEMENT_3D('',#249033,#127170,#127171);
#103271=AXIS2_PLACEMENT_3D('',#249034,#127172,#127173);
#103272=AXIS2_PLACEMENT_3D('',#249035,#127174,#127175);
#103273=AXIS2_PLACEMENT_3D('',#249036,#127176,#127177);
#103274=AXIS2_PLACEMENT_3D('',#249037,#127178,#127179);
#103275=AXIS2_PLACEMENT_3D('',#249038,#127180,#127181);
#103276=AXIS2_PLACEMENT_3D('',#249039,#127182,#127183);
#103277=AXIS2_PLACEMENT_3D('',#249040,#127184,#127185);
#103278=AXIS2_PLACEMENT_3D('',#249069,#127186,#127187);
#103279=AXIS2_PLACEMENT_3D('',#249070,#127188,#127189);
#103280=AXIS2_PLACEMENT_3D('',#249130,#127190,#127191);
#103281=AXIS2_PLACEMENT_3D('',#249131,#127192,#127193);
#103282=AXIS2_PLACEMENT_3D('',#249163,#127194,#127195);
#103283=AXIS2_PLACEMENT_3D('',#249166,#127197,#127198);
#103284=AXIS2_PLACEMENT_3D('',#249167,#127199,#127200);
#103285=AXIS2_PLACEMENT_3D('',#249168,#127201,#127202);
#103286=AXIS2_PLACEMENT_3D('',#249169,#127203,#127204);
#103287=AXIS2_PLACEMENT_3D('',#249170,#127205,#127206);
#103288=AXIS2_PLACEMENT_3D('',#249171,#127207,#127208);
#103289=AXIS2_PLACEMENT_3D('',#250187,#127209,#127210);
#103290=AXIS2_PLACEMENT_3D('',#251467,#127213,#127214);
#103291=AXIS2_PLACEMENT_3D('',#252037,#127217,#127218);
#103292=AXIS2_PLACEMENT_3D('',#252038,#127219,#127220);
#103293=AXIS2_PLACEMENT_3D('',#254404,#127221,#127222);
#103294=AXIS2_PLACEMENT_3D('',#255719,#127224,#127225);
#103295=AXIS2_PLACEMENT_3D('',#256139,#127228,#127229);
#103296=AXIS2_PLACEMENT_3D('',#258537,#127230,#127231);
#103297=AXIS2_PLACEMENT_3D('',#258652,#127232,#127233);
#103298=AXIS2_PLACEMENT_3D('',#259889,#127235,#127236);
#103299=AXIS2_PLACEMENT_3D('',#260277,#127239,#127240);
#103300=AXIS2_PLACEMENT_3D('',#262605,#127241,#127242);
#103301=AXIS2_PLACEMENT_3D('',#262658,#127243,#127244);
#103302=AXIS2_PLACEMENT_3D('',#263854,#127247,#127248);
#103303=AXIS2_PLACEMENT_3D('',#264398,#127251,#127252);
#103304=AXIS2_PLACEMENT_3D('',#264399,#127253,#127254);
#103305=AXIS2_PLACEMENT_3D('',#264428,#127255,#127256);
#103306=AXIS2_PLACEMENT_3D('',#266693,#127257,#127258);
#103307=AXIS2_PLACEMENT_3D('',#266694,#127259,#127260);
#103308=AXIS2_PLACEMENT_3D('',#266705,#127261,#127262);
#103309=AXIS2_PLACEMENT_3D('',#266970,#127263,#127264);
#103310=AXIS2_PLACEMENT_3D('',#271074,#127267,#127268);
#103311=AXIS2_PLACEMENT_3D('',#271075,#127269,#127270);
#103312=AXIS2_PLACEMENT_3D('',#271079,#127273,#127274);
#103313=AXIS2_PLACEMENT_3D('',#271080,#127275,#127276);
#103314=AXIS2_PLACEMENT_3D('',#271129,#127277,#127278);
#103315=AXIS2_PLACEMENT_3D('',#271178,#127279,#127280);
#103316=AXIS2_PLACEMENT_3D('',#271179,#127281,#127282);
#103317=AXIS2_PLACEMENT_3D('',#271180,#127283,#127284);
#103318=AXIS2_PLACEMENT_3D('',#271181,#127285,#127286);
#103319=AXIS2_PLACEMENT_3D('',#271182,#127287,#127288);
#103320=AXIS2_PLACEMENT_3D('',#271183,#127289,#127290);
#103321=AXIS2_PLACEMENT_3D('',#271184,#127291,#127292);
#103322=AXIS2_PLACEMENT_3D('',#271185,#127293,#127294);
#103323=AXIS2_PLACEMENT_3D('',#271186,#127295,#127296);
#103324=AXIS2_PLACEMENT_3D('',#271187,#127297,#127298);
#103325=AXIS2_PLACEMENT_3D('',#271188,#127299,#127300);
#103326=AXIS2_PLACEMENT_3D('',#271189,#127301,#127302);
#103327=AXIS2_PLACEMENT_3D('',#271190,#127303,#127304);
#103328=AXIS2_PLACEMENT_3D('',#271191,#127305,#127306);
#103329=AXIS2_PLACEMENT_3D('',#271192,#127307,#127308);
#103330=AXIS2_PLACEMENT_3D('',#271193,#127309,#127310);
#103331=AXIS2_PLACEMENT_3D('',#271194,#127311,#127312);
#103332=AXIS2_PLACEMENT_3D('',#271195,#127313,#127314);
#103333=AXIS2_PLACEMENT_3D('',#271196,#127315,#127316);
#103334=AXIS2_PLACEMENT_3D('',#271205,#127321,#127322);
#103335=AXIS2_PLACEMENT_3D('',#271211,#127326,#127327);
#103336=AXIS2_PLACEMENT_3D('',#271217,#127331,#127332);
#103337=AXIS2_PLACEMENT_3D('',#271220,#127335,#127336);
#103338=AXIS2_PLACEMENT_3D('',#271221,#127337,#127338);
#103339=AXIS2_PLACEMENT_3D('',#271222,#127339,#127340);
#103340=AXIS2_PLACEMENT_3D('',#271223,#127341,#127342);
#103341=AXIS2_PLACEMENT_3D('',#271224,#127343,#127344);
#103342=AXIS2_PLACEMENT_3D('',#271226,#127345,#127346);
#103343=AXIS2_PLACEMENT_3D('',#271228,#127347,#127348);
#103344=AXIS2_PLACEMENT_3D('',#271229,#127349,#127350);
#103345=AXIS2_PLACEMENT_3D('',#271230,#127351,#127352);
#103346=AXIS2_PLACEMENT_3D('',#271233,#127354,#127355);
#103347=AXIS2_PLACEMENT_3D('',#271234,#127356,#127357);
#103348=AXIS2_PLACEMENT_3D('',#271255,#127360,#127361);
#103349=AXIS2_PLACEMENT_3D('',#271272,#127363,#127364);
#103350=AXIS2_PLACEMENT_3D('',#271289,#127366,#127367);
#103351=AXIS2_PLACEMENT_3D('',#271290,#127368,#127369);
#103352=AXIS2_PLACEMENT_3D('',#271293,#127370,#127371);
#103353=AXIS2_PLACEMENT_3D('',#271309,#127373,#127374);
#103354=AXIS2_PLACEMENT_3D('',#271325,#127376,#127377);
#103355=AXIS2_PLACEMENT_3D('',#271328,#127378,#127379);
#103356=AXIS2_PLACEMENT_3D('',#271344,#127381,#127382);
#103357=AXIS2_PLACEMENT_3D('',#271360,#127384,#127385);
#103358=AXIS2_PLACEMENT_3D('',#271370,#127386,#127387);
#103359=AXIS2_PLACEMENT_3D('',#271386,#127389,#127390);
#103360=AXIS2_PLACEMENT_3D('',#271395,#127392,#127393);
#103361=AXIS2_PLACEMENT_3D('',#271398,#127394,#127395);
#103362=AXIS2_PLACEMENT_3D('',#271414,#127397,#127398);
#103363=AXIS2_PLACEMENT_3D('',#271430,#127400,#127401);
#103364=AXIS2_PLACEMENT_3D('',#271433,#127402,#127403);
#103365=AXIS2_PLACEMENT_3D('',#271449,#127405,#127406);
#103366=AXIS2_PLACEMENT_3D('',#271465,#127408,#127409);
#103367=AXIS2_PLACEMENT_3D('',#271486,#127412,#127413);
#103368=AXIS2_PLACEMENT_3D('',#271489,#127414,#127415);
#103369=AXIS2_PLACEMENT_3D('',#271493,#127417,#127418);
#103370=AXIS2_PLACEMENT_3D('',#271495,#127420,#127421);
#103371=AXIS2_PLACEMENT_3D('',#271498,#127422,#127423);
#103372=AXIS2_PLACEMENT_3D('',#271500,#127424,#127425);
#103373=AXIS2_PLACEMENT_3D('',#271502,#127426,#127427);
#103374=AXIS2_PLACEMENT_3D('',#271504,#127428,#127429);
#103375=AXIS2_PLACEMENT_3D('',#271506,#127430,#127431);
#103376=AXIS2_PLACEMENT_3D('',#271508,#127432,#127433);
#103377=AXIS2_PLACEMENT_3D('',#271510,#127434,#127435);
#103378=AXIS2_PLACEMENT_3D('',#271512,#127436,#127437);
#103379=AXIS2_PLACEMENT_3D('',#271514,#127438,#127439);
#103380=AXIS2_PLACEMENT_3D('',#271515,#127440,#127441);
#103381=AXIS2_PLACEMENT_3D('',#271516,#127442,#127443);
#103382=AXIS2_PLACEMENT_3D('',#271517,#127444,#127445);
#103383=AXIS2_PLACEMENT_3D('',#271518,#127446,#127447);
#103384=AXIS2_PLACEMENT_3D('',#271519,#127448,#127449);
#103385=AXIS2_PLACEMENT_3D('',#271520,#127450,#127451);
#103386=AXIS2_PLACEMENT_3D('',#271522,#127452,#127453);
#103387=AXIS2_PLACEMENT_3D('',#271524,#127454,#127455);
#103388=AXIS2_PLACEMENT_3D('',#271526,#127456,#127457);
#103389=AXIS2_PLACEMENT_3D('',#271528,#127458,#127459);
#103390=AXIS2_PLACEMENT_3D('',#271530,#127460,#127461);
#103391=AXIS2_PLACEMENT_3D('',#271532,#127462,#127463);
#103392=AXIS2_PLACEMENT_3D('',#271534,#127464,#127465);
#103393=AXIS2_PLACEMENT_3D('',#271536,#127466,#127467);
#103394=AXIS2_PLACEMENT_3D('',#271537,#127468,#127469);
#103395=AXIS2_PLACEMENT_3D('',#271543,#127473,#127474);
#103396=AXIS2_PLACEMENT_3D('',#271549,#127478,#127479);
#103397=AXIS2_PLACEMENT_3D('',#271561,#127480,#127481);
#103398=AXIS2_PLACEMENT_3D('',#271581,#127482,#127483);
#103399=AXIS2_PLACEMENT_3D('',#271606,#127484,#127485);
#103400=AXIS2_PLACEMENT_3D('',#271613,#127486,#127487);
#103401=AXIS2_PLACEMENT_3D('',#271638,#127488,#127489);
#103402=AXIS2_PLACEMENT_3D('',#271645,#127490,#127491);
#103403=AXIS2_PLACEMENT_3D('',#271670,#127492,#127493);
#103404=AXIS2_PLACEMENT_3D('',#271677,#127494,#127495);
#103405=AXIS2_PLACEMENT_3D('',#271679,#127496,#127497);
#103406=AXIS2_PLACEMENT_3D('',#271699,#127498,#127499);
#103407=AXIS2_PLACEMENT_3D('',#271724,#127500,#127501);
#103408=AXIS2_PLACEMENT_3D('',#271731,#127502,#127503);
#103409=AXIS2_PLACEMENT_3D('',#271743,#127504,#127505);
#103410=AXIS2_PLACEMENT_3D('',#271763,#127506,#127507);
#103411=AXIS2_PLACEMENT_3D('',#271774,#127508,#127509);
#103412=AXIS2_PLACEMENT_3D('',#271781,#127510,#127511);
#103413=AXIS2_PLACEMENT_3D('',#271799,#127512,#127513);
#103414=AXIS2_PLACEMENT_3D('',#271806,#127514,#127515);
#103415=AXIS2_PLACEMENT_3D('',#271817,#127516,#127517);
#103416=AXIS2_PLACEMENT_3D('',#271824,#127518,#127519);
#103417=AXIS2_PLACEMENT_3D('',#271835,#127520,#127521);
#103418=AXIS2_PLACEMENT_3D('',#271842,#127522,#127523);
#103419=AXIS2_PLACEMENT_3D('',#271853,#127524,#127525);
#103420=AXIS2_PLACEMENT_3D('',#271860,#127526,#127527);
#103421=AXIS2_PLACEMENT_3D('',#271871,#127528,#127529);
#103422=AXIS2_PLACEMENT_3D('',#271885,#127530,#127531);
#103423=AXIS2_PLACEMENT_3D('',#271896,#127532,#127533);
#103424=AXIS2_PLACEMENT_3D('',#271903,#127534,#127535);
#103425=AXIS2_PLACEMENT_3D('',#271907,#127537,#127538);
#103426=AXIS2_PLACEMENT_3D('',#271909,#127540,#127541);
#103427=AXIS2_PLACEMENT_3D('',#271914,#127544,#127545);
#103428=AXIS2_PLACEMENT_3D('',#271915,#127546,#127547);
#103429=AXIS2_PLACEMENT_3D('',#271920,#127550,#127551);
#103430=AXIS2_PLACEMENT_3D('',#271921,#127552,#127553);
#103431=AXIS2_PLACEMENT_3D('',#271926,#127556,#127557);
#103432=AXIS2_PLACEMENT_3D('',#271927,#127558,#127559);
#103433=AXIS2_PLACEMENT_3D('',#271929,#127560,#127561);
#103434=AXIS2_PLACEMENT_3D('',#271931,#127563,#127564);
#103435=AXIS2_PLACEMENT_3D('',#271936,#127567,#127568);
#103436=AXIS2_PLACEMENT_3D('',#271937,#127569,#127570);
#103437=AXIS2_PLACEMENT_3D('',#271941,#127572,#127573);
#103438=AXIS2_PLACEMENT_3D('',#271943,#127575,#127576);
#103439=AXIS2_PLACEMENT_3D('',#271947,#127578,#127579);
#103440=AXIS2_PLACEMENT_3D('',#271949,#127581,#127582);
#103441=AXIS2_PLACEMENT_3D('',#271954,#127585,#127586);
#103442=AXIS2_PLACEMENT_3D('',#271955,#127587,#127588);
#103443=AXIS2_PLACEMENT_3D('',#271959,#127590,#127591);
#103444=AXIS2_PLACEMENT_3D('',#271961,#127593,#127594);
#103445=AXIS2_PLACEMENT_3D('',#271965,#127596,#127597);
#103446=AXIS2_PLACEMENT_3D('',#271967,#127599,#127600);
#103447=AXIS2_PLACEMENT_3D('',#271972,#127603,#127604);
#103448=AXIS2_PLACEMENT_3D('',#271973,#127605,#127606);
#103449=AXIS2_PLACEMENT_3D('',#271977,#127608,#127609);
#103450=AXIS2_PLACEMENT_3D('',#271979,#127611,#127612);
#103451=AXIS2_PLACEMENT_3D('',#271984,#127615,#127616);
#103452=AXIS2_PLACEMENT_3D('',#271985,#127617,#127618);
#103453=AXIS2_PLACEMENT_3D('',#272001,#127619,#127620);
#103454=AXIS2_PLACEMENT_3D('',#272015,#127621,#127622);
#103455=AXIS2_PLACEMENT_3D('',#272044,#127623,#127624);
#103456=AXIS2_PLACEMENT_3D('',#272045,#127625,#127626);
#103457=AXIS2_PLACEMENT_3D('',#272074,#127627,#127628);
#103458=AXIS2_PLACEMENT_3D('',#272075,#127629,#127630);
#103459=AXIS2_PLACEMENT_3D('',#272104,#127631,#127632);
#103460=AXIS2_PLACEMENT_3D('',#272105,#127633,#127634);
#103461=AXIS2_PLACEMENT_3D('',#272114,#127635,#127636);
#103462=AXIS2_PLACEMENT_3D('',#272128,#127637,#127638);
#103463=AXIS2_PLACEMENT_3D('',#272157,#127639,#127640);
#103464=AXIS2_PLACEMENT_3D('',#272158,#127641,#127642);
#103465=AXIS2_PLACEMENT_3D('',#272174,#127643,#127644);
#103466=AXIS2_PLACEMENT_3D('',#272188,#127645,#127646);
#103467=AXIS2_PLACEMENT_3D('',#272195,#127647,#127648);
#103468=AXIS2_PLACEMENT_3D('',#272204,#127649,#127650);
#103469=AXIS2_PLACEMENT_3D('',#272227,#127651,#127652);
#103470=AXIS2_PLACEMENT_3D('',#272228,#127653,#127654);
#103471=AXIS2_PLACEMENT_3D('',#272235,#127655,#127656);
#103472=AXIS2_PLACEMENT_3D('',#272244,#127657,#127658);
#103473=AXIS2_PLACEMENT_3D('',#272251,#127659,#127660);
#103474=AXIS2_PLACEMENT_3D('',#272260,#127661,#127662);
#103475=AXIS2_PLACEMENT_3D('',#272275,#127663,#127664);
#103476=AXIS2_PLACEMENT_3D('',#272276,#127665,#127666);
#103477=AXIS2_PLACEMENT_3D('',#272284,#127667,#127668);
#103478=AXIS2_PLACEMENT_3D('',#272298,#127669,#127670);
#103479=AXIS2_PLACEMENT_3D('',#272313,#127671,#127672);
#103480=AXIS2_PLACEMENT_3D('',#272314,#127673,#127674);
#103481=AXIS2_PLACEMENT_3D('',#272337,#127675,#127676);
#103482=AXIS2_PLACEMENT_3D('',#272338,#127677,#127678);
#103483=AXIS2_PLACEMENT_3D('',#272341,#127680,#127681);
#103484=AXIS2_PLACEMENT_3D('',#272342,#127682,#127683);
#103485=AXIS2_PLACEMENT_3D('',#272362,#127684,#127685);
#103486=AXIS2_PLACEMENT_3D('',#272363,#127686,#127687);
#103487=AXIS2_PLACEMENT_3D('',#272364,#127688,#127689);
#103488=AXIS2_PLACEMENT_3D('',#272365,#127690,#127691);
#103489=AXIS2_PLACEMENT_3D('',#272366,#127692,#127693);
#103490=AXIS2_PLACEMENT_3D('',#272367,#127694,#127695);
#103491=AXIS2_PLACEMENT_3D('',#272368,#127696,#127697);
#103492=AXIS2_PLACEMENT_3D('',#272369,#127698,#127699);
#103493=AXIS2_PLACEMENT_3D('',#272370,#127700,#127701);
#103494=AXIS2_PLACEMENT_3D('',#272371,#127702,#127703);
#103495=AXIS2_PLACEMENT_3D('',#272372,#127704,#127705);
#103496=AXIS2_PLACEMENT_3D('',#272373,#127706,#127707);
#103497=AXIS2_PLACEMENT_3D('',#272375,#127709,#127710);
#103498=AXIS2_PLACEMENT_3D('',#272377,#127712,#127713);
#103499=AXIS2_PLACEMENT_3D('',#272378,#127714,#127715);
#103500=AXIS2_PLACEMENT_3D('',#272380,#127717,#127718);
#103501=AXIS2_PLACEMENT_3D('',#272381,#127719,#127720);
#103502=AXIS2_PLACEMENT_3D('',#272382,#127721,#127722);
#103503=AXIS2_PLACEMENT_3D('',#272383,#127723,#127724);
#103504=AXIS2_PLACEMENT_3D('',#272384,#127725,#127726);
#103505=AXIS2_PLACEMENT_3D('',#272385,#127727,#127728);
#103506=AXIS2_PLACEMENT_3D('',#272386,#127729,#127730);
#103507=AXIS2_PLACEMENT_3D('',#272387,#127731,#127732);
#103508=AXIS2_PLACEMENT_3D('',#272388,#127733,#127734);
#103509=AXIS2_PLACEMENT_3D('',#272389,#127735,#127736);
#103510=AXIS2_PLACEMENT_3D('',#272391,#127738,#127739);
#103511=AXIS2_PLACEMENT_3D('',#272393,#127741,#127742);
#103512=AXIS2_PLACEMENT_3D('',#272394,#127743,#127744);
#103513=AXIS2_PLACEMENT_3D('',#272395,#127745,#127746);
#103514=AXIS2_PLACEMENT_3D('',#272396,#127747,#127748);
#103515=AXIS2_PLACEMENT_3D('',#272397,#127749,#127750);
#103516=AXIS2_PLACEMENT_3D('',#272398,#127751,#127752);
#103517=AXIS2_PLACEMENT_3D('',#272400,#127754,#127755);
#103518=AXIS2_PLACEMENT_3D('',#272402,#127757,#127758);
#103519=AXIS2_PLACEMENT_3D('',#272403,#127759,#127760);
#103520=AXIS2_PLACEMENT_3D('',#272405,#127762,#127763);
#103521=AXIS2_PLACEMENT_3D('',#272407,#127765,#127766);
#103522=AXIS2_PLACEMENT_3D('',#272408,#127767,#127768);
#103523=AXIS2_PLACEMENT_3D('',#272410,#127770,#127771);
#103524=AXIS2_PLACEMENT_3D('',#272411,#127772,#127773);
#103525=AXIS2_PLACEMENT_3D('',#272413,#127775,#127776);
#103526=AXIS2_PLACEMENT_3D('',#272415,#127778,#127779);
#103527=AXIS2_PLACEMENT_3D('',#272416,#127780,#127781);
#103528=AXIS2_PLACEMENT_3D('',#272418,#127783,#127784);
#103529=AXIS2_PLACEMENT_3D('',#272420,#127786,#127787);
#103530=AXIS2_PLACEMENT_3D('',#272421,#127788,#127789);
#103531=AXIS2_PLACEMENT_3D('',#272423,#127791,#127792);
#103532=AXIS2_PLACEMENT_3D('',#272425,#127794,#127795);
#103533=AXIS2_PLACEMENT_3D('',#272426,#127796,#127797);
#103534=AXIS2_PLACEMENT_3D('',#272429,#127800,#127801);
#103535=AXIS2_PLACEMENT_3D('',#272430,#127802,#127803);
#103536=AXIS2_PLACEMENT_3D('',#272431,#127804,#127805);
#103537=AXIS2_PLACEMENT_3D('',#272433,#127806,#127807);
#103538=AXIS2_PLACEMENT_3D('',#272436,#127809,#127810);
#103539=AXIS2_PLACEMENT_3D('',#272437,#127811,#127812);
#103540=AXIS2_PLACEMENT_3D('',#272440,#127813,#127814);
#103541=AXIS2_PLACEMENT_3D('',#272444,#127816,#127817);
#103542=AXIS2_PLACEMENT_3D('',#272446,#127819,#127820);
#103543=AXIS2_PLACEMENT_3D('',#272452,#127824,#127825);
#103544=AXIS2_PLACEMENT_3D('',#272458,#127829,#127830);
#103545=AXIS2_PLACEMENT_3D('',#272461,#127833,#127834);
#103546=AXIS2_PLACEMENT_3D('',#272462,#127835,#127836);
#103547=AXIS2_PLACEMENT_3D('',#272463,#127837,#127838);
#103548=AXIS2_PLACEMENT_3D('',#272464,#127839,#127840);
#103549=AXIS2_PLACEMENT_3D('',#272466,#127841,#127842);
#103550=AXIS2_PLACEMENT_3D('',#272468,#127843,#127844);
#103551=AXIS2_PLACEMENT_3D('',#272469,#127845,#127846);
#103552=AXIS2_PLACEMENT_3D('',#272470,#127847,#127848);
#103553=AXIS2_PLACEMENT_3D('',#272473,#127850,#127851);
#103554=AXIS2_PLACEMENT_3D('',#272474,#127852,#127853);
#103555=AXIS2_PLACEMENT_3D('',#272495,#127856,#127857);
#103556=AXIS2_PLACEMENT_3D('',#272516,#127860,#127861);
#103557=AXIS2_PLACEMENT_3D('',#272519,#127862,#127863);
#103558=AXIS2_PLACEMENT_3D('',#272539,#127865,#127866);
#103559=AXIS2_PLACEMENT_3D('',#272559,#127868,#127869);
#103560=AXIS2_PLACEMENT_3D('',#272562,#127870,#127871);
#103561=AXIS2_PLACEMENT_3D('',#272582,#127873,#127874);
#103562=AXIS2_PLACEMENT_3D('',#272602,#127876,#127877);
#103563=AXIS2_PLACEMENT_3D('',#272605,#127878,#127879);
#103564=AXIS2_PLACEMENT_3D('',#272625,#127881,#127882);
#103565=AXIS2_PLACEMENT_3D('',#272645,#127884,#127885);
#103566=AXIS2_PLACEMENT_3D('',#272648,#127886,#127887);
#103567=AXIS2_PLACEMENT_3D('',#272668,#127889,#127890);
#103568=AXIS2_PLACEMENT_3D('',#272688,#127892,#127893);
#103569=AXIS2_PLACEMENT_3D('',#272705,#127895,#127896);
#103570=AXIS2_PLACEMENT_3D('',#272726,#127898,#127899);
#103571=AXIS2_PLACEMENT_3D('',#272727,#127900,#127901);
#103572=AXIS2_PLACEMENT_3D('',#272744,#127903,#127904);
#103573=AXIS2_PLACEMENT_3D('',#272765,#127906,#127907);
#103574=AXIS2_PLACEMENT_3D('',#272766,#127908,#127909);
#103575=AXIS2_PLACEMENT_3D('',#272776,#127910,#127911);
#103576=AXIS2_PLACEMENT_3D('',#272796,#127913,#127914);
#103577=AXIS2_PLACEMENT_3D('',#272805,#127916,#127917);
#103578=AXIS2_PLACEMENT_3D('',#272808,#127918,#127919);
#103579=AXIS2_PLACEMENT_3D('',#272828,#127921,#127922);
#103580=AXIS2_PLACEMENT_3D('',#272848,#127924,#127925);
#103581=AXIS2_PLACEMENT_3D('',#272858,#127926,#127927);
#103582=AXIS2_PLACEMENT_3D('',#272878,#127929,#127930);
#103583=AXIS2_PLACEMENT_3D('',#272887,#127932,#127933);
#103584=AXIS2_PLACEMENT_3D('',#272890,#127934,#127935);
#103585=AXIS2_PLACEMENT_3D('',#272910,#127937,#127938);
#103586=AXIS2_PLACEMENT_3D('',#272930,#127940,#127941);
#103587=AXIS2_PLACEMENT_3D('',#272933,#127942,#127943);
#103588=AXIS2_PLACEMENT_3D('',#272953,#127945,#127946);
#103589=AXIS2_PLACEMENT_3D('',#272973,#127948,#127949);
#103590=AXIS2_PLACEMENT_3D('',#272976,#127950,#127951);
#103591=AXIS2_PLACEMENT_3D('',#272996,#127953,#127954);
#103592=AXIS2_PLACEMENT_3D('',#273016,#127956,#127957);
#103593=AXIS2_PLACEMENT_3D('',#273019,#127958,#127959);
#103594=AXIS2_PLACEMENT_3D('',#273039,#127960,#127961);
#103595=AXIS2_PLACEMENT_3D('',#273053,#127962,#127963);
#103596=AXIS2_PLACEMENT_3D('',#273056,#127964,#127965);
#103597=AXIS2_PLACEMENT_3D('',#273059,#127968,#127969);
#103598=AXIS2_PLACEMENT_3D('',#273062,#127970,#127971);
#103599=AXIS2_PLACEMENT_3D('',#273095,#127972,#127973);
#103600=AXIS2_PLACEMENT_3D('',#273098,#127974,#127975);
#103601=AXIS2_PLACEMENT_3D('',#273102,#127977,#127978);
#103602=AXIS2_PLACEMENT_3D('',#273104,#127980,#127981);
#103603=AXIS2_PLACEMENT_3D('',#273106,#127982,#127983);
#103604=AXIS2_PLACEMENT_3D('',#273108,#127984,#127985);
#103605=AXIS2_PLACEMENT_3D('',#273110,#127986,#127987);
#103606=AXIS2_PLACEMENT_3D('',#273112,#127988,#127989);
#103607=AXIS2_PLACEMENT_3D('',#273114,#127990,#127991);
#103608=AXIS2_PLACEMENT_3D('',#273116,#127992,#127993);
#103609=AXIS2_PLACEMENT_3D('',#273118,#127994,#127995);
#103610=AXIS2_PLACEMENT_3D('',#273120,#127996,#127997);
#103611=AXIS2_PLACEMENT_3D('',#273122,#127998,#127999);
#103612=AXIS2_PLACEMENT_3D('',#273124,#128000,#128001);
#103613=AXIS2_PLACEMENT_3D('',#273126,#128002,#128003);
#103614=AXIS2_PLACEMENT_3D('',#273128,#128004,#128005);
#103615=AXIS2_PLACEMENT_3D('',#273130,#128006,#128007);
#103616=AXIS2_PLACEMENT_3D('',#273132,#128008,#128009);
#103617=AXIS2_PLACEMENT_3D('',#273134,#128010,#128011);
#103618=AXIS2_PLACEMENT_3D('',#273136,#128012,#128013);
#103619=AXIS2_PLACEMENT_3D('',#273138,#128014,#128015);
#103620=AXIS2_PLACEMENT_3D('',#273139,#128016,#128017);
#103621=AXIS2_PLACEMENT_3D('',#273140,#128018,#128019);
#103622=AXIS2_PLACEMENT_3D('',#273141,#128020,#128021);
#103623=AXIS2_PLACEMENT_3D('',#273142,#128022,#128023);
#103624=AXIS2_PLACEMENT_3D('',#273143,#128024,#128025);
#103625=AXIS2_PLACEMENT_3D('',#273144,#128026,#128027);
#103626=AXIS2_PLACEMENT_3D('',#273145,#128028,#128029);
#103627=AXIS2_PLACEMENT_3D('',#273146,#128030,#128031);
#103628=AXIS2_PLACEMENT_3D('',#273147,#128032,#128033);
#103629=AXIS2_PLACEMENT_3D('',#273148,#128034,#128035);
#103630=AXIS2_PLACEMENT_3D('',#273149,#128036,#128037);
#103631=AXIS2_PLACEMENT_3D('',#273150,#128038,#128039);
#103632=AXIS2_PLACEMENT_3D('',#273152,#128040,#128041);
#103633=AXIS2_PLACEMENT_3D('',#273154,#128042,#128043);
#103634=AXIS2_PLACEMENT_3D('',#273156,#128044,#128045);
#103635=AXIS2_PLACEMENT_3D('',#273158,#128046,#128047);
#103636=AXIS2_PLACEMENT_3D('',#273160,#128048,#128049);
#103637=AXIS2_PLACEMENT_3D('',#273162,#128050,#128051);
#103638=AXIS2_PLACEMENT_3D('',#273164,#128052,#128053);
#103639=AXIS2_PLACEMENT_3D('',#273166,#128054,#128055);
#103640=AXIS2_PLACEMENT_3D('',#273168,#128056,#128057);
#103641=AXIS2_PLACEMENT_3D('',#273170,#128058,#128059);
#103642=AXIS2_PLACEMENT_3D('',#273172,#128060,#128061);
#103643=AXIS2_PLACEMENT_3D('',#273174,#128062,#128063);
#103644=AXIS2_PLACEMENT_3D('',#273176,#128064,#128065);
#103645=AXIS2_PLACEMENT_3D('',#273178,#128066,#128067);
#103646=AXIS2_PLACEMENT_3D('',#273180,#128068,#128069);
#103647=AXIS2_PLACEMENT_3D('',#273182,#128070,#128071);
#103648=AXIS2_PLACEMENT_3D('',#273184,#128072,#128073);
#103649=AXIS2_PLACEMENT_3D('',#273185,#128074,#128075);
#103650=AXIS2_PLACEMENT_3D('',#273191,#128079,#128080);
#103651=AXIS2_PLACEMENT_3D('',#273197,#128084,#128085);
#103652=AXIS2_PLACEMENT_3D('',#273209,#128086,#128087);
#103653=AXIS2_PLACEMENT_3D('',#273233,#128088,#128089);
#103654=AXIS2_PLACEMENT_3D('',#273262,#128090,#128091);
#103655=AXIS2_PLACEMENT_3D('',#273269,#128092,#128093);
#103656=AXIS2_PLACEMENT_3D('',#273298,#128094,#128095);
#103657=AXIS2_PLACEMENT_3D('',#273305,#128096,#128097);
#103658=AXIS2_PLACEMENT_3D('',#273334,#128098,#128099);
#103659=AXIS2_PLACEMENT_3D('',#273341,#128100,#128101);
#103660=AXIS2_PLACEMENT_3D('',#273353,#128102,#128103);
#103661=AXIS2_PLACEMENT_3D('',#273377,#128104,#128105);
#103662=AXIS2_PLACEMENT_3D('',#273404,#128106,#128107);
#103663=AXIS2_PLACEMENT_3D('',#273405,#128108,#128109);
#103664=AXIS2_PLACEMENT_3D('',#273434,#128110,#128111);
#103665=AXIS2_PLACEMENT_3D('',#273441,#128112,#128113);
#103666=AXIS2_PLACEMENT_3D('',#273453,#128114,#128115);
#103667=AXIS2_PLACEMENT_3D('',#273477,#128116,#128117);
#103668=AXIS2_PLACEMENT_3D('',#273506,#128118,#128119);
#103669=AXIS2_PLACEMENT_3D('',#273513,#128120,#128121);
#103670=AXIS2_PLACEMENT_3D('',#273532,#128122,#128123);
#103671=AXIS2_PLACEMENT_3D('',#273539,#128124,#128125);
#103672=AXIS2_PLACEMENT_3D('',#273551,#128126,#128127);
#103673=AXIS2_PLACEMENT_3D('',#273575,#128128,#128129);
#103674=AXIS2_PLACEMENT_3D('',#273604,#128130,#128131);
#103675=AXIS2_PLACEMENT_3D('',#273611,#128132,#128133);
#103676=AXIS2_PLACEMENT_3D('',#273623,#128134,#128135);
#103677=AXIS2_PLACEMENT_3D('',#273647,#128136,#128137);
#103678=AXIS2_PLACEMENT_3D('',#273676,#128138,#128139);
#103679=AXIS2_PLACEMENT_3D('',#273683,#128140,#128141);
#103680=AXIS2_PLACEMENT_3D('',#273694,#128142,#128143);
#103681=AXIS2_PLACEMENT_3D('',#273701,#128144,#128145);
#103682=AXIS2_PLACEMENT_3D('',#273712,#128146,#128147);
#103683=AXIS2_PLACEMENT_3D('',#273719,#128148,#128149);
#103684=AXIS2_PLACEMENT_3D('',#273730,#128150,#128151);
#103685=AXIS2_PLACEMENT_3D('',#273737,#128152,#128153);
#103686=AXIS2_PLACEMENT_3D('',#273748,#128154,#128155);
#103687=AXIS2_PLACEMENT_3D('',#273755,#128156,#128157);
#103688=AXIS2_PLACEMENT_3D('',#273766,#128158,#128159);
#103689=AXIS2_PLACEMENT_3D('',#273773,#128160,#128161);
#103690=AXIS2_PLACEMENT_3D('',#273784,#128162,#128163);
#103691=AXIS2_PLACEMENT_3D('',#273791,#128164,#128165);
#103692=AXIS2_PLACEMENT_3D('',#273809,#128166,#128167);
#103693=AXIS2_PLACEMENT_3D('',#273816,#128168,#128169);
#103694=AXIS2_PLACEMENT_3D('',#273827,#128170,#128171);
#103695=AXIS2_PLACEMENT_3D('',#273834,#128172,#128173);
#103696=AXIS2_PLACEMENT_3D('',#273845,#128174,#128175);
#103697=AXIS2_PLACEMENT_3D('',#273852,#128176,#128177);
#103698=AXIS2_PLACEMENT_3D('',#273863,#128178,#128179);
#103699=AXIS2_PLACEMENT_3D('',#273870,#128180,#128181);
#103700=AXIS2_PLACEMENT_3D('',#273881,#128182,#128183);
#103701=AXIS2_PLACEMENT_3D('',#273899,#128184,#128185);
#103702=AXIS2_PLACEMENT_3D('',#273911,#128186,#128187);
#103703=AXIS2_PLACEMENT_3D('',#273935,#128188,#128189);
#103704=AXIS2_PLACEMENT_3D('',#273946,#128190,#128191);
#103705=AXIS2_PLACEMENT_3D('',#273953,#128192,#128193);
#103706=AXIS2_PLACEMENT_3D('',#273964,#128194,#128195);
#103707=AXIS2_PLACEMENT_3D('',#273971,#128196,#128197);
#103708=AXIS2_PLACEMENT_3D('',#273975,#128199,#128200);
#103709=AXIS2_PLACEMENT_3D('',#273977,#128202,#128203);
#103710=AXIS2_PLACEMENT_3D('',#273982,#128206,#128207);
#103711=AXIS2_PLACEMENT_3D('',#273983,#128208,#128209);
#103712=AXIS2_PLACEMENT_3D('',#273988,#128212,#128213);
#103713=AXIS2_PLACEMENT_3D('',#273989,#128214,#128215);
#103714=AXIS2_PLACEMENT_3D('',#273994,#128218,#128219);
#103715=AXIS2_PLACEMENT_3D('',#273995,#128220,#128221);
#103716=AXIS2_PLACEMENT_3D('',#273999,#128223,#128224);
#103717=AXIS2_PLACEMENT_3D('',#274001,#128226,#128227);
#103718=AXIS2_PLACEMENT_3D('',#274004,#128229,#128230);
#103719=AXIS2_PLACEMENT_3D('',#274005,#128231,#128232);
#103720=AXIS2_PLACEMENT_3D('',#274010,#128235,#128236);
#103721=AXIS2_PLACEMENT_3D('',#274011,#128237,#128238);
#103722=AXIS2_PLACEMENT_3D('',#274015,#128240,#128241);
#103723=AXIS2_PLACEMENT_3D('',#274017,#128243,#128244);
#103724=AXIS2_PLACEMENT_3D('',#274022,#128247,#128248);
#103725=AXIS2_PLACEMENT_3D('',#274023,#128249,#128250);
#103726=AXIS2_PLACEMENT_3D('',#274026,#128252,#128253);
#103727=AXIS2_PLACEMENT_3D('',#274027,#128254,#128255);
#103728=AXIS2_PLACEMENT_3D('',#274031,#128257,#128258);
#103729=AXIS2_PLACEMENT_3D('',#274033,#128260,#128261);
#103730=AXIS2_PLACEMENT_3D('',#274038,#128264,#128265);
#103731=AXIS2_PLACEMENT_3D('',#274039,#128266,#128267);
#103732=AXIS2_PLACEMENT_3D('',#274043,#128269,#128270);
#103733=AXIS2_PLACEMENT_3D('',#274045,#128272,#128273);
#103734=AXIS2_PLACEMENT_3D('',#274050,#128276,#128277);
#103735=AXIS2_PLACEMENT_3D('',#274051,#128278,#128279);
#103736=AXIS2_PLACEMENT_3D('',#274055,#128281,#128282);
#103737=AXIS2_PLACEMENT_3D('',#274057,#128284,#128285);
#103738=AXIS2_PLACEMENT_3D('',#274062,#128288,#128289);
#103739=AXIS2_PLACEMENT_3D('',#274063,#128290,#128291);
#103740=AXIS2_PLACEMENT_3D('',#274068,#128294,#128295);
#103741=AXIS2_PLACEMENT_3D('',#274069,#128296,#128297);
#103742=AXIS2_PLACEMENT_3D('',#274073,#128299,#128300);
#103743=AXIS2_PLACEMENT_3D('',#274075,#128302,#128303);
#103744=AXIS2_PLACEMENT_3D('',#274080,#128306,#128307);
#103745=AXIS2_PLACEMENT_3D('',#274081,#128308,#128309);
#103746=AXIS2_PLACEMENT_3D('',#274085,#128311,#128312);
#103747=AXIS2_PLACEMENT_3D('',#274087,#128314,#128315);
#103748=AXIS2_PLACEMENT_3D('',#274092,#128318,#128319);
#103749=AXIS2_PLACEMENT_3D('',#274093,#128320,#128321);
#103750=AXIS2_PLACEMENT_3D('',#274097,#128323,#128324);
#103751=AXIS2_PLACEMENT_3D('',#274099,#128326,#128327);
#103752=AXIS2_PLACEMENT_3D('',#274104,#128330,#128331);
#103753=AXIS2_PLACEMENT_3D('',#274105,#128332,#128333);
#103754=AXIS2_PLACEMENT_3D('',#274110,#128336,#128337);
#103755=AXIS2_PLACEMENT_3D('',#274111,#128338,#128339);
#103756=AXIS2_PLACEMENT_3D('',#274115,#128341,#128342);
#103757=AXIS2_PLACEMENT_3D('',#274117,#128344,#128345);
#103758=AXIS2_PLACEMENT_3D('',#274121,#128347,#128348);
#103759=AXIS2_PLACEMENT_3D('',#274123,#128350,#128351);
#103760=AXIS2_PLACEMENT_3D('',#274128,#128354,#128355);
#103761=AXIS2_PLACEMENT_3D('',#274129,#128356,#128357);
#103762=AXIS2_PLACEMENT_3D('',#274134,#128360,#128361);
#103763=AXIS2_PLACEMENT_3D('',#274135,#128362,#128363);
#103764=AXIS2_PLACEMENT_3D('',#274155,#128364,#128365);
#103765=AXIS2_PLACEMENT_3D('',#274169,#128366,#128367);
#103766=AXIS2_PLACEMENT_3D('',#274202,#128368,#128369);
#103767=AXIS2_PLACEMENT_3D('',#274203,#128370,#128371);
#103768=AXIS2_PLACEMENT_3D('',#274236,#128372,#128373);
#103769=AXIS2_PLACEMENT_3D('',#274237,#128374,#128375);
#103770=AXIS2_PLACEMENT_3D('',#274270,#128376,#128377);
#103771=AXIS2_PLACEMENT_3D('',#274271,#128378,#128379);
#103772=AXIS2_PLACEMENT_3D('',#274291,#128380,#128381);
#103773=AXIS2_PLACEMENT_3D('',#274305,#128382,#128383);
#103774=AXIS2_PLACEMENT_3D('',#274329,#128384,#128385);
#103775=AXIS2_PLACEMENT_3D('',#274330,#128386,#128387);
#103776=AXIS2_PLACEMENT_3D('',#274363,#128388,#128389);
#103777=AXIS2_PLACEMENT_3D('',#274364,#128390,#128391);
#103778=AXIS2_PLACEMENT_3D('',#274384,#128392,#128393);
#103779=AXIS2_PLACEMENT_3D('',#274398,#128394,#128395);
#103780=AXIS2_PLACEMENT_3D('',#274431,#128396,#128397);
#103781=AXIS2_PLACEMENT_3D('',#274432,#128398,#128399);
#103782=AXIS2_PLACEMENT_3D('',#274458,#128400,#128401);
#103783=AXIS2_PLACEMENT_3D('',#274459,#128402,#128403);
#103784=AXIS2_PLACEMENT_3D('',#274479,#128404,#128405);
#103785=AXIS2_PLACEMENT_3D('',#274493,#128406,#128407);
#103786=AXIS2_PLACEMENT_3D('',#274526,#128408,#128409);
#103787=AXIS2_PLACEMENT_3D('',#274527,#128410,#128411);
#103788=AXIS2_PLACEMENT_3D('',#274547,#128412,#128413);
#103789=AXIS2_PLACEMENT_3D('',#274561,#128414,#128415);
#103790=AXIS2_PLACEMENT_3D('',#274594,#128416,#128417);
#103791=AXIS2_PLACEMENT_3D('',#274595,#128418,#128419);
#103792=AXIS2_PLACEMENT_3D('',#274602,#128420,#128421);
#103793=AXIS2_PLACEMENT_3D('',#274611,#128422,#128423);
#103794=AXIS2_PLACEMENT_3D('',#274626,#128424,#128425);
#103795=AXIS2_PLACEMENT_3D('',#274627,#128426,#128427);
#103796=AXIS2_PLACEMENT_3D('',#274642,#128428,#128429);
#103797=AXIS2_PLACEMENT_3D('',#274643,#128430,#128431);
#103798=AXIS2_PLACEMENT_3D('',#274650,#128432,#128433);
#103799=AXIS2_PLACEMENT_3D('',#274659,#128434,#128435);
#103800=AXIS2_PLACEMENT_3D('',#274674,#128436,#128437);
#103801=AXIS2_PLACEMENT_3D('',#274675,#128438,#128439);
#103802=AXIS2_PLACEMENT_3D('',#274682,#128440,#128441);
#103803=AXIS2_PLACEMENT_3D('',#274691,#128442,#128443);
#103804=AXIS2_PLACEMENT_3D('',#274718,#128444,#128445);
#103805=AXIS2_PLACEMENT_3D('',#274719,#128446,#128447);
#103806=AXIS2_PLACEMENT_3D('',#274726,#128448,#128449);
#103807=AXIS2_PLACEMENT_3D('',#274735,#128450,#128451);
#103808=AXIS2_PLACEMENT_3D('',#274750,#128452,#128453);
#103809=AXIS2_PLACEMENT_3D('',#274751,#128454,#128455);
#103810=AXIS2_PLACEMENT_3D('',#274766,#128456,#128457);
#103811=AXIS2_PLACEMENT_3D('',#274767,#128458,#128459);
#103812=AXIS2_PLACEMENT_3D('',#274775,#128460,#128461);
#103813=AXIS2_PLACEMENT_3D('',#274789,#128462,#128463);
#103814=AXIS2_PLACEMENT_3D('',#274809,#128464,#128465);
#103815=AXIS2_PLACEMENT_3D('',#274823,#128466,#128467);
#103816=AXIS2_PLACEMENT_3D('',#274838,#128468,#128469);
#103817=AXIS2_PLACEMENT_3D('',#274839,#128470,#128471);
#103818=AXIS2_PLACEMENT_3D('',#274854,#128472,#128473);
#103819=AXIS2_PLACEMENT_3D('',#274855,#128474,#128475);
#103820=AXIS2_PLACEMENT_3D('',#274884,#128476,#128477);
#103821=AXIS2_PLACEMENT_3D('',#274891,#128478,#128479);
#103822=AXIS2_PLACEMENT_3D('',#274896,#128482,#128483);
#103823=AXIS2_PLACEMENT_3D('',#274897,#128484,#128485);
#103824=AXIS2_PLACEMENT_3D('',#274930,#128486,#128487);
#103825=AXIS2_PLACEMENT_3D('',#274931,#128488,#128489);
#103826=AXIS2_PLACEMENT_3D('',#274932,#128490,#128491);
#103827=AXIS2_PLACEMENT_3D('',#274933,#128492,#128493);
#103828=AXIS2_PLACEMENT_3D('',#274934,#128494,#128495);
#103829=AXIS2_PLACEMENT_3D('',#274935,#128496,#128497);
#103830=AXIS2_PLACEMENT_3D('',#274936,#128498,#128499);
#103831=AXIS2_PLACEMENT_3D('',#274937,#128500,#128501);
#103832=AXIS2_PLACEMENT_3D('',#274938,#128502,#128503);
#103833=AXIS2_PLACEMENT_3D('',#274939,#128504,#128505);
#103834=AXIS2_PLACEMENT_3D('',#274940,#128506,#128507);
#103835=AXIS2_PLACEMENT_3D('',#274941,#128508,#128509);
#103836=AXIS2_PLACEMENT_3D('',#274942,#128510,#128511);
#103837=AXIS2_PLACEMENT_3D('',#274943,#128512,#128513);
#103838=AXIS2_PLACEMENT_3D('',#274944,#128514,#128515);
#103839=AXIS2_PLACEMENT_3D('',#274945,#128516,#128517);
#103840=AXIS2_PLACEMENT_3D('',#274946,#128518,#128519);
#103841=AXIS2_PLACEMENT_3D('',#274947,#128520,#128521);
#103842=AXIS2_PLACEMENT_3D('',#274948,#128522,#128523);
#103843=AXIS2_PLACEMENT_3D('',#274949,#128524,#128525);
#103844=AXIS2_PLACEMENT_3D('',#274950,#128526,#128527);
#103845=AXIS2_PLACEMENT_3D('',#274952,#128529,#128530);
#103846=AXIS2_PLACEMENT_3D('',#274954,#128532,#128533);
#103847=AXIS2_PLACEMENT_3D('',#274955,#128534,#128535);
#103848=AXIS2_PLACEMENT_3D('',#274957,#128537,#128538);
#103849=AXIS2_PLACEMENT_3D('',#274959,#128540,#128541);
#103850=AXIS2_PLACEMENT_3D('',#274960,#128542,#128543);
#103851=AXIS2_PLACEMENT_3D('',#274961,#128544,#128545);
#103852=AXIS2_PLACEMENT_3D('',#274962,#128546,#128547);
#103853=AXIS2_PLACEMENT_3D('',#274963,#128548,#128549);
#103854=AXIS2_PLACEMENT_3D('',#274964,#128550,#128551);
#103855=AXIS2_PLACEMENT_3D('',#274965,#128552,#128553);
#103856=AXIS2_PLACEMENT_3D('',#274966,#128554,#128555);
#103857=AXIS2_PLACEMENT_3D('',#274968,#128557,#128558);
#103858=AXIS2_PLACEMENT_3D('',#274970,#128560,#128561);
#103859=AXIS2_PLACEMENT_3D('',#274971,#128562,#128563);
#103860=AXIS2_PLACEMENT_3D('',#274972,#128564,#128565);
#103861=AXIS2_PLACEMENT_3D('',#274973,#128566,#128567);
#103862=AXIS2_PLACEMENT_3D('',#274974,#128568,#128569);
#103863=AXIS2_PLACEMENT_3D('',#274975,#128570,#128571);
#103864=AXIS2_PLACEMENT_3D('',#274976,#128572,#128573);
#103865=AXIS2_PLACEMENT_3D('',#274977,#128574,#128575);
#103866=AXIS2_PLACEMENT_3D('',#274979,#128577,#128578);
#103867=AXIS2_PLACEMENT_3D('',#274981,#128580,#128581);
#103868=AXIS2_PLACEMENT_3D('',#274982,#128582,#128583);
#103869=AXIS2_PLACEMENT_3D('',#274983,#128584,#128585);
#103870=AXIS2_PLACEMENT_3D('',#274984,#128586,#128587);
#103871=AXIS2_PLACEMENT_3D('',#274985,#128588,#128589);
#103872=AXIS2_PLACEMENT_3D('',#274986,#128590,#128591);
#103873=AXIS2_PLACEMENT_3D('',#274987,#128592,#128593);
#103874=AXIS2_PLACEMENT_3D('',#274988,#128594,#128595);
#103875=AXIS2_PLACEMENT_3D('',#274989,#128596,#128597);
#103876=AXIS2_PLACEMENT_3D('',#274990,#128598,#128599);
#103877=AXIS2_PLACEMENT_3D('',#274991,#128600,#128601);
#103878=AXIS2_PLACEMENT_3D('',#274992,#128602,#128603);
#103879=AXIS2_PLACEMENT_3D('',#274993,#128604,#128605);
#103880=AXIS2_PLACEMENT_3D('',#274994,#128606,#128607);
#103881=AXIS2_PLACEMENT_3D('',#274996,#128609,#128610);
#103882=AXIS2_PLACEMENT_3D('',#274998,#128612,#128613);
#103883=AXIS2_PLACEMENT_3D('',#274999,#128614,#128615);
#103884=AXIS2_PLACEMENT_3D('',#275001,#128617,#128618);
#103885=AXIS2_PLACEMENT_3D('',#275003,#128620,#128621);
#103886=AXIS2_PLACEMENT_3D('',#275004,#128622,#128623);
#103887=AXIS2_PLACEMENT_3D('',#275006,#128625,#128626);
#103888=AXIS2_PLACEMENT_3D('',#275008,#128628,#128629);
#103889=AXIS2_PLACEMENT_3D('',#275009,#128630,#128631);
#103890=AXIS2_PLACEMENT_3D('',#275011,#128633,#128634);
#103891=AXIS2_PLACEMENT_3D('',#275012,#128635,#128636);
#103892=AXIS2_PLACEMENT_3D('',#275014,#128638,#128639);
#103893=AXIS2_PLACEMENT_3D('',#275016,#128641,#128642);
#103894=AXIS2_PLACEMENT_3D('',#275017,#128643,#128644);
#103895=AXIS2_PLACEMENT_3D('',#275019,#128646,#128647);
#103896=AXIS2_PLACEMENT_3D('',#275021,#128649,#128650);
#103897=AXIS2_PLACEMENT_3D('',#275022,#128651,#128652);
#103898=AXIS2_PLACEMENT_3D('',#275024,#128654,#128655);
#103899=AXIS2_PLACEMENT_3D('',#275026,#128657,#128658);
#103900=AXIS2_PLACEMENT_3D('',#275027,#128659,#128660);
#103901=AXIS2_PLACEMENT_3D('',#275029,#128662,#128663);
#103902=AXIS2_PLACEMENT_3D('',#275031,#128665,#128666);
#103903=AXIS2_PLACEMENT_3D('',#275032,#128667,#128668);
#103904=AXIS2_PLACEMENT_3D('',#275034,#128670,#128671);
#103905=AXIS2_PLACEMENT_3D('',#275036,#128673,#128674);
#103906=AXIS2_PLACEMENT_3D('',#275037,#128675,#128676);
#103907=AXIS2_PLACEMENT_3D('',#275039,#128678,#128679);
#103908=AXIS2_PLACEMENT_3D('',#275040,#128680,#128681);
#103909=AXIS2_PLACEMENT_3D('',#275042,#128683,#128684);
#103910=AXIS2_PLACEMENT_3D('',#275044,#128686,#128687);
#103911=AXIS2_PLACEMENT_3D('',#275045,#128688,#128689);
#103912=AXIS2_PLACEMENT_3D('',#275047,#128691,#128692);
#103913=AXIS2_PLACEMENT_3D('',#275049,#128694,#128695);
#103914=AXIS2_PLACEMENT_3D('',#275050,#128696,#128697);
#103915=AXIS2_PLACEMENT_3D('',#275052,#128699,#128700);
#103916=AXIS2_PLACEMENT_3D('',#275054,#128702,#128703);
#103917=AXIS2_PLACEMENT_3D('',#275055,#128704,#128705);
#103918=AXIS2_PLACEMENT_3D('',#275057,#128707,#128708);
#103919=AXIS2_PLACEMENT_3D('',#275059,#128710,#128711);
#103920=AXIS2_PLACEMENT_3D('',#275060,#128712,#128713);
#103921=AXIS2_PLACEMENT_3D('',#275063,#128716,#128717);
#103922=AXIS2_PLACEMENT_3D('',#275064,#128718,#128719);
#103923=AXIS2_PLACEMENT_3D('',#275065,#128720,#128721);
#103924=AXIS2_PLACEMENT_3D('',#275066,#128722,#128723);
#103925=AXIS2_PLACEMENT_3D('',#275068,#128724,#128725);
#103926=AXIS2_PLACEMENT_3D('',#275071,#128727,#128728);
#103927=AXIS2_PLACEMENT_3D('',#275072,#128729,#128730);
#103928=AXIS2_PLACEMENT_3D('',#275075,#128731,#128732);
#103929=AXIS2_PLACEMENT_3D('',#275079,#128734,#128735);
#103930=AXIS2_PLACEMENT_3D('',#275081,#128737,#128738);
#103931=AXIS2_PLACEMENT_3D('',#275083,#128739,#128740);
#103932=AXIS2_PLACEMENT_3D('',#275086,#128742,#128743);
#103933=AXIS2_PLACEMENT_3D('',#275087,#128744,#128745);
#103934=AXIS2_PLACEMENT_3D('',#275089,#128746,#128747);
#103935=AXIS2_PLACEMENT_3D('',#275092,#128749,#128750);
#103936=AXIS2_PLACEMENT_3D('',#275093,#128751,#128752);
#103937=AXIS2_PLACEMENT_3D('',#275095,#128753,#128754);
#103938=AXIS2_PLACEMENT_3D('',#275098,#128756,#128757);
#103939=AXIS2_PLACEMENT_3D('',#275099,#128758,#128759);
#103940=AXIS2_PLACEMENT_3D('',#275100,#128760,#128761);
#103941=AXIS2_PLACEMENT_3D('',#275101,#128762,#128763);
#103942=AXIS2_PLACEMENT_3D('',#275102,#128764,#128765);
#103943=AXIS2_PLACEMENT_3D('',#275103,#128766,#128767);
#103944=AXIS2_PLACEMENT_3D('',#275104,#128768,#128769);
#103945=AXIS2_PLACEMENT_3D('',#275106,#128770,#128771);
#103946=AXIS2_PLACEMENT_3D('',#275109,#128773,#128774);
#103947=AXIS2_PLACEMENT_3D('',#275110,#128775,#128776);
#103948=AXIS2_PLACEMENT_3D('',#275112,#128777,#128778);
#103949=AXIS2_PLACEMENT_3D('',#275115,#128780,#128781);
#103950=AXIS2_PLACEMENT_3D('',#275116,#128782,#128783);
#103951=AXIS2_PLACEMENT_3D('',#275119,#128784,#128785);
#103952=AXIS2_PLACEMENT_3D('',#275123,#128787,#128788);
#103953=AXIS2_PLACEMENT_3D('',#275125,#128790,#128791);
#103954=AXIS2_PLACEMENT_3D('',#275127,#128792,#128793);
#103955=AXIS2_PLACEMENT_3D('',#275129,#128794,#128795);
#103956=AXIS2_PLACEMENT_3D('',#275130,#128796,#128797);
#103957=AXIS2_PLACEMENT_3D('',#275131,#128798,#128799);
#103958=AXIS2_PLACEMENT_3D('',#275133,#128800,#128801);
#103959=AXIS2_PLACEMENT_3D('',#275135,#128802,#128803);
#103960=AXIS2_PLACEMENT_3D('',#275136,#128804,#128805);
#103961=AXIS2_PLACEMENT_3D('',#275137,#128806,#128807);
#103962=AXIS2_PLACEMENT_3D('',#275139,#128809,#128810);
#103963=AXIS2_PLACEMENT_3D('',#275141,#128812,#128813);
#103964=AXIS2_PLACEMENT_3D('',#275142,#128814,#128815);
#103965=AXIS2_PLACEMENT_3D('',#275144,#128816,#128817);
#103966=AXIS2_PLACEMENT_3D('',#275147,#128819,#128820);
#103967=AXIS2_PLACEMENT_3D('',#275148,#128821,#128822);
#103968=AXIS2_PLACEMENT_3D('',#275149,#128823,#128824);
#103969=AXIS2_PLACEMENT_3D('',#275150,#128825,#128826);
#103970=AXIS2_PLACEMENT_3D('',#275152,#128827,#128828);
#103971=AXIS2_PLACEMENT_3D('',#275155,#128830,#128831);
#103972=AXIS2_PLACEMENT_3D('',#275156,#128832,#128833);
#103973=AXIS2_PLACEMENT_3D('',#275157,#128834,#128835);
#103974=AXIS2_PLACEMENT_3D('',#275158,#128836,#128837);
#103975=AXIS2_PLACEMENT_3D('',#275159,#128838,#128839);
#103976=AXIS2_PLACEMENT_3D('',#275160,#128840,#128841);
#103977=AXIS2_PLACEMENT_3D('',#275161,#128842,#128843);
#103978=AXIS2_PLACEMENT_3D('',#275162,#128844,#128845);
#103979=AXIS2_PLACEMENT_3D('',#275163,#128846,#128847);
#103980=AXIS2_PLACEMENT_3D('',#275164,#128848,#128849);
#103981=AXIS2_PLACEMENT_3D('',#275165,#128850,#128851);
#103982=AXIS2_PLACEMENT_3D('',#275166,#128852,#128853);
#103983=AXIS2_PLACEMENT_3D('',#275167,#128854,#128855);
#103984=AXIS2_PLACEMENT_3D('',#275168,#128856,#128857);
#103985=AXIS2_PLACEMENT_3D('',#275169,#128858,#128859);
#103986=AXIS2_PLACEMENT_3D('',#275170,#128860,#128861);
#103987=AXIS2_PLACEMENT_3D('',#275171,#128862,#128863);
#103988=AXIS2_PLACEMENT_3D('',#275172,#128864,#128865);
#103989=AXIS2_PLACEMENT_3D('',#275173,#128866,#128867);
#103990=AXIS2_PLACEMENT_3D('',#275174,#128868,#128869);
#103991=AXIS2_PLACEMENT_3D('',#275175,#128870,#128871);
#103992=AXIS2_PLACEMENT_3D('',#275176,#128872,#128873);
#103993=AXIS2_PLACEMENT_3D('',#275177,#128874,#128875);
#103994=AXIS2_PLACEMENT_3D('',#275178,#128876,#128877);
#103995=AXIS2_PLACEMENT_3D('',#275179,#128878,#128879);
#103996=AXIS2_PLACEMENT_3D('',#275180,#128880,#128881);
#103997=AXIS2_PLACEMENT_3D('',#275181,#128882,#128883);
#103998=AXIS2_PLACEMENT_3D('',#275182,#128884,#128885);
#103999=AXIS2_PLACEMENT_3D('',#275183,#128886,#128887);
#104000=AXIS2_PLACEMENT_3D('',#275184,#128888,#128889);
#104001=AXIS2_PLACEMENT_3D('',#275185,#128890,#128891);
#104002=AXIS2_PLACEMENT_3D('',#275186,#128892,#128893);
#104003=AXIS2_PLACEMENT_3D('',#275187,#128894,#128895);
#104004=AXIS2_PLACEMENT_3D('',#275188,#128896,#128897);
#104005=AXIS2_PLACEMENT_3D('',#275189,#128898,#128899);
#104006=AXIS2_PLACEMENT_3D('',#275190,#128900,#128901);
#104007=AXIS2_PLACEMENT_3D('',#275191,#128902,#128903);
#104008=AXIS2_PLACEMENT_3D('',#275192,#128904,#128905);
#104009=AXIS2_PLACEMENT_3D('',#275193,#128906,#128907);
#104010=AXIS2_PLACEMENT_3D('',#275194,#128908,#128909);
#104011=AXIS2_PLACEMENT_3D('',#275195,#128910,#128911);
#104012=AXIS2_PLACEMENT_3D('',#275196,#128912,#128913);
#104013=AXIS2_PLACEMENT_3D('',#275197,#128914,#128915);
#104014=AXIS2_PLACEMENT_3D('',#275198,#128916,#128917);
#104015=AXIS2_PLACEMENT_3D('',#275199,#128918,#128919);
#104016=AXIS2_PLACEMENT_3D('',#275200,#128920,#128921);
#104017=AXIS2_PLACEMENT_3D('',#275201,#128922,#128923);
#104018=AXIS2_PLACEMENT_3D('',#275202,#128924,#128925);
#104019=AXIS2_PLACEMENT_3D('',#275203,#128926,#128927);
#104020=AXIS2_PLACEMENT_3D('',#275204,#128928,#128929);
#104021=AXIS2_PLACEMENT_3D('',#275205,#128930,#128931);
#104022=AXIS2_PLACEMENT_3D('',#275206,#128932,#128933);
#104023=AXIS2_PLACEMENT_3D('',#275207,#128934,#128935);
#104024=AXIS2_PLACEMENT_3D('',#275208,#128936,#128937);
#104025=AXIS2_PLACEMENT_3D('',#275209,#128938,#128939);
#104026=AXIS2_PLACEMENT_3D('',#275210,#128940,#128941);
#104027=AXIS2_PLACEMENT_3D('',#275211,#128942,#128943);
#104028=AXIS2_PLACEMENT_3D('',#275212,#128944,#128945);
#104029=AXIS2_PLACEMENT_3D('',#275213,#128946,#128947);
#104030=AXIS2_PLACEMENT_3D('',#275214,#128948,#128949);
#104031=AXIS2_PLACEMENT_3D('',#275215,#128950,#128951);
#104032=AXIS2_PLACEMENT_3D('',#275216,#128952,#128953);
#104033=AXIS2_PLACEMENT_3D('',#275217,#128954,#128955);
#104034=AXIS2_PLACEMENT_3D('',#275218,#128956,#128957);
#104035=AXIS2_PLACEMENT_3D('',#275219,#128958,#128959);
#104036=AXIS2_PLACEMENT_3D('',#275220,#128960,#128961);
#104037=AXIS2_PLACEMENT_3D('',#275221,#128962,#128963);
#104038=AXIS2_PLACEMENT_3D('',#275222,#128964,#128965);
#104039=AXIS2_PLACEMENT_3D('',#275223,#128966,#128967);
#104040=AXIS2_PLACEMENT_3D('',#275224,#128968,#128969);
#104041=AXIS2_PLACEMENT_3D('',#275225,#128970,#128971);
#104042=AXIS2_PLACEMENT_3D('',#275226,#128972,#128973);
#104043=AXIS2_PLACEMENT_3D('',#275227,#128974,#128975);
#104044=AXIS2_PLACEMENT_3D('',#275228,#128976,#128977);
#104045=AXIS2_PLACEMENT_3D('',#275229,#128978,#128979);
#104046=AXIS2_PLACEMENT_3D('',#275230,#128980,#128981);
#104047=AXIS2_PLACEMENT_3D('',#275231,#128982,#128983);
#104048=AXIS2_PLACEMENT_3D('',#275232,#128984,#128985);
#104049=AXIS2_PLACEMENT_3D('',#275233,#128986,#128987);
#104050=AXIS2_PLACEMENT_3D('',#275234,#128988,#128989);
#104051=AXIS2_PLACEMENT_3D('',#275235,#128990,#128991);
#104052=AXIS2_PLACEMENT_3D('',#275236,#128992,#128993);
#104053=AXIS2_PLACEMENT_3D('',#275237,#128994,#128995);
#104054=AXIS2_PLACEMENT_3D('',#275238,#128996,#128997);
#104055=AXIS2_PLACEMENT_3D('',#275239,#128998,#128999);
#104056=AXIS2_PLACEMENT_3D('',#275240,#129000,#129001);
#104057=AXIS2_PLACEMENT_3D('',#275241,#129002,#129003);
#104058=AXIS2_PLACEMENT_3D('',#275242,#129004,#129005);
#104059=AXIS2_PLACEMENT_3D('',#275243,#129006,#129007);
#104060=AXIS2_PLACEMENT_3D('',#275244,#129008,#129009);
#104061=AXIS2_PLACEMENT_3D('',#275245,#129010,#129011);
#104062=AXIS2_PLACEMENT_3D('',#275246,#129012,#129013);
#104063=AXIS2_PLACEMENT_3D('',#275247,#129014,#129015);
#104064=AXIS2_PLACEMENT_3D('',#275248,#129016,#129017);
#104065=AXIS2_PLACEMENT_3D('',#275249,#129018,#129019);
#104066=AXIS2_PLACEMENT_3D('',#275250,#129020,#129021);
#104067=AXIS2_PLACEMENT_3D('',#275251,#129022,#129023);
#104068=AXIS2_PLACEMENT_3D('',#275252,#129024,#129025);
#104069=AXIS2_PLACEMENT_3D('',#275253,#129026,#129027);
#104070=AXIS2_PLACEMENT_3D('',#275254,#129028,#129029);
#104071=AXIS2_PLACEMENT_3D('',#275255,#129030,#129031);
#104072=AXIS2_PLACEMENT_3D('',#275256,#129032,#129033);
#104073=AXIS2_PLACEMENT_3D('',#275257,#129034,#129035);
#104074=AXIS2_PLACEMENT_3D('',#275258,#129036,#129037);
#104075=AXIS2_PLACEMENT_3D('',#275259,#129038,#129039);
#104076=AXIS2_PLACEMENT_3D('',#275260,#129040,#129041);
#104077=AXIS2_PLACEMENT_3D('',#275261,#129042,#129043);
#104078=AXIS2_PLACEMENT_3D('',#275262,#129044,#129045);
#104079=AXIS2_PLACEMENT_3D('',#275263,#129046,#129047);
#104080=AXIS2_PLACEMENT_3D('',#275264,#129048,#129049);
#104081=AXIS2_PLACEMENT_3D('',#275265,#129050,#129051);
#104082=AXIS2_PLACEMENT_3D('',#275266,#129052,#129053);
#104083=AXIS2_PLACEMENT_3D('',#275267,#129054,#129055);
#104084=AXIS2_PLACEMENT_3D('',#275268,#129056,#129057);
#104085=AXIS2_PLACEMENT_3D('',#275269,#129058,#129059);
#104086=AXIS2_PLACEMENT_3D('',#275270,#129060,#129061);
#104087=AXIS2_PLACEMENT_3D('',#275271,#129062,#129063);
#104088=AXIS2_PLACEMENT_3D('',#275272,#129064,#129065);
#104089=AXIS2_PLACEMENT_3D('',#275273,#129066,#129067);
#104090=AXIS2_PLACEMENT_3D('',#275274,#129068,#129069);
#104091=AXIS2_PLACEMENT_3D('',#275275,#129070,#129071);
#104092=AXIS2_PLACEMENT_3D('',#275276,#129072,#129073);
#104093=AXIS2_PLACEMENT_3D('',#275277,#129074,#129075);
#104094=AXIS2_PLACEMENT_3D('',#275278,#129076,#129077);
#104095=AXIS2_PLACEMENT_3D('',#275279,#129078,#129079);
#104096=AXIS2_PLACEMENT_3D('',#275280,#129080,#129081);
#104097=AXIS2_PLACEMENT_3D('',#275281,#129082,#129083);
#104098=AXIS2_PLACEMENT_3D('',#275282,#129084,#129085);
#104099=AXIS2_PLACEMENT_3D('',#275283,#129086,#129087);
#104100=AXIS2_PLACEMENT_3D('',#275284,#129088,#129089);
#104101=AXIS2_PLACEMENT_3D('',#275285,#129090,#129091);
#104102=AXIS2_PLACEMENT_3D('',#275286,#129092,#129093);
#104103=AXIS2_PLACEMENT_3D('',#275287,#129094,#129095);
#104104=AXIS2_PLACEMENT_3D('',#275288,#129096,#129097);
#104105=AXIS2_PLACEMENT_3D('',#275289,#129098,#129099);
#104106=AXIS2_PLACEMENT_3D('',#275290,#129100,#129101);
#104107=AXIS2_PLACEMENT_3D('',#275291,#129102,#129103);
#104108=AXIS2_PLACEMENT_3D('',#275292,#129104,#129105);
#104109=AXIS2_PLACEMENT_3D('',#275293,#129106,#129107);
#104110=AXIS2_PLACEMENT_3D('',#275294,#129108,#129109);
#104111=AXIS2_PLACEMENT_3D('',#275295,#129110,#129111);
#104112=AXIS2_PLACEMENT_3D('',#275296,#129112,#129113);
#104113=AXIS2_PLACEMENT_3D('',#275297,#129114,#129115);
#104114=AXIS2_PLACEMENT_3D('',#275299,#129116,#129117);
#104115=AXIS2_PLACEMENT_3D('',#275302,#129119,#129120);
#104116=AXIS2_PLACEMENT_3D('',#275303,#129121,#129122);
#104117=AXIS2_PLACEMENT_3D('',#275305,#129123,#129124);
#104118=AXIS2_PLACEMENT_3D('',#275308,#129126,#129127);
#104119=AXIS2_PLACEMENT_3D('',#275309,#129128,#129129);
#104120=AXIS2_PLACEMENT_3D('',#275311,#129130,#129131);
#104121=AXIS2_PLACEMENT_3D('',#275314,#129133,#129134);
#104122=AXIS2_PLACEMENT_3D('',#275315,#129135,#129136);
#104123=AXIS2_PLACEMENT_3D('',#275317,#129137,#129138);
#104124=AXIS2_PLACEMENT_3D('',#275320,#129140,#129141);
#104125=AXIS2_PLACEMENT_3D('',#275321,#129142,#129143);
#104126=AXIS2_PLACEMENT_3D('',#275322,#129144,#129145);
#104127=AXIS2_PLACEMENT_3D('',#275323,#129146,#129147);
#104128=AXIS2_PLACEMENT_3D('',#275324,#129148,#129149);
#104129=AXIS2_PLACEMENT_3D('',#275325,#129150,#129151);
#104130=AXIS2_PLACEMENT_3D('',#275326,#129152,#129153);
#104131=AXIS2_PLACEMENT_3D('',#275328,#129154,#129155);
#104132=AXIS2_PLACEMENT_3D('',#275330,#129156,#129157);
#104133=AXIS2_PLACEMENT_3D('',#275331,#129158,#129159);
#104134=AXIS2_PLACEMENT_3D('',#275332,#129160,#129161);
#104135=AXIS2_PLACEMENT_3D('',#275334,#129162,#129163);
#104136=AXIS2_PLACEMENT_3D('',#275336,#129164,#129165);
#104137=AXIS2_PLACEMENT_3D('',#275337,#129166,#129167);
#104138=AXIS2_PLACEMENT_3D('',#275338,#129168,#129169);
#104139=AXIS2_PLACEMENT_3D('',#275340,#129170,#129171);
#104140=AXIS2_PLACEMENT_3D('',#275342,#129172,#129173);
#104141=AXIS2_PLACEMENT_3D('',#275343,#129174,#129175);
#104142=AXIS2_PLACEMENT_3D('',#275344,#129176,#129177);
#104143=AXIS2_PLACEMENT_3D('',#275347,#129179,#129180);
#104144=AXIS2_PLACEMENT_3D('',#275348,#129181,#129182);
#104145=AXIS2_PLACEMENT_3D('',#275350,#129183,#129184);
#104146=AXIS2_PLACEMENT_3D('',#275351,#129185,#129186);
#104147=AXIS2_PLACEMENT_3D('',#275352,#129187,#129188);
#104148=AXIS2_PLACEMENT_3D('',#275354,#129189,#129190);
#104149=AXIS2_PLACEMENT_3D('',#275356,#129191,#129192);
#104150=AXIS2_PLACEMENT_3D('',#275357,#129193,#129194);
#104151=AXIS2_PLACEMENT_3D('',#275358,#129195,#129196);
#104152=AXIS2_PLACEMENT_3D('',#275360,#129198,#129199);
#104153=AXIS2_PLACEMENT_3D('',#275362,#129201,#129202);
#104154=AXIS2_PLACEMENT_3D('',#275365,#129204,#129205);
#104155=AXIS2_PLACEMENT_3D('',#275366,#129206,#129207);
#104156=AXIS2_PLACEMENT_3D('',#275368,#129208,#129209);
#104157=AXIS2_PLACEMENT_3D('',#275369,#129210,#129211);
#104158=AXIS2_PLACEMENT_3D('',#275370,#129212,#129213);
#104159=AXIS2_PLACEMENT_3D('',#275371,#129214,#129215);
#104160=AXIS2_PLACEMENT_3D('',#275372,#129216,#129217);
#104161=AXIS2_PLACEMENT_3D('',#275375,#129218,#129219);
#104162=AXIS2_PLACEMENT_3D('',#275377,#129220,#129221);
#104163=AXIS2_PLACEMENT_3D('',#275379,#129222,#129223);
#104164=AXIS2_PLACEMENT_3D('',#275380,#129224,#129225);
#104165=AXIS2_PLACEMENT_3D('',#275382,#129226,#129227);
#104166=AXIS2_PLACEMENT_3D('',#275384,#129228,#129229);
#104167=AXIS2_PLACEMENT_3D('',#275385,#129230,#129231);
#104168=AXIS2_PLACEMENT_3D('',#275386,#129232,#129233);
#104169=AXIS2_PLACEMENT_3D('',#275389,#129235,#129236);
#104170=AXIS2_PLACEMENT_3D('',#275390,#129237,#129238);
#104171=AXIS2_PLACEMENT_3D('',#275392,#129239,#129240);
#104172=AXIS2_PLACEMENT_3D('',#275393,#129241,#129242);
#104173=AXIS2_PLACEMENT_3D('',#275394,#129243,#129244);
#104174=AXIS2_PLACEMENT_3D('',#275395,#129245,#129246);
#104175=AXIS2_PLACEMENT_3D('',#275396,#129247,#129248);
#104176=AXIS2_PLACEMENT_3D('',#275399,#129249,#129250);
#104177=AXIS2_PLACEMENT_3D('',#275400,#129251,#129252);
#104178=AXIS2_PLACEMENT_3D('',#275403,#129253,#129254);
#104179=AXIS2_PLACEMENT_3D('',#275404,#129255,#129256);
#104180=AXIS2_PLACEMENT_3D('',#275407,#129257,#129258);
#104181=AXIS2_PLACEMENT_3D('',#275408,#129259,#129260);
#104182=AXIS2_PLACEMENT_3D('',#275411,#129261,#129262);
#104183=AXIS2_PLACEMENT_3D('',#275412,#129263,#129264);
#104184=AXIS2_PLACEMENT_3D('',#275415,#129265,#129266);
#104185=AXIS2_PLACEMENT_3D('',#275416,#129267,#129268);
#104186=AXIS2_PLACEMENT_3D('',#275419,#129269,#129270);
#104187=AXIS2_PLACEMENT_3D('',#275420,#129271,#129272);
#104188=AXIS2_PLACEMENT_3D('',#275423,#129273,#129274);
#104189=AXIS2_PLACEMENT_3D('',#275424,#129275,#129276);
#104190=AXIS2_PLACEMENT_3D('',#275427,#129277,#129278);
#104191=AXIS2_PLACEMENT_3D('',#275428,#129279,#129280);
#104192=AXIS2_PLACEMENT_3D('',#275431,#129281,#129282);
#104193=AXIS2_PLACEMENT_3D('',#275432,#129283,#129284);
#104194=AXIS2_PLACEMENT_3D('',#275435,#129285,#129286);
#104195=AXIS2_PLACEMENT_3D('',#275436,#129287,#129288);
#104196=AXIS2_PLACEMENT_3D('',#275439,#129289,#129290);
#104197=AXIS2_PLACEMENT_3D('',#275440,#129291,#129292);
#104198=AXIS2_PLACEMENT_3D('',#275443,#129293,#129294);
#104199=AXIS2_PLACEMENT_3D('',#275444,#129295,#129296);
#104200=AXIS2_PLACEMENT_3D('',#275447,#129297,#129298);
#104201=AXIS2_PLACEMENT_3D('',#275448,#129299,#129300);
#104202=AXIS2_PLACEMENT_3D('',#275451,#129301,#129302);
#104203=AXIS2_PLACEMENT_3D('',#275452,#129303,#129304);
#104204=AXIS2_PLACEMENT_3D('',#275455,#129305,#129306);
#104205=AXIS2_PLACEMENT_3D('',#275456,#129307,#129308);
#104206=AXIS2_PLACEMENT_3D('',#275459,#129309,#129310);
#104207=AXIS2_PLACEMENT_3D('',#275460,#129311,#129312);
#104208=AXIS2_PLACEMENT_3D('',#275463,#129313,#129314);
#104209=AXIS2_PLACEMENT_3D('',#275464,#129315,#129316);
#104210=AXIS2_PLACEMENT_3D('',#275467,#129317,#129318);
#104211=AXIS2_PLACEMENT_3D('',#275468,#129319,#129320);
#104212=AXIS2_PLACEMENT_3D('',#275471,#129321,#129322);
#104213=AXIS2_PLACEMENT_3D('',#275472,#129323,#129324);
#104214=AXIS2_PLACEMENT_3D('',#275475,#129325,#129326);
#104215=AXIS2_PLACEMENT_3D('',#275476,#129327,#129328);
#104216=AXIS2_PLACEMENT_3D('',#275479,#129329,#129330);
#104217=AXIS2_PLACEMENT_3D('',#275480,#129331,#129332);
#104218=AXIS2_PLACEMENT_3D('',#275483,#129333,#129334);
#104219=AXIS2_PLACEMENT_3D('',#275484,#129335,#129336);
#104220=AXIS2_PLACEMENT_3D('',#275487,#129337,#129338);
#104221=AXIS2_PLACEMENT_3D('',#275488,#129339,#129340);
#104222=AXIS2_PLACEMENT_3D('',#275491,#129341,#129342);
#104223=AXIS2_PLACEMENT_3D('',#275492,#129343,#129344);
#104224=AXIS2_PLACEMENT_3D('',#275493,#129345,#129346);
#104225=AXIS2_PLACEMENT_3D('',#275495,#129347,#129348);
#104226=AXIS2_PLACEMENT_3D('',#275498,#129350,#129351);
#104227=AXIS2_PLACEMENT_3D('',#275499,#129352,#129353);
#104228=AXIS2_PLACEMENT_3D('',#275501,#129354,#129355);
#104229=AXIS2_PLACEMENT_3D('',#275504,#129357,#129358);
#104230=AXIS2_PLACEMENT_3D('',#275505,#129359,#129360);
#104231=AXIS2_PLACEMENT_3D('',#275507,#129361,#129362);
#104232=AXIS2_PLACEMENT_3D('',#275510,#129364,#129365);
#104233=AXIS2_PLACEMENT_3D('',#275511,#129366,#129367);
#104234=AXIS2_PLACEMENT_3D('',#275513,#129368,#129369);
#104235=AXIS2_PLACEMENT_3D('',#275516,#129371,#129372);
#104236=AXIS2_PLACEMENT_3D('',#275517,#129373,#129374);
#104237=AXIS2_PLACEMENT_3D('',#275526,#129379,#129380);
#104238=AXIS2_PLACEMENT_3D('',#275532,#129384,#129385);
#104239=AXIS2_PLACEMENT_3D('',#275538,#129389,#129390);
#104240=AXIS2_PLACEMENT_3D('',#275544,#129394,#129395);
#104241=AXIS2_PLACEMENT_3D('',#275550,#129399,#129400);
#104242=AXIS2_PLACEMENT_3D('',#275553,#129403,#129404);
#104243=AXIS2_PLACEMENT_3D('',#275554,#129405,#129406);
#104244=AXIS2_PLACEMENT_3D('',#275555,#129407,#129408);
#104245=AXIS2_PLACEMENT_3D('',#275556,#129409,#129410);
#104246=AXIS2_PLACEMENT_3D('',#275557,#129411,#129412);
#104247=AXIS2_PLACEMENT_3D('',#275558,#129413,#129414);
#104248=AXIS2_PLACEMENT_3D('',#275559,#129415,#129416);
#104249=AXIS2_PLACEMENT_3D('',#275560,#129417,#129418);
#104250=AXIS2_PLACEMENT_3D('',#275565,#129420,#129421);
#104251=AXIS2_PLACEMENT_3D('',#275569,#129422,#129423);
#104252=AXIS2_PLACEMENT_3D('',#275593,#129425,#129426);
#104253=AXIS2_PLACEMENT_3D('',#275615,#129427,#129428);
#104254=AXIS2_PLACEMENT_3D('',#275661,#129430,#129431);
#104255=AXIS2_PLACEMENT_3D('',#275707,#129433,#129434);
#104256=AXIS2_PLACEMENT_3D('',#275722,#129436,#129437);
#104257=AXIS2_PLACEMENT_3D('',#275734,#129438,#129439);
#104258=AXIS2_PLACEMENT_3D('',#275745,#129441,#129442);
#104259=AXIS2_PLACEMENT_3D('',#275763,#129444,#129445);
#104260=AXIS2_PLACEMENT_3D('',#275768,#129447,#129448);
#104261=AXIS2_PLACEMENT_3D('',#275777,#129449,#129450);
#104262=AXIS2_PLACEMENT_3D('',#275818,#129452,#129453);
#104263=AXIS2_PLACEMENT_3D('',#275855,#129454,#129455);
#104264=AXIS2_PLACEMENT_3D('',#275931,#129457,#129458);
#104265=AXIS2_PLACEMENT_3D('',#276007,#129460,#129461);
#104266=AXIS2_PLACEMENT_3D('',#276083,#129463,#129464);
#104267=AXIS2_PLACEMENT_3D('',#276109,#129466,#129467);
#104268=AXIS2_PLACEMENT_3D('',#276134,#129468,#129469);
#104269=AXIS2_PLACEMENT_3D('',#276211,#129470,#129471);
#104270=AXIS2_PLACEMENT_3D('',#276222,#129473,#129474);
#104271=AXIS2_PLACEMENT_3D('',#276261,#129475,#129476);
#104272=AXIS2_PLACEMENT_3D('',#276279,#129478,#129479);
#104273=AXIS2_PLACEMENT_3D('',#276318,#129480,#129481);
#104274=AXIS2_PLACEMENT_3D('',#276321,#129482,#129483);
#104275=AXIS2_PLACEMENT_3D('',#276323,#129484,#129485);
#104276=AXIS2_PLACEMENT_3D('',#276325,#129486,#129487);
#104277=AXIS2_PLACEMENT_3D('',#276327,#129488,#129489);
#104278=AXIS2_PLACEMENT_3D('',#276329,#129490,#129491);
#104279=AXIS2_PLACEMENT_3D('',#276330,#129492,#129493);
#104280=AXIS2_PLACEMENT_3D('',#276331,#129494,#129495);
#104281=AXIS2_PLACEMENT_3D('',#276351,#129498,#129499);
#104282=AXIS2_PLACEMENT_3D('',#276368,#129501,#129502);
#104283=AXIS2_PLACEMENT_3D('',#276385,#129504,#129505);
#104284=AXIS2_PLACEMENT_3D('',#276402,#129507,#129508);
#104285=AXIS2_PLACEMENT_3D('',#276419,#129510,#129511);
#104286=AXIS2_PLACEMENT_3D('',#276433,#129512,#129513);
#104287=AXIS2_PLACEMENT_3D('',#276434,#129514,#129515);
#104288=AXIS2_PLACEMENT_3D('',#276435,#129516,#129517);
#104289=AXIS2_PLACEMENT_3D('',#276436,#129518,#129519);
#104290=AXIS2_PLACEMENT_3D('',#276437,#129520,#129521);
#104291=AXIS2_PLACEMENT_3D('',#276438,#129522,#129523);
#104292=AXIS2_PLACEMENT_3D('',#276439,#129524,#129525);
#104293=AXIS2_PLACEMENT_3D('',#276440,#129526,#129527);
#104294=AXIS2_PLACEMENT_3D('',#276441,#129528,#129529);
#104295=AXIS2_PLACEMENT_3D('',#276442,#129530,#129531);
#104296=AXIS2_PLACEMENT_3D('',#276443,#129532,#129533);
#104297=AXIS2_PLACEMENT_3D('',#276444,#129534,#129535);
#104298=AXIS2_PLACEMENT_3D('',#276445,#129536,#129537);
#104299=AXIS2_PLACEMENT_3D('',#276446,#129538,#129539);
#104300=AXIS2_PLACEMENT_3D('',#276447,#129540,#129541);
#104301=AXIS2_PLACEMENT_3D('',#276448,#129542,#129543);
#104302=AXIS2_PLACEMENT_3D('',#276449,#129544,#129545);
#104303=AXIS2_PLACEMENT_3D('',#276450,#129546,#129547);
#104304=AXIS2_PLACEMENT_3D('',#276451,#129548,#129549);
#104305=AXIS2_PLACEMENT_3D('',#280642,#129550,#129551);
#104306=AXIS2_PLACEMENT_3D('',#280643,#129552,#129553);
#104307=AXIS2_PLACEMENT_3D('',#280658,#129555,#129556);
#104308=AXIS2_PLACEMENT_3D('',#280672,#129557,#129558);
#104309=AXIS2_PLACEMENT_3D('',#280718,#129560,#129561);
#104310=AXIS2_PLACEMENT_3D('',#280764,#129563,#129564);
#104311=AXIS2_PLACEMENT_3D('',#280810,#129566,#129567);
#104312=AXIS2_PLACEMENT_3D('',#280856,#129569,#129570);
#104313=AXIS2_PLACEMENT_3D('',#280861,#129572,#129573);
#104314=AXIS2_PLACEMENT_3D('',#280867,#129574,#129575);
#104315=AXIS2_PLACEMENT_3D('',#280872,#129577,#129578);
#104316=AXIS2_PLACEMENT_3D('',#280881,#129579,#129580);
#104317=AXIS2_PLACEMENT_3D('',#280957,#129582,#129583);
#104318=AXIS2_PLACEMENT_3D('',#281033,#129585,#129586);
#104319=AXIS2_PLACEMENT_3D('',#281109,#129588,#129589);
#104320=AXIS2_PLACEMENT_3D('',#281185,#129591,#129592);
#104321=AXIS2_PLACEMENT_3D('',#281263,#129594,#129595);
#104322=AXIS2_PLACEMENT_3D('',#281273,#129597,#129598);
#104323=AXIS2_PLACEMENT_3D('',#281282,#129599,#129600);
#104324=AXIS2_PLACEMENT_3D('',#281357,#129601,#129602);
#104325=AXIS2_PLACEMENT_3D('',#281359,#129603,#129604);
#104326=AXIS2_PLACEMENT_3D('',#281360,#129605,#129606);
#104327=AXIS2_PLACEMENT_3D('',#281362,#129607,#129608);
#104328=AXIS2_PLACEMENT_3D('',#281365,#129609,#129610);
#104329=AXIS2_PLACEMENT_3D('',#281367,#129611,#129612);
#104330=AXIS2_PLACEMENT_3D('',#281369,#129613,#129614);
#104331=AXIS2_PLACEMENT_3D('',#281371,#129615,#129616);
#104332=AXIS2_PLACEMENT_3D('',#281373,#129617,#129618);
#104333=AXIS2_PLACEMENT_3D('',#281374,#129619,#129620);
#104334=AXIS2_PLACEMENT_3D('',#281375,#129621,#129622);
#104335=AXIS2_PLACEMENT_3D('',#281395,#129624,#129625);
#104336=AXIS2_PLACEMENT_3D('',#281407,#129626,#129627);
#104337=AXIS2_PLACEMENT_3D('',#281423,#129629,#129630);
#104338=AXIS2_PLACEMENT_3D('',#281468,#129631,#129632);
#104339=AXIS2_PLACEMENT_3D('',#281469,#129633,#129634);
#104340=AXIS2_PLACEMENT_3D('',#281472,#129637,#129638);
#104341=AXIS2_PLACEMENT_3D('',#281474,#129640,#129641);
#104342=AXIS2_PLACEMENT_3D('',#281476,#129643,#129644);
#104343=AXIS2_PLACEMENT_3D('',#281478,#129646,#129647);
#104344=AXIS2_PLACEMENT_3D('',#281480,#129649,#129650);
#104345=AXIS2_PLACEMENT_3D('',#281481,#129651,#129652);
#104346=AXIS2_PLACEMENT_3D('',#281482,#129653,#129654);
#104347=AXIS2_PLACEMENT_3D('',#285705,#129655,#129656);
#104348=AXIS2_PLACEMENT_3D('',#285706,#129657,#129658);
#104349=AXIS2_PLACEMENT_3D('',#285725,#129660,#129661);
#104350=AXIS2_PLACEMENT_3D('',#285737,#129662,#129663);
#104351=AXIS2_PLACEMENT_3D('',#285766,#129665,#129666);
#104352=AXIS2_PLACEMENT_3D('',#285800,#129667,#129668);
#104353=AXIS2_PLACEMENT_3D('',#285801,#129669,#129670);
#104354=AXIS2_PLACEMENT_3D('',#285804,#129671,#129672);
#104355=AXIS2_PLACEMENT_3D('',#290036,#129673,#129674);
#104356=AXIS2_PLACEMENT_3D('',#290037,#129675,#129676);
#104357=AXIS2_PLACEMENT_3D('',#290038,#129677,#129678);
#104358=AXIS2_PLACEMENT_3D('',#290039,#129679,#129680);
#104359=AXIS2_PLACEMENT_3D('',#290049,#129682,#129683);
#104360=AXIS2_PLACEMENT_3D('',#290050,#129684,#129685);
#104361=AXIS2_PLACEMENT_3D('',#290096,#129687,#129688);
#104362=AXIS2_PLACEMENT_3D('',#290142,#129690,#129691);
#104363=AXIS2_PLACEMENT_3D('',#290188,#129693,#129694);
#104364=AXIS2_PLACEMENT_3D('',#290234,#129696,#129697);
#104365=AXIS2_PLACEMENT_3D('',#290280,#129699,#129700);
#104366=AXIS2_PLACEMENT_3D('',#290326,#129702,#129703);
#104367=AXIS2_PLACEMENT_3D('',#290372,#129705,#129706);
#104368=AXIS2_PLACEMENT_3D('',#290418,#129708,#129709);
#104369=AXIS2_PLACEMENT_3D('',#290464,#129711,#129712);
#104370=AXIS2_PLACEMENT_3D('',#290510,#129714,#129715);
#104371=AXIS2_PLACEMENT_3D('',#290556,#129717,#129718);
#104372=AXIS2_PLACEMENT_3D('',#290602,#129720,#129721);
#104373=AXIS2_PLACEMENT_3D('',#290648,#129723,#129724);
#104374=AXIS2_PLACEMENT_3D('',#290694,#129726,#129727);
#104375=AXIS2_PLACEMENT_3D('',#290740,#129729,#129730);
#104376=AXIS2_PLACEMENT_3D('',#290786,#129732,#129733);
#104377=AXIS2_PLACEMENT_3D('',#290832,#129735,#129736);
#104378=AXIS2_PLACEMENT_3D('',#290878,#129738,#129739);
#104379=AXIS2_PLACEMENT_3D('',#290924,#129741,#129742);
#104380=AXIS2_PLACEMENT_3D('',#290943,#129744,#129745);
#104381=AXIS2_PLACEMENT_3D('',#290955,#129746,#129747);
#104382=AXIS2_PLACEMENT_3D('',#291001,#129749,#129750);
#104383=AXIS2_PLACEMENT_3D('',#291047,#129752,#129753);
#104384=AXIS2_PLACEMENT_3D('',#291093,#129755,#129756);
#104385=AXIS2_PLACEMENT_3D('',#291139,#129758,#129759);
#104386=AXIS2_PLACEMENT_3D('',#291185,#129761,#129762);
#104387=AXIS2_PLACEMENT_3D('',#291231,#129764,#129765);
#104388=AXIS2_PLACEMENT_3D('',#291277,#129767,#129768);
#104389=AXIS2_PLACEMENT_3D('',#291323,#129770,#129771);
#104390=AXIS2_PLACEMENT_3D('',#291369,#129773,#129774);
#104391=AXIS2_PLACEMENT_3D('',#291415,#129776,#129777);
#104392=AXIS2_PLACEMENT_3D('',#291461,#129779,#129780);
#104393=AXIS2_PLACEMENT_3D('',#291507,#129782,#129783);
#104394=AXIS2_PLACEMENT_3D('',#291521,#129785,#129786);
#104395=AXIS2_PLACEMENT_3D('',#291526,#129787,#129788);
#104396=AXIS2_PLACEMENT_3D('',#291604,#129790,#129791);
#104397=AXIS2_PLACEMENT_3D('',#291682,#129793,#129794);
#104398=AXIS2_PLACEMENT_3D('',#291758,#129796,#129797);
#104399=AXIS2_PLACEMENT_3D('',#291834,#129799,#129800);
#104400=AXIS2_PLACEMENT_3D('',#291910,#129802,#129803);
#104401=AXIS2_PLACEMENT_3D('',#291986,#129805,#129806);
#104402=AXIS2_PLACEMENT_3D('',#292064,#129808,#129809);
#104403=AXIS2_PLACEMENT_3D('',#292140,#129811,#129812);
#104404=AXIS2_PLACEMENT_3D('',#292216,#129814,#129815);
#104405=AXIS2_PLACEMENT_3D('',#292294,#129817,#129818);
#104406=AXIS2_PLACEMENT_3D('',#292370,#129820,#129821);
#104407=AXIS2_PLACEMENT_3D('',#292446,#129823,#129824);
#104408=AXIS2_PLACEMENT_3D('',#292474,#129826,#129827);
#104409=AXIS2_PLACEMENT_3D('',#292493,#129828,#129829);
#104410=AXIS2_PLACEMENT_3D('',#292571,#129831,#129832);
#104411=AXIS2_PLACEMENT_3D('',#292649,#129834,#129835);
#104412=AXIS2_PLACEMENT_3D('',#292725,#129837,#129838);
#104413=AXIS2_PLACEMENT_3D('',#292801,#129840,#129841);
#104414=AXIS2_PLACEMENT_3D('',#292877,#129843,#129844);
#104415=AXIS2_PLACEMENT_3D('',#292953,#129846,#129847);
#104416=AXIS2_PLACEMENT_3D('',#293029,#129849,#129850);
#104417=AXIS2_PLACEMENT_3D('',#293105,#129852,#129853);
#104418=AXIS2_PLACEMENT_3D('',#293183,#129855,#129856);
#104419=AXIS2_PLACEMENT_3D('',#293261,#129858,#129859);
#104420=AXIS2_PLACEMENT_3D('',#293337,#129861,#129862);
#104421=AXIS2_PLACEMENT_3D('',#293413,#129864,#129865);
#104422=AXIS2_PLACEMENT_3D('',#293489,#129867,#129868);
#104423=AXIS2_PLACEMENT_3D('',#293565,#129870,#129871);
#104424=AXIS2_PLACEMENT_3D('',#293641,#129873,#129874);
#104425=AXIS2_PLACEMENT_3D('',#293717,#129876,#129877);
#104426=AXIS2_PLACEMENT_3D('',#293793,#129879,#129880);
#104427=AXIS2_PLACEMENT_3D('',#293871,#129882,#129883);
#104428=AXIS2_PLACEMENT_3D('',#293881,#129884,#129885);
#104429=AXIS2_PLACEMENT_3D('',#293882,#129886,#129887);
#104430=AXIS2_PLACEMENT_3D('',#293904,#129889,#129890);
#104431=AXIS2_PLACEMENT_3D('',#293933,#129891,#129892);
#104432=AXIS2_PLACEMENT_3D('',#293946,#129893,#129894);
#104433=AXIS2_PLACEMENT_3D('',#293960,#129895,#129896);
#104434=AXIS2_PLACEMENT_3D('',#294011,#129898,#129899);
#104435=AXIS2_PLACEMENT_3D('',#294012,#129900,#129901);
#104436=AXIS2_PLACEMENT_3D('',#294037,#129902,#129903);
#104437=AXIS2_PLACEMENT_3D('',#298268,#129904,#129905);
#104438=AXIS2_PLACEMENT_3D('',#298269,#129906,#129907);
#104439=AXIS2_PLACEMENT_3D('',#298270,#129908,#129909);
#104440=AXIS2_PLACEMENT_3D('',#298279,#129914,#129915);
#104441=AXIS2_PLACEMENT_3D('',#298290,#129920,#129921);
#104442=AXIS2_PLACEMENT_3D('',#298292,#129922,#129923);
#104443=AXIS2_PLACEMENT_3D('',#298294,#129924,#129925);
#104444=AXIS2_PLACEMENT_3D('',#298296,#129926,#129927);
#104445=AXIS2_PLACEMENT_3D('',#298298,#129928,#129929);
#104446=AXIS2_PLACEMENT_3D('',#298299,#129930,#129931);
#104447=AXIS2_PLACEMENT_3D('',#298300,#129932,#129933);
#104448=AXIS2_PLACEMENT_3D('',#298303,#129936,#129937);
#104449=AXIS2_PLACEMENT_3D('',#298305,#129939,#129940);
#104450=AXIS2_PLACEMENT_3D('',#298307,#129942,#129943);
#104451=AXIS2_PLACEMENT_3D('',#298308,#129944,#129945);
#104452=AXIS2_PLACEMENT_3D('',#298328,#129948,#129949);
#104453=AXIS2_PLACEMENT_3D('',#298345,#129951,#129952);
#104454=AXIS2_PLACEMENT_3D('',#298362,#129954,#129955);
#104455=AXIS2_PLACEMENT_3D('',#298379,#129957,#129958);
#104456=AXIS2_PLACEMENT_3D('',#298396,#129960,#129961);
#104457=AXIS2_PLACEMENT_3D('',#298410,#129962,#129963);
#104458=AXIS2_PLACEMENT_3D('',#298411,#129964,#129965);
#104459=AXIS2_PLACEMENT_3D('',#298412,#129966,#129967);
#104460=AXIS2_PLACEMENT_3D('',#298413,#129968,#129969);
#104461=AXIS2_PLACEMENT_3D('',#298414,#129970,#129971);
#104462=AXIS2_PLACEMENT_3D('',#298415,#129972,#129973);
#104463=AXIS2_PLACEMENT_3D('',#298416,#129974,#129975);
#104464=AXIS2_PLACEMENT_3D('',#298417,#129976,#129977);
#104465=AXIS2_PLACEMENT_3D('',#298418,#129978,#129979);
#104466=AXIS2_PLACEMENT_3D('',#298419,#129980,#129981);
#104467=AXIS2_PLACEMENT_3D('',#298420,#129982,#129983);
#104468=AXIS2_PLACEMENT_3D('',#298421,#129984,#129985);
#104469=AXIS2_PLACEMENT_3D('',#298422,#129986,#129987);
#104470=AXIS2_PLACEMENT_3D('',#298423,#129988,#129989);
#104471=AXIS2_PLACEMENT_3D('',#298424,#129990,#129991);
#104472=AXIS2_PLACEMENT_3D('',#298425,#129992,#129993);
#104473=AXIS2_PLACEMENT_3D('',#298426,#129994,#129995);
#104474=AXIS2_PLACEMENT_3D('',#298427,#129996,#129997);
#104475=AXIS2_PLACEMENT_3D('',#298428,#129998,#129999);
#104476=AXIS2_PLACEMENT_3D('',#298429,#130000,#130001);
#104477=AXIS2_PLACEMENT_3D('',#302622,#130002,#130003);
#104478=AXIS2_PLACEMENT_3D('',#302623,#130004,#130005);
#104479=AXIS2_PLACEMENT_3D('',#302625,#130006,#130007);
#104480=AXIS2_PLACEMENT_3D('',#302628,#130009,#130010);
#104481=AXIS2_PLACEMENT_3D('',#302629,#130011,#130012);
#104482=AXIS2_PLACEMENT_3D('',#302631,#130013,#130014);
#104483=AXIS2_PLACEMENT_3D('',#302634,#130016,#130017);
#104484=AXIS2_PLACEMENT_3D('',#302635,#130018,#130019);
#104485=AXIS2_PLACEMENT_3D('',#302637,#130020,#130021);
#104486=AXIS2_PLACEMENT_3D('',#302640,#130023,#130024);
#104487=AXIS2_PLACEMENT_3D('',#302641,#130025,#130026);
#104488=AXIS2_PLACEMENT_3D('',#302643,#130027,#130028);
#104489=AXIS2_PLACEMENT_3D('',#302646,#130030,#130031);
#104490=AXIS2_PLACEMENT_3D('',#302647,#130032,#130033);
#104491=AXIS2_PLACEMENT_3D('',#302649,#130034,#130035);
#104492=AXIS2_PLACEMENT_3D('',#302652,#130037,#130038);
#104493=AXIS2_PLACEMENT_3D('',#302653,#130039,#130040);
#104494=AXIS2_PLACEMENT_3D('',#302655,#130041,#130042);
#104495=AXIS2_PLACEMENT_3D('',#302658,#130044,#130045);
#104496=AXIS2_PLACEMENT_3D('',#302659,#130046,#130047);
#104497=AXIS2_PLACEMENT_3D('',#302661,#130048,#130049);
#104498=AXIS2_PLACEMENT_3D('',#302664,#130051,#130052);
#104499=AXIS2_PLACEMENT_3D('',#302665,#130053,#130054);
#104500=AXIS2_PLACEMENT_3D('',#302667,#130055,#130056);
#104501=AXIS2_PLACEMENT_3D('',#302670,#130058,#130059);
#104502=AXIS2_PLACEMENT_3D('',#302671,#130060,#130061);
#104503=AXIS2_PLACEMENT_3D('',#302673,#130062,#130063);
#104504=AXIS2_PLACEMENT_3D('',#302676,#130065,#130066);
#104505=AXIS2_PLACEMENT_3D('',#302677,#130067,#130068);
#104506=AXIS2_PLACEMENT_3D('',#302679,#130069,#130070);
#104507=AXIS2_PLACEMENT_3D('',#302682,#130072,#130073);
#104508=AXIS2_PLACEMENT_3D('',#302683,#130074,#130075);
#104509=AXIS2_PLACEMENT_3D('',#302685,#130076,#130077);
#104510=AXIS2_PLACEMENT_3D('',#302688,#130079,#130080);
#104511=AXIS2_PLACEMENT_3D('',#302689,#130081,#130082);
#104512=AXIS2_PLACEMENT_3D('',#302691,#130083,#130084);
#104513=AXIS2_PLACEMENT_3D('',#302693,#130085,#130086);
#104514=AXIS2_PLACEMENT_3D('',#302694,#130087,#130088);
#104515=AXIS2_PLACEMENT_3D('',#302696,#130089,#130090);
#104516=AXIS2_PLACEMENT_3D('',#302698,#130091,#130092);
#104517=AXIS2_PLACEMENT_3D('',#302699,#130093,#130094);
#104518=AXIS2_PLACEMENT_3D('',#302700,#130095,#130096);
#104519=AXIS2_PLACEMENT_3D('',#302702,#130097,#130098);
#104520=AXIS2_PLACEMENT_3D('',#302704,#130099,#130100);
#104521=AXIS2_PLACEMENT_3D('',#302706,#130101,#130102);
#104522=AXIS2_PLACEMENT_3D('',#302707,#130103,#130104);
#104523=AXIS2_PLACEMENT_3D('',#302708,#130105,#130106);
#104524=AXIS2_PLACEMENT_3D('',#302710,#130108,#130109);
#104525=AXIS2_PLACEMENT_3D('',#302712,#130110,#130111);
#104526=AXIS2_PLACEMENT_3D('',#302714,#130112,#130113);
#104527=AXIS2_PLACEMENT_3D('',#302715,#130114,#130115);
#104528=AXIS2_PLACEMENT_3D('',#302716,#130116,#130117);
#104529=AXIS2_PLACEMENT_3D('',#302718,#130119,#130120);
#104530=AXIS2_PLACEMENT_3D('',#302719,#130121,#130122);
#104531=AXIS2_PLACEMENT_3D('',#302720,#130123,#130124);
#104532=AXIS2_PLACEMENT_3D('',#302721,#130125,#130126);
#104533=AXIS2_PLACEMENT_3D('',#302722,#130127,#130128);
#104534=AXIS2_PLACEMENT_3D('',#302723,#130129,#130130);
#104535=AXIS2_PLACEMENT_3D('',#302724,#130131,#130132);
#104536=AXIS2_PLACEMENT_3D('',#302725,#130133,#130134);
#104537=AXIS2_PLACEMENT_3D('',#302726,#130135,#130136);
#104538=AXIS2_PLACEMENT_3D('',#302727,#130137,#130138);
#104539=AXIS2_PLACEMENT_3D('',#302728,#130139,#130140);
#104540=AXIS2_PLACEMENT_3D('',#302729,#130141,#130142);
#104541=AXIS2_PLACEMENT_3D('',#302730,#130143,#130144);
#104542=AXIS2_PLACEMENT_3D('',#302731,#130145,#130146);
#104543=AXIS2_PLACEMENT_3D('',#302732,#130147,#130148);
#104544=AXIS2_PLACEMENT_3D('',#302733,#130149,#130150);
#104545=AXIS2_PLACEMENT_3D('',#302750,#130159,#130160);
#104546=AXIS2_PLACEMENT_3D('',#302767,#130169,#130170);
#104547=AXIS2_PLACEMENT_3D('',#302770,#130173,#130174);
#104548=AXIS2_PLACEMENT_3D('',#302772,#130176,#130177);
#104549=AXIS2_PLACEMENT_3D('',#302774,#130179,#130180);
#104550=AXIS2_PLACEMENT_3D('',#302775,#130181,#130182);
#104551=AXIS2_PLACEMENT_3D('',#302778,#130185,#130186);
#104552=AXIS2_PLACEMENT_3D('',#302780,#130188,#130189);
#104553=AXIS2_PLACEMENT_3D('',#302782,#130191,#130192);
#104554=AXIS2_PLACEMENT_3D('',#302783,#130193,#130194);
#104555=AXIS2_PLACEMENT_3D('',#302784,#130195,#130196);
#104556=AXIS2_PLACEMENT_3D('',#302793,#130201,#130202);
#104557=AXIS2_PLACEMENT_3D('',#302799,#130206,#130207);
#104558=AXIS2_PLACEMENT_3D('',#302805,#130211,#130212);
#104559=AXIS2_PLACEMENT_3D('',#302808,#130215,#130216);
#104560=AXIS2_PLACEMENT_3D('',#302809,#130217,#130218);
#104561=AXIS2_PLACEMENT_3D('',#302810,#130219,#130220);
#104562=AXIS2_PLACEMENT_3D('',#302811,#130221,#130222);
#104563=AXIS2_PLACEMENT_3D('',#302812,#130223,#130224);
#104564=AXIS2_PLACEMENT_3D('',#302814,#130225,#130226);
#104565=AXIS2_PLACEMENT_3D('',#302817,#130228,#130229);
#104566=AXIS2_PLACEMENT_3D('',#302818,#130230,#130231);
#104567=AXIS2_PLACEMENT_3D('',#302820,#130232,#130233);
#104568=AXIS2_PLACEMENT_3D('',#302823,#130235,#130236);
#104569=AXIS2_PLACEMENT_3D('',#302824,#130237,#130238);
#104570=AXIS2_PLACEMENT_3D('',#302826,#130239,#130240);
#104571=AXIS2_PLACEMENT_3D('',#302829,#130242,#130243);
#104572=AXIS2_PLACEMENT_3D('',#302830,#130244,#130245);
#104573=AXIS2_PLACEMENT_3D('',#302832,#130246,#130247);
#104574=AXIS2_PLACEMENT_3D('',#302835,#130249,#130250);
#104575=AXIS2_PLACEMENT_3D('',#302836,#130251,#130252);
#104576=AXIS2_PLACEMENT_3D('',#302838,#130253,#130254);
#104577=AXIS2_PLACEMENT_3D('',#302841,#130256,#130257);
#104578=AXIS2_PLACEMENT_3D('',#302842,#130258,#130259);
#104579=AXIS2_PLACEMENT_3D('',#302844,#130260,#130261);
#104580=AXIS2_PLACEMENT_3D('',#302847,#130263,#130264);
#104581=AXIS2_PLACEMENT_3D('',#302848,#130265,#130266);
#104582=AXIS2_PLACEMENT_3D('',#302850,#130267,#130268);
#104583=AXIS2_PLACEMENT_3D('',#302853,#130270,#130271);
#104584=AXIS2_PLACEMENT_3D('',#302854,#130272,#130273);
#104585=AXIS2_PLACEMENT_3D('',#302856,#130274,#130275);
#104586=AXIS2_PLACEMENT_3D('',#302859,#130277,#130278);
#104587=AXIS2_PLACEMENT_3D('',#302860,#130279,#130280);
#104588=AXIS2_PLACEMENT_3D('',#302877,#130289,#130290);
#104589=AXIS2_PLACEMENT_3D('',#302894,#130299,#130300);
#104590=AXIS2_PLACEMENT_3D('',#302897,#130303,#130304);
#104591=AXIS2_PLACEMENT_3D('',#302900,#130307,#130308);
#104592=AXIS2_PLACEMENT_3D('',#302903,#130311,#130312);
#104593=AXIS2_PLACEMENT_3D('',#302904,#130313,#130314);
#104594=AXIS2_PLACEMENT_3D('',#302905,#130315,#130316);
#104595=AXIS2_PLACEMENT_3D('',#302907,#130318,#130319);
#104596=AXIS2_PLACEMENT_3D('',#302909,#130321,#130322);
#104597=AXIS2_PLACEMENT_3D('',#302910,#130323,#130324);
#104598=AXIS2_PLACEMENT_3D('',#302911,#130325,#130326);
#104599=AXIS2_PLACEMENT_3D('',#302913,#130327,#130328);
#104600=AXIS2_PLACEMENT_3D('',#302916,#130330,#130331);
#104601=AXIS2_PLACEMENT_3D('',#302917,#130332,#130333);
#104602=AXIS2_PLACEMENT_3D('',#302919,#130334,#130335);
#104603=AXIS2_PLACEMENT_3D('',#302922,#130337,#130338);
#104604=AXIS2_PLACEMENT_3D('',#302923,#130339,#130340);
#104605=AXIS2_PLACEMENT_3D('',#302932,#130345,#130346);
#104606=AXIS2_PLACEMENT_3D('',#302941,#130351,#130352);
#104607=AXIS2_PLACEMENT_3D('',#302947,#130356,#130357);
#104608=AXIS2_PLACEMENT_3D('',#302953,#130361,#130362);
#104609=AXIS2_PLACEMENT_3D('',#302959,#130366,#130367);
#104610=AXIS2_PLACEMENT_3D('',#302965,#130371,#130372);
#104611=AXIS2_PLACEMENT_3D('',#302968,#130375,#130376);
#104612=AXIS2_PLACEMENT_3D('',#302971,#130379,#130380);
#104613=AXIS2_PLACEMENT_3D('',#302975,#130382,#130383);
#104614=AXIS2_PLACEMENT_3D('',#302976,#130384,#130385);
#104615=AXIS2_PLACEMENT_3D('',#302977,#130386,#130387);
#104616=AXIS2_PLACEMENT_3D('',#302983,#130391,#130392);
#104617=AXIS2_PLACEMENT_3D('',#302985,#130393,#130394);
#104618=AXIS2_PLACEMENT_3D('',#302988,#130396,#130397);
#104619=AXIS2_PLACEMENT_3D('',#302989,#130398,#130399);
#104620=AXIS2_PLACEMENT_3D('',#302990,#130400,#130401);
#104621=AXIS2_PLACEMENT_3D('',#302991,#130402,#130403);
#104622=AXIS2_PLACEMENT_3D('',#302992,#130404,#130405);
#104623=AXIS2_PLACEMENT_3D('',#302996,#130407,#130408);
#104624=AXIS2_PLACEMENT_3D('',#302997,#130409,#130410);
#104625=AXIS2_PLACEMENT_3D('',#302998,#130411,#130412);
#104626=AXIS2_PLACEMENT_3D('',#303001,#130415,#130416);
#104627=AXIS2_PLACEMENT_3D('',#303003,#130418,#130419);
#104628=AXIS2_PLACEMENT_3D('',#303005,#130421,#130422);
#104629=AXIS2_PLACEMENT_3D('',#303006,#130423,#130424);
#104630=AXIS2_PLACEMENT_3D('',#303008,#130426,#130427);
#104631=AXIS2_PLACEMENT_3D('',#303010,#130429,#130430);
#104632=AXIS2_PLACEMENT_3D('',#303011,#130431,#130432);
#104633=AXIS2_PLACEMENT_3D('',#303012,#130433,#130434);
#104634=AXIS2_PLACEMENT_3D('',#303013,#130435,#130436);
#104635=AXIS2_PLACEMENT_3D('',#303014,#130437,#130438);
#104636=AXIS2_PLACEMENT_3D('',#303015,#130439,#130440);
#104637=AXIS2_PLACEMENT_3D('',#303016,#130441,#130442);
#104638=AXIS2_PLACEMENT_3D('',#303017,#130443,#130444);
#104639=AXIS2_PLACEMENT_3D('',#303039,#130446,#130447);
#104640=AXIS2_PLACEMENT_3D('',#303041,#130448,#130449);
#104641=AXIS2_PLACEMENT_3D('',#303054,#130450,#130451);
#104642=AXIS2_PLACEMENT_3D('',#303059,#130453,#130454);
#104643=AXIS2_PLACEMENT_3D('',#303120,#130455,#130456);
#104644=AXIS2_PLACEMENT_3D('',#303142,#130458,#130459);
#104645=AXIS2_PLACEMENT_3D('',#303155,#130460,#130461);
#104646=AXIS2_PLACEMENT_3D('',#303231,#130463,#130464);
#104647=AXIS2_PLACEMENT_3D('',#303309,#130466,#130467);
#104648=AXIS2_PLACEMENT_3D('',#303385,#130469,#130470);
#104649=AXIS2_PLACEMENT_3D('',#303461,#130472,#130473);
#104650=AXIS2_PLACEMENT_3D('',#303537,#130475,#130476);
#104651=AXIS2_PLACEMENT_3D('',#303613,#130478,#130479);
#104652=AXIS2_PLACEMENT_3D('',#303689,#130481,#130482);
#104653=AXIS2_PLACEMENT_3D('',#303765,#130484,#130485);
#104654=AXIS2_PLACEMENT_3D('',#303843,#130487,#130488);
#104655=AXIS2_PLACEMENT_3D('',#303921,#130490,#130491);
#104656=AXIS2_PLACEMENT_3D('',#303997,#130493,#130494);
#104657=AXIS2_PLACEMENT_3D('',#304073,#130496,#130497);
#104658=AXIS2_PLACEMENT_3D('',#304149,#130499,#130500);
#104659=AXIS2_PLACEMENT_3D('',#304225,#130502,#130503);
#104660=AXIS2_PLACEMENT_3D('',#304301,#130505,#130506);
#104661=AXIS2_PLACEMENT_3D('',#304303,#130507,#130508);
#104662=AXIS2_PLACEMENT_3D('',#304307,#130510,#130511);
#104663=AXIS2_PLACEMENT_3D('',#304325,#130513,#130514);
#104664=AXIS2_PLACEMENT_3D('',#304326,#130515,#130516);
#104665=AXIS2_PLACEMENT_3D('',#304332,#130518,#130519);
#104666=AXIS2_PLACEMENT_3D('',#304378,#130521,#130522);
#104667=AXIS2_PLACEMENT_3D('',#304424,#130524,#130525);
#104668=AXIS2_PLACEMENT_3D('',#304470,#130527,#130528);
#104669=AXIS2_PLACEMENT_3D('',#304516,#130530,#130531);
#104670=AXIS2_PLACEMENT_3D('',#304562,#130533,#130534);
#104671=AXIS2_PLACEMENT_3D('',#304608,#130536,#130537);
#104672=AXIS2_PLACEMENT_3D('',#304654,#130539,#130540);
#104673=AXIS2_PLACEMENT_3D('',#304700,#130542,#130543);
#104674=AXIS2_PLACEMENT_3D('',#304746,#130545,#130546);
#104675=AXIS2_PLACEMENT_3D('',#304792,#130548,#130549);
#104676=AXIS2_PLACEMENT_3D('',#304838,#130551,#130552);
#104677=AXIS2_PLACEMENT_3D('',#304884,#130554,#130555);
#104678=AXIS2_PLACEMENT_3D('',#304930,#130557,#130558);
#104679=AXIS2_PLACEMENT_3D('',#304976,#130560,#130561);
#104680=AXIS2_PLACEMENT_3D('',#305022,#130563,#130564);
#104681=AXIS2_PLACEMENT_3D('',#305027,#130566,#130567);
#104682=AXIS2_PLACEMENT_3D('',#305068,#130568,#130569);
#104683=AXIS2_PLACEMENT_3D('',#305070,#130570,#130571);
#104684=AXIS2_PLACEMENT_3D('',#305071,#130572,#130573);
#104685=AXIS2_PLACEMENT_3D('',#305073,#130574,#130575);
#104686=AXIS2_PLACEMENT_3D('',#306683,#130577,#130578);
#104687=AXIS2_PLACEMENT_3D('',#306684,#130579,#130580);
#104688=AXIS2_PLACEMENT_3D('',#306765,#130581,#130582);
#104689=AXIS2_PLACEMENT_3D('',#306814,#130583,#130584);
#104690=AXIS2_PLACEMENT_3D('',#306895,#130585,#130586);
#104691=AXIS2_PLACEMENT_3D('',#307696,#130603,#130604);
#104692=AXIS2_PLACEMENT_3D('',#307841,#130605,#130606);
#104693=AXIS2_PLACEMENT_3D('',#307986,#130607,#130608);
#104694=AXIS2_PLACEMENT_3D('',#308843,#130629,#130630);
#104695=AXIS2_PLACEMENT_3D('',#308849,#130634,#130635);
#104696=AXIS2_PLACEMENT_3D('',#308853,#130638,#130639);
#104697=AXIS2_PLACEMENT_3D('',#308857,#130642,#130643);
#104698=AXIS2_PLACEMENT_3D('',#308859,#130645,#130646);
#104699=AXIS2_PLACEMENT_3D('',#308862,#130647,#130648);
#104700=AXIS2_PLACEMENT_3D('',#308864,#130649,#130650);
#104701=AXIS2_PLACEMENT_3D('',#308866,#130651,#130652);
#104702=AXIS2_PLACEMENT_3D('',#308868,#130653,#130654);
#104703=AXIS2_PLACEMENT_3D('',#308870,#130655,#130656);
#104704=AXIS2_PLACEMENT_3D('',#308871,#130657,#130658);
#104705=AXIS2_PLACEMENT_3D('',#308872,#130659,#130660);
#104706=AXIS2_PLACEMENT_3D('',#308880,#130661,#130662);
#104707=AXIS2_PLACEMENT_3D('',#308888,#130663,#130664);
#104708=AXIS2_PLACEMENT_3D('',#308896,#130665,#130666);
#104709=AXIS2_PLACEMENT_3D('',#308904,#130667,#130668);
#104710=AXIS2_PLACEMENT_3D('',#308912,#130669,#130670);
#104711=AXIS2_PLACEMENT_3D('',#308920,#130671,#130672);
#104712=AXIS2_PLACEMENT_3D('',#308926,#130676,#130677);
#104713=AXIS2_PLACEMENT_3D('',#308930,#130680,#130681);
#104714=AXIS2_PLACEMENT_3D('',#308934,#130684,#130685);
#104715=AXIS2_PLACEMENT_3D('',#308938,#130688,#130689);
#104716=AXIS2_PLACEMENT_3D('',#308942,#130692,#130693);
#104717=AXIS2_PLACEMENT_3D('',#308944,#130695,#130696);
#104718=AXIS2_PLACEMENT_3D('',#308945,#130697,#130698);
#104719=AXIS2_PLACEMENT_3D('',#308946,#130699,#130700);
#104720=AXIS2_PLACEMENT_3D('',#308947,#130701,#130702);
#104721=AXIS2_PLACEMENT_3D('',#308948,#130703,#130704);
#104722=AXIS2_PLACEMENT_3D('',#308962,#130706,#130707);
#104723=AXIS2_PLACEMENT_3D('',#308977,#130708,#130709);
#104724=AXIS2_PLACEMENT_3D('',#308999,#130711,#130712);
#104725=AXIS2_PLACEMENT_3D('',#309020,#130713,#130714);
#104726=AXIS2_PLACEMENT_3D('',#309096,#130716,#130717);
#104727=AXIS2_PLACEMENT_3D('',#309172,#130719,#130720);
#104728=AXIS2_PLACEMENT_3D('',#309248,#130722,#130723);
#104729=AXIS2_PLACEMENT_3D('',#309272,#130725,#130726);
#104730=AXIS2_PLACEMENT_3D('',#309274,#130727,#130728);
#104731=AXIS2_PLACEMENT_3D('',#309297,#130729,#130730);
#104732=AXIS2_PLACEMENT_3D('',#309329,#130732,#130733);
#104733=AXIS2_PLACEMENT_3D('',#309375,#130735,#130736);
#104734=AXIS2_PLACEMENT_3D('',#309421,#130738,#130739);
#104735=AXIS2_PLACEMENT_3D('',#309426,#130741,#130742);
#104736=AXIS2_PLACEMENT_3D('',#309818,#130743,#130744);
#104737=AXIS2_PLACEMENT_3D('',#309841,#130745,#130746);
#104738=AXIS2_PLACEMENT_3D('',#310210,#130747,#130748);
#104739=AXIS2_PLACEMENT_3D('',#310237,#130751,#130752);
#104740=AXIS2_PLACEMENT_3D('',#310264,#130755,#130756);
#104741=AXIS2_PLACEMENT_3D('',#310291,#130759,#130760);
#104742=AXIS2_PLACEMENT_3D('',#310318,#130763,#130764);
#104743=AXIS2_PLACEMENT_3D('',#310345,#130767,#130768);
#104744=AXIS2_PLACEMENT_3D('',#310372,#130771,#130772);
#104745=AXIS2_PLACEMENT_3D('',#310381,#130773,#130774);
#104746=AXIS2_PLACEMENT_3D('',#310382,#130775,#130776);
#104747=AXIS2_PLACEMENT_3D('',#310390,#130777,#130778);
#104748=AXIS2_PLACEMENT_3D('',#310391,#130779,#130780);
#104749=AXIS2_PLACEMENT_3D('',#310399,#130781,#130782);
#104750=AXIS2_PLACEMENT_3D('',#310400,#130783,#130784);
#104751=AXIS2_PLACEMENT_3D('',#310408,#130785,#130786);
#104752=AXIS2_PLACEMENT_3D('',#310409,#130787,#130788);
#104753=AXIS2_PLACEMENT_3D('',#310417,#130789,#130790);
#104754=AXIS2_PLACEMENT_3D('',#310418,#130791,#130792);
#104755=AXIS2_PLACEMENT_3D('',#310425,#130793,#130794);
#104756=AXIS2_PLACEMENT_3D('',#310426,#130795,#130796);
#104757=AXIS2_PLACEMENT_3D('',#310435,#130797,#130798);
#104758=AXIS2_PLACEMENT_3D('',#310436,#130799,#130800);
#104759=AXIS2_PLACEMENT_3D('',#310444,#130801,#130802);
#104760=AXIS2_PLACEMENT_3D('',#310445,#130803,#130804);
#104761=AXIS2_PLACEMENT_3D('',#310453,#130805,#130806);
#104762=AXIS2_PLACEMENT_3D('',#310454,#130807,#130808);
#104763=AXIS2_PLACEMENT_3D('',#310462,#130809,#130810);
#104764=AXIS2_PLACEMENT_3D('',#310463,#130811,#130812);
#104765=AXIS2_PLACEMENT_3D('',#310471,#130813,#130814);
#104766=AXIS2_PLACEMENT_3D('',#310472,#130815,#130816);
#104767=AXIS2_PLACEMENT_3D('',#310479,#130817,#130818);
#104768=AXIS2_PLACEMENT_3D('',#310480,#130819,#130820);
#104769=AXIS2_PLACEMENT_3D('',#310481,#130821,#130822);
#104770=AXIS2_PLACEMENT_3D('',#310482,#130823,#130824);
#104771=AXIS2_PLACEMENT_3D('',#310483,#130825,#130826);
#104772=AXIS2_PLACEMENT_3D('',#310484,#130827,#130828);
#104773=AXIS2_PLACEMENT_3D('',#310485,#130829,#130830);
#104774=AXIS2_PLACEMENT_3D('',#310486,#130831,#130832);
#104775=AXIS2_PLACEMENT_3D('',#310487,#130833,#130834);
#104776=AXIS2_PLACEMENT_3D('',#310489,#130835,#130836);
#104777=AXIS2_PLACEMENT_3D('',#310490,#130837,#130838);
#104778=AXIS2_PLACEMENT_3D('',#310492,#130839,#130840);
#104779=AXIS2_PLACEMENT_3D('',#310493,#130841,#130842);
#104780=AXIS2_PLACEMENT_3D('',#310495,#130844,#130845);
#104781=AXIS2_PLACEMENT_3D('',#310497,#130847,#130848);
#104782=AXIS2_PLACEMENT_3D('',#310498,#130849,#130850);
#104783=AXIS2_PLACEMENT_3D('',#310499,#130851,#130852);
#104784=AXIS2_PLACEMENT_3D('',#310500,#130853,#130854);
#104785=AXIS2_PLACEMENT_3D('',#310501,#130855,#130856);
#104786=AXIS2_PLACEMENT_3D('',#310502,#130857,#130858);
#104787=AXIS2_PLACEMENT_3D('',#310503,#130859,#130860);
#104788=AXIS2_PLACEMENT_3D('',#310504,#130861,#130862);
#104789=AXIS2_PLACEMENT_3D('',#310505,#130863,#130864);
#104790=AXIS2_PLACEMENT_3D('',#310506,#130865,#130866);
#104791=AXIS2_PLACEMENT_3D('',#310507,#130867,#130868);
#104792=AXIS2_PLACEMENT_3D('',#310508,#130869,#130870);
#104793=AXIS2_PLACEMENT_3D('',#310509,#130871,#130872);
#104794=AXIS2_PLACEMENT_3D('',#310510,#130873,#130874);
#104795=AXIS2_PLACEMENT_3D('',#310511,#130875,#130876);
#104796=AXIS2_PLACEMENT_3D('',#310512,#130877,#130878);
#104797=AXIS2_PLACEMENT_3D('',#310513,#130879,#130880);
#104798=AXIS2_PLACEMENT_3D('',#310514,#130881,#130882);
#104799=AXIS2_PLACEMENT_3D('',#310515,#130883,#130884);
#104800=AXIS2_PLACEMENT_3D('',#310516,#130885,#130886);
#104801=AXIS2_PLACEMENT_3D('',#310517,#130887,#130888);
#104802=AXIS2_PLACEMENT_3D('',#310518,#130889,#130890);
#104803=AXIS2_PLACEMENT_3D('',#310519,#130891,#130892);
#104804=AXIS2_PLACEMENT_3D('',#310520,#130893,#130894);
#104805=AXIS2_PLACEMENT_3D('',#310521,#130895,#130896);
#104806=AXIS2_PLACEMENT_3D('',#310522,#130897,#130898);
#104807=AXIS2_PLACEMENT_3D('',#310523,#130899,#130900);
#104808=AXIS2_PLACEMENT_3D('',#310524,#130901,#130902);
#104809=AXIS2_PLACEMENT_3D('',#310525,#130903,#130904);
#104810=AXIS2_PLACEMENT_3D('',#310526,#130905,#130906);
#104811=AXIS2_PLACEMENT_3D('',#310527,#130907,#130908);
#104812=AXIS2_PLACEMENT_3D('',#310528,#130909,#130910);
#104813=AXIS2_PLACEMENT_3D('',#310529,#130911,#130912);
#104814=AXIS2_PLACEMENT_3D('',#310530,#130913,#130914);
#104815=AXIS2_PLACEMENT_3D('',#310531,#130915,#130916);
#104816=AXIS2_PLACEMENT_3D('',#310532,#130917,#130918);
#104817=AXIS2_PLACEMENT_3D('',#310533,#130919,#130920);
#104818=AXIS2_PLACEMENT_3D('',#310534,#130921,#130922);
#104819=AXIS2_PLACEMENT_3D('',#310535,#130923,#130924);
#104820=AXIS2_PLACEMENT_3D('',#310536,#130925,#130926);
#104821=AXIS2_PLACEMENT_3D('',#310537,#130927,#130928);
#104822=AXIS2_PLACEMENT_3D('',#310538,#130929,#130930);
#104823=AXIS2_PLACEMENT_3D('',#310539,#130931,#130932);
#104824=AXIS2_PLACEMENT_3D('',#310540,#130933,#130934);
#104825=AXIS2_PLACEMENT_3D('',#310541,#130935,#130936);
#104826=AXIS2_PLACEMENT_3D('',#310542,#130937,#130938);
#104827=AXIS2_PLACEMENT_3D('',#310543,#130939,#130940);
#104828=AXIS2_PLACEMENT_3D('',#310544,#130941,#130942);
#104829=AXIS2_PLACEMENT_3D('',#310545,#130943,#130944);
#104830=AXIS2_PLACEMENT_3D('',#310546,#130945,#130946);
#104831=AXIS2_PLACEMENT_3D('',#310547,#130947,#130948);
#104832=AXIS2_PLACEMENT_3D('',#310548,#130949,#130950);
#104833=AXIS2_PLACEMENT_3D('',#310549,#130951,#130952);
#104834=AXIS2_PLACEMENT_3D('',#310550,#130953,#130954);
#104835=AXIS2_PLACEMENT_3D('',#310551,#130955,#130956);
#104836=AXIS2_PLACEMENT_3D('',#310552,#130957,#130958);
#104837=AXIS2_PLACEMENT_3D('',#310553,#130959,#130960);
#104838=AXIS2_PLACEMENT_3D('',#310554,#130961,#130962);
#104839=AXIS2_PLACEMENT_3D('',#310555,#130963,#130964);
#104840=AXIS2_PLACEMENT_3D('',#310556,#130965,#130966);
#104841=AXIS2_PLACEMENT_3D('',#310557,#130967,#130968);
#104842=AXIS2_PLACEMENT_3D('',#310558,#130969,#130970);
#104843=AXIS2_PLACEMENT_3D('',#310559,#130971,#130972);
#104844=AXIS2_PLACEMENT_3D('',#310560,#130973,#130974);
#104845=AXIS2_PLACEMENT_3D('',#310561,#130975,#130976);
#104846=AXIS2_PLACEMENT_3D('',#310562,#130977,#130978);
#104847=AXIS2_PLACEMENT_3D('',#310563,#130979,#130980);
#104848=AXIS2_PLACEMENT_3D('',#310564,#130981,#130982);
#104849=AXIS2_PLACEMENT_3D('',#310565,#130983,#130984);
#104850=AXIS2_PLACEMENT_3D('',#310566,#130985,#130986);
#104851=AXIS2_PLACEMENT_3D('',#310567,#130987,#130988);
#104852=AXIS2_PLACEMENT_3D('',#310568,#130989,#130990);
#104853=AXIS2_PLACEMENT_3D('',#310569,#130991,#130992);
#104854=AXIS2_PLACEMENT_3D('',#310570,#130993,#130994);
#104855=AXIS2_PLACEMENT_3D('',#310571,#130995,#130996);
#104856=AXIS2_PLACEMENT_3D('',#310572,#130997,#130998);
#104857=AXIS2_PLACEMENT_3D('',#310573,#130999,#131000);
#104858=AXIS2_PLACEMENT_3D('',#310574,#131001,#131002);
#104859=AXIS2_PLACEMENT_3D('',#310575,#131003,#131004);
#104860=AXIS2_PLACEMENT_3D('',#310576,#131005,#131006);
#104861=AXIS2_PLACEMENT_3D('',#310577,#131007,#131008);
#104862=AXIS2_PLACEMENT_3D('',#310578,#131009,#131010);
#104863=AXIS2_PLACEMENT_3D('',#310579,#131011,#131012);
#104864=DIRECTION('axis',(0.,0.,1.));
#104865=DIRECTION('refdir',(1.,0.,0.));
#104866=DIRECTION('axis',(0.,0.,1.));
#104867=DIRECTION('refdir',(1.,0.,0.));
#104868=DIRECTION('center_axis',(1.,0.,-2.89120579329468E-17));
#104869=DIRECTION('ref_axis',(-2.89120579329468E-17,0.,-1.));
#104870=DIRECTION('center_axis',(1.,0.,-5.33761069531325E-17));
#104871=DIRECTION('ref_axis',(-5.33761069531325E-17,0.,-1.));
#104872=DIRECTION('',(1.,0.,-2.89120579329468E-17));
#104873=DIRECTION('center_axis',(1.,0.,-2.89120579329468E-17));
#104874=DIRECTION('ref_axis',(-2.89120579329468E-17,0.,-1.));
#104875=DIRECTION('center_axis',(1.,0.,-2.89120579329468E-17));
#104876=DIRECTION('ref_axis',(-2.89120579329468E-17,0.,-1.));
#104877=DIRECTION('center_axis',(1.,0.,-5.33761069531325E-17));
#104878=DIRECTION('ref_axis',(-5.33761069531325E-17,0.,-1.));
#104879=DIRECTION('',(1.,0.,-2.89120579329468E-17));
#104880=DIRECTION('center_axis',(1.,0.,-2.89120579329468E-17));
#104881=DIRECTION('ref_axis',(-2.89120579329468E-17,0.,-1.));
#104882=DIRECTION('center_axis',(1.,0.,-2.89120579329468E-17));
#104883=DIRECTION('ref_axis',(-2.89120579329468E-17,0.,-1.));
#104884=DIRECTION('center_axis',(1.,0.,-5.33761069531325E-17));
#104885=DIRECTION('ref_axis',(-5.33761069531325E-17,0.,-1.));
#104886=DIRECTION('',(1.,0.,-2.89120579329468E-17));
#104887=DIRECTION('center_axis',(1.,0.,-2.89120579329468E-17));
#104888=DIRECTION('ref_axis',(-2.89120579329468E-17,0.,-1.));
#104889=DIRECTION('center_axis',(1.,0.,-2.89120579329468E-17));
#104890=DIRECTION('ref_axis',(-2.89120579329468E-17,0.,-1.));
#104891=DIRECTION('center_axis',(1.,0.,-5.33761069531325E-17));
#104892=DIRECTION('ref_axis',(-5.33761069531325E-17,0.,-1.));
#104893=DIRECTION('',(1.,0.,-2.89120579329468E-17));
#104894=DIRECTION('center_axis',(1.,0.,-2.89120579329468E-17));
#104895=DIRECTION('ref_axis',(-2.89120579329468E-17,0.,-1.));
#104896=DIRECTION('center_axis',(1.,0.,-2.89120579329468E-17));
#104897=DIRECTION('ref_axis',(-2.89120579329468E-17,0.,-1.));
#104898=DIRECTION('center_axis',(1.,0.,-5.33761069531325E-17));
#104899=DIRECTION('ref_axis',(-5.33761069531325E-17,0.,-1.));
#104900=DIRECTION('',(1.,0.,-2.89120579329468E-17));
#104901=DIRECTION('center_axis',(1.,0.,-2.89120579329468E-17));
#104902=DIRECTION('ref_axis',(-2.89120579329468E-17,0.,-1.));
#104903=DIRECTION('center_axis',(1.,0.,-2.89120579329468E-17));
#104904=DIRECTION('ref_axis',(-2.89120579329468E-17,0.,-1.));
#104905=DIRECTION('center_axis',(1.,0.,-5.33761069531325E-17));
#104906=DIRECTION('ref_axis',(-5.33761069531325E-17,0.,-1.));
#104907=DIRECTION('',(1.,0.,-2.89120579329468E-17));
#104908=DIRECTION('center_axis',(1.,0.,-2.89120579329468E-17));
#104909=DIRECTION('ref_axis',(-2.89120579329468E-17,0.,-1.));
#104910=DIRECTION('center_axis',(1.,0.,-2.89120579329468E-17));
#104911=DIRECTION('ref_axis',(-2.89120579329468E-17,0.,-1.));
#104912=DIRECTION('center_axis',(1.,0.,-5.33761069531325E-17));
#104913=DIRECTION('ref_axis',(-5.33761069531325E-17,0.,-1.));
#104914=DIRECTION('',(1.,0.,-2.89120579329468E-17));
#104915=DIRECTION('center_axis',(1.,0.,-2.89120579329468E-17));
#104916=DIRECTION('ref_axis',(-2.89120579329468E-17,0.,-1.));
#104917=DIRECTION('center_axis',(1.,0.,-2.89120579329468E-17));
#104918=DIRECTION('ref_axis',(-2.89120579329468E-17,0.,-1.));
#104919=DIRECTION('center_axis',(1.,0.,-5.33761069531325E-17));
#104920=DIRECTION('ref_axis',(-5.33761069531325E-17,0.,-1.));
#104921=DIRECTION('',(1.,0.,-2.89120579329468E-17));
#104922=DIRECTION('center_axis',(1.,0.,-2.89120579329468E-17));
#104923=DIRECTION('ref_axis',(-2.89120579329468E-17,0.,-1.));
#104924=DIRECTION('center_axis',(1.,0.,-2.89120579329468E-17));
#104925=DIRECTION('ref_axis',(-2.89120579329468E-17,0.,-1.));
#104926=DIRECTION('center_axis',(1.,0.,-5.33761069531325E-17));
#104927=DIRECTION('ref_axis',(-5.33761069531325E-17,0.,-1.));
#104928=DIRECTION('',(1.,0.,-2.89120579329468E-17));
#104929=DIRECTION('center_axis',(1.,0.,-2.89120579329468E-17));
#104930=DIRECTION('ref_axis',(-2.89120579329468E-17,0.,-1.));
#104931=DIRECTION('center_axis',(1.,0.,-2.89120579329468E-17));
#104932=DIRECTION('ref_axis',(-2.89120579329468E-17,0.,-1.));
#104933=DIRECTION('center_axis',(1.,0.,-5.33761069531325E-17));
#104934=DIRECTION('ref_axis',(-5.33761069531325E-17,0.,-1.));
#104935=DIRECTION('',(1.,0.,-2.89120579329468E-17));
#104936=DIRECTION('center_axis',(1.,0.,-2.89120579329468E-17));
#104937=DIRECTION('ref_axis',(-2.89120579329468E-17,0.,-1.));
#104938=DIRECTION('center_axis',(1.,0.,-2.89120579329468E-17));
#104939=DIRECTION('ref_axis',(-2.89120579329468E-17,0.,-1.));
#104940=DIRECTION('center_axis',(1.,0.,-5.33761069531325E-17));
#104941=DIRECTION('ref_axis',(-5.33761069531325E-17,0.,-1.));
#104942=DIRECTION('',(1.,0.,-2.89120579329468E-17));
#104943=DIRECTION('center_axis',(1.,0.,-2.89120579329468E-17));
#104944=DIRECTION('ref_axis',(-2.89120579329468E-17,0.,-1.));
#104945=DIRECTION('center_axis',(1.,0.,-2.89120579329468E-17));
#104946=DIRECTION('ref_axis',(-2.89120579329468E-17,0.,-1.));
#104947=DIRECTION('center_axis',(1.,0.,-5.33761069531325E-17));
#104948=DIRECTION('ref_axis',(-5.33761069531325E-17,0.,-1.));
#104949=DIRECTION('',(1.,0.,-2.89120579329468E-17));
#104950=DIRECTION('center_axis',(1.,0.,-2.89120579329468E-17));
#104951=DIRECTION('ref_axis',(-2.89120579329468E-17,0.,-1.));
#104952=DIRECTION('center_axis',(-1.,0.,0.));
#104953=DIRECTION('ref_axis',(0.,0.,1.));
#104954=DIRECTION('',(0.,0.,-1.));
#104955=DIRECTION('',(0.,-1.,0.));
#104956=DIRECTION('',(0.,0.,-1.));
#104957=DIRECTION('',(0.,-1.,0.));
#104958=DIRECTION('center_axis',(1.22464679914735E-16,0.,1.));
#104959=DIRECTION('ref_axis',(1.,0.,-1.22464679914735E-16));
#104960=DIRECTION('',(-1.,0.,1.22464679914735E-16));
#104961=DIRECTION('',(0.,1.,0.));
#104962=DIRECTION('',(-1.,0.,1.22464679914735E-16));
#104963=DIRECTION('center_axis',(1.,0.,-5.33761069531325E-17));
#104964=DIRECTION('ref_axis',(-5.33761069531325E-17,0.,-1.));
#104965=DIRECTION('',(5.33761069531325E-17,0.,1.));
#104966=DIRECTION('',(0.,1.,0.));
#104967=DIRECTION('',(5.33761069531325E-17,0.,1.));
#104968=DIRECTION('',(0.,-1.,0.));
#104969=DIRECTION('center_axis',(0.,0.,-1.));
#104970=DIRECTION('ref_axis',(-1.,0.,0.));
#104971=DIRECTION('',(1.,0.,0.));
#104972=DIRECTION('',(0.,-1.,0.));
#104973=DIRECTION('',(1.,0.,0.));
#104974=DIRECTION('',(0.,-1.,0.));
#104975=DIRECTION('center_axis',(-1.,0.,0.));
#104976=DIRECTION('ref_axis',(0.,0.,1.));
#104977=DIRECTION('',(0.,0.,-1.));
#104978=DIRECTION('',(0.,-1.,0.));
#104979=DIRECTION('',(0.,0.,-1.));
#104980=DIRECTION('center_axis',(0.,0.,1.));
#104981=DIRECTION('ref_axis',(1.,0.,0.));
#104982=DIRECTION('',(-1.,0.,0.));
#104983=DIRECTION('',(0.,1.,0.));
#104984=DIRECTION('',(-1.,0.,0.));
#104985=DIRECTION('center_axis',(-1.,0.,5.78241158658936E-17));
#104986=DIRECTION('ref_axis',(5.78241158658936E-17,0.,1.));
#104987=DIRECTION('',(-5.78241158658936E-17,0.,-1.));
#104988=DIRECTION('',(0.,1.,0.));
#104989=DIRECTION('',(-5.78241158658936E-17,0.,-1.));
#104990=DIRECTION('',(0.,-1.,0.));
#104991=DIRECTION('center_axis',(-7.70988211545248E-17,0.,-1.));
#104992=DIRECTION('ref_axis',(-1.,0.,7.70988211545248E-17));
#104993=DIRECTION('',(1.,0.,-7.70988211545248E-17));
#104994=DIRECTION('',(0.,-1.,0.));
#104995=DIRECTION('',(1.,0.,-7.70988211545248E-17));
#104996=DIRECTION('center_axis',(0.,1.,0.));
#104997=DIRECTION('ref_axis',(0.,0.,1.));
#104998=DIRECTION('center_axis',(0.,1.,0.));
#104999=DIRECTION('ref_axis',(0.,0.,1.));
#105000=DIRECTION('center_axis',(0.,-1.,0.));
#105001=DIRECTION('ref_axis',(0.,0.,1.));
#105002=DIRECTION('center_axis',(0.,-1.,0.));
#105003=DIRECTION('ref_axis',(0.,0.,1.));
#105004=DIRECTION('center_axis',(0.,1.,0.));
#105005=DIRECTION('ref_axis',(0.,0.,1.));
#105006=DIRECTION('center_axis',(0.,1.,0.));
#105007=DIRECTION('ref_axis',(0.,0.,1.));
#105008=DIRECTION('center_axis',(0.,-1.,0.));
#105009=DIRECTION('ref_axis',(0.,0.,1.));
#105010=DIRECTION('center_axis',(0.,-1.,0.));
#105011=DIRECTION('ref_axis',(0.,0.,1.));
#105012=DIRECTION('center_axis',(0.,1.,0.));
#105013=DIRECTION('ref_axis',(0.,0.,1.));
#105014=DIRECTION('center_axis',(0.,1.,0.));
#105015=DIRECTION('ref_axis',(0.,0.,1.));
#105016=DIRECTION('center_axis',(0.,-1.,0.));
#105017=DIRECTION('ref_axis',(0.,0.,-1.));
#105018=DIRECTION('center_axis',(0.,-1.,0.));
#105019=DIRECTION('ref_axis',(0.,0.,-1.));
#105020=DIRECTION('center_axis',(0.,1.,0.));
#105021=DIRECTION('ref_axis',(0.,0.,1.));
#105022=DIRECTION('center_axis',(0.,1.,0.));
#105023=DIRECTION('ref_axis',(0.,0.,1.));
#105024=DIRECTION('axis',(0.,0.,1.));
#105025=DIRECTION('refdir',(1.,0.,0.));
#105026=DIRECTION('center_axis',(1.,0.,-2.89120579329468E-17));
#105027=DIRECTION('ref_axis',(-2.89120579329468E-17,0.,-1.));
#105028=DIRECTION('center_axis',(1.,0.,-5.33761069531325E-17));
#105029=DIRECTION('ref_axis',(-5.33761069531325E-17,0.,-1.));
#105030=DIRECTION('',(1.,0.,-2.89120579329468E-17));
#105031=DIRECTION('center_axis',(1.,0.,-2.96720509643778E-17));
#105032=DIRECTION('ref_axis',(-2.96720509643778E-17,0.,-1.));
#105033=DIRECTION('center_axis',(1.,0.,-2.89120579329468E-17));
#105034=DIRECTION('ref_axis',(-2.89120579329468E-17,0.,-1.));
#105035=DIRECTION('center_axis',(1.,0.,-5.33761069531325E-17));
#105036=DIRECTION('ref_axis',(-5.33761069531325E-17,0.,-1.));
#105037=DIRECTION('',(1.,0.,-2.89120579329468E-17));
#105038=DIRECTION('center_axis',(1.,0.,-2.89120579329468E-17));
#105039=DIRECTION('ref_axis',(-2.89120579329468E-17,0.,-1.));
#105040=DIRECTION('center_axis',(1.,0.,-2.89120579329468E-17));
#105041=DIRECTION('ref_axis',(-2.89120579329468E-17,0.,-1.));
#105042=DIRECTION('center_axis',(1.,0.,-5.33761069531325E-17));
#105043=DIRECTION('ref_axis',(-5.33761069531325E-17,0.,-1.));
#105044=DIRECTION('',(1.,0.,-2.89120579329468E-17));
#105045=DIRECTION('center_axis',(1.,0.,-2.89120579329468E-17));
#105046=DIRECTION('ref_axis',(-2.89120579329468E-17,0.,-1.));
#105047=DIRECTION('center_axis',(1.,0.,-2.89120579329468E-17));
#105048=DIRECTION('ref_axis',(-2.89120579329468E-17,0.,-1.));
#105049=DIRECTION('center_axis',(1.,0.,-5.33761069531325E-17));
#105050=DIRECTION('ref_axis',(-5.33761069531325E-17,0.,-1.));
#105051=DIRECTION('',(1.,0.,-2.89120579329468E-17));
#105052=DIRECTION('center_axis',(1.,0.,-2.96720509643778E-17));
#105053=DIRECTION('ref_axis',(-2.96720509643778E-17,0.,-1.));
#105054=DIRECTION('center_axis',(1.,0.,-2.89120579329468E-17));
#105055=DIRECTION('ref_axis',(-2.89120579329468E-17,0.,-1.));
#105056=DIRECTION('center_axis',(1.,0.,-5.33761069531325E-17));
#105057=DIRECTION('ref_axis',(-5.33761069531325E-17,0.,-1.));
#105058=DIRECTION('',(1.,0.,-2.89120579329468E-17));
#105059=DIRECTION('center_axis',(1.,0.,-2.96720509643778E-17));
#105060=DIRECTION('ref_axis',(-2.96720509643778E-17,0.,-1.));
#105061=DIRECTION('center_axis',(1.,0.,-2.89120579329468E-17));
#105062=DIRECTION('ref_axis',(-2.89120579329468E-17,0.,-1.));
#105063=DIRECTION('center_axis',(1.,0.,-5.33761069531325E-17));
#105064=DIRECTION('ref_axis',(-5.33761069531325E-17,0.,-1.));
#105065=DIRECTION('',(1.,0.,-2.89120579329468E-17));
#105066=DIRECTION('center_axis',(1.,0.,-2.96720509643778E-17));
#105067=DIRECTION('ref_axis',(-2.96720509643778E-17,0.,-1.));
#105068=DIRECTION('center_axis',(1.,0.,-2.89120579329468E-17));
#105069=DIRECTION('ref_axis',(-2.89120579329468E-17,0.,-1.));
#105070=DIRECTION('center_axis',(1.,0.,-5.33761069531325E-17));
#105071=DIRECTION('ref_axis',(-5.33761069531325E-17,0.,-1.));
#105072=DIRECTION('',(1.,0.,-2.89120579329468E-17));
#105073=DIRECTION('center_axis',(1.,0.,-2.96720509643778E-17));
#105074=DIRECTION('ref_axis',(-2.96720509643778E-17,0.,-1.));
#105075=DIRECTION('center_axis',(1.,0.,-2.89120579329468E-17));
#105076=DIRECTION('ref_axis',(-2.89120579329468E-17,0.,-1.));
#105077=DIRECTION('center_axis',(1.,0.,-5.33761069531325E-17));
#105078=DIRECTION('ref_axis',(-5.33761069531325E-17,0.,-1.));
#105079=DIRECTION('',(1.,0.,-2.89120579329468E-17));
#105080=DIRECTION('center_axis',(1.,0.,-2.96720509643778E-17));
#105081=DIRECTION('ref_axis',(-2.96720509643778E-17,0.,-1.));
#105082=DIRECTION('center_axis',(1.,0.,-2.89120579329468E-17));
#105083=DIRECTION('ref_axis',(-2.89120579329468E-17,0.,-1.));
#105084=DIRECTION('center_axis',(1.,0.,-5.33761069531325E-17));
#105085=DIRECTION('ref_axis',(-5.33761069531325E-17,0.,-1.));
#105086=DIRECTION('',(1.,0.,-2.89120579329468E-17));
#105087=DIRECTION('center_axis',(1.,0.,-2.96720509643778E-17));
#105088=DIRECTION('ref_axis',(-2.96720509643778E-17,0.,-1.));
#105089=DIRECTION('center_axis',(1.,0.,-2.89120579329468E-17));
#105090=DIRECTION('ref_axis',(-2.89120579329468E-17,0.,-1.));
#105091=DIRECTION('center_axis',(1.,0.,-5.33761069531325E-17));
#105092=DIRECTION('ref_axis',(-5.33761069531325E-17,0.,-1.));
#105093=DIRECTION('',(1.,0.,-2.89120579329468E-17));
#105094=DIRECTION('center_axis',(1.,0.,-2.96720509643778E-17));
#105095=DIRECTION('ref_axis',(-2.96720509643778E-17,0.,-1.));
#105096=DIRECTION('center_axis',(1.,0.,-2.89120579329468E-17));
#105097=DIRECTION('ref_axis',(-2.89120579329468E-17,0.,-1.));
#105098=DIRECTION('center_axis',(1.,0.,-5.33761069531325E-17));
#105099=DIRECTION('ref_axis',(-5.33761069531325E-17,0.,-1.));
#105100=DIRECTION('',(1.,0.,-2.89120579329468E-17));
#105101=DIRECTION('center_axis',(1.,0.,-2.96720509643778E-17));
#105102=DIRECTION('ref_axis',(-2.96720509643778E-17,0.,-1.));
#105103=DIRECTION('center_axis',(1.,0.,-2.89120579329468E-17));
#105104=DIRECTION('ref_axis',(-2.89120579329468E-17,0.,-1.));
#105105=DIRECTION('center_axis',(1.,0.,-5.33761069531325E-17));
#105106=DIRECTION('ref_axis',(-5.33761069531325E-17,0.,-1.));
#105107=DIRECTION('',(1.,0.,-2.89120579329468E-17));
#105108=DIRECTION('center_axis',(1.,0.,-2.96720509643778E-17));
#105109=DIRECTION('ref_axis',(-2.96720509643778E-17,0.,-1.));
#105110=DIRECTION('center_axis',(-1.,0.,0.));
#105111=DIRECTION('ref_axis',(0.,0.,1.));
#105112=DIRECTION('',(0.,0.,-1.));
#105113=DIRECTION('',(0.,-1.,0.));
#105114=DIRECTION('',(0.,0.,-1.));
#105115=DIRECTION('',(0.,-1.,0.));
#105116=DIRECTION('center_axis',(1.22464679914735E-16,0.,1.));
#105117=DIRECTION('ref_axis',(1.,0.,-1.22464679914735E-16));
#105118=DIRECTION('',(-1.,0.,1.22464679914735E-16));
#105119=DIRECTION('',(0.,1.,0.));
#105120=DIRECTION('',(-1.,0.,1.22464679914735E-16));
#105121=DIRECTION('center_axis',(1.,0.,-5.33761069531325E-17));
#105122=DIRECTION('ref_axis',(-5.33761069531325E-17,0.,-1.));
#105123=DIRECTION('',(5.33761069531325E-17,0.,1.));
#105124=DIRECTION('',(0.,1.,0.));
#105125=DIRECTION('',(5.33761069531325E-17,0.,1.));
#105126=DIRECTION('',(0.,-1.,0.));
#105127=DIRECTION('center_axis',(0.,0.,-1.));
#105128=DIRECTION('ref_axis',(-1.,0.,0.));
#105129=DIRECTION('',(1.,0.,0.));
#105130=DIRECTION('',(0.,-1.,0.));
#105131=DIRECTION('',(1.,0.,0.));
#105132=DIRECTION('',(0.,-1.,0.));
#105133=DIRECTION('center_axis',(-1.,0.,0.));
#105134=DIRECTION('ref_axis',(0.,0.,1.));
#105135=DIRECTION('',(0.,0.,-1.));
#105136=DIRECTION('',(0.,-1.,0.));
#105137=DIRECTION('',(0.,0.,-1.));
#105138=DIRECTION('center_axis',(0.,0.,1.));
#105139=DIRECTION('ref_axis',(1.,0.,0.));
#105140=DIRECTION('',(-1.,0.,0.));
#105141=DIRECTION('',(0.,1.,0.));
#105142=DIRECTION('',(-1.,0.,0.));
#105143=DIRECTION('center_axis',(-1.,0.,5.78241158658936E-17));
#105144=DIRECTION('ref_axis',(5.78241158658936E-17,0.,1.));
#105145=DIRECTION('',(-5.78241158658936E-17,0.,-1.));
#105146=DIRECTION('',(0.,1.,0.));
#105147=DIRECTION('',(-5.78241158658936E-17,0.,-1.));
#105148=DIRECTION('',(0.,-1.,0.));
#105149=DIRECTION('center_axis',(-7.70988211545248E-17,0.,-1.));
#105150=DIRECTION('ref_axis',(-1.,0.,7.70988211545248E-17));
#105151=DIRECTION('',(1.,0.,-7.70988211545248E-17));
#105152=DIRECTION('',(0.,-1.,0.));
#105153=DIRECTION('',(1.,0.,-7.70988211545248E-17));
#105154=DIRECTION('center_axis',(0.,1.,0.));
#105155=DIRECTION('ref_axis',(0.,0.,1.));
#105156=DIRECTION('center_axis',(0.,1.,0.));
#105157=DIRECTION('ref_axis',(0.,0.,1.));
#105158=DIRECTION('center_axis',(0.,-1.,0.));
#105159=DIRECTION('ref_axis',(0.,0.,1.));
#105160=DIRECTION('center_axis',(0.,-1.,0.));
#105161=DIRECTION('ref_axis',(0.,0.,1.));
#105162=DIRECTION('center_axis',(0.,1.,0.));
#105163=DIRECTION('ref_axis',(0.,0.,1.));
#105164=DIRECTION('center_axis',(0.,1.,0.));
#105165=DIRECTION('ref_axis',(0.,0.,1.));
#105166=DIRECTION('center_axis',(0.,-1.,0.));
#105167=DIRECTION('ref_axis',(0.,0.,1.));
#105168=DIRECTION('center_axis',(0.,-1.,0.));
#105169=DIRECTION('ref_axis',(0.,0.,1.));
#105170=DIRECTION('center_axis',(0.,1.,0.));
#105171=DIRECTION('ref_axis',(0.,0.,1.));
#105172=DIRECTION('center_axis',(0.,1.,0.));
#105173=DIRECTION('ref_axis',(0.,0.,1.));
#105174=DIRECTION('center_axis',(0.,-1.,0.));
#105175=DIRECTION('ref_axis',(0.,0.,-1.));
#105176=DIRECTION('center_axis',(0.,-1.,0.));
#105177=DIRECTION('ref_axis',(0.,0.,-1.));
#105178=DIRECTION('center_axis',(0.,1.,0.));
#105179=DIRECTION('ref_axis',(0.,0.,1.));
#105180=DIRECTION('center_axis',(0.,1.,0.));
#105181=DIRECTION('ref_axis',(0.,0.,1.));
#105182=DIRECTION('axis',(0.,0.,1.));
#105183=DIRECTION('refdir',(1.,0.,0.));
#105184=DIRECTION('center_axis',(0.,0.,-1.));
#105185=DIRECTION('ref_axis',(1.,0.,0.));
#105186=DIRECTION('center_axis',(0.,0.,1.));
#105187=DIRECTION('ref_axis',(-1.,0.,0.));
#105188=DIRECTION('',(0.707106781186552,-8.65956056235499E-17,0.707106781186543));
#105189=DIRECTION('center_axis',(0.,0.,-1.));
#105190=DIRECTION('ref_axis',(-1.,0.,0.));
#105191=DIRECTION('center_axis',(0.,0.,1.));
#105192=DIRECTION('ref_axis',(1.,0.,0.));
#105193=DIRECTION('center_axis',(0.,0.,-1.));
#105194=DIRECTION('ref_axis',(1.,0.,0.));
#105195=DIRECTION('center_axis',(0.,0.,-1.));
#105196=DIRECTION('ref_axis',(-1.,0.,0.));
#105197=DIRECTION('',(0.,0.,1.));
#105198=DIRECTION('center_axis',(0.,1.23467863058847E-16,-1.));
#105199=DIRECTION('ref_axis',(-1.,0.,0.));
#105200=DIRECTION('center_axis',(0.,0.,1.));
#105201=DIRECTION('ref_axis',(0.,1.,0.));
#105202=DIRECTION('center_axis',(0.,0.,-1.));
#105203=DIRECTION('ref_axis',(1.,0.,0.));
#105204=DIRECTION('center_axis',(0.,0.,-1.));
#105205=DIRECTION('ref_axis',(-1.,0.,0.));
#105206=DIRECTION('',(0.,0.,1.));
#105207=DIRECTION('center_axis',(0.,0.,1.));
#105208=DIRECTION('ref_axis',(1.,0.,0.));
#105209=DIRECTION('center_axis',(0.,0.,-1.));
#105210=DIRECTION('ref_axis',(-1.,0.,0.));
#105211=DIRECTION('center_axis',(0.,0.,-1.));
#105212=DIRECTION('ref_axis',(1.,0.,0.));
#105213=DIRECTION('',(-0.707106781186552,8.65956056235499E-17,0.707106781186543));
#105214=DIRECTION('center_axis',(0.,0.,1.));
#105215=DIRECTION('ref_axis',(1.,0.,0.));
#105216=DIRECTION('center_axis',(0.,0.,1.));
#105217=DIRECTION('ref_axis',(1.,0.,0.));
#105218=DIRECTION('center_axis',(0.,0.,-1.));
#105219=DIRECTION('ref_axis',(-1.,0.,0.));
#105220=DIRECTION('center_axis',(0.,0.,1.));
#105221=DIRECTION('ref_axis',(1.,0.,0.));
#105222=DIRECTION('',(0.,0.,1.));
#105223=DIRECTION('center_axis',(0.,1.23467863058847E-16,-1.));
#105224=DIRECTION('ref_axis',(-1.,0.,0.));
#105225=DIRECTION('center_axis',(0.,0.,-1.));
#105226=DIRECTION('ref_axis',(0.,1.,0.));
#105227=DIRECTION('center_axis',(0.,0.,-1.));
#105228=DIRECTION('ref_axis',(-1.,0.,0.));
#105229=DIRECTION('center_axis',(0.,0.,1.));
#105230=DIRECTION('ref_axis',(1.,0.,0.));
#105231=DIRECTION('',(0.,0.,1.));
#105232=DIRECTION('center_axis',(0.,0.,1.));
#105233=DIRECTION('ref_axis',(1.,0.,0.));
#105234=DIRECTION('center_axis',(0.,0.,-1.));
#105235=DIRECTION('ref_axis',(0.,1.,0.));
#105236=DIRECTION('',(-1.54660695142382E-33,-1.23467863058847E-16,1.));
#105237=DIRECTION('center_axis',(0.,0.,1.));
#105238=DIRECTION('ref_axis',(0.,1.,0.));
#105239=DIRECTION('',(0.,1.23467863058847E-16,-1.));
#105240=DIRECTION('center_axis',(0.,0.,1.));
#105241=DIRECTION('ref_axis',(1.,0.,0.));
#105242=DIRECTION('center_axis',(0.,0.,-1.));
#105243=DIRECTION('ref_axis',(0.,1.,0.));
#105244=DIRECTION('center_axis',(0.,0.,1.));
#105245=DIRECTION('ref_axis',(1.,0.,0.));
#105246=DIRECTION('',(0.,-1.23467863058847E-16,1.));
#105247=DIRECTION('center_axis',(0.,0.,1.));
#105248=DIRECTION('ref_axis',(0.,1.,0.));
#105249=DIRECTION('',(-5.86299591403052E-36,1.23467863058847E-16,-1.));
#105250=DIRECTION('center_axis',(0.,0.,-1.));
#105251=DIRECTION('ref_axis',(1.,0.,0.));
#105252=DIRECTION('center_axis',(-0.911086081553275,0.412216147184822,0.));
#105253=DIRECTION('ref_axis',(-0.412216147184823,-0.911086081553275,0.));
#105254=DIRECTION('center_axis',(-0.970284356147939,0.241967494127993,-1.34486472837252E-14));
#105255=DIRECTION('ref_axis',(-0.241967494127993,-0.970284356147939,-2.62269727666659E-30));
#105256=DIRECTION('center_axis',(0.,0.,-1.));
#105257=DIRECTION('ref_axis',(1.,-5.55111512312579E-15,0.));
#105258=DIRECTION('center_axis',(-0.919081670180344,0.0804092269952343,
-0.385776152389619));
#105259=DIRECTION('ref_axis',(-0.387029378450866,1.43097488374089E-17,0.922067383771889));
#105260=DIRECTION('center_axis',(5.61645494961161E-33,0.,-1.));
#105261=DIRECTION('ref_axis',(0.,1.,0.));
#105262=DIRECTION('',(-6.15711282612512E-33,-1.23467863058847E-16,1.));
#105263=DIRECTION('center_axis',(0.,0.,-1.));
#105264=DIRECTION('ref_axis',(0.,1.,0.));
#105265=DIRECTION('',(1.23259516440783E-32,1.23467863058847E-16,-1.));
#105266=DIRECTION('center_axis',(0.,0.,-1.));
#105267=DIRECTION('ref_axis',(0.,1.,0.));
#105268=DIRECTION('center_axis',(-0.0871557427476402,-0.996194698091747,
-1.22998030563942E-16));
#105269=DIRECTION('ref_axis',(-0.996194698091747,0.0871557427476402,1.12142775393191E-33));
#105270=DIRECTION('',(-0.996194698091747,0.0871557427476402,1.07609333103578E-17));
#105271=DIRECTION('',(-6.16356212163056E-32,1.23467863058847E-16,-1.));
#105272=DIRECTION('',(-0.996194698091747,0.0871557427476402,1.54074395550979E-33));
#105273=DIRECTION('',(6.16356212163056E-32,-1.23467863058847E-16,1.));
#105274=DIRECTION('',(-0.996194698091747,0.0871557427476402,1.07609333103578E-17));
#105275=DIRECTION('',(-6.16356212163056E-32,1.23467863058847E-16,-1.));
#105276=DIRECTION('',(0.996194698091747,-0.0871557427476402,0.));
#105277=DIRECTION('',(-0.996194698091747,0.0871557427476402,1.07609333103578E-17));
#105278=DIRECTION('',(1.13659195805196E-16,1.13523971920422E-16,-1.));
#105279=DIRECTION('',(-0.996194698091747,0.0871557427476402,1.54074395550979E-33));
#105280=DIRECTION('',(1.13659195805196E-16,-1.33411754197273E-16,1.));
#105281=DIRECTION('center_axis',(0.,1.23467863058847E-16,-1.));
#105282=DIRECTION('ref_axis',(0.,1.,0.));
#105283=DIRECTION('center_axis',(0.996194698091747,-0.0871557427476394,
-1.20952890408421E-15));
#105284=DIRECTION('ref_axis',(0.0871557427476394,0.996194698091747,1.39857739234396E-32));
#105285=DIRECTION('center_axis',(0.707106781186544,-0.707106781186551,0.));
#105286=DIRECTION('ref_axis',(0.707106781186551,0.707106781186544,0.));
#105287=DIRECTION('center_axis',(0.,0.,1.));
#105288=DIRECTION('ref_axis',(0.,1.,0.));
#105289=DIRECTION('center_axis',(-1.35502005093696E-32,0.,-1.));
#105290=DIRECTION('ref_axis',(0.,1.,0.));
#105291=DIRECTION('',(8.71576399210526E-33,-1.23467863058847E-16,1.));
#105292=DIRECTION('center_axis',(-2.85576800769162E-31,6.6052904065149E-46,
-1.));
#105293=DIRECTION('ref_axis',(2.31296463463574E-15,1.,3.11150763893057E-61));
#105294=DIRECTION('',(1.54660695142382E-33,1.23467863058847E-16,-1.));
#105295=DIRECTION('center_axis',(-2.85576800769162E-31,6.6052904065149E-46,
-1.));
#105296=DIRECTION('ref_axis',(2.31296463463574E-15,1.,3.11150763893057E-61));
#105297=DIRECTION('center_axis',(-0.707106781186548,-0.707106781186547,
-8.7304963227523E-17));
#105298=DIRECTION('ref_axis',(-0.707106781186547,0.707106781186548,3.47167550285579E-33));
#105299=DIRECTION('',(0.707106781186547,-0.707106781186548,0.));
#105300=DIRECTION('',(-0.707106781186547,0.707106781186548,8.73049632275231E-17));
#105301=DIRECTION('center_axis',(0.,1.23467863058847E-16,-1.));
#105302=DIRECTION('ref_axis',(0.,1.,0.));
#105303=DIRECTION('center_axis',(0.707106781186548,-0.707106781186548,0.));
#105304=DIRECTION('ref_axis',(0.707106781186548,0.707106781186548,0.));
#105305=DIRECTION('center_axis',(0.0871557427476394,-0.996194698091747,
0.));
#105306=DIRECTION('ref_axis',(0.996194698091747,0.0871557427476394,0.));
#105307=DIRECTION('center_axis',(0.,0.,1.));
#105308=DIRECTION('ref_axis',(0.,1.,0.));
#105309=DIRECTION('center_axis',(-0.996194698091747,-0.0871557427476402,
-1.07609333103578E-17));
#105310=DIRECTION('ref_axis',(-0.0871557427476402,0.996194698091747,1.81609423396931E-34));
#105311=DIRECTION('',(-0.0871557427476402,0.996194698091747,1.22998030563942E-16));
#105312=DIRECTION('',(1.08020383274181E-17,4.42963887209064E-33,-1.));
#105313=DIRECTION('',(-0.0871557427476402,0.996194698091747,0.));
#105314=DIRECTION('',(-1.08020383274181E-17,-4.42963887209064E-33,1.));
#105315=DIRECTION('',(-0.0871557427476402,0.996194698091747,1.22998030563942E-16));
#105316=DIRECTION('',(1.08020383274181E-17,4.42963887209064E-33,-1.));
#105317=DIRECTION('',(-0.0871557427476402,0.996194698091747,0.));
#105318=DIRECTION('',(-1.08020383274181E-17,-4.62223186652937E-33,1.));
#105319=DIRECTION('',(-0.0871557427476402,0.996194698091747,1.22998030563942E-16));
#105320=DIRECTION('',(0.0871557427476402,-0.996194698091747,0.));
#105321=DIRECTION('center_axis',(-0.996194698091748,-0.0871557427476319,
-1.23112093893486E-14));
#105322=DIRECTION('ref_axis',(0.0399152964550247,-0.45623392616117,-0.888964213975159));
#105323=DIRECTION('',(-1.08020383274181E-17,-4.42963887209064E-33,1.));
#105324=DIRECTION('center_axis',(0.,-1.38777878078144E-14,1.));
#105325=DIRECTION('ref_axis',(0.,1.,1.38777878078144E-14));
#105326=DIRECTION('center_axis',(0.999990739418254,-0.00427492665558239,
-0.00049606433434234));
#105327=DIRECTION('ref_axis',(0.00427492718156908,0.999990862457049,1.90763185875202E-22));
#105328=DIRECTION('center_axis',(0.,0.,-1.));
#105329=DIRECTION('ref_axis',(0.,1.,0.));
#105330=DIRECTION('center_axis',(0.,0.,1.));
#105331=DIRECTION('ref_axis',(1.,0.,0.));
#105332=DIRECTION('',(6.19323182390956E-32,-1.23467863058847E-16,1.));
#105333=DIRECTION('',(0.,1.23467863058847E-16,-1.));
#105334=DIRECTION('center_axis',(0.,-1.23467863058847E-16,1.));
#105335=DIRECTION('ref_axis',(0.,-1.,-1.21694324257719E-16));
#105336=DIRECTION('center_axis',(-1.73309037721552E-31,-1.19033121480991E-16,
1.));
#105337=DIRECTION('ref_axis',(3.90798504668055E-14,-1.,-1.19033121480991E-16));
#105338=DIRECTION('center_axis',(0.999944632572398,0.0105228573644618,3.55322387352642E-5));
#105339=DIRECTION('ref_axis',(0.00955105836032764,-0.906170827987028,-0.422803982702979));
#105340=DIRECTION('center_axis',(0.,1.18842113532929E-16,-1.));
#105341=DIRECTION('ref_axis',(0.,-1.,-1.18842113532929E-16));
#105342=DIRECTION('center_axis',(-0.998402993028371,-0.0564930323058765,
-2.85110252341697E-5));
#105343=DIRECTION('ref_axis',(0.0553356758873256,-0.977847117549328,-0.201873667610621));
#105344=DIRECTION('center_axis',(0.,0.,-1.));
#105345=DIRECTION('ref_axis',(0.,1.,0.));
#105346=DIRECTION('center_axis',(-5.55111512312579E-13,6.5495003047383E-14,
1.));
#105347=DIRECTION('ref_axis',(1.,7.99467207819295E-41,5.55111512312579E-13));
#105348=DIRECTION('',(-6.19323182390956E-32,1.23467863058847E-16,-1.));
#105349=DIRECTION('center_axis',(0.,0.,1.));
#105350=DIRECTION('ref_axis',(1.,0.,0.));
#105351=DIRECTION('center_axis',(0.,0.,1.));
#105352=DIRECTION('ref_axis',(1.,0.,0.));
#105353=DIRECTION('',(0.,-1.23467863058847E-16,1.));
#105354=DIRECTION('center_axis',(-5.55111512312579E-13,6.5495003047383E-14,
1.));
#105355=DIRECTION('ref_axis',(1.,7.99467207819295E-41,5.55111512312579E-13));
#105356=DIRECTION('center_axis',(-0.99074835547853,0.134685218959648,0.0166609696710313));
#105357=DIRECTION('ref_axis',(-0.13470391634661,-0.99088589399632,2.11341644556228E-18));
#105358=DIRECTION('center_axis',(0.003518046819505,0.149207652782245,-0.988799625656174));
#105359=DIRECTION('ref_axis',(-0.14424605496163,-0.978388820119907,-0.148149898050531));
#105360=DIRECTION('center_axis',(-0.989538255790606,0.14315195982541,0.0179320028170335));
#105361=DIRECTION('ref_axis',(-0.143174981115239,-0.989697390510176,-2.48873089681965E-18));
#105362=DIRECTION('center_axis',(-0.0109903293950669,-0.174043205665198,
0.98467668562913));
#105363=DIRECTION('ref_axis',(-0.115491862188353,-0.977924987362897,-0.174138878081674));
#105364=DIRECTION('center_axis',(0.,-1.38777878078144E-14,1.));
#105365=DIRECTION('ref_axis',(0.,1.,1.38777878078144E-14));
#105366=DIRECTION('center_axis',(0.,0.,-1.));
#105367=DIRECTION('ref_axis',(0.,1.,0.));
#105368=DIRECTION('center_axis',(0.,0.,1.));
#105369=DIRECTION('ref_axis',(1.,0.,0.));
#105370=DIRECTION('',(6.19323182390956E-32,-1.23467863058847E-16,1.));
#105371=DIRECTION('',(0.,1.23467863058847E-16,-1.));
#105372=DIRECTION('center_axis',(0.,-1.23467863058847E-16,1.));
#105373=DIRECTION('ref_axis',(0.,-1.,-1.21694324257719E-16));
#105374=DIRECTION('center_axis',(-6.69603100287811E-32,-1.19033121480991E-16,
1.));
#105375=DIRECTION('ref_axis',(1.50990331349022E-14,-1.,-1.19033121480991E-16));
#105376=DIRECTION('center_axis',(0.997043106246102,0.0768439138394239,0.00023915050274134));
#105377=DIRECTION('ref_axis',(0.0767329141488397,-0.995425758077136,-0.0569176602012574));
#105378=DIRECTION('center_axis',(0.,1.18842113532929E-16,-1.));
#105379=DIRECTION('ref_axis',(0.,-1.,-1.18842113532929E-16));
#105380=DIRECTION('center_axis',(-0.993203928613398,-0.116387082026082,
-5.76573235384675E-5));
#105381=DIRECTION('ref_axis',(0.115222785780397,-0.983198120721487,-0.141580948742201));
#105382=DIRECTION('center_axis',(0.,0.,-1.));
#105383=DIRECTION('ref_axis',(0.,1.,0.));
#105384=DIRECTION('center_axis',(0.,0.,1.));
#105385=DIRECTION('ref_axis',(1.,0.,0.));
#105386=DIRECTION('',(-6.19323182390956E-32,1.23467863058847E-16,-1.));
#105387=DIRECTION('center_axis',(0.,0.,1.));
#105388=DIRECTION('ref_axis',(1.,0.,0.));
#105389=DIRECTION('center_axis',(0.,0.,1.));
#105390=DIRECTION('ref_axis',(1.,0.,0.));
#105391=DIRECTION('',(0.,-1.23467863058847E-16,1.));
#105392=DIRECTION('center_axis',(-0.962140601075499,0.272553597962085,-1.24636926569648E-14));
#105393=DIRECTION('ref_axis',(-0.272553597962085,-0.962140601075499,-4.52904126028793E-31));
#105394=DIRECTION('center_axis',(0.,0.,-1.));
#105395=DIRECTION('ref_axis',(1.,0.,0.));
#105396=DIRECTION('center_axis',(0.,0.,-1.));
#105397=DIRECTION('ref_axis',(1.,0.,0.));
#105398=DIRECTION('center_axis',(-0.959694777166788,0.28104436425374,1.95400042656926E-13));
#105399=DIRECTION('ref_axis',(-0.28104436425374,-0.959694777166788,-3.56742184214581E-30));
#105400=DIRECTION('center_axis',(0.,0.,1.));
#105401=DIRECTION('ref_axis',(1.,0.,0.));
#105402=DIRECTION('center_axis',(0.,0.,1.));
#105403=DIRECTION('ref_axis',(1.,0.,0.));
#105404=DIRECTION('center_axis',(0.,0.,-1.));
#105405=DIRECTION('ref_axis',(0.,1.,0.));
#105406=DIRECTION('center_axis',(0.,0.,1.));
#105407=DIRECTION('ref_axis',(1.,0.,0.));
#105408=DIRECTION('',(6.19323182390956E-32,-1.23467863058847E-16,1.));
#105409=DIRECTION('',(0.,1.23467863058847E-16,-1.));
#105410=DIRECTION('center_axis',(0.,-1.23467863058847E-16,1.));
#105411=DIRECTION('ref_axis',(0.,-1.,-1.21694324257719E-16));
#105412=DIRECTION('center_axis',(-5.51437847295852E-32,-1.19033121480991E-16,
1.));
#105413=DIRECTION('ref_axis',(1.24344978758017E-14,-1.,-1.19033121480991E-16));
#105414=DIRECTION('center_axis',(0.991081580819709,0.133256151528742,0.000313432060176465));
#105415=DIRECTION('ref_axis',(0.133155408522202,-0.990235223988547,-0.0412775768866911));
#105416=DIRECTION('center_axis',(0.,1.18842113532929E-16,-1.));
#105417=DIRECTION('ref_axis',(0.,-1.,-1.18842113532929E-16));
#105418=DIRECTION('center_axis',(-0.986714641503604,-0.162462950731673,
-7.66940215737917E-5));
#105419=DIRECTION('ref_axis',(0.162365053105111,-0.986103455739161,-0.0351790293990564));
#105420=DIRECTION('center_axis',(0.,0.,-1.));
#105421=DIRECTION('ref_axis',(0.,1.,0.));
#105422=DIRECTION('center_axis',(0.,0.,1.));
#105423=DIRECTION('ref_axis',(1.,0.,0.));
#105424=DIRECTION('',(-6.19323182390956E-32,1.23467863058847E-16,-1.));
#105425=DIRECTION('center_axis',(0.,0.,1.));
#105426=DIRECTION('ref_axis',(1.,0.,0.));
#105427=DIRECTION('',(0.,-1.23467863058847E-16,1.));
#105428=DIRECTION('center_axis',(-0.911656491798923,0.41095308851605,-5.08035184938228E-15));
#105429=DIRECTION('ref_axis',(-0.41095308851605,-0.911656491798923,7.81754519040083E-31));
#105430=DIRECTION('center_axis',(0.,0.,-1.));
#105431=DIRECTION('ref_axis',(1.,0.,0.));
#105432=DIRECTION('center_axis',(0.,0.,-1.));
#105433=DIRECTION('ref_axis',(1.,0.,0.));
#105434=DIRECTION('center_axis',(0.,0.,1.));
#105435=DIRECTION('ref_axis',(1.,0.,0.));
#105436=DIRECTION('center_axis',(0.,0.,-1.));
#105437=DIRECTION('ref_axis',(0.,1.,0.));
#105438=DIRECTION('',(-1.54074395550979E-33,-1.23467863058847E-16,1.));
#105439=DIRECTION('center_axis',(0.,0.,1.));
#105440=DIRECTION('ref_axis',(0.,1.,0.));
#105441=DIRECTION('',(0.,1.23467863058847E-16,-1.));
#105442=DIRECTION('center_axis',(0.,1.23467863058847E-16,-1.));
#105443=DIRECTION('ref_axis',(0.,1.,1.21694324257719E-16));
#105444=DIRECTION('center_axis',(0.,-1.19212619247436E-16,1.));
#105445=DIRECTION('ref_axis',(0.,1.,1.19212619247436E-16));
#105446=DIRECTION('center_axis',(-0.913306614095669,-0.407272671129681,
-2.94898912583324E-15));
#105447=DIRECTION('ref_axis',(0.407272671129681,-0.913306614095669,-7.93980541862816E-31));
#105448=DIRECTION('center_axis',(4.39608526712911E-31,1.18842113532929E-16,
-1.));
#105449=DIRECTION('ref_axis',(-9.50350909079134E-14,1.,1.18842113532929E-16));
#105450=DIRECTION('center_axis',(0.,0.,-1.));
#105451=DIRECTION('ref_axis',(0.,1.,0.));
#105452=DIRECTION('center_axis',(0.,0.,-1.));
#105453=DIRECTION('ref_axis',(-1.,0.,0.));
#105454=DIRECTION('',(0.,1.23467863058847E-16,-1.));
#105455=DIRECTION('center_axis',(0.,0.,-1.));
#105456=DIRECTION('ref_axis',(-1.,0.,0.));
#105457=DIRECTION('',(0.,-1.23467863058847E-16,1.));
#105458=DIRECTION('center_axis',(-0.930967150605313,-0.365102950541111,
0.));
#105459=DIRECTION('ref_axis',(0.365102950541111,-0.930967150605313,0.));
#105460=DIRECTION('center_axis',(0.,0.,1.));
#105461=DIRECTION('ref_axis',(-1.,0.,0.));
#105462=DIRECTION('center_axis',(-0.934252508717439,-0.356612184249462,
0.));
#105463=DIRECTION('ref_axis',(0.356612184249462,-0.934252508717439,0.));
#105464=DIRECTION('center_axis',(0.,0.,1.));
#105465=DIRECTION('ref_axis',(-1.,-1.23459581198307E-13,0.));
#105466=DIRECTION('center_axis',(0.,0.,-1.));
#105467=DIRECTION('ref_axis',(-1.,0.,0.));
#105468=DIRECTION('center_axis',(0.,0.,1.));
#105469=DIRECTION('ref_axis',(1.,0.,0.));
#105470=DIRECTION('center_axis',(0.,0.,-1.));
#105471=DIRECTION('ref_axis',(-0.574616980402509,-0.818422461711006,0.));
#105472=DIRECTION('',(0.,1.23467863058847E-16,-1.));
#105473=DIRECTION('center_axis',(0.,0.,-1.));
#105474=DIRECTION('ref_axis',(-1.,0.,0.));
#105475=DIRECTION('',(1.87032180698308E-16,-1.23467863058847E-16,1.));
#105476=DIRECTION('center_axis',(0.,-1.23467863058847E-16,1.));
#105477=DIRECTION('ref_axis',(0.,-1.,-1.21694324257719E-16));
#105478=DIRECTION('center_axis',(0.,-1.19033121480991E-16,1.));
#105479=DIRECTION('ref_axis',(0.,-1.,-1.19033121480991E-16));
#105480=DIRECTION('center_axis',(-0.989231081512618,0.146362093675256,-7.00312215489063E-5));
#105481=DIRECTION('ref_axis',(0.145905880903543,0.986109658115763,-0.0793676010004968));
#105482=DIRECTION('center_axis',(0.,1.18842113532929E-16,-1.));
#105483=DIRECTION('ref_axis',(0.,-1.,-1.18842113532929E-16));
#105484=DIRECTION('center_axis',(0.993897575431132,-0.11030651249529,0.000287842394383403));
#105485=DIRECTION('ref_axis',(0.11019840995775,0.99280107613086,-0.0469290280763431));
#105486=DIRECTION('center_axis',(0.,0.,-1.));
#105487=DIRECTION('ref_axis',(0.,1.,0.));
#105488=DIRECTION('center_axis',(2.7755575615626E-13,-5.13478148889134E-13,
-1.));
#105489=DIRECTION('ref_axis',(1.14794370197489E-40,-1.,5.13478148889134E-13));
#105490=DIRECTION('',(0.,1.23467863058847E-16,-1.));
#105491=DIRECTION('center_axis',(0.,0.,-1.));
#105492=DIRECTION('ref_axis',(-1.,0.,0.));
#105493=DIRECTION('',(0.,-1.23467863058847E-16,1.));
#105494=DIRECTION('center_axis',(-0.974807460973989,-0.220687770576049,
0.0323623538639763));
#105495=DIRECTION('ref_axis',(0.220803427003966,-0.975318330917298,-7.28333184199878E-18));
#105496=DIRECTION('center_axis',(-0.976728808322011,-0.212349635823786,
0.0301407889639504));
#105497=DIRECTION('ref_axis',(0.212446157929364,-0.977172773863994,-1.17576428045677E-20));
#105498=DIRECTION('center_axis',(-0.049502590584409,0.39010562996265,0.91943846504096));
#105499=DIRECTION('ref_axis',(-0.184301157644048,0.901190701629574,-0.392286123368467));
#105500=DIRECTION('center_axis',(0.0251527414239362,-0.254018072308455,
-0.966872358969661));
#105501=DIRECTION('ref_axis',(-0.21303056621937,0.943601106365043,-0.253446108518006));
#105502=DIRECTION('center_axis',(0.,1.38777878078144E-14,1.));
#105503=DIRECTION('ref_axis',(0.,1.,-1.38777878078144E-14));
#105504=DIRECTION('center_axis',(0.,0.,-1.));
#105505=DIRECTION('ref_axis',(-0.634315526883886,-0.773074260568814,0.));
#105506=DIRECTION('center_axis',(0.,0.,1.));
#105507=DIRECTION('ref_axis',(1.,0.,0.));
#105508=DIRECTION('',(1.87032180698308E-16,-1.23467863058847E-16,1.));
#105509=DIRECTION('',(0.,1.23467863058847E-16,-1.));
#105510=DIRECTION('center_axis',(0.,-1.23467863058847E-16,1.));
#105511=DIRECTION('ref_axis',(0.,-1.,-1.21694324257719E-16));
#105512=DIRECTION('center_axis',(0.,-1.19033121480991E-16,1.));
#105513=DIRECTION('ref_axis',(0.,-1.,-1.19033121480991E-16));
#105514=DIRECTION('center_axis',(-0.995792071114552,0.0916414155502236,
-4.54020018912243E-5));
#105515=DIRECTION('ref_axis',(0.0902737810735944,0.980845595415019,-0.172605221258321));
#105516=DIRECTION('center_axis',(0.,1.18842113532929E-16,-1.));
#105517=DIRECTION('ref_axis',(0.,-1.,-1.18842113532929E-16));
#105518=DIRECTION('center_axis',(0.99894947983821,-0.0458248384975214,0.000144594765933473));
#105519=DIRECTION('ref_axis',(0.0458248568623928,0.998949481468877,-0.000126359025533782));
#105520=DIRECTION('center_axis',(0.,0.,-1.));
#105521=DIRECTION('ref_axis',(0.,1.,0.));
#105522=DIRECTION('center_axis',(0.,0.,-1.));
#105523=DIRECTION('ref_axis',(-1.,0.,0.));
#105524=DIRECTION('',(0.,1.23467863058847E-16,-1.));
#105525=DIRECTION('center_axis',(0.,0.,-1.));
#105526=DIRECTION('ref_axis',(-1.,0.,0.));
#105527=DIRECTION('',(0.,-1.23467863058847E-16,1.));
#105528=DIRECTION('center_axis',(-0.996993498376656,-0.0769676640255834,
0.00894107874490511));
#105529=DIRECTION('ref_axis',(0.07697074071877,-0.997033352036532,7.99587428479913E-19));
#105530=DIRECTION('center_axis',(-0.997624402707396,-0.0684293228260734,
0.00793592466417746));
#105531=DIRECTION('ref_axis',(0.0684314777296081,-0.997655818835204,-3.0788904879186E-19));
#105532=DIRECTION('center_axis',(-0.00150472629281886,0.0576832079807129,
0.998333803552618));
#105533=DIRECTION('ref_axis',(-0.0662281834101546,0.996137339756707,-0.0576561190561847));
#105534=DIRECTION('center_axis',(0.000120245183265025,-0.117893637115676,
-0.993026221138562));
#105535=DIRECTION('ref_axis',(-0.0688956039870738,0.990665697053924,-0.117621734521805));
#105536=DIRECTION('center_axis',(0.,-4.63518112781003E-12,1.));
#105537=DIRECTION('ref_axis',(0.,1.,4.63518112781003E-12));
#105538=DIRECTION('center_axis',(0.,0.,-1.));
#105539=DIRECTION('ref_axis',(-0.688859710772107,-0.724894681229604,0.));
#105540=DIRECTION('center_axis',(0.,0.,1.));
#105541=DIRECTION('ref_axis',(1.,0.,0.));
#105542=DIRECTION('',(1.87032180698308E-16,-1.23467863058847E-16,1.));
#105543=DIRECTION('',(0.,1.23467863058847E-16,-1.));
#105544=DIRECTION('center_axis',(-0.0690733635565107,0.78951215817867,0.609835570080205));
#105545=DIRECTION('ref_axis',(-3.95541556389227E-18,0.611295598907861,-0.791402357057319));
#105546=DIRECTION('center_axis',(-0.222999209171599,0.974818625544692,0.));
#105547=DIRECTION('ref_axis',(-0.974818625544692,-0.222999209171599,0.));
#105548=DIRECTION('center_axis',(0.,0.,-1.));
#105549=DIRECTION('ref_axis',(1.,0.,0.));
#105550=DIRECTION('center_axis',(-0.334110320282714,0.942533974921107,0.));
#105551=DIRECTION('ref_axis',(-0.942533974921107,-0.334110320282714,0.));
#105552=DIRECTION('center_axis',(0.,0.,-1.));
#105553=DIRECTION('ref_axis',(1.,-1.5419764230905E-14,0.));
#105554=DIRECTION('center_axis',(-0.388071473886494,0.870248040119286,-0.303428541544968));
#105555=DIRECTION('ref_axis',(-0.913306614096678,-0.407272671127417,-4.84423453041484E-17));
#105556=DIRECTION('center_axis',(0.,0.,-1.));
#105557=DIRECTION('ref_axis',(0.,1.,0.));
#105558=DIRECTION('',(0.,-1.23467863058847E-16,1.));
#105559=DIRECTION('center_axis',(0.,0.,1.));
#105560=DIRECTION('ref_axis',(0.,1.,0.));
#105561=DIRECTION('',(0.,1.23467863058847E-16,-1.));
#105562=DIRECTION('center_axis',(0.,0.,1.));
#105563=DIRECTION('ref_axis',(1.,0.,0.));
#105564=DIRECTION('center_axis',(-0.886046769573674,0.368569282539184,0.281207763222511));
#105565=DIRECTION('ref_axis',(0.259553330905099,-0.108212392885459,0.959646886329587));
#105566=DIRECTION('center_axis',(0.,1.18842113532929E-16,-1.));
#105567=DIRECTION('ref_axis',(0.,1.,1.18842113532929E-16));
#105568=DIRECTION('center_axis',(0.,0.,-1.));
#105569=DIRECTION('ref_axis',(1.,1.78263170299393E-15,0.));
#105570=DIRECTION('',(0.,-1.23467863058847E-16,1.));
#105571=DIRECTION('center_axis',(0.,1.18842113532929E-16,-1.));
#105572=DIRECTION('ref_axis',(0.,-1.,-1.18842113532929E-16));
#105573=DIRECTION('',(0.,1.23467863058847E-16,-1.));
#105574=DIRECTION('center_axis',(0.,0.,-1.));
#105575=DIRECTION('ref_axis',(1.,0.,0.));
#105576=DIRECTION('',(0.,-1.23467863058847E-16,1.));
#105577=DIRECTION('center_axis',(0.,1.18842113532929E-16,-1.));
#105578=DIRECTION('ref_axis',(0.,-1.,-1.18842113532929E-16));
#105579=DIRECTION('',(0.,1.23467863058847E-16,-1.));
#105580=DIRECTION('center_axis',(0.14258112270268,-0.00286725800189432,
-0.989778966376026));
#105581=DIRECTION('ref_axis',(-0.97964031348631,0.142384138292289,-0.141533082193549));
#105582=DIRECTION('',(0.,-1.23467863058847E-16,1.));
#105583=DIRECTION('center_axis',(0.,1.18842113532929E-16,-1.));
#105584=DIRECTION('ref_axis',(0.,-1.,-1.18842113532929E-16));
#105585=DIRECTION('',(0.,1.23467863058847E-16,-1.));
#105586=DIRECTION('center_axis',(0.115833335784744,6.92921622240005E-10,
-0.993268663716408));
#105587=DIRECTION('ref_axis',(-0.99326587756307,0.00236855704116508,-0.115833010866533));
#105588=DIRECTION('',(0.,-1.23467863058847E-16,1.));
#105589=DIRECTION('center_axis',(0.,1.18842113532929E-16,-1.));
#105590=DIRECTION('ref_axis',(0.,-1.,-1.18842113532929E-16));
#105591=DIRECTION('',(0.,1.23467863058847E-16,-1.));
#105592=DIRECTION('center_axis',(0.145269618857488,0.00325155863830722,
-0.989386762193341));
#105593=DIRECTION('ref_axis',(-0.979906495318529,-0.13766658060369,-0.144330083549635));
#105594=DIRECTION('',(0.,-1.23467863058847E-16,1.));
#105595=DIRECTION('center_axis',(0.,1.18842113532929E-16,-1.));
#105596=DIRECTION('ref_axis',(0.,-1.,-1.18842113532929E-16));
#105597=DIRECTION('',(0.,1.23467863058847E-16,-1.));
#105598=DIRECTION('center_axis',(0.,0.,-1.));
#105599=DIRECTION('ref_axis',(1.,0.,0.));
#105600=DIRECTION('',(0.,-1.23467863058847E-16,1.));
#105601=DIRECTION('center_axis',(0.,1.18842113532929E-16,-1.));
#105602=DIRECTION('ref_axis',(0.,-1.,-1.18842113532929E-16));
#105603=DIRECTION('',(0.,1.23467863058847E-16,-1.));
#105604=DIRECTION('center_axis',(-0.384110320270104,-0.923287204428827,
0.));
#105605=DIRECTION('ref_axis',(0.923287204428827,-0.384110320270104,0.));
#105606=DIRECTION('center_axis',(-0.405419774737912,-0.90915150463265,-0.0952803645860425));
#105607=DIRECTION('ref_axis',(0.913306614095667,-0.407272671129684,-4.7539503937481E-18));
#105608=DIRECTION('center_axis',(0.,0.,-1.));
#105609=DIRECTION('ref_axis',(1.,0.,0.));
#105610=DIRECTION('center_axis',(0.272999209159005,0.962014257585904,0.));
#105611=DIRECTION('ref_axis',(-0.962014257585904,0.272999209159004,0.));
#105612=DIRECTION('center_axis',(0.,0.,-1.));
#105613=DIRECTION('ref_axis',(1.,2.69845874040837E-15,0.));
#105614=DIRECTION('center_axis',(0.0479130906931042,0.547649132616206,-0.835335120346889));
#105615=DIRECTION('ref_axis',(-2.39380283931159E-17,-0.836295598856108,
-0.54827882626808));
#105616=DIRECTION('center_axis',(4.26141870503966E-34,0.,-1.));
#105617=DIRECTION('ref_axis',(0.,1.,0.));
#105618=DIRECTION('',(0.,-1.23467863058847E-16,1.));
#105619=DIRECTION('center_axis',(-2.85576800769162E-31,6.6052904065149E-46,
-1.));
#105620=DIRECTION('ref_axis',(2.31296463463574E-15,1.,3.11150763893057E-61));
#105621=DIRECTION('',(-1.23259516440783E-32,1.23467863058847E-16,-1.));
#105622=DIRECTION('center_axis',(-2.85576800769162E-31,6.6052904065149E-46,
-1.));
#105623=DIRECTION('ref_axis',(2.31296463463574E-15,1.,3.11150763893057E-61));
#105624=DIRECTION('center_axis',(-0.996194698091746,0.0871557427476566,
1.07609333103598E-17));
#105625=DIRECTION('ref_axis',(1.08020383274202E-17,1.24308539071746E-35,
1.));
#105626=DIRECTION('',(0.0871557427476566,0.996194698091746,1.22998030563941E-16));
#105627=DIRECTION('',(-1.08020383274202E-17,-4.37133056147834E-33,-1.));
#105628=DIRECTION('',(0.0871557427476566,0.996194698091746,0.));
#105629=DIRECTION('',(1.08020383274202E-17,4.37133056147834E-33,1.));
#105630=DIRECTION('',(0.0871557427476566,0.996194698091746,1.22998030563941E-16));
#105631=DIRECTION('',(-1.08020383274202E-17,-4.37133056147834E-33,-1.));
#105632=DIRECTION('center_axis',(-0.996194698091723,0.0871557427479135,
1.21464724749175E-13));
#105633=DIRECTION('ref_axis',(-0.0257890725821804,-0.294770448454491,0.955220030387392));
#105634=DIRECTION('',(-0.0871557427476566,-0.996194698091746,-3.51482972517089E-16));
#105635=DIRECTION('',(0.0871557427476566,0.996194698091746,1.22998030563941E-16));
#105636=DIRECTION('',(-1.08020383274202E-17,-4.56392355591706E-33,-1.));
#105637=DIRECTION('',(0.0871557427476566,0.996194698091746,0.));
#105638=DIRECTION('',(1.08020383274202E-17,4.37133056147834E-33,1.));
#105639=DIRECTION('center_axis',(0.,1.23467863058847E-16,-1.));
#105640=DIRECTION('ref_axis',(0.,1.,0.));
#105641=DIRECTION('center_axis',(-0.0871557427476572,-0.996194698091746,
0.));
#105642=DIRECTION('ref_axis',(0.996194698091746,-0.0871557427476572,0.));
#105643=DIRECTION('center_axis',(-0.707106781186544,-0.707106781186551,
0.));
#105644=DIRECTION('ref_axis',(0.707106781186551,-0.707106781186544,0.));
#105645=DIRECTION('center_axis',(0.,0.,1.));
#105646=DIRECTION('ref_axis',(0.,1.,0.));
#105647=DIRECTION('center_axis',(1.67127905768941E-33,0.,-1.));
#105648=DIRECTION('ref_axis',(0.,1.,0.));
#105649=DIRECTION('',(1.23259516440783E-32,-1.23467863058847E-16,1.));
#105650=DIRECTION('center_axis',(5.71153601538325E-31,2.64211616260596E-45,
-1.));
#105651=DIRECTION('ref_axis',(-4.62592926927148E-15,1.,1.24460305557223E-60));
#105652=DIRECTION('',(3.08148791101958E-33,1.23467863058847E-16,-1.));
#105653=DIRECTION('center_axis',(5.71153601538325E-31,2.64211616260596E-45,
-1.));
#105654=DIRECTION('ref_axis',(-4.62592926927148E-15,1.,1.24460305557223E-60));
#105655=DIRECTION('center_axis',(-0.707106781186548,0.707106781186547,8.73049632275231E-17));
#105656=DIRECTION('ref_axis',(1.23467863058847E-16,2.16153073061992E-33,
1.));
#105657=DIRECTION('',(-0.707106781186547,-0.707106781186548,0.));
#105658=DIRECTION('',(0.707106781186547,0.707106781186548,8.73049632275231E-17));
#105659=DIRECTION('center_axis',(0.,1.23467863058847E-16,-1.));
#105660=DIRECTION('ref_axis',(0.,1.,0.));
#105661=DIRECTION('center_axis',(-0.707106781186548,-0.707106781186548,
0.));
#105662=DIRECTION('ref_axis',(0.707106781186548,-0.707106781186548,0.));
#105663=DIRECTION('center_axis',(-0.996194698091746,-0.0871557427476538,
0.));
#105664=DIRECTION('ref_axis',(0.0871557427476538,-0.996194698091746,0.));
#105665=DIRECTION('center_axis',(0.,0.,1.));
#105666=DIRECTION('ref_axis',(0.,1.,0.));
#105667=DIRECTION('center_axis',(-0.0871557427476569,0.996194698091746,
1.22998030563941E-16));
#105668=DIRECTION('ref_axis',(1.41124413247282E-15,-4.52989727324155E-33,
1.));
#105669=DIRECTION('',(0.996194698091746,0.0871557427476568,1.07609333103598E-17));
#105670=DIRECTION('',(-1.87032180698308E-16,1.07104667533214E-16,-1.));
#105671=DIRECTION('',(0.996194698091746,0.0871557427476568,1.54074395550979E-33));
#105672=DIRECTION('',(5.23852944873328E-32,-1.23467863058847E-16,1.));
#105673=DIRECTION('',(0.996194698091746,0.0871557427476568,1.07609333103598E-17));
#105674=DIRECTION('',(-0.996194698091746,-0.0871557427476568,0.));
#105675=DIRECTION('',(-1.87032180698308E-16,1.07104667533214E-16,-1.));
#105676=DIRECTION('',(0.996194698091746,0.0871557427476568,1.54074395550979E-33));
#105677=DIRECTION('',(-1.54074395550979E-33,-1.23467863058847E-16,1.));
#105678=DIRECTION('center_axis',(0.,0.,-1.));
#105679=DIRECTION('ref_axis',(-1.,0.,0.));
#105680=DIRECTION('center_axis',(0.,0.,-1.));
#105681=DIRECTION('ref_axis',(0.,1.,0.));
#105682=DIRECTION('center_axis',(0.,0.,-1.));
#105683=DIRECTION('ref_axis',(-1.,0.,0.));
#105684=DIRECTION('',(-5.16102651992463E-32,-2.15733828054269E-47,1.));
#105685=DIRECTION('center_axis',(0.,-1.23467863058847E-16,1.));
#105686=DIRECTION('ref_axis',(0.,-1.,-1.21694324257719E-16));
#105687=DIRECTION('center_axis',(9.84710441599736E-32,-1.19033121480991E-16,
1.));
#105688=DIRECTION('ref_axis',(-2.22044604925031E-14,-1.,-1.19033121480991E-16));
#105689=DIRECTION('center_axis',(-0.162977314581735,-0.986629813581626,
-7.67047044552073E-5));
#105690=DIRECTION('ref_axis',(0.982479968620953,-0.162284694779714,-0.0916339953228362));
#105691=DIRECTION('center_axis',(0.133849112401615,0.991001679892255,0.000292506460560356));
#105692=DIRECTION('ref_axis',(0.990279721870948,-0.133762854809558,0.0381257278539607));
#105693=DIRECTION('center_axis',(0.,0.,-1.));
#105694=DIRECTION('ref_axis',(0.,1.,0.));
#105695=DIRECTION('center_axis',(0.,0.,-1.));
#105696=DIRECTION('ref_axis',(-1.,0.,0.));
#105697=DIRECTION('',(5.16102651992463E-32,2.15733828054269E-47,-1.));
#105698=DIRECTION('center_axis',(0.,0.,-1.));
#105699=DIRECTION('ref_axis',(-1.,0.,0.));
#105700=DIRECTION('center_axis',(0.282954786668892,-0.959133248668381,0.));
#105701=DIRECTION('ref_axis',(0.959133248668381,0.282954786668892,0.));
#105702=DIRECTION('center_axis',(0.,0.,-1.));
#105703=DIRECTION('ref_axis',(1.,0.,0.));
#105704=DIRECTION('center_axis',(0.274464020377229,-0.96159736975429,0.));
#105705=DIRECTION('ref_axis',(0.96159736975429,0.274464020377229,0.));
#105706=DIRECTION('center_axis',(0.,0.,1.));
#105707=DIRECTION('ref_axis',(1.,0.,0.));
#105708=DIRECTION('center_axis',(0.,0.,1.));
#105709=DIRECTION('ref_axis',(1.,0.,0.));
#105710=DIRECTION('center_axis',(0.,0.,-1.));
#105711=DIRECTION('ref_axis',(0.,1.,0.));
#105712=DIRECTION('center_axis',(0.,0.,1.));
#105713=DIRECTION('ref_axis',(1.,0.,0.));
#105714=DIRECTION('',(-5.16102651992463E-32,-2.15733828054269E-47,1.));
#105715=DIRECTION('center_axis',(0.,-1.23467863058847E-16,1.));
#105716=DIRECTION('ref_axis',(0.,-1.,-1.21694324257719E-16));
#105717=DIRECTION('center_axis',(0.,-1.19033121480991E-16,1.));
#105718=DIRECTION('ref_axis',(0.,-1.,-1.19033121480991E-16));
#105719=DIRECTION('center_axis',(-0.117127826816072,-0.99311684553817,-5.73904025634227E-5));
#105720=DIRECTION('ref_axis',(0.983475565813904,-0.115998770283216,0.138996750824625));
#105721=DIRECTION('center_axis',(0.0776595476784529,0.996979910344055,0.000230271010090371));
#105722=DIRECTION('ref_axis',(0.995508289094979,-0.0775574567760436,0.05429629123265));
#105723=DIRECTION('center_axis',(0.,0.,-1.));
#105724=DIRECTION('ref_axis',(0.,1.,0.));
#105725=DIRECTION('center_axis',(0.,0.,1.));
#105726=DIRECTION('ref_axis',(1.,0.,0.));
#105727=DIRECTION('center_axis',(1.18805075949821E-12,-7.25808302348696E-12,
1.));
#105728=DIRECTION('ref_axis',(5.87747175411144E-39,1.,7.25808302348696E-12));
#105729=DIRECTION('',(5.16102651992463E-32,2.15733828054269E-47,-1.));
#105730=DIRECTION('center_axis',(-0.14514509610524,0.989248239790814,-0.0179114808817288));
#105731=DIRECTION('ref_axis',(-0.989406963861029,-0.145168384517086,-1.21343959465114E-18));
#105732=DIRECTION('center_axis',(-0.136675079747296,0.990475586151279,-0.0166744059669382));
#105733=DIRECTION('ref_axis',(-0.990613308713893,-0.136694083993833,9.06110283290218E-19));
#105734=DIRECTION('center_axis',(-0.16767237013086,-0.0112896091060275,
0.98577812971324));
#105735=DIRECTION('ref_axis',(-0.977934730745161,-0.124494525481806,-0.167764047183683));
#105736=DIRECTION('center_axis',(6.61970478432749E-12,0.,1.));
#105737=DIRECTION('ref_axis',(1.,0.,-6.61970478432749E-12));
#105738=DIRECTION('center_axis',(0.,0.,-1.));
#105739=DIRECTION('ref_axis',(0.,1.,0.));
#105740=DIRECTION('center_axis',(0.,0.,1.));
#105741=DIRECTION('ref_axis',(1.,0.,0.));
#105742=DIRECTION('',(-5.16102651992463E-32,-2.15733828054269E-47,1.));
#105743=DIRECTION('center_axis',(0.,-1.23467863058847E-16,1.));
#105744=DIRECTION('ref_axis',(0.,-1.,-1.21694324257719E-16));
#105745=DIRECTION('center_axis',(-1.96942088319945E-31,-1.19033121480991E-16,
1.));
#105746=DIRECTION('ref_axis',(4.44089209850063E-14,-1.,-1.19033121480991E-16));
#105747=DIRECTION('center_axis',(-0.0573840568526241,-0.998352176938356,
-2.86632424776913E-5));
#105748=DIRECTION('ref_axis',(0.978156398817009,-0.0562289739133945,0.200120868342077));
#105749=DIRECTION('center_axis',(0.0114617529384933,0.99993431126188,3.71591962562455E-5));
#105750=DIRECTION('ref_axis',(-0.999934311920365,0.0114617532273491,-7.56982004799599E-6));
#105751=DIRECTION('center_axis',(0.,0.,-1.));
#105752=DIRECTION('ref_axis',(0.,1.,0.));
#105753=DIRECTION('center_axis',(0.,0.,1.));
#105754=DIRECTION('ref_axis',(1.,0.,0.));
#105755=DIRECTION('center_axis',(0.,0.,1.));
#105756=DIRECTION('ref_axis',(1.,0.,0.));
#105757=DIRECTION('',(5.16102651992463E-32,2.15733828054269E-47,-1.));
#105758=DIRECTION('center_axis',(-0.00620231251671424,0.999980508301815,
-0.000717172147678158));
#105759=DIRECTION('ref_axis',(-0.999980765464846,-0.00620231411175082,5.84684475171815E-22));
#105760=DIRECTION('center_axis',(0.00235261362124023,0.999997195602435,
0.000272022820600068));
#105761=DIRECTION('ref_axis',(-0.999997232600541,0.00235261370828272,8.12493746167259E-22));
#105762=DIRECTION('center_axis',(-0.0305144215778958,-2.78804702901659E-8,
0.999534326612031));
#105763=DIRECTION('ref_axis',(-0.99952008198814,-0.00533875532879332,-0.0305139868578466));
#105764=DIRECTION('center_axis',(3.91353616180368E-12,0.,1.));
#105765=DIRECTION('ref_axis',(1.,0.,-3.91353616180368E-12));
#105766=DIRECTION('center_axis',(0.,0.,-1.));
#105767=DIRECTION('ref_axis',(0.,1.,0.));
#105768=DIRECTION('center_axis',(0.,0.,1.));
#105769=DIRECTION('ref_axis',(1.,0.,0.));
#105770=DIRECTION('',(-5.16102651992463E-32,-2.15733828054269E-47,1.));
#105771=DIRECTION('center_axis',(0.,-1.23467863058847E-16,1.));
#105772=DIRECTION('ref_axis',(0.,-1.,-1.21694324257719E-16));
#105773=DIRECTION('center_axis',(0.,-1.19033121480991E-16,1.));
#105774=DIRECTION('ref_axis',(0.,-1.,-1.19033121480991E-16));
#105775=DIRECTION('center_axis',(0.00957667179610246,-0.999954142104087,
3.23448419023486E-5));
#105776=DIRECTION('ref_axis',(-0.906194367619744,-0.0086923991525787,-0.422772054766189));
#105777=DIRECTION('center_axis',(-0.055599347306662,0.998453159538039,-2.80638595116041E-5));
#105778=DIRECTION('ref_axis',(0.977793822426841,0.0544546102272507,0.202370789020812));
#105779=DIRECTION('center_axis',(0.,0.,-1.));
#105780=DIRECTION('ref_axis',(0.,1.,0.));
#105781=DIRECTION('center_axis',(0.,0.,1.));
#105782=DIRECTION('ref_axis',(1.,0.,0.));
#105783=DIRECTION('center_axis',(0.,0.,1.));
#105784=DIRECTION('ref_axis',(1.,0.,0.));
#105785=DIRECTION('',(5.16102651992463E-32,2.15733828054269E-47,-1.));
#105786=DIRECTION('center_axis',(0.132860127107541,0.991003467296,0.0161342626814395));
#105787=DIRECTION('ref_axis',(-0.991132478736687,0.132877423188709,7.57324997548269E-19));
#105788=DIRECTION('center_axis',(0.141334929101325,0.989809819863889,0.0173481502454526));
#105789=DIRECTION('ref_axis',(-0.989958799240908,0.1413562018643,-1.53957070961197E-18));
#105790=DIRECTION('center_axis',(-0.159896444557162,0.0103428845664614,
0.987079607608638));
#105791=DIRECTION('ref_axis',(-0.980515938222932,0.113929190724357,-0.16002698019927));
#105792=DIRECTION('center_axis',(0.,0.,1.));
#105793=DIRECTION('ref_axis',(1.,0.,0.));
#105794=DIRECTION('center_axis',(0.,0.,-1.));
#105795=DIRECTION('ref_axis',(0.,1.,0.));
#105796=DIRECTION('center_axis',(0.,0.,1.));
#105797=DIRECTION('ref_axis',(1.,0.,0.));
#105798=DIRECTION('',(-5.16102651992463E-32,-2.15733828054269E-47,1.));
#105799=DIRECTION('center_axis',(0.,-1.23467863058847E-16,1.));
#105800=DIRECTION('ref_axis',(0.,-1.,-1.21694324257719E-16));
#105801=DIRECTION('center_axis',(-4.72661011967866E-32,-1.19033121480991E-16,
1.));
#105802=DIRECTION('ref_axis',(1.06581410364015E-14,-1.,-1.19033121480991E-16));
#105803=DIRECTION('center_axis',(0.0759780984300171,-0.997109458589618,
0.000236960074453804));
#105804=DIRECTION('ref_axis',(0.995484288532962,0.0758678217481024,0.0570535266852247));
#105805=DIRECTION('center_axis',(-0.115641121459685,0.993291058926343,-5.73108184457433E-5));
#105806=DIRECTION('ref_axis',(0.983116729805053,0.114464840497617,0.142756071209856));
#105807=DIRECTION('center_axis',(0.,0.,-1.));
#105808=DIRECTION('ref_axis',(0.,1.,0.));
#105809=DIRECTION('center_axis',(0.,0.,-1.));
#105810=DIRECTION('ref_axis',(-1.,0.,0.));
#105811=DIRECTION('',(5.16102651992463E-32,2.15733828054269E-47,-1.));
#105812=DIRECTION('center_axis',(0.,0.,-1.));
#105813=DIRECTION('ref_axis',(-1.,0.,0.));
#105814=DIRECTION('center_axis',(-0.270643175546941,-0.962679734662503,
0.));
#105815=DIRECTION('ref_axis',(0.962679734662504,-0.270643175546941,0.));
#105816=DIRECTION('center_axis',(0.,0.,-1.));
#105817=DIRECTION('ref_axis',(1.,0.,0.));
#105818=DIRECTION('center_axis',(-0.279133941838593,-0.960252176521172,
-2.49865799020366E-15));
#105819=DIRECTION('ref_axis',(0.960252176521172,-0.279133941838593,3.84227067759201E-30));
#105820=DIRECTION('center_axis',(0.,0.,1.));
#105821=DIRECTION('ref_axis',(1.,0.,0.));
#105822=DIRECTION('center_axis',(0.,0.,1.));
#105823=DIRECTION('ref_axis',(1.,0.,0.));
#105824=DIRECTION('center_axis',(0.,0.,-1.));
#105825=DIRECTION('ref_axis',(0.,1.,0.));
#105826=DIRECTION('center_axis',(0.,0.,1.));
#105827=DIRECTION('ref_axis',(1.,0.,0.));
#105828=DIRECTION('',(-5.16102651992463E-32,-2.15733828054269E-47,1.));
#105829=DIRECTION('center_axis',(0.,-1.23467863058847E-16,1.));
#105830=DIRECTION('ref_axis',(0.,-1.,-1.21694324257719E-16));
#105831=DIRECTION('center_axis',(0.,-1.19033121480991E-16,1.));
#105832=DIRECTION('ref_axis',(0.,-1.,-1.19033121480991E-16));
#105833=DIRECTION('center_axis',(0.132576902561935,-0.991172672369243,0.000313776189307544));
#105834=DIRECTION('ref_axis',(0.99031382809775,0.132475188409534,0.0415793979542594));
#105835=DIRECTION('center_axis',(-0.161944455651288,0.986799872024417,-7.65271292523058E-5));
#105836=DIRECTION('ref_axis',(0.98612977255929,0.161837341642917,0.0368340402632872));
#105837=DIRECTION('center_axis',(0.,0.,-1.));
#105838=DIRECTION('ref_axis',(0.,1.,0.));
#105839=DIRECTION('center_axis',(0.,0.,-1.));
#105840=DIRECTION('ref_axis',(-1.,0.,0.));
#105841=DIRECTION('',(5.16102651992463E-32,2.15733828054269E-47,-1.));
#105842=DIRECTION('center_axis',(0.,0.,-1.));
#105843=DIRECTION('ref_axis',(-1.,0.,0.));
#105844=DIRECTION('center_axis',(0.996194698091747,-0.0871557427476409,
-1.07609333103578E-17));
#105845=DIRECTION('ref_axis',(-0.0871557427476409,-0.996194698091747,2.79703111108876E-34));
#105846=DIRECTION('',(0.996194698091747,-0.0871557427476402,-1.07609333103578E-17));
#105847=DIRECTION('center_axis',(1.13659195805196E-16,0.,1.));
#105848=DIRECTION('ref_axis',(-0.675590207615648,0.737277336810136,7.678703969146E-17));
#105849=DIRECTION('center_axis',(0.,0.,1.));
#105850=DIRECTION('ref_axis',(1.,0.,0.));
#105851=DIRECTION('center_axis',(0.,0.,1.));
#105852=DIRECTION('ref_axis',(1.,0.,0.));
#105853=DIRECTION('',(-1.13659195805196E-16,1.33411754197273E-16,-1.));
#105854=DIRECTION('center_axis',(-0.996194698091747,0.0871557427476457,
0.));
#105855=DIRECTION('ref_axis',(-0.0871557427476457,-0.996194698091747,0.));
#105856=DIRECTION('center_axis',(-0.996194698091747,0.0871557427476457,
0.));
#105857=DIRECTION('ref_axis',(0.0871557427476457,0.996194698091747,0.));
#105858=DIRECTION('center_axis',(-0.996194698091747,0.0871557427476457,
-1.3824978635387E-14));
#105859=DIRECTION('ref_axis',(-0.0871557427476457,-0.996194698091747,6.24837364119099E-31));
#105860=DIRECTION('',(0.996194698091747,-0.0871557427476402,0.));
#105861=DIRECTION('center_axis',(0.,0.,-1.));
#105862=DIRECTION('ref_axis',(-1.,0.,0.));
#105863=DIRECTION('center_axis',(0.,1.13523971920422E-16,-1.));
#105864=DIRECTION('ref_axis',(1.,0.,0.));
#105865=DIRECTION('center_axis',(0.,0.,-1.));
#105866=DIRECTION('ref_axis',(-1.,0.,0.));
#105867=DIRECTION('',(-1.13659195805196E-16,-1.13523971920422E-16,1.));
#105868=DIRECTION('center_axis',(0.996194698091747,-0.0871557427476409,
-1.07609333103578E-17));
#105869=DIRECTION('ref_axis',(-0.0871557427476409,-0.996194698091747,2.79703111108876E-34));
#105870=DIRECTION('',(0.996194698091747,-0.0871557427476402,-1.07609333103578E-17));
#105871=DIRECTION('center_axis',(0.,0.,1.));
#105872=DIRECTION('ref_axis',(1.,0.,0.));
#105873=DIRECTION('center_axis',(-6.19323182390956E-32,0.,-1.));
#105874=DIRECTION('ref_axis',(0.,1.,0.));
#105875=DIRECTION('center_axis',(0.,0.,1.));
#105876=DIRECTION('ref_axis',(1.,0.,0.));
#105877=DIRECTION('',(6.19323182390956E-32,-1.23467863058847E-16,1.));
#105878=DIRECTION('center_axis',(-0.996194698091747,0.08715574274764,0.));
#105879=DIRECTION('ref_axis',(-0.08715574274764,-0.996194698091747,0.));
#105880=DIRECTION('center_axis',(0.996194698091747,-0.0871557427476409,
-1.07609333103578E-17));
#105881=DIRECTION('ref_axis',(-0.0871557427476409,-0.996194698091747,2.79703111108876E-34));
#105882=DIRECTION('',(0.996194698091747,-0.0871557427476402,-1.07609333103578E-17));
#105883=DIRECTION('center_axis',(6.19323182390956E-32,0.,1.));
#105884=DIRECTION('ref_axis',(-0.675590207615642,0.737277336810141,4.18408677372686E-32));
#105885=DIRECTION('center_axis',(0.,0.,1.));
#105886=DIRECTION('ref_axis',(1.,0.,0.));
#105887=DIRECTION('center_axis',(0.,0.,1.));
#105888=DIRECTION('ref_axis',(1.,0.,0.));
#105889=DIRECTION('',(-6.19323182390956E-32,1.23467863058847E-16,-1.));
#105890=DIRECTION('center_axis',(-0.996194698091747,0.0871557427476457,
0.));
#105891=DIRECTION('ref_axis',(-0.0871557427476457,-0.996194698091747,0.));
#105892=DIRECTION('center_axis',(-0.996194698091747,0.0871557427476457,
0.));
#105893=DIRECTION('ref_axis',(0.0871557427476457,0.996194698091747,0.));
#105894=DIRECTION('center_axis',(-0.996194698091747,0.0871557427476457,
-3.00690150789426E-14));
#105895=DIRECTION('ref_axis',(-0.0871557427476457,-0.996194698091747,1.22577679051452E-30));
#105896=DIRECTION('',(0.996194698091747,-0.0871557427476402,0.));
#105897=DIRECTION('center_axis',(0.,0.,1.));
#105898=DIRECTION('ref_axis',(1.,0.,0.));
#105899=DIRECTION('center_axis',(-6.19323182390956E-32,0.,-1.));
#105900=DIRECTION('ref_axis',(0.,1.,0.));
#105901=DIRECTION('center_axis',(0.,0.,1.));
#105902=DIRECTION('ref_axis',(1.,0.,0.));
#105903=DIRECTION('',(6.19323182390956E-32,-1.23467863058847E-16,1.));
#105904=DIRECTION('center_axis',(0.707106781186548,-0.707106781186548,-8.7304963227523E-17));
#105905=DIRECTION('ref_axis',(-0.707106781186548,-0.707106781186548,-2.5701266908181E-33));
#105906=DIRECTION('',(0.707106781186547,-0.707106781186548,-8.73049632275231E-17));
#105907=DIRECTION('center_axis',(-0.955086750882198,-0.0835592633859996,
0.284301156859545));
#105908=DIRECTION('ref_axis',(0.28529890144429,-2.70823414235005E-19,0.958438593147564));
#105909=DIRECTION('center_axis',(-0.996194698091746,-0.0871557427476572,
-1.07609333103598E-17));
#105910=DIRECTION('ref_axis',(-0.0871557427476572,0.996194698091746,-1.48387871229006E-34));
#105911=DIRECTION('',(-0.996194698091746,-0.0871557427476568,-1.07609333103598E-17));
#105912=DIRECTION('center_axis',(0.,0.,1.));
#105913=DIRECTION('ref_axis',(0.,-1.,0.));
#105914=DIRECTION('center_axis',(0.,0.,-1.));
#105915=DIRECTION('ref_axis',(-1.,0.,0.));
#105916=DIRECTION('',(0.,1.23467863058847E-16,-1.));
#105917=DIRECTION('center_axis',(0.,0.,-1.));
#105918=DIRECTION('ref_axis',(-1.,0.,0.));
#105919=DIRECTION('center_axis',(-0.996194698091746,-0.0871557427476538,
0.));
#105920=DIRECTION('ref_axis',(0.0871557427476538,-0.996194698091746,0.));
#105921=DIRECTION('center_axis',(0.996194698091746,0.0871557427476572,0.));
#105922=DIRECTION('ref_axis',(0.0871557427476572,-0.996194698091746,0.));
#105923=DIRECTION('center_axis',(-0.996194698091745,-0.0871557427476607,
0.));
#105924=DIRECTION('ref_axis',(0.0871557427476607,-0.996194698091745,0.));
#105925=DIRECTION('',(-0.996194698091746,-0.0871557427476568,0.));
#105926=DIRECTION('center_axis',(0.,0.,1.));
#105927=DIRECTION('ref_axis',(1.,0.,0.));
#105928=DIRECTION('center_axis',(0.,1.07104667533214E-16,-1.));
#105929=DIRECTION('ref_axis',(1.,0.,0.));
#105930=DIRECTION('center_axis',(0.,0.,-1.));
#105931=DIRECTION('ref_axis',(-1.,0.,0.));
#105932=DIRECTION('',(1.87032180698308E-16,-1.07104667533214E-16,1.));
#105933=DIRECTION('center_axis',(-0.996194698091746,-0.0871557427476572,
-1.07609333103598E-17));
#105934=DIRECTION('ref_axis',(-0.0871557427476572,0.996194698091746,-1.48387871229006E-34));
#105935=DIRECTION('',(-0.996194698091746,-0.0871557427476568,-1.07609333103598E-17));
#105936=DIRECTION('center_axis',(5.40794518211031E-32,0.,1.));
#105937=DIRECTION('ref_axis',(0.,-1.,0.));
#105938=DIRECTION('center_axis',(0.,0.,1.));
#105939=DIRECTION('ref_axis',(1.,0.,0.));
#105940=DIRECTION('center_axis',(0.,0.,1.));
#105941=DIRECTION('ref_axis',(1.,0.,0.));
#105942=DIRECTION('',(-5.40794518211031E-32,1.23467863058847E-16,-1.));
#105943=DIRECTION('center_axis',(0.996194698091745,0.0871557427476607,0.));
#105944=DIRECTION('ref_axis',(-0.0871557427476607,0.996194698091745,0.));
#105945=DIRECTION('center_axis',(0.996194698091746,0.0871557427476572,0.));
#105946=DIRECTION('ref_axis',(0.0871557427476572,-0.996194698091746,0.));
#105947=DIRECTION('center_axis',(0.996194698091745,0.0871557427476607,1.2095289040845E-15));
#105948=DIRECTION('ref_axis',(-0.0871557427476607,0.996194698091745,-5.51367835803032E-32));
#105949=DIRECTION('',(-0.996194698091746,-0.0871557427476568,0.));
#105950=DIRECTION('center_axis',(0.,0.,-1.));
#105951=DIRECTION('ref_axis',(-1.,0.,0.));
#105952=DIRECTION('center_axis',(0.,-1.07104667533214E-16,1.));
#105953=DIRECTION('ref_axis',(-1.,0.,0.));
#105954=DIRECTION('center_axis',(0.,0.,-1.));
#105955=DIRECTION('ref_axis',(-1.,0.,0.));
#105956=DIRECTION('',(1.87032180698308E-16,-1.07104667533214E-16,1.));
#105957=DIRECTION('center_axis',(-0.707106781186548,-0.707106781186548,
-8.7304963227523E-17));
#105958=DIRECTION('ref_axis',(-0.707106781186548,0.707106781186548,2.5701266908181E-33));
#105959=DIRECTION('',(-0.707106781186547,-0.707106781186548,-8.73049632275231E-17));
#105960=DIRECTION('center_axis',(-0.0871557427476572,-0.996194698091746,
-1.22998030563942E-16));
#105961=DIRECTION('ref_axis',(-0.996194698091746,0.0871557427476572,1.44426287624373E-33));
#105962=DIRECTION('',(-0.0871557427476566,-0.996194698091746,-1.22998030563941E-16));
#105963=DIRECTION('center_axis',(0.,4.51531312650048E-33,1.));
#105964=DIRECTION('ref_axis',(0.737277336810104,0.675590207615682,-3.05050133258228E-33));
#105965=DIRECTION('center_axis',(0.,0.,-1.));
#105966=DIRECTION('ref_axis',(-1.,0.,0.));
#105967=DIRECTION('',(-1.08020383274202E-17,-4.51531312650048E-33,-1.));
#105968=DIRECTION('center_axis',(0.,0.,-1.));
#105969=DIRECTION('ref_axis',(-1.,0.,0.));
#105970=DIRECTION('center_axis',(-0.0871557427476538,-0.996194698091746,
0.));
#105971=DIRECTION('ref_axis',(0.996194698091746,-0.0871557427476538,0.));
#105972=DIRECTION('center_axis',(0.0871557427476538,0.996194698091746,0.));
#105973=DIRECTION('ref_axis',(0.996194698091746,-0.0871557427476538,0.));
#105974=DIRECTION('center_axis',(-0.0871557427476538,-0.996194698091746,
0.));
#105975=DIRECTION('ref_axis',(0.996194698091746,-0.0871557427476538,0.));
#105976=DIRECTION('',(-0.0871557427476566,-0.996194698091746,0.));
#105977=DIRECTION('center_axis',(0.,0.,1.));
#105978=DIRECTION('ref_axis',(1.,0.,0.));
#105979=DIRECTION('center_axis',(0.,-4.73133896404282E-33,-1.));
#105980=DIRECTION('ref_axis',(1.,0.,0.));
#105981=DIRECTION('center_axis',(0.,0.,1.));
#105982=DIRECTION('ref_axis',(1.,0.,0.));
#105983=DIRECTION('',(1.08020383274202E-17,4.73133896404282E-33,1.));
#105984=DIRECTION('center_axis',(-0.0871557427476572,-0.996194698091746,
-1.22998030563942E-16));
#105985=DIRECTION('ref_axis',(-0.996194698091746,0.0871557427476572,1.44426287624373E-33));
#105986=DIRECTION('',(-0.0871557427476566,-0.996194698091746,-1.22998030563941E-16));
#105987=DIRECTION('center_axis',(0.,0.,-1.));
#105988=DIRECTION('ref_axis',(-1.,0.,0.));
#105989=DIRECTION('center_axis',(0.985034259191114,-0.172358661574676,4.57699418854155E-11));
#105990=DIRECTION('ref_axis',(0.0566495632167467,0.323753735284747,-0.944443934744951));
#105991=DIRECTION('center_axis',(0.,4.51531312650048E-33,1.));
#105992=DIRECTION('ref_axis',(-1.,0.,0.));
#105993=DIRECTION('center_axis',(0.,0.,-1.));
#105994=DIRECTION('ref_axis',(-1.,0.,0.));
#105995=DIRECTION('',(1.08020383274202E-17,4.51531312650048E-33,1.));
#105996=DIRECTION('center_axis',(0.0871557427476607,0.996194698091745,0.));
#105997=DIRECTION('ref_axis',(-0.996194698091745,0.0871557427476607,0.));
#105998=DIRECTION('center_axis',(0.0835592633859915,0.955086750882199,0.284301156859544));
#105999=DIRECTION('ref_axis',(-2.48475885091778E-18,0.285298901444289,-0.958438593147564));
#106000=DIRECTION('center_axis',(-0.0871557427476572,-0.996194698091746,
-1.22998030563942E-16));
#106001=DIRECTION('ref_axis',(-0.996194698091746,0.0871557427476572,1.44426287624373E-33));
#106002=DIRECTION('',(-0.0871557427476566,-0.996194698091746,-1.22998030563941E-16));
#106003=DIRECTION('center_axis',(0.,4.51531312650048E-33,1.));
#106004=DIRECTION('ref_axis',(0.737277336810102,0.675590207615684,-3.05050133258228E-33));
#106005=DIRECTION('center_axis',(0.,0.,1.));
#106006=DIRECTION('ref_axis',(1.,0.,0.));
#106007=DIRECTION('center_axis',(0.,0.,1.));
#106008=DIRECTION('ref_axis',(1.,0.,0.));
#106009=DIRECTION('',(-1.08020383274202E-17,-4.51531312650048E-33,-1.));
#106010=DIRECTION('center_axis',(0.0871557427476538,0.996194698091746,6.91248931769351E-15));
#106011=DIRECTION('ref_axis',(-0.996194698091746,0.0871557427476538,2.78649888037662E-32));
#106012=DIRECTION('center_axis',(0.0871557427476538,0.996194698091746,0.));
#106013=DIRECTION('ref_axis',(0.996194698091746,-0.0871557427476538,0.));
#106014=DIRECTION('center_axis',(0.0871557427476538,0.996194698091746,6.91248931769351E-15));
#106015=DIRECTION('ref_axis',(-0.996194698091746,0.0871557427476538,2.78649888037662E-32));
#106016=DIRECTION('',(-0.0871557427476566,-0.996194698091746,0.));
#106017=DIRECTION('center_axis',(0.,0.,1.));
#106018=DIRECTION('ref_axis',(1.,0.,0.));
#106019=DIRECTION('center_axis',(0.,-4.51531312650048E-33,-1.));
#106020=DIRECTION('ref_axis',(1.,0.,0.));
#106021=DIRECTION('center_axis',(0.,0.,1.));
#106022=DIRECTION('ref_axis',(1.,0.,0.));
#106023=DIRECTION('',(1.08020383274202E-17,4.51531312650048E-33,1.));
#106024=DIRECTION('center_axis',(0.0871557427476394,-0.996194698091747,
0.));
#106025=DIRECTION('ref_axis',(0.996194698091747,0.0871557427476394,0.));
#106026=DIRECTION('center_axis',(0.,4.51531312649963E-33,-1.));
#106027=DIRECTION('ref_axis',(1.,0.,0.));
#106028=DIRECTION('center_axis',(0.,0.,-1.));
#106029=DIRECTION('ref_axis',(-1.,0.,0.));
#106030=DIRECTION('',(1.08020383274181E-17,4.51531312649963E-33,-1.));
#106031=DIRECTION('center_axis',(1.38777878078144E-14,0.,-1.));
#106032=DIRECTION('ref_axis',(-1.,0.,-1.38777878078144E-14));
#106033=DIRECTION('center_axis',(0.985034259178149,0.172358661648767,3.69403275210692E-11));
#106034=DIRECTION('ref_axis',(-0.0885145471782662,0.505862951942684,0.858060515808564));
#106035=DIRECTION('center_axis',(0.0871557427476394,-0.996194698091747,
-1.22998030563942E-16));
#106036=DIRECTION('ref_axis',(-0.996194698091747,-0.0871557427476394,8.16488070285074E-35));
#106037=DIRECTION('',(0.0871557427476402,-0.996194698091747,-1.22998030563942E-16));
#106038=DIRECTION('center_axis',(0.,-4.73133896404192E-33,1.));
#106039=DIRECTION('ref_axis',(-1.,0.,0.));
#106040=DIRECTION('center_axis',(0.,0.,1.));
#106041=DIRECTION('ref_axis',(1.,0.,0.));
#106042=DIRECTION('center_axis',(0.,0.,1.));
#106043=DIRECTION('ref_axis',(1.,0.,0.));
#106044=DIRECTION('',(1.08020383274181E-17,4.73133896404192E-33,-1.));
#106045=DIRECTION('center_axis',(-0.0871557427476469,0.996194698091747,
-1.3824978635387E-14));
#106046=DIRECTION('ref_axis',(-0.996194698091747,-0.0871557427476469,-9.13671722807069E-31));
#106047=DIRECTION('center_axis',(-0.0871557427476469,0.996194698091747,
0.));
#106048=DIRECTION('ref_axis',(0.996194698091747,0.0871557427476469,0.));
#106049=DIRECTION('center_axis',(-0.0871557427476469,0.996194698091747,
0.));
#106050=DIRECTION('ref_axis',(-0.996194698091747,-0.0871557427476469,0.));
#106051=DIRECTION('',(0.0871557427476402,-0.996194698091747,0.));
#106052=DIRECTION('center_axis',(0.,0.,-1.));
#106053=DIRECTION('ref_axis',(-1.,0.,0.));
#106054=DIRECTION('center_axis',(0.,-4.51531312649963E-33,1.));
#106055=DIRECTION('ref_axis',(0.737277336810104,-0.675590207615683,-3.0505013325817E-33));
#106056=DIRECTION('center_axis',(0.,0.,-1.));
#106057=DIRECTION('ref_axis',(-1.,0.,0.));
#106058=DIRECTION('',(-1.08020383274181E-17,-4.51531312649963E-33,1.));
#106059=DIRECTION('center_axis',(0.0871557427476394,-0.996194698091747,
-1.22998030563942E-16));
#106060=DIRECTION('ref_axis',(-0.996194698091747,-0.0871557427476394,8.16488070285074E-35));
#106061=DIRECTION('',(0.0871557427476402,-0.996194698091747,-1.22998030563942E-16));
#106062=DIRECTION('center_axis',(0.,-4.51531312649963E-33,1.));
#106063=DIRECTION('ref_axis',(-1.,0.,0.));
#106064=DIRECTION('center_axis',(0.,0.,1.));
#106065=DIRECTION('ref_axis',(1.,0.,0.));
#106066=DIRECTION('center_axis',(0.,0.,1.));
#106067=DIRECTION('ref_axis',(1.,0.,0.));
#106068=DIRECTION('',(1.08020383274181E-17,4.51531312649963E-33,-1.));
#106069=DIRECTION('center_axis',(-0.0871557427476469,0.996194698091747,
0.));
#106070=DIRECTION('ref_axis',(-0.996194698091747,-0.0871557427476469,0.));
#106071=DIRECTION('center_axis',(-0.0871557427476469,0.996194698091747,
0.));
#106072=DIRECTION('ref_axis',(0.996194698091747,0.0871557427476469,0.));
#106073=DIRECTION('center_axis',(-0.0871557427476469,0.996194698091747,
-1.3824978635387E-14));
#106074=DIRECTION('ref_axis',(-0.996194698091747,-0.0871557427476469,-9.13671722807069E-31));
#106075=DIRECTION('',(0.0871557427476402,-0.996194698091747,0.));
#106076=DIRECTION('center_axis',(0.,0.,1.));
#106077=DIRECTION('ref_axis',(1.,0.,0.));
#106078=DIRECTION('center_axis',(0.,0.,1.));
#106079=DIRECTION('ref_axis',(1.,0.,0.));
#106080=DIRECTION('center_axis',(0.,4.51531312649963E-33,-1.));
#106081=DIRECTION('ref_axis',(1.,0.,0.));
#106082=DIRECTION('center_axis',(0.,0.,1.));
#106083=DIRECTION('ref_axis',(1.,0.,0.));
#106084=DIRECTION('center_axis',(0.,0.,1.));
#106085=DIRECTION('ref_axis',(1.,0.,0.));
#106086=DIRECTION('',(-1.08020383274181E-17,-4.51531312649963E-33,1.));
#106087=DIRECTION('center_axis',(0.0871557427476394,-0.996194698091747,
-1.22998030563942E-16));
#106088=DIRECTION('ref_axis',(-0.996194698091747,-0.0871557427476394,8.16488070285074E-35));
#106089=DIRECTION('',(0.0871557427476402,-0.996194698091747,-1.22998030563942E-16));
#106090=DIRECTION('center_axis',(0.,1.23467863058847E-16,-1.));
#106091=DIRECTION('ref_axis',(-1.,0.,0.));
#106092=DIRECTION('',(-4.38004274807345E-16,1.,1.23467863058847E-16));
#106093=DIRECTION('center_axis',(0.,0.,1.));
#106094=DIRECTION('ref_axis',(0.,1.,0.));
#106095=DIRECTION('center_axis',(1.76945321870477E-31,1.17608371252665E-16,
-1.));
#106096=DIRECTION('ref_axis',(-3.01980662698042E-14,1.,1.17608371252665E-16));
#106097=DIRECTION('center_axis',(0.,0.,1.));
#106098=DIRECTION('ref_axis',(0.,1.,0.));
#106099=DIRECTION('',(1.,4.38004274807345E-16,5.40794518211031E-32));
#106100=DIRECTION('center_axis',(0.,0.,1.));
#106101=DIRECTION('ref_axis',(0.,1.,0.));
#106102=DIRECTION('',(1.,4.38004274807345E-16,5.40794518211031E-32));
#106103=DIRECTION('center_axis',(0.,1.23467863058847E-16,-1.));
#106104=DIRECTION('ref_axis',(-1.,0.,0.));
#106105=DIRECTION('',(-1.,-4.38004274807345E-16,-5.40794518211031E-32));
#106106=DIRECTION('center_axis',(0.,0.,1.));
#106107=DIRECTION('ref_axis',(0.,1.,0.));
#106108=DIRECTION('center_axis',(0.,0.,1.));
#106109=DIRECTION('ref_axis',(0.,1.,0.));
#106110=DIRECTION('',(-4.38004274807345E-16,1.,1.23467863058847E-16));
#106111=DIRECTION('center_axis',(0.,0.,-1.));
#106112=DIRECTION('ref_axis',(0.,-1.,0.));
#106113=DIRECTION('',(-5.01606788234257E-16,1.,0.));
#106114=DIRECTION('',(-1.,-5.01606788234257E-16,0.));
#106115=DIRECTION('',(5.01606788234257E-16,-1.,0.));
#106116=DIRECTION('center_axis',(0.,-1.,0.));
#106117=DIRECTION('ref_axis',(-1.,0.,0.));
#106118=DIRECTION('',(5.01606788234257E-16,-1.,0.));
#106119=DIRECTION('center_axis',(0.,-1.,0.));
#106120=DIRECTION('ref_axis',(0.,0.,1.));
#106121=DIRECTION('center_axis',(6.703313282803E-15,-0.423071618151431,
-0.90609624539269));
#106122=DIRECTION('ref_axis',(9.44993610611347E-31,-0.90609624539269,0.423071618151431));
#106123=DIRECTION('center_axis',(1.,0.,0.));
#106124=DIRECTION('ref_axis',(0.,0.97671957347062,-0.214520103485359));
#106125=DIRECTION('center_axis',(-0.999690759108302,0.0248673681371606,
-1.24658621679628E-5));
#106126=DIRECTION('ref_axis',(0.0242993767343897,0.976750214327029,-0.212998965026647));
#106127=DIRECTION('center_axis',(0.,-0.423401464461212,-0.905942161449671));
#106128=DIRECTION('ref_axis',(0.,-0.905942161449671,0.423401464461211));
#106129=DIRECTION('center_axis',(0.,1.,0.));
#106130=DIRECTION('ref_axis',(0.,0.,-1.));
#106131=DIRECTION('center_axis',(0.,0.,-1.));
#106132=DIRECTION('ref_axis',(1.,0.,0.));
#106133=DIRECTION('center_axis',(0.,1.,0.));
#106134=DIRECTION('ref_axis',(0.,0.,-1.));
#106135=DIRECTION('center_axis',(0.,0.,1.));
#106136=DIRECTION('ref_axis',(1.,0.,0.));
#106137=DIRECTION('center_axis',(-1.,0.,0.));
#106138=DIRECTION('ref_axis',(0.,0.,1.));
#106139=DIRECTION('center_axis',(0.,0.,-1.));
#106140=DIRECTION('ref_axis',(1.,0.,0.));
#106141=DIRECTION('center_axis',(-1.,0.,0.));
#106142=DIRECTION('ref_axis',(0.,0.,-1.));
#106143=DIRECTION('',(-1.,0.,0.));
#106144=DIRECTION('center_axis',(-1.,0.,0.));
#106145=DIRECTION('ref_axis',(0.,0.,1.));
#106146=DIRECTION('',(1.,0.,0.));
#106147=DIRECTION('center_axis',(0.,-1.,0.));
#106148=DIRECTION('ref_axis',(0.,0.,-1.));
#106149=DIRECTION('',(0.,-1.,0.));
#106150=DIRECTION('',(0.,1.,0.));
#106151=DIRECTION('center_axis',(0.,-1.,0.));
#106152=DIRECTION('ref_axis',(0.,0.,-1.));
#106153=DIRECTION('',(0.,-1.,0.));
#106154=DIRECTION('center_axis',(9.37295054023422E-45,-1.,2.02617679489732E-30));
#106155=DIRECTION('ref_axis',(-1.,-4.97841222228891E-60,4.62592926927148E-15));
#106156=DIRECTION('center_axis',(0.,-1.,0.));
#106157=DIRECTION('ref_axis',(0.,0.,-1.));
#106158=DIRECTION('',(0.,1.,0.));
#106159=DIRECTION('center_axis',(0.,1.,0.));
#106160=DIRECTION('ref_axis',(0.,0.,-1.));
#106161=DIRECTION('',(0.,-1.,0.));
#106162=DIRECTION('center_axis',(0.,0.,-1.));
#106163=DIRECTION('ref_axis',(1.,0.,0.));
#106164=DIRECTION('center_axis',(0.,0.,1.));
#106165=DIRECTION('ref_axis',(1.,0.,0.));
#106166=DIRECTION('center_axis',(-1.,0.,0.));
#106167=DIRECTION('ref_axis',(0.,0.,1.));
#106168=DIRECTION('center_axis',(0.,0.,-1.));
#106169=DIRECTION('ref_axis',(1.,0.,0.));
#106170=DIRECTION('center_axis',(-1.,0.,0.));
#106171=DIRECTION('ref_axis',(0.,0.,-1.));
#106172=DIRECTION('',(-1.,0.,0.));
#106173=DIRECTION('center_axis',(-1.,0.,0.));
#106174=DIRECTION('ref_axis',(0.,0.,1.));
#106175=DIRECTION('',(1.,0.,0.));
#106176=DIRECTION('center_axis',(0.,0.,-1.));
#106177=DIRECTION('ref_axis',(1.,0.,0.));
#106178=DIRECTION('center_axis',(0.,0.,1.));
#106179=DIRECTION('ref_axis',(1.,0.,0.));
#106180=DIRECTION('center_axis',(0.,-1.,0.));
#106181=DIRECTION('ref_axis',(0.,0.,1.));
#106182=DIRECTION('center_axis',(0.,0.,-1.));
#106183=DIRECTION('ref_axis',(1.,0.,0.));
#106184=DIRECTION('center_axis',(0.,-1.,0.));
#106185=DIRECTION('ref_axis',(0.,0.,-1.));
#106186=DIRECTION('',(0.,-1.,0.));
#106187=DIRECTION('center_axis',(0.,-1.,0.));
#106188=DIRECTION('ref_axis',(0.,0.,1.));
#106189=DIRECTION('',(0.,1.,0.));
#106190=DIRECTION('center_axis',(0.,0.,-1.));
#106191=DIRECTION('ref_axis',(1.,0.,0.));
#106192=DIRECTION('center_axis',(0.991696083061511,0.128603555318137,6.6332437503331E-5));
#106193=DIRECTION('ref_axis',(-0.0239412820628473,0.184110745713541,0.982613885677376));
#106194=DIRECTION('center_axis',(0.,0.,-1.));
#106195=DIRECTION('ref_axis',(0.,-1.,0.));
#106196=DIRECTION('center_axis',(-0.998076762506053,-0.0619901273296905,
-1.60961186456236E-5));
#106197=DIRECTION('ref_axis',(0.0113170760680052,-0.181956139738737,-0.983241520177341));
#106198=DIRECTION('center_axis',(0.,0.,1.));
#106199=DIRECTION('ref_axis',(1.,0.,0.));
#106200=DIRECTION('center_axis',(0.,-1.,0.));
#106201=DIRECTION('ref_axis',(0.,0.,-1.));
#106202=DIRECTION('center_axis',(0.,1.,0.));
#106203=DIRECTION('ref_axis',(0.,0.,-1.));
#106204=DIRECTION('',(0.,1.,0.));
#106205=DIRECTION('center_axis',(0.,1.,0.));
#106206=DIRECTION('ref_axis',(0.,0.,-1.));
#106207=DIRECTION('',(0.,-1.,0.));
#106208=DIRECTION('center_axis',(0.,0.,-1.));
#106209=DIRECTION('ref_axis',(1.,0.,0.));
#106210=DIRECTION('center_axis',(0.,0.,1.));
#106211=DIRECTION('ref_axis',(1.,0.,0.));
#106212=DIRECTION('center_axis',(-1.,0.,0.));
#106213=DIRECTION('ref_axis',(0.,0.,1.));
#106214=DIRECTION('center_axis',(0.,0.,-1.));
#106215=DIRECTION('ref_axis',(1.,0.,0.));
#106216=DIRECTION('center_axis',(-1.,0.,0.));
#106217=DIRECTION('ref_axis',(0.,0.,-1.));
#106218=DIRECTION('',(-1.,0.,0.));
#106219=DIRECTION('center_axis',(-1.,0.,0.));
#106220=DIRECTION('ref_axis',(0.,0.,1.));
#106221=DIRECTION('',(1.,0.,0.));
#106222=DIRECTION('center_axis',(0.,0.,-1.));
#106223=DIRECTION('ref_axis',(1.,0.,0.));
#106224=DIRECTION('center_axis',(0.,0.,1.));
#106225=DIRECTION('ref_axis',(1.,0.,0.));
#106226=DIRECTION('center_axis',(0.,-1.,0.));
#106227=DIRECTION('ref_axis',(0.,0.,1.));
#106228=DIRECTION('center_axis',(0.,0.,-1.));
#106229=DIRECTION('ref_axis',(1.,0.,0.));
#106230=DIRECTION('center_axis',(0.,-1.,0.));
#106231=DIRECTION('ref_axis',(0.,0.,-1.));
#106232=DIRECTION('',(0.,-1.,0.));
#106233=DIRECTION('center_axis',(0.,-1.,0.));
#106234=DIRECTION('ref_axis',(0.,0.,1.));
#106235=DIRECTION('',(0.,1.,0.));
#106236=DIRECTION('center_axis',(0.,0.,-1.));
#106237=DIRECTION('ref_axis',(1.,0.,0.));
#106238=DIRECTION('center_axis',(0.,0.,1.));
#106239=DIRECTION('ref_axis',(1.,0.,0.));
#106240=DIRECTION('center_axis',(0.950554487276066,0.310557831521497,-3.79371153572051E-14));
#106241=DIRECTION('ref_axis',(-0.310557831521497,0.950554487276066,1.69736969313821E-30));
#106242=DIRECTION('center_axis',(-0.988230180462193,-0.15293610778742,0.00341428740686027));
#106243=DIRECTION('ref_axis',(0.0254252921822052,-0.186218180898005,-0.982179384644418));
#106244=DIRECTION('center_axis',(1.,0.,1.73472347597681E-14));
#106245=DIRECTION('ref_axis',(1.73472347597681E-14,0.,-1.));
#106246=DIRECTION('center_axis',(-1.,0.,0.));
#106247=DIRECTION('ref_axis',(0.,1.,0.));
#106248=DIRECTION('',(1.,4.38004274807345E-16,0.));
#106249=DIRECTION('',(-1.,-4.38004274807345E-16,0.));
#106250=DIRECTION('center_axis',(1.,0.,0.));
#106251=DIRECTION('ref_axis',(0.,0.,-1.));
#106252=DIRECTION('center_axis',(0.,-1.,0.));
#106253=DIRECTION('ref_axis',(0.,0.,-1.));
#106254=DIRECTION('center_axis',(0.,1.,0.));
#106255=DIRECTION('ref_axis',(0.,0.,-1.));
#106256=DIRECTION('',(0.,1.,0.));
#106257=DIRECTION('center_axis',(0.,1.,0.));
#106258=DIRECTION('ref_axis',(0.,0.,-1.));
#106259=DIRECTION('',(0.,-1.,0.));
#106260=DIRECTION('center_axis',(0.,0.,-1.));
#106261=DIRECTION('ref_axis',(1.,0.,0.));
#106262=DIRECTION('center_axis',(0.,0.,1.));
#106263=DIRECTION('ref_axis',(1.,0.,0.));
#106264=DIRECTION('center_axis',(-1.,0.,0.));
#106265=DIRECTION('ref_axis',(0.,0.,1.));
#106266=DIRECTION('center_axis',(0.,0.,-1.));
#106267=DIRECTION('ref_axis',(1.,0.,0.));
#106268=DIRECTION('center_axis',(-1.,0.,0.));
#106269=DIRECTION('ref_axis',(0.,0.,-1.));
#106270=DIRECTION('',(-1.,0.,0.));
#106271=DIRECTION('center_axis',(-1.,0.,0.));
#106272=DIRECTION('ref_axis',(0.,0.,1.));
#106273=DIRECTION('',(1.,0.,0.));
#106274=DIRECTION('center_axis',(0.,0.,-1.));
#106275=DIRECTION('ref_axis',(1.,0.,0.));
#106276=DIRECTION('center_axis',(0.,0.,1.));
#106277=DIRECTION('ref_axis',(1.,0.,0.));
#106278=DIRECTION('center_axis',(0.,-1.,0.));
#106279=DIRECTION('ref_axis',(0.,0.,1.));
#106280=DIRECTION('center_axis',(0.,0.,-1.));
#106281=DIRECTION('ref_axis',(1.,0.,0.));
#106282=DIRECTION('center_axis',(0.,-1.,0.));
#106283=DIRECTION('ref_axis',(0.,0.,-1.));
#106284=DIRECTION('',(0.,-1.,0.));
#106285=DIRECTION('center_axis',(0.,-1.,0.));
#106286=DIRECTION('ref_axis',(0.,0.,1.));
#106287=DIRECTION('',(0.,1.,0.));
#106288=DIRECTION('center_axis',(-1.,0.,0.));
#106289=DIRECTION('ref_axis',(0.,1.,0.));
#106290=DIRECTION('',(-1.,-4.38004274807345E-16,0.));
#106291=DIRECTION('center_axis',(1.,0.,0.));
#106292=DIRECTION('ref_axis',(0.,0.,-1.));
#106293=DIRECTION('',(1.,4.38004274807345E-16,0.));
#106294=DIRECTION('center_axis',(-1.,0.,0.));
#106295=DIRECTION('ref_axis',(0.,0.,1.));
#106296=DIRECTION('center_axis',(0.,-1.,0.));
#106297=DIRECTION('ref_axis',(0.,0.,-1.));
#106298=DIRECTION('center_axis',(0.,1.,0.));
#106299=DIRECTION('ref_axis',(0.,0.,-1.));
#106300=DIRECTION('',(0.,1.,0.));
#106301=DIRECTION('center_axis',(0.,1.,0.));
#106302=DIRECTION('ref_axis',(0.,0.,-1.));
#106303=DIRECTION('',(0.,-1.,0.));
#106304=DIRECTION('center_axis',(0.,0.,-1.));
#106305=DIRECTION('ref_axis',(1.,0.,0.));
#106306=DIRECTION('center_axis',(0.,0.,1.));
#106307=DIRECTION('ref_axis',(1.,0.,0.));
#106308=DIRECTION('center_axis',(-1.,0.,0.));
#106309=DIRECTION('ref_axis',(0.,0.,1.));
#106310=DIRECTION('center_axis',(0.,0.,-1.));
#106311=DIRECTION('ref_axis',(1.,0.,0.));
#106312=DIRECTION('center_axis',(-1.,0.,0.));
#106313=DIRECTION('ref_axis',(0.,0.,-1.));
#106314=DIRECTION('',(-1.,0.,0.));
#106315=DIRECTION('center_axis',(-1.,0.,0.));
#106316=DIRECTION('ref_axis',(0.,0.,1.));
#106317=DIRECTION('',(1.,0.,0.));
#106318=DIRECTION('center_axis',(0.,0.,-1.));
#106319=DIRECTION('ref_axis',(1.,0.,0.));
#106320=DIRECTION('center_axis',(0.,0.,1.));
#106321=DIRECTION('ref_axis',(1.,0.,0.));
#106322=DIRECTION('center_axis',(0.,-1.,0.));
#106323=DIRECTION('ref_axis',(0.,0.,1.));
#106324=DIRECTION('center_axis',(0.,0.,-1.));
#106325=DIRECTION('ref_axis',(1.,0.,0.));
#106326=DIRECTION('center_axis',(0.,-1.,0.));
#106327=DIRECTION('ref_axis',(0.,0.,-1.));
#106328=DIRECTION('',(0.,-1.,0.));
#106329=DIRECTION('center_axis',(0.,-1.,0.));
#106330=DIRECTION('ref_axis',(0.,0.,1.));
#106331=DIRECTION('',(0.,1.,0.));
#106332=DIRECTION('center_axis',(-1.,0.,0.));
#106333=DIRECTION('ref_axis',(0.,1.,0.));
#106334=DIRECTION('',(-1.,-4.38004274807345E-16,0.));
#106335=DIRECTION('center_axis',(1.,0.,0.));
#106336=DIRECTION('ref_axis',(0.,0.,-1.));
#106337=DIRECTION('',(1.,4.38004274807345E-16,0.));
#106338=DIRECTION('center_axis',(-1.,0.,0.));
#106339=DIRECTION('ref_axis',(0.,0.,1.));
#106340=DIRECTION('center_axis',(0.,-1.,0.));
#106341=DIRECTION('ref_axis',(0.,0.,-1.));
#106342=DIRECTION('center_axis',(0.,1.,0.));
#106343=DIRECTION('ref_axis',(0.,0.,-1.));
#106344=DIRECTION('',(0.,1.,0.));
#106345=DIRECTION('',(0.,-1.,0.));
#106346=DIRECTION('center_axis',(1.,0.,-1.6326809185664E-16));
#106347=DIRECTION('ref_axis',(-1.6326809185664E-16,0.,-1.));
#106348=DIRECTION('',(-1.6326809185664E-16,-7.15121221728469E-32,-1.));
#106349=DIRECTION('',(-1.6326809185664E-16,0.,-1.));
#106350=DIRECTION('',(0.,1.,0.));
#106351=DIRECTION('',(-1.6326809185664E-16,1.00522029149049E-16,-1.));
#106352=DIRECTION('',(2.0158362407235E-32,1.,1.23467863058847E-16));
#106353=DIRECTION('',(2.0158362407235E-32,1.,1.23467863058847E-16));
#106354=DIRECTION('center_axis',(0.,-1.,0.));
#106355=DIRECTION('ref_axis',(0.,0.,-1.));
#106356=DIRECTION('center_axis',(0.,-1.,0.));
#106357=DIRECTION('ref_axis',(0.,0.,-1.));
#106358=DIRECTION('',(0.,-1.,0.));
#106359=DIRECTION('center_axis',(0.,0.,1.));
#106360=DIRECTION('ref_axis',(-1.,0.,0.));
#106361=DIRECTION('center_axis',(0.990268068741571,0.139173100960059,0.));
#106362=DIRECTION('ref_axis',(-0.139173100960059,0.990268068741571,0.));
#106363=DIRECTION('center_axis',(0.,0.,1.));
#106364=DIRECTION('ref_axis',(-1.,-1.5419764230905E-15,0.));
#106365=DIRECTION('center_axis',(0.904824724134427,0.425784239486454,0.));
#106366=DIRECTION('ref_axis',(-0.425784239486454,0.904824724134427,0.));
#106367=DIRECTION('center_axis',(0.,0.,-1.));
#106368=DIRECTION('ref_axis',(-1.,0.,0.));
#106369=DIRECTION('center_axis',(-0.990268068741572,-0.139173100960052,
0.));
#106370=DIRECTION('ref_axis',(-0.139173100960052,0.990268068741572,0.));
#106371=DIRECTION('center_axis',(0.990268068741572,0.139173100960052,0.));
#106372=DIRECTION('ref_axis',(-0.139173100960052,0.990268068741572,0.));
#106373=DIRECTION('',(0.990268068741571,0.139173100960059,0.));
#106374=DIRECTION('',(-0.990268068741571,-0.139173100960059,0.));
#106375=DIRECTION('center_axis',(0.,0.,1.));
#106376=DIRECTION('ref_axis',(0.,-1.,0.));
#106377=DIRECTION('',(0.,1.23467863058847E-16,-1.));
#106378=DIRECTION('center_axis',(0.,0.,1.));
#106379=DIRECTION('ref_axis',(0.,-1.,0.));
#106380=DIRECTION('',(3.43088182518023E-33,-1.23467863058847E-16,1.));
#106381=DIRECTION('center_axis',(0.,-1.23467863058847E-16,1.));
#106382=DIRECTION('ref_axis',(0.,-1.,0.));
#106383=DIRECTION('center_axis',(-0.990268068741572,-0.139173100960051,
-1.7605559658208E-14));
#106384=DIRECTION('ref_axis',(0.139173100960051,-0.990268068741572,2.08829111071605E-30));
#106385=DIRECTION('center_axis',(-0.904824724134424,-0.42578423948646,0.));
#106386=DIRECTION('ref_axis',(0.42578423948646,-0.904824724134424,0.));
#106387=DIRECTION('center_axis',(0.,0.,-1.));
#106388=DIRECTION('ref_axis',(0.,-1.,0.));
#106389=DIRECTION('center_axis',(0.990268068741571,0.139173100960064,1.71834053708117E-17));
#106390=DIRECTION('ref_axis',(0.139173100960064,-0.990268068741571,7.54967553857625E-35));
#106391=DIRECTION('center_axis',(-0.990268068741571,-0.139173100960064,
-3.86282952735861E-15));
#106392=DIRECTION('ref_axis',(0.139173100960064,-0.990268068741571,3.33751075060364E-33));
#106393=DIRECTION('',(0.990268068741571,0.139173100960059,1.71834053708117E-17));
#106394=DIRECTION('',(-0.990268068741571,-0.139173100960059,-1.71834053708117E-17));
#106395=DIRECTION('center_axis',(0.,-1.23467863058847E-16,1.));
#106396=DIRECTION('ref_axis',(0.,-1.,0.));
#106397=DIRECTION('center_axis',(-0.728126055379271,-0.685443248911113,
1.18468586241421E-15));
#106398=DIRECTION('ref_axis',(0.685443248911113,-0.728126055379271,2.48798705504199E-31));
#106399=DIRECTION('center_axis',(0.,0.,-1.));
#106400=DIRECTION('ref_axis',(0.,-1.,0.));
#106401=DIRECTION('center_axis',(3.11538328111815E-31,-7.86084147552189E-46,
1.));
#106402=DIRECTION('ref_axis',(-2.52323414687536E-15,-1.,3.11150763893057E-61));
#106403=DIRECTION('center_axis',(0.,-1.23467863058847E-16,1.));
#106404=DIRECTION('ref_axis',(0.,-1.,0.));
#106405=DIRECTION('center_axis',(-0.685443248911113,-0.728126055379271,
-1.18468586241421E-15));
#106406=DIRECTION('ref_axis',(0.728126055379271,-0.685443248911113,2.6468713136043E-31));
#106407=DIRECTION('center_axis',(0.,0.,-1.));
#106408=DIRECTION('ref_axis',(0.,-1.,0.));
#106409=DIRECTION('center_axis',(0.,0.,1.));
#106410=DIRECTION('ref_axis',(0.,-1.,0.));
#106411=DIRECTION('center_axis',(0.,-1.23467863058847E-16,1.));
#106412=DIRECTION('ref_axis',(0.,-1.,0.));
#106413=DIRECTION('center_axis',(-0.139173100960068,-0.99026806874157,-2.36226307343407E-14));
#106414=DIRECTION('ref_axis',(0.99026806874157,-0.139173100960068,-1.46728138438144E-30));
#106415=DIRECTION('center_axis',(0.,0.,-1.));
#106416=DIRECTION('ref_axis',(0.,-1.,0.));
#106417=DIRECTION('center_axis',(-6.23076656223629E-31,-3.14433659020876E-45,
1.));
#106418=DIRECTION('ref_axis',(5.04646829375071E-15,-1.,1.86690458335834E-60));
#106419=DIRECTION('center_axis',(0.139173100960068,0.99026806874157,1.22266282302933E-16));
#106420=DIRECTION('ref_axis',(0.99026806874157,-0.139173100960068,-6.9848527780828E-33));
#106421=DIRECTION('center_axis',(-0.139173100960068,-0.99026806874157,0.));
#106422=DIRECTION('ref_axis',(0.99026806874157,-0.139173100960068,0.));
#106423=DIRECTION('',(0.139173100960067,0.99026806874157,1.22266282302933E-16));
#106424=DIRECTION('',(-0.139173100960067,-0.99026806874157,-1.22266282302933E-16));
#106425=DIRECTION('center_axis',(0.,-1.23467863058847E-16,1.));
#106426=DIRECTION('ref_axis',(0.,-1.,0.));
#106427=DIRECTION('center_axis',(-0.425784239486454,-0.904824724134427,
0.));
#106428=DIRECTION('ref_axis',(0.904824724134427,-0.425784239486454,0.));
#106429=DIRECTION('center_axis',(0.,0.,1.));
#106430=DIRECTION('ref_axis',(0.,-1.,0.));
#106431=DIRECTION('center_axis',(0.,0.,-1.));
#106432=DIRECTION('ref_axis',(0.,-1.,0.));
#106433=DIRECTION('center_axis',(0.,-1.23467863058847E-16,1.));
#106434=DIRECTION('ref_axis',(0.,-1.,0.));
#106435=DIRECTION('center_axis',(0.425784239486448,-0.90482472413443,1.18178866550092E-14));
#106436=DIRECTION('ref_axis',(0.90482472413443,0.425784239486448,3.74967935723291E-30));
#106437=DIRECTION('center_axis',(0.,0.,-1.));
#106438=DIRECTION('ref_axis',(0.,-1.,0.));
#106439=DIRECTION('center_axis',(-2.19322982990717E-31,-3.89595880873225E-46,
1.));
#106440=DIRECTION('ref_axis',(1.77635683940025E-15,-1.,-5.4451383681285E-61));
#106441=DIRECTION('center_axis',(0.,-1.23467863058847E-16,1.));
#106442=DIRECTION('ref_axis',(0.,-1.,0.));
#106443=DIRECTION('center_axis',(0.139173100960068,-0.99026806874157,0.));
#106444=DIRECTION('ref_axis',(0.99026806874157,0.139173100960068,0.));
#106445=DIRECTION('center_axis',(0.,0.,1.));
#106446=DIRECTION('ref_axis',(0.,-1.,0.));
#106447=DIRECTION('center_axis',(0.,0.,-1.));
#106448=DIRECTION('ref_axis',(0.,-1.,0.));
#106449=DIRECTION('center_axis',(-0.139173100960064,0.990268068741571,1.22266282302934E-16));
#106450=DIRECTION('ref_axis',(0.990268068741571,0.139173100960064,-6.46427645420959E-34));
#106451=DIRECTION('center_axis',(0.139173100960064,-0.990268068741571,-3.86282952735861E-15));
#106452=DIRECTION('ref_axis',(0.990268068741571,0.139173100960064,3.00533800087463E-32));
#106453=DIRECTION('',(-0.139173100960065,0.99026806874157,1.22266282302933E-16));
#106454=DIRECTION('',(0.139173100960065,-0.99026806874157,-1.22266282302933E-16));
#106455=DIRECTION('center_axis',(0.,-1.23467863058847E-16,1.));
#106456=DIRECTION('ref_axis',(0.,-1.,0.));
#106457=DIRECTION('center_axis',(0.685443248911113,-0.728126055379271,-1.18468586241421E-15));
#106458=DIRECTION('ref_axis',(0.728126055379271,0.685443248911113,-2.6468713136043E-31));
#106459=DIRECTION('center_axis',(0.,0.,-1.));
#106460=DIRECTION('ref_axis',(0.,-1.,0.));
#106461=DIRECTION('center_axis',(-1.24615331244726E-30,-1.2577346360835E-44,
1.));
#106462=DIRECTION('ref_axis',(1.00929365875014E-14,-1.,-9.95682444457783E-60));
#106463=DIRECTION('center_axis',(0.,-1.23467863058847E-16,1.));
#106464=DIRECTION('ref_axis',(0.,-1.,0.));
#106465=DIRECTION('center_axis',(0.728126055379271,-0.685443248911113,0.));
#106466=DIRECTION('ref_axis',(0.685443248911113,0.728126055379271,0.));
#106467=DIRECTION('center_axis',(0.,0.,-1.));
#106468=DIRECTION('ref_axis',(0.,-1.,0.));
#106469=DIRECTION('center_axis',(0.,0.,1.));
#106470=DIRECTION('ref_axis',(0.,-1.,0.));
#106471=DIRECTION('center_axis',(0.,-1.23467863058847E-16,1.));
#106472=DIRECTION('ref_axis',(0.,-1.,0.));
#106473=DIRECTION('center_axis',(0.990268068741571,-0.139173100960064,-7.72565905471723E-15));
#106474=DIRECTION('ref_axis',(0.139173100960064,0.990268068741571,-6.67502150120727E-33));
#106475=DIRECTION('center_axis',(0.,0.,-1.));
#106476=DIRECTION('ref_axis',(0.,-1.,0.));
#106477=DIRECTION('center_axis',(3.11538328111815E-31,-7.86084147552191E-46,
1.));
#106478=DIRECTION('ref_axis',(-2.52323414687536E-15,-1.,-6.22301527786114E-61));
#106479=DIRECTION('center_axis',(-0.990268068741571,0.139173100960064,1.71834053708117E-17));
#106480=DIRECTION('ref_axis',(0.139173100960064,0.990268068741571,-7.54967553857625E-35));
#106481=DIRECTION('center_axis',(0.990268068741571,-0.139173100960064,0.));
#106482=DIRECTION('ref_axis',(0.139173100960064,0.990268068741571,0.));
#106483=DIRECTION('',(-0.990268068741571,0.139173100960059,1.71834053708117E-17));
#106484=DIRECTION('',(0.990268068741571,-0.139173100960059,-1.71834053708117E-17));
#106485=DIRECTION('center_axis',(0.,-1.23467863058847E-16,1.));
#106486=DIRECTION('ref_axis',(0.,-1.,0.));
#106487=DIRECTION('center_axis',(0.902736181373369,-0.430194591829591,1.25279811715363E-14));
#106488=DIRECTION('ref_axis',(0.430194591829591,0.902736181373369,2.66752875008673E-30));
#106489=DIRECTION('center_axis',(1.5706724042304E-30,-1.99810034797076E-44,
1.));
#106490=DIRECTION('ref_axis',(-1.27213054904966E-14,-1.,2.98704733337335E-59));
#106491=DIRECTION('center_axis',(0.,0.,-1.));
#106492=DIRECTION('ref_axis',(0.,-1.,0.));
#106493=DIRECTION('center_axis',(0.,0.,-1.));
#106494=DIRECTION('ref_axis',(0.,1.,0.));
#106495=DIRECTION('center_axis',(0.,0.,1.));
#106496=DIRECTION('ref_axis',(0.,-1.,0.));
#106497=DIRECTION('',(0.,0.,-1.));
#106498=DIRECTION('center_axis',(0.,0.,1.));
#106499=DIRECTION('ref_axis',(0.,-1.,0.));
#106500=DIRECTION('center_axis',(0.,0.,1.));
#106501=DIRECTION('ref_axis',(0.,-1.,0.));
#106502=DIRECTION('center_axis',(0.,0.,1.));
#106503=DIRECTION('ref_axis',(0.,-1.,0.));
#106504=DIRECTION('center_axis',(0.,0.,-1.));
#106505=DIRECTION('ref_axis',(0.,1.,0.));
#106506=DIRECTION('center_axis',(0.,0.,1.));
#106507=DIRECTION('ref_axis',(0.,1.,0.));
#106508=DIRECTION('',(0.,0.,-1.));
#106509=DIRECTION('center_axis',(0.,0.,1.));
#106510=DIRECTION('ref_axis',(0.,1.,0.));
#106511=DIRECTION('center_axis',(0.,0.,1.));
#106512=DIRECTION('ref_axis',(0.,1.,0.));
#106513=DIRECTION('center_axis',(0.,0.,1.));
#106514=DIRECTION('ref_axis',(1.,0.,0.));
#106515=DIRECTION('center_axis',(-0.91200931366711,0.410169491533009,5.52463721181358E-12));
#106516=DIRECTION('ref_axis',(-0.410169491533009,-0.91200931366711,-2.38205677224627E-27));
#106517=DIRECTION('center_axis',(0.,0.,1.));
#106518=DIRECTION('ref_axis',(-0.550808342809401,0.834631756819474,0.));
#106519=DIRECTION('',(0.,-1.23467863058847E-16,1.));
#106520=DIRECTION('center_axis',(0.,0.,1.));
#106521=DIRECTION('ref_axis',(1.,0.,0.));
#106522=DIRECTION('',(-6.19323182390956E-32,1.23467863058847E-16,-1.));
#106523=DIRECTION('center_axis',(0.,-6.17339315294237E-17,1.));
#106524=DIRECTION('ref_axis',(0.,-1.,0.));
#106525=DIRECTION('center_axis',(1.37076864369198E-30,-3.04371781932207E-44,
1.));
#106526=DIRECTION('ref_axis',(-2.22044604925031E-14,-1.,3.98272977783113E-59));
#106527=DIRECTION('center_axis',(0.991119122260598,0.132976688396752,-0.000292971696495811));
#106528=DIRECTION('ref_axis',(0.132889234509439,-0.990382454371073,0.0385103288147991));
#106529=DIRECTION('center_axis',(0.,0.,-1.));
#106530=DIRECTION('ref_axis',(0.,-1.,0.));
#106531=DIRECTION('center_axis',(-0.98674762086852,-0.162262524904213,7.56440721780465E-5));
#106532=DIRECTION('ref_axis',(0.162172283364071,-0.986183084450869,0.0338093840738556));
#106533=DIRECTION('center_axis',(0.,0.,1.));
#106534=DIRECTION('ref_axis',(0.,-1.,0.));
#106535=DIRECTION('center_axis',(0.,0.,1.));
#106536=DIRECTION('ref_axis',(1.,0.,0.));
#106537=DIRECTION('',(6.19323182390956E-32,-1.23467863058847E-16,1.));
#106538=DIRECTION('center_axis',(0.,0.,1.));
#106539=DIRECTION('ref_axis',(1.,0.,0.));
#106540=DIRECTION('',(0.,1.23467863058847E-16,-1.));
#106541=DIRECTION('center_axis',(-0.959851548777671,0.280508474576272,0.));
#106542=DIRECTION('ref_axis',(-0.280508474576272,-0.959851548777671,0.));
#106543=DIRECTION('center_axis',(0.,0.,1.));
#106544=DIRECTION('ref_axis',(-1.,0.,0.));
#106545=DIRECTION('center_axis',(-0.962287669136798,0.272033898305467,2.53734057564779E-13));
#106546=DIRECTION('ref_axis',(-0.272033898305467,-0.962287669136798,2.03523668564842E-29));
#106547=DIRECTION('center_axis',(0.,0.,-1.));
#106548=DIRECTION('ref_axis',(-1.,0.,0.));
#106549=DIRECTION('center_axis',(0.,0.,1.));
#106550=DIRECTION('ref_axis',(-1.,0.,0.));
#106551=DIRECTION('center_axis',(0.,0.,1.));
#106552=DIRECTION('ref_axis',(1.,0.,0.));
#106553=DIRECTION('center_axis',(0.,0.,1.));
#106554=DIRECTION('ref_axis',(-0.610293066582434,0.792175720961838,0.));
#106555=DIRECTION('',(0.,-1.23467863058847E-16,1.));
#106556=DIRECTION('center_axis',(0.,0.,1.));
#106557=DIRECTION('ref_axis',(1.,0.,0.));
#106558=DIRECTION('',(-6.19323182390956E-32,1.23467863058847E-16,-1.));
#106559=DIRECTION('center_axis',(0.,-6.17339315294237E-17,1.));
#106560=DIRECTION('ref_axis',(0.,-1.,0.));
#106561=DIRECTION('center_axis',(2.19322982990717E-31,-7.79191761746451E-46,
1.));
#106562=DIRECTION('ref_axis',(-3.5527136788005E-15,-1.,-1.0890276736257E-60));
#106563=DIRECTION('center_axis',(0.997057160474908,0.0766613778272904,-0.000227805474783485));
#106564=DIRECTION('ref_axis',(0.0765600400510118,-0.995577374783063,0.0544449362884298));
#106565=DIRECTION('center_axis',(0.,0.,-1.));
#106566=DIRECTION('ref_axis',(0.,-1.,0.));
#106567=DIRECTION('center_axis',(-0.993225936104905,-0.116199124850017,
5.68561820310259E-5));
#106568=DIRECTION('ref_axis',(0.115054757945929,-0.983375585734681,0.140480817391474));
#106569=DIRECTION('center_axis',(0.,0.,1.));
#106570=DIRECTION('ref_axis',(0.,-1.,0.));
#106571=DIRECTION('center_axis',(0.,0.,1.));
#106572=DIRECTION('ref_axis',(1.,0.,0.));
#106573=DIRECTION('',(6.19323182390956E-32,-1.23467863058847E-16,1.));
#106574=DIRECTION('center_axis',(0.,0.,1.));
#106575=DIRECTION('ref_axis',(1.,0.,0.));
#106576=DIRECTION('',(0.,1.23467863058847E-16,-1.));
#106577=DIRECTION('center_axis',(-0.989571111262359,0.142966967401199,-0.017591531686721));
#106578=DIRECTION('ref_axis',(-0.142989093957737,-0.989724264130745,-6.72869096378782E-19));
#106579=DIRECTION('center_axis',(-0.99077695153738,0.134510490459868,-0.0163694917007939));
#106580=DIRECTION('ref_axis',(-0.134528515815408,-0.990909722645057,-8.11100475129765E-19));
#106581=DIRECTION('center_axis',(-0.0107641901120226,-0.163472360314363,
-0.986489188802636));
#106582=DIRECTION('ref_axis',(-0.12265200609037,-0.978880947255001,0.163549920523247));
#106583=DIRECTION('center_axis',(0.00303671056267577,0.143796114116046,
0.989602675801801));
#106584=DIRECTION('ref_axis',(-0.135485018598508,-0.980423214391085,0.142878026366596));
#106585=DIRECTION('center_axis',(-1.66533453693774E-13,1.96105155259282E-14,
1.));
#106586=DIRECTION('ref_axis',(1.,3.15330219577248E-42,1.66533453693774E-13));
#106587=DIRECTION('center_axis',(0.,0.,1.));
#106588=DIRECTION('ref_axis',(-0.664473794614039,0.747311565728258,0.));
#106589=DIRECTION('',(0.,-1.23467863058847E-16,1.));
#106590=DIRECTION('center_axis',(0.,0.,1.));
#106591=DIRECTION('ref_axis',(1.,0.,0.));
#106592=DIRECTION('',(-6.19323182390956E-32,1.23467863058847E-16,-1.));
#106593=DIRECTION('center_axis',(0.,-6.17339315294237E-17,1.));
#106594=DIRECTION('ref_axis',(0.,-1.,0.));
#106595=DIRECTION('center_axis',(-8.2246118621519E-31,-1.09573841495595E-44,
1.));
#106596=DIRECTION('ref_axis',(1.33226762955019E-14,-1.,1.36906336112945E-59));
#106597=DIRECTION('center_axis',(0.999944906622129,0.0104967882139315,-3.40243194832232E-5));
#106598=DIRECTION('ref_axis',(0.0104967884357142,-0.99994490717852,6.34634886399102E-6));
#106599=DIRECTION('center_axis',(0.,0.,-1.));
#106600=DIRECTION('ref_axis',(0.,-1.,0.));
#106601=DIRECTION('center_axis',(-0.998408840407527,-0.0563895966071302,
2.81172984632072E-5));
#106602=DIRECTION('ref_axis',(0.0552480255757205,-0.978096630168846,0.20068541980506));
#106603=DIRECTION('center_axis',(0.,0.,1.));
#106604=DIRECTION('ref_axis',(0.,-1.,0.));
#106605=DIRECTION('center_axis',(0.,0.,1.));
#106606=DIRECTION('ref_axis',(1.,0.,0.));
#106607=DIRECTION('',(6.19323182390956E-32,-1.23467863058847E-16,1.));
#106608=DIRECTION('center_axis',(0.,0.,1.));
#106609=DIRECTION('ref_axis',(1.,0.,0.));
#106610=DIRECTION('',(0.,1.23467863058847E-16,-1.));
#106611=DIRECTION('center_axis',(-0.999990764844661,0.00426925256430225,
-0.000493667835992639));
#106612=DIRECTION('ref_axis',(-0.00426925308452771,-0.999990886697524,1.74890393922737E-21));
#106613=DIRECTION('center_axis',(0.,0.,1.));
#106614=DIRECTION('ref_axis',(0.,-1.,0.));
#106615=DIRECTION('',(0.,1.23467863058847E-16,-1.));
#106616=DIRECTION('',(3.43088182518023E-33,1.23467863058847E-16,-1.));
#106617=DIRECTION('',(0.,-1.23467863058847E-16,1.));
#106618=DIRECTION('center_axis',(-0.908150397510606,0.418644067796653,0.));
#106619=DIRECTION('ref_axis',(-0.418644067796653,-0.908150397510606,0.));
#106620=DIRECTION('center_axis',(-0.691017694403315,0.329301163645224,0.643471281133376));
#106621=DIRECTION('ref_axis',(0.681480917945783,1.81728452038657E-16,0.731835882200219));
#106622=DIRECTION('center_axis',(0.,0.,1.));
#106623=DIRECTION('ref_axis',(-1.,0.,0.));
#106624=DIRECTION('center_axis',(0.,0.,-1.));
#106625=DIRECTION('ref_axis',(-1.,0.,0.));
#106626=DIRECTION('center_axis',(0.,0.,1.));
#106627=DIRECTION('ref_axis',(-1.,0.,0.));
#106628=DIRECTION('center_axis',(1.0547118733939E-12,0.,-1.));
#106629=DIRECTION('ref_axis',(-1.,0.,-1.0547118733939E-12));
#106630=DIRECTION('center_axis',(-2.85977186515575E-47,0.,1.));
#106631=DIRECTION('ref_axis',(0.,-1.,0.));
#106632=DIRECTION('',(-2.85977186515575E-47,5.70122241611331E-32,1.));
#106633=DIRECTION('center_axis',(0.,0.,-1.));
#106634=DIRECTION('ref_axis',(-1.,0.,0.));
#106635=DIRECTION('',(2.85977186515575E-47,-5.70122241611331E-32,-1.));
#106636=DIRECTION('center_axis',(0.,-0.422696864907095,0.906271129628277));
#106637=DIRECTION('ref_axis',(0.,0.906271129628277,0.422696864907095));
#106638=DIRECTION('center_axis',(-1.,0.,0.));
#106639=DIRECTION('ref_axis',(0.,0.976478786201388,0.215613497023408));
#106640=DIRECTION('center_axis',(1.,5.01606788234257E-16,0.));
#106641=DIRECTION('ref_axis',(-5.01606788234257E-16,1.,0.));
#106642=DIRECTION('center_axis',(1.,0.,0.));
#106643=DIRECTION('ref_axis',(0.,0.976373434674102,0.216090064701498));
#106644=DIRECTION('',(0.,0.,1.));
#106645=DIRECTION('center_axis',(1.,-6.16404235248998E-16,2.09401852497606E-16));
#106646=DIRECTION('ref_axis',(6.47177887660072E-16,0.976105817825534,-0.21729572569921));
#106647=DIRECTION('center_axis',(-1.,0.,0.));
#106648=DIRECTION('ref_axis',(0.,0.976212736710707,-0.216814881140091));
#106649=DIRECTION('center_axis',(0.,-1.18842113532926E-16,1.));
#106650=DIRECTION('ref_axis',(0.,1.,1.18842113532926E-16));
#106651=DIRECTION('center_axis',(-1.25618648527741E-14,-0.425033206427438,
0.905177757920515));
#106652=DIRECTION('ref_axis',(-2.68759262534439E-30,0.905177757920515,0.425033206427438));
#106653=DIRECTION('center_axis',(1.,0.,0.));
#106654=DIRECTION('ref_axis',(0.,0.97773854081723,0.20982694250404));
#106655=DIRECTION('center_axis',(-1.,-5.01606788234257E-16,0.));
#106656=DIRECTION('ref_axis',(-5.01606788234257E-16,1.,0.));
#106657=DIRECTION('',(-2.85977186515575E-47,5.70122241611331E-32,1.));
#106658=DIRECTION('center_axis',(1.,0.,0.));
#106659=DIRECTION('ref_axis',(0.,0.978009404010872,-0.20856079609145));
#106660=DIRECTION('',(0.,0.,-1.));
#106661=DIRECTION('center_axis',(0.,0.,1.));
#106662=DIRECTION('ref_axis',(1.,0.,0.));
#106663=DIRECTION('center_axis',(0.,0.,-1.));
#106664=DIRECTION('ref_axis',(-1.,0.,0.));
#106665=DIRECTION('center_axis',(0.,-0.427133403156944,0.904188617439729));
#106666=DIRECTION('ref_axis',(0.,0.904188617439729,0.427133403156944));
#106667=DIRECTION('center_axis',(-0.999999999999896,4.44492331285301E-7,
9.98246615501751E-8));
#106668=DIRECTION('ref_axis',(-3.30569704855731E-8,-0.289344971701435,0.957224888597812));
#106669=DIRECTION('center_axis',(1.,5.01606788234257E-16,0.));
#106670=DIRECTION('ref_axis',(-5.01606788234257E-16,1.,0.));
#106671=DIRECTION('',(2.85977186515575E-47,-5.70122241611331E-32,-1.));
#106672=DIRECTION('',(0.,0.,1.));
#106673=DIRECTION('center_axis',(-1.,0.,0.));
#106674=DIRECTION('ref_axis',(0.,0.979170381919184,-0.203040299379802));
#106675=DIRECTION('center_axis',(0.,-1.18842113532926E-16,1.));
#106676=DIRECTION('ref_axis',(0.,1.,1.18842113532926E-16));
#106677=DIRECTION('center_axis',(4.39817443652073E-16,-0.434491800625061,
0.900675788055609));
#106678=DIRECTION('ref_axis',(9.63119795361041E-32,0.900675788055609,0.434491800625061));
#106679=DIRECTION('center_axis',(0.999999999999961,2.70500792618992E-7,
6.20337317877928E-8));
#106680=DIRECTION('ref_axis',(1.37645772676246E-7,-0.677526578069449,0.735498290962993));
#106681=DIRECTION('center_axis',(-1.,-5.01606788234257E-16,0.));
#106682=DIRECTION('ref_axis',(-5.01606788234257E-16,1.,0.));
#106683=DIRECTION('',(-5.01606788234257E-16,1.,0.));
#106684=DIRECTION('center_axis',(-1.,-6.93889390390722E-16,0.));
#106685=DIRECTION('ref_axis',(-6.93889390390722E-16,1.,0.));
#106686=DIRECTION('',(-2.85977186515575E-47,5.70122241611331E-32,1.));
#106687=DIRECTION('center_axis',(-1.,-6.93889390390722E-16,0.));
#106688=DIRECTION('ref_axis',(-6.93889390390722E-16,1.,0.));
#106689=DIRECTION('',(5.01606788234257E-16,-1.,0.));
#106690=DIRECTION('center_axis',(0.999999999999962,2.70358791824049E-7,
-6.1992890822951E-8));
#106691=DIRECTION('ref_axis',(-1.37951269970466E-7,0.678661255727541,0.734451427920388));
#106692=DIRECTION('',(0.,0.,-1.));
#106693=DIRECTION('center_axis',(0.,-1.,0.));
#106694=DIRECTION('ref_axis',(-1.,0.,0.));
#106695=DIRECTION('',(5.01606788234257E-16,-1.,0.));
#106696=DIRECTION('center_axis',(0.,1.,0.));
#106697=DIRECTION('ref_axis',(0.,0.,-1.));
#106698=DIRECTION('center_axis',(0.,0.,-1.));
#106699=DIRECTION('ref_axis',(0.,-1.,0.));
#106700=DIRECTION('',(-5.01606788234257E-16,1.,0.));
#106701=DIRECTION('',(-1.,-5.01606788234257E-16,0.));
#106702=DIRECTION('center_axis',(0.,-1.,0.));
#106703=DIRECTION('ref_axis',(-1.,0.,0.));
#106704=DIRECTION('',(5.01606788234257E-16,-1.,0.));
#106705=DIRECTION('center_axis',(0.,-1.,0.));
#106706=DIRECTION('ref_axis',(0.,0.,1.));
#106707=DIRECTION('center_axis',(0.,-0.439015545441723,0.898479466020513));
#106708=DIRECTION('ref_axis',(0.,0.898479466020513,0.439015545441723));
#106709=DIRECTION('center_axis',(-0.999999999999983,1.80161300130019E-7,
4.18470807107139E-8));
#106710=DIRECTION('ref_axis',(1.57783577724163E-7,0.949012697225746,-0.315237847512461));
#106711=DIRECTION('center_axis',(1.,5.01606788234257E-16,0.));
#106712=DIRECTION('ref_axis',(-5.01606788234257E-16,1.,0.));
#106713=DIRECTION('',(-5.01606788234257E-16,1.,0.));
#106714=DIRECTION('center_axis',(1.,0.,0.));
#106715=DIRECTION('ref_axis',(0.,-1.,0.));
#106716=DIRECTION('',(2.85977186515575E-47,-5.70122241611331E-32,-1.));
#106717=DIRECTION('center_axis',(1.,0.,0.));
#106718=DIRECTION('ref_axis',(0.,-1.,0.));
#106719=DIRECTION('',(0.,0.,1.));
#106720=DIRECTION('center_axis',(-0.999999999999982,1.83115484047939E-7,
-4.25253431652647E-8));
#106721=DIRECTION('ref_axis',(1.60098072209542E-7,0.948126339374677,0.317893763046633));
#106722=DIRECTION('center_axis',(0.,-1.18842113532926E-16,1.));
#106723=DIRECTION('ref_axis',(0.,1.,1.18842113532926E-16));
#106724=DIRECTION('center_axis',(-1.87193934265674E-16,-0.452600956351886,
0.8917131681821));
#106725=DIRECTION('ref_axis',(4.92064035297146E-32,0.8917131681821,0.452600956351886));
#106726=DIRECTION('center_axis',(1.,2.12837658787934E-8,5.13482592661443E-9));
#106727=DIRECTION('ref_axis',(2.11054534386375E-8,-0.99947069068166,0.0325321144152161));
#106728=DIRECTION('center_axis',(-1.,-5.01606788234257E-16,0.));
#106729=DIRECTION('ref_axis',(-5.01606788234257E-16,1.,0.));
#106730=DIRECTION('',(-5.01606788234257E-16,1.,0.));
#106731=DIRECTION('center_axis',(-1.,0.,0.));
#106732=DIRECTION('ref_axis',(0.,1.,0.));
#106733=DIRECTION('',(-2.85977186515575E-47,5.70122241611331E-32,1.));
#106734=DIRECTION('center_axis',(-1.,0.,0.));
#106735=DIRECTION('ref_axis',(0.,1.,0.));
#106736=DIRECTION('',(5.01606788234257E-16,-1.,0.));
#106737=DIRECTION('center_axis',(1.,2.01124692837111E-8,-4.85055393716843E-9));
#106738=DIRECTION('ref_axis',(1.99358965914732E-8,-0.999421676179656,-0.0340046053093633));
#106739=DIRECTION('',(0.,0.,-1.));
#106740=DIRECTION('center_axis',(0.,-1.,0.));
#106741=DIRECTION('ref_axis',(-1.,0.,0.));
#106742=DIRECTION('center_axis',(0.,1.,0.));
#106743=DIRECTION('ref_axis',(0.,0.,-1.));
#106744=DIRECTION('center_axis',(0.,1.23467863058847E-16,-1.));
#106745=DIRECTION('ref_axis',(0.,1.,1.1837531408762E-16));
#106746=DIRECTION('center_axis',(0.,-1.19392659184112E-16,1.));
#106747=DIRECTION('ref_axis',(0.,1.,1.19392659184112E-16));
#106748=DIRECTION('center_axis',(-0.982083847990974,-0.18844354663646,-0.00058757664438451));
#106749=DIRECTION('ref_axis',(0.152822052410976,-0.798257081809623,0.582607116020463));
#106750=DIRECTION('center_axis',(-1.,0.,0.));
#106751=DIRECTION('ref_axis',(0.,-0.558140143889771,-0.829746696154137));
#106752=DIRECTION('center_axis',(0.,-0.605101105507222,-0.796148636947862));
#106753=DIRECTION('ref_axis',(0.,-0.796148636947862,0.605101105507222));
#106754=DIRECTION('center_axis',(1.,0.,0.));
#106755=DIRECTION('ref_axis',(0.,1.,0.));
#106756=DIRECTION('',(0.,-1.,0.));
#106757=DIRECTION('center_axis',(1.,0.,0.));
#106758=DIRECTION('ref_axis',(0.,0.,1.));
#106759=DIRECTION('',(0.,0.,1.));
#106760=DIRECTION('center_axis',(1.,0.,0.));
#106761=DIRECTION('ref_axis',(0.,0.,1.));
#106762=DIRECTION('',(0.,0.,-1.));
#106763=DIRECTION('center_axis',(1.,0.,0.));
#106764=DIRECTION('ref_axis',(0.,-0.892435299537675,0.45117539398675));
#106765=DIRECTION('center_axis',(0.,-1.,0.));
#106766=DIRECTION('ref_axis',(0.,0.,-1.));
#106767=DIRECTION('',(0.,1.,0.));
#106768=DIRECTION('center_axis',(0.,-1.,0.));
#106769=DIRECTION('ref_axis',(0.,0.,1.));
#106770=DIRECTION('center_axis',(0.,0.,1.));
#106771=DIRECTION('ref_axis',(1.,0.,0.));
#106772=DIRECTION('',(0.,-1.,0.));
#106773=DIRECTION('',(1.,0.,0.));
#106774=DIRECTION('center_axis',(0.,-1.,0.));
#106775=DIRECTION('ref_axis',(0.,0.,-1.));
#106776=DIRECTION('',(0.,1.,0.));
#106777=DIRECTION('center_axis',(0.,1.,0.));
#106778=DIRECTION('ref_axis',(0.,0.,-1.));
#106779=DIRECTION('center_axis',(-1.,0.,1.87032180698308E-16));
#106780=DIRECTION('ref_axis',(0.,1.,0.));
#106781=DIRECTION('center_axis',(0.999999999999995,-9.86470856182844E-8,
2.32552699791497E-8));
#106782=DIRECTION('ref_axis',(9.49367918032427E-8,0.992051753940111,0.125830511023124));
#106783=DIRECTION('',(1.87032180698308E-16,8.19208946723987E-32,1.));
#106784=DIRECTION('center_axis',(-1.,0.,0.));
#106785=DIRECTION('ref_axis',(0.,0.,-1.));
#106786=DIRECTION('',(-1.87032180698308E-16,0.,-1.));
#106787=DIRECTION('center_axis',(-1.,0.,0.));
#106788=DIRECTION('ref_axis',(0.,0.,-1.));
#106789=DIRECTION('center_axis',(-1.85986770746484E-14,-0.444295746197836,
-0.895880176089698));
#106790=DIRECTION('ref_axis',(8.37014173169963E-31,-0.895880176089698,0.444295746197836));
#106791=DIRECTION('center_axis',(0.,-1.18842113532926E-16,1.));
#106792=DIRECTION('ref_axis',(0.,1.,1.18842113532926E-16));
#106793=DIRECTION('center_axis',(-0.999999999999951,-3.06438046744071E-7,
6.9946007058117E-8));
#106794=DIRECTION('ref_axis',(1.06561695484496E-7,-0.539875486220256,-0.841744889725165));
#106795=DIRECTION('center_axis',(0.,-0.432834338283548,-0.901473480254768));
#106796=DIRECTION('ref_axis',(0.,-0.901473480254768,0.432834338283548));
#106797=DIRECTION('center_axis',(1.,0.,0.));
#106798=DIRECTION('ref_axis',(0.,1.,0.));
#106799=DIRECTION('',(0.,0.,1.));
#106800=DIRECTION('center_axis',(1.,0.,0.));
#106801=DIRECTION('ref_axis',(0.,0.000252653767746131,-0.999999968083036));
#106802=DIRECTION('center_axis',(0.,0.,1.));
#106803=DIRECTION('ref_axis',(1.,0.,0.));
#106804=DIRECTION('center_axis',(3.552570199055E-14,1.,2.23044154114413E-16));
#106805=DIRECTION('ref_axis',(0.00256148703537234,1.37530068325002E-16,
-0.999996719386703));
#106806=DIRECTION('center_axis',(0.,0.,1.));
#106807=DIRECTION('ref_axis',(1.,0.,0.));
#106808=DIRECTION('center_axis',(0.,-0.429430624963615,-0.903099849597684));
#106809=DIRECTION('ref_axis',(0.,-0.903099849597684,0.429430624963615));
#106810=DIRECTION('center_axis',(0.999999999999922,-3.86396202578527E-7,
8.73478327237184E-8));
#106811=DIRECTION('ref_axis',(-5.51687521210774E-8,-0.354181556455975,-0.935176681203301));
#106812=DIRECTION('center_axis',(-1.,0.,1.87032180698308E-16));
#106813=DIRECTION('ref_axis',(0.,1.,0.));
#106814=DIRECTION('',(-1.87032180698308E-16,0.,-1.));
#106815=DIRECTION('center_axis',(0.,-1.18842113532926E-16,1.));
#106816=DIRECTION('ref_axis',(0.,1.,1.18842113532926E-16));
#106817=DIRECTION('center_axis',(-1.,1.54885822040769E-14,-1.69750672317071E-15));
#106818=DIRECTION('ref_axis',(1.54954772622702E-14,0.977150339649803,-0.212549320681755));
#106819=DIRECTION('center_axis',(0.,-0.424147858891027,-0.905592951495404));
#106820=DIRECTION('ref_axis',(0.,-0.905592951495404,0.424147858891027));
#106821=DIRECTION('center_axis',(1.,0.,0.));
#106822=DIRECTION('ref_axis',(0.,1.,0.));
#106823=DIRECTION('',(0.,0.,1.));
#106824=DIRECTION('center_axis',(0.,0.,1.));
#106825=DIRECTION('ref_axis',(1.,0.,0.));
#106826=DIRECTION('center_axis',(0.,0.,1.));
#106827=DIRECTION('ref_axis',(1.,0.,0.));
#106828=DIRECTION('center_axis',(-1.,0.,1.87032180698308E-16));
#106829=DIRECTION('ref_axis',(0.,1.,0.));
#106830=DIRECTION('',(-1.87032180698308E-16,0.,-1.));
#106831=DIRECTION('center_axis',(-1.,0.,0.));
#106832=DIRECTION('ref_axis',(0.,1.,0.));
#106833=DIRECTION('',(-1.,-4.18005656861881E-16,0.));
#106834=DIRECTION('center_axis',(1.,0.,0.));
#106835=DIRECTION('ref_axis',(0.,0.,-1.));
#106836=DIRECTION('',(1.,4.18005656861881E-16,0.));
#106837=DIRECTION('center_axis',(0.,0.,-1.));
#106838=DIRECTION('ref_axis',(0.,-1.,0.));
#106839=DIRECTION('',(1.,4.18005656861881E-16,0.));
#106840=DIRECTION('',(-4.18005656861881E-16,1.,0.));
#106841=DIRECTION('center_axis',(-1.,0.,0.));
#106842=DIRECTION('ref_axis',(0.,1.,0.));
#106843=DIRECTION('',(-1.,-4.18005656861881E-16,0.));
#106844=DIRECTION('center_axis',(-1.,0.,0.));
#106845=DIRECTION('ref_axis',(0.,0.,1.));
#106846=DIRECTION('center_axis',(-1.,0.,0.));
#106847=DIRECTION('ref_axis',(0.,1.,0.));
#106848=DIRECTION('',(-1.,-4.18005656861881E-16,0.));
#106849=DIRECTION('center_axis',(1.,0.,0.));
#106850=DIRECTION('ref_axis',(0.,0.,-1.));
#106851=DIRECTION('',(1.,4.18005656861881E-16,0.));
#106852=DIRECTION('center_axis',(0.,0.,-1.));
#106853=DIRECTION('ref_axis',(0.,-1.,0.));
#106854=DIRECTION('',(1.,4.18005656861881E-16,0.));
#106855=DIRECTION('',(-4.18005656861881E-16,1.,0.));
#106856=DIRECTION('center_axis',(-1.,0.,0.));
#106857=DIRECTION('ref_axis',(0.,1.,0.));
#106858=DIRECTION('',(-1.,-4.18005656861881E-16,0.));
#106859=DIRECTION('center_axis',(-1.,0.,0.));
#106860=DIRECTION('ref_axis',(0.,0.,1.));
#106861=DIRECTION('center_axis',(4.18005656861882E-16,-1.,0.));
#106862=DIRECTION('ref_axis',(0.,0.,-1.));
#106863=DIRECTION('',(1.,4.18005656861881E-16,0.));
#106864=DIRECTION('center_axis',(0.,-1.,0.));
#106865=DIRECTION('ref_axis',(-1.,0.,0.));
#106866=DIRECTION('',(0.,0.,-1.));
#106867=DIRECTION('center_axis',(0.,-1.,0.));
#106868=DIRECTION('ref_axis',(-1.,0.,0.));
#106869=DIRECTION('center_axis',(0.,1.,0.));
#106870=DIRECTION('ref_axis',(0.949353414912971,0.,-0.314210269712943));
#106871=DIRECTION('',(0.,0.,1.));
#106872=DIRECTION('center_axis',(2.01185813448618E-8,1.,-4.85634575709083E-9));
#106873=DIRECTION('ref_axis',(0.999508172274741,-1.99563942566965E-8,0.0313594253136996));
#106874=DIRECTION('',(-5.16102651992463E-32,-2.15733828054269E-47,1.));
#106875=DIRECTION('center_axis',(0.452924541251067,-1.8658316499269E-14,
-0.891548854484436));
#106876=DIRECTION('ref_axis',(-0.891548854484436,-1.10243984483832E-29,
-0.452924541251067));
#106877=DIRECTION('center_axis',(0.,-1.18842113532926E-16,1.));
#106878=DIRECTION('ref_axis',(0.,1.,1.18842113532926E-16));
#106879=DIRECTION('center_axis',(1.78035353894022E-7,-0.999999999999983,
4.13792904095341E-8));
#106880=DIRECTION('ref_axis',(0.953984227728196,1.57435058485391E-7,-0.299856787893509));
#106881=DIRECTION('center_axis',(0.439239043992112,0.,-0.898370225593489));
#106882=DIRECTION('ref_axis',(-0.898370225593489,0.,-0.439239043992112));
#106883=DIRECTION('center_axis',(-4.18005656861882E-16,1.,0.));
#106884=DIRECTION('ref_axis',(1.,4.18005656861882E-16,0.));
#106885=DIRECTION('',(1.,4.18005656861881E-16,0.));
#106886=DIRECTION('center_axis',(0.,1.,0.));
#106887=DIRECTION('ref_axis',(1.,0.,0.));
#106888=DIRECTION('',(0.,0.,1.));
#106889=DIRECTION('center_axis',(0.,1.,0.));
#106890=DIRECTION('ref_axis',(1.,0.,0.));
#106891=DIRECTION('',(-1.,-4.18005656861881E-16,0.));
#106892=DIRECTION('',(5.16102651992463E-32,2.15733828054269E-47,-1.));
#106893=DIRECTION('center_axis',(1.77394867447905E-7,-0.999999999999983,
-4.1222642628058E-8));
#106894=DIRECTION('ref_axis',(0.952173814166433,1.56314884088295E-7,0.305556913873213));
#106895=DIRECTION('',(0.,0.,-1.));
#106896=DIRECTION('center_axis',(-1.,0.,0.));
#106897=DIRECTION('ref_axis',(0.,1.,0.));
#106898=DIRECTION('',(-1.,-4.18005656861881E-16,0.));
#106899=DIRECTION('center_axis',(1.,0.,0.));
#106900=DIRECTION('ref_axis',(0.,0.,-1.));
#106901=DIRECTION('center_axis',(0.,0.,-1.));
#106902=DIRECTION('ref_axis',(0.,-1.,0.));
#106903=DIRECTION('',(1.,4.18005656861881E-16,0.));
#106904=DIRECTION('',(-4.18005656861881E-16,1.,0.));
#106905=DIRECTION('center_axis',(-1.,0.,0.));
#106906=DIRECTION('ref_axis',(0.,1.,0.));
#106907=DIRECTION('',(-1.,-4.18005656861881E-16,0.));
#106908=DIRECTION('center_axis',(-1.,0.,0.));
#106909=DIRECTION('ref_axis',(0.,0.,1.));
#106910=DIRECTION('center_axis',(-0.434677673768106,0.,0.900586098009262));
#106911=DIRECTION('ref_axis',(0.900586098009262,0.,0.434677673768106));
#106912=DIRECTION('center_axis',(2.65375153024716E-7,0.999999999999963,
6.08903066929881E-8));
#106913=DIRECTION('ref_axis',(-0.69985050026065,1.42229635936985E-7,0.714289351233027));
#106914=DIRECTION('center_axis',(4.18005656861882E-16,-1.,0.));
#106915=DIRECTION('ref_axis',(0.,0.,-1.));
#106916=DIRECTION('',(0.,0.,1.));
#106917=DIRECTION('center_axis',(2.67568067369228E-7,0.999999999999962,
-6.13851229161734E-8));
#106918=DIRECTION('ref_axis',(0.690330185099942,-1.40298517037424E-7,0.723494461305586));
#106919=DIRECTION('',(-5.16102651992463E-32,-2.15733828054269E-47,1.));
#106920=DIRECTION('center_axis',(0.,-1.,0.));
#106921=DIRECTION('ref_axis',(-1.,0.,0.));
#106922=DIRECTION('',(0.,0.,-1.));
#106923=DIRECTION('center_axis',(0.,-1.,0.));
#106924=DIRECTION('ref_axis',(-1.,0.,0.));
#106925=DIRECTION('center_axis',(0.,-1.18842113532926E-16,1.));
#106926=DIRECTION('ref_axis',(0.,1.,1.18842113532926E-16));
#106927=DIRECTION('center_axis',(-0.427243916491378,0.,0.904136403327014));
#106928=DIRECTION('ref_axis',(0.904136403327014,0.,0.427243916491378));
#106929=DIRECTION('center_axis',(0.,-1.,0.));
#106930=DIRECTION('ref_axis',(0.979260396969467,0.,0.202605712967828));
#106931=DIRECTION('center_axis',(-4.18005656861882E-16,1.,0.));
#106932=DIRECTION('ref_axis',(1.,4.18005656861882E-16,0.));
#106933=DIRECTION('',(0.,0.,1.));
#106934=DIRECTION('',(5.16102651992463E-32,2.15733828054269E-47,-1.));
#106935=DIRECTION('center_axis',(4.42078072401712E-7,-0.999999999999897,
-9.93087227438785E-8));
#106936=DIRECTION('ref_axis',(-0.291484561136116,-3.38626385168455E-8,-0.956575533148995));
#106937=DIRECTION('',(0.,0.,-1.));
#106938=DIRECTION('center_axis',(0.,0.,1.));
#106939=DIRECTION('ref_axis',(1.,0.,0.));
#106940=DIRECTION('center_axis',(0.,0.,-1.));
#106941=DIRECTION('ref_axis',(-1.,0.,0.));
#106942=DIRECTION('center_axis',(-0.425113301005477,0.,0.905140144567805));
#106943=DIRECTION('ref_axis',(0.905140144567805,0.,0.425113301005477));
#106944=DIRECTION('center_axis',(0.,1.,0.));
#106945=DIRECTION('ref_axis',(0.978069789124882,0.,0.208277429408972));
#106946=DIRECTION('center_axis',(4.18005656861882E-16,-1.,0.));
#106947=DIRECTION('ref_axis',(0.,0.,-1.));
#106948=DIRECTION('',(0.,0.,-1.));
#106949=DIRECTION('',(0.,0.,1.));
#106950=DIRECTION('center_axis',(0.,1.,0.));
#106951=DIRECTION('ref_axis',(0.977785987053698,0.,-0.209605733512769));
#106952=DIRECTION('',(-5.16102651992463E-32,-2.15733828054269E-47,1.));
#106953=DIRECTION('center_axis',(0.,-1.18842113532926E-16,1.));
#106954=DIRECTION('ref_axis',(0.,1.,1.18842113532926E-16));
#106955=DIRECTION('center_axis',(-0.422711655064036,-5.86630265286877E-15,
0.906264231156137));
#106956=DIRECTION('ref_axis',(0.906264231156137,8.13850067779198E-31,0.422711655064036));
#106957=DIRECTION('center_axis',(0.,-1.,0.));
#106958=DIRECTION('ref_axis',(0.976222312485803,0.,0.216771761548571));
#106959=DIRECTION('center_axis',(-4.18005656861882E-16,1.,0.));
#106960=DIRECTION('ref_axis',(1.,4.18005656861882E-16,0.));
#106961=DIRECTION('',(0.,0.,1.));
#106962=DIRECTION('',(5.16102651992463E-32,2.15733828054269E-47,-1.));
#106963=DIRECTION('center_axis',(0.,-1.,0.));
#106964=DIRECTION('ref_axis',(0.976488023107232,0.,-0.21557166030842));
#106965=DIRECTION('center_axis',(0.,1.,0.));
#106966=DIRECTION('ref_axis',(0.976392755984516,0.,-0.216002745494037));
#106967=DIRECTION('',(0.,0.,-1.));
#106968=DIRECTION('center_axis',(0.,1.,0.));
#106969=DIRECTION('ref_axis',(0.976124389191499,0.,0.217212285162516));
#106970=DIRECTION('center_axis',(0.,0.,1.));
#106971=DIRECTION('ref_axis',(1.,0.,0.));
#106972=DIRECTION('center_axis',(1.,0.,0.));
#106973=DIRECTION('ref_axis',(0.,-0.0033149217825888,0.999994505631694));
#106974=DIRECTION('center_axis',(0.,0.,1.));
#106975=DIRECTION('ref_axis',(1.,0.,0.));
#106976=DIRECTION('center_axis',(-0.422683349901129,0.,0.906277433083468));
#106977=DIRECTION('ref_axis',(0.906277433083468,0.,0.422683349901129));
#106978=DIRECTION('center_axis',(0.,1.,0.));
#106979=DIRECTION('ref_axis',(0.976470143643405,0.,0.215652634050752));
#106980=DIRECTION('center_axis',(4.18005656861882E-16,-1.,0.));
#106981=DIRECTION('ref_axis',(0.,0.,-1.));
#106982=DIRECTION('center_axis',(0.,-1.,0.));
#106983=DIRECTION('ref_axis',(0.976404651458869,0.,0.21594896760458));
#106984=DIRECTION('',(0.,0.,1.));
#106985=DIRECTION('center_axis',(0.,-1.,0.));
#106986=DIRECTION('ref_axis',(0.976137352210661,0.,-0.217154022802156));
#106987=DIRECTION('center_axis',(0.,1.,0.));
#106988=DIRECTION('ref_axis',(0.976204192855077,0.,-0.216853346416809));
#106989=DIRECTION('',(-5.16102651992463E-32,-2.15733828054269E-47,1.));
#106990=DIRECTION('',(0.,0.,-1.));
#106991=DIRECTION('center_axis',(0.,-1.18842113532926E-16,1.));
#106992=DIRECTION('ref_axis',(0.,1.,1.18842113532926E-16));
#106993=DIRECTION('center_axis',(-0.424954451342053,5.8974277037113E-15,
0.905214733797774));
#106994=DIRECTION('ref_axis',(0.905214733797774,1.745344269554E-30,0.424954451342053));
#106995=DIRECTION('center_axis',(0.,-1.,0.));
#106996=DIRECTION('ref_axis',(0.977685721591009,0.,0.210072915429545));
#106997=DIRECTION('center_axis',(-4.18005656861882E-16,1.,0.));
#106998=DIRECTION('ref_axis',(1.,4.18005656861882E-16,0.));
#106999=DIRECTION('',(0.,0.,1.));
#107000=DIRECTION('',(5.16102651992463E-32,2.15733828054269E-47,-1.));
#107001=DIRECTION('center_axis',(0.,-1.,0.));
#107002=DIRECTION('ref_axis',(0.977956433447826,0.,-0.208809037826448));
#107003=DIRECTION('',(0.,0.,-1.));
#107004=DIRECTION('center_axis',(0.,0.,1.));
#107005=DIRECTION('ref_axis',(1.,0.,0.));
#107006=DIRECTION('center_axis',(0.,0.,1.));
#107007=DIRECTION('ref_axis',(1.,0.,0.));
#107008=DIRECTION('center_axis',(-0.427024288778512,0.,0.904240154380022));
#107009=DIRECTION('ref_axis',(0.904240154380022,0.,0.427024288778512));
#107010=DIRECTION('center_axis',(4.47342289204968E-7,0.999999999999895,
1.00433397542106E-7));
#107011=DIRECTION('ref_axis',(-0.286876404864124,3.21200065696789E-8,0.957967602965901));
#107012=DIRECTION('center_axis',(4.18005656861882E-16,-1.,0.));
#107013=DIRECTION('ref_axis',(0.,0.,-1.));
#107014=DIRECTION('',(0.,0.,1.));
#107015=DIRECTION('center_axis',(0.,1.,0.));
#107016=DIRECTION('ref_axis',(0.979094017787432,0.,-0.203408220907771));
#107017=DIRECTION('',(-5.16102651992463E-32,-2.15733828054269E-47,1.));
#107018=DIRECTION('',(0.,0.,-1.));
#107019=DIRECTION('center_axis',(0.,-1.18842113532926E-16,1.));
#107020=DIRECTION('ref_axis',(0.,1.,1.18842113532926E-16));
#107021=DIRECTION('center_axis',(2.74436147249853E-7,-0.99999999999996,
6.29034153387369E-8));
#107022=DIRECTION('ref_axis',(0.660475707126984,1.34027541627577E-7,-0.750847414788845));
#107023=DIRECTION('center_axis',(0.434307547312743,0.,-0.900764649809921));
#107024=DIRECTION('ref_axis',(-0.900764649809921,0.,-0.434307547312743));
#107025=DIRECTION('center_axis',(-4.18005656861882E-16,1.,0.));
#107026=DIRECTION('ref_axis',(1.,4.18005656861882E-16,0.));
#107027=DIRECTION('',(1.,4.18005656861881E-16,0.));
#107028=DIRECTION('center_axis',(-3.46944695195361E-16,1.,0.));
#107029=DIRECTION('ref_axis',(1.,3.46944695195361E-16,0.));
#107030=DIRECTION('',(0.,0.,1.));
#107031=DIRECTION('center_axis',(-3.46944695195361E-16,1.,0.));
#107032=DIRECTION('ref_axis',(1.,3.46944695195361E-16,0.));
#107033=DIRECTION('',(5.16102651992463E-32,2.15733828054269E-47,-1.));
#107034=DIRECTION('center_axis',(2.74310940053038E-7,-0.99999999999996,
-6.28664519205214E-8));
#107035=DIRECTION('ref_axis',(-0.661953171072186,-1.34459749665864E-7,-0.749545194973231));
#107036=DIRECTION('',(0.,0.,-1.));
#107037=DIRECTION('center_axis',(-1.,0.,0.));
#107038=DIRECTION('ref_axis',(0.,1.,0.));
#107039=DIRECTION('',(-1.,-4.18005656861881E-16,0.));
#107040=DIRECTION('center_axis',(1.,0.,0.));
#107041=DIRECTION('ref_axis',(0.,0.,-1.));
#107042=DIRECTION('center_axis',(0.,0.,-1.));
#107043=DIRECTION('ref_axis',(0.,-1.,0.));
#107044=DIRECTION('',(1.,4.18005656861881E-16,0.));
#107045=DIRECTION('',(-4.18005656861881E-16,1.,0.));
#107046=DIRECTION('center_axis',(-1.,0.,0.));
#107047=DIRECTION('ref_axis',(0.,1.,0.));
#107048=DIRECTION('',(-1.,-4.18005656861881E-16,0.));
#107049=DIRECTION('center_axis',(-1.,0.,0.));
#107050=DIRECTION('ref_axis',(0.,0.,1.));
#107051=DIRECTION('center_axis',(-0.438793812561498,0.,0.898587775377423));
#107052=DIRECTION('ref_axis',(0.898587775377423,0.,0.438793812561498));
#107053=DIRECTION('center_axis',(1.84116539076111E-7,0.999999999999982,
4.27391046394982E-8));
#107054=DIRECTION('ref_axis',(0.944128962664186,-1.59743963387227E-7,-0.329576245895577));
#107055=DIRECTION('center_axis',(4.18005656861882E-16,-1.,0.));
#107056=DIRECTION('ref_axis',(0.,0.,-1.));
#107057=DIRECTION('',(0.,0.,1.));
#107058=DIRECTION('center_axis',(1.87037537959256E-7,0.999999999999982,
-4.3409180827419E-8));
#107059=DIRECTION('ref_axis',(0.943089040549533,-1.61957749522192E-7,0.332540315744325));
#107060=DIRECTION('',(-5.16102651992463E-32,-2.15733828054269E-47,1.));
#107061=DIRECTION('',(1.,4.18005656861881E-16,0.));
#107062=DIRECTION('center_axis',(3.46944695195361E-16,-1.,0.));
#107063=DIRECTION('ref_axis',(-1.,-3.46944695195361E-16,0.));
#107064=DIRECTION('',(0.,0.,-1.));
#107065=DIRECTION('center_axis',(3.46944695195361E-16,-1.,0.));
#107066=DIRECTION('ref_axis',(-1.,-3.46944695195361E-16,0.));
#107067=DIRECTION('center_axis',(0.,-1.18842113532926E-16,1.));
#107068=DIRECTION('ref_axis',(0.,1.,1.18842113532926E-16));
#107069=DIRECTION('center_axis',(2.32689124945317E-8,-1.,5.60875666134475E-9));
#107070=DIRECTION('ref_axis',(0.999404101599166,2.30614476367381E-8,-0.0345172667916152));
#107071=DIRECTION('center_axis',(0.452279624303263,0.,-0.891876191766604));
#107072=DIRECTION('ref_axis',(-0.891876191766604,0.,-0.452279624303263));
#107073=DIRECTION('center_axis',(-4.18005656861882E-16,1.,0.));
#107074=DIRECTION('ref_axis',(1.,4.18005656861882E-16,0.));
#107075=DIRECTION('center_axis',(2.20735454691794E-8,-1.,-5.3187770880344E-9));
#107076=DIRECTION('ref_axis',(0.999350588277669,2.18675573381274E-8,0.0360333416307286));
#107077=DIRECTION('',(0.,0.,-1.));
#107078=DIRECTION('center_axis',(-6.93889390390722E-16,1.,0.));
#107079=DIRECTION('ref_axis',(1.,6.93889390390722E-16,0.));
#107080=DIRECTION('',(0.,0.,1.));
#107081=DIRECTION('center_axis',(-6.93889390390722E-16,1.,0.));
#107082=DIRECTION('ref_axis',(1.,6.93889390390722E-16,0.));
#107083=DIRECTION('',(-1.,-4.18005656861881E-16,0.));
#107084=DIRECTION('',(5.16102651992463E-32,2.15733828054269E-47,-1.));
#107085=DIRECTION('center_axis',(0.,1.23467863058847E-16,-1.));
#107086=DIRECTION('ref_axis',(-1.,0.,0.));
#107087=DIRECTION('center_axis',(0.,1.17559414210783E-16,-1.));
#107088=DIRECTION('ref_axis',(0.,1.,1.17559414210783E-16));
#107089=DIRECTION('',(-5.01606788234257E-16,1.,1.23467863058847E-16));
#107090=DIRECTION('',(5.01606788234257E-16,-1.,-1.23467863058847E-16));
#107091=DIRECTION('center_axis',(0.,-1.,0.));
#107092=DIRECTION('ref_axis',(0.,0.,1.));
#107093=DIRECTION('center_axis',(0.,-1.,0.));
#107094=DIRECTION('ref_axis',(0.,0.,1.));
#107095=DIRECTION('center_axis',(-1.,-5.01606788234257E-16,1.13659195805196E-16));
#107096=DIRECTION('ref_axis',(-5.01606788234257E-16,1.,5.42661491374937E-48));
#107097=DIRECTION('',(5.01606788234257E-16,-1.,-1.23467863058847E-16));
#107098=DIRECTION('',(-1.13659195805196E-16,-4.9783213633841E-32,-1.));
#107099=DIRECTION('',(-5.01606788234257E-16,1.,1.23467863058847E-16));
#107100=DIRECTION('',(-5.01606788234257E-16,1.,0.));
#107101=DIRECTION('center_axis',(-1.,0.,1.13659195805196E-16));
#107102=DIRECTION('ref_axis',(0.,1.,0.));
#107103=DIRECTION('',(1.13659195805196E-16,1.14024448322266E-31,1.));
#107104=DIRECTION('center_axis',(-1.,0.,1.13659195805196E-16));
#107105=DIRECTION('ref_axis',(0.,1.,0.));
#107106=DIRECTION('',(5.01606788234257E-16,-1.,0.));
#107107=DIRECTION('',(-1.13659195805196E-16,1.39441621308911E-16,-1.));
#107108=DIRECTION('center_axis',(0.,-1.,0.));
#107109=DIRECTION('ref_axis',(-1.,0.,0.));
#107110=DIRECTION('',(5.01606788234257E-16,-1.,0.));
#107111=DIRECTION('center_axis',(0.,1.,0.));
#107112=DIRECTION('ref_axis',(0.,0.,-1.));
#107113=DIRECTION('center_axis',(0.,0.,-1.));
#107114=DIRECTION('ref_axis',(0.,-1.,0.));
#107115=DIRECTION('',(-4.38004274807345E-16,1.,0.));
#107116=DIRECTION('',(-1.,-5.01606788234257E-16,0.));
#107117=DIRECTION('center_axis',(0.,1.,0.));
#107118=DIRECTION('ref_axis',(1.,0.,0.));
#107119=DIRECTION('',(4.38004274807345E-16,-1.,0.));
#107120=DIRECTION('center_axis',(0.,1.,0.));
#107121=DIRECTION('ref_axis',(0.,0.,-1.));
#107122=DIRECTION('center_axis',(1.,4.38004274807345E-16,1.13659195805196E-16));
#107123=DIRECTION('ref_axis',(-4.38004274807345E-16,1.,-1.29211895128087E-48));
#107124=DIRECTION('',(-4.38004274807345E-16,1.,1.23467863058847E-16));
#107125=DIRECTION('',(-1.13659195805196E-16,-1.07494104808783E-16,1.));
#107126=DIRECTION('',(-4.38004274807345E-16,1.,0.));
#107127=DIRECTION('center_axis',(1.,0.,1.13659195805196E-16));
#107128=DIRECTION('ref_axis',(0.,-1.,0.));
#107129=DIRECTION('',(1.13659195805196E-16,0.,-1.));
#107130=DIRECTION('center_axis',(1.,0.,1.13659195805196E-16));
#107131=DIRECTION('ref_axis',(0.,-1.,0.));
#107132=DIRECTION('',(4.38004274807345E-16,-1.,-1.23467863058847E-16));
#107133=DIRECTION('',(4.38004274807345E-16,-1.,-1.23467863058847E-16));
#107134=DIRECTION('',(-1.13659195805196E-16,-4.9783213633841E-32,1.));
#107135=DIRECTION('',(-4.38004274807345E-16,1.,1.23467863058847E-16));
#107136=DIRECTION('center_axis',(0.,1.,2.77555756156289E-14));
#107137=DIRECTION('ref_axis',(0.,2.77555756156289E-14,-1.));
#107138=DIRECTION('center_axis',(0.,-0.800147951883018,0.599802680135236));
#107139=DIRECTION('ref_axis',(0.,0.599802680135236,0.800147951883018));
#107140=DIRECTION('center_axis',(1.,5.01606788234257E-16,0.));
#107141=DIRECTION('ref_axis',(-5.01606788234257E-16,1.,0.));
#107142=DIRECTION('',(-5.01606788234257E-16,1.,0.));
#107143=DIRECTION('center_axis',(1.,0.,0.));
#107144=DIRECTION('ref_axis',(0.,-1.,0.));
#107145=DIRECTION('',(2.85977186515575E-47,-5.70122241611331E-32,-1.));
#107146=DIRECTION('center_axis',(1.,0.,0.));
#107147=DIRECTION('ref_axis',(0.,-1.,0.));
#107148=DIRECTION('center_axis',(1.,0.,0.));
#107149=DIRECTION('ref_axis',(0.,0.919361469721465,0.393413888915463));
#107150=DIRECTION('',(0.,0.,1.));
#107151=DIRECTION('',(6.19323182390956E-32,-1.23467863058847E-16,1.));
#107152=DIRECTION('center_axis',(0.,1.23467863058847E-16,-1.));
#107153=DIRECTION('ref_axis',(0.,1.,1.1837531408762E-16));
#107154=DIRECTION('center_axis',(0.,-1.19392659184112E-16,1.));
#107155=DIRECTION('ref_axis',(0.,1.,1.19392659184112E-16));
#107156=DIRECTION('center_axis',(-0.976975053597396,0.213351911799271,-0.000840464134822775));
#107157=DIRECTION('ref_axis',(0.178869337010668,0.821208026530106,0.541870037407396));
#107158=DIRECTION('center_axis',(0.,1.17559414210783E-16,-1.));
#107159=DIRECTION('ref_axis',(0.,1.,1.17559414210783E-16));
#107160=DIRECTION('center_axis',(0.,1.23467863058847E-16,-1.));
#107161=DIRECTION('ref_axis',(-1.,0.,0.));
#107162=DIRECTION('',(5.01606788234257E-16,-1.,-1.23467863058847E-16));
#107163=DIRECTION('center_axis',(0.,-1.,0.));
#107164=DIRECTION('ref_axis',(0.,0.,1.));
#107165=DIRECTION('center_axis',(-1.,-5.01606788234257E-16,0.));
#107166=DIRECTION('ref_axis',(-5.01606788234257E-16,1.,0.));
#107167=DIRECTION('',(-5.01606788234257E-16,1.,0.));
#107168=DIRECTION('center_axis',(-1.,0.,0.));
#107169=DIRECTION('ref_axis',(0.,1.,0.));
#107170=DIRECTION('',(-2.85977186515575E-47,5.70122241611331E-32,1.));
#107171=DIRECTION('center_axis',(-1.,0.,0.));
#107172=DIRECTION('ref_axis',(0.,1.,0.));
#107173=DIRECTION('',(5.01606788234257E-16,-1.,0.));
#107174=DIRECTION('',(-6.19323182390956E-32,1.23467863058847E-16,-1.));
#107175=DIRECTION('',(5.01606788234257E-16,-1.,-1.23467863058847E-16));
#107176=DIRECTION('',(0.,0.,-1.));
#107177=DIRECTION('',(-5.01606788234257E-16,1.,1.23467863058847E-16));
#107178=DIRECTION('center_axis',(0.,-1.,0.));
#107179=DIRECTION('ref_axis',(-1.,0.,0.));
#107180=DIRECTION('',(5.01606788234257E-16,-1.,0.));
#107181=DIRECTION('center_axis',(0.,1.,0.));
#107182=DIRECTION('ref_axis',(0.,0.,-1.));
#107183=DIRECTION('center_axis',(0.,0.,-1.));
#107184=DIRECTION('ref_axis',(0.,-1.,0.));
#107185=DIRECTION('',(-5.01606788234257E-16,1.,0.));
#107186=DIRECTION('',(-1.,-5.01606788234257E-16,0.));
#107187=DIRECTION('center_axis',(0.,-1.,0.));
#107188=DIRECTION('ref_axis',(-1.,0.,0.));
#107189=DIRECTION('',(5.01606788234257E-16,-1.,0.));
#107190=DIRECTION('center_axis',(0.,-1.,0.));
#107191=DIRECTION('ref_axis',(0.,0.,1.));
#107192=DIRECTION('center_axis',(1.,5.01606788234257E-16,0.));
#107193=DIRECTION('ref_axis',(-5.01606788234257E-16,1.,0.));
#107194=DIRECTION('',(-5.01606788234257E-16,1.,0.));
#107195=DIRECTION('center_axis',(1.,0.,0.));
#107196=DIRECTION('ref_axis',(0.,-1.,0.));
#107197=DIRECTION('',(2.85977186515575E-47,-5.70122241611331E-32,-1.));
#107198=DIRECTION('center_axis',(1.,0.,0.));
#107199=DIRECTION('ref_axis',(0.,-1.,0.));
#107200=DIRECTION('',(5.01606788234257E-16,-1.,-1.23467863058847E-16));
#107201=DIRECTION('',(0.,0.,1.));
#107202=DIRECTION('',(-5.01606788234257E-16,1.,1.23467863058847E-16));
#107203=DIRECTION('',(6.19323182390956E-32,-1.23467863058847E-16,1.));
#107204=DIRECTION('center_axis',(0.,1.23467863058847E-16,-1.));
#107205=DIRECTION('ref_axis',(-1.,0.,0.));
#107206=DIRECTION('center_axis',(2.62387838037626E-32,1.17559414210783E-16,
-1.));
#107207=DIRECTION('ref_axis',(-4.44089209850062E-15,1.,1.17559414210783E-16));
#107208=DIRECTION('',(-2.30924636740563E-32,-1.,-1.23467863058847E-16));
#107209=DIRECTION('',(0.,1.,1.23467863058847E-16));
#107210=DIRECTION('center_axis',(0.,-1.,0.));
#107211=DIRECTION('ref_axis',(0.,0.,1.));
#107212=DIRECTION('center_axis',(0.,-1.,0.));
#107213=DIRECTION('ref_axis',(0.,0.,1.));
#107214=DIRECTION('center_axis',(1.,0.,0.));
#107215=DIRECTION('ref_axis',(0.,1.,0.));
#107216=DIRECTION('',(0.,-1.,0.));
#107217=DIRECTION('center_axis',(1.,0.,0.));
#107218=DIRECTION('ref_axis',(0.,0.,1.));
#107219=DIRECTION('',(0.,0.,1.));
#107220=DIRECTION('center_axis',(1.,0.,0.));
#107221=DIRECTION('ref_axis',(0.,0.,1.));
#107222=DIRECTION('',(0.,0.,-1.));
#107223=DIRECTION('',(0.,-1.,-1.23467863058847E-16));
#107224=DIRECTION('center_axis',(0.,-1.,0.));
#107225=DIRECTION('ref_axis',(0.,0.,-1.));
#107226=DIRECTION('',(0.,1.,0.));
#107227=DIRECTION('center_axis',(0.,-1.,0.));
#107228=DIRECTION('ref_axis',(0.,0.,1.));
#107229=DIRECTION('center_axis',(0.,0.,1.));
#107230=DIRECTION('ref_axis',(1.,0.,0.));
#107231=DIRECTION('',(0.,-1.,0.));
#107232=DIRECTION('',(1.,0.,0.));
#107233=DIRECTION('center_axis',(0.,-1.,0.));
#107234=DIRECTION('ref_axis',(0.,0.,-1.));
#107235=DIRECTION('',(0.,1.,0.));
#107236=DIRECTION('center_axis',(0.,1.,0.));
#107237=DIRECTION('ref_axis',(0.,0.,-1.));
#107238=DIRECTION('center_axis',(-1.,0.,1.87032180698308E-16));
#107239=DIRECTION('ref_axis',(0.,1.,0.));
#107240=DIRECTION('',(1.87032180698308E-16,8.19208946723987E-32,1.));
#107241=DIRECTION('center_axis',(-1.,0.,0.));
#107242=DIRECTION('ref_axis',(0.,0.,-1.));
#107243=DIRECTION('',(-1.87032180698308E-16,0.,-1.));
#107244=DIRECTION('center_axis',(-1.,0.,0.));
#107245=DIRECTION('ref_axis',(0.,0.,-1.));
#107246=DIRECTION('center_axis',(3.33932916167122E-16,-0.999710458475598,
-0.0240624025090732));
#107247=DIRECTION('ref_axis',(2.2263435019713E-33,-0.0240624025090732,0.999710458475598));
#107248=DIRECTION('center_axis',(0.,1.,0.));
#107249=DIRECTION('ref_axis',(0.,0.,-1.));
#107250=DIRECTION('center_axis',(-1.,-4.38004274807345E-16,0.));
#107251=DIRECTION('ref_axis',(-4.38004274807345E-16,1.,0.));
#107252=DIRECTION('',(-5.40794518211031E-32,1.23467863058847E-16,-1.));
#107253=DIRECTION('',(4.38004274807345E-16,-1.,-1.23467863058847E-16));
#107254=DIRECTION('',(4.38004274807345E-16,-1.,0.));
#107255=DIRECTION('center_axis',(1.,0.,0.));
#107256=DIRECTION('ref_axis',(0.,1.,0.));
#107257=DIRECTION('',(0.,0.,1.));
#107258=DIRECTION('',(-4.38004274807345E-16,1.,0.));
#107259=DIRECTION('center_axis',(-4.38004274807346E-16,1.,0.));
#107260=DIRECTION('ref_axis',(1.,4.38004274807346E-16,0.));
#107261=DIRECTION('',(-4.38004274807345E-16,1.,0.));
#107262=DIRECTION('center_axis',(0.,-1.,0.));
#107263=DIRECTION('ref_axis',(0.,0.,1.));
#107264=DIRECTION('center_axis',(0.,0.,1.));
#107265=DIRECTION('ref_axis',(1.,0.,0.));
#107266=DIRECTION('',(0.,-1.,0.));
#107267=DIRECTION('',(1.,0.,0.));
#107268=DIRECTION('center_axis',(0.,-1.,0.));
#107269=DIRECTION('ref_axis',(0.,0.,-1.));
#107270=DIRECTION('',(0.,1.,0.));
#107271=DIRECTION('center_axis',(0.,1.,0.));
#107272=DIRECTION('ref_axis',(0.,0.,-1.));
#107273=DIRECTION('center_axis',(-1.,0.,1.87032180698308E-16));
#107274=DIRECTION('ref_axis',(0.,1.,0.));
#107275=DIRECTION('',(-1.87032180698308E-16,0.,-1.));
#107276=DIRECTION('center_axis',(-1.,0.,0.));
#107277=DIRECTION('ref_axis',(0.,0.,-1.));
#107278=DIRECTION('',(2.30924636740563E-32,1.,1.23467863058847E-16));
#107279=DIRECTION('',(1.87032180698308E-16,8.19208946723987E-32,1.));
#107280=DIRECTION('center_axis',(-1.,0.,0.));
#107281=DIRECTION('ref_axis',(0.,0.,-1.));
#107282=DIRECTION('center_axis',(0.,1.23467863058847E-16,-1.));
#107283=DIRECTION('ref_axis',(-1.,0.,0.));
#107284=DIRECTION('center_axis',(5.24775676075252E-32,1.17559414210783E-16,
-1.));
#107285=DIRECTION('ref_axis',(-8.88178419700125E-15,1.,1.17559414210783E-16));
#107286=DIRECTION('',(1.,4.18005656861881E-16,5.16102651992463E-32));
#107287=DIRECTION('',(-1.,-4.18005656861881E-16,-5.16102651992463E-32));
#107288=DIRECTION('center_axis',(1.,0.,0.));
#107289=DIRECTION('ref_axis',(0.,0.,-1.));
#107290=DIRECTION('center_axis',(-1.,0.,0.));
#107291=DIRECTION('ref_axis',(0.,0.,1.));
#107292=DIRECTION('center_axis',(-4.18005656861882E-16,1.,0.));
#107293=DIRECTION('ref_axis',(1.,4.18005656861882E-16,0.));
#107294=DIRECTION('',(-1.,-4.18005656861881E-16,-5.16102651992463E-32));
#107295=DIRECTION('',(0.,0.,-1.));
#107296=DIRECTION('',(1.,4.18005656861881E-16,5.16102651992463E-32));
#107297=DIRECTION('',(1.,4.18005656861881E-16,0.));
#107298=DIRECTION('center_axis',(0.,1.,0.));
#107299=DIRECTION('ref_axis',(1.,0.,0.));
#107300=DIRECTION('',(0.,0.,1.));
#107301=DIRECTION('center_axis',(0.,1.,0.));
#107302=DIRECTION('ref_axis',(1.,0.,0.));
#107303=DIRECTION('',(-1.,-4.18005656861881E-16,0.));
#107304=DIRECTION('',(-1.73522765332111E-17,-7.25334975031394E-33,-1.));
#107305=DIRECTION('center_axis',(-1.,0.,0.));
#107306=DIRECTION('ref_axis',(0.,1.,0.));
#107307=DIRECTION('',(-1.,-4.18005656861881E-16,0.));
#107308=DIRECTION('center_axis',(1.,0.,0.));
#107309=DIRECTION('ref_axis',(0.,0.,-1.));
#107310=DIRECTION('center_axis',(0.,0.,-1.));
#107311=DIRECTION('ref_axis',(0.,-1.,0.));
#107312=DIRECTION('',(1.,4.38004274807345E-16,0.));
#107313=DIRECTION('',(-4.18005656861881E-16,1.,0.));
#107314=DIRECTION('center_axis',(1.,0.,0.));
#107315=DIRECTION('ref_axis',(0.,-1.,0.));
#107316=DIRECTION('',(-1.,-4.38004274807345E-16,0.));
#107317=DIRECTION('center_axis',(-1.,0.,0.));
#107318=DIRECTION('ref_axis',(0.,0.,1.));
#107319=DIRECTION('center_axis',(-1.,0.,0.));
#107320=DIRECTION('ref_axis',(0.,0.,1.));
#107321=DIRECTION('center_axis',(4.38004274807345E-16,-1.,0.));
#107322=DIRECTION('ref_axis',(0.,0.,-1.));
#107323=DIRECTION('',(1.6326809185664E-16,7.15121221728469E-32,1.));
#107324=DIRECTION('',(1.,4.38004274807345E-16,5.40794518211031E-32));
#107325=DIRECTION('',(1.,4.38004274807345E-16,5.40794518211031E-32));
#107326=DIRECTION('',(1.73522765332111E-17,7.60037129918566E-33,1.));
#107327=DIRECTION('',(1.,4.38004274807345E-16,0.));
#107328=DIRECTION('center_axis',(0.,-1.,0.));
#107329=DIRECTION('ref_axis',(-1.,0.,0.));
#107330=DIRECTION('',(0.,0.,-1.));
#107331=DIRECTION('center_axis',(0.,-1.,0.));
#107332=DIRECTION('ref_axis',(-1.,0.,0.));
#107333=DIRECTION('',(-1.,-4.38004274807345E-16,-5.40794518211031E-32));
#107334=DIRECTION('',(-1.,-4.38004274807345E-16,-5.40794518211031E-32));
#107335=DIRECTION('',(-5.40794518211031E-32,-2.3687031076881E-47,1.));
#107336=DIRECTION('center_axis',(0.,1.,0.));
#107337=DIRECTION('ref_axis',(-1.,0.,0.));
#107338=DIRECTION('center_axis',(4.18005656861882E-16,-1.,0.));
#107339=DIRECTION('ref_axis',(0.,0.,-1.));
#107340=DIRECTION('',(1.,4.18005656861881E-16,0.));
#107341=DIRECTION('center_axis',(6.93889390390722E-16,-1.,0.));
#107342=DIRECTION('ref_axis',(-1.,-6.93889390390722E-16,0.));
#107343=DIRECTION('',(0.,0.,-1.));
#107344=DIRECTION('center_axis',(6.93889390390722E-16,-1.,0.));
#107345=DIRECTION('ref_axis',(-1.,-6.93889390390722E-16,0.));
#107346=DIRECTION('center_axis',(0.,1.,0.));
#107347=DIRECTION('ref_axis',(0.964920734332925,0.,0.262541380461079));
#107348=DIRECTION('center_axis',(0.,1.,0.));
#107349=DIRECTION('ref_axis',(-0.285513244926914,0.,0.958374763321376));
#107350=DIRECTION('center_axis',(0.,-1.,0.));
#107351=DIRECTION('ref_axis',(0.882822386976779,0.,0.469706965088471));
#107352=DIRECTION('',(0.,0.,1.));
#107353=DIRECTION('',(-5.16102651992463E-32,-2.15733828054269E-47,1.));
#107354=DIRECTION('center_axis',(0.403600920616143,-3.09956391918065E-14,
-0.91493513260657));
#107355=DIRECTION('ref_axis',(-0.91493513260657,-7.63177238048844E-30,-0.403600920616143));
#107356=DIRECTION('center_axis',(0.,1.23467863058847E-16,-1.));
#107357=DIRECTION('ref_axis',(0.,1.,1.1837531408762E-16));
#107358=DIRECTION('center_axis',(0.,-1.19392659184112E-16,1.));
#107359=DIRECTION('ref_axis',(0.,1.,1.19392659184112E-16));
#107360=DIRECTION('center_axis',(0.212543372582222,0.977151310604023,-0.000794327523214365));
#107361=DIRECTION('ref_axis',(0.808607924198044,-0.175426436275447,0.561585959920498));
#107362=DIRECTION('center_axis',(-3.98829513817191E-31,1.17559414210783E-16,
-1.));
#107363=DIRECTION('ref_axis',(6.75015598972095E-14,1.,1.17559414210783E-16));
#107364=DIRECTION('center_axis',(0.,1.23467863058847E-16,-1.));
#107365=DIRECTION('ref_axis',(-1.,0.,0.));
#107366=DIRECTION('',(-1.,-4.18005656861881E-16,-5.16102651992463E-32));
#107367=DIRECTION('center_axis',(-1.,0.,0.));
#107368=DIRECTION('ref_axis',(0.,0.,1.));
#107369=DIRECTION('center_axis',(-4.18005656861882E-16,1.,0.));
#107370=DIRECTION('ref_axis',(1.,4.18005656861882E-16,0.));
#107371=DIRECTION('',(1.,4.18005656861881E-16,0.));
#107372=DIRECTION('center_axis',(0.,1.,0.));
#107373=DIRECTION('ref_axis',(1.,0.,0.));
#107374=DIRECTION('',(0.,0.,1.));
#107375=DIRECTION('center_axis',(0.,1.,0.));
#107376=DIRECTION('ref_axis',(1.,0.,0.));
#107377=DIRECTION('',(-1.,-4.18005656861881E-16,0.));
#107378=DIRECTION('',(-1.73522765332111E-17,-7.25334975031394E-33,-1.));
#107379=DIRECTION('',(-1.,-4.18005656861881E-16,-5.16102651992463E-32));
#107380=DIRECTION('',(0.,0.,-1.));
#107381=DIRECTION('',(1.,4.18005656861881E-16,5.16102651992463E-32));
#107382=DIRECTION('center_axis',(-1.,0.,0.));
#107383=DIRECTION('ref_axis',(0.,1.,0.));
#107384=DIRECTION('',(-1.,-4.18005656861881E-16,0.));
#107385=DIRECTION('center_axis',(1.,0.,0.));
#107386=DIRECTION('ref_axis',(0.,0.,-1.));
#107387=DIRECTION('center_axis',(0.,0.,-1.));
#107388=DIRECTION('ref_axis',(0.,-1.,0.));
#107389=DIRECTION('',(1.,4.18005656861881E-16,0.));
#107390=DIRECTION('',(-4.18005656861881E-16,1.,0.));
#107391=DIRECTION('center_axis',(-1.,0.,0.));
#107392=DIRECTION('ref_axis',(0.,1.,0.));
#107393=DIRECTION('',(-1.,-4.18005656861881E-16,0.));
#107394=DIRECTION('center_axis',(-1.,0.,0.));
#107395=DIRECTION('ref_axis',(0.,0.,1.));
#107396=DIRECTION('center_axis',(4.18005656861882E-16,-1.,0.));
#107397=DIRECTION('ref_axis',(0.,0.,-1.));
#107398=DIRECTION('',(1.,4.18005656861881E-16,0.));
#107399=DIRECTION('center_axis',(0.,-1.,0.));
#107400=DIRECTION('ref_axis',(-1.,0.,0.));
#107401=DIRECTION('',(0.,0.,-1.));
#107402=DIRECTION('center_axis',(0.,-1.,0.));
#107403=DIRECTION('ref_axis',(-1.,0.,0.));
#107404=DIRECTION('',(-1.,-4.18005656861881E-16,-5.16102651992463E-32));
#107405=DIRECTION('',(0.,0.,1.));
#107406=DIRECTION('',(1.,4.18005656861881E-16,5.16102651992463E-32));
#107407=DIRECTION('',(1.73522765332111E-17,7.25334975031394E-33,1.));
#107408=DIRECTION('center_axis',(0.,1.23467863058847E-16,-1.));
#107409=DIRECTION('ref_axis',(0.,1.,1.1837531408762E-16));
#107410=DIRECTION('center_axis',(0.,-1.19392659184112E-16,1.));
#107411=DIRECTION('ref_axis',(0.,1.,1.19392659184112E-16));
#107412=DIRECTION('center_axis',(0.,1.17559414210783E-16,-1.));
#107413=DIRECTION('ref_axis',(0.,1.,1.17559414210783E-16));
#107414=DIRECTION('center_axis',(0.214155640377145,-0.97679914458343,-0.000890413238434334));
#107415=DIRECTION('ref_axis',(0.833617683430173,0.18323919483608,-0.52106137387868));
#107416=DIRECTION('center_axis',(0.817080261705548,0.,-0.576523933528517));
#107417=DIRECTION('ref_axis',(-0.576523933528517,0.,-0.817080261705548));
#107418=DIRECTION('center_axis',(-4.18005656861882E-16,1.,0.));
#107419=DIRECTION('ref_axis',(1.,4.18005656861882E-16,0.));
#107420=DIRECTION('',(0.,0.,-1.));
#107421=DIRECTION('center_axis',(0.,1.,0.));
#107422=DIRECTION('ref_axis',(0.979462303582526,0.,-0.201627368828764));
#107423=DIRECTION('center_axis',(0.,1.,0.));
#107424=DIRECTION('ref_axis',(1.,0.,0.));
#107425=DIRECTION('',(0.,0.,1.));
#107426=DIRECTION('center_axis',(0.,1.,0.));
#107427=DIRECTION('ref_axis',(1.,0.,0.));
#107428=DIRECTION('',(-1.,-4.18005656861881E-16,0.));
#107429=DIRECTION('',(5.16102651992463E-32,2.15733828054269E-47,-1.));
#107430=DIRECTION('center_axis',(-1.,0.,0.));
#107431=DIRECTION('ref_axis',(0.,0.,1.));
#107432=DIRECTION('center_axis',(-4.38004274807345E-16,1.,0.));
#107433=DIRECTION('ref_axis',(1.,4.38004274807345E-16,0.));
#107434=DIRECTION('',(-1.,-4.38004274807345E-16,-5.40794518211031E-32));
#107435=DIRECTION('',(-1.,-4.38004274807345E-16,-5.40794518211031E-32));
#107436=DIRECTION('',(1.13659195805196E-16,4.9783213633841E-32,-1.));
#107437=DIRECTION('',(1.,4.38004274807345E-16,5.40794518211031E-32));
#107438=DIRECTION('',(1.,4.38004274807345E-16,5.40794518211031E-32));
#107439=DIRECTION('',(1.,4.38004274807345E-16,0.));
#107440=DIRECTION('center_axis',(0.,1.,0.));
#107441=DIRECTION('ref_axis',(1.,0.,0.));
#107442=DIRECTION('',(0.,0.,1.));
#107443=DIRECTION('center_axis',(0.,1.,0.));
#107444=DIRECTION('ref_axis',(1.,0.,0.));
#107445=DIRECTION('',(-1.,-4.38004274807345E-16,0.));
#107446=DIRECTION('',(1.73522765332109E-17,7.60037129918555E-33,-1.));
#107447=DIRECTION('center_axis',(1.,0.,0.));
#107448=DIRECTION('ref_axis',(0.,-1.,0.));
#107449=DIRECTION('',(-1.,-4.38004274807345E-16,0.));
#107450=DIRECTION('center_axis',(-1.,0.,0.));
#107451=DIRECTION('ref_axis',(0.,0.,1.));
#107452=DIRECTION('center_axis',(0.,0.,-1.));
#107453=DIRECTION('ref_axis',(0.,-1.,0.));
#107454=DIRECTION('',(1.,4.18005656861881E-16,0.));
#107455=DIRECTION('',(-4.18005656861881E-16,1.,0.));
#107456=DIRECTION('center_axis',(-1.,0.,0.));
#107457=DIRECTION('ref_axis',(0.,1.,0.));
#107458=DIRECTION('',(-1.,-4.18005656861881E-16,0.));
#107459=DIRECTION('center_axis',(-1.,0.,0.));
#107460=DIRECTION('ref_axis',(0.,0.,1.));
#107461=DIRECTION('center_axis',(4.18005656861882E-16,-1.,0.));
#107462=DIRECTION('ref_axis',(0.,0.,-1.));
#107463=DIRECTION('',(1.,4.18005656861881E-16,0.));
#107464=DIRECTION('center_axis',(0.,-1.,0.));
#107465=DIRECTION('ref_axis',(-1.,0.,0.));
#107466=DIRECTION('',(0.,0.,-1.));
#107467=DIRECTION('center_axis',(0.,-1.,0.));
#107468=DIRECTION('ref_axis',(-1.,0.,0.));
#107469=DIRECTION('',(-1.,-4.18005656861881E-16,-5.16102651992463E-32));
#107470=DIRECTION('',(0.,0.,1.));
#107471=DIRECTION('',(1.,4.18005656861881E-16,5.16102651992463E-32));
#107472=DIRECTION('',(-1.73522765332109E-17,-7.25334975031383E-33,1.));
#107473=DIRECTION('center_axis',(1.,-1.38777878078144E-14,1.38777878078144E-14));
#107474=DIRECTION('ref_axis',(1.38777878078144E-14,4.48415508583941E-44,
-1.));
#107475=DIRECTION('center_axis',(0.,1.23467863058847E-16,-1.));
#107476=DIRECTION('ref_axis',(-1.,0.,0.));
#107477=DIRECTION('center_axis',(8.39641081720404E-32,1.17559414210783E-16,
-1.));
#107478=DIRECTION('ref_axis',(-1.4210854715202E-14,1.,1.17559414210783E-16));
#107479=DIRECTION('',(1.,4.18005656861881E-16,5.16102651992463E-32));
#107480=DIRECTION('',(-1.,-4.18005656861881E-16,-5.16102651992463E-32));
#107481=DIRECTION('center_axis',(-1.,0.,0.));
#107482=DIRECTION('ref_axis',(0.,0.,1.));
#107483=DIRECTION('center_axis',(-4.18005656861882E-16,1.,0.));
#107484=DIRECTION('ref_axis',(1.,4.18005656861882E-16,0.));
#107485=DIRECTION('',(1.,4.18005656861881E-16,0.));
#107486=DIRECTION('center_axis',(0.,1.,0.));
#107487=DIRECTION('ref_axis',(1.,0.,0.));
#107488=DIRECTION('',(0.,0.,1.));
#107489=DIRECTION('center_axis',(0.,1.,0.));
#107490=DIRECTION('ref_axis',(1.,0.,0.));
#107491=DIRECTION('',(-1.,-4.18005656861881E-16,0.));
#107492=DIRECTION('',(1.73522765332109E-17,7.25334975031383E-33,-1.));
#107493=DIRECTION('',(-1.,-4.18005656861881E-16,-5.16102651992463E-32));
#107494=DIRECTION('',(0.,0.,-1.));
#107495=DIRECTION('',(1.,4.18005656861881E-16,5.16102651992463E-32));
#107496=DIRECTION('center_axis',(-1.,0.,0.));
#107497=DIRECTION('ref_axis',(0.,1.,0.));
#107498=DIRECTION('',(-1.,-4.18005656861881E-16,0.));
#107499=DIRECTION('center_axis',(1.,0.,0.));
#107500=DIRECTION('ref_axis',(0.,0.,-1.));
#107501=DIRECTION('center_axis',(0.,0.,-1.));
#107502=DIRECTION('ref_axis',(0.,-1.,0.));
#107503=DIRECTION('',(1.,4.18005656861881E-16,0.));
#107504=DIRECTION('',(-4.18005656861881E-16,1.,0.));
#107505=DIRECTION('center_axis',(-1.,0.,0.));
#107506=DIRECTION('ref_axis',(0.,1.,0.));
#107507=DIRECTION('',(-1.,-4.18005656861881E-16,0.));
#107508=DIRECTION('center_axis',(-1.,0.,0.));
#107509=DIRECTION('ref_axis',(0.,0.,1.));
#107510=DIRECTION('center_axis',(-1.,0.,0.));
#107511=DIRECTION('ref_axis',(0.,0.,1.));
#107512=DIRECTION('center_axis',(4.18005656861882E-16,-1.,0.));
#107513=DIRECTION('ref_axis',(0.,0.,-1.));
#107514=DIRECTION('',(1.,4.18005656861881E-16,0.));
#107515=DIRECTION('center_axis',(0.,-1.,0.));
#107516=DIRECTION('ref_axis',(-1.,0.,0.));
#107517=DIRECTION('',(0.,0.,-1.));
#107518=DIRECTION('center_axis',(0.,-1.,0.));
#107519=DIRECTION('ref_axis',(-1.,0.,0.));
#107520=DIRECTION('',(-1.,-4.18005656861881E-16,-5.16102651992463E-32));
#107521=DIRECTION('',(0.,0.,1.));
#107522=DIRECTION('',(1.,4.18005656861881E-16,5.16102651992463E-32));
#107523=DIRECTION('',(-1.73522765332109E-17,-7.25334975031383E-33,1.));
#107524=DIRECTION('center_axis',(0.,1.23467863058847E-16,-1.));
#107525=DIRECTION('ref_axis',(-1.,0.,0.));
#107526=DIRECTION('',(1.,4.18005656861881E-16,5.16102651992463E-32));
#107527=DIRECTION('center_axis',(1.,4.38004274807346E-16,5.40794518211031E-32));
#107528=DIRECTION('ref_axis',(4.38004274807346E-16,-1.,-5.80597460094347E-63));
#107529=DIRECTION('center_axis',(-1.,-4.38004274807345E-16,0.));
#107530=DIRECTION('ref_axis',(0.,0.,-1.));
#107531=DIRECTION('center_axis',(0.,0.,-1.));
#107532=DIRECTION('ref_axis',(0.,1.,0.));
#107533=DIRECTION('center_axis',(0.,0.,-1.));
#107534=DIRECTION('ref_axis',(1.,0.,0.));
#107535=DIRECTION('',(0.,0.,-1.));
#107536=DIRECTION('center_axis',(0.,0.,1.));
#107537=DIRECTION('ref_axis',(0.,1.,0.));
#107538=DIRECTION('center_axis',(0.,1.23467863058847E-16,-1.));
#107539=DIRECTION('ref_axis',(-1.,0.,0.));
#107540=DIRECTION('center_axis',(0.,0.,1.));
#107541=DIRECTION('ref_axis',(0.,1.,0.));
#107542=DIRECTION('center_axis',(0.,0.,-1.));
#107543=DIRECTION('ref_axis',(0.,1.,0.));
#107544=DIRECTION('',(0.,0.,-1.));
#107545=DIRECTION('center_axis',(1.,4.38004274807346E-16,5.40794518211031E-32));
#107546=DIRECTION('ref_axis',(4.38004274807346E-16,-1.,-5.80597460094347E-63));
#107547=DIRECTION('center_axis',(1.,4.38004274807345E-16,-4.02455846426619E-13));
#107548=DIRECTION('ref_axis',(-4.02455846426619E-13,-4.48415508583941E-44,
-1.));
#107549=DIRECTION('center_axis',(1.,0.,0.));
#107550=DIRECTION('ref_axis',(0.,0.,-1.));
#107551=DIRECTION('center_axis',(0.71239495798367,0.701778757044872,0.));
#107552=DIRECTION('ref_axis',(-0.701778757044872,0.71239495798367,0.));
#107553=DIRECTION('center_axis',(-1.71346080461497E-30,2.37790454634537E-44,
-1.));
#107554=DIRECTION('ref_axis',(1.38777878078144E-14,1.,2.48920611114446E-59));
#107555=DIRECTION('center_axis',(0.,1.23467863058847E-16,-1.));
#107556=DIRECTION('ref_axis',(0.,1.,1.19418947186571E-16));
#107557=DIRECTION('center_axis',(0.740307041655026,0.672268907563025,0.));
#107558=DIRECTION('ref_axis',(-0.672268907563025,0.740307041655026,0.));
#107559=DIRECTION('center_axis',(0.,-1.18613571006961E-16,1.));
#107560=DIRECTION('ref_axis',(0.,1.,1.18613571006961E-16));
#107561=DIRECTION('center_axis',(0.,1.,0.));
#107562=DIRECTION('ref_axis',(0.,0.,-1.));
#107563=DIRECTION('center_axis',(-8.56730402307488E-31,5.94476136586342E-45,
-1.));
#107564=DIRECTION('ref_axis',(6.93889390390722E-15,1.,9.95682444457783E-60));
#107565=DIRECTION('center_axis',(0.,1.,1.23467863058847E-16));
#107566=DIRECTION('ref_axis',(1.,0.,0.));
#107567=DIRECTION('center_axis',(0.,1.,1.23467863058847E-16));
#107568=DIRECTION('ref_axis',(1.,0.,0.));
#107569=DIRECTION('center_axis',(0.,1.,0.));
#107570=DIRECTION('ref_axis',(0.,0.,-1.));
#107571=DIRECTION('center_axis',(0.,0.,-1.));
#107572=DIRECTION('ref_axis',(0.,1.,0.));
#107573=DIRECTION('center_axis',(0.,0.,-1.));
#107574=DIRECTION('ref_axis',(1.,0.,0.));
#107575=DIRECTION('',(0.,0.,-1.));
#107576=DIRECTION('center_axis',(0.,0.,1.));
#107577=DIRECTION('ref_axis',(0.,1.,0.));
#107578=DIRECTION('center_axis',(0.,1.23467863058847E-16,-1.));
#107579=DIRECTION('ref_axis',(-1.,0.,0.));
#107580=DIRECTION('center_axis',(0.,0.,1.));
#107581=DIRECTION('ref_axis',(0.,1.,0.));
#107582=DIRECTION('center_axis',(0.,0.,-1.));
#107583=DIRECTION('ref_axis',(0.,1.,0.));
#107584=DIRECTION('',(0.,0.,-1.));
#107585=DIRECTION('center_axis',(0.,0.,1.));
#107586=DIRECTION('ref_axis',(0.,1.,0.));
#107587=DIRECTION('center_axis',(-1.,-4.38004274807346E-16,-5.40794518211031E-32));
#107588=DIRECTION('ref_axis',(-4.38004274807346E-16,1.,5.80597460094347E-63));
#107589=DIRECTION('center_axis',(-1.,-4.38004274807345E-16,0.));
#107590=DIRECTION('ref_axis',(0.,0.,1.));
#107591=DIRECTION('center_axis',(-1.,-5.01606788234257E-16,0.));
#107592=DIRECTION('ref_axis',(-5.01606788234257E-16,1.,0.));
#107593=DIRECTION('center_axis',(-1.,0.,0.));
#107594=DIRECTION('ref_axis',(0.,-1.,0.));
#107595=DIRECTION('',(1.,5.01606788234257E-16,0.));
#107596=DIRECTION('center_axis',(1.,0.,0.));
#107597=DIRECTION('ref_axis',(0.,1.,0.));
#107598=DIRECTION('center_axis',(1.,5.01606788234257E-16,0.));
#107599=DIRECTION('ref_axis',(0.,-1.,0.));
#107600=DIRECTION('center_axis',(0.,0.,-1.));
#107601=DIRECTION('ref_axis',(-1.,0.,0.));
#107602=DIRECTION('center_axis',(0.,0.,1.));
#107603=DIRECTION('ref_axis',(-1.,0.,0.));
#107604=DIRECTION('',(1.87032180698308E-16,0.,1.));
#107605=DIRECTION('center_axis',(0.,0.,-1.));
#107606=DIRECTION('ref_axis',(-1.,0.,0.));
#107607=DIRECTION('center_axis',(0.,1.,0.));
#107608=DIRECTION('ref_axis',(1.,0.,0.));
#107609=DIRECTION('',(0.,0.,-1.));
#107610=DIRECTION('',(-1.,0.,0.));
#107611=DIRECTION('center_axis',(0.,-1.,0.));
#107612=DIRECTION('ref_axis',(0.,0.,1.));
#107613=DIRECTION('center_axis',(-0.488849591387095,-0.481564692142823,
-0.727407399111432));
#107614=DIRECTION('ref_axis',(-0.82998476161361,2.33877977530395E-17,0.557786066058662));
#107615=DIRECTION('center_axis',(-0.366954554655378,-9.16653140031321E-14,
-0.930238869762855));
#107616=DIRECTION('ref_axis',(-0.930238869762855,-2.79622788237931E-29,
0.366954554655378));
#107617=DIRECTION('center_axis',(4.38004274807345E-16,-1.,0.));
#107618=DIRECTION('ref_axis',(-1.,0.,0.));
#107619=DIRECTION('center_axis',(0.,0.,-1.));
#107620=DIRECTION('ref_axis',(-1.,0.,0.));
#107621=DIRECTION('center_axis',(0.,-1.,0.));
#107622=DIRECTION('ref_axis',(0.,0.,-1.));
#107623=DIRECTION('center_axis',(0.,-1.,0.));
#107624=DIRECTION('ref_axis',(0.,0.,1.));
#107625=DIRECTION('center_axis',(-0.716305556970081,-0.650473286312467,
-0.252568511195758));
#107626=DIRECTION('ref_axis',(0.672268907563029,-0.740307041655023,-6.62280424422414E-17));
#107627=DIRECTION('center_axis',(0.,0.,1.));
#107628=DIRECTION('ref_axis',(-1.,0.,0.));
#107629=DIRECTION('',(1.87032180698308E-16,0.,1.));
#107630=DIRECTION('center_axis',(0.,1.,0.));
#107631=DIRECTION('ref_axis',(1.,0.,0.));
#107632=DIRECTION('',(0.,0.,-1.));
#107633=DIRECTION('center_axis',(0.,0.,-1.));
#107634=DIRECTION('ref_axis',(1.,0.,0.));
#107635=DIRECTION('center_axis',(0.,-0.425268108821871,-0.905067420482623));
#107636=DIRECTION('ref_axis',(0.,-0.905067420482623,0.425268108821871));
#107637=DIRECTION('center_axis',(0.,-0.434584798675586,-0.900630919278314));
#107638=DIRECTION('ref_axis',(0.,-0.900630919278314,0.434584798675586));
#107639=DIRECTION('center_axis',(0.,0.,1.));
#107640=DIRECTION('ref_axis',(-1.,0.,0.));
#107641=DIRECTION('',(1.87032180698308E-16,0.,1.));
#107642=DIRECTION('center_axis',(0.,1.,0.));
#107643=DIRECTION('ref_axis',(1.,0.,0.));
#107644=DIRECTION('',(0.,0.,-1.));
#107645=DIRECTION('center_axis',(0.,0.,-1.));
#107646=DIRECTION('ref_axis',(1.,0.,0.));
#107647=DIRECTION('center_axis',(1.79937481368581E-15,-0.983475799774124,
0.181039640020212));
#107648=DIRECTION('ref_axis',(3.24346588047852E-31,0.181039640020212,0.983475799774124));
#107649=DIRECTION('center_axis',(0.,-0.425920949091245,-0.904760379948864));
#107650=DIRECTION('ref_axis',(0.,-0.904760379948864,0.425920949091245));
#107651=DIRECTION('center_axis',(-6.15557891118828E-9,1.,-7.98957508368948E-9));
#107652=DIRECTION('ref_axis',(0.717962811307083,-1.14191836379562E-9,-0.696081461885051));
#107653=DIRECTION('center_axis',(-0.998868362320773,0.00644281759551,0.0471220209249073));
#107654=DIRECTION('ref_axis',(0.0465471507530001,0.335857313107545,0.940762046422451));
#107655=DIRECTION('center_axis',(4.38004274807345E-16,-1.,0.));
#107656=DIRECTION('ref_axis',(0.,0.,-1.));
#107657=DIRECTION('',(-1.87032180698308E-16,-8.19208946723987E-32,-1.));
#107658=DIRECTION('center_axis',(0.,0.,-1.));
#107659=DIRECTION('ref_axis',(-1.,0.,0.));
#107660=DIRECTION('center_axis',(0.,0.,1.));
#107661=DIRECTION('ref_axis',(-1.,0.,0.));
#107662=DIRECTION('',(1.87032180698308E-16,0.,1.));
#107663=DIRECTION('center_axis',(0.,0.,-1.));
#107664=DIRECTION('ref_axis',(-1.,0.,0.));
#107665=DIRECTION('center_axis',(0.,1.,0.));
#107666=DIRECTION('ref_axis',(1.,0.,0.));
#107667=DIRECTION('',(0.,0.,-1.));
#107668=DIRECTION('',(-1.,0.,0.));
#107669=DIRECTION('center_axis',(0.,0.,-1.));
#107670=DIRECTION('ref_axis',(1.,0.,0.));
#107671=DIRECTION('center_axis',(0.,0.,1.));
#107672=DIRECTION('ref_axis',(1.,0.,0.));
#107673=DIRECTION('center_axis',(0.,0.,-1.));
#107674=DIRECTION('ref_axis',(-1.,0.,0.));
#107675=DIRECTION('center_axis',(4.38004274807345E-16,-1.,0.));
#107676=DIRECTION('ref_axis',(0.,0.,-1.));
#107677=DIRECTION('',(-1.87032180698308E-16,-8.19208946723987E-32,-1.));
#107678=DIRECTION('',(0.,0.,1.));
#107679=DIRECTION('center_axis',(0.,0.,-1.));
#107680=DIRECTION('ref_axis',(-1.,0.,0.));
#107681=DIRECTION('center_axis',(0.,0.,1.));
#107682=DIRECTION('ref_axis',(-1.,0.,0.));
#107683=DIRECTION('',(1.87032180698308E-16,0.,1.));
#107684=DIRECTION('center_axis',(0.,0.,-1.));
#107685=DIRECTION('ref_axis',(-1.,0.,0.));
#107686=DIRECTION('center_axis',(0.,1.,0.));
#107687=DIRECTION('ref_axis',(1.,0.,0.));
#107688=DIRECTION('',(0.,0.,-1.));
#107689=DIRECTION('',(-1.,0.,0.));
#107690=DIRECTION('center_axis',(0.,0.,-1.));
#107691=DIRECTION('ref_axis',(1.,0.,0.));
#107692=DIRECTION('center_axis',(0.,0.,1.));
#107693=DIRECTION('ref_axis',(1.,0.,0.));
#107694=DIRECTION('center_axis',(0.,0.,-1.));
#107695=DIRECTION('ref_axis',(-1.,0.,0.));
#107696=DIRECTION('center_axis',(4.38004274807345E-16,-1.,0.));
#107697=DIRECTION('ref_axis',(0.,0.,-1.));
#107698=DIRECTION('',(-1.87032180698308E-16,-8.19208946723987E-32,-1.));
#107699=DIRECTION('',(0.,0.,1.));
#107700=DIRECTION('center_axis',(0.,0.,-1.));
#107701=DIRECTION('ref_axis',(-1.,0.,0.));
#107702=DIRECTION('center_axis',(0.,7.15121221728469E-32,1.));
#107703=DIRECTION('ref_axis',(-1.,0.,0.));
#107704=DIRECTION('center_axis',(0.,7.15121221728469E-32,1.));
#107705=DIRECTION('ref_axis',(-1.,0.,0.));
#107706=DIRECTION('center_axis',(-2.0158362407235E-32,-1.,0.));
#107707=DIRECTION('ref_axis',(0.,0.,-1.));
#107708=DIRECTION('center_axis',(0.,1.,0.));
#107709=DIRECTION('ref_axis',(0.,0.,-1.));
#107710=DIRECTION('center_axis',(0.,1.,0.));
#107711=DIRECTION('ref_axis',(0.,0.,-1.));
#107712=DIRECTION('',(-2.0158362407235E-32,-1.,-1.23467863058847E-16));
#107713=DIRECTION('center_axis',(-1.41612495910826E-31,1.,0.));
#107714=DIRECTION('ref_axis',(0.,0.,-1.));
#107715=DIRECTION('center_axis',(-2.0158362407235E-32,-1.,0.));
#107716=DIRECTION('ref_axis',(0.,0.,-1.));
#107717=DIRECTION('center_axis',(0.,1.,0.));
#107718=DIRECTION('ref_axis',(0.,0.,-1.));
#107719=DIRECTION('',(-2.0158362407235E-32,-1.,-1.23467863058847E-16));
#107720=DIRECTION('center_axis',(0.,0.,-1.));
#107721=DIRECTION('ref_axis',(-1.,0.,0.));
#107722=DIRECTION('center_axis',(0.,-1.0052202914905E-16,1.));
#107723=DIRECTION('ref_axis',(-1.,0.,0.));
#107724=DIRECTION('center_axis',(0.,0.,-1.));
#107725=DIRECTION('ref_axis',(-1.,0.,0.));
#107726=DIRECTION('',(1.6326809185664E-16,-1.0052202914905E-16,1.));
#107727=DIRECTION('center_axis',(-0.139173100960059,0.990268068741571,1.22266282302934E-16));
#107728=DIRECTION('ref_axis',(8.78519494496445E-16,-5.20658772030138E-33,
1.));
#107729=DIRECTION('',(-3.43088182518023E-33,1.23467863058847E-16,-1.));
#107730=DIRECTION('',(-0.990268068741571,-0.139173100960059,-1.71834053708117E-17));
#107731=DIRECTION('center_axis',(0.,0.,-1.));
#107732=DIRECTION('ref_axis',(0.,1.,0.));
#107733=DIRECTION('',(0.,-1.23467863058847E-16,1.));
#107734=DIRECTION('center_axis',(0.,0.,1.));
#107735=DIRECTION('ref_axis',(0.,1.,0.));
#107736=DIRECTION('center_axis',(0.,0.,-1.));
#107737=DIRECTION('ref_axis',(0.,1.,0.));
#107738=DIRECTION('',(0.,1.23467863058847E-16,-1.));
#107739=DIRECTION('center_axis',(0.,0.,1.));
#107740=DIRECTION('ref_axis',(0.,1.,0.));
#107741=DIRECTION('center_axis',(0.,0.,-1.));
#107742=DIRECTION('ref_axis',(0.,1.,0.));
#107743=DIRECTION('',(3.05149908249585E-33,-1.23467863058847E-16,1.));
#107744=DIRECTION('center_axis',(0.,0.,1.));
#107745=DIRECTION('ref_axis',(0.,1.,0.));
#107746=DIRECTION('center_axis',(-0.99026806874157,0.139173100960067,1.71834053708127E-17));
#107747=DIRECTION('ref_axis',(1.73522765332111E-17,-1.01418524800046E-34,
1.));
#107748=DIRECTION('',(-0.139173100960067,-0.99026806874157,-1.22266282302933E-16));
#107749=DIRECTION('',(-3.05149908249585E-33,1.23467863058847E-16,-1.));
#107750=DIRECTION('',(-0.139173100960067,-0.99026806874157,-1.22266282302933E-16));
#107751=DIRECTION('',(1.73522765332111E-17,6.55191041448207E-33,1.));
#107752=DIRECTION('',(-0.139173100960067,-0.99026806874157,0.));
#107753=DIRECTION('',(-1.73522765332111E-17,-6.55191041448207E-33,-1.));
#107754=DIRECTION('',(-0.139173100960067,-0.99026806874157,-1.22266282302933E-16));
#107755=DIRECTION('',(1.73522765332111E-17,6.93709640335951E-33,1.));
#107756=DIRECTION('',(-0.139173100960067,-0.99026806874157,0.));
#107757=DIRECTION('',(-1.73522765332111E-17,-6.93709640335951E-33,-1.));
#107758=DIRECTION('center_axis',(0.,0.,1.));
#107759=DIRECTION('ref_axis',(0.,-1.,0.));
#107760=DIRECTION('',(0.,1.23467863058847E-16,-1.));
#107761=DIRECTION('',(0.,-1.23467863058847E-16,1.));
#107762=DIRECTION('center_axis',(0.,0.,1.));
#107763=DIRECTION('ref_axis',(0.,-1.,0.));
#107764=DIRECTION('',(0.,1.23467863058847E-16,-1.));
#107765=DIRECTION('center_axis',(-0.907068166518068,-0.420531768759975,
0.0195031472628737));
#107766=DIRECTION('ref_axis',(0.0518039117125095,-0.157474353828549,-0.986163365075769));
#107767=DIRECTION('center_axis',(0.,0.,1.));
#107768=DIRECTION('ref_axis',(-1.,0.,0.));
#107769=DIRECTION('',(0.,1.23467863058847E-16,-1.));
#107770=DIRECTION('center_axis',(1.3159378979443E-30,-2.80509034228723E-44,
1.));
#107771=DIRECTION('ref_axis',(-2.1316282072803E-14,-1.,-5.4762534445178E-59));
#107772=DIRECTION('',(0.,-1.23467863058847E-16,1.));
#107773=DIRECTION('center_axis',(0.,0.,1.));
#107774=DIRECTION('ref_axis',(-1.,-1.77920356510442E-15,0.));
#107775=DIRECTION('center_axis',(-0.966107498808678,-0.25814005491211,0.000113117697403614));
#107776=DIRECTION('ref_axis',(0.25388184709702,-0.950091406535467,0.181301756588465));
#107777=DIRECTION('',(0.,1.23467863058847E-16,-1.));
#107778=DIRECTION('center_axis',(0.,0.,1.));
#107779=DIRECTION('ref_axis',(0.,-1.,0.));
#107780=DIRECTION('',(0.,-1.23467863058847E-16,1.));
#107781=DIRECTION('center_axis',(0.14008961833327,0.00275771348606123,0.990134987691864));
#107782=DIRECTION('ref_axis',(-0.979470506182107,-0.146013776318751,0.13898742621009));
#107783=DIRECTION('',(0.,1.23467863058847E-16,-1.));
#107784=DIRECTION('center_axis',(-6.57968948972152E-31,-7.01272585571806E-45,
1.));
#107785=DIRECTION('ref_axis',(1.06581410364015E-14,-1.,0.));
#107786=DIRECTION('',(0.,-1.23467863058847E-16,1.));
#107787=DIRECTION('center_axis',(0.115800998570926,-7.45156346442165E-10,
0.99327243429483));
#107788=DIRECTION('ref_axis',(-0.993253120969688,-0.00623601609274104,0.115798746915784));
#107789=DIRECTION('',(0.,1.23467863058847E-16,-1.));
#107790=DIRECTION('center_axis',(0.,0.,1.));
#107791=DIRECTION('ref_axis',(0.,-1.,0.));
#107792=DIRECTION('',(0.,-1.23467863058847E-16,1.));
#107793=DIRECTION('center_axis',(0.137684637338237,-0.0024146994890512,
0.990473174733882));
#107794=DIRECTION('ref_axis',(-0.981548350661306,0.133629566375757,0.136769785787277));
#107795=DIRECTION('',(0.,1.23467863058847E-16,-1.));
#107796=DIRECTION('center_axis',(-1.8642453554211E-30,-5.62966047861811E-44,
1.));
#107797=DIRECTION('ref_axis',(3.01980662698043E-14,-1.,-9.95682444457782E-59));
#107798=DIRECTION('',(0.,-1.23467863058847E-16,1.));
#107799=DIRECTION('center_axis',(0.,0.,1.));
#107800=DIRECTION('ref_axis',(-1.,1.13691107810172E-13,0.));
#107801=DIRECTION('',(0.,1.23467863058847E-16,-1.));
#107802=DIRECTION('center_axis',(1.15144566070127E-30,-2.14764729331365E-44,
1.));
#107803=DIRECTION('ref_axis',(-1.86517468137027E-14,-1.,3.73380916671668E-59));
#107804=DIRECTION('',(0.,-1.23467863058847E-16,1.));
#107805=DIRECTION('center_axis',(0.,0.,1.));
#107806=DIRECTION('ref_axis',(-1.,-1.0479508998465E-13,0.));
#107807=DIRECTION('center_axis',(0.,0.,1.));
#107808=DIRECTION('ref_axis',(0.,-1.,0.));
#107809=DIRECTION('',(3.79382742684518E-34,-1.23467863058847E-16,1.));
#107810=DIRECTION('',(0.,-1.23467863058847E-16,1.));
#107811=DIRECTION('center_axis',(-0.99026806874157,-0.139173100960065,-1.71834053708124E-17));
#107812=DIRECTION('ref_axis',(-0.139173100960065,0.99026806874157,2.95927408114303E-34));
#107813=DIRECTION('',(0.139173100960065,-0.99026806874157,-1.22266282302933E-16));
#107814=DIRECTION('',(-1.73522765332109E-17,-6.98077064262961E-33,1.));
#107815=DIRECTION('',(0.139173100960065,-0.99026806874157,-3.85185988877447E-34));
#107816=DIRECTION('',(1.73522765332109E-17,6.98077064262961E-33,-1.));
#107817=DIRECTION('',(0.139173100960065,-0.99026806874157,-1.22266282302933E-16));
#107818=DIRECTION('',(-3.79382742684518E-34,1.23467863058847E-16,-1.));
#107819=DIRECTION('',(0.139173100960065,-0.99026806874157,-1.22266282302933E-16));
#107820=DIRECTION('',(-1.73522765332109E-17,-7.36595663150706E-33,1.));
#107821=DIRECTION('',(0.139173100960065,-0.99026806874157,-3.85185988877447E-34));
#107822=DIRECTION('',(1.73522765332109E-17,6.98077064262961E-33,-1.));
#107823=DIRECTION('center_axis',(0.,0.,-1.));
#107824=DIRECTION('ref_axis',(0.,1.,0.));
#107825=DIRECTION('',(0.,-1.23467863058847E-16,1.));
#107826=DIRECTION('center_axis',(0.,0.,1.));
#107827=DIRECTION('ref_axis',(0.,1.,0.));
#107828=DIRECTION('center_axis',(0.,0.,-1.));
#107829=DIRECTION('ref_axis',(0.,1.,0.));
#107830=DIRECTION('',(0.,1.23467863058847E-16,-1.));
#107831=DIRECTION('center_axis',(0.,0.,1.));
#107832=DIRECTION('ref_axis',(0.,1.,0.));
#107833=DIRECTION('center_axis',(0.,0.,-1.));
#107834=DIRECTION('ref_axis',(0.,1.,0.));
#107835=DIRECTION('',(-3.43088182518023E-33,-1.23467863058847E-16,1.));
#107836=DIRECTION('center_axis',(0.,0.,1.));
#107837=DIRECTION('ref_axis',(0.,1.,0.));
#107838=DIRECTION('center_axis',(-0.139173100960059,-0.990268068741571,
-1.22266282302934E-16));
#107839=DIRECTION('ref_axis',(-0.990268068741571,0.139173100960059,3.29749813286563E-34));
#107840=DIRECTION('',(0.990268068741571,-0.139173100960059,-1.71834053708117E-17));
#107841=DIRECTION('',(0.990268068741571,-0.139173100960059,-1.71834053708117E-17));
#107842=DIRECTION('',(5.85782591378957E-32,-1.23467863058847E-16,1.));
#107843=DIRECTION('',(0.990268068741571,-0.139173100960059,0.));
#107844=DIRECTION('',(-5.85782591378957E-32,1.23467863058847E-16,-1.));
#107845=DIRECTION('',(0.990268068741571,-0.139173100960059,-1.71834053708117E-17));
#107846=DIRECTION('',(1.13659195805196E-16,-1.39441621308911E-16,1.));
#107847=DIRECTION('',(0.990268068741571,-0.139173100960059,0.));
#107848=DIRECTION('',(1.13659195805196E-16,1.07494104808783E-16,-1.));
#107849=DIRECTION('center_axis',(0.,1.,0.));
#107850=DIRECTION('ref_axis',(0.,0.,-1.));
#107851=DIRECTION('center_axis',(-4.38004274807345E-16,1.,0.));
#107852=DIRECTION('ref_axis',(0.,0.,-1.));
#107853=DIRECTION('center_axis',(0.,1.23467863058847E-16,-1.));
#107854=DIRECTION('ref_axis',(-1.,0.,0.));
#107855=DIRECTION('',(-0.139173100960065,0.99026806874157,1.22266282302933E-16));
#107856=DIRECTION('center_axis',(4.28365201153744E-31,1.48619034146585E-45,
-1.));
#107857=DIRECTION('ref_axis',(-3.46944695195361E-15,1.,1.24460305557223E-60));
#107858=DIRECTION('center_axis',(0.,0.,-1.));
#107859=DIRECTION('ref_axis',(0.,1.,0.));
#107860=DIRECTION('center_axis',(0.,0.,-1.));
#107861=DIRECTION('ref_axis',(0.,1.,0.));
#107862=DIRECTION('',(-0.990268068741571,0.139173100960059,1.71834053708117E-17));
#107863=DIRECTION('',(4.38004274807345E-16,-1.,-1.23467863058847E-16));
#107864=DIRECTION('',(1.,4.38004274807345E-16,5.40794518211031E-32));
#107865=DIRECTION('center_axis',(-1.,0.,0.));
#107866=DIRECTION('ref_axis',(0.,0.,1.));
#107867=DIRECTION('center_axis',(-1.,-4.38004274807345E-16,0.));
#107868=DIRECTION('ref_axis',(0.,0.,1.));
#107869=DIRECTION('center_axis',(0.,1.23467863058847E-16,-1.));
#107870=DIRECTION('ref_axis',(-1.,0.,0.));
#107871=DIRECTION('',(4.38004274807345E-16,-1.,-1.23467863058847E-16));
#107872=DIRECTION('center_axis',(0.,0.,-1.));
#107873=DIRECTION('ref_axis',(0.,1.,0.));
#107874=DIRECTION('',(1.,4.38004274807345E-16,5.40794518211031E-32));
#107875=DIRECTION('center_axis',(1.,0.,0.));
#107876=DIRECTION('ref_axis',(0.,0.,-1.));
#107877=DIRECTION('center_axis',(1.,0.,4.33680868994201E-16));
#107878=DIRECTION('ref_axis',(0.,1.,0.));
#107879=DIRECTION('center_axis',(0.,1.23467863058847E-16,-1.));
#107880=DIRECTION('ref_axis',(-1.,0.,0.));
#107881=DIRECTION('',(0.990268068741571,0.139173100960059,1.71834053708117E-17));
#107882=DIRECTION('center_axis',(0.,0.,-1.));
#107883=DIRECTION('ref_axis',(0.,1.,0.));
#107884=DIRECTION('center_axis',(-6.14104352374008E-30,3.05443170604608E-43,
-1.));
#107885=DIRECTION('ref_axis',(4.9737991503207E-14,1.,0.));
#107886=DIRECTION('center_axis',(-4.28365201153744E-31,1.48619034146585E-45,
-1.));
#107887=DIRECTION('ref_axis',(3.46944695195361E-15,1.,1.24460305557223E-60));
#107888=DIRECTION('',(0.139173100960067,0.99026806874157,1.22266282302933E-16));
#107889=DIRECTION('',(-1.,-4.38004274807345E-16,-5.40794518211031E-32));
#107890=DIRECTION('center_axis',(0.,1.23467863058847E-16,-1.));
#107891=DIRECTION('ref_axis',(-1.,0.,0.));
#107892=DIRECTION('',(-1.,-4.38004274807345E-16,-5.40794518211031E-32));
#107893=DIRECTION('center_axis',(0.,-1.,0.));
#107894=DIRECTION('ref_axis',(-1.,0.,0.));
#107895=DIRECTION('center_axis',(0.,-1.,0.));
#107896=DIRECTION('ref_axis',(0.,0.,1.));
#107897=DIRECTION('',(-5.01606788234257E-16,1.,0.));
#107898=DIRECTION('center_axis',(0.,0.452474032063612,0.891777578944491));
#107899=DIRECTION('ref_axis',(0.,0.891777578944491,-0.452474032063612));
#107900=DIRECTION('center_axis',(0.,0.,-1.));
#107901=DIRECTION('ref_axis',(-1.,0.,0.));
#107902=DIRECTION('center_axis',(0.,0.438949247410394,0.898511857572202));
#107903=DIRECTION('ref_axis',(0.,0.898511857572202,-0.438949247410394));
#107904=DIRECTION('center_axis',(0.,-1.,0.));
#107905=DIRECTION('ref_axis',(-1.,0.,0.));
#107906=DIRECTION('',(5.01606788234257E-16,-1.,0.));
#107907=DIRECTION('center_axis',(0.,1.,0.));
#107908=DIRECTION('ref_axis',(0.,0.,-1.));
#107909=DIRECTION('center_axis',(0.,0.,1.));
#107910=DIRECTION('ref_axis',(1.,0.,0.));
#107911=DIRECTION('',(-5.01606788234257E-16,1.,0.));
#107912=DIRECTION('',(1.,5.01606788234257E-16,0.));
#107913=DIRECTION('center_axis',(0.,-1.,0.));
#107914=DIRECTION('ref_axis',(-1.,0.,0.));
#107915=DIRECTION('center_axis',(0.,-1.,0.));
#107916=DIRECTION('ref_axis',(0.,0.,1.));
#107917=DIRECTION('center_axis',(0.,0.434444534286154,0.900698588113075));
#107918=DIRECTION('ref_axis',(0.,0.900698588113075,-0.434444534286154));
#107919=DIRECTION('center_axis',(0.,0.,-1.));
#107920=DIRECTION('ref_axis',(-1.,0.,0.));
#107921=DIRECTION('center_axis',(0.,0.427115883537276,0.904196893397767));
#107922=DIRECTION('ref_axis',(0.,0.904196893397767,-0.427115883537276));
#107923=DIRECTION('center_axis',(0.,0.,-1.));
#107924=DIRECTION('ref_axis',(-1.,0.,0.));
#107925=DIRECTION('center_axis',(0.,0.,1.));
#107926=DIRECTION('ref_axis',(1.,0.,0.));
#107927=DIRECTION('center_axis',(0.,0.425023904828957,0.905182125499585));
#107928=DIRECTION('ref_axis',(0.,0.905182125499585,-0.425023904828957));
#107929=DIRECTION('center_axis',(0.,0.,-1.));
#107930=DIRECTION('ref_axis',(-1.,0.,0.));
#107931=DIRECTION('center_axis',(0.,0.422696564637279,0.906271269678038));
#107932=DIRECTION('ref_axis',(0.,0.906271269678038,-0.422696564637279));
#107933=DIRECTION('center_axis',(0.,0.,1.));
#107934=DIRECTION('ref_axis',(0.,-1.,0.));
#107935=DIRECTION('center_axis',(0.,0.,1.));
#107936=DIRECTION('ref_axis',(1.,0.,0.));
#107937=DIRECTION('center_axis',(0.,-4.38538094726937E-12,1.));
#107938=DIRECTION('ref_axis',(0.,1.,4.38538094726937E-12));
#107939=DIRECTION('center_axis',(-0.939797023107103,0.132079858078289,-0.315176881209658));
#107940=DIRECTION('ref_axis',(-0.317962525883615,-4.30796627806664E-16,
0.948103281364278));
#107941=DIRECTION('center_axis',(0.,-1.,0.));
#107942=DIRECTION('ref_axis',(-1.,0.,0.));
#107943=DIRECTION('',(5.01606788234257E-16,-1.,0.));
#107944=DIRECTION('center_axis',(0.,1.,0.));
#107945=DIRECTION('ref_axis',(0.,0.,-1.));
#107946=DIRECTION('center_axis',(0.,0.,1.));
#107947=DIRECTION('ref_axis',(1.,0.,0.));
#107948=DIRECTION('',(1.,5.01606788234257E-16,0.));
#107949=DIRECTION('center_axis',(0.,-0.422768104239746,0.906237899250264));
#107950=DIRECTION('ref_axis',(0.,0.906237899250264,0.422768104239746));
#107951=DIRECTION('center_axis',(0.,0.422768104239797,0.90623789925024));
#107952=DIRECTION('ref_axis',(0.,0.90623789925024,-0.422768104239797));
#107953=DIRECTION('center_axis',(0.,0.,1.));
#107954=DIRECTION('ref_axis',(1.,0.,0.));
#107955=DIRECTION('center_axis',(-0.999980556584797,-0.00245118997350333,
-0.0057339445474203));
#107956=DIRECTION('ref_axis',(-0.00114511081840959,0.976049495468532,-0.217545561013868));
#107957=DIRECTION('center_axis',(0.,0.,1.));
#107958=DIRECTION('ref_axis',(-1.,0.,0.));
#107959=DIRECTION('center_axis',(0.,0.,1.));
#107960=DIRECTION('ref_axis',(1.,0.,0.));
#107961=DIRECTION('',(0.,0.,-1.));
#107962=DIRECTION('center_axis',(-0.99998055646326,-0.00245129305198786,
0.00573392167742329));
#107963=DIRECTION('ref_axis',(0.00115277299597243,-0.976316950640099,-0.216342050945344));
#107964=DIRECTION('center_axis',(5.9276100702047E-15,-0.42712932005395,
0.904190546262374));
#107965=DIRECTION('ref_axis',(-3.36279389150844E-29,0.904190546262374,0.42712932005395));
#107966=DIRECTION('center_axis',(0.,0.,1.));
#107967=DIRECTION('ref_axis',(1.,0.,0.));
#107968=DIRECTION('center_axis',(0.,0.,-1.));
#107969=DIRECTION('ref_axis',(1.,0.,0.));
#107970=DIRECTION('center_axis',(0.,0.,1.));
#107971=DIRECTION('ref_axis',(1.,0.,0.));
#107972=DIRECTION('',(0.,0.,1.));
#107973=DIRECTION('center_axis',(-5.01926581554439E-14,0.427129320053956,
0.904190546262371));
#107974=DIRECTION('ref_axis',(3.44539770291064E-30,0.904190546262371,-0.427129320053956));
#107975=DIRECTION('center_axis',(2.85977186515575E-47,0.,-1.));
#107976=DIRECTION('ref_axis',(0.,1.,0.));
#107977=DIRECTION('',(2.85977186515575E-47,-5.70122241611331E-32,-1.));
#107978=DIRECTION('center_axis',(5.01606788234257E-16,-1.,5.70122241611331E-32));
#107979=DIRECTION('ref_axis',(-4.59816715307009E-64,-5.70122241611331E-32,
-1.));
#107980=DIRECTION('',(-2.85977186515575E-47,5.70122241611331E-32,1.));
#107981=DIRECTION('center_axis',(-2.85977186515575E-47,0.,1.));
#107982=DIRECTION('ref_axis',(0.,-1.,0.));
#107983=DIRECTION('center_axis',(0.,-0.430903547306764,0.902397990311618));
#107984=DIRECTION('ref_axis',(0.,0.902397990311618,0.430903547306764));
#107985=DIRECTION('center_axis',(0.,0.430903547308298,0.902397990310886));
#107986=DIRECTION('ref_axis',(0.,0.902397990310886,-0.430903547308298));
#107987=DIRECTION('center_axis',(0.,0.,1.));
#107988=DIRECTION('ref_axis',(1.,0.,0.));
#107989=DIRECTION('center_axis',(0.,0.,1.));
#107990=DIRECTION('ref_axis',(-1.,0.,0.));
#107991=DIRECTION('center_axis',(0.,0.,1.));
#107992=DIRECTION('ref_axis',(1.,0.,0.));
#107993=DIRECTION('',(0.,0.,-1.));
#107994=DIRECTION('center_axis',(3.10313574260842E-14,-0.443150313610309,
0.896447321122153));
#107995=DIRECTION('ref_axis',(1.13003852554043E-30,0.896447321122153,0.443150313610309));
#107996=DIRECTION('center_axis',(0.,0.,1.));
#107997=DIRECTION('ref_axis',(1.,0.,0.));
#107998=DIRECTION('center_axis',(0.,0.,-1.));
#107999=DIRECTION('ref_axis',(1.,0.,0.));
#108000=DIRECTION('center_axis',(0.,0.,1.));
#108001=DIRECTION('ref_axis',(1.,0.,0.));
#108002=DIRECTION('',(0.,0.,1.));
#108003=DIRECTION('center_axis',(6.14994601925012E-15,0.443150313610303,
0.896447321122156));
#108004=DIRECTION('ref_axis',(3.80752501607971E-29,0.896447321122156,-0.443150313610303));
#108005=DIRECTION('center_axis',(-1.,-5.01606788234257E-16,0.));
#108006=DIRECTION('ref_axis',(0.,1.,0.));
#108007=DIRECTION('center_axis',(0.,0.,1.));
#108008=DIRECTION('ref_axis',(1.,0.,0.));
#108009=DIRECTION('center_axis',(1.,0.,0.));
#108010=DIRECTION('ref_axis',(0.,1.,0.));
#108011=DIRECTION('center_axis',(2.85977186515575E-47,0.,-1.));
#108012=DIRECTION('ref_axis',(0.,1.,0.));
#108013=DIRECTION('center_axis',(0.,0.,1.));
#108014=DIRECTION('ref_axis',(1.,0.,0.));
#108015=DIRECTION('',(2.85977186515575E-47,-5.70122241611331E-32,-1.));
#108016=DIRECTION('center_axis',(-1.,-5.01606788234257E-16,0.));
#108017=DIRECTION('ref_axis',(0.,1.,0.));
#108018=DIRECTION('center_axis',(1.,0.,0.));
#108019=DIRECTION('ref_axis',(0.,1.,0.));
#108020=DIRECTION('center_axis',(-1.,-5.01606788234257E-16,0.));
#108021=DIRECTION('ref_axis',(-5.01606788234257E-16,1.,0.));
#108022=DIRECTION('center_axis',(-1.,0.,0.));
#108023=DIRECTION('ref_axis',(0.,-1.,0.));
#108024=DIRECTION('',(1.,5.01606788234257E-16,0.));
#108025=DIRECTION('center_axis',(1.,5.01606788234257E-16,0.));
#108026=DIRECTION('ref_axis',(0.,-1.,0.));
#108027=DIRECTION('center_axis',(0.,0.,-1.));
#108028=DIRECTION('ref_axis',(-1.,0.,0.));
#108029=DIRECTION('center_axis',(0.,-0.450013465461336,0.893021769557427));
#108030=DIRECTION('ref_axis',(0.,0.893021769557427,0.450013465461336));
#108031=DIRECTION('center_axis',(0.,0.450013465459867,0.893021769558168));
#108032=DIRECTION('ref_axis',(0.,0.893021769558168,-0.450013465459867));
#108033=DIRECTION('center_axis',(0.,0.,1.));
#108034=DIRECTION('ref_axis',(1.,0.,0.));
#108035=DIRECTION('center_axis',(0.,0.,1.));
#108036=DIRECTION('ref_axis',(-1.,0.,0.));
#108037=DIRECTION('center_axis',(0.,0.,1.));
#108038=DIRECTION('ref_axis',(1.,0.,0.));
#108039=DIRECTION('',(0.,0.,-1.));
#108040=DIRECTION('center_axis',(-2.85977186515575E-47,0.,1.));
#108041=DIRECTION('ref_axis',(0.,-1.,0.));
#108042=DIRECTION('center_axis',(0.,0.,-1.));
#108043=DIRECTION('ref_axis',(-1.,0.,0.));
#108044=DIRECTION('',(-2.85977186515575E-47,5.70122241611331E-32,1.));
#108045=DIRECTION('center_axis',(1.,5.01606788234257E-16,0.));
#108046=DIRECTION('ref_axis',(0.,-1.,0.));
#108047=DIRECTION('center_axis',(-1.,0.,0.));
#108048=DIRECTION('ref_axis',(0.,-1.,0.));
#108049=DIRECTION('center_axis',(6.4968286789753E-15,-0.468145843483567,
0.883651214693365));
#108050=DIRECTION('ref_axis',(8.06613026210763E-31,0.883651214693365,0.468145843483567));
#108051=DIRECTION('center_axis',(0.,0.,1.));
#108052=DIRECTION('ref_axis',(1.,0.,0.));
#108053=DIRECTION('center_axis',(0.,0.,-1.));
#108054=DIRECTION('ref_axis',(1.,0.,0.));
#108055=DIRECTION('center_axis',(0.,0.,1.));
#108056=DIRECTION('ref_axis',(1.,0.,0.));
#108057=DIRECTION('',(0.,0.,1.));
#108058=DIRECTION('center_axis',(6.4968286789756E-15,0.468145843483589,
0.883651214693354));
#108059=DIRECTION('ref_axis',(-1.16233255777344E-30,0.883651214693354,-0.468145843483589));
#108060=DIRECTION('center_axis',(-1.,-5.01606788234257E-16,0.));
#108061=DIRECTION('ref_axis',(0.,1.,0.));
#108062=DIRECTION('center_axis',(0.,0.,1.));
#108063=DIRECTION('ref_axis',(1.,0.,0.));
#108064=DIRECTION('center_axis',(1.,0.,0.));
#108065=DIRECTION('ref_axis',(0.,1.,0.));
#108066=DIRECTION('center_axis',(2.85977186515575E-47,0.,-1.));
#108067=DIRECTION('ref_axis',(0.,1.,0.));
#108068=DIRECTION('center_axis',(0.,0.,1.));
#108069=DIRECTION('ref_axis',(1.,0.,0.));
#108070=DIRECTION('',(2.85977186515575E-47,-5.70122241611331E-32,-1.));
#108071=DIRECTION('center_axis',(-1.,-5.01606788234257E-16,0.));
#108072=DIRECTION('ref_axis',(0.,1.,0.));
#108073=DIRECTION('center_axis',(0.,-1.18842113532926E-16,1.));
#108074=DIRECTION('ref_axis',(0.,1.,1.18842113532926E-16));
#108075=DIRECTION('center_axis',(0.,-0.450823097219337,-0.892613317743783));
#108076=DIRECTION('ref_axis',(0.,-0.892613317743783,0.450823097219337));
#108077=DIRECTION('center_axis',(-1.22429528305785E-14,-0.470879150309884,
-0.882197724891332));
#108078=DIRECTION('ref_axis',(-1.13789948105108E-30,-0.882197724891332,
0.470879150309884));
#108079=DIRECTION('center_axis',(0.,-0.466134040541469,-0.884714109895668));
#108080=DIRECTION('ref_axis',(0.,-0.884714109895668,0.466134040541469));
#108081=DIRECTION('center_axis',(0.,0.,-1.));
#108082=DIRECTION('ref_axis',(-1.,0.,0.));
#108083=DIRECTION('center_axis',(0.,0.,-1.));
#108084=DIRECTION('ref_axis',(1.,0.,0.));
#108085=DIRECTION('center_axis',(1.,0.,0.));
#108086=DIRECTION('ref_axis',(0.,0.,1.));
#108087=DIRECTION('center_axis',(-1.,0.,0.));
#108088=DIRECTION('ref_axis',(0.,0.,1.));
#108089=DIRECTION('center_axis',(1.,0.,0.));
#108090=DIRECTION('ref_axis',(0.,0.,1.));
#108091=DIRECTION('center_axis',(1.,0.,0.));
#108092=DIRECTION('ref_axis',(0.,0.,-1.));
#108093=DIRECTION('center_axis',(-1.,0.,1.87032180698308E-16));
#108094=DIRECTION('ref_axis',(0.,0.,-1.));
#108095=DIRECTION('center_axis',(0.,8.19208946723988E-32,1.));
#108096=DIRECTION('ref_axis',(-1.,0.,0.));
#108097=DIRECTION('center_axis',(0.,0.,-1.));
#108098=DIRECTION('ref_axis',(-1.,0.,0.));
#108099=DIRECTION('center_axis',(0.,-0.457805146562934,-0.88905255625328));
#108100=DIRECTION('ref_axis',(0.,-0.88905255625328,0.457805146562934));
#108101=DIRECTION('center_axis',(0.,-0.440696042277477,-0.89765639212394));
#108102=DIRECTION('ref_axis',(0.,-0.89765639212394,0.440696042277477));
#108103=DIRECTION('center_axis',(-4.18005656861882E-16,1.,0.));
#108104=DIRECTION('ref_axis',(1.,5.9211894646675E-16,0.));
#108105=DIRECTION('center_axis',(5.78241158658935E-16,-1.,0.));
#108106=DIRECTION('ref_axis',(1.,5.78241158658935E-16,0.));
#108107=DIRECTION('center_axis',(0.,0.,1.));
#108108=DIRECTION('ref_axis',(1.,0.,0.));
#108109=DIRECTION('center_axis',(-4.18005656861881E-16,1.,0.));
#108110=DIRECTION('ref_axis',(1.,4.18005656861881E-16,0.));
#108111=DIRECTION('center_axis',(-5.78241158658935E-16,1.,0.));
#108112=DIRECTION('ref_axis',(-1.,-5.78241158658935E-16,0.));
#108113=DIRECTION('',(4.18005656861881E-16,-1.,0.));
#108114=DIRECTION('center_axis',(4.18005656861882E-16,-1.,0.));
#108115=DIRECTION('ref_axis',(-1.,-5.9211894646675E-16,0.));
#108116=DIRECTION('center_axis',(0.,0.,-1.));
#108117=DIRECTION('ref_axis',(-1.,0.,0.));
#108118=DIRECTION('center_axis',(-4.18005656861882E-16,1.,0.));
#108119=DIRECTION('ref_axis',(1.,0.,0.));
#108120=DIRECTION('center_axis',(0.,-1.,0.));
#108121=DIRECTION('ref_axis',(1.,0.,0.));
#108122=DIRECTION('center_axis',(0.,0.,1.));
#108123=DIRECTION('ref_axis',(1.,0.,0.));
#108124=DIRECTION('center_axis',(-4.18005656861881E-16,1.,0.));
#108125=DIRECTION('ref_axis',(1.,4.18005656861881E-16,0.));
#108126=DIRECTION('center_axis',(0.,1.,0.));
#108127=DIRECTION('ref_axis',(-1.,0.,0.));
#108128=DIRECTION('',(4.18005656861881E-16,-1.,0.));
#108129=DIRECTION('center_axis',(4.18005656861882E-16,-1.,0.));
#108130=DIRECTION('ref_axis',(-1.,0.,0.));
#108131=DIRECTION('center_axis',(0.,0.,-1.));
#108132=DIRECTION('ref_axis',(-1.,0.,0.));
#108133=DIRECTION('center_axis',(-1.,0.,0.));
#108134=DIRECTION('ref_axis',(0.,1.,0.));
#108135=DIRECTION('',(-1.,-4.18005656861881E-16,0.));
#108136=DIRECTION('center_axis',(1.,0.,0.));
#108137=DIRECTION('ref_axis',(0.,0.,-1.));
#108138=DIRECTION('center_axis',(0.,0.,1.));
#108139=DIRECTION('ref_axis',(0.,-1.,0.));
#108140=DIRECTION('center_axis',(0.,0.,-1.));
#108141=DIRECTION('ref_axis',(-1.,0.,0.));
#108142=DIRECTION('center_axis',(0.,0.,-1.));
#108143=DIRECTION('ref_axis',(-1.,0.,0.));
#108144=DIRECTION('center_axis',(-0.452796108559755,-6.28380831479673E-15,
-0.891614089207401));
#108145=DIRECTION('ref_axis',(-0.891614089207401,-8.65475050140857E-31,
0.452796108559755));
#108146=DIRECTION('center_axis',(-0.162781055433294,-0.986662212774382,
7.66497430181043E-5));
#108147=DIRECTION('ref_axis',(0.986085660689183,-0.162688589397824,-0.0341685917609087));
#108148=DIRECTION('center_axis',(-0.473890079491229,-6.57654596740791E-15,
-0.880584006531913));
#108149=DIRECTION('ref_axis',(-0.880584006531913,4.48746122839123E-29,0.473890079491229));
#108150=DIRECTION('center_axis',(0.,0.,-1.));
#108151=DIRECTION('ref_axis',(-1.,0.,0.));
#108152=DIRECTION('center_axis',(0.,0.,1.));
#108153=DIRECTION('ref_axis',(-1.,0.,0.));
#108154=DIRECTION('center_axis',(0.,0.,-1.));
#108155=DIRECTION('ref_axis',(-1.,0.,0.));
#108156=DIRECTION('',(0.,0.,-1.));
#108157=DIRECTION('center_axis',(0.473890079491223,6.57654596740749E-15,
-0.880584006531917));
#108158=DIRECTION('ref_axis',(-0.880584006531917,-2.59399416170326E-30,
-0.473890079491223));
#108159=DIRECTION('center_axis',(0.,0.,1.));
#108160=DIRECTION('ref_axis',(-1.,0.,0.));
#108161=DIRECTION('center_axis',(0.,0.,-1.));
#108162=DIRECTION('ref_axis',(-1.,0.,0.));
#108163=DIRECTION('',(0.,0.,1.));
#108164=DIRECTION('center_axis',(4.18005656861882E-16,-1.,0.));
#108165=DIRECTION('ref_axis',(-1.,0.,0.));
#108166=DIRECTION('center_axis',(0.,1.,0.));
#108167=DIRECTION('ref_axis',(-1.,0.,0.));
#108168=DIRECTION('center_axis',(0.453758938247698,0.,-0.891124472764788));
#108169=DIRECTION('ref_axis',(-0.891124472764788,0.,-0.453758938247698));
#108170=DIRECTION('center_axis',(0.,0.,1.));
#108171=DIRECTION('ref_axis',(1.,0.,0.));
#108172=DIRECTION('center_axis',(0.,0.,-1.));
#108173=DIRECTION('ref_axis',(1.,0.,0.));
#108174=DIRECTION('center_axis',(0.,0.,1.));
#108175=DIRECTION('ref_axis',(1.,0.,0.));
#108176=DIRECTION('',(0.,0.,1.));
#108177=DIRECTION('center_axis',(0.453758938247726,-6.29717026090114E-15,
0.891124472764774));
#108178=DIRECTION('ref_axis',(0.891124472764774,1.97126653384901E-30,-0.453758938247726));
#108179=DIRECTION('center_axis',(0.439171790863778,-6.20608564480709E-14,
0.898403104463415));
#108180=DIRECTION('ref_axis',(0.898403104463415,-1.60954096059593E-29,-0.439171790863778));
#108181=DIRECTION('center_axis',(0.,0.,1.));
#108182=DIRECTION('ref_axis',(1.,0.,0.));
#108183=DIRECTION('center_axis',(0.133735125220376,0.991017062579732,-0.000312982633993186));
#108184=DIRECTION('ref_axis',(0.990180089850999,-0.133635142118712,-0.0410492198900214));
#108185=DIRECTION('center_axis',(0.,0.,1.));
#108186=DIRECTION('ref_axis',(0.,-1.,0.));
#108187=DIRECTION('center_axis',(0.,0.,1.));
#108188=DIRECTION('ref_axis',(1.,0.,0.));
#108189=DIRECTION('center_axis',(-1.,0.,0.));
#108190=DIRECTION('ref_axis',(0.,1.,0.));
#108191=DIRECTION('center_axis',(-1.,0.,0.));
#108192=DIRECTION('ref_axis',(0.,0.,1.));
#108193=DIRECTION('',(1.,4.18005656861881E-16,0.));
#108194=DIRECTION('center_axis',(-4.18005656861882E-16,1.,0.));
#108195=DIRECTION('ref_axis',(1.,0.,0.));
#108196=DIRECTION('center_axis',(0.,0.,1.));
#108197=DIRECTION('ref_axis',(1.,0.,0.));
#108198=DIRECTION('center_axis',(0.,-1.,0.));
#108199=DIRECTION('ref_axis',(1.,0.,0.));
#108200=DIRECTION('center_axis',(0.,0.,-1.));
#108201=DIRECTION('ref_axis',(1.,0.,0.));
#108202=DIRECTION('center_axis',(0.,0.,1.));
#108203=DIRECTION('ref_axis',(1.,0.,0.));
#108204=DIRECTION('',(0.,0.,-1.));
#108205=DIRECTION('center_axis',(-4.18005656861882E-16,1.,0.));
#108206=DIRECTION('ref_axis',(1.,0.,0.));
#108207=DIRECTION('center_axis',(0.,-1.,0.));
#108208=DIRECTION('ref_axis',(1.,0.,0.));
#108209=DIRECTION('center_axis',(-4.18005656861881E-16,1.,0.));
#108210=DIRECTION('ref_axis',(1.,4.18005656861881E-16,0.));
#108211=DIRECTION('center_axis',(0.,1.,0.));
#108212=DIRECTION('ref_axis',(-1.,0.,0.));
#108213=DIRECTION('',(4.18005656861881E-16,-1.,0.));
#108214=DIRECTION('center_axis',(4.18005656861882E-16,-1.,0.));
#108215=DIRECTION('ref_axis',(-1.,0.,0.));
#108216=DIRECTION('center_axis',(0.,0.,-1.));
#108217=DIRECTION('ref_axis',(-1.,0.,0.));
#108218=DIRECTION('center_axis',(-0.446066534667472,0.,0.894999802597606));
#108219=DIRECTION('ref_axis',(0.894999802597606,0.,0.446066534667472));
#108220=DIRECTION('center_axis',(0.,0.,1.));
#108221=DIRECTION('ref_axis',(-1.,0.,0.));
#108222=DIRECTION('center_axis',(0.,0.,-1.));
#108223=DIRECTION('ref_axis',(-1.,0.,0.));
#108224=DIRECTION('',(0.,0.,1.));
#108225=DIRECTION('center_axis',(4.18005656861882E-16,-1.,0.));
#108226=DIRECTION('ref_axis',(-1.,0.,0.));
#108227=DIRECTION('center_axis',(1.,0.,0.));
#108228=DIRECTION('ref_axis',(0.,0.,-1.));
#108229=DIRECTION('center_axis',(0.,1.,0.));
#108230=DIRECTION('ref_axis',(-1.,0.,0.));
#108231=DIRECTION('center_axis',(0.,0.,1.));
#108232=DIRECTION('ref_axis',(0.,-1.,0.));
#108233=DIRECTION('center_axis',(0.,0.,-1.));
#108234=DIRECTION('ref_axis',(-1.,0.,0.));
#108235=DIRECTION('center_axis',(0.,0.,-1.));
#108236=DIRECTION('ref_axis',(-1.,0.,0.));
#108237=DIRECTION('center_axis',(-0.434629636675507,0.,-0.90060928205483));
#108238=DIRECTION('ref_axis',(-0.90060928205483,0.,0.434629636675507));
#108239=DIRECTION('center_axis',(-0.116944233518957,-0.993138481232708,
5.78053165623419E-5));
#108240=DIRECTION('ref_axis',(0.983258715661079,-0.115789058593805,-0.140695387225332));
#108241=DIRECTION('center_axis',(-0.446066534667672,4.96824693939355E-14,
-0.894999802597506));
#108242=DIRECTION('ref_axis',(-0.894999802597506,-9.63397512853712E-30,
0.446066534667672));
#108243=DIRECTION('center_axis',(0.,0.,1.));
#108244=DIRECTION('ref_axis',(1.,0.,0.));
#108245=DIRECTION('center_axis',(0.,0.,1.));
#108246=DIRECTION('ref_axis',(-1.,0.,0.));
#108247=DIRECTION('center_axis',(0.,0.,1.));
#108248=DIRECTION('ref_axis',(1.,0.,0.));
#108249=DIRECTION('',(0.,0.,-1.));
#108250=DIRECTION('center_axis',(-0.432211889750627,1.54100116546287E-13,
0.901772078941343));
#108251=DIRECTION('ref_axis',(0.901772078941343,9.67025840811756E-28,0.432211889750627));
#108252=DIRECTION('center_axis',(0.,0.,1.));
#108253=DIRECTION('ref_axis',(1.,0.,0.));
#108254=DIRECTION('center_axis',(0.,0.,-1.));
#108255=DIRECTION('ref_axis',(1.,0.,0.));
#108256=DIRECTION('center_axis',(0.,0.,1.));
#108257=DIRECTION('ref_axis',(1.,0.,0.));
#108258=DIRECTION('',(0.,0.,1.));
#108259=DIRECTION('center_axis',(0.432211889750627,-1.1996289787948E-14,
0.901772078941343));
#108260=DIRECTION('ref_axis',(0.901772078941343,7.55282579686682E-29,-0.432211889750627));
#108261=DIRECTION('center_axis',(0.42722596110711,0.,0.904144887811741));
#108262=DIRECTION('ref_axis',(0.904144887811741,0.,-0.42722596110711));
#108263=DIRECTION('center_axis',(0.,0.,1.));
#108264=DIRECTION('ref_axis',(1.,0.,0.));
#108265=DIRECTION('center_axis',(0.0775715986932,0.996986754706871,-0.000240863536308724));
#108266=DIRECTION('ref_axis',(0.995376869740143,-0.0774600592983714,-0.0567875549729645));
#108267=DIRECTION('center_axis',(0.,0.,1.));
#108268=DIRECTION('ref_axis',(0.,-1.,0.));
#108269=DIRECTION('center_axis',(0.,0.,1.));
#108270=DIRECTION('ref_axis',(1.,0.,0.));
#108271=DIRECTION('center_axis',(0.,0.,1.));
#108272=DIRECTION('ref_axis',(1.,0.,0.));
#108273=DIRECTION('center_axis',(0.,0.,-1.));
#108274=DIRECTION('ref_axis',(1.,0.,0.));
#108275=DIRECTION('',(0.,0.,-1.));
#108276=DIRECTION('center_axis',(-1.,-4.18005656861882E-16,0.));
#108277=DIRECTION('ref_axis',(-4.18005656861882E-16,1.,0.));
#108278=DIRECTION('',(0.,0.,1.));
#108279=DIRECTION('center_axis',(0.,0.,1.));
#108280=DIRECTION('ref_axis',(-1.,0.,0.));
#108281=DIRECTION('center_axis',(0.,0.,-1.));
#108282=DIRECTION('ref_axis',(-1.,0.,0.));
#108283=DIRECTION('center_axis',(-0.427895220819097,0.,0.903828346534991));
#108284=DIRECTION('ref_axis',(0.903828346534991,0.,0.427895220819097));
#108285=DIRECTION('center_axis',(0.,0.,1.));
#108286=DIRECTION('ref_axis',(0.,-1.,0.));
#108287=DIRECTION('center_axis',(0.,0.,1.));
#108288=DIRECTION('ref_axis',(1.,0.,0.));
#108289=DIRECTION('center_axis',(0.,0.,1.));
#108290=DIRECTION('ref_axis',(1.,0.,0.));
#108291=DIRECTION('center_axis',(0.425103688199478,0.,0.905144659310986));
#108292=DIRECTION('ref_axis',(0.905144659310986,0.,-0.425103688199478));
#108293=DIRECTION('center_axis',(-0.0572816986700422,-0.998358055091024,
2.88503434636003E-5));
#108294=DIRECTION('ref_axis',(0.977894907203397,-0.0561134278004395,-0.20142699343967));
#108295=DIRECTION('center_axis',(0.427895220819092,0.,0.903828346534994));
#108296=DIRECTION('ref_axis',(0.903828346534994,0.,-0.427895220819092));
#108297=DIRECTION('center_axis',(0.,0.,1.));
#108298=DIRECTION('ref_axis',(1.,0.,0.));
#108299=DIRECTION('center_axis',(0.,0.,1.));
#108300=DIRECTION('ref_axis',(-1.,0.,0.));
#108301=DIRECTION('center_axis',(0.,0.,1.));
#108302=DIRECTION('ref_axis',(1.,0.,0.));
#108303=DIRECTION('',(0.,0.,-1.));
#108304=DIRECTION('center_axis',(-0.00301258321928094,-0.999973601321737,
0.00661218587031605));
#108305=DIRECTION('ref_axis',(0.976036390081241,-0.00150160440505745,0.217602183861723));
#108306=DIRECTION('center_axis',(-0.422820321921619,0.,0.906213537401698));
#108307=DIRECTION('ref_axis',(0.906213537401698,0.,0.422820321921619));
#108308=DIRECTION('center_axis',(0.,0.,1.));
#108309=DIRECTION('ref_axis',(1.,0.,0.));
#108310=DIRECTION('center_axis',(0.,0.,-1.));
#108311=DIRECTION('ref_axis',(1.,0.,0.));
#108312=DIRECTION('center_axis',(0.,0.,1.));
#108313=DIRECTION('ref_axis',(1.,0.,0.));
#108314=DIRECTION('',(0.,0.,1.));
#108315=DIRECTION('center_axis',(0.422820321921648,-5.86781070846046E-15,
0.906213537401685));
#108316=DIRECTION('ref_axis',(0.906213537401684,-2.1653413854129E-31,-0.422820321921648));
#108317=DIRECTION('center_axis',(-0.00301263259095615,-0.999973601245449,
-0.0066121749130267));
#108318=DIRECTION('ref_axis',(0.976304654845778,-0.00151044331358758,-0.216395331482594));
#108319=DIRECTION('center_axis',(0.422711298276089,-5.8662977014411E-15,
0.906264397573767));
#108320=DIRECTION('ref_axis',(0.906264397573767,-1.10286040862995E-31,-0.422711298276089));
#108321=DIRECTION('center_axis',(0.,0.,1.));
#108322=DIRECTION('ref_axis',(1.,0.,0.));
#108323=DIRECTION('center_axis',(0.0114473717304193,0.999934475947494,-3.86273995495549E-5));
#108324=DIRECTION('ref_axis',(-0.906145684596772,0.0103900004240839,0.422838085060741));
#108325=DIRECTION('center_axis',(0.,0.,1.));
#108326=DIRECTION('ref_axis',(0.,-1.,0.));
#108327=DIRECTION('center_axis',(8.20654853338604E-14,-3.5527136788005E-12,
1.));
#108328=DIRECTION('ref_axis',(1.83670992315982E-40,1.,3.5527136788005E-12));
#108329=DIRECTION('center_axis',(0.,5.55111512312578E-14,1.));
#108330=DIRECTION('ref_axis',(0.,1.,-5.55111512312578E-14));
#108331=DIRECTION('center_axis',(0.,0.,-1.));
#108332=DIRECTION('ref_axis',(1.,0.,0.));
#108333=DIRECTION('',(0.,0.,-1.));
#108334=DIRECTION('center_axis',(-1.,-4.18005656861882E-16,0.));
#108335=DIRECTION('ref_axis',(-4.18005656861882E-16,1.,0.));
#108336=DIRECTION('',(0.,0.,1.));
#108337=DIRECTION('center_axis',(1.,0.,0.));
#108338=DIRECTION('ref_axis',(0.,0.00139138517159681,-0.999999032023184));
#108339=DIRECTION('center_axis',(0.,0.,1.));
#108340=DIRECTION('ref_axis',(-1.,0.,0.));
#108341=DIRECTION('center_axis',(4.44089209850062E-13,0.,1.));
#108342=DIRECTION('ref_axis',(1.,0.,-4.44089209850062E-13));
#108343=DIRECTION('center_axis',(-0.422759120858735,0.,0.906242090023824));
#108344=DIRECTION('ref_axis',(0.906242090023824,0.,0.422759120858735));
#108345=DIRECTION('center_axis',(0.,0.,1.));
#108346=DIRECTION('ref_axis',(0.,-1.,0.));
#108347=DIRECTION('center_axis',(0.,0.,1.));
#108348=DIRECTION('ref_axis',(1.,0.,0.));
#108349=DIRECTION('center_axis',(0.,0.,1.));
#108350=DIRECTION('ref_axis',(1.,0.,0.));
#108351=DIRECTION('center_axis',(0.422683101271474,0.,0.906277549043078));
#108352=DIRECTION('ref_axis',(0.906277549043078,0.,-0.422683101271474));
#108353=DIRECTION('center_axis',(0.00955294373602,-0.999954369112247,-3.0972651916074E-5));
#108354=DIRECTION('ref_axis',(-0.99995436957652,-0.0095529439031991,5.25421246130079E-6));
#108355=DIRECTION('center_axis',(0.422759120858763,0.,0.906242090023811));
#108356=DIRECTION('ref_axis',(0.906242090023811,0.,-0.422759120858763));
#108357=DIRECTION('center_axis',(0.,0.,1.));
#108358=DIRECTION('ref_axis',(1.,0.,0.));
#108359=DIRECTION('center_axis',(-0.00252660201784237,0.999981531120523,
-0.0055275401488527));
#108360=DIRECTION('ref_axis',(0.976075629574813,0.00126433814704904,-0.217427612779938));
#108361=DIRECTION('center_axis',(0.,0.,1.));
#108362=DIRECTION('ref_axis',(-1.,0.,0.));
#108363=DIRECTION('center_axis',(0.,0.,1.));
#108364=DIRECTION('ref_axis',(1.,0.,0.));
#108365=DIRECTION('',(0.,0.,-1.));
#108366=DIRECTION('center_axis',(-0.00252663505004111,0.999981531077572,
0.0055275328202581));
#108367=DIRECTION('ref_axis',(0.976342845954299,0.00127169757905682,0.21622448968405));
#108368=DIRECTION('center_axis',(-0.427566573571512,0.,0.903983863331817));
#108369=DIRECTION('ref_axis',(0.903983863331817,0.,0.427566573571512));
#108370=DIRECTION('center_axis',(0.,0.,1.));
#108371=DIRECTION('ref_axis',(1.,0.,0.));
#108372=DIRECTION('center_axis',(0.,0.,-1.));
#108373=DIRECTION('ref_axis',(1.,0.,0.));
#108374=DIRECTION('center_axis',(0.,0.,1.));
#108375=DIRECTION('ref_axis',(1.,0.,0.));
#108376=DIRECTION('',(0.,0.,1.));
#108377=DIRECTION('center_axis',(0.427566573571518,4.42475067662884E-14,
0.903983863331814));
#108378=DIRECTION('ref_axis',(0.903983863331814,-2.72495173441675E-28,-0.427566573571518));
#108379=DIRECTION('center_axis',(0.424945455576639,5.89730286238743E-15,
0.905218956819157));
#108380=DIRECTION('ref_axis',(0.905218956819157,3.24660130849529E-29,-0.424945455576639));
#108381=DIRECTION('center_axis',(0.,0.,1.));
#108382=DIRECTION('ref_axis',(1.,0.,0.));
#108383=DIRECTION('center_axis',(-0.0554974440951108,0.998458828862227,
2.76763464500059E-5));
#108384=DIRECTION('ref_axis',(0.978043885168222,0.0543682946724248,-0.201182124502805));
#108385=DIRECTION('center_axis',(0.,0.,1.));
#108386=DIRECTION('ref_axis',(0.,-1.,0.));
#108387=DIRECTION('center_axis',(3.85729088923276E-14,3.33066907387548E-13,
1.));
#108388=DIRECTION('ref_axis',(-1.00445073922803E-41,1.,-3.33066907387547E-13));
#108389=DIRECTION('center_axis',(0.,0.,1.));
#108390=DIRECTION('ref_axis',(1.,0.,0.));
#108391=DIRECTION('center_axis',(0.,0.,-1.));
#108392=DIRECTION('ref_axis',(1.,0.,0.));
#108393=DIRECTION('',(0.,0.,-1.));
#108394=DIRECTION('center_axis',(-1.,-4.18005656861882E-16,0.));
#108395=DIRECTION('ref_axis',(-4.18005656861882E-16,1.,0.));
#108396=DIRECTION('',(0.,0.,1.));
#108397=DIRECTION('center_axis',(0.,0.,1.));
#108398=DIRECTION('ref_axis',(-1.,0.,0.));
#108399=DIRECTION('center_axis',(0.,0.,1.));
#108400=DIRECTION('ref_axis',(1.,0.,0.));
#108401=DIRECTION('center_axis',(-0.431774610811204,0.,0.901981532770396));
#108402=DIRECTION('ref_axis',(0.901981532770396,0.,0.431774610811205));
#108403=DIRECTION('center_axis',(0.,0.,1.));
#108404=DIRECTION('ref_axis',(0.,-1.,0.));
#108405=DIRECTION('center_axis',(0.,0.,1.));
#108406=DIRECTION('ref_axis',(1.,0.,0.));
#108407=DIRECTION('center_axis',(0.,0.,1.));
#108408=DIRECTION('ref_axis',(1.,0.,0.));
#108409=DIRECTION('center_axis',(0.427007199080172,0.,0.904248224733511));
#108410=DIRECTION('ref_axis',(0.904248224733511,0.,-0.427007199080172));
#108411=DIRECTION('center_axis',(0.0757974280411721,-0.997123211513648,
-0.000225749977414995));
#108412=DIRECTION('ref_axis',(0.995635758500845,0.0756967156000945,-0.054584280171167));
#108413=DIRECTION('center_axis',(0.43177461081284,0.,0.901981532769613));
#108414=DIRECTION('ref_axis',(0.901981532769613,0.,-0.43177461081284));
#108415=DIRECTION('center_axis',(0.,0.,1.));
#108416=DIRECTION('ref_axis',(1.,0.,0.));
#108417=DIRECTION('center_axis',(0.,0.,1.));
#108418=DIRECTION('ref_axis',(-1.,0.,0.));
#108419=DIRECTION('center_axis',(0.,0.,1.));
#108420=DIRECTION('ref_axis',(1.,0.,0.));
#108421=DIRECTION('',(0.,0.,-1.));
#108422=DIRECTION('center_axis',(0.44541715199073,0.,-0.895323159933031));
#108423=DIRECTION('ref_axis',(-0.895323159933031,0.,-0.44541715199073));
#108424=DIRECTION('center_axis',(0.,0.,1.));
#108425=DIRECTION('ref_axis',(1.,0.,0.));
#108426=DIRECTION('center_axis',(0.,0.,-1.));
#108427=DIRECTION('ref_axis',(1.,0.,0.));
#108428=DIRECTION('center_axis',(0.,0.,1.));
#108429=DIRECTION('ref_axis',(1.,0.,0.));
#108430=DIRECTION('',(0.,0.,1.));
#108431=DIRECTION('center_axis',(0.445417151990703,0.,0.895323159933044));
#108432=DIRECTION('ref_axis',(0.895323159933044,0.,-0.445417151990703));
#108433=DIRECTION('center_axis',(0.434261044064412,6.0265826227258E-15,
0.90078707007155));
#108434=DIRECTION('ref_axis',(0.90078707007155,1.10802520916158E-30,-0.434261044064412));
#108435=DIRECTION('center_axis',(0.,0.,1.));
#108436=DIRECTION('ref_axis',(1.,0.,0.));
#108437=DIRECTION('center_axis',(-0.115453898308443,0.993312838018061,5.65145097326706E-5));
#108438=DIRECTION('ref_axis',(0.983295509889155,0.114297632119478,-0.141654479363368));
#108439=DIRECTION('center_axis',(0.,0.,1.));
#108440=DIRECTION('ref_axis',(0.,-1.,0.));
#108441=DIRECTION('center_axis',(0.,0.,1.));
#108442=DIRECTION('ref_axis',(1.,0.,0.));
#108443=DIRECTION('center_axis',(-4.18005656861882E-16,1.,0.));
#108444=DIRECTION('ref_axis',(1.,2.96059473233375E-16,0.));
#108445=DIRECTION('center_axis',(0.,0.,1.));
#108446=DIRECTION('ref_axis',(1.,0.,0.));
#108447=DIRECTION('center_axis',(4.33680868994202E-16,-1.,0.));
#108448=DIRECTION('ref_axis',(1.,4.33680868994202E-16,0.));
#108449=DIRECTION('center_axis',(-1.,0.,0.));
#108450=DIRECTION('ref_axis',(0.,0.,1.));
#108451=DIRECTION('center_axis',(0.,0.,-1.));
#108452=DIRECTION('ref_axis',(1.,0.,0.));
#108453=DIRECTION('center_axis',(0.,0.,1.));
#108454=DIRECTION('ref_axis',(1.,0.,0.));
#108455=DIRECTION('',(0.,0.,-1.));
#108456=DIRECTION('center_axis',(-4.18005656861882E-16,1.,0.));
#108457=DIRECTION('ref_axis',(1.,2.96059473233375E-16,0.));
#108458=DIRECTION('center_axis',(4.33680868994202E-16,-1.,0.));
#108459=DIRECTION('ref_axis',(1.,4.33680868994202E-16,0.));
#108460=DIRECTION('center_axis',(-4.18005656861881E-16,1.,0.));
#108461=DIRECTION('ref_axis',(1.,4.18005656861881E-16,0.));
#108462=DIRECTION('center_axis',(-4.33680868994202E-16,1.,0.));
#108463=DIRECTION('ref_axis',(-1.,-4.33680868994202E-16,0.));
#108464=DIRECTION('',(4.18005656861881E-16,-1.,0.));
#108465=DIRECTION('center_axis',(4.18005656861882E-16,-1.,0.));
#108466=DIRECTION('ref_axis',(-1.,-2.96059473233375E-16,0.));
#108467=DIRECTION('center_axis',(0.,0.,-1.));
#108468=DIRECTION('ref_axis',(-1.,0.,0.));
#108469=DIRECTION('center_axis',(-0.453032377894844,0.,0.891494063120413));
#108470=DIRECTION('ref_axis',(0.891494063120413,0.,0.453032377894844));
#108471=DIRECTION('center_axis',(0.,0.,1.));
#108472=DIRECTION('ref_axis',(-1.,0.,0.));
#108473=DIRECTION('center_axis',(0.,0.,-1.));
#108474=DIRECTION('ref_axis',(-1.,0.,0.));
#108475=DIRECTION('',(0.,0.,1.));
#108476=DIRECTION('center_axis',(4.18005656861882E-16,-1.,0.));
#108477=DIRECTION('ref_axis',(-1.,-2.96059473233375E-16,0.));
#108478=DIRECTION('center_axis',(1.,0.,0.));
#108479=DIRECTION('ref_axis',(0.,0.,-1.));
#108480=DIRECTION('center_axis',(-4.33680868994202E-16,1.,0.));
#108481=DIRECTION('ref_axis',(-1.,-4.33680868994202E-16,0.));
#108482=DIRECTION('center_axis',(-1.,0.,0.));
#108483=DIRECTION('ref_axis',(0.,1.,0.));
#108484=DIRECTION('',(-1.,-4.18005656861881E-16,0.));
#108485=DIRECTION('center_axis',(0.,0.,1.));
#108486=DIRECTION('ref_axis',(0.,-1.,0.));
#108487=DIRECTION('center_axis',(0.,0.,-1.));
#108488=DIRECTION('ref_axis',(-1.,0.,0.));
#108489=DIRECTION('center_axis',(0.,0.,-1.));
#108490=DIRECTION('ref_axis',(-1.,0.,0.));
#108491=DIRECTION('center_axis',(-0.438728460697982,-6.08858048281589E-15,
-0.898619684724066));
#108492=DIRECTION('ref_axis',(-0.898619684724066,-1.57717257184587E-30,
0.438728460697982));
#108493=DIRECTION('center_axis',(0.132298166463164,-0.991209921788581,-0.000293425222152531));
#108494=DIRECTION('ref_axis',(0.990461456417794,0.132209758351032,-0.0388160166362208));
#108495=DIRECTION('center_axis',(-0.45303237789485,-6.28708721049444E-15,
-0.89149406312041));
#108496=DIRECTION('ref_axis',(-0.89149406312041,3.90721898735751E-30,0.45303237789485));
#108497=DIRECTION('center_axis',(0.,0.,1.));
#108498=DIRECTION('ref_axis',(1.,0.,0.));
#108499=DIRECTION('center_axis',(0.,0.,1.));
#108500=DIRECTION('ref_axis',(-1.,0.,0.));
#108501=DIRECTION('center_axis',(0.,0.,1.));
#108502=DIRECTION('ref_axis',(1.,0.,0.));
#108503=DIRECTION('',(0.,0.,-1.));
#108504=DIRECTION('center_axis',(0.473027330271434,0.,-0.881047753993096));
#108505=DIRECTION('ref_axis',(-0.881047753993096,0.,-0.473027330271434));
#108506=DIRECTION('center_axis',(-0.452154194923616,0.,-0.891939787212666));
#108507=DIRECTION('ref_axis',(-0.891939787212666,0.,0.452154194923616));
#108508=DIRECTION('center_axis',(0.,0.,-1.));
#108509=DIRECTION('ref_axis',(-1.,0.,0.));
#108510=DIRECTION('center_axis',(-0.16174361462519,0.986832811286145,7.54788824122006E-5));
#108511=DIRECTION('ref_axis',(0.98621116070404,0.16164443851147,-0.0354770630281384));
#108512=DIRECTION('center_axis',(0.,0.,1.));
#108513=DIRECTION('ref_axis',(0.,-1.,0.));
#108514=DIRECTION('center_axis',(0.,0.,-1.));
#108515=DIRECTION('ref_axis',(-1.,0.,0.));
#108516=DIRECTION('center_axis',(-1.,0.,0.));
#108517=DIRECTION('ref_axis',(0.,1.,0.));
#108518=DIRECTION('center_axis',(-1.,0.,0.));
#108519=DIRECTION('ref_axis',(0.,0.,1.));
#108520=DIRECTION('',(1.,4.18005656861881E-16,0.));
#108521=DIRECTION('center_axis',(-4.18005656861882E-16,1.,0.));
#108522=DIRECTION('ref_axis',(1.,5.9211894646675E-16,0.));
#108523=DIRECTION('center_axis',(0.,0.,1.));
#108524=DIRECTION('ref_axis',(1.,0.,0.));
#108525=DIRECTION('center_axis',(5.78241158658935E-16,-1.,0.));
#108526=DIRECTION('ref_axis',(1.,5.78241158658935E-16,0.));
#108527=DIRECTION('center_axis',(0.,0.,-1.));
#108528=DIRECTION('ref_axis',(1.,0.,0.));
#108529=DIRECTION('',(0.,0.,-1.));
#108530=DIRECTION('center_axis',(0.,0.,-1.));
#108531=DIRECTION('ref_axis',(-1.,0.,0.));
#108532=DIRECTION('center_axis',(0.,0.,-1.));
#108533=DIRECTION('ref_axis',(1.,0.,0.));
#108534=DIRECTION('center_axis',(0.,0.,-1.));
#108535=DIRECTION('ref_axis',(-1.,0.,0.));
#108536=DIRECTION('',(0.,0.,1.));
#108537=DIRECTION('center_axis',(-0.473027330271494,0.,-0.881047753993064));
#108538=DIRECTION('ref_axis',(-0.881047753993064,0.,0.473027330271494));
#108539=DIRECTION('center_axis',(-0.744016723942684,0.668160994441905,0.));
#108540=DIRECTION('ref_axis',(-0.668160994441905,-0.744016723942684,0.));
#108541=DIRECTION('center_axis',(0.,-1.,-1.23467863058847E-16));
#108542=DIRECTION('ref_axis',(-1.,0.,0.));
#108543=DIRECTION('center_axis',(0.,-1.,0.));
#108544=DIRECTION('ref_axis',(0.,0.,1.));
#108545=DIRECTION('center_axis',(0.,-1.,-1.23467863058847E-16));
#108546=DIRECTION('ref_axis',(-1.,0.,0.));
#108547=DIRECTION('center_axis',(0.,-1.,0.));
#108548=DIRECTION('ref_axis',(0.,0.,1.));
#108549=DIRECTION('center_axis',(0.,1.23467863058847E-16,-1.));
#108550=DIRECTION('ref_axis',(0.,1.,1.1837531408762E-16));
#108551=DIRECTION('center_axis',(0.,-1.19392659184112E-16,1.));
#108552=DIRECTION('ref_axis',(0.,1.,1.19392659184112E-16));
#108553=DIRECTION('center_axis',(0.,-1.,0.));
#108554=DIRECTION('ref_axis',(0.,0.,1.));
#108555=DIRECTION('center_axis',(0.,0.,-1.));
#108556=DIRECTION('ref_axis',(-1.,0.,0.));
#108557=DIRECTION('center_axis',(0.,0.,-1.));
#108558=DIRECTION('ref_axis',(-1.,0.,0.));
#108559=DIRECTION('center_axis',(-1.13659195805196E-16,0.,-1.));
#108560=DIRECTION('ref_axis',(0.,1.,0.));
#108561=DIRECTION('center_axis',(0.,0.,-1.));
#108562=DIRECTION('ref_axis',(-1.,0.,0.));
#108563=DIRECTION('center_axis',(0.,-1.,0.));
#108564=DIRECTION('ref_axis',(-1.,0.,0.));
#108565=DIRECTION('center_axis',(0.,-1.,0.));
#108566=DIRECTION('ref_axis',(0.,0.,1.));
#108567=DIRECTION('',(-5.01606788234257E-16,1.,0.));
#108568=DIRECTION('center_axis',(-1.,-5.01606788234257E-16,1.13659195805196E-16));
#108569=DIRECTION('ref_axis',(0.,1.,0.));
#108570=DIRECTION('center_axis',(0.,0.,1.));
#108571=DIRECTION('ref_axis',(1.,0.,0.));
#108572=DIRECTION('center_axis',(1.,0.,-1.13659195805196E-16));
#108573=DIRECTION('ref_axis',(0.,1.,0.));
#108574=DIRECTION('center_axis',(0.,-1.14024448322266E-31,-1.));
#108575=DIRECTION('ref_axis',(1.,0.,0.));
#108576=DIRECTION('center_axis',(0.,0.,1.));
#108577=DIRECTION('ref_axis',(1.,0.,0.));
#108578=DIRECTION('',(-1.13659195805196E-16,-1.14024448322266E-31,-1.));
#108579=DIRECTION('center_axis',(-1.,-5.01606788234257E-16,1.13659195805196E-16));
#108580=DIRECTION('ref_axis',(0.,1.,0.));
#108581=DIRECTION('center_axis',(1.,0.,-1.13659195805196E-16));
#108582=DIRECTION('ref_axis',(0.,1.,0.));
#108583=DIRECTION('center_axis',(-6.24334907322839E-14,-0.457979853752065,
0.888962571516505));
#108584=DIRECTION('ref_axis',(-1.27562203883084E-29,0.888962571516505,0.457979853752065));
#108585=DIRECTION('center_axis',(0.,0.,1.));
#108586=DIRECTION('ref_axis',(1.,0.,0.));
#108587=DIRECTION('center_axis',(0.,-4.9783213633841E-32,-1.));
#108588=DIRECTION('ref_axis',(1.,0.,0.));
#108589=DIRECTION('center_axis',(0.,1.11022302462516E-13,-1.));
#108590=DIRECTION('ref_axis',(0.,-1.,-1.11022302462516E-13));
#108591=DIRECTION('',(1.13659195805196E-16,4.9783213633841E-32,1.));
#108592=DIRECTION('center_axis',(0.,-0.489712654585584,-0.871883889023499));
#108593=DIRECTION('ref_axis',(0.,-0.871883889023499,0.489712654585584));
#108594=DIRECTION('center_axis',(0.,-0.973635916817664,-0.228107653274998));
#108595=DIRECTION('ref_axis',(0.,-0.228107653274998,0.973635916817664));
#108596=DIRECTION('center_axis',(0.,-1.,0.));
#108597=DIRECTION('ref_axis',(0.,0.,1.));
#108598=DIRECTION('center_axis',(0.952431113365324,-0.30470794606498,-0.00529546018307552));
#108599=DIRECTION('ref_axis',(0.0463072011468755,0.161873964053018,-0.985724334123747));
#108600=DIRECTION('center_axis',(0.,1.,1.23467863058847E-16));
#108601=DIRECTION('ref_axis',(1.,0.,0.));
#108602=DIRECTION('',(-5.01606788234257E-16,1.,1.23467863058847E-16));
#108603=DIRECTION('center_axis',(-1.,-5.01606788234257E-16,0.));
#108604=DIRECTION('ref_axis',(-5.01606788234257E-16,1.,0.));
#108605=DIRECTION('',(1.,5.01606788234257E-16,0.));
#108606=DIRECTION('center_axis',(-1.,0.,-1.13659195805196E-16));
#108607=DIRECTION('ref_axis',(0.,-1.,0.));
#108608=DIRECTION('center_axis',(1.,4.38004274807345E-16,1.13659195805196E-16));
#108609=DIRECTION('ref_axis',(0.,-1.,0.));
#108610=DIRECTION('center_axis',(0.,0.,1.));
#108611=DIRECTION('ref_axis',(1.,0.,0.));
#108612=DIRECTION('center_axis',(0.,-1.,-1.23467863058847E-16));
#108613=DIRECTION('ref_axis',(-1.,0.,0.));
#108614=DIRECTION('center_axis',(0.,1.,0.));
#108615=DIRECTION('ref_axis',(0.,0.,-1.));
#108616=DIRECTION('center_axis',(0.,4.9783213633841E-32,-1.));
#108617=DIRECTION('ref_axis',(1.,0.,0.));
#108618=DIRECTION('center_axis',(0.,0.,-1.));
#108619=DIRECTION('ref_axis',(0.,1.,0.));
#108620=DIRECTION('center_axis',(0.,0.,1.));
#108621=DIRECTION('ref_axis',(0.,1.,0.));
#108622=DIRECTION('center_axis',(0.,1.,1.23467863058847E-16));
#108623=DIRECTION('ref_axis',(1.,0.,0.));
#108624=DIRECTION('center_axis',(-4.38004274807345E-16,1.,0.));
#108625=DIRECTION('ref_axis',(0.,0.,-1.));
#108626=DIRECTION('',(-4.38004274807345E-16,1.,1.23467863058847E-16));
#108627=DIRECTION('center_axis',(0.,1.,0.));
#108628=DIRECTION('ref_axis',(0.,0.,-1.));
#108629=DIRECTION('center_axis',(1.13659195805195E-16,0.,-1.));
#108630=DIRECTION('ref_axis',(1.,0.,1.13659195805195E-16));
#108631=DIRECTION('center_axis',(0.,0.,1.));
#108632=DIRECTION('ref_axis',(1.,0.,0.));
#108633=DIRECTION('',(-1.13659195805196E-16,0.,1.));
#108634=DIRECTION('center_axis',(1.,4.38004274807345E-16,1.13659195805196E-16));
#108635=DIRECTION('ref_axis',(0.,-1.,0.));
#108636=DIRECTION('center_axis',(0.,-1.,0.));
#108637=DIRECTION('ref_axis',(0.,0.,1.));
#108638=DIRECTION('center_axis',(-1.,0.,-1.13659195805196E-16));
#108639=DIRECTION('ref_axis',(0.,-1.,0.));
#108640=DIRECTION('center_axis',(0.,1.,0.));
#108641=DIRECTION('ref_axis',(1.,0.,0.));
#108642=DIRECTION('',(4.38004274807345E-16,-1.,0.));
#108643=DIRECTION('center_axis',(0.,1.07494104808783E-16,-1.));
#108644=DIRECTION('ref_axis',(1.,0.,0.));
#108645=DIRECTION('center_axis',(0.,0.,1.));
#108646=DIRECTION('ref_axis',(1.,0.,0.));
#108647=DIRECTION('center_axis',(0.,0.,1.));
#108648=DIRECTION('ref_axis',(1.,0.,0.));
#108649=DIRECTION('center_axis',(0.,1.,0.));
#108650=DIRECTION('ref_axis',(0.,0.,-1.));
#108651=DIRECTION('center_axis',(0.,-1.,-1.23467863058847E-16));
#108652=DIRECTION('ref_axis',(-1.,0.,0.));
#108653=DIRECTION('center_axis',(0.,-0.460605100635463,0.887605171947863));
#108654=DIRECTION('ref_axis',(0.,0.887605171947863,0.460605100635463));
#108655=DIRECTION('center_axis',(0.,0.635616055211064,0.772005330524295));
#108656=DIRECTION('ref_axis',(0.,0.772005330524295,-0.635616055211064));
#108657=DIRECTION('center_axis',(0.,0.46043947842117,0.887691098700016));
#108658=DIRECTION('ref_axis',(0.,0.887691098700016,-0.46043947842117));
#108659=DIRECTION('center_axis',(-0.976945182380867,0.213489703311671,0.000507151563339024));
#108660=DIRECTION('ref_axis',(0.169470879268944,0.776952017533326,-0.606321023493912));
#108661=DIRECTION('center_axis',(0.,0.477110018651024,0.878843575446063));
#108662=DIRECTION('ref_axis',(0.,0.878843575446063,-0.477110018651024));
#108663=DIRECTION('center_axis',(0.,0.,1.));
#108664=DIRECTION('ref_axis',(1.,0.,0.));
#108665=DIRECTION('center_axis',(0.,0.,1.));
#108666=DIRECTION('ref_axis',(-1.,0.,0.));
#108667=DIRECTION('center_axis',(0.,0.,1.));
#108668=DIRECTION('ref_axis',(1.,0.,0.));
#108669=DIRECTION('',(0.,0.,-1.));
#108670=DIRECTION('center_axis',(0.,-0.477110018651003,0.878843575446074));
#108671=DIRECTION('ref_axis',(0.,0.878843575446074,0.477110018651003));
#108672=DIRECTION('center_axis',(-2.85977186515575E-47,0.,1.));
#108673=DIRECTION('ref_axis',(0.,-1.,0.));
#108674=DIRECTION('center_axis',(0.,0.,-1.));
#108675=DIRECTION('ref_axis',(-1.,0.,0.));
#108676=DIRECTION('',(-2.85977186515575E-47,5.70122241611331E-32,1.));
#108677=DIRECTION('center_axis',(1.,5.01606788234257E-16,0.));
#108678=DIRECTION('ref_axis',(0.,-1.,0.));
#108679=DIRECTION('center_axis',(-1.,0.,0.));
#108680=DIRECTION('ref_axis',(0.,-1.,0.));
#108681=DIRECTION('center_axis',(0.,-1.18842113532926E-16,1.));
#108682=DIRECTION('ref_axis',(0.,1.,1.18842113532926E-16));
#108683=DIRECTION('center_axis',(1.88564486786379E-14,-0.483290003559882,
0.875460320322451));
#108684=DIRECTION('ref_axis',(-3.50034193199929E-30,0.875460320322451,0.483290003559882));
#108685=DIRECTION('center_axis',(0.,-1.,0.));
#108686=DIRECTION('ref_axis',(0.,0.,1.));
#108687=DIRECTION('center_axis',(0.,1.,1.23467863058847E-16));
#108688=DIRECTION('ref_axis',(1.,0.,0.));
#108689=DIRECTION('center_axis',(0.,-0.498898715136559,0.866660297945562));
#108690=DIRECTION('ref_axis',(0.,0.866660297945562,0.498898715136559));
#108691=DIRECTION('center_axis',(-1.60982338570647E-12,0.,1.));
#108692=DIRECTION('ref_axis',(1.,0.,1.60982338570648E-12));
#108693=DIRECTION('center_axis',(0.,0.,-1.));
#108694=DIRECTION('ref_axis',(1.,0.,0.));
#108695=DIRECTION('center_axis',(0.,0.,1.));
#108696=DIRECTION('ref_axis',(1.,0.,0.));
#108697=DIRECTION('',(0.,0.,1.));
#108698=DIRECTION('center_axis',(6.92361050625672E-15,0.498898715136586,
0.866660297945547));
#108699=DIRECTION('ref_axis',(-2.25138771964303E-30,0.866660297945547,-0.498898715136586));
#108700=DIRECTION('center_axis',(6.20126212581678E-14,0.483005416470283,
0.875617363727084));
#108701=DIRECTION('ref_axis',(-9.99028424960391E-30,0.875617363727084,-0.483005416470283));
#108702=DIRECTION('center_axis',(0.,1.,0.));
#108703=DIRECTION('ref_axis',(0.,0.,-1.));
#108704=DIRECTION('center_axis',(0.,-1.,-1.23467863058847E-16));
#108705=DIRECTION('ref_axis',(-1.,0.,0.));
#108706=DIRECTION('center_axis',(0.,1.,0.));
#108707=DIRECTION('ref_axis',(0.,0.,-1.));
#108708=DIRECTION('',(-5.01606788234257E-16,1.,1.23467863058847E-16));
#108709=DIRECTION('center_axis',(0.,0.,1.));
#108710=DIRECTION('ref_axis',(1.,0.,0.));
#108711=DIRECTION('center_axis',(6.19323182390956E-32,0.,1.));
#108712=DIRECTION('ref_axis',(-0.656059028990495,0.754709580222783,4.06312565670714E-32));
#108713=DIRECTION('center_axis',(0.,0.,1.));
#108714=DIRECTION('ref_axis',(1.,0.,0.));
#108715=DIRECTION('center_axis',(0.,-1.,0.));
#108716=DIRECTION('ref_axis',(-1.,0.,0.));
#108717=DIRECTION('center_axis',(0.,-1.,0.));
#108718=DIRECTION('ref_axis',(0.,0.,1.));
#108719=DIRECTION('',(-5.01606788234257E-16,1.,0.));
#108720=DIRECTION('center_axis',(-1.,-5.01606788234257E-16,0.));
#108721=DIRECTION('ref_axis',(0.,1.,0.));
#108722=DIRECTION('center_axis',(0.,0.,1.));
#108723=DIRECTION('ref_axis',(1.,0.,0.));
#108724=DIRECTION('center_axis',(1.,0.,0.));
#108725=DIRECTION('ref_axis',(0.,1.,0.));
#108726=DIRECTION('center_axis',(2.85977186515575E-47,0.,-1.));
#108727=DIRECTION('ref_axis',(0.,1.,0.));
#108728=DIRECTION('center_axis',(0.,0.,1.));
#108729=DIRECTION('ref_axis',(1.,0.,0.));
#108730=DIRECTION('',(2.85977186515575E-47,-5.70122241611331E-32,-1.));
#108731=DIRECTION('center_axis',(-1.,-5.01606788234257E-16,0.));
#108732=DIRECTION('ref_axis',(0.,1.,0.));
#108733=DIRECTION('center_axis',(1.,0.,0.));
#108734=DIRECTION('ref_axis',(0.,1.,0.));
#108735=DIRECTION('center_axis',(-1.,-5.01606788234257E-16,0.));
#108736=DIRECTION('ref_axis',(-5.01606788234257E-16,1.,0.));
#108737=DIRECTION('center_axis',(-1.,0.,0.));
#108738=DIRECTION('ref_axis',(0.,-1.,0.));
#108739=DIRECTION('',(1.,5.01606788234257E-16,0.));
#108740=DIRECTION('center_axis',(1.,5.01606788234257E-16,0.));
#108741=DIRECTION('ref_axis',(0.,-1.,0.));
#108742=DIRECTION('center_axis',(0.,0.,-1.));
#108743=DIRECTION('ref_axis',(-1.,0.,0.));
#108744=DIRECTION('center_axis',(0.,-1.,0.));
#108745=DIRECTION('ref_axis',(-1.,0.,0.));
#108746=DIRECTION('',(5.01606788234257E-16,-1.,0.));
#108747=DIRECTION('center_axis',(0.,1.,0.));
#108748=DIRECTION('ref_axis',(0.,0.,-1.));
#108749=DIRECTION('center_axis',(-6.19323182390956E-32,0.,-1.));
#108750=DIRECTION('ref_axis',(0.,1.,0.));
#108751=DIRECTION('center_axis',(0.,0.,1.));
#108752=DIRECTION('ref_axis',(1.,0.,0.));
#108753=DIRECTION('center_axis',(0.,0.,1.));
#108754=DIRECTION('ref_axis',(1.,0.,0.));
#108755=DIRECTION('center_axis',(0.,1.,0.));
#108756=DIRECTION('ref_axis',(0.,0.,-1.));
#108757=DIRECTION('center_axis',(0.,1.,1.23467863058847E-16));
#108758=DIRECTION('ref_axis',(1.,0.,0.));
#108759=DIRECTION('center_axis',(0.,1.,0.));
#108760=DIRECTION('ref_axis',(0.,0.,-1.));
#108761=DIRECTION('',(5.01606788234257E-16,-1.,-1.23467863058847E-16));
#108762=DIRECTION('center_axis',(0.,0.495757141593727,0.86846120037617));
#108763=DIRECTION('ref_axis',(0.,0.86846120037617,-0.495757141593727));
#108764=DIRECTION('center_axis',(0.,0.509034676478003,0.860746012562902));
#108765=DIRECTION('ref_axis',(0.,0.860746012562902,-0.509034676478003));
#108766=DIRECTION('center_axis',(0.,0.,1.));
#108767=DIRECTION('ref_axis',(1.,0.,0.));
#108768=DIRECTION('center_axis',(0.,0.,1.));
#108769=DIRECTION('ref_axis',(-1.,0.,0.));
#108770=DIRECTION('center_axis',(0.,-1.9151347174784E-12,1.));
#108771=DIRECTION('ref_axis',(0.,1.,1.9151347174784E-12));
#108772=DIRECTION('',(0.,0.,-1.));
#108773=DIRECTION('center_axis',(0.,-0.509034676477531,0.860746012563181));
#108774=DIRECTION('ref_axis',(0.,0.860746012563181,0.509034676477531));
#108775=DIRECTION('center_axis',(0.,-0.496115977596257,0.868256262156346));
#108776=DIRECTION('ref_axis',(0.,0.868256262156346,0.496115977596257));
#108777=DIRECTION('center_axis',(-2.85977186515575E-47,0.,1.));
#108778=DIRECTION('ref_axis',(0.,-1.,0.));
#108779=DIRECTION('center_axis',(0.,0.,-1.));
#108780=DIRECTION('ref_axis',(-1.,0.,0.));
#108781=DIRECTION('',(-2.85977186515575E-47,5.70122241611331E-32,1.));
#108782=DIRECTION('center_axis',(1.,5.01606788234257E-16,0.));
#108783=DIRECTION('ref_axis',(0.,-1.,0.));
#108784=DIRECTION('center_axis',(-1.,0.,0.));
#108785=DIRECTION('ref_axis',(0.,-1.,0.));
#108786=DIRECTION('center_axis',(0.,1.23467863058847E-16,-1.));
#108787=DIRECTION('ref_axis',(0.,1.,1.1837531408762E-16));
#108788=DIRECTION('center_axis',(0.,-1.19392659184112E-16,1.));
#108789=DIRECTION('ref_axis',(0.,1.,1.19392659184112E-16));
#108790=DIRECTION('center_axis',(0.,-1.,0.));
#108791=DIRECTION('ref_axis',(0.,0.,-1.));
#108792=DIRECTION('center_axis',(0.,-1.,0.));
#108793=DIRECTION('ref_axis',(0.,0.,1.));
#108794=DIRECTION('center_axis',(-2.30924636740563E-32,-1.,0.));
#108795=DIRECTION('ref_axis',(0.,0.,-1.));
#108796=DIRECTION('center_axis',(0.,-1.,0.));
#108797=DIRECTION('ref_axis',(0.,0.,1.));
#108798=DIRECTION('center_axis',(0.,-0.481647286662901,-0.876365158624112));
#108799=DIRECTION('ref_axis',(0.,-0.876365158624112,0.481647286662901));
#108800=DIRECTION('center_axis',(0.,-0.498146280733357,-0.867093007117186));
#108801=DIRECTION('ref_axis',(0.,-0.867093007117186,0.498146280733357));
#108802=DIRECTION('center_axis',(0.,0.,-1.));
#108803=DIRECTION('ref_axis',(-1.,0.,0.));
#108804=DIRECTION('center_axis',(0.,0.,-1.));
#108805=DIRECTION('ref_axis',(1.,0.,0.));
#108806=DIRECTION('center_axis',(1.,0.,0.));
#108807=DIRECTION('ref_axis',(0.,0.,1.));
#108808=DIRECTION('center_axis',(-1.,0.,0.));
#108809=DIRECTION('ref_axis',(0.,0.,1.));
#108810=DIRECTION('center_axis',(1.,0.,0.));
#108811=DIRECTION('ref_axis',(0.,0.,1.));
#108812=DIRECTION('center_axis',(1.,0.,0.));
#108813=DIRECTION('ref_axis',(0.,0.,-1.));
#108814=DIRECTION('center_axis',(-1.,0.,1.87032180698308E-16));
#108815=DIRECTION('ref_axis',(0.,0.,-1.));
#108816=DIRECTION('center_axis',(0.,8.19208946723987E-32,1.));
#108817=DIRECTION('ref_axis',(-1.,0.,0.));
#108818=DIRECTION('center_axis',(0.,0.,-1.));
#108819=DIRECTION('ref_axis',(-1.,0.,0.));
#108820=DIRECTION('center_axis',(0.,-0.488256551855887,-0.872700142987154));
#108821=DIRECTION('ref_axis',(0.,-0.872700142987154,0.488256551855887));
#108822=DIRECTION('center_axis',(0.,0.,1.));
#108823=DIRECTION('ref_axis',(0.,-1.,0.));
#108824=DIRECTION('',(0.,-1.23467863058847E-16,1.));
#108825=DIRECTION('center_axis',(0.,0.,1.));
#108826=DIRECTION('ref_axis',(-1.,0.,0.));
#108827=DIRECTION('center_axis',(0.,0.,1.));
#108828=DIRECTION('ref_axis',(1.,0.,0.));
#108829=DIRECTION('center_axis',(-1.,-4.38004274807345E-16,0.));
#108830=DIRECTION('ref_axis',(0.,1.,0.));
#108831=DIRECTION('center_axis',(-1.,0.,0.));
#108832=DIRECTION('ref_axis',(0.,1.,0.));
#108833=DIRECTION('center_axis',(1.,0.,0.));
#108834=DIRECTION('ref_axis',(0.,0.,1.));
#108835=DIRECTION('center_axis',(1.,0.,0.));
#108836=DIRECTION('ref_axis',(0.,0.,-1.));
#108837=DIRECTION('center_axis',(-1.,0.,1.87032180698308E-16));
#108838=DIRECTION('ref_axis',(0.,0.,-1.));
#108839=DIRECTION('center_axis',(0.,8.19208946723988E-32,1.));
#108840=DIRECTION('ref_axis',(-1.,0.,0.));
#108841=DIRECTION('center_axis',(0.,0.,-1.));
#108842=DIRECTION('ref_axis',(-1.,0.,0.));
#108843=DIRECTION('center_axis',(-1.44372869288582E-12,-0.522894079854115,
-0.852397666147391));
#108844=DIRECTION('ref_axis',(-4.54659658509035E-27,-0.852397666147391,
0.522894079854115));
#108845=DIRECTION('center_axis',(-1.90454958189083E-14,-0.515457402104623,
-0.856915203865326));
#108846=DIRECTION('ref_axis',(-1.04773227122123E-29,-0.856915203865326,
0.515457402104623));
#108847=DIRECTION('center_axis',(0.,1.23467863058847E-16,-1.));
#108848=DIRECTION('ref_axis',(0.,1.,1.1837531408762E-16));
#108849=DIRECTION('center_axis',(0.,-1.19392659184112E-16,1.));
#108850=DIRECTION('ref_axis',(0.,1.,1.19392659184112E-16));
#108851=DIRECTION('center_axis',(-1.,-4.1800565686188E-16,-5.16102651992463E-32));
#108852=DIRECTION('ref_axis',(-4.1800565686188E-16,1.,-8.08534226092968E-63));
#108853=DIRECTION('center_axis',(1.,0.,0.));
#108854=DIRECTION('ref_axis',(0.,0.,-1.));
#108855=DIRECTION('center_axis',(-1.,0.,-5.16102651992463E-32));
#108856=DIRECTION('ref_axis',(0.,1.,0.));
#108857=DIRECTION('center_axis',(-1.,0.,0.));
#108858=DIRECTION('ref_axis',(0.,0.,1.));
#108859=DIRECTION('center_axis',(-1.,0.,0.));
#108860=DIRECTION('ref_axis',(0.,0.,1.));
#108861=DIRECTION('center_axis',(0.,0.,-1.));
#108862=DIRECTION('ref_axis',(-1.,0.,0.));
#108863=DIRECTION('center_axis',(0.,0.,-1.));
#108864=DIRECTION('ref_axis',(-1.,0.,0.));
#108865=DIRECTION('center_axis',(0.,-7.68642463345396E-33,-1.));
#108866=DIRECTION('ref_axis',(1.,0.,0.));
#108867=DIRECTION('center_axis',(0.,0.,-1.));
#108868=DIRECTION('ref_axis',(-1.,0.,0.));
#108869=DIRECTION('center_axis',(-1.,0.,0.));
#108870=DIRECTION('ref_axis',(0.,1.,0.));
#108871=DIRECTION('center_axis',(-1.,0.,0.));
#108872=DIRECTION('ref_axis',(0.,0.,1.));
#108873=DIRECTION('',(1.,4.18005656861881E-16,0.));
#108874=DIRECTION('center_axis',(-4.18005656861882E-16,1.,0.));
#108875=DIRECTION('ref_axis',(1.,0.,0.));
#108876=DIRECTION('center_axis',(0.,0.,1.));
#108877=DIRECTION('ref_axis',(1.,0.,0.));
#108878=DIRECTION('center_axis',(0.,-1.,0.));
#108879=DIRECTION('ref_axis',(1.,0.,0.));
#108880=DIRECTION('center_axis',(0.,0.,-1.));
#108881=DIRECTION('ref_axis',(1.,0.,0.));
#108882=DIRECTION('center_axis',(0.,0.,1.));
#108883=DIRECTION('ref_axis',(1.,0.,0.));
#108884=DIRECTION('',(0.,0.,-1.));
#108885=DIRECTION('center_axis',(-4.18005656861882E-16,1.,0.));
#108886=DIRECTION('ref_axis',(1.,0.,0.));
#108887=DIRECTION('center_axis',(0.,-1.,0.));
#108888=DIRECTION('ref_axis',(1.,0.,0.));
#108889=DIRECTION('center_axis',(0.533061469511947,0.,-0.846076515287928));
#108890=DIRECTION('ref_axis',(-0.846076515287928,0.,-0.533061469511947));
#108891=DIRECTION('center_axis',(0.542737080693052,0.,-0.839902649859366));
#108892=DIRECTION('ref_axis',(-0.839902649859366,0.,-0.542737080693052));
#108893=DIRECTION('center_axis',(-1.11022302462516E-13,0.,-1.));
#108894=DIRECTION('ref_axis',(-1.,0.,1.11022302462516E-13));
#108895=DIRECTION('center_axis',(0.,0.,-1.));
#108896=DIRECTION('ref_axis',(1.,0.,0.));
#108897=DIRECTION('center_axis',(0.,0.,-1.));
#108898=DIRECTION('ref_axis',(-1.,0.,0.));
#108899=DIRECTION('',(0.,0.,1.));
#108900=DIRECTION('center_axis',(-0.542737080693356,0.,-0.839902649859169));
#108901=DIRECTION('ref_axis',(-0.839902649859169,0.,0.542737080693356));
#108902=DIRECTION('center_axis',(-0.532459169918176,0.,-0.846455688367706));
#108903=DIRECTION('ref_axis',(-0.846455688367706,0.,0.532459169918176));
#108904=DIRECTION('center_axis',(-1.,0.,0.));
#108905=DIRECTION('ref_axis',(0.,0.,1.));
#108906=DIRECTION('center_axis',(1.,0.,5.16102651992463E-32));
#108907=DIRECTION('ref_axis',(0.,-1.,0.));
#108908=DIRECTION('',(1.,4.18005656861881E-16,5.16102651992463E-32));
#108909=DIRECTION('center_axis',(-4.18005656861881E-16,1.,0.));
#108910=DIRECTION('ref_axis',(1.,4.18005656861881E-16,0.));
#108911=DIRECTION('',(4.18005656861881E-16,-1.,0.));
#108912=DIRECTION('center_axis',(0.,1.,0.));
#108913=DIRECTION('ref_axis',(-1.,0.,0.));
#108914=DIRECTION('center_axis',(4.38004274807345E-16,-1.,0.));
#108915=DIRECTION('ref_axis',(-1.,0.,0.));
#108916=DIRECTION('center_axis',(0.,0.,-1.));
#108917=DIRECTION('ref_axis',(-1.,0.,0.));
#108918=DIRECTION('center_axis',(0.,0.,1.));
#108919=DIRECTION('ref_axis',(0.,-1.,0.));
#108920=DIRECTION('',(0.,1.23467863058847E-16,-1.));
#108921=DIRECTION('center_axis',(0.,0.,-1.));
#108922=DIRECTION('ref_axis',(1.,0.,0.));
#108923=DIRECTION('center_axis',(0.,0.,-1.));
#108924=DIRECTION('ref_axis',(-1.,0.,0.));
#108925=DIRECTION('',(0.,0.,1.));
#108926=DIRECTION('center_axis',(4.38004274807345E-16,-1.,0.));
#108927=DIRECTION('ref_axis',(-1.,0.,0.));
#108928=DIRECTION('center_axis',(1.,0.,0.));
#108929=DIRECTION('ref_axis',(0.,0.,-1.));
#108930=DIRECTION('center_axis',(0.,1.,0.));
#108931=DIRECTION('ref_axis',(-1.,0.,0.));
#108932=DIRECTION('center_axis',(1.,0.,0.));
#108933=DIRECTION('ref_axis',(0.,-1.,0.));
#108934=DIRECTION('',(-1.,-4.38004274807345E-16,0.));
#108935=DIRECTION('center_axis',(0.,-7.60037129918566E-33,-1.));
#108936=DIRECTION('ref_axis',(1.,0.,0.));
#108937=DIRECTION('center_axis',(0.,0.,1.));
#108938=DIRECTION('ref_axis',(1.,0.,0.));
#108939=DIRECTION('center_axis',(0.,0.,1.));
#108940=DIRECTION('ref_axis',(1.,0.,0.));
#108941=DIRECTION('center_axis',(1.,0.,0.));
#108942=DIRECTION('ref_axis',(0.,0.,-1.));
#108943=DIRECTION('center_axis',(-1.,0.,-5.40794518211031E-32));
#108944=DIRECTION('ref_axis',(0.,1.,0.));
#108945=DIRECTION('center_axis',(-1.,0.,-5.40794518211031E-32));
#108946=DIRECTION('ref_axis',(0.,1.,0.));
#108947=DIRECTION('center_axis',(-1.,0.,-5.40794518211031E-32));
#108948=DIRECTION('ref_axis',(0.,1.,0.));
#108949=DIRECTION('center_axis',(-1.,0.,0.));
#108950=DIRECTION('ref_axis',(0.,1.,0.));
#108951=DIRECTION('',(-1.,-4.18005656861881E-16,0.));
#108952=DIRECTION('center_axis',(1.,0.,0.));
#108953=DIRECTION('ref_axis',(0.,0.,-1.));
#108954=DIRECTION('center_axis',(0.,0.,1.));
#108955=DIRECTION('ref_axis',(0.,-1.,0.));
#108956=DIRECTION('center_axis',(0.,0.,-1.));
#108957=DIRECTION('ref_axis',(-1.,0.,0.));
#108958=DIRECTION('center_axis',(0.,0.,-1.));
#108959=DIRECTION('ref_axis',(-1.,0.,0.));
#108960=DIRECTION('center_axis',(-0.639652375806928,0.,-0.768664320834884));
#108961=DIRECTION('ref_axis',(-0.768664320834884,0.,0.639652375806928));
#108962=DIRECTION('center_axis',(-0.460063868749635,-6.3846687485495E-15,
-0.887885824118799));
#108963=DIRECTION('ref_axis',(-0.887885824118799,1.45303619130616E-30,0.460063868749635));
#108964=DIRECTION('center_axis',(0.212606354611556,0.977137797844532,0.000511861626231249));
#108965=DIRECTION('ref_axis',(0.773811164394419,-0.168046480235339,-0.610718152947059));
#108966=DIRECTION('center_axis',(-0.482846004727867,-1.73271215008562E-12,
-0.875705279028473));
#108967=DIRECTION('ref_axis',(-0.875705279028473,2.53817490248555E-28,0.482846004727867));
#108968=DIRECTION('center_axis',(0.,0.,-1.));
#108969=DIRECTION('ref_axis',(-1.,0.,0.));
#108970=DIRECTION('center_axis',(0.,0.,1.));
#108971=DIRECTION('ref_axis',(-1.,0.,0.));
#108972=DIRECTION('center_axis',(0.,0.,-1.));
#108973=DIRECTION('ref_axis',(-1.,0.,0.));
#108974=DIRECTION('',(0.,0.,-1.));
#108975=DIRECTION('center_axis',(0.482846004726866,0.,-0.875705279029025));
#108976=DIRECTION('ref_axis',(-0.875705279029025,0.,-0.482846004726866));
#108977=DIRECTION('center_axis',(0.460227641765603,-1.23207131288176E-14,
-0.887800944894108));
#108978=DIRECTION('ref_axis',(-0.887800944894108,7.43200893707752E-29,-0.460227641765603));
#108979=DIRECTION('center_axis',(0.782801330915055,-1.71942202750291E-12,
-0.622271706184379));
#108980=DIRECTION('ref_axis',(-0.622271706184379,-5.64324648533862E-28,
-0.782801330915055));
#108981=DIRECTION('center_axis',(0.,0.,1.));
#108982=DIRECTION('ref_axis',(-1.,0.,0.));
#108983=DIRECTION('center_axis',(0.,0.,-1.));
#108984=DIRECTION('ref_axis',(-1.,0.,0.));
#108985=DIRECTION('',(0.,0.,1.));
#108986=DIRECTION('center_axis',(4.18005656861882E-16,-1.,0.));
#108987=DIRECTION('ref_axis',(-1.,-5.9211894646675E-16,0.));
#108988=DIRECTION('center_axis',(-5.78241158658935E-16,1.,0.));
#108989=DIRECTION('ref_axis',(-1.,-5.78241158658935E-16,0.));
#108990=DIRECTION('center_axis',(0.,-1.18842113532926E-16,1.));
#108991=DIRECTION('ref_axis',(0.,1.,1.18842113532926E-16));
#108992=DIRECTION('center_axis',(-0.482758140724685,-1.88531393333386E-14,
0.875753719697522));
#108993=DIRECTION('ref_axis',(0.875753719697522,-7.73315028487173E-30,0.482758140724685));
#108994=DIRECTION('center_axis',(-1.,0.,0.));
#108995=DIRECTION('ref_axis',(0.,0.,1.));
#108996=DIRECTION('center_axis',(1.,0.,5.16102651992463E-32));
#108997=DIRECTION('ref_axis',(0.,-1.,0.));
#108998=DIRECTION('center_axis',(-0.506538210354814,0.,0.862217514001277));
#108999=DIRECTION('ref_axis',(0.862217514001277,0.,0.506538210354814));
#109000=DIRECTION('center_axis',(0.,1.77635683940025E-12,1.));
#109001=DIRECTION('ref_axis',(0.,1.,-1.77635683940025E-12));
#109002=DIRECTION('center_axis',(0.,0.,-1.));
#109003=DIRECTION('ref_axis',(1.,0.,0.));
#109004=DIRECTION('center_axis',(0.,0.,1.));
#109005=DIRECTION('ref_axis',(1.,0.,0.));
#109006=DIRECTION('',(0.,0.,1.));
#109007=DIRECTION('center_axis',(0.50653821035484,0.,0.862217514001262));
#109008=DIRECTION('ref_axis',(0.862217514001262,0.,-0.50653821035484));
#109009=DIRECTION('center_axis',(0.482476521947278,-1.33914135876736E-14,
0.875908902666058));
#109010=DIRECTION('ref_axis',(0.875908902666058,-3.49403168495695E-30,-0.482476521947278));
#109011=DIRECTION('center_axis',(1.,0.,0.));
#109012=DIRECTION('ref_axis',(0.,0.,-1.));
#109013=DIRECTION('center_axis',(-1.,-4.1800565686188E-16,-5.16102651992463E-32));
#109014=DIRECTION('ref_axis',(-4.1800565686188E-16,1.,-8.08534226092968E-63));
#109015=DIRECTION('center_axis',(1.,0.,0.));
#109016=DIRECTION('ref_axis',(0.,0.,-1.));
#109017=DIRECTION('',(1.,4.18005656861881E-16,5.16102651992463E-32));
#109018=DIRECTION('center_axis',(0.,0.,1.));
#109019=DIRECTION('ref_axis',(1.,0.,0.));
#109020=DIRECTION('center_axis',(0.,7.25334975031394E-33,1.));
#109021=DIRECTION('ref_axis',(0.754709580222751,0.656059028990531,-4.75862559411968E-33));
#109022=DIRECTION('center_axis',(0.,0.,1.));
#109023=DIRECTION('ref_axis',(1.,0.,0.));
#109024=DIRECTION('center_axis',(-1.,0.,0.));
#109025=DIRECTION('ref_axis',(0.,1.,0.));
#109026=DIRECTION('center_axis',(-1.,0.,0.));
#109027=DIRECTION('ref_axis',(0.,0.,1.));
#109028=DIRECTION('',(1.,4.18005656861881E-16,0.));
#109029=DIRECTION('center_axis',(-4.18005656861882E-16,1.,0.));
#109030=DIRECTION('ref_axis',(1.,0.,0.));
#109031=DIRECTION('center_axis',(0.,0.,1.));
#109032=DIRECTION('ref_axis',(1.,0.,0.));
#109033=DIRECTION('center_axis',(0.,-1.,0.));
#109034=DIRECTION('ref_axis',(1.,0.,0.));
#109035=DIRECTION('center_axis',(0.,0.,-1.));
#109036=DIRECTION('ref_axis',(1.,0.,0.));
#109037=DIRECTION('center_axis',(0.,0.,1.));
#109038=DIRECTION('ref_axis',(1.,0.,0.));
#109039=DIRECTION('',(0.,0.,-1.));
#109040=DIRECTION('center_axis',(-4.18005656861882E-16,1.,0.));
#109041=DIRECTION('ref_axis',(1.,0.,0.));
#109042=DIRECTION('center_axis',(0.,-1.,0.));
#109043=DIRECTION('ref_axis',(1.,0.,0.));
#109044=DIRECTION('center_axis',(-4.18005656861881E-16,1.,0.));
#109045=DIRECTION('ref_axis',(1.,4.18005656861881E-16,0.));
#109046=DIRECTION('center_axis',(0.,1.,0.));
#109047=DIRECTION('ref_axis',(-1.,0.,0.));
#109048=DIRECTION('',(4.18005656861881E-16,-1.,0.));
#109049=DIRECTION('center_axis',(4.18005656861882E-16,-1.,0.));
#109050=DIRECTION('ref_axis',(-1.,0.,0.));
#109051=DIRECTION('center_axis',(0.,0.,-1.));
#109052=DIRECTION('ref_axis',(-1.,0.,0.));
#109053=DIRECTION('center_axis',(-1.,0.,0.));
#109054=DIRECTION('ref_axis',(0.,1.,0.));
#109055=DIRECTION('',(-1.,-4.18005656861881E-16,0.));
#109056=DIRECTION('center_axis',(1.,0.,0.));
#109057=DIRECTION('ref_axis',(0.,0.,-1.));
#109058=DIRECTION('center_axis',(0.,-7.25334975031394E-33,-1.));
#109059=DIRECTION('ref_axis',(1.,0.,0.));
#109060=DIRECTION('center_axis',(0.,0.,1.));
#109061=DIRECTION('ref_axis',(1.,0.,0.));
#109062=DIRECTION('center_axis',(0.,0.,1.));
#109063=DIRECTION('ref_axis',(1.,0.,0.));
#109064=DIRECTION('center_axis',(1.,0.,0.));
#109065=DIRECTION('ref_axis',(0.,0.,-1.));
#109066=DIRECTION('center_axis',(1.,4.1800565686188E-16,5.16102651992463E-32));
#109067=DIRECTION('ref_axis',(4.1800565686188E-16,-1.,8.08534226092968E-63));
#109068=DIRECTION('center_axis',(1.,0.,0.));
#109069=DIRECTION('ref_axis',(0.,0.,-1.));
#109070=DIRECTION('',(-1.,-4.18005656861881E-16,-5.16102651992463E-32));
#109071=DIRECTION('center_axis',(0.495139693244723,0.,0.868813377068702));
#109072=DIRECTION('ref_axis',(0.868813377068702,0.,-0.495139693244723));
#109073=DIRECTION('center_axis',(0.517480097907924,0.,0.855695242635604));
#109074=DIRECTION('ref_axis',(0.855695242635604,0.,-0.517480097907924));
#109075=DIRECTION('center_axis',(0.,0.,1.));
#109076=DIRECTION('ref_axis',(1.,0.,0.));
#109077=DIRECTION('center_axis',(0.,0.,1.));
#109078=DIRECTION('ref_axis',(-1.,0.,0.));
#109079=DIRECTION('center_axis',(-1.11022302462516E-12,0.,1.));
#109080=DIRECTION('ref_axis',(1.,0.,1.11022302462516E-12));
#109081=DIRECTION('',(0.,0.,-1.));
#109082=DIRECTION('center_axis',(-0.517480097905755,0.,0.855695242636916));
#109083=DIRECTION('ref_axis',(0.855695242636916,0.,0.517480097905755));
#109084=DIRECTION('center_axis',(-0.49549481432688,0.,0.868610896187223));
#109085=DIRECTION('ref_axis',(0.868610896187223,0.,0.49549481432688));
#109086=DIRECTION('center_axis',(0.,0.,1.));
#109087=DIRECTION('ref_axis',(-1.,0.,0.));
#109088=DIRECTION('center_axis',(0.,0.,-1.));
#109089=DIRECTION('ref_axis',(-1.,0.,0.));
#109090=DIRECTION('',(0.,0.,1.));
#109091=DIRECTION('center_axis',(4.18005656861882E-16,-1.,0.));
#109092=DIRECTION('ref_axis',(-1.,0.,0.));
#109093=DIRECTION('center_axis',(0.,1.,0.));
#109094=DIRECTION('ref_axis',(-1.,0.,0.));
#109095=DIRECTION('center_axis',(0.,-1.18842113532926E-16,1.));
#109096=DIRECTION('ref_axis',(0.,1.,1.18842113532926E-16));
#109097=DIRECTION('center_axis',(0.460985151818831,0.,-0.887407848625743));
#109098=DIRECTION('ref_axis',(-0.887407848625743,0.,-0.460985151818831));
#109099=DIRECTION('center_axis',(-0.483825549717016,0.,0.87516446308167));
#109100=DIRECTION('ref_axis',(0.87516446308167,0.,0.483825549717016));
#109101=DIRECTION('center_axis',(-1.,0.,0.));
#109102=DIRECTION('ref_axis',(0.,0.,1.));
#109103=DIRECTION('center_axis',(-0.661718432379332,0.,-0.749752436641215));
#109104=DIRECTION('ref_axis',(-0.749752436641215,0.,0.661718432379332));
#109105=DIRECTION('center_axis',(0.,0.,-1.));
#109106=DIRECTION('ref_axis',(-1.,0.,0.));
#109107=DIRECTION('center_axis',(0.,0.,1.));
#109108=DIRECTION('ref_axis',(0.,-1.,0.));
#109109=DIRECTION('center_axis',(0.,0.,-1.));
#109110=DIRECTION('ref_axis',(-1.,0.,0.));
#109111=DIRECTION('center_axis',(-1.,0.,0.));
#109112=DIRECTION('ref_axis',(0.,1.,0.));
#109113=DIRECTION('center_axis',(-1.,0.,0.));
#109114=DIRECTION('ref_axis',(0.,0.,1.));
#109115=DIRECTION('',(1.,4.18005656861881E-16,0.));
#109116=DIRECTION('center_axis',(0.732878068742756,0.679645439025561,-0.0311739244825062));
#109117=DIRECTION('ref_axis',(0.680359513835124,-0.732052760892824,0.0347805578337564));
#109118=DIRECTION('center_axis',(-4.18005656861882E-16,1.,0.));
#109119=DIRECTION('ref_axis',(1.,0.,0.));
#109120=DIRECTION('center_axis',(0.,0.,1.));
#109121=DIRECTION('ref_axis',(1.,0.,0.));
#109122=DIRECTION('center_axis',(0.,-1.,0.));
#109123=DIRECTION('ref_axis',(1.,0.,0.));
#109124=DIRECTION('center_axis',(0.,0.,-1.));
#109125=DIRECTION('ref_axis',(1.,0.,0.));
#109126=DIRECTION('',(0.,0.,-1.));
#109127=DIRECTION('center_axis',(0.483753083973024,0.,-0.875204521095834));
#109128=DIRECTION('ref_axis',(-0.875204521095834,0.,-0.483753083973024));
#109129=DIRECTION('center_axis',(0.,0.,-1.));
#109130=DIRECTION('ref_axis',(-1.,0.,0.));
#109131=DIRECTION('center_axis',(0.,0.,-1.));
#109132=DIRECTION('ref_axis',(1.,0.,0.));
#109133=DIRECTION('center_axis',(0.,0.,-1.));
#109134=DIRECTION('ref_axis',(-1.,0.,0.));
#109135=DIRECTION('',(0.,0.,1.));
#109136=DIRECTION('center_axis',(-0.48375308397303,0.,-0.875204521095831));
#109137=DIRECTION('ref_axis',(-0.875204521095831,0.,0.48375308397303));
#109138=DIRECTION('center_axis',(-0.460817663464343,0.,-0.887494834373285));
#109139=DIRECTION('ref_axis',(-0.887494834373285,0.,0.460817663464343));
#109140=DIRECTION('center_axis',(0.214288672238559,-0.976770219107516,0.000551375454002857));
#109141=DIRECTION('ref_axis',(0.837939441759682,0.183541158169798,-0.513974839074017));
#109142=DIRECTION('center_axis',(-1.,0.,0.));
#109143=DIRECTION('ref_axis',(0.,0.,1.));
#109144=DIRECTION('center_axis',(0.,0.,-1.));
#109145=DIRECTION('ref_axis',(-1.,0.,0.));
#109146=DIRECTION('center_axis',(0.,-7.60037129918555E-33,1.));
#109147=DIRECTION('ref_axis',(-1.,0.,0.));
#109148=DIRECTION('center_axis',(0.,0.,-1.));
#109149=DIRECTION('ref_axis',(-1.,0.,0.));
#109150=DIRECTION('center_axis',(1.,0.,0.));
#109151=DIRECTION('ref_axis',(0.,-1.,0.));
#109152=DIRECTION('center_axis',(1.,0.,0.));
#109153=DIRECTION('ref_axis',(0.,0.,-1.));
#109154=DIRECTION('',(1.,4.38004274807345E-16,0.));
#109155=DIRECTION('center_axis',(-4.38004274807345E-16,1.,0.));
#109156=DIRECTION('ref_axis',(1.,0.,0.));
#109157=DIRECTION('center_axis',(0.,0.,-1.));
#109158=DIRECTION('ref_axis',(-1.,0.,0.));
#109159=DIRECTION('center_axis',(0.,-1.,0.));
#109160=DIRECTION('ref_axis',(1.,0.,0.));
#109161=DIRECTION('center_axis',(0.,0.,1.));
#109162=DIRECTION('ref_axis',(-1.,0.,0.));
#109163=DIRECTION('center_axis',(0.,0.,-1.));
#109164=DIRECTION('ref_axis',(-1.,0.,0.));
#109165=DIRECTION('',(0.,0.,-1.));
#109166=DIRECTION('center_axis',(-4.38004274807345E-16,1.,0.));
#109167=DIRECTION('ref_axis',(1.,0.,0.));
#109168=DIRECTION('center_axis',(0.,-1.,0.));
#109169=DIRECTION('ref_axis',(1.,0.,0.));
#109170=DIRECTION('center_axis',(-1.,0.,0.));
#109171=DIRECTION('ref_axis',(0.,0.,1.));
#109172=DIRECTION('center_axis',(-1.,-4.38004274807346E-16,-5.40794518211031E-32));
#109173=DIRECTION('ref_axis',(-4.38004274807346E-16,1.,5.80597460094347E-63));
#109174=DIRECTION('center_axis',(-1.,0.,0.));
#109175=DIRECTION('ref_axis',(0.,0.,1.));
#109176=DIRECTION('',(-1.,-4.38004274807345E-16,-5.40794518211031E-32));
#109177=DIRECTION('center_axis',(1.,0.,5.40794518211031E-32));
#109178=DIRECTION('ref_axis',(0.,-1.,0.));
#109179=DIRECTION('center_axis',(-1.,0.,0.));
#109180=DIRECTION('ref_axis',(0.,0.,1.));
#109181=DIRECTION('center_axis',(1.,0.,5.40794518211031E-32));
#109182=DIRECTION('ref_axis',(0.,-1.,0.));
#109183=DIRECTION('center_axis',(-4.18005656861881E-16,1.,0.));
#109184=DIRECTION('ref_axis',(1.,4.18005656861881E-16,0.));
#109185=DIRECTION('center_axis',(0.,1.,0.));
#109186=DIRECTION('ref_axis',(-1.,0.,0.));
#109187=DIRECTION('',(4.18005656861881E-16,-1.,0.));
#109188=DIRECTION('center_axis',(4.18005656861882E-16,-1.,0.));
#109189=DIRECTION('ref_axis',(-1.,0.,0.));
#109190=DIRECTION('center_axis',(0.,0.,-1.));
#109191=DIRECTION('ref_axis',(-1.,0.,0.));
#109192=DIRECTION('center_axis',(-1.,0.,0.));
#109193=DIRECTION('ref_axis',(0.,1.,0.));
#109194=DIRECTION('',(-1.,-4.18005656861881E-16,0.));
#109195=DIRECTION('center_axis',(1.,0.,0.));
#109196=DIRECTION('ref_axis',(0.,0.,-1.));
#109197=DIRECTION('center_axis',(0.,7.25334975031382E-33,-1.));
#109198=DIRECTION('ref_axis',(1.,0.,0.));
#109199=DIRECTION('center_axis',(0.,0.,1.));
#109200=DIRECTION('ref_axis',(1.,0.,0.));
#109201=DIRECTION('center_axis',(0.,0.,1.));
#109202=DIRECTION('ref_axis',(1.,0.,0.));
#109203=DIRECTION('center_axis',(0.,0.,1.));
#109204=DIRECTION('ref_axis',(1.,0.,0.));
#109205=DIRECTION('center_axis',(1.,0.,0.));
#109206=DIRECTION('ref_axis',(0.,0.,-1.));
#109207=DIRECTION('center_axis',(-1.,0.,-5.16102651992463E-32));
#109208=DIRECTION('ref_axis',(0.,1.,0.));
#109209=DIRECTION('center_axis',(1.,0.,-1.38777878078144E-14));
#109210=DIRECTION('ref_axis',(-1.38777878078144E-14,0.,-1.));
#109211=DIRECTION('',(-1.,-4.18005656861881E-16,-5.16102651992463E-32));
#109212=DIRECTION('center_axis',(0.534259922646944,0.,0.845320255910907));
#109213=DIRECTION('ref_axis',(0.845320255910907,0.,-0.534259922646944));
#109214=DIRECTION('center_axis',(0.543750575738856,0.,0.839246871536417));
#109215=DIRECTION('ref_axis',(0.839246871536417,0.,-0.543750575738856));
#109216=DIRECTION('center_axis',(0.,-1.66533453693774E-12,-1.));
#109217=DIRECTION('ref_axis',(0.,-1.,1.66533453693774E-12));
#109218=DIRECTION('center_axis',(0.,0.,1.));
#109219=DIRECTION('ref_axis',(-1.,0.,0.));
#109220=DIRECTION('center_axis',(0.,0.,-1.));
#109221=DIRECTION('ref_axis',(-1.,0.,0.));
#109222=DIRECTION('',(0.,0.,-1.));
#109223=DIRECTION('center_axis',(0.543750575738856,0.,-0.839246871536417));
#109224=DIRECTION('ref_axis',(-0.839246871536417,0.,-0.543750575738856));
#109225=DIRECTION('center_axis',(0.534875344054122,-1.17257728967007E-14,
-0.844930983171398));
#109226=DIRECTION('ref_axis',(-0.844930983171398,-8.89670234612257E-31,
-0.534875344054122));
#109227=DIRECTION('center_axis',(1.,0.,0.));
#109228=DIRECTION('ref_axis',(0.,0.,-1.));
#109229=DIRECTION('center_axis',(1.,4.1800565686188E-16,5.16102651992463E-32));
#109230=DIRECTION('ref_axis',(4.1800565686188E-16,-1.,8.08534226092968E-63));
#109231=DIRECTION('center_axis',(0.,0.,1.));
#109232=DIRECTION('ref_axis',(-1.,0.,0.));
#109233=DIRECTION('center_axis',(0.,0.,-1.));
#109234=DIRECTION('ref_axis',(-1.,0.,0.));
#109235=DIRECTION('',(0.,0.,1.));
#109236=DIRECTION('center_axis',(4.18005656861882E-16,-1.,0.));
#109237=DIRECTION('ref_axis',(-1.,0.,0.));
#109238=DIRECTION('center_axis',(0.,1.,0.));
#109239=DIRECTION('ref_axis',(-1.,0.,0.));
#109240=DIRECTION('center_axis',(0.,1.23467863058847E-16,-1.));
#109241=DIRECTION('ref_axis',(0.,1.,1.1837531408762E-16));
#109242=DIRECTION('center_axis',(0.,-1.19392659184112E-16,1.));
#109243=DIRECTION('ref_axis',(0.,1.,1.19392659184112E-16));
#109244=DIRECTION('center_axis',(1.,0.,5.16102651992463E-32));
#109245=DIRECTION('ref_axis',(0.,-1.,0.));
#109246=DIRECTION('center_axis',(-1.,0.,0.));
#109247=DIRECTION('ref_axis',(0.,0.,1.));
#109248=DIRECTION('center_axis',(-0.496741562438066,-1.20445113324067E-14,
0.867898507975782));
#109249=DIRECTION('ref_axis',(0.867898507975782,5.70559822356712E-31,0.496741562438066));
#109250=DIRECTION('center_axis',(-0.518474310548575,0.,0.855093205037428));
#109251=DIRECTION('ref_axis',(0.855093205037428,0.,0.518474310548575));
#109252=DIRECTION('center_axis',(0.,0.,1.));
#109253=DIRECTION('ref_axis',(1.,0.,0.));
#109254=DIRECTION('center_axis',(0.,0.,-1.));
#109255=DIRECTION('ref_axis',(1.,0.,0.));
#109256=DIRECTION('center_axis',(-2.72711680125255E-25,-1.11022302462516E-13,
1.));
#109257=DIRECTION('ref_axis',(-1.56607307231965E-53,1.,1.11022302462516E-13));
#109258=DIRECTION('',(0.,0.,1.));
#109259=DIRECTION('center_axis',(0.518474310548581,-7.19527646559628E-15,
0.855093205037424));
#109260=DIRECTION('ref_axis',(0.855093205037424,3.43699106634736E-31,-0.518474310548581));
#109261=DIRECTION('center_axis',(0.496378972716316,-6.19668439877561E-14,
0.868105935612178));
#109262=DIRECTION('ref_axis',(0.868105935612178,3.44724486393529E-29,-0.496378972716316));
#109263=DIRECTION('center_axis',(1.,0.,0.));
#109264=DIRECTION('ref_axis',(0.,0.,-1.));
#109265=DIRECTION('center_axis',(-1.,-4.1800565686188E-16,-5.16102651992463E-32));
#109266=DIRECTION('ref_axis',(-4.1800565686188E-16,1.,-8.08534226092968E-63));
#109267=DIRECTION('center_axis',(1.,0.,0.));
#109268=DIRECTION('ref_axis',(0.,0.,-1.));
#109269=DIRECTION('',(1.,4.18005656861881E-16,5.16102651992463E-32));
#109270=DIRECTION('center_axis',(0.,0.,1.));
#109271=DIRECTION('ref_axis',(1.,0.,0.));
#109272=DIRECTION('center_axis',(0.,-7.25334975031382E-33,1.));
#109273=DIRECTION('ref_axis',(-1.,0.,0.));
#109274=DIRECTION('center_axis',(0.,0.,1.));
#109275=DIRECTION('ref_axis',(1.,0.,0.));
#109276=DIRECTION('center_axis',(-1.,0.,0.));
#109277=DIRECTION('ref_axis',(0.,1.,0.));
#109278=DIRECTION('center_axis',(-1.,0.,0.));
#109279=DIRECTION('ref_axis',(0.,0.,1.));
#109280=DIRECTION('',(1.,4.18005656861881E-16,0.));
#109281=DIRECTION('center_axis',(-4.18005656861882E-16,1.,0.));
#109282=DIRECTION('ref_axis',(1.,0.,0.));
#109283=DIRECTION('center_axis',(0.,0.,1.));
#109284=DIRECTION('ref_axis',(1.,0.,0.));
#109285=DIRECTION('center_axis',(0.,-1.,0.));
#109286=DIRECTION('ref_axis',(1.,0.,0.));
#109287=DIRECTION('center_axis',(0.,0.,-1.));
#109288=DIRECTION('ref_axis',(1.,0.,0.));
#109289=DIRECTION('center_axis',(0.,0.,1.));
#109290=DIRECTION('ref_axis',(1.,0.,0.));
#109291=DIRECTION('',(0.,0.,-1.));
#109292=DIRECTION('center_axis',(-4.18005656861882E-16,1.,0.));
#109293=DIRECTION('ref_axis',(1.,0.,0.));
#109294=DIRECTION('center_axis',(0.,-1.,0.));
#109295=DIRECTION('ref_axis',(1.,0.,0.));
#109296=DIRECTION('center_axis',(-4.18005656861881E-16,1.,0.));
#109297=DIRECTION('ref_axis',(1.,4.18005656861881E-16,0.));
#109298=DIRECTION('center_axis',(0.,1.,0.));
#109299=DIRECTION('ref_axis',(-1.,0.,0.));
#109300=DIRECTION('',(4.18005656861881E-16,-1.,0.));
#109301=DIRECTION('center_axis',(4.18005656861882E-16,-1.,0.));
#109302=DIRECTION('ref_axis',(-1.,0.,0.));
#109303=DIRECTION('center_axis',(0.,0.,-1.));
#109304=DIRECTION('ref_axis',(-1.,0.,0.));
#109305=DIRECTION('center_axis',(-1.,0.,-5.16102651992463E-32));
#109306=DIRECTION('ref_axis',(0.,1.,0.));
#109307=DIRECTION('center_axis',(-1.,0.,0.));
#109308=DIRECTION('ref_axis',(0.,1.,0.));
#109309=DIRECTION('',(-1.,-4.18005656861881E-16,0.));
#109310=DIRECTION('center_axis',(1.,0.,0.));
#109311=DIRECTION('ref_axis',(0.,0.,-1.));
#109312=DIRECTION('center_axis',(0.,7.25334975031382E-33,-1.));
#109313=DIRECTION('ref_axis',(1.,0.,0.));
#109314=DIRECTION('center_axis',(0.,0.,1.));
#109315=DIRECTION('ref_axis',(1.,0.,0.));
#109316=DIRECTION('center_axis',(0.,0.,1.));
#109317=DIRECTION('ref_axis',(1.,0.,0.));
#109318=DIRECTION('center_axis',(0.,0.,1.));
#109319=DIRECTION('ref_axis',(1.,0.,0.));
#109320=DIRECTION('center_axis',(1.,0.,0.));
#109321=DIRECTION('ref_axis',(0.,0.,-1.));
#109322=DIRECTION('center_axis',(1.,4.1800565686188E-16,5.16102651992463E-32));
#109323=DIRECTION('ref_axis',(4.1800565686188E-16,-1.,8.08534226092968E-63));
#109324=DIRECTION('center_axis',(1.,0.,0.));
#109325=DIRECTION('ref_axis',(0.,0.,-1.));
#109326=DIRECTION('',(-1.,-4.18005656861881E-16,-5.16102651992463E-32));
#109327=DIRECTION('center_axis',(0.483537964931496,0.,0.875323389650881));
#109328=DIRECTION('ref_axis',(0.875323389650881,0.,-0.483537964931496));
#109329=DIRECTION('center_axis',(0.507514080295474,0.,0.861643463563578));
#109330=DIRECTION('ref_axis',(0.861643463563578,0.,-0.507514080295474));
#109331=DIRECTION('center_axis',(1.11022302462516E-13,0.,1.));
#109332=DIRECTION('ref_axis',(1.,0.,-1.11022302462516E-13));
#109333=DIRECTION('center_axis',(0.,0.,1.));
#109334=DIRECTION('ref_axis',(-1.,0.,0.));
#109335=DIRECTION('center_axis',(0.,0.,1.));
#109336=DIRECTION('ref_axis',(1.,0.,0.));
#109337=DIRECTION('',(0.,0.,-1.));
#109338=DIRECTION('center_axis',(-0.507514080295481,0.,0.861643463563574));
#109339=DIRECTION('ref_axis',(0.861643463563574,0.,0.507514080295481));
#109340=DIRECTION('center_axis',(0.,0.,1.));
#109341=DIRECTION('ref_axis',(-1.,0.,0.));
#109342=DIRECTION('center_axis',(0.,0.,-1.));
#109343=DIRECTION('ref_axis',(-1.,0.,0.));
#109344=DIRECTION('',(0.,0.,1.));
#109345=DIRECTION('center_axis',(4.18005656861882E-16,-1.,0.));
#109346=DIRECTION('ref_axis',(-1.,0.,0.));
#109347=DIRECTION('center_axis',(0.,1.,0.));
#109348=DIRECTION('ref_axis',(-1.,0.,0.));
#109349=DIRECTION('center_axis',(0.,1.23467863058847E-16,-1.));
#109350=DIRECTION('ref_axis',(-1.,0.,0.));
#109351=DIRECTION('center_axis',(0.,0.,1.));
#109352=DIRECTION('ref_axis',(0.,1.,0.));
#109353=DIRECTION('center_axis',(0.,0.,1.));
#109354=DIRECTION('ref_axis',(0.,-1.,0.));
#109355=DIRECTION('center_axis',(5.01606788234257E-16,-1.,5.70122241611331E-32));
#109356=DIRECTION('ref_axis',(-4.59816715307009E-64,-5.70122241611331E-32,
-1.));
#109357=DIRECTION('',(-1.,-5.01606788234257E-16,0.));
#109358=DIRECTION('center_axis',(0.,0.,-1.));
#109359=DIRECTION('ref_axis',(-1.,0.,0.));
#109360=DIRECTION('center_axis',(0.990268068741571,0.139173100960059,1.71834053708117E-17));
#109361=DIRECTION('ref_axis',(0.139173100960059,-0.990268068741571,4.14246685971564E-34));
#109362=DIRECTION('center_axis',(-0.990268068741571,-0.139173100960059,
0.));
#109363=DIRECTION('ref_axis',(0.139173100960059,-0.990268068741571,0.));
#109364=DIRECTION('center_axis',(0.,1.23467863058847E-16,-1.));
#109365=DIRECTION('ref_axis',(0.,1.,0.));
#109366=DIRECTION('center_axis',(-0.728126055379271,-0.685443248911113,
0.));
#109367=DIRECTION('ref_axis',(0.685443248911113,-0.728126055379271,0.));
#109368=DIRECTION('center_axis',(0.,1.23467863058847E-16,-1.));
#109369=DIRECTION('ref_axis',(0.,1.,0.));
#109370=DIRECTION('center_axis',(-0.685443248911109,-0.728126055379275,
0.));
#109371=DIRECTION('ref_axis',(0.728126055379275,-0.685443248911109,0.));
#109372=DIRECTION('center_axis',(0.,1.23467863058847E-16,-1.));
#109373=DIRECTION('ref_axis',(0.,1.,0.));
#109374=DIRECTION('center_axis',(-0.139173100960066,-0.99026806874157,0.));
#109375=DIRECTION('ref_axis',(0.99026806874157,-0.139173100960066,0.));
#109376=DIRECTION('center_axis',(0.139173100960066,0.99026806874157,1.22266282302933E-16));
#109377=DIRECTION('ref_axis',(0.99026806874157,-0.139173100960066,-9.57340194962255E-34));
#109378=DIRECTION('center_axis',(0.139173100960066,0.99026806874157,0.));
#109379=DIRECTION('ref_axis',(-0.99026806874157,0.139173100960066,0.));
#109380=DIRECTION('center_axis',(-0.139173100960066,-0.99026806874157,0.));
#109381=DIRECTION('ref_axis',(-0.99026806874157,0.139173100960066,0.));
#109382=DIRECTION('center_axis',(0.139173100960066,0.99026806874157,0.));
#109383=DIRECTION('ref_axis',(-0.99026806874157,0.139173100960066,0.));
#109384=DIRECTION('',(0.139173100960067,0.99026806874157,0.));
#109385=DIRECTION('center_axis',(0.139173100960066,0.99026806874157,1.22266282302933E-16));
#109386=DIRECTION('ref_axis',(0.99026806874157,-0.139173100960066,-9.57340194962255E-34));
#109387=DIRECTION('',(0.139173100960067,0.99026806874157,1.22266282302933E-16));
#109388=DIRECTION('center_axis',(0.139173100960066,0.99026806874157,0.));
#109389=DIRECTION('ref_axis',(-0.99026806874157,0.139173100960066,0.));
#109390=DIRECTION('center_axis',(-0.139173100960066,-0.99026806874157,0.));
#109391=DIRECTION('ref_axis',(-0.99026806874157,0.139173100960066,0.));
#109392=DIRECTION('center_axis',(0.139173100960066,0.99026806874157,0.));
#109393=DIRECTION('ref_axis',(-0.99026806874157,0.139173100960066,0.));
#109394=DIRECTION('',(0.139173100960067,0.99026806874157,0.));
#109395=DIRECTION('center_axis',(0.139173100960066,0.99026806874157,1.22266282302933E-16));
#109396=DIRECTION('ref_axis',(0.99026806874157,-0.139173100960066,-9.57340194962255E-34));
#109397=DIRECTION('center_axis',(0.139173100960066,0.99026806874157,0.));
#109398=DIRECTION('ref_axis',(-0.99026806874157,0.139173100960066,0.));
#109399=DIRECTION('',(0.139173100960067,0.99026806874157,1.22266282302933E-16));
#109400=DIRECTION('center_axis',(0.133528512868191,0.950104737537312,-0.281906232567436));
#109401=DIRECTION('ref_axis',(2.32560161936155E-16,-0.284453521859895,-0.958689831958962));
#109402=DIRECTION('center_axis',(0.369731042763204,0.785707308414229,0.495946551073502));
#109403=DIRECTION('ref_axis',(-1.91361720426385E-15,0.533770129672178,-0.845629616717477));
#109404=DIRECTION('center_axis',(0.416737288136069,0.909026970269307,0.));
#109405=DIRECTION('ref_axis',(-0.909026970269307,0.416737288136069,0.));
#109406=DIRECTION('center_axis',(0.,0.,1.));
#109407=DIRECTION('ref_axis',(-1.,0.,0.));
#109408=DIRECTION('center_axis',(0.40826271186488,0.912864479591979,-3.16713488626711E-15));
#109409=DIRECTION('ref_axis',(-0.912864479591979,0.40826271186488,6.04208104977424E-31));
#109410=DIRECTION('center_axis',(0.,0.,-1.));
#109411=DIRECTION('ref_axis',(-1.,0.,0.));
#109412=DIRECTION('center_axis',(0.,-6.17339315294237E-17,1.));
#109413=DIRECTION('ref_axis',(0.,-1.,0.));
#109414=DIRECTION('center_axis',(0.,0.,-1.));
#109415=DIRECTION('ref_axis',(0.,-1.,0.));
#109416=DIRECTION('center_axis',(-0.278601694915732,-0.960406734456856,
8.33020054374265E-16));
#109417=DIRECTION('ref_axis',(0.960406734456856,-0.278601694915732,-5.45700864471184E-31));
#109418=DIRECTION('center_axis',(0.,0.,1.));
#109419=DIRECTION('ref_axis',(-1.,0.,0.));
#109420=DIRECTION('center_axis',(-0.270127118644541,-0.962824667202081,
4.0829772679528E-16));
#109421=DIRECTION('ref_axis',(0.962824667202081,-0.270127118644541,5.77560433057458E-31));
#109422=DIRECTION('center_axis',(0.,0.,-1.));
#109423=DIRECTION('ref_axis',(-1.,0.,0.));
#109424=DIRECTION('center_axis',(-0.185959552881302,-0.695904038033425,
0.693640118895209));
#109425=DIRECTION('ref_axis',(-3.15382046976506E-16,0.705953788300242,0.708257897085897));
#109426=DIRECTION('center_axis',(0.,-6.17339315294237E-17,1.));
#109427=DIRECTION('ref_axis',(0.,-1.,0.));
#109428=DIRECTION('center_axis',(0.,0.,-1.));
#109429=DIRECTION('ref_axis',(0.,-1.,0.));
#109430=DIRECTION('center_axis',(0.141151402782332,0.989840911569284,-0.0170660855578596));
#109431=DIRECTION('ref_axis',(-0.989985089278404,0.141171962536586,2.4318092123443E-19));
#109432=DIRECTION('center_axis',(0.1326869973619,0.991030504325029,-0.0158965476868861));
#109433=DIRECTION('ref_axis',(-0.991155744879145,0.132703765557229,-2.90070390844182E-17));
#109434=DIRECTION('center_axis',(-0.1499957800683,0.0101893565027498,-0.988634129987308));
#109435=DIRECTION('ref_axis',(-0.981224439714038,0.121089666642347,0.150119590794534));
#109436=DIRECTION('center_axis',(0.,-6.17339315294237E-17,1.));
#109437=DIRECTION('ref_axis',(0.,-1.,0.));
#109438=DIRECTION('center_axis',(0.,0.,-1.));
#109439=DIRECTION('ref_axis',(0.,-1.,0.));
#109440=DIRECTION('center_axis',(0.00234948403731584,0.999997203076769,
-0.000271594180011335));
#109441=DIRECTION('ref_axis',(-0.999997239958367,0.00234948412396881,6.81083076705817E-23));
#109442=DIRECTION('center_axis',(-0.00619406208384126,0.999980560265093,
0.000716021516796888));
#109443=DIRECTION('ref_axis',(-0.999980816603614,-0.00619406367164884,-2.43997512021813E-21));
#109444=DIRECTION('center_axis',(-0.0216109392502409,-2.83714134350443E-8,
-0.99976645638105));
#109445=DIRECTION('ref_axis',(-0.999764411688039,0.00202245879910768,0.021610894994789));
#109446=DIRECTION('center_axis',(0.,-6.17339315294237E-17,1.));
#109447=DIRECTION('ref_axis',(0.,-1.,0.));
#109448=DIRECTION('center_axis',(0.,0.,-1.));
#109449=DIRECTION('ref_axis',(0.,-1.,0.));
#109450=DIRECTION('center_axis',(-0.136497250965888,0.990504401193308,0.0164174204868685));
#109451=DIRECTION('ref_axis',(-0.990637914348733,-0.136515649853022,4.14575077332242E-19));
#109452=DIRECTION('center_axis',(-0.144956948347396,0.989281282708723,0.017607578141073));
#109453=DIRECTION('ref_axis',(-0.989434670234472,-0.144979423843532,1.06064347286242E-18));
#109454=DIRECTION('center_axis',(-0.157548218657054,-0.0111059690216339,
-0.98744884234581));
#109455=DIRECTION('ref_axis',(-0.980524532402052,-0.11697738133772,0.157759099937552));
#109456=DIRECTION('center_axis',(0.,-6.17339315294237E-17,1.));
#109457=DIRECTION('ref_axis',(0.,-1.,0.));
#109458=DIRECTION('center_axis',(0.,0.,-1.));
#109459=DIRECTION('ref_axis',(0.,-1.,0.));
#109460=DIRECTION('center_axis',(0.0971107883155516,-0.363411229368455,
-0.926553707650906));
#109461=DIRECTION('ref_axis',(-3.86068458172679E-17,-0.930953788243945,
0.365137021067773));
#109462=DIRECTION('center_axis',(0.273940677965627,-0.961746590820957,0.));
#109463=DIRECTION('ref_axis',(0.961746590820957,0.273940677965627,0.));
#109464=DIRECTION('center_axis',(0.,0.,1.));
#109465=DIRECTION('ref_axis',(-1.,0.,0.));
#109466=DIRECTION('center_axis',(0.282415254236812,-0.959292251701408,0.));
#109467=DIRECTION('ref_axis',(0.959292251701408,0.282415254236812,0.));
#109468=DIRECTION('center_axis',(0.,0.,-1.));
#109469=DIRECTION('ref_axis',(-1.,0.,0.));
#109470=DIRECTION('center_axis',(0.,-6.17339315294237E-17,1.));
#109471=DIRECTION('ref_axis',(0.,-1.,0.));
#109472=DIRECTION('center_axis',(0.,0.,-1.));
#109473=DIRECTION('ref_axis',(0.,-1.,0.));
#109474=DIRECTION('center_axis',(-0.412076271185962,0.911149354785193,0.));
#109475=DIRECTION('ref_axis',(-0.911149354785193,-0.412076271185962,0.));
#109476=DIRECTION('center_axis',(0.,0.,1.));
#109477=DIRECTION('ref_axis',(-1.,0.,0.));
#109478=DIRECTION('center_axis',(-0.42055084745715,0.907268970428876,0.));
#109479=DIRECTION('ref_axis',(-0.907268970428876,-0.42055084745715,0.));
#109480=DIRECTION('center_axis',(0.,0.,-1.));
#109481=DIRECTION('ref_axis',(-1.,0.,0.));
#109482=DIRECTION('center_axis',(-0.408524918701489,0.868147321075037,-0.281829061152641));
#109483=DIRECTION('ref_axis',(-0.904824724134437,-0.425784239486432,-2.46811619432984E-17));
#109484=DIRECTION('center_axis',(0.133528512868198,-0.950104737537311,-0.281906232567435));
#109485=DIRECTION('ref_axis',(-1.78830809785603E-17,-0.284453521859893,
0.958689831958962));
#109486=DIRECTION('center_axis',(-0.139173100960066,0.99026806874157,1.22266282302934E-16));
#109487=DIRECTION('ref_axis',(0.99026806874157,0.139173100960066,1.22723965167578E-33));
#109488=DIRECTION('',(-0.139173100960065,0.99026806874157,1.22266282302933E-16));
#109489=DIRECTION('center_axis',(-0.139173100960066,0.99026806874157,0.));
#109490=DIRECTION('ref_axis',(-0.99026806874157,-0.139173100960066,0.));
#109491=DIRECTION('center_axis',(0.139173100960066,-0.99026806874157,0.));
#109492=DIRECTION('ref_axis',(-0.99026806874157,-0.139173100960066,0.));
#109493=DIRECTION('center_axis',(-0.139173100960039,0.990268068741574,2.74854602616996E-14));
#109494=DIRECTION('ref_axis',(-0.990268068741574,-0.139173100960039,-5.80135260633727E-30));
#109495=DIRECTION('',(-0.139173100960065,0.99026806874157,0.));
#109496=DIRECTION('center_axis',(-0.139173100960066,0.99026806874157,1.22266282302934E-16));
#109497=DIRECTION('ref_axis',(0.99026806874157,0.139173100960066,1.22723965167578E-33));
#109498=DIRECTION('center_axis',(0.139173100960066,-0.99026806874157,0.));
#109499=DIRECTION('ref_axis',(0.99026806874157,0.139173100960066,0.));
#109500=DIRECTION('center_axis',(0.139173100960073,-0.990268068741569,0.));
#109501=DIRECTION('ref_axis',(0.990268068741569,0.139173100960073,0.));
#109502=DIRECTION('center_axis',(-0.139173100960066,0.99026806874157,1.22266282302934E-16));
#109503=DIRECTION('ref_axis',(0.99026806874157,0.139173100960066,1.22723965167578E-33));
#109504=DIRECTION('',(-0.139173100960065,0.99026806874157,1.22266282302933E-16));
#109505=DIRECTION('center_axis',(-0.139173100960066,0.99026806874157,0.));
#109506=DIRECTION('ref_axis',(-0.99026806874157,-0.139173100960066,0.));
#109507=DIRECTION('center_axis',(0.139173100960066,-0.99026806874157,0.));
#109508=DIRECTION('ref_axis',(-0.99026806874157,-0.139173100960066,0.));
#109509=DIRECTION('center_axis',(-0.139173100960066,0.99026806874157,0.));
#109510=DIRECTION('ref_axis',(-0.99026806874157,-0.139173100960066,0.));
#109511=DIRECTION('',(-0.139173100960065,0.99026806874157,0.));
#109512=DIRECTION('center_axis',(0.,1.23467863058847E-16,-1.));
#109513=DIRECTION('ref_axis',(0.,1.,0.));
#109514=DIRECTION('center_axis',(0.685443248911109,-0.728126055379275,0.));
#109515=DIRECTION('ref_axis',(0.728126055379275,0.685443248911109,0.));
#109516=DIRECTION('center_axis',(0.,1.23467863058847E-16,-1.));
#109517=DIRECTION('ref_axis',(0.,1.,0.));
#109518=DIRECTION('center_axis',(0.728126055379271,-0.685443248911113,0.));
#109519=DIRECTION('ref_axis',(0.685443248911113,0.728126055379271,0.));
#109520=DIRECTION('center_axis',(0.,1.23467863058847E-16,-1.));
#109521=DIRECTION('ref_axis',(0.,1.,0.));
#109522=DIRECTION('center_axis',(0.990268068741571,-0.139173100960059,0.));
#109523=DIRECTION('ref_axis',(0.139173100960059,0.990268068741571,0.));
#109524=DIRECTION('center_axis',(-0.990268068741571,0.139173100960059,1.71834053708117E-17));
#109525=DIRECTION('ref_axis',(0.139173100960059,0.990268068741571,-4.14246685971564E-34));
#109526=DIRECTION('center_axis',(-0.990268068741571,0.139173100960064,0.));
#109527=DIRECTION('ref_axis',(-0.139173100960064,-0.990268068741571,0.));
#109528=DIRECTION('center_axis',(0.990268068741572,-0.139173100960051,0.));
#109529=DIRECTION('ref_axis',(-0.139173100960051,-0.990268068741572,0.));
#109530=DIRECTION('center_axis',(-0.990268068741572,0.139173100960051,0.));
#109531=DIRECTION('ref_axis',(-0.139173100960051,-0.990268068741572,0.));
#109532=DIRECTION('',(-0.990268068741571,0.139173100960059,0.));
#109533=DIRECTION('center_axis',(-0.990268068741571,0.139173100960059,1.71834053708117E-17));
#109534=DIRECTION('ref_axis',(0.139173100960059,0.990268068741571,-4.14246685971564E-34));
#109535=DIRECTION('',(-0.990268068741571,0.139173100960059,1.71834053708117E-17));
#109536=DIRECTION('center_axis',(-0.990268068741572,0.139173100960051,0.));
#109537=DIRECTION('ref_axis',(-0.139173100960051,-0.990268068741572,0.));
#109538=DIRECTION('center_axis',(0.990268068741572,-0.139173100960051,0.));
#109539=DIRECTION('ref_axis',(-0.139173100960051,-0.990268068741572,0.));
#109540=DIRECTION('center_axis',(-0.990268068741572,0.139173100960051,1.37427301308497E-14));
#109541=DIRECTION('ref_axis',(-0.139173100960051,-0.990268068741572,1.93598700157835E-30));
#109542=DIRECTION('',(-0.990268068741571,0.139173100960059,0.));
#109543=DIRECTION('center_axis',(-0.990268068741571,0.139173100960059,1.71834053708117E-17));
#109544=DIRECTION('ref_axis',(0.139173100960059,0.990268068741571,-4.14246685971564E-34));
#109545=DIRECTION('center_axis',(-0.990268068741571,0.139173100960059,0.));
#109546=DIRECTION('ref_axis',(-0.139173100960059,-0.990268068741571,0.));
#109547=DIRECTION('',(-0.990268068741571,0.139173100960059,1.71834053708117E-17));
#109548=DIRECTION('center_axis',(1.,5.01606788234257E-16,0.));
#109549=DIRECTION('ref_axis',(5.01606788234257E-16,-1.,0.));
#109550=DIRECTION('',(-1.,-5.01606788234257E-16,0.));
#109551=DIRECTION('center_axis',(0.,1.23467863058847E-16,-1.));
#109552=DIRECTION('ref_axis',(0.,1.,0.));
#109553=DIRECTION('center_axis',(0.,0.,1.));
#109554=DIRECTION('ref_axis',(0.,1.,0.));
#109555=DIRECTION('center_axis',(0.,0.,-1.));
#109556=DIRECTION('ref_axis',(1.,8.87756872621991E-15,0.));
#109557=DIRECTION('center_axis',(1.,5.01606788234257E-16,0.));
#109558=DIRECTION('ref_axis',(5.01606788234257E-16,-1.,0.));
#109559=DIRECTION('center_axis',(-4.38004274807345E-16,1.,0.));
#109560=DIRECTION('ref_axis',(1.,4.38004274807345E-16,0.));
#109561=DIRECTION('center_axis',(-4.38004274807345E-16,1.,0.));
#109562=DIRECTION('ref_axis',(1.,4.38004274807345E-16,0.));
#109563=DIRECTION('center_axis',(5.01606788234257E-16,-1.,5.70122241611331E-32));
#109564=DIRECTION('ref_axis',(-4.59816715307009E-64,-5.70122241611331E-32,
-1.));
#109565=DIRECTION('center_axis',(-4.38004274807345E-16,1.,0.));
#109566=DIRECTION('ref_axis',(1.,4.38004274807345E-16,0.));
#109567=DIRECTION('center_axis',(-1.,-4.18005656861882E-16,0.));
#109568=DIRECTION('ref_axis',(-4.18005656861882E-16,1.,0.));
#109569=DIRECTION('',(-4.18005656861881E-16,1.,0.));
#109570=DIRECTION('center_axis',(-1.,-4.18005656861882E-16,0.));
#109571=DIRECTION('ref_axis',(-4.18005656861882E-16,1.,0.));
#109572=DIRECTION('',(-4.18005656861881E-16,1.,0.));
#109573=DIRECTION('center_axis',(0.,0.,1.));
#109574=DIRECTION('ref_axis',(1.,0.,0.));
#109575=DIRECTION('',(4.18005656861881E-16,-1.,0.));
#109576=DIRECTION('center_axis',(0.,0.,-1.));
#109577=DIRECTION('ref_axis',(-1.,0.,0.));
#109578=DIRECTION('center_axis',(-1.,-4.38004274807345E-16,0.));
#109579=DIRECTION('ref_axis',(-4.38004274807345E-16,1.,0.));
#109580=DIRECTION('center_axis',(4.18005656861881E-16,-1.,0.));
#109581=DIRECTION('ref_axis',(-1.,-4.18005656861881E-16,0.));
#109582=DIRECTION('center_axis',(0.,0.,1.));
#109583=DIRECTION('ref_axis',(1.,0.,0.));
#109584=DIRECTION('',(4.18005656861881E-16,-1.,0.));
#109585=DIRECTION('',(-1.,-4.18005656861881E-16,0.));
#109586=DIRECTION('center_axis',(4.18005656861881E-16,-1.,0.));
#109587=DIRECTION('ref_axis',(-1.,-4.18005656861881E-16,0.));
#109588=DIRECTION('',(-4.18005656861881E-16,1.,0.));
#109589=DIRECTION('center_axis',(-1.,-4.18005656861882E-16,0.));
#109590=DIRECTION('ref_axis',(-4.18005656861882E-16,1.,0.));
#109591=DIRECTION('center_axis',(-1.,0.,0.));
#109592=DIRECTION('ref_axis',(0.,1.,0.));
#109593=DIRECTION('center_axis',(0.,0.,-1.));
#109594=DIRECTION('ref_axis',(-1.,0.,0.));
#109595=DIRECTION('center_axis',(-1.,-4.38004274807345E-16,0.));
#109596=DIRECTION('ref_axis',(-4.38004274807345E-16,1.,0.));
#109597=DIRECTION('center_axis',(0.,0.,-1.));
#109598=DIRECTION('ref_axis',(-1.,0.,0.));
#109599=DIRECTION('center_axis',(-1.,-4.38004274807345E-16,0.));
#109600=DIRECTION('ref_axis',(-4.38004274807345E-16,1.,0.));
#109601=DIRECTION('center_axis',(0.,0.,-1.));
#109602=DIRECTION('ref_axis',(-1.,0.,0.));
#109603=DIRECTION('center_axis',(-1.,-4.38004274807345E-16,0.));
#109604=DIRECTION('ref_axis',(-4.38004274807345E-16,1.,0.));
#109605=DIRECTION('center_axis',(0.,0.,-1.));
#109606=DIRECTION('ref_axis',(-1.,0.,0.));
#109607=DIRECTION('center_axis',(-1.,-4.38004274807345E-16,0.));
#109608=DIRECTION('ref_axis',(-4.38004274807345E-16,1.,0.));
#109609=DIRECTION('center_axis',(-1.,0.,0.));
#109610=DIRECTION('ref_axis',(0.,1.,0.));
#109611=DIRECTION('',(1.,4.18005656861881E-16,0.));
#109612=DIRECTION('center_axis',(4.18005656861881E-16,-1.,0.));
#109613=DIRECTION('ref_axis',(-1.,-4.18005656861881E-16,0.));
#109614=DIRECTION('',(-4.18005656861881E-16,1.,0.));
#109615=DIRECTION('',(4.18005656861881E-16,-1.,0.));
#109616=DIRECTION('center_axis',(-1.,-4.18005656861882E-16,0.));
#109617=DIRECTION('ref_axis',(-4.18005656861882E-16,1.,0.));
#109618=DIRECTION('center_axis',(0.,0.,1.));
#109619=DIRECTION('ref_axis',(1.,0.,0.));
#109620=DIRECTION('center_axis',(0.,0.,-1.));
#109621=DIRECTION('ref_axis',(-1.,0.,0.));
#109622=DIRECTION('center_axis',(-1.,-4.38004274807345E-16,0.));
#109623=DIRECTION('ref_axis',(-4.38004274807345E-16,1.,0.));
#109624=DIRECTION('center_axis',(0.,0.,1.));
#109625=DIRECTION('ref_axis',(1.,0.,0.));
#109626=DIRECTION('',(4.18005656861881E-16,-1.,0.));
#109627=DIRECTION('center_axis',(4.18005656861881E-16,-1.,0.));
#109628=DIRECTION('ref_axis',(-1.,-4.18005656861881E-16,0.));
#109629=DIRECTION('center_axis',(0.,-1.18842113532926E-16,1.));
#109630=DIRECTION('ref_axis',(0.,1.,1.18842113532926E-16));
#109631=DIRECTION('center_axis',(0.,0.,1.));
#109632=DIRECTION('ref_axis',(1.,0.,0.));
#109633=DIRECTION('',(1.,5.01606788234257E-16,0.));
#109634=DIRECTION('center_axis',(1.,5.01606788234257E-16,0.));
#109635=DIRECTION('ref_axis',(5.01606788234257E-16,-1.,0.));
#109636=DIRECTION('',(-1.,-5.01606788234257E-16,0.));
#109637=DIRECTION('center_axis',(5.01606788234257E-16,-1.,5.70122241611331E-32));
#109638=DIRECTION('ref_axis',(-4.59816715307009E-64,-5.70122241611331E-32,
-1.));
#109639=DIRECTION('center_axis',(-4.38004274807345E-16,1.,0.));
#109640=DIRECTION('ref_axis',(1.,4.38004274807345E-16,0.));
#109641=DIRECTION('center_axis',(0.0999814467122865,-0.00101927549405267,
0.994988779530094));
#109642=DIRECTION('ref_axis',(0.648676516536244,0.758334173982988,-0.0644054148650803));
#109643=DIRECTION('center_axis',(-0.742683090861321,0.669643059061075,-1.01363406279984E-15));
#109644=DIRECTION('ref_axis',(-0.669643059061075,-0.742683090861321,-3.71575034000761E-31));
#109645=DIRECTION('center_axis',(0.,1.23467863058847E-16,-1.));
#109646=DIRECTION('ref_axis',(0.,1.,0.));
#109647=DIRECTION('center_axis',(0.,0.,1.));
#109648=DIRECTION('ref_axis',(0.,1.,0.));
#109649=DIRECTION('center_axis',(0.,0.,-1.));
#109650=DIRECTION('ref_axis',(1.,-7.98385375378166E-15,0.));
#109651=DIRECTION('center_axis',(0.,1.23467863058847E-16,-1.));
#109652=DIRECTION('ref_axis',(-1.,0.,0.));
#109653=DIRECTION('center_axis',(0.,0.,-1.));
#109654=DIRECTION('ref_axis',(-1.,0.,0.));
#109655=DIRECTION('center_axis',(-4.38004274807345E-16,1.,0.));
#109656=DIRECTION('ref_axis',(1.,4.38004274807345E-16,0.));
#109657=DIRECTION('center_axis',(0.,1.23467863058847E-16,-1.));
#109658=DIRECTION('ref_axis',(-1.,0.,0.));
#109659=DIRECTION('center_axis',(0.,0.,1.));
#109660=DIRECTION('ref_axis',(1.,0.,0.));
#109661=DIRECTION('',(1.,5.01606788234257E-16,0.));
#109662=DIRECTION('center_axis',(1.,5.01606788234257E-16,0.));
#109663=DIRECTION('ref_axis',(5.01606788234257E-16,-1.,0.));
#109664=DIRECTION('',(-1.,-5.01606788234257E-16,0.));
#109665=DIRECTION('center_axis',(5.01606788234257E-16,-1.,5.70122241611331E-32));
#109666=DIRECTION('ref_axis',(-4.59816715307009E-64,-5.70122241611331E-32,
-1.));
#109667=DIRECTION('center_axis',(0.,0.,-1.));
#109668=DIRECTION('ref_axis',(-1.,0.,0.));
#109669=DIRECTION('center_axis',(0.,-1.18842113532926E-16,1.));
#109670=DIRECTION('ref_axis',(0.,1.,1.18842113532926E-16));
#109671=DIRECTION('center_axis',(0.,-1.18842113532926E-16,1.));
#109672=DIRECTION('ref_axis',(0.,1.,1.18842113532926E-16));
#109673=DIRECTION('center_axis',(0.,0.,1.));
#109674=DIRECTION('ref_axis',(1.,0.,0.));
#109675=DIRECTION('',(4.18005656861881E-16,-1.,0.));
#109676=DIRECTION('center_axis',(4.18005656861881E-16,-1.,0.));
#109677=DIRECTION('ref_axis',(-1.,-4.18005656861881E-16,0.));
#109678=DIRECTION('',(-4.18005656861881E-16,1.,0.));
#109679=DIRECTION('center_axis',(-1.,-4.18005656861882E-16,0.));
#109680=DIRECTION('ref_axis',(-4.18005656861882E-16,1.,0.));
#109681=DIRECTION('center_axis',(-1.,-4.38004274807345E-16,0.));
#109682=DIRECTION('ref_axis',(-4.38004274807345E-16,1.,0.));
#109683=DIRECTION('center_axis',(0.,0.,-1.));
#109684=DIRECTION('ref_axis',(-1.,0.,0.));
#109685=DIRECTION('center_axis',(0.,0.,-1.));
#109686=DIRECTION('ref_axis',(1.,0.,0.));
#109687=DIRECTION('center_axis',(0.,1.23467863058847E-16,-1.));
#109688=DIRECTION('ref_axis',(0.,1.,0.));
#109689=DIRECTION('center_axis',(0.,0.,1.));
#109690=DIRECTION('ref_axis',(0.,1.,0.));
#109691=DIRECTION('center_axis',(0.,1.23467863058847E-16,-1.));
#109692=DIRECTION('ref_axis',(-1.,0.,0.));
#109693=DIRECTION('center_axis',(0.,1.23467863058847E-16,-1.));
#109694=DIRECTION('ref_axis',(0.,1.,0.));
#109695=DIRECTION('center_axis',(0.,0.,1.));
#109696=DIRECTION('ref_axis',(0.,1.,0.));
#109697=DIRECTION('center_axis',(0.,0.,-1.));
#109698=DIRECTION('ref_axis',(1.,0.,0.));
#109699=DIRECTION('center_axis',(0.,0.,-1.));
#109700=DIRECTION('ref_axis',(-1.,0.,0.));
#109701=DIRECTION('center_axis',(-1.,-4.38004274807345E-16,0.));
#109702=DIRECTION('ref_axis',(-4.38004274807345E-16,1.,0.));
#109703=DIRECTION('center_axis',(0.,1.23467863058847E-16,-1.));
#109704=DIRECTION('ref_axis',(-1.,0.,0.));
#109705=DIRECTION('center_axis',(0.,0.,1.));
#109706=DIRECTION('ref_axis',(1.,0.,0.));
#109707=DIRECTION('',(4.18005656861881E-16,-1.,0.));
#109708=DIRECTION('center_axis',(4.18005656861881E-16,-1.,0.));
#109709=DIRECTION('ref_axis',(-1.,-4.18005656861881E-16,0.));
#109710=DIRECTION('',(-4.18005656861881E-16,1.,0.));
#109711=DIRECTION('center_axis',(-1.,-4.18005656861882E-16,0.));
#109712=DIRECTION('ref_axis',(-4.18005656861882E-16,1.,0.));
#109713=DIRECTION('center_axis',(-1.,-4.38004274807345E-16,0.));
#109714=DIRECTION('ref_axis',(-4.38004274807345E-16,1.,0.));
#109715=DIRECTION('center_axis',(0.,0.,-1.));
#109716=DIRECTION('ref_axis',(-1.,0.,0.));
#109717=DIRECTION('center_axis',(0.,0.,-1.));
#109718=DIRECTION('ref_axis',(1.,-1.06649986710964E-14,0.));
#109719=DIRECTION('center_axis',(0.,1.23467863058847E-16,-1.));
#109720=DIRECTION('ref_axis',(0.,1.,0.));
#109721=DIRECTION('center_axis',(0.,0.,1.));
#109722=DIRECTION('ref_axis',(0.,1.,0.));
#109723=DIRECTION('center_axis',(0.,0.,1.));
#109724=DIRECTION('ref_axis',(1.,0.,0.));
#109725=DIRECTION('',(4.18005656861881E-16,-1.,0.));
#109726=DIRECTION('center_axis',(4.18005656861881E-16,-1.,0.));
#109727=DIRECTION('ref_axis',(-1.,-4.18005656861881E-16,0.));
#109728=DIRECTION('',(-4.18005656861881E-16,1.,0.));
#109729=DIRECTION('center_axis',(-1.,-4.18005656861882E-16,0.));
#109730=DIRECTION('ref_axis',(-4.18005656861882E-16,1.,0.));
#109731=DIRECTION('center_axis',(0.,1.23467863058847E-16,-1.));
#109732=DIRECTION('ref_axis',(-1.,0.,0.));
#109733=DIRECTION('center_axis',(0.,0.,1.));
#109734=DIRECTION('ref_axis',(0.,1.,0.));
#109735=DIRECTION('center_axis',(0.,1.23467863058847E-16,-1.));
#109736=DIRECTION('ref_axis',(0.,1.,0.));
#109737=DIRECTION('center_axis',(0.,0.,-1.));
#109738=DIRECTION('ref_axis',(1.,0.,0.));
#109739=DIRECTION('center_axis',(0.,0.,-1.));
#109740=DIRECTION('ref_axis',(-1.,0.,0.));
#109741=DIRECTION('center_axis',(-1.,-4.38004274807345E-16,0.));
#109742=DIRECTION('ref_axis',(-4.38004274807345E-16,1.,0.));
#109743=DIRECTION('center_axis',(0.,-1.18842113532926E-16,1.));
#109744=DIRECTION('ref_axis',(0.,1.,1.18842113532926E-16));
#109745=DIRECTION('center_axis',(0.,0.,1.));
#109746=DIRECTION('ref_axis',(1.,0.,0.));
#109747=DIRECTION('',(4.18005656861881E-16,-1.,0.));
#109748=DIRECTION('center_axis',(4.18005656861881E-16,-1.,0.));
#109749=DIRECTION('ref_axis',(-1.,-4.18005656861881E-16,0.));
#109750=DIRECTION('',(-4.18005656861881E-16,1.,0.));
#109751=DIRECTION('center_axis',(-1.,-4.18005656861882E-16,0.));
#109752=DIRECTION('ref_axis',(-4.18005656861882E-16,1.,0.));
#109753=DIRECTION('center_axis',(0.,1.23467863058847E-16,-1.));
#109754=DIRECTION('ref_axis',(-1.,0.,0.));
#109755=DIRECTION('center_axis',(0.,1.23467863058847E-16,-1.));
#109756=DIRECTION('ref_axis',(-1.,0.,0.));
#109757=DIRECTION('center_axis',(0.,0.,-1.));
#109758=DIRECTION('ref_axis',(0.,1.,0.));
#109759=DIRECTION('',(1.,-4.18005656861881E-16,-5.16102651992463E-32));
#109760=DIRECTION('',(0.139173100960065,0.99026806874157,1.22266282302933E-16));
#109761=DIRECTION('center_axis',(1.,-4.18005656861882E-16,0.));
#109762=DIRECTION('ref_axis',(-4.18005656861882E-16,-1.,0.));
#109763=DIRECTION('',(-4.18005656861881E-16,-1.,0.));
#109764=DIRECTION('',(0.,0.,-1.));
#109765=DIRECTION('',(4.18005656861881E-16,1.,0.));
#109766=DIRECTION('',(0.,0.,1.));
#109767=DIRECTION('center_axis',(-4.18005656861881E-16,-1.,0.));
#109768=DIRECTION('ref_axis',(1.,-4.18005656861881E-16,0.));
#109769=DIRECTION('center_axis',(0.,1.,0.));
#109770=DIRECTION('ref_axis',(-1.,0.,0.));
#109771=DIRECTION('',(-4.18005656861881E-16,-1.,0.));
#109772=DIRECTION('center_axis',(0.,-1.,0.));
#109773=DIRECTION('ref_axis',(1.,0.,0.));
#109774=DIRECTION('center_axis',(0.,0.,1.));
#109775=DIRECTION('ref_axis',(1.,0.,0.));
#109776=DIRECTION('',(-1.,4.18005656861881E-16,0.));
#109777=DIRECTION('',(0.139173100960065,0.99026806874157,0.));
#109778=DIRECTION('',(1.,-4.18005656861881E-16,0.));
#109779=DIRECTION('center_axis',(0.,-1.18842113532926E-16,1.));
#109780=DIRECTION('ref_axis',(0.,1.,1.18842113532926E-16));
#109781=DIRECTION('center_axis',(0.,1.19392659184112E-16,-1.));
#109782=DIRECTION('ref_axis',(0.,1.,1.19392659184112E-16));
#109783=DIRECTION('center_axis',(1.,-4.38004274807345E-16,0.));
#109784=DIRECTION('ref_axis',(-4.38004274807345E-16,-1.,0.));
#109785=DIRECTION('',(0.,0.,1.));
#109786=DIRECTION('',(0.,0.,-1.));
#109787=DIRECTION('center_axis',(0.,0.,-1.));
#109788=DIRECTION('ref_axis',(1.,0.,0.));
#109789=DIRECTION('center_axis',(0.,0.,1.));
#109790=DIRECTION('ref_axis',(-1.,0.,0.));
#109791=DIRECTION('center_axis',(0.,1.23467863058847E-16,-1.));
#109792=DIRECTION('ref_axis',(0.,1.,0.));
#109793=DIRECTION('center_axis',(0.,0.,-1.));
#109794=DIRECTION('ref_axis',(0.,1.,0.));
#109795=DIRECTION('center_axis',(0.,1.23467863058847E-16,-1.));
#109796=DIRECTION('ref_axis',(-1.,0.,0.));
#109797=DIRECTION('',(0.139173100960065,0.99026806874157,1.22266282302933E-16));
#109798=DIRECTION('',(-1.,4.18005656861881E-16,5.16102651992463E-32));
#109799=DIRECTION('',(1.,-4.18005656861881E-16,-5.16102651992463E-32));
#109800=DIRECTION('center_axis',(1.,-4.18005656861882E-16,0.));
#109801=DIRECTION('ref_axis',(-4.18005656861882E-16,-1.,0.));
#109802=DIRECTION('',(-4.18005656861881E-16,-1.,0.));
#109803=DIRECTION('',(0.,0.,-1.));
#109804=DIRECTION('',(4.18005656861881E-16,1.,0.));
#109805=DIRECTION('',(0.,0.,1.));
#109806=DIRECTION('center_axis',(-4.18005656861881E-16,-1.,0.));
#109807=DIRECTION('ref_axis',(1.,-4.18005656861881E-16,0.));
#109808=DIRECTION('center_axis',(0.,1.,0.));
#109809=DIRECTION('ref_axis',(-1.,0.,0.));
#109810=DIRECTION('',(-4.18005656861881E-16,-1.,0.));
#109811=DIRECTION('center_axis',(0.,-1.,0.));
#109812=DIRECTION('ref_axis',(1.,0.,0.));
#109813=DIRECTION('center_axis',(0.,0.,1.));
#109814=DIRECTION('ref_axis',(1.,0.,0.));
#109815=DIRECTION('',(-1.,4.38004274807345E-16,0.));
#109816=DIRECTION('',(0.139173100960065,0.99026806874157,0.));
#109817=DIRECTION('',(1.,-4.18005656861881E-16,0.));
#109818=DIRECTION('center_axis',(0.,1.23467863058847E-16,-1.));
#109819=DIRECTION('ref_axis',(0.,1.,0.));
#109820=DIRECTION('center_axis',(0.214612320896177,0.976699255456037,-0.000340750905301442));
#109821=DIRECTION('ref_axis',(-0.880441023637846,0.193310232164562,-0.432960457820371));
#109822=DIRECTION('center_axis',(0.,0.,1.));
#109823=DIRECTION('ref_axis',(-1.,-1.06649986710964E-14,0.));
#109824=DIRECTION('center_axis',(0.,0.,-1.));
#109825=DIRECTION('ref_axis',(1.,0.,0.));
#109826=DIRECTION('center_axis',(1.,-4.38004274807345E-16,0.));
#109827=DIRECTION('ref_axis',(-4.38004274807345E-16,-1.,0.));
#109828=DIRECTION('',(0.,0.,1.));
#109829=DIRECTION('',(0.,0.,-1.));
#109830=DIRECTION('center_axis',(1.,-4.18005656861882E-16,0.));
#109831=DIRECTION('ref_axis',(-4.18005656861882E-16,-1.,0.));
#109832=DIRECTION('',(-4.18005656861881E-16,-1.,0.));
#109833=DIRECTION('',(0.,0.,-1.));
#109834=DIRECTION('',(4.18005656861881E-16,1.,0.));
#109835=DIRECTION('',(0.,0.,1.));
#109836=DIRECTION('center_axis',(-4.18005656861881E-16,-1.,0.));
#109837=DIRECTION('ref_axis',(1.,-4.18005656861881E-16,0.));
#109838=DIRECTION('center_axis',(0.,1.,0.));
#109839=DIRECTION('ref_axis',(-1.,0.,0.));
#109840=DIRECTION('',(-4.18005656861881E-16,-1.,0.));
#109841=DIRECTION('center_axis',(0.,-1.,0.));
#109842=DIRECTION('ref_axis',(1.,0.,0.));
#109843=DIRECTION('center_axis',(0.,0.,1.));
#109844=DIRECTION('ref_axis',(1.,0.,0.));
#109845=DIRECTION('',(-1.,4.18005656861881E-16,0.));
#109846=DIRECTION('',(-0.139173100960067,0.99026806874157,0.));
#109847=DIRECTION('',(1.,-4.18005656861881E-16,0.));
#109848=DIRECTION('center_axis',(0.,1.23467863058847E-16,-1.));
#109849=DIRECTION('ref_axis',(-1.,0.,0.));
#109850=DIRECTION('',(-0.139173100960067,0.99026806874157,1.22266282302933E-16));
#109851=DIRECTION('',(-1.,4.18005656861881E-16,5.16102651992463E-32));
#109852=DIRECTION('center_axis',(0.,0.,-1.));
#109853=DIRECTION('ref_axis',(0.,1.,0.));
#109854=DIRECTION('center_axis',(1.,-4.38004274807345E-16,0.));
#109855=DIRECTION('ref_axis',(-4.38004274807345E-16,-1.,0.));
#109856=DIRECTION('',(0.,0.,1.));
#109857=DIRECTION('',(0.,0.,-1.));
#109858=DIRECTION('center_axis',(0.,0.,-1.));
#109859=DIRECTION('ref_axis',(1.,0.,0.));
#109860=DIRECTION('center_axis',(0.,0.,1.));
#109861=DIRECTION('ref_axis',(-1.,0.,0.));
#109862=DIRECTION('center_axis',(0.,1.23467863058847E-16,-1.));
#109863=DIRECTION('ref_axis',(0.,1.,0.));
#109864=DIRECTION('center_axis',(0.212854559998133,-0.977083829553736,-0.000355404849016026));
#109865=DIRECTION('ref_axis',(-0.773913504202019,-0.168372497077826,-0.610498640654939));
#109866=DIRECTION('center_axis',(0.,1.23467863058847E-16,-1.));
#109867=DIRECTION('ref_axis',(-1.,0.,0.));
#109868=DIRECTION('',(-0.139173100960067,0.99026806874157,1.22266282302933E-16));
#109869=DIRECTION('',(-1.,4.18005656861881E-16,5.16102651992463E-32));
#109870=DIRECTION('center_axis',(0.,0.,-1.));
#109871=DIRECTION('ref_axis',(0.,1.,0.));
#109872=DIRECTION('',(1.,-4.18005656861881E-16,-5.16102651992463E-32));
#109873=DIRECTION('center_axis',(0.,1.23467863058847E-16,-1.));
#109874=DIRECTION('ref_axis',(0.,1.,0.));
#109875=DIRECTION('center_axis',(0.,0.,1.));
#109876=DIRECTION('ref_axis',(-1.,0.,0.));
#109877=DIRECTION('center_axis',(0.,0.,-1.));
#109878=DIRECTION('ref_axis',(1.,0.,0.));
#109879=DIRECTION('center_axis',(1.,-4.38004274807345E-16,0.));
#109880=DIRECTION('ref_axis',(-4.38004274807345E-16,-1.,0.));
#109881=DIRECTION('',(0.,0.,1.));
#109882=DIRECTION('',(0.,0.,-1.));
#109883=DIRECTION('center_axis',(1.,-4.18005656861882E-16,0.));
#109884=DIRECTION('ref_axis',(-4.18005656861882E-16,-1.,0.));
#109885=DIRECTION('',(4.18005656861881E-16,1.,0.));
#109886=DIRECTION('',(0.,0.,1.));
#109887=DIRECTION('',(-4.18005656861881E-16,-1.,0.));
#109888=DIRECTION('',(0.,0.,-1.));
#109889=DIRECTION('center_axis',(-4.18005656861881E-16,-1.,0.));
#109890=DIRECTION('ref_axis',(1.,-4.18005656861881E-16,0.));
#109891=DIRECTION('',(-4.18005656861881E-16,-1.,0.));
#109892=DIRECTION('center_axis',(0.,-1.,0.));
#109893=DIRECTION('ref_axis',(1.,0.,0.));
#109894=DIRECTION('center_axis',(0.,1.,0.));
#109895=DIRECTION('ref_axis',(-1.,0.,0.));
#109896=DIRECTION('center_axis',(0.,0.,1.));
#109897=DIRECTION('ref_axis',(1.,0.,0.));
#109898=DIRECTION('',(-1.,4.18005656861881E-16,0.));
#109899=DIRECTION('',(-0.139173100960067,0.99026806874157,0.));
#109900=DIRECTION('',(1.,-4.38004274807345E-16,0.));
#109901=DIRECTION('center_axis',(0.,-1.18842113532926E-16,1.));
#109902=DIRECTION('ref_axis',(0.,1.,1.18842113532926E-16));
#109903=DIRECTION('center_axis',(0.,1.19392659184112E-16,-1.));
#109904=DIRECTION('ref_axis',(0.,1.,1.19392659184112E-16));
#109905=DIRECTION('center_axis',(0.,-1.18842113532926E-16,1.));
#109906=DIRECTION('ref_axis',(0.,1.,1.18842113532926E-16));
#109907=DIRECTION('center_axis',(0.,1.19392659184112E-16,-1.));
#109908=DIRECTION('ref_axis',(0.,1.,1.19392659184112E-16));
#109909=DIRECTION('center_axis',(0.,0.,-1.));
#109910=DIRECTION('ref_axis',(1.,0.,0.));
#109911=DIRECTION('center_axis',(0.,0.,1.));
#109912=DIRECTION('ref_axis',(-1.,-7.98385375378166E-15,0.));
#109913=DIRECTION('center_axis',(-5.01606788234257E-16,-1.,5.70122241611331E-32));
#109914=DIRECTION('ref_axis',(-1.,5.01606788234257E-16,0.));
#109915=DIRECTION('',(-1.,5.01606788234257E-16,0.));
#109916=DIRECTION('',(-2.85977186515575E-47,-5.70122241611331E-32,-1.));
#109917=DIRECTION('',(1.,-5.01606788234257E-16,0.));
#109918=DIRECTION('',(2.85977186515575E-47,5.70122241611331E-32,1.));
#109919=DIRECTION('center_axis',(-1.,5.01606788234257E-16,0.));
#109920=DIRECTION('ref_axis',(-5.01606788234257E-16,-1.,0.));
#109921=DIRECTION('center_axis',(1.,0.,0.));
#109922=DIRECTION('ref_axis',(0.,1.,0.));
#109923=DIRECTION('',(-1.,5.01606788234257E-16,0.));
#109924=DIRECTION('center_axis',(-1.,0.,0.));
#109925=DIRECTION('ref_axis',(0.,-1.,0.));
#109926=DIRECTION('center_axis',(0.,0.,1.));
#109927=DIRECTION('ref_axis',(1.,0.,0.));
#109928=DIRECTION('',(5.01606788234257E-16,1.,0.));
#109929=DIRECTION('',(0.990268068741571,0.139173100960059,0.));
#109930=DIRECTION('',(-5.01606788234257E-16,-1.,0.));
#109931=DIRECTION('center_axis',(0.,1.23467863058847E-16,-1.));
#109932=DIRECTION('ref_axis',(-1.,0.,0.));
#109933=DIRECTION('',(0.990268068741571,0.139173100960059,1.71834053708117E-17));
#109934=DIRECTION('',(5.01606788234257E-16,1.,1.23467863058847E-16));
#109935=DIRECTION('center_axis',(0.,0.,-1.));
#109936=DIRECTION('ref_axis',(0.,1.,0.));
#109937=DIRECTION('center_axis',(4.38004274807345E-16,1.,0.));
#109938=DIRECTION('ref_axis',(1.,-4.38004274807345E-16,0.));
#109939=DIRECTION('',(0.,0.,1.));
#109940=DIRECTION('',(0.,0.,-1.));
#109941=DIRECTION('center_axis',(0.,0.,-1.));
#109942=DIRECTION('ref_axis',(1.,0.,0.));
#109943=DIRECTION('center_axis',(0.,0.,1.));
#109944=DIRECTION('ref_axis',(-1.,8.87756872621991E-15,0.));
#109945=DIRECTION('center_axis',(0.,-1.,0.));
#109946=DIRECTION('ref_axis',(0.,0.,-1.));
#109947=DIRECTION('center_axis',(0.,0.,1.));
#109948=DIRECTION('ref_axis',(0.,1.,0.));
#109949=DIRECTION('center_axis',(-1.,0.,0.));
#109950=DIRECTION('ref_axis',(0.,0.,1.));
#109951=DIRECTION('center_axis',(0.,0.,-1.));
#109952=DIRECTION('ref_axis',(0.,1.,0.));
#109953=DIRECTION('center_axis',(0.,1.23467863058847E-16,-1.));
#109954=DIRECTION('ref_axis',(-1.,0.,0.));
#109955=DIRECTION('',(0.990268068741571,0.139173100960059,1.71834053708117E-17));
#109956=DIRECTION('',(5.01606788234257E-16,1.,1.23467863058847E-16));
#109957=DIRECTION('center_axis',(0.,0.,-1.));
#109958=DIRECTION('ref_axis',(0.,1.,0.));
#109959=DIRECTION('',(-5.01606788234257E-16,-1.,-1.23467863058847E-16));
#109960=DIRECTION('center_axis',(0.,1.23467863058847E-16,-1.));
#109961=DIRECTION('ref_axis',(0.,1.,0.));
#109962=DIRECTION('center_axis',(0.952430221804268,0.304711142119182,0.00527185567859643));
#109963=DIRECTION('ref_axis',(0.0463243094405771,-0.161849302626711,0.985727579807982));
#109964=DIRECTION('center_axis',(-0.742683090861321,-0.669643059061075,
1.01363406279984E-15));
#109965=DIRECTION('ref_axis',(0.669643059061075,-0.742683090861321,-3.71575034000761E-31));
#109966=DIRECTION('center_axis',(0.0999814466925417,0.0010192755153814,
-0.994988779532056));
#109967=DIRECTION('ref_axis',(-0.648676516538678,0.75833417398337,-0.0644054148360687));
#109968=DIRECTION('center_axis',(4.38004274807345E-16,1.,0.));
#109969=DIRECTION('ref_axis',(1.,-4.38004274807345E-16,0.));
#109970=DIRECTION('',(-1.13659195805196E-16,4.9783213633841E-32,1.));
#109971=DIRECTION('',(0.,0.,-1.));
#109972=DIRECTION('center_axis',(-5.01606788234257E-16,-1.,5.70122241611331E-32));
#109973=DIRECTION('ref_axis',(-1.,5.01606788234257E-16,0.));
#109974=DIRECTION('',(1.,-5.01606788234257E-16,0.));
#109975=DIRECTION('',(1.13659195805196E-16,0.,1.));
#109976=DIRECTION('',(-1.,5.01606788234257E-16,0.));
#109977=DIRECTION('',(1.13659195805196E-16,-1.14024448322266E-31,-1.));
#109978=DIRECTION('center_axis',(-1.,5.01606788234257E-16,0.));
#109979=DIRECTION('ref_axis',(-5.01606788234257E-16,-1.,0.));
#109980=DIRECTION('',(-1.,5.01606788234257E-16,0.));
#109981=DIRECTION('center_axis',(-1.,0.,1.13659195805196E-16));
#109982=DIRECTION('ref_axis',(0.,-1.,0.));
#109983=DIRECTION('center_axis',(1.,0.,1.13659195805196E-16));
#109984=DIRECTION('ref_axis',(0.,1.,0.));
#109985=DIRECTION('center_axis',(0.,0.,1.));
#109986=DIRECTION('ref_axis',(1.,0.,0.));
#109987=DIRECTION('',(5.01606788234257E-16,1.,0.));
#109988=DIRECTION('',(0.990268068741571,0.139173100960059,0.));
#109989=DIRECTION('',(-4.38004274807345E-16,-1.,0.));
#109990=DIRECTION('center_axis',(0.,-1.18842113532926E-16,1.));
#109991=DIRECTION('ref_axis',(0.,1.,1.18842113532926E-16));
#109992=DIRECTION('center_axis',(0.,1.19392659184112E-16,-1.));
#109993=DIRECTION('ref_axis',(0.,1.,1.19392659184112E-16));
#109994=DIRECTION('center_axis',(-4.18005656861881E-16,-1.,0.));
#109995=DIRECTION('ref_axis',(1.,-4.18005656861881E-16,0.));
#109996=DIRECTION('',(4.18005656861881E-16,1.,0.));
#109997=DIRECTION('center_axis',(5.78241158658935E-16,1.,0.));
#109998=DIRECTION('ref_axis',(-1.,5.78241158658935E-16,0.));
#109999=DIRECTION('',(-4.18005656861881E-16,-1.,0.));
#110000=DIRECTION('center_axis',(-5.78241158658935E-16,-1.,0.));
#110001=DIRECTION('ref_axis',(1.,-5.78241158658935E-16,0.));
#110002=DIRECTION('center_axis',(0.,0.,1.));
#110003=DIRECTION('ref_axis',(1.,0.,0.));
#110004=DIRECTION('',(-1.,4.18005656861881E-16,0.));
#110005=DIRECTION('center_axis',(0.,0.,1.));
#110006=DIRECTION('ref_axis',(1.,0.,0.));
#110007=DIRECTION('',(1.,-4.18005656861881E-16,0.));
#110008=DIRECTION('center_axis',(1.,-4.38004274807345E-16,0.));
#110009=DIRECTION('ref_axis',(-4.38004274807345E-16,-1.,0.));
#110010=DIRECTION('',(0.,0.,1.));
#110011=DIRECTION('',(0.,0.,-1.));
#110012=DIRECTION('center_axis',(0.,0.,-1.));
#110013=DIRECTION('ref_axis',(1.,0.,0.));
#110014=DIRECTION('center_axis',(0.,0.,1.));
#110015=DIRECTION('ref_axis',(0.,-1.,0.));
#110016=DIRECTION('center_axis',(0.,0.,1.));
#110017=DIRECTION('ref_axis',(1.,0.,0.));
#110018=DIRECTION('',(-1.,4.18005656861881E-16,0.));
#110019=DIRECTION('center_axis',(0.,0.,1.));
#110020=DIRECTION('ref_axis',(1.,0.,0.));
#110021=DIRECTION('',(1.,-4.18005656861881E-16,0.));
#110022=DIRECTION('',(-4.18005656861881E-16,-1.,0.));
#110023=DIRECTION('center_axis',(1.,-4.18005656861882E-16,0.));
#110024=DIRECTION('ref_axis',(-4.18005656861882E-16,-1.,0.));
#110025=DIRECTION('',(-4.18005656861881E-16,-1.,0.));
#110026=DIRECTION('',(0.,0.,-1.));
#110027=DIRECTION('',(4.18005656861881E-16,1.,0.));
#110028=DIRECTION('',(0.,0.,1.));
#110029=DIRECTION('center_axis',(-4.18005656861881E-16,-1.,0.));
#110030=DIRECTION('ref_axis',(1.,-4.18005656861881E-16,0.));
#110031=DIRECTION('center_axis',(4.33680868994202E-16,1.,0.));
#110032=DIRECTION('ref_axis',(-1.,4.33680868994202E-16,0.));
#110033=DIRECTION('center_axis',(-4.33680868994202E-16,-1.,0.));
#110034=DIRECTION('ref_axis',(1.,-4.33680868994202E-16,0.));
#110035=DIRECTION('center_axis',(1.,0.,0.));
#110036=DIRECTION('ref_axis',(0.,1.,0.));
#110037=DIRECTION('center_axis',(-1.,0.,0.));
#110038=DIRECTION('ref_axis',(0.,0.,1.));
#110039=DIRECTION('center_axis',(1.,-4.38004274807345E-16,0.));
#110040=DIRECTION('ref_axis',(-4.38004274807345E-16,-1.,0.));
#110041=DIRECTION('',(0.,0.,-1.));
#110042=DIRECTION('',(0.,0.,1.));
#110043=DIRECTION('center_axis',(0.,0.,-1.));
#110044=DIRECTION('ref_axis',(1.,0.,0.));
#110045=DIRECTION('center_axis',(0.,0.,1.));
#110046=DIRECTION('ref_axis',(0.,-1.,0.));
#110047=DIRECTION('center_axis',(-0.149968574026289,-0.0101861056380938,
0.988638290810371));
#110048=DIRECTION('ref_axis',(0.981228608534593,0.121089848369309,0.150092193052014));
#110049=DIRECTION('center_axis',(1.,-4.38004274807345E-16,0.));
#110050=DIRECTION('ref_axis',(-4.38004274807345E-16,-1.,0.));
#110051=DIRECTION('',(0.,0.,1.));
#110052=DIRECTION('',(0.,0.,-1.));
#110053=DIRECTION('center_axis',(-0.00252744588198969,-0.999981530022895,
0.00552735292733838));
#110054=DIRECTION('ref_axis',(0.976049181036949,-0.00126447960099768,0.217546310675312));
#110055=DIRECTION('center_axis',(0.,0.,-1.));
#110056=DIRECTION('ref_axis',(1.,0.,0.));
#110057=DIRECTION('center_axis',(0.,0.,1.));
#110058=DIRECTION('ref_axis',(0.,-1.,0.));
#110059=DIRECTION('center_axis',(-0.0216109392502409,2.83714134350443E-8,
0.99976645638105));
#110060=DIRECTION('ref_axis',(0.999764411688039,0.00202245879910768,0.021610894994789));
#110061=DIRECTION('center_axis',(1.,0.,0.));
#110062=DIRECTION('ref_axis',(0.,0.00139138517159681,-0.999999032023184));
#110063=DIRECTION('center_axis',(1.,-4.38004274807345E-16,0.));
#110064=DIRECTION('ref_axis',(-4.38004274807345E-16,-1.,0.));
#110065=DIRECTION('',(0.,0.,1.));
#110066=DIRECTION('',(0.,0.,-1.));
#110067=DIRECTION('center_axis',(-0.00301392117783963,0.999973599253448,
0.00661188893112461));
#110068=DIRECTION('ref_axis',(0.976327184229521,0.00151250353879502,0.216293646849601));
#110069=DIRECTION('center_axis',(0.,0.,-1.));
#110070=DIRECTION('ref_axis',(1.,0.,0.));
#110071=DIRECTION('center_axis',(0.,0.,1.));
#110072=DIRECTION('ref_axis',(0.,-1.,0.));
#110073=DIRECTION('center_axis',(-0.157518537373542,0.0111023184919509,
0.987453618610922));
#110074=DIRECTION('ref_axis',(0.98052929088236,-0.116977821119357,0.157729195420202));
#110075=DIRECTION('center_axis',(1.,-4.38004274807345E-16,0.));
#110076=DIRECTION('ref_axis',(-4.38004274807345E-16,-1.,0.));
#110077=DIRECTION('',(0.,0.,1.));
#110078=DIRECTION('',(0.,0.,-1.));
#110079=DIRECTION('center_axis',(0.,0.,-1.));
#110080=DIRECTION('ref_axis',(1.,0.,0.));
#110081=DIRECTION('center_axis',(0.,0.,1.));
#110082=DIRECTION('ref_axis',(0.,-1.,0.));
#110083=DIRECTION('center_axis',(1.,0.,0.));
#110084=DIRECTION('ref_axis',(0.,1.,0.));
#110085=DIRECTION('',(1.,-4.18005656861881E-16,0.));
#110086=DIRECTION('center_axis',(1.,0.,0.));
#110087=DIRECTION('ref_axis',(0.,0.,-1.));
#110088=DIRECTION('center_axis',(1.,-4.18005656861882E-16,0.));
#110089=DIRECTION('ref_axis',(-4.18005656861882E-16,-1.,0.));
#110090=DIRECTION('',(-4.18005656861881E-16,-1.,0.));
#110091=DIRECTION('',(0.,0.,-1.));
#110092=DIRECTION('',(4.18005656861881E-16,1.,0.));
#110093=DIRECTION('',(0.,0.,1.));
#110094=DIRECTION('center_axis',(-4.18005656861881E-16,-1.,0.));
#110095=DIRECTION('ref_axis',(1.,-4.18005656861881E-16,0.));
#110096=DIRECTION('center_axis',(0.,1.,0.));
#110097=DIRECTION('ref_axis',(-1.,0.,0.));
#110098=DIRECTION('',(-4.18005656861881E-16,-1.,0.));
#110099=DIRECTION('center_axis',(0.,-1.,0.));
#110100=DIRECTION('ref_axis',(1.,0.,0.));
#110101=DIRECTION('center_axis',(0.,0.,1.));
#110102=DIRECTION('ref_axis',(1.,0.,0.));
#110103=DIRECTION('',(-1.,4.18005656861881E-16,0.));
#110104=DIRECTION('center_axis',(0.,0.,1.));
#110105=DIRECTION('ref_axis',(1.,0.,0.));
#110106=DIRECTION('center_axis',(-4.18005656861881E-16,-1.,0.));
#110107=DIRECTION('ref_axis',(1.,-4.18005656861881E-16,0.));
#110108=DIRECTION('',(4.18005656861881E-16,1.,0.));
#110109=DIRECTION('center_axis',(0.,1.,0.));
#110110=DIRECTION('ref_axis',(-1.,0.,0.));
#110111=DIRECTION('',(-4.18005656861881E-16,-1.,0.));
#110112=DIRECTION('center_axis',(0.,-1.,0.));
#110113=DIRECTION('ref_axis',(1.,0.,0.));
#110114=DIRECTION('center_axis',(1.,-4.38004274807345E-16,0.));
#110115=DIRECTION('ref_axis',(-4.38004274807345E-16,-1.,0.));
#110116=DIRECTION('',(0.,0.,-1.));
#110117=DIRECTION('',(0.,0.,1.));
#110118=DIRECTION('center_axis',(0.,0.,-1.));
#110119=DIRECTION('ref_axis',(1.,0.,0.));
#110120=DIRECTION('center_axis',(0.,0.,1.));
#110121=DIRECTION('ref_axis',(0.,-1.,0.));
#110122=DIRECTION('center_axis',(0.,0.,1.));
#110123=DIRECTION('ref_axis',(1.,0.,0.));
#110124=DIRECTION('',(-1.,4.18005656861881E-16,0.));
#110125=DIRECTION('center_axis',(0.,0.,1.));
#110126=DIRECTION('ref_axis',(1.,0.,0.));
#110127=DIRECTION('',(1.,-4.18005656861881E-16,0.));
#110128=DIRECTION('center_axis',(1.,-4.18005656861882E-16,0.));
#110129=DIRECTION('ref_axis',(-4.18005656861882E-16,-1.,0.));
#110130=DIRECTION('',(-4.18005656861881E-16,-1.,0.));
#110131=DIRECTION('',(0.,0.,-1.));
#110132=DIRECTION('',(0.,0.,1.));
#110133=DIRECTION('center_axis',(1.,-4.18005656861882E-16,0.));
#110134=DIRECTION('ref_axis',(-4.18005656861882E-16,-1.,0.));
#110135=DIRECTION('',(-4.18005656861881E-16,-1.,0.));
#110136=DIRECTION('',(0.,0.,-1.));
#110137=DIRECTION('',(0.,0.,1.));
#110138=DIRECTION('center_axis',(4.38004274807345E-16,1.,0.));
#110139=DIRECTION('ref_axis',(1.,-4.38004274807345E-16,0.));
#110140=DIRECTION('',(0.,0.,1.));
#110141=DIRECTION('',(0.,0.,-1.));
#110142=DIRECTION('center_axis',(-5.01606788234257E-16,-1.,5.70122241611331E-32));
#110143=DIRECTION('ref_axis',(-1.,5.01606788234257E-16,0.));
#110144=DIRECTION('',(-1.,5.01606788234257E-16,0.));
#110145=DIRECTION('',(-2.85977186515575E-47,-5.70122241611331E-32,-1.));
#110146=DIRECTION('',(1.,-5.01606788234257E-16,0.));
#110147=DIRECTION('',(2.85977186515575E-47,5.70122241611331E-32,1.));
#110148=DIRECTION('center_axis',(4.38004274807345E-16,1.,0.));
#110149=DIRECTION('ref_axis',(1.,-4.38004274807345E-16,0.));
#110150=DIRECTION('',(0.,0.,1.));
#110151=DIRECTION('',(0.,0.,-1.));
#110152=DIRECTION('center_axis',(4.38004274807345E-16,1.,0.));
#110153=DIRECTION('ref_axis',(1.,-4.38004274807345E-16,0.));
#110154=DIRECTION('',(0.,0.,1.));
#110155=DIRECTION('',(0.,0.,-1.));
#110156=DIRECTION('center_axis',(-1.,5.01606788234257E-16,0.));
#110157=DIRECTION('ref_axis',(-5.01606788234257E-16,-1.,0.));
#110158=DIRECTION('',(1.,-5.01606788234257E-16,0.));
#110159=DIRECTION('center_axis',(1.,0.,0.));
#110160=DIRECTION('ref_axis',(0.,1.,0.));
#110161=DIRECTION('',(-1.,5.01606788234257E-16,0.));
#110162=DIRECTION('center_axis',(-1.,0.,0.));
#110163=DIRECTION('ref_axis',(0.,-1.,0.));
#110164=DIRECTION('center_axis',(0.,1.23467863058847E-16,-1.));
#110165=DIRECTION('ref_axis',(0.,1.,0.));
#110166=DIRECTION('center_axis',(-0.976893716583792,-0.213725378195426,
-0.000359463945942464));
#110167=DIRECTION('ref_axis',(-0.169779058278416,0.777043764862974,-0.606117198945607));
#110168=DIRECTION('center_axis',(-0.999980560004511,0.00244828575950157,
0.00573458890456878));
#110169=DIRECTION('ref_axis',(-0.00114118854494862,-0.976015867166676,0.217696404948694));
#110170=DIRECTION('center_axis',(-1.,5.01606788234257E-16,0.));
#110171=DIRECTION('ref_axis',(-5.01606788234257E-16,-1.,0.));
#110172=DIRECTION('center_axis',(1.,0.,0.));
#110173=DIRECTION('ref_axis',(0.,1.,0.));
#110174=DIRECTION('',(-1.,5.01606788234257E-16,0.));
#110175=DIRECTION('center_axis',(-1.,0.,0.));
#110176=DIRECTION('ref_axis',(0.,-1.,0.));
#110177=DIRECTION('center_axis',(0.,-1.,0.));
#110178=DIRECTION('ref_axis',(0.,0.,-1.));
#110179=DIRECTION('center_axis',(0.,0.,1.));
#110180=DIRECTION('ref_axis',(0.,1.,0.));
#110181=DIRECTION('center_axis',(-1.,0.,0.));
#110182=DIRECTION('ref_axis',(0.,0.,1.));
#110183=DIRECTION('center_axis',(0.,0.,-1.));
#110184=DIRECTION('ref_axis',(0.,1.,0.));
#110185=DIRECTION('center_axis',(-0.990268068741571,-0.139173100960059,
0.));
#110186=DIRECTION('ref_axis',(0.139173100960059,-0.990268068741571,0.));
#110187=DIRECTION('center_axis',(-0.939797023107103,-0.132079858078289,
0.315176881209658));
#110188=DIRECTION('ref_axis',(0.317962525883615,-4.30796627806664E-16,0.948103281364278));
#110189=DIRECTION('center_axis',(0.990268068741571,0.139173100960059,1.71834053708117E-17));
#110190=DIRECTION('ref_axis',(-0.139173100960059,0.990268068741571,-4.14246685971564E-34));
#110191=DIRECTION('',(-0.990268068741571,-0.139173100960059,-1.71834053708117E-17));
#110192=DIRECTION('center_axis',(-0.990268068741572,-0.139173100960051,
-1.37427301308497E-14));
#110193=DIRECTION('ref_axis',(0.139173100960051,-0.990268068741572,1.93598700157835E-30));
#110194=DIRECTION('center_axis',(0.,0.,-1.));
#110195=DIRECTION('ref_axis',(-1.,0.,0.));
#110196=DIRECTION('center_axis',(-0.990268068741572,-0.139173100960051,
0.));
#110197=DIRECTION('ref_axis',(0.139173100960051,-0.990268068741572,0.));
#110198=DIRECTION('',(-0.990268068741571,-0.139173100960059,0.));
#110199=DIRECTION('center_axis',(-0.990268068741572,-0.139173100960051,
0.));
#110200=DIRECTION('ref_axis',(0.139173100960051,-0.990268068741572,0.));
#110201=DIRECTION('center_axis',(0.,0.,-1.));
#110202=DIRECTION('ref_axis',(-1.,0.,0.));
#110203=DIRECTION('center_axis',(0.990268068741571,0.139173100960059,1.71834053708117E-17));
#110204=DIRECTION('ref_axis',(-0.139173100960059,0.990268068741571,-4.14246685971564E-34));
#110205=DIRECTION('',(-0.990268068741571,-0.139173100960059,-1.71834053708117E-17));
#110206=DIRECTION('center_axis',(0.,0.,1.));
#110207=DIRECTION('ref_axis',(1.,0.,0.));
#110208=DIRECTION('center_axis',(-0.990268068741572,-0.139173100960051,
0.));
#110209=DIRECTION('ref_axis',(0.139173100960051,-0.990268068741572,0.));
#110210=DIRECTION('center_axis',(-0.990268068741572,-0.139173100960051,
0.));
#110211=DIRECTION('ref_axis',(0.139173100960051,-0.990268068741572,0.));
#110212=DIRECTION('',(-0.990268068741571,-0.139173100960059,0.));
#110213=DIRECTION('center_axis',(-0.990268068741571,-0.139173100960064,
0.));
#110214=DIRECTION('ref_axis',(0.139173100960064,-0.990268068741571,0.));
#110215=DIRECTION('center_axis',(0.,0.,-1.));
#110216=DIRECTION('ref_axis',(-1.,0.,0.));
#110217=DIRECTION('center_axis',(0.990268068741571,0.139173100960059,1.71834053708117E-17));
#110218=DIRECTION('ref_axis',(-0.139173100960059,0.990268068741571,-4.14246685971564E-34));
#110219=DIRECTION('',(0.990268068741571,0.139173100960059,1.71834053708117E-17));
#110220=DIRECTION('',(-0.990268068741571,-0.139173100960059,-1.71834053708117E-17));
#110221=DIRECTION('center_axis',(0.990268068741571,0.139173100960059,0.));
#110222=DIRECTION('ref_axis',(-0.139173100960059,0.990268068741571,0.));
#110223=DIRECTION('center_axis',(0.,1.23467863058847E-16,-1.));
#110224=DIRECTION('ref_axis',(0.,1.,0.));
#110225=DIRECTION('center_axis',(0.,0.,-1.));
#110226=DIRECTION('ref_axis',(0.,1.,0.));
#110227=DIRECTION('center_axis',(0.728126055379271,0.685443248911113,0.));
#110228=DIRECTION('ref_axis',(-0.685443248911113,0.728126055379271,0.));
#110229=DIRECTION('center_axis',(0.,0.,1.));
#110230=DIRECTION('ref_axis',(0.,1.,0.));
#110231=DIRECTION('center_axis',(0.,1.23467863058847E-16,-1.));
#110232=DIRECTION('ref_axis',(0.,1.,0.));
#110233=DIRECTION('center_axis',(0.,0.,-1.));
#110234=DIRECTION('ref_axis',(0.,1.,0.));
#110235=DIRECTION('center_axis',(0.685443248911109,0.728126055379275,0.));
#110236=DIRECTION('ref_axis',(-0.728126055379275,0.685443248911109,0.));
#110237=DIRECTION('center_axis',(0.,0.,1.));
#110238=DIRECTION('ref_axis',(0.,1.,0.));
#110239=DIRECTION('center_axis',(0.,1.23467863058847E-16,-1.));
#110240=DIRECTION('ref_axis',(0.,1.,0.));
#110241=DIRECTION('center_axis',(0.,0.,-1.));
#110242=DIRECTION('ref_axis',(0.,1.,0.));
#110243=DIRECTION('center_axis',(0.139173100960066,0.99026806874157,0.));
#110244=DIRECTION('ref_axis',(-0.99026806874157,0.139173100960066,0.));
#110245=DIRECTION('center_axis',(4.28365201153744E-31,-1.48619034146585E-45,
1.));
#110246=DIRECTION('ref_axis',(3.46944695195361E-15,1.,1.24460305557223E-60));
#110247=DIRECTION('center_axis',(-0.139173100960066,-0.99026806874157,0.));
#110248=DIRECTION('ref_axis',(0.99026806874157,-0.139173100960066,0.));
#110249=DIRECTION('center_axis',(0.,0.,-1.));
#110250=DIRECTION('ref_axis',(-1.,0.,0.));
#110251=DIRECTION('center_axis',(-0.139173100960066,-0.99026806874157,0.));
#110252=DIRECTION('ref_axis',(0.99026806874157,-0.139173100960066,0.));
#110253=DIRECTION('',(-0.139173100960065,-0.99026806874157,-3.85185988877447E-34));
#110254=DIRECTION('center_axis',(-0.139173100960066,-0.99026806874157,0.));
#110255=DIRECTION('ref_axis',(0.99026806874157,-0.139173100960066,0.));
#110256=DIRECTION('center_axis',(0.,0.,-1.));
#110257=DIRECTION('ref_axis',(-1.,0.,0.));
#110258=DIRECTION('center_axis',(0.139173100960066,0.99026806874157,1.22266282302934E-16));
#110259=DIRECTION('ref_axis',(-0.99026806874157,0.139173100960066,1.22723965167578E-33));
#110260=DIRECTION('',(-0.139173100960065,-0.99026806874157,-1.22266282302933E-16));
#110261=DIRECTION('center_axis',(0.139173100960073,0.990268068741569,0.));
#110262=DIRECTION('ref_axis',(-0.990268068741569,0.139173100960073,0.));
#110263=DIRECTION('center_axis',(0.133528512868198,0.950104737537311,0.281906232567435));
#110264=DIRECTION('ref_axis',(1.78830809785603E-17,-0.284453521859893,0.958689831958962));
#110265=DIRECTION('center_axis',(0.139173100960066,0.99026806874157,1.22266282302934E-16));
#110266=DIRECTION('ref_axis',(-0.99026806874157,0.139173100960066,1.22723965167578E-33));
#110267=DIRECTION('',(-0.139173100960065,-0.99026806874157,-1.22266282302933E-16));
#110268=DIRECTION('',(0.139173100960065,0.99026806874157,1.22266282302933E-16));
#110269=DIRECTION('center_axis',(0.,0.,1.));
#110270=DIRECTION('ref_axis',(1.,0.,0.));
#110271=DIRECTION('center_axis',(-0.139173100960039,-0.990268068741574,
-2.74854602616996E-14));
#110272=DIRECTION('ref_axis',(0.990268068741574,-0.139173100960039,-5.80135260633727E-30));
#110273=DIRECTION('center_axis',(-0.139173100960066,-0.99026806874157,0.));
#110274=DIRECTION('ref_axis',(0.99026806874157,-0.139173100960066,0.));
#110275=DIRECTION('',(-0.139173100960065,-0.99026806874157,-3.85185988877447E-34));
#110276=DIRECTION('center_axis',(-0.139173100960066,-0.99026806874157,0.));
#110277=DIRECTION('ref_axis',(0.99026806874157,-0.139173100960066,0.));
#110278=DIRECTION('center_axis',(0.,0.,-1.));
#110279=DIRECTION('ref_axis',(-1.,0.,0.));
#110280=DIRECTION('center_axis',(0.139173100960066,0.99026806874157,1.22266282302934E-16));
#110281=DIRECTION('ref_axis',(-0.99026806874157,0.139173100960066,1.22723965167578E-33));
#110282=DIRECTION('',(-0.139173100960065,-0.99026806874157,-1.22266282302933E-16));
#110283=DIRECTION('center_axis',(0.,0.,1.));
#110284=DIRECTION('ref_axis',(1.,0.,0.));
#110285=DIRECTION('center_axis',(-0.408524918701489,-0.868147321075037,
0.281829061152641));
#110286=DIRECTION('ref_axis',(0.904824724134437,-0.425784239486432,-2.46811619432984E-17));
#110287=DIRECTION('center_axis',(-0.907068166518068,0.420531768759975,-0.0195031472628737));
#110288=DIRECTION('ref_axis',(0.0518039117125095,0.157474353828549,0.986163365075769));
#110289=DIRECTION('center_axis',(-0.42055084745715,-0.907268970428876,0.));
#110290=DIRECTION('ref_axis',(0.907268970428876,-0.42055084745715,0.));
#110291=DIRECTION('center_axis',(0.732902040696953,-0.679599705515257,0.0316044143406873));
#110292=DIRECTION('ref_axis',(-0.11008573061797,-0.164305835944245,-0.980247277062768));
#110293=DIRECTION('center_axis',(0.,0.,1.));
#110294=DIRECTION('ref_axis',(1.,0.,0.));
#110295=DIRECTION('center_axis',(0.,0.,-1.));
#110296=DIRECTION('ref_axis',(1.,0.,0.));
#110297=DIRECTION('center_axis',(-0.412076271185962,-0.911149354785193,
0.));
#110298=DIRECTION('ref_axis',(0.911149354785193,-0.412076271185962,0.));
#110299=DIRECTION('center_axis',(0.,0.,1.));
#110300=DIRECTION('ref_axis',(1.,0.,0.));
#110301=DIRECTION('center_axis',(0.,-6.17339315294237E-17,1.));
#110302=DIRECTION('ref_axis',(0.,-1.,0.));
#110303=DIRECTION('center_axis',(1.3159378979443E-30,2.80509034228723E-44,
-1.));
#110304=DIRECTION('ref_axis',(2.1316282072803E-14,-1.,-5.4762534445178E-59));
#110305=DIRECTION('center_axis',(0.132724703727513,-0.991152939252941,6.34877946761353E-5));
#110306=DIRECTION('ref_axis',(0.985065037121742,0.131916564409429,0.1106566431569));
#110307=DIRECTION('center_axis',(-0.162778679587413,0.986662604791219,-7.60156866848099E-5));
#110308=DIRECTION('ref_axis',(0.986084783174683,0.162685986477531,0.0342062888248791));
#110309=DIRECTION('center_axis',(0.282415254236812,0.959292251701408,0.));
#110310=DIRECTION('ref_axis',(-0.959292251701408,0.282415254236812,0.));
#110311=DIRECTION('center_axis',(0.,0.,-1.));
#110312=DIRECTION('ref_axis',(-1.,0.,0.));
#110313=DIRECTION('center_axis',(0.,0.,1.));
#110314=DIRECTION('ref_axis',(1.,0.,0.));
#110315=DIRECTION('center_axis',(0.273940677965627,0.961746590820957,0.));
#110316=DIRECTION('ref_axis',(-0.961746590820957,0.273940677965627,0.));
#110317=DIRECTION('center_axis',(0.,0.,-1.));
#110318=DIRECTION('ref_axis',(1.,-1.77920356510442E-15,0.));
#110319=DIRECTION('center_axis',(0.0971107883155516,0.363411229368455,0.926553707650906));
#110320=DIRECTION('ref_axis',(3.86068458172679E-17,-0.930953788243945,0.365137021067773));
#110321=DIRECTION('center_axis',(0.,0.,1.));
#110322=DIRECTION('ref_axis',(1.,0.,0.));
#110323=DIRECTION('center_axis',(-0.966107498808678,0.25814005491211,-0.000113117697403614));
#110324=DIRECTION('ref_axis',(0.25388184709702,0.950091406535467,-0.181301756588465));
#110325=DIRECTION('center_axis',(0.,-6.17339315294237E-17,1.));
#110326=DIRECTION('ref_axis',(0.,-1.,0.));
#110327=DIRECTION('center_axis',(0.,0.,-1.));
#110328=DIRECTION('ref_axis',(0.,-1.,0.));
#110329=DIRECTION('center_axis',(0.0766838736637995,-0.997055455878901,
3.77098383583762E-5));
#110330=DIRECTION('ref_axis',(0.97952184613108,0.0753424193663023,0.186709594815031));
#110331=DIRECTION('center_axis',(-0.116942841787273,0.993138645130569,-5.74711537241093E-5));
#110332=DIRECTION('ref_axis',(0.983260089651775,0.115787775552541,0.140686840644664));
#110333=DIRECTION('center_axis',(-0.144956948347396,-0.989281282708723,
-0.017607578141073));
#110334=DIRECTION('ref_axis',(0.989434670234472,-0.144979423843532,1.06064347286242E-18));
#110335=DIRECTION('center_axis',(0.,0.,-1.));
#110336=DIRECTION('ref_axis',(-1.,0.,0.));
#110337=DIRECTION('center_axis',(0.140089618365222,-0.00275771349061114,
-0.990134987687331));
#110338=DIRECTION('ref_axis',(0.979470506177534,-0.146013776318709,0.138987426242359));
#110339=DIRECTION('center_axis',(-0.136497250965888,-0.990504401193308,
-0.0164174204868685));
#110340=DIRECTION('ref_axis',(0.990637914348733,-0.136515649853022,4.14575077332242E-19));
#110341=DIRECTION('center_axis',(0.,0.,-1.));
#110342=DIRECTION('ref_axis',(-1.,0.,0.));
#110343=DIRECTION('center_axis',(0.,-6.17339315294237E-17,1.));
#110344=DIRECTION('ref_axis',(0.,-1.,0.));
#110345=DIRECTION('center_axis',(-6.57968948972152E-31,7.01272585571806E-45,
-1.));
#110346=DIRECTION('ref_axis',(-1.06581410364015E-14,-1.,0.));
#110347=DIRECTION('center_axis',(0.0112985155260908,-0.999936169720593,
5.60510491874375E-6));
#110348=DIRECTION('ref_axis',(0.976494079513853,0.0110348444394294,0.2152615731676));
#110349=DIRECTION('center_axis',(-0.0572811109810715,0.99835808881386,-2.87177830595105E-5));
#110350=DIRECTION('ref_axis',(0.977895626960296,0.0561128647169375,0.201423655972154));
#110351=DIRECTION('center_axis',(-0.00619406208384126,-0.999980560265093,
-0.000716021516796888));
#110352=DIRECTION('ref_axis',(0.999980816603614,-0.00619406367164884,-2.43997512021813E-21));
#110353=DIRECTION('center_axis',(8.20654853338604E-14,3.5527136788005E-12,
-1.));
#110354=DIRECTION('ref_axis',(-1.83670992315982E-40,1.,3.5527136788005E-12));
#110355=DIRECTION('center_axis',(0.115801534012589,-2.98133654443904E-10,
-0.993272371870038));
#110356=DIRECTION('ref_axis',(0.99325305842217,-0.00623603598024155,0.115799282339136));
#110357=DIRECTION('center_axis',(0.00234948403731584,-0.999997203076769,
0.000271594180011335));
#110358=DIRECTION('ref_axis',(0.999997239958367,0.00234948412396881,6.81083076705817E-23));
#110359=DIRECTION('center_axis',(0.,0.,-1.));
#110360=DIRECTION('ref_axis',(-1.,0.,0.));
#110361=DIRECTION('center_axis',(0.,-6.17339315294237E-17,1.));
#110362=DIRECTION('ref_axis',(0.,-1.,0.));
#110363=DIRECTION('center_axis',(0.,0.,-1.));
#110364=DIRECTION('ref_axis',(0.,-1.,0.));
#110365=DIRECTION('center_axis',(-0.0554962509005653,-0.998458895190388,
-2.74074994885905E-5));
#110366=DIRECTION('ref_axis',(0.978041961940448,-0.0543669614620168,0.201191834290228));
#110367=DIRECTION('center_axis',(0.00943472545585777,0.999955491976012,
4.75229707891771E-6));
#110368=DIRECTION('ref_axis',(0.976210029853252,-0.00921171311038235,0.216631304190978));
#110369=DIRECTION('center_axis',(0.1326869973619,-0.991030504325029,0.0158965476868861));
#110370=DIRECTION('ref_axis',(0.991155744879145,0.132703765557229,-2.90070390844182E-17));
#110371=DIRECTION('center_axis',(3.85729088923276E-14,-3.33066907387548E-13,
-1.));
#110372=DIRECTION('ref_axis',(1.00445073922803E-41,1.,-3.33066907387547E-13));
#110373=DIRECTION('center_axis',(0.137685287328068,0.00241479086434434,
-0.99047308415649));
#110374=DIRECTION('ref_axis',(0.981548262063148,0.133629545123289,0.136770442387809));
#110375=DIRECTION('center_axis',(0.141151402782332,-0.989840911569284,0.0170660855578596));
#110376=DIRECTION('ref_axis',(0.989985089278404,0.141171962536586,2.4318092123443E-19));
#110377=DIRECTION('center_axis',(0.,0.,-1.));
#110378=DIRECTION('ref_axis',(-1.,0.,0.));
#110379=DIRECTION('center_axis',(0.,-6.17339315294237E-17,1.));
#110380=DIRECTION('ref_axis',(0.,-1.,0.));
#110381=DIRECTION('center_axis',(-1.8642453554211E-30,5.62966047861811E-44,
-1.));
#110382=DIRECTION('ref_axis',(-3.01980662698043E-14,-1.,-9.95682444457782E-59));
#110383=DIRECTION('center_axis',(-0.115451282615198,-0.993313142075069,
-5.58879192006845E-5));
#110384=DIRECTION('ref_axis',(0.983286165238662,-0.114293836168303,0.14172239154128));
#110385=DIRECTION('center_axis',(0.0749734441413244,0.997185530014467,3.74613657666356E-5));
#110386=DIRECTION('ref_axis',(0.979143860919972,-0.0736240940087581,0.189358898402267));
#110387=DIRECTION('center_axis',(-0.185959552881302,0.695904038033425,-0.693640118895209));
#110388=DIRECTION('ref_axis',(3.15382046976506E-16,0.705953788300242,0.708257897085897));
#110389=DIRECTION('center_axis',(0.,0.,-1.));
#110390=DIRECTION('ref_axis',(-1.,0.,0.));
#110391=DIRECTION('center_axis',(-0.270127118644541,0.962824667202081,-4.0829772679528E-16));
#110392=DIRECTION('ref_axis',(-0.962824667202081,-0.270127118644541,5.77560433057458E-31));
#110393=DIRECTION('center_axis',(0.,0.,1.));
#110394=DIRECTION('ref_axis',(1.,0.,0.));
#110395=DIRECTION('center_axis',(-0.278601694915732,0.960406734456856,-8.33020054374265E-16));
#110396=DIRECTION('ref_axis',(-0.960406734456856,-0.278601694915732,-5.45700864471184E-31));
#110397=DIRECTION('center_axis',(0.,0.,-1.));
#110398=DIRECTION('ref_axis',(1.,1.13691107810172E-13,0.));
#110399=DIRECTION('center_axis',(0.,0.,1.));
#110400=DIRECTION('ref_axis',(1.,0.,0.));
#110401=DIRECTION('center_axis',(0.,-6.17339315294237E-17,1.));
#110402=DIRECTION('ref_axis',(0.,-1.,0.));
#110403=DIRECTION('center_axis',(1.15144566070127E-30,2.14764729331365E-44,
-1.));
#110404=DIRECTION('ref_axis',(1.86517468137027E-14,-1.,3.73380916671668E-59));
#110405=DIRECTION('center_axis',(-0.161739700498652,-0.986833452889392,
-7.44379325117182E-5));
#110406=DIRECTION('ref_axis',(0.986200813837069,-0.161638712068232,0.0357894055276974));
#110407=DIRECTION('center_axis',(0.131366277566232,0.991333897851926,6.39382359252622E-5));
#110408=DIRECTION('ref_axis',(0.984780382030639,-0.130505244040753,0.114786673640506));
#110409=DIRECTION('center_axis',(0.,0.,1.));
#110410=DIRECTION('ref_axis',(1.,0.,0.));
#110411=DIRECTION('center_axis',(0.40826271186488,-0.912864479591979,3.16713488626711E-15));
#110412=DIRECTION('ref_axis',(0.912864479591979,0.40826271186488,6.04208104977424E-31));
#110413=DIRECTION('center_axis',(0.,0.,1.));
#110414=DIRECTION('ref_axis',(1.,0.,0.));
#110415=DIRECTION('center_axis',(0.,0.,-1.));
#110416=DIRECTION('ref_axis',(1.,-1.0479508998465E-13,0.));
#110417=DIRECTION('center_axis',(0.416737288136069,-0.909026970269307,0.));
#110418=DIRECTION('ref_axis',(0.909026970269307,0.416737288136069,0.));
#110419=DIRECTION('center_axis',(0.369731042763204,-0.785707308414229,-0.495946551073502));
#110420=DIRECTION('ref_axis',(1.91361720426385E-15,0.533770129672178,-0.845629616717477));
#110421=DIRECTION('center_axis',(0.133528512868191,-0.950104737537312,0.281906232567436));
#110422=DIRECTION('ref_axis',(-2.32560161936155E-16,-0.284453521859895,
-0.958689831958962));
#110423=DIRECTION('center_axis',(0.,0.,1.));
#110424=DIRECTION('ref_axis',(1.,0.,0.));
#110425=DIRECTION('center_axis',(0.139173100960066,-0.99026806874157,0.));
#110426=DIRECTION('ref_axis',(0.99026806874157,0.139173100960066,0.));
#110427=DIRECTION('center_axis',(-0.139173100960066,0.99026806874157,1.22266282302933E-16));
#110428=DIRECTION('ref_axis',(-0.99026806874157,-0.139173100960066,-9.57340194962255E-34));
#110429=DIRECTION('',(0.139173100960067,-0.99026806874157,-1.22266282302933E-16));
#110430=DIRECTION('center_axis',(0.139173100960066,-0.99026806874157,0.));
#110431=DIRECTION('ref_axis',(0.99026806874157,0.139173100960066,0.));
#110432=DIRECTION('center_axis',(0.,0.,-1.));
#110433=DIRECTION('ref_axis',(-1.,0.,0.));
#110434=DIRECTION('center_axis',(0.139173100960066,-0.99026806874157,0.));
#110435=DIRECTION('ref_axis',(0.99026806874157,0.139173100960066,0.));
#110436=DIRECTION('',(0.139173100960067,-0.99026806874157,0.));
#110437=DIRECTION('center_axis',(0.139173100960066,-0.99026806874157,0.));
#110438=DIRECTION('ref_axis',(0.99026806874157,0.139173100960066,0.));
#110439=DIRECTION('center_axis',(0.,0.,-1.));
#110440=DIRECTION('ref_axis',(-1.,0.,0.));
#110441=DIRECTION('center_axis',(-0.139173100960066,0.99026806874157,1.22266282302933E-16));
#110442=DIRECTION('ref_axis',(-0.99026806874157,-0.139173100960066,-9.57340194962255E-34));
#110443=DIRECTION('',(0.139173100960067,-0.99026806874157,-1.22266282302933E-16));
#110444=DIRECTION('center_axis',(0.,0.,1.));
#110445=DIRECTION('ref_axis',(1.,0.,0.));
#110446=DIRECTION('center_axis',(0.139173100960066,-0.99026806874157,0.));
#110447=DIRECTION('ref_axis',(0.99026806874157,0.139173100960066,0.));
#110448=DIRECTION('center_axis',(0.139173100960066,-0.99026806874157,0.));
#110449=DIRECTION('ref_axis',(0.99026806874157,0.139173100960066,0.));
#110450=DIRECTION('',(0.139173100960067,-0.99026806874157,0.));
#110451=DIRECTION('center_axis',(0.139173100960066,-0.99026806874157,0.));
#110452=DIRECTION('ref_axis',(0.99026806874157,0.139173100960066,0.));
#110453=DIRECTION('center_axis',(0.,0.,-1.));
#110454=DIRECTION('ref_axis',(-1.,0.,0.));
#110455=DIRECTION('center_axis',(-0.139173100960066,0.99026806874157,1.22266282302933E-16));
#110456=DIRECTION('ref_axis',(-0.99026806874157,-0.139173100960066,-9.57340194962255E-34));
#110457=DIRECTION('',(-0.139173100960067,0.99026806874157,1.22266282302933E-16));
#110458=DIRECTION('',(0.139173100960067,-0.99026806874157,-1.22266282302933E-16));
#110459=DIRECTION('center_axis',(-0.139173100960066,0.99026806874157,0.));
#110460=DIRECTION('ref_axis',(-0.99026806874157,-0.139173100960066,0.));
#110461=DIRECTION('center_axis',(0.,1.23467863058847E-16,-1.));
#110462=DIRECTION('ref_axis',(0.,1.,0.));
#110463=DIRECTION('center_axis',(0.,0.,-1.));
#110464=DIRECTION('ref_axis',(0.,1.,0.));
#110465=DIRECTION('center_axis',(-0.685443248911109,0.728126055379275,0.));
#110466=DIRECTION('ref_axis',(-0.728126055379275,-0.685443248911109,0.));
#110467=DIRECTION('center_axis',(-4.28365201153744E-31,-1.48619034146585E-45,
1.));
#110468=DIRECTION('ref_axis',(-3.46944695195361E-15,1.,1.24460305557223E-60));
#110469=DIRECTION('center_axis',(0.,1.23467863058847E-16,-1.));
#110470=DIRECTION('ref_axis',(0.,1.,0.));
#110471=DIRECTION('center_axis',(0.,0.,-1.));
#110472=DIRECTION('ref_axis',(0.,1.,0.));
#110473=DIRECTION('center_axis',(-0.728126055379271,0.685443248911113,0.));
#110474=DIRECTION('ref_axis',(-0.685443248911113,-0.728126055379271,0.));
#110475=DIRECTION('center_axis',(-6.14104352374008E-30,-3.05443170604608E-43,
1.));
#110476=DIRECTION('ref_axis',(-4.9737991503207E-14,1.,0.));
#110477=DIRECTION('center_axis',(0.,1.23467863058847E-16,-1.));
#110478=DIRECTION('ref_axis',(0.,1.,0.));
#110479=DIRECTION('center_axis',(0.,0.,-1.));
#110480=DIRECTION('ref_axis',(0.,1.,0.));
#110481=DIRECTION('center_axis',(-0.990268068741571,0.139173100960059,0.));
#110482=DIRECTION('ref_axis',(-0.139173100960059,-0.990268068741571,0.));
#110483=DIRECTION('center_axis',(0.,0.,1.));
#110484=DIRECTION('ref_axis',(0.,1.,0.));
#110485=DIRECTION('center_axis',(-0.990268068741571,0.139173100960059,1.71834053708117E-17));
#110486=DIRECTION('ref_axis',(-0.139173100960059,-0.990268068741571,4.14246685971564E-34));
#110487=DIRECTION('',(0.990268068741571,-0.139173100960059,-1.71834053708117E-17));
#110488=DIRECTION('',(-0.990268068741571,0.139173100960059,1.71834053708117E-17));
#110489=DIRECTION('center_axis',(0.,0.,-1.));
#110490=DIRECTION('ref_axis',(1.,0.,0.));
#110491=DIRECTION('center_axis',(0.,-7.15121221728469E-32,-1.));
#110492=DIRECTION('ref_axis',(1.,0.,0.));
#110493=DIRECTION('center_axis',(-1.,0.,5.40794518211031E-32));
#110494=DIRECTION('ref_axis',(0.,1.,0.));
#110495=DIRECTION('center_axis',(0.,-1.,0.));
#110496=DIRECTION('ref_axis',(0.,0.,-1.));
#110497=DIRECTION('center_axis',(-5.01606788234257E-16,-1.,5.70122241611331E-32));
#110498=DIRECTION('ref_axis',(-1.,5.01606788234257E-16,0.));
#110499=DIRECTION('',(-1.,5.01606788234257E-16,0.));
#110500=DIRECTION('',(-2.85977186515575E-47,-5.70122241611331E-32,-1.));
#110501=DIRECTION('',(2.85977186515575E-47,5.70122241611331E-32,1.));
#110502=DIRECTION('center_axis',(0.,0.,1.));
#110503=DIRECTION('ref_axis',(0.,-1.,0.));
#110504=DIRECTION('',(0.,1.23467863058847E-16,-1.));
#110505=DIRECTION('',(0.,-1.23467863058847E-16,1.));
#110506=DIRECTION('center_axis',(0.,1.18613571006961E-16,-1.));
#110507=DIRECTION('ref_axis',(0.,1.,1.18613571006961E-16));
#110508=DIRECTION('center_axis',(0.,1.23467863058847E-16,-1.));
#110509=DIRECTION('ref_axis',(-1.,0.,0.));
#110510=DIRECTION('center_axis',(0.,0.,-1.));
#110511=DIRECTION('ref_axis',(0.,1.,0.));
#110512=DIRECTION('',(4.38004274807345E-16,1.,1.23467863058847E-16));
#110513=DIRECTION('',(1.,-4.38004274807345E-16,-5.40794518211031E-32));
#110514=DIRECTION('center_axis',(-4.18005656861882E-16,-1.,0.));
#110515=DIRECTION('ref_axis',(1.,0.,0.));
#110516=DIRECTION('center_axis',(1.,0.,0.));
#110517=DIRECTION('ref_axis',(0.,0.,-1.));
#110518=DIRECTION('center_axis',(0.,1.,0.));
#110519=DIRECTION('ref_axis',(1.,0.,0.));
#110520=DIRECTION('center_axis',(0.,0.,1.));
#110521=DIRECTION('ref_axis',(1.,0.,0.));
#110522=DIRECTION('center_axis',(0.,0.,1.));
#110523=DIRECTION('ref_axis',(1.,0.,0.));
#110524=DIRECTION('',(0.,0.,-1.));
#110525=DIRECTION('center_axis',(0.,0.,1.));
#110526=DIRECTION('ref_axis',(1.,0.,0.));
#110527=DIRECTION('center_axis',(-0.507514080295481,0.,-0.861643463563574));
#110528=DIRECTION('ref_axis',(-0.861643463563574,0.,0.507514080295481));
#110529=DIRECTION('center_axis',(-0.483825549717016,0.,-0.87516446308167));
#110530=DIRECTION('ref_axis',(-0.87516446308167,0.,0.483825549717016));
#110531=DIRECTION('center_axis',(0.,0.,-1.));
#110532=DIRECTION('ref_axis',(-1.,0.,0.));
#110533=DIRECTION('center_axis',(0.,0.,1.));
#110534=DIRECTION('ref_axis',(-0.707106781193192,-0.707106781179903,0.));
#110535=DIRECTION('center_axis',(1.11022302462516E-13,0.,-1.));
#110536=DIRECTION('ref_axis',(-1.,0.,-1.11022302462516E-13));
#110537=DIRECTION('',(0.,0.,1.));
#110538=DIRECTION('center_axis',(0.507514080295474,0.,-0.861643463563578));
#110539=DIRECTION('ref_axis',(-0.861643463563578,0.,-0.507514080295474));
#110540=DIRECTION('center_axis',(0.483537964931496,0.,-0.875323389650881));
#110541=DIRECTION('ref_axis',(-0.875323389650881,0.,-0.483537964931496));
#110542=DIRECTION('center_axis',(1.,0.,0.));
#110543=DIRECTION('ref_axis',(0.,0.,-1.));
#110544=DIRECTION('center_axis',(-1.,4.1800565686188E-16,5.16102651992463E-32));
#110545=DIRECTION('ref_axis',(-4.1800565686188E-16,-1.,8.08534226092968E-63));
#110546=DIRECTION('center_axis',(1.,0.,0.));
#110547=DIRECTION('ref_axis',(0.,0.,-1.));
#110548=DIRECTION('',(-1.,4.18005656861881E-16,5.16102651992463E-32));
#110549=DIRECTION('center_axis',(0.,0.,-1.));
#110550=DIRECTION('ref_axis',(-1.,0.,0.));
#110551=DIRECTION('center_axis',(0.,0.,-1.));
#110552=DIRECTION('ref_axis',(-1.,0.,0.));
#110553=DIRECTION('center_axis',(0.,7.25334975031382E-33,-1.));
#110554=DIRECTION('ref_axis',(-1.,0.,0.));
#110555=DIRECTION('',(1.73522765332109E-17,-7.25334975031383E-33,1.));
#110556=DIRECTION('',(-1.73522765332109E-17,6.98077064262961E-33,-1.));
#110557=DIRECTION('center_axis',(1.,0.,0.));
#110558=DIRECTION('ref_axis',(0.,1.,0.));
#110559=DIRECTION('',(-1.,4.18005656861881E-16,0.));
#110560=DIRECTION('center_axis',(1.,0.,-5.16102651992463E-32));
#110561=DIRECTION('ref_axis',(0.,1.,0.));
#110562=DIRECTION('center_axis',(-1.,0.,0.));
#110563=DIRECTION('ref_axis',(0.,0.,1.));
#110564=DIRECTION('',(-1.,4.18005656861881E-16,5.16102651992463E-32));
#110565=DIRECTION('center_axis',(-1.,0.,0.));
#110566=DIRECTION('ref_axis',(0.,0.,1.));
#110567=DIRECTION('',(1.,-4.18005656861881E-16,-5.16102651992463E-32));
#110568=DIRECTION('center_axis',(-4.18005656861882E-16,-1.,0.));
#110569=DIRECTION('ref_axis',(1.,0.,0.));
#110570=DIRECTION('center_axis',(0.,1.,0.));
#110571=DIRECTION('ref_axis',(1.,0.,0.));
#110572=DIRECTION('center_axis',(-1.,0.,0.));
#110573=DIRECTION('ref_axis',(0.,0.,1.));
#110574=DIRECTION('center_axis',(0.,-1.,0.));
#110575=DIRECTION('ref_axis',(1.,0.,0.));
#110576=DIRECTION('center_axis',(4.18005656861881E-16,1.,0.));
#110577=DIRECTION('ref_axis',(-1.,4.18005656861881E-16,0.));
#110578=DIRECTION('',(4.18005656861881E-16,1.,0.));
#110579=DIRECTION('center_axis',(0.,1.,0.));
#110580=DIRECTION('ref_axis',(-1.,0.,0.));
#110581=DIRECTION('center_axis',(4.18005656861882E-16,1.,0.));
#110582=DIRECTION('ref_axis',(-1.,0.,0.));
#110583=DIRECTION('center_axis',(1.,0.,0.));
#110584=DIRECTION('ref_axis',(0.,0.,-1.));
#110585=DIRECTION('center_axis',(0.,-1.,0.));
#110586=DIRECTION('ref_axis',(-1.,0.,0.));
#110587=DIRECTION('center_axis',(0.,0.,-1.));
#110588=DIRECTION('ref_axis',(-1.,0.,0.));
#110589=DIRECTION('center_axis',(0.,0.,-1.));
#110590=DIRECTION('ref_axis',(-1.,0.,0.));
#110591=DIRECTION('',(0.,0.,1.));
#110592=DIRECTION('center_axis',(0.,0.,-1.));
#110593=DIRECTION('ref_axis',(-1.,0.,0.));
#110594=DIRECTION('center_axis',(4.18005656861882E-16,1.,0.));
#110595=DIRECTION('ref_axis',(-1.,0.,0.));
#110596=DIRECTION('center_axis',(0.,-1.,0.));
#110597=DIRECTION('ref_axis',(-1.,0.,0.));
#110598=DIRECTION('center_axis',(-1.,0.,0.));
#110599=DIRECTION('ref_axis',(0.,0.,1.));
#110600=DIRECTION('center_axis',(1.,0.,0.));
#110601=DIRECTION('ref_axis',(0.,1.,0.));
#110602=DIRECTION('',(1.,-4.18005656861881E-16,0.));
#110603=DIRECTION('center_axis',(0.,-7.25334975031382E-33,1.));
#110604=DIRECTION('ref_axis',(1.,0.,0.));
#110605=DIRECTION('',(-1.73522765332109E-17,7.25334975031383E-33,-1.));
#110606=DIRECTION('center_axis',(0.,0.,-1.));
#110607=DIRECTION('ref_axis',(-1.,0.,0.));
#110608=DIRECTION('',(1.73522765332109E-17,-6.98077064262961E-33,1.));
#110609=DIRECTION('center_axis',(1.,0.,0.));
#110610=DIRECTION('ref_axis',(0.,0.,-1.));
#110611=DIRECTION('center_axis',(1.,-4.1800565686188E-16,-5.16102651992463E-32));
#110612=DIRECTION('ref_axis',(4.1800565686188E-16,1.,-8.08534226092968E-63));
#110613=DIRECTION('',(1.,-4.18005656861881E-16,-5.16102651992463E-32));
#110614=DIRECTION('center_axis',(1.,0.,0.));
#110615=DIRECTION('ref_axis',(0.,0.,-1.));
#110616=DIRECTION('center_axis',(0.496378972716316,6.19668439877561E-14,
-0.868105935612178));
#110617=DIRECTION('ref_axis',(-0.868105935612178,3.44724486393529E-29,-0.496378972716316));
#110618=DIRECTION('center_axis',(0.518474310548581,7.19527646559628E-15,
-0.855093205037424));
#110619=DIRECTION('ref_axis',(-0.855093205037424,3.43699106634736E-31,-0.518474310548581));
#110620=DIRECTION('center_axis',(-2.72711680125255E-25,1.11022302462516E-13,
-1.));
#110621=DIRECTION('ref_axis',(1.56607307231965E-53,1.,1.11022302462516E-13));
#110622=DIRECTION('center_axis',(0.,0.,-1.));
#110623=DIRECTION('ref_axis',(-1.,0.,0.));
#110624=DIRECTION('',(0.,0.,-1.));
#110625=DIRECTION('center_axis',(0.,0.,-1.));
#110626=DIRECTION('ref_axis',(-1.,0.,0.));
#110627=DIRECTION('center_axis',(-0.518474310548575,0.,-0.855093205037428));
#110628=DIRECTION('ref_axis',(-0.855093205037428,0.,0.518474310548575));
#110629=DIRECTION('center_axis',(-0.496741562438066,1.20445113324067E-14,
-0.867898507975782));
#110630=DIRECTION('ref_axis',(-0.867898507975782,5.70559822356712E-31,0.496741562438066));
#110631=DIRECTION('center_axis',(-1.,0.,0.));
#110632=DIRECTION('ref_axis',(0.,0.,1.));
#110633=DIRECTION('center_axis',(-1.,0.,5.16102651992463E-32));
#110634=DIRECTION('ref_axis',(0.,-1.,0.));
#110635=DIRECTION('',(-1.,4.18005656861881E-16,5.16102651992463E-32));
#110636=DIRECTION('center_axis',(-1.,0.,0.));
#110637=DIRECTION('ref_axis',(0.,0.,1.));
#110638=DIRECTION('',(1.,-4.18005656861881E-16,-5.16102651992463E-32));
#110639=DIRECTION('center_axis',(0.,1.23467863058847E-16,-1.));
#110640=DIRECTION('ref_axis',(0.,1.,1.1837531408762E-16));
#110641=DIRECTION('center_axis',(8.39641081720404E-32,-1.17559414210783E-16,
1.));
#110642=DIRECTION('ref_axis',(1.4210854715202E-14,1.,1.17559414210783E-16));
#110643=DIRECTION('center_axis',(-4.18005656861882E-16,-1.,0.));
#110644=DIRECTION('ref_axis',(1.,0.,0.));
#110645=DIRECTION('center_axis',(1.,0.,0.));
#110646=DIRECTION('ref_axis',(0.,0.,-1.));
#110647=DIRECTION('center_axis',(0.,1.,0.));
#110648=DIRECTION('ref_axis',(1.,0.,0.));
#110649=DIRECTION('center_axis',(0.,0.,1.));
#110650=DIRECTION('ref_axis',(1.,0.,0.));
#110651=DIRECTION('center_axis',(0.,0.,1.));
#110652=DIRECTION('ref_axis',(1.,0.,0.));
#110653=DIRECTION('',(0.,0.,-1.));
#110654=DIRECTION('center_axis',(0.,0.,1.));
#110655=DIRECTION('ref_axis',(1.,0.,0.));
#110656=DIRECTION('center_axis',(-1.,4.1800565686188E-16,5.16102651992463E-32));
#110657=DIRECTION('ref_axis',(-4.1800565686188E-16,-1.,8.08534226092968E-63));
#110658=DIRECTION('center_axis',(1.,1.38777878078144E-14,-1.38777878078144E-14));
#110659=DIRECTION('ref_axis',(-1.38777878078144E-14,4.48415508583941E-44,
-1.));
#110660=DIRECTION('',(1.,-4.18005656861881E-16,-5.16102651992463E-32));
#110661=DIRECTION('center_axis',(1.,0.,0.));
#110662=DIRECTION('ref_axis',(0.,0.,-1.));
#110663=DIRECTION('',(-1.,4.18005656861881E-16,5.16102651992463E-32));
#110664=DIRECTION('center_axis',(0.534875344054122,1.17257728967007E-14,
0.844930983171398));
#110665=DIRECTION('ref_axis',(0.844930983171398,-8.89670234612257E-31,-0.534875344054122));
#110666=DIRECTION('center_axis',(0.543750575738856,0.,0.839246871536417));
#110667=DIRECTION('ref_axis',(0.839246871536417,0.,-0.543750575738856));
#110668=DIRECTION('center_axis',(0.,0.,1.));
#110669=DIRECTION('ref_axis',(1.,0.,0.));
#110670=DIRECTION('center_axis',(0.,0.,1.));
#110671=DIRECTION('ref_axis',(1.,0.,0.));
#110672=DIRECTION('',(0.,0.,1.));
#110673=DIRECTION('center_axis',(0.,1.66533453693774E-12,1.));
#110674=DIRECTION('ref_axis',(0.,-1.,1.66533453693774E-12));
#110675=DIRECTION('center_axis',(0.543750575738856,0.,-0.839246871536417));
#110676=DIRECTION('ref_axis',(-0.839246871536417,0.,-0.543750575738856));
#110677=DIRECTION('center_axis',(0.534259922646944,0.,-0.845320255910907));
#110678=DIRECTION('ref_axis',(-0.845320255910907,0.,-0.534259922646944));
#110679=DIRECTION('center_axis',(1.,0.,1.38777878078144E-14));
#110680=DIRECTION('ref_axis',(1.38777878078144E-14,0.,-1.));
#110681=DIRECTION('center_axis',(1.,0.,-5.16102651992463E-32));
#110682=DIRECTION('ref_axis',(0.,1.,0.));
#110683=DIRECTION('center_axis',(1.,0.,0.));
#110684=DIRECTION('ref_axis',(0.,0.,-1.));
#110685=DIRECTION('',(-1.,4.18005656861881E-16,5.16102651992463E-32));
#110686=DIRECTION('center_axis',(0.,0.,-1.));
#110687=DIRECTION('ref_axis',(-1.,0.,0.));
#110688=DIRECTION('center_axis',(0.,0.,-1.));
#110689=DIRECTION('ref_axis',(-1.,0.,0.));
#110690=DIRECTION('center_axis',(0.,7.25334975031382E-33,-1.));
#110691=DIRECTION('ref_axis',(-1.,0.,0.));
#110692=DIRECTION('',(1.73522765332109E-17,-7.25334975031383E-33,1.));
#110693=DIRECTION('',(-1.73522765332109E-17,6.98077064262961E-33,-1.));
#110694=DIRECTION('center_axis',(1.,0.,0.));
#110695=DIRECTION('ref_axis',(0.,1.,0.));
#110696=DIRECTION('',(-1.,4.18005656861881E-16,0.));
#110697=DIRECTION('center_axis',(-4.18005656861882E-16,-1.,0.));
#110698=DIRECTION('ref_axis',(1.,0.,0.));
#110699=DIRECTION('center_axis',(0.,1.,0.));
#110700=DIRECTION('ref_axis',(1.,0.,0.));
#110701=DIRECTION('center_axis',(-1.,0.,0.));
#110702=DIRECTION('ref_axis',(0.,0.,1.));
#110703=DIRECTION('center_axis',(0.,-1.,0.));
#110704=DIRECTION('ref_axis',(1.,0.,0.));
#110705=DIRECTION('center_axis',(4.18005656861881E-16,1.,0.));
#110706=DIRECTION('ref_axis',(-1.,4.18005656861881E-16,0.));
#110707=DIRECTION('',(4.18005656861881E-16,1.,0.));
#110708=DIRECTION('center_axis',(0.,1.,0.));
#110709=DIRECTION('ref_axis',(-1.,0.,0.));
#110710=DIRECTION('center_axis',(-1.,0.,5.40794518211031E-32));
#110711=DIRECTION('ref_axis',(0.,-1.,0.));
#110712=DIRECTION('center_axis',(-1.,4.38004274807345E-16,0.));
#110713=DIRECTION('ref_axis',(0.,0.,1.));
#110714=DIRECTION('',(-1.,4.38004274807345E-16,5.40794518211031E-32));
#110715=DIRECTION('center_axis',(-1.,0.,0.));
#110716=DIRECTION('ref_axis',(0.,0.,1.));
#110717=DIRECTION('',(1.,-4.38004274807345E-16,-5.40794518211031E-32));
#110718=DIRECTION('center_axis',(-1.,0.,5.40794518211031E-32));
#110719=DIRECTION('ref_axis',(0.,-1.,0.));
#110720=DIRECTION('',(-1.,4.38004274807345E-16,5.40794518211031E-32));
#110721=DIRECTION('center_axis',(-1.,0.,0.));
#110722=DIRECTION('ref_axis',(0.,0.,1.));
#110723=DIRECTION('',(1.,-4.38004274807345E-16,-5.40794518211031E-32));
#110724=DIRECTION('center_axis',(1.,-4.38004274807346E-16,-5.40794518211031E-32));
#110725=DIRECTION('ref_axis',(4.38004274807346E-16,1.,5.80597460094347E-63));
#110726=DIRECTION('',(-1.,4.38004274807345E-16,5.40794518211031E-32));
#110727=DIRECTION('center_axis',(-1.,0.,0.));
#110728=DIRECTION('ref_axis',(0.,0.,1.));
#110729=DIRECTION('center_axis',(-1.,4.38004274807345E-16,0.));
#110730=DIRECTION('ref_axis',(0.,0.,1.));
#110731=DIRECTION('center_axis',(4.38004274807345E-16,1.,0.));
#110732=DIRECTION('ref_axis',(-1.,0.,0.));
#110733=DIRECTION('center_axis',(0.,0.,1.));
#110734=DIRECTION('ref_axis',(1.,0.,0.));
#110735=DIRECTION('center_axis',(-1.,0.,0.));
#110736=DIRECTION('ref_axis',(0.,0.,1.));
#110737=DIRECTION('center_axis',(0.,-1.,0.));
#110738=DIRECTION('ref_axis',(-1.,0.,0.));
#110739=DIRECTION('center_axis',(0.,0.,1.));
#110740=DIRECTION('ref_axis',(1.,0.,0.));
#110741=DIRECTION('center_axis',(0.,0.,1.));
#110742=DIRECTION('ref_axis',(1.,0.,0.));
#110743=DIRECTION('',(0.,0.,1.));
#110744=DIRECTION('center_axis',(4.38004274807345E-16,1.,0.));
#110745=DIRECTION('ref_axis',(-1.,0.,0.));
#110746=DIRECTION('center_axis',(1.,0.,0.));
#110747=DIRECTION('ref_axis',(0.,0.,-1.));
#110748=DIRECTION('center_axis',(0.,-1.,0.));
#110749=DIRECTION('ref_axis',(-1.,0.,0.));
#110750=DIRECTION('center_axis',(-1.,0.,0.));
#110751=DIRECTION('ref_axis',(0.,-1.,0.));
#110752=DIRECTION('',(1.,-4.38004274807345E-16,0.));
#110753=DIRECTION('center_axis',(0.,-7.60037129918555E-33,1.));
#110754=DIRECTION('ref_axis',(1.,0.,0.));
#110755=DIRECTION('center_axis',(0.,0.,1.));
#110756=DIRECTION('ref_axis',(1.,0.,0.));
#110757=DIRECTION('',(1.73522765332109E-17,-7.36595663150706E-33,1.));
#110758=DIRECTION('',(-1.73522765332109E-17,7.60037129918555E-33,-1.));
#110759=DIRECTION('center_axis',(-0.460817663464343,0.,0.887494834373285));
#110760=DIRECTION('ref_axis',(0.887494834373285,0.,0.460817663464343));
#110761=DIRECTION('center_axis',(-0.661718432379332,0.,0.749752436641215));
#110762=DIRECTION('ref_axis',(0.749752436641215,0.,0.661718432379332));
#110763=DIRECTION('center_axis',(-0.48375308397303,0.,0.875204521095831));
#110764=DIRECTION('ref_axis',(0.875204521095831,0.,0.48375308397303));
#110765=DIRECTION('center_axis',(0.,0.,1.));
#110766=DIRECTION('ref_axis',(1.,0.,0.));
#110767=DIRECTION('center_axis',(0.,0.,-1.));
#110768=DIRECTION('ref_axis',(-1.,0.,0.));
#110769=DIRECTION('center_axis',(0.,0.,1.));
#110770=DIRECTION('ref_axis',(1.,0.,0.));
#110771=DIRECTION('',(0.,0.,-1.));
#110772=DIRECTION('center_axis',(0.483753083973024,0.,0.875204521095834));
#110773=DIRECTION('ref_axis',(0.875204521095834,0.,-0.483753083973024));
#110774=DIRECTION('center_axis',(0.460985151818831,0.,0.887407848625743));
#110775=DIRECTION('ref_axis',(0.887407848625743,0.,-0.460985151818831));
#110776=DIRECTION('center_axis',(0.,0.,-1.));
#110777=DIRECTION('ref_axis',(-1.,0.,0.));
#110778=DIRECTION('center_axis',(0.,0.,-1.));
#110779=DIRECTION('ref_axis',(-1.,0.,0.));
#110780=DIRECTION('',(0.,0.,1.));
#110781=DIRECTION('center_axis',(0.,0.,-1.));
#110782=DIRECTION('ref_axis',(-1.,0.,0.));
#110783=DIRECTION('center_axis',(4.18005656861882E-16,1.,0.));
#110784=DIRECTION('ref_axis',(-1.,0.,0.));
#110785=DIRECTION('center_axis',(0.,-1.,0.));
#110786=DIRECTION('ref_axis',(-1.,0.,0.));
#110787=DIRECTION('center_axis',(-1.,0.,0.));
#110788=DIRECTION('ref_axis',(0.,0.,1.));
#110789=DIRECTION('center_axis',(1.,0.,0.));
#110790=DIRECTION('ref_axis',(0.,1.,0.));
#110791=DIRECTION('',(1.,-4.18005656861881E-16,0.));
#110792=DIRECTION('center_axis',(0.,0.,1.));
#110793=DIRECTION('ref_axis',(0.,-1.,0.));
#110794=DIRECTION('center_axis',(0.,0.,1.));
#110795=DIRECTION('ref_axis',(1.,0.,0.));
#110796=DIRECTION('',(0.,-1.23467863058847E-16,1.));
#110797=DIRECTION('',(-5.16102651992463E-32,2.15733828054269E-47,-1.));
#110798=DIRECTION('center_axis',(0.817080261705548,0.,0.576523933528517));
#110799=DIRECTION('ref_axis',(0.576523933528517,0.,-0.817080261705548));
#110800=DIRECTION('center_axis',(0.214170029765708,0.976796000598309,0.000878387901143853));
#110801=DIRECTION('ref_axis',(0.840875521369131,-0.184825863749487,0.50869220325404));
#110802=DIRECTION('center_axis',(0.,-1.,0.));
#110803=DIRECTION('ref_axis',(0.979462303532354,0.,0.201627369072492));
#110804=DIRECTION('center_axis',(0.,-1.18842113532926E-16,1.));
#110805=DIRECTION('ref_axis',(0.,1.,1.18842113532926E-16));
#110806=DIRECTION('center_axis',(0.,1.19392659184112E-16,-1.));
#110807=DIRECTION('ref_axis',(0.,1.,1.19392659184112E-16));
#110808=DIRECTION('center_axis',(-4.18005656861882E-16,-1.,0.));
#110809=DIRECTION('ref_axis',(1.,0.,0.));
#110810=DIRECTION('center_axis',(1.,0.,0.));
#110811=DIRECTION('ref_axis',(0.,0.,-1.));
#110812=DIRECTION('center_axis',(0.,1.,0.));
#110813=DIRECTION('ref_axis',(1.,0.,0.));
#110814=DIRECTION('center_axis',(0.,0.,1.));
#110815=DIRECTION('ref_axis',(1.,0.,0.));
#110816=DIRECTION('center_axis',(0.,0.,1.));
#110817=DIRECTION('ref_axis',(1.,0.,0.));
#110818=DIRECTION('',(0.,0.,-1.));
#110819=DIRECTION('center_axis',(0.,0.,1.));
#110820=DIRECTION('ref_axis',(1.,0.,0.));
#110821=DIRECTION('center_axis',(-0.49549481432688,0.,-0.868610896187223));
#110822=DIRECTION('ref_axis',(-0.868610896187223,0.,0.49549481432688));
#110823=DIRECTION('center_axis',(-1.,0.,0.));
#110824=DIRECTION('ref_axis',(0.,0.,1.));
#110825=DIRECTION('center_axis',(-0.517480097905755,0.,-0.855695242636916));
#110826=DIRECTION('ref_axis',(-0.855695242636916,0.,0.517480097905755));
#110827=DIRECTION('center_axis',(-1.11022302462516E-12,0.,-1.));
#110828=DIRECTION('ref_axis',(-1.,0.,1.11022302462516E-12));
#110829=DIRECTION('center_axis',(0.,0.,1.));
#110830=DIRECTION('ref_axis',(1.,0.,0.));
#110831=DIRECTION('center_axis',(0.,0.,-1.));
#110832=DIRECTION('ref_axis',(-1.,0.,0.));
#110833=DIRECTION('',(0.,0.,1.));
#110834=DIRECTION('center_axis',(0.517480097907924,0.,-0.855695242635604));
#110835=DIRECTION('ref_axis',(-0.855695242635604,0.,-0.517480097907924));
#110836=DIRECTION('center_axis',(0.495139693244723,0.,-0.868813377068702));
#110837=DIRECTION('ref_axis',(-0.868813377068702,0.,-0.495139693244723));
#110838=DIRECTION('center_axis',(1.,0.,0.));
#110839=DIRECTION('ref_axis',(0.,0.,-1.));
#110840=DIRECTION('center_axis',(-1.,4.1800565686188E-16,5.16102651992463E-32));
#110841=DIRECTION('ref_axis',(-4.1800565686188E-16,-1.,8.08534226092968E-63));
#110842=DIRECTION('center_axis',(1.,0.,0.));
#110843=DIRECTION('ref_axis',(0.,0.,-1.));
#110844=DIRECTION('',(-1.,4.18005656861881E-16,5.16102651992463E-32));
#110845=DIRECTION('center_axis',(0.,0.,-1.));
#110846=DIRECTION('ref_axis',(-1.,0.,0.));
#110847=DIRECTION('center_axis',(0.,-7.25334975031394E-33,-1.));
#110848=DIRECTION('ref_axis',(-1.,0.,0.));
#110849=DIRECTION('',(1.73522765332111E-17,-6.55191041448207E-33,-1.));
#110850=DIRECTION('',(-1.73522765332111E-17,7.25334975031394E-33,1.));
#110851=DIRECTION('center_axis',(1.,0.,0.));
#110852=DIRECTION('ref_axis',(0.,1.,0.));
#110853=DIRECTION('',(-1.,4.18005656861881E-16,0.));
#110854=DIRECTION('center_axis',(-4.18005656861882E-16,-1.,0.));
#110855=DIRECTION('ref_axis',(1.,0.,0.));
#110856=DIRECTION('center_axis',(0.,1.,0.));
#110857=DIRECTION('ref_axis',(1.,0.,0.));
#110858=DIRECTION('center_axis',(-1.,0.,0.));
#110859=DIRECTION('ref_axis',(0.,0.,1.));
#110860=DIRECTION('center_axis',(0.,-1.,0.));
#110861=DIRECTION('ref_axis',(1.,0.,0.));
#110862=DIRECTION('center_axis',(4.18005656861881E-16,1.,0.));
#110863=DIRECTION('ref_axis',(-1.,4.18005656861881E-16,0.));
#110864=DIRECTION('',(4.18005656861881E-16,1.,0.));
#110865=DIRECTION('center_axis',(0.,1.,0.));
#110866=DIRECTION('ref_axis',(-1.,0.,0.));
#110867=DIRECTION('center_axis',(4.18005656861882E-16,1.,0.));
#110868=DIRECTION('ref_axis',(-1.,0.,0.));
#110869=DIRECTION('center_axis',(1.,0.,0.));
#110870=DIRECTION('ref_axis',(0.,0.,-1.));
#110871=DIRECTION('center_axis',(0.,-1.,0.));
#110872=DIRECTION('ref_axis',(-1.,0.,0.));
#110873=DIRECTION('center_axis',(0.,0.,-1.));
#110874=DIRECTION('ref_axis',(-1.,0.,0.));
#110875=DIRECTION('center_axis',(0.,0.,-1.));
#110876=DIRECTION('ref_axis',(-1.,0.,0.));
#110877=DIRECTION('',(0.,0.,1.));
#110878=DIRECTION('center_axis',(0.,0.,-1.));
#110879=DIRECTION('ref_axis',(-1.,0.,0.));
#110880=DIRECTION('center_axis',(4.18005656861882E-16,1.,0.));
#110881=DIRECTION('ref_axis',(-1.,0.,0.));
#110882=DIRECTION('center_axis',(0.,-1.,0.));
#110883=DIRECTION('ref_axis',(-1.,0.,0.));
#110884=DIRECTION('center_axis',(-1.,0.,0.));
#110885=DIRECTION('ref_axis',(0.,0.,1.));
#110886=DIRECTION('center_axis',(1.,0.,0.));
#110887=DIRECTION('ref_axis',(0.,1.,0.));
#110888=DIRECTION('',(1.,-4.18005656861881E-16,0.));
#110889=DIRECTION('center_axis',(0.,7.25334975031394E-33,1.));
#110890=DIRECTION('ref_axis',(-0.754709580222751,0.656059028990531,-4.75862559411968E-33));
#110891=DIRECTION('',(1.73522765332111E-17,-7.25334975031394E-33,-1.));
#110892=DIRECTION('center_axis',(0.,0.,-1.));
#110893=DIRECTION('ref_axis',(-1.,0.,0.));
#110894=DIRECTION('',(-1.73522765332111E-17,6.55191041448207E-33,1.));
#110895=DIRECTION('center_axis',(1.,0.,0.));
#110896=DIRECTION('ref_axis',(0.,0.,-1.));
#110897=DIRECTION('center_axis',(1.,-4.1800565686188E-16,-5.16102651992463E-32));
#110898=DIRECTION('ref_axis',(4.1800565686188E-16,1.,-8.08534226092968E-63));
#110899=DIRECTION('',(1.,-4.18005656861881E-16,-5.16102651992463E-32));
#110900=DIRECTION('center_axis',(1.,0.,0.));
#110901=DIRECTION('ref_axis',(0.,0.,-1.));
#110902=DIRECTION('center_axis',(0.482476521947278,1.33914135876736E-14,
-0.875908902666058));
#110903=DIRECTION('ref_axis',(-0.875908902666058,-3.49403168495695E-30,
-0.482476521947278));
#110904=DIRECTION('center_axis',(0.50653821035484,0.,-0.862217514001262));
#110905=DIRECTION('ref_axis',(-0.862217514001262,0.,-0.50653821035484));
#110906=DIRECTION('center_axis',(0.,0.,-1.));
#110907=DIRECTION('ref_axis',(-1.,0.,0.));
#110908=DIRECTION('center_axis',(0.,0.,-1.));
#110909=DIRECTION('ref_axis',(-1.,0.,0.));
#110910=DIRECTION('',(0.,0.,-1.));
#110911=DIRECTION('center_axis',(0.,-1.77635683940025E-12,-1.));
#110912=DIRECTION('ref_axis',(0.,1.,-1.77635683940025E-12));
#110913=DIRECTION('center_axis',(-0.506538210354814,0.,-0.862217514001277));
#110914=DIRECTION('ref_axis',(-0.862217514001277,0.,0.506538210354814));
#110915=DIRECTION('center_axis',(-0.482758140724685,1.88531393333386E-14,
-0.875753719697522));
#110916=DIRECTION('ref_axis',(-0.875753719697522,-7.73315028487173E-30,
0.482758140724685));
#110917=DIRECTION('center_axis',(-1.,0.,5.16102651992463E-32));
#110918=DIRECTION('ref_axis',(0.,-1.,0.));
#110919=DIRECTION('center_axis',(-1.,0.,0.));
#110920=DIRECTION('ref_axis',(0.,0.,1.));
#110921=DIRECTION('',(-1.,4.18005656861881E-16,5.16102651992463E-32));
#110922=DIRECTION('center_axis',(-1.,0.,0.));
#110923=DIRECTION('ref_axis',(0.,0.,1.));
#110924=DIRECTION('',(1.,-4.18005656861881E-16,-5.16102651992463E-32));
#110925=DIRECTION('center_axis',(0.,-1.18842113532926E-16,1.));
#110926=DIRECTION('ref_axis',(0.,1.,1.18842113532926E-16));
#110927=DIRECTION('center_axis',(0.,1.19392659184112E-16,-1.));
#110928=DIRECTION('ref_axis',(0.,1.,1.19392659184112E-16));
#110929=DIRECTION('center_axis',(-4.18005656861882E-16,-1.,0.));
#110930=DIRECTION('ref_axis',(1.,-5.9211894646675E-16,0.));
#110931=DIRECTION('center_axis',(1.,0.,0.));
#110932=DIRECTION('ref_axis',(0.,0.,-1.));
#110933=DIRECTION('center_axis',(6.93889390390722E-16,1.,0.));
#110934=DIRECTION('ref_axis',(1.,-6.93889390390722E-16,0.));
#110935=DIRECTION('center_axis',(0.,0.,1.));
#110936=DIRECTION('ref_axis',(1.,0.,0.));
#110937=DIRECTION('center_axis',(0.,0.,1.));
#110938=DIRECTION('ref_axis',(1.,0.,0.));
#110939=DIRECTION('',(0.,0.,-1.));
#110940=DIRECTION('center_axis',(0.,0.,1.));
#110941=DIRECTION('ref_axis',(1.,0.,0.));
#110942=DIRECTION('center_axis',(0.403600920616143,3.09956391918065E-14,
0.91493513260657));
#110943=DIRECTION('ref_axis',(0.91493513260657,-7.63177238048844E-30,-0.403600920616143));
#110944=DIRECTION('center_axis',(0.,-1.,0.));
#110945=DIRECTION('ref_axis',(-0.285513245062781,0.,-0.9583747632809));
#110946=DIRECTION('center_axis',(0.782801330915055,1.71942202750291E-12,
0.622271706184379));
#110947=DIRECTION('ref_axis',(0.622271706184379,-5.64324648533862E-28,-0.782801330915055));
#110948=DIRECTION('center_axis',(0.,1.,0.));
#110949=DIRECTION('ref_axis',(0.882822386979436,0.,-0.469706965083476));
#110950=DIRECTION('center_axis',(0.460227641765603,1.23207131288176E-14,
0.887800944894108));
#110951=DIRECTION('ref_axis',(0.887800944894108,7.43200893707752E-29,-0.460227641765603));
#110952=DIRECTION('center_axis',(0.213575684387547,-0.976926520634823,-1.78530135123478E-5));
#110953=DIRECTION('ref_axis',(0.953391643317273,0.20842650212588,0.218180584984919));
#110954=DIRECTION('center_axis',(0.482846004726866,0.,0.875705279029025));
#110955=DIRECTION('ref_axis',(0.875705279029025,0.,-0.482846004726866));
#110956=DIRECTION('center_axis',(0.,0.,1.));
#110957=DIRECTION('ref_axis',(1.,0.,0.));
#110958=DIRECTION('center_axis',(0.,0.,1.));
#110959=DIRECTION('ref_axis',(1.,0.,0.));
#110960=DIRECTION('',(0.,0.,1.));
#110961=DIRECTION('center_axis',(0.,0.,1.));
#110962=DIRECTION('ref_axis',(1.,0.,0.));
#110963=DIRECTION('center_axis',(-0.482846004727867,1.73271215008562E-12,
0.875705279028473));
#110964=DIRECTION('ref_axis',(0.875705279028473,2.53817490248555E-28,0.482846004727867));
#110965=DIRECTION('center_axis',(-0.460063868749635,6.3846687485495E-15,
0.887885824118799));
#110966=DIRECTION('ref_axis',(0.887885824118799,1.45303619130616E-30,0.460063868749635));
#110967=DIRECTION('center_axis',(-0.639652375806928,0.,0.768664320834884));
#110968=DIRECTION('ref_axis',(0.768664320834884,0.,0.639652375806928));
#110969=DIRECTION('center_axis',(0.,0.,1.));
#110970=DIRECTION('ref_axis',(1.,0.,0.));
#110971=DIRECTION('center_axis',(0.,0.,1.));
#110972=DIRECTION('ref_axis',(0.,-1.,0.));
#110973=DIRECTION('',(5.16102651992463E-32,-2.15733828054269E-47,1.));
#110974=DIRECTION('',(0.,1.23467863058847E-16,-1.));
#110975=DIRECTION('center_axis',(1.,0.,0.));
#110976=DIRECTION('ref_axis',(0.,1.,0.));
#110977=DIRECTION('',(-1.,4.18005656861881E-16,0.));
#110978=DIRECTION('center_axis',(1.,0.,-5.40794518211031E-32));
#110979=DIRECTION('ref_axis',(0.,1.,0.));
#110980=DIRECTION('',(1.,-4.38004274807345E-16,-5.40794518211031E-32));
#110981=DIRECTION('',(-1.,4.38004274807345E-16,5.40794518211031E-32));
#110982=DIRECTION('center_axis',(1.,0.,-4.33680868994201E-16));
#110983=DIRECTION('ref_axis',(0.,1.,0.));
#110984=DIRECTION('center_axis',(1.,0.,-5.40794518211031E-32));
#110985=DIRECTION('ref_axis',(0.,1.,0.));
#110986=DIRECTION('center_axis',(1.,0.,0.));
#110987=DIRECTION('ref_axis',(0.,0.,-1.));
#110988=DIRECTION('',(1.,-4.38004274807345E-16,-5.40794518211031E-32));
#110989=DIRECTION('center_axis',(1.,0.,0.));
#110990=DIRECTION('ref_axis',(0.,0.,-1.));
#110991=DIRECTION('',(-1.,4.38004274807345E-16,5.40794518211031E-32));
#110992=DIRECTION('center_axis',(0.,0.,-1.));
#110993=DIRECTION('ref_axis',(-1.,0.,0.));
#110994=DIRECTION('center_axis',(0.,-7.60037129918566E-33,-1.));
#110995=DIRECTION('ref_axis',(-1.,0.,0.));
#110996=DIRECTION('',(1.73522765332111E-17,-6.93709640335951E-33,-1.));
#110997=DIRECTION('',(-1.73522765332111E-17,7.60037129918566E-33,1.));
#110998=DIRECTION('center_axis',(-1.,0.,0.));
#110999=DIRECTION('ref_axis',(0.,-1.,0.));
#111000=DIRECTION('',(-1.,4.38004274807345E-16,0.));
#111001=DIRECTION('center_axis',(1.,0.,0.));
#111002=DIRECTION('ref_axis',(0.,0.,-1.));
#111003=DIRECTION('center_axis',(-4.38004274807345E-16,-1.,0.));
#111004=DIRECTION('ref_axis',(1.,0.,0.));
#111005=DIRECTION('center_axis',(0.,1.,0.));
#111006=DIRECTION('ref_axis',(1.,0.,0.));
#111007=DIRECTION('center_axis',(0.,0.,1.));
#111008=DIRECTION('ref_axis',(1.,0.,0.));
#111009=DIRECTION('center_axis',(0.,0.,-1.));
#111010=DIRECTION('ref_axis',(-1.,0.,0.));
#111011=DIRECTION('',(0.,0.,-1.));
#111012=DIRECTION('center_axis',(0.,0.,1.));
#111013=DIRECTION('ref_axis',(1.,0.,0.));
#111014=DIRECTION('center_axis',(-1.,4.38004274807345E-16,0.));
#111015=DIRECTION('ref_axis',(0.,0.,-1.));
#111016=DIRECTION('center_axis',(1.,-4.38004274807345E-16,4.02455846426619E-13));
#111017=DIRECTION('ref_axis',(4.02455846426619E-13,-4.48415508583941E-44,
-1.));
#111018=DIRECTION('center_axis',(0.,0.,1.));
#111019=DIRECTION('ref_axis',(0.,-1.,0.));
#111020=DIRECTION('',(5.40794518211031E-32,-2.3687031076881E-47,1.));
#111021=DIRECTION('center_axis',(-1.71346080461497E-30,-2.37790454634537E-44,
1.));
#111022=DIRECTION('ref_axis',(-1.38777878078144E-14,1.,2.48920611114446E-59));
#111023=DIRECTION('center_axis',(-4.38004274807345E-16,-1.,0.));
#111024=DIRECTION('ref_axis',(1.,0.,0.));
#111025=DIRECTION('center_axis',(0.,1.,0.));
#111026=DIRECTION('ref_axis',(1.,0.,0.));
#111027=DIRECTION('center_axis',(-1.,0.,0.));
#111028=DIRECTION('ref_axis',(0.,0.,1.));
#111029=DIRECTION('center_axis',(0.,-1.,0.));
#111030=DIRECTION('ref_axis',(1.,0.,0.));
#111031=DIRECTION('center_axis',(4.18005656861881E-16,1.,0.));
#111032=DIRECTION('ref_axis',(-1.,4.18005656861881E-16,0.));
#111033=DIRECTION('',(4.18005656861881E-16,1.,0.));
#111034=DIRECTION('center_axis',(0.,1.,0.));
#111035=DIRECTION('ref_axis',(-1.,0.,0.));
#111036=DIRECTION('center_axis',(-1.,0.,5.16102651992463E-32));
#111037=DIRECTION('ref_axis',(0.,-1.,0.));
#111038=DIRECTION('center_axis',(-1.,0.,0.));
#111039=DIRECTION('ref_axis',(0.,0.,1.));
#111040=DIRECTION('center_axis',(-1.,0.,0.));
#111041=DIRECTION('ref_axis',(0.,0.,1.));
#111042=DIRECTION('',(1.,-4.18005656861881E-16,-5.16102651992463E-32));
#111043=DIRECTION('center_axis',(-0.532459169918176,0.,0.846455688367706));
#111044=DIRECTION('ref_axis',(0.846455688367706,0.,0.532459169918176));
#111045=DIRECTION('center_axis',(-0.542737080693356,0.,0.839902649859169));
#111046=DIRECTION('ref_axis',(0.839902649859169,0.,0.542737080693356));
#111047=DIRECTION('center_axis',(0.,0.,1.));
#111048=DIRECTION('ref_axis',(1.,0.,0.));
#111049=DIRECTION('center_axis',(0.,0.,-1.));
#111050=DIRECTION('ref_axis',(-1.,0.,0.));
#111051=DIRECTION('center_axis',(-1.11022302462516E-13,0.,1.));
#111052=DIRECTION('ref_axis',(1.,0.,1.11022302462516E-13));
#111053=DIRECTION('',(0.,0.,-1.));
#111054=DIRECTION('center_axis',(0.542737080693052,0.,0.839902649859366));
#111055=DIRECTION('ref_axis',(0.839902649859366,0.,-0.542737080693052));
#111056=DIRECTION('center_axis',(0.533061469511947,0.,0.846076515287928));
#111057=DIRECTION('ref_axis',(0.846076515287928,0.,-0.533061469511947));
#111058=DIRECTION('center_axis',(1.,0.,0.));
#111059=DIRECTION('ref_axis',(0.,0.,-1.));
#111060=DIRECTION('center_axis',(4.18005656861882E-16,1.,0.));
#111061=DIRECTION('ref_axis',(-1.,0.,0.));
#111062=DIRECTION('center_axis',(1.,0.,0.));
#111063=DIRECTION('ref_axis',(0.,0.,-1.));
#111064=DIRECTION('center_axis',(0.,-1.,0.));
#111065=DIRECTION('ref_axis',(-1.,0.,0.));
#111066=DIRECTION('center_axis',(0.,0.,-1.));
#111067=DIRECTION('ref_axis',(-1.,0.,0.));
#111068=DIRECTION('center_axis',(0.,0.,-1.));
#111069=DIRECTION('ref_axis',(-1.,0.,0.));
#111070=DIRECTION('',(0.,0.,1.));
#111071=DIRECTION('center_axis',(0.,0.,-1.));
#111072=DIRECTION('ref_axis',(-1.,0.,0.));
#111073=DIRECTION('center_axis',(4.18005656861882E-16,1.,0.));
#111074=DIRECTION('ref_axis',(-1.,0.,0.));
#111075=DIRECTION('center_axis',(0.,-1.,0.));
#111076=DIRECTION('ref_axis',(-1.,0.,0.));
#111077=DIRECTION('center_axis',(-1.,0.,0.));
#111078=DIRECTION('ref_axis',(0.,0.,1.));
#111079=DIRECTION('center_axis',(1.,0.,0.));
#111080=DIRECTION('ref_axis',(0.,1.,0.));
#111081=DIRECTION('',(1.,-4.18005656861881E-16,0.));
#111082=DIRECTION('center_axis',(0.,-7.68642463345396E-33,-1.));
#111083=DIRECTION('ref_axis',(-1.,0.,0.));
#111084=DIRECTION('center_axis',(0.,0.,1.));
#111085=DIRECTION('ref_axis',(1.,0.,0.));
#111086=DIRECTION('',(-1.73522765332111E-17,6.93709640335951E-33,1.));
#111087=DIRECTION('',(1.73522765332111E-17,-7.25334975031394E-33,-1.));
#111088=DIRECTION('center_axis',(0.,0.,1.));
#111089=DIRECTION('ref_axis',(1.,0.,0.));
#111090=DIRECTION('center_axis',(1.,0.,-5.16102651992463E-32));
#111091=DIRECTION('ref_axis',(0.,1.,0.));
#111092=DIRECTION('',(-1.,4.18005656861881E-16,5.16102651992463E-32));
#111093=DIRECTION('center_axis',(-1.,0.,0.));
#111094=DIRECTION('ref_axis',(0.,0.,1.));
#111095=DIRECTION('',(1.,-4.18005656861881E-16,-5.16102651992463E-32));
#111096=DIRECTION('center_axis',(1.,-4.1800565686188E-16,-5.16102651992463E-32));
#111097=DIRECTION('ref_axis',(4.1800565686188E-16,1.,-8.08534226092968E-63));
#111098=DIRECTION('center_axis',(1.,0.,0.));
#111099=DIRECTION('ref_axis',(0.,0.,-1.));
#111100=DIRECTION('',(1.,-4.18005656861881E-16,-5.16102651992463E-32));
#111101=DIRECTION('',(-1.,4.18005656861881E-16,5.16102651992463E-32));
#111102=DIRECTION('center_axis',(0.,1.23467863058847E-16,-1.));
#111103=DIRECTION('ref_axis',(0.,1.,1.1837531408762E-16));
#111104=DIRECTION('center_axis',(5.24775676075252E-32,-1.17559414210783E-16,
1.));
#111105=DIRECTION('ref_axis',(8.88178419700125E-15,1.,1.17559414210783E-16));
#111106=DIRECTION('center_axis',(0.,1.,0.));
#111107=DIRECTION('ref_axis',(0.,0.,1.));
#111108=DIRECTION('center_axis',(-1.90454958189083E-14,0.515457402104623,
0.856915203865326));
#111109=DIRECTION('ref_axis',(1.04773227122123E-29,-0.856915203865326,0.515457402104623));
#111110=DIRECTION('center_axis',(-1.44372869288582E-12,0.522894079854115,
0.852397666147391));
#111111=DIRECTION('ref_axis',(4.54659658509035E-27,-0.852397666147391,0.522894079854115));
#111112=DIRECTION('center_axis',(0.,0.,1.));
#111113=DIRECTION('ref_axis',(1.,0.,0.));
#111114=DIRECTION('center_axis',(0.,8.19208946723988E-32,1.));
#111115=DIRECTION('ref_axis',(1.,0.,0.));
#111116=DIRECTION('',(-1.87032180698308E-16,8.19208946723987E-32,1.));
#111117=DIRECTION('center_axis',(0.,0.,1.));
#111118=DIRECTION('ref_axis',(1.,0.,0.));
#111119=DIRECTION('',(1.87032180698308E-16,-8.19208946723987E-32,-1.));
#111120=DIRECTION('center_axis',(1.,0.,1.87032180698308E-16));
#111121=DIRECTION('ref_axis',(0.,0.,-1.));
#111122=DIRECTION('center_axis',(0.,0.,1.));
#111123=DIRECTION('ref_axis',(1.,0.,0.));
#111124=DIRECTION('center_axis',(-1.,0.,0.));
#111125=DIRECTION('ref_axis',(0.,0.,-1.));
#111126=DIRECTION('center_axis',(0.,-1.,0.));
#111127=DIRECTION('ref_axis',(0.,0.,-1.));
#111128=DIRECTION('center_axis',(1.,0.,0.));
#111129=DIRECTION('ref_axis',(0.,0.,-1.));
#111130=DIRECTION('center_axis',(-1.,0.,0.));
#111131=DIRECTION('ref_axis',(0.,0.,1.));
#111132=DIRECTION('',(-1.,0.,0.));
#111133=DIRECTION('center_axis',(-1.,0.,0.));
#111134=DIRECTION('ref_axis',(0.,1.,0.));
#111135=DIRECTION('',(1.,0.,0.));
#111136=DIRECTION('center_axis',(1.,-4.38004274807345E-16,0.));
#111137=DIRECTION('ref_axis',(0.,1.,0.));
#111138=DIRECTION('center_axis',(0.,1.,0.));
#111139=DIRECTION('ref_axis',(0.,0.,1.));
#111140=DIRECTION('center_axis',(1.,0.,0.));
#111141=DIRECTION('ref_axis',(0.,1.,0.));
#111142=DIRECTION('center_axis',(0.,0.,-1.));
#111143=DIRECTION('ref_axis',(-1.,0.,0.));
#111144=DIRECTION('center_axis',(0.,0.,1.));
#111145=DIRECTION('ref_axis',(1.,0.,0.));
#111146=DIRECTION('',(0.,0.,1.));
#111147=DIRECTION('',(0.,0.,-1.));
#111148=DIRECTION('center_axis',(0.,0.,1.));
#111149=DIRECTION('ref_axis',(0.,-1.,0.));
#111150=DIRECTION('',(5.40794518211031E-32,1.23467863058847E-16,-1.));
#111151=DIRECTION('center_axis',(-8.56730402307488E-31,-5.94476136586342E-45,
1.));
#111152=DIRECTION('ref_axis',(-6.93889390390722E-15,1.,9.95682444457783E-60));
#111153=DIRECTION('center_axis',(-1.22429528305785E-14,0.470879150309884,
0.882197724891332));
#111154=DIRECTION('ref_axis',(1.13789948105108E-30,-0.882197724891332,0.470879150309884));
#111155=DIRECTION('center_axis',(0.,0.488256551855887,0.872700142987154));
#111156=DIRECTION('ref_axis',(0.,-0.872700142987154,0.488256551855887));
#111157=DIRECTION('center_axis',(0.,0.,1.));
#111158=DIRECTION('ref_axis',(1.,0.,0.));
#111159=DIRECTION('center_axis',(0.,8.19208946723987E-32,1.));
#111160=DIRECTION('ref_axis',(1.,0.,0.));
#111161=DIRECTION('',(-1.87032180698308E-16,8.19208946723987E-32,1.));
#111162=DIRECTION('center_axis',(0.,0.,1.));
#111163=DIRECTION('ref_axis',(1.,0.,0.));
#111164=DIRECTION('',(1.87032180698308E-16,-8.19208946723987E-32,-1.));
#111165=DIRECTION('center_axis',(1.,0.,1.87032180698308E-16));
#111166=DIRECTION('ref_axis',(0.,0.,-1.));
#111167=DIRECTION('center_axis',(0.,0.,1.));
#111168=DIRECTION('ref_axis',(1.,0.,0.));
#111169=DIRECTION('center_axis',(-1.,0.,0.));
#111170=DIRECTION('ref_axis',(0.,0.,-1.));
#111171=DIRECTION('center_axis',(0.,-1.,0.));
#111172=DIRECTION('ref_axis',(0.,0.,-1.));
#111173=DIRECTION('center_axis',(1.,0.,0.));
#111174=DIRECTION('ref_axis',(0.,0.,-1.));
#111175=DIRECTION('center_axis',(-1.,0.,0.));
#111176=DIRECTION('ref_axis',(0.,0.,1.));
#111177=DIRECTION('',(1.,0.,0.));
#111178=DIRECTION('',(-1.,0.,0.));
#111179=DIRECTION('center_axis',(-1.,0.,0.));
#111180=DIRECTION('ref_axis',(0.,0.,1.));
#111181=DIRECTION('center_axis',(-1.,0.,0.));
#111182=DIRECTION('ref_axis',(0.,0.,1.));
#111183=DIRECTION('center_axis',(0.,1.,0.));
#111184=DIRECTION('ref_axis',(0.,0.,1.));
#111185=DIRECTION('center_axis',(1.,0.,0.));
#111186=DIRECTION('ref_axis',(0.,0.,1.));
#111187=DIRECTION('center_axis',(0.,0.,-1.));
#111188=DIRECTION('ref_axis',(-1.,0.,0.));
#111189=DIRECTION('center_axis',(0.,0.,-1.));
#111190=DIRECTION('ref_axis',(-1.,0.,0.));
#111191=DIRECTION('center_axis',(0.,0.,1.));
#111192=DIRECTION('ref_axis',(1.,0.,0.));
#111193=DIRECTION('',(0.,0.,1.));
#111194=DIRECTION('center_axis',(0.,0.,1.));
#111195=DIRECTION('ref_axis',(1.,0.,0.));
#111196=DIRECTION('',(0.,0.,-1.));
#111197=DIRECTION('center_axis',(0.,0.498146280733357,0.867093007117186));
#111198=DIRECTION('ref_axis',(0.,-0.867093007117186,0.498146280733357));
#111199=DIRECTION('center_axis',(0.,0.481647286662901,0.876365158624112));
#111200=DIRECTION('ref_axis',(0.,-0.876365158624112,0.481647286662901));
#111201=DIRECTION('center_axis',(0.,1.,0.));
#111202=DIRECTION('ref_axis',(0.,0.,1.));
#111203=DIRECTION('center_axis',(2.30924636740563E-32,-1.,0.));
#111204=DIRECTION('ref_axis',(0.,0.,-1.));
#111205=DIRECTION('center_axis',(0.,1.,0.));
#111206=DIRECTION('ref_axis',(0.,0.,1.));
#111207=DIRECTION('',(-2.30924636740563E-32,1.,1.23467863058847E-16));
#111208=DIRECTION('',(2.30924636740563E-32,-1.,-1.23467863058847E-16));
#111209=DIRECTION('center_axis',(0.,-1.,0.));
#111210=DIRECTION('ref_axis',(0.,0.,-1.));
#111211=DIRECTION('center_axis',(0.,1.,0.));
#111212=DIRECTION('ref_axis',(0.,0.,1.));
#111213=DIRECTION('',(0.,1.,1.23467863058847E-16));
#111214=DIRECTION('',(0.,-1.,-1.23467863058847E-16));
#111215=DIRECTION('center_axis',(0.,1.23467863058847E-16,-1.));
#111216=DIRECTION('ref_axis',(0.,1.,1.1837531408762E-16));
#111217=DIRECTION('center_axis',(2.62387838037626E-32,-1.17559414210783E-16,
1.));
#111218=DIRECTION('ref_axis',(4.44089209850062E-15,1.,1.17559414210783E-16));
#111219=DIRECTION('center_axis',(-1.,5.01606788234257E-16,0.));
#111220=DIRECTION('ref_axis',(0.,-1.,0.));
#111221=DIRECTION('center_axis',(0.,-1.,0.));
#111222=DIRECTION('ref_axis',(0.,0.,-1.));
#111223=DIRECTION('center_axis',(1.,0.,0.));
#111224=DIRECTION('ref_axis',(0.,-1.,0.));
#111225=DIRECTION('center_axis',(0.,0.,1.));
#111226=DIRECTION('ref_axis',(1.,0.,0.));
#111227=DIRECTION('center_axis',(2.85977186515575E-47,0.,1.));
#111228=DIRECTION('ref_axis',(0.,-1.,0.));
#111229=DIRECTION('',(-2.85977186515575E-47,-5.70122241611331E-32,-1.));
#111230=DIRECTION('center_axis',(0.,0.,1.));
#111231=DIRECTION('ref_axis',(1.,0.,0.));
#111232=DIRECTION('center_axis',(0.,0.496115977596257,-0.868256262156346));
#111233=DIRECTION('ref_axis',(0.,0.868256262156346,0.496115977596257));
#111234=DIRECTION('center_axis',(0.,1.,0.));
#111235=DIRECTION('ref_axis',(0.,0.,1.));
#111236=DIRECTION('center_axis',(0.,0.509034676477531,-0.860746012563181));
#111237=DIRECTION('ref_axis',(0.,0.860746012563181,0.509034676477531));
#111238=DIRECTION('center_axis',(0.,1.9151347174784E-12,-1.));
#111239=DIRECTION('ref_axis',(0.,1.,1.9151347174784E-12));
#111240=DIRECTION('center_axis',(0.,0.,1.));
#111241=DIRECTION('ref_axis',(1.,0.,0.));
#111242=DIRECTION('center_axis',(0.,0.,-1.));
#111243=DIRECTION('ref_axis',(-1.,0.,0.));
#111244=DIRECTION('',(0.,0.,1.));
#111245=DIRECTION('center_axis',(0.,-0.509034676478003,-0.860746012562902));
#111246=DIRECTION('ref_axis',(0.,0.860746012562902,-0.509034676478003));
#111247=DIRECTION('center_axis',(0.,-0.495757141593727,-0.86846120037617));
#111248=DIRECTION('ref_axis',(0.,0.86846120037617,-0.495757141593727));
#111249=DIRECTION('center_axis',(0.,-1.,0.));
#111250=DIRECTION('ref_axis',(0.,0.,-1.));
#111251=DIRECTION('center_axis',(0.,1.,1.23467863058847E-16));
#111252=DIRECTION('ref_axis',(-1.,0.,0.));
#111253=DIRECTION('center_axis',(0.,-1.,0.));
#111254=DIRECTION('ref_axis',(0.,0.,-1.));
#111255=DIRECTION('',(5.01606788234257E-16,1.,1.23467863058847E-16));
#111256=DIRECTION('center_axis',(0.,0.,-1.));
#111257=DIRECTION('ref_axis',(-1.,0.,0.));
#111258=DIRECTION('center_axis',(6.19323182390956E-32,0.,-1.));
#111259=DIRECTION('ref_axis',(0.,1.,0.));
#111260=DIRECTION('',(5.85782591378957E-32,1.23467863058847E-16,-1.));
#111261=DIRECTION('',(-6.19323182390956E-32,-1.23467863058847E-16,1.));
#111262=DIRECTION('center_axis',(0.,-1.,0.));
#111263=DIRECTION('ref_axis',(1.,0.,0.));
#111264=DIRECTION('',(5.01606788234257E-16,1.,0.));
#111265=DIRECTION('center_axis',(-1.,5.01606788234257E-16,0.));
#111266=DIRECTION('ref_axis',(0.,-1.,0.));
#111267=DIRECTION('center_axis',(1.,0.,0.));
#111268=DIRECTION('ref_axis',(0.,-1.,0.));
#111269=DIRECTION('center_axis',(0.,1.,0.));
#111270=DIRECTION('ref_axis',(0.,0.,1.));
#111271=DIRECTION('center_axis',(-1.,0.,0.));
#111272=DIRECTION('ref_axis',(0.,-1.,0.));
#111273=DIRECTION('center_axis',(1.,-5.01606788234257E-16,0.));
#111274=DIRECTION('ref_axis',(5.01606788234257E-16,1.,0.));
#111275=DIRECTION('',(1.,-5.01606788234257E-16,0.));
#111276=DIRECTION('center_axis',(1.,0.,0.));
#111277=DIRECTION('ref_axis',(0.,1.,0.));
#111278=DIRECTION('center_axis',(1.,-5.01606788234257E-16,0.));
#111279=DIRECTION('ref_axis',(0.,1.,0.));
#111280=DIRECTION('center_axis',(0.,-1.,0.));
#111281=DIRECTION('ref_axis',(0.,0.,-1.));
#111282=DIRECTION('center_axis',(-1.,0.,0.));
#111283=DIRECTION('ref_axis',(0.,1.,0.));
#111284=DIRECTION('center_axis',(0.,0.,-1.));
#111285=DIRECTION('ref_axis',(-1.,0.,0.));
#111286=DIRECTION('center_axis',(-2.85977186515575E-47,0.,-1.));
#111287=DIRECTION('ref_axis',(0.,1.,0.));
#111288=DIRECTION('',(2.85977186515575E-47,5.70122241611331E-32,1.));
#111289=DIRECTION('center_axis',(0.,0.,-1.));
#111290=DIRECTION('ref_axis',(-1.,0.,0.));
#111291=DIRECTION('center_axis',(1.,-5.01606788234257E-16,0.));
#111292=DIRECTION('ref_axis',(0.,1.,0.));
#111293=DIRECTION('center_axis',(-1.,0.,0.));
#111294=DIRECTION('ref_axis',(0.,1.,0.));
#111295=DIRECTION('center_axis',(0.,1.,0.));
#111296=DIRECTION('ref_axis',(0.,0.,1.));
#111297=DIRECTION('center_axis',(0.,-1.,0.));
#111298=DIRECTION('ref_axis',(1.,0.,0.));
#111299=DIRECTION('',(-5.01606788234257E-16,-1.,0.));
#111300=DIRECTION('center_axis',(-6.19323182390956E-32,0.,1.));
#111301=DIRECTION('ref_axis',(0.656059028990495,0.754709580222783,4.06312565670714E-32));
#111302=DIRECTION('',(6.19323182390956E-32,1.23467863058847E-16,-1.));
#111303=DIRECTION('center_axis',(0.,0.,-1.));
#111304=DIRECTION('ref_axis',(-1.,0.,0.));
#111305=DIRECTION('',(-5.85782591378957E-32,-1.23467863058847E-16,1.));
#111306=DIRECTION('center_axis',(0.,-1.,0.));
#111307=DIRECTION('ref_axis',(0.,0.,-1.));
#111308=DIRECTION('center_axis',(0.,-1.,-1.23467863058847E-16));
#111309=DIRECTION('ref_axis',(1.,0.,0.));
#111310=DIRECTION('',(-5.01606788234257E-16,-1.,-1.23467863058847E-16));
#111311=DIRECTION('center_axis',(0.,-1.,0.));
#111312=DIRECTION('ref_axis',(0.,0.,-1.));
#111313=DIRECTION('center_axis',(6.20126212581678E-14,-0.483005416470283,
-0.875617363727084));
#111314=DIRECTION('ref_axis',(9.99028424960391E-30,0.875617363727084,-0.483005416470283));
#111315=DIRECTION('center_axis',(6.92361050625672E-15,-0.498898715136586,
-0.866660297945547));
#111316=DIRECTION('ref_axis',(2.25138771964303E-30,0.866660297945547,-0.498898715136586));
#111317=DIRECTION('center_axis',(0.,0.,-1.));
#111318=DIRECTION('ref_axis',(-1.,0.,0.));
#111319=DIRECTION('center_axis',(0.,0.,-1.));
#111320=DIRECTION('ref_axis',(-1.,0.,0.));
#111321=DIRECTION('',(0.,0.,-1.));
#111322=DIRECTION('center_axis',(-1.60982338570647E-12,0.,-1.));
#111323=DIRECTION('ref_axis',(-1.,0.,1.60982338570648E-12));
#111324=DIRECTION('center_axis',(0.,0.498898715136559,-0.866660297945562));
#111325=DIRECTION('ref_axis',(0.,0.866660297945562,0.498898715136559));
#111326=DIRECTION('center_axis',(1.88564486786379E-14,0.483290003559882,
-0.875460320322451));
#111327=DIRECTION('ref_axis',(3.50034193199929E-30,0.875460320322451,0.483290003559882));
#111328=DIRECTION('center_axis',(0.,1.,1.23467863058847E-16));
#111329=DIRECTION('ref_axis',(-1.,0.,0.));
#111330=DIRECTION('center_axis',(0.,1.,0.));
#111331=DIRECTION('ref_axis',(0.,0.,1.));
#111332=DIRECTION('',(5.01606788234257E-16,1.,1.23467863058847E-16));
#111333=DIRECTION('center_axis',(0.,1.,0.));
#111334=DIRECTION('ref_axis',(0.,0.,1.));
#111335=DIRECTION('',(-5.01606788234257E-16,-1.,-1.23467863058847E-16));
#111336=DIRECTION('center_axis',(0.,-1.18842113532926E-16,1.));
#111337=DIRECTION('ref_axis',(0.,1.,1.18842113532926E-16));
#111338=DIRECTION('center_axis',(0.,1.19392659184112E-16,-1.));
#111339=DIRECTION('ref_axis',(0.,1.,1.19392659184112E-16));
#111340=DIRECTION('center_axis',(-1.,5.01606788234257E-16,0.));
#111341=DIRECTION('ref_axis',(0.,-1.,0.));
#111342=DIRECTION('center_axis',(0.,-1.,0.));
#111343=DIRECTION('ref_axis',(0.,0.,-1.));
#111344=DIRECTION('center_axis',(1.,0.,0.));
#111345=DIRECTION('ref_axis',(0.,-1.,0.));
#111346=DIRECTION('center_axis',(0.,0.,1.));
#111347=DIRECTION('ref_axis',(1.,0.,0.));
#111348=DIRECTION('center_axis',(2.85977186515575E-47,0.,1.));
#111349=DIRECTION('ref_axis',(0.,-1.,0.));
#111350=DIRECTION('',(-2.85977186515575E-47,-5.70122241611331E-32,-1.));
#111351=DIRECTION('center_axis',(0.,0.,1.));
#111352=DIRECTION('ref_axis',(1.,0.,0.));
#111353=DIRECTION('center_axis',(0.,0.477110018651003,-0.878843575446074));
#111354=DIRECTION('ref_axis',(0.,0.878843575446074,0.477110018651003));
#111355=DIRECTION('center_axis',(0.,0.460605100635463,-0.887605171947863));
#111356=DIRECTION('ref_axis',(0.,0.887605171947863,0.460605100635463));
#111357=DIRECTION('center_axis',(0.,0.,-1.));
#111358=DIRECTION('ref_axis',(-1.,0.,0.));
#111359=DIRECTION('center_axis',(0.,0.,1.));
#111360=DIRECTION('ref_axis',(1.,0.,0.));
#111361=DIRECTION('center_axis',(0.,0.,-1.));
#111362=DIRECTION('ref_axis',(-1.,0.,0.));
#111363=DIRECTION('',(0.,0.,1.));
#111364=DIRECTION('center_axis',(0.,-0.477110018651024,-0.878843575446063));
#111365=DIRECTION('ref_axis',(0.,0.878843575446063,-0.477110018651024));
#111366=DIRECTION('center_axis',(0.,-0.46043947842117,-0.887691098700016));
#111367=DIRECTION('ref_axis',(0.,0.887691098700016,-0.46043947842117));
#111368=DIRECTION('center_axis',(0.,-0.635616055211064,-0.772005330524295));
#111369=DIRECTION('ref_axis',(0.,0.772005330524295,-0.635616055211064));
#111370=DIRECTION('center_axis',(0.,4.38538094726937E-12,-1.));
#111371=DIRECTION('ref_axis',(0.,1.,4.38538094726937E-12));
#111372=DIRECTION('center_axis',(0.,0.800147951883018,-0.599802680135236));
#111373=DIRECTION('ref_axis',(0.,0.599802680135236,0.800147951883018));
#111374=DIRECTION('center_axis',(1.,0.,0.));
#111375=DIRECTION('ref_axis',(0.,0.919361469586663,0.393413889230479));
#111376=DIRECTION('center_axis',(0.,-1.,-1.23467863058847E-16));
#111377=DIRECTION('ref_axis',(1.,0.,0.));
#111378=DIRECTION('center_axis',(0.,-1.,0.));
#111379=DIRECTION('ref_axis',(0.,0.,-1.));
#111380=DIRECTION('',(-4.38004274807345E-16,-1.,-1.23467863058847E-16));
#111381=DIRECTION('center_axis',(0.,-1.,0.));
#111382=DIRECTION('ref_axis',(0.,0.,-1.));
#111383=DIRECTION('',(4.38004274807345E-16,1.,1.23467863058847E-16));
#111384=DIRECTION('center_axis',(0.,0.,-1.));
#111385=DIRECTION('ref_axis',(-1.,0.,0.));
#111386=DIRECTION('center_axis',(0.,1.07494104808783E-16,-1.));
#111387=DIRECTION('ref_axis',(-1.,0.,0.));
#111388=DIRECTION('',(-1.13659195805196E-16,1.07494104808783E-16,-1.));
#111389=DIRECTION('',(1.13659195805196E-16,-1.07494104808783E-16,1.));
#111390=DIRECTION('center_axis',(0.,1.,0.));
#111391=DIRECTION('ref_axis',(-1.,0.,0.));
#111392=DIRECTION('',(4.38004274807345E-16,1.,0.));
#111393=DIRECTION('center_axis',(0.,1.,0.));
#111394=DIRECTION('ref_axis',(0.,0.,1.));
#111395=DIRECTION('center_axis',(-1.,4.38004274807345E-16,1.13659195805196E-16));
#111396=DIRECTION('ref_axis',(0.,-1.,0.));
#111397=DIRECTION('center_axis',(0.,0.,-1.));
#111398=DIRECTION('ref_axis',(-1.,0.,0.));
#111399=DIRECTION('center_axis',(1.,0.,-1.13659195805196E-16));
#111400=DIRECTION('ref_axis',(0.,-1.,0.));
#111401=DIRECTION('center_axis',(-1.13659195805195E-16,0.,-1.));
#111402=DIRECTION('ref_axis',(-1.,0.,1.13659195805195E-16));
#111403=DIRECTION('center_axis',(0.,0.,-1.));
#111404=DIRECTION('ref_axis',(-1.,0.,0.));
#111405=DIRECTION('',(-1.13659195805196E-16,0.,-1.));
#111406=DIRECTION('center_axis',(0.,-1.,0.));
#111407=DIRECTION('ref_axis',(0.,0.,-1.));
#111408=DIRECTION('center_axis',(-4.38004274807345E-16,-1.,0.));
#111409=DIRECTION('ref_axis',(0.,0.,-1.));
#111410=DIRECTION('center_axis',(0.,1.,1.23467863058847E-16));
#111411=DIRECTION('ref_axis',(-1.,0.,0.));
#111412=DIRECTION('',(-4.38004274807345E-16,-1.,-1.23467863058847E-16));
#111413=DIRECTION('center_axis',(0.,4.9783213633841E-32,-1.));
#111414=DIRECTION('ref_axis',(-1.,0.,0.));
#111415=DIRECTION('',(1.13659195805196E-16,-4.9783213633841E-32,1.));
#111416=DIRECTION('',(-1.13659195805196E-16,4.9783213633841E-32,-1.));
#111417=DIRECTION('center_axis',(0.,-1.,-1.23467863058847E-16));
#111418=DIRECTION('ref_axis',(1.,0.,0.));
#111419=DIRECTION('center_axis',(-4.38004274807345E-16,-1.,0.));
#111420=DIRECTION('ref_axis',(0.,0.,-1.));
#111421=DIRECTION('',(-4.38004274807345E-16,-1.,-1.23467863058847E-16));
#111422=DIRECTION('',(4.38004274807345E-16,1.,1.23467863058847E-16));
#111423=DIRECTION('center_axis',(-1.,4.38004274807345E-16,1.13659195805196E-16));
#111424=DIRECTION('ref_axis',(0.,-1.,0.));
#111425=DIRECTION('center_axis',(0.,-1.,0.));
#111426=DIRECTION('ref_axis',(0.,0.,-1.));
#111427=DIRECTION('center_axis',(-1.,0.,1.13659195805196E-16));
#111428=DIRECTION('ref_axis',(0.,-1.,0.));
#111429=DIRECTION('center_axis',(1.,0.,-1.13659195805196E-16));
#111430=DIRECTION('ref_axis',(0.,-1.,0.));
#111431=DIRECTION('center_axis',(1.,-5.01606788234257E-16,0.));
#111432=DIRECTION('ref_axis',(5.01606788234257E-16,1.,0.));
#111433=DIRECTION('',(1.,-5.01606788234257E-16,0.));
#111434=DIRECTION('center_axis',(1.,0.,1.13659195805196E-16));
#111435=DIRECTION('ref_axis',(0.,1.,0.));
#111436=DIRECTION('center_axis',(0.,1.,1.23467863058847E-16));
#111437=DIRECTION('ref_axis',(-1.,0.,0.));
#111438=DIRECTION('center_axis',(0.,1.,0.));
#111439=DIRECTION('ref_axis',(0.,0.,1.));
#111440=DIRECTION('center_axis',(0.,1.,0.));
#111441=DIRECTION('ref_axis',(0.,0.,1.));
#111442=DIRECTION('',(-5.01606788234257E-16,-1.,-1.23467863058847E-16));
#111443=DIRECTION('center_axis',(0.,0.973635916817664,0.228107653274998));
#111444=DIRECTION('ref_axis',(0.,-0.228107653274998,0.973635916817664));
#111445=DIRECTION('center_axis',(0.,0.489712654585584,0.871883889023499));
#111446=DIRECTION('ref_axis',(0.,-0.871883889023499,0.489712654585584));
#111447=DIRECTION('center_axis',(0.,-1.11022302462516E-13,1.));
#111448=DIRECTION('ref_axis',(0.,-1.,-1.11022302462516E-13));
#111449=DIRECTION('center_axis',(0.,-4.9783213633841E-32,-1.));
#111450=DIRECTION('ref_axis',(-1.,0.,0.));
#111451=DIRECTION('',(1.13659195805196E-16,-4.9783213633841E-32,-1.));
#111452=DIRECTION('center_axis',(0.,0.,-1.));
#111453=DIRECTION('ref_axis',(-1.,0.,0.));
#111454=DIRECTION('center_axis',(-6.24334907322839E-14,0.457979853752065,
-0.888962571516505));
#111455=DIRECTION('ref_axis',(1.27562203883084E-29,0.888962571516505,0.457979853752065));
#111456=DIRECTION('center_axis',(0.,1.,0.));
#111457=DIRECTION('ref_axis',(0.,0.,1.));
#111458=DIRECTION('center_axis',(1.,-5.01606788234257E-16,1.13659195805196E-16));
#111459=DIRECTION('ref_axis',(0.,1.,0.));
#111460=DIRECTION('center_axis',(0.,-1.,0.));
#111461=DIRECTION('ref_axis',(0.,0.,-1.));
#111462=DIRECTION('center_axis',(-1.,0.,-1.13659195805196E-16));
#111463=DIRECTION('ref_axis',(0.,1.,0.));
#111464=DIRECTION('center_axis',(0.,0.,-1.));
#111465=DIRECTION('ref_axis',(-1.,0.,0.));
#111466=DIRECTION('center_axis',(0.,-1.14024448322266E-31,-1.));
#111467=DIRECTION('ref_axis',(-1.,0.,0.));
#111468=DIRECTION('',(-1.13659195805196E-16,1.14024448322266E-31,1.));
#111469=DIRECTION('center_axis',(0.,0.,-1.));
#111470=DIRECTION('ref_axis',(-1.,0.,0.));
#111471=DIRECTION('center_axis',(1.,-5.01606788234257E-16,1.13659195805196E-16));
#111472=DIRECTION('ref_axis',(0.,1.,0.));
#111473=DIRECTION('center_axis',(-1.,0.,-1.13659195805196E-16));
#111474=DIRECTION('ref_axis',(0.,1.,0.));
#111475=DIRECTION('center_axis',(0.,1.,0.));
#111476=DIRECTION('ref_axis',(0.,0.,1.));
#111477=DIRECTION('center_axis',(0.,-1.,0.));
#111478=DIRECTION('ref_axis',(1.,0.,0.));
#111479=DIRECTION('',(-5.01606788234257E-16,-1.,0.));
#111480=DIRECTION('center_axis',(1.13659195805196E-16,0.,-1.));
#111481=DIRECTION('ref_axis',(0.,1.,0.));
#111482=DIRECTION('center_axis',(0.,0.,1.));
#111483=DIRECTION('ref_axis',(1.,0.,0.));
#111484=DIRECTION('',(-1.13659195805196E-16,-1.39441621308911E-16,1.));
#111485=DIRECTION('',(1.13659195805196E-16,1.39441621308911E-16,-1.));
#111486=DIRECTION('center_axis',(0.,0.,1.));
#111487=DIRECTION('ref_axis',(1.,0.,0.));
#111488=DIRECTION('center_axis',(0.,1.23467863058847E-16,-1.));
#111489=DIRECTION('ref_axis',(0.,1.,1.1837531408762E-16));
#111490=DIRECTION('center_axis',(0.,-1.17559414210783E-16,1.));
#111491=DIRECTION('ref_axis',(0.,1.,1.17559414210783E-16));
#111492=DIRECTION('center_axis',(-0.744016723942684,-0.668160994441905,
0.));
#111493=DIRECTION('ref_axis',(0.668160994441905,-0.744016723942684,0.));
#111494=DIRECTION('center_axis',(0.,-1.,-1.23467863058847E-16));
#111495=DIRECTION('ref_axis',(1.,0.,0.));
#111496=DIRECTION('',(5.01606788234257E-16,1.,1.23467863058847E-16));
#111497=DIRECTION('center_axis',(0.,1.,0.));
#111498=DIRECTION('ref_axis',(0.,0.,1.));
#111499=DIRECTION('',(-5.01606788234257E-16,-1.,-1.23467863058847E-16));
#111500=DIRECTION('center_axis',(0.,-1.,-1.23467863058847E-16));
#111501=DIRECTION('ref_axis',(1.,0.,0.));
#111502=DIRECTION('',(5.01606788234257E-16,1.,1.23467863058847E-16));
#111503=DIRECTION('center_axis',(0.,1.,0.));
#111504=DIRECTION('ref_axis',(0.,0.,1.));
#111505=DIRECTION('',(-5.01606788234257E-16,-1.,-1.23467863058847E-16));
#111506=DIRECTION('center_axis',(-0.473027330271494,0.,0.881047753993064));
#111507=DIRECTION('ref_axis',(0.881047753993064,0.,0.473027330271494));
#111508=DIRECTION('center_axis',(-0.452154194923616,0.,0.891939787212666));
#111509=DIRECTION('ref_axis',(0.891939787212666,0.,0.452154194923616));
#111510=DIRECTION('center_axis',(0.,0.,1.));
#111511=DIRECTION('ref_axis',(1.,0.,0.));
#111512=DIRECTION('center_axis',(0.,0.,-1.));
#111513=DIRECTION('ref_axis',(-1.,0.,0.));
#111514=DIRECTION('center_axis',(0.,0.,1.));
#111515=DIRECTION('ref_axis',(1.,0.,0.));
#111516=DIRECTION('',(0.,0.,-1.));
#111517=DIRECTION('center_axis',(0.473027330271434,0.,0.881047753993096));
#111518=DIRECTION('ref_axis',(0.881047753993096,0.,-0.473027330271434));
#111519=DIRECTION('center_axis',(0.,0.,-1.));
#111520=DIRECTION('ref_axis',(-1.,0.,0.));
#111521=DIRECTION('center_axis',(0.,0.,-1.));
#111522=DIRECTION('ref_axis',(-1.,0.,0.));
#111523=DIRECTION('',(0.,0.,1.));
#111524=DIRECTION('center_axis',(0.,0.,-1.));
#111525=DIRECTION('ref_axis',(-1.,0.,0.));
#111526=DIRECTION('center_axis',(4.18005656861882E-16,1.,0.));
#111527=DIRECTION('ref_axis',(-1.,5.9211894646675E-16,0.));
#111528=DIRECTION('center_axis',(-6.93889390390722E-16,-1.,0.));
#111529=DIRECTION('ref_axis',(-1.,6.93889390390722E-16,0.));
#111530=DIRECTION('center_axis',(-1.,0.,0.));
#111531=DIRECTION('ref_axis',(0.,0.,1.));
#111532=DIRECTION('center_axis',(1.,0.,0.));
#111533=DIRECTION('ref_axis',(0.,1.,0.));
#111534=DIRECTION('',(1.,-4.18005656861881E-16,0.));
#111535=DIRECTION('center_axis',(0.,0.,1.));
#111536=DIRECTION('ref_axis',(0.,-1.,0.));
#111537=DIRECTION('center_axis',(0.,0.,1.));
#111538=DIRECTION('ref_axis',(1.,0.,0.));
#111539=DIRECTION('',(0.,-1.23467863058847E-16,1.));
#111540=DIRECTION('',(-5.16102651992463E-32,2.15733828054269E-47,-1.));
#111541=DIRECTION('center_axis',(2.20736287103737E-8,1.,5.31880064827284E-9));
#111542=DIRECTION('ref_axis',(0.999350588281835,-2.18676396770165E-8,-0.0360333415151705));
#111543=DIRECTION('center_axis',(0.452279624303263,0.,0.891876191766604));
#111544=DIRECTION('ref_axis',(0.891876191766604,0.,-0.452279624303263));
#111545=DIRECTION('center_axis',(0.,0.,-1.));
#111546=DIRECTION('ref_axis',(-1.,0.,0.));
#111547=DIRECTION('center_axis',(-0.453032377894844,0.,-0.891494063120413));
#111548=DIRECTION('ref_axis',(-0.891494063120413,0.,0.453032377894844));
#111549=DIRECTION('center_axis',(0.,0.,1.));
#111550=DIRECTION('ref_axis',(1.,0.,0.));
#111551=DIRECTION('center_axis',(0.,0.,-1.));
#111552=DIRECTION('ref_axis',(-1.,0.,0.));
#111553=DIRECTION('',(0.,0.,1.));
#111554=DIRECTION('center_axis',(-0.45303237789485,6.28708721049444E-15,
0.89149406312041));
#111555=DIRECTION('ref_axis',(0.89149406312041,3.90721898735751E-30,0.45303237789485));
#111556=DIRECTION('center_axis',(-0.438728460697982,6.08858048281589E-15,
0.898619684724066));
#111557=DIRECTION('ref_axis',(0.898619684724066,-1.57717257184587E-30,0.438728460697982));
#111558=DIRECTION('center_axis',(1.87037530511154E-7,-0.999999999999982,
4.34091799744689E-8));
#111559=DIRECTION('ref_axis',(0.943089040187619,1.61957742669363E-7,-0.332540316770719));
#111560=DIRECTION('center_axis',(0.,0.,1.));
#111561=DIRECTION('ref_axis',(1.,0.,0.));
#111562=DIRECTION('center_axis',(0.,0.,1.));
#111563=DIRECTION('ref_axis',(0.,-1.,0.));
#111564=DIRECTION('',(5.16102651992463E-32,-2.15733828054269E-47,1.));
#111565=DIRECTION('',(0.,1.23467863058847E-16,-1.));
#111566=DIRECTION('center_axis',(1.,0.,0.));
#111567=DIRECTION('ref_axis',(0.,1.,0.));
#111568=DIRECTION('',(-1.,4.18005656861881E-16,0.));
#111569=DIRECTION('center_axis',(1.,0.,0.));
#111570=DIRECTION('ref_axis',(0.,0.,-1.));
#111571=DIRECTION('center_axis',(-4.18005656861882E-16,-1.,0.));
#111572=DIRECTION('ref_axis',(1.,-2.96059473233375E-16,0.));
#111573=DIRECTION('center_axis',(3.46944695195361E-16,1.,0.));
#111574=DIRECTION('ref_axis',(1.,-3.46944695195361E-16,0.));
#111575=DIRECTION('center_axis',(0.,0.,1.));
#111576=DIRECTION('ref_axis',(1.,0.,0.));
#111577=DIRECTION('center_axis',(0.,0.,1.));
#111578=DIRECTION('ref_axis',(1.,0.,0.));
#111579=DIRECTION('',(0.,0.,-1.));
#111580=DIRECTION('center_axis',(0.,0.,1.));
#111581=DIRECTION('ref_axis',(1.,0.,0.));
#111582=DIRECTION('center_axis',(-0.438793812561498,0.,-0.898587775377423));
#111583=DIRECTION('ref_axis',(-0.898587775377423,0.,0.438793812561498));
#111584=DIRECTION('center_axis',(-4.18005656861882E-16,-1.,0.));
#111585=DIRECTION('ref_axis',(1.,-2.96059473233375E-16,0.));
#111586=DIRECTION('center_axis',(3.46944695195361E-16,1.,0.));
#111587=DIRECTION('ref_axis',(1.,-3.46944695195361E-16,0.));
#111588=DIRECTION('center_axis',(-1.,0.,0.));
#111589=DIRECTION('ref_axis',(0.,0.,1.));
#111590=DIRECTION('center_axis',(-4.33680868994202E-16,-1.,0.));
#111591=DIRECTION('ref_axis',(1.,-4.33680868994202E-16,0.));
#111592=DIRECTION('center_axis',(4.18005656861881E-16,1.,0.));
#111593=DIRECTION('ref_axis',(-1.,4.18005656861881E-16,0.));
#111594=DIRECTION('',(4.18005656861881E-16,1.,0.));
#111595=DIRECTION('center_axis',(4.33680868994202E-16,1.,0.));
#111596=DIRECTION('ref_axis',(-1.,4.33680868994202E-16,0.));
#111597=DIRECTION('center_axis',(4.18005656861882E-16,1.,0.));
#111598=DIRECTION('ref_axis',(-1.,2.96059473233375E-16,0.));
#111599=DIRECTION('center_axis',(1.,0.,0.));
#111600=DIRECTION('ref_axis',(0.,0.,-1.));
#111601=DIRECTION('center_axis',(-3.46944695195361E-16,-1.,0.));
#111602=DIRECTION('ref_axis',(-1.,3.46944695195361E-16,0.));
#111603=DIRECTION('center_axis',(0.,0.,-1.));
#111604=DIRECTION('ref_axis',(-1.,0.,0.));
#111605=DIRECTION('center_axis',(0.,0.,-1.));
#111606=DIRECTION('ref_axis',(-1.,0.,0.));
#111607=DIRECTION('',(0.,0.,1.));
#111608=DIRECTION('center_axis',(0.,0.,-1.));
#111609=DIRECTION('ref_axis',(-1.,0.,0.));
#111610=DIRECTION('center_axis',(4.18005656861882E-16,1.,0.));
#111611=DIRECTION('ref_axis',(-1.,2.96059473233375E-16,0.));
#111612=DIRECTION('center_axis',(-3.46944695195361E-16,-1.,0.));
#111613=DIRECTION('ref_axis',(-1.,3.46944695195361E-16,0.));
#111614=DIRECTION('center_axis',(0.,0.,1.));
#111615=DIRECTION('ref_axis',(0.,-1.,0.));
#111616=DIRECTION('',(-5.16102651992463E-32,2.15733828054269E-47,-1.));
#111617=DIRECTION('center_axis',(0.,0.,-1.));
#111618=DIRECTION('ref_axis',(-1.,0.,0.));
#111619=DIRECTION('',(0.,-1.23467863058847E-16,1.));
#111620=DIRECTION('center_axis',(2.74310936473999E-7,0.99999999999996,6.28664506624393E-8));
#111621=DIRECTION('ref_axis',(-0.661953171810168,1.34459748483106E-7,0.74954519432149));
#111622=DIRECTION('center_axis',(0.434261044064412,-6.0265826227258E-15,
-0.90078707007155));
#111623=DIRECTION('ref_axis',(-0.90078707007155,1.10802520916158E-30,-0.434261044064412));
#111624=DIRECTION('center_axis',(0.445417151990703,0.,-0.895323159933044));
#111625=DIRECTION('ref_axis',(-0.895323159933044,0.,-0.445417151990703));
#111626=DIRECTION('center_axis',(0.,0.,-1.));
#111627=DIRECTION('ref_axis',(-1.,0.,0.));
#111628=DIRECTION('center_axis',(0.,0.,-1.));
#111629=DIRECTION('ref_axis',(-1.,0.,0.));
#111630=DIRECTION('',(0.,0.,-1.));
#111631=DIRECTION('center_axis',(0.,0.,-1.));
#111632=DIRECTION('ref_axis',(-1.,0.,0.));
#111633=DIRECTION('center_axis',(0.44541715199073,0.,0.895323159933031));
#111634=DIRECTION('ref_axis',(0.895323159933031,0.,-0.44541715199073));
#111635=DIRECTION('center_axis',(0.434307547312743,0.,0.900764649809921));
#111636=DIRECTION('ref_axis',(0.900764649809921,0.,-0.434307547312743));
#111637=DIRECTION('center_axis',(0.,0.,-1.));
#111638=DIRECTION('ref_axis',(-1.,0.,0.));
#111639=DIRECTION('center_axis',(-0.431774610811204,0.,-0.901981532770396));
#111640=DIRECTION('ref_axis',(-0.901981532770396,0.,0.431774610811205));
#111641=DIRECTION('center_axis',(0.,0.,1.));
#111642=DIRECTION('ref_axis',(1.,0.,0.));
#111643=DIRECTION('center_axis',(0.,0.,-1.));
#111644=DIRECTION('ref_axis',(-1.,0.,0.));
#111645=DIRECTION('',(0.,0.,1.));
#111646=DIRECTION('center_axis',(0.43177461081284,0.,-0.901981532769613));
#111647=DIRECTION('ref_axis',(-0.901981532769613,0.,-0.43177461081284));
#111648=DIRECTION('center_axis',(0.427007199080172,0.,-0.904248224733511));
#111649=DIRECTION('ref_axis',(-0.904248224733511,0.,-0.427007199080172));
#111650=DIRECTION('center_axis',(0.,0.,-1.));
#111651=DIRECTION('ref_axis',(-1.,0.,0.));
#111652=DIRECTION('center_axis',(0.,-1.,0.));
#111653=DIRECTION('ref_axis',(0.979094017787432,0.,0.203408220907771));
#111654=DIRECTION('center_axis',(0.,0.,1.));
#111655=DIRECTION('ref_axis',(0.,-1.,0.));
#111656=DIRECTION('',(0.,1.23467863058847E-16,-1.));
#111657=DIRECTION('',(5.16102651992463E-32,-2.15733828054269E-47,1.));
#111658=DIRECTION('center_axis',(0.,0.,-1.));
#111659=DIRECTION('ref_axis',(-1.,0.,0.));
#111660=DIRECTION('center_axis',(-0.427024288778512,0.,-0.904240154380022));
#111661=DIRECTION('ref_axis',(-0.904240154380022,0.,0.427024288778512));
#111662=DIRECTION('center_axis',(0.,0.,1.));
#111663=DIRECTION('ref_axis',(1.,0.,0.));
#111664=DIRECTION('center_axis',(0.,0.,-1.));
#111665=DIRECTION('ref_axis',(-1.,0.,0.));
#111666=DIRECTION('',(0.,0.,1.));
#111667=DIRECTION('',(0.,0.,-1.));
#111668=DIRECTION('center_axis',(1.,-4.18005656861882E-16,0.));
#111669=DIRECTION('ref_axis',(-4.18005656861882E-16,-1.,0.));
#111670=DIRECTION('',(0.,0.,-1.));
#111671=DIRECTION('center_axis',(0.,0.,-1.));
#111672=DIRECTION('ref_axis',(-1.,0.,0.));
#111673=DIRECTION('center_axis',(0.,0.,-1.));
#111674=DIRECTION('ref_axis',(-1.,0.,0.));
#111675=DIRECTION('',(0.,0.,1.));
#111676=DIRECTION('center_axis',(0.,0.,-1.));
#111677=DIRECTION('ref_axis',(-1.,0.,0.));
#111678=DIRECTION('center_axis',(0.,0.,1.));
#111679=DIRECTION('ref_axis',(0.,-1.,0.));
#111680=DIRECTION('',(-5.16102651992463E-32,2.15733828054269E-47,-1.));
#111681=DIRECTION('center_axis',(0.,0.,-1.));
#111682=DIRECTION('ref_axis',(-1.,0.,0.));
#111683=DIRECTION('',(0.,-1.23467863058847E-16,1.));
#111684=DIRECTION('center_axis',(0.,1.,0.));
#111685=DIRECTION('ref_axis',(0.977956433447826,0.,0.208809037826448));
#111686=DIRECTION('center_axis',(0.424945455576639,-5.89730286238743E-15,
-0.905218956819157));
#111687=DIRECTION('ref_axis',(-0.905218956819157,3.24660130849529E-29,-0.424945455576639));
#111688=DIRECTION('center_axis',(0.427566573571518,-4.42475067662884E-14,
-0.903983863331814));
#111689=DIRECTION('ref_axis',(-0.903983863331814,-2.72495173441675E-28,
-0.427566573571518));
#111690=DIRECTION('center_axis',(0.,0.,-1.));
#111691=DIRECTION('ref_axis',(-1.,0.,0.));
#111692=DIRECTION('center_axis',(0.,0.,-1.));
#111693=DIRECTION('ref_axis',(-1.,0.,0.));
#111694=DIRECTION('',(0.,0.,-1.));
#111695=DIRECTION('center_axis',(0.,0.,-1.));
#111696=DIRECTION('ref_axis',(-1.,0.,0.));
#111697=DIRECTION('center_axis',(-0.427566573571512,0.,-0.903983863331817));
#111698=DIRECTION('ref_axis',(-0.903983863331817,0.,0.427566573571512));
#111699=DIRECTION('center_axis',(-0.424954451342053,-5.8974277037113E-15,
-0.905214733797774));
#111700=DIRECTION('ref_axis',(-0.905214733797774,1.745344269554E-30,0.424954451342053));
#111701=DIRECTION('center_axis',(-0.00252749518976105,-0.999981529958737,
-0.00552734198781944));
#111702=DIRECTION('ref_axis',(0.976364750278453,-0.00127318089754541,-0.216125550141799));
#111703=DIRECTION('center_axis',(0.,0.,-1.));
#111704=DIRECTION('ref_axis',(-1.,0.,0.));
#111705=DIRECTION('center_axis',(-0.422759120858735,0.,-0.906242090023824));
#111706=DIRECTION('ref_axis',(-0.906242090023824,0.,0.422759120858735));
#111707=DIRECTION('center_axis',(0.,1.,0.));
#111708=DIRECTION('ref_axis',(0.976404651458723,0.,-0.21594896760524));
#111709=DIRECTION('center_axis',(0.,0.,1.));
#111710=DIRECTION('ref_axis',(1.,0.,0.));
#111711=DIRECTION('center_axis',(0.,0.,-1.));
#111712=DIRECTION('ref_axis',(-1.,0.,0.));
#111713=DIRECTION('',(0.,0.,1.));
#111714=DIRECTION('center_axis',(0.422759120858763,0.,-0.906242090023811));
#111715=DIRECTION('ref_axis',(-0.906242090023811,0.,-0.422759120858763));
#111716=DIRECTION('center_axis',(0.,1.,0.));
#111717=DIRECTION('ref_axis',(0.976137352210977,0.,0.217154022800736));
#111718=DIRECTION('center_axis',(0.422683101271474,0.,-0.906277549043078));
#111719=DIRECTION('ref_axis',(-0.906277549043078,0.,-0.422683101271474));
#111720=DIRECTION('center_axis',(0.,0.,-1.));
#111721=DIRECTION('ref_axis',(-1.,0.,0.));
#111722=DIRECTION('center_axis',(0.,-1.,0.));
#111723=DIRECTION('ref_axis',(0.976204192855077,0.,0.216853346416809));
#111724=DIRECTION('center_axis',(0.,0.,1.));
#111725=DIRECTION('ref_axis',(0.,-1.,0.));
#111726=DIRECTION('',(0.,1.23467863058847E-16,-1.));
#111727=DIRECTION('',(5.16102651992463E-32,-2.15733828054269E-47,1.));
#111728=DIRECTION('center_axis',(4.44089209850062E-13,0.,-1.));
#111729=DIRECTION('ref_axis',(-1.,0.,-4.44089209850062E-13));
#111730=DIRECTION('center_axis',(-0.422683349901129,0.,-0.906277433083468));
#111731=DIRECTION('ref_axis',(-0.906277433083468,0.,0.422683349901129));
#111732=DIRECTION('center_axis',(0.,0.,1.));
#111733=DIRECTION('ref_axis',(1.,0.,0.));
#111734=DIRECTION('center_axis',(0.,0.,-1.));
#111735=DIRECTION('ref_axis',(-1.,0.,0.));
#111736=DIRECTION('',(0.,0.,1.));
#111737=DIRECTION('',(0.,0.,-1.));
#111738=DIRECTION('center_axis',(1.,-4.18005656861882E-16,0.));
#111739=DIRECTION('ref_axis',(-4.18005656861882E-16,-1.,0.));
#111740=DIRECTION('center_axis',(1.,0.,0.));
#111741=DIRECTION('ref_axis',(0.,-0.00331492178303338,0.999994505631692));
#111742=DIRECTION('',(0.,0.,-1.));
#111743=DIRECTION('center_axis',(0.,0.,-1.));
#111744=DIRECTION('ref_axis',(-1.,0.,0.));
#111745=DIRECTION('center_axis',(0.,0.,-1.));
#111746=DIRECTION('ref_axis',(-1.,0.,0.));
#111747=DIRECTION('',(0.,0.,1.));
#111748=DIRECTION('center_axis',(0.,-5.55111512312578E-14,-1.));
#111749=DIRECTION('ref_axis',(0.,1.,-5.55111512312578E-14));
#111750=DIRECTION('center_axis',(0.,0.,1.));
#111751=DIRECTION('ref_axis',(0.,-1.,0.));
#111752=DIRECTION('',(-5.16102651992463E-32,2.15733828054269E-47,-1.));
#111753=DIRECTION('center_axis',(0.,0.,-1.));
#111754=DIRECTION('ref_axis',(-1.,0.,0.));
#111755=DIRECTION('',(0.,-1.23467863058847E-16,1.));
#111756=DIRECTION('center_axis',(0.,1.,0.));
#111757=DIRECTION('ref_axis',(0.976488023107232,0.,0.21557166030842));
#111758=DIRECTION('center_axis',(0.422711298276089,5.8662977014411E-15,
-0.906264397573767));
#111759=DIRECTION('ref_axis',(-0.906264397573767,-1.10286040862995E-31,
-0.422711298276089));
#111760=DIRECTION('center_axis',(0.422820321921648,5.86781070846046E-15,
-0.906213537401685));
#111761=DIRECTION('ref_axis',(-0.906213537401684,-2.1653413854129E-31,-0.422820321921648));
#111762=DIRECTION('center_axis',(-1.03393670705645E-14,-1.,-1.1317479530313E-15));
#111763=DIRECTION('ref_axis',(0.976392755984668,-1.03397437742268E-14,0.216002745493349));
#111764=DIRECTION('center_axis',(0.,0.,-1.));
#111765=DIRECTION('ref_axis',(-1.,0.,0.));
#111766=DIRECTION('center_axis',(0.,0.,-1.));
#111767=DIRECTION('ref_axis',(-1.,0.,0.));
#111768=DIRECTION('',(0.,0.,-1.));
#111769=DIRECTION('center_axis',(0.,0.,-1.));
#111770=DIRECTION('ref_axis',(-1.,0.,0.));
#111771=DIRECTION('center_axis',(0.,-1.,0.));
#111772=DIRECTION('ref_axis',(0.976124389191106,0.,-0.217212285164286));
#111773=DIRECTION('center_axis',(-0.422820321921619,0.,-0.906213537401698));
#111774=DIRECTION('ref_axis',(-0.906213537401698,0.,0.422820321921619));
#111775=DIRECTION('center_axis',(-0.00301385145090742,0.999973599361283,
-0.0066119044059187));
#111776=DIRECTION('ref_axis',(0.976009136147408,0.0015020133499738,-0.21772439025678));
#111777=DIRECTION('center_axis',(-0.422711655064036,5.86630265286877E-15,
-0.906264231156137));
#111778=DIRECTION('ref_axis',(-0.906264231156137,8.13850067779198E-31,0.422711655064036));
#111779=DIRECTION('center_axis',(0.,0.,-1.));
#111780=DIRECTION('ref_axis',(-1.,0.,0.));
#111781=DIRECTION('center_axis',(-0.427895220819097,0.,-0.903828346534991));
#111782=DIRECTION('ref_axis',(-0.903828346534991,0.,0.427895220819097));
#111783=DIRECTION('center_axis',(0.,0.,1.));
#111784=DIRECTION('ref_axis',(1.,0.,0.));
#111785=DIRECTION('center_axis',(0.,0.,-1.));
#111786=DIRECTION('ref_axis',(-1.,0.,0.));
#111787=DIRECTION('',(0.,0.,1.));
#111788=DIRECTION('center_axis',(0.427895220819092,0.,-0.903828346534994));
#111789=DIRECTION('ref_axis',(-0.903828346534994,0.,-0.427895220819092));
#111790=DIRECTION('center_axis',(0.425103688199478,0.,-0.905144659310986));
#111791=DIRECTION('ref_axis',(-0.905144659310986,0.,-0.425103688199478));
#111792=DIRECTION('center_axis',(0.,0.,-1.));
#111793=DIRECTION('ref_axis',(-1.,0.,0.));
#111794=DIRECTION('center_axis',(0.,-1.,0.));
#111795=DIRECTION('ref_axis',(0.977785987053698,0.,0.209605733512769));
#111796=DIRECTION('center_axis',(0.,0.,1.));
#111797=DIRECTION('ref_axis',(0.,-1.,0.));
#111798=DIRECTION('',(0.,1.23467863058847E-16,-1.));
#111799=DIRECTION('',(5.16102651992463E-32,-2.15733828054269E-47,1.));
#111800=DIRECTION('center_axis',(0.,0.,1.));
#111801=DIRECTION('ref_axis',(1.,0.,0.));
#111802=DIRECTION('center_axis',(-0.425113301005477,0.,-0.905140144567805));
#111803=DIRECTION('ref_axis',(-0.905140144567805,0.,0.425113301005477));
#111804=DIRECTION('center_axis',(0.,0.,1.));
#111805=DIRECTION('ref_axis',(1.,0.,0.));
#111806=DIRECTION('',(0.,0.,-1.));
#111807=DIRECTION('center_axis',(0.,0.,1.));
#111808=DIRECTION('ref_axis',(1.,0.,0.));
#111809=DIRECTION('',(0.,0.,1.));
#111810=DIRECTION('center_axis',(1.,-4.18005656861882E-16,0.));
#111811=DIRECTION('ref_axis',(-4.18005656861882E-16,-1.,0.));
#111812=DIRECTION('',(0.,0.,-1.));
#111813=DIRECTION('center_axis',(0.,0.,-1.));
#111814=DIRECTION('ref_axis',(-1.,0.,0.));
#111815=DIRECTION('center_axis',(0.,0.,-1.));
#111816=DIRECTION('ref_axis',(-1.,0.,0.));
#111817=DIRECTION('',(0.,0.,1.));
#111818=DIRECTION('center_axis',(0.,0.,-1.));
#111819=DIRECTION('ref_axis',(-1.,0.,0.));
#111820=DIRECTION('center_axis',(0.,0.,1.));
#111821=DIRECTION('ref_axis',(0.,-1.,0.));
#111822=DIRECTION('',(-5.16102651992463E-32,2.15733828054269E-47,-1.));
#111823=DIRECTION('center_axis',(0.,0.,-1.));
#111824=DIRECTION('ref_axis',(-1.,0.,0.));
#111825=DIRECTION('',(0.,-1.23467863058847E-16,1.));
#111826=DIRECTION('center_axis',(4.4207807240187E-7,0.999999999999897,9.93087227439201E-8));
#111827=DIRECTION('ref_axis',(-0.291484561047742,3.38626384751091E-8,0.956575533175924));
#111828=DIRECTION('center_axis',(0.42722596110711,0.,-0.904144887811741));
#111829=DIRECTION('ref_axis',(-0.904144887811741,0.,-0.42722596110711));
#111830=DIRECTION('center_axis',(0.432211889750627,1.1996289787948E-14,
-0.901772078941343));
#111831=DIRECTION('ref_axis',(-0.901772078941343,7.55282579686682E-29,-0.432211889750627));
#111832=DIRECTION('center_axis',(0.,0.,-1.));
#111833=DIRECTION('ref_axis',(-1.,0.,0.));
#111834=DIRECTION('center_axis',(0.,0.,-1.));
#111835=DIRECTION('ref_axis',(-1.,0.,0.));
#111836=DIRECTION('',(0.,0.,-1.));
#111837=DIRECTION('center_axis',(0.,0.,-1.));
#111838=DIRECTION('ref_axis',(-1.,0.,0.));
#111839=DIRECTION('center_axis',(-0.432211889750627,-1.54100116546287E-13,
-0.901772078941343));
#111840=DIRECTION('ref_axis',(-0.901772078941343,9.67025840811756E-28,0.432211889750627));
#111841=DIRECTION('center_axis',(-0.427243916491378,0.,-0.904136403327014));
#111842=DIRECTION('ref_axis',(-0.904136403327014,0.,0.427243916491378));
#111843=DIRECTION('center_axis',(0.,0.,-1.));
#111844=DIRECTION('ref_axis',(-1.,0.,0.));
#111845=DIRECTION('center_axis',(-0.446066534667472,0.,-0.894999802597606));
#111846=DIRECTION('ref_axis',(-0.894999802597606,0.,0.446066534667472));
#111847=DIRECTION('center_axis',(0.,0.,1.));
#111848=DIRECTION('ref_axis',(1.,0.,0.));
#111849=DIRECTION('center_axis',(0.,0.,-1.));
#111850=DIRECTION('ref_axis',(-1.,0.,0.));
#111851=DIRECTION('',(0.,0.,1.));
#111852=DIRECTION('center_axis',(-0.446066534667672,-4.96824693939355E-14,
0.894999802597506));
#111853=DIRECTION('ref_axis',(0.894999802597506,-9.63397512853712E-30,0.446066534667672));
#111854=DIRECTION('center_axis',(-0.434629636675507,0.,0.90060928205483));
#111855=DIRECTION('ref_axis',(0.90060928205483,0.,0.434629636675507));
#111856=DIRECTION('center_axis',(2.67568127619604E-7,-0.999999999999962,
6.13851297333844E-8));
#111857=DIRECTION('ref_axis',(0.690330186704652,1.40298554221222E-7,-0.723494459774435));
#111858=DIRECTION('center_axis',(0.,0.,1.));
#111859=DIRECTION('ref_axis',(1.,0.,0.));
#111860=DIRECTION('center_axis',(0.,0.,1.));
#111861=DIRECTION('ref_axis',(0.,-1.,0.));
#111862=DIRECTION('',(5.16102651992463E-32,-2.15733828054269E-47,1.));
#111863=DIRECTION('',(0.,1.23467863058847E-16,-1.));
#111864=DIRECTION('center_axis',(-4.18005656861882E-16,-1.,0.));
#111865=DIRECTION('ref_axis',(1.,0.,0.));
#111866=DIRECTION('center_axis',(0.,1.,0.));
#111867=DIRECTION('ref_axis',(1.,0.,0.));
#111868=DIRECTION('center_axis',(0.,0.,1.));
#111869=DIRECTION('ref_axis',(1.,0.,0.));
#111870=DIRECTION('center_axis',(0.,0.,1.));
#111871=DIRECTION('ref_axis',(1.,0.,0.));
#111872=DIRECTION('',(0.,0.,-1.));
#111873=DIRECTION('center_axis',(0.,0.,1.));
#111874=DIRECTION('ref_axis',(1.,0.,0.));
#111875=DIRECTION('center_axis',(-0.434677673768106,0.,-0.900586098009262));
#111876=DIRECTION('ref_axis',(-0.900586098009262,0.,0.434677673768106));
#111877=DIRECTION('center_axis',(-4.18005656861882E-16,-1.,0.));
#111878=DIRECTION('ref_axis',(1.,0.,0.));
#111879=DIRECTION('center_axis',(0.,1.,0.));
#111880=DIRECTION('ref_axis',(1.,0.,0.));
#111881=DIRECTION('center_axis',(-1.,0.,0.));
#111882=DIRECTION('ref_axis',(0.,0.,1.));
#111883=DIRECTION('center_axis',(0.,-1.,0.));
#111884=DIRECTION('ref_axis',(1.,0.,0.));
#111885=DIRECTION('center_axis',(4.18005656861881E-16,1.,0.));
#111886=DIRECTION('ref_axis',(-1.,4.18005656861881E-16,0.));
#111887=DIRECTION('',(4.18005656861881E-16,1.,0.));
#111888=DIRECTION('center_axis',(0.,1.,0.));
#111889=DIRECTION('ref_axis',(-1.,0.,0.));
#111890=DIRECTION('center_axis',(4.18005656861882E-16,1.,0.));
#111891=DIRECTION('ref_axis',(-1.,0.,0.));
#111892=DIRECTION('center_axis',(1.,0.,0.));
#111893=DIRECTION('ref_axis',(0.,0.,-1.));
#111894=DIRECTION('center_axis',(0.,-1.,0.));
#111895=DIRECTION('ref_axis',(-1.,0.,0.));
#111896=DIRECTION('center_axis',(0.,0.,-1.));
#111897=DIRECTION('ref_axis',(-1.,0.,0.));
#111898=DIRECTION('center_axis',(0.,0.,-1.));
#111899=DIRECTION('ref_axis',(-1.,0.,0.));
#111900=DIRECTION('',(0.,0.,1.));
#111901=DIRECTION('center_axis',(0.,0.,-1.));
#111902=DIRECTION('ref_axis',(-1.,0.,0.));
#111903=DIRECTION('center_axis',(4.18005656861882E-16,1.,0.));
#111904=DIRECTION('ref_axis',(-1.,0.,0.));
#111905=DIRECTION('center_axis',(0.,-1.,0.));
#111906=DIRECTION('ref_axis',(-1.,0.,0.));
#111907=DIRECTION('center_axis',(-1.,0.,0.));
#111908=DIRECTION('ref_axis',(0.,0.,1.));
#111909=DIRECTION('center_axis',(1.,0.,0.));
#111910=DIRECTION('ref_axis',(0.,1.,0.));
#111911=DIRECTION('',(1.,-4.18005656861881E-16,0.));
#111912=DIRECTION('center_axis',(0.,0.,1.));
#111913=DIRECTION('ref_axis',(0.,-1.,0.));
#111914=DIRECTION('',(-5.16102651992463E-32,2.15733828054269E-47,-1.));
#111915=DIRECTION('center_axis',(0.,0.,-1.));
#111916=DIRECTION('ref_axis',(-1.,0.,0.));
#111917=DIRECTION('',(0.,-1.23467863058847E-16,1.));
#111918=DIRECTION('center_axis',(1.7739481101835E-7,0.999999999999983,4.12226225097212E-8));
#111919=DIRECTION('ref_axis',(0.952173814460364,-1.56314836594747E-7,-0.30555691295727));
#111920=DIRECTION('center_axis',(0.439171790863778,6.20608564480709E-14,
-0.898403104463415));
#111921=DIRECTION('ref_axis',(-0.898403104463415,-1.60954096059593E-29,
-0.439171790863778));
#111922=DIRECTION('center_axis',(0.453758938247726,6.29717026090114E-15,
-0.891124472764774));
#111923=DIRECTION('ref_axis',(-0.891124472764774,1.97126653384901E-30,-0.453758938247726));
#111924=DIRECTION('center_axis',(0.,0.,-1.));
#111925=DIRECTION('ref_axis',(-1.,0.,0.));
#111926=DIRECTION('center_axis',(0.,0.,-1.));
#111927=DIRECTION('ref_axis',(-1.,0.,0.));
#111928=DIRECTION('',(0.,0.,-1.));
#111929=DIRECTION('center_axis',(0.,0.,-1.));
#111930=DIRECTION('ref_axis',(-1.,0.,0.));
#111931=DIRECTION('center_axis',(0.453758938247698,0.,0.891124472764788));
#111932=DIRECTION('ref_axis',(0.891124472764788,0.,-0.453758938247698));
#111933=DIRECTION('center_axis',(0.439239043992112,0.,0.898370225593489));
#111934=DIRECTION('ref_axis',(0.898370225593489,0.,-0.439239043992112));
#111935=DIRECTION('center_axis',(-4.18005656861882E-16,-1.,0.));
#111936=DIRECTION('ref_axis',(1.,0.,0.));
#111937=DIRECTION('center_axis',(1.,0.,0.));
#111938=DIRECTION('ref_axis',(0.,0.,-1.));
#111939=DIRECTION('center_axis',(0.,1.,0.));
#111940=DIRECTION('ref_axis',(1.,0.,0.));
#111941=DIRECTION('center_axis',(0.,0.,1.));
#111942=DIRECTION('ref_axis',(1.,0.,0.));
#111943=DIRECTION('center_axis',(0.,0.,1.));
#111944=DIRECTION('ref_axis',(1.,0.,0.));
#111945=DIRECTION('',(0.,0.,-1.));
#111946=DIRECTION('center_axis',(0.,0.,1.));
#111947=DIRECTION('ref_axis',(1.,0.,0.));
#111948=DIRECTION('center_axis',(0.452924541251067,1.8658316499269E-14,
0.891548854484436));
#111949=DIRECTION('ref_axis',(0.891548854484436,-1.10243984483832E-29,-0.452924541251067));
#111950=DIRECTION('center_axis',(0.473890079491223,-6.57654596740749E-15,
0.880584006531917));
#111951=DIRECTION('ref_axis',(0.880584006531917,-2.59399416170326E-30,-0.473890079491223));
#111952=DIRECTION('center_axis',(0.,0.,1.));
#111953=DIRECTION('ref_axis',(1.,0.,0.));
#111954=DIRECTION('center_axis',(0.,0.,1.));
#111955=DIRECTION('ref_axis',(1.,0.,0.));
#111956=DIRECTION('',(0.,0.,1.));
#111957=DIRECTION('center_axis',(0.,0.,1.));
#111958=DIRECTION('ref_axis',(1.,0.,0.));
#111959=DIRECTION('center_axis',(-0.473890079491229,6.57654596740791E-15,
0.880584006531913));
#111960=DIRECTION('ref_axis',(0.880584006531913,4.48746122839123E-29,0.473890079491229));
#111961=DIRECTION('center_axis',(-0.452796108559755,6.28380831479673E-15,
0.891614089207401));
#111962=DIRECTION('ref_axis',(0.891614089207401,-8.65475050140857E-31,0.452796108559755));
#111963=DIRECTION('center_axis',(2.01185813448576E-8,-1.,4.8563457570887E-9));
#111964=DIRECTION('ref_axis',(0.999508172280242,1.99563942576545E-8,-0.031359425138364));
#111965=DIRECTION('center_axis',(0.,0.,1.));
#111966=DIRECTION('ref_axis',(1.,0.,0.));
#111967=DIRECTION('center_axis',(0.,0.,1.));
#111968=DIRECTION('ref_axis',(0.,-1.,0.));
#111969=DIRECTION('',(5.16102651992463E-32,-2.15733828054269E-47,1.));
#111970=DIRECTION('',(0.,1.23467863058847E-16,-1.));
#111971=DIRECTION('center_axis',(1.,0.,0.));
#111972=DIRECTION('ref_axis',(0.,1.,0.));
#111973=DIRECTION('',(-1.,4.18005656861881E-16,0.));
#111974=DIRECTION('center_axis',(-4.18005656861882E-16,-1.,0.));
#111975=DIRECTION('ref_axis',(1.,0.,0.));
#111976=DIRECTION('center_axis',(0.,1.,0.));
#111977=DIRECTION('ref_axis',(1.,0.,0.));
#111978=DIRECTION('center_axis',(-1.,0.,0.));
#111979=DIRECTION('ref_axis',(0.,0.,1.));
#111980=DIRECTION('center_axis',(0.,-1.,0.));
#111981=DIRECTION('ref_axis',(1.,0.,0.));
#111982=DIRECTION('center_axis',(4.18005656861881E-16,1.,0.));
#111983=DIRECTION('ref_axis',(-1.,4.18005656861881E-16,0.));
#111984=DIRECTION('',(4.18005656861881E-16,1.,0.));
#111985=DIRECTION('center_axis',(0.,1.,0.));
#111986=DIRECTION('ref_axis',(-1.,0.,0.));
#111987=DIRECTION('center_axis',(4.18005656861882E-16,1.,0.));
#111988=DIRECTION('ref_axis',(-1.,0.,0.));
#111989=DIRECTION('center_axis',(1.,0.,0.));
#111990=DIRECTION('ref_axis',(0.,0.,-1.));
#111991=DIRECTION('center_axis',(0.,-1.,0.));
#111992=DIRECTION('ref_axis',(-1.,0.,0.));
#111993=DIRECTION('center_axis',(-4.18005656861882E-16,-1.,0.));
#111994=DIRECTION('ref_axis',(1.,-5.9211894646675E-16,0.));
#111995=DIRECTION('center_axis',(6.93889390390722E-16,1.,0.));
#111996=DIRECTION('ref_axis',(1.,-6.93889390390722E-16,0.));
#111997=DIRECTION('center_axis',(-1.,0.,0.));
#111998=DIRECTION('ref_axis',(0.,0.,1.));
#111999=DIRECTION('center_axis',(-5.78241158658935E-16,-1.,0.));
#112000=DIRECTION('ref_axis',(1.,-5.78241158658935E-16,0.));
#112001=DIRECTION('center_axis',(4.18005656861881E-16,1.,0.));
#112002=DIRECTION('ref_axis',(-1.,4.18005656861881E-16,0.));
#112003=DIRECTION('',(4.18005656861881E-16,1.,0.));
#112004=DIRECTION('center_axis',(5.78241158658935E-16,1.,0.));
#112005=DIRECTION('ref_axis',(-1.,5.78241158658935E-16,0.));
#112006=DIRECTION('center_axis',(4.18005656861882E-16,1.,0.));
#112007=DIRECTION('ref_axis',(-1.,5.9211894646675E-16,0.));
#112008=DIRECTION('center_axis',(1.,0.,0.));
#112009=DIRECTION('ref_axis',(0.,0.,-1.));
#112010=DIRECTION('center_axis',(-6.93889390390722E-16,-1.,0.));
#112011=DIRECTION('ref_axis',(-1.,6.93889390390722E-16,0.));
#112012=DIRECTION('center_axis',(0.,0.424147858891027,0.905592951495404));
#112013=DIRECTION('ref_axis',(0.,-0.905592951495404,0.424147858891027));
#112014=DIRECTION('center_axis',(0.,0.425268108821871,0.905067420482623));
#112015=DIRECTION('ref_axis',(0.,-0.905067420482623,0.425268108821871));
#112016=DIRECTION('center_axis',(0.,0.429430624963615,0.903099849597684));
#112017=DIRECTION('ref_axis',(0.,-0.903099849597684,0.429430624963615));
#112018=DIRECTION('center_axis',(0.,0.434584798675586,0.900630919278314));
#112019=DIRECTION('ref_axis',(0.,-0.900630919278314,0.434584798675586));
#112020=DIRECTION('center_axis',(0.,0.440696042277477,0.89765639212394));
#112021=DIRECTION('ref_axis',(0.,-0.89765639212394,0.440696042277477));
#112022=DIRECTION('center_axis',(-0.998868362320773,-0.00644281759551,-0.0471220209249073));
#112023=DIRECTION('ref_axis',(0.0465471507530001,-0.335857313107545,-0.940762046422451));
#112024=DIRECTION('center_axis',(0.,0.425920949091245,0.904760379948864));
#112025=DIRECTION('ref_axis',(0.,-0.904760379948864,0.425920949091245));
#112026=DIRECTION('center_axis',(0.,0.432834338283548,0.901473480254768));
#112027=DIRECTION('ref_axis',(0.,-0.901473480254768,0.432834338283548));
#112028=DIRECTION('center_axis',(-1.85986770746484E-14,0.444295746197836,
0.895880176089698));
#112029=DIRECTION('ref_axis',(-8.37014173169963E-31,-0.895880176089698,
0.444295746197836));
#112030=DIRECTION('center_axis',(0.,0.457805146562934,0.88905255625328));
#112031=DIRECTION('ref_axis',(0.,-0.88905255625328,0.457805146562934));
#112032=DIRECTION('center_axis',(0.,0.,1.));
#112033=DIRECTION('ref_axis',(1.,0.,0.));
#112034=DIRECTION('center_axis',(0.,8.19208946723988E-32,1.));
#112035=DIRECTION('ref_axis',(1.,0.,0.));
#112036=DIRECTION('',(-1.87032180698308E-16,8.19208946723987E-32,1.));
#112037=DIRECTION('center_axis',(0.,0.,1.));
#112038=DIRECTION('ref_axis',(1.,0.,0.));
#112039=DIRECTION('',(1.87032180698308E-16,-8.19208946723987E-32,-1.));
#112040=DIRECTION('center_axis',(1.,0.,1.87032180698308E-16));
#112041=DIRECTION('ref_axis',(0.,0.,-1.));
#112042=DIRECTION('center_axis',(0.,0.,1.));
#112043=DIRECTION('ref_axis',(1.,0.,0.));
#112044=DIRECTION('center_axis',(-1.,0.,0.));
#112045=DIRECTION('ref_axis',(0.,0.,-1.));
#112046=DIRECTION('center_axis',(0.,-1.,0.));
#112047=DIRECTION('ref_axis',(0.,0.,-1.));
#112048=DIRECTION('center_axis',(1.,0.,0.));
#112049=DIRECTION('ref_axis',(0.,0.,-1.));
#112050=DIRECTION('center_axis',(-1.,0.,0.));
#112051=DIRECTION('ref_axis',(0.,0.,1.));
#112052=DIRECTION('',(1.,0.,0.));
#112053=DIRECTION('',(-1.,0.,0.));
#112054=DIRECTION('center_axis',(-1.,0.,0.));
#112055=DIRECTION('ref_axis',(0.,0.,1.));
#112056=DIRECTION('center_axis',(-1.,0.,0.));
#112057=DIRECTION('ref_axis',(0.,0.,1.));
#112058=DIRECTION('center_axis',(0.,1.,0.));
#112059=DIRECTION('ref_axis',(0.,0.,1.));
#112060=DIRECTION('center_axis',(1.,0.,0.));
#112061=DIRECTION('ref_axis',(0.,0.,1.));
#112062=DIRECTION('center_axis',(0.,0.,-1.));
#112063=DIRECTION('ref_axis',(-1.,0.,0.));
#112064=DIRECTION('center_axis',(0.,0.,-1.));
#112065=DIRECTION('ref_axis',(-1.,0.,0.));
#112066=DIRECTION('center_axis',(0.,0.,1.));
#112067=DIRECTION('ref_axis',(1.,0.,0.));
#112068=DIRECTION('',(0.,0.,1.));
#112069=DIRECTION('center_axis',(0.,0.,1.));
#112070=DIRECTION('ref_axis',(1.,0.,0.));
#112071=DIRECTION('',(0.,0.,-1.));
#112072=DIRECTION('center_axis',(0.,0.466134040541469,0.884714109895668));
#112073=DIRECTION('ref_axis',(0.,-0.884714109895668,0.466134040541469));
#112074=DIRECTION('center_axis',(0.,0.450823097219337,0.892613317743783));
#112075=DIRECTION('ref_axis',(0.,-0.892613317743783,0.450823097219337));
#112076=DIRECTION('center_axis',(3.33932916167122E-16,0.999710458475598,
0.0240624025090732));
#112077=DIRECTION('ref_axis',(-2.2263435019713E-33,-0.0240624025090732,
0.999710458475598));
#112078=DIRECTION('center_axis',(0.,0.605101105507222,0.796148636947862));
#112079=DIRECTION('ref_axis',(0.,-0.796148636947862,0.605101105507222));
#112080=DIRECTION('center_axis',(-0.98202959189485,0.188726538511571,0.0004174976347577));
#112081=DIRECTION('ref_axis',(-0.153131413400455,-0.798101172975176,0.58273946830949));
#112082=DIRECTION('center_axis',(1.,0.,0.));
#112083=DIRECTION('ref_axis',(0.,-0.892435299537773,0.451175393986558));
#112084=DIRECTION('center_axis',(0.,-1.18842113532926E-16,1.));
#112085=DIRECTION('ref_axis',(0.,1.,1.18842113532926E-16));
#112086=DIRECTION('center_axis',(0.,1.19392659184112E-16,-1.));
#112087=DIRECTION('ref_axis',(0.,1.,1.19392659184112E-16));
#112088=DIRECTION('center_axis',(1.,-5.01606788234257E-16,0.));
#112089=DIRECTION('ref_axis',(0.,1.,0.));
#112090=DIRECTION('center_axis',(0.,-1.,0.));
#112091=DIRECTION('ref_axis',(0.,0.,-1.));
#112092=DIRECTION('center_axis',(-1.,0.,0.));
#112093=DIRECTION('ref_axis',(0.,1.,0.));
#112094=DIRECTION('center_axis',(0.,0.,-1.));
#112095=DIRECTION('ref_axis',(-1.,0.,0.));
#112096=DIRECTION('center_axis',(1.,0.,0.));
#112097=DIRECTION('ref_axis',(0.,1.,0.));
#112098=DIRECTION('center_axis',(-2.85977186515575E-47,0.,-1.));
#112099=DIRECTION('ref_axis',(0.,1.,0.));
#112100=DIRECTION('',(2.85977186515575E-47,5.70122241611331E-32,1.));
#112101=DIRECTION('center_axis',(0.,0.,-1.));
#112102=DIRECTION('ref_axis',(-1.,0.,0.));
#112103=DIRECTION('center_axis',(1.,-5.01606788234257E-16,0.));
#112104=DIRECTION('ref_axis',(0.,1.,0.));
#112105=DIRECTION('center_axis',(-1.,0.,0.));
#112106=DIRECTION('ref_axis',(0.,1.,0.));
#112107=DIRECTION('center_axis',(0.,1.,0.));
#112108=DIRECTION('ref_axis',(0.,0.,1.));
#112109=DIRECTION('center_axis',(0.,-0.452474032063612,-0.891777578944491));
#112110=DIRECTION('ref_axis',(0.,0.891777578944491,-0.452474032063612));
#112111=DIRECTION('center_axis',(6.4968286789756E-15,-0.468145843483589,
-0.883651214693354));
#112112=DIRECTION('ref_axis',(1.16233255777344E-30,0.883651214693354,-0.468145843483589));
#112113=DIRECTION('center_axis',(0.,0.,-1.));
#112114=DIRECTION('ref_axis',(-1.,0.,0.));
#112115=DIRECTION('center_axis',(0.,0.,-1.));
#112116=DIRECTION('ref_axis',(-1.,0.,0.));
#112117=DIRECTION('',(0.,0.,-1.));
#112118=DIRECTION('center_axis',(0.,0.,-1.));
#112119=DIRECTION('ref_axis',(-1.,0.,0.));
#112120=DIRECTION('center_axis',(6.4968286789753E-15,0.468145843483567,
-0.883651214693365));
#112121=DIRECTION('ref_axis',(-8.06613026210763E-31,0.883651214693365,0.468145843483567));
#112122=DIRECTION('center_axis',(-1.87193934265674E-16,0.452600956351886,
-0.8917131681821));
#112123=DIRECTION('ref_axis',(-4.92064035297146E-32,0.8917131681821,0.452600956351886));
#112124=DIRECTION('center_axis',(-1.,5.01606788234257E-16,0.));
#112125=DIRECTION('ref_axis',(0.,-1.,0.));
#112126=DIRECTION('center_axis',(0.,-1.,0.));
#112127=DIRECTION('ref_axis',(0.,0.,-1.));
#112128=DIRECTION('center_axis',(1.,0.,0.));
#112129=DIRECTION('ref_axis',(0.,-1.,0.));
#112130=DIRECTION('center_axis',(0.,0.,1.));
#112131=DIRECTION('ref_axis',(1.,0.,0.));
#112132=DIRECTION('center_axis',(2.85977186515575E-47,0.,1.));
#112133=DIRECTION('ref_axis',(0.,-1.,0.));
#112134=DIRECTION('',(-2.85977186515575E-47,-5.70122241611331E-32,-1.));
#112135=DIRECTION('center_axis',(0.,0.,1.));
#112136=DIRECTION('ref_axis',(1.,0.,0.));
#112137=DIRECTION('center_axis',(0.,0.,-1.));
#112138=DIRECTION('ref_axis',(-1.,0.,0.));
#112139=DIRECTION('center_axis',(0.,0.450013465461336,-0.893021769557427));
#112140=DIRECTION('ref_axis',(0.,0.893021769557427,0.450013465461336));
#112141=DIRECTION('center_axis',(0.,0.,1.));
#112142=DIRECTION('ref_axis',(1.,0.,0.));
#112143=DIRECTION('center_axis',(0.,0.,-1.));
#112144=DIRECTION('ref_axis',(-1.,0.,0.));
#112145=DIRECTION('',(0.,0.,1.));
#112146=DIRECTION('center_axis',(0.,-0.450013465459867,-0.893021769558168));
#112147=DIRECTION('ref_axis',(0.,0.893021769558168,-0.450013465459867));
#112148=DIRECTION('center_axis',(0.,-0.438949247410394,-0.898511857572202));
#112149=DIRECTION('ref_axis',(0.,0.898511857572202,-0.438949247410394));
#112150=DIRECTION('center_axis',(0.,0.439015545441723,-0.898479466020513));
#112151=DIRECTION('ref_axis',(0.,0.898479466020513,0.439015545441723));
#112152=DIRECTION('center_axis',(-1.,5.01606788234257E-16,0.));
#112153=DIRECTION('ref_axis',(0.,-1.,0.));
#112154=DIRECTION('center_axis',(1.,0.,0.));
#112155=DIRECTION('ref_axis',(0.,-1.,0.));
#112156=DIRECTION('center_axis',(0.,1.,0.));
#112157=DIRECTION('ref_axis',(0.,0.,1.));
#112158=DIRECTION('center_axis',(-1.,0.,0.));
#112159=DIRECTION('ref_axis',(0.,-1.,0.));
#112160=DIRECTION('center_axis',(1.,-5.01606788234257E-16,0.));
#112161=DIRECTION('ref_axis',(5.01606788234257E-16,1.,0.));
#112162=DIRECTION('',(1.,-5.01606788234257E-16,0.));
#112163=DIRECTION('center_axis',(1.,0.,0.));
#112164=DIRECTION('ref_axis',(0.,1.,0.));
#112165=DIRECTION('center_axis',(1.,-5.01606788234257E-16,0.));
#112166=DIRECTION('ref_axis',(0.,1.,0.));
#112167=DIRECTION('center_axis',(0.,-1.,0.));
#112168=DIRECTION('ref_axis',(0.,0.,-1.));
#112169=DIRECTION('center_axis',(-1.,6.93889390390722E-16,0.));
#112170=DIRECTION('ref_axis',(6.93889390390722E-16,1.,0.));
#112171=DIRECTION('center_axis',(0.,0.,-1.));
#112172=DIRECTION('ref_axis',(-1.,0.,0.));
#112173=DIRECTION('center_axis',(-2.85977186515575E-47,0.,-1.));
#112174=DIRECTION('ref_axis',(0.,1.,0.));
#112175=DIRECTION('',(2.85977186515575E-47,5.70122241611331E-32,1.));
#112176=DIRECTION('center_axis',(0.,0.,-1.));
#112177=DIRECTION('ref_axis',(-1.,0.,0.));
#112178=DIRECTION('center_axis',(1.,-5.01606788234257E-16,0.));
#112179=DIRECTION('ref_axis',(0.,1.,0.));
#112180=DIRECTION('center_axis',(-1.,6.93889390390722E-16,0.));
#112181=DIRECTION('ref_axis',(6.93889390390722E-16,1.,0.));
#112182=DIRECTION('center_axis',(0.,1.,0.));
#112183=DIRECTION('ref_axis',(0.,0.,1.));
#112184=DIRECTION('center_axis',(0.,-0.434444534286154,-0.900698588113075));
#112185=DIRECTION('ref_axis',(0.,0.900698588113075,-0.434444534286154));
#112186=DIRECTION('center_axis',(6.14994601925012E-15,-0.443150313610303,
-0.896447321122156));
#112187=DIRECTION('ref_axis',(-3.80752501607971E-29,0.896447321122156,-0.443150313610303));
#112188=DIRECTION('center_axis',(0.,0.,-1.));
#112189=DIRECTION('ref_axis',(-1.,0.,0.));
#112190=DIRECTION('center_axis',(0.,0.,-1.));
#112191=DIRECTION('ref_axis',(-1.,0.,0.));
#112192=DIRECTION('',(0.,0.,-1.));
#112193=DIRECTION('center_axis',(0.,0.,-1.));
#112194=DIRECTION('ref_axis',(-1.,0.,0.));
#112195=DIRECTION('center_axis',(3.10313574260842E-14,0.443150313610309,
-0.896447321122153));
#112196=DIRECTION('ref_axis',(-1.13003852554043E-30,0.896447321122153,0.443150313610309));
#112197=DIRECTION('center_axis',(4.39817443652073E-16,0.434491800625061,
-0.900675788055609));
#112198=DIRECTION('ref_axis',(-9.63119795361041E-32,0.900675788055609,0.434491800625061));
#112199=DIRECTION('center_axis',(0.,0.,-1.));
#112200=DIRECTION('ref_axis',(-1.,0.,0.));
#112201=DIRECTION('center_axis',(0.,0.430903547306764,-0.902397990311618));
#112202=DIRECTION('ref_axis',(0.,0.902397990311618,0.430903547306764));
#112203=DIRECTION('center_axis',(0.,0.,1.));
#112204=DIRECTION('ref_axis',(1.,0.,0.));
#112205=DIRECTION('center_axis',(0.,0.,-1.));
#112206=DIRECTION('ref_axis',(-1.,0.,0.));
#112207=DIRECTION('',(0.,0.,1.));
#112208=DIRECTION('center_axis',(0.,-0.430903547308298,-0.902397990310886));
#112209=DIRECTION('ref_axis',(0.,0.902397990310886,-0.430903547308298));
#112210=DIRECTION('center_axis',(0.,-0.427115883537276,-0.904196893397767));
#112211=DIRECTION('ref_axis',(0.,0.904196893397767,-0.427115883537276));
#112212=DIRECTION('center_axis',(0.,0.427133403156944,-0.904188617439729));
#112213=DIRECTION('ref_axis',(0.,0.904188617439729,0.427133403156944));
#112214=DIRECTION('center_axis',(2.85977186515575E-47,0.,1.));
#112215=DIRECTION('ref_axis',(0.,-1.,0.));
#112216=DIRECTION('center_axis',(0.,0.,1.));
#112217=DIRECTION('ref_axis',(1.,0.,0.));
#112218=DIRECTION('',(-2.85977186515575E-47,-5.70122241611331E-32,-1.));
#112219=DIRECTION('center_axis',(0.,0.,1.));
#112220=DIRECTION('ref_axis',(1.,0.,0.));
#112221=DIRECTION('',(2.85977186515575E-47,5.70122241611331E-32,1.));
#112222=DIRECTION('center_axis',(-5.01606788234257E-16,-1.,5.70122241611331E-32));
#112223=DIRECTION('ref_axis',(-1.,5.01606788234257E-16,0.));
#112224=DIRECTION('',(-2.85977186515575E-47,-5.70122241611331E-32,-1.));
#112225=DIRECTION('center_axis',(-2.85977186515575E-47,0.,-1.));
#112226=DIRECTION('ref_axis',(0.,1.,0.));
#112227=DIRECTION('center_axis',(0.,0.,-1.));
#112228=DIRECTION('ref_axis',(-1.,0.,0.));
#112229=DIRECTION('',(2.85977186515575E-47,5.70122241611331E-32,1.));
#112230=DIRECTION('center_axis',(0.,0.,-1.));
#112231=DIRECTION('ref_axis',(-1.,0.,0.));
#112232=DIRECTION('center_axis',(0.,-0.425023904828957,-0.905182125499585));
#112233=DIRECTION('ref_axis',(0.,0.905182125499585,-0.425023904828957));
#112234=DIRECTION('center_axis',(-5.01926581554439E-14,-0.427129320053956,
-0.904190546262371));
#112235=DIRECTION('ref_axis',(-3.44539770291064E-30,0.904190546262371,-0.427129320053956));
#112236=DIRECTION('center_axis',(0.,0.,-1.));
#112237=DIRECTION('ref_axis',(-1.,0.,0.));
#112238=DIRECTION('center_axis',(0.,0.,-1.));
#112239=DIRECTION('ref_axis',(-1.,0.,0.));
#112240=DIRECTION('',(0.,0.,-1.));
#112241=DIRECTION('center_axis',(0.,0.,-1.));
#112242=DIRECTION('ref_axis',(-1.,0.,0.));
#112243=DIRECTION('center_axis',(5.9276100702047E-15,0.42712932005395,-0.904190546262374));
#112244=DIRECTION('ref_axis',(3.36279389150844E-29,0.904190546262374,0.42712932005395));
#112245=DIRECTION('center_axis',(-1.25618648527741E-14,0.425033206427438,
-0.905177757920515));
#112246=DIRECTION('ref_axis',(2.68759262534439E-30,0.905177757920515,0.425033206427438));
#112247=DIRECTION('center_axis',(-0.999980559779821,0.00244847680975066,
-0.00573454651630453));
#112248=DIRECTION('ref_axis',(0.00115079471073239,0.976348942497979,0.216197636792386));
#112249=DIRECTION('center_axis',(0.,0.,-1.));
#112250=DIRECTION('ref_axis',(-1.,0.,0.));
#112251=DIRECTION('center_axis',(0.,0.422768104239746,-0.906237899250264));
#112252=DIRECTION('ref_axis',(0.,0.906237899250264,0.422768104239746));
#112253=DIRECTION('center_axis',(1.,0.,0.));
#112254=DIRECTION('ref_axis',(0.,0.976373434674857,0.216090064698084));
#112255=DIRECTION('center_axis',(0.,0.,1.));
#112256=DIRECTION('ref_axis',(1.,0.,0.));
#112257=DIRECTION('center_axis',(0.,0.,-1.));
#112258=DIRECTION('ref_axis',(-1.,0.,0.));
#112259=DIRECTION('',(0.,0.,1.));
#112260=DIRECTION('center_axis',(0.,-0.422768104239797,-0.90623789925024));
#112261=DIRECTION('ref_axis',(0.,0.90623789925024,-0.422768104239797));
#112262=DIRECTION('center_axis',(1.,0.,0.));
#112263=DIRECTION('ref_axis',(0.,0.976105817825331,-0.217295725700119));
#112264=DIRECTION('center_axis',(0.,-0.422696564637279,-0.906271269678038));
#112265=DIRECTION('ref_axis',(0.,0.906271269678038,-0.422696564637279));
#112266=DIRECTION('center_axis',(0.,0.422696864907095,-0.906271129628277));
#112267=DIRECTION('ref_axis',(0.,0.906271129628277,0.422696864907095));
#112268=DIRECTION('center_axis',(0.,0.,1.));
#112269=DIRECTION('ref_axis',(1.,0.,0.));
#112270=DIRECTION('',(5.01606788234257E-16,1.,0.));
#112271=DIRECTION('center_axis',(0.,0.,1.));
#112272=DIRECTION('ref_axis',(1.,0.,0.));
#112273=DIRECTION('',(-5.01606788234257E-16,-1.,0.));
#112274=DIRECTION('center_axis',(0.,-1.,0.));
#112275=DIRECTION('ref_axis',(1.,0.,0.));
#112276=DIRECTION('',(5.01606788234257E-16,1.,0.));
#112277=DIRECTION('center_axis',(-0.691017694403315,-0.329301163645224,
-0.643471281133376));
#112278=DIRECTION('ref_axis',(-0.681480917945783,1.81728452038657E-16,0.731835882200219));
#112279=DIRECTION('center_axis',(0.,0.,-1.));
#112280=DIRECTION('ref_axis',(-1.,0.,0.));
#112281=DIRECTION('center_axis',(0.,0.,1.));
#112282=DIRECTION('ref_axis',(0.,-1.,0.));
#112283=DIRECTION('',(0.,1.23467863058847E-16,-1.));
#112284=DIRECTION('',(-6.19323182390956E-32,-1.23467863058847E-16,1.));
#112285=DIRECTION('center_axis',(0.,0.,-1.));
#112286=DIRECTION('ref_axis',(-1.,0.,0.));
#112287=DIRECTION('center_axis',(0.999946261821081,-0.0103669398946897,
5.22173233649368E-6));
#112288=DIRECTION('ref_axis',(0.0101220853315265,0.976219669473995,-0.216547224227478));
#112289=DIRECTION('center_axis',(-1.,0.,0.));
#112290=DIRECTION('ref_axis',(0.,0.976212736710707,-0.216814881140091));
#112291=DIRECTION('center_axis',(0.,0.,-1.));
#112292=DIRECTION('ref_axis',(1.,0.,0.));
#112293=DIRECTION('center_axis',(0.,0.,1.));
#112294=DIRECTION('ref_axis',(0.,-1.,0.));
#112295=DIRECTION('center_axis',(0.,0.,-1.));
#112296=DIRECTION('ref_axis',(-1.,0.,0.));
#112297=DIRECTION('center_axis',(1.,0.,0.));
#112298=DIRECTION('ref_axis',(0.,0.978009404010872,-0.20856079609145));
#112299=DIRECTION('center_axis',(-0.998408908923169,0.0563883836225873,
-2.7843844968591E-5));
#112300=DIRECTION('ref_axis',(0.055246667114195,0.978094652824472,-0.200695430662856));
#112301=DIRECTION('center_axis',(-0.0107605169339556,0.163442104496002,
0.986494242128778));
#112302=DIRECTION('ref_axis',(0.12265223013178,-0.978886010491001,0.163519445047717));
#112303=DIRECTION('center_axis',(0.,0.,-1.));
#112304=DIRECTION('ref_axis',(-1.,0.,0.));
#112305=DIRECTION('center_axis',(0.997120695413915,-0.0758308469044614,
3.78816969998108E-5));
#112306=DIRECTION('ref_axis',(0.0744761237692872,0.979212817695212,-0.188667868620245));
#112307=DIRECTION('center_axis',(-1.,0.,0.));
#112308=DIRECTION('ref_axis',(0.,0.979170381919184,-0.203040299379802));
#112309=DIRECTION('center_axis',(0.,0.,-1.));
#112310=DIRECTION('ref_axis',(1.,0.,0.));
#112311=DIRECTION('center_axis',(0.,0.,1.));
#112312=DIRECTION('ref_axis',(0.,-1.,0.));
#112313=DIRECTION('center_axis',(0.,0.,-1.));
#112314=DIRECTION('ref_axis',(-1.,0.,0.));
#112315=DIRECTION('center_axis',(0.999999999999962,-2.70358732879246E-7,
6.19928773069953E-8));
#112316=DIRECTION('ref_axis',(-1.37951239417795E-7,-0.67866125427495,-0.734451429262638));
#112317=DIRECTION('center_axis',(-0.9932262444019,0.116196489921731,-5.62242552552882E-5));
#112318=DIRECTION('ref_axis',(0.11505091787893,0.983366096661123,-0.140550369023647));
#112319=DIRECTION('center_axis',(0.,-1.,0.));
#112320=DIRECTION('ref_axis',(1.,0.,0.));
#112321=DIRECTION('',(-5.01606788234257E-16,-1.,0.));
#112322=DIRECTION('',(5.01606788234257E-16,1.,0.));
#112323=DIRECTION('center_axis',(0.,0.,1.));
#112324=DIRECTION('ref_axis',(1.,0.,0.));
#112325=DIRECTION('center_axis',(0.,0.,1.));
#112326=DIRECTION('ref_axis',(1.,0.,0.));
#112327=DIRECTION('',(-5.01606788234257E-16,-1.,0.));
#112328=DIRECTION('center_axis',(0.,-1.,0.));
#112329=DIRECTION('ref_axis',(1.,0.,0.));
#112330=DIRECTION('',(5.01606788234257E-16,1.,0.));
#112331=DIRECTION('center_axis',(0.,0.,-1.));
#112332=DIRECTION('ref_axis',(-1.,0.,0.));
#112333=DIRECTION('center_axis',(0.991243176770489,-0.132049083222371,6.42345784418605E-5));
#112334=DIRECTION('ref_axis',(0.131204337993624,0.984846821255349,-0.113411464830016));
#112335=DIRECTION('center_axis',(-0.999999999999982,-1.83115630218257E-7,
4.25253736080571E-8));
#112336=DIRECTION('ref_axis',(1.60098201248805E-7,-0.948126339790581,-0.317893761806189));
#112337=DIRECTION('center_axis',(0.,0.,-1.));
#112338=DIRECTION('ref_axis',(1.,0.,0.));
#112339=DIRECTION('center_axis',(0.,0.,1.));
#112340=DIRECTION('ref_axis',(0.,-1.,0.));
#112341=DIRECTION('center_axis',(0.,0.,-1.));
#112342=DIRECTION('ref_axis',(-1.,0.,0.));
#112343=DIRECTION('center_axis',(1.,-2.01122486990919E-8,4.85048672787675E-9));
#112344=DIRECTION('ref_axis',(1.993567842142E-8,0.999421676189316,0.0340046050254766));
#112345=DIRECTION('center_axis',(-0.986748267175955,0.162258595028188,-7.45971144795321E-5));
#112346=DIRECTION('ref_axis',(0.162166590547152,0.986173067657473,-0.0341273722598251));
#112347=DIRECTION('center_axis',(0.,-1.,0.));
#112348=DIRECTION('ref_axis',(1.,0.,0.));
#112349=DIRECTION('',(-5.01606788234257E-16,-1.,0.));
#112350=DIRECTION('center_axis',(0.,1.23467863058847E-16,-1.));
#112351=DIRECTION('ref_axis',(-1.,0.,0.));
#112352=DIRECTION('center_axis',(0.,0.,-1.));
#112353=DIRECTION('ref_axis',(0.,1.,0.));
#112354=DIRECTION('',(2.0158362407235E-32,-1.,-1.23467863058847E-16));
#112355=DIRECTION('center_axis',(0.,1.23467863058847E-16,-1.));
#112356=DIRECTION('ref_axis',(-1.,0.,0.));
#112357=DIRECTION('',(2.0158362407235E-32,-1.,-1.23467863058847E-16));
#112358=DIRECTION('center_axis',(0.,0.,-1.));
#112359=DIRECTION('ref_axis',(0.,1.,0.));
#112360=DIRECTION('center_axis',(0.,1.23467863058847E-16,-1.));
#112361=DIRECTION('ref_axis',(-1.,0.,0.));
#112362=DIRECTION('center_axis',(0.,0.,-1.));
#112363=DIRECTION('ref_axis',(0.,-1.,0.));
#112364=DIRECTION('center_axis',(0.,1.23467863058847E-16,-1.));
#112365=DIRECTION('ref_axis',(-1.,0.,0.));
#112366=DIRECTION('center_axis',(0.,0.,-1.));
#112367=DIRECTION('ref_axis',(0.,-1.,0.));
#112368=DIRECTION('center_axis',(0.,0.,-1.));
#112369=DIRECTION('ref_axis',(0.,-1.,0.));
#112370=DIRECTION('center_axis',(0.139173100960059,-0.990268068741571,-1.22266282302934E-16));
#112371=DIRECTION('ref_axis',(6.9401346861194E-34,1.23467863058847E-16,
-1.));
#112372=DIRECTION('',(-3.43088182518023E-33,1.23467863058847E-16,-1.));
#112373=DIRECTION('',(0.990268068741571,0.139173100960059,1.71834053708117E-17));
#112374=DIRECTION('',(3.43088182518023E-33,-1.23467863058847E-16,1.));
#112375=DIRECTION('center_axis',(0.,0.,-1.));
#112376=DIRECTION('ref_axis',(0.,1.,0.));
#112377=DIRECTION('center_axis',(0.,0.,1.));
#112378=DIRECTION('ref_axis',(0.,-1.,0.));
#112379=DIRECTION('',(0.,1.23467863058847E-16,-1.));
#112380=DIRECTION('center_axis',(0.,0.,-1.));
#112381=DIRECTION('ref_axis',(0.,1.,0.));
#112382=DIRECTION('center_axis',(0.,0.,1.));
#112383=DIRECTION('ref_axis',(0.,-1.,0.));
#112384=DIRECTION('',(0.,-1.23467863058847E-16,1.));
#112385=DIRECTION('center_axis',(0.,0.,-1.));
#112386=DIRECTION('ref_axis',(0.,1.,0.));
#112387=DIRECTION('center_axis',(0.,0.,1.));
#112388=DIRECTION('ref_axis',(0.,-1.,0.));
#112389=DIRECTION('',(3.79382742684518E-34,1.23467863058847E-16,-1.));
#112390=DIRECTION('center_axis',(0.99026806874157,-0.139173100960065,-1.71834053708124E-17));
#112391=DIRECTION('ref_axis',(2.50622989185404E-33,1.23467863058847E-16,
-1.));
#112392=DIRECTION('',(0.139173100960065,0.99026806874157,1.22266282302933E-16));
#112393=DIRECTION('',(-3.79382742684518E-34,-1.23467863058847E-16,1.));
#112394=DIRECTION('center_axis',(0.,0.,1.));
#112395=DIRECTION('ref_axis',(0.,-1.,0.));
#112396=DIRECTION('',(0.,1.23467863058847E-16,-1.));
#112397=DIRECTION('center_axis',(0.,0.,-1.));
#112398=DIRECTION('ref_axis',(0.,-1.,0.));
#112399=DIRECTION('center_axis',(0.,0.,1.));
#112400=DIRECTION('ref_axis',(0.,-1.,0.));
#112401=DIRECTION('',(0.,-1.23467863058847E-16,1.));
#112402=DIRECTION('center_axis',(0.,0.,1.));
#112403=DIRECTION('ref_axis',(0.,-1.,0.));
#112404=DIRECTION('center_axis',(0.,0.,1.));
#112405=DIRECTION('ref_axis',(0.,-1.,0.));
#112406=DIRECTION('center_axis',(0.,0.,-1.));
#112407=DIRECTION('ref_axis',(0.,-1.,0.));
#112408=DIRECTION('',(3.05149908249585E-33,1.23467863058847E-16,-1.));
#112409=DIRECTION('center_axis',(0.99026806874157,0.139173100960067,1.71834053708127E-17));
#112410=DIRECTION('ref_axis',(1.48746998541713E-33,1.23467863058847E-16,
-1.));
#112411=DIRECTION('',(-0.139173100960067,0.99026806874157,1.22266282302933E-16));
#112412=DIRECTION('',(-3.05149908249585E-33,-1.23467863058847E-16,1.));
#112413=DIRECTION('center_axis',(0.,0.,-1.));
#112414=DIRECTION('ref_axis',(0.,1.,0.));
#112415=DIRECTION('center_axis',(0.,0.,1.));
#112416=DIRECTION('ref_axis',(0.,-1.,0.));
#112417=DIRECTION('',(0.,1.23467863058847E-16,-1.));
#112418=DIRECTION('center_axis',(0.,0.,-1.));
#112419=DIRECTION('ref_axis',(0.,1.,0.));
#112420=DIRECTION('center_axis',(0.,0.,1.));
#112421=DIRECTION('ref_axis',(0.,-1.,0.));
#112422=DIRECTION('',(0.,-1.23467863058847E-16,1.));
#112423=DIRECTION('center_axis',(0.,0.,-1.));
#112424=DIRECTION('ref_axis',(0.,1.,0.));
#112425=DIRECTION('center_axis',(0.,0.,1.));
#112426=DIRECTION('ref_axis',(0.,-1.,0.));
#112427=DIRECTION('',(3.43088182518023E-33,1.23467863058847E-16,-1.));
#112428=DIRECTION('center_axis',(0.139173100960059,0.990268068741571,1.22266282302934E-16));
#112429=DIRECTION('ref_axis',(8.78519494496445E-16,5.20658772030138E-33,
-1.));
#112430=DIRECTION('',(-3.43088182518023E-33,-1.23467863058847E-16,1.));
#112431=DIRECTION('',(0.990268068741571,-0.139173100960059,0.));
#112432=DIRECTION('',(-1.6326809185664E-16,-1.0052202914905E-16,1.));
#112433=DIRECTION('',(-0.990268068741571,0.139173100960059,1.71834053708117E-17));
#112434=DIRECTION('center_axis',(0.,0.,1.));
#112435=DIRECTION('ref_axis',(1.,0.,0.));
#112436=DIRECTION('center_axis',(0.990268068741572,-0.139173100960052,0.));
#112437=DIRECTION('ref_axis',(0.139173100960052,0.990268068741572,0.));
#112438=DIRECTION('center_axis',(0.,-1.0052202914905E-16,1.));
#112439=DIRECTION('ref_axis',(1.,0.,0.));
#112440=DIRECTION('center_axis',(0.,0.,1.));
#112441=DIRECTION('ref_axis',(1.,0.,0.));
#112442=DIRECTION('',(1.6326809185664E-16,1.00522029149049E-16,-1.));
#112443=DIRECTION('center_axis',(0.,-1.,0.));
#112444=DIRECTION('ref_axis',(0.,0.,-1.));
#112445=DIRECTION('center_axis',(2.0158362407235E-32,-1.,0.));
#112446=DIRECTION('ref_axis',(0.,0.,-1.));
#112447=DIRECTION('center_axis',(-1.41612495910826E-31,-1.,0.));
#112448=DIRECTION('ref_axis',(0.,0.,-1.));
#112449=DIRECTION('',(-2.0158362407235E-32,1.,1.23467863058847E-16));
#112450=DIRECTION('center_axis',(0.,-1.,0.));
#112451=DIRECTION('ref_axis',(0.,0.,-1.));
#112452=DIRECTION('center_axis',(2.0158362407235E-32,-1.,0.));
#112453=DIRECTION('ref_axis',(0.,0.,-1.));
#112454=DIRECTION('',(-2.0158362407235E-32,1.,1.23467863058847E-16));
#112455=DIRECTION('center_axis',(0.,7.15121221728469E-32,1.));
#112456=DIRECTION('ref_axis',(1.,0.,0.));
#112457=DIRECTION('',(-1.6326809185664E-16,7.15121221728469E-32,1.));
#112458=DIRECTION('',(1.6326809185664E-16,-7.15121221728469E-32,-1.));
#112459=DIRECTION('center_axis',(0.,0.,1.));
#112460=DIRECTION('ref_axis',(1.,0.,0.));
#112461=DIRECTION('center_axis',(-1.,0.,0.));
#112462=DIRECTION('ref_axis',(0.,0.,-1.));
#112463=DIRECTION('center_axis',(0.,-1.,0.));
#112464=DIRECTION('ref_axis',(0.,0.,-1.));
#112465=DIRECTION('center_axis',(1.,0.,0.));
#112466=DIRECTION('ref_axis',(0.,0.,-1.));
#112467=DIRECTION('center_axis',(-4.38004274807345E-16,-1.,0.));
#112468=DIRECTION('ref_axis',(-1.,4.38004274807345E-16,0.));
#112469=DIRECTION('',(-1.,4.38004274807345E-16,0.));
#112470=DIRECTION('center_axis',(-1.,0.,0.));
#112471=DIRECTION('ref_axis',(0.,0.,1.));
#112472=DIRECTION('center_axis',(0.,1.,0.));
#112473=DIRECTION('ref_axis',(0.,0.,1.));
#112474=DIRECTION('center_axis',(1.,0.,0.));
#112475=DIRECTION('ref_axis',(0.,0.,1.));
#112476=DIRECTION('center_axis',(0.,0.,-1.));
#112477=DIRECTION('ref_axis',(-1.,0.,0.));
#112478=DIRECTION('',(0.,0.,1.));
#112479=DIRECTION('center_axis',(0.,0.,1.));
#112480=DIRECTION('ref_axis',(-1.,0.,0.));
#112481=DIRECTION('',(0.,0.,-1.));
#112482=DIRECTION('center_axis',(0.,1.,0.));
#112483=DIRECTION('ref_axis',(1.,0.,0.));
#112484=DIRECTION('',(-1.,0.,0.));
#112485=DIRECTION('',(-1.87032180698308E-16,0.,1.));
#112486=DIRECTION('center_axis',(0.,0.,1.));
#112487=DIRECTION('ref_axis',(1.,0.,0.));
#112488=DIRECTION('center_axis',(0.,0.,1.));
#112489=DIRECTION('ref_axis',(-1.,0.,0.));
#112490=DIRECTION('',(1.87032180698308E-16,0.,-1.));
#112491=DIRECTION('center_axis',(-1.,0.,0.));
#112492=DIRECTION('ref_axis',(0.,0.,-1.));
#112493=DIRECTION('center_axis',(0.,-1.,0.));
#112494=DIRECTION('ref_axis',(0.,0.,-1.));
#112495=DIRECTION('center_axis',(1.,0.,0.));
#112496=DIRECTION('ref_axis',(0.,0.,-1.));
#112497=DIRECTION('center_axis',(-4.38004274807345E-16,-1.,0.));
#112498=DIRECTION('ref_axis',(-1.,4.38004274807345E-16,0.));
#112499=DIRECTION('',(-1.,4.38004274807345E-16,0.));
#112500=DIRECTION('center_axis',(-1.,0.,0.));
#112501=DIRECTION('ref_axis',(0.,0.,1.));
#112502=DIRECTION('center_axis',(0.,1.,0.));
#112503=DIRECTION('ref_axis',(0.,0.,1.));
#112504=DIRECTION('center_axis',(1.,0.,0.));
#112505=DIRECTION('ref_axis',(0.,0.,1.));
#112506=DIRECTION('center_axis',(0.,0.,-1.));
#112507=DIRECTION('ref_axis',(-1.,0.,0.));
#112508=DIRECTION('',(0.,0.,1.));
#112509=DIRECTION('center_axis',(0.,0.,1.));
#112510=DIRECTION('ref_axis',(-1.,0.,0.));
#112511=DIRECTION('',(0.,0.,-1.));
#112512=DIRECTION('center_axis',(0.,1.,0.));
#112513=DIRECTION('ref_axis',(1.,0.,0.));
#112514=DIRECTION('',(-1.,0.,0.));
#112515=DIRECTION('',(-1.87032180698308E-16,0.,1.));
#112516=DIRECTION('center_axis',(0.,0.,1.));
#112517=DIRECTION('ref_axis',(1.,0.,0.));
#112518=DIRECTION('center_axis',(0.,0.,1.));
#112519=DIRECTION('ref_axis',(-1.,0.,0.));
#112520=DIRECTION('',(1.87032180698308E-16,0.,-1.));
#112521=DIRECTION('center_axis',(-1.,0.,0.));
#112522=DIRECTION('ref_axis',(0.,0.,-1.));
#112523=DIRECTION('center_axis',(0.,-1.,0.));
#112524=DIRECTION('ref_axis',(0.,0.,-1.));
#112525=DIRECTION('center_axis',(1.,0.,0.));
#112526=DIRECTION('ref_axis',(0.,0.,-1.));
#112527=DIRECTION('center_axis',(-4.38004274807345E-16,-1.,0.));
#112528=DIRECTION('ref_axis',(-1.,4.38004274807345E-16,0.));
#112529=DIRECTION('center_axis',(-6.15557891118788E-9,-1.,7.989575083689E-9));
#112530=DIRECTION('ref_axis',(0.717962811290552,1.14191836403356E-9,0.696081461902102));
#112531=DIRECTION('',(-1.,4.38004274807345E-16,0.));
#112532=DIRECTION('center_axis',(1.79937481368581E-15,0.983475799774124,
-0.181039640020212));
#112533=DIRECTION('ref_axis',(-3.24346588047852E-31,0.181039640020212,0.983475799774124));
#112534=DIRECTION('center_axis',(0.,1.,0.));
#112535=DIRECTION('ref_axis',(0.,0.,1.));
#112536=DIRECTION('center_axis',(1.,0.,0.));
#112537=DIRECTION('ref_axis',(0.,0.000252653767738075,-0.999999968083036));
#112538=DIRECTION('center_axis',(-0.988033841711791,0.154018907555706,0.00820388612708266));
#112539=DIRECTION('ref_axis',(-0.0369034044335798,-0.184421063066604,-0.982154270081129));
#112540=DIRECTION('center_axis',(0.,0.,-1.));
#112541=DIRECTION('ref_axis',(-1.,0.,0.));
#112542=DIRECTION('',(0.,0.,1.));
#112543=DIRECTION('center_axis',(0.,0.,1.));
#112544=DIRECTION('ref_axis',(-1.,0.,0.));
#112545=DIRECTION('',(0.,0.,-1.));
#112546=DIRECTION('center_axis',(0.,0.,-1.));
#112547=DIRECTION('ref_axis',(-1.,0.,0.));
#112548=DIRECTION('center_axis',(0.,1.,0.));
#112549=DIRECTION('ref_axis',(1.,0.,0.));
#112550=DIRECTION('',(-1.,0.,0.));
#112551=DIRECTION('',(-1.87032180698308E-16,0.,1.));
#112552=DIRECTION('center_axis',(3.552570199055E-14,-1.,-2.23044154114413E-16));
#112553=DIRECTION('ref_axis',(-0.00256148703537234,1.37530068325002E-16,
-0.999996719386703));
#112554=DIRECTION('center_axis',(0.,0.,1.));
#112555=DIRECTION('ref_axis',(1.,0.,0.));
#112556=DIRECTION('center_axis',(0.,0.,1.));
#112557=DIRECTION('ref_axis',(-1.,0.,0.));
#112558=DIRECTION('',(1.87032180698308E-16,0.,-1.));
#112559=DIRECTION('center_axis',(0.,0.,-1.));
#112560=DIRECTION('ref_axis',(-1.,0.,0.));
#112561=DIRECTION('center_axis',(0.,-1.,0.));
#112562=DIRECTION('ref_axis',(0.,0.,-1.));
#112563=DIRECTION('center_axis',(0.991674892658728,-0.128766868407894,-2.95080255278421E-5));
#112564=DIRECTION('ref_axis',(-0.0290207967337628,-0.223275175385041,-0.974323349516841));
#112565=DIRECTION('center_axis',(-0.998076185175213,0.0619994224918331,
1.40275800867403E-5));
#112566=DIRECTION('ref_axis',(0.0133447743819902,0.214605257625009,0.976609697062443));
#112567=DIRECTION('center_axis',(0.,1.,0.));
#112568=DIRECTION('ref_axis',(0.,0.,1.));
#112569=DIRECTION('center_axis',(0.,0.,-1.));
#112570=DIRECTION('ref_axis',(-1.,0.,0.));
#112571=DIRECTION('',(0.,0.,1.));
#112572=DIRECTION('center_axis',(0.,0.,1.));
#112573=DIRECTION('ref_axis',(-1.,0.,0.));
#112574=DIRECTION('',(0.,0.,-1.));
#112575=DIRECTION('center_axis',(0.,0.,-1.));
#112576=DIRECTION('ref_axis',(-1.,0.,0.));
#112577=DIRECTION('center_axis',(0.,1.,0.));
#112578=DIRECTION('ref_axis',(1.,0.,0.));
#112579=DIRECTION('',(-1.,0.,0.));
#112580=DIRECTION('',(-1.87032180698308E-16,0.,1.));
#112581=DIRECTION('center_axis',(0.,0.,1.));
#112582=DIRECTION('ref_axis',(1.,0.,0.));
#112583=DIRECTION('center_axis',(0.,0.,1.));
#112584=DIRECTION('ref_axis',(-1.,0.,0.));
#112585=DIRECTION('',(1.87032180698308E-16,0.,-1.));
#112586=DIRECTION('center_axis',(0.,0.,-1.));
#112587=DIRECTION('ref_axis',(-1.,0.,0.));
#112588=DIRECTION('center_axis',(-0.716305556970081,0.650473286312467,0.252568511195758));
#112589=DIRECTION('ref_axis',(-0.672268907563029,-0.740307041655023,-6.62280424422414E-17));
#112590=DIRECTION('center_axis',(-0.488849591387095,0.481564692142823,0.727407399111432));
#112591=DIRECTION('ref_axis',(0.82998476161361,2.33877977530395E-17,0.557786066058662));
#112592=DIRECTION('center_axis',(0.,1.,0.));
#112593=DIRECTION('ref_axis',(0.,0.,1.));
#112594=DIRECTION('center_axis',(0.,-1.,0.));
#112595=DIRECTION('ref_axis',(0.,0.,-1.));
#112596=DIRECTION('center_axis',(0.,1.,0.));
#112597=DIRECTION('ref_axis',(0.,0.,1.));
#112598=DIRECTION('',(4.38004274807345E-16,1.,0.));
#112599=DIRECTION('',(0.,-1.,0.));
#112600=DIRECTION('center_axis',(-4.38004274807345E-16,-1.,0.));
#112601=DIRECTION('ref_axis',(1.,0.,0.));
#112602=DIRECTION('center_axis',(-0.366954554655378,9.16653140031321E-14,
0.930238869762855));
#112603=DIRECTION('ref_axis',(0.930238869762855,-2.79622788237931E-29,0.366954554655378));
#112604=DIRECTION('center_axis',(0.,-1.,0.));
#112605=DIRECTION('ref_axis',(1.,0.,0.));
#112606=DIRECTION('center_axis',(9.37295054023422E-45,1.,-2.02617679489732E-30));
#112607=DIRECTION('ref_axis',(1.,-4.97841222228891E-60,4.62592926927148E-15));
#112608=DIRECTION('center_axis',(-1.,0.,0.));
#112609=DIRECTION('ref_axis',(0.,0.,1.));
#112610=DIRECTION('center_axis',(0.,1.,0.));
#112611=DIRECTION('ref_axis',(1.,0.,0.));
#112612=DIRECTION('',(-1.,0.,0.));
#112613=DIRECTION('',(-1.87032180698308E-16,0.,1.));
#112614=DIRECTION('center_axis',(0.,0.,1.));
#112615=DIRECTION('ref_axis',(1.,0.,0.));
#112616=DIRECTION('center_axis',(0.,0.,1.));
#112617=DIRECTION('ref_axis',(-1.,0.,0.));
#112618=DIRECTION('',(1.87032180698308E-16,0.,-1.));
#112619=DIRECTION('center_axis',(-1.,5.01606788234257E-16,0.));
#112620=DIRECTION('ref_axis',(0.,-1.,0.));
#112621=DIRECTION('center_axis',(1.,0.,0.));
#112622=DIRECTION('ref_axis',(0.,-1.,0.));
#112623=DIRECTION('center_axis',(0.,1.,0.));
#112624=DIRECTION('ref_axis',(0.,0.,1.));
#112625=DIRECTION('center_axis',(-1.,0.,0.));
#112626=DIRECTION('ref_axis',(0.,-1.,0.));
#112627=DIRECTION('center_axis',(1.,-5.01606788234257E-16,0.));
#112628=DIRECTION('ref_axis',(5.01606788234257E-16,1.,0.));
#112629=DIRECTION('',(1.,-5.01606788234257E-16,0.));
#112630=DIRECTION('center_axis',(1.,-4.38004274807346E-16,-5.40794518211031E-32));
#112631=DIRECTION('ref_axis',(4.38004274807346E-16,1.,5.80597460094347E-63));
#112632=DIRECTION('',(-1.,4.38004274807345E-16,5.40794518211031E-32));
#112633=DIRECTION('center_axis',(-1.,0.,0.));
#112634=DIRECTION('ref_axis',(0.,0.,1.));
#112635=DIRECTION('',(1.,-4.38004274807345E-16,-5.40794518211031E-32));
#112636=DIRECTION('center_axis',(0.,0.,-1.));
#112637=DIRECTION('ref_axis',(0.,1.,0.));
#112638=DIRECTION('center_axis',(0.,0.,-1.));
#112639=DIRECTION('ref_axis',(0.,1.,0.));
#112640=DIRECTION('',(0.,0.,-1.));
#112641=DIRECTION('center_axis',(0.,0.,-1.));
#112642=DIRECTION('ref_axis',(0.,1.,0.));
#112643=DIRECTION('center_axis',(0.,0.,-1.));
#112644=DIRECTION('ref_axis',(0.,1.,0.));
#112645=DIRECTION('center_axis',(0.,1.23467863058847E-16,-1.));
#112646=DIRECTION('ref_axis',(-1.,0.,0.));
#112647=DIRECTION('center_axis',(0.,0.,-1.));
#112648=DIRECTION('ref_axis',(0.,1.,0.));
#112649=DIRECTION('center_axis',(0.,0.,-1.));
#112650=DIRECTION('ref_axis',(0.,1.,0.));
#112651=DIRECTION('center_axis',(0.,0.,1.));
#112652=DIRECTION('ref_axis',(-1.,0.,0.));
#112653=DIRECTION('',(0.,0.,-1.));
#112654=DIRECTION('center_axis',(0.,1.,1.23467863058847E-16));
#112655=DIRECTION('ref_axis',(-1.,0.,0.));
#112656=DIRECTION('center_axis',(0.,-1.,-2.77555756156289E-14));
#112657=DIRECTION('ref_axis',(0.,2.77555756156289E-14,-1.));
#112658=DIRECTION('',(-4.38004274807345E-16,-1.,-1.23467863058847E-16));
#112659=DIRECTION('',(4.38004274807345E-16,1.,1.23467863058847E-16));
#112660=DIRECTION('center_axis',(0.,1.,1.23467863058847E-16));
#112661=DIRECTION('ref_axis',(-1.,0.,0.));
#112662=DIRECTION('center_axis',(0.,-1.,0.));
#112663=DIRECTION('ref_axis',(0.,0.,-1.));
#112664=DIRECTION('',(-4.38004274807345E-16,-1.,-1.23467863058847E-16));
#112665=DIRECTION('center_axis',(0.,-1.,0.));
#112666=DIRECTION('ref_axis',(0.,0.,-1.));
#112667=DIRECTION('',(4.38004274807345E-16,1.,1.23467863058847E-16));
#112668=DIRECTION('center_axis',(0.740307041655026,-0.672268907563025,0.));
#112669=DIRECTION('ref_axis',(0.672268907563025,0.740307041655026,0.));
#112670=DIRECTION('center_axis',(0.,0.,-1.));
#112671=DIRECTION('ref_axis',(0.,1.,0.));
#112672=DIRECTION('center_axis',(0.,1.23467863058847E-16,-1.));
#112673=DIRECTION('ref_axis',(0.,1.,1.19418947186571E-16));
#112674=DIRECTION('center_axis',(0.71239495798367,-0.701778757044872,0.));
#112675=DIRECTION('ref_axis',(0.701778757044872,0.71239495798367,0.));
#112676=DIRECTION('center_axis',(1.76945321870477E-31,-1.17608371252665E-16,
1.));
#112677=DIRECTION('ref_axis',(3.01980662698042E-14,1.,1.17608371252665E-16));
#112678=DIRECTION('center_axis',(1.,0.,0.));
#112679=DIRECTION('ref_axis',(0.,0.,-1.));
#112680=DIRECTION('center_axis',(0.,0.,-1.));
#112681=DIRECTION('ref_axis',(0.,1.,0.));
#112682=DIRECTION('center_axis',(-1.,4.38004274807346E-16,5.40794518211031E-32));
#112683=DIRECTION('ref_axis',(-4.38004274807346E-16,-1.,-5.80597460094347E-63));
#112684=DIRECTION('',(1.,-4.38004274807345E-16,-5.40794518211031E-32));
#112685=DIRECTION('',(-1.,4.38004274807345E-16,5.40794518211031E-32));
#112686=DIRECTION('center_axis',(0.,0.,-1.));
#112687=DIRECTION('ref_axis',(0.,1.,0.));
#112688=DIRECTION('center_axis',(0.,0.,-1.));
#112689=DIRECTION('ref_axis',(0.,1.,0.));
#112690=DIRECTION('',(0.,0.,-1.));
#112691=DIRECTION('center_axis',(0.,0.,-1.));
#112692=DIRECTION('ref_axis',(0.,1.,0.));
#112693=DIRECTION('center_axis',(0.,1.23467863058847E-16,-1.));
#112694=DIRECTION('ref_axis',(-1.,0.,0.));
#112695=DIRECTION('center_axis',(0.,0.,-1.));
#112696=DIRECTION('ref_axis',(0.,1.,0.));
#112697=DIRECTION('center_axis',(0.,0.,-1.));
#112698=DIRECTION('ref_axis',(0.,1.,0.));
#112699=DIRECTION('center_axis',(0.,0.,1.));
#112700=DIRECTION('ref_axis',(-1.,0.,0.));
#112701=DIRECTION('',(0.,0.,-1.));
#112702=DIRECTION('center_axis',(-1.,4.38004274807346E-16,5.40794518211031E-32));
#112703=DIRECTION('ref_axis',(-4.38004274807346E-16,-1.,-5.80597460094347E-63));
#112704=DIRECTION('',(-1.,4.38004274807345E-16,5.40794518211031E-32));
#112705=DIRECTION('center_axis',(-1.,0.,0.));
#112706=DIRECTION('ref_axis',(0.,0.,1.));
#112707=DIRECTION('',(1.,-4.38004274807345E-16,-5.40794518211031E-32));
#112708=DIRECTION('center_axis',(0.,1.23467863058847E-16,-1.));
#112709=DIRECTION('ref_axis',(-1.,0.,0.));
#112710=DIRECTION('',(-0.0871557427476402,-0.996194698091747,-1.22998030563942E-16));
#112711=DIRECTION('center_axis',(0.,-1.17559414210783E-16,1.));
#112712=DIRECTION('ref_axis',(0.,1.,1.17559414210783E-16));
#112713=DIRECTION('center_axis',(-4.18005656861882E-16,-1.,0.));
#112714=DIRECTION('ref_axis',(-1.,4.18005656861882E-16,0.));
#112715=DIRECTION('',(1.08020383274181E-17,-4.51531312649963E-33,1.));
#112716=DIRECTION('',(1.,-4.18005656861881E-16,0.));
#112717=DIRECTION('center_axis',(0.,0.,-1.));
#112718=DIRECTION('ref_axis',(-1.,0.,0.));
#112719=DIRECTION('center_axis',(0.,0.,-1.));
#112720=DIRECTION('ref_axis',(-1.,0.,0.));
#112721=DIRECTION('center_axis',(1.,0.,0.));
#112722=DIRECTION('ref_axis',(0.,1.,0.));
#112723=DIRECTION('',(-1.,4.18005656861881E-16,0.));
#112724=DIRECTION('center_axis',(0.,0.,-1.));
#112725=DIRECTION('ref_axis',(0.,-1.,0.));
#112726=DIRECTION('',(-0.0871557427476402,-0.996194698091747,0.));
#112727=DIRECTION('',(1.,-4.18005656861881E-16,0.));
#112728=DIRECTION('center_axis',(1.,0.,0.));
#112729=DIRECTION('ref_axis',(0.,1.,0.));
#112730=DIRECTION('',(-1.,4.18005656861881E-16,0.));
#112731=DIRECTION('center_axis',(4.18005656861882E-16,1.,0.));
#112732=DIRECTION('ref_axis',(1.,-4.18005656861882E-16,0.));
#112733=DIRECTION('',(-1.08020383274181E-17,4.51531312649963E-33,-1.));
#112734=DIRECTION('center_axis',(0.,0.,-1.));
#112735=DIRECTION('ref_axis',(-1.,0.,0.));
#112736=DIRECTION('center_axis',(0.,1.23467863058847E-16,-1.));
#112737=DIRECTION('ref_axis',(-1.,0.,0.));
#112738=DIRECTION('',(-0.0871557427476402,-0.996194698091747,-1.22998030563942E-16));
#112739=DIRECTION('center_axis',(0.,0.,1.));
#112740=DIRECTION('ref_axis',(1.,0.,0.));
#112741=DIRECTION('center_axis',(-4.18005656861882E-16,-1.,0.));
#112742=DIRECTION('ref_axis',(-1.,4.18005656861882E-16,0.));
#112743=DIRECTION('',(1.08020383274181E-17,-4.51531312649963E-33,1.));
#112744=DIRECTION('',(1.,-4.18005656861881E-16,0.));
#112745=DIRECTION('center_axis',(1.,0.,0.));
#112746=DIRECTION('ref_axis',(0.,1.,0.));
#112747=DIRECTION('',(-1.,4.18005656861881E-16,0.));
#112748=DIRECTION('center_axis',(0.,0.,-1.));
#112749=DIRECTION('ref_axis',(0.,-1.,0.));
#112750=DIRECTION('',(-0.0871557427476402,-0.996194698091747,0.));
#112751=DIRECTION('',(1.,-4.38004274807345E-16,0.));
#112752=DIRECTION('center_axis',(-1.,0.,0.));
#112753=DIRECTION('ref_axis',(0.,-1.,0.));
#112754=DIRECTION('',(-1.,4.38004274807345E-16,0.));
#112755=DIRECTION('center_axis',(4.38004274807345E-16,1.,0.));
#112756=DIRECTION('ref_axis',(1.,-4.38004274807345E-16,0.));
#112757=DIRECTION('',(-1.08020383274181E-17,4.73133896404192E-33,-1.));
#112758=DIRECTION('center_axis',(0.,0.,-1.));
#112759=DIRECTION('ref_axis',(-1.,0.,0.));
#112760=DIRECTION('center_axis',(4.18005656861882E-16,1.,0.));
#112761=DIRECTION('ref_axis',(1.,-4.18005656861882E-16,0.));
#112762=DIRECTION('',(-1.,4.18005656861881E-16,0.));
#112763=DIRECTION('',(-1.08020383274181E-17,4.51531312649963E-33,-1.));
#112764=DIRECTION('center_axis',(1.38777878078144E-14,0.,1.));
#112765=DIRECTION('ref_axis',(1.,0.,-1.38777878078144E-14));
#112766=DIRECTION('center_axis',(0.,1.23467863058847E-16,-1.));
#112767=DIRECTION('ref_axis',(0.,1.,1.1837531408762E-16));
#112768=DIRECTION('center_axis',(-4.18005656861882E-16,-1.,0.));
#112769=DIRECTION('ref_axis',(-1.,4.18005656861882E-16,0.));
#112770=DIRECTION('',(-1.08020383274202E-17,4.51531312650048E-33,1.));
#112771=DIRECTION('',(1.,-4.18005656861881E-16,0.));
#112772=DIRECTION('center_axis',(1.,0.,0.));
#112773=DIRECTION('ref_axis',(0.,1.,0.));
#112774=DIRECTION('',(-1.,4.18005656861881E-16,0.));
#112775=DIRECTION('center_axis',(0.,0.,-1.));
#112776=DIRECTION('ref_axis',(0.,-1.,0.));
#112777=DIRECTION('',(0.0871557427476566,-0.996194698091746,0.));
#112778=DIRECTION('',(1.,-4.18005656861881E-16,0.));
#112779=DIRECTION('center_axis',(1.,0.,0.));
#112780=DIRECTION('ref_axis',(0.,1.,0.));
#112781=DIRECTION('',(-1.,4.18005656861881E-16,0.));
#112782=DIRECTION('center_axis',(4.18005656861882E-16,1.,0.));
#112783=DIRECTION('ref_axis',(1.,-4.18005656861882E-16,0.));
#112784=DIRECTION('',(1.08020383274202E-17,-4.51531312650048E-33,-1.));
#112785=DIRECTION('center_axis',(0.,0.,-1.));
#112786=DIRECTION('ref_axis',(-1.,0.,0.));
#112787=DIRECTION('center_axis',(0.,1.23467863058847E-16,-1.));
#112788=DIRECTION('ref_axis',(-1.,0.,0.));
#112789=DIRECTION('center_axis',(-3.98829513817191E-31,-1.17559414210783E-16,
1.));
#112790=DIRECTION('ref_axis',(-6.75015598972095E-14,1.,1.17559414210783E-16));
#112791=DIRECTION('',(0.0871557427476566,-0.996194698091746,-1.22998030563941E-16));
#112792=DIRECTION('center_axis',(0.,1.23467863058847E-16,-1.));
#112793=DIRECTION('ref_axis',(0.,1.,1.1837531408762E-16));
#112794=DIRECTION('center_axis',(0.0835592633859915,-0.955086750882199,
-0.284301156859544));
#112795=DIRECTION('ref_axis',(2.48475885091778E-18,0.285298901444289,-0.958438593147564));
#112796=DIRECTION('center_axis',(0.,0.,1.));
#112797=DIRECTION('ref_axis',(1.,0.,0.));
#112798=DIRECTION('center_axis',(0.,-1.,0.));
#112799=DIRECTION('ref_axis',(0.964920734333665,0.,-0.26254138045836));
#112800=DIRECTION('center_axis',(-4.18005656861882E-16,-1.,0.));
#112801=DIRECTION('ref_axis',(-1.,4.18005656861882E-16,0.));
#112802=DIRECTION('',(-1.08020383274202E-17,4.51531312650048E-33,1.));
#112803=DIRECTION('',(1.,-4.18005656861881E-16,0.));
#112804=DIRECTION('center_axis',(-4.38004274807345E-16,-1.,0.));
#112805=DIRECTION('ref_axis',(-1.,4.38004274807345E-16,0.));
#112806=DIRECTION('',(-1.08020383274202E-17,4.73133896404282E-33,1.));
#112807=DIRECTION('',(1.,-4.38004274807345E-16,0.));
#112808=DIRECTION('center_axis',(0.,0.,-1.));
#112809=DIRECTION('ref_axis',(-1.,0.,0.));
#112810=DIRECTION('center_axis',(-1.,0.,0.));
#112811=DIRECTION('ref_axis',(0.,-1.,0.));
#112812=DIRECTION('',(-1.,4.38004274807345E-16,0.));
#112813=DIRECTION('center_axis',(0.,0.,-1.));
#112814=DIRECTION('ref_axis',(0.,-1.,0.));
#112815=DIRECTION('',(0.0871557427476566,-0.996194698091746,0.));
#112816=DIRECTION('',(1.,-4.18005656861881E-16,0.));
#112817=DIRECTION('center_axis',(1.,0.,0.));
#112818=DIRECTION('ref_axis',(0.,1.,0.));
#112819=DIRECTION('',(-1.,4.18005656861881E-16,0.));
#112820=DIRECTION('center_axis',(4.18005656861882E-16,1.,0.));
#112821=DIRECTION('ref_axis',(1.,-4.18005656861882E-16,0.));
#112822=DIRECTION('',(1.08020383274202E-17,-4.51531312650048E-33,-1.));
#112823=DIRECTION('center_axis',(0.,0.,-1.));
#112824=DIRECTION('ref_axis',(-1.,0.,0.));
#112825=DIRECTION('center_axis',(0.,0.,1.));
#112826=DIRECTION('ref_axis',(1.,0.,0.));
#112827=DIRECTION('center_axis',(0.,1.23467863058847E-16,-1.));
#112828=DIRECTION('ref_axis',(-1.,0.,0.));
#112829=DIRECTION('',(0.0871557427476566,-0.996194698091746,-1.22998030563941E-16));
#112830=DIRECTION('center_axis',(1.,0.,1.87032180698308E-16));
#112831=DIRECTION('ref_axis',(-1.87032180698308E-16,0.,1.));
#112832=DIRECTION('',(0.,-1.,0.));
#112833=DIRECTION('',(-1.87032180698308E-16,-1.07104667533214E-16,1.));
#112834=DIRECTION('',(0.,1.,0.));
#112835=DIRECTION('center_axis',(0.,-1.,0.));
#112836=DIRECTION('ref_axis',(0.,0.,-1.));
#112837=DIRECTION('',(0.,-1.,0.));
#112838=DIRECTION('center_axis',(0.,0.,1.));
#112839=DIRECTION('ref_axis',(1.,0.,0.));
#112840=DIRECTION('',(0.996194698091746,-0.0871557427476568,0.));
#112841=DIRECTION('',(4.38004274807345E-16,1.,0.));
#112842=DIRECTION('center_axis',(4.38004274807346E-16,1.,0.));
#112843=DIRECTION('ref_axis',(-1.,4.38004274807346E-16,0.));
#112844=DIRECTION('',(-4.38004274807345E-16,-1.,0.));
#112845=DIRECTION('center_axis',(1.,-4.38004274807345E-16,0.));
#112846=DIRECTION('ref_axis',(-4.38004274807345E-16,-1.,0.));
#112847=DIRECTION('',(5.40794518211031E-32,1.23467863058847E-16,-1.));
#112848=DIRECTION('center_axis',(0.,0.,-1.));
#112849=DIRECTION('ref_axis',(-1.,0.,0.));
#112850=DIRECTION('center_axis',(0.,0.,1.));
#112851=DIRECTION('ref_axis',(1.,0.,0.));
#112852=DIRECTION('center_axis',(1.,0.,1.87032180698308E-16));
#112853=DIRECTION('ref_axis',(-1.87032180698308E-16,0.,1.));
#112854=DIRECTION('',(-1.87032180698308E-16,-1.07104667533214E-16,1.));
#112855=DIRECTION('',(0.,1.,0.));
#112856=DIRECTION('',(0.,-1.,0.));
#112857=DIRECTION('center_axis',(0.,-1.,0.));
#112858=DIRECTION('ref_axis',(0.,0.,-1.));
#112859=DIRECTION('',(0.,-1.,0.));
#112860=DIRECTION('center_axis',(0.,0.,1.));
#112861=DIRECTION('ref_axis',(1.,0.,0.));
#112862=DIRECTION('',(0.996194698091746,-0.0871557427476568,0.));
#112863=DIRECTION('',(0.,1.,0.));
#112864=DIRECTION('center_axis',(0.,-1.,0.));
#112865=DIRECTION('ref_axis',(0.,0.,-1.));
#112866=DIRECTION('',(0.,-1.,0.));
#112867=DIRECTION('center_axis',(-1.,0.,0.));
#112868=DIRECTION('ref_axis',(0.,0.,1.));
#112869=DIRECTION('',(0.,1.23467863058847E-16,-1.));
#112870=DIRECTION('',(0.,1.,0.));
#112871=DIRECTION('center_axis',(0.,0.,1.));
#112872=DIRECTION('ref_axis',(1.,0.,0.));
#112873=DIRECTION('center_axis',(0.,0.,1.));
#112874=DIRECTION('ref_axis',(1.,0.,0.));
#112875=DIRECTION('center_axis',(0.,1.23467863058847E-16,-1.));
#112876=DIRECTION('ref_axis',(-1.,0.,0.));
#112877=DIRECTION('',(0.996194698091746,-0.0871557427476568,-1.07609333103598E-17));
#112878=DIRECTION('center_axis',(-1.,5.01606788234257E-16,0.));
#112879=DIRECTION('ref_axis',(0.,0.,1.));
#112880=DIRECTION('',(-6.19323182390956E-32,-1.23467863058847E-16,1.));
#112881=DIRECTION('',(-5.01606788234257E-16,-1.,0.));
#112882=DIRECTION('center_axis',(0.,-1.,0.));
#112883=DIRECTION('ref_axis',(1.,0.,0.));
#112884=DIRECTION('',(5.01606788234257E-16,1.,0.));
#112885=DIRECTION('center_axis',(0.,0.,-1.));
#112886=DIRECTION('ref_axis',(0.,-1.,0.));
#112887=DIRECTION('',(-0.996194698091747,-0.0871557427476402,0.));
#112888=DIRECTION('',(-5.01606788234257E-16,-1.,0.));
#112889=DIRECTION('center_axis',(0.,-1.,0.));
#112890=DIRECTION('ref_axis',(1.,0.,0.));
#112891=DIRECTION('',(5.01606788234257E-16,1.,0.));
#112892=DIRECTION('center_axis',(1.,-5.01606788234257E-16,0.));
#112893=DIRECTION('ref_axis',(-5.01606788234257E-16,-1.,0.));
#112894=DIRECTION('',(6.19323182390956E-32,1.23467863058847E-16,-1.));
#112895=DIRECTION('center_axis',(0.,0.,-1.));
#112896=DIRECTION('ref_axis',(-1.,0.,0.));
#112897=DIRECTION('center_axis',(0.,1.23467863058847E-16,-1.));
#112898=DIRECTION('ref_axis',(-1.,0.,0.));
#112899=DIRECTION('center_axis',(0.,-1.17559414210783E-16,1.));
#112900=DIRECTION('ref_axis',(0.,1.,1.17559414210783E-16));
#112901=DIRECTION('',(-0.996194698091747,-0.0871557427476402,-1.07609333103578E-17));
#112902=DIRECTION('center_axis',(0.,1.23467863058847E-16,-1.));
#112903=DIRECTION('ref_axis',(0.,1.,1.1837531408762E-16));
#112904=DIRECTION('center_axis',(-1.,5.01606788234257E-16,0.));
#112905=DIRECTION('ref_axis',(0.,0.,1.));
#112906=DIRECTION('',(-6.19323182390956E-32,-1.23467863058847E-16,1.));
#112907=DIRECTION('',(-5.01606788234257E-16,-1.,0.));
#112908=DIRECTION('center_axis',(0.,0.,-1.));
#112909=DIRECTION('ref_axis',(-1.,0.,0.));
#112910=DIRECTION('center_axis',(0.,0.,1.));
#112911=DIRECTION('ref_axis',(1.,0.,0.));
#112912=DIRECTION('center_axis',(-1.,4.38004274807345E-16,1.13659195805196E-16));
#112913=DIRECTION('ref_axis',(1.13659195805196E-16,0.,1.));
#112914=DIRECTION('',(1.13659195805196E-16,-1.13523971920422E-16,1.));
#112915=DIRECTION('',(-4.38004274807345E-16,-1.,0.));
#112916=DIRECTION('center_axis',(0.,1.,0.));
#112917=DIRECTION('ref_axis',(-1.,0.,0.));
#112918=DIRECTION('',(4.38004274807345E-16,1.,0.));
#112919=DIRECTION('center_axis',(0.,0.,-1.));
#112920=DIRECTION('ref_axis',(0.,-1.,0.));
#112921=DIRECTION('',(-0.996194698091747,-0.0871557427476402,0.));
#112922=DIRECTION('',(-5.01606788234257E-16,-1.,0.));
#112923=DIRECTION('center_axis',(0.,-1.,0.));
#112924=DIRECTION('ref_axis',(1.,0.,0.));
#112925=DIRECTION('',(5.01606788234257E-16,1.,0.));
#112926=DIRECTION('center_axis',(1.,-5.01606788234257E-16,1.13659195805196E-16));
#112927=DIRECTION('ref_axis',(-5.01606788234257E-16,-1.,-5.42661491374937E-48));
#112928=DIRECTION('',(1.13659195805196E-16,1.33411754197273E-16,-1.));
#112929=DIRECTION('center_axis',(0.,0.,-1.));
#112930=DIRECTION('ref_axis',(-1.,0.,0.));
#112931=DIRECTION('center_axis',(0.,0.,-1.));
#112932=DIRECTION('ref_axis',(-1.,0.,0.));
#112933=DIRECTION('center_axis',(0.,1.23467863058847E-16,-1.));
#112934=DIRECTION('ref_axis',(-1.,0.,0.));
#112935=DIRECTION('',(-0.996194698091747,-0.0871557427476402,-1.07609333103578E-17));
#112936=DIRECTION('center_axis',(4.18005656861882E-16,1.,0.));
#112937=DIRECTION('ref_axis',(1.,-4.18005656861882E-16,0.));
#112938=DIRECTION('',(-1.,4.18005656861881E-16,0.));
#112939=DIRECTION('',(-5.16102651992463E-32,2.15733828054269E-47,-1.));
#112940=DIRECTION('center_axis',(2.32688276946506E-8,1.,-5.60873972379676E-9));
#112941=DIRECTION('ref_axis',(0.999404101594694,-2.30613634711969E-8,0.0345172669210846));
#112942=DIRECTION('center_axis',(0.,0.,1.));
#112943=DIRECTION('ref_axis',(1.,0.,0.));
#112944=DIRECTION('center_axis',(-0.161942099399832,-0.986800258756125,
7.590006713781E-5));
#112945=DIRECTION('ref_axis',(0.986128889721933,-0.161834757970274,-0.0368690109508116));
#112946=DIRECTION('center_axis',(0.,-1.18842113532926E-16,1.));
#112947=DIRECTION('ref_axis',(0.,1.,1.18842113532926E-16));
#112948=DIRECTION('center_axis',(0.,1.19033121480991E-16,-1.));
#112949=DIRECTION('ref_axis',(0.,-1.,-1.19033121480991E-16));
#112950=DIRECTION('center_axis',(-4.18005656861882E-16,-1.,0.));
#112951=DIRECTION('ref_axis',(-1.,4.18005656861882E-16,0.));
#112952=DIRECTION('center_axis',(1.8411653907608E-7,-0.999999999999982,
-4.27391046394874E-8));
#112953=DIRECTION('ref_axis',(0.944128962271366,1.59743963266783E-7,0.329576247020879));
#112954=DIRECTION('',(5.16102651992463E-32,-2.15733828054269E-47,1.));
#112955=DIRECTION('',(1.,-4.18005656861881E-16,0.));
#112956=DIRECTION('center_axis',(0.131559425275772,0.991308283854165,-6.31127399035659E-5));
#112957=DIRECTION('ref_axis',(0.984955559835192,-0.130723532319353,-0.113021693703886));
#112958=DIRECTION('center_axis',(0.,0.,-1.));
#112959=DIRECTION('ref_axis',(-1.,0.,0.));
#112960=DIRECTION('center_axis',(1.,0.,0.));
#112961=DIRECTION('ref_axis',(0.,1.,0.));
#112962=DIRECTION('',(-1.,4.18005656861881E-16,0.));
#112963=DIRECTION('center_axis',(0.,0.,-1.));
#112964=DIRECTION('ref_axis',(0.,-1.,0.));
#112965=DIRECTION('center_axis',(0.,0.,-1.));
#112966=DIRECTION('ref_axis',(-1.,0.,0.));
#112967=DIRECTION('',(1.,-4.18005656861881E-16,0.));
#112968=DIRECTION('center_axis',(1.,0.,0.));
#112969=DIRECTION('ref_axis',(0.,1.,0.));
#112970=DIRECTION('',(-1.,4.18005656861881E-16,0.));
#112971=DIRECTION('center_axis',(4.18005656861882E-16,1.,0.));
#112972=DIRECTION('ref_axis',(1.,-4.18005656861882E-16,0.));
#112973=DIRECTION('',(-5.16102651992463E-32,2.15733828054269E-47,-1.));
#112974=DIRECTION('center_axis',(2.74436147249812E-7,0.99999999999996,-6.29034153387323E-8));
#112975=DIRECTION('ref_axis',(0.660475707378147,-1.3402754171038E-7,0.750847414567913));
#112976=DIRECTION('center_axis',(0.,0.,1.));
#112977=DIRECTION('ref_axis',(1.,0.,0.));
#112978=DIRECTION('center_axis',(-0.115639749300789,-0.993291218694044,
5.69820218245346E-5));
#112979=DIRECTION('ref_axis',(0.983118122834487,-0.114463578413279,-0.142747489544376));
#112980=DIRECTION('center_axis',(0.,-1.18842113532926E-16,1.));
#112981=DIRECTION('ref_axis',(0.,1.,1.18842113532926E-16));
#112982=DIRECTION('center_axis',(-4.72661011967866E-32,1.19033121480991E-16,
-1.));
#112983=DIRECTION('ref_axis',(-1.06581410364015E-14,-1.,-1.19033121480991E-16));
#112984=DIRECTION('center_axis',(-4.18005656861882E-16,-1.,0.));
#112985=DIRECTION('ref_axis',(-1.,4.18005656861882E-16,0.));
#112986=DIRECTION('center_axis',(4.47342289204968E-7,-0.999999999999895,
-1.00433397542106E-7));
#112987=DIRECTION('ref_axis',(-0.286876404864124,-3.21200065696789E-8,-0.957967602965901));
#112988=DIRECTION('',(5.16102651992463E-32,-2.15733828054269E-47,1.));
#112989=DIRECTION('center_axis',(0.0751032200622623,0.997175764329397,-3.7018408260164E-5));
#112990=DIRECTION('ref_axis',(0.979395211524647,-0.0737710402502458,-0.187996950142784));
#112991=DIRECTION('center_axis',(0.,0.,-1.));
#112992=DIRECTION('ref_axis',(-1.,0.,0.));
#112993=DIRECTION('center_axis',(-0.159867238682005,-0.0103393831144628,
-0.987084374890517));
#112994=DIRECTION('ref_axis',(0.98052069011386,0.11392960656718,-0.159997565625503));
#112995=DIRECTION('center_axis',(4.18005656861882E-16,1.,0.));
#112996=DIRECTION('ref_axis',(1.,-4.18005656861882E-16,0.));
#112997=DIRECTION('',(-5.16102651992463E-32,2.15733828054269E-47,-1.));
#112998=DIRECTION('center_axis',(0.,1.,0.));
#112999=DIRECTION('ref_axis',(0.977685721591009,0.,-0.210072915429545));
#113000=DIRECTION('center_axis',(0.,0.,-1.));
#113001=DIRECTION('ref_axis',(-1.,0.,0.));
#113002=DIRECTION('center_axis',(-0.0555987775761959,-0.998453191267193,
2.79354816923995E-5));
#113003=DIRECTION('ref_axis',(0.977794512058442,-0.054454062847614,-0.20236760419539));
#113004=DIRECTION('center_axis',(0.,-1.18842113532926E-16,1.));
#113005=DIRECTION('ref_axis',(0.,1.,1.18842113532926E-16));
#113006=DIRECTION('center_axis',(0.,1.19033121480991E-16,-1.));
#113007=DIRECTION('ref_axis',(0.,-1.,-1.19033121480991E-16));
#113008=DIRECTION('center_axis',(-4.18005656861882E-16,-1.,0.));
#113009=DIRECTION('ref_axis',(-1.,4.18005656861882E-16,0.));
#113010=DIRECTION('center_axis',(0.,-1.,0.));
#113011=DIRECTION('ref_axis',(0.976470143643405,0.,-0.215652634050752));
#113012=DIRECTION('',(5.16102651992463E-32,-2.15733828054269E-47,1.));
#113013=DIRECTION('center_axis',(0.00945202350686712,0.99995532861701,-4.69828733081355E-6));
#113014=DIRECTION('ref_axis',(0.976474172799545,-0.00923108138389767,-0.215436712265873));
#113015=DIRECTION('center_axis',(0.,0.,-1.));
#113016=DIRECTION('ref_axis',(-1.,0.,0.));
#113017=DIRECTION('center_axis',(-0.0305144215778958,2.78804702901659E-8,
-0.999534326612031));
#113018=DIRECTION('ref_axis',(0.99952008198814,-0.00533875532879332,-0.0305139868578466));
#113019=DIRECTION('center_axis',(4.18005656861882E-16,1.,0.));
#113020=DIRECTION('ref_axis',(1.,-4.18005656861882E-16,0.));
#113021=DIRECTION('',(-5.16102651992463E-32,2.15733828054269E-47,-1.));
#113022=DIRECTION('center_axis',(0.,1.,0.));
#113023=DIRECTION('ref_axis',(0.976222312485803,0.,-0.216771761548571));
#113024=DIRECTION('center_axis',(0.,0.,-1.));
#113025=DIRECTION('ref_axis',(-1.,0.,0.));
#113026=DIRECTION('center_axis',(0.0113199996393415,-0.999935926735075,
-5.71253473801473E-6));
#113027=DIRECTION('ref_axis',(0.976230462447886,0.0110528731720008,-0.216453039210427));
#113028=DIRECTION('center_axis',(0.,-1.18842113532926E-16,1.));
#113029=DIRECTION('ref_axis',(0.,1.,1.18842113532926E-16));
#113030=DIRECTION('center_axis',(-1.96942088319945E-31,1.19033121480991E-16,
-1.));
#113031=DIRECTION('ref_axis',(-4.44089209850063E-14,-1.,-1.19033121480991E-16));
#113032=DIRECTION('center_axis',(-4.18005656861882E-16,-1.,0.));
#113033=DIRECTION('ref_axis',(-1.,4.18005656861882E-16,0.));
#113034=DIRECTION('center_axis',(0.,-1.,0.));
#113035=DIRECTION('ref_axis',(0.978069789124882,0.,-0.208277429408972));
#113036=DIRECTION('',(5.16102651992463E-32,-2.15733828054269E-47,1.));
#113037=DIRECTION('center_axis',(-0.0573828197059871,0.998352248055229,
2.83841706920683E-5));
#113038=DIRECTION('ref_axis',(0.978154360176249,0.0562275849658862,-0.200131222844156));
#113039=DIRECTION('center_axis',(0.,0.,-1.));
#113040=DIRECTION('ref_axis',(-1.,0.,0.));
#113041=DIRECTION('center_axis',(-0.167640680088922,0.0112856983933777,
-0.985783564171719));
#113042=DIRECTION('ref_axis',(0.977940174982197,-0.124494780023978,-0.167732119472009));
#113043=DIRECTION('center_axis',(4.18005656861882E-16,1.,0.));
#113044=DIRECTION('ref_axis',(1.,-4.18005656861882E-16,0.));
#113045=DIRECTION('',(-5.16102651992463E-32,2.15733828054269E-47,-1.));
#113046=DIRECTION('center_axis',(0.,1.,0.));
#113047=DIRECTION('ref_axis',(0.979260396969467,0.,-0.202605712967828));
#113048=DIRECTION('center_axis',(0.,0.,-1.));
#113049=DIRECTION('ref_axis',(-1.,0.,0.));
#113050=DIRECTION('center_axis',(0.0768213995086415,-0.997044869150772,
-3.84402733247989E-5));
#113051=DIRECTION('ref_axis',(0.979293407027384,0.0754609081712752,-0.187856525813356));
#113052=DIRECTION('center_axis',(0.,-1.18842113532926E-16,1.));
#113053=DIRECTION('ref_axis',(0.,1.,1.18842113532926E-16));
#113054=DIRECTION('center_axis',(0.,1.19033121480991E-16,-1.));
#113055=DIRECTION('ref_axis',(0.,-1.,-1.19033121480991E-16));
#113056=DIRECTION('center_axis',(-4.18005656861882E-16,-1.,0.));
#113057=DIRECTION('ref_axis',(-1.,4.18005656861882E-16,0.));
#113058=DIRECTION('center_axis',(2.65375038641309E-7,-0.999999999999963,
-6.08902664370013E-8));
#113059=DIRECTION('ref_axis',(-0.699850500391891,-1.4222958468278E-7,-0.714289351104438));
#113060=DIRECTION('',(5.16102651992463E-32,-2.15733828054269E-47,1.));
#113061=DIRECTION('',(1.,-4.18005656861881E-16,0.));
#113062=DIRECTION('center_axis',(-0.117125163318625,0.993117159703197,5.67506910983411E-5));
#113063=DIRECTION('ref_axis',(0.98346589789016,0.115994870303608,-0.139068392348335));
#113064=DIRECTION('center_axis',(0.,0.,-1.));
#113065=DIRECTION('ref_axis',(-1.,0.,0.));
#113066=DIRECTION('center_axis',(1.,0.,0.));
#113067=DIRECTION('ref_axis',(0.,1.,0.));
#113068=DIRECTION('',(-1.,4.18005656861881E-16,0.));
#113069=DIRECTION('center_axis',(0.,0.,-1.));
#113070=DIRECTION('ref_axis',(0.,-1.,0.));
#113071=DIRECTION('center_axis',(0.,0.,-1.));
#113072=DIRECTION('ref_axis',(-1.,0.,0.));
#113073=DIRECTION('',(1.,-4.18005656861881E-16,0.));
#113074=DIRECTION('center_axis',(1.,0.,0.));
#113075=DIRECTION('ref_axis',(0.,1.,0.));
#113076=DIRECTION('',(-1.,4.18005656861881E-16,0.));
#113077=DIRECTION('center_axis',(4.18005656861882E-16,1.,0.));
#113078=DIRECTION('ref_axis',(1.,-4.18005656861882E-16,0.));
#113079=DIRECTION('',(-5.16102651992463E-32,2.15733828054269E-47,-1.));
#113080=DIRECTION('center_axis',(1.78035294390513E-7,0.999999999999983,
-4.13792835849922E-8));
#113081=DIRECTION('ref_axis',(0.953984227519048,-1.57435003701598E-7,0.299856788558906));
#113082=DIRECTION('center_axis',(0.,0.,1.));
#113083=DIRECTION('ref_axis',(1.,0.,0.));
#113084=DIRECTION('center_axis',(0.132927043042659,-0.991125823009864,-6.47375843459798E-5));
#113085=DIRECTION('ref_axis',(0.984931431928559,0.132103559132877,-0.111618654639735));
#113086=DIRECTION('center_axis',(0.,-1.18842113532926E-16,1.));
#113087=DIRECTION('ref_axis',(0.,1.,1.18842113532926E-16));
#113088=DIRECTION('center_axis',(9.84710441599736E-32,1.19033121480991E-16,
-1.));
#113089=DIRECTION('ref_axis',(2.22044604925031E-14,-1.,-1.19033121480991E-16));
#113090=DIRECTION('center_axis',(0.,0.,1.));
#113091=DIRECTION('ref_axis',(1.,0.,0.));
#113092=DIRECTION('center_axis',(0.,-1.,0.));
#113093=DIRECTION('ref_axis',(0.949353414893388,0.,0.314210269772112));
#113094=DIRECTION('center_axis',(-4.18005656861882E-16,-1.,0.));
#113095=DIRECTION('ref_axis',(-1.,4.18005656861882E-16,0.));
#113096=DIRECTION('',(5.16102651992463E-32,-2.15733828054269E-47,1.));
#113097=DIRECTION('',(1.,-4.18005656861881E-16,0.));
#113098=DIRECTION('center_axis',(1.,0.,0.));
#113099=DIRECTION('ref_axis',(0.,1.,0.));
#113100=DIRECTION('',(-1.,4.18005656861881E-16,0.));
#113101=DIRECTION('center_axis',(0.,0.,-1.));
#113102=DIRECTION('ref_axis',(0.,-1.,0.));
#113103=DIRECTION('center_axis',(0.,0.,1.));
#113104=DIRECTION('ref_axis',(-1.,-1.5419764230905E-14,0.));
#113105=DIRECTION('',(1.,-4.18005656861881E-16,0.));
#113106=DIRECTION('center_axis',(1.,0.,0.));
#113107=DIRECTION('ref_axis',(0.,1.,0.));
#113108=DIRECTION('center_axis',(0.985034259178296,-0.172358661647933,-3.73628995927113E-11));
#113109=DIRECTION('ref_axis',(-0.0884978163252629,-0.505767334680601,-0.858118604667059));
#113110=DIRECTION('center_axis',(1.,0.,0.));
#113111=DIRECTION('ref_axis',(0.,1.,0.));
#113112=DIRECTION('center_axis',(0.985034259164998,0.172358661723926,1.4184662739622E-13));
#113113=DIRECTION('ref_axis',(0.0566474313388088,-0.323741551509226,0.944448239105306));
#113114=DIRECTION('',(-1.,4.18005656861881E-16,0.));
#113115=DIRECTION('center_axis',(0.,0.,-1.));
#113116=DIRECTION('ref_axis',(0.,-1.,0.));
#113117=DIRECTION('center_axis',(0.,0.,1.));
#113118=DIRECTION('ref_axis',(-1.,2.69845874040837E-15,0.));
#113119=DIRECTION('',(1.,-4.18005656861881E-16,0.));
#113120=DIRECTION('center_axis',(1.,0.,0.));
#113121=DIRECTION('ref_axis',(0.,1.,0.));
#113122=DIRECTION('center_axis',(1.,0.,1.87032180698308E-16));
#113123=DIRECTION('ref_axis',(-1.87032180698308E-16,0.,1.));
#113124=DIRECTION('center_axis',(1.,0.,0.));
#113125=DIRECTION('ref_axis',(0.,0.97671957347062,-0.214520103485359));
#113126=DIRECTION('',(-1.87032180698308E-16,-1.23467863058847E-16,1.));
#113127=DIRECTION('',(0.,-1.,0.));
#113128=DIRECTION('center_axis',(-0.00150472629281886,-0.0576832079807129,
-0.998333803552618));
#113129=DIRECTION('ref_axis',(0.0662281834101546,0.996137339756707,-0.0576561190561847));
#113130=DIRECTION('center_axis',(-1.,0.,0.));
#113131=DIRECTION('ref_axis',(0.,0.,1.));
#113132=DIRECTION('',(0.,1.23467863058847E-16,-1.));
#113133=DIRECTION('center_axis',(-1.,0.,0.));
#113134=DIRECTION('ref_axis',(0.,0.977150339649859,-0.212549320681494));
#113135=DIRECTION('',(0.,1.,0.));
#113136=DIRECTION('center_axis',(0.,0.,1.));
#113137=DIRECTION('ref_axis',(1.,0.,0.));
#113138=DIRECTION('center_axis',(0.998974276838322,0.045281273125727,-2.27917889832281E-5));
#113139=DIRECTION('ref_axis',(0.0443009274833836,-0.977241931984893,0.207450317412498));
#113140=DIRECTION('center_axis',(0.,-1.18842113532926E-16,1.));
#113141=DIRECTION('ref_axis',(0.,1.,1.18842113532926E-16));
#113142=DIRECTION('center_axis',(0.,0.,1.));
#113143=DIRECTION('ref_axis',(0.,-1.,0.));
#113144=DIRECTION('center_axis',(0.,1.19033121480991E-16,-1.));
#113145=DIRECTION('ref_axis',(0.,-1.,-1.19033121480991E-16));
#113146=DIRECTION('center_axis',(1.,0.,1.87032180698308E-16));
#113147=DIRECTION('ref_axis',(-1.87032180698308E-16,0.,1.));
#113148=DIRECTION('center_axis',(0.999999999999922,3.86396291419339E-7,
-8.7347856309549E-8));
#113149=DIRECTION('ref_axis',(-5.51687615636349E-8,0.354181556536311,0.935176681172875));
#113150=DIRECTION('',(-1.87032180698308E-16,-1.23467863058847E-16,1.));
#113151=DIRECTION('',(0.,-1.,0.));
#113152=DIRECTION('center_axis',(-0.995792257730495,-0.0916393879573366,
4.49311545952089E-5));
#113153=DIRECTION('ref_axis',(0.0902711933575697,-0.980840233260372,0.172637042570649));
#113154=DIRECTION('center_axis',(0.,0.,-1.));
#113155=DIRECTION('ref_axis',(-1.,0.,0.));
#113156=DIRECTION('center_axis',(-0.049502590584409,-0.39010562996265,-0.91943846504096));
#113157=DIRECTION('ref_axis',(0.184301157644048,0.901190701629574,-0.392286123368467));
#113158=DIRECTION('center_axis',(-1.,0.,0.));
#113159=DIRECTION('ref_axis',(0.,0.,1.));
#113160=DIRECTION('',(0.,1.23467863058847E-16,-1.));
#113161=DIRECTION('center_axis',(-0.999999999999951,3.06438016471383E-7,
-6.99460036508937E-8));
#113162=DIRECTION('ref_axis',(1.06561681951965E-7,0.539875486057826,0.841744889829344));
#113163=DIRECTION('',(0.,1.,0.));
#113164=DIRECTION('center_axis',(0.,0.,1.));
#113165=DIRECTION('ref_axis',(1.,0.,0.));
#113166=DIRECTION('center_axis',(0.994006408314,0.109321806185977,-5.40642036517117E-5));
#113167=DIRECTION('ref_axis',(0.10805711689382,-0.982431998566189,0.152154617681619));
#113168=DIRECTION('center_axis',(0.,-1.18842113532926E-16,1.));
#113169=DIRECTION('ref_axis',(0.,1.,1.18842113532926E-16));
#113170=DIRECTION('center_axis',(0.,1.19033121480991E-16,-1.));
#113171=DIRECTION('ref_axis',(0.,-1.,-1.19033121480991E-16));
#113172=DIRECTION('center_axis',(0.,0.,1.));
#113173=DIRECTION('ref_axis',(1.,0.,0.));
#113174=DIRECTION('center_axis',(0.999999999999995,9.8647085618326E-8,-2.32552699791606E-8));
#113175=DIRECTION('ref_axis',(9.49367917791162E-8,-0.992051753854412,-0.125830511698778));
#113176=DIRECTION('center_axis',(-0.989231594111401,-0.146358629503497,
6.91496543724644E-5));
#113177=DIRECTION('ref_axis',(0.145900204554444,-0.986095533541962,0.0795533094193093));
#113178=DIRECTION('center_axis',(1.,0.,1.87032180698308E-16));
#113179=DIRECTION('ref_axis',(-1.87032180698308E-16,0.,1.));
#113180=DIRECTION('',(-1.87032180698308E-16,-1.23467863058847E-16,1.));
#113181=DIRECTION('',(0.,1.,0.));
#113182=DIRECTION('',(0.,-1.,0.));
#113183=DIRECTION('center_axis',(0.,-1.,0.));
#113184=DIRECTION('ref_axis',(0.,0.,-1.));
#113185=DIRECTION('',(0.,-1.,0.));
#113186=DIRECTION('center_axis',(0.,0.,1.));
#113187=DIRECTION('ref_axis',(1.,0.,0.));
#113188=DIRECTION('center_axis',(0.,0.,-1.));
#113189=DIRECTION('ref_axis',(1.,-1.23459581198307E-13,0.));
#113190=DIRECTION('',(0.,1.,0.));
#113191=DIRECTION('center_axis',(0.,-1.,0.));
#113192=DIRECTION('ref_axis',(0.,0.,-1.));
#113193=DIRECTION('',(0.,-1.,0.));
#113194=DIRECTION('center_axis',(-1.,0.,0.));
#113195=DIRECTION('ref_axis',(0.,0.,1.));
#113196=DIRECTION('',(0.,1.23467863058847E-16,-1.));
#113197=DIRECTION('center_axis',(-1.,0.,0.));
#113198=DIRECTION('ref_axis',(0.,-0.558140143909497,-0.829746696140868));
#113199=DIRECTION('',(0.,1.,0.));
#113200=DIRECTION('center_axis',(0.,0.,1.));
#113201=DIRECTION('ref_axis',(1.,0.,0.));
#113202=DIRECTION('center_axis',(0.,1.23467863058847E-16,-1.));
#113203=DIRECTION('ref_axis',(0.,1.,1.1837531408762E-16));
#113204=DIRECTION('center_axis',(0.,1.19212619247436E-16,-1.));
#113205=DIRECTION('ref_axis',(0.,1.,1.19212619247436E-16));
#113206=DIRECTION('center_axis',(0.,-1.,0.));
#113207=DIRECTION('ref_axis',(1.,0.,0.));
#113208=DIRECTION('',(-5.01606788234257E-16,-1.,0.));
#113209=DIRECTION('',(5.01606788234257E-16,1.,0.));
#113210=DIRECTION('center_axis',(1.,-5.01606788234257E-16,0.));
#113211=DIRECTION('ref_axis',(-5.01606788234257E-16,-1.,0.));
#113212=DIRECTION('',(6.19323182390956E-32,1.23467863058847E-16,-1.));
#113213=DIRECTION('center_axis',(1.,-2.12838232963581E-8,-5.13483277355434E-9));
#113214=DIRECTION('ref_axis',(2.11055106046707E-8,0.999470690690628,-0.0325321141397118));
#113215=DIRECTION('',(6.19323182390956E-32,1.23467863058847E-16,-1.));
#113216=DIRECTION('center_axis',(0.,0.,-1.));
#113217=DIRECTION('ref_axis',(-1.,0.,0.));
#113218=DIRECTION('center_axis',(-0.986715031900344,0.162460579946267,7.60619890862346E-5));
#113219=DIRECTION('ref_axis',(0.162362454938592,0.986102575671949,0.0352156709358418));
#113220=DIRECTION('center_axis',(0.,-1.18842113532926E-16,1.));
#113221=DIRECTION('ref_axis',(0.,1.,1.18842113532926E-16));
#113222=DIRECTION('center_axis',(-5.51437847295852E-32,1.19033121480991E-16,
-1.));
#113223=DIRECTION('ref_axis',(-1.24344978758017E-14,-1.,-1.19033121480991E-16));
#113224=DIRECTION('center_axis',(-1.,5.01606788234257E-16,0.));
#113225=DIRECTION('ref_axis',(0.,0.,1.));
#113226=DIRECTION('',(-6.19323182390956E-32,-1.23467863058847E-16,1.));
#113227=DIRECTION('center_axis',(-0.999999999999983,-1.80161300130045E-7,
-4.18470807107181E-8));
#113228=DIRECTION('ref_axis',(1.57783577543169E-7,-0.949012696634457,0.315237849292515));
#113229=DIRECTION('',(-6.19323182390956E-32,-1.23467863058847E-16,1.));
#113230=DIRECTION('',(-5.01606788234257E-16,-1.,0.));
#113231=DIRECTION('center_axis',(0.991217376526726,-0.132242612086272,-6.34040519857628E-5));
#113232=DIRECTION('ref_axis',(0.131422968750417,0.985020258821126,0.111638223726418));
#113233=DIRECTION('center_axis',(0.,0.,-1.));
#113234=DIRECTION('ref_axis',(-1.,0.,0.));
#113235=DIRECTION('center_axis',(0.,-1.,0.));
#113236=DIRECTION('ref_axis',(1.,0.,0.));
#113237=DIRECTION('',(5.01606788234257E-16,1.,0.));
#113238=DIRECTION('center_axis',(0.,0.,-1.));
#113239=DIRECTION('ref_axis',(0.,-1.,0.));
#113240=DIRECTION('center_axis',(0.,0.,-1.));
#113241=DIRECTION('ref_axis',(-1.,0.,0.));
#113242=DIRECTION('',(-5.01606788234257E-16,-1.,0.));
#113243=DIRECTION('center_axis',(0.,-1.,0.));
#113244=DIRECTION('ref_axis',(1.,0.,0.));
#113245=DIRECTION('',(5.01606788234257E-16,1.,0.));
#113246=DIRECTION('center_axis',(1.,-5.01606788234257E-16,0.));
#113247=DIRECTION('ref_axis',(-5.01606788234257E-16,-1.,0.));
#113248=DIRECTION('',(6.19323182390956E-32,1.23467863058847E-16,-1.));
#113249=DIRECTION('center_axis',(0.999999999999961,-2.7050082141817E-7,
-6.20337418949715E-8));
#113250=DIRECTION('ref_axis',(1.37645784434391E-7,0.677526577092017,-0.735498291863385));
#113251=DIRECTION('',(6.19323182390956E-32,1.23467863058847E-16,-1.));
#113252=DIRECTION('center_axis',(0.,0.,-1.));
#113253=DIRECTION('ref_axis',(-1.,0.,0.));
#113254=DIRECTION('center_axis',(0.,0.,-1.));
#113255=DIRECTION('ref_axis',(-1.,0.,0.));
#113256=DIRECTION('center_axis',(-0.993204090877291,0.116385697482287,5.73251750129611E-5));
#113257=DIRECTION('ref_axis',(0.115221510518281,0.983199503181504,0.141572385928648));
#113258=DIRECTION('center_axis',(0.,-1.18842113532926E-16,1.));
#113259=DIRECTION('ref_axis',(0.,1.,1.18842113532926E-16));
#113260=DIRECTION('center_axis',(-6.69603100287811E-32,1.19033121480991E-16,
-1.));
#113261=DIRECTION('ref_axis',(-1.50990331349022E-14,-1.,-1.19033121480991E-16));
#113262=DIRECTION('center_axis',(-1.,5.01606788234257E-16,0.));
#113263=DIRECTION('ref_axis',(0.,0.,1.));
#113264=DIRECTION('',(-6.19323182390956E-32,-1.23467863058847E-16,1.));
#113265=DIRECTION('center_axis',(-0.999999999999896,-4.44492331285063E-7,
-9.98246615501216E-8));
